#176108=CARTESIAN_POINT('Ctrl Pts',(-21.845742680186,-3.12619666607363,
135.830257907741));
#176109=CARTESIAN_POINT('Ctrl Pts',(-21.8383408585105,-3.25770653532805,
135.743518308122));
#176110=CARTESIAN_POINT('Ctrl Pts',(-21.8309429441991,-3.38914698154654,
135.656824497663));
#176111=CARTESIAN_POINT('Ctrl Pts',(-21.8235450298877,-3.51719526162264,
135.564833503806));
#176112=CARTESIAN_POINT('Ctrl Pts',(-21.8161471155763,-3.64140375070958,
135.467847433975));
#176113=CARTESIAN_POINT('Ctrl Pts',(-21.8087504306641,-3.7655915985983,
135.37087748147));
#176114=CARTESIAN_POINT('Ctrl Pts',(-21.8013537457518,-3.88594062800541,
135.268914329994));
#176115=CARTESIAN_POINT('Ctrl Pts',(-21.7939570608396,-4.0020340600782,
135.162302097723));
#176116=CARTESIAN_POINT('Ctrl Pts',(-21.7865607039042,-4.11812234444605,
135.055694592751));
#176117=CARTESIAN_POINT('Ctrl Pts',(-21.7791643469687,-4.22995513172452,
134.944438669363));
#176118=CARTESIAN_POINT('Ctrl Pts',(-21.7717679900333,-4.33715068128002,
134.828917056526));
#176119=CARTESIAN_POINT('Ctrl Pts',(-21.7643705006967,-4.44436264274842,
134.713377757034));
#176120=CARTESIAN_POINT('Ctrl Pts',(-21.75697301136,-4.54693569891078,134.593571741362));
#176121=CARTESIAN_POINT('Ctrl Pts',(-21.7495755220234,-4.64452686892937,
134.469916608994));
#176122=CARTESIAN_POINT('Ctrl Pts',(-21.7421754395084,-4.74215224938077,
134.346218129512));
#176123=CARTESIAN_POINT('Ctrl Pts',(-21.7347753569935,-4.83479203551193,
134.218668139732));
#176124=CARTESIAN_POINT('Ctrl Pts',(-21.7273752744785,-4.92214531890378,
134.087715003266));
#176125=CARTESIAN_POINT('Ctrl Pts',(-21.719967054812,-5.00959465621136,
133.956617870363));
#176126=CARTESIAN_POINT('Ctrl Pts',(-21.7125588351455,-5.09174567445106,
133.822110428272));
#176127=CARTESIAN_POINT('Ctrl Pts',(-21.705150615479,-5.16834199435097,
133.684668169188));
#176128=CARTESIAN_POINT('Ctrl Pts',(-21.697737836177,-5.24498545800748,
133.547141316687));
#176129=CARTESIAN_POINT('Ctrl Pts',(-21.690325056875,-5.31606724272622,
133.406676380159));
#176130=CARTESIAN_POINT('Ctrl Pts',(-21.6829122775729,-5.38137848385342,
133.263770338621));
#176131=CARTESIAN_POINT('Ctrl Pts',(-21.6754889065441,-5.446783044745,133.120660106229));
#176132=CARTESIAN_POINT('Ctrl Pts',(-21.6680655355153,-5.50640045337233,
132.975102147108));
#176133=CARTESIAN_POINT('Ctrl Pts',(-21.6606421644865,-5.56007092836429,
132.827610931803));
#176134=CARTESIAN_POINT('Ctrl Pts',(-21.6567061150459,-5.58852830200886,
132.749407550449));
#176135=CARTESIAN_POINT('Ctrl Pts',(-21.6527700656052,-5.61531462151302,
132.670660884153));
#176136=CARTESIAN_POINT('Ctrl Pts',(-21.6488340161646,-5.64041188726546,
132.591448837127));
#176137=CARTESIAN_POINT('Ctrl Pts',(-21.6398564824062,-5.69765495647397,
132.410778132406));
#176138=CARTESIAN_POINT('Ctrl Pts',(-21.6308789486478,-5.74624880988774,
132.227243494478));
#176139=CARTESIAN_POINT('Ctrl Pts',(-21.6219014148894,-5.78594647018682,
132.041597056826));
#176140=CARTESIAN_POINT('Ctrl Pts',(-21.6129769272198,-5.82540956655472,
131.857047559343));
#176141=CARTESIAN_POINT('Ctrl Pts',(-21.6040524395501,-5.85608123096748,
131.670411147484));
#176142=CARTESIAN_POINT('Ctrl Pts',(-21.5951279518804,-5.8777655631654,
131.482448035947));
#176143=CARTESIAN_POINT('Ctrl Pts',(-21.5862995925613,-5.8992163268758,
131.296509531821));
#176144=CARTESIAN_POINT('Ctrl Pts',(-21.5774712332422,-5.91187226502017,
131.109272779503));
#176145=CARTESIAN_POINT('Ctrl Pts',(-21.5686428739231,-5.91559043864777,
130.921494407222));
#176146=CARTESIAN_POINT('Ctrl Pts',(-21.5668869983483,-5.91632994754399,
130.884147098912));
#176147=CARTESIAN_POINT('Ctrl Pts',(-21.5651311227735,-5.91671605321219,
130.846778431061));
#176148=CARTESIAN_POINT('Ctrl Pts',(-21.5633752471987,-5.91674785866266,
130.809394454159));
#176149=CARTESIAN_POINT('',(-19.8133751630259,-5.91241589777291,130.801494312422));
#176150=CARTESIAN_POINT('Ctrl Pts',(-21.5633751922043,-5.91249924175333,
130.809389669497));
#176151=CARTESIAN_POINT('Ctrl Pts',(-21.4990455922534,-5.90151877568405,
129.440734853295));
#176152=CARTESIAN_POINT('Ctrl Pts',(-21.3419001176983,-4.74664212764213,
126.080642320765));
#176153=CARTESIAN_POINT('Ctrl Pts',(-21.0919387685389,0.850611657590301,
123.857849238585));
#176154=CARTESIAN_POINT('Ctrl Pts',(-20.813491144726,6.30407313683402,127.765245217356));
#176155=CARTESIAN_POINT('Ctrl Pts',(-20.5350435209133,5.96439937442269,
134.46543977988));
#176156=CARTESIAN_POINT('Ctrl Pts',(-20.2565958971003,0.143733964024427,
137.801281445897));
#176157=CARTESIAN_POINT('Ctrl Pts',(-20.0160397875307,-4.99895800061713,
135.128328424986));
#176158=CARTESIAN_POINT('Ctrl Pts',(-19.8682995525653,-5.90317744802826,
131.97214796945));
#176159=CARTESIAN_POINT('Ctrl Pts',(-19.8133751922042,-5.90827769618411,
130.801496940956));
#176160=CARTESIAN_POINT('',(-18.0633751922043,-5.91997941989959,130.800355646857));
#176161=CARTESIAN_POINT('Ctrl Pts',(-19.8133751324712,-5.91674930439072,
130.801491559896));
#176162=CARTESIAN_POINT('Ctrl Pts',(-19.805254061995,-5.91666525141781,
130.628152287518));
#176163=CARTESIAN_POINT('Ctrl Pts',(-19.7971329915187,-5.90895978560523,
130.455069894106));
#176164=CARTESIAN_POINT('Ctrl Pts',(-19.7890119210425,-5.89372508479234,
130.282886565106));
#176165=CARTESIAN_POINT('Ctrl Pts',(-19.780850939307,-5.8784155125575,130.109857035655));
#176166=CARTESIAN_POINT('Ctrl Pts',(-19.7726899575716,-5.85550259932545,
129.937735664064));
#176167=CARTESIAN_POINT('Ctrl Pts',(-19.764528975836,-5.82513029749076,
129.767158814755));
#176168=CARTESIAN_POINT('Ctrl Pts',(-19.7563478049367,-5.79468285869375,
129.596159981416));
#176169=CARTESIAN_POINT('Ctrl Pts',(-19.7481666340374,-5.75673919147736,
129.426713542274));
#176170=CARTESIAN_POINT('Ctrl Pts',(-19.7399854631381,-5.7114933612633,
129.259441801982));
#176171=CARTESIAN_POINT('Ctrl Pts',(-19.7317751853,-5.6660865556063,129.091574942928));
#176172=CARTESIAN_POINT('Ctrl Pts',(-19.7235649074619,-5.61332565032963,
128.925898501203));
#176173=CARTESIAN_POINT('Ctrl Pts',(-19.7153546296238,-5.5534544170368,
128.763019244744));
#176174=CARTESIAN_POINT('Ctrl Pts',(-19.7101366362407,-5.5154036098262,
128.659502299372));
#176175=CARTESIAN_POINT('Ctrl Pts',(-19.7049186428575,-5.47448177662029,
128.557114725779));
#176176=CARTESIAN_POINT('Ctrl Pts',(-19.6997006494744,-5.43076109945184,
128.456007057477));
#176177=CARTESIAN_POINT('Ctrl Pts',(-19.692277383069,-5.36856281551098,
128.312168401059));
#176178=CARTESIAN_POINT('Ctrl Pts',(-19.6848541166636,-5.30055198667891,
128.170585018124));
#176179=CARTESIAN_POINT('Ctrl Pts',(-19.6774308502582,-5.22691332803574,
128.031761183154));
#176180=CARTESIAN_POINT('Ctrl Pts',(-19.6700163575372,-5.15336170417167,
127.893101426428));
#176181=CARTESIAN_POINT('Ctrl Pts',(-19.6626018648161,-5.07419566381752,
127.757195052076));
#176182=CARTESIAN_POINT('Ctrl Pts',(-19.6551873720952,-4.98964822034993,
127.624527099965));
#176183=CARTESIAN_POINT('Ctrl Pts',(-19.6477800257414,-4.90518226689174,
127.491987018222));
#176184=CARTESIAN_POINT('Ctrl Pts',(-19.6403726793877,-4.81534543548999,
127.362679457492));
#176185=CARTESIAN_POINT('Ctrl Pts',(-19.632965333034,-4.72041689796875,
127.237065441684));
#176186=CARTESIAN_POINT('Ctrl Pts',(-19.6255635113586,-4.62555916173197,
127.111545113548));
#176187=CARTESIAN_POINT('Ctrl Pts',(-19.6181616896832,-4.52561750498102,
126.989713141722));
#176188=CARTESIAN_POINT('Ctrl Pts',(-19.6107598680078,-4.42091463852936,
126.872001996924));
#176189=CARTESIAN_POINT('Ctrl Pts',(-19.6033619536965,-4.31626704390605,
126.754352990923));
#176190=CARTESIAN_POINT('Ctrl Pts',(-19.5959640393852,-4.20686349262083,
126.640820757849));
#176191=CARTESIAN_POINT('Ctrl Pts',(-19.5885661250739,-4.09306716331315,
126.531804970286));
#176192=CARTESIAN_POINT('Ctrl Pts',(-19.5811694401617,-3.97928974489091,
126.422807299169));
#176193=CARTESIAN_POINT('Ctrl Pts',(-19.5737727552495,-3.86112126657913,
126.318324841927));
#176194=CARTESIAN_POINT('Ctrl Pts',(-19.5663760703374,-3.73896205988283,
126.218720719225));
#176195=CARTESIAN_POINT('Ctrl Pts',(-19.5589797134019,-3.61680826985394,
126.119121013074));
#176196=CARTESIAN_POINT('Ctrl Pts',(-19.5515833564665,-3.49066439259866,
126.024399447261));
#176197=CARTESIAN_POINT('Ctrl Pts',(-19.5441869995311,-3.36096394646326,
125.934878929226));
#176198=CARTESIAN_POINT('Ctrl Pts',(-19.5367895101945,-3.23124364285826,
125.845344705372));
#176199=CARTESIAN_POINT('Ctrl Pts',(-19.529392020858,-3.09796599340552,
125.761013326884));
#176200=CARTESIAN_POINT('Ctrl Pts',(-19.5219945315215,-2.96159346797302,
125.682164341264));
#176201=CARTESIAN_POINT('Ctrl Pts',(-19.5145944490065,-2.82517313736313,
125.603287715255));
#176202=CARTESIAN_POINT('Ctrl Pts',(-19.5071943664916,-2.68565609370416,
125.529897495227));
#176203=CARTESIAN_POINT('Ctrl Pts',(-19.4997942839766,-2.54352921937556,
125.462227179259));
#176204=CARTESIAN_POINT('Ctrl Pts',(-19.4923860643102,-2.40124606193763,
125.394482452821));
#176205=CARTESIAN_POINT('Ctrl Pts',(-19.4849778446437,-2.25634767994791,
125.332470351808));
#176206=CARTESIAN_POINT('Ctrl Pts',(-19.4775696249772,-2.10934141801378,
125.276376414916));
#176207=CARTESIAN_POINT('Ctrl Pts',(-19.4701568456752,-1.96224467617836,
125.220247953141));
#176208=CARTESIAN_POINT('Ctrl Pts',(-19.4627440663732,-1.81303782222359,
125.170045032456));
#176209=CARTESIAN_POINT('Ctrl Pts',(-19.4553312870711,-1.66224265139249,
125.125903086652));
#176210=CARTESIAN_POINT('Ctrl Pts',(-19.4479079160424,-1.51123201734951,
125.081698068766));
#176211=CARTESIAN_POINT('Ctrl Pts',(-19.4404845450136,-1.35862889501245,
125.043571412378));
#176212=CARTESIAN_POINT('Ctrl Pts',(-19.4330611739849,-1.20496535129876,
125.01160746689));
#176213=CARTESIAN_POINT('Ctrl Pts',(-19.4291251245438,-1.12348925330885,
124.994659416026));
#176214=CARTESIAN_POINT('Ctrl Pts',(-19.4251890751027,-1.04171513246566,
124.979443058799));
#176215=CARTESIAN_POINT('Ctrl Pts',(-19.4212530256616,-0.959722669037745,
124.965965036498));
#176216=CARTESIAN_POINT('Ctrl Pts',(-19.4138297592562,-0.805087441922301,
124.940545907076));
#176217=CARTESIAN_POINT('Ctrl Pts',(-19.4064064928507,-0.649207817768075,
124.921236066696));
#176218=CARTESIAN_POINT('Ctrl Pts',(-19.3989832264453,-0.492607899991114,
124.908152682006));
#176219=CARTESIAN_POINT('Ctrl Pts',(-19.3915687337243,-0.336193070312152,
124.895084760789));
#176220=CARTESIAN_POINT('Ctrl Pts',(-19.3841542410033,-0.179060009951245,
124.888228677603));
#176221=CARTESIAN_POINT('Ctrl Pts',(-19.3767397482823,-0.0217427461081744,
124.88765056759));
#176222=CARTESIAN_POINT('Ctrl Pts',(-19.3693324019285,0.135422889433114,
124.88707301478));
#176223=CARTESIAN_POINT('Ctrl Pts',(-19.3619250555747,0.292772004215519,
124.892761390263));
#176224=CARTESIAN_POINT('Ctrl Pts',(-19.354517709221,0.449765826577879,
124.904730013558));
#176225=CARTESIAN_POINT('Ctrl Pts',(-19.3471158875456,0.606642557024484,
124.916689710203));
#176226=CARTESIAN_POINT('Ctrl Pts',(-19.3397140658702,0.763164152067051,
124.93492029984));
#176227=CARTESIAN_POINT('Ctrl Pts',(-19.3323122441948,0.918792328765516,
124.959384037707));
#176228=CARTESIAN_POINT('Ctrl Pts',(-19.3249143298834,1.07433835056069,
124.983834861357));
#176229=CARTESIAN_POINT('Ctrl Pts',(-19.3175164155721,1.22899152544658,
125.014512222368));
#176230=CARTESIAN_POINT('Ctrl Pts',(-19.3101185012607,1.38221929063171,
125.051326601057));
#176231=CARTESIAN_POINT('Ctrl Pts',(-19.3027218163485,1.53542159214232,
125.088134861865));
#176232=CARTESIAN_POINT('Ctrl Pts',(-19.2953251314363,1.68719859146999,
125.13107802911));
#176233=CARTESIAN_POINT('Ctrl Pts',(-19.2879284465241,1.83702839595899,
125.180015568146));
#176234=CARTESIAN_POINT('Ctrl Pts',(-19.2805320895887,1.98685155683745,
125.22895093724));
#176235=CARTESIAN_POINT('Ctrl Pts',(-19.2731357326532,2.13472733970239,
125.283880033731));
#176236=CARTESIAN_POINT('Ctrl Pts',(-19.2657393757178,2.28014974612413,
125.344612665714));
#176237=CARTESIAN_POINT('Ctrl Pts',(-19.2583418863812,2.42559441708775,
125.405354596019));
#176238=CARTESIAN_POINT('Ctrl Pts',(-19.2509443970446,2.56858461921539,
125.471901687142));
#176239=CARTESIAN_POINT('Ctrl Pts',(-19.2435469077081,2.70863518501748,
125.544015952339));
#176240=CARTESIAN_POINT('Ctrl Pts',(-19.2361468251931,2.8487348453281,125.616155497079));
#176241=CARTESIAN_POINT('Ctrl Pts',(-19.228746742678,2.98589248594806,125.693865930657));
#176242=CARTESIAN_POINT('Ctrl Pts',(-19.2213466601631,3.11964848651157,
125.776863836552));
#176243=CARTESIAN_POINT('Ctrl Pts',(-19.2139384404966,3.25355156554814,
125.859953007177));
#176244=CARTESIAN_POINT('Ctrl Pts',(-19.2065302208301,3.38404521721012,
125.948341064354));
#176245=CARTESIAN_POINT('Ctrl Pts',(-19.1991220011637,3.51069911038355,
126.041701452892));
#176246=CARTESIAN_POINT('Ctrl Pts',(-19.1917092218616,3.63743095691508,
126.135119303192));
#176247=CARTESIAN_POINT('Ctrl Pts',(-19.1842964425595,3.76031804505089,
126.233515350278));
#176248=CARTESIAN_POINT('Ctrl Pts',(-19.1768836632575,3.87896438743185,
126.336523798306));
#176249=CARTESIAN_POINT('Ctrl Pts',(-19.1694602922287,3.99778025727076,
126.439679429635));
#176250=CARTESIAN_POINT('Ctrl Pts',(-19.1620369212,4.11234300825503,126.54746036933));
#176251=CARTESIAN_POINT('Ctrl Pts',(-19.1546135501712,4.2222940796779,126.659464567335));
#176252=CARTESIAN_POINT('Ctrl Pts',(-19.1506775007304,4.28059277598683,
126.718851880623));
#176253=CARTESIAN_POINT('Ctrl Pts',(-19.1467414512895,4.33759563802791,
126.779425951686));
#176254=CARTESIAN_POINT('Ctrl Pts',(-19.1428054018486,4.39325400916325,
126.841123333038));
#176255=CARTESIAN_POINT('Ctrl Pts',(-19.1353821354432,4.49822396008497,
126.957482668758));
#176256=CARTESIAN_POINT('Ctrl Pts',(-19.1279588690378,4.59872662010651,
127.078191170905));
#176257=CARTESIAN_POINT('Ctrl Pts',(-19.1205356026323,4.69438012291138,
127.202871227867));
#176258=CARTESIAN_POINT('Ctrl Pts',(-19.1131211099113,4.78992057121961,
127.327403923355));
#176259=CARTESIAN_POINT('Ctrl Pts',(-19.1057066171903,4.8806230454924,127.455898536846));
#176260=CARTESIAN_POINT('Ctrl Pts',(-19.0982921244693,4.96614324961477,
127.58794152379));
#176261=CARTESIAN_POINT('Ctrl Pts',(-19.0908847781155,5.0515810261445,127.719857242733));
#176262=CARTESIAN_POINT('Ctrl Pts',(-19.0834774317617,5.13184627475372,
127.855314215252));
#176263=CARTESIAN_POINT('Ctrl Pts',(-19.0760700854079,5.20663572878033,
127.993866897543));
#176264=CARTESIAN_POINT('Ctrl Pts',(-19.0686682637325,5.28136940201058,
128.132316242016));
#176265=CARTESIAN_POINT('Ctrl Pts',(-19.0612664420571,5.35063523600553,
128.273856371853));
#176266=CARTESIAN_POINT('Ctrl Pts',(-19.0538646203816,5.41417403142384,
128.418014012407));
#176267=CARTESIAN_POINT('Ctrl Pts',(-19.0464667060703,5.47767928520665,
128.562095553263));
#176268=CARTESIAN_POINT('Ctrl Pts',(-19.0390687917589,5.53546337120056,
128.708791512263));
#176269=CARTESIAN_POINT('Ctrl Pts',(-19.0316708774475,5.58731374165029,
128.857605441673));
#176270=CARTESIAN_POINT('Ctrl Pts',(-19.0242741925353,5.63915549550904,
129.006394640907));
#176271=CARTESIAN_POINT('Ctrl Pts',(-19.0168775076232,5.68506536818857,
129.157300759831));
#176272=CARTESIAN_POINT('Ctrl Pts',(-19.009480822711,5.72487949973719,129.309808752963));
#176273=CARTESIAN_POINT('Ctrl Pts',(-19.0020844657755,5.76469186588549,
129.462309983731));
#176274=CARTESIAN_POINT('Ctrl Pts',(-18.99468810884,5.79840893404005,129.616412586286));
#176275=CARTESIAN_POINT('Ctrl Pts',(-18.9872917519045,5.82591721352525,
129.77158804645));
#176276=CARTESIAN_POINT('Ctrl Pts',(-18.9798942625679,5.85342970459826,
129.926787264372));
#176277=CARTESIAN_POINT('Ctrl Pts',(-18.9724967732313,5.87473144910435,
130.083059299371));
#176278=CARTESIAN_POINT('Ctrl Pts',(-18.9650992838947,5.88976042715353,
130.239867328645));
#176279=CARTESIAN_POINT('Ctrl Pts',(-18.9576992013797,5.90479467358766,
130.396730326732));
#176280=CARTESIAN_POINT('Ctrl Pts',(-18.9502991188648,5.91355173996144,
130.554129321824));
#176281=CARTESIAN_POINT('Ctrl Pts',(-18.9428990363498,5.91602163658517,
130.711524428738));
#176282=CARTESIAN_POINT('Ctrl Pts',(-18.9354908166833,5.91849424911415,
130.869092607753));
#176283=CARTESIAN_POINT('Ctrl Pts',(-18.9280825970168,5.91466587953959,
131.026656516571));
#176284=CARTESIAN_POINT('Ctrl Pts',(-18.9206743773503,5.90457866351184,
131.183677594382));
#176285=CARTESIAN_POINT('Ctrl Pts',(-18.9132615980483,5.89448523897093,
131.340795316047));
#176286=CARTESIAN_POINT('Ctrl Pts',(-18.9058488187462,5.87812533065798,
131.497369170545));
#176287=CARTESIAN_POINT('Ctrl Pts',(-18.8984360394441,5.85559265213575,
131.65286828091));
#176288=CARTESIAN_POINT('Ctrl Pts',(-18.8910126684153,5.83302777786578,
131.808589575696));
#176289=CARTESIAN_POINT('Ctrl Pts',(-18.8835892973866,5.80427258604344,
131.963232693286));
#176290=CARTESIAN_POINT('Ctrl Pts',(-18.8761659263578,5.76947152194551,
132.116278648527));
#176291=CARTESIAN_POINT('Ctrl Pts',(-18.8722298769172,5.75101916272129,
132.19742728628));
#176292=CARTESIAN_POINT('Ctrl Pts',(-18.8682938274765,5.7308679204954,132.27812717353));
#176293=CARTESIAN_POINT('Ctrl Pts',(-18.8643577780358,5.70904487533382,
132.358303079154));
#176294=CARTESIAN_POINT('Ctrl Pts',(-18.8569345116303,5.66788729323179,
132.509512334959));
#176295=CARTESIAN_POINT('Ctrl Pts',(-18.8495112452249,5.62065595438862,
132.659313963098));
#176296=CARTESIAN_POINT('Ctrl Pts',(-18.8420879788194,5.56746214607701,
132.807182580322));
#176297=CARTESIAN_POINT('Ctrl Pts',(-18.8346734860984,5.51433120842935,
132.954876429122));
#176298=CARTESIAN_POINT('Ctrl Pts',(-18.8272589933775,5.45525195381932,
133.100641466801));
#176299=CARTESIAN_POINT('Ctrl Pts',(-18.8198445006565,5.39038620852657,
133.24396449636));
#176300=CARTESIAN_POINT('Ctrl Pts',(-18.8124371543027,5.32558298328118,
133.387149385787));
#176301=CARTESIAN_POINT('Ctrl Pts',(-18.8050298079489,5.25500452342057,
133.527896615039));
#176302=CARTESIAN_POINT('Ctrl Pts',(-18.7976224615952,5.17886175452877,
133.665710209975));
#176303=CARTESIAN_POINT('Ctrl Pts',(-18.7902206399198,5.10277577578681,
133.803421018332));
#176304=CARTESIAN_POINT('Ctrl Pts',(-18.7828188182444,5.02113393111676,
133.938202223669));
#176305=CARTESIAN_POINT('Ctrl Pts',(-18.775416996569,4.93419429630813,134.069579937731));
#176306=CARTESIAN_POINT('Ctrl Pts',(-18.7680190822576,4.84730055625585,
134.200888298521));
#176307=CARTESIAN_POINT('Ctrl Pts',(-18.7606211679462,4.7551148012385,134.328796435686));
#176308=CARTESIAN_POINT('Ctrl Pts',(-18.7532232536348,4.65793981954055,
134.452857184652));
#176309=CARTESIAN_POINT('Ctrl Pts',(-18.7458265687226,4.56078098656177,
134.576897316972));
#176310=CARTESIAN_POINT('Ctrl Pts',(-18.7384298838105,4.4586348024227,134.697091036458));
#176311=CARTESIAN_POINT('Ctrl Pts',(-18.7310331988983,4.3518460191663,134.813022088427));
#176312=CARTESIAN_POINT('Ctrl Pts',(-18.7236368419628,4.24506197103646,
134.928947999892));
#176313=CARTESIAN_POINT('Ctrl Pts',(-18.7162404850274,4.13363598601705,
135.040611345094));
#176314=CARTESIAN_POINT('Ctrl Pts',(-18.7088441280919,4.0179513735731,135.14763096629));
#176315=CARTESIAN_POINT('Ctrl Pts',(-18.7014466387554,3.90224904951965,
135.254666972462));
#176316=CARTESIAN_POINT('Ctrl Pts',(-18.6940491494187,3.78228707385151,
135.357057585485));
#176317=CARTESIAN_POINT('Ctrl Pts',(-18.6866516600822,3.65848356752733,
135.454460460433));
#176318=CARTESIAN_POINT('Ctrl Pts',(-18.6792515775672,3.53463666207592,
135.551897479808));
#176319=CARTESIAN_POINT('Ctrl Pts',(-18.6718514950523,3.40694583801266,
135.644343049292));
#176320=CARTESIAN_POINT('Ctrl Pts',(-18.6644514125373,3.27585991636076,
135.731496943149));
#176321=CARTESIAN_POINT('Ctrl Pts',(-18.6570431928708,3.14462985226186,
135.818746671672));
#176322=CARTESIAN_POINT('Ctrl Pts',(-18.6496349732043,3.00999754606355,
135.900692897353));
#176323=CARTESIAN_POINT('Ctrl Pts',(-18.6422267535379,2.87243887957627,
135.977079964834));
#176324=CARTESIAN_POINT('Ctrl Pts',(-18.6348139742358,2.73479554802506,
136.05351404728));
#176325=CARTESIAN_POINT('Ctrl Pts',(-18.6274011949337,2.59422259977726,
136.124381985966));
#176326=CARTESIAN_POINT('Ctrl Pts',(-18.6199884156316,2.45121733113151,
136.189475672796));
#176327=CARTESIAN_POINT('Ctrl Pts',(-18.6125650446028,2.30800772985163,
136.254662368538));
#176328=CARTESIAN_POINT('Ctrl Pts',(-18.6051416735741,2.1623592117385,136.314058193694));
#176329=CARTESIAN_POINT('Ctrl Pts',(-18.5977183025454,2.01478648989958,
136.367504150014));
#176330=CARTESIAN_POINT('Ctrl Pts',(-18.5937822531046,1.9365398918211,136.395842478473));
#176331=CARTESIAN_POINT('Ctrl Pts',(-18.5898462036637,1.85775255249047,
136.42250892794));
#176332=CARTESIAN_POINT('Ctrl Pts',(-18.5859101542229,1.77850240341984,
136.44748561738));
#176333=CARTESIAN_POINT('Ctrl Pts',(-18.5784868878175,1.62903909558629,
136.494590874169));
#176334=CARTESIAN_POINT('Ctrl Pts',(-18.571063621412,1.47747705089621,136.535825250256));
#176335=CARTESIAN_POINT('Ctrl Pts',(-18.5636403550066,1.32431844264458,
136.570998392298));
#176336=CARTESIAN_POINT('Ctrl Pts',(-18.5562258622856,1.17134085514886,
136.606129962608));
#176337=CARTESIAN_POINT('Ctrl Pts',(-18.5488113695646,1.01677082046078,
136.635214475868));
#176338=CARTESIAN_POINT('Ctrl Pts',(-18.5413968768436,0.861127576809288,
136.658110685596));
#176339=CARTESIAN_POINT('Ctrl Pts',(-18.5339895304898,0.705634347975893,
136.680984827095));
#176340=CARTESIAN_POINT('Ctrl Pts',(-18.526582184136,0.549070336308056,
136.697682485281));
#176341=CARTESIAN_POINT('Ctrl Pts',(-18.5191748377823,0.391966829328503,
136.708113031684));
#176342=CARTESIAN_POINT('Ctrl Pts',(-18.5117730161069,0.234980496071408,
136.718535798592));
#176343=CARTESIAN_POINT('Ctrl Pts',(-18.5043711944314,0.0774558395621827,
136.722700736153));
#176344=CARTESIAN_POINT('Ctrl Pts',(-18.496969372756,-0.0800689483216963,
136.720568822659));
#176345=CARTESIAN_POINT('Ctrl Pts',(-18.4895714584446,-0.237510580095773,
136.718438034587));
#176346=CARTESIAN_POINT('Ctrl Pts',(-18.4821735441333,-0.394951970787518,
136.710017020522));
#176347=CARTESIAN_POINT('Ctrl Pts',(-18.474775629822,-0.551853243714099,
136.695318821449));
#176348=CARTESIAN_POINT('Ctrl Pts',(-18.4673789449098,-0.708728442495824,
136.680623064951));
#176349=CARTESIAN_POINT('Ctrl Pts',(-18.4599822599976,-0.86506333034826,
136.659652228581));
#176350=CARTESIAN_POINT('Ctrl Pts',(-18.4525855750854,-1.02032135351922,
136.632471366175));
#176351=CARTESIAN_POINT('Ctrl Pts',(-18.4451892181499,-1.17557249238673,
136.605291708997));
#176352=CARTESIAN_POINT('Ctrl Pts',(-18.4377928612145,-1.32974649380934,
136.571902637663));
#176353=CARTESIAN_POINT('Ctrl Pts',(-18.430396504279,-1.48231549085407,
136.532420616211));
#176354=CARTESIAN_POINT('Ctrl Pts',(-18.4229990149425,-1.63490784660174,
136.492932549961));
#176355=CARTESIAN_POINT('Ctrl Pts',(-18.415601525606,-1.78589434727353,
136.4473497697));
#176356=CARTESIAN_POINT('Ctrl Pts',(-18.4082040362694,-1.9347609637968,
136.395839006639));
#176357=CARTESIAN_POINT('Ctrl Pts',(-18.4008039537544,-2.08367976528151,
136.344310186559));
#176358=CARTESIAN_POINT('Ctrl Pts',(-18.3934038712394,-2.23047685051118,
136.286849368298));
#176359=CARTESIAN_POINT('Ctrl Pts',(-18.3860037887244,-2.37465703234387,
136.223671878348));
#176360=CARTESIAN_POINT('Ctrl Pts',(-18.378595569058,-2.51899575510878,
136.160424918253));
#176361=CARTESIAN_POINT('Ctrl Pts',(-18.3711873493915,-2.66071148568839,
136.091448882692));
#176362=CARTESIAN_POINT('Ctrl Pts',(-18.3637791297251,-2.79933190824786,
136.017005956544));
#176363=CARTESIAN_POINT('Ctrl Pts',(-18.356366350423,-2.93803764936441,
135.942517212017));
#176364=CARTESIAN_POINT('Ctrl Pts',(-18.348953571121,-3.07364396547769,
135.862555061328));
#176365=CARTESIAN_POINT('Ctrl Pts',(-18.341540791819,-3.20570696855736,
135.77742540643));
#176366=CARTESIAN_POINT('Ctrl Pts',(-18.3341174207902,-3.33795866944916,
135.692174114289));
#176367=CARTESIAN_POINT('Ctrl Pts',(-18.3266940497614,-3.46665664103307,
135.601740785341));
#176368=CARTESIAN_POINT('Ctrl Pts',(-18.3192706787326,-3.59138889857157,
135.506472519862));
#176369=CARTESIAN_POINT('Ctrl Pts',(-18.3153346292918,-3.65752493442915,
135.455958999574));
#176370=CARTESIAN_POINT('Ctrl Pts',(-18.3113985798509,-3.72254665499518,
135.404086846922));
#176371=CARTESIAN_POINT('Ctrl Pts',(-18.30746253041,-3.78639689256382,135.35091196276));
#176372=CARTESIAN_POINT('Ctrl Pts',(-18.3001424141559,-3.9051431555055,
135.252019319332));
#176373=CARTESIAN_POINT('Ctrl Pts',(-18.2928222979017,-4.02021616790234,
135.148301554346));
#176374=CARTESIAN_POINT('Ctrl Pts',(-18.2855021816476,-4.13119046426338,
135.040065507012));
#176375=CARTESIAN_POINT('Ctrl Pts',(-18.2781907686664,-4.24203281742192,
134.931958147232));
#176376=CARTESIAN_POINT('Ctrl Pts',(-18.2708793556851,-4.34878587753108,
134.819343458631));
#176377=CARTESIAN_POINT('Ctrl Pts',(-18.2635679427039,-4.45105574861657,
134.702569601857));
#176378=CARTESIAN_POINT('Ctrl Pts',(-18.2562635213531,-4.55322782285328,
134.585907411551));
#176379=CARTESIAN_POINT('Ctrl Pts',(-18.2489591000023,-4.65092498734133,
134.465094254707));
#176380=CARTESIAN_POINT('Ctrl Pts',(-18.2416546786515,-4.74378905259512,
134.34051615529));
#176381=CARTESIAN_POINT('Ctrl Pts',(-18.2342263667162,-4.8382281889974,
134.213825081716));
#176382=CARTESIAN_POINT('Ctrl Pts',(-18.226798054781,-4.92766849113517,
134.083240461263));
#176383=CARTESIAN_POINT('Ctrl Pts',(-18.2193697428457,-5.01177438429781,
133.949205301075));
#176384=CARTESIAN_POINT('Ctrl Pts',(-18.212073836435,-5.09438113673903,
133.817559242996));
#176385=CARTESIAN_POINT('Ctrl Pts',(-18.2047779300244,-5.17184184502397,
133.682584966104));
#176386=CARTESIAN_POINT('Ctrl Pts',(-18.1974820236138,-5.24388129092448,
133.544732776451));
#176387=CARTESIAN_POINT('Ctrl Pts',(-18.1901875500544,-5.31590658891714,
133.406907659745));
#176388=CARTESIAN_POINT('Ctrl Pts',(-18.1828930764951,-5.38251256475605,
133.266206095432));
#176389=CARTESIAN_POINT('Ctrl Pts',(-18.1755986029358,-5.4434696449894,
133.123103549971));
#176390=CARTESIAN_POINT('Ctrl Pts',(-18.1683040281309,-5.50442757129209,
132.979999018282));
#176391=CARTESIAN_POINT('Ctrl Pts',(-18.161009453326,-5.55973629600026,
132.834493793265));
#176392=CARTESIAN_POINT('Ctrl Pts',(-18.1537148785212,-5.60921426509306,
132.687083616516));
#176393=CARTESIAN_POINT('Ctrl Pts',(-18.1461865713281,-5.66027760470986,
132.534950130517));
#176394=CARTESIAN_POINT('Ctrl Pts',(-18.138658264135,-5.70513013885221,
132.380787987925));
#176395=CARTESIAN_POINT('Ctrl Pts',(-18.1311299569419,-5.7436280871913,
132.225158618172));
#176396=CARTESIAN_POINT('Ctrl Pts',(-18.1238273542451,-5.78097183714094,
132.07419513779));
#176397=CARTESIAN_POINT('Ctrl Pts',(-18.1165247515484,-5.81233652687398,
131.921851535299));
#176398=CARTESIAN_POINT('Ctrl Pts',(-18.1092221488516,-5.83764314806235,
131.768649494605));
#176399=CARTESIAN_POINT('Ctrl Pts',(-18.1015809894104,-5.86412301222138,
131.608344837722));
#176400=CARTESIAN_POINT('Ctrl Pts',(-18.0939398299692,-5.88396960496991,
131.447100723953));
#176401=CARTESIAN_POINT('Ctrl Pts',(-18.086298670528,-5.89715334372373,
131.285518599011));
#176402=CARTESIAN_POINT('Ctrl Pts',(-18.0786575110868,-5.91033708247756,
131.123936474068));
#176403=CARTESIAN_POINT('Ctrl Pts',(-18.0710163516455,-5.91685801118231,
130.962016816047));
#176404=CARTESIAN_POINT('Ctrl Pts',(-18.0633751922043,-5.91674864602274,
130.800357832532));
#176405=CARTESIAN_POINT('',(-16.3133751922043,-5.92097783986537,130.809153648924));
#176406=CARTESIAN_POINT('Ctrl Pts',(-18.0633751922043,-5.92301518338556,
130.800353593109));
#176407=CARTESIAN_POINT('Ctrl Pts',(-18.0519217636686,-5.92489819397444,
130.557782917589));
#176408=CARTESIAN_POINT('Ctrl Pts',(-17.9476524605274,-5.80104331945593,
128.351415487931));
#176409=CARTESIAN_POINT('Ctrl Pts',(-17.7505672827852,-3.02951815479332,
124.495669764465));
#176410=CARTESIAN_POINT('Ctrl Pts',(-17.4721196589708,3.6701517233714,124.845539689074));
#176411=CARTESIAN_POINT('Ctrl Pts',(-17.1936720351586,6.99713146463687,
130.671274942398));
#176412=CARTESIAN_POINT('Ctrl Pts',(-16.9152244113454,3.89408921877592,
136.619309429597));
#176413=CARTESIAN_POINT('Ctrl Pts',(-16.6367767875328,-2.78743078230602,
137.223690034585));
#176414=CARTESIAN_POINT('Ctrl Pts',(-16.4361603811523,-5.75582047298202,
133.408977741301));
#176415=CARTESIAN_POINT('Ctrl Pts',(-16.3283598493761,-5.92377094759506,
131.126796202098));
#176416=CARTESIAN_POINT('Ctrl Pts',(-16.3133751922043,-5.92097783986537,
130.809153648924));
#176417=CARTESIAN_POINT('',(-14.5633751922042,-5.90740060865866,130.806092547028));
#176418=CARTESIAN_POINT('Ctrl Pts',(-16.3133751922043,-5.92097783986537,
130.809153648924));
#176419=CARTESIAN_POINT('Ctrl Pts',(-16.2355439747718,-5.90647026905285,
129.159298978353));
#176420=CARTESIAN_POINT('Ctrl Pts',(-16.064896882735,-4.32853530421092,
125.517624031903));
#176421=CARTESIAN_POINT('Ctrl Pts',(-15.8014339160941,1.84829460391826,
124.054444500495));
#176422=CARTESIAN_POINT('Ctrl Pts',(-15.522986292281,6.67794397737314,128.710888677124));
#176423=CARTESIAN_POINT('Ctrl Pts',(-15.2445386684683,5.37088907132037,
135.291131295225));
#176424=CARTESIAN_POINT('Ctrl Pts',(-14.9660910446553,-0.871750508755442,
137.748250851493));
#176425=CARTESIAN_POINT('Ctrl Pts',(-14.7390365525673,-5.30894723277776,
134.548523582037));
#176426=CARTESIAN_POINT('Ctrl Pts',(-14.6047979350836,-5.90970731248103,
131.689299166102));
#176427=CARTESIAN_POINT('Ctrl Pts',(-14.5633751922042,-5.90740060865866,
130.806092547028));
#176428=CARTESIAN_POINT('',(-12.8133751922043,-5.9146051397711,130.798967998767));
#176429=CARTESIAN_POINT('Ctrl Pts',(-14.5633751922042,-5.90740060865866,
130.806092547028));
#176430=CARTESIAN_POINT('Ctrl Pts',(-14.5119820604793,-5.90453868486625,
129.710299488454));
#176431=CARTESIAN_POINT('Ctrl Pts',(-14.3677730541501,-5.08582181367531,
126.631532353636));
#176432=CARTESIAN_POINT('Ctrl Pts',(-14.1307481732166,-0.122437078091865,
123.80703472175));
#176433=CARTESIAN_POINT('Ctrl Pts',(-13.8523005494037,5.82086821931613,
126.919125270293));
#176434=CARTESIAN_POINT('Ctrl Pts',(-13.5738529255909,6.41507998839504,
133.601557298682));
#176435=CARTESIAN_POINT('Ctrl Pts',(-13.2954053017781,1.11414664221958,
137.713502227777));
#176436=CARTESIAN_POINT('Ctrl Pts',(-13.0419127239824,-4.643793337457,135.676787665054));
#176437=CARTESIAN_POINT('Ctrl Pts',(-12.8812360207912,-5.90184908491918,
132.241450451055));
#176438=CARTESIAN_POINT('Ctrl Pts',(-12.8133751922043,-5.9146051397711,
130.798967998767));
#176439=CARTESIAN_POINT('',(-11.0633751922043,-5.92207844733352,130.804950250625));
#176440=CARTESIAN_POINT('Ctrl Pts',(-12.8133751922043,-5.9146051397711,
130.798967998767));
#176441=CARTESIAN_POINT('Ctrl Pts',(-12.7884201461869,-5.91929603350845,
130.268511522982));
#176442=CARTESIAN_POINT('Ctrl Pts',(-12.6706492255654,-5.61047757032242,
127.770484247143));
#176443=CARTESIAN_POINT('Ctrl Pts',(-12.4600624303391,-2.08330682229084,
124.123238465223));
#176444=CARTESIAN_POINT('Ctrl Pts',(-12.1816148065263,4.49493906093286,
125.440305866834));
#176445=CARTESIAN_POINT('Ctrl Pts',(-11.9031671827135,6.94255553713972,
131.686677535726));
#176446=CARTESIAN_POINT('Ctrl Pts',(-11.6247195589006,3.01030263740934,
137.122243060405));
#176447=CARTESIAN_POINT('Ctrl Pts',(-11.3462719350876,-3.6882713246427,
136.751983265833));
#176448=CARTESIAN_POINT('Ctrl Pts',(-11.159157146189,-5.91205182492537,
132.830344731594));
#176449=CARTESIAN_POINT('Ctrl Pts',(-11.0648582318944,-5.92650494164408,
130.836311522113));
#176450=CARTESIAN_POINT('Ctrl Pts',(-11.0633751922043,-5.92646057751854,
130.804950686933));
#176451=CARTESIAN_POINT('',(-9.31337521180815,-5.91431177079138,130.809468401107));
#176452=CARTESIAN_POINT('Ctrl Pts',(-11.0633751922043,-5.91674997067294,
130.804949720094));
#176453=CARTESIAN_POINT('Ctrl Pts',(-11.0559725385279,-5.91676553096338,
130.648667335256));
#176454=CARTESIAN_POINT('Ctrl Pts',(-11.0485698848515,-5.91058485695991,
130.492142119407));
#176455=CARTESIAN_POINT('Ctrl Pts',(-11.0411672311751,-5.89817619223044,
130.33590766592));
#176456=CARTESIAN_POINT('Ctrl Pts',(-11.0337733149295,-5.88578217357992,
130.17985761762));
#176457=CARTESIAN_POINT('Ctrl Pts',(-11.026379398684,-5.86717482433238,
130.024098019341));
#176458=CARTESIAN_POINT('Ctrl Pts',(-11.0189854824384,-5.8423743511813,
129.869164112462));
#176459=CARTESIAN_POINT('Ctrl Pts',(-11.0115986568399,-5.81759766128598,
129.714378784714));
#176460=CARTESIAN_POINT('Ctrl Pts',(-11.0042118312414,-5.78663972892824,
129.56041794053));
#176461=CARTESIAN_POINT('Ctrl Pts',(-10.9968250056428,-5.74957266881999,
129.407813200377));
#176462=CARTESIAN_POINT('Ctrl Pts',(-10.9894436296807,-5.71253295496425,
129.25532104449));
#176463=CARTESIAN_POINT('Ctrl Pts',(-10.9820622537184,-5.66939317491942,
129.104183364184));
#176464=CARTESIAN_POINT('Ctrl Pts',(-10.9746808777562,-5.62027675265298,
128.954922922998));
#176465=CARTESIAN_POINT('Ctrl Pts',(-10.9669598698273,-5.56890038492651,
128.798794708451));
#176466=CARTESIAN_POINT('Ctrl Pts',(-10.9592388618985,-5.51098439803554,
128.644721000573));
#176467=CARTESIAN_POINT('Ctrl Pts',(-10.9515178539696,-5.44672909903955,
128.493284529642));
#176468=CARTESIAN_POINT('Ctrl Pts',(-10.9441414338751,-5.38534150780139,
128.34860665371));
#176469=CARTESIAN_POINT('Ctrl Pts',(-10.9367650137806,-5.31816835142111,
128.206336096069));
#176470=CARTESIAN_POINT('Ctrl Pts',(-10.9293885936862,-5.24543405326975,
128.066961823949));
#176471=CARTESIAN_POINT('Ctrl Pts',(-10.9220123116993,-5.17270111691086,
127.92759016131));
#176472=CARTESIAN_POINT('Ctrl Pts',(-10.9146360297123,-5.0944074193427,
127.791115009524));
#176473=CARTESIAN_POINT('Ctrl Pts',(-10.9072597477254,-5.01082368071441,
127.658001355929));
#176474=CARTESIAN_POINT('Ctrl Pts',(-10.8998821260389,-4.92722476138972,
127.524863525884));
#176475=CARTESIAN_POINT('Ctrl Pts',(-10.8925045043525,-4.83833408803295,
127.395088727551));
#176476=CARTESIAN_POINT('Ctrl Pts',(-10.885126882666,-4.74446599590369,
127.269113387709));
#176477=CARTESIAN_POINT('Ctrl Pts',(-10.8777464429199,-4.65056204860439,
127.143089928563));
#176478=CARTESIAN_POINT('Ctrl Pts',(-10.8703660031739,-4.55167712190346,
127.020869117988));
#176479=CARTESIAN_POINT('Ctrl Pts',(-10.8629855634278,-4.4481660206591,
126.90285454745));
#176480=CARTESIAN_POINT('Ctrl Pts',(-10.8555969500128,-4.34454028322792,
126.784709278463));
#176481=CARTESIAN_POINT('Ctrl Pts',(-10.8482083365977,-4.23627838943202,
126.670779832888));
#176482=CARTESIAN_POINT('Ctrl Pts',(-10.8408197231827,-4.12377266546004,
126.561433612997));
#176483=CARTESIAN_POINT('Ctrl Pts',(-10.8334263149394,-4.01119393108678,
126.452016433059));
#176484=CARTESIAN_POINT('Ctrl Pts',(-10.8260329066962,-3.89436615855799,
126.34718865428));
#176485=CARTESIAN_POINT('Ctrl Pts',(-10.8186394984529,-3.77371450048516,
126.24727718281));
#176486=CARTESIAN_POINT('Ctrl Pts',(-10.8112359444123,-3.65289727502847,
126.147228605218));
#176487=CARTESIAN_POINT('Ctrl Pts',(-10.8038323903717,-3.52824598511995,
126.052110030891));
#176488=CARTESIAN_POINT('Ctrl Pts',(-10.7964288363311,-3.40021498322093,
125.96220524724));
#176489=CARTESIAN_POINT('Ctrl Pts',(-10.7940781200414,-3.35956362036101,
125.93365941124));
#176490=CARTESIAN_POINT('Ctrl Pts',(-10.7917274037517,-3.31857172301088,
125.905638850208));
#176491=CARTESIAN_POINT('Ctrl Pts',(-10.7893766874619,-3.27725432932366,
125.878151667123));
#176492=CARTESIAN_POINT('Ctrl Pts',(-10.7819534210565,-3.14677919633695,
125.791350599861));
#176493=CARTESIAN_POINT('Ctrl Pts',(-10.7745301546511,-3.01265587994184,
125.709605488931));
#176494=CARTESIAN_POINT('Ctrl Pts',(-10.7671068882456,-2.87531383550085,
125.633238794414));
#176495=CARTESIAN_POINT('Ctrl Pts',(-10.7596923955246,-2.73813411795046,
125.556962358988));
#176496=CARTESIAN_POINT('Ctrl Pts',(-10.7522779028036,-2.59774356784212,
125.486051866285));
#176497=CARTESIAN_POINT('Ctrl Pts',(-10.7448634100826,-2.45460168509987,
125.420787349744));
#176498=CARTESIAN_POINT('Ctrl Pts',(-10.7374560637288,-2.31159776789361,
125.355585737602));
#176499=CARTESIAN_POINT('Ctrl Pts',(-10.7300487173751,-2.16584813471945,
125.296019421885));
#176500=CARTESIAN_POINT('Ctrl Pts',(-10.7226413710213,-2.017837932274,125.242323163397));
#176501=CARTESIAN_POINT('Ctrl Pts',(-10.7152395493459,-1.86993812142143,
125.188666953605));
#176502=CARTESIAN_POINT('Ctrl Pts',(-10.7078377276705,-1.71978144779477,
125.140872210394));
#176503=CARTESIAN_POINT('Ctrl Pts',(-10.7004359059951,-1.56787403763929,
125.099126041793));
#176504=CARTESIAN_POINT('Ctrl Pts',(-10.6930379916837,-1.41604681822383,
125.05740191067));
#176505=CARTESIAN_POINT('Ctrl Pts',(-10.6856400773724,-1.26247106191039,
125.021720093822));
#176506=CARTESIAN_POINT('Ctrl Pts',(-10.678242163061,-1.10766898746678,
124.992218157448));
#176507=CARTESIAN_POINT('Ctrl Pts',(-10.6708454781488,-0.952892638319105,
124.96272112376));
#176508=CARTESIAN_POINT('Ctrl Pts',(-10.6634487932367,-0.796890741846708,
124.939402002103));
#176509=CARTESIAN_POINT('Ctrl Pts',(-10.6560521083244,-0.640196785166688,
124.922347472497));
#176510=CARTESIAN_POINT('Ctrl Pts',(-10.648655751389,-0.483509776461135,
124.905293699108));
#176511=CARTESIAN_POINT('Ctrl Pts',(-10.6412593944536,-0.326131139669395,
124.894504005844));
#176512=CARTESIAN_POINT('Ctrl Pts',(-10.6338630375182,-0.168600310285228,
124.890013274209));
#176513=CARTESIAN_POINT('Ctrl Pts',(-10.6264655481816,-0.0110453625287005,
124.885521855032));
#176514=CARTESIAN_POINT('Ctrl Pts',(-10.619068058845,0.146661451045509,
124.887331328345));
#176515=CARTESIAN_POINT('Ctrl Pts',(-10.6116705695084,0.303980012317705,
124.895424443041));
#176516=CARTESIAN_POINT('Ctrl Pts',(-10.6042704869934,0.461353721367905,
124.903520394766));
#176517=CARTESIAN_POINT('Ctrl Pts',(-10.5968704044785,0.61833853456716,
124.917904354309));
#176518=CARTESIAN_POINT('Ctrl Pts',(-10.5894703219635,0.774398922773036,
124.938507152732));
#176519=CARTESIAN_POINT('Ctrl Pts',(-10.582062102297,0.930630915418698,
124.959132606049));
#176520=CARTESIAN_POINT('Ctrl Pts',(-10.5746538826305,1.08593608273927,
124.985990505799));
#176521=CARTESIAN_POINT('Ctrl Pts',(-10.567245662964,1.23978783797754,125.018960313412));
#176522=CARTESIAN_POINT('Ctrl Pts',(-10.559832883662,1.39373428640401,125.051950413392));
#176523=CARTESIAN_POINT('Ctrl Pts',(-10.55242010436,1.54622517948682,125.091059824526));
#176524=CARTESIAN_POINT('Ctrl Pts',(-10.5450073250579,1.69674908362636,
125.136118111311));
#176525=CARTESIAN_POINT('Ctrl Pts',(-10.5375839540292,1.84748806337922,
125.181240779489));
#176526=CARTESIAN_POINT('Ctrl Pts',(-10.5301605830004,1.99625408881397,
125.232329178865));
#176527=CARTESIAN_POINT('Ctrl Pts',(-10.5227372119717,2.14255491820914,
125.289164430216));
#176528=CARTESIAN_POINT('Ctrl Pts',(-10.5188011625308,2.22012712839686,
125.319299844227));
#176529=CARTESIAN_POINT('Ctrl Pts',(-10.5148651130899,2.29700667109292,
125.351050124242));
#176530=CARTESIAN_POINT('Ctrl Pts',(-10.510929063649,2.37312309110805,125.384377466582));
#176531=CARTESIAN_POINT('Ctrl Pts',(-10.5035057972436,2.51667628374082,
125.447231794123));
#176532=CARTESIAN_POINT('Ctrl Pts',(-10.4960825308381,2.65794768936465,
125.515888309583));
#176533=CARTESIAN_POINT('Ctrl Pts',(-10.4886592644326,2.79643388206537,
125.590159997554));
#176534=CARTESIAN_POINT('Ctrl Pts',(-10.4812447717116,2.93475639558649,
125.664343902557));
#176535=CARTESIAN_POINT('Ctrl Pts',(-10.4738302789907,3.07029992295007,
125.744129595039));
#176536=CARTESIAN_POINT('Ctrl Pts',(-10.4664157862697,3.20258049315985,
125.829281849613));
#176537=CARTESIAN_POINT('Ctrl Pts',(-10.4590084399159,3.33473356637598,
125.914352031239));
#176538=CARTESIAN_POINT('Ctrl Pts',(-10.4516010935622,3.46362963165732,
126.00477827684));
#176539=CARTESIAN_POINT('Ctrl Pts',(-10.4441937472084,3.58880894445214,
126.100279312707));
#176540=CARTESIAN_POINT('Ctrl Pts',(-10.436791925533,3.71389489379274,126.195709120299));
#176541=CARTESIAN_POINT('Ctrl Pts',(-10.4293901038576,3.8352693147493,126.296205956322));
#176542=CARTESIAN_POINT('Ctrl Pts',(-10.4219882821822,3.95250121443982,
126.401445138891));
#176543=CARTESIAN_POINT('Ctrl Pts',(-10.4145903678708,4.06967122832319,
126.506628766516));
#176544=CARTESIAN_POINT('Ctrl Pts',(-10.4071924535595,4.18270279898259,
126.616549506211));
#176545=CARTESIAN_POINT('Ctrl Pts',(-10.3997945392481,4.29119791608063,
126.730842358429));
#176546=CARTESIAN_POINT('Ctrl Pts',(-10.3923978543359,4.39967500325837,
126.845116217247));
#176547=CARTESIAN_POINT('Ctrl Pts',(-10.3850011694237,4.50361687634247,
126.963760476095));
#176548=CARTESIAN_POINT('Ctrl Pts',(-10.3776044845115,4.60266224615703,
127.086373149822));
#176549=CARTESIAN_POINT('Ctrl Pts',(-10.3702081275761,4.70170322419625,
127.208980386774));
#176550=CARTESIAN_POINT('Ctrl Pts',(-10.3628117706406,4.79584789609205,
127.33555539834));
#176551=CARTESIAN_POINT('Ctrl Pts',(-10.3554154137051,4.88477533698727,
127.465663196466));
#176552=CARTESIAN_POINT('Ctrl Pts',(-10.3480179243686,4.97371639290084,
127.595790914427));
#176553=CARTESIAN_POINT('Ctrl Pts',(-10.340620435032,5.05743841669607,127.729452187701));
#176554=CARTESIAN_POINT('Ctrl Pts',(-10.3332229456954,5.13566397518045,
127.866183274972));
#176555=CARTESIAN_POINT('Ctrl Pts',(-10.3258228631804,5.21391695551287,
128.002962293113));
#176556=CARTESIAN_POINT('Ctrl Pts',(-10.3184227806654,5.28666944907581,
128.142812943979));
#176557=CARTESIAN_POINT('Ctrl Pts',(-10.3110226981504,5.3536901830731,128.285247284235));
#176558=CARTESIAN_POINT('Ctrl Pts',(-10.3036144784839,5.42078461325731,
128.427838245691));
#176559=CARTESIAN_POINT('Ctrl Pts',(-10.2962062588175,5.48213453801958,
128.573018232284));
#176560=CARTESIAN_POINT('Ctrl Pts',(-10.288798039151,5.53755673686508,128.720279057622));
#176561=CARTESIAN_POINT('Ctrl Pts',(-10.2813852598489,5.59301304714952,
128.867630519541));
#176562=CARTESIAN_POINT('Ctrl Pts',(-10.2739724805468,5.64253424443491,
129.017065018678));
#176563=CARTESIAN_POINT('Ctrl Pts',(-10.2665597012447,5.6859872785842,129.168060146907));
#176564=CARTESIAN_POINT('Ctrl Pts',(-10.2591363302159,5.72950240046618,
129.319271024056));
#176565=CARTESIAN_POINT('Ctrl Pts',(-10.2517129591872,5.76693195373218,
129.472046622293));
#176566=CARTESIAN_POINT('Ctrl Pts',(-10.2442895881585,5.79819401899688,
129.625854495151));
#176567=CARTESIAN_POINT('Ctrl Pts',(-10.2403535387177,5.81476991612321,
129.70740711991));
#176568=CARTESIAN_POINT('Ctrl Pts',(-10.2364174892769,5.82961277704559,
129.789249858412));
#176569=CARTESIAN_POINT('Ctrl Pts',(-10.2324814398361,5.84271632432023,
129.871303000898));
#176570=CARTESIAN_POINT('Ctrl Pts',(-10.2250581734307,5.86742920553252,
130.026052666836));
#176571=CARTESIAN_POINT('Ctrl Pts',(-10.2176349070252,5.88602718010824,
130.182018825036));
#176572=CARTESIAN_POINT('Ctrl Pts',(-10.2102116406198,5.89839547540299,
130.338676842623));
#176573=CARTESIAN_POINT('Ctrl Pts',(-10.2027971478988,5.91074915239983,
130.495149703442));
#176574=CARTESIAN_POINT('Ctrl Pts',(-10.1953826551778,5.91688777704139,
130.652312427466));
#176575=CARTESIAN_POINT('Ctrl Pts',(-10.1879681624568,5.91674765296144,
130.809630691122));
#176576=CARTESIAN_POINT('Ctrl Pts',(-10.180560816103,5.91660766393836,130.966797325512));
#176577=CARTESIAN_POINT('Ctrl Pts',(-10.1731534697492,5.91020097425619,
131.12411883029));
#176578=CARTESIAN_POINT('Ctrl Pts',(-10.1657461233955,5.89751572429131,
131.281056374036));
#176579=CARTESIAN_POINT('Ctrl Pts',(-10.1583443017201,5.8848399354645,131.43787686784));
#176580=CARTESIAN_POINT('Ctrl Pts',(-10.1509424800447,5.86589494036225,
131.594313600335));
#176581=CARTESIAN_POINT('Ctrl Pts',(-10.1435406583693,5.84072094086921,
131.749828466513));
#176582=CARTESIAN_POINT('Ctrl Pts',(-10.136142744058,5.81556023053434,131.905261237605));
#176583=CARTESIAN_POINT('Ctrl Pts',(-10.1287448297466,5.78417712400211,
132.05977274399));
#176584=CARTESIAN_POINT('Ctrl Pts',(-10.1213469154352,5.74666357142174,
132.212830837128));
#176585=CARTESIAN_POINT('Ctrl Pts',(-10.113950230523,5.70915625291342,132.365863494788));
#176586=CARTESIAN_POINT('Ctrl Pts',(-10.1065535456107,5.66552059908761,
132.517442856355));
#176587=CARTESIAN_POINT('Ctrl Pts',(-10.0991568606985,5.6158995258123,132.667047676221));
#176588=CARTESIAN_POINT('Ctrl Pts',(-10.0917605037631,5.56628065278753,
132.816645862452));
#176589=CARTESIAN_POINT('Ctrl Pts',(-10.0843641468277,5.5106770055377,132.964269326751));
#176590=CARTESIAN_POINT('Ctrl Pts',(-10.0769677898923,5.44928108410796,
133.109412944279));
#176591=CARTESIAN_POINT('Ctrl Pts',(-10.0695703005556,5.38787576280555,
133.254578783665));
#176592=CARTESIAN_POINT('Ctrl Pts',(-10.0621728112191,5.32067654700163,
133.397263676478));
#176593=CARTESIAN_POINT('Ctrl Pts',(-10.0547753218825,5.24792363598143,
133.536983546806));
#176594=CARTESIAN_POINT('Ctrl Pts',(-10.0473752393675,5.17514522154135,
133.676752395717));
#176595=CARTESIAN_POINT('Ctrl Pts',(-10.0399751568525,5.09680940804071,
133.813553821845));
#176596=CARTESIAN_POINT('Ctrl Pts',(-10.0325750743375,5.01320170743094,
133.946929503543));
#176597=CARTESIAN_POINT('Ctrl Pts',(-10.025166854671,4.92950207155915,134.080451845515));
#176598=CARTESIAN_POINT('Ctrl Pts',(-10.0177586350045,4.8405191700166,134.21054060371));
#176599=CARTESIAN_POINT('Ctrl Pts',(-10.010350415338,4.74658151925483,134.336766942378));
#176600=CARTESIAN_POINT('Ctrl Pts',(-10.002937636036,4.65258605143658,134.46307097125));
#176601=CARTESIAN_POINT('Ctrl Pts',(-9.99552485673399,4.55362999186371,
134.585507553963));
#176602=CARTESIAN_POINT('Ctrl Pts',(-9.98811207743194,4.45008094043782,
134.703682377315));
#176603=CARTESIAN_POINT('Ctrl Pts',(-9.98068870640318,4.34638393327112,
134.822026054397));
#176604=CARTESIAN_POINT('Ctrl Pts',(-9.97326533537441,4.23808108345211,
134.936095540218));
#176605=CARTESIAN_POINT('Ctrl Pts',(-9.96584196434566,4.12557607384473,
135.045534113359));
#176606=CARTESIAN_POINT('Ctrl Pts',(-9.96190591490489,4.06592321823056,
135.103561070781));
#176607=CARTESIAN_POINT('Ctrl Pts',(-9.95796986546407,4.00508953330804,
135.160286789327));
#176608=CARTESIAN_POINT('Ctrl Pts',(-9.9540338160233,3.94313868804302,135.215662902533));
#176609=CARTESIAN_POINT('Ctrl Pts',(-9.94661054961786,3.82630132729226,
135.320100523812));
#176610=CARTESIAN_POINT('Ctrl Pts',(-9.93918728321246,3.7051352407465,135.420051044737));
#176611=CARTESIAN_POINT('Ctrl Pts',(-9.93176401680702,3.58001977948435,
135.515134326948));
#176612=CARTESIAN_POINT('Ctrl Pts',(-9.924349524086,3.45505219430705,135.610105228615));
#176613=CARTESIAN_POINT('Ctrl Pts',(-9.91693503136498,3.32614482006905,
135.700220118628));
#176614=CARTESIAN_POINT('Ctrl Pts',(-9.90952053864396,3.193712768883,135.785136592489));
#176615=CARTESIAN_POINT('Ctrl Pts',(-9.90211319229019,3.06140836069405,
135.869971220656));
#176616=CARTESIAN_POINT('Ctrl Pts',(-9.89470584593635,2.92558635088209,
135.949617207303));
#176617=CARTESIAN_POINT('Ctrl Pts',(-9.88729849958258,2.78669366316633,
136.02377332305));
#176618=CARTESIAN_POINT('Ctrl Pts',(-9.87989667790721,2.64790456685758,
136.097874130368));
#176619=CARTESIAN_POINT('Ctrl Pts',(-9.87249485623189,2.50604968068134,
136.166493044531));
#176620=CARTESIAN_POINT('Ctrl Pts',(-9.86509303455651,2.36160345772091,
136.229373029624));
#176621=CARTESIAN_POINT('Ctrl Pts',(-9.85769512024507,2.21723348679515,
136.292219820863));
#176622=CARTESIAN_POINT('Ctrl Pts',(-9.85029720593362,2.07027524482308,
136.349333567877));
#176623=CARTESIAN_POINT('Ctrl Pts',(-9.84289929162219,1.9212261447454,136.400503991645));
#176624=CARTESIAN_POINT('Ctrl Pts',(-9.83550260670999,1.77220181392583,
136.451665911817));
#176625=CARTESIAN_POINT('Ctrl Pts',(-9.8281059217978,1.6210876673359,136.496886347886));
#176626=CARTESIAN_POINT('Ctrl Pts',(-9.82070923688559,1.46839949318662,
136.536003793036));
#176627=CARTESIAN_POINT('Ctrl Pts',(-9.81331287995015,1.315718089391,136.575119503677));
#176628=CARTESIAN_POINT('Ctrl Pts',(-9.80591652301471,1.16146315842902,
136.608132668826));
#176629=CARTESIAN_POINT('Ctrl Pts',(-9.79852016607927,1.00616372711077,
136.634932211908));
#176630=CARTESIAN_POINT('Ctrl Pts',(-9.7911226767427,0.850840519053114,
136.661735858068));
#176631=CARTESIAN_POINT('Ctrl Pts',(-9.78372518740613,0.694472860110188,
136.682323924469));
#176632=CARTESIAN_POINT('Ctrl Pts',(-9.77632769806957,0.537597850636254,
136.696636842718));
#176633=CARTESIAN_POINT('Ctrl Pts',(-9.76892761555455,0.380667848870265,
136.710954778338));
#176634=CARTESIAN_POINT('Ctrl Pts',(-9.76152753303949,0.223230513995242,
136.718993152237));
#176635=CARTESIAN_POINT('Ctrl Pts',(-9.75412745052446,0.0658257711749089,
136.720744439661));
#176636=CARTESIAN_POINT('Ctrl Pts',(-9.746719230858,-0.091752054341082,
136.722497652806));
#176637=CARTESIAN_POINT('Ctrl Pts',(-9.73931101119156,-0.249296842727074,
136.71794996901));
#176638=CARTESIAN_POINT('Ctrl Pts',(-9.7319027915251,-0.406270231155212,
136.707145982271));
#176639=CARTESIAN_POINT('Ctrl Pts',(-9.72449001222301,-0.563340234085357,
136.696335345859));
#176640=CARTESIAN_POINT('Ctrl Pts',(-9.71707723292087,-0.719837766041626,
136.679260773995));
#176641=CARTESIAN_POINT('Ctrl Pts',(-9.70966445361879,-0.875232383435107,
136.656018402971));
#176642=CARTESIAN_POINT('Ctrl Pts',(-9.70224108259003,-1.03084903594476,
136.632742822157));
#176643=CARTESIAN_POINT('Ctrl Pts',(-9.69481771156129,-1.18535926075348,
136.603281910697));
#176644=CARTESIAN_POINT('Ctrl Pts',(-9.68739434053253,-1.33824473757904,
136.567782481775));
#176645=CARTESIAN_POINT('Ctrl Pts',(-9.68345829109182,-1.41930828582709,
136.548959832764));
#176646=CARTESIAN_POINT('Ctrl Pts',(-9.67952224165109,-1.49991533204027,
136.528440367216));
#176647=CARTESIAN_POINT('Ctrl Pts',(-9.67558619221037,-1.5799907695123,
136.506251508381));
#176648=CARTESIAN_POINT('Ctrl Pts',(-9.66816292580495,-1.73101054551834,
136.464404013107));
#176649=CARTESIAN_POINT('Ctrl Pts',(-9.66073965939949,-1.88059497894224,
136.416489250882));
#176650=CARTESIAN_POINT('Ctrl Pts',(-9.65331639299407,-2.02821920009124,
136.362620906441));
#176651=CARTESIAN_POINT('Ctrl Pts',(-9.64590190027308,-2.17566894167027,
136.308816229909));
#176652=CARTESIAN_POINT('Ctrl Pts',(-9.63848740755215,-2.32116273533804,
136.249072104348));
#176653=CARTESIAN_POINT('Ctrl Pts',(-9.63107291483115,-2.4641881282552,
136.183552697337));
#176654=CARTESIAN_POINT('Ctrl Pts',(-9.62366556847732,-2.60707566791507,
136.118096440396));
#176655=CARTESIAN_POINT('Ctrl Pts',(-9.61625822212349,-2.7474992061147,
136.046876138106));
#176656=CARTESIAN_POINT('Ctrl Pts',(-9.60885087576966,-2.88496373685656,
135.97010497821));
#176657=CARTESIAN_POINT('Ctrl Pts',(-9.60144905409428,-3.02232574136377,
135.893391077142));
#176658=CARTESIAN_POINT('Ctrl Pts',(-9.59404723241887,-3.15673280821445,
135.811134743078));
#176659=CARTESIAN_POINT('Ctrl Pts',(-9.5866454107435,-3.2877122323319,135.723596212643));
#176660=CARTESIAN_POINT('Ctrl Pts',(-9.57924749643216,-3.41862251343128,
135.636103893117));
#176661=CARTESIAN_POINT('Ctrl Pts',(-9.57184958212081,-3.54610844577842,
135.543335137415));
#176662=CARTESIAN_POINT('Ctrl Pts',(-9.56445166780946,-3.66972425183371,
135.445594772185));
#176663=CARTESIAN_POINT('Ctrl Pts',(-9.55705498289727,-3.79331951518448,
135.347870649631));
#176664=CARTESIAN_POINT('Ctrl Pts',(-9.54965829798511,-3.91304563615874,
135.245176788596));
#176665=CARTESIAN_POINT('Ctrl Pts',(-9.54226161307292,-4.02848793837069,
135.137859837931));
#176666=CARTESIAN_POINT('Ctrl Pts',(-9.5348652561375,-4.14392512174999,
135.030547645812));
#176667=CARTESIAN_POINT('Ctrl Pts',(-9.52746889920204,-4.25507859064215,
134.918613025821));
#176668=CARTESIAN_POINT('Ctrl Pts',(-9.5200725422666,-4.36156894126619,
134.802441023596));
#176669=CARTESIAN_POINT('Ctrl Pts',(-9.51267505293002,-4.46807559583507,
134.68625123514));
#176670=CARTESIAN_POINT('Ctrl Pts',(-9.50527756359342,-4.56991745833369,
134.565823047891));
#176671=CARTESIAN_POINT('Ctrl Pts',(-9.49788007425684,-4.66675409632555,
134.441576141415));
#176672=CARTESIAN_POINT('Ctrl Pts',(-9.49047999174186,-4.76362468025047,
134.317285680379));
#176673=CARTESIAN_POINT('Ctrl Pts',(-9.48307990922691,-4.85548631699029,
134.189174129133));
#176674=CARTESIAN_POINT('Ctrl Pts',(-9.47567982671194,-4.94204083301768,
134.057691674696));
#176675=CARTESIAN_POINT('Ctrl Pts',(-9.4682716070455,-5.02869052463333,
133.926064641783));
#176676=CARTESIAN_POINT('Ctrl Pts',(-9.46086338737904,-5.11002123582678,
133.791059615239));
#176677=CARTESIAN_POINT('Ctrl Pts',(-9.4534551677126,-5.1857794865322,133.653153639104));
#176678=CARTESIAN_POINT('Ctrl Pts',(-9.44604238841058,-5.26158436517683,
133.515162784141));
#176679=CARTESIAN_POINT('Ctrl Pts',(-9.43862960910857,-5.33180978297738,
133.374267755105));
#176680=CARTESIAN_POINT('Ctrl Pts',(-9.43121682980654,-5.39624990440219,
133.230966793224));
#176681=CARTESIAN_POINT('Ctrl Pts',(-9.42379345877782,-5.46078210089444,
133.087461076208));
#176682=CARTESIAN_POINT('Ctrl Pts',(-9.41637008774905,-5.51951235233774,
132.941542905853));
#176683=CARTESIAN_POINT('Ctrl Pts',(-9.40894671672032,-5.57228401204957,
132.793727715805));
#176684=CARTESIAN_POINT('Ctrl Pts',(-9.40501066727938,-5.60026481226855,
132.715352555262));
#176685=CARTESIAN_POINT('Ctrl Pts',(-9.4010746178385,-5.62657128217795,
132.636444292024));
#176686=CARTESIAN_POINT('Ctrl Pts',(-9.39713856839757,-5.651185896725,132.557080938426));
#176687=CARTESIAN_POINT('Ctrl Pts',(-9.38809573540457,-5.70773646903769,
132.374748484753));
#176688=CARTESIAN_POINT('Ctrl Pts',(-9.37905290241155,-5.75549286966623,
132.189567681947));
#176689=CARTESIAN_POINT('Ctrl Pts',(-9.37001006941856,-5.7942091403477,
132.00230510727));
#176690=CARTESIAN_POINT('Ctrl Pts',(-9.36057093182716,-5.83462216204914,
131.806835699677));
#176691=CARTESIAN_POINT('Ctrl Pts',(-9.35113179423582,-5.86518480503675,
131.609097826369));
#176692=CARTESIAN_POINT('Ctrl Pts',(-9.34169265664443,-5.8856728759424,
131.409988688164));
#176693=CARTESIAN_POINT('Ctrl Pts',(-9.3328127637492,-5.90494708118736,
131.222676255793));
#176694=CARTESIAN_POINT('Ctrl Pts',(-9.32393287085396,-5.91530547341419,
131.034150421048));
#176695=CARTESIAN_POINT('Ctrl Pts',(-9.31505297795874,-5.91660919492221,
130.845179694748));
#176696=CARTESIAN_POINT('Ctrl Pts',(-9.31449373326259,-5.9166913016939,
130.833278551608));
#176697=CARTESIAN_POINT('Ctrl Pts',(-9.31393448856645,-5.91673751044455,
130.821375650849));
#176698=CARTESIAN_POINT('Ctrl Pts',(-9.3133752438703,-5.91674779288229,
130.809471187257));
#176699=CARTESIAN_POINT('',(-7.56337516349587,-5.91244826925484,130.801667160838));
#176700=CARTESIAN_POINT('Ctrl Pts',(-9.3133751922043,-5.9128223061593,130.809466697563));
#176701=CARTESIAN_POINT('Ctrl Pts',(-9.24848044299772,-5.90153186961771,
129.428978555947));
#176702=CARTESIAN_POINT('Ctrl Pts',(-9.09076981918684,-4.73048501898084,
126.056784170589));
#176703=CARTESIAN_POINT('Ctrl Pts',(-8.84024332077167,0.892881284146524,
123.863155855944));
#176704=CARTESIAN_POINT('Ctrl Pts',(-8.56179569695882,6.32245629500537,
127.80367620762));
#176705=CARTESIAN_POINT('Ctrl Pts',(-8.28334807314588,5.9420028399166,134.501678940454));
#176706=CARTESIAN_POINT('Ctrl Pts',(-8.00490044933302,0.101139057920626,
137.802026758594));
#176707=CARTESIAN_POINT('Ctrl Pts',(-7.76490948901916,-5.01314309408,135.104171354005));
#176708=CARTESIAN_POINT('Ctrl Pts',(-7.61773440330959,-5.90337292098504,
131.960358330193));
#176709=CARTESIAN_POINT('Ctrl Pts',(-7.56337519220432,-5.90810821042033,
130.801669750358));
#176710=CARTESIAN_POINT('',(-5.81337519220429,-5.91970862835117,130.800211422335));
#176711=CARTESIAN_POINT('Ctrl Pts',(-7.56337513504499,-5.9167493857658,
130.801664594553));
#176712=CARTESIAN_POINT('Ctrl Pts',(-7.55528446404787,-5.91667068981716,
130.628956793656));
#176713=CARTESIAN_POINT('Ctrl Pts',(-7.5471937930507,-5.90902596019284,
130.456497795035));
#176714=CARTESIAN_POINT('Ctrl Pts',(-7.53910312205358,-5.89390511114336,
130.284925247825));
#176715=CARTESIAN_POINT('Ctrl Pts',(-7.53097456335621,-5.87871345286232,
130.112549245717));
#176716=CARTESIAN_POINT('Ctrl Pts',(-7.52284600465886,-5.85597557211895,
129.941068258802));
#176717=CARTESIAN_POINT('Ctrl Pts',(-7.51471744596151,-5.82583314817139,
129.771113942194));
#176718=CARTESIAN_POINT('Ctrl Pts',(-7.50656981588184,-5.79562000348323,
129.600760875467));
#176719=CARTESIAN_POINT('Ctrl Pts',(-7.49842218580217,-5.75796764258631,
129.431941879387));
#176720=CARTESIAN_POINT('Ctrl Pts',(-7.49027455572249,-5.71306787093264,
129.265274504115));
#176721=CARTESIAN_POINT('Ctrl Pts',(-7.48209847134111,-5.66801129397036,
129.098025069553));
#176722=CARTESIAN_POINT('Ctrl Pts',(-7.47392238695973,-5.61565671350522,
128.932942534547));
#176723=CARTESIAN_POINT('Ctrl Pts',(-7.46574630257834,-5.55624564874628,
128.770628862076));
#176724=CARTESIAN_POINT('Ctrl Pts',(-7.45983260228799,-5.51327407280285,
128.653228604539));
#176725=CARTESIAN_POINT('Ctrl Pts',(-7.45391890199762,-5.46661188495489,
128.53727643129));
#176726=CARTESIAN_POINT('Ctrl Pts',(-7.44800520170728,-5.41636538536468,
128.422991982784));
#176727=CARTESIAN_POINT('Ctrl Pts',(-7.4405819353018,-5.35329266708549,
128.27953460997));
#176728=CARTESIAN_POINT('Ctrl Pts',(-7.43315866889636,-5.28442124009781,
128.138367851464));
#176729=CARTESIAN_POINT('Ctrl Pts',(-7.42573540249089,-5.20993888572132,
127.999994847994));
#176730=CARTESIAN_POINT('Ctrl Pts',(-7.41832090976983,-5.13554456330222,
127.861785389922));
#176731=CARTESIAN_POINT('Ctrl Pts',(-7.41090641704874,-5.05555268903511,
127.726363439756));
#176732=CARTESIAN_POINT('Ctrl Pts',(-7.40349192432768,-4.97019922455477,
127.59421260996));
#176733=CARTESIAN_POINT('Ctrl Pts',(-7.39608457797386,-4.884928026957,127.462189152109));
#176734=CARTESIAN_POINT('Ctrl Pts',(-7.38867723162001,-4.79430572819841,
127.333430849439));
#176735=CARTESIAN_POINT('Ctrl Pts',(-7.38126988526619,-4.69861430131405,
127.208397017919));
#176736=CARTESIAN_POINT('Ctrl Pts',(-7.37386806359074,-4.60299424470596,
127.083456441347));
#176737=CARTESIAN_POINT('Ctrl Pts',(-7.36646624191535,-4.50231281384863,
126.962235100016));
#176738=CARTESIAN_POINT('Ctrl Pts',(-7.35906442023989,-4.39689534614848,
126.845163492199));
#176739=CARTESIAN_POINT('Ctrl Pts',(-7.35166650592851,-4.29153352750941,
126.728153685572));
#176740=CARTESIAN_POINT('Ctrl Pts',(-7.34426859161715,-4.18144090029054,
126.615289526455));
#176741=CARTESIAN_POINT('Ctrl Pts',(-7.33687067730577,-4.06698306932293,
126.506968469258));
#176742=CARTESIAN_POINT('Ctrl Pts',(-7.32947399239352,-3.95254425917018,
126.398665413055));
#176743=CARTESIAN_POINT('Ctrl Pts',(-7.32207730748121,-3.83374195587244,
126.294904216699));
#176744=CARTESIAN_POINT('Ctrl Pts',(-7.31468062256897,-3.71097869393608,
126.196045557194));
#176745=CARTESIAN_POINT('Ctrl Pts',(-7.30728426563349,-3.58822087545141,
126.097191281186));
#176746=CARTESIAN_POINT('Ctrl Pts',(-7.29988790869808,-3.46150273829219,
126.003239343929));
#176747=CARTESIAN_POINT('Ctrl Pts',(-7.29249155176259,-3.33125975840187,
125.914510007931));
#176748=CARTESIAN_POINT('Ctrl Pts',(-7.28509406242597,-3.20099683797864,
125.825767087244));
#176749=CARTESIAN_POINT('Ctrl Pts',(-7.27769657308931,-3.06720830881352,
125.742248570103));
#176750=CARTESIAN_POINT('Ctrl Pts',(-7.27029908375269,-2.93035833389096,
125.664231183642));
#176751=CARTESIAN_POINT('Ctrl Pts',(-7.26289900123764,-2.79346038642164,
125.586186448306));
#176752=CARTESIAN_POINT('Ctrl Pts',(-7.25549891872264,-2.65349918058857,
125.513646867873));
#176753=CARTESIAN_POINT('Ctrl Pts',(-7.24809883620759,-2.51096301111948,
125.446842972304));
#176754=CARTESIAN_POINT('Ctrl Pts',(-7.24069061654108,-2.36827010847918,
125.379965618985));
#176755=CARTESIAN_POINT('Ctrl Pts',(-7.23328239687457,-2.2229969258592,
125.31883670449));
#176756=CARTESIAN_POINT('Ctrl Pts',(-7.22587417720806,-2.07565192789372,
125.263638675731));
#176757=CARTESIAN_POINT('Ctrl Pts',(-7.21846139790595,-1.92821624154057,
125.208406673506));
#176758=CARTESIAN_POINT('Ctrl Pts',(-7.21104861860382,-1.77870655261404,
125.159112947436));
#176759=CARTESIAN_POINT('Ctrl Pts',(-7.20363583930171,-1.62764547111343,
125.115889752486));
#176760=CARTESIAN_POINT('Ctrl Pts',(-7.19621246827291,-1.47636854645551,
125.072604798209));
#176761=CARTESIAN_POINT('Ctrl Pts',(-7.18878909724414,-1.32353616372034,
125.035407786739));
#176762=CARTESIAN_POINT('Ctrl Pts',(-7.18136572621535,-1.16968089342613,
125.004379827076));
#176763=CARTESIAN_POINT('Ctrl Pts',(-7.17742967677499,-1.08810313741903,
124.987928058359));
#176764=CARTESIAN_POINT('Ctrl Pts',(-7.17349362733462,-1.00623790539112,
124.973209765342));
#176765=CARTESIAN_POINT('Ctrl Pts',(-7.16955757789427,-0.924164916562035,
124.960231104157));
#176766=CARTESIAN_POINT('Ctrl Pts',(-7.16213431148884,-0.769377821023641,
124.935753754211));
#176767=CARTESIAN_POINT('Ctrl Pts',(-7.15471104508342,-0.613383540478684,
124.917393155114));
#176768=CARTESIAN_POINT('Ctrl Pts',(-7.14728777867799,-0.456706881859427,
124.905263280976));
#176769=CARTESIAN_POINT('Ctrl Pts',(-7.13987328595699,-0.30021540203947,
124.893147743342));
#176770=CARTESIAN_POINT('Ctrl Pts',(-7.13245879323596,-0.143043518065936,
124.887248300721));
#176771=CARTESIAN_POINT('Ctrl Pts',(-7.12504430051496,0.0142743501722947,
124.887627836256));
#176772=CARTESIAN_POINT('Ctrl Pts',(-7.11763695416119,0.171440589526204,
124.88800700598));
#176773=CARTESIAN_POINT('Ctrl Pts',(-7.11022960780743,0.328752162237795,
124.894653104793));
#176774=CARTESIAN_POINT('Ctrl Pts',(-7.10282226145367,0.4856702194611,124.907577172294));
#176775=CARTESIAN_POINT('Ctrl Pts',(-7.09542043977828,0.642471241277148,
124.920491600539));
#176776=CARTESIAN_POINT('Ctrl Pts',(-7.08801861810287,0.798878961563464,
124.93967464378));
#176777=CARTESIAN_POINT('Ctrl Pts',(-7.08061679642748,0.954355337116193,
124.965085281275));
#176778=CARTESIAN_POINT('Ctrl Pts',(-7.07321888211614,1.10974963790049,
124.990482504692));
#176779=CARTESIAN_POINT('Ctrl Pts',(-7.06582096780479,1.26421320561768,
125.022100715093));
#176780=CARTESIAN_POINT('Ctrl Pts',(-7.05842305349344,1.41721403227515,
125.059847152596));
#176781=CARTESIAN_POINT('Ctrl Pts',(-7.05102636858124,1.57018943297094,
125.097587317325));
#176782=CARTESIAN_POINT('Ctrl Pts',(-7.04362968366908,1.72170221297456,
125.141453598607));
#176783=CARTESIAN_POINT('Ctrl Pts',(-7.03623299875687,1.87123134477403,
125.19130228749));
#176784=CARTESIAN_POINT('Ctrl Pts',(-7.02883664182143,2.02075384629509,
125.24114876603));
#176785=CARTESIAN_POINT('Ctrl Pts',(-7.02144028488599,2.16829252036316,
125.296977006675));
#176786=CARTESIAN_POINT('Ctrl Pts',(-7.01404392795055,2.31334253567563,
125.358593740887));
#176787=CARTESIAN_POINT('Ctrl Pts',(-7.00664643861397,2.45841475851594,
125.420219908779));
#176788=CARTESIAN_POINT('Ctrl Pts',(-6.9992489492774,2.60099722033429,125.487636188884));
#176789=CARTESIAN_POINT('Ctrl Pts',(-6.99185145994082,2.74060621132301,
125.560601645516));
#176790=CARTESIAN_POINT('Ctrl Pts',(-6.98445137742582,2.8802641420271,125.633592680075));
#176791=CARTESIAN_POINT('Ctrl Pts',(-6.97705129491078,3.01694619596777,
125.712136591347));
#176792=CARTESIAN_POINT('Ctrl Pts',(-6.96965121239577,3.15019448653172,
125.795947170223));
#176793=CARTESIAN_POINT('Ctrl Pts',(-6.96224299272931,3.28358929728922,
125.879849907447));
#176794=CARTESIAN_POINT('Ctrl Pts',(-6.95483477306293,3.41354248801447,
125.969030678893));
#176795=CARTESIAN_POINT('Ctrl Pts',(-6.94742655339647,3.53962572340069,
126.063160315877));
#176796=CARTESIAN_POINT('Ctrl Pts',(-6.94001377409441,3.66578656091466,
126.157347888081));
#176797=CARTESIAN_POINT('Ctrl Pts',(-6.93260099479233,3.78807240757056,
126.256490160701));
#176798=CARTESIAN_POINT('Ctrl Pts',(-6.92518821549027,3.90608951004912,
126.360218934183));
#176799=CARTESIAN_POINT('Ctrl Pts',(-6.91776484446151,4.02427524089816,
126.464095920201));
#176800=CARTESIAN_POINT('Ctrl Pts',(-6.91034147343269,4.13817977612814,
126.572572238946));
#176801=CARTESIAN_POINT('Ctrl Pts',(-6.90291810240393,4.24744700906844,
126.685243665153));
#176802=CARTESIAN_POINT('Ctrl Pts',(-6.89898205296311,4.30538311780511,
126.744984758842));
#176803=CARTESIAN_POINT('Ctrl Pts',(-6.89504600352228,4.36201619215133,
126.805904700208));
#176804=CARTESIAN_POINT('Ctrl Pts',(-6.89110995408146,4.41729796259356,
126.867939746754));
#176805=CARTESIAN_POINT('Ctrl Pts',(-6.88368668767603,4.52155765636165,
126.98493590849));
#176806=CARTESIAN_POINT('Ctrl Pts',(-6.8762634212706,4.62132366738767,127.106253962405));
#176807=CARTESIAN_POINT('Ctrl Pts',(-6.86884015486518,4.7162164350593,127.231513979355));
#176808=CARTESIAN_POINT('Ctrl Pts',(-6.86142566214419,4.81099704735989,
127.356625949367));
#176809=CARTESIAN_POINT('Ctrl Pts',(-6.85401116942323,4.90091565794216,
127.485670313854));
#176810=CARTESIAN_POINT('Ctrl Pts',(-6.84659667670223,4.98563049443313,
127.618231440103));
#176811=CARTESIAN_POINT('Ctrl Pts',(-6.83918933034846,5.07026367957537,
127.750664798949));
#176812=CARTESIAN_POINT('Ctrl Pts',(-6.83178198399465,5.14970287601641,
127.886607859114));
#176813=CARTESIAN_POINT('Ctrl Pts',(-6.82437463764089,5.22364753486462,
128.025613238979));
#176814=CARTESIAN_POINT('Ctrl Pts',(-6.81697281596549,5.29753704299648,
128.164514943387));
#176815=CARTESIAN_POINT('Ctrl Pts',(-6.80957099429009,5.36593999871168,
128.306474091605));
#176816=CARTESIAN_POINT('Ctrl Pts',(-6.8021691726147,5.42860008842839,128.451015839932));
#176817=CARTESIAN_POINT('Ctrl Pts',(-6.79477125830335,5.49122710037147,
128.595481285796));
#176818=CARTESIAN_POINT('Ctrl Pts',(-6.78737334399204,5.5481171358204,128.742526274992));
#176819=CARTESIAN_POINT('Ctrl Pts',(-6.77997542968069,5.59906067297614,
128.891653075146));
#176820=CARTESIAN_POINT('Ctrl Pts',(-6.7725787447685,5.64999574424015,129.04075509313));
#176821=CARTESIAN_POINT('Ctrl Pts',(-6.76518205985623,5.69498615793799,
129.191937882538));
#176822=CARTESIAN_POINT('Ctrl Pts',(-6.75778537494404,5.73387119238194,
129.344685409969));
#176823=CARTESIAN_POINT('Ctrl Pts',(-6.7503890180086,5.77275450262271,129.497426164415));
#176824=CARTESIAN_POINT('Ctrl Pts',(-6.7429926610732,5.80553287979693,129.65173115717));
#176825=CARTESIAN_POINT('Ctrl Pts',(-6.73559630413777,5.83209605254753,
129.807071192996));
#176826=CARTESIAN_POINT('Ctrl Pts',(-6.7281988148012,5.85866329218773,129.962435011778));
#176827=CARTESIAN_POINT('Ctrl Pts',(-6.72080132546463,5.87901336978973,
130.118833821182));
#176828=CARTESIAN_POINT('Ctrl Pts',(-6.71340383612807,5.89308753440536,
130.275730430823));
#176829=CARTESIAN_POINT('Ctrl Pts',(-6.70600375361309,5.90716663269756,
130.432682040326));
#176830=CARTESIAN_POINT('Ctrl Pts',(-6.69860367109814,5.91496540446514,
130.590131425927));
#176831=CARTESIAN_POINT('Ctrl Pts',(-6.69120358858316,5.91647714663784,
130.747538651636));
#176832=CARTESIAN_POINT('Ctrl Pts',(-6.6837953689167,5.91799055112647,130.905118962771));
#176833=CARTESIAN_POINT('Ctrl Pts',(-6.67638714925018,5.9132031162481,131.062656647922));
#176834=CARTESIAN_POINT('Ctrl Pts',(-6.66897892958372,5.9021602552449,131.219613412749));
#176835=CARTESIAN_POINT('Ctrl Pts',(-6.66156615028166,5.89111059754501,
131.376666781846));
#176836=CARTESIAN_POINT('Ctrl Pts',(-6.65415337097965,5.87379788285035,
131.533138147988));
#176837=CARTESIAN_POINT('Ctrl Pts',(-6.6467405916776,5.85031905458617,131.688497214504));
#176838=CARTESIAN_POINT('Ctrl Pts',(-6.63931722064885,5.82680667867113,
131.844078265341));
#176839=CARTESIAN_POINT('Ctrl Pts',(-6.6318938496201,5.7971106630666,131.998543476737));
#176840=CARTESIAN_POINT('Ctrl Pts',(-6.62447047859135,5.76137860958308,
132.151374752436));
#176841=CARTESIAN_POINT('Ctrl Pts',(-6.62053442915043,5.74243261744663,
132.23240956195));
#176842=CARTESIAN_POINT('Ctrl Pts',(-6.61659837970951,5.72179050545635,
132.312985287692));
#176843=CARTESIAN_POINT('Ctrl Pts',(-6.61266233026859,5.6994798111297,132.393026864776));
#176844=CARTESIAN_POINT('Ctrl Pts',(-6.60523906386315,5.65740253792386,
132.54398278114));
#176845=CARTESIAN_POINT('Ctrl Pts',(-6.59781579745767,5.60926018913864,
132.693494123237));
#176846=CARTESIAN_POINT('Ctrl Pts',(-6.59039253105223,5.55516724814181,
132.841036194989));
#176847=CARTESIAN_POINT('Ctrl Pts',(-6.58297803833122,5.5011382405091,132.988403884266));
#176848=CARTESIAN_POINT('Ctrl Pts',(-6.57556354561025,5.44117276734328,
133.133806589066));
#176849=CARTESIAN_POINT('Ctrl Pts',(-6.56814905288923,5.37543577590156,
133.276732106978));
#176850=CARTESIAN_POINT('Ctrl Pts',(-6.56074170653544,5.30976214424714,
133.419519867895));
#176851=CARTESIAN_POINT('Ctrl Pts',(-6.55333436018166,5.23832822370858,
133.55983485831));
#176852=CARTESIAN_POINT('Ctrl Pts',(-6.54592701382788,5.16134795509735,
133.697182397232));
#176853=CARTESIAN_POINT('Ctrl Pts',(-6.53852519215247,5.08442510127475,
133.834427497179));
#176854=CARTESIAN_POINT('Ctrl Pts',(-6.53112337047707,5.00196431778647,
133.968709228251));
#176855=CARTESIAN_POINT('Ctrl Pts',(-6.52372154880166,4.91422656033279,
134.099555281955));
#176856=CARTESIAN_POINT('Ctrl Pts',(-6.51632363449031,4.82653511895844,
134.230332263046));
#176857=CARTESIAN_POINT('Ctrl Pts',(-6.50892572017889,4.73357245879413,
134.357676869513));
#176858=CARTESIAN_POINT('Ctrl Pts',(-6.50152780586754,4.63564408453204,
134.481143788225));
#176859=CARTESIAN_POINT('Ctrl Pts',(-6.49413112095533,4.53773198418901,
134.604590188976));
#176860=CARTESIAN_POINT('Ctrl Pts',(-6.48673443604315,4.43485603929642,
134.724159888735));
#176861=CARTESIAN_POINT('Ctrl Pts',(-6.47933775113094,4.32736352937015,
134.839438739137));
#176862=CARTESIAN_POINT('Ctrl Pts',(-6.47194139419549,4.21987578577442,
134.954712477953));
#176863=CARTESIAN_POINT('Ctrl Pts',(-6.46454503726002,4.10777213874416,
135.065695472695));
#176864=CARTESIAN_POINT('Ctrl Pts',(-6.45714868032456,3.99143821085792,
135.172008905993));
#176865=CARTESIAN_POINT('Ctrl Pts',(-6.44975119098798,3.87508647195033,
135.27833861615));
#176866=CARTESIAN_POINT('Ctrl Pts',(-6.44235370165139,3.75450343817615,
135.379997089517));
#176867=CARTESIAN_POINT('Ctrl Pts',(-6.4349562123148,3.63010930669793,135.476644532733));
#176868=CARTESIAN_POINT('Ctrl Pts',(-6.4275561297998,3.50567156904975,135.57332585556));
#176869=CARTESIAN_POINT('Ctrl Pts',(-6.42015604728487,3.37742036838085,
135.664992421953));
#176870=CARTESIAN_POINT('Ctrl Pts',(-6.41275596476987,3.24580634495809,
135.751346743838));
#176871=CARTESIAN_POINT('Ctrl Pts',(-6.4053477451034,3.11404759838633,135.837796021178));
#176872=CARTESIAN_POINT('Ctrl Pts',(-6.39793952543684,2.97891895667795,
135.918921183524));
#176873=CARTESIAN_POINT('Ctrl Pts',(-6.39053130577037,2.84089784907312,
135.994469477083));
#176874=CARTESIAN_POINT('Ctrl Pts',(-6.38311852646829,2.70279179177936,
136.070064269356));
#176875=CARTESIAN_POINT('Ctrl Pts',(-6.37570574716627,2.56179005476495,
136.140075187587));
#176876=CARTESIAN_POINT('Ctrl Pts',(-6.36829296786419,2.41839119192782,
136.204297154721));
#176877=CARTESIAN_POINT('Ctrl Pts',(-6.36086959683542,2.27478743407074,
136.268610885214));
#176878=CARTESIAN_POINT('Ctrl Pts',(-6.35344622580663,2.12878005524076,
136.327119006033));
#176879=CARTESIAN_POINT('Ctrl Pts',(-6.34602285477786,1.98088472687642,
136.37966565508));
#176880=CARTESIAN_POINT('Ctrl Pts',(-6.34208680533712,1.90246707507912,
136.407527149243));
#176881=CARTESIAN_POINT('Ctrl Pts',(-6.33815075589638,1.82351886925034,
136.433713503745));
#176882=CARTESIAN_POINT('Ctrl Pts',(-6.33421470645564,1.74411814830525,
136.458207312273));
#176883=CARTESIAN_POINT('Ctrl Pts',(-6.32679144005021,1.59437086661246,
136.504401870733));
#176884=CARTESIAN_POINT('Ctrl Pts',(-6.31936817364477,1.44256062466505,
136.544712881658));
#176885=CARTESIAN_POINT('Ctrl Pts',(-6.31194490723934,1.28919074518874,
136.578953052104));
#176886=CARTESIAN_POINT('Ctrl Pts',(-6.30453041451832,1.13600213617317,
136.613152753511));
#176887=CARTESIAN_POINT('Ctrl Pts',(-6.29711592179732,0.981257919622204,
136.641295816229));
#176888=CARTESIAN_POINT('Ctrl Pts',(-6.2897014290763,0.82547818395196,136.663244157142));
#176889=CARTESIAN_POINT('Ctrl Pts',(-6.28229408272252,0.669848594655958,
136.685171343418));
#176890=CARTESIAN_POINT('Ctrl Pts',(-6.27488673636877,0.513185840371659,
136.700915642659));
#176891=CARTESIAN_POINT('Ctrl Pts',(-6.26747939001498,0.356021750459489,
136.710389662169));
#176892=CARTESIAN_POINT('Ctrl Pts',(-6.26007756833959,0.198974879455262,
136.719856615599));
#176893=CARTESIAN_POINT('Ctrl Pts',(-6.25267574666416,0.0414277883562145,
136.723062578698));
#176894=CARTESIAN_POINT('Ctrl Pts',(-6.24527392498877,-0.116081103395428,
136.719971806609));
#176895=CARTESIAN_POINT('Ctrl Pts',(-6.23787601067742,-0.273506847429162,
136.716882666115));
#176896=CARTESIAN_POINT('Ctrl Pts',(-6.23047809636608,-0.430894059994037,
136.70750341764));
#176897=CARTESIAN_POINT('Ctrl Pts',(-6.22308018205473,-0.587702953794054,
136.691850388309));
#176898=CARTESIAN_POINT('Ctrl Pts',(-6.21568349714252,-0.744485788800949,
136.676199960227));
#176899=CARTESIAN_POINT('Ctrl Pts',(-6.20828681223032,-0.900690124697001,
136.654277857563));
#176900=CARTESIAN_POINT('Ctrl Pts',(-6.2008901273181,-1.05577981367228,
136.6261523991));
#176901=CARTESIAN_POINT('Ctrl Pts',(-6.19349377038265,-1.21086262580822,
136.59802818775));
#176902=CARTESIAN_POINT('Ctrl Pts',(-6.18609741344724,-1.36483052198972,
136.563701234132));
#176903=CARTESIAN_POINT('Ctrl Pts',(-6.17870105651178,-1.51715635401359,
136.523291213401));
#176904=CARTESIAN_POINT('Ctrl Pts',(-6.1713035671752,-1.66950550751121,
136.482875005793));
#176905=CARTESIAN_POINT('Ctrl Pts',(-6.16390607783857,-1.82021173543165,
136.436373972391));
#176906=CARTESIAN_POINT('Ctrl Pts',(-6.15650858850199,-1.96876203316624,
136.383957970356));
#176907=CARTESIAN_POINT('Ctrl Pts',(-6.14910850598699,-2.11736440497743,
136.331523593973));
#176908=CARTESIAN_POINT('Ctrl Pts',(-6.14170842347198,-2.26380899008739,
136.273170244804));
#176909=CARTESIAN_POINT('Ctrl Pts',(-6.13430834095698,-2.40760192128238,
136.209116259696));
#176910=CARTESIAN_POINT('Ctrl Pts',(-6.1269001212905,-2.55155296758749,
136.144991840647));
#176911=CARTESIAN_POINT('Ctrl Pts',(-6.11949190162403,-2.69284619579678,
136.075154419176));
#176912=CARTESIAN_POINT('Ctrl Pts',(-6.11208368195756,-2.83101089482012,
135.999869050425));
#176913=CARTESIAN_POINT('Ctrl Pts',(-6.10467090265549,-2.96926063191031,
135.924537344786));
#176914=CARTESIAN_POINT('Ctrl Pts',(-6.09725812335342,-3.10437768324554,
135.843751201475));
#176915=CARTESIAN_POINT('Ctrl Pts',(-6.08984534405135,-3.23592003113169,
135.757819218849));
#176916=CARTESIAN_POINT('Ctrl Pts',(-6.0824219730226,-3.36765033289323,
135.671764452575));
#176917=CARTESIAN_POINT('Ctrl Pts',(-6.07499860199389,-3.49579542666038,
135.580549378065));
#176918=CARTESIAN_POINT('Ctrl Pts',(-6.06757523096513,-3.61994544822661,
135.484523597032));
#176919=CARTESIAN_POINT('Ctrl Pts',(-6.06363918152437,-3.68577276859955,
135.433608423821));
#176920=CARTESIAN_POINT('Ctrl Pts',(-6.05970313208357,-3.75047752394584,
135.381341426573));
#176921=CARTESIAN_POINT('Ctrl Pts',(-6.0557670826428,-3.8140028879032,135.327778853101));
#176922=CARTESIAN_POINT('Ctrl Pts',(-6.04844892319008,-3.93211338161724,
135.228191828275));
#176923=CARTESIAN_POINT('Ctrl Pts',(-6.04113076373738,-4.04652378683626,
135.123804285533));
#176924=CARTESIAN_POINT('Ctrl Pts',(-6.03381260428466,-4.15681063084074,
135.014925418377));
#176925=CARTESIAN_POINT('Ctrl Pts',(-6.02650314913099,-4.26696629846438,
134.906176052939));
#176926=CARTESIAN_POINT('Ctrl Pts',(-6.01919369397733,-4.37300789179196,
134.792946258656));
#176927=CARTESIAN_POINT('Ctrl Pts',(-6.01188423882365,-4.4745437509958,
134.675586364397));
#176928=CARTESIAN_POINT('Ctrl Pts',(-6.0045817750019,-4.57598249339982,
134.558338722276));
#176929=CARTESIAN_POINT('Ctrl Pts',(-5.99727931118016,-4.67292382734191,
134.436969129899));
#176930=CARTESIAN_POINT('Ctrl Pts',(-5.98997684735841,-4.76501202442191,
134.311865566902));
#176931=CARTESIAN_POINT('Ctrl Pts',(-5.98261844506032,-4.85780563731206,
134.185803683142));
#176932=CARTESIAN_POINT('Ctrl Pts',(-5.97526004276216,-4.94567115456138,
134.055950647106));
#176933=CARTESIAN_POINT('Ctrl Pts',(-5.96790164046408,-5.02828466217561,
133.922739029278));
#176934=CARTESIAN_POINT('Ctrl Pts',(-5.96060768547709,-5.11017461347822,
133.790694122677));
#176935=CARTESIAN_POINT('Ctrl Pts',(-5.95331373049013,-5.18690398224569,
133.655349566142));
#176936=CARTESIAN_POINT('Ctrl Pts',(-5.94601977550315,-5.25819998616286,
133.517156862774));
#176937=CARTESIAN_POINT('Ctrl Pts',(-5.93872726715306,-5.32948184968156,
133.378991567674));
#176938=CARTESIAN_POINT('Ctrl Pts',(-5.93143475880301,-5.39533231605664,
133.237979591406));
#176939=CARTESIAN_POINT('Ctrl Pts',(-5.92414225045292,-5.45552437627061,
133.094597361315));
#176940=CARTESIAN_POINT('Ctrl Pts',(-5.91684965354754,-5.51571716741625,
132.951213390087));
#176941=CARTESIAN_POINT('Ctrl Pts',(-5.90955705664208,-5.5702512675601,
132.805459462894));
#176942=CARTESIAN_POINT('Ctrl Pts',(-5.9022644597367,-5.61894779131388,
132.657832031154));
#176943=CARTESIAN_POINT('Ctrl Pts',(-5.89485702077567,-5.6684111761685,
132.507879798256));
#176944=CARTESIAN_POINT('Ctrl Pts',(-5.88744958181468,-5.71185143378304,
132.355994940758));
#176945=CARTESIAN_POINT('Ctrl Pts',(-5.88004214285365,-5.74913392966919,
132.202713084302));
#176946=CARTESIAN_POINT('Ctrl Pts',(-5.87274168883747,-5.78587795797063,
132.051645063295));
#176947=CARTESIAN_POINT('Ctrl Pts',(-5.86544123482127,-5.8166408791501,
131.899220517167));
#176948=CARTESIAN_POINT('Ctrl Pts',(-5.85814078080509,-5.84134564715325,
131.745961166092));
#176949=CARTESIAN_POINT('Ctrl Pts',(-5.85067984937163,-5.86659347143138,
131.589332892374));
#176950=CARTESIAN_POINT('Ctrl Pts',(-5.84321891793812,-5.88551366306476,
131.431833112249));
#176951=CARTESIAN_POINT('Ctrl Pts',(-5.83575798650466,-5.89808008625693,
131.274022047321));
#176952=CARTESIAN_POINT('Ctrl Pts',(-5.82829705507119,-5.91064650944911,
131.116210982393));
#176953=CARTESIAN_POINT('Ctrl Pts',(-5.82083612363776,-5.91685920350292,
130.958089057843));
#176954=CARTESIAN_POINT('Ctrl Pts',(-5.81337519220429,-5.91674854661678,
130.800213497092));
#176955=CARTESIAN_POINT('',(-4.06337519220434,-5.92132048307296,130.809046855528));
#176956=CARTESIAN_POINT('Ctrl Pts',(-5.81337519220429,-5.92270786400364,
130.800209320135));
#176957=CARTESIAN_POINT('Ctrl Pts',(-5.80135661441281,-5.92473620102161,
130.545634893806));
#176958=CARTESIAN_POINT('Ctrl Pts',(-5.69652216201681,-5.79401867711778,
128.327156252607));
#176959=CARTESIAN_POINT('Ctrl Pts',(-5.49887183501715,-2.99105923299359,
124.477345113001));
#176960=CARTESIAN_POINT('Ctrl Pts',(-5.22042421120391,3.70635675827079,
124.86799134748));
#176961=CARTESIAN_POINT('Ctrl Pts',(-4.94197658739132,6.99781195427446,
130.713870933415));
#176962=CARTESIAN_POINT('Ctrl Pts',(-4.66352896357833,3.85861982642432,
136.642906118412));
#176963=CARTESIAN_POINT('Ctrl Pts',(-4.38508133976539,-2.82645541785551,
137.20660321694));
#176964=CARTESIAN_POINT('Ctrl Pts',(-4.18503008264081,-5.7632723015822,
133.384689163164));
#176965=CARTESIAN_POINT('Ctrl Pts',(-4.07779470012041,-5.92396940801648,
131.114663565642));
#176966=CARTESIAN_POINT('Ctrl Pts',(-4.06337519220434,-5.92132048307296,
130.809046855528));
#176967=CARTESIAN_POINT('',(-2.31337593551284,-5.91165713928214,130.806298299166));
#176968=CARTESIAN_POINT('Ctrl Pts',(-4.06337519220434,-5.92132048307296,
130.809046855528));
#176969=CARTESIAN_POINT('Ctrl Pts',(-3.98497882551612,-5.90691873702097,
129.147461743774));
#176970=CARTESIAN_POINT('Ctrl Pts',(-3.81376658422367,-4.30954189761841,
125.494430884269));
#176971=CARTESIAN_POINT('Ctrl Pts',(-3.54973846832673,1.88934901456002,
124.065820654671));
#176972=CARTESIAN_POINT('Ctrl Pts',(-3.27129084451378,6.6905638084388,128.751578004728));
#176973=CARTESIAN_POINT('Ctrl Pts',(-2.99284322070105,5.34347731457243,
135.323742291973));
#176974=CARTESIAN_POINT('Ctrl Pts',(-2.7143955968881,-0.914003788003028,
137.74281560451));
#176975=CARTESIAN_POINT('Ctrl Pts',(-2.48790670352819,-5.32063620302637,
134.524174883853));
#176976=CARTESIAN_POINT('Ctrl Pts',(-2.35423368477254,-5.91003297744418,
131.677416134064));
#176977=CARTESIAN_POINT('Ctrl Pts',(-2.31337654062121,-5.90751142670208,
130.806309852799));
#176978=CARTESIAN_POINT('',(-0.563374439001446,-5.91502852340845,130.79899021336));
#176979=CARTESIAN_POINT('Ctrl Pts',(-2.31337519220432,-5.91674968734432,
130.80628410681));
#176980=CARTESIAN_POINT('Ctrl Pts',(-2.3057930075727,-5.91680232326788,
130.644373357754));
#176981=CARTESIAN_POINT('Ctrl Pts',(-2.29821082294107,-5.91020461859756,
130.482517862187));
#176982=CARTESIAN_POINT('Ctrl Pts',(-2.29062863830944,-5.89699648063777,
130.321283946792));
#176983=CARTESIAN_POINT('Ctrl Pts',(-2.28304210500759,-5.88378076731029,
130.159957557637));
#176984=CARTESIAN_POINT('Ctrl Pts',(-2.27545557170574,-5.86394708961438,
129.999253804566));
#176985=CARTESIAN_POINT('Ctrl Pts',(-2.26786903840389,-5.83758710464856,
129.839732524392));
#176986=CARTESIAN_POINT('Ctrl Pts',(-2.26027699856307,-5.81120798679575,
129.680095458771));
#176987=CARTESIAN_POINT('Ctrl Pts',(-2.25268495872227,-5.77829317310447,
129.521642918593));
#176988=CARTESIAN_POINT('Ctrl Pts',(-2.24509291888145,-5.73898519239538,
129.364923392826));
#176989=CARTESIAN_POINT('Ctrl Pts',(-2.23748852633052,-5.6996132552133,
129.207948874869));
#176990=CARTESIAN_POINT('Ctrl Pts',(-2.22988413377958,-5.65382744716086,
129.052713342816));
#176991=CARTESIAN_POINT('Ctrl Pts',(-2.22227974122865,-5.60182027501037,
128.899750376865));
#176992=CARTESIAN_POINT('Ctrl Pts',(-2.2146688457404,-5.54976862864605,
128.746656603808));
#176993=CARTESIAN_POINT('Ctrl Pts',(-2.20705795025213,-5.49148513093914,
128.595839595603));
#176994=CARTESIAN_POINT('Ctrl Pts',(-2.19944705476388,-5.4272100320278,
128.447811905836));
#176995=CARTESIAN_POINT('Ctrl Pts',(-2.191821899877,-5.36281451045945,128.299506878686));
#176996=CARTESIAN_POINT('Ctrl Pts',(-2.18419674499019,-5.29240509848426,
128.154001928447));
#176997=CARTESIAN_POINT('Ctrl Pts',(-2.17657159010332,-5.21626825515832,
128.011785452467));
#176998=CARTESIAN_POINT('Ctrl Pts',(-2.170214509823,-5.15279308219536,127.89321978811));
#176999=CARTESIAN_POINT('Ctrl Pts',(-2.16385742954263,-5.08533789991428,
127.776939382873));
#177000=CARTESIAN_POINT('Ctrl Pts',(-2.15750034926231,-5.01409095860777,
127.663210761015));
#177001=CARTESIAN_POINT('Ctrl Pts',(-2.15007708285687,-4.93089474233096,
127.530407992961));
#177002=CARTESIAN_POINT('Ctrl Pts',(-2.14265381645139,-4.84229297604232,
127.400711986189));
#177003=CARTESIAN_POINT('Ctrl Pts',(-2.13523055004595,-4.7485443720732,
127.274593357682));
#177004=CARTESIAN_POINT('Ctrl Pts',(-2.12781605732493,-4.65490657116863,
127.148623790919));
#177005=CARTESIAN_POINT('Ctrl Pts',(-2.12040156460396,-4.55613426162116,
127.026223482906));
#177006=CARTESIAN_POINT('Ctrl Pts',(-2.11298707188294,-4.45253099752081,
126.907836746394));
#177007=CARTESIAN_POINT('Ctrl Pts',(-2.10557972552916,-4.349027590147,126.789564115475));
#177008=CARTESIAN_POINT('Ctrl Pts',(-2.09817237917537,-4.24070274209709,
126.675297633804));
#177009=CARTESIAN_POINT('Ctrl Pts',(-2.09076503282159,-4.12790201220618,
126.565450906317));
#177010=CARTESIAN_POINT('Ctrl Pts',(-2.08336321114618,-4.01518541335518,
126.455686106663));
#177011=CARTESIAN_POINT('Ctrl Pts',(-2.07596138947079,-3.89799984592126,
126.350334756892));
#177012=CARTESIAN_POINT('Ctrl Pts',(-2.06855956779538,-3.77672959920243,
126.249775664246));
#177013=CARTESIAN_POINT('Ctrl Pts',(-2.06116165348401,-3.65552337010287,
126.149269655962));
#177014=CARTESIAN_POINT('Ctrl Pts',(-2.0537637391726,-3.53023704266339,
126.053551104272));
#177015=CARTESIAN_POINT('Ctrl Pts',(-2.04636582486123,-3.40128995994975,
125.962960285963));
#177016=CARTESIAN_POINT('Ctrl Pts',(-2.03896913994901,-3.27236430590211,
125.872384522205));
#177017=CARTESIAN_POINT('Ctrl Pts',(-2.03157245503679,-3.13977940913043,
125.786935014975));
#177018=CARTESIAN_POINT('Ctrl Pts',(-2.02417577012457,-3.00398582290172,
125.706910300171));
#177019=CARTESIAN_POINT('Ctrl Pts',(-2.0167794131891,-2.86819825790272,
125.626889133748));
#177020=CARTESIAN_POINT('Ctrl Pts',(-2.00938305625366,-2.72920260794733,
125.552292471002));
#177021=CARTESIAN_POINT('Ctrl Pts',(-2.00198669931819,-2.58747616329207,
125.483374086208));
#177022=CARTESIAN_POINT('Ctrl Pts',(-1.99458920998161,-2.44572801995653,
125.414445149833));
#177023=CARTESIAN_POINT('Ctrl Pts',(-1.98719172064502,-2.30124858517679,
125.351196385678));
#177024=CARTESIAN_POINT('Ctrl Pts',(-1.97979423130843,-2.15453722444724,
125.293834334989));
#177025=CARTESIAN_POINT('Ctrl Pts',(-1.97239414879345,-2.00777443427803,
125.236452176123));
#177026=CARTESIAN_POINT('Ctrl Pts',(-1.96499406627848,-1.85877850786164,
125.184960975141));
#177027=CARTESIAN_POINT('Ctrl Pts',(-1.9575939837635,-1.70806599298024,
125.139518066698));
#177028=CARTESIAN_POINT('Ctrl Pts',(-1.95018576409703,-1.55718775419468,
125.094025189105));
#177029=CARTESIAN_POINT('Ctrl Pts',(-1.94277754443058,-1.40458951497581,
125.054593993804));
#177030=CARTESIAN_POINT('Ctrl Pts',(-1.93536932476411,-1.25080081208395,
125.021331317019));
#177031=CARTESIAN_POINT('Ctrl Pts',(-1.92795654546203,-1.09691745481113,
124.98804816761));
#177032=CARTESIAN_POINT('Ctrl Pts',(-1.92054376615991,-0.941842540717448,
124.960941166087));
#177033=CARTESIAN_POINT('Ctrl Pts',(-1.91313098685782,-0.786112328983106,
124.940065436667));
#177034=CARTESIAN_POINT('Ctrl Pts',(-1.90570761582904,-0.630159602619215,
124.919159879025));
#177035=CARTESIAN_POINT('Ctrl Pts',(-1.89828424480029,-0.473550079262816,
124.904503410531));
#177036=CARTESIAN_POINT('Ctrl Pts',(-1.89086087377152,-0.316822461589335,
124.896099105892));
#177037=CARTESIAN_POINT('Ctrl Pts',(-1.88692482433083,-0.233721718073758,
124.891642941914));
#177038=CARTESIAN_POINT('Ctrl Pts',(-1.88298877489015,-0.150587741872396,
124.888943614882));
#177039=CARTESIAN_POINT('Ctrl Pts',(-1.87905272544947,-0.0675003028066515,
124.887995663338));
#177040=CARTESIAN_POINT('Ctrl Pts',(-1.87162945904403,0.0892000142053658,
124.886207856309));
#177041=CARTESIAN_POINT('Ctrl Pts',(-1.86420619263863,0.246208356781524,
124.890647171959));
#177042=CARTESIAN_POINT('Ctrl Pts',(-1.85678292623319,0.402988941192107,
124.901350328249));
#177043=CARTESIAN_POINT('Ctrl Pts',(-1.84936843351219,0.559584223971734,
124.912040834298));
#177044=CARTESIAN_POINT('Ctrl Pts',(-1.84195394079111,0.715951915618239,
124.928980419423));
#177045=CARTESIAN_POINT('Ctrl Pts',(-1.8345394480701,0.871554124829254,
124.952153856865));
#177046=CARTESIAN_POINT('Ctrl Pts',(-1.82713210171632,1.02700635877293,
124.975304958876));
#177047=CARTESIAN_POINT('Ctrl Pts',(-1.81972475536254,1.18169421235017,
125.004677897003));
#177048=CARTESIAN_POINT('Ctrl Pts',(-1.81231740900876,1.33508292502333,
125.04020550638));
#177049=CARTESIAN_POINT('Ctrl Pts',(-1.80491558733332,1.4883572346082,125.075706617926));
#177050=CARTESIAN_POINT('Ctrl Pts',(-1.79751376565783,1.64033397049057,
125.117353176775));
#177051=CARTESIAN_POINT('Ctrl Pts',(-1.7901119439824,1.79048671365771,125.165026624024));
#177052=CARTESIAN_POINT('Ctrl Pts',(-1.78271402967108,1.94056019235902,
125.212674904831));
#177053=CARTESIAN_POINT('Ctrl Pts',(-1.77531611535977,2.08881124105536,
125.266343625154));
#177054=CARTESIAN_POINT('Ctrl Pts',(-1.76791820104845,2.2347269100769,125.325863907712));
#177055=CARTESIAN_POINT('Ctrl Pts',(-1.76052151613624,2.38061833056206,
125.38537429908));
#177056=CARTESIAN_POINT('Ctrl Pts',(-1.75312483122411,2.52417479632223,
125.450734181854));
#177057=CARTESIAN_POINT('Ctrl Pts',(-1.7457281463119,2.66490160560296,125.521725858759));
#177058=CARTESIAN_POINT('Ctrl Pts',(-1.73833178937645,2.8056221749097,125.592714387819));
#177059=CARTESIAN_POINT('Ctrl Pts',(-1.73093543244098,2.94351300392341,
125.669334046348));
#177060=CARTESIAN_POINT('Ctrl Pts',(-1.72353907550553,3.07810259811792,
125.751320447732));
#177061=CARTESIAN_POINT('Ctrl Pts',(-1.71614158616895,3.2127127983229,125.833319401442));
#177062=CARTESIAN_POINT('Ctrl Pts',(-1.70874409683235,3.34402043850989,
125.92068653983));
#177063=CARTESIAN_POINT('Ctrl Pts',(-1.70134660749576,3.47158183043043,
126.01311337315));
#177064=CARTESIAN_POINT('Ctrl Pts',(-1.69394652498075,3.59918793879934,
126.105572606553));
#177065=CARTESIAN_POINT('Ctrl Pts',(-1.6865464424657,3.7230448821481,126.203094847359));
#177066=CARTESIAN_POINT('Ctrl Pts',(-1.67914635995069,3.84274108368343,
126.305330552511));
#177067=CARTESIAN_POINT('Ctrl Pts',(-1.67173814028423,3.96256890349707,
126.40767867633));
#177068=CARTESIAN_POINT('Ctrl Pts',(-1.6643299206178,4.07822656056999,126.514750372571));
#177069=CARTESIAN_POINT('Ctrl Pts',(-1.65692170095133,4.18933794300868,
126.626157874547));
#177070=CARTESIAN_POINT('Ctrl Pts',(-1.64950892164925,4.30051771264958,
126.737633945983));
#177071=CARTESIAN_POINT('Ctrl Pts',(-1.64209614234712,4.40714537972399,
126.853450866711));
#177072=CARTESIAN_POINT('Ctrl Pts',(-1.63468336304504,4.50888470548128,
126.973187262682));
#177073=CARTESIAN_POINT('Ctrl Pts',(-1.62725999201627,4.61076940115831,
127.09309474363));
#177074=CARTESIAN_POINT('Ctrl Pts',(-1.61983662098756,4.70775157596957,
127.216932591816));
#177075=CARTESIAN_POINT('Ctrl Pts',(-1.61241324995879,4.79953746112196,
127.344249243378));
#177076=CARTESIAN_POINT('Ctrl Pts',(-1.60847720051802,4.8482045398015,127.411755586956));
#177077=CARTESIAN_POINT('Ctrl Pts',(-1.60454115107726,4.89541150488017,
127.480239503417));
#177078=CARTESIAN_POINT('Ctrl Pts',(-1.60060510163649,4.94111983370151,
127.549630928098));
#177079=CARTESIAN_POINT('Ctrl Pts',(-1.59318183523107,5.02732431535081,
127.680500989416));
#177080=CARTESIAN_POINT('Ctrl Pts',(-1.5857585688257,5.10845623767103,127.814996113277));
#177081=CARTESIAN_POINT('Ctrl Pts',(-1.57833530242027,5.18419510460719,
127.952685376613));
#177082=CARTESIAN_POINT('Ctrl Pts',(-1.57092080969925,5.25984445449256,
128.090211902674));
#177083=CARTESIAN_POINT('Ctrl Pts',(-1.56350631697814,5.33011325860168,
128.230924729751));
#177084=CARTESIAN_POINT('Ctrl Pts',(-1.55609182425712,5.39472358424925,
128.374363084225));
#177085=CARTESIAN_POINT('Ctrl Pts',(-1.54868447790336,5.45927163603234,
128.517663187412));
#177086=CARTESIAN_POINT('Ctrl Pts',(-1.54127713154963,5.51817191462117,
128.663683250145));
#177087=CARTESIAN_POINT('Ctrl Pts',(-1.53386978519586,5.57119187658512,
128.811937058989));
#177088=CARTESIAN_POINT('Ctrl Pts',(-1.52646796352046,5.62417229426118,
128.96008029455));
#177089=CARTESIAN_POINT('Ctrl Pts',(-1.51906614184496,5.67128100279193,
129.110453608984));
#177090=CARTESIAN_POINT('Ctrl Pts',(-1.51166432016956,5.71233320680563,
129.262550027083));
#177091=CARTESIAN_POINT('Ctrl Pts',(-1.50426640585821,5.75336373968031,
129.414566154667));
#177092=CARTESIAN_POINT('Ctrl Pts',(-1.49686849154693,5.78834403834904,
129.56830321489));
#177093=CARTESIAN_POINT('Ctrl Pts',(-1.48947057723558,5.81713892222552,
129.723238366371));
#177094=CARTESIAN_POINT('Ctrl Pts',(-1.48207389232338,5.84592902091465,
129.878147770441));
#177095=CARTESIAN_POINT('Ctrl Pts',(-1.47467720741118,5.86853567675316,
130.034254503959));
#177096=CARTESIAN_POINT('Ctrl Pts',(-1.46728052249898,5.88487464624398,
130.191024689632));
#177097=CARTESIAN_POINT('Ctrl Pts',(-1.45988416556353,5.90121289124782,
130.347787923951));
#177098=CARTESIAN_POINT('Ctrl Pts',(-1.45248780862806,5.911283963798,130.505214180646));
#177099=CARTESIAN_POINT('Ctrl Pts',(-1.4450914516926,5.91505544553447,130.662763870594));
#177100=CARTESIAN_POINT('Ctrl Pts',(-1.43769396235606,5.91882750469441,
130.820337681801));
#177101=CARTESIAN_POINT('Ctrl Pts',(-1.43029647301953,5.91629804369174,
130.978034590675));
#177102=CARTESIAN_POINT('Ctrl Pts',(-1.42289898368298,5.90748677934887,
131.135314563483));
#177103=CARTESIAN_POINT('Ctrl Pts',(-1.41549890116797,5.89867242623088,
131.292649670544));
#177104=CARTESIAN_POINT('Ctrl Pts',(-1.40809881865298,5.88357190632204,
131.449567178063));
#177105=CARTESIAN_POINT('Ctrl Pts',(-1.40069873613797,5.86225683278428,
131.605531878268));
#177106=CARTESIAN_POINT('Ctrl Pts',(-1.3932905164715,5.84091832113198,131.761668077693));
#177107=CARTESIAN_POINT('Ctrl Pts',(-1.38588229680507,5.81335165939988,
131.916849007374));
#177108=CARTESIAN_POINT('Ctrl Pts',(-1.37847407713861,5.77967978901732,
132.070548636355));
#177109=CARTESIAN_POINT('Ctrl Pts',(-1.37106129783653,5.74598719416029,
132.224342864894));
#177110=CARTESIAN_POINT('Ctrl Pts',(-1.36364851853442,5.70618199722547,
132.376653615695));
#177111=CARTESIAN_POINT('Ctrl Pts',(-1.35623573923235,5.6604369668774,132.526970238608));
#177112=CARTESIAN_POINT('Ctrl Pts',(-1.34881236820361,5.61462657388495,
132.677501640961));
#177113=CARTESIAN_POINT('Ctrl Pts',(-1.34138899717489,5.56285951934267,
132.826032873159));
#177114=CARTESIAN_POINT('Ctrl Pts',(-1.33396562614615,5.50535692750925,
132.9720726979));
#177115=CARTESIAN_POINT('Ctrl Pts',(-1.3300295767053,5.47486767356284,133.049506517156));
#177116=CARTESIAN_POINT('Ctrl Pts',(-1.32609352726445,5.44276673279752,
133.126240303509));
#177117=CARTESIAN_POINT('Ctrl Pts',(-1.32215747782359,5.40909223016113,
133.202203775095));
#177118=CARTESIAN_POINT('Ctrl Pts',(-1.31473421141816,5.34558316913515,
133.345468511766));
#177119=CARTESIAN_POINT('Ctrl Pts',(-1.30731094501272,5.27628239810198,
133.486424995463));
#177120=CARTESIAN_POINT('Ctrl Pts',(-1.29988767860729,5.2013792288988,133.624570659332));
#177121=CARTESIAN_POINT('Ctrl Pts',(-1.29247318588628,5.1265645890212,133.7625530465));
#177122=CARTESIAN_POINT('Ctrl Pts',(-1.2850586931653,5.04616090743831,133.89773090165));
#177123=CARTESIAN_POINT('Ctrl Pts',(-1.27764420044429,4.96040561664195,
134.029621332747));
#177124=CARTESIAN_POINT('Ctrl Pts',(-1.27023685409053,4.87473298002385,
134.161384642879));
#177125=CARTESIAN_POINT('Ctrl Pts',(-1.26282950773677,4.78371920504016,
134.289866526044));
#177126=CARTESIAN_POINT('Ctrl Pts',(-1.25542216138302,4.68764766141966,
134.414608526628));
#177127=CARTESIAN_POINT('Ctrl Pts',(-1.24802033970763,4.59164777158069,
134.539257489922));
#177128=CARTESIAN_POINT('Ctrl Pts',(-1.24061851803223,4.49059785100919,
134.660171830121));
#177129=CARTESIAN_POINT('Ctrl Pts',(-1.23321669635683,4.38482454589331,
134.776922041161));
#177130=CARTESIAN_POINT('Ctrl Pts',(-1.22581878204542,4.27910707768095,
134.893610620674));
#177131=CARTESIAN_POINT('Ctrl Pts',(-1.21842086773407,4.1686714407265,135.006139172925));
#177132=CARTESIAN_POINT('Ctrl Pts',(-1.21102295342266,4.05388444788204,
135.114111358122));
#177133=CARTESIAN_POINT('Ctrl Pts',(-1.20362626851044,3.93911653055418,
135.222065600299));
#177134=CARTESIAN_POINT('Ctrl Pts',(-1.19622958359819,3.81999896415178,
135.325464722696));
#177135=CARTESIAN_POINT('Ctrl Pts',(-1.18883289868597,3.69693537909345,
135.423949275153));
#177136=CARTESIAN_POINT('Ctrl Pts',(-1.18143654175054,3.57387725080378,
135.522429460702));
#177137=CARTESIAN_POINT('Ctrl Pts',(-1.17404018481509,3.44687374321637,
135.615995276359));
#177138=CARTESIAN_POINT('Ctrl Pts',(-1.16664382787965,3.31636130502646,
135.70432778654));
#177139=CARTESIAN_POINT('Ctrl Pts',(-1.15924633854305,3.18582888504832,
135.792673820654));
#177140=CARTESIAN_POINT('Ctrl Pts',(-1.15184884920649,3.05178677394595,
135.875784744682));
#177141=CARTESIAN_POINT('Ctrl Pts',(-1.14445135986989,2.91469997481603,
135.953385245523));
#177142=CARTESIAN_POINT('Ctrl Pts',(-1.13705127735488,2.77756512012139,
136.031012949099));
#177143=CARTESIAN_POINT('Ctrl Pts',(-1.12965119483986,2.63738377704964,
136.103126199768));
#177144=CARTESIAN_POINT('Ctrl Pts',(-1.12225111232485,2.49464493972069,
136.169495954836));
#177145=CARTESIAN_POINT('Ctrl Pts',(-1.11484289265838,2.35174914636659,
136.235938690273));
#177146=CARTESIAN_POINT('Ctrl Pts',(-1.10743467299194,2.20629058125491,
136.296625160027));
#177147=CARTESIAN_POINT('Ctrl Pts',(-1.10002645332548,2.0587782619703,136.351374465623));
#177148=CARTESIAN_POINT('Ctrl Pts',(-1.09261367402341,1.91117515131413,
136.406157468504));
#177149=CARTESIAN_POINT('Ctrl Pts',(-1.0852008947213,1.76151612176115,136.454995910186));
#177150=CARTESIAN_POINT('Ctrl Pts',(-1.07778811541922,1.6103241834286,136.49775912696));
#177151=CARTESIAN_POINT('Ctrl Pts',(-1.07036474439047,1.45891621496458,
136.540583445823));
#177152=CARTESIAN_POINT('Ctrl Pts',(-1.06294137336175,1.30597132523184,
136.577315115797));
#177153=CARTESIAN_POINT('Ctrl Pts',(-1.055518002333,1.15202232914964,136.607874649223));
#177154=CARTESIAN_POINT('Ctrl Pts',(-1.05158195289228,1.07039487747272,
136.624078047111));
#177155=CARTESIAN_POINT('Ctrl Pts',(-1.04764590345148,0.988485227210227,
136.638547102349));
#177156=CARTESIAN_POINT('Ctrl Pts',(-1.04370985401076,0.906373115949746,
136.651275901473));
#177157=CARTESIAN_POINT('Ctrl Pts',(-1.03628658760532,0.751512236741009,
136.675282019368));
#177158=CARTESIAN_POINT('Ctrl Pts',(-1.02886332119983,0.595462795402828,
136.693167740489));
#177159=CARTESIAN_POINT('Ctrl Pts',(-1.0214400547944,0.438749943334577,
136.704820688588));
#177160=CARTESIAN_POINT('Ctrl Pts',(-1.01402556207338,0.282222312843054,
136.716459863869));
#177161=CARTESIAN_POINT('Ctrl Pts',(-1.00661106935241,0.125033201004514,
136.721880902015));
#177162=CARTESIAN_POINT('Ctrl Pts',(-0.999196576631391,-0.0322827833728939,
136.721022546762));
#177163=CARTESIAN_POINT('Ctrl Pts',(-0.991789230277595,-0.189447140681941,
136.720165018825));
#177164=CARTESIAN_POINT('Ctrl Pts',(-0.984381883923756,-0.346737756299064,
136.713040148482));
#177165=CARTESIAN_POINT('Ctrl Pts',(-0.976974537569959,-0.503615750273477,
136.699638536255));
#177166=CARTESIAN_POINT('Ctrl Pts',(-0.969572715894546,-0.660376738721094,
136.686246919456));
#177167=CARTESIAN_POINT('Ctrl Pts',(-0.962170894219245,-0.816725347952993,
136.66658791377));
#177168=CARTESIAN_POINT('Ctrl Pts',(-0.954769072543826,-0.972123662110491,
136.64070417737));
#177169=CARTESIAN_POINT('Ctrl Pts',(-0.94737115823238,-1.12743994270911,
136.614834104792));
#177170=CARTESIAN_POINT('Ctrl Pts',(-0.939973243920947,-1.28180656000724,
136.582745906877));
#177171=CARTESIAN_POINT('Ctrl Pts',(-0.932575329609506,-1.43469179080562,
136.544533962326));
#177172=CARTESIAN_POINT('Ctrl Pts',(-0.925178644697286,-1.58755161485074,
136.506328367908));
#177173=CARTESIAN_POINT('Ctrl Pts',(-0.917781959785012,-1.73893017918694,
136.462001137028));
#177174=CARTESIAN_POINT('Ctrl Pts',(-0.910385274872795,-1.88830689611621,
136.411697563798));
#177175=CARTESIAN_POINT('Ctrl Pts',(-0.902988917937337,-2.03767698952532,
136.361396221082));
#177176=CARTESIAN_POINT('Ctrl Pts',(-0.895592561001907,-2.18504505824414,
136.305119182057));
#177177=CARTESIAN_POINT('Ctrl Pts',(-0.888196204066446,-2.32990686155138,
136.243061250897));
#177178=CARTESIAN_POINT('Ctrl Pts',(-0.880798714729856,-2.47479084357051,
136.18099381851));
#177179=CARTESIAN_POINT('Ctrl Pts',(-0.873401225393216,-2.6171674529902,
136.113143878704));
#177180=CARTESIAN_POINT('Ctrl Pts',(-0.866003736056626,-2.75655371556865,
136.039753838298));
#177181=CARTESIAN_POINT('Ctrl Pts',(-0.858603653541681,-2.89598883978418,
135.966338071128));
#177182=CARTESIAN_POINT('Ctrl Pts',(-0.851203571026781,-3.03243119997379,
135.887378510511));
#177183=CARTESIAN_POINT('Ctrl Pts',(-0.843803488511838,-3.16542378276714,
135.803162757878));
#177184=CARTESIAN_POINT('Ctrl Pts',(-0.836395268845371,-3.29856260457818,
135.718854401368));
#177185=CARTESIAN_POINT('Ctrl Pts',(-0.828987049178865,-3.42824375777772,
135.62927851019));
#177186=CARTESIAN_POINT('Ctrl Pts',(-0.82157882951239,-3.55403991091922,
135.534765555211));
#177187=CARTESIAN_POINT('Ctrl Pts',(-0.814166050210334,-3.67991348949378,
135.440194429085));
#177188=CARTESIAN_POINT('Ctrl Pts',(-0.806753270908295,-3.80189701475527,
135.340680419632));
#177189=CARTESIAN_POINT('Ctrl Pts',(-0.799340491606245,-3.91959785588101,
135.236592923151));
#177190=CARTESIAN_POINT('Ctrl Pts',(-0.791917120577471,-4.03746687348868,
135.132356701573));
#177191=CARTESIAN_POINT('Ctrl Pts',(-0.78449374954874,-4.15104071652076,
135.023534199059));
#177192=CARTESIAN_POINT('Ctrl Pts',(-0.777070378519966,-4.25996451027873,
134.910530722867));
#177193=CARTESIAN_POINT('Ctrl Pts',(-0.773134329079252,-4.31771851931851,
134.85061356831));
#177194=CARTESIAN_POINT('Ctrl Pts',(-0.769198279638492,-4.37416591199664,
134.789521537525));
#177195=CARTESIAN_POINT('Ctrl Pts',(-0.765262230197777,-4.42925861303343,
134.72731851963));
#177196=CARTESIAN_POINT('Ctrl Pts',(-0.757905128544479,-4.53223562284684,
134.611051198123));
#177197=CARTESIAN_POINT('Ctrl Pts',(-0.750548026891183,-4.63080249576435,
134.490533175901));
#177198=CARTESIAN_POINT('Ctrl Pts',(-0.743190925237883,-4.72458291754208,
134.366136413117));
#177199=CARTESIAN_POINT('Ctrl Pts',(-0.735698603028151,-4.8200869855888,
134.239453288083));
#177200=CARTESIAN_POINT('Ctrl Pts',(-0.728206280818478,-4.91062661734549,
134.108747682586));
#177201=CARTESIAN_POINT('Ctrl Pts',(-0.720713958608741,-4.99584315379781,
133.974452374148));
#177202=CARTESIAN_POINT('Ctrl Pts',(-0.71337486278037,-5.07931691662832,
133.842903555193));
#177203=CARTESIAN_POINT('Ctrl Pts',(-0.706035766951913,-5.15768296477155,
133.707910767536));
#177204=CARTESIAN_POINT('Ctrl Pts',(-0.698696671123543,-5.23064471034456,
133.569914174568));
#177205=CARTESIAN_POINT('Ctrl Pts',(-0.691362564756517,-5.30355685310305,
133.432011398151));
#177206=CARTESIAN_POINT('Ctrl Pts',(-0.68402845838953,-5.37107182671326,
133.291109214693));
#177207=CARTESIAN_POINT('Ctrl Pts',(-0.676694352022508,-5.43293719121724,
133.147675372094));
#177208=CARTESIAN_POINT('Ctrl Pts',(-0.669363719094841,-5.4947732562291,
133.004309459891));
#177209=CARTESIAN_POINT('Ctrl Pts',(-0.66203308616718,-5.55096488716106,
132.858414623623));
#177210=CARTESIAN_POINT('Ctrl Pts',(-0.654702453239508,-5.60130642736868,
132.710481513317));
#177211=CARTESIAN_POINT('Ctrl Pts',(-0.647091848153241,-5.6535706159776,
132.556898529033));
#177212=CARTESIAN_POINT('Ctrl Pts',(-0.639481243066946,-5.69952882857686,
132.401118882871));
#177213=CARTESIAN_POINT('Ctrl Pts',(-0.631870637980683,-5.73900659669919,
132.243712501416));
#177214=CARTESIAN_POINT('Ctrl Pts',(-0.624540907355159,-5.77702741143781,
132.092115307537));
#177215=CARTESIAN_POINT('Ctrl Pts',(-0.617211176729692,-5.80903751536817,
131.939009708147));
#177216=CARTESIAN_POINT('Ctrl Pts',(-0.609881446104168,-5.83493256653342,
131.784917860417));
#177217=CARTESIAN_POINT('Ctrl Pts',(-0.60255090713329,-5.86083047348497,
131.630809018962));
#177218=CARTESIAN_POINT('Ctrl Pts',(-0.595220368162337,-5.88061192932304,
131.475714089102));
#177219=CARTESIAN_POINT('Ctrl Pts',(-0.587889829191454,-5.8942242033676,
131.320162520369));
#177220=CARTESIAN_POINT('Ctrl Pts',(-0.580555320412306,-5.9078438490554,
131.164526713642));
#177221=CARTESIAN_POINT('Ctrl Pts',(-0.57322081163314,-5.91528762124507,
131.008434154064));
#177222=CARTESIAN_POINT('Ctrl Pts',(-0.565886302853983,-5.91655484099832,
130.852416584515));
#177223=CARTESIAN_POINT('Ctrl Pts',(-0.565049265970727,-5.9166994600457,
130.83461137573));
#177224=CARTESIAN_POINT('Ctrl Pts',(-0.564212229087517,-5.91676369097117,
130.816807141521));
#177225=CARTESIAN_POINT('Ctrl Pts',(-0.563375192204262,-5.91674757584986,
130.79900466996));
#177226=CARTESIAN_POINT('',(1.18662480779564,-5.92210060015532,130.804726096251));
#177227=CARTESIAN_POINT('Ctrl Pts',(-0.563374100425627,-5.91425578389467,
130.798983714904));
#177228=CARTESIAN_POINT('Ctrl Pts',(-0.537854269078733,-5.91899404643966,
130.256440525358));
#177229=CARTESIAN_POINT('Ctrl Pts',(-0.419518563127545,-5.60142465403446,
127.746111889883));
#177230=CARTESIAN_POINT('Ctrl Pts',(-0.2083669825721,-2.04259833657134,
124.110680571));
#177231=CARTESIAN_POINT('Ctrl Pts',(0.0700806412408244,4.5275083038907,
125.467767220224));
#177232=CARTESIAN_POINT('Ctrl Pts',(0.348528265053751,6.93705599415352,
131.728922494524));
#177233=CARTESIAN_POINT('Ctrl Pts',(0.626975888866651,2.97178811981426,
137.140450571258));
#177234=CARTESIAN_POINT('Ctrl Pts',(0.905423512679459,-3.72440785671249,
136.72942151575));
#177235=CARTESIAN_POINT('Ctrl Pts',(1.09197315232256,-5.91763069388933,
132.806204183693));
#177236=CARTESIAN_POINT('Ctrl Pts',(1.18570691736122,-5.92652215037093,
130.824135984152));
#177237=CARTESIAN_POINT('Ctrl Pts',(1.18662480779563,-5.92650486509969,
130.804726368057));
#177238=CARTESIAN_POINT('',(2.93662479004875,-5.91447619583082,130.809538251585));
#177239=CARTESIAN_POINT('Ctrl Pts',(1.18662480779565,-5.91674998873255,
130.804725766041));
#177240=CARTESIAN_POINT('Ctrl Pts',(1.1940350854322,-5.91675964326844,130.648286730755));
#177241=CARTESIAN_POINT('Ctrl Pts',(1.20144536306876,-5.91056063453475,
130.491606878693));
#177242=CARTESIAN_POINT('Ctrl Pts',(1.20885564070531,-5.89812159424516,
130.335220742903));
#177243=CARTESIAN_POINT('Ctrl Pts',(1.21625716100478,-5.88569725419679,
130.179019421525));
#177244=CARTESIAN_POINT('Ctrl Pts',(1.2236586813042,-5.86704758979576,130.023111495431));
#177245=CARTESIAN_POINT('Ctrl Pts',(1.23106020160367,-5.84219319642566,
129.868033101075));
#177246=CARTESIAN_POINT('Ctrl Pts',(1.23845460439431,-5.817362703735,129.713103834439));
#177247=CARTESIAN_POINT('Ctrl Pts',(1.24584900718498,-5.78633941867362,
129.559002879114));
#177248=CARTESIAN_POINT('Ctrl Pts',(1.25324340997562,-5.74919584151621,
129.40626271742));
#177249=CARTESIAN_POINT('Ctrl Pts',(1.2606323293674,-5.71207980857768,129.253635821835));
#177250=CARTESIAN_POINT('Ctrl Pts',(1.26802124875918,-5.66885260811299,
129.102368073306));
#177251=CARTESIAN_POINT('Ctrl Pts',(1.27541016815096,-5.61963804525913,
128.952983075632));
#177252=CARTESIAN_POINT('Ctrl Pts',(1.28279523383285,-5.57044915038689,
128.803675990088));
#177253=CARTESIAN_POINT('Ctrl Pts',(1.29018029951475,-5.51527922885192,
128.656250054947));
#177254=CARTESIAN_POINT('Ctrl Pts',(1.29756536519665,-5.45430225584897,
128.51121486024));
#177255=CARTESIAN_POINT('Ctrl Pts',(1.30494927592191,-5.39333481908606,
128.366202347709));
#177256=CARTESIAN_POINT('Ctrl Pts',(1.31233318664717,-5.32656227780676,
128.223580178958));
#177257=CARTESIAN_POINT('Ctrl Pts',(1.31971709737243,-5.2542072203174,128.083839151291));
#177258=CARTESIAN_POINT('Ctrl Pts',(1.3271007517007,-5.18185467526619,127.944102975955));
#177259=CARTESIAN_POINT('Ctrl Pts',(1.33448440602898,-5.10392017165668,
127.807248075647));
#177260=CARTESIAN_POINT('Ctrl Pts',(1.34186806035726,-5.02067271393934,
127.673741499563));
#177261=CARTESIAN_POINT('Ctrl Pts',(1.34925292985532,-4.93741155571667,
127.540212951547));
#177262=CARTESIAN_POINT('Ctrl Pts',(1.35663779935341,-4.84883590086788,
127.410034142876));
#177263=CARTESIAN_POINT('Ctrl Pts',(1.36402266885148,-4.75525851876446,
127.283643789672));
#177264=CARTESIAN_POINT('Ctrl Pts',(1.37141022555093,-4.66164708578567,
127.15720744563));
#177265=CARTESIAN_POINT('Ctrl Pts',(1.37879778225042,-4.56303052504015,
127.034562602469));
#177266=CARTESIAN_POINT('Ctrl Pts',(1.38618533894987,-4.45976225609666,
126.916115360179));
#177267=CARTESIAN_POINT('Ctrl Pts',(1.39358103742541,-4.35638017589496,
126.797537577986));
#177268=CARTESIAN_POINT('Ctrl Pts',(1.40097673590085,-4.24833639680506,
126.683166916957));
#177269=CARTESIAN_POINT('Ctrl Pts',(1.40837243437639,-4.13602208551581,
126.57337351399));
#177270=CARTESIAN_POINT('Ctrl Pts',(1.41577279822131,-4.02363692388693,
126.463510850928));
#177271=CARTESIAN_POINT('Ctrl Pts',(1.42317316206625,-3.90697614011333,
126.358231449219));
#177272=CARTESIAN_POINT('Ctrl Pts',(1.43057352591117,-3.78646397365026,
126.257865138766));
#177273=CARTESIAN_POINT('Ctrl Pts',(1.43798426079176,-3.66578291873755,
126.157358172717));
#177274=CARTESIAN_POINT('Ctrl Pts',(1.44539499567228,-3.54123999963713,
126.061778274154));
#177275=CARTESIAN_POINT('Ctrl Pts',(1.45280573055285,-3.41328899580607,
125.971412366901));
#177276=CARTESIAN_POINT('Ctrl Pts',(1.45597674047032,-3.35853951297656,
125.932745326085));
#177277=CARTESIAN_POINT('Ctrl Pts',(1.45914775038788,-3.30316634952253,
125.895032363853));
#177278=CARTESIAN_POINT('Ctrl Pts',(1.46231876030535,-3.24720637728398,
125.858293361066));
#177279=CARTESIAN_POINT('Ctrl Pts',(1.46974202671077,-3.11620527896578,
125.772288141195));
#177280=CARTESIAN_POINT('Ctrl Pts',(1.4771652931162,-2.9815868418728,125.691360991508));
#177281=CARTESIAN_POINT('Ctrl Pts',(1.48458855952163,-2.84378247631683,
125.615831751896));
#177282=CARTESIAN_POINT('Ctrl Pts',(1.49200305224264,-2.7061409840766,125.540391781573));
#177283=CARTESIAN_POINT('Ctrl Pts',(1.49941754496364,-2.56532138278411,
125.470337199803));
#177284=CARTESIAN_POINT('Ctrl Pts',(1.50683203768466,-2.42178486849296,
125.405945237731));
#177285=CARTESIAN_POINT('Ctrl Pts',(1.51423938403844,-2.27838670009834,
125.341615339057));
#177286=CARTESIAN_POINT('Ctrl Pts',(1.52164673039226,-2.13227717025643,
125.282937346352));
#177287=CARTESIAN_POINT('Ctrl Pts',(1.52905407674604,-1.98394284573079,
125.230143062844));
#177288=CARTESIAN_POINT('Ctrl Pts',(1.53645589842143,-1.83571915454092,
125.177388155304));
#177289=CARTESIAN_POINT('Ctrl Pts',(1.54385772009686,-1.68527432280217,
125.130508343911));
#177290=CARTESIAN_POINT('Ctrl Pts',(1.55125954177225,-1.53311560636215,
125.089687652292));
#177291=CARTESIAN_POINT('Ctrl Pts',(1.5586574560836,-1.38103721332414,125.048888509599));
#177292=CARTESIAN_POINT('Ctrl Pts',(1.56605537039489,-1.22724709706649,
125.014142213072));
#177293=CARTESIAN_POINT('Ctrl Pts',(1.57345328470623,-1.072268304086,124.985583147465));
#177294=CARTESIAN_POINT('Ctrl Pts',(1.58084996961843,-0.917315265769306,
124.957028827857));
#177295=CARTESIAN_POINT('Ctrl Pts',(1.58824665453057,-0.76117430953846,
124.934659766071));
#177296=CARTESIAN_POINT('Ctrl Pts',(1.59564333944277,-0.604379440272201,
124.918559393036));
#177297=CARTESIAN_POINT('Ctrl Pts',(1.60303969637822,-0.447591523454532,
124.902459733909));
#177298=CARTESIAN_POINT('Ctrl Pts',(1.61043605331375,-0.290150122598635,
124.892628248985));
#177299=CARTESIAN_POINT('Ctrl Pts',(1.61783241024921,-0.132594875537374,
124.889096535424));
#177300=CARTESIAN_POINT('Ctrl Pts',(1.62522989958578,0.0249844936342075,
124.885564281149));
#177301=CARTESIAN_POINT('Ctrl Pts',(1.63262738892231,0.182677370488753,
124.888333727073));
#177302=CARTESIAN_POINT('Ctrl Pts',(1.64002487825888,0.339943751926087,
124.897384334557));
#177303=CARTESIAN_POINT('Ctrl Pts',(1.64742496077388,0.497265262849863,
124.906438114718));
#177304=CARTESIAN_POINT('Ctrl Pts',(1.6548250432889,0.654159608239698,124.921777418875));
#177305=CARTESIAN_POINT('Ctrl Pts',(1.6622251258039,0.810091689926226,124.943329819454));
#177306=CARTESIAN_POINT('Ctrl Pts',(1.66963334547036,0.966195234966553,
124.964905919114));
#177307=CARTESIAN_POINT('Ctrl Pts',(1.67704156513685,1.12133403318331,124.992708707882));
#177308=CARTESIAN_POINT('Ctrl Pts',(1.68444978480332,1.27498224132818,125.026614443945));
#177309=CARTESIAN_POINT('Ctrl Pts',(1.6918625641054,1.42872501738185,125.060541048421));
#177310=CARTESIAN_POINT('Ctrl Pts',(1.69927534340744,1.58097501507603,125.100577990297));
#177311=CARTESIAN_POINT('Ctrl Pts',(1.70668812270952,1.73122184777611,125.146551723985));
#177312=CARTESIAN_POINT('Ctrl Pts',(1.71411149373828,1.88168336019642,125.192591147099));
#177313=CARTESIAN_POINT('Ctrl Pts',(1.72153486476699,2.03013563975381,125.244584180947));
#177314=CARTESIAN_POINT('Ctrl Pts',(1.72895823579574,2.17608778622686,125.302308953947));
#177315=CARTESIAN_POINT('Ctrl Pts',(1.73289428523654,2.25347511636075,125.332916013678));
#177316=CARTESIAN_POINT('Ctrl Pts',(1.73683033467736,2.33015996168881,125.365133693031));
#177317=CARTESIAN_POINT('Ctrl Pts',(1.74076638411816,2.40607209844888,125.398923760145));
#177318=CARTESIAN_POINT('Ctrl Pts',(1.74818965052359,2.54924001924134,125.46265077217));
#177319=CARTESIAN_POINT('Ctrl Pts',(1.755612916929,2.69009087573639,125.532165974727));
#177320=CARTESIAN_POINT('Ctrl Pts',(1.76303618333444,2.82812238976302,125.607279291377));
#177321=CARTESIAN_POINT('Ctrl Pts',(1.77045067605546,2.96599076200327,125.682303830325));
#177322=CARTESIAN_POINT('Ctrl Pts',(1.77786516877653,3.10104609990376,125.762913136486));
#177323=CARTESIAN_POINT('Ctrl Pts',(1.78527966149755,3.2328058733188,125.848869042764));
#177324=CARTESIAN_POINT('Ctrl Pts',(1.79268700785134,3.36443865170356,125.934742101503));
#177325=CARTESIAN_POINT('Ctrl Pts',(1.80009435420517,3.49278187861667,126.025951298649));
#177326=CARTESIAN_POINT('Ctrl Pts',(1.80750170055896,3.61737753021731,126.122212567111));
#177327=CARTESIAN_POINT('Ctrl Pts',(1.81490352223436,3.74188025368009,126.218402040287));
#177328=CARTESIAN_POINT('Ctrl Pts',(1.82230534390971,3.86264067308458,126.319635854887));
#177329=CARTESIAN_POINT('Ctrl Pts',(1.82970716558512,3.97922977996487,126.425586711466));
#177330=CARTESIAN_POINT('Ctrl Pts',(1.83710507989642,4.09575734036218,126.531481637412));
#177331=CARTESIAN_POINT('Ctrl Pts',(1.84450299420769,4.20811769806562,126.642088395783));
#177332=CARTESIAN_POINT('Ctrl Pts',(1.85190090851899,4.31591507196789,126.75703957099));
#177333=CARTESIAN_POINT('Ctrl Pts',(1.8592975934312,4.42369453190318,126.871971643398));
#177334=CARTESIAN_POINT('Ctrl Pts',(1.86669427834345,4.52691225790639,126.991246427726));
#177335=CARTESIAN_POINT('Ctrl Pts',(1.87409096325567,4.62520941449318,127.114459747003));
#177336=CARTESIAN_POINT('Ctrl Pts',(1.88148732019112,4.72350221248104,127.237667602871));
#177337=CARTESIAN_POINT('Ctrl Pts',(1.88888367712659,4.81687464207243,127.364813354635));
#177338=CARTESIAN_POINT('Ctrl Pts',(1.89628003406204,4.90500843225194,127.495460068738));
#177339=CARTESIAN_POINT('Ctrl Pts',(1.90367752339863,4.99315571593972,127.626126785186));
#177340=CARTESIAN_POINT('Ctrl Pts',(1.9110750127352,5.07606255445162,127.760295221747));
#177341=CARTESIAN_POINT('Ctrl Pts',(1.91847250207178,5.15345434266035,127.897499956885));
#177342=CARTESIAN_POINT('Ctrl Pts',(1.92587258458679,5.23087326044057,128.03475278893));
#177343=CARTESIAN_POINT('Ctrl Pts',(1.93327266710181,5.30277309546234,128.175043713766));
#177344=CARTESIAN_POINT('Ctrl Pts',(1.94067274961682,5.36892554946398,128.317883389274));
#177345=CARTESIAN_POINT('Ctrl Pts',(1.9480809692833,5.43515074488934,128.46088013169));
#177346=CARTESIAN_POINT('Ctrl Pts',(1.95548918894971,5.49561578119426,128.60643088284));
#177347=CARTESIAN_POINT('Ctrl Pts',(1.96289740861619,5.55014053475337,128.754026350431));
#177348=CARTESIAN_POINT('Ctrl Pts',(1.97031018791826,5.60469884738858,128.90171266057));
#177349=CARTESIAN_POINT('Ctrl Pts',(1.97772296722037,5.6533094769499,129.051445840615));
#177350=CARTESIAN_POINT('Ctrl Pts',(1.98513574652245,5.69584255581191,129.202702682206));
#177351=CARTESIAN_POINT('Ctrl Pts',(1.99255911755121,5.73843640793154,129.354175646665));
#177352=CARTESIAN_POINT('Ctrl Pts',(1.99998248857994,5.77493527928529,129.507176258639));
#177353=CARTESIAN_POINT('Ctrl Pts',(2.0074058596087,5.80526049315837,129.661171582859));
#177354=CARTESIAN_POINT('Ctrl Pts',(2.01134190904947,5.82133964919735,129.742823598827));
#177355=CARTESIAN_POINT('Ctrl Pts',(2.0152779584903,5.83568403513684,129.82475517368));
#177356=CARTESIAN_POINT('Ctrl Pts',(2.01921400793108,5.84828785886529,129.906886560922));
#177357=CARTESIAN_POINT('Ctrl Pts',(2.02663727433653,5.87205827706538,130.061783794029));
#177358=CARTESIAN_POINT('Ctrl Pts',(2.03406054074194,5.88970649679028,130.217860273688));
#177359=CARTESIAN_POINT('Ctrl Pts',(2.04148380714739,5.90112094111124,130.374590678089));
#177360=CARTESIAN_POINT('Ctrl Pts',(2.04889829986839,5.91252189450691,130.531135840167));
#177361=CARTESIAN_POINT('Ctrl Pts',(2.05631279258944,5.9177037113047,130.68833301988));
#177362=CARTESIAN_POINT('Ctrl Pts',(2.06372728531045,5.9166059488978,130.845647515817));
#177363=CARTESIAN_POINT('Ctrl Pts',(2.07113463166422,5.91550924455563,131.00281038612));
#177364=CARTESIAN_POINT('Ctrl Pts',(2.07854197801803,5.90814501292183,131.160089976757));
#177365=CARTESIAN_POINT('Ctrl Pts',(2.0859493243718,5.89450467461231,131.316947394096));
#177366=CARTESIAN_POINT('Ctrl Pts',(2.09335114604718,5.88087450978173,131.473687821256));
#177367=CARTESIAN_POINT('Ctrl Pts',(2.10075296772251,5.86097759089359,131.630006331778));
#177368=CARTESIAN_POINT('Ctrl Pts',(2.1081547893979,5.83485739468559,131.785365075345));
#177369=CARTESIAN_POINT('Ctrl Pts',(2.11555270370928,5.80875098712571,131.940641806242));
#177370=CARTESIAN_POINT('Ctrl Pts',(2.12295061802067,5.77642790665482,132.09495941201));
#177371=CARTESIAN_POINT('Ctrl Pts',(2.13034853233205,5.73798334105775,132.247786313694));
#177372=CARTESIAN_POINT('Ctrl Pts',(2.13774521724426,5.69954516425014,132.400587818319));
#177373=CARTESIAN_POINT('Ctrl Pts',(2.14514190215647,5.65498761229471,132.551898748862));
#177374=CARTESIAN_POINT('Ctrl Pts',(2.15253858706868,5.60445677138152,132.70119873934));
#177375=CARTESIAN_POINT('Ctrl Pts',(2.1599349440041,5.55392817105891,132.8504921097));
#177376=CARTESIAN_POINT('Ctrl Pts',(2.16733130093954,5.49742692808816,132.997774363695));
#177377=CARTESIAN_POINT('Ctrl Pts',(2.17472765787497,5.43514861378607,133.142541557647));
#177378=CARTESIAN_POINT('Ctrl Pts',(2.18212514721153,5.37286076451498,133.287330915827));
#177379=CARTESIAN_POINT('Ctrl Pts',(2.18952263654819,5.30479423031583,133.429604104318));
#177380=CARTESIAN_POINT('Ctrl Pts',(2.19692012588476,5.231192152731,133.568878518341));
#177381=CARTESIAN_POINT('Ctrl Pts',(2.2043202083997,5.15756427405248,133.708201754793));
#177382=CARTESIAN_POINT('Ctrl Pts',(2.21172029091452,5.07839716282394,133.844523793975));
#177383=CARTESIAN_POINT('Ctrl Pts',(2.21912037342946,4.99397911564089,133.977388060725));
#177384=CARTESIAN_POINT('Ctrl Pts',(2.22652859309594,4.90946824213586,134.110398425397));
#177385=CARTESIAN_POINT('Ctrl Pts',(2.23393681276249,4.81969510204575,134.239943109171));
#177386=CARTESIAN_POINT('Ctrl Pts',(2.24134503242897,4.72499081618039,134.365595284014));
#177387=CARTESIAN_POINT('Ctrl Pts',(2.24875781173106,4.63022824140704,134.491324795675));
#177388=CARTESIAN_POINT('Ctrl Pts',(2.25617059103314,4.5305287090298,134.6131567363));
#177389=CARTESIAN_POINT('Ctrl Pts',(2.26358337033523,4.42626221243583,134.73069903768));
#177390=CARTESIAN_POINT('Ctrl Pts',(2.27100674136397,4.32184673498236,134.848409289012));
#177391=CARTESIAN_POINT('Ctrl Pts',(2.27843011239267,4.21285151842754,134.961817391203));
#177392=CARTESIAN_POINT('Ctrl Pts',(2.28585348342142,4.09968240962053,135.070569086775));
#177393=CARTESIAN_POINT('Ctrl Pts',(2.28978953286226,4.03967743267468,135.128231845229));
#177394=CARTESIAN_POINT('Ctrl Pts',(2.29372558230313,3.97849956930882,135.184586200873));
#177395=CARTESIAN_POINT('Ctrl Pts',(2.29766163174398,3.9162127817296,135.23958417571));
#177396=CARTESIAN_POINT('Ctrl Pts',(2.3050848981494,3.79874184426099,135.343308639825));
#177397=CARTESIAN_POINT('Ctrl Pts',(2.31250816455476,3.67696957545211,135.442519736538));
#177398=CARTESIAN_POINT('Ctrl Pts',(2.3199314309602,3.55127763336318,135.53683964375));
#177399=CARTESIAN_POINT('Ctrl Pts',(2.32734592368122,3.42573424871136,135.631048072665));
#177400=CARTESIAN_POINT('Ctrl Pts',(2.3347604164023,3.29628070791526,135.720376597284));
#177401=CARTESIAN_POINT('Ctrl Pts',(2.34217490912332,3.16333419970981,135.804485346355));
#177402=CARTESIAN_POINT('Ctrl Pts',(2.34958225547707,3.03051583035488,135.888513028247));
#177403=CARTESIAN_POINT('Ctrl Pts',(2.3569896018308,2.8942115092836,135.967330752114));
#177404=CARTESIAN_POINT('Ctrl Pts',(2.36439694818455,2.75486998560348,136.040640014707));
#177405=CARTESIAN_POINT('Ctrl Pts',(2.37179876985996,2.61563238808818,136.113894600486));
#177406=CARTESIAN_POINT('Ctrl Pts',(2.37920059153536,2.47336242734692,136.181648732345));
#177407=CARTESIAN_POINT('Ctrl Pts',(2.38660241321077,2.32853611232308,136.243648267259));
#177408=CARTESIAN_POINT('Ctrl Pts',(2.39400032752223,2.18378624998154,136.305615073103));
#177409=CARTESIAN_POINT('Ctrl Pts',(2.40139824183376,2.03648306321578,136.361833185401));
#177410=CARTESIAN_POINT('Ctrl Pts',(2.40879615614523,1.88712523577866,136.412095356923));
#177411=CARTESIAN_POINT('Ctrl Pts',(2.41619284105743,1.73779222890518,136.462349175782));
#177412=CARTESIAN_POINT('Ctrl Pts',(2.42358952596956,1.58640561248091,136.50664889932));
#177413=CARTESIAN_POINT('Ctrl Pts',(2.43098621088177,1.43348214829835,136.54483616346));
#177414=CARTESIAN_POINT('Ctrl Pts',(2.43838256781722,1.28056546490244,136.583021734337));
#177415=CARTESIAN_POINT('Ctrl Pts',(2.44577892475267,1.12611243142052,136.615095294281));
#177416=CARTESIAN_POINT('Ctrl Pts',(2.45317528168812,0.97065274101566,136.640948989111));
#177417=CARTESIAN_POINT('Ctrl Pts',(2.46057277102466,0.815169249335995,
136.666806642208));
#177418=CARTESIAN_POINT('Ctrl Pts',(2.46797026036123,0.658679162120519,
136.686442472838));
#177419=CARTESIAN_POINT('Ctrl Pts',(2.47536774969777,0.501719932381965,
136.699800183192));
#177420=CARTESIAN_POINT('Ctrl Pts',(2.48276783221279,0.3447056808274,136.713162576072));
#177421=CARTESIAN_POINT('Ctrl Pts',(2.49016791472778,0.187222331038063,
136.720242435294));
#177422=CARTESIAN_POINT('Ctrl Pts',(2.49756799724281,0.0298098439794243,
136.721035522925));
#177423=CARTESIAN_POINT('Ctrl Pts',(2.50497621690927,-0.127775734290234,
136.721829482636));
#177424=CARTESIAN_POINT('Ctrl Pts',(2.51238443657572,-0.285289920693903,
136.716322863255));
#177425=CARTESIAN_POINT('Ctrl Pts',(2.51979265624217,-0.442194633834676,
136.70456353512));
#177426=CARTESIAN_POINT('Ctrl Pts',(2.52720543554424,-0.599195919208739,
136.692796969314));
#177427=CARTESIAN_POINT('Ctrl Pts',(2.53461821484636,-0.755586613862468,
136.674770068906));
#177428=CARTESIAN_POINT('Ctrl Pts',(2.54203099414843,-0.910836869243758,
136.650582197367));
#177429=CARTESIAN_POINT('Ctrl Pts',(2.54945436517718,-1.06630895347023,
136.626359765062));
#177430=CARTESIAN_POINT('Ctrl Pts',(2.55687773620583,-1.22063697863208,
136.595958851851));
#177431=CARTESIAN_POINT('Ctrl Pts',(2.56430110723457,-1.37330352774386,
136.55952942336));
#177432=CARTESIAN_POINT('Ctrl Pts',(2.56823715667533,-1.45425099526594,
136.540213666262));
#177433=CARTESIAN_POINT('Ctrl Pts',(2.57217320611614,-1.5347316402072,136.519203902923));
#177434=CARTESIAN_POINT('Ctrl Pts',(2.5761092555569,-1.614670524186,136.49652801328));
#177435=CARTESIAN_POINT('Ctrl Pts',(2.58353252196235,-1.76543276456432,
136.453761993102));
#177436=CARTESIAN_POINT('Ctrl Pts',(2.59095578836782,-1.91472275577802,
136.404937555722));
#177437=CARTESIAN_POINT('Ctrl Pts',(2.59837905477326,-2.06201632989022,
136.350171578802));
#177438=CARTESIAN_POINT('Ctrl Pts',(2.60579354749427,-2.20913581522959,
136.295470330719));
#177439=CARTESIAN_POINT('Ctrl Pts',(2.61320804021524,-2.35426323378479,
136.234841650059));
#177440=CARTESIAN_POINT('Ctrl Pts',(2.62062253293624,-2.49688714154573,
136.168452820808));
#177441=CARTESIAN_POINT('Ctrl Pts',(2.62802987929002,-2.63937358301488,
136.102127979611));
#177442=CARTESIAN_POINT('Ctrl Pts',(2.63543722564383,-2.77936098129598,
136.030054198934));
#177443=CARTESIAN_POINT('Ctrl Pts',(2.64284457199761,-2.91635563729711,
135.952447675814));
#177444=CARTESIAN_POINT('Ctrl Pts',(2.65024639367301,-3.05324811751509,
135.874899034568));
#177445=CARTESIAN_POINT('Ctrl Pts',(2.65764821534844,-3.18715197646189,
135.791826050558));
#177446=CARTESIAN_POINT('Ctrl Pts',(2.66505003702383,-3.31759610195315,
135.703491833078));
#177447=CARTESIAN_POINT('Ctrl Pts',(2.67244795133514,-3.4479713670052,135.615204246545));
#177448=CARTESIAN_POINT('Ctrl Pts',(2.67984586564639,-3.57489022758569,
135.521661166579));
#177449=CARTESIAN_POINT('Ctrl Pts',(2.6872437799577,-3.69790876998053,135.423170127754));
#177450=CARTESIAN_POINT('Ctrl Pts',(2.6946404648699,-3.8209068689261,135.324695456352));
#177451=CARTESIAN_POINT('Ctrl Pts',(2.70203714978218,-3.94000564497269,
135.221274691116));
#177452=CARTESIAN_POINT('Ctrl Pts',(2.70943383469438,-4.05479253956745,
135.113256998725));
#177453=CARTESIAN_POINT('Ctrl Pts',(2.71683019162982,-4.16957434439101,
135.005244095952));
#177454=CARTESIAN_POINT('Ctrl Pts',(2.7242265485652,-4.28004437606428,134.892634927137));
#177455=CARTESIAN_POINT('Ctrl Pts',(2.73162290550064,-4.38582558171782,
134.77581684032));
#177456=CARTESIAN_POINT('Ctrl Pts',(2.73902039483721,-4.49162298274399,
134.658980868355));
#177457=CARTESIAN_POINT('Ctrl Pts',(2.74641788417378,-4.59272987779126,
134.537934972038));
#177458=CARTESIAN_POINT('Ctrl Pts',(2.75381537351035,-4.68880839543919,
134.413100895469));
#177459=CARTESIAN_POINT('Ctrl Pts',(2.76121545602542,-4.78492059326364,
134.288223058507));
#177460=CARTESIAN_POINT('Ctrl Pts',(2.76861553854049,-4.8760006766464,134.159554693013));
#177461=CARTESIAN_POINT('Ctrl Pts',(2.77601562105556,-4.96175321800073,
134.027547792733));
#177462=CARTESIAN_POINT('Ctrl Pts',(2.78342384072205,-5.04760005308911,
133.895395737296));
#177463=CARTESIAN_POINT('Ctrl Pts',(2.79083206038853,-5.1281074434976,133.759898128959));
#177464=CARTESIAN_POINT('Ctrl Pts',(2.79824028005501,-5.20302481775922,
133.621533545926));
#177465=CARTESIAN_POINT('Ctrl Pts',(2.80565305935704,-5.2779883024141,133.483083801801));
#177466=CARTESIAN_POINT('Ctrl Pts',(2.81306583865903,-5.34735475106751,
133.341763901173));
#177467=CARTESIAN_POINT('Ctrl Pts',(2.82047861796104,-5.41092136493723,
133.198073329018));
#177468=CARTESIAN_POINT('Ctrl Pts',(2.82790198898978,-5.4745788057661,133.054177445034));
#177469=CARTESIAN_POINT('Ctrl Pts',(2.83532536001858,-5.53241972375438,
132.907904470494));
#177470=CARTESIAN_POINT('Ctrl Pts',(2.84274873104732,-5.58429061271274,
132.759770783048));
#177471=CARTESIAN_POINT('Ctrl Pts',(2.84668478048813,-5.61179380266354,
132.681226747544));
#177472=CARTESIAN_POINT('Ctrl Pts',(2.8506208299289,-5.63761944817894,132.602159811346));
#177473=CARTESIAN_POINT('Ctrl Pts',(2.85455687936971,-5.66175049941405,
132.522648092026));
#177474=CARTESIAN_POINT('Ctrl Pts',(2.86366808789622,-5.71760930989739,
132.33859353023));
#177475=CARTESIAN_POINT('Ctrl Pts',(2.87277929642273,-5.76452188978835,
132.151705729902));
#177476=CARTESIAN_POINT('Ctrl Pts',(2.88189050494924,-5.80224320684398,
131.962766561583));
#177477=CARTESIAN_POINT('Ctrl Pts',(2.89101288072823,-5.84001075744482,
131.773595817903));
#177478=CARTESIAN_POINT('Ctrl Pts',(2.90013525650721,-5.86856438465176,
131.582368600916));
#177479=CARTESIAN_POINT('Ctrl Pts',(2.9092576322862,-5.88770617541872,131.38989161968));
#177480=CARTESIAN_POINT('Ctrl Pts',(2.91838000806519,-5.90684796618569,
131.197414638443));
#177481=CARTESIAN_POINT('Ctrl Pts',(2.92750238384411,-5.91657775146001,
131.00368782821));
#177482=CARTESIAN_POINT('Ctrl Pts',(2.9366247596231,-5.9167477322684,130.809540887515));
#177483=CARTESIAN_POINT('',(4.68662480779567,-5.90794960642534,130.801846066134));
#177484=CARTESIAN_POINT('Ctrl Pts',(2.93662480779568,-5.91315123421776,
130.809536714076));
#177485=CARTESIAN_POINT('Ctrl Pts',(3.002084706258,-5.90155967865228,129.41722218474));
#177486=CARTESIAN_POINT('Ctrl Pts',(3.16036047932472,-4.71421286616052,
126.032947503737));
#177487=CARTESIAN_POINT('Ctrl Pts',(3.41145212699552,0.935117824657439,
123.868719682199));
#177488=CARTESIAN_POINT('Ctrl Pts',(3.6898997508085,6.34060517223504,127.842218389349));
#177489=CARTESIAN_POINT('Ctrl Pts',(3.96834737462117,5.91938612231001,134.537781095536));
#177490=CARTESIAN_POINT('Ctrl Pts',(4.24679499843421,0.0585404040744741,
137.802512770201));
#177491=CARTESIAN_POINT('Ctrl Pts',(4.48622080949229,-5.02721977015144,
135.080001576444));
#177492=CARTESIAN_POINT('Ctrl Pts',(4.63283074594615,-5.90357735060225,
131.948565170342));
#177493=CARTESIAN_POINT('Ctrl Pts',(4.68662480779567,-5.90794960642534,
130.801846066134));
#177494=CARTESIAN_POINT('',(6.43662480779561,-5.92239257047651,130.800071874156));
#177495=CARTESIAN_POINT('Ctrl Pts',(4.68662480779567,-5.90794960642534,
130.801846066134));
#177496=CARTESIAN_POINT('Ctrl Pts',(4.72564662055044,-5.91112120831184,
129.970024548512));
#177497=CARTESIAN_POINT('Ctrl Pts',(4.85748430790944,-5.357959038813,127.163691475044));
#177498=CARTESIAN_POINT('Ctrl Pts',(5.082137869873,-1.05101382462193,123.885333917891));
#177499=CARTESIAN_POINT('Ctrl Pts',(5.36058549368563,5.25307447480259,126.180209982854));
#177500=CARTESIAN_POINT('Ctrl Pts',(5.63903311749881,6.72984395884472,132.724454578803));
#177501=CARTESIAN_POINT('Ctrl Pts',(5.91748074131143,2.02221561585842,137.504226626174));
#177502=CARTESIAN_POINT('Ctrl Pts',(6.18334463807725,-4.24699899157585,
136.189382608541));
#177503=CARTESIAN_POINT('Ctrl Pts',(6.35639266023856,-5.90852833851104,
132.49976478573));
#177504=CARTESIAN_POINT('Ctrl Pts',(6.43662480779561,-5.92239257047651,
130.800071874156));
#177505=CARTESIAN_POINT('',(8.18662480779565,-5.92165762541258,130.808932636213));
#177506=CARTESIAN_POINT('Ctrl Pts',(6.43662480779561,-5.92239257047651,
130.800071874156));
#177507=CARTESIAN_POINT('Ctrl Pts',(6.44920853484286,-5.92456705683997,
130.53348955878));
#177508=CARTESIAN_POINT('Ctrl Pts',(6.55460813649462,-5.78691335188716,
128.302891236576));
#177509=CARTESIAN_POINT('Ctrl Pts',(6.75282361275006,-2.95248947639563,
124.459254911432));
#177510=CARTESIAN_POINT('Ctrl Pts',(7.03127123656321,3.74242445275167,124.890662980229));
#177511=CARTESIAN_POINT('Ctrl Pts',(7.30971886037598,6.99823313741991,130.756470277563));
#177512=CARTESIAN_POINT('Ctrl Pts',(7.588166484189,3.82300745149239,136.66628645778));
#177513=CARTESIAN_POINT('Ctrl Pts',(7.86661410800171,-2.86537531805696,
137.189279161839));
#177514=CARTESIAN_POINT('Ctrl Pts',(8.06610021587067,-5.77064201872146,
133.360405977193));
#177515=CARTESIAN_POINT('Ctrl Pts',(8.17277044913534,-5.92416113212367,
131.102527757664));
#177516=CARTESIAN_POINT('Ctrl Pts',(8.18662480779565,-5.92165762541258,
130.808932636213));
#177517=CARTESIAN_POINT('',(9.93662400132317,-5.91171822603858,130.806485822397));
#177518=CARTESIAN_POINT('Ctrl Pts',(8.18662480779565,-5.92165762541258,
130.808932636213));
#177519=CARTESIAN_POINT('Ctrl Pts',(8.26558632373962,-5.90738914211935,
129.135616935941));
#177520=CARTESIAN_POINT('Ctrl Pts',(8.4373637142878,-4.29042602827262,125.471272957867));
#177521=CARTESIAN_POINT('Ctrl Pts',(8.70195697944047,1.93033341467937,124.077446507921));
#177522=CARTESIAN_POINT('Ctrl Pts',(8.98040460325343,6.7029357182005,128.792343398947));
#177523=CARTESIAN_POINT('Ctrl Pts',(9.25885222706628,5.3158675533077,135.356185821374));
#177524=CARTESIAN_POINT('Ctrl Pts',(9.53729985087913,-0.956223198505886,
137.737123250526));
#177525=CARTESIAN_POINT('Ctrl Pts',(9.76322355739578,-5.33223384913622,
134.499816419021));
#177526=CARTESIAN_POINT('Ctrl Pts',(9.89633138930801,-5.91036449412479,
131.665510020757));
#177527=CARTESIAN_POINT('Ctrl Pts',(9.93662334661598,-5.90763365731545,
130.806498324047));
#177528=CARTESIAN_POINT('',(11.6866256258633,-5.91485588054631,130.79903509886));
#177529=CARTESIAN_POINT('Ctrl Pts',(9.93662480779568,-5.91674962384094,
130.806470422784));
#177530=CARTESIAN_POINT('Ctrl Pts',(9.94419276580098,-5.91680724575811,
130.644875194101));
#177531=CARTESIAN_POINT('Ctrl Pts',(9.95176072380631,-5.91024040341668,
130.48332735637));
#177532=CARTESIAN_POINT('Ctrl Pts',(9.9593286818116,-5.89708709072551,130.322391316782));
#177533=CARTESIAN_POINT('Ctrl Pts',(9.96690056530931,-5.88392695542389,
130.161371799827));
#177534=CARTESIAN_POINT('Ctrl Pts',(9.97447244880701,-5.86417356697056,
130.000965061026));
#177535=CARTESIAN_POINT('Ctrl Pts',(9.98204433230472,-5.83791669394471,
129.841729204687));
#177536=CARTESIAN_POINT('Ctrl Pts',(9.98962133024956,-5.81164208565014,
129.682385792102));
#177537=CARTESIAN_POINT('Ctrl Pts',(9.99719832819441,-5.77885529158964,
129.524215182232));
#177538=CARTESIAN_POINT('Ctrl Pts',(10.0047753261393,-5.73969699141968,
129.367764289717));
#177539=CARTESIAN_POINT('Ctrl Pts',(10.0123643149607,-5.70047672180609,
129.211065807938));
#177540=CARTESIAN_POINT('Ctrl Pts',(10.0199533037822,-5.65486488004793,
129.056092820959));
#177541=CARTESIAN_POINT('Ctrl Pts',(10.0275422926037,-5.6030521688323,128.9033774625));
#177542=CARTESIAN_POINT('Ctrl Pts',(10.0351374993923,-5.5511970053554,128.750536978138));
#177543=CARTESIAN_POINT('Ctrl Pts',(10.042732706181,-5.49313096425641,128.599958136316));
#177544=CARTESIAN_POINT('Ctrl Pts',(10.0503279129696,-5.42909254872292,
128.452152153186));
#177545=CARTESIAN_POINT('Ctrl Pts',(10.0579373914952,-5.3649338021114,128.304068435931));
#177546=CARTESIAN_POINT('Ctrl Pts',(10.0655468700207,-5.2947803979279,128.158768307418));
#177547=CARTESIAN_POINT('Ctrl Pts',(10.0731563485463,-5.21891713299337,
128.016738957181));
#177548=CARTESIAN_POINT('Ctrl Pts',(10.0801692651992,-5.14900133623913,
127.885844311493));
#177549=CARTESIAN_POINT('Ctrl Pts',(10.0871821818521,-5.07423647615101,
127.75772757786));
#177550=CARTESIAN_POINT('Ctrl Pts',(10.0941950985049,-4.99487698837381,
127.632746764413));
#177551=CARTESIAN_POINT('Ctrl Pts',(10.1016183649104,-4.9108739053874,127.500452895869));
#177552=CARTESIAN_POINT('Ctrl Pts',(10.1090416313157,-4.82148428427923,
127.371298636164));
#177553=CARTESIAN_POINT('Ctrl Pts',(10.1164648977212,-4.72696969736647,
127.245753018704));
#177554=CARTESIAN_POINT('Ctrl Pts',(10.1238793904422,-4.63256681884621,
127.120355785738));
#177555=CARTESIAN_POINT('Ctrl Pts',(10.1312938831632,-4.53305125390469,
126.998559000602));
#177556=CARTESIAN_POINT('Ctrl Pts',(10.1387083758842,-4.4287292556656,126.880805119996));
#177557=CARTESIAN_POINT('Ctrl Pts',(10.146115722238,-4.32450780689622,126.763164735014));
#177558=CARTESIAN_POINT('Ctrl Pts',(10.1535230685917,-4.21548939334842,
126.649559774533));
#177559=CARTESIAN_POINT('Ctrl Pts',(10.1609304149455,-4.10202208518554,
126.54040173231));
#177560=CARTESIAN_POINT('Ctrl Pts',(10.1683322366209,-3.98863940522165,
126.431325104274));
#177561=CARTESIAN_POINT('Ctrl Pts',(10.1757340582964,-3.87081470539658,
126.32668904823));
#177562=CARTESIAN_POINT('Ctrl Pts',(10.1831358799718,-3.74893457379556,
126.226870025123));
#177563=CARTESIAN_POINT('Ctrl Pts',(10.1905337942832,-3.62711878176765,
126.127103695702));
#177564=CARTESIAN_POINT('Ctrl Pts',(10.1979317085945,-3.50125210960173,
126.032149570891));
#177565=CARTESIAN_POINT('Ctrl Pts',(10.2053296229059,-3.3717559639555,125.942345368512));
#177566=CARTESIAN_POINT('Ctrl Pts',(10.2127263078181,-3.24228133821939,
125.852556089963));
#177567=CARTESIAN_POINT('Ctrl Pts',(10.2201229927302,-3.10917874253501,
125.767915247813));
#177568=CARTESIAN_POINT('Ctrl Pts',(10.2275196776424,-2.97290053909443,
125.688718629785));
#177569=CARTESIAN_POINT('Ctrl Pts',(10.2349160345779,-2.8366283783722,125.609525523417));
#177570=CARTESIAN_POINT('Ctrl Pts',(10.2423123915133,-2.69718121262551,
125.535776348748));
#177571=CARTESIAN_POINT('Ctrl Pts',(10.2497087484487,-2.55503786806384,
125.467721969947));
#177572=CARTESIAN_POINT('Ctrl Pts',(10.2571062377853,-2.41287276099325,
125.399657171847));
#177573=CARTESIAN_POINT('Ctrl Pts',(10.2645037271219,-2.26801098990349,
125.337289066872));
#177574=CARTESIAN_POINT('Ctrl Pts',(10.2719012164585,-2.12095316831205,
125.280821152664));
#177575=CARTESIAN_POINT('Ctrl Pts',(10.2793012989735,-1.97384379582901,
125.224333443716));
#177576=CARTESIAN_POINT('Ctrl Pts',(10.2867013814885,-1.82453718840631,
125.173750177241));
#177577=CARTESIAN_POINT('Ctrl Pts',(10.2941014640035,-1.67355084199639,
125.129225540605));
#177578=CARTESIAN_POINT('Ctrl Pts',(10.30150968367,-1.52239847057702,125.084651944553));
#177579=CARTESIAN_POINT('Ctrl Pts',(10.3089179033365,-1.36956302977261,
125.046150388616));
#177580=CARTESIAN_POINT('Ctrl Pts',(10.3163261230029,-1.21557469687477,
125.013824483596));
#177581=CARTESIAN_POINT('Ctrl Pts',(10.323738902305,-1.06149158672746,124.98147868252));
#177582=CARTESIAN_POINT('Ctrl Pts',(10.331151681607,-0.90625453780127,124.955316168244));
#177583=CARTESIAN_POINT('Ctrl Pts',(10.3385644609091,-0.7504001348975,124.935388799603));
#177584=CARTESIAN_POINT('Ctrl Pts',(10.3459878319378,-0.59432303991357,
124.915432957802));
#177585=CARTESIAN_POINT('Ctrl Pts',(10.3534112029666,-0.437627200085401,
124.901730087478));
#177586=CARTESIAN_POINT('Ctrl Pts',(10.3608345739954,-0.280851326824123,
124.894279984045));
#177587=CARTESIAN_POINT('Ctrl Pts',(10.3647706234362,-0.197724997035228,
124.890329760442));
#177588=CARTESIAN_POINT('Ctrl Pts',(10.368706672877,-0.114576129541411,
124.888136543532));
#177589=CARTESIAN_POINT('Ctrl Pts',(10.3726427223178,-0.0314844594406813,
124.887694386375));
#177590=CARTESIAN_POINT('Ctrl Pts',(10.3800659887232,0.125223837166229,
124.886860491777));
#177591=CARTESIAN_POINT('Ctrl Pts',(10.3874892551287,0.28220224736707,124.892255479522));
#177592=CARTESIAN_POINT('Ctrl Pts',(10.3949125215341,0.438914773846293,
124.903912805425));
#177593=CARTESIAN_POINT('Ctrl Pts',(10.4023270142551,0.595442079133384,
124.915556353337));
#177594=CARTESIAN_POINT('Ctrl Pts',(10.4097415069761,0.751703757586047,
124.933447479131));
#177595=CARTESIAN_POINT('Ctrl Pts',(10.4171559996971,0.907162020557403,
124.957567682036));
#177596=CARTESIAN_POINT('Ctrl Pts',(10.4245633460509,1.06247044700223,124.981664636982));
#177597=CARTESIAN_POINT('Ctrl Pts',(10.4319706924046,1.2169766331604,125.011978659766));
#177598=CARTESIAN_POINT('Ctrl Pts',(10.4393780387584,1.37014623725376,125.04843933153));
#177599=CARTESIAN_POINT('Ctrl Pts',(10.4467798604338,1.52320160167784,125.08487280955));
#177600=CARTESIAN_POINT('Ctrl Pts',(10.4541816821093,1.67492200735845,125.127443722312));
#177601=CARTESIAN_POINT('Ctrl Pts',(10.4615835037847,1.82478176673787,125.176030308648));
#177602=CARTESIAN_POINT('Ctrl Pts',(10.4689814180961,1.97456241631661,125.224591246504));
#177603=CARTESIAN_POINT('Ctrl Pts',(10.4763793324075,2.1224840215316,125.279161418682));
#177604=CARTESIAN_POINT('Ctrl Pts',(10.4837772467188,2.26803467022076,125.339568828561));
#177605=CARTESIAN_POINT('Ctrl Pts',(10.491173931631,2.41356113103246,125.399966199824));
#177606=CARTESIAN_POINT('Ctrl Pts',(10.4985706165432,2.55671707286601,125.466198740585));
#177607=CARTESIAN_POINT('Ctrl Pts',(10.5059673014554,2.69700912831771,125.538045746209));
#177608=CARTESIAN_POINT('Ctrl Pts',(10.5133636583908,2.83729496307266,125.609889566063));
#177609=CARTESIAN_POINT('Ctrl Pts',(10.5207600153262,2.97471683167974,125.687347185622));
#177610=CARTESIAN_POINT('Ctrl Pts',(10.5281563722617,3.10880485774485,125.770151353048));
#177611=CARTESIAN_POINT('Ctrl Pts',(10.5355538615983,3.24291341302963,125.852968198003));
#177612=CARTESIAN_POINT('Ctrl Pts',(10.542951350935,3.37368679182139,125.941133024556));
#177613=CARTESIAN_POINT('Ctrl Pts',(10.5503488402716,3.5006831919568,126.03433464782));
#177614=CARTESIAN_POINT('Ctrl Pts',(10.5577489227866,3.62772411048287,126.127568942768));
#177615=CARTESIAN_POINT('Ctrl Pts',(10.5651490053016,3.75098511348906,126.225843329081));
#177616=CARTESIAN_POINT('Ctrl Pts',(10.5725490878166,3.87005675957541,126.328805764795));
#177617=CARTESIAN_POINT('Ctrl Pts',(10.579957307483,3.9892593371775,126.431881418291));
#177618=CARTESIAN_POINT('Ctrl Pts',(10.5873655271494,4.10426307557628,126.539655171727));
#177619=CARTESIAN_POINT('Ctrl Pts',(10.5947737468159,4.21469423029261,126.651736976103));
#177620=CARTESIAN_POINT('Ctrl Pts',(10.602186526118,4.32519335354219,126.763887764959));
#177621=CARTESIAN_POINT('Ctrl Pts',(10.60959930542,4.43111403458347,126.880351612742));
#177622=CARTESIAN_POINT('Ctrl Pts',(10.6170120847221,4.53212260591901,127.000705106427));
#177623=CARTESIAN_POINT('Ctrl Pts',(10.6244354557508,4.6332755030381,127.121230566828));
#177624=CARTESIAN_POINT('Ctrl Pts',(10.6318588267796,4.72950204486285,127.245656478611));
#177625=CARTESIAN_POINT('Ctrl Pts',(10.6392821978083,4.8205112168404,127.373529498024));
#177626=CARTESIAN_POINT('Ctrl Pts',(10.6432182472491,4.86876646355787,127.441330841188));
#177627=CARTESIAN_POINT('Ctrl Pts',(10.64715429669,4.91555567296337,127.510100850996));
#177628=CARTESIAN_POINT('Ctrl Pts',(10.6510903461308,4.96084074961768,127.579769229586));
#177629=CARTESIAN_POINT('Ctrl Pts',(10.6585136125362,5.04624699088922,127.711161617332));
#177630=CARTESIAN_POINT('Ctrl Pts',(10.6659368789416,5.12655870002981,127.84614812235));
#177631=CARTESIAN_POINT('Ctrl Pts',(10.6733601453471,5.20145801007354,127.984295878603));
#177632=CARTESIAN_POINT('Ctrl Pts',(10.6807746380681,5.2762687953528,128.122280355681));
#177633=CARTESIAN_POINT('Ctrl Pts',(10.6881891307891,5.34567973862619,128.263418321831));
#177634=CARTESIAN_POINT('Ctrl Pts',(10.6956036235102,5.40941571721768,128.407247320115));
#177635=CARTESIAN_POINT('Ctrl Pts',(10.7030109698639,5.47309026467339,128.550937690595));
#177636=CARTESIAN_POINT('Ctrl Pts',(10.7104183162176,5.5311005864092,128.697313590628));
#177637=CARTESIAN_POINT('Ctrl Pts',(10.7178256625714,5.58321710302218,128.84588740023));
#177638=CARTESIAN_POINT('Ctrl Pts',(10.7252274842468,5.63529474917068,128.99435039788));
#177639=CARTESIAN_POINT('Ctrl Pts',(10.7326293059222,5.68148721984,129.145007690324));
#177640=CARTESIAN_POINT('Ctrl Pts',(10.7400311275976,5.72161280918421,129.297351186846));
#177641=CARTESIAN_POINT('Ctrl Pts',(10.747429041909,5.76171721654226,129.449614262423));
#177642=CARTESIAN_POINT('Ctrl Pts',(10.7548269562203,5.79576102598574,129.603561409261));
#177643=CARTESIAN_POINT('Ctrl Pts',(10.7622248705317,5.82361224211681,129.758668972784));
#177644=CARTESIAN_POINT('Ctrl Pts',(10.7696215554439,5.85145882988107,129.913750760244));
#177645=CARTESIAN_POINT('Ctrl Pts',(10.7770182403562,5.87311480087535,130.069992214597));
#177646=CARTESIAN_POINT('Ctrl Pts',(10.7844149252684,5.88849916302601,130.226858955627));
#177647=CARTESIAN_POINT('Ctrl Pts',(10.7918112822038,5.90388284301787,130.383718741021));
#177648=CARTESIAN_POINT('Ctrl Pts',(10.7992076391392,5.91299543066692,130.541203386449));
#177649=CARTESIAN_POINT('Ctrl Pts',(10.8066039960746,5.91580779284587,130.698773115445));
#177650=CARTESIAN_POINT('Ctrl Pts',(10.8140014854112,5.91862058560467,130.856366968771));
#177651=CARTESIAN_POINT('Ctrl Pts',(10.8213989747479,5.9151312256229,131.01404555834));
#177652=CARTESIAN_POINT('Ctrl Pts',(10.8287964640845,5.90536271669626,131.171268980449));
#177653=CARTESIAN_POINT('Ctrl Pts',(10.8361965465995,5.89559078343395,131.328547516986));
#177654=CARTESIAN_POINT('Ctrl Pts',(10.8435966291146,5.87953534189579,131.485370196036));
#177655=CARTESIAN_POINT('Ctrl Pts',(10.8509967116296,5.85727126187853,131.641202255674));
#177656=CARTESIAN_POINT('Ctrl Pts',(10.8584049312961,5.83498270021658,131.797205668681));
#177657=CARTESIAN_POINT('Ctrl Pts',(10.8658131509625,5.80647191886609,131.952215917124));
#177658=CARTESIAN_POINT('Ctrl Pts',(10.873221370629,5.77186505907829,132.105707728175));
#177659=CARTESIAN_POINT('Ctrl Pts',(10.8806341499311,5.7372368993457,132.259294010875));
#177660=CARTESIAN_POINT('Ctrl Pts',(10.8880469292331,5.69650528113772,132.411359634179));
#177661=CARTESIAN_POINT('Ctrl Pts',(10.8954597085352,5.64984607839031,132.56139500909));
#177662=CARTESIAN_POINT('Ctrl Pts',(10.902883079564,5.60312020678591,132.71164476158));
#177663=CARTESIAN_POINT('Ctrl Pts',(10.9103064505928,5.55044995959825,132.859858121085));
#177664=CARTESIAN_POINT('Ctrl Pts',(10.9177298216216,5.49205944728994,133.005545205449));
#177665=CARTESIAN_POINT('Ctrl Pts',(10.9216658710623,5.46109939660376,133.08279199329));
#177666=CARTESIAN_POINT('Ctrl Pts',(10.9256019205029,5.42853195025858,133.159328950403));
#177667=CARTESIAN_POINT('Ctrl Pts',(10.9295379699436,5.39439566032155,133.235086028303));
#177668=CARTESIAN_POINT('Ctrl Pts',(10.936961236349,5.33001568285598,133.377961512929));
#177669=CARTESIAN_POINT('Ctrl Pts',(10.9443845027544,5.25985815368121,133.518493531566));
#177670=CARTESIAN_POINT('Ctrl Pts',(10.9518077691599,5.18411544039399,133.656180679065));
#177671=CARTESIAN_POINT('Ctrl Pts',(10.9592222618809,5.10846224870362,133.793705091791));
#177672=CARTESIAN_POINT('Ctrl Pts',(10.966636754602,5.02723719084237,133.928391002378));
#177673=CARTESIAN_POINT('Ctrl Pts',(10.974051247323,4.94068063440387,134.059756973054));
#177674=CARTESIAN_POINT('Ctrl Pts',(10.9814585936767,4.85420750443351,134.190996328262));
#177675=CARTESIAN_POINT('Ctrl Pts',(10.9888659400305,4.76241331003379,134.318921804274));
#177676=CARTESIAN_POINT('Ctrl Pts',(10.9962732863842,4.66558420643275,134.443076678924));
#177677=CARTESIAN_POINT('Ctrl Pts',(11.0036751080596,4.56882732163019,134.567138954184));
#177678=CARTESIAN_POINT('Ctrl Pts',(11.011076929735,4.46704323337127,134.687435934572));
#177679=CARTESIAN_POINT('Ctrl Pts',(11.0184787514104,4.36056119631744,134.803540110371));
#177680=CARTESIAN_POINT('Ctrl Pts',(11.0258766657218,4.25413537030136,134.919582995679));
#177681=CARTESIAN_POINT('Ctrl Pts',(11.0332745800332,4.14301678622663,135.03143720997));
#177682=CARTESIAN_POINT('Ctrl Pts',(11.0406724943446,4.02757466278196,135.138708653686));
#177683=CARTESIAN_POINT('Ctrl Pts',(11.0480691792568,3.9121517237247,135.245962270834));
#177684=CARTESIAN_POINT('Ctrl Pts',(11.0554658641691,3.79240694448886,135.348634375047));
#177685=CARTESIAN_POINT('Ctrl Pts',(11.0628625490813,3.6687461360898,135.446367979842));
#177686=CARTESIAN_POINT('Ctrl Pts',(11.0702589060167,3.54509081094057,135.544097251027));
#177687=CARTESIAN_POINT('Ctrl Pts',(11.0776552629521,3.41752009475671,135.636888226728));
#177688=CARTESIAN_POINT('Ctrl Pts',(11.0850516198875,3.28647236959852,135.724424634057));
#177689=CARTESIAN_POINT('Ctrl Pts',(11.0924491092241,3.15540458069868,135.811974443433));
#177690=CARTESIAN_POINT('Ctrl Pts',(11.0998465985608,3.02085903330203,135.894267875232));
#177691=CARTESIAN_POINT('Ctrl Pts',(11.1072440878974,2.88330239779886,135.971032452059));
#177692=CARTESIAN_POINT('Ctrl Pts',(11.1146441704124,2.74569754202996,136.04782393859));
#177693=CARTESIAN_POINT('Ctrl Pts',(11.1220442529274,2.60507982236836,136.119082529544));
#177694=CARTESIAN_POINT('Ctrl Pts',(11.1294443354424,2.46193961812188,136.184582163118));
#177695=CARTESIAN_POINT('Ctrl Pts',(11.1368525551089,2.31864201650667,136.250153820272));
#177696=CARTESIAN_POINT('Ctrl Pts',(11.1442607747753,2.17281673063916,136.309953718074));
#177697=CARTESIAN_POINT('Ctrl Pts',(11.1516689944418,2.02497386985343,136.363804059936));
#177698=CARTESIAN_POINT('Ctrl Pts',(11.1590817737438,1.87704001425334,136.417687545785));
#177699=CARTESIAN_POINT('Ctrl Pts',(11.166494553046,1.72708646407916,136.465614065613));
#177700=CARTESIAN_POINT('Ctrl Pts',(11.173907332348,1.57563701514503,136.507456141841));
#177701=CARTESIAN_POINT('Ctrl Pts',(11.1813307033768,1.42397116813621,136.54935800399));
#177702=CARTESIAN_POINT('Ctrl Pts',(11.1887540744055,1.27080551601733,136.585157974457));
#177703=CARTESIAN_POINT('Ctrl Pts',(11.1961774454342,1.11667334769981,136.61477981045));
#177704=CARTESIAN_POINT('Ctrl Pts',(11.200113494875,1.03494877370778,136.63048601866));
#177705=CARTESIAN_POINT('Ctrl Pts',(11.2040495443158,0.952952563794645,
136.64445619853));
#177706=CARTESIAN_POINT('Ctrl Pts',(11.2079855937565,0.870764490067564,
136.656684922091));
#177707=CARTESIAN_POINT('Ctrl Pts',(11.215408860162,0.71576034801899,136.679747913082));
#177708=CARTESIAN_POINT('Ctrl Pts',(11.2228321265674,0.559604922454607,
136.696683385581));
#177709=CARTESIAN_POINT('Ctrl Pts',(11.2302553929728,0.402824039110081,
136.707382162166));
#177710=CARTESIAN_POINT('Ctrl Pts',(11.2376698856938,0.246228457749604,
136.718068293686));
#177711=CARTESIAN_POINT('Ctrl Pts',(11.2450843784149,0.0890092588634893,
136.722532376653));
#177712=CARTESIAN_POINT('Ctrl Pts',(11.2524988711359,-0.0682985857609222,
136.720716410255));
#177713=CARTESIAN_POINT('Ctrl Pts',(11.2599062174897,-0.225454811162149,
136.718902194154));
#177714=CARTESIAN_POINT('Ctrl Pts',(11.2673135638434,-0.382699141440079,
136.710819983197));
#177715=CARTESIAN_POINT('Ctrl Pts',(11.2747209101972,-0.53949264941082,
136.696463658394));
#177716=CARTESIAN_POINT('Ctrl Pts',(11.2821227318726,-0.696169214867613,
136.68211804108));
#177717=CARTESIAN_POINT('Ctrl Pts',(11.2895245535481,-0.852395257374062,
136.661507661269));
#177718=CARTESIAN_POINT('Ctrl Pts',(11.2969263752234,-1.00763313071025,
136.634678450789));
#177719=CARTESIAN_POINT('Ctrl Pts',(11.3043242895348,-1.16278905518213,
136.60786340324));
#177720=CARTESIAN_POINT('Ctrl Pts',(11.3117222038461,-1.31695748245476,
136.574836126431));
#177721=CARTESIAN_POINT('Ctrl Pts',(11.3191201181575,-1.46960727369043,
136.535694234065));
#177722=CARTESIAN_POINT('Ctrl Pts',(11.3265168030697,-1.6222316972995,136.496558846373));
#177723=CARTESIAN_POINT('Ctrl Pts',(11.333913487982,-1.77333762450528,136.451310952486));
#177724=CARTESIAN_POINT('Ctrl Pts',(11.3413101728942,-1.92240536170159,
136.400099012792));
#177725=CARTESIAN_POINT('Ctrl Pts',(11.3487065298296,-2.07146648907822,
136.348889343888));
#177726=CARTESIAN_POINT('Ctrl Pts',(11.356102886765,-2.21848925309794,136.291716276284));
#177727=CARTESIAN_POINT('Ctrl Pts',(11.3634992437005,-2.36297060821013,
136.228777680001));
#177728=CARTESIAN_POINT('Ctrl Pts',(11.3708967330371,-2.50747408378725,
136.165829447658));
#177729=CARTESIAN_POINT('Ctrl Pts',(11.3782942223737,-2.64943503345679,
136.097114078121));
#177730=CARTESIAN_POINT('Ctrl Pts',(11.3856917117103,-2.78837196752447,
136.02287691372));
#177731=CARTESIAN_POINT('Ctrl Pts',(11.3930917942253,-2.927357605719,135.948613725596));
#177732=CARTESIAN_POINT('Ctrl Pts',(11.4004918767404,-3.0633167886923,135.868825064542));
#177733=CARTESIAN_POINT('Ctrl Pts',(11.4078919592554,-3.19579426225298,
135.783801308633));
#177734=CARTESIAN_POINT('Ctrl Pts',(11.4153001789218,-3.32841740841409,
135.698684060363));
#177735=CARTESIAN_POINT('Ctrl Pts',(11.4227083985882,-3.45755088504768,
135.608320422832));
#177736=CARTESIAN_POINT('Ctrl Pts',(11.4301166182547,-3.58276938029463,
135.51304346207));
#177737=CARTESIAN_POINT('Ctrl Pts',(11.4375293975567,-3.70806494543602,
135.417707859928));
#177738=CARTESIAN_POINT('Ctrl Pts',(11.4449421768588,-3.82944044060424,
135.317453145898));
#177739=CARTESIAN_POINT('Ctrl Pts',(11.4523549561609,-3.94650549087129,
135.21265109949));
#177740=CARTESIAN_POINT('Ctrl Pts',(11.4597783271896,-4.06373780917214,
135.107699307003));
#177741=CARTESIAN_POINT('Ctrl Pts',(11.4672016982183,-4.17664711448327,
134.998187464499));
#177742=CARTESIAN_POINT('Ctrl Pts',(11.474625069247,-4.28488100590149,134.884523031952));
#177743=CARTESIAN_POINT('Ctrl Pts',(11.4785611186878,-4.34226921216777,
134.824255422475));
#177744=CARTESIAN_POINT('Ctrl Pts',(11.4824971681286,-4.39834367447588,
134.762820912282));
#177745=CARTESIAN_POINT('Ctrl Pts',(11.4864332175694,-4.45305670734803,
134.700283681956));
#177746=CARTESIAN_POINT('Ctrl Pts',(11.4937956702431,-4.55539843887839,
134.583306645577));
#177747=CARTESIAN_POINT('Ctrl Pts',(11.5011581229168,-4.65329686455237,
134.462100747582));
#177748=CARTESIAN_POINT('Ctrl Pts',(11.5085205755906,-4.74637765054397,
134.337040869289));
#177749=CARTESIAN_POINT('Ctrl Pts',(11.5159415852658,-4.8401987512058,134.210986331771));
#177750=CARTESIAN_POINT('Ctrl Pts',(11.523362594941,-4.92912493136729,134.081016476417));
#177751=CARTESIAN_POINT('Ctrl Pts',(11.5307836046162,-5.01281050267483,
133.947553488959));
#177752=CARTESIAN_POINT('Ctrl Pts',(11.5381280065076,-5.09563217992484,
133.815468252527));
#177753=CARTESIAN_POINT('Ctrl Pts',(11.5454724083989,-5.1733207042299,133.679961977886));
#177754=CARTESIAN_POINT('Ctrl Pts',(11.5528168102903,-5.24558146672041,
133.541476917342));
#177755=CARTESIAN_POINT('Ctrl Pts',(11.5601561603024,-5.3177925243272,133.403087114356));
#177756=CARTESIAN_POINT('Ctrl Pts',(11.5674955103146,-5.38458307413891,
133.261722937933));
#177757=CARTESIAN_POINT('Ctrl Pts',(11.5748348603267,-5.44570279726505,
133.117853994768));
#177758=CARTESIAN_POINT('Ctrl Pts',(11.5821706709072,-5.50679304515347,
132.974054432993));
#177759=CARTESIAN_POINT('Ctrl Pts',(11.5895064814877,-5.56221776140611,
132.827752857696));
#177760=CARTESIAN_POINT('Ctrl Pts',(11.5968422920681,-5.61177352462589,
132.679441541368));
#177761=CARTESIAN_POINT('Ctrl Pts',(11.6043241683788,-5.66231600889853,
132.528177149784));
#177762=CARTESIAN_POINT('Ctrl Pts',(11.6118060446894,-5.70675318012188,
132.374822504533));
#177763=CARTESIAN_POINT('Ctrl Pts',(11.619287921,-5.74492160186354,132.21991928853));
#177764=CARTESIAN_POINT('Ctrl Pts',(11.6266225812379,-5.78233900809533,
132.068064003577));
#177765=CARTESIAN_POINT('Ctrl Pts',(11.6339572414757,-5.8137320057929,131.914720911414));
#177766=CARTESIAN_POINT('Ctrl Pts',(11.6412919017136,-5.83899770548043,
131.760413104564));
#177767=CARTESIAN_POINT('Ctrl Pts',(11.6488473860606,-5.86502407784319,
131.601459563231));
#177768=CARTESIAN_POINT('Ctrl Pts',(11.6564028704076,-5.88454831827244,
131.44148272438));
#177769=CARTESIAN_POINT('Ctrl Pts',(11.6639583547546,-5.8975152635197,131.28106207451));
#177770=CARTESIAN_POINT('Ctrl Pts',(11.6715138391016,-5.91048220876697,
131.120641424639));
#177771=CARTESIAN_POINT('Ctrl Pts',(11.6790693234486,-5.9168918570892,130.959777403725));
#177772=CARTESIAN_POINT('Ctrl Pts',(11.6866248077956,-5.91674761742372,
130.799050795463));
#177773=CARTESIAN_POINT('',(13.4366248077956,-5.9221125045945,130.804501180565));
#177774=CARTESIAN_POINT('Ctrl Pts',(11.6866260347045,-5.91391045748492,
130.799027254254));
#177775=CARTESIAN_POINT('Ctrl Pts',(11.7127109702638,-5.91868981499976,
130.244388001879));
#177776=CARTESIAN_POINT('Ctrl Pts',(11.8316117804274,-5.59228796829895,
127.72174242367));
#177777=CARTESIAN_POINT('Ctrl Pts',(12.0433284651951,-2.00181416161862,
124.098370713555));
#177778=CARTESIAN_POINT('Ctrl Pts',(12.3217760890081,4.55990977836376,125.495426323045));
#177779=CARTESIAN_POINT('Ctrl Pts',(12.600223712821,6.93129939600614,131.771133193343));
#177780=CARTESIAN_POINT('Ctrl Pts',(12.8786713366339,2.93316348151725,137.158423295966));
#177781=CARTESIAN_POINT('Ctrl Pts',(13.1571189604468,-3.76040637948188,
136.706640210358));
#177782=CARTESIAN_POINT('Ctrl Pts',(13.343103450834,-5.92313498158111,132.782070348646));
#177783=CARTESIAN_POINT('Ctrl Pts',(13.436272066617,-5.92653126023725,130.811960232984));
#177784=CARTESIAN_POINT('Ctrl Pts',(13.4366248077956,-5.92652866437588,
130.804501285384));
#177785=CARTESIAN_POINT('',(15.186624792037,-5.91464336866557,130.809600954502));
#177786=CARTESIAN_POINT('Ctrl Pts',(13.4366248077956,-5.91674999833336,
130.804501053285));
#177787=CARTESIAN_POINT('Ctrl Pts',(13.4440429936624,-5.9167537153653,130.647897384805));
#177788=CARTESIAN_POINT('Ctrl Pts',(13.4514611795291,-5.91053569384905,
130.491055185319));
#177789=CARTESIAN_POINT('Ctrl Pts',(13.4588793653959,-5.89806501653408,
130.334509978281));
#177790=CARTESIAN_POINT('Ctrl Pts',(13.4662887814253,-5.8856090821513,130.17814984021));
#177791=CARTESIAN_POINT('Ctrl Pts',(13.4736981974548,-5.86691523469698,
130.022086364759));
#177792=CARTESIAN_POINT('Ctrl Pts',(13.4811076134842,-5.84200452152495,
129.866856626651));
#177793=CARTESIAN_POINT('Ctrl Pts',(13.4885098919879,-5.81711780496167,
129.711776422089));
#177794=CARTESIAN_POINT('Ctrl Pts',(13.4959121704916,-5.78602620363372,
129.557528722674));
#177795=CARTESIAN_POINT('Ctrl Pts',(13.5033144489953,-5.7488026662856,129.404646908764));
#177796=CARTESIAN_POINT('Ctrl Pts',(13.5107112166218,-5.71160684126162,
129.251878912903));
#177797=CARTESIAN_POINT('Ctrl Pts',(13.5181079842483,-5.66828825786702,
129.100475139549));
#177798=CARTESIAN_POINT('Ctrl Pts',(13.5255047518748,-5.61897116429073,
128.95096006254));
#177799=CARTESIAN_POINT('Ctrl Pts',(13.5328976308802,-5.56967999764619,
128.801523588445));
#177800=CARTESIAN_POINT('Ctrl Pts',(13.5402905098857,-5.51439671792575,
128.653974187445));
#177801=CARTESIAN_POINT('Ctrl Pts',(13.5476833888911,-5.45329573856649,
128.508822303742));
#177802=CARTESIAN_POINT('Ctrl Pts',(13.5550750649302,-5.39220470153485,
128.363694039098));
#177803=CARTESIAN_POINT('Ctrl Pts',(13.5624667409693,-5.32529798838409,
128.220962861824));
#177804=CARTESIAN_POINT('Ctrl Pts',(13.5698584170083,-5.25279862348526,
128.081120418169));
#177805=CARTESIAN_POINT('Ctrl Pts',(13.5772497912476,-5.18030221871185,
127.941283684235));
#177806=CARTESIAN_POINT('Ctrl Pts',(13.5846411654869,-5.10221378826202,
127.804335781348));
#177807=CARTESIAN_POINT('Ctrl Pts',(13.5920325397262,-5.01880277670205,
127.670744615075));
#177808=CARTESIAN_POINT('Ctrl Pts',(13.5994250770067,-4.9353786403247,127.53713242808));
#177809=CARTESIAN_POINT('Ctrl Pts',(13.6068176142871,-4.84663045333017,
127.406878346496));
#177810=CARTESIAN_POINT('Ctrl Pts',(13.6142101515676,-4.75287143714511,
127.28042195969));
#177811=CARTESIAN_POINT('Ctrl Pts',(13.6216053171532,-4.65907908635613,
127.153920613224));
#177812=CARTESIAN_POINT('Ctrl Pts',(13.6290004827387,-4.56027258201902,
127.031219949844));
#177813=CARTESIAN_POINT('Ctrl Pts',(13.6363956483242,-4.4568058175647,126.912726967411));
#177814=CARTESIAN_POINT('Ctrl Pts',(13.6437989522555,-4.35322518841236,
126.794103583996));
#177815=CARTESIAN_POINT('Ctrl Pts',(13.6512022561868,-4.24497430347026,
126.67969741039));
#177816=CARTESIAN_POINT('Ctrl Pts',(13.658605560118,-4.13244484685284,126.569879521821));
#177817=CARTESIAN_POINT('Ctrl Pts',(13.6660134637275,-4.01984547560077,
126.459993403317));
#177818=CARTESIAN_POINT('Ctrl Pts',(13.673421367337,-3.90296251305144,126.354701499595));
#177819=CARTESIAN_POINT('Ctrl Pts',(13.6808292709464,-3.78222076458437,
126.254334612097));
#177820=CARTESIAN_POINT('Ctrl Pts',(13.6882476815014,-3.66130776294873,
126.153825369964));
#177821=CARTESIAN_POINT('Ctrl Pts',(13.6956660920563,-3.53652534116423,
126.058255321024));
#177822=CARTESIAN_POINT('Ctrl Pts',(13.7030845026112,-3.40832794592024,
125.967912419192));
#177823=CARTESIAN_POINT('Ctrl Pts',(13.706727737765,-3.34536927660466,125.923544365764));
#177824=CARTESIAN_POINT('Ctrl Pts',(13.7103709729188,-3.28158735658004,
125.88043633549));
#177825=CARTESIAN_POINT('Ctrl Pts',(13.7140142080725,-3.21703809881979,
125.838618333351));
#177826=CARTESIAN_POINT('Ctrl Pts',(13.721437474478,-3.08551588946378,125.753412147826));
#177827=CARTESIAN_POINT('Ctrl Pts',(13.7288607408834,-2.95040732000841,
125.673305958167));
#177828=CARTESIAN_POINT('Ctrl Pts',(13.7362840072888,-2.81214573972864,
125.598616972223));
#177829=CARTESIAN_POINT('Ctrl Pts',(13.7436985000098,-2.67404757315466,
125.524016262459));
#177830=CARTESIAN_POINT('Ctrl Pts',(13.7511129927308,-2.53280413880009,
125.45482018752));
#177831=CARTESIAN_POINT('Ctrl Pts',(13.7585274854519,-2.38887831175831,
125.391303165986));
#177832=CARTESIAN_POINT('Ctrl Pts',(13.7659348318056,-2.24509120584755,
125.327847364547));
#177833=CARTESIAN_POINT('Ctrl Pts',(13.7733421781595,-2.09862719348059,
125.270059869189));
#177834=CARTESIAN_POINT('Ctrl Pts',(13.7807495245132,-1.94997424345807,
125.218169516972));
#177835=CARTESIAN_POINT('Ctrl Pts',(13.7881513461886,-1.80143216441404,
125.166317866538));
#177836=CARTESIAN_POINT('Ctrl Pts',(13.795553167864,-1.65070474935151,125.120354724112));
#177837=CARTESIAN_POINT('Ctrl Pts',(13.8029549895394,-1.49830036492387,
125.080461022101));
#177838=CARTESIAN_POINT('Ctrl Pts',(13.8103529038507,-1.34597643358468,
125.040588379664));
#177839=CARTESIAN_POINT('Ctrl Pts',(13.8177508181621,-1.19197765613274,
125.006778890994));
#177840=CARTESIAN_POINT('Ctrl Pts',(13.8251487324734,-1.03682788741214,
124.979163754422));
#177841=CARTESIAN_POINT('Ctrl Pts',(13.8325454173856,-0.881703901768178,
124.951553206984));
#177842=CARTESIAN_POINT('Ctrl Pts',(13.8399421022978,-0.725429671639387,
124.930135033964));
#177843=CARTESIAN_POINT('Ctrl Pts',(13.84733878721,-0.568539699878368,124.914989414104));
#177844=CARTESIAN_POINT('Ctrl Pts',(13.8547351441455,-0.411656684782658,
124.899844465818));
#177845=CARTESIAN_POINT('Ctrl Pts',(13.8621315010809,-0.254158353911757,
124.890971553542));
#177846=CARTESIAN_POINT('Ctrl Pts',(13.8695278580164,-0.0965845274411798,
124.888398988924));
#177847=CARTESIAN_POINT('Ctrl Pts',(13.8769253473529,0.061013423984047,
124.88582603044));
#177848=CARTESIAN_POINT('Ctrl Pts',(13.8843228366896,0.218686520751447,
124.889555346353));
#177849=CARTESIAN_POINT('Ctrl Pts',(13.8917203260261,0.375894894790388,
124.899563111252));
#177850=CARTESIAN_POINT('Ctrl Pts',(13.8991204085411,0.533158377980696,
124.909574384358));
#177851=CARTESIAN_POINT('Ctrl Pts',(13.906520491056,0.689956441782852,124.925868464725));
#177852=CARTESIAN_POINT('Ctrl Pts',(13.913920573571,0.845754438828811,124.948369668828));
#177853=CARTESIAN_POINT('Ctrl Pts',(13.9213287932375,1.00172375178961,124.970895615318));
#177854=CARTESIAN_POINT('Ctrl Pts',(13.928737012904,1.15669043217741,124.999642262864));
#177855=CARTESIAN_POINT('Ctrl Pts',(13.9361452325704,1.3101293997381,125.034482670985));
#177856=CARTESIAN_POINT('Ctrl Pts',(13.9435580118725,1.46366280642284,125.069344522796));
#177857=CARTESIAN_POINT('Ctrl Pts',(13.9509707911745,1.61566626704777,125.110307511829));
#177858=CARTESIAN_POINT('Ctrl Pts',(13.9583835704766,1.76563046085579,125.157194988846));
#177859=CARTESIAN_POINT('Ctrl Pts',(13.9658069415053,1.91580893053656,125.204149460888));
#177860=CARTESIAN_POINT('Ctrl Pts',(13.973230312534,2.06394196326246,125.257045202587));
#177861=CARTESIAN_POINT('Ctrl Pts',(13.9806536835628,2.20954001850263,125.315657358222));
#177862=CARTESIAN_POINT('Ctrl Pts',(13.9845897330036,2.28673960096969,125.346734929519));
#177863=CARTESIAN_POINT('Ctrl Pts',(13.9885257824445,2.36322690734754,125.379418814373));
#177864=CARTESIAN_POINT('Ctrl Pts',(13.9924618318854,2.43893194790328,125.413670354158));
#177865=CARTESIAN_POINT('Ctrl Pts',(13.9998850982908,2.58170929171549,125.478267689239));
#177866=CARTESIAN_POINT('Ctrl Pts',(14.0073083646962,2.72213437980149,125.548639002982));
#177867=CARTESIAN_POINT('Ctrl Pts',(14.0147316311016,2.85970610034554,125.62459116496));
#177868=CARTESIAN_POINT('Ctrl Pts',(14.0221461238226,2.99711522254071,125.700453557791));
#177869=CARTESIAN_POINT('Ctrl Pts',(14.0295606165437,3.131677366452,125.781883490623));
#177870=CARTESIAN_POINT('Ctrl Pts',(14.0369751092647,3.26291146066457,125.868639863475));
#177871=CARTESIAN_POINT('Ctrl Pts',(14.0443824556184,3.39401906651588,125.955312617269));
#177872=CARTESIAN_POINT('Ctrl Pts',(14.0517898019722,3.52180469925431,126.04730138617));
#177873=CARTESIAN_POINT('Ctrl Pts',(14.0591971483259,3.64581207272215,126.144319320228));
#177874=CARTESIAN_POINT('Ctrl Pts',(14.0665989700013,3.76972695681267,126.241264894652));
#177875=CARTESIAN_POINT('Ctrl Pts',(14.0740007916767,3.88986889984315,126.343231936572));
#177876=CARTESIAN_POINT('Ctrl Pts',(14.0814026133521,4.00581089366082,126.449890541113));
#177877=CARTESIAN_POINT('Ctrl Pts',(14.0888005276634,4.12169168260212,126.556492841406));
#177878=CARTESIAN_POINT('Ctrl Pts',(14.0961984419748,4.23337666379677,126.667781519879));
#177879=CARTESIAN_POINT('Ctrl Pts',(14.1035963562861,4.34047230003337,126.783386758519));
#177880=CARTESIAN_POINT('Ctrl Pts',(14.1109930411983,4.44755013891845,126.898972785665));
#177881=CARTESIAN_POINT('Ctrl Pts',(14.1183897261105,4.55003989306975,127.018873675703));
#177882=CARTESIAN_POINT('Ctrl Pts',(14.1257864110227,4.64758519399128,127.142683074814));
#177883=CARTESIAN_POINT('Ctrl Pts',(14.1331827679581,4.74512616965181,127.266486984086));
#177884=CARTESIAN_POINT('Ctrl Pts',(14.1405791248936,4.8377228969889,127.394198764614));
#177885=CARTESIAN_POINT('Ctrl Pts',(14.147975481829,4.92505977062255,127.525379553532));
#177886=CARTESIAN_POINT('Ctrl Pts',(14.1553729711656,5.01241001575426,127.656580426562));
#177887=CARTESIAN_POINT('Ctrl Pts',(14.1627704605021,5.09449859683924,127.791251054751));
#177888=CARTESIAN_POINT('Ctrl Pts',(14.1701679498386,5.17105374699097,127.928924353583));
#177889=CARTESIAN_POINT('Ctrl Pts',(14.1775680323536,5.24763573343257,128.066645913577));
#177890=CARTESIAN_POINT('Ctrl Pts',(14.1849681148686,5.31868024563838,128.20737191385));
#177891=CARTESIAN_POINT('Ctrl Pts',(14.1923681973836,5.38396196834096,128.350611631635));
#177892=CARTESIAN_POINT('Ctrl Pts',(14.1997764170501,5.44931547500848,128.494008856214));
#177893=CARTESIAN_POINT('Ctrl Pts',(14.2071846367166,5.50889338230191,128.639924978483));
#177894=CARTESIAN_POINT('Ctrl Pts',(14.2145928563831,5.5625186701399,128.787849619122));
#177895=CARTESIAN_POINT('Ctrl Pts',(14.2220056356851,5.61617696344769,128.935865304909));
#177896=CARTESIAN_POINT('Ctrl Pts',(14.2294184149872,5.66387522400035,129.085891617444));
#177897=CARTESIAN_POINT('Ctrl Pts',(14.2368311942892,5.70548677149639,129.237404567519));
#177898=CARTESIAN_POINT('Ctrl Pts',(14.244254565318,5.74715777552295,129.389134006402));
#177899=CARTESIAN_POINT('Ctrl Pts',(14.2516779363467,5.7827246124855,129.542353962618));
#177900=CARTESIAN_POINT('Ctrl Pts',(14.2591013073754,5.8121118512552,129.696531031845));
#177901=CARTESIAN_POINT('Ctrl Pts',(14.2630373568164,5.82769367038867,129.77827941338));
#177902=CARTESIAN_POINT('Ctrl Pts',(14.2669734062573,5.84153904980948,129.860296788583));
#177903=CARTESIAN_POINT('Ctrl Pts',(14.2709094556983,5.85364268295297,129.942503377177));
#177904=CARTESIAN_POINT('Ctrl Pts',(14.2783327221038,5.87646975731931,130.09754243768));
#177905=CARTESIAN_POINT('Ctrl Pts',(14.2857559885092,5.89316756823212,130.253723455326));
#177906=CARTESIAN_POINT('Ctrl Pts',(14.2931792549146,5.90362773861287,130.410520438838));
#177907=CARTESIAN_POINT('Ctrl Pts',(14.3005937476357,5.9140755459409,130.567132101337));
#177908=CARTESIAN_POINT('Ctrl Pts',(14.3080082403568,5.9183003628808,130.72435791174));
#177909=CARTESIAN_POINT('Ctrl Pts',(14.3154227330778,5.91624500282486,130.881662810613));
#177910=CARTESIAN_POINT('Ctrl Pts',(14.3228300794316,5.91419162380233,131.038816093102));
#177911=CARTESIAN_POINT('Ctrl Pts',(14.3302374257853,5.9058701231011,131.196047941545));
#177912=CARTESIAN_POINT('Ctrl Pts',(14.3376447721391,5.89127520189453,131.352819420069));
#177913=CARTESIAN_POINT('Ctrl Pts',(14.3450465938145,5.8766911661309,131.509473972509));
#177914=CARTESIAN_POINT('Ctrl Pts',(14.3524484154899,5.85584306074447,131.665668468618));
#177915=CARTESIAN_POINT('Ctrl Pts',(14.3598502371653,5.82877763571499,131.8208653327));
#177916=CARTESIAN_POINT('Ctrl Pts',(14.3672481514766,5.80172649831251,131.975980269566));
#177917=CARTESIAN_POINT('Ctrl Pts',(14.374646065788,5.76846464164647,132.130098256421));
#177918=CARTESIAN_POINT('Ctrl Pts',(14.3820439800994,5.72909048761005,132.282688303594));
#177919=CARTESIAN_POINT('Ctrl Pts',(14.3894406650116,5.68972287684377,132.435252993069));
#177920=CARTESIAN_POINT('Ctrl Pts',(14.3968373499239,5.64424507785501,132.586289885705));
#177921=CARTESIAN_POINT('Ctrl Pts',(14.4042340348361,5.59280634174263,132.735279514429));
#177922=CARTESIAN_POINT('Ctrl Pts',(14.4116303917716,5.54136988647778,132.884262536797));
#177923=CARTESIAN_POINT('Ctrl Pts',(14.419026748707,5.48397314146012,133.031198122891));
#177924=CARTESIAN_POINT('Ctrl Pts',(14.4264231056425,5.42081474203117,133.175583528867));
#177925=CARTESIAN_POINT('Ctrl Pts',(14.4338205949791,5.35764667288985,133.319991040617));
#177926=CARTESIAN_POINT('Ctrl Pts',(14.4412180843157,5.28871534252514,133.461847252803));
#177927=CARTESIAN_POINT('Ctrl Pts',(14.4486155736523,5.21426682572683,133.600671049658));
#177928=CARTESIAN_POINT('Ctrl Pts',(14.4560156561673,5.13979221111637,133.739543510979));
#177929=CARTESIAN_POINT('Ctrl Pts',(14.4634157386823,5.05979673572452,133.875381111754));
#177930=CARTESIAN_POINT('Ctrl Pts',(14.4708158211974,4.97457147010795,134.007729040225));
#177931=CARTESIAN_POINT('Ctrl Pts',(14.4782240408639,4.88925249055057,134.140222498849));
#177932=CARTESIAN_POINT('Ctrl Pts',(14.4856322605304,4.79869243848905,134.269218307875));
#177933=CARTESIAN_POINT('Ctrl Pts',(14.4930404801969,4.70322502682163,134.394291662806));
#177934=CARTESIAN_POINT('Ctrl Pts',(14.5004532594989,4.60769885655543,134.5194419983));
#177935=CARTESIAN_POINT('Ctrl Pts',(14.507866038801,4.5072595457769,134.64066478231));
#177936=CARTESIAN_POINT('Ctrl Pts',(14.5152788181031,4.40227946764858,134.757570206143));
#177937=CARTESIAN_POINT('Ctrl Pts',(14.5227021891319,4.29714938906111,134.87464266993));
#177938=CARTESIAN_POINT('Ctrl Pts',(14.5301255601606,4.18746584462711,134.987385186112));
#177939=CARTESIAN_POINT('Ctrl Pts',(14.5375489311894,4.07363683014216,135.09544597428));
#177940=CARTESIAN_POINT('Ctrl Pts',(14.54148498063,4.01328195537579,135.152742397047));
#177941=CARTESIAN_POINT('Ctrl Pts',(14.5454210300707,3.95176218053971,135.208723301553));
#177942=CARTESIAN_POINT('Ctrl Pts',(14.5493570795113,3.88914175871114,135.263341100047));
#177943=CARTESIAN_POINT('Ctrl Pts',(14.5567803459167,3.77104159745337,135.366348563449));
#177944=CARTESIAN_POINT('Ctrl Pts',(14.564203612322,3.64866765869746,135.464816559647));
#177945=CARTESIAN_POINT('Ctrl Pts',(14.5716268787275,3.52240389334273,135.558369596803));
#177946=CARTESIAN_POINT('Ctrl Pts',(14.5790413714485,3.39628936127274,135.651812062038));
#177947=CARTESIAN_POINT('Ctrl Pts',(14.5864558641695,3.26629445086713,135.740350911159));
#177948=CARTESIAN_POINT('Ctrl Pts',(14.5938703568906,3.13283841202407,135.82364881876));
#177949=CARTESIAN_POINT('Ctrl Pts',(14.6012777032443,2.99951100313579,135.906866440701));
#177950=CARTESIAN_POINT('Ctrl Pts',(14.6086850495981,2.862729421611,135.984852981169));
#177951=CARTESIAN_POINT('Ctrl Pts',(14.6160923959519,2.72294422531694,136.057312674106));
#177952=CARTESIAN_POINT('Ctrl Pts',(14.6234942176273,2.58326328609667,136.129718323871));
#177953=CARTESIAN_POINT('Ctrl Pts',(14.6308960393026,2.44058352265737,136.19660516277));
#177954=CARTESIAN_POINT('Ctrl Pts',(14.638297860978,2.29538248216377,136.257721950091));
#177955=CARTESIAN_POINT('Ctrl Pts',(14.6456957752894,2.15025809216776,136.318806474335));
#177956=CARTESIAN_POINT('Ctrl Pts',(14.6530936896008,2.00261541898403,136.374126868734));
#177957=CARTESIAN_POINT('Ctrl Pts',(14.6604916039122,1.85295439869872,136.423478925525));
#177958=CARTESIAN_POINT('Ctrl Pts',(14.6678882888244,1.70331824936092,136.4728227809));
#177959=CARTESIAN_POINT('Ctrl Pts',(14.6752849737366,1.55166477278916,136.516200150363));
#177960=CARTESIAN_POINT('Ctrl Pts',(14.6826816586488,1.3985116852086,136.553455818451));
#177961=CARTESIAN_POINT('Ctrl Pts',(14.6900780155843,1.24536538859666,136.590709834583));
#177962=CARTESIAN_POINT('Ctrl Pts',(14.6974743725197,1.09071997590906,136.621842600824));
#177963=CARTESIAN_POINT('Ctrl Pts',(14.7048707294551,0.935105787033889,
136.646749489385));
#177964=CARTESIAN_POINT('Ctrl Pts',(14.7122682187917,0.779467773228917,
136.671660191255));
#177965=CARTESIAN_POINT('Ctrl Pts',(14.7196657081283,0.62286105653735,136.690343058499));
#177966=CARTESIAN_POINT('Ctrl Pts',(14.7270631974649,0.465823422714856,
136.702745065985));
#177967=CARTESIAN_POINT('Ctrl Pts',(14.7344632799798,0.30873073959416,136.715151420975));
#177968=CARTESIAN_POINT('Ctrl Pts',(14.7418633624948,0.151207210495546,
136.721272503175));
#177969=CARTESIAN_POINT('Ctrl Pts',(14.7492634450097,-0.00620718782220476,
136.721107361624));
#177970=CARTESIAN_POINT('Ctrl Pts',(14.7566716646762,-0.163794679454623,
136.720942038482));
#177971=CARTESIAN_POINT('Ctrl Pts',(14.7640798843426,-0.321272427130523,
136.714476687566));
#177972=CARTESIAN_POINT('Ctrl Pts',(14.7714881040091,-0.478102650822751,
136.70176245378));
#177973=CARTESIAN_POINT('Ctrl Pts',(14.7789008833112,-0.635029400900809,
136.689040394595));
#177974=CARTESIAN_POINT('Ctrl Pts',(14.7863136626133,-0.791307463137764,
136.670061833636));
#177975=CARTESIAN_POINT('Ctrl Pts',(14.7937264419153,-0.946407603652012,
136.644929357873));
#177976=CARTESIAN_POINT('Ctrl Pts',(14.8011498129441,-1.10172935852028,
136.61976097165));
#177977=CARTESIAN_POINT('Ctrl Pts',(14.8085731839728,-1.25586946535376,
136.588421183204));
#177978=CARTESIAN_POINT('Ctrl Pts',(14.8159965550016,-1.40831142963687,
136.55106310505));
#177979=CARTESIAN_POINT('Ctrl Pts',(14.8199326044424,-1.48913981689591,
136.531254955617));
#177980=CARTESIAN_POINT('Ctrl Pts',(14.8238686538833,-1.56949107832643,
136.509755673011));
#177981=CARTESIAN_POINT('Ctrl Pts',(14.8278047033241,-1.64929044664833,
136.486593592823));
#177982=CARTESIAN_POINT('Ctrl Pts',(14.8352279697296,-1.7997895648476,136.442910632452));
#177983=CARTESIAN_POINT('Ctrl Pts',(14.842651236135,-1.94877958185454,136.393178329126));
#177984=CARTESIAN_POINT('Ctrl Pts',(14.8500745025404,-2.09573705091141,
136.3375167491));
#177985=CARTESIAN_POINT('Ctrl Pts',(14.8574889952614,-2.24252082844392,
136.28192095644));
#177986=CARTESIAN_POINT('Ctrl Pts',(14.8649034879824,-2.38727649413616,
136.2204099673));
#177987=CARTESIAN_POINT('Ctrl Pts',(14.8723179807034,-2.52949363175903,
136.153154175873));
#177988=CARTESIAN_POINT('Ctrl Pts',(14.8797253270571,-2.67157369515048,
136.08596320811));
#177989=CARTESIAN_POINT('Ctrl Pts',(14.8871326734108,-2.81111976622904,
136.013038619768));
#177990=CARTESIAN_POINT('Ctrl Pts',(14.8945400197646,-2.94763947110261,
135.934599609163));
#177991=CARTESIAN_POINT('Ctrl Pts',(14.90194184144,-3.08405735442892,135.856219101331));
#177992=CARTESIAN_POINT('Ctrl Pts',(14.9093436631153,-3.21745304361395,
135.772332545676));
#177993=CARTESIAN_POINT('Ctrl Pts',(14.9167454847906,-3.34735703682289,
135.68320591441));
#177994=CARTESIAN_POINT('Ctrl Pts',(14.9241433991019,-3.4771924547259,135.594126332397));
#177995=CARTESIAN_POINT('Ctrl Pts',(14.9315413134133,-3.60353954051628,
135.499812394439));
#177996=CARTESIAN_POINT('Ctrl Pts',(14.9389392277246,-3.72595626075486,
135.40057433164));
#177997=CARTESIAN_POINT('Ctrl Pts',(14.9463359126368,-3.84835263755524,
135.301352760407));
#177998=CARTESIAN_POINT('Ctrl Pts',(14.9537325975491,-3.96681965542502,
135.197208923264));
#177999=CARTESIAN_POINT('Ctrl Pts',(14.9611292824613,-4.08094688893181,
135.088494491784));
#178000=CARTESIAN_POINT('Ctrl Pts',(14.9685256393967,-4.1950690619173,134.979784880815));
#178001=CARTESIAN_POINT('Ctrl Pts',(14.9759219963321,-4.30485156286373,
134.866505335949));
#178002=CARTESIAN_POINT('Ctrl Pts',(14.9833183532675,-4.40991970378503,
134.749045493278));
#178003=CARTESIAN_POINT('Ctrl Pts',(14.9907158426041,-4.51500393090708,
134.631567667204));
#178004=CARTESIAN_POINT('Ctrl Pts',(14.9981133319406,-4.61537211194998,
134.50990854722));
#178005=CARTESIAN_POINT('Ctrl Pts',(15.0055108212772,-4.71068894902936,
134.38449192633));
#178006=CARTESIAN_POINT('Ctrl Pts',(15.0129109037922,-4.80603919927794,
134.259031340839));
#178007=CARTESIAN_POINT('Ctrl Pts',(15.0203109863071,-4.89633435429538,
134.129810928955));
#178008=CARTESIAN_POINT('Ctrl Pts',(15.027711068822,-4.98128174338273,133.9972844744));
#178009=CARTESIAN_POINT('Ctrl Pts',(15.0351192884885,-5.06632254085743,
133.864612293385));
#178010=CARTESIAN_POINT('Ctrl Pts',(15.042527508155,-5.14600362724973,133.728627124168));
#178011=CARTESIAN_POINT('Ctrl Pts',(15.0499357278214,-5.22007734897655,
133.58980906139));
#178012=CARTESIAN_POINT('Ctrl Pts',(15.0573485071235,-5.29419666184331,
133.45090555841));
#178013=CARTESIAN_POINT('Ctrl Pts',(15.0647612864255,-5.36270157095136,
133.30916602285));
#178014=CARTESIAN_POINT('Ctrl Pts',(15.0721740657276,-5.4253923217827,133.165091164927));
#178015=CARTESIAN_POINT('Ctrl Pts',(15.0795974367563,-5.48817264809856,
133.02081044609));
#178016=CARTESIAN_POINT('Ctrl Pts',(15.0870208077851,-5.54512208931563,
132.874188087565));
#178017=CARTESIAN_POINT('Ctrl Pts',(15.0944441788138,-5.596090285426,132.725741391869));
#178018=CARTESIAN_POINT('Ctrl Pts',(15.0983802282549,-5.62311484597069,
132.647031391876));
#178019=CARTESIAN_POINT('Ctrl Pts',(15.1023162776959,-5.64845871011584,
132.567808712566));
#178020=CARTESIAN_POINT('Ctrl Pts',(15.1062523271369,-5.67210530385628,
132.488151573851));
#178021=CARTESIAN_POINT('Ctrl Pts',(15.1154352247266,-5.72727337324023,
132.302309561938));
#178022=CARTESIAN_POINT('Ctrl Pts',(15.1246181223163,-5.77333541830667,
132.113648895864));
#178023=CARTESIAN_POINT('Ctrl Pts',(15.1338010199059,-5.81004723006746,
131.922967674081));
#178024=CARTESIAN_POINT('Ctrl Pts',(15.1428586604398,-5.84625828339016,
131.734887392601));
#178025=CARTESIAN_POINT('Ctrl Pts',(15.1519163009736,-5.87337244800413,
131.544841256533));
#178026=CARTESIAN_POINT('Ctrl Pts',(15.1609739415075,-5.89120098166726,
131.353616073709));
#178027=CARTESIAN_POINT('Ctrl Pts',(15.1695242154695,-5.90803084443243,
131.173102429403));
#178028=CARTESIAN_POINT('Ctrl Pts',(15.1780744894315,-5.91658646534607,
130.991538235456));
#178029=CARTESIAN_POINT('Ctrl Pts',(15.1866247633935,-5.91674767718177,
130.80960342827));
#178030=CARTESIAN_POINT('',(16.9366248077956,-5.90780204387767,130.802025653359));
#178031=CARTESIAN_POINT('Ctrl Pts',(15.1866248077956,-5.91348565267583,
130.809599593522));
#178032=CARTESIAN_POINT('Ctrl Pts',(15.2526498555137,-5.9016025138533,129.405465492393));
#178033=CARTESIAN_POINT('Ctrl Pts',(15.4114907778362,-4.69782533091822,
126.00913283962));
#178034=CARTESIAN_POINT('Ctrl Pts',(15.6631475747628,0.977319714034647,
123.874540511177));
#178035=CARTESIAN_POINT('Ctrl Pts',(15.9415951985758,6.35851909600637,127.880870334347));
#178036=CARTESIAN_POINT('Ctrl Pts',(16.2200428223884,5.89655005967416,134.57374490735));
#178037=CARTESIAN_POINT('Ctrl Pts',(16.4984904462014,0.0159395809900309,
137.802739462705));
#178038=CARTESIAN_POINT('Ctrl Pts',(16.7373511080038,-5.04118839832629,
135.055819514375));
#178039=CARTESIAN_POINT('Ctrl Pts',(16.8833958952019,-5.90379043459487,
131.936768349731));
#178040=CARTESIAN_POINT('Ctrl Pts',(16.9366248077956,-5.90780204387767,
130.802025653359));
#178041=CARTESIAN_POINT('',(18.6866248077956,-5.92206989474538,130.799941417168));
#178042=CARTESIAN_POINT('Ctrl Pts',(16.9366248077956,-5.90780204387767,
130.802025653359));
#178043=CARTESIAN_POINT('Ctrl Pts',(16.9762117698061,-5.91078552440622,
129.958104298891));
#178044=CARTESIAN_POINT('Ctrl Pts',(17.1086146064211,-5.34658274166464,
127.139324596949));
#178045=CARTESIAN_POINT('Ctrl Pts',(17.33383331764,-1.00887627239691,123.879064291967));
#178046=CARTESIAN_POINT('Ctrl Pts',(17.6122809414531,5.28112566490743,126.212272612985));
#178047=CARTESIAN_POINT('Ctrl Pts',(17.8907285652659,6.7180311134912,132.765385474242));
#178048=CARTESIAN_POINT('Ctrl Pts',(18.1691761890789,1.98139416284149,137.516412293604));
#178049=CARTESIAN_POINT('Ctrl Pts',(18.4344749365886,-4.26639119716458,
136.166306194459));
#178050=CARTESIAN_POINT('Ctrl Pts',(18.6069578094943,-5.90800757224012,
132.487901526767));
#178051=CARTESIAN_POINT('Ctrl Pts',(18.6866248077956,-5.92206989474538,
130.799941417168));
#178052=CARTESIAN_POINT('',(20.4366248077956,-5.92198869469903,130.808811111152));
#178053=CARTESIAN_POINT('Ctrl Pts',(18.6866248077956,-5.92206989474538,
130.799941417168));
#178054=CARTESIAN_POINT('Ctrl Pts',(18.6997736840986,-5.92439085252084,
130.521347028541));
#178055=CARTESIAN_POINT('Ctrl Pts',(18.8057384350059,-5.7797270106078,128.27862052501));
#178056=CARTESIAN_POINT('Ctrl Pts',(19.0045190605175,-2.91381031421446,
124.441399830078));
#178057=CARTESIAN_POINT('Ctrl Pts',(19.2829666843302,3.77835347032134,124.913553747223));
#178058=CARTESIAN_POINT('Ctrl Pts',(19.5614143081434,6.99839499846111,130.799071396303));
#178059=CARTESIAN_POINT('Ctrl Pts',(19.839861931956,3.78725341361693,136.689449581327));
#178060=CARTESIAN_POINT('Ctrl Pts',(20.1183095557691,-2.9041890407256,137.171718511235));
#178061=CARTESIAN_POINT('Ctrl Pts',(20.3172305143822,-5.7779299637371,133.336128281175));
#178062=CARTESIAN_POINT('Ctrl Pts',(20.423335598391,-5.92434601569743,131.090388889328));
#178063=CARTESIAN_POINT('Ctrl Pts',(20.4366248077956,-5.92198869469903,
130.808811111152));
#178064=CARTESIAN_POINT('',(22.1866248077956,-5.90776713110451,130.806650508727));
#178065=CARTESIAN_POINT('Ctrl Pts',(20.4366248077956,-5.92198869469903,
130.808811111152));
#178066=CARTESIAN_POINT('Ctrl Pts',(20.5161514729953,-5.90788176989252,
129.123764167348));
#178067=CARTESIAN_POINT('Ctrl Pts',(20.6884940127994,-4.27118742048918,
125.448150887193));
#178068=CARTESIAN_POINT('Ctrl Pts',(20.9536524272077,1.97124628558328,124.089321629448));
#178069=CARTESIAN_POINT('Ctrl Pts',(21.2321000510206,6.71505924821413,128.8331833492));
#178070=CARTESIAN_POINT('Ctrl Pts',(21.5105476748335,5.28806081061698,135.388460681217));
#178071=CARTESIAN_POINT('Ctrl Pts',(21.7889952986464,-0.99840717580492,
137.731174000475));
#178072=CARTESIAN_POINT('Ctrl Pts',(22.0143543429672,-5.34374262142005,
134.475446717348));
#178073=CARTESIAN_POINT('Ctrl Pts',(22.1468975126835,-5.9107024042326,131.653576004858));
#178074=CARTESIAN_POINT('Ctrl Pts',(22.1866248077956,-5.90776713110451,
130.806650508727));
#178075=CARTESIAN_POINT('',(23.9366248230411,-5.91468528336671,130.799105832252));
#178076=CARTESIAN_POINT('Ctrl Pts',(22.1866248077956,-5.90776713110451,
130.806650508727));
#178077=CARTESIAN_POINT('Ctrl Pts',(22.2397133872878,-5.90384465210482,
129.674882755639));
#178078=CARTESIAN_POINT('Ctrl Pts',(22.3856178413844,-5.04464026757503,
126.558908262004));
#178079=CARTESIAN_POINT('Ctrl Pts',(22.6243381700852,0.00536115071223864,
123.805965673837));
#178080=CARTESIAN_POINT('Ctrl Pts',(22.9027857938979,5.89084570391381,127.026067693108));
#178081=CARTESIAN_POINT('Ctrl Pts',(23.1812334177107,6.36293083903494,133.718236330083));
#178082=CARTESIAN_POINT('Ctrl Pts',(23.4596810415237,0.987793379532795,
137.732695537999));
#178083=CARTESIAN_POINT('Ctrl Pts',(23.7114781715519,-4.69373819460421,
135.605498381351));
#178084=CARTESIAN_POINT('Ctrl Pts',(23.8704594269759,-5.90161551527517,
132.206175144537));
#178085=CARTESIAN_POINT('Ctrl Pts',(23.9366248077956,-5.91356949928869,
130.799107147868));
#178086=CARTESIAN_POINT('',(25.6866248077955,-5.92211383359681,130.804275968097));
#178087=CARTESIAN_POINT('Ctrl Pts',(23.9366248512203,-5.91674766439881,
130.799103400509));
#178088=CARTESIAN_POINT('Ctrl Pts',(23.9456716507033,-5.91657663065078,
130.606613054719));
#178089=CARTESIAN_POINT('Ctrl Pts',(23.9547184501863,-5.90700848198333,
130.414538242424));
#178090=CARTESIAN_POINT('Ctrl Pts',(23.9637652496693,-5.88818678512448,
130.22368261214));
#178091=CARTESIAN_POINT('Ctrl Pts',(23.9729451091623,-5.86908825940729,
130.030019883928));
#178092=CARTESIAN_POINT('Ctrl Pts',(23.9821249686552,-5.84046202858799,
129.837612422055));
#178093=CARTESIAN_POINT('Ctrl Pts',(23.9913048281483,-5.80250701712613,
129.647276835508));
#178094=CARTESIAN_POINT('Ctrl Pts',(23.999728648482,-5.76767792224026,129.472616996169));
#178095=CARTESIAN_POINT('Ctrl Pts',(24.0081524688158,-5.72499397722651,
129.299701495139));
#178096=CARTESIAN_POINT('Ctrl Pts',(24.0165762891496,-5.6746439613045,129.129145265759));
#178097=CARTESIAN_POINT('Ctrl Pts',(24.023999555555,-5.63027435619705,128.97884714951));
#178098=CARTESIAN_POINT('Ctrl Pts',(24.0314228219604,-5.57986236094382,
128.83008573685));
#178099=CARTESIAN_POINT('Ctrl Pts',(24.0388460883658,-5.52353043033182,
128.683383920924));
#178100=CARTESIAN_POINT('Ctrl Pts',(24.0462605810868,-5.46726507938364,
128.536855494361));
#178101=CARTESIAN_POINT('Ctrl Pts',(24.0536750738078,-5.40509385289825,
128.392382164185));
#178102=CARTESIAN_POINT('Ctrl Pts',(24.0610895665288,-5.33718947358348,
128.250473563374));
#178103=CARTESIAN_POINT('Ctrl Pts',(24.0684969128826,-5.26935054306615,
128.108701739416));
#178104=CARTESIAN_POINT('Ctrl Pts',(24.0759042592364,-5.19578962060363,
127.969490058064));
#178105=CARTESIAN_POINT('Ctrl Pts',(24.0833116055901,-5.11672815014872,
127.833329887335));
#178106=CARTESIAN_POINT('Ctrl Pts',(24.0907134272655,-5.03772564672119,
127.697271269999));
#178107=CARTESIAN_POINT('Ctrl Pts',(24.0981152489409,-4.95323095060532,
127.564259953031));
#178108=CARTESIAN_POINT('Ctrl Pts',(24.1055170706163,-4.86351217474033,
127.434764219086));
#178109=CARTESIAN_POINT('Ctrl Pts',(24.1129149849276,-4.77384076071849,
127.305336844929));
#178110=CARTESIAN_POINT('Ctrl Pts',(24.120312899239,-4.67895097119628,127.179421663853));
#178111=CARTESIAN_POINT('Ctrl Pts',(24.1277108135503,-4.57915505213842,
127.057459288337));
#178112=CARTESIAN_POINT('Ctrl Pts',(24.1351074984625,-4.47937571735225,
126.935517180756));
#178113=CARTESIAN_POINT('Ctrl Pts',(24.1425041833746,-4.37469210734596,
126.817526863637));
#178114=CARTESIAN_POINT('Ctrl Pts',(24.1499008682868,-4.26545776381407,
126.703897152588));
#178115=CARTESIAN_POINT('Ctrl Pts',(24.1572972252222,-4.15622826384744,
126.590272479999));
#178116=CARTESIAN_POINT('Ctrl Pts',(24.1646935821577,-4.04244869027558,
126.481008298142));
#178117=CARTESIAN_POINT('Ctrl Pts',(24.1720899390931,-3.92451038575863,
126.376477512224));
#178118=CARTESIAN_POINT('Ctrl Pts',(24.1794874284297,-3.80655402458584,
126.271930722375));
#178119=CARTESIAN_POINT('Ctrl Pts',(24.1868849177662,-3.68443794406968,
126.17211901905));
#178120=CARTESIAN_POINT('Ctrl Pts',(24.1942824071028,-3.55858746359443,
126.07737576182));
#178121=CARTESIAN_POINT('Ctrl Pts',(24.2016824896177,-3.4326928664287,125.982599292489));
#178122=CARTESIAN_POINT('Ctrl Pts',(24.2090825721327,-3.30306156096661,
125.892895031101));
#178123=CARTESIAN_POINT('Ctrl Pts',(24.2164826546477,-3.17014866238169,
125.808553573564));
#178124=CARTESIAN_POINT('Ctrl Pts',(24.2238908743141,-3.03708961240101,
125.724119373924));
#178125=CARTESIAN_POINT('Ctrl Pts',(24.2312990939805,-2.90074207837538,
125.645059954875));
#178126=CARTESIAN_POINT('Ctrl Pts',(24.238707313647,-2.76158728059598,125.571620775557));
#178127=CARTESIAN_POINT('Ctrl Pts',(24.246120092949,-2.62234683536006,125.498136395649));
#178128=CARTESIAN_POINT('Ctrl Pts',(24.2535328722511,-2.48029601952231,
125.430279308824));
#178129=CARTESIAN_POINT('Ctrl Pts',(24.2609456515532,-2.33593645005443,
125.368246981538));
#178130=CARTESIAN_POINT('Ctrl Pts',(24.2683690225819,-2.19137061286431,
125.306126019554));
#178131=CARTESIAN_POINT('Ctrl Pts',(24.2757923936106,-2.04448978115152,
125.249846572598));
#178132=CARTESIAN_POINT('Ctrl Pts',(24.2832157646394,-1.895811938507,125.19955663738));
#178133=CARTESIAN_POINT('Ctrl Pts',(24.2871518140804,-1.81697937885602,
125.172891707034));
#178134=CARTESIAN_POINT('Ctrl Pts',(24.2910878635214,-1.73764181840951,
125.147909796198));
#178135=CARTESIAN_POINT('Ctrl Pts',(24.2950239129624,-1.65787755193035,
125.124627121591));
#178136=CARTESIAN_POINT('Ctrl Pts',(24.3024471793678,-1.50744463471726,
125.080716723912));
#178137=CARTESIAN_POINT('Ctrl Pts',(24.3098704457732,-1.3550385302888,125.042720586018));
#178138=CARTESIAN_POINT('Ctrl Pts',(24.3172937121787,-1.20116535325871,
125.010818319746));
#178139=CARTESIAN_POINT('Ctrl Pts',(24.3247082048997,-1.04747404154529,
124.978953759303));
#178140=CARTESIAN_POINT('Ctrl Pts',(24.3321226976207,-0.892319470638296,
124.953168809008));
#178141=CARTESIAN_POINT('Ctrl Pts',(24.3395371903417,-0.736223770039259,
124.933593621429));
#178142=CARTESIAN_POINT('Ctrl Pts',(24.3469445366954,-0.580278520353359,
124.914037301153));
#178143=CARTESIAN_POINT('Ctrl Pts',(24.3543518830492,-0.423394314735643,
124.900678874369));
#178144=CARTESIAN_POINT('Ctrl Pts',(24.361759229403,-0.266104250879958,
124.893597630424));
#178145=CARTESIAN_POINT('Ctrl Pts',(24.3691610510784,-0.108931499888111,
124.886521667938));
#178146=CARTESIAN_POINT('Ctrl Pts',(24.3765628727537,0.0486461353012634,
124.885713582992));
#178147=CARTESIAN_POINT('Ctrl Pts',(24.3839646944291,0.206089753637759,
124.891200922788));
#178148=CARTESIAN_POINT('Ctrl Pts',(24.3913626087405,0.363450258713448,
124.89668536586));
#178149=CARTESIAN_POINT('Ctrl Pts',(24.3987605230519,0.520676515704192,
124.908458602183));
#178150=CARTESIAN_POINT('Ctrl Pts',(24.4061584373632,0.677229048280863,
124.926496092191));
#178151=CARTESIAN_POINT('Ctrl Pts',(24.4135551222754,0.833755564666995,
124.944530584695));
#178152=CARTESIAN_POINT('Ctrl Pts',(24.4209518071876,0.98960820836661,124.968827222111));
#178153=CARTESIAN_POINT('Ctrl Pts',(24.4283484920998,1.1442519333095,124.99930953462));
#178154=CARTESIAN_POINT('Ctrl Pts',(24.4357448490353,1.29888880118756,125.029790495511));
#178155=CARTESIAN_POINT('Ctrl Pts',(24.4431412059707,1.4523164906429,125.066456513942));
#178156=CARTESIAN_POINT('Ctrl Pts',(24.4505375629061,1.60400973569663,125.109179906624));
#178157=CARTESIAN_POINT('Ctrl Pts',(24.4579350522427,1.75572620537343,125.151909840366));
#178158=CARTESIAN_POINT('Ctrl Pts',(24.4653325415793,1.90570734256569,125.200698893727));
#178159=CARTESIAN_POINT('Ctrl Pts',(24.4727300309159,2.05344278690677,125.255369422457));
#178160=CARTESIAN_POINT('Ctrl Pts',(24.4801301134309,2.20123001967885,125.310059115855));
#178161=CARTESIAN_POINT('Ctrl Pts',(24.4875301959458,2.34676964236528,125.370634260061));
#178162=CARTESIAN_POINT('Ctrl Pts',(24.4949302784608,2.48957116752841,125.436869027977));
#178163=CARTESIAN_POINT('Ctrl Pts',(24.5023384981273,2.63252971764881,125.503176627829));
#178164=CARTESIAN_POINT('Ctrl Pts',(24.5097467177938,2.77274381858923,125.575156122638));
#178165=CARTESIAN_POINT('Ctrl Pts',(24.5171549374602,2.90974684729997,125.652535324805));
#178166=CARTESIAN_POINT('Ctrl Pts',(24.5245677167623,3.04683419908907,125.729962152581));
#178167=CARTESIAN_POINT('Ctrl Pts',(24.5319804960644,3.18070622379183,125.812795114103));
#178168=CARTESIAN_POINT('Ctrl Pts',(24.5393932753664,3.3109256510603,125.900718920251));
#178169=CARTESIAN_POINT('Ctrl Pts',(24.5468166463952,3.44133114195296,125.988768356055));
#178170=CARTESIAN_POINT('Ctrl Pts',(24.5542400174239,3.56807331189845,126.081922943875));
#178171=CARTESIAN_POINT('Ctrl Pts',(24.5616633884526,3.69074766429063,126.179826885282));
#178172=CARTESIAN_POINT('Ctrl Pts',(24.5655994378935,3.75579254946112,126.23173790419));
#178173=CARTESIAN_POINT('Ctrl Pts',(24.5695354873344,3.81969442791911,126.284983507724));
#178174=CARTESIAN_POINT('Ctrl Pts',(24.5734715367753,3.88239733584584,126.339506589816));
#178175=CARTESIAN_POINT('Ctrl Pts',(24.5808948031808,4.00065306330287,126.442335421033));
#178176=CARTESIAN_POINT('Ctrl Pts',(24.5883180695862,4.11499951238944,126.550021152415));
#178177=CARTESIAN_POINT('Ctrl Pts',(24.5957413359917,4.22501200326998,126.66223505999));
#178178=CARTESIAN_POINT('Ctrl Pts',(24.6031558287127,4.33489446852228,126.774316340045));
#178179=CARTESIAN_POINT('Ctrl Pts',(24.6105703214338,4.44045291290973,126.890914879288));
#178180=CARTESIAN_POINT('Ctrl Pts',(24.6179848141548,4.5412956116416,127.011661746025));
#178181=CARTESIAN_POINT('Ctrl Pts',(24.6253921605086,4.64204111438377,127.132292232387));
#178182=CARTESIAN_POINT('Ctrl Pts',(24.6327995068624,4.73807968241352,127.257062801791));
#178183=CARTESIAN_POINT('Ctrl Pts',(24.6402068532162,4.82905645503334,127.385567801878));
#178184=CARTESIAN_POINT('Ctrl Pts',(24.6476086748916,4.91996537374391,127.513976958088));
#178185=CARTESIAN_POINT('Ctrl Pts',(24.655010496567,5.0058197993633,127.646114695752));
#178186=CARTESIAN_POINT('Ctrl Pts',(24.6624123182425,5.08630526646846,127.78154251209));
#178187=CARTESIAN_POINT('Ctrl Pts',(24.6698102325539,5.16674824592203,127.916898837137));
#178188=CARTESIAN_POINT('Ctrl Pts',(24.6772081468652,5.24182772113697,128.055541461833));
#178189=CARTESIAN_POINT('Ctrl Pts',(24.6846060611766,5.31127273781135,128.197003245229));
#178190=CARTESIAN_POINT('Ctrl Pts',(24.6920027460888,5.38070621398372,128.338441520242));
#178191=CARTESIAN_POINT('Ctrl Pts',(24.6993994310011,5.44450692564126,128.482697689365));
#178192=CARTESIAN_POINT('Ctrl Pts',(24.7067961159133,5.50245000353816,128.62928026938));
#178193=CARTESIAN_POINT('Ctrl Pts',(24.7141924728488,5.56039051217835,128.775856349771));
#178194=CARTESIAN_POINT('Ctrl Pts',(24.7215888297843,5.61247376626662,128.924758288788));
#178195=CARTESIAN_POINT('Ctrl Pts',(24.7289851867198,5.65852327027925,129.07547514935));
#178196=CARTESIAN_POINT('Ctrl Pts',(24.7363826760564,5.70457982458843,129.226215085048));
#178197=CARTESIAN_POINT('Ctrl Pts',(24.743780165393,5.74460068036273,129.378770138535));
#178198=CARTESIAN_POINT('Ctrl Pts',(24.7511776547296,5.77845943249758,129.532614908126));
#178199=CARTESIAN_POINT('Ctrl Pts',(24.7585777372446,5.81233005376556,129.686513607762));
#178200=CARTESIAN_POINT('Ctrl Pts',(24.7659778197597,5.84003419043265,129.841702559298));
#178201=CARTESIAN_POINT('Ctrl Pts',(24.7733779022747,5.86149671679066,129.997647036701));
#178202=CARTESIAN_POINT('Ctrl Pts',(24.7807861219412,5.8829828434028,130.153762991088));
#178203=CARTESIAN_POINT('Ctrl Pts',(24.7881943416076,5.89821360233257,130.31063576042));
#178204=CARTESIAN_POINT('Ctrl Pts',(24.7956025612741,5.90716577155861,130.467725637467));
#178205=CARTESIAN_POINT('Ctrl Pts',(24.8030153405762,5.91612345069544,130.624912200711));
#178206=CARTESIAN_POINT('Ctrl Pts',(24.8104281198783,5.9187948335726,130.782315765558));
#178207=CARTESIAN_POINT('Ctrl Pts',(24.8178408991804,5.91520882655381,130.939398022606));
#178208=CARTESIAN_POINT('Ctrl Pts',(24.8252642702092,5.91161769568003,131.096704726149));
#178209=CARTESIAN_POINT('Ctrl Pts',(24.832687641238,5.90175134137646,131.253688833394));
#178210=CARTESIAN_POINT('Ctrl Pts',(24.8401110122668,5.885690466642,131.409817712148));
#178211=CARTESIAN_POINT('Ctrl Pts',(24.8440470617073,5.87717460548304,131.492600989918));
#178212=CARTESIAN_POINT('Ctrl Pts',(24.8479831111478,5.86691809743371,131.575143999358));
#178213=CARTESIAN_POINT('Ctrl Pts',(24.8519191605883,5.85493873763482,131.657368789299));
#178214=CARTESIAN_POINT('Ctrl Pts',(24.8593424269937,5.83234603891552,131.812442176991));
#178215=CARTESIAN_POINT('Ctrl Pts',(24.8667656933991,5.80355403208354,131.966851851249));
#178216=CARTESIAN_POINT('Ctrl Pts',(24.8741889598045,5.76860973210365,132.120062833563));
#178217=CARTESIAN_POINT('Ctrl Pts',(24.8816034525255,5.73370673338439,132.273092733219));
#178218=CARTESIAN_POINT('Ctrl Pts',(24.8890179452466,5.69266599767656,132.424926400591));
#178219=CARTESIAN_POINT('Ctrl Pts',(24.8964324379676,5.64558618084606,132.575034849925));
#178220=CARTESIAN_POINT('Ctrl Pts',(24.9038397843214,5.59855174131547,132.724998619084));
#178221=CARTESIAN_POINT('Ctrl Pts',(24.9112471306751,5.54548991948243,132.873240126774));
#178222=CARTESIAN_POINT('Ctrl Pts',(24.9186544770289,5.48655019129086,133.019241553631));
#178223=CARTESIAN_POINT('Ctrl Pts',(24.9260562987043,5.42765442257233,133.165134087116));
#178224=CARTESIAN_POINT('Ctrl Pts',(24.9334581203797,5.36288961569906,133.308789521764));
#178225=CARTESIAN_POINT('Ctrl Pts',(24.9408599420551,5.29245471923663,133.449706267444));
#178226=CARTESIAN_POINT('Ctrl Pts',(24.9482578563664,5.22205700480778,133.590548624272));
#178227=CARTESIAN_POINT('Ctrl Pts',(24.9556557706778,5.14599532836024,133.728654838313));
#178228=CARTESIAN_POINT('Ctrl Pts',(24.9630536849891,5.06451625138588,133.863544446947));
#178229=CARTESIAN_POINT('Ctrl Pts',(24.9704503699014,4.98305071475594,133.998411639375));
#178230=CARTESIAN_POINT('Ctrl Pts',(24.9778470548135,4.89616975719619,134.130062968087));
#178231=CARTESIAN_POINT('Ctrl Pts',(24.9852437397257,4.80416533013663,134.258043585531));
#178232=CARTESIAN_POINT('Ctrl Pts',(24.9926400966611,4.71216498264979,134.386018528181));
#178233=CARTESIAN_POINT('Ctrl Pts',(25.0000364535966,4.61504183527233,134.510322780091));
#178234=CARTESIAN_POINT('Ctrl Pts',(25.0074328105321,4.5131303536997,134.630531676603));
#178235=CARTESIAN_POINT('Ctrl Pts',(25.0148302998686,4.41120326921907,134.750758977405));
#178236=CARTESIAN_POINT('Ctrl Pts',(25.0222277892052,4.30448663224654,134.866889389592));
#178237=CARTESIAN_POINT('Ctrl Pts',(25.0296252785417,4.1933541530555,134.978532572523));
#178238=CARTESIAN_POINT('Ctrl Pts',(25.0370253610567,4.08218271654616,135.0902148918));
#178239=CARTESIAN_POINT('Ctrl Pts',(25.0444254435717,3.96659261901945,135.197406585606));
#178240=CARTESIAN_POINT('Ctrl Pts',(25.0518255260867,3.84699313335238,135.299755416073));
#178241=CARTESIAN_POINT('Ctrl Pts',(25.0592337457532,3.72726213575569,135.4022167896));
#178242=CARTESIAN_POINT('Ctrl Pts',(25.0666419654197,3.60351322928271,135.4998244221));
#178243=CARTESIAN_POINT('Ctrl Pts',(25.0740501850862,3.47618793284358,135.592267051286));
#178244=CARTESIAN_POINT('Ctrl Pts',(25.0814629643882,3.34878426980885,135.684766577367));
#178245=CARTESIAN_POINT('Ctrl Pts',(25.0888757436903,3.21780014050114,135.772094559034));
#178246=CARTESIAN_POINT('Ctrl Pts',(25.0962885229924,3.08370406445976,135.853984346651));
#178247=CARTESIAN_POINT('Ctrl Pts',(25.1037118940211,2.94941638565646,135.935991142236));
#178248=CARTESIAN_POINT('Ctrl Pts',(25.1111352650498,2.81200820471106,136.012544043446));
#178249=CARTESIAN_POINT('Ctrl Pts',(25.1185586360786,2.6719712621141,136.083423047291));
#178250=CARTESIAN_POINT('Ctrl Pts',(25.1224946855194,2.59772031500809,136.121004795849));
#178251=CARTESIAN_POINT('Ctrl Pts',(25.1264307349603,2.52273065029043,136.156992217978));
#178252=CARTESIAN_POINT('Ctrl Pts',(25.1303667844011,2.44707746919643,136.191358150724));
#178253=CARTESIAN_POINT('Ctrl Pts',(25.1377900508066,2.30439793070983,136.256171227358));
#178254=CARTESIAN_POINT('Ctrl Pts',(25.145213317212,2.15892591567081,136.315409897181));
#178255=CARTESIAN_POINT('Ctrl Pts',(25.1526365836174,2.01113692938864,136.368824546261));
#178256=CARTESIAN_POINT('Ctrl Pts',(25.1600510763384,1.86352261741495,136.422176063662));
#178257=CARTESIAN_POINT('Ctrl Pts',(25.1674655690594,1.71359713277626,136.469717136335));
#178258=CARTESIAN_POINT('Ctrl Pts',(25.1748800617804,1.56185885207399,136.511244836533));
#178259=CARTESIAN_POINT('Ctrl Pts',(25.1822874081341,1.41026682243951,136.552732510771));
#178260=CARTESIAN_POINT('Ctrl Pts',(25.189694754488,1.25686583279447,136.588218253181));
#178261=CARTESIAN_POINT('Ctrl Pts',(25.1971021008418,1.10217233463407,136.617547928093));
#178262=CARTESIAN_POINT('Ctrl Pts',(25.2045039225171,0.947594212721068,
136.646855727826));
#178263=CARTESIAN_POINT('Ctrl Pts',(25.2119057441925,0.791725866935453,
136.670016532975));
#178264=CARTESIAN_POINT('Ctrl Pts',(25.2193075658679,0.63509683581886,136.686926602885));
#178265=CARTESIAN_POINT('Ctrl Pts',(25.2267054801792,0.478550487948597,
136.7038277461));
#178266=CARTESIAN_POINT('Ctrl Pts',(25.2341033944905,0.321244624674761,
136.714484685648));
#178267=CARTESIAN_POINT('Ctrl Pts',(25.2415013088019,0.163716745317209,
136.71884515891));
#178268=CARTESIAN_POINT('Ctrl Pts',(25.2488979937141,0.00621504423535982,
136.723204907542));
#178269=CARTESIAN_POINT('Ctrl Pts',(25.2562946786262,-0.151508226914853,
136.721270256281));
#178270=CARTESIAN_POINT('Ctrl Pts',(25.2636913635384,-0.308912585129157,
136.713040975924));
#178271=CARTESIAN_POINT('Ctrl Pts',(25.2710877204738,-0.466309963869269,
136.704812060463));
#178272=CARTESIAN_POINT('Ctrl Pts',(25.2784840774093,-0.623388085001987,
136.690289090361));
#178273=CARTESIAN_POINT('Ctrl Pts',(25.2858804343447,-0.779608879247233,
136.669523919461));
#178274=CARTESIAN_POINT('Ctrl Pts',(25.2932779236813,-0.935853591294892,
136.648755569361));
#178275=CARTESIAN_POINT('Ctrl Pts',(25.3006754130179,-1.0912403450341,136.621743164734));
#178276=CARTESIAN_POINT('Ctrl Pts',(25.3080729023544,-1.24523873629802,
136.588590129966));
#178277=CARTESIAN_POINT('Ctrl Pts',(25.3154729848694,-1.39929111145949,
136.555425473454));
#178278=CARTESIAN_POINT('Ctrl Pts',(25.3228730673844,-1.5519537904435,136.516115979528));
#178279=CARTESIAN_POINT('Ctrl Pts',(25.3302731498994,-1.70270920356773,
136.470815587879));
#178280=CARTESIAN_POINT('Ctrl Pts',(25.3376813695658,-1.85363038776651,
136.425465383793));
#178281=CARTESIAN_POINT('Ctrl Pts',(25.3450895892323,-2.00263976006402,
136.374111233591));
#178282=CARTESIAN_POINT('Ctrl Pts',(25.3524978088987,-2.14923679492765,
136.316956354769));
#178283=CARTESIAN_POINT('Ctrl Pts',(25.3599105882008,-2.29592405782034,
136.259766298072));
#178284=CARTESIAN_POINT('Ctrl Pts',(25.3673233675028,-2.44019568341001,
136.196768547618));
#178285=CARTESIAN_POINT('Ctrl Pts',(25.3747361468049,-2.58157408554993,
136.128213151523));
#178286=CARTESIAN_POINT('Ctrl Pts',(25.3821595178337,-2.72315449578081,
136.059559800262));
#178287=CARTESIAN_POINT('Ctrl Pts',(25.3895828888624,-2.86183309784256,
135.985333119044));
#178288=CARTESIAN_POINT('Ctrl Pts',(25.3970062598912,-2.99715899924097,
135.905827906079));
#178289=CARTESIAN_POINT('Ctrl Pts',(25.4009423093321,-3.06891203926582,
135.863672334462));
#178290=CARTESIAN_POINT('Ctrl Pts',(25.404878358773,-3.13972302222651,135.820033486419));
#178291=CARTESIAN_POINT('Ctrl Pts',(25.408814408214,-3.20952844705469,135.774959948637));
#178292=CARTESIAN_POINT('Ctrl Pts',(25.4162346050843,-3.34112486183839,
135.68998781376));
#178293=CARTESIAN_POINT('Ctrl Pts',(25.4236548019546,-3.4695443034646,135.599657033977));
#178294=CARTESIAN_POINT('Ctrl Pts',(25.4310749988249,-3.59431996881035,
135.504232373722));
#178295=CARTESIAN_POINT('Ctrl Pts',(25.4384864234167,-3.71894812231803,
135.408920526065));
#178296=CARTESIAN_POINT('Ctrl Pts',(25.4458978480086,-3.83994078008817,
135.308527009478));
#178297=CARTESIAN_POINT('Ctrl Pts',(25.4533092726004,-3.9568580362525,135.203361077153));
#178298=CARTESIAN_POINT('Ctrl Pts',(25.4607135552692,-4.07366262662126,
135.098296486613));
#178299=CARTESIAN_POINT('Ctrl Pts',(25.4681178379381,-4.18639935763738,
134.988468883858));
#178300=CARTESIAN_POINT('Ctrl Pts',(25.4755221206069,-4.29465958995777,
134.874229112847));
#178301=CARTESIAN_POINT('Ctrl Pts',(25.4829208860585,-4.40283915339494,
134.760074466305));
#178302=CARTESIAN_POINT('Ctrl Pts',(25.4903196515101,-4.50654860379132,
134.64151446767));
#178303=CARTESIAN_POINT('Ctrl Pts',(25.4977184169617,-4.60541461751424,
134.518938219836));
#178304=CARTESIAN_POINT('Ctrl Pts',(25.5051132855161,-4.70422855894348,
134.396426532371));
#178305=CARTESIAN_POINT('Ctrl Pts',(25.5125081540706,-4.79820391012449,
134.269903098562));
#178306=CARTESIAN_POINT('Ctrl Pts',(25.519903022625,-4.88700634916399,134.139791550104));
#178307=CARTESIAN_POINT('Ctrl Pts',(25.527296676565,-4.97579420231431,134.009701372598));
#178308=CARTESIAN_POINT('Ctrl Pts',(25.5346903305049,-5.05941061909563,
133.876024558373));
#178309=CARTESIAN_POINT('Ctrl Pts',(25.5420839844448,-5.13756344001877,
133.739215377564));
#178310=CARTESIAN_POINT('Ctrl Pts',(25.5494773254721,-5.21571295337497,
133.602411986764));
#178311=CARTESIAN_POINT('Ctrl Pts',(25.5568706664994,-5.28839914527273,
133.462476817398));
#178312=CARTESIAN_POINT('Ctrl Pts',(25.5642640075267,-5.35537498064481,
133.319890259447));
#178313=CARTESIAN_POINT('Ctrl Pts',(25.5716584987318,-5.42236123540883,
133.177281519388));
#178314=CARTESIAN_POINT('Ctrl Pts',(25.5790529899368,-5.48363520598969,
133.032020907689));
#178315=CARTESIAN_POINT('Ctrl Pts',(25.5864474811419,-5.53899739066159,
132.884610234498));
#178316=CARTESIAN_POINT('Ctrl Pts',(25.5938445860284,-5.5943791438355,132.737147457039));
#178317=CARTESIAN_POINT('Ctrl Pts',(25.601241690915,-5.64384481952122,132.587533454593));
#178318=CARTESIAN_POINT('Ctrl Pts',(25.6086387958015,-5.68724435633118,
132.436286533127));
#178319=CARTESIAN_POINT('Ctrl Pts',(25.6160440377224,-5.73069163391611,
132.28487323557));
#178320=CARTESIAN_POINT('Ctrl Pts',(25.6234492796433,-5.76805934356134,
132.131823791191));
#178321=CARTESIAN_POINT('Ctrl Pts',(25.6308545215641,-5.79924809922357,
131.977668780902));
#178322=CARTESIAN_POINT('Ctrl Pts',(25.6382643467168,-5.83045615814433,
131.82341836142));
#178323=CARTESIAN_POINT('Ctrl Pts',(25.6456741718695,-5.85547758370099,
131.668061380605));
#178324=CARTESIAN_POINT('Ctrl Pts',(25.6530839970223,-5.87426478966554,
131.512134411511));
#178325=CARTESIAN_POINT('Ctrl Pts',(25.6605043622138,-5.89307871932133,
131.355985645511));
#178326=CARTESIAN_POINT('Ctrl Pts',(25.6679247274053,-5.90564068938807,
131.199265643398));
#178327=CARTESIAN_POINT('Ctrl Pts',(25.6753450925968,-5.91195518967298,
131.042512665214));
#178328=CARTESIAN_POINT('Ctrl Pts',(25.6791049976631,-5.91515475209332,
130.963085803919));
#178329=CARTESIAN_POINT('Ctrl Pts',(25.6828649027293,-5.91675113395662,
130.883650431332));
#178330=CARTESIAN_POINT('Ctrl Pts',(25.6866248077955,-5.91674999939557,
130.804276044766));
#178331=CARTESIAN_POINT('',(27.4366239742277,-5.91481336151323,130.809673827526));
#178332=CARTESIAN_POINT('Ctrl Pts',(25.6866248077955,-5.92653132131743,
130.804275904954));
#178333=CARTESIAN_POINT('Ctrl Pts',(25.6868372158726,-5.92653226647307,
130.799784399869));
#178334=CARTESIAN_POINT('Ctrl Pts',(25.6870496239497,-5.92652760397538,
130.795292896806));
#178335=CARTESIAN_POINT('Ctrl Pts',(25.7800779066311,-5.92202701559398,
128.828156677032));
#178336=CARTESIAN_POINT('Ctrl Pts',(25.9657096558399,-3.76932368489478,
124.907771816502));
#178337=CARTESIAN_POINT('Ctrl Pts',(26.2441572796525,2.92355563587315,124.445871569505));
#178338=CARTESIAN_POINT('Ctrl Pts',(26.5226049034657,6.92983015090643,129.827112128218));
#178339=CARTESIAN_POINT('Ctrl Pts',(26.8010525272784,4.56792929827948,136.1063963074));
#178340=CARTESIAN_POINT('Ctrl Pts',(27.0795001510913,-1.99167542371128,
137.513368706464));
#178341=CARTESIAN_POINT('Ctrl Pts',(27.2913571581557,-5.59000537624551,
133.893030412084));
#178342=CARTESIAN_POINT('Ctrl Pts',(27.4103982906157,-5.91861368694706,
131.367325223928));
#178343=CARTESIAN_POINT('Ctrl Pts',(27.4366235484716,-5.91382540835153,
130.809681996055));
#178344=CARTESIAN_POINT('',(29.1866256294184,-5.9117342771041,130.802189275152));
#178345=CARTESIAN_POINT('Ctrl Pts',(27.4366248077956,-5.91674762872223,
130.809657834746));
#178346=CARTESIAN_POINT('Ctrl Pts',(27.443965016876,-5.91688743308838,130.65350279638));
#178347=CARTESIAN_POINT('Ctrl Pts',(27.4513052259564,-5.91084113374822,
130.497219595639));
#178348=CARTESIAN_POINT('Ctrl Pts',(27.4586454350368,-5.89860518297208,
130.341340685042));
#178349=CARTESIAN_POINT('Ctrl Pts',(27.4660516835234,-5.88625914610499,
130.184059341544));
#178350=CARTESIAN_POINT('Ctrl Pts',(27.4734579320102,-5.86761150181308,
130.027189989693));
#178351=CARTESIAN_POINT('Ctrl Pts',(27.4808641804968,-5.84271241096424,
129.871278496172));
#178352=CARTESIAN_POINT('Ctrl Pts',(27.4882001791284,-5.81804949333168,
129.716845856602));
#178353=CARTESIAN_POINT('Ctrl Pts',(27.4955361777599,-5.78725328873107,
129.563353362203));
#178354=CARTESIAN_POINT('Ctrl Pts',(27.5028721763914,-5.75042446463643,
129.411324710272));
#178355=CARTESIAN_POINT('Ctrl Pts',(27.5102083131135,-5.71359494728757,
129.259293196601));
#178356=CARTESIAN_POINT('Ctrl Pts',(27.5175444498355,-5.67073267353985,
129.108725949671));
#178357=CARTESIAN_POINT('Ctrl Pts',(27.5248805865576,-5.62198896756605,
128.960134326932));
#178358=CARTESIAN_POINT('Ctrl Pts',(27.5322183682366,-5.57323433195728,
128.811509386));
#178359=CARTESIAN_POINT('Ctrl Pts',(27.5395561499156,-5.51859575789823,
128.664861311901));
#178360=CARTESIAN_POINT('Ctrl Pts',(27.5468939315946,-5.45827368163428,
128.520683981333));
#178361=CARTESIAN_POINT('Ctrl Pts',(27.5543523871881,-5.39695957516337,
128.374135574105));
#178362=CARTESIAN_POINT('Ctrl Pts',(27.5618108427816,-5.3297735441911,128.230140266825));
#178363=CARTESIAN_POINT('Ctrl Pts',(27.5692692983752,-5.25697551298712,
128.089192295278));
#178364=CARTESIAN_POINT('Ctrl Pts',(27.5766186203589,-5.18524267709565,
127.950306702565));
#178365=CARTESIAN_POINT('Ctrl Pts',(27.5839679423425,-5.10806120040344,
127.814380171892));
#178366=CARTESIAN_POINT('Ctrl Pts',(27.5913172643262,-5.02572412757875,
127.681857205883));
#178367=CARTESIAN_POINT('Ctrl Pts',(27.5988302867247,-4.94155306067873,
127.546382394172));
#178368=CARTESIAN_POINT('Ctrl Pts',(27.6063433091232,-4.85199427692997,
127.414464896858));
#178369=CARTESIAN_POINT('Ctrl Pts',(27.6138563315217,-4.75740460400089,
127.286544249941));
#178370=CARTESIAN_POINT('Ctrl Pts',(27.6213693539202,-4.66281493107167,
127.158623603023));
#178371=CARTESIAN_POINT('Ctrl Pts',(27.6288823763187,-4.56319468257101,
127.034700088833));
#178372=CARTESIAN_POINT('Ctrl Pts',(27.6363953987172,-4.45894050967834,
126.915173029695));
#178373=CARTESIAN_POINT('Ctrl Pts',(27.6438186651226,-4.3559318324494,126.797073927153));
#178374=CARTESIAN_POINT('Ctrl Pts',(27.651241931528,-4.2480722099351,126.68289148983));
#178375=CARTESIAN_POINT('Ctrl Pts',(27.6586651979334,-4.13569101201919,
126.573049896808));
#178376=CARTESIAN_POINT('Ctrl Pts',(27.6660796906545,-4.02344263934621,
126.463338127426));
#178377=CARTESIAN_POINT('Ctrl Pts',(27.6734941833755,-3.90668359313888,
126.357957248402));
#178378=CARTESIAN_POINT('Ctrl Pts',(27.6809086760965,-3.78578340080344,
126.257298422621));
#178379=CARTESIAN_POINT('Ctrl Pts',(27.6883160224503,-3.66499973662536,
126.156736615606));
#178380=CARTESIAN_POINT('Ctrl Pts',(27.6957233688041,-3.54008315735201,
126.060888038354));
#178381=CARTESIAN_POINT('Ctrl Pts',(27.7031307151579,-3.41143985491094,
125.970106933819));
#178382=CARTESIAN_POINT('Ctrl Pts',(27.7105325368333,-3.28289249949808,
125.879393537256));
#178383=CARTESIAN_POINT('Ctrl Pts',(27.7179343585087,-3.15062425902694,
125.793740302197));
#178384=CARTESIAN_POINT('Ctrl Pts',(27.7253361801841,-3.01507411433273,
125.713461026376));
#178385=CARTESIAN_POINT('Ctrl Pts',(27.7327340944955,-2.87959552550517,
125.633224129359));
#178386=CARTESIAN_POINT('Ctrl Pts',(27.7401320088068,-2.74083880317532,
125.558355731559));
#178387=CARTESIAN_POINT('Ctrl Pts',(27.7475299231182,-2.59927150009754,
125.489126076054));
#178388=CARTESIAN_POINT('Ctrl Pts',(27.7549266080304,-2.45772772293704,
125.419907925262));
#178389=CARTESIAN_POINT('Ctrl Pts',(27.7623232929426,-2.31337462703835,
125.356326820817));
#178390=CARTESIAN_POINT('Ctrl Pts',(27.7697199778548,-2.16670403726219,
125.298606883752));
#178391=CARTESIAN_POINT('Ctrl Pts',(27.7771163347903,-2.02003995101388,
125.240889506048));
#178392=CARTESIAN_POINT('Ctrl Pts',(27.7845126917257,-1.87105892257703,
125.189032915675));
#178393=CARTESIAN_POINT('Ctrl Pts',(27.7919090486611,-1.72027215703767,
125.143212830392));
#178394=CARTESIAN_POINT('Ctrl Pts',(27.7993065379977,-1.56946230565956,
125.097385729937));
#178395=CARTESIAN_POINT('Ctrl Pts',(27.8067040273342,-1.41684652389887,
125.057597083329));
#178396=CARTESIAN_POINT('Ctrl Pts',(27.8141015166708,-1.26295040520195,
125.023972495952));
#178397=CARTESIAN_POINT('Ctrl Pts',(27.8215015991858,-1.10900033845896,
124.990336121528));
#178398=CARTESIAN_POINT('Ctrl Pts',(27.8289016817008,-0.953769405649258,
124.962868188108));
#178399=CARTESIAN_POINT('Ctrl Pts',(27.8363017642158,-0.797792446516978,
124.941643007551));
#178400=CARTESIAN_POINT('Ctrl Pts',(27.8437099838823,-0.641643974683311,
124.920394487726));
#178401=CARTESIAN_POINT('Ctrl Pts',(27.8511182035487,-0.484748208384811,
124.905402480083));
#178402=CARTESIAN_POINT('Ctrl Pts',(27.8585264232152,-0.32764488956888,
124.896689385275));
#178403=CARTESIAN_POINT('Ctrl Pts',(27.8659392025172,-0.170444876281628,
124.887970927702));
#178404=CARTESIAN_POINT('Ctrl Pts',(27.8733519818193,-0.0130374283167435,
124.885539089349));
#178405=CARTESIAN_POINT('Ctrl Pts',(27.8807647611214,0.144039189540048,
124.88936414467));
#178406=CARTESIAN_POINT('Ctrl Pts',(27.8881881321502,0.301340245834596,
124.893194665409));
#178407=CARTESIAN_POINT('Ctrl Pts',(27.8956115031789,0.458309156382128,
124.903299911375));
#178408=CARTESIAN_POINT('Ctrl Pts',(27.9030348742077,0.614413412423298,
124.919598369086));
#178409=CARTESIAN_POINT('Ctrl Pts',(27.9069709236484,0.697183634646086,
124.928240202441));
#178410=CARTESIAN_POINT('Ctrl Pts',(27.9109069730892,0.779710939849281,
124.938622315023));
#178411=CARTESIAN_POINT('Ctrl Pts',(27.91484302253,0.861917404034309,124.950726793084));
#178412=CARTESIAN_POINT('Ctrl Pts',(27.9222662889354,1.01695622991221,124.973555460939));
#178413=CARTESIAN_POINT('Ctrl Pts',(27.9296895553408,1.17132190883347,125.002582419669));
#178414=CARTESIAN_POINT('Ctrl Pts',(27.9371128217462,1.32447953445568,125.037759840218));
#178415=CARTESIAN_POINT('Ctrl Pts',(27.9445273144673,1.47745614048356,125.072895683977));
#178416=CARTESIAN_POINT('Ctrl Pts',(27.9519418071883,1.62922717502141,125.114167437156));
#178417=CARTESIAN_POINT('Ctrl Pts',(27.9593562999093,1.7792638030657,125.161475638976));
#178418=CARTESIAN_POINT('Ctrl Pts',(27.9667636462631,1.92915582015953,125.20873824337));
#178419=CARTESIAN_POINT('Ctrl Pts',(27.9741709926169,2.0773164051288,125.262025602098));
#178420=CARTESIAN_POINT('Ctrl Pts',(27.9815783389707,2.22322796668605,125.321187451356));
#178421=CARTESIAN_POINT('Ctrl Pts',(27.9889801606462,2.36903070189555,125.380305175475));
#178422=CARTESIAN_POINT('Ctrl Pts',(27.9963819823215,2.51258740918187,125.445288526469));
#178423=CARTESIAN_POINT('Ctrl Pts',(28.003783803997,2.65339680176143,125.515937792668));
#178424=CARTESIAN_POINT('Ctrl Pts',(28.0111817183084,2.79413186215931,125.58654976367));
#178425=CARTESIAN_POINT('Ctrl Pts',(28.0185796326198,2.93212216335348,125.662821526187));
#178426=CARTESIAN_POINT('Ctrl Pts',(28.0259775469312,3.0668876185034,125.744505787833));
#178427=CARTESIAN_POINT('Ctrl Pts',(28.0333742318434,3.20163067807899,125.826176475036));
#178428=CARTESIAN_POINT('Ctrl Pts',(28.0407709167557,3.33314963631253,125.913257682901));
#178429=CARTESIAN_POINT('Ctrl Pts',(28.0481676016679,3.46099009048201,126.005456768135));
#178430=CARTESIAN_POINT('Ctrl Pts',(28.0555639586034,3.58882487607142,126.097651765164));
#178431=CARTESIAN_POINT('Ctrl Pts',(28.0629603155388,3.71298117914123,126.194963969986));
#178432=CARTESIAN_POINT('Ctrl Pts',(28.0703566724743,3.83303484452738,126.297058271024));
#178433=CARTESIAN_POINT('Ctrl Pts',(28.0777541618109,3.95310689043654,126.399168202961));
#178434=CARTESIAN_POINT('Ctrl Pts',(28.0851516511474,4.0690747635913,126.506061447077));
#178435=CARTESIAN_POINT('Ctrl Pts',(28.092549140484,4.1805486925268,126.617363699498));
#178436=CARTESIAN_POINT('Ctrl Pts',(28.099949222999,4.29206169847481,126.728704968751));
#178437=CARTESIAN_POINT('Ctrl Pts',(28.107349305514,4.3990773597029,126.844458059937));
#178438=CARTESIAN_POINT('Ctrl Pts',(28.114749388029,4.50124406159337,126.964213164607));
#178439=CARTESIAN_POINT('Ctrl Pts',(28.1221576076954,4.60352310627586,127.084099952326));
#178440=CARTESIAN_POINT('Ctrl Pts',(28.1295658273619,4.70094230097773,127.207997257701));
#178441=CARTESIAN_POINT('Ctrl Pts',(28.1369740470284,4.79319105568959,127.335463088645));
#178442=CARTESIAN_POINT('Ctrl Pts',(28.1443868263304,4.88549658797059,127.46300737268));
#178443=CARTESIAN_POINT('Ctrl Pts',(28.1517996056325,4.9726251329659,127.594124248633));
#178444=CARTESIAN_POINT('Ctrl Pts',(28.1592123849345,5.05431075435431,127.72834479171));
#178445=CARTESIAN_POINT('Ctrl Pts',(28.1666357559633,5.13611309198947,127.862757115393));
#178446=CARTESIAN_POINT('Ctrl Pts',(28.1740591269921,5.21245679269273,128.000281637707));
#178447=CARTESIAN_POINT('Ctrl Pts',(28.1814824980209,5.28312260207257,128.140426283921));
#178448=CARTESIAN_POINT('Ctrl Pts',(28.1854185474616,5.32059130980751,128.214734338067));
#178449=CARTESIAN_POINT('Ctrl Pts',(28.1893545969023,5.35646456875852,128.289778682676));
#178450=CARTESIAN_POINT('Ctrl Pts',(28.1932906463429,5.39071533044503,128.365484075261));
#178451=CARTESIAN_POINT('Ctrl Pts',(28.2007139127484,5.45531119805775,128.508262082997));
#178452=CARTESIAN_POINT('Ctrl Pts',(28.2081371791538,5.51432841563994,128.653824080753));
#178453=CARTESIAN_POINT('Ctrl Pts',(28.2155604455592,5.56751809318757,128.801694183901));
#178454=CARTESIAN_POINT('Ctrl Pts',(28.2229749382802,5.62064490495354,128.949389516867));
#178455=CARTESIAN_POINT('Ctrl Pts',(28.2303894310012,5.66795776150901,129.099387177314));
#178456=CARTESIAN_POINT('Ctrl Pts',(28.2378039237222,5.70925449378641,129.251188480396));
#178457=CARTESIAN_POINT('Ctrl Pts',(28.245211270076,5.75051142271838,129.402843471667));
#178458=CARTESIAN_POINT('Ctrl Pts',(28.2526186164298,5.78576367384332,129.556298286936));
#178459=CARTESIAN_POINT('Ctrl Pts',(28.2600259627835,5.81485789762128,129.711036240736));
#178460=CARTESIAN_POINT('Ctrl Pts',(28.2674277844589,5.84393042182966,129.865658785133));
#178461=CARTESIAN_POINT('Ctrl Pts',(28.2748296061344,5.8668539950702,130.021562197229));
#178462=CARTESIAN_POINT('Ctrl Pts',(28.2822314278098,5.88352568267587,130.17821678122));
#178463=CARTESIAN_POINT('Ctrl Pts',(28.2896293421211,5.90018856942726,130.334788668475));
#178464=CARTESIAN_POINT('Ctrl Pts',(28.2970272564324,5.91060610388832,130.492110567638));
#178465=CARTESIAN_POINT('Ctrl Pts',(28.3044251707437,5.91472684148525,130.649644900478));
#178466=CARTESIAN_POINT('Ctrl Pts',(28.3118218556558,5.91884689429037,130.807153053971));
#178467=CARTESIAN_POINT('Ctrl Pts',(28.3192185405681,5.9166722173005,130.964873198271));
#178468=CARTESIAN_POINT('Ctrl Pts',(28.3266152254803,5.90820340383502,131.122264850649));
#178469=CARTESIAN_POINT('Ctrl Pts',(28.3340115824157,5.89973496588562,131.279649524117));
#178470=CARTESIAN_POINT('Ctrl Pts',(28.3414079393512,5.88497296644016,131.436705361867));
#178471=CARTESIAN_POINT('Ctrl Pts',(28.3488042962866,5.8639700781312,131.592894374156));
#178472=CARTESIAN_POINT('Ctrl Pts',(28.3562017856231,5.84296397422646,131.749107299381));
#178473=CARTESIAN_POINT('Ctrl Pts',(28.3635992749596,5.81571512869173,131.904452764903));
#178474=CARTESIAN_POINT('Ctrl Pts',(28.3709967642961,5.78232777297846,132.058400524563));
#178475=CARTESIAN_POINT('Ctrl Pts',(28.3783968468111,5.7489287133792,132.212402250373));
#178476=CARTESIAN_POINT('Ctrl Pts',(28.3857969293261,5.70938693836345,132.365004930219));
#178477=CARTESIAN_POINT('Ctrl Pts',(28.3931970118411,5.66385717509631,132.515691229286));
#178478=CARTESIAN_POINT('Ctrl Pts',(28.4006052315076,5.61827734717395,132.66654322343));
#178479=CARTESIAN_POINT('Ctrl Pts',(28.408013451174,5.56669648954086,132.815474270903));
#178480=CARTESIAN_POINT('Ctrl Pts',(28.4154216708405,5.50931858117112,132.961984156014));
#178481=CARTESIAN_POINT('Ctrl Pts',(28.4228344501426,5.45190535765593,133.108584215514));
#178482=CARTESIAN_POINT('Ctrl Pts',(28.4302472294447,5.38868812329735,133.252759802188));
#178483=CARTESIAN_POINT('Ctrl Pts',(28.4376600087468,5.31991765272615,133.394033710972));
#178484=CARTESIAN_POINT('Ctrl Pts',(28.4450833797755,5.25104891968187,133.535509478542));
#178485=CARTESIAN_POINT('Ctrl Pts',(28.4525067508043,5.17661127919204,133.674074959643));
#178486=CARTESIAN_POINT('Ctrl Pts',(28.459930121833,5.09690021530756,133.809279710936));
#178487=CARTESIAN_POINT('Ctrl Pts',(28.4638661712739,5.05463549659387,133.880968514267));
#178488=CARTESIAN_POINT('Ctrl Pts',(28.4678022207148,5.01088893682213,133.951713004331));
#178489=CARTESIAN_POINT('Ctrl Pts',(28.4717382701558,4.96570921926207,134.021449754074));
#178490=CARTESIAN_POINT('Ctrl Pts',(28.4791615365612,4.88050168195686,134.152971087675));
#178491=CARTESIAN_POINT('Ctrl Pts',(28.4865848029667,4.78993649839303,134.281303759618));
#178492=CARTESIAN_POINT('Ctrl Pts',(28.4940080693721,4.69427951265969,134.405981144429));
#178493=CARTESIAN_POINT('Ctrl Pts',(28.5014225620932,4.59873558553967,134.530511170925));
#178494=CARTESIAN_POINT('Ctrl Pts',(28.5088370548142,4.49811206029958,134.651394216484));
#178495=CARTESIAN_POINT('Ctrl Pts',(28.5162515475352,4.39271921730441,134.768190639202));
#178496=CARTESIAN_POINT('Ctrl Pts',(28.523658893889,4.28742795589973,134.884874489131));
#178497=CARTESIAN_POINT('Ctrl Pts',(28.5310662402428,4.17737677656537,134.997479282392));
#178498=CARTESIAN_POINT('Ctrl Pts',(28.5384735865966,4.06291749224456,135.105596720562));
#178499=CARTESIAN_POINT('Ctrl Pts',(28.5458754082719,3.9485435759763,135.213633520666));
#178500=CARTESIAN_POINT('Ctrl Pts',(28.5532772299473,3.82976837124208,135.317189374453));
#178501=CARTESIAN_POINT('Ctrl Pts',(28.5606790516227,3.70698188742178,135.41589136655));
#178502=CARTESIAN_POINT('Ctrl Pts',(28.5680769659341,3.58426022163018,135.514541254634));
#178503=CARTESIAN_POINT('Ctrl Pts',(28.5754748802455,3.45753178411389,135.608342150716));
#178504=CARTESIAN_POINT('Ctrl Pts',(28.5828727945568,3.32722104761594,135.696960198852));
#178505=CARTESIAN_POINT('Ctrl Pts',(28.5902694794691,3.19693196639815,135.785563520277));
#178506=CARTESIAN_POINT('Ctrl Pts',(28.5976661643813,3.06306207609928,135.868985493458));
#178507=CARTESIAN_POINT('Ctrl Pts',(28.6050628492935,2.92606642084863,135.946934473456));
#178508=CARTESIAN_POINT('Ctrl Pts',(28.612459206229,2.7890768401287,136.024879997115));
#178509=CARTESIAN_POINT('Ctrl Pts',(28.6198555631645,2.64896209449349,136.097352825506));
#178510=CARTESIAN_POINT('Ctrl Pts',(28.6272519201,2.50620328079606,136.16410647701));
#178511=CARTESIAN_POINT('Ctrl Pts',(28.6346494094366,2.36342261035959,136.230870348669));
#178512=CARTESIAN_POINT('Ctrl Pts',(28.6420468987732,2.2179974040005,136.291913141832));
#178513=CARTESIAN_POINT('Ctrl Pts',(28.6494443881098,2.07043011247464,136.347035938371));
#178514=CARTESIAN_POINT('Ctrl Pts',(28.6568444706249,1.92281109146329,136.402178058121));
#178515=CARTESIAN_POINT('Ctrl Pts',(28.6642445531399,1.77304883971829,136.451395918903));
#178516=CARTESIAN_POINT('Ctrl Pts',(28.671644635655,1.62166223948166,136.494540064959));
#178517=CARTESIAN_POINT('Ctrl Pts',(28.6790528553215,1.47010917411581,136.53773165244));
#178518=CARTESIAN_POINT('Ctrl Pts',(28.6864610749879,1.31692855244665,136.574836085069));
#178519=CARTESIAN_POINT('Ctrl Pts',(28.6938692946544,1.16265147571948,136.605754597336));
#178520=CARTESIAN_POINT('Ctrl Pts',(28.7012820739565,1.0082794440254,136.636692139431));
#178521=CARTESIAN_POINT('Ctrl Pts',(28.7086948532586,0.852809980353635,
136.661436116041));
#178522=CARTESIAN_POINT('Ctrl Pts',(28.7161076325607,0.696780120652307,
136.679939569973));
#178523=CARTESIAN_POINT('Ctrl Pts',(28.7235310035895,0.540527318170587,
136.698469462507));
#178524=CARTESIAN_POINT('Ctrl Pts',(28.7309543746183,0.383712891615819,
136.710740994564));
#178525=CARTESIAN_POINT('Ctrl Pts',(28.7383777456471,0.226875528073778,
136.716759289616));
#178526=CARTESIAN_POINT('Ctrl Pts',(28.7423137950877,0.143716594668171,
136.71995033406));
#178527=CARTESIAN_POINT('Ctrl Pts',(28.7462498445283,0.0605511674709851,
136.721384239266));
#178528=CARTESIAN_POINT('Ctrl Pts',(28.7501858939688,-0.0225410760443611,
136.721067679978));
#178529=CARTESIAN_POINT('Ctrl Pts',(28.7576091603742,-0.179250454103204,
136.720470659038));
#178530=CARTESIAN_POINT('Ctrl Pts',(28.7650324267796,-0.336173059472607,
136.713642549052));
#178531=CARTESIAN_POINT('Ctrl Pts',(28.7724556931851,-0.492772611700997,
136.700554789713));
#178532=CARTESIAN_POINT('Ctrl Pts',(28.7798701859061,-0.649187076263437,
136.687482499018));
#178533=CARTESIAN_POINT('Ctrl Pts',(28.7872846786271,-0.805278879335282,
136.668165316284));
#178534=CARTESIAN_POINT('Ctrl Pts',(28.7946991713481,-0.960510423616398,
136.642626651983));
#178535=CARTESIAN_POINT('Ctrl Pts',(28.8021065177018,-1.11559234989033,
136.617112602807));
#178536=CARTESIAN_POINT('Ctrl Pts',(28.8095138640555,-1.26981530217414,
136.585389070105));
#178537=CARTESIAN_POINT('Ctrl Pts',(28.8169212104093,-1.42264560394922,
136.547531348797));
#178538=CARTESIAN_POINT('Ctrl Pts',(28.8243230320847,-1.57536191912015,
136.509701863205));
#178539=CARTESIAN_POINT('Ctrl Pts',(28.8317248537601,-1.72668729116989,
136.465747388037));
#178540=CARTESIAN_POINT('Ctrl Pts',(28.8391266754356,-1.87609716623874,
136.415794479364));
#178541=CARTESIAN_POINT('Ctrl Pts',(28.8465245897469,-2.02542816899692,
136.365867940442));
#178542=CARTESIAN_POINT('Ctrl Pts',(28.8539225040582,-2.17284533544077,
136.309949392371));
#178543=CARTESIAN_POINT('Ctrl Pts',(28.8613204183695,-2.31783834522459,
136.248215498797));
#178544=CARTESIAN_POINT('Ctrl Pts',(28.8687171032817,-2.46280725980105,
136.186491864277));
#178545=CARTESIAN_POINT('Ctrl Pts',(28.8761137881939,-2.60535247413135,
136.118954948376));
#178546=CARTESIAN_POINT('Ctrl Pts',(28.8835104731061,-2.74498265660099,
136.045829951394));
#178547=CARTESIAN_POINT('Ctrl Pts',(28.8909068300416,-2.88460664772181,
135.972708196851));
#178548=CARTESIAN_POINT('Ctrl Pts',(28.898303186977,-3.02131553329272,135.893999027086));
#178549=CARTESIAN_POINT('Ctrl Pts',(28.9056995439125,-3.15464189674526,
135.80997397317));
#178550=CARTESIAN_POINT('Ctrl Pts',(28.9130970332491,-3.28798867280498,
135.725936054803));
#178551=CARTESIAN_POINT('Ctrl Pts',(28.9204945225856,-3.41795157975971,
135.636580830796));
#178552=CARTESIAN_POINT('Ctrl Pts',(28.9278920119222,-3.54409167524775,
135.542223507091));
#178553=CARTESIAN_POINT('Ctrl Pts',(28.9352920944372,-3.67027598895036,
135.447833106573));
#178554=CARTESIAN_POINT('Ctrl Pts',(28.9426921769522,-3.79263452436216,
135.34843733866));
#178555=CARTESIAN_POINT('Ctrl Pts',(28.9500922594672,-3.91076107159585,
135.244391969188));
#178556=CARTESIAN_POINT('Ctrl Pts',(28.9575004791336,-4.02901751111209,
135.140232191137));
#178557=CARTESIAN_POINT('Ctrl Pts',(28.9649086988002,-4.143032388792,135.031412847989));
#178558=CARTESIAN_POINT('Ctrl Pts',(28.9723169184666,-4.25243553721774,
134.918327385092));
#178559=CARTESIAN_POINT('Ctrl Pts',(28.9797296977688,-4.36190602145663,
134.805172319978));
#178560=CARTESIAN_POINT('Ctrl Pts',(28.9871424770708,-4.46675887243248,
134.687746180831));
#178561=CARTESIAN_POINT('Ctrl Pts',(28.994555256373,-4.56666430268049,134.566475409691));
#178562=CARTESIAN_POINT('Ctrl Pts',(29.0019786274017,-4.66671248249163,
134.445031361187));
#178563=CARTESIAN_POINT('Ctrl Pts',(29.0094019984305,-4.761798897917,134.319732005737));
#178564=CARTESIAN_POINT('Ctrl Pts',(29.0168253694593,-4.85163668595149,
134.191033325406));
#178565=CARTESIAN_POINT('Ctrl Pts',(29.0207614189,-4.899270836795,134.122794197013));
#178566=CARTESIAN_POINT('Ctrl Pts',(29.0246974683408,-4.94543016668652,
134.053599828531));
#178567=CARTESIAN_POINT('Ctrl Pts',(29.0286335177815,-4.99007722365454,
133.983520862735));
#178568=CARTESIAN_POINT('Ctrl Pts',(29.0362400418879,-5.07635889267805,
133.848091328453));
#178569=CARTESIAN_POINT('Ctrl Pts',(29.0438465659943,-5.15724064230757,
133.708963349913));
#178570=CARTESIAN_POINT('Ctrl Pts',(29.0514530901007,-5.2323984196574,133.566594738792));
#178571=CARTESIAN_POINT('Ctrl Pts',(29.0590492970541,-5.30745425632099,
133.424419230161));
#178572=CARTESIAN_POINT('Ctrl Pts',(29.0666455040075,-5.37680142326697,
133.279012149228));
#178573=CARTESIAN_POINT('Ctrl Pts',(29.0742417109609,-5.44015902814017,
133.130860200855));
#178574=CARTESIAN_POINT('Ctrl Pts',(29.0818288199004,-5.50344074930285,
132.98288569479));
#178575=CARTESIAN_POINT('Ctrl Pts',(29.0894159288399,-5.56074706272857,
132.83217318864));
#178576=CARTESIAN_POINT('Ctrl Pts',(29.0970030377794,-5.61184284714001,
132.679234059029));
#178577=CARTESIAN_POINT('Ctrl Pts',(29.1045799859559,-5.66287020335803,
132.526499747652));
#178578=CARTESIAN_POINT('Ctrl Pts',(29.1121569341324,-5.7077035037439,132.371545087259));
#178579=CARTESIAN_POINT('Ctrl Pts',(29.1197338823088,-5.74615574642359,
132.214901187824));
#178580=CARTESIAN_POINT('Ctrl Pts',(29.1273048899565,-5.78457784152278,
132.05838010137));
#178581=CARTESIAN_POINT('Ctrl Pts',(29.1348758976042,-5.81662876103272,
131.900172750996));
#178582=CARTESIAN_POINT('Ctrl Pts',(29.1424469052518,-5.84217110628933,
131.740825954532));
#178583=CARTESIAN_POINT('Ctrl Pts',(29.1500122319244,-5.86769428561259,
131.5815987254));
#178584=CARTESIAN_POINT('Ctrl Pts',(29.1575775585969,-5.88671857053288,
131.421234097781));
#178585=CARTESIAN_POINT('Ctrl Pts',(29.1651428852695,-5.89915750936803,
131.260289605641));
#178586=CARTESIAN_POINT('Ctrl Pts',(29.1723035261115,-5.91093106222438,
131.107954385549));
#178587=CARTESIAN_POINT('Ctrl Pts',(29.1794641669536,-5.91680531166713,
130.955100016775));
#178588=CARTESIAN_POINT('Ctrl Pts',(29.1866248077956,-5.91674960731476,
130.802204964392));
#178589=CARTESIAN_POINT('',(30.9366248077955,-5.92174042288377,130.7998180981));
#178590=CARTESIAN_POINT('Ctrl Pts',(29.1866262959298,-5.90766577404403,
130.80217654783));
#178591=CARTESIAN_POINT('Ctrl Pts',(29.2267779111514,-5.91044712185902,
129.946168516127));
#178592=CARTESIAN_POINT('Ctrl Pts',(29.3597454009771,-5.33509832877074,
127.114953888422));
#178593=CARTESIAN_POINT('Ctrl Pts',(29.5855287654075,-0.96670133588667,
123.873051285443));
#178594=CARTESIAN_POINT('Ctrl Pts',(29.8639763892201,5.30898116095411,126.244505404626));
#178595=CARTESIAN_POINT('Ctrl Pts',(30.1424240130331,6.70596932902698,132.806243703186));
#178596=CARTESIAN_POINT('Ctrl Pts',(30.420871636846,1.94049928853783,137.528349243488));
#178597=CARTESIAN_POINT('Ctrl Pts',(30.6856052351002,-4.28566032468232,
136.143193126057));
#178598=CARTESIAN_POINT('Ctrl Pts',(30.85752295875,-5.90750938229346,132.476046720674));
#178599=CARTESIAN_POINT('Ctrl Pts',(30.9366248077955,-5.92174042288377,
130.7998180981));
#178600=CARTESIAN_POINT('',(32.6866248077956,-5.92231311245214,130.808682413197));
#178601=CARTESIAN_POINT('Ctrl Pts',(30.9366248077955,-5.92174042288377,
130.7998180981));
#178602=CARTESIAN_POINT('Ctrl Pts',(30.9503388333543,-5.92420768321634,
130.509207417696));
#178603=CARTESIAN_POINT('Ctrl Pts',(31.0568687335175,-5.77245931818093,
128.254344206899));
#178604=CARTESIAN_POINT('Ctrl Pts',(31.2562145082845,-2.87502317972114,
124.423780530593));
#178605=CARTESIAN_POINT('Ctrl Pts',(31.5346621320976,3.8141424796121,124.936662800225));
#178606=CARTESIAN_POINT('Ctrl Pts',(31.8131097559105,6.99829753140275,130.841672711039));
#178607=CARTESIAN_POINT('Ctrl Pts',(32.0915573797234,3.75135903767198,136.712394630739));
#178608=CARTESIAN_POINT('Ctrl Pts',(32.3700050035363,-2.94289514760019,
137.153921915842));
#178609=CARTESIAN_POINT('Ctrl Pts',(32.5683608128937,-5.78513647409968,
133.311856168978));
#178610=CARTESIAN_POINT('Ctrl Pts',(32.6739007476468,-5.92452395854052,
131.07824707337));
#178611=CARTESIAN_POINT('Ctrl Pts',(32.6866248077956,-5.92231311245214,
130.808682413197));
#178612=CARTESIAN_POINT('',(34.4366248077956,-5.90791192852897,130.806830871508));
#178613=CARTESIAN_POINT('Ctrl Pts',(32.6866248077956,-5.92231311245214,
130.808682413197));
#178614=CARTESIAN_POINT('Ctrl Pts',(32.7667166222511,-5.90839690389693,
129.111903044516));
#178615=CARTESIAN_POINT('Ctrl Pts',(32.939624311311,-4.25182580178573,125.425065311405));
#178616=CARTESIAN_POINT('Ctrl Pts',(33.2053478749749,2.01208611123176,124.101445579217));
#178617=CARTESIAN_POINT('Ctrl Pts',(33.4837954987878,6.7269339492388,128.874096342156));
#178618=CARTESIAN_POINT('Ctrl Pts',(33.7622431226007,5.26005811688714,135.420565675545));
#178619=CARTESIAN_POINT('Ctrl Pts',(34.0406907464136,-1.0405541567591,137.724968074804));
#178620=CARTESIAN_POINT('Ctrl Pts',(34.2654846414787,-5.35514334605665,
134.451080629057));
#178621=CARTESIAN_POINT('Ctrl Pts',(34.3974626619392,-5.91103772112295,
131.641657145399));
#178622=CARTESIAN_POINT('Ctrl Pts',(34.4366248077956,-5.90791192852897,
130.806830871508));
#178623=CARTESIAN_POINT('',(36.1866248250608,-5.91451745769036,130.799166741936));
#178624=CARTESIAN_POINT('Ctrl Pts',(34.4366248077956,-5.90791192852897,
130.806830871508));
#178625=CARTESIAN_POINT('Ctrl Pts',(34.4902785365435,-5.90362946585253,
129.663085004891));
#178626=CARTESIAN_POINT('Ctrl Pts',(34.6367481398959,-5.03069841154749,
126.53472321439));
#178627=CARTESIAN_POINT('Ctrl Pts',(34.8760336178522,0.047962267785614,
123.806127972732));
#178628=CARTESIAN_POINT('Ctrl Pts',(35.1544812416653,5.91373610162903,127.061996945949));
#178629=CARTESIAN_POINT('Ctrl Pts',(35.432928865478,6.34507536014334,133.756915308749));
#178630=CARTESIAN_POINT('Ctrl Pts',(35.711376489291,0.945600336853253,137.73858015067));
#178631=CARTESIAN_POINT('Ctrl Pts',(35.9626084700635,-4.71015443282379,
135.581689261836));
#178632=CARTESIAN_POINT('Ctrl Pts',(36.1210245762317,-5.90156890071962,
132.19441833346));
#178633=CARTESIAN_POINT('Ctrl Pts',(36.1866248077956,-5.91323377650414,
130.799168236558));
#178634=CARTESIAN_POINT('',(37.9366248077955,-5.92210452553072,130.804050934745));
#178635=CARTESIAN_POINT('Ctrl Pts',(36.1866248550572,-5.91674771806056,
130.799164145188));
#178636=CARTESIAN_POINT('Ctrl Pts',(36.1956075840384,-5.91657982411567,
130.607998669251));
#178637=CARTESIAN_POINT('Ctrl Pts',(36.2045903130197,-5.90714364554391,
130.417241009972));
#178638=CARTESIAN_POINT('Ctrl Pts',(36.2135730420009,-5.88857986329382,
130.227682409108));
#178639=CARTESIAN_POINT('Ctrl Pts',(36.2226894911536,-5.86973973382792,
130.035301969952));
#178640=CARTESIAN_POINT('Ctrl Pts',(36.2318059403062,-5.84149826826958,
129.8441565403));
#178641=CARTESIAN_POINT('Ctrl Pts',(36.2409223894589,-5.80405176354405,
129.655050525119));
#178642=CARTESIAN_POINT('Ctrl Pts',(36.2500388386115,-5.76660525881853,
129.465944509937));
#178643=CARTESIAN_POINT('Ctrl Pts',(36.2591552877641,-5.71995381969959,
129.278877833967));
#178644=CARTESIAN_POINT('Ctrl Pts',(36.2682717369168,-5.66434131196571,
129.09463313517));
#178645=CARTESIAN_POINT('Ctrl Pts',(36.2756950033222,-5.61905762163104,
128.944607893977));
#178646=CARTESIAN_POINT('Ctrl Pts',(36.2831182697276,-5.56774100745304,
128.796156109647));
#178647=CARTESIAN_POINT('Ctrl Pts',(36.290541536133,-5.51051710494887,128.649799920216));
#178648=CARTESIAN_POINT('Ctrl Pts',(36.297956028854,-5.45336083634523,128.503616711647));
#178649=CARTESIAN_POINT('Ctrl Pts',(36.305370521575,-5.3903113115816,128.359524512129));
#178650=CARTESIAN_POINT('Ctrl Pts',(36.3127850142959,-5.32154435244625,
128.218031893786));
#178651=CARTESIAN_POINT('Ctrl Pts',(36.3201923606497,-5.25284367349506,
128.076675651357));
#178652=CARTESIAN_POINT('Ctrl Pts',(36.3275997070035,-5.17843669292861,
127.937914335489));
#178653=CARTESIAN_POINT('Ctrl Pts',(36.3350070533572,-5.09854784169346,
127.802237957103));
#178654=CARTESIAN_POINT('Ctrl Pts',(36.3424088750326,-5.01871857457771,
127.66666277128));
#178655=CARTESIAN_POINT('Ctrl Pts',(36.3498106967079,-4.93341576631353,
127.534168261902));
#178656=CARTESIAN_POINT('Ctrl Pts',(36.3572125183833,-4.84291037544202,
127.405221070867));
#178657=CARTESIAN_POINT('Ctrl Pts',(36.3646104326946,-4.752452761662,127.27634195005));
#178658=CARTESIAN_POINT('Ctrl Pts',(36.3720083470059,-4.65679824878223,
127.151006722973));
#178659=CARTESIAN_POINT('Ctrl Pts',(36.3794062613172,-4.55626175911545,
127.029654093222));
#178660=CARTESIAN_POINT('Ctrl Pts',(36.3868029462294,-4.45574197678934,
126.908321630078));
#178661=CARTESIAN_POINT('Ctrl Pts',(36.3941996311416,-4.35034206577818,
126.790970737893));
#178662=CARTESIAN_POINT('Ctrl Pts',(36.4015963160537,-4.2404180498028,126.678008072593));
#178663=CARTESIAN_POINT('Ctrl Pts',(36.4089926729892,-4.13049890797349,
126.565050416175));
#178664=CARTESIAN_POINT('Ctrl Pts',(36.4163890299246,-4.01605632038603,
126.456480867289));
#178665=CARTESIAN_POINT('Ctrl Pts',(36.42378538686,-3.8974838924297,126.352669942019));
#178666=CARTESIAN_POINT('Ctrl Pts',(36.4311828761966,-3.77889331073178,
126.248843123031));
#178667=CARTESIAN_POINT('Ctrl Pts',(36.4385803655331,-3.65617191057611,
126.149776624228));
#178668=CARTESIAN_POINT('Ctrl Pts',(36.4459778548697,-3.52974703272114,
126.055801209967));
#178669=CARTESIAN_POINT('Ctrl Pts',(36.4533779373846,-3.40327783682139,
125.961792852771));
#178670=CARTESIAN_POINT('Ctrl Pts',(36.4607780198996,-3.27310287782725,
125.872879355944));
#178671=CARTESIAN_POINT('Ctrl Pts',(36.4681781024146,-3.13967903141979,
125.789348539598));
#178672=CARTESIAN_POINT('Ctrl Pts',(36.475586322081,-3.00610847177691,125.705725872533));
#178673=CARTESIAN_POINT('Ctrl Pts',(36.4829945417474,-2.86928220683207,
125.62749790441));
#178674=CARTESIAN_POINT('Ctrl Pts',(36.4904027614138,-2.72968294214001,
125.554907160501));
#178675=CARTESIAN_POINT('Ctrl Pts',(36.4978155407158,-2.58999775642967,
125.4822717382));
#178676=CARTESIAN_POINT('Ctrl Pts',(36.5052283200179,-2.44753650711736,
125.415280612245));
#178677=CARTESIAN_POINT('Ctrl Pts',(36.5126410993199,-2.30280200391537,
125.354128191947));
#178678=CARTESIAN_POINT('Ctrl Pts',(36.5200644703487,-2.15786069726782,
125.292888394204));
#178679=CARTESIAN_POINT('Ctrl Pts',(36.5274878413774,-2.01063999794909,
125.237504095288));
#178680=CARTESIAN_POINT('Ctrl Pts',(36.5349112124061,-1.86165878085102,
125.188120136053));
#178681=CARTESIAN_POINT('Ctrl Pts',(36.5388472618473,-1.78266536478243,
125.161935575913));
#178682=CARTESIAN_POINT('Ctrl Pts',(36.5427833112885,-1.7031772022922,125.137437078181));
#178683=CARTESIAN_POINT('Ctrl Pts',(36.5467193607296,-1.6232726854084,125.114640382677));
#178684=CARTESIAN_POINT('Ctrl Pts',(36.5541426271351,-1.47257526031468,
125.071646526421));
#178685=CARTESIAN_POINT('Ctrl Pts',(36.5615658935405,-1.31994068634216,
125.034578831723));
#178686=CARTESIAN_POINT('Ctrl Pts',(36.5689891599459,-1.16587616207567,
125.003613826229));
#178687=CARTESIAN_POINT('Ctrl Pts',(36.5764036526669,-1.01199372928239,
124.9726854188));
#178688=CARTESIAN_POINT('Ctrl Pts',(36.583818145388,-0.85668507271891,124.947845416152));
#178689=CARTESIAN_POINT('Ctrl Pts',(36.591232638109,-0.700473104488531,
124.929220790091));
#178690=CARTESIAN_POINT('Ctrl Pts',(36.5986399844627,-0.544411699234631,
124.910614115145));
#178691=CARTESIAN_POINT('Ctrl Pts',(36.6060473308166,-0.387449083782456,
124.898210934551));
#178692=CARTESIAN_POINT('Ctrl Pts',(36.6134546771703,-0.230118828605541,
124.892087291068));
#178693=CARTESIAN_POINT('Ctrl Pts',(36.6208564988457,-0.0729059162684447,
124.885968214829));
#178694=CARTESIAN_POINT('Ctrl Pts',(36.6282583205211,0.0846737184149918,
124.886119364646));
#178695=CARTESIAN_POINT('Ctrl Pts',(36.6356601421965,0.242081016691307,
124.892565006767));
#178696=CARTESIAN_POINT('Ctrl Pts',(36.6430580565079,0.399405220879894,
124.899007246284));
#178697=CARTESIAN_POINT('Ctrl Pts',(36.6504559708192,0.556556897801354,
124.911737345329));
#178698=CARTESIAN_POINT('Ctrl Pts',(36.6578538851306,0.712996730501101,
124.930727480844));
#178699=CARTESIAN_POINT('Ctrl Pts',(36.6652505700428,0.869410565738761,
124.949714460544));
#178700=CARTESIAN_POINT('Ctrl Pts',(36.672647254955,1.02511242132171,124.974959367078));
#178701=CARTESIAN_POINT('Ctrl Pts',(36.6800439398672,1.1795677265864,125.006382475067));
#178702=CARTESIAN_POINT('Ctrl Pts',(36.6874402968026,1.33401618314101,125.037804189723));
#178703=CARTESIAN_POINT('Ctrl Pts',(36.6948366537381,1.48721783347539,125.075403486711));
#178704=CARTESIAN_POINT('Ctrl Pts',(36.7022330106735,1.63864819858704,125.119049487666));
#178705=CARTESIAN_POINT('Ctrl Pts',(36.7096305000101,1.79010174807438,125.162702170934));
#178706=CARTESIAN_POINT('Ctrl Pts',(36.7170279893467,1.93978311364797,125.2124032981));
#178707=CARTESIAN_POINT('Ctrl Pts',(36.7244254786833,2.08718302576793,125.267972121493));
#178708=CARTESIAN_POINT('Ctrl Pts',(36.7318255611983,2.23463460869859,125.323560424452));
#178709=CARTESIAN_POINT('Ctrl Pts',(36.7392256437132,2.37980279677705,125.385020387333));
#178710=CARTESIAN_POINT('Ctrl Pts',(36.7466257262282,2.52219848632689,125.452123201488));
#178711=CARTESIAN_POINT('Ctrl Pts',(36.7540339458947,2.66475075457582,125.519299802084));
#178712=CARTESIAN_POINT('Ctrl Pts',(36.7614421655612,2.80452409805858,125.59213148631));
#178713=CARTESIAN_POINT('Ctrl Pts',(36.7688503852277,2.94105355925407,125.670343231142));
#178714=CARTESIAN_POINT('Ctrl Pts',(36.7762631645297,3.07766705205501,125.748603113999));
#178715=CARTESIAN_POINT('Ctrl Pts',(36.7836759438318,3.21103236867163,125.83224945783));
#178716=CARTESIAN_POINT('Ctrl Pts',(36.7910887231338,3.34071416611194,125.920964317568));
#178717=CARTESIAN_POINT('Ctrl Pts',(36.7985120941626,3.4705812589859,126.009805937257));
#178718=CARTESIAN_POINT('Ctrl Pts',(36.8059354651913,3.5967540222762,126.1037303147));
#178719=CARTESIAN_POINT('Ctrl Pts',(36.8133588362201,3.7188301327171,126.202379195777));
#178720=CARTESIAN_POINT('Ctrl Pts',(36.8172948856609,3.7835578156491,126.254685199571));
#178721=CARTESIAN_POINT('Ctrl Pts',(36.8212309351017,3.84713438905048,126.308318805457));
#178722=CARTESIAN_POINT('Ctrl Pts',(36.8251669845425,3.90950423776022,126.36322256776));
#178723=CARTESIAN_POINT('Ctrl Pts',(36.8325902509479,4.02713182593014,126.466769349974));
#178724=CARTESIAN_POINT('Ctrl Pts',(36.8400135173534,4.14082064282964,126.575149145481));
#178725=CARTESIAN_POINT('Ctrl Pts',(36.8474367837588,4.25014801752764,126.688030651248));
#178726=CARTESIAN_POINT('Ctrl Pts',(36.8548512764798,4.35934617634797,126.80077874045));
#178727=CARTESIAN_POINT('Ctrl Pts',(36.8622657692008,4.46419289657875,126.918017683605));
#178728=CARTESIAN_POINT('Ctrl Pts',(36.8696802619218,4.56429870647891,127.039376171312));
#178729=CARTESIAN_POINT('Ctrl Pts',(36.8770876082756,4.66430803063057,127.16061768914));
#178730=CARTESIAN_POINT('Ctrl Pts',(36.8844949546294,4.75958530541786,127.285970560856));
#178731=CARTESIAN_POINT('Ctrl Pts',(36.8919023009832,4.84977814603905,127.41502698148));
#178732=CARTESIAN_POINT('Ctrl Pts',(36.8993041226586,4.93990371743693,127.543987146957));
#178733=CARTESIAN_POINT('Ctrl Pts',(36.906705944334,5.02495219245812,127.676645056671));
#178734=CARTESIAN_POINT('Ctrl Pts',(36.9141077660094,5.10461178079674,127.812560301728));
#178735=CARTESIAN_POINT('Ctrl Pts',(36.9215056803208,5.18422931745863,127.948403798184));
#178736=CARTESIAN_POINT('Ctrl Pts',(36.9289035946321,5.25846344461655,128.087500884228));
#178737=CARTESIAN_POINT('Ctrl Pts',(36.9363015089434,5.32704605660825,128.229382778191));
#178738=CARTESIAN_POINT('Ctrl Pts',(36.9436981938556,5.39561727141405,128.371241093956));
#178739=CARTESIAN_POINT('Ctrl Pts',(36.9510948787679,5.45853867274588,128.515882963387));
#178740=CARTESIAN_POINT('Ctrl Pts',(36.9584915636801,5.51558838732208,128.662815543528));
#178741=CARTESIAN_POINT('Ctrl Pts',(36.9658879206155,5.57263557225415,128.809741608524));
#178742=CARTESIAN_POINT('Ctrl Pts',(36.973284277551,5.62381145299412,128.958957834283));
#178743=CARTESIAN_POINT('Ctrl Pts',(36.9806806344864,5.66894264750733,129.109952218811));
#178744=CARTESIAN_POINT('Ctrl Pts',(36.988078123823,5.71408075172164,129.260969720964));
#178745=CARTESIAN_POINT('Ctrl Pts',(36.9954756131596,5.75317222009143,129.413765566268));
#178746=CARTESIAN_POINT('Ctrl Pts',(37.0028731024962,5.78609384812336,129.567813593305));
#178747=CARTESIAN_POINT('Ctrl Pts',(37.0102731850112,5.81902701678101,129.721915621639));
#178748=CARTESIAN_POINT('Ctrl Pts',(37.0176732675261,5.84578596095896,129.877270340826));
#178749=CARTESIAN_POINT('Ctrl Pts',(37.0250733500411,5.86629881137007,130.033342577428));
#178750=CARTESIAN_POINT('Ctrl Pts',(37.0324815697076,5.88683421776897,130.189586431498));
#178751=CARTESIAN_POINT('Ctrl Pts',(37.0398897893741,5.90110976543565,130.346549008294));
#178752=CARTESIAN_POINT('Ctrl Pts',(37.0472980090406,5.9091055181301,130.503690469223));
#178753=CARTESIAN_POINT('Ctrl Pts',(37.0547107883427,5.91710619207691,130.6609286481));
#178754=CARTESIAN_POINT('Ctrl Pts',(37.0621235676446,5.91881936528427,130.818345558087));
#178755=CARTESIAN_POINT('Ctrl Pts',(37.0695363469467,5.91427722042245,130.975403075722));
#178756=CARTESIAN_POINT('Ctrl Pts',(37.0769597179755,5.90972858553104,131.132685004503));
#178757=CARTESIAN_POINT('Ctrl Pts',(37.0843830890043,5.89890680721048,131.289606143896));
#178758=CARTESIAN_POINT('Ctrl Pts',(37.091806460033,5.88189582924777,131.44563436284));
#178759=CARTESIAN_POINT('Ctrl Pts',(37.0957425094738,5.87287620055913,131.528364268369));
#178760=CARTESIAN_POINT('Ctrl Pts',(37.0996785589146,5.86211741981153,131.610843314209));
#178761=CARTESIAN_POINT('Ctrl Pts',(37.1036146083554,5.84963775632701,131.692993658958));
#178762=CARTESIAN_POINT('Ctrl Pts',(37.1110378747608,5.82610150047212,131.84792664533));
#178763=CARTESIAN_POINT('Ctrl Pts',(37.1184611411662,5.79637009157543,132.002158193617));
#178764=CARTESIAN_POINT('Ctrl Pts',(37.1258844075717,5.76049380029665,132.155153621414));
#178765=CARTESIAN_POINT('Ctrl Pts',(37.1332989002927,5.72465991181477,132.307968221321));
#178766=CARTESIAN_POINT('Ctrl Pts',(37.1407133930137,5.68269568186778,132.45954924896));
#178767=CARTESIAN_POINT('Ctrl Pts',(37.1481278857347,5.63470298458015,132.609368328924));
#178768=CARTESIAN_POINT('Ctrl Pts',(37.1555352320885,5.58675654446106,132.759043007619));
#178769=CARTESIAN_POINT('Ctrl Pts',(37.1629425784423,5.53279331760733,132.906958766367));
#178770=CARTESIAN_POINT('Ctrl Pts',(37.1703499247961,5.4729659293069,133.052598705302));
#178771=CARTESIAN_POINT('Ctrl Pts',(37.1777517464715,5.41318316252982,133.198130020475));
#178772=CARTESIAN_POINT('Ctrl Pts',(37.1851535681469,5.34754508419324,133.341388551759));
#178773=CARTESIAN_POINT('Ctrl Pts',(37.1925553898223,5.27625369249818,133.481873929372));
#178774=CARTESIAN_POINT('Ctrl Pts',(37.1999533041337,5.20499993497386,133.622285145848));
#178775=CARTESIAN_POINT('Ctrl Pts',(37.207351218445,5.12809897604868,133.759925792089));
#178776=CARTESIAN_POINT('Ctrl Pts',(37.2147491327564,5.04580029735864,133.894316915263));
#178777=CARTESIAN_POINT('Ctrl Pts',(37.2221458176686,4.96351529521606,134.02868570507));
#178778=CARTESIAN_POINT('Ctrl Pts',(37.2295425025809,4.87583454835409,134.159805725539));
#178779=CARTESIAN_POINT('Ctrl Pts',(37.2369391874931,4.78305277157969,134.287223914737));
#178780=CARTESIAN_POINT('Ctrl Pts',(37.2443355444285,4.69027510884636,134.41463645408));
#178781=CARTESIAN_POINT('Ctrl Pts',(37.251731901364,4.59239708567242,134.538347186755));
#178782=CARTESIAN_POINT('Ctrl Pts',(37.2591282582995,4.48975574661072,134.657933491961));
#178783=CARTESIAN_POINT('Ctrl Pts',(37.266525747636,4.38709869289799,134.777538106136));
#178784=CARTESIAN_POINT('Ctrl Pts',(37.2739232369726,4.27967711435648,134.893016752237));
#178785=CARTESIAN_POINT('Ctrl Pts',(37.2813207263092,4.16786709044987,135.003981371735));
#178786=CARTESIAN_POINT('Ctrl Pts',(37.2887208088242,4.05601787171271,135.114984889708));
#178787=CARTESIAN_POINT('Ctrl Pts',(37.2961208913392,3.93977740953756,135.221470967769));
#178788=CARTESIAN_POINT('Ctrl Pts',(37.3035209738543,3.81955711339041,135.323089865933));
#178789=CARTESIAN_POINT('Ctrl Pts',(37.3109291935207,3.69920462266887,135.424820504523));
#178790=CARTESIAN_POINT('Ctrl Pts',(37.3183374131872,3.57486384361288,135.521673033861));
#178791=CARTESIAN_POINT('Ctrl Pts',(37.3257456328536,3.44697818169413,135.61333888508));
#178792=CARTESIAN_POINT('Ctrl Pts',(37.3331584121557,3.31901380828399,135.705061155101));
#178793=CARTESIAN_POINT('Ctrl Pts',(37.3405711914578,3.18750051559732,135.791590181211));
#178794=CARTESIAN_POINT('Ctrl Pts',(37.3479839707599,3.05290843766486,135.872662170723));
#178795=CARTESIAN_POINT('Ctrl Pts',(37.3554073417886,2.91812404825991,135.953849999696));
#178796=CARTESIAN_POINT('Ctrl Pts',(37.3628307128174,2.78025241393159,136.02956503996));
#178797=CARTESIAN_POINT('Ctrl Pts',(37.3702540838461,2.63978660528028,136.099590285964));
#178798=CARTESIAN_POINT('Ctrl Pts',(37.3741901332869,2.56530826310386,136.136719351627));
#178799=CARTESIAN_POINT('Ctrl Pts',(37.3781261827276,2.49010092212003,136.172249623619));
#178800=CARTESIAN_POINT('Ctrl Pts',(37.3820622321684,2.41423994751945,136.206154397256));
#178801=CARTESIAN_POINT('Ctrl Pts',(37.3894854985738,2.27116851696018,136.270097742207));
#178802=CARTESIAN_POINT('Ctrl Pts',(37.3969087649793,2.12533859458309,136.328449785029));
#178803=CARTESIAN_POINT('Ctrl Pts',(37.4043320313847,1.97722719635829,136.380963810952));
#178804=CARTESIAN_POINT('Ctrl Pts',(37.4117465241057,1.8292908535063,136.433415769657));
#178805=CARTESIAN_POINT('Ctrl Pts',(37.4191610168267,1.67907875063627,136.480043322525));
#178806=CARTESIAN_POINT('Ctrl Pts',(37.4265755095477,1.52709049039462,136.520646579329));
#178807=CARTESIAN_POINT('Ctrl Pts',(37.4339828559015,1.37524872216024,136.561210701185));
#178808=CARTESIAN_POINT('Ctrl Pts',(37.4413902022553,1.22163456289373,136.595761990761));
#178809=CARTESIAN_POINT('Ctrl Pts',(37.4487975486091,1.06676539278921,136.624149459032));
#178810=CARTESIAN_POINT('Ctrl Pts',(37.4561993702845,0.912011729954633,
136.652515754857));
#178811=CARTESIAN_POINT('Ctrl Pts',(37.4636011919599,0.75600528565307,136.674727316029));
#178812=CARTESIAN_POINT('Ctrl Pts',(37.4710030136353,0.599276220113848,
136.690683627265));
#178813=CARTESIAN_POINT('Ctrl Pts',(37.4784009279467,0.44262989062857,136.706631515288));
#178814=CARTESIAN_POINT('Ctrl Pts',(37.485798842258,0.28526207005183,136.716330691948));
#178815=CARTESIAN_POINT('Ctrl Pts',(37.4931967565693,0.127710565882259,
136.719732167508));
#178816=CARTESIAN_POINT('Ctrl Pts',(37.5005934414816,-0.0298147560858202,
136.723133077804));
#178817=CARTESIAN_POINT('Ctrl Pts',(37.5079901263939,-0.187523328218363,
136.720238356069));
#178818=CARTESIAN_POINT('Ctrl Pts',(37.5153868113061,-0.344874676129766,
136.711051063176));
#178819=CARTESIAN_POINT('Ctrl Pts',(37.5227831682415,-0.50221904691751,
136.701864177658));
#178820=CARTESIAN_POINT('Ctrl Pts',(37.530179525177,-0.659205852315889,
136.686385297525));
#178821=CARTESIAN_POINT('Ctrl Pts',(37.5375758821124,-0.815297348663056,
136.664669551041));
#178822=CARTESIAN_POINT('Ctrl Pts',(37.544973371449,-0.971412743016796,
136.64295047982));
#178823=CARTESIAN_POINT('Ctrl Pts',(37.5523708607856,-1.12663218562586,
136.614992692396));
#178824=CARTESIAN_POINT('Ctrl Pts',(37.5597683501222,-1.28042591172418,
136.580902839959));
#178825=CARTESIAN_POINT('Ctrl Pts',(37.5671684326372,-1.43427354997455,
136.546801037377));
#178826=CARTESIAN_POINT('Ctrl Pts',(37.5745685151522,-1.58669411242584,
136.506562970707));
#178827=CARTESIAN_POINT('Ctrl Pts',(37.5819685976672,-1.73717097605971,
136.46034572738));
#178828=CARTESIAN_POINT('Ctrl Pts',(37.5893768173337,-1.88781330447453,
136.414077663443));
#178829=CARTESIAN_POINT('Ctrl Pts',(37.5967850370001,-2.03650730868539,
136.361817402371));
#178830=CARTESIAN_POINT('Ctrl Pts',(37.6041932566666,-2.18275370947581,
136.303771204735));
#178831=CARTESIAN_POINT('Ctrl Pts',(37.6116060359687,-2.32909012248588,
136.245689280633));
#178832=CARTESIAN_POINT('Ctrl Pts',(37.6190188152708,-2.47297558986873,
136.181814475047));
#178833=CARTESIAN_POINT('Ctrl Pts',(37.6264315945728,-2.61393405644007,
136.112399738662));
#178834=CARTESIAN_POINT('Ctrl Pts',(37.6338549656016,-2.75509393107895,
136.042885819246));
#178835=CARTESIAN_POINT('Ctrl Pts',(37.6412783366304,-2.8933181248711,135.967816337263));
#178836=CARTESIAN_POINT('Ctrl Pts',(37.6487017076592,-3.02815754819667,
135.887488830173));
#178837=CARTESIAN_POINT('Ctrl Pts',(37.6526377570999,-3.09965264586894,
135.844897258483));
#178838=CARTESIAN_POINT('Ctrl Pts',(37.6565738065405,-3.17019667480669,
135.800828172418));
#178839=CARTESIAN_POINT('Ctrl Pts',(37.6605098559812,-3.2397264308791,135.755330544314));
#178840=CARTESIAN_POINT('Ctrl Pts',(37.6679221115746,-3.37066287645052,
135.669650713946));
#178841=CARTESIAN_POINT('Ctrl Pts',(37.675334367168,-3.49839897233822,135.578641572179));
#178842=CARTESIAN_POINT('Ctrl Pts',(37.6827466227614,-3.62247011547864,
135.482569764768));
#178843=CARTESIAN_POINT('Ctrl Pts',(37.6901501101258,-3.74639449031427,
135.386611604221));
#178844=CARTESIAN_POINT('Ctrl Pts',(37.6975535974902,-3.86666224837065,
135.285602925195));
#178845=CARTESIAN_POINT('Ctrl Pts',(37.7049570848546,-3.98283590640176,
135.179854727398));
#178846=CARTESIAN_POINT('Ctrl Pts',(37.7123534420334,-4.09889767935609,
135.074208374077));
#178847=CARTESIAN_POINT('Ctrl Pts',(37.7197497992122,-4.21087292643776,
134.963831839071));
#178848=CARTESIAN_POINT('Ctrl Pts',(37.7271461563909,-4.3183556485216,134.849077548994));
#178849=CARTESIAN_POINT('Ctrl Pts',(37.734537015717,-4.42575847665778,134.734408557959));
#178850=CARTESIAN_POINT('Ctrl Pts',(37.7419278750431,-4.52867517368807,
134.615368563017));
#178851=CARTESIAN_POINT('Ctrl Pts',(37.7493187343692,-4.6267352650982,134.492348056427));
#178852=CARTESIAN_POINT('Ctrl Pts',(37.756705723756,-4.72474401111272,134.369391964794));
#178853=CARTESIAN_POINT('Ctrl Pts',(37.7640927131428,-4.81790098287275,
134.242459804359));
#178854=CARTESIAN_POINT('Ctrl Pts',(37.7714797025296,-4.90587490393759,
134.111976373577));
#178855=CARTESIAN_POINT('Ctrl Pts',(37.7788655139203,-4.9938347958847,133.981513750864));
#178856=CARTESIAN_POINT('Ctrl Pts',(37.7862513253109,-5.07661306799916,
133.847501291781));
#178857=CARTESIAN_POINT('Ctrl Pts',(37.7936371367016,-5.15392078710318,
133.710394182886));
#178858=CARTESIAN_POINT('Ctrl Pts',(37.8010226735015,-5.2312256320508,133.573292171376));
#178859=CARTESIAN_POINT('Ctrl Pts',(37.8084082103015,-5.30306014434898,
133.433096065046));
#178860=CARTESIAN_POINT('Ctrl Pts',(37.8157937471015,-5.36918067557369,
133.290286890718));
#178861=CARTESIAN_POINT('Ctrl Pts',(37.8231804792538,-5.43531190843543,
133.147454602662));
#178862=CARTESIAN_POINT('Ctrl Pts',(37.8305672114062,-5.49572716160444,
133.002008744488));
#178863=CARTESIAN_POINT('Ctrl Pts',(37.8379539435586,-5.55023045568705,
132.854451457325));
#178864=CARTESIAN_POINT('Ctrl Pts',(37.8453433414564,-5.60475341907727,
132.706840919258));
#178865=CARTESIAN_POINT('Ctrl Pts',(37.8527327393541,-5.65336004616993,
132.557117786319));
#178866=CARTESIAN_POINT('Ctrl Pts',(37.8601221372519,-5.69590390508168,
132.405800365598));
#178867=CARTESIAN_POINT('Ctrl Pts',(37.8675196661198,-5.7384945773941,132.254316441808));
#178868=CARTESIAN_POINT('Ctrl Pts',(37.8749171949877,-5.77500905850871,
132.101235087859));
#178869=CARTESIAN_POINT('Ctrl Pts',(37.8823147238556,-5.80535167515036,
131.947086520978));
#178870=CARTESIAN_POINT('Ctrl Pts',(37.8897168959795,-5.83571333714352,
131.792841198643));
#178871=CARTESIAN_POINT('Ctrl Pts',(37.8971190681034,-5.85989535865037,
131.637527697812));
#178872=CARTESIAN_POINT('Ctrl Pts',(37.9045212402273,-5.87785390268125,
131.481681856887));
#178873=CARTESIAN_POINT('Ctrl Pts',(37.911933808771,-5.89583766965469,131.325617129025));
#178874=CARTESIAN_POINT('Ctrl Pts',(37.9193463773147,-5.90758047647729,
131.16901894028));
#178875=CARTESIAN_POINT('Ctrl Pts',(37.9267589458584,-5.91309056511575,
131.012424384809));
#178876=CARTESIAN_POINT('Ctrl Pts',(37.9300475665041,-5.91553514166833,
130.94295047909));
#178877=CARTESIAN_POINT('Ctrl Pts',(37.9333361871498,-5.91675362238445,
130.873477241184));
#178878=CARTESIAN_POINT('Ctrl Pts',(37.9366248077955,-5.91674999191025,
130.804051214748));
#178879=CARTESIAN_POINT('',(39.6866240381297,-5.91498544959244,130.809720579457));
#178880=CARTESIAN_POINT('Ctrl Pts',(37.9366248077955,-5.92651271267239,
130.804050704229));
#178881=CARTESIAN_POINT('Ctrl Pts',(37.9374023651284,-5.92652516855156,
130.787608616101));
#178882=CARTESIAN_POINT('Ctrl Pts',(37.9381799224613,-5.92646268754296,
130.771166625385));
#178883=CARTESIAN_POINT('Ctrl Pts',(38.0317733543984,-5.90988757984946,
128.792144232197));
#178884=CARTESIAN_POINT('Ctrl Pts',(38.217405103607,-3.7333596383727,124.884936123503));
#178885=CARTESIAN_POINT('Ctrl Pts',(38.4958527274199,2.96220739674919,124.46378589054));
#178886=CARTESIAN_POINT('Ctrl Pts',(38.7743003512328,6.93565054613509,129.869314077418));
#178887=CARTESIAN_POINT('Ctrl Pts',(39.0527479750457,4.53556966898844,136.134104355128));
#178888=CARTESIAN_POINT('Ctrl Pts',(39.3311955988587,-2.03247815906468,
137.501120510476));
#178889=CARTESIAN_POINT('Ctrl Pts',(39.5424875011082,-5.59916423616403,
133.868660331039));
#178890=CARTESIAN_POINT('Ctrl Pts',(39.6609635287535,-5.91891885957568,
131.355273964503));
#178891=CARTESIAN_POINT('Ctrl Pts',(39.6866236817946,-5.9141696267495,130.80972741823));
#178892=CARTESIAN_POINT('',(41.4366255671013,-5.91167177449429,130.80237612265));
#178893=CARTESIAN_POINT('Ctrl Pts',(39.6866248077955,-5.91674758557763,
130.809705808054));
#178894=CARTESIAN_POINT('Ctrl Pts',(39.6939603857742,-5.91688853801437,
130.653681435918));
#178895=CARTESIAN_POINT('Ctrl Pts',(39.701295963753,-5.91085373526745,130.497522968287));
#178896=CARTESIAN_POINT('Ctrl Pts',(39.7086315417317,-5.89863824892961,
130.34176211912));
#178897=CARTESIAN_POINT('Ctrl Pts',(39.716109012763,-5.88618647682792,130.182988367297));
#178898=CARTESIAN_POINT('Ctrl Pts',(39.7235864837944,-5.86731242361618,
130.024628175413));
#178899=CARTESIAN_POINT('Ctrl Pts',(39.7310639548258,-5.84206663858188,
129.867243787673));
#178900=CARTESIAN_POINT('Ctrl Pts',(39.7383948603265,-5.81731569490013,
129.712944283338));
#178901=CARTESIAN_POINT('Ctrl Pts',(39.7457257658273,-5.78644057510626,
129.55958307169));
#178902=CARTESIAN_POINT('Ctrl Pts',(39.7530566713281,-5.74954111903638,
129.407683316609));
#178903=CARTESIAN_POINT('Ctrl Pts',(39.7603875560361,-5.71264176762486,
129.255783992362));
#178904=CARTESIAN_POINT('Ctrl Pts',(39.7677184407442,-5.66971820337799,
129.105346486387));
#178905=CARTESIAN_POINT('Ctrl Pts',(39.7750493254522,-5.62092094437509,
128.956881713874));
#178906=CARTESIAN_POINT('Ctrl Pts',(39.7823816999613,-5.57211376866862,
128.808386769972));
#178907=CARTESIAN_POINT('Ctrl Pts',(39.7897140744705,-5.51743064147151,
128.661865718906));
#178908=CARTESIAN_POINT('Ctrl Pts',(39.7970464489796,-5.45707122236629,
128.517812075216));
#178909=CARTESIAN_POINT('Ctrl Pts',(39.804633482105,-5.39461547742173,128.368755345348));
#178910=CARTESIAN_POINT('Ctrl Pts',(39.8122205152304,-5.32608221199373,
128.222340914693));
#178911=CARTESIAN_POINT('Ctrl Pts',(39.8198075483558,-5.2517452856169,128.079089618656));
#178912=CARTESIAN_POINT('Ctrl Pts',(39.8271512980281,-5.17979202408456,
127.940431774284));
#178913=CARTESIAN_POINT('Ctrl Pts',(39.8344950477005,-5.10240180354443,
127.804737635045));
#178914=CARTESIAN_POINT('Ctrl Pts',(39.8418387973729,-5.01986775780857,
127.672450935501));
#178915=CARTESIAN_POINT('Ctrl Pts',(39.8495474722248,-4.93323243509578,
127.533590653014));
#178916=CARTESIAN_POINT('Ctrl Pts',(39.8572561470767,-4.84092929066518,
127.398485515014));
#178917=CARTESIAN_POINT('Ctrl Pts',(39.8649648219286,-4.74334534328168,
127.267609917154));
#178918=CARTESIAN_POINT('Ctrl Pts',(39.8726734967805,-4.64576139589804,
127.136734319293));
#178919=CARTESIAN_POINT('Ctrl Pts',(39.8803821716324,-4.54289700502975,
127.010088583274));
#178920=CARTESIAN_POINT('Ctrl Pts',(39.8880908464843,-4.43518330710743,
126.888102250852));
#178921=CARTESIAN_POINT('Ctrl Pts',(39.8955141128897,-4.33145763563316,
126.770632379469));
#178922=CARTESIAN_POINT('Ctrl Pts',(39.9029373792952,-4.22290495060319,
126.657108629819));
#178923=CARTESIAN_POINT('Ctrl Pts',(39.9103606457006,-4.10985719789727,
126.547953168156));
#178924=CARTESIAN_POINT('Ctrl Pts',(39.9177751384216,-3.99694305824686,
126.438926719184));
#178925=CARTESIAN_POINT('Ctrl Pts',(39.9251896311426,-3.87954469199329,
126.334258538078));
#178926=CARTESIAN_POINT('Ctrl Pts',(39.9326041238636,-3.75803400081586,
126.234337531058));
#178927=CARTESIAN_POINT('Ctrl Pts',(39.9400114702173,-3.63664042621773,
126.134512831667));
#178928=CARTESIAN_POINT('Ctrl Pts',(39.9474188165711,-3.51114270386505,
126.039426432942));
#178929=CARTESIAN_POINT('Ctrl Pts',(39.9548261629248,-3.38194917453696,
125.949430098666));
#178930=CARTESIAN_POINT('Ctrl Pts',(39.9622279846002,-3.25285200261651,
125.859500887051));
#178931=CARTESIAN_POINT('Ctrl Pts',(39.9696298062757,-3.12006481721647,
125.77465439327));
#178932=CARTESIAN_POINT('Ctrl Pts',(39.9770316279511,-2.98402850121463,
125.695201737042));
#178933=CARTESIAN_POINT('Ctrl Pts',(39.9844295422624,-2.84806399772568,
125.615791023253));
#178934=CARTESIAN_POINT('Ctrl Pts',(39.9918274565738,-2.70885410104915,
125.541768664143));
#178935=CARTESIAN_POINT('Ctrl Pts',(39.9992253708851,-2.56686800032308,
125.473402051659));
#178936=CARTESIAN_POINT('Ctrl Pts',(40.0066220557973,-2.42490549511085,
125.405046800465));
#178937=CARTESIAN_POINT('Ctrl Pts',(40.0140187407095,-2.28016803751169,
125.342345592298));
#178938=CARTESIAN_POINT('Ctrl Pts',(40.0214154256217,-2.13314880756229,
125.285519550159));
#178939=CARTESIAN_POINT('Ctrl Pts',(40.0288117825571,-1.98613609659962,
125.228696027746));
#178940=CARTESIAN_POINT('Ctrl Pts',(40.0362081394926,-1.83684216265196,
125.177747287962));
#178941=CARTESIAN_POINT('Ctrl Pts',(40.0436044964281,-1.68577927097773,
125.132845933459));
#178942=CARTESIAN_POINT('Ctrl Pts',(40.0510019857646,-1.53469325118937,
125.087937704444));
#178943=CARTESIAN_POINT('Ctrl Pts',(40.0583994751012,-1.3818380922606,125.049078810608));
#178944=CARTESIAN_POINT('Ctrl Pts',(40.0657969644377,-1.22774014249539,
125.016391655572));
#178945=CARTESIAN_POINT('Ctrl Pts',(40.0731970469527,-1.07358817393255,
124.983693042105));
#178946=CARTESIAN_POINT('Ctrl Pts',(40.0805971294677,-0.918192912085663,
124.95717055235));
#178947=CARTESIAN_POINT('Ctrl Pts',(40.0879972119827,-0.762089639146931,
124.936895241068));
#178948=CARTESIAN_POINT('Ctrl Pts',(40.0954054316492,-0.605814714611795,
124.916597634997));
#178949=CARTESIAN_POINT('Ctrl Pts',(40.1028136513156,-0.448830594622927,
124.902560974183));
#178950=CARTESIAN_POINT('Ctrl Pts',(40.1102218709821,-0.291677147486677,
124.894804373301));
#178951=CARTESIAN_POINT('Ctrl Pts',(40.1176346502841,-0.134426975026185,
124.88704299836));
#178952=CARTESIAN_POINT('Ctrl Pts',(40.1250474295862,0.0229923598331128,
124.885569388876));
#178953=CARTESIAN_POINT('Ctrl Pts',(40.1324602088882,0.180042783226127,
124.890350543284));
#178954=CARTESIAN_POINT('Ctrl Pts',(40.1398835799169,0.337317607629243,
124.89513852923));
#178955=CARTESIAN_POINT('Ctrl Pts',(40.1473069509458,0.494222096405806,
124.90619910228));
#178956=CARTESIAN_POINT('Ctrl Pts',(40.1547303219745,0.650224246858324,
124.923447508932));
#178957=CARTESIAN_POINT('Ctrl Pts',(40.1586663714154,0.732940330251242,
124.93259302801));
#178958=CARTESIAN_POINT('Ctrl Pts',(40.1626024208563,0.81540290755164,124.943477315367));
#178959=CARTESIAN_POINT('Ctrl Pts',(40.1665384702972,0.897534165250741,
124.956081983241));
#178960=CARTESIAN_POINT('Ctrl Pts',(40.1739617367026,1.05243115403726,124.979853993472));
#178961=CARTESIAN_POINT('Ctrl Pts',(40.1813850031081,1.20661727758316,125.009820082102));
#178962=CARTESIAN_POINT('Ctrl Pts',(40.1888082695135,1.35955793060564,125.045929164833));
#178963=CARTESIAN_POINT('Ctrl Pts',(40.1962227622345,1.51231782047762,125.081995569627));
#178964=CARTESIAN_POINT('Ctrl Pts',(40.2036372549555,1.66383481017379,125.1241904315));
#178965=CARTESIAN_POINT('Ctrl Pts',(40.2110517476765,1.81358067993473,125.172411072349));
#178966=CARTESIAN_POINT('Ctrl Pts',(40.2184590940303,1.96318221898834,125.220585236329));
#178967=CARTESIAN_POINT('Ctrl Pts',(40.2258664403841,2.11101568360718,125.274773503299));
#178968=CARTESIAN_POINT('Ctrl Pts',(40.2332737867379,2.25656440679198,125.334822461515));
#178969=CARTESIAN_POINT('Ctrl Pts',(40.2406756084133,2.40200457424758,125.394826632952));
#178970=CARTESIAN_POINT('Ctrl Pts',(40.2480774300886,2.54516304965807,125.460682650378));
#178971=CARTESIAN_POINT('Ctrl Pts',(40.255479251764,2.68553977122917,125.532187754349));
#178972=CARTESIAN_POINT('Ctrl Pts',(40.2628771660754,2.82584238902285,125.603655111332));
#178973=CARTESIAN_POINT('Ctrl Pts',(40.2702750803868,2.96336584570946,125.68076544684));
#178974=CARTESIAN_POINT('Ctrl Pts',(40.2776729946982,3.09763156868231,125.763268550642));
#178975=CARTESIAN_POINT('Ctrl Pts',(40.2850696796104,3.23187497912706,125.845757943925));
#178976=CARTESIAN_POINT('Ctrl Pts',(40.2924663645227,3.36286141258997,125.933638131604));
#178977=CARTESIAN_POINT('Ctrl Pts',(40.2998630494349,3.4901382561708,126.026613709732));
#178978=CARTESIAN_POINT('Ctrl Pts',(40.3072594063703,3.61740945616265,126.119585165226));
#178979=CARTESIAN_POINT('Ctrl Pts',(40.3146557633057,3.74097109189239,126.217651341734));
#178980=CARTESIAN_POINT('Ctrl Pts',(40.3220521202412,3.8604010559739,126.320474551938));
#178981=CARTESIAN_POINT('Ctrl Pts',(40.3294496095777,3.97984930508813,126.423313504638));
#178982=CARTESIAN_POINT('Ctrl Pts',(40.3368470989143,4.0951643401099,126.530910697628));
#178983=CARTESIAN_POINT('Ctrl Pts',(40.3442445882509,4.20595867528984,126.642889461322));
#178984=CARTESIAN_POINT('Ctrl Pts',(40.3516446707659,4.3167918492519,126.754907478997));
#178985=CARTESIAN_POINT('Ctrl Pts',(40.3590447532808,4.42310090580708,126.871309860251));
#178986=CARTESIAN_POINT('Ctrl Pts',(40.3664448357958,4.52453673147266,126.991684663849));
#178987=CARTESIAN_POINT('Ctrl Pts',(40.3738530554623,4.62608409625671,127.112191831918));
#178988=CARTESIAN_POINT('Ctrl Pts',(40.3812612751288,4.7227472879426,127.236679860052));
#178989=CARTESIAN_POINT('Ctrl Pts',(40.3886694947953,4.81421841280676,127.364704873703));
#178990=CARTESIAN_POINT('Ctrl Pts',(40.3960822740973,4.905745836622,127.492808684613));
#178991=CARTESIAN_POINT('Ctrl Pts',(40.4034950533994,4.99207462168811,127.624453507457));
#178992=CARTESIAN_POINT('Ctrl Pts',(40.4109078327014,5.07294169108934,127.759168807301));
#178993=CARTESIAN_POINT('Ctrl Pts',(40.4183312037302,5.15392430715175,127.894076594683));
#178994=CARTESIAN_POINT('Ctrl Pts',(40.425754574759,5.22942944258174,128.03206329476));
#178995=CARTESIAN_POINT('Ctrl Pts',(40.4331779457878,5.29924084244862,128.172635507258));
#178996=CARTESIAN_POINT('Ctrl Pts',(40.4371139952286,5.33625652175943,128.247170267308));
#178997=CARTESIAN_POINT('Ctrl Pts',(40.4410500446693,5.37167229983716,128.32243159223));
#178998=CARTESIAN_POINT('Ctrl Pts',(40.4449860941101,5.40546158672476,128.39834407628));
#178999=CARTESIAN_POINT('Ctrl Pts',(40.4524093605156,5.46918712726751,128.541512652051));
#179000=CARTESIAN_POINT('Ctrl Pts',(40.459832626921,5.5273171742017,128.687431207435));
#179001=CARTESIAN_POINT('Ctrl Pts',(40.4672558933265,5.57960573897948,128.835622351557));
#179002=CARTESIAN_POINT('Ctrl Pts',(40.4746703860475,5.63183250301585,128.983638346053));
#179003=CARTESIAN_POINT('Ctrl Pts',(40.4820848787685,5.67823140463998,129.133921234178));
#179004=CARTESIAN_POINT('Ctrl Pts',(40.4894993714894,5.71860331416626,129.285971109664));
#179005=CARTESIAN_POINT('Ctrl Pts',(40.4969067178432,5.75893631172639,129.437874433757));
#179006=CARTESIAN_POINT('Ctrl Pts',(40.504314064197,5.79325378669266,129.591540996322));
#179007=CARTESIAN_POINT('Ctrl Pts',(40.5117214105508,5.82140553757743,129.746453187985));
#179008=CARTESIAN_POINT('Ctrl Pts',(40.5191232322262,5.84953629182421,129.901249840291));
#179009=CARTESIAN_POINT('Ctrl Pts',(40.5265250539017,5.87151041202376,130.057289906154));
#179010=CARTESIAN_POINT('Ctrl Pts',(40.5339268755771,5.88722818982492,130.214043072993));
#179011=CARTESIAN_POINT('Ctrl Pts',(40.5413247898884,5.90293767033347,130.370713491055));
#179012=CARTESIAN_POINT('Ctrl Pts',(40.5487227041997,5.91239734872819,130.528095889897));
#179013=CARTESIAN_POINT('Ctrl Pts',(40.5561206185111,5.9155590537797,130.685652388091));
#179014=CARTESIAN_POINT('Ctrl Pts',(40.5635173034233,5.9187202334132,130.843182703254));
#179015=CARTESIAN_POINT('Ctrl Pts',(40.5709139883355,5.91558550943023,131.000886687489));
#179016=CARTESIAN_POINT('Ctrl Pts',(40.5783106732477,5.90615876521095,131.158223871694));
#179017=CARTESIAN_POINT('Ctrl Pts',(40.5857070301832,5.8967324389834,131.315554079403));
#179018=CARTESIAN_POINT('Ctrl Pts',(40.5931033871186,5.88101466958121,131.472517146792));
#179019=CARTESIAN_POINT('Ctrl Pts',(40.600499744054,5.85906140355735,131.628575414718));
#179020=CARTESIAN_POINT('Ctrl Pts',(40.6078972333906,5.83710477643234,131.784657575564));
#179021=CARTESIAN_POINT('Ctrl Pts',(40.6152947227272,5.80891080381423,131.939834291438));
#179022=CARTESIAN_POINT('Ctrl Pts',(40.6226922120638,5.77458694298216,132.093575960494));
#179023=CARTESIAN_POINT('Ctrl Pts',(40.6300922945788,5.74025104997384,132.247371523453));
#179024=CARTESIAN_POINT('Ctrl Pts',(40.6374923770939,5.69978107174915,132.399730673917));
#179025=CARTESIAN_POINT('Ctrl Pts',(40.6448924596089,5.65333488177034,132.550137028524));
#179026=CARTESIAN_POINT('Ctrl Pts',(40.6523006792754,5.60683761943092,132.700708770381));
#179027=CARTESIAN_POINT('Ctrl Pts',(40.6597088989418,5.55435113191353,132.849323071186));
#179028=CARTESIAN_POINT('Ctrl Pts',(40.6671171186083,5.4960824393679,132.995480966194));
#179029=CARTESIAN_POINT('Ctrl Pts',(40.6745298979104,5.43777788341435,133.141728818948));
#179030=CARTESIAN_POINT('Ctrl Pts',(40.6819426772125,5.37368418260655,133.285516913133));
#179031=CARTESIAN_POINT('Ctrl Pts',(40.6893554565146,5.30405501181169,133.426369579064));
#179032=CARTESIAN_POINT('Ctrl Pts',(40.6967788275433,5.23432635159222,133.56742350189));
#179033=CARTESIAN_POINT('Ctrl Pts',(40.7042021985721,5.15904660284588,133.705533292648));
#179034=CARTESIAN_POINT('Ctrl Pts',(40.7116255696009,5.07851398612542,133.84025031504));
#179035=CARTESIAN_POINT('Ctrl Pts',(40.7155616190416,5.03581366038748,133.911680512801));
#179036=CARTESIAN_POINT('Ctrl Pts',(40.7194976684823,4.99163726934961,133.982157394404));
#179037=CARTESIAN_POINT('Ctrl Pts',(40.723433717923,4.94603388147802,134.051617830318));
#179038=CARTESIAN_POINT('Ctrl Pts',(40.7308569843284,4.86002731518371,134.182618044669));
#179039=CARTESIAN_POINT('Ctrl Pts',(40.7382802507339,4.76868261218417,134.310397042927));
#179040=CARTESIAN_POINT('Ctrl Pts',(40.7457035171393,4.67226845212472,134.434489826531));
#179041=CARTESIAN_POINT('Ctrl Pts',(40.7531180098603,4.57596824559563,134.55843594277));
#179042=CARTESIAN_POINT('Ctrl Pts',(40.7605325025813,4.4746107352678,134.678704224687));
#179043=CARTESIAN_POINT('Ctrl Pts',(40.7679469953023,4.36850887198248,134.794856927289));
#179044=CARTESIAN_POINT('Ctrl Pts',(40.7753543416561,4.26250927366765,134.910897677542));
#179045=CARTESIAN_POINT('Ctrl Pts',(40.7827616880099,4.15177467598909,135.022830471733));
#179046=CARTESIAN_POINT('Ctrl Pts',(40.7901690343636,4.03665937080015,135.130249160586));
#179047=CARTESIAN_POINT('Ctrl Pts',(40.797570856039,3.92162992294871,135.237587732528));
#179048=CARTESIAN_POINT('Ctrl Pts',(40.8049726777144,3.80222654496907,135.340418649281));
#179049=CARTESIAN_POINT('Ctrl Pts',(40.8123744993898,3.67884150905682,135.438371376481));
#179050=CARTESIAN_POINT('Ctrl Pts',(40.8197724137012,3.55552160714426,135.536272395199));
#179051=CARTESIAN_POINT('Ctrl Pts',(40.8271703280126,3.42822452493381,135.629300121399));
#179052=CARTESIAN_POINT('Ctrl Pts',(40.834568242324,3.29737675957992,135.717123289208));
#179053=CARTESIAN_POINT('Ctrl Pts',(40.8419649272362,3.16655073875137,135.8049318624));
#179054=CARTESIAN_POINT('Ctrl Pts',(40.8493616121484,3.03217551552328,135.887537385946));
#179055=CARTESIAN_POINT('Ctrl Pts',(40.8567582970606,2.89470790091954,135.964650990293));
#179056=CARTESIAN_POINT('Ctrl Pts',(40.864154653996,2.75724638177389,136.041761175341));
#179057=CARTESIAN_POINT('Ctrl Pts',(40.8715510109314,2.61669306946448,136.113379742752));
#179058=CARTESIAN_POINT('Ctrl Pts',(40.8789473678669,2.47353055233435,136.179263144047));
#179059=CARTESIAN_POINT('Ctrl Pts',(40.8863448572035,2.33034611665716,136.245156632258));
#179060=CARTESIAN_POINT('Ctrl Pts',(40.8937423465401,2.18455201988314,136.305313049932));
#179061=CARTESIAN_POINT('Ctrl Pts',(40.9011398358766,2.03665191433,136.359536541185));
#179062=CARTESIAN_POINT('Ctrl Pts',(40.9085399183916,1.88869996262476,136.413779040399));
#179063=CARTESIAN_POINT('Ctrl Pts',(40.9159400009066,1.73864088254088,136.462084343953));
#179064=CARTESIAN_POINT('Ctrl Pts',(40.9233400834216,1.58699445648627,136.504306157445));
#179065=CARTESIAN_POINT('Ctrl Pts',(40.930748303088,1.43518127959615,136.54657439816));
#179066=CARTESIAN_POINT('Ctrl Pts',(40.9381565227545,1.2817776307969,136.582745689409));
#179067=CARTESIAN_POINT('Ctrl Pts',(40.9455647424209,1.12731520270745,136.612724500472));
#179068=CARTESIAN_POINT('Ctrl Pts',(40.952977521723,0.972757705570631,136.642721762993));
#179069=CARTESIAN_POINT('Ctrl Pts',(40.9603903010251,0.817140498780058,
136.666518894402));
#179070=CARTESIAN_POINT('Ctrl Pts',(40.9678030803271,0.661000894175588,
136.684072207466));
#179071=CARTESIAN_POINT('Ctrl Pts',(40.9752264513559,0.504638189981837,
136.701650601526));
#179072=CARTESIAN_POINT('Ctrl Pts',(40.9826498223847,0.347751968537191,
136.712967332296));
#179073=CARTESIAN_POINT('Ctrl Pts',(40.9900731934134,0.190880875758771,
136.718030802296));
#179074=CARTESIAN_POINT('Ctrl Pts',(40.9940092428542,0.107704058296784,
136.720715575587));
#179075=CARTESIAN_POINT('Ctrl Pts',(40.9979452922951,0.0245314433688089,
136.721643202666));
#179076=CARTESIAN_POINT('Ctrl Pts',(41.0018813417359,-0.0585573336590143,
136.720820843172));
#179077=CARTESIAN_POINT('Ctrl Pts',(41.0093046081413,-0.215260174020292,
136.71926989883));
#179078=CARTESIAN_POINT('Ctrl Pts',(41.0167278745468,-0.372138307333893,
136.711486682914));
#179079=CARTESIAN_POINT('Ctrl Pts',(41.0241511409522,-0.528655289229605,
136.697445900138));
#179080=CARTESIAN_POINT('Ctrl Pts',(41.0315656336732,-0.684987281050643,
136.683421712401));
#179081=CARTESIAN_POINT('Ctrl Pts',(41.0389801263942,-0.840958602928902,
136.663154712461));
#179082=CARTESIAN_POINT('Ctrl Pts',(41.0463946191152,-0.996031810030865,
136.636671582862));
#179083=CARTESIAN_POINT('Ctrl Pts',(41.053801965469,-1.15095555173808,136.6102139787));
#179084=CARTESIAN_POINT('Ctrl Pts',(41.0612093118228,-1.30498253648128,
136.577552234876));
#179085=CARTESIAN_POINT('Ctrl Pts',(41.0686166581766,-1.45757955597116,
136.538764893558));
#179086=CARTESIAN_POINT('Ctrl Pts',(41.076018479852,-1.61006276284655,136.500006481302));
#179087=CARTESIAN_POINT('Ctrl Pts',(41.0834203015274,-1.76111776782164,
136.455131660018));
#179088=CARTESIAN_POINT('Ctrl Pts',(41.0908221232029,-1.91022079713827,
136.404270176539));
#179089=CARTESIAN_POINT('Ctrl Pts',(41.0982200375142,-2.05924511612529,
136.353435542442));
#179090=CARTESIAN_POINT('Ctrl Pts',(41.1056179518255,-2.20631915919651,
136.296620660277));
#179091=CARTESIAN_POINT('Ctrl Pts',(41.1130158661368,-2.35093369086305,
136.234005296886));
#179092=CARTESIAN_POINT('Ctrl Pts',(41.120412551049,-2.49552419021863,136.171400339031));
#179093=CARTESIAN_POINT('Ctrl Pts',(41.1278092359612,-2.63765564713984,
136.102996961254));
#179094=CARTESIAN_POINT('Ctrl Pts',(41.1352059208734,-2.77683810997354,
136.029023350556));
#179095=CARTESIAN_POINT('Ctrl Pts',(41.1426022778088,-2.91601440131099,
135.955053019926));
#179096=CARTESIAN_POINT('Ctrl Pts',(41.1499986347443,-3.05224162892631,
135.87551312267));
#179097=CARTESIAN_POINT('Ctrl Pts',(41.1573949916798,-3.1850540377979,135.790678030127));
#179098=CARTESIAN_POINT('Ctrl Pts',(41.1647924810163,-3.31788678058872,
135.705829949114));
#179099=CARTESIAN_POINT('Ctrl Pts',(41.1721899703529,-3.44730334902115,
135.615685259549));
#179100=CARTESIAN_POINT('Ctrl Pts',(41.1795874596895,-3.5728667276141,135.520561833503));
#179101=CARTESIAN_POINT('Ctrl Pts',(41.1869875422044,-3.69847412225334,
135.425405062089));
#179102=CARTESIAN_POINT('Ctrl Pts',(41.1943876247194,-3.82022534039261,
135.325266304615));
#179103=CARTESIAN_POINT('Ctrl Pts',(41.2017877072343,-3.9377163453184,135.220503793043));
#179104=CARTESIAN_POINT('Ctrl Pts',(41.2091959269008,-4.0553365436833,135.115626084319));
#179105=CARTESIAN_POINT('Ctrl Pts',(41.2166041465672,-4.16868689470295,
135.00611471642));
#179106=CARTESIAN_POINT('Ctrl Pts',(41.2240123662337,-4.27739963283134,
134.892365380718));
#179107=CARTESIAN_POINT('Ctrl Pts',(41.2314251455357,-4.38617928183638,
134.778546034198));
#179108=CARTESIAN_POINT('Ctrl Pts',(41.2388379248378,-4.49031538389258,
134.660483801621));
#179109=CARTESIAN_POINT('Ctrl Pts',(41.2462507041399,-4.5894807535191,134.538607124638));
#179110=CARTESIAN_POINT('Ctrl Pts',(41.2536740751686,-4.68878781527613,
134.416556304543));
#179111=CARTESIAN_POINT('Ctrl Pts',(41.2610974461973,-4.78310973622976,
134.290680452602));
#179112=CARTESIAN_POINT('Ctrl Pts',(41.2685208172261,-4.87216243438203,
134.161437288644));
#179113=CARTESIAN_POINT('Ctrl Pts',(41.272456866667,-4.91938031173366,134.092909461965));
#179114=CARTESIAN_POINT('Ctrl Pts',(41.2763929161079,-4.96511758064068,
134.023435390549));
#179115=CARTESIAN_POINT('Ctrl Pts',(41.2803289655488,-5.00933721984806,
133.953085943844));
#179116=CARTESIAN_POINT('Ctrl Pts',(41.2879507990617,-5.09496488614177,
133.816860071033));
#179117=CARTESIAN_POINT('Ctrl Pts',(41.2955726325746,-5.17514684997344,
133.676956375135));
#179118=CARTESIAN_POINT('Ctrl Pts',(41.3031944660875,-5.24956106473146,
133.533836609429));
#179119=CARTESIAN_POINT('Ctrl Pts',(41.3108058128407,-5.32387289415342,
133.390913759935));
#179120=CARTESIAN_POINT('Ctrl Pts',(41.3184171595939,-5.39243262360372,
133.244783959347));
#179121=CARTESIAN_POINT('Ctrl Pts',(41.3260285063472,-5.45496157201488,
133.095937544126));
#179122=CARTESIAN_POINT('Ctrl Pts',(41.3336305557737,-5.51741414076793,
132.947272946105));
#179123=CARTESIAN_POINT('Ctrl Pts',(41.3412326052003,-5.57385047090191,
132.795898661498));
#179124=CARTESIAN_POINT('Ctrl Pts',(41.3488346546268,-5.62403781503907,
132.642329392467));
#179125=CARTESIAN_POINT('Ctrl Pts',(41.3564261680854,-5.67415560263751,
132.488972960895));
#179126=CARTESIAN_POINT('Ctrl Pts',(41.3640176815441,-5.7180415659947,132.333427938303));
#179127=CARTESIAN_POINT('Ctrl Pts',(41.3716091950027,-5.75551120804998,
132.176228430626));
#179128=CARTESIAN_POINT('Ctrl Pts',(41.3791945469146,-5.79295043838896,
132.019156511754));
#179129=CARTESIAN_POINT('Ctrl Pts',(41.3867798988264,-5.823983640756,131.860433118151));
#179130=CARTESIAN_POINT('Ctrl Pts',(41.3943652507382,-5.84847600411157,
131.700607788737));
#179131=CARTESIAN_POINT('Ctrl Pts',(41.4019444458498,-5.87294848775788,
131.5409121847));
#179132=CARTESIAN_POINT('Ctrl Pts',(41.4095236409613,-5.89089066382546,
131.380116769395));
#179133=CARTESIAN_POINT('Ctrl Pts',(41.4171028360728,-5.90221872705661,
131.218781491174));
#179134=CARTESIAN_POINT('Ctrl Pts',(41.4236101599804,-5.91194474355384,
131.080262704199));
#179135=CARTESIAN_POINT('Ctrl Pts',(41.430117483888,-5.91679593767829,130.941346268479));
#179136=CARTESIAN_POINT('Ctrl Pts',(41.4366248077955,-5.91674967204228,
130.802390620728));
#179137=CARTESIAN_POINT('',(43.1866248077955,-5.92140473490589,130.799702052978));
#179138=CARTESIAN_POINT('Ctrl Pts',(41.4366261848254,-5.90754071104223,
130.802364327911));
#179139=CARTESIAN_POINT('Ctrl Pts',(41.4773429863376,-5.91011510315806,
129.934261000353));
#179140=CARTESIAN_POINT('Ctrl Pts',(41.6108756624536,-5.32352528808913,
127.090594479252));
#179141=CARTESIAN_POINT('Ctrl Pts',(41.8372242131748,-0.924490577904954,
123.867295121138));
#179142=CARTESIAN_POINT('Ctrl Pts',(42.1156718369874,5.33663993075326,126.276907163378));
#179143=CARTESIAN_POINT('Ctrl Pts',(42.3941194608004,6.69365905240206,132.847027751616));
#179144=CARTESIAN_POINT('Ctrl Pts',(42.6725670846133,1.8995325083189,137.540037033501));
#179145=CARTESIAN_POINT('Ctrl Pts',(42.9367355336118,-4.30480664579817,
136.120044043652));
#179146=CARTESIAN_POINT('Ctrl Pts',(43.1080881080057,-5.90703348562082,
132.464199972487));
#179147=CARTESIAN_POINT('Ctrl Pts',(43.1866248077955,-5.92140473490589,
130.799702052978));
#179148=CARTESIAN_POINT('',(44.9366248077955,-5.92016258122845,130.808544943896));
#179149=CARTESIAN_POINT('Ctrl Pts',(43.1866248077955,-5.92140473490589,
130.799702052978));
#179150=CARTESIAN_POINT('Ctrl Pts',(43.20090398261,-5.92401764812218,130.497070839358));
#179151=CARTESIAN_POINT('Ctrl Pts',(43.3079990320291,-5.76510993760414,
128.23006237518));
#179152=CARTESIAN_POINT('Ctrl Pts',(43.5079099560517,-2.83612951018477,
124.406397665834));
#179153=CARTESIAN_POINT('Ctrl Pts',(43.786357579865,3.84979015445499,124.959989282935));
#179154=CARTESIAN_POINT('Ctrl Pts',(44.0648052036776,6.99794073985275,130.884272643158));
#179155=CARTESIAN_POINT('Ctrl Pts',(44.3432528274906,3.71532565374068,136.735120755777));
#179156=CARTESIAN_POINT('Ctrl Pts',(44.6217004513035,-2.981492204414,137.135890035122));
#179157=CARTESIAN_POINT('Ctrl Pts',(44.8194911114051,-5.79226188538465,
133.287589730583));
#179158=CARTESIAN_POINT('Ctrl Pts',(44.9244658969025,-5.92469486449521,
131.06610242403));
#179159=CARTESIAN_POINT('Ctrl Pts',(44.9366248077955,-5.92263029408517,
130.808546688057));
#179160=CARTESIAN_POINT('',(46.6866247826357,-5.91193532425354,130.807010291797));
#179161=CARTESIAN_POINT('Ctrl Pts',(44.9366248077955,-5.91674852212777,
130.808542530865));
#179162=CARTESIAN_POINT('Ctrl Pts',(44.9439356290697,-5.91685786750848,
130.653836042839));
#179163=CARTESIAN_POINT('Ctrl Pts',(44.9512464503438,-5.91089535321625,
130.498893564097));
#179164=CARTESIAN_POINT('Ctrl Pts',(44.9585572716179,-5.89883200535206,
130.344239399696));
#179165=CARTESIAN_POINT('Ctrl Pts',(44.9658607352432,-5.88678079810431,
130.189740880055));
#179166=CARTESIAN_POINT('Ctrl Pts',(44.9731641988686,-5.86864100352846,
130.035530478046));
#179167=CARTESIAN_POINT('Ctrl Pts',(44.9804676624939,-5.84443566142174,
129.882133768032));
#179168=CARTESIAN_POINT('Ctrl Pts',(44.9877654758338,-5.82024904564804,
129.728855732559));
#179169=CARTESIAN_POINT('Ctrl Pts',(44.9950632891737,-5.79000628061789,
129.576390514602));
#179170=CARTESIAN_POINT('Ctrl Pts',(45.0023611025136,-5.75378230755912,
129.425259562632));
#179171=CARTESIAN_POINT('Ctrl Pts',(45.0097042106975,-5.71733350561856,
129.273190596412));
#179172=CARTESIAN_POINT('Ctrl Pts',(45.0170473188815,-5.67482902238523,
129.122472908791));
#179173=CARTESIAN_POINT('Ctrl Pts',(45.0243904270655,-5.62639776554055,
128.973628865938));
#179174=CARTESIAN_POINT('Ctrl Pts',(45.0316830372035,-5.57829956709244,
128.82580841325));
#179175=CARTESIAN_POINT('Ctrl Pts',(45.0389756473414,-5.52435599133673,
128.679836282438));
#179176=CARTESIAN_POINT('Ctrl Pts',(45.0462682574794,-5.46474358155259,
128.536209795777));
#179177=CARTESIAN_POINT('Ctrl Pts',(45.0535606612411,-5.40513285876214,
128.392587373657));
#179178=CARTESIAN_POINT('Ctrl Pts',(45.0608530650027,-5.33985376844323,
128.251310819223));
#179179=CARTESIAN_POINT('Ctrl Pts',(45.0681454687644,-5.26913108006282,
128.112857650149));
#179180=CARTESIAN_POINT('Ctrl Pts',(45.0754392015105,-5.19839550301742,
127.974379249052));
#179181=CARTESIAN_POINT('Ctrl Pts',(45.0827329342566,-5.12221452936977,
127.838725599691));
#179182=CARTESIAN_POINT('Ctrl Pts',(45.0900266670027,-5.04085882516912,
127.7063495028));
#179183=CARTESIAN_POINT('Ctrl Pts',(45.0974074196632,-4.95853248403015,
127.572394055934));
#179184=CARTESIAN_POINT('Ctrl Pts',(45.1047881723237,-4.87090734677987,
127.441795221017));
#179185=CARTESIAN_POINT('Ctrl Pts',(45.1121689249843,-4.77830835698527,
127.314991074502));
#179186=CARTESIAN_POINT('Ctrl Pts',(45.1194735190076,-4.68666485414325,
127.189495362429));
#179187=CARTESIAN_POINT('Ctrl Pts',(45.126778113031,-4.59014995067122,127.067716658515));
#179188=CARTESIAN_POINT('Ctrl Pts',(45.1340827070544,-4.48911806096891,
126.950044906939));
#179189=CARTESIAN_POINT('Ctrl Pts',(45.1415015390335,-4.38650611404346,
126.830532864129));
#179190=CARTESIAN_POINT('Ctrl Pts',(45.1489203710127,-4.27923500777099,
126.715257603372));
#179191=CARTESIAN_POINT('Ctrl Pts',(45.1563392029919,-4.16771300727604,
126.604586950869));
#179192=CARTESIAN_POINT('Ctrl Pts',(45.163758034971,-4.05619100678108,126.493916298365));
#179193=CARTESIAN_POINT('Ctrl Pts',(45.1711768669501,-3.94041845823231,
126.387850480556));
#179194=CARTESIAN_POINT('Ctrl Pts',(45.1785956989293,-3.82083591173472,
126.286712612453));
#179195=CARTESIAN_POINT('Ctrl Pts',(45.1860189653347,-3.70118188768014,
126.185514291651));
#179196=CARTESIAN_POINT('Ctrl Pts',(45.1934422317401,-3.5773236613378,126.088919949533));
#179197=CARTESIAN_POINT('Ctrl Pts',(45.2008654981455,-3.44965085327522,
125.997299191601));
#179198=CARTESIAN_POINT('Ctrl Pts',(45.2082799908665,-3.32212894386903,
125.905786721796));
#179199=CARTESIAN_POINT('Ctrl Pts',(45.2156944835875,-3.19080172729827,
125.819236350781));
#179200=CARTESIAN_POINT('Ctrl Pts',(45.2231089763085,-3.05609353823588,
125.737978984877));
#179201=CARTESIAN_POINT('Ctrl Pts',(45.2305163226623,-2.92151518599797,
125.65679993788));
#179202=CARTESIAN_POINT('Ctrl Pts',(45.2379236690161,-2.78356266621654,
125.580903931238));
#179203=CARTESIAN_POINT('Ctrl Pts',(45.2453310153699,-2.64269098546984,
125.510579840294));
#179204=CARTESIAN_POINT('Ctrl Pts',(45.2527328370453,-2.50192437213682,
125.44030819971));
#179205=CARTESIAN_POINT('Ctrl Pts',(45.2601346587207,-2.35824326553433,
125.37560036619));
#179206=CARTESIAN_POINT('Ctrl Pts',(45.2675364803961,-2.21212898083884,
125.316700284179));
#179207=CARTESIAN_POINT('Ctrl Pts',(45.2749343947074,-2.06609182873709,
125.257831295062));
#179208=CARTESIAN_POINT('Ctrl Pts',(45.2823323090188,-1.91762440194704,
125.204764090846));
#179209=CARTESIAN_POINT('Ctrl Pts',(45.2897302233302,-1.76722968623992,
125.157695247759));
#179210=CARTESIAN_POINT('Ctrl Pts',(45.2971269082424,-1.61685996340631,
125.110634226661));
#179211=CARTESIAN_POINT('Ctrl Pts',(45.3045235931546,-1.46456394322652,
125.069569699691));
#179212=CARTESIAN_POINT('Ctrl Pts',(45.3119202780668,-1.31086164400109,
125.034648985882));
#179213=CARTESIAN_POINT('Ctrl Pts',(45.3193166350022,-1.15716616009645,
124.999729820494));
#179214=CARTESIAN_POINT('Ctrl Pts',(45.3267129919377,-1.00206488515139,
124.970954009303));
#179215=CARTESIAN_POINT('Ctrl Pts',(45.3341093488732,-0.846089689838693,
124.94841809742));
#179216=CARTESIAN_POINT('Ctrl Pts',(45.3415068382097,-0.690090614325849,
124.925878735232));
#179217=CARTESIAN_POINT('Ctrl Pts',(45.3489043275463,-0.533217721518071,
124.909581227955));
#179218=CARTESIAN_POINT('Ctrl Pts',(45.3563018168828,-0.376009541818982,
124.899570410712));
#179219=CARTESIAN_POINT('Ctrl Pts',(45.3637018993978,-0.218746253035978,
124.889556084192));
#179220=CARTESIAN_POINT('Ctrl Pts',(45.3711019819128,-0.0611478156626729,
124.885832859144));
#179221=CARTESIAN_POINT('Ctrl Pts',(45.3785020644278,0.096245841597927,
124.888393469206));
#179222=CARTESIAN_POINT('Ctrl Pts',(45.3859102840943,0.253812569365371,
124.890956894922));
#179223=CARTESIAN_POINT('Ctrl Pts',(45.3933185037608,0.411173693849745,
124.899817948841));
#179224=CARTESIAN_POINT('Ctrl Pts',(45.4007267234272,0.567792275605391,
124.914917308198));
#179225=CARTESIAN_POINT('Ctrl Pts',(45.4081395027293,0.724507253484786,
124.930025960958));
#179226=CARTESIAN_POINT('Ctrl Pts',(45.4155522820314,0.88047840897048,124.951380519465));
#179227=CARTESIAN_POINT('Ctrl Pts',(45.4229650613335,1.03517813060349,124.9788703549));
#179228=CARTESIAN_POINT('Ctrl Pts',(45.4303884323622,1.19009889445346,125.0063994691));
#179229=CARTESIAN_POINT('Ctrl Pts',(45.437811803391,1.3437442324516,125.040081288913));
#179230=CARTESIAN_POINT('Ctrl Pts',(45.4452351744197,1.49560003991316,125.07975485969));
#179231=CARTESIAN_POINT('Ctrl Pts',(45.4491712238606,1.57611763276001,125.10079073887));
#179232=CARTESIAN_POINT('Ctrl Pts',(45.4531072733014,1.65613241984305,125.123510294631));
#179233=CARTESIAN_POINT('Ctrl Pts',(45.4570433227422,1.73557007374295,125.147884056877));
#179234=CARTESIAN_POINT('Ctrl Pts',(45.4644665891476,1.88538700983267,125.193852211792));
#179235=CARTESIAN_POINT('Ctrl Pts',(45.4718898555531,2.03360296229411,125.245846044098));
#179236=CARTESIAN_POINT('Ctrl Pts',(45.4793131219585,2.17969637211682,125.30373753578));
#179237=CARTESIAN_POINT('Ctrl Pts',(45.4867276146795,2.32561711166163,125.361560604525));
#179238=CARTESIAN_POINT('Ctrl Pts',(45.4941421074005,2.46941995843265,125.425267321563));
#179239=CARTESIAN_POINT('Ctrl Pts',(45.5015566001215,2.61059714831543,125.494679545062));
#179240=CARTESIAN_POINT('Ctrl Pts',(45.5089639464753,2.75163826630716,125.564024866447));
#179241=CARTESIAN_POINT('Ctrl Pts',(45.5163712928292,2.890058432802,125.639064582904));
#179242=CARTESIAN_POINT('Ctrl Pts',(45.5237786391829,3.0253686666206,125.719572028693));
#179243=CARTESIAN_POINT('Ctrl Pts',(45.5311804608583,3.16057798096165,125.800019428992));
#179244=CARTESIAN_POINT('Ctrl Pts',(45.5385822825336,3.29268166164688,125.885926248643));
#179245=CARTESIAN_POINT('Ctrl Pts',(45.545984104209,3.4212143086976,125.977019401486));
#179246=CARTESIAN_POINT('Ctrl Pts',(45.5533820185204,3.54967910436535,126.068064466964));
#179247=CARTESIAN_POINT('Ctrl Pts',(45.5607799328318,3.67457631691279,126.164290197822));
#179248=CARTESIAN_POINT('Ctrl Pts',(45.5681778471432,3.79546868509539,126.265379672138));
#179249=CARTESIAN_POINT('Ctrl Pts',(45.5755745320554,3.91634096315892,126.366452347217));
#179250=CARTESIAN_POINT('Ctrl Pts',(45.5829712169676,4.03320943165098,126.472386922357));
#179251=CARTESIAN_POINT('Ctrl Pts',(45.5903679018798,4.14566906430304,126.582825520971));
#179252=CARTESIAN_POINT('Ctrl Pts',(45.5977642588152,4.25812371037713,126.693259222622));
#179253=CARTESIAN_POINT('Ctrl Pts',(45.6051606157507,4.3661696429725,126.808196289093));
#179254=CARTESIAN_POINT('Ctrl Pts',(45.6125569726861,4.46943814686197,126.927241427513));
#179255=CARTESIAN_POINT('Ctrl Pts',(45.6199544620227,4.57272246142317,127.046304792049));
#179256=CARTESIAN_POINT('Ctrl Pts',(45.6273519513593,4.67122764626124,127.169477198867));
#179257=CARTESIAN_POINT('Ctrl Pts',(45.6347494406959,4.76462489147967,127.296329801568));
#179258=CARTESIAN_POINT('Ctrl Pts',(45.6421495232109,4.85805487695762,127.423226872252));
#179259=CARTESIAN_POINT('Ctrl Pts',(45.6495496057259,4.94637313659405,127.55380640695));
#179260=CARTESIAN_POINT('Ctrl Pts',(45.6569496882409,5.02929393913205,127.687610220709));
#179261=CARTESIAN_POINT('Ctrl Pts',(45.6643579079074,5.11230592161691,127.821561165516));
#179262=CARTESIAN_POINT('Ctrl Pts',(45.6717661275738,5.18990839753916,127.95874315233));
#179263=CARTESIAN_POINT('Ctrl Pts',(45.6791743472403,5.26186104793697,128.098672373384));
#179264=CARTESIAN_POINT('Ctrl Pts',(45.6865871265424,5.3338579839904,128.238687718539));
#179265=CARTESIAN_POINT('Ctrl Pts',(45.6939999058444,5.40019800847263,128.381453329469));
#179266=CARTESIAN_POINT('Ctrl Pts',(45.7014126851465,5.46068900966242,128.526465514131));
#179267=CARTESIAN_POINT('Ctrl Pts',(45.7088360561752,5.52126644323154,128.671684899004));
#179268=CARTESIAN_POINT('Ctrl Pts',(45.716259427204,5.57597803248774,128.819156919657));
#179269=CARTESIAN_POINT('Ctrl Pts',(45.7236827982327,5.6246813069971,128.96836204534));
#179270=CARTESIAN_POINT('Ctrl Pts',(45.7276188476735,5.65050495176093,129.047474183104));
#179271=CARTESIAN_POINT('Ctrl Pts',(45.7315548971143,5.67464029293529,129.127073364458));
#179272=CARTESIAN_POINT('Ctrl Pts',(45.7354909465551,5.69707194876263,129.20708112633));
#179273=CARTESIAN_POINT('Ctrl Pts',(45.7429142129605,5.73937735158505,129.357973268265));
#179274=CARTESIAN_POINT('Ctrl Pts',(45.750337479366,5.77574781060515,129.510775483146));
#179275=CARTESIAN_POINT('Ctrl Pts',(45.7577607457714,5.80600911562059,129.664979771742));
#179276=CARTESIAN_POINT('Ctrl Pts',(45.7651752384924,5.83623465428658,129.819001803675));
#179277=CARTESIAN_POINT('Ctrl Pts',(45.7725897312134,5.86036534023474,129.974422248053));
#179278=CARTESIAN_POINT('Ctrl Pts',(45.7800042239344,5.87827659032461,130.130717618536));
#179279=CARTESIAN_POINT('Ctrl Pts',(45.7874115702882,5.89617057687732,130.286862345657));
#179280=CARTESIAN_POINT('Ctrl Pts',(45.794818916642,5.90785701927774,130.443879951684));
#179281=CARTESIAN_POINT('Ctrl Pts',(45.8022262629957,5.91326231156118,130.601236524534));
#179282=CARTESIAN_POINT('Ctrl Pts',(45.8096280846711,5.9186635723737,130.758475734914));
#179283=CARTESIAN_POINT('Ctrl Pts',(45.8170299063465,5.91779299821617,130.916053037257));
#179284=CARTESIAN_POINT('Ctrl Pts',(45.8244317280219,5.91062878415207,131.073429267641));
#179285=CARTESIAN_POINT('Ctrl Pts',(45.8318296423332,5.90346835202084,131.230722420336));
#179286=CARTESIAN_POINT('Ctrl Pts',(45.8392275566445,5.89002091356227,131.387814340496));
#179287=CARTESIAN_POINT('Ctrl Pts',(45.8466254709558,5.87031675378085,131.544165843811));
#179288=CARTESIAN_POINT('Ctrl Pts',(45.854022155868,5.85061586847319,131.700491364344));
#179289=CARTESIAN_POINT('Ctrl Pts',(45.8614188407802,5.82466037207562,131.856076342233));
#179290=CARTESIAN_POINT('Ctrl Pts',(45.8688155256924,5.79253242970573,132.010386576369));
#179291=CARTESIAN_POINT('Ctrl Pts',(45.8762118826278,5.76040591192252,132.164689968228));
#179292=CARTESIAN_POINT('Ctrl Pts',(45.8836082395633,5.72210756845078,132.317718363261));
#179293=CARTESIAN_POINT('Ctrl Pts',(45.8910045964987,5.67777067078999,132.468947885455));
#179294=CARTESIAN_POINT('Ctrl Pts',(45.8984020858353,5.63342698503679,132.620200561275));
#179295=CARTESIAN_POINT('Ctrl Pts',(45.9057995751719,5.58304300928447,132.76965345763));
#179296=CARTESIAN_POINT('Ctrl Pts',(45.9131970645085,5.52680181437526,132.916798135487));
#179297=CARTESIAN_POINT('Ctrl Pts',(45.9205971470234,5.47054090420276,133.063994394681));
#179298=CARTESIAN_POINT('Ctrl Pts',(45.9279972295384,5.40841882008364,133.208880475903));
#179299=CARTESIAN_POINT('Ctrl Pts',(45.9353973120533,5.34066660127346,133.350968325192));
#179300=CARTESIAN_POINT('Ctrl Pts',(45.9428055317198,5.27283988193331,133.49321241468));
#179301=CARTESIAN_POINT('Ctrl Pts',(45.9502137513862,5.19937082501298,133.632651790219));
#179302=CARTESIAN_POINT('Ctrl Pts',(45.9576219710527,5.12053657342015,133.768822754745));
#179303=CARTESIAN_POINT('Ctrl Pts',(45.9650347503548,5.04165380066066,133.905077530227));
#179304=CARTESIAN_POINT('Ctrl Pts',(45.9724475296569,4.95739945253087,134.038059571623));
#179305=CARTESIAN_POINT('Ctrl Pts',(45.9798603089589,4.86809345833394,134.167334992049));
#179306=CARTESIAN_POINT('Ctrl Pts',(45.9872836799877,4.77865985954472,134.296795127256));
#179307=CARTESIAN_POINT('Ctrl Pts',(45.9947070510164,4.68416042234265,134.422537766178));
#179308=CARTESIAN_POINT('Ctrl Pts',(46.0021304220451,4.58495523391334,134.54416222534));
#179309=CARTESIAN_POINT('Ctrl Pts',(46.0060664714861,4.53235426261025,134.60865043193));
#179310=CARTESIAN_POINT('Ctrl Pts',(46.010002520927,4.47843095841243,134.67198147985));
#179311=CARTESIAN_POINT('Ctrl Pts',(46.0139385703679,4.42324302030786,134.734100016788));
#179312=CARTESIAN_POINT('Ctrl Pts',(46.0213618367734,4.31916029140282,134.851253638795));
#179313=CARTESIAN_POINT('Ctrl Pts',(46.0287851031789,4.2102625819376,134.964446465579));
#179314=CARTESIAN_POINT('Ctrl Pts',(46.0362083695843,4.09688312118325,135.073257343169));
#179315=CARTESIAN_POINT('Ctrl Pts',(46.0436228623053,3.98363766553642,135.181939615337));
#179316=CARTESIAN_POINT('Ctrl Pts',(46.0510373550263,3.86592126912529,135.286249991384));
#179317=CARTESIAN_POINT('Ctrl Pts',(46.0584518477473,3.74410701560329,135.38580069883));
#179318=CARTESIAN_POINT('Ctrl Pts',(46.0658591941011,3.62241017124454,135.485255455557));
#179319=CARTESIAN_POINT('Ctrl Pts',(46.0732665404548,3.49662361989866,135.579959441951));
#179320=CARTESIAN_POINT('Ctrl Pts',(46.0806738868086,3.36715677110134,135.669562138708));
#179321=CARTESIAN_POINT('Ctrl Pts',(46.088075708484,3.23778648356381,135.759098006394));
#179322=CARTESIAN_POINT('Ctrl Pts',(46.0954775301595,3.10474166968327,135.843539948656));
#179323=CARTESIAN_POINT('Ctrl Pts',(46.1028793518349,2.96846415723677,135.922578189114));
#179324=CARTESIAN_POINT('Ctrl Pts',(46.1102772661463,2.83225858462753,136.0015747059));
#179325=CARTESIAN_POINT('Ctrl Pts',(46.1176751804578,2.69282403416121,136.075173015105));
#179326=CARTESIAN_POINT('Ctrl Pts',(46.1250730947692,2.55063050665169,136.14310715407));
#179327=CARTESIAN_POINT('Ctrl Pts',(46.1324697796814,2.40846060912821,136.211030003614));
#179328=CARTESIAN_POINT('Ctrl Pts',(46.1398664645937,2.26353298103326,136.27329039032));
#179329=CARTESIAN_POINT('Ctrl Pts',(46.1472631495059,2.1163414731415,136.329668693281));
#179330=CARTESIAN_POINT('Ctrl Pts',(46.1546595064414,1.96915649187545,136.386044496369));
#179331=CARTESIAN_POINT('Ctrl Pts',(46.1620558633768,1.81970817900835,136.436538600782));
#179332=CARTESIAN_POINT('Ctrl Pts',(46.1694522203123,1.66850932276898,136.480979963826));
#179333=CARTESIAN_POINT('Ctrl Pts',(46.1768497096488,1.51728731759851,136.525428130956));
#179334=CARTESIAN_POINT('Ctrl Pts',(46.1842471989854,1.36431459357758,136.563821606276));
#179335=CARTESIAN_POINT('Ctrl Pts',(46.191644688322,1.21011786912664,136.596039588756));
#179336=CARTESIAN_POINT('Ctrl Pts',(46.199044770837,1.05586709125386,136.628268865198));
#179337=CARTESIAN_POINT('Ctrl Pts',(46.206444853352,0.900391823851985,136.654318262379));
#179338=CARTESIAN_POINT('Ctrl Pts',(46.213844935867,0.744227562900071,136.674118355081));
#179339=CARTESIAN_POINT('Ctrl Pts',(46.2212531555334,0.587891583288495,
136.693940220021));
#179340=CARTESIAN_POINT('Ctrl Pts',(46.2286613751999,0.430865467671833,
136.707499010156));
#179341=CARTESIAN_POINT('Ctrl Pts',(46.2360695948664,0.27368914003429,136.714777254075));
#179342=CARTESIAN_POINT('Ctrl Pts',(46.2434823741684,0.116416072989489,
136.722059977632));
#179343=CARTESIAN_POINT('Ctrl Pts',(46.2508951534706,-0.0410070178754066,
136.723054449985));
#179344=CARTESIAN_POINT('Ctrl Pts',(46.2583079327727,-0.198042161633038,
136.717795310257));
#179345=CARTESIAN_POINT('Ctrl Pts',(46.2657313038014,-0.355301684568288,
136.712528656023));
#179346=CARTESIAN_POINT('Ctrl Pts',(46.2731546748302,-0.512171781994873,
136.700990570913));
#179347=CARTESIAN_POINT('Ctrl Pts',(46.280578045859,-0.668120711639999,
136.683267427269));
#179348=CARTESIAN_POINT('Ctrl Pts',(46.2845140952996,-0.750808576077483,
136.673870191249));
#179349=CARTESIAN_POINT('Ctrl Pts',(46.2884501447402,-0.833237643384159,
136.662734966589));
#179350=CARTESIAN_POINT('Ctrl Pts',(46.2923861941809,-0.915330156377743,
136.649880377803));
#179351=CARTESIAN_POINT('Ctrl Pts',(46.2998094605863,-1.07015407387049,
136.625637024531));
#179352=CARTESIAN_POINT('Ctrl Pts',(46.3072327269918,-1.22424827677132,
136.595201785179));
#179353=CARTESIAN_POINT('Ctrl Pts',(46.3146559933972,-1.37707831775669,
136.558627370964));
#179354=CARTESIAN_POINT('Ctrl Pts',(46.3220704861182,-1.52972772632494,
136.52209618467));
#179355=CARTESIAN_POINT('Ctrl Pts',(46.3294849788391,-1.68111558755918,
136.479440352643));
#179356=CARTESIAN_POINT('Ctrl Pts',(46.3368994715601,-1.83071399666345,
136.430764160232));
#179357=CARTESIAN_POINT('Ctrl Pts',(46.3443068179139,-1.98016821718939,
136.382134883767));
#179358=CARTESIAN_POINT('Ctrl Pts',(46.3517141642678,-2.12783606660938,
136.327496913579));
#179359=CARTESIAN_POINT('Ctrl Pts',(46.3591215106215,-2.27320134724993,
136.267005233259));
#179360=CARTESIAN_POINT('Ctrl Pts',(46.3665233322969,-2.41845820897882,
136.206558669917));
#179361=CARTESIAN_POINT('Ctrl Pts',(46.3739251539723,-2.56141557822503,
136.140267232377));
#179362=CARTESIAN_POINT('Ctrl Pts',(46.3813269756476,-2.7015740126405,136.06833520116));
#179363=CARTESIAN_POINT('Ctrl Pts',(46.3887248899591,-2.84165845851243,
135.996441142302));
#179364=CARTESIAN_POINT('Ctrl Pts',(46.3961228042706,-2.97894658086459,
135.918912589866));
#179365=CARTESIAN_POINT('Ctrl Pts',(46.4035207185821,-3.11296057086087,
135.836001209537));
#179366=CARTESIAN_POINT('Ctrl Pts',(46.4109174034943,-3.24695229016116,
135.753103607576));
#179367=CARTESIAN_POINT('Ctrl Pts',(46.4183140884065,-3.3776706398419,135.664825149305));
#179368=CARTESIAN_POINT('Ctrl Pts',(46.4257107733187,-3.50466390820735,
135.571462614902));
#179369=CARTESIAN_POINT('Ctrl Pts',(46.4331071302542,-3.63165154555802,
135.478104220293));
#179370=CARTESIAN_POINT('Ctrl Pts',(46.4405034871896,-3.75491412925077,
135.379662418904));
#179371=CARTESIAN_POINT('Ctrl Pts',(46.4478998441251,-3.87403058165865,
135.276476181242));
#179372=CARTESIAN_POINT('Ctrl Pts',(46.4552973334616,-3.99316527109948,
135.173274145503));
#179373=CARTESIAN_POINT('Ctrl Pts',(46.4626948227982,-4.10815228314594,
135.065326471596));
#179374=CARTESIAN_POINT('Ctrl Pts',(46.4700923121348,-4.21860528029612,
134.953011006736));
#179375=CARTESIAN_POINT('Ctrl Pts',(46.4774923946498,-4.32909699657292,
134.840656169864));
#179376=CARTESIAN_POINT('Ctrl Pts',(46.4848924771647,-4.43505127190368,
134.723930759578));
#179377=CARTESIAN_POINT('Ctrl Pts',(46.4922925596797,-4.53612024823016,
134.603247777788));
#179378=CARTESIAN_POINT('Ctrl Pts',(46.4997007793462,-4.63730036028668,
134.482432092651));
#179379=CARTESIAN_POINT('Ctrl Pts',(46.5071089990127,-4.73358420549952,
134.357650431633));
#179380=CARTESIAN_POINT('Ctrl Pts',(46.5145172186791,-4.8246652425727,134.229347604346));
#179381=CARTESIAN_POINT('Ctrl Pts',(46.5219299979812,-4.91580233850455,
134.100965808809));
#179382=CARTESIAN_POINT('Ctrl Pts',(46.5293427772834,-5.00173004214471,
133.969058840609));
#179383=CARTESIAN_POINT('Ctrl Pts',(46.5367555565854,-5.08218670994251,
133.834098033215));
#179384=CARTESIAN_POINT('Ctrl Pts',(46.5441789276142,-5.16275833800006,
133.698944387491));
#179385=CARTESIAN_POINT('Ctrl Pts',(46.5516022986429,-5.23784313964544,
133.560728514899));
#179386=CARTESIAN_POINT('Ctrl Pts',(46.5590256696716,-5.30722636269027,
133.419944471635));
#179387=CARTESIAN_POINT('Ctrl Pts',(46.5629617191124,-5.34401501237569,
133.345297393831));
#179388=CARTESIAN_POINT('Ctrl Pts',(46.5668977685531,-5.37920155682514,
133.269928624069));
#179389=CARTESIAN_POINT('Ctrl Pts',(46.5708338179938,-5.41275963571393,
133.193913648676));
#179390=CARTESIAN_POINT('Ctrl Pts',(46.5790075004481,-5.48244704303539,
133.036059363562));
#179391=CARTESIAN_POINT('Ctrl Pts',(46.5871811829024,-5.54529049275333,
132.875006885446));
#179392=CARTESIAN_POINT('Ctrl Pts',(46.5953548653567,-5.60101427766594,
132.711339805675));
#179393=CARTESIAN_POINT('Ctrl Pts',(46.6034977581387,-5.65652815509931,
132.548289247991));
#179394=CARTESIAN_POINT('Ctrl Pts',(46.6116406509207,-5.70497578329349,
132.382643967415));
#179395=CARTESIAN_POINT('Ctrl Pts',(46.6197835437026,-5.74613022296392,
132.215005159341));
#179396=CARTESIAN_POINT('Ctrl Pts',(46.6279070867468,-5.78718686844328,
132.04776470687));
#179397=CARTESIAN_POINT('Ctrl Pts',(46.6360306297911,-5.8209848249271,131.878540410804));
#179398=CARTESIAN_POINT('Ctrl Pts',(46.6441541728353,-5.84734612825664,
131.707950025905));
#179399=CARTESIAN_POINT('Ctrl Pts',(46.6522457214236,-5.87360360797701,
131.538031508751));
#179400=CARTESIAN_POINT('Ctrl Pts',(46.6603372700119,-5.89248280272631,
131.366757875198));
#179401=CARTESIAN_POINT('Ctrl Pts',(46.6684288186002,-5.90385647684864,
131.1947569076));
#179402=CARTESIAN_POINT('Ctrl Pts',(46.6744941295062,-5.91238202284796,
131.065827403781));
#179403=CARTESIAN_POINT('Ctrl Pts',(46.6805594404121,-5.91669136066497,
130.936489603205));
#179404=CARTESIAN_POINT('Ctrl Pts',(46.6866247513181,-5.91674940543741,
130.807013117524));
#179405=CARTESIAN_POINT('',(48.4366248414426,-5.9154484603631,130.799233570558));
#179406=CARTESIAN_POINT('Ctrl Pts',(46.6866248077955,-5.90806780525821,
130.807008021674));
#179407=CARTESIAN_POINT('Ctrl Pts',(46.7408436857992,-5.90342285908467,
129.651290948913));
#179408=CARTESIAN_POINT('Ctrl Pts',(46.8878784384072,-5.01664859954711,
126.510550347247));
#179409=CARTESIAN_POINT('Ctrl Pts',(47.1277290656195,0.0905616076009186,
123.806549593712));
#179410=CARTESIAN_POINT('Ctrl Pts',(47.4061766894324,5.9364073636732,127.098064873448));
#179411=CARTESIAN_POINT('Ctrl Pts',(47.6846243132453,6.32698476215336,133.795484879415));
#179412=CARTESIAN_POINT('Ctrl Pts',(47.9630719370583,0.903372254600805,
137.744207813289));
#179413=CARTESIAN_POINT('Ctrl Pts',(48.2137387685748,-4.72645520494283,
135.557858009853));
#179414=CARTESIAN_POINT('Ctrl Pts',(48.3715897254874,-5.9015373895361,132.182661905809));
#179415=CARTESIAN_POINT('Ctrl Pts',(48.4366248077955,-5.91290344989438,
130.799236492267));
#179416=CARTESIAN_POINT('',(50.1866248077955,-5.92098875812942,130.803826647697));
#179417=CARTESIAN_POINT('Ctrl Pts',(48.4366248586207,-5.91674777733439,
130.799232078923));
#179418=CARTESIAN_POINT('Ctrl Pts',(48.445546196015,-5.91658317823966,130.609335619975));
#179419=CARTESIAN_POINT('Ctrl Pts',(48.4544675334093,-5.90727285882511,
130.419839250733));
#179420=CARTESIAN_POINT('Ctrl Pts',(48.4633888708036,-5.88895466743454,
130.231522518797));
#179421=CARTESIAN_POINT('Ctrl Pts',(48.4728185897837,-5.86959261560288,
130.03247457532));
#179422=CARTESIAN_POINT('Ctrl Pts',(48.4822483087638,-5.84016649034169,
129.834744725379));
#179423=CARTESIAN_POINT('Ctrl Pts',(48.4916780277439,-5.80089613338642,
129.639227744387));
#179424=CARTESIAN_POINT('Ctrl Pts',(48.501107746724,-5.76162577643119,129.443710763395));
#179425=CARTESIAN_POINT('Ctrl Pts',(48.5105374657041,-5.71251132052502,
129.250406591543));
#179426=CARTESIAN_POINT('Ctrl Pts',(48.5199671846841,-5.6538287683761,129.060184359161));
#179427=CARTESIAN_POINT('Ctrl Pts',(48.5273904510895,-5.6076326708179,128.910437552264));
#179428=CARTESIAN_POINT('Ctrl Pts',(48.5348137174949,-5.555413339271,128.762300897197));
#179429=CARTESIAN_POINT('Ctrl Pts',(48.5422369839003,-5.49729958532726,
128.616295757545));
#179430=CARTESIAN_POINT('Ctrl Pts',(48.5496514766213,-5.43925451701456,
128.470463183842));
#179431=CARTESIAN_POINT('Ctrl Pts',(48.5570659693423,-5.37532903029584,
128.326757454371));
#179432=CARTESIAN_POINT('Ctrl Pts',(48.5644804620632,-5.3057020395247,128.185686061558));
#179433=CARTESIAN_POINT('Ctrl Pts',(48.571887808417,-5.23614215786867,128.044750638665));
#179434=CARTESIAN_POINT('Ctrl Pts',(48.5792951547707,-5.16089187637648,
127.906444830133));
#179435=CARTESIAN_POINT('Ctrl Pts',(48.5867025011244,-5.08017860467204,
127.771257271629));
#179436=CARTESIAN_POINT('Ctrl Pts',(48.5941043227998,-4.99952553197077,
127.636170541107));
#179437=CARTESIAN_POINT('Ctrl Pts',(48.6015061444752,-4.91341777248504,
127.504197748952));
#179438=CARTESIAN_POINT('Ctrl Pts',(48.6089079661506,-4.82212912031739,
127.375803879012));
#179439=CARTESIAN_POINT('Ctrl Pts',(48.6163058804619,-4.73088865871902,
127.247477787197));
#179440=CARTESIAN_POINT('Ctrl Pts',(48.6237037947732,-4.63447296699451,
127.122727158461));
#179441=CARTESIAN_POINT('Ctrl Pts',(48.6311017090845,-4.53319963213509,
127.001988771243));
#179442=CARTESIAN_POINT('Ctrl Pts',(48.6384983939967,-4.43194312706619,
126.881270448554));
#179443=CARTESIAN_POINT('Ctrl Pts',(48.6458950789088,-4.32583082068225,
126.764563329783));
#179444=CARTESIAN_POINT('Ctrl Pts',(48.653291763821,-4.21522120553785,126.652271896105));
#179445=CARTESIAN_POINT('Ctrl Pts',(48.6606881207564,-4.1046164949397,126.539985441546));
#179446=CARTESIAN_POINT('Ctrl Pts',(48.6680844776919,-3.98951513404839,
126.432114548716));
#179447=CARTESIAN_POINT('Ctrl Pts',(48.6754808346273,-3.87031297639719,
126.329027330845));
#179448=CARTESIAN_POINT('Ctrl Pts',(48.6828783239638,-3.75109256859135,
126.225924330058));
#179449=CARTESIAN_POINT('Ctrl Pts',(48.6902758133004,-3.62777039628237,
126.127606706723));
#179450=CARTESIAN_POINT('Ctrl Pts',(48.697673302637,-3.50077580576758,126.034402617724));
#179451=CARTESIAN_POINT('Ctrl Pts',(48.7050733851519,-3.37373669749576,
125.941165856177));
#179452=CARTESIAN_POINT('Ctrl Pts',(48.7124734676669,-3.2430229086499,125.853046418634));
#179453=CARTESIAN_POINT('Ctrl Pts',(48.7198735501819,-3.10909305848895,
125.770329338744));
#179454=CARTESIAN_POINT('Ctrl Pts',(48.7272817698484,-2.97501593868961,
125.687521302921));
#179455=CARTESIAN_POINT('Ctrl Pts',(48.7346899895148,-2.83771601297265,
125.610127684493));
#179456=CARTESIAN_POINT('Ctrl Pts',(48.7420982091813,-2.69767745426955,
125.538388065869));
#179457=CARTESIAN_POINT('Ctrl Pts',(48.7495109884833,-2.55755270417024,
125.466604292707));
#179458=CARTESIAN_POINT('Ctrl Pts',(48.7569237677852,-2.41468630033689,
125.400481610002));
#179459=CARTESIAN_POINT('Ctrl Pts',(48.7643365470873,-2.26958222659054,
125.340211362719));
#179460=CARTESIAN_POINT('Ctrl Pts',(48.771759918116,-2.12427082133892,125.27985499848));
#179461=CARTESIAN_POINT('Ctrl Pts',(48.7791832891448,-1.97671570973133,
125.22536789989));
#179462=CARTESIAN_POINT('Ctrl Pts',(48.7866066601735,-1.82743663873346,
125.17689174658));
#179463=CARTESIAN_POINT('Ctrl Pts',(48.7905427096146,-1.7482852933807,125.151188526923));
#179464=CARTESIAN_POINT('Ctrl Pts',(48.7944787590558,-1.66864947431325,
125.127174350099));
#179465=CARTESIAN_POINT('Ctrl Pts',(48.7984148084969,-1.58860766791951,
125.104864478439));
#179466=CARTESIAN_POINT('Ctrl Pts',(48.8058380749024,-1.43765131909392,
125.062788756759));
#179467=CARTESIAN_POINT('Ctrl Pts',(48.8132613413078,-1.28479393150785,
125.026650878815));
#179468=CARTESIAN_POINT('Ctrl Pts',(48.8206846077132,-1.13054376892283,
124.996624281518));
#179469=CARTESIAN_POINT('Ctrl Pts',(48.8280991004342,-0.976475917220308,
124.966633173166));
#179470=CARTESIAN_POINT('Ctrl Pts',(48.8355135931552,-0.821018930020202,
124.94273903862));
#179471=CARTESIAN_POINT('Ctrl Pts',(48.8429280858763,-0.664696482650895,
124.925065664219));
#179472=CARTESIAN_POINT('Ctrl Pts',(48.85033543223,-0.508524704741576,124.907409324081));
#179473=CARTESIAN_POINT('Ctrl Pts',(48.8577427785838,-0.351489495762193,
124.895961849281));
#179474=CARTESIAN_POINT('Ctrl Pts',(48.8651501249376,-0.194124879194325,
124.890796033174));
#179475=CARTESIAN_POINT('Ctrl Pts',(48.872551946613,-0.0368776310945197,
124.885634069927));
#179476=CARTESIAN_POINT('Ctrl Pts',(48.8799537682885,0.120698163911409,
124.886744448906));
#179477=CARTESIAN_POINT('Ctrl Pts',(48.8873555899639,0.278063309341962,
124.894148154507));
#179478=CARTESIAN_POINT('Ctrl Pts',(48.8947535042752,0.435345382937171,
124.901547951749));
#179479=CARTESIAN_POINT('Ctrl Pts',(48.9021514185865,0.592416656476129,
124.915234441797));
#179480=CARTESIAN_POINT('Ctrl Pts',(48.9095493328979,0.74873799236339,124.935176519134));
#179481=CARTESIAN_POINT('Ctrl Pts',(48.9169460178101,0.905033350480361,
124.955115282459));
#179482=CARTESIAN_POINT('Ctrl Pts',(48.9243427027223,1.0605786483571,124.981307522652));
#179483=CARTESIAN_POINT('Ctrl Pts',(48.9317393876345,1.21483981054544,125.013670261726));
#179484=CARTESIAN_POINT('Ctrl Pts',(48.9391357445699,1.36909413263219,125.046031565803));
#179485=CARTESIAN_POINT('Ctrl Pts',(48.9465321015054,1.52206406690208,125.084562748093));
#179486=CARTESIAN_POINT('Ctrl Pts',(48.9539284584408,1.67322594076375,125.129129740002));
#179487=CARTESIAN_POINT('Ctrl Pts',(48.9613259477774,1.82441095789421,125.173703555231));
#179488=CARTESIAN_POINT('Ctrl Pts',(48.968723437114,1.97378700535063,125.224314914506));
#179489=CARTESIAN_POINT('Ctrl Pts',(48.9761209264506,2.12084592329109,125.28077997344));
#179490=CARTESIAN_POINT('Ctrl Pts',(48.9835210089656,2.26795639250747,125.337264826113));
#179491=CARTESIAN_POINT('Ctrl Pts',(48.9909210914806,2.41274776671714,125.399607330248));
#179492=CARTESIAN_POINT('Ctrl Pts',(48.9983211739956,2.55473234412884,125.467575704122));
#179493=CARTESIAN_POINT('Ctrl Pts',(49.0057293936621,2.69687304817977,125.53561881621));
#179494=CARTESIAN_POINT('Ctrl Pts',(49.0131376133285,2.83620045485241,125.609299991048));
#179495=CARTESIAN_POINT('Ctrl Pts',(49.020545832995,2.97225128938345,125.68834138038));
#179496=CARTESIAN_POINT('Ctrl Pts',(49.027958612297,3.10838586093301,125.767431418368));
#179497=CARTESIAN_POINT('Ctrl Pts',(49.0353713915991,3.24123952756261,125.851888044962));
#179498=CARTESIAN_POINT('Ctrl Pts',(49.0427841709011,3.37037888976805,125.941390670928));
#179499=CARTESIAN_POINT('Ctrl Pts',(49.0502075419299,3.49970277235025,126.031021182443));
#179500=CARTESIAN_POINT('Ctrl Pts',(49.0576309129587,3.62530145360704,126.125711869107));
#179501=CARTESIAN_POINT('Ctrl Pts',(49.0650542839875,3.74677479852134,126.225102034382));
#179502=CARTESIAN_POINT('Ctrl Pts',(49.0689903334282,3.81118288070779,126.277801084845));
#179503=CARTESIAN_POINT('Ctrl Pts',(49.072926382869,3.87443179320028,126.331820705672));
#179504=CARTESIAN_POINT('Ctrl Pts',(49.0768624323098,3.93646627155632,126.387103113707));
#179505=CARTESIAN_POINT('Ctrl Pts',(49.0842856987152,4.05346136170605,126.491364009955));
#179506=CARTESIAN_POINT('Ctrl Pts',(49.0917089651207,4.16648833363798,126.600433853532));
#179507=CARTESIAN_POINT('Ctrl Pts',(49.0991322315261,4.27512654098774,126.713978774627));
#179508=CARTESIAN_POINT('Ctrl Pts',(49.1065467242471,4.3836363469984,126.827389495055));
#179509=CARTESIAN_POINT('Ctrl Pts',(49.1139612169682,4.48776745793892,126.945264497789));
#179510=CARTESIAN_POINT('Ctrl Pts',(49.1213757096892,4.58713266954996,127.067230109483));
#179511=CARTESIAN_POINT('Ctrl Pts',(49.128783056043,4.68640210922901,127.189078166128));
#179512=CARTESIAN_POINT('Ctrl Pts',(49.1361904023967,4.78091456023954,127.315008695161));
#179513=CARTESIAN_POINT('Ctrl Pts',(49.1435977487505,4.87032012673337,127.444611754089));
#179514=CARTESIAN_POINT('Ctrl Pts',(49.1509995704259,4.95965901118264,127.574118150166));
#179515=CARTESIAN_POINT('Ctrl Pts',(49.1584013921013,5.04389838410333,127.707291316244));
#179516=CARTESIAN_POINT('Ctrl Pts',(49.1658032137767,5.12272914186027,127.84368895363));
#179517=CARTESIAN_POINT('Ctrl Pts',(49.1732011280881,5.20151828547382,127.980014587765));
#179518=CARTESIAN_POINT('Ctrl Pts',(49.1805990423994,5.27490431380218,128.119560980864));
#179519=CARTESIAN_POINT('Ctrl Pts',(49.1879969567108,5.34262197975757,128.26185772791));
#179520=CARTESIAN_POINT('Ctrl Pts',(49.195393641623,5.4103283922654,128.404130827817));
#179521=CARTESIAN_POINT('Ctrl Pts',(49.2027903265353,5.47236815169598,128.549153037798));
#179522=CARTESIAN_POINT('Ctrl Pts',(49.2101870114475,5.52852238895339,128.696430173424));
#179523=CARTESIAN_POINT('Ctrl Pts',(49.2175833683829,5.58467413627307,128.843700778627));
#179524=CARTESIAN_POINT('Ctrl Pts',(49.2249797253184,5.63494074732371,128.993225761867));
#179525=CARTESIAN_POINT('Ctrl Pts',(49.2323760822538,5.67915195998449,129.14449207521));
#179526=CARTESIAN_POINT('Ctrl Pts',(49.2397735715904,5.72336994149479,129.295781547811));
#179527=CARTESIAN_POINT('Ctrl Pts',(49.247171060927,5.7615305739112,129.448812523025));
#179528=CARTESIAN_POINT('Ctrl Pts',(49.2545685502636,5.79351385791696,129.603058099203));
#179529=CARTESIAN_POINT('Ctrl Pts',(49.2619686327786,5.82550835361335,129.757357745929));
#179530=CARTESIAN_POINT('Ctrl Pts',(49.2693687152936,5.85132111373933,129.912872476042));
#179531=CARTESIAN_POINT('Ctrl Pts',(49.2767687978086,5.87088352809197,130.069066688529));
#179532=CARTESIAN_POINT('Ctrl Pts',(49.2841770174751,5.89046745333025,130.22543265261));
#179533=CARTESIAN_POINT('Ctrl Pts',(49.2915852371415,5.90378726074775,130.382479220564));
#179534=CARTESIAN_POINT('Ctrl Pts',(49.2989934568079,5.91082630062458,130.539666442442));
#179535=CARTESIAN_POINT('Ctrl Pts',(49.30640623611,5.917869672913,130.696950410432));
#179536=CARTESIAN_POINT('Ctrl Pts',(49.3138190154121,5.91862457296778,130.854374832421));
#179537=CARTESIAN_POINT('Ctrl Pts',(49.3212317947142,5.91312645857319,131.011401790818));
#179538=CARTESIAN_POINT('Ctrl Pts',(49.328655165743,5.90762048821491,131.168653116698));
#179539=CARTESIAN_POINT('Ctrl Pts',(49.3360785367717,5.8958436868817,131.32550547347));
#179540=CARTESIAN_POINT('Ctrl Pts',(49.3435019078005,5.87788323603809,131.481427250921));
#179541=CARTESIAN_POINT('Ctrl Pts',(49.3474379572412,5.86836017404581,131.564100718616));
#179542=CARTESIAN_POINT('Ctrl Pts',(49.351374006682,5.8570995192712,131.646512744557));
#179543=CARTESIAN_POINT('Ctrl Pts',(49.3553100561227,5.84412001454051,131.728585599996));
#179544=CARTESIAN_POINT('Ctrl Pts',(49.3627333225281,5.81964107369463,131.883372443948));
#179545=CARTESIAN_POINT('Ctrl Pts',(49.3701565889336,5.7889713644415,132.037420151157));
#179546=CARTESIAN_POINT('Ctrl Pts',(49.377579855339,5.75216441127301,132.190194355135));
#179547=CARTESIAN_POINT('Ctrl Pts',(49.38499434806,5.71540096086654,132.342787992691));
#179548=CARTESIAN_POINT('Ctrl Pts',(49.392408840781,5.67251479168054,132.494110763706));
#179549=CARTESIAN_POINT('Ctrl Pts',(49.399823333502,5.62361099232305,132.643634922699));
#179550=CARTESIAN_POINT('Ctrl Pts',(49.4072306798558,5.57475432828858,132.793014964679));
#179551=CARTESIAN_POINT('Ctrl Pts',(49.4146380262096,5.51989169604158,132.940599493412));
#179552=CARTESIAN_POINT('Ctrl Pts',(49.4220453725634,5.45917886455839,133.085872547681));
#179553=CARTESIAN_POINT('Ctrl Pts',(49.4294471942388,5.39851131499548,133.231037251826));
#179554=CARTESIAN_POINT('Ctrl Pts',(49.4368490159141,5.33200239743908,133.373893571248));
#179555=CARTESIAN_POINT('Ctrl Pts',(49.4442508375895,5.25985715224054,133.513942375056));
#179556=CARTESIAN_POINT('Ctrl Pts',(49.4516487519009,5.18774999195535,133.653917248191));
#179557=CARTESIAN_POINT('Ctrl Pts',(49.4590466662122,5.1100126001463,133.791087226305));
#179558=CARTESIAN_POINT('Ctrl Pts',(49.4664445805236,5.02689736934888,133.924974884106));
#179559=CARTESIAN_POINT('Ctrl Pts',(49.4738412654358,4.94379595079495,134.058840292208));
#179560=CARTESIAN_POINT('Ctrl Pts',(49.481237950348,4.85531866367337,134.189424145733));
#179561=CARTESIAN_POINT('Ctrl Pts',(49.4886346352602,4.76176297524727,134.316275185158));
#179562=CARTESIAN_POINT('Ctrl Pts',(49.4960309921956,4.66821143517857,134.443120599875));
#179563=CARTESIAN_POINT('Ctrl Pts',(49.503427349131,4.56958216311505,134.566233229168));
#179564=CARTESIAN_POINT('Ctrl Pts',(49.5108237060665,4.46621476997766,134.685192511752));
#179565=CARTESIAN_POINT('Ctrl Pts',(49.518221195403,4.36283155102836,134.804170007307));
#179566=CARTESIAN_POINT('Ctrl Pts',(49.5256186847396,4.25470901146467,134.918992608217));
#179567=CARTESIAN_POINT('Ctrl Pts',(49.5330161740762,4.14222558600479,135.029274552446));
#179568=CARTESIAN_POINT('Ctrl Pts',(49.5404162565912,4.02970272965449,135.139595155841));
#179569=CARTESIAN_POINT('Ctrl Pts',(49.5478163391062,3.91281621016474,135.245371672274));
#179570=CARTESIAN_POINT('Ctrl Pts',(49.5552164216212,3.79197955834561,135.346256872611));
#179571=CARTESIAN_POINT('Ctrl Pts',(49.5626246412877,3.67101003420549,135.447253006596));
#179572=CARTESIAN_POINT('Ctrl Pts',(49.5700328609541,3.54608199006025,135.543346843867));
#179573=CARTESIAN_POINT('Ctrl Pts',(49.5774410806205,3.41764070151259,135.634232520408));
#179574=CARTESIAN_POINT('Ctrl Pts',(49.5848538599226,3.28912035949482,135.725174135567));
#179575=CARTESIAN_POINT('Ctrl Pts',(49.5922666392247,3.15708277670348,135.810900999753));
#179576=CARTESIAN_POINT('Ctrl Pts',(49.5996794185268,3.0219996842398,135.891152187009));
#179577=CARTESIAN_POINT('Ctrl Pts',(49.6071027895555,2.88672357871883,135.971518040925));
#179578=CARTESIAN_POINT('Ctrl Pts',(49.6145261605842,2.74839359989224,136.046392414594));
#179579=CARTESIAN_POINT('Ctrl Pts',(49.621949531613,2.60750413019932,136.115561307946));
#179580=CARTESIAN_POINT('Ctrl Pts',(49.6258855810538,2.53280115277032,136.152236314887));
#179581=CARTESIAN_POINT('Ctrl Pts',(49.6298216304947,2.4573789223514,136.187308120155));
#179582=CARTESIAN_POINT('Ctrl Pts',(49.6337576799356,2.38131296529585,136.220750478332));
#179583=CARTESIAN_POINT('Ctrl Pts',(49.641180946341,2.23785494422899,136.283821722154));
#179584=CARTESIAN_POINT('Ctrl Pts',(49.6486042127465,2.09167251829583,136.341284975719));
#179585=CARTESIAN_POINT('Ctrl Pts',(49.6560274791519,1.94324419645132,136.392896432559));
#179586=CARTESIAN_POINT('Ctrl Pts',(49.6634419718729,1.79499130455702,136.444446888943));
#179587=CARTESIAN_POINT('Ctrl Pts',(49.6708564645939,1.64449814962074,136.490159194205));
#179588=CARTESIAN_POINT('Ctrl Pts',(49.6782709573149,1.49226554182097,136.529836503044));
#179589=CARTESIAN_POINT('Ctrl Pts',(49.6856783036687,1.34017966153985,136.5694755694));
#179590=CARTESIAN_POINT('Ctrl Pts',(49.6930856500225,1.18635802488163,136.603091125833));
#179591=CARTESIAN_POINT('Ctrl Pts',(49.7004929963763,1.03131892156764,136.630535335554));
#179592=CARTESIAN_POINT('Ctrl Pts',(49.7078948180517,0.87639545226619,136.657959076347));
#179593=CARTESIAN_POINT('Ctrl Pts',(49.7152966397271,0.720256690325655,
136.679220570484));
#179594=CARTESIAN_POINT('Ctrl Pts',(49.7226984614025,0.563433398017768,
136.694222531779));
#179595=CARTESIAN_POINT('Ctrl Pts',(49.7300963757139,0.406692891505404,
136.709216573656));
#179596=CARTESIAN_POINT('Ctrl Pts',(49.7374942900252,0.249268944948803,
136.717957628023));
#179597=CARTESIAN_POINT('Ctrl Pts',(49.7448922043366,0.0916996540967001,
136.720399979837));
#179598=CARTESIAN_POINT('Ctrl Pts',(49.7522888892488,-0.0658434515980862,
136.722841925776));
#179599=CARTESIAN_POINT('Ctrl Pts',(49.759685574161,-0.223531480763051,
136.718987240832));
#179600=CARTESIAN_POINT('Ctrl Pts',(49.7670822590732,-0.380823987658732,
136.708842275842));
#179601=CARTESIAN_POINT('Ctrl Pts',(49.7744786160086,-0.538109520039827,
136.698697760691));
#179602=CARTESIAN_POINT('Ctrl Pts',(49.7818749729441,-0.694999192499319,
136.682263544104));
#179603=CARTESIAN_POINT('Ctrl Pts',(49.7892713298795,-0.850955606919887,
136.65959802672));
#179604=CARTESIAN_POINT('Ctrl Pts',(49.7966688192161,-1.00693589866586,
136.636929039187));
#179605=CARTESIAN_POINT('Ctrl Pts',(49.8040663085527,-1.16198227843079,
136.608026904952));
#179606=CARTESIAN_POINT('Ctrl Pts',(49.8114637978893,-1.31556564047997,
136.573001498058));
#179607=CARTESIAN_POINT('Ctrl Pts',(49.8188638804043,-1.4692028409384,136.537963813063));
#179608=CARTESIAN_POINT('Ctrl Pts',(49.8262639629193,-1.62137563885699,
136.496798664685));
#179609=CARTESIAN_POINT('Ctrl Pts',(49.8336640454343,-1.77156837702499,
136.449666282278));
#179610=CARTESIAN_POINT('Ctrl Pts',(49.8410722651008,-1.92192626754878,
136.40248207297));
#179611=CARTESIAN_POINT('Ctrl Pts',(49.8484804847673,-2.0702993937618,136.349317637552));
#179612=CARTESIAN_POINT('Ctrl Pts',(49.8558887044338,-2.21618974126468,
136.290382272027));
#179613=CARTESIAN_POINT('Ctrl Pts',(49.8633014837358,-2.36216988184215,
136.231410632767));
#179614=CARTESIAN_POINT('Ctrl Pts',(49.8707142630379,-2.50566385928894,
136.166661138954));
#179615=CARTESIAN_POINT('Ctrl Pts',(49.87812704234,-2.64619716702359,136.096389634468));
#179616=CARTESIAN_POINT('Ctrl Pts',(49.8855504133687,-2.78693127533868,
136.026017722762));
#179617=CARTESIAN_POINT('Ctrl Pts',(49.8929737843975,-2.92469593891223,
135.950108221743));
#179618=CARTESIAN_POINT('Ctrl Pts',(49.9003971554262,-3.05904388763994,
135.868961397094));
#179619=CARTESIAN_POINT('Ctrl Pts',(49.904333204867,-3.13027839368957,135.825935403574));
#179620=CARTESIAN_POINT('Ctrl Pts',(49.9082692543077,-3.20055285457639,
135.781437712479));
#179621=CARTESIAN_POINT('Ctrl Pts',(49.9122053037485,-3.26980436544908,
135.735517679979));
#179622=CARTESIAN_POINT('Ctrl Pts',(49.9196099432231,-3.40008282836062,
135.649131243417));
#179623=CARTESIAN_POINT('Ctrl Pts',(49.9270145826977,-3.52713740843895,
135.557444507087));
#179624=CARTESIAN_POINT('Ctrl Pts',(49.9344192221724,-3.65050568465854,
135.460726025132));
#179625=CARTESIAN_POINT('Ctrl Pts',(49.9418150978359,-3.77372794752092,
135.36412201499));
#179626=CARTESIAN_POINT('Ctrl Pts',(49.9492109734994,-3.89327229771408,
135.262498341619));
#179627=CARTESIAN_POINT('Ctrl Pts',(49.956606849163,-4.00870365838643,135.156167775718));
#179628=CARTESIAN_POINT('Ctrl Pts',(49.963995606204,-4.12402391493515,135.049939554311));
#179629=CARTESIAN_POINT('Ctrl Pts',(49.971384363245,-4.23523878823535,134.939013711422));
#179630=CARTESIAN_POINT('Ctrl Pts',(49.978773120286,-4.34194490417043,134.823744278234));
#179631=CARTESIAN_POINT('Ctrl Pts',(49.9861563981161,-4.44857189105712,
134.708560324314));
#179632=CARTESIAN_POINT('Ctrl Pts',(49.9935396759461,-4.55069652350319,
134.589039467391));
#179633=CARTESIAN_POINT('Ctrl Pts',(50.0009229537762,-4.64795116117806,
134.465573608612));
#179634=CARTESIAN_POINT('Ctrl Pts',(50.008660531027,-4.74987273169511,134.336183025985));
#179635=CARTESIAN_POINT('Ctrl Pts',(50.0163981082779,-4.84644505124757,
134.202459754589));
#179636=CARTESIAN_POINT('Ctrl Pts',(50.0241356855287,-4.93729087406291,
134.06489575576));
#179637=CARTESIAN_POINT('Ctrl Pts',(50.0315139282383,-5.02391779979922,
133.933720254881));
#179638=CARTESIAN_POINT('Ctrl Pts',(50.0388921709478,-5.10533787375355,
133.799053048601));
#179639=CARTESIAN_POINT('Ctrl Pts',(50.0462704136574,-5.18126751669558,
133.661351601615));
#179640=CARTESIAN_POINT('Ctrl Pts',(50.0536484892962,-5.25719544030873,
133.5236532727));
#179641=CARTESIAN_POINT('Ctrl Pts',(50.061026564935,-5.3276329986223,133.38292116834));
#179642=CARTESIAN_POINT('Ctrl Pts',(50.0684046405738,-5.39234218173474,
133.239638087914));
#179643=CARTESIAN_POINT('Ctrl Pts',(50.0757840254405,-5.45706284739009,
133.096329582131));
#179644=CARTESIAN_POINT('Ctrl Pts',(50.0831634103072,-5.51605295970531,
132.950469541257));
#179645=CARTESIAN_POINT('Ctrl Pts',(50.090542795174,-5.56912241309877,132.802561335818));
#179646=CARTESIAN_POINT('Ctrl Pts',(50.0979249660981,-5.62221190265312,
132.654597288224));
#179647=CARTESIAN_POINT('Ctrl Pts',(50.1053071370221,-5.66937615664302,
132.504583889727));
#179648=CARTESIAN_POINT('Ctrl Pts',(50.1126893079463,-5.71047479811216,
132.35304010107));
#179649=CARTESIAN_POINT('Ctrl Pts',(50.1200796238243,-5.75161878485249,
132.201329109947));
#179650=CARTESIAN_POINT('Ctrl Pts',(50.1274699397025,-5.78668369838023,
132.048084719622));
#179651=CARTESIAN_POINT('Ctrl Pts',(50.1348602555805,-5.81558005653692,
131.893837174684));
#179652=CARTESIAN_POINT('Ctrl Pts',(50.1422553353984,-5.84449504184223,
131.73949019881));
#179653=CARTESIAN_POINT('Ctrl Pts',(50.1496504152164,-5.86723349559764,
131.584139150302));
#179654=CARTESIAN_POINT('Ctrl Pts',(50.1570454950343,-5.88375782693143,
131.428319267256));
#179655=CARTESIAN_POINT('Ctrl Pts',(50.1644507263577,-5.90030484183908,
131.272285484371));
#179656=CARTESIAN_POINT('Ctrl Pts',(50.171855957681,-5.91062067882276,131.115781955036));
#179657=CARTESIAN_POINT('Ctrl Pts',(50.1792611890044,-5.91471982211213,
130.959344450316));
#179658=CARTESIAN_POINT('Ctrl Pts',(50.1817157286014,-5.91607852504501,
130.907491640724));
#179659=CARTESIAN_POINT('Ctrl Pts',(50.1841702681985,-5.91675464911097,
130.855646046806));
#179660=CARTESIAN_POINT('Ctrl Pts',(50.1866248077955,-5.91674997593985,
130.803827029961));
#179661=CARTESIAN_POINT('',(51.9366241057987,-5.91515969554757,130.80975978087));
#179662=CARTESIAN_POINT('Ctrl Pts',(50.1866248077955,-5.92647345050323,
130.803826153073));
#179663=CARTESIAN_POINT('Ctrl Pts',(50.1879675143841,-5.92650997018912,
130.775433012952));
#179664=CARTESIAN_POINT('Ctrl Pts',(50.1893102209727,-5.92632365013767,
130.747040365475));
#179665=CARTESIAN_POINT('Ctrl Pts',(50.2834688021656,-5.89752915104776,
128.756206350782));
#179666=CARTESIAN_POINT('Ctrl Pts',(50.4691005513741,-3.69725725083763,
124.862319776956));
#179667=CARTESIAN_POINT('Ctrl Pts',(50.7475481751871,3.00074939194039,124.481935163904));
#179668=CARTESIAN_POINT('Ctrl Pts',(51.025995799,6.94121393828233,129.911550675113));
#179669=CARTESIAN_POINT('Ctrl Pts',(51.3044434228129,4.50304197249439,136.161614907245));
#179670=CARTESIAN_POINT('Ctrl Pts',(51.5828910466258,-2.07320558018495,
137.488624163583));
#179671=CARTESIAN_POINT('Ctrl Pts',(51.7936178464117,-5.60823393350386,
133.844292795978));
#179672=CARTESIAN_POINT('Ctrl Pts',(51.9115287715932,-5.91922017290752,
131.343217642334));
#179673=CARTESIAN_POINT('Ctrl Pts',(51.9366238221706,-5.91451815454292,
130.809765226023));
#179674=CARTESIAN_POINT('',(53.686625479034,-5.9116149950419,130.802566075556));
#179675=CARTESIAN_POINT('Ctrl Pts',(51.9366248077955,-5.9167475488552,130.809746303783));
#179676=CARTESIAN_POINT('Ctrl Pts',(51.9439560591643,-5.91688945578099,
130.653846494255));
#179677=CARTESIAN_POINT('Ctrl Pts',(51.951287310533,-5.91086546482152,130.497806767427));
#179678=CARTESIAN_POINT('Ctrl Pts',(51.9586185619018,-5.89866929285895,
130.342158133818));
#179679=CARTESIAN_POINT('Ctrl Pts',(51.9661672174164,-5.88611145026003,
130.181893827313));
#179680=CARTESIAN_POINT('Ctrl Pts',(51.9737158729309,-5.86700965347304,
130.022044579614));
#179681=CARTESIAN_POINT('Ctrl Pts',(51.9812645284455,-5.84141482151809,
129.863189301891));
#179682=CARTESIAN_POINT('Ctrl Pts',(51.9885906513572,-5.81657451923583,
129.709017040682));
#179683=CARTESIAN_POINT('Ctrl Pts',(51.9959167742689,-5.78561867600374,
129.555781372117));
#179684=CARTESIAN_POINT('Ctrl Pts',(52.0032428971806,-5.74864632721248,
129.404004960197));
#179685=CARTESIAN_POINT('Ctrl Pts',(52.010568844207,-5.71167486605228,129.25223219212));
#179686=CARTESIAN_POINT('Ctrl Pts',(52.0178947912334,-5.66868727655011,
129.101918981409));
#179687=CARTESIAN_POINT('Ctrl Pts',(52.0252207382597,-5.61983329325566,
128.953575833072));
#179688=CARTESIAN_POINT('Ctrl Pts',(52.0325480234181,-5.57097038646265,
128.805205588892));
#179689=CARTESIAN_POINT('Ctrl Pts',(52.0398753085765,-5.51623907267722,
128.658806485197));
#179690=CARTESIAN_POINT('Ctrl Pts',(52.0472025937348,-5.45583825678566,
128.514871705539));
#179691=CARTESIAN_POINT('Ctrl Pts',(52.0549179021112,-5.39223885936663,
128.363314725409));
#179692=CARTESIAN_POINT('Ctrl Pts',(52.0626332104877,-5.32235333157764,
128.214490617775));
#179693=CARTESIAN_POINT('Ctrl Pts',(52.0703485188641,-5.24646991932888,
128.068947678341));
#179694=CARTESIAN_POINT('Ctrl Pts',(52.0776870150263,-5.17429261903222,
127.930512991046));
#179695=CARTESIAN_POINT('Ctrl Pts',(52.0850255111885,-5.09668961357051,
127.79504689232));
#179696=CARTESIAN_POINT('Ctrl Pts',(52.0923640073507,-5.01395414508074,
127.662992381665));
#179697=CARTESIAN_POINT('Ctrl Pts',(52.0997074671847,-4.93116271530131,
127.530848550905));
#179698=CARTESIAN_POINT('Ctrl Pts',(52.1070509270187,-4.84323212316322,
127.402121216907));
#179699=CARTESIAN_POINT('Ctrl Pts',(52.1143943868527,-4.75049683159906,
127.277221491381));
#179700=CARTESIAN_POINT('Ctrl Pts',(52.1217476746734,-4.65763742943423,
127.152154608565));
#179701=CARTESIAN_POINT('Ctrl Pts',(52.1291009624941,-4.55996073382341,
127.030925851244));
#179702=CARTESIAN_POINT('Ctrl Pts',(52.1364542503148,-4.45783936112482,
126.913910927247));
#179703=CARTESIAN_POINT('Ctrl Pts',(52.1375649316271,-4.44241438348144,
126.89623634514));
#179704=CARTESIAN_POINT('Ctrl Pts',(52.1386756129393,-4.42688806529473,
126.878657827617));
#179705=CARTESIAN_POINT('Ctrl Pts',(52.1397862942516,-4.41126175718772,
126.861176590403));
#179706=CARTESIAN_POINT('Ctrl Pts',(52.147209560657,-4.30682293506047,126.744340303067));
#179707=CARTESIAN_POINT('Ctrl Pts',(52.1546328270625,-4.19758120997391,
126.631479447753));
#179708=CARTESIAN_POINT('Ctrl Pts',(52.1620560934679,-4.08387109150341,
126.523014162246));
#179709=CARTESIAN_POINT('Ctrl Pts',(52.1694705861889,-3.97029536895008,
126.414677073698));
#179710=CARTESIAN_POINT('Ctrl Pts',(52.1768850789099,-3.85226203288944,
126.310725469028));
#179711=CARTESIAN_POINT('Ctrl Pts',(52.1842995716309,-3.73014534549287,
126.211545983379));
#179712=CARTESIAN_POINT('Ctrl Pts',(52.1917069179847,-3.60814635875687,
126.112462090653));
#179713=CARTESIAN_POINT('Ctrl Pts',(52.1991142643386,-3.48207214368769,
126.018141393914));
#179714=CARTESIAN_POINT('Ctrl Pts',(52.2065216106924,-3.35233317478483,
125.928933164743));
#179715=CARTESIAN_POINT('Ctrl Pts',(52.2139234323678,-3.22269097010012,
125.839791470436));
#179716=CARTESIAN_POINT('Ctrl Pts',(52.2213252540432,-3.08938976024935,
125.755754861952));
#179717=CARTESIAN_POINT('Ctrl Pts',(52.2287270757186,-2.9528723138158,125.677131769465));
#179718=CARTESIAN_POINT('Ctrl Pts',(52.2361249900299,-2.81642693387919,
125.598550181496));
#179719=CARTESIAN_POINT('Ctrl Pts',(52.2435229043413,-2.67676902132893,
125.525376604003));
#179720=CARTESIAN_POINT('Ctrl Pts',(52.2509208186527,-2.53436938430073,
125.457875567889));
#179721=CARTESIAN_POINT('Ctrl Pts',(52.2583175035649,-2.39199341150901,
125.390385749223));
#179722=CARTESIAN_POINT('Ctrl Pts',(52.2657141884771,-2.24687695550852,
125.32856676075));
#179723=CARTESIAN_POINT('Ctrl Pts',(52.2731108733894,-2.09951453323692,
125.272636719248));
#179724=CARTESIAN_POINT('Ctrl Pts',(52.2805072303248,-1.95215864516933,
125.216709157742));
#179725=CARTESIAN_POINT('Ctrl Pts',(52.2879035872603,-1.80255733785183,
125.16667015647));
#179726=CARTESIAN_POINT('Ctrl Pts',(52.2952999441957,-1.65122391773314,
125.122689196584));
#179727=CARTESIAN_POINT('Ctrl Pts',(52.3026974335323,-1.49986732808149,
125.0787015031));
#179728=CARTESIAN_POINT('Ctrl Pts',(52.3100949228689,-1.34677845608772,
125.040773801967));
#179729=CARTESIAN_POINT('Ctrl Pts',(52.3174924122055,-1.19248438540936,
125.009025290507));
#179730=CARTESIAN_POINT('Ctrl Pts',(52.3248924947206,-1.03813622718349,
124.977265649656));
#179731=CARTESIAN_POINT('Ctrl Pts',(52.3322925772356,-0.88258239452695,
124.951689586367));
#179732=CARTESIAN_POINT('Ctrl Pts',(52.3396926597507,-0.726358592244894,
124.932364895669));
#179733=CARTESIAN_POINT('Ctrl Pts',(52.3471008794171,-0.569963005832477,
124.913018955488));
#179734=CARTESIAN_POINT('Ctrl Pts',(52.3545090990836,-0.412896349256926,
124.899938161637));
#179735=CARTESIAN_POINT('Ctrl Pts',(52.36191731875,-0.255698597178542,124.893138342105));
#179736=CARTESIAN_POINT('Ctrl Pts',(52.3693300980521,-0.098404092506292,
124.886334337398));
#179737=CARTESIAN_POINT('Ctrl Pts',(52.3767428773542,0.0590212960175399,
124.88581901139));
#179738=CARTESIAN_POINT('Ctrl Pts',(52.3841556566563,0.216039705387039,
124.891556087718));
#179739=CARTESIAN_POINT('Ctrl Pts',(52.3915790276851,0.37328247002283,124.897301361449));
#179740=CARTESIAN_POINT('Ctrl Pts',(52.3990023987139,0.53011672287545,124.909316851731));
#179741=CARTESIAN_POINT('Ctrl Pts',(52.4064257697426,0.686010987022784,
124.92751456818));
#179742=CARTESIAN_POINT('Ctrl Pts',(52.4103618191833,0.768669866501998,
124.937163434089));
#179743=CARTESIAN_POINT('Ctrl Pts',(52.4142978686239,0.851064660209557,
124.948549492898));
#179744=CARTESIAN_POINT('Ctrl Pts',(52.4182339180645,0.933117668009956,
124.961653883513));
#179745=CARTESIAN_POINT('Ctrl Pts',(52.42565718447,1.08786707994086,124.98636835524));
#179746=CARTESIAN_POINT('Ctrl Pts',(52.4330804508755,1.24186793468851,125.017272463365));
#179747=CARTESIAN_POINT('Ctrl Pts',(52.4405037172809,1.39458594783973,125.054311870243));
#179748=CARTESIAN_POINT('Ctrl Pts',(52.4479182100019,1.54712346098142,125.091307499619));
#179749=CARTESIAN_POINT('Ctrl Pts',(52.4553327027228,1.69838079131768,125.134423906641));
#179750=CARTESIAN_POINT('Ctrl Pts',(52.4627471954438,1.84783035390649,125.183555199685));
#179751=CARTESIAN_POINT('Ctrl Pts',(52.4701545417976,1.99713587138085,125.232639138139));
#179752=CARTESIAN_POINT('Ctrl Pts',(52.4775618881514,2.14463673762683,125.287726305386));
#179753=CARTESIAN_POINT('Ctrl Pts',(52.4849692345052,2.28981722907865,125.348660147423));
#179754=CARTESIAN_POINT('Ctrl Pts',(52.4923710561806,2.43488943944198,125.409548542702));
#179755=CARTESIAN_POINT('Ctrl Pts',(52.499772877856,2.57764437818717,125.476274786242));
#179756=CARTESIAN_POINT('Ctrl Pts',(52.5071746995314,2.71758322703924,125.548633078337));
#179757=CARTESIAN_POINT('Ctrl Pts',(52.5145726138428,2.85744820326268,125.620953173052));
#179758=CARTESIAN_POINT('Ctrl Pts',(52.5219705281541,2.99449971945855,125.698899224199));
#179759=CARTESIAN_POINT('Ctrl Pts',(52.5293684424655,3.1282607349877,125.782218112974));
#179760=CARTESIAN_POINT('Ctrl Pts',(52.5367651273777,3.26199952186255,125.865523155661));
#179761=CARTESIAN_POINT('Ctrl Pts',(52.5441618122898,3.39244857680424,125.954199066723));
#179762=CARTESIAN_POINT('Ctrl Pts',(52.551558497202,3.51915709350606,126.047947692501));
#179763=CARTESIAN_POINT('Ctrl Pts',(52.5589548541375,3.64585999181964,126.141692161367));
#179764=CARTESIAN_POINT('Ctrl Pts',(52.5663512110729,3.76882238158787,126.240508675684));
#179765=CARTESIAN_POINT('Ctrl Pts',(52.5737475680084,3.88762421884382,126.344056984902));
#179766=CARTESIAN_POINT('Ctrl Pts',(52.581145057345,4.00644424496435,126.44762114763));
#179767=CARTESIAN_POINT('Ctrl Pts',(52.5885425466816,4.12110216881211,126.555918302442));
#179768=CARTESIAN_POINT('Ctrl Pts',(52.5959400360182,4.23121280471162,126.668569427994));
#179769=CARTESIAN_POINT('Ctrl Pts',(52.6033401185331,4.34136203972353,126.781260043223));
#179770=CARTESIAN_POINT('Ctrl Pts',(52.6107402010482,4.44696055228445,126.898307401211));
#179771=CARTESIAN_POINT('Ctrl Pts',(52.6181402835632,4.54766174298314,127.019297443205));
#179772=CARTESIAN_POINT('Ctrl Pts',(52.6255485032296,4.64847366499349,127.140420526187));
#179773=CARTESIAN_POINT('Ctrl Pts',(52.632956722896,4.74437727177301,127.26549466413));
#179774=CARTESIAN_POINT('Ctrl Pts',(52.6403649425625,4.83506737729302,127.394074116473));
#179775=CARTESIAN_POINT('Ctrl Pts',(52.6477777218646,4.92581330106,127.522732707324));
#179776=CARTESIAN_POINT('Ctrl Pts',(52.6551905011666,5.01133912725185,127.654900598912));
#179777=CARTESIAN_POINT('Ctrl Pts',(52.6626032804687,5.09138464810678,127.790105663598));
#179778=CARTESIAN_POINT('Ctrl Pts',(52.6700266514975,5.17154454175555,127.92550391562));
#179779=CARTESIAN_POINT('Ctrl Pts',(52.6774500225262,5.24620831404149,128.063947680314));
#179780=CARTESIAN_POINT('Ctrl Pts',(52.684873393555,5.3151627175081,128.20494225014));
#179781=CARTESIAN_POINT('Ctrl Pts',(52.6888094429958,5.35172399676439,128.27970095418));
#179782=CARTESIAN_POINT('Ctrl Pts',(52.6927454924366,5.38668098162346,128.355176470578));
#179783=CARTESIAN_POINT('Ctrl Pts',(52.6966815418774,5.42000754163706,128.431293233125));
#179784=CARTESIAN_POINT('Ctrl Pts',(52.7041048082828,5.48286039373613,128.574847071766));
#179785=CARTESIAN_POINT('Ctrl Pts',(52.7115280746882,5.54010111599179,128.721116777712));
#179786=CARTESIAN_POINT('Ctrl Pts',(52.7189513410937,5.59148663042751,128.86962347153));
#179787=CARTESIAN_POINT('Ctrl Pts',(52.7263658338147,5.64281141145248,129.017954642769));
#179788=CARTESIAN_POINT('Ctrl Pts',(52.7337803265356,5.68829463881708,129.168517189784));
#179789=CARTESIAN_POINT('Ctrl Pts',(52.7411948192566,5.72774022959643,129.32081000341));
#179790=CARTESIAN_POINT('Ctrl Pts',(52.7486021656104,5.76714780123039,129.472956031489));
#179791=CARTESIAN_POINT('Ctrl Pts',(52.7560095119642,5.80052922839119,129.626828647179));
#179792=CARTESIAN_POINT('Ctrl Pts',(52.763416858318,5.82773746320924,129.781909336376));
#179793=CARTESIAN_POINT('Ctrl Pts',(52.7708186799934,5.85492540509926,129.936874360544));
#179794=CARTESIAN_POINT('Ctrl Pts',(52.7782205016688,5.87594925799897,130.093045298053));
#179795=CARTESIAN_POINT('Ctrl Pts',(52.7856223233442,5.89071254356778,130.249891239193));
#179796=CARTESIAN_POINT('Ctrl Pts',(52.7930202376556,5.90546803571309,130.406654382583));
#179797=CARTESIAN_POINT('Ctrl Pts',(52.8004181519669,5.91396950750976,130.564091449242));
#179798=CARTESIAN_POINT('Ctrl Pts',(52.8078160662783,5.91617206285784,130.721664274476));
#179799=CARTESIAN_POINT('Ctrl Pts',(52.8152127511905,5.91837425218116,130.879210913964));
#179800=CARTESIAN_POINT('Ctrl Pts',(52.8226094361027,5.91427959736362,131.036892894355));
#179801=CARTESIAN_POINT('Ctrl Pts',(52.8300061210149,5.90389527170223,131.194169780198));
#179802=CARTESIAN_POINT('Ctrl Pts',(52.8374024779504,5.89351140649271,131.35143969222));
#179803=CARTESIAN_POINT('Ctrl Pts',(52.8447988348858,5.87683844956178,131.508304172924));
#179804=CARTESIAN_POINT('Ctrl Pts',(52.8521951918212,5.8539356193096,131.66422591369));
#179805=CARTESIAN_POINT('Ctrl Pts',(52.8595926811578,5.83102928257562,131.820171526473));
#179806=CARTESIAN_POINT('Ctrl Pts',(52.8669901704944,5.80189122761264,131.975173742568));
#179807=CARTESIAN_POINT('Ctrl Pts',(52.874387659831,5.76663213354565,132.128703624063));
#179808=CARTESIAN_POINT('Ctrl Pts',(52.881787742346,5.731360679458,132.28228732522));
#179809=CARTESIAN_POINT('Ctrl Pts',(52.8891878248609,5.68996399765501,132.434397300576));
#179810=CARTESIAN_POINT('Ctrl Pts',(52.8965879073759,5.64260310204595,132.584518137361));
#179811=CARTESIAN_POINT('Ctrl Pts',(52.9039961270424,5.59519012826335,132.734804047438));
#179812=CARTESIAN_POINT('Ctrl Pts',(52.9114043467088,5.54179995576858,132.883096094616));
#179813=CARTESIAN_POINT('Ctrl Pts',(52.9188125663753,5.48264263821576,133.028896583586));
#179814=CARTESIAN_POINT('Ctrl Pts',(52.9262253456773,5.42344891032091,133.174786810325));
#179815=CARTESIAN_POINT('Ctrl Pts',(52.9336381249794,5.35848111807983,133.318182083901));
#179816=CARTESIAN_POINT('Ctrl Pts',(52.9410509042814,5.28799582719607,133.458608287633));
#179817=CARTESIAN_POINT('Ctrl Pts',(52.9484742753102,5.21740982362327,133.59923513891));
#179818=CARTESIAN_POINT('Ctrl Pts',(52.955897646339,5.14129075613998,133.736884121616));
#179819=CARTESIAN_POINT('Ctrl Pts',(52.9633210173677,5.05993957075007,133.871108423118));
#179820=CARTESIAN_POINT('Ctrl Pts',(52.9672570668085,5.01680522026109,133.942277368443));
#179821=CARTESIAN_POINT('Ctrl Pts',(52.9711931162494,4.97220063492622,134.012484030043));
#179822=CARTESIAN_POINT('Ctrl Pts',(52.9751291656902,4.92617526658991,134.081665578252));
#179823=CARTESIAN_POINT('Ctrl Pts',(52.9825524320956,4.83937285831089,134.212139819091));
#179824=CARTESIAN_POINT('Ctrl Pts',(52.9899756985011,4.74725202068656,134.339360408767));
#179825=CARTESIAN_POINT('Ctrl Pts',(52.9973989649065,4.6500842589625,134.462863992862));
#179826=CARTESIAN_POINT('Ctrl Pts',(53.0048134576275,4.55303134146338,134.586221605976));
#179827=CARTESIAN_POINT('Ctrl Pts',(53.0122279503485,4.45094360188705,134.705870667667));
#179828=CARTESIAN_POINT('Ctrl Pts',(53.0196424430696,4.34413664995451,134.821375346071));
#179829=CARTESIAN_POINT('Ctrl Pts',(53.0270497894233,4.23743264258361,134.936768696717));
#179830=CARTESIAN_POINT('Ctrl Pts',(53.0344571357771,4.12601872987208,135.048025344126));
#179831=CARTESIAN_POINT('Ctrl Pts',(53.0418644821309,4.01025166945499,135.154741303223));
#179832=CARTESIAN_POINT('Ctrl Pts',(53.0492663038063,3.89457095247904,135.261377669531));
#179833=CARTESIAN_POINT('Ctrl Pts',(53.0566681254817,3.77454382579025,135.363479838813));
#179834=CARTESIAN_POINT('Ctrl Pts',(53.0640699471571,3.65056480986416,135.460679671441));
#179835=CARTESIAN_POINT('Ctrl Pts',(53.0714678614684,3.52665124149642,135.557828193034));
#179836=CARTESIAN_POINT('Ctrl Pts',(53.0788657757797,3.39879023163356,135.650079302173));
#179837=CARTESIAN_POINT('Ctrl Pts',(53.086263690091,3.26741028603743,135.737104335336));
#179838=CARTESIAN_POINT('Ctrl Pts',(53.0936603750032,3.13605217340384,135.824114906517));
#179839=CARTESIAN_POINT('Ctrl Pts',(53.1010570599155,3.00117659656919,135.90590091945));
#179840=CARTESIAN_POINT('Ctrl Pts',(53.1084537448277,2.8632421165247,135.982176290672));
#179841=CARTESIAN_POINT('Ctrl Pts',(53.1158501017631,2.7253137526396,136.058448279764));
#179842=CARTESIAN_POINT('Ctrl Pts',(53.1232464586986,2.58432708190977,136.129209932343));
#179843=CARTESIAN_POINT('Ctrl Pts',(53.130642815634,2.4407661662857,136.194220642095));
#179844=CARTESIAN_POINT('Ctrl Pts',(53.1380403049706,2.29718327111916,136.259241305152));
#179845=CARTESIAN_POINT('Ctrl Pts',(53.1454377943071,2.1510256863835,136.318509118218));
#179846=CARTESIAN_POINT('Ctrl Pts',(53.1528352836437,2.00279824729528,136.371831294914));
#179847=CARTESIAN_POINT('Ctrl Pts',(53.1602353661587,1.85451884730828,136.425172163616));
#179848=CARTESIAN_POINT('Ctrl Pts',(53.1676354486737,1.70416849937797,136.472563119973));
#179849=CARTESIAN_POINT('Ctrl Pts',(53.1750355311887,1.5522678668175,136.513861036354));
#179850=CARTESIAN_POINT('Ctrl Pts',(53.1824437508552,1.40020020389534,136.55520436404));
#179851=CARTESIAN_POINT('Ctrl Pts',(53.1898519705216,1.24657921239373,136.590441173567));
#179852=CARTESIAN_POINT('Ctrl Pts',(53.1972601901881,1.09193715660315,136.619479172551));
#179853=CARTESIAN_POINT('Ctrl Pts',(53.2046729694902,0.937199921207133,
136.648535043939));
#179854=CARTESIAN_POINT('Ctrl Pts',(53.2120857487923,0.781440737749198,
136.671384448335));
#179855=CARTESIAN_POINT('Ctrl Pts',(53.2194985280944,0.62519717405066,136.687986970085));
#179856=CARTESIAN_POINT('Ctrl Pts',(53.2269218991231,0.468730362221436,
136.704613214297));
#179857=CARTESIAN_POINT('Ctrl Pts',(53.2343452701519,0.311778159362604,
136.714974724435));
#179858=CARTESIAN_POINT('Ctrl Pts',(53.2417686411807,0.154879150262876,
136.719083181754));
#179859=CARTESIAN_POINT('Ctrl Pts',(53.2457046906215,0.0716875308978307,
136.721261584405));
#179860=CARTESIAN_POINT('Ctrl Pts',(53.2496407400623,-0.0114891897633528,
136.721682898984));
#179861=CARTESIAN_POINT('Ctrl Pts',(53.2535767895031,-0.0945714214127198,
136.720354769756));
#179862=CARTESIAN_POINT('Ctrl Pts',(53.2610000559085,-0.251261917394923,
136.717849959484));
#179863=CARTESIAN_POINT('Ctrl Pts',(53.268423322314,-0.408089765475678,
136.709111926048));
#179864=CARTESIAN_POINT('Ctrl Pts',(53.2758465887194,-0.564518377244247,
136.694118640121));
#179865=CARTESIAN_POINT('Ctrl Pts',(53.2832610814404,-0.72076210338496,
136.679143075013));
#179866=CARTESIAN_POINT('Ctrl Pts',(53.2906755741615,-0.87660716449545,
136.657927008867));
#179867=CARTESIAN_POINT('Ctrl Pts',(53.2980900668825,-1.03151628812405,
136.630500395312));
#179868=CARTESIAN_POINT('Ctrl Pts',(53.3054974132363,-1.18627610450663,
136.60310021656));
#179869=CARTESIAN_POINT('Ctrl Pts',(53.3129047595901,-1.34010141418094,
136.569501471909));
#179870=CARTESIAN_POINT('Ctrl Pts',(53.3203121059439,-1.49245949684531,
136.52978594786));
#179871=CARTESIAN_POINT('Ctrl Pts',(53.3277139276193,-1.64470394510392,
136.490100045148));
#179872=CARTESIAN_POINT('Ctrl Pts',(53.3351157492948,-1.79548298560572,
136.444306540601));
#179873=CARTESIAN_POINT('Ctrl Pts',(53.3425175709702,-1.94427364410263,
136.392538367007));
#179874=CARTESIAN_POINT('Ctrl Pts',(53.3499154852815,-2.09298575716804,
136.34079752143));
#179875=CARTESIAN_POINT('Ctrl Pts',(53.3573133995928,-2.23971122698436,
136.283088410468));
#179876=CARTESIAN_POINT('Ctrl Pts',(53.3647113139041,-2.38394192178945,
136.219593897494));
#179877=CARTESIAN_POINT('Ctrl Pts',(53.3721079988163,-2.52814864807028,
136.156109936155));
#179878=CARTESIAN_POINT('Ctrl Pts',(53.3795046837286,-2.66986108084924,
136.086842631213));
#179879=CARTESIAN_POINT('Ctrl Pts',(53.3869013686408,-2.8085906665899,136.012023147919));
#179880=CARTESIAN_POINT('Ctrl Pts',(53.3942977255762,-2.94731410091516,
135.937206982199));
#179881=CARTESIAN_POINT('Ctrl Pts',(53.4016940825117,-3.08305462262472,
135.856839304833));
#179882=CARTESIAN_POINT('Ctrl Pts',(53.4090904394471,-3.21534815550256,
135.771197317258));
#179883=CARTESIAN_POINT('Ctrl Pts',(53.4164879287837,-3.34766194285783,
135.685542217676));
#179884=CARTESIAN_POINT('Ctrl Pts',(53.4238854181202,-3.47652737718893,
135.594611402899));
#179885=CARTESIAN_POINT('Ctrl Pts',(53.4312829074568,-3.60150938608916,
135.498725399346));
#179886=CARTESIAN_POINT('Ctrl Pts',(53.4386829899718,-3.72653520723922,
135.402805783102));
#179887=CARTESIAN_POINT('Ctrl Pts',(53.4460830724868,-3.84767459657205,
135.301927746744));
#179888=CARTESIAN_POINT('Ctrl Pts',(53.4534831550018,-3.96452570551961,
135.196451975083));
#179889=CARTESIAN_POINT('Ctrl Pts',(53.4608913746683,-4.08150530427405,
135.090860221967));
#179890=CARTESIAN_POINT('Ctrl Pts',(53.4682995943347,-4.19418692839497,
134.980660887301));
#179891=CARTESIAN_POINT('Ctrl Pts',(53.4757078140012,-4.30220522783594,
134.866251893817));
#179892=CARTESIAN_POINT('Ctrl Pts',(53.4831205933033,-4.41029001073799,
134.751772483506));
#179893=CARTESIAN_POINT('Ctrl Pts',(53.4905333726054,-4.51370550507364,
134.633078532338));
#179894=CARTESIAN_POINT('Ctrl Pts',(53.4979461519075,-4.61212713946999,
134.510600465696));
#179895=CARTESIAN_POINT('Ctrl Pts',(53.5053695229362,-4.7106894033128,134.387947396649));
#179896=CARTESIAN_POINT('Ctrl Pts',(53.5127928939649,-4.8042433346608,134.26149971259));
#179897=CARTESIAN_POINT('Ctrl Pts',(53.5202162649937,-4.89250764304995,
134.13171685416));
#179898=CARTESIAN_POINT('Ctrl Pts',(53.5241523144345,-4.93930749723082,
134.062902868523));
#179899=CARTESIAN_POINT('Ctrl Pts',(53.5280883638753,-4.9846210103391,133.993151668565));
#179900=CARTESIAN_POINT('Ctrl Pts',(53.532024413316,-5.02841159320816,133.922534347779));
#179901=CARTESIAN_POINT('Ctrl Pts',(53.5396620524379,-5.11338427302963,
133.785506187936));
#179902=CARTESIAN_POINT('Ctrl Pts',(53.5472996915599,-5.1928647323864,133.644820790303));
#179903=CARTESIAN_POINT('Ctrl Pts',(53.5549373306818,-5.26653292943453,
133.500943912345));
#179904=CARTESIAN_POINT('Ctrl Pts',(53.5625643034415,-5.34009824499512,
133.357267965967));
#179905=CARTESIAN_POINT('Ctrl Pts',(53.5701912762012,-5.40786731261599,
133.21040972157));
#179906=CARTESIAN_POINT('Ctrl Pts',(53.5778182489609,-5.46956365958501,
133.060863207028));
#179907=CARTESIAN_POINT('Ctrl Pts',(53.5854357124241,-5.53118308365448,
132.911503146823));
#179908=CARTESIAN_POINT('Ctrl Pts',(53.5930531758872,-5.58674474131301,
132.759461810151));
#179909=CARTESIAN_POINT('Ctrl Pts',(53.6006706393504,-5.63601825436551,
132.60525728283));
#179910=CARTESIAN_POINT('Ctrl Pts',(53.608277176095,-5.68522108800988,132.451273951118));
#179911=CARTESIAN_POINT('Ctrl Pts',(53.6158837128396,-5.72815365873106,
132.295133942283));
#179912=CARTESIAN_POINT('Ctrl Pts',(53.6234902495842,-5.76463396731877,
132.137374415445));
#179913=CARTESIAN_POINT('Ctrl Pts',(53.631090387928,-5.80108358971582,131.979747591401));
#179914=CARTESIAN_POINT('Ctrl Pts',(53.6386905262718,-5.83109168432949,
131.82050429686));
#179915=CARTESIAN_POINT('Ctrl Pts',(53.6462906646155,-5.85452601886792,
131.660196850089));
#179916=CARTESIAN_POINT('Ctrl Pts',(53.6538841673983,-5.8779398932582,131.500029365223));
#179917=CARTESIAN_POINT('Ctrl Pts',(53.6614776701811,-5.89479140087716,
131.33879992004));
#179918=CARTESIAN_POINT('Ctrl Pts',(53.6690711729639,-5.90499937150216,
131.177070940819));
#179919=CARTESIAN_POINT('Ctrl Pts',(53.6749223845744,-5.91286517440627,
131.052449865664));
#179920=CARTESIAN_POINT('Ctrl Pts',(53.680773596185,-5.91678736038817,130.927532467533));
#179921=CARTESIAN_POINT('Ctrl Pts',(53.6866248077955,-5.91674973171695,
130.802578841105));
#179922=CARTESIAN_POINT('',(55.4366248077955,-5.92106340457748,130.79959340511));
#179923=CARTESIAN_POINT('Ctrl Pts',(53.686626026497,-5.90742709745722,130.802555663958));
#179924=CARTESIAN_POINT('Ctrl Pts',(53.727908030041,-5.90978532495469,129.922359697697));
#179925=CARTESIAN_POINT('Ctrl Pts',(53.8620059081893,-5.31185327642548,
127.066239178578));
#179926=CARTESIAN_POINT('Ctrl Pts',(54.0889196609419,-0.882245562582123,
123.861796012345));
#179927=CARTESIAN_POINT('Ctrl Pts',(54.3673672847546,5.36410094939406,126.309476688583));
#179928=CARTESIAN_POINT('Ctrl Pts',(54.6458149085676,6.68110073978089,132.887736108264));
#179929=CARTESIAN_POINT('Ctrl Pts',(54.9242625323805,1.858495340223,137.551475230548));
#179930=CARTESIAN_POINT('Ctrl Pts',(55.1878658321232,-4.32383043540707,
136.096859582895));
#179931=CARTESIAN_POINT('Ctrl Pts',(55.3586532572615,-5.90657959716367,
132.452360893221));
#179932=CARTESIAN_POINT('Ctrl Pts',(55.4366248077955,-5.92106340457748,
130.79959340511));
#179933=CARTESIAN_POINT('',(57.1866248077955,-5.92031730829855,130.808402304245));
#179934=CARTESIAN_POINT('Ctrl Pts',(55.4366248077955,-5.92106340457748,
130.79959340511));
#179935=CARTESIAN_POINT('Ctrl Pts',(55.4514691318657,-5.92382085046061,
130.48493740509));
#179936=CARTESIAN_POINT('Ctrl Pts',(55.5591293305407,-5.75767852999927,
128.205775126642));
#179937=CARTESIAN_POINT('Ctrl Pts',(55.7596054038189,-2.79713074682738,
124.389251879948));
#179938=CARTESIAN_POINT('Ctrl Pts',(56.0380530276321,3.88529517390352,124.983532330973));
#179939=CARTESIAN_POINT('Ctrl Pts',(56.3165006514451,6.99732463703978,130.926869614113));
#179940=CARTESIAN_POINT('Ctrl Pts',(56.5949482752577,3.6791545970478,136.757627114317));
#179941=CARTESIAN_POINT('Ctrl Pts',(56.8733958990709,-3.01997878093501,
137.117623537249));
#179942=CARTESIAN_POINT('Ctrl Pts',(57.0706214099165,-5.7993065312336,133.263329052102));
#179943=CARTESIAN_POINT('Ctrl Pts',(57.1750310461582,-5.92485864146025,
131.053955056992));
#179944=CARTESIAN_POINT('Ctrl Pts',(57.1866248077955,-5.9229396490959,130.808404094467));
#179945=CARTESIAN_POINT('',(58.9366247815215,-5.91201869214909,130.807184091162));
#179946=CARTESIAN_POINT('Ctrl Pts',(57.1866248077955,-5.91674862124091,
130.808399867971));
#179947=CARTESIAN_POINT('Ctrl Pts',(57.1939380426069,-5.91685425135328,
130.653671450818));
#179948=CARTESIAN_POINT('Ctrl Pts',(57.2012512774183,-5.91088629876316,
130.498704782712));
#179949=CARTESIAN_POINT('Ctrl Pts',(57.2085645122297,-5.89881522288282,
130.344024296181));
#179950=CARTESIAN_POINT('Ctrl Pts',(57.2158702793011,-5.88675647310165,
130.189501758042));
#179951=CARTESIAN_POINT('Ctrl Pts',(57.2231760463724,-5.86860702960594,
130.035265200377));
#179952=CARTESIAN_POINT('Ctrl Pts',(57.2304818134437,-5.84438936097259,
129.881840395646));
#179953=CARTESIAN_POINT('Ctrl Pts',(57.2377818193403,-5.82019078988507,
129.728536578501));
#179954=CARTESIAN_POINT('Ctrl Pts',(57.2450818252368,-5.78993357634959,
129.576043618411));
#179955=CARTESIAN_POINT('Ctrl Pts',(57.2523818311334,-5.75369209415274,
129.4248832353));
#179956=CARTESIAN_POINT('Ctrl Pts',(57.2597947192818,-5.71689019869302,
129.271385412372));
#179957=CARTESIAN_POINT('Ctrl Pts',(57.2672076074303,-5.67391745113027,
129.119262122311));
#179958=CARTESIAN_POINT('Ctrl Pts',(57.2746204955787,-5.62490602073945,
128.96905061096));
#179959=CARTESIAN_POINT('Ctrl Pts',(57.281915036378,-5.57667706173495,128.82123723834));
#179960=CARTESIAN_POINT('Ctrl Pts',(57.2892095771774,-5.52260093667172,
128.675275429644));
#179961=CARTESIAN_POINT('Ctrl Pts',(57.2965041179767,-5.46285411060139,
128.53166276506));
#179962=CARTESIAN_POINT('Ctrl Pts',(57.3037983637164,-5.40310970125243,
128.388055909517));
#179963=CARTESIAN_POINT('Ctrl Pts',(57.3110926094561,-5.33769519475609,
128.246798364337));
#179964=CARTESIAN_POINT('Ctrl Pts',(57.3183868551958,-5.26683529508206,
128.108367936386));
#179965=CARTESIAN_POINT('Ctrl Pts',(57.3256823401667,-5.19596335690571,
127.969913990266));
#179966=CARTESIAN_POINT('Ctrl Pts',(57.3329778251376,-5.11964436033471,
127.834288459341));
#179967=CARTESIAN_POINT('Ctrl Pts',(57.3402733101084,-5.03814892406815,
127.701944465369));
#179968=CARTESIAN_POINT('Ctrl Pts',(57.3477747964908,-4.95435231454629,
127.565863495766));
#179969=CARTESIAN_POINT('Ctrl Pts',(57.3552762828731,-4.86508283881317,
127.433252493631));
#179970=CARTESIAN_POINT('Ctrl Pts',(57.3627777692554,-4.77068175052153,
127.304571167079));
#179971=CARTESIAN_POINT('Ctrl Pts',(57.370084061884,-4.6787370424514,127.179238215753));
#179972=CARTESIAN_POINT('Ctrl Pts',(57.3773903545127,-4.58192475377393,
127.057633233637));
#179973=CARTESIAN_POINT('Ctrl Pts',(57.3846966471413,-4.48059993087497,
126.940145972655));
#179974=CARTESIAN_POINT('Ctrl Pts',(57.3922957304005,-4.37521464115621,
126.817950555159));
#179975=CARTESIAN_POINT('Ctrl Pts',(57.3998948136597,-4.26494798228707,
126.700210065349));
#179976=CARTESIAN_POINT('Ctrl Pts',(57.4074938969189,-4.15023953349525,
126.587318718662));
#179977=CARTESIAN_POINT('Ctrl Pts',(57.4150929801781,-4.03553108470327,
126.474427371975));
#179978=CARTESIAN_POINT('Ctrl Pts',(57.4226920634373,-3.91638123640206,
126.366385422119));
#179979=CARTESIAN_POINT('Ctrl Pts',(57.4302911466965,-3.79326491482562,
126.26353780133));
#179980=CARTESIAN_POINT('Ctrl Pts',(57.437714413102,-3.67299708478074,126.163069723505));
#179981=CARTESIAN_POINT('Ctrl Pts',(57.4451376795074,-3.54855315606726,
126.067231131235));
#179982=CARTESIAN_POINT('Ctrl Pts',(57.4525609459128,-3.42032499192752,
125.976389251444));
#179983=CARTESIAN_POINT('Ctrl Pts',(57.4599754386338,-3.29224838282892,
125.885654739211));
#179984=CARTESIAN_POINT('Ctrl Pts',(57.4673899313548,-3.16039674277302,
125.799905397816));
#179985=CARTESIAN_POINT('Ctrl Pts',(57.4748044240758,-3.02519641289154,
125.719469544403));
#179986=CARTESIAN_POINT('Ctrl Pts',(57.4822117704296,-2.89012639417781,
125.639111218095));
#179987=CARTESIAN_POINT('Ctrl Pts',(57.4896191167834,-2.75171442980218,
125.564056373772));
#179988=CARTESIAN_POINT('Ctrl Pts',(57.4970264631372,-2.6104172763789,125.494591111676));
#179989=CARTESIAN_POINT('Ctrl Pts',(57.5044282848126,-2.46922550770409,
125.425177659393));
#179990=CARTESIAN_POINT('Ctrl Pts',(57.511830106488,-2.32515316823143,125.361345652437));
#179991=CARTESIAN_POINT('Ctrl Pts',(57.5192319281634,-2.17868304917881,
125.303336100831));
#179992=CARTESIAN_POINT('Ctrl Pts',(57.5266298424747,-2.03229025056129,
125.245357172015));
#179993=CARTESIAN_POINT('Ctrl Pts',(57.5340277567861,-1.88350253939427,
125.193194714378));
#179994=CARTESIAN_POINT('Ctrl Pts',(57.5414256710974,-1.73282408874509,
125.14704223869));
#179995=CARTESIAN_POINT('Ctrl Pts',(57.5488223560096,-1.58217067812126,
125.100897432707));
#179996=CARTESIAN_POINT('Ctrl Pts',(57.5562190409218,-1.42962750820282,
125.060760735669));
#179997=CARTESIAN_POINT('Ctrl Pts',(57.563615725834,-1.27571548442838,125.026776298381));
#179998=CARTESIAN_POINT('Ctrl Pts',(57.5710120827695,-1.12181028527413,
124.992793367999));
#179999=CARTESIAN_POINT('Ctrl Pts',(57.578408439705,-0.966536717466216,
124.964962235441));
#180000=CARTESIAN_POINT('Ctrl Pts',(57.5858047966404,-0.810427229520558,
124.943376206381));
#180001=CARTESIAN_POINT('Ctrl Pts',(57.593202285977,-0.65429384081399,124.921786872445));
#180002=CARTESIAN_POINT('Ctrl Pts',(57.6005997753136,-0.497324646944804,
124.906444596948));
#180003=CARTESIAN_POINT('Ctrl Pts',(57.6079972646502,-0.340058441262998,
124.897390935993));
#180004=CARTESIAN_POINT('Ctrl Pts',(57.6153973471651,-0.182737106157256,
124.888334101291));
#180005=CARTESIAN_POINT('Ctrl Pts',(57.6227974296801,-0.0251189243910171,
124.885570291646));
#180006=CARTESIAN_POINT('Ctrl Pts',(57.630197512195,0.132256229568732,124.889088954131));
#180007=CARTESIAN_POINT('Ctrl Pts',(57.6376057318615,0.289804433689493,
124.892611485747));
#180008=CARTESIAN_POINT('Ctrl Pts',(57.645013951528,0.447108702886177,124.902430277321));
#180009=CARTESIAN_POINT('Ctrl Pts',(57.6524221711944,0.603632468775904,
124.918482738682));
#180010=CARTESIAN_POINT('Ctrl Pts',(57.6598349504965,0.760252572432243,
124.934545080065));
#180011=CARTESIAN_POINT('Ctrl Pts',(57.6672477297986,0.916090846875104,
124.956848683615));
#180012=CARTESIAN_POINT('Ctrl Pts',(57.6746605091007,1.07062036384995,124.985279710841));
#180013=CARTESIAN_POINT('Ctrl Pts',(57.6820838801294,1.22537067984492,125.013751361652));
#180014=CARTESIAN_POINT('Ctrl Pts',(57.6895072511581,1.37880814035333,125.048367840201));
#180015=CARTESIAN_POINT('Ctrl Pts',(57.6969306221869,1.53041962999226,125.08896506532));
#180016=CARTESIAN_POINT('Ctrl Pts',(57.7008666716277,1.61080767966777,125.110490688195));
#180017=CARTESIAN_POINT('Ctrl Pts',(57.7048027210686,1.69068268387806,125.133696895736));
#180018=CARTESIAN_POINT('Ctrl Pts',(57.7087387705094,1.76997049597375,125.158553765939));
#180019=CARTESIAN_POINT('Ctrl Pts',(57.7161620369149,1.91950483509634,125.205433047384));
#180020=CARTESIAN_POINT('Ctrl Pts',(57.7235853033203,2.06740154024459,125.258328148936));
#180021=CARTESIAN_POINT('Ctrl Pts',(57.7310085697257,2.21313984135335,125.317107880074));
#180022=CARTESIAN_POINT('Ctrl Pts',(57.7384230624467,2.35870589189342,125.375818138451));
#180023=CARTESIAN_POINT('Ctrl Pts',(57.7458375551678,2.50211827346222,125.440399043895));
#180024=CARTESIAN_POINT('Ctrl Pts',(57.7532520478888,2.64287031575285,125.510669366972));
#180025=CARTESIAN_POINT('Ctrl Pts',(57.7606593942426,2.7834866959255,125.580871960867));
#180026=CARTESIAN_POINT('Ctrl Pts',(57.7680667405963,2.92144750976236,125.656752889853));
#180027=CARTESIAN_POINT('Ctrl Pts',(57.7754740869501,3.05626516492244,125.738082515825));
#180028=CARTESIAN_POINT('Ctrl Pts',(57.7828759086255,3.19098226798874,125.819351483093));
#180029=CARTESIAN_POINT('Ctrl Pts',(57.7902777303009,3.32256056190424,125.906060863689));
#180030=CARTESIAN_POINT('Ctrl Pts',(57.7976795519763,3.45053631766601,125.997934743492));
#180031=CARTESIAN_POINT('Ctrl Pts',(57.8050774662877,3.57844451602229,126.089760123789));
#180032=CARTESIAN_POINT('Ctrl Pts',(57.812475380599,3.70275366117676,126.186744356588));
#180033=CARTESIAN_POINT('Ctrl Pts',(57.8198732949103,3.82302842918003,126.288567864108));
#180034=CARTESIAN_POINT('Ctrl Pts',(57.8272699798225,3.94328320969938,126.390374450409));
#180035=CARTESIAN_POINT('Ctrl Pts',(57.8346666647347,4.05950465906293,126.497018474366));
#180036=CARTESIAN_POINT('Ctrl Pts',(57.8420633496469,4.17128993700269,126.608139600513));
#180037=CARTESIAN_POINT('Ctrl Pts',(57.8494597065824,4.28307025826609,126.719255799432));
#180038=CARTESIAN_POINT('Ctrl Pts',(57.8568560635178,4.39041453447414,126.834848442644));
#180039=CARTESIAN_POINT('Ctrl Pts',(57.8642524204533,4.492956463491,126.954520000128));
#180040=CARTESIAN_POINT('Ctrl Pts',(57.8716499097899,4.59551409193883,127.074209879633));
#180041=CARTESIAN_POINT('Ctrl Pts',(57.8790473991264,4.69326766630308,127.197979633371));
#180042=CARTESIAN_POINT('Ctrl Pts',(57.886444888463,4.7858909932891,127.325398421328));
#180043=CARTESIAN_POINT('Ctrl Pts',(57.893844970978,4.87854678923855,127.452861875742));
#180044=CARTESIAN_POINT('Ctrl Pts',(57.9012450534929,4.96606853785129,127.583976609418));
#180045=CARTESIAN_POINT('Ctrl Pts',(57.9086451360079,5.04817330226624,127.718282706562));
#180046=CARTESIAN_POINT('Ctrl Pts',(57.9160533556744,5.13036834931048,127.852736487067));
#180047=CARTESIAN_POINT('Ctrl Pts',(57.9234615753408,5.20713432174797,127.990388320514));
#180048=CARTESIAN_POINT('Ctrl Pts',(57.9308697950073,5.27823385014464,128.130752945209));
#180049=CARTESIAN_POINT('Ctrl Pts',(57.9382825743094,5.34937713911489,128.271203961989));
#180050=CARTESIAN_POINT('Ctrl Pts',(57.9456953536114,5.41484687967498,128.414370758362));
#180051=CARTESIAN_POINT('Ctrl Pts',(57.9531081329135,5.4744540297795,128.559748482178));
#180052=CARTESIAN_POINT('Ctrl Pts',(57.9605315039422,5.53414634937529,128.705333928504));
#180053=CARTESIAN_POINT('Ctrl Pts',(57.967954874971,5.5879592209053,128.853136261815));
#180054=CARTESIAN_POINT('Ctrl Pts',(57.9753782459998,5.6357533391064,129.002635093728));
#180055=CARTESIAN_POINT('Ctrl Pts',(57.9793142954406,5.66109492738108,129.081902961584));
#180056=CARTESIAN_POINT('Ctrl Pts',(57.9832503448815,5.68474527857404,129.161647586823));
#180057=CARTESIAN_POINT('Ctrl Pts',(57.9871863943223,5.70668948883968,129.241790414194));
#180058=CARTESIAN_POINT('Ctrl Pts',(57.9946096607278,5.74807558454479,129.392937285441));
#180059=CARTESIAN_POINT('Ctrl Pts',(58.0020329271332,5.78351521925214,129.545958066559));
#180060=CARTESIAN_POINT('Ctrl Pts',(58.0094561935386,5.81283727832263,129.700343707259));
#180061=CARTESIAN_POINT('Ctrl Pts',(58.0168706862596,5.84212468115439,129.854546876954));
#180062=CARTESIAN_POINT('Ctrl Pts',(58.0242851789807,5.86530883165831,130.010111332086));
#180063=CARTESIAN_POINT('Ctrl Pts',(58.0316996717017,5.88226833561215,130.166512837641));
#180064=CARTESIAN_POINT('Ctrl Pts',(58.0391070180555,5.89921149335756,130.322763597537));
#180065=CARTESIAN_POINT('Ctrl Pts',(58.0465143644092,5.90994190850043,130.479849433084));
#180066=CARTESIAN_POINT('Ctrl Pts',(58.053921710763,5.91438922651423,130.637235994029));
#180067=CARTESIAN_POINT('Ctrl Pts',(58.0613235324384,5.91883322755047,130.794505170139));
#180068=CARTESIAN_POINT('Ctrl Pts',(58.0687253541138,5.91700345175747,130.952074253508));
#180069=CARTESIAN_POINT('Ctrl Pts',(58.0761271757892,5.90888137664651,131.10940395747));
#180070=CARTESIAN_POINT('Ctrl Pts',(58.0835250901006,5.90076358911575,131.266650608307));
#180071=CARTESIAN_POINT('Ctrl Pts',(58.090923004412,5.88636013670069,131.423657759545));
#180072=CARTESIAN_POINT('Ctrl Pts',(58.0983209187234,5.86570458601269,131.579886421218));
#180073=CARTESIAN_POINT('Ctrl Pts',(58.1057176036356,5.84505246790256,131.736089120521));
#180074=CARTESIAN_POINT('Ctrl Pts',(58.1131142885478,5.81815036247924,131.891513217307));
#180075=CARTESIAN_POINT('Ctrl Pts',(58.12051097346,5.78508368517174,132.045625020528));
#180076=CARTESIAN_POINT('Ctrl Pts',(58.1279073303955,5.75201847407532,132.19972999027));
#180077=CARTESIAN_POINT('Ctrl Pts',(58.1353036873309,5.71278931290752,132.352522417155));
#180078=CARTESIAN_POINT('Ctrl Pts',(58.1427000442664,5.66753265968059,132.503479246136));
#180079=CARTESIAN_POINT('Ctrl Pts',(58.150097533603,5.62226907754451,132.654459186993));
#180080=CARTESIAN_POINT('Ctrl Pts',(58.1574950229396,5.57097627309034,132.803602612771));
#180081=CARTESIAN_POINT('Ctrl Pts',(58.1648925122762,5.51384040878113,132.950402208261));
#180082=CARTESIAN_POINT('Ctrl Pts',(58.1722925947912,5.45668451558301,133.097253264122));
#180083=CARTESIAN_POINT('Ctrl Pts',(58.1796926773062,5.39368161974116,133.241758506183));
#180084=CARTESIAN_POINT('Ctrl Pts',(58.1870927598213,5.32506572715347,133.38343129593));
#180085=CARTESIAN_POINT('Ctrl Pts',(58.1945009794877,5.25637438433838,133.525259869472));
#180086=CARTESIAN_POINT('Ctrl Pts',(58.2019091991542,5.18205788157243,133.66424943452));
#180087=CARTESIAN_POINT('Ctrl Pts',(58.2093174188207,5.10239617928412,133.799937989648));
#180088=CARTESIAN_POINT('Ctrl Pts',(58.2167301981228,5.02268544654705,133.935710058817));
#180089=CARTESIAN_POINT('Ctrl Pts',(58.2241429774249,4.93762316002383,134.068176756233));
#180090=CARTESIAN_POINT('Ctrl Pts',(58.231555756727,4.84753188428267,134.196906150549));
#180091=CARTESIAN_POINT('Ctrl Pts',(58.2389791277557,4.75731188190199,134.32581947946));
#180092=CARTESIAN_POINT('Ctrl Pts',(58.2464024987845,4.66204876442175,134.450984543766));
#180093=CARTESIAN_POINT('Ctrl Pts',(58.2538258698133,4.56210505142999,134.572002859369));
#180094=CARTESIAN_POINT('Ctrl Pts',(58.2577619192539,4.50911249668749,134.636169674094));
#180095=CARTESIAN_POINT('Ctrl Pts',(58.2616979686946,4.45480467750348,134.699171302174));
#180096=CARTESIAN_POINT('Ctrl Pts',(58.2656340181352,4.39923962874216,134.760952743551));
#180097=CARTESIAN_POINT('Ctrl Pts',(58.2730572845406,4.29444568089989,134.877470613859));
#180098=CARTESIAN_POINT('Ctrl Pts',(58.2804805509461,4.18486095219262,134.989998452176));
#180099=CARTESIAN_POINT('Ctrl Pts',(58.2879038173515,4.07082122940121,135.098117140793));
#180100=CARTESIAN_POINT('Ctrl Pts',(58.2953183100725,3.95691629209141,135.2061080421));
#180101=CARTESIAN_POINT('Ctrl Pts',(58.3027328027936,3.83856710982604,135.3096999124));
#180102=CARTESIAN_POINT('Ctrl Pts',(58.3101472955146,3.71614911982727,135.408507257467));
#180103=CARTESIAN_POINT('Ctrl Pts',(58.3175546418684,3.59384912089656,135.507219368293));
#180104=CARTESIAN_POINT('Ctrl Pts',(58.3249619882221,3.46748841003899,135.601155901602));
#180105=CARTESIAN_POINT('Ctrl Pts',(58.3323693345759,3.33747852291532,135.689968836773));
#180106=CARTESIAN_POINT('Ctrl Pts',(58.3397711562512,3.20756560207102,135.778715531905));
#180107=CARTESIAN_POINT('Ctrl Pts',(58.3471729779266,3.07400923113412,135.862346028108));
#180108=CARTESIAN_POINT('Ctrl Pts',(58.3545747996019,2.9372531153924,135.940553244271));
#180109=CARTESIAN_POINT('Ctrl Pts',(58.3619727139134,2.80056919213752,136.018719175454));
#180110=CARTESIAN_POINT('Ctrl Pts',(58.3693706282249,2.66068921127279,136.091467343368));
#180111=CARTESIAN_POINT('Ctrl Pts',(58.3767685425363,2.51808478389424,136.15853465131));
#180112=CARTESIAN_POINT('Ctrl Pts',(58.3841652274485,2.37550405478604,136.225590813882));
#180113=CARTESIAN_POINT('Ctrl Pts',(58.3915619123607,2.23020011521923,136.286967831439));
#180114=CARTESIAN_POINT('Ctrl Pts',(58.3989585972729,2.08266814371336,136.342449093355));
#180115=CARTESIAN_POINT('Ctrl Pts',(58.4063549542083,1.9351427139295,136.397927895172));
#180116=CARTESIAN_POINT('Ctrl Pts',(58.4137513111438,1.78538979804815,136.447511329748));
#180117=CARTESIAN_POINT('Ctrl Pts',(58.4211476680793,1.63392321598273,136.491031479043));
#180118=CARTESIAN_POINT('Ctrl Pts',(58.4285451574158,1.48243344399757,136.534558291384));
#180119=CARTESIAN_POINT('Ctrl Pts',(58.4359426467523,1.32922984222628,136.572019866972));
#180120=CARTESIAN_POINT('Ctrl Pts',(58.4433401360889,1.17483985468064,136.603298613299));
#180121=CARTESIAN_POINT('Ctrl Pts',(58.4507402186039,1.02039574596376,136.634588324342));
#180122=CARTESIAN_POINT('Ctrl Pts',(58.4581403011189,0.86476478908387,136.659690816806));
#180123=CARTESIAN_POINT('Ctrl Pts',(58.4655403836339,0.708482892709509,
136.678539926477));
#180124=CARTESIAN_POINT('Ctrl Pts',(58.4729486033004,0.552029148323692,
136.697409762682));
#180125=CARTESIAN_POINT('Ctrl Pts',(58.4803568229668,0.394923405833401,
136.71001243907));
#180126=CARTESIAN_POINT('Ctrl Pts',(58.4877650426333,0.23770568557277,136.716333771222));
#180127=CARTESIAN_POINT('Ctrl Pts',(58.4951778219354,0.08039120042774,136.722658994048));
#180128=CARTESIAN_POINT('Ctrl Pts',(58.5025906012376,-0.0770350273878875,
136.72269516894));
#180129=CARTESIAN_POINT('Ctrl Pts',(58.5100033805397,-0.234035247772293,
136.716480209159));
#180130=CARTESIAN_POINT('Ctrl Pts',(58.5174267515684,-0.391259797433267,
136.710256369153));
#180131=CARTESIAN_POINT('Ctrl Pts',(58.5248501225971,-0.548056752820933,
136.697763585009));
#180132=CARTESIAN_POINT('Ctrl Pts',(58.5322734936259,-0.703894907287435,
136.679091464336));
#180133=CARTESIAN_POINT('Ctrl Pts',(58.5362095430666,-0.78652403606943,
136.669191057924));
#180134=CARTESIAN_POINT('Ctrl Pts',(58.5401455925074,-0.868883792885377,
136.657554270445));
#180135=CARTESIAN_POINT('Ctrl Pts',(58.5440816419481,-0.950896535366328,
136.644200199398));
#180136=CARTESIAN_POINT('Ctrl Pts',(58.5515049083535,-1.10557000815762,
136.619014838168));
#180137=CARTESIAN_POINT('Ctrl Pts',(58.5589281747589,-1.25947608810888,
136.587642147561));
#180138=CARTESIAN_POINT('Ctrl Pts',(58.5663514411644,-1.41208065866681,
136.550138091148));
#180139=CARTESIAN_POINT('Ctrl Pts',(58.5737659338854,-1.56450486329579,
136.512678361414));
#180140=CARTESIAN_POINT('Ctrl Pts',(58.5811804266064,-1.71563026150735,
136.469101778821));
#180141=CARTESIAN_POINT('Ctrl Pts',(58.5885949193274,-1.8649295931009,136.419515840289));
#180142=CARTESIAN_POINT('Ctrl Pts',(58.5960022656812,-2.01408502437742,
136.369977694552));
#180143=CARTESIAN_POINT('Ctrl Pts',(58.603409612035,-2.16141754102118,136.314441840567));
#180144=CARTESIAN_POINT('Ctrl Pts',(58.6108169583887,-2.30641189835171,
136.253066401295));
#180145=CARTESIAN_POINT('Ctrl Pts',(58.6182187800641,-2.45129811342042,
136.191736738141));
#180146=CARTESIAN_POINT('Ctrl Pts',(58.6256206017395,-2.59384929920243,
136.124576306744));
#180147=CARTESIAN_POINT('Ctrl Pts',(58.633022423415,-2.73356726611679,136.05179242409));
#180148=CARTESIAN_POINT('Ctrl Pts',(58.6404203377263,-2.87321147700378,
135.97904696348));
#180149=CARTESIAN_POINT('Ctrl Pts',(58.6478182520377,-3.01002511741883,
135.900684135702));
#180150=CARTESIAN_POINT('Ctrl Pts',(58.655216166349,-3.14353191933897,135.816958510335));
#180151=CARTESIAN_POINT('Ctrl Pts',(58.6626128512612,-3.27701653485051,
135.733246798649));
#180152=CARTESIAN_POINT('Ctrl Pts',(58.6700095361734,-3.40719508659085,
135.644174256277));
#180153=CARTESIAN_POINT('Ctrl Pts',(58.6774062210856,-3.5336176778186,135.550040407597));
#180154=CARTESIAN_POINT('Ctrl Pts',(58.684802578021,-3.66003466333635,135.45591073291));
#180155=CARTESIAN_POINT('Ctrl Pts',(58.6921989349565,-3.78269572007288,
135.356720421088));
#180156=CARTESIAN_POINT('Ctrl Pts',(58.6995952918919,-3.90118184161253,
135.252810999572));
#180157=CARTESIAN_POINT('Ctrl Pts',(58.7069927812285,-4.01968610367937,
135.14888566926));
#180158=CARTESIAN_POINT('Ctrl Pts',(58.714390270565,-4.13401387715223,135.040240036794));
#180159=CARTESIAN_POINT('Ctrl Pts',(58.7217877599015,-4.24378113175039,
134.927254294136));
#180160=CARTESIAN_POINT('Ctrl Pts',(58.7291878424165,-4.35358686508995,
134.8142289445));
#180161=CARTESIAN_POINT('Ctrl Pts',(58.7365879249314,-4.45882863663084,
134.696860723119));
#180162=CARTESIAN_POINT('Ctrl Pts',(58.7439880074464,-4.55916110881966,
134.575564741758));
#180163=CARTESIAN_POINT('Ctrl Pts',(58.7513962271129,-4.65960390687621,
134.454135382997));
#180164=CARTESIAN_POINT('Ctrl Pts',(58.7588044467794,-4.7551263867847,134.328769926799));
#180165=CARTESIAN_POINT('Ctrl Pts',(58.7662126664459,-4.84542472061101,
134.199915040542));
#180166=CARTESIAN_POINT('Ctrl Pts',(58.773625445748,-4.93577863155494,134.070980846253));
#180167=CARTESIAN_POINT('Ctrl Pts',(58.78103822505,-5.02090178799864,133.938553255662));
#180168=CARTESIAN_POINT('Ctrl Pts',(58.7884510043521,-5.10053542037966,
133.803105186207));
#180169=CARTESIAN_POINT('Ctrl Pts',(58.7958743753808,-5.18028283702907,
133.667463582198));
#180170=CARTESIAN_POINT('Ctrl Pts',(58.8032977464095,-5.25452488828037,
133.528793207927));
#180171=CARTESIAN_POINT('Ctrl Pts',(58.8107211174382,-5.32304983338438,
133.387589417693));
#180172=CARTESIAN_POINT('Ctrl Pts',(58.8146571668791,-5.35938340351294,
133.312719779971));
#180173=CARTESIAN_POINT('Ctrl Pts',(58.81859321632,-5.39411050494493,133.237138216132));
#180174=CARTESIAN_POINT('Ctrl Pts',(58.8225292657609,-5.42720523735072,
133.160920371566));
#180175=CARTESIAN_POINT('Ctrl Pts',(58.8307364137368,-5.49621183143824,
133.001996776182));
#180176=CARTESIAN_POINT('Ctrl Pts',(58.8389435617126,-5.55829734966145,
132.839894260625));
#180177=CARTESIAN_POINT('Ctrl Pts',(58.8471507096885,-5.61318787800807,
132.67520331771));
#180178=CARTESIAN_POINT('Ctrl Pts',(58.8553258331378,-5.66786422194073,
132.511155003572));
#180179=CARTESIAN_POINT('Ctrl Pts',(58.8635009565872,-5.71540149870125,
132.344538634856));
#180180=CARTESIAN_POINT('Ctrl Pts',(58.8716760800365,-5.75557476425497,
132.1759617606));
#180181=CARTESIAN_POINT('Ctrl Pts',(58.879830802216,-5.79564777619953,132.007805575074));
#180182=CARTESIAN_POINT('Ctrl Pts',(58.8879855243955,-5.8283933671508,131.837698871199));
#180183=CARTESIAN_POINT('Ctrl Pts',(58.896140246575,-5.85363568991775,131.666265352569));
#180184=CARTESIAN_POINT('Ctrl Pts',(58.9042614198469,-5.87877416459087,
131.495537119436));
#180185=CARTESIAN_POINT('Ctrl Pts',(58.9123825931188,-5.89647088813332,
131.323493192654));
#180186=CARTESIAN_POINT('Ctrl Pts',(58.9205037663907,-5.90660082279266,
131.150766856951));
#180187=CARTESIAN_POINT('Ctrl Pts',(58.9258774271522,-5.91330365138323,
131.036476384186));
#180188=CARTESIAN_POINT('Ctrl Pts',(58.9312510879138,-5.91669453246377,
130.921887482986));
#180189=CARTESIAN_POINT('Ctrl Pts',(58.9366247486753,-5.91674932490583,
130.807187051078));
#180190=CARTESIAN_POINT('',(60.6866248421796,-5.91522241010308,130.799308802059));
#180191=CARTESIAN_POINT('Ctrl Pts',(58.9366248077955,-5.90823460448425,
130.807181723492));
#180192=CARTESIAN_POINT('Ctrl Pts',(58.9914088350549,-5.90322513381588,
129.639500448815));
#180193=CARTESIAN_POINT('Ctrl Pts',(59.1390087369187,-5.00249046179937,
126.486390081414));
#180194=CARTESIAN_POINT('Ctrl Pts',(59.3794245133868,0.133157591622454,
123.807230521151));
#180195=CARTESIAN_POINT('Ctrl Pts',(59.6578721371997,5.95885864996216,127.134270139101));
#180196=CARTESIAN_POINT('Ctrl Pts',(59.9363197610124,6.30865971541475,133.83394361287));
#180197=CARTESIAN_POINT('Ctrl Pts',(60.2147673848254,0.861110697562879,
137.749578317314));
#180198=CARTESIAN_POINT('Ctrl Pts',(60.4648690670865,-4.74264084872292,
135.534005146028));
#180199=CARTESIAN_POINT('Ctrl Pts',(60.6221548747431,-5.90152067071388,
132.170905612889));
#180200=CARTESIAN_POINT('Ctrl Pts',(60.6866248077955,-5.91257889518605,
130.79931179142));
#180201=CARTESIAN_POINT('',(62.4366248077954,-5.92102293431065,130.803603394944));
#180202=CARTESIAN_POINT('Ctrl Pts',(60.6866248620209,-5.9167478418662,130.799307077057));
#180203=CARTESIAN_POINT('Ctrl Pts',(60.6954873200923,-5.91658668901759,
130.610627325191));
#180204=CARTESIAN_POINT('Ctrl Pts',(60.7043497781637,-5.90739656084578,
130.422339921947));
#180205=CARTESIAN_POINT('Ctrl Pts',(60.7132122362351,-5.88931252189037,
130.235213376507));
#180206=CARTESIAN_POINT('Ctrl Pts',(60.7221443094069,-5.87108643180472,
130.04661694166));
#180207=CARTESIAN_POINT('Ctrl Pts',(60.7310763825786,-5.84382625345664,
129.859199684484));
#180208=CARTESIAN_POINT('Ctrl Pts',(60.7400084557503,-5.80771882203087,
129.673726880793));
#180209=CARTESIAN_POINT('Ctrl Pts',(60.7490150007341,-5.77131034226002,
129.486707684064));
#180210=CARTESIAN_POINT('Ctrl Pts',(60.7580215457179,-5.72590651421125,
129.30166550607));
#180211=CARTESIAN_POINT('Ctrl Pts',(60.7670280907016,-5.67174697298224,
129.119363039833));
#180212=CARTESIAN_POINT('Ctrl Pts',(60.7685729379515,-5.66245725994887,
129.088093616972));
#180213=CARTESIAN_POINT('Ctrl Pts',(60.7701177852014,-5.65291005942039,
129.056904746874));
#180214=CARTESIAN_POINT('Ctrl Pts',(60.7716626324512,-5.64310672008258,
129.025800214246));
#180215=CARTESIAN_POINT('Ctrl Pts',(60.7790858988566,-5.59599992711428,
128.876337390568));
#180216=CARTESIAN_POINT('Ctrl Pts',(60.786509165262,-5.54287981320506,128.728521354023));
#180217=CARTESIAN_POINT('Ctrl Pts',(60.7939324316674,-5.48387836124831,
128.582872674422));
#180218=CARTESIAN_POINT('Ctrl Pts',(60.8013469243884,-5.42494664410802,
128.437396139466));
#180219=CARTESIAN_POINT('Ctrl Pts',(60.8087614171094,-5.36014756421678,
128.294082205112));
#180220=CARTESIAN_POINT('Ctrl Pts',(60.8161759098303,-5.28966312186374,
128.15343726528));
#180221=CARTESIAN_POINT('Ctrl Pts',(60.8235832561841,-5.21924661506993,
128.012927884337));
#180222=CARTESIAN_POINT('Ctrl Pts',(60.8309906025378,-5.1431558210789,127.875082708114));
#180223=CARTESIAN_POINT('Ctrl Pts',(60.8383979488915,-5.06162111976517,
127.740388978917));
#180224=CARTESIAN_POINT('Ctrl Pts',(60.8457997705669,-4.98014723010781,
127.605795709385));
#180225=CARTESIAN_POINT('Ctrl Pts',(60.8532015922422,-4.8932377101554,127.474349524752));
#180226=CARTESIAN_POINT('Ctrl Pts',(60.8606034139176,-4.80116917942636,
127.346513733589));
#180227=CARTESIAN_POINT('Ctrl Pts',(60.8680013282289,-4.70914925095804,
127.218745425946));
#180228=CARTESIAN_POINT('Ctrl Pts',(60.8753992425403,-4.61197595310718,
127.094584018232));
#180229=CARTESIAN_POINT('Ctrl Pts',(60.8827971568516,-4.50996952577516,
126.97446434755));
#180230=CARTESIAN_POINT('Ctrl Pts',(60.8901938417637,-4.40798005006093,
126.854364638579));
#180231=CARTESIAN_POINT('Ctrl Pts',(60.8975905266759,-4.3011592803352,126.738305617849));
#180232=CARTESIAN_POINT('Ctrl Pts',(60.9049872115881,-4.18986816470222,
126.626689576793));
#180233=CARTESIAN_POINT('Ctrl Pts',(60.9123835685235,-4.07858198383394,
126.515078484909));
#180234=CARTESIAN_POINT('Ctrl Pts',(60.9197799254589,-3.96282611476256,
126.40791024533));
#180235=CARTESIAN_POINT('Ctrl Pts',(60.9271762823943,-3.84299864449683,
126.305550554794));
#180236=CARTESIAN_POINT('Ctrl Pts',(60.9345737717309,-3.72315282833915,
126.203175192728));
#180237=CARTESIAN_POINT('Ctrl Pts',(60.9419712610674,-3.59923445362533,
126.105610088057));
#180238=CARTESIAN_POINT('Ctrl Pts',(60.949368750404,-3.471674856282,126.013180778032));
#180239=CARTESIAN_POINT('Ctrl Pts',(60.9567688329189,-3.34407054311992,
125.920719067056));
#180240=CARTESIAN_POINT('Ctrl Pts',(60.9641689154339,-3.21282276807083,
125.833396954096));
#180241=CARTESIAN_POINT('Ctrl Pts',(60.9715689979489,-3.07839187697724,
125.751496675774));
#180242=CARTESIAN_POINT('Ctrl Pts',(60.9789772176153,-2.94381316529887,
125.669506339676));
#180243=CARTESIAN_POINT('Ctrl Pts',(60.9863854372817,-2.80604466650949,
125.59294993879));
#180244=CARTESIAN_POINT('Ctrl Pts',(60.9937936569482,-2.6655720029761,125.52206410379));
#180245=CARTESIAN_POINT('Ctrl Pts',(61.0012064362502,-2.52501288086183,
125.451134639741));
#180246=CARTESIAN_POINT('Ctrl Pts',(61.0086192155523,-2.38174661647441,
125.385882850486));
#180247=CARTESIAN_POINT('Ctrl Pts',(61.0160319948543,-2.23627834906836,
125.326497009553));
#180248=CARTESIAN_POINT('Ctrl Pts',(61.023455365883,-2.09060222978048,125.267026315346));
#180249=CARTESIAN_POINT('Ctrl Pts',(61.0308787369117,-1.9427181735932,125.213438436121));
#180250=CARTESIAN_POINT('Ctrl Pts',(61.0383021079405,-1.79314678028665,
125.165871885038));
#180251=CARTESIAN_POINT('Ctrl Pts',(61.0422381573817,-1.7138404386294,125.140650958306));
#180252=CARTESIAN_POINT('Ctrl Pts',(61.046174206823,-1.63405991391674,125.117121992242));
#180253=CARTESIAN_POINT('Ctrl Pts',(61.0501102562642,-1.55388378398904,
125.095299771126));
#180254=CARTESIAN_POINT('Ctrl Pts',(61.0575335226697,-1.40267410517459,
125.054143743153));
#180255=CARTESIAN_POINT('Ctrl Pts',(61.0649567890751,-1.24959956816168,
125.018937021065));
#180256=CARTESIAN_POINT('Ctrl Pts',(61.0723800554806,-1.09516948305461,
124.989849944613));
#180257=CARTESIAN_POINT('Ctrl Pts',(61.0797945482016,-0.940921921483288,
124.96079724667));
#180258=CARTESIAN_POINT('Ctrl Pts',(61.0872090409226,-0.785322364161935,
124.937849865632));
#180259=CARTESIAN_POINT('Ctrl Pts',(61.0946235336436,-0.628895230239016,
124.921128397784));
#180260=CARTESIAN_POINT('Ctrl Pts',(61.1020308799974,-0.47261886667715,
124.904423046716));
#180261=CARTESIAN_POINT('Ctrl Pts',(61.1094382263512,-0.315516883168193,
124.8939317019));
#180262=CARTESIAN_POINT('Ctrl Pts',(61.116845572705,-0.158123736413326,
124.88972390459));
#180263=CARTESIAN_POINT('Ctrl Pts',(61.1242473943804,-0.00084797940541162,
124.885519245614));
#180264=CARTESIAN_POINT('Ctrl Pts',(61.1316492160557,0.156718136893979,
124.88758881261));
#180265=CARTESIAN_POINT('Ctrl Pts',(61.1390510377312,0.314035298255438,
124.895950307343));
#180266=CARTESIAN_POINT('Ctrl Pts',(61.1464489520425,0.47126941311197,124.904307388108));
#180267=CARTESIAN_POINT('Ctrl Pts',(61.1538468663538,0.628254462934403,
124.918949762001));
#180268=CARTESIAN_POINT('Ctrl Pts',(61.1612447806652,0.784451509464366,
124.939843042198));
#180269=CARTESIAN_POINT('Ctrl Pts',(61.1686414655774,0.940622598878676,
124.960732850311));
#180270=CARTESIAN_POINT('Ctrl Pts',(61.1760381504896,1.096005575261,124.9878714536));
#180271=CARTESIAN_POINT('Ctrl Pts',(61.1834348354018,1.25006687816888,125.021172624546));
#180272=CARTESIAN_POINT('Ctrl Pts',(61.1908311923373,1.40412134983736,125.054472318884));
#180273=CARTESIAN_POINT('Ctrl Pts',(61.1982275492727,1.55685389968581,125.093933958689));
#180274=CARTESIAN_POINT('Ctrl Pts',(61.2056239062081,1.70774168093889,125.139420290106));
#180275=CARTESIAN_POINT('Ctrl Pts',(61.2130213955447,1.85865256349626,125.184913585596));
#180276=CARTESIAN_POINT('Ctrl Pts',(61.2204188848813,2.00771775765134,125.236433301559));
#180277=CARTESIAN_POINT('Ctrl Pts',(61.2278163742178,2.1544302320902,125.2937925037));
#180278=CARTESIAN_POINT('Ctrl Pts',(61.2352164567328,2.30119413635954,125.351171813021));
#180279=CARTESIAN_POINT('Ctrl Pts',(61.2426165392478,2.44560333140259,125.414394548285));
#180280=CARTESIAN_POINT('Ctrl Pts',(61.2500166217628,2.5871715353852,125.483225963285));
#180281=CARTESIAN_POINT('Ctrl Pts',(61.2574248414292,2.72889540816165,125.552133065502));
#180282=CARTESIAN_POINT('Ctrl Pts',(61.2648330610957,2.86777171519548,125.626661000668));
#180283=CARTESIAN_POINT('Ctrl Pts',(61.2722412807622,3.00333888164796,125.706529105591));
#180284=CARTESIAN_POINT('Ctrl Pts',(61.2796540600642,3.13898948742954,125.786446368001));
#180285=CARTESIAN_POINT('Ctrl Pts',(61.2870668393663,3.27132658113066,125.871710147787));
#180286=CARTESIAN_POINT('Ctrl Pts',(61.2944796186683,3.39991872279468,125.961997223428));
#180287=CARTESIAN_POINT('Ctrl Pts',(61.3019029896971,3.52869460294108,126.052413305476));
#180288=CARTESIAN_POINT('Ctrl Pts',(61.3093263607259,3.65371454805904,126.147866792564));
#180289=CARTESIAN_POINT('Ctrl Pts',(61.3167497317546,3.77458062620727,126.247994559098));
#180290=CARTESIAN_POINT('Ctrl Pts',(61.3206857811954,3.83866672098319,126.301084703447));
#180291=CARTESIAN_POINT('Ctrl Pts',(61.3246218306362,3.90158562885523,126.355488337498));
#180292=CARTESIAN_POINT('Ctrl Pts',(61.328557880077,3.96328243814734,126.411147342755));
#180293=CARTESIAN_POINT('Ctrl Pts',(61.3359811464824,4.07964069498093,126.516118489612));
#180294=CARTESIAN_POINT('Ctrl Pts',(61.3434044128879,4.19200163368944,126.625874339636));
#180295=CARTESIAN_POINT('Ctrl Pts',(61.3508276792933,4.29994664806236,126.740078468611));
#180296=CARTESIAN_POINT('Ctrl Pts',(61.3582421720143,4.40776408039256,126.854147617789));
#180297=CARTESIAN_POINT('Ctrl Pts',(61.3656566647354,4.51117572342619,126.9726543122));
#180298=CARTESIAN_POINT('Ctrl Pts',(61.3730711574564,4.60979665473362,127.095222528399));
#180299=CARTESIAN_POINT('Ctrl Pts',(61.3804785038101,4.70832253147444,127.217672608738));
#180300=CARTESIAN_POINT('Ctrl Pts',(61.3878858501639,4.80206665651455,127.344176128685));
#180301=CARTESIAN_POINT('Ctrl Pts',(61.3952931965177,4.89068163592486,127.474321023428));
#180302=CARTESIAN_POINT('Ctrl Pts',(61.4026950181931,4.97923052294039,127.604368851199));
#180303=CARTESIAN_POINT('Ctrl Pts',(61.4100968398685,5.06265767223972,127.738052338859));
#180304=CARTESIAN_POINT('Ctrl Pts',(61.4174986615439,5.14065667831233,127.87492731431));
#180305=CARTESIAN_POINT('Ctrl Pts',(61.4248965758553,5.21861450931679,128.011730034527));
#180306=CARTESIAN_POINT('Ctrl Pts',(61.4322944901667,5.29114971946928,128.15172056374));
#180307=CARTESIAN_POINT('Ctrl Pts',(61.4396924044781,5.35799993008529,128.294426891009));
#180308=CARTESIAN_POINT('Ctrl Pts',(61.4470890893903,5.42483903140899,128.437109503076));
#180309=CARTESIAN_POINT('Ctrl Pts',(61.4544857743025,5.48599485003209,128.582506679756));
#180310=CARTESIAN_POINT('Ctrl Pts',(61.4618824592147,5.54125152915468,128.730122913459));
#180311=CARTESIAN_POINT('Ctrl Pts',(61.4692788161501,5.59650575813822,128.877732601703));
#180312=CARTESIAN_POINT('Ctrl Pts',(61.4766751730856,5.64586123685168,129.027560801719));
#180313=CARTESIAN_POINT('Ctrl Pts',(61.4840715300211,5.68915082939721,129.179093438648));
#180314=CARTESIAN_POINT('Ctrl Pts',(61.4914690193577,5.73244704968986,129.33064927561));
#180315=CARTESIAN_POINT('Ctrl Pts',(61.4988665086943,5.76967543209657,129.483909710115));
#180316=CARTESIAN_POINT('Ctrl Pts',(61.5062639980309,5.80071918692378,129.638347119808));
#180317=CARTESIAN_POINT('Ctrl Pts',(61.5136640805459,5.83177382409111,129.792838667295));
#180318=CARTESIAN_POINT('Ctrl Pts',(61.5210641630609,5.85663944366383,129.948507645677));
#180319=CARTESIAN_POINT('Ctrl Pts',(61.5284642455759,5.87525069706555,130.104818046216));
#180320=CARTESIAN_POINT('Ctrl Pts',(61.5358724652423,5.8938824154537,130.26130032611));
#180321=CARTESIAN_POINT('Ctrl Pts',(61.5432806849089,5.90624598905169,130.418425065803));
#180322=CARTESIAN_POINT('Ctrl Pts',(61.5506889045753,5.91232805527671,130.575652223999));
#180323=CARTESIAN_POINT('Ctrl Pts',(61.5581016838774,5.918413864912,130.732976152888));
#180324=CARTESIAN_POINT('Ctrl Pts',(61.5655144631794,5.91821046384112,130.890402253458));
#180325=CARTESIAN_POINT('Ctrl Pts',(61.5729272424815,5.91175658364844,131.047392833927));
#180326=CARTESIAN_POINT('Ctrl Pts',(61.5803506135103,5.90529348184907,131.2046077299));
#180327=CARTESIAN_POINT('Ctrl Pts',(61.5877739845391,5.89256209389692,131.361385491828));
#180328=CARTESIAN_POINT('Ctrl Pts',(61.5951973555678,5.87365283570351,131.517195050048));
#180329=CARTESIAN_POINT('Ctrl Pts',(61.5991334050085,5.8636266932882,131.599809016413));
#180330=CARTESIAN_POINT('Ctrl Pts',(61.6030694544492,5.85186458175435,131.682150968647));
#180331=CARTESIAN_POINT('Ctrl Pts',(61.6070055038899,5.83838571673788,131.764143293535));
#180332=CARTESIAN_POINT('Ctrl Pts',(61.6144287702953,5.81296499797722,131.918778259385));
#180333=CARTESIAN_POINT('Ctrl Pts',(61.6218520367008,5.78135812484507,132.072636417221));
#180334=CARTESIAN_POINT('Ctrl Pts',(61.6292753031062,5.74362187368212,132.225183736276));
#180335=CARTESIAN_POINT('Ctrl Pts',(61.6366897958272,5.7059302236342,132.377550757068));
#180336=CARTESIAN_POINT('Ctrl Pts',(61.6441042885482,5.66212370437189,132.528609664138));
#180337=CARTESIAN_POINT('Ctrl Pts',(61.6515187812692,5.61231061509273,132.677833361488));
#180338=CARTESIAN_POINT('Ctrl Pts',(61.658926127623,5.56254553754444,132.82691323142));
#180339=CARTESIAN_POINT('Ctrl Pts',(61.6663334739767,5.50678553285906,132.974161061339));
#180340=CARTESIAN_POINT('Ctrl Pts',(61.6737408203305,5.44518950792927,133.119061847798));
#180341=CARTESIAN_POINT('Ctrl Pts',(61.6811426420059,5.38363942363875,133.263854561783));
#180342=CARTESIAN_POINT('Ctrl Pts',(61.6885444636813,5.31626213137478,133.406303375749));
#180343=CARTESIAN_POINT('Ctrl Pts',(61.6959462853567,5.24326570604115,133.545910416193));
#180344=CARTESIAN_POINT('Ctrl Pts',(61.703344199668,5.17030781495226,133.685443759167));
#180345=CARTESIAN_POINT('Ctrl Pts',(61.7107421139794,5.09173687084677,133.82213798627));
#180346=CARTESIAN_POINT('Ctrl Pts',(61.7181400282907,5.00780816780718,133.955517217442));
#180347=CARTESIAN_POINT('Ctrl Pts',(61.7255367132029,4.92389341219542,134.088874283406));
#180348=CARTESIAN_POINT('Ctrl Pts',(61.7329333981151,4.83462286337252,134.218917131155));
#180349=CARTESIAN_POINT('Ctrl Pts',(61.7403300830273,4.74029673003504,134.345196320295));
#180350=CARTESIAN_POINT('Ctrl Pts',(61.7477264399628,4.64597477921716,134.471469910083));
#180351=CARTESIAN_POINT('Ctrl Pts',(61.7551227968982,4.54659791300742,134.59397987401));
#180352=CARTESIAN_POINT('Ctrl Pts',(61.7625191538336,4.44250829611049,134.712307725894));
#180353=CARTESIAN_POINT('Ctrl Pts',(61.7699166431702,4.33840274282749,134.830653694074));
#180354=CARTESIAN_POINT('Ctrl Pts',(61.7773141325067,4.22958324876174,134.944815995));
#180355=CARTESIAN_POINT('Ctrl Pts',(61.7847116218433,4.11643058986292,135.054411177423));
#180356=CARTESIAN_POINT('Ctrl Pts',(61.7921117043583,4.00323826547494,135.164044778268));
#180357=CARTESIAN_POINT('Ctrl Pts',(61.7995117868733,3.88571001994317,135.269107813487));
#180358=CARTESIAN_POINT('Ctrl Pts',(61.8069118693883,3.76426149009823,135.369255577657));
#180359=CARTESIAN_POINT('Ctrl Pts',(61.8143200890548,3.64267941510951,135.469513464589));
#180360=CARTESIAN_POINT('Ctrl Pts',(61.8217283087212,3.51716873512941,135.564845049001));
#180361=CARTESIAN_POINT('Ctrl Pts',(61.8291365283877,3.38817657939181,135.654947183061));
#180362=CARTESIAN_POINT('Ctrl Pts',(61.8365493076898,3.25910503113451,135.745104773482));
#180363=CARTESIAN_POINT('Ctrl Pts',(61.8439620869918,3.12654805093928,135.830026299104));
#180364=CARTESIAN_POINT('Ctrl Pts',(61.8513748662939,2.99097894949759,135.909453710367));
#180365=CARTESIAN_POINT('Ctrl Pts',(61.8587982373226,2.8552161405664,135.988994611239));
#180366=CARTESIAN_POINT('Ctrl Pts',(61.8662216083514,2.71643294310971,136.063025543815));
#180367=CARTESIAN_POINT('Ctrl Pts',(61.8736449793801,2.57512503308625,136.131335521437));
#180368=CARTESIAN_POINT('Ctrl Pts',(61.877581028821,2.50020018855354,136.167555110648));
#180369=CARTESIAN_POINT('Ctrl Pts',(61.8815170782618,2.42456586350064,136.202167149593));
#180370=CARTESIAN_POINT('Ctrl Pts',(61.8854531277027,2.34829774264479,136.23514585309));
#180371=CARTESIAN_POINT('Ctrl Pts',(61.8928763941081,2.2044584469599,136.297342658656));
#180372=CARTESIAN_POINT('Ctrl Pts',(61.9002996605136,2.05792893431406,136.353914993641));
#180373=CARTESIAN_POINT('Ctrl Pts',(61.907722926919,1.90918918891571,136.404621968916));
#180374=CARTESIAN_POINT('Ctrl Pts',(61.91513741964,1.76062524154414,136.455269012758));
#180375=CARTESIAN_POINT('Ctrl Pts',(61.922551912361,1.60985661112041,136.500064376527));
#180376=CARTESIAN_POINT('Ctrl Pts',(61.929966405082,1.45738529679739,136.538814267146));
#180377=CARTESIAN_POINT('Ctrl Pts',(61.9373737514358,1.30506094006778,136.577526809161));
#180378=CARTESIAN_POINT('Ctrl Pts',(61.9447810977896,1.15103752593519,136.610205386813));
#180379=CARTESIAN_POINT('Ctrl Pts',(61.9521884441434,0.99583423444274,136.636705321029));
#180380=CARTESIAN_POINT('Ctrl Pts',(61.9595902658188,0.840746699420133,
136.663185490594));
#180381=CARTESIAN_POINT('Ctrl Pts',(61.9669920874942,0.684481405619452,
136.683496129843));
#180382=CARTESIAN_POINT('Ctrl Pts',(61.9743939091696,0.527569697687247,
136.697543185295));
#180383=CARTESIAN_POINT('Ctrl Pts',(61.981791823481,0.370740822224485,136.711582825415));
#180384=CARTESIAN_POINT('Ctrl Pts',(61.9891897377924,0.213266583089832,
136.719365433586));
#180385=CARTESIAN_POINT('Ctrl Pts',(61.9965876521038,0.0556853443427907,
136.720848571152));
#180386=CARTESIAN_POINT('Ctrl Pts',(62.003984337016,-0.10186970726096,136.722331462247));
#180387=CARTESIAN_POINT('Ctrl Pts',(62.0113810219281,-0.259531350270411,
136.717516956931));
#180388=CARTESIAN_POINT('Ctrl Pts',(62.0187777068403,-0.416759187618657,
136.706414695769));
#180389=CARTESIAN_POINT('Ctrl Pts',(62.0261740637758,-0.573980053319833,
136.695312926894));
#180390=CARTESIAN_POINT('Ctrl Pts',(62.0335704207112,-0.730766779235901,
136.677923982828));
#180391=CARTESIAN_POINT('Ctrl Pts',(62.0409667776467,-0.886582332707555,
136.654309534423));
#180392=CARTESIAN_POINT('Ctrl Pts',(62.0483642669833,-1.04242174193845,
136.630691470585));
#180393=CARTESIAN_POINT('Ctrl Pts',(62.0557617563198,-1.19728931355836,
136.600846060519));
#180394=CARTESIAN_POINT('Ctrl Pts',(62.0631592456564,-1.3506566204702,136.564886397048));
#180395=CARTESIAN_POINT('Ctrl Pts',(62.0705593281714,-1.50407769005373,
136.528914127973));
#180396=CARTESIAN_POINT('Ctrl Pts',(62.0779594106865,-1.6559970846206,136.486823423278));
#180397=CARTESIAN_POINT('Ctrl Pts',(62.0853594932015,-1.80590013187556,
136.438777648297));
#180398=CARTESIAN_POINT('Ctrl Pts',(62.092767712868,-1.95596801294138,136.390679042047));
#180399=CARTESIAN_POINT('Ctrl Pts',(62.1001759325344,-2.10401476313579,
136.336612402311));
#180400=CARTESIAN_POINT('Ctrl Pts',(62.1075841522009,-2.24954365133065,
136.276790052767));
#180401=CARTESIAN_POINT('Ctrl Pts',(62.1149969315029,-2.39516211012792,
136.216930883566));
#180402=CARTESIAN_POINT('Ctrl Pts',(62.122409710805,-2.53825928041674,136.151309100842));
#180403=CARTESIAN_POINT('Ctrl Pts',(62.1298224901071,-2.67836222180148,
136.080183432192));
#180404=CARTESIAN_POINT('Ctrl Pts',(62.1372458611359,-2.81866534883903,
136.008956135851));
#180405=CARTESIAN_POINT('Ctrl Pts',(62.1446692321646,-2.95596537727408,
135.93220942865));
#180406=CARTESIAN_POINT('Ctrl Pts',(62.1520926031934,-3.08981687309164,
135.850246293367));
#180407=CARTESIAN_POINT('Ctrl Pts',(62.1560286526342,-3.16078814789647,
135.806787472362));
#180408=CARTESIAN_POINT('Ctrl Pts',(62.1599647020749,-3.23079043668502,
135.761862825116));
#180409=CARTESIAN_POINT('Ctrl Pts',(62.1639007515157,-3.2997611362165,135.715522089806));
#180410=CARTESIAN_POINT('Ctrl Pts',(62.1712980963833,-3.4293835044989,135.628430094224));
#180411=CARTESIAN_POINT('Ctrl Pts',(62.1786954412508,-3.55575829884785,
135.536066499443));
#180412=CARTESIAN_POINT('Ctrl Pts',(62.1860927861183,-3.67842526326733,
135.43870179459));
#180413=CARTESIAN_POINT('Ctrl Pts',(62.1934813718664,-3.80094697900442,
135.341452378275));
#180414=CARTESIAN_POINT('Ctrl Pts',(62.2008699576145,-3.91976931110266,
135.239213869239));
#180415=CARTESIAN_POINT('Ctrl Pts',(62.2082585433626,-4.03445957380163,
135.132300833172));
#180416=CARTESIAN_POINT('Ctrl Pts',(62.2156400218208,-4.14903951268851,
135.025490639782));
#180417=CARTESIAN_POINT('Ctrl Pts',(62.223021500279,-4.25949502084972,134.914015124824));
#180418=CARTESIAN_POINT('Ctrl Pts',(62.2304029787372,-4.36542533481602,
134.798229945504));
#180419=CARTESIAN_POINT('Ctrl Pts',(62.2377789958862,-4.47127727448394,
134.682530431769));
#180420=CARTESIAN_POINT('Ctrl Pts',(62.2451550130352,-4.57261043273816,
134.562527878227));
#180421=CARTESIAN_POINT('Ctrl Pts',(62.2525310301842,-4.6690599892814,134.438615613984));
#180422=CARTESIAN_POINT('Ctrl Pts',(62.2602016042513,-4.76936120228845,
134.309754986156));
#180423=CARTESIAN_POINT('Ctrl Pts',(62.2678721783185,-4.86438039852302,
134.176666214058));
#180424=CARTESIAN_POINT('Ctrl Pts',(62.2755427523856,-4.95375217877916,
134.0398312037));
#180425=CARTESIAN_POINT('Ctrl Pts',(62.2829137966036,-5.03963406171821,
133.908339492247));
#180426=CARTESIAN_POINT('Ctrl Pts',(62.2902848408216,-5.1203010331985,133.773388936696));
#180427=CARTESIAN_POINT('Ctrl Pts',(62.2976558850396,-5.19547235895497,
133.635437714686));
#180428=CARTESIAN_POINT('Ctrl Pts',(62.3050267840442,-5.27064220379776,
133.497489210385));
#180429=CARTESIAN_POINT('Ctrl Pts',(62.3123976830489,-5.34031643794952,
133.356540487433));
#180430=CARTESIAN_POINT('Ctrl Pts',(62.3197685820535,-5.40426003168304,
133.213074812412));
#180431=CARTESIAN_POINT('Ctrl Pts',(62.3271408180326,-5.4682152238599,133.069583114792));
#180432=CARTESIAN_POINT('Ctrl Pts',(62.3345130540117,-5.52643755324915,
132.923573899925));
#180433=CARTESIAN_POINT('Ctrl Pts',(62.3418852899909,-5.57874000795137,
132.775550736804));
#180434=CARTESIAN_POINT('Ctrl Pts',(62.3492603456933,-5.63106246722916,
132.627470957975));
#180435=CARTESIAN_POINT('Ctrl Pts',(62.3566354013958,-5.677460419311,132.477376051935));
#180436=CARTESIAN_POINT('Ctrl Pts',(62.3640104570983,-5.71779666927694,
132.32578488821));
#180437=CARTESIAN_POINT('Ctrl Pts',(62.3713936318705,-5.75817732471455,
132.174026840426));
#180438=CARTESIAN_POINT('Ctrl Pts',(62.3787768066428,-5.79248285793303,
132.020769609828));
#180439=CARTESIAN_POINT('Ctrl Pts',(62.386159981415,-5.82062703583033,131.866543027635));
#180440=CARTESIAN_POINT('Ctrl Pts',(62.3935479622602,-5.84878953416268,
131.712216051745));
#180441=CARTESIAN_POINT('Ctrl Pts',(62.4009359431054,-5.87078263465548,
131.556918838468));
#180442=CARTESIAN_POINT('Ctrl Pts',(62.4083239239507,-5.8865720210988,131.401185887571));
#180443=CARTESIAN_POINT('Ctrl Pts',(62.415721914078,-5.90238279910038,131.245241948711));
#180444=CARTESIAN_POINT('Ctrl Pts',(62.4231199042053,-5.91197306176435,
131.088861467507));
#180445=CARTESIAN_POINT('Ctrl Pts',(62.4305178943326,-5.91536056244642,
130.932579098112));
#180446=CARTESIAN_POINT('Ctrl Pts',(62.4325535321535,-5.91629267027411,
130.889576296485));
#180447=CARTESIAN_POINT('Ctrl Pts',(62.4345891699745,-5.91675544781438,
130.846580893109));
#180448=CARTESIAN_POINT('Ctrl Pts',(62.4366248077954,-5.91674995161543,
130.803603941404));
#180449=CARTESIAN_POINT('',(64.1866248077954,-5.91487042073829,130.809777511898));
#180450=CARTESIAN_POINT('Ctrl Pts',(62.4366248077954,-5.92641419966217,
130.803602705471));
#180451=CARTESIAN_POINT('Ctrl Pts',(62.4385326636398,-5.9264866793447,130.763257721606));
#180452=CARTESIAN_POINT('Ctrl Pts',(62.4404405194842,-5.9261104867987,130.722914125487));
#180453=CARTESIAN_POINT('Ctrl Pts',(62.5351642499328,-5.88495218713434,
128.720344364475));
#180454=CARTESIAN_POINT('Ctrl Pts',(62.7207959991417,-3.66101786007206,
124.839923614913));
#180455=CARTESIAN_POINT('Ctrl Pts',(62.9992436229541,3.03918019325866,124.50031871707));
#180456=CARTESIAN_POINT('Ctrl Pts',(63.2776912467674,6.94652012119423,129.953820356205));
#180457=CARTESIAN_POINT('Ctrl Pts',(63.55613887058,4.4703474141243,136.188926944336));
#180458=CARTESIAN_POINT('Ctrl Pts',(63.8345864943932,-2.113856177913,137.475880128848));
#180459=CARTESIAN_POINT('Ctrl Pts',(64.0447484734647,-5.61721949372411,
133.819923126594));
#180460=CARTESIAN_POINT('Ctrl Pts',(64.1620945779322,-5.91951888618433,
131.331144473255));
#180461=CARTESIAN_POINT('Ctrl Pts',(64.1866248077954,-5.91487042073829,
130.809777511898));
#180462=CARTESIAN_POINT('',(65.9366248077954,-5.90732499563075,130.802771912788));
#180463=CARTESIAN_POINT('Ctrl Pts',(64.1866248077954,-5.91487042073829,
130.809777511898));
#180464=CARTESIAN_POINT('Ctrl Pts',(64.2549104525365,-5.90193032756302,
129.358430365884));
#180465=CARTESIAN_POINT('Ctrl Pts',(64.416011971882,-4.63111467414602,125.91410477066));
#180466=CARTESIAN_POINT('Ctrl Pts',(64.6699293658316,1.14574950453723,123.90038939781));
#180467=CARTESIAN_POINT('Ctrl Pts',(64.9483769896447,6.42781211149671,128.036547041898));
#180468=CARTESIAN_POINT('Ctrl Pts',(65.2268246134574,5.80302940406682,134.716190146808));
#180469=CARTESIAN_POINT('Ctrl Pts',(65.5052722372703,-0.154453831949839,
137.801053017846));
#180470=CARTESIAN_POINT('Ctrl Pts',(65.7418723020498,-5.0959898596557,134.958976688939));
#180471=CARTESIAN_POINT('Ctrl Pts',(65.8856564922247,-5.90472330876078,
131.889541835793));
#180472=CARTESIAN_POINT('Ctrl Pts',(65.9366248077954,-5.90732499563075,
130.802771912788));
#180473=CARTESIAN_POINT('',(67.6866248077955,-5.92071699922957,130.79949226525));
#180474=CARTESIAN_POINT('Ctrl Pts',(65.9366248077954,-5.90732499563075,
130.802771912788));
#180475=CARTESIAN_POINT('Ctrl Pts',(65.978472366829,-5.90946111183665,129.910478965698));
#180476=CARTESIAN_POINT('Ctrl Pts',(66.1131358004669,-5.30008853599008,
127.041893018253));
#180477=CARTESIAN_POINT('Ctrl Pts',(66.3406151087089,-0.839967855329431,
123.856554162838));
#180478=CARTESIAN_POINT('Ctrl Pts',(66.619062732522,5.39136319930542,126.342212773363));
#180479=CARTESIAN_POINT('Ctrl Pts',(66.8975103563348,6.66829485651329,132.928367264669));
#180480=CARTESIAN_POINT('Ctrl Pts',(67.1759579801478,1.81738930489791,137.562663410783));
#180481=CARTESIAN_POINT('Ctrl Pts',(67.4389961306345,-4.3427319715742,136.073640374768));
#180482=CARTESIAN_POINT('Ctrl Pts',(67.6092184065172,-5.90614742993307,
132.440529099857));
#180483=CARTESIAN_POINT('Ctrl Pts',(67.6866248077955,-5.92071699922957,
130.79949226525));
#180484=CARTESIAN_POINT('',(69.4366248077955,-5.9204678244194,130.808252981436));
#180485=CARTESIAN_POINT('Ctrl Pts',(67.6866248077955,-5.92071699922957,
130.79949226525));
#180486=CARTESIAN_POINT('Ctrl Pts',(67.7020342811215,-5.92361739746199,
130.472807224837));
#180487=CARTESIAN_POINT('Ctrl Pts',(67.8102596290518,-5.75016475465227,
128.181482562032));
#180488=CARTESIAN_POINT('Ctrl Pts',(68.0113008515862,-2.75802833476207,
124.372343808279));
#180489=CARTESIAN_POINT('Ctrl Pts',(68.2897484753995,3.92065622231303,125.00729107194));
#180490=CARTESIAN_POINT('Ctrl Pts',(68.5681960992121,6.99644924578514,130.969462045448));
#180491=CARTESIAN_POINT('Ctrl Pts',(68.8466437230252,3.64284720793011,136.77991287238));
#180492=CARTESIAN_POINT('Ctrl Pts',(69.1250913468378,-3.05835345103424,
137.099123099097));
#180493=CARTESIAN_POINT('Ctrl Pts',(69.3217517084282,-5.80627074332086,
133.239074215812));
#180494=CARTESIAN_POINT('Ctrl Pts',(69.4255961954139,-5.92501520140697,
131.041805089321));
#180495=CARTESIAN_POINT('Ctrl Pts',(69.4366248077955,-5.92324058126049,
130.808254804363));
#180496=CARTESIAN_POINT('',(71.1866247805454,-5.91210743526078,130.807354196885));
#180497=CARTESIAN_POINT('Ctrl Pts',(69.4366248077955,-5.91674872130226,
130.808250536342));
#180498=CARTESIAN_POINT('Ctrl Pts',(69.4439407278742,-5.91685046494537,
130.653493687942));
#180499=CARTESIAN_POINT('Ctrl Pts',(69.451256647953,-5.91087639187094,130.498496518504));
#180500=CARTESIAN_POINT('Ctrl Pts',(69.4585725680317,-5.89879643630179,
130.343783625551));
#180501=CARTESIAN_POINT('Ctrl Pts',(69.4658809137479,-5.88672898742519,
130.189230910885));
#180502=CARTESIAN_POINT('Ctrl Pts',(69.473189259464,-5.86856826374107,130.034962267138));
#180503=CARTESIAN_POINT('Ctrl Pts',(69.4804976051802,-5.84433620417594,
129.881503697422));
#180504=CARTESIAN_POINT('Ctrl Pts',(69.4878000820948,-5.82012360361777,
129.728168359136));
#180505=CARTESIAN_POINT('Ctrl Pts',(69.4951025590094,-5.78984942927961,
129.575642178058));
#180506=CARTESIAN_POINT('Ctrl Pts',(69.5024050359239,-5.75358752863028,
129.424447173581));
#180507=CARTESIAN_POINT('Ctrl Pts',(69.5098876008631,-5.71643136509835,
129.269523515115));
#180508=CARTESIAN_POINT('Ctrl Pts',(69.5173701658022,-5.67298833895637,
129.115997951889));
#180509=CARTESIAN_POINT('Ctrl Pts',(69.5248527307414,-5.62339394741176,
128.964422826576));
#180510=CARTESIAN_POINT('Ctrl Pts',(69.5321494851218,-5.57503110703688,
128.8166116858));
#180511=CARTESIAN_POINT('Ctrl Pts',(69.5394462395022,-5.52081893454438,
128.670655641708));
#180512=CARTESIAN_POINT('Ctrl Pts',(69.5467429938826,-5.46093385327126,
128.527052554809));
#180513=CARTESIAN_POINT('Ctrl Pts',(69.5540393668669,-5.40105190214901,
128.383456973943));
#180514=CARTESIAN_POINT('Ctrl Pts',(69.5613357398511,-5.3354977798605,128.242214460549));
#180515=CARTESIAN_POINT('Ctrl Pts',(69.5686321128354,-5.26449616021194,
128.103803130377));
#180516=CARTESIAN_POINT('Ctrl Pts',(69.5759296374804,-5.19348333365522,
127.965369953336));
#180517=CARTESIAN_POINT('Ctrl Pts',(69.5832271621254,-5.11702147458102,
127.829769190646));
#180518=CARTESIAN_POINT('Ctrl Pts',(69.5905246867704,-5.03538118839708,
127.69745430259));
#180519=CARTESIAN_POINT('Ctrl Pts',(69.5981465124115,-4.95011281907282,
127.559259359025));
#180520=CARTESIAN_POINT('Ctrl Pts',(69.6057683380526,-4.85919544818148,
127.424649435827));
#180521=CARTESIAN_POINT('Ctrl Pts',(69.6133901636938,-4.76298711651232,
127.294106454341));
#180522=CARTESIAN_POINT('Ctrl Pts',(69.6206984429048,-4.6707366002486,127.168933746034));
#180523=CARTESIAN_POINT('Ctrl Pts',(69.6280067221158,-4.57362205408285,
127.047500299789));
#180524=CARTESIAN_POINT('Ctrl Pts',(69.6353150013268,-4.47199918411649,
126.930195693384));
#180525=CARTESIAN_POINT('Ctrl Pts',(69.6426281226757,-4.37030898339657,
126.812813366211));
#180526=CARTESIAN_POINT('Ctrl Pts',(69.6499412440246,-4.26410477346076,
126.699565604616));
#180527=CARTESIAN_POINT('Ctrl Pts',(69.6572543653735,-4.15377803744627,
126.5908040939));
#180528=CARTESIAN_POINT('Ctrl Pts',(69.6645770915714,-4.04330640138201,
126.481899738858));
#180529=CARTESIAN_POINT('Ctrl Pts',(69.6718998177694,-3.92870171892136,
126.377493647466));
#180530=CARTESIAN_POINT('Ctrl Pts',(69.6792225439673,-3.8103876164212,126.277896569866));
#180531=CARTESIAN_POINT('Ctrl Pts',(69.6801438941328,-3.79550125921326,
126.265365200885));
#180532=CARTESIAN_POINT('Ctrl Pts',(69.6810652442983,-3.78055621475712,
126.252909905282));
#180533=CARTESIAN_POINT('Ctrl Pts',(69.6819865944638,-3.76555335708998,
126.240531252065));
#180534=CARTESIAN_POINT('Ctrl Pts',(69.6894098608692,-3.64467617762322,
126.140797140098));
#180535=CARTESIAN_POINT('Ctrl Pts',(69.6968331272747,-3.51965115785384,
126.045717849011));
#180536=CARTESIAN_POINT('Ctrl Pts',(69.7042563936801,-3.3908723891784,125.95565821354));
#180537=CARTESIAN_POINT('Ctrl Pts',(69.7116708864011,-3.26224582631312,
125.865705021079));
#180538=CARTESIAN_POINT('Ctrl Pts',(69.7190853791222,-3.12987464858298,
125.780759886778));
#180539=CARTESIAN_POINT('Ctrl Pts',(69.7264998718432,-2.99418718778021,
125.701148526438));
#180540=CARTESIAN_POINT('Ctrl Pts',(69.7339072181969,-2.8586305076609,125.621613898525));
#180541=CARTESIAN_POINT('Ctrl Pts',(69.7413145645506,-2.71976422759838,
125.547402997708));
#180542=CARTESIAN_POINT('Ctrl Pts',(69.7487219109044,-2.57804683731763,
125.47879913852));
#180543=CARTESIAN_POINT('Ctrl Pts',(69.7561237325798,-2.43643514521304,
125.410246446678));
#180544=CARTESIAN_POINT('Ctrl Pts',(69.7635255542552,-2.29197691152282,
125.347292631605));
#180545=CARTESIAN_POINT('Ctrl Pts',(69.7709273759306,-2.14515638561624,
125.290175759969));
#180546=CARTESIAN_POINT('Ctrl Pts',(69.778325290242,-1.99841336512276,125.233089039885));
#180547=CARTESIAN_POINT('Ctrl Pts',(69.7857232045533,-1.84931088296295,
125.181833261727));
#180548=CARTESIAN_POINT('Ctrl Pts',(69.7931211188647,-1.69835428081799,
125.136598863635));
#180549=CARTESIAN_POINT('Ctrl Pts',(69.8005178037769,-1.54742276492156,
125.091371982678));
#180550=CARTESIAN_POINT('Ctrl Pts',(69.807914488689,-1.39463809780787,125.052164602853));
#180551=CARTESIAN_POINT('Ctrl Pts',(69.8153111736012,-1.24052205275116,
125.019117701392));
#180552=CARTESIAN_POINT('Ctrl Pts',(69.8227075305367,-1.08641284136107,
124.986072265266));
#180553=CARTESIAN_POINT('Ctrl Pts',(69.8301038874722,-0.930972734409442,
124.959186842633));
#180554=CARTESIAN_POINT('Ctrl Pts',(69.8375002444076,-0.774734738525306,
124.938551496275));
#180555=CARTESIAN_POINT('Ctrl Pts',(69.8448977337442,-0.618472822205254,
124.917912990592));
#180556=CARTESIAN_POINT('Ctrl Pts',(69.8522952230807,-0.461413143825941,
124.903526515388));
#180557=CARTESIAN_POINT('Ctrl Pts',(69.8596927124173,-0.304094739718604,
124.895430346208));
#180558=CARTESIAN_POINT('Ctrl Pts',(69.8670927949323,-0.14672118788802,
124.887331338928));
#180559=CARTESIAN_POINT('Ctrl Pts',(69.8744928774473,0.0109108976734853,
124.885527047099));
#180560=CARTESIAN_POINT('Ctrl Pts',(69.8818929599623,0.168261716740211,
124.890003631622));
#180561=CARTESIAN_POINT('Ctrl Pts',(69.8893011796288,0.325785559207997,
124.89448513861));
#180562=CARTESIAN_POINT('Ctrl Pts',(69.8967093992953,0.483027144149797,
124.905261304));
#180563=CARTESIAN_POINT('Ctrl Pts',(69.9041176189618,0.639450294128235,
124.922266272536));
#180564=CARTESIAN_POINT('Ctrl Pts',(69.9115303982638,0.795969719945647,
124.939281707346));
#180565=CARTESIAN_POINT('Ctrl Pts',(69.9189431775659,0.951669338700781,
124.962533529471));
#180566=CARTESIAN_POINT('Ctrl Pts',(69.926355956868,1.10602292486905,124.991904694966));
#180567=CARTESIAN_POINT('Ctrl Pts',(69.9337793278967,1.26059705867981,125.02131782736));
#180568=CARTESIAN_POINT('Ctrl Pts',(69.9412026989255,1.4138209560176,125.05686768192));
#180569=CARTESIAN_POINT('Ctrl Pts',(69.9486260699543,1.56518250981502,125.098387057036));
#180570=CARTESIAN_POINT('Ctrl Pts',(69.9525621193951,1.64543803750871,125.120401625966));
#180571=CARTESIAN_POINT('Ctrl Pts',(69.9564981688358,1.72517029904688,125.144093625371));
#180572=CARTESIAN_POINT('Ctrl Pts',(69.9604342182766,1.80430533129763,125.16943268245));
#180573=CARTESIAN_POINT('Ctrl Pts',(69.967857484682,1.95355153240296,125.217221353296));
#180574=CARTESIAN_POINT('Ctrl Pts',(69.9752807510875,2.10112350987105,125.271015764047));
#180575=CARTESIAN_POINT('Ctrl Pts',(69.9827040174929,2.24650130187933,125.330681556536));
#180576=CARTESIAN_POINT('Ctrl Pts',(69.9901185102139,2.39170726941065,125.390276829014));
#180577=CARTESIAN_POINT('Ctrl Pts',(69.9975330029349,2.53472387157822,125.455729529795));
#180578=CARTESIAN_POINT('Ctrl Pts',(70.0049474956559,2.67504555065757,125.526855348558));
#180579=CARTESIAN_POINT('Ctrl Pts',(70.0123548420097,2.81523198241931,125.597912613578));
#180580=CARTESIAN_POINT('Ctrl Pts',(70.0197621883634,2.95272833140933,125.674631943299));
#180581=CARTESIAN_POINT('Ctrl Pts',(70.0271695347172,3.08704841219299,125.756780735754));
#180582=CARTESIAN_POINT('Ctrl Pts',(70.0345713563926,3.22126831199298,125.83886825854));
#180583=CARTESIAN_POINT('Ctrl Pts',(70.041973178068,3.35231634345692,125.926376987033));
#180584=CARTESIAN_POINT('Ctrl Pts',(70.0493749997434,3.47973046574129,126.019028189375));
#180585=CARTESIAN_POINT('Ctrl Pts',(70.0567729140548,3.60707732710293,126.11163048187));
#180586=CARTESIAN_POINT('Ctrl Pts',(70.0641708283662,3.73079379854535,126.209369622826));
#180587=CARTESIAN_POINT('Ctrl Pts',(70.0715687426776,3.85044650954543,126.311923390444));
#180588=CARTESIAN_POINT('Ctrl Pts',(70.0789654275898,3.9700793364348,126.414460115486));
#180589=CARTESIAN_POINT('Ctrl Pts',(70.086362112502,4.08564946004065,126.521809636526));
#180590=CARTESIAN_POINT('Ctrl Pts',(70.0937587974142,4.19675624102293,126.63360917257));
#180591=CARTESIAN_POINT('Ctrl Pts',(70.1011551543496,4.30785809541419,126.745403751306));
#180592=CARTESIAN_POINT('Ctrl Pts',(70.108551511285,4.41449673755278,126.861647687931));
#180593=CARTESIAN_POINT('Ctrl Pts',(70.1159478682204,4.51630829196768,126.981941230005));
#180594=CARTESIAN_POINT('Ctrl Pts',(70.123345357557,4.61813543399169,127.102253189327));
#180595=CARTESIAN_POINT('Ctrl Pts',(70.1307428468936,4.71513377558765,127.226615703652));
#180596=CARTESIAN_POINT('Ctrl Pts',(70.1381403362302,4.80697975214996,127.354595955314));
#180597=CARTESIAN_POINT('Ctrl Pts',(70.1455404187452,4.89885792517665,127.482621070255));
#180598=CARTESIAN_POINT('Ctrl Pts',(70.1529405012601,4.98557991961542,127.614266144404));
#180599=CARTESIAN_POINT('Ctrl Pts',(70.1603405837751,5.06686560348531,127.749069548172));
#180600=CARTESIAN_POINT('Ctrl Pts',(70.1677488034416,5.14824066932122,127.884021182141));
#180601=CARTESIAN_POINT('Ctrl Pts',(70.175157023108,5.2241672936826,128.022137761481));
#180602=CARTESIAN_POINT('Ctrl Pts',(70.1825652427745,5.29441106545892,128.162932588555));
#180603=CARTESIAN_POINT('Ctrl Pts',(70.1899780220765,5.36469807110454,128.303814072495));
#180604=CARTESIAN_POINT('Ctrl Pts',(70.1973908013786,5.42929510173657,128.447376749211));
#180605=CARTESIAN_POINT('Ctrl Pts',(70.2048035806806,5.4880161919904,128.593114625156));
#180606=CARTESIAN_POINT('Ctrl Pts',(70.2122269517094,5.54682118569186,128.739060738212));
#180607=CARTESIAN_POINT('Ctrl Pts',(70.2196503227381,5.5997333454398,128.887187907311));
#180608=CARTESIAN_POINT('Ctrl Pts',(70.2270736937669,5.64661653630389,129.036974905719));
#180609=CARTESIAN_POINT('Ctrl Pts',(70.2310097432078,5.67147512904752,129.116395566368));
#180610=CARTESIAN_POINT('Ctrl Pts',(70.2349457926487,5.69463961388656,129.196282680525));
#180611=CARTESIAN_POINT('Ctrl Pts',(70.2388818420896,5.71609556543968,129.276557603673));
#180612=CARTESIAN_POINT('Ctrl Pts',(70.246305108495,5.75656082045037,129.42795360343));
#180613=CARTESIAN_POINT('Ctrl Pts',(70.2537283749005,5.79106831761621,129.581187280543));
#180614=CARTESIAN_POINT('Ctrl Pts',(70.2611516413059,5.81945004420199,129.735748552531));
#180615=CARTESIAN_POINT('Ctrl Pts',(70.2685661340269,5.84779822594401,129.890127145933));
#180616=CARTESIAN_POINT('Ctrl Pts',(70.275980626748,5.87003498190646,130.045829847321));
#180617=CARTESIAN_POINT('Ctrl Pts',(70.283395119469,5.88604211128355,130.202331692433));
#180618=CARTESIAN_POINT('Ctrl Pts',(70.2908024658228,5.90203381238663,130.358682695174));
#180619=CARTESIAN_POINT('Ctrl Pts',(70.2982098121765,5.91180780265241,130.515830939367));
#180620=CARTESIAN_POINT('Ctrl Pts',(70.3056171585303,5.91529698159951,130.67324165639));
#180621=CARTESIAN_POINT('Ctrl Pts',(70.3130189802057,5.91878355818531,130.830534970562));
#180622=CARTESIAN_POINT('Ctrl Pts',(70.3204208018811,5.91599464855981,130.988089996177));
#180623=CARTESIAN_POINT('Ctrl Pts',(70.3278226235566,5.90691501336847,131.145367343808));
#180624=CARTESIAN_POINT('Ctrl Pts',(70.3352205378679,5.8978401712459,131.302561665951));
#180625=CARTESIAN_POINT('Ctrl Pts',(70.3426184521793,5.88248123859997,131.459478230305));
#180626=CARTESIAN_POINT('Ctrl Pts',(70.3500163664906,5.86087506240501,131.615578261222));
#180627=CARTESIAN_POINT('Ctrl Pts',(70.3574130514028,5.83927247676453,131.771652351146));
#180628=CARTESIAN_POINT('Ctrl Pts',(70.3648097363151,5.81142475918317,131.926909807532));
#180629=CARTESIAN_POINT('Ctrl Pts',(70.3722064212272,5.77742057223629,132.080817469168));
#180630=CARTESIAN_POINT('Ctrl Pts',(70.3796027781627,5.74341789307072,132.234718306376));
#180631=CARTESIAN_POINT('Ctrl Pts',(70.3869991350981,5.70325936785843,132.387269103333));
#180632=CARTESIAN_POINT('Ctrl Pts',(70.3943954920335,5.65708463606796,132.537947645339));
#180633=CARTESIAN_POINT('Ctrl Pts',(70.4017929813701,5.61090283480805,132.688649256616));
#180634=CARTESIAN_POINT('Ctrl Pts',(70.4091904707067,5.55870310232612,132.837477685252));
#180635=CARTESIAN_POINT('Ctrl Pts',(70.4165879600433,5.50067468580775,132.983926758662));
#180636=CARTESIAN_POINT('Ctrl Pts',(70.4239880425583,5.44262592751775,133.130427169569));
#180637=CARTESIAN_POINT('Ctrl Pts',(70.4313881250733,5.37874455454987,133.274546217773));
#180638=CARTESIAN_POINT('Ctrl Pts',(70.4387882075884,5.30926753077319,133.415798698237));
#180639=CARTESIAN_POINT('Ctrl Pts',(70.4461964272549,5.23971410986665,133.557206500324));
#180640=CARTESIAN_POINT('Ctrl Pts',(70.4536046469213,5.16455291508093,133.695741104571));
#180641=CARTESIAN_POINT('Ctrl Pts',(70.4610128665878,5.08406671399133,133.830942222312));
#180642=CARTESIAN_POINT('Ctrl Pts',(70.4684256458899,5.00353097498771,133.966226554085));
#180643=CARTESIAN_POINT('Ctrl Pts',(70.475838425192,4.91766390208587,134.098172998918));
#180644=CARTESIAN_POINT('Ctrl Pts',(70.4832512044941,4.82679068316633,134.22635159701));
#180645=CARTESIAN_POINT('Ctrl Pts',(70.4906745755229,4.73578762033045,134.354713342694));
#180646=CARTESIAN_POINT('Ctrl Pts',(70.4980979465516,4.63976435258281,134.479296194346));
#180647=CARTESIAN_POINT('Ctrl Pts',(70.5055213175804,4.53908581848059,134.599703882011));
#180648=CARTESIAN_POINT('Ctrl Pts',(70.509457367021,4.48570364395298,134.663546927152));
#180649=CARTESIAN_POINT('Ctrl Pts',(70.5133934164617,4.43101332217446,134.726216800849));
#180650=CARTESIAN_POINT('Ctrl Pts',(70.5173294659024,4.37507322173496,134.787658857336));
#180651=CARTESIAN_POINT('Ctrl Pts',(70.5247527323078,4.26957193813348,134.903536658334));
#180652=CARTESIAN_POINT('Ctrl Pts',(70.5321759987133,4.15930425088632,135.015395338423));
#180653=CARTESIAN_POINT('Ctrl Pts',(70.5395992651187,4.04460849184142,135.122817831691));
#180654=CARTESIAN_POINT('Ctrl Pts',(70.5470137578397,3.93004829365897,135.230113360492));
#180655=CARTESIAN_POINT('Ctrl Pts',(70.5544282505607,3.81107071101288,135.33298288641));
#180656=CARTESIAN_POINT('Ctrl Pts',(70.5618427432817,3.68805352078212,135.431043207754));
#180657=CARTESIAN_POINT('Ctrl Pts',(70.5692500896354,3.56515489915108,135.529009014867));
#180658=CARTESIAN_POINT('Ctrl Pts',(70.5766574359892,3.4382247111246,135.622174614237));
#180659=CARTESIAN_POINT('Ctrl Pts',(70.5840647823429,3.30767660323895,135.710194496825));
#180660=CARTESIAN_POINT('Ctrl Pts',(70.5914666040183,3.17722586305691,135.798148730865));
#180661=CARTESIAN_POINT('Ctrl Pts',(70.5988684256938,3.04316288404195,135.880964682051));
#180662=CARTESIAN_POINT('Ctrl Pts',(70.6062702473692,2.90593323255091,135.958337975923));
#180663=CARTESIAN_POINT('Ctrl Pts',(70.6136681616805,2.76877602352488,136.035670425036));
#180664=CARTESIAN_POINT('Ctrl Pts',(70.6210660759918,2.62845579556738,136.107565755947));
#180665=CARTESIAN_POINT('Ctrl Pts',(70.6284639903032,2.48544575258087,136.173763747661));
#180666=CARTESIAN_POINT('Ctrl Pts',(70.6358606752154,2.34245947526874,136.239950738471));
#180667=CARTESIAN_POINT('Ctrl Pts',(70.6432573601277,2.1967846085204,136.300442112532));
#180668=CARTESIAN_POINT('Ctrl Pts',(70.6506540450399,2.04891764025126,136.355024277523));
#180669=CARTESIAN_POINT('Ctrl Pts',(70.6580504019754,1.90105722855834,136.409604022284));
#180670=CARTESIAN_POINT('Ctrl Pts',(70.6654467589108,1.75100525881178,136.458274949689));
#180671=CARTESIAN_POINT('Ctrl Pts',(70.6728431158463,1.59927656356989,136.500872272581));
#180672=CARTESIAN_POINT('Ctrl Pts',(70.6802406051828,1.44752463827816,136.54347611723));
#180673=CARTESIAN_POINT('Ctrl Pts',(70.6876380945194,1.29409583577123,136.580004404934));
#180674=CARTESIAN_POINT('Ctrl Pts',(70.6950355838559,1.13951830610753,136.610342756063));
#180675=CARTESIAN_POINT('Ctrl Pts',(70.7024356663709,0.984886589529773,
136.640691742254));
#180676=CARTESIAN_POINT('Ctrl Pts',(70.709835748886,0.829105710134168,136.664846399819));
#180677=CARTESIAN_POINT('Ctrl Pts',(70.717235831401,0.672711969420469,136.682743827999));
#180678=CARTESIAN_POINT('Ctrl Pts',(70.7246440510675,0.516146257711301,
136.700660936241));
#180679=CARTESIAN_POINT('Ctrl Pts',(70.732052270734,0.358966709958309,136.712307031883));
#180680=CARTESIAN_POINT('Ctrl Pts',(70.7394604904004,0.201713422834879,
136.717671218029));
#180681=CARTESIAN_POINT('Ctrl Pts',(70.7468732697025,0.0443633489371363,
136.723038705742));
#180682=CARTESIAN_POINT('Ctrl Pts',(70.7542860490046,-0.113060182341062,
136.722116581831));
#180683=CARTESIAN_POINT('Ctrl Pts',(70.7616988283066,-0.270019661649939,
136.714946032296));
#180684=CARTESIAN_POINT('Ctrl Pts',(70.7691221993354,-0.427203412023969,
136.707765237144));
#180685=CARTESIAN_POINT('Ctrl Pts',(70.7765455703642,-0.583921415204719,
136.694318216891));
#180686=CARTESIAN_POINT('Ctrl Pts',(70.783968941393,-0.739643019853316,
136.674697811091));
#180687=CARTESIAN_POINT('Ctrl Pts',(70.7879049908338,-0.822210351126378,
136.664294601151));
#180688=CARTESIAN_POINT('Ctrl Pts',(70.7918410402745,-0.904497745579814,
136.652156682058));
#180689=CARTESIAN_POINT('Ctrl Pts',(70.7957770897153,-0.98642767853512,
136.638303623589));
#180690=CARTESIAN_POINT('Ctrl Pts',(70.8032003561208,-1.14094497514307,
136.612177187655));
#180691=CARTESIAN_POINT('Ctrl Pts',(70.8106236225262,-1.29465722909891,
136.579868208319));
#180692=CARTESIAN_POINT('Ctrl Pts',(70.8180468889316,-1.4470306744114,136.541435899433));
#180693=CARTESIAN_POINT('Ctrl Pts',(70.8254613816527,-1.59922402696579,
136.503049014345));
#180694=CARTESIAN_POINT('Ctrl Pts',(70.8328758743737,-1.7500813621471,136.458553295931));
#180695=CARTESIAN_POINT('Ctrl Pts',(70.8402903670947,-1.89907608388792,
136.408059448705));
#180696=CARTESIAN_POINT('Ctrl Pts',(70.8476977134485,-2.04792719890596,
136.357614269349));
#180697=CARTESIAN_POINT('Ctrl Pts',(70.8551050598022,-2.19491892331317,
136.301182589468));
#180698=CARTESIAN_POINT('Ctrl Pts',(70.862512406156,-2.3395369845147,136.238925665533));
#180699=CARTESIAN_POINT('Ctrl Pts',(70.8699142278314,-2.48404718411098,
136.176715175161));
#180700=CARTESIAN_POINT('Ctrl Pts',(70.8773160495068,-2.62618690414198,
136.108688238563));
#180701=CARTESIAN_POINT('Ctrl Pts',(70.8847178711823,-2.76545922625434,
136.035055201503));
#180702=CARTESIAN_POINT('Ctrl Pts',(70.8921157854936,-2.90465802759125,
135.96146103475));
#180703=CARTESIAN_POINT('Ctrl Pts',(70.899513699805,-3.04099211639179,135.882266835393));
#180704=CARTESIAN_POINT('Ctrl Pts',(70.9069116141163,-3.17398678309439,
135.797730067471));
#180705=CARTESIAN_POINT('Ctrl Pts',(70.9143082990285,-3.30695934849587,
135.713207348026));
#180706=CARTESIAN_POINT('Ctrl Pts',(70.9217049839407,-3.43659327848189,
135.623344022168));
#180707=CARTESIAN_POINT('Ctrl Pts',(70.9291016688529,-3.5624405079365,135.528442347375));
#180708=CARTESIAN_POINT('Ctrl Pts',(70.9364980257884,-3.68828215719317,
135.433544880621));
#180709=CARTESIAN_POINT('Ctrl Pts',(70.9438943827238,-3.81033714172265,
135.333609733897));
#180710=CARTESIAN_POINT('Ctrl Pts',(70.9512907396592,-3.928188541847,135.228980978931));
#180711=CARTESIAN_POINT('Ctrl Pts',(70.9586882289958,-4.04605798532149,
135.124336205035));
#180712=CARTESIAN_POINT('Ctrl Pts',(70.9660857183324,-4.15972228376363,
135.014996639913));
#180713=CARTESIAN_POINT('Ctrl Pts',(70.9734832076689,-4.26879972834428,
134.901344806184));
#180714=CARTESIAN_POINT('Ctrl Pts',(70.9808832901838,-4.37791540985311,
134.787653131982));
#180715=CARTESIAN_POINT('Ctrl Pts',(70.9882833726988,-4.48244077783003,
134.669646448629));
#180716=CARTESIAN_POINT('Ctrl Pts',(70.9956834552137,-4.58203302802309,
134.547741962367));
#180717=CARTESIAN_POINT('Ctrl Pts',(71.0030916748801,-4.68173479013442,
134.42570342959));
#180718=CARTESIAN_POINT('Ctrl Pts',(71.0104998945465,-4.77649236511753,
134.299758823676));
#180719=CARTESIAN_POINT('Ctrl Pts',(71.017908114213,-4.86600464965862,134.170356653214));
#180720=CARTESIAN_POINT('Ctrl Pts',(71.025320893515,-4.95557202751718,134.040874837876));
#180721=CARTESIAN_POINT('Ctrl Pts',(71.0327336728171,-5.03988748249446,
133.907931532048));
#180722=CARTESIAN_POINT('Ctrl Pts',(71.0401464521191,-5.11869512860509,
133.772001219609));
#180723=CARTESIAN_POINT('Ctrl Pts',(71.0475698231479,-5.19761537877647,
133.635876683564));
#180724=CARTESIAN_POINT('Ctrl Pts',(71.0549931941766,-5.27101192856715,
133.496756946096));
#180725=CARTESIAN_POINT('Ctrl Pts',(71.0624165652054,-5.33867605651321,
133.355138641251));
#180726=CARTESIAN_POINT('Ctrl Pts',(71.0663526146463,-5.37455320072993,
133.280049217935));
#180727=CARTESIAN_POINT('Ctrl Pts',(71.0702886640872,-5.40881957231786,
133.204257660723));
#180728=CARTESIAN_POINT('Ctrl Pts',(71.0742247135281,-5.44144973190216,
133.127839771267));
#180729=CARTESIAN_POINT('Ctrl Pts',(71.0824664643207,-5.50977449449734,
132.967827248446));
#180730=CARTESIAN_POINT('Ctrl Pts',(71.0907082151132,-5.57109886347091,
132.804654973488));
#180731=CARTESIAN_POINT('Ctrl Pts',(71.0989499659057,-5.62515069641183,
132.638920566207));
#180732=CARTESIAN_POINT('Ctrl Pts',(71.1071583725541,-5.67898384861912,
132.473856680531));
#180733=CARTESIAN_POINT('Ctrl Pts',(71.1153667792024,-5.72560307789162,
132.306251557788));
#180734=CARTESIAN_POINT('Ctrl Pts',(71.1235751858508,-5.76478541520492,
132.136719307687));
#180735=CARTESIAN_POINT('Ctrl Pts',(71.1317620467689,-5.80386490526583,
131.967632052125));
#180736=CARTESIAN_POINT('Ctrl Pts',(71.139948907687,-5.83554637754198,131.796627980267));
#180737=CARTESIAN_POINT('Ctrl Pts',(71.1481357686052,-5.85965608173033,
131.624336938164));
#180738=CARTESIAN_POINT('Ctrl Pts',(71.1562874406351,-5.88366215722719,
131.452786439997));
#180739=CARTESIAN_POINT('Ctrl Pts',(71.164439112665,-5.90016132245018,131.279960230598));
#180740=CARTESIAN_POINT('Ctrl Pts',(71.172590784695,-5.90903071560393,131.106497282917));
#180741=CARTESIAN_POINT('Ctrl Pts',(71.1772687719017,-5.91412058030319,
131.006952373956));
#180742=CARTESIAN_POINT('Ctrl Pts',(71.1819467591085,-5.91669867470891,
130.907198071244));
#180743=CARTESIAN_POINT('Ctrl Pts',(71.1866247463153,-5.91674924113994,
130.807357277356));
#180744=CARTESIAN_POINT('',(72.9366248426605,-5.91499535916685,130.799390962839));
#180745=CARTESIAN_POINT('Ctrl Pts',(71.1866248077955,-5.90841215785675,
130.807351744564));
#180746=CARTESIAN_POINT('Ctrl Pts',(71.2419739843107,-5.90303659312473,
129.627713360534));
#180747=CARTESIAN_POINT('Ctrl Pts',(71.3901390354303,-4.98822362966825,
126.46224284269));
#180748=CARTESIAN_POINT('Ctrl Pts',(71.6311199611539,0.175748641439395,
123.808170729825));
#180749=CARTESIAN_POINT('Ctrl Pts',(71.9095675849669,5.98108912855082,127.170611401303));
#180750=CARTESIAN_POINT('Ctrl Pts',(72.1880152087798,6.29010089897139,133.872290084015));
#180751=CARTESIAN_POINT('Ctrl Pts',(72.4664628325927,0.818817231748582,
137.754691463744));
#180752=CARTESIAN_POINT('Ctrl Pts',(72.7159993655978,-4.75871170394957,
135.510131186065));
#180753=CARTESIAN_POINT('Ctrl Pts',(72.8727200239988,-5.90151843304881,
132.159149211696));
#180754=CARTESIAN_POINT('Ctrl Pts',(72.9366248077954,-5.91226047810136,
130.799394002698));
#180755=CARTESIAN_POINT('',(74.6866248077955,-5.92105151543396,130.803381673069));
#180756=CARTESIAN_POINT('Ctrl Pts',(72.9366248650027,-5.91674791128255,
130.799389014852));
#180757=CARTESIAN_POINT('Ctrl Pts',(72.945430803682,-5.91659035247599,130.611876899878));
#180758=CARTESIAN_POINT('Ctrl Pts',(72.9542367423612,-5.90751514879322,
130.424749374994));
#180759=CARTESIAN_POINT('Ctrl Pts',(72.9630426810405,-5.88965462586106,
130.238764515587));
#180760=CARTESIAN_POINT('Ctrl Pts',(72.9719130074933,-5.87166350932068,
130.051419761291));
#180761=CARTESIAN_POINT('Ctrl Pts',(72.9807833339461,-5.84475822811481,
129.865234475));
#180762=CARTESIAN_POINT('Ctrl Pts',(72.989653660399,-5.80912273554289,129.680962377449));
#180763=CARTESIAN_POINT('Ctrl Pts',(72.998594956327,-5.77320213145674,129.495215960533));
#180764=CARTESIAN_POINT('Ctrl Pts',(73.007536252255,-5.72841111589955,129.311413496325));
#180765=CARTESIAN_POINT('Ctrl Pts',(73.0164775481831,-5.67498623746573,
129.130305132501));
#180766=CARTESIAN_POINT('Ctrl Pts',(73.0187710588615,-5.66128234821181,
129.083849454294));
#180767=CARTESIAN_POINT('Ctrl Pts',(73.02106456954,-5.64701062660013,129.037570925487));
#180768=CARTESIAN_POINT('Ctrl Pts',(73.0233580802185,-5.63217556439491,
128.991481974542));
#180769=CARTESIAN_POINT('Ctrl Pts',(73.0307813466239,-5.58415982157597,
128.842308672483));
#180770=CARTESIAN_POINT('Ctrl Pts',(73.0382046130293,-5.53014089368967,
128.694818731837));
#180771=CARTESIAN_POINT('Ctrl Pts',(73.0456278794347,-5.4702539300403,128.549531909354));
#180772=CARTESIAN_POINT('Ctrl Pts',(73.0530423721557,-5.41043774780861,
128.404416803829));
#180773=CARTESIAN_POINT('Ctrl Pts',(73.0604568648767,-5.34476747589827,
128.261499975141));
#180774=CARTESIAN_POINT('Ctrl Pts',(73.0678713575977,-5.27342819378993,
128.121286699941));
#180775=CARTESIAN_POINT('Ctrl Pts',(73.0752787039515,-5.20215767116756,
127.981208567574));
#180776=CARTESIAN_POINT('Ctrl Pts',(73.0826860503052,-5.12522918424966,
127.843829131562));
#180777=CARTESIAN_POINT('Ctrl Pts',(73.090093396659,-5.04287607462456,127.709634222797));
#180778=CARTESIAN_POINT('Ctrl Pts',(73.0974952183343,-4.96058438705569,
127.575539401658));
#180779=CARTESIAN_POINT('Ctrl Pts',(73.1048970400097,-4.87287632710042,
127.444624695334));
#180780=CARTESIAN_POINT('Ctrl Pts',(73.1122988616851,-4.78003132944284,
127.317351719951));
#180781=CARTESIAN_POINT('Ctrl Pts',(73.1196967759964,-4.6872353439367,127.190145930981));
#180782=CARTESIAN_POINT('Ctrl Pts',(73.1270946903077,-4.58930804075162,
127.066578345136));
#180783=CARTESIAN_POINT('Ctrl Pts',(73.1344926046191,-4.48657230083255,
126.947081842069));
#180784=CARTESIAN_POINT('Ctrl Pts',(73.1418892895313,-4.38385363372979,
126.827605197153));
#180785=CARTESIAN_POINT('Ctrl Pts',(73.1492859744434,-4.27632835894441,
126.712198575072));
#180786=CARTESIAN_POINT('Ctrl Pts',(73.1566826593556,-4.16435986675526,
126.601262062612));
#180787=CARTESIAN_POINT('Ctrl Pts',(73.164079016291,-4.05239633936639,126.490330469193));
#180788=CARTESIAN_POINT('Ctrl Pts',(73.1714753732265,-3.9359902514904,126.383868854023));
#180789=CARTESIAN_POINT('Ctrl Pts',(73.1788717301619,-3.81554190886022,
126.282240483798));
#180790=CARTESIAN_POINT('Ctrl Pts',(73.1862692194984,-3.6950751252813,126.18059655401));
#180791=CARTESIAN_POINT('Ctrl Pts',(73.193666708835,-3.57056514000339,126.083787583313));
#180792=CARTESIAN_POINT('Ctrl Pts',(73.2010641981715,-3.44244526259913,
125.992136477264));
#180793=CARTESIAN_POINT('Ctrl Pts',(73.2084642806865,-3.31428047297036,
125.900453243061));
#180794=CARTESIAN_POINT('Ctrl Pts',(73.2158643632015,-3.1825035751514,125.813931690438));
#180795=CARTESIAN_POINT('Ctrl Pts',(73.2232644457165,-3.04757662451002,
125.732851248528));
#180796=CARTESIAN_POINT('Ctrl Pts',(73.2306726653829,-2.91250130781558,
125.651681650337));
#180797=CARTESIAN_POINT('Ctrl Pts',(73.2380808850493,-2.77426934101548,
125.57596530382));
#180798=CARTESIAN_POINT('Ctrl Pts',(73.2454891047157,-2.63336777791731,
125.505935879144));
#180799=CARTESIAN_POINT('Ctrl Pts',(73.2529018840178,-2.49237949225783,
125.435863352525));
#180800=CARTESIAN_POINT('Ctrl Pts',(73.2603146633198,-2.34871867610027,
125.37148487465));
#180801=CARTESIAN_POINT('Ctrl Pts',(73.2677274426219,-2.2028916054145,125.312985640632));
#180802=CARTESIAN_POINT('Ctrl Pts',(73.2751508136506,-2.05685617017173,
125.254402820165));
#180803=CARTESIAN_POINT('Ctrl Pts',(73.2825741846794,-1.90864864930206,
125.201716146024));
#180804=CARTESIAN_POINT('Ctrl Pts',(73.2899975557081,-1.75879047610902,
125.155060959763));
#180805=CARTESIAN_POINT('Ctrl Pts',(73.2939336051492,-1.67933207687891,
125.13032326053));
#180806=CARTESIAN_POINT('Ctrl Pts',(73.2978696545902,-1.59940980282377,
125.107280377103));
#180807=CARTESIAN_POINT('Ctrl Pts',(73.3018057040313,-1.51910232032421,
125.085946615162));
#180808=CARTESIAN_POINT('Ctrl Pts',(73.3092289704367,-1.36764491465122,
125.045711805949));
#180809=CARTESIAN_POINT('Ctrl Pts',(73.3166522368422,-1.2143589004448,125.011437544314));
#180810=CARTESIAN_POINT('Ctrl Pts',(73.3240755032476,-1.05975461527935,
124.983291066539));
#180811=CARTESIAN_POINT('Ctrl Pts',(73.3314899959686,-0.905333059539768,
124.955177855563));
#180812=CARTESIAN_POINT('Ctrl Pts',(73.3389044886896,-0.749596697896401,
124.933178078357));
#180813=CARTESIAN_POINT('Ctrl Pts',(73.3463189814106,-0.593070673885265,
124.917409136682));
#180814=CARTESIAN_POINT('Ctrl Pts',(73.3537263277644,-0.436695515549284,
124.901655393708));
#180815=CARTESIAN_POINT('Ctrl Pts',(73.3611336741181,-0.27953257898284,
124.892120567636));
#180816=CARTESIAN_POINT('Ctrl Pts',(73.3685410204719,-0.122116734302222,
124.888870945045));
#180817=CARTESIAN_POINT('Ctrl Pts',(73.3759428421473,0.0351817037025853,
124.885623746145));
#180818=CARTESIAN_POINT('Ctrl Pts',(73.3833446638227,0.192732302624848,
124.888652424469));
#180819=CARTESIAN_POINT('Ctrl Pts',(73.3907464854981,0.349995650471745,
124.897971398496));
#180820=CARTESIAN_POINT('Ctrl Pts',(73.3981443998094,0.507175980221113,
124.907285453109));
#180821=CARTESIAN_POINT('Ctrl Pts',(73.4055423141208,0.664068989187735,
124.922883168268));
#180822=CARTESIAN_POINT('Ctrl Pts',(73.4129402284321,0.820135958420872,
124.944726877117));
#180823=CARTESIAN_POINT('Ctrl Pts',(73.4203369133443,0.976176992155399,
124.966566955938));
#180824=CARTESIAN_POINT('Ctrl Pts',(73.4277335982566,1.13139188926999,124.994650916692));
#180825=CARTESIAN_POINT('Ctrl Pts',(73.4351302831688,1.28524762409922,125.028889285523));
#180826=CARTESIAN_POINT('Ctrl Pts',(73.4425266401042,1.43909653680393,125.06312613619));
#180827=CARTESIAN_POINT('Ctrl Pts',(73.4499229970396,1.59158604266972,125.103516771243));
#180828=CARTESIAN_POINT('Ctrl Pts',(73.457319353975,1.7421941401116,125.149920756655));
#180829=CARTESIAN_POINT('Ctrl Pts',(73.4647168433116,1.89282529603757,125.196331846635));
#180830=CARTESIAN_POINT('Ctrl Pts',(73.4721143326482,2.04157411322565,125.248758010204));
#180831=CARTESIAN_POINT('Ctrl Pts',(73.4795118219848,2.18793470767816,125.307009230085));
#180832=CARTESIAN_POINT('Ctrl Pts',(73.4869119044998,2.33434660861027,125.365280869842));
#180833=CARTESIAN_POINT('Ctrl Pts',(73.4943119870148,2.47836827335111,125.429381493493));
#180834=CARTESIAN_POINT('Ctrl Pts',(73.5017120695298,2.61951485804302,125.499073399046));
#180835=CARTESIAN_POINT('Ctrl Pts',(73.5091202891963,2.76081664791502,125.568841938013));
#180836=CARTESIAN_POINT('Ctrl Pts',(73.5165285088627,2.89923670919764,125.644213871848));
#180837=CARTESIAN_POINT('Ctrl Pts',(73.5239367285292,3.0343151840806,125.724905732821));
#180838=CARTESIAN_POINT('Ctrl Pts',(73.5313495078312,3.16947679751105,125.805647258289));
#180839=CARTESIAN_POINT('Ctrl Pts',(73.5387622871333,3.30129241448396,125.891715031785));
#180840=CARTESIAN_POINT('Ctrl Pts',(73.5461750664354,3.42933257057741,125.98278321148));
#180841=CARTESIAN_POINT('Ctrl Pts',(73.5535984374641,3.55755567645037,126.073981513662));
#180842=CARTESIAN_POINT('Ctrl Pts',(73.5610218084928,3.68199225276942,126.170194264108));
#180843=CARTESIAN_POINT('Ctrl Pts',(73.5684451795216,3.80224658541458,126.271055921629));
#180844=CARTESIAN_POINT('Ctrl Pts',(73.5723812289625,3.86600831804772,126.324535192591));
#180845=CARTESIAN_POINT('Ctrl Pts',(73.5763172784034,3.92859488981757,126.379320823921));
#180846=CARTESIAN_POINT('Ctrl Pts',(73.5802533278442,3.98995174384923,126.435354363936));
#180847=CARTESIAN_POINT('Ctrl Pts',(73.5876765942497,4.10566885566872,126.541031871657));
#180848=CARTESIAN_POINT('Ctrl Pts',(73.5950998606552,4.21735959757791,126.651469661085));
#180849=CARTESIAN_POINT('Ctrl Pts',(73.6025231270606,4.32460741903181,126.766328766063));
#180850=CARTESIAN_POINT('Ctrl Pts',(73.6099376197817,4.4317284824672,126.881052117117));
#180851=CARTESIAN_POINT('Ctrl Pts',(73.6173521125027,4.53441682563771,127.000186111896));
#180852=CARTESIAN_POINT('Ctrl Pts',(73.6247666052237,4.63228982220687,127.123352390792));
#180853=CARTESIAN_POINT('Ctrl Pts',(73.6321739515775,4.73006848509707,127.246399957391));
#180854=CARTESIAN_POINT('Ctrl Pts',(73.6395812979313,4.82304081044393,127.373471780618));
#180855=CARTESIAN_POINT('Ctrl Pts',(73.6469886442851,4.91086191911022,127.504153688609));
#180856=CARTESIAN_POINT('Ctrl Pts',(73.6543904659605,4.99861752748036,127.634738129104));
#180857=CARTESIAN_POINT('Ctrl Pts',(73.661792287636,5.08122936173455,127.768926984656));
#180858=CARTESIAN_POINT('Ctrl Pts',(73.6691941093114,5.15839372584091,127.90627422622));
#180859=CARTESIAN_POINT('Ctrl Pts',(73.6765920236228,5.23551735548016,128.043548963244));
#180860=CARTESIAN_POINT('Ctrl Pts',(73.6839899379341,5.30719905963787,128.183978441169));
#180861=CARTESIAN_POINT('Ctrl Pts',(73.6913878522455,5.37317933775536,128.327089060627));
#180862=CARTESIAN_POINT('Ctrl Pts',(73.6987845371577,5.43914865114758,128.470175897697));
#180863=CARTESIAN_POINT('Ctrl Pts',(73.70618122207,5.49941826281195,128.61594265333));
#180864=CARTESIAN_POINT('Ctrl Pts',(73.7135779069822,5.55377533624324,128.763892515136));
#180865=CARTESIAN_POINT('Ctrl Pts',(73.7209742639176,5.6081299994249,128.911835816689));
#180866=CARTESIAN_POINT('Ctrl Pts',(73.7283706208531,5.6565725169158,129.061961681544));
#180867=CARTESIAN_POINT('Ctrl Pts',(73.7357669777886,5.6989388852343,129.213755026961));
#180868=CARTESIAN_POINT('Ctrl Pts',(73.7431644671252,5.74131173995197,129.365571612326));
#180869=CARTESIAN_POINT('Ctrl Pts',(73.7505619564618,5.7776064928376,129.519055827002));
#180870=CARTESIAN_POINT('Ctrl Pts',(73.7579594457983,5.80770956814848,129.673679347474));
#180871=CARTESIAN_POINT('Ctrl Pts',(73.7653595283134,5.83782319604574,129.828357070982));
#180872=CARTESIAN_POINT('Ctrl Pts',(73.7727596108284,5.86174075366047,129.984174529263));
#180873=CARTESIAN_POINT('Ctrl Pts',(73.7801596933434,5.87940015646438,130.140595325715));
#180874=CARTESIAN_POINT('Ctrl Pts',(73.7875679130099,5.89707897759708,130.297188122912));
#180875=CARTESIAN_POINT('Ctrl Pts',(73.7949761326763,5.90848585923868,130.454385212029));
#180876=CARTESIAN_POINT('Ctrl Pts',(73.8023843523428,5.91361072643859,130.611646480434));
#180877=CARTESIAN_POINT('Ctrl Pts',(73.8097971316449,5.91873874790875,130.769004540526));
#180878=CARTESIAN_POINT('Ctrl Pts',(73.817209910947,5.9175770532492,130.926426486195));
#180879=CARTESIAN_POINT('Ctrl Pts',(73.8246226902491,5.91016764640917,131.083374871392));
#180880=CARTESIAN_POINT('Ctrl Pts',(73.8320460612779,5.90274765266118,131.240547511802));
#180881=CARTESIAN_POINT('Ctrl Pts',(73.8394694323067,5.88906214985623,131.39724486943));
#180882=CARTESIAN_POINT('Ctrl Pts',(73.8468928033354,5.86920478500243,131.552936434838));
#180883=CARTESIAN_POINT('Ctrl Pts',(73.850828852776,5.85867593368659,131.635487838581));
#180884=CARTESIAN_POINT('Ctrl Pts',(73.8547649022166,5.84641280124301,131.717756665896));
#180885=CARTESIAN_POINT('Ctrl Pts',(73.8587009516572,5.83243507540528,131.799665421976));
#180886=CARTESIAN_POINT('Ctrl Pts',(73.8661242180626,5.80607352070382,131.954142779668));
#180887=CARTESIAN_POINT('Ctrl Pts',(73.873547484468,5.77353065489684,132.107805686861));
#180888=CARTESIAN_POINT('Ctrl Pts',(73.8809707508734,5.73486650406995,132.260120468296));
#180889=CARTESIAN_POINT('Ctrl Pts',(73.8883852435944,5.69624805105844,132.412255226308));
#180890=CARTESIAN_POINT('Ctrl Pts',(73.8957997363155,5.65152280498643,132.56304467189));
#180891=CARTESIAN_POINT('Ctrl Pts',(73.9032142290365,5.60080227162785,132.711962378057));
#180892=CARTESIAN_POINT('Ctrl Pts',(73.9106215753903,5.55013062462896,132.860736551732));
#180893=CARTESIAN_POINT('Ctrl Pts',(73.918028921744,5.49347531371264,133.007642226515));
#180894=CARTESIAN_POINT('Ctrl Pts',(73.9254362680978,5.43099837779956,133.152165375811));
#180895=CARTESIAN_POINT('Ctrl Pts',(73.9328380897732,5.36856803954236,133.29658073429));
#180896=CARTESIAN_POINT('Ctrl Pts',(73.9402399114486,5.30032486926107,133.438616764308));
#180897=CARTESIAN_POINT('Ctrl Pts',(73.947641733124,5.22647996870166,133.577776868196));
#180898=CARTESIAN_POINT('Ctrl Pts',(73.9550396474354,5.1526740502905,133.716863510549));
#180899=CARTESIAN_POINT('Ctrl Pts',(73.9624375617467,5.07327246536376,133.853076921387));
#180900=CARTESIAN_POINT('Ctrl Pts',(73.9698354760581,4.98853340009094,133.985942783514));
#180901=CARTESIAN_POINT('Ctrl Pts',(73.9772321609703,4.90380841691344,134.118786565745));
#180902=CARTESIAN_POINT('Ctrl Pts',(73.9846288458825,4.8137479143422,134.248283588933));
#180903=CARTESIAN_POINT('Ctrl Pts',(73.9920255307947,4.71865483138288,134.373986248464));
#180904=CARTESIAN_POINT('Ctrl Pts',(73.9994218877301,4.6235659649505,134.499683334209));
#180905=CARTESIAN_POINT('Ctrl Pts',(74.0068182446656,4.523445187041,134.621586093119));
#180906=CARTESIAN_POINT('Ctrl Pts',(74.014214601601,4.4186372034637,134.73927812962));
#180907=CARTESIAN_POINT('Ctrl Pts',(74.0216120909376,4.31381317351656,134.856988185071));
#180908=CARTESIAN_POINT('Ctrl Pts',(74.0290095802742,4.20430075729512,134.970485955687));
#180909=CARTESIAN_POINT('Ctrl Pts',(74.0364070696108,4.09048305787075,135.079390315214));
#180910=CARTESIAN_POINT('Ctrl Pts',(74.0438071521258,3.97662545982813,135.188332850996));
#180911=CARTESIAN_POINT('Ctrl Pts',(74.0512072346407,3.85845984330652,135.292678511851));
#180912=CARTESIAN_POINT('Ctrl Pts',(74.0586073171557,3.73640393575553,135.392085128843));
#180913=CARTESIAN_POINT('Ctrl Pts',(74.0660155368222,3.61421381518662,135.491601053629));
#180914=CARTESIAN_POINT('Ctrl Pts',(74.0734237564887,3.48812515021597,135.586166852634));
#180915=CARTESIAN_POINT('Ctrl Pts',(74.0808319761552,3.35858690714007,135.675482105446));
#180916=CARTESIAN_POINT('Ctrl Pts',(74.0882447554572,3.22896893543684,135.764852330306));
#180917=CARTESIAN_POINT('Ctrl Pts',(74.0956575347593,3.09589746978524,135.848965370567));
#180918=CARTESIAN_POINT('Ctrl Pts',(74.1030703140613,2.95984738292835,135.927566062624));
#180919=CARTESIAN_POINT('Ctrl Pts',(74.1104936850901,2.82360290132734,136.006279063036));
#180920=CARTESIAN_POINT('Ctrl Pts',(74.1179170561189,2.68437162790257,136.079463811276));
#180921=CARTESIAN_POINT('Ctrl Pts',(74.1253404271476,2.5426505137647,136.146912341916));
#180922=CARTESIAN_POINT('Ctrl Pts',(74.1292764765885,2.46750657849685,136.182675171266));
#180923=CARTESIAN_POINT('Ctrl Pts',(74.1332125260293,2.3916629614686,136.216826161325));
#180924=CARTESIAN_POINT('Ctrl Pts',(74.1371485754701,2.31519550295665,136.249339988104));
#180925=CARTESIAN_POINT('Ctrl Pts',(74.1445718418755,2.17098026267194,136.310660050688));
#180926=CARTESIAN_POINT('Ctrl Pts',(74.1519951082809,2.0241090930186,136.366339370785));
#180927=CARTESIAN_POINT('Ctrl Pts',(74.1594183746864,1.87506343567259,136.41613998553));
#180928=CARTESIAN_POINT('Ctrl Pts',(74.1668328674074,1.726193937916,136.465881740083));
#180929=CARTESIAN_POINT('Ctrl Pts',(74.1742473601283,1.57515541879241,136.509758502452));
#180930=CARTESIAN_POINT('Ctrl Pts',(74.1816618528493,1.4224510478273,136.547579538958));
#180931=CARTESIAN_POINT('Ctrl Pts',(74.1890691992031,1.26989385908415,136.585364122125));
#180932=CARTESIAN_POINT('Ctrl Pts',(74.1964765455569,1.11567437487134,136.61710451008));
#180933=CARTESIAN_POINT('Ctrl Pts',(74.2038838919107,0.960312646315376,
136.642659186826));
#180934=CARTESIAN_POINT('Ctrl Pts',(74.2112857135861,0.805066792397916,
136.668194803931));
#180935=CARTESIAN_POINT('Ctrl Pts',(74.2186875352614,0.648680757205681,
136.687553835673));
#180936=CARTESIAN_POINT('Ctrl Pts',(74.2260893569368,0.491686448070869,
136.700645464763));
#180937=CARTESIAN_POINT('Ctrl Pts',(74.2334872712482,0.334775015009695,
136.713730182883));
#180938=CARTESIAN_POINT('Ctrl Pts',(74.2408851855595,0.177256318563158,
136.72055405647));
#180939=CARTESIAN_POINT('Ctrl Pts',(74.2482830998709,0.0196689711522565,
136.72107792483));
#180940=CARTESIAN_POINT('Ctrl Pts',(74.2556797847831,-0.137892188100206,
136.721601706132));
#180941=CARTESIAN_POINT('Ctrl Pts',(74.2630764696953,-0.295521602744105,
136.715827558846));
#180942=CARTESIAN_POINT('Ctrl Pts',(74.2704731546075,-0.452678944409718,
136.703768412912));
#180943=CARTESIAN_POINT('Ctrl Pts',(74.2778695115429,-0.609829317554113,
136.691709801693));
#180944=CARTESIAN_POINT('Ctrl Pts',(74.2852658684783,-0.76650728713711,
136.673366774501));
#180945=CARTESIAN_POINT('Ctrl Pts',(74.2926622254137,-0.922176205857355,
136.648804270118));
#180946=CARTESIAN_POINT('Ctrl Pts',(74.3000597147503,-1.07786895788646,
136.624238005152));
#180947=CARTESIAN_POINT('Ctrl Pts',(74.3074572040869,-1.23255198268647,
136.593450425187));
#180948=CARTESIAN_POINT('Ctrl Pts',(74.3148546934235,-1.38569755137894,
136.556557837638));
#180949=CARTESIAN_POINT('Ctrl Pts',(74.3222547759385,-1.53889680501311,
136.519652317449));
#180950=CARTESIAN_POINT('Ctrl Pts',(74.3296548584534,-1.69055716679896,
136.476637616123));
#180951=CARTESIAN_POINT('Ctrl Pts',(74.3370549409684,-1.84016496842807,
136.427680228923));
#180952=CARTESIAN_POINT('Ctrl Pts',(74.3444631606348,-1.98993727921513,
136.378669008043));
#180953=CARTESIAN_POINT('Ctrl Pts',(74.3518713803013,-2.13765216746389,
136.323702167447));
#180954=CARTESIAN_POINT('Ctrl Pts',(74.3592795999678,-2.28281420372402,
136.262995050625));
#180955=CARTESIAN_POINT('Ctrl Pts',(74.3666923792698,-2.42806558479541,
136.202250569585));
#180956=CARTESIAN_POINT('Ctrl Pts',(74.3741051585719,-2.57076064540786,
136.13575892959));
#180957=CARTESIAN_POINT('Ctrl Pts',(74.3815179378739,-2.71042802887655,
136.063781732364));
#180958=CARTESIAN_POINT('Ctrl Pts',(74.3889413089027,-2.85029497565258,
135.991701690743));
#180959=CARTESIAN_POINT('Ctrl Pts',(74.3963646799315,-2.98712528124606,
135.914120621237));
#180960=CARTESIAN_POINT('Ctrl Pts',(74.4037880509602,-3.12047536423706,
135.831344212495));
#180961=CARTESIAN_POINT('Ctrl Pts',(74.4077241004011,-3.19118077793225,
135.787454174387));
#180962=CARTESIAN_POINT('Ctrl Pts',(74.411660149842,-3.26090830066379,135.742104235688));
#180963=CARTESIAN_POINT('Ctrl Pts',(74.4155961992829,-3.32959563312116,
135.695344514738));
#180964=CARTESIAN_POINT('Ctrl Pts',(74.4229865676082,-3.45856369964765,
135.607547964975));
#180965=CARTESIAN_POINT('Ctrl Pts',(74.4303769359336,-3.58426034178358,
135.514508215958));
#180966=CARTESIAN_POINT('Ctrl Pts',(74.4377673042589,-3.70622745252568,
135.41649771794));
#180967=CARTESIAN_POINT('Ctrl Pts',(74.4451489183431,-3.82805008745028,
135.318603317997));
#180968=CARTESIAN_POINT('Ctrl Pts',(74.4525305324272,-3.94615169233114,
135.215750121195));
#180969=CARTESIAN_POINT('Ctrl Pts',(74.4599121465114,-4.06010195808091,
135.108254511761));
#180970=CARTESIAN_POINT('Ctrl Pts',(74.4672866643554,-4.1739426788938,135.000862242145));
#180971=CARTESIAN_POINT('Ctrl Pts',(74.4746611821994,-4.2836397319908,134.888836700284));
#180972=CARTESIAN_POINT('Ctrl Pts',(74.4820357000435,-4.38879495099896,
134.772535190413));
#180973=CARTESIAN_POINT('Ctrl Pts',(74.4894047737232,-4.49387254021456,
134.656319538972));
#180974=CARTESIAN_POINT('Ctrl Pts',(74.4967738474029,-4.59441471883195,
134.53583448246));
#180975=CARTESIAN_POINT('Ctrl Pts',(74.5041429210826,-4.69005947318445,
134.411474796587));
#180976=CARTESIAN_POINT('Ctrl Pts',(74.511746333029,-4.7887457530969,134.283160443615));
#180977=CARTESIAN_POINT('Ctrl Pts',(74.5193497449753,-4.88221766942739,
134.1507212306));
#180978=CARTESIAN_POINT('Ctrl Pts',(74.5269531569216,-4.97012145377866,
134.014629032697));
#180979=CARTESIAN_POINT('Ctrl Pts',(74.5343173147514,-5.05525919803919,
133.882819204185));
#180980=CARTESIAN_POINT('Ctrl Pts',(74.5416814725812,-5.13517372494517,
133.747583154343));
#180981=CARTESIAN_POINT('Ctrl Pts',(74.549045630411,-5.20958712413971,133.609379790138));
#180982=CARTESIAN_POINT('Ctrl Pts',(74.5564096624141,-5.28399925187906,
133.471178787328));
#180983=CARTESIAN_POINT('Ctrl Pts',(74.5637736944171,-5.35291025985287,
133.330010902823));
#180984=CARTESIAN_POINT('Ctrl Pts',(74.5711377264201,-5.41608807588343,
133.18635988641));
#180985=CARTESIAN_POINT('Ctrl Pts',(74.5785031202411,-5.47927757528023,
133.042682304859));
#180986=CARTESIAN_POINT('Ctrl Pts',(74.585868514062,-5.53673162053088,132.896521022438));
#180987=CARTESIAN_POINT('Ctrl Pts',(74.593233907883,-5.58826626889062,132.748379822841));
#180988=CARTESIAN_POINT('Ctrl Pts',(74.6006021517574,-5.63982085868267,
132.60018129972));
#180989=CARTESIAN_POINT('Ctrl Pts',(74.6079703956318,-5.68545136843434,
132.450001690142));
#180990=CARTESIAN_POINT('Ctrl Pts',(74.6153386395062,-5.72502375860916,
132.298359789541));
#180991=CARTESIAN_POINT('Ctrl Pts',(74.6227149696233,-5.76463957730755,
132.146551470286));
#180992=CARTESIAN_POINT('Ctrl Pts',(74.6300912997405,-5.79818390819066,
131.993278020939));
#180993=CARTESIAN_POINT('Ctrl Pts',(74.6374676298576,-5.82557373822989,
131.839068877389));
#180994=CARTESIAN_POINT('Ctrl Pts',(74.6448488045965,-5.85298155734553,
131.684758452449));
#180995=CARTESIAN_POINT('Ctrl Pts',(74.6522299793354,-5.87422677263048,
131.529511481286));
#180996=CARTESIAN_POINT('Ctrl Pts',(74.6596111540743,-5.88927831124794,
131.373861745892));
#180997=CARTESIAN_POINT('Ctrl Pts',(74.6670021893174,-5.9043499572014,131.218004078166));
#180998=CARTESIAN_POINT('Ctrl Pts',(74.6743932245606,-5.91321138974546,
131.061742946688));
#180999=CARTESIAN_POINT('Ctrl Pts',(74.6817842598037,-5.91588359738916,
130.905611912086));
#181000=CARTESIAN_POINT('Ctrl Pts',(74.683397775801,-5.91646695948111,130.871527387562));
#181001=CARTESIAN_POINT('Ctrl Pts',(74.6850112917982,-5.91675555147155,
130.837449041975));
#181002=CARTESIAN_POINT('Ctrl Pts',(74.6866248077955,-5.91674991913294,
130.803382384264));
#181003=CARTESIAN_POINT('',(76.4366248077954,-5.91522634936544,130.8098031079));
#181004=CARTESIAN_POINT('Ctrl Pts',(74.6866248077955,-5.92633562348113,
130.803380799432));
#181005=CARTESIAN_POINT('Ctrl Pts',(74.6890978128956,-5.92645530821839,
130.751082873092));
#181006=CARTESIAN_POINT('Ctrl Pts',(74.6915708179957,-5.92582318992127,
130.698787913914));
#181007=CARTESIAN_POINT('Ctrl Pts',(74.7868596977001,-5.87215715415332,
128.684559602157));
#181008=CARTESIAN_POINT('Ctrl Pts',(74.9724914469087,-3.62464280894678,
124.817748467285));
#181009=CARTESIAN_POINT('Ctrl Pts',(75.2509390707216,3.07749837663965,124.518935868821));
#181010=CARTESIAN_POINT('Ctrl Pts',(75.5293866945345,6.95156889824953,129.996121554386));
#181011=CARTESIAN_POINT('Ctrl Pts',(75.8078343183472,4.43748720538687,136.216039454336));
#181012=CARTESIAN_POINT('Ctrl Pts',(76.0862819421603,-2.1544284459224,137.462888878506));
#181013=CARTESIAN_POINT('Ctrl Pts',(76.2958787719761,-5.62611108597975,
133.795562092127));
#181014=CARTESIAN_POINT('Ctrl Pts',(76.412659727188,-5.91981165034088,131.319080415719));
#181015=CARTESIAN_POINT('Ctrl Pts',(76.4366248077954,-5.91522634936544,
130.8098031079));
#181016=CARTESIAN_POINT('',(78.1866248462858,-5.91289176011554,130.802962071976));
#181017=CARTESIAN_POINT('Ctrl Pts',(76.4366248077954,-5.91522634936544,
130.8098031079));
#181018=CARTESIAN_POINT('Ctrl Pts',(76.5054756017923,-5.9020529485309,129.346668158248));
#181019=CARTESIAN_POINT('Ctrl Pts',(76.6671422703935,-4.61414522720397,
125.890408083284));
#181020=CARTESIAN_POINT('Ctrl Pts',(76.9216248135988,1.18775470884825,123.907491814845));
#181021=CARTESIAN_POINT('Ctrl Pts',(77.200072437412,6.444541485859,128.075726239824));
#181022=CARTESIAN_POINT('Ctrl Pts',(77.4785200612247,5.77910947071827,134.751442356751));
#181023=CARTESIAN_POINT('Ctrl Pts',(77.7569676850376,-0.197041822817637,
137.799983181025));
#181024=CARTESIAN_POINT('Ctrl Pts',(77.9930026005611,-5.10942382781107,
134.934739361913));
#181025=CARTESIAN_POINT('Ctrl Pts',(78.1362216414804,-5.9049751713417,131.877724787875));
#181026=CARTESIAN_POINT('Ctrl Pts',(78.1866248077954,-5.90723462883533,
130.802964231305));
#181027=CARTESIAN_POINT('',(79.9366248077955,-5.91765730409607,130.799401002026));
#181028=CARTESIAN_POINT('Ctrl Pts',(78.1866248725357,-5.91674983436422,
130.802960599348));
#181029=CARTESIAN_POINT('Ctrl Pts',(78.1945270335779,-5.91670989979542,
130.634189328837));
#181030=CARTESIAN_POINT('Ctrl Pts',(78.2024291946202,-5.90944460636754,
130.465609897226));
#181031=CARTESIAN_POINT('Ctrl Pts',(78.2103313556624,-5.89502840903797,
130.297832613271));
#181032=CARTESIAN_POINT('Ctrl Pts',(78.2182492070647,-5.88058358721903,
130.129722194372));
#181033=CARTESIAN_POINT('Ctrl Pts',(78.2261670584669,-5.85895952068674,
129.962417391742));
#181034=CARTESIAN_POINT('Ctrl Pts',(78.2340849098691,-5.83028189352874,
129.79651955644));
#181035=CARTESIAN_POINT('Ctrl Pts',(78.2420266193473,-5.80151785492241,
129.630121837653));
#181036=CARTESIAN_POINT('Ctrl Pts',(78.2499683288254,-5.76565778336446,
129.465139853294));
#181037=CARTESIAN_POINT('Ctrl Pts',(78.2579100383036,-5.72287817090009,
129.302163558743));
#181038=CARTESIAN_POINT('Ctrl Pts',(78.2658646621798,-5.68002899243783,
129.138922240554));
#181039=CARTESIAN_POINT('Ctrl Pts',(78.2738192860561,-5.63023788296061,
128.977693401605));
#181040=CARTESIAN_POINT('Ctrl Pts',(78.2817739099323,-5.57373019043886,
128.819048972839));
#181041=CARTESIAN_POINT('Ctrl Pts',(78.2897479198207,-5.51708478445259,
128.660017915758));
#181042=CARTESIAN_POINT('Ctrl Pts',(78.2977219297091,-5.45369016527998,
128.503584133401));
#181043=CARTESIAN_POINT('Ctrl Pts',(78.3056959395974,-5.38381942457843,
128.350298889322));
#181044=CARTESIAN_POINT('Ctrl Pts',(78.3084182706194,-5.35996551825003,
128.297967229215));
#181045=CARTESIAN_POINT('Ctrl Pts',(78.3111406016414,-5.33535717654536,
128.246002314849));
#181046=CARTESIAN_POINT('Ctrl Pts',(78.3138629326633,-5.31000644233234,
128.19442534157));
#181047=CARTESIAN_POINT('Ctrl Pts',(78.3212861990688,-5.24087992828296,
128.05378498228));
#181048=CARTESIAN_POINT('Ctrl Pts',(78.3287094654741,-5.1660575455445,127.915680173518));
#181049=CARTESIAN_POINT('Ctrl Pts',(78.3361327318796,-5.08574833795125,
127.780605600121));
#181050=CARTESIAN_POINT('Ctrl Pts',(78.3435472246006,-5.0055340491721,127.645690673652));
#181051=CARTESIAN_POINT('Ctrl Pts',(78.3509617173216,-4.91984603282031,
127.513799171315));
#181052=CARTESIAN_POINT('Ctrl Pts',(78.3583762100426,-4.82894063743904,
127.385404215008));
#181053=CARTESIAN_POINT('Ctrl Pts',(78.3657835563964,-4.73812286010017,
127.257133010595));
#181054=CARTESIAN_POINT('Ctrl Pts',(78.3731909027502,-4.64209792915583,
127.132351945622));
#181055=CARTESIAN_POINT('Ctrl Pts',(78.380598249104,-4.54116712779319,127.01150790754));
#181056=CARTESIAN_POINT('Ctrl Pts',(78.3880000707794,-4.44031160443018,
126.890753999501));
#181057=CARTESIAN_POINT('Ctrl Pts',(78.3954018924548,-4.33455773444595,
126.773931556894));
#181058=CARTESIAN_POINT('Ctrl Pts',(78.4028037141302,-4.22424889844974,
126.661456828381));
#181059=CARTESIAN_POINT('Ctrl Pts',(78.4102016284416,-4.11399829362917,
126.549041474401));
#181060=CARTESIAN_POINT('Ctrl Pts',(78.417599542753,-3.99919777225675,126.440969529504));
#181061=CARTESIAN_POINT('Ctrl Pts',(78.4249974570644,-3.88022953820049,
126.337622513157));
#181062=CARTESIAN_POINT('Ctrl Pts',(78.4323941419766,-3.76128107450676,
126.23429267121));
#181063=CARTESIAN_POINT('Ctrl Pts',(78.4397908268889,-3.63816655426999,
126.135686443999));
#181064=CARTESIAN_POINT('Ctrl Pts',(78.4471875118011,-3.51130351085463,
126.042147033826));
#181065=CARTESIAN_POINT('Ctrl Pts',(78.4545838687365,-3.38444609267964,
125.948611771288));
#181066=CARTESIAN_POINT('Ctrl Pts',(78.461980225672,-3.2538407822705,125.860143100606));
#181067=CARTESIAN_POINT('Ctrl Pts',(78.4693765826074,-3.11993630293593,
125.77704244302));
#181068=CARTESIAN_POINT('Ctrl Pts',(78.476774071944,-2.98601132248373,125.69392906251));
#181069=CARTESIAN_POINT('Ctrl Pts',(78.4841715612806,-2.84878648456505,
125.616185528377));
#181070=CARTESIAN_POINT('Ctrl Pts',(78.4915690506172,-2.7087373189545,125.544068543983));
#181071=CARTESIAN_POINT('Ctrl Pts',(78.4989691331322,-2.56863905932585,
125.471926279092));
#181072=CARTESIAN_POINT('Ctrl Pts',(78.5063692156472,-2.42571483246961,
125.405414661724));
#181073=CARTESIAN_POINT('Ctrl Pts',(78.5137692981623,-2.28046231007505,
125.34474321203));
#181074=CARTESIAN_POINT('Ctrl Pts',(78.5211775178287,-2.1350500675999,125.284005047841));
#181075=CARTESIAN_POINT('Ctrl Pts',(78.5285857374952,-1.98730476136634,
125.229120020179));
#181076=CARTESIAN_POINT('Ctrl Pts',(78.5359939571617,-1.83774216640246,
125.180248750584));
#181077=CARTESIAN_POINT('Ctrl Pts',(78.5434067364638,-1.68808751815687,
125.131347401538));
#181078=CARTESIAN_POINT('Ctrl Pts',(78.5508195157658,-1.53661371075818,
125.088467287444));
#181079=CARTESIAN_POINT('Ctrl Pts',(78.5582322950679,-1.38384851366532,
125.051718280889));
#181080=CARTESIAN_POINT('Ctrl Pts',(78.5656556660967,-1.23086503849498,
125.014916765631));
#181081=CARTESIAN_POINT('Ctrl Pts',(78.5730790371254,-1.07658685352688,
124.984263926978));
#181082=CARTESIAN_POINT('Ctrl Pts',(78.5805024081542,-0.921549500963253,
124.959818113676));
#181083=CARTESIAN_POINT('Ctrl Pts',(78.5844384575949,-0.839344976565465,
124.946856356895));
#181084=CARTESIAN_POINT('Ctrl Pts',(78.5883745070356,-0.756927080310396,
124.935638748306));
#181085=CARTESIAN_POINT('Ctrl Pts',(78.5923105564763,-0.674375721295938,
124.926168042545));
#181086=CARTESIAN_POINT('Ctrl Pts',(78.5997338228818,-0.518686434531233,
124.908306587052));
#181087=CARTESIAN_POINT('Ctrl Pts',(78.6071570892872,-0.362051622079567,
124.896607754196));
#181088=CARTESIAN_POINT('Ctrl Pts',(78.6145803556926,-0.205000469604143,
124.891163058718));
#181089=CARTESIAN_POINT('Ctrl Pts',(78.6219948484136,-0.0481349385484352,
124.885724798418));
#181090=CARTESIAN_POINT('Ctrl Pts',(78.6294093411346,0.109145583613756,
124.886525974743));
#181091=CARTESIAN_POINT('Ctrl Pts',(78.6368238338557,0.266304483379695,
124.893606648348));
#181092=CARTESIAN_POINT('Ctrl Pts',(78.6442311802094,0.423311907481,124.900680497332));
#181093=CARTESIAN_POINT('Ctrl Pts',(78.6516385265633,0.580197572140323,
124.914021777738));
#181094=CARTESIAN_POINT('Ctrl Pts',(78.659045872917,0.736422647367805,124.93361856507));
#181095=CARTESIAN_POINT('Ctrl Pts',(78.6664476945924,0.892531204040482,
124.953200736379));
#181096=CARTESIAN_POINT('Ctrl Pts',(78.6738495162679,1.04797978349757,124.979029078526));
#181097=CARTESIAN_POINT('Ctrl Pts',(78.6812513379433,1.20223257834504,125.011039688249));
#181098=CARTESIAN_POINT('Ctrl Pts',(78.6886492522546,1.35640394434237,125.04303339982));
#181099=CARTESIAN_POINT('Ctrl Pts',(78.696047166566,1.50938041830019,125.081202803749));
#181100=CARTESIAN_POINT('Ctrl Pts',(78.7034450808773,1.66063442655972,125.125432561689));
#181101=CARTESIAN_POINT('Ctrl Pts',(78.7108417657895,1.81186329914721,125.169654969446));
#181102=CARTESIAN_POINT('Ctrl Pts',(78.7182384507017,1.96136991620067,125.219935627707));
#181103=CARTESIAN_POINT('Ctrl Pts',(78.7256351356139,2.10863984492123,125.276108763054));
#181104=CARTESIAN_POINT('Ctrl Pts',(78.7330314925494,2.25590324353882,125.332279407626));
#181105=CARTESIAN_POINT('Ctrl Pts',(78.7404278494848,2.40092980223452,125.394341876737));
#181106=CARTESIAN_POINT('Ctrl Pts',(78.7478242064203,2.54322338087415,125.462081572301));
#181107=CARTESIAN_POINT('Ctrl Pts',(78.7552216957569,2.68553874502392,125.529831638986));
#181108=CARTESIAN_POINT('Ctrl Pts',(78.7626191850934,2.82511995890015,125.603260502345));
#181109=CARTESIAN_POINT('Ctrl Pts',(78.77001667443,2.96149401523343,125.682106840152));
#181110=CARTESIAN_POINT('Ctrl Pts',(78.777416756945,3.09791587728085,125.76098081742));
#181111=CARTESIAN_POINT('Ctrl Pts',(78.78481683946,3.23112802041357,125.845275863474));
#181112=CARTESIAN_POINT('Ctrl Pts',(78.792216921975,3.36068516568954,125.934686523788));
#181113=CARTESIAN_POINT('Ctrl Pts',(78.7996251416415,3.49038477236554,126.024195500314));
#181114=CARTESIAN_POINT('Ctrl Pts',(78.807033361308,3.61642104746169,126.11883111272));
#181115=CARTESIAN_POINT('Ctrl Pts',(78.8144415809744,3.73838006652545,126.218246244733));
#181116=CARTESIAN_POINT('Ctrl Pts',(78.8218543602765,3.86041414933046,126.317722565101));
#181117=CARTESIAN_POINT('Ctrl Pts',(78.8292671395786,3.97836569659867,126.421984020153));
#181118=CARTESIAN_POINT('Ctrl Pts',(78.8366799188806,4.09185699712507,126.530645971315));
#181119=CARTESIAN_POINT('Ctrl Pts',(78.8441032899094,4.20551045934395,126.639463183769));
#181120=CARTESIAN_POINT('Ctrl Pts',(78.8515266609381,4.31469068806539,126.752693182139));
#181121=CARTESIAN_POINT('Ctrl Pts',(78.8589500319669,4.41905911919642,126.869916938525));
#181122=CARTESIAN_POINT('Ctrl Pts',(78.8628860814077,4.47439776566789,126.932071786906));
#181123=CARTESIAN_POINT('Ctrl Pts',(78.8668221308484,4.52838434356865,126.995348905774));
#181124=CARTESIAN_POINT('Ctrl Pts',(78.8707581802892,4.5809733425261,127.059682554292));
#181125=CARTESIAN_POINT('Ctrl Pts',(78.8781814466946,4.68015455331391,127.181013807612));
#181126=CARTESIAN_POINT('Ctrl Pts',(78.8856047131,4.77466205487176,127.306471606538));
#181127=CARTESIAN_POINT('Ctrl Pts',(78.8930279795055,4.86413281547984,127.435660198135));
#181128=CARTESIAN_POINT('Ctrl Pts',(78.9004424722265,4.95349782907904,127.564696099546));
#181129=CARTESIAN_POINT('Ctrl Pts',(78.9078569649475,5.03783774076514,127.69745371263));
#181130=CARTESIAN_POINT('Ctrl Pts',(78.9152714576685,5.11682879366983,127.833503223013));
#181131=CARTESIAN_POINT('Ctrl Pts',(78.9226788040223,5.19574371202383,127.969421603755));
#181132=CARTESIAN_POINT('Ctrl Pts',(78.9300861503761,5.2693198488673,128.108625244604));
#181133=CARTESIAN_POINT('Ctrl Pts',(78.9374934967298,5.33727598584508,128.250654367149));
#181134=CARTESIAN_POINT('Ctrl Pts',(78.9448953184052,5.40518143857207,128.392577559015));
#181135=CARTESIAN_POINT('Ctrl Pts',(78.9522971400807,5.46747507706612,128.537321701267));
#181136=CARTESIAN_POINT('Ctrl Pts',(78.9596989617561,5.52392104796787,128.684401462696));
#181137=CARTESIAN_POINT('Ctrl Pts',(78.9670968760674,5.58033722148095,128.831403581864));
#181138=CARTESIAN_POINT('Ctrl Pts',(78.9744947903788,5.63091174177378,128.980738517087));
#181139=CARTESIAN_POINT('Ctrl Pts',(78.9818927046902,5.67545647981579,129.13190006251));
#181140=CARTESIAN_POINT('Ctrl Pts',(78.9892893896024,5.71999381533041,129.283036487627));
#181141=CARTESIAN_POINT('Ctrl Pts',(78.9966860745146,5.75850325193283,129.435998562765));
#181142=CARTESIAN_POINT('Ctrl Pts',(79.0040827594268,5.79084619600052,129.590263876459));
#181143=CARTESIAN_POINT('Ctrl Pts',(79.0114791163622,5.82318770594818,129.744522349868));
#181144=CARTESIAN_POINT('Ctrl Pts',(79.0188754732976,5.84936319043042,129.900083581578));
#181145=CARTESIAN_POINT('Ctrl Pts',(79.0262718302331,5.86928502103311,130.056414159338));
#181146=CARTESIAN_POINT('Ctrl Pts',(79.0336693195697,5.88920990171894,130.212768671708));
#181147=CARTESIAN_POINT('Ctrl Pts',(79.0410668089063,5.90287917492191,130.369892394333));
#181148=CARTESIAN_POINT('Ctrl Pts',(79.0484642982428,5.91025702645075,130.527246121753));
#181149=CARTESIAN_POINT('Ctrl Pts',(79.0558643807578,5.91763746427399,130.684655009279));
#181150=CARTESIAN_POINT('Ctrl Pts',(79.0632644632728,5.91872207191936,130.842293689474));
#181151=CARTESIAN_POINT('Ctrl Pts',(79.0706645457878,5.91352715278672,130.99962243092));
#181152=CARTESIAN_POINT('Ctrl Pts',(79.0780727654543,5.90832652130644,131.157124171491));
#181153=CARTESIAN_POINT('Ctrl Pts',(79.0854809851207,5.89683258566624,131.314314919371));
#181154=CARTESIAN_POINT('Ctrl Pts',(79.0928892047872,5.87911364833969,131.47065880337));
#181155=CARTESIAN_POINT('Ctrl Pts',(79.1003019840893,5.86138380530286,131.627098914422));
#181156=CARTESIAN_POINT('Ctrl Pts',(79.1077147633914,5.83742138275471,131.782690754884));
#181157=CARTESIAN_POINT('Ctrl Pts',(79.1151275426934,5.80734582588931,131.936908639076));
#181158=CARTESIAN_POINT('Ctrl Pts',(79.1225509137222,5.77722729565787,132.091346877013));
#181159=CARTESIAN_POINT('Ctrl Pts',(79.129974284751,5.74097827168832,132.244406875497));
#181160=CARTESIAN_POINT('Ctrl Pts',(79.1373976557797,5.69876829185863,132.395577296151));
#181161=CARTESIAN_POINT('Ctrl Pts',(79.1413337052205,5.67638754773837,132.475731480466));
#181162=CARTESIAN_POINT('Ctrl Pts',(79.1452697546613,5.65233177958366,132.555354745812));
#181163=CARTESIAN_POINT('Ctrl Pts',(79.1492058041021,5.62663169755628,132.634373268494));
#181164=CARTESIAN_POINT('Ctrl Pts',(79.1566290705075,5.57816214492473,132.783399736188));
#181165=CARTESIAN_POINT('Ctrl Pts',(79.1640523369129,5.52369455860523,132.930724578636));
#181166=CARTESIAN_POINT('Ctrl Pts',(79.1714756033183,5.4633656692368,133.075828452844));
#181167=CARTESIAN_POINT('Ctrl Pts',(79.1788900960393,5.40310808360552,133.220760826324));
#181168=CARTESIAN_POINT('Ctrl Pts',(79.1863045887604,5.33700312620981,133.363477115313));
#181169=CARTESIAN_POINT('Ctrl Pts',(79.1937190814814,5.26523741356136,133.50347260882));
#181170=CARTESIAN_POINT('Ctrl Pts',(79.2011264278352,5.19354087140873,133.6433331694));
#181171=CARTESIAN_POINT('Ctrl Pts',(79.208533774189,5.11619460507125,133.780477825228));
#181172=CARTESIAN_POINT('Ctrl Pts',(79.2159411205427,5.03343343375855,133.914421457875));
#181173=CARTESIAN_POINT('Ctrl Pts',(79.2233429422181,4.95073398884981,134.048265190307));
#181174=CARTESIAN_POINT('Ctrl Pts',(79.2307447638935,4.86262787581848,134.178912337079));
#181175=CARTESIAN_POINT('Ctrl Pts',(79.2381465855689,4.76939593305506,134.305902134706));
#181176=CARTESIAN_POINT('Ctrl Pts',(79.2455444998803,4.67621320670851,134.432824895408));
#181177=CARTESIAN_POINT('Ctrl Pts',(79.2529424141917,4.57791025988974,134.556093851872));
#181178=CARTESIAN_POINT('Ctrl Pts',(79.260340328503,4.47481128958491,134.675277109187));
#181179=CARTESIAN_POINT('Ctrl Pts',(79.2677370134152,4.37172945245855,134.794440560407));
#181180=CARTESIAN_POINT('Ctrl Pts',(79.2751336983274,4.26385341766289,134.909519377983));
#181181=CARTESIAN_POINT('Ctrl Pts',(79.2825303832396,4.15154779152017,135.020114583018));
#181182=CARTESIAN_POINT('Ctrl Pts',(79.289926740175,4.03924714512659,135.130704884146));
#181183=CARTESIAN_POINT('Ctrl Pts',(79.2973230971105,3.9225175638997,135.236811706103));
#181184=CARTESIAN_POINT('Ctrl Pts',(79.3047194540459,3.80176045737709,135.338073002271));
#181185=CARTESIAN_POINT('Ctrl Pts',(79.3121169433825,3.68098486263312,135.439349801801));
#181186=CARTESIAN_POINT('Ctrl Pts',(79.3195144327191,3.5561808008703,135.53577935852));
#181187=CARTESIAN_POINT('Ctrl Pts',(79.3269119220557,3.42778256246763,135.627040087212));
#181188=CARTESIAN_POINT('Ctrl Pts',(79.3343120045707,3.29933931426163,135.718332807211));
#181189=CARTESIAN_POINT('Ctrl Pts',(79.3417120870857,3.16729968497964,135.804452875525));
#181190=CARTESIAN_POINT('Ctrl Pts',(79.3491121696007,3.03212657833541,135.88512227065));
#181191=CARTESIAN_POINT('Ctrl Pts',(79.3565203892671,2.89680483496421,135.965880370069));
#181192=CARTESIAN_POINT('Ctrl Pts',(79.3639286089336,2.75834305393096,136.041175635316));
#181193=CARTESIAN_POINT('Ctrl Pts',(79.3713368286001,2.61722899799891,136.110775879731));
#181194=CARTESIAN_POINT('Ctrl Pts',(79.3787496079022,2.47602808871995,136.180418961934));
#181195=CARTESIAN_POINT('Ctrl Pts',(79.3861623872043,2.3321719920476,136.244359887505));
#181196=CARTESIAN_POINT('Ctrl Pts',(79.3935751665063,2.18616754527691,136.302415003117));
#181197=CARTESIAN_POINT('Ctrl Pts',(79.4009985375351,2.03995448050585,136.360553070601));
#181198=CARTESIAN_POINT('Ctrl Pts',(79.4084219085638,1.89158728601007,136.412788407988));
#181199=CARTESIAN_POINT('Ctrl Pts',(79.4158452795926,1.741587804611,136.458987261415));
#181200=CARTESIAN_POINT('Ctrl Pts',(79.4197813290334,1.66205448038528,136.483483002028));
#181201=CARTESIAN_POINT('Ctrl Pts',(79.4237173784741,1.58206244191956,136.506282522811));
#181202=CARTESIAN_POINT('Ctrl Pts',(79.4276534279149,1.50169039877162,136.527371757581));
#181203=CARTESIAN_POINT('Ctrl Pts',(79.4350766943203,1.35011123372,136.567145396185));
#181204=CARTESIAN_POINT('Ctrl Pts',(79.4424999607257,1.19672161046144,136.600952949165));
#181205=CARTESIAN_POINT('Ctrl Pts',(79.4499232271312,1.04203237321619,136.628628734306));
#181206=CARTESIAN_POINT('Ctrl Pts',(79.4573377198522,0.887525965802995,
136.656271808966));
#181207=CARTESIAN_POINT('Ctrl Pts',(79.4647522125732,0.731723365765574,
136.677797476357));
#181208=CARTESIAN_POINT('Ctrl Pts',(79.4721667052942,0.575150071538092,
136.693089933616));
#181209=CARTESIAN_POINT('Ctrl Pts',(79.479574051648,0.418727688546467,136.708367651429));
#181210=CARTESIAN_POINT('Ctrl Pts',(79.4869813980017,0.261536459217152,
136.717424083419));
#181211=CARTESIAN_POINT('Ctrl Pts',(79.4943887443555,0.104111452942493,
136.720194571276));
#181212=CARTESIAN_POINT('Ctrl Pts',(79.5017905660309,-0.0531961398232929,
136.722962992798));
#181213=CARTESIAN_POINT('Ctrl Pts',(79.5091923877063,-0.210736790727082,
136.719454798675));
#181214=CARTESIAN_POINT('Ctrl Pts',(79.5165942093817,-0.367971046389676,
136.709657212278));
#181215=CARTESIAN_POINT('Ctrl Pts',(79.5239921236931,-0.525122299312614,
136.699864797951));
#181216=CARTESIAN_POINT('Ctrl Pts',(79.5313900380044,-0.681967107482434,
136.683789626689));
#181217=CARTESIAN_POINT('Ctrl Pts',(79.5387879523158,-0.837966869088659,
136.661471004848));
#181218=CARTESIAN_POINT('Ctrl Pts',(79.546184637228,-0.993940706364406,
136.639156091958));
#181219=CARTESIAN_POINT('Ctrl Pts',(79.5535813221401,-1.14906940661803,
136.610599840533));
#181220=CARTESIAN_POINT('Ctrl Pts',(79.5609780070523,-1.30282021898066,
136.575893346358));
#181221=CARTESIAN_POINT('Ctrl Pts',(79.5683743639878,-1.45656421387115,
136.541188391105));
#181222=CARTESIAN_POINT('Ctrl Pts',(79.5757707209233,-1.60893007821654,
136.500333817537));
#181223=CARTESIAN_POINT('Ctrl Pts',(79.5831670778587,-1.75939624028258,
136.453471647824));
#181224=CARTESIAN_POINT('Ctrl Pts',(79.5905645671953,-1.90988543910226,
136.406602303393));
#181225=CARTESIAN_POINT('Ctrl Pts',(79.5979620565318,-2.058474000088,136.353723642426));
#181226=CARTESIAN_POINT('Ctrl Pts',(79.6053595458684,-2.20465661993256,
136.295027221057));
#181227=CARTESIAN_POINT('Ctrl Pts',(79.6127596283834,-2.350890483868,136.236310223747));
#181228=CARTESIAN_POINT('Ctrl Pts',(79.6201597108984,-2.49471638126169,
136.171771544599));
#181229=CARTESIAN_POINT('Ctrl Pts',(79.6275597934134,-2.63565019398481,
136.101650360203));
#181230=CARTESIAN_POINT('Ctrl Pts',(79.6349680130798,-2.77673897792317,
136.031452070356));
#181231=CARTESIAN_POINT('Ctrl Pts',(79.6423762327463,-2.91492899181364,
135.955659182587));
#181232=CARTESIAN_POINT('Ctrl Pts',(79.6497844524127,-3.04976124275421,
135.87455656296));
#181233=CARTESIAN_POINT('Ctrl Pts',(79.6571972317148,-3.18467648069582,
135.793404026024));
#181234=CARTESIAN_POINT('Ctrl Pts',(79.6646100110169,-3.31622952641147,
135.706935449793));
#181235=CARTESIAN_POINT('Ctrl Pts',(79.672022790319,-3.4439919092189,135.615477981727));
#181236=CARTESIAN_POINT('Ctrl Pts',(79.6794461613477,-3.57193684491018,
135.523889834943));
#181237=CARTESIAN_POINT('Ctrl Pts',(79.6868695323765,-3.69608000633086,
135.427298788013));
#181238=CARTESIAN_POINT('Ctrl Pts',(79.6942929034052,-3.81602679377552,
135.326071584853));
#181239=CARTESIAN_POINT('Ctrl Pts',(79.6982289528461,-3.87962545856341,
135.272398492824));
#181240=CARTESIAN_POINT('Ctrl Pts',(79.702165002287,-3.94204499181968,135.217422623261));
#181241=CARTESIAN_POINT('Ctrl Pts',(79.7061010517278,-4.00323101482898,
135.161202593632));
#181242=CARTESIAN_POINT('Ctrl Pts',(79.7134134904188,-4.11690312406568,
135.056756364984));
#181243=CARTESIAN_POINT('Ctrl Pts',(79.7207259291098,-4.22668148481328,
134.947677566942));
#181244=CARTESIAN_POINT('Ctrl Pts',(79.7280383678008,-4.3321564831283,134.834292474085));
#181245=CARTESIAN_POINT('Ctrl Pts',(79.7353420711127,-4.43750548187835,
134.721042830127));
#181246=CARTESIAN_POINT('Ctrl Pts',(79.7426457744246,-4.53856108607832,
134.60349740517));
#181247=CARTESIAN_POINT('Ctrl Pts',(79.7499494777365,-4.63494720400953,
134.482022235843));
#181248=CARTESIAN_POINT('Ctrl Pts',(79.7572461627114,-4.73124070176747,
134.360663795474));
#181249=CARTESIAN_POINT('Ctrl Pts',(79.7645428476862,-4.82287340406486,
134.235383424818));
#181250=CARTESIAN_POINT('Ctrl Pts',(79.771839532661,-4.90950671483698,134.106583259889));
#181251=CARTESIAN_POINT('Ctrl Pts',(79.7791305735189,-4.99607301318684,
133.977882724201));
#181252=CARTESIAN_POINT('Ctrl Pts',(79.7864216143768,-5.07764740490519,
133.845668133241));
#181253=CARTESIAN_POINT('Ctrl Pts',(79.7937126552347,-5.15393239403828,
133.71037359761));
#181254=CARTESIAN_POINT('Ctrl Pts',(79.8010006578554,-5.23018559458332,
133.575135440335));
#181255=CARTESIAN_POINT('Ctrl Pts',(79.8082886604761,-5.30115358817978,
133.436820226451));
#181256=CARTESIAN_POINT('Ctrl Pts',(79.8155766630968,-5.36658298783485,
133.295889786005));
#181257=CARTESIAN_POINT('Ctrl Pts',(79.8228631672246,-5.43199893449135,
133.154988322395));
#181258=CARTESIAN_POINT('Ctrl Pts',(79.8301496713525,-5.49187839129512,
133.011473051662));
#181259=CARTESIAN_POINT('Ctrl Pts',(79.8374361754803,-5.54601474745979,
132.865828779692));
#181260=CARTESIAN_POINT('Ctrl Pts',(79.8447227195084,-5.60015140007108,
132.720183710184));
#181261=CARTESIAN_POINT('Ctrl Pts',(79.8520092635366,-5.64854475669413,
132.572409977985));
#181262=CARTESIAN_POINT('Ctrl Pts',(79.8592958075647,-5.69103712586775,
132.423010361796));
#181263=CARTESIAN_POINT('Ctrl Pts',(79.866586863467,-5.733555806585,132.273518236419));
#181264=CARTESIAN_POINT('Ctrl Pts',(79.8738779193693,-5.77016609637652,
132.122398587331));
#181265=CARTESIAN_POINT('Ctrl Pts',(79.8811689752716,-5.80076069769532,
131.970167587254));
#181266=CARTESIAN_POINT('Ctrl Pts',(79.8884625230659,-5.83136575544766,
131.817884558608));
#181267=CARTESIAN_POINT('Ctrl Pts',(79.8957560708601,-5.85595096667871,
131.664489802451));
#181268=CARTESIAN_POINT('Ctrl Pts',(79.9030496186544,-5.87446066816507,
131.510506792718));
#181269=CARTESIAN_POINT('Ctrl Pts',(79.9103508269902,-5.89298981071651,
131.356362051921));
#181270=CARTESIAN_POINT('Ctrl Pts',(79.917652035326,-5.90543066925387,131.201628207417));
#181271=CARTESIAN_POINT('Ctrl Pts',(79.9249532436618,-5.91177963798963,
131.046831387663));
#181272=CARTESIAN_POINT('Ctrl Pts',(79.9288437650397,-5.91516274903892,
130.964346364803));
#181273=CARTESIAN_POINT('Ctrl Pts',(79.9327342864175,-5.91681701672771,
130.88184344256));
#181274=CARTESIAN_POINT('Ctrl Pts',(79.9366248077954,-5.91674792198156,
130.799401764183));
#181275=CARTESIAN_POINT('',(81.6866248077954,-5.92353248883006,130.808099003046));
#181276=CARTESIAN_POINT('Ctrl Pts',(79.9366248077954,-5.92036607957503,
130.799398731789));
#181277=CARTESIAN_POINT('Ctrl Pts',(79.9525994303772,-5.92340740034602,
130.460680406864));
#181278=CARTESIAN_POINT('Ctrl Pts',(80.061389927564,-5.74256826904676,128.157184786054));
#181279=CARTESIAN_POINT('Ctrl Pts',(80.2629962993529,-2.71882372294293,
124.355674077366));
#181280=CARTESIAN_POINT('Ctrl Pts',(80.5414439231668,3.95587198936288,125.031264625449));
#181281=CARTESIAN_POINT('Ctrl Pts',(80.8198915469792,6.99531459853266,131.012048358891));
#181282=CARTESIAN_POINT('Ctrl Pts',(81.0983391707924,3.60640483176838,136.801977204155));
#181283=CARTESIAN_POINT('Ctrl Pts',(81.3767867946052,-3.09661479272062,
137.080389406207));
#181284=CARTESIAN_POINT('Ctrl Pts',(81.5728820069396,-5.81315485131558,
133.214825300187));
#181285=CARTESIAN_POINT('Ctrl Pts',(81.6761613446696,-5.92516446039476,
131.029652639399));
#181286=CARTESIAN_POINT('Ctrl Pts',(81.6866248077954,-5.92353248883006,
130.808099003046));
#181287=CARTESIAN_POINT('',(83.4366248077954,-5.90860028553273,130.807517856062));
#181288=CARTESIAN_POINT('Ctrl Pts',(81.6866248077954,-5.92353248883006,
130.808099003046));
#181289=CARTESIAN_POINT('Ctrl Pts',(81.7689772192739,-5.91068809952968,
129.064366932107));
#181290=CARTESIAN_POINT('Ctrl Pts',(81.944145505357,-4.17314388298674,125.333100902792));
#181291=CARTESIAN_POINT('Ctrl Pts',(82.2121296660436,2.17468473634867,124.152420537573));
#181292=CARTESIAN_POINT('Ctrl Pts',(82.4905772898569,6.77193580165642,129.038448380621));
#181293=CARTESIAN_POINT('Ctrl Pts',(82.7690249136695,5.1461086926968,135.547263299818));
#181294=CARTESIAN_POINT('Ctrl Pts',(83.0474725374827,-1.20874090346615,
137.697582357697));
#181295=CARTESIAN_POINT('Ctrl Pts',(83.2700058355244,-5.39976777314671,
134.353588453385));
#181296=CARTESIAN_POINT('Ctrl Pts',(83.3997232589621,-5.91239030108813,
131.593925525655));
#181297=CARTESIAN_POINT('Ctrl Pts',(83.4366248077954,-5.90860028553273,
130.807517856062));
#181298=CARTESIAN_POINT('',(85.1866248077954,-5.91194855424759,130.79948298725));
#181299=CARTESIAN_POINT('Ctrl Pts',(83.4366248077954,-5.90860028553273,
130.807517856062));
#181300=CARTESIAN_POINT('Ctrl Pts',(83.4925391335664,-5.90285754109132,
129.615929534796));
#181301=CARTESIAN_POINT('Ctrl Pts',(83.6412693339418,-4.97384773570943,
126.438109061856));
#181302=CARTESIAN_POINT('Ctrl Pts',(83.8828154089211,0.218333178828223,
123.80937018488));
#181303=CARTESIAN_POINT('Ctrl Pts',(84.1612630327344,6.00309797568514,127.207087313424));
#181304=CARTESIAN_POINT('Ctrl Pts',(84.4397106565468,6.27130900052438,133.910522871902));
#181305=CARTESIAN_POINT('Ctrl Pts',(84.71815828036,0.776493424362582,137.759547063109));
#181306=CARTESIAN_POINT('Ctrl Pts',(84.9671296641093,-4.7746681124197,135.486236640735));
#181307=CARTESIAN_POINT('Ctrl Pts',(85.1232851732545,-5.90153036521254,
132.147392464895));
#181308=CARTESIAN_POINT('Ctrl Pts',(85.1866248077954,-5.91194855424759,
130.79948298725));
#181309=CARTESIAN_POINT('',(86.9366241207765,-5.92196730184553,130.803176251173));
#181310=CARTESIAN_POINT('Ctrl Pts',(85.1866248077954,-5.91194855424759,
130.79948298725));
#181311=CARTESIAN_POINT('Ctrl Pts',(85.2161010478588,-5.91679684620963,
130.172209027827));
#181312=CARTESIAN_POINT('Ctrl Pts',(85.3383931625264,-5.53558770671179,
127.575492174767));
#181313=CARTESIAN_POINT('Ctrl Pts',(85.5535011517986,-1.75560445854355,
124.029745239887));
#181314=CARTESIAN_POINT('Ctrl Pts',(85.8319487756115,4.7507286914536,125.665475774475));
#181315=CARTESIAN_POINT('Ctrl Pts',(86.1103963994243,6.8913742600039,132.023590431382));
#181316=CARTESIAN_POINT('Ctrl Pts',(86.3888440232373,2.69918354595779,137.261292452082));
#181317=CARTESIAN_POINT('Ctrl Pts',(86.6642530762223,-3.90060987699965,
136.572983623696));
#181318=CARTESIAN_POINT('Ctrl Pts',(86.846846254603,-5.92098433078664,132.701838245013));
#181319=CARTESIAN_POINT('Ctrl Pts',(86.9366235583794,-5.9262383104758,130.803187280332));
#181320=CARTESIAN_POINT('',(88.6866248062304,-5.91569305183782,130.809821120246));
#181321=CARTESIAN_POINT('Ctrl Pts',(86.9366248077953,-5.91674987874936,
130.803162778058));
#181322=CARTESIAN_POINT('Ctrl Pts',(86.9396629621512,-5.91673689178478,
130.739013432001));
#181323=CARTESIAN_POINT('Ctrl Pts',(86.9427011165071,-5.91568067838148,
130.67487583135));
#181324=CARTESIAN_POINT('Ctrl Pts',(86.945739270863,-5.91358218154266,130.610772537765));
#181325=CARTESIAN_POINT('Ctrl Pts',(86.9531625372684,-5.90845482484487,
130.454145925023));
#181326=CARTESIAN_POINT('Ctrl Pts',(86.9605858036738,-5.89709281915318,
130.297486319545));
#181327=CARTESIAN_POINT('Ctrl Pts',(86.9680090700793,-5.87948312036875,
130.141330603314));
#181328=CARTESIAN_POINT('Ctrl Pts',(86.9754235628003,-5.86189423478589,
129.985359450172));
#181329=CARTESIAN_POINT('Ctrl Pts',(86.9828380555213,-5.83807239593259,
129.829891368147));
#181330=CARTESIAN_POINT('Ctrl Pts',(86.9902525482423,-5.80805654683473,
129.675463053006));
#181331=CARTESIAN_POINT('Ctrl Pts',(86.9976598945961,-5.77806962814226,
129.521183581689));
#181332=CARTESIAN_POINT('Ctrl Pts',(87.0050672409499,-5.74190065508616,
129.367942246121));
#181333=CARTESIAN_POINT('Ctrl Pts',(87.0124745873037,-5.69964032010081,
129.21627032291));
#181334=CARTESIAN_POINT('Ctrl Pts',(87.0198764089791,-5.65741150446767,
129.064711522341));
#181335=CARTESIAN_POINT('Ctrl Pts',(87.0272782306545,-5.60910047272904,
128.914720161505));
#181336=CARTESIAN_POINT('Ctrl Pts',(87.0346800523299,-5.55484889329824,
128.766816916164));
#181337=CARTESIAN_POINT('Ctrl Pts',(87.0420779666413,-5.50062595285393,
128.618991747795));
#181338=CARTESIAN_POINT('Ctrl Pts',(87.0494758809526,-5.44046883837646,
128.473252849217));
#181339=CARTESIAN_POINT('Ctrl Pts',(87.056873795264,-5.37456889341132,128.330105219982));
#181340=CARTESIAN_POINT('Ctrl Pts',(87.0642704801762,-5.30867989982158,
128.186981379285));
#181341=CARTESIAN_POINT('Ctrl Pts',(87.0716671650885,-5.23705012580709,
128.046448292034));
#181342=CARTESIAN_POINT('Ctrl Pts',(87.0790638500007,-5.15991888229762,
127.908990573753));
#181343=CARTESIAN_POINT('Ctrl Pts',(87.0864602069362,-5.08279105886826,
127.771538950492));
#181344=CARTESIAN_POINT('Ctrl Pts',(87.0938565638716,-5.00016243365457,
127.637162750611));
#181345=CARTESIAN_POINT('Ctrl Pts',(87.1012529208071,-4.91231793758966,
127.506321345129));
#181346=CARTESIAN_POINT('Ctrl Pts',(87.1086504101436,-4.82445999230827,
127.375459907495));
#181347=CARTESIAN_POINT('Ctrl Pts',(87.1160478994802,-4.73138479422256,
127.248134651781));
#181348=CARTESIAN_POINT('Ctrl Pts',(87.1234453888168,-4.63342010767118,
127.124775224029));
#181349=CARTESIAN_POINT('Ctrl Pts',(87.1308454713318,-4.53542107975067,
127.001372552822));
#181350=CARTESIAN_POINT('Ctrl Pts',(87.1382455538468,-4.4325293828044,126.881938769633));
#181351=CARTESIAN_POINT('Ctrl Pts',(87.1456456363618,-4.32511237779127,
126.766869629096));
#181352=CARTESIAN_POINT('Ctrl Pts',(87.1530538560283,-4.21757725673839,
126.65167395821));
#181353=CARTESIAN_POINT('Ctrl Pts',(87.1604620756948,-4.10550714502573,
126.540852787686));
#181354=CARTESIAN_POINT('Ctrl Pts',(87.1678702953613,-3.9893060253567,126.434764755412));
#181355=CARTESIAN_POINT('Ctrl Pts',(87.1752830746634,-3.87303338583718,
126.328611427724));
#181356=CARTESIAN_POINT('Ctrl Pts',(87.1826958539654,-3.75262495683606,
126.227197283059));
#181357=CARTESIAN_POINT('Ctrl Pts',(87.1901086332675,-3.62851653654409,
126.130839642271));
#181358=CARTESIAN_POINT('Ctrl Pts',(87.1975320042963,-3.50423078432128,
126.034344321167));
#181359=CARTESIAN_POINT('Ctrl Pts',(87.204955375325,-3.37623478500182,125.942920150223));
#181360=CARTESIAN_POINT('Ctrl Pts',(87.2123787463538,-3.2449926234718,125.856840689752));
#181361=CARTESIAN_POINT('Ctrl Pts',(87.2163147957945,-3.17540488031723,
125.811199294363));
#181362=CARTESIAN_POINT('Ctrl Pts',(87.2202508452353,-3.10490493454365,
125.767059720152));
#181363=CARTESIAN_POINT('Ctrl Pts',(87.224186894676,-3.03356448216249,125.724457361099));
#181364=CARTESIAN_POINT('Ctrl Pts',(87.2316101610815,-2.89901861542882,
125.644110641499));
#181365=CARTESIAN_POINT('Ctrl Pts',(87.2390334274869,-2.76107501090047,
125.568991475291));
#181366=CARTESIAN_POINT('Ctrl Pts',(87.2464566938924,-2.62017831194225,
125.499401034673));
#181367=CARTESIAN_POINT('Ctrl Pts',(87.2538711866134,-2.47944814118135,
125.429892844177));
#181368=CARTESIAN_POINT('Ctrl Pts',(87.2612856793344,-2.33577215490723,
125.36590053602));
#181369=CARTESIAN_POINT('Ctrl Pts',(87.2687001720554,-2.18962294012674,
125.307681443504));
#181370=CARTESIAN_POINT('Ctrl Pts',(87.2761075184092,-2.04361458946177,
125.249518464741));
#181371=CARTESIAN_POINT('Ctrl Pts',(87.2835148647629,-1.89513810041531,
125.19711776113));
#181372=CARTESIAN_POINT('Ctrl Pts',(87.2909222111167,-1.74468947252004,
125.150690198539));
#181373=CARTESIAN_POINT('Ctrl Pts',(87.2983240327921,-1.59435305488766,
125.104297263377));
#181374=CARTESIAN_POINT('Ctrl Pts',(87.3057258544675,-1.44204778232258,
125.063868708343));
#181375=CARTESIAN_POINT('Ctrl Pts',(87.3131276761429,-1.28828828932917,
125.029566781759));
#181376=CARTESIAN_POINT('Ctrl Pts',(87.3205255904543,-1.13460996477558,
124.995282962894));
#181377=CARTESIAN_POINT('Ctrl Pts',(87.3279235047656,-0.979479312067915,
124.96711941249));
#181378=CARTESIAN_POINT('Ctrl Pts',(87.335321419077,-0.823424627491789,
124.945188112396));
#181379=CARTESIAN_POINT('Ctrl Pts',(87.3427181039892,-0.667395876372897,
124.923260456886));
#181380=CARTESIAN_POINT('Ctrl Pts',(87.3501147889014,-0.510443767454701,
124.907563048054));
#181381=CARTESIAN_POINT('Ctrl Pts',(87.3575114738136,-0.353105374908404,
124.898156493367));
#181382=CARTESIAN_POINT('Ctrl Pts',(87.364907830749,-0.195773958911312,
124.888750355776));
#181383=CARTESIAN_POINT('Ctrl Pts',(87.3723041876844,-0.0380566659750203,
124.885634539975));
#181384=CARTESIAN_POINT('Ctrl Pts',(87.3797005446199,0.119506009921639,
124.888817626758));
#181385=CARTESIAN_POINT('Ctrl Pts',(87.3870980339564,0.277092809066217,
124.89200120088));
#181386=CARTESIAN_POINT('Ctrl Pts',(87.3944955232931,0.434524570790814,
124.90148559025));
#181387=CARTESIAN_POINT('Ctrl Pts',(87.4018930126296,0.591262657080174,
124.917227271629));
#181388=CARTESIAN_POINT('Ctrl Pts',(87.4092930951446,0.748055687662819,
124.93297447123));
#181389=CARTESIAN_POINT('Ctrl Pts',(87.4166931776596,0.904154187469182,
124.954983292769));
#181390=CARTESIAN_POINT('Ctrl Pts',(87.4240932601746,1.05902662934586,124.983158580114));
#181391=CARTESIAN_POINT('Ctrl Pts',(87.4315014798411,1.21406936939365,125.011364849084));
#181392=CARTESIAN_POINT('Ctrl Pts',(87.4389096995075,1.36788299161932,125.045751058433));
#181393=CARTESIAN_POINT('Ctrl Pts',(87.446317919174,1.51994740129198,125.086171178608));
#181394=CARTESIAN_POINT('Ctrl Pts',(87.4537306984761,1.67210540407156,125.126616176694));
#181395=CARTESIAN_POINT('Ctrl Pts',(87.4611434777781,1.82251169319055,125.173102375787));
#181396=CARTESIAN_POINT('Ctrl Pts',(87.4685562570802,1.97066373806021,125.225434646199));
#181397=CARTESIAN_POINT('Ctrl Pts',(87.4759796281089,2.11902746951911,125.277841691413));
#181398=CARTESIAN_POINT('Ctrl Pts',(87.4834029991377,2.26513017790937,125.336111353121));
#181399=CARTESIAN_POINT('Ctrl Pts',(87.4908263701665,2.40849085997515,125.400001049595));
#181400=CARTESIAN_POINT('Ctrl Pts',(87.4947624196073,2.48450413349837,125.433876899678));
#181401=CARTESIAN_POINT('Ctrl Pts',(87.498698469048,2.55974695012835,125.46933198269));
#181402=CARTESIAN_POINT('Ctrl Pts',(87.5026345184888,2.63415077846103,125.506325110056));
#181403=CARTESIAN_POINT('Ctrl Pts',(87.5100577848942,2.77447407663323,125.576092993754));
#181404=CARTESIAN_POINT('Ctrl Pts',(87.5174810512996,2.91223584635632,125.651545110787));
#181405=CARTESIAN_POINT('Ctrl Pts',(87.5249043177051,3.04694236233204,125.732470161027));
#181406=CARTESIAN_POINT('Ctrl Pts',(87.5323188104261,3.18148966639265,125.813299564579));
#181407=CARTESIAN_POINT('Ctrl Pts',(87.5397333031471,3.31298858766372,125.899588835289));
#181408=CARTESIAN_POINT('Ctrl Pts',(87.5471477958681,3.44096717952954,125.991079467259));
#181409=CARTESIAN_POINT('Ctrl Pts',(87.5545551422219,3.56882242081021,126.082481917114));
#181410=CARTESIAN_POINT('Ctrl Pts',(87.5619624885757,3.69316378589292,126.179075532161));
#181411=CARTESIAN_POINT('Ctrl Pts',(87.5693698349295,3.81354576748629,126.280556992099));
#181412=CARTESIAN_POINT('Ctrl Pts',(87.5767716566049,3.93383796365611,126.381962763336));
#181413=CARTESIAN_POINT('Ctrl Pts',(87.5841734782803,4.05017637208661,126.488248881137));
#181414=CARTESIAN_POINT('Ctrl Pts',(87.5915752999557,4.1621463161506,126.599070068097));
#181415=CARTESIAN_POINT('Ctrl Pts',(87.598973214267,4.27405715215269,126.709832753415));
#181416=CARTESIAN_POINT('Ctrl Pts',(87.6063711285784,4.38160385180637,126.825125478141));
#181417=CARTESIAN_POINT('Ctrl Pts',(87.6137690428898,4.48440664456365,126.94456430057));
#181418=CARTESIAN_POINT('Ctrl Pts',(87.621165727802,4.58719235336167,127.063983274434));
#181419=CARTESIAN_POINT('Ctrl Pts',(87.6285624127141,4.68523547662453,127.187546695878));
#181420=CARTESIAN_POINT('Ctrl Pts',(87.6359590976264,4.7781947218654,127.314835469005));
#181421=CARTESIAN_POINT('Ctrl Pts',(87.6433554545618,4.87114984519592,127.442118598015));
#181422=CARTESIAN_POINT('Ctrl Pts',(87.6507518114973,4.95902131856453,127.5731264488));
#181423=CARTESIAN_POINT('Ctrl Pts',(87.6581481684327,5.04150977250863,127.707408926596));
#181424=CARTESIAN_POINT('Ctrl Pts',(87.6655456577693,5.12401085564567,127.841711963383));
#181425=CARTESIAN_POINT('Ctrl Pts',(87.6729431471059,5.20112708295338,127.979290307344));
#181426=CARTESIAN_POINT('Ctrl Pts',(87.6803406364425,5.272603924762,128.11966726169));
#181427=CARTESIAN_POINT('Ctrl Pts',(87.6877407189575,5.34410582266671,128.260093424959));
#181428=CARTESIAN_POINT('Ctrl Pts',(87.6951408014724,5.40996422984681,128.403319819423));
#181429=CARTESIAN_POINT('Ctrl Pts',(87.7025408839874,5.46997190044179,128.548847822019));
#181430=CARTESIAN_POINT('Ctrl Pts',(87.7099491036539,5.53004555563953,128.694535847614));
#181431=CARTESIAN_POINT('Ctrl Pts',(87.7173573233204,5.58425548376604,128.842530190304));
#181432=CARTESIAN_POINT('Ctrl Pts',(87.7247655429869,5.63244341971258,128.99231434712));
#181433=CARTESIAN_POINT('Ctrl Pts',(87.7321783222889,5.68066101452968,129.142190693586));
#181434=CARTESIAN_POINT('Ctrl Pts',(87.739591101591,5.72284913182212,129.293858690448));
#181435=CARTESIAN_POINT('Ctrl Pts',(87.7470038808931,5.75890030966424,129.446790072125));
#181436=CARTESIAN_POINT('Ctrl Pts',(87.7544272519218,5.79500299911989,129.599939969332));
#181437=CARTESIAN_POINT('Ctrl Pts',(87.7618506229506,5.82495116508458,129.754356491213));
#181438=CARTESIAN_POINT('Ctrl Pts',(87.7692739939793,5.84868890442652,129.909503834758));
#181439=CARTESIAN_POINT('Ctrl Pts',(87.7732100434201,5.86127522340487,129.991766679014));
#181440=CARTESIAN_POINT('Ctrl Pts',(87.7771460928609,5.87211643822368,130.074234930039));
#181441=CARTESIAN_POINT('Ctrl Pts',(87.7810821423017,5.88121015909862,130.156828666991));
#181442=CARTESIAN_POINT('Ctrl Pts',(87.7885054087072,5.89836063286343,130.31259787722));
#181443=CARTESIAN_POINT('Ctrl Pts',(87.7959286751126,5.90934423144243,130.469284467981));
#181444=CARTESIAN_POINT('Ctrl Pts',(87.8033519415181,5.91407185703321,130.626358841317));
#181445=CARTESIAN_POINT('Ctrl Pts',(87.8107664342391,5.91879389496316,130.783247565789));
#181446=CARTESIAN_POINT('Ctrl Pts',(87.8181809269601,5.91727466666259,130.940522791048));
#181447=CARTESIAN_POINT('Ctrl Pts',(87.8255954196811,5.90947656179092,131.09764772629));
#181448=CARTESIAN_POINT('Ctrl Pts',(87.8330027660349,5.90168597302632,131.254621218604));
#181449=CARTESIAN_POINT('Ctrl Pts',(87.8404101123887,5.88762857404784,131.411444338941));
#181450=CARTESIAN_POINT('Ctrl Pts',(87.8478174587424,5.86731874924192,131.56757831737));
#181451=CARTESIAN_POINT('Ctrl Pts',(87.8552192804178,5.84702407226958,131.723595845187));
#181452=CARTESIAN_POINT('Ctrl Pts',(87.8626211020932,5.82048630266507,131.878924885928));
#181453=CARTESIAN_POINT('Ctrl Pts',(87.8700229237686,5.78777178924067,132.033029929533));
#181454=CARTESIAN_POINT('Ctrl Pts',(87.87742083808,5.75507454555326,132.187053622285));
#181455=CARTESIAN_POINT('Ctrl Pts',(87.8848187523914,5.71620712911922,132.33985424048));
#181456=CARTESIAN_POINT('Ctrl Pts',(87.8922166667027,5.67128728570899,132.490904742531));
#181457=CARTESIAN_POINT('Ctrl Pts',(87.8996133516149,5.62637490716184,132.64193014273));
#181458=CARTESIAN_POINT('Ctrl Pts',(87.9070100365271,5.57541220416368,132.791205646551));
#181459=CARTESIAN_POINT('Ctrl Pts',(87.9144067214393,5.51856729703439,132.938217583392));
#181460=CARTESIAN_POINT('Ctrl Pts',(87.9218030783748,5.46172491046786,133.085223001569));
#181461=CARTESIAN_POINT('Ctrl Pts',(87.9291994353102,5.39900097300319,133.229964704157));
#181462=CARTESIAN_POINT('Ctrl Pts',(87.9365957922457,5.33061234560512,133.371947535936));
#181463=CARTESIAN_POINT('Ctrl Pts',(87.9439932815823,5.26221324773357,133.513952105648));
#181464=CARTESIAN_POINT('Ctrl Pts',(87.9513907709188,5.18814789506565,133.653196627176));
#181465=CARTESIAN_POINT('Ctrl Pts',(87.9587882602554,5.10867976660914,133.789209291241));
#181466=CARTESIAN_POINT('Ctrl Pts',(87.9661883427704,5.0291837807234,133.925269634334));
#181467=CARTESIAN_POINT('Ctrl Pts',(87.9735884252854,4.94428143644078,134.058095542208));
#181468=CARTESIAN_POINT('Ctrl Pts',(87.9809885078004,4.85428021801495,134.187243135108));
#181469=CARTESIAN_POINT('Ctrl Pts',(87.9883967274669,4.76418003399711,134.316532739062));
#181470=CARTESIAN_POINT('Ctrl Pts',(87.9958049471333,4.66896999237839,134.442135644086));
#181471=CARTESIAN_POINT('Ctrl Pts',(88.0032131667998,4.56899909557546,134.563639514792));
#181472=CARTESIAN_POINT('Ctrl Pts',(88.0106259461019,4.46896666835359,134.685218169103));
#181473=CARTESIAN_POINT('Ctrl Pts',(88.018038725404,4.3641677950318,134.802692484011));
#181474=CARTESIAN_POINT('Ctrl Pts',(88.0254515047061,4.25498883460737,134.915686508306));
#181475=CARTESIAN_POINT('Ctrl Pts',(88.0328748757348,4.14565387416439,135.028841983761));
#181476=CARTESIAN_POINT('Ctrl Pts',(88.0402982467635,4.03192659623113,135.137504125873));
#181477=CARTESIAN_POINT('Ctrl Pts',(88.0477216177923,3.91422757004694,135.241336287139));
#181478=CARTESIAN_POINT('Ctrl Pts',(88.051657667233,3.85182072221531,135.296390590461));
#181479=CARTESIAN_POINT('Ctrl Pts',(88.0555937166738,3.7882977884274,135.350087715604));
#181480=CARTESIAN_POINT('Ctrl Pts',(88.0595297661146,3.72372471661368,135.40238245281));
#181481=CARTESIAN_POINT('Ctrl Pts',(88.06695303252,3.60194191842861,135.501008695118));
#181482=CARTESIAN_POINT('Ctrl Pts',(88.0743762989254,3.47605395534822,135.594942437263));
#181483=CARTESIAN_POINT('Ctrl Pts',(88.0817995653309,3.34645823359367,135.683822458109));
#181484=CARTESIAN_POINT('Ctrl Pts',(88.0892140580519,3.2170156832198,135.772597430151));
#181485=CARTESIAN_POINT('Ctrl Pts',(88.0966285507728,3.0838744019375,135.856330361269));
#181486=CARTESIAN_POINT('Ctrl Pts',(88.1040430434938,2.94746567774693,135.934699460275));
#181487=CARTESIAN_POINT('Ctrl Pts',(88.1114503898476,2.81118842942062,136.012993024192));
#181488=CARTESIAN_POINT('Ctrl Pts',(88.1188577362013,2.67165032930038,136.085932863465));
#181489=CARTESIAN_POINT('Ctrl Pts',(88.1262650825551,2.52931243490207,136.153239861777));
#181490=CARTESIAN_POINT('Ctrl Pts',(88.1336669042305,2.38708070147531,136.22049665999));
#181491=CARTESIAN_POINT('Ctrl Pts',(88.1410687259059,2.24205366766045,136.282128823476));
#181492=CARTESIAN_POINT('Ctrl Pts',(88.1484705475813,2.09471773639211,136.337902717103));
#181493=CARTESIAN_POINT('Ctrl Pts',(88.1558684618926,1.94745958261503,136.393647168125));
#181494=CARTESIAN_POINT('Ctrl Pts',(88.163266376204,1.79789530701756,136.443539376393));
#181495=CARTESIAN_POINT('Ctrl Pts',(88.1706642905153,1.64653196907772,136.487393525909));
#181496=CARTESIAN_POINT('Ctrl Pts',(88.1780609754275,1.49519378497874,136.53124038766));
#181497=CARTESIAN_POINT('Ctrl Pts',(88.1854576603397,1.34205749010861,136.569051078361));
#181498=CARTESIAN_POINT('Ctrl Pts',(88.1928543452519,1.18764612323309,136.60068939089));
#181499=CARTESIAN_POINT('Ctrl Pts',(88.2002507021873,1.0332416031195,136.632326300544));
#181500=CARTESIAN_POINT('Ctrl Pts',(88.2076470591228,0.877562489117202,
136.657791301282));
#181501=CARTESIAN_POINT('Ctrl Pts',(88.2150434160582,0.721142587985943,
136.676999200886));
#181502=CARTESIAN_POINT('Ctrl Pts',(88.2224409053948,0.564698738568276,
136.696210041267));
#181503=CARTESIAN_POINT('Ctrl Pts',(88.2298383947314,0.407514246733144,
136.709161827551));
#181504=CARTESIAN_POINT('Ctrl Pts',(88.2372358840679,0.250128475829376,
136.715821207647));
#181505=CARTESIAN_POINT('Ctrl Pts',(88.2446359665829,0.0926875335874854,
136.722482922179));
#181506=CARTESIAN_POINT('Ctrl Pts',(88.2520360490979,-0.0649544554721071,
136.722847823034));
#181507=CARTESIAN_POINT('Ctrl Pts',(88.2594361316129,-0.222257839989229,
136.716934677573));
#181508=CARTESIAN_POINT('Ctrl Pts',(88.2668443512794,-0.379734195748697,
136.71101503));
#181509=CARTESIAN_POINT('Ctrl Pts',(88.2742525709459,-0.536870830133897,
136.698803563685));
#181510=CARTESIAN_POINT('Ctrl Pts',(88.2816607906123,-0.693132189373962,
136.680371026896));
#181511=CARTESIAN_POINT('Ctrl Pts',(88.2890735699144,-0.849489724873278,
136.661927145188));
#181512=CARTESIAN_POINT('Ctrl Pts',(88.2964863492164,-1.00497054393579,
136.637254621682));
#181513=CARTESIAN_POINT('Ctrl Pts',(88.3038991285185,-1.15904951168507,
136.606475300331));
#181514=CARTESIAN_POINT('Ctrl Pts',(88.3113224995472,-1.31334863468906,
136.575652000044));
#181515=CARTESIAN_POINT('Ctrl Pts',(88.318745870576,-1.46624154398572,136.538704562227));
#181516=CARTESIAN_POINT('Ctrl Pts',(88.3261692416047,-1.61721768054957,
136.495804857495));
#181517=CARTESIAN_POINT('Ctrl Pts',(88.3301052910456,-1.69726885078065,
136.473058404681));
#181518=CARTESIAN_POINT('Ctrl Pts',(88.3340413404865,-1.77678146029476,
136.448639369187));
#181519=CARTESIAN_POINT('Ctrl Pts',(88.3379773899274,-1.85568182637297,
136.422578797894));
#181520=CARTESIAN_POINT('Ctrl Pts',(88.3454006563329,-2.00448545439682,
136.37342937376));
#181521=CARTESIAN_POINT('Ctrl Pts',(88.3528239227383,-2.15156009103515,
136.318289747177));
#181522=CARTESIAN_POINT('Ctrl Pts',(88.3602471891438,-2.2963870229461,136.257299018405));
#181523=CARTESIAN_POINT('Ctrl Pts',(88.3676616818648,-2.44104278145067,
136.19638037561));
#181524=CARTESIAN_POINT('Ctrl Pts',(88.3750761745858,-2.5834557825298,136.12962453947));
#181525=CARTESIAN_POINT('Ctrl Pts',(88.3824906673068,-2.72312217244512,
136.057220428796));
#181526=CARTESIAN_POINT('Ctrl Pts',(88.3898980136606,-2.86265394663559,
135.984886103931));
#181527=CARTESIAN_POINT('Ctrl Pts',(88.3973053600144,-2.9994440507029,135.906914513157));
#181528=CARTESIAN_POINT('Ctrl Pts',(88.4047127063682,-3.13300844333492,
135.823542688032));
#181529=CARTESIAN_POINT('Ctrl Pts',(88.4121145280437,-3.26647321860391,
135.740233044761));
#181530=CARTESIAN_POINT('Ctrl Pts',(88.4195163497191,-3.39671675751825,
135.651531383647));
#181531=CARTESIAN_POINT('Ctrl Pts',(88.4269181713945,-3.52327958355582,
135.557720643758));
#181532=CARTESIAN_POINT('Ctrl Pts',(88.4343160857059,-3.64977559806242,
135.463959425829));
#181533=CARTESIAN_POINT('Ctrl Pts',(88.4417140000172,-3.77259447017055,
135.365094722142));
#181534=CARTESIAN_POINT('Ctrl Pts',(88.4491119143286,-3.89130578958367,
135.261452698111));
#181535=CARTESIAN_POINT('Ctrl Pts',(88.4565085992408,-4.00999738132931,
135.157827897503));
#181536=CARTESIAN_POINT('Ctrl Pts',(88.463905284153,-4.12458249421014,135.049427597485));
#181537=CARTESIAN_POINT('Ctrl Pts',(88.4713019690653,-4.23466381808838,
134.936618222105));
#181538=CARTESIAN_POINT('Ctrl Pts',(88.4786983260007,-4.34474026084537,
134.823813848812));
#181539=CARTESIAN_POINT('Ctrl Pts',(88.4860946829362,-4.45031305096526,
134.706601056056));
#181540=CARTESIAN_POINT('Ctrl Pts',(88.4934910398717,-4.55102197822761,
134.585382902106));
#181541=CARTESIAN_POINT('Ctrl Pts',(88.5008885292083,-4.65174632428396,
134.464146189347));
#181542=CARTESIAN_POINT('Ctrl Pts',(88.5082860185449,-4.74760508617959,
134.338903181521));
#181543=CARTESIAN_POINT('Ctrl Pts',(88.5156835078815,-4.83827866479283,
134.210089632668));
#181544=CARTESIAN_POINT('Ctrl Pts',(88.5230835903965,-4.92898402888836,
134.081230928426));
#181545=CARTESIAN_POINT('Ctrl Pts',(88.5304836729115,-5.0145003760186,133.948799496202));
#181546=CARTESIAN_POINT('Ctrl Pts',(88.5378837554266,-5.09455180095346,
133.813259504186));
#181547=CARTESIAN_POINT('Ctrl Pts',(88.5452919750931,-5.17469125065952,
133.677570472014));
#181548=CARTESIAN_POINT('Ctrl Pts',(88.5527001947595,-5.24935358736278,
133.53876637534));
#181549=CARTESIAN_POINT('Ctrl Pts',(88.560108414426,-5.31830885369035,133.397336031884));
#181550=CARTESIAN_POINT('Ctrl Pts',(88.5675211937281,-5.38730656083386,
133.255818640412));
#181551=CARTESIAN_POINT('Ctrl Pts',(88.5749339730302,-5.45059004857925,
133.111672122273));
#181552=CARTESIAN_POINT('Ctrl Pts',(88.5823467523323,-5.50797797946812,
132.965404147945));
#181553=CARTESIAN_POINT('Ctrl Pts',(88.5897701233611,-5.56544790892379,
132.818927179077));
#181554=CARTESIAN_POINT('Ctrl Pts',(88.5971934943899,-5.61700533517418,
132.670323051701));
#181555=CARTESIAN_POINT('Ctrl Pts',(88.6046168654186,-5.66251888820989,
132.520114213851));
#181556=CARTESIAN_POINT('Ctrl Pts',(88.6085529148593,-5.68665126611114,
132.440469883815));
#181557=CARTESIAN_POINT('Ctrl Pts',(88.6124889642999,-5.70908534761106,
132.360374588369));
#181558=CARTESIAN_POINT('Ctrl Pts',(88.6164250137405,-5.72980742602137,
132.27990710047));
#181559=CARTESIAN_POINT('Ctrl Pts',(88.6261250355039,-5.78087502936128,
132.081602583305));
#181560=CARTESIAN_POINT('Ctrl Pts',(88.6358250572672,-5.82166799180386,
131.880551790034));
#181561=CARTESIAN_POINT('Ctrl Pts',(88.6455250790304,-5.85194413610283,
131.677676362547));
#181562=CARTESIAN_POINT('Ctrl Pts',(88.6550245796708,-5.88159440485232,
131.478994823436));
#181563=CARTESIAN_POINT('Ctrl Pts',(88.6645240803113,-5.90115822620598,
131.278563068723));
#181564=CARTESIAN_POINT('Ctrl Pts',(88.6740235809517,-5.91045275283364,
131.077268695536));
#181565=CARTESIAN_POINT('Ctrl Pts',(88.678223984272,-5.91456252259787,130.988262169246));
#181566=CARTESIAN_POINT('Ctrl Pts',(88.6824243875923,-5.91666507788678,
130.899087300844));
#181567=CARTESIAN_POINT('Ctrl Pts',(88.6866247909126,-5.9167474790821,130.80982241906));
#181568=CARTESIAN_POINT('',(90.4366248408691,-5.91280601562254,130.803156497514));
#181569=CARTESIAN_POINT('Ctrl Pts',(88.6866248077954,-5.91558532475283,
130.809820987551));
#181570=CARTESIAN_POINT('Ctrl Pts',(88.756040751048,-5.90219245444721,129.3349040253));
#181571=CARTESIAN_POINT('Ctrl Pts',(88.918272568905,-4.59705841354693,125.866736618183));
#181572=CARTESIAN_POINT('Ctrl Pts',(89.1733202613661,1.22971590047256,123.914849797887));
#181573=CARTESIAN_POINT('Ctrl Pts',(89.451767885179,6.46103205536798,128.115006548304));
#181574=CARTESIAN_POINT('Ctrl Pts',(89.7302155089922,5.75497539034297,134.786548306122));
#181575=CARTESIAN_POINT('Ctrl Pts',(90.0086631328047,-0.239622512229257,
137.79865411884));
#181576=CARTESIAN_POINT('Ctrl Pts',(90.2441328990728,-5.12275198661228,
134.910492178741));
#181577=CARTESIAN_POINT('Ctrl Pts',(90.3867867907362,-5.90523390002275,
131.865903345122));
#181578=CARTESIAN_POINT('Ctrl Pts',(90.4366248077954,-5.90715601702778,
130.803158353846));
#181579=CARTESIAN_POINT('',(92.1866248077953,-5.91752627892735,130.799315009708));
#181580=CARTESIAN_POINT('Ctrl Pts',(90.4366248639554,-5.91674987721069,
130.80315520174));
#181581=CARTESIAN_POINT('Ctrl Pts',(90.4445032138975,-5.91671559555037,
130.634884630583));
#181582=CARTESIAN_POINT('Ctrl Pts',(90.4523815638397,-5.90949872441783,
130.466797726228));
#181583=CARTESIAN_POINT('Ctrl Pts',(90.4602599137817,-5.89517156383314,
130.29950143376));
#181584=CARTESIAN_POINT('Ctrl Pts',(90.4681529579633,-5.88081768106298,
130.131893109991));
#181585=CARTESIAN_POINT('Ctrl Pts',(90.4760460021448,-5.85932704389707,
129.965078635201));
#181586=CARTESIAN_POINT('Ctrl Pts',(90.4839390463263,-5.83082321380477,
129.799656077985));
#181587=CARTESIAN_POINT('Ctrl Pts',(90.491854985065,-5.80223670552753,129.633753696242));
#181588=CARTESIAN_POINT('Ctrl Pts',(90.4997709238037,-5.76659635918975,
129.46925159903));
#181589=CARTESIAN_POINT('Ctrl Pts',(90.5076868625424,-5.72407656219687,
129.306736474929));
#181590=CARTESIAN_POINT('Ctrl Pts',(90.5156151112129,-5.6814906434436,129.143968626525));
#181591=CARTESIAN_POINT('Ctrl Pts',(90.5235433598835,-5.6320039940697,128.983194201965));
#181592=CARTESIAN_POINT('Ctrl Pts',(90.531471608554,-5.57583988714239,128.824981898005));
#181593=CARTESIAN_POINT('Ctrl Pts',(90.5394190372223,-5.5195399081597,128.666386847268));
#181594=CARTESIAN_POINT('Ctrl Pts',(90.5473664658905,-5.45653027275169,
128.510366586071));
#181595=CARTESIAN_POINT('Ctrl Pts',(90.5553138945588,-5.38708203898443,
128.357469188068));
#181596=CARTESIAN_POINT('Ctrl Pts',(90.5587287231827,-5.3572417187441,128.291772667468));
#181597=CARTESIAN_POINT('Ctrl Pts',(90.5621435518066,-5.32621325346571,
128.226652364695));
#181598=CARTESIAN_POINT('Ctrl Pts',(90.5655583804305,-5.2940206433992,128.162150181253));
#181599=CARTESIAN_POINT('Ctrl Pts',(90.572981646836,-5.22403929231815,128.021933220414));
#181600=CARTESIAN_POINT('Ctrl Pts',(90.5804049132415,-5.14837761269494,
127.884286435494));
#181601=CARTESIAN_POINT('Ctrl Pts',(90.5878281796469,-5.06724765577779,
127.749703229656));
#181602=CARTESIAN_POINT('Ctrl Pts',(90.595242672368,-4.98621358773235,127.615279089991));
#181603=CARTESIAN_POINT('Ctrl Pts',(90.6026571650891,-4.89972429797056,
127.483911638574));
#181604=CARTESIAN_POINT('Ctrl Pts',(90.6100716578101,-4.80803901031332,
127.356072428072));
#181605=CARTESIAN_POINT('Ctrl Pts',(90.6174790041639,-4.71644209238809,
127.228356433814));
#181606=CARTESIAN_POINT('Ctrl Pts',(90.6248863505178,-4.61965936280325,
127.104162211755));
#181607=CARTESIAN_POINT('Ctrl Pts',(90.6322936968716,-4.51799481949465,
126.983934807068));
#181608=CARTESIAN_POINT('Ctrl Pts',(90.639695518547,-4.41640610143804,126.863797072516));
#181609=CARTESIAN_POINT('Ctrl Pts',(90.6470973402225,-4.30994305946116,
126.747620548181));
#181610=CARTESIAN_POINT('Ctrl Pts',(90.6544991618979,-4.19895160163495,
126.635819384757));
#181611=CARTESIAN_POINT('Ctrl Pts',(90.6618970762093,-4.08801873533561,
126.524077240298));
#181612=CARTESIAN_POINT('Ctrl Pts',(90.6692949905207,-3.97256247634775,
126.416706121082));
#181613=CARTESIAN_POINT('Ctrl Pts',(90.6766929048321,-3.85296734387529,
126.314085212924));
#181614=CARTESIAN_POINT('Ctrl Pts',(90.6840895897443,-3.73339208594409,
126.2114813585));
#181615=CARTESIAN_POINT('Ctrl Pts',(90.6914862746566,-3.60967960264082,
126.113626391262));
#181616=CARTESIAN_POINT('Ctrl Pts',(90.6988829595688,-3.48224950876385,
126.020860965511));
#181617=CARTESIAN_POINT('Ctrl Pts',(90.7062793165043,-3.35482506527059,
125.928099653075));
#181618=CARTESIAN_POINT('Ctrl Pts',(90.7136756734398,-3.22368364076562,
125.840427653108));
#181619=CARTESIAN_POINT('Ctrl Pts',(90.7210720303753,-3.08927578508048,
125.758143649756));
#181620=CARTESIAN_POINT('Ctrl Pts',(90.7284695197119,-2.9548473512095,125.675847048513));
#181621=CARTESIAN_POINT('Ctrl Pts',(90.7358670090485,-2.81715180878977,
125.598940281324));
#181622=CARTESIAN_POINT('Ctrl Pts',(90.7432644983851,-2.67666624141168,
125.527677152113));
#181623=CARTESIAN_POINT('Ctrl Pts',(90.7506645809002,-2.53613142703582,
125.456389041722));
#181624=CARTESIAN_POINT('Ctrl Pts',(90.7580646634152,-2.39280497314063,
125.390748676996));
#181625=CARTESIAN_POINT('Ctrl Pts',(90.7654647459302,-2.24718581760332,
125.330962544736));
#181626=CARTESIAN_POINT('Ctrl Pts',(90.7728729655967,-2.10140653883449,
125.271110671477));
#181627=CARTESIAN_POINT('Ctrl Pts',(90.7802811852632,-1.95332986923686,
125.217126028321));
#181628=CARTESIAN_POINT('Ctrl Pts',(90.7876894049297,-1.80347255203134,
125.169166094165));
#181629=CARTESIAN_POINT('Ctrl Pts',(90.7951021842319,-1.65352300014715,
125.121176641469));
#181630=CARTESIAN_POINT('Ctrl Pts',(90.802514963534,-1.50179097578084,125.079219385903));
#181631=CARTESIAN_POINT('Ctrl Pts',(90.8099277428361,-1.34880490743863,
125.043400985337));
#181632=CARTESIAN_POINT('Ctrl Pts',(90.8173511138649,-1.19560024542797,
125.007531405761));
#181633=CARTESIAN_POINT('Ctrl Pts',(90.8247744848937,-1.04113832634722,
124.977818270137));
#181634=CARTESIAN_POINT('Ctrl Pts',(90.8321978559225,-0.885955037661632,
124.954316666129));
#181635=CARTESIAN_POINT('Ctrl Pts',(90.8361339053628,-0.803673134438044,
124.941855551773));
#181636=CARTESIAN_POINT('Ctrl Pts',(90.8400699548032,-0.721188480435601,
124.931139852149));
#181637=CARTESIAN_POINT('Ctrl Pts',(90.8440060042436,-0.63858100003989,
124.922171835413));
#181638=CARTESIAN_POINT('Ctrl Pts',(90.851429270649,-0.48278587008773,124.905258435729));
#181639=CARTESIAN_POINT('Ctrl Pts',(90.8588525370545,-0.326082745600167,
124.894513300188));
#181640=CARTESIAN_POINT('Ctrl Pts',(90.8662758034599,-0.16900135951202,
124.890024720529));
#181641=CARTESIAN_POINT('Ctrl Pts',(90.8736902961809,-0.0121056305772075,
124.885541445998));
#181642=CARTESIAN_POINT('Ctrl Pts',(90.881104788902,0.14516710055356,124.88730001866));
#181643=CARTESIAN_POINT('Ctrl Pts',(90.888519281623,0.302279986459184,124.895337231905));
#181644=CARTESIAN_POINT('Ctrl Pts',(90.8959266279768,0.459241441050176,
124.903366698582));
#181645=CARTESIAN_POINT('Ctrl Pts',(90.9033339743306,0.616042986821128,
124.917662739376));
#181646=CARTESIAN_POINT('Ctrl Pts',(90.9107413206843,0.772145876353247,
124.93821015));
#181647=CARTESIAN_POINT('Ctrl Pts',(90.9181431423597,0.928132338460816,
124.958742235589));
#181648=CARTESIAN_POINT('Ctrl Pts',(90.9255449640351,1.08342081336588,124.985516358822));
#181649=CARTESIAN_POINT('Ctrl Pts',(90.9329467857105,1.23747589259897,125.018465356007));
#181650=CARTESIAN_POINT('Ctrl Pts',(90.9403447000218,1.39144964735457,125.051396959672));
#181651=CARTESIAN_POINT('Ctrl Pts',(90.9477426143332,1.54419093901699,125.090496867628));
#181652=CARTESIAN_POINT('Ctrl Pts',(90.9551405286445,1.69517290579942,125.135646532172));
#181653=CARTESIAN_POINT('Ctrl Pts',(90.9625372135568,1.84612978211828,125.180788693661));
#181654=CARTESIAN_POINT('Ctrl Pts',(90.969933898469,1.99532755652216,125.231978509551));
#181655=CARTESIAN_POINT('Ctrl Pts',(90.9773305833812,2.14225281485328,125.289047077997));
#181656=CARTESIAN_POINT('Ctrl Pts',(90.9847269403166,2.28917155836448,125.346113115963));
#181657=CARTESIAN_POINT('Ctrl Pts',(90.992123297252,2.43381763818899,125.409057253026));
#181658=CARTESIAN_POINT('Ctrl Pts',(90.9995196541875,2.5756962297044,125.477661874931));
#181659=CARTESIAN_POINT('Ctrl Pts',(91.006917143524,2.71759654319447,125.546277000379));
#181660=CARTESIAN_POINT('Ctrl Pts',(91.0143146328607,2.85672818862127,125.620554173739));
#181661=CARTESIAN_POINT('Ctrl Pts',(91.0217121221972,2.9926197582217,125.700229198294));
#181662=CARTESIAN_POINT('Ctrl Pts',(91.0291122047122,3.12855896440119,125.779932152805));
#181663=CARTESIAN_POINT('Ctrl Pts',(91.0365122872273,3.26125551155026,125.865036537193));
#181664=CARTESIAN_POINT('Ctrl Pts',(91.0439123697423,3.39026598836524,125.95523419205));
#181665=CARTESIAN_POINT('Ctrl Pts',(91.0513205894087,3.51941832546209,126.045531028502));
#181666=CARTESIAN_POINT('Ctrl Pts',(91.0587288090752,3.64487619156441,126.140932106109));
#181667=CARTESIAN_POINT('Ctrl Pts',(91.0661370287417,3.76622778288404,126.241087795355));
#181668=CARTESIAN_POINT('Ctrl Pts',(91.0735498080438,3.88765406408343,126.341305128756));
#181669=CARTESIAN_POINT('Ctrl Pts',(91.0809625873458,4.00496875691294,126.446282656632));
#181670=CARTESIAN_POINT('Ctrl Pts',(91.0883753666479,4.11779649856984,126.555633448299));
#181671=CARTESIAN_POINT('Ctrl Pts',(91.0957987376766,4.23078545379503,126.665140485505));
#181672=CARTESIAN_POINT('Ctrl Pts',(91.1032221087054,4.33927439652106,126.779032997027));
#181673=CARTESIAN_POINT('Ctrl Pts',(91.1106454797341,4.44292731966955,126.896889901792));
#181674=CARTESIAN_POINT('Ctrl Pts',(91.1145815291749,4.49788658664,126.959380460635));
#181675=CARTESIAN_POINT('Ctrl Pts',(91.1185175786157,4.55148697851146,127.022985038748));
#181676=CARTESIAN_POINT('Ctrl Pts',(91.1224536280564,4.60368338593768,127.087637619475));
#181677=CARTESIAN_POINT('Ctrl Pts',(91.1298768944618,4.70212418135033,127.209570368989));
#181678=CARTESIAN_POINT('Ctrl Pts',(91.1373001608672,4.79586623467169,127.335601137458));
#181679=CARTESIAN_POINT('Ctrl Pts',(91.1447234272727,4.88454892996854,127.465331969405));
#181680=CARTESIAN_POINT('Ctrl Pts',(91.1521379199937,4.97312680968425,127.594909470281));
#181681=CARTESIAN_POINT('Ctrl Pts',(91.1595524127147,5.05665702547508,127.728178024655));
#181682=CARTESIAN_POINT('Ctrl Pts',(91.1669669054357,5.13481844287327,127.864705855314));
#181683=CARTESIAN_POINT('Ctrl Pts',(91.1743742517894,5.21290452535465,128.00110209531));
#181684=CARTESIAN_POINT('Ctrl Pts',(91.1817815981432,5.28563192693006,128.140751035867));
#181685=CARTESIAN_POINT('Ctrl Pts',(91.189188944497,5.35272223325634,128.283191195234));
#181686=CARTESIAN_POINT('Ctrl Pts',(91.1965907661724,5.41976250110099,128.425525117356));
#181687=CARTESIAN_POINT('Ctrl Pts',(91.2039925878478,5.48117388676096,128.570645776893));
#181688=CARTESIAN_POINT('Ctrl Pts',(91.2113944095231,5.53672349559555,128.71806641592));
#181689=CARTESIAN_POINT('Ctrl Pts',(91.2187923238345,5.59224378022399,128.86540923274));
#181690=CARTESIAN_POINT('Ctrl Pts',(91.2261902381458,5.64190831935104,129.015049262592));
#181691=CARTESIAN_POINT('Ctrl Pts',(91.2335881524572,5.68553206885048,129.166479163805));
#181692=CARTESIAN_POINT('Ctrl Pts',(91.2409848373694,5.72914856887417,129.317883900117));
#181693=CARTESIAN_POINT('Ctrl Pts',(91.2483815222816,5.76672616841884,129.471077559092));
#181694=CARTESIAN_POINT('Ctrl Pts',(91.2557782071938,5.79812945649661,129.625536895288));
#181695=CARTESIAN_POINT('Ctrl Pts',(91.2631745641292,5.82953135211968,129.779989382594));
#181696=CARTESIAN_POINT('Ctrl Pts',(91.2705709210646,5.85475940625998,129.935707069719));
#181697=CARTESIAN_POINT('Ctrl Pts',(91.277967278,5.8737292391587,130.092156020872));
#181698=CARTESIAN_POINT('Ctrl Pts',(91.2853647673366,5.89270197638728,130.248628924759));
#181699=CARTESIAN_POINT('Ctrl Pts',(91.2927622566732,5.90541453963378,130.405832944991));
#181700=CARTESIAN_POINT('Ctrl Pts',(91.3001597460097,5.91183439766716,130.563228668087));
#181701=CARTESIAN_POINT('Ctrl Pts',(91.3075598285247,5.91825650617181,130.72067956601));
#181702=CARTESIAN_POINT('Ctrl Pts',(91.3149599110397,5.91838150233257,130.87832192784));
#181703=CARTESIAN_POINT('Ctrl Pts',(91.3223599935547,5.91222897474555,131.035616131401));
#181704=CARTESIAN_POINT('Ctrl Pts',(91.3297682132211,5.90606968182196,131.19308329611));
#181705=CARTESIAN_POINT('Ctrl Pts',(91.3371764328876,5.89361909443958,131.35020116476));
#181706=CARTESIAN_POINT('Ctrl Pts',(91.344584652554,5.87494877580655,131.506434291869));
#181707=CARTESIAN_POINT('Ctrl Pts',(91.3519974318561,5.85626696590393,131.66276357786));
#181708=CARTESIAN_POINT('Ctrl Pts',(91.3594102111581,5.83135785562912,131.818206669498));
#181709=CARTESIAN_POINT('Ctrl Pts',(91.3668229904602,5.8003440879611,131.972238617939));
#181710=CARTESIAN_POINT('Ctrl Pts',(91.3742463614889,5.76928600636741,132.126490654451));
#181711=CARTESIAN_POINT('Ctrl Pts',(91.3816697325177,5.73210593435422,132.27932715899));
#181712=CARTESIAN_POINT('Ctrl Pts',(91.3890931035464,5.6889765193202,132.430237834678));
#181713=CARTESIAN_POINT('Ctrl Pts',(91.3930291529874,5.6661082685921,132.510254295983));
#181714=CARTESIAN_POINT('Ctrl Pts',(91.3969652024283,5.64156825671818,132.589729651809));
#181715=CARTESIAN_POINT('Ctrl Pts',(91.4009012518693,5.61538764267704,132.66859026677));
#181716=CARTESIAN_POINT('Ctrl Pts',(91.4083245182747,5.56601182166638,132.817318925424));
#181717=CARTESIAN_POINT('Ctrl Pts',(91.4157477846802,5.51064843637328,132.964309478627));
#181718=CARTESIAN_POINT('Ctrl Pts',(91.4231710510857,5.44943737629167,133.109043425324));
#181719=CARTESIAN_POINT('Ctrl Pts',(91.4305855438067,5.38829866259978,133.253606308515));
#181720=CARTESIAN_POINT('Ctrl Pts',(91.4380000365277,5.32132617541701,133.395917553664));
#181721=CARTESIAN_POINT('Ctrl Pts',(91.4454145292487,5.24870960011652,133.535473595116));
#181722=CARTESIAN_POINT('Ctrl Pts',(91.4528218756025,5.17616301540528,133.674895127202));
#181723=CARTESIAN_POINT('Ctrl Pts',(91.4602292219562,5.09798334366856,133.811566413381));
#181724=CARTESIAN_POINT('Ctrl Pts',(91.46763656831,5.01440835281893,133.945003773622));
#181725=CARTESIAN_POINT('Ctrl Pts',(91.4750383899854,4.93089569535057,134.078341611245));
#181726=CARTESIAN_POINT('Ctrl Pts',(91.4824402116608,4.84199592845688,134.208450010511));
#181727=CARTESIAN_POINT('Ctrl Pts',(91.4898420333362,4.74799269012315,134.334869926014));
#181728=CARTESIAN_POINT('Ctrl Pts',(91.4972399476476,4.65403907536715,134.461223105428));
#181729=CARTESIAN_POINT('Ctrl Pts',(91.504637861959,4.55498757674822,134.583891380064));
#181730=CARTESIAN_POINT('Ctrl Pts',(91.5120357762703,4.45116501431281,134.702444836494));
#181731=CARTESIAN_POINT('Ctrl Pts',(91.5194324611825,4.34735970530389,134.82097859149));
#181732=CARTESIAN_POINT('Ctrl Pts',(91.5268291460947,4.23878515177542,134.93539860488));
#181733=CARTESIAN_POINT('Ctrl Pts',(91.5342258310069,4.12580838199207,135.04530812462));
#181734=CARTESIAN_POINT('Ctrl Pts',(91.5416221879424,4.01283662171701,135.155212770856));
#181735=CARTESIAN_POINT('Ctrl Pts',(91.5490185448779,3.8954633008768,135.260607060807));
#181736=CARTESIAN_POINT('Ctrl Pts',(91.5564149018133,3.77409202545241,135.361131398055));
#181737=CARTESIAN_POINT('Ctrl Pts',(91.5638123911499,3.65270216777599,135.461671125835));
#181738=CARTESIAN_POINT('Ctrl Pts',(91.5712098804865,3.5273134242617,135.55733917819));
#181739=CARTESIAN_POINT('Ctrl Pts',(91.578607369823,3.39836203482263,135.647816619511));
#181740=CARTESIAN_POINT('Ctrl Pts',(91.5860074523381,3.2693654416738,135.738325777559));
#181741=CARTESIAN_POINT('Ctrl Pts',(91.5934075348531,3.13680402148058,135.823640487567));
#181742=CARTESIAN_POINT('Ctrl Pts',(91.6008076173681,3.00114236177598,135.903485551008));
#181743=CARTESIAN_POINT('Ctrl Pts',(91.6082158370345,2.86533152813027,135.983418412306));
#181744=CARTESIAN_POINT('Ctrl Pts',(91.615624056701,2.7264139688223,136.057869426345));
#181745=CARTESIAN_POINT('Ctrl Pts',(91.6230322763675,2.58487885096429,136.126609379916));
#181746=CARTESIAN_POINT('Ctrl Pts',(91.6304450556695,2.44325662060257,136.195391641782));
#181747=CARTESIAN_POINT('Ctrl Pts',(91.6378578349716,2.29901396268784,136.258455689784));
#181748=CARTESIAN_POINT('Ctrl Pts',(91.6452706142737,2.15265882307452,136.315620959261));
#181749=CARTESIAN_POINT('Ctrl Pts',(91.6526939853025,2.00609456437444,136.372867909156));
#181750=CARTESIAN_POINT('Ctrl Pts',(91.6601173563312,1.85741214745418,136.424199125519));
#181751=CARTESIAN_POINT('Ctrl Pts',(91.66754072736,1.70713421966435,136.46948403357));
#181752=CARTESIAN_POINT('Ctrl Pts',(91.6714767768007,1.62745325648183,136.493495178414));
#181753=CARTESIAN_POINT('Ctrl Pts',(91.6754128262415,1.54732391292978,136.515807342531));
#181754=CARTESIAN_POINT('Ctrl Pts',(91.6793488756822,1.46682498273252,136.536406939128));
#181755=CARTESIAN_POINT('Ctrl Pts',(91.6867721420876,1.31500651266434,136.575257135418));
#181756=CARTESIAN_POINT('Ctrl Pts',(91.6941954084931,1.1614139351894,136.608130335848));
#181757=CARTESIAN_POINT('Ctrl Pts',(91.7016186748985,1.00655909361785,136.634863970927));
#181758=CARTESIAN_POINT('Ctrl Pts',(91.7090331676195,0.851887277608911,
136.661566009069));
#181759=CARTESIAN_POINT('Ctrl Pts',(91.7164476603405,0.695956531385569,
136.682142862991));
#181760=CARTESIAN_POINT('Ctrl Pts',(91.7238621530615,0.539293048570612,
136.696481930834));
#181761=CARTESIAN_POINT('Ctrl Pts',(91.7312694994153,0.382780563918668,
136.710807178143));
#181762=CARTESIAN_POINT('Ctrl Pts',(91.7386768457691,0.225537117906594,
136.718906574708));
#181763=CARTESIAN_POINT('Ctrl Pts',(91.7460841921229,0.0680981636066172,
136.720718720539));
#181764=CARTESIAN_POINT('Ctrl Pts',(91.7534860137983,-0.0892233667816346,
136.722529514803));
#181765=CARTESIAN_POINT('Ctrl Pts',(91.7608878354737,-0.246739743448905,
136.71806239102));
#181766=CARTESIAN_POINT('Ctrl Pts',(91.7682896571491,-0.403911445235869,
136.707307856607));
#181767=CARTESIAN_POINT('Ctrl Pts',(91.7756875714605,-0.561000177304546,
136.69655899943));
#181768=CARTESIAN_POINT('Ctrl Pts',(91.7830854857718,-0.717744225373094,
136.679529367138));
#181769=CARTESIAN_POINT('Ctrl Pts',(91.7904834000831,-0.873605236879032,
136.656261543983));
#181770=CARTESIAN_POINT('Ctrl Pts',(91.7978800849954,-1.02944034711246,
136.632997587518));
#181771=CARTESIAN_POINT('Ctrl Pts',(91.8052767699075,-1.18439234318304,
136.603497552744));
#181772=CARTESIAN_POINT('Ctrl Pts',(91.8126734548197,-1.33792903861843,
136.567855776766));
#181773=CARTESIAN_POINT('Ctrl Pts',(91.8200698117552,-1.49145892607585,
136.532215581181));
#181774=CARTESIAN_POINT('Ctrl Pts',(91.8274661686906,-1.64357327404957,
136.49043427029));
#181775=CARTESIAN_POINT('Ctrl Pts',(91.8348625256261,-1.79375138499813,
136.442657038589));
#181776=CARTESIAN_POINT('Ctrl Pts',(91.8422600149627,-1.94395248859886,
136.394872492071));
#181777=CARTESIAN_POINT('Ctrl Pts',(91.8496575042993,-2.09221640916468,
136.341090310078));
#181778=CARTESIAN_POINT('Ctrl Pts',(91.8570549936358,-2.23803901880698,
136.281505121119));
#181779=CARTESIAN_POINT('Ctrl Pts',(91.8644550761508,-2.38391274633883,
136.221899044663));
#181780=CARTESIAN_POINT('Ctrl Pts',(91.8718551586658,-2.52734311371323,
136.156486052207));
#181781=CARTESIAN_POINT('Ctrl Pts',(91.8792552411808,-2.66784746770677,
136.085508262875));
#181782=CARTESIAN_POINT('Ctrl Pts',(91.8866634608472,-2.80850632068193,
136.014452426166));
#181783=CARTESIAN_POINT('Ctrl Pts',(91.8940716805137,-2.94623240141119,
135.937819740826));
#181784=CARTESIAN_POINT('Ctrl Pts',(91.9014799001802,-3.08056845955723,
135.855897861661));
#181785=CARTESIAN_POINT('Ctrl Pts',(91.9088926794822,-3.21498719930563,
135.773925560947));
#181786=CARTESIAN_POINT('Ctrl Pts',(91.9163054587843,-3.34601144888164,
135.686657786049));
#181787=CARTESIAN_POINT('Ctrl Pts',(91.9237182380863,-3.47321473698105,
135.594424286591));
#181788=CARTESIAN_POINT('Ctrl Pts',(91.9311416091151,-3.60059977910374,
135.502058999584));
#181789=CARTESIAN_POINT('Ctrl Pts',(91.9385649801439,-3.72415266332074,
135.404714047604));
#181790=CARTESIAN_POINT('Ctrl Pts',(91.9459883511726,-3.84348102971194,
135.302758569809));
#181791=CARTESIAN_POINT('Ctrl Pts',(91.9499244006134,-3.90675179281829,
135.248699329093));
#181792=CARTESIAN_POINT('Ctrl Pts',(91.9538604500543,-3.968835515863,135.193344512691));
#181793=CARTESIAN_POINT('Ctrl Pts',(91.9577964994951,-4.02967817795937,
135.136753068));
#181794=CARTESIAN_POINT('Ctrl Pts',(91.9651092607808,-4.14271737387972,
135.031612181927));
#181795=CARTESIAN_POINT('Ctrl Pts',(91.9724220220665,-4.25183428317431,
134.921862168348));
#181796=CARTESIAN_POINT('Ctrl Pts',(91.9797347833521,-4.35662126326586,
134.807831827773));
#181797=CARTESIAN_POINT('Ctrl Pts',(91.9870388008535,-4.46128295077362,
134.693937831962));
#181798=CARTESIAN_POINT('Ctrl Pts',(91.9943428183548,-4.5616247513243,134.575773972212));
#181799=CARTESIAN_POINT('Ctrl Pts',(92.0016468358561,-4.6572727888953,134.453708604853));
#181800=CARTESIAN_POINT('Ctrl Pts',(92.008943826474,-4.7528288075724,134.331760671373));
#181801=CARTESIAN_POINT('Ctrl Pts',(92.0162408170919,-4.84369981294541,
134.205919000611));
#181802=CARTESIAN_POINT('Ctrl Pts',(92.0235378077098,-4.92954964602831,
134.076587817783));
#181803=CARTESIAN_POINT('Ctrl Pts',(92.030829124937,-5.01533273109574,133.947357189604));
#181804=CARTESIAN_POINT('Ctrl Pts',(92.0381204421642,-5.09610220423257,
133.814642770773));
#181805=CARTESIAN_POINT('Ctrl Pts',(92.0454117593914,-5.17156320462958,
133.67888050496));
#181806=CARTESIAN_POINT('Ctrl Pts',(92.0527000265024,-5.24699263805258,
133.543175031448));
#181807=CARTESIAN_POINT('Ctrl Pts',(92.0599882936134,-5.31711782937492,
133.404424583361));
#181808=CARTESIAN_POINT('Ctrl Pts',(92.0672765607244,-5.38168819565519,
133.263092552374));
#181809=CARTESIAN_POINT('Ctrl Pts',(92.0745633173205,-5.44624517953679,
133.121789812867));
#181810=CARTESIAN_POINT('Ctrl Pts',(92.0818500739167,-5.50524946949846,
132.97790690556));
#181811=CARTESIAN_POINT('Ctrl Pts',(92.0891368305128,-5.55849739808825,
132.831929910573));
#181812=CARTESIAN_POINT('Ctrl Pts',(92.0964236148311,-5.61174552925784,
132.685952360223));
#181813=CARTESIAN_POINT('Ctrl Pts',(92.1037103991495,-5.65923712502633,
132.537881068885));
#181814=CARTESIAN_POINT('Ctrl Pts',(92.1109971834678,-5.70081754541245,
132.388219789468));
#181815=CARTESIAN_POINT('Ctrl Pts',(92.1182883586633,-5.74242302136636,
132.23846832702));
#181816=CARTESIAN_POINT('Ctrl Pts',(92.1255795338589,-5.7781101049333,132.08712533467));
#181817=CARTESIAN_POINT('Ctrl Pts',(92.1328707090544,-5.80777463398576,
131.934707627706));
#181818=CARTESIAN_POINT('Ctrl Pts',(92.140164370051,-5.8374492766502,131.78223795654));
#181819=CARTESIAN_POINT('Ctrl Pts',(92.1474580310474,-5.86109721452016,
131.628693221285));
#181820=CARTESIAN_POINT('Ctrl Pts',(92.154751692044,-5.87866595867811,131.474597224131));
#181821=CARTESIAN_POINT('Ctrl Pts',(92.1620527420383,-5.89625250122448,
131.320345116762));
#181822=CARTESIAN_POINT('Ctrl Pts',(92.1693537920326,-5.90774752402002,
131.16554101612));
#181823=CARTESIAN_POINT('Ctrl Pts',(92.1766548420269,-5.91315060519789,
131.010711005857));
#181824=CARTESIAN_POINT('Ctrl Pts',(92.1799781639497,-5.91561000187961,
130.940234845878));
#181825=CARTESIAN_POINT('Ctrl Pts',(92.1833014858725,-5.91680790818329,
130.869753291447));
#181826=CARTESIAN_POINT('Ctrl Pts',(92.1866248077953,-5.91674784920219,
130.79931567344));
#181827=CARTESIAN_POINT('',(93.9366248077954,-5.92381476472989,130.807936889348));
#181828=CARTESIAN_POINT('Ctrl Pts',(92.1866248077953,-5.92001119952791,
130.799312890928));
#181829=CARTESIAN_POINT('Ctrl Pts',(92.2031645796329,-5.92319097430219,
130.448557057701));
#181830=CARTESIAN_POINT('Ctrl Pts',(92.3125202260744,-5.73488872890447,
128.132881907437));
#181831=CARTESIAN_POINT('Ctrl Pts',(92.514691747121,-2.67951836410898,124.339243304882));
#181832=CARTESIAN_POINT('Ctrl Pts',(92.7931393709338,3.99094117012314,125.055452103163));
#181833=CARTESIAN_POINT('Ctrl Pts',(93.0715869947465,6.99392073732381,131.054626976383));
#181834=CARTESIAN_POINT('Ctrl Pts',(93.3500346185597,3.56982881895088,136.823819292042));
#181835=CARTESIAN_POINT('Ctrl Pts',(93.6284822423723,-3.13476138820806,
137.061423152762));
#181836=CARTESIAN_POINT('Ctrl Pts',(93.8240123054511,-5.8199591828543,133.190582379912));
#181837=CARTESIAN_POINT('Ctrl Pts',(93.9267264939254,-5.92530633858584,
131.017497826861));
#181838=CARTESIAN_POINT('Ctrl Pts',(93.9366248077954,-5.92381476472989,
130.807936889348));
#181839=CARTESIAN_POINT('',(95.6866248077953,-5.90879879622959,130.807679832969));
#181840=CARTESIAN_POINT('Ctrl Pts',(93.9366248077954,-5.92381476472989,
130.807936889348));
#181841=CARTESIAN_POINT('Ctrl Pts',(94.0195423685297,-5.91131994314571,
129.052457926775));
#181842=CARTESIAN_POINT('Ctrl Pts',(94.1952758038683,-4.15316323793241,
125.310207551055));
#181843=CARTESIAN_POINT('Ctrl Pts',(94.463825113811,2.21513669179455,124.165781705854));
#181844=CARTESIAN_POINT('Ctrl Pts',(94.7422727376241,6.78255994238161,129.079703794217));
#181845=CARTESIAN_POINT('Ctrl Pts',(95.0207203614368,5.11714195239869,135.578501249066));
#181846=CARTESIAN_POINT('Ctrl Pts',(95.2991679852499,-1.25067950555994,
137.690096693304));
#181847=CARTESIAN_POINT('Ctrl Pts',(95.521136134036,-5.41068117704307,134.329209871018));
#181848=CARTESIAN_POINT('Ctrl Pts',(95.6502884082178,-5.91273003071525,
131.581978529553));
#181849=CARTESIAN_POINT('Ctrl Pts',(95.6866248077953,-5.90879879622959,
130.807679832969));
#181850=CARTESIAN_POINT('',(97.4366248077953,-5.91164346900976,130.799578598919));
#181851=CARTESIAN_POINT('Ctrl Pts',(95.6866248077953,-5.90879879622959,
130.807679832969));
#181852=CARTESIAN_POINT('Ctrl Pts',(95.743104282822,-5.90268828273519,129.60414881709));
#181853=CARTESIAN_POINT('Ctrl Pts',(95.8923996324532,-4.95936241370667,
126.413989174633));
#181854=CARTESIAN_POINT('Ctrl Pts',(96.1345108566885,0.26090962579987,123.810828841882));
#181855=CARTESIAN_POINT('Ctrl Pts',(96.4129584805014,6.02488437581224,127.243696523827));
#181856=CARTESIAN_POINT('Ctrl Pts',(96.6914061043143,6.25228471641837,133.94864055981));
#181857=CARTESIAN_POINT('Ctrl Pts',(96.969853728127,0.734140843724936,137.764144935481));
#181858=CARTESIAN_POINT('Ctrl Pts',(97.2182599626209,-4.79051041786796,
135.462322015875));
#181859=CARTESIAN_POINT('Ctrl Pts',(97.3738503225103,-5.90155615582126,
132.135635140803));
#181860=CARTESIAN_POINT('Ctrl Pts',(97.4366248077953,-5.91164346900976,
130.799578598919));
#181861=CARTESIAN_POINT('',(99.1866239901644,-5.92190965301424,130.802961585215));
#181862=CARTESIAN_POINT('Ctrl Pts',(97.4366248077953,-5.91164346900976,
130.799578598919));
#181863=CARTESIAN_POINT('Ctrl Pts',(97.4666661971145,-5.9164708586937,130.160194706803));
#181864=CARTESIAN_POINT('Ctrl Pts',(97.5895234610379,-5.52581770990293,
127.551110354335));
#181865=CARTESIAN_POINT('Ctrl Pts',(97.8051965995659,-1.71433292458932,
124.019183895178));
#181866=CARTESIAN_POINT('Ctrl Pts',(98.0836442233787,4.78192252208498,125.694490020073));
#181867=CARTESIAN_POINT('Ctrl Pts',(98.3620918471916,6.88382478086414,132.065517593005));
#181868=CARTESIAN_POINT('Ctrl Pts',(98.6405394710045,2.6598283595664,137.277603516453));
#181869=CARTESIAN_POINT('Ctrl Pts',(98.9153832961096,-3.92211680638712,
136.550627681392));
#181870=CARTESIAN_POINT('Ctrl Pts',(99.0974112466104,-5.92004009495408,
132.689770205197));
#181871=CARTESIAN_POINT('Ctrl Pts',(99.1866233225069,-5.92612303819684,
130.802974698158));
#181872=CARTESIAN_POINT('',(100.936624807795,-5.91594690676652,130.809831085281));
#181873=CARTESIAN_POINT('Ctrl Pts',(99.1866248077953,-5.91674983077855,
130.802945526759));
#181874=CARTESIAN_POINT('Ctrl Pts',(99.190228111407,-5.91673163312845,130.7268578703));
#181875=CARTESIAN_POINT('Ctrl Pts',(99.1938314150186,-5.91524580007589,
130.650789527188));
#181876=CARTESIAN_POINT('Ctrl Pts',(99.1974347186303,-5.91229419097278,
130.574778471288));
#181877=CARTESIAN_POINT('Ctrl Pts',(99.2048579850357,-5.90621349862531,
130.41818597215));
#181878=CARTESIAN_POINT('Ctrl Pts',(99.2122812514411,-5.89389807196139,
130.261598432965));
#181879=CARTESIAN_POINT('Ctrl Pts',(99.2197045178466,-5.8753381352769,130.105552805173));
#181880=CARTESIAN_POINT('Ctrl Pts',(99.2271190105676,-5.85680013489626,
129.949691610355));
#181881=CARTESIAN_POINT('Ctrl Pts',(99.2345335032886,-5.83203235906404,
129.794371419087));
#181882=CARTESIAN_POINT('Ctrl Pts',(99.2419479960096,-5.80107701710407,
129.640128680138));
#181883=CARTESIAN_POINT('Ctrl Pts',(99.2493553423634,-5.77015151106811,
129.486034606148));
#181884=CARTESIAN_POINT('Ctrl Pts',(99.2567626887172,-5.73305038463465,
129.333016280592));
#181885=CARTESIAN_POINT('Ctrl Pts',(99.264170035071,-5.68986756258922,129.181604418165));
#181886=CARTESIAN_POINT('Ctrl Pts',(99.2715718567464,-5.64671694792167,
129.030305484417));
#181887=CARTESIAN_POINT('Ctrl Pts',(99.2789736784218,-5.59749377128855,
128.880610985535));
#181888=CARTESIAN_POINT('Ctrl Pts',(99.2863755000972,-5.54234286797957,
128.733040725262));
#181889=CARTESIAN_POINT('Ctrl Pts',(99.2937734144086,-5.48722107840303,
128.585548366179));
#181890=CARTESIAN_POINT('Ctrl Pts',(99.3011713287199,-5.42617792445619,
128.440178361236));
#181891=CARTESIAN_POINT('Ctrl Pts',(99.3085692430313,-5.35940782021498,
128.297434535864));
#181892=CARTESIAN_POINT('Ctrl Pts',(99.3159659279435,-5.29264881195401,
128.154714431927));
#181893=CARTESIAN_POINT('Ctrl Pts',(99.3233626128557,-5.22016490028322,
128.014619979193));
#181894=CARTESIAN_POINT('Ctrl Pts',(99.3307592977679,-5.14219834169077,
127.877634327457));
#181895=CARTESIAN_POINT('Ctrl Pts',(99.3381556547034,-5.06423524021717,
127.740654749809));
#181896=CARTESIAN_POINT('Ctrl Pts',(99.3455520116389,-4.98079015985139,
127.606784023502));
#181897=CARTESIAN_POINT('Ctrl Pts',(99.3529483685743,-4.8921508225692,127.47647977659));
#181898=CARTESIAN_POINT('Ctrl Pts',(99.3603458579109,-4.80349791437826,
127.346155579765));
#181899=CARTESIAN_POINT('Ctrl Pts',(99.3677433472474,-4.70964937578964,
127.219399258241));
#181900=CARTESIAN_POINT('Ctrl Pts',(99.375140836584,-4.61093558044671,127.096638454907));
#181901=CARTESIAN_POINT('Ctrl Pts',(99.382540919099,-4.51218718113584,126.973834617964));
#181902=CARTESIAN_POINT('Ctrl Pts',(99.389941001614,-4.40857036319694,126.85502937857));
#181903=CARTESIAN_POINT('Ctrl Pts',(99.397341084129,-4.30045488985332,126.740616247796));
#181904=CARTESIAN_POINT('Ctrl Pts',(99.4047493037955,-4.19222053243215,
126.626077308023));
#181905=CARTESIAN_POINT('Ctrl Pts',(99.4121575234619,-4.0794778971994,126.515940393338));
#181906=CARTESIAN_POINT('Ctrl Pts',(99.4195657431284,-3.96263314250425,
126.410561675827));
#181907=CARTESIAN_POINT('Ctrl Pts',(99.4269785224305,-3.84571647181216,
126.305118099473));
#181908=CARTESIAN_POINT('Ctrl Pts',(99.4343913017325,-3.72469293701729,
126.204438794061));
#181909=CARTESIAN_POINT('Ctrl Pts',(99.4418040810346,-3.60000025985815,
126.108838421737));
#181910=CARTESIAN_POINT('Ctrl Pts',(99.4492274520634,-3.47512941595448,
126.013101451118));
#181911=CARTESIAN_POINT('Ctrl Pts',(99.4566508230921,-3.34657926322684,
125.92245812203));
#181912=CARTESIAN_POINT('Ctrl Pts',(99.4640741941209,-3.21481554320218,
125.837179164701));
#181913=CARTESIAN_POINT('Ctrl Pts',(99.4680102435616,-3.14495125721809,
125.791962215285));
#181914=CARTESIAN_POINT('Ctrl Pts',(99.4719462930024,-3.07418392752774,
125.748252612057));
#181915=CARTESIAN_POINT('Ctrl Pts',(99.4758823424432,-3.00258546426742,
125.706085311909));
#181916=CARTESIAN_POINT('Ctrl Pts',(99.4833056088486,-2.8675529970698,125.626559099827));
#181917=CARTESIAN_POINT('Ctrl Pts',(99.4907288752541,-2.72915467663098,
125.552281027277));
#181918=CARTESIAN_POINT('Ctrl Pts',(99.4981521416595,-2.58783697139819,
125.483549554207));
#181919=CARTESIAN_POINT('Ctrl Pts',(99.5055666343805,-2.44668629195717,
125.41489931603));
#181920=CARTESIAN_POINT('Ctrl Pts',(99.5129811271015,-2.30262342832347,
125.35178279001));
#181921=CARTESIAN_POINT('Ctrl Pts',(99.5203956198226,-2.15612252520884,
125.294454427912));
#181922=CARTESIAN_POINT('Ctrl Pts',(99.5278029661763,-2.00976282518029,
125.237181321047));
#181923=CARTESIAN_POINT('Ctrl Pts',(99.5352103125301,-1.86097010910352,
125.185685406831));
#181924=CARTESIAN_POINT('Ctrl Pts',(99.5426176588839,-1.71024165092188,
125.140174527937));
#181925=CARTESIAN_POINT('Ctrl Pts',(99.5500194805593,-1.5596256117108,125.094697592772));
#181926=CARTESIAN_POINT('Ctrl Pts',(99.5574213022347,-1.40707706092008,
125.05519691221));
#181927=CARTESIAN_POINT('Ctrl Pts',(99.5648231239101,-1.25311161117067,
125.021831598836));
#181928=CARTESIAN_POINT('Ctrl Pts',(99.5722210382215,-1.09922743858373,
124.988483898752));
#181929=CARTESIAN_POINT('Ctrl Pts',(99.5796189525328,-0.943928220562229,
124.961265194468));
#181930=CARTESIAN_POINT('Ctrl Pts',(99.5870168668442,-0.787742925268995,
124.940284249868));
#181931=CARTESIAN_POINT('Ctrl Pts',(99.5944135517564,-0.631583585138571,
124.919306791921));
#181932=CARTESIAN_POINT('Ctrl Pts',(99.6018102366686,-0.474538829596409,
124.904565085961));
#181933=CARTESIAN_POINT('Ctrl Pts',(99.6092069215808,-0.317146091797828,
124.896116469009));
#181934=CARTESIAN_POINT('Ctrl Pts',(99.6166032785163,-0.159760332958178,
124.887668226678));
#181935=CARTESIAN_POINT('Ctrl Pts',(99.6239996354517,-0.00202699530287781,
124.885512538533));
#181936=CARTESIAN_POINT('Ctrl Pts',(99.6313959923871,0.155513384969617,
124.889654695071));
#181937=CARTESIAN_POINT('Ctrl Pts',(99.6387934817237,0.313077885076512,
124.893797485784));
#181938=CARTESIAN_POINT('Ctrl Pts',(99.6461909710603,0.470448995785109,
124.904240031248));
#181939=CARTESIAN_POINT('Ctrl Pts',(99.6535884603969,0.627088353998179,
124.920935530189));
#181940=CARTESIAN_POINT('Ctrl Pts',(99.6609885429119,0.783782621895561,
124.937636881711));
#181941=CARTESIAN_POINT('Ctrl Pts',(99.6683886254269,0.939744255614704,
124.960595511352));
#181942=CARTESIAN_POINT('Ctrl Pts',(99.6757887079419,1.09444231709256,124.989713029186));
#181943=CARTESIAN_POINT('Ctrl Pts',(99.6831969276084,1.24931048499225,125.018862564724));
#181944=CARTESIAN_POINT('Ctrl Pts',(99.6906051472749,1.40291193879136,125.054184444152));
#181945=CARTESIAN_POINT('Ctrl Pts',(99.6980133669413,1.55472748231848,125.095529474659));
#181946=CARTESIAN_POINT('Ctrl Pts',(99.7054261462434,1.70663646577957,125.136899952343));
#181947=CARTESIAN_POINT('Ctrl Pts',(99.7128389255454,1.85675699353004,125.184300855926));
#181948=CARTESIAN_POINT('Ctrl Pts',(99.7202517048475,2.00458773210166,125.23753400029));
#181949=CARTESIAN_POINT('Ctrl Pts',(99.7276750758762,2.15262969816523,125.290843206668));
#181950=CARTESIAN_POINT('Ctrl Pts',(99.735098446905,2.29837499564107,125.350001157429));
#181951=CARTESIAN_POINT('Ctrl Pts',(99.7425218179338,2.44134410684905,125.414762347337));
#181952=CARTESIAN_POINT('Ctrl Pts',(99.7464578673746,2.51714976010779,125.44910028415));
#181953=CARTESIAN_POINT('Ctrl Pts',(99.7503939168153,2.592175357509,125.485012734642));
#181954=CARTESIAN_POINT('Ctrl Pts',(99.7543299662561,2.66635261964488,125.522458093833));
#181955=CARTESIAN_POINT('Ctrl Pts',(99.7617532326615,2.8062486210409,125.593078872639));
#181956=CARTESIAN_POINT('Ctrl Pts',(99.7691764990669,2.9435485399053,125.669368186712));
#181957=CARTESIAN_POINT('Ctrl Pts',(99.7765997654724,3.07775994633127,125.751111734396));
#181958=CARTESIAN_POINT('Ctrl Pts',(99.7840142581934,3.2118127260205,125.832758667995));
#181959=CARTESIAN_POINT('Ctrl Pts',(99.7914287509144,3.34278394363856,125.919846811222));
#181960=CARTESIAN_POINT('Ctrl Pts',(99.7988432436354,3.4702032349126,126.012114790096));
#181961=CARTESIAN_POINT('Ctrl Pts',(99.8062505899892,3.59749971467655,126.104293837619));
#181962=CARTESIAN_POINT('Ctrl Pts',(99.813657936343,3.72125078325056,126.201642564191));
#181963=CARTESIAN_POINT('Ctrl Pts',(99.8210652826968,3.84101278799423,126.303854943204));
#181964=CARTESIAN_POINT('Ctrl Pts',(99.8284671043722,3.96068546971632,126.405991088368));
#181965=CARTESIAN_POINT('Ctrl Pts',(99.8358689260476,4.07637472889887,126.512983421846));
#181966=CARTESIAN_POINT('Ctrl Pts',(99.843270747723,4.18766799839924,126.624484148377));
#181967=CARTESIAN_POINT('Ctrl Pts',(99.8506686620344,4.29890251704895,126.735926014542));
#181968=CARTESIAN_POINT('Ctrl Pts',(99.8580665763457,4.40574540457195,126.851871270446));
#181969=CARTESIAN_POINT('Ctrl Pts',(99.865464490657,4.50781923461863,126.97193366973));
#181970=CARTESIAN_POINT('Ctrl Pts',(99.8728611755693,4.60987610184649,127.09197611682));
#181971=CARTESIAN_POINT('Ctrl Pts',(99.8802578604815,4.70716524297956,127.216134065239));
#181972=CARTESIAN_POINT('Ctrl Pts',(99.8876545453937,4.79934792301003,127.343986349311));
#181973=CARTESIAN_POINT('Ctrl Pts',(99.8950509023291,4.89152651556394,127.47183296428));
#181974=CARTESIAN_POINT('Ctrl Pts',(99.9024472592646,4.97859887890554,127.603373286392));
#181975=CARTESIAN_POINT('Ctrl Pts',(99.9098436162,5.06026838897342,127.738155406877));
#181976=CARTESIAN_POINT('Ctrl Pts',(99.9172411055366,5.14195040285179,127.872958162849));
#181977=CARTESIAN_POINT('Ctrl Pts',(99.9246385948732,5.21822772294531,128.011003386167));
#181978=CARTESIAN_POINT('Ctrl Pts',(99.9320360842097,5.28884872608873,128.151812839476));
#181979=CARTESIAN_POINT('Ctrl Pts',(99.9394361667247,5.35949448531528,128.292671653321));
#181980=CARTESIAN_POINT('Ctrl Pts',(99.9468362492398,5.42447981257595,128.436296292949));
#181981=CARTESIAN_POINT('Ctrl Pts',(99.9542363317547,5.48360050111013,128.582186882971));
#181982=CARTESIAN_POINT('Ctrl Pts',(99.9616445514212,5.54278619891914,128.728237894695));
#181983=CARTESIAN_POINT('Ctrl Pts',(99.9690527710876,5.59609423909144,128.876559486611));
#181984=CARTESIAN_POINT('Ctrl Pts',(99.9764609907541,5.64336950355073,129.026634201918));
#181985=CARTESIAN_POINT('Ctrl Pts',(99.9838737700562,5.69067386514649,129.176801285708));
#181986=CARTESIAN_POINT('Ctrl Pts',(99.9912865493583,5.73193795464536,129.328723283557));
#181987=CARTESIAN_POINT('Ctrl Pts',(99.9986993286603,5.76705752781521,129.481871285522));
#181988=CARTESIAN_POINT('Ctrl Pts',(100.006122699689,5.80222728147815,129.635238112534));
#181989=CARTESIAN_POINT('Ctrl Pts',(100.013546070718,5.83123491537528,129.789834076422));
#181990=CARTESIAN_POINT('Ctrl Pts',(100.020969441747,5.85402778899558,129.945123043802));
#181991=CARTESIAN_POINT('Ctrl Pts',(100.024905491187,5.86611311749639,130.027460980414));
#181992=CARTESIAN_POINT('Ctrl Pts',(100.028841540628,5.87645212380115,130.109993697044));
#181993=CARTESIAN_POINT('Ctrl Pts',(100.032777590069,5.88504290467065,130.192641259784));
#181994=CARTESIAN_POINT('Ctrl Pts',(100.040200856474,5.90124484928165,130.348511983771));
#181995=CARTESIAN_POINT('Ctrl Pts',(100.04762412288,5.91127444860908,130.505262531775));
#181996=CARTESIAN_POINT('Ctrl Pts',(100.055047389285,5.91504583031439,130.662362773285));
#181997=CARTESIAN_POINT('Ctrl Pts',(100.062461882006,5.91881275455972,130.819277335357));
#181998=CARTESIAN_POINT('Ctrl Pts',(100.069876374727,5.91633617547076,130.976540398697));
#181999=CARTESIAN_POINT('Ctrl Pts',(100.077290867448,5.90758175100173,131.1336149535));
#182000=CARTESIAN_POINT('Ctrl Pts',(100.084698213802,5.89883576437661,131.290538113933));
#182001=CARTESIAN_POINT('Ctrl Pts',(100.092105560156,5.88382399900399,131.447272757324));
#182002=CARTESIAN_POINT('Ctrl Pts',(100.099512906509,5.86256411864931,131.603280211283));
#182003=CARTESIAN_POINT('Ctrl Pts',(100.106914728185,5.8413200947155,131.759171308998));
#182004=CARTESIAN_POINT('Ctrl Pts',(100.11431654986,5.81383728483579,131.914335928916));
#182005=CARTESIAN_POINT('Ctrl Pts',(100.121718371535,5.78018529639496,132.068238974782));
#182006=CARTESIAN_POINT('Ctrl Pts',(100.129116285847,5.7465510725769,132.222060776429));
#182007=CARTESIAN_POINT('Ctrl Pts',(100.136514200158,5.70675423553321,132.374621966586));
#182008=CARTESIAN_POINT('Ctrl Pts',(100.14391211447,5.66091573710451,132.525396230185));
#182009=CARTESIAN_POINT('Ctrl Pts',(100.151308799382,5.61508485620265,132.676145437837));
#182010=CARTESIAN_POINT('Ctrl Pts',(100.158705484294,5.56321441506422,132.82510795149));
#182011=CARTESIAN_POINT('Ctrl Pts',(100.166102169206,5.50547565775297,132.971771133456));
#182012=CARTESIAN_POINT('Ctrl Pts',(100.173498526141,5.44773946063873,133.118427812222));
#182013=CARTESIAN_POINT('Ctrl Pts',(100.180894883077,5.38413560147719,133.262785014671));
#182014=CARTESIAN_POINT('Ctrl Pts',(100.188291240012,5.31488395136552,133.404348914851));
#182015=CARTESIAN_POINT('Ctrl Pts',(100.195688729349,5.24562169864942,133.545934488824));
#182016=CARTESIAN_POINT('Ctrl Pts',(100.203086218685,5.17071009731625,133.68472557365));
#182017=CARTESIAN_POINT('Ctrl Pts',(100.210483708022,5.09041549352912,133.820251972661));
#182018=CARTESIAN_POINT('Ctrl Pts',(100.217883790537,5.01009274259305,133.955825880242));
#182019=CARTESIAN_POINT('Ctrl Pts',(100.225283873052,4.92438342235262,134.088132502492));
#182020=CARTESIAN_POINT('Ctrl Pts',(100.232683955567,4.8335977133866,134.216729839623));
#182021=CARTESIAN_POINT('Ctrl Pts',(100.240092175233,4.74271217620058,134.345468582747));
#182022=CARTESIAN_POINT('Ctrl Pts',(100.2475003949,4.6467393180703,134.470489590093));
#182023=CARTESIAN_POINT('Ctrl Pts',(100.254908614566,4.54603064494879,134.59138265839));
#182024=CARTESIAN_POINT('Ctrl Pts',(100.262321393868,4.4452599873193,134.712350134353));
#182025=CARTESIAN_POINT('Ctrl Pts',(100.269734173171,4.33974795618001,134.829184332247));
#182026=CARTESIAN_POINT('Ctrl Pts',(100.277146952473,4.22988319189158,134.941511659703));
#182027=CARTESIAN_POINT('Ctrl Pts',(100.284570323501,4.11986144767587,135.053999485712));
#182028=CARTESIAN_POINT('Ctrl Pts',(100.29199369453,4.00547481954478,135.161967324346));
#182029=CARTESIAN_POINT('Ctrl Pts',(100.299417065559,3.88714591821438,135.265081094463));
#182030=CARTESIAN_POINT('Ctrl Pts',(100.303353115,3.82440509546536,135.319754489561));
#182031=CARTESIAN_POINT('Ctrl Pts',(100.30728916444,3.76055646896729,135.373063937694));
#182032=CARTESIAN_POINT('Ctrl Pts',(100.311225213881,3.69566626063343,135.424964631385));
#182033=CARTESIAN_POINT('Ctrl Pts',(100.318648480287,3.57328535287096,135.522847719918));
#182034=CARTESIAN_POINT('Ctrl Pts',(100.326071746692,3.44682792085274,135.616013405926));
#182035=CARTESIAN_POINT('Ctrl Pts',(100.333495013098,3.3166935622925,135.704102894089));
#182036=CARTESIAN_POINT('Ctrl Pts',(100.340909505819,3.18671301173692,135.792088267793));
#182037=CARTESIAN_POINT('Ctrl Pts',(100.34832399854,3.05306449113602,135.875009178764));
#182038=CARTESIAN_POINT('Ctrl Pts',(100.355738491261,2.9161812393335,135.95254646715));
#182039=CARTESIAN_POINT('Ctrl Pts',(100.363145837614,2.77942992076272,136.030009022179));
#182040=CARTESIAN_POINT('Ctrl Pts',(100.370553183968,2.63945040045551,136.102098102025));
#182041=CARTESIAN_POINT('Ctrl Pts',(100.377960530322,2.49670542644565,136.16853740213));
#182042=CARTESIAN_POINT('Ctrl Pts',(100.385362351997,2.35406691702286,136.234927149299));
#182043=CARTESIAN_POINT('Ctrl Pts',(100.392764173673,2.20866739775046,136.295675350166));
#182044=CARTESIAN_POINT('Ctrl Pts',(100.400165995348,2.06099468475453,136.350551334798));
#182045=CARTESIAN_POINT('Ctrl Pts',(100.40756390966,1.9133999270344,136.405398350826));
#182046=CARTESIAN_POINT('Ctrl Pts',(100.414961823971,1.76353471448369,136.45437919451));
#182047=CARTESIAN_POINT('Ctrl Pts',(100.422359738282,1.6119072283005,136.49731113991));
#182048=CARTESIAN_POINT('Ctrl Pts',(100.429756423194,1.4603049398546,136.540235950799));
#182049=CARTESIAN_POINT('Ctrl Pts',(100.437153108107,1.30694131783884,136.577113756863));
#182050=CARTESIAN_POINT('Ctrl Pts',(100.444549793019,1.15234022045967,136.60781153739));
#182051=CARTESIAN_POINT('Ctrl Pts',(100.451946149954,0.997745978255167,
136.638507956746));
#182052=CARTESIAN_POINT('Ctrl Pts',(100.45934250689,0.841914735938592,136.663024822723));
#182053=CARTESIAN_POINT('Ctrl Pts',(100.466738863825,0.685380808968709,
136.681280194113));
#182054=CARTESIAN_POINT('Ctrl Pts',(100.474136353162,0.528822916254995,
136.699538360446));
#182055=CARTESIAN_POINT('Ctrl Pts',(100.481533842498,0.371562495485032,
136.711533080147));
#182056=CARTESIAN_POINT('Ctrl Pts',(100.488931331835,0.21413910303813,136.717234285001));
#182057=CARTESIAN_POINT('Ctrl Pts',(100.49633141435,0.0566605260651548,
136.722937488404));
#182058=CARTESIAN_POINT('Ctrl Pts',(100.503731496865,-0.10098076350849,
136.722342770967));
#182059=CARTESIAN_POINT('Ctrl Pts',(100.51113157938,-0.258245238563375,
136.715472184713));
#182060=CARTESIAN_POINT('Ctrl Pts',(100.518539799047,-0.415682642075875,
136.708594043543));
#182061=CARTESIAN_POINT('Ctrl Pts',(100.525948018713,-0.572742030421845,
136.695426268184));
#182062=CARTESIAN_POINT('Ctrl Pts',(100.533356238379,-0.728888290417765,
136.676042865661));
#182063=CARTESIAN_POINT('Ctrl Pts',(100.540769017682,-0.885130655831496,
136.656647532977));
#182064=CARTESIAN_POINT('Ctrl Pts',(100.548181796984,-1.04045840554142,
136.631029010719));
#182065=CARTESIAN_POINT('Ctrl Pts',(100.555594576286,-1.19434715609937,
136.599312337228));
#182066=CARTESIAN_POINT('Ctrl Pts',(100.563017947314,-1.34845579012067,
136.567550345468));
#182067=CARTESIAN_POINT('Ctrl Pts',(100.570441318343,-1.50112095712515,
136.529672889666));
#182068=CARTESIAN_POINT('Ctrl Pts',(100.577864689372,-1.651833153772,136.48585494517));
#182069=CARTESIAN_POINT('Ctrl Pts',(100.581800738813,-1.73174437672379,
136.462621619602));
#182070=CARTESIAN_POINT('Ctrl Pts',(100.585736788254,-1.81110686745139,
136.437719020714));
#182071=CARTESIAN_POINT('Ctrl Pts',(100.589672837694,-1.88984713359227,
136.411178643341));
#182072=CARTESIAN_POINT('Ctrl Pts',(100.5970961041,-2.0383488181342,136.361124319913));
#182073=CARTESIAN_POINT('Ctrl Pts',(100.604519370505,-2.18508507926232,
136.305090429881));
#182074=CARTESIAN_POINT('Ctrl Pts',(100.611942636911,-2.32953805998807,
136.243219228485));
#182075=CARTESIAN_POINT('Ctrl Pts',(100.619357129632,-2.47382030928688,
136.181421153711));
#182076=CARTESIAN_POINT('Ctrl Pts',(100.626771622353,-2.61582431006067,
136.113799646043));
#182077=CARTESIAN_POINT('Ctrl Pts',(100.634186115074,-2.75504736790875,
136.040546687892));
#182078=CARTESIAN_POINT('Ctrl Pts',(100.641593461428,-2.89413623733203,
135.967364333701));
#182079=CARTESIAN_POINT('Ctrl Pts',(100.649000807781,-3.0304491717913,135.888561507371));
#182080=CARTESIAN_POINT('Ctrl Pts',(100.656408154135,-3.16350358182101,
135.804378182566));
#182081=CARTESIAN_POINT('Ctrl Pts',(100.663809975811,-3.29645875485178,
135.72025764486));
#182082=CARTESIAN_POINT('Ctrl Pts',(100.671211797486,-3.42615992846691,
135.630764797794));
#182083=CARTESIAN_POINT('Ctrl Pts',(100.678613619161,-3.55214935698775,
135.536185372156));
#182084=CARTESIAN_POINT('Ctrl Pts',(100.686011533473,-3.67807227667005,
135.441655874261));
#182085=CARTESIAN_POINT('Ctrl Pts',(100.693409447784,-3.80028705571648,
135.342045368973));
#182086=CARTESIAN_POINT('Ctrl Pts',(100.700807362095,-3.91836527726643,
135.237682635693));
#182087=CARTESIAN_POINT('Ctrl Pts',(100.708204047008,-4.03642387635795,
135.133337245606));
#182088=CARTESIAN_POINT('Ctrl Pts',(100.71560073192,-4.15034700284785,135.024241441889));
#182089=CARTESIAN_POINT('Ctrl Pts',(100.722997416832,-4.2597395844868,134.910764060344));
#182090=CARTESIAN_POINT('Ctrl Pts',(100.730393773767,-4.36912731554406,
134.797291710504));
#182091=CARTESIAN_POINT('Ctrl Pts',(100.737790130703,-4.47398464210597,
134.679438437891));
#182092=CARTESIAN_POINT('Ctrl Pts',(100.745186487638,-4.57395381415604,
134.557609486009));
#182093=CARTESIAN_POINT('Ctrl Pts',(100.752583976975,-4.6739382917417,134.435761881803));
#182094=CARTESIAN_POINT('Ctrl Pts',(100.759981466312,-4.76903288785948,
134.309937674948));
#182095=CARTESIAN_POINT('Ctrl Pts',(100.767378955648,-4.85892066186766,
134.180574556903));
#182096=CARTESIAN_POINT('Ctrl Pts',(100.774779038163,-4.94883994589581,
134.051166090818));
#182097=CARTESIAN_POINT('Ctrl Pts',(100.782179120678,-5.03354856088985,
133.918216549965));
#182098=CARTESIAN_POINT('Ctrl Pts',(100.789579203193,-5.11277343225509,
133.782191773445));
#182099=CARTESIAN_POINT('Ctrl Pts',(100.79698742286,-5.19208541951074,133.646017423701));
#182100=CARTESIAN_POINT('Ctrl Pts',(100.804395642526,-5.26590143296005,
133.50676140791));
#182101=CARTESIAN_POINT('Ctrl Pts',(100.811803862193,-5.33399449506292,
133.364913934554));
#182102=CARTESIAN_POINT('Ctrl Pts',(100.819216641495,-5.40212946730932,
133.222979156445));
#182103=CARTESIAN_POINT('Ctrl Pts',(100.826629420797,-5.46453432178863,
133.078450084456));
#182104=CARTESIAN_POINT('Ctrl Pts',(100.834042200099,-5.52103081473653,
132.931835483511));
#182105=CARTESIAN_POINT('Ctrl Pts',(100.841465571127,-5.57760803252298,
132.78501139275));
#182106=CARTESIAN_POINT('Ctrl Pts',(100.848888942156,-5.62825990803157,
132.636096173978));
#182107=CARTESIAN_POINT('Ctrl Pts',(100.856312313185,-5.67285825397636,
132.485613065235));
#182108=CARTESIAN_POINT('Ctrl Pts',(100.860248362626,-5.69650536711889,
132.405823310187));
#182109=CARTESIAN_POINT('Ctrl Pts',(100.864184412066,-5.71845147017101,
132.325592936097));
#182110=CARTESIAN_POINT('Ctrl Pts',(100.868120461507,-5.73868333621174,
132.245000797898));
#182111=CARTESIAN_POINT('Ctrl Pts',(100.877925013815,-5.78908015969434,
132.044248788432));
#182112=CARTESIAN_POINT('Ctrl Pts',(100.887729566123,-5.82896187484381,
131.840759098584));
#182113=CARTESIAN_POINT('Ctrl Pts',(100.897534118431,-5.85808598425451,
131.635479841012));
#182114=CARTESIAN_POINT('Ctrl Pts',(100.907119184766,-5.88655811759235,
131.434795991399));
#182115=CARTESIAN_POINT('Ctrl Pts',(100.9167042511,-5.90474895845509,131.232401516521));
#182116=CARTESIAN_POINT('Ctrl Pts',(100.926289317435,-5.91247627987531,
131.029204568812));
#182117=CARTESIAN_POINT('Ctrl Pts',(100.929734473082,-5.91525370718769,
130.956169590497));
#182118=CARTESIAN_POINT('Ctrl Pts',(100.933179628729,-5.91667977690174,
130.883031174209));
#182119=CARTESIAN_POINT('Ctrl Pts',(100.936624784376,-5.91674746993127,
130.809832323138));
#182120=CARTESIAN_POINT('',(102.686624807795,-5.90708923804999,130.803354028443));
#182121=CARTESIAN_POINT('Ctrl Pts',(100.936624807795,-5.91594690676652,
130.809831085281));
#182122=CARTESIAN_POINT('Ctrl Pts',(101.006605900304,-5.90234915318238,
129.323137679429));
#182123=CARTESIAN_POINT('Ctrl Pts',(101.169402867416,-4.57985391044984,
125.843090929061));
#182124=CARTESIAN_POINT('Ctrl Pts',(101.425015709134,1.27163152452042,123.922463074289));
#182125=CARTESIAN_POINT('Ctrl Pts',(101.703463332946,6.47728320895777,128.154386511786));
#182126=CARTESIAN_POINT('Ctrl Pts',(101.981910956759,5.73062805723803,134.821506694067));
#182127=CARTESIAN_POINT('Ctrl Pts',(102.260358580572,-0.282194322339087,
137.797065880537));
#182128=CARTESIAN_POINT('Ctrl Pts',(102.495263197585,-5.13597471230578,
134.886235526842));
#182129=CARTESIAN_POINT('Ctrl Pts',(102.637351939992,-5.90549920155596,
131.854077402682));
#182130=CARTESIAN_POINT('Ctrl Pts',(102.686624807795,-5.90708923804999,
130.803354028443));
#182131=CARTESIAN_POINT('',(104.436623928268,-5.91867361597261,130.799254319557));
#182132=CARTESIAN_POINT('Ctrl Pts',(102.686624807795,-5.90708923804999,
130.803354028443));
#182133=CARTESIAN_POINT('Ctrl Pts',(102.730167814596,-5.90849437180735,
129.874817552491));
#182134=CARTESIAN_POINT('Ctrl Pts',(102.866526696002,-5.26416868365254,
126.968865704744));
#182135=CARTESIAN_POINT('Ctrl Pts',(103.09570145201,-0.712954253829686,
123.842374064699));
#182136=CARTESIAN_POINT('Ctrl Pts',(103.374149075824,5.47194727155702,126.441408224103));
#182137=CARTESIAN_POINT('Ctrl Pts',(103.652596699636,6.62839657387416,133.049782491025));
#182138=CARTESIAN_POINT('Ctrl Pts',(103.931044323449,1.69367323997139,137.594723751195));
#182139=CARTESIAN_POINT('Ctrl Pts',(104.192386583952,-4.39869557774552,
136.00378319751));
#182140=CARTESIAN_POINT('Ctrl Pts',(104.36091296985,-5.90497045334534,132.405092580601));
#182141=CARTESIAN_POINT('Ctrl Pts',(104.436623481144,-5.91965264882207,
130.799262955289));
#182142=CARTESIAN_POINT('',(106.186626238041,-5.92089107076249,130.807736560839));
#182143=CARTESIAN_POINT('Ctrl Pts',(104.436624807795,-5.91674778188568,
130.799237332397));
#182144=CARTESIAN_POINT('Ctrl Pts',(104.447754512545,-5.9165434785673,130.563292783946));
#182145=CARTESIAN_POINT('Ctrl Pts',(104.458884217295,-5.90222283262232,
130.32793572196));
#182146=CARTESIAN_POINT('Ctrl Pts',(104.470013922045,-5.87401388310876,
130.094507489415));
#182147=CARTESIAN_POINT('Ctrl Pts',(104.475989138389,-5.85886931459173,
129.969186627684));
#182148=CARTESIAN_POINT('Ctrl Pts',(104.481964354732,-5.83972243368569,
129.844421012513));
#182149=CARTESIAN_POINT('Ctrl Pts',(104.487939571075,-5.81661343588987,
129.720414724117));
#182150=CARTESIAN_POINT('Ctrl Pts',(104.49536283748,-5.78790414117255,129.566356416966));
#182151=CARTESIAN_POINT('Ctrl Pts',(104.502786103886,-5.7530266451983,129.413206531442));
#182152=CARTESIAN_POINT('Ctrl Pts',(104.510209370291,-5.71204908842056,
129.261497767545));
#182153=CARTESIAN_POINT('Ctrl Pts',(104.517623863012,-5.67111996371195,
129.109968310809));
#182154=CARTESIAN_POINT('Ctrl Pts',(104.525038355733,-5.62410522566874,
128.959876942165));
#182155=CARTESIAN_POINT('Ctrl Pts',(104.532452848454,-5.57112437816934,
128.811748330776));
#182156=CARTESIAN_POINT('Ctrl Pts',(104.539860194807,-5.51819459560541,
128.663762491319));
#182157=CARTESIAN_POINT('Ctrl Pts',(104.547267541161,-5.45931027629513,
128.517735992088));
#182158=CARTESIAN_POINT('Ctrl Pts',(104.554674887515,-5.39464126270649,
128.374180334294));
#182159=CARTESIAN_POINT('Ctrl Pts',(104.56207670919,-5.330020481708,128.230731745725));
#182160=CARTESIAN_POINT('Ctrl Pts',(104.569478530866,-5.2596237497342,128.089750668129));
#182161=CARTESIAN_POINT('Ctrl Pts',(104.576880352541,-5.18366970116864,
127.951730429181));
#182162=CARTESIAN_POINT('Ctrl Pts',(104.584278266852,-5.10775574815394,
127.813783050043));
#182163=CARTESIAN_POINT('Ctrl Pts',(104.591676181164,-5.02629050060196,
127.678793722975));
#182164=CARTESIAN_POINT('Ctrl Pts',(104.599074095475,-4.93953933280967,
127.547232781247));
#182165=CARTESIAN_POINT('Ctrl Pts',(104.606470780387,-4.85280258148795,
127.41569370256));
#182166=CARTESIAN_POINT('Ctrl Pts',(104.613867465299,-4.76078185863432,
127.287582189795));
#182167=CARTESIAN_POINT('Ctrl Pts',(104.621264150212,-4.66378687969518,
127.163341185692));
#182168=CARTESIAN_POINT('Ctrl Pts',(104.628660507147,-4.56679620161498,
127.039105690566));
#182169=CARTESIAN_POINT('Ctrl Pts',(104.636056864082,-4.46483193572243,
126.918740657105));
#182170=CARTESIAN_POINT('Ctrl Pts',(104.643453221018,-4.35824508450094,
126.802657187035));
#182171=CARTESIAN_POINT('Ctrl Pts',(104.650850710355,-4.25164191456034,
126.686555944289));
#182172=CARTESIAN_POINT('Ctrl Pts',(104.658248199691,-4.14041500259756,
126.574737845144));
#182173=CARTESIAN_POINT('Ctrl Pts',(104.665645689028,-4.02495320719324,
126.467578141766));
#182174=CARTESIAN_POINT('Ctrl Pts',(104.673045771543,-3.90945093683552,
126.36038087372));
#182175=CARTESIAN_POINT('Ctrl Pts',(104.680445854058,-3.78971110078864,
126.257845506502));
#182176=CARTESIAN_POINT('Ctrl Pts',(104.687845936573,-3.66615658516074,
126.160307812571));
#182177=CARTESIAN_POINT('Ctrl Pts',(104.695254156239,-3.54246620864119,
126.062662865918));
#182178=CARTESIAN_POINT('Ctrl Pts',(104.702662375906,-3.41495306876543,
125.970026798783));
#182179=CARTESIAN_POINT('Ctrl Pts',(104.710070595572,-3.28407065155395,
125.882693164547));
#182180=CARTESIAN_POINT('Ctrl Pts',(104.717483374874,-3.15310767839848,
125.795305777918));
#182181=CARTESIAN_POINT('Ctrl Pts',(104.724896154176,-3.01877161353898,
125.713227521416));
#182182=CARTESIAN_POINT('Ctrl Pts',(104.732308933478,-2.88154115773741,
125.636706302621));
#182183=CARTESIAN_POINT('Ctrl Pts',(104.739732304507,-2.74411462062511,
125.560075746721));
#182184=CARTESIAN_POINT('Ctrl Pts',(104.747155675536,-2.60378576492046,
125.489018254992));
#182185=CARTESIAN_POINT('Ctrl Pts',(104.754579046565,-2.46105464894796,
125.423734206321));
#182186=CARTESIAN_POINT('Ctrl Pts',(104.758515096006,-2.38537518646285,
125.389119037241));
#182187=CARTESIAN_POINT('Ctrl Pts',(104.762451145447,-2.30902065175045,
125.356126168367));
#182188=CARTESIAN_POINT('Ctrl Pts',(104.766387194889,-2.23206726167876,
125.324779766639));
#182189=CARTESIAN_POINT('Ctrl Pts',(104.773810461294,-2.08693556965547,
125.265661431276));
#182190=CARTESIAN_POINT('Ctrl Pts',(104.7812337277,-1.939234095028,125.212223602401));
#182191=CARTESIAN_POINT('Ctrl Pts',(104.788656994105,-1.78944784497462,
125.164696888884));
#182192=CARTESIAN_POINT('Ctrl Pts',(104.796071486826,-1.63983862982983,
125.117226347995));
#182193=CARTESIAN_POINT('Ctrl Pts',(104.803485979547,-1.48814989626871,
125.0756531277));
#182194=CARTESIAN_POINT('Ctrl Pts',(104.810900472268,-1.33488765808264,
125.040160282498));
#182195=CARTESIAN_POINT('Ctrl Pts',(104.818307818622,-1.18177313981183,
125.004701646637));
#182196=CARTESIAN_POINT('Ctrl Pts',(104.825715164976,-1.02708849740593,
124.975311802433));
#182197=CARTESIAN_POINT('Ctrl Pts',(104.83312251133,-0.871355875321791,
124.952124335507));
#182198=CARTESIAN_POINT('Ctrl Pts',(104.840524333005,-0.715739404502658,
124.928954162669));
#182199=CARTESIAN_POINT('Ctrl Pts',(104.84792615468,-0.559076877960228,
124.911977210923));
#182200=CARTESIAN_POINT('Ctrl Pts',(104.855327976356,-0.401901523465638,
124.901276192629));
#182201=CARTESIAN_POINT('Ctrl Pts',(104.862725890667,-0.244809140617348,
124.890580823319));
#182202=CARTESIAN_POINT('Ctrl Pts',(104.870123804979,-0.0872048404574969,
124.886154814723));
#182203=CARTESIAN_POINT('Ctrl Pts',(104.87752171929,0.0703722310258373,
124.888029126549));
#182204=CARTESIAN_POINT('Ctrl Pts',(104.884918404202,0.22792311605863,124.889903126898));
#182205=CARTESIAN_POINT('Ctrl Pts',(104.892315089114,0.385446408489498,
124.89807536525));
#182206=CARTESIAN_POINT('Ctrl Pts',(104.899711774026,0.542402039280793,
124.9125246906));
#182207=CARTESIAN_POINT('Ctrl Pts',(104.907108130962,0.69935071049494,124.926973375252));
#182208=CARTESIAN_POINT('Ctrl Pts',(104.914504487897,0.855731398391698,
124.947698559261));
#182209=CARTESIAN_POINT('Ctrl Pts',(104.921900844833,1.01100850603132,124.974627144822));
#182210=CARTESIAN_POINT('Ctrl Pts',(104.929298334169,1.16630938699253,125.001559853218));
#182211=CARTESIAN_POINT('Ctrl Pts',(104.936695823506,1.32050598344136,125.034697790466));
#182212=CARTESIAN_POINT('Ctrl Pts',(104.944093312842,1.47307239754155,125.073916631791));
#182213=CARTESIAN_POINT('Ctrl Pts',(104.951493395357,1.62569229356169,125.113149221221));
#182214=CARTESIAN_POINT('Ctrl Pts',(104.958893477872,1.77668050814672,125.15846686595));
#182215=CARTESIAN_POINT('Ctrl Pts',(104.966293560387,1.92552596614671,125.209695273133));
#182216=CARTESIAN_POINT('Ctrl Pts',(104.973701780054,2.07453509502946,125.260980011217));
#182217=CARTESIAN_POINT('Ctrl Pts',(104.98110999972,2.22139640868509,125.318188370107));
#182218=CARTESIAN_POINT('Ctrl Pts',(104.988518219387,2.36561781206822,125.381097491945));
#182219=CARTESIAN_POINT('Ctrl Pts',(104.995930998689,2.50992798131898,125.444045333297));
#182220=CARTESIAN_POINT('Ctrl Pts',(105.003343777991,2.65159466748911,125.512700766747));
#182221=CARTESIAN_POINT('Ctrl Pts',(105.010756557293,2.79015054945589,125.58679504789));
#182222=CARTESIAN_POINT('Ctrl Pts',(105.018179928322,2.92890440656424,125.660995198416));
#182223=CARTESIAN_POINT('Ctrl Pts',(105.02560329935,3.06453826104044,125.740649529086));
#182224=CARTESIAN_POINT('Ctrl Pts',(105.033026670379,3.19661323471266,125.825445636352));
#182225=CARTESIAN_POINT('Ctrl Pts',(105.03696271982,3.2666425548477,125.870406567078));
#182226=CARTESIAN_POINT('Ctrl Pts',(105.04089876926,3.3356718809024,125.916812348075));
#182227=CARTESIAN_POINT('Ctrl Pts',(105.044834818701,3.40363968346692,125.964611918756));
#182228=CARTESIAN_POINT('Ctrl Pts',(105.052258085107,3.53182483790369,126.054760417289));
#182229=CARTESIAN_POINT('Ctrl Pts',(105.059681351512,3.65661985161943,126.150141399217));
#182230=CARTESIAN_POINT('Ctrl Pts',(105.067104617917,3.77756854861396,126.250471463994));
#182231=CARTESIAN_POINT('Ctrl Pts',(105.074519110638,3.89837429429289,126.350682946966));
#182232=CARTESIAN_POINT('Ctrl Pts',(105.081933603359,4.0153424876353,126.455831633507));
#182233=CARTESIAN_POINT('Ctrl Pts',(105.08934809608,4.128045606891,126.565590745312));
#182234=CARTESIAN_POINT('Ctrl Pts',(105.096755442434,4.24064009863725,126.675244067153));
#182235=CARTESIAN_POINT('Ctrl Pts',(105.104162788788,4.34897743453195,126.789498709027));
#182236=CARTESIAN_POINT('Ctrl Pts',(105.111570135142,4.45266299337704,126.907987582305));
#182237=CARTESIAN_POINT('Ctrl Pts',(105.118971956817,4.55627121962051,127.02638808211));
#182238=CARTESIAN_POINT('Ctrl Pts',(105.126373778493,4.65523433222816,127.1490162455));
#182239=CARTESIAN_POINT('Ctrl Pts',(105.133775600168,4.74919452031331,127.275468160898));
#182240=CARTESIAN_POINT('Ctrl Pts',(105.141173514479,4.84310510754649,127.401853323315));
#182241=CARTESIAN_POINT('Ctrl Pts',(105.148571428791,4.93201780786472,127.532057918868));
#182242=CARTESIAN_POINT('Ctrl Pts',(105.155969343102,5.01561515241312,127.665645083246));
#182243=CARTESIAN_POINT('Ctrl Pts',(105.163366028014,5.09919860459946,127.79921004786));
#182244=CARTESIAN_POINT('Ctrl Pts',(105.170762712927,5.17746825630318,127.936156149521));
#182245=CARTESIAN_POINT('Ctrl Pts',(105.178159397839,5.25014998195715,128.076017580216));
#182246=CARTESIAN_POINT('Ctrl Pts',(105.185555754774,5.32282848482725,128.215872809309));
#182247=CARTESIAN_POINT('Ctrl Pts',(105.19295211171,5.38991938217132,128.358642779165));
#182248=CARTESIAN_POINT('Ctrl Pts',(105.200348468645,5.45119467001556,128.503837365761));
#182249=CARTESIAN_POINT('Ctrl Pts',(105.207745957982,5.51247933926285,128.649054182019));
#182250=CARTESIAN_POINT('Ctrl Pts',(105.215143447318,5.56794648098274,128.796696010208));
#182251=CARTESIAN_POINT('Ctrl Pts',(105.222540936655,5.61741643250335,128.946253197006));
#182252=CARTESIAN_POINT('Ctrl Pts',(105.22994101917,5.66690372563873,129.095862810843));
#182253=CARTESIAN_POINT('Ctrl Pts',(105.237341101685,5.71038952574151,129.247388765903));
#182254=CARTESIAN_POINT('Ctrl Pts',(105.2447411842,5.74774422171534,129.400306870647));
#182255=CARTESIAN_POINT('Ctrl Pts',(105.252149403867,5.78513999301754,129.553393124567));
#182256=CARTESIAN_POINT('Ctrl Pts',(105.259557623533,5.81639110777643,129.707874222446));
#182257=CARTESIAN_POINT('Ctrl Pts',(105.2669658432,5.84141907322822,129.863215690668));
#182258=CARTESIAN_POINT('Ctrl Pts',(105.274378622502,5.86646244297514,130.018652768972));
#182259=CARTESIAN_POINT('Ctrl Pts',(105.281791401804,5.88527498666656,130.174950903038));
#182260=CARTESIAN_POINT('Ctrl Pts',(105.289204181106,5.89783020810086,130.331571659454));
#182261=CARTESIAN_POINT('Ctrl Pts',(105.296627552135,5.91040336902432,130.488416202951));
#182262=CARTESIAN_POINT('Ctrl Pts',(105.304050923163,5.91670133608945,130.645583917464));
#182263=CARTESIAN_POINT('Ctrl Pts',(105.311474294192,5.91674971887665,130.802536700609));
#182264=CARTESIAN_POINT('Ctrl Pts',(105.315410343633,5.91677537259135,130.885756832263));
#182265=CARTESIAN_POINT('Ctrl Pts',(105.319346393074,5.91504491162565,130.96891661744));
#182266=CARTESIAN_POINT('Ctrl Pts',(105.323282442514,5.91156803654956,131.051936690209));
#182267=CARTESIAN_POINT('Ctrl Pts',(105.33070570892,5.90501075866559,131.208509956486));
#182268=CARTESIAN_POINT('Ctrl Pts',(105.338128975325,5.89221879044042,131.365059286446));
#182269=CARTESIAN_POINT('Ctrl Pts',(105.345552241731,5.87318399051068,131.521047701382));
#182270=CARTESIAN_POINT('Ctrl Pts',(105.352966734452,5.85417168813369,131.676851750967));
#182271=CARTESIAN_POINT('Ctrl Pts',(105.360381227173,5.82893128578972,131.832095838212));
#182272=CARTESIAN_POINT('Ctrl Pts',(105.367795719894,5.79750662537259,131.986243645306));
#182273=CARTESIAN_POINT('Ctrl Pts',(105.375203066248,5.76611225322631,132.140242878941));
#182274=CARTESIAN_POINT('Ctrl Pts',(105.382610412601,5.72854556349577,132.293147572659));
#182275=CARTESIAN_POINT('Ctrl Pts',(105.390017758955,5.68490209584444,132.444427300102));
#182276=CARTESIAN_POINT('Ctrl Pts',(105.397419580631,5.64129117913782,132.595594197416));
#182277=CARTESIAN_POINT('Ctrl Pts',(105.404821402306,5.59161261194114,132.745138184505));
#182278=CARTESIAN_POINT('Ctrl Pts',(105.412223223981,5.53601281097703,132.892539900865));
#182279=CARTESIAN_POINT('Ctrl Pts',(105.419621138293,5.4804423607151,133.039863805006));
#182280=CARTESIAN_POINT('Ctrl Pts',(105.427019052604,5.41895703322618,133.185047342242));
#182281=CARTESIAN_POINT('Ctrl Pts',(105.434416966915,5.35175277515702,133.327587281205));
#182282=CARTESIAN_POINT('Ctrl Pts',(105.441813651828,5.28455968521634,133.470103532616));
#182283=CARTESIAN_POINT('Ctrl Pts',(105.44921033674,5.21164970996226,133.609976720348));
#182284=CARTESIAN_POINT('Ctrl Pts',(105.456607021652,5.13326657530261,133.74672443419));
#182285=CARTESIAN_POINT('Ctrl Pts',(105.464003378588,5.05488691623329,133.883466084496));
#182286=CARTESIAN_POINT('Ctrl Pts',(105.471399735523,4.97103476593801,134.017082212602));
#182287=CARTESIAN_POINT('Ctrl Pts',(105.478796092458,4.88199923792222,134.147116068302));
#182288=CARTESIAN_POINT('Ctrl Pts',(105.486193581795,4.7929500783398,134.277169832517));
#182289=CARTESIAN_POINT('Ctrl Pts',(105.493591071132,4.69871617181061,134.403639924246));
#182290=CARTESIAN_POINT('Ctrl Pts',(105.500988560468,4.59962919204559,134.526099708123));
#182291=CARTESIAN_POINT('Ctrl Pts',(105.508388642983,4.50050747749342,134.648602420088));
#182292=CARTESIAN_POINT('Ctrl Pts',(105.515788725498,4.39652953721887,134.767091735234));
#182293=CARTESIAN_POINT('Ctrl Pts',(105.523188808013,4.28806633044486,134.881175269743));
#182294=CARTESIAN_POINT('Ctrl Pts',(105.53059702768,4.17948385722472,134.995384250827));
#182295=CARTESIAN_POINT('Ctrl Pts',(105.538005247346,4.06640652532517,135.105177505565));
#182296=CARTESIAN_POINT('Ctrl Pts',(105.545413467012,3.94924157527939,135.210200099729));
#182297=CARTESIAN_POINT('Ctrl Pts',(105.552826246315,3.83200451216169,135.315287333547));
#182298=CARTESIAN_POINT('Ctrl Pts',(105.560239025617,3.71067510476582,135.415597818611));
#182299=CARTESIAN_POINT('Ctrl Pts',(105.567651804919,3.58569203052612,135.510818226503));
#182300=CARTESIAN_POINT('Ctrl Pts',(105.575075175947,3.46053037460892,135.60617468978));
#182301=CARTESIAN_POINT('Ctrl Pts',(105.582498546976,3.33170493020274,135.696426336569));
#182302=CARTESIAN_POINT('Ctrl Pts',(105.589921918005,3.19968226068691,135.781303855453));
#182303=CARTESIAN_POINT('Ctrl Pts',(105.593857967446,3.12968067347,135.826307952573));
#182304=CARTESIAN_POINT('Ctrl Pts',(105.597794016886,3.05878063457298,135.869801961931));
#182305=CARTESIAN_POINT('Ctrl Pts',(105.601730066327,2.98705416019581,135.911751145669));
#182306=CARTESIAN_POINT('Ctrl Pts',(105.609153332733,2.85178026802552,135.99086599701));
#182307=CARTESIAN_POINT('Ctrl Pts',(105.616576599138,2.71315651173587,136.064722488628));
#182308=CARTESIAN_POINT('Ctrl Pts',(105.623999865543,2.57163026611553,136.133023520856));
#182309=CARTESIAN_POINT('Ctrl Pts',(105.631414358264,2.43027129276448,136.201243826935));
#182310=CARTESIAN_POINT('Ctrl Pts',(105.638828850985,2.28601699142607,136.263921582802));
#182311=CARTESIAN_POINT('Ctrl Pts',(105.646243343706,2.1393422790795,136.320803781004));
#182312=CARTESIAN_POINT('Ctrl Pts',(105.65365069006,1.9928089373428,136.377631154002));
#182313=CARTESIAN_POINT('Ctrl Pts',(105.661058036414,1.84386017461458,136.428673955848));
#182314=CARTESIAN_POINT('Ctrl Pts',(105.668465382768,1.69299389513649,136.473725858361));
#182315=CARTESIAN_POINT('Ctrl Pts',(105.675867204443,1.54224013742148,136.518744159465));
#182316=CARTESIAN_POINT('Ctrl Pts',(105.683269026118,1.38957206674136,136.557780351749));
#182317=CARTESIAN_POINT('Ctrl Pts',(105.690670847794,1.23550577761279,136.590676892709));
#182318=CARTESIAN_POINT('Ctrl Pts',(105.698068762105,1.08152081887889,136.623556067841));
#182319=CARTESIAN_POINT('Ctrl Pts',(105.705466676416,0.926139475819769,
136.650301968651));
#182320=CARTESIAN_POINT('Ctrl Pts',(105.712864590728,0.769891045187945,
136.670807441755));
#182321=CARTESIAN_POINT('Ctrl Pts',(105.72026127564,0.61366858021088,136.691309507221));
#182322=CARTESIAN_POINT('Ctrl Pts',(105.727657960552,0.456579683407301,
136.705573154684));
#182323=CARTESIAN_POINT('Ctrl Pts',(105.735054645464,0.299161959957347,
136.71354268315));
#182324=CARTESIAN_POINT('Ctrl Pts',(105.7424510024,0.141751216574213,136.721511858238));
#182325=CARTESIAN_POINT('Ctrl Pts',(105.749847359335,-0.0159879516442059,
136.723187450375));
#182326=CARTESIAN_POINT('Ctrl Pts',(105.757243716271,-0.17351499490074,
136.718565814297));
#182327=CARTESIAN_POINT('Ctrl Pts',(105.764641205607,-0.331066155949856,
136.713943470636));
#182328=CARTESIAN_POINT('Ctrl Pts',(105.772038694944,-0.488404754209991,
136.703021990012));
#182329=CARTESIAN_POINT('Ctrl Pts',(105.77943618428,-0.644992571524573,
136.685849812079));
#182330=CARTESIAN_POINT('Ctrl Pts',(105.786836266795,-0.801635280455549,
136.668671614466));
#182331=CARTESIAN_POINT('Ctrl Pts',(105.79423634931,-0.957526313599619,
136.645238397603));
#182332=CARTESIAN_POINT('Ctrl Pts',(105.801636431825,-1.11213503481809,
136.615650166954));
#182333=CARTESIAN_POINT('Ctrl Pts',(105.809044651492,-1.26691376421993,
136.586029401004));
#182334=CARTESIAN_POINT('Ctrl Pts',(105.816452871158,-1.42040699889691,
136.550240175196));
#182335=CARTESIAN_POINT('Ctrl Pts',(105.823861090825,-1.57209599917411,
136.508433261904));
#182336=CARTESIAN_POINT('Ctrl Pts',(105.831273870127,-1.7238783614999,136.466600617154));
#182337=CARTESIAN_POINT('Ctrl Pts',(105.838686649429,-1.87385392185703,
136.418743017881));
#182338=CARTESIAN_POINT('Ctrl Pts',(105.846099428731,-2.02152195230672,
136.365060174172));
#182339=CARTESIAN_POINT('Ctrl Pts',(105.853522799759,-2.16940097776336,
136.311300625899));
#182340=CARTESIAN_POINT('Ctrl Pts',(105.860946170788,-2.31496554370426,
136.251699350603));
#182341=CARTESIAN_POINT('Ctrl Pts',(105.868369541817,-2.45773688190387,
136.186503311868));
#182342=CARTESIAN_POINT('Ctrl Pts',(105.872305591258,-2.53343767116798,
136.151934807774));
#182343=CARTESIAN_POINT('Ctrl Pts',(105.876241640698,-2.6083536159097,136.115794171515));
#182344=CARTESIAN_POINT('Ctrl Pts',(105.880177690139,-2.68241656366872,
136.078123215698));
#182345=CARTESIAN_POINT('Ctrl Pts',(105.887600956545,-2.82209697171773,
136.007076968697));
#182346=CARTESIAN_POINT('Ctrl Pts',(105.89502422295,-2.95916405618854,135.930370114267));
#182347=CARTESIAN_POINT('Ctrl Pts',(105.902447489356,-3.09312604171576,
135.848218451859));
#182348=CARTESIAN_POINT('Ctrl Pts',(105.909861982077,-3.22692969530103,
135.766163885894));
#182349=CARTESIAN_POINT('Ctrl Pts',(105.917276474798,-3.35763523991832,
135.678677514719));
#182350=CARTESIAN_POINT('Ctrl Pts',(105.924690967519,-3.48477310900594,
135.586022142732));
#182351=CARTESIAN_POINT('Ctrl Pts',(105.932098313872,-3.6117884378286,135.49345607548));
#182352=CARTESIAN_POINT('Ctrl Pts',(105.939505660226,-3.7352426371587,135.395731144136));
#182353=CARTESIAN_POINT('Ctrl Pts',(105.94691300658,-3.85469298785055,135.293154724218));
#182354=CARTESIAN_POINT('Ctrl Pts',(105.954314828255,-3.97405424796441,
135.190654809664));
#182355=CARTESIAN_POINT('Ctrl Pts',(105.961716649931,-4.08941732342291,
135.083310853458));
#182356=CARTESIAN_POINT('Ctrl Pts',(105.969118471606,-4.20037070756353,
134.971471904962));
#182357=CARTESIAN_POINT('Ctrl Pts',(105.976516385917,-4.311265520276,134.859691995376));
#182358=CARTESIAN_POINT('Ctrl Pts',(105.983914300229,-4.41775501543425,
134.743422083526));
#182359=CARTESIAN_POINT('Ctrl Pts',(105.99131221454,-4.51946294403796,134.623049562737));
#182360=CARTESIAN_POINT('Ctrl Pts',(105.998708899452,-4.62115397062931,
134.502697045676));
#182361=CARTESIAN_POINT('Ctrl Pts',(106.006105584365,-4.7180647670393,134.378243557669));
#182362=CARTESIAN_POINT('Ctrl Pts',(106.013502269277,-4.80985788171252,
134.250111293432));
#182363=CARTESIAN_POINT('Ctrl Pts',(106.020898626212,-4.90164692618279,
134.121984710713));
#182364=CARTESIAN_POINT('Ctrl Pts',(106.028294983148,-4.98831852271849,
133.990179979564));
#182365=CARTESIAN_POINT('Ctrl Pts',(106.035691340083,-5.06957742408703,
133.855149909485));
#182366=CARTESIAN_POINT('Ctrl Pts',(106.04308882942,-5.15084876640076,133.720099165958));
#182367=CARTESIAN_POINT('Ctrl Pts',(106.050486318756,-5.22670557100859,
133.581822420132));
#182368=CARTESIAN_POINT('Ctrl Pts',(106.057883808093,-5.29689767150079,
133.440798673002));
#182369=CARTESIAN_POINT('Ctrl Pts',(106.065283890608,-5.3671143777252,133.299725490215));
#182370=CARTESIAN_POINT('Ctrl Pts',(106.072683973123,-5.43166225998016,
133.155903722865));
#182371=CARTESIAN_POINT('Ctrl Pts',(106.080084055638,-5.49033863389968,
133.009833865558));
#182372=CARTESIAN_POINT('Ctrl Pts',(106.087492275304,-5.54907952852431,
132.863603389427));
#182373=CARTESIAN_POINT('Ctrl Pts',(106.094900494971,-5.60193588187207,
132.71512023319));
#182374=CARTESIAN_POINT('Ctrl Pts',(106.102308714637,-5.64875415154569,
132.564902323376));
#182375=CARTESIAN_POINT('Ctrl Pts',(106.10972149394,-5.69560123708312,132.414591956945));
#182376=CARTESIAN_POINT('Ctrl Pts',(106.117134273242,-5.73640273714705,
132.262545069094));
#182377=CARTESIAN_POINT('Ctrl Pts',(106.124547052544,-5.77105601780815,
132.1092908846));
#182378=CARTESIAN_POINT('Ctrl Pts',(106.131970423572,-5.80575881270173,
131.95581772334));
#182379=CARTESIAN_POINT('Ctrl Pts',(106.139393794601,-5.83429577530219,
131.801134186271));
#182380=CARTESIAN_POINT('Ctrl Pts',(106.14681716563,-5.85661589714791,131.645776564512));
#182381=CARTESIAN_POINT('Ctrl Pts',(106.150753215071,-5.86845056131456,
131.563402225699));
#182382=CARTESIAN_POINT('Ctrl Pts',(106.154689264512,-5.87853831853057,
131.480838422975));
#182383=CARTESIAN_POINT('Ctrl Pts',(106.158625313952,-5.88687750885685,
131.398165095669));
#182384=CARTESIAN_POINT('Ctrl Pts',(106.167958478567,-5.90665140581494,
131.202130014161));
#182385=CARTESIAN_POINT('Ctrl Pts',(106.177291643181,-5.91663550124626,
131.005090988402));
#182386=CARTESIAN_POINT('Ctrl Pts',(106.186624807795,-5.91674902090619,
130.807764454462));
#182387=CARTESIAN_POINT('',(107.936623643011,-5.91240499895973,130.80786427171));
#182388=CARTESIAN_POINT('Ctrl Pts',(106.186627341394,-5.92408642895685,
130.80771504248));
#182389=CARTESIAN_POINT('Ctrl Pts',(106.270109206851,-5.91195890497154,
129.040502122754));
#182390=CARTESIAN_POINT('Ctrl Pts',(106.446406946912,-4.13303796844123,
125.287351149234));
#182391=CARTESIAN_POINT('Ctrl Pts',(106.715520561579,2.25550656452963,124.17938886912));
#182392=CARTESIAN_POINT('Ctrl Pts',(106.993968185391,6.79293275285633,129.121023115604));
#182393=CARTESIAN_POINT('Ctrl Pts',(107.272415809204,5.0879855945222,135.609562290782));
#182394=CARTESIAN_POINT('Ctrl Pts',(107.550863433017,-1.29257176326585,
137.682355875427));
#182395=CARTESIAN_POINT('Ctrl Pts',(107.772265740639,-5.42148536177523,
134.304840178653));
#182396=CARTESIAN_POINT('Ctrl Pts',(107.900852173658,-5.9130646159241,131.570055323628));
#182397=CARTESIAN_POINT('Ctrl Pts',(107.936622732073,-5.90900772285622,
130.807881682323));
#182398=CARTESIAN_POINT('',(109.686626001159,-5.91357378928978,130.799653518455));
#182399=CARTESIAN_POINT('Ctrl Pts',(107.936624807795,-5.91674897578147,
130.807842009375));
#182400=CARTESIAN_POINT('Ctrl Pts',(107.94409446103,-5.91684274612946,130.648475973948));
#182401=CARTESIAN_POINT('Ctrl Pts',(107.951564114265,-5.91049345477139,
130.489096138341));
#182402=CARTESIAN_POINT('Ctrl Pts',(107.9590337675,-5.89772439811517,130.330253576512));
#182403=CARTESIAN_POINT('Ctrl Pts',(107.966504510164,-5.88495347912462,
130.1713878479));
#182404=CARTESIAN_POINT('Ctrl Pts',(107.973975252829,-5.86576095780414,
130.013059911091));
#182405=CARTESIAN_POINT('Ctrl Pts',(107.981445995494,-5.84022206841509,
129.855816072435));
#182406=CARTESIAN_POINT('Ctrl Pts',(107.98891919135,-5.81467479273977,129.69852059912));
#182407=CARTESIAN_POINT('Ctrl Pts',(107.996392387206,-5.7827770550703,129.542310291412));
#182408=CARTESIAN_POINT('Ctrl Pts',(108.003865583063,-5.74465529499681,
129.38772160068));
#182409=CARTESIAN_POINT('Ctrl Pts',(108.011342597095,-5.70651405790379,
129.233053928102));
#182410=CARTESIAN_POINT('Ctrl Pts',(108.018819611127,-5.6621425497145,129.080009875145));
#182411=CARTESIAN_POINT('Ctrl Pts',(108.026296625159,-5.61171717273773,
128.929111051321));
#182412=CARTESIAN_POINT('Ctrl Pts',(108.033783535364,-5.5612250554452,128.778012505934));
#182413=CARTESIAN_POINT('Ctrl Pts',(108.04127044557,-5.50466317855855,128.629065205899));
#182414=CARTESIAN_POINT('Ctrl Pts',(108.048757355775,-5.44225660651554,
128.482772025387));
#182415=CARTESIAN_POINT('Ctrl Pts',(108.056249706816,-5.37980468279946,
128.336372531704));
#182416=CARTESIAN_POINT('Ctrl Pts',(108.063742057857,-5.31149975231297,
128.192631329411));
#182417=CARTESIAN_POINT('Ctrl Pts',(108.071234408898,-5.23761287276468,
128.052026706582));
#182418=CARTESIAN_POINT('Ctrl Pts',(108.078738864129,-5.16360662604355,
127.911194931432));
#182419=CARTESIAN_POINT('Ctrl Pts',(108.086243319359,-5.08400059452109,
127.773510173305));
#182420=CARTESIAN_POINT('Ctrl Pts',(108.093747774589,-4.99910978103279,
127.639422709852));
#182421=CARTESIAN_POINT('Ctrl Pts',(108.098418076607,-4.94627906576286,
127.55597508682));
#182422=CARTESIAN_POINT('Ctrl Pts',(108.103088378625,-4.89140236815802,
127.473920090637));
#182423=CARTESIAN_POINT('Ctrl Pts',(108.107758680642,-4.83456333426392,
127.39335960181));
#182424=CARTESIAN_POINT('Ctrl Pts',(108.115181947048,-4.74421986413769,
127.265311786478));
#182425=CARTESIAN_POINT('Ctrl Pts',(108.122605213453,-4.64864907589165,
127.14066207089));
#182426=CARTESIAN_POINT('Ctrl Pts',(108.130028479859,-4.54813506396797,
127.019866199231));
#182427=CARTESIAN_POINT('Ctrl Pts',(108.13744297258,-4.44773985125906,126.899213098261));
#182428=CARTESIAN_POINT('Ctrl Pts',(108.144857465301,-4.34241328079953,
126.782405058767));
#182429=CARTESIAN_POINT('Ctrl Pts',(108.152271958022,-4.23248278113099,
126.669869104704));
#182430=CARTESIAN_POINT('Ctrl Pts',(108.159679304375,-4.122658236617,126.55744161703));
#182431=CARTESIAN_POINT('Ctrl Pts',(108.167086650729,-4.00823885606507,
126.449278282703));
#182432=CARTESIAN_POINT('Ctrl Pts',(108.174493997083,-3.88959232822549,
126.345773163819));
#182433=CARTESIAN_POINT('Ctrl Pts',(108.181895818758,-3.77103429144233,
126.242345242957));
#182434=CARTESIAN_POINT('Ctrl Pts',(108.189297640434,-3.64825566504315,
126.143568864137));
#182435=CARTESIAN_POINT('Ctrl Pts',(108.196699462109,-3.52166090466189,
126.049801223145));
#182436=CARTESIAN_POINT('Ctrl Pts',(108.204097376421,-3.39513297266975,
125.956083081362));
#182437=CARTESIAN_POINT('Ctrl Pts',(108.211495290732,-3.26479321789758,
125.867368633233));
#182438=CARTESIAN_POINT('Ctrl Pts',(108.218893205043,-3.13107898728395,
125.783974682412));
#182439=CARTESIAN_POINT('Ctrl Pts',(108.226289889956,-2.99738697754934,
125.700594590154));
#182440=CARTESIAN_POINT('Ctrl Pts',(108.233686574868,-2.86032192138361,
125.622533437739));
#182441=CARTESIAN_POINT('Ctrl Pts',(108.24108325978,-2.72035004343166,125.550064641538));
#182442=CARTESIAN_POINT('Ctrl Pts',(108.248479616715,-2.58038437197945,
125.47759905868));
#182443=CARTESIAN_POINT('Ctrl Pts',(108.255875973651,-2.43751246652316,
125.410725510616));
#182444=CARTESIAN_POINT('Ctrl Pts',(108.263272330586,-2.29222479750266,
125.349671255172));
#182445=CARTESIAN_POINT('Ctrl Pts',(108.270669819923,-2.14691488456913,
125.288607652166));
#182446=CARTESIAN_POINT('Ctrl Pts',(108.27806730926,-1.99918881579962,125.233365260405));
#182447=CARTESIAN_POINT('Ctrl Pts',(108.285464798596,-1.84955651734156,
125.184122966749));
#182448=CARTESIAN_POINT('Ctrl Pts',(108.292864881111,-1.69987176551313,
125.134863411283));
#182449=CARTESIAN_POINT('Ctrl Pts',(108.300264963626,-1.5482798079326,125.091608258246));
#182450=CARTESIAN_POINT('Ctrl Pts',(108.307665046141,-1.39530503277655,
125.054486320852));
#182451=CARTESIAN_POINT('Ctrl Pts',(108.315073265808,-1.24216204612914,
125.017323564072));
#182452=CARTESIAN_POINT('Ctrl Pts',(108.322481485474,-1.08763356825991,
124.986307579436));
#182453=CARTESIAN_POINT('Ctrl Pts',(108.329889705141,-0.932254191617432,
124.961516046237));
#182454=CARTESIAN_POINT('Ctrl Pts',(108.337302484443,-0.776779181561499,
124.936709254263));
#182455=CARTESIAN_POINT('Ctrl Pts',(108.344715263745,-0.620452598997422,
124.91813459151));
#182456=CARTESIAN_POINT('Ctrl Pts',(108.352128043047,-0.463812917036198,
124.905817734744));
#182457=CARTESIAN_POINT('Ctrl Pts',(108.359551414076,-0.306949420951381,
124.893483279076));
#182458=CARTESIAN_POINT('Ctrl Pts',(108.366974785105,-0.149772304001651,
124.88742450181));
#182459=CARTESIAN_POINT('Ctrl Pts',(108.374398156133,0.00718037102544568,
124.887614974497));
#182460=CARTESIAN_POINT('Ctrl Pts',(108.378334205574,0.0904004453502009,
124.887715967686));
#182461=CARTESIAN_POINT('Ctrl Pts',(108.382270255015,0.173557500760324,
124.889572981685));
#182462=CARTESIAN_POINT('Ctrl Pts',(108.386206304455,0.256572186180075,
124.893176195153));
#182463=CARTESIAN_POINT('Ctrl Pts',(108.393629570861,0.41313529208642,124.899971743302));
#182464=CARTESIAN_POINT('Ctrl Pts',(108.401052837266,0.56966497356679,124.913001938145));
#182465=CARTESIAN_POINT('Ctrl Pts',(108.408476103672,0.725624240145992,
124.932274103846));
#182466=CARTESIAN_POINT('Ctrl Pts',(108.415890596393,0.881399175823931,
124.951523491448));
#182467=CARTESIAN_POINT('Ctrl Pts',(108.423305089114,1.03660467170355,124.977000119638));
#182468=CARTESIAN_POINT('Ctrl Pts',(108.430719581835,1.19070447731366,125.008659330387));
#182469=CARTESIAN_POINT('Ctrl Pts',(108.438126928189,1.34465575572914,125.040288026798));
#182470=CARTESIAN_POINT('Ctrl Pts',(108.445534274542,1.49750310227977,125.078087367941));
#182471=CARTESIAN_POINT('Ctrl Pts',(108.452941620896,1.64871623661404,125.121961007047));
#182472=CARTESIAN_POINT('Ctrl Pts',(108.460343442572,1.79981659048746,125.165801923537));
#182473=CARTESIAN_POINT('Ctrl Pts',(108.467745264247,1.94928480208421,125.215708013698));
#182474=CARTESIAN_POINT('Ctrl Pts',(108.475147085922,2.09660173432233,125.271532070599));
#182475=CARTESIAN_POINT('Ctrl Pts',(108.482545000234,2.24384089909842,125.327326658414));
#182476=CARTESIAN_POINT('Ctrl Pts',(108.489942914545,2.38893069801256,125.389032859332));
#182477=CARTESIAN_POINT('Ctrl Pts',(108.497340828856,2.53136819847509,125.456453961102));
#182478=CARTESIAN_POINT('Ctrl Pts',(108.504737513769,2.67378202840953,125.523863858708));
#182479=CARTESIAN_POINT('Ctrl Pts',(108.512134198681,2.81354409759998,125.596986612715));
#182480=CARTESIAN_POINT('Ctrl Pts',(108.519530883593,2.95017236730276,125.67557776335));
#182481=CARTESIAN_POINT('Ctrl Pts',(108.526927240528,3.08679457876498,125.754165429171));
#182482=CARTESIAN_POINT('Ctrl Pts',(108.534323597464,3.22028294344749,125.838220823368));
#182483=CARTESIAN_POINT('Ctrl Pts',(108.541719954399,3.35018115165315,125.927454137674));
#182484=CARTESIAN_POINT('Ctrl Pts',(108.549117443736,3.480099247606,126.016701113829));
#182485=CARTESIAN_POINT('Ctrl Pts',(108.556514933072,3.60642578491945,126.111127377187));
#182486=CARTESIAN_POINT('Ctrl Pts',(108.563912422409,3.72873463347499,126.210400605156));
#182487=CARTESIAN_POINT('Ctrl Pts',(108.571312504924,3.85108635720804,126.309708633201));
#182488=CARTESIAN_POINT('Ctrl Pts',(108.578712587439,3.96941729841992,126.413866773637));
#182489=CARTESIAN_POINT('Ctrl Pts',(108.586112669954,4.0833356382855,126.522503470532));
#182490=CARTESIAN_POINT('Ctrl Pts',(108.59352088962,4.19737924307678,126.631259624643));
#182491=CARTESIAN_POINT('Ctrl Pts',(108.600929109287,4.30700028622644,126.744503912244));
#182492=CARTESIAN_POINT('Ctrl Pts',(108.608337328953,4.41184445366697,126.861828553125));
#182493=CARTESIAN_POINT('Ctrl Pts',(108.615750108256,4.51675315094359,126.979225405365));
#182494=CARTESIAN_POINT('Ctrl Pts',(108.623162887558,4.61687887714527,127.100707327746));
#182495=CARTESIAN_POINT('Ctrl Pts',(108.63057566686,4.71190897181134,127.225835166509));
#182496=CARTESIAN_POINT('Ctrl Pts',(108.637999037888,4.80707484993294,127.351141793796));
#182497=CARTESIAN_POINT('Ctrl Pts',(108.645422408917,4.8971303418157,127.480104436667));
#182498=CARTESIAN_POINT('Ctrl Pts',(108.652845779946,4.98180684638433,127.612256122438));
#182499=CARTESIAN_POINT('Ctrl Pts',(108.656781829387,5.02670436089111,127.682326117169));
#182500=CARTESIAN_POINT('Ctrl Pts',(108.660717878828,5.07009042209485,127.753292264444));
#182501=CARTESIAN_POINT('Ctrl Pts',(108.664653928268,5.11193040177253,127.82508249528));
#182502=CARTESIAN_POINT('Ctrl Pts',(108.672077194674,5.19083929766396,127.960476630141));
#182503=CARTESIAN_POINT('Ctrl Pts',(108.679500461079,5.26448474199825,128.099212622914));
#182504=CARTESIAN_POINT('Ctrl Pts',(108.686923727485,5.33257031628044,128.240842647193));
#182505=CARTESIAN_POINT('Ctrl Pts',(108.694338220206,5.40057541906814,128.382305276546));
#182506=CARTESIAN_POINT('Ctrl Pts',(108.701752712927,5.46303357186457,128.526654795715));
#182507=CARTESIAN_POINT('Ctrl Pts',(108.709167205648,5.51969249025468,128.673415903237));
#182508=CARTESIAN_POINT('Ctrl Pts',(108.716574552001,5.57629679864595,128.820035556878));
#182509=CARTESIAN_POINT('Ctrl Pts',(108.723981898355,5.62711286672333,128.969061825581));
#182510=CARTESIAN_POINT('Ctrl Pts',(108.731389244709,5.67193512427151,129.119996491685));
#182511=CARTESIAN_POINT('Ctrl Pts',(108.738791066384,5.71672395168899,129.27081858502));
#182512=CARTESIAN_POINT('Ctrl Pts',(108.74619288806,5.75552776395484,129.423545885352));
#182513=CARTESIAN_POINT('Ctrl Pts',(108.753594709735,5.78818980415609,129.57766205901));
#182514=CARTESIAN_POINT('Ctrl Pts',(108.760992624046,5.82083460232035,129.731696875938));
#182515=CARTESIAN_POINT('Ctrl Pts',(108.768390538358,5.8473440082055,129.887118741775));
#182516=CARTESIAN_POINT('Ctrl Pts',(108.775788452669,5.86761167405109,130.043398197312));
#182517=CARTESIAN_POINT('Ctrl Pts',(108.783185137581,5.88787597177845,130.199651682039));
#182518=CARTESIAN_POINT('Ctrl Pts',(108.790581822493,5.90190054016471,130.35676210378));
#182519=CARTESIAN_POINT('Ctrl Pts',(108.797978507406,5.90963049642396,130.514191773208));
#182520=CARTESIAN_POINT('Ctrl Pts',(108.805374864341,5.91736010992885,130.67161446204));
#182521=CARTESIAN_POINT('Ctrl Pts',(108.812771221277,5.91879564796385,130.829355997565));
#182522=CARTESIAN_POINT('Ctrl Pts',(108.820167578212,5.91393428789429,130.986875825065));
#182523=CARTESIAN_POINT('Ctrl Pts',(108.827565067549,5.90907218353808,131.144419769252));
#182524=CARTESIAN_POINT('Ctrl Pts',(108.834962556885,5.89791127299929,131.301741564682));
#182525=CARTESIAN_POINT('Ctrl Pts',(108.842360046222,5.88050081494962,131.458303067539));
#182526=CARTESIAN_POINT('Ctrl Pts',(108.849760128737,5.86308425369089,131.614919452788));
#182527=CARTESIAN_POINT('Ctrl Pts',(108.857160211252,5.83941382434853,131.770774644046));
#182528=CARTESIAN_POINT('Ctrl Pts',(108.864560293767,5.80959033980777,131.92533815798));
#182529=CARTESIAN_POINT('Ctrl Pts',(108.871968513433,5.77973406127979,132.080071630387));
#182530=CARTESIAN_POINT('Ctrl Pts',(108.8793767331,5.74371128634123,132.233510222212));
#182531=CARTESIAN_POINT('Ctrl Pts',(108.886784952766,5.7016735766245,132.385135423831));
#182532=CARTESIAN_POINT('Ctrl Pts',(108.894197732068,5.65960999339889,132.536853948231));
#182533=CARTESIAN_POINT('Ctrl Pts',(108.90161051137,5.61152421227203,132.6867565038));
#182534=CARTESIAN_POINT('Ctrl Pts',(108.909023290672,5.55761670512263,132.834342667103));
#182535=CARTESIAN_POINT('Ctrl Pts',(108.916446661701,5.50363217239908,132.982139708437));
#182536=CARTESIAN_POINT('Ctrl Pts',(108.92387003273,5.44380944163022,133.127613402821));
#182537=CARTESIAN_POINT('Ctrl Pts',(108.931293403759,5.3783962047193,133.270285358421));
#182538=CARTESIAN_POINT('Ctrl Pts',(108.9352294532,5.34371253693922,133.345933452649));
#182539=CARTESIAN_POINT('Ctrl Pts',(108.939165502641,5.30745793321449,133.420794310745));
#182540=CARTESIAN_POINT('Ctrl Pts',(108.943101552081,5.2696743098201,133.49479984396));
#182541=CARTESIAN_POINT('Ctrl Pts',(108.950524818487,5.19841557528643,133.634371969968));
#182542=CARTESIAN_POINT('Ctrl Pts',(108.957948084892,5.12150021691154,133.771322160943));
#182543=CARTESIAN_POINT('Ctrl Pts',(108.965371351298,5.03914478229674,133.905158970499));
#182544=CARTESIAN_POINT('Ctrl Pts',(108.972785844019,4.95688668496634,134.038837596061));
#182545=CARTESIAN_POINT('Ctrl Pts',(108.98020033674,4.86920150351011,134.169409849959));
#182546=CARTESIAN_POINT('Ctrl Pts',(108.987614829461,4.77635275662183,134.29640656612));
#182547=CARTESIAN_POINT('Ctrl Pts',(108.995022175815,4.68359350085161,134.423280878064));
#182548=CARTESIAN_POINT('Ctrl Pts',(109.002429522168,4.58568080639566,134.546586213726));
#182549=CARTESIAN_POINT('Ctrl Pts',(109.009836868522,4.48292272216005,134.665880322247));
#182550=CARTESIAN_POINT('Ctrl Pts',(109.017238690197,4.3802412787808,134.785085456721));
#182551=CARTESIAN_POINT('Ctrl Pts',(109.024640511873,4.27272188391508,134.900285039362));
#182552=CARTESIAN_POINT('Ctrl Pts',(109.032042333548,4.16071421276395,135.011068095179));
#182553=CARTESIAN_POINT('Ctrl Pts',(109.03944024786,4.04876566958952,135.121792669484));
#182554=CARTESIAN_POINT('Ctrl Pts',(109.046838162171,3.93233383349262,135.228105098317));
#182555=CARTESIAN_POINT('Ctrl Pts',(109.054236076482,3.81180666993848,135.329629722659));
#182556=CARTESIAN_POINT('Ctrl Pts',(109.061632761395,3.69129953581284,135.431137475451));
#182557=CARTESIAN_POINT('Ctrl Pts',(109.069029446307,3.56669871018576,135.527858762617));
#182558=CARTESIAN_POINT('Ctrl Pts',(109.076426131219,3.43842690082814,135.619456775501));
#182559=CARTESIAN_POINT('Ctrl Pts',(109.083822488154,3.31016077917751,135.711050726833));
#182560=CARTESIAN_POINT('Ctrl Pts',(109.09121884509,3.17822430124098,135.797521638641));
#182561=CARTESIAN_POINT('Ctrl Pts',(109.098615202025,3.04307072530972,135.878574953132));
#182562=CARTESIAN_POINT('Ctrl Pts',(109.106012691362,2.90789645702027,135.959640677093));
#182563=CARTESIAN_POINT('Ctrl Pts',(109.113410180699,2.76950443017307,136.035286960192));
#182564=CARTESIAN_POINT('Ctrl Pts',(109.120807670035,2.62837402591716,136.105264365266));
#182565=CARTESIAN_POINT('Ctrl Pts',(109.12820775255,2.48719414861702,136.175266300812));
#182566=CARTESIAN_POINT('Ctrl Pts',(109.135607835065,2.34327431692121,136.239595236074));
#182567=CARTESIAN_POINT('Ctrl Pts',(109.14300791758,2.19711533330873,136.29804924859));
#182568=CARTESIAN_POINT('Ctrl Pts',(109.150416137247,2.05079563286817,136.356567537302));
#182569=CARTESIAN_POINT('Ctrl Pts',(109.157824356913,1.9022322101993,136.409197863355));
#182570=CARTESIAN_POINT('Ctrl Pts',(109.16523257658,1.75194322489847,136.455787472727));
#182571=CARTESIAN_POINT('Ctrl Pts',(109.172645355882,1.60156173923575,136.502405757225));
#182572=CARTESIAN_POINT('Ctrl Pts',(109.180058135184,1.44945293451599,136.542975820561));
#182573=CARTESIAN_POINT('Ctrl Pts',(109.187470914486,1.29614619109431,136.577395834314));
#182574=CARTESIAN_POINT('Ctrl Pts',(109.194894285514,1.14262039580749,136.611865028997));
#182575=CARTESIAN_POINT('Ctrl Pts',(109.202317656543,0.987893609460659,
136.64016655654));
#182576=CARTESIAN_POINT('Ctrl Pts',(109.209741027572,0.832502200176965,
136.662250224686));
#182577=CARTESIAN_POINT('Ctrl Pts',(109.213677077013,0.750109946408958,
136.673959515427));
#182578=CARTESIAN_POINT('Ctrl Pts',(109.217613126454,0.667530887443442,
136.683921612908));
#182579=CARTESIAN_POINT('Ctrl Pts',(109.221549175894,0.584844965044413,
136.692134978847));
#182580=CARTESIAN_POINT('Ctrl Pts',(109.2289724423,0.428901895939548,136.707625130678));
#182581=CARTESIAN_POINT('Ctrl Pts',(109.236395708705,0.272107191678051,
136.716938984737));
#182582=CARTESIAN_POINT('Ctrl Pts',(109.243818975111,0.114991369290807,
136.719993089879));
#182583=CARTESIAN_POINT('Ctrl Pts',(109.251233467832,-0.0419387552421442,
136.723043585323));
#182584=CARTESIAN_POINT('Ctrl Pts',(109.258647960553,-0.199188872851643,
136.719849051427));
#182585=CARTESIAN_POINT('Ctrl Pts',(109.266062453274,-0.356221822541083,
136.710377598209));
#182586=CARTESIAN_POINT('Ctrl Pts',(109.273469799627,-0.513103417961313,
136.700915273934));
#182587=CARTESIAN_POINT('Ctrl Pts',(109.280877145981,-0.669767892046414,
136.685188096883));
#182588=CARTESIAN_POINT('Ctrl Pts',(109.288284492335,-0.825676658664553,
136.663216189931));
#182589=CARTESIAN_POINT('Ctrl Pts',(109.29568631401,-0.981469142642558,
136.641260670457));
#182590=CARTESIAN_POINT('Ctrl Pts',(109.303088135686,-1.1365066733729,136.613069746773));
#182591=CARTESIAN_POINT('Ctrl Pts',(109.310489957361,-1.29025447796769,
136.578715468507));
#182592=CARTESIAN_POINT('Ctrl Pts',(109.317887871672,-1.44392112029299,
136.544379325597));
#182593=CARTESIAN_POINT('Ctrl Pts',(109.325285785984,-1.59629902900928,
136.503886388978));
#182594=CARTESIAN_POINT('Ctrl Pts',(109.332683700295,-1.74686244673501,
136.457360012108));
#182595=CARTESIAN_POINT('Ctrl Pts',(109.340080385207,-1.89740084355233,
136.410841367077));
#182596=CARTESIAN_POINT('Ctrl Pts',(109.34747707012,-2.04612499152957,136.358291381861));
#182597=CARTESIAN_POINT('Ctrl Pts',(109.354873755032,-2.19252304013005,
136.299883639172));
#182598=CARTESIAN_POINT('Ctrl Pts',(109.362270111967,-2.33891459728753,
136.241478486343));
#182599=CARTESIAN_POINT('Ctrl Pts',(109.369666468903,-2.48297991342709,
136.177216230822));
#182600=CARTESIAN_POINT('Ctrl Pts',(109.377062825838,-2.6242261715584,136.107318995963));
#182601=CARTESIAN_POINT('Ctrl Pts',(109.384460315175,-2.76549405485232,
136.037411059659));
#182602=CARTESIAN_POINT('Ctrl Pts',(109.391857804511,-2.90394168616086,
135.961866591785));
#182603=CARTESIAN_POINT('Ctrl Pts',(109.399255293848,-3.03910008971452,
135.8809540824));
#182604=CARTESIAN_POINT('Ctrl Pts',(109.406655376363,-3.17430587283665,
135.800013209261));
#182605=CARTESIAN_POINT('Ctrl Pts',(109.414055458878,-3.30621981243113,
135.713700739666));
#182606=CARTESIAN_POINT('Ctrl Pts',(109.421455541392,-3.43440132943781,
135.622328868899));
#182607=CARTESIAN_POINT('Ctrl Pts',(109.428863761059,-3.56272379520065,
135.530856525367));
#182608=CARTESIAN_POINT('Ctrl Pts',(109.436271980725,-3.68730533789365,
135.434313887141));
#182609=CARTESIAN_POINT('Ctrl Pts',(109.443680200392,-3.80773736331207,
135.333054329282));
#182610=CARTESIAN_POINT('Ctrl Pts',(109.451092979694,-3.92824351263296,
135.231732447855));
#182611=CARTESIAN_POINT('Ctrl Pts',(109.458505758996,-4.04459478033752,
135.125688112711));
#182612=CARTESIAN_POINT('Ctrl Pts',(109.465918538298,-4.15641935227887,
135.015311665786));
#182613=CARTESIAN_POINT('Ctrl Pts',(109.473341909327,-4.26840370441258,
134.904777507817));
#182614=CARTESIAN_POINT('Ctrl Pts',(109.480765280356,-4.37584818850849,
134.789899147314));
#182615=CARTESIAN_POINT('Ctrl Pts',(109.488188651384,-4.47842065632573,
134.671100715826));
#182616=CARTESIAN_POINT('Ctrl Pts',(109.492124700825,-4.53280703995719,
134.60811093692));
#182617=CARTESIAN_POINT('Ctrl Pts',(109.496060750266,-4.58582443318841,
134.544019592876));
#182618=CARTESIAN_POINT('Ctrl Pts',(109.499996799707,-4.63742833134212,
134.478893109485));
#182619=CARTESIAN_POINT('Ctrl Pts',(109.507772966711,-4.73937840491298,
134.350227446411));
#182620=CARTESIAN_POINT('Ctrl Pts',(109.515549133715,-4.83613835824615,
134.217102726659));
#182621=CARTESIAN_POINT('Ctrl Pts',(109.523325300718,-4.92729617052023,
134.079980102561));
#182622=CARTESIAN_POINT('Ctrl Pts',(109.530729946761,-5.01409874736348,
133.949408768976));
#182623=CARTESIAN_POINT('Ctrl Pts',(109.538134592803,-5.09582174505376,
133.815213002727));
#182624=CARTESIAN_POINT('Ctrl Pts',(109.545539238845,-5.17214874724491,
133.677826799527));
#182625=CARTESIAN_POINT('Ctrl Pts',(109.552936918627,-5.24840394130658,
133.540569848701));
#182626=CARTESIAN_POINT('Ctrl Pts',(109.560334598409,-5.31927306273739,
133.400128758789));
#182627=CARTESIAN_POINT('Ctrl Pts',(109.567732278191,-5.38448260220117,
133.256966918849));
#182628=CARTESIAN_POINT('Ctrl Pts',(109.575124465065,-5.44964372243038,
133.113911379103));
#182629=CARTESIAN_POINT('Ctrl Pts',(109.582516651939,-5.50915347148947,
132.968139449289));
#182630=CARTESIAN_POINT('Ctrl Pts',(109.589908838812,-5.56278404411905,
132.820139435044));
#182631=CARTESIAN_POINT('Ctrl Pts',(109.597297002377,-5.616385427498,132.672219972047));
#182632=CARTESIAN_POINT('Ctrl Pts',(109.604685165941,-5.6641138786913,132.522075189744));
#182633=CARTESIAN_POINT('Ctrl Pts',(109.612073329506,-5.70578961301687,
132.370213565479));
#182634=CARTESIAN_POINT('Ctrl Pts',(109.619459567761,-5.74745448690789,
132.2183915154));
#182635=CARTESIAN_POINT('Ctrl Pts',(109.626845806016,-5.78306968274208,
132.064853873456));
#182636=CARTESIAN_POINT('Ctrl Pts',(109.634232044272,-5.8125052155614,131.910124462865));
#182637=CARTESIAN_POINT('Ctrl Pts',(109.641617182809,-5.84193636580126,
131.755418089532));
#182638=CARTESIAN_POINT('Ctrl Pts',(109.649002321347,-5.86518961886955,
131.599520668681));
#182639=CARTESIAN_POINT('Ctrl Pts',(109.656387459885,-5.88218612271177,
131.442966114158));
#182640=CARTESIAN_POINT('Ctrl Pts',(109.663774300717,-5.8991865442944,131.286375473383));
#182641=CARTESIAN_POINT('Ctrl Pts',(109.671161141549,-5.90992729760968,
131.129127768272));
#182642=CARTESIAN_POINT('Ctrl Pts',(109.678547982381,-5.91438139765927,
130.971762067745));
#182643=CARTESIAN_POINT('Ctrl Pts',(109.681240257519,-5.9160047794402,130.914407134462));
#182644=CARTESIAN_POINT('Ctrl Pts',(109.683932532657,-5.91679355703985,
130.857036545142));
#182645=CARTESIAN_POINT('Ctrl Pts',(109.686624807795,-5.91674814578703,
130.79967640731));
#182646=CARTESIAN_POINT('',(111.436624807795,-5.92599054836748,130.802728473828));
#182647=CARTESIAN_POINT('Ctrl Pts',(109.686626838718,-5.9113458756003,130.799637453972));
#182648=CARTESIAN_POINT('Ctrl Pts',(109.717232700319,-5.91613812751391,
130.148157013076));
#182649=CARTESIAN_POINT('Ctrl Pts',(109.840654436524,-5.5159435970196,127.526716476239));
#182650=CARTESIAN_POINT('Ctrl Pts',(110.056892047334,-1.67299786539814,
124.008873977688));
#182651=CARTESIAN_POINT('Ctrl Pts',(110.335339671146,4.81293915681766,125.723693613804));
#182652=CARTESIAN_POINT('Ctrl Pts',(110.613787294959,6.87602021906624,132.107398021992));
#182653=CARTESIAN_POINT('Ctrl Pts',(110.892234918771,2.62037461225579,137.293674712428));
#182654=CARTESIAN_POINT('Ctrl Pts',(111.166514089717,-3.94351033188604,
136.528222003439));
#182655=CARTESIAN_POINT('Ctrl Pts',(111.347977386058,-5.9191353605258,132.677693844969));
#182656=CARTESIAN_POINT('Ctrl Pts',(111.436624807795,-5.92599054836748,
130.802728473828));
#182657=CARTESIAN_POINT('',(113.186624807795,-5.9163106462342,130.809833344935));
#182658=CARTESIAN_POINT('Ctrl Pts',(111.436624807795,-5.92599054836748,
130.802728473828));
#182659=CARTESIAN_POINT('Ctrl Pts',(111.440793260663,-5.92631289871739,
130.714562291163));
#182660=CARTESIAN_POINT('Ctrl Pts',(111.44496171353,-5.92451638237235,130.626409536429));
#182661=CARTESIAN_POINT('Ctrl Pts',(111.541946041002,-5.83246842234974,
128.577681904707));
#182662=CARTESIAN_POINT('Ctrl Pts',(111.72757779021,-3.51471719713118,124.752557286777));
#182663=CARTESIAN_POINT('Ctrl Pts',(112.006025414023,3.19176304137608,124.57618197385));
#182664=CARTESIAN_POINT('Ctrl Pts',(112.284473037836,6.96516897115486,130.123198571052));
#182665=CARTESIAN_POINT('Ctrl Pts',(112.562920661649,4.33792488386143,136.296169812387));
#182666=CARTESIAN_POINT('Ctrl Pts',(112.841368285462,-2.27566025228867,
137.422436693472));
#182667=CARTESIAN_POINT('Ctrl Pts',(113.049269667511,-5.65225878233849,
133.722498405386));
#182668=CARTESIAN_POINT('Ctrl Pts',(113.164355174955,-5.92066294021549,
131.282860026435));
#182669=CARTESIAN_POINT('Ctrl Pts',(113.186624807795,-5.9163106462342,130.809833344935));
#182670=CARTESIAN_POINT('',(114.936624807795,-5.90703435793375,130.803551001656));
#182671=CARTESIAN_POINT('Ctrl Pts',(113.186624807795,-5.9163106462342,130.809833344935));
#182672=CARTESIAN_POINT('Ctrl Pts',(113.257171049559,-5.90252335186627,
129.311368827196));
#182673=CARTESIAN_POINT('Ctrl Pts',(113.420533165929,-4.56253139760311,
125.819471574505));
#182674=CARTESIAN_POINT('Ctrl Pts',(113.676711156899,1.31350002779897,123.93033136193));
#182675=CARTESIAN_POINT('Ctrl Pts',(113.955158780714,6.49329434443499,128.193864671035));
#182676=CARTESIAN_POINT('Ctrl Pts',(114.233606404526,5.70606837360377,134.856316225183));
#182677=CARTESIAN_POINT('Ctrl Pts',(114.512054028339,-0.324755675635378,
137.795218524968));
#182678=CARTESIAN_POINT('Ctrl Pts',(114.746393496096,-5.14909238192378,
134.861969788687));
#182679=CARTESIAN_POINT('Ctrl Pts',(114.887917089248,-5.90577078422116,
131.842246860606));
#182680=CARTESIAN_POINT('Ctrl Pts',(114.936624807795,-5.90703435793375,
130.803551001656));
#182681=CARTESIAN_POINT('',(116.686624005233,-5.91849301305788,130.799182298099));
#182682=CARTESIAN_POINT('Ctrl Pts',(114.936624807795,-5.90703435793375,
130.803551001656));
#182683=CARTESIAN_POINT('Ctrl Pts',(114.980732963852,-5.9081786099777,129.86294116798));
#182684=CARTESIAN_POINT('Ctrl Pts',(115.117656994514,-5.25199350988407,
126.944533803055));
#182685=CARTESIAN_POINT('Ctrl Pts',(115.347396899778,-0.670561456245021,
123.838163099281));
#182686=CARTESIAN_POINT('Ctrl Pts',(115.625844523592,5.49840441862291,126.474798355674));
#182687=CARTESIAN_POINT('Ctrl Pts',(115.904292147403,6.61460524476664,133.09008981987));
#182688=CARTESIAN_POINT('Ctrl Pts',(116.182739771217,1.65230699240024,137.604907811225));
#182689=CARTESIAN_POINT('Ctrl Pts',(116.443516934764,-4.41711217639929,
135.980430952529));
#182690=CARTESIAN_POINT('Ctrl Pts',(116.611478223709,-5.90462326373388,
132.393283988731));
#182691=CARTESIAN_POINT('Ctrl Pts',(116.686623638048,-5.91929151057414,
130.799189386355));
#182692=CARTESIAN_POINT('',(118.436626221702,-5.92102170304425,130.807562845889));
#182693=CARTESIAN_POINT('Ctrl Pts',(116.686624807795,-5.91674772039611,
130.79916680515));
#182694=CARTESIAN_POINT('Ctrl Pts',(116.697559326435,-5.91654419251059,
130.567309538048));
#182695=CARTESIAN_POINT('Ctrl Pts',(116.708493845074,-5.9027089717455,130.336026612641));
#182696=CARTESIAN_POINT('Ctrl Pts',(116.719428363714,-5.87546247901726,
130.10659903926));
#182697=CARTESIAN_POINT('Ctrl Pts',(116.726163915423,-5.85867891800975,
129.965273999261));
#182698=CARTESIAN_POINT('Ctrl Pts',(116.732899467133,-5.8368073903389,129.824652131221));
#182699=CARTESIAN_POINT('Ctrl Pts',(116.739635018842,-5.80990738120078,
129.685027430187));
#182700=CARTESIAN_POINT('Ctrl Pts',(116.747058285247,-5.78026082175766,
129.531146739006));
#182701=CARTESIAN_POINT('Ctrl Pts',(116.754481551653,-5.74445170516041,
129.378212000212));
#182702=CARTESIAN_POINT('Ctrl Pts',(116.761904818058,-5.70255141329609,
129.226755489147));
#182703=CARTESIAN_POINT('Ctrl Pts',(116.769319310779,-5.66070064409708,
129.0754779871));
#182704=CARTESIAN_POINT('Ctrl Pts',(116.7767338035,-5.6127731283662,128.925675591356));
#182705=CARTESIAN_POINT('Ctrl Pts',(116.784148296221,-5.55889156157783,
128.777872233904));
#182706=CARTESIAN_POINT('Ctrl Pts',(116.791555642575,-5.50506192787217,
128.630211334891));
#182707=CARTESIAN_POINT('Ctrl Pts',(116.798962988928,-5.44528979480404,
128.484545986759));
#182708=CARTESIAN_POINT('Ctrl Pts',(116.806370335282,-5.37974811534769,
128.34138664736));
#182709=CARTESIAN_POINT('Ctrl Pts',(116.813772156957,-5.31425531934863,
128.198334081597));
#182710=CARTESIAN_POINT('Ctrl Pts',(116.821173978633,-5.24300169982891,
128.057784140942));
#182711=CARTESIAN_POINT('Ctrl Pts',(116.828575800308,-5.16620889014691,
127.920228813042));
#182712=CARTESIAN_POINT('Ctrl Pts',(116.835973714619,-5.08945661879133,
127.782746099529));
#182713=CARTESIAN_POINT('Ctrl Pts',(116.843371628931,-5.00717116225369,
127.648255175586));
#182714=CARTESIAN_POINT('Ctrl Pts',(116.850769543242,-4.91962075296629,
127.517224750358));
#182715=CARTESIAN_POINT('Ctrl Pts',(116.858166228154,-4.83208489296877,
127.386216100011));
#182716=CARTESIAN_POINT('Ctrl Pts',(116.865562913066,-4.73928602390572,
127.258667117113));
#182717=CARTESIAN_POINT('Ctrl Pts',(116.872959597979,-4.64153655180344,
127.135018850876));
#182718=CARTESIAN_POINT('Ctrl Pts',(116.880355954914,-4.54379141401512,
127.011376067333));
#182719=CARTESIAN_POINT('Ctrl Pts',(116.887752311849,-4.44109634116225,
126.891633949385));
#182720=CARTESIAN_POINT('Ctrl Pts',(116.895148668785,-4.33380483171786,
126.776201454489));
#182721=CARTESIAN_POINT('Ctrl Pts',(116.902546158121,-4.22649689566947,
126.660751286584));
#182722=CARTESIAN_POINT('Ctrl Pts',(116.909943647458,-4.11459137597694,
126.549612328952));
#182723=CARTESIAN_POINT('Ctrl Pts',(116.917341136794,-3.99847940828271,
126.443157459716));
#182724=CARTESIAN_POINT('Ctrl Pts',(116.924741219309,-3.88232673771803,
126.336665272891));
#182725=CARTESIAN_POINT('Ctrl Pts',(116.932141301824,-3.76196495829002,
126.234860695784));
#182726=CARTESIAN_POINT('Ctrl Pts',(116.939541384339,-3.63781899221396,
126.138076920405));
#182727=CARTESIAN_POINT('Ctrl Pts',(116.946949604006,-3.51353651488587,
126.041186721316));
#182728=CARTESIAN_POINT('Ctrl Pts',(116.954357823672,-3.38546183549985,
125.949328579188));
#182729=CARTESIAN_POINT('Ctrl Pts',(116.961766043339,-3.25405021861709,
125.862793281465));
#182730=CARTESIAN_POINT('Ctrl Pts',(116.969178822641,-3.12255772007668,
125.776204722711));
#182731=CARTESIAN_POINT('Ctrl Pts',(116.976591601943,-2.98772451050982,
125.694945728685));
#182732=CARTESIAN_POINT('Ctrl Pts',(116.984004381245,-2.85003079089306,
125.619261288386));
#182733=CARTESIAN_POINT('Ctrl Pts',(116.991427752274,-2.71214032803271,
125.54346870661));
#182734=CARTESIAN_POINT('Ctrl Pts',(116.998851123302,-2.57138152517667,
125.473266752986));
#182735=CARTESIAN_POINT('Ctrl Pts',(117.006274494331,-2.42825565114771,
125.408852758692));
#182736=CARTESIAN_POINT('Ctrl Pts',(117.010210543773,-2.35236687846472,
125.374698913318));
#182737=CARTESIAN_POINT('Ctrl Pts',(117.014146593214,-2.2758129214637,125.342171447449));
#182738=CARTESIAN_POINT('Ctrl Pts',(117.018082642656,-2.19867014271157,
125.311294063623));
#182739=CARTESIAN_POINT('Ctrl Pts',(117.025505909061,-2.05318126955525,
125.253060281388));
#182740=CARTESIAN_POINT('Ctrl Pts',(117.032929175466,-1.90515724026218,
125.20052254339));
#182741=CARTESIAN_POINT('Ctrl Pts',(117.040352441872,-1.75508445680622,
125.153908501852));
#182742=CARTESIAN_POINT('Ctrl Pts',(117.047766934593,-1.60518904691754,
125.10734955424));
#182743=CARTESIAN_POINT('Ctrl Pts',(117.055181427314,-1.4532500558055,125.066700476575));
#182744=CARTESIAN_POINT('Ctrl Pts',(117.062595920035,-1.29977460219091,
125.032141239718));
#182745=CARTESIAN_POINT('Ctrl Pts',(117.070003266389,-1.14644707399665,
124.997615312355));
#182746=CARTESIAN_POINT('Ctrl Pts',(117.077410612743,-0.991586393215401,
124.969167622001));
#182747=CARTESIAN_POINT('Ctrl Pts',(117.084817959096,-0.835715507803487,
124.946928573358));
#182748=CARTESIAN_POINT('Ctrl Pts',(117.092219780772,-0.679960876778697,
124.924706111436));
#182749=CARTESIAN_POINT('Ctrl Pts',(117.099621602447,-0.523197909306233,
124.908683123499));
#182750=CARTESIAN_POINT('Ctrl Pts',(117.107023424123,-0.365960326771369,
124.898939074464));
#182751=CARTESIAN_POINT('Ctrl Pts',(117.114421338434,-0.20880574873239,
124.889200169237));
#182752=CARTESIAN_POINT('Ctrl Pts',(117.121819252745,-0.0511774262446159,
124.885733624754));
#182753=CARTESIAN_POINT('Ctrl Pts',(117.129217167057,0.106385316232477,
124.888567118213));
#182754=CARTESIAN_POINT('Ctrl Pts',(117.136613851969,0.263921874640249,
124.891400140796));
#182755=CARTESIAN_POINT('Ctrl Pts',(117.144010536881,0.421392501794947,
124.900531116727));
#182756=CARTESIAN_POINT('Ctrl Pts',(117.151407221793,0.578257267417322,
124.915935607839));
#182757=CARTESIAN_POINT('Ctrl Pts',(117.158803578729,0.735115077491607,
124.931339415899));
#182758=CARTESIAN_POINT('Ctrl Pts',(117.166199935664,0.891366707938846,
124.953016149552));
#182759=CARTESIAN_POINT('Ctrl Pts',(117.1735962926,1.04647701670976,124.980889452015));
#182760=CARTESIAN_POINT('Ctrl Pts',(117.180993781936,1.20161107326492,125.008767021953));
#182761=CARTESIAN_POINT('Ctrl Pts',(117.188391271273,1.35560309277827,125.04284298368));
#182762=CARTESIAN_POINT('Ctrl Pts',(117.195788760609,1.50792794395739,125.082989813438));
#182763=CARTESIAN_POINT('Ctrl Pts',(117.203188843124,1.66030619237707,125.123150716604));
#182764=CARTESIAN_POINT('Ctrl Pts',(117.210588925639,1.81101574813416,125.169386629819));
#182765=CARTESIAN_POINT('Ctrl Pts',(117.217989008154,1.95954660651778,125.22152015241));
#182766=CARTESIAN_POINT('Ctrl Pts',(117.225397227821,2.10824078984943,125.273711001168));
#182767=CARTESIAN_POINT('Ctrl Pts',(117.232805447487,2.25475113898685,125.33181228662));
#182768=CARTESIAN_POINT('Ctrl Pts',(117.240213667154,2.39858692460105,125.395598159514));
#182769=CARTESIAN_POINT('Ctrl Pts',(117.247626446456,2.54251123874147,125.459423291549));
#182770=CARTESIAN_POINT('Ctrl Pts',(117.255039225758,2.68375737504578,125.528939818301));
#182771=CARTESIAN_POINT('Ctrl Pts',(117.26245200506,2.82185965697311,125.603876155629));
#182772=CARTESIAN_POINT('Ctrl Pts',(117.269875376089,2.96015926591721,125.67891956551));
#182773=CARTESIAN_POINT('Ctrl Pts',(117.277298747117,3.09530572889295,125.759398062139));
#182774=CARTESIAN_POINT('Ctrl Pts',(117.284722118146,3.22686207754897,125.844996576182));
#182775=CARTESIAN_POINT('Ctrl Pts',(117.288658167587,3.29661641025614,125.890382962234));
#182776=CARTESIAN_POINT('Ctrl Pts',(117.292594217028,3.36536197219685,125.937208084541));
#182777=CARTESIAN_POINT('Ctrl Pts',(117.296530266468,3.43303754592154,125.985420508912));
#182778=CARTESIAN_POINT('Ctrl Pts',(117.303953532874,3.56067156588671,126.07634763662));
#182779=CARTESIAN_POINT('Ctrl Pts',(117.311376799279,3.68488365633071,126.17248651403));
#182780=CARTESIAN_POINT('Ctrl Pts',(117.318800065685,3.80521937484481,126.273550968971));
#182781=CARTESIAN_POINT('Ctrl Pts',(117.326214558406,3.92541286653305,126.374495974119));
#182782=CARTESIAN_POINT('Ctrl Pts',(117.333629051127,4.04173882282624,126.480354731091));
#182783=CARTESIAN_POINT('Ctrl Pts',(117.341043543848,4.15377171908746,126.59079786519));
#182784=CARTESIAN_POINT('Ctrl Pts',(117.348450890201,4.2656966338253,126.701134550039));
#182785=CARTESIAN_POINT('Ctrl Pts',(117.355858236555,4.37333646204576,126.816046555153));
#182786=CARTESIAN_POINT('Ctrl Pts',(117.363265582909,4.47629882443489,126.935164396532));
#182787=CARTESIAN_POINT('Ctrl Pts',(117.370667404584,4.5791843936096,127.054193395332));
#182788=CARTESIAN_POINT('Ctrl Pts',(117.37806922626,4.67739920022347,127.177421703261));
#182789=CARTESIAN_POINT('Ctrl Pts',(117.385471047935,4.77058789874365,127.304443238133));
#182790=CARTESIAN_POINT('Ctrl Pts',(117.392868962247,4.86372740367526,127.431397719325));
#182791=CARTESIAN_POINT('Ctrl Pts',(117.400266876558,4.95184586431757,127.562141139332));
#182792=CARTESIAN_POINT('Ctrl Pts',(117.407664790869,5.03462847701474,127.696234709413));
#182793=CARTESIAN_POINT('Ctrl Pts',(117.415061475782,5.11739733274345,127.830305995576));
#182794=CARTESIAN_POINT('Ctrl Pts',(117.422458160694,5.19483190450104,127.967726009528));
#182795=CARTESIAN_POINT('Ctrl Pts',(117.429854845606,5.2666609073049,128.108027283209));
#182796=CARTESIAN_POINT('Ctrl Pts',(117.437251202542,5.33848672513551,128.248322335784));
#182797=CARTESIAN_POINT('Ctrl Pts',(117.444647559477,5.40470729811113,128.391498061778));
#182798=CARTESIAN_POINT('Ctrl Pts',(117.452043916412,5.46509761000641,128.537062958324));
#182799=CARTESIAN_POINT('Ctrl Pts',(117.459441405749,5.52549716781264,128.682650141228));
#182800=CARTESIAN_POINT('Ctrl Pts',(117.466838895086,5.58006454414085,128.830626878191));
#182801=CARTESIAN_POINT('Ctrl Pts',(117.474236384422,5.6286231820523,128.980482431677));
#182802=CARTESIAN_POINT('Ctrl Pts',(117.481636466937,5.677198842119,129.130390516794));
#182803=CARTESIAN_POINT('Ctrl Pts',(117.489036549452,5.71976145503388,129.282178374837));
#182804=CARTESIAN_POINT('Ctrl Pts',(117.496436631967,5.75618460300468,129.435321035));
#182805=CARTESIAN_POINT('Ctrl Pts',(117.503844851634,5.79264780197107,129.588632091261));
#182806=CARTESIAN_POINT('Ctrl Pts',(117.5112530713,5.82295796742928,129.743300561369));
#182807=CARTESIAN_POINT('Ctrl Pts',(117.518661290967,5.84703986156242,129.898791503804));
#182808=CARTESIAN_POINT('Ctrl Pts',(117.526074070269,5.87113657769958,130.054378148319));
#182809=CARTESIAN_POINT('Ctrl Pts',(117.533486849571,5.88899734173318,130.210787903836));
#182810=CARTESIAN_POINT('Ctrl Pts',(117.540899628873,5.90059893554949,130.367482185628));
#182811=CARTESIAN_POINT('Ctrl Pts',(117.548322999902,5.91221710626711,130.524400359559));
#182812=CARTESIAN_POINT('Ctrl Pts',(117.555746370931,5.91755823215747,130.681603499632));
#182813=CARTESIAN_POINT('Ctrl Pts',(117.563169741959,5.91665119790844,130.838553669326));
#182814=CARTESIAN_POINT('Ctrl Pts',(117.5671057914,5.91617026658563,130.921772415262));
#182815=CARTESIAN_POINT('Ctrl Pts',(117.571041840841,5.91393362046543,131.00492012587));
#182816=CARTESIAN_POINT('Ctrl Pts',(117.574977890281,5.90995144306108,131.087917495741));
#182817=CARTESIAN_POINT('Ctrl Pts',(117.582401156687,5.90244118075565,131.244447945065));
#182818=CARTESIAN_POINT('Ctrl Pts',(117.589824423092,5.88869648933059,131.400916506187));
#182819=CARTESIAN_POINT('Ctrl Pts',(117.597247689498,5.86871249631517,131.556786160789));
#182820=CARTESIAN_POINT('Ctrl Pts',(117.604662182219,5.84875212271991,131.712471590403));
#182821=CARTESIAN_POINT('Ctrl Pts',(117.61207667494,5.82256717319967,131.867559155842));
#182822=CARTESIAN_POINT('Ctrl Pts',(117.619491167661,5.79020475355474,132.021512816107));
#182823=CARTESIAN_POINT('Ctrl Pts',(117.626898514014,5.75787352602829,132.175318090037));
#182824=CARTESIAN_POINT('Ctrl Pts',(117.634305860368,5.7193767580515,132.327991271683));
#182825=CARTESIAN_POINT('Ctrl Pts',(117.641713206722,5.6748132163735,132.479002526086));
#182826=CARTESIAN_POINT('Ctrl Pts',(117.649115028397,5.63028291186618,132.629901150599));
#182827=CARTESIAN_POINT('Ctrl Pts',(117.656516850073,5.57969494840352,132.779139959445));
#182828=CARTESIAN_POINT('Ctrl Pts',(117.663918671748,5.5231989014902,132.926200493023));
#182829=CARTESIAN_POINT('Ctrl Pts',(117.671316586059,5.46673267840028,133.073183394489));
#182830=CARTESIAN_POINT('Ctrl Pts',(117.678714500371,5.40436471669324,133.217989963171));
#182831=CARTESIAN_POINT('Ctrl Pts',(117.686112414682,5.33629402269755,133.360118169804));
#182832=CARTESIAN_POINT('Ctrl Pts',(117.693509099594,5.26823464081633,133.502222757308));
#182833=CARTESIAN_POINT('Ctrl Pts',(117.700905784506,5.19447456862119,133.6416495298));
#182834=CARTESIAN_POINT('Ctrl Pts',(117.708302469419,5.11526046407216,133.777917569635));
#182835=CARTESIAN_POINT('Ctrl Pts',(117.715698826354,5.03604987195955,133.914179567203));
#182836=CARTESIAN_POINT('Ctrl Pts',(117.72309518329,4.95138591595434,134.047282787873));
#182837=CARTESIAN_POINT('Ctrl Pts',(117.730491540225,4.86156048457356,134.176772249816));
#182838=CARTESIAN_POINT('Ctrl Pts',(117.737889029561,4.77172130068986,134.306281536926));
#182839=CARTESIAN_POINT('Ctrl Pts',(117.745286518898,4.67671928075236,134.43217565692));
#182840=CARTESIAN_POINT('Ctrl Pts',(117.752684008235,4.57688868937742,134.554030001332));
#182841=CARTESIAN_POINT('Ctrl Pts',(117.76008409075,4.4770231025435,134.675927061594));
#182842=CARTESIAN_POINT('Ctrl Pts',(117.767484173265,4.37232581064742,134.793781238172));
#182843=CARTESIAN_POINT('Ctrl Pts',(117.77488425578,4.26317015459075,134.907202412652));
#182844=CARTESIAN_POINT('Ctrl Pts',(117.782292475446,4.1538944706687,135.020748305374));
#182845=CARTESIAN_POINT('Ctrl Pts',(117.789700695112,4.04015089112619,135.129851192083));
#182846=CARTESIAN_POINT('Ctrl Pts',(117.797108914779,3.92234880953655,135.234158624115));
#182847=CARTESIAN_POINT('Ctrl Pts',(117.804521694081,3.80447422273125,135.338530255631));
#182848=CARTESIAN_POINT('Ctrl Pts',(117.811934473383,3.68253644489493,135.438100315633));
#182849=CARTESIAN_POINT('Ctrl Pts',(117.819347252685,3.55697605265327,135.532558151865));
#182850=CARTESIAN_POINT('Ctrl Pts',(117.826770623714,3.43123625383499,135.627150953883));
#182851=CARTESIAN_POINT('Ctrl Pts',(117.834193994743,3.30186380887613,135.716616731473));
#182852=CARTESIAN_POINT('Ctrl Pts',(117.841617365771,3.16932691188674,135.800689018311));
#182853=CARTESIAN_POINT('Ctrl Pts',(117.845553415212,3.09905266891977,135.845266162082));
#182854=CARTESIAN_POINT('Ctrl Pts',(117.849489464653,3.02788918325162,135.88832777694));
#182855=CARTESIAN_POINT('Ctrl Pts',(117.853425514094,2.95590868120716,135.929839564051));
#182856=CARTESIAN_POINT('Ctrl Pts',(117.8608487805,2.82015570079294,136.008129499001));
#182857=CARTESIAN_POINT('Ctrl Pts',(117.868272046905,2.68108492745272,136.081140780079));
#182858=CARTESIAN_POINT('Ctrl Pts',(117.875695313311,2.53914553621633,136.148579036419));
#182859=CARTESIAN_POINT('Ctrl Pts',(117.883109806032,2.39737390555306,136.215937586342));
#182860=CARTESIAN_POINT('Ctrl Pts',(117.890524298753,2.25274073962245,136.277736064058));
#182861=CARTESIAN_POINT('Ctrl Pts',(117.897938791474,2.10572248673276,136.33372435776));
#182862=CARTESIAN_POINT('Ctrl Pts',(117.905346137827,1.95884593557024,136.389658687836));
#182863=CARTESIAN_POINT('Ctrl Pts',(117.912753484181,1.80958922049484,136.439793850581));
#182864=CARTESIAN_POINT('Ctrl Pts',(117.920160830535,1.65845149250135,136.483926552523));
#182865=CARTESIAN_POINT('Ctrl Pts',(117.927562652211,1.50742648872749,136.52802633863));
#182866=CARTESIAN_POINT('Ctrl Pts',(117.934964473886,1.35452362225062,136.566132473785));
#182867=CARTESIAN_POINT('Ctrl Pts',(117.942366295561,1.2002599370313,136.598090560017));
#182868=CARTESIAN_POINT('Ctrl Pts',(117.949764209873,1.04607768641041,136.630031775825));
#182869=CARTESIAN_POINT('Ctrl Pts',(117.957162124184,0.890536412317678,
136.655831330758));
#182870=CARTESIAN_POINT('Ctrl Pts',(117.964560038495,0.734166053972068,
136.675385295397));
#182871=CARTESIAN_POINT('Ctrl Pts',(117.971956723408,0.577821681543391,
136.694936010521));
#182872=CARTESIAN_POINT('Ctrl Pts',(117.97935340832,0.420648868362236,136.70824314901));
#182873=CARTESIAN_POINT('Ctrl Pts',(117.986750093232,0.263185548715929,
136.715254283455));
#182874=CARTESIAN_POINT('Ctrl Pts',(117.994146450168,0.105729211158112,
136.722265107019));
#182875=CARTESIAN_POINT('Ctrl Pts',(118.001542807103,-0.0520172343242812,
136.722980465023));
#182876=CARTESIAN_POINT('Ctrl Pts',(118.008939164039,-0.209513225759455,
136.71740000275));
#182877=CARTESIAN_POINT('Ctrl Pts',(118.016336653375,-0.367033330232874,
136.711818686093));
#182878=CARTESIAN_POINT('Ctrl Pts',(118.023734142712,-0.524302531221012,
136.699939643114));
#182879=CARTESIAN_POINT('Ctrl Pts',(118.031131632048,-0.680782915405135,
136.681814588853));
#182880=CARTESIAN_POINT('Ctrl Pts',(118.038531714563,-0.837318153545358,
136.663683180882));
#182881=CARTESIAN_POINT('Ctrl Pts',(118.045931797078,-0.993063653747919,
136.639301445216));
#182882=CARTESIAN_POINT('Ctrl Pts',(118.053331879593,-1.14748939846722,
136.608772615599));
#182883=CARTESIAN_POINT('Ctrl Pts',(118.06074009926,-1.3020849501683,136.578210216395));
#182884=CARTESIAN_POINT('Ctrl Pts',(118.068148318926,-1.45535748179579,
136.541487296792));
#182885=CARTESIAN_POINT('Ctrl Pts',(118.075556538593,-1.60678918108002,
136.498757784085));
#182886=CARTESIAN_POINT('Ctrl Pts',(118.082969317895,-1.75831408404838,
136.456001972077));
#182887=CARTESIAN_POINT('Ctrl Pts',(118.090382097197,-1.90799554291565,
136.40723231569));
#182888=CARTESIAN_POINT('Ctrl Pts',(118.097794876499,-2.05533405471236,
136.352651569385));
#182889=CARTESIAN_POINT('Ctrl Pts',(118.105218247528,-2.20288309068433,
136.297992835551));
#182890=CARTESIAN_POINT('Ctrl Pts',(118.112641618557,-2.34808214977163,
136.237506571698));
#182891=CARTESIAN_POINT('Ctrl Pts',(118.120064989585,-2.49045397595665,
136.171442651236));
#182892=CARTESIAN_POINT('Ctrl Pts',(118.124001039026,-2.56594293436141,
136.136413975426));
#182893=CARTESIAN_POINT('Ctrl Pts',(118.127937088467,-2.64063749277048,
136.099817974152));
#182894=CARTESIAN_POINT('Ctrl Pts',(118.131873137907,-2.71446975451147,
136.061696874107));
#182895=CARTESIAN_POINT('Ctrl Pts',(118.139296404313,-2.85371509593537,
135.989801669139));
#182896=CARTESIAN_POINT('Ctrl Pts',(118.146719670718,-2.99031270447579,
135.912261869661));
#182897=CARTESIAN_POINT('Ctrl Pts',(118.154142937123,-3.12377212751132,
135.829296264705));
#182898=CARTESIAN_POINT('Ctrl Pts',(118.161557429844,-3.25707381259186,
135.746428718203));
#182899=CARTESIAN_POINT('Ctrl Pts',(118.168971922565,-3.38724438116514,
135.658148326199));
#182900=CARTESIAN_POINT('Ctrl Pts',(118.176386415286,-3.51381587513444,
135.564720746606));
#182901=CARTESIAN_POINT('Ctrl Pts',(118.18379376164,-3.6402653747327,135.471383216031));
#182902=CARTESIAN_POINT('Ctrl Pts',(118.191201107994,-3.76312240734789,
135.372908594552));
#182903=CARTESIAN_POINT('Ctrl Pts',(118.198608454348,-3.88194613311887,
135.269606946948));
#182904=CARTESIAN_POINT('Ctrl Pts',(118.206010276023,-4.00068123567213,
135.166382345611));
#182905=CARTESIAN_POINT('Ctrl Pts',(118.213412097698,-4.11538874059069,
135.058338130456));
#182906=CARTESIAN_POINT('Ctrl Pts',(118.220813919374,-4.22565927359882,
134.945825849335));
#182907=CARTESIAN_POINT('Ctrl Pts',(118.228211833685,-4.33587159565062,
134.833372962571));
#182908=CARTESIAN_POINT('Ctrl Pts',(118.235609747996,-4.44165134985032,
134.71645697315));
#182909=CARTESIAN_POINT('Ctrl Pts',(118.243007662308,-4.54262465234175,
134.595467557556));
#182910=CARTESIAN_POINT('Ctrl Pts',(118.25040434722,-4.64358117490245,134.474498248207));
#182911=CARTESIAN_POINT('Ctrl Pts',(118.257801032132,-4.73973259207421,
134.34945714251));
#182912=CARTESIAN_POINT('Ctrl Pts',(118.265197717044,-4.83074402857291,
134.220768481523));
#182913=CARTESIAN_POINT('Ctrl Pts',(118.27259407398,-4.92175142952915,134.092085526726));
#182914=CARTESIAN_POINT('Ctrl Pts',(118.279990430915,-5.0076190874318,133.959755643005));
#182915=CARTESIAN_POINT('Ctrl Pts',(118.287386787851,-5.08805451689844,
133.824233428724));
#182916=CARTESIAN_POINT('Ctrl Pts',(118.294784277187,-5.16850226123474,
133.688690465645));
#182917=CARTESIAN_POINT('Ctrl Pts',(118.302181766524,-5.24351593059231,
133.549954519867));
#182918=CARTESIAN_POINT('Ctrl Pts',(118.30957925586,-5.31284827901142,133.408506106341));
#182919=CARTESIAN_POINT('Ctrl Pts',(118.316979338375,-5.38220493177775,
133.267008108293));
#182920=CARTESIAN_POINT('Ctrl Pts',(118.32437942089,-5.44587613419044,133.122796084346));
#182921=CARTESIAN_POINT('Ctrl Pts',(118.331779503405,-5.50366225229148,
132.976371753634));
#182922=CARTESIAN_POINT('Ctrl Pts',(118.339187723072,-5.56151191216997,
132.829786414316));
#182923=CARTESIAN_POINT('Ctrl Pts',(118.346595942738,-5.61346342709531,
132.680984257502));
#182924=CARTESIAN_POINT('Ctrl Pts',(118.354004162405,-5.65936641028078,
132.530484134782));
#182925=CARTESIAN_POINT('Ctrl Pts',(118.361416941707,-5.70529764598653,
132.379891381747));
#182926=CARTESIAN_POINT('Ctrl Pts',(118.368829721009,-5.7451728375307,132.227598940661));
#182927=CARTESIAN_POINT('Ctrl Pts',(118.376242500311,-5.77889257442692,
132.074136651256));
#182928=CARTESIAN_POINT('Ctrl Pts',(118.38366587134,-5.81266049166447,131.920455087736));
#182929=CARTESIAN_POINT('Ctrl Pts',(118.391089242369,-5.84025532294638,
131.765600704004));
#182930=CARTESIAN_POINT('Ctrl Pts',(118.398512613398,-5.86162932531237,
131.610110091744));
#182931=CARTESIAN_POINT('Ctrl Pts',(118.402448662838,-5.87296233422877,
131.527665238179));
#182932=CARTESIAN_POINT('Ctrl Pts',(118.406384712279,-5.88254731524014,
131.445041558131));
#182933=CARTESIAN_POINT('Ctrl Pts',(118.41032076172,-5.89038309505153,131.362318999554));
#182934=CARTESIAN_POINT('Ctrl Pts',(118.419088777078,-5.90783822074711,
131.178044722765));
#182935=CARTESIAN_POINT('Ctrl Pts',(118.427856792437,-5.91664794092523,
130.992938687461));
#182936=CARTESIAN_POINT('Ctrl Pts',(118.436624807795,-5.91674911845536,
130.807590440738));
#182937=CARTESIAN_POINT('',(120.186623619739,-5.91251430151314,130.808017835056));
#182938=CARTESIAN_POINT('Ctrl Pts',(118.436627322331,-5.92434761776706,
130.807541365187));
#182939=CARTESIAN_POINT('Ctrl Pts',(118.520674343399,-5.91263932333013,
129.028571282425));
#182940=CARTESIAN_POINT('Ctrl Pts',(118.69753723907,-4.11280805307987,125.264539470063));
#182941=CARTESIAN_POINT('Ctrl Pts',(118.967216009345,2.29579285864173,124.193241523149));
#182942=CARTESIAN_POINT('Ctrl Pts',(119.245663633159,6.80305384870884,129.162404813681));
#182943=CARTESIAN_POINT('Ctrl Pts',(119.524111256971,5.05864069946902,135.640445273981));
#182944=CARTESIAN_POINT('Ctrl Pts',(119.802558880784,-1.33441612424553,
137.674360190906));
#182945=CARTESIAN_POINT('Ctrl Pts',(120.023396027555,-5.4322063654912,134.280458789483));
#182946=CARTESIAN_POINT('Ctrl Pts',(120.151417299721,-5.91340439953517,
131.558097539106));
#182947=CARTESIAN_POINT('Ctrl Pts',(120.186622697283,-5.90922639532864,
130.808035468526));
#182948=CARTESIAN_POINT('',(121.936626022957,-5.91342861064485,130.799761379028));
#182949=CARTESIAN_POINT('Ctrl Pts',(120.186624807795,-5.91674888370799,
130.807995124438));
#182950=CARTESIAN_POINT('Ctrl Pts',(120.194083991,-5.9168466282442,130.648873159404));
#182951=CARTESIAN_POINT('Ctrl Pts',(120.201543174204,-5.91052102208661,
130.489729998654));
#182952=CARTESIAN_POINT('Ctrl Pts',(120.209002357409,-5.89779360542141,
130.331115279131));
#182953=CARTESIAN_POINT('Ctrl Pts',(120.216462331572,-5.88506483916271,
130.172483740374));
#182954=CARTESIAN_POINT('Ctrl Pts',(120.223922305736,-5.86593293838123,
130.014381117835));
#182955=CARTESIAN_POINT('Ctrl Pts',(120.231382279899,-5.84047139694184,
129.857352473987));
#182956=CARTESIAN_POINT('Ctrl Pts',(120.238844423679,-5.81500245041472,
129.700278160835));
#182957=CARTESIAN_POINT('Ctrl Pts',(120.246306567458,-5.78320025401866,
129.544278808323));
#182958=CARTESIAN_POINT('Ctrl Pts',(120.253768711238,-5.74518954052248,
129.389889795678));
#182959=CARTESIAN_POINT('Ctrl Pts',(120.261234404323,-5.70716074755135,
129.235427349203));
#182960=CARTESIAN_POINT('Ctrl Pts',(120.268700097408,-5.66291764158275,
129.082577121966));
#182961=CARTESIAN_POINT('Ctrl Pts',(120.276165790493,-5.61263496516564,
128.931859800397));
#182962=CARTESIAN_POINT('Ctrl Pts',(120.28364116073,-5.56228711153645,128.780947116616));
#182963=CARTESIAN_POINT('Ctrl Pts',(120.291116530966,-5.50588416412254,
128.63217320733));
#182964=CARTESIAN_POINT('Ctrl Pts',(120.298591901202,-5.44364958479852,
128.486040156451));
#182965=CARTESIAN_POINT('Ctrl Pts',(120.306072502209,-5.38137145782292,
128.339804851307));
#182966=CARTESIAN_POINT('Ctrl Pts',(120.313553103216,-5.3132537206381,128.196214416576));
#182967=CARTESIAN_POINT('Ctrl Pts',(120.321033704224,-5.23956589460368,
128.05574645792));
#182968=CARTESIAN_POINT('Ctrl Pts',(120.32852648743,-5.16575806754871,127.915049746439));
#182969=CARTESIAN_POINT('Ctrl Pts',(120.336019270636,-5.08636220911963,
127.777485986279));
#182970=CARTESIAN_POINT('Ctrl Pts',(120.343512053842,-5.00169188693494,
127.64350490579));
#182971=CARTESIAN_POINT('Ctrl Pts',(120.348826078698,-4.94164207843157,
127.548482966356));
#182972=CARTESIAN_POINT('Ctrl Pts',(120.354140103554,-4.87894016049074,
127.455262458878));
#182973=CARTESIAN_POINT('Ctrl Pts',(120.359454128411,-4.81371002966179,
127.363993440529));
#182974=CARTESIAN_POINT('Ctrl Pts',(120.366877394816,-4.72258876999511,
127.236497943973));
#182975=CARTESIAN_POINT('Ctrl Pts',(120.374300661221,-4.6262609742564,127.11243230437));
#182976=CARTESIAN_POINT('Ctrl Pts',(120.381723927627,-4.52501350586842,
126.9922505281));
#182977=CARTESIAN_POINT('Ctrl Pts',(120.389138420348,-4.42388570358,126.872210796709));
#182978=CARTESIAN_POINT('Ctrl Pts',(120.396552913069,-4.3178500408882,126.756046074127));
#182979=CARTESIAN_POINT('Ctrl Pts',(120.40396740579,-4.20723653968417,126.644181383249));
#182980=CARTESIAN_POINT('Ctrl Pts',(120.411374752144,-4.09672965193697,
126.53242451177));
#182981=CARTESIAN_POINT('Ctrl Pts',(120.418782098497,-3.98165397039524,
126.424959684706));
#182982=CARTESIAN_POINT('Ctrl Pts',(120.426189444851,-3.8623795757647,126.322178718623));
#182983=CARTESIAN_POINT('Ctrl Pts',(120.433591266527,-3.7431941404779,126.219474410462));
#182984=CARTESIAN_POINT('Ctrl Pts',(120.440993088202,-3.61981650902956,
126.121447250087));
#182985=CARTESIAN_POINT('Ctrl Pts',(120.448394909877,-3.49265330391212,
126.028451964632));
#182986=CARTESIAN_POINT('Ctrl Pts',(120.455792824189,-3.36555722726127,
125.935505770664));
#182987=CARTESIAN_POINT('Ctrl Pts',(120.4631907385,-3.23467985735817,125.847586381291));
#182988=CARTESIAN_POINT('Ctrl Pts',(120.470588652811,-3.10046046151212,
125.765007932042));
#182989=CARTESIAN_POINT('Ctrl Pts',(120.477985337723,-2.96626337049419,
125.682443205833));
#182990=CARTESIAN_POINT('Ctrl Pts',(120.485382022635,-2.82872567343642,
125.605217853611));
#182991=CARTESIAN_POINT('Ctrl Pts',(120.492778707548,-2.68831525070869,
125.533602448639));
#182992=CARTESIAN_POINT('Ctrl Pts',(120.500175064483,-2.54791105392604,
125.461990219169));
#182993=CARTESIAN_POINT('Ctrl Pts',(120.507571421418,-2.40463471728811,
125.395987611958));
#182994=CARTESIAN_POINT('Ctrl Pts',(120.514967778354,-2.25897808553035,
125.335818894986));
#182995=CARTESIAN_POINT('Ctrl Pts',(120.52236526769,-2.11329915337054,125.275640966031));
#182996=CARTESIAN_POINT('Ctrl Pts',(120.529762757027,-1.96523954550562,
125.221298848294));
#182997=CARTESIAN_POINT('Ctrl Pts',(120.537160246363,-1.81531026757037,
125.172968321255));
#182998=CARTESIAN_POINT('Ctrl Pts',(120.544560328878,-1.66532843215927,
125.124620852024));
#182999=CARTESIAN_POINT('Ctrl Pts',(120.551960411393,-1.513475976834,125.082289283677));
#183000=CARTESIAN_POINT('Ctrl Pts',(120.559360493908,-1.36027806417806,
125.046099234942));
#183001=CARTESIAN_POINT('Ctrl Pts',(120.566768713574,-1.20691169466769,
125.009869391529));
#183002=CARTESIAN_POINT('Ctrl Pts',(120.574176933241,-1.05219727675213,
124.979794640251));
#183003=CARTESIAN_POINT('Ctrl Pts',(120.581585152907,-0.896669865831108,
124.955949404748));
#183004=CARTESIAN_POINT('Ctrl Pts',(120.588997932209,-0.74104673038411,
124.932089492902));
#183005=CARTESIAN_POINT('Ctrl Pts',(120.596410711511,-0.584609974946085,
124.914466778572));
#183006=CARTESIAN_POINT('Ctrl Pts',(120.603823490813,-0.427898218953112,
124.903103660212));
#183007=CARTESIAN_POINT('Ctrl Pts',(120.611246861842,-0.270962545854011,
124.891724305696));
#183008=CARTESIAN_POINT('Ctrl Pts',(120.618670232871,-0.113751459536328,
124.886622422408));
#183009=CARTESIAN_POINT('Ctrl Pts',(120.626093603899,0.0431971480589227,
124.887768307046));
#183010=CARTESIAN_POINT('Ctrl Pts',(120.630029653341,0.126415065745407,
124.888375882577));
#183011=CARTESIAN_POINT('Ctrl Pts',(120.633965702782,0.209559276287754,
124.890739062768));
#183012=CARTESIAN_POINT('Ctrl Pts',(120.637901752223,0.292550489865668,
124.89484754343));
#183013=CARTESIAN_POINT('Ctrl Pts',(120.645325018628,0.449069328589629,
124.902596009737));
#183014=CARTESIAN_POINT('Ctrl Pts',(120.652748285034,0.605516791442864,
124.91657880376));
#183015=CARTESIAN_POINT('Ctrl Pts',(120.660171551439,0.761355853315115,
124.936799980715));
#183016=CARTESIAN_POINT('Ctrl Pts',(120.66758604416,0.917010726358304,124.956997257918));
#183017=CARTESIAN_POINT('Ctrl Pts',(120.675000536881,1.07205826317264,124.983418193991));
#183018=CARTESIAN_POINT('Ctrl Pts',(120.682415029602,1.22596249506846,125.016014867424));
#183019=CARTESIAN_POINT('Ctrl Pts',(120.689822375956,1.37971838827108,125.048580122956));
#183020=CARTESIAN_POINT('Ctrl Pts',(120.69722972231,1.53233280759622,125.087309188948));
#183021=CARTESIAN_POINT('Ctrl Pts',(120.704637068663,1.68327606900739,125.132102492444));
#183022=CARTESIAN_POINT('Ctrl Pts',(120.712038890339,1.83410675123923,125.176862387406));
#183023=CARTESIAN_POINT('Ctrl Pts',(120.719440712014,1.98326840100057,125.227677408351));
#183024=CARTESIAN_POINT('Ctrl Pts',(120.72684253369,2.13024278691824,125.284397190941));
#183025=CARTESIAN_POINT('Ctrl Pts',(120.734240448001,2.27713958620143,125.341087031599));
#183026=CARTESIAN_POINT('Ctrl Pts',(120.741638362312,2.42185107377855,125.403675292032));
#183027=CARTESIAN_POINT('Ctrl Pts',(120.749036276624,2.56387552382144,125.471962202139));
#183028=CARTESIAN_POINT('Ctrl Pts',(120.756432961536,2.70587637197733,125.5402377642));
#183029=CARTESIAN_POINT('Ctrl Pts',(120.763829646448,2.84519073274181,125.614209934796));
#183030=CARTESIAN_POINT('Ctrl Pts',(120.77122633136,2.98133806439828,125.693631324376));
#183031=CARTESIAN_POINT('Ctrl Pts',(120.778622688295,3.11747935913958,125.773049192329));
#183032=CARTESIAN_POINT('Ctrl Pts',(120.786019045231,3.25045358154954,125.857915610738));
#183033=CARTESIAN_POINT('Ctrl Pts',(120.793415402166,3.37980619453057,125.947937999021));
#183034=CARTESIAN_POINT('Ctrl Pts',(120.800812891503,3.5091786117264,126.037974169961));
#183035=CARTESIAN_POINT('Ctrl Pts',(120.808210380839,3.63492800903486,126.133167669307));
#183036=CARTESIAN_POINT('Ctrl Pts',(120.815607870176,3.75663028717459,126.233183586649));
#183037=CARTESIAN_POINT('Ctrl Pts',(120.823007952691,3.87837522785968,126.333234564416));
#183038=CARTESIAN_POINT('Ctrl Pts',(120.830408035206,3.99606993650866,126.438111089069));
#183039=CARTESIAN_POINT('Ctrl Pts',(120.837808117721,4.10932486332231,126.547439226445));
#183040=CARTESIAN_POINT('Ctrl Pts',(120.845216337387,4.22270432557088,126.656887581348));
#183041=CARTESIAN_POINT('Ctrl Pts',(120.852624557054,4.33163398757523,126.770797065199));
#183042=CARTESIAN_POINT('Ctrl Pts',(120.86003277672,4.43576202410635,126.888757748531));
#183043=CARTESIAN_POINT('Ctrl Pts',(120.867445556022,4.53995414970641,127.006791034695));
#183044=CARTESIAN_POINT('Ctrl Pts',(120.874858335325,4.63933852586753,127.128880200011));
#183045=CARTESIAN_POINT('Ctrl Pts',(120.882271114627,4.73360517117553,127.254584195604));
#183046=CARTESIAN_POINT('Ctrl Pts',(120.889694485655,4.82800650908714,127.38046780296));
#183047=CARTESIAN_POINT('Ctrl Pts',(120.897117856684,4.917275300239,127.509976249791));
#183048=CARTESIAN_POINT('Ctrl Pts',(120.904541227713,5.00114579112764,127.642640937015));
#183049=CARTESIAN_POINT('Ctrl Pts',(120.908477277154,5.04561593784276,127.712982937428));
#183050=CARTESIAN_POINT('Ctrl Pts',(120.912413326595,5.08856920412359,127.784211873135));
#183051=CARTESIAN_POINT('Ctrl Pts',(120.916349376036,5.12997140109303,127.856255465699));
#183052=CARTESIAN_POINT('Ctrl Pts',(120.923772642441,5.20805465245714,127.992127432866));
#183053=CARTESIAN_POINT('Ctrl Pts',(120.931195908846,5.28085420694602,128.131309155906));
#183054=CARTESIAN_POINT('Ctrl Pts',(120.938619175252,5.34807637760309,128.273351012325));
#183055=CARTESIAN_POINT('Ctrl Pts',(120.946033667973,5.41521909723699,128.415224987065));
#183056=CARTESIAN_POINT('Ctrl Pts',(120.953448160694,5.47679739633404,128.559952032276));
#183057=CARTESIAN_POINT('Ctrl Pts',(120.960862653415,5.53256188844834,128.707055319573));
#183058=CARTESIAN_POINT('Ctrl Pts',(120.968269999769,5.58827263264549,128.854016823183));
#183059=CARTESIAN_POINT('Ctrl Pts',(120.975677346123,5.63818059402247,129.003349662604));
#183060=CARTESIAN_POINT('Ctrl Pts',(120.983084692476,5.68208323896502,129.154554378042));
#183061=CARTESIAN_POINT('Ctrl Pts',(120.990486514152,5.72595313965853,129.305646319298));
#183062=CARTESIAN_POINT('Ctrl Pts',(120.997888335827,5.76382653855316,129.458606999766));
#183063=CARTESIAN_POINT('Ctrl Pts',(121.005290157503,5.79554982470989,129.612919141116));
#183064=CARTESIAN_POINT('Ctrl Pts',(121.012688071814,5.82725636439077,129.767149822288));
#183065=CARTESIAN_POINT('Ctrl Pts',(121.020085986125,5.85281918210673,129.922730178796));
#183066=CARTESIAN_POINT('Ctrl Pts',(121.027483900437,5.87213515503615,130.079130113872));
#183067=CARTESIAN_POINT('Ctrl Pts',(121.034880585349,5.89144791800142,130.235504058116));
#183068=CARTESIAN_POINT('Ctrl Pts',(121.042277270261,5.90451585081448,130.392696940494));
#183069=CARTESIAN_POINT('Ctrl Pts',(121.049673955173,5.91128734477379,130.550170747553));
#183070=CARTESIAN_POINT('Ctrl Pts',(121.057070312109,5.91805853847797,130.707637572059));
#183071=CARTESIAN_POINT('Ctrl Pts',(121.064466669044,5.91853383241655,130.865384923527));
#183072=CARTESIAN_POINT('Ctrl Pts',(121.07186302598,5.91271369451713,131.022872240071));
#183073=CARTESIAN_POINT('Ctrl Pts',(121.079260515317,5.90689266553974,131.180383668325));
#183074=CARTESIAN_POINT('Ctrl Pts',(121.086658004653,5.89477429936458,131.337634609316));
#183075=CARTESIAN_POINT('Ctrl Pts',(121.09405549399,5.87641112958486,131.494087229051));
#183076=CARTESIAN_POINT('Ctrl Pts',(121.101455576505,5.8580415226243,131.650594693011));
#183077=CARTESIAN_POINT('Ctrl Pts',(121.10885565902,5.83342279705357,131.806302908013));
#183078=CARTESIAN_POINT('Ctrl Pts',(121.116255741535,5.80265899309267,131.960682014229));
#183079=CARTESIAN_POINT('Ctrl Pts',(121.123663961202,5.77186136116694,132.115230876142));
#183080=CARTESIAN_POINT('Ctrl Pts',(121.131072180868,5.73490522938715,132.26844734425));
#183081=CARTESIAN_POINT('Ctrl Pts',(121.138480400535,5.69194531289289,132.419813841134));
#183082=CARTESIAN_POINT('Ctrl Pts',(121.145893179837,5.64895895528682,132.571273501572));
#183083=CARTESIAN_POINT('Ctrl Pts',(121.153305959139,5.59996156567458,132.720880567995));
#183084=CARTESIAN_POINT('Ctrl Pts',(121.160718738441,5.54515665844007,132.868135846572));
#183085=CARTESIAN_POINT('Ctrl Pts',(121.16814210947,5.49027344338409,133.015601530396));
#183086=CARTESIAN_POINT('Ctrl Pts',(121.175565480498,5.42956628132339,133.160708371548));
#183087=CARTESIAN_POINT('Ctrl Pts',(121.182988851527,5.36328577167897,133.302979494827));
#183088=CARTESIAN_POINT('Ctrl Pts',(121.186924900968,5.32814225508741,133.378415058137));
#183089=CARTESIAN_POINT('Ctrl Pts',(121.190860950409,5.29143262378694,133.453053837168));
#183090=CARTESIAN_POINT('Ctrl Pts',(121.194796999849,5.25319920775148,133.526827999589));
#183091=CARTESIAN_POINT('Ctrl Pts',(121.202220266255,5.18109217833081,133.665963767506));
#183092=CARTESIAN_POINT('Ctrl Pts',(121.20964353266,5.10334459033582,133.802443215493));
#183093=CARTESIAN_POINT('Ctrl Pts',(121.217066799066,5.0201759789293,133.935776224457));
#183094=CARTESIAN_POINT('Ctrl Pts',(121.224481291787,4.93710566591456,134.068951644878));
#183095=CARTESIAN_POINT('Ctrl Pts',(121.231895784508,4.84862727869129,134.198987714987));
#183096=CARTESIAN_POINT('Ctrl Pts',(121.239310277229,4.75500718701793,134.325416881517));
#183097=CARTESIAN_POINT('Ctrl Pts',(121.246717623582,4.66147732991412,134.451724190855));
#183098=CARTESIAN_POINT('Ctrl Pts',(121.254124969936,4.56281585497749,134.574431219593));
#183099=CARTESIAN_POINT('Ctrl Pts',(121.26153231629,4.45933349751323,134.693097600245));
#183100=CARTESIAN_POINT('Ctrl Pts',(121.268934137965,4.35592832109475,134.811675475034));
#183101=CARTESIAN_POINT('Ctrl Pts',(121.276335959641,4.2477096657567,134.92621842222));
#183102=CARTESIAN_POINT('Ctrl Pts',(121.283737781316,4.13502970194288,135.036317602998));
#183103=CARTESIAN_POINT('Ctrl Pts',(121.291135695627,4.02240922100567,135.146358663275));
#183104=CARTESIAN_POINT('Ctrl Pts',(121.298533609938,3.9053323881929,135.25196036875));
#183105=CARTESIAN_POINT('Ctrl Pts',(121.30593152425,3.78418944852479,135.352749429022));
#183106=CARTESIAN_POINT('Ctrl Pts',(121.313328209162,3.66306664061498,135.45352173998));
#183107=CARTESIAN_POINT('Ctrl Pts',(121.320724894074,3.53787935362518,135.549482754533));
#183108=CARTESIAN_POINT('Ctrl Pts',(121.328121578986,3.40905233774438,135.640298243406));
#183109=CARTESIAN_POINT('Ctrl Pts',(121.335517935922,3.28023103418856,135.731109705426));
#183110=CARTESIAN_POINT('Ctrl Pts',(121.342914292857,3.1477706277457,135.816775880339));
#183111=CARTESIAN_POINT('Ctrl Pts',(121.350310649792,3.01212616136603,135.897004974922));
#183112=CARTESIAN_POINT('Ctrl Pts',(121.357708139129,2.87646092747217,135.977246352785));
#183113=CARTESIAN_POINT('Ctrl Pts',(121.365105628466,2.73761098431293,136.052048802786));
#183114=CARTESIAN_POINT('Ctrl Pts',(121.372503117802,2.59605722255035,136.121165810513));
#183115=CARTESIAN_POINT('Ctrl Pts',(121.379903200317,2.4544538393353,136.1903070471));
#183116=CARTESIAN_POINT('Ctrl Pts',(121.387303282832,2.31014508565248,136.253758709631));
#183117=CARTESIAN_POINT('Ctrl Pts',(121.394703365347,2.16363298386153,136.311321927912));
#183118=CARTESIAN_POINT('Ctrl Pts',(121.402111585013,2.0169597769537,136.368948442868));
#183119=CARTESIAN_POINT('Ctrl Pts',(121.40951980468,1.86807873108844,136.420673446083));
#183120=CARTESIAN_POINT('Ctrl Pts',(121.416928024346,1.71750892611891,136.466347340546));
#183121=CARTESIAN_POINT('Ctrl Pts',(121.424340803648,1.5668464479467,136.512049346529));
#183122=CARTESIAN_POINT('Ctrl Pts',(121.43175358295,1.41449349995957,136.551692728728));
#183123=CARTESIAN_POINT('Ctrl Pts',(121.439166362252,1.26098007256295,136.585178883097));
#183124=CARTESIAN_POINT('Ctrl Pts',(121.446589733281,1.10724729798208,136.618712884054));
#183125=CARTESIAN_POINT('Ctrl Pts',(121.45401310431,0.952351098933248,136.64607202137));
#183126=CARTESIAN_POINT('Ctrl Pts',(121.461436475339,0.796828139136472,
136.667209368743));
#183127=CARTESIAN_POINT('Ctrl Pts',(121.465372524779,0.714366134128753,
136.678416897504));
#183128=CARTESIAN_POINT('Ctrl Pts',(121.46930857422,0.631727963045877,136.687876128241));
#183129=CARTESIAN_POINT('Ctrl Pts',(121.473244623661,0.54899357553466,136.695586009326));
#183130=CARTESIAN_POINT('Ctrl Pts',(121.480667890067,0.392959102742847,
136.710126604437));
#183131=CARTESIAN_POINT('Ctrl Pts',(121.488091156472,0.236110607450815,
136.718485832063));
#183132=CARTESIAN_POINT('Ctrl Pts',(121.495514422877,0.078979104850994,
136.720583472014));
#183133=CARTESIAN_POINT('Ctrl Pts',(121.502928915598,-0.0779666813618246,
136.722678632729));
#183134=CARTESIAN_POINT('Ctrl Pts',(121.510343408319,-0.23519443945632,
136.718526931922));
#183135=CARTESIAN_POINT('Ctrl Pts',(121.51775790104,-0.392166824264851,
136.708099750052));
#183136=CARTESIAN_POINT('Ctrl Pts',(121.525165247394,-0.548987913178997,
136.697682618292));
#183137=CARTESIAN_POINT('Ctrl Pts',(121.532572593748,-0.705553748843742,
136.681002071509));
#183138=CARTESIAN_POINT('Ctrl Pts',(121.539979940102,-0.861325877599658,
136.658081510731));
#183139=CARTESIAN_POINT('Ctrl Pts',(121.547381761777,-1.01698182562545,
136.635178044972));
#183140=CARTESIAN_POINT('Ctrl Pts',(121.554783583453,-1.17184487771584,
136.606043886146));
#183141=CARTESIAN_POINT('Ctrl Pts',(121.562185405128,-1.32538070947762,
136.57075433786));
#183142=CARTESIAN_POINT('Ctrl Pts',(121.569583319439,-1.47883549086751,
136.535483418652));
#183143=CARTESIAN_POINT('Ctrl Pts',(121.576981233751,-1.63096408437483,
136.494063664693));
#183144=CARTESIAN_POINT('Ctrl Pts',(121.584379148062,-1.78124149324664,
136.44662162759));
#183145=CARTESIAN_POINT('Ctrl Pts',(121.591775832974,-1.93149392874036,
136.399187474493));
#183146=CARTESIAN_POINT('Ctrl Pts',(121.599172517886,-2.07989543452824,
136.345733136804));
#183147=CARTESIAN_POINT('Ctrl Pts',(121.606569202799,-2.2259352262042,136.286435309801));
#183148=CARTESIAN_POINT('Ctrl Pts',(121.613965559734,-2.37196854232265,
136.227140112126));
#183149=CARTESIAN_POINT('Ctrl Pts',(121.621361916669,-2.5156400066765,136.162002080765));
#183150=CARTESIAN_POINT('Ctrl Pts',(121.628758273605,-2.6564581635341,136.091246334876));
#183151=CARTESIAN_POINT('Ctrl Pts',(121.636155762941,-2.7972978800106,136.020479756102));
#183152=CARTESIAN_POINT('Ctrl Pts',(121.643553252278,-2.93528308558697,
135.944093917864));
#183153=CARTESIAN_POINT('Ctrl Pts',(121.650950741615,-3.06994644755794,
135.862360160036));
#183154=CARTESIAN_POINT('Ctrl Pts',(121.65835082413,-3.20465701556178,135.780597750566));
#183155=CARTESIAN_POINT('Ctrl Pts',(121.665750906645,-3.33604310259594,
135.693483882548));
#183156=CARTESIAN_POINT('Ctrl Pts',(121.67315098916,-3.46366603818448,135.601333427415));
#183157=CARTESIAN_POINT('Ctrl Pts',(121.680559208826,-3.59142930831138,
135.509081643382));
#183158=CARTESIAN_POINT('Ctrl Pts',(121.687967428493,-3.71542086035615,
135.411782430656));
#183159=CARTESIAN_POINT('Ctrl Pts',(121.695375648159,-3.83523425877866,
135.309791644981));
#183160=CARTESIAN_POINT('Ctrl Pts',(121.702788427461,-3.95512140034852,
135.207738085679));
#183161=CARTESIAN_POINT('Ctrl Pts',(121.710201206763,-4.07082499036623,
135.1009874521));
#183162=CARTESIAN_POINT('Ctrl Pts',(121.717613986065,-4.18197559769595,
134.989932342286));
#183163=CARTESIAN_POINT('Ctrl Pts',(121.725037357094,-4.29328502222603,
134.878718551723));
#183164=CARTESIAN_POINT('Ctrl Pts',(121.732460728123,-4.4000282184377,134.763188274579));
#183165=CARTESIAN_POINT('Ctrl Pts',(121.739884099152,-4.50187562605314,
134.643767656426));
#183166=CARTESIAN_POINT('Ctrl Pts',(121.743820148593,-4.5558775653682,134.58044797922));
#183167=CARTESIAN_POINT('Ctrl Pts',(121.747756198034,-4.60850383410758,
134.51603509072));
#183168=CARTESIAN_POINT('Ctrl Pts',(121.751692247475,-4.65971033277122,
134.450595686396));
#183169=CARTESIAN_POINT('Ctrl Pts',(121.759397770821,-4.75995624605906,
134.322486305309));
#183170=CARTESIAN_POINT('Ctrl Pts',(121.767103294168,-4.855078114618,134.190031390031));
#183171=CARTESIAN_POINT('Ctrl Pts',(121.774808817515,-4.94467841284417,
134.05368146292));
#183172=CARTESIAN_POINT('Ctrl Pts',(121.782221809932,-5.03087714347355,
133.92250789686));
#183173=CARTESIAN_POINT('Ctrl Pts',(121.789634802349,-5.11196556567067,
133.787729956513));
#183174=CARTESIAN_POINT('Ctrl Pts',(121.797047794766,-5.18762905297334,
133.649784201366));
#183175=CARTESIAN_POINT('Ctrl Pts',(121.804453731265,-5.26322052139986,
133.511969747308));
#183176=CARTESIAN_POINT('Ctrl Pts',(121.811859667764,-5.33339715386406,
133.370993803931));
#183177=CARTESIAN_POINT('Ctrl Pts',(121.819265604263,-5.39788738894737,
133.22732209038));
#183178=CARTESIAN_POINT('Ctrl Pts',(121.826665950708,-5.46232894634043,
133.083758821266));
#183179=CARTESIAN_POINT('Ctrl Pts',(121.834066297153,-5.52109249856701,
132.937504171086));
#183180=CARTESIAN_POINT('Ctrl Pts',(121.841466643598,-5.5739523158509,132.789048538404));
#183181=CARTESIAN_POINT('Ctrl Pts',(121.848862862064,-5.62678264746364,
132.64067571558));
#183182=CARTESIAN_POINT('Ctrl Pts',(121.856259080531,-5.67371567677217,
132.490104705223));
#183183=CARTESIAN_POINT('Ctrl Pts',(121.863655298998,-5.71457379272419,
132.337845840843));
#183184=CARTESIAN_POINT('Ctrl Pts',(121.871049372158,-5.75542005759352,
132.185631139841));
#183185=CARTESIAN_POINT('Ctrl Pts',(121.878443445317,-5.79019481915347,
132.031729918762));
#183186=CARTESIAN_POINT('Ctrl Pts',(121.885837518477,-5.81877034216444,
131.876667601432));
#183187=CARTESIAN_POINT('Ctrl Pts',(121.893230393674,-5.84734123546433,
131.721630406781));
#183188=CARTESIAN_POINT('Ctrl Pts',(121.90062326887,-5.86971482614708,131.565432857629));
#183189=CARTESIAN_POINT('Ctrl Pts',(121.908016144067,-5.8858145526158,131.408610247037));
#183190=CARTESIAN_POINT('Ctrl Pts',(121.915410427234,-5.9019173452718,131.251757769634));
#183191=CARTESIAN_POINT('Ctrl Pts',(121.922804710401,-5.91174385098551,
131.094280364091));
#183192=CARTESIAN_POINT('Ctrl Pts',(121.930198993569,-5.91526939587632,
130.93671822675));
#183193=CARTESIAN_POINT('Ctrl Pts',(121.932340931644,-5.916290657663,130.891076433814));
#183194=CARTESIAN_POINT('Ctrl Pts',(121.93448286972,-5.91678353011378,130.845427540589));
#183195=CARTESIAN_POINT('Ctrl Pts',(121.936624807795,-5.91674823051506,
130.799784680839));
#183196=CARTESIAN_POINT('',(123.686624807795,-5.92584126535119,130.802516799045));
#183197=CARTESIAN_POINT('Ctrl Pts',(121.936626891659,-5.91105546203302,
130.799744720898));
#183198=CARTESIAN_POINT('Ctrl Pts',(121.967797884869,-5.91580744003664,
130.136152748363));
#183199=CARTESIAN_POINT('Ctrl Pts',(122.091784752684,-5.50598867124265,
127.502332575195));
#183200=CARTESIAN_POINT('Ctrl Pts',(122.308587495099,-1.63160081265663,
123.998815869465));
#183201=CARTESIAN_POINT('Ctrl Pts',(122.587035118914,4.84377744631919,125.753085473515));
#183202=CARTESIAN_POINT('Ctrl Pts',(122.865482742726,6.86796086381084,132.14923016645));
#183203=CARTESIAN_POINT('Ctrl Pts',(123.143930366539,2.58082376599965,137.309505444483));
#183204=CARTESIAN_POINT('Ctrl Pts',(123.417644388228,-3.96476507443635,
136.505770194011));
#183205=CARTESIAN_POINT('Ctrl Pts',(123.598542535314,-5.91824650158347,
132.665654016414));
#183206=CARTESIAN_POINT('Ctrl Pts',(123.686624807795,-5.92584126535119,
130.802516799045));
#183207=CARTESIAN_POINT('',(125.436624807795,-5.91667608508364,130.809827719978));
#183208=CARTESIAN_POINT('Ctrl Pts',(123.686624807795,-5.92584126535119,
130.802516799045));
#183209=CARTESIAN_POINT('Ctrl Pts',(123.691358409918,-5.92624941319846,
130.702390518927));
#183210=CARTESIAN_POINT('Ctrl Pts',(123.696092012042,-5.92393242245176,
130.602283526104));
#183211=CARTESIAN_POINT('Ctrl Pts',(123.793641488769,-5.81880593488637,
128.542219269167));
#183212=CARTESIAN_POINT('Ctrl Pts',(123.979273237977,-3.47781303298138,
124.731274331503));
#183213=CARTESIAN_POINT('Ctrl Pts',(124.257720861791,3.22961659657427,124.595726535137));
#183214=CARTESIAN_POINT('Ctrl Pts',(124.536168485603,6.96918634942095,130.16561015189));
#183215=CARTESIAN_POINT('Ctrl Pts',(124.814616109416,4.30441431082963,136.322474241898));
#183216=CARTESIAN_POINT('Ctrl Pts',(125.093063733229,-2.31590419708269,
137.408461485986));
#183217=CARTESIAN_POINT('Ctrl Pts',(125.300399966022,-5.66080020113054,
133.698150859813));
#183218=CARTESIAN_POINT('Ctrl Pts',(125.414920324211,-5.92093715202594,
131.270777417702));
#183219=CARTESIAN_POINT('Ctrl Pts',(125.436624807795,-5.91667608508364,
130.809827719978));
#183220=CARTESIAN_POINT('',(127.186624807795,-5.90699143088146,130.803749018818));
#183221=CARTESIAN_POINT('Ctrl Pts',(125.436624807795,-5.91667608508364,
130.809827719978));
#183222=CARTESIAN_POINT('Ctrl Pts',(125.507736198815,-5.90271535681672,
129.299597169321));
#183223=CARTESIAN_POINT('Ctrl Pts',(125.671663464439,-4.54509055714801,
125.795879117947));
#183224=CARTESIAN_POINT('Ctrl Pts',(125.928406604669,1.35531985884536,123.938454369257));
#183225=CARTESIAN_POINT('Ctrl Pts',(126.206854228481,6.50906486850591,128.23343956317));
#183226=CARTESIAN_POINT('Ctrl Pts',(126.485301852293,5.68129724950531,134.890975609601));
#183227=CARTESIAN_POINT('Ctrl Pts',(126.763749476106,-0.367304994988542,
137.793112120586));
#183228=CARTESIAN_POINT('Ctrl Pts',(126.997523794607,-5.16210537323063,
134.837695341821));
#183229=CARTESIAN_POINT('Ctrl Pts',(127.138482238503,-5.90604835788347,
131.830411623805));
#183230=CARTESIAN_POINT('Ctrl Pts',(127.186624807795,-5.90699143088146,
130.803749018818));
#183231=CARTESIAN_POINT('',(128.936624084929,-5.91831124264779,130.799118091926));
#183232=CARTESIAN_POINT('Ctrl Pts',(127.186624807795,-5.90699143088146,
130.803749018818));
#183233=CARTESIAN_POINT('Ctrl Pts',(127.231298113108,-5.90786654387585,
129.851070076254));
#183234=CARTESIAN_POINT('Ctrl Pts',(127.368787293024,-5.23971675382112,
126.920207720007));
#183235=CARTESIAN_POINT('Ctrl Pts',(127.599092347546,-0.628143810757646,
123.834210268875));
#183236=CARTESIAN_POINT('Ctrl Pts',(127.877539971358,5.52465782028921,126.508348920764));
#183237=CARTESIAN_POINT('Ctrl Pts',(128.155987595171,6.60056880902916,133.130312450174));
#183238=CARTESIAN_POINT('Ctrl Pts',(128.434435218984,1.61087951798409,137.614839874481));
#183239=CARTESIAN_POINT('Ctrl Pts',(128.694647287185,-4.43540799159065,
135.957047019246));
#183240=CARTESIAN_POINT('Ctrl Pts',(128.862043480784,-5.90429634502181,
132.381480787606));
#183241=CARTESIAN_POINT('Ctrl Pts',(128.936623799777,-5.9189280327544,130.799123593926));
#183242=CARTESIAN_POINT('',(130.686626174971,-5.92114659639425,130.807384154776));
#183243=CARTESIAN_POINT('Ctrl Pts',(128.936624807795,-5.91674766505958,
130.799104144226));
#183244=CARTESIAN_POINT('Ctrl Pts',(128.947379588894,-5.91654502312587,
130.571008021481));
#183245=CARTESIAN_POINT('Ctrl Pts',(128.958134369993,-5.90314918816152,
130.343473921271));
#183246=CARTESIAN_POINT('Ctrl Pts',(128.968889151092,-5.87677360007643,
130.117729263822));
#183247=CARTESIAN_POINT('Ctrl Pts',(128.976369589598,-5.85842818114997,
129.960713606087));
#183248=CARTESIAN_POINT('Ctrl Pts',(128.983850028104,-5.8338043041974,129.804562724547));
#183249=CARTESIAN_POINT('Ctrl Pts',(128.99133046661,-5.80298603825706,129.649681613559));
#183250=CARTESIAN_POINT('Ctrl Pts',(128.998753733015,-5.77240331265216,
129.495984240453));
#183251=CARTESIAN_POINT('Ctrl Pts',(129.006176999421,-5.73566390235169,
129.343270315442));
#183252=CARTESIAN_POINT('Ctrl Pts',(129.013600265826,-5.69284242803125,
129.192071669484));
#183253=CARTESIAN_POINT('Ctrl Pts',(129.021014758547,-5.65007156513736,
129.04105172777));
#183254=CARTESIAN_POINT('Ctrl Pts',(129.028429251268,-5.60123304769037,
128.891543855909));
#183255=CARTESIAN_POINT('Ctrl Pts',(129.035843743989,-5.54645275821413,
128.744071229301));
#183256=CARTESIAN_POINT('Ctrl Pts',(129.043251090343,-5.49172526804333,
128.596740742362));
#183257=CARTESIAN_POINT('Ctrl Pts',(129.050658436697,-5.43106753609541,
128.45144194301));
#183258=CARTESIAN_POINT('Ctrl Pts',(129.05806578305,-5.36465561944204,128.308684226828));
#183259=CARTESIAN_POINT('Ctrl Pts',(129.065467604726,-5.29829323530168,
128.166032984736));
#183260=CARTESIAN_POINT('Ctrl Pts',(129.072869426401,-5.22618536856474,
128.025919389152));
#183261=CARTESIAN_POINT('Ctrl Pts',(129.080271248076,-5.14855664335168,
127.888834069462));
#183262=CARTESIAN_POINT('Ctrl Pts',(129.087669162388,-5.07096889773812,
127.751821116045));
#183263=CARTESIAN_POINT('Ctrl Pts',(129.095067076699,-4.98786628133185,
127.617833578836));
#183264=CARTESIAN_POINT('Ctrl Pts',(129.10246499101,-4.89951987476105,127.48733852549));
#183265=CARTESIAN_POINT('Ctrl Pts',(129.109861675922,-4.81118814976063,
127.356865158054));
#183266=CARTESIAN_POINT('Ctrl Pts',(129.117258360835,-4.71761457318377,
127.2298834314));
#183267=CARTESIAN_POINT('Ctrl Pts',(129.124655045747,-4.61911423006035,
127.10683248486));
#183268=CARTESIAN_POINT('Ctrl Pts',(129.132051402682,-4.52061825454543,
126.983786994528));
#183269=CARTESIAN_POINT('Ctrl Pts',(129.139447759617,-4.41719618013541,
126.864672229181));
#183270=CARTESIAN_POINT('Ctrl Pts',(129.146844116553,-4.30920398819393,
126.749894986853));
#183271=CARTESIAN_POINT('Ctrl Pts',(129.154241605889,-4.20119526237202,
126.635100171836));
#183272=CARTESIAN_POINT('Ctrl Pts',(129.161639095226,-4.08861528164914,
126.524644474013));
#183273=CARTESIAN_POINT('Ctrl Pts',(129.169036584562,-3.97185744423585,
126.418898383643));
#183274=CARTESIAN_POINT('Ctrl Pts',(129.176436667077,-3.8550586775434,126.313115224144));
#183275=CARTESIAN_POINT('Ctrl Pts',(129.183836749592,-3.7340794147835,126.212045209555));
#183276=CARTESIAN_POINT('Ctrl Pts',(129.191236832107,-3.60934659853295,
126.116018939087));
#183277=CARTESIAN_POINT('Ctrl Pts',(129.198645051773,-3.48447662572835,
126.019887077865));
#183278=CARTESIAN_POINT('Ctrl Pts',(129.20605327144,-3.35584515268553,125.92881026458));
#183279=CARTESIAN_POINT('Ctrl Pts',(129.213461491106,-3.22390920563638,
125.843076509967));
#183280=CARTESIAN_POINT('Ctrl Pts',(129.220874270408,-3.0918920542133,125.757289987659));
#183281=CARTESIAN_POINT('Ctrl Pts',(129.22828704971,-2.95656669623262,125.676853267191));
#183282=CARTESIAN_POINT('Ctrl Pts',(129.235699829012,-2.81841481509146,
125.602008409903));
#183283=CARTESIAN_POINT('Ctrl Pts',(129.243123200041,-2.68006553606374,
125.527056610774));
#183284=CARTESIAN_POINT('Ctrl Pts',(129.250546571069,-2.5388820019244,125.457712796615));
#183285=CARTESIAN_POINT('Ctrl Pts',(129.257969942098,-2.39536667341973,
125.394171243582));
#183286=CARTESIAN_POINT('Ctrl Pts',(129.261905991539,-2.31927140263232,
125.3604799875));
#183287=CARTESIAN_POINT('Ctrl Pts',(129.265842040981,-2.24252086008494,
125.328419129956));
#183288=CARTESIAN_POINT('Ctrl Pts',(129.269778090422,-2.16519155121374,
125.298011908208));
#183289=CARTESIAN_POINT('Ctrl Pts',(129.277201356828,-2.01935088806817,
125.240664836975));
#183290=CARTESIAN_POINT('Ctrl Pts',(129.284624623233,-1.87100978919444,
125.189029136661));
#183291=CARTESIAN_POINT('Ctrl Pts',(129.292047889638,-1.72065603333818,
125.143329494402));
#183292=CARTESIAN_POINT('Ctrl Pts',(129.299462382359,-1.57047998313492,
125.097683865324));
#183293=CARTESIAN_POINT('Ctrl Pts',(129.30687687508,-1.41829636462693,125.057960436557));
#183294=CARTESIAN_POINT('Ctrl Pts',(129.314291367801,-1.26461338267296,
125.024336088651));
#183295=CARTESIAN_POINT('Ctrl Pts',(129.321698714155,-1.11107852616328,
124.990744149157));
#183296=CARTESIAN_POINT('Ctrl Pts',(129.329106060509,-0.956047545426268,
124.963239666791));
#183297=CARTESIAN_POINT('Ctrl Pts',(129.336513406863,-0.800044172539664,
124.941949860507));
#183298=CARTESIAN_POINT('Ctrl Pts',(129.343915228538,-0.644157152854006,
124.920675932963));
#183299=CARTESIAN_POINT('Ctrl Pts',(129.351317050214,-0.487299553360572,
124.905607502572));
#183300=CARTESIAN_POINT('Ctrl Pts',(129.358718871889,-0.330005569281536,
124.896820783867));
#183301=CARTESIAN_POINT('Ctrl Pts',(129.3661167862,-0.172794619472546,124.888038703602));
#183302=CARTESIAN_POINT('Ctrl Pts',(129.373514700512,-0.0151481156323031,
124.885531751684));
#183303=CARTESIAN_POINT('Ctrl Pts',(129.380912614823,0.142394459293183,
124.88932432178));
#183304=CARTESIAN_POINT('Ctrl Pts',(129.388309299735,0.29991085350083,124.89311626162));
#183305=CARTESIAN_POINT('Ctrl Pts',(129.395705984648,0.457322980247357,
124.903205636778));
#183306=CARTESIAN_POINT('Ctrl Pts',(129.40310266956,0.614091068019229,124.919564722832));
#183307=CARTESIAN_POINT('Ctrl Pts',(129.410499026495,0.770852204529808,
124.935923083507));
#183308=CARTESIAN_POINT('Ctrl Pts',(129.417895383431,0.926968987565892,
124.958550563564));
#183309=CARTESIAN_POINT('Ctrl Pts',(129.425291740366,1.08190674979855,124.987367550075));
#183310=CARTESIAN_POINT('Ctrl Pts',(129.432689229703,1.23686823339825,125.01618894854));
#183311=CARTESIAN_POINT('Ctrl Pts',(129.44008671904,1.39064996974529,125.05120167205));
#183312=CARTESIAN_POINT('Ctrl Pts',(129.447484208376,1.54272761355005,125.092275002583));
#183313=CARTESIAN_POINT('Ctrl Pts',(129.454884290891,1.6948585679371,125.13336273131));
#183314=CARTESIAN_POINT('Ctrl Pts',(129.462284373406,1.84528388026811,125.180515199723));
#183315=CARTESIAN_POINT('Ctrl Pts',(129.469684455921,1.99349463516965,125.233551905893));
#183316=CARTESIAN_POINT('Ctrl Pts',(129.477092675588,2.14186836303254,125.286646931374));
#183317=CARTESIAN_POINT('Ctrl Pts',(129.484500895254,2.28802231865685,125.345638990424));
#183318=CARTESIAN_POINT('Ctrl Pts',(129.491909114921,2.43146715661416,125.410299250766));
#183319=CARTESIAN_POINT('Ctrl Pts',(129.499321894223,2.57500028247584,125.474999308419));
#183320=CARTESIAN_POINT('Ctrl Pts',(129.506734673525,2.71582063498677,125.545374352514));
#183321=CARTESIAN_POINT('Ctrl Pts',(129.514147452827,2.85346419944377,125.621149969233));
#183322=CARTESIAN_POINT('Ctrl Pts',(129.521570823856,2.9913044354806,125.697033857707));
#183323=CARTESIAN_POINT('Ctrl Pts',(129.528994194885,3.12595849905387,125.778333538135));
#183324=CARTESIAN_POINT('Ctrl Pts',(129.536417565913,3.25699134782469,125.86473128707));
#183325=CARTESIAN_POINT('Ctrl Pts',(129.540353615354,3.32646810833134,125.91054144664));
#183326=CARTESIAN_POINT('Ctrl Pts',(129.544289664795,3.39492735876577,125.957784175133));
#183327=CARTESIAN_POINT('Ctrl Pts',(129.548225714235,3.46230819590717,126.006407666666));
#183328=CARTESIAN_POINT('Ctrl Pts',(129.555648980641,3.5893863518749,126.098110054211));
#183329=CARTESIAN_POINT('Ctrl Pts',(129.563072247046,3.7130109163222,126.19500326464));
#183330=CARTESIAN_POINT('Ctrl Pts',(129.570495513452,3.83272919727131,126.296798364764));
#183331=CARTESIAN_POINT('Ctrl Pts',(129.577910006173,3.95230598115442,126.398473151534));
#183332=CARTESIAN_POINT('Ctrl Pts',(129.585324498894,4.06798538989691,126.505038056301));
#183333=CARTESIAN_POINT('Ctrl Pts',(129.592738991615,4.17934391174314,126.616161120183));
#183334=CARTESIAN_POINT('Ctrl Pts',(129.600146337969,4.29059510205344,126.727177079473));
#183335=CARTESIAN_POINT('Ctrl Pts',(129.607553684322,4.39753343396602,126.842742189719));
#183336=CARTESIAN_POINT('Ctrl Pts',(129.614961030676,4.49976878459078,126.962484585245));
#183337=CARTESIAN_POINT('Ctrl Pts',(129.622362852352,4.601927884234,127.082137672375));
#183338=CARTESIAN_POINT('Ctrl Pts',(129.629764674027,4.69939074546822,127.205961558573));
#183339=CARTESIAN_POINT('Ctrl Pts',(129.637166495702,4.79180450128185,127.333548006088));
#183340=CARTESIAN_POINT('Ctrl Pts',(129.644564410014,4.88416947259307,127.46106710171));
#183341=CARTESIAN_POINT('Ctrl Pts',(129.651962324325,4.97149042829734,127.592344501425));
#183342=CARTESIAN_POINT('Ctrl Pts',(129.659360238637,5.053455241603,127.726939508323));
#183343=CARTESIAN_POINT('Ctrl Pts',(129.666756923549,5.13540643384361,127.861512147972));
#183344=CARTESIAN_POINT('Ctrl Pts',(129.674153608461,5.21200305628852,127.999400982067));
#183345=CARTESIAN_POINT('Ctrl Pts',(129.681550293373,5.28297667459216,128.140136899817));
#183346=CARTESIAN_POINT('Ctrl Pts',(129.688946650309,5.35394714585119,128.280866577189));
#183347=CARTESIAN_POINT('Ctrl Pts',(129.696343007244,5.41929494063072,128.424442753893));
#183348=CARTESIAN_POINT('Ctrl Pts',(129.703739364179,5.47879803879187,128.570372566427));
#183349=CARTESIAN_POINT('Ctrl Pts',(129.711136853516,5.53831024702926,128.716324721189));
#183350=CARTESIAN_POINT('Ctrl Pts',(129.718534342853,5.59197583595167,128.864630883593));
#183351=CARTESIAN_POINT('Ctrl Pts',(129.725931832189,5.6396213608959,129.014779250814));
#183352=CARTESIAN_POINT('Ctrl Pts',(129.733331914704,5.68728358790507,129.164980252312));
#183353=CARTESIAN_POINT('Ctrl Pts',(129.740731997219,5.72892143645894,129.317024388783));
#183354=CARTESIAN_POINT('Ctrl Pts',(129.748132079734,5.76441168675377,129.470385929607));
#183355=CARTESIAN_POINT('Ctrl Pts',(129.755540299401,5.79994096222729,129.62391610721));
#183356=CARTESIAN_POINT('Ctrl Pts',(129.762948519067,5.82930905523075,129.77876621825));
#183357=CARTESIAN_POINT('Ctrl Pts',(129.770356738734,5.85244398568209,129.934400873122));
#183358=CARTESIAN_POINT('Ctrl Pts',(129.777769518036,5.87559315529713,130.090131318527));
#183359=CARTESIAN_POINT('Ctrl Pts',(129.785182297338,5.89250147783606,130.246646899673));
#183360=CARTESIAN_POINT('Ctrl Pts',(129.79259507664,5.90314901413344,130.403408900479));
#183361=CARTESIAN_POINT('Ctrl Pts',(129.800018447669,5.91381176413,130.560394890182));
#183362=CARTESIAN_POINT('Ctrl Pts',(129.807441818697,5.91819585092863,130.717627630594));
#183363=CARTESIAN_POINT('Ctrl Pts',(129.814865189726,5.91633343325431,130.874569370989));
#183364=CARTESIAN_POINT('Ctrl Pts',(129.818801239167,5.9153459347153,130.957783647511));
#183365=CARTESIAN_POINT('Ctrl Pts',(129.822737288608,5.91260318632033,131.040916202488));
#183366=CARTESIAN_POINT('Ctrl Pts',(129.826673338048,5.90811585414848,131.123887793968));
#183367=CARTESIAN_POINT('Ctrl Pts',(129.834096604454,5.8996528857171,131.280369626048));
#183368=CARTESIAN_POINT('Ctrl Pts',(129.841519870859,5.88495598040664,131.436751620332));
#183369=CARTESIAN_POINT('Ctrl Pts',(129.848943137265,5.86402353481957,131.592496738793));
#183370=CARTESIAN_POINT('Ctrl Pts',(129.856357629986,5.84311582964484,131.748057779458));
#183371=CARTESIAN_POINT('Ctrl Pts',(129.863772122707,5.81598730324102,131.902983076263));
#183372=CARTESIAN_POINT('Ctrl Pts',(129.871186615428,5.78268832356932,132.056736884889));
#183373=CARTESIAN_POINT('Ctrl Pts',(129.878593961781,5.74942143870794,132.210342499806));
#183374=CARTESIAN_POINT('Ctrl Pts',(129.886001308135,5.70999601899646,132.362778512018));
#183375=CARTESIAN_POINT('Ctrl Pts',(129.893408654489,5.66451405460985,132.513515697606));
#183376=CARTESIAN_POINT('Ctrl Pts',(129.900810476164,5.61906601238819,132.664140457715));
#183377=CARTESIAN_POINT('Ctrl Pts',(129.90821229784,5.56757052721464,132.813068558219));
#183378=CARTESIAN_POINT('Ctrl Pts',(129.915614119515,5.51018032783333,132.959782459633));
#183379=CARTESIAN_POINT('Ctrl Pts',(129.923012033827,5.45282042429159,133.10641891192));
#183380=CARTESIAN_POINT('Ctrl Pts',(129.930409948138,5.38957213943364,133.250843146186));
#183381=CARTESIAN_POINT('Ctrl Pts',(129.937807862449,5.32063753189545,133.392554353878));
#183382=CARTESIAN_POINT('Ctrl Pts',(129.945204547361,5.25171438003843,133.534242011739));
#183383=CARTESIAN_POINT('Ctrl Pts',(129.952601232274,5.1771069441081,133.673217202481));
#183384=CARTESIAN_POINT('Ctrl Pts',(129.959997917186,5.09706480497668,133.809000518847));
#183385=CARTESIAN_POINT('Ctrl Pts',(129.967394274121,5.01702621499759,133.944777814438));
#183386=CARTESIAN_POINT('Ctrl Pts',(129.974790631057,4.93155359053565,134.077363195483));
#183387=CARTESIAN_POINT('Ctrl Pts',(129.982186987992,4.84094158430336,134.20630346539));
#183388=CARTESIAN_POINT('Ctrl Pts',(129.989584477329,4.75031570514154,134.335263476382));
#183389=CARTESIAN_POINT('Ctrl Pts',(129.996981966665,4.65454909212963,134.46057695959));
#183390=CARTESIAN_POINT('Ctrl Pts',(130.004379456002,4.55397858840311,134.581821349177));
#183391=CARTESIAN_POINT('Ctrl Pts',(130.011779538517,4.45337282984241,134.703108240798));
#183392=CARTESIAN_POINT('Ctrl Pts',(130.019179621032,4.34796006592033,134.820322911678));
#183393=CARTESIAN_POINT('Ctrl Pts',(130.026579703547,4.23811600538281,134.933077523267));
#183394=CARTESIAN_POINT('Ctrl Pts',(130.033987923213,4.12815116000849,135.045956120142));
#183395=CARTESIAN_POINT('Ctrl Pts',(130.04139614288,4.01374554763212,135.154364595974));
#183396=CARTESIAN_POINT('Ctrl Pts',(130.048804362546,3.89531069969698,135.257953000724));
#183397=CARTESIAN_POINT('Ctrl Pts',(130.056217141848,3.77680295708913,135.361605162409));
#183398=CARTESIAN_POINT('Ctrl Pts',(130.063629921151,3.65426132726043,135.460431107745));
#183399=CARTESIAN_POINT('Ctrl Pts',(130.071042700453,3.52812826970216,135.554122872146));
#183400=CARTESIAN_POINT('Ctrl Pts',(130.078466071481,3.4018149873162,135.647948507733));
#183401=CARTESIAN_POINT('Ctrl Pts',(130.08588944251,3.2719003357471,135.736625100936));
#183402=CARTESIAN_POINT('Ctrl Pts',(130.093312813539,3.13885412248647,135.819889040399));
#183403=CARTESIAN_POINT('Ctrl Pts',(130.09724886298,3.06830982781482,135.864037578994));
#183404=CARTESIAN_POINT('Ctrl Pts',(130.101184912421,2.99688553237233,135.906665203682));
#183405=CARTESIAN_POINT('Ctrl Pts',(130.105120961861,2.92465366993242,135.947738055928));
#183406=CARTESIAN_POINT('Ctrl Pts',(130.112544228267,2.78842663165143,136.025200173423));
#183407=CARTESIAN_POINT('Ctrl Pts',(130.119967494672,2.64891399457985,136.097363538501));
#183408=CARTESIAN_POINT('Ctrl Pts',(130.127390761078,2.50656671734434,136.163936520005));
#183409=CARTESIAN_POINT('Ctrl Pts',(130.134805253799,2.36438768276912,136.230430817773));
#183410=CARTESIAN_POINT('Ctrl Pts',(130.14221974652,2.21938101168184,136.291347727374));
#183411=CARTESIAN_POINT('Ctrl Pts',(130.149634239241,2.07202466606484,136.346440041908));
#183412=CARTESIAN_POINT('Ctrl Pts',(130.157041585595,1.92481034804172,136.401479256396));
#183413=CARTESIAN_POINT('Ctrl Pts',(130.164448931948,1.77525121138219,136.450704922263));
#183414=CARTESIAN_POINT('Ctrl Pts',(130.171856278302,1.62384763533801,136.49391678828));
#183415=CARTESIAN_POINT('Ctrl Pts',(130.179258099978,1.47255698179307,136.537096425256));
#183416=CARTESIAN_POINT('Ctrl Pts',(130.186659921653,1.31942498539211,136.574271091245));
#183417=CARTESIAN_POINT('Ctrl Pts',(130.194061743328,1.16496962038035,136.605289538531));
#183418=CARTESIAN_POINT('Ctrl Pts',(130.20145965764,1.01059579115362,136.63629161142));
#183419=CARTESIAN_POINT('Ctrl Pts',(130.208857571951,0.854900349667567,
136.661143864464));
#183420=CARTESIAN_POINT('Ctrl Pts',(130.216255486262,0.698413857970478,
136.679745596058));
#183421=CARTESIAN_POINT('Ctrl Pts',(130.223652171175,0.541953371489244,
136.698344236383));
#183422=CARTESIAN_POINT('Ctrl Pts',(130.231048856087,0.384702466027742,
136.710694372796));
#183423=CARTESIAN_POINT('Ctrl Pts',(130.238445540999,0.227199385047126,
136.716746853422));
#183424=CARTESIAN_POINT('Ctrl Pts',(130.245841897934,0.0697032879180588,
136.722799065674));
#183425=CARTESIAN_POINT('Ctrl Pts',(130.25323825487,-0.0880445894748271,
136.722554163036));
#183426=CARTESIAN_POINT('Ctrl Pts',(130.260634611805,-0.245503693015841,
136.716015081353));
#183427=CARTESIAN_POINT('Ctrl Pts',(130.268032101142,-0.40298690394747,
136.709474998521));
#183428=CARTESIAN_POINT('Ctrl Pts',(130.275429590478,-0.56018087999485,
136.696638833368));
#183429=CARTESIAN_POINT('Ctrl Pts',(130.282827079815,-0.716548032609668,
136.677561574409));
#183430=CARTESIAN_POINT('Ctrl Pts',(130.29022716233,-0.872969999487436,
136.658477627947));
#183431=CARTESIAN_POINT('Ctrl Pts',(130.297627244845,-1.02856419554083,
136.633148276953));
#183432=CARTESIAN_POINT('Ctrl Pts',(130.30502732736,-1.18280124145736,136.601679979625));
#183433=CARTESIAN_POINT('Ctrl Pts',(130.312435547026,-1.33720788686194,
136.57017707967));
#183434=CARTESIAN_POINT('Ctrl Pts',(130.319843766693,-1.4902540358692,136.532521827054));
#183435=CARTESIAN_POINT('Ctrl Pts',(130.327251986359,-1.64142282280249,
136.488871298292));
#183436=CARTESIAN_POINT('Ctrl Pts',(130.334664765661,-1.79268465160185,
136.445193903357));
#183437=CARTESIAN_POINT('Ctrl Pts',(130.342077544964,-1.9420664624772,136.395513997035));
#183438=CARTESIAN_POINT('Ctrl Pts',(130.349490324266,-2.0890699959377,136.340037370644));
#183439=CARTESIAN_POINT('Ctrl Pts',(130.356913695294,-2.23628357494058,
136.284481476649));
#183440=CARTESIAN_POINT('Ctrl Pts',(130.364337066323,-2.38111174676919,
136.223112465582));
#183441=CARTESIAN_POINT('Ctrl Pts',(130.371760437352,-2.52307878529869,
136.156183111416));
#183442=CARTESIAN_POINT('Ctrl Pts',(130.375696486793,-2.59835311557997,
136.120695561889));
#183443=CARTESIAN_POINT('Ctrl Pts',(130.379632536234,-2.67282351982889,
136.083645551673));
#183444=CARTESIAN_POINT('Ctrl Pts',(130.383568585674,-2.74642235967692,
136.045075719989));
#183445=CARTESIAN_POINT('Ctrl Pts',(130.39099185208,-2.88522747468796,135.972334221157));
#183446=CARTESIAN_POINT('Ctrl Pts',(130.398415118485,-3.02135054562298,
135.893964349898));
#183447=CARTESIAN_POINT('Ctrl Pts',(130.405838384891,-3.15430246077847,
135.810187876714));
#183448=CARTESIAN_POINT('Ctrl Pts',(130.413252877612,-3.28709723781139,
135.726510420364));
#183449=CARTESIAN_POINT('Ctrl Pts',(130.420667370333,-3.41672800682248,
135.637439278793));
#183450=CARTESIAN_POINT('Ctrl Pts',(130.428081863054,-3.5427284355203,135.543242953587));
#183451=CARTESIAN_POINT('Ctrl Pts',(130.435489209407,-3.66860742026092,
135.449137418347));
#183452=CARTESIAN_POINT('Ctrl Pts',(130.442896555761,-3.79086273364817,
135.349916755745));
#183453=CARTESIAN_POINT('Ctrl Pts',(130.450303902115,-3.90905543144098,
135.245893708338));
#183454=CARTESIAN_POINT('Ctrl Pts',(130.45770572379,-4.0271599766607,135.141948245244));
#183455=CARTESIAN_POINT('Ctrl Pts',(130.465107545466,-4.1412076605105,135.033207774757));
#183456=CARTESIAN_POINT('Ctrl Pts',(130.472509367141,-4.25079125627099,
134.920026330195));
#183457=CARTESIAN_POINT('Ctrl Pts',(130.479907281453,-4.36031700370395,
134.806904633237));
#183458=CARTESIAN_POINT('Ctrl Pts',(130.487305195764,-4.4653830972374,134.689346898611));
#183459=CARTESIAN_POINT('Ctrl Pts',(130.494703110075,-4.56561803201373,
134.567745071518));
#183460=CARTESIAN_POINT('Ctrl Pts',(130.502099794987,-4.66583630956262,
134.446163452443));
#183461=CARTESIAN_POINT('Ctrl Pts',(130.5094964799,-4.76122478456999,134.320539362502));
#183462=CARTESIAN_POINT('Ctrl Pts',(130.516893164812,-4.8514511704319,134.191299073372));
#183463=CARTESIAN_POINT('Ctrl Pts',(130.524289521747,-4.94167355556137,
134.062064514891));
#183464=CARTESIAN_POINT('Ctrl Pts',(130.531685878683,-5.02673409297332,
133.929214382131));
#183465=CARTESIAN_POINT('Ctrl Pts',(130.539082235618,-5.10634306997367,
133.793205045473));
#183466=CARTESIAN_POINT('Ctrl Pts',(130.546479724955,-5.18596423531163,
133.657174885439));
#183467=CARTESIAN_POINT('Ctrl Pts',(130.553877214291,-5.26013198975974,
133.517984880619));
#183468=CARTESIAN_POINT('Ctrl Pts',(130.561274703628,-5.32860201697006,
133.376117042122));
#183469=CARTESIAN_POINT('Ctrl Pts',(130.568674786143,-5.39709604624213,
133.234199472073));
#183470=CARTESIAN_POINT('Ctrl Pts',(130.576074868658,-5.45988820945286,
133.089602535361));
#183471=CARTESIAN_POINT('Ctrl Pts',(130.583474951173,-5.51678193044974,
132.94282915705));
#183472=CARTESIAN_POINT('Ctrl Pts',(130.590883170839,-5.5737382119418,132.795894386321));
#183473=CARTESIAN_POINT('Ctrl Pts',(130.598291390506,-5.62478296336238,
132.646778742849));
#183474=CARTESIAN_POINT('Ctrl Pts',(130.605699610172,-5.66976895910799,
132.496001984061));
#183475=CARTESIAN_POINT('Ctrl Pts',(130.613112389474,-5.71478264298338,
132.345132424692));
#183476=CARTESIAN_POINT('Ctrl Pts',(130.620525168776,-5.75373004841809,
132.192600073624));
#183477=CARTESIAN_POINT('Ctrl Pts',(130.627937948079,-5.78651499205246,
132.038935365911));
#183478=CARTESIAN_POINT('Ctrl Pts',(130.635361319107,-5.81934678035175,
131.885051094858));
#183479=CARTESIAN_POINT('Ctrl Pts',(130.642784690136,-5.8459984577789,131.730031602649));
#183480=CARTESIAN_POINT('Ctrl Pts',(130.650208061165,-5.86642554864406,
131.574413761652));
#183481=CARTESIAN_POINT('Ctrl Pts',(130.654144110606,-5.87725648236231,
131.491901448354));
#183482=CARTESIAN_POINT('Ctrl Pts',(130.658080160047,-5.88633833199474,
131.409220952629));
#183483=CARTESIAN_POINT('Ctrl Pts',(130.662016209487,-5.89367041093406,
131.326452228091));
#183484=CARTESIAN_POINT('Ctrl Pts',(130.67021907559,-5.9089507224997,131.153959281779));
#183485=CARTESIAN_POINT('Ctrl Pts',(130.678421941693,-5.91665983543796,
130.980785795447));
#183486=CARTESIAN_POINT('Ctrl Pts',(130.686624807795,-5.91674921377853,
130.807410822667));
#183487=CARTESIAN_POINT('',(132.436623601775,-5.91262847433545,130.80816648937));
#183488=CARTESIAN_POINT('Ctrl Pts',(130.686627247827,-5.92459733177465,
130.807363227819));
#183489=CARTESIAN_POINT('Ctrl Pts',(130.771239442985,-5.91334481668904,
129.016629511582));
#183490=CARTESIAN_POINT('Ctrl Pts',(130.948667512746,-4.09245350856522,
125.241769634098));
#183491=CARTESIAN_POINT('Ctrl Pts',(131.218911457113,2.33599408130523,124.207339154629));
#183492=CARTESIAN_POINT('Ctrl Pts',(131.497359080925,6.81292285489911,129.203847355033));
#183493=CARTESIAN_POINT('Ctrl Pts',(131.775806704738,5.02910835462435,135.671149054285));
#183494=CARTESIAN_POINT('Ctrl Pts',(132.054254328551,-1.37621103794747,
137.666109936025));
#183495=CARTESIAN_POINT('Ctrl Pts',(132.274526317919,-5.44283188373582,
134.256076213049));
#183496=CARTESIAN_POINT('Ctrl Pts',(132.401982432682,-5.91374388142558,
131.546133979802));
#183497=CARTESIAN_POINT('Ctrl Pts',(132.43662267284,-5.90945480774847,130.808184249578));
#183498=CARTESIAN_POINT('',(134.186626039157,-5.9132873379319,130.799875516716));
#183499=CARTESIAN_POINT('Ctrl Pts',(132.436624807795,-5.91674879074801,
130.8081434316));
#183500=CARTESIAN_POINT('Ctrl Pts',(132.44407390138,-5.91685037237187,130.649258288229));
#183501=CARTESIAN_POINT('Ctrl Pts',(132.451522994964,-5.91054770060562,
130.490344618787));
#183502=CARTESIAN_POINT('Ctrl Pts',(132.458972088549,-5.89786057853249,
130.331950669859));
#183503=CARTESIAN_POINT('Ctrl Pts',(132.466421684772,-5.88517260037755,
130.173546033072));
#183504=CARTESIAN_POINT('Ctrl Pts',(132.473871280995,-5.86609934203964,
130.015661551399));
#183505=CARTESIAN_POINT('Ctrl Pts',(132.481320877217,-5.84071257509522,
129.858841089674));
#183506=CARTESIAN_POINT('Ctrl Pts',(132.488772368481,-5.81531935022228,
129.701980735697));
#183507=CARTESIAN_POINT('Ctrl Pts',(132.496223859745,-5.78360947568675,
129.546185301953));
#183508=CARTESIAN_POINT('Ctrl Pts',(132.503675351009,-5.74570599473036,
129.391989142132));
#183509=CARTESIAN_POINT('Ctrl Pts',(132.511130130572,-5.70778578719094,
129.237724936454));
#183510=CARTESIAN_POINT('Ctrl Pts',(132.518584910135,-5.66366661589122,
129.085061765474));
#183511=CARTESIAN_POINT('Ctrl Pts',(132.526039689697,-5.61352158044227,
128.934519440244));
#183512=CARTESIAN_POINT('Ctrl Pts',(132.53350393347,-5.56331288340478,128.783785994129));
#183513=CARTESIAN_POINT('Ctrl Pts',(132.540968177242,-5.50706315523841,
128.635179119972));
#183514=CARTESIAN_POINT('Ctrl Pts',(132.548432421014,-5.44499427198543,
128.489200160806));
#183515=CARTESIAN_POINT('Ctrl Pts',(132.555901690165,-5.38288360022045,
128.343122919809));
#183516=CARTESIAN_POINT('Ctrl Pts',(132.563370959316,-5.31494612024657,
128.199677450412));
#183517=CARTESIAN_POINT('Ctrl Pts',(132.570840228467,-5.24144983426337,
128.059340727401));
#183518=CARTESIAN_POINT('Ctrl Pts',(132.578321762038,-5.16783286855118,
127.91877357373));
#183519=CARTESIAN_POINT('Ctrl Pts',(132.58580329561,-5.08863904046948,127.781325683021));
#183520=CARTESIAN_POINT('Ctrl Pts',(132.593284829182,-5.00418050062325,
127.647446288719));
#183521=CARTESIAN_POINT('Ctrl Pts',(132.599239744847,-4.93695584979939,
127.54088518133));
#183522=CARTESIAN_POINT('Ctrl Pts',(132.605194660512,-4.86639670527273,
127.436584300791));
#183523=CARTESIAN_POINT('Ctrl Pts',(132.611149576177,-4.79267835126431,
127.334754763319));
#183524=CARTESIAN_POINT('Ctrl Pts',(132.618572842582,-4.7007826785881,127.20781630993));
#183525=CARTESIAN_POINT('Ctrl Pts',(132.625996108988,-4.60370144481768,
127.08433934361));
#183526=CARTESIAN_POINT('Ctrl Pts',(132.633419375393,-4.50172427172658,
126.964776116107));
#183527=CARTESIAN_POINT('Ctrl Pts',(132.640833868114,-4.39986762718525,
126.845354202409));
#183528=CARTESIAN_POINT('Ctrl Pts',(132.648248360835,-4.29312680145029,
126.729837101266));
#183529=CARTESIAN_POINT('Ctrl Pts',(132.655662853556,-4.18183439753327,
126.618647818758));
#183530=CARTESIAN_POINT('Ctrl Pts',(132.66307019991,-4.07064926142554,126.507565704667));
#183531=CARTESIAN_POINT('Ctrl Pts',(132.670477546264,-3.95492154306506,
126.400803367012));
#183532=CARTESIAN_POINT('Ctrl Pts',(132.677884892618,-3.83502370139943,
126.298750362317));
#183533=CARTESIAN_POINT('Ctrl Pts',(132.685286714293,-3.71521528406725,
126.196773472603));
#183534=CARTESIAN_POINT('Ctrl Pts',(132.692688535969,-3.59124321937131,
126.099499163105));
#183535=CARTESIAN_POINT('Ctrl Pts',(132.700090357644,-3.463516281595,126.007279679159));
#183536=CARTESIAN_POINT('Ctrl Pts',(132.707488271955,-3.335856769874,125.91510887716));
#183537=CARTESIAN_POINT('Ctrl Pts',(132.714886186267,-3.20444663454561,
125.827987804427));
#183538=CARTESIAN_POINT('Ctrl Pts',(132.722284100578,-3.06972704701265,
125.746227916723));
#183539=CARTESIAN_POINT('Ctrl Pts',(132.72968078549,-2.93502984743204,125.66448161603));
#183540=CARTESIAN_POINT('Ctrl Pts',(132.737077470403,-2.79702460599024,
125.588094925615));
#183541=CARTESIAN_POINT('Ctrl Pts',(132.744474155315,-2.65618084144462,
125.517335565607));
#183542=CARTESIAN_POINT('Ctrl Pts',(132.75187051225,-2.51534332205942,125.446579343143));
#183543=CARTESIAN_POINT('Ctrl Pts',(132.759266869186,-2.37166786339592,
125.381450122535));
#183544=CARTESIAN_POINT('Ctrl Pts',(132.766663226121,-2.22564766625974,
125.322169173611));
#183545=CARTESIAN_POINT('Ctrl Pts',(132.774060715458,-2.07960511305829,
125.262879148622));
#183546=CARTESIAN_POINT('Ctrl Pts',(132.781458204794,-1.93121745249945,
125.209439318576));
#183547=CARTESIAN_POINT('Ctrl Pts',(132.788855694131,-1.7809967507698,125.16202234906));
#183548=CARTESIAN_POINT('Ctrl Pts',(132.796255776646,-1.63072338940593,
125.114588757598));
#183549=CARTESIAN_POINT('Ctrl Pts',(132.803655859161,-1.47861606328235,
125.073182342554));
#183550=CARTESIAN_POINT('Ctrl Pts',(132.811055941676,-1.32520068992937,
125.037925523514));
#183551=CARTESIAN_POINT('Ctrl Pts',(132.818464161342,-1.17161662060201,
125.002629935978));
#183552=CARTESIAN_POINT('Ctrl Pts',(132.825872381009,-1.01672199563854,
124.973497532491));
#183553=CARTESIAN_POINT('Ctrl Pts',(132.833280600675,-0.861052313563191,
124.950599478281));
#183554=CARTESIAN_POINT('Ctrl Pts',(132.840693379978,-0.705286819396123,
124.9276873307));
#183555=CARTESIAN_POINT('Ctrl Pts',(132.84810615928,-0.548745687904146,
124.911017217811));
#183556=CARTESIAN_POINT('Ctrl Pts',(132.855518938582,-0.391967664889735,
124.900608258923));
#183557=CARTESIAN_POINT('Ctrl Pts',(132.86294230961,-0.234965630083658,
124.890184427226));
#183558=CARTESIAN_POINT('Ctrl Pts',(132.870365680639,-0.0777263999109395,
124.88603962697));
#183559=CARTESIAN_POINT('Ctrl Pts',(132.877789051668,0.0792123244657625,
124.8881408811));
#183560=CARTESIAN_POINT('Ctrl Pts',(132.881725101109,0.162425001823287,
124.889255016459));
#183561=CARTESIAN_POINT('Ctrl Pts',(132.88566115055,0.245553286538442,124.892124275274));
#183562=CARTESIAN_POINT('Ctrl Pts',(132.88959719999,0.328517952984534,124.896737870888));
#183563=CARTESIAN_POINT('Ctrl Pts',(132.897020466396,0.484986724663619,
124.90543896823));
#183564=CARTESIAN_POINT('Ctrl Pts',(132.904443732801,0.641346171672067,
124.920373843296));
#183565=CARTESIAN_POINT('Ctrl Pts',(132.911866999207,0.79705925416422,124.941543282201));
#183566=CARTESIAN_POINT('Ctrl Pts',(132.919281491928,0.952588296724034,
124.962687700588));
#183567=CARTESIAN_POINT('Ctrl Pts',(132.926695984649,1.10747212912949,124.990051965506));
#183568=CARTESIAN_POINT('Ctrl Pts',(132.93411047737,1.26117508433303,125.023584893742));
#183569=CARTESIAN_POINT('Ctrl Pts',(132.941517823724,1.41472989484175,125.057085501678));
#183570=CARTESIAN_POINT('Ctrl Pts',(132.948925170077,1.5671057317581,125.096742857397));
#183571=CARTESIAN_POINT('Ctrl Pts',(132.956332516431,1.71777352698821,125.142454165453));
#183572=CARTESIAN_POINT('Ctrl Pts',(132.963734338107,1.86832894849248,125.188131380291));
#183573=CARTESIAN_POINT('Ctrl Pts',(132.971136159782,2.01717850917903,125.239853449051));
#183574=CARTESIAN_POINT('Ctrl Pts',(132.978537981457,2.16380490258672,125.297466855558));
#183575=CARTESIAN_POINT('Ctrl Pts',(132.985935895769,2.31035389306298,125.355049848397));
#183576=CARTESIAN_POINT('Ctrl Pts',(132.99333381008,2.45468170696657,125.418517849114));
#183577=CARTESIAN_POINT('Ctrl Pts',(133.000731724392,2.59628784382242,125.487668037162));
#183578=CARTESIAN_POINT('Ctrl Pts',(133.008128409304,2.73787044830651,125.556806733703));
#183579=CARTESIAN_POINT('Ctrl Pts',(133.015525094216,2.87673193830053,125.631625579822));
#183580=CARTESIAN_POINT('Ctrl Pts',(133.022921779128,3.0123932869216,125.711874265359));
#183581=CARTESIAN_POINT('Ctrl Pts',(133.030318136064,3.1480486201766,125.792119392586));
#183582=CARTESIAN_POINT('Ctrl Pts',(133.037714492999,3.28050377290562,125.877793690452));
#183583=CARTESIAN_POINT('Ctrl Pts',(133.045110849935,3.40930599745367,125.968601816899));
#183584=CARTESIAN_POINT('Ctrl Pts',(133.052508339271,3.53812794195056,126.059423846302));
#183585=CARTESIAN_POINT('Ctrl Pts',(133.059905828608,3.66329553956439,126.155381054207));
#183586=CARTESIAN_POINT('Ctrl Pts',(133.067303317944,3.7843867375661,126.256135954796));
#183587=CARTESIAN_POINT('Ctrl Pts',(133.074703400459,3.90552038390059,126.35692617486));
#183588=CARTESIAN_POINT('Ctrl Pts',(133.082103482974,4.02257449876675,126.462517197492));
#183589=CARTESIAN_POINT('Ctrl Pts',(133.089503565489,4.13516181582623,126.572532724157));
#183590=CARTESIAN_POINT('Ctrl Pts',(133.096911785156,4.24787293421459,126.682669224204));
#183591=CARTESIAN_POINT('Ctrl Pts',(133.104320004822,4.35610717864507,126.797239683346));
#183592=CARTESIAN_POINT('Ctrl Pts',(133.111728224489,4.45951522576416,126.915832038055));
#183593=CARTESIAN_POINT('Ctrl Pts',(133.119141003791,4.56298691881095,127.034497384378));
#183594=CARTESIAN_POINT('Ctrl Pts',(133.126553783093,4.66162626220762,127.157189268572));
#183595=CARTESIAN_POINT('Ctrl Pts',(133.133966562395,4.75512596507289,127.283464762987));
#183596=CARTESIAN_POINT('Ctrl Pts',(133.141389933424,4.84875926469812,127.40992068575));
#183597=CARTESIAN_POINT('Ctrl Pts',(133.148813304453,4.93723804723103,127.53997013756));
#183598=CARTESIAN_POINT('Ctrl Pts',(133.156236675481,5.0202994165876,127.673142910298));
#183599=CARTESIAN_POINT('Ctrl Pts',(133.160172724922,5.06434054764887,127.743754309837));
#183600=CARTESIAN_POINT('Ctrl Pts',(133.164108774363,5.10685942735345,127.815243394556));
#183601=CARTESIAN_POINT('Ctrl Pts',(133.168044823803,5.14782230743705,127.887537679238));
#183602=CARTESIAN_POINT('Ctrl Pts',(133.175468090209,5.22507702087024,128.023882443928));
#183603=CARTESIAN_POINT('Ctrl Pts',(133.182891356614,5.29702798789942,128.163504739803));
#183604=CARTESIAN_POINT('Ctrl Pts',(133.19031462302,5.3633842639891,128.305953164949));
#183605=CARTESIAN_POINT('Ctrl Pts',(133.197729115741,5.42966211247099,128.448233227885));
#183606=CARTESIAN_POINT('Ctrl Pts',(133.205143608462,5.4903582760621,128.593332436224));
#183607=CARTESIAN_POINT('Ctrl Pts',(133.212558101183,5.5452262755268,128.740772452329));
#183608=CARTESIAN_POINT('Ctrl Pts',(133.219965447537,5.60004139114794,128.888070360196));
#183609=CARTESIAN_POINT('Ctrl Pts',(133.22737279389,5.64903939646685,129.037704236752));
#183610=CARTESIAN_POINT('Ctrl Pts',(133.234780140244,5.69202080197526,129.189173398578));
#183611=CARTESIAN_POINT('Ctrl Pts',(133.24218196192,5.73497015032987,129.340529588989));
#183612=CARTESIAN_POINT('Ctrl Pts',(133.249583783595,5.77191173244081,129.49371798158));
#183613=CARTESIAN_POINT('Ctrl Pts',(133.256985605271,5.80269508903512,129.648220372532));
#183614=CARTESIAN_POINT('Ctrl Pts',(133.264383519582,5.83346219533502,129.802641202874));
#183615=CARTESIAN_POINT('Ctrl Pts',(133.271781433893,5.858077477642,129.958374284966));
#183616=CARTESIAN_POINT('Ctrl Pts',(133.279179348205,5.87644104189458,130.114888904124));
#183617=CARTESIAN_POINT('Ctrl Pts',(133.286576033117,5.89480155445593,130.271377513391));
#183618=CARTESIAN_POINT('Ctrl Pts',(133.293972718029,5.90691236745847,130.428647031564));
#183619=CARTESIAN_POINT('Ctrl Pts',(133.301369402941,5.91272514819743,130.586159141004));
#183620=CARTESIAN_POINT('Ctrl Pts',(133.308765759877,5.91853767119159,130.743664266192));
#183621=CARTESIAN_POINT('Ctrl Pts',(133.316162116812,5.91805270342139,130.901411588216));
#183622=CARTESIAN_POINT('Ctrl Pts',(133.323558473748,5.91127400335937,131.058860558053));
#183623=CARTESIAN_POINT('Ctrl Pts',(133.330955963084,5.90449426546107,131.216333633729));
#183624=CARTESIAN_POINT('Ctrl Pts',(133.338353452421,5.89141889269998,131.37350789329));
#183625=CARTESIAN_POINT('Ctrl Pts',(133.345750941757,5.87210369164419,131.529845832494));
#183626=CARTESIAN_POINT('Ctrl Pts',(133.353151024272,5.85278171967458,131.68623857572));
#183627=CARTESIAN_POINT('Ctrl Pts',(133.360551106787,5.82721561013181,131.841794044638));
#183628=CARTESIAN_POINT('Ctrl Pts',(133.367951189302,5.79551262671546,131.995983022559));
#183629=CARTESIAN_POINT('Ctrl Pts',(133.375359408969,5.7637747826097,132.150341547113));
#183630=CARTESIAN_POINT('Ctrl Pts',(133.382767628635,5.72588666341188,132.303330214011));
#183631=CARTESIAN_POINT('Ctrl Pts',(133.390175848302,5.68200613203574,132.454432397219));
#183632=CARTESIAN_POINT('Ctrl Pts',(133.397588627604,5.63809859292471,132.6056275813));
#183633=CARTESIAN_POINT('Ctrl Pts',(133.405001406906,5.58819141044362,132.754933614834));
#183634=CARTESIAN_POINT('Ctrl Pts',(133.412414186208,5.53249113394025,132.901852552085));
#183635=CARTESIAN_POINT('Ctrl Pts',(133.419837557237,5.47671127026969,133.048981414004));
#183636=CARTESIAN_POINT('Ctrl Pts',(133.427260928266,5.41512192644351,133.193716024936));
#183637=CARTESIAN_POINT('Ctrl Pts',(133.434684299295,5.34797660011437,133.335581043987));
#183638=CARTESIAN_POINT('Ctrl Pts',(133.438620348735,5.31237453696658,133.410801281088));
#183639=CARTESIAN_POINT('Ctrl Pts',(133.442556398176,5.27521123837849,133.485215215288));
#183640=CARTESIAN_POINT('Ctrl Pts',(133.446492447616,5.2365294464544,133.558755273187));
#183641=CARTESIAN_POINT('Ctrl Pts',(133.453915714022,5.1635767940994,133.697449527286));
#183642=CARTESIAN_POINT('Ctrl Pts',(133.461338980427,5.08499985744994,133.833453174989));
#183643=CARTESIAN_POINT('Ctrl Pts',(133.468762246833,5.00102115109538,133.966277442657));
#183644=CARTESIAN_POINT('Ctrl Pts',(133.476176739554,4.91714170059768,134.098944723072));
#183645=CARTESIAN_POINT('Ctrl Pts',(133.483591232275,4.82787338620697,134.228439790858));
#183646=CARTESIAN_POINT('Ctrl Pts',(133.491005724996,4.73348541887591,134.354296722877));
#183647=CARTESIAN_POINT('Ctrl Pts',(133.498413071349,4.63918842622115,134.480032349247));
#183648=CARTESIAN_POINT('Ctrl Pts',(133.505820417703,4.53978182674042,134.602136524107));
#183649=CARTESIAN_POINT('Ctrl Pts',(133.513227764057,4.43557903062356,134.720170779664));
#183650=CARTESIAN_POINT('Ctrl Pts',(133.520629585732,4.33145395288362,134.838117000821));
#183651=CARTESIAN_POINT('Ctrl Pts',(133.528031407408,4.22254004715631,134.95199906812));
#183652=CARTESIAN_POINT('Ctrl Pts',(133.535433229083,4.1091919660784,135.061410294093));
#183653=CARTESIAN_POINT('Ctrl Pts',(133.542831143395,3.99590372056947,135.170763762732));
#183654=CARTESIAN_POINT('Ctrl Pts',(133.550229057706,3.8781862293635,135.275650831741));
#183655=CARTESIAN_POINT('Ctrl Pts',(133.557626972017,3.75643200257498,135.375700593167));
#183656=CARTESIAN_POINT('Ctrl Pts',(133.56502365693,3.63469800913089,135.475733728138));
#183657=CARTESIAN_POINT('Ctrl Pts',(133.572420341842,3.50892889963901,135.570930914207));
#183658=CARTESIAN_POINT('Ctrl Pts',(133.579817026754,3.37955145096719,135.660960513869));
#183659=CARTESIAN_POINT('Ctrl Pts',(133.587213383689,3.25017973902701,135.750986121523));
#183660=CARTESIAN_POINT('Ctrl Pts',(133.594609740625,3.11720031244699,135.83584438515));
#183661=CARTESIAN_POINT('Ctrl Pts',(133.60200609756,2.98106998197459,135.915246286906));
#183662=CARTESIAN_POINT('Ctrl Pts',(133.609403586897,2.84491880960145,135.994660345297));
#183663=CARTESIAN_POINT('Ctrl Pts',(133.616801076233,2.70561609526588,136.068616190367));
#183664=CARTESIAN_POINT('Ctrl Pts',(133.62419856557,2.56364422132333,136.13687023959));
#183665=CARTESIAN_POINT('Ctrl Pts',(133.631598648085,2.42162257935944,136.205148215164));
#183666=CARTESIAN_POINT('Ctrl Pts',(133.6389987306,2.2769302511042,136.26772025374));
#183667=CARTESIAN_POINT('Ctrl Pts',(133.646398813115,2.13007046019527,136.324390544759));
#183668=CARTESIAN_POINT('Ctrl Pts',(133.653807032781,1.98304918184942,136.381123150588));
#183669=CARTESIAN_POINT('Ctrl Pts',(133.661215252448,1.83385602962931,136.431940914274));
#183670=CARTESIAN_POINT('Ctrl Pts',(133.668623472114,1.68301098441021,136.476697401366));
#183671=CARTESIAN_POINT('Ctrl Pts',(133.676036251416,1.53207309658211,136.52148143533));
#183672=CARTESIAN_POINT('Ctrl Pts',(133.683449030718,1.3794816508222,136.560196667391));
#183673=CARTESIAN_POINT('Ctrl Pts',(133.69086181002,1.22576722794721,136.592747721535));
#183674=CARTESIAN_POINT('Ctrl Pts',(133.698285181049,1.07183317069698,136.62534528615));
#183675=CARTESIAN_POINT('Ctrl Pts',(133.705708552078,0.916773298681986,
136.651761019437));
#183676=CARTESIAN_POINT('Ctrl Pts',(133.713131923107,0.761124551332805,
136.671951262785));
#183677=CARTESIAN_POINT('Ctrl Pts',(133.717067972547,0.678595850746283,
136.682656614266));
#183678=CARTESIAN_POINT('Ctrl Pts',(133.721004021988,0.595901629734843,
136.691612627742));
#183679=CARTESIAN_POINT('Ctrl Pts',(133.724940071429,0.513121842865592,
136.698818738282));
#183680=CARTESIAN_POINT('Ctrl Pts',(133.732363337835,0.357001748301379,
136.712409237865));
#183681=CARTESIAN_POINT('Ctrl Pts',(133.73978660424,0.200105274057244,136.719813529305));
#183682=CARTESIAN_POINT('Ctrl Pts',(133.747209870645,0.0429639138102346,
136.720954626336));
#183683=CARTESIAN_POINT('Ctrl Pts',(133.754624363366,-0.113991718398853,
136.722094374685));
#183684=CARTESIAN_POINT('Ctrl Pts',(133.762038856087,-0.271191290846173,
136.716985660809));
#183685=CARTESIAN_POINT('Ctrl Pts',(133.769453348808,-0.428097294104577,
136.70560313667));
#183686=CARTESIAN_POINT('Ctrl Pts',(133.776860695162,-0.584852065449522,
136.694231583436));
#183687=CARTESIAN_POINT('Ctrl Pts',(133.784268041516,-0.741313461089294,
136.676598285024));
#183688=CARTESIAN_POINT('Ctrl Pts',(133.79167538787,-0.896943179789474,
136.65272991975));
#183689=CARTESIAN_POINT('Ctrl Pts',(133.799077209545,-1.05245682397432,
136.628879356404));
#183690=CARTESIAN_POINT('Ctrl Pts',(133.80647903122,-1.20713965891711,136.598803042012));
#183691=CARTESIAN_POINT('Ctrl Pts',(133.813880852896,-1.36045782851884,
136.562579531373));
#183692=CARTESIAN_POINT('Ctrl Pts',(133.821278767207,-1.5136950626515,136.526375142843));
#183693=CARTESIAN_POINT('Ctrl Pts',(133.828676681518,-1.66556870377039,
136.484030106367));
#183694=CARTESIAN_POINT('Ctrl Pts',(133.83607459583,-1.81555453520508,136.435674167014));
#183695=CARTESIAN_POINT('Ctrl Pts',(133.843471280742,-1.96551544171603,
136.38732626354));
#183696=CARTESIAN_POINT('Ctrl Pts',(133.850867965654,-2.11358880624222,
136.332969554149));
#183697=CARTESIAN_POINT('Ctrl Pts',(133.858264650566,-2.25926492943554,
136.272783840134));
#183698=CARTESIAN_POINT('Ctrl Pts',(133.865661007502,-2.40493459319669,
136.212600794817));
#183699=CARTESIAN_POINT('Ctrl Pts',(133.873057364437,-2.54820688196584,
136.14658940133));
#183700=CARTESIAN_POINT('Ctrl Pts',(133.880453721372,-2.68859171948106,
136.074977766291));
#183701=CARTESIAN_POINT('Ctrl Pts',(133.887851210709,-2.8289980502734,136.003355167328));
#183702=CARTESIAN_POINT('Ctrl Pts',(133.895248700046,-2.96651571702576,
135.926130789232));
#183703=CARTESIAN_POINT('Ctrl Pts',(133.902646189382,-3.10067904741429,
135.843578811634));
#183704=CARTESIAN_POINT('Ctrl Pts',(133.910046271897,-3.23488940854992,
135.760997895569));
#183705=CARTESIAN_POINT('Ctrl Pts',(133.917446354412,-3.36574277446368,
135.673085857166));
#183706=CARTESIAN_POINT('Ctrl Pts',(133.924846436927,-3.49280239951895,
135.580160232334));
#183707=CARTESIAN_POINT('Ctrl Pts',(133.932254656593,-3.62000173969448,
135.487132426224));
#183708=CARTESIAN_POINT('Ctrl Pts',(133.93966287626,-3.74339870653799,135.389080244456));
#183709=CARTESIAN_POINT('Ctrl Pts',(133.947071095926,-3.86258903823458,
135.286362010271));
#183710=CARTESIAN_POINT('Ctrl Pts',(133.954483875228,-3.98185272959161,
135.183580554726));
#183711=CARTESIAN_POINT('Ctrl Pts',(133.96189665453,-4.09690435448368,135.076127578396));
#183712=CARTESIAN_POINT('Ctrl Pts',(133.969309433832,-4.20737687847538,
134.964397920881));
#183713=CARTESIAN_POINT('Ctrl Pts',(133.976732804861,-4.31800725079001,
134.852508618791));
#183714=CARTESIAN_POINT('Ctrl Pts',(133.98415617589,-4.42404520370888,134.736330706023));
#183715=CARTESIAN_POINT('Ctrl Pts',(133.991579546919,-4.52516377712922,
134.616292326379));
#183716=CARTESIAN_POINT('Ctrl Pts',(133.99551559636,-4.57877927106441,134.55264509721));
#183717=CARTESIAN_POINT('Ctrl Pts',(133.9994516458,-4.63101246522455,134.487913051098));
#183718=CARTESIAN_POINT('Ctrl Pts',(134.003387695241,-4.68181966692091,
134.422163150725));
#183719=CARTESIAN_POINT('Ctrl Pts',(134.011022574931,-4.7803720042715,134.294625987765));
#183720=CARTESIAN_POINT('Ctrl Pts',(134.018657454621,-4.87386670141188,
134.162855095918));
#183721=CARTESIAN_POINT('Ctrl Pts',(134.02629233431,-4.96192037701707,134.027290454631));
#183722=CARTESIAN_POINT('Ctrl Pts',(134.033714027795,-5.04751535913498,
133.895511139718));
#183723=CARTESIAN_POINT('Ctrl Pts',(134.041135721279,-5.12796884959424,
133.760147423981));
#183724=CARTESIAN_POINT('Ctrl Pts',(134.048557414764,-5.20296800714661,
133.62163846668));
#183725=CARTESIAN_POINT('Ctrl Pts',(134.05597195836,-5.27789491224383,133.483262945708));
#183726=CARTESIAN_POINT('Ctrl Pts',(134.063386501956,-5.34737776716814,
133.341748538514));
#183727=CARTESIAN_POINT('Ctrl Pts',(134.070801045553,-5.41114695277371,
133.197563328994));
#183728=CARTESIAN_POINT('Ctrl Pts',(134.078209897014,-5.47486718285919,
133.053488810271));
#183729=CARTESIAN_POINT('Ctrl Pts',(134.085618748475,-5.53288232615693,
132.906747909422));
#183730=CARTESIAN_POINT('Ctrl Pts',(134.093027599936,-5.58496872146775,
132.757833151984));
#183731=CARTESIAN_POINT('Ctrl Pts',(134.100432213184,-5.63702532090011,
132.609003580822));
#183732=CARTESIAN_POINT('Ctrl Pts',(134.107836826432,-5.68315980345566,
132.458002979346));
#183733=CARTESIAN_POINT('Ctrl Pts',(134.11524143968,-5.72319672339956,132.305343571423));
#183734=CARTESIAN_POINT('Ctrl Pts',(134.12264368252,-5.7632208264932,132.152733033712));
#183735=CARTESIAN_POINT('Ctrl Pts',(134.130045925361,-5.79715115857646,
131.998465105857));
#183736=CARTESIAN_POINT('Ctrl Pts',(134.137448168201,-5.82486222414745,
131.843066847546));
#183737=CARTESIAN_POINT('Ctrl Pts',(134.144849108908,-5.85256841504679,
131.687695925445));
#183738=CARTESIAN_POINT('Ctrl Pts',(134.152250049615,-5.87405745611901,
131.531195435284));
#183739=CARTESIAN_POINT('Ctrl Pts',(134.159650990322,-5.88925506503365,
131.374102086546));
#183740=CARTESIAN_POINT('Ctrl Pts',(134.167053047952,-5.90445496751447,
131.216985029869));
#183741=CARTESIAN_POINT('Ctrl Pts',(134.174455105581,-5.91336150741497,
131.0592753061));
#183742=CARTESIAN_POINT('Ctrl Pts',(134.18185716321,-5.91595230949239,130.901514280964));
#183743=CARTESIAN_POINT('Ctrl Pts',(134.183446378072,-5.91650855227934,
130.867643136172));
#183744=CARTESIAN_POINT('Ctrl Pts',(134.185035592933,-5.91677385779731,
130.833769631019));
#183745=CARTESIAN_POINT('Ctrl Pts',(134.186624807795,-5.91674831791726,
130.799899124178));
#183746=CARTESIAN_POINT('',(135.936624807795,-5.92567594249246,130.802308620648));
#183747=CARTESIAN_POINT('Ctrl Pts',(134.186626933769,-5.91077285849561,
130.799858365367));
#183748=CARTESIAN_POINT('Ctrl Pts',(134.218363062198,-5.91547483959939,
130.124154099521));
#183749=CARTESIAN_POINT('Ctrl Pts',(134.342915065229,-5.49594096797783,
127.477948136323));
#183750=CARTESIAN_POINT('Ctrl Pts',(134.560282942868,-1.5901433003448,123.989009943189));
#183751=CARTESIAN_POINT('Ctrl Pts',(134.83873056668,4.87443624786771,125.782664510092));
#183752=CARTESIAN_POINT('Ctrl Pts',(135.117178190494,6.8596470137397,132.19101247627));
#183753=CARTESIAN_POINT('Ctrl Pts',(135.395625814306,2.54117728637125,137.325095126005));
#183754=CARTESIAN_POINT('Ctrl Pts',(135.66877468674,-3.98589310494111,136.483271655578));
#183755=CARTESIAN_POINT('Ctrl Pts',(135.84910768457,-5.91738414547342,132.653629227728));
#183756=CARTESIAN_POINT('Ctrl Pts',(135.936624807795,-5.92567594249246,
130.802308620648));
#183757=CARTESIAN_POINT('',(137.686624807795,-5.91704275648427,130.809814173709));
#183758=CARTESIAN_POINT('Ctrl Pts',(135.936624807795,-5.92567594249246,
130.802308620648));
#183759=CARTESIAN_POINT('Ctrl Pts',(135.941923559174,-5.92617797191561,
130.690219840098));
#183760=CARTESIAN_POINT('Ctrl Pts',(135.947222310553,-5.92327425135077,
130.578157588943));
#183761=CARTESIAN_POINT('Ctrl Pts',(136.045336936536,-5.80492782942922,
128.506840458106));
#183762=CARTESIAN_POINT('Ctrl Pts',(136.230968685746,-3.44077999718933,
124.710216416672));
#183763=CARTESIAN_POINT('Ctrl Pts',(136.509416309557,3.26735047713948,124.615501159646));
#183764=CARTESIAN_POINT('Ctrl Pts',(136.787863933371,6.97294548192195,130.208045401854));
#183765=CARTESIAN_POINT('Ctrl Pts',(137.066311557183,4.27074423614178,136.348574195687));
#183766=CARTESIAN_POINT('Ctrl Pts',(137.344759180996,-2.35606232519568,
137.394241561112));
#183767=CARTESIAN_POINT('Ctrl Pts',(137.551530264534,-5.66925498345734,
133.67380708407));
#183768=CARTESIAN_POINT('Ctrl Pts',(137.665485473467,-5.92120632191818,
131.258690372421));
#183769=CARTESIAN_POINT('Ctrl Pts',(137.686624807795,-5.91704275648427,
130.809814173709));
#183770=CARTESIAN_POINT('',(139.436624807833,-5.91674998555252,130.803947139341));
#183771=CARTESIAN_POINT('Ctrl Pts',(137.686624807795,-5.91674748693855,
130.809813901568));
#183772=CARTESIAN_POINT('Ctrl Pts',(137.69393408468,-5.91689052743576,130.654616684241));
#183773=CARTESIAN_POINT('Ctrl Pts',(137.701243361564,-5.91092312658041,
130.499242156393));
#183774=CARTESIAN_POINT('Ctrl Pts',(137.708552638449,-5.89883028694207,
130.344217369919));
#183775=CARTESIAN_POINT('Ctrl Pts',(137.715856751963,-5.8867459898465,130.189302095017));
#183776=CARTESIAN_POINT('Ctrl Pts',(137.723160865477,-5.86854489581824,
130.034736451036));
#183777=CARTESIAN_POINT('Ctrl Pts',(137.730464978992,-5.84426407875375,
129.881047052038));
#183778=CARTESIAN_POINT('Ctrl Pts',(137.737766293394,-5.81999256668224,
129.727416550513));
#183779=CARTESIAN_POINT('Ctrl Pts',(137.745067607796,-5.78964602436644,
129.574662004816));
#183780=CARTESIAN_POINT('Ctrl Pts',(137.752368922199,-5.7533133206347,129.423304356182));
#183781=CARTESIAN_POINT('Ctrl Pts',(137.759668915328,-5.71698719180307,
129.271974097787));
#183782=CARTESIAN_POINT('Ctrl Pts',(137.766968908458,-5.67467714561526,
129.122040606972));
#183783=CARTESIAN_POINT('Ctrl Pts',(137.774268901587,-5.62652299648003,
128.974013783608));
#183784=CARTESIAN_POINT('Ctrl Pts',(137.781569104416,-5.57836746407182,
128.825982708035));
#183785=CARTESIAN_POINT('Ctrl Pts',(137.788869307244,-5.52436761338954,
128.679858774188));
#183786=CARTESIAN_POINT('Ctrl Pts',(137.796169510073,-5.46471278755805,
128.536135604037));
#183787=CARTESIAN_POINT('Ctrl Pts',(137.80347145356,-5.40504373764388,128.392378164567));
#183788=CARTESIAN_POINT('Ctrl Pts',(137.810773397047,-5.33971717708414,
128.251022982321));
#183789=CARTESIAN_POINT('Ctrl Pts',(137.818075340535,-5.26897000914988,
128.112542346364));
#183790=CARTESIAN_POINT('Ctrl Pts',(137.825384779612,-5.19815021783941,
127.973919557277));
#183791=CARTESIAN_POINT('Ctrl Pts',(137.83269421869,-5.12189888135447,127.838177549932));
#183792=CARTESIAN_POINT('Ctrl Pts',(137.840003657768,-5.04049846765269,
127.705763231636));
#183793=CARTESIAN_POINT('Ctrl Pts',(137.847317023562,-4.95905432468774,
127.573277778806));
#183794=CARTESIAN_POINT('Ctrl Pts',(137.854630389357,-4.87245580897648,
127.444123893767));
#183795=CARTESIAN_POINT('Ctrl Pts',(137.861943755151,-4.78102743035337,
127.318717596155));
#183796=CARTESIAN_POINT('Ctrl Pts',(137.869268052795,-4.68946238671831,
127.19312384413));
#183797=CARTESIAN_POINT('Ctrl Pts',(137.876592350438,-4.59305329741779,
127.07128916947));
#183798=CARTESIAN_POINT('Ctrl Pts',(137.883916648082,-4.49216403964663,
126.95359539447));
#183799=CARTESIAN_POINT('Ctrl Pts',(137.889829241595,-4.4107204391639,126.858586223006));
#183800=CARTESIAN_POINT('Ctrl Pts',(137.895741835109,-4.3263580580978,126.766274891852));
#183801=CARTESIAN_POINT('Ctrl Pts',(137.901654428623,-4.23928440043606,
126.676843405643));
#183802=CARTESIAN_POINT('Ctrl Pts',(137.909077695028,-4.12996334593991,
126.564562095313));
#183803=CARTESIAN_POINT('Ctrl Pts',(137.916500961434,-4.01601309505411,
126.456457204189));
#183804=CARTESIAN_POINT('Ctrl Pts',(137.923924227839,-3.89778575089131,
126.352934239129));
#183805=CARTESIAN_POINT('Ctrl Pts',(137.93133872056,-3.77969814163099,126.249533629616));
#183806=CARTESIAN_POINT('Ctrl Pts',(137.938753213281,-3.65734377954116,
126.150704410188));
#183807=CARTESIAN_POINT('Ctrl Pts',(137.946167706002,-3.53111305708877,
126.056816922079));
#183808=CARTESIAN_POINT('Ctrl Pts',(137.953575052356,-3.40500400055936,
125.963019926266));
#183809=CARTESIAN_POINT('Ctrl Pts',(137.96098239871,-3.27502631919018,125.874155400811));
#183810=CARTESIAN_POINT('Ctrl Pts',(137.968389745063,-3.14160499327923,
125.790554814715));
#183811=CARTESIAN_POINT('Ctrl Pts',(137.975791566739,-3.00828317802684,
125.70701658109));
#183812=CARTESIAN_POINT('Ctrl Pts',(137.983193388414,-2.87152314723186,
125.628734666894));
#183813=CARTESIAN_POINT('Ctrl Pts',(137.990595210089,-2.73178040618521,
125.55599836112));
#183814=CARTESIAN_POINT('Ctrl Pts',(137.997993124401,-2.5921114342442,125.483300452276));
#183815=CARTESIAN_POINT('Ctrl Pts',(138.005391038712,-2.44946321813233,
125.416142493546));
#183816=CARTESIAN_POINT('Ctrl Pts',(138.012788953023,-2.30431740720409,
125.354768720061));
#183817=CARTESIAN_POINT('Ctrl Pts',(138.020185637936,-2.15919571687599,
125.293405145783));
#183818=CARTESIAN_POINT('Ctrl Pts',(138.027582322848,-2.01157759898021,
125.237823994241));
#183819=CARTESIAN_POINT('Ctrl Pts',(138.03497900776,-1.86196641298671,125.188222118614));
#183820=CARTESIAN_POINT('Ctrl Pts',(138.042375364695,-1.71236186091009,
125.138622442387));
#183821=CARTESIAN_POINT('Ctrl Pts',(138.049771721631,-1.56076477078605,
125.095001632386));
#183822=CARTESIAN_POINT('Ctrl Pts',(138.057168078566,-1.40769520274225,
125.057507149913));
#183823=CARTESIAN_POINT('Ctrl Pts',(138.064565567903,-1.25460219935681,
125.020006926938));
#183824=CARTESIAN_POINT('Ctrl Pts',(138.071963057239,-1.10003663177245,
124.988634987906));
#183825=CARTESIAN_POINT('Ctrl Pts',(138.079360546576,-0.944530182811315,
124.963487969043));
#183826=CARTESIAN_POINT('Ctrl Pts',(138.086760629091,-0.788969221304679,
124.938332134932));
#183827=CARTESIAN_POINT('Ctrl Pts',(138.094160711606,-0.632467090023876,
124.919405625163));
#183828=CARTESIAN_POINT('Ctrl Pts',(138.101560794121,-0.475561895459883,
124.906753353083));
#183829=CARTESIAN_POINT('Ctrl Pts',(138.108969013787,-0.31848416750478,
124.894087168528));
#183830=CARTESIAN_POINT('Ctrl Pts',(138.116377233454,-0.161002863466468,
124.887709029779));
#183831=CARTESIAN_POINT('Ctrl Pts',(138.12378545312,-0.00365814210466802,
124.887611748424));
#183832=CARTESIAN_POINT('Ctrl Pts',(138.131198232422,0.153783422307805,
124.887514407193));
#183833=CARTESIAN_POINT('Ctrl Pts',(138.138611011724,0.311087864390723,
124.893705611727));
#183834=CARTESIAN_POINT('Ctrl Pts',(138.146023791026,0.4677193546816,124.906126206511));
#183835=CARTESIAN_POINT('Ctrl Pts',(138.153447162055,0.624574647391092,
124.918564548423));
#183836=CARTESIAN_POINT('Ctrl Pts',(138.160870533084,0.780754698214678,
124.937250013342));
#183837=CARTESIAN_POINT('Ctrl Pts',(138.168293904113,0.935732260909257,
124.962072050712));
#183838=CARTESIAN_POINT('Ctrl Pts',(138.172229953553,1.01790508328725,124.975233290522));
#183839=CARTESIAN_POINT('Ctrl Pts',(138.176166002994,1.09974005804813,124.990118896725));
#183840=CARTESIAN_POINT('Ctrl Pts',(138.180102052435,1.18116035903808,125.006706715449));
#183841=CARTESIAN_POINT('Ctrl Pts',(138.187525318841,1.33471650566103,125.037990823872));
#183842=CARTESIAN_POINT('Ctrl Pts',(138.194948585246,1.48726110624673,125.07542706292));
#183843=CARTESIAN_POINT('Ctrl Pts',(138.202371851651,1.63826267605801,125.118938384632));
#183844=CARTESIAN_POINT('Ctrl Pts',(138.209786344373,1.7890857745541,125.162398279576));
#183845=CARTESIAN_POINT('Ctrl Pts',(138.217200837094,1.93836911722859,125.211918862519));
#183846=CARTESIAN_POINT('Ctrl Pts',(138.224615329815,2.08559010884906,125.267371863706));
#183847=CARTESIAN_POINT('Ctrl Pts',(138.232022676168,2.23266920333493,125.322771417202));
#183848=CARTESIAN_POINT('Ctrl Pts',(138.239430022522,2.37768955703574,125.384091875053));
#183849=CARTESIAN_POINT('Ctrl Pts',(138.246837368876,2.52014258346241,125.451154856387));
#183850=CARTESIAN_POINT('Ctrl Pts',(138.254239190551,2.66248936304763,125.51816781962));
#183851=CARTESIAN_POINT('Ctrl Pts',(138.261641012227,2.80227229171358,125.590914620009));
#183852=CARTESIAN_POINT('Ctrl Pts',(138.269042833902,2.93900177070275,125.669168395818));
#183853=CARTESIAN_POINT('Ctrl Pts',(138.276440748213,3.07565907126367,125.747380862067));
#183854=CARTESIAN_POINT('Ctrl Pts',(138.283838662525,3.20926580914066,125.831094329171));
#183855=CARTESIAN_POINT('Ctrl Pts',(138.291236576836,3.33935615915975,125.920035586942));
#183856=CARTESIAN_POINT('Ctrl Pts',(138.298633261748,3.46942489052312,126.008962064289));
#183857=CARTESIAN_POINT('Ctrl Pts',(138.306029946661,3.59597808595126,126.103114397584));
#183858=CARTESIAN_POINT('Ctrl Pts',(138.313426631573,3.71857804920002,126.2021755002));
#183859=CARTESIAN_POINT('Ctrl Pts',(138.320822988508,3.84117257623801,126.301232210343));
#183860=CARTESIAN_POINT('Ctrl Pts',(138.328219345444,3.95981392927376,126.405197022414));
#183861=CARTESIAN_POINT('Ctrl Pts',(138.335615702379,4.07409693973764,126.513712101535));
#183862=CARTESIAN_POINT('Ctrl Pts',(138.343013191716,4.18839744722169,126.62224379459));
#183863=CARTESIAN_POINT('Ctrl Pts',(138.350410681052,4.29833801278211,126.735326884774));
#183864=CARTESIAN_POINT('Ctrl Pts',(138.357808170389,4.4035499460711,126.852566286511));
#183865=CARTESIAN_POINT('Ctrl Pts',(138.365208252904,4.50879876124089,126.96984678634));
#183866=CARTESIAN_POINT('Ctrl Pts',(138.372608335419,4.60931539467053,127.091286220921));
#183867=CARTESIAN_POINT('Ctrl Pts',(138.380008417934,4.70477119978698,127.216456142785));
#183868=CARTESIAN_POINT('Ctrl Pts',(138.3874166376,4.80033196837398,127.341763701845));
#183869=CARTESIAN_POINT('Ctrl Pts',(138.394824857267,4.89082056866922,127.470809643247));
#183870=CARTESIAN_POINT('Ctrl Pts',(138.402233076933,4.97595107948322,127.603135630613));
#183871=CARTESIAN_POINT('Ctrl Pts',(138.409645856235,5.06113398670645,127.735543062418));
#183872=CARTESIAN_POINT('Ctrl Pts',(138.417058635538,5.14095204430903,127.871234241915));
#183873=CARTESIAN_POINT('Ctrl Pts',(138.42447141484,5.21516539258678,128.009726385602));
#183874=CARTESIAN_POINT('Ctrl Pts',(138.431894785868,5.28948478037655,128.148416413358));
#183875=CARTESIAN_POINT('Ctrl Pts',(138.439318156897,5.35818330192005,128.289915063571));
#183876=CARTESIAN_POINT('Ctrl Pts',(138.446741527926,5.4210689770581,128.433718993769));
#183877=CARTESIAN_POINT('Ctrl Pts',(138.450677577367,5.45441247093785,128.509967288089));
#183878=CARTESIAN_POINT('Ctrl Pts',(138.454613626808,5.48612259164549,128.586863403795));
#183879=CARTESIAN_POINT('Ctrl Pts',(138.458549676248,5.51617645144817,128.664330730161));
#183880=CARTESIAN_POINT('Ctrl Pts',(138.465972942654,5.57285709308646,128.810431690011));
#183881=CARTESIAN_POINT('Ctrl Pts',(138.473396209059,5.62381500765201,128.959006984408));
#183882=CARTESIAN_POINT('Ctrl Pts',(138.480819475465,5.66882773729218,129.109567813886));
#183883=CARTESIAN_POINT('Ctrl Pts',(138.488233968186,5.71378726562398,129.259950692966));
#183884=CARTESIAN_POINT('Ctrl Pts',(138.495648460907,5.75281548986186,129.412314081771));
#183885=CARTESIAN_POINT('Ctrl Pts',(138.503062953628,5.78573785149633,129.566148973192));
#183886=CARTESIAN_POINT('Ctrl Pts',(138.510470299982,5.81862848131925,129.719835592754));
#183887=CARTESIAN_POINT('Ctrl Pts',(138.517877646335,5.84542488693863,129.874990528817));
#183888=CARTESIAN_POINT('Ctrl Pts',(138.525284992689,5.86600224181193,130.031089473945));
#183889=CARTESIAN_POINT('Ctrl Pts',(138.532686814365,5.88656424931753,130.18707199459));
#183890=CARTESIAN_POINT('Ctrl Pts',(138.54008863604,5.90091639318574,130.343996753884));
#183891=CARTESIAN_POINT('Ctrl Pts',(138.547490457715,5.90898489853239,130.501329214216));
#183892=CARTESIAN_POINT('Ctrl Pts',(138.554888372027,5.91704914457791,130.658578619969));
#183893=CARTESIAN_POINT('Ctrl Pts',(138.562286286338,5.91883633916288,130.81623492627));
#183894=CARTESIAN_POINT('Ctrl Pts',(138.569684200649,5.91432455187191,130.973758544428));
#183895=CARTESIAN_POINT('Ctrl Pts',(138.577080885562,5.90981351435814,131.131255985018));
#183896=CARTESIAN_POINT('Ctrl Pts',(138.584477570474,5.89900558318721,131.288620408449));
#183897=CARTESIAN_POINT('Ctrl Pts',(138.591874255386,5.8819309468065,131.445312175408));
#183898=CARTESIAN_POINT('Ctrl Pts',(138.599270612322,5.86485706753306,131.601996994489));
#183899=CARTESIAN_POINT('Ctrl Pts',(138.606666969257,5.84151707599249,131.758008845303));
#183900=CARTESIAN_POINT('Ctrl Pts',(138.614063326192,5.81199302529507,131.912813429562));
#183901=CARTESIAN_POINT('Ctrl Pts',(138.621460815529,5.7824644543901,132.067641714798));
#183902=CARTESIAN_POINT('Ctrl Pts',(138.628858304866,5.74675000907169,132.221261998736));
#183903=CARTESIAN_POINT('Ctrl Pts',(138.636255794202,5.70498279988453,132.37315053834));
#183904=CARTESIAN_POINT('Ctrl Pts',(138.643655876717,5.66320094926714,132.525092322235));
#183905=CARTESIAN_POINT('Ctrl Pts',(138.651055959232,5.61536220923463,132.675300793432));
#183906=CARTESIAN_POINT('Ctrl Pts',(138.658456041747,5.56164940327724,132.823267865937));
#183907=CARTESIAN_POINT('Ctrl Pts',(138.665864261414,5.50787753456762,132.971397643451));
#183908=CARTESIAN_POINT('Ctrl Pts',(138.67327248108,5.44821882806217,133.1172807491));
#183909=CARTESIAN_POINT('Ctrl Pts',(138.680680700747,5.38290434774678,133.260428887283));
#183910=CARTESIAN_POINT('Ctrl Pts',(138.688093480049,5.31754966745868,133.403665130756));
#183911=CARTESIAN_POINT('Ctrl Pts',(138.695506259351,5.24653244497277,133.544162720141));
#183912=CARTESIAN_POINT('Ctrl Pts',(138.702919038653,5.17012920969352,133.681458898399));
#183913=CARTESIAN_POINT('Ctrl Pts',(138.710342409682,5.09361680588854,133.818951251876));
#183914=CARTESIAN_POINT('Ctrl Pts',(138.71776578071,5.01170321296263,133.953232740431));
#183915=CARTESIAN_POINT('Ctrl Pts',(138.725189151739,4.92470813722807,134.083869776818));
#183916=CARTESIAN_POINT('Ctrl Pts',(138.72912520118,4.87858126065594,134.153136668103));
#183917=CARTESIAN_POINT('Ctrl Pts',(138.733061250621,4.83102647550725,134.221379519561));
#183918=CARTESIAN_POINT('Ctrl Pts',(138.736997300061,4.78209586517842,134.288537665126));
#183919=CARTESIAN_POINT('Ctrl Pts',(138.744420566467,4.6898142611695,134.415195831729));
#183920=CARTESIAN_POINT('Ctrl Pts',(138.751843832872,4.59235765566148,134.53837674423));
#183921=CARTESIAN_POINT('Ctrl Pts',(138.759267099278,4.49001704558511,134.657629034489));
#183922=CARTESIAN_POINT('Ctrl Pts',(138.766681591999,4.38779739361071,134.776740378444));
#183923=CARTESIAN_POINT('Ctrl Pts',(138.77409608472,4.28070546797207,134.891932062163));
#183924=CARTESIAN_POINT('Ctrl Pts',(138.781510577441,4.16907515762518,135.002782093856));
#183925=CARTESIAN_POINT('Ctrl Pts',(138.788917923794,4.05755244077452,135.113525284114));
#183926=CARTESIAN_POINT('Ctrl Pts',(138.796325270148,3.94150031062554,135.219934891887));
#183927=CARTESIAN_POINT('Ctrl Pts',(138.803732616502,3.82129241007672,135.321622496093));
#183928=CARTESIAN_POINT('Ctrl Pts',(138.811134438177,3.70117416511497,135.423234257847));
#183929=CARTESIAN_POINT('Ctrl Pts',(138.818536259853,3.57690660511175,135.520130788457));
#183930=CARTESIAN_POINT('Ctrl Pts',(138.825938081528,3.44889957457064,135.611961088386));
#183931=CARTESIAN_POINT('Ctrl Pts',(138.83333599584,3.32096011794519,135.703742911814));
#183932=CARTESIAN_POINT('Ctrl Pts',(138.840733910151,3.18928542472388,135.790463613759));
#183933=CARTESIAN_POINT('Ctrl Pts',(138.848131824462,3.05431761223031,135.871813082673));
#183934=CARTESIAN_POINT('Ctrl Pts',(138.855528509374,2.91937222893831,135.953149032781));
#183935=CARTESIAN_POINT('Ctrl Pts',(138.862925194287,2.78113513191781,136.029115328895));
#183936=CARTESIAN_POINT('Ctrl Pts',(138.870321879199,2.64007665259938,136.099445681179));
#183937=CARTESIAN_POINT('Ctrl Pts',(138.877718236134,2.49902442796164,136.169772914942));
#183938=CARTESIAN_POINT('Ctrl Pts',(138.88511459307,2.35515140384878,136.234464535202));
#183939=CARTESIAN_POINT('Ctrl Pts',(138.892510950005,2.20895145225117,136.29330077429));
#183940=CARTESIAN_POINT('Ctrl Pts',(138.899908439342,2.06272911706785,136.352146021356));
#183941=CARTESIAN_POINT('Ctrl Pts',(138.907305928678,1.91417949137052,136.405133962877));
#183942=CARTESIAN_POINT('Ctrl Pts',(138.914703418015,1.7638151645086,136.452093492619));
#183943=CARTESIAN_POINT('Ctrl Pts',(138.92210350053,1.61339812766402,136.499069483951));
#183944=CARTESIAN_POINT('Ctrl Pts',(138.929503583045,1.46116547920626,136.540012744826));
#183945=CARTESIAN_POINT('Ctrl Pts',(138.93690366556,1.30764350683274,136.574802456935));
#183946=CARTESIAN_POINT('Ctrl Pts',(138.944311885226,1.15395272126881,136.609630423908));
#183947=CARTESIAN_POINT('Ctrl Pts',(138.951720104893,0.998970144751367,
136.638291246499));
#183948=CARTESIAN_POINT('Ctrl Pts',(138.959128324559,0.843231489926721,
136.660715389683));
#183949=CARTESIAN_POINT('Ctrl Pts',(138.966541103861,0.687396980558781,
136.683153334553));
#183950=CARTESIAN_POINT('Ctrl Pts',(138.973953883163,0.530805836065061,
136.69934691287));
#183951=CARTESIAN_POINT('Ctrl Pts',(138.981366662465,0.373996857945198,
136.709278645172));
#183952=CARTESIAN_POINT('Ctrl Pts',(138.988790033494,0.216963823803561,
136.719224568399));
#183953=CARTESIAN_POINT('Ctrl Pts',(138.996213404523,0.0597127066057581,
136.722890767328));
#183954=CARTESIAN_POINT('Ctrl Pts',(139.003636775552,-0.0972188953469484,
136.720311855439));
#183955=CARTESIAN_POINT('Ctrl Pts',(139.007572824993,-0.180427796224534,
136.718944454475));
#183956=CARTESIAN_POINT('Ctrl Pts',(139.011508874433,-0.263546962858581,
136.715822195045));
#183957=CARTESIAN_POINT('Ctrl Pts',(139.015444923874,-0.346497202820251,
136.710956104895));
#183958=CARTESIAN_POINT('Ctrl Pts',(139.022868190279,-0.502938766598866,
136.701778810738));
#183959=CARTESIAN_POINT('Ctrl Pts',(139.030291456685,-0.659252032738175,
136.686368100478));
#183960=CARTESIAN_POINT('Ctrl Pts',(139.03771472309,-0.814899961487367,
136.664724822568));
#183961=CARTESIAN_POINT('Ctrl Pts',(139.045129215811,-0.970363927311087,
136.643107125215));
#183962=CARTESIAN_POINT('Ctrl Pts',(139.052543708532,-1.12516375489571,
136.615271573938));
#183963=CARTESIAN_POINT('Ctrl Pts',(139.059958201253,-1.27876393545895,
136.581270982101));
#183964=CARTESIAN_POINT('Ctrl Pts',(139.067365547607,-1.43221607038478,
136.547303161314));
#183965=CARTESIAN_POINT('Ctrl Pts',(139.074772893961,-1.58447049815674,
136.507182209653));
#183966=CARTESIAN_POINT('Ctrl Pts',(139.082180240315,-1.73499846600558,
136.461012532388));
#183967=CARTESIAN_POINT('Ctrl Pts',(139.08958206199,-1.8854141644169,136.41487729021));
#183968=CARTESIAN_POINT('Ctrl Pts',(139.096983883665,-2.03410561145598,
136.362702414163));
#183969=CARTESIAN_POINT('Ctrl Pts',(139.104385705341,-2.18055597030818,
136.304642994213));
#183970=CARTESIAN_POINT('Ctrl Pts',(139.111783619652,-2.32692901915716,
136.246614223378));
#183971=CARTESIAN_POINT('Ctrl Pts',(139.119181533963,-2.47106298978218,
136.182707232422));
#183972=CARTESIAN_POINT('Ctrl Pts',(139.126579448275,-2.61245800134243,
136.113126364302));
#183973=CARTESIAN_POINT('Ctrl Pts',(139.133976133187,-2.75382951561592,
136.043557059261));
#183974=CARTESIAN_POINT('Ctrl Pts',(139.141372818099,-2.89246263958192,
135.968315913089));
#183975=CARTESIAN_POINT('Ctrl Pts',(139.148769503011,-3.02787911043441,
135.887654692779));
#183976=CARTESIAN_POINT('Ctrl Pts',(139.156165859947,-3.16328957677839,
135.806997049072));
#183977=CARTESIAN_POINT('Ctrl Pts',(139.163562216882,-3.29548335289159,
135.720920000121));
#183978=CARTESIAN_POINT('Ctrl Pts',(139.170958573817,-3.42400859213571,
135.629720264627));
#183979=CARTESIAN_POINT('Ctrl Pts',(139.178356063154,-3.55255350892234,
135.538506566219));
#183980=CARTESIAN_POINT('Ctrl Pts',(139.185753552491,-3.67742846603564,
135.44216883567));
#183981=CARTESIAN_POINT('Ctrl Pts',(139.193151041827,-3.79821243989223,
135.341045841818));
#183982=CARTESIAN_POINT('Ctrl Pts',(139.200551124342,-3.91903875438439,
135.239887399457));
#183983=CARTESIAN_POINT('Ctrl Pts',(139.207951206857,-4.03577094431272,
135.133940593454));
#183984=CARTESIAN_POINT('Ctrl Pts',(139.215351289372,-4.14802289045598,
135.023582899309));
#183985=CARTESIAN_POINT('Ctrl Pts',(139.222759509039,-4.26039826915299,
134.913103855534));
#183986=CARTESIAN_POINT('Ctrl Pts',(139.230167728705,-4.36828329918245,
134.798204499265));
#183987=CARTESIAN_POINT('Ctrl Pts',(139.237575948372,-4.47132991298856,
134.679297955345));
#183988=CARTESIAN_POINT('Ctrl Pts',(139.244988727674,-4.57443995026648,
134.56031822643));
#183989=CARTESIAN_POINT('Ctrl Pts',(139.252401506976,-4.6727054048812,134.437326686306));
#183990=CARTESIAN_POINT('Ctrl Pts',(139.259814286278,-4.7658203354942,134.310767195858));
#183991=CARTESIAN_POINT('Ctrl Pts',(139.267237657306,-4.85906831308645,
134.184026871275));
#183992=CARTESIAN_POINT('Ctrl Pts',(139.274661028335,-4.94715085999547,
134.053708722867));
#183993=CARTESIAN_POINT('Ctrl Pts',(139.282084399364,-5.02980651250673,
133.920283756741));
#183994=CARTESIAN_POINT('Ctrl Pts',(139.286020448805,-5.0736325227633,133.849538638213));
#183995=CARTESIAN_POINT('Ctrl Pts',(139.289956498246,-5.11593361734224,
133.77792047178));
#183996=CARTESIAN_POINT('Ctrl Pts',(139.293892547686,-5.15667626875567,
133.70550184504));
#183997=CARTESIAN_POINT('Ctrl Pts',(139.301655844179,-5.23703534137144,
133.562666426064));
#183998=CARTESIAN_POINT('Ctrl Pts',(139.309419140672,-5.31155351039293,
133.416316834427));
#183999=CARTESIAN_POINT('Ctrl Pts',(139.317182437165,-5.37992469322463,
133.26694886121));
#184000=CARTESIAN_POINT('Ctrl Pts',(139.324933467789,-5.44818785081589,
133.117816886707));
#184001=CARTESIAN_POINT('Ctrl Pts',(139.332684498413,-5.5103232440121,132.965676328053));
#184002=CARTESIAN_POINT('Ctrl Pts',(139.340435529037,-5.56606974513515,
132.81104897274));
#184003=CARTESIAN_POINT('Ctrl Pts',(139.348451302267,-5.62372031227101,
132.65114019732));
#184004=CARTESIAN_POINT('Ctrl Pts',(139.356467075497,-5.67453761797106,
132.488572011555));
#184005=CARTESIAN_POINT('Ctrl Pts',(139.364482848727,-5.71828491622516,
132.323948778671));
#184006=CARTESIAN_POINT('Ctrl Pts',(139.37220791147,-5.76044561790614,132.165295986652));
#184007=CARTESIAN_POINT('Ctrl Pts',(139.379932974214,-5.79603998975774,
132.004734941028));
#184008=CARTESIAN_POINT('Ctrl Pts',(139.387658036958,-5.82490506791931,
131.842826559342));
#184009=CARTESIAN_POINT('Ctrl Pts',(139.395374508062,-5.85373804299438,
131.681098248492));
#184010=CARTESIAN_POINT('Ctrl Pts',(139.403090979166,-5.87585658124932,
131.518025905713));
#184011=CARTESIAN_POINT('Ctrl Pts',(139.41080745027,-5.89114804590412,131.354183556102));
#184012=CARTESIAN_POINT('Ctrl Pts',(139.418513889541,-5.90641963082197,
131.190554210469));
#184013=CARTESIAN_POINT('Ctrl Pts',(139.426220328812,-5.91488181128325,
131.026157176566));
#184014=CARTESIAN_POINT('Ctrl Pts',(139.433926768083,-5.91647336974226,
130.861574493773));
#184015=CARTESIAN_POINT('Ctrl Pts',(139.434826114654,-5.91665910566928,
130.84236758561));
#184016=CARTESIAN_POINT('Ctrl Pts',(139.435725461224,-5.9167513280669,130.82315815739));
#184017=CARTESIAN_POINT('Ctrl Pts',(139.436624807795,-5.91674998555258,
130.80394714016));
#184018=CARTESIAN_POINT('',(141.186624807795,-5.91699976706494,130.799049164418));
#184019=CARTESIAN_POINT('Ctrl Pts',(139.436624807833,-5.91674998555252,
130.803947139341));
#184020=CARTESIAN_POINT('Ctrl Pts',(139.444414740142,-5.9167383569805,130.637545744475));
#184021=CARTESIAN_POINT('Ctrl Pts',(139.452204672452,-5.90970268366904,
130.471295336118));
#184022=CARTESIAN_POINT('Ctrl Pts',(139.459994604761,-5.8957067789312,130.30579052283));
#184023=CARTESIAN_POINT('Ctrl Pts',(139.467795773126,-5.8816906867568,130.140046988432));
#184024=CARTESIAN_POINT('Ctrl Pts',(139.475596941491,-5.86069434653312,
129.975051505079));
#184025=CARTESIAN_POINT('Ctrl Pts',(139.483398109855,-5.83283296513644,
129.811390243729));
#184026=CARTESIAN_POINT('Ctrl Pts',(139.491218767466,-5.80490197912712,
129.647320116124));
#184027=CARTESIAN_POINT('Ctrl Pts',(139.499039425076,-5.77007170382882,
129.484591184027));
#184028=CARTESIAN_POINT('Ctrl Pts',(139.506860082686,-5.72850826458461,
129.323778426303));
#184029=CARTESIAN_POINT('Ctrl Pts',(139.514690882978,-5.68689092134039,
129.162757109059));
#184030=CARTESIAN_POINT('Ctrl Pts',(139.52252168327,-5.63852307109696,129.003657224133));
#184031=CARTESIAN_POINT('Ctrl Pts',(139.530352483562,-5.58361987152639,
128.847035991247));
#184032=CARTESIAN_POINT('Ctrl Pts',(139.538201730399,-5.5285873397904,128.690045815141));
#184033=CARTESIAN_POINT('Ctrl Pts',(139.546050977236,-5.46698878344372,
128.535546258075));
#184034=CARTESIAN_POINT('Ctrl Pts',(139.553900224074,-5.39908734484855,
128.384074187162));
#184035=CARTESIAN_POINT('Ctrl Pts',(139.560046873215,-5.34591455923882,
128.265458262093));
#184036=CARTESIAN_POINT('Ctrl Pts',(139.566193522357,-5.28887763188302,
128.148698427508));
#184037=CARTESIAN_POINT('Ctrl Pts',(139.572340171499,-5.22812176134569,
128.034040525764));
#184038=CARTESIAN_POINT('Ctrl Pts',(139.579763437905,-5.15474730930144,
127.895568956866));
#184039=CARTESIAN_POINT('Ctrl Pts',(139.58718670431,-5.07575678829435,127.759805100288));
#184040=CARTESIAN_POINT('Ctrl Pts',(139.594609970715,-4.99137419954193,
127.627237050147));
#184041=CARTESIAN_POINT('Ctrl Pts',(139.602024463436,-4.90709134400182,
127.494825684433));
#184042=CARTESIAN_POINT('Ctrl Pts',(139.609438956157,-4.81742930465359,
127.365602918501));
#184043=CARTESIAN_POINT('Ctrl Pts',(139.616853448878,-4.72265870931268,
127.240033853947));
#184044=CARTESIAN_POINT('Ctrl Pts',(139.624260795232,-4.62797945743952,
127.114585817584));
#184045=CARTESIAN_POINT('Ctrl Pts',(139.631668141586,-4.52820167529697,
126.992784767797));
#184046=CARTESIAN_POINT('Ctrl Pts',(139.63907548794,-4.42364010616832,126.875068216433));
#184047=CARTESIAN_POINT('Ctrl Pts',(139.646477309615,-4.3191565230031,126.757439462515));
#184048=CARTESIAN_POINT('Ctrl Pts',(139.653879131291,-4.20989650391839,
126.643889419174));
#184049=CARTESIAN_POINT('Ctrl Pts',(139.661280952966,-4.09621593772498,
126.534823692556));
#184050=CARTESIAN_POINT('Ctrl Pts',(139.668678867277,-3.98259538261721,
126.425815540885));
#184051=CARTESIAN_POINT('Ctrl Pts',(139.676076781589,-3.8645591965125,126.321287249256));
#184052=CARTESIAN_POINT('Ctrl Pts',(139.6834746959,-3.74250101662348,126.221608529238));
#184053=CARTESIAN_POINT('Ctrl Pts',(139.690871380812,-3.62046312058982,
126.121946374016));
#184054=CARTESIAN_POINT('Ctrl Pts',(139.698268065725,-3.49440484616371,
126.0271324268));
#184055=CARTESIAN_POINT('Ctrl Pts',(139.705664750637,-3.36475397762668,
125.937497024599));
#184056=CARTESIAN_POINT('Ctrl Pts',(139.713061107572,-3.23510885794502,
125.847865596926));
#184057=CARTESIAN_POINT('Ctrl Pts',(139.720457464508,-3.10187176795193,
125.763412469989));
#184058=CARTESIAN_POINT('Ctrl Pts',(139.727853821443,-2.96550039594985,
125.684425269915));
#184059=CARTESIAN_POINT('Ctrl Pts',(139.73525131078,-2.82910814514249,125.6054259767));
#184060=CARTESIAN_POINT('Ctrl Pts',(139.742648800116,-2.68958097989421,
125.531894463733));
#184061=CARTESIAN_POINT('Ctrl Pts',(139.750046289453,-2.5474020217075,125.464072844206));
#184062=CARTESIAN_POINT('Ctrl Pts',(139.757446371968,-2.40517322290756,
125.396227449915));
#184063=CARTESIAN_POINT('Ctrl Pts',(139.764846454483,-2.26029111709618,
125.334096094844));
#184064=CARTESIAN_POINT('Ctrl Pts',(139.772246536998,-2.11325952156014,
125.277873057005));
#184065=CARTESIAN_POINT('Ctrl Pts',(139.779654756665,-1.96606624966948,
125.221588196156));
#184066=CARTESIAN_POINT('Ctrl Pts',(139.787062976331,-1.81671911670941,
125.171224760489));
#184067=CARTESIAN_POINT('Ctrl Pts',(139.794471195998,-1.66573854684275,
125.126927601135));
#184068=CARTESIAN_POINT('Ctrl Pts',(139.8018839753,-1.51466505095442,125.082603177618));
#184069=CARTESIAN_POINT('Ctrl Pts',(139.809296754602,-1.36195647613885,
125.044352560755));
#184070=CARTESIAN_POINT('Ctrl Pts',(139.816709533904,-1.20814369104697,
125.012269511214));
#184071=CARTESIAN_POINT('Ctrl Pts',(139.824132904933,-1.05411113103469,
124.980140619907));
#184072=CARTESIAN_POINT('Ctrl Pts',(139.831556275961,-0.898971576840442,
124.954196957889));
#184073=CARTESIAN_POINT('Ctrl Pts',(139.83897964699,-0.743262098289538,
124.934480549307));
#184074=CARTESIAN_POINT('Ctrl Pts',(139.842915696431,-0.660701196564727,
124.924026436388));
#184075=CARTESIAN_POINT('Ctrl Pts',(139.846851745872,-0.577980099564831,
124.915322157159));
#184076=CARTESIAN_POINT('Ctrl Pts',(139.850787795312,-0.495178763206054,
124.908368033194));
#184077=CARTESIAN_POINT('Ctrl Pts',(139.858211061718,-0.339018026973734,
124.895252772426));
#184078=CARTESIAN_POINT('Ctrl Pts',(139.865634328123,-0.182099743347254,
124.88832605418));
#184079=CARTESIAN_POINT('Ctrl Pts',(139.873057594529,-0.0249556378615223,
124.887663246681));
#184080=CARTESIAN_POINT('Ctrl Pts',(139.88047208725,0.132002736341643,124.887001222565));
#184081=CARTESIAN_POINT('Ctrl Pts',(139.887886579971,0.289186031483495,
124.892588374202));
#184082=CARTESIAN_POINT('Ctrl Pts',(139.895301072692,0.446056663475881,
124.904448413518));
#184083=CARTESIAN_POINT('Ctrl Pts',(139.902708419046,0.60277609764719,124.916297021683));
#184084=CARTESIAN_POINT('Ctrl Pts',(139.910115765399,0.759183098873836,
124.934406453087));
#184085=CARTESIAN_POINT('Ctrl Pts',(139.917523111753,0.914739449614415,
124.958748391133));
#184086=CARTESIAN_POINT('Ctrl Pts',(139.924924933429,1.07017978055975,124.983072174044));
#184087=CARTESIAN_POINT('Ctrl Pts',(139.932326755104,1.22477035706669,125.013619150465));
#184088=CARTESIAN_POINT('Ctrl Pts',(139.939728576779,1.37797756460276,125.050309141089));
#184089=CARTESIAN_POINT('Ctrl Pts',(139.947126491091,1.53110389524665,125.086979763352));
#184090=CARTESIAN_POINT('Ctrl Pts',(139.954524405402,1.68284794917277,125.129786854809));
#184091=CARTESIAN_POINT('Ctrl Pts',(139.961922319713,1.83268590703819,125.17859907546));
#184092=CARTESIAN_POINT('Ctrl Pts',(139.969319004626,1.98249896455313,125.227403184404));
#184093=CARTESIAN_POINT('Ctrl Pts',(139.976715689538,2.13040620008801,125.282210326405));
#184094=CARTESIAN_POINT('Ctrl Pts',(139.98411237445,2.27589846390889,125.342839149653));
#184095=CARTESIAN_POINT('Ctrl Pts',(139.991508731385,2.42138427645033,125.403465284555));
#184096=CARTESIAN_POINT('Ctrl Pts',(139.998905088321,2.56445498561727,125.469912443845));
#184097=CARTESIAN_POINT('Ctrl Pts',(140.006301445256,2.70462121169588,125.541951030338));
#184098=CARTESIAN_POINT('Ctrl Pts',(140.013698934593,2.84480889758158,125.614000646124));
#184099=CARTESIAN_POINT('Ctrl Pts',(140.021096423929,2.98209088291864,125.691643222996));
#184100=CARTESIAN_POINT('Ctrl Pts',(140.028493913266,3.11600233204865,125.774603165246));
#184101=CARTESIAN_POINT('Ctrl Pts',(140.035893995781,3.24996072362956,125.857592188976));
#184102=CARTESIAN_POINT('Ctrl Pts',(140.043294078296,3.38054590943538,125.94590209281));
#184103=CARTESIAN_POINT('Ctrl Pts',(140.050694160811,3.50732211232254,126.03921401301));
#184104=CARTESIAN_POINT('Ctrl Pts',(140.058102380477,3.63423771867769,126.132628539258));
#184105=CARTESIAN_POINT('Ctrl Pts',(140.065510600144,3.75733567684197,126.231055844775));
#184106=CARTESIAN_POINT('Ctrl Pts',(140.07291881981,3.87621281748567,126.334136377546));
#184107=CARTESIAN_POINT('Ctrl Pts',(140.080331599112,3.99516312502599,126.437280354666));
#184108=CARTESIAN_POINT('Ctrl Pts',(140.087744378415,4.10988716710901,126.545083010852));
#184109=CARTESIAN_POINT('Ctrl Pts',(140.095157157717,4.22001911275532,126.657148391205));
#184110=CARTESIAN_POINT('Ctrl Pts',(140.102580528745,4.33030842009029,126.769373895829));
#184111=CARTESIAN_POINT('Ctrl Pts',(140.110003899774,4.43599227624557,126.885874013523));
#184112=CARTESIAN_POINT('Ctrl Pts',(140.117427270803,4.53674502575533,127.006219607311));
#184113=CARTESIAN_POINT('Ctrl Pts',(140.121363320244,4.59016655107471,127.07002972879));
#184114=CARTESIAN_POINT('Ctrl Pts',(140.125299369685,4.64220248121217,127.134920454943));
#184115=CARTESIAN_POINT('Ctrl Pts',(140.129235419125,4.69280932749273,127.200824690411));
#184116=CARTESIAN_POINT('Ctrl Pts',(140.136658685531,4.78825226019181,127.325118021702));
#184117=CARTESIAN_POINT('Ctrl Pts',(140.144081951936,4.87889806966939,127.453393757467));
#184118=CARTESIAN_POINT('Ctrl Pts',(140.151505218342,4.96439593586349,127.585245280322));
#184119=CARTESIAN_POINT('Ctrl Pts',(140.158919711063,5.04979275068001,127.716940965626));
#184120=CARTESIAN_POINT('Ctrl Pts',(140.166334203784,5.1300535322111,127.852203715424));
#184121=CARTESIAN_POINT('Ctrl Pts',(140.173748696505,5.20486775361052,127.990594061875));
#184122=CARTESIAN_POINT('Ctrl Pts',(140.181156042858,5.27960986624664,128.128851022499));
#184123=CARTESIAN_POINT('Ctrl Pts',(140.188563389212,5.348915693337,128.270229252329));
#184124=CARTESIAN_POINT('Ctrl Pts',(140.195970735566,5.41251813870924,128.414260627891));
#184125=CARTESIAN_POINT('Ctrl Pts',(140.203372557241,5.47607314697814,128.558184579419));
#184126=CARTESIAN_POINT('Ctrl Pts',(140.210774378917,5.5339330932668,128.704757396574));
#184127=CARTESIAN_POINT('Ctrl Pts',(140.218176200592,5.58587700300791,128.853486795463));
#184128=CARTESIAN_POINT('Ctrl Pts',(140.225574114904,5.63779349196338,129.00213768126));
#184129=CARTESIAN_POINT('Ctrl Pts',(140.232972029215,5.68380004126205,129.152942529997));
#184130=CARTESIAN_POINT('Ctrl Pts',(140.240369943526,5.72372401381683,129.305389645146));
#184131=CARTESIAN_POINT('Ctrl Pts',(140.247766628439,5.76364135173166,129.457811426351));
#184132=CARTESIAN_POINT('Ctrl Pts',(140.255163313351,5.79747802458901,129.611874571548));
#184133=CARTESIAN_POINT('Ctrl Pts',(140.262559998263,5.82511140093468,129.767052693562));
#184134=CARTESIAN_POINT('Ctrl Pts',(140.269956355198,5.85274355198747,129.922223934816));
#184135=CARTESIAN_POINT('Ctrl Pts',(140.277352712134,5.87417288799663,130.07850968707));
#184136=CARTESIAN_POINT('Ctrl Pts',(140.284749069069,5.88932805388643,130.235374118424));
#184137=CARTESIAN_POINT('Ctrl Pts',(140.292146558406,5.90448554007083,130.392262566123));
#184138=CARTESIAN_POINT('Ctrl Pts',(140.299544047743,5.91336690756985,130.54972949774));
#184139=CARTESIAN_POINT('Ctrl Pts',(140.306941537079,5.91595276783079,130.707234867658));
#184140=CARTESIAN_POINT('Ctrl Pts',(140.314341619594,5.91853953456102,130.864795450839));
#184141=CARTESIAN_POINT('Ctrl Pts',(140.321741702109,5.91482639404668,131.022394126134));
#184142=CARTESIAN_POINT('Ctrl Pts',(140.329141784624,5.90484606719343,131.17949190825));
#184143=CARTESIAN_POINT('Ctrl Pts',(140.336550004291,5.89485476594481,131.336762435527));
#184144=CARTESIAN_POINT('Ctrl Pts',(140.343958223957,5.87858253942994,131.493530596899));
#184145=CARTESIAN_POINT('Ctrl Pts',(140.351366443624,5.85611396607032,131.649262847943));
#184146=CARTESIAN_POINT('Ctrl Pts',(140.358779222926,5.83363156367869,131.805090949589));
#184147=CARTESIAN_POINT('Ctrl Pts',(140.366192002228,5.80494528293594,131.959881504242));
#184148=CARTESIAN_POINT('Ctrl Pts',(140.37360478153,5.77019051133239,132.113112704643));
#184149=CARTESIAN_POINT('Ctrl Pts',(140.381028152559,5.73538608048134,132.26656284897));
#184150=CARTESIAN_POINT('Ctrl Pts',(140.388451523587,5.69449593773427,132.418448829562));
#184151=CARTESIAN_POINT('Ctrl Pts',(140.395874894616,5.64770510344878,132.568264704238));
#184152=CARTESIAN_POINT('Ctrl Pts',(140.399810944057,5.62289548038023,132.647700675773));
#184153=CARTESIAN_POINT('Ctrl Pts',(140.403746993498,5.59642776595489,132.72655500006));
#184154=CARTESIAN_POINT('Ctrl Pts',(140.407683042938,5.56833490270679,132.804754822166));
#184155=CARTESIAN_POINT('Ctrl Pts',(140.415106309344,5.5153526393686,132.952237246126));
#184156=CARTESIAN_POINT('Ctrl Pts',(140.422529575749,5.45642690408131,133.097836301353));
#184157=CARTESIAN_POINT('Ctrl Pts',(140.429952842155,5.39171016875434,133.241037046362));
#184158=CARTESIAN_POINT('Ctrl Pts',(140.437367334876,5.32706992323409,133.384068539983));
#184159=CARTESIAN_POINT('Ctrl Pts',(140.444781827597,5.25665245388446,133.524707028831));
#184160=CARTESIAN_POINT('Ctrl Pts',(140.452196320318,5.18065965010269,133.662453714772));
#184161=CARTESIAN_POINT('Ctrl Pts',(140.459603666671,5.10474009104626,133.800067635271));
#184162=CARTESIAN_POINT('Ctrl Pts',(140.467011013025,5.02325607468222,133.934794977023));
#184163=CARTESIAN_POINT('Ctrl Pts',(140.474418359379,4.93645707454128,134.066157992283));
#184164=CARTESIAN_POINT('Ctrl Pts',(140.481820181054,4.84972281236938,134.19742303205));
#184165=CARTESIAN_POINT('Ctrl Pts',(140.48922200273,4.757681664416,134.325328431454));
#184166=CARTESIAN_POINT('Ctrl Pts',(140.496623824405,4.66062836091113,134.449422186864));
#184167=CARTESIAN_POINT('Ctrl Pts',(140.504021738717,4.56362629108983,134.573450434146));
#184168=CARTESIAN_POINT('Ctrl Pts',(140.511419653028,4.4616175645007,134.6936707514));
#184169=CARTESIAN_POINT('Ctrl Pts',(140.518817567339,4.35493937136174,134.809661309682));
#184170=CARTESIAN_POINT('Ctrl Pts',(140.526214252251,4.2482789062031,134.925632592438));
#184171=CARTESIAN_POINT('Ctrl Pts',(140.533610937164,4.13695076704041,135.037375236797));
#184172=CARTESIAN_POINT('Ctrl Pts',(140.541007622076,4.02133153301469,135.14450154432));
#184173=CARTESIAN_POINT('Ctrl Pts',(140.548403979011,3.90571742566694,135.251623101749));
#184174=CARTESIAN_POINT('Ctrl Pts',(140.555800335947,3.78581287560716,135.354128475629));
#184175=CARTESIAN_POINT('Ctrl Pts',(140.563196692882,3.66203012422643,135.451668002682));
#184176=CARTESIAN_POINT('Ctrl Pts',(140.570594182219,3.53822842139034,135.549222463287));
#184177=CARTESIAN_POINT('Ctrl Pts',(140.577991671555,3.41054762819856,135.641809332179));
#184178=CARTESIAN_POINT('Ctrl Pts',(140.585389160892,3.27943162033682,135.729120389376));
#184179=CARTESIAN_POINT('Ctrl Pts',(140.592789243407,3.14826964996188,135.816462053328));
#184180=CARTESIAN_POINT('Ctrl Pts',(140.600189325922,3.01367037786306,135.89852401661));
#184181=CARTESIAN_POINT('Ctrl Pts',(140.607589408437,2.87610495408147,135.975042473531));
#184182=CARTESIAN_POINT('Ctrl Pts',(140.614997628103,2.73838826297432,136.051645070362));
#184183=CARTESIAN_POINT('Ctrl Pts',(140.62240584777,2.59769923300498,136.122691805838));
#184184=CARTESIAN_POINT('Ctrl Pts',(140.629814067436,2.45453246690868,136.187965444389));
#184185=CARTESIAN_POINT('Ctrl Pts',(140.637226846738,2.31127758405667,136.253279257775));
#184186=CARTESIAN_POINT('Ctrl Pts',(140.644639626041,2.16554227108809,136.312812753108));
#184187=CARTESIAN_POINT('Ctrl Pts',(140.652052405343,2.01783871947345,136.366397786149));
#184188=CARTESIAN_POINT('Ctrl Pts',(140.659475776371,1.8699241220977,136.420059383997));
#184189=CARTESIAN_POINT('Ctrl Pts',(140.6668991474,1.72003602403849,136.467755431367));
#184190=CARTESIAN_POINT('Ctrl Pts',(140.674322518429,1.56870009680697,136.509368117016));
#184191=CARTESIAN_POINT('Ctrl Pts',(140.67825856787,1.48845815693258,136.53143216143));
#184192=CARTESIAN_POINT('Ctrl Pts',(140.682194617311,1.40780933448111,136.55178681208));
#184193=CARTESIAN_POINT('Ctrl Pts',(140.686130666751,1.32683273061614,136.570420404584));
#184194=CARTESIAN_POINT('Ctrl Pts',(140.693553933157,1.17411338292093,136.605562778511));
#184195=CARTESIAN_POINT('Ctrl Pts',(140.700977199562,1.01976597491551,136.634686734355));
#184196=CARTESIAN_POINT('Ctrl Pts',(140.708400465968,0.864306156244563,
136.657642212601));
#184197=CARTESIAN_POINT('Ctrl Pts',(140.715814958689,0.7090300781691,136.680570559379));
#184198=CARTESIAN_POINT('Ctrl Pts',(140.72322945141,0.552644572186405,136.697344886597));
#184199=CARTESIAN_POINT('Ctrl Pts',(140.730643944131,0.395678417444024,
136.707865436948));
#184200=CARTESIAN_POINT('Ctrl Pts',(140.738051290484,0.238863552591311,
136.718375847197));
#184201=CARTESIAN_POINT('Ctrl Pts',(140.745458636838,0.081469523095977,
136.722644455598));
#184202=CARTESIAN_POINT('Ctrl Pts',(140.752865983192,-0.0759668817954667,
136.720622916972));
#184203=CARTESIAN_POINT('Ctrl Pts',(140.760267804867,-0.233285864676519,
136.718602886085));
#184204=CARTESIAN_POINT('Ctrl Pts',(140.767669626543,-0.390646788362894,
136.710302054212));
#184205=CARTESIAN_POINT('Ctrl Pts',(140.775071448218,-0.547510060510293,
136.695724067239));
#184206=CARTESIAN_POINT('Ctrl Pts',(140.78246936253,-0.704290525757123,
136.681153775871));
#184207=CARTESIAN_POINT('Ctrl Pts',(140.789867276841,-0.860573491901972,
136.660312963175));
#184208=CARTESIAN_POINT('Ctrl Pts',(140.797265191152,-1.01582180275943,
136.633257307982));
#184209=CARTESIAN_POINT('Ctrl Pts',(140.804661876065,-1.17104431416416,
136.606206148948));
#184210=CARTESIAN_POINT('Ctrl Pts',(140.812058560977,-1.32523214413837,
136.572942261236));
#184211=CARTESIAN_POINT('Ctrl Pts',(140.819455245889,-1.47785556077945,
136.533572911064));
#184212=CARTESIAN_POINT('Ctrl Pts',(140.826851602824,-1.63047220993841,
136.494205306571));
#184213=CARTESIAN_POINT('Ctrl Pts',(140.83424795976,-1.78152422222521,136.448732871148));
#184214=CARTESIAN_POINT('Ctrl Pts',(140.841644316695,-1.93049458948127,
136.397313433609));
#184215=CARTESIAN_POINT('Ctrl Pts',(140.849041806032,-2.07948776448096,
136.345886123623));
#184216=CARTESIAN_POINT('Ctrl Pts',(140.856439295368,-2.22639830697387,
136.2885101204));
#184217=CARTESIAN_POINT('Ctrl Pts',(140.863836784705,-2.37072697710647,
136.225392268693));
#184218=CARTESIAN_POINT('Ctrl Pts',(140.87123686722,-2.51510624143075,136.162252291121));
#184219=CARTESIAN_POINT('Ctrl Pts',(140.878636949735,-2.65690148959547,
136.093366607084));
#184220=CARTESIAN_POINT('Ctrl Pts',(140.88603703225,-2.79563610629492,136.018989015034));
#184221=CARTESIAN_POINT('Ctrl Pts',(140.893445251916,-2.9345232759676,135.944529637176));
#184222=CARTESIAN_POINT('Ctrl Pts',(140.900853471583,-3.07034276389088,
135.86456646768));
#184223=CARTESIAN_POINT('Ctrl Pts',(140.908261691249,-3.2026444587668,135.779398208703));
#184224=CARTESIAN_POINT('Ctrl Pts',(140.915674470551,-3.33502758312833,
135.694177530085));
#184225=CARTESIAN_POINT('Ctrl Pts',(140.923087249853,-3.46388829527051,
135.603745592259));
#184226=CARTESIAN_POINT('Ctrl Pts',(140.930500029155,-3.58880827868209,
135.50844243035));
#184227=CARTESIAN_POINT('Ctrl Pts',(140.937923400184,-3.71390675362418,
135.413003094813));
#184228=CARTESIAN_POINT('Ctrl Pts',(140.945346771213,-3.83505296731995,
135.312678871508));
#184229=CARTESIAN_POINT('Ctrl Pts',(140.952770142242,-3.95186366354295,
135.207848342912));
#184230=CARTESIAN_POINT('Ctrl Pts',(140.956706191682,-4.01379949751447,
135.152264681276));
#184231=CARTESIAN_POINT('Ctrl Pts',(140.960642241123,-4.0745171000723,135.095414728721));
#184232=CARTESIAN_POINT('Ctrl Pts',(140.964578290564,-4.13396390152835,
135.037358730412));
#184233=CARTESIAN_POINT('Ctrl Pts',(140.971895211055,-4.24447255398932,
134.929435511951));
#184234=CARTESIAN_POINT('Ctrl Pts',(140.979212131547,-4.35094241740044,
134.816995737345));
#184235=CARTESIAN_POINT('Ctrl Pts',(140.986529052038,-4.45297372612522,
134.70037852781));
#184236=CARTESIAN_POINT('Ctrl Pts',(140.993837183181,-4.55488247116387,
134.58390140307));
#184237=CARTESIAN_POINT('Ctrl Pts',(141.001145314324,-4.65236301871726,
134.463257114099));
#184238=CARTESIAN_POINT('Ctrl Pts',(141.008453445466,-4.74505034526125,
134.338823488136));
#184239=CARTESIAN_POINT('Ctrl Pts',(141.01587725223,-4.83920475878625,134.212420283812));
#184240=CARTESIAN_POINT('Ctrl Pts',(141.023301058994,-4.92841261661277,
134.082107020091));
#184241=CARTESIAN_POINT('Ctrl Pts',(141.030724865757,-5.01233110107955,
133.948317916203));
#184242=CARTESIAN_POINT('Ctrl Pts',(141.038020045489,-5.09479558950856,
133.81684688119));
#184243=CARTESIAN_POINT('Ctrl Pts',(141.04531522522,-5.17215228161119,133.682019809762));
#184244=CARTESIAN_POINT('Ctrl Pts',(141.052610404951,-5.24411756057458,
133.544280611539));
#184245=CARTESIAN_POINT('Ctrl Pts',(141.05990249636,-5.31605237394326,133.406599723472));
#184246=CARTESIAN_POINT('Ctrl Pts',(141.067194587769,-5.38260013705376,
133.266009501727));
#184247=CARTESIAN_POINT('Ctrl Pts',(141.074486679178,-5.4435222173952,133.122980127366));
#184248=CARTESIAN_POINT('Ctrl Pts',(141.081777219704,-5.50443134082765,
132.979981172494));
#184249=CARTESIAN_POINT('Ctrl Pts',(141.089067760231,-5.55971701232054,
132.834544451499));
#184250=CARTESIAN_POINT('Ctrl Pts',(141.096358300758,-5.60918809127039,
132.687161594635));
#184251=CARTESIAN_POINT('Ctrl Pts',(141.103880509677,-5.6602311915705,132.535095415664));
#184252=CARTESIAN_POINT('Ctrl Pts',(141.111402718597,-5.70508387488403,
132.380957767139));
#184253=CARTESIAN_POINT('Ctrl Pts',(141.118924927517,-5.74359140978907,
132.225306879709));
#184254=CARTESIAN_POINT('Ctrl Pts',(141.126219416928,-5.78093320773838,
132.074368004931));
#184255=CARTESIAN_POINT('Ctrl Pts',(141.133513906339,-5.81230840630384,
131.922006577658));
#184256=CARTESIAN_POINT('Ctrl Pts',(141.14080839575,-5.83762777962395,131.768742527943));
#184257=CARTESIAN_POINT('Ctrl Pts',(141.148444464425,-5.86413278395792,
131.608301578218));
#184258=CARTESIAN_POINT('Ctrl Pts',(141.156080533099,-5.88400104460627,
131.44687190088));
#184259=CARTESIAN_POINT('Ctrl Pts',(141.163716601773,-5.89719109893007,
131.285055640632));
#184260=CARTESIAN_POINT('Ctrl Pts',(141.171352670447,-5.91038115325386,
131.123239380383));
#184261=CARTESIAN_POINT('Ctrl Pts',(141.178988739121,-5.91689302595348,
130.961037018775));
#184262=CARTESIAN_POINT('Ctrl Pts',(141.186624807795,-5.91674761616294,
130.799049390764));
#184263=CARTESIAN_POINT('',(142.936624807795,-5.92483523511467,130.807229770117));
#184264=CARTESIAN_POINT('Ctrl Pts',(141.186624807795,-5.91856290585919,
130.799047761251));
#184265=CARTESIAN_POINT('Ctrl Pts',(141.205425176656,-5.92226342242035,
130.400100415301));
#184266=CARTESIAN_POINT('Ctrl Pts',(141.317041420117,-5.70333307753058,
128.03562168117));
#184267=CARTESIAN_POINT('Ctrl Pts',(141.521473538194,-2.52131864300096,
124.275921843184));
#184268=CARTESIAN_POINT('Ctrl Pts',(141.799921162,4.12972612270149,125.154323212222));
#184269=CARTESIAN_POINT('Ctrl Pts',(142.078368785816,6.98575432998188,131.22483293709));
#184270=CARTESIAN_POINT('Ctrl Pts',(142.356816409628,3.42221558107838,136.908949141534));
#184271=CARTESIAN_POINT('Ctrl Pts',(142.635264033442,-3.28617210231038,
136.983246718178));
#184272=CARTESIAN_POINT('Ctrl Pts',(142.828533499497,-5.84638522401492,
133.093672015244));
#184273=CARTESIAN_POINT('Ctrl Pts',(142.928987090948,-5.92579859098698,
130.968857383612));
#184274=CARTESIAN_POINT('Ctrl Pts',(142.936624807795,-5.92483523511467,
130.807229770117));
#184275=CARTESIAN_POINT('',(144.686624807795,-5.90969244644754,130.808282040953));
#184276=CARTESIAN_POINT('Ctrl Pts',(142.936624807795,-5.92483523511467,
130.807229770117));
#184277=CARTESIAN_POINT('Ctrl Pts',(143.021802965552,-5.91409159534479,
129.004709116883));
#184278=CARTESIAN_POINT('Ctrl Pts',(143.199796997915,-4.07199242933219,
125.219045149632));
#184279=CARTESIAN_POINT('Ctrl Pts',(143.47060690488,2.37610874285143,124.221681241164));
#184280=CARTESIAN_POINT('Ctrl Pts',(143.749054528693,6.82253940572497,129.245349203993));
#184281=CARTESIAN_POINT('Ctrl Pts',(144.027502152506,4.99938965432202,135.701672493953));
#184282=CARTESIAN_POINT('Ctrl Pts',(144.305949776318,-1.41795495564429,
137.6576054165));
#184283=CARTESIAN_POINT('Ctrl Pts',(144.525657328082,-5.45337545441397,
134.231681535502));
#184284=CARTESIAN_POINT('Ctrl Pts',(144.652549005241,-5.91408802850884,
131.534134200586));
#184285=CARTESIAN_POINT('Ctrl Pts',(144.686624807795,-5.90969244644754,
130.808282040953));
#184286=CARTESIAN_POINT('',(146.436624824885,-5.9136271076536,130.800021490431));
#184287=CARTESIAN_POINT('Ctrl Pts',(144.686624807795,-5.90969244644754,
130.808282040953));
#184288=CARTESIAN_POINT('Ctrl Pts',(144.745364879845,-5.90211531582624,
129.557053751139));
#184289=CARTESIAN_POINT('Ctrl Pts',(144.8969208265,-4.90031956675752,126.317657450322));
#184290=CARTESIAN_POINT('Ctrl Pts',(145.141292647757,0.431102961529391,
123.819254264266));
#184291=CARTESIAN_POINT('Ctrl Pts',(145.419740271571,6.10978948450507,127.391439143905));
#184292=CARTESIAN_POINT('Ctrl Pts',(145.698187895383,6.17387795102984,134.099932127357));
#184293=CARTESIAN_POINT('Ctrl Pts',(145.976635519196,0.564474191264713,
137.779955890925));
#184294=CARTESIAN_POINT('Ctrl Pts',(146.222781156667,-4.85274554974043,
135.366472664822));
#184295=CARTESIAN_POINT('Ctrl Pts',(146.376110919533,-5.90179167691209,
132.088595634264));
#184296=CARTESIAN_POINT('Ctrl Pts',(146.436624807795,-5.91049805840725,
130.800024150482));
#184297=CARTESIAN_POINT('',(148.186624807795,-5.92111847692839,130.802105950051));
#184298=CARTESIAN_POINT('Ctrl Pts',(146.436624841933,-5.916748406975,130.800018836969));
#184299=CARTESIAN_POINT('Ctrl Pts',(146.445134157759,-5.91661530346575,
130.618632431374));
#184300=CARTESIAN_POINT('Ctrl Pts',(146.453643473586,-5.90813728831268,
130.437583582325));
#184301=CARTESIAN_POINT('Ctrl Pts',(146.462152789412,-5.89143102435819,
130.257578167473));
#184302=CARTESIAN_POINT('Ctrl Pts',(146.47070354915,-5.87464339393995,130.076696051277));
#184303=CARTESIAN_POINT('Ctrl Pts',(146.479254308889,-5.84954727551356,
129.896867686644));
#184304=CARTESIAN_POINT('Ctrl Pts',(146.487805068627,-5.81631051165087,
129.718790447305));
#184305=CARTESIAN_POINT('Ctrl Pts',(146.496410202756,-5.78286239478047,
129.539580812518));
#184306=CARTESIAN_POINT('Ctrl Pts',(146.505015336886,-5.74116985229078,
129.362144772545));
#184307=CARTESIAN_POINT('Ctrl Pts',(146.513620471015,-5.6914525224521,129.187172085831));
#184308=CARTESIAN_POINT('Ctrl Pts',(146.520257236284,-5.65310771073977,
129.052223271231));
#184309=CARTESIAN_POINT('Ctrl Pts',(146.526894001554,-5.60999045453091,
128.918739338434));
#184310=CARTESIAN_POINT('Ctrl Pts',(146.533530766823,-5.56222059870605,
128.787027582633));
#184311=CARTESIAN_POINT('Ctrl Pts',(146.540954033228,-5.50878969501127,
128.639707101586));
#184312=CARTESIAN_POINT('Ctrl Pts',(146.548377299634,-5.44942107922372,
128.494288070434));
#184313=CARTESIAN_POINT('Ctrl Pts',(146.555800566039,-5.38426878985133,
128.351284964201));
#184314=CARTESIAN_POINT('Ctrl Pts',(146.56321505876,-5.31919350507435,128.208450875764));
#184315=CARTESIAN_POINT('Ctrl Pts',(146.570629551481,-5.24834830671106,
128.068027364898));
#184316=CARTESIAN_POINT('Ctrl Pts',(146.578044044202,-5.17193660139352,
127.930512612945));
#184317=CARTESIAN_POINT('Ctrl Pts',(146.585451390556,-5.09559854455438,
127.793130402887));
#184318=CARTESIAN_POINT('Ctrl Pts',(146.59285873691,-5.01370484193458,127.658651694499));
#184319=CARTESIAN_POINT('Ctrl Pts',(146.600266083264,-4.92650642000909,
127.527553474002));
#184320=CARTESIAN_POINT('Ctrl Pts',(146.607667904939,-4.83937303395645,
127.396553031505));
#184321=CARTESIAN_POINT('Ctrl Pts',(146.615069726615,-4.74694301229305,
127.268928366144));
#184322=CARTESIAN_POINT('Ctrl Pts',(146.62247154829,-4.64951245962729,127.145130582399));
#184323=CARTESIAN_POINT('Ctrl Pts',(146.629869462601,-4.55213333979178,
127.02139815054));
#184324=CARTESIAN_POINT('Ctrl Pts',(146.637267376913,-4.44975917640805,
126.901488869612));
#184325=CARTESIAN_POINT('Ctrl Pts',(146.644665291224,-4.34272844203446,
126.785823540315));
#184326=CARTESIAN_POINT('Ctrl Pts',(146.652061976136,-4.23571549422752,
126.670177432496));
#184327=CARTESIAN_POINT('Ctrl Pts',(146.659458661048,-4.12404776455757,
126.558774150282));
#184328=CARTESIAN_POINT('Ctrl Pts',(146.666855345961,-4.00810301044205,
126.452000244138));
#184329=CARTESIAN_POINT('Ctrl Pts',(146.674251702896,-3.8921633974384,126.345231072461));
#184330=CARTESIAN_POINT('Ctrl Pts',(146.681648059831,-3.77194741167059,
126.243091121585));
#184331=CARTESIAN_POINT('Ctrl Pts',(146.689044416767,-3.64786835687497,
126.145928798444));
#184332=CARTESIAN_POINT('Ctrl Pts',(146.696441906103,-3.52377030525935,
126.048751599503));
#184333=CARTESIAN_POINT('Ctrl Pts',(146.70383939544,-3.39580830089613,125.956553775881));
#184334=CARTESIAN_POINT('Ctrl Pts',(146.711236884776,-3.26442715553067,
125.86964219513));
#184335=CARTESIAN_POINT('Ctrl Pts',(146.718636967291,-3.13299995470803,
125.782700147658));
#184336=CARTESIAN_POINT('Ctrl Pts',(146.726037049806,-2.99815153767556,
125.701048238365));
#184337=CARTESIAN_POINT('Ctrl Pts',(146.733437132321,-2.86035385522582,
125.624948837702));
#184338=CARTESIAN_POINT('Ctrl Pts',(146.740845351987,-2.72240465005856,
125.548765757924));
#184339=CARTESIAN_POINT('Ctrl Pts',(146.748253571654,-2.58150002992763,
125.478147560544));
#184340=CARTESIAN_POINT('Ctrl Pts',(146.75566179132,-2.43813525646765,125.413309974726));
#184341=CARTESIAN_POINT('Ctrl Pts',(146.763074570622,-2.29468224438167,
125.348432482455));
#184342=CARTESIAN_POINT('Ctrl Pts',(146.770487349924,-2.14876640696812,
125.289342831039));
#184343=CARTESIAN_POINT('Ctrl Pts',(146.777900129226,-2.0009004450983,125.236207605004));
#184344=CARTESIAN_POINT('Ctrl Pts',(146.785323500255,-1.85282320540788,
125.182996456866));
#184345=CARTESIAN_POINT('Ctrl Pts',(146.792746871284,-1.70279063125872,
125.135756838232));
#184346=CARTESIAN_POINT('Ctrl Pts',(146.800170242312,-1.551328750304,125.094604959836));
#184347=CARTESIAN_POINT('Ctrl Pts',(146.804106291753,-1.47102002674315,
125.072785246484));
#184348=CARTESIAN_POINT('Ctrl Pts',(146.808042341194,-1.39030962529649,
125.052676157388));
#184349=CARTESIAN_POINT('Ctrl Pts',(146.811978390635,-1.30927668226356,
125.034289116122));
#184350=CARTESIAN_POINT('Ctrl Pts',(146.81940165704,-1.1564510806562,124.999611730133));
#184351=CARTESIAN_POINT('Ctrl Pts',(146.826824923445,-1.00201574427408,
124.970957689606));
#184352=CARTESIAN_POINT('Ctrl Pts',(146.834248189851,-0.846486777102989,
124.9484754839));
#184353=CARTESIAN_POINT('Ctrl Pts',(146.841662682572,-0.691141632255162,
124.926019850294));
#184354=CARTESIAN_POINT('Ctrl Pts',(146.849077175293,-0.534705795357542,
124.909721584459));
#184355=CARTESIAN_POINT('Ctrl Pts',(146.856491668014,-0.37770834673534,
124.89967883382));
#184356=CARTESIAN_POINT('Ctrl Pts',(146.863899014368,-0.22086221816497,
124.889645762761));
#184357=CARTESIAN_POINT('Ctrl Pts',(146.871306360721,-0.0634559255323632,
124.885856227417));
#184358=CARTESIAN_POINT('Ctrl Pts',(146.878713707075,0.0939735972562396,
124.88835693894));
#184359=CARTESIAN_POINT('Ctrl Pts',(146.88611552875,0.251285703167327,124.890855785338));
#184360=CARTESIAN_POINT('Ctrl Pts',(146.893517350426,0.40862063309177,124.899635531284));
#184361=CARTESIAN_POINT('Ctrl Pts',(146.900919172101,0.565438808281448,
124.914690888575));
#184362=CARTESIAN_POINT('Ctrl Pts',(146.908317086413,0.722174200377338,
124.92973829826));
#184363=CARTESIAN_POINT('Ctrl Pts',(146.915715000724,0.878393010365668,
124.951054686014));
#184364=CARTESIAN_POINT('Ctrl Pts',(146.923112915035,1.0335582540163,124.978582738342));
#184365=CARTESIAN_POINT('Ctrl Pts',(146.930509599948,1.18869771201809,125.006106216007));
#184366=CARTESIAN_POINT('Ctrl Pts',(146.93790628486,1.34278358397292,125.03983924436));
#184367=CARTESIAN_POINT('Ctrl Pts',(146.945302969772,1.49528646691333,125.079672945355));
#184368=CARTESIAN_POINT('Ctrl Pts',(146.952699326707,1.64778258771611,125.119504880082));
#184369=CARTESIAN_POINT('Ctrl Pts',(146.960095683643,1.79869549788864,125.165436855246));
#184370=CARTESIAN_POINT('Ctrl Pts',(146.967492040578,1.9475086720437,125.217309469168));
#184371=CARTESIAN_POINT('Ctrl Pts',(146.974889529915,2.09634462987568,125.269190024919));
#184372=CARTESIAN_POINT('Ctrl Pts',(146.982287019251,2.24307985907154,125.327012907538));
#184373=CARTESIAN_POINT('Ctrl Pts',(146.989684508588,2.38721575165447,125.390569753712));
#184374=CARTESIAN_POINT('Ctrl Pts',(146.997084591103,2.53140217085101,125.45414887964));
#184375=CARTESIAN_POINT('Ctrl Pts',(147.004484673618,2.67298709790295,125.523465820563));
#184376=CARTESIAN_POINT('Ctrl Pts',(147.011884756133,2.8114946921874,125.598265328551));
#184377=CARTESIAN_POINT('Ctrl Pts',(147.0192929758,2.9501545898108,125.673147086288));
#184378=CARTESIAN_POINT('Ctrl Pts',(147.026701195466,3.08573006824559,125.753523273201));
#184379=CARTESIAN_POINT('Ctrl Pts',(147.034109415132,3.21777192742527,125.839093818534));
#184380=CARTESIAN_POINT('Ctrl Pts',(147.041522194435,3.34989505616613,125.924717031109));
#184381=CARTESIAN_POINT('Ctrl Pts',(147.048934973737,3.47847992772278,126.015540757741));
#184382=CARTESIAN_POINT('Ctrl Pts',(147.056347753039,3.60310926247154,126.111223691672));
#184383=CARTESIAN_POINT('Ctrl Pts',(147.063771124068,3.72791667345833,126.207043341866));
#184384=CARTESIAN_POINT('Ctrl Pts',(147.071194495096,3.84875697358736,126.307735827878));
#184385=CARTESIAN_POINT('Ctrl Pts',(147.078617866125,3.96524806068224,126.412921402484));
#184386=CARTESIAN_POINT('Ctrl Pts',(147.082553915566,4.02701443022521,126.468693318034));
#184387=CARTESIAN_POINT('Ctrl Pts',(147.086489965007,4.0875587198433,126.52572781076));
#184388=CARTESIAN_POINT('Ctrl Pts',(147.090426014447,4.14682854345745,126.583964475772));
#184389=CARTESIAN_POINT('Ctrl Pts',(147.097849280853,4.25860958104587,126.693797008481));
#184390=CARTESIAN_POINT('Ctrl Pts',(147.105272547258,4.36619310847296,126.808239621997));
#184391=CARTESIAN_POINT('Ctrl Pts',(147.112695813664,4.4691752306249,126.926938365545));
#184392=CARTESIAN_POINT('Ctrl Pts',(147.120110306385,4.5720356364607,127.045496817035));
#184393=CARTESIAN_POINT('Ctrl Pts',(147.127524799106,4.67030522009927,127.168301106319));
#184394=CARTESIAN_POINT('Ctrl Pts',(147.134939291827,4.76361542649413,127.294959154215));
#184395=CARTESIAN_POINT('Ctrl Pts',(147.142346638181,4.85683569699896,127.421495124316));
#184396=CARTESIAN_POINT('Ctrl Pts',(147.149753984534,4.94510588643994,127.551877159868));
#184397=CARTESIAN_POINT('Ctrl Pts',(147.157161330888,5.02809646950872,127.685678771687));
#184398=CARTESIAN_POINT('Ctrl Pts',(147.164563152564,5.11102515506961,127.819380589217));
#184399=CARTESIAN_POINT('Ctrl Pts',(147.171964974239,5.18868187889322,127.95649658886));
#184400=CARTESIAN_POINT('Ctrl Pts',(147.179366795914,5.2607794346013,128.096569949332));
#184401=CARTESIAN_POINT('Ctrl Pts',(147.186764710226,5.33283893057094,128.236569366167));
#184402=CARTESIAN_POINT('Ctrl Pts',(147.194162624537,5.39934493249765,128.379522703619));
#184403=CARTESIAN_POINT('Ctrl Pts',(147.201560538848,5.46005540675389,128.524947202304));
#184404=CARTESIAN_POINT('Ctrl Pts',(147.208957223761,5.52075579203069,128.670347534075));
#184405=CARTESIAN_POINT('Ctrl Pts',(147.216353908673,5.57566241745714,128.818217867889));
#184406=CARTESIAN_POINT('Ctrl Pts',(147.223750593585,5.62458072998013,128.968053950793));
#184407=CARTESIAN_POINT('Ctrl Pts',(147.23114695052,5.67349687341389,129.117883389808));
#184408=CARTESIAN_POINT('Ctrl Pts',(147.238543307456,5.71642511604805,129.269678049739));
#184409=CARTESIAN_POINT('Ctrl Pts',(147.245939664391,5.75322037244169,129.422917202647));
#184410=CARTESIAN_POINT('Ctrl Pts',(147.253337153728,5.79002126228304,129.576179816861));
#184411=CARTESIAN_POINT('Ctrl Pts',(147.260734643065,5.82068720909482,129.730887001399));
#184412=CARTESIAN_POINT('Ctrl Pts',(147.268132132401,5.84512400504113,129.886506637789));
#184413=CARTESIAN_POINT('Ctrl Pts',(147.275532214916,5.86956936726836,130.042180826402));
#184414=CARTESIAN_POINT('Ctrl Pts',(147.282932297431,5.88778117318749,130.198767735153));
#184415=CARTESIAN_POINT('Ctrl Pts',(147.290332379946,5.89971696663163,130.355729058111));
#184416=CARTESIAN_POINT('Ctrl Pts',(147.297740599613,5.9116658847077,130.51286297618));
#184417=CARTESIAN_POINT('Ctrl Pts',(147.305148819279,5.91732497999493,130.670371758208));
#184418=CARTESIAN_POINT('Ctrl Pts',(147.312557038945,5.91670390691144,130.827715283885));
#184419=CARTESIAN_POINT('Ctrl Pts',(147.319969818248,5.91608245156783,130.985155651876));
#184420=CARTESIAN_POINT('Ctrl Pts',(147.32738259755,5.90917314202703,131.142430188767));
#184421=CARTESIAN_POINT('Ctrl Pts',(147.334795376852,5.89603757950191,131.299003340752));
#184422=CARTESIAN_POINT('Ctrl Pts',(147.34221874788,5.88288324826905,131.4558002118));
#184423=CARTESIAN_POINT('Ctrl Pts',(147.349642118909,5.86348494193607,131.611893326914));
#184424=CARTESIAN_POINT('Ctrl Pts',(147.357065489938,5.83795561703674,131.766755950062));
#184425=CARTESIAN_POINT('Ctrl Pts',(147.361001539379,5.82441935640741,131.848867828732));
#184426=CARTESIAN_POINT('Ctrl Pts',(147.36493758882,5.80916028979156,131.930633990754));
#184427=CARTESIAN_POINT('Ctrl Pts',(147.36887363826,5.79220092157807,132.011977711918));
#184428=CARTESIAN_POINT('Ctrl Pts',(147.376296904666,5.7602160824111,132.165389431382));
#184429=CARTESIAN_POINT('Ctrl Pts',(147.383720171071,5.72208379492518,132.317761527952));
#184430=CARTESIAN_POINT('Ctrl Pts',(147.391143437477,5.67788353275672,132.468562874189));
#184431=CARTESIAN_POINT('Ctrl Pts',(147.398557930198,5.63373551162751,132.619185985759));
#184432=CARTESIAN_POINT('Ctrl Pts',(147.405972422919,5.58353389537917,132.768241687633));
#184433=CARTESIAN_POINT('Ctrl Pts',(147.41338691564,5.52740933832674,132.915207975638));
#184434=CARTESIAN_POINT('Ctrl Pts',(147.420794261993,5.47133887623547,133.062032612001));
#184435=CARTESIAN_POINT('Ctrl Pts',(147.428201608347,5.40935697062705,133.206771497293));
#184436=CARTESIAN_POINT('Ctrl Pts',(147.435608954701,5.34164432245116,133.348916864719));
#184437=CARTESIAN_POINT('Ctrl Pts',(147.443010776376,5.27398217692291,133.490956214767));
#184438=CARTESIAN_POINT('Ctrl Pts',(147.450412598052,5.20059795919364,133.630405562924));
#184439=CARTESIAN_POINT('Ctrl Pts',(147.457814419727,5.12172076388581,133.766776351267));
#184440=CARTESIAN_POINT('Ctrl Pts',(147.465212334039,5.04288520723543,133.903075150533));
#184441=CARTESIAN_POINT('Ctrl Pts',(147.47261024835,4.95856263432894,134.036298304224));
#184442=CARTESIAN_POINT('Ctrl Pts',(147.480008162661,4.86902837922111,134.165981239355));
#184443=CARTESIAN_POINT('Ctrl Pts',(147.487404847574,4.77950900308215,134.295642623536));
#184444=CARTESIAN_POINT('Ctrl Pts',(147.494801532486,4.68477987555104,134.421764649904));
#184445=CARTESIAN_POINT('Ctrl Pts',(147.502198217398,4.58516007824034,134.543911074427));
#184446=CARTESIAN_POINT('Ctrl Pts',(147.509594574333,4.48554469817586,134.66605208285));
#184447=CARTESIAN_POINT('Ctrl Pts',(147.516990931269,4.38103931545204,134.784217550653));
#184448=CARTESIAN_POINT('Ctrl Pts',(147.524387288204,4.27200361100666,134.898003947174));
#184449=CARTESIAN_POINT('Ctrl Pts',(147.531784777541,4.16295121291654,135.011807764683));
#184450=CARTESIAN_POINT('Ctrl Pts',(147.539182266877,4.04936737033896,135.121230906417));
#184451=CARTESIAN_POINT('Ctrl Pts',(147.546579756214,3.93164884797777,135.225906489622));
#184452=CARTESIAN_POINT('Ctrl Pts',(147.553979838729,3.81388905957093,135.330618766691));
#184453=CARTESIAN_POINT('Ctrl Pts',(147.561379921244,3.69199198441348,135.430579923824));
#184454=CARTESIAN_POINT('Ctrl Pts',(147.568780003759,3.56638756593778,135.52546327394));
#184455=CARTESIAN_POINT('Ctrl Pts',(147.576188223426,3.44064503249161,135.620450958054));
#184456=CARTESIAN_POINT('Ctrl Pts',(147.583596443092,3.31118731252439,135.710349459245));
#184457=CARTESIAN_POINT('Ctrl Pts',(147.591004662759,3.17847404300024,135.794874951828));
#184458=CARTESIAN_POINT('Ctrl Pts',(147.598417442061,3.04567909067309,135.879452468441));
#184459=CARTESIAN_POINT('Ctrl Pts',(147.605830221363,2.90962491796424,135.958650199476));
#184460=CARTESIAN_POINT('Ctrl Pts',(147.613243000665,2.77079539841787,136.032230491865));
#184461=CARTESIAN_POINT('Ctrl Pts',(147.620666371694,2.6317675127435,136.105915919227));
#184462=CARTESIAN_POINT('Ctrl Pts',(147.628089742722,2.48995669580852,136.173967716226));
#184463=CARTESIAN_POINT('Ctrl Pts',(147.635513113751,2.34586716132055,136.236196202701));
#184464=CARTESIAN_POINT('Ctrl Pts',(147.639449163192,2.2694674327546,136.269191239382));
#184465=CARTESIAN_POINT('Ctrl Pts',(147.643385212633,2.19242734667834,136.300549962301));
#184466=CARTESIAN_POINT('Ctrl Pts',(147.647321262073,2.11482361751463,136.330249833729));
#184467=CARTESIAN_POINT('Ctrl Pts',(147.654744528479,1.96846540624065,136.38626286434));
#184468=CARTESIAN_POINT('Ctrl Pts',(147.662167794884,1.81965901317569,136.436541931007));
#184469=CARTESIAN_POINT('Ctrl Pts',(147.66959106129,1.66889424831701,136.480866809797));
#184470=CARTESIAN_POINT('Ctrl Pts',(147.677005554011,1.51830767489006,136.525139300261));
#184471=CARTESIAN_POINT('Ctrl Pts',(147.684420046732,1.365767691602,136.563471506478));
#184472=CARTESIAN_POINT('Ctrl Pts',(147.691834539453,1.21178409719669,136.595691195618));
#184473=CARTESIAN_POINT('Ctrl Pts',(147.699241885806,1.05794891797699,136.627879830208));
#184474=CARTESIAN_POINT('Ctrl Pts',(147.70664923216,0.90267326058903,136.653967600545));
#184475=CARTESIAN_POINT('Ctrl Pts',(147.714056578514,0.746481996895511,
136.6738320751));
#184476=CARTESIAN_POINT('Ctrl Pts',(147.721458400189,0.590407226539157,
136.693681733981));
#184477=CARTESIAN_POINT('Ctrl Pts',(147.728860221865,0.433418578332028,
136.707317292175));
#184478=CARTESIAN_POINT('Ctrl Pts',(147.73626204354,0.276050921131112,136.714667415985));
#184479=CARTESIAN_POINT('Ctrl Pts',(147.743659957852,0.118766337091485,
136.722013659723));
#184480=CARTESIAN_POINT('Ctrl Pts',(147.751057872163,-0.0388964855337151,
136.723081059724));
#184481=CARTESIAN_POINT('Ctrl Pts',(147.758455786474,-0.196397863552939,
136.71785014928));
#184482=CARTESIAN_POINT('Ctrl Pts',(147.765852471386,-0.353873067700333,
136.712620108119));
#184483=CARTESIAN_POINT('Ctrl Pts',(147.773249156299,-0.51118650776281,
136.701093846212));
#184484=CARTESIAN_POINT('Ctrl Pts',(147.780645841211,-0.667798687876059,
136.683304015403));
#184485=CARTESIAN_POINT('Ctrl Pts',(147.788042198146,-0.824403923641123,
136.665514973413));
#184486=CARTESIAN_POINT('Ctrl Pts',(147.795438555082,-0.980307590371243,
136.641462956881));
#184487=CARTESIAN_POINT('Ctrl Pts',(147.802834912017,-1.13497576996038,
136.611232457387));
#184488=CARTESIAN_POINT('Ctrl Pts',(147.810232401354,-1.2896676296426,136.580997329526));
#184489=CARTESIAN_POINT('Ctrl Pts',(147.81762989069,-1.44312325915959,136.544581906819));
#184490=CARTESIAN_POINT('Ctrl Pts',(147.825027380027,-1.59481952864751,
136.502121689561));
#184491=CARTESIAN_POINT('Ctrl Pts',(147.832427462542,-1.74656897502743,
136.45964658794));
#184492=CARTESIAN_POINT('Ctrl Pts',(147.839827545057,-1.89655747419436,
136.411122573423));
#184493=CARTESIAN_POINT('Ctrl Pts',(147.847227627572,-2.04427778012711,
136.35673478725));
#184494=CARTESIAN_POINT('Ctrl Pts',(147.854635847238,-2.19216051972247,
136.302287196115));
#184495=CARTESIAN_POINT('Ctrl Pts',(147.862044066905,-2.33776973465519,
136.241963085661));
#184496=CARTESIAN_POINT('Ctrl Pts',(147.869452286571,-2.48061818933069,
136.175995746767));
#184497=CARTESIAN_POINT('Ctrl Pts',(147.876865065873,-2.62355456484653,
136.109987806076));
#184498=CARTESIAN_POINT('Ctrl Pts',(147.884277845175,-2.76372646261958,
136.038329885458));
#184499=CARTESIAN_POINT('Ctrl Pts',(147.891690624477,-2.90067239292292,
135.961300624143));
#184500=CARTESIAN_POINT('Ctrl Pts',(147.899113995506,-3.03781399799365,
135.884161299807));
#184501=CARTESIAN_POINT('Ctrl Pts',(147.906537366535,-3.17172011261075,
135.801635501764));
#184502=CARTESIAN_POINT('Ctrl Pts',(147.913960737564,-3.30195861365784,
135.714044912527));
#184503=CARTESIAN_POINT('Ctrl Pts',(147.917896787004,-3.37101419194558,
135.667602280405));
#184504=CARTESIAN_POINT('Ctrl Pts',(147.921832836445,-3.43903922199857,
135.619736429816));
#184505=CARTESIAN_POINT('Ctrl Pts',(147.925768885886,-3.50597327616687,
135.570499720583));
#184506=CARTESIAN_POINT('Ctrl Pts',(147.933123905128,-3.63104824377164,
135.478494538933));
#184507=CARTESIAN_POINT('Ctrl Pts',(147.940478924369,-3.75270524870596,
135.381410785428));
#184508=CARTESIAN_POINT('Ctrl Pts',(147.947833943611,-3.8704987908315,135.279533203363));
#184509=CARTESIAN_POINT('Ctrl Pts',(147.955180237663,-3.98815259559593,
135.177776477707));
#184510=CARTESIAN_POINT('Ctrl Pts',(147.962526531715,-4.10195177232589,
135.071237486037));
#184511=CARTESIAN_POINT('Ctrl Pts',(147.969872825766,-4.21148001421642,
134.960243995665));
#184512=CARTESIAN_POINT('Ctrl Pts',(147.97721208139,-4.3209033179346,134.849356847308));
#184513=CARTESIAN_POINT('Ctrl Pts',(147.984551337014,-4.42606356485535,
134.734023963175));
#184514=CARTESIAN_POINT('Ctrl Pts',(147.991890592638,-4.52657792759927,
134.614612948826));
#184515=CARTESIAN_POINT('Ctrl Pts',(147.999224490157,-4.62701890873292,
134.495289111794));
#184516=CARTESIAN_POINT('Ctrl Pts',(148.006558387677,-4.72282051299202,
134.37189336114));
#184517=CARTESIAN_POINT('Ctrl Pts',(148.013892285197,-4.81363732265844,
134.244829522877));
#184518=CARTESIAN_POINT('Ctrl Pts',(148.021223039868,-4.90441521392979,
134.117820136214));
#184519=CARTESIAN_POINT('Ctrl Pts',(148.028553794539,-4.99021233941579,
133.987146098375));
#184520=CARTESIAN_POINT('Ctrl Pts',(148.035884549209,-5.07072415600133,
133.853243543532));
#184521=CARTESIAN_POINT('Ctrl Pts',(148.043213762271,-5.15121904148193,
133.719369147514));
#184522=CARTESIAN_POINT('Ctrl Pts',(148.050542975332,-5.22643063297417,
133.582267911324));
#184523=CARTESIAN_POINT('Ctrl Pts',(148.057872188393,-5.29609838416044,
133.442403920431));
#184524=CARTESIAN_POINT('Ctrl Pts',(148.065201372892,-5.36576586384708,
133.302540474598));
#184525=CARTESIAN_POINT('Ctrl Pts',(148.072530557391,-5.42988937632489,
133.159914636398));
#184526=CARTESIAN_POINT('Ctrl Pts',(148.07985974189,-5.48825502631292,133.015013762827));
#184527=CARTESIAN_POINT('Ctrl Pts',(148.087190410633,-5.54663249601668,
132.870083545161));
#184528=CARTESIAN_POINT('Ctrl Pts',(148.094521079376,-5.59924964074774,
132.72287772861));
#184529=CARTESIAN_POINT('Ctrl Pts',(148.101851748119,-5.64594135944282,
132.573902006806));
#184530=CARTESIAN_POINT('Ctrl Pts',(148.109189520302,-5.69267832254938,
132.424781927093));
#184531=CARTESIAN_POINT('Ctrl Pts',(148.116527292484,-5.73347827712869,
132.273888880453));
#184532=CARTESIAN_POINT('Ctrl Pts',(148.123865064667,-5.76822634556614,
132.1217426384));
#184533=CARTESIAN_POINT('Ctrl Pts',(148.13120651168,-5.80299181618652,131.969520199975));
#184534=CARTESIAN_POINT('Ctrl Pts',(148.138547958692,-5.83169929265059,
131.816043689774));
#184535=CARTESIAN_POINT('Ctrl Pts',(148.145889405705,-5.85428548751921,
131.661840642477));
#184536=CARTESIAN_POINT('Ctrl Pts',(148.153241485596,-5.87690439477602,
131.50741425743));
#184537=CARTESIAN_POINT('Ctrl Pts',(148.160593565487,-5.89338426854782,
131.352259611532));
#184538=CARTESIAN_POINT('Ctrl Pts',(148.167945645379,-5.90371385336624,
131.196907812272));
#184539=CARTESIAN_POINT('Ctrl Pts',(148.174172032851,-5.91246185372226,
131.065342253818));
#184540=CARTESIAN_POINT('Ctrl Pts',(148.180398420323,-5.91679965474399,
130.93363543647));
#184541=CARTESIAN_POINT('Ctrl Pts',(148.186624807795,-5.91674957104603,
130.802107613661));
#184542=CARTESIAN_POINT('',(149.936624807795,-5.91741018499184,130.809792679456));
#184543=CARTESIAN_POINT('Ctrl Pts',(148.186624807795,-5.92549522901829,
130.802104283454));
#184544=CARTESIAN_POINT('Ctrl Pts',(148.19248870843,-5.9260986124455,130.678050383426));
#184545=CARTESIAN_POINT('Ctrl Pts',(148.198352609065,-5.92254184562957,
130.554031734584));
#184546=CARTESIAN_POINT('Ctrl Pts',(148.297032384304,-5.79083462023666,
128.4715467825));
#184547=CARTESIAN_POINT('Ctrl Pts',(148.482664133512,-3.40361946202966,
124.689384322596));
#184548=CARTESIAN_POINT('Ctrl Pts',(148.761111757326,3.30496328483161,124.635505114617));
#184549=CARTESIAN_POINT('Ctrl Pts',(149.039559381138,6.97644622936501,130.250502748502));
#184550=CARTESIAN_POINT('Ctrl Pts',(149.31800700495,4.23691590745723,136.374468706597));
#184551=CARTESIAN_POINT('Ctrl Pts',(149.596454628764,-2.39613314855434,
137.379777445777));
#184552=CARTESIAN_POINT('Ctrl Pts',(149.802660563045,-5.67762348943452,
133.649467228661));
#184553=CARTESIAN_POINT('Ctrl Pts',(149.916050622722,-5.92147029572398,
131.246598976015));
#184554=CARTESIAN_POINT('Ctrl Pts',(149.936624807795,-5.91741018499184,
130.809792679456));
#184555=CARTESIAN_POINT('',(151.686624807835,-5.91674999613679,130.804146806335));
#184556=CARTESIAN_POINT('Ctrl Pts',(149.936624807795,-5.91674750701871,
130.809792071131));
#184557=CARTESIAN_POINT('Ctrl Pts',(149.943932106311,-5.91688990486533,
130.654671145612));
#184558=CARTESIAN_POINT('Ctrl Pts',(149.951239404828,-5.91092786845665,
130.499368082824));
#184559=CARTESIAN_POINT('Ctrl Pts',(149.958546703344,-5.89884527149,130.344409505468));
#184560=CARTESIAN_POINT('Ctrl Pts',(149.965848675255,-5.88677148205011,
130.189563884111));
#184561=CARTESIAN_POINT('Ctrl Pts',(149.973150647166,-5.86858604119047,
130.035062629882));
#184562=CARTESIAN_POINT('Ctrl Pts',(149.980452619077,-5.84432489231685,
129.881432063698));
#184563=CARTESIAN_POINT('Ctrl Pts',(149.987751576981,-5.82007375762373,
129.727864911008));
#184564=CARTESIAN_POINT('Ctrl Pts',(149.995050534885,-5.78975196218206,
129.575168110421));
#184565=CARTESIAN_POINT('Ctrl Pts',(150.002349492789,-5.75344725503109,
129.423862429927));
#184566=CARTESIAN_POINT('Ctrl Pts',(150.009646984945,-5.7171498384515,129.272587134056));
#184567=CARTESIAN_POINT('Ctrl Pts',(150.016944477101,-5.67487198927059,
129.122702776197));
#184568=CARTESIAN_POINT('Ctrl Pts',(150.024241969256,-5.62675242818888,
128.974719211615));
#184569=CARTESIAN_POINT('Ctrl Pts',(150.031539528218,-5.57863242658976,
128.826734292296));
#184570=CARTESIAN_POINT('Ctrl Pts',(150.038837087179,-5.52467072538557,
128.680650566464));
#184571=CARTESIAN_POINT('Ctrl Pts',(150.046134646141,-5.46505561347183,
128.536961732464));
#184572=CARTESIAN_POINT('Ctrl Pts',(150.053433804352,-5.40542743699231,
128.393241409264));
#184573=CARTESIAN_POINT('Ctrl Pts',(150.060732962563,-5.34014353216303,
128.251917377002));
#184574=CARTESIAN_POINT('Ctrl Pts',(150.068032120774,-5.26943979956252,
128.113462113109));
#184575=CARTESIAN_POINT('Ctrl Pts',(150.075338692602,-5.1986642545184,127.974866222825));
#184576=CARTESIAN_POINT('Ctrl Pts',(150.082645264429,-5.12245806211543,
127.839145263181));
#184577=CARTESIAN_POINT('Ctrl Pts',(150.089951836257,-5.0411027552245,127.706746443114));
#184578=CARTESIAN_POINT('Ctrl Pts',(150.097262210755,-4.95970510735594,
127.574278716719));
#184579=CARTESIAN_POINT('Ctrl Pts',(150.104572585253,-4.87315322139015,
127.445136892233));
#184580=CARTESIAN_POINT('Ctrl Pts',(150.111882959752,-4.78177074702681,
127.319737383215));
#184581=CARTESIAN_POINT('Ctrl Pts',(150.119204413597,-4.69024977658409,
127.19414782309));
#184582=CARTESIAN_POINT('Ctrl Pts',(150.126525867443,-4.59388383081696,
127.072312209756));
#184583=CARTESIAN_POINT('Ctrl Pts',(150.133847321289,-4.49303604899263,
126.95461288233));
#184584=CARTESIAN_POINT('Ctrl Pts',(150.140348172989,-4.40349147386482,
126.850105514131));
#184585=CARTESIAN_POINT('Ctrl Pts',(150.146849024689,-4.31041409756609,
126.748858792964));
#184586=CARTESIAN_POINT('Ctrl Pts',(150.153349876389,-4.21408048751599,
126.651114151579));
#184587=CARTESIAN_POINT('Ctrl Pts',(150.160773142795,-4.10407797028059,
126.539500389849));
#184588=CARTESIAN_POINT('Ctrl Pts',(150.1681964092,-3.98947176547295,126.432091149178));
#184589=CARTESIAN_POINT('Ctrl Pts',(150.175619675606,-3.87061643811742,
126.32928978556));
#184590=CARTESIAN_POINT('Ctrl Pts',(150.183034168327,-3.75190158788854,
126.226609924616));
#184591=CARTESIAN_POINT('Ctrl Pts',(150.190448661048,-3.62894789123219,
126.128527341995));
#184592=CARTESIAN_POINT('Ctrl Pts',(150.197863153769,-3.50214798775444,
126.03540999564));
#184593=CARTESIAN_POINT('Ctrl Pts',(150.205270500122,-3.37547029879769,
125.942382399289));
#184594=CARTESIAN_POINT('Ctrl Pts',(150.212677846476,-3.2449540820249,125.854310731327));
#184595=CARTESIAN_POINT('Ctrl Pts',(150.22008519283,-3.11102632760607,125.771523867636));
#184596=CARTESIAN_POINT('Ctrl Pts',(150.227487014505,-2.97719846155896,
125.688798749512));
#184597=CARTESIAN_POINT('Ctrl Pts',(150.234888836181,-2.83996444037969,
125.611350782824));
#184598=CARTESIAN_POINT('Ctrl Pts',(150.242290657856,-2.69978152190396,
125.539466478413));
#184599=CARTESIAN_POINT('Ctrl Pts',(150.249688572167,-2.55967260489901,
125.467620121167));
#184600=CARTESIAN_POINT('Ctrl Pts',(150.257086486479,-2.41661822217042,
125.401331746898));
#184601=CARTESIAN_POINT('Ctrl Pts',(150.26448440079,-2.27110150087739,125.340842654274));
#184602=CARTESIAN_POINT('Ctrl Pts',(150.271881085702,-2.12560896182449,
125.280363613841));
#184603=CARTESIAN_POINT('Ctrl Pts',(150.279277770615,-1.97765524070537,
125.225682085472));
#184604=CARTESIAN_POINT('Ctrl Pts',(150.286674455527,-1.82774488596508,
125.176991854607));
#184605=CARTESIAN_POINT('Ctrl Pts',(150.294070812462,-1.67784117840697,
125.128303782718));
#184606=CARTESIAN_POINT('Ctrl Pts',(150.301467169398,-1.52598136477429,
125.085606595426));
#184607=CARTESIAN_POINT('Ctrl Pts',(150.308863526333,-1.37268639319796,
125.049044585546));
#184608=CARTESIAN_POINT('Ctrl Pts',(150.31626101567,-1.21936795177014,125.012476977928));
#184609=CARTESIAN_POINT('Ctrl Pts',(150.323658505006,-1.06461427803038,
124.982046504626));
#184610=CARTESIAN_POINT('Ctrl Pts',(150.331055994343,-0.908957633202125,
124.957846563573));
#184611=CARTESIAN_POINT('Ctrl Pts',(150.338456076858,-0.753246423178655,
124.933638139267));
#184612=CARTESIAN_POINT('Ctrl Pts',(150.345856159373,-0.596631980484085,
124.915664653056));
#184613=CARTESIAN_POINT('Ctrl Pts',(150.353256241888,-0.439652675039819,
124.903967741847));
#184614=CARTESIAN_POINT('Ctrl Pts',(150.360664461554,-0.282500754710905,
124.892257968682));
#184615=CARTESIAN_POINT('Ctrl Pts',(150.368072681221,-0.124983542895683,
124.886838581501));
#184616=CARTESIAN_POINT('Ctrl Pts',(150.375480900887,0.0323588554119081,
124.887699103927));
#184617=CARTESIAN_POINT('Ctrl Pts',(150.382893680189,0.189798095340595,
124.88856015599));
#184618=CARTESIAN_POINT('Ctrl Pts',(150.390306459491,0.347061935317314,
124.895708802602));
#184619=CARTESIAN_POINT('Ctrl Pts',(150.397719238793,0.503614915903667,
124.9090826276));
#184620=CARTESIAN_POINT('Ctrl Pts',(150.405142609822,0.660391586730009,
124.922475561746));
#184621=CARTESIAN_POINT('Ctrl Pts',(150.412565980851,0.816455000170236,
124.942111392765));
#184622=CARTESIAN_POINT('Ctrl Pts',(150.41998935188,0.9712785927025,124.967876362652));
#184623=CARTESIAN_POINT('Ctrl Pts',(150.423925401321,1.05336977640659,124.981537567908));
#184624=CARTESIAN_POINT('Ctrl Pts',(150.427861450762,1.1351126220454,124.996921051034));
#184625=CARTESIAN_POINT('Ctrl Pts',(150.431797500202,1.21643043974548,125.014004190906));
#184626=CARTESIAN_POINT('Ctrl Pts',(150.439220766608,1.36979330608149,125.046222459557));
#184627=CARTESIAN_POINT('Ctrl Pts',(150.446644033013,1.52210719535654,125.084586587279));
#184628=CARTESIAN_POINT('Ctrl Pts',(150.454067299419,1.67284110169347,125.129016292242));
#184629=CARTESIAN_POINT('Ctrl Pts',(150.46148179214,1.82339685307062,125.173393484984));
#184630=CARTESIAN_POINT('Ctrl Pts',(150.468896284861,1.9723759840262,125.223821880504));
#184631=CARTESIAN_POINT('Ctrl Pts',(150.476310777582,2.11925668982468,125.280170030237));
#184632=CARTESIAN_POINT('Ctrl Pts',(150.483718123936,2.26599582646911,125.336463869502));
#184633=CARTESIAN_POINT('Ctrl Pts',(150.491125470289,2.41064021824683,125.398665971281));
#184634=CARTESIAN_POINT('Ctrl Pts',(150.498532816643,2.55268237394668,125.466594862098));
#184635=CARTESIAN_POINT('Ctrl Pts',(150.505934638318,2.6946185892478,125.534473088986));
#184636=CARTESIAN_POINT('Ctrl Pts',(150.513336459994,2.83395609763766,125.608069439907));
#184637=CARTESIAN_POINT('Ctrl Pts',(150.520738281669,2.97020669040165,125.687154077002));
#184638=CARTESIAN_POINT('Ctrl Pts',(150.528136195981,3.10638535753878,125.766196965932));
#184639=CARTESIAN_POINT('Ctrl Pts',(150.535534110292,3.23948003235821,125.850722184156));
#184640=CARTESIAN_POINT('Ctrl Pts',(150.542932024603,3.36902656142461,125.940453690936));
#184641=CARTESIAN_POINT('Ctrl Pts',(150.550328709516,3.49855156220764,126.030170285968));
#184642=CARTESIAN_POINT('Ctrl Pts',(150.557725394428,3.62452928092174,126.125091240058));
#184643=CARTESIAN_POINT('Ctrl Pts',(150.56512207934,3.74652395962857,126.224896808076));
#184644=CARTESIAN_POINT('Ctrl Pts',(150.572518436275,3.86851322896337,126.32469795061));
#184645=CARTESIAN_POINT('Ctrl Pts',(150.579914793211,3.98651952052958,126.429383040045));
#184646=CARTESIAN_POINT('Ctrl Pts',(150.587311150146,4.10013985150687,126.538591781754));
#184647=CARTESIAN_POINT('Ctrl Pts',(150.594708639483,4.21377757804723,126.647817243601));
#184648=CARTESIAN_POINT('Ctrl Pts',(150.602106128819,4.32302773779736,126.761567478045));
#184649=CARTESIAN_POINT('Ctrl Pts',(150.609503618156,4.42752405223851,126.879445162508));
#184650=CARTESIAN_POINT('Ctrl Pts',(150.616903700671,4.5320569977008,126.997364168812));
#184651=CARTESIAN_POINT('Ctrl Pts',(150.624303783186,4.63183253248303,127.119413226679));
#184652=CARTESIAN_POINT('Ctrl Pts',(150.631703865701,4.72652462418257,127.245161896014));
#184653=CARTESIAN_POINT('Ctrl Pts',(150.639112085368,4.82132083957137,127.371048838938));
#184654=CARTESIAN_POINT('Ctrl Pts',(150.646520305034,4.91102222404954,127.500643219211));
#184655=CARTESIAN_POINT('Ctrl Pts',(150.653928524701,4.99534565174867,127.633484968466));
#184656=CARTESIAN_POINT('Ctrl Pts',(150.661341304003,5.07972097911038,127.766408479601));
#184657=CARTESIAN_POINT('Ctrl Pts',(150.668754083305,5.15871156714548,127.902583020226));
#184658=CARTESIAN_POINT('Ctrl Pts',(150.676166862607,5.23208049943405,128.041524355689));
#184659=CARTESIAN_POINT('Ctrl Pts',(150.683590233635,5.30555426469391,128.180664217048));
#184660=CARTESIAN_POINT('Ctrl Pts',(150.691013604664,5.37339017096703,128.322578433019));
#184661=CARTESIAN_POINT('Ctrl Pts',(150.698436975693,5.43539930563968,128.466762501817));
#184662=CARTESIAN_POINT('Ctrl Pts',(150.702373025134,5.46827803673185,128.543212354743));
#184663=CARTESIAN_POINT('Ctrl Pts',(150.706309074575,5.49951948144194,128.620300074247));
#184664=CARTESIAN_POINT('Ctrl Pts',(150.710245124015,5.52910121881237,128.697948911696));
#184665=CARTESIAN_POINT('Ctrl Pts',(150.717668390421,5.58489145227859,128.844392195787));
#184666=CARTESIAN_POINT('Ctrl Pts',(150.725091656826,5.63494400272429,128.993274932717));
#184667=CARTESIAN_POINT('Ctrl Pts',(150.732514923232,5.6790393918795,129.144106977913));
#184668=CARTESIAN_POINT('Ctrl Pts',(150.739929415953,5.72308266394661,129.294760752157));
#184669=CARTESIAN_POINT('Ctrl Pts',(150.747343908674,5.76118268588832,129.447358893899));
#184670=CARTESIAN_POINT('Ctrl Pts',(150.754758401395,5.79316800090004,129.601391342876));
#184671=CARTESIAN_POINT('Ctrl Pts',(150.762165747748,5.82512248726093,129.75527532958));
#184672=CARTESIAN_POINT('Ctrl Pts',(150.769573094102,5.85097392427088,129.910590508307));
#184673=CARTESIAN_POINT('Ctrl Pts',(150.776980440456,5.87060067930828,130.066811821482));
#184674=CARTESIAN_POINT('Ctrl Pts',(150.784382262131,5.89021279597131,130.222916618908));
#184675=CARTESIAN_POINT('Ctrl Pts',(150.791784083807,5.90360942837723,130.379925836323));
#184676=CARTESIAN_POINT('Ctrl Pts',(150.799185905482,5.91072005689088,130.537304496932));
#184677=CARTESIAN_POINT('Ctrl Pts',(150.806583819794,5.91782693175914,130.694600078573));
#184678=CARTESIAN_POINT('Ctrl Pts',(150.813981734105,5.91865439454688,130.852264343029));
#184679=CARTESIAN_POINT('Ctrl Pts',(150.821379648416,5.91318379987458,131.00975757811));
#184680=CARTESIAN_POINT('Ctrl Pts',(150.828776333329,5.9077141143159,131.167224640672));
#184681=CARTESIAN_POINT('Ctrl Pts',(150.836173018241,5.89594846148009,131.32452035756));
#184682=CARTESIAN_POINT('Ctrl Pts',(150.843569703153,5.87792031419289,131.481105283225));
#184683=CARTESIAN_POINT('Ctrl Pts',(150.850966060088,5.85989296629269,131.637683265751));
#184684=CARTESIAN_POINT('Ctrl Pts',(150.858362417024,5.8356037187708,131.793550148872));
#184685=CARTESIAN_POINT('Ctrl Pts',(150.865758773959,5.80513787564255,131.948172143684));
#184686=CARTESIAN_POINT('Ctrl Pts',(150.873156263296,5.77466736811589,132.102817811518));
#184687=CARTESIAN_POINT('Ctrl Pts',(150.880553752633,5.7380184542325,132.256217845262));
#184688=CARTESIAN_POINT('Ctrl Pts',(150.887951241969,5.69532743024335,132.407849321866));
#184689=CARTESIAN_POINT('Ctrl Pts',(150.895351324484,5.65262144098211,132.559533952648));
#184690=CARTESIAN_POINT('Ctrl Pts',(150.902751406999,5.60386922569224,132.709448432841));
#184691=CARTESIAN_POINT('Ctrl Pts',(150.910151489514,5.54925669734036,132.857085798764));
#184692=CARTESIAN_POINT('Ctrl Pts',(150.917559709181,5.49458411689897,133.004885507149));
#184693=CARTESIAN_POINT('Ctrl Pts',(150.924967928847,5.43403848386057,133.150402750441));
#184694=CARTESIAN_POINT('Ctrl Pts',(150.932376148513,5.36785383032385,133.293150648641));
#184695=CARTESIAN_POINT('Ctrl Pts',(150.939788927816,5.30162844123736,133.43598640579));
#184696=CARTESIAN_POINT('Ctrl Pts',(150.947201707118,5.22975728583163,133.576049090089));
#184697=CARTESIAN_POINT('Ctrl Pts',(150.95461448642,5.15251970532112,133.712877636388));
#184698=CARTESIAN_POINT('Ctrl Pts',(150.962037857448,5.0751717641333,133.849901689731));
#184699=CARTESIAN_POINT('Ctrl Pts',(150.969461228477,4.99244227934222,133.983682059071));
#184700=CARTESIAN_POINT('Ctrl Pts',(150.976884599506,4.90465359070537,134.113787111338));
#184701=CARTESIAN_POINT('Ctrl Pts',(150.980820648947,4.85810592152945,134.182771931878));
#184702=CARTESIAN_POINT('Ctrl Pts',(150.984756698388,4.81013660385384,134.25072403948));
#184703=CARTESIAN_POINT('Ctrl Pts',(150.988692747828,4.76079808940158,134.317583086248));
#184704=CARTESIAN_POINT('Ctrl Pts',(150.996116014234,4.66774719094704,134.443677161852));
#184705=CARTESIAN_POINT('Ctrl Pts',(151.003539280639,4.56954255390688,134.566262546077));
#184706=CARTESIAN_POINT('Ctrl Pts',(151.010962547045,4.46647791742634,134.684889650526));
#184707=CARTESIAN_POINT('Ctrl Pts',(151.018377039766,4.36353509478691,134.803376547588));
#184708=CARTESIAN_POINT('Ctrl Pts',(151.025791532487,4.25574394883958,134.917914198125));
#184709=CARTESIAN_POINT('Ctrl Pts',(151.033206025208,4.14344093113797,135.02808265064));
#184710=CARTESIAN_POINT('Ctrl Pts',(151.040613371561,4.03124615531315,135.138144918652));
#184711=CARTESIAN_POINT('Ctrl Pts',(151.048020717915,3.91454842985615,135.243846112645));
#184712=CARTESIAN_POINT('Ctrl Pts',(151.055428064269,3.79372375517209,135.344800093205));
#184713=CARTESIAN_POINT('Ctrl Pts',(151.062829885944,3.67298919608848,135.445678778479));
#184714=CARTESIAN_POINT('Ctrl Pts',(151.07023170762,3.54813410179089,135.541817061911));
#184715=CARTESIAN_POINT('Ctrl Pts',(151.077633529295,3.41957044582327,135.632866445309));
#184716=CARTESIAN_POINT('Ctrl Pts',(151.085031443607,3.29107465760982,135.723867764447));
#184717=CARTESIAN_POINT('Ctrl Pts',(151.092429357918,3.15887451048879,135.809785318427));
#184718=CARTESIAN_POINT('Ctrl Pts',(151.099827272229,3.02341400132938,135.89031169274));
#184719=CARTESIAN_POINT('Ctrl Pts',(151.107223957141,2.88797600324841,135.970824685032));
#184720=CARTESIAN_POINT('Ctrl Pts',(151.114620642054,2.74927903903473,136.04594808522));
#184721=CARTESIAN_POINT('Ctrl Pts',(151.122017326966,2.60779505238653,136.115418471445));
#184722=CARTESIAN_POINT('Ctrl Pts',(151.129413683901,2.46631733928662,136.18488577728));
#184723=CARTESIAN_POINT('Ctrl Pts',(151.136810040837,2.32205318455341,136.24870040302));
#184724=CARTESIAN_POINT('Ctrl Pts',(151.144206397772,2.1754977888152,136.306645591407));
#184725=CARTESIAN_POINT('Ctrl Pts',(151.151603887109,2.02891995507124,136.364599651351));
#184726=CARTESIAN_POINT('Ctrl Pts',(151.159001376445,1.88005052901395,136.416682347392));
#184727=CARTESIAN_POINT('Ctrl Pts',(151.166398865782,1.7294031320678,136.462725696747));
#184728=CARTESIAN_POINT('Ctrl Pts',(151.173798948297,1.57870292591083,136.508785186526));
#184729=CARTESIAN_POINT('Ctrl Pts',(151.181199030812,1.42622386472237,136.548801005477));
#184730=CARTESIAN_POINT('Ctrl Pts',(151.188599113327,1.27249296190427,136.582655541192));
#184731=CARTESIAN_POINT('Ctrl Pts',(151.196007332993,1.11859301615438,136.61654730345));
#184732=CARTESIAN_POINT('Ctrl Pts',(151.20341555266,0.963438844543162,136.644264172089));
#184733=CARTESIAN_POINT('Ctrl Pts',(151.210823772326,0.807566573070859,
136.66573987441));
#184734=CARTESIAN_POINT('Ctrl Pts',(151.218236551628,0.6515983648165,136.687228794667));
#184735=CARTESIAN_POINT('Ctrl Pts',(151.225649330931,0.494911546686642,
136.702468858212));
#184736=CARTESIAN_POINT('Ctrl Pts',(151.233062110233,0.338045016600596,
136.711445865745));
#184737=CARTESIAN_POINT('Ctrl Pts',(151.240485481261,0.180954348259829,
136.720435700046));
#184738=CARTESIAN_POINT('Ctrl Pts',(151.24790885229,0.0236838273676483,
136.723144598866));
#184739=CARTESIAN_POINT('Ctrl Pts',(151.255332223319,-0.133229168437175,
136.719610447554));
#184740=CARTESIAN_POINT('Ctrl Pts',(151.25926827276,-0.21642820388921,136.717736555728));
#184741=CARTESIAN_POINT('Ctrl Pts',(151.2632043222,-0.299526824438706,136.714108384187));
#184742=CARTESIAN_POINT('Ctrl Pts',(151.267140371641,-0.382445906253092,
136.70873744254));
#184743=CARTESIAN_POINT('Ctrl Pts',(151.274563638047,-0.538828706737724,
136.698608014215));
#184744=CARTESIAN_POINT('Ctrl Pts',(151.281986904452,-0.695045267387024,
136.682246066261));
#184745=CARTESIAN_POINT('Ctrl Pts',(151.289410170858,-0.850558563565077,
136.659655716231));
#184746=CARTESIAN_POINT('Ctrl Pts',(151.296824663579,-1.00588805594146,
136.637092066118));
#184747=CARTESIAN_POINT('Ctrl Pts',(151.3042391563,-1.16051557254203,136.608314720081));
#184748=CARTESIAN_POINT('Ctrl Pts',(151.311653649021,-1.31390593599615,
136.5733797503));
#184749=CARTESIAN_POINT('Ctrl Pts',(151.319060995374,-1.46714845604283,
136.538478452159));
#184750=CARTESIAN_POINT('Ctrl Pts',(151.326468341728,-1.61915583527227,
136.497431427929));
#184751=CARTESIAN_POINT('Ctrl Pts',(151.333875688082,-1.76939996625633,
136.450346299616));
#184752=CARTESIAN_POINT('Ctrl Pts',(151.341277509757,-1.91953203949932,
136.403296289168));
#184753=CARTESIAN_POINT('Ctrl Pts',(151.348679331433,-2.06790312835083,
136.350217252759));
#184754=CARTESIAN_POINT('Ctrl Pts',(151.356081153108,-2.21399734964868,
136.291267423613));
#184755=CARTESIAN_POINT('Ctrl Pts',(151.363479067419,-2.36001444894535,
136.232348713624));
#184756=CARTESIAN_POINT('Ctrl Pts',(151.370876981731,-2.50375672910866,
136.167565522326));
#184757=CARTESIAN_POINT('Ctrl Pts',(151.378274896042,-2.64472556245306,
136.097125231811));
#184758=CARTESIAN_POINT('Ctrl Pts',(151.385671580954,-2.78567096933374,
136.026696647195));
#184759=CARTESIAN_POINT('Ctrl Pts',(151.393068265867,-2.92384351053614,
135.950612995893));
#184760=CARTESIAN_POINT('Ctrl Pts',(151.400464950779,-3.0587664646925,135.869128951555));
#184761=CARTESIAN_POINT('Ctrl Pts',(151.407861307714,-3.19368343622383,
135.787648520304));
#184762=CARTESIAN_POINT('Ctrl Pts',(151.41525766465,-3.32535078766426,135.700768365125));
#184763=CARTESIAN_POINT('Ctrl Pts',(151.422654021585,-3.4533184869581,135.608787949739));
#184764=CARTESIAN_POINT('Ctrl Pts',(151.430051510922,-3.58130577843335,
135.516793451917));
#184765=CARTESIAN_POINT('Ctrl Pts',(151.437449000258,-3.7055919867931,135.419697356975));
#184766=CARTESIAN_POINT('Ctrl Pts',(151.444846489595,-3.82575815843665,
135.317840990367));
#184767=CARTESIAN_POINT('Ctrl Pts',(151.45224657211,-3.94596645414534,135.215948918166));
#184768=CARTESIAN_POINT('Ctrl Pts',(151.459646654625,-4.06205155301634,
135.109293493141));
#184769=CARTESIAN_POINT('Ctrl Pts',(151.46704673714,-4.17362964078278,134.998254534212));
#184770=CARTESIAN_POINT('Ctrl Pts',(151.474454956806,-4.28533042012754,
134.887093476532));
#184771=CARTESIAN_POINT('Ctrl Pts',(151.481863176473,-4.3925140263037,134.771539522283));
#184772=CARTESIAN_POINT('Ctrl Pts',(151.489271396139,-4.49483491301252,
134.652007907439));
#184773=CARTESIAN_POINT('Ctrl Pts',(151.496684175441,-4.59721877651929,
134.532402722881));
#184774=CARTESIAN_POINT('Ctrl Pts',(151.504096954743,-4.69473372608831,
134.408815291793));
#184775=CARTESIAN_POINT('Ctrl Pts',(151.511509734045,-4.78707652795662,
134.281691329188));
#184776=CARTESIAN_POINT('Ctrl Pts',(151.518933105074,-4.87955127355102,
134.154385725903));
#184777=CARTESIAN_POINT('Ctrl Pts',(151.526356476103,-4.96683890493653,
134.023533808525));
#184778=CARTESIAN_POINT('Ctrl Pts',(151.533779847131,-5.04868083039081,
133.889608166037));
#184779=CARTESIAN_POINT('Ctrl Pts',(151.537715896572,-5.09207538303798,
133.818597576886));
#184780=CARTESIAN_POINT('Ctrl Pts',(151.541651946013,-5.13393973377019,
133.7467232386));
#184781=CARTESIAN_POINT('Ctrl Pts',(151.545587995454,-5.17424079758205,
133.674057941525));
#184782=CARTESIAN_POINT('Ctrl Pts',(151.553371571041,-5.25393653848299,
133.53036161839));
#184783=CARTESIAN_POINT('Ctrl Pts',(151.561155146628,-5.32773786595042,
133.38317140476));
#184784=CARTESIAN_POINT('Ctrl Pts',(151.568938722215,-5.39534067565741,
133.23298771041));
#184785=CARTESIAN_POINT('Ctrl Pts',(151.576709743611,-5.46283444825421,
133.083046248537));
#184786=CARTESIAN_POINT('Ctrl Pts',(151.584480765007,-5.52414949831497,
132.930121219899));
#184787=CARTESIAN_POINT('Ctrl Pts',(151.592251786403,-5.57902686897509,
132.774738692392));
#184788=CARTESIAN_POINT('Ctrl Pts',(151.600116204852,-5.63456379060807,
132.617488679326));
#184789=CARTESIAN_POINT('Ctrl Pts',(151.607980623302,-5.6835070853738,132.457721980328));
#184790=CARTESIAN_POINT('Ctrl Pts',(151.615845041751,-5.72563672666113,
132.296008912845));
#184791=CARTESIAN_POINT('Ctrl Pts',(151.623589367304,-5.76712303104186,
132.136765270247));
#184792=CARTESIAN_POINT('Ctrl Pts',(151.631333692857,-5.80200216877751,
131.97563459611));
#184793=CARTESIAN_POINT('Ctrl Pts',(151.63907801841,-5.83011250681481,131.8131810775));
#184794=CARTESIAN_POINT('Ctrl Pts',(151.647002483308,-5.85887671429841,
131.646948757222));
#184795=CARTESIAN_POINT('Ctrl Pts',(151.654926948205,-5.8805532369963,131.479331604281));
#184796=CARTESIAN_POINT('Ctrl Pts',(151.662851413103,-5.89502310973353,
131.310950291965));
#184797=CARTESIAN_POINT('Ctrl Pts',(151.670775878,-5.90949298247077,131.142568979649));
#184798=CARTESIAN_POINT('Ctrl Pts',(151.678700342898,-5.91675611320991,
130.973423862282));
#184799=CARTESIAN_POINT('Ctrl Pts',(151.686624807795,-5.91674999613682,
130.804146807182));
#184800=CARTESIAN_POINT('',(153.436624807795,-5.91686882972502,130.799002464883));
#184801=CARTESIAN_POINT('Ctrl Pts',(151.686624807835,-5.91674999613679,
130.804146806335));
#184802=CARTESIAN_POINT('Ctrl Pts',(151.694394241467,-5.91674399871208,
130.638181424187));
#184803=CARTESIAN_POINT('Ctrl Pts',(151.702163675099,-5.90975068576896,
130.472358873233));
#184804=CARTESIAN_POINT('Ctrl Pts',(151.709933108731,-5.89583178258735,
130.307270933572));
#184805=CARTESIAN_POINT('Ctrl Pts',(151.717713027261,-5.88189409576128,
130.141960206734));
#184806=CARTESIAN_POINT('Ctrl Pts',(151.725492945791,-5.86101218853056,
129.977386382935));
#184807=CARTESIAN_POINT('Ctrl Pts',(151.733272864321,-5.83329921270253,
129.814132937896));
#184808=CARTESIAN_POINT('Ctrl Pts',(151.741071519732,-5.8055194939216,129.650486319022));
#184809=CARTESIAN_POINT('Ctrl Pts',(151.748870175143,-5.77087585845673,
129.488166749331));
#184810=CARTESIAN_POINT('Ctrl Pts',(151.756668830555,-5.72953240368024,
129.327746586183));
#184811=CARTESIAN_POINT('Ctrl Pts',(151.764477142575,-5.68813775577232,
129.167127784325));
#184812=CARTESIAN_POINT('Ctrl Pts',(151.772285454596,-5.64002681891617,
129.008413384443));
#184813=CARTESIAN_POINT('Ctrl Pts',(151.780093766616,-5.58541276505045,
128.852158064932));
#184814=CARTESIAN_POINT('Ctrl Pts',(151.787920366743,-5.53067079780044,
128.695536774662));
#184815=CARTESIAN_POINT('Ctrl Pts',(151.79574696687,-5.46939536664615,128.541386377018));
#184816=CARTESIAN_POINT('Ctrl Pts',(151.803573566996,-5.40184768559138,
128.390241286594));
#184817=CARTESIAN_POINT('Ctrl Pts',(151.810394251087,-5.34298158970802,
128.25852216247));
#184818=CARTESIAN_POINT('Ctrl Pts',(151.817214935177,-5.27935270885023,
128.129085204907));
#184819=CARTESIAN_POINT('Ctrl Pts',(151.824035619267,-5.21116117164875,
128.002266792299));
#184820=CARTESIAN_POINT('Ctrl Pts',(151.831458885672,-5.13694516332012,
127.864244440074));
#184821=CARTESIAN_POINT('Ctrl Pts',(151.838882152078,-5.05712967269481,
127.728963936607));
#184822=CARTESIAN_POINT('Ctrl Pts',(151.846305418483,-4.97194166800753,
127.596912003413));
#184823=CARTESIAN_POINT('Ctrl Pts',(151.853719911204,-4.88685434846738,
127.465016144638));
#184824=CARTESIAN_POINT('Ctrl Pts',(151.861134403925,-4.79640735469481,
127.336341571188));
#184825=CARTESIAN_POINT('Ctrl Pts',(151.868548896646,-4.70087414069661,
127.21135172865));
#184826=CARTESIAN_POINT('Ctrl Pts',(151.875956243,-4.60543300520682,127.086482356028));
#184827=CARTESIAN_POINT('Ctrl Pts',(151.883363589354,-4.50491563415403,
126.965290938613));
#184828=CARTESIAN_POINT('Ctrl Pts',(151.890770935708,-4.39963942824886,
126.848213064213));
#184829=CARTESIAN_POINT('Ctrl Pts',(151.898172757383,-4.29444174130989,
126.73122251091));
#184830=CARTESIAN_POINT('Ctrl Pts',(151.905574579058,-4.18449253521667,
126.618339668136));
#184831=CARTESIAN_POINT('Ctrl Pts',(151.912976400734,-4.07015016122592,
126.509967968125));
#184832=CARTESIAN_POINT('Ctrl Pts',(151.920374315045,-3.95586814768432,
126.401653476691));
#184833=CARTESIAN_POINT('Ctrl Pts',(151.927772229356,-3.83719785513682,
126.297845641497));
#184834=CARTESIAN_POINT('Ctrl Pts',(151.935170143668,-3.71453516404212,
126.198911771081));
#184835=CARTESIAN_POINT('Ctrl Pts',(151.94256682858,-3.59189285726126,126.099994341679));
#184836=CARTESIAN_POINT('Ctrl Pts',(151.949963513492,-3.46525975899447,
126.005949503642));
#184837=CARTESIAN_POINT('Ctrl Pts',(151.957360198404,-3.33506565645255,
125.917104983813));
#184838=CARTESIAN_POINT('Ctrl Pts',(151.96475655534,-3.20487732685367,125.828264403444));
#184839=CARTESIAN_POINT('Ctrl Pts',(151.972152912275,-3.0711286152806,125.744623893211));
#184840=CARTESIAN_POINT('Ctrl Pts',(151.979549269211,-2.93427895241776,
125.666468287836));
#184841=CARTESIAN_POINT('Ctrl Pts',(151.986946758547,-2.79740833752209,
125.588300716638));
#184842=CARTESIAN_POINT('Ctrl Pts',(151.994344247884,-2.65743615019851,
125.515619907497));
#184843=CARTESIAN_POINT('Ctrl Pts',(152.001741737221,-2.51484697681013,
125.448665028221));
#184844=CARTESIAN_POINT('Ctrl Pts',(152.009141819736,-2.37220781900786,
125.381686678016));
#184845=CARTESIAN_POINT('Ctrl Pts',(152.016541902251,-2.22695018633235,
125.320438412596));
#184846=CARTESIAN_POINT('Ctrl Pts',(152.023941984766,-2.07957906936119,
125.265111439494));
#184847=CARTESIAN_POINT('Ctrl Pts',(152.031350204432,-1.93204590269703,
125.209723628697));
#184848=CARTESIAN_POINT('Ctrl Pts',(152.038758424098,-1.78239496026529,
125.160270244536));
#184849=CARTESIAN_POINT('Ctrl Pts',(152.046166643765,-1.6311475383365,125.116892967488));
#184850=CARTESIAN_POINT('Ctrl Pts',(152.053579423067,-1.47980702614295,
125.07348899245));
#184851=CARTESIAN_POINT('Ctrl Pts',(152.060992202369,-1.32686843830145,
125.036168664721));
#184852=CARTESIAN_POINT('Ctrl Pts',(152.068404981671,-1.17286320437495,
125.005022511685));
#184853=CARTESIAN_POINT('Ctrl Pts',(152.0758283527,-1.01863792054824,124.973831855565));
#184854=CARTESIAN_POINT('Ctrl Pts',(152.083251723729,-0.86334331429587,
124.948833052723));
#184855=CARTESIAN_POINT('Ctrl Pts',(152.090675094757,-0.707516701305408,
124.930064857232));
#184856=CARTESIAN_POINT('Ctrl Pts',(152.094611144198,-0.624893692094613,
124.920113509647));
#184857=CARTESIAN_POINT('Ctrl Pts',(152.098547193639,-0.542121142311129,
124.911912938485));
#184858=CARTESIAN_POINT('Ctrl Pts',(152.102483243079,-0.459279008347264,
124.905462978601));
#184859=CARTESIAN_POINT('Ctrl Pts',(152.109906509485,-0.303041329096324,
124.893298555553));
#184860=CARTESIAN_POINT('Ctrl Pts',(152.11732977589,-0.146083787901677,
124.887327171775));
#184861=CARTESIAN_POINT('Ctrl Pts',(152.124753042296,0.0110614407656326,
124.887620957328));
#184862=CARTESIAN_POINT('Ctrl Pts',(152.132167535017,0.168020936822925,
124.887914395652));
#184863=CARTESIAN_POINT('Ctrl Pts',(152.139582027738,0.325167309145095,
124.894458263104));
#184864=CARTESIAN_POINT('Ctrl Pts',(152.146996520459,0.481962839262947,
124.907272998744));
#184865=CARTESIAN_POINT('Ctrl Pts',(152.154403866812,0.638607243945569,
124.920075383059));
#184866=CARTESIAN_POINT('Ctrl Pts',(152.161811213166,0.794901110064077,
124.939136572747));
#184867=CARTESIAN_POINT('Ctrl Pts',(152.16921855952,0.950306402420161,124.964424975453));
#184868=CARTESIAN_POINT('Ctrl Pts',(152.176620381195,1.1055957876461,124.989694517115));
#184869=CARTESIAN_POINT('Ctrl Pts',(152.184022202871,1.25999755183236,125.021181964288));
#184870=CARTESIAN_POINT('Ctrl Pts',(152.191424024546,1.41297857840731,125.058803890889));
#184871=CARTESIAN_POINT('Ctrl Pts',(152.198821938858,1.56587884748914,125.096405957168));
#184872=CARTESIAN_POINT('Ctrl Pts',(152.206219853169,1.71735951103385,125.140135964636));
#184873=CARTESIAN_POINT('Ctrl Pts',(152.21361776748,1.86689755890752,125.189859387087));
#184874=CARTESIAN_POINT('Ctrl Pts',(152.221014452393,2.01641075627049,125.239574546408));
#184875=CARTESIAN_POINT('Ctrl Pts',(152.228411137305,2.16398162479775,125.295281026284));
#184876=CARTESIAN_POINT('Ctrl Pts',(152.235807822217,2.30910212812869,125.356794378926));
#184877=CARTESIAN_POINT('Ctrl Pts',(152.243204179153,2.45421619666444,125.418305004001));
#184878=CARTESIAN_POINT('Ctrl Pts',(152.250600536088,2.59687977234429,125.485621844194));
#184879=CARTESIAN_POINT('Ctrl Pts',(152.257996893024,2.7366048821447,125.558512327583));
#184880=CARTESIAN_POINT('Ctrl Pts',(152.26539438236,2.87635138421607,125.63141397069));
#184881=CARTESIAN_POINT('Ctrl Pts',(152.272791871697,3.01315819363307,125.709890783435));
#184882=CARTESIAN_POINT('Ctrl Pts',(152.280189361033,3.14656216097893,125.79366434563));
#184883=CARTESIAN_POINT('Ctrl Pts',(152.287589443548,3.28001289287883,125.877467274517));
#184884=CARTESIAN_POINT('Ctrl Pts',(152.294989526063,3.41005809179386,125.966570451265));
#184885=CARTESIAN_POINT('Ctrl Pts',(152.302389608579,3.53626392966847,126.060652365341));
#184886=CARTESIAN_POINT('Ctrl Pts',(152.309797828245,3.66260854383611,126.154837732154));
#184887=CARTESIAN_POINT('Ctrl Pts',(152.317206047912,3.78510506633482,126.254012546252));
#184888=CARTESIAN_POINT('Ctrl Pts',(152.324614267578,3.90335252399985,126.357814808077));
#184889=CARTESIAN_POINT('Ctrl Pts',(152.33202704688,4.02167276100213,126.461680958462));
#184890=CARTESIAN_POINT('Ctrl Pts',(152.339439826182,4.13573845214823,126.570179975122));
#184891=CARTESIAN_POINT('Ctrl Pts',(152.346852605484,4.24518618352658,126.682913683576));
#184892=CARTESIAN_POINT('Ctrl Pts',(152.354275976513,4.35479029895607,126.795808471239));
#184893=CARTESIAN_POINT('Ctrl Pts',(152.361699347542,4.45976302775116,126.912949758086));
#184894=CARTESIAN_POINT('Ctrl Pts',(152.369122718571,4.55978133275822,127.033906432732));
#184895=CARTESIAN_POINT('Ctrl Pts',(152.373058768011,4.61281343797622,127.098040563942));
#184896=CARTESIAN_POINT('Ctrl Pts',(152.376994817452,4.66445339573696,127.163246845292));
#184897=CARTESIAN_POINT('Ctrl Pts',(152.380930866892,4.71465812659974,127.229457917941));
#184898=CARTESIAN_POINT('Ctrl Pts',(152.388354133298,4.80934268217594,127.354329934586));
#184899=CARTESIAN_POINT('Ctrl Pts',(152.395777399703,4.89920596138387,127.483155080469));
#184900=CARTESIAN_POINT('Ctrl Pts',(152.403200666109,4.98389962585687,127.615524610198));
#184901=CARTESIAN_POINT('Ctrl Pts',(152.41061515883,5.06849318945193,127.747737690136));
#184902=CARTESIAN_POINT('Ctrl Pts',(152.418029651551,5.14792910118636,127.883486503988));
#184903=CARTESIAN_POINT('Ctrl Pts',(152.425444144272,5.22189951513272,128.022329701786));
#184904=CARTESIAN_POINT('Ctrl Pts',(152.432851490626,5.29579863360919,128.161039077283));
#184905=CARTESIAN_POINT('Ctrl Pts',(152.440258836979,5.36424256721013,128.302836571942));
#184906=CARTESIAN_POINT('Ctrl Pts',(152.447666183333,5.42696707431228,128.447252445074));
#184907=CARTESIAN_POINT('Ctrl Pts',(152.455068005008,5.48964479911058,128.591560607398));
#184908=CARTESIAN_POINT('Ctrl Pts',(152.462469826684,5.54661144304806,128.738482918814));
#184909=CARTESIAN_POINT('Ctrl Pts',(152.469871648359,5.59764903232333,128.887525759413));
#184910=CARTESIAN_POINT('Ctrl Pts',(152.477269562671,5.6486596792525,129.036489921457));
#184911=CARTESIAN_POINT('Ctrl Pts',(152.484667476982,5.69374738423859,129.187572031053));
#184912=CARTESIAN_POINT('Ctrl Pts',(152.492065391293,5.73274262823508,129.340259350264));
#184913=CARTESIAN_POINT('Ctrl Pts',(152.499462076206,5.77173139192943,129.492921295612));
#184914=CARTESIAN_POINT('Ctrl Pts',(152.506858761118,5.80462961177846,129.647187559806));
#184915=CARTESIAN_POINT('Ctrl Pts',(152.51425544603,5.83131786286819,129.802531018934));
#184916=CARTESIAN_POINT('Ctrl Pts',(152.521651802965,5.8580049305729,129.957867589971));
#184917=CARTESIAN_POINT('Ctrl Pts',(152.529048159901,5.87848251381301,130.114280893062));
#184918=CARTESIAN_POINT('Ctrl Pts',(152.536444516836,5.89268252059566,130.271234671877));
#184919=CARTESIAN_POINT('Ctrl Pts',(152.543842006173,5.90688470143562,130.428212480717));
#184920=CARTESIAN_POINT('Ctrl Pts',(152.551239495509,5.91480735847635,130.585730558241));
#184921=CARTESIAN_POINT('Ctrl Pts',(152.558636984846,5.91643439093532,130.743248750815));
#184922=CARTESIAN_POINT('Ctrl Pts',(152.566037067361,5.918061993748,130.900822161147));
#184923=CARTESIAN_POINT('Ctrl Pts',(152.573437149876,5.91338957416129,131.058395313563));
#184924=CARTESIAN_POINT('Ctrl Pts',(152.580837232391,5.90245313343109,131.215429431938));
#184925=CARTESIAN_POINT('Ctrl Pts',(152.588245452057,5.89150466696001,131.37263622547));
#184926=CARTESIAN_POINT('Ctrl Pts',(152.595653671724,5.87427844963756,131.529302428629));
#184927=CARTESIAN_POINT('Ctrl Pts',(152.60306189139,5.85086230615452,131.684895021732));
#184928=CARTESIAN_POINT('Ctrl Pts',(152.610474670692,5.82743175042586,131.84058337948));
#184929=CARTESIAN_POINT('Ctrl Pts',(152.617887449994,5.79780374713262,131.995196444689));
#184930=CARTESIAN_POINT('Ctrl Pts',(152.625300229297,5.76211685764562,132.148213243912));
#184931=CARTESIAN_POINT('Ctrl Pts',(152.632723600325,5.72637897705737,132.301448680713));
#184932=CARTESIAN_POINT('Ctrl Pts',(152.640146971354,5.68456501883588,132.453082937305));
#184933=CARTESIAN_POINT('Ctrl Pts',(152.647570342383,5.63686307972441,132.60261120715));
#184934=CARTESIAN_POINT('Ctrl Pts',(152.651506391824,5.61157036701482,132.681894683705));
#184935=CARTESIAN_POINT('Ctrl Pts',(152.655442441264,5.58462313432085,132.760586430516));
#184936=CARTESIAN_POINT('Ctrl Pts',(152.659378490705,5.55605476705483,132.83861379453));
#184937=CARTESIAN_POINT('Ctrl Pts',(152.666801757111,5.50217571798014,132.985770967907));
#184938=CARTESIAN_POINT('Ctrl Pts',(152.674225023516,5.44236477167517,133.131008627844));
#184939=CARTESIAN_POINT('Ctrl Pts',(152.681648289922,5.37677753181936,133.273812770539));
#184940=CARTESIAN_POINT('Ctrl Pts',(152.689062782643,5.31126781063433,133.416448130596));
#184941=CARTESIAN_POINT('Ctrl Pts',(152.696477275364,5.23999553955777,133.556655362616));
#184942=CARTESIAN_POINT('Ctrl Pts',(152.703891768085,5.16316564057221,133.693936906664));
#184943=CARTESIAN_POINT('Ctrl Pts',(152.711299114438,5.08640979313591,133.83108613359));
#184944=CARTESIAN_POINT('Ctrl Pts',(152.718706460792,5.00410716291266,133.965314962822));
#184945=CARTESIAN_POINT('Ctrl Pts',(152.726113807146,4.91651012699712,134.096147174078));
#184946=CARTESIAN_POINT('Ctrl Pts',(152.733515628821,4.82897842425573,134.226881805736));
#184947=CARTESIAN_POINT('Ctrl Pts',(152.740917450497,4.73616038514163,134.354224554757));
#184948=CARTESIAN_POINT('Ctrl Pts',(152.748319272172,4.63835348589855,134.477725219992));
#184949=CARTESIAN_POINT('Ctrl Pts',(152.755717186483,4.54059821815634,134.601160690186));
#184950=CARTESIAN_POINT('Ctrl Pts',(152.763115100795,4.43785956635898,134.720757823964));
#184951=CARTESIAN_POINT('Ctrl Pts',(152.770513015106,4.33047728226959,134.836096852769));
#184952=CARTESIAN_POINT('Ctrl Pts',(152.777909700018,4.22311284316767,134.95141671432));
#184953=CARTESIAN_POINT('Ctrl Pts',(152.785306384931,4.11110655746502,135.062479602365));
#184954=CARTESIAN_POINT('Ctrl Pts',(152.792703069843,3.99483735735602,135.168900117991));
#184955=CARTESIAN_POINT('Ctrl Pts',(152.800099426778,3.87857331274518,135.27531591482));
#184956=CARTESIAN_POINT('Ctrl Pts',(152.807495783714,3.7580470049338,135.377089496483));
#184957=CARTESIAN_POINT('Ctrl Pts',(152.814892140649,3.63367279617466,135.473873715614));
#184958=CARTESIAN_POINT('Ctrl Pts',(152.822289629986,3.50927954540669,135.570672752655));
#184959=CARTESIAN_POINT('Ctrl Pts',(152.829687119322,3.38103751529433,135.662480676899));
#184960=CARTESIAN_POINT('Ctrl Pts',(152.837084608659,3.24939244952186,135.748991976069));
#184961=CARTESIAN_POINT('Ctrl Pts',(152.844484691174,3.11770123577574,135.83553360164));
#184962=CARTESIAN_POINT('Ctrl Pts',(152.851884773689,2.98260492302754,135.916774700531));
#184963=CARTESIAN_POINT('Ctrl Pts',(152.859284856204,2.84457625844915,135.992454339962));
#184964=CARTESIAN_POINT('Ctrl Pts',(152.86669307587,2.70639581716417,136.068217196937));
#184965=CARTESIAN_POINT('Ctrl Pts',(152.874101295537,2.56527691219257,136.138406202024));
#184966=CARTESIAN_POINT('Ctrl Pts',(152.881509515203,2.42171545948031,136.202807134465));
#184967=CARTESIAN_POINT('Ctrl Pts',(152.888922294505,2.27806564708916,136.267247704605));
#184968=CARTESIAN_POINT('Ctrl Pts',(152.896335073807,2.13197063697471,136.325892964705));
#184969=CARTESIAN_POINT('Ctrl Pts',(152.903747853109,1.98394363465944,136.378577891497));
#184970=CARTESIAN_POINT('Ctrl Pts',(152.911171224138,1.83570512442169,136.431338096984));
#184971=CARTESIAN_POINT('Ctrl Pts',(152.918594595167,1.68552946406388,136.47812084926));
#184972=CARTESIAN_POINT('Ctrl Pts',(152.926017966196,1.53394303250813,136.518811539179));
#184973=CARTESIAN_POINT('Ctrl Pts',(152.929954015637,1.45356826922851,136.540386719334));
#184974=CARTESIAN_POINT('Ctrl Pts',(152.933890065077,1.3727970364754,136.560250060588));
#184975=CARTESIAN_POINT('Ctrl Pts',(152.937826114518,1.29170850495124,136.578390380283));
#184976=CARTESIAN_POINT('Ctrl Pts',(152.945249380924,1.1387780651872,136.612602457086));
#184977=CARTESIAN_POINT('Ctrl Pts',(152.952672647329,0.984256231096225,
136.640786316849));
#184978=CARTESIAN_POINT('Ctrl Pts',(152.960095913735,0.828659556224084,
136.662795041743));
#184979=CARTESIAN_POINT('Ctrl Pts',(152.967510406456,0.673246783700032,
136.684777754151));
#184980=CARTESIAN_POINT('Ctrl Pts',(152.974924899177,0.516762065087655,
136.700599807618));
#184981=CARTESIAN_POINT('Ctrl Pts',(152.982339391898,0.35973477698849,136.710164665511));
#184982=CARTESIAN_POINT('Ctrl Pts',(152.989746738251,0.202858837701513,
136.719720304435));
#184983=CARTESIAN_POINT('Ctrl Pts',(152.997154084605,0.0454417401219702,
136.723030731617));
#184984=CARTESIAN_POINT('Ctrl Pts',(153.004561430959,-0.11197944215825,
136.720050870363));
#184985=CARTESIAN_POINT('Ctrl Pts',(153.011963252634,-0.269283213781397,
136.717073231602));
#184986=CARTESIAN_POINT('Ctrl Pts',(153.01936507431,-0.426590692414489,
136.707814652917));
#184987=CARTESIAN_POINT('Ctrl Pts',(153.026766895985,-0.583362317904174,
136.692282064779));
#184988=CARTESIAN_POINT('Ctrl Pts',(153.034164810297,-0.740051184873071,
136.676757676173));
#184989=CARTESIAN_POINT('Ctrl Pts',(153.041562724608,-0.896204391514378,
136.654965910835));
#184990=CARTESIAN_POINT('Ctrl Pts',(153.048960638919,-1.0512851305278,136.626965716388));
#184991=CARTESIAN_POINT('Ctrl Pts',(153.056357323832,-1.2063400979359,136.598970175065));
#184992=CARTESIAN_POINT('Ctrl Pts',(153.063754008744,-1.36032258444087,
136.564768318571));
#184993=CARTESIAN_POINT('Ctrl Pts',(153.071150693656,-1.51270352091475,
136.524470635766));
#184994=CARTESIAN_POINT('Ctrl Pts',(153.078547050591,-1.66507770065822,
136.484174739802));
#184995=CARTESIAN_POINT('Ctrl Pts',(153.085943407527,-1.81585011068001,
136.437783650405));
#184996=CARTESIAN_POINT('Ctrl Pts',(153.093339764462,-1.96450471314927,
136.385458340641));
#184997=CARTESIAN_POINT('Ctrl Pts',(153.100737253799,-2.11318207501793,
136.333125019739));
#184998=CARTESIAN_POINT('Ctrl Pts',(153.108134743135,-2.25974063158198,
136.274855793389));
#184999=CARTESIAN_POINT('Ctrl Pts',(153.115532232472,-2.40368241136039,
136.210860541529));
#185000=CARTESIAN_POINT('Ctrl Pts',(153.122932314987,-2.5476746497063,136.146842856234));
#185001=CARTESIAN_POINT('Ctrl Pts',(153.130332397502,-2.68904794402243,
136.077095300567));
#185002=CARTESIAN_POINT('Ctrl Pts',(153.137732480017,-2.82732723277683,
136.001874569572));
#185003=CARTESIAN_POINT('Ctrl Pts',(153.145140699683,-2.96575857382483,
135.926571125651));
#185004=CARTESIAN_POINT('Ctrl Pts',(153.15254891935,-3.10108878681862,135.845782665914));
#185005=CARTESIAN_POINT('Ctrl Pts',(153.159957139016,-3.23286958708453,
135.75981062694));
#185006=CARTESIAN_POINT('Ctrl Pts',(153.167369918318,-3.36473149623409,
135.67378567361));
#185007=CARTESIAN_POINT('Ctrl Pts',(153.174782697621,-3.4930393360125,135.582570999549));
#185008=CARTESIAN_POINT('Ctrl Pts',(153.182195476923,-3.61737686754928,
135.486509179991));
#185009=CARTESIAN_POINT('Ctrl Pts',(153.189618847951,-3.74189205838202,
135.3903101028));
#185010=CARTESIAN_POINT('Ctrl Pts',(153.19704221898,-3.86242532549634,135.289250286883));
#185011=CARTESIAN_POINT('Ctrl Pts',(153.204465590009,-3.97859572430564,
135.18371064069));
#185012=CARTESIAN_POINT('Ctrl Pts',(153.20840163945,-4.04019205722495,135.12775098789));
#185013=CARTESIAN_POINT('Ctrl Pts',(153.21233768889,-4.10056247302935,135.070532483352));
#185014=CARTESIAN_POINT('Ctrl Pts',(153.216273738331,-4.15965476973412,
135.012115691133));
#185015=CARTESIAN_POINT('Ctrl Pts',(153.223592420534,-4.26953086420184,
134.90349562831));
#185016=CARTESIAN_POINT('Ctrl Pts',(153.230911102736,-4.37533843268223,
134.790381873428));
#185017=CARTESIAN_POINT('Ctrl Pts',(153.238229784938,-4.47667967794884,
134.673116182801));
#185018=CARTESIAN_POINT('Ctrl Pts',(153.245539663129,-4.57789901472265,
134.555991556986));
#185019=CARTESIAN_POINT('Ctrl Pts',(153.252849541319,-4.67466246908713,
134.434725220875));
#185020=CARTESIAN_POINT('Ctrl Pts',(153.26015941951,-4.76660722913028,134.309697418175));
#185021=CARTESIAN_POINT('Ctrl Pts',(153.267512144022,-4.85909091672224,
134.183936774069));
#185022=CARTESIAN_POINT('Ctrl Pts',(153.274864868534,-4.94669893677471,
134.054370679206));
#185023=CARTESIAN_POINT('Ctrl Pts',(153.282217593045,-5.02910073848491,
133.921422747949));
#185024=CARTESIAN_POINT('Ctrl Pts',(153.289514502521,-5.11087702246753,
133.789484033556));
#185025=CARTESIAN_POINT('Ctrl Pts',(153.296811411997,-5.18752564005307,
133.654214974863));
#185026=CARTESIAN_POINT('Ctrl Pts',(153.304108321473,-5.25876516238274,
133.516061104237));
#185027=CARTESIAN_POINT('Ctrl Pts',(153.311402106787,-5.32997418361129,
133.377966383996));
#185028=CARTESIAN_POINT('Ctrl Pts',(153.318695892102,-5.39577854117277,
133.236989650387));
#185029=CARTESIAN_POINT('Ctrl Pts',(153.325989677416,-5.45594192358712,
133.093602476554));
#185030=CARTESIAN_POINT('Ctrl Pts',(153.333281875092,-5.51609221023646,
132.950246513812));
#185031=CARTESIAN_POINT('Ctrl Pts',(153.340574072768,-5.57060381713691,
132.804481509788));
#185032=CARTESIAN_POINT('Ctrl Pts',(153.347866270444,-5.61928803196595,
132.656800245814));
#185033=CARTESIAN_POINT('Ctrl Pts',(153.355262815223,-5.66866888956578,
132.507005748932));
#185034=CARTESIAN_POINT('Ctrl Pts',(153.362659360003,-5.71205414157252,
132.355240103339));
#185035=CARTESIAN_POINT('Ctrl Pts',(153.370055904782,-5.74929893923802,
132.202034495757));
#185036=CARTESIAN_POINT('Ctrl Pts',(153.377351841901,-5.78603713388111,
132.050912787906));
#185037=CARTESIAN_POINT('Ctrl Pts',(153.38464777902,-5.81680082570675,131.898390434799));
#185038=CARTESIAN_POINT('Ctrl Pts',(153.391943716139,-5.84150245883854,
131.744987847601));
#185039=CARTESIAN_POINT('Ctrl Pts',(153.399390564749,-5.86671502842724,
131.58841223237));
#185040=CARTESIAN_POINT('Ctrl Pts',(153.406837413358,-5.8856119489608,131.430919987324));
#185041=CARTESIAN_POINT('Ctrl Pts',(153.414284261967,-5.89815585201501,
131.273069597468));
#185042=CARTESIAN_POINT('Ctrl Pts',(153.421731110576,-5.91069975506921,
131.115219207613));
#185043=CARTESIAN_POINT('Ctrl Pts',(153.429177959186,-5.91689066209841,
130.957011097166));
#185044=CARTESIAN_POINT('Ctrl Pts',(153.436624807795,-5.91674757395282,
130.799002574689));
#185045=CARTESIAN_POINT('',(155.186624807795,-5.92506007442198,130.807039561929));
#185046=CARTESIAN_POINT('Ctrl Pts',(153.436624807795,-5.91819628231606,
130.799001262779));
#185047=CARTESIAN_POINT('Ctrl Pts',(153.455990325912,-5.92201671705791,
130.387995942853));
#185048=CARTESIAN_POINT('Ctrl Pts',(153.568171718631,-5.69523304119842,
128.011295060988));
#185049=CARTESIAN_POINT('Ctrl Pts',(153.773168985959,-2.48153146899543,
124.260694817819));
#185050=CARTESIAN_POINT('Ctrl Pts',(154.05161660977,4.16404298980398,125.179566709394));
#185051=CARTESIAN_POINT('Ctrl Pts',(154.330064233584,6.98306536577905,131.267349416113));
#185052=CARTESIAN_POINT('Ctrl Pts',(154.608511857395,3.38499181231609,136.92966803523));
#185053=CARTESIAN_POINT('Ctrl Pts',(154.886959481209,-3.32372385062522,
136.963128375415));
#185054=CARTESIAN_POINT('Ctrl Pts',(155.079663798008,-5.85279551419678,
133.069460061617));
#185055=CARTESIAN_POINT('Ctrl Pts',(155.179552240204,-5.92590251216317,
130.956692591981));
#185056=CARTESIAN_POINT('Ctrl Pts',(155.186624807795,-5.92506007442198,
130.807039561929));
#185057=CARTESIAN_POINT('',(156.936624807795,-5.90993960677025,130.808420119559));
#185058=CARTESIAN_POINT('Ctrl Pts',(155.186624807795,-5.92506007442198,
130.807039561929));
#185059=CARTESIAN_POINT('Ctrl Pts',(155.272368114808,-5.91484689555162,
128.992741496091));
#185060=CARTESIAN_POINT('Ctrl Pts',(155.450927296425,-4.05138645339299,
125.196360691353));
#185061=CARTESIAN_POINT('Ctrl Pts',(155.722302352647,2.41613535680962,124.236267251306));
#185062=CARTESIAN_POINT('Ctrl Pts',(156.00074997646,6.83190314484835,129.286908822695));
#185063=CARTESIAN_POINT('Ctrl Pts',(156.279197600274,4.96948569979414,135.732014461931));
#185064=CARTESIAN_POINT('Ctrl Pts',(156.557645224086,-1.45964633049555,
137.648846947465));
#185065=CARTESIAN_POINT('Ctrl Pts',(156.776787626594,-5.46381109745409,
134.20729724922));
#185066=CARTESIAN_POINT('Ctrl Pts',(156.903114154496,-5.9144261227287,131.522159083227));
#185067=CARTESIAN_POINT('Ctrl Pts',(156.936624807795,-5.90993960677025,
130.808420119559));
#185068=CARTESIAN_POINT('',(158.686624841308,-5.91340240352139,130.800147492464));
#185069=CARTESIAN_POINT('Ctrl Pts',(156.936624807795,-5.90993960677025,
130.808420119559));
#185070=CARTESIAN_POINT('Ctrl Pts',(156.995930029101,-5.90199962961032,
129.545286070295));
#185071=CARTESIAN_POINT('Ctrl Pts',(157.148051125009,-4.88528165776799,
126.293613740952));
#185072=CARTESIAN_POINT('Ctrl Pts',(157.392988095525,0.473615299172821,
123.822007928195));
#185073=CARTESIAN_POINT('Ctrl Pts',(157.671435719337,6.13045170597051,127.428694400194));
#185074=CARTESIAN_POINT('Ctrl Pts',(157.94988334315,6.15370248419541,134.13745321549));
#185075=CARTESIAN_POINT('Ctrl Pts',(158.228330966963,0.522001304524755,
137.783262763922));
#185076=CARTESIAN_POINT('Ctrl Pts',(158.473911455178,-4.86802256101213,
135.342465056774));
#185077=CARTESIAN_POINT('Ctrl Pts',(158.626676068789,-5.90188209181897,
132.076832144556));
#185078=CARTESIAN_POINT('Ctrl Pts',(158.686624807795,-5.91023198214956,
130.800150465391));
#185079=CARTESIAN_POINT('',(160.436624807795,-5.92111242539784,130.80190585319));
#185080=CARTESIAN_POINT('Ctrl Pts',(158.686624876677,-5.91674849775012,
130.800144354807));
#185081=CARTESIAN_POINT('Ctrl Pts',(158.695090859125,-5.91661988002312,
130.619653055616));
#185082=CARTESIAN_POINT('Ctrl Pts',(158.703556841572,-5.90822844586705,
130.43949138511));
#185083=CARTESIAN_POINT('Ctrl Pts',(158.712022824019,-5.89168835379828,
130.260357948255));
#185084=CARTESIAN_POINT('Ctrl Pts',(158.720527460507,-5.87507274286249,
130.080406622712));
#185085=CARTESIAN_POINT('Ctrl Pts',(158.729032096996,-5.85023399995928,
129.901493083318));
#185086=CARTESIAN_POINT('Ctrl Pts',(158.737536733484,-5.81733743584099,
129.724307044791));
#185087=CARTESIAN_POINT('Ctrl Pts',(158.746093572354,-5.78423894904418,
129.546033419143));
#185088=CARTESIAN_POINT('Ctrl Pts',(158.754650411224,-5.74298350254313,
129.369508707574));
#185089=CARTESIAN_POINT('Ctrl Pts',(158.763207250093,-5.69378812398778,
129.195414576943));
#185090=CARTESIAN_POINT('Ctrl Pts',(158.770546904925,-5.65159063687621,
129.04608480148));
#185091=CARTESIAN_POINT('Ctrl Pts',(158.777886559757,-5.60355225430021,
128.898543003698));
#185092=CARTESIAN_POINT('Ctrl Pts',(158.785226214589,-5.54983746486989,
128.753206143611));
#185093=CARTESIAN_POINT('Ctrl Pts',(158.792649480994,-5.49551076954329,
128.606213641147));
#185094=CARTESIAN_POINT('Ctrl Pts',(158.8000727474,-5.43525804680119,128.461158697887));
#185095=CARTESIAN_POINT('Ctrl Pts',(158.807496013805,-5.36923646405302,
128.318554841649));
#185096=CARTESIAN_POINT('Ctrl Pts',(158.814910506526,-5.30329291333286,
128.176119531326));
#185097=CARTESIAN_POINT('Ctrl Pts',(158.822324999247,-5.23159422979941,
128.036129877013));
#185098=CARTESIAN_POINT('Ctrl Pts',(158.829739491968,-5.15434684888729,
127.899082812628));
#185099=CARTESIAN_POINT('Ctrl Pts',(158.837146838322,-5.07717392190918,
127.762167839363));
#185100=CARTESIAN_POINT('Ctrl Pts',(158.844554184676,-4.99446312652244,
127.628190132767));
#185101=CARTESIAN_POINT('Ctrl Pts',(158.85196153103,-4.90646828810346,127.497625142761));
#185102=CARTESIAN_POINT('Ctrl Pts',(158.859363352705,-4.81853907955477,
127.36715753305));
#185103=CARTESIAN_POINT('Ctrl Pts',(158.866765174381,-4.7253338828433,127.240097880055));
#185104=CARTESIAN_POINT('Ctrl Pts',(158.874166996056,-4.62715154309232,
127.116895477425));
#185105=CARTESIAN_POINT('Ctrl Pts',(158.881564910367,-4.5290210330342,126.993758112383));
#185106=CARTESIAN_POINT('Ctrl Pts',(158.888962824679,-4.42591884457932,
126.874474233687));
#185107=CARTESIAN_POINT('Ctrl Pts',(158.89636073899,-4.31818600554819,126.759462573859));
#185108=CARTESIAN_POINT('Ctrl Pts',(158.903757423902,-4.21047106976063,
126.644470026882));
#185109=CARTESIAN_POINT('Ctrl Pts',(158.911154108815,-4.09812726563609,
126.533748561878));
#185110=CARTESIAN_POINT('Ctrl Pts',(158.918550793727,-3.98153469663544,
126.427682422635));
#185111=CARTESIAN_POINT('Ctrl Pts',(158.925947150662,-3.86494729747148,
126.321620986475));
#185112=CARTESIAN_POINT('Ctrl Pts',(158.933343507598,-3.74411178415559,
126.220214716842));
#185113=CARTESIAN_POINT('Ctrl Pts',(158.940739864533,-3.61944357361845,
126.123809498318));
#185114=CARTESIAN_POINT('Ctrl Pts',(158.94813735387,-3.49475627605998,126.027389519909));
#185115=CARTESIAN_POINT('Ctrl Pts',(158.955534843206,-3.36623540821487,
125.935972345539));
#185116=CARTESIAN_POINT('Ctrl Pts',(158.962932332543,-3.23432764157704,
125.849862129381));
#185117=CARTESIAN_POINT('Ctrl Pts',(158.970332415058,-3.10237363487604,
125.763721727419));
#185118=CARTESIAN_POINT('Ctrl Pts',(158.977732497573,-2.96703067792505,
125.682892191536));
#185119=CARTESIAN_POINT('Ctrl Pts',(158.985132580088,-2.82877230989586,
125.607633014423));
#185120=CARTESIAN_POINT('Ctrl Pts',(158.992540799755,-2.69036191257786,
125.532291082108));
#185121=CARTESIAN_POINT('Ctrl Pts',(158.999949019421,-2.54903003007183,
125.462531919536));
#185122=CARTESIAN_POINT('Ctrl Pts',(159.007357239088,-2.40527322804099,
125.398568237075));
#185123=CARTESIAN_POINT('Ctrl Pts',(159.01477001839,-2.26142794609707,125.334565186036));
#185124=CARTESIAN_POINT('Ctrl Pts',(159.022182797692,-2.11515511668609,
125.276364860532));
#185125=CARTESIAN_POINT('Ctrl Pts',(159.029595576994,-1.96696844522749,
125.224130721049));
#185126=CARTESIAN_POINT('Ctrl Pts',(159.037018948023,-1.81857003770349,
125.171821946978));
#185127=CARTESIAN_POINT('Ctrl Pts',(159.044442319051,-1.6682526823436,125.125496494448));
#185128=CARTESIAN_POINT('Ctrl Pts',(159.05186569008,-1.5165431044626,125.08526736996));
#185129=CARTESIAN_POINT('Ctrl Pts',(159.055801739521,-1.43610304604864,
125.063936922872));
#185130=CARTESIAN_POINT('Ctrl Pts',(159.059737788962,-1.35527173024639,
125.044319513473));
#185131=CARTESIAN_POINT('Ctrl Pts',(159.063673838402,-1.27412836142776,
125.0264260834));
#185132=CARTESIAN_POINT('Ctrl Pts',(159.071097104808,-1.12109450023375,
124.992679632717));
#185133=CARTESIAN_POINT('Ctrl Pts',(159.078520371213,-0.966487599903085,
124.96496621481));
#185134=CARTESIAN_POINT('Ctrl Pts',(159.085943637619,-0.810824658756232,
124.943431174615));
#185135=CARTESIAN_POINT('Ctrl Pts',(159.09335813034,-0.655345698278701,
124.921921587048));
#185136=CARTESIAN_POINT('Ctrl Pts',(159.100772623061,-0.498813547604672,
124.906575892524));
#185137=CARTESIAN_POINT('Ctrl Pts',(159.108187115782,-0.341757874707942,
124.897489015984));
#185138=CARTESIAN_POINT('Ctrl Pts',(159.115594462136,-0.184853577981791,
124.888410897718));
#185139=CARTESIAN_POINT('Ctrl Pts',(159.123001808489,-0.0274271337459625,
124.885579609365));
#185140=CARTESIAN_POINT('Ctrl Pts',(159.130409154843,0.129984249697388,
124.889038592745));
#185141=CARTESIAN_POINT('Ctrl Pts',(159.137810976519,0.287278229792342,
124.892494996285));
#185142=CARTESIAN_POINT('Ctrl Pts',(159.145212798194,0.444556799859494,
124.902232321938));
#185143=CARTESIAN_POINT('Ctrl Pts',(159.152614619869,0.601280423338662,
124.918241997031));
#185144=CARTESIAN_POINT('Ctrl Pts',(159.160012534181,0.757921313636707,
124.934243220741));
#185145=CARTESIAN_POINT('Ctrl Pts',(159.167410448492,0.914007470349413,
124.956510161788));
#185146=CARTESIAN_POINT('Ctrl Pts',(159.174808362803,1.06900226807922,124.984982238964));
#185147=CARTESIAN_POINT('Ctrl Pts',(159.182205047716,1.22397130848554,125.013449584598));
#185148=CARTESIAN_POINT('Ctrl Pts',(159.189601732628,1.37784898306789,125.048119952392));
#185149=CARTESIAN_POINT('Ctrl Pts',(159.19699841754,1.53010656143899,125.088881243695));
#185150=CARTESIAN_POINT('Ctrl Pts',(159.204394774475,1.68235738854946,125.1296407276));
#185151=CARTESIAN_POINT('Ctrl Pts',(159.211791131411,1.83298790168538,125.17649050147));
#185152=CARTESIAN_POINT('Ctrl Pts',(159.219187488346,1.9814825553528,125.229268022341));
#185153=CARTESIAN_POINT('Ctrl Pts',(159.226584977683,2.12999994393089,125.282053623586));
#185154=CARTESIAN_POINT('Ctrl Pts',(159.233982467019,2.27638047016422,125.340768653868));
#185155=CARTESIAN_POINT('Ctrl Pts',(159.241379956356,2.42012680368066,125.40520171857));
#185156=CARTESIAN_POINT('Ctrl Pts',(159.248780038871,2.56392352725143,125.469657370183));
#185157=CARTESIAN_POINT('Ctrl Pts',(159.256180121386,2.70508387916875,125.539834894461));
#185158=CARTESIAN_POINT('Ctrl Pts',(159.263580203901,2.84313358139258,125.615476151628));
#185159=CARTESIAN_POINT('Ctrl Pts',(159.270988423567,2.98133508345591,125.691200584132));
#185160=CARTESIAN_POINT('Ctrl Pts',(159.278396643234,3.11641877732786,125.772400568279));
#185161=CARTESIAN_POINT('Ctrl Pts',(159.2858048629,3.24793729788046,125.858773304462));
#185162=CARTESIAN_POINT('Ctrl Pts',(159.293217642202,3.379536765888,125.945199201623));
#185163=CARTESIAN_POINT('Ctrl Pts',(159.300630421504,3.5075663852619,126.036803978112));
#185164=CARTESIAN_POINT('Ctrl Pts',(159.308043200806,3.6316109617408,126.133243793394));
#185165=CARTESIAN_POINT('Ctrl Pts',(159.315466571835,3.75583277892774,126.229821406407));
#185166=CARTESIAN_POINT('Ctrl Pts',(159.322889942864,3.8760578964236,126.331247616026));
#185167=CARTESIAN_POINT('Ctrl Pts',(159.330313313893,3.99190653076059,126.437140356099));
#185168=CARTESIAN_POINT('Ctrl Pts',(159.334249363333,4.05333225643613,126.493287227747));
#185169=CARTESIAN_POINT('Ctrl Pts',(159.338185412774,4.11352823916345,126.550689214031));
#185170=CARTESIAN_POINT('Ctrl Pts',(159.342121462215,4.1724424615358,126.609285592293));
#185171=CARTESIAN_POINT('Ctrl Pts',(159.34954472862,4.28355284627977,126.719796532962));
#185172=CARTESIAN_POINT('Ctrl Pts',(159.356967995026,4.39043773576217,126.834891917589));
#185173=CARTESIAN_POINT('Ctrl Pts',(159.364391261431,4.49269539695125,126.954215343331));
#185174=CARTESIAN_POINT('Ctrl Pts',(159.371805754152,4.59483219807689,127.073397738694));
#185175=CARTESIAN_POINT('Ctrl Pts',(159.379220246873,4.69235241644284,127.196797947547));
#185176=CARTESIAN_POINT('Ctrl Pts',(159.386634739594,4.78488989052833,127.324021654474));
#185177=CARTESIAN_POINT('Ctrl Pts',(159.394042085948,4.87733817351233,127.451122738402));
#185178=CARTESIAN_POINT('Ctrl Pts',(159.401449432302,4.96481305505397,127.582039683973));
#185179=CARTESIAN_POINT('Ctrl Pts',(159.408856778656,5.04698761211093,127.716344003994));
#185180=CARTESIAN_POINT('Ctrl Pts',(159.416258600331,5.12910088028297,127.850548154785));
#185181=CARTESIAN_POINT('Ctrl Pts',(159.423660422006,5.20592150129936,127.988134332506));
#185182=CARTESIAN_POINT('Ctrl Pts',(159.431062243682,5.27716505490398,128.128643976029));
#185183=CARTESIAN_POINT('Ctrl Pts',(159.438460157993,5.3483709995912,128.269079445604));
#185184=CARTESIAN_POINT('Ctrl Pts',(159.445858072304,5.41400557177566,128.412434975372));
#185185=CARTESIAN_POINT('Ctrl Pts',(159.453255986616,5.47382968100753,128.558226341566));
#185186=CARTESIAN_POINT('Ctrl Pts',(159.460652671528,5.53364384855771,128.70399347988));
#185187=CARTESIAN_POINT('Ctrl Pts',(159.46804935644,5.587649327999,128.852195306212));
#185188=CARTESIAN_POINT('Ctrl Pts',(159.475446041352,5.63565463941373,129.002326392654));
#185189=CARTESIAN_POINT('Ctrl Pts',(159.482842398288,5.68365782222265,129.152450822126));
#185190=CARTESIAN_POINT('Ctrl Pts',(159.490238755223,5.72566125231639,129.304503986051));
#185191=CARTESIAN_POINT('Ctrl Pts',(159.497635112159,5.7615230167609,129.457964282962));
#185192=CARTESIAN_POINT('Ctrl Pts',(159.505032601495,5.79739027173312,129.611448075037));
#185193=CARTESIAN_POINT('Ctrl Pts',(159.512430090832,5.82711390383247,129.766339065531));
#185194=CARTESIAN_POINT('Ctrl Pts',(159.519827580168,5.85060294612467,129.922104572363));
#185195=CARTESIAN_POINT('Ctrl Pts',(159.527227662683,5.87410022246421,130.077924682551));
#185196=CARTESIAN_POINT('Ctrl Pts',(159.534627745198,5.89135850200246,130.234619550542));
#185197=CARTESIAN_POINT('Ctrl Pts',(159.542027827713,5.90233860618015,130.391650621933));
#185198=CARTESIAN_POINT('Ctrl Pts',(159.54943604738,5.91333078411117,130.54885436513));
#185199=CARTESIAN_POINT('Ctrl Pts',(159.556844267046,5.91803097388586,130.706394677405));
#185200=CARTESIAN_POINT('Ctrl Pts',(159.564252486713,5.91645211760912,130.863731507222));
#185201=CARTESIAN_POINT('Ctrl Pts',(159.571665266015,5.91487228957268,131.021165175233));
#185202=CARTESIAN_POINT('Ctrl Pts',(159.579078045317,5.90700573329939,131.178394739263));
#185203=CARTESIAN_POINT('Ctrl Pts',(159.586490824619,5.89291730892882,131.334885030413));
#185204=CARTESIAN_POINT('Ctrl Pts',(159.593914195648,5.87880875435682,131.491598922231));
#185205=CARTESIAN_POINT('Ctrl Pts',(159.601337566676,5.85846062433322,131.647571062304));
#185206=CARTESIAN_POINT('Ctrl Pts',(159.608760937705,5.83198907969069,131.802275411959));
#185207=CARTESIAN_POINT('Ctrl Pts',(159.612696987146,5.81795323154548,131.884303370225));
#185208=CARTESIAN_POINT('Ctrl Pts',(159.616633036587,5.80219671380875,131.965975131038));
#185209=CARTESIAN_POINT('Ctrl Pts',(159.620569086027,5.78474249749451,132.047214108602));
#185210=CARTESIAN_POINT('Ctrl Pts',(159.627992352433,5.75182439025273,132.200428284909));
#185211=CARTESIAN_POINT('Ctrl Pts',(159.635415618838,5.71276527706964,132.352565436319));
#185212=CARTESIAN_POINT('Ctrl Pts',(159.642838885244,5.66764786323264,132.503094929015));
#185213=CARTESIAN_POINT('Ctrl Pts',(159.650253377965,5.62258377443199,132.653446508352));
#185214=CARTESIAN_POINT('Ctrl Pts',(159.657667870686,5.57147574393903,132.802193857082));
#185215=CARTESIAN_POINT('Ctrl Pts',(159.665082363407,5.51445760123563,132.948815776033));
#185216=CARTESIAN_POINT('Ctrl Pts',(159.67248970976,5.45749441476486,133.095296375258));
#185217=CARTESIAN_POINT('Ctrl Pts',(159.679897056114,5.39463259086107,133.239655277422));
#185218=CARTESIAN_POINT('Ctrl Pts',(159.687304402468,5.3260559180466,133.381385825115));
#185219=CARTESIAN_POINT('Ctrl Pts',(159.694706224143,5.25753039230196,133.523010664818));
#185220=CARTESIAN_POINT('Ctrl Pts',(159.702108045819,5.18329866644969,133.662010718739));
#185221=CARTESIAN_POINT('Ctrl Pts',(159.709509867494,5.1035928048584,133.797898832571));
#185222=CARTESIAN_POINT('Ctrl Pts',(159.716907781805,5.02392901937096,133.933715212126));
#185223=CARTESIAN_POINT('Ctrl Pts',(159.724305696117,4.93879704161671,134.066422602066));
#185224=CARTESIAN_POINT('Ctrl Pts',(159.731703610428,4.8484750285367,134.19555811405));
#185225=CARTESIAN_POINT('Ctrl Pts',(159.73910029534,4.75816802533676,134.324672166054));
#185226=CARTESIAN_POINT('Ctrl Pts',(159.746496980253,4.66267291234489,134.450215212586));
#185227=CARTESIAN_POINT('Ctrl Pts',(159.753893665165,4.56231142080306,134.571752960037));
#185228=CARTESIAN_POINT('Ctrl Pts',(159.7612900221,4.46195437939494,134.693285318378));
#185229=CARTESIAN_POINT('Ctrl Pts',(159.768686379036,4.35673162617207,134.810812442921));
#185230=CARTESIAN_POINT('Ctrl Pts',(159.776082735971,4.24700529181384,134.923932999963));
#185231=CARTESIAN_POINT('Ctrl Pts',(159.783480225308,4.13726215807369,135.037070876051));
#185232=CARTESIAN_POINT('Ctrl Pts',(159.790877714644,4.02301433022011,135.145800573338));
#185233=CARTESIAN_POINT('Ctrl Pts',(159.798275203981,3.90466079892524,135.249757631089));
#185234=CARTESIAN_POINT('Ctrl Pts',(159.805675286496,3.78626577898337,135.353751130825));
#185235=CARTESIAN_POINT('Ctrl Pts',(159.813075369011,3.6637624703608,135.452968413815));
#185236=CARTESIAN_POINT('Ctrl Pts',(159.820475451526,3.53758279716106,135.547085416216));
#185237=CARTESIAN_POINT('Ctrl Pts',(159.827883671192,3.41126437643905,135.641305909937));
#185238=CARTESIAN_POINT('Ctrl Pts',(159.835291890859,3.28126181733074,135.730414699631));
#185239=CARTESIAN_POINT('Ctrl Pts',(159.842700110525,3.14803647601173,135.814130762812));
#185240=CARTESIAN_POINT('Ctrl Pts',(159.850112889827,3.01472913671803,135.897898351833));
#185241=CARTESIAN_POINT('Ctrl Pts',(159.857525669129,2.87819538571021,135.976266415152));
#185242=CARTESIAN_POINT('Ctrl Pts',(159.864938448432,2.73892053422907,136.049000249579));
#185243=CARTESIAN_POINT('Ctrl Pts',(159.87236181946,2.59944668030884,136.121838009519));
#185244=CARTESIAN_POINT('Ctrl Pts',(159.879785190489,2.45722424019631,136.189025302982));
#185245=CARTESIAN_POINT('Ctrl Pts',(159.887208561518,2.31275857289416,136.250375522614));
#185246=CARTESIAN_POINT('Ctrl Pts',(159.891144610959,2.23615940968312,136.282904881142));
#185247=CARTESIAN_POINT('Ctrl Pts',(159.8950806604,2.1589298615324,136.313794058186));
#185248=CARTESIAN_POINT('Ctrl Pts',(159.89901670984,2.08114677863706,136.343020983419));
#185249=CARTESIAN_POINT('Ctrl Pts',(159.906439976246,1.93445031182582,136.398142052265));
#185250=CARTESIAN_POINT('Ctrl Pts',(159.913863242651,1.78534061284876,136.447514360626));
#185251=CARTESIAN_POINT('Ctrl Pts',(159.921286509057,1.63430882319367,136.490920670263));
#185252=CARTESIAN_POINT('Ctrl Pts',(159.928701001778,1.48345554057138,136.534275677247));
#185253=CARTESIAN_POINT('Ctrl Pts',(159.936115494499,1.33068504447641,136.571678619083));
#185254=CARTESIAN_POINT('Ctrl Pts',(159.94352998722,1.17650817263736,136.602960369421));
#185255=CARTESIAN_POINT('Ctrl Pts',(159.950937333574,1.02247990227215,136.634211969231));
#185256=CARTESIAN_POINT('Ctrl Pts',(159.958344679927,0.86704831811973,136.659354049223));
#185257=CARTESIAN_POINT('Ctrl Pts',(159.965752026281,0.710739027593632,
136.678267375181));
#185258=CARTESIAN_POINT('Ctrl Pts',(159.973153847957,0.554546318433565,
136.697166594867));
#185259=CARTESIAN_POINT('Ctrl Pts',(159.980555669632,0.397477575349415,
136.709846265965));
#185260=CARTESIAN_POINT('Ctrl Pts',(159.987957491307,0.240068091516747,
136.716238311999));
#185261=CARTESIAN_POINT('Ctrl Pts',(159.995355405619,0.0827417029254899,
136.722626983722));
#185262=CARTESIAN_POINT('Ctrl Pts',(160.00275331993,-0.0749246961394813,
136.722734625595));
#185263=CARTESIAN_POINT('Ctrl Pts',(160.010151234241,-0.232391313986322,
136.716545056476));
#185264=CARTESIAN_POINT('Ctrl Pts',(160.017547919154,-0.389831763738124,
136.71035651595));
#185265=CARTESIAN_POINT('Ctrl Pts',(160.024944604066,-0.547072125519367,
136.697872856038));
#185266=CARTESIAN_POINT('Ctrl Pts',(160.032341288978,-0.703573112222377,
136.679130012041));
#185267=CARTESIAN_POINT('Ctrl Pts',(160.039737645913,-0.860067159507634,
136.660387999121));
#185268=CARTESIAN_POINT('Ctrl Pts',(160.047134002849,-1.01582152625271,
136.635387398346));
#185269=CARTESIAN_POINT('Ctrl Pts',(160.054530359784,-1.17030281856806,
136.604215949844));
#185270=CARTESIAN_POINT('Ctrl Pts',(160.061927849121,-1.3248077623638,136.573039728913));
#185271=CARTESIAN_POINT('Ctrl Pts',(160.069325338457,-1.47803887768987,
136.535690852927));
#185272=CARTESIAN_POINT('Ctrl Pts',(160.076722827794,-1.62947386920359,
136.492308004109));
#185273=CARTESIAN_POINT('Ctrl Pts',(160.084122910309,-1.7809619460186,136.448909947501));
#185274=CARTESIAN_POINT('Ctrl Pts',(160.091522992824,-1.93065228679722,
136.399473809455));
#185275=CARTESIAN_POINT('Ctrl Pts',(160.098923075339,-2.0780387819236,136.344187815532));
#185276=CARTESIAN_POINT('Ctrl Pts',(160.106331295005,-2.22558734365329,
136.288841028974));
#185277=CARTESIAN_POINT('Ctrl Pts',(160.113739514672,-2.37082665080243,
136.227631671566));
#185278=CARTESIAN_POINT('Ctrl Pts',(160.121147734338,-2.51327089691157,
136.160795995804));
#185279=CARTESIAN_POINT('Ctrl Pts',(160.12856051364,-2.65580281507737,136.093919183799));
#185280=CARTESIAN_POINT('Ctrl Pts',(160.135973292943,-2.79553591368827,
136.021409324709));
#185281=CARTESIAN_POINT('Ctrl Pts',(160.143386072245,-2.93201040772376,
135.94354786182));
#185282=CARTESIAN_POINT('Ctrl Pts',(160.150809443273,-3.06867990291634,
135.865575146821));
#185283=CARTESIAN_POINT('Ctrl Pts',(160.158232814302,-3.20208117860711,
135.782235753263));
#185284=CARTESIAN_POINT('Ctrl Pts',(160.165656185331,-3.33178407785868,
135.693853988154));
#185285=CARTESIAN_POINT('Ctrl Pts',(160.169592234772,-3.40055566722048,
135.646991855602));
#185286=CARTESIAN_POINT('Ctrl Pts',(160.173528284212,-3.4682880639065,135.598712804192));
#185287=CARTESIAN_POINT('Ctrl Pts',(160.177464333653,-3.5349211601155,135.549069560617));
#185288=CARTESIAN_POINT('Ctrl Pts',(160.184814521984,-3.65935196658665,
135.456365646416));
#185289=CARTESIAN_POINT('Ctrl Pts',(160.192164710316,-3.78033979812036,
135.358609719615));
#185290=CARTESIAN_POINT('Ctrl Pts',(160.199514898647,-3.89744121542264,
135.256088656746));
#185291=CARTESIAN_POINT('Ctrl Pts',(160.206856366003,-4.01440369225802,
135.1536892348));
#185292=CARTESIAN_POINT('Ctrl Pts',(160.214197833358,-4.12748864631828,
135.046536175349));
#185293=CARTESIAN_POINT('Ctrl Pts',(160.221539300714,-4.23628206835796,
134.93495921823));
#185294=CARTESIAN_POINT('Ctrl Pts',(160.228873737485,-4.3449713039615,134.82348911321));
#185295=CARTESIAN_POINT('Ctrl Pts',(160.236208174257,-4.44937692219924,
134.70760381301));
#185296=CARTESIAN_POINT('Ctrl Pts',(160.243542611028,-4.54911861775299,
134.587672706743));
#185297=CARTESIAN_POINT('Ctrl Pts',(160.250871701082,-4.64878760279232,
134.467829028831));
#185298=CARTESIAN_POINT('Ctrl Pts',(160.258200791136,-4.74379918996974,
134.343945707568));
#185299=CARTESIAN_POINT('Ctrl Pts',(160.26552988119,-4.83381069254079,134.216428136121));
#185300=CARTESIAN_POINT('Ctrl Pts',(160.272855833505,-4.9237836592839,134.088965157643));
#185301=CARTESIAN_POINT('Ctrl Pts',(160.280181785821,-5.00876058062966,
133.957871335271));
#185302=CARTESIAN_POINT('Ctrl Pts',(160.287507738136,-5.08843983619722,
133.823584126335));
#185303=CARTESIAN_POINT('Ctrl Pts',(160.294832163464,-5.16810248378662,
133.689324907607));
#185304=CARTESIAN_POINT('Ctrl Pts',(160.302156588792,-5.24246946773354,
133.551873954233));
#185305=CARTESIAN_POINT('Ctrl Pts',(160.309481014119,-5.31128333298679,
133.411696407072));
#185306=CARTESIAN_POINT('Ctrl Pts',(160.316805428625,-5.38009709656539,
133.271519067027));
#185307=CARTESIAN_POINT('Ctrl Pts',(160.32412984313,-5.4433575896976,133.1286154836));
#185308=CARTESIAN_POINT('Ctrl Pts',(160.331454257636,-5.5008541512746,132.983473778672));
#185309=CARTESIAN_POINT('Ctrl Pts',(160.338780177261,-5.55836252802465,
132.838302248058));
#185310=CARTESIAN_POINT('Ctrl Pts',(160.346106096887,-5.6101044760651,132.690892035358));
#185311=CARTESIAN_POINT('Ctrl Pts',(160.353432016512,-5.65591824276781,
132.541749288424));
#185312=CARTESIAN_POINT('Ctrl Pts',(160.360764971615,-5.70177600690807,
132.392463311645));
#185313=CARTESIAN_POINT('Ctrl Pts',(160.368097926717,-5.74169410699057,
132.24144184254));
#185314=CARTESIAN_POINT('Ctrl Pts',(160.375430881819,-5.77556110624976,
132.08920476005));
#185315=CARTESIAN_POINT('Ctrl Pts',(160.382767538779,-5.8094452024113,131.936890824499));
#185316=CARTESIAN_POINT('Ctrl Pts',(160.39010419574,-5.83727204445423,131.783360427865));
#185317=CARTESIAN_POINT('Ctrl Pts',(160.3974408527,-5.85898183122031,131.62914086947));
#185318=CARTESIAN_POINT('Ctrl Pts',(160.404787910665,-5.88072239543675,
131.47470267766));
#185319=CARTESIAN_POINT('Ctrl Pts',(160.412134968629,-5.89632854334946,
131.319573751473));
#185320=CARTESIAN_POINT('Ctrl Pts',(160.419482026594,-5.90579252285111,
131.16428455333));
#185321=CARTESIAN_POINT('Ctrl Pts',(160.425196286995,-5.91315324377544,
131.04350656032));
#185322=CARTESIAN_POINT('Ctrl Pts',(160.430910547395,-5.91679954108405,
130.922631689549));
#185323=CARTESIAN_POINT('Ctrl Pts',(160.436624807795,-5.91674949152901,
130.801907661968));
#185324=CARTESIAN_POINT('',(162.186624807795,-5.91777788669619,130.809763220789));
#185325=CARTESIAN_POINT('Ctrl Pts',(160.436624807795,-5.92529977099551,
130.801904117208));
#185326=CARTESIAN_POINT('Ctrl Pts',(160.443053857686,-5.92601137657551,
130.665882277054));
#185327=CARTESIAN_POINT('Ctrl Pts',(160.449482907576,-5.9217351792167,130.529905972966));
#185328=CARTESIAN_POINT('Ctrl Pts',(160.548727832071,-5.77652682953759,
128.436339550169));
#185329=CARTESIAN_POINT('Ctrl Pts',(160.734359581279,-3.3663328045,124.668778821217));
#185330=CARTESIAN_POINT('Ctrl Pts',(161.012807205092,3.34245362589332,124.655737658797));
#185331=CARTESIAN_POINT('Ctrl Pts',(161.291254828905,6.97968846202762,130.292980618556));
#185332=CARTESIAN_POINT('Ctrl Pts',(161.569702452718,4.20293057829504,136.400156815103));
#185333=CARTESIAN_POINT('Ctrl Pts',(161.848150076531,-2.43611518231675,
137.365069675955));
#185334=CARTESIAN_POINT('Ctrl Pts',(162.053790861556,-5.68590607778289,
133.625131439863));
#185335=CARTESIAN_POINT('Ctrl Pts',(162.166615771978,-5.92172892300598,
131.234503316265));
#185336=CARTESIAN_POINT('Ctrl Pts',(162.186624807795,-5.91777788669619,
130.809763220789));
#185337=CARTESIAN_POINT('',(163.936624807795,-5.90693473238044,130.804346773966));
#185338=CARTESIAN_POINT('Ctrl Pts',(162.186624807795,-5.91777788669619,
130.809763220789));
#185339=CARTESIAN_POINT('Ctrl Pts',(162.259431646582,-5.90340125874275,
129.264262281094));
#185340=CARTESIAN_POINT('Ctrl Pts',(162.425054359975,-4.4920549294218,125.725268843379));
#185341=CARTESIAN_POINT('Ctrl Pts',(162.683492947968,1.48047183150485,123.96434865219));
#185342=CARTESIAN_POINT('Ctrl Pts',(162.961940571783,6.5549269731353,128.352729954683));
#185343=CARTESIAN_POINT('Ctrl Pts',(163.240388195595,5.60572445244513,134.994040067549));
#185344=CARTESIAN_POINT('Ctrl Pts',(163.518835819408,-0.49486498518204,
137.785239443099));
#185345=CARTESIAN_POINT('Ctrl Pts',(163.750914690142,-5.20052006496424,
134.764823450537));
#185346=CARTESIAN_POINT('Ctrl Pts',(163.89017768627,-5.90691414848796,131.794876866286));
#185347=CARTESIAN_POINT('Ctrl Pts',(163.936624807795,-5.90693473238044,
130.804346773966));
#185348=CARTESIAN_POINT('',(165.686624807795,-5.9178288693344,130.79896272858));
#185349=CARTESIAN_POINT('Ctrl Pts',(163.936624807795,-5.90693473238044,
130.804346773966));
#185350=CARTESIAN_POINT('Ctrl Pts',(163.982993560875,-5.90695528154252,
129.815487965044));
#185351=CARTESIAN_POINT('Ctrl Pts',(164.122178188557,-5.20227317339492,
126.847267783513));
#185352=CARTESIAN_POINT('Ctrl Pts',(164.354178690849,-0.500757509154189,
123.823902004597));
#185353=CARTESIAN_POINT('Ctrl Pts',(164.632626314658,5.60218586257347,126.609950755435));
#185354=CARTESIAN_POINT('Ctrl Pts',(164.911073938473,6.55699410858763,133.250457261255));
#185355=CARTESIAN_POINT('Ctrl Pts',(165.189521562285,1.48624509578439,137.643120449992));
#185356=CARTESIAN_POINT('Ctrl Pts',(165.448038518726,-4.48957751367164,
135.886709966933));
#185357=CARTESIAN_POINT('Ctrl Pts',(165.613739600563,-5.90343703981052,
132.346093050683));
#185358=CARTESIAN_POINT('Ctrl Pts',(165.686624807795,-5.9178288693344,130.79896272858));
#185359=CARTESIAN_POINT('',(167.436624807795,-5.92148368288513,130.806842939611));
#185360=CARTESIAN_POINT('Ctrl Pts',(165.686624807795,-5.9178288693344,130.79896272858));
#185361=CARTESIAN_POINT('Ctrl Pts',(165.706555475167,-5.92176435608143,
130.375895538377));
#185362=CARTESIAN_POINT('Ctrl Pts',(165.819302017143,-5.6870478495866,127.986964075457));
#185363=CARTESIAN_POINT('Ctrl Pts',(166.024864433725,-2.44165234092735,
124.245710270396));
#185364=CARTESIAN_POINT('Ctrl Pts',(166.303312057537,4.19820555675649,125.205018635372));
#185365=CARTESIAN_POINT('Ctrl Pts',(166.581759681351,6.98011764152404,131.309848738916));
#185366=CARTESIAN_POINT('Ctrl Pts',(166.860207305163,3.34764261143406,136.950159953411));
#185367=CARTESIAN_POINT('Ctrl Pts',(167.138654928975,-3.36115243712761,
136.942781817248));
#185368=CARTESIAN_POINT('Ctrl Pts',(167.33079409652,-5.85912794910789,133.045254473615));
#185369=CARTESIAN_POINT('Ctrl Pts',(167.43011738946,-5.92599866040667,130.944526178327));
#185370=CARTESIAN_POINT('Ctrl Pts',(167.436624807795,-5.92527153925886,
130.806844527503));
#185371=CARTESIAN_POINT('',(169.186624778302,-5.9129989234673,130.808555423824));
#185372=CARTESIAN_POINT('Ctrl Pts',(167.436624807795,-5.91674948011374,
130.806840955004));
#185373=CARTESIAN_POINT('Ctrl Pts',(167.443972012379,-5.91681455163261,
130.651615351601));
#185374=CARTESIAN_POINT('Ctrl Pts',(167.451319216962,-5.91076692399308,
130.496140163611));
#185375=CARTESIAN_POINT('Ctrl Pts',(167.458666421546,-5.89857393061799,
130.34094272027));
#185376=CARTESIAN_POINT('Ctrl Pts',(167.466005334366,-5.88639469777177,
130.185920426611));
#185377=CARTESIAN_POINT('Ctrl Pts',(167.473344247186,-5.86808392919402,
130.031175630505));
#185378=CARTESIAN_POINT('Ctrl Pts',(167.480683160006,-5.84366093305929,
129.877237399252));
#185379=CARTESIAN_POINT('Ctrl Pts',(167.488015470109,-5.81925990995148,
129.723437664066));
#185380=CARTESIAN_POINT('Ctrl Pts',(167.495347780212,-5.78875766286815,
129.570443423924));
#185381=CARTESIAN_POINT('Ctrl Pts',(167.502680090315,-5.75222542074246,
129.418780135795));
#185382=CARTESIAN_POINT('Ctrl Pts',(167.510007480636,-5.71571769076565,
129.267218609641));
#185383=CARTESIAN_POINT('Ctrl Pts',(167.517334870957,-5.67318810855586,
129.116986627315));
#185384=CARTESIAN_POINT('Ctrl Pts',(167.524662261277,-5.62475920940763,
128.96860072077));
#185385=CARTESIAN_POINT('Ctrl Pts',(167.531987158873,-5.57634678541911,
128.820265294032));
#185386=CARTESIAN_POINT('Ctrl Pts',(167.539312056469,-5.5220391529434,128.673775056407));
#185387=CARTESIAN_POINT('Ctrl Pts',(167.546636954065,-5.46200904102642,
128.529632546291));
#185388=CARTESIAN_POINT('Ctrl Pts',(167.553960722033,-5.40198818680619,
128.38551226548));
#185389=CARTESIAN_POINT('Ctrl Pts',(167.561284490001,-5.33624675509488,
128.243739344073));
#185390=CARTESIAN_POINT('Ctrl Pts',(167.568608257969,-5.26500596497368,
128.104797180399));
#185391=CARTESIAN_POINT('Ctrl Pts',(167.575932412763,-5.19376141206259,
127.965847678088));
#185392=CARTESIAN_POINT('Ctrl Pts',(167.583256567557,-5.117017096654,127.829729570625));
#185393=CARTESIAN_POINT('Ctrl Pts',(167.590580722352,-5.03504049750885,
127.696902210613));
#185394=CARTESIAN_POINT('Ctrl Pts',(167.597906780482,-4.95304259501328,
127.564040332606));
#185395=CARTESIAN_POINT('Ctrl Pts',(167.605232838613,-4.86580990330667,
127.434471228328));
#185396=CARTESIAN_POINT('Ctrl Pts',(167.612558896743,-4.77365342222497,
127.308625563678));
#185397=CARTESIAN_POINT('Ctrl Pts',(167.619892590845,-4.68140088617454,
127.182648729726));
#185398=CARTESIAN_POINT('Ctrl Pts',(167.627226284948,-4.5842145368701,127.060403394326));
#185399=CARTESIAN_POINT('Ctrl Pts',(167.63455997905,-4.48244629727542,126.942287889802));
#185400=CARTESIAN_POINT('Ctrl Pts',(167.641897718933,-4.38062191517208,
126.824107224469));
#185401=CARTESIAN_POINT('Ctrl Pts',(167.649235458816,-4.27421086771408,
126.710061206532));
#185402=CARTESIAN_POINT('Ctrl Pts',(167.656573198699,-4.16360166614498,
126.600510985601));
#185403=CARTESIAN_POINT('Ctrl Pts',(167.663921850295,-4.0528279812466,126.490797856116));
#185404=CARTESIAN_POINT('Ctrl Pts',(167.671270501891,-3.93784395315123,
126.385594134857));
#185405=CARTESIAN_POINT('Ctrl Pts',(167.678619153487,-3.81907152118827,
126.285220956242));
#185406=CARTESIAN_POINT('Ctrl Pts',(167.684262827859,-3.72785574894204,
126.208135585093));
#185407=CARTESIAN_POINT('Ctrl Pts',(167.68990650223,-3.63440624112913,126.133898470931));
#185408=CARTESIAN_POINT('Ctrl Pts',(167.695550176602,-3.53892500501756,
126.062637262987));
#185409=CARTESIAN_POINT('Ctrl Pts',(167.702973443007,-3.41333614114691,
125.968905609436));
#185410=CARTESIAN_POINT('Ctrl Pts',(167.710396709413,-3.28383094794813,
125.880025172351));
#185411=CARTESIAN_POINT('Ctrl Pts',(167.717819975818,-3.15082080951499,
125.796341169837));
#185412=CARTESIAN_POINT('Ctrl Pts',(167.725234468539,-3.01796787801939,
125.712756074865));
#185413=CARTESIAN_POINT('Ctrl Pts',(167.73264896126,-2.88161855994549,125.634355386119));
#185414=CARTESIAN_POINT('Ctrl Pts',(167.740063453981,-2.74221653490598,
125.561443582347));
#185415=CARTESIAN_POINT('Ctrl Pts',(167.747470800335,-2.60294887078684,
125.488602053717));
#185416=CARTESIAN_POINT('Ctrl Pts',(167.754878146689,-2.46063468583382,
125.421239049779));
#185417=CARTESIAN_POINT('Ctrl Pts',(167.762285493042,-2.3157457177737,125.359615230212));
#185418=CARTESIAN_POINT('Ctrl Pts',(167.769687314718,-2.17096481337226,
125.298037372015));
#185419=CARTESIAN_POINT('Ctrl Pts',(167.777089136393,-2.02361329162015,
125.242190320611));
#185420=CARTESIAN_POINT('Ctrl Pts',(167.784490958069,-1.8741864167139,125.192288287499));
#185421=CARTESIAN_POINT('Ctrl Pts',(167.79188887238,-1.72483842309231,125.142412597282));
#185422=CARTESIAN_POINT('Ctrl Pts',(167.799286786691,-1.57341761136135,
125.098475793171));
#185423=CARTESIAN_POINT('Ctrl Pts',(167.806684701002,-1.42043799449899,
125.060643487842));
#185424=CARTESIAN_POINT('Ctrl Pts',(167.814081385915,-1.26748380007303,
125.022817469556));
#185425=CARTESIAN_POINT('Ctrl Pts',(167.821478070827,-1.11297167666974,
124.991094026185));
#185426=CARTESIAN_POINT('Ctrl Pts',(167.828874755739,-0.957429641656374,
124.965588568258));
#185427=CARTESIAN_POINT('Ctrl Pts',(167.836271112675,-0.801894503539834,
124.940084241271));
#185428=CARTESIAN_POINT('Ctrl Pts',(167.84366746961,-0.645329912993157,
124.920797411925));
#185429=CARTESIAN_POINT('Ctrl Pts',(167.851063826545,-0.488272628939536,
124.907792089826));
#185430=CARTESIAN_POINT('Ctrl Pts',(167.858461315882,-0.331191299014834,
124.89478477658));
#185431=CARTESIAN_POINT('Ctrl Pts',(167.865858805218,-0.1736174974353,124.888060916291));
#185432=CARTESIAN_POINT('Ctrl Pts',(167.873256294555,-0.0160914847102347,
124.887632499204));
#185433=CARTESIAN_POINT('Ctrl Pts',(167.88065637707,0.14148974851462,124.887203931936));
#185434=CARTESIAN_POINT('Ctrl Pts',(167.888056459585,0.29902278646763,124.893075202722));
#185435=CARTESIAN_POINT('Ctrl Pts',(167.8954565421,0.45596914255646,124.90520621176));
#185436=CARTESIAN_POINT('Ctrl Pts',(167.902864761766,0.613088077298231,
124.91735056009));
#185437=CARTESIAN_POINT('Ctrl Pts',(167.910272981433,0.769618669418635,
124.935768364139));
#185438=CARTESIAN_POINT('Ctrl Pts',(167.917681201099,0.925028582930064,
124.96036774597));
#185439=CARTESIAN_POINT('Ctrl Pts',(167.925093980401,1.08053414865005,124.984982268311));
#185440=CARTESIAN_POINT('Ctrl Pts',(167.932506759704,1.23491729609663,125.015785876818));
#185441=CARTESIAN_POINT('Ctrl Pts',(167.939919539006,1.38765812122744,125.052636050004));
#185442=CARTESIAN_POINT('Ctrl Pts',(167.947342910034,1.5406171896123,125.089538876447));
#185443=CARTESIAN_POINT('Ctrl Pts',(167.954766281063,1.69192889079118,125.132505421117));
#185444=CARTESIAN_POINT('Ctrl Pts',(167.962189652092,1.84108986408209,125.181343751606));
#185445=CARTESIAN_POINT('Ctrl Pts',(167.966125701533,1.92017859118967,125.20723900629));
#185446=CARTESIAN_POINT('Ctrl Pts',(167.970061750973,1.99866301631166,125.234784230544));
#185447=CARTESIAN_POINT('Ctrl Pts',(167.973997800414,2.07647074253002,125.263945487098));
#185448=CARTESIAN_POINT('Ctrl Pts',(167.98142106682,2.22321368588102,125.318942706867));
#185449=CARTESIAN_POINT('Ctrl Pts',(167.988844333225,2.36799203508985,125.379857046413));
#185450=CARTESIAN_POINT('Ctrl Pts',(167.996267599631,2.51029298523497,125.446528995465));
#185451=CARTESIAN_POINT('Ctrl Pts',(168.003682092352,2.65242574747452,125.513122143811));
#185452=CARTESIAN_POINT('Ctrl Pts',(168.011096585073,2.79208660427583,125.585459199409));
#185453=CARTESIAN_POINT('Ctrl Pts',(168.018511077794,2.92877956937595,125.663331460237));
#185454=CARTESIAN_POINT('Ctrl Pts',(168.025918424147,3.06534078464996,125.741128664848));
#185455=CARTESIAN_POINT('Ctrl Pts',(168.033325770501,3.19893948086716,125.824450270135));
#185456=CARTESIAN_POINT('Ctrl Pts',(168.040733116855,3.32910137189247,125.913040282711));
#185457=CARTESIAN_POINT('Ctrl Pts',(168.04813493853,3.45916618326872,126.001564221514));
#185458=CARTESIAN_POINT('Ctrl Pts',(168.055536760206,3.58579898605364,126.095348534552));
#185459=CARTESIAN_POINT('Ctrl Pts',(168.062938581881,3.70855185565093,126.194092328578));
#185460=CARTESIAN_POINT('Ctrl Pts',(168.070336496192,3.83123992496291,126.292783996523));
#185461=CARTESIAN_POINT('Ctrl Pts',(168.077734410504,3.95005185001548,126.396429698054));
#185462=CARTESIAN_POINT('Ctrl Pts',(168.085132324815,4.06457045960395,126.504686497192));
#185463=CARTESIAN_POINT('Ctrl Pts',(168.092529009727,4.17907003827798,126.612925306015));
#185464=CARTESIAN_POINT('Ctrl Pts',(168.09992569464,4.28927744650871,126.725773435414));
#185465=CARTESIAN_POINT('Ctrl Pts',(168.107322379552,4.3948101798645,126.842849031636));
#185466=CARTESIAN_POINT('Ctrl Pts',(168.114718736487,4.50033823378823,126.959919436603));
#185467=CARTESIAN_POINT('Ctrl Pts',(168.122115093423,4.60119177504133,127.081216658401));
#185468=CARTESIAN_POINT('Ctrl Pts',(168.129511450358,4.69702681922106,127.206323705301));
#185469=CARTESIAN_POINT('Ctrl Pts',(168.136908939695,4.79287653599075,127.331449906411));
#185470=CARTESIAN_POINT('Ctrl Pts',(168.144306429031,4.88370599878966,127.460386797676));
#185471=CARTESIAN_POINT('Ctrl Pts',(168.151703918368,4.96921309588313,127.59268632365));
#185472=CARTESIAN_POINT('Ctrl Pts',(168.159104000883,5.05475016735696,127.725032227017));
#185473=CARTESIAN_POINT('Ctrl Pts',(168.166504083398,5.13496095593303,127.860742798688));
#185474=CARTESIAN_POINT('Ctrl Pts',(168.173904165913,5.20958813355524,127.999343319719));
#185475=CARTESIAN_POINT('Ctrl Pts',(168.181312385579,5.28429737143119,128.138096246271));
#185476=CARTESIAN_POINT('Ctrl Pts',(168.188720605246,5.35341055977898,128.279745139567));
#185477=CARTESIAN_POINT('Ctrl Pts',(168.196128824912,5.41671725750466,128.423792467995));
#185478=CARTESIAN_POINT('Ctrl Pts',(168.203541604214,5.48006291944636,128.56792845515));
#185479=CARTESIAN_POINT('Ctrl Pts',(168.210954383516,5.53759483341865,128.714465472273));
#185480=CARTESIAN_POINT('Ctrl Pts',(168.218367162819,5.58915188595099,128.862889073023));
#185481=CARTESIAN_POINT('Ctrl Pts',(168.225790533847,5.64078260561777,129.011524748374));
#185482=CARTESIAN_POINT('Ctrl Pts',(168.233213904876,5.68642130519154,129.162052034856));
#185483=CARTESIAN_POINT('Ctrl Pts',(168.240637275905,5.72595738410117,129.313943696716));
#185484=CARTESIAN_POINT('Ctrl Pts',(168.244573325346,5.74692036179461,129.394480300425));
#185485=CARTESIAN_POINT('Ctrl Pts',(168.248509374786,5.76616853337601,129.475400336614));
#185486=CARTESIAN_POINT('Ctrl Pts',(168.252445424227,5.78369131892802,129.556624551783));
#185487=CARTESIAN_POINT('Ctrl Pts',(168.259868690633,5.81673874561114,129.709810886667));
#185488=CARTESIAN_POINT('Ctrl Pts',(168.267291957038,5.8437460207227,129.864542700632));
#185489=CARTESIAN_POINT('Ctrl Pts',(168.274715223444,5.86457016118434,130.020302337177));
#185490=CARTESIAN_POINT('Ctrl Pts',(168.282129716165,5.88536968924135,130.175877878767));
#185491=CARTESIAN_POINT('Ctrl Pts',(168.289544208886,5.90000058018201,130.332478458477));
#185492=CARTESIAN_POINT('Ctrl Pts',(168.296958701607,5.90837032823849,130.489573980475));
#185493=CARTESIAN_POINT('Ctrl Pts',(168.30436604796,5.91673200921669,130.646518087894));
#185494=CARTESIAN_POINT('Ctrl Pts',(168.311773394314,5.91884454153348,130.803955817635));
#185495=CARTESIAN_POINT('Ctrl Pts',(168.319180740668,5.91466693643344,130.961349768659));
#185496=CARTESIAN_POINT('Ctrl Pts',(168.326582562343,5.91049244714892,131.118626329337));
#185497=CARTESIAN_POINT('Ctrl Pts',(168.333984384019,5.90003717156359,131.275858804753));
#185498=CARTESIAN_POINT('Ctrl Pts',(168.341386205694,5.88331214550307,131.432507703109));
#185499=CARTESIAN_POINT('Ctrl Pts',(168.348784120006,5.86659594845354,131.589073907731));
#185500=CARTESIAN_POINT('Ctrl Pts',(168.356182034317,5.84361663198994,131.745056778573));
#185501=CARTESIAN_POINT('Ctrl Pts',(168.363579948628,5.81443722663803,131.89991997241));
#185502=CARTESIAN_POINT('Ctrl Pts',(168.370976633541,5.78526267037401,132.054757430793));
#185503=CARTESIAN_POINT('Ctrl Pts',(168.378373318453,5.74989013919929,132.208475214983));
#185504=CARTESIAN_POINT('Ctrl Pts',(168.385770003365,5.70843414450413,132.360545111885));
#185505=CARTESIAN_POINT('Ctrl Pts',(168.3931663603,5.66697998801119,132.512608265849));
#185506=CARTESIAN_POINT('Ctrl Pts',(168.400562717236,5.61944300252852,132.663023317657));
#185507=CARTESIAN_POINT('Ctrl Pts',(168.407959074171,5.56598808303539,132.811275469274));
#185508=CARTESIAN_POINT('Ctrl Pts',(168.415356563508,5.51252497945723,132.959550318676));
#185509=CARTESIAN_POINT('Ctrl Pts',(168.422754052845,5.4531422644287,133.105661257341));
#185510=CARTESIAN_POINT('Ctrl Pts',(168.430151542181,5.38805360091495,133.249111925198));
#185511=CARTESIAN_POINT('Ctrl Pts',(168.437551624696,5.32294212067166,133.392612879463));
#185512=CARTESIAN_POINT('Ctrl Pts',(168.444951707211,5.25212086368438,133.533451366482));
#185513=CARTESIAN_POINT('Ctrl Pts',(168.452351789726,5.17585013234562,133.67115429169));
#185514=CARTESIAN_POINT('Ctrl Pts',(168.459760009393,5.09949553349667,133.809008635421));
#185515=CARTESIAN_POINT('Ctrl Pts',(168.467168229059,5.01767967434691,133.943720204958));
#185516=CARTESIAN_POINT('Ctrl Pts',(168.474576448726,4.9307073937808,134.07484302226));
#185517=CARTESIAN_POINT('Ctrl Pts',(168.481989228028,4.84368158322695,134.206046543469));
#185518=CARTESIAN_POINT('Ctrl Pts',(168.48940200733,4.75149324537416,134.333656609204));
#185519=CARTESIAN_POINT('Ctrl Pts',(168.496814786632,4.6544881127323,134.457259599325));
#185520=CARTESIAN_POINT('Ctrl Pts',(168.504238157661,4.5573443746082,134.581039199194));
#185521=CARTESIAN_POINT('Ctrl Pts',(168.511661528689,4.45537033724308,134.700800004877));
#185522=CARTESIAN_POINT('Ctrl Pts',(168.519084899718,4.34894979669837,134.816163981179));
#185523=CARTESIAN_POINT('Ctrl Pts',(168.523020949159,4.2925230725765,134.877332729534));
#185524=CARTESIAN_POINT('Ctrl Pts',(168.5269569986,4.23484686126025,134.937266017562));
#185525=CARTESIAN_POINT('Ctrl Pts',(168.53089304804,4.17598212226016,134.995912105627));
#185526=CARTESIAN_POINT('Ctrl Pts',(168.538316314446,4.06496506161014,135.106516797436));
#185527=CARTESIAN_POINT('Ctrl Pts',(168.545739580851,3.94938289617561,135.212875107856));
#185528=CARTESIAN_POINT('Ctrl Pts',(168.553162847257,3.82959385918532,135.31458693519));
#185529=CARTESIAN_POINT('Ctrl Pts',(168.560577339978,3.70994640288897,135.416178547591));
#185530=CARTESIAN_POINT('Ctrl Pts',(168.567991832699,3.58610225395346,135.513134369022));
#185531=CARTESIAN_POINT('Ctrl Pts',(168.57540632542,3.45845739538752,135.605090042017));
#185532=CARTESIAN_POINT('Ctrl Pts',(168.582813671773,3.33093556574234,135.696957084672));
#185533=CARTESIAN_POINT('Ctrl Pts',(168.590221018127,3.19962062016315,135.783833356494));
#185534=CARTESIAN_POINT('Ctrl Pts',(168.597628364481,3.064942533938,135.865393894097));
#185535=CARTESIAN_POINT('Ctrl Pts',(168.605030186156,2.93036489571015,135.946893600775));
#185536=CARTESIAN_POINT('Ctrl Pts',(168.612432007832,2.79242942924893,136.023085274895));
#185537=CARTESIAN_POINT('Ctrl Pts',(168.619833829507,2.65159598941728,136.093686592717));
#185538=CARTESIAN_POINT('Ctrl Pts',(168.627231743819,2.51083689446027,136.164250640653));
#185539=CARTESIAN_POINT('Ctrl Pts',(168.63462965813,2.36718320570566,136.229230042688));
#185540=CARTESIAN_POINT('Ctrl Pts',(168.642027572441,2.22112023343574,136.288387921576));
#185541=CARTESIAN_POINT('Ctrl Pts',(168.649424257354,2.07508153418408,136.347535969496));
#185542=CARTESIAN_POINT('Ctrl Pts',(168.656820942266,1.92663469170935,136.400864274336));
#185543=CARTESIAN_POINT('Ctrl Pts',(168.664217627178,1.77628600285024,136.448183665694));
#185544=CARTESIAN_POINT('Ctrl Pts',(168.671613984114,1.62594398060959,136.49550095886));
#185545=CARTESIAN_POINT('Ctrl Pts',(168.679010341049,1.47370063573898,136.53680975625));
#185546=CARTESIAN_POINT('Ctrl Pts',(168.686406697984,1.32007821216927,136.571970527768));
#185547=CARTESIAN_POINT('Ctrl Pts',(168.693804187321,1.16643226861439,136.607136682489));
#185548=CARTESIAN_POINT('Ctrl Pts',(168.701201676658,1.01140718986344,136.636152853836));
#185549=CARTESIAN_POINT('Ctrl Pts',(168.708599165994,0.855536067754428,
136.658930507769));
#185550=CARTESIAN_POINT('Ctrl Pts',(168.715999248509,0.699610305265305,
136.681716146373));
#185551=CARTESIAN_POINT('Ctrl Pts',(168.723399331024,0.542838278075566,
136.698258859513));
#185552=CARTESIAN_POINT('Ctrl Pts',(168.730799413539,0.385758713844092,
136.708521927794));
#185553=CARTESIAN_POINT('Ctrl Pts',(168.738207633206,0.228506424483239,
136.718796281374));
#185554=CARTESIAN_POINT('Ctrl Pts',(168.745615852872,0.0709462954679959,
136.722777175773));
#185555=CARTESIAN_POINT('Ctrl Pts',(168.753024072538,-0.0863816863814132,
136.720480018555));
#185556=CARTESIAN_POINT('Ctrl Pts',(168.760436851841,-0.243806500978941,
136.718181447475));
#185557=CARTESIAN_POINT('Ctrl Pts',(168.767849631143,-0.400998511820644,
136.709597145508));
#185558=CARTESIAN_POINT('Ctrl Pts',(168.775262410445,-0.55742285170284,
136.69479441542));
#185559=CARTESIAN_POINT('Ctrl Pts',(168.782685781474,-0.714070698017043,
136.679970534497));
#185560=CARTESIAN_POINT('Ctrl Pts',(168.790109152502,-0.869948313691009,
136.658910529599));
#185561=CARTESIAN_POINT('Ctrl Pts',(168.797532523531,-1.02453019586171,
136.631732961965));
#185562=CARTESIAN_POINT('Ctrl Pts',(168.801468572972,-1.1064932189296,136.617322763489));
#185563=CARTESIAN_POINT('Ctrl Pts',(168.805404622413,-1.18809219258352,
136.601193539564));
#185564=CARTESIAN_POINT('Ctrl Pts',(168.809340671853,-1.26925063669719,
136.583368610617));
#185565=CARTESIAN_POINT('Ctrl Pts',(168.816763938259,-1.42231292942813,
136.549751350918));
#185566=CARTESIAN_POINT('Ctrl Pts',(168.824187204664,-1.57427017187731,
136.509998066409));
#185567=CARTESIAN_POINT('Ctrl Pts',(168.83161047107,-1.72459211334545,136.464193884111));
#185568=CARTESIAN_POINT('Ctrl Pts',(168.839024963791,-1.87473638676212,
136.418443838552));
#185569=CARTESIAN_POINT('Ctrl Pts',(168.846439456512,-2.02324885282527,
136.366657238365));
#185570=CARTESIAN_POINT('Ctrl Pts',(168.853853949233,-2.16960892878973,
136.308970291159));
#185571=CARTESIAN_POINT('Ctrl Pts',(168.861261295586,-2.31582793740229,
136.251338944805));
#185572=CARTESIAN_POINT('Ctrl Pts',(168.86866864194,-2.45989834098218,136.187818709047));
#185573=CARTESIAN_POINT('Ctrl Pts',(168.876075988294,-2.60131432648213,
136.118595683626));
#185574=CARTESIAN_POINT('Ctrl Pts',(168.883477809969,-2.74262483860503,
136.049424287348));
#185575=CARTESIAN_POINT('Ctrl Pts',(168.890879631645,-2.88128454078637,
135.974558733826));
#185576=CARTESIAN_POINT('Ctrl Pts',(168.89828145332,-3.01680734327979,135.894233309101));
#185577=CARTESIAN_POINT('Ctrl Pts',(168.905679367632,-3.15225860434103,
135.813950287542));
#185578=CARTESIAN_POINT('Ctrl Pts',(168.913077281943,-3.28457594329207,
135.72821332472));
#185579=CARTESIAN_POINT('Ctrl Pts',(168.920475196254,-3.41329774653486,
135.637302687982));
#185580=CARTESIAN_POINT('Ctrl Pts',(168.927871881166,-3.54199815854864,
135.546407158943));
#185581=CARTESIAN_POINT('Ctrl Pts',(168.935268566079,-3.66710391612022,
135.450339877519));
#185582=CARTESIAN_POINT('Ctrl Pts',(168.942665250991,-3.78818219902325,
135.349424554355));
#185583=CARTESIAN_POINT('Ctrl Pts',(168.950061607926,-3.90925511318838,
135.248513705883));
#185584=CARTESIAN_POINT('Ctrl Pts',(168.957457964862,-4.02630062101159,
135.1427554821));
#185585=CARTESIAN_POINT('Ctrl Pts',(168.964854321797,-4.1389190462698,135.032513842193));
#185586=CARTESIAN_POINT('Ctrl Pts',(168.972251811134,-4.25155471369718,
134.922255324009));
#185587=CARTESIAN_POINT('Ctrl Pts',(168.97964930047,-4.35976168219568,134.807512284089));
#185588=CARTESIAN_POINT('Ctrl Pts',(168.987046789807,-4.4631773164106,134.688685372884));
#185589=CARTESIAN_POINT('Ctrl Pts',(168.994446872322,-4.56662920281481,
134.569816807091));
#185590=CARTESIAN_POINT('Ctrl Pts',(169.001846954837,-4.66528616595876,
134.446861801133));
#185591=CARTESIAN_POINT('Ctrl Pts',(169.009247037352,-4.7588261173174,134.320253754116));
#185592=CARTESIAN_POINT('Ctrl Pts',(169.016655257018,-4.85246892546906,
134.193506488535));
#185593=CARTESIAN_POINT('Ctrl Pts',(169.024063476685,-4.94098326302515,
134.063098460322));
#185594=CARTESIAN_POINT('Ctrl Pts',(169.031471696351,-5.02409021673763,
133.929492303844));
#185595=CARTESIAN_POINT('Ctrl Pts',(169.038884475653,-5.10724832139393,
133.795803915006));
#185596=CARTESIAN_POINT('Ctrl Pts',(169.046297254955,-5.18499222651813,
133.658913799479));
#185597=CARTESIAN_POINT('Ctrl Pts',(169.053710034257,-5.25708944704321,
133.519308334979));
#185598=CARTESIAN_POINT('Ctrl Pts',(169.061133405286,-5.32928968345753,
133.379503395645));
#185599=CARTESIAN_POINT('Ctrl Pts',(169.068556776315,-5.39582696368089,
133.236975695829));
#185600=CARTESIAN_POINT('Ctrl Pts',(169.075980147344,-5.45651698950754,
133.092231441217));
#185601=CARTESIAN_POINT('Ctrl Pts',(169.079916196784,-5.48869629743827,
133.015484564331));
#185602=CARTESIAN_POINT('Ctrl Pts',(169.083852246225,-5.51923256297325,
132.938114797283));
#185603=CARTESIAN_POINT('Ctrl Pts',(169.087788295666,-5.54810406687026,
132.860199090228));
#185604=CARTESIAN_POINT('Ctrl Pts',(169.096337488275,-5.61081365713913,
132.690964329118));
#185605=CARTESIAN_POINT('Ctrl Pts',(169.104886680883,-5.66582349201742,
132.518730504111));
#185606=CARTESIAN_POINT('Ctrl Pts',(169.113435873491,-5.71287611630099,
132.344158345288));
#185607=CARTESIAN_POINT('Ctrl Pts',(169.1219544283,-5.75976011777493,132.170211801898));
#185608=CARTESIAN_POINT('Ctrl Pts',(169.130472983109,-5.79874374486091,
131.993943781956));
#185609=CARTESIAN_POINT('Ctrl Pts',(169.138991537918,-5.82961881215657,
131.816030063309));
#185610=CARTESIAN_POINT('Ctrl Pts',(169.147449767728,-5.86027523457195,
131.639376258474));
#185611=CARTESIAN_POINT('Ctrl Pts',(169.155907997538,-5.88293745840983,
131.461100123086));
#185612=CARTESIAN_POINT('Ctrl Pts',(169.164366227348,-5.89744884930004,
131.281883006978));
#185613=CARTESIAN_POINT('Ctrl Pts',(169.171785731182,-5.91017814641917,
131.124674925614));
#185614=CARTESIAN_POINT('Ctrl Pts',(169.179205235017,-5.91663626882271,
130.966743136856));
#185615=CARTESIAN_POINT('Ctrl Pts',(169.186624738851,-5.91674851051812,
130.808558924556));
#185616=CARTESIAN_POINT('',(170.936624807795,-5.90997459655701,130.800282389652));
#185617=CARTESIAN_POINT('Ctrl Pts',(169.186624807795,-5.91019576558979,
130.808552806709));
#185618=CARTESIAN_POINT('Ctrl Pts',(169.246495178356,-5.90189558337006,
129.533520458627));
#185619=CARTESIAN_POINT('Ctrl Pts',(169.399181423523,-4.87013215197593,
126.269586643864));
#185620=CARTESIAN_POINT('Ctrl Pts',(169.64468354329,0.516110086827318,123.825020325773));
#185621=CARTESIAN_POINT('Ctrl Pts',(169.923131167105,6.15088676129293,127.466074743035));
#185622=CARTESIAN_POINT('Ctrl Pts',(170.201578790917,6.13329898965285,134.174850794656));
#185623=CARTESIAN_POINT('Ctrl Pts',(170.48002641473,0.479509074835291,137.786311031131));
#185624=CARTESIAN_POINT('Ctrl Pts',(170.72504175369,-4.88318756993693,135.318440300322));
#185625=CARTESIAN_POINT('Ctrl Pts',(170.877241218044,-5.9019844995111,132.065066804779));
#185626=CARTESIAN_POINT('Ctrl Pts',(170.936624807795,-5.90997459655701,
130.800282389652));
#185627=CARTESIAN_POINT('',(172.686624807795,-5.92509021110593,130.801708436727));
#185628=CARTESIAN_POINT('Ctrl Pts',(170.936624807795,-5.90997459655701,
130.800282389652));
#185629=CARTESIAN_POINT('Ctrl Pts',(170.970057092649,-5.91447293021401,
130.088223165501));
#185630=CARTESIAN_POINT('Ctrl Pts',(171.096305252108,-5.46525073119121,
127.404805355658));
#185631=CARTESIAN_POINT('Ctrl Pts',(171.315369286168,-1.46542337909948,
123.961108842987));
#185632=CARTESIAN_POINT('Ctrl Pts',(171.593816909983,4.96532439755938,125.872513685901));
#185633=CARTESIAN_POINT('Ctrl Pts',(171.872264533795,6.83318162244277,132.316044924908));
#185634=CARTESIAN_POINT('Ctrl Pts',(172.150712157608,2.4216787557808,137.370412135345));
#185635=CARTESIAN_POINT('Ctrl Pts',(172.422165582275,-4.04851912677806,
136.415502720852));
#185636=CARTESIAN_POINT('Ctrl Pts',(172.600803132337,-5.91495363718931,
132.617640293932));
#185637=CARTESIAN_POINT('Ctrl Pts',(172.686624807795,-5.92509021110593,
130.801708436727));
#185638=CARTESIAN_POINT('',(174.436624807795,-5.9179196420516,130.809725587076));
#185639=CARTESIAN_POINT('Ctrl Pts',(172.686624807795,-5.92509021110593,
130.801708436727));
#185640=CARTESIAN_POINT('Ctrl Pts',(172.693619006941,-5.92591631029654,
130.653715648455));
#185641=CARTESIAN_POINT('Ctrl Pts',(172.793429080688,-5.85367826635182,
128.542618109344));
#185642=CARTESIAN_POINT('Ctrl Pts',(172.986055029049,-3.32892140626788,
124.648400676076));
#185643=CARTESIAN_POINT('Ctrl Pts',(173.264502652858,3.37982011111009,124.676198042461));
#185644=CARTESIAN_POINT('Ctrl Pts',(173.542950276673,6.9826720597651,130.335477437983));
#185645=CARTESIAN_POINT('Ctrl Pts',(173.821397900485,4.16878950799601,136.425637569324));
#185646=CARTESIAN_POINT('Ctrl Pts',(174.099845524299,-2.47600694493612,
137.350118796645));
#185647=CARTESIAN_POINT('Ctrl Pts',(174.304921160068,-5.69410310579832,
133.600799859742));
#185648=CARTESIAN_POINT('Ctrl Pts',(174.417180921234,-5.92198205708473,
131.22240348325));
#185649=CARTESIAN_POINT('Ctrl Pts',(174.436624807795,-5.91814536937201,
130.809725791712));
#185650=CARTESIAN_POINT('',(176.18662480776,-5.91674999707342,130.804546713429));
#185651=CARTESIAN_POINT('Ctrl Pts',(174.436624807795,-5.91674756863957,
130.809724524517));
#185652=CARTESIAN_POINT('Ctrl Pts',(174.443929001547,-5.9168880736424,130.654738123466));
#185653=CARTESIAN_POINT('Ctrl Pts',(174.451233195298,-5.91093472951897,
130.49956034794));
#185654=CARTESIAN_POINT('Ctrl Pts',(174.45853738905,-5.8988692447101,130.344717064023));
#185655=CARTESIAN_POINT('Ctrl Pts',(174.46583594041,-5.88681308032585,130.18999339446));
#185656=CARTESIAN_POINT('Ctrl Pts',(174.47313449177,-5.86865420127859,130.035604084019));
#185657=CARTESIAN_POINT('Ctrl Pts',(174.48043304313,-5.84442638127245,129.882074958789));
#185658=CARTESIAN_POINT('Ctrl Pts',(174.487779198497,-5.82004053794948,
129.727544456563));
#185659=CARTESIAN_POINT('Ctrl Pts',(174.495125353863,-5.78950629686442,
129.57388579532));
#185660=CARTESIAN_POINT('Ctrl Pts',(174.502471509229,-5.75291125004384,
129.421630451692));
#185661=CARTESIAN_POINT('Ctrl Pts',(174.509764874657,-5.71657917755128,
129.270469224622));
#185662=CARTESIAN_POINT('Ctrl Pts',(174.517058240085,-5.67427322768761,
129.120691588368));
#185663=CARTESIAN_POINT('Ctrl Pts',(174.524351605513,-5.62613037306831,
128.972807291086));
#185664=CARTESIAN_POINT('Ctrl Pts',(174.531644770911,-5.57798883883177,
128.824927049732));
#185665=CARTESIAN_POINT('Ctrl Pts',(174.538937936308,-5.52401083722427,
128.678940410037));
#185666=CARTESIAN_POINT('Ctrl Pts',(174.546231101706,-5.46438297325061,
128.535341163231));
#185667=CARTESIAN_POINT('Ctrl Pts',(174.553525601954,-5.40474419573206,
128.391715633801));
#185668=CARTESIAN_POINT('Ctrl Pts',(174.560820102202,-5.33945364616344,
128.25047872192));
#185669=CARTESIAN_POINT('Ctrl Pts',(174.56811460245,-5.26874562569991,128.112103182964));
#185670=CARTESIAN_POINT('Ctrl Pts',(174.575500116573,-5.1971553774347,127.972001124914));
#185671=CARTESIAN_POINT('Ctrl Pts',(174.582885630696,-5.12001174020782,
127.83483268724));
#185672=CARTESIAN_POINT('Ctrl Pts',(174.590271144818,-5.0376047641483,127.701060953864));
#185673=CARTESIAN_POINT('Ctrl Pts',(174.59757652405,-4.95609192679949,127.568740681165));
#185674=CARTESIAN_POINT('Ctrl Pts',(174.604881903281,-4.86942966911613,
127.439744052297));
#185675=CARTESIAN_POINT('Ctrl Pts',(174.612187282513,-4.77794074362902,
127.314487724054));
#185676=CARTESIAN_POINT('Ctrl Pts',(174.619612864081,-4.68494646403069,
127.187170434578));
#185677=CARTESIAN_POINT('Ctrl Pts',(174.62703844565,-4.58696555586886,127.063717931935));
#185678=CARTESIAN_POINT('Ctrl Pts',(174.634464027218,-4.48437712179394,
126.944530000553));
#185679=CARTESIAN_POINT('Ctrl Pts',(174.641889608787,-4.38178868771901,
126.825342069171));
#185680=CARTESIAN_POINT('Ctrl Pts',(174.649315190355,-4.27459305631298,
126.710418962902));
#185681=CARTESIAN_POINT('Ctrl Pts',(174.656740771924,-4.16320513849686,
126.60011829138));
#185682=CARTESIAN_POINT('Ctrl Pts',(174.664164038329,-4.05185194943482,
126.489852009629));
#185683=CARTESIAN_POINT('Ctrl Pts',(174.671587304735,-3.93594660125779,
126.383845984206));
#185684=CARTESIAN_POINT('Ctrl Pts',(174.67901057114,-3.81584854330713,126.282499224617));
#185685=CARTESIAN_POINT('Ctrl Pts',(174.686425063861,-3.69589243128723,
126.181272248482));
#185686=CARTESIAN_POINT('Ctrl Pts',(174.693839556582,-3.57175375582001,
126.084693815132));
#185687=CARTESIAN_POINT('Ctrl Pts',(174.701254049303,-3.44382960705885,
125.993127075111));
#185688=CARTESIAN_POINT('Ctrl Pts',(174.708661395657,-3.3160287564088,125.901648590562));
#185689=CARTESIAN_POINT('Ctrl Pts',(174.716068742011,-3.18444999758383,
125.815172398668));
#185690=CARTESIAN_POINT('Ctrl Pts',(174.723476088364,-3.04952429295717,
125.734022152615));
#185691=CARTESIAN_POINT('Ctrl Pts',(174.73087791004,-2.91469922101105,125.652932431477));
#185692=CARTESIAN_POINT('Ctrl Pts',(174.738279731715,-2.77653249221001,
125.577160938383));
#185693=CARTESIAN_POINT('Ctrl Pts',(174.745681553391,-2.63548481858331,
125.506988596128));
#185694=CARTESIAN_POINT('Ctrl Pts',(174.753079467702,-2.49451160292591,
125.436853297306));
#185695=CARTESIAN_POINT('Ctrl Pts',(174.760477382013,-2.35066080461964,
125.372311428666));
#185696=CARTESIAN_POINT('Ctrl Pts',(174.767875296325,-2.20441845267172,
125.313598389239));
#185697=CARTESIAN_POINT('Ctrl Pts',(174.775271981237,-2.05820040354942,
125.254895106854));
#185698=CARTESIAN_POINT('Ctrl Pts',(174.782668666149,-1.90959193565443,
125.202018870151));
#185699=CARTESIAN_POINT('Ctrl Pts',(174.790065351061,-1.75909991924992,
125.155157307665));
#185700=CARTESIAN_POINT('Ctrl Pts',(174.797461707997,-1.6086145758194,125.10829782307));
#185701=CARTESIAN_POINT('Ctrl Pts',(174.804858064932,-1.45624620636001,
125.067452593391));
#185702=CARTESIAN_POINT('Ctrl Pts',(174.812254421867,-1.30251747706525,
125.03275955855));
#185703=CARTESIAN_POINT('Ctrl Pts',(174.819651911204,-1.14876521150936,
124.998061212116));
#185704=CARTESIAN_POINT('Ctrl Pts',(174.827049400541,-0.993652535579348,
124.969517018183));
#185705=CARTESIAN_POINT('Ctrl Pts',(174.834446889877,-0.837712808111135,
124.947213887833));
#185706=CARTESIAN_POINT('Ctrl Pts',(174.841846972392,-0.681718416213029,
124.924902939155));
#185707=CARTESIAN_POINT('Ctrl Pts',(174.849247054907,-0.524896764851784,
124.908837462763));
#185708=CARTESIAN_POINT('Ctrl Pts',(174.856647137422,-0.367786690952134,
124.89905253818));
#185709=CARTESIAN_POINT('Ctrl Pts',(174.864055357088,-0.210503858375036,
124.889256854067));
#185710=CARTESIAN_POINT('Ctrl Pts',(174.871463576755,-0.0529323426943236,
124.885755536941));
#185711=CARTESIAN_POINT('Ctrl Pts',(174.878871796421,0.104387918666272,
124.888531535777));
#185712=CARTESIAN_POINT('Ctrl Pts',(174.886284575723,0.261805008023041,
124.891309243195));
#185713=CARTESIAN_POINT('Ctrl Pts',(174.893697355026,0.418970163099699,
124.900371943808));
#185714=CARTESIAN_POINT('Ctrl Pts',(174.901110134328,0.575348724016495,
124.915650707214));
#185715=CARTESIAN_POINT('Ctrl Pts',(174.908533505356,0.73195072595411,124.930951301634));
#185716=CARTESIAN_POINT('Ctrl Pts',(174.915956876385,0.887763520202904,
124.952485646826));
#185717=CARTESIAN_POINT('Ctrl Pts',(174.923380247414,1.04226196719356,124.98013358265));
#185718=CARTESIAN_POINT('Ctrl Pts',(174.927316296855,1.12418075092763,124.994793181628));
#185719=CARTESIAN_POINT('Ctrl Pts',(174.931252346295,1.20573025481183,125.01117069005));
#185720=CARTESIAN_POINT('Ctrl Pts',(174.935188395736,1.28683407005348,125.02924255482));
#185721=CARTESIAN_POINT('Ctrl Pts',(174.942611662142,1.43979333443543,125.063325527774));
#185722=CARTESIAN_POINT('Ctrl Pts',(174.950034928547,1.59162887770532,125.103541133724));
#185723=CARTESIAN_POINT('Ctrl Pts',(174.957458194952,1.74181071071733,125.149802632141));
#185724=CARTESIAN_POINT('Ctrl Pts',(174.964872687674,1.89181504127466,125.19600945331));
#185725=CARTESIAN_POINT('Ctrl Pts',(174.972287180395,2.04016919884106,125.248247834485));
#185726=CARTESIAN_POINT('Ctrl Pts',(174.979701673116,2.18635301765181,125.306379984215));
#185727=CARTESIAN_POINT('Ctrl Pts',(174.987109019469,2.33239593899437,125.36445610399));
#185728=CARTESIAN_POINT('Ctrl Pts',(174.994516365823,2.47627234150279,125.428414546277));
#185729=CARTESIAN_POINT('Ctrl Pts',(175.001923712177,2.61747698089627,125.498067672677));
#185730=CARTESIAN_POINT('Ctrl Pts',(175.009325533852,2.75857630454238,125.567668849148));
#185731=CARTESIAN_POINT('Ctrl Pts',(175.016727355528,2.89700749946936,125.642956088335));
#185732=CARTESIAN_POINT('Ctrl Pts',(175.024129177203,3.03228519126849,125.723693625791));
#185733=CARTESIAN_POINT('Ctrl Pts',(175.031527091514,3.16749147102659,125.804388542529));
#185734=CARTESIAN_POINT('Ctrl Pts',(175.038925005826,3.29954724326952,125.890527836688));
#185735=CARTESIAN_POINT('Ctrl Pts',(175.046322920137,3.42799174957475,125.981829837224));
#185736=CARTESIAN_POINT('Ctrl Pts',(175.053719605049,3.55641491073356,126.073116665024));
#185737=CARTESIAN_POINT('Ctrl Pts',(175.061116289962,3.6812276930651,126.169564280363));
#185738=CARTESIAN_POINT('Ctrl Pts',(175.068512974874,3.80199826361165,126.270847656738));
#185739=CARTESIAN_POINT('Ctrl Pts',(175.075909331809,3.92276347906459,126.372126542102));
#185740=CARTESIAN_POINT('Ctrl Pts',(175.083305688745,4.03948655308724,126.478240522284));
#185741=CARTESIAN_POINT('Ctrl Pts',(175.09070204568,4.15176891907437,126.588824423307));
#185742=CARTESIAN_POINT('Ctrl Pts',(175.098099535017,4.26406847577848,126.699425255008));
#185743=CARTESIAN_POINT('Ctrl Pts',(175.105497024353,4.37192570472563,126.814497108236));
#185744=CARTESIAN_POINT('Ctrl Pts',(175.11289451369,4.47497919168296,126.933638230659));
#185745=CARTESIAN_POINT('Ctrl Pts',(175.120294596205,4.57806880388083,127.052821117818));
#185746=CARTESIAN_POINT('Ctrl Pts',(175.12769467872,4.6763510773099,127.176075832118));
#185747=CARTESIAN_POINT('Ctrl Pts',(175.135094761235,4.76950524405483,127.302967996132));
#185748=CARTESIAN_POINT('Ctrl Pts',(175.142502980902,4.86276184338219,127.429999691124));
#185749=CARTESIAN_POINT('Ctrl Pts',(175.149911200568,4.95087885376649,127.560676522493));
#185750=CARTESIAN_POINT('Ctrl Pts',(175.157319420235,5.03357877135145,127.694535009095));
#185751=CARTESIAN_POINT('Ctrl Pts',(175.164732199537,5.11632958935577,127.828475883363));
#185752=CARTESIAN_POINT('Ctrl Pts',(175.172144978839,5.19365648795154,127.965601990528));
#185753=CARTESIAN_POINT('Ctrl Pts',(175.179557758141,5.26532846351507,128.105426247523));
#185754=CARTESIAN_POINT('Ctrl Pts',(175.18698112917,5.33710284735834,128.245450291974));
#185755=CARTESIAN_POINT('Ctrl Pts',(175.194404500198,5.40320601409473,128.388179848205));
#185756=CARTESIAN_POINT('Ctrl Pts',(175.201827871227,5.46345520708816,128.533108151934));
#185757=CARTESIAN_POINT('Ctrl Pts',(175.205763920668,5.49540077487273,128.609952616077));
#185758=CARTESIAN_POINT('Ctrl Pts',(175.209699970109,5.52570141200866,128.687414966641));
#185759=CARTESIAN_POINT('Ctrl Pts',(175.213636019549,5.55433563356411,128.765418187722));
#185760=CARTESIAN_POINT('Ctrl Pts',(175.221059285955,5.60833888177444,128.912529828282));
#185761=CARTESIAN_POINT('Ctrl Pts',(175.22848255236,5.6565751734508,129.062010888378));
#185762=CARTESIAN_POINT('Ctrl Pts',(175.235905818766,5.6988310137765,129.213368587756));
#185763=CARTESIAN_POINT('Ctrl Pts',(175.243320311487,5.74103691120799,129.364547394903));
#185764=CARTESIAN_POINT('Ctrl Pts',(175.250734804208,5.77727632757357,129.51759807029));
#185765=CARTESIAN_POINT('Ctrl Pts',(175.258149296929,5.80738402842343,129.672008504082));
#185766=CARTESIAN_POINT('Ctrl Pts',(175.265556643283,5.8374627103377,129.826270111284));
#185767=CARTESIAN_POINT('Ctrl Pts',(175.272963989636,5.86142137137703,129.981888503833));
#185768=CARTESIAN_POINT('Ctrl Pts',(175.28037133599,5.87914478016453,130.138337182269));
#185769=CARTESIAN_POINT('Ctrl Pts',(175.287773157665,5.89685497016506,130.294669175379));
#185770=CARTESIAN_POINT('Ctrl Pts',(175.295174979341,5.90833912582,130.451829852019));
#185771=CARTESIAN_POINT('Ctrl Pts',(175.302576801016,5.91353324571094,130.609283416511));
#185772=CARTESIAN_POINT('Ctrl Pts',(175.309974715328,5.91872462366646,130.766653862494));
#185773=CARTESIAN_POINT('Ctrl Pts',(175.317372629639,5.9176325664383,130.924316516258));
#185774=CARTESIAN_POINT('Ctrl Pts',(175.32477054395,5.91024500066961,131.081731478616));
#185775=CARTESIAN_POINT('Ctrl Pts',(175.332167228863,5.90285866258037,131.239120281463));
#185776=CARTESIAN_POINT('Ctrl Pts',(175.339563913775,5.88917890982933,131.396261102075));
#185777=CARTESIAN_POINT('Ctrl Pts',(175.346960598687,5.86924578015624,131.55261494239));
#185778=CARTESIAN_POINT('Ctrl Pts',(175.354356955622,5.84931353433896,131.708961849813));
#185779=CARTESIAN_POINT('Ctrl Pts',(175.361753312558,5.82312851013706,131.864521476024));
#185780=CARTESIAN_POINT('Ctrl Pts',(175.369149669493,5.79078250377275,132.018761110196));
#185781=CARTESIAN_POINT('Ctrl Pts',(175.37654715883,5.75843154515223,132.17302435885));
#185782=CARTESIAN_POINT('Ctrl Pts',(175.383944648166,5.71991780283251,132.325966847695));
#185783=CARTESIAN_POINT('Ctrl Pts',(175.391342137503,5.67538392920773,132.477067351752));
#185784=CARTESIAN_POINT('Ctrl Pts',(175.398742220018,5.63083444430259,132.628220823857));
#185785=CARTESIAN_POINT('Ctrl Pts',(175.406142302533,5.58026073187371,132.777530667734));
#185786=CARTESIAN_POINT('Ctrl Pts',(175.413542385048,5.52385486305895,132.924492220642));
#185787=CARTESIAN_POINT('Ctrl Pts',(175.420950604715,5.46738697019292,133.071615372885));
#185788=CARTESIAN_POINT('Ctrl Pts',(175.428358824381,5.40507424749297,133.216384728638));
#185789=CARTESIAN_POINT('Ctrl Pts',(175.435767044047,5.33715663715738,133.358316293169));
#185790=CARTESIAN_POINT('Ctrl Pts',(175.44317982335,5.26919722466591,133.500335214211));
#185791=CARTESIAN_POINT('Ctrl Pts',(175.450592602652,5.19562622460076,133.639512534424));
#185792=CARTESIAN_POINT('Ctrl Pts',(175.458005381954,5.11672857063927,133.775390623625));
#185793=CARTESIAN_POINT('Ctrl Pts',(175.465428752982,5.03771818400969,133.911462861812));
#185794=CARTESIAN_POINT('Ctrl Pts',(175.472852124011,4.95336614232203,134.044226139633));
#185795=CARTESIAN_POINT('Ctrl Pts',(175.48027549504,4.86400001629385,134.17325278028));
#185796=CARTESIAN_POINT('Ctrl Pts',(175.484211544481,4.81661595196297,134.241665801102));
#185797=CARTESIAN_POINT('Ctrl Pts',(175.488147593921,4.76782291709144,134.309028877887));
#185798=CARTESIAN_POINT('Ctrl Pts',(175.492083643362,4.71767409421103,134.375282305773));
#185799=CARTESIAN_POINT('Ctrl Pts',(175.499506909768,4.62309497934961,134.500234203069));
#185800=CARTESIAN_POINT('Ctrl Pts',(175.506930176173,4.52340522385552,134.621614925639));
#185801=CARTESIAN_POINT('Ctrl Pts',(175.514353442579,4.41890401854798,134.738978494484));
#185802=CARTESIAN_POINT('Ctrl Pts',(175.5217679353,4.31452632498669,134.856203349337));
#185803=CARTESIAN_POINT('Ctrl Pts',(175.529182428021,4.20534874690522,134.969420225197));
#185804=CARTESIAN_POINT('Ctrl Pts',(175.536596920742,4.09171282355591,135.078213297765));
#185805=CARTESIAN_POINT('Ctrl Pts',(175.544004267095,3.97818642678798,135.186901511475));
#185806=CARTESIAN_POINT('Ctrl Pts',(175.551411613449,3.8602105073087,135.291174153915));
#185807=CARTESIAN_POINT('Ctrl Pts',(175.558818959803,3.73816573865111,135.390649691848));
#185808=CARTESIAN_POINT('Ctrl Pts',(175.566220781478,3.6162119955864,135.490051037171));
#185809=CARTESIAN_POINT('Ctrl Pts',(175.573622603154,3.49019573395453,135.584662167159));
#185810=CARTESIAN_POINT('Ctrl Pts',(175.581024424829,3.36053313950423,135.674139624954));
#185811=CARTESIAN_POINT('Ctrl Pts',(175.588422339141,3.2309389929287,135.763569848295));
#185812=CARTESIAN_POINT('Ctrl Pts',(175.595820253452,3.097702653472,135.847871585104));
#185813=CARTESIAN_POINT('Ctrl Pts',(175.603218167763,2.96127182766808,135.926742849024));
#185814=CARTESIAN_POINT('Ctrl Pts',(175.610614852676,2.82486367419191,136.005601005972));
#185815=CARTESIAN_POINT('Ctrl Pts',(175.618011537588,2.68526241084319,136.07903029447));
#185816=CARTESIAN_POINT('Ctrl Pts',(175.6254082225,2.54294315333224,136.146773057786));
#185817=CARTESIAN_POINT('Ctrl Pts',(175.632804579435,2.4006302064062,136.214512817317));
#185818=CARTESIAN_POINT('Ctrl Pts',(175.640200936371,2.25559984201149,136.27656639258));
#185819=CARTESIAN_POINT('Ctrl Pts',(175.647597293306,2.108349862954,136.332723071121));
#185820=CARTESIAN_POINT('Ctrl Pts',(175.654994782643,1.96107733954886,136.388888347394));
#185821=CARTESIAN_POINT('Ctrl Pts',(175.66239227198,1.81158487365314,136.439154796263));
#185822=CARTESIAN_POINT('Ctrl Pts',(175.669789761316,1.66038809370673,136.483360700395));
#185823=CARTESIAN_POINT('Ctrl Pts',(175.677189843831,1.50913831196425,136.527582100839));
#185824=CARTESIAN_POINT('Ctrl Pts',(175.684589926346,1.35618338473752,136.565738621961));
#185825=CARTESIAN_POINT('Ctrl Pts',(175.691990008861,1.20205171822511,136.597719076112));
#185826=CARTESIAN_POINT('Ctrl Pts',(175.699398228528,1.04775056809937,136.629734696061));
#185827=CARTESIAN_POINT('Ctrl Pts',(175.706806448194,0.89227046033038,136.655560610638));
#185828=CARTESIAN_POINT('Ctrl Pts',(175.71421466786,0.736148288012586,136.675137079037));
#185829=CARTESIAN_POINT('Ctrl Pts',(175.721627447163,0.579930025102714,
136.694725596425));
#185830=CARTESIAN_POINT('Ctrl Pts',(175.729040226465,0.423069281292891,
136.708056971602));
#185831=CARTESIAN_POINT('Ctrl Pts',(175.736453005767,0.266105087431851,
136.715123567046));
#185832=CARTESIAN_POINT('Ctrl Pts',(175.743876376796,0.108916615769398,
136.722200259573));
#185833=CARTESIAN_POINT('Ctrl Pts',(175.751299747824,-0.0483752288583152,
136.722994292513));
#185834=CARTESIAN_POINT('Ctrl Pts',(175.758723118853,-0.205233569866812,
136.717550090625));
#185835=CARTESIAN_POINT('Ctrl Pts',(175.762659168294,-0.288403626033039,
136.714663444153));
#185836=CARTESIAN_POINT('Ctrl Pts',(175.766595217735,-0.371451917537092,
136.710023870462));
#185837=CARTESIAN_POINT('Ctrl Pts',(175.770531267175,-0.454299466532195,
136.703643841586));
#185838=CARTESIAN_POINT('Ctrl Pts',(175.777954533581,-0.610547358354118,
136.691611306242));
#185839=CARTESIAN_POINT('Ctrl Pts',(175.785377799986,-0.766553145834642,
136.673348737022));
#185840=CARTESIAN_POINT('Ctrl Pts',(175.792801066392,-0.921779894265251,
136.648866789094));
#185841=CARTESIAN_POINT('Ctrl Pts',(175.800215559113,-1.07682317756969,
136.624413776796));
#185842=CARTESIAN_POINT('Ctrl Pts',(175.807630051834,-1.2310888894619,136.593756075164));
#185843=CARTESIAN_POINT('Ctrl Pts',(175.815044544555,-1.38404257487515,
136.556956267656));
#185844=CARTESIAN_POINT('Ctrl Pts',(175.822451890908,-1.53684883776815,
136.520191929188));
#185845=CARTESIAN_POINT('Ctrl Pts',(175.829859237262,-1.68834523120841,
136.477297357118));
#185846=CARTESIAN_POINT('Ctrl Pts',(175.837266583616,-1.83800499713292,
136.428386594837));
#185847=CARTESIAN_POINT('Ctrl Pts',(175.844668405291,-1.98755314115846,
136.379512312047));
#185848=CARTESIAN_POINT('Ctrl Pts',(175.852070226967,-2.13526703187452,
136.324630888933));
#185849=CARTESIAN_POINT('Ctrl Pts',(175.859472048642,-2.2806327507365,136.263906827533));
#185850=CARTESIAN_POINT('Ctrl Pts',(175.866869962954,-2.42592173216508,
136.203214821893));
#185851=CARTESIAN_POINT('Ctrl Pts',(175.874267877265,-2.56886466684566,
136.136686463989));
#185852=CARTESIAN_POINT('Ctrl Pts',(175.881665791576,-2.70896548878649,
136.064535191006));
#185853=CARTESIAN_POINT('Ctrl Pts',(175.889062476488,-2.84904302851353,
135.992395908255));
#185854=CARTESIAN_POINT('Ctrl Pts',(175.896459161401,-2.98627906134308,
135.91463573573));
#185855=CARTESIAN_POINT('Ctrl Pts',(175.903855846313,-3.12020000172131,
135.831515131977));
#185856=CARTESIAN_POINT('Ctrl Pts',(175.911252203248,-3.25411500390483,
135.748398213878));
#185857=CARTESIAN_POINT('Ctrl Pts',(175.918648560184,-3.38471488874059,
135.659921534012));
#185858=CARTESIAN_POINT('Ctrl Pts',(175.926044917119,-3.51155330329859,
135.56639001275));
#185859=CARTESIAN_POINT('Ctrl Pts',(175.933442406456,-3.63841113714163,
135.472844171573));
#185860=CARTESIAN_POINT('Ctrl Pts',(175.940839895792,-3.76150605356803,
135.374242169608));
#185861=CARTESIAN_POINT('Ctrl Pts',(175.948237385129,-3.88042328543855,
135.270930407497));
#185862=CARTESIAN_POINT('Ctrl Pts',(175.955637467644,-3.99938220356058,
135.167582429608));
#185863=CARTESIAN_POINT('Ctrl Pts',(175.963037550159,-4.11416023972835,
135.059521649114));
#185864=CARTESIAN_POINT('Ctrl Pts',(175.970437632674,-4.224378232165,134.947132529476));
#185865=CARTESIAN_POINT('Ctrl Pts',(175.97784585234,-4.33471742061488,134.834619826447));
#185866=CARTESIAN_POINT('Ctrl Pts',(175.985254072007,-4.44048629003844,
134.717769546018));
#185867=CARTESIAN_POINT('Ctrl Pts',(175.992662291673,-4.5413443749702,134.597001100188));
#185868=CARTESIAN_POINT('Ctrl Pts',(176.000075070975,-4.64226453636987,
134.476158323397));
#185869=CARTESIAN_POINT('Ctrl Pts',(176.007487850277,-4.73826766343565,
134.351392871023));
#185870=CARTESIAN_POINT('Ctrl Pts',(176.014900629579,-4.82905597116431,
134.223154116721));
#185871=CARTESIAN_POINT('Ctrl Pts',(176.022324000608,-4.9199740014849,134.094732128872));
#185872=CARTESIAN_POINT('Ctrl Pts',(176.029747371637,-5.00566212797293,
133.96282723945));
#185873=CARTESIAN_POINT('Ctrl Pts',(176.037170742666,-5.08586753153024,
133.827915150599));
#185874=CARTESIAN_POINT('Ctrl Pts',(176.041106792106,-5.12839436099982,
133.756381523917));
#185875=CARTESIAN_POINT('Ctrl Pts',(176.045042841547,-5.16938058638033,
133.684002841315));
#185876=CARTESIAN_POINT('Ctrl Pts',(176.048978890988,-5.20879401129288,
133.610852290531));
#185877=CARTESIAN_POINT('Ctrl Pts',(176.056804946312,-5.28715980636309,
133.465406897628));
#185878=CARTESIAN_POINT('Ctrl Pts',(176.064631001636,-5.35952100433335,
133.316508050305));
#185879=CARTESIAN_POINT('Ctrl Pts',(176.07245705696,-5.42557744025171,133.164665683089));
#185880=CARTESIAN_POINT('Ctrl Pts',(176.080269925152,-5.49152256914748,
133.013079174693));
#185881=CARTESIAN_POINT('Ctrl Pts',(176.088082793345,-5.55118398804998,
132.858559319343));
#185882=CARTESIAN_POINT('Ctrl Pts',(176.095895661537,-5.60430706077633,
132.701641021469));
#185883=CARTESIAN_POINT('Ctrl Pts',(176.103690540573,-5.65730781744522,
132.545084028514));
#185884=CARTESIAN_POINT('Ctrl Pts',(176.11148541961,-5.70380015565364,132.386139904117));
#185885=CARTESIAN_POINT('Ctrl Pts',(176.119280298646,-5.74357746203557,
132.225363256584));
#185886=CARTESIAN_POINT('Ctrl Pts',(176.127064591086,-5.78330074496215,
132.064804967479));
#185887=CARTESIAN_POINT('Ctrl Pts',(176.134848883526,-5.81632709643767,
131.902419418109));
#185888=CARTESIAN_POINT('Ctrl Pts',(176.142633175966,-5.84249900201333,
131.738778069229));
#185889=CARTESIAN_POINT('Ctrl Pts',(176.150402849986,-5.86862175837175,
131.575444028665));
#185890=CARTESIAN_POINT('Ctrl Pts',(176.158172524007,-5.88791569417547,
131.410859201104));
#185891=CARTESIAN_POINT('Ctrl Pts',(176.165942198028,-5.9002739477779,131.245606471567));
#185892=CARTESIAN_POINT('Ctrl Pts',(176.172836401272,-5.91123969895993,
131.098974077335));
#185893=CARTESIAN_POINT('Ctrl Pts',(176.179730604516,-5.91674536509889,
130.951816162445));
#185894=CARTESIAN_POINT('Ctrl Pts',(176.18662480776,-5.91674999707342,130.804546713429));
#185895=CARTESIAN_POINT('',(177.936624807795,-5.91674751037323,130.798932819469));
#185896=CARTESIAN_POINT('Ctrl Pts',(176.186624807795,-5.91674999707345,
130.804546712692));
#185897=CARTESIAN_POINT('Ctrl Pts',(176.194355043842,-5.91675519072865,
130.639418479146));
#185898=CARTESIAN_POINT('Ctrl Pts',(176.202085279889,-5.90984332064331,
130.474416800835));
#185899=CARTESIAN_POINT('Ctrl Pts',(176.209815515936,-5.89607197714202,
130.310128078309));
#185900=CARTESIAN_POINT('Ctrl Pts',(176.217554849163,-5.88228442709847,
130.145646015741));
#185901=CARTESIAN_POINT('Ctrl Pts',(176.225294182391,-5.86162132030127,
129.981878903413));
#185902=CARTESIAN_POINT('Ctrl Pts',(176.233033515618,-5.8341917385858,129.819405126228));
#185903=CARTESIAN_POINT('Ctrl Pts',(176.240899598884,-5.80631293205789,
129.654270453487));
#185904=CARTESIAN_POINT('Ctrl Pts',(176.248765682149,-5.77144417701273,
129.490472187952));
#185905=CARTESIAN_POINT('Ctrl Pts',(176.256631765414,-5.72975279112999,
129.328601993997));
#185906=CARTESIAN_POINT('Ctrl Pts',(176.264397304788,-5.68859430250429,
129.168800816951));
#185907=CARTESIAN_POINT('Ctrl Pts',(176.272162844161,-5.64078673126599,
129.010878994164));
#185908=CARTESIAN_POINT('Ctrl Pts',(176.279928383534,-5.5865400071046,128.855386191998));
#185909=CARTESIAN_POINT('Ctrl Pts',(176.287844738745,-5.53123974824816,
128.696873538136));
#185910=CARTESIAN_POINT('Ctrl Pts',(176.295761093957,-5.46924781901711,
128.540885545812));
#185911=CARTESIAN_POINT('Ctrl Pts',(176.303677449168,-5.40083612746166,
128.387979089991));
#185912=CARTESIAN_POINT('Ctrl Pts',(176.311593804379,-5.3324244359062,128.23507263417));
#185913=CARTESIAN_POINT('Ctrl Pts',(176.31951015959,-5.25759319491068,128.085247996554));
#185914=CARTESIAN_POINT('Ctrl Pts',(176.327426514802,-5.17666132341062,
127.939031996761));
#185915=CARTESIAN_POINT('Ctrl Pts',(176.334849781207,-5.10077048390061,
127.801923404455));
#185916=CARTESIAN_POINT('Ctrl Pts',(176.342273047613,-5.01931395727661,
127.667624627721));
#185917=CARTESIAN_POINT('Ctrl Pts',(176.349696314018,-4.93252462046695,
127.536619588814));
#185918=CARTESIAN_POINT('Ctrl Pts',(176.357110806739,-4.84583786144609,
127.405769386985));
#185919=CARTESIAN_POINT('Ctrl Pts',(176.36452529946,-4.75383104242812,127.278205482258));
#185920=CARTESIAN_POINT('Ctrl Pts',(176.371939792181,-4.65678323929925,
127.154387956753));
#185921=CARTESIAN_POINT('Ctrl Pts',(176.379347138535,-4.55982897449686,
127.030689771241));
#185922=CARTESIAN_POINT('Ctrl Pts',(176.386754484889,-4.45784362701647,
126.91073106819));
#185923=CARTESIAN_POINT('Ctrl Pts',(176.394161831242,-4.35114987704113,
126.794943538984));
#185924=CARTESIAN_POINT('Ctrl Pts',(176.401563652918,-4.24453570328974,
126.679242368485));
#185925=CARTESIAN_POINT('Ctrl Pts',(176.408965474593,-4.13322037119265,
126.567706450713));
#185926=CARTESIAN_POINT('Ctrl Pts',(176.416367296269,-4.01756711697121,
126.460734825312));
#185927=CARTESIAN_POINT('Ctrl Pts',(176.42376521058,-3.90197491520212,126.353819669399));
#185928=CARTESIAN_POINT('Ctrl Pts',(176.431163124891,-3.78204962521748,
126.251464260148));
#185929=CARTESIAN_POINT('Ctrl Pts',(176.438561039203,-3.65819156987707,
126.154031059289));
#185930=CARTESIAN_POINT('Ctrl Pts',(176.445957724115,-3.53435409749872,
126.056614050062));
#185931=CARTESIAN_POINT('Ctrl Pts',(176.453354409027,-3.40658544998641,
125.964117856352));
#185932=CARTESIAN_POINT('Ctrl Pts',(176.460751093939,-3.27531937255807,
125.87686494834));
#185933=CARTESIAN_POINT('Ctrl Pts',(176.468147450875,-3.1440591156053,125.789615909212));
#185934=CARTESIAN_POINT('Ctrl Pts',(176.47554380781,-3.00930204797122,125.707609900153));
#185935=CARTESIAN_POINT('Ctrl Pts',(176.482940164745,-2.87151103396717,
125.631126141505));
#185936=CARTESIAN_POINT('Ctrl Pts',(176.490337654082,-2.73369892380657,
125.554630672999));
#185937=CARTESIAN_POINT('Ctrl Pts',(176.497735143419,-2.59285226879406,
125.483659319529));
#185938=CARTESIAN_POINT('Ctrl Pts',(176.505132632755,-2.44945853109072,
125.418445331659));
#185939=CARTESIAN_POINT('Ctrl Pts',(176.51253271527,-2.30601452693502,125.353208483127));
#185940=CARTESIAN_POINT('Ctrl Pts',(176.519932797785,-2.16002200197382,
125.293733172932));
#185941=CARTESIAN_POINT('Ctrl Pts',(176.5273328803,-2.01198823718576,125.240204446508));
#185942=CARTESIAN_POINT('Ctrl Pts',(176.534741099967,-1.86379169405521,
125.186616859746));
#185943=CARTESIAN_POINT('Ctrl Pts',(176.542149319633,-1.71354977984559,
125.138989042347));
#185944=CARTESIAN_POINT('Ctrl Pts',(176.549557539299,-1.56178547706073,
125.097456317848));
#185945=CARTESIAN_POINT('Ctrl Pts',(176.556970318601,-1.4099277658798,125.055898030649));
#185946=CARTESIAN_POINT('Ctrl Pts',(176.564383097904,-1.25654616188793,
125.02044239542));
#185947=CARTESIAN_POINT('Ctrl Pts',(176.571795877206,-1.10217315737517,
124.99117346303));
#185948=CARTESIAN_POINT('Ctrl Pts',(176.579219248234,-0.947579577474068,
124.961862709817));
#185949=CARTESIAN_POINT('Ctrl Pts',(176.586642619263,-0.791992136134873,
124.9387563693));
#185950=CARTESIAN_POINT('Ctrl Pts',(176.594065990292,-0.635948581030021,
124.921886651216));
#185951=CARTESIAN_POINT('Ctrl Pts',(176.598002039733,-0.553210543900006,
124.912941921905));
#185952=CARTESIAN_POINT('Ctrl Pts',(176.601938089173,-0.470344291830868,
124.905749659825));
#185953=CARTESIAN_POINT('Ctrl Pts',(176.605874138614,-0.387429773278801,
124.900308726426));
#185954=CARTESIAN_POINT('Ctrl Pts',(176.61329740502,-0.231055578962694,
124.890047295841));
#185955=CARTESIAN_POINT('Ctrl Pts',(176.620720671425,-0.0740369722305812,
124.885987209403));
#185956=CARTESIAN_POINT('Ctrl Pts',(176.62814393783,0.0830930337498934,
124.888194112958));
#185957=CARTESIAN_POINT('Ctrl Pts',(176.635558430551,0.240037325112162,
124.890398408136));
#185958=CARTESIAN_POINT('Ctrl Pts',(176.642972923272,0.397092384027427,
124.898854944318));
#185959=CARTESIAN_POINT('Ctrl Pts',(176.650387415993,0.553720283044722,
124.913577612681));
#185960=CARTESIAN_POINT('Ctrl Pts',(176.657794762347,0.710197218196119,
124.928286090781));
#185961=CARTESIAN_POINT('Ctrl Pts',(176.665202108701,0.866247443924086,
124.949248642838));
#185962=CARTESIAN_POINT('Ctrl Pts',(176.672609455055,1.02133334952026,124.976427128613));
#185963=CARTESIAN_POINT('Ctrl Pts',(176.68001127673,1.17630358619691,125.003585343648));
#185964=CARTESIAN_POINT('Ctrl Pts',(176.687413098406,1.33031056870666,125.036950197183));
#185965=CARTESIAN_POINT('Ctrl Pts',(176.694814920081,1.4828222356449,125.076431778974));
#185966=CARTESIAN_POINT('Ctrl Pts',(176.702212834392,1.63525339286118,125.115892518745));
#185967=CARTESIAN_POINT('Ctrl Pts',(176.709610748704,1.78619044609497,125.161463462799));
#185968=CARTESIAN_POINT('Ctrl Pts',(176.717008663015,1.93511206174074,125.213003727597));
#185969=CARTESIAN_POINT('Ctrl Pts',(176.724405347927,2.08400892931559,125.264535427338));
#185970=CARTESIAN_POINT('Ctrl Pts',(176.73180203284,2.23089067161478,125.322034357041));
#185971=CARTESIAN_POINT('Ctrl Pts',(176.739198717752,2.37525153545877,125.385309897578));
#185972=CARTESIAN_POINT('Ctrl Pts',(176.746595074687,2.51960599819104,125.448582632412));
#185973=CARTESIAN_POINT('Ctrl Pts',(176.753991431623,2.66143946282441,125.517631318926));
#185974=CARTESIAN_POINT('Ctrl Pts',(176.761387788558,2.8002668239092,125.592217461683));
#185975=CARTESIAN_POINT('Ctrl Pts',(176.768785277895,2.93911543981793,125.66681502377));
#185976=CARTESIAN_POINT('Ctrl Pts',(176.776182767231,3.0749567069106,125.746951553495));
#185977=CARTESIAN_POINT('Ctrl Pts',(176.783580256568,3.20733089967709,125.832343012762));
#185978=CARTESIAN_POINT('Ctrl Pts',(176.790980339083,3.33975149601111,125.917764405874));
#185979=CARTESIAN_POINT('Ctrl Pts',(176.798380421598,3.4687022847138,126.008444193921));
#185980=CARTESIAN_POINT('Ctrl Pts',(176.805780504113,3.59375338405989,126.104055608627));
#185981=CARTESIAN_POINT('Ctrl Pts',(176.81318872378,3.71894198994533,126.199772157913));
#185982=CARTESIAN_POINT('Ctrl Pts',(176.820596943446,3.84022204610599,126.300430936731));
#185983=CARTESIAN_POINT('Ctrl Pts',(176.828005163113,3.95719701619971,126.405665090767));
#185984=CARTESIAN_POINT('Ctrl Pts',(176.835417942415,4.07424398243563,126.510964014669));
#185985=CARTESIAN_POINT('Ctrl Pts',(176.842830721717,4.18698031602106,126.620843665207));
#185986=CARTESIAN_POINT('Ctrl Pts',(176.850243501019,4.29504747748942,126.734901473084));
#185987=CARTESIAN_POINT('Ctrl Pts',(176.857666872048,4.4032690503861,126.849122252105));
#185988=CARTESIAN_POINT('Ctrl Pts',(176.865090243076,4.50680788154691,126.967532831516));
#185989=CARTESIAN_POINT('Ctrl Pts',(176.872513614105,4.60534620625596,127.089698199119));
#185990=CARTESIAN_POINT('Ctrl Pts',(176.876449663546,4.65759359041109,127.154473208339));
#185991=CARTESIAN_POINT('Ctrl Pts',(176.880385712987,4.70843587755835,127.220303339764));
#185992=CARTESIAN_POINT('Ctrl Pts',(176.884321762427,4.75783081149922,127.287120715079));
#185993=CARTESIAN_POINT('Ctrl Pts',(176.891745028833,4.850988115349,127.413136199624));
#185994=CARTESIAN_POINT('Ctrl Pts',(176.899168295238,4.93927637338779,127.543045824573));
#185995=CARTESIAN_POINT('Ctrl Pts',(176.906591561644,5.02235224927055,127.676436634035));
#185996=CARTESIAN_POINT('Ctrl Pts',(176.914006054365,5.10532993636708,127.809669786638));
#185997=CARTESIAN_POINT('Ctrl Pts',(176.921420547086,5.18310730860256,127.946375620103));
#185998=CARTESIAN_POINT('Ctrl Pts',(176.928835039807,5.25538191600952,128.08610906935));
#185999=CARTESIAN_POINT('Ctrl Pts',(176.936242386161,5.32758686242861,128.225707838237));
#186000=CARTESIAN_POINT('Ctrl Pts',(176.943649732514,5.39429943243706,128.368328084139));
#186001=CARTESIAN_POINT('Ctrl Pts',(176.951057078868,5.45526112277846,128.513496884211));
#186002=CARTESIAN_POINT('Ctrl Pts',(176.958458900543,5.51617734559132,128.658557411914));
#186003=CARTESIAN_POINT('Ctrl Pts',(176.965860722219,5.57135108524651,128.806162366322));
#186004=CARTESIAN_POINT('Ctrl Pts',(176.973262543894,5.62057039359431,128.955815510421));
#186005=CARTESIAN_POINT('Ctrl Pts',(176.980660458206,5.66976371945242,129.10538965379));
#186006=CARTESIAN_POINT('Ctrl Pts',(176.988058372517,5.7130087576989,129.257009479828));
#186007=CARTESIAN_POINT('Ctrl Pts',(176.995456286828,5.75014224409737,129.410160224815));
#186008=CARTESIAN_POINT('Ctrl Pts',(177.002852971741,5.78726955958403,129.563285518926));
#186009=CARTESIAN_POINT('Ctrl Pts',(177.010249656653,5.81828725106939,129.717940864624));
#186010=CARTESIAN_POINT('Ctrl Pts',(177.017646341565,5.84308231987691,129.873597723139));
#186011=CARTESIAN_POINT('Ctrl Pts',(177.0250426985,5.86787628924509,130.029247679666));
#186012=CARTESIAN_POINT('Ctrl Pts',(177.032439055436,5.88644812582946,130.185898692064));
#186013=CARTESIAN_POINT('Ctrl Pts',(177.039835412371,5.89873627125152,130.343013714768));
#186014=CARTESIAN_POINT('Ctrl Pts',(177.047232901708,5.91102629802002,130.500152792183));
#186015=CARTESIAN_POINT('Ctrl Pts',(177.054630391044,5.91703068894933,130.657755649171));
#186016=CARTESIAN_POINT('Ctrl Pts',(177.062027880381,5.91673992046528,130.815281976114));
#186017=CARTESIAN_POINT('Ctrl Pts',(177.069427962896,5.91644905005278,130.972863523666));
#186018=CARTESIAN_POINT('Ctrl Pts',(177.076828045411,5.90985862727574,131.130368114695));
#186019=CARTESIAN_POINT('Ctrl Pts',(177.084228127926,5.89701120996687,131.287257451295));
#186020=CARTESIAN_POINT('Ctrl Pts',(177.091636347592,5.88414966560198,131.444319303847));
#186021=CARTESIAN_POINT('Ctrl Pts',(177.099044567259,5.86501741696226,131.600764178604));
#186022=CARTESIAN_POINT('Ctrl Pts',(177.106452786925,5.83970877139378,131.75606016459));
#186023=CARTESIAN_POINT('Ctrl Pts',(177.113865566227,5.81438454877628,131.911451732665));
#186024=CARTESIAN_POINT('Ctrl Pts',(177.121278345529,5.78287642886657,132.065692638045));
#186025=CARTESIAN_POINT('Ctrl Pts',(177.128691124831,5.74532930527565,132.218263632783));
#186026=CARTESIAN_POINT('Ctrl Pts',(177.13611449586,5.70772853259378,132.371052628114));
#186027=CARTESIAN_POINT('Ctrl Pts',(177.143537866889,5.66407162589269,132.522166589652));
#186028=CARTESIAN_POINT('Ctrl Pts',(177.150961237918,5.61455281366331,132.671103038224));
#186029=CARTESIAN_POINT('Ctrl Pts',(177.154897287358,5.58829675123149,132.750072716939));
#186030=CARTESIAN_POINT('Ctrl Pts',(177.158833336799,5.5603934953522,132.828430567071));
#186031=CARTESIAN_POINT('Ctrl Pts',(177.16276938624,5.53087731346671,132.906104347396));
#186032=CARTESIAN_POINT('Ctrl Pts',(177.170192652645,5.47521071559956,133.052594672972));
#186033=CARTESIAN_POINT('Ctrl Pts',(177.177615919051,5.4136360289286,133.197093410418));
#186034=CARTESIAN_POINT('Ctrl Pts',(177.185039185456,5.34631510325961,133.339088488395));
#186035=CARTESIAN_POINT('Ctrl Pts',(177.192453678177,5.27907374533417,133.480915739982));
#186036=CARTESIAN_POINT('Ctrl Pts',(177.199868170898,5.20609982544146,133.620244888226));
#186037=CARTESIAN_POINT('Ctrl Pts',(177.207282663619,5.12760430784209,133.756580904858));
#186038=CARTESIAN_POINT('Ctrl Pts',(177.214690009973,5.04918444717779,133.892785515704));
#186039=CARTESIAN_POINT('Ctrl Pts',(177.222097356327,4.96525376871951,134.026002416854));
#186040=CARTESIAN_POINT('Ctrl Pts',(177.22950470268,4.8760704285268,134.155758495847));
#186041=CARTESIAN_POINT('Ctrl Pts',(177.236906524356,4.78695360463412,134.28541779786));
#186042=CARTESIAN_POINT('Ctrl Pts',(177.244308346031,4.69259213007899,134.411621110942));
#186043=CARTESIAN_POINT('Ctrl Pts',(177.251710167707,4.59328893996197,134.533921888885));
#186044=CARTESIAN_POINT('Ctrl Pts',(177.259108082018,4.49403817122483,134.656158105201));
#186045=CARTESIAN_POINT('Ctrl Pts',(177.266505996329,4.38985111697191,134.774495600136));
#186046=CARTESIAN_POINT('Ctrl Pts',(177.273903910641,4.28107261419333,134.888518772499));
#186047=CARTESIAN_POINT('Ctrl Pts',(177.281300595553,4.17231218842958,135.002522996278));
#186048=CARTESIAN_POINT('Ctrl Pts',(177.288697280465,4.05896208592436,135.112214050608));
#186049=CARTESIAN_POINT('Ctrl Pts',(177.296093965377,3.94140590276758,135.217211178386));
#186050=CARTESIAN_POINT('Ctrl Pts',(177.303490322313,3.82385493217522,135.322203650482));
#186051=CARTESIAN_POINT('Ctrl Pts',(177.310886679248,3.70209853017439,135.422502361196));
#186052=CARTESIAN_POINT('Ctrl Pts',(177.318283036184,3.57655525460029,135.517765233477));
#186053=CARTESIAN_POINT('Ctrl Pts',(177.32568052552,3.4509927580304,135.613042690747));
#186054=CARTESIAN_POINT('Ctrl Pts',(177.333078014857,3.32164253086402,135.703282548755));
#186055=CARTESIAN_POINT('Ctrl Pts',(177.340475504193,3.18895400316233,135.788184744501));
#186056=CARTESIAN_POINT('Ctrl Pts',(177.347875586708,3.05621896170209,135.87311670258));
#186057=CARTESIAN_POINT('Ctrl Pts',(177.355275669223,2.92014360401691,135.952707071962));
#186058=CARTESIAN_POINT('Ctrl Pts',(177.362675751738,2.78120381892832,136.026700694589));
#186059=CARTESIAN_POINT('Ctrl Pts',(177.370083971405,2.64211125526319,136.10077568081));
#186060=CARTESIAN_POINT('Ctrl Pts',(177.377492191071,2.50014830366085,136.169241454361));
#186061=CARTESIAN_POINT('Ctrl Pts',(177.384900410737,2.35581345131169,136.231889847807));
#186062=CARTESIAN_POINT('Ctrl Pts',(177.39231319004,2.21138976326912,136.294576800294));
#186063=CARTESIAN_POINT('Ctrl Pts',(177.399725969342,2.06459161280398,136.351439103559));
#186064=CARTESIAN_POINT('Ctrl Pts',(177.407138748644,1.91593417645481,136.402317994502));
#186065=CARTESIAN_POINT('Ctrl Pts',(177.414562119672,1.76706433138938,136.45326958359));
#186066=CARTESIAN_POINT('Ctrl Pts',(177.421985490701,1.61633025132645,136.49822057893));
#186067=CARTESIAN_POINT('Ctrl Pts',(177.42940886173,1.46425967146917,136.537062788184));
#186068=CARTESIAN_POINT('Ctrl Pts',(177.433344911171,1.38362820114492,136.557657859537));
#186069=CARTESIAN_POINT('Ctrl Pts',(177.437280960611,1.30262113124199,136.576536392097));
#186070=CARTESIAN_POINT('Ctrl Pts',(177.441217010052,1.22131776273696,136.593688167889));
#186071=CARTESIAN_POINT('Ctrl Pts',(177.448640276458,1.06798214712807,136.626035881742));
#186072=CARTESIAN_POINT('Ctrl Pts',(177.456063542863,0.913128644707063,
136.652336451127));
#186073=CARTESIAN_POINT('Ctrl Pts',(177.463486809269,0.757275559365821,
136.672449257804));
#186074=CARTESIAN_POINT('Ctrl Pts',(177.47090130199,0.601606679428604,136.692538292813));
#186075=CARTESIAN_POINT('Ctrl Pts',(177.478315794711,0.444940934814573,
136.706454075208));
#186076=CARTESIAN_POINT('Ctrl Pts',(177.485730287432,0.287808838163108,
136.714106520325));
#186077=CARTESIAN_POINT('Ctrl Pts',(177.493137633785,0.130828191341923,
136.721751589727));
#186078=CARTESIAN_POINT('Ctrl Pts',(177.500544980139,-0.0266175423223238,
136.723145321975));
#186079=CARTESIAN_POINT('Ctrl Pts',(177.507952326493,-0.18399078026119,
136.718249182231));
#186080=CARTESIAN_POINT('Ctrl Pts',(177.515354148168,-0.341246643301121,
136.713356694213));
#186081=CARTESIAN_POINT('Ctrl Pts',(177.522755969844,-0.498429746764934,
136.702183686622));
#186082=CARTESIAN_POINT('Ctrl Pts',(177.530157791519,-0.655000654859997,
136.684743658205));
#186083=CARTESIAN_POINT('Ctrl Pts',(177.537555705831,-0.811488910392845,
136.667312836243));
#186084=CARTESIAN_POINT('Ctrl Pts',(177.544953620142,-0.96736524410747,
136.643621623335));
#186085=CARTESIAN_POINT('Ctrl Pts',(177.552351534454,-1.12209360613494,
136.613735498013));
#186086=CARTESIAN_POINT('Ctrl Pts',(177.559748219366,-1.27679625511462,
136.583854339223));
#186087=CARTESIAN_POINT('Ctrl Pts',(177.567144904278,-1.4303509448687,136.547780381962));
#186088=CARTESIAN_POINT('Ctrl Pts',(177.57454158919,-1.58222999060772,136.505630547969));
#186089=CARTESIAN_POINT('Ctrl Pts',(177.581937946126,-1.73410230187086,
136.463482582945));
#186090=CARTESIAN_POINT('Ctrl Pts',(177.589334303061,-1.88429875714948,
136.415259376694));
#186091=CARTESIAN_POINT('Ctrl Pts',(177.596730659997,-2.03230531659756,
136.361128172776));
#186092=CARTESIAN_POINT('Ctrl Pts',(177.604128149333,-2.18033453622717,
136.306988681232));
#186093=CARTESIAN_POINT('Ctrl Pts',(177.61152563867,-2.32617284183337,136.246939519212));
#186094=CARTESIAN_POINT('Ctrl Pts',(177.618923128006,-2.46932485398994,
136.181196613574));
#186095=CARTESIAN_POINT('Ctrl Pts',(177.626323210521,-2.61252704786361,
136.115430661862));
#186096=CARTESIAN_POINT('Ctrl Pts',(177.633723293036,-2.75304073439541,
136.04396714834));
#186097=CARTESIAN_POINT('Ctrl Pts',(177.641123375552,-2.89039401235355,
135.96706853259));
#186098=CARTESIAN_POINT('Ctrl Pts',(177.648531595218,-3.02789832436052,
135.890085358907));
#186099=CARTESIAN_POINT('Ctrl Pts',(177.655939814885,-3.16223496167907,
135.807655330097));
#186100=CARTESIAN_POINT('Ctrl Pts',(177.663348034551,-3.29295934264992,
135.720085317969));
#186101=CARTESIAN_POINT('Ctrl Pts',(177.670760813853,-3.42376418229605,
135.63246140796));
#186102=CARTESIAN_POINT('Ctrl Pts',(177.678173593155,-3.55095203452769,
135.539691430287));
#186103=CARTESIAN_POINT('Ctrl Pts',(177.685586372457,-3.67411086194991,
135.44212300223));
#186104=CARTESIAN_POINT('Ctrl Pts',(177.693009743486,-3.79744566448051,
135.344415163826));
#186105=CARTESIAN_POINT('Ctrl Pts',(177.700433114515,-3.91673966209711,
135.241895424228));
#186106=CARTESIAN_POINT('Ctrl Pts',(177.707856485544,-4.03161657575471,
135.134949301406));
#186107=CARTESIAN_POINT('Ctrl Pts',(177.711792534984,-4.09252707180661,
135.078243900951));
#186108=CARTESIAN_POINT('Ctrl Pts',(177.715728584425,-4.15219641590479,
135.020294666788));
#186109=CARTESIAN_POINT('Ctrl Pts',(177.719664633866,-4.21057314726077,
134.961162794007));
#186110=CARTESIAN_POINT('Ctrl Pts',(177.726987714394,-4.31918395389978,
134.851147035132));
#186111=CARTESIAN_POINT('Ctrl Pts',(177.734310794923,-4.42366599101378,
134.736683004449));
#186112=CARTESIAN_POINT('Ctrl Pts',(177.741633875452,-4.52362539881567,
134.61811779569));
#186113=CARTESIAN_POINT('Ctrl Pts',(177.748948118279,-4.62346417276795,
134.499695674788));
#186114=CARTESIAN_POINT('Ctrl Pts',(177.756262361106,-4.71879093201483,
134.377182514416));
#186115=CARTESIAN_POINT('Ctrl Pts',(177.763576603933,-4.80924728733108,
134.250963451053));
#186116=CARTESIAN_POINT('Ctrl Pts',(177.770882500434,-4.89960042235674,
134.124888417022));
#186117=CARTESIAN_POINT('Ctrl Pts',(177.778188396935,-4.985093998768,133.995116211621));
#186118=CARTESIAN_POINT('Ctrl Pts',(177.785494293436,-5.06540902935797,
133.862065954546));
#186119=CARTESIAN_POINT('Ctrl Pts',(177.792795471415,-5.14567218839746,
133.729101628126));
#186120=CARTESIAN_POINT('Ctrl Pts',(177.800096649395,-5.22076325672502,
133.592863788803));
#186121=CARTESIAN_POINT('Ctrl Pts',(177.807397827374,-5.29040573463265,
133.453801638888));
#186122=CARTESIAN_POINT('Ctrl Pts',(177.814695823601,-5.36001786330739,
133.314800090344));
#186123=CARTESIAN_POINT('Ctrl Pts',(177.821993819828,-5.42418595412213,
133.172977022927));
#186124=CARTESIAN_POINT('Ctrl Pts',(177.829291816054,-5.48267892226044,
133.028807155));
#186125=CARTESIAN_POINT('Ctrl Pts',(177.836588164671,-5.54115868490669,
132.884669835157));
#186126=CARTESIAN_POINT('Ctrl Pts',(177.843884513287,-5.59396573107036,
132.738187125347));
#186127=CARTESIAN_POINT('Ctrl Pts',(177.851180861903,-5.64091681357705,
132.589854404955));
#186128=CARTESIAN_POINT('Ctrl Pts',(177.85847957844,-5.68788313335843,132.441473545386));
#186129=CARTESIAN_POINT('Ctrl Pts',(177.865778294978,-5.72898957039591,
132.291241840484));
#186130=CARTESIAN_POINT('Ctrl Pts',(177.873077011515,-5.76410247697536,
132.139670767841));
#186131=CARTESIAN_POINT('Ctrl Pts',(177.88037674119,-5.79922025759192,131.988078655554));
#186132=CARTESIAN_POINT('Ctrl Pts',(177.887676470866,-5.82834277242975,
131.835147181732));
#186133=CARTESIAN_POINT('Ctrl Pts',(177.894976200541,-5.85138751742267,
131.681398064572));
#186134=CARTESIAN_POINT('Ctrl Pts',(177.902282487808,-5.87445296428058,
131.527510829438));
#186135=CARTESIAN_POINT('Ctrl Pts',(177.909588775074,-5.89142968455054,
131.372804865184));
#186136=CARTESIAN_POINT('Ctrl Pts',(177.916895062341,-5.90228702617907,
131.217807619125));
#186137=CARTESIAN_POINT('Ctrl Pts',(177.923471644159,-5.91206000566133,
131.078290511037));
#186138=CARTESIAN_POINT('Ctrl Pts',(177.930048225977,-5.91687557850981,
130.938537649031));
#186139=CARTESIAN_POINT('Ctrl Pts',(177.936624807795,-5.91674751037323,
130.798932819469));
#186140=CARTESIAN_POINT('',(179.686624807795,-5.92158244890185,130.806643466513));
#186141=CARTESIAN_POINT('Ctrl Pts',(177.936624807795,-5.91746116842021,
130.798932164786));
#186142=CARTESIAN_POINT('Ctrl Pts',(177.957120624423,-5.9215064818599,130.363799294495));
#186143=CARTESIAN_POINT('Ctrl Pts',(178.070432315656,-5.6787771470729,127.962628861881));
#186144=CARTESIAN_POINT('Ctrl Pts',(178.276559881491,-2.40168273653391,
124.230968756176));
#186145=CARTESIAN_POINT('Ctrl Pts',(178.555007505305,4.23221255766007,125.230678047027));
#186146=CARTESIAN_POINT('Ctrl Pts',(178.833455129117,6.97691126644166,131.352329330672));
#186147=CARTESIAN_POINT('Ctrl Pts',(179.11190275293,3.31016936242742,136.970424136732));
#186148=CARTESIAN_POINT('Ctrl Pts',(179.390350376743,-3.39845647489431,
136.922207797627));
#186149=CARTESIAN_POINT('Ctrl Pts',(179.581924395032,-5.86538284120287,
133.021055300245));
#186150=CARTESIAN_POINT('Ctrl Pts',(179.680682538715,-5.92608698495012,
130.932358269279));
#186151=CARTESIAN_POINT('Ctrl Pts',(179.686624807795,-5.92546899106887,
130.806644964827));
#186152=CARTESIAN_POINT('',(181.436624793272,-5.91313131605275,130.808682171932));
#186153=CARTESIAN_POINT('Ctrl Pts',(179.686624807795,-5.9167495603248,130.80664160337));
#186154=CARTESIAN_POINT('Ctrl Pts',(179.693977154138,-5.91680943647244,
130.651326226339));
#186155=CARTESIAN_POINT('Ctrl Pts',(179.701329500482,-5.91074953815374,
130.495761078002));
#186156=CARTESIAN_POINT('Ctrl Pts',(179.708681846825,-5.89853708827506,
130.340474014242));
#186157=CARTESIAN_POINT('Ctrl Pts',(179.716025830516,-5.88633852899205,
130.185363575961));
#186158=CARTESIAN_POINT('Ctrl Pts',(179.723369814208,-5.86800137290794,
130.030530968938));
#186159=CARTESIAN_POINT('Ctrl Pts',(179.730713797899,-5.84354481501677,
129.876505802743));
#186160=CARTESIAN_POINT('Ctrl Pts',(179.738051104691,-5.81911049219403,
129.722620670976));
#186161=CARTESIAN_POINT('Ctrl Pts',(179.745388411482,-5.78856789958858,
129.569541892852));
#186162=CARTESIAN_POINT('Ctrl Pts',(179.752725718274,-5.75198815284064,
129.417795490325));
#186163=CARTESIAN_POINT('Ctrl Pts',(179.760058027822,-5.71543331957921,
129.266152438212));
#186164=CARTESIAN_POINT('Ctrl Pts',(179.767390337371,-5.6728496059675,129.11584032425));
#186165=CARTESIAN_POINT('Ctrl Pts',(179.774722646919,-5.62435943793095,
128.96737627483));
#186166=CARTESIAN_POINT('Ctrl Pts',(179.782052360326,-5.57588643874756,
128.818964791891));
#186167=CARTESIAN_POINT('Ctrl Pts',(179.789382073733,-5.52151126173289,
128.672400433808));
#186168=CARTESIAN_POINT('Ctrl Pts',(179.796711787139,-5.46140653421223,
128.528186364447));
#186169=CARTESIAN_POINT('Ctrl Pts',(179.804040294966,-5.40131169262705,
128.383996015199));
#186170=CARTESIAN_POINT('Ctrl Pts',(179.811368802792,-5.33548932152652,
128.24215553726));
#186171=CARTESIAN_POINT('Ctrl Pts',(179.818697310619,-5.26416055459471,
128.103148997209));
#186172=CARTESIAN_POINT('Ctrl Pts',(179.826026126248,-5.19282879179809,
127.964136618774));
#186173=CARTESIAN_POINT('Ctrl Pts',(179.833354941878,-5.11599034668846,
127.827958754184));
#186174=CARTESIAN_POINT('Ctrl Pts',(179.840683757508,-5.03391263741617,
127.695075471208));
#186175=CARTESIAN_POINT('Ctrl Pts',(179.848014394317,-4.95181453217909,
127.562159167297));
#186176=CARTESIAN_POINT('Ctrl Pts',(179.855345031126,-4.86447477205808,
127.432539398244));
#186177=CARTESIAN_POINT('Ctrl Pts',(179.862675667936,-4.77220433056239,
127.306647594766));
#186178=CARTESIAN_POINT('Ctrl Pts',(179.870013917591,-4.67983806647012,
127.180625053001));
#186179=CARTESIAN_POINT('Ctrl Pts',(179.877352167246,-4.58253111937658,
127.058338516905));
#186180=CARTESIAN_POINT('Ctrl Pts',(179.884690416902,-4.48063543929967,
126.940187145452));
#186181=CARTESIAN_POINT('Ctrl Pts',(179.892032632595,-4.37868468856922,
126.821971917776));
#186182=CARTESIAN_POINT('Ctrl Pts',(179.899374848289,-4.27214052426441,
126.707896584654));
#186183=CARTESIAN_POINT('Ctrl Pts',(179.906717063983,-4.16139154293925,
126.598323172553));
#186184=CARTESIAN_POINT('Ctrl Pts',(179.914070345708,-4.05047564310977,
126.48858461374));
#186185=CARTESIAN_POINT('Ctrl Pts',(179.921423627433,-3.93534254692211,
126.383361787399));
#186186=CARTESIAN_POINT('Ctrl Pts',(179.928776909158,-3.81641438967868,
126.282976784186));
#186187=CARTESIAN_POINT('Ctrl Pts',(179.934933147562,-3.71684658903447,
126.198933490997));
#186188=CARTESIAN_POINT('Ctrl Pts',(179.941089385965,-3.61461941093371,
126.118280447087));
#186189=CARTESIAN_POINT('Ctrl Pts',(179.947245624368,-3.50999522101216,
126.041182675165));
#186190=CARTESIAN_POINT('Ctrl Pts',(179.954668890774,-3.38383811283284,
125.948217253306));
#186191=CARTESIAN_POINT('Ctrl Pts',(179.962092157179,-3.25379427861745,
125.860126797838));
#186192=CARTESIAN_POINT('Ctrl Pts',(179.969515423585,-3.12027719627839,
125.777254016261));
#186193=CARTESIAN_POINT('Ctrl Pts',(179.976929916306,-2.98691792004263,
125.694479183429));
#186194=CARTESIAN_POINT('Ctrl Pts',(179.984344409027,-2.85009388096072,
125.616909944266));
#186195=CARTESIAN_POINT('Ctrl Pts',(179.991758901748,-2.71025060387357,
125.544848071074));
#186196=CARTESIAN_POINT('Ctrl Pts',(179.999166248101,-2.5705421130023,125.47285565383));
#186197=CARTESIAN_POINT('Ctrl Pts',(180.006573594455,-2.42782050707694,
125.406360204809));
#186198=CARTESIAN_POINT('Ctrl Pts',(180.013980940809,-2.28255910179349,
125.345619507262));
#186199=CARTESIAN_POINT('Ctrl Pts',(180.021382762484,-2.13740603794629,
125.284924112419));
#186200=CARTESIAN_POINT('Ctrl Pts',(180.02878458416,-1.98971728942356,125.229975066268));
#186201=CARTESIAN_POINT('Ctrl Pts',(180.036186405835,-1.83998941521192,
125.180983561525));
#186202=CARTESIAN_POINT('Ctrl Pts',(180.043584320146,-1.69034058117979,
125.132017919016));
#186203=CARTESIAN_POINT('Ctrl Pts',(180.050982234458,-1.53865511912818,
125.089003670412));
#186204=CARTESIAN_POINT('Ctrl Pts',(180.058380148769,-1.38544804064297,
125.052103296376));
#186205=CARTESIAN_POINT('Ctrl Pts',(180.065776833681,-1.23226642239424,
125.015209054514));
#186206=CARTESIAN_POINT('Ctrl Pts',(180.073173518594,-1.07756405213862,
124.984426758055));
#186207=CARTESIAN_POINT('Ctrl Pts',(180.080570203506,-0.921869639997064,
124.959868601201));
#186208=CARTESIAN_POINT('Ctrl Pts',(180.087966560441,-0.76618213150912,
124.935311533282));
#186209=CARTESIAN_POINT('Ctrl Pts',(180.095362917377,-0.609503037337292,
124.916978114377));
#186210=CARTESIAN_POINT('Ctrl Pts',(180.102759274312,-0.452369496104509,
124.904929085503));
#186211=CARTESIAN_POINT('Ctrl Pts',(180.110156763649,-0.295211897325392,
124.892878211893));
#186212=CARTESIAN_POINT('Ctrl Pts',(180.117554252985,-0.137600085177405,
124.887113672636));
#186213=CARTESIAN_POINT('Ctrl Pts',(180.124951742322,0.0199256168518951,
124.887644169037));
#186214=CARTESIAN_POINT('Ctrl Pts',(180.132351824837,0.177506539271902,
124.888174851403));
#186215=CARTESIAN_POINT('Ctrl Pts',(180.139751907352,0.335000918410661,
124.895004961724));
#186216=CARTESIAN_POINT('Ctrl Pts',(180.147151989867,0.491870521751642,
124.908091123018));
#186217=CARTESIAN_POINT('Ctrl Pts',(180.154560209533,0.648912619348167,
124.921191673893));
#186218=CARTESIAN_POINT('Ctrl Pts',(180.1619684292,0.805328196918372,124.940561982845));
#186219=CARTESIAN_POINT('Ctrl Pts',(180.169376648866,0.960585487624677,
124.966106933161));
#186220=CARTESIAN_POINT('Ctrl Pts',(180.176789428168,1.115938336603,124.991667605968));
#186221=CARTESIAN_POINT('Ctrl Pts',(180.184202207471,1.27013111337955,125.023410417793));
#186222=CARTESIAN_POINT('Ctrl Pts',(180.191614986773,1.42264479111333,125.061189684987));
#186223=CARTESIAN_POINT('Ctrl Pts',(180.199038357801,1.57537638754186,125.09902293297));
#186224=CARTESIAN_POINT('Ctrl Pts',(180.20646172883,1.72642373571236,125.142909758842));
#186225=CARTESIAN_POINT('Ctrl Pts',(180.213885099859,1.87528465261602,125.192655169651));
#186226=CARTESIAN_POINT('Ctrl Pts',(180.2178211493,1.95421428262784,125.219031380086));
#186227=CARTESIAN_POINT('Ctrl Pts',(180.221757198741,2.03252957801731,125.247053850963));
#186228=CARTESIAN_POINT('Ctrl Pts',(180.225693248181,2.11015834979351,125.276688204941));
#186229=CARTESIAN_POINT('Ctrl Pts',(180.233116514587,2.25656379065098,125.332577671686));
#186230=CARTESIAN_POINT('Ctrl Pts',(180.240539780992,2.40096865457811,125.394372189534));
#186231=CARTESIAN_POINT('Ctrl Pts',(180.247963047398,2.5428611171387,125.461909129584));
#186232=CARTESIAN_POINT('Ctrl Pts',(180.255377540119,2.68458587459203,125.529366246579));
#186233=CARTESIAN_POINT('Ctrl Pts',(180.26279203284,2.82380380761203,125.602552117214));
#186234=CARTESIAN_POINT('Ctrl Pts',(180.270206525561,2.9600202095537,125.681255024126));
#186235=CARTESIAN_POINT('Ctrl Pts',(180.277613871915,3.09610532099887,125.759882074213));
#186236=CARTESIAN_POINT('Ctrl Pts',(180.285021218268,3.22919433968091,125.844015388928));
#186237=CARTESIAN_POINT('Ctrl Pts',(180.292428564622,3.35881454655656,125.933396092511));
#186238=CARTESIAN_POINT('Ctrl Pts',(180.299830386298,3.48833807779142,126.022710132594));
#186239=CARTESIAN_POINT('Ctrl Pts',(180.307232207973,3.61439764263109,126.11726355784));
#186240=CARTESIAN_POINT('Ctrl Pts',(180.314634029648,3.73654715640086,126.21675275393));
#186241=CARTESIAN_POINT('Ctrl Pts',(180.32203194396,3.8586321883935,126.316189430449));
#186242=CARTESIAN_POINT('Ctrl Pts',(180.329429858271,3.97681099133407,126.420556453577));
#186243=CARTESIAN_POINT('Ctrl Pts',(180.336827772583,4.09066848929571,126.529508354249));
#186244=CARTESIAN_POINT('Ctrl Pts',(180.344224457495,4.20450706620659,126.638442149092));
#186245=CARTESIAN_POINT('Ctrl Pts',(180.351621142407,4.31402549395549,126.751959051452));
#186246=CARTESIAN_POINT('Ctrl Pts',(180.359017827319,4.4188435996499,126.869674886236));
#186247=CARTESIAN_POINT('Ctrl Pts',(180.366414184255,4.52365705759943,126.987385501376));
#186248=CARTESIAN_POINT('Ctrl Pts',(180.37381054119,4.62377035965245,127.109294399949));
#186249=CARTESIAN_POINT('Ctrl Pts',(180.381206898125,4.71884206612648,127.234982504021));
#186250=CARTESIAN_POINT('Ctrl Pts',(180.388604387462,4.81392832832141,127.360689851263));
#186251=CARTESIAN_POINT('Ctrl Pts',(180.396001876799,4.90397123280667,127.490177258346));
#186252=CARTESIAN_POINT('Ctrl Pts',(180.403399366135,4.98867140088571,127.622994839086));
#186253=CARTESIAN_POINT('Ctrl Pts',(180.41079944865,5.07340126047743,127.755858978823));
#186254=CARTESIAN_POINT('Ctrl Pts',(180.418199531165,5.15278445416412,127.892055301928));
#186255=CARTESIAN_POINT('Ctrl Pts',(180.42559961368,5.22656654840633,128.031107531824));
#186256=CARTESIAN_POINT('Ctrl Pts',(180.433007833347,5.30042977364622,128.170312663941));
#186257=CARTESIAN_POINT('Ctrl Pts',(180.440416053013,5.36867942446826,128.312379644405));
#186258=CARTESIAN_POINT('Ctrl Pts',(180.44782427268,5.43110809229362,128.456809669807));
#186259=CARTESIAN_POINT('Ctrl Pts',(180.455237051982,5.49357518392232,128.60132858948));
#186260=CARTESIAN_POINT('Ctrl Pts',(180.462649831284,5.55021401954599,128.748213104701));
#186261=CARTESIAN_POINT('Ctrl Pts',(180.470062610586,5.60086662026004,128.896947797918));
#186262=CARTESIAN_POINT('Ctrl Pts',(180.477485981615,5.65159159578549,129.04589501024));
#186263=CARTESIAN_POINT('Ctrl Pts',(180.484909352643,5.69631314746229,129.196697323519));
#186264=CARTESIAN_POINT('Ctrl Pts',(180.492332723672,5.73492388620217,129.348826838512));
#186265=CARTESIAN_POINT('Ctrl Pts',(180.496268773113,5.75539622633393,129.429489557658));
#186266=CARTESIAN_POINT('Ctrl Pts',(180.500204822554,5.77415145806278,129.510525263669));
#186267=CARTESIAN_POINT('Ctrl Pts',(180.504140871994,5.79117948410592,129.591854640108));
#186268=CARTESIAN_POINT('Ctrl Pts',(180.5115641384,5.82329380979685,129.745239305871));
#186269=CARTESIAN_POINT('Ctrl Pts',(180.518987404805,5.84935868805641,129.900132653963));
#186270=CARTESIAN_POINT('Ctrl Pts',(180.526410671211,5.86923428957744,130.056016167097));
#186271=CARTESIAN_POINT('Ctrl Pts',(180.533825163932,5.88908639978802,130.211715438863));
#186272=CARTESIAN_POINT('Ctrl Pts',(180.541239656653,5.90276374747488,130.368402179512));
#186273=CARTESIAN_POINT('Ctrl Pts',(180.548654149374,5.91017705542789,130.525545739925));
#186274=CARTESIAN_POINT('Ctrl Pts',(180.556061495727,5.91758321815559,130.682537839459));
#186275=CARTESIAN_POINT('Ctrl Pts',(180.563468842081,5.91873734318499,130.839985511826));
#186276=CARTESIAN_POINT('Ctrl Pts',(180.570876188435,5.91360171383272,130.997351116438));
#186277=CARTESIAN_POINT('Ctrl Pts',(180.57827801011,5.90846991482658,131.154599351844));
#186278=CARTESIAN_POINT('Ctrl Pts',(180.585679831786,5.89705771424754,131.311765269877));
#186279=CARTESIAN_POINT('Ctrl Pts',(180.593081653461,5.87937943175644,131.468309455911));
#186280=CARTESIAN_POINT('Ctrl Pts',(180.600479567773,5.86171048149293,131.624771003489));
#186281=CARTESIAN_POINT('Ctrl Pts',(180.607877482084,5.83778207877467,131.780611102708));
#186282=CARTESIAN_POINT('Ctrl Pts',(180.615275396395,5.80766051783306,131.935293803967));
#186283=CARTESIAN_POINT('Ctrl Pts',(180.622672081308,5.77754396254863,132.089950799766));
#186284=CARTESIAN_POINT('Ctrl Pts',(180.63006876622,5.74123636296223,132.243450413284));
#186285=CARTESIAN_POINT('Ctrl Pts',(180.637465451132,5.69885544372551,132.395265138277));
#186286=CARTESIAN_POINT('Ctrl Pts',(180.644861808067,5.65647640370319,132.547073131647));
#186287=CARTESIAN_POINT('Ctrl Pts',(180.652258165003,5.60802467985748,132.697196025489));
#186288=CARTESIAN_POINT('Ctrl Pts',(180.659654521938,5.55366829783429,132.84512003507));
#186289=CARTESIAN_POINT('Ctrl Pts',(180.667052011275,5.49930359371009,132.993066692195));
#186290=CARTESIAN_POINT('Ctrl Pts',(180.674449500611,5.4390325601511,133.138813444321));
#186291=CARTESIAN_POINT('Ctrl Pts',(180.681846989948,5.37307187764845,133.281865241199));
#186292=CARTESIAN_POINT('Ctrl Pts',(180.689247072463,5.30708807273077,133.424967184663));
#186293=CARTESIAN_POINT('Ctrl Pts',(180.696647154978,5.23541080405183,133.56537195318));
#186294=CARTESIAN_POINT('Ctrl Pts',(180.704047237493,5.15830324904222,133.702608045482));
#186295=CARTESIAN_POINT('Ctrl Pts',(180.71145545716,5.08111090634927,133.839995042975));
#186296=CARTESIAN_POINT('Ctrl Pts',(180.718863676826,4.99847653549861,133.974206080262));
#186297=CARTESIAN_POINT('Ctrl Pts',(180.726271896493,4.91070768452162,134.104797043204));
#186298=CARTESIAN_POINT('Ctrl Pts',(180.733684675795,4.82288481328128,134.235468382706));
#186299=CARTESIAN_POINT('Ctrl Pts',(180.741097455097,4.72992138477512,134.362514907542));
#186300=CARTESIAN_POINT('Ctrl Pts',(180.748510234399,4.6321656429306,134.485525109809));
#186301=CARTESIAN_POINT('Ctrl Pts',(180.755933605427,4.53427022309773,134.608711074823));
#186302=CARTESIAN_POINT('Ctrl Pts',(180.763356976456,4.43156905705897,134.727848916707));
#186303=CARTESIAN_POINT('Ctrl Pts',(180.770780347485,4.32444823497244,134.842562943545));
#186304=CARTESIAN_POINT('Ctrl Pts',(180.774716396926,4.26765020477355,134.9033870731));
#186305=CARTESIAN_POINT('Ctrl Pts',(180.778652446367,4.20961023112803,134.962968159235));
#186306=CARTESIAN_POINT('Ctrl Pts',(180.782588495807,4.15038958737084,135.02125483435));
#186307=CARTESIAN_POINT('Ctrl Pts',(180.790011762213,4.03870130145738,135.131181684552));
#186308=CARTESIAN_POINT('Ctrl Pts',(180.797435028618,3.92247384426901,135.236834442952));
#186309=CARTESIAN_POINT('Ctrl Pts',(180.804858295024,3.80206787792984,135.337815195933));
#186310=CARTESIAN_POINT('Ctrl Pts',(180.812272787745,3.68180422144385,135.43867659805));
#186311=CARTESIAN_POINT('Ctrl Pts',(180.819687280466,3.5573721694491,135.534876748629));
#186312=CARTESIAN_POINT('Ctrl Pts',(180.827101773187,3.42916991556503,135.626053707414));
#186313=CARTESIAN_POINT('Ctrl Pts',(180.83450911954,3.30109122784012,135.717142786413));
#186314=CARTESIAN_POINT('Ctrl Pts',(180.841916465894,3.16924987469744,135.803218097274));
#186315=CARTESIAN_POINT('Ctrl Pts',(180.849323812248,3.03407780160299,135.883957300012));
#186316=CARTESIAN_POINT('Ctrl Pts',(180.856725633923,2.89900654493989,135.964636284407));
#186317=CARTESIAN_POINT('Ctrl Pts',(180.864127455599,2.76060983375698,136.039986894538));
#186318=CARTESIAN_POINT('Ctrl Pts',(180.871529277274,2.61934923298189,136.109729611159));
#186319=CARTESIAN_POINT('Ctrl Pts',(180.878927191586,2.47816320257805,136.179435511143));
#186320=CARTESIAN_POINT('Ctrl Pts',(180.886325105897,2.33411662733151,136.243539248482));
#186321=CARTESIAN_POINT('Ctrl Pts',(180.893723020208,2.18769625047188,136.301806904541));
#186322=CARTESIAN_POINT('Ctrl Pts',(180.901119705121,2.04130020602305,136.360064877571));
#186323=CARTESIAN_POINT('Ctrl Pts',(180.908516390033,1.8925314893964,136.412488556298));
#186324=CARTESIAN_POINT('Ctrl Pts',(180.915913074945,1.74189753958409,136.458891855794));
#186325=CARTESIAN_POINT('Ctrl Pts',(180.92330943188,1.59127026903901,136.505293097718));
#186326=CARTESIAN_POINT('Ctrl Pts',(180.930705788816,1.43877828651029,136.5456743813));
#186327=CARTESIAN_POINT('Ctrl Pts',(180.938102145751,1.28494467561209,136.579899358075));
#186328=CARTESIAN_POINT('Ctrl Pts',(180.945499635088,1.13108751239619,136.61412957478));
#186329=CARTESIAN_POINT('Ctrl Pts',(180.952897124424,0.97588867623078,136.642201526869));
#186330=CARTESIAN_POINT('Ctrl Pts',(180.960294613761,0.819881788008743,
136.664029927023));
#186331=CARTESIAN_POINT('Ctrl Pts',(180.967694696276,0.663820211813073,
136.685865979089));
#186332=CARTESIAN_POINT('Ctrl Pts',(180.975094778791,0.50695038905536,136.701454069904));
#186333=CARTESIAN_POINT('Ctrl Pts',(180.982494861306,0.34981126093449,136.710760760142));
#186334=CARTESIAN_POINT('Ctrl Pts',(180.989903080972,0.192499342187787,
136.720077684043));
#186335=CARTESIAN_POINT('Ctrl Pts',(180.997311300639,0.0349178995625732,
136.72309939146));
#186336=CARTESIAN_POINT('Ctrl Pts',(181.004719520305,-0.122393183915837,
136.719844576722));
#186337=CARTESIAN_POINT('Ctrl Pts',(181.012132299607,-0.279801089741335,
136.7165877587));
#186338=CARTESIAN_POINT('Ctrl Pts',(181.01954507891,-0.436937933096332,
136.707046743394));
#186339=CARTESIAN_POINT('Ctrl Pts',(181.026957858212,-0.593269266378005,
136.691292088211));
#186340=CARTESIAN_POINT('Ctrl Pts',(181.03438122924,-0.749823973199911,
136.675514922038));
#186341=CARTESIAN_POINT('Ctrl Pts',(181.041804600269,-0.905570502595506,
136.653506436043));
#186342=CARTESIAN_POINT('Ctrl Pts',(181.049227971298,-1.05998408315404,
136.625388388154));
#186343=CARTESIAN_POINT('Ctrl Pts',(181.053164020739,-1.14185786866959,
136.61047952448));
#186344=CARTESIAN_POINT('Ctrl Pts',(181.05710007018,-1.22335714732034,136.59385388328));
#186345=CARTESIAN_POINT('Ctrl Pts',(181.06103611962,-1.30440558235503,136.575535250101));
#186346=CARTESIAN_POINT('Ctrl Pts',(181.068459386026,-1.45726040139478,
136.540986879633));
#186347=CARTESIAN_POINT('Ctrl Pts',(181.075882652431,-1.60897283890215,
136.500309324795));
#186348=CARTESIAN_POINT('Ctrl Pts',(181.083305918837,-1.75901317219453,
136.453590938817));
#186349=CARTESIAN_POINT('Ctrl Pts',(181.090720411558,-1.90887617027225,
136.406927770093));
#186350=CARTESIAN_POINT('Ctrl Pts',(181.098134904279,-2.05707064500866,
136.354238091858));
#186351=CARTESIAN_POINT('Ctrl Pts',(181.105549397,-2.20307685243817,136.295661278134));
#186352=CARTESIAN_POINT('Ctrl Pts',(181.112956743353,-2.34894233358859,
136.237140922947));
#186353=CARTESIAN_POINT('Ctrl Pts',(181.120364089707,-2.49262340217373,
136.172744866634));
#186354=CARTESIAN_POINT('Ctrl Pts',(181.127771436061,-2.6336153873598,136.102662284512));
#186355=CARTESIAN_POINT('Ctrl Pts',(181.135173257736,-2.77450221540357,
136.032631972624));
#186356=CARTESIAN_POINT('Ctrl Pts',(181.142575079412,-2.91270362066783,
135.956923745224));
#186357=CARTESIAN_POINT('Ctrl Pts',(181.149976901087,-3.04773494857795,
135.875774842979));
#186358=CARTESIAN_POINT('Ctrl Pts',(181.157374815399,-3.1826949945026,135.794668778606));
#186359=CARTESIAN_POINT('Ctrl Pts',(181.16477272971,-3.31448797669285,135.708127951092));
#186360=CARTESIAN_POINT('Ctrl Pts',(181.172170644021,-3.44265399617015,
135.616435432566));
#186361=CARTESIAN_POINT('Ctrl Pts',(181.179567328934,-3.57079871677919,
135.524758151673));
#186362=CARTESIAN_POINT('Ctrl Pts',(181.186964013846,-3.69531736762194,
135.427931095897));
#186363=CARTESIAN_POINT('Ctrl Pts',(181.194360698758,-3.81577910700978,
135.326280604586));
#186364=CARTESIAN_POINT('Ctrl Pts',(181.201757055694,-3.93623550499821,
135.224634620564));
#186365=CARTESIAN_POINT('Ctrl Pts',(181.209153412629,-4.0526350639138,135.118165867008));
#186366=CARTESIAN_POINT('Ctrl Pts',(181.216549769564,-4.16458033046145,
135.007240729303));
#186367=CARTESIAN_POINT('Ctrl Pts',(181.223947258901,-4.27654273611478,
134.896298608676));
#186368=CARTESIAN_POINT('Ctrl Pts',(181.231344748238,-4.38404922633616,
134.78089900815));
#186369=CARTESIAN_POINT('Ctrl Pts',(181.238742237574,-4.48673961136266,
134.661444778215));
#186370=CARTESIAN_POINT('Ctrl Pts',(181.246142320089,-4.58946599434432,
134.541948673785));
#186371=CARTESIAN_POINT('Ctrl Pts',(181.253542402604,-4.68737266758336,
134.418395392961));
#186372=CARTESIAN_POINT('Ctrl Pts',(181.260942485119,-4.78014018674565,
134.291220287464));
#186373=CARTESIAN_POINT('Ctrl Pts',(181.268350704786,-4.87300971333234,
134.163905339864));
#186374=CARTESIAN_POINT('Ctrl Pts',(181.275758924452,-4.96072858024092,
134.032960915913));
#186375=CARTESIAN_POINT('Ctrl Pts',(181.283167144119,-5.04302069557768,
133.898851339232));
#186376=CARTESIAN_POINT('Ctrl Pts',(181.290579923421,-5.12536346033855,
133.764659220344));
#186377=CARTESIAN_POINT('Ctrl Pts',(181.297992702723,-5.20227263606082,
133.627298391857));
#186378=CARTESIAN_POINT('Ctrl Pts',(181.305405482025,-5.27351870270403,
133.487256637678));
#186379=CARTESIAN_POINT('Ctrl Pts',(181.312828853054,-5.34486656906833,
133.347014785273));
#186380=CARTESIAN_POINT('Ctrl Pts',(181.320252224083,-5.4105350099472,133.204084694854));
#186381=CARTESIAN_POINT('Ctrl Pts',(181.327675595111,-5.47034281196722,
133.058973684604));
#186382=CARTESIAN_POINT('Ctrl Pts',(181.331611644552,-5.50205434366603,
132.982032345081));
#186383=CARTESIAN_POINT('Ctrl Pts',(181.335547693993,-5.53211907170173,
132.904478128601));
#186384=CARTESIAN_POINT('Ctrl Pts',(181.339483743433,-5.56051574565194,
132.826388116107));
#186385=CARTESIAN_POINT('Ctrl Pts',(181.348080014218,-5.622533640077,132.655840742883));
#186386=CARTESIAN_POINT('Ctrl Pts',(181.356676285003,-5.67674712583689,
132.482312359138));
#186387=CARTESIAN_POINT('Ctrl Pts',(181.365272555788,-5.7229002646624,132.306473503879));
#186388=CARTESIAN_POINT('Ctrl Pts',(181.373836240798,-5.76887845136683,
132.13130119875));
#186389=CARTESIAN_POINT('Ctrl Pts',(181.382399925807,-5.8068571937891,131.953836020863));
#186390=CARTESIAN_POINT('Ctrl Pts',(181.390963610817,-5.83663002103799,
131.774762884679));
#186391=CARTESIAN_POINT('Ctrl Pts',(181.399463586485,-5.86618135400975,
131.597021959055));
#186392=CARTESIAN_POINT('Ctrl Pts',(181.407963562153,-5.88764834009424,
131.417697041437));
#186393=CARTESIAN_POINT('Ctrl Pts',(181.416463537821,-5.90087621830845,
131.237477713398));
#186394=CARTESIAN_POINT('Ctrl Pts',(181.423183949748,-5.91133469418984,
131.094989291209));
#186395=CARTESIAN_POINT('Ctrl Pts',(181.429904361675,-5.91664371146173,
130.95194217167));
#186396=CARTESIAN_POINT('Ctrl Pts',(181.436624773602,-5.91674841954496,
130.808685234569));
#186397=CARTESIAN_POINT('',(183.186624807795,-5.9097261727316,130.800419732287));
#186398=CARTESIAN_POINT('Ctrl Pts',(181.436624807795,-5.91046065331948,
130.808679910655));
#186399=CARTESIAN_POINT('Ctrl Pts',(181.497060327612,-5.90180348691877,
129.521756724088));
#186400=CARTESIAN_POINT('Ctrl Pts',(181.650311722033,-4.85487069311502,
126.24557662955));
#186401=CARTESIAN_POINT('Ctrl Pts',(181.89637899106,0.558585749835051,123.828291345372));
#186402=CARTESIAN_POINT('Ctrl Pts',(182.174826614872,6.17109389324245,127.503578787286));
#186403=CARTESIAN_POINT('Ctrl Pts',(182.453274238685,6.11266822346165,134.212123479067));
#186404=CARTESIAN_POINT('Ctrl Pts',(182.731721862497,0.436999076760051,
137.789100579601));
#186405=CARTESIAN_POINT('Ctrl Pts',(182.976172052201,-4.89824093256168,
135.294398866638));
#186406=CARTESIAN_POINT('Ctrl Pts',(183.1278063673,-5.90209859011289,132.053299422131));
#186407=CARTESIAN_POINT('Ctrl Pts',(183.186624807795,-5.9097261727316,130.800419732287));
#186408=CARTESIAN_POINT('',(184.936624807795,-5.92486718842363,130.801517542038));
#186409=CARTESIAN_POINT('Ctrl Pts',(183.186624807795,-5.9097261727316,130.800419732287));
#186410=CARTESIAN_POINT('Ctrl Pts',(183.220622241905,-5.91413496418055,
130.076247273033));
#186411=CARTESIAN_POINT('Ctrl Pts',(183.347435550617,-5.4548282023846,127.380421002293));
#186412=CARTESIAN_POINT('Ctrl Pts',(183.567064733937,-1.42373941229825,
123.952315184543));
#186413=CARTESIAN_POINT('Ctrl Pts',(183.845512357749,4.99525395369783,125.90283040054));
#186414=CARTESIAN_POINT('Ctrl Pts',(184.123959981563,6.82385296796736,132.357612432922));
#186415=CARTESIAN_POINT('Ctrl Pts',(184.402407605375,2.38166446842562,137.385031927559));
#186416=CARTESIAN_POINT('Ctrl Pts',(184.673295880787,-4.06914253102304,
136.392824298985));
#186417=CARTESIAN_POINT('Ctrl Pts',(184.851368281593,-5.91419482002716,
132.605670887374));
#186418=CARTESIAN_POINT('Ctrl Pts',(184.936624807795,-5.92486718842363,
130.801517542038));
#186419=CARTESIAN_POINT('',(186.686624807795,-5.91810304431807,130.809680029163));
#186420=CARTESIAN_POINT('Ctrl Pts',(184.936624807795,-5.92486718842363,
130.801517542038));
#186421=CARTESIAN_POINT('Ctrl Pts',(184.944184156197,-5.92581346379487,
130.641550624367));
#186422=CARTESIAN_POINT('Ctrl Pts',(185.044559379204,-5.84727879099301,
128.518407035367));
#186423=CARTESIAN_POINT('Ctrl Pts',(185.237750476814,-3.29138665363019,
124.628250642296));
#186424=CARTESIAN_POINT('Ctrl Pts',(185.516198100626,3.4170613558443,124.696885507443));
#186425=CARTESIAN_POINT('Ctrl Pts',(185.794645724439,6.98539691202545,130.377991632052));
#186426=CARTESIAN_POINT('Ctrl Pts',(186.073093348252,4.13449396166582,136.450910025061));
#186427=CARTESIAN_POINT('Ctrl Pts',(186.351540972065,-2.5158069582057,137.334925361857));
#186428=CARTESIAN_POINT('Ctrl Pts',(186.55605145858,-5.7022149293107,133.576472626177));
#186429=CARTESIAN_POINT('Ctrl Pts',(186.667746070489,-5.92222955506447,
131.210299569289));
#186430=CARTESIAN_POINT('Ctrl Pts',(186.686624807795,-5.91851213263273,
130.809680396867));
#186431=CARTESIAN_POINT('',(188.436624807759,-5.91674998742092,130.804746434304));
#186432=CARTESIAN_POINT('Ctrl Pts',(186.686624807795,-5.91674760990531,
130.809678810848));
#186433=CARTESIAN_POINT('Ctrl Pts',(186.693927872074,-5.91688686513407,
130.654750624113));
#186434=CARTESIAN_POINT('Ctrl Pts',(186.701230936354,-5.91093684901184,
130.499626658566));
#186435=CARTESIAN_POINT('Ctrl Pts',(186.708534000633,-5.89887823475046,
130.344832452937));
#186436=CARTESIAN_POINT('Ctrl Pts',(186.71583126983,-5.88682918916652,130.190161078655));
#186437=CARTESIAN_POINT('Ctrl Pts',(186.723128539027,-5.86868122137412,
130.035819325382));
#186438=CARTESIAN_POINT('Ctrl Pts',(186.730425808224,-5.84446706708341,
129.882332817401));
#186439=CARTESIAN_POINT('Ctrl Pts',(186.737842908702,-5.81985528279573,
129.726325848082));
#186440=CARTESIAN_POINT('Ctrl Pts',(186.745260009179,-5.78897632400346,
129.57120286325));
#186441=CARTESIAN_POINT('Ctrl Pts',(186.752677109657,-5.75191958714079,
129.417511085149));
#186442=CARTESIAN_POINT('Ctrl Pts',(186.759968840886,-5.71548921030546,
129.266417117715));
#186443=CARTESIAN_POINT('Ctrl Pts',(186.767260572116,-5.67308835349849,
129.116706741788));
#186444=CARTESIAN_POINT('Ctrl Pts',(186.774552303345,-5.62485348468246,
128.968889604895));
#186445=CARTESIAN_POINT('Ctrl Pts',(186.781843715033,-5.57662072963386,
128.821078945703));
#186446=CARTESIAN_POINT('Ctrl Pts',(186.789135126721,-5.52255459037707,
128.675161726577));
#186447=CARTESIAN_POINT('Ctrl Pts',(186.796426538409,-5.46284118724312,
128.531631701602));
#186448=CARTESIAN_POINT('Ctrl Pts',(186.803719166403,-5.40311782310642,
128.388077733878));
#186449=CARTESIAN_POINT('Ctrl Pts',(186.811011794397,-5.33774546886925,
128.246912107963));
#186450=CARTESIAN_POINT('Ctrl Pts',(186.818304422391,-5.26695796755661,
128.108607600227));
#186451=CARTESIAN_POINT('Ctrl Pts',(186.8258154055,-5.19405095418979,127.966161993203));
#186452=CARTESIAN_POINT('Ctrl Pts',(186.833326388608,-5.11539964036747,
127.826751909787));
#186453=CARTESIAN_POINT('Ctrl Pts',(186.840837371716,-5.03130930734334,
127.690864637748));
#186454=CARTESIAN_POINT('Ctrl Pts',(186.84814077682,-4.949542944875,127.558732827339));
#186455=CARTESIAN_POINT('Ctrl Pts',(186.855444181923,-4.86263449198645,
127.429931967507));
#186456=CARTESIAN_POINT('Ctrl Pts',(186.862747587026,-4.77090702822886,
127.30487827149));
#186457=CARTESIAN_POINT('Ctrl Pts',(186.870362359137,-4.6752689357269,127.174493145188));
#186458=CARTESIAN_POINT('Ctrl Pts',(186.877977131248,-4.57439219292684,
127.048182094909));
#186459=CARTESIAN_POINT('Ctrl Pts',(186.885591903359,-4.46868683856503,
126.926375509119));
#186460=CARTESIAN_POINT('Ctrl Pts',(186.89320667547,-4.3629814842032,126.80456892333));
#186461=CARTESIAN_POINT('Ctrl Pts',(186.900821447581,-4.25244789244555,
126.687267089292));
#186462=CARTESIAN_POINT('Ctrl Pts',(186.908436219692,-4.13753558760197,
126.574853574916));
#186463=CARTESIAN_POINT('Ctrl Pts',(186.915859486097,-4.02551323950221,
126.465267174611));
#186464=CARTESIAN_POINT('Ctrl Pts',(186.923282752503,-3.9089647500179,126.359968661986));
#186465=CARTESIAN_POINT('Ctrl Pts',(186.930706018908,-3.78825199071475,
126.259354851085));
#186466=CARTESIAN_POINT('Ctrl Pts',(186.938120511629,-3.66768190386831,
126.158859957352));
#186467=CARTESIAN_POINT('Ctrl Pts',(186.94553500435,-3.54295762806711,126.063038980729));
#186468=CARTESIAN_POINT('Ctrl Pts',(186.952949497071,-3.4144784567078,125.972252647831));
#186469=CARTESIAN_POINT('Ctrl Pts',(186.960356843425,-3.28612311841112,
125.881553818218));
#186470=CARTESIAN_POINT('Ctrl Pts',(186.967764189779,-3.15402039231062,
125.795880185779));
#186471=CARTESIAN_POINT('Ctrl Pts',(186.975171536132,-3.01860320296358,
125.715552774313));
#186472=CARTESIAN_POINT('Ctrl Pts',(186.982573357808,-2.88328701286552,
125.63528527406));
#186473=CARTESIAN_POINT('Ctrl Pts',(186.989975179483,-2.74466160138934,
125.560356244931));
#186474=CARTESIAN_POINT('Ctrl Pts',(186.997377001159,-2.60318938208514,
125.491043800031));
#186475=CARTESIAN_POINT('Ctrl Pts',(187.00477491547,-2.46179184486368,125.421767944631));
#186476=CARTESIAN_POINT('Ctrl Pts',(187.012172829781,-2.3175508271054,125.358102932441));
#186477=CARTESIAN_POINT('Ctrl Pts',(187.019570744093,-2.17095378175324,
125.300281199535));
#186478=CARTESIAN_POINT('Ctrl Pts',(187.026967429005,-2.02438109817091,
125.242469075553));
#186479=CARTESIAN_POINT('Ctrl Pts',(187.034364113917,-1.87545351098578,
125.190498440448));
#186480=CARTESIAN_POINT('Ctrl Pts',(187.041760798829,-1.72467902321808,
125.144553833817));
#186481=CARTESIAN_POINT('Ctrl Pts',(187.049157155765,-1.573911220949,125.098611264417));
#186482=CARTESIAN_POINT('Ctrl Pts',(187.0565535127,-1.42129703801589,125.058694301019));
#186483=CARTESIAN_POINT('Ctrl Pts',(187.063949869636,-1.2673599706079,125.024937699367));
#186484=CARTESIAN_POINT('Ctrl Pts',(187.071347358972,-1.11339933504184,
124.991175929494));
#186485=CARTESIAN_POINT('Ctrl Pts',(187.078744848309,-0.958115776379954,
124.963576479304));
#186486=CARTESIAN_POINT('Ctrl Pts',(187.086142337645,-0.802043172628662,
124.942223011561));
#186487=CARTESIAN_POINT('Ctrl Pts',(187.09354242016,-0.645915857868791,
124.920862058393));
#186488=CARTESIAN_POINT('Ctrl Pts',(187.100942502675,-0.488999316935465,
124.905751497561));
#186489=CARTESIAN_POINT('Ctrl Pts',(187.10834258519,-0.331832590309043,
124.896923127883));
#186490=CARTESIAN_POINT('Ctrl Pts',(187.115750804857,-0.174493042708975,
124.888085050506));
#186491=CARTESIAN_POINT('Ctrl Pts',(187.123159024523,-0.016903132952331,
124.885542980791));
#186492=CARTESIAN_POINT('Ctrl Pts',(187.13056724419,0.140397315335382,124.889276581278));
#186493=CARTESIAN_POINT('Ctrl Pts',(187.137980023492,0.297794579424681,
124.893012479734));
#186494=CARTESIAN_POINT('Ctrl Pts',(187.145392802794,0.454901655364147,
124.903031721345));
#186495=CARTESIAN_POINT('Ctrl Pts',(187.152805582096,0.611184312778971,
124.919262122357));
#186496=CARTESIAN_POINT('Ctrl Pts',(187.160228953124,0.767690274183362,
124.935515714127));
#186497=CARTESIAN_POINT('Ctrl Pts',(187.167652324153,0.923369095910833,
124.957998137041));
#186498=CARTESIAN_POINT('Ctrl Pts',(187.175075695182,1.07769637957054,124.986586036512));
#186499=CARTESIAN_POINT('Ctrl Pts',(187.179011744623,1.15952440839869,125.001744026769));
#186500=CARTESIAN_POINT('Ctrl Pts',(187.182947794064,1.24097270681647,125.01861764673));
#186501=CARTESIAN_POINT('Ctrl Pts',(187.186883843504,1.32196501082129,125.037182878614));
#186502=CARTESIAN_POINT('Ctrl Pts',(187.19430710991,1.47471396849223,125.072196326546));
#186503=CARTESIAN_POINT('Ctrl Pts',(187.201730376315,1.62630189479336,125.113335453442));
#186504=CARTESIAN_POINT('Ctrl Pts',(187.209153642721,1.77619933841254,125.160510294185));
#186505=CARTESIAN_POINT('Ctrl Pts',(187.216568135442,1.92591961570148,125.207629378185));
#186506=CARTESIAN_POINT('Ctrl Pts',(187.223982628163,2.07395303475566,125.260769865369));
#186507=CARTESIAN_POINT('Ctrl Pts',(187.231397120884,2.21978027822349,125.319790800442));
#186508=CARTESIAN_POINT('Ctrl Pts',(187.238804467237,2.36546696790406,125.378754848915));
#186509=CARTESIAN_POINT('Ctrl Pts',(187.246211813591,2.50895137152433,125.443587922699));
#186510=CARTESIAN_POINT('Ctrl Pts',(187.253619159945,2.64972939637269,125.514099311307));
#186511=CARTESIAN_POINT('Ctrl Pts',(187.26102098162,2.79040242365833,125.584558109861));
#186512=CARTESIAN_POINT('Ctrl Pts',(187.268422803296,2.92837275898145,125.660686624124));
#186513=CARTESIAN_POINT('Ctrl Pts',(187.275824624971,3.0631564720913,125.742246139407));
#186514=CARTESIAN_POINT('Ctrl Pts',(187.283222539282,3.19786903392806,125.823762600057));
#186515=CARTESIAN_POINT('Ctrl Pts',(187.290620453594,3.3293980051506,125.910704159221));
#186516=CARTESIAN_POINT('Ctrl Pts',(187.298018367905,3.45728435048477,126.002786346309));
#186517=CARTESIAN_POINT('Ctrl Pts',(187.305415052817,3.58514944342875,126.094853231009));
#186518=CARTESIAN_POINT('Ctrl Pts',(187.31281173773,3.70937280925888,126.192058830229));
#186519=CARTESIAN_POINT('Ctrl Pts',(187.320208422642,3.82952460154685,126.2940754948));
#186520=CARTESIAN_POINT('Ctrl Pts',(187.327604779577,3.94967106617857,126.396087635844));
#186521=CARTESIAN_POINT('Ctrl Pts',(187.335001136513,4.06574603167699,126.502910176461));
#186522=CARTESIAN_POINT('Ctrl Pts',(187.342397493448,4.17735316173905,126.614175523252));
#186523=CARTESIAN_POINT('Ctrl Pts',(187.349794982785,4.28897737913757,126.725457905052));
#186524=CARTESIAN_POINT('Ctrl Pts',(187.357192472121,4.39613213470813,126.841184183831));
#186525=CARTESIAN_POINT('Ctrl Pts',(187.364589961458,4.4984584664945,126.96095041467));
#186526=CARTESIAN_POINT('Ctrl Pts',(187.371990043973,4.6008206686173,127.080758629375));
#186527=CARTESIAN_POINT('Ctrl Pts',(187.379390126488,4.69835083467273,127.204609332144));
#186528=CARTESIAN_POINT('Ctrl Pts',(187.386790209003,4.79073084686722,127.332066200991));
#186529=CARTESIAN_POINT('Ctrl Pts',(187.394198428669,4.88321244038255,127.45966322177));
#186530=CARTESIAN_POINT('Ctrl Pts',(187.401606648336,4.97053235119977,127.590874025252));
#186531=CARTESIAN_POINT('Ctrl Pts',(187.409014868002,5.05241590194538,127.725233449638));
#186532=CARTESIAN_POINT('Ctrl Pts',(187.416427647304,5.13434985065019,127.859675570009));
#186533=CARTESIAN_POINT('Ctrl Pts',(187.423840426606,5.21084059102242,127.997269847324));
#186534=CARTESIAN_POINT('Ctrl Pts',(187.431253205909,5.28166008873117,128.137527801358));
#186535=CARTESIAN_POINT('Ctrl Pts',(187.438676576937,5.35258077665936,128.277986162534));
#186536=CARTESIAN_POINT('Ctrl Pts',(187.446099947966,5.41781388333707,128.421115463055));
#186537=CARTESIAN_POINT('Ctrl Pts',(187.453523318995,5.47717974033229,128.566407835537));
#186538=CARTESIAN_POINT('Ctrl Pts',(187.457459368436,5.50865694217581,128.64344533767));
#186539=CARTESIAN_POINT('Ctrl Pts',(187.461395417877,5.53848548259736,128.721090701616));
#186540=CARTESIAN_POINT('Ctrl Pts',(187.465331467317,5.56664434588085,128.799266782113));
#186541=CARTESIAN_POINT('Ctrl Pts',(187.472754733723,5.61975108322465,128.946704430135));
#186542=CARTESIAN_POINT('Ctrl Pts',(187.480178000128,5.66707654755361,129.096476348691));
#186543=CARTESIAN_POINT('Ctrl Pts',(187.487601266534,5.70841024769987,129.248088467055));
#186544=CARTESIAN_POINT('Ctrl Pts',(187.495015759255,5.74969509484514,129.399521392486));
#186545=CARTESIAN_POINT('Ctrl Pts',(187.502430251976,5.78500217687627,129.552789831813));
#186546=CARTESIAN_POINT('Ctrl Pts',(187.509844744697,5.81416937976279,129.707380678858));
#186547=CARTESIAN_POINT('Ctrl Pts',(187.517252091051,5.84330847020106,129.861822525424));
#186548=CARTESIAN_POINT('Ctrl Pts',(187.524659437404,5.86631939401667,130.017583877895));
#186549=CARTESIAN_POINT('Ctrl Pts',(187.532066783758,5.88309012691937,130.17413754512));
#186550=CARTESIAN_POINT('Ctrl Pts',(187.539468605433,5.89984835157674,130.330574448713));
#186551=CARTESIAN_POINT('Ctrl Pts',(187.546870427109,5.91037561281063,130.487802120845));
#186552=CARTESIAN_POINT('Ctrl Pts',(187.554272248784,5.91461117192879,130.64528438617));
#186553=CARTESIAN_POINT('Ctrl Pts',(187.561670163096,5.91884449512825,130.802683517833));
#186554=CARTESIAN_POINT('Ctrl Pts',(187.569068077407,5.91679272080989,130.960336602811));
#186555=CARTESIAN_POINT('Ctrl Pts',(187.576465991718,5.90844706236015,131.117703678424));
#186556=CARTESIAN_POINT('Ctrl Pts',(187.583862676631,5.90010279080743,131.275044602484));
#186557=CARTESIAN_POINT('Ctrl Pts',(187.591259361543,5.88546673073356,131.432099239102));
#186558=CARTESIAN_POINT('Ctrl Pts',(187.598656046455,5.86458220017064,131.588328843926));
#186559=CARTESIAN_POINT('Ctrl Pts',(187.60605240339,5.84369859564966,131.744551521365));
#186560=CARTESIAN_POINT('Ctrl Pts',(187.613448760326,5.81656712099775,131.899948869742));
#186561=CARTESIAN_POINT('Ctrl Pts',(187.620845117261,5.78328281349836,132.053988746889));
#186562=CARTESIAN_POINT('Ctrl Pts',(187.628242606598,5.74999341008647,132.208052207934));
#186563=CARTESIAN_POINT('Ctrl Pts',(187.635640095934,5.71054937699733,132.360757419028));
#186564=CARTESIAN_POINT('Ctrl Pts',(187.643037585271,5.66509653682644,132.511584033214));
#186565=CARTESIAN_POINT('Ctrl Pts',(187.650437667786,5.61962776323287,132.662463519436));
#186566=CARTESIAN_POINT('Ctrl Pts',(187.657837750301,5.56814609641887,132.811462740405));
#186567=CARTESIAN_POINT('Ctrl Pts',(187.665237832816,5.51084667598898,132.958078211923));
#186568=CARTESIAN_POINT('Ctrl Pts',(187.672646052482,5.45348424895594,133.104854902223));
#186569=CARTESIAN_POINT('Ctrl Pts',(187.680054272149,5.39029142860743,133.249242260506));
#186570=CARTESIAN_POINT('Ctrl Pts',(187.687462491815,5.3215110989095,133.390757761603));
#186571=CARTESIAN_POINT('Ctrl Pts',(187.694875271117,5.2526884360661,133.53236036313));
#186572=CARTESIAN_POINT('Ctrl Pts',(187.702288050419,5.17827158724947,133.671087257152));
#186573=CARTESIAN_POINT('Ctrl Pts',(187.709700829722,5.09854826658263,133.806482556433));
#186574=CARTESIAN_POINT('Ctrl Pts',(187.71712420075,5.01871103349667,133.942071314867));
#186575=CARTESIAN_POINT('Ctrl Pts',(187.724547571779,4.93355238690208,134.074318658072));
#186576=CARTESIAN_POINT('Ctrl Pts',(187.731970942808,4.84340249483737,134.20279891118));
#186577=CARTESIAN_POINT('Ctrl Pts',(187.735906992249,4.79560285894802,134.270922224219));
#186578=CARTESIAN_POINT('Ctrl Pts',(187.739843041689,4.74640066993037,134.337987035869));
#186579=CARTESIAN_POINT('Ctrl Pts',(187.74377909113,4.69584947277127,134.403933966114));
#186580=CARTESIAN_POINT('Ctrl Pts',(187.751202357536,4.6005114925774,134.528307818423));
#186581=CARTESIAN_POINT('Ctrl Pts',(187.758625623941,4.50008470519337,134.649079452252));
#186582=CARTESIAN_POINT('Ctrl Pts',(187.766048890346,4.39487101069584,134.765804718124));
#186583=CARTESIAN_POINT('Ctrl Pts',(187.773463383067,4.28978167004782,134.882392024425));
#186584=CARTESIAN_POINT('Ctrl Pts',(187.780877875788,4.17991693151612,134.994942207732));
#186585=CARTESIAN_POINT('Ctrl Pts',(187.788292368509,4.06562085926568,135.103041530498));
#186586=CARTESIAN_POINT('Ctrl Pts',(187.795699714863,3.95143494987295,135.211036663066));
#186587=CARTESIAN_POINT('Ctrl Pts',(187.803107061217,3.83282647904385,135.314589220668));
#186588=CARTESIAN_POINT('Ctrl Pts',(187.810514407571,3.71017843575953,135.413319994402));
#186589=CARTESIAN_POINT('Ctrl Pts',(187.817916229246,3.58762186801298,135.511977131));
#186590=CARTESIAN_POINT('Ctrl Pts',(187.825318050921,3.4610320163687,135.60581941131));
#186591=CARTESIAN_POINT('Ctrl Pts',(187.832719872597,3.33082714958386,135.69450591828));
#186592=CARTESIAN_POINT('Ctrl Pts',(187.840117786908,3.20069101693379,135.783145608334));
#186593=CARTESIAN_POINT('Ctrl Pts',(187.847515701219,3.06694397743706,135.866634735812));
#186594=CARTESIAN_POINT('Ctrl Pts',(187.854913615531,2.93003556760929,135.944674045271));
#186595=CARTESIAN_POINT('Ctrl Pts',(187.862310300443,2.79314990947657,136.022700386012));
#186596=CARTESIAN_POINT('Ctrl Pts',(187.869706985355,2.65310424769539,136.095278521522));
#186597=CARTESIAN_POINT('Ctrl Pts',(187.877103670267,2.51037525760295,136.162153692006));
#186598=CARTESIAN_POINT('Ctrl Pts',(187.884500027203,2.36765259626331,136.229025897175));
#186599=CARTESIAN_POINT('Ctrl Pts',(187.891896384138,2.22224718122004,136.290195481735));
#186600=CARTESIAN_POINT('Ctrl Pts',(187.899292741074,2.0746580887224,136.345454767407));
#186601=CARTESIAN_POINT('Ctrl Pts',(187.90669023041,1.92704639995784,136.400722513416));
#186602=CARTESIAN_POINT('Ctrl Pts',(187.914087719747,1.77725071766979,136.450078027893));
#186603=CARTESIAN_POINT('Ctrl Pts',(187.921485209083,1.62578764516406,136.493362735278));
#186604=CARTESIAN_POINT('Ctrl Pts',(187.928885291598,1.47427147751353,136.53666261605));
#186605=CARTESIAN_POINT('Ctrl Pts',(187.936285374113,1.32108711461301,136.573887350165));
#186606=CARTESIAN_POINT('Ctrl Pts',(187.943685456628,1.16676362970169,136.60492896859));
#186607=CARTESIAN_POINT('Ctrl Pts',(187.951093676295,1.01227045025355,136.636004720467));
#186608=CARTESIAN_POINT('Ctrl Pts',(187.958501895961,0.856636013498965,
136.660883705003));
#186609=CARTESIAN_POINT('Ctrl Pts',(187.965910115627,0.700397566244245,
136.679509450719));
#186610=CARTESIAN_POINT('Ctrl Pts',(187.973322894929,0.544062956832329,
136.698146660271));
#186611=CARTESIAN_POINT('Ctrl Pts',(187.980735674231,0.387123967424787,
136.710522932578));
#186612=CARTESIAN_POINT('Ctrl Pts',(187.988148453534,0.23011966537511,136.716633911495));
#186613=CARTESIAN_POINT('Ctrl Pts',(187.995571824562,0.072891028215697,
136.722753622065));
#186614=CARTESIAN_POINT('Ctrl Pts',(188.002995195591,-0.0844027356615752,
136.72259016019));
#186615=CARTESIAN_POINT('Ctrl Pts',(188.01041856662,-0.241225030045429,
136.716191217928));
#186616=CARTESIAN_POINT('Ctrl Pts',(188.014354616061,-0.324375973428068,
136.7127983452));
#186617=CARTESIAN_POINT('Ctrl Pts',(188.018290665501,-0.407394483839031,
136.707653318947));
#186618=CARTESIAN_POINT('Ctrl Pts',(188.022226714942,-0.490201660815617,
136.700769091733));
#186619=CARTESIAN_POINT('Ctrl Pts',(188.029649981348,-0.646373412268205,
136.687785654058));
#186620=CARTESIAN_POINT('Ctrl Pts',(188.037073247753,-0.80226513988054,
136.668573771693));
#186621=CARTESIAN_POINT('Ctrl Pts',(188.044496514159,-0.957339983753277,
136.643147368083));
#186622=CARTESIAN_POINT('Ctrl Pts',(188.051911006879,-1.11223154203839,
136.61775101637));
#186623=CARTESIAN_POINT('Ctrl Pts',(188.0593254996,-1.26630777361279,136.58615482358));
#186624=CARTESIAN_POINT('Ctrl Pts',(188.066739992321,-1.41903461427524,
136.548424625391));
#186625=CARTESIAN_POINT('Ctrl Pts',(188.074147338675,-1.57161425105952,
136.510730792987));
#186626=CARTESIAN_POINT('Ctrl Pts',(188.081554685029,-1.72284672618799,
136.466914814107));
#186627=CARTESIAN_POINT('Ctrl Pts',(188.088962031383,-1.87220598557174,
136.417093936555));
#186628=CARTESIAN_POINT('Ctrl Pts',(188.096363853058,-2.02145384718316,
136.367310217293));
#186629=CARTESIAN_POINT('Ctrl Pts',(188.103765674734,-2.16883092230147,
136.311530634628));
#186630=CARTESIAN_POINT('Ctrl Pts',(188.111167496409,-2.31382430327432,
136.249922815914));
#186631=CARTESIAN_POINT('Ctrl Pts',(188.11856541072,-2.45874114337115,136.188347519488));
#186632=CARTESIAN_POINT('Ctrl Pts',(188.125963325032,-2.60127645265397,
136.120950259984));
#186633=CARTESIAN_POINT('Ctrl Pts',(188.133361239343,-2.7409354735747,136.047947490328));
#186634=CARTESIAN_POINT('Ctrl Pts',(188.140757924255,-2.88057128569987,
135.974956852407));
#186635=CARTESIAN_POINT('Ctrl Pts',(188.148154609167,-3.01733142762264,
135.896362725914));
#186636=CARTESIAN_POINT('Ctrl Pts',(188.15555129408,-3.1507439080487,135.812428447418));
#186637=CARTESIAN_POINT('Ctrl Pts',(188.162947651015,-3.28415047282601,
135.728497890655));
#186638=CARTESIAN_POINT('Ctrl Pts',(188.170344007951,-3.41420935528581,
135.639227851488));
#186639=CARTESIAN_POINT('Ctrl Pts',(188.177740364886,-3.54047606690486,
135.544925961718));
#186640=CARTESIAN_POINT('Ctrl Pts',(188.185137854223,-3.66676211027926,
135.450609634088));
#186641=CARTESIAN_POINT('Ctrl Pts',(188.192535343559,-3.78925452766934,
135.351260145295));
#186642=CARTESIAN_POINT('Ctrl Pts',(188.199932832896,-3.90754066825958,
135.247226414368));
#186643=CARTESIAN_POINT('Ctrl Pts',(188.207332915411,-4.02586827387267,
135.143156214579));
#186644=CARTESIAN_POINT('Ctrl Pts',(188.214732997926,-4.13998638682651,
135.034398749718));
#186645=CARTESIAN_POINT('Ctrl Pts',(188.222133080441,-4.24951819270741,
134.921340784187));
#186646=CARTESIAN_POINT('Ctrl Pts',(188.229541300107,-4.35917044006939,
134.808158499799));
#186647=CARTESIAN_POINT('Ctrl Pts',(188.236949519774,-4.4642260490177,134.690666539206));
#186648=CARTESIAN_POINT('Ctrl Pts',(188.24435773944,-4.56434711347478,134.569286379147));
#186649=CARTESIAN_POINT('Ctrl Pts',(188.251770518742,-4.66452980077634,
134.447831511624));
#186650=CARTESIAN_POINT('Ctrl Pts',(188.259183298044,-4.75977166640558,
134.322483972582));
#186651=CARTESIAN_POINT('Ctrl Pts',(188.266596077347,-4.84977766634151,
134.193694940048));
#186652=CARTESIAN_POINT('Ctrl Pts',(188.274019448375,-4.93991227107106,
134.064721887705));
#186653=CARTESIAN_POINT('Ctrl Pts',(188.281442819404,-5.02479586745561,
133.932297834228));
#186654=CARTESIAN_POINT('Ctrl Pts',(188.288866190433,-5.10417853681512,
133.796900011929));
#186655=CARTESIAN_POINT('Ctrl Pts',(188.292802239874,-5.14626913287155,
133.725108837719));
#186656=CARTESIAN_POINT('Ctrl Pts',(188.296738289315,-5.18681400928749,
133.652482001339));
#186657=CARTESIAN_POINT('Ctrl Pts',(188.300674338755,-5.22578141579513,
133.579092885161));
#186658=CARTESIAN_POINT('Ctrl Pts',(188.308522635262,-5.30348058216972,
133.432758457005));
#186659=CARTESIAN_POINT('Ctrl Pts',(188.316370931769,-5.37511838685106,
133.282990724991));
#186660=CARTESIAN_POINT('Ctrl Pts',(188.324219228275,-5.44039662476336,
133.130304539453));
#186661=CARTESIAN_POINT('Ctrl Pts',(188.332053990155,-5.50556228836188,
132.977881665902));
#186662=CARTESIAN_POINT('Ctrl Pts',(188.339888752035,-5.56439012663925,
132.822550655319));
#186663=CARTESIAN_POINT('Ctrl Pts',(188.347723513915,-5.61662765213832,
132.664850977588));
#186664=CARTESIAN_POINT('Ctrl Pts',(188.355539641514,-5.6687409353559,132.507526374433));
#186665=CARTESIAN_POINT('Ctrl Pts',(188.363355769114,-5.71429507358988,
132.347844634376));
#186666=CARTESIAN_POINT('Ctrl Pts',(188.371171896713,-5.75308575484795,
132.1863645466));
#186667=CARTESIAN_POINT('Ctrl Pts',(188.378976980979,-5.7918216291147,132.025112612533));
#186668=CARTESIAN_POINT('Ctrl Pts',(188.386782065244,-5.82381301965768,
131.862067694374));
#186669=CARTESIAN_POINT('Ctrl Pts',(188.39458714951,-5.8489048080885,131.697805136503));
#186670=CARTESIAN_POINT('Ctrl Pts',(188.402376866656,-5.87394719429565,
131.533865988645));
#186671=CARTESIAN_POINT('Ctrl Pts',(188.410166583802,-5.89211702687552,
131.368714288067));
#186672=CARTESIAN_POINT('Ctrl Pts',(188.417956300948,-5.90330990566078,
131.20293648265));
#186673=CARTESIAN_POINT('Ctrl Pts',(188.424179136552,-5.91225136570458,
131.070504455847));
#186674=CARTESIAN_POINT('Ctrl Pts',(188.430401972156,-5.91674131959235,
130.937673208914));
#186675=CARTESIAN_POINT('Ctrl Pts',(188.436624807759,-5.91674998742092,
130.804746434304));
#186676=CARTESIAN_POINT('',(190.186624807795,-5.9167474892903,130.798909885783));
#186677=CARTESIAN_POINT('Ctrl Pts',(188.436624807795,-5.91674998742097,
130.80474643354));
#186678=CARTESIAN_POINT('Ctrl Pts',(188.444336312247,-5.91676072880488,
130.640020016287));
#186679=CARTESIAN_POINT('Ctrl Pts',(188.452047816698,-5.9098880006331,130.475412038668));
#186680=CARTESIAN_POINT('Ctrl Pts',(188.45975932115,-5.89618734660479,130.311506342716));
#186681=CARTESIAN_POINT('Ctrl Pts',(188.467479281045,-5.88247167020258,
130.147420928874));
#186682=CARTESIAN_POINT('Ctrl Pts',(188.47519924094,-5.86191315565751,129.984039656638));
#186683=CARTESIAN_POINT('Ctrl Pts',(188.482919200835,-5.83461887000143,
129.821938506494));
#186684=CARTESIAN_POINT('Ctrl Pts',(188.490936097646,-5.80627474974523,
129.65360237375));
#186685=CARTESIAN_POINT('Ctrl Pts',(188.498952994457,-5.77066650315088,
129.486647185334));
#186686=CARTESIAN_POINT('Ctrl Pts',(188.506969891268,-5.72797103557548,
129.321701392353));
#186687=CARTESIAN_POINT('Ctrl Pts',(188.514715160958,-5.6867221685032,129.162344264416));
#186688=CARTESIAN_POINT('Ctrl Pts',(188.522460430647,-5.63885863849107,
129.004862872487));
#186689=CARTESIAN_POINT('Ctrl Pts',(188.530205700337,-5.5845895056426,128.849804244379));
#186690=CARTESIAN_POINT('Ctrl Pts',(188.538358410709,-5.52746553966337,
128.686588741718));
#186691=CARTESIAN_POINT('Ctrl Pts',(188.546511121081,-5.46324405110737,
128.526058178221));
#186692=CARTESIAN_POINT('Ctrl Pts',(188.554663831453,-5.39222426567471,
128.368822067026));
#186693=CARTESIAN_POINT('Ctrl Pts',(188.562816541824,-5.32120448024206,
128.21158595583));
#186694=CARTESIAN_POINT('Ctrl Pts',(188.570969252196,-5.24338665044448,
128.057644630733));
#186695=CARTESIAN_POINT('Ctrl Pts',(188.579121962568,-5.15912334327355,
127.907573277876));
#186696=CARTESIAN_POINT('Ctrl Pts',(188.586545228974,-5.08239929092767,
127.770929194955));
#186697=CARTESIAN_POINT('Ctrl Pts',(188.593968495379,-5.00012675873199,
127.637128755464));
#186698=CARTESIAN_POINT('Ctrl Pts',(188.601391761784,-4.91254156507233,
127.506654455104));
#186699=CARTESIAN_POINT('Ctrl Pts',(188.608806254505,-4.82505988983811,
127.376334364533));
#186700=CARTESIAN_POINT('Ctrl Pts',(188.616220747226,-4.73227825779838,
127.249332894892));
#186701=CARTESIAN_POINT('Ctrl Pts',(188.623635239947,-4.6344785403192,127.126108420962));
#186702=CARTESIAN_POINT('Ctrl Pts',(188.631042586301,-4.53677308588965,
127.00300271542));
#186703=CARTESIAN_POINT('Ctrl Pts',(188.638449932655,-4.43405940528752,
126.883667048682));
#186704=CARTESIAN_POINT('Ctrl Pts',(188.645857279009,-4.32666280054533,
126.76853113989));
#186705=CARTESIAN_POINT('Ctrl Pts',(188.653259100684,-4.21934629624284,
126.653481103803));
#186706=CARTESIAN_POINT('Ctrl Pts',(188.66066092236,-4.10735407577181,126.542624860554));
#186707=CARTESIAN_POINT('Ctrl Pts',(188.668062744035,-3.99105179769123,
126.436359231274));
#186708=CARTESIAN_POINT('Ctrl Pts',(188.675460658346,-3.87481091467824,
126.330149698793));
#186709=CARTESIAN_POINT('Ctrl Pts',(188.682858572658,-3.75426478020397,
126.22852620523));
#186710=CARTESIAN_POINT('Ctrl Pts',(188.690256486969,-3.62981591611858,
126.131848768722));
#186711=CARTESIAN_POINT('Ctrl Pts',(188.697653171881,-3.50538773317637,
126.035187398249));
#186712=CARTESIAN_POINT('Ctrl Pts',(188.705049856793,-3.3770584023365,125.943470682302));
#186713=CARTESIAN_POINT('Ctrl Pts',(188.712446541706,-3.24526362374814,
125.857018444755));
#186714=CARTESIAN_POINT('Ctrl Pts',(188.719842898641,-3.11347468907845,
125.77057004059));
#186715=CARTESIAN_POINT('Ctrl Pts',(188.727239255577,-2.97822092432744,
125.689385855431));
#186716=CARTESIAN_POINT('Ctrl Pts',(188.734635612512,-2.83996688492409,
125.613742286863));
#186717=CARTESIAN_POINT('Ctrl Pts',(188.742033101849,-2.70169167847449,
125.53808713707));
#186718=CARTESIAN_POINT('Ctrl Pts',(188.749430591185,-2.56041561025224,
125.467974472102));
#186719=CARTESIAN_POINT('Ctrl Pts',(188.756828080522,-2.41662755324927,
125.403634570878));
#186720=CARTESIAN_POINT('Ctrl Pts',(188.764228163037,-2.27278909156605,
125.339272115401));
#186721=CARTESIAN_POINT('Ctrl Pts',(188.771628245552,-2.1264372284147,125.280686605083));
#186722=CARTESIAN_POINT('Ctrl Pts',(188.779028328067,-1.97808036179923,
125.228059993966));
#186723=CARTESIAN_POINT('Ctrl Pts',(188.786436547733,-1.82956036155703,
125.175375514479));
#186724=CARTESIAN_POINT('Ctrl Pts',(188.7938447674,-1.67903130693944,125.128663144689));
#186725=CARTESIAN_POINT('Ctrl Pts',(188.801252987066,-1.52701699451342,
125.088055022082));
#186726=CARTESIAN_POINT('Ctrl Pts',(188.808665766368,-1.37490911981405,
125.047421905852));
#186727=CARTESIAN_POINT('Ctrl Pts',(188.81607854567,-1.22131452911263,125.012900604892));
#186728=CARTESIAN_POINT('Ctrl Pts',(188.823491324972,-1.06676621647483,
124.984571927082));
#186729=CARTESIAN_POINT('Ctrl Pts',(188.830914696001,-0.911997077960795,
124.956202771929));
#186730=CARTESIAN_POINT('Ctrl Pts',(188.83833806703,-0.75627186444372,124.934043964435));
#186731=CARTESIAN_POINT('Ctrl Pts',(188.845761438059,-0.600128509702636,
124.918124440318));
#186732=CARTESIAN_POINT('Ctrl Pts',(188.8496974875,-0.517337556408728,124.909683526647));
#186733=CARTESIAN_POINT('Ctrl Pts',(188.853633536941,-0.434429058316661,
124.90299582822));
#186734=CARTESIAN_POINT('Ctrl Pts',(188.857569586381,-0.3514829554707,124.898059719837));
#186735=CARTESIAN_POINT('Ctrl Pts',(188.864992852787,-0.195049194165717,
124.888750373478));
#186736=CARTESIAN_POINT('Ctrl Pts',(188.872416119192,-0.0380087817261698,
124.885646179091));
#186737=CARTESIAN_POINT('Ctrl Pts',(188.879839385598,0.1191048789509,124.888809536702));
#186738=CARTESIAN_POINT('Ctrl Pts',(188.887253878319,0.276032844328527,
124.891969155487));
#186739=CARTESIAN_POINT('Ctrl Pts',(188.89466837104,0.433033516041292,124.90138157371));
#186740=CARTESIAN_POINT('Ctrl Pts',(188.902082863761,0.589568892045253,
124.917057407774));
#186741=CARTESIAN_POINT('Ctrl Pts',(188.909490210115,0.745953393360701,
124.932718132878));
#186742=CARTESIAN_POINT('Ctrl Pts',(188.916897556468,0.901873122835364,
124.954630218564));
#186743=CARTESIAN_POINT('Ctrl Pts',(188.924304902822,1.05679071189202,124.98275225271));
#186744=CARTESIAN_POINT('Ctrl Pts',(188.931706724498,1.21159275756575,125.010853312383));
#186745=CARTESIAN_POINT('Ctrl Pts',(188.939108546173,1.36539378534926,125.045155031959));
#186746=CARTESIAN_POINT('Ctrl Pts',(188.946510367848,1.51766229100495,125.085564264052));
#186747=CARTESIAN_POINT('Ctrl Pts',(188.95390828216,1.66985041530155,125.125952164426));
#186748=CARTESIAN_POINT('Ctrl Pts',(188.961306196471,1.8205072687502,125.17244106084));
#186749=CARTESIAN_POINT('Ctrl Pts',(188.968704110782,1.96911238500255,125.22488689886));
#186750=CARTESIAN_POINT('Ctrl Pts',(188.976100795695,2.11769280578066,125.277324021333));
#186751=CARTESIAN_POINT('Ctrl Pts',(188.983497480607,2.26422181439622,125.33571599657));
#186752=CARTESIAN_POINT('Ctrl Pts',(188.990894165519,2.40819482739287,125.39986913031));
#186753=CARTESIAN_POINT('Ctrl Pts',(188.998290522454,2.55216145647515,125.464019419434));
#186754=CARTESIAN_POINT('Ctrl Pts',(189.00568687939,2.69357197430951,125.533930207192));
#186755=CARTESIAN_POINT('Ctrl Pts',(189.013083236325,2.83194273622357,125.609360049592));
#186756=CARTESIAN_POINT('Ctrl Pts',(189.020480725662,2.97033468305507,125.684801440493));
#186757=CARTESIAN_POINT('Ctrl Pts',(189.027878214998,3.10568561952156,125.765763389823));
#186758=CARTESIAN_POINT('Ctrl Pts',(189.035275704335,3.23753755765109,125.851959066268));
#186759=CARTESIAN_POINT('Ctrl Pts',(189.04267578685,3.36943571627262,125.938184958474));
#186760=CARTESIAN_POINT('Ctrl Pts',(189.050075869365,3.49783212220785,126.029648026486));
#186761=CARTESIAN_POINT('Ctrl Pts',(189.05747595188,3.62229889082746,126.126018891269));
#186762=CARTESIAN_POINT('Ctrl Pts',(189.064884171547,3.74690252345494,126.222495725726));
#186763=CARTESIAN_POINT('Ctrl Pts',(189.072292391213,3.86756759402008,126.323890905695));
#186764=CARTESIAN_POINT('Ctrl Pts',(189.079700610879,3.98389980667395,126.429835169831));
#186765=CARTESIAN_POINT('Ctrl Pts',(189.087113390182,4.10030361986379,126.535844640893));
#186766=CARTESIAN_POINT('Ctrl Pts',(189.094526169484,4.21236899608596,126.646408513676));
#186767=CARTESIAN_POINT('Ctrl Pts',(189.101938948786,4.31973985307035,126.761122043812));
#186768=CARTESIAN_POINT('Ctrl Pts',(189.109362319814,4.42726412657015,126.875999482018));
#186769=CARTESIAN_POINT('Ctrl Pts',(189.116785690843,4.53008024059027,126.995038137808));
#186770=CARTESIAN_POINT('Ctrl Pts',(189.124209061872,4.627873084345,127.11780107272));
#186771=CARTESIAN_POINT('Ctrl Pts',(189.128145111313,4.6797251966109,127.182892926467));
#186772=CARTESIAN_POINT('Ctrl Pts',(189.132081160754,4.73016581507376,127.249031329645));
#186773=CARTESIAN_POINT('Ctrl Pts',(189.136017210194,4.77915309751256,127.316148147971));
#186774=CARTESIAN_POINT('Ctrl Pts',(189.1434404766,4.87154158335144,127.442728372691));
#186775=CARTESIAN_POINT('Ctrl Pts',(189.150863743005,4.95903740885353,127.573173026402));
#186776=CARTESIAN_POINT('Ctrl Pts',(189.158287009411,5.04129975781475,127.707067070878));
#186777=CARTESIAN_POINT('Ctrl Pts',(189.165701502132,5.12346487951111,127.840802863713));
#186778=CARTESIAN_POINT('Ctrl Pts',(189.173115994853,5.20040864350211,127.977979617276));
#186779=CARTESIAN_POINT('Ctrl Pts',(189.180530487574,5.27183131466145,128.118150433635));
#186780=CARTESIAN_POINT('Ctrl Pts',(189.187937833927,5.34318514596105,128.258186148084));
#186781=CARTESIAN_POINT('Ctrl Pts',(189.195345180281,5.40902831002284,128.401209849912));
#186782=CARTESIAN_POINT('Ctrl Pts',(189.202752526635,5.46910518719545,128.546747051454));
#186783=CARTESIAN_POINT('Ctrl Pts',(189.21015434831,5.52913725676648,128.692175705861));
#186784=CARTESIAN_POINT('Ctrl Pts',(189.217556169986,5.58341146092722,128.840113783703));
#186785=CARTESIAN_POINT('Ctrl Pts',(189.224957991661,5.6317188761904,128.990063766976));
#186786=CARTESIAN_POINT('Ctrl Pts',(189.232355905972,5.68000079034474,129.139934592819));
#186787=CARTESIAN_POINT('Ctrl Pts',(189.239753820284,5.72232207444452,129.291814854514));
#186788=CARTESIAN_POINT('Ctrl Pts',(189.247151734595,5.75852260079111,129.445188804042));
#186789=CARTESIAN_POINT('Ctrl Pts',(189.254548419507,5.79471711126733,129.598537265604));
#186790=CARTESIAN_POINT('Ctrl Pts',(189.26194510442,5.82479279708112,129.753378559388));
#186791=CARTESIAN_POINT('Ctrl Pts',(189.269341789332,5.84863987901503,129.909183468564));
#186792=CARTESIAN_POINT('Ctrl Pts',(189.276738146267,5.8724859035443,130.064981469187));
#186793=CARTESIAN_POINT('Ctrl Pts',(189.284134503203,5.89010381686027,130.221742631245));
#186794=CARTESIAN_POINT('Ctrl Pts',(189.291530860138,5.90143533087373,130.3789295444));
#186795=CARTESIAN_POINT('Ctrl Pts',(189.298928349475,5.91276857977092,130.536140523273));
#186796=CARTESIAN_POINT('Ctrl Pts',(189.306325838811,5.9178134861293,130.693777010678));
#186797=CARTESIAN_POINT('Ctrl Pts',(189.313723328148,5.91656381556915,130.851298649032));
#186798=CARTESIAN_POINT('Ctrl Pts',(189.321123410663,5.91531370693891,131.008875506353));
#186799=CARTESIAN_POINT('Ctrl Pts',(189.328523493178,5.90776463111646,131.166337061412));
#186800=CARTESIAN_POINT('Ctrl Pts',(189.335923575693,5.89396242191814,131.323145285339));
#186801=CARTESIAN_POINT('Ctrl Pts',(189.343331795359,5.88014503577195,131.480125936029));
#186802=CARTESIAN_POINT('Ctrl Pts',(189.350740015026,5.86006081725151,131.636451448796));
#186803=CARTESIAN_POINT('Ctrl Pts',(189.358148234692,5.83380730984865,131.791590496599));
#186804=CARTESIAN_POINT('Ctrl Pts',(189.365561013994,5.80753764385015,131.946825029897));
#186805=CARTESIAN_POINT('Ctrl Pts',(189.372973793296,5.77509119954317,132.100871278681));
#186806=CARTESIAN_POINT('Ctrl Pts',(189.380386572599,5.7366160286638,132.253210886634));
#186807=CARTESIAN_POINT('Ctrl Pts',(189.387809943627,5.69808588265588,132.405768164563));
#186808=CARTESIAN_POINT('Ctrl Pts',(189.395233314656,5.65350991124101,132.556613574327));
#186809=CARTESIAN_POINT('Ctrl Pts',(189.402656685685,5.60308539804483,132.705245828387));
#186810=CARTESIAN_POINT('Ctrl Pts',(189.406592735126,5.57634911122828,132.784054215872));
#186811=CARTESIAN_POINT('Ctrl Pts',(189.410528784567,5.54796938585717,132.862240759177));
#186812=CARTESIAN_POINT('Ctrl Pts',(189.414464834007,5.51798092849068,132.93973342701));
#186813=CARTESIAN_POINT('Ctrl Pts',(189.421888100413,5.46142363380593,133.085882180079));
#186814=CARTESIAN_POINT('Ctrl Pts',(189.429311366818,5.39897048314281,133.230003417703));
#186815=CARTESIAN_POINT('Ctrl Pts',(189.436734633224,5.33078644043194,133.371586063258));
#186816=CARTESIAN_POINT('Ctrl Pts',(189.444149125945,5.26268298559709,133.513001369884));
#186817=CARTESIAN_POINT('Ctrl Pts',(189.451563618666,5.18886228167012,133.651883723719));
#186818=CARTESIAN_POINT('Ctrl Pts',(189.458978111387,5.10953830238054,133.787739389865));
#186819=CARTESIAN_POINT('Ctrl Pts',(189.466385457741,5.03029077852894,133.923464113205));
#186820=CARTESIAN_POINT('Ctrl Pts',(189.473792804094,4.94555072602297,134.056167636292));
#186821=CARTESIAN_POINT('Ctrl Pts',(189.481200150448,4.85557917610903,134.1853784269));
#186822=CARTESIAN_POINT('Ctrl Pts',(189.488601972123,4.76567473037149,134.314492847226));
#186823=CARTESIAN_POINT('Ctrl Pts',(189.496003793799,4.67054676872829,134.440119416974));
#186824=CARTESIAN_POINT('Ctrl Pts',(189.503405615474,4.57050093892078,134.561813442263));
#186825=CARTESIAN_POINT('Ctrl Pts',(189.510803529786,4.470507922528,134.683443226223));
#186826=CARTESIAN_POINT('Ctrl Pts',(189.518201444097,4.36560244470111,134.801144312466));
#186827=CARTESIAN_POINT('Ctrl Pts',(189.525599358408,4.25613186592361,134.914503206622));
#186828=CARTESIAN_POINT('Ctrl Pts',(189.53299604332,4.1466794791702,135.027843262585));
#186829=CARTESIAN_POINT('Ctrl Pts',(189.540392728233,4.03266375619807,135.136842290347));
#186830=CARTESIAN_POINT('Ctrl Pts',(189.547789413145,3.9144706037665,135.241121874919));
#186831=CARTESIAN_POINT('Ctrl Pts',(189.55518577008,3.79628269214324,135.345396835624));
#186832=CARTESIAN_POINT('Ctrl Pts',(189.562582127016,3.67391799928616,135.444952522259));
#186833=CARTESIAN_POINT('Ctrl Pts',(189.569978483951,3.5477971575957,135.539449411987));
#186834=CARTESIAN_POINT('Ctrl Pts',(189.577375973288,3.42165700648274,135.633960769431));
#186835=CARTESIAN_POINT('Ctrl Pts',(189.584773462624,3.2917598602477,135.723411563957));
#186836=CARTESIAN_POINT('Ctrl Pts',(189.592170951961,3.15855696719353,135.807504473932));
#186837=CARTESIAN_POINT('Ctrl Pts',(189.599571034476,3.02530738007121,135.891626862547));
#186838=CARTESIAN_POINT('Ctrl Pts',(189.606971116991,2.88875005437881,135.970387427978));
#186839=CARTESIAN_POINT('Ctrl Pts',(189.614371199506,2.74936242334025,136.043533913767));
#186840=CARTESIAN_POINT('Ctrl Pts',(189.621779419172,2.6098215212719,136.116760831637));
#186841=CARTESIAN_POINT('Ctrl Pts',(189.629187638839,2.46744442931756,136.184361167894));
#186842=CARTESIAN_POINT('Ctrl Pts',(189.636595858505,2.3227308926061,136.246129793398));
#186843=CARTESIAN_POINT('Ctrl Pts',(189.644008637807,2.17792828712777,136.307936436459));
#186844=CARTESIAN_POINT('Ctrl Pts',(189.651421417109,2.03078671951321,136.363904084189));
#186845=CARTESIAN_POINT('Ctrl Pts',(189.658834196411,1.88182232319197,136.413877112455));
#186846=CARTESIAN_POINT('Ctrl Pts',(189.66625756744,1.73264507955527,136.463921544528));
#186847=CARTESIAN_POINT('Ctrl Pts',(189.673680938469,1.58164016277834,136.507954145901));
#186848=CARTESIAN_POINT('Ctrl Pts',(189.681104309498,1.42933595688406,136.545869938717));
#186849=CARTESIAN_POINT('Ctrl Pts',(189.685040358939,1.3485806124279,136.565973801845));
#186850=CARTESIAN_POINT('Ctrl Pts',(189.688976408379,1.26746012441086,136.584358871603));
#186851=CARTESIAN_POINT('Ctrl Pts',(189.69291245782,1.18605385454001,136.601015412931));
#186852=CARTESIAN_POINT('Ctrl Pts',(189.700335724226,1.03252417016951,136.632429130043));
#186853=CARTESIAN_POINT('Ctrl Pts',(189.707758990631,0.877513437794605,
136.657786574917));
#186854=CARTESIAN_POINT('Ctrl Pts',(189.715182257037,0.721540807687306,
136.676950286983));
#186855=CARTESIAN_POINT('Ctrl Pts',(189.722596749758,0.56575252427599,136.696091349132));
#186856=CARTESIAN_POINT('Ctrl Pts',(189.730011242479,0.409004972998288,
136.709053204846));
#186857=CARTESIAN_POINT('Ctrl Pts',(189.7374257352,0.251829205035335,136.715749000509));
#186858=CARTESIAN_POINT('Ctrl Pts',(189.744833081553,0.0948049289951359,
136.722438342512));
#186859=CARTESIAN_POINT('Ctrl Pts',(189.752240427907,-0.0626463716075346,
136.722873632068));
#186860=CARTESIAN_POINT('Ctrl Pts',(189.759647774261,-0.219986889591926,
136.717019607471));
#186861=CARTESIAN_POINT('Ctrl Pts',(189.767049595936,-0.377210057081186,
136.711169949027));
#186862=CARTESIAN_POINT('Ctrl Pts',(189.774451417612,-0.534322235037135,
136.699040330281));
#186863=CARTESIAN_POINT('Ctrl Pts',(189.781853239287,-0.690784079832339,
136.68064753343));
#186864=CARTESIAN_POINT('Ctrl Pts',(189.789251153599,-0.847163329639719,
136.662264445992));
#186865=CARTESIAN_POINT('Ctrl Pts',(189.79664906791,-1.00289256018978,136.637624808542));
#186866=CARTESIAN_POINT('Ctrl Pts',(189.804046982221,-1.15743613013174,
136.606797361484));
#186867=CARTESIAN_POINT('Ctrl Pts',(189.811443667134,-1.31195401773457,
136.575975037388));
#186868=CARTESIAN_POINT('Ctrl Pts',(189.818840352046,-1.4652862700588,136.538967017513));
#186869=CARTESIAN_POINT('Ctrl Pts',(189.826237036958,-1.61690592382758,
136.4958934336));
#186870=CARTESIAN_POINT('Ctrl Pts',(189.833633393893,-1.76851885462208,
136.452821759614));
#186871=CARTESIAN_POINT('Ctrl Pts',(189.841029750829,-1.91841897876412,
136.403685158374));
#186872=CARTESIAN_POINT('Ctrl Pts',(189.848426107764,-2.0660932839906,136.348653999445));
#186873=CARTESIAN_POINT('Ctrl Pts',(189.855823597101,-2.21379019853027,
136.293614415105));
#186874=CARTESIAN_POINT('Ctrl Pts',(189.863221086437,-2.35926026579751,
136.232678606497));
#186875=CARTESIAN_POINT('Ctrl Pts',(189.870618575774,-2.50200942995244,
136.166065511994));
#186876=CARTESIAN_POINT('Ctrl Pts',(189.878018658289,-2.64480863460694,
136.099429066372));
#186877=CARTESIAN_POINT('Ctrl Pts',(189.885418740804,-2.78488469905547,
136.027111530211));
#186878=CARTESIAN_POINT('Ctrl Pts',(189.892818823319,-2.92176732847544,
135.949378230826));
#186879=CARTESIAN_POINT('Ctrl Pts',(189.900227042986,-3.05880047441704,
135.871559455687));
#186880=CARTESIAN_POINT('Ctrl Pts',(189.907635262652,-3.19263284780672,
135.788313208874));
#186881=CARTESIAN_POINT('Ctrl Pts',(189.915043482319,-3.32282174323811,
135.699949062806));
#186882=CARTESIAN_POINT('Ctrl Pts',(189.922456261621,-3.45309076776235,
135.611530530079));
#186883=CARTESIAN_POINT('Ctrl Pts',(189.929869040923,-3.579711546312,135.517988042663));
#186884=CARTESIAN_POINT('Ctrl Pts',(189.937281820225,-3.70227416517129,
135.419671719583));
#186885=CARTESIAN_POINT('Ctrl Pts',(189.944705191254,-3.82501190724813,
135.321214917531));
#186886=CARTESIAN_POINT('Ctrl Pts',(189.952128562282,-3.94367962786938,
135.217970900963));
#186887=CARTESIAN_POINT('Ctrl Pts',(189.959551933311,-4.05790340171897,
135.110327471226));
#186888=CARTESIAN_POINT('Ctrl Pts',(189.963487982752,-4.1184675873743,135.053252341912));
#186889=CARTESIAN_POINT('Ctrl Pts',(189.967424032192,-4.17778307250271,
134.994940957179));
#186890=CARTESIAN_POINT('Ctrl Pts',(189.971360081633,-4.23579876978104,
134.935454824241));
#186891=CARTESIAN_POINT('Ctrl Pts',(189.97868580183,-4.34377677455446,134.824740065172));
#186892=CARTESIAN_POINT('Ctrl Pts',(189.986011522027,-4.44759549208393,
134.709599597571));
#186893=CARTESIAN_POINT('Ctrl Pts',(189.993337242224,-4.54686303201109,
134.590383217952));
#186894=CARTESIAN_POINT('Ctrl Pts',(190.000654105557,-4.6460105565541,134.471310972051));
#186895=CARTESIAN_POINT('Ctrl Pts',(190.00797096889,-4.74061760854022,134.348172911224));
#186896=CARTESIAN_POINT('Ctrl Pts',(190.015287832222,-4.83032801012746,
134.221356648743));
#186897=CARTESIAN_POINT('Ctrl Pts',(190.022596306275,-4.91993555265535,
134.094685789707));
#186898=CARTESIAN_POINT('Ctrl Pts',(190.029904780328,-5.00465740532908,
133.964345439033));
#186899=CARTESIAN_POINT('Ctrl Pts',(190.037213254381,-5.08417700870137,
133.830756941033));
#186900=CARTESIAN_POINT('Ctrl Pts',(190.044516984866,-5.16364499985177,
133.697255148686));
#186901=CARTESIAN_POINT('Ctrl Pts',(190.051820715352,-5.23791726272298,
133.560509731128));
#186902=CARTESIAN_POINT('Ctrl Pts',(190.059124445837,-5.30671991172705,
133.420971849862));
#186903=CARTESIAN_POINT('Ctrl Pts',(190.06642496806,-5.3754923382356,133.281495262502));
#186904=CARTESIAN_POINT('Ctrl Pts',(190.073725490283,-5.43879976191837,
133.139228995741));
#186905=CARTESIAN_POINT('Ctrl Pts',(190.081026012506,-5.49641386784294,
132.994649446895));
#186906=CARTESIAN_POINT('Ctrl Pts',(190.088324859137,-5.55401475037018,
132.850103081465));
#186907=CARTESIAN_POINT('Ctrl Pts',(190.095623705769,-5.60592477449524,
132.703244847386));
#186908=CARTESIAN_POINT('Ctrl Pts',(190.1029225524,-5.65196358703582,132.554571511522));
#186909=CARTESIAN_POINT('Ctrl Pts',(190.110223624323,-5.69801643600718,
132.405852847751));
#186910=CARTESIAN_POINT('Ctrl Pts',(190.117524696245,-5.73819437761977,
132.255318341899));
#186911=CARTESIAN_POINT('Ctrl Pts',(190.124825768168,-5.77236675875697,
132.103480536934));
#186912=CARTESIAN_POINT('Ctrl Pts',(190.132127831751,-5.80654378132449,
131.951622108746));
#186913=CARTESIAN_POINT('Ctrl Pts',(190.139429895335,-5.83471354286302,
131.79846040554));
#186914=CARTESIAN_POINT('Ctrl Pts',(190.146731958918,-5.85679658929349,
131.644517908875));
#186915=CARTESIAN_POINT('Ctrl Pts',(190.154040273153,-5.87889853906686,
131.490443635655));
#186916=CARTESIAN_POINT('Ctrl Pts',(190.161348587387,-5.89490331910291,
131.33558761541));
#186917=CARTESIAN_POINT('Ctrl Pts',(190.168656901621,-5.90478335808391,
131.180477695875));
#186918=CARTESIAN_POINT('Ctrl Pts',(190.174646203679,-5.91288023732375,
131.053362176412));
#186919=CARTESIAN_POINT('Ctrl Pts',(190.180635505737,-5.91686463980822,
130.926076303123));
#186920=CARTESIAN_POINT('Ctrl Pts',(190.186624807795,-5.9167474892903,130.798909885783));
#186921=CARTESIAN_POINT('',(191.936624807795,-5.92167388468568,130.806439789968));
#186922=CARTESIAN_POINT('Ctrl Pts',(190.186624807795,-5.91709367293974,
130.798909566865));
#186923=CARTESIAN_POINT('Ctrl Pts',(190.207685773679,-5.92124324054971,
130.351707301601));
#186924=CARTESIAN_POINT('Ctrl Pts',(190.321562614164,-5.67042057656234,
127.938289561738));
#186925=CARTESIAN_POINT('Ctrl Pts',(190.52825532926,-2.36162413690314,124.216470821409));
#186926=CARTESIAN_POINT('Ctrl Pts',(190.80670295307,4.26606273237082,125.256543993538));
#186927=CARTESIAN_POINT('Ctrl Pts',(191.085150576885,6.97344635934664,131.394789617243));
#186928=CARTESIAN_POINT('Ctrl Pts',(191.363598200697,3.27257345387652,136.990459834304));
#186929=CARTESIAN_POINT('Ctrl Pts',(191.64204582451,-3.43563458160472,136.901407078928));
#186930=CARTESIAN_POINT('Ctrl Pts',(191.833054693543,-5.87156050063434,
132.996862586964));
#186931=CARTESIAN_POINT('Ctrl Pts',(191.931247687971,-5.92616743922034,
130.920188992212));
#186932=CARTESIAN_POINT('Ctrl Pts',(191.936624807795,-5.92565178765728,
130.806441186659));
#186933=CARTESIAN_POINT('',(193.686624807763,-5.91674833022066,130.808805764476));
#186934=CARTESIAN_POINT('Ctrl Pts',(191.936624807795,-5.91674963529206,
130.806438061004));
#186935=CARTESIAN_POINT('Ctrl Pts',(191.943982571507,-5.91680420246894,
130.651025731606));
#186936=CARTESIAN_POINT('Ctrl Pts',(191.95134033522,-5.91073134974623,130.495363673782));
#186937=CARTESIAN_POINT('Ctrl Pts',(191.958698098932,-5.89849824070525,
130.3399803134));
#186938=CARTESIAN_POINT('Ctrl Pts',(191.966047433817,-5.88627914553708,
130.184774955408));
#186939=CARTESIAN_POINT('Ctrl Pts',(191.973396768702,-5.86791386650228,
130.029848035039));
#186940=CARTESIAN_POINT('Ctrl Pts',(191.980746103587,-5.84342153691622,
129.875729741274));
#186941=CARTESIAN_POINT('Ctrl Pts',(191.988088691781,-5.81895169129261,
129.721752928126));
#186942=CARTESIAN_POINT('Ctrl Pts',(191.995431279975,-5.7883660488743,129.568583637425));
#186943=CARTESIAN_POINT('Ctrl Pts',(192.00277386817,-5.7517356631725,129.416748487506));
#186944=CARTESIAN_POINT('Ctrl Pts',(192.010111385737,-5.71513057359504,
129.265018191543));
#186945=CARTESIAN_POINT('Ctrl Pts',(192.017448903304,-5.67248913923677,
129.114620570674));
#186946=CARTESIAN_POINT('Ctrl Pts',(192.024786420871,-5.62393372693014,
128.966073371895));
#186947=CARTESIAN_POINT('Ctrl Pts',(192.032121243465,-5.57539614838435,
128.817580732537));
#186948=CARTESIAN_POINT('Ctrl Pts',(192.03945606606,-5.52094902955856,128.670937524576));
#186949=CARTESIAN_POINT('Ctrl Pts',(192.046790888654,-5.46076494507694,
128.52664755901));
#186950=CARTESIAN_POINT('Ctrl Pts',(192.054124432835,-5.40059135029389,
128.382382742256));
#186951=CARTESIAN_POINT('Ctrl Pts',(192.061457977017,-5.33468292520694,
128.240470702987));
#186952=CARTESIAN_POINT('Ctrl Pts',(192.068791521199,-5.2632607654466,128.101396193566));
#186953=CARTESIAN_POINT('Ctrl Pts',(192.076125297015,-5.19183634977695,
127.962317291398));
#186954=CARTESIAN_POINT('Ctrl Pts',(192.083459072831,-5.11489802642811,
127.826076435999));
#186955=CARTESIAN_POINT('Ctrl Pts',(192.090792848647,-5.03271319836429,
127.693134424325));
#186956=CARTESIAN_POINT('Ctrl Pts',(192.098128366077,-4.95050885317121,
127.560160841782));
#186957=CARTESIAN_POINT('Ctrl Pts',(192.105463883507,-4.86305572373874,
127.43048798552));
#186958=CARTESIAN_POINT('Ctrl Pts',(192.112799400937,-4.77066480062535,
127.304548062218));
#186959=CARTESIAN_POINT('Ctrl Pts',(192.120142509709,-4.67817826447584,
127.178477806865));
#186960=CARTESIAN_POINT('Ctrl Pts',(192.12748561848,-4.58074395310877,127.056148507902));
#186961=CARTESIAN_POINT('Ctrl Pts',(192.134828727252,-4.47871388483845,
126.937960159743));
#186962=CARTESIAN_POINT('Ctrl Pts',(192.142175724157,-4.37662979224858,
126.81970923155));
#186963=CARTESIAN_POINT('Ctrl Pts',(192.149522721062,-4.26994535451669,
126.705603899663));
#186964=CARTESIAN_POINT('Ctrl Pts',(192.156869717967,-4.15904929270293,
126.596007074508));
#186965=CARTESIAN_POINT('Ctrl Pts',(192.164227936362,-4.04798385296286,
126.486242855825));
#186966=CARTESIAN_POINT('Ctrl Pts',(192.171586154757,-3.93269421798494,
126.381001158029));
#186967=CARTESIAN_POINT('Ctrl Pts',(192.178944373152,-3.81360275633488,
126.280605034052));
#186968=CARTESIAN_POINT('Ctrl Pts',(192.18560993948,-3.70572174572714,126.189659510622));
#186969=CARTESIAN_POINT('Ctrl Pts',(192.192275505808,-3.59472154676677,
126.102689823874));
#186970=CARTESIAN_POINT('Ctrl Pts',(192.198941072137,-3.48093537284348,
126.019904588655));
#186971=CARTESIAN_POINT('Ctrl Pts',(192.206364338542,-3.35421469515357,
125.927708843354));
#186972=CARTESIAN_POINT('Ctrl Pts',(192.213787604947,-3.22363703874374,
125.840411633728));
#186973=CARTESIAN_POINT('Ctrl Pts',(192.221210871353,-3.08961796002339,
125.758353143969));
#186974=CARTESIAN_POINT('Ctrl Pts',(192.228625364074,-2.95575728072412,
125.676391640529));
#186975=CARTESIAN_POINT('Ctrl Pts',(192.236039856795,-2.8184635906989,125.599656725305));
#186976=CARTESIAN_POINT('Ctrl Pts',(192.243454349516,-2.67818424350777,
125.528447452973));
#186977=CARTESIAN_POINT('Ctrl Pts',(192.25086169587,-2.53804010283326,125.457306814819));
#186978=CARTESIAN_POINT('Ctrl Pts',(192.258269042224,-2.39491636453648,
125.39168138473));
#186979=CARTESIAN_POINT('Ctrl Pts',(192.265676388577,-2.24928790474382,
125.331826059971));
#186980=CARTESIAN_POINT('Ctrl Pts',(192.273078210253,-2.10376806015,125.272015377571));
#186981=CARTESIAN_POINT('Ctrl Pts',(192.280480031928,-1.95574755751648,
125.21796637283));
#186982=CARTESIAN_POINT('Ctrl Pts',(192.287881853604,-1.80572423221982,
125.169887211854));
#186983=CARTESIAN_POINT('Ctrl Pts',(192.295279767915,-1.65578010306985,
125.121833431494));
#186984=CARTESIAN_POINT('Ctrl Pts',(192.302677682226,-1.5038356114583,125.079743332305));
#186985=CARTESIAN_POINT('Ctrl Pts',(192.310075596538,-1.35040674849502,
125.04377625692));
#186986=CARTESIAN_POINT('Ctrl Pts',(192.31747228145,-1.19700338262484,125.007815158611));
#186987=CARTESIAN_POINT('Ctrl Pts',(192.324868966362,-1.04211649807024,
124.977975149715));
#186988=CARTESIAN_POINT('Ctrl Pts',(192.332265651274,-0.886275478114352,
124.954365203944));
#186989=CARTESIAN_POINT('Ctrl Pts',(192.33966200821,-0.73044136831249,124.930756305064));
#186990=CARTESIAN_POINT('Ctrl Pts',(192.347058365145,-0.573653576316578,
124.913376975953));
#186991=CARTESIAN_POINT('Ctrl Pts',(192.354454722081,-0.416449600545396,
124.902284686785));
#186992=CARTESIAN_POINT('Ctrl Pts',(192.361852211417,-0.259221556444396,
124.891190699359));
#186993=CARTESIAN_POINT('Ctrl Pts',(192.369249700754,-0.10157757409154,
124.886385694742));
#186994=CARTESIAN_POINT('Ctrl Pts',(192.37664719009,0.0559419800692496,
124.887875084974));
#186995=CARTESIAN_POINT('Ctrl Pts',(192.384047272605,0.213516752465648,
124.88936499731));
#186996=CARTESIAN_POINT('Ctrl Pts',(192.39144735512,0.370966636778287,124.897153694073));
#186997=CARTESIAN_POINT('Ctrl Pts',(192.398847437635,0.527753674510833,
124.911194522712));
#186998=CARTESIAN_POINT('Ctrl Pts',(192.406255657302,0.684713115709465,
124.925250790685));
#186999=CARTESIAN_POINT('Ctrl Pts',(192.413663876968,0.841007882692738,
124.945572886768));
#187000=CARTESIAN_POINT('Ctrl Pts',(192.421072096635,0.996106797477932,
124.972062458991));
#187001=CARTESIAN_POINT('Ctrl Pts',(192.428484875937,1.15130117305738,124.998568335104));
#187002=CARTESIAN_POINT('Ctrl Pts',(192.435897655239,1.30529786549359,125.031249174006));
#187003=CARTESIAN_POINT('Ctrl Pts',(192.443310434541,1.45757874437968,125.069956135283));
#187004=CARTESIAN_POINT('Ctrl Pts',(192.45073380557,1.61007720932673,125.108718402881));
#187005=CARTESIAN_POINT('Ctrl Pts',(192.458157176598,1.76085460737413,125.153523883713));
#187006=CARTESIAN_POINT('Ctrl Pts',(192.465580547627,1.90940995179483,125.204174531507));
#187007=CARTESIAN_POINT('Ctrl Pts',(192.469516597068,1.9881775599421,125.231030720313));
#187008=CARTESIAN_POINT('Ctrl Pts',(192.473452646509,2.06632082359468,125.259529399429));
#187009=CARTESIAN_POINT('Ctrl Pts',(192.477388695949,2.14376776436376,125.289635752718));
#187010=CARTESIAN_POINT('Ctrl Pts',(192.484811962355,2.28983027762013,125.346415395433));
#187011=CARTESIAN_POINT('Ctrl Pts',(192.49223522876,2.43385630529008,125.409087801767));
#187012=CARTESIAN_POINT('Ctrl Pts',(192.499658495166,2.57533502238865,125.477487230207));
#187013=CARTESIAN_POINT('Ctrl Pts',(192.507072987887,2.71664652339273,125.545805816202));
#187014=CARTESIAN_POINT('Ctrl Pts',(192.514487480608,2.85541637385971,125.619837789946));
#187015=CARTESIAN_POINT('Ctrl Pts',(192.521901973329,2.99115116509402,125.699368426577));
#187016=CARTESIAN_POINT('Ctrl Pts',(192.529309319682,3.1267551300262,125.778822408586));
#187017=CARTESIAN_POINT('Ctrl Pts',(192.536716666036,3.25932953951027,125.863764315137));
#187018=CARTESIAN_POINT('Ctrl Pts',(192.54412401239,3.38840325911156,125.953932397693));
#187019=CARTESIAN_POINT('Ctrl Pts',(192.551525834065,3.51738071066331,126.044033229491));
#187020=CARTESIAN_POINT('Ctrl Pts',(192.558927655741,3.64286236637453,126.139352263232));
#187021=CARTESIAN_POINT('Ctrl Pts',(192.566329477416,3.76440399802195,126.239583174779));
#187022=CARTESIAN_POINT('Ctrl Pts',(192.573727391728,3.88588146878789,126.339761175208));
#187023=CARTESIAN_POINT('Ctrl Pts',(192.581125306039,4.00342277045593,126.444845652573));
#187024=CARTESIAN_POINT('Ctrl Pts',(192.58852322035,4.11661493775789,126.554488617525));
#187025=CARTESIAN_POINT('Ctrl Pts',(192.595919905262,4.22978829457512,126.664113361806));
#187026=CARTESIAN_POINT('Ctrl Pts',(192.603316590175,4.33861368359645,126.778294830715));
#187027=CARTESIAN_POINT('Ctrl Pts',(192.610713275087,4.44271327755592,126.896646542057));
#187028=CARTESIAN_POINT('Ctrl Pts',(192.618109632022,4.54680825563025,127.01499300556));
#187029=CARTESIAN_POINT('Ctrl Pts',(192.625505988958,4.64617760874819,127.137509063529));
#187030=CARTESIAN_POINT('Ctrl Pts',(192.632902345893,4.74048245459971,127.263773567354));
#187031=CARTESIAN_POINT('Ctrl Pts',(192.64029983523,4.83480173876412,127.390057402596));
#187032=CARTESIAN_POINT('Ctrl Pts',(192.647697324566,4.92405474836339,127.520090527295));
#187033=CARTESIAN_POINT('Ctrl Pts',(192.655094813903,5.00794484883268,127.653421241197));
#187034=CARTESIAN_POINT('Ctrl Pts',(192.662494896418,5.09186435684631,127.786798693974));
#187035=CARTESIAN_POINT('Ctrl Pts',(192.669894978933,5.1704170140703,127.923475721708));
#187036=CARTESIAN_POINT('Ctrl Pts',(192.677295061448,5.24335129090999,128.062974507837));
#187037=CARTESIAN_POINT('Ctrl Pts',(192.684703281114,5.31636576648502,128.202626687223));
#187038=CARTESIAN_POINT('Ctrl Pts',(192.692111500781,5.38374935076555,128.345106490511));
#187039=CARTESIAN_POINT('Ctrl Pts',(192.699519720447,5.4452976753735,128.48991386098));
#187040=CARTESIAN_POINT('Ctrl Pts',(192.706932499749,5.50688388194844,128.634810357969));
#187041=CARTESIAN_POINT('Ctrl Pts',(192.714345279052,5.56262754045087,128.782036928429));
#187042=CARTESIAN_POINT('Ctrl Pts',(192.721758058354,5.61237381239609,128.931077202695));
#187043=CARTESIAN_POINT('Ctrl Pts',(192.729181429382,5.66219116414747,129.080330432694));
#187044=CARTESIAN_POINT('Ctrl Pts',(192.736604800411,5.70599391075369,129.231402184733));
#187045=CARTESIAN_POINT('Ctrl Pts',(192.74402817144,5.74367787858866,129.383763915644));
#187046=CARTESIAN_POINT('Ctrl Pts',(192.747964220881,5.76365882254902,129.464549761242));
#187047=CARTESIAN_POINT('Ctrl Pts',(192.751900270321,5.7819204194436,129.545698134267));
#187048=CARTESIAN_POINT('Ctrl Pts',(192.755836319762,5.79845305499836,129.627129658289));
#187049=CARTESIAN_POINT('Ctrl Pts',(192.763259586168,5.82963308968896,129.780706971204));
#187050=CARTESIAN_POINT('Ctrl Pts',(192.770682852573,5.85475460525286,129.935756113794));
#187051=CARTESIAN_POINT('Ctrl Pts',(192.778106118978,5.87368093133555,130.091757727195));
#187052=CARTESIAN_POINT('Ctrl Pts',(192.785520611699,5.89258488807253,130.247574959644));
#187053=CARTESIAN_POINT('Ctrl Pts',(192.79293510442,5.90530818568646,130.404342055148));
#187054=CARTESIAN_POINT('Ctrl Pts',(192.800349597141,5.91176477883311,130.561527830965));
#187055=CARTESIAN_POINT('Ctrl Pts',(192.807756943495,5.91821514887222,130.718562105214));
#187056=CARTESIAN_POINT('Ctrl Pts',(192.815164289849,5.91841082384763,130.876013885927));
#187057=CARTESIAN_POINT('Ctrl Pts',(192.822571636203,5.91231736054565,131.033345312885));
#187058=CARTESIAN_POINT('Ctrl Pts',(192.829973457878,5.90622844197851,131.190559396129));
#187059=CARTESIAN_POINT('Ctrl Pts',(192.837375279553,5.89385973928897,131.347652932937));
#187060=CARTESIAN_POINT('Ctrl Pts',(192.844777101229,5.8752288554425,131.504086605847));
#187061=CARTESIAN_POINT('Ctrl Pts',(192.85217501554,5.8566078066946,131.660437698638));
#187062=CARTESIAN_POINT('Ctrl Pts',(192.859572929851,5.83173120439777,131.816129251521));
#187063=CARTESIAN_POINT('Ctrl Pts',(192.866970844163,5.80066860403245,131.970625728376));
#187064=CARTESIAN_POINT('Ctrl Pts',(192.874367529075,5.76961116570776,132.125096530719));
#187065=CARTESIAN_POINT('Ctrl Pts',(192.881764213987,5.73236984310127,132.278372285581));
#187066=CARTESIAN_POINT('Ctrl Pts',(192.889160898899,5.6890655697637,132.429926213114));
#187067=CARTESIAN_POINT('Ctrl Pts',(192.896557255835,5.64576321658296,132.581473420587));
#187068=CARTESIAN_POINT('Ctrl Pts',(192.90395361277,5.5963985497707,132.731298593605));
#187069=CARTESIAN_POINT('Ctrl Pts',(192.911349969705,5.54114271941322,132.878888979771));
#187070=CARTESIAN_POINT('Ctrl Pts',(192.918747459042,5.48587842924699,133.026501962402));
#187071=CARTESIAN_POINT('Ctrl Pts',(192.926144948379,5.42472131052274,133.17187912729));
#187072=CARTESIAN_POINT('Ctrl Pts',(192.933542437715,5.35789105322837,133.314526752354));
#187073=CARTESIAN_POINT('Ctrl Pts',(192.94094252023,5.29103736869093,133.457224382321));
#187074=CARTESIAN_POINT('Ctrl Pts',(192.948342602745,5.21850674434839,133.597190229583));
#187075=CARTESIAN_POINT('Ctrl Pts',(192.95574268526,5.14056522291733,133.733954403645));
#187076=CARTESIAN_POINT('Ctrl Pts',(192.963150904926,5.06253799677085,133.870868963976));
#187077=CARTESIAN_POINT('Ctrl Pts',(192.970559124593,4.97908817626604,134.004574495774));
#187078=CARTESIAN_POINT('Ctrl Pts',(192.977967344259,4.89052600718495,134.13462876526));
#187079=CARTESIAN_POINT('Ctrl Pts',(192.985380123561,4.80190932956638,134.26476308098));
#187080=CARTESIAN_POINT('Ctrl Pts',(192.992792902864,4.70817425520031,134.391241357163));
#187081=CARTESIAN_POINT('Ctrl Pts',(193.000205682166,4.60967152652743,134.51365421339));
#187082=CARTESIAN_POINT('Ctrl Pts',(193.007629053194,4.51102805253667,134.636241978846));
#187083=CARTESIAN_POINT('Ctrl Pts',(193.015052424223,4.40760356345385,134.754752442234));
#187084=CARTESIAN_POINT('Ctrl Pts',(193.022475795252,4.29978642922707,134.868812268839));
#187085=CARTESIAN_POINT('Ctrl Pts',(193.026411844693,4.24261919762311,134.929289525733));
#187086=CARTESIAN_POINT('Ctrl Pts',(193.030347894133,4.18421761234096,134.988516202176));
#187087=CARTESIAN_POINT('Ctrl Pts',(193.034283943574,4.12464325826948,135.046441304506));
#187088=CARTESIAN_POINT('Ctrl Pts',(193.04170720998,4.01228788574312,135.155686239721));
#187089=CARTESIAN_POINT('Ctrl Pts',(193.049130476385,3.89541944365211,135.260629531099));
#187090=CARTESIAN_POINT('Ctrl Pts',(193.05655374279,3.77440100965145,135.360875467848));
#187091=CARTESIAN_POINT('Ctrl Pts',(193.063968235512,3.65352560938941,135.461002922225));
#187092=CARTESIAN_POINT('Ctrl Pts',(193.071382728233,3.52851026521044,135.55644383722));
#187093=CARTESIAN_POINT('Ctrl Pts',(193.078797220954,3.39975536658942,135.6468387032));
#187094=CARTESIAN_POINT('Ctrl Pts',(193.086204567307,3.27112456678774,135.737146443204));
#187095=CARTESIAN_POINT('Ctrl Pts',(193.093611913661,3.13876169151149,135.822417603552));
#187096=CARTESIAN_POINT('Ctrl Pts',(193.101019260015,3.0031006403987,135.902332479605));
#187097=CARTESIAN_POINT('Ctrl Pts',(193.10842108169,2.86754077041626,135.982187752127));
#187098=CARTESIAN_POINT('Ctrl Pts',(193.115822903366,2.72868794285352,136.056694506122));
#187099=CARTESIAN_POINT('Ctrl Pts',(193.123224725041,2.58700541559937,136.125576037201));
#187100=CARTESIAN_POINT('Ctrl Pts',(193.130622639352,2.44539768144717,136.194421206256));
#187101=CARTESIAN_POINT('Ctrl Pts',(193.138020553664,2.30096355740562,136.257646903513));
#187102=CARTESIAN_POINT('Ctrl Pts',(193.145418467975,2.15419120161526,136.315022177613));
#187103=CARTESIAN_POINT('Ctrl Pts',(193.152815152887,2.00744323672871,136.372387916984));
#187104=CARTESIAN_POINT('Ctrl Pts',(193.1602118378,1.85835815862988,136.423905027017));
#187105=CARTESIAN_POINT('Ctrl Pts',(193.167608522712,1.70744452966099,136.46939051516));
#187106=CARTESIAN_POINT('Ctrl Pts',(193.175004879647,1.55653759236051,136.514873986428));
#187107=CARTESIAN_POINT('Ctrl Pts',(193.182401236583,1.40380262282025,136.554326259858));
#187108=CARTESIAN_POINT('Ctrl Pts',(193.189797593518,1.24976352495471,136.58761417367));
#187109=CARTESIAN_POINT('Ctrl Pts',(193.197195082855,1.09570084331009,136.620907183947));
#187110=CARTESIAN_POINT('Ctrl Pts',(193.204592572191,0.94033400067869,136.648033876561));
#187111=CARTESIAN_POINT('Ctrl Pts',(193.211990061528,0.78419712723474,136.668912214077));
#187112=CARTESIAN_POINT('Ctrl Pts',(193.219390144043,0.628005520252473,
136.689797870461));
#187113=CARTESIAN_POINT('Ctrl Pts',(193.226790226558,0.471043714796622,
136.704430761329));
#187114=CARTESIAN_POINT('Ctrl Pts',(193.234190309073,0.313850845635412,
136.712780728661));
#187115=CARTESIAN_POINT('Ctrl Pts',(193.241598528739,0.156485126754066,
136.721139877641));
#187116=CARTESIAN_POINT('Ctrl Pts',(193.249006748406,-0.00111179024260466,
136.723202286104));
#187117=CARTESIAN_POINT('Ctrl Pts',(193.256414968072,-0.15840014612975,
136.718989934455));
#187118=CARTESIAN_POINT('Ctrl Pts',(193.263827747375,-0.315785310375573,
136.714774990174));
#187119=CARTESIAN_POINT('Ctrl Pts',(193.271240526677,-0.472861163480505,
136.704277615075));
#187120=CARTESIAN_POINT('Ctrl Pts',(193.278653305979,-0.629093697246785,
136.687571618591));
#187121=CARTESIAN_POINT('Ctrl Pts',(193.286076677007,-0.785549463383723,
136.670841751796));
#187122=CARTESIAN_POINT('Ctrl Pts',(193.293500048036,-0.941159135255626,
136.647885600237));
#187123=CARTESIAN_POINT('Ctrl Pts',(193.300923419065,-1.09539869234955,
136.618828114018));
#187124=CARTESIAN_POINT('Ctrl Pts',(193.304859468506,-1.17718020644852,
136.6034211376));
#187125=CARTESIAN_POINT('Ctrl Pts',(193.308795517947,-1.25857677010934,
136.586299695192));
#187126=CARTESIAN_POINT('Ctrl Pts',(193.312731567387,-1.33951219278451,
136.567488036588));
#187127=CARTESIAN_POINT('Ctrl Pts',(193.320154833793,-1.49215387404138,
136.532009835551));
#187128=CARTESIAN_POINT('Ctrl Pts',(193.327578100198,-1.64361588484665,
136.490409517706));
#187129=CARTESIAN_POINT('Ctrl Pts',(193.335001366604,-1.79336905016339,
136.442778659217));
#187130=CARTESIAN_POINT('Ctrl Pts',(193.342415859325,-1.94294521967514,
136.395204096447));
#187131=CARTESIAN_POINT('Ctrl Pts',(193.349830352046,-2.0908162116855,136.3416132926));
#187132=CARTESIAN_POINT('Ctrl Pts',(193.357244844767,-2.23646314026778,
136.282148782941));
#187133=CARTESIAN_POINT('Ctrl Pts',(193.364652191121,-2.38196968885627,
136.222741587416));
#187134=CARTESIAN_POINT('Ctrl Pts',(193.372059537474,-2.52525609829113,
136.157472096766));
#187135=CARTESIAN_POINT('Ctrl Pts',(193.379466883828,-2.66581885865279,
136.08653255488));
#187136=CARTESIAN_POINT('Ctrl Pts',(193.386868705504,-2.80627678200372,
136.015645922381));
#187137=CARTESIAN_POINT('Ctrl Pts',(193.394270527179,-2.94401476924652,
135.9390978265));
#187138=CARTESIAN_POINT('Ctrl Pts',(193.401672348854,-3.07854961893739,
135.857128453737));
#187139=CARTESIAN_POINT('Ctrl Pts',(193.409070263166,-3.21301344872921,
135.775202351967));
#187140=CARTESIAN_POINT('Ctrl Pts',(193.416468177477,-3.34427719051927,
135.687860866565));
#187141=CARTESIAN_POINT('Ctrl Pts',(193.423866091788,-3.47188267699022,
135.595389863951));
#187142=CARTESIAN_POINT('Ctrl Pts',(193.4312627767,-3.59946695774474,135.502934228339));
#187143=CARTESIAN_POINT('Ctrl Pts',(193.438659461613,-3.72339388777422,
135.405350986174));
#187144=CARTESIAN_POINT('Ctrl Pts',(193.446056146525,-3.84323461989282,
135.302969093412));
#187145=CARTESIAN_POINT('Ctrl Pts',(193.45345250346,-3.96307003814781,135.200591740371));
#187146=CARTESIAN_POINT('Ctrl Pts',(193.460848860396,-4.07881933492679,
135.093416402282));
#187147=CARTESIAN_POINT('Ctrl Pts',(193.468245217331,-4.19008729459038,
134.981811877151));
#187148=CARTESIAN_POINT('Ctrl Pts',(193.475642706668,-4.30137228966243,
134.870190265084));
#187149=CARTESIAN_POINT('Ctrl Pts',(193.483040196004,-4.40817431791499,
134.754138380124));
#187150=CARTESIAN_POINT('Ctrl Pts',(193.490437685341,-4.51013564852389,
134.634061257879));
#187151=CARTESIAN_POINT('Ctrl Pts',(193.497837767856,-4.61213272151835,
134.513942042786));
#187152=CARTESIAN_POINT('Ctrl Pts',(193.505237850371,-4.70928547688403,
134.389795065409));
#187153=CARTESIAN_POINT('Ctrl Pts',(193.512637932886,-4.80127712631488,
134.262057613953));
#187154=CARTESIAN_POINT('Ctrl Pts',(193.520046152552,-4.89336993002218,
134.134179702037));
#187155=CARTESIAN_POINT('Ctrl Pts',(193.527454372219,-4.98029007582845,
134.002703734542));
#187156=CARTESIAN_POINT('Ctrl Pts',(193.534862591885,-5.06176430342499,
133.868095707138));
#187157=CARTESIAN_POINT('Ctrl Pts',(193.542275371188,-5.14328867704949,
133.733404830738));
#187158=CARTESIAN_POINT('Ctrl Pts',(193.54968815049,-5.21936027347246,133.595578379247));
#187159=CARTESIAN_POINT('Ctrl Pts',(193.557100929792,-5.28975254618504,
133.455105524687));
#187160=CARTESIAN_POINT('Ctrl Pts',(193.564524300821,-5.36024539867765,
133.314431955926));
#187161=CARTESIAN_POINT('Ctrl Pts',(193.571947671849,-5.42504256684365,
133.171104771232));
#187162=CARTESIAN_POINT('Ctrl Pts',(193.579371042878,-5.48396592885686,
133.025632382487));
#187163=CARTESIAN_POINT('Ctrl Pts',(193.583307092319,-5.51520850924322,
132.948499431412));
#187164=CARTESIAN_POINT('Ctrl Pts',(193.58724314176,-5.54480058572185,132.870763639298));
#187165=CARTESIAN_POINT('Ctrl Pts',(193.591179191201,-5.57272137747765,
132.792502215014));
#187166=CARTESIAN_POINT('Ctrl Pts',(193.59982438893,-5.63404702115283,132.62060765482));
#187167=CARTESIAN_POINT('Ctrl Pts',(193.60846958666,-5.6874596691831,132.445749915596));
#187168=CARTESIAN_POINT('Ctrl Pts',(193.61711478439,-5.7327048543804,132.268609781835));
#187169=CARTESIAN_POINT('Ctrl Pts',(193.625725250551,-5.77776826973561,
132.092181298032));
#187170=CARTESIAN_POINT('Ctrl Pts',(193.634335716713,-5.81472962923724,
131.913488824043));
#187171=CARTESIAN_POINT('Ctrl Pts',(193.642946182875,-5.84338413695381,
131.733226803029));
#187172=CARTESIAN_POINT('Ctrl Pts',(193.651489290023,-5.87181448266578,
131.554374957907));
#187173=CARTESIAN_POINT('Ctrl Pts',(193.660032397172,-5.89206736515099,
131.373978144609));
#187174=CARTESIAN_POINT('Ctrl Pts',(193.668575504321,-5.90398986112245,
131.192734512496));
#187175=CARTESIAN_POINT('Ctrl Pts',(193.674591938801,-5.91238621090631,
131.065094718366));
#187176=CARTESIAN_POINT('Ctrl Pts',(193.680608373282,-5.91665199363111,
130.937035352127));
#187177=CARTESIAN_POINT('Ctrl Pts',(193.686624807763,-5.91674833022066,
130.808805764476));
#187178=CARTESIAN_POINT('',(195.436626015881,-5.91264468443637,130.800534531502));
#187179=CARTESIAN_POINT('Ctrl Pts',(193.686624807795,-5.91674833022117,
130.808805763797));
#187180=CARTESIAN_POINT('Ctrl Pts',(193.694249891429,-5.91687042486749,
130.646290683926));
#187181=CARTESIAN_POINT('Ctrl Pts',(193.701874975063,-5.91029198571113,
130.483707620702));
#187182=CARTESIAN_POINT('Ctrl Pts',(193.709500058697,-5.89702633263468,
130.321648493507));
#187183=CARTESIAN_POINT('Ctrl Pts',(193.716903394445,-5.8841464629385,130.164302267934));
#187184=CARTESIAN_POINT('Ctrl Pts',(193.724306730192,-5.86496295699468,
130.007450318832));
#187185=CARTESIAN_POINT('Ctrl Pts',(193.731710065939,-5.839540805705,129.851630991173));
#187186=CARTESIAN_POINT('Ctrl Pts',(193.739114086533,-5.81411630273351,
129.695797249413));
#187187=CARTESIAN_POINT('Ctrl Pts',(193.746518107128,-5.78245206455313,
129.540996686389));
#187188=CARTESIAN_POINT('Ctrl Pts',(193.753922127722,-5.74466447835844,
129.387758840923));
#187189=CARTESIAN_POINT('Ctrl Pts',(193.761328280158,-5.70686601197486,
129.234476873648));
#187190=CARTESIAN_POINT('Ctrl Pts',(193.768734432594,-5.66294077563007,
129.082758880831));
#187191=CARTESIAN_POINT('Ctrl Pts',(193.776140585029,-5.61305539489754,
128.933120468277));
#187192=CARTESIAN_POINT('Ctrl Pts',(193.783931104195,-5.56058104765214,
128.775716076322));
#187193=CARTESIAN_POINT('Ctrl Pts',(193.79172162336,-5.50151156375219,128.620613319595));
#187194=CARTESIAN_POINT('Ctrl Pts',(193.799512142525,-5.43609843388967,
128.468388789919));
#187195=CARTESIAN_POINT('Ctrl Pts',(193.806931140232,-5.37380478565584,
128.32342368392));
#187196=CARTESIAN_POINT('Ctrl Pts',(193.814350137939,-5.3057587036248,128.181068965662));
#187197=CARTESIAN_POINT('Ctrl Pts',(193.821769135646,-5.23222448513309,
128.041797043696));
#187198=CARTESIAN_POINT('Ctrl Pts',(193.829193605055,-5.15863603325452,
127.902422405087));
#187199=CARTESIAN_POINT('Ctrl Pts',(193.836618074465,-5.07955156595895,
127.766135413061));
#187200=CARTESIAN_POINT('Ctrl Pts',(193.844042543874,-4.99527888296432,
127.633379784462));
#187201=CARTESIAN_POINT('Ctrl Pts',(193.851477405336,-4.91088824323663,
127.500438337403));
#187202=CARTESIAN_POINT('Ctrl Pts',(193.858912266798,-4.82129510231583,
127.371038424274));
#187203=CARTESIAN_POINT('Ctrl Pts',(193.86634712826,-4.72684806539047,127.245591458262));
#187204=CARTESIAN_POINT('Ctrl Pts',(193.867440357178,-4.71296048557474,
127.227145620151));
#187205=CARTESIAN_POINT('Ctrl Pts',(193.868533586096,-4.69896802508309,
127.20878518446));
#187206=CARTESIAN_POINT('Ctrl Pts',(193.869626815014,-4.68487185884326,
127.190511391503));
#187207=CARTESIAN_POINT('Ctrl Pts',(193.877050081419,-4.58915576902482,
127.066428291302));
#187208=CARTESIAN_POINT('Ctrl Pts',(193.884473347825,-4.48836185950119,
126.945962881474));
#187209=CARTESIAN_POINT('Ctrl Pts',(193.89189661423,-4.38279338078887,126.82955839056));
#187210=CARTESIAN_POINT('Ctrl Pts',(193.899311106951,-4.27734967525132,
126.713291480087));
#187211=CARTESIAN_POINT('Ctrl Pts',(193.906725599672,-4.16714288156309,
126.601076208577));
#187212=CARTESIAN_POINT('Ctrl Pts',(193.914140092393,-4.0525183215702,126.493325264447));
#187213=CARTESIAN_POINT('Ctrl Pts',(193.921547438747,-3.93800424104399,
126.385678174735));
#187214=CARTESIAN_POINT('Ctrl Pts',(193.928954785101,-3.81908114123644,
126.282487100167));
#187215=CARTESIAN_POINT('Ctrl Pts',(193.936362131454,-3.69613316353616,
126.184130082202));
#187216=CARTESIAN_POINT('Ctrl Pts',(193.94376395313,-3.57327688507596,126.085846422612));
#187217=CARTESIAN_POINT('Ctrl Pts',(193.951165774805,-3.44640199616621,
125.992389872936));
#187218=CARTESIAN_POINT('Ctrl Pts',(193.958567596481,-3.31592780126095,
125.904100075582));
#187219=CARTESIAN_POINT('Ctrl Pts',(193.965965510792,-3.18552248266734,
125.815856885725));
#187220=CARTESIAN_POINT('Ctrl Pts',(193.973363425103,-3.05152195049331,
125.732775224944));
#187221=CARTESIAN_POINT('Ctrl Pts',(193.980761339415,-2.91437665000294,
125.655152979063));
#187222=CARTESIAN_POINT('Ctrl Pts',(193.988158024327,-2.77725414057385,
125.577543632592));
#187223=CARTESIAN_POINT('Ctrl Pts',(193.995554709239,-2.63698822459584,
125.505392084079));
#187224=CARTESIAN_POINT('Ctrl Pts',(194.002951394151,-2.49405635059935,
125.438951641306));
#187225=CARTESIAN_POINT('Ctrl Pts',(194.010347751087,-2.35113081435208,
125.372514144571));
#187226=CARTESIAN_POINT('Ctrl Pts',(194.017744108022,-2.20553989364301,
125.31178740741));
#187227=CARTESIAN_POINT('Ctrl Pts',(194.025140464957,-2.057783294511,125.256977588125));
#187228=CARTESIAN_POINT('Ctrl Pts',(194.032537954294,-1.9100040734663,125.202159377317));
#187229=CARTESIAN_POINT('Ctrl Pts',(194.039935443631,-1.76005886381328,
125.15326001798));
#187230=CARTESIAN_POINT('Ctrl Pts',(194.047332932967,-1.60846474911433,
125.110436512579));
#187231=CARTESIAN_POINT('Ctrl Pts',(194.054733015482,-1.45681749333343,
125.067597995464));
#187232=CARTESIAN_POINT('Ctrl Pts',(194.062133097997,-1.30352054068615,
125.030839674279));
#187233=CARTESIAN_POINT('Ctrl Pts',(194.069533180512,-1.14910329058166,
125.000267907239));
#187234=CARTESIAN_POINT('Ctrl Pts',(194.076941400178,-0.994516242836139,
124.969662523398));
#187235=CARTESIAN_POINT('Ctrl Pts',(194.084349619845,-0.838806803898584,
124.945257351789));
#187236=CARTESIAN_POINT('Ctrl Pts',(194.091757839511,-0.68251238996658,
124.927107228436));
#187237=CARTESIAN_POINT('Ctrl Pts',(194.099170618813,-0.526121779430448,
124.908945933984));
#187238=CARTESIAN_POINT('Ctrl Pts',(194.106583398116,-0.369145847837443,
124.897047387302));
#187239=CARTESIAN_POINT('Ctrl Pts',(194.113996177418,-0.212123673302736,
124.891414303779));
#187240=CARTESIAN_POINT('Ctrl Pts',(194.121419548446,-0.0548771381217091,
124.885773171442));
#187241=CARTESIAN_POINT('Ctrl Pts',(194.128842919475,0.102415399659899,
124.886415380671));
#187242=CARTESIAN_POINT('Ctrl Pts',(194.136266290504,0.259217491474521,
124.893291606413));
#187243=CARTESIAN_POINT('Ctrl Pts',(194.140202339945,0.342357722969995,
124.896937546294));
#187244=CARTESIAN_POINT('Ctrl Pts',(194.144138389385,0.425360189154594,
124.902335228505));
#187245=CARTESIAN_POINT('Ctrl Pts',(194.148074438826,0.508146029354237,
124.909471460393));
#187246=CARTESIAN_POINT('Ctrl Pts',(194.155497705232,0.664277540311929,
124.922930171021));
#187247=CARTESIAN_POINT('Ctrl Pts',(194.162920971637,0.820110071483281,
124.942616445193));
#187248=CARTESIAN_POINT('Ctrl Pts',(194.170344238043,0.975106807833801,
124.968514725511));
#187249=CARTESIAN_POINT('Ctrl Pts',(194.177758730764,1.12992035091363,124.994382396213));
#187250=CARTESIAN_POINT('Ctrl Pts',(194.185173223485,1.28389970087569,125.0264473977));
#187251=CARTESIAN_POINT('Ctrl Pts',(194.192587716206,1.43651099637365,125.064642269093));
#187252=CARTESIAN_POINT('Ctrl Pts',(194.199995062559,1.58897519935966,125.102800326831));
#187253=CARTESIAN_POINT('Ctrl Pts',(194.207402408913,1.74007361322188,125.147076402391));
#187254=CARTESIAN_POINT('Ctrl Pts',(194.214809755267,1.88928054317001,125.197351647384));
#187255=CARTESIAN_POINT('Ctrl Pts',(194.222211576942,2.03837618896044,125.247589395203));
#187256=CARTESIAN_POINT('Ctrl Pts',(194.229613398618,2.18558280757734,125.303817284624));
#187257=CARTESIAN_POINT('Ctrl Pts',(194.237015220293,2.33038800394414,125.365866127951));
#187258=CARTESIAN_POINT('Ctrl Pts',(194.244413134605,2.47511675877508,125.427882216177));
#187259=CARTESIAN_POINT('Ctrl Pts',(194.251811048916,2.61744627377012,125.495712991953));
#187260=CARTESIAN_POINT('Ctrl Pts',(194.259208963227,2.75688245248113,125.569140497485));
#187261=CARTESIAN_POINT('Ctrl Pts',(194.26660564814,2.89629545942845,125.642555800698));
#187262=CARTESIAN_POINT('Ctrl Pts',(194.274002333052,3.03281575440156,125.721565813977));
#187263=CARTESIAN_POINT('Ctrl Pts',(194.281399017964,3.16597214979834,125.805905765394));
#187264=CARTESIAN_POINT('Ctrl Pts',(194.2887953749,3.29912264090107,125.89024197709));
#187265=CARTESIAN_POINT('Ctrl Pts',(194.296191731835,3.42890921364481,125.979907457263));
#187266=CARTESIAN_POINT('Ctrl Pts',(194.30358808877,3.55488831789053,126.07459322267));
#187267=CARTESIAN_POINT('Ctrl Pts',(194.310985578107,3.68088670985897,126.169293484709));
#187268=CARTESIAN_POINT('Ctrl Pts',(194.318383067444,3.80307617420363,126.269015338105));
#187269=CARTESIAN_POINT('Ctrl Pts',(194.32578055678,3.92104512400985,126.373408609478));
#187270=CARTESIAN_POINT('Ctrl Pts',(194.333180639295,4.03905542764841,126.477838475751));
#187271=CARTESIAN_POINT('Ctrl Pts',(194.34058072181,4.15284199170322,126.586942773136));
#187272=CARTESIAN_POINT('Ctrl Pts',(194.347980804325,4.26202918068377,126.700333592131));
#187273=CARTESIAN_POINT('Ctrl Pts',(194.355389023992,4.37133643220337,126.813849095989));
#187274=CARTESIAN_POINT('Ctrl Pts',(194.362797243658,4.47603394942869,126.931660265503));
#187275=CARTESIAN_POINT('Ctrl Pts',(194.370205463325,4.57578511067753,127.053344597419));
#187276=CARTESIAN_POINT('Ctrl Pts',(194.377618242627,4.67559766710175,127.17510382401));
#187277=CARTESIAN_POINT('Ctrl Pts',(194.385031021929,4.77045757678608,127.300740665929));
#187278=CARTESIAN_POINT('Ctrl Pts',(194.392443801231,4.86007117030686,127.429803049224));
#187279=CARTESIAN_POINT('Ctrl Pts',(194.39986717226,4.94981280793254,127.559049842905));
#187280=CARTESIAN_POINT('Ctrl Pts',(194.407290543289,5.03429295787514,127.691731639473));
#187281=CARTESIAN_POINT('Ctrl Pts',(194.414713914317,5.11326315514323,127.827370448158));
#187282=CARTESIAN_POINT('Ctrl Pts',(194.418649963758,5.15513504859709,127.899289399128));
#187283=CARTESIAN_POINT('Ctrl Pts',(194.422586013199,5.19545868610213,127.972039303758));
#187284=CARTESIAN_POINT('Ctrl Pts',(194.426522062639,5.23420254088829,128.04554668338));
#187285=CARTESIAN_POINT('Ctrl Pts',(194.433945329045,5.30727224186316,128.184179307264));
#187286=CARTESIAN_POINT('Ctrl Pts',(194.44136859545,5.37494091137785,128.325926541199));
#187287=CARTESIAN_POINT('Ctrl Pts',(194.448791861856,5.4369314766717,128.470328338338));
#187288=CARTESIAN_POINT('Ctrl Pts',(194.456206354577,5.49884877426541,128.614559464546));
#187289=CARTESIAN_POINT('Ctrl Pts',(194.463620847298,5.55510118019554,128.761438569126));
#187290=CARTESIAN_POINT('Ctrl Pts',(194.471035340019,5.60545688611216,128.910480035154));
#187291=CARTESIAN_POINT('Ctrl Pts',(194.478442686372,5.6557640573036,129.059377849406));
#187292=CARTESIAN_POINT('Ctrl Pts',(194.485850032726,5.70018572444837,129.21043352466));
#187293=CARTESIAN_POINT('Ctrl Pts',(194.49325737908,5.73853772718516,129.363140538545));
#187294=CARTESIAN_POINT('Ctrl Pts',(194.500659200755,5.77686112555123,129.515733657777));
#187295=CARTESIAN_POINT('Ctrl Pts',(194.508061022431,5.80912378280913,129.669975302801));
#187296=CARTESIAN_POINT('Ctrl Pts',(194.515462844106,5.83519107930323,129.825342931045));
#187297=CARTESIAN_POINT('Ctrl Pts',(194.522860758417,5.86124461507446,129.980628541928));
#187298=CARTESIAN_POINT('Ctrl Pts',(194.530258672729,5.88110924179336,130.13703858504));
#187299=CARTESIAN_POINT('Ctrl Pts',(194.53765658704,5.8947012623256,130.294039551533));
#187300=CARTESIAN_POINT('Ctrl Pts',(194.545053271952,5.90829102411064,130.451014427314));
#187301=CARTESIAN_POINT('Ctrl Pts',(194.552449956865,5.91561021638582,130.608579660035));
#187302=CARTESIAN_POINT('Ctrl Pts',(194.559846641777,5.91662691086489,130.766195710526));
#187303=CARTESIAN_POINT('Ctrl Pts',(194.567242998712,5.91764356026267,130.923804772156));
#187304=CARTESIAN_POINT('Ctrl Pts',(194.574639355648,5.91235826511605,131.081464273787));
#187305=CARTESIAN_POINT('Ctrl Pts',(194.582035712583,5.90079123209493,131.238634031134));
#187306=CARTESIAN_POINT('Ctrl Pts',(194.58943320192,5.88922242813151,131.395827851571));
#187307=CARTESIAN_POINT('Ctrl Pts',(194.596830691256,5.87136999872203,131.552531406112));
#187308=CARTESIAN_POINT('Ctrl Pts',(194.604228180593,5.84730608186697,131.708209137763));
#187309=CARTESIAN_POINT('Ctrl Pts',(194.611628263108,5.82323372944323,131.863941442));
#187310=CARTESIAN_POINT('Ctrl Pts',(194.619028345623,5.79294561132196,132.0186468387));
#187311=CARTESIAN_POINT('Ctrl Pts',(194.626428428138,5.75656504659628,132.171799620522));
#187312=CARTESIAN_POINT('Ctrl Pts',(194.633836647804,5.72014447769965,132.325120809573));
#187313=CARTESIAN_POINT('Ctrl Pts',(194.641244867471,5.67761816964086,132.476885610823));
#187314=CARTESIAN_POINT('Ctrl Pts',(194.648653087137,5.62915963413416,132.626582441586));
#187315=CARTESIAN_POINT('Ctrl Pts',(194.656065866439,5.58067127320736,132.776371408251));
#187316=CARTESIAN_POINT('Ctrl Pts',(194.663478645741,5.52624353814764,132.924089518748));
#187317=CARTESIAN_POINT('Ctrl Pts',(194.670891425043,5.46609803607665,133.069245343661));
#187318=CARTESIAN_POINT('Ctrl Pts',(194.678314796072,5.4058665952918,133.214608574024));
#187319=CARTESIAN_POINT('Ctrl Pts',(194.685738167101,5.33990122668302,133.35740186875));
#187320=CARTESIAN_POINT('Ctrl Pts',(194.69316153813,5.26846977602395,133.49715782152));
#187321=CARTESIAN_POINT('Ctrl Pts',(194.697097587571,5.23059510690934,133.571259781079));
#187322=CARTESIAN_POINT('Ctrl Pts',(194.701033637011,5.19118446278821,133.644508299809));
#187323=CARTESIAN_POINT('Ctrl Pts',(194.704969686452,5.15028262235604,133.716837136331));
#187324=CARTESIAN_POINT('Ctrl Pts',(194.712392952858,5.07314302780579,133.853247064702));
#187325=CARTESIAN_POINT('Ctrl Pts',(194.719816219263,4.99046363417835,133.986796475152));
#187326=CARTESIAN_POINT('Ctrl Pts',(194.727239485669,4.90248172731818,134.117003591961));
#187327=CARTESIAN_POINT('Ctrl Pts',(194.73465397839,4.81460380776549,134.247056814772));
#187328=CARTESIAN_POINT('Ctrl Pts',(194.742068471111,4.7214360566969,134.373775300779));
#187329=CARTESIAN_POINT('Ctrl Pts',(194.749482963832,4.62326173930799,134.496701535243));
#187330=CARTESIAN_POINT('Ctrl Pts',(194.756890310185,4.52518204602216,134.619509288774));
#187331=CARTESIAN_POINT('Ctrl Pts',(194.764297656539,4.4221056244628,134.738531777645));
#187332=CARTESIAN_POINT('Ctrl Pts',(194.771705002893,4.31435908307288,134.853340274814));
#187333=CARTESIAN_POINT('Ctrl Pts',(194.779106824568,4.2066929031187,134.968063143474));
#187334=CARTESIAN_POINT('Ctrl Pts',(194.786508646244,4.0943637931164,135.078578007448));
#187335=CARTESIAN_POINT('Ctrl Pts',(194.793910467919,3.97773861771825,135.184489160384));
#187336=CARTESIAN_POINT('Ctrl Pts',(194.801308382231,3.86117500784292,135.290344403647));
#187337=CARTESIAN_POINT('Ctrl Pts',(194.808706296542,3.74032012477287,135.39160052553));
#187338=CARTESIAN_POINT('Ctrl Pts',(194.816104210853,3.61557758426522,135.487898734701));
#187339=CARTESIAN_POINT('Ctrl Pts',(194.823500895765,3.49085577370419,135.584180940857));
#187340=CARTESIAN_POINT('Ctrl Pts',(194.830897580678,3.36224788314285,135.675506641639));
#187341=CARTESIAN_POINT('Ctrl Pts',(194.83829426559,3.23019058414608,135.761557340775));
#187342=CARTESIAN_POINT('Ctrl Pts',(194.845690622525,3.09813914070806,135.847604224333));
#187343=CARTESIAN_POINT('Ctrl Pts',(194.853086979461,2.96263890570939,135.928376367518));
#187344=CARTESIAN_POINT('Ctrl Pts',(194.860483336396,2.82415527368646,136.003598787972));
#187345=CARTESIAN_POINT('Ctrl Pts',(194.867880825733,2.68565043946621,136.078832725171));
#187346=CARTESIAN_POINT('Ctrl Pts',(194.875278315069,2.54416162679036,136.148515069628));
#187347=CARTESIAN_POINT('Ctrl Pts',(194.882675804406,2.40017840727624,136.212417031449));
#187348=CARTESIAN_POINT('Ctrl Pts',(194.890075886921,2.25614471466828,136.276341394004));
#187349=CARTESIAN_POINT('Ctrl Pts',(194.897475969436,2.10961521526799,136.33448118823));
#187350=CARTESIAN_POINT('Ctrl Pts',(194.904876051951,1.96109885853,136.386656008315));
#187351=CARTESIAN_POINT('Ctrl Pts',(194.912284271617,1.81241919278925,136.438888199978));
#187352=CARTESIAN_POINT('Ctrl Pts',(194.919692491284,1.66174865902651,136.485142194737));
#187353=CARTESIAN_POINT('Ctrl Pts',(194.92710071095,1.50961145356359,136.525287449974));
#187354=CARTESIAN_POINT('Ctrl Pts',(194.934513490252,1.35738061018877,136.565457413946));
#187355=CARTESIAN_POINT('Ctrl Pts',(194.941926269555,1.20368165996157,136.599511065906));
#187356=CARTESIAN_POINT('Ctrl Pts',(194.949339048857,1.04904784043026,136.627369220598));
#187357=CARTESIAN_POINT('Ctrl Pts',(194.956762419885,0.894193072846361,
136.655267180328));
#187358=CARTESIAN_POINT('Ctrl Pts',(194.964185790914,0.738401136849904,
136.676951911201));
#187359=CARTESIAN_POINT('Ctrl Pts',(194.971609161943,0.582210051798615,
136.692396114919));
#187360=CARTESIAN_POINT('Ctrl Pts',(194.975545211384,0.499393790750225,
136.700585002308));
#187361=CARTESIAN_POINT('Ctrl Pts',(194.979481260825,0.416465321632257,
136.70702032481));
#187362=CARTESIAN_POINT('Ctrl Pts',(194.983417310265,0.333504579172153,
136.711703950924));
#187363=CARTESIAN_POINT('Ctrl Pts',(194.990840576671,0.177043208009956,
136.720537123605));
#187364=CARTESIAN_POINT('Ctrl Pts',(194.998263843076,0.0199940748712888,
136.723163326617));
#187365=CARTESIAN_POINT('Ctrl Pts',(195.005687109482,-0.137109229893286,
136.71952178372));
#187366=CARTESIAN_POINT('Ctrl Pts',(195.013101602203,-0.294026851598554,
136.715884544824));
#187367=CARTESIAN_POINT('Ctrl Pts',(195.020516094924,-0.450998147931574,
136.70599431416));
#187368=CARTESIAN_POINT('Ctrl Pts',(195.027930587645,-0.607485087027711,
136.689842112868));
#187369=CARTESIAN_POINT('Ctrl Pts',(195.035337933998,-0.763821198120527,
136.673705479675));
#187370=CARTESIAN_POINT('Ctrl Pts',(195.042745280352,-0.919673512534122,
136.651318929462));
#187371=CARTESIAN_POINT('Ctrl Pts',(195.050152626706,-1.07450479022457,
136.622725509723));
#187372=CARTESIAN_POINT('Ctrl Pts',(195.057554448381,-1.22922058890767,
136.594153416035));
#187373=CARTESIAN_POINT('Ctrl Pts',(195.064956270057,-1.38291650166136,
136.559383737918));
#187374=CARTESIAN_POINT('Ctrl Pts',(195.072358091732,-1.53506131021855,
136.518511240044));
#187375=CARTESIAN_POINT('Ctrl Pts',(195.079756006044,-1.68712580271452,
136.477660318445));
#187376=CARTESIAN_POINT('Ctrl Pts',(195.087153920355,-1.83764046212198,
136.430713089725));
#187377=CARTESIAN_POINT('Ctrl Pts',(195.094551834666,-1.98608526295548,
136.377815191775));
#187378=CARTESIAN_POINT('Ctrl Pts',(195.101948519579,-2.13450539495601,
136.324926084496));
#187379=CARTESIAN_POINT('Ctrl Pts',(195.109345204491,-2.28085599977257,
136.266088395828));
#187380=CARTESIAN_POINT('Ctrl Pts',(195.116741889403,-2.42463308582467,
136.201497354913));
#187381=CARTESIAN_POINT('Ctrl Pts',(195.124138246339,-2.56840379665031,
136.136909178033));
#187382=CARTESIAN_POINT('Ctrl Pts',(195.131534603274,-2.70960087509142,
136.066568309123));
#187383=CARTESIAN_POINT('Ctrl Pts',(195.138930960209,-2.84774141358831,
135.990717663107));
#187384=CARTESIAN_POINT('Ctrl Pts',(195.146328449546,-2.98590310175456,
135.914855404164));
#187385=CARTESIAN_POINT('Ctrl Pts',(195.153725938883,-3.1210069909607,135.833481868153));
#187386=CARTESIAN_POINT('Ctrl Pts',(195.161123428219,-3.25259596837197,
135.746885279015));
#187387=CARTESIAN_POINT('Ctrl Pts',(195.168523510734,-3.38423107409569,
135.660258333577));
#187388=CARTESIAN_POINT('Ctrl Pts',(195.175923593249,-3.51234850319129,
135.568404894722));
#187389=CARTESIAN_POINT('Ctrl Pts',(195.183323675764,-3.63652137552785,
135.471655642292));
#187390=CARTESIAN_POINT('Ctrl Pts',(195.190731895431,-3.76083078870214,
135.374800004113));
#187391=CARTESIAN_POINT('Ctrl Pts',(195.198140115097,-3.88118668830531,
135.273038030831));
#187392=CARTESIAN_POINT('Ctrl Pts',(195.205548334764,-3.99719590421933,
135.166740182184));
#187393=CARTESIAN_POINT('Ctrl Pts',(195.212961114066,-4.11327652186949,
135.060376908984));
#187394=CARTESIAN_POINT('Ctrl Pts',(195.220373893368,-4.2250048606152,134.949472459869));
#187395=CARTESIAN_POINT('Ctrl Pts',(195.22778667267,-4.33202607173832,134.834432661125));
#187396=CARTESIAN_POINT('Ctrl Pts',(195.235210043698,-4.43920019978721,
134.719228488122));
#187397=CARTESIAN_POINT('Ctrl Pts',(195.242633414727,-4.54165352484936,
134.599877446827));
#187398=CARTESIAN_POINT('Ctrl Pts',(195.250056785756,-4.63907226748901,
134.476817432767));
#187399=CARTESIAN_POINT('Ctrl Pts',(195.253992835197,-4.6907260223665,134.411568060529));
#187400=CARTESIAN_POINT('Ctrl Pts',(195.257928884637,-4.7409651046425,134.345276439808));
#187401=CARTESIAN_POINT('Ctrl Pts',(195.261864934078,-4.78974787966705,
134.278010831926));
#187402=CARTESIAN_POINT('Ctrl Pts',(195.269344497194,-4.88244840344199,
134.150187905093));
#187403=CARTESIAN_POINT('Ctrl Pts',(195.27682406031,-4.97016722581075,134.018460598548));
#187404=CARTESIAN_POINT('Ctrl Pts',(195.284303623426,-5.05256043017122,
133.883250622416));
#187405=CARTESIAN_POINT('Ctrl Pts',(195.291774119838,-5.13485375774175,
133.748204547404));
#187406=CARTESIAN_POINT('Ctrl Pts',(195.29924461625,-5.21183412944589,133.609684515291));
#187407=CARTESIAN_POINT('Ctrl Pts',(195.306715112662,-5.28319868593022,
133.468144056114));
#187408=CARTESIAN_POINT('Ctrl Pts',(195.314177953125,-5.35449010624771,
133.326748651109));
#187409=CARTESIAN_POINT('Ctrl Pts',(195.321640793587,-5.42017700590164,
133.182339305798));
#187410=CARTESIAN_POINT('Ctrl Pts',(195.329103634049,-5.48000059220959,
133.03539716408));
#187411=CARTESIAN_POINT('Ctrl Pts',(195.336560224284,-5.53977407546993,
132.888578088357));
#187412=CARTESIAN_POINT('Ctrl Pts',(195.344016814518,-5.59369388645601,
132.739230777314));
#187413=CARTESIAN_POINT('Ctrl Pts',(195.351473404753,-5.64154786489769,
132.587859496334));
#187414=CARTESIAN_POINT('Ctrl Pts',(195.358924751708,-5.68936819367592,
132.436594655673));
#187415=CARTESIAN_POINT('Ctrl Pts',(195.366376098664,-5.73113107811833,
132.28330902832));
#187416=CARTESIAN_POINT('Ctrl Pts',(195.373827445619,-5.76667310995969,
132.128525186405));
#187417=CARTESIAN_POINT('Ctrl Pts',(195.381275645374,-5.80220013002815,
131.97380672004));
#187418=CARTESIAN_POINT('Ctrl Pts',(195.388723845128,-5.83151144890194,
131.817591655312));
#187419=CARTESIAN_POINT('Ctrl Pts',(195.396172044882,-5.85449396429676,
131.660416097376));
#187420=CARTESIAN_POINT('Ctrl Pts',(195.403619442704,-5.87747400521164,
131.503257462208));
#187421=CARTESIAN_POINT('Ctrl Pts',(195.411066840526,-5.89412654082032,
131.345138900639));
#187422=CARTESIAN_POINT('Ctrl Pts',(195.418514238348,-5.90438986155658,
131.186605205818));
#187423=CARTESIAN_POINT('Ctrl Pts',(195.424551094831,-5.91270930356792,
131.058097882038));
#187424=CARTESIAN_POINT('Ctrl Pts',(195.430587951313,-5.91683153852153,
130.929318034017));
#187425=CARTESIAN_POINT('Ctrl Pts',(195.436624807795,-5.91674877781543,
130.800557629312));
#187426=CARTESIAN_POINT('',(197.186623444831,-5.92116344383671,130.801362336707));
#187427=CARTESIAN_POINT('Ctrl Pts',(195.436626945312,-5.90948723714756,
130.800516761409));
#187428=CARTESIAN_POINT('Ctrl Pts',(195.471188816171,-5.9137909198465,130.064246680543));
#187429=CARTESIAN_POINT('Ctrl Pts',(195.598566561638,-5.44429779229546,
127.356026198653));
#187430=CARTESIAN_POINT('Ctrl Pts',(195.818760181701,-1.38200268831043,
123.943775431166));
#187431=CARTESIAN_POINT('Ctrl Pts',(196.097207805517,5.0249984088633,125.933328743181));
#187432=CARTESIAN_POINT('Ctrl Pts',(196.375655429329,6.81427145311116,132.39912238462));
#187433=CARTESIAN_POINT('Ctrl Pts',(196.654103053143,2.34156192761705,137.399407870579));
#187434=CARTESIAN_POINT('Ctrl Pts',(196.924425368086,-4.08962105397609,
136.370105731155));
#187435=CARTESIAN_POINT('Ctrl Pts',(197.101931808425,-5.91344458449586,
132.593748677927));
#187436=CARTESIAN_POINT('Ctrl Pts',(197.18662237416,-5.92463101698242,130.801383223244));
#187437=CARTESIAN_POINT('',(198.936625519421,-5.91828595945227,130.809611426597));
#187438=CARTESIAN_POINT('Ctrl Pts',(197.186624807795,-5.91674922678536,
130.801335748166));
#187439=CARTESIAN_POINT('Ctrl Pts',(197.194749305453,-5.91666143946249,
130.629620706627));
#187440=CARTESIAN_POINT('Ctrl Pts',(197.20287380311,-5.90909912685711,130.458101858393));
#187441=CARTESIAN_POINT('Ctrl Pts',(197.210998300767,-5.89410901923282,
130.287244158827));
#187442=CARTESIAN_POINT('Ctrl Pts',(197.218421567172,-5.88041271860844,
130.131133310534));
#187443=CARTESIAN_POINT('Ctrl Pts',(197.225844833577,-5.86048931664855,
129.975330918972));
#187444=CARTESIAN_POINT('Ctrl Pts',(197.233268099982,-5.83435518767231,
129.820373774879));
#187445=CARTESIAN_POINT('Ctrl Pts',(197.240682592703,-5.80825194706619,
129.665599777262));
#187446=CARTESIAN_POINT('Ctrl Pts',(197.248097085424,-5.77595265235115,
129.511669403079));
#187447=CARTESIAN_POINT('Ctrl Pts',(197.255511578145,-5.73752557677412,
129.359116410395));
#187448=CARTESIAN_POINT('Ctrl Pts',(197.262918924498,-5.69913553865926,
129.206710454028));
#187449=CARTESIAN_POINT('Ctrl Pts',(197.270326270852,-5.65462956830657,
129.055679595785));
#187450=CARTESIAN_POINT('Ctrl Pts',(197.277733617205,-5.60412731398305,
128.906549348981));
#187451=CARTESIAN_POINT('Ctrl Pts',(197.285135438881,-5.55366272614622,
128.757530329141));
#187452=CARTESIAN_POINT('Ctrl Pts',(197.292537260556,-5.49721087842226,
128.610409450263));
#187453=CARTESIAN_POINT('Ctrl Pts',(197.299939082232,-5.43494173808804,
128.465698849356));
#187454=CARTESIAN_POINT('Ctrl Pts',(197.307336996543,-5.37270546914825,
128.321064640048));
#187455=CARTESIAN_POINT('Ctrl Pts',(197.314734910855,-5.3046581706263,128.178838516762));
#187456=CARTESIAN_POINT('Ctrl Pts',(197.322132825166,-5.23101855199436,
128.03951424368));
#187457=CARTESIAN_POINT('Ctrl Pts',(197.329529510078,-5.15739117093109,
127.900213123764));
#187458=CARTESIAN_POINT('Ctrl Pts',(197.336926194991,-5.07817348849507,
127.76381322667));
#187459=CARTESIAN_POINT('Ctrl Pts',(197.344322879903,-4.9936309933754,127.630785336515));
#187460=CARTESIAN_POINT('Ctrl Pts',(197.351719236839,-4.90909224695859,
127.497763344956));
#187461=CARTESIAN_POINT('Ctrl Pts',(197.359115593775,-4.81922935754628,
127.368113378099));
#187462=CARTESIAN_POINT('Ctrl Pts',(197.36651195071,-4.72435198303289,127.242278515352));
#187463=CARTESIAN_POINT('Ctrl Pts',(197.373909440047,-4.62946008255125,
127.116424386966));
#187464=CARTESIAN_POINT('Ctrl Pts',(197.381306929384,-4.52955239306734,
126.9943868238));
#187465=CARTESIAN_POINT('Ctrl Pts',(197.388704418721,-4.42497971392021,
126.876576879388));
#187466=CARTESIAN_POINT('Ctrl Pts',(197.396104501236,-4.32037037698219,
126.758725636883));
#187467=CARTESIAN_POINT('Ctrl Pts',(197.403504583751,-4.21109304215689,
126.645105242758));
#187468=CARTESIAN_POINT('Ctrl Pts',(197.410904666267,-4.09753619015153,
126.536090741738));
#187469=CARTESIAN_POINT('Ctrl Pts',(197.418312885934,-3.9838544707137,126.426956368068));
#187470=CARTESIAN_POINT('Ctrl Pts',(197.4257211056,-3.86588410582371,126.322438260625));
#187471=CARTESIAN_POINT('Ctrl Pts',(197.433129325267,-3.74404811053006,
126.222872397726));
#187472=CARTESIAN_POINT('Ctrl Pts',(197.440542104569,-3.62213712721409,
126.123245253698));
#187473=CARTESIAN_POINT('Ctrl Pts',(197.447954883872,-3.49635607014594,
126.028576651746));
#187474=CARTESIAN_POINT('Ctrl Pts',(197.455367663174,-3.36715745966806,
125.939159572974));
#187475=CARTESIAN_POINT('Ctrl Pts',(197.462791034203,-3.23777424415678,
125.849614730886));
#187476=CARTESIAN_POINT('Ctrl Pts',(197.470214405232,-3.10496403682583,
125.765336597878));
#187477=CARTESIAN_POINT('Ctrl Pts',(197.477637776261,-2.96920520601125,
125.686572911233));
#187478=CARTESIAN_POINT('Ctrl Pts',(197.481573825702,-2.89722261642787,
125.644810514667));
#187479=CARTESIAN_POINT('Ctrl Pts',(197.485509875143,-2.82441143032903,
125.604597636826));
#187480=CARTESIAN_POINT('Ctrl Pts',(197.489445924583,-2.75084517427645,
125.565965692624));
#187481=CARTESIAN_POINT('Ctrl Pts',(197.496869190989,-2.61210151128014,
125.493107051516));
#187482=CARTESIAN_POINT('Ctrl Pts',(197.504292457394,-2.47025146129094,
125.425654175521));
#187483=CARTESIAN_POINT('Ctrl Pts',(197.5117157238,-2.32575549227818,125.363883436965));
#187484=CARTESIAN_POINT('Ctrl Pts',(197.519130216521,-2.18143030550119,
125.302185706292));
#187485=CARTESIAN_POINT('Ctrl Pts',(197.526544709242,-2.03446576441921,
125.246156890495));
#187486=CARTESIAN_POINT('Ctrl Pts',(197.533959201963,-1.88534783816607,
125.19602805863));
#187487=CARTESIAN_POINT('Ctrl Pts',(197.541366548317,-1.73637363738422,
125.14594754282));
#187488=CARTESIAN_POINT('Ctrl Pts',(197.548773894671,-1.58525053483429,
125.101755808138));
#187489=CARTESIAN_POINT('Ctrl Pts',(197.556181241024,-1.432485332562,125.063636243892));
#187490=CARTESIAN_POINT('Ctrl Pts',(197.5635830627,-1.27983406834118,125.025545110655));
#187491=CARTESIAN_POINT('Ctrl Pts',(197.570984884375,-1.12554350365379,
124.993517220284));
#187492=CARTESIAN_POINT('Ctrl Pts',(197.57838670605,-0.970136385334234,
124.967686397057));
#187493=CARTESIAN_POINT('Ctrl Pts',(197.585784620362,-0.814811305222937,
124.941869209721));
#187494=CARTESIAN_POINT('Ctrl Pts',(197.593182534673,-0.658371212651233,
124.922242635465));
#187495=CARTESIAN_POINT('Ctrl Pts',(197.600580448984,-0.501349743220964,
124.908889559417));
#187496=CARTESIAN_POINT('Ctrl Pts',(197.607977133896,-0.3443543679101,124.895538702408));
#187497=CARTESIAN_POINT('Ctrl Pts',(197.615373818808,-0.186778179082625,
124.88845930607));
#187498=CARTESIAN_POINT('Ctrl Pts',(197.622770503721,-0.0291607638722707,
124.887682477566));
#187499=CARTESIAN_POINT('Ctrl Pts',(197.630166860656,0.128449662416806,
124.886905683508));
#187500=CARTESIAN_POINT('Ctrl Pts',(197.637563217591,0.286100938161007,
124.892430903457));
#187501=CARTESIAN_POINT('Ctrl Pts',(197.644959574526,0.443252910452061,
124.9042371087));
#187502=CARTESIAN_POINT('Ctrl Pts',(197.652357063863,0.600428943111264,
124.916045121502));
#187503=CARTESIAN_POINT('Ctrl Pts',(197.659754553199,0.757105147833064,
124.934136006373));
#187504=CARTESIAN_POINT('Ctrl Pts',(197.667152042536,0.912746078026357,
124.958436810369));
#187505=CARTESIAN_POINT('Ctrl Pts',(197.674552125051,1.06844156790636,124.982746132975));
#187506=CARTESIAN_POINT('Ctrl Pts',(197.681952207565,1.2231006920997,125.013269651301));
#187507=CARTESIAN_POINT('Ctrl Pts',(197.68935229008,1.37619793154745,125.049883246362));
#187508=CARTESIAN_POINT('Ctrl Pts',(197.696760509747,1.52946351714884,125.086537101834));
#187509=CARTESIAN_POINT('Ctrl Pts',(197.704168729413,1.68116342485591,125.12929432084));
#187510=CARTESIAN_POINT('Ctrl Pts',(197.711576949079,1.83078633663098,125.177980613327));
#187511=CARTESIAN_POINT('Ctrl Pts',(197.718989728381,1.98050133881175,125.226696871413));
#187512=CARTESIAN_POINT('Ctrl Pts',(197.726402507683,2.12813644850627,125.281349345265));
#187513=CARTESIAN_POINT('Ctrl Pts',(197.733815286985,2.27320057411559,125.341715680144));
#187514=CARTESIAN_POINT('Ctrl Pts',(197.741238658014,2.41847197415036,125.402168269274));
#187515=CARTESIAN_POINT('Ctrl Pts',(197.748662029042,2.56116471546263,125.468350868582));
#187516=CARTESIAN_POINT('Ctrl Pts',(197.756085400071,2.7008117998894,125.539994921295));
#187517=CARTESIAN_POINT('Ctrl Pts',(197.760021449512,2.77485603483877,125.577982317118));
#187518=CARTESIAN_POINT('Ctrl Pts',(197.763957498952,2.84804449245546,125.617504387378));
#187519=CARTESIAN_POINT('Ctrl Pts',(197.767893548393,2.92031099958208,125.658516252623));
#187520=CARTESIAN_POINT('Ctrl Pts',(197.775316814799,3.05660337666153,125.735863350536));
#187521=CARTESIAN_POINT('Ctrl Pts',(197.782740081204,3.19002680850025,125.818745887891));
#187522=CARTESIAN_POINT('Ctrl Pts',(197.790163347609,3.32009988104743,125.906925845936));
#187523=CARTESIAN_POINT('Ctrl Pts',(197.79757784033,3.4500192180248,125.995001582594));
#187524=CARTESIAN_POINT('Ctrl Pts',(197.804992333051,3.57659577183659,126.08836206974));
#187525=CARTESIAN_POINT('Ctrl Pts',(197.812406825772,3.69937245935516,126.186723346248));
#187526=CARTESIAN_POINT('Ctrl Pts',(197.819814172126,3.82203081007992,126.284989818454));
#187527=CARTESIAN_POINT('Ctrl Pts',(197.82722151848,3.94089629635784,126.38824725262));
#187528=CARTESIAN_POINT('Ctrl Pts',(197.834628864833,4.05554068868584,126.49616838823));
#187529=CARTESIAN_POINT('Ctrl Pts',(197.842030686509,4.17009957490073,126.604009032185));
#187530=CARTESIAN_POINT('Ctrl Pts',(197.849432508184,4.28044336511714,126.716506196922));
#187531=CARTESIAN_POINT('Ctrl Pts',(197.85683432986,4.38617691174633,126.833292416016));
#187532=CARTESIAN_POINT('Ctrl Pts',(197.864232244171,4.49185464245934,126.950016984573));
#187533=CARTESIAN_POINT('Ctrl Pts',(197.871630158482,4.59292672653128,127.071025822277));
#187534=CARTESIAN_POINT('Ctrl Pts',(197.879028072794,4.68903498727919,127.195914767817));
#187535=CARTESIAN_POINT('Ctrl Pts',(197.886424757706,4.78512727657764,127.32078295908));
#187536=CARTESIAN_POINT('Ctrl Pts',(197.893821442618,4.87625715228911,127.449529682885));
#187537=CARTESIAN_POINT('Ctrl Pts',(197.90121812753,4.96210678305087,127.581717783478));
#187538=CARTESIAN_POINT('Ctrl Pts',(197.908614484466,5.04795260715005,127.713900022711));
#187539=CARTESIAN_POINT('Ctrl Pts',(197.916010841401,5.12851844851035,127.849523022255));
#187540=CARTESIAN_POINT('Ctrl Pts',(197.923407198337,5.20353003334438,127.988120969634));
#187541=CARTESIAN_POINT('Ctrl Pts',(197.930804687674,5.27855310264355,128.126740136713));
#187542=CARTESIAN_POINT('Ctrl Pts',(197.93820217701,5.34802004452218,128.268334830214));
#187543=CARTESIAN_POINT('Ctrl Pts',(197.945599666347,5.41170281439631,128.412415130906));
#187544=CARTESIAN_POINT('Ctrl Pts',(197.952999748862,5.47540790816671,128.556545938723));
#187545=CARTESIAN_POINT('Ctrl Pts',(197.960399831377,5.5333246421133,128.703163747315));
#187546=CARTESIAN_POINT('Ctrl Pts',(197.967799913892,5.58527338516755,128.851759333269));
#187547=CARTESIAN_POINT('Ctrl Pts',(197.975208133559,5.63727925120526,129.000518315345));
#187548=CARTESIAN_POINT('Ctrl Pts',(197.982616353225,5.68330389749944,129.15125906534));
#187549=CARTESIAN_POINT('Ctrl Pts',(197.990024572892,5.72321757932056,129.303457188875));
#187550=CARTESIAN_POINT('Ctrl Pts',(197.997437352194,5.76315582734688,129.455748987816));
#187551=CARTESIAN_POINT('Ctrl Pts',(198.004850131496,5.79697553623499,129.609499583923));
#187552=CARTESIAN_POINT('Ctrl Pts',(198.012262910798,5.82459833231772,129.76417561976));
#187553=CARTESIAN_POINT('Ctrl Pts',(198.019686281827,5.85226059714686,129.91907266397));
#187554=CARTESIAN_POINT('Ctrl Pts',(198.027109652855,5.87370821410285,130.074897420031));
#187555=CARTESIAN_POINT('Ctrl Pts',(198.034533023884,5.88891470369336,130.231111827664));
#187556=CARTESIAN_POINT('Ctrl Pts',(198.038469073325,5.89697754934896,130.313940454904));
#187557=CARTESIAN_POINT('Ctrl Pts',(198.042405122766,5.90328666138535,130.396878621457));
#187558=CARTESIAN_POINT('Ctrl Pts',(198.046341172207,5.90784402994841,130.479846395531));
#187559=CARTESIAN_POINT('Ctrl Pts',(198.053764438612,5.91643908482775,130.636321028099));
#187560=CARTESIAN_POINT('Ctrl Pts',(198.061187705018,5.9188262827532,130.793373976012));
#187561=CARTESIAN_POINT('Ctrl Pts',(198.068610971423,5.91494565958679,130.950471557045));
#187562=CARTESIAN_POINT('Ctrl Pts',(198.076025464144,5.91106962299469,131.107383461784));
#187563=CARTESIAN_POINT('Ctrl Pts',(198.083439956865,5.90094052019157,131.264339525099));
#187564=CARTESIAN_POINT('Ctrl Pts',(198.090854449586,5.88455019112052,131.420801702085));
#187565=CARTESIAN_POINT('Ctrl Pts',(198.09826179594,5.86817565966571,131.577113074935));
#187566=CARTESIAN_POINT('Ctrl Pts',(198.105669142294,5.84555195468406,131.732931140355));
#187567=CARTESIAN_POINT('Ctrl Pts',(198.113076488647,5.81672294120831,131.887718724436));
#187568=CARTESIAN_POINT('Ctrl Pts',(198.120478310323,5.78791542949845,132.042390862097));
#187569=CARTESIAN_POINT('Ctrl Pts',(198.127880131998,5.75291189262878,132.196033683341));
#187570=CARTESIAN_POINT('Ctrl Pts',(198.135281953674,5.71180790358625,132.348116114732));
#187571=CARTESIAN_POINT('Ctrl Pts',(198.142679867985,5.67072561301959,132.500118262991));
#187572=CARTESIAN_POINT('Ctrl Pts',(198.150077782296,5.6235493809752,132.650561302415));
#187573=CARTESIAN_POINT('Ctrl Pts',(198.157475696608,5.57042563656271,132.798925429756));
#187574=CARTESIAN_POINT('Ctrl Pts',(198.16487238152,5.5173107203528,132.94726490167));
#187575=CARTESIAN_POINT('Ctrl Pts',(198.172269066432,5.45825037911139,133.093525796069));
#187576=CARTESIAN_POINT('Ctrl Pts',(198.179665751344,5.39344060874215,133.237204419061));
#187577=CARTESIAN_POINT('Ctrl Pts',(198.18706210828,5.32863371210605,133.380876671192));
#187578=CARTESIAN_POINT('Ctrl Pts',(198.194458465215,5.25807804673258,133.5219665393));
#187579=CARTESIAN_POINT('Ctrl Pts',(198.20185482215,5.18201726216687,133.659991486062));
#187580=CARTESIAN_POINT('Ctrl Pts',(198.209252311487,5.1059448325008,133.798037564794));
#187581=CARTESIAN_POINT('Ctrl Pts',(198.216649800824,5.02436578559861,133.933017460883));
#187582=CARTESIAN_POINT('Ctrl Pts',(198.22404729016,4.93756904071554,134.064474500649));
#187583=CARTESIAN_POINT('Ctrl Pts',(198.231447372675,4.85074186936809,134.195977622476));
#187584=CARTESIAN_POINT('Ctrl Pts',(198.23884745519,4.75869356396067,134.323955117915));
#187585=CARTESIAN_POINT('Ctrl Pts',(198.246247537705,4.66175545359166,134.447980610569));
#187586=CARTESIAN_POINT('Ctrl Pts',(198.253655757372,4.56471074980486,134.572142482001));
#187587=CARTESIAN_POINT('Ctrl Pts',(198.261063977038,4.4627657331708,134.692343377834));
#187588=CARTESIAN_POINT('Ctrl Pts',(198.268472196704,4.35629146133617,134.808190692181));
#187589=CARTESIAN_POINT('Ctrl Pts',(198.275884976006,4.24975165636372,134.924109308617));
#187590=CARTESIAN_POINT('Ctrl Pts',(198.283297755308,4.13867730416189,135.035668740291));
#187591=CARTESIAN_POINT('Ctrl Pts',(198.290710534611,4.0234747705666,135.142514756496));
#187592=CARTESIAN_POINT('Ctrl Pts',(198.298133905639,3.9081076301889,135.249513439299));
#187593=CARTESIAN_POINT('Ctrl Pts',(198.305557276668,3.7886008105804,135.351785013754));
#187594=CARTESIAN_POINT('Ctrl Pts',(198.312980647697,3.6653926842793,135.449016367192));
#187595=CARTESIAN_POINT('Ctrl Pts',(198.316916697138,3.60006477937584,135.500570763819));
#187596=CARTESIAN_POINT('Ctrl Pts',(198.320852746578,3.53369678008804,135.550708903358));
#187597=CARTESIAN_POINT('Ctrl Pts',(198.324788796019,3.4663570110182,135.599389255089));
#187598=CARTESIAN_POINT('Ctrl Pts',(198.332212062425,3.33935630815509,135.691198879192));
#187599=CARTESIAN_POINT('Ctrl Pts',(198.33963532883,3.2085135538949,135.778098250994));
#187600=CARTESIAN_POINT('Ctrl Pts',(198.347058595235,3.07424533812585,135.859748452689));
#187601=CARTESIAN_POINT('Ctrl Pts',(198.354473087956,2.94013581623739,135.941302150627));
#187602=CARTESIAN_POINT('Ctrl Pts',(198.361887580677,2.80260920746114,136.017618835655));
#187603=CARTESIAN_POINT('Ctrl Pts',(198.369302073398,2.66211377350456,136.088400816071));
#187604=CARTESIAN_POINT('Ctrl Pts',(198.376709419752,2.52175375433678,136.15911457415));
#187605=CARTESIAN_POINT('Ctrl Pts',(198.384116766106,2.37843093774423,136.22430408084));
#187606=CARTESIAN_POINT('Ctrl Pts',(198.39152411246,2.23262097347329,136.283715885415));
#187607=CARTESIAN_POINT('Ctrl Pts',(198.398925934135,2.08691975977482,136.343083378425));
#187608=CARTESIAN_POINT('Ctrl Pts',(198.406327755811,1.93873543618441,136.396681609322));
#187609=CARTESIAN_POINT('Ctrl Pts',(198.413729577486,1.7885664693587,136.444303928202));
#187610=CARTESIAN_POINT('Ctrl Pts',(198.421127491797,1.63847677556185,136.49190110763));
#187611=CARTESIAN_POINT('Ctrl Pts',(198.428525406109,1.48640487996303,136.533528545095));
#187612=CARTESIAN_POINT('Ctrl Pts',(198.43592332042,1.33286725626621,136.569028469201));
#187613=CARTESIAN_POINT('Ctrl Pts',(198.443320005332,1.17935514773689,136.604522493864));
#187614=CARTESIAN_POINT('Ctrl Pts',(198.450716690245,1.02437815788533,136.633890942145));
#187615=CARTESIAN_POINT('Ctrl Pts',(198.458113375157,0.868465999221073,
136.657026452098));
#187616=CARTESIAN_POINT('Ctrl Pts',(198.465509732092,0.712560753865369,
136.680160936198));
#187617=CARTESIAN_POINT('Ctrl Pts',(198.472906089028,0.555720791400502,
136.697062976703));
#187618=CARTESIAN_POINT('Ctrl Pts',(198.480302445963,0.398483782675044,
136.707676739666));
#187619=CARTESIAN_POINT('Ctrl Pts',(198.4876999353,0.241222700562017,136.718292127623));
#187620=CARTESIAN_POINT('Ctrl Pts',(198.495097424636,0.0835648236240816,
136.722617295928));
#187621=CARTESIAN_POINT('Ctrl Pts',(198.502494913973,-0.0739494677253907,
136.720648477257));
#187622=CARTESIAN_POINT('Ctrl Pts',(198.509894996488,-0.231518975465559,
136.718678968419));
#187623=CARTESIAN_POINT('Ctrl Pts',(198.517295079003,-0.388944424367331,
136.710411084445));
#187624=CARTESIAN_POINT('Ctrl Pts',(198.524695161518,-0.545688000420484,
136.695893115032));
#187625=CARTESIAN_POINT('Ctrl Pts',(198.532103381184,-0.702603932149111,
136.681359181619));
#187626=CARTESIAN_POINT('Ctrl Pts',(198.539511600851,-0.858836121715699,
136.660561472159));
#187627=CARTESIAN_POINT('Ctrl Pts',(198.546919820517,-1.01385369294746,
136.633599954889));
#187628=CARTESIAN_POINT('Ctrl Pts',(198.55433259982,-1.16896667490789,136.606621843255));
#187629=CARTESIAN_POINT('Ctrl Pts',(198.561745379122,-1.32286318481004,
136.573472442769));
#187630=CARTESIAN_POINT('Ctrl Pts',(198.569158158424,-1.47502554766598,
136.534302170168));
#187631=CARTESIAN_POINT('Ctrl Pts',(198.576581529452,-1.62740532724162,
136.495075929244));
#187632=CARTESIAN_POINT('Ctrl Pts',(198.584004900481,-1.77804565442718,
136.449811741413));
#187633=CARTESIAN_POINT('Ctrl Pts',(198.59142827151,-1.92644614760085,136.398709176862));
#187634=CARTESIAN_POINT('Ctrl Pts',(198.595364320951,-2.00513164990258,
136.371613370947));
#187635=CARTESIAN_POINT('Ctrl Pts',(198.599300370392,-2.083187811426,136.34287698262));
#187636=CARTESIAN_POINT('Ctrl Pts',(198.603236419832,-2.16054276008407,
136.312535046934));
#187637=CARTESIAN_POINT('Ctrl Pts',(198.610659686238,-2.30643177908773,
136.255311103171));
#187638=CARTESIAN_POINT('Ctrl Pts',(198.618082952643,-2.4502663863924,136.192200621447));
#187639=CARTESIAN_POINT('Ctrl Pts',(198.625506219049,-2.59153626383937,
136.12337089728));
#187640=CARTESIAN_POINT('Ctrl Pts',(198.63292071177,-2.73263917202303,136.054622524132));
#187641=CARTESIAN_POINT('Ctrl Pts',(198.640335204491,-2.87118305185535,
135.980168525608));
#187642=CARTESIAN_POINT('Ctrl Pts',(198.647749697212,-3.00667515047484,
135.900225127344));
#187643=CARTESIAN_POINT('Ctrl Pts',(198.655157043566,-3.14203665670858,
135.820358781537));
#187644=CARTESIAN_POINT('Ctrl Pts',(198.662564389919,-3.27435191817235,
135.735013757533));
#187645=CARTESIAN_POINT('Ctrl Pts',(198.669971736273,-3.40315059928627,
135.644453236626));
#187646=CARTESIAN_POINT('Ctrl Pts',(198.677373557949,-3.53185321748438,
135.553960259172));
#187647=CARTESIAN_POINT('Ctrl Pts',(198.684775379624,-3.65704417362253,
135.458259743947));
#187648=CARTESIAN_POINT('Ctrl Pts',(198.692177201299,-3.77828017388039,
135.357659365744));
#187649=CARTESIAN_POINT('Ctrl Pts',(198.699575115611,-3.89945217459736,
135.257112093699));
#187650=CARTESIAN_POINT('Ctrl Pts',(198.706973029922,-4.01667309082048,
135.151670347788));
#187651=CARTESIAN_POINT('Ctrl Pts',(198.714370944233,-4.12953101835425,
135.041683372673));
#187652=CARTESIAN_POINT('Ctrl Pts',(198.721767629146,-4.24237019094798,
134.931714675399));
#187653=CARTESIAN_POINT('Ctrl Pts',(198.729164314058,-4.35084754678297,
134.81720250832));
#187654=CARTESIAN_POINT('Ctrl Pts',(198.73656099897,-4.45458643666219,134.69853450182));
#187655=CARTESIAN_POINT('Ctrl Pts',(198.743957355906,-4.55832072665023,
134.579871757183));
#187656=CARTESIAN_POINT('Ctrl Pts',(198.751353712841,-4.65731672275938,
134.457053820572));
#187657=CARTESIAN_POINT('Ctrl Pts',(198.758750069776,-4.75123682608077,
134.330502870084));
#187658=CARTESIAN_POINT('Ctrl Pts',(198.766147559113,-4.84517130880985,
134.203932544323));
#187659=CARTESIAN_POINT('Ctrl Pts',(198.77354504845,-4.93402812889303,134.073628366469));
#187660=CARTESIAN_POINT('Ctrl Pts',(198.780942537786,-5.01751202795966,
133.940042937537));
#187661=CARTESIAN_POINT('Ctrl Pts',(198.788342620301,-5.10102519217775,
133.80641068044));
#187662=CARTESIAN_POINT('Ctrl Pts',(198.795742702816,-5.17916148769389,
133.669495198516));
#187663=CARTESIAN_POINT('Ctrl Pts',(198.803142785331,-5.25167084038773,
133.529775071685));
#187664=CARTESIAN_POINT('Ctrl Pts',(198.810551004998,-5.32425992456896,
133.389901308211));
#187665=CARTESIAN_POINT('Ctrl Pts',(198.817959224664,-5.39120953722308,
133.247217072428));
#187666=CARTESIAN_POINT('Ctrl Pts',(198.825367444331,-5.45231683291927,
133.102223040768));
#187667=CARTESIAN_POINT('Ctrl Pts',(198.832780223633,-5.51346173913636,
132.957139767702));
#187668=CARTESIAN_POINT('Ctrl Pts',(198.840193002935,-5.56875703240109,
132.809744214664));
#187669=CARTESIAN_POINT('Ctrl Pts',(198.847605782237,-5.61804944659764,
132.660553220203));
#187670=CARTESIAN_POINT('Ctrl Pts',(198.855029153265,-5.66741229210717,
132.511149054653));
#187671=CARTESIAN_POINT('Ctrl Pts',(198.862452524294,-5.71075502537524,
132.359944681874));
#187672=CARTESIAN_POINT('Ctrl Pts',(198.869875895323,-5.74797508196189,
132.207468959657));
#187673=CARTESIAN_POINT('Ctrl Pts',(198.873811944764,-5.76771004904698,
132.126622673133));
#187674=CARTESIAN_POINT('Ctrl Pts',(198.877747994205,-5.78572457362142,
132.045419093963));
#187675=CARTESIAN_POINT('Ctrl Pts',(198.881684043645,-5.80200928305024,
131.96393762747));
#187676=CARTESIAN_POINT('Ctrl Pts',(198.892415019576,-5.84640680080297,
131.741792131358));
#187677=CARTESIAN_POINT('Ctrl Pts',(198.903145995507,-5.87805736973165,
131.517021225439));
#187678=CARTESIAN_POINT('Ctrl Pts',(198.913876971438,-5.89671799543621,
131.290824845232));
#187679=CARTESIAN_POINT('Ctrl Pts',(198.921459583557,-5.90990377532492,
131.130992279687));
#187680=CARTESIAN_POINT('Ctrl Pts',(198.929042195676,-5.91660456247561,
130.970448251875));
#187681=CARTESIAN_POINT('Ctrl Pts',(198.936624807795,-5.91674765788855,
130.809625156515));
#187682=CARTESIAN_POINT('',(200.686624807795,-5.90698642445631,130.80494468951));
#187683=CARTESIAN_POINT('Ctrl Pts',(198.936625793059,-5.9188774747153,130.809606147102));
#187684=CARTESIAN_POINT('Ctrl Pts',(199.011127751193,-5.90425259497605,
129.228876773919));
#187685=CARTESIAN_POINT('Ctrl Pts',(199.178445583929,-4.43793552679426,
125.654919300417));
#187686=CARTESIAN_POINT('Ctrl Pts',(199.438579291272,1.60513008150291,123.992524011201));
#187687=CARTESIAN_POINT('Ctrl Pts',(199.717026915084,6.59860307470548,128.472837940681));
#187688=CARTESIAN_POINT('Ctrl Pts',(199.995474538897,5.52828220193623,135.095707309003));
#187689=CARTESIAN_POINT('Ctrl Pts',(200.27392216271,-0.622259942815148,
137.775038711833));
#187690=CARTESIAN_POINT('Ctrl Pts',(200.504305585676,-5.2380063121806,134.691886300211));
#187691=CARTESIAN_POINT('Ctrl Pts',(200.641873134038,-5.90782357734734,
131.759296891607));
#187692=CARTESIAN_POINT('Ctrl Pts',(200.686624807795,-5.90698642445631,
130.80494468951));
#187693=CARTESIAN_POINT('',(202.436624807795,-5.91672686803579,130.798894919773));
#187694=CARTESIAN_POINT('Ctrl Pts',(200.686624807795,-5.90698642445631,
130.80494468951));
#187695=CARTESIAN_POINT('Ctrl Pts',(200.734689008642,-5.90608730535493,
129.77995116259));
#187696=CARTESIAN_POINT('Ctrl Pts',(200.875569084094,-5.16390162333142,
126.774392662908));
#187697=CARTESIAN_POINT('Ctrl Pts',(201.109265034148,-0.373204209884669,
123.815921653964));
#187698=CARTESIAN_POINT('Ctrl Pts',(201.387712657962,5.67784563147399,126.712951384136));
#187699=CARTESIAN_POINT('Ctrl Pts',(201.666160281774,6.5112327157493,133.369786323417));
#187700=CARTESIAN_POINT('Ctrl Pts',(201.944607905587,1.36111502553663,137.669120366955));
#187701=CARTESIAN_POINT('Ctrl Pts',(202.201429414261,-4.54266270085758,
135.816111494225));
#187702=CARTESIAN_POINT('Ctrl Pts',(202.36543504833,-5.90274340491685,132.310756663458));
#187703=CARTESIAN_POINT('Ctrl Pts',(202.436624807795,-5.91672686803579,
130.798894919773));
#187704=CARTESIAN_POINT('',(204.186624807795,-5.92581928566479,130.806233519117));
#187705=CARTESIAN_POINT('Ctrl Pts',(202.436624807795,-5.91672686803579,
130.798894919773));
#187706=CARTESIAN_POINT('Ctrl Pts',(202.458250922934,-5.9209747821421,130.339619647749));
#187707=CARTESIAN_POINT('Ctrl Pts',(202.572692912681,-5.66197777958727,
127.913946320691));
#187708=CARTESIAN_POINT('Ctrl Pts',(202.779950777024,-2.32147802600033,
124.202217003606));
#187709=CARTESIAN_POINT('Ctrl Pts',(203.058398400839,4.2997548257633,125.28261551589));
#187710=CARTESIAN_POINT('Ctrl Pts',(203.336846024651,6.96972305013295,131.437228026285));
#187711=CARTESIAN_POINT('Ctrl Pts',(203.615293648464,3.23485627607878,137.010266301744));
#187712=CARTESIAN_POINT('Ctrl Pts',(203.893741272277,-3.4726853742618,136.880380435614));
#187713=CARTESIAN_POINT('Ctrl Pts',(204.084184992054,-5.87766124044895,
132.972676372107));
#187714=CARTESIAN_POINT('Ctrl Pts',(204.181812837227,-5.92623998325372,
130.908018473525));
#187715=CARTESIAN_POINT('Ctrl Pts',(204.186624807795,-5.92581928566479,
130.806233519117));
#187716=CARTESIAN_POINT('',(205.936623590202,-5.91340924895264,130.808944439334));
#187717=CARTESIAN_POINT('Ctrl Pts',(204.186624807795,-5.92581928566479,
130.806233519117));
#187718=CARTESIAN_POINT('Ctrl Pts',(204.274628711831,-5.91812534204668,
128.944735566654));
#187719=CARTESIAN_POINT('Ctrl Pts',(204.455448490471,-3.96770241261772,
125.106068119418));
#187720=CARTESIAN_POINT('Ctrl Pts',(204.729084143717,2.57533168687046,124.297039558175));
#187721=CARTESIAN_POINT('Ctrl Pts',(205.007531767529,6.86682325353852,129.453694210665));
#187722=CARTESIAN_POINT('Ctrl Pts',(205.285979391342,4.84803947518153,135.851545143624));
#187723=CARTESIAN_POINT('Ctrl Pts',(205.564427015155,-1.62585529160082,
137.611280375001));
#187724=CARTESIAN_POINT('Ctrl Pts',(205.781308123836,-5.50460122239126,
134.109769780245));
#187725=CARTESIAN_POINT('Ctrl Pts',(205.905373357914,-5.91576144076024,
131.474232650613));
#187726=CARTESIAN_POINT('Ctrl Pts',(205.936622717388,-5.911015738934,130.80896117583));
#187727=CARTESIAN_POINT('',(207.686626030528,-5.91241378256136,130.800689035563));
#187728=CARTESIAN_POINT('Ctrl Pts',(205.936624807795,-5.91674824245351,
130.808921091594));
#187729=CARTESIAN_POINT('Ctrl Pts',(205.944320535086,-5.91687464410253,
130.644927890423));
#187730=CARTESIAN_POINT('Ctrl Pts',(205.952016262377,-5.91017796225583,
130.480857837863));
#187731=CARTESIAN_POINT('Ctrl Pts',(205.959711989668,-5.89667042808694,
130.31732014181));
#187732=CARTESIAN_POINT('Ctrl Pts',(205.967107144318,-5.8836904587688,130.160169750732));
#187733=CARTESIAN_POINT('Ctrl Pts',(205.974502298968,-5.86442165241146,
130.003511317041));
#187734=CARTESIAN_POINT('Ctrl Pts',(205.981897453618,-5.83892794642443,
129.847882181341));
#187735=CARTESIAN_POINT('Ctrl Pts',(205.989293079306,-5.81343261660182,
129.692243132757));
#187736=CARTESIAN_POINT('Ctrl Pts',(205.996688704995,-5.78171165733105,
129.53763388078));
#187737=CARTESIAN_POINT('Ctrl Pts',(206.004084330683,-5.74388042102671,
129.384583074623));
#187738=CARTESIAN_POINT('Ctrl Pts',(206.011481882822,-5.70603933025007,
129.231492401015));
#187739=CARTESIAN_POINT('Ctrl Pts',(206.01887943496,-5.66208488256809,129.079961343446));
#187740=CARTESIAN_POINT('Ctrl Pts',(206.026276987099,-5.61218269697228,
128.930504716408));
#187741=CARTESIAN_POINT('Ctrl Pts',(206.033677921977,-5.56225769219368,
128.780979746109));
#187742=CARTESIAN_POINT('Ctrl Pts',(206.041078856855,-5.50637965184727,
128.633531448377));
#187743=CARTESIAN_POINT('Ctrl Pts',(206.048479791733,-5.44476278582211,
128.488655807227));
#187744=CARTESIAN_POINT('Ctrl Pts',(206.055889603669,-5.38307201339005,
128.343606394855));
#187745=CARTESIAN_POINT('Ctrl Pts',(206.063299415605,-5.31562881696656,
128.201136143459));
#187746=CARTESIAN_POINT('Ctrl Pts',(206.070709227541,-5.24269425134762,
128.06171817835));
#187747=CARTESIAN_POINT('Ctrl Pts',(206.078124284764,-5.16970805651977,
127.922201521501));
#187748=CARTESIAN_POINT('Ctrl Pts',(206.085539341988,-5.09122293266157,
127.785741777807));
#187749=CARTESIAN_POINT('Ctrl Pts',(206.092954399211,-5.00754363174057,
127.652783656945));
#187750=CARTESIAN_POINT('Ctrl Pts',(206.100380033849,-4.92374496414771,
127.519635874265));
#187751=CARTESIAN_POINT('Ctrl Pts',(206.107805668488,-4.83473753693092,
127.389999992524));
#187752=CARTESIAN_POINT('Ctrl Pts',(206.115231303126,-4.74086717656672,
127.264288728938));
#187753=CARTESIAN_POINT('Ctrl Pts',(206.117261623011,-4.71520110645441,
127.229916706794));
#187754=CARTESIAN_POINT('Ctrl Pts',(206.119291942896,-4.68917170648531,
127.195837875561));
#187755=CARTESIAN_POINT('Ctrl Pts',(206.121322262781,-4.66278652276695,
127.162060189869));
#187756=CARTESIAN_POINT('Ctrl Pts',(206.128745542087,-4.56631670550191,
127.038561820438));
#187757=CARTESIAN_POINT('Ctrl Pts',(206.136168821393,-4.46479117026267,
126.918712002184));
#187758=CARTESIAN_POINT('Ctrl Pts',(206.1435921007,-4.35851586193957,126.802952110088));
#187759=CARTESIAN_POINT('Ctrl Pts',(206.151006606373,-4.25236616125308,
126.687329035533));
#187760=CARTESIAN_POINT('Ctrl Pts',(206.158421112046,-4.14147811176257,
126.575786537499));
#187761=CARTESIAN_POINT('Ctrl Pts',(206.165835617719,-4.02619954292322,
126.4687351952));
#187762=CARTESIAN_POINT('Ctrl Pts',(206.173242977064,-3.9110320831151,126.361787032278));
#187763=CARTESIAN_POINT('Ctrl Pts',(206.180650336408,-3.79148280018012,
126.259321659787));
#187764=CARTESIAN_POINT('Ctrl Pts',(206.188057695753,-3.66793813141363,
126.161714774232));
#187765=CARTESIAN_POINT('Ctrl Pts',(206.195459530445,-3.54448560632645,
126.064180687105));
#187766=CARTESIAN_POINT('Ctrl Pts',(206.202861365137,-3.41704392042245,
125.971498102217));
#187767=CARTESIAN_POINT('Ctrl Pts',(206.210263199829,-3.28603443959317,
125.884004103622));
#187768=CARTESIAN_POINT('Ctrl Pts',(206.217661127171,-3.15509411728722,
125.796556292186));
#187769=CARTESIAN_POINT('Ctrl Pts',(206.225059054513,-3.02059006058692,
125.714291818989));
#187770=CARTESIAN_POINT('Ctrl Pts',(206.232456981854,-2.88297452136991,
125.637505822661));
#187771=CARTESIAN_POINT('Ctrl Pts',(206.239853679775,-2.74538185171612,
125.560732586972));
#187772=CARTESIAN_POINT('Ctrl Pts',(206.247250377697,-2.60467905146201,
125.489436202917));
#187773=CARTESIAN_POINT('Ctrl Pts',(206.254647075618,-2.4613451038374,125.423867067499));
#187774=CARTESIAN_POINT('Ctrl Pts',(206.262043445548,-2.3180175120597,125.358300839608));
#187775=CARTESIAN_POINT('Ctrl Pts',(206.269439815478,-2.1720593443594,125.298461510681));
#187776=CARTESIAN_POINT('Ctrl Pts',(206.276836185407,-2.02397155401354,
125.244552193614));
#187777=CARTESIAN_POINT('Ctrl Pts',(206.284233687713,-1.87586109160203,
125.190634623095));
#187778=CARTESIAN_POINT('Ctrl Pts',(206.291631190018,-1.72562070814953,
125.142648999845));
#187779=CARTESIAN_POINT('Ctrl Pts',(206.299028692324,-1.57376843488975,
125.100749176045));
#187780=CARTESIAN_POINT('Ctrl Pts',(206.306428787771,-1.42186293089913,
125.058834664561));
#187781=CARTESIAN_POINT('Ctrl Pts',(206.313828883218,-1.26834477174244,
125.023010299208));
#187782=CARTESIAN_POINT('Ctrl Pts',(206.321228978665,-1.1137439959854,124.993379213887));
#187783=CARTESIAN_POINT('Ctrl Pts',(206.328637211142,-0.958973223613178,
124.963715546683));
#187784=CARTESIAN_POINT('Ctrl Pts',(206.336045443619,-0.803117824125187,
124.940258829909));
#187785=CARTESIAN_POINT('Ctrl Pts',(206.343453676096,-0.646715539100822,
124.923060627429));
#187786=CARTESIAN_POINT('Ctrl Pts',(206.35086646816,-0.490216992290331,
124.905851839875));
#187787=CARTESIAN_POINT('Ctrl Pts',(206.358279260223,-0.333171260766503,
124.894909268023));
#187788=CARTESIAN_POINT('Ctrl Pts',(206.365692052287,-0.176117430763197,
124.890232345954));
#187789=CARTESIAN_POINT('Ctrl Pts',(206.373115435889,-0.0188391992448544,
124.885548741409));
#187790=CARTESIAN_POINT('Ctrl Pts',(206.380538819491,0.13844678157505,124.887148662973));
#187791=CARTESIAN_POINT('Ctrl Pts',(206.387962203094,0.295204371712296,
124.894979521256));
#187792=CARTESIAN_POINT('Ctrl Pts',(206.391898097594,0.378317594721756,
124.899131459738));
#187793=CARTESIAN_POINT('Ctrl Pts',(206.395833992093,0.461282402246363,
124.905034131635));
#187794=CARTESIAN_POINT('Ctrl Pts',(206.399769886593,0.544020024813092,
124.912673866295));
#187795=CARTESIAN_POINT('Ctrl Pts',(206.407193124759,0.700066147897168,
124.927082679821));
#187796=CARTESIAN_POINT('Ctrl Pts',(206.414616362924,0.855775400938864,
124.947717077111));
#187797=CARTESIAN_POINT('Ctrl Pts',(206.42203960109,1.0106110768226,124.974558235503));
#187798=CARTESIAN_POINT('Ctrl Pts',(206.429454065568,1.1652637490334,125.001367669744));
#187799=CARTESIAN_POINT('Ctrl Pts',(206.436868530046,1.31904453505951,125.034369199787));
#187800=CARTESIAN_POINT('Ctrl Pts',(206.444282994524,1.47141999714576,125.07349211842));
#187801=CARTESIAN_POINT('Ctrl Pts',(206.451690312658,1.62364859393998,125.11257732889));
#187802=CARTESIAN_POINT('Ctrl Pts',(206.459097630792,1.77447420420068,125.157772089943));
#187803=CARTESIAN_POINT('Ctrl Pts',(206.466504948926,1.92337186920565,125.208954357494));
#187804=CARTESIAN_POINT('Ctrl Pts',(206.47390674243,2.07215848127999,125.260098451574));
#187805=CARTESIAN_POINT('Ctrl Pts',(206.481308535935,2.21901965969763,125.317221039542));
#187806=CARTESIAN_POINT('Ctrl Pts',(206.48871032944,2.36344405149433,125.380149819859));
#187807=CARTESIAN_POINT('Ctrl Pts',(206.496108215656,2.50779220395472,125.443045381076));
#187808=CARTESIAN_POINT('Ctrl Pts',(206.503506101871,2.64970579024399,125.511740881817));
#187809=CARTESIAN_POINT('Ctrl Pts',(206.510903988087,2.78869205246822,125.586015362698));
#187810=CARTESIAN_POINT('Ctrl Pts',(206.518300645105,2.92765522138042,125.660277502477));
#187811=CARTESIAN_POINT('Ctrl Pts',(206.525697302122,3.06369170265306,125.740116606851));
#187812=CARTESIAN_POINT('Ctrl Pts',(206.533093959139,3.19633193171053,125.825265042582));
#187813=CARTESIAN_POINT('Ctrl Pts',(206.540490288307,3.32896628161558,125.910409704189));
#187814=CARTESIAN_POINT('Ctrl Pts',(206.547886617474,3.45820436447894,126.000863027573));
#187815=CARTESIAN_POINT('Ctrl Pts',(206.555282946642,3.58360452178626,126.096313337224));
#187816=CARTESIAN_POINT('Ctrl Pts',(206.562680408361,3.70902388080001,126.191778262557));
#187817=CARTESIAN_POINT('Ctrl Pts',(206.57007787008,3.83060384705553,126.292241471571));
#187818=CARTESIAN_POINT('Ctrl Pts',(206.577475331799,3.94793497542389,126.397350293965));
#187819=CARTESIAN_POINT('Ctrl Pts',(206.584875386871,4.06530723695059,126.502495964703));
#187820=CARTESIAN_POINT('Ctrl Pts',(206.592275441942,4.17842741707443,126.612290242479));
#187821=CARTESIAN_POINT('Ctrl Pts',(206.599675497014,4.28692225118017,126.726342940454));
#187822=CARTESIAN_POINT('Ctrl Pts',(206.607083689639,4.39553639284793,126.840521057759));
#187823=CARTESIAN_POINT('Ctrl Pts',(206.614491882264,4.49951477334651,126.958966676524));
#187824=CARTESIAN_POINT('Ctrl Pts',(206.621900074889,4.59852335176967,127.081255254334));
#187825=CARTESIAN_POINT('Ctrl Pts',(206.629312827337,4.69759287104336,127.203619102085));
#187826=CARTESIAN_POINT('Ctrl Pts',(206.636725579785,4.79168627026316,127.329830323613));
#187827=CARTESIAN_POINT('Ctrl Pts',(206.644138332232,4.88051264007905,127.459435067942));
#187828=CARTESIAN_POINT('Ctrl Pts',(206.651561676931,4.96946593591552,127.589225007439));
#187829=CARTESIAN_POINT('Ctrl Pts',(206.658985021629,5.05313697283413,127.722417839174));
#187830=CARTESIAN_POINT('Ctrl Pts',(206.666408366327,5.13128020290801,127.85853407112));
#187831=CARTESIAN_POINT('Ctrl Pts',(206.670344747687,5.17271725948344,127.930712505499));
#187832=CARTESIAN_POINT('Ctrl Pts',(206.674281129047,5.21260076983565,128.003712593246));
#187833=CARTESIAN_POINT('Ctrl Pts',(206.678217510406,5.25089964747057,128.077460646043));
#187834=CARTESIAN_POINT('Ctrl Pts',(206.685640788461,5.32312415823054,128.216535662379));
#187835=CARTESIAN_POINT('Ctrl Pts',(206.693064066516,5.38992876580882,128.358692359875));
#187836=CARTESIAN_POINT('Ctrl Pts',(206.70048734457,5.45103920233565,128.503469012753));
#187837=CARTESIAN_POINT('Ctrl Pts',(206.707901848764,5.51207741006388,128.648074548481));
#187838=CARTESIAN_POINT('Ctrl Pts',(206.715316352958,5.56743469941649,128.795293535183));
#187839=CARTESIAN_POINT('Ctrl Pts',(206.722730857152,5.61688222173231,128.944638952992));
#187840=CARTESIAN_POINT('Ctrl Pts',(206.730138214794,5.66628208350656,129.093840422567));
#187841=CARTESIAN_POINT('Ctrl Pts',(206.737545572436,5.70978340170099,129.245163890933));
#187842=CARTESIAN_POINT('Ctrl Pts',(206.744952930079,5.74720510199896,129.398101723174));
#187843=CARTESIAN_POINT('Ctrl Pts',(206.752354762849,5.78459889084789,129.550925484796));
#187844=CARTESIAN_POINT('Ctrl Pts',(206.75975659562,5.81592200238041,129.705360851741));
#187845=CARTESIAN_POINT('Ctrl Pts',(206.76715842839,5.84104299956862,129.860884470708));
#187846=CARTESIAN_POINT('Ctrl Pts',(206.774556353595,5.86615073491324,130.016325985852));
#187847=CARTESIAN_POINT('Ctrl Pts',(206.7819542788,5.88506281728915,130.172854241269));
#187848=CARTESIAN_POINT('Ctrl Pts',(206.789352204005,5.89769879798555,130.3299352275));
#187849=CARTESIAN_POINT('Ctrl Pts',(206.796748899477,5.91033267824449,130.486990102675));
#187850=CARTESIAN_POINT('Ctrl Pts',(206.804145594949,5.916692497478,130.644597154582));
#187851=CARTESIAN_POINT('Ctrl Pts',(206.811542290421,5.91674961156377,130.802216658626));
#187852=CARTESIAN_POINT('Ctrl Pts',(206.818938657709,5.91680672311545,130.959829169243));
#187853=CARTESIAN_POINT('Ctrl Pts',(206.826335024996,5.91056168541346,131.117453757603));
#187854=CARTESIAN_POINT('Ctrl Pts',(206.833731392284,5.89803799224905,131.274550371269));
#187855=CARTESIAN_POINT('Ctrl Pts',(206.841128891757,5.88551238204311,131.431671032212));
#187856=CARTESIAN_POINT('Ctrl Pts',(206.84852639123,5.86670623237614,131.588263185401));
#187857=CARTESIAN_POINT('Ctrl Pts',(206.855923890704,5.84169493924943,131.743791721611));
#187858=CARTESIAN_POINT('Ctrl Pts',(206.863323983131,5.81667487922173,131.899374773326));
#187859=CARTESIAN_POINT('Ctrl Pts',(206.870724075559,5.78544540453325,132.053893097456));
#187860=CARTESIAN_POINT('Ctrl Pts',(206.878124167987,5.74813303139715,132.206821745677));
#187861=CARTESIAN_POINT('Ctrl Pts',(206.885532397177,5.71077963148513,132.359918546412));
#187862=CARTESIAN_POINT('Ctrl Pts',(206.892940626368,5.66733006440155,132.511421817633));
#187863=CARTESIAN_POINT('Ctrl Pts',(206.900348855559,5.61796095210065,132.660821040837));
#187864=CARTESIAN_POINT('Ctrl Pts',(206.907761644179,5.56856145534386,132.810312212507));
#187865=CARTESIAN_POINT('Ctrl Pts',(206.9151744328,5.51323528469942,132.957696407142));
#187866=CARTESIAN_POINT('Ctrl Pts',(206.922587221421,5.4522070340239,133.102483551754));
#187867=CARTESIAN_POINT('Ctrl Pts',(206.930010601367,5.39109158672778,133.247477566947));
#187868=CARTESIAN_POINT('Ctrl Pts',(206.937433981314,5.32425794604404,133.389866784103));
#187869=CARTESIAN_POINT('Ctrl Pts',(206.944857361261,5.25197679745634,133.529185434225));
#187870=CARTESIAN_POINT('Ctrl Pts',(206.948793285581,5.21365286245805,133.603053088456));
#187871=CARTESIAN_POINT('Ctrl Pts',(206.9527292099,5.17379827248528,133.67605802251));
#187872=CARTESIAN_POINT('Ctrl Pts',(206.956665134219,5.13245820404137,133.748134275011));
#187873=CARTESIAN_POINT('Ctrl Pts',(206.964088477532,5.05448883884311,133.884073567444));
#187874=CARTESIAN_POINT('Ctrl Pts',(206.971511820845,4.97099709000868,134.017118578131));
#187875=CARTESIAN_POINT('Ctrl Pts',(206.978935164159,4.8822231829641,134.146788979435));
#187876=CARTESIAN_POINT('Ctrl Pts',(206.986349734158,4.79355419377888,134.276306129166));
#187877=CARTESIAN_POINT('Ctrl Pts',(206.993764304158,4.69961568142008,134.402456303235));
#187878=CARTESIAN_POINT('Ctrl Pts',(207.001178874158,4.60069370173865,134.524783715183));
#187879=CARTESIAN_POINT('Ctrl Pts',(207.008586298086,4.50186706186089,134.646993229456));
#187880=CARTESIAN_POINT('Ctrl Pts',(207.015993722013,4.39806674964955,134.76538702808));
#187881=CARTESIAN_POINT('Ctrl Pts',(207.02340114594,4.2896219877561,134.879538376224));
#187882=CARTESIAN_POINT('Ctrl Pts',(207.030803045408,4.18125810400504,134.993604590251));
#187883=CARTESIAN_POINT('Ctrl Pts',(207.038204944876,4.06825692352974,135.103434384324));
#187884=CARTESIAN_POINT('Ctrl Pts',(207.045606844344,3.9509877230448,135.208634289223));
#187885=CARTESIAN_POINT('Ctrl Pts',(207.053004836591,3.8337804251313,135.313778662536));
#187886=CARTESIAN_POINT('Ctrl Pts',(207.060402828839,3.71230987122733,135.414297765317));
#187887=CARTESIAN_POINT('Ctrl Pts',(207.067800821086,3.58698186339951,135.509835266753));
#187888=CARTESIAN_POINT('Ctrl Pts',(207.0751975839,3.46167468317873,135.605356891311));
#187889=CARTESIAN_POINT('Ctrl Pts',(207.082594346714,3.33251161790928,135.695898331514));
#187890=CARTESIAN_POINT('Ctrl Pts',(207.089991109528,3.19993127924519,135.781143752344));
#187891=CARTESIAN_POINT('Ctrl Pts',(207.097387544336,3.06735681979036,135.866385393008));
#187892=CARTESIAN_POINT('Ctrl Pts',(207.104783979144,2.93136570223466,135.946331279376));
#187893=CARTESIAN_POINT('Ctrl Pts',(207.112180413952,2.79242499555474,136.020709264532));
#187894=CARTESIAN_POINT('Ctrl Pts',(207.119577981065,2.65346301872775,136.095098636061));
#187895=CARTESIAN_POINT('Ctrl Pts',(207.126975548178,2.51155088280885,136.163918232992));
#187896=CARTESIAN_POINT('Ctrl Pts',(207.134373115291,2.36717955207727,136.226942247263));
#187897=CARTESIAN_POINT('Ctrl Pts',(207.141773275419,2.22275761591827,136.289988352881));
#187898=CARTESIAN_POINT('Ctrl Pts',(207.149173435547,2.07587511060173,136.347234681915));
#187899=CARTESIAN_POINT('Ctrl Pts',(207.156573595675,1.92704208331791,136.398503927459));
#187900=CARTESIAN_POINT('Ctrl Pts',(207.163981892314,1.7780454134245,136.449829543778));
#187901=CARTESIAN_POINT('Ctrl Pts',(207.171390188953,1.62709429179282,136.495164830576));
#187902=CARTESIAN_POINT('Ctrl Pts',(207.178798485592,1.47471370865867,136.534382436023));
#187903=CARTESIAN_POINT('Ctrl Pts',(207.186211341619,1.32223934388331,136.573624177691));
#187904=CARTESIAN_POINT('Ctrl Pts',(207.193624197646,1.16833412867738,136.606740657254));
#187905=CARTESIAN_POINT('Ctrl Pts',(207.201037053673,1.01353178190939,136.633655934288));
#187906=CARTESIAN_POINT('Ctrl Pts',(207.208460500376,0.858508270520578,
136.660609664919));
#187907=CARTESIAN_POINT('Ctrl Pts',(207.215883947078,0.702585436732427,
136.681344449338));
#187908=CARTESIAN_POINT('Ctrl Pts',(207.223307393781,0.546301465452972,
136.695836262202));
#187909=CARTESIAN_POINT('Ctrl Pts',(207.227242515198,0.463456336076836,
136.703518279122));
#187910=CARTESIAN_POINT('Ctrl Pts',(207.231177636615,0.38050972967095,136.709446907009));
#187911=CARTESIAN_POINT('Ctrl Pts',(207.235112758032,0.297541510646655,
136.713624498283));
#187912=CARTESIAN_POINT('Ctrl Pts',(207.242535825934,0.141033322402311,
136.72150495238));
#187913=CARTESIAN_POINT('Ctrl Pts',(207.249958893836,-0.0160248826544751,
136.723175299195));
#187914=CARTESIAN_POINT('Ctrl Pts',(207.257381961737,-0.17309917929533,
136.71857799915));
#187915=CARTESIAN_POINT('Ctrl Pts',(207.264796255826,-0.329987819465992,
136.713986132956));
#187916=CARTESIAN_POINT('Ctrl Pts',(207.272210549914,-0.486892143847507,
136.703141376656));
#187917=CARTESIAN_POINT('Ctrl Pts',(207.279624844002,-0.643274099441511,
136.68603801398));
#187918=CARTESIAN_POINT('Ctrl Pts',(207.28703199178,-0.799505325385146,
136.668951136479));
#187919=CARTESIAN_POINT('Ctrl Pts',(207.294439139558,-0.955214816271548,
136.645617702214));
#187920=CARTESIAN_POINT('Ctrl Pts',(207.301846287336,-1.10986562624154,
136.616084015508));
#187921=CARTESIAN_POINT('Ctrl Pts',(207.309247910677,-1.26440109375863,
136.586572355766));
#187922=CARTESIAN_POINT('Ctrl Pts',(207.316649534019,-1.41787908742527,
136.550869720914));
#187923=CARTESIAN_POINT('Ctrl Pts',(207.32405115736,-1.56976899679204,136.509074094964));
#187924=CARTESIAN_POINT('Ctrl Pts',(207.331448873763,-1.72157873124577,
136.467300530788));
#187925=CARTESIAN_POINT('Ctrl Pts',(207.338846590166,-1.87180169182007,
136.419440479476));
#187926=CARTESIAN_POINT('Ctrl Pts',(207.34624430657,-2.01991876954609,136.365642729358));
#187927=CARTESIAN_POINT('Ctrl Pts',(207.353640794833,-2.16801125746096,
136.311853910529));
#187928=CARTESIAN_POINT('Ctrl Pts',(207.361037283097,-2.31399820584744,
136.252129476629));
#187929=CARTESIAN_POINT('Ctrl Pts',(207.36843377136,-2.4573768406137,136.186667708927));
#187930=CARTESIAN_POINT('Ctrl Pts',(207.375829932446,-2.60074913313828,
136.121208836875));
#187931=CARTESIAN_POINT('Ctrl Pts',(207.383226093531,-2.7415130018506,136.050013290682));
#187932=CARTESIAN_POINT('Ctrl Pts',(207.390622254617,-2.87918704637743,
135.973326908274));
#187933=CARTESIAN_POINT('Ctrl Pts',(207.398019549068,-3.01688218766657,
135.896628774672));
#187934=CARTESIAN_POINT('Ctrl Pts',(207.40541684352,-3.15148623585924,135.814438311193));
#187935=CARTESIAN_POINT('Ctrl Pts',(207.412814137971,-3.28254386071344,
135.727046506894));
#187936=CARTESIAN_POINT('Ctrl Pts',(207.420214026732,-3.41364744886641,
135.639624053363));
#187937=CARTESIAN_POINT('Ctrl Pts',(207.427613915493,-3.5412018269446,135.546996834099));
#187938=CARTESIAN_POINT('Ctrl Pts',(207.435013804254,-3.66478215559698,
135.449498109021));
#187939=CARTESIAN_POINT('Ctrl Pts',(207.442421832859,-3.78849842204456,
135.351892135792));
#187940=CARTESIAN_POINT('Ctrl Pts',(207.449829861464,-3.90823161575698,
135.249404186581));
#187941=CARTESIAN_POINT('Ctrl Pts',(207.457237890069,-4.02359084921884,
135.142407095024));
#187942=CARTESIAN_POINT('Ctrl Pts',(207.464650479546,-4.13902110546382,
135.035344128971));
#187943=CARTESIAN_POINT('Ctrl Pts',(207.472063069024,-4.25007177278625,
134.923766752786));
#187944=CARTESIAN_POINT('Ctrl Pts',(207.479475658502,-4.35639050034371,
134.80808293199));
#187945=CARTESIAN_POINT('Ctrl Pts',(207.486898843278,-4.4628611961998,134.692233756756));
#187946=CARTESIAN_POINT('Ctrl Pts',(207.494322028054,-4.56458620292865,
134.572266697968));
#187947=CARTESIAN_POINT('Ctrl Pts',(207.501745212829,-4.66125443395861,
134.448621539125));
#187948=CARTESIAN_POINT('Ctrl Pts',(207.505683602501,-4.71254201121785,
134.383021283805));
#187949=CARTESIAN_POINT('Ctrl Pts',(207.509621992173,-4.76240691754465,
134.316386173422));
#187950=CARTESIAN_POINT('Ctrl Pts',(207.513560381845,-4.81080786236673,
134.248784847229));
#187951=CARTESIAN_POINT('Ctrl Pts',(207.521051269147,-4.90286732147384,
134.120205920782));
#187952=CARTESIAN_POINT('Ctrl Pts',(207.528542156449,-4.98990483109686,
133.987743324545));
#187953=CARTESIAN_POINT('Ctrl Pts',(207.53603304375,-5.07157846591888,133.851822254163));
#187954=CARTESIAN_POINT('Ctrl Pts',(207.54351476451,-5.15315215733145,133.716067509366));
#187955=CARTESIAN_POINT('Ctrl Pts',(207.55099648527,-5.22937485457269,133.576863024161));
#187956=CARTESIAN_POINT('Ctrl Pts',(207.558478206029,-5.29994590927854,
133.43466552788));
#187957=CARTESIAN_POINT('Ctrl Pts',(207.565952157474,-5.37044368021443,
133.292615695094));
#187958=CARTESIAN_POINT('Ctrl Pts',(207.57342610892,-5.43530133283299,133.14757936331));
#187959=CARTESIAN_POINT('Ctrl Pts',(207.580900060365,-5.49426246614916,
133.000040584129));
#187960=CARTESIAN_POINT('Ctrl Pts',(207.588367634612,-5.55317329048832,
132.852627693386));
#187961=CARTESIAN_POINT('Ctrl Pts',(207.595835208858,-5.60619748008959,
132.702716943955));
#187962=CARTESIAN_POINT('Ctrl Pts',(207.603302783105,-5.65312540941891,
132.550815216999));
#187963=CARTESIAN_POINT('Ctrl Pts',(207.610764849886,-5.70001872858317,
132.399025520213));
#187964=CARTESIAN_POINT('Ctrl Pts',(207.618226916666,-5.74082463923422,
132.245248118835));
#187965=CARTESIAN_POINT('Ctrl Pts',(207.625688983447,-5.7753823822878,132.090007886789));
#187966=CARTESIAN_POINT('Ctrl Pts',(207.633147775048,-5.80992495758146,
131.934835791327));
#187967=CARTESIAN_POINT('Ctrl Pts',(207.640606566648,-5.83822474834227,
131.77820249896));
#187968=CARTESIAN_POINT('Ctrl Pts',(207.648065358248,-5.86017137152786,
131.620646142873));
#187969=CARTESIAN_POINT('Ctrl Pts',(207.655522975005,-5.88211453787134,
131.463114603699));
#187970=CARTESIAN_POINT('Ctrl Pts',(207.662980591761,-5.89770647524173,
131.304660650403));
#187971=CARTESIAN_POINT('Ctrl Pts',(207.670438208517,-5.9068882401741,131.145830792827));
#187972=CARTESIAN_POINT('Ctrl Pts',(207.67583374161,-5.9135311823046,131.030918511774));
#187973=CARTESIAN_POINT('Ctrl Pts',(207.681229274702,-5.91681984302548,
130.91580966449));
#187974=CARTESIAN_POINT('Ctrl Pts',(207.686624807795,-5.91674887527788,
130.800712412811));
#187975=CARTESIAN_POINT('Ctrl Pts',(207.686626923708,-5.90924709096476,
130.800671958988));
#187976=CARTESIAN_POINT('Ctrl Pts',(207.721753951025,-5.91343857842015,
130.052291188706));
#187977=CARTESIAN_POINT('Ctrl Pts',(207.849696852946,-5.433669738664,127.331654299026));
#187978=CARTESIAN_POINT('Ctrl Pts',(208.070455629472,-1.34028874287017,
123.935438990336));
#187979=CARTESIAN_POINT('Ctrl Pts',(208.348903253284,5.054696368039,125.964103710928));
#187980=CARTESIAN_POINT('Ctrl Pts',(208.627350877096,6.80417363260146,132.440391727885));
#187981=CARTESIAN_POINT('Ctrl Pts',(208.90579850091,2.30187076695336,137.413882217603));
#187982=CARTESIAN_POINT('Ctrl Pts',(209.175555710051,-4.11089059224102,
136.346724719354));
#187983=CARTESIAN_POINT('Ctrl Pts',(209.352497044589,-5.91202822503604,
132.582291201825));
#187984=CARTESIAN_POINT('Ctrl Pts',(209.436622504522,-5.92383576977198,
130.80157570118));
#187985=CARTESIAN_POINT('Origin',(213.235140564004,0.,130.804360617566));
#187986=CARTESIAN_POINT('',(-258.389859436029,-4.91824857376509,130.800615065845));
#187987=CARTESIAN_POINT('Ctrl Pts',(-258.319801180436,-4.76405452823419,
129.582490119309));
#187988=CARTESIAN_POINT('Ctrl Pts',(-258.327575080909,-4.79806489326847,
129.715096016398));
#187989=CARTESIAN_POINT('Ctrl Pts',(-258.335348981381,-4.82649184728085,
129.8489564752));
#187990=CARTESIAN_POINT('Ctrl Pts',(-258.343122881853,-4.84927537315292,
129.983561362064));
#187991=CARTESIAN_POINT('Ctrl Pts',(-258.34504967233,-4.85492235574935,
130.016923689642));
#187992=CARTESIAN_POINT('Ctrl Pts',(-258.346976462806,-4.86022290448851,
130.050331736036));
#187993=CARTESIAN_POINT('Ctrl Pts',(-258.348903253283,-4.86517660022172,
130.08377772077));
#187994=CARTESIAN_POINT('Ctrl Pts',(-258.362555314187,-4.90027546368103,
130.320755547965));
#187995=CARTESIAN_POINT('Ctrl Pts',(-258.376207375092,-4.91806560196264,
130.560356557379));
#187996=CARTESIAN_POINT('Ctrl Pts',(-258.389859435997,-4.91824857376465,
130.800615065277));
#187997=CARTESIAN_POINT('',(-259.999992532581,-4.31287516290238,128.44040399958));
#187998=CARTESIAN_POINT('Ctrl Pts',(-258.389859436029,-4.91824857376509,
130.800615065845));
#187999=CARTESIAN_POINT('Ctrl Pts',(-258.397511447859,-4.91835112986932,
130.935280517276));
#188000=CARTESIAN_POINT('Ctrl Pts',(-258.40516345969,-4.91291866327918,
131.070155068034));
#188001=CARTESIAN_POINT('Ctrl Pts',(-258.41281547152,-4.90192624921011,
131.204738076728));
#188002=CARTESIAN_POINT('Ctrl Pts',(-258.420459778954,-4.89094490280721,
131.339185581082));
#188003=CARTESIAN_POINT('Ctrl Pts',(-258.428104086388,-4.87441477518558,
131.473341728033));
#188004=CARTESIAN_POINT('Ctrl Pts',(-258.435748393821,-4.85236297429289,
131.606705074898));
#188005=CARTESIAN_POINT('Ctrl Pts',(-258.443731830625,-4.82933287505326,
131.745984906426));
#188006=CARTESIAN_POINT('Ctrl Pts',(-258.451715267428,-4.80027990481861,
131.884399532785));
#188007=CARTESIAN_POINT('Ctrl Pts',(-258.459698704231,-4.76529553161854,
132.02138221098));
#188008=CARTESIAN_POINT('Ctrl Pts',(-258.467334088494,-4.73183636620147,
132.152392878594));
#188009=CARTESIAN_POINT('Ctrl Pts',(-258.474969472757,-4.69295217675676,
132.282093385481));
#188010=CARTESIAN_POINT('Ctrl Pts',(-258.48260485702,-4.64877526646828,
132.409998056209));
#188011=CARTESIAN_POINT('Ctrl Pts',(-258.490238971884,-4.60460570069148,
132.537881462495));
#188012=CARTESIAN_POINT('Ctrl Pts',(-258.497873086747,-4.55514529512487,
132.663969245013));
#188013=CARTESIAN_POINT('Ctrl Pts',(-258.50550720161,-4.50057593422793,
132.787791816965));
#188014=CARTESIAN_POINT('Ctrl Pts',(-258.513141812779,-4.44600302568972,
132.91162243882));
#188015=CARTESIAN_POINT('Ctrl Pts',(-258.520776423949,-4.3863206644437,
133.033187188249));
#188016=CARTESIAN_POINT('Ctrl Pts',(-258.528411035118,-4.32175826677667,
133.152037883727));
#188017=CARTESIAN_POINT('Ctrl Pts',(-258.536047908509,-4.25717673853753,
133.270923796016));
#188018=CARTESIAN_POINT('Ctrl Pts',(-258.543684781901,-4.18771249147707,
133.387093701195));
#188019=CARTESIAN_POINT('Ctrl Pts',(-258.551321655292,-4.11363984045046,
133.50012587544));
#188020=CARTESIAN_POINT('Ctrl Pts',(-258.558966652433,-4.03948839439416,
133.613278288037));
#188021=CARTESIAN_POINT('Ctrl Pts',(-258.566611649574,-3.96071898158943,
133.723285970572));
#188022=CARTESIAN_POINT('Ctrl Pts',(-258.574256646714,-3.87764815134681,
133.829757761224));
#188023=CARTESIAN_POINT('Ctrl Pts',(-258.581906426395,-3.79452535384532,
133.936296158255));
#188024=CARTESIAN_POINT('Ctrl Pts',(-258.589556206076,-3.70709604330389,
134.039293954262));
#188025=CARTESIAN_POINT('Ctrl Pts',(-258.597205985756,-3.61571472858466,
134.13839571996));
#188026=CARTESIAN_POINT('Ctrl Pts',(-258.604866500394,-3.52420517820673,
134.237636555448));
#188027=CARTESIAN_POINT('Ctrl Pts',(-258.612527015032,-3.42873284137469,
134.332970167501));
#188028=CARTESIAN_POINT('Ctrl Pts',(-258.62018752967,-3.32968663806097,
134.424080213725));
#188029=CARTESIAN_POINT('Ctrl Pts',(-258.622575312145,-3.2988139356827,
134.452479215874));
#188030=CARTESIAN_POINT('Ctrl Pts',(-258.624963094621,-3.26759422865444,
134.48046818036));
#188031=CARTESIAN_POINT('Ctrl Pts',(-258.627350877096,-3.23603986999501,
134.508038387338));
#188032=CARTESIAN_POINT('Ctrl Pts',(-258.635127709651,-3.13326963599956,
134.597832531249));
#188033=CARTESIAN_POINT('Ctrl Pts',(-258.642904542206,-3.02659721906916,
134.683487383169));
#188034=CARTESIAN_POINT('Ctrl Pts',(-258.650681374762,-2.91639018574448,
134.764644868348));
#188035=CARTESIAN_POINT('Ctrl Pts',(-258.658448646073,-2.80631864669946,
134.845702574279));
#188036=CARTESIAN_POINT('Ctrl Pts',(-258.666215917384,-2.69272144950787,
134.922273685838));
#188037=CARTESIAN_POINT('Ctrl Pts',(-258.673983188696,-2.57600128484593,
134.994038462338));
#188038=CARTESIAN_POINT('Ctrl Pts',(-258.681742765027,-2.45939675401745,
135.065732141986));
#188039=CARTESIAN_POINT('Ctrl Pts',(-258.689502341359,-2.33967574347888,
135.132628759213));
#188040=CARTESIAN_POINT('Ctrl Pts',(-258.69726191769,-2.21727186503747,
135.194450427469));
#188041=CARTESIAN_POINT('Ctrl Pts',(-258.705015658649,-2.09496003701437,
135.256225604465));
#188042=CARTESIAN_POINT('Ctrl Pts',(-258.712769399607,-1.96996970432977,
135.312933253643));
#188043=CARTESIAN_POINT('Ctrl Pts',(-258.720523140566,-1.84276084284099,
135.36434039149));
#188044=CARTESIAN_POINT('Ctrl Pts',(-258.728273599587,-1.71560582524482,
135.415725770157));
#188045=CARTESIAN_POINT('Ctrl Pts',(-258.736024058607,-1.58623450800852,
135.461814953734));
#188046=CARTESIAN_POINT('Ctrl Pts',(-258.743774517628,-1.45512850411597,
135.502422356093));
#188047=CARTESIAN_POINT('Ctrl Pts',(-258.751523363193,-1.32404979326963,
135.543021304989));
#188048=CARTESIAN_POINT('Ctrl Pts',(-258.759272208759,-1.19123748701413,
135.578140627048));
#188049=CARTESIAN_POINT('Ctrl Pts',(-258.767021054325,-1.05718970734705,
135.60764418042));
#188050=CARTESIAN_POINT('Ctrl Pts',(-258.774769961837,-0.923140856050142,
135.637147969654));
#188051=CARTESIAN_POINT('Ctrl Pts',(-258.78251886935,-0.7878568931795,135.661035816665));
#188052=CARTESIAN_POINT('Ctrl Pts',(-258.790267776863,-0.651847129970203,
135.679222500907));
#188053=CARTESIAN_POINT('Ctrl Pts',(-258.79801842141,-0.515806878143327,
135.697413261966));
#188054=CARTESIAN_POINT('Ctrl Pts',(-258.805769065956,-0.379040889373938,
135.709900265377));
#188055=CARTESIAN_POINT('Ctrl Pts',(-258.813519710502,-0.24206421517884,
135.716650101934));
#188056=CARTESIAN_POINT('Ctrl Pts',(-258.821278578715,-0.104942204614877,
135.72340710027));
#188057=CARTESIAN_POINT('Ctrl Pts',(-258.829037446928,0.032390547106922,
135.724414752418));
#188058=CARTESIAN_POINT('Ctrl Pts',(-258.836796315141,0.169417802337889,
135.719691803839));
#188059=CARTESIAN_POINT('Ctrl Pts',(-258.844559321162,0.306518134269045,
135.71496633651));
#188060=CARTESIAN_POINT('Ctrl Pts',(-258.852322327183,0.443312255718664,
135.704504208516));
#188061=CARTESIAN_POINT('Ctrl Pts',(-258.860085333204,0.579289416653436,
135.688376059214));
#188062=CARTESIAN_POINT('Ctrl Pts',(-258.867860767497,0.715484271752939,
135.67222208937));
#188063=CARTESIAN_POINT('Ctrl Pts',(-258.87563620179,0.85085916677422,135.650384033521));
#188064=CARTESIAN_POINT('Ctrl Pts',(-258.883411636083,0.984913016375688,
135.622983803983));
#188065=CARTESIAN_POINT('Ctrl Pts',(-258.890873924358,1.11356801266962,
135.596687084864));
#188066=CARTESIAN_POINT('Ctrl Pts',(-258.898336212633,1.24100602086473,
135.565267616871));
#188067=CARTESIAN_POINT('Ctrl Pts',(-258.905798500908,1.36679936031642,
135.528875679574));
#188068=CARTESIAN_POINT('Ctrl Pts',(-258.913563209033,1.49769065382591,
135.49100890724));
#188069=CARTESIAN_POINT('Ctrl Pts',(-258.921327917158,1.6272174403873,135.447637701225));
#188070=CARTESIAN_POINT('Ctrl Pts',(-258.929092625283,1.75488088859039,
135.398876492972));
#188071=CARTESIAN_POINT('Ctrl Pts',(-258.936847736376,1.88238654720433,
135.350175552643));
#188072=CARTESIAN_POINT('Ctrl Pts',(-258.94460284747,2.00803308696774,135.296098003159));
#188073=CARTESIAN_POINT('Ctrl Pts',(-258.952357958563,2.13133483328165,
135.236808574501));
#188074=CARTESIAN_POINT('Ctrl Pts',(-258.960105351597,2.25451386693592,
135.177578152011));
#188075=CARTESIAN_POINT('Ctrl Pts',(-258.96785274463,2.37535239987729,135.1131463409));
#188076=CARTESIAN_POINT('Ctrl Pts',(-258.975600137663,2.49338316794614,
135.043726541888));
#188077=CARTESIAN_POINT('Ctrl Pts',(-258.983341684822,2.61132487469468,
134.974359124294));
#188078=CARTESIAN_POINT('Ctrl Pts',(-258.991083231981,2.72646269683481,
134.900011407841));
#188079=CARTESIAN_POINT('Ctrl Pts',(-258.99882477914,2.83835282906841,134.820943279509));
#188080=CARTESIAN_POINT('Ctrl Pts',(-259.006563070912,2.95019591054144,
134.741908400003));
#188081=CARTESIAN_POINT('Ctrl Pts',(-259.014301362683,3.05879369856792,
134.658157281911));
#188082=CARTESIAN_POINT('Ctrl Pts',(-259.022039654455,3.16373051564571,
134.569993670171));
#188083=CARTESIAN_POINT('Ctrl Pts',(-259.029776350361,3.26864569163368,
134.481848240388));
#188084=CARTESIAN_POINT('Ctrl Pts',(-259.037513046267,3.36990109832788,
134.389292378848));
#188085=CARTESIAN_POINT('Ctrl Pts',(-259.045249742173,3.46711370159911,
134.292670472307));
#188086=CARTESIAN_POINT('Ctrl Pts',(-259.052986528804,3.56432744483308,
134.19604743273));
#188087=CARTESIAN_POINT('Ctrl Pts',(-259.060723315434,3.65749801206921,
134.095358529446));
#188088=CARTESIAN_POINT('Ctrl Pts',(-259.068460102065,3.74627914665232,
133.99098510405));
#188089=CARTESIAN_POINT('Ctrl Pts',(-259.076198665721,3.83508067295352,
133.886587705616));
#188090=CARTESIAN_POINT('Ctrl Pts',(-259.083937229377,3.91949050655106,
133.778504399685));
#188091=CARTESIAN_POINT('Ctrl Pts',(-259.091675793033,3.99920287563806,
133.667149366669));
#188092=CARTESIAN_POINT('Ctrl Pts',(-259.099422711592,4.07900130579743,
133.555674109731));
#188093=CARTESIAN_POINT('Ctrl Pts',(-259.107169630151,4.1540919119548,133.440920388912));
#188094=CARTESIAN_POINT('Ctrl Pts',(-259.11491654871,4.22421216047996,133.323331575269));
#188095=CARTESIAN_POINT('Ctrl Pts',(-259.122667657237,4.29437033396256,
133.205679163011));
#188096=CARTESIAN_POINT('Ctrl Pts',(-259.130418765763,4.35955260727491,
133.085188947405));
#188097=CARTESIAN_POINT('Ctrl Pts',(-259.138169874289,4.41954308950522,
132.96232770316));
#188098=CARTESIAN_POINT('Ctrl Pts',(-259.145933621294,4.47963138850846,
132.839266128962));
#188099=CARTESIAN_POINT('Ctrl Pts',(-259.153697368299,4.53451082282979,
132.713826159953));
#188100=CARTESIAN_POINT('Ctrl Pts',(-259.161461115304,4.58401387421637,
132.586494132063));
#188101=CARTESIAN_POINT('Ctrl Pts',(-259.169056118443,4.63244098427488,
132.461929646523));
#188102=CARTESIAN_POINT('Ctrl Pts',(-259.176651121582,4.67572299195017,
132.33555485375));
#188103=CARTESIAN_POINT('Ctrl Pts',(-259.184246124721,4.71375015242697,
132.207835791196));
#188104=CARTESIAN_POINT('Ctrl Pts',(-259.192031309133,4.75272952499007,
132.076918603052));
#188105=CARTESIAN_POINT('Ctrl Pts',(-259.199816493545,4.78631181980715,
131.944171146245));
#188106=CARTESIAN_POINT('Ctrl Pts',(-259.207601677957,4.81432412344634,
131.810077425073));
#188107=CARTESIAN_POINT('Ctrl Pts',(-259.215377243051,4.84230181528276,
131.676149389148));
#188108=CARTESIAN_POINT('Ctrl Pts',(-259.223152808144,4.86472313132261,
131.540878776735));
#188109=CARTESIAN_POINT('Ctrl Pts',(-259.230928373238,4.88146463124323,
131.404765577923));
#188110=CARTESIAN_POINT('Ctrl Pts',(-259.238696177382,4.89818942113344,
131.268788236454));
#188111=CARTESIAN_POINT('Ctrl Pts',(-259.246463981527,4.90924563005071,
131.131970366726));
#188112=CARTESIAN_POINT('Ctrl Pts',(-259.254231785671,4.91456074023952,
130.994822668895));
#188113=CARTESIAN_POINT('Ctrl Pts',(-259.26199368058,4.91987180704147,130.857779304028));
#188114=CARTESIAN_POINT('Ctrl Pts',(-259.269755575489,4.91945045365875,
130.720406998459));
#188115=CARTESIAN_POINT('Ctrl Pts',(-259.277517470398,4.9132759609789,130.583221761263));
#188116=CARTESIAN_POINT('Ctrl Pts',(-259.285275943259,4.90710419049708,
130.446097006021));
#188117=CARTESIAN_POINT('Ctrl Pts',(-259.293034416119,4.89518434386338,
130.309159543684));
#188118=CARTESIAN_POINT('Ctrl Pts',(-259.300792888979,4.87754780323644,
130.172925355925));
#188119=CARTESIAN_POINT('Ctrl Pts',(-259.308549661931,4.8599151268374,130.036721017555));
#188120=CARTESIAN_POINT('Ctrl Pts',(-259.316306434883,4.83656829808708,
129.901220033568));
#188121=CARTESIAN_POINT('Ctrl Pts',(-259.324063207834,4.80759053215213,
129.766932866992));
#188122=CARTESIAN_POINT('Ctrl Pts',(-259.331819949055,4.77861288475751,
129.632646249749));
#188123=CARTESIAN_POINT('Ctrl Pts',(-259.339576690276,4.74400442807287,
129.499573821107));
#188124=CARTESIAN_POINT('Ctrl Pts',(-259.347333431497,4.7038993472714,129.368215084119));
#188125=CARTESIAN_POINT('Ctrl Pts',(-259.355091808782,4.66378580744186,
129.236828640735));
#188126=CARTESIAN_POINT('Ctrl Pts',(-259.362850186067,4.61817345026256,
129.107156981035));
#188127=CARTESIAN_POINT('Ctrl Pts',(-259.370608563352,4.56724598277686,
128.979683332316));
#188128=CARTESIAN_POINT('Ctrl Pts',(-259.378374961998,4.51626586154739,
128.852077889003));
#188129=CARTESIAN_POINT('Ctrl Pts',(-259.386141360644,4.45995979725993,
128.726675358917));
#188130=CARTESIAN_POINT('Ctrl Pts',(-259.393907759291,4.39855943860582,
128.603938401819));
#188131=CARTESIAN_POINT('Ctrl Pts',(-259.401678197314,4.33712714504929,
128.481137608079));
#188132=CARTESIAN_POINT('Ctrl Pts',(-259.409448635337,4.27059546581696,
128.361005491011));
#188133=CARTESIAN_POINT('Ctrl Pts',(-259.41721907336,4.19924100054342,128.243978208266));
#188134=CARTESIAN_POINT('Ctrl Pts',(-259.425001697521,4.12777463226247,
128.126767395242));
#188135=CARTESIAN_POINT('Ctrl Pts',(-259.432784321682,4.05147058038222,
128.012671471211));
#188136=CARTESIAN_POINT('Ctrl Pts',(-259.440566945844,3.97064809108426,
127.902096535979));
#188137=CARTESIAN_POINT('Ctrl Pts',(-259.447942546741,3.8940525351133,127.797304556493));
#188138=CARTESIAN_POINT('Ctrl Pts',(-259.455318147638,3.81339932404087,
127.695674852864));
#188139=CARTESIAN_POINT('Ctrl Pts',(-259.462693748534,3.72899119397172,
127.597522963773));
#188140=CARTESIAN_POINT('Ctrl Pts',(-259.470480941117,3.639872710803,127.493893758047));
#188141=CARTESIAN_POINT('Ctrl Pts',(-259.4782681337,3.54629431034451,127.393823152026));
#188142=CARTESIAN_POINT('Ctrl Pts',(-259.486055326282,3.44857082400634,
127.297718016115));
#188143=CARTESIAN_POINT('Ctrl Pts',(-259.493833075873,3.35096584020889,
127.201729420282));
#188144=CARTESIAN_POINT('Ctrl Pts',(-259.501610825463,3.24922604762373,
127.109696996534));
#188145=CARTESIAN_POINT('Ctrl Pts',(-259.509388575054,3.14370639443858,
127.021994536914));
#188146=CARTESIAN_POINT('Ctrl Pts',(-259.517158735265,3.03828970530945,
126.934377655674));
#188147=CARTESIAN_POINT('Ctrl Pts',(-259.524928895477,2.92910079372457,
126.851082577125));
#188148=CARTESIAN_POINT('Ctrl Pts',(-259.532699055688,2.81653106311716,
126.772445956639));
#188149=CARTESIAN_POINT('Ctrl Pts',(-259.540463473649,2.70404452301452,
126.693867449646));
#188150=CARTESIAN_POINT('Ctrl Pts',(-259.548227891611,2.58818245534753,
126.619940769906));
#188151=CARTESIAN_POINT('Ctrl Pts',(-259.555992309572,2.46936864366422,
126.550961792604));
#188152=CARTESIAN_POINT('Ctrl Pts',(-259.563753547399,2.35060349549515,
126.482011067568));
#188153=CARTESIAN_POINT('Ctrl Pts',(-259.571514785227,2.2288893440266,126.418004209507));
#188154=CARTESIAN_POINT('Ctrl Pts',(-259.579276023054,2.10467803831177,
126.359193194673));
#188155=CARTESIAN_POINT('Ctrl Pts',(-259.587035707387,1.98049159479754,
126.300393951483));
#188156=CARTESIAN_POINT('Ctrl Pts',(-259.594795391721,1.85380934306757,
126.246788649275));
#188157=CARTESIAN_POINT('Ctrl Pts',(-259.602555076055,1.72510641635312,
126.198582625222));
#188158=CARTESIAN_POINT('Ctrl Pts',(-259.610314871376,1.59640164878467,
126.150375911673));
#188159=CARTESIAN_POINT('Ctrl Pts',(-259.618074666698,1.46567651331978,
126.107568766764));
#188160=CARTESIAN_POINT('Ctrl Pts',(-259.625834462019,1.33342438310065,
126.070317686091));
#188161=CARTESIAN_POINT('Ctrl Pts',(-259.63359603252,1.20114199805461,126.033058083626));
#188162=CARTESIAN_POINT('Ctrl Pts',(-259.641357603021,1.06733229784172,
126.001357180389));
#188163=CARTESIAN_POINT('Ctrl Pts',(-259.649119173522,0.932501642178328,
125.975320987387));
#188164=CARTESIAN_POINT('Ctrl Pts',(-259.656888964626,0.797528181744626,
125.949257218368));
#188165=CARTESIAN_POINT('Ctrl Pts',(-259.66465875573,0.661531988718544,
125.92887021873));
#188166=CARTESIAN_POINT('Ctrl Pts',(-259.672428546834,0.525027960616441,
125.914214535589));
#188167=CARTESIAN_POINT('Ctrl Pts',(-259.680202491048,0.388450968345654,
125.899551018689));
#188168=CARTESIAN_POINT('Ctrl Pts',(-259.687976435263,0.251365988490296,
125.890624948406));
#188169=CARTESIAN_POINT('Ctrl Pts',(-259.695750379478,0.114289834376831,
125.887438725136));
#188170=CARTESIAN_POINT('Ctrl Pts',(-259.703536666297,-0.0230039540221484,
125.884247443135));
#188171=CARTESIAN_POINT('Ctrl Pts',(-259.711322953117,-0.160288499093245,
125.8868142119));
#188172=CARTESIAN_POINT('Ctrl Pts',(-259.719109239936,-0.297049294226065,
125.895089309184));
#188173=CARTESIAN_POINT('Ctrl Pts',(-259.726453284073,-0.426042399538032,
125.902894400508));
#188174=CARTESIAN_POINT('Ctrl Pts',(-259.73379732821,-0.554569337392523,
125.915777299511));
#188175=CARTESIAN_POINT('Ctrl Pts',(-259.741141372348,-0.682206894920373,
125.933654630235));
#188176=CARTESIAN_POINT('Ctrl Pts',(-259.748774629122,-0.814870892104533,
125.952235980417));
#188177=CARTESIAN_POINT('Ctrl Pts',(-259.756407885897,-0.947026750298924,
125.976276897283));
#188178=CARTESIAN_POINT('Ctrl Pts',(-259.764041142672,-1.07817805427494,
126.005744656085));
#188179=CARTESIAN_POINT('Ctrl Pts',(-259.771664808356,-1.209164568287,126.035175389019));
#188180=CARTESIAN_POINT('Ctrl Pts',(-259.77928847404,-1.33914864612342,
126.070019318878));
#188181=CARTESIAN_POINT('Ctrl Pts',(-259.786912139724,-1.46763882087358,
126.110191963378));
#188182=CARTESIAN_POINT('Ctrl Pts',(-259.794528200188,-1.5960008163482,
126.150324532435));
#188183=CARTESIAN_POINT('Ctrl Pts',(-259.802144260653,-1.72287148776318,
126.195775124874));
#188184=CARTESIAN_POINT('Ctrl Pts',(-259.809760321117,-1.8477699479343,
126.246408305177));
#188185=CARTESIAN_POINT('Ctrl Pts',(-259.817686663262,-1.97775682674349,
126.299104303693));
#188186=CARTESIAN_POINT('Ctrl Pts',(-259.825613005406,-2.10560695858319,
126.357414024714));
#188187=CARTESIAN_POINT('Ctrl Pts',(-259.83353934755,-2.23079566345197,
126.42112736226));
#188188=CARTESIAN_POINT('Ctrl Pts',(-259.841146810408,-2.35094798656864,
126.482277491799));
#188189=CARTESIAN_POINT('Ctrl Pts',(-259.848754273265,-2.46864846641231,
126.548404698225));
#188190=CARTESIAN_POINT('Ctrl Pts',(-259.856361736122,-2.58345457280964,
126.619274533299));
#188191=CARTESIAN_POINT('Ctrl Pts',(-259.863968055281,-2.69824341935702,
126.690133713862));
#188192=CARTESIAN_POINT('Ctrl Pts',(-259.871574374439,-2.81013841209187,
126.765733892621));
#188193=CARTESIAN_POINT('Ctrl Pts',(-259.879180693597,-2.91872362369027,
126.845795792909));
#188194=CARTESIAN_POINT('Ctrl Pts',(-259.886787647209,-3.0273178925455,
126.925864371281));
#188195=CARTESIAN_POINT('Ctrl Pts',(-259.894394600822,-3.13260150486788,
127.010395169864));
#188196=CARTESIAN_POINT('Ctrl Pts',(-259.902001554435,-3.2341898996486,
127.099067274859));
#188197=CARTESIAN_POINT('Ctrl Pts',(-259.9096109211,-3.33581051996215,127.187767508124));
#188198=CARTESIAN_POINT('Ctrl Pts',(-259.917220287765,-3.43373328697769,
127.280611392494));
#188199=CARTESIAN_POINT('Ctrl Pts',(-259.92482965443,-3.52760937784773,
127.377240085717));
#188200=CARTESIAN_POINT('Ctrl Pts',(-259.932447357799,-3.62158831789155,
127.473974643821));
#188201=CARTESIAN_POINT('Ctrl Pts',(-259.940065061167,-3.71151145141156,
127.574501994588));
#188202=CARTESIAN_POINT('Ctrl Pts',(-259.947682764535,-3.79706912348943,
127.678428895032));
#188203=CARTESIAN_POINT('Ctrl Pts',(-259.955305402399,-3.88268221700061,
127.782423115889));
#188204=CARTESIAN_POINT('Ctrl Pts',(-259.962928040264,-3.96392397811463,
127.889820945947));
#188205=CARTESIAN_POINT('Ctrl Pts',(-259.970550678129,-4.04052803945671,
128.000200097042));
#188206=CARTESIAN_POINT('Ctrl Pts',(-259.978184189506,-4.1172413746782,
128.110736701382));
#188207=CARTESIAN_POINT('Ctrl Pts',(-259.985817700883,-4.18930359531733,
128.224262770745));
#188208=CARTESIAN_POINT('Ctrl Pts',(-259.99345121226,-4.25649411764769,
128.340331216579));
#188209=CARTESIAN_POINT('Ctrl Pts',(-259.995631652367,-4.27568645292739,
128.373485067011));
#188210=CARTESIAN_POINT('Ctrl Pts',(-259.997812092474,-4.29448160516882,
128.406846227114));
#188211=CARTESIAN_POINT('Ctrl Pts',(-259.999992532581,-4.31287516290238,
128.44040399958));
#188212=CARTESIAN_POINT('',(-260.,0.837162017623962,125.957883255734));
#188213=CARTESIAN_POINT('Origin',(-260.,0.,130.804360617566));
#188214=CARTESIAN_POINT('',(-258.735140563986,-4.91824979995562,130.802957857252));
#188215=CARTESIAN_POINT('Ctrl Pts',(-258.735140564015,-4.91824979995577,
130.802957857762));
#188216=CARTESIAN_POINT('Ctrl Pts',(-258.743125920418,-4.91829022612684,
130.944697025984));
#188217=CARTESIAN_POINT('Ctrl Pts',(-258.751111276821,-4.91219912563647,
131.086370582116));
#188218=CARTESIAN_POINT('Ctrl Pts',(-258.759096633224,-4.9000197173338,
131.227432517176));
#188219=CARTESIAN_POINT('Ctrl Pts',(-258.767087865585,-4.88783134691572,
131.368598251478));
#188220=CARTESIAN_POINT('Ctrl Pts',(-258.775079097945,-4.86954576746095,
131.509151113065));
#188221=CARTESIAN_POINT('Ctrl Pts',(-258.783070330306,-4.84525785291376,
131.64855218426));
#188222=CARTESIAN_POINT('Ctrl Pts',(-258.791068654905,-4.82094838278348,
131.788076974244));
#188223=CARTESIAN_POINT('Ctrl Pts',(-258.799066979503,-4.79062601762179,
131.926447585823));
#188224=CARTESIAN_POINT('Ctrl Pts',(-258.807065304102,-4.75443630802797,
132.06313718845));
#188225=CARTESIAN_POINT('Ctrl Pts',(-258.815077527633,-4.71818371047263,
132.200064320765));
#188226=CARTESIAN_POINT('Ctrl Pts',(-258.823089751164,-4.67604348840026,
132.335304263536));
#188227=CARTESIAN_POINT('Ctrl Pts',(-258.831101974695,-4.62821082354395,
132.468346084849));
#188228=CARTESIAN_POINT('Ctrl Pts',(-258.83912215898,-4.58033063329716,
132.601520093331));
#188229=CARTESIAN_POINT('Ctrl Pts',(-258.847142343264,-4.52674685385319,
132.732491295973));
#188230=CARTESIAN_POINT('Ctrl Pts',(-258.855162527549,-4.46770190836591,
132.860770771325));
#188231=CARTESIAN_POINT('Ctrl Pts',(-258.863196907718,-4.40855245215567,
132.989277303889));
#188232=CARTESIAN_POINT('Ctrl Pts',(-258.871231287888,-4.34392267902974,
133.115082274356));
#188233=CARTESIAN_POINT('Ctrl Pts',(-258.879265668057,-4.27410033019235,
133.237722372413));
#188234=CARTESIAN_POINT('Ctrl Pts',(-258.881580280287,-4.25398531706869,
133.273053569701));
#188235=CARTESIAN_POINT('Ctrl Pts',(-258.883894892518,-4.23343961435544,
133.30812229263));
#188236=CARTESIAN_POINT('Ctrl Pts',(-258.886209504748,-4.2124707400616,
133.342917949325));
#188237=CARTESIAN_POINT('Ctrl Pts',(-258.89399669733,-4.14192386389677,
133.459983121708));
#188238=CARTESIAN_POINT('Ctrl Pts',(-258.901783889913,-4.06638508417377,
133.574285072608));
#188239=CARTESIAN_POINT('Ctrl Pts',(-258.909571082495,-3.98609680935438,
133.685370039445));
#188240=CARTESIAN_POINT('Ctrl Pts',(-258.917348832086,-3.90590589459564,
133.796320301194));
#188241=CARTESIAN_POINT('Ctrl Pts',(-258.925126581676,-3.82097717117305,
133.904061028655));
#188242=CARTESIAN_POINT('Ctrl Pts',(-258.932904331267,-3.73159812815367,
134.008164368182));
#188243=CARTESIAN_POINT('Ctrl Pts',(-258.940674491478,-3.64230629949165,
134.112166125665));
#188244=CARTESIAN_POINT('Ctrl Pts',(-258.94844465169,-3.54857304588502,
134.212537265401));
#188245=CARTESIAN_POINT('Ctrl Pts',(-258.956214811901,-3.45072800518379,
134.308880455823));
#188246=CARTESIAN_POINT('Ctrl Pts',(-258.963979229863,-3.35295527324923,
134.405152447366));
#188247=CARTESIAN_POINT('Ctrl Pts',(-258.971743647824,-3.25107707939238,
134.497402142855));
#188248=CARTESIAN_POINT('Ctrl Pts',(-258.979508065785,-3.14546180132275,
134.585267006108));
#188249=CARTESIAN_POINT('Ctrl Pts',(-258.987269303613,-3.03988978093909,
134.673095881854));
#188250=CARTESIAN_POINT('Ctrl Pts',(-258.99503054144,-2.93058401949167,
134.756543248864));
#188251=CARTESIAN_POINT('Ctrl Pts',(-259.002791779267,-2.8179479018152,
134.835285162277));
#188252=CARTESIAN_POINT('Ctrl Pts',(-259.010551463601,-2.70533432944358,
134.914011314667));
#188253=CARTESIAN_POINT('Ctrl Pts',(-259.018311147935,-2.58939204584363,
134.988033664008));
#188254=CARTESIAN_POINT('Ctrl Pts',(-259.026070832268,-2.47055518681673,
135.057070357413));
#188255=CARTESIAN_POINT('Ctrl Pts',(-259.03383062759,-2.35171662805145,
135.12610803826));
#188256=CARTESIAN_POINT('Ctrl Pts',(-259.041590422911,-2.22998374808351,
135.190159725453));
#188257=CARTESIAN_POINT('Ctrl Pts',(-259.049350218233,-2.1058168284298,
135.248988672601));
#188258=CARTESIAN_POINT('Ctrl Pts',(-259.057111788734,-1.98162150357265,
135.307831077827));
#188259=CARTESIAN_POINT('Ctrl Pts',(-259.064873359235,-1.85499138276835,
135.361448198621));
#188260=CARTESIAN_POINT('Ctrl Pts',(-259.072634929736,-1.72640798836747,
135.409650892913));
#188261=CARTESIAN_POINT('Ctrl Pts',(-259.08040472084,-1.59768840593121,
135.457904640688));
#188262=CARTESIAN_POINT('Ctrl Pts',(-259.088174511943,-1.46701178244654,
135.500732369397));
#188263=CARTESIAN_POINT('Ctrl Pts',(-259.095944303047,-1.33487665854731,
135.537994250302));
#188264=CARTESIAN_POINT('Ctrl Pts',(-259.103718247262,-1.20267090574684,
135.575276048436));
#188265=CARTESIAN_POINT('Ctrl Pts',(-259.111492191477,-1.06900547771351,
135.60698598034));
#188266=CARTESIAN_POINT('Ctrl Pts',(-259.119266135692,-0.934389518613181,
135.633035310482));
#188267=CARTESIAN_POINT('Ctrl Pts',(-259.127052422511,-0.79955983125197,
135.659125998855));
#188268=CARTESIAN_POINT('Ctrl Pts',(-259.134838709331,-0.6637769823593,
135.679538067927));
#188269=CARTESIAN_POINT('Ctrl Pts',(-259.14262499615,-0.527556552464962,
135.694234557296));
#188270=CARTESIAN_POINT('Ctrl Pts',(-259.149969040287,-0.399073120923145,
135.708096320816));
#188271=CARTESIAN_POINT('Ctrl Pts',(-259.157313084425,-0.270200707173242,
135.716873781456));
#188272=CARTESIAN_POINT('Ctrl Pts',(-259.164657128562,-0.141370506025531,
135.72057841609));
#188273=CARTESIAN_POINT('Ctrl Pts',(-259.172363388608,-0.00618626512051576,
135.724465767165));
#188274=CARTESIAN_POINT('Ctrl Pts',(-259.180069648654,0.129394565249223,
135.722779750212));
#188275=CARTESIAN_POINT('Ctrl Pts',(-259.187775908701,0.264868809592343,
135.715473279296));
#188276=CARTESIAN_POINT('Ctrl Pts',(-259.195472507276,0.400173207544053,
135.708175968628));
#188277=CARTESIAN_POINT('Ctrl Pts',(-259.203169105852,0.535370891849149,
135.695272240219));
#188278=CARTESIAN_POINT('Ctrl Pts',(-259.210865704427,0.669955370441971,
135.676766887995));
#188279=CARTESIAN_POINT('Ctrl Pts',(-259.218554573727,0.804404693166619,
135.65828011969));
#188280=CARTESIAN_POINT('Ctrl Pts',(-259.226243443028,0.938241643463367,
135.634202972054));
#188281=CARTESIAN_POINT('Ctrl Pts',(-259.233932312328,1.07096199527409,
135.604592223143));
#188282=CARTESIAN_POINT('Ctrl Pts',(-259.241615376899,1.20358214954474,
135.575003828936));
#188283=CARTESIAN_POINT('Ctrl Pts',(-259.249298441469,1.33508699557577,
135.539890232041));
#188284=CARTESIAN_POINT('Ctrl Pts',(-259.256981506039,1.4649801353849,135.499359687367));
#188285=CARTESIAN_POINT('Ctrl Pts',(-259.264736641303,1.59609173282675,
135.458448947467));
#188286=CARTESIAN_POINT('Ctrl Pts',(-259.272491776567,1.72556082352701,
135.412019167305));
#188287=CARTESIAN_POINT('Ctrl Pts',(-259.280246911831,1.85288991576312,
135.360233972101));
#188288=CARTESIAN_POINT('Ctrl Pts',(-259.287925523627,1.97896259357931,
135.308959765116));
#188289=CARTESIAN_POINT('Ctrl Pts',(-259.295604135422,2.10293694822109,
135.252435530452));
#188290=CARTESIAN_POINT('Ctrl Pts',(-259.303282747218,2.22434846112939,
135.190869136419));
#188291=CARTESIAN_POINT('Ctrl Pts',(-259.310961664611,2.34576480604577,
135.12930029213));
#188292=CARTESIAN_POINT('Ctrl Pts',(-259.318640582005,2.46461775081044,
135.06268906903));
#188293=CARTESIAN_POINT('Ctrl Pts',(-259.326319499398,2.58046650838747,
134.991289762129));
#188294=CARTESIAN_POINT('Ctrl Pts',(-259.334000455379,2.69634602131912,
134.919871500247));
#188295=CARTESIAN_POINT('Ctrl Pts',(-259.34168141136,2.80921942148387,134.843662834839));
#188296=CARTESIAN_POINT('Ctrl Pts',(-259.349362367341,2.91867451310751,
134.762961651901));
#188297=CARTESIAN_POINT('Ctrl Pts',(-259.35717423276,3.02999508926459,134.680885048172));
#188298=CARTESIAN_POINT('Ctrl Pts',(-259.36498609818,3.13777942900704,134.594161648671));
#188299=CARTESIAN_POINT('Ctrl Pts',(-259.372797963599,3.24162963026778,
134.503146959418));
#188300=CARTESIAN_POINT('Ctrl Pts',(-259.380492559669,3.34392086386956,
134.413498555019));
#188301=CARTESIAN_POINT('Ctrl Pts',(-259.388187155739,3.44239501607596,
134.319687131659));
#188302=CARTESIAN_POINT('Ctrl Pts',(-259.395881751809,3.53671030809215,
134.222088409409));
#188303=CARTESIAN_POINT('Ctrl Pts',(-259.403752251903,3.63318171581071,
134.122258509869));
#188304=CARTESIAN_POINT('Ctrl Pts',(-259.411622751998,3.72530153017333,
134.01846640365));
#188305=CARTESIAN_POINT('Ctrl Pts',(-259.419493252092,3.8127493250714,133.911147647066));
#188306=CARTESIAN_POINT('Ctrl Pts',(-259.427363752186,3.90019711996948,
133.803828890482));
#188307=CARTESIAN_POINT('Ctrl Pts',(-259.43523425228,3.98297269501011,133.69298387897));
#188308=CARTESIAN_POINT('Ctrl Pts',(-259.443104752374,4.06080482670846,
133.579076318657));
#188309=CARTESIAN_POINT('Ctrl Pts',(-259.450996306946,4.13884516815917,
133.464864042741));
#188310=CARTESIAN_POINT('Ctrl Pts',(-259.458887861518,4.21217532934342,
133.347193335508));
#188311=CARTESIAN_POINT('Ctrl Pts',(-259.46677941609,4.28047914998072,133.226483923486));
#188312=CARTESIAN_POINT('Ctrl Pts',(-259.474660674075,4.3486938505123,133.105932008299));
#188313=CARTESIAN_POINT('Ctrl Pts',(-259.482541932061,4.41189508226405,
132.98234960711));
#188314=CARTESIAN_POINT('Ctrl Pts',(-259.490423190047,4.46980916533012,
132.856186411348));
#188315=CARTESIAN_POINT('Ctrl Pts',(-259.498295871439,4.52766022475709,
132.730160509718));
#188316=CARTESIAN_POINT('Ctrl Pts',(-259.506168552831,4.58023543508844,
132.601559746475));
#188317=CARTESIAN_POINT('Ctrl Pts',(-259.514041234222,4.62730647137447,
132.470859307177));
#188318=CARTESIAN_POINT('Ctrl Pts',(-259.52190705186,4.67433646903304,132.340272818348));
#188319=CARTESIAN_POINT('Ctrl Pts',(-259.529772869497,4.71587172181415,
132.207590652673));
#188320=CARTESIAN_POINT('Ctrl Pts',(-259.537638687135,4.75173165413759,
132.073308744783));
#188321=CARTESIAN_POINT('Ctrl Pts',(-259.545499205399,4.78756742684223,
131.939117305544));
#188322=CARTESIAN_POINT('Ctrl Pts',(-259.553359723664,4.8177353988466,131.803328634847));
#188323=CARTESIAN_POINT('Ctrl Pts',(-259.561220241928,4.84210463919843,
131.666454420788));
#188324=CARTESIAN_POINT('Ctrl Pts',(-259.569077860488,4.8664648898651,131.529630698909));
#188325=CARTESIAN_POINT('Ctrl Pts',(-259.576935479049,4.88503060150653,
131.391722602004));
#188326=CARTESIAN_POINT('Ctrl Pts',(-259.584793097609,4.89772182492112,
131.253252573599));
#188327=CARTESIAN_POINT('Ctrl Pts',(-259.592649357877,4.91041085449106,
131.114806481558));
#188328=CARTESIAN_POINT('Ctrl Pts',(-259.600505618145,4.91722738378753,
130.97579902716));
#188329=CARTESIAN_POINT('Ctrl Pts',(-259.608361878413,4.9181432943351,130.836758131155));
#188330=CARTESIAN_POINT('Ctrl Pts',(-259.616218320535,4.91905922608383,
130.69771401668));
#188331=CARTESIAN_POINT('Ctrl Pts',(-259.624074762657,4.91407426562755,
130.558636836429));
#188332=CARTESIAN_POINT('Ctrl Pts',(-259.631931204778,4.90321241491024,
130.420054649918));
#188333=CARTESIAN_POINT('Ctrl Pts',(-259.639792798094,4.89234344245782,
130.28138159992));
#188334=CARTESIAN_POINT('Ctrl Pts',(-259.64765439141,4.87558990925817,130.143204568982));
#188335=CARTESIAN_POINT('Ctrl Pts',(-259.655515984725,4.85302777544528,
130.006047099419));
#188336=CARTESIAN_POINT('Ctrl Pts',(-259.66338015352,4.83045825021641,129.868844696698));
#188337=CARTESIAN_POINT('Ctrl Pts',(-259.671244322315,4.80207640315996,
129.732662891872));
#188338=CARTESIAN_POINT('Ctrl Pts',(-259.67910849111,4.76800926284416,129.598014592608));
#188339=CARTESIAN_POINT('Ctrl Pts',(-259.68698147486,4.73390393663589,129.463215365927));
#188340=CARTESIAN_POINT('Ctrl Pts',(-259.69485445861,4.69410068626818,129.32995344318));
#188341=CARTESIAN_POINT('Ctrl Pts',(-259.70272744236,4.64877652418144,129.198726820363));
#188342=CARTESIAN_POINT('Ctrl Pts',(-259.709002420302,4.61265195865421,
129.094135703471));
#188343=CARTESIAN_POINT('Ctrl Pts',(-259.715277398245,4.57302122015438,
128.990837253891));
#188344=CARTESIAN_POINT('Ctrl Pts',(-259.721552376188,4.52999553129857,
128.88907381165));
#188345=CARTESIAN_POINT('Ctrl Pts',(-259.729340865402,4.47659213822368,
128.762765244579));
#188346=CARTESIAN_POINT('Ctrl Pts',(-259.737129354617,4.41784166832893,
128.63854916123));
#188347=CARTESIAN_POINT('Ctrl Pts',(-259.744917843832,4.35393345271473,
128.51690645369));
#188348=CARTESIAN_POINT('Ctrl Pts',(-259.752699932249,4.29007775865146,
128.395363715515));
#188349=CARTESIAN_POINT('Ctrl Pts',(-259.760482020667,4.2210729339634,128.276390486525));
#188350=CARTESIAN_POINT('Ctrl Pts',(-259.768264109084,4.14715602421871,
128.160446857005));
#188351=CARTESIAN_POINT('Ctrl Pts',(-259.776041625002,4.07328254561895,
128.044571352147));
#188352=CARTESIAN_POINT('Ctrl Pts',(-259.78381914092,3.99450293455686,127.931722230335));
#188353=CARTESIAN_POINT('Ctrl Pts',(-259.791596656838,3.91109954323073,
127.822333886391));
#188354=CARTESIAN_POINT('Ctrl Pts',(-259.799371306898,3.82772688437878,
127.712985849855));
#188355=CARTESIAN_POINT('Ctrl Pts',(-259.807145956958,3.73973407267837,
127.607096360549));
#188356=CARTESIAN_POINT('Ctrl Pts',(-259.814920607018,3.64744583509542,
127.505069490287));
#188357=CARTESIAN_POINT('Ctrl Pts',(-259.822696039392,3.55514831113214,
127.403032353707));
#188358=CARTESIAN_POINT('Ctrl Pts',(-259.830471471765,3.45855475148024,
127.304858906876));
#188359=CARTESIAN_POINT('Ctrl Pts',(-259.838246904139,3.35802912226606,
127.210918886229));
#188360=CARTESIAN_POINT('Ctrl Pts',(-259.845756665457,3.26093825380846,
127.120188609196));
#188361=CARTESIAN_POINT('Ctrl Pts',(-259.853266426776,3.16017986615663,
127.03340743426));
#188362=CARTESIAN_POINT('Ctrl Pts',(-259.860776188094,3.05611296324695,
126.950874323523));
#188363=CARTESIAN_POINT('Ctrl Pts',(-259.86984693344,2.93041464406388,126.851185825005));
#188364=CARTESIAN_POINT('Ctrl Pts',(-259.878917678785,2.79997527753095,
126.757761425072));
#188365=CARTESIAN_POINT('Ctrl Pts',(-259.887988424131,2.66539424307775,
126.670977428039));
#188366=CARTESIAN_POINT('Ctrl Pts',(-259.89732272212,2.52690292495375,126.58167190152));
#188367=CARTESIAN_POINT('Ctrl Pts',(-259.906657020109,2.38402579214265,
126.499398505981));
#188368=CARTESIAN_POINT('Ctrl Pts',(-259.915991318098,2.2374405325973,126.424515537476));
#188369=CARTESIAN_POINT('Ctrl Pts',(-259.925109869169,2.09424334979852,
126.351363365404));
#188370=CARTESIAN_POINT('Ctrl Pts',(-259.93422842024,1.9475076731623,126.285263762748));
#188371=CARTESIAN_POINT('Ctrl Pts',(-259.943346971312,1.79788636277355,
126.226502200243));
#188372=CARTESIAN_POINT('Ctrl Pts',(-259.95278914276,1.64295494286366,126.165655170556));
#188373=CARTESIAN_POINT('Ctrl Pts',(-259.962231314208,1.48492941989842,
126.112676642776));
#188374=CARTESIAN_POINT('Ctrl Pts',(-259.971673485656,1.32455638043327,
126.067828821246));
#188375=CARTESIAN_POINT('Ctrl Pts',(-259.981115657104,1.16418334096776,
126.022980999715));
#188376=CARTESIAN_POINT('Ctrl Pts',(-259.990557828552,1.00146289783601,
125.986263963227));
#188377=CARTESIAN_POINT('Ctrl Pts',(-260.,0.837162017624996,125.957883255734));
#188378=CARTESIAN_POINT('Ctrl Pts',(-258.665423831404,-4.76405452823398,
129.582490119308));
#188379=CARTESIAN_POINT('Ctrl Pts',(-258.673755749879,-4.80055740878989,
129.724814296587));
#188380=CARTESIAN_POINT('Ctrl Pts',(-258.682087668354,-4.83071962826672,
129.868936410275));
#188381=CARTESIAN_POINT('Ctrl Pts',(-258.690419586829,-4.8543766360945,
130.014290660258));
#188382=CARTESIAN_POINT('Ctrl Pts',(-258.698727113262,-4.87796438703723,
130.159219379564));
#188383=CARTESIAN_POINT('Ctrl Pts',(-258.707034639695,-4.89508485697752,
130.305372751092));
#188384=CARTESIAN_POINT('Ctrl Pts',(-258.715342166129,-4.90562406003518,
130.452173672743));
#188385=CARTESIAN_POINT('Ctrl Pts',(-258.721941632081,-4.9139963610206,
130.568791740947));
#188386=CARTESIAN_POINT('Ctrl Pts',(-258.728541098034,-4.91821638989561,
130.685818086956));
#188387=CARTESIAN_POINT('Ctrl Pts',(-258.735140563986,-4.91824979995562,
130.802957857252));
#188388=CARTESIAN_POINT('Origin',(212.,0.,130.804360617566));
#188389=CARTESIAN_POINT('',(212.,-9.,130.804360617566));
#188390=CARTESIAN_POINT('Origin',(212.,0.,130.804360617566));
#188391=CARTESIAN_POINT('',(212.,-7.,130.804360617566));
#188392=CARTESIAN_POINT('Origin',(212.,0.,130.804360617566));
#188393=CARTESIAN_POINT('Origin',(210.,0.,130.804360617566));
#188394=CARTESIAN_POINT('',(210.,-9.,130.804360617566));
#188395=CARTESIAN_POINT('',(210.,-9.,130.804360617566));
#188396=CARTESIAN_POINT('Origin',(210.,0.,130.804360617566));
#188397=CARTESIAN_POINT('Origin',(210.,0.,130.804360617566));
#188398=CARTESIAN_POINT('Ctrl Pts',(210.,-2.8641783061622,134.81100053397));
#188399=CARTESIAN_POINT('Ctrl Pts',(210.,-2.96502472716555,134.75378484428));
#188400=CARTESIAN_POINT('Ctrl Pts',(210.,-3.06346128541938,134.692924280852));
#188401=CARTESIAN_POINT('Ctrl Pts',(210.,-3.15926168328819,134.628476370697));
#188402=CARTESIAN_POINT('Ctrl Pts',(210.,-3.27563203468335,134.550190412411));
#188403=CARTESIAN_POINT('Ctrl Pts',(210.,-3.38811397812997,134.466613066522));
#188404=CARTESIAN_POINT('Ctrl Pts',(210.,-3.49662687492886,134.378182862155));
#188405=CARTESIAN_POINT('Ctrl Pts',(210.,-3.60844752995494,134.287057072797));
#188406=CARTESIAN_POINT('Ctrl Pts',(210.,-3.7160539550275,134.190777777457));
#188407=CARTESIAN_POINT('Ctrl Pts',(210.,-3.81933617822931,134.089772607624));
#188408=CARTESIAN_POINT('Ctrl Pts',(210.,-3.92261840143113,133.988767437792));
#188409=CARTESIAN_POINT('Ctrl Pts',(210.,-4.02157682130595,133.883035820798));
#188410=CARTESIAN_POINT('Ctrl Pts',(210.,-4.11607356234994,133.772960819414));
#188411=CARTESIAN_POINT('Ctrl Pts',(210.,-4.169132731693,133.711154580655));
#188412=CARTESIAN_POINT('Ctrl Pts',(210.,-4.22078471769379,133.647978234656));
#188413=CARTESIAN_POINT('Ctrl Pts',(210.,-4.27100052841727,133.583494472577));
#188414=CARTESIAN_POINT('Ctrl Pts',(210.,-4.28346862121088,133.567483787542));
#188415=CARTESIAN_POINT('Ctrl Pts',(210.,-4.29584950541028,133.551390713183));
#188416=CARTESIAN_POINT('Ctrl Pts',(210.,-4.30813839293311,133.535221857428));
#188417=CARTESIAN_POINT('Ctrl Pts',(210.,-4.40009216432484,133.414235538449));
#188418=CARTESIAN_POINT('Ctrl Pts',(210.,-4.48665891050019,133.289326577391));
#188419=CARTESIAN_POINT('Ctrl Pts',(210.,-4.56773849979461,133.160993194298));
#188420=CARTESIAN_POINT('Ctrl Pts',(210.,-4.64849084265369,133.03317777932));
#188421=CARTESIAN_POINT('Ctrl Pts',(210.,-4.72380062867781,132.901964837969));
#188422=CARTESIAN_POINT('Ctrl Pts',(210.,-4.79353962578297,132.767799500622));
#188423=CARTESIAN_POINT('Ctrl Pts',(210.,-4.86402484104165,132.632198573225));
#188424=CARTESIAN_POINT('Ctrl Pts',(210.,-4.928819916136,132.493581111616));
#188425=CARTESIAN_POINT('Ctrl Pts',(210.,-4.98775557446357,132.352368204748));
#188426=CARTESIAN_POINT('Ctrl Pts',(210.,-5.04615226330057,132.21244669685));
#188427=CARTESIAN_POINT('Ctrl Pts',(210.,-5.09879659579809,132.069976268777));
#188428=CARTESIAN_POINT('Ctrl Pts',(210.,-5.14548145371836,131.925339242337));
#188429=CARTESIAN_POINT('Ctrl Pts',(210.,-5.15890833504517,131.88374065393));
#188430=CARTESIAN_POINT('Ctrl Pts',(210.,-5.17184197206715,131.84196271352));
#188431=CARTESIAN_POINT('Ctrl Pts',(210.,-5.18427670924701,131.800014223967));
#188432=CARTESIAN_POINT('Ctrl Pts',(210.,-5.19020423391478,131.780017765416));
#188433=CARTESIAN_POINT('Ctrl Pts',(210.,-5.19601887800011,131.75998081631));
#188434=CARTESIAN_POINT('Ctrl Pts',(210.,-5.20171845467757,131.739909779336));
#188435=CARTESIAN_POINT('Ctrl Pts',(210.,-5.244666117862,131.588669751436));
#188436=CARTESIAN_POINT('Ctrl Pts',(210.,-5.28095619241888,131.4359495813));
#188437=CARTESIAN_POINT('Ctrl Pts',(210.,-5.31045568168286,131.282214375908));
#188438=CARTESIAN_POINT('Ctrl Pts',(210.,-5.34002140650602,131.128133987004));
#188439=CARTESIAN_POINT('Ctrl Pts',(210.,-5.36276647177015,130.973033269566));
#188440=CARTESIAN_POINT('Ctrl Pts',(210.,-5.37851503032129,130.817349238262));
#188441=CARTESIAN_POINT('Ctrl Pts',(210.,-5.39406434679863,130.663634835425));
#188442=CARTESIAN_POINT('Ctrl Pts',(210.,-5.40279340123895,130.509351025403));
#188443=CARTESIAN_POINT('Ctrl Pts',(210.,-5.40448640685994,130.354899211369));
#188444=CARTESIAN_POINT('Ctrl Pts',(210.,-5.40520651984511,130.289203766836));
#188445=CARTESIAN_POINT('Ctrl Pts',(210.,-5.40465306852236,130.223477753562));
#188446=CARTESIAN_POINT('Ctrl Pts',(210.,-5.40280661787305,130.157751497854));
#188447=CARTESIAN_POINT('Ctrl Pts',(210.,-5.39955346179212,130.041952156823));
#188448=CARTESIAN_POINT('Ctrl Pts',(210.,-5.39228769078652,129.926152028858));
#188449=CARTESIAN_POINT('Ctrl Pts',(210.,-5.38110695373693,129.810516944227));
#188450=CARTESIAN_POINT('Ctrl Pts',(210.,-5.37798956653967,129.778275837868));
#188451=CARTESIAN_POINT('Ctrl Pts',(210.,-5.37456773065206,129.746047563338));
#188452=CARTESIAN_POINT('Ctrl Pts',(210.,-5.37084332865221,129.713835726721));
#188453=CARTESIAN_POINT('Ctrl Pts',(210.,-5.36786151250135,129.688046412175));
#188454=CARTESIAN_POINT('Ctrl Pts',(210.,-5.36468519189614,129.662263949371));
#188455=CARTESIAN_POINT('Ctrl Pts',(210.,-5.36131905158111,129.636517152514));
#188456=CARTESIAN_POINT('Ctrl Pts',(210.,-5.34132632447221,129.483597596195));
#188457=CARTESIAN_POINT('Ctrl Pts',(210.,-5.31462277703016,129.331755121105));
#188458=CARTESIAN_POINT('Ctrl Pts',(210.,-5.28154289170897,129.181379978409));
#188459=CARTESIAN_POINT('Ctrl Pts',(210.,-5.24788597458129,129.028381754061));
#188460=CARTESIAN_POINT('Ctrl Pts',(210.,-5.20762823228242,128.876901854454));
#188461=CARTESIAN_POINT('Ctrl Pts',(210.,-5.16106759031274,128.727341113289));
#188462=CARTESIAN_POINT('Ctrl Pts',(210.,-5.1136565897567,128.575048874982));
#188463=CARTESIAN_POINT('Ctrl Pts',(210.,-5.05971025362034,128.424745789725));
#188464=CARTESIAN_POINT('Ctrl Pts',(210.,-4.99948878343386,128.276855218127));
#188465=CARTESIAN_POINT('Ctrl Pts',(210.,-4.94601440467812,128.145534006347));
#188466=CARTESIAN_POINT('Ctrl Pts',(210.,-4.88759133985197,128.01611464299));
#188467=CARTESIAN_POINT('Ctrl Pts',(210.,-4.82436816053947,127.88890102204));
#188468=CARTESIAN_POINT('Ctrl Pts',(210.,-4.79249149405723,127.824760841));
#188469=CARTESIAN_POINT('Ctrl Pts',(210.,-4.75939410526878,127.761181537784));
#188470=CARTESIAN_POINT('Ctrl Pts',(210.,-4.7250921856227,127.698203303454));
#188471=CARTESIAN_POINT('Ctrl Pts',(210.,-4.71478448273727,127.679278388044));
#188472=CARTESIAN_POINT('Ctrl Pts',(210.,-4.70436799826693,127.660407756002));
#188473=CARTESIAN_POINT('Ctrl Pts',(210.,-4.69384313927245,127.641592516773));
#188474=CARTESIAN_POINT('Ctrl Pts',(210.,-4.68242422337511,127.621178976367));
#188475=CARTESIAN_POINT('Ctrl Pts',(210.,-4.67088203968081,127.60083836979));
#188476=CARTESIAN_POINT('Ctrl Pts',(210.,-4.65921993791005,127.580576301963));
#188477=CARTESIAN_POINT('Ctrl Pts',(210.,-4.64586056367047,127.5573653446));
#188478=CARTESIAN_POINT('Ctrl Pts',(210.,-4.63234280926635,127.534255628605));
#188479=CARTESIAN_POINT('Ctrl Pts',(210.,-4.61866803274399,127.511249065334));
#188480=CARTESIAN_POINT('Ctrl Pts',(210.,-4.53526957206909,127.370938767826));
#188481=CARTESIAN_POINT('Ctrl Pts',(210.,-4.44603502941789,127.234464045224));
#188482=CARTESIAN_POINT('Ctrl Pts',(210.,-4.35129440682451,127.102081779137));
#188483=CARTESIAN_POINT('Ctrl Pts',(210.,-4.25655378423112,126.969699513049));
#188484=CARTESIAN_POINT('Ctrl Pts',(210.,-4.15630670922515,126.841409133477));
#188485=CARTESIAN_POINT('Ctrl Pts',(210.,-4.05083428316753,126.71748608273));
#188486=CARTESIAN_POINT('Ctrl Pts',(210.,-3.99881145153813,126.656362732817));
#188487=CARTESIAN_POINT('Ctrl Pts',(210.,-3.94551667042523,126.596302213789));
#188488=CARTESIAN_POINT('Ctrl Pts',(210.,-3.8909797140714,126.537339895932));
#188489=CARTESIAN_POINT('Ctrl Pts',(210.,-3.86497510378344,126.509225160529));
#188490=CARTESIAN_POINT('Ctrl Pts',(210.,-3.8386880328713,126.481360140095));
#188491=CARTESIAN_POINT('Ctrl Pts',(210.,-3.81212153503869,126.453748815486));
#188492=CARTESIAN_POINT('Ctrl Pts',(210.,-3.79363314055594,126.43453329582));
#188493=CARTESIAN_POINT('Ctrl Pts',(210.,-3.77500857133956,126.41543988829));
#188494=CARTESIAN_POINT('Ctrl Pts',(210.,-3.75626121342458,126.396482227117));
#188495=CARTESIAN_POINT('Ctrl Pts',(210.,-3.6393612358576,126.278270894304));
#188496=CARTESIAN_POINT('Ctrl Pts',(210.,-3.51758395568067,126.165223350996));
#188497=CARTESIAN_POINT('Ctrl Pts',(210.,-3.39124299655272,126.057613808602));
#188498=CARTESIAN_POINT('Ctrl Pts',(210.,-3.26529717903502,125.950340823791));
#188499=CARTESIAN_POINT('Ctrl Pts',(210.,-3.13481576057488,125.848471304097));
#188500=CARTESIAN_POINT('Ctrl Pts',(210.,-3.00006601075642,125.752304395756));
#188501=CARTESIAN_POINT('Ctrl Pts',(210.,-2.86552956545396,125.656289716534));
#188502=CARTESIAN_POINT('Ctrl Pts',(210.,-2.72673788371416,125.565959020801));
#188503=CARTESIAN_POINT('Ctrl Pts',(210.,-2.58391981636417,125.481646183644));
#188504=CARTESIAN_POINT('Ctrl Pts',(210.,2.59168471337878,125.476247689738));
#188505=CARTESIAN_POINT('Ctrl Pts',(210.,2.71111266644001,125.545959660002));
#188506=CARTESIAN_POINT('Ctrl Pts',(210.,2.82764132334605,125.619975219606));
#188507=CARTESIAN_POINT('Ctrl Pts',(210.,2.94101107271424,125.698291576074));
#188508=CARTESIAN_POINT('Ctrl Pts',(210.,3.07489319746795,125.790777978005));
#188509=CARTESIAN_POINT('Ctrl Pts',(210.,3.20437111666488,125.889261565323));
#188510=CARTESIAN_POINT('Ctrl Pts',(210.,3.32928169753943,125.993299430327));
#188511=CARTESIAN_POINT('Ctrl Pts',(210.,3.45638475582413,126.099163406996));
#188512=CARTESIAN_POINT('Ctrl Pts',(210.,3.57875916616007,126.210779035122));
#188513=CARTESIAN_POINT('Ctrl Pts',(210.,3.69619194875321,126.327715160383));
#188514=CARTESIAN_POINT('Ctrl Pts',(210.,3.81326715672415,126.444295223309));
#188515=CARTESIAN_POINT('Ctrl Pts',(210.,3.9254310827064,126.566164219876));
#188516=CARTESIAN_POINT('Ctrl Pts',(210.,4.03242689161515,126.692918634597));
#188517=CARTESIAN_POINT('Ctrl Pts',(210.,4.08855183263102,126.759408005744));
#188518=CARTESIAN_POINT('Ctrl Pts',(210.,4.14325394828036,126.827241949012));
#188519=CARTESIAN_POINT('Ctrl Pts',(210.,4.19649068322839,126.896363740591));
#188520=CARTESIAN_POINT('Ctrl Pts',(210.,4.213627944191,126.918614507503));
#188521=CARTESIAN_POINT('Ctrl Pts',(210.,4.23061332624127,126.940998731528));
#188522=CARTESIAN_POINT('Ctrl Pts',(210.,4.24744532208237,126.963514532833));
#188523=CARTESIAN_POINT('Ctrl Pts',(210.,4.25948801745557,126.979623789201));
#188524=CARTESIAN_POINT('Ctrl Pts',(210.,4.2714501552323,126.995797726654));
#188525=CARTESIAN_POINT('Ctrl Pts',(210.,4.28332546167438,127.012027509189));
#188526=CARTESIAN_POINT('Ctrl Pts',(210.,4.37956101060926,127.143551023039));
#188527=CARTESIAN_POINT('Ctrl Pts',(210.,4.47021273499132,127.278892841946));
#188528=CARTESIAN_POINT('Ctrl Pts',(210.,4.55510872905159,127.417626057086));
#188529=CARTESIAN_POINT('Ctrl Pts',(210.,4.64006233451871,127.556453418196));
#188530=CARTESIAN_POINT('Ctrl Pts',(210.,4.71925268848836,127.69867755979));
#188531=CARTESIAN_POINT('Ctrl Pts',(210.,4.79246067878325,127.843893787959));
#188532=CARTESIAN_POINT('Ctrl Pts',(210.,4.86453983676611,127.986870851115));
#188533=CARTESIAN_POINT('Ctrl Pts',(210.,4.93081984635459,128.1327491888));
#188534=CARTESIAN_POINT('Ctrl Pts',(210.,4.99104310450031,128.281153501978));
#188535=CARTESIAN_POINT('Ctrl Pts',(210.,5.05072900641638,128.428233642658));
#188536=CARTESIAN_POINT('Ctrl Pts',(210.,5.10446594616894,128.577795554527));
#188537=CARTESIAN_POINT('Ctrl Pts',(210.,5.15195263203104,128.729474268576));
#188538=CARTESIAN_POINT('Ctrl Pts',(210.,5.16621208753242,128.775020843036));
#188539=CARTESIAN_POINT('Ctrl Pts',(210.,5.17990759903754,128.820758254765));
#188540=CARTESIAN_POINT('Ctrl Pts',(210.,5.1930300689057,128.866676489988));
#188541=CARTESIAN_POINT('Ctrl Pts',(210.,5.19914764870326,128.888083166548));
#188542=CARTESIAN_POINT('Ctrl Pts',(210.,5.2051406806358,128.90952914099));
#188543=CARTESIAN_POINT('Ctrl Pts',(210.,5.21100820960353,128.931013391454));
#188544=CARTESIAN_POINT('Ctrl Pts',(210.,5.21620337908719,128.950035764076));
#188545=CARTESIAN_POINT('Ctrl Pts',(210.,5.22129750196036,128.96907841561));
#188546=CARTESIAN_POINT('Ctrl Pts',(210.,5.22629012191461,128.988140212046));
#188547=CARTESIAN_POINT('Ctrl Pts',(210.,5.26614820913265,129.140318177088));
#188548=CARTESIAN_POINT('Ctrl Pts',(210.,5.29954350738592,129.293724156363));
#188549=CARTESIAN_POINT('Ctrl Pts',(210.,5.32627173644381,129.447991892391));
#188550=CARTESIAN_POINT('Ctrl Pts',(210.,5.35267492411837,129.600383582004));
#188551=CARTESIAN_POINT('Ctrl Pts',(210.,5.37257233544242,129.753616870713));
#188552=CARTESIAN_POINT('Ctrl Pts',(210.,5.38571671980561,129.907341042028));
#188553=CARTESIAN_POINT('Ctrl Pts',(210.,5.39854800023754,130.057403448666));
#188554=CARTESIAN_POINT('Ctrl Pts',(210.,5.40494414667608,130.207934192936));
#188555=CARTESIAN_POINT('Ctrl Pts',(210.,5.40462612405376,130.358600246709));
#188556=CARTESIAN_POINT('Ctrl Pts',(210.,5.4044980822189,130.41926120798));
#188557=CARTESIAN_POINT('Ctrl Pts',(210.,5.40328109662435,130.479943979233));
#188558=CARTESIAN_POINT('Ctrl Pts',(210.,5.40095462579041,130.540626197016));
#188559=CARTESIAN_POINT('Ctrl Pts',(210.,5.39555663845411,130.681423940254));
#188560=CARTESIAN_POINT('Ctrl Pts',(210.,5.38418746158711,130.82222005765));
#188561=CARTESIAN_POINT('Ctrl Pts',(210.,5.36695826250822,130.962655854025));
#188562=CARTESIAN_POINT('Ctrl Pts',(210.,5.36453283903126,130.982425564501));
#188563=CARTESIAN_POINT('Ctrl Pts',(210.,5.36199124033403,131.002188101967));
#188564=CARTESIAN_POINT('Ctrl Pts',(210.,5.35933373296221,131.021942432198));
#188565=CARTESIAN_POINT('Ctrl Pts',(210.,5.35674292549998,131.041200954947));
#188566=CARTESIAN_POINT('Ctrl Pts',(210.,5.35404312369154,131.060442922715));
#188567=CARTESIAN_POINT('Ctrl Pts',(210.,5.35123522163466,131.079665129237));
#188568=CARTESIAN_POINT('Ctrl Pts',(210.,5.32917189754803,131.23070521666));
#188569=CARTESIAN_POINT('Ctrl Pts',(210.,5.30043229141883,131.380573392734));
#188570=CARTESIAN_POINT('Ctrl Pts',(210.,5.26526672076462,131.52884789957));
#188571=CARTESIAN_POINT('Ctrl Pts',(210.,5.22989628612353,131.677986208872));
#188572=CARTESIAN_POINT('Ctrl Pts',(210.,5.18802438233364,131.825513008037));
#188573=CARTESIAN_POINT('Ctrl Pts',(210.,5.13985568266502,131.970981511079));
#188574=CARTESIAN_POINT('Ctrl Pts',(210.,5.09214210403352,132.115075557753));
#188575=CARTESIAN_POINT('Ctrl Pts',(210.,5.03824965696429,132.257150705429));
#188576=CARTESIAN_POINT('Ctrl Pts',(210.,4.97833532758118,132.396744612767));
#188577=CARTESIAN_POINT('Ctrl Pts',(210.,4.92981628697671,132.509788729726));
#188578=CARTESIAN_POINT('Ctrl Pts',(210.,4.87734729734596,132.621205309558));
#188579=CARTESIAN_POINT('Ctrl Pts',(210.,4.82099454674417,132.730730504221));
#188580=CARTESIAN_POINT('Ctrl Pts',(210.,4.79165588826149,132.787752073659));
#188581=CARTESIAN_POINT('Ctrl Pts',(210.,4.76126429707162,132.844260685062));
#188582=CARTESIAN_POINT('Ctrl Pts',(210.,4.72982767878697,132.900216977775));
#188583=CARTESIAN_POINT('Ctrl Pts',(210.,4.71933699539195,132.91889009794));
#188584=CARTESIAN_POINT('Ctrl Pts',(210.,4.70872882129724,132.937503608749));
#188585=CARTESIAN_POINT('Ctrl Pts',(210.,4.69800701316631,132.956049819302));
#188586=CARTESIAN_POINT('Ctrl Pts',(210.,4.67896109085937,132.988994792853));
#188587=CARTESIAN_POINT('Ctrl Pts',(210.,4.65956569768156,133.021711868397));
#188588=CARTESIAN_POINT('Ctrl Pts',(210.,4.63982391216924,133.054194020027));
#188589=CARTESIAN_POINT('Ctrl Pts',(210.,4.56178429176233,133.182596528585));
#188590=CARTESIAN_POINT('Ctrl Pts',(210.,4.47833472600848,133.30733089509));
#188591=CARTESIAN_POINT('Ctrl Pts',(210.,4.3897187404882,133.4281029892));
#188592=CARTESIAN_POINT('Ctrl Pts',(210.,4.30158605741235,133.548216404765));
#188593=CARTESIAN_POINT('Ctrl Pts',(210.,4.20834258956795,133.66441109461));
#188594=CARTESIAN_POINT('Ctrl Pts',(210.,4.11019598182694,133.776357668134));
#188595=CARTESIAN_POINT('Ctrl Pts',(210.,4.06527327633945,133.827596759005));
#188596=CARTESIAN_POINT('Ctrl Pts',(210.,4.01932297958479,133.877945279926));
#188597=CARTESIAN_POINT('Ctrl Pts',(210.,3.9723632412024,133.927368436226));
#188598=CARTESIAN_POINT('Ctrl Pts',(210.,3.95145209377834,133.949376542386));
#188599=CARTESIAN_POINT('Ctrl Pts',(210.,3.93034076955951,133.971201128248));
#188600=CARTESIAN_POINT('Ctrl Pts',(210.,3.90903081243557,133.992838982041));
#188601=CARTESIAN_POINT('Ctrl Pts',(210.,3.89187183158307,134.010261988421));
#188602=CARTESIAN_POINT('Ctrl Pts',(210.,3.87458340886331,134.027564474838));
#188603=CARTESIAN_POINT('Ctrl Pts',(210.,3.85717820998098,134.044733292105));
#188604=CARTESIAN_POINT('Ctrl Pts',(210.,3.75307497292274,134.147422693473));
#188605=CARTESIAN_POINT('Ctrl Pts',(210.,3.64469941185318,134.245433426635));
#188606=CARTESIAN_POINT('Ctrl Pts',(210.,3.5322642813685,134.338467234451));
#188607=CARTESIAN_POINT('Ctrl Pts',(210.000000000001,3.42170402111848,134.429949691579));
#188608=CARTESIAN_POINT('Ctrl Pts',(210.000000000001,3.30721789468442,134.516620114227));
#188609=CARTESIAN_POINT('Ctrl Pts',(210.000000000001,3.18898565748847,134.598150619545));
#188610=CARTESIAN_POINT('Ctrl Pts',(210.000000000001,3.0814058769606,134.672335411075));
#188611=CARTESIAN_POINT('Ctrl Pts',(210.000000000001,2.97072408738642,134.742264450146));
#188612=CARTESIAN_POINT('Ctrl Pts',(210.000000000001,2.85706463458494,134.807654853105));
#188613=CARTESIAN_POINT('Origin',(236.,4.44872159004524,125.399836936956));
#188614=CARTESIAN_POINT('',(236.,4.44872159004524,125.399836936956));
#188615=CARTESIAN_POINT('',(236.,4.44872159004524,136.208884298175));
#188616=CARTESIAN_POINT('',(236.,4.44872159004524,128.102098777261));
#188617=CARTESIAN_POINT('',(224.,4.44872159004524,125.399836936956));
#188618=CARTESIAN_POINT('',(210.,4.44872159004524,125.399836936956));
#188619=CARTESIAN_POINT('',(224.,4.44872159004524,136.208884298175));
#188620=CARTESIAN_POINT('',(224.,4.44872159004524,143.664891345585));
#188621=CARTESIAN_POINT('',(210.,4.44872159004524,136.208884298175));
#188622=CARTESIAN_POINT('Origin',(224.,5.72436079502262,130.804360617566));
#188623=CARTESIAN_POINT('Origin',(224.,0.,130.804360617566));
#188624=CARTESIAN_POINT('Origin',(236.,-4.44872159004524,136.208884298175));
#188625=CARTESIAN_POINT('',(236.,-4.44872159004524,136.208884298175));
#188626=CARTESIAN_POINT('',(236.,-4.44872159004524,125.399836936956));
#188627=CARTESIAN_POINT('',(236.,-4.44872159004524,133.50662245787));
#188628=CARTESIAN_POINT('',(224.,-4.44872159004524,136.208884298175));
#188629=CARTESIAN_POINT('',(210.,-4.44872159004524,136.208884298175));
#188630=CARTESIAN_POINT('',(224.,-4.44872159004524,125.399836936956));
#188631=CARTESIAN_POINT('',(224.,-4.44872159004524,117.943829889547));
#188632=CARTESIAN_POINT('',(210.,-4.44872159004524,125.399836936956));
#188633=CARTESIAN_POINT('Origin',(224.,-5.72436079502262,130.804360617566));
#188634=CARTESIAN_POINT('',(224.,-7.,130.804360617566));
#188635=CARTESIAN_POINT('Origin',(224.,0.,130.804360617566));
#188636=CARTESIAN_POINT('Origin',(224.,0.,130.804360617566));
#188637=CARTESIAN_POINT('Origin',(210.,0.,130.804360617566));
#188638=CARTESIAN_POINT('',(210.,-7.,130.804360617566));
#188639=CARTESIAN_POINT('Origin',(236.,0.,130.804360617566));
#188640=CARTESIAN_POINT('Origin',(236.,0.,130.804360617566));
#188641=CARTESIAN_POINT('Origin',(236.,0.,130.804360617566));
#188642=CARTESIAN_POINT('Ctrl Pts',(210.579426101437,-2.14555810197798,
126.384433368448));
#188643=CARTESIAN_POINT('Ctrl Pts',(210.533016425084,-2.88204635455982,
126.741945114569));
#188644=CARTESIAN_POINT('Ctrl Pts',(210.440198811428,-4.16073755837059,
127.832228156677));
#188645=CARTESIAN_POINT('Ctrl Pts',(210.254565323169,-5.41774734084591,
130.983824311839));
#188646=CARTESIAN_POINT('Ctrl Pts',(210.022525636658,-3.70466367662459,
135.280954889074));
#188647=CARTESIAN_POINT('Ctrl Pts',(209.744078012845,1.77278938863763,136.341871604603));
#188648=CARTESIAN_POINT('Ctrl Pts',(209.465630389032,5.61248518735455,132.305536381355));
#188649=CARTESIAN_POINT('Ctrl Pts',(209.187182765219,4.2990952821384,126.894094626803));
#188650=CARTESIAN_POINT('Ctrl Pts',(208.908735141406,-0.967335548355457,
125.073681250508));
#188651=CARTESIAN_POINT('Ctrl Pts',(208.630287517594,-5.34357155608916,
128.520706403956));
#188652=CARTESIAN_POINT('Ctrl Pts',(208.351839893781,-4.80999390579215,
134.065650134797));
#188653=CARTESIAN_POINT('Ctrl Pts',(208.073392269968,0.144086686833323,
136.613971320579));
#188654=CARTESIAN_POINT('Ctrl Pts',(207.794944646155,4.96557142732685,133.823362329787));
#188655=CARTESIAN_POINT('Ctrl Pts',(207.516497022342,5.22403776314189,128.258534510045));
#188656=CARTESIAN_POINT('Ctrl Pts',(207.238049398529,0.681816090004523,
125.033145533949));
#188657=CARTESIAN_POINT('Ctrl Pts',(206.959601774716,-4.48693345015888,
127.111248278652));
#188658=CARTESIAN_POINT('Ctrl Pts',(206.681154150904,-5.53242507739068,
132.583126545744));
#188659=CARTESIAN_POINT('Ctrl Pts',(206.40270652709,-1.49388053201802,136.420413394932));
#188660=CARTESIAN_POINT('Ctrl Pts',(206.124258903278,3.91746311099657,135.0968180907));
#188661=CARTESIAN_POINT('Ctrl Pts',(205.845811279465,5.72885172159717,129.828666190814));
#188662=CARTESIAN_POINT('Ctrl Pts',(205.567363655652,2.27570431130586,125.457128678938));
#188663=CARTESIAN_POINT('Ctrl Pts',(205.288916031839,-3.26870357308214,
125.999436687584));
#188664=CARTESIAN_POINT('Ctrl Pts',(205.010468408026,-5.80933288384994,
130.9572347388));
#188665=CARTESIAN_POINT('Ctrl Pts',(204.732020784213,-3.01146890392974,
135.774549108008));
#188666=CARTESIAN_POINT('Ctrl Pts',(204.4535731604,2.5537877891123,136.024502973214));
#188667=CARTESIAN_POINT('Ctrl Pts',(204.175125536587,5.77223831170541,131.477401078575));
#188668=CARTESIAN_POINT('Ctrl Pts',(203.896677912775,3.6862837897924,126.311807855303));
#188669=CARTESIAN_POINT('Ctrl Pts',(203.618230288961,-1.78718543642468,
125.274651160291));
#188670=CARTESIAN_POINT('Ctrl Pts',(203.339782665149,-5.61831856260093,
129.319027308227));
#188671=CARTESIAN_POINT('Ctrl Pts',(203.061335041336,-4.28649139606962,
134.728352208566));
#188672=CARTESIAN_POINT('Ctrl Pts',(202.782887417523,0.984411954691954,
136.531720532469));
#188673=CARTESIAN_POINT('Ctrl Pts',(202.50443979371,5.3506888113544,133.071924892697));
#188674=CARTESIAN_POINT('Ctrl Pts',(202.225992169897,4.79994404549834,127.528348460205));
#188675=CARTESIAN_POINT('Ctrl Pts',(201.947544546084,-0.161714807569177,
124.995267158526));
#188676=CARTESIAN_POINT('Ctrl Pts',(201.669096922271,-4.97476565284641,
127.800458955558));
#188677=CARTESIAN_POINT('Ctrl Pts',(201.390649298458,-5.21624989388704,
133.366089631302));
#188678=CARTESIAN_POINT('Ctrl Pts',(201.112201674645,-0.664255310463968,
136.577616490799));
#188679=CARTESIAN_POINT('Ctrl Pts',(200.833754050833,4.49815745262305,134.483803242045));
#188680=CARTESIAN_POINT('Ctrl Pts',(200.55530642702,5.52698326394509,129.008761972148));
#188681=CARTESIAN_POINT('Ctrl Pts',(200.276858803207,1.47678146385132,125.183788137525));
#188682=CARTESIAN_POINT('Ctrl Pts',(199.998411179394,-3.93051035674001,
126.523845831826));
#188683=CARTESIAN_POINT('Ctrl Pts',(199.719963555581,-5.7258551755912,131.79748749945));
#188684=CARTESIAN_POINT('Ctrl Pts',(199.441515931768,-2.25941881165118,
136.158494079568));
#188685=CARTESIAN_POINT('Ctrl Pts',(199.163068307955,3.28331306145151,135.599313572066));
#188686=CARTESIAN_POINT('Ctrl Pts',(198.884620684142,5.80884062984016,130.633805545853));
#188687=CARTESIAN_POINT('Ctrl Pts',(198.606173060329,2.99632743704681,125.825029298466));
#188688=CARTESIAN_POINT('Ctrl Pts',(198.327725436517,-2.56966429165962,
125.592015279473));
#188689=CARTESIAN_POINT('Ctrl Pts',(198.049277812704,-5.77426007141042,
130.148891988961));
#188690=CARTESIAN_POINT('Ctrl Pts',(197.770830188891,-3.6725929338218,135.308112346714));
#188691=CARTESIAN_POINT('Ctrl Pts',(197.492382565078,1.80400769380988,136.328604885883));
#188692=CARTESIAN_POINT('Ctrl Pts',(197.213934941265,5.62281338150559,132.272586816804));
#188693=CARTESIAN_POINT('Ctrl Pts',(196.935487317452,4.27452826130232,126.867340597462));
#188694=CARTESIAN_POINT('Ctrl Pts',(196.657039693639,-1.00183950872307,
125.080023442474));
#188695=CARTESIAN_POINT('Ctrl Pts',(196.378592069827,-5.35756571281285,
128.553092501978));
#188696=CARTESIAN_POINT('Ctrl Pts',(196.100144446013,-4.78995075846325,
134.094966979145));
#188697=CARTESIAN_POINT('Ctrl Pts',(195.821696822201,0.179394940810534,
136.612934965078));
#188698=CARTESIAN_POINT('Ctrl Pts',(195.543249198387,4.98388545340951,133.79310689028));
#188699=CARTESIAN_POINT('Ctrl Pts',(195.264801574575,5.20842871066526,128.22676699923));
#188700=CARTESIAN_POINT('Ctrl Pts',(194.986353950762,0.64668042870769,125.029109720981));
#188701=CARTESIAN_POINT('Ctrl Pts',(194.70790632695,-4.50933557513701,127.138625880003));
#188702=CARTESIAN_POINT('Ctrl Pts',(194.429458703136,-5.52149247872048,
132.616773181746));
#188703=CARTESIAN_POINT('Ctrl Pts',(194.151011079324,-1.4596675342632,136.429401878284));
#188704=CARTESIAN_POINT('Ctrl Pts',(193.87256345551,3.9435205654586,135.072892454764));
#188705=CARTESIAN_POINT('Ctrl Pts',(193.594115831698,5.72280591721378,129.793810802232));
#188706=CARTESIAN_POINT('Ctrl Pts',(193.315668207884,2.24311220566103,125.443375061888));
#188707=CARTESIAN_POINT('Ctrl Pts',(193.037220584072,-3.29789204077089,
126.019423148508));
#188708=CARTESIAN_POINT('Ctrl Pts',(192.758772960259,-5.80829461271728,
130.992595012001));
#188709=CARTESIAN_POINT('Ctrl Pts',(192.480325336446,-2.98115818654302,
135.792788662769));
#188710=CARTESIAN_POINT('Ctrl Pts',(192.201877712633,2.58551697539033,136.008860638253));
#188711=CARTESIAN_POINT('Ctrl Pts',(191.92343008882,5.77622834646622,131.442251348686));
#188712=CARTESIAN_POINT('Ctrl Pts',(191.644982465007,3.658868051582,126.289451639914));
#188713=CARTESIAN_POINT('Ctrl Pts',(191.366534841194,-1.82081323706467,
125.285632716038));
#188714=CARTESIAN_POINT('Ctrl Pts',(191.088087217381,-5.6272561125207,129.35325512882));
#188715=CARTESIAN_POINT('Ctrl Pts',(190.809639593569,-4.26252552731426,
134.754372595315));
#188716=CARTESIAN_POINT('Ctrl Pts',(190.531191969755,1.01925778154541,136.525622023071));
#188717=CARTESIAN_POINT('Ctrl Pts',(190.252744345943,5.36439298267566,133.039311718326));
#188718=CARTESIAN_POINT('Ctrl Pts',(189.974296722129,4.77991309789331,127.499190535413));
#188719=CARTESIAN_POINT('Ctrl Pts',(189.695849098317,-0.197073412116412,
124.996359191464));
#188720=CARTESIAN_POINT('Ctrl Pts',(189.417401474504,-4.99295908396257,
127.830797421458));
#188721=CARTESIAN_POINT('Ctrl Pts',(189.138953850692,-5.20055927725872,
133.397794962038));
#188722=CARTESIAN_POINT('Ctrl Pts',(188.860506226878,-0.629099556198964,
136.581553036358));
#188723=CARTESIAN_POINT('Ctrl Pts',(188.582058603065,4.52047192378579,134.456353509349));
#188724=CARTESIAN_POINT('Ctrl Pts',(188.303610979253,5.51595054314194,128.975150924561));
#188725=CARTESIAN_POINT('Ctrl Pts',(188.02516335544,1.44254008251539,125.174902685784));
#188726=CARTESIAN_POINT('Ctrl Pts',(187.746715731627,-3.95649424194195,
126.547851272005));
#188727=CARTESIAN_POINT('Ctrl Pts',(187.468268107814,-5.71970364354381,
131.832324004755));
#188728=CARTESIAN_POINT('Ctrl Pts',(187.189820484001,-2.22678481978599,
136.172148603481));
#188729=CARTESIAN_POINT('Ctrl Pts',(186.911372860188,3.312440468869,135.579238274173));
#188730=CARTESIAN_POINT('Ctrl Pts',(186.632925236375,5.80769478834652,130.598448644184));
#188731=CARTESIAN_POINT('Ctrl Pts',(186.354477612562,2.96596131899707,125.806882058373));
#188732=CARTESIAN_POINT('Ctrl Pts',(186.076029988749,-2.60134570724499,
125.607754128061));
#188733=CARTESIAN_POINT('Ctrl Pts',(185.797582364937,-5.7781431113317,130.184053693262));
#188734=CARTESIAN_POINT('Ctrl Pts',(185.519134741124,-3.64510927408837,
135.33038501822));
#188735=CARTESIAN_POINT('Ctrl Pts',(185.240687117311,1.83760191255446,136.317521027561));
#188736=CARTESIAN_POINT('Ctrl Pts',(184.962239493498,5.63164671340385,132.238331952975));
#188737=CARTESIAN_POINT('Ctrl Pts',(184.683791869685,4.25048330587202,126.841393274542));
#188738=CARTESIAN_POINT('Ctrl Pts',(184.405344245872,-1.03666661210287,
125.086227982629));
#188739=CARTESIAN_POINT('Ctrl Pts',(184.126896622059,-5.37117055753467,
128.585747235914));
#188740=CARTESIAN_POINT('Ctrl Pts',(183.848448998247,-4.7698311568614,134.124063801647));
#188741=CARTESIAN_POINT('Ctrl Pts',(183.570001374433,0.214750057761129,
136.611735317726));
#188742=CARTESIAN_POINT('Ctrl Pts',(183.291553750621,5.00198646042476,133.762713190383));
#188743=CARTESIAN_POINT('Ctrl Pts',(183.013106126807,5.19264166658148,128.195109572179));
#188744=CARTESIAN_POINT('Ctrl Pts',(182.734658502995,0.611512855797894,
125.025280195685));
#188745=CARTESIAN_POINT('Ctrl Pts',(182.456210879182,-4.53156639540017,
127.166143403126));
#188746=CARTESIAN_POINT('Ctrl Pts',(182.177763255369,-5.5103575085511,132.650350493844));
#188747=CARTESIAN_POINT('Ctrl Pts',(181.899315631556,-1.42539926727337,
136.438183069882));
#188748=CARTESIAN_POINT('Ctrl Pts',(181.620868007743,3.96943126600311,135.048808039769));
#188749=CARTESIAN_POINT('Ctrl Pts',(181.34242038393,5.71654838332065,129.758993181434));
#188750=CARTESIAN_POINT('Ctrl Pts',(181.063972760118,2.21043680528058,125.429819927867));
#188751=CARTESIAN_POINT('Ctrl Pts',(180.785525136304,-3.32695821097111,
126.039587007222));
#188752=CARTESIAN_POINT('Ctrl Pts',(180.507077512492,-5.80704116228462,
131.027948262352));
#188753=CARTESIAN_POINT('Ctrl Pts',(180.228629888679,-2.95073697519064,
135.810843394787));
#188754=CARTESIAN_POINT('Ctrl Pts',(179.950182264866,2.61715034058839,135.993025435236));
#188755=CARTESIAN_POINT('Ctrl Pts',(179.671734641053,5.78000434826875,131.407077988614));
#188756=CARTESIAN_POINT('Ctrl Pts',(179.39328701724,3.63131672880039,126.26726272238));
#188757=CARTESIAN_POINT('Ctrl Pts',(179.114839393428,-1.8543735647511,125.296818772266));
#188758=CARTESIAN_POINT('Ctrl Pts',(178.836391769614,-5.63598514348121,
129.387536719606));
#188759=CARTESIAN_POINT('Ctrl Pts',(178.557944145802,-4.23840170853308,
134.780246613475));
#188760=CARTESIAN_POINT('Ctrl Pts',(178.279496521988,1.05406583912245,136.519311509933));
#188761=CARTESIAN_POINT('Ctrl Pts',(178.001048898175,5.3778983746034,133.006615727177));
#188762=CARTESIAN_POINT('Ctrl Pts',(177.722601274363,4.75970502876524,127.470155084831));
#188763=CARTESIAN_POINT('Ctrl Pts',(177.44415365055,-0.232424713990654,
124.997666442073));
#188764=CARTESIAN_POINT('Ctrl Pts',(177.165706026737,-5.01096749916768,
127.861246073811));
#188765=CARTESIAN_POINT('Ctrl Pts',(176.887258402924,-5.18467595198119,
133.429404192122));
#188766=CARTESIAN_POINT('Ctrl Pts',(176.608810779111,-0.593920490425269,
136.585275505922));
#188767=CARTESIAN_POINT('Ctrl Pts',(176.330363155298,4.54261888720253,134.428768450716));
#188768=CARTESIAN_POINT('Ctrl Pts',(176.051915531486,5.50471342676105,128.941607659011));
#188769=CARTESIAN_POINT('Ctrl Pts',(175.773467907672,1.40824524732727,125.166225835676));
#188770=CARTESIAN_POINT('Ctrl Pts',(175.49502028386,-3.98233151779528,126.572014438702));
#188771=CARTESIAN_POINT('Ctrl Pts',(175.216572660047,-5.7133401657742,131.867122418498));
#188772=CARTESIAN_POINT('Ctrl Pts',(174.938125036234,-2.19406831359054,
136.185604222037));
#188773=CARTESIAN_POINT('Ctrl Pts',(174.659677412421,3.34144513258691,135.558986041432));
#188774=CARTESIAN_POINT('Ctrl Pts',(174.381229788608,5.80633374058666,130.563099372659));
#188775=CARTESIAN_POINT('Ctrl Pts',(174.102782164795,2.93548529615992,125.788920001687));
#188776=CARTESIAN_POINT('Ctrl Pts',(173.824334540982,-2.63293072900865,
125.623685538813));
#188777=CARTESIAN_POINT('Ctrl Pts',(173.54588691717,-5.7818120400351,130.219238383264));
#188778=CARTESIAN_POINT('Ctrl Pts',(173.267439293356,-3.61749054349026,
135.352489976228));
#188779=CARTESIAN_POINT('Ctrl Pts',(172.988991669544,1.87112803828436,136.306232877052));
#188780=CARTESIAN_POINT('Ctrl Pts',(172.71054404573,5.64027136256211,132.204023952811));
#188781=CARTESIAN_POINT('Ctrl Pts',(172.432096421918,4.22628084721974,126.815592800833));
#188782=CARTESIAN_POINT('Ctrl Pts',(172.153648798105,-1.07145530142008,
125.092644410292));
#188783=CARTESIAN_POINT('Ctrl Pts',(171.875201174292,-5.38457637155629,
128.618484181386));
#188784=CARTESIAN_POINT('Ctrl Pts',(171.596753550479,-4.74953480741189,
134.153037611328));
#188785=CARTESIAN_POINT('Ctrl Pts',(171.318305926666,0.25009721706947,136.610320475968));
#188786=CARTESIAN_POINT('Ctrl Pts',(171.039858302853,5.01990211699227,133.732209867644));
#188787=CARTESIAN_POINT('Ctrl Pts',(170.76141067904,5.1766622072511,128.163548831885));
#188788=CARTESIAN_POINT('Ctrl Pts',(170.482963055228,0.576322623054293,
125.021664816339));
#188789=CARTESIAN_POINT('Ctrl Pts',(170.204515431414,-4.55362929680409,
127.193795741725));
#188790=CARTESIAN_POINT('Ctrl Pts',(169.926067807602,-5.4990183500578,132.683859402108));
#188791=CARTESIAN_POINT('Ctrl Pts',(169.647620183788,-1.39107818158956,
136.446755498118));
#188792=CARTESIAN_POINT('Ctrl Pts',(169.369172559976,3.99519487781229,135.024566345214));
#188793=CARTESIAN_POINT('Ctrl Pts',(169.090724936163,5.71007902062496,129.724214297113));
#188794=CARTESIAN_POINT('Ctrl Pts',(168.81227731235,2.17767949635139,125.416463949427));
#188795=CARTESIAN_POINT('Ctrl Pts',(168.533829688537,-3.35590109951139,
126.059927426375));
#188796=CARTESIAN_POINT('Ctrl Pts',(168.255382064725,-5.80557252980615,
131.063293227581));
#188797=CARTESIAN_POINT('Ctrl Pts',(167.976934440911,-2.92020642319446,
135.828712609743));
#188798=CARTESIAN_POINT('Ctrl Pts',(167.698486817099,2.64868672631821,135.976997964335));
#188799=CARTESIAN_POINT('Ctrl Pts',(167.420039193286,5.78356616988455,131.371882294628));
#188800=CARTESIAN_POINT('Ctrl Pts',(167.141591569473,3.60363084624196,126.245241928676));
#188801=CARTESIAN_POINT('Ctrl Pts',(166.86314394566,-1.88786517794308,125.308208912483));
#188802=CARTESIAN_POINT('Ctrl Pts',(166.584696321847,-5.64450533093961,
129.421870811324));
#188803=CARTESIAN_POINT('Ctrl Pts',(166.306248698034,-4.21412083421794,
134.805973303719));
#188804=CARTESIAN_POINT('Ctrl Pts',(166.027801074221,1.08883483790225,136.512789227187));
#188805=CARTESIAN_POINT('Ctrl Pts',(165.749353450409,5.3912044865292,132.973838130654));
#188806=CARTESIAN_POINT('Ctrl Pts',(165.470905826595,4.73932058701693,127.441243184462));
#188807=CARTESIAN_POINT('Ctrl Pts',(165.192458202783,-0.267767403281747,
124.999188861871));
#188808=CARTESIAN_POINT('Ctrl Pts',(164.914010578969,-5.02879023112935,
127.891803784357));
#188809=CARTESIAN_POINT('Ctrl Pts',(164.635562955157,-5.16860050662956,
133.46091615025));
#188810=CARTESIAN_POINT('Ctrl Pts',(164.357115331344,-0.55871941670932,
136.588783761558));
#188811=CARTESIAN_POINT('Ctrl Pts',(164.078667707531,4.56459752220588,134.401049088318));
#188812=CARTESIAN_POINT('Ctrl Pts',(163.800220083718,5.49327233119978,128.908133418456));
#188813=CARTESIAN_POINT('Ctrl Pts',(163.521772459905,1.37389822909362,125.157757908727));
#188814=CARTESIAN_POINT('Ctrl Pts',(163.243324836092,-4.00802122688977,
126.596334436543));
#188815=CARTESIAN_POINT('Ctrl Pts',(162.964877212279,-5.70676497808368,
131.901881451211));
#188816=CARTESIAN_POINT('Ctrl Pts',(162.686429588467,-2.16127050538683,
136.198860436632));
#188817=CARTESIAN_POINT('Ctrl Pts',(162.407981964654,3.37032597782655,135.538557624299));
#188818=CARTESIAN_POINT('Ctrl Pts',(162.129534340841,5.80475753699479,130.527759041158));
#188819=CARTESIAN_POINT('Ctrl Pts',(161.851086717028,2.90490049783562,125.771143793998));
#188820=CARTESIAN_POINT('Ctrl Pts',(161.572639093215,-2.66441818655578,
125.639808921385));
#188821=CARTESIAN_POINT('Ctrl Pts',(161.294191469402,-5.7852667215671,130.254444755185));
#188822=CARTESIAN_POINT('Ctrl Pts',(161.015743845589,-3.58973776544978,
135.37442640163));
#188823=CARTESIAN_POINT('Ctrl Pts',(160.737296221776,1.90458482867669,136.294740852644));
#188824=CARTESIAN_POINT('Ctrl Pts',(160.458848597964,5.64868700939082,132.169664087608));
#188825=CARTESIAN_POINT('Ctrl Pts',(160.18040097415,4.20192178217643,126.789940132385));
#188826=CARTESIAN_POINT('Ctrl Pts',(159.901953350338,-1.10620428756715,
125.099272487699));
#188827=CARTESIAN_POINT('Ctrl Pts',(159.623505726525,-5.39778265812024,
128.651302125312));
#188828=CARTESIAN_POINT('Ctrl Pts',(159.345058102712,-4.72906246220349,
134.18188733455));
#188829=CARTESIAN_POINT('Ctrl Pts',(159.066610478899,0.285435108933367,
136.608690492233));
#188830=CARTESIAN_POINT('Ctrl Pts',(158.788162855086,5.03763175924073,133.701598052375));
#188831=CARTESIAN_POINT('Ctrl Pts',(158.509715231273,5.16049092479898,128.132085947844));
#188832=CARTESIAN_POINT('Ctrl Pts',(158.23126760746,0.541111034464008,125.018263716911));
#188833=CARTESIAN_POINT('Ctrl Pts',(157.952819983648,-4.57552346179978,
127.221581871133));
#188834=CARTESIAN_POINT('Ctrl Pts',(157.674372359834,-5.48747542341729,
132.717298664853));
#188835=CARTESIAN_POINT('Ctrl Pts',(157.395924736022,-1.35670554899215,
136.455118845335));
#188836=CARTESIAN_POINT('Ctrl Pts',(157.117477112209,4.02081044620608,135.000168269382));
#188837=CARTESIAN_POINT('Ctrl Pts',(156.839029488396,5.70339806885126,129.68947543801));
#188838=CARTESIAN_POINT('Ctrl Pts',(156.560581864583,2.1448414927076,125.403307621479));
#188839=CARTESIAN_POINT('Ctrl Pts',(156.28213424077,-3.38471963390224,126.080443652244));
#188840=CARTESIAN_POINT('Ctrl Pts',(156.003686616957,-5.8038887697026,131.098628597966));
#188841=CARTESIAN_POINT('Ctrl Pts',(155.725238993144,-2.88956766187541,
135.846395645489));
#188842=CARTESIAN_POINT('Ctrl Pts',(155.446791369331,2.68012496398725,135.960778819456));
#188843=CARTESIAN_POINT('Ctrl Pts',(155.168343745519,5.78691367932904,131.336665570917));
#188844=CARTESIAN_POINT('Ctrl Pts',(154.889896121706,3.57581142981733,126.223390074792));
#188845=CARTESIAN_POINT('Ctrl Pts',(154.611448497893,-1.92128683559663,
125.319802714623));
#188846=CARTESIAN_POINT('Ctrl Pts',(154.33300087408,-5.65281635917722,129.456256131708));
#188847=CARTESIAN_POINT('Ctrl Pts',(154.054553250267,-4.18968380410554,
134.831551712731));
#188848=CARTESIAN_POINT('Ctrl Pts',(153.776105626454,1.12356348950664,136.50605541652));
#188849=CARTESIAN_POINT('Ctrl Pts',(153.497658002641,5.40431082539012,132.940980143345));
#188850=CARTESIAN_POINT('Ctrl Pts',(153.219210378828,4.71876052800142,127.412455905645));
#188851=CARTESIAN_POINT('Ctrl Pts',(152.940762755016,-0.303100170353132,
125.000926394444));
#188852=CARTESIAN_POINT('Ctrl Pts',(152.662315131202,-5.04642661941966,
127.922469420767));
#188853=CARTESIAN_POINT('Ctrl Pts',(152.38386750739,-5.15233353688545,133.492329668737));
#188854=CARTESIAN_POINT('Ctrl Pts',(152.105419883576,-0.523497639439988,
136.592077673268));
#188855=CARTESIAN_POINT('Ctrl Pts',(151.826972259764,4.58640701436939,134.373196449306));
#188856=CARTESIAN_POINT('Ctrl Pts',(151.548524635951,5.48162768041213,128.874729443297));
#188857=CARTESIAN_POINT('Ctrl Pts',(151.270077012138,1.33950030055583,125.149499218718));
#188858=CARTESIAN_POINT('Ctrl Pts',(150.991629388325,-4.03356241728369,
126.620810364342));
#188859=CARTESIAN_POINT('Ctrl Pts',(150.713181764512,-5.69997832411825,
131.936599814887));
#188860=CARTESIAN_POINT('Ctrl Pts',(150.434734140699,-2.1283926105098,136.211916756054));
#188861=CARTESIAN_POINT('Ctrl Pts',(150.156286516886,3.39908193439765,135.517953779753));
#188862=CARTESIAN_POINT('Ctrl Pts',(149.877838893074,5.8029662359777,130.49242895923));
#188863=CARTESIAN_POINT('Ctrl Pts',(149.599391269261,2.87420805735513,125.753554094008));
#188864=CARTESIAN_POINT('Ctrl Pts',(149.320943645448,-2.69580691310719,
125.65612367832));
#188865=CARTESIAN_POINT('Ctrl Pts',(149.042496021635,-5.7885070279132,130.289671504441));
#188866=CARTESIAN_POINT('Ctrl Pts',(148.764048397822,-3.56185196835627,
135.396193481562));
#188867=CARTESIAN_POINT('Ctrl Pts',(148.485600774009,1.93797104397778,136.283045380177));
#188868=CARTESIAN_POINT('Ctrl Pts',(148.207153150196,5.6568933420451,132.135253630582));
#188869=CARTESIAN_POINT('Ctrl Pts',(147.928705526383,4.17740701337624,126.764436219762));
#188870=CARTESIAN_POINT('Ctrl Pts',(147.65025790257,-1.14091228290746,125.106111969245));
#188871=CARTESIAN_POINT('Ctrl Pts',(147.371810278758,-5.41078892786276,
128.684199851613));
#188872=CARTESIAN_POINT('Ctrl Pts',(147.093362654945,-4.70841487984645,
134.210611902278));
#188873=CARTESIAN_POINT('Ctrl Pts',(146.814915031132,0.320762423894332,
136.60684542692));
#188874=CARTESIAN_POINT('Ctrl Pts',(146.536467407319,5.05517473019176,133.670878878906));
#188875=CARTESIAN_POINT('Ctrl Pts',(146.258019783506,5.14412841845787,128.100722085923));
#188876=CARTESIAN_POINT('Ctrl Pts',(145.979572159693,0.505879394805349,
125.015077023433));
#188877=CARTESIAN_POINT('Ctrl Pts',(145.70112453588,-4.59724807909095,127.249500761725));
#188878=CARTESIAN_POINT('Ctrl Pts',(145.422676912067,-5.47572915635697,
132.750667042976));
#188879=CARTESIAN_POINT('Ctrl Pts',(145.144229288255,-1.32228264317164,
136.463272801628));
#188880=CARTESIAN_POINT('Ctrl Pts',(144.865781664442,4.0462770219901,134.975614716357));
#188881=CARTESIAN_POINT('Ctrl Pts',(144.587334040629,5.69650577556471,129.654777891387));
#188882=CARTESIAN_POINT('Ctrl Pts',(144.308886416816,2.11192401117359,125.390351431538));
#188883=CARTESIAN_POINT('Ctrl Pts',(144.030438793003,-3.41341274626234,
126.101134924595));
#188884=CARTESIAN_POINT('Ctrl Pts',(143.75199116919,-5.80198994436631,131.133953064144));
#188885=CARTESIAN_POINT('Ctrl Pts',(143.473543545377,-2.85882182656403,
135.863891846773));
#188886=CARTESIAN_POINT('Ctrl Pts',(143.195095921564,2.71146388864014,135.944368601604));
#188887=CARTESIAN_POINT('Ctrl Pts',(142.916648297751,5.790046752559,131.301429122451));
#188888=CARTESIAN_POINT('Ctrl Pts',(142.638200673938,3.54785951038517,126.201707970457));
#188889=CARTESIAN_POINT('Ctrl Pts',(142.359753050125,-1.95463729925998,
125.331599749072));
#188890=CARTESIAN_POINT('Ctrl Pts',(142.081305426313,-5.66091792022584,
129.490691406602));
#188891=CARTESIAN_POINT('Ctrl Pts',(141.8028578025,-4.16509152371897,134.856980892698));
#188892=CARTESIAN_POINT('Ctrl Pts',(141.524410178687,1.15825050705268,136.499110327454));
#188893=CARTESIAN_POINT('Ctrl Pts',(141.245962554874,5.41721690552589,132.908042982814));
#188894=CARTESIAN_POINT('Ctrl Pts',(140.967514931061,4.69802561357932,127.383794315106));
#188895=CARTESIAN_POINT('Ctrl Pts',(140.689067307248,-0.338421705936203,
125.002878975406));
#188896=CARTESIAN_POINT('Ctrl Pts',(140.410619683435,-5.06387601051571,
127.953241846716));
#188897=CARTESIAN_POINT('Ctrl Pts',(140.132172059623,-5.13587564552739,
133.523643583541));
#188898=CARTESIAN_POINT('Ctrl Pts',(139.85372443581,-0.48825646377323,136.595157118993));
#188899=CARTESIAN_POINT('Ctrl Pts',(139.575276811997,4.60804655553434,134.34521156577));
#188900=CARTESIAN_POINT('Ctrl Pts',(139.296829188184,5.46977990589493,128.841396971331));
#188901=CARTESIAN_POINT('Ctrl Pts',(139.018381564371,1.30505273634171,125.141450071677));
#188902=CARTESIAN_POINT('Ctrl Pts',(138.739933940558,-4.05895414253892,
126.645441315135));
#188903=CARTESIAN_POINT('Ctrl Pts',(138.461486316745,-5.69298045535984,
131.971276223022));
#188904=CARTESIAN_POINT('Ctrl Pts',(138.183038692932,-2.09543584726193,
136.224772696493));
#188905=CARTESIAN_POINT('Ctrl Pts',(137.904591069119,3.42771193673771,135.49717527128));
#188906=CARTESIAN_POINT('Ctrl Pts',(137.626143445306,5.80095990391266,130.457110436044));
#188907=CARTESIAN_POINT('Ctrl Pts',(137.347695821494,2.84340911203807,125.736151553513));
#188908=CARTESIAN_POINT('Ctrl Pts',(137.069248197681,-2.727095745542,125.672629205068));
#188909=CARTESIAN_POINT('Ctrl Pts',(136.790800573868,-5.7915328390027,130.324917325691));
#188910=CARTESIAN_POINT('Ctrl Pts',(136.512352950055,-3.53383418552815,
135.417790409441));
#188911=CARTESIAN_POINT('Ctrl Pts',(136.233905326242,1.97128544704926,136.271146893031));
#188912=CARTESIAN_POINT('Ctrl Pts',(135.955457702429,5.66489005643625,132.100793856825));
#188913=CARTESIAN_POINT('Ctrl Pts',(135.677010078616,4.15273744922295,126.739082008025));
#188914=CARTESIAN_POINT('Ctrl Pts',(135.398562454803,-1.17557800132362,
125.113162601491));
#188915=CARTESIAN_POINT('Ctrl Pts',(135.12011483099,-5.42359469883174,128.717176141249));
#188916=CARTESIAN_POINT('Ctrl Pts',(134.841667207177,-4.68759282544451,
134.239210250113));
#188917=CARTESIAN_POINT('Ctrl Pts',(134.563219583365,0.356077852885664,
136.604785348398));
#188918=CARTESIAN_POINT('Ctrl Pts',(134.284771959552,5.0725303797842,133.640053485549));
#188919=CARTESIAN_POINT('Ctrl Pts',(134.006324335739,5.12757529454644,128.069458408322));
#188920=CARTESIAN_POINT('Ctrl Pts',(133.727876711926,0.470629009599695,
125.012104853988));
#188921=CARTESIAN_POINT('Ctrl Pts',(133.449429088113,-4.61880234366392,
127.277551378957));
#188922=CARTESIAN_POINT('Ctrl Pts',(133.1709814643,-5.46377998413907,132.783963299997));
#188923=CARTESIAN_POINT('Ctrl Pts',(132.892533840487,-1.28781073968153,
136.47121706485));
#188924=CARTESIAN_POINT('Ctrl Pts',(132.614086216674,4.07159366149105,134.950906595976));
#188925=CARTESIAN_POINT('Ctrl Pts',(132.335638592862,5.68940239616175,129.620122942976));
#188926=CARTESIAN_POINT('Ctrl Pts',(132.057190969048,2.07892827151876,125.377595859696));
#188927=CARTESIAN_POINT('Ctrl Pts',(131.778743345236,-3.44197937335791,
126.122000476702));
#188928=CARTESIAN_POINT('Ctrl Pts',(131.500295721423,-5.79987612415893,
131.169265317152));
#188929=CARTESIAN_POINT('Ctrl Pts',(131.22184809761,-2.82797005655853,135.881200565267));
#188930=CARTESIAN_POINT('Ctrl Pts',(130.943400473797,2.74270233900145,135.927767918864));
#188931=CARTESIAN_POINT('Ctrl Pts',(130.664952849984,5.79296527347731,131.26617425493));
#188932=CARTESIAN_POINT('Ctrl Pts',(130.386505226171,3.51977612371406,126.180196419108));
#188933=CARTESIAN_POINT('Ctrl Pts',(130.108057602358,-1.98791533311939,
125.343599578688));
#188934=CARTESIAN_POINT('Ctrl Pts',(129.829609978546,-5.66880971387908,
129.52517535999));
#188935=CARTESIAN_POINT('Ctrl Pts',(129.551162354732,-4.14034490433441,
134.882259901329));
#188936=CARTESIAN_POINT('Ctrl Pts',(129.27271473092,1.19289460520041,136.491954217345));
#188937=CARTESIAN_POINT('Ctrl Pts',(128.994267107107,5.42992224869717,132.875027869557));
#188938=CARTESIAN_POINT('Ctrl Pts',(128.715819483294,4.67711661209022,127.355259474909));
#188939=CARTESIAN_POINT('Ctrl Pts',(128.437371859481,-0.373730701178542,
125.005046532403));
#188940=CARTESIAN_POINT('Ctrl Pts',(128.158924235668,-5.0811377578241,127.984119921918));
#188941=CARTESIAN_POINT('Ctrl Pts',(127.880476611855,-5.11922744240848,
133.554856734316));
#188942=CARTESIAN_POINT('Ctrl Pts',(127.602028988042,-0.452997195583419,
136.598021984625));
#188943=CARTESIAN_POINT('Ctrl Pts',(127.323581364229,4.62951534383955,134.3170954747));
#188944=CARTESIAN_POINT('Ctrl Pts',(127.045133740417,5.45772944667181,128.808137237705));
#188945=CARTESIAN_POINT('Ctrl Pts',(126.766686116604,1.2705568129186,125.133610765869));
#188946=CARTESIAN_POINT('Ctrl Pts',(126.488238492791,-4.08419546175569,
126.67022637621));
#188947=CARTESIAN_POINT('Ctrl Pts',(126.209790868978,-5.68577163111709,
132.005909390672));
#188948=CARTESIAN_POINT('Ctrl Pts',(125.931343245165,-2.06240143686808,
136.237427781569));
#188949=CARTESIAN_POINT('Ctrl Pts',(125.652895621352,3.45621492395137,135.476222868834));
#188950=CARTESIAN_POINT('Ctrl Pts',(125.374447997539,5.79873861514512,130.421804780342));
#188951=CARTESIAN_POINT('Ctrl Pts',(125.096000373726,2.8125048031507,125.718936817367));
#188952=CARTESIAN_POINT('Ctrl Pts',(124.817552749914,-2.75828352444112,
125.68932489001));
#188953=CARTESIAN_POINT('Ctrl Pts',(124.5391051261,-5.79434404271298,130.36018091289));
#188954=CARTESIAN_POINT('Ctrl Pts',(124.260657502288,-3.50568545517477,
135.439216384981));
#188955=CARTESIAN_POINT('Ctrl Pts',(123.982209878475,2.00452680341345,136.25904583211));
#188956=CARTESIAN_POINT('Ctrl Pts',(123.703762254662,5.67267685624313,132.066286043259));
#188957=CARTESIAN_POINT('Ctrl Pts',(123.425314630849,4.12791400385628,126.71387843668));
#188958=CARTESIAN_POINT('Ctrl Pts',(123.146867007036,-1.21020015826455,
125.120424123171));
#188959=CARTESIAN_POINT('Ctrl Pts',(122.868419383223,-5.43619949650465,
128.750229772276));
#188960=CARTESIAN_POINT('Ctrl Pts',(122.58997175941,-4.66659707056658,134.267681318331));
#188961=CARTESIAN_POINT('Ctrl Pts',(122.311524135597,0.391380087281262,
136.602510333005));
#188962=CARTESIAN_POINT('Ctrl Pts',(122.033076511785,5.08969806489794,133.609123014551));
#188963=CARTESIAN_POINT('Ctrl Pts',(121.754628887972,5.11083216644683,128.038296073528));
#188964=CARTESIAN_POINT('Ctrl Pts',(121.476181264159,0.435361185062875,
125.00934731871));
#188965=CARTESIAN_POINT('Ctrl Pts',(121.197733640346,-4.64018545681751,
127.305732683402));
#188966=CARTESIAN_POINT('Ctrl Pts',(120.919286016533,-5.45162834954452,
132.817186202114));
#188967=CARTESIAN_POINT('Ctrl Pts',(120.64083839272,-1.25329111589093,136.478951340622));
#188968=CARTESIAN_POINT('Ctrl Pts',(120.362390768907,4.09675942659154,134.92604482381));
#188969=CARTESIAN_POINT('Ctrl Pts',(120.083943145094,5.68208819386074,129.585511876926));
#188970=CARTESIAN_POINT('Ctrl Pts',(119.805495521281,2.04585549641223,125.36504137862));
#188971=CARTESIAN_POINT('Ctrl Pts',(119.527047897469,-3.47041845664194,
126.143039535386));
#188972=CARTESIAN_POINT('Ctrl Pts',(119.248600273655,-5.79754738740892,
131.204564048482));
#188973=CARTESIAN_POINT('Ctrl Pts',(118.970152649843,-2.7970134950826,135.898321159589));
#188974=CARTESIAN_POINT('Ctrl Pts',(118.69170502603,2.77383915751901,135.910977386384));
#188975=CARTESIAN_POINT('Ctrl Pts',(118.413257402217,5.795669133937,131.230902274733));
#188976=CARTESIAN_POINT('Ctrl Pts',(118.134809778404,3.49156231044436,126.158856217863));
#188977=CARTESIAN_POINT('Ctrl Pts',(117.856362154591,-2.02111970404504,
125.355801758813));
#188978=CARTESIAN_POINT('Ctrl Pts',(117.577914530778,-5.67649144770371,
129.559706714059));
#188979=CARTESIAN_POINT('Ctrl Pts',(117.299466906965,-4.11544486294674,
134.907387801903));
#188980=CARTESIAN_POINT('Ctrl Pts',(117.021019283153,1.22749450019975,136.484587351363));
#188981=CARTESIAN_POINT('Ctrl Pts',(116.74257165934,5.44242638410263,132.841936026965));
#188982=CARTESIAN_POINT('Ctrl Pts',(116.464124035527,4.65603429832517,127.326852442422));
#188983=CARTESIAN_POINT('Ctrl Pts',(116.185676411714,-0.409025847692317,
125.007428985116));
#188984=CARTESIAN_POINT('Ctrl Pts',(115.907228787901,-5.09821122170419,
128.015102502178));
#188985=CARTESIAN_POINT('Ctrl Pts',(115.628781164088,-5.10238954443416,
133.585967964446));
#188986=CARTESIAN_POINT('Ctrl Pts',(115.350333540275,-0.417721141415912,
136.600672164005));
#188987=CARTESIAN_POINT('Ctrl Pts',(115.071885916462,4.65081258375125,134.288849217947));
#188988=CARTESIAN_POINT('Ctrl Pts',(114.793438292649,5.44547674927697,128.77495147487));
#188989=CARTESIAN_POINT('Ctrl Pts',(114.514990668836,1.23601380854556,125.125981591782));
#188990=CARTESIAN_POINT('Ctrl Pts',(114.236543045024,-4.10928543960769,
126.695164629152));
#188991=CARTESIAN_POINT('Ctrl Pts',(113.958095421211,-5.67835211851559,
132.040498034489));
#188992=CARTESIAN_POINT('Ctrl Pts',(113.679647797398,-2.02929060343055,
136.249881542344));
#188993=CARTESIAN_POINT('Ctrl Pts',(113.401200173585,3.48458983985001,135.455097348814));
#188994=CARTESIAN_POINT('Ctrl Pts',(113.122752549772,5.79630245198571,130.386513300387));
#188995=CARTESIAN_POINT('Ctrl Pts',(112.844304925959,2.78149627586357,125.701910523471));
#188996=CARTESIAN_POINT('Ctrl Pts',(112.565857302146,-2.78936909412988,
125.706210114483));
#188997=CARTESIAN_POINT('Ctrl Pts',(112.287409678333,-5.7969405348739,130.395460959329));
#188998=CARTESIAN_POINT('Ctrl Pts',(112.008962054521,-3.47740682035766,
135.460470614237));
#188999=CARTESIAN_POINT('Ctrl Pts',(111.730514430707,2.03769388129978,136.246742645822));
#189000=CARTESIAN_POINT('Ctrl Pts',(111.452066806895,5.68025345292297,132.031731468582));
#189001=CARTESIAN_POINT('Ctrl Pts',(111.173619183082,4.10293759711819,126.688826439658));
#189002=CARTESIAN_POINT('Ctrl Pts',(110.895171559269,-1.24477747079359,
125.127896265209));
#189003=CARTESIAN_POINT('Ctrl Pts',(110.616723935456,-5.44860285380605,
128.783359519875));
#189004=CARTESIAN_POINT('Ctrl Pts',(110.338276311643,-4.64542839321807,
134.296024051927));
#189005=CARTESIAN_POINT('Ctrl Pts',(110.05982868783,0.426667818943798,136.600020465042));
#189006=CARTESIAN_POINT('Ctrl Pts',(109.781381064017,5.10667714937814,133.57808861205));
#189007=CARTESIAN_POINT('Ctrl Pts',(109.502933440204,5.0938996545818,128.007236236273));
#189008=CARTESIAN_POINT('Ctrl Pts',(109.224485816392,0.400077228057368,
125.006804519781));
#189009=CARTESIAN_POINT('Ctrl Pts',(108.946038192578,-4.66139662619255,
127.334043630792));
#189010=CARTESIAN_POINT('Ctrl Pts',(108.667590568766,-5.43927470285667,
132.850334518237));
#189011=CARTESIAN_POINT('Ctrl Pts',(108.389142944953,-1.21872505093712,
136.486475342347));
#189012=CARTESIAN_POINT('Ctrl Pts',(108.11069532114,4.1217733847649,134.901030321119));
#189013=CARTESIAN_POINT('Ctrl Pts',(107.832247697327,5.67456343969215,129.550945975765));
#189014=CARTESIAN_POINT('Ctrl Pts',(107.553800073514,2.01270691137792,125.352688453517));
#189015=CARTESIAN_POINT('Ctrl Pts',(107.275352449701,-3.49872894229381,
126.164251321038));
#189016=CARTESIAN_POINT('Ctrl Pts',(106.996904825888,-5.7950038204084,131.239847950126));
#189017=CARTESIAN_POINT('Ctrl Pts',(106.718457202076,-2.76595328924301,
135.91525299533));
#189018=CARTESIAN_POINT('Ctrl Pts',(106.440009578262,2.80487319040651,135.893997626342));
#189019=CARTESIAN_POINT('Ctrl Pts',(106.16156195445,5.7981582337456,131.195614488879));
#189020=CARTESIAN_POINT('Ctrl Pts',(105.883114330637,3.46321911604922,126.137688157493));
#189021=CARTESIAN_POINT('Ctrl Pts',(105.604666706824,-2.05424918163679,
125.36820583729));
#189022=CARTESIAN_POINT('Ctrl Pts',(105.326219083011,-5.68396283705021,
129.594284189235));
#189023=CARTESIAN_POINT('Ctrl Pts',(105.047771459198,-4.09039232223623,
134.932363663296));
#189024=CARTESIAN_POINT('Ctrl Pts',(104.769323835385,1.26204890993897,136.47701000249));
#189025=CARTESIAN_POINT('Ctrl Pts',(104.490876211572,5.45472884839698,132.808768681268));
#189026=CARTESIAN_POINT('Ctrl Pts',(104.21242858776,4.63477945349693,127.29857427028));
#189027=CARTESIAN_POINT('Ctrl Pts',(103.933980963947,-0.444305837602887,
125.010026245263));
#189028=CARTESIAN_POINT('Ctrl Pts',(103.655533340134,-5.1150957694926,128.046188439421));
#189029=CARTESIAN_POINT('Ctrl Pts',(103.377085716321,-5.08536257553889,
133.616976121092));
#189030=CARTESIAN_POINT('Ctrl Pts',(103.098638092508,-0.38242960843803,
136.603107558928));
#189031=CARTESIAN_POINT('Ctrl Pts',(102.820190468695,4.6719374860923,134.260473842188));
#189032=CARTESIAN_POINT('Ctrl Pts',(102.541742844882,5.4330222677386,128.741840912539));
#189033=CARTESIAN_POINT('Ctrl Pts',(102.263295221069,1.2014250032263,125.118562832119));
#189034=CARTESIAN_POINT('Ctrl Pts',(101.984847597256,-4.13422314637653,
126.720255149861));
#189035=CARTESIAN_POINT('Ctrl Pts',(101.706399973443,-5.67072219248816,
132.07504087278));
#189036=CARTESIAN_POINT('Ctrl Pts',(101.427952349631,-1.99610457388343,
136.262133517338));
#189037=CARTESIAN_POINT('Ctrl Pts',(101.149504725818,3.51283563299066,135.433799494034));
#189038=CARTESIAN_POINT('Ctrl Pts',(100.871057102005,5.7936515047074,130.351237303918));
#189039=CARTESIAN_POINT('Ctrl Pts',(100.592609478192,2.75038467920892,125.685073302739));
#189040=CARTESIAN_POINT('Ctrl Pts',(100.314161854379,-2.82035130272114,
125.723284252797));
#189041=CARTESIAN_POINT('Ctrl Pts',(100.035714230566,-5.79932221927147,
130.430756157697));
#189042=CARTESIAN_POINT('Ctrl Pts',(99.7572666067534,-3.44899932895201,
135.481552309624));
#189043=CARTESIAN_POINT('Ctrl Pts',(99.4788189829407,2.07078545168999,136.234237790066));
#189044=CARTESIAN_POINT('Ctrl Pts',(99.2003713591278,5.6876195657222,131.997131413226));
#189045=CARTESIAN_POINT('Ctrl Pts',(98.9219237353147,4.07780915451857,126.663926945268));
#189046=CARTESIAN_POINT('Ctrl Pts',(98.6434761115021,-1.27930865763567,
125.13557875072));
#189047=CARTESIAN_POINT('Ctrl Pts',(98.3650284876889,-5.460804311125,128.816564156414));
#189048=CARTESIAN_POINT('Ctrl Pts',(98.0865808638763,-4.62408757781209,
134.324237400649));
#189049=CARTESIAN_POINT('Ctrl Pts',(97.8081332400632,0.461939740273397,
136.597315836771));
#189050=CARTESIAN_POINT('Ctrl Pts',(97.5296856162504,5.12346700405862,133.546951428038));
#189051=CARTESIAN_POINT('Ctrl Pts',(97.2512379924375,5.07677838639178,127.97628004749));
#189052=CARTESIAN_POINT('Ctrl Pts',(96.9727903686245,0.364778446043045,
125.004476551425));
#189053=CARTESIAN_POINT('Ctrl Pts',(96.6943427448119,-4.68243506580139,
127.362483172053));
#189054=CARTESIAN_POINT('Ctrl Pts',(96.4158951209985,-5.42671950184442,
132.883407020047));
#189055=CARTESIAN_POINT('Ctrl Pts',(96.1374474971861,-1.18411382567837,
136.493788791223));
#189056=CARTESIAN_POINT('Ctrl Pts',(95.8589998733729,4.14663460910971,134.875864014826));
#189057=CARTESIAN_POINT('Ctrl Pts',(95.5805522495601,5.66682841248846,129.516426520346));
#189058=CARTESIAN_POINT('Ctrl Pts',(95.3021046257473,1.97948374474885,125.340537542131));
#189059=CARTESIAN_POINT('Ctrl Pts',(95.0236570019342,-3.52690978125809,
126.185635047646));
#189060=CARTESIAN_POINT('Ctrl Pts',(94.7452093781216,-5.79224551741027,
131.275115714627));
#189061=CARTESIAN_POINT('Ctrl Pts',(94.4667617543085,-2.73479058998699,
135.931995445075));
#189062=CARTESIAN_POINT('Ctrl Pts',(94.1883141304955,2.8358032876865,135.876829267928));
#189063=CARTESIAN_POINT('Ctrl Pts',(93.909866506683,5.80043248066857,131.160312204968));
#189064=CARTESIAN_POINT('Ctrl Pts',(93.6314188828698,3.43474759079615,126.116693022386));
#189065=CARTESIAN_POINT('Ctrl Pts',(93.352971259057,-2.08730253826965,125.380811354481));
#189066=CARTESIAN_POINT('Ctrl Pts',(93.0745236352441,-5.69122360506351,
129.628906504239));
#189067=CARTESIAN_POINT('Ctrl Pts',(92.7960760114314,-4.06518821053398,
134.957186560018));
#189068=CARTESIAN_POINT('Ctrl Pts',(92.5176283876181,1.29655655399172,136.469222451509));
#189069=CARTESIAN_POINT('Ctrl Pts',(92.2391807638055,5.46682918570788,132.775527061492));
#189070=CARTESIAN_POINT('Ctrl Pts',(91.9607331399925,4.61335286521161,127.270426006341));
#189071=CARTESIAN_POINT('Ctrl Pts',(91.6822855161797,-0.479569363597252,
125.012838216602));
#189072=CARTESIAN_POINT('Ctrl Pts',(91.4038378923669,-5.13179077552621,
128.077376581749));
#189073=CARTESIAN_POINT('Ctrl Pts',(91.1253902685539,-5.06814716666323,
133.647880055237));
#189074=CARTESIAN_POINT('Ctrl Pts',(90.846942644741,-0.347123904390365,
136.605328079151));
#189075=CARTESIAN_POINT('Ctrl Pts',(90.5684950209282,4.69288926807169,134.231970398883));
#189076=CARTESIAN_POINT('Ctrl Pts',(90.2900473971151,5.42036646356212,128.708806777632));
#189077=CARTESIAN_POINT('Ctrl Pts',(90.0115997733025,1.16679167866171,125.111354761782));
#189078=CARTESIAN_POINT('Ctrl Pts',(89.7331521494893,-4.15900765798632,
126.7454970086));
#189079=CARTESIAN_POINT('Ctrl Pts',(89.4547045256766,-5.66288213576447,
132.109536625546));
#189080=CARTESIAN_POINT('Ctrl Pts',(89.1762569018636,-1.96284457794726,
136.274183252551));
#189081=CARTESIAN_POINT('Ctrl Pts',(88.8978092780507,3.5409512567151,135.412330093694));
#189082=CARTESIAN_POINT('Ctrl Pts',(88.619361654238,5.79078587154194,130.3159780981));
#189083=CARTESIAN_POINT('Ctrl Pts',(88.3409140304249,2.71917116603865,125.668425779081));
#189084=CARTESIAN_POINT('Ctrl Pts',(88.0624664066122,-2.85122900215762,
125.740546672265));
#189085=CARTESIAN_POINT('Ctrl Pts',(87.7840187827991,-5.80148900765152,
130.466065200115));
#189086=CARTESIAN_POINT('Ctrl Pts',(87.5055711589863,-3.42046403360785,
135.502460689953));
#189087=CARTESIAN_POINT('Ctrl Pts',(87.2271235351733,2.10380028836375,136.221531728214));
#189088=CARTESIAN_POINT('Ctrl Pts',(86.9486759113605,5.69477492168681,131.962487159311));
#189089=CARTESIAN_POINT('Ctrl Pts',(86.6702282875477,4.05252960720113,126.63918087617));
#189090=CARTESIAN_POINT('Ctrl Pts',(86.3917806637346,-1.31379243922498,
125.14347129503));
#189091=CARTESIAN_POINT('Ctrl Pts',(86.113333039922,-5.47280341633199,128.849842451481));
#189092=CARTESIAN_POINT('Ctrl Pts',(85.8348854161089,-4.6025754151404,134.352320319043));
#189093=CARTESIAN_POINT('Ctrl Pts',(85.5564377922961,0.497194544256039,
136.594396548415));
#189094=CARTESIAN_POINT('Ctrl Pts',(85.2779901684829,5.1400670067851,133.515712616316));
#189095=CARTESIAN_POINT('Ctrl Pts',(84.9995425446705,5.05946899631168,127.945428654274));
#189096=CARTESIAN_POINT('Ctrl Pts',(84.7210949208572,0.329466147029263,
125.002363499906));
#189097=CARTESIAN_POINT('Ctrl Pts',(84.4426472970446,-4.70329999605691,
127.391050253351));
#189098=CARTESIAN_POINT('Ctrl Pts',(84.1641996732315,-5.41396321174535,
132.916402482027));
#189099=CARTESIAN_POINT('Ctrl Pts',(83.8857520494189,-1.14945872264635,
136.500891416245));
#189100=CARTESIAN_POINT('Ctrl Pts',(83.6073044256056,4.17134217838416,134.850546837477));
#189101=CARTESIAN_POINT('Ctrl Pts',(83.328856801793,5.65888339887398,129.481954789796));
#189102=CARTESIAN_POINT('Ctrl Pts',(83.05040917798,1.94618722762166,125.328589094719));
#189103=CARTESIAN_POINT('Ctrl Pts',(82.7719615541671,-3.5549599292834,126.207189922827));
#189104=CARTESIAN_POINT('Ctrl Pts',(82.4935139303543,-5.78927258062435,
131.310366035126));
#189105=CARTESIAN_POINT('Ctrl Pts',(82.2150663065413,-2.70352655206008,
135.948547888425));
#189106=CARTESIAN_POINT('Ctrl Pts',(81.9366186827285,2.86662830323276,135.859472947324));
#189107=CARTESIAN_POINT('Ctrl Pts',(81.6581710589156,5.80249179043285,131.124996731141));
#189108=CARTESIAN_POINT('Ctrl Pts',(81.3797234351026,3.40614878970799,126.095871590527));
#189109=CARTESIAN_POINT('Ctrl Pts',(81.1012758112897,-2.12027854913937,
125.393617843285));
#189110=CARTESIAN_POINT('Ctrl Pts',(80.822828187477,-5.6982734826932,129.663572376127));
#189111=CARTESIAN_POINT('Ctrl Pts',(80.5443805636639,-4.03983346178761,
134.981855572247));
#189112=CARTESIAN_POINT('Ctrl Pts',(80.2659329398512,1.33101615366455,136.461224986989));
#189113=CARTESIAN_POINT('Ctrl Pts',(79.9874853160382,5.47872694765296,132.742212399419));
#189114=CARTESIAN_POINT('Ctrl Pts',(79.7090376922254,4.59175532743923,127.242408693648));
#189115=CARTESIAN_POINT('Ctrl Pts',(79.4305900684125,-0.514815118972584,
125.015864794932));
#189116=CARTESIAN_POINT('Ctrl Pts',(79.1521424445996,-5.1482956211654,128.108665773475));
#189117=CARTESIAN_POINT('Ctrl Pts',(78.8736948207867,-5.05074395573051,
133.678678621723));
#189118=CARTESIAN_POINT('Ctrl Pts',(78.5952471969738,-0.31180533753877,
136.607333642391));
#189119=CARTESIAN_POINT('Ctrl Pts',(78.3167995731609,4.71366715331346,134.203339944237));
#189120=CARTESIAN_POINT('Ctrl Pts',(78.0383519493481,5.407509805713,128.675850294243));
#189121=CARTESIAN_POINT('Ctrl Pts',(77.7599043255351,1.1321151182024,125.104357647873));
#189122=CARTESIAN_POINT('Ctrl Pts',(77.4814567017223,-4.18363805603787,
126.770889270024));
#189123=CARTESIAN_POINT('Ctrl Pts',(77.2030090779094,-5.65483223886072,
132.143984014535));
#189124=CARTESIAN_POINT('Ctrl Pts',(76.9245614540965,-1.92951184808342,
136.286030301474));
#189125=CARTESIAN_POINT('Ctrl Pts',(76.6461138302835,3.56893566918854,135.390689943351));
#189126=CARTESIAN_POINT('Ctrl Pts',(76.3676662064707,5.78770565867644,130.280736989476));
#189127=CARTESIAN_POINT('Ctrl Pts',(76.0892185826578,2.68785689298084,125.651968569378));
#189128=CARTESIAN_POINT('Ctrl Pts',(75.8107709588449,-2.8820010482549,125.75799673322));
#189129=CARTESIAN_POINT('Ctrl Pts',(75.532323335032,-5.8034408197229,130.501386778194));
#189130=CARTESIAN_POINT('Ctrl Pts',(75.2538757112192,-3.39180199171105,
135.523194980456));
#189131=CARTESIAN_POINT('Ctrl Pts',(74.9754280874062,2.13673716794415,136.208624931095));
#189132=CARTESIAN_POINT('Ctrl Pts',(74.6969804635933,5.70171925567246,131.92779999059));
#189133=CARTESIAN_POINT('Ctrl Pts',(74.4185328397805,4.02709989190878,126.61458914934));
#189134=CARTESIAN_POINT('Ctrl Pts',(74.1400852159675,-1.34822753775231,
125.151573605674));
#189135=CARTESIAN_POINT('Ctrl Pts',(73.8616375921548,-5.48459972479585,
128.883193171938));
#189136=CARTESIAN_POINT('Ctrl Pts',(73.5831899683417,-4.58089270234404,
134.380271766487));
#189137=CARTESIAN_POINT('Ctrl Pts',(73.3047423445289,0.532430924512096,
136.591262708148));
#189138=CARTESIAN_POINT('Ctrl Pts',(73.026294720716,5.15647654243839,133.484373334449));
#189139=CARTESIAN_POINT('Ctrl Pts',(72.7478470969032,5.04197212574731,127.914683199832));
#189140=CARTESIAN_POINT('Ctrl Pts',(72.46939947309,0.294141639526237,125.000465443524));
#189141=CARTESIAN_POINT('Ctrl Pts',(72.1909518492774,-4.72399064380143,
127.419743816117));
#189142=CARTESIAN_POINT('Ctrl Pts',(71.9125042254643,-5.40100630524849,
132.949319681519));
#189143=CARTESIAN_POINT('Ctrl Pts',(71.6340566016516,-1.11476102599866,
136.507782954223));
#189144=CARTESIAN_POINT('Ctrl Pts',(71.3556089778387,4.19589517704018,134.82507972721));
#189145=CARTESIAN_POINT('Ctrl Pts',(71.0771613540258,5.65072869325411,129.447532061481));
#189146=CARTESIAN_POINT('Ctrl Pts',(70.7987137302128,1.91281859381102,125.316843554035));
#189147=CARTESIAN_POINT('Ctrl Pts',(70.5202661064001,-3.58287834696108,
126.22891514786));
#189148=CARTESIAN_POINT('Ctrl Pts',(70.241818482587,-5.78608512021397,131.345597605407));
#189149=CARTESIAN_POINT('Ctrl Pts',(69.9633708587742,-2.67216233396265,
135.964909712024));
#189150=CARTESIAN_POINT('Ctrl Pts',(69.6849232349613,2.89734709481291,135.841929307673));
#189151=CARTESIAN_POINT('Ctrl Pts',(69.4064756111484,5.80433608672999,131.089669376025));
#189152=CARTESIAN_POINT('Ctrl Pts',(69.1280279873355,3.37742377252397,126.07522463346));
#189153=CARTESIAN_POINT('Ctrl Pts',(68.8495803635227,-2.15317599230747,
125.406624829152));
#189154=CARTESIAN_POINT('Ctrl Pts',(68.5711327397097,-5.70511220870344,
129.698280520343));
#189155=CARTESIAN_POINT('Ctrl Pts',(68.2926851158969,-4.01432901552682,
135.006369785865));
#189156=CARTESIAN_POINT('Ctrl Pts',(68.014237492084,1.36542643204398,136.45301790528));
#189157=CARTESIAN_POINT('Ctrl Pts',(67.735789868271,5.49042169335597,132.708825929535));
#189158=CARTESIAN_POINT('Ctrl Pts',(67.4573422444582,4.56998764048497,127.214523370394));
#189159=CARTESIAN_POINT('Ctrl Pts',(67.1788946206453,-0.550041797684044,
125.019105868103));
#189160=CARTESIAN_POINT('Ctrl Pts',(66.9004469968323,-5.164609694817,128.140054855163));
#189161=CARTESIAN_POINT('Ctrl Pts',(66.6219993730196,-5.03315358762317,
133.709370679297));
#189162=CARTESIAN_POINT('Ctrl Pts',(66.3435517492066,-0.2764752166261,136.609124174332));
#189163=CARTESIAN_POINT('Ctrl Pts',(66.0651041253938,4.73427037188528,134.174583539162));
#189164=CARTESIAN_POINT('Ctrl Pts',(65.7866565015808,5.39445277059944,128.642972683589));
#189165=CARTESIAN_POINT('Ctrl Pts',(65.508208877768,1.0973966068015,125.097571749668));
#189166=CARTESIAN_POINT('Ctrl Pts',(65.2297612539551,-4.20811342784249,
126.796430993211));
#189167=CARTESIAN_POINT('Ctrl Pts',(64.9513136301422,-5.64657280006891,
132.178381763287));
#189168=CARTESIAN_POINT('Ctrl Pts',(64.6728660063292,-1.89610761944867,
136.297674225111));
#189169=CARTESIAN_POINT('Ctrl Pts',(64.3944183825164,3.59678783343796,135.368879844889));
#189170=CARTESIAN_POINT('Ctrl Pts',(64.1159707587035,5.78441098024938,130.245515283918));
#189171=CARTESIAN_POINT('Ctrl Pts',(63.8375231348906,2.65644302039782,125.635702283457));
#189172=CARTESIAN_POINT('Ctrl Pts',(63.5590755110777,-2.91266630074331,
125.775633789045));
#189173=CARTESIAN_POINT('Ctrl Pts',(63.2806278872649,-5.80517758316048,
130.53671958308));
#189174=CARTESIAN_POINT('Ctrl Pts',(63.0021802634519,-3.36301426534433,
135.543754412816));
#189175=CARTESIAN_POINT('Ctrl Pts',(62.723732639639,2.16959486994269,136.195517876976));
#189176=CARTESIAN_POINT('Ctrl Pts',(62.4452850158262,5.70845231035428,131.893071192411));
#189177=CARTESIAN_POINT('Ctrl Pts',(62.1668373920132,4.00152095094907,126.590152676031));
#189178=CARTESIAN_POINT('Ctrl Pts',(61.8883897682004,-1.38261267721222,
125.159885382419));
#189179=CARTESIAN_POINT('Ctrl Pts',(61.6099421443874,-5.49619279939966,
128.916615081961));
#189180=CARTESIAN_POINT('Ctrl Pts',(61.3314945205747,-4.55904024288434,
134.408090707227));
#189181=CARTESIAN_POINT('Ctrl Pts',(61.0530468967616,0.567647575344072,
136.587914432096));
#189182=CARTESIAN_POINT('Ctrl Pts',(60.7745992729488,5.17269500295686,133.452934743723));
#189183=CARTESIAN_POINT('Ctrl Pts',(60.496151649136,5.02428842305186,127.884044823451));
#189184=CARTESIAN_POINT('Ctrl Pts',(60.2177040253229,0.258806232497024,
124.998782452612));
#189185=CARTESIAN_POINT('Ctrl Pts',(59.9392564015102,-4.74450624233532,
127.448562797104));
#189186=CARTESIAN_POINT('Ctrl Pts',(59.6608087776971,-5.38784926247686,
132.982157398764));
#189187=CARTESIAN_POINT('Ctrl Pts',(59.3823611538844,-1.08002202147149,
136.514463149789));
#189188=CARTESIAN_POINT('Ctrl Pts',(59.1039135300714,4.22029269525717,134.799463627718));
#189189=CARTESIAN_POINT('Ctrl Pts',(58.8254659062585,5.64236459780459,129.413159610949));
#189190=CARTESIAN_POINT('Ctrl Pts',(58.5470182824457,1.8793790798041,125.305301355313));
#189191=CARTESIAN_POINT('Ctrl Pts',(58.2685706586328,-3.61066399976409,
126.250809917708));
#189192=CARTESIAN_POINT('Ctrl Pts',(57.9901230348199,-5.78268325429153,
131.380809119953));
#189193=CARTESIAN_POINT('Ctrl Pts',(57.711675411007,-2.64069909790739,135.981080309579));
#189194=CARTESIAN_POINT('Ctrl Pts',(57.4332277871941,2.92795852413098,135.824198999061));
#189195=CARTESIAN_POINT('Ctrl Pts',(57.1547801633813,5.80596530121877,131.054331448687));
#189196=CARTESIAN_POINT('Ctrl Pts',(56.8763325395683,3.34857360366007,126.054752916266));
#189197=CARTESIAN_POINT('Ctrl Pts',(56.5978849157555,-2.18599364874745,
125.419831830104));
#189198=CARTESIAN_POINT('Ctrl Pts',(56.3194372919424,-5.71173952968275,
129.733029650764));
#189199=CARTESIAN_POINT('Ctrl Pts',(56.0409896681298,-3.98867581682796,
135.030728292487));
#189200=CARTESIAN_POINT('Ctrl Pts',(55.7625420443167,1.39978611404518,136.444601510497));
#189201=CARTESIAN_POINT('Ctrl Pts',(55.4840944205039,5.50191298946419,132.675368888989));
#189202=CARTESIAN_POINT('Ctrl Pts',(55.2056467966909,4.54805061095778,127.186771069878));
#189203=CARTESIAN_POINT('Ctrl Pts',(54.9271991728781,-0.585248094394635,
125.022561316018));
#189204=CARTESIAN_POINT('Ctrl Pts',(54.6487515490652,-5.18073239195715,
128.171542663682));
#189205=CARTESIAN_POINT('Ctrl Pts',(54.3703039252523,-5.01537671415865,
133.739955090657));
#189206=CARTESIAN_POINT('Ctrl Pts',(54.0918563014394,-0.241134850822232,
136.610699608625));
#189207=CARTESIAN_POINT('Ctrl Pts',(53.8134086776265,4.75469816032759,134.145702249237));
#189208=CARTESIAN_POINT('Ctrl Pts',(53.5349610538137,5.38119584205463,128.610175163959));
#189209=CARTESIAN_POINT('Ctrl Pts',(53.2565134300007,1.06263743096531,125.090997318624));
#189210=CARTESIAN_POINT('Ctrl Pts',(52.9780658061879,-4.23243286645675,
126.822121231705));
#189211=CARTESIAN_POINT('Ctrl Pts',(52.6996181823749,-5.63810412544538,
132.21272859718));
#189212=CARTESIAN_POINT('Ctrl Pts',(52.4211705585621,-1.86263312984859,
136.309114591992));
#189213=CARTESIAN_POINT('Ctrl Pts',(52.1427229347491,3.62450671739182,135.346900606486));
#189214=CARTESIAN_POINT('Ctrl Pts',(51.8642753109363,5.7809019583462,130.210314286579));
#189215=CARTESIAN_POINT('Ctrl Pts',(51.5858276871234,2.62493071234137,125.619627524071));
#189216=CARTESIAN_POINT('Ctrl Pts',(51.3073800633105,-2.94322362331098,
125.793457186192));
#189217=CARTESIAN_POINT('Ctrl Pts',(51.0289324394976,-5.80669923360788,
130.572062305503));
#189218=CARTESIAN_POINT('Ctrl Pts',(50.7504848156848,-3.33410192124705,
135.564138225197));
#189219=CARTESIAN_POINT('Ctrl Pts',(50.4720371918718,2.20237217680579,136.182211051539));
#189220=CARTESIAN_POINT('Ctrl Pts',(50.193589568059,5.71497383623647,131.858302051661));
#189221=CARTESIAN_POINT('Ctrl Pts',(49.915141944246,3.97579373215887,126.565872361749));
#189222=CARTESIAN_POINT('Ctrl Pts',(49.6366943204332,-1.41694658345112,
125.168406317271));
#189223=CARTESIAN_POINT('Ctrl Pts',(49.3582466966203,-5.50758221055828,
128.950106943089));
#189224=CARTESIAN_POINT('Ctrl Pts',(49.0797990728074,-4.53701884651156,
134.435776110423));
#189225=CARTESIAN_POINT('Ctrl Pts',(48.8013514489945,0.602843191786665,
136.584351844331));
#189226=CARTESIAN_POINT('Ctrl Pts',(48.5229038251815,5.18872178735999,133.421398009111));
#189227=CARTESIAN_POINT('Ctrl Pts',(48.2444562013688,5.006418543501,127.853514660444));
#189228=CARTESIAN_POINT('Ctrl Pts',(47.9660085775558,0.223461235307256,
124.997314589534));
#189229=CARTESIAN_POINT('Ctrl Pts',(47.6875609537429,-4.7648460314457,127.477506128414));
#189230=CARTESIAN_POINT('Ctrl Pts',(47.40911332993,-5.37449257096935,133.014914416948));
#189231=CARTESIAN_POINT('Ctrl Pts',(47.1306657061172,-1.04524299633083,
136.520931755405));
#189232=CARTESIAN_POINT('Ctrl Pts',(46.8522180823042,4.24453382897653,134.773699488214));
#189233=CARTESIAN_POINT('Ctrl Pts',(46.5737704584914,5.6337914224598,129.378838711881));
#189234=CARTESIAN_POINT('Ctrl Pts',(46.2953228346785,1.84586992471411,125.293962926255));
#189235=CARTESIAN_POINT('Ctrl Pts',(46.0168752108656,-3.63831585808481,
126.272873421051));
#189236=CARTESIAN_POINT('Ctrl Pts',(45.7384275870526,-5.77906710891461,
131.415999273987));
#189237=CARTESIAN_POINT('Ctrl Pts',(45.4599799632399,-2.60913800977569,
135.997059081882));
#189238=CARTESIAN_POINT('Ctrl Pts',(45.1815323394269,2.95846145686929,135.806282678493));
#189239=CARTESIAN_POINT('Ctrl Pts',(44.903084715614,5.80737937352832,131.018984258588));
#189240=CARTESIAN_POINT('Ctrl Pts',(44.6246370918012,3.31959935216964,126.034457197533));
#189241=CARTESIAN_POINT('Ctrl Pts',(44.3461894679882,-2.21873030238901,
125.43323835675));
#189242=CARTESIAN_POINT('Ctrl Pts',(44.0677418441753,-5.7181552000533,129.767818479747));
#189243=CARTESIAN_POINT('Ctrl Pts',(43.7892942203624,-3.96287481627985,
135.054930189501));
#189244=CARTESIAN_POINT('Ctrl Pts',(43.5108465965496,1.43409392645716,136.435976114513));
#189245=CARTESIAN_POINT('Ctrl Pts',(43.2323989727367,5.51320041016325,132.641842517543));
#189246=CARTESIAN_POINT('Ctrl Pts',(42.9539513489238,4.52594505174265,127.159152820475));
#189247=CARTESIAN_POINT('Ctrl Pts',(42.6755037251109,-0.620432704521861,
125.026231010632));
#189248=CARTESIAN_POINT('Ctrl Pts',(42.397056101298,-5.19666311515333,128.203128032237));
#189249=CARTESIAN_POINT('Ctrl Pts',(42.1186084774851,-4.99741399406557,
133.770430722483));
#189250=CARTESIAN_POINT('Ctrl Pts',(41.8401608536722,-0.205785549677785,
136.612059886891));
#189251=CARTESIAN_POINT('Ctrl Pts',(41.5617132298594,4.77494976168102,134.11669714467));
#189252=CARTESIAN_POINT('Ctrl Pts',(41.2832656060464,5.36773951131901,128.577458950676));
#189253=CARTESIAN_POINT('Ctrl Pts',(41.0048179822336,1.02783887870806,125.084634598359));
#189254=CARTESIAN_POINT('Ctrl Pts',(40.7263703584206,-4.25659547071474,
126.847959033542));
#189255=CARTESIAN_POINT('Ctrl Pts',(40.4479227346078,-5.62942652880005,
132.24702324348));
#189256=CARTESIAN_POINT('Ctrl Pts',(40.1694751107948,-1.82908961969292,
136.320350978189));
#189257=CARTESIAN_POINT('Ctrl Pts',(39.891027486982,3.65209129391637,135.324753042595));
#189258=CARTESIAN_POINT('Ctrl Pts',(39.6125798631691,5.77717872299504,130.175135301845));
#189259=CARTESIAN_POINT('Ctrl Pts',(39.3341322393562,2.59332113651206,125.603744886877));
#189260=CARTESIAN_POINT('Ctrl Pts',(39.0556846155433,-2.97367188364494,
125.811466264208));
#189261=CARTESIAN_POINT('Ctrl Pts',(38.7772369917304,-5.80800571467979,
130.607413635826));
#189262=CARTESIAN_POINT('Ctrl Pts',(38.4987893679175,-3.30506603077697,
135.584345662267));
#189263=CARTESIAN_POINT('Ctrl Pts',(38.2203417441046,2.23506787395795,136.16870494788));
#189264=CARTESIAN_POINT('Ctrl Pts',(37.9418941202917,5.72128359166147,131.823493856722));
#189265=CARTESIAN_POINT('Ctrl Pts',(37.6634464964789,3.94991918886983,126.541749106207));
#189266=CARTESIAN_POINT('Ctrl Pts',(37.3849988726659,-1.45122798421329,
125.177136094481));
#189267=CARTESIAN_POINT('Ctrl Pts',(37.1065512488531,-5.51876753623267,
128.983667514269));
#189268=CARTESIAN_POINT('Ctrl Pts',(36.8281036250402,-4.51482932923697,
134.463326950183));
#189269=CARTESIAN_POINT('Ctrl Pts',(36.5496560012273,0.6380164696531,136.580575076865));
#189270=CARTESIAN_POINT('Ctrl Pts',(36.2712083774144,5.20455630176915,133.389764299214));
#189271=CARTESIAN_POINT('Ctrl Pts',(35.9927607536015,4.9883631492699,127.82309384212));
#189272=CARTESIAN_POINT('Ctrl Pts',(35.7143131297886,0.188107957679239,
124.996061908681));
#189273=CARTESIAN_POINT('Ctrl Pts',(35.4358655059757,-4.78500925743413,
127.50657273754));
#189274=CARTESIAN_POINT('Ctrl Pts',(35.1574178821628,-5.36093672566315,
133.047589522248));
#189275=CARTESIAN_POINT('Ctrl Pts',(34.87897025835,-1.01042523932657,136.527188531377));
#189276=CARTESIAN_POINT('Ctrl Pts',(34.6005226345371,4.26861767993396,134.747788263399));
#189277=CARTESIAN_POINT('Ctrl Pts',(34.3220750107242,5.62500948490202,129.34457063605));
#189278=CARTESIAN_POINT('Ctrl Pts',(34.0436273869112,1.81229237023524,125.282828687009));
#189279=CARTESIAN_POINT('Ctrl Pts',(33.7651797630984,-3.66583289727342,
126.295104840318));
#189280=CARTESIAN_POINT('Ctrl Pts',(33.4867321392855,-5.77523681808073,
131.451166763527));
#189281=CARTESIAN_POINT('Ctrl Pts',(33.2082845154725,-2.57748023907555,
136.012845436834));
#189282=CARTESIAN_POINT('Ctrl Pts',(32.9298368916598,2.98885476273036,135.788181009863));
#189283=CARTESIAN_POINT('Ctrl Pts',(32.6513892678468,5.80857825125962,130.983629115531));
#189284=CARTESIAN_POINT('Ctrl Pts',(32.3729416440339,3.29050209170421,126.014338229324));
#189285=CARTESIAN_POINT('Ctrl Pts',(32.094494020221,-2.25138474016344,125.446843912307));
#189286=CARTESIAN_POINT('Ctrl Pts',(31.8160463964081,-5.72435898208005,
129.802645718181));
#189287=CARTESIAN_POINT('Ctrl Pts',(31.5375987725953,-3.93692696994811,
135.078974580096));
#189288=CARTESIAN_POINT('Ctrl Pts',(31.2591511487823,1.46834859799131,136.427142036947));
#189289=CARTESIAN_POINT('Ctrl Pts',(30.9807035249695,5.52428353719365,132.608248057529));
#189290=CARTESIAN_POINT('Ctrl Pts',(30.7022559011566,4.50367178196922,127.131669645585));
#189291=CARTESIAN_POINT('Ctrl Pts',(30.4238082773436,-0.655594324287056,
125.030114815962));
#189292=CARTESIAN_POINT('Ctrl Pts',(30.1453606535308,-5.21240127408669,
128.234809790423));
#189293=CARTESIAN_POINT('Ctrl Pts',(29.8669130297179,-4.97926609295916,
133.80079644549));
#189294=CARTESIAN_POINT('Ctrl Pts',(29.588465405905,-0.170428623074124,
136.613204958723));
#189295=CARTESIAN_POINT('Ctrl Pts',(29.3100177820921,4.79502442551506,134.087569300254));
#189296=CARTESIAN_POINT('Ctrl Pts',(29.0315701582792,5.35408427702179,128.544825256054));
#189297=CARTESIAN_POINT('Ctrl Pts',(28.7531225344664,0.99300223950345,125.078483824645));
#189298=CARTESIAN_POINT('Ctrl Pts',(28.4746749106534,-4.28060034526213,
126.873943441297));
#189299=CARTESIAN_POINT('Ctrl Pts',(28.1962272868406,-5.6205403316845,132.281264431386));
#189300=CARTESIAN_POINT('Ctrl Pts',(27.9177796630277,-1.79547833194873,
136.331382967337));
#189301=CARTESIAN_POINT('Ctrl Pts',(27.6393320392148,3.67954054085496,135.3024379739));
#189302=CARTESIAN_POINT('Ctrl Pts',(27.3608844154018,5.77324141216173,130.139979633288));
#189303=CARTESIAN_POINT('Ctrl Pts',(27.082436791589,2.56161546421434,125.58805496041));
#189304=CARTESIAN_POINT('Ctrl Pts',(26.8039891677761,-3.00400995347367,
125.82966035576));
#189305=CARTESIAN_POINT('Ctrl Pts',(26.5255415439632,-5.80909697796402,
130.642772264091));
#189306=CARTESIAN_POINT('Ctrl Pts',(26.2470939201503,-3.27590766986969,
135.604375975235));
#189307=CARTESIAN_POINT('Ctrl Pts',(25.9686462963375,2.2676807498481,136.155000066467));
#189308=CARTESIAN_POINT('Ctrl Pts',(25.6901986725246,5.727381342819,131.788647897428));
#189309=CARTESIAN_POINT('Ctrl Pts',(25.4117510487116,3.92389827987267,126.517783803302));
#189310=CARTESIAN_POINT('Ctrl Pts',(25.1333034248988,-1.48545560918882,
125.186074390566));
#189311=CARTESIAN_POINT('Ctrl Pts',(24.8548558010858,-5.5297483619465,129.017295551901));
#189312=CARTESIAN_POINT('Ctrl Pts',(24.576408177273,-4.49247251330123,134.490742205601));
#189313=CARTESIAN_POINT('Ctrl Pts',(24.2979605534601,0.673166105584617,
136.576584269648));
#189314=CARTESIAN_POINT('Ctrl Pts',(24.0195129296472,5.22019795943058,133.358034786234));
#189315=CARTESIAN_POINT('Ctrl Pts',(23.7410653058343,4.97012290940784,127.792783495733));
#189316=CARTESIAN_POINT('Ctrl Pts',(23.4626176820214,0.152747709641667,
124.995024456474));
#189317=CARTESIAN_POINT('Ctrl Pts',(23.1841700582085,-4.80499517314482,
127.53576154741));
#189318=CARTESIAN_POINT('Ctrl Pts',(22.9057224343956,-5.34718222887511,
133.080181503877));
#189319=CARTESIAN_POINT('Ctrl Pts',(22.6272748105827,-0.975570040643468,
136.533233245855));
#189320=CARTESIAN_POINT('Ctrl Pts',(22.3488271867698,4.29254335569345,134.721730913422));
#189321=CARTESIAN_POINT('Ctrl Pts',(22.070379562957,5.61601911054919,129.310356653276));
#189322=CARTESIAN_POINT('Ctrl Pts',(21.791931939144,1.77864766059611,125.27189905016));
#189323=CARTESIAN_POINT('Ctrl Pts',(21.5134843153312,-3.69321409767591,
126.317503351717));
#189324=CARTESIAN_POINT('Ctrl Pts',(21.2350366915183,-5.77119252372273,
131.486310285425));
#189325=CARTESIAN_POINT('Ctrl Pts',(20.9565890677054,-2.54572695889727,
136.028438789465));
#189326=CARTESIAN_POINT('Ctrl Pts',(20.6781414438925,3.01913731547902,135.769894663934));
#189327=CARTESIAN_POINT('Ctrl Pts',(20.3996938200796,5.80956188998761,130.948267329615));
#189328=CARTESIAN_POINT('Ctrl Pts',(20.1212461962667,3.26128290047392,125.994396757156));
#189329=CARTESIAN_POINT('Ctrl Pts',(19.8427985724538,-2.28395575204823,
125.460647992615));
#189330=CARTESIAN_POINT('Ctrl Pts',(19.5643509486409,-5.7303506458796,129.837510075529));
#189331=CARTESIAN_POINT('Ctrl Pts',(19.285903324828,-3.91083323933969,135.102860573299));
#189332=CARTESIAN_POINT('Ctrl Pts',(19.0074557010152,1.50254885932817,136.418099605148));
#189333=CARTESIAN_POINT('Ctrl Pts',(18.7290080772022,5.53516195986603,132.574586753804));
#189334=CARTESIAN_POINT('Ctrl Pts',(18.4505604533894,4.48123162698169,127.104322563612));
#189335=CARTESIAN_POINT('Ctrl Pts',(18.1721128295765,-0.690731650763477,
125.034212588094));
#189336=CARTESIAN_POINT('Ctrl Pts',(17.8936652057636,-5.22794628557398,
128.26658676426));
#189337=CARTESIAN_POINT('Ctrl Pts',(17.6152175819507,-4.96093368331654,
133.831051134467));
#189338=CARTESIAN_POINT('Ctrl Pts',(17.3367699581378,-0.135065381175154,
136.614134781694));
#189339=CARTESIAN_POINT('Ctrl Pts',(17.0583223343249,4.81492140795562,134.058319795333));
#189340=CARTESIAN_POINT('Ctrl Pts',(16.779874710512,5.34023064516271,128.512275289347));
#189341=CARTESIAN_POINT('Ctrl Pts',(16.5014270866992,0.958128804235671,
125.0725452254));
#189342=CARTESIAN_POINT('Ctrl Pts',(16.2229794628862,-4.30444660058956,
126.900073492105));
#189343=CARTESIAN_POINT('Ctrl Pts',(15.9445318390734,-5.61144586338,132.315450892077));
#189344=CARTESIAN_POINT('Ctrl Pts',(15.6660842152604,-1.76180051209467,
136.342210150638));
#189345=CARTESIAN_POINT('Ctrl Pts',(15.3876365914476,3.70685344106567,135.279956227294));
#189346=CARTESIAN_POINT('Ctrl Pts',(15.1091889676347,5.76909017174479,130.104848583611));
#189347=CARTESIAN_POINT('Ctrl Pts',(14.8307413438218,2.52981487031356,125.572558326068));
#189348=CARTESIAN_POINT('Ctrl Pts',(14.5522937200089,-3.03423670860886,
125.848038786661));
#189349=CARTESIAN_POINT('Ctrl Pts',(14.273846096196,-5.80997298302346,130.678136880072));
#189350=CARTESIAN_POINT('Ctrl Pts',(13.9953984723831,-3.24662791899898,
135.624228421867));
#189351=CARTESIAN_POINT('Ctrl Pts',(13.7169508485702,2.30020959599411,136.141096915141));
#189352=CARTESIAN_POINT('Ctrl Pts',(13.4385032247574,5.73326686375462,131.753765465006));
#189353=CARTESIAN_POINT('Ctrl Pts',(13.1600556009444,3.89773196938174,126.493977341077));
#189354=CARTESIAN_POINT('Ctrl Pts',(12.8816079771316,-1.51962819006047,
125.195220874312));
#189355=CARTESIAN_POINT('Ctrl Pts',(12.6031603533186,-5.54052428080121,
129.050989809886));
#189356=CARTESIAN_POINT('Ctrl Pts',(12.3247127295058,-4.46994922714442,
134.518020860792));
#189357=CARTESIAN_POINT('Ctrl Pts',(12.0462651056929,0.708290797098533,
136.572379570561));
#189358=CARTESIAN_POINT('Ctrl Pts',(11.76781748188,5.23564618073708,133.326210645918));
#189359=CARTESIAN_POINT('Ctrl Pts',(11.4893698580671,4.95169849981347,127.762584744442));
#189360=CARTESIAN_POINT('Ctrl Pts',(11.2109222342542,0.117381801481337,
124.994202271355));
#189361=CARTESIAN_POINT('Ctrl Pts',(10.9324746104413,-4.82480303799234,
127.565071476419));
#189362=CARTESIAN_POINT('Ctrl Pts',(10.6540269866284,-5.33322959028317,
133.112689154126));
#189363=CARTESIAN_POINT('Ctrl Pts',(10.3755793628155,-0.940678691853753,
136.539065674851));
#189364=CARTESIAN_POINT('Ctrl Pts',(10.0971317390026,4.31630996968034,134.695528403849));
#189365=CARTESIAN_POINT('Ctrl Pts',(9.81868411518972,5.60682063254294,129.276198031366));
#189366=CARTESIAN_POINT('Ctrl Pts',(9.54023649137686,1.74493704251384,125.261174420708));
#189367=CARTESIAN_POINT('Ctrl Pts',(9.26178886756394,-3.72045844467185,
126.340068125262));
#189368=CARTESIAN_POINT('Ctrl Pts',(8.98334124375105,-5.76693437570339,
131.52142853743));
#189369=CARTESIAN_POINT('Ctrl Pts',(8.70489361993813,-2.51387934587036,
136.043838561958));
#189370=CARTESIAN_POINT('Ctrl Pts',(8.42644599612531,3.0493079929842,135.751424318317));
#189371=CARTESIAN_POINT('Ctrl Pts',(8.14799837231237,5.81033025326331,130.912900211183));
#189372=CARTESIAN_POINT('Ctrl Pts',(7.86955074849947,3.23194286120641,125.974633519968));
#189373=CARTESIAN_POINT('Ctrl Pts',(7.59110312468663,-2.3164421311127,125.47465008616));
#189374=CARTESIAN_POINT('Ctrl Pts',(7.31265550087371,-5.73612996942864,
129.872410259879));
#189375=CARTESIAN_POINT('Ctrl Pts',(7.0342078770608,-3.88459459136738,135.126587284006));
#189376=CARTESIAN_POINT('Ctrl Pts',(6.75576025324794,1.53669344316449,136.408849154185));
#189377=CARTESIAN_POINT('Ctrl Pts',(6.47731262943506,5.54583527507644,132.540859853697));
#189378=CARTESIAN_POINT('Ctrl Pts',(6.19886500562214,4.45862541830825,127.077112587908));
#189379=CARTESIAN_POINT('Ctrl Pts',(5.92041738180924,-0.725843381924555,
125.038524175185));
#189380=CARTESIAN_POINT('Ctrl Pts',(5.64196975799638,-5.24329757358911,
128.29845777624));
#189381=CARTESIAN_POINT('Ctrl Pts',(5.36352213418349,-4.94241744445191,
133.861193668313));
#189382=CARTESIAN_POINT('Ctrl Pts',(5.08507451037056,-0.0996971343788212,
136.614849321347));
#189383=CARTESIAN_POINT('Ctrl Pts',(4.80662688655771,4.83463997171276,134.028949713759));
#189384=CARTESIAN_POINT('Ctrl Pts',(4.5281792627448,5.32617912909322,128.479810256704));
#189385=CARTESIAN_POINT('Ctrl Pts',(4.24973163893191,0.923219865152705,
125.066819020683));
#189386=CARTESIAN_POINT('Ctrl Pts',(3.97128401511898,-4.32813335306523,
126.926348217707));
#189387=CARTESIAN_POINT('Ctrl Pts',(3.69283639130614,-5.60214346088543,
132.349581358763));
#189388=CARTESIAN_POINT('Ctrl Pts',(3.41438876749324,-1.72805740807474,
136.352832126888));
#189389=CARTESIAN_POINT('Ctrl Pts',(3.13594114368033,3.73402898245891,135.257308635848));
#189390=CARTESIAN_POINT('Ctrl Pts',(2.85749351986744,5.76472515556999,130.06974345461));
#189391=CARTESIAN_POINT('Ctrl Pts',(2.5790458960546,2.49792053319242,125.557255558086));
#189392=CARTESIAN_POINT('Ctrl Pts',(2.30059827224166,-3.06435102898697,
125.866600875889));
#189393=CARTESIAN_POINT('Ctrl Pts',(2.02215064842876,-5.81063369739741,
130.713506173321));
#189394=CARTESIAN_POINT('Ctrl Pts',(1.74370302461591,-3.21722786313679,
135.643902266527));
#189395=CARTESIAN_POINT('Ctrl Pts',(1.46525540080302,2.33265320702766,136.12699600909));
#189396=CARTESIAN_POINT('Ctrl Pts',(1.18680777699008,5.73893993637821,131.718847852038));
#189397=CARTESIAN_POINT('Ctrl Pts',(0.908360153177235,3.87142122699929,
126.47033060169));
#189398=CARTESIAN_POINT('Ctrl Pts',(0.629912529364331,-1.55374446055069,
125.204575206795));
#189399=CARTESIAN_POINT('Ctrl Pts',(0.351464905551429,-5.55109489349118,
129.084749039672));
#189400=CARTESIAN_POINT('Ctrl Pts',(0.0730172817385382,-4.44726030537518,
134.545161904937));
#189401=CARTESIAN_POINT('Ctrl Pts',(-0.205430342074321,0.743389242636492,
136.56796113541));
#189402=CARTESIAN_POINT('Ctrl Pts',(-0.48387796588724,5.25090039324876,
133.294293057522));
#189403=CARTESIAN_POINT('Ctrl Pts',(-0.762325589700153,4.93309060321035,
127.732498707276));
#189404=CARTESIAN_POINT('Ctrl Pts',(-1.040773213513,0.0820115436953976,
124.993595383789));
#189405=CARTESIAN_POINT('Ctrl Pts',(-1.3192208373259,-4.84443211798899,
127.594501438479));
#189406=CARTESIAN_POINT('Ctrl Pts',(-1.5976684611388,-5.31907932690746,
133.145111268411));
#189407=CARTESIAN_POINT('Ctrl Pts',(-1.8761160849517,-0.905752485869179,
136.544685602242));
#189408=CARTESIAN_POINT('Ctrl Pts',(-2.15456370876455,4.33991664121397,
134.669181705622));
#189409=CARTESIAN_POINT('Ctrl Pts',(-2.43301133257747,5.59741439173625,
129.242096036083));
#189410=CARTESIAN_POINT('Ctrl Pts',(-2.71145895639038,1.71116176514775,
125.250655196059));
#189411=CARTESIAN_POINT('Ctrl Pts',(-2.98990658020324,-3.74756492871192,
126.362798324807));
#189412=CARTESIAN_POINT('Ctrl Pts',(-3.26835420401613,-5.76246253181,131.556520218218));
#189413=CARTESIAN_POINT('Ctrl Pts',(-3.54680182782904,-2.48193858011979,
136.059044183669));
#189414=CARTESIAN_POINT('Ctrl Pts',(-3.82524945164193,3.0793656772603,135.732770657435));
#189415=CARTESIAN_POINT('Ctrl Pts',(-4.1036970754548,5.81088331261472,130.877529070775));
#189416=CARTESIAN_POINT('Ctrl Pts',(-4.38214469926771,3.20248306110764,
125.955049250094));
#189417=CARTESIAN_POINT('Ctrl Pts',(-4.66059232308062,-2.34884267356213,
125.488849674089));
#189418=CARTESIAN_POINT('Ctrl Pts',(-4.93903994689347,-5.7416967385722,
129.907344977992));
#189419=CARTESIAN_POINT('Ctrl Pts',(-5.21748757070636,-3.85821199831392,
135.150153833014));
#189420=CARTESIAN_POINT('Ctrl Pts',(-5.49593519451928,1.57078108426016,
136.399391026839));
#189421=CARTESIAN_POINT('Ctrl Pts',(-5.77438281833216,5.55630308732125,
132.507068606974));
#189422=CARTESIAN_POINT('Ctrl Pts',(-6.05283044214503,4.43585399363028,
127.050040726751));
#189423=CARTESIAN_POINT('Ctrl Pts',(-6.33127806595794,-0.76092821669219,
125.043049417465));
#189424=CARTESIAN_POINT('Ctrl Pts',(-6.60972568977086,-5.25845456928442,
128.330421645371));
#189425=CARTESIAN_POINT('Ctrl Pts',(-6.88817331358369,-4.92371806249131,
133.891222930087));
#189426=CARTESIAN_POINT('Ctrl Pts',(-7.16662093739661,-0.0643251932685087,
136.615348551203));
#189427=CARTESIAN_POINT('Ctrl Pts',(-7.44506856120951,4.8541793861078,133.999460143849));
#189428=CARTESIAN_POINT('Ctrl Pts',(-7.72351618502242,5.3119302494974,128.44743136113));
#189429=CARTESIAN_POINT('Ctrl Pts',(-8.00196380883526,0.888276715818123,
125.06130542268));
#189430=CARTESIAN_POINT('Ctrl Pts',(-8.28041143264819,-4.35165972496785,
126.952766644486));
#189431=CARTESIAN_POINT('Ctrl Pts',(-8.55885905646108,-5.59263346890473,
132.383654566726));
#189432=CARTESIAN_POINT('Ctrl Pts',(-8.83730668027396,-1.69425027025207,
136.363248502487));
#189433=CARTESIAN_POINT('Ctrl Pts',(-9.11575430408684,3.76106615803527,
135.234496038775));
#189434=CARTESIAN_POINT('Ctrl Pts',(-9.39420192789976,5.7601465253845,130.034665547118));
#189435=CARTESIAN_POINT('Ctrl Pts',(-9.67264955171265,2.4659336347071,125.542147223509));
#189436=CARTESIAN_POINT('Ctrl Pts',(-9.95109717552551,-3.09435179871079,
125.885345935621));
#189437=CARTESIAN_POINT('Ctrl Pts',(-10.2295447993384,-5.81107909660284,
130.748878833214));
#189438=CARTESIAN_POINT('Ctrl Pts',(-10.5079924231513,-3.18770859171301,
135.663396780189));
#189439=CARTESIAN_POINT('Ctrl Pts',(-10.7864400469642,2.36501038073878,
136.112697870828));
#189440=CARTESIAN_POINT('Ctrl Pts',(-11.0648876707771,5.74440035047196,
131.683896352409));
#189441=CARTESIAN_POINT('Ctrl Pts',(-11.34333529459,3.84496702767957,126.446844461378));
#189442=CARTESIAN_POINT('Ctrl Pts',(-11.6217829184029,-1.58780315646856,
125.214137041385));
#189443=CARTESIAN_POINT('Ctrl Pts',(-11.9002305422157,-5.56145980831845,
129.118571990297));
#189444=CARTESIAN_POINT('Ctrl Pts',(-12.1786781660286,-4.42440658873985,
134.572164332316));
#189445=CARTESIAN_POINT('Ctrl Pts',(-12.4571257898416,0.778460141612691,
136.563329127923));
#189446=CARTESIAN_POINT('Ctrl Pts',(-12.7355734136544,5.26596003171537,
133.262283203764));
#189447=CARTESIAN_POINT('Ctrl Pts',(-13.0140210374673,4.91429990912079,
127.702526499083));
#189448=CARTESIAN_POINT('Ctrl Pts',(-13.2924686612802,0.0466382469415425,
124.993203816266));
#189449=CARTESIAN_POINT('Ctrl Pts',(-13.5709162850931,-4.86388168577195,
127.624050343051));
#189450=CARTESIAN_POINT('Ctrl Pts',(-13.849363908906,-5.30473196309121,
133.177446645321));
#189451=CARTESIAN_POINT('Ctrl Pts',(-14.1278115327188,-0.87079271689315,
136.550092819781));
#189452=CARTESIAN_POINT('Ctrl Pts',(-14.4062591565318,4.36336249554048,
134.642691795028));
#189453=CARTESIAN_POINT('Ctrl Pts',(-14.6847067803446,5.58780073668082,
129.20805193109));
#189454=CARTESIAN_POINT('Ctrl Pts',(-14.9631544041576,1.67732308005318,
125.240341766008));
#189455=CARTESIAN_POINT('Ctrl Pts',(-15.2416020279704,-3.77453254535539,
126.385693108075));
#189456=CARTESIAN_POINT('Ctrl Pts',(-15.5200496517834,-5.75777715774833,
131.591584027456));
#189457=CARTESIAN_POINT('Ctrl Pts',(-15.7984972755962,-2.44990584522241,
136.074055091149));
#189458=CARTESIAN_POINT('Ctrl Pts',(-16.0769448994091,3.1093092545088,135.713934372506));
#189459=CARTESIAN_POINT('Ctrl Pts',(-16.355392523222,5.81122104754806,130.842155219084));
#189460=CARTESIAN_POINT('Ctrl Pts',(-16.6338401470349,3.17290459182133,
125.935644673236));
#189461=CARTESIAN_POINT('Ctrl Pts',(-16.9122877708478,-2.38115617878252,
125.50324623023));
#189462=CARTESIAN_POINT('Ctrl Pts',(-17.1907353946607,-5.74705074703162,
129.94231293535));
#189463=CARTESIAN_POINT('Ctrl Pts',(-17.4691830184736,-3.83168643779603,
135.173559347056));
#189464=CARTESIAN_POINT('Ctrl Pts',(-17.7476306422864,1.6048105194851,136.389725573584));
#189465=CARTESIAN_POINT('Ctrl Pts',(-18.0260782660994,5.56656500871184,
132.473214265779));
#189466=CARTESIAN_POINT('Ctrl Pts',(-18.3045258899123,4.4129181967513,127.023107983299));
#189467=CARTESIAN_POINT('Ctrl Pts',(-18.5829735137251,-0.795984854984928,
125.047788147249));
#189468=CARTESIAN_POINT('Ctrl Pts',(-18.861421137538,-5.27341671101187,
128.362477187221));
#189469=CARTESIAN_POINT('Ctrl Pts',(-19.1398687613509,-4.90483623034722,
133.921137807042));
#189470=CARTESIAN_POINT('Ctrl Pts',(-19.4183163851638,-0.0289508685644962,
136.615632452765));
#189471=CARTESIAN_POINT('Ctrl Pts',(-19.6967640089767,4.87353892710056,
133.969852178351));
#189472=CARTESIAN_POINT('Ctrl Pts',(-19.9752116327896,5.29748453437273,
128.415139802436));
#189473=CARTESIAN_POINT('Ctrl Pts',(-20.2536592566025,0.853300651063172,
125.056004635698));
#189474=CARTESIAN_POINT('Ctrl Pts',(-20.5321068804154,-4.37502484451904,
126.979327793496));
#189475=CARTESIAN_POINT('Ctrl Pts',(-20.8105545042282,-5.58291623983416,
132.417669253371));
#189476=CARTESIAN_POINT('Ctrl Pts',(-21.0890021280412,-1.66038035136256,
136.37345889145));
#189477=CARTESIAN_POINT('Ctrl Pts',(-21.367449751854,3.78796396592178,135.211519281404));
#189478=CARTESIAN_POINT('Ctrl Pts',(-21.6458973756669,5.75535445085128,
129.999616160961));
#189479=CARTESIAN_POINT('Ctrl Pts',(-21.9243449994798,2.43385536014432,
125.527233882186));
#189480=CARTESIAN_POINT('Ctrl Pts',(-22.2027926232928,-3.12423790609075,
125.904273271251));
#189481=CARTESIAN_POINT('Ctrl Pts',(-22.4812402471056,-5.81130916413533,
130.784253549004));
#189482=CARTESIAN_POINT('Ctrl Pts',(-22.7596878709185,-3.15807119857507,
135.682711240481));
#189483=CARTESIAN_POINT('Ctrl Pts',(-23.0381354947314,2.39727991812053,
136.098203030175));
#189484=CARTESIAN_POINT('Ctrl Pts',(-23.3165831185443,5.74964790369824,
131.648912261261));
#189485=CARTESIAN_POINT('Ctrl Pts',(-23.5950307423572,3.81837035169266,
126.423519790431));
#189486=CARTESIAN_POINT('Ctrl Pts',(-23.8734783661701,-1.62180301575654,
125.223906023766));
#189487=CARTESIAN_POINT('Ctrl Pts',(-24.151925989983,-5.57161864120731,
129.15245740844));
#189488=CARTESIAN_POINT('Ctrl Pts',(-24.4303736137958,-4.4013889240913,
134.599027142342));
#189489=CARTESIAN_POINT('Ctrl Pts',(-24.7088212376087,0.813502194462058,
136.558483719739));
#189490=CARTESIAN_POINT('Ctrl Pts',(-24.9872688614217,5.28082453809644,
133.230182270781));
#189491=CARTESIAN_POINT('Ctrl Pts',(-25.2657164852345,4.89532711384086,
127.672669230493));
#189492=CARTESIAN_POINT('Ctrl Pts',(-25.5441641090475,0.0112632219902977,
124.993027583295));
#189493=CARTESIAN_POINT('Ctrl Pts',(-25.8226117328602,-4.88315102063038,
127.65371709519));
#189494=CARTESIAN_POINT('Ctrl Pts',(-26.1010593566733,-5.29018803048126,
133.209694086655));
#189495=CARTESIAN_POINT('Ctrl Pts',(-26.3795069804861,-0.835800680372761,
136.555287127099));
#189496=CARTESIAN_POINT('Ctrl Pts',(-26.6579546042989,4.38664666386508,
134.616059653661));
#189497=CARTESIAN_POINT('Ctrl Pts',(-26.9364022281119,5.57798002361419,
129.174066977901));
#189498=CARTESIAN_POINT('Ctrl Pts',(-27.2148498519247,1.64342224113504,
125.23023451272));
#189499=CARTESIAN_POINT('Ctrl Pts',(-27.4932974757377,-3.80136029530733,
126.408751626694));
#189500=CARTESIAN_POINT('Ctrl Pts',(-27.7717450995505,-5.75287842713667,
131.626618665841));
#189501=CARTESIAN_POINT('Ctrl Pts',(-28.0501927233634,-2.41778232816299,
136.088870728161));
#189502=CARTESIAN_POINT('Ctrl Pts',(-28.3286403471763,3.13913761515943,
135.694916161515));
#189503=CARTESIAN_POINT('Ctrl Pts',(-28.6070879709892,5.8113434455484,130.8067799669));
#189504=CARTESIAN_POINT('Ctrl Pts',(-28.8855355948021,3.14320854938853,
125.916420508438));
#189505=CARTESIAN_POINT('Ctrl Pts',(-29.163983218615,-2.41338144938502,
125.517839221114));
#189506=CARTESIAN_POINT('Ctrl Pts',(-29.4424308424279,-5.75219179641212,
129.977312836202));
#189507=CARTESIAN_POINT('Ctrl Pts',(-29.7208784662408,-3.80501889272807,
135.196802958832));
#189508=CARTESIAN_POINT('Ctrl Pts',(-29.9993260900537,1.6387804878663,136.379853152576));
#189509=CARTESIAN_POINT('Ctrl Pts',(-30.2777737138665,5.576620658989,132.439298084597));
#189510=CARTESIAN_POINT('Ctrl Pts',(-30.5562213376795,4.38981887756547,
126.996315355552));
#189511=CARTESIAN_POINT('Ctrl Pts',(-30.8346689614924,-0.831011997766135,
125.052740188944));
#189512=CARTESIAN_POINT('Ctrl Pts',(-31.1131165853052,-5.2881834443438,
128.394623213959));
#189513=CARTESIAN_POINT('Ctrl Pts',(-31.3915642091181,-4.88577264769286,
133.950937190672));
#189514=CARTESIAN_POINT('Ctrl Pts',(-31.670011832931,0.00642452892459172,
136.615701015511));
#189515=CARTESIAN_POINT('Ctrl Pts',(-31.9484594567439,4.89271787731614,
133.940126914399));
#189516=CARTESIAN_POINT('Ctrl Pts',(-32.2269070805568,5.28284251901049,
128.382936777197));
#189517=CARTESIAN_POINT('Ctrl Pts',(-32.5053547043697,0.818292966938792,
125.050916856162));
#189518=CARTESIAN_POINT('Ctrl Pts',(-32.7838023281826,-4.3982278459157,
127.006030680504));
#189519=CARTESIAN_POINT('Ctrl Pts',(-33.0622499519955,-5.57299213374921,
132.451624158271));
#189520=CARTESIAN_POINT('Ctrl Pts',(-33.3406975758084,-1.62644890646854,
136.383462915428));
#189521=CARTESIAN_POINT('Ctrl Pts',(-33.6191451996212,3.81472140941051,
135.188379215148));
#189522=CARTESIAN_POINT('Ctrl Pts',(-33.8975928234342,5.75034910954236,
129.964596594906));
#189523=CARTESIAN_POINT('Ctrl Pts',(-34.176040447247,2.40168689817613,125.512516086734));
#189524=CARTESIAN_POINT('Ctrl Pts',(-34.4544880710599,-3.15400824368619,
125.923382181419));
#189525=CARTESIAN_POINT('Ctrl Pts',(-34.7329356948729,-5.81132389146964,
130.81962900987));
#189526=CARTESIAN_POINT('Ctrl Pts',(-35.0113833186857,-3.1283167819475,
135.701844931696));
#189527=CARTESIAN_POINT('Ctrl Pts',(-35.2898309424986,2.42946062341331,
136.083512024245));
#189528=CARTESIAN_POINT('Ctrl Pts',(-35.5682785663115,5.75468240160701,
131.613896874941));
#189529=CARTESIAN_POINT('Ctrl Pts',(-35.8467261901244,3.79163218458816,
126.400357453152));
#189530=CARTESIAN_POINT('Ctrl Pts',(-36.1251738139373,-1.65574277853735,
125.233881791944));
#189531=CARTESIAN_POINT('Ctrl Pts',(-36.4036214377501,-5.58157101571846,
129.186404038463));
#189532=CARTESIAN_POINT('Ctrl Pts',(-36.6820690615631,-4.37820816435757,
134.625749339604));
#189533=CARTESIAN_POINT('Ctrl Pts',(-36.960516685376,0.848514102688449,
136.553425090409));
#189534=CARTESIAN_POINT('Ctrl Pts',(-37.2389643091888,5.29549336158222,
133.197991448084));
#189535=CARTESIAN_POINT('Ctrl Pts',(-37.5174119330018,4.87617292041449,
127.64292800788));
#189536=CARTESIAN_POINT('Ctrl Pts',(-37.7958595568146,-0.0241122203237842,
124.993066691407));
#189537=CARTESIAN_POINT('Ctrl Pts',(-38.0743071806275,-4.90223940853195,
127.683500595584));
#189538=CARTESIAN_POINT('Ctrl Pts',(-38.3527548044404,-5.27544806800837,
133.241852397473));
#189539=CARTESIAN_POINT('Ctrl Pts',(-38.6312024282533,-0.800777672950798,
136.560268331721));
#189540=CARTESIAN_POINT('Ctrl Pts',(-38.9096500520661,4.40976828338437,
134.589286268384));
#189541=CARTESIAN_POINT('Ctrl Pts',(-39.1880976758791,5.56795261644649,
129.140142435842));
#189542=CARTESIAN_POINT('Ctrl Pts',(-39.4665452996919,1.6094605046014,125.220333810727));
#189543=CARTESIAN_POINT('Ctrl Pts',(-39.7449929235049,-3.82804718445556,
126.43197302622));
#189544=CARTESIAN_POINT('Ctrl Pts',(-40.0234405473177,-5.74776652149929,
131.661622835152));
#189545=CARTESIAN_POINT('Ctrl Pts',(-40.3018881711306,-2.38556921929025,
136.103490545709));
#189546=CARTESIAN_POINT('Ctrl Pts',(-40.5803357949436,3.16884965391132,
135.675716729192));
#189547=CARTESIAN_POINT('Ctrl Pts',(-40.8587834187564,5.81125050208024,
130.771404625066));
#189548=CARTESIAN_POINT('Ctrl Pts',(-41.1372310425694,3.11339603420704,
125.897377468058));
#189549=CARTESIAN_POINT('Ctrl Pts',(-41.4156786663821,-2.4455172912504,
125.532628105994));
#189550=CARTESIAN_POINT('Ctrl Pts',(-41.6941262901951,-5.75711969621025,
130.012343383614));
#189551=CARTESIAN_POINT('Ctrl Pts',(-41.9725739140079,-3.77821035128576,
135.219883807042));
#189552=CARTESIAN_POINT('Ctrl Pts',(-42.2510215378209,1.67268973063362,
136.369774129642));
#189553=CARTESIAN_POINT('Ctrl Pts',(-42.5294691616338,5.58646966553678,
132.405321320208));
#189554=CARTESIAN_POINT('Ctrl Pts',(-42.8079167854466,4.366556892027,126.969663836325));
#189555=CARTESIAN_POINT('Ctrl Pts',(-43.0863644092596,-0.866008347092154,
125.057905359049));
#189556=CARTESIAN_POINT('Ctrl Pts',(-43.3648120330724,-5.3027542220935,
128.426858534403));
#189557=CARTESIAN_POINT('Ctrl Pts',(-43.6432596568854,-4.86652802093628,
133.98061997675));
#189558=CARTESIAN_POINT('Ctrl Pts',(-43.9217072806982,0.0417996883503892,
136.615554236903));
#189559=CARTESIAN_POINT('Ctrl Pts',(-44.2001549045111,4.9117155260715,133.910285453475));
#189560=CARTESIAN_POINT('Ctrl Pts',(-44.478602528324,5.26800474597596,128.350823478709));
#189561=CARTESIAN_POINT('Ctrl Pts',(-44.7570501521369,0.783254960667603,
125.046042272601));
#189562=CARTESIAN_POINT('Ctrl Pts',(-45.0354977759497,-4.42126786936209,
127.032874316024));
#189563=CARTESIAN_POINT('Ctrl Pts',(-45.3139453997627,-5.56286151839129,
132.485518023215));
#189564=CARTESIAN_POINT('Ctrl Pts',(-45.5923930235756,-1.59245719291215,
136.393260203719));
#189565=CARTESIAN_POINT('Ctrl Pts',(-45.8708406473885,3.84133749699455,
135.165076697471));
#189566=CARTESIAN_POINT('Ctrl Pts',(-46.1492882712014,5.74513068693249,
129.929608146614));
#189567=CARTESIAN_POINT('Ctrl Pts',(-46.4277358950142,2.3694294408167,125.497994382526));
#189568=CARTESIAN_POINT('Ctrl Pts',(-46.7061835188271,-3.18366170834627,
125.942671958037));
#189569=CARTESIAN_POINT('Ctrl Pts',(-46.98463114264,-5.81112327806003,130.85500390496));
#189570=CARTESIAN_POINT('Ctrl Pts',(-47.263078766453,-3.09844644439114,
135.720797144829));
#189571=CARTESIAN_POINT('Ctrl Pts',(-47.5415263902657,2.46155130414924,
136.068625397419));
#189572=CARTESIAN_POINT('Ctrl Pts',(-47.8199740140787,5.75950365764311,
131.578851490957));
#189573=CARTESIAN_POINT('Ctrl Pts',(-48.0984216378915,3.76475351715869,
126.377358307829));
#189574=CARTESIAN_POINT('Ctrl Pts',(-48.3768692617045,-1.6896211871606,
125.244063976264));
#189575=CARTESIAN_POINT('Ctrl Pts',(-48.6553168855173,-5.59131656306301,
129.220410622463));
#189576=CARTESIAN_POINT('Ctrl Pts',(-48.9337645093303,-4.35486516851022,
134.652329933902));
#189577=CARTESIAN_POINT('Ctrl Pts',(-49.2122121331431,0.883494568912716,
136.548153427379));
#189578=CARTESIAN_POINT('Ctrl Pts',(-49.4906597569561,5.3099659586141,133.165711928516));
#189579=CARTESIAN_POINT('Ctrl Pts',(-49.7691073807689,4.85683803860733,
127.613303933314));
#189580=CARTESIAN_POINT('Ctrl Pts',(-50.0475550045819,-0.0594867691506708,
124.993321139153));
#189581=CARTESIAN_POINT('Ctrl Pts',(-50.3260026283946,-4.92114614214944,
127.713399740592));
#189582=CARTESIAN_POINT('Ctrl Pts',(-50.6044502522077,-5.26051262186729,
133.273920386136));
#189583=CARTESIAN_POINT('Ctrl Pts',(-50.8828978760204,-0.765724992417492,
136.565036249065));
#189584=CARTESIAN_POINT('Ctrl Pts',(-51.1613454998334,4.4327264973184,134.562372631296));
#189585=CARTESIAN_POINT('Ctrl Pts',(-51.4397931236463,5.55771888674681,
129.106279562002));
#189586=CARTESIAN_POINT('Ctrl Pts',(-51.7182407474591,1.57543912891688,
125.210640026899));
#189587=CARTESIAN_POINT('Ctrl Pts',(-51.9966883712721,-3.85459222390762,
126.455356446176));
#189588=CARTESIAN_POINT('Ctrl Pts',(-52.2751359950849,-5.7424416302597,
131.696595238295));
#189589=CARTESIAN_POINT('Ctrl Pts',(-52.5535836188979,-2.35326771227282,
136.117914002047));
#189590=CARTESIAN_POINT('Ctrl Pts',(-52.8320312427106,3.19844426977395,
135.656336786975));
#189591=CARTESIAN_POINT('Ctrl Pts',(-53.1104788665238,5.81094222058764,
130.736030504428));
#189592=CARTESIAN_POINT('Ctrl Pts',(-53.3889264903363,3.08346815099054,
125.878516257743));
#189593=CARTESIAN_POINT('Ctrl Pts',(-53.6673741141495,-2.47756251357323,
125.547612336859));
#189594=CARTESIAN_POINT('Ctrl Pts',(-53.9458217379622,-5.76183426382087,
130.047403279515));
#189595=CARTESIAN_POINT('Ctrl Pts',(-54.2242693617753,-3.75126180686946,
135.242801036416));
#189596=CARTESIAN_POINT('Ctrl Pts',(-54.502716985588,1.70653699126786,136.359488878264));
#189597=CARTESIAN_POINT('Ctrl Pts',(-54.7811646094011,5.59611166339667,
132.371285231631));
#189598=CARTESIAN_POINT('Ctrl Pts',(-55.0596122332138,4.3431331021171,126.943154413196));
#189599=CARTESIAN_POINT('Ctrl Pts',(-55.3380598570268,-0.900972606160421,
125.063283466166));
#189600=CARTESIAN_POINT('Ctrl Pts',(-55.6165074808396,-5.31712850433539,
128.459181954061));
#189601=CARTESIAN_POINT('Ctrl Pts',(-55.8949551046525,-4.84710306319425,
134.01018506537));
#189602=CARTESIAN_POINT('Ctrl Pts',(-56.1734027284654,0.0771732988733811,
136.615192122377));
#189603=CARTESIAN_POINT('Ctrl Pts',(-56.4518503522783,4.93053116940174,
133.880328901363));
#189604=CARTESIAN_POINT('Ctrl Pts',(-56.7302979760911,5.25297176508825,
128.318801096944));
#189605=CARTESIAN_POINT('Ctrl Pts',(-57.0087455999042,0.748187930595796,
125.041381065643));
#189606=CARTESIAN_POINT('Ctrl Pts',(-57.2871932237169,-4.44414406110167,
127.059857705357));
#189607=CARTESIAN_POINT('Ctrl Pts',(-57.5656408475299,-5.55252476915405,
132.519349592253));
#189608=CARTESIAN_POINT('Ctrl Pts',(-57.8440884713427,-1.55840647026886,
136.402850393281));
#189609=CARTESIAN_POINT('Ctrl Pts',(-58.1225360951557,3.867811242405,135.141612591857));
#189610=CARTESIAN_POINT('Ctrl Pts',(-58.4009837189685,5.73969937639226,
129.894652112598));
#189611=CARTESIAN_POINT('Ctrl Pts',(-58.6794313427815,2.33708418337799,
125.483669307672));
#189612=CARTESIAN_POINT('Ctrl Pts',(-58.9578789665944,-3.21319720125095,
125.962141886319));
#189613=CARTESIAN_POINT('Ctrl Pts',(-59.2363265904072,-5.81070733134035,
130.890376923444));
#189614=CARTESIAN_POINT('Ctrl Pts',(-59.5147742142201,-3.06846129276222,
135.739567177598));
#189615=CARTESIAN_POINT('Ctrl Pts',(-59.793221838033,2.49355077119662,136.053543701326));
#189616=CARTESIAN_POINT('Ctrl Pts',(-60.071669461846,5.76411149315304,131.543777407928));
#189617=CARTESIAN_POINT('Ctrl Pts',(-60.3501170856587,3.73773534540316,
126.354523206705));
#189618=CARTESIAN_POINT('Ctrl Pts',(-60.6285647094717,-1.72343698624942,
125.254452199421));
#189619=CARTESIAN_POINT('Ctrl Pts',(-60.9070123332846,-5.6008549221161,
129.254475900312));
#189620=CARTESIAN_POINT('Ctrl Pts',(-61.1854599570975,-4.33136080153256,
134.678767940282));
#189621=CARTESIAN_POINT('Ctrl Pts',(-61.4639075809103,0.918442296920838,
136.542668925995));
#189622=CARTESIAN_POINT('Ctrl Pts',(-61.7423552047232,5.32424179290464,
133.133344908207));
#189623=CARTESIAN_POINT('Ctrl Pts',(-62.0208028285362,4.83732318488056,
127.583798104527));
#189624=CARTESIAN_POINT('Ctrl Pts',(-62.299250452349,-0.0948591136734494,
124.993790917104));
#189625=CARTESIAN_POINT('Ctrl Pts',(-62.5776980761619,-4.93987052088691,
127.743413422294));
#189626=CARTESIAN_POINT('Ctrl Pts',(-62.8561456999749,-5.24538224549645,
133.305896864355));
#189627=CARTESIAN_POINT('Ctrl Pts',(-63.1345933237877,-0.730643937663188,
136.569590702456));
#189628=CARTESIAN_POINT('Ctrl Pts',(-63.4130409476006,4.45552045494177,
134.53531973969));
#189629=CARTESIAN_POINT('Ctrl Pts',(-63.6914885714135,5.5472792137301,129.072479611178));
#189630=CARTESIAN_POINT('Ctrl Pts',(-63.9699361952264,1.54135937475606,
125.201153520444));
#189631=CARTESIAN_POINT('Ctrl Pts',(-64.2483838190392,-3.88099443002729,
126.478901020081));
#189632=CARTESIAN_POINT('Ctrl Pts',(-64.5268314428522,-5.73690395073373,
131.731534579357));
#189633=CARTESIAN_POINT('Ctrl Pts',(-64.805279066665,-2.32087900405488,
136.132140562712));
#189634=CARTESIAN_POINT('Ctrl Pts',(-65.083726690478,3.22792036610792,135.636777052998));
#189635=CARTESIAN_POINT('Ctrl Pts',(-65.3621743142908,5.81041861249411,
130.700658915789));
#189636=CARTESIAN_POINT('Ctrl Pts',(-65.6406219381037,3.05342600872776,
125.859837576403));
#189637=CARTESIAN_POINT('Ctrl Pts',(-65.9190695619166,-2.50951592890599,
125.562791358466));
#189638=CARTESIAN_POINT('Ctrl Pts',(-66.1975171857295,-5.76633532454392,
130.082491224748));
#189639=CARTESIAN_POINT('Ctrl Pts',(-66.4759648095424,-3.72417425806736,
135.26555379775));
#189640=CARTESIAN_POINT('Ctrl Pts',(-66.7544124333553,1.74032101554631,
136.348997779564));
#189641=CARTESIAN_POINT('Ctrl Pts',(-67.0328600571681,5.60554629528092,
132.337191080086));
#189642=CARTESIAN_POINT('Ctrl Pts',(-67.3113076809811,4.31954837581292,
126.916788068483));
#189643=CARTESIAN_POINT('Ctrl Pts',(-67.5897553047939,-0.935903479357421,
125.068874311009));
#189644=CARTESIAN_POINT('Ctrl Pts',(-67.8682029286069,-5.33130575842519,
128.491592275178));
#189645=CARTESIAN_POINT('Ctrl Pts',(-68.1466505524197,-4.82749849426569,
134.039631360986));
#189646=CARTESIAN_POINT('Ctrl Pts',(-68.4250981762326,0.112544049711387,
136.614614685353));
#189647=CARTESIAN_POINT('Ctrl Pts',(-68.7035458000455,4.94916411008632,
133.850258368115));
#189648=CARTESIAN_POINT('Ctrl Pts',(-68.9819934238584,5.23774413340002,
128.286870818499));
#189649=CARTESIAN_POINT('Ctrl Pts',(-69.2604410476712,0.713093176145084,
125.036933408012));
#189650=CARTESIAN_POINT('Ctrl Pts',(-69.5388886714842,-4.46685557344872,
127.086979848621));
#189651=CARTESIAN_POINT('Ctrl Pts',(-69.8173362952971,-5.54198226906957,
132.553117611744));
#189652=CARTESIAN_POINT('Ctrl Pts',(-70.09578391911,-1.52429800030071,136.412233128746));
#189653=CARTESIAN_POINT('Ctrl Pts',(-70.3742315429229,3.89414166464747,
135.117987767775));
#189654=CARTESIAN_POINT('Ctrl Pts',(-70.6526791667357,5.73405537918087,
129.859729788164));
#189655=CARTESIAN_POINT('Ctrl Pts',(-70.9311267905487,2.3046523244254,125.469541392991));
#189656=CARTESIAN_POINT('Ctrl Pts',(-71.2095744143614,-3.24261362795168,
125.981791244794));
#189657=CARTESIAN_POINT('Ctrl Pts',(-71.4880220381746,-5.81007606672361,
130.925746754563));
#189658=CARTESIAN_POINT('Ctrl Pts',(-71.7664696619872,-3.03836243817177,
135.758154334473));
#189659=CARTESIAN_POINT('Ctrl Pts',(-72.0449172858002,2.52545783880292,
136.038267494822));
#189660=CARTESIAN_POINT('Ctrl Pts',(-72.3233649096131,5.76850573739207,
131.508675925537));
#189661=CARTESIAN_POINT('Ctrl Pts',(-72.601812533426,3.71057867048956,126.331852995942));
#189662=CARTESIAN_POINT('Ctrl Pts',(-72.8802601572389,-1.75718892274731,
125.265046076474));
#189663=CARTESIAN_POINT('Ctrl Pts',(-73.1587077810518,-5.61018573943046,
129.28859860971));
#189664=CARTESIAN_POINT('Ctrl Pts',(-73.4371554048648,-4.30769593438731,
134.705062379074));
#189665=CARTESIAN_POINT('Ctrl Pts',(-73.7156030286775,0.953355991712339,
136.536971789486));
#189666=CARTESIAN_POINT('Ctrl Pts',(-73.9940506524905,5.33832033545752,
133.100891586529));
#189667=CARTESIAN_POINT('Ctrl Pts',(-74.2724982763033,4.81762908236426,
127.554411614868));
#189668=CARTESIAN_POINT('Ctrl Pts',(-74.5509459001162,-0.130227943157576,
124.994476007852));
#189669=CARTESIAN_POINT('Ctrl Pts',(-74.8293935239292,-4.95841185090586,
127.77354052852));
#189670=CARTESIAN_POINT('Ctrl Pts',(-75.107841147742,-5.23005749955717,
133.337780647228));
#189671=CARTESIAN_POINT('Ctrl Pts',(-75.3862887715549,-0.695535808628632,
136.573931523126));
#189672=CARTESIAN_POINT('Ctrl Pts',(-75.6647363953679,4.4781493116164,134.508128596022));
#189673=CARTESIAN_POINT('Ctrl Pts',(-75.9431840191806,5.53663398424198,
129.038743835842));
#189674=CARTESIAN_POINT('Ctrl Pts',(-76.2216316429937,1.50722250495638,
125.191874642891));
#189675=CARTESIAN_POINT('Ctrl Pts',(-76.5000792668064,-3.90725282447187,
126.502605875483));
#189676=CARTESIAN_POINT('Ctrl Pts',(-76.7785268906195,-5.73115368812196,
131.766439563647));
#189677=CARTESIAN_POINT('Ctrl Pts',(-77.0569745144322,-2.28840429481114,
136.146169700531));
#189678=CARTESIAN_POINT('Ctrl Pts',(-77.3354221382452,3.25727685066645,
135.617038252052));
#189679=CARTESIAN_POINT('Ctrl Pts',(-77.613869762058,5.80967969720196,130.665291169852));
#189680=CARTESIAN_POINT('Ctrl Pts',(-77.8923173858709,3.0232707206408,125.841342116181));
#189681=CARTESIAN_POINT('Ctrl Pts',(-78.1707650096839,-2.54137635320382,
125.57816460835));
#189682=CARTESIAN_POINT('Ctrl Pts',(-78.4492126334967,-5.77062271159095,
130.117605919119));
#189683=CARTESIAN_POINT('Ctrl Pts',(-78.7276602573096,-3.69694870861804,
135.288141247929));
#189684=CARTESIAN_POINT('Ctrl Pts',(-79.0061078811224,1.77404055158998,
136.338301222296));
#189685=CARTESIAN_POINT('Ctrl Pts',(-79.2845555049354,5.61477321158579,
132.303040128944));
#189686=CARTESIAN_POINT('Ctrl Pts',(-79.5630031287483,4.29580358705489,
126.8905657792));
#189687=CARTESIAN_POINT('Ctrl Pts',(-79.8414507525611,-0.970799672307275,
125.074677686406));
#189688=CARTESIAN_POINT('Ctrl Pts',(-80.1198983763742,-5.34528545901998,
128.524088296775));
#189689=CARTESIAN_POINT('Ctrl Pts',(-80.3983460001869,-4.80771504060458,
134.068957772455));
#189690=CARTESIAN_POINT('Ctrl Pts',(-80.6767936239998,0.147910630189091,
136.613821947228));
#189691=CARTESIAN_POINT('Ctrl Pts',(-80.9552412478128,4.96761365767528,
133.820074968005));
#189692=CARTESIAN_POINT('Ctrl Pts',(-81.2336888716256,5.22232241517632,
128.255033826564));
#189693=CARTESIAN_POINT('Ctrl Pts',(-81.5121364954386,0.6779719977639,125.032699464516));
#189694=CARTESIAN_POINT('Ctrl Pts',(-81.7905841192513,-4.48940156482041,
127.114239740797));
#189695=CARTESIAN_POINT('Ctrl Pts',(-82.0690317430644,-5.53123440879372,
132.586820830401));
#189696=CARTESIAN_POINT('Ctrl Pts',(-82.3474793668772,-1.490133046909,136.421408062431));
#189697=CARTESIAN_POINT('Ctrl Pts',(-82.62592699069,3.92032778803891,135.094203100652));
#189698=CARTESIAN_POINT('Ctrl Pts',(-82.9043746145031,5.72819890443852,
129.824842467372));
#189699=CARTESIAN_POINT('Ctrl Pts',(-83.1828222383158,2.27213506573304,
125.455611161998));
#189700=CARTESIAN_POINT('Ctrl Pts',(-83.4612698621288,-3.27190989841242,
126.001619305352));
#189701=CARTESIAN_POINT('Ctrl Pts',(-83.7397174859417,-5.80922950760163,
130.961112087674));
#189702=CARTESIAN_POINT('Ctrl Pts',(-84.0181651097544,-3.00815099594316,
135.776557926701));
#189703=CARTESIAN_POINT('Ctrl Pts',(-84.2966127335676,2.55727132464077,
136.022797343974));
#189704=CARTESIAN_POINT('Ctrl Pts',(-84.5750603573801,5.77268622752965,
131.473548344486));
#189705=CARTESIAN_POINT('Ctrl Pts',(-84.8535079811934,3.68328449871872,
126.309348515594));
#189706=CARTESIAN_POINT('Ctrl Pts',(-85.131955605006,-1.79087574596318,
125.275845214866));
#189707=CARTESIAN_POINT('Ctrl Pts',(-85.4104032288191,-5.61930866924928,
129.322777486226));
#189708=CARTESIAN_POINT('Ctrl Pts',(-85.6888508526319,-4.28387144398495,
134.731212275928));
#189709=CARTESIAN_POINT('Ctrl Pts',(-85.9672984764448,0.98823435954663,
136.531062228962));
#189710=CARTESIAN_POINT('Ctrl Pts',(-86.2457461002577,5.35220106458756,
133.068353166051));
#189711=CARTESIAN_POINT('Ctrl Pts',(-86.5241937240705,4.79775646083024,
127.525145553266));
#189712=CARTESIAN_POINT('Ctrl Pts',(-86.8026413478836,-0.165591946996939,
124.995376386011));
#189713=CARTESIAN_POINT('Ctrl Pts',(-87.0810889716963,-4.97676944515001,
127.803779942897));
#189714=CARTESIAN_POINT('Ctrl Pts',(-87.3595365955093,-5.21453895191432,
133.36957055329));
#189715=CARTESIAN_POINT('Ctrl Pts',(-87.6379842193221,-0.660401906259044,
136.578058550223));
#189716=CARTESIAN_POINT('Ctrl Pts',(-87.916431843135,4.50061222882128,134.480800207869));
#189717=CARTESIAN_POINT('Ctrl Pts',(-88.1948794669479,5.52578359274576,
129.005073486085));
#189718=CARTESIAN_POINT('Ctrl Pts',(-88.4733270907608,1.47302978447255,
125.182803738068));
#189719=CARTESIAN_POINT('Ctrl Pts',(-88.7517747145737,-3.93336643422502,
126.526470133988));
#189720=CARTESIAN_POINT('Ctrl Pts',(-89.0302223383866,-5.7251910555031,
131.801308897747));
#189721=CARTESIAN_POINT('Ctrl Pts',(-89.3086699621995,-2.25584478790559,
136.16000089565));
#189722=CARTESIAN_POINT('Ctrl Pts',(-89.5871175860123,3.28651263563227,
135.597121115567));
#189723=CARTESIAN_POINT('Ctrl Pts',(-89.8655652098253,5.80872550209253,
130.629928577187));
#189724=CARTESIAN_POINT('Ctrl Pts',(-90.1440128336381,2.99300340414587,
125.823030562435));
#189725=CARTESIAN_POINT('Ctrl Pts',(-90.4224604574511,-2.57314260586573,
125.593731516848));
#189726=CARTESIAN_POINT('Ctrl Pts',(-90.7009080812639,-5.77469626609129,
130.152746061436));
#189727=CARTESIAN_POINT('Ctrl Pts',(-90.9793557050769,-3.66958616737523,
135.310562549967));
#189728=CARTESIAN_POINT('Ctrl Pts',(-91.2578033288896,1.80769434990835,
136.327399602824));
#189729=CARTESIAN_POINT('Ctrl Pts',(-91.5362509527026,5.62379207040447,
132.268833643682));
#189730=CARTESIAN_POINT('Ctrl Pts',(-91.8146985765155,4.27189961571542,
126.864488517025));
#189731=CARTESIAN_POINT('Ctrl Pts',(-92.0931462003284,-1.00565989191805,
125.080693377311));
#189732=CARTESIAN_POINT('Ctrl Pts',(-92.3715938241412,-5.3590670880956,
128.556668814702));
#189733=CARTESIAN_POINT('Ctrl Pts',(-92.6500414479542,-4.78775343529548,
134.098163213075));
#189734=CARTESIAN_POINT('Ctrl Pts',(-92.928489071767,0.183271729783054,
136.612813937377));
#189735=CARTESIAN_POINT('Ctrl Pts',(-93.2069366955801,4.98587912851244,
133.789779819492));
#189736=CARTESIAN_POINT('Ctrl Pts',(-93.4853843193926,5.2067071818758,128.223291300872));
#189737=CARTESIAN_POINT('Ctrl Pts',(-93.7638319432059,0.642825696881324,
125.028679392048));
#189738=CARTESIAN_POINT('Ctrl Pts',(-94.0422795670186,-4.51178119976554,
127.14163637176));
#189739=CARTESIAN_POINT('Ctrl Pts',(-94.3207271908314,-5.52028158659305,
132.62045799934));
#189740=CARTESIAN_POINT('Ctrl Pts',(-94.5991748146444,-1.45591287608963,
136.430374854359));
#189741=CARTESIAN_POINT('Ctrl Pts',(-94.8776224384574,3.94636864224209,
135.07025947184));
#189742=CARTESIAN_POINT('Ctrl Pts',(-95.1560700622702,5.7221301691794,129.789991442987));
#189743=CARTESIAN_POINT('Ctrl Pts',(-95.4345176860831,2.23953361224044,
125.441879130882));
#189744=CARTESIAN_POINT('Ctrl Pts',(-95.7129653098959,-3.30108492704829,
126.021625333256));
#189745=CARTESIAN_POINT('Ctrl Pts',(-95.9914129337089,-5.80816768534362,
130.996471612301));
#189746=CARTESIAN_POINT('Ctrl Pts',(-96.2698605575217,-2.97782808557417,
135.794777272329));
#189747=CARTESIAN_POINT('Ctrl Pts',(-96.5483081813347,2.58899004984866,
136.007133822036));
#189748=CARTESIAN_POINT('Ctrl Pts',(-96.8267558051475,5.77665280865574,
131.438395966436));
#189749=CARTESIAN_POINT('Ctrl Pts',(-97.1052034289604,3.65585384148698,
126.287010599573));
#189750=CARTESIAN_POINT('Ctrl Pts',(-97.3836510527732,-1.82449620761995,
125.286849214428));
#189751=CARTESIAN_POINT('Ctrl Pts',(-97.6620986765863,-5.62822337351841,
129.35701126335));
#189752=CARTESIAN_POINT('Ctrl Pts',(-97.9405463003989,-4.25988821315111,
134.757216661848));
#189753=CARTESIAN_POINT('Ctrl Pts',(-98.2189939242121,1.02307610799351,
136.524940463405));
#189754=CARTESIAN_POINT('Ctrl Pts',(-98.4974415480248,5.36588346593846,
133.035730852497));
#189755=CARTESIAN_POINT('Ctrl Pts',(-98.7758891718378,4.77770605666655,
127.496001004183));
#189756=CARTESIAN_POINT('Ctrl Pts',(-99.0543367956506,-0.200949814765295,
124.996492018215));
#189757=CARTESIAN_POINT('Ctrl Pts',(-99.3327844194636,-4.99494262337204,
127.834130544897));
#189758=CARTESIAN_POINT('Ctrl Pts',(-99.6112320432764,-5.19882717761281,
133.401265404553));
#189759=CARTESIAN_POINT('Ctrl Pts',(-99.8896796670892,-0.625243532454567,
136.581971630822));
#189760=CARTESIAN_POINT('Ctrl Pts',(-100.168127290903,4.5229083741848,134.453335587896));
#189761=CARTESIAN_POINT('Ctrl Pts',(-100.446574914715,5.51472844130613,
128.971469809575));
#189762=CARTESIAN_POINT('Ctrl Pts',(-100.725022538528,1.43878248032906,
125.173941142103));
#189763=CARTESIAN_POINT('Ctrl Pts',(-101.003470162341,-3.95933429163924,
126.550492911299));
#189764=CARTESIAN_POINT('Ctrl Pts',(-101.281917786154,-5.71901627382367,
131.836141289563));
#189765=CARTESIAN_POINT('Ctrl Pts',(-101.560365409967,-2.22320168984167,
136.17363363555));
#189766=CARTESIAN_POINT('Ctrl Pts',(-101.83881303378,3.31562663766449,135.577026381578));
#189767=CARTESIAN_POINT('Ctrl Pts',(-102.117260657593,5.80755606252295,
130.594572448163));
#189768=CARTESIAN_POINT('Ctrl Pts',(-102.395708281405,2.96262518080941,
125.804903593708));
#189769=CARTESIAN_POINT('Ctrl Pts',(-102.674155905219,-2.60481350978186,
125.609491507123));
#189770=CARTESIAN_POINT('Ctrl Pts',(-102.952603529031,-5.77855583709781,
130.187910349571));
#189771=CARTESIAN_POINT('Ctrl Pts',(-103.231051152844,-3.64208764826766,
135.332816873036));
#189772=CARTESIAN_POINT('Ctrl Pts',(-103.509498776657,1.84128116344741,
136.316293325111));
#189773=CARTESIAN_POINT('Ctrl Pts',(-103.78794640047,5.63260253753978,132.234572891835));
#189774=CARTESIAN_POINT('Ctrl Pts',(-104.066394024283,4.24783734756473,
126.838557248259));
#189775=CARTESIAN_POINT('Ctrl Pts',(-104.344841648096,-1.04048284643121,
125.086921160811));
#189776=CARTESIAN_POINT('Ctrl Pts',(-104.623289271909,-5.3726501349701,
128.589332621676));
#189777=CARTESIAN_POINT('Ctrl Pts',(-104.901736895722,-4.76761441802147,
134.12724660063));
#189778=CARTESIAN_POINT('Ctrl Pts',(-105.180184519534,0.218626038175886,
136.611590693152));
#189779=CARTESIAN_POINT('Ctrl Pts',(-105.458632143348,5.00395984576562,
133.759374045173));
#189780=CARTESIAN_POINT('Ctrl Pts',(-105.73707976716,5.1908990121252,128.191644417652));
#189781=CARTESIAN_POINT('Ctrl Pts',(-106.015527390973,0.607655575856702,
125.024873339572));
#189782=CARTESIAN_POINT('Ctrl Pts',(-106.293975014786,-4.53399364899913,
127.169168726316));
#189783=CARTESIAN_POINT('Ctrl Pts',(-106.572422638599,-5.50912420832816,
132.654027872123));
#189784=CARTESIAN_POINT('Ctrl Pts',(-106.850870262412,-1.42163875588365,
136.43913317226));
#189785=CARTESIAN_POINT('Ctrl Pts',(-107.129317886225,3.97226326230387,
135.046157768576));
#189786=CARTESIAN_POINT('Ctrl Pts',(-107.407765510038,5.71584939828273,
129.755178006424));
#189787=CARTESIAN_POINT('Ctrl Pts',(-107.686213133851,2.20684917200607,
125.428345808491));
#189788=CARTESIAN_POINT('Ctrl Pts',(-107.964660757664,-3.3301376327682,
126.041808587174));
#189789=CARTESIAN_POINT('Ctrl Pts',(-108.243108381476,-5.80689063929651,
131.031824018185));
#189790=CARTESIAN_POINT('Ctrl Pts',(-108.521556005289,-2.94739483068967,
135.812811696231));
#189791=CARTESIAN_POINT('Ctrl Pts',(-108.800003629102,2.62061283907833,
135.991277509423));
#189792=CARTESIAN_POINT('Ctrl Pts',(-109.078451252915,5.7804053337882,131.403220093974));
#189793=CARTESIAN_POINT('Ctrl Pts',(-109.356898876728,3.62828771524594,
126.264840075618));
#189794=CARTESIAN_POINT('Ctrl Pts',(-109.635346500541,-1.85804906189805,
125.298057667405));
#189795=CARTESIAN_POINT('Ctrl Pts',(-109.913794124354,-5.636929521901,129.391298672536));
#189796=CARTESIAN_POINT('Ctrl Pts',(-110.192241748167,-4.2357471305931,
134.783074573235));
#189797=CARTESIAN_POINT('Ctrl Pts',(-110.470689371979,1.05787994597834,
136.518606719657));
#189798=CARTESIAN_POINT('Ctrl Pts',(-110.749136995792,5.37936703250445,
133.003025854698));
#189799=CARTESIAN_POINT('Ctrl Pts',(-111.027584619605,4.75747861284798,
127.466979047582));
#189800=CARTESIAN_POINT('Ctrl Pts',(-111.306032243418,-0.23630023626489,
124.997822863128));
#189801=CARTESIAN_POINT('Ctrl Pts',(-111.584479867231,-5.01293071215839,
127.864591209862));
#189802=CARTESIAN_POINT('Ctrl Pts',(-111.862927491044,-5.18292275885852,
133.432864026556));
#189803=CARTESIAN_POINT('Ctrl Pts',(-112.141375114857,-0.590061990020461,
136.585670619917));
#189804=CARTESIAN_POINT('Ctrl Pts',(-112.41982273867,4.54503692151536,134.425735753813));
#189805=CARTESIAN_POINT('Ctrl Pts',(-112.698270362483,5.50346893957634,
128.937934051507));
#189806=CARTESIAN_POINT('Ctrl Pts',(-112.976717986295,1.40448186157095,
125.165287183403));
#189807=CARTESIAN_POINT('Ctrl Pts',(-113.255165610108,-3.98515543446448,
126.574673317241));
#189808=CARTESIAN_POINT('Ctrl Pts',(-113.533613233921,-5.71262957189362,
131.870935448366));
#189809=CARTESIAN_POINT('Ctrl Pts',(-113.812060857734,-2.19047621022174,
136.187067415062));
#189810=CARTESIAN_POINT('Ctrl Pts',(-114.090508481547,3.34461777793161,
135.556754794705));
#189811=CARTESIAN_POINT('Ctrl Pts',(-114.36895610536,5.80617142182825,130.559224092919));
#189812=CARTESIAN_POINT('Ctrl Pts',(-114.647403729173,2.9321371763071,125.786961881698));
#189813=CARTESIAN_POINT('Ctrl Pts',(-114.925851352986,-2.63638789137572,
125.625443995184));
#189814=CARTESIAN_POINT('Ctrl Pts',(-115.204298976799,-5.78220128159277,
130.223097480497));
#189815=CARTESIAN_POINT('Ctrl Pts',(-115.482746600612,-3.61445417026275,
135.354903392492));
#189816=CARTESIAN_POINT('Ctrl Pts',(-115.761194224424,1.87479974763623,
136.304982800703));
#189817=CARTESIAN_POINT('Ctrl Pts',(-116.039641848237,5.64120428651674,
132.200259142944));
#189818=CARTESIAN_POINT('Ctrl Pts',(-116.31808947205,4.22361767423897,126.812772933795));
#189819=CARTESIAN_POINT('Ctrl Pts',(-116.596537095863,-1.07526724547036,
125.093360806132));
#189820=CARTESIAN_POINT('Ctrl Pts',(-116.874984719676,-5.38603409631742,
128.622078507325));
#189821=CARTESIAN_POINT('Ctrl Pts',(-117.153432343489,-4.7472987350426,
134.156206857421));
#189822=CARTESIAN_POINT('Ctrl Pts',(-117.431879967302,0.253972245300257,
136.610152259881));
#189823=CARTESIAN_POINT('Ctrl Pts',(-117.710327591115,5.02185513944583,
133.728858771743));
#189824=CARTESIAN_POINT('Ctrl Pts',(-117.988775214928,5.17489849170343,
128.160094349593));
#189825=CARTESIAN_POINT('Ctrl Pts',(-118.26722283874,0.572462937930709,
125.021281448121));
#189826=CARTESIAN_POINT('Ctrl Pts',(-118.545670462553,-4.55603808943068,
127.196835784245));
#189827=CARTESIAN_POINT('Ctrl Pts',(-118.824118086366,-5.49776268743969,
132.687529204804));
#189828=CARTESIAN_POINT('Ctrl Pts',(-119.102565710179,-1.38731195633035,
136.447682691592));
#189829=CARTESIAN_POINT('Ctrl Pts',(-119.381013333992,3.99801068868978,
135.021898883958));
#189830=CARTESIAN_POINT('Ctrl Pts',(-119.659460957805,5.70935682448427,
129.720403447709));
#189831=CARTESIAN_POINT('Ctrl Pts',(-119.937908581618,2.17408295616475,
125.415011696306));
#189832=CARTESIAN_POINT('Ctrl Pts',(-120.216356205431,-3.3590669390133,
126.062168319208));
#189833=CARTESIAN_POINT('Ctrl Pts',(-120.494803829244,-5.80539841678086,
131.067167995328));
#189834=CARTESIAN_POINT('Ctrl Pts',(-120.773251453056,-2.91685235900652,
135.830660530138));
#189835=CARTESIAN_POINT('Ctrl Pts',(-121.051699076869,2.65213852053535,
135.975228993696));
#189836=CARTESIAN_POINT('Ctrl Pts',(-121.330146700682,5.78394366387473,
131.368022030553));
#189837=CARTESIAN_POINT('Ctrl Pts',(-121.608594324495,3.60058714147007,
126.242837765265));
#189838=CARTESIAN_POINT('Ctrl Pts',(-121.887041948308,-1.89153306548558,
125.309470158462));
#189839=CARTESIAN_POINT('Ctrl Pts',(-122.165489572121,-5.64542679178685,
129.425638443252));
#189840=CARTESIAN_POINT('Ctrl Pts',(-122.443937195934,-4.21144909086733,
134.808785051914));
#189841=CARTESIAN_POINT('Ctrl Pts',(-122.722384819747,1.09264458383337,
136.512061232418));
#189842=CARTESIAN_POINT('Ctrl Pts',(-123.00083244356,5.39265126464657,132.97023938455));
#189843=CARTESIAN_POINT('Ctrl Pts',(-123.279280067372,4.73707487890982,
127.438080758883));
#189844=CARTESIAN_POINT('Ctrl Pts',(-123.557727691185,-0.27164190157181,
124.999368871432));
#189845=CARTESIAN_POINT('Ctrl Pts',(-123.836175314998,-5.03073304495359,
127.895160809065));
#189846=CARTESIAN_POINT('Ctrl Pts',(-124.114622938811,-5.16682628499523,
133.464365248398));
#189847=CARTESIAN_POINT('Ctrl Pts',(-124.393070562624,-0.554858582622917,
136.589155380447));
#189848=CARTESIAN_POINT('Ctrl Pts',(-124.671518186437,4.56699705083122,
134.398001728342));
#189849=CARTESIAN_POINT('Ctrl Pts',(-124.94996581025,5.49200550478084,128.904467454562));
#189850=CARTESIAN_POINT('Ctrl Pts',(-125.228413434063,1.37012919922165,
125.156842182641));
#189851=CARTESIAN_POINT('Ctrl Pts',(-125.506861057876,-4.0108289058903,
126.599010455801));
#189852=CARTESIAN_POINT('Ctrl Pts',(-125.785308681688,-5.70603118637341,
131.905690084846));
#189853=CARTESIAN_POINT('Ctrl Pts',(-126.063756305501,-2.1576695617001,
136.200301736396));
#189854=CARTESIAN_POINT('Ctrl Pts',(-126.342203929314,3.37348498215772,
135.536307106118));
#189855=CARTESIAN_POINT('Ctrl Pts',(-126.620651553127,5.8045716313158,130.523884821299));
#189856=CARTESIAN_POINT('Ctrl Pts',(-126.89909917694,2.90154052038371,125.769206091244));
#189857=CARTESIAN_POINT('Ctrl Pts',(-127.177546800753,-2.66786458064647,
125.641588389905));
#189858=CARTESIAN_POINT('Ctrl Pts',(-127.455994424566,-5.7856324644928,
130.258306150342));
#189859=CARTESIAN_POINT('Ctrl Pts',(-127.734442048379,-3.5866867573295,
135.376821289913));
#189860=CARTESIAN_POINT('Ctrl Pts',(-128.012889672192,1.90824886043053,
136.293468448719));
#189861=CARTESIAN_POINT('Ctrl Pts',(-128.291337296005,5.64959699859458,
132.16589366852));
#189862=CARTESIAN_POINT('Ctrl Pts',(-128.569784919818,4.19924149320669,
126.787136529081));
#189863=CARTESIAN_POINT('Ctrl Pts',(-128.84823254363,-1.11001180008614,
125.100012074652));
#189864=CARTESIAN_POINT('Ctrl Pts',(-129.126680167443,-5.39921847619124,
128.654905258242));
#189865=CARTESIAN_POINT('Ctrl Pts',(-129.405127791256,-4.72680713916258,
134.185042910317));
#189866=CARTESIAN_POINT('Ctrl Pts',(-129.683575415069,0.289309041389885,
136.608498690867));
#189867=CARTESIAN_POINT('Ctrl Pts',(-129.962023038882,5.03956434643776,
133.69823512996));
#189868=CARTESIAN_POINT('Ctrl Pts',(-130.240470662695,5.15870621351431,
128.128642265792));
#189869=CARTESIAN_POINT('Ctrl Pts',(-130.518918286508,0.537249087180579,
125.017903850796));
#189870=CARTESIAN_POINT('Ctrl Pts',(-130.79736591032,-4.57791370419536,
127.224636520332));
#189871=CARTESIAN_POINT('Ctrl Pts',(-131.075813534134,-5.4861974449331,
132.720960755981));
#189872=CARTESIAN_POINT('Ctrl Pts',(-131.354261157946,-1.35293374942274,
136.456023095549));
#189873=CARTESIAN_POINT('Ctrl Pts',(-131.632708781759,4.02360996731925,
134.99748371691));
#189874=CARTESIAN_POINT('Ctrl Pts',(-131.911156405572,5.7026526883694,129.685669055425));
#189875=CARTESIAN_POINT('Ctrl Pts',(-132.189604029385,2.1412361788793,125.401877288427));
#189876=CARTESIAN_POINT('Ctrl Pts',(-132.468051653198,-3.38787177379785,
126.082703774923));
#189877=CARTESIAN_POINT('Ctrl Pts',(-132.746499277011,-5.80369107309236,
131.102502234048));
#189878=CARTESIAN_POINT('Ctrl Pts',(-133.024946900823,-2.88620180228584,
135.848323112653));
#189879=CARTESIAN_POINT('Ctrl Pts',(-133.303394524637,2.68356592602436,
135.95898886954));
#189880=CARTESIAN_POINT('Ctrl Pts',(-133.581842148449,5.78726766780228,
131.332803080451));
#189881=CARTESIAN_POINT('Ctrl Pts',(-133.860289772262,3.57275314661281,
126.221004483821));
#189882=CARTESIAN_POINT('Ctrl Pts',(-134.138737396075,-1.92494697761906,
125.321086264707));
#189883=CARTESIAN_POINT('Ctrl Pts',(-134.417185019888,-5.65371486830715,
129.460029303025));
#189884=CARTESIAN_POINT('Ctrl Pts',(-134.695632643701,-4.1869949943469,
134.834347145171));
#189885=CARTESIAN_POINT('Ctrl Pts',(-134.974080267514,1.1273687333409,136.505304244234));
#189886=CARTESIAN_POINT('Ctrl Pts',(-135.252527891327,5.40573567011315,
132.937372656969));
#189887=CARTESIAN_POINT('Ctrl Pts',(-135.53097551514,4.71649561092,127.409307208922));
#189888=CARTESIAN_POINT('Ctrl Pts',(-135.809423138953,-0.306973501088704,
125.001129985841));
#189889=CARTESIAN_POINT('Ctrl Pts',(-136.087870762765,-5.04834896208586,
127.925838209736));
#189890=CARTESIAN_POINT('Ctrl Pts',(-136.366318386578,-5.15053835248403,
133.49576790279));
#189891=CARTESIAN_POINT('Ctrl Pts',(-136.644766010391,-0.519634614735935,
136.592425783278));
#189892=CARTESIAN_POINT('Ctrl Pts',(-136.923213634204,4.58878794839197,
134.37013453918));
#189893=CARTESIAN_POINT('Ctrl Pts',(-137.201661258017,5.48033856170195,
128.871071258858));
#189894=CARTESIAN_POINT('Ctrl Pts',(-137.48010888183,1.33572576623031,125.148606452753));
#189895=CARTESIAN_POINT('Ctrl Pts',(-137.758556505643,-4.03635375457527,
126.623503425159));
#189896=CARTESIAN_POINT('Ctrl Pts',(-138.037004129456,-5.69922136176977,
131.940403911158));
#189897=CARTESIAN_POINT('Ctrl Pts',(-138.315451753269,-2.12478295993955,
136.213336109146));
#189898=CARTESIAN_POINT('Ctrl Pts',(-138.593899377082,3.40222718065648,
135.515684073514));
#189899=CARTESIAN_POINT('Ctrl Pts',(-138.872347000894,5.80275675026745,
130.488555942812));
#189900=CARTESIAN_POINT('Ctrl Pts',(-139.150794624707,2.870836346809,125.751636880291));
#189901=CARTESIAN_POINT('Ctrl Pts',(-139.42924224852,-2.69924241121433,
125.65792409305));
#189902=CARTESIAN_POINT('Ctrl Pts',(-139.707689872333,-5.78884925865424,
130.293535054436));
#189903=CARTESIAN_POINT('Ctrl Pts',(-139.986137496146,-3.55878643839929,
135.398569753122));
#189904=CARTESIAN_POINT('Ctrl Pts',(-140.264585119959,1.94162726236197,
136.281750695826));
#189905=CARTESIAN_POINT('Ctrl Pts',(-140.543032743772,5.65778036277742,
132.131477741989));
#189906=CARTESIAN_POINT('Ctrl Pts',(-140.821480367585,4.17470970773734,
126.761648984083));
#189907=CARTESIAN_POINT('Ctrl Pts',(-141.099927991397,-1.14471522280625,
125.106874719905));
#189908=CARTESIAN_POINT('Ctrl Pts',(-141.37837561521,-5.41220278603824,
128.687811658017));
#189909=CARTESIAN_POINT('Ctrl Pts',(-141.656823239023,-4.70614038970644,
134.213753690789));
#189910=CARTESIAN_POINT('Ctrl Pts',(-141.935270862836,0.324635117026387,
136.60663004738));
#189911=CARTESIAN_POINT('Ctrl Pts',(-142.213718486649,5.05708681051884,
133.667504254592));
#189912=CARTESIAN_POINT('Ctrl Pts',(-142.492166110462,5.14232277757003,
128.097289331719));
#189913=CARTESIAN_POINT('Ctrl Pts',(-142.770613734275,0.502015328467386,
125.014740672754));
#189914=CARTESIAN_POINT('Ctrl Pts',(-143.049061358088,-4.59961968268416,
127.252569904414));
#189915=CARTESIAN_POINT('Ctrl Pts',(-143.327508981901,-5.4744289093626,
132.754321286837));
#189916=CARTESIAN_POINT('Ctrl Pts',(-143.605956605714,-1.31850540905707,
136.464154075075));
#189917=CARTESIAN_POINT('Ctrl Pts',(-143.884404229526,4.04906014960179,
134.972913172143));
#189918=CARTESIAN_POINT('Ctrl Pts',(-144.162851853339,5.69573723836169,
129.650976116669));
#189919=CARTESIAN_POINT('Ctrl Pts',(-144.441299477152,2.10831005730047,
125.388943071553));
#189920=CARTESIAN_POINT('Ctrl Pts',(-144.719747100965,-3.41655106974776,
126.103414193369));
#189921=CARTESIAN_POINT('Ctrl Pts',(-144.998194724778,-5.80176867149642,
131.13782542502));
#189922=CARTESIAN_POINT('Ctrl Pts',(-145.276642348591,-2.85544429629671,
135.865798789283));
#189923=CARTESIAN_POINT('Ctrl Pts',(-145.555089972404,2.71489389099137,
135.942557738738));
#189924=CARTESIAN_POINT('Ctrl Pts',(-145.833537596217,5.79037722239768,
131.29756454872));
#189925=CARTESIAN_POINT('Ctrl Pts',(-146.111985220029,3.54478676207412,
126.199341040322));
#189926=CARTESIAN_POINT('Ctrl Pts',(-146.390432843843,-1.95828956013508,
125.332905555698));
#189927=CARTESIAN_POINT('Ctrl Pts',(-146.668880467655,-5.66179344434354,
129.49446997749));
#189928=CARTESIAN_POINT('Ctrl Pts',(-146.947328091469,-4.16238574718705,
134.859759905796));
#189929=CARTESIAN_POINT('Ctrl Pts',(-147.225775715281,1.16205110778606,
136.498336005488));
#189930=CARTESIAN_POINT('Ctrl Pts',(-147.504223339094,5.41861976405632,
132.904426889841));
#189931=CARTESIAN_POINT('Ctrl Pts',(-147.782670962907,4.6957415714508,127.380659463914));
#189932=CARTESIAN_POINT('Ctrl Pts',(-148.06111858672,-0.342293725589094,
125.003106141093));
#189933=CARTESIAN_POINT('Ctrl Pts',(-148.339566210533,-5.06577781079073,
127.956622275114));
#189934=CARTESIAN_POINT('Ctrl Pts',(-148.618013834346,-5.1340595648799,
133.527070826096));
#189935=CARTESIAN_POINT('Ctrl Pts',(-148.896461458158,-0.48439139159784,
136.595481707227));
#189936=CARTESIAN_POINT('Ctrl Pts',(-149.174909081971,4.61040880672808,
134.342135218952));
#189937=CARTESIAN_POINT('Ctrl Pts',(-149.453356705784,5.4684685426618,128.837746701901));
#189938=CARTESIAN_POINT('Ctrl Pts',(-149.731804329597,1.30127283742975,
125.140580298914));
#189939=CARTESIAN_POINT('Ctrl Pts',(-150.01025195341,-4.06172903468827,
126.648151317718));
#189940=CARTESIAN_POINT('Ctrl Pts',(-150.288699577223,-5.69220035042211,
131.975075640969));
#189941=CARTESIAN_POINT('Ctrl Pts',(-150.567147201036,-2.09181762356486,
136.226170050321));
#189942=CARTESIAN_POINT('Ctrl Pts',(-150.845594824849,3.43084330837664,
135.494886461086));
#189943=CARTESIAN_POINT('Ctrl Pts',(-151.124042448661,5.80072684593324,
130.453238766583));
#189944=CARTESIAN_POINT('Ctrl Pts',(-151.402490072475,2.84002579333802,
125.734254899877));
#189945=CARTESIAN_POINT('Ctrl Pts',(-151.680937696287,-2.73052022036177,
125.674450499292));
#189946=CARTESIAN_POINT('Ctrl Pts',(-151.9593853201,-5.79185154487752,130.32878288736));
#189947=CARTESIAN_POINT('Ctrl Pts',(-152.237832943913,-3.53075424732904,
135.420147976222));
#189948=CARTESIAN_POINT('Ctrl Pts',(-152.516280567726,1.97493371658077,
136.269829976228));
#189949=CARTESIAN_POINT('Ctrl Pts',(-152.794728191539,5.66575407582884,
132.097012638644));
#189950=CARTESIAN_POINT('Ctrl Pts',(-153.073175815352,4.15002322686382,
126.736311243251));
#189951=CARTESIAN_POINT('Ctrl Pts',(-153.351623439165,-1.17937622768304,
125.113948487592));
#189952=CARTESIAN_POINT('Ctrl Pts',(-153.630071062978,-5.42498654472129,
128.720796487292));
#189953=CARTESIAN_POINT('Ctrl Pts',(-153.90851868679,-4.6852992524868,134.242338134946));
#189954=CARTESIAN_POINT('Ctrl Pts',(-154.186966310604,0.359949163189457,
136.604546398667));
#189955=CARTESIAN_POINT('Ctrl Pts',(-154.465413934416,5.0744218823891,133.636667284384));
#189956=CARTESIAN_POINT('Ctrl Pts',(-154.743861558229,5.12574879096345,
128.066036709167));
#189957=CARTESIAN_POINT('Ctrl Pts',(-155.022309182042,0.466762967392146,
125.011792031209));
#189958=CARTESIAN_POINT('Ctrl Pts',(-155.300756805855,-4.62115522057418,
127.280634901405));
#189959=CARTESIAN_POINT('Ctrl Pts',(-155.579204429668,-5.46245751681569,
132.787609561181));
#189960=CARTESIAN_POINT('Ctrl Pts',(-155.857652053481,-1.28402821098903,
136.472075328871));
#189961=CARTESIAN_POINT('Ctrl Pts',(-156.136099677293,4.07436029247137,
134.948188160129));
#189962=CARTESIAN_POINT('Ctrl Pts',(-156.414547301107,5.68861073071636,
129.616325916999));
#189963=CARTESIAN_POINT('Ctrl Pts',(-156.692994924919,2.07530581151645,
125.376209524969));
#189964=CARTESIAN_POINT('Ctrl Pts',(-156.971442548732,-3.44510376414151,
126.124298807112));
#189965=CARTESIAN_POINT('Ctrl Pts',(-157.249890172545,-5.79963128322921,
131.173136259331));
#189966=CARTESIAN_POINT('Ctrl Pts',(-157.528337796358,-2.82458098076833,
135.883086912459));
#189967=CARTESIAN_POINT('Ctrl Pts',(-157.806785420171,2.74612125456611,
135.925936210153));
#189968=CARTESIAN_POINT('Ctrl Pts',(-158.085233043984,5.79327221243612,
131.262307741136));
#189969=CARTESIAN_POINT('Ctrl Pts',(-158.363680667797,3.51668902415852,
126.177848237519));
#189970=CARTESIAN_POINT('Ctrl Pts',(-158.64212829161,-1.9915595775106,125.344927593469));
#189971=CARTESIAN_POINT('Ctrl Pts',(-158.920575915422,-5.66966222054205,
129.528959190434));
#189972=CARTESIAN_POINT('Ctrl Pts',(-159.199023539236,-4.13762226129274,
134.885022392109));
#189973=CARTESIAN_POINT('Ctrl Pts',(-159.477471163048,1.19669042199943,
136.491156774389));
#189974=CARTESIAN_POINT('Ctrl Pts',(-159.755918786861,5.43130306905165,
132.871403303985));
#189975=CARTESIAN_POINT('Ctrl Pts',(-160.034366410674,4.67481352955083,
127.352138585409));
#189976=CARTESIAN_POINT('Ctrl Pts',(-160.312814034487,-0.377601266270116,
125.005297263965));
#189977=CARTESIAN_POINT('Ctrl Pts',(-160.5912616583,-5.08301894523598,127.987511864483));
#189978=CARTESIAN_POINT('Ctrl Pts',(-160.869709282113,-5.1173905328107,
133.558272858373));
#189979=CARTESIAN_POINT('Ctrl Pts',(-161.148156905926,-0.449130219157962,
136.598323039052));
#189980=CARTESIAN_POINT('Ctrl Pts',(-161.426604529739,4.63185882466967,
134.314004805186));
#189981=CARTESIAN_POINT('Ctrl Pts',(-161.705052153551,5.45639588750942,
128.804495018547));
#189982=CARTESIAN_POINT('Ctrl Pts',(-161.983499777364,1.26677168948586,
125.13276401854));
#189983=CARTESIAN_POINT('Ctrl Pts',(-162.261947401177,-4.08695380593746,
126.67295322014));
#189984=CARTESIAN_POINT('Ctrl Pts',(-162.54039502499,-5.68496841249774,
132.009703989503));
#189985=CARTESIAN_POINT('Ctrl Pts',(-162.818842648803,-2.05877477411906,
136.238803084352));
#189986=CARTESIAN_POINT('Ctrl Pts',(-163.097290272616,3.45933230493559,
135.473915039499));
#189987=CARTESIAN_POINT('Ctrl Pts',(-163.375737896429,5.79848199353304,
130.417934601304));
#189988=CARTESIAN_POINT('Ctrl Pts',(-163.654185520242,2.80911000166655,
125.717060794092));
#189989=CARTESIAN_POINT('Ctrl Pts',(-163.932633144055,-2.76169684907854,
125.691166996241));
#189990=CARTESIAN_POINT('Ctrl Pts',(-164.211080767867,-5.79463921191188,
130.36404834299));
#189991=CARTESIAN_POINT('Ctrl Pts',(-164.489528391681,-3.50259122286156,
135.441555159625));
#189992=CARTESIAN_POINT('Ctrl Pts',(-164.767976015493,2.00816698890481,
136.257706731653));
#189993=CARTESIAN_POINT('Ctrl Pts',(-165.046423639306,5.67351784227885,
132.062499635604));
#189994=CARTESIAN_POINT('Ctrl Pts',(-165.324871263119,4.12518296535417,
126.711124245485));
#189995=CARTESIAN_POINT('Ctrl Pts',(-165.603318886932,-1.21399353033979,
125.121233115594));
#189996=CARTESIAN_POINT('Ctrl Pts',(-165.881766510745,-5.43756927853226,
128.753858523801));
#189997=CARTESIAN_POINT('Ctrl Pts',(-166.160214134558,-4.66428449978105,
134.270795183582));
#189998=CARTESIAN_POINT('Ctrl Pts',(-166.438661758371,0.395249871304121,
136.602247821935));
#189999=CARTESIAN_POINT('Ctrl Pts',(-166.717109382183,5.09156891968999,
133.60572536201));
#190000=CARTESIAN_POINT('Ctrl Pts',(-166.995557005996,5.10898486785074,
128.034885556215));
#190001=CARTESIAN_POINT('Ctrl Pts',(-167.274004629809,0.431493310242956,
125.009058035423));
#190002=CARTESIAN_POINT('Ctrl Pts',(-167.552452253622,-4.64251951985801,
127.30883047135));
#190003=CARTESIAN_POINT('Ctrl Pts',(-167.830899877435,-5.45028371089662,
132.820824345507));
#190004=CARTESIAN_POINT('Ctrl Pts',(-168.109347501248,-1.24950343278299,
136.479786563416));
#190005=CARTESIAN_POINT('Ctrl Pts',(-168.387795125061,4.09950945842204,
134.923309597059));
#190006=CARTESIAN_POINT('Ctrl Pts',(-168.666242748874,5.68127342950807,
129.581719740392));
#190007=CARTESIAN_POINT('Ctrl Pts',(-168.944690372687,2.04222466451309,
125.36367712052));
#190008=CARTESIAN_POINT('Ctrl Pts',(-169.223137996499,-3.47352879894819,
126.145356842267));
#190009=CARTESIAN_POINT('Ctrl Pts',(-169.501585620313,-5.79727898749155,
131.208433428525));
#190010=CARTESIAN_POINT('Ctrl Pts',(-169.780033244125,-2.79361299935373,
135.900186841566));
#190011=CARTESIAN_POINT('Ctrl Pts',(-170.058480867939,2.77724685960862,
135.909124899701));
#190012=CARTESIAN_POINT('Ctrl Pts',(-170.336928491751,5.79595253064181,
131.227033964152));
#190013=CARTESIAN_POINT('Ctrl Pts',(-170.615376115564,3.48846097403773,
126.156526871832));
#190014=CARTESIAN_POINT('Ctrl Pts',(-170.893823739377,-2.02475579691427,
125.357151932539));
#190015=CARTESIAN_POINT('Ctrl Pts',(-171.17227136319,-5.67732090532164,
129.563495663847));
#190016=CARTESIAN_POINT('Ctrl Pts',(-171.450718987003,-4.11270545428381,
134.910133667999));
#190017=CARTESIAN_POINT('Ctrl Pts',(-171.729166610815,1.23128539240979,
136.483766816968));
#190018=CARTESIAN_POINT('Ctrl Pts',(-172.007614234629,5.44378511511418,
132.838303123102));
#190019=CARTESIAN_POINT('Ctrl Pts',(-172.286061858441,4.65371226071637,
127.323745630264));
#190020=CARTESIAN_POINT('Ctrl Pts',(-172.564509482254,-0.412894814796852,
125.00770327326));
#190021=CARTESIAN_POINT('Ctrl Pts',(-172.842957106067,-5.10007172654484,
128.018505833219));
#190022=CARTESIAN_POINT('Ctrl Pts',(-173.12140472988,-5.10053187395325,
133.589372843419));
#190023=CARTESIAN_POINT('Ctrl Pts',(-173.399852353693,-0.413852404033268,
136.600949673471));
#190024=CARTESIAN_POINT('Ctrl Pts',(-173.678299977506,4.65313720737985,
134.285744340263));
#190025=CARTESIAN_POINT('Ctrl Pts',(-173.956747601319,5.44412104360021,
128.771317440947));
#190026=CARTESIAN_POINT('Ctrl Pts',(-174.235195225131,1.23222360085094,
125.125157901261));
#190027=CARTESIAN_POINT('Ctrl Pts',(-174.513642848945,-4.11202713361109,
126.697908213384));
#190028=CARTESIAN_POINT('Ctrl Pts',(-174.792090472757,-5.67752581597763,
132.044287673595));
#190029=CARTESIAN_POINT('Ctrl Pts',(-175.070538096571,-2.02565563601667,
136.251234743121));
#190030=CARTESIAN_POINT('Ctrl Pts',(-175.348985720383,3.48769311466452,
135.452770585855));
#190031=CARTESIAN_POINT('Ctrl Pts',(-175.627433344196,5.79602227624969,
130.382644755183));
#190032=CARTESIAN_POINT('Ctrl Pts',(-175.905880968009,2.77809011739122,
125.700055200075));
#190033=CARTESIAN_POINT('Ctrl Pts',(-176.184328591822,-2.79277114210269,
125.708072964459));
#190034=CARTESIAN_POINT('Ctrl Pts',(-176.462776215635,-5.79721215645926,
130.399330114555));
#190035=CARTESIAN_POINT('Ctrl Pts',(-176.741223839448,-3.47429840858841,
135.462790510077));
#190036=CARTESIAN_POINT('Ctrl Pts',(-177.019671463261,2.04132584786218,
136.245381411334));
#190037=CARTESIAN_POINT('Ctrl Pts',(-177.298119087073,5.68107137443935,
132.02794001176));
#190038=CARTESIAN_POINT('Ctrl Pts',(-177.576566710886,4.10018984367198,
126.686088924097));
#190039=CARTESIAN_POINT('Ctrl Pts',(-177.855014334699,-1.24856584802001,
125.128728333976));
#190040=CARTESIAN_POINT('Ctrl Pts',(-178.133461958512,-5.4499505212146,
128.786996542421));
#190041=CARTESIAN_POINT('Ctrl Pts',(-178.411909582325,-4.64309691029714,
134.29912378221));
#190042=CARTESIAN_POINT('Ctrl Pts',(-178.690357206138,0.430535933288815,
136.599734402363));
#190043=CARTESIAN_POINT('Ctrl Pts',(-178.968804829951,5.10852728703229,
133.574679634036));
#190044=CARTESIAN_POINT('Ctrl Pts',(-179.247252453763,5.09203162942501,
128.00383702718));
#190045=CARTESIAN_POINT('Ctrl Pts',(-179.525700077576,0.396207663951002,
125.006538786706));
#190046=CARTESIAN_POINT('Ctrl Pts',(-179.80414770139,-4.66371178887382,
127.337155569449));
#190047=CARTESIAN_POINT('Ctrl Pts',(-180.082595325202,-5.43790794271038,
132.853964409027));
#190048=CARTESIAN_POINT('Ctrl Pts',(-180.361042949015,-1.2149323537682,
136.487287492965));
#190049=CARTESIAN_POINT('Ctrl Pts',(-180.639490572828,4.12450671554208,
134.898278404822));
#190050=CARTESIAN_POINT('Ctrl Pts',(-180.917938196641,5.67372560662389,
129.547158869193));
#190051=CARTESIAN_POINT('Ctrl Pts',(-181.196385820454,2.00906784212309,
125.351346322599));
#190052=CARTESIAN_POINT('Ctrl Pts',(-181.474833444267,-3.50182512086801,
126.166587518521));
#190053=CARTESIAN_POINT('Ctrl Pts',(-181.75328106808,-5.79471187144949,
131.243715624654));
#190054=CARTESIAN_POINT('Ctrl Pts',(-182.031728691892,-2.76254149958135,
135.917097942958));
#190055=CARTESIAN_POINT('Ctrl Pts',(-182.310176315705,2.80826955274668,
135.892124430331));
#190056=CARTESIAN_POINT('Ctrl Pts',(-182.588623939518,5.79841807769547,
131.191744524852));
#190057=CARTESIAN_POINT('Ctrl Pts',(-182.867071563331,3.46010365771282,
126.135377733334));
#190058=CARTESIAN_POINT('Ctrl Pts',(-183.145519187144,-2.05787698824661,
125.369578119929));
#190059=CARTESIAN_POINT('Ctrl Pts',(-183.423966810957,-5.68476921488759,
129.598078117967));
#190060=CARTESIAN_POINT('Ctrl Pts',(-183.70241443477,-4.08763624946197,
134.93509280296));
#190061=CARTESIAN_POINT('Ctrl Pts',(-183.980862058583,1.26583473708647,
136.476166407061));
#190062=CARTESIAN_POINT('Ctrl Pts',(-184.259309682396,5.45606543971754,
132.805127573733));
#190063=CARTESIAN_POINT('Ctrl Pts',(-184.537757306209,4.63243854686269,
127.295481650585));
#190064=CARTESIAN_POINT('Ctrl Pts',(-184.816204930021,-0.448173063354899,
125.010324079826));
#190065=CARTESIAN_POINT('Ctrl Pts',(-185.094652553834,-5.11693552282041,
128.049603032828));
#190066=CARTESIAN_POINT('Ctrl Pts',(-185.373100177647,-5.08348421301165,
133.620369628814));
#190067=CARTESIAN_POINT('Ctrl Pts',(-185.65154780146,-0.378559253454916,
136.60336151315));
#190068=CARTESIAN_POINT('Ctrl Pts',(-185.929995425273,4.67424316637891,
134.257354871388));
#190069=CARTESIAN_POINT('Ctrl Pts',(-186.208443049086,5.4316444657843,128.73821519851));
#190070=CARTESIAN_POINT('Ctrl Pts',(-186.486890672899,1.19762985171755,
125.117762228929));
#190071=CARTESIAN_POINT('Ctrl Pts',(-186.765338296712,-4.13694808860639,
126.72301537273));
#190072=CARTESIAN_POINT('Ctrl Pts',(-187.043785920525,-5.66987283665109,
132.078825411735));
#190073=CARTESIAN_POINT('Ctrl Pts',(-187.322233544337,-1.99246143649967,
136.263464565965));
#190074=CARTESIAN_POINT('Ctrl Pts',(-187.600681168151,3.51592468664221,
135.43145388367));
#190075=CARTESIAN_POINT('Ctrl Pts',(-187.879128791963,5.79334778522967,
130.347370535898));
#190076=CARTESIAN_POINT('Ctrl Pts',(-188.157576415776,2.74696728996466,
125.683238747971));
#190077=CARTESIAN_POINT('Ctrl Pts',(-188.436024039589,-2.82374194796541,
125.72516777749));
#190078=CARTESIAN_POINT('Ctrl Pts',(-188.714471663402,-5.79957028317828,
130.434626894674));
#190079=CARTESIAN_POINT('Ctrl Pts',(-188.992919287215,-3.44587685290989,
135.483853240698));
#190080=CARTESIAN_POINT('Ctrl Pts',(-189.271366911028,2.07440906473995,
136.232854471987));
#190081=CARTESIAN_POINT('Ctrl Pts',(-189.54981453484,5.68841439241029,131.993335047731));
#190082=CARTESIAN_POINT('Ctrl Pts',(-189.828262158654,4.07504478794802,
126.661206206783));
#190083=CARTESIAN_POINT('Ctrl Pts',(-190.106709782466,-1.28309189963338,
125.136433864998));
#190084=CARTESIAN_POINT('Ctrl Pts',(-190.385157406279,-5.46212981397553,
128.820209315208));
#190085=CARTESIAN_POINT('Ctrl Pts',(-190.663605030092,-4.62173726915045,
134.327322881104));
#190086=CARTESIAN_POINT('Ctrl Pts',(-190.942052653905,0.465806041606811,
136.597006233083));
#190087=CARTESIAN_POINT('Ctrl Pts',(-191.220500277718,5.12529635601715,
133.543531250871));
#190088=CARTESIAN_POINT('Ctrl Pts',(-191.49894790153,5.07488970389458,127.972892272577));
#190089=CARTESIAN_POINT('Ctrl Pts',(-191.777395525344,0.360907336037817,
125.004234378408));
#190090=CARTESIAN_POINT('Ctrl Pts',(-192.055843149156,-4.68473124233415,
127.365609146106));
#190091=CARTESIAN_POINT('Ctrl Pts',(-192.33429077297,-5.42533067084548,
132.887028523726));
#190092=CARTESIAN_POINT('Ctrl Pts',(-192.612738396782,-1.1803162549878,
136.494577839569));
#190093=CARTESIAN_POINT('Ctrl Pts',(-192.891186020595,4.14935113754904,
134.873095510955));
#190094=CARTESIAN_POINT('Ctrl Pts',(-193.169633644408,5.66596754175055,
129.512644584067));
#190095=CARTESIAN_POINT('Ctrl Pts',(-193.448081268221,1.97583657298603,
125.339217588127));
#190096=CARTESIAN_POINT('Ctrl Pts',(-193.726528892034,-3.52999168137001,
126.187990049162));
#190097=CARTESIAN_POINT('Ctrl Pts',(-194.004976515847,-5.79193003022761,
131.27898154032));
#190098=CARTESIAN_POINT('Ctrl Pts',(-194.28342413966,-2.73136763281852,
135.933819589987));
#190099=CARTESIAN_POINT('Ctrl Pts',(-194.561871763472,2.83918818442447,
135.874935432001));
#190100=CARTESIAN_POINT('Ctrl Pts',(-194.840319387286,5.80066876223446,
131.156440730899));
#190101=CARTESIAN_POINT('Ctrl Pts',(-195.118767011098,3.43161812597426,
126.114401605713));
#190102=CARTESIAN_POINT('Ctrl Pts',(-195.397214634911,-2.09092192419104,
125.382205695184));
#190103=CARTESIAN_POINT('Ctrl Pts',(-195.675662258724,-5.69200687323938,
129.63270527133));
#190104=CARTESIAN_POINT('Ctrl Pts',(-195.954109882537,-4.06241557577554,
134.95989887212));
#190105=CARTESIAN_POINT('Ctrl Pts',(-196.23255750635,1.30033717579212,136.468355826305));
#190106=CARTESIAN_POINT('Ctrl Pts',(-196.511005130163,5.46814358780935,
132.771877885207));
#190107=CARTESIAN_POINT('Ctrl Pts',(-196.789452753976,4.61099317629508,
127.267347693709));
#190108=CARTESIAN_POINT('Ctrl Pts',(-197.067900377789,-0.483434704694746,
125.013159586548));
#190109=CARTESIAN_POINT('Ctrl Pts',(-197.346348001602,-5.13360970916836,
128.080802310993));
#190110=CARTESIAN_POINT('Ctrl Pts',(-197.624795625414,-5.06624818169292,
133.651262065958));
#190111=CARTESIAN_POINT('Ctrl Pts',(-197.903243249227,-0.343252075224855,
136.605558468718));
#190112=CARTESIAN_POINT('Ctrl Pts',(-198.18169087304,4.69517591957924,134.228837450539));
#190113=CARTESIAN_POINT('Ctrl Pts',(-198.460138496853,5.41896661638458,
128.705189517851));
#190114=CARTESIAN_POINT('Ctrl Pts',(-198.738586120666,1.1629917239694,125.110577275591));
#190115=CARTESIAN_POINT('Ctrl Pts',(-199.017033744479,-4.16171574746965,
126.748273767825));
#190116=CARTESIAN_POINT('Ctrl Pts',(-199.295481368292,-5.6620097581009,
132.113315924113));
#190117=CARTESIAN_POINT('Ctrl Pts',(-199.573928992105,-1.95919340559182,
136.275492099704));
#190118=CARTESIAN_POINT('Ctrl Pts',(-199.852376615917,3.54402597473752,
135.409965722843));
#190119=CARTESIAN_POINT('Ctrl Pts',(-200.13082423973,5.79045861957696,130.312113250549));
#190120=CARTESIAN_POINT('Ctrl Pts',(-200.409271863544,2.71574267265526,
125.666612060922));
#190121=CARTESIAN_POINT('Ctrl Pts',(-200.687719487356,-2.85460811903155,
125.742450801881));
#190122=CARTESIAN_POINT('Ctrl Pts',(-200.966167111169,-5.80171350468764,
130.469937375411));
#190123=CARTESIAN_POINT('Ctrl Pts',(-201.244614734982,-3.41732760899753,
135.504742570997));
#190124=CARTESIAN_POINT('Ctrl Pts',(-201.523062358795,2.10741541362659,
136.220126377805));
#190125=CARTESIAN_POINT('Ctrl Pts',(-201.801509982608,5.69554662409457,
131.958686025817));
#190126=CARTESIAN_POINT('Ctrl Pts',(-202.079957606421,4.04974872994014,
126.636477015578));
#190127=CARTESIAN_POINT('Ctrl Pts',(-202.358405230234,-1.31757040580477,
125.144349423131));
#190128=CARTESIAN_POINT('Ctrl Pts',(-202.636852854047,-5.47410670550813,
128.853495611451));
#190129=CARTESIAN_POINT('Ctrl Pts',(-202.915300477859,-4.6002063678289,
134.355391435336));
#190130=CARTESIAN_POINT('Ctrl Pts',(-203.193748101672,0.501058889310003,
136.594063415189));
#190131=CARTESIAN_POINT('Ctrl Pts',(-203.472195725485,5.14187550526088,
133.512281366733));
#190132=CARTESIAN_POINT('Ctrl Pts',(-203.750643349298,5.05755972645996,
127.942052439074));
#190133=CARTESIAN_POINT('Ctrl Pts',(-204.029090973111,0.325593634571106,
125.002144895921));
#190134=CARTESIAN_POINT('Ctrl Pts',(-204.307538596924,-4.70557710135553,
127.394190146963));
#190135=CARTESIAN_POINT('Ctrl Pts',(-204.585986220737,-5.41255236135747,
132.920015464399));
#190136=CARTESIAN_POINT('Ctrl Pts',(-204.864433844549,-1.14565641915494,
136.50165733308));
#190137=CARTESIAN_POINT('Ctrl Pts',(-205.142881468362,4.17404180382362,
134.847761848621));
#190138=CARTESIAN_POINT('Ctrl Pts',(-205.421329092175,5.6579995223666,129.478178163952));
#190139=CARTESIAN_POINT('Ctrl Pts',(-205.699776715988,1.94253208849746,
125.327291366541));
#190140=CARTESIAN_POINT('Ctrl Pts',(-205.978224339801,-3.55802743673226,
126.209563641112));
#190141=CARTESIAN_POINT('Ctrl Pts',(-206.256671963614,-5.78893356690891,
131.314229868733));
#190142=CARTESIAN_POINT('Ctrl Pts',(-206.535119587427,-2.70009255422283,
135.950351163029));
#190143=CARTESIAN_POINT('Ctrl Pts',(-206.81356721124,2.87000160893922,135.857558541658));
#190144=CARTESIAN_POINT('Ctrl Pts',(-207.092014835053,5.80270450085972,
131.121123890489));
#190145=CARTESIAN_POINT('Ctrl Pts',(-207.370462458865,3.40300543436423,
126.09359926625));
#190146=CARTESIAN_POINT('Ctrl Pts',(-207.648910082679,-2.12388938025395,
125.395034190384));
#190147=CARTESIAN_POINT('Ctrl Pts',(-207.927357706491,-5.69903361218359,
129.667375840811));
#190148=CARTESIAN_POINT('Ctrl Pts',(-208.205805330304,-4.03704436778601,
134.984550956282));
#190149=CARTESIAN_POINT('Ctrl Pts',(-208.484252954117,1.33479143002538,
136.460335364123));
#190150=CARTESIAN_POINT('Ctrl Pts',(-208.76270057793,5.48001911182977,132.738555289606));
#190151=CARTESIAN_POINT('Ctrl Pts',(-209.041148201743,4.58937694367963,
127.239344802146));
#190152=CARTESIAN_POINT('Ctrl Pts',(-209.319595825556,-0.518678432184342,
125.016209688352));
#190153=CARTESIAN_POINT('Ctrl Pts',(-209.598043449369,-5.15009366772074,
128.112102511612));
#190154=CARTESIAN_POINT('Ctrl Pts',(-209.876491073182,-5.04882441868487,
133.682049010123));
#190155=CARTESIAN_POINT('Ctrl Pts',(-210.154938696994,-0.307932177662294,
136.607540458767));
#190156=CARTESIAN_POINT('Ctrl Pts',(-210.433386320807,4.71593469130848,
134.200193134443));
#190157=CARTESIAN_POINT('Ctrl Pts',(-210.71183394462,5.40608796518471,128.672241622749));
#190158=CARTESIAN_POINT('Ctrl Pts',(-210.990281568433,1.12831050113542,
125.103603307488));
#190159=CARTESIAN_POINT('Ctrl Pts',(-211.268729192246,-4.18632919242468,
126.773682462711));
#190160=CARTESIAN_POINT('Ctrl Pts',(-211.547176816059,-5.65393687169752,
132.14775793267));
#190161=CARTESIAN_POINT('Ctrl Pts',(-211.825624439872,-1.92585277605142,
136.287316898656));
#190162=CARTESIAN_POINT('Ctrl Pts',(-212.104072063685,3.57199593764717,
135.388306899624));
#190163=CARTESIAN_POINT('Ctrl Pts',(-212.382519687498,5.78735488635066,
130.276874205606));
#190164=CARTESIAN_POINT('Ctrl Pts',(-212.660967311311,2.68441742250212,
125.650175755035));
#190165=CARTESIAN_POINT('Ctrl Pts',(-212.939414935123,-2.88536851154432,
125.759921397201));
#190166=CARTESIAN_POINT('Ctrl Pts',(-213.217862558936,-5.80364174156953,
130.505260248325));
#190167=CARTESIAN_POINT('Ctrl Pts',(-213.496310182749,-3.38865173475374,
135.525457726916));
#190168=CARTESIAN_POINT('Ctrl Pts',(-213.774757806562,2.14034367146046,
136.20719760043));
#190169=CARTESIAN_POINT('Ctrl Pts',(-214.053205430375,5.7024678052036,131.923994229952));
#190170=CARTESIAN_POINT('Ctrl Pts',(-214.331653054188,4.02430260700449,
126.611902266833));
#190171=CARTESIAN_POINT('Ctrl Pts',(-214.610100678001,-1.35200008892003,
125.152474715061));
#190172=CARTESIAN_POINT('Ctrl Pts',(-214.888548301814,-5.48588075200302,
128.886854197714));
#190173=CARTESIAN_POINT('Ctrl Pts',(-215.166995925626,-4.5785050041694,
134.383328404815));
#190174=CARTESIAN_POINT('Ctrl Pts',(-215.445443549439,0.536293170092427,
136.59090605773));
#190175=CARTESIAN_POINT('Ctrl Pts',(-215.723891173253,5.15826412041666,
133.480931139593));
#190176=CARTESIAN_POINT('Ctrl Pts',(-216.002338797065,5.04004233928969,
127.911318669453));
#190177=CARTESIAN_POINT('Ctrl Pts',(-216.280786420879,0.290267868112,125.000270416672));
#190178=CARTESIAN_POINT('Ctrl Pts',(-216.559234044691,-4.72624859348692,
127.422897512942));
#190179=CARTESIAN_POINT('Ctrl Pts',(-216.837681668504,-5.39957348775117,
132.952924008705));
#190180=CARTESIAN_POINT('Ctrl Pts',(-217.116129292317,-1.11095413060172,
136.508525711168));
#190181=CARTESIAN_POINT('Ctrl Pts',(-217.39457691613,4.19857779944424,134.822278356567));
#190182=CARTESIAN_POINT('Ctrl Pts',(-217.673024539943,5.64982184372931,
129.443760886018));
#190183=CARTESIAN_POINT('Ctrl Pts',(-217.951472163756,1.90915562276867,
125.315568099769));
#190184=CARTESIAN_POINT('Ctrl Pts',(-218.229919787568,-3.58593134807924,
126.231307494954));
#190185=CARTESIAN_POINT('Ctrl Pts',(-218.508367411381,-5.78572259252759,
131.349459303753));
#190186=CARTESIAN_POINT('Ctrl Pts',(-218.786815035194,-2.66871742270537,
135.966692049498));
#190187=CARTESIAN_POINT('Ctrl Pts',(-219.065262659007,2.90070868448967,
135.839994403207));
#190188=CARTESIAN_POINT('Ctrl Pts',(-219.34371028282,5.80452521813531,131.085795312298));
#190189=CARTESIAN_POINT('Ctrl Pts',(-219.622157906633,3.37426664313623,
126.07297148578));
#190190=CARTESIAN_POINT('Ctrl Pts',(-219.900605530446,-2.15677813481551,
125.408063130162));
#190191=CARTESIAN_POINT('Ctrl Pts',(-220.179053154259,-5.70584917134113,
129.702088541682));
#190192=CARTESIAN_POINT('Ctrl Pts',(-220.457500778071,-4.01152356563293,
135.009048141953));
#190193=CARTESIAN_POINT('Ctrl Pts',(-220.735948401884,1.36919622307095,
136.452105317718));
#190194=CARTESIAN_POINT('Ctrl Pts',(-221.014396025697,5.49169157172664,
132.705161021709));
#190195=CARTESIAN_POINT('Ctrl Pts',(-221.29284364951,4.56759065001379,127.211474013555));
#190196=CARTESIAN_POINT('Ctrl Pts',(-221.571291273323,-0.553902939853376,
125.019474272218));
#190197=CARTESIAN_POINT('Ctrl Pts',(-221.849738897136,-5.16638678765824,
128.143502474846));
#190198=CARTESIAN_POINT('Ctrl Pts',(-222.128186520948,-5.03121356963114,
133.712729320486));
#190199=CARTESIAN_POINT('Ctrl Pts',(-222.406634144762,-0.272600869560251,
136.609307409853));
#190200=CARTESIAN_POINT('Ctrl Pts',(-222.685081768574,4.73651871234416,
134.171422984523));
#190201=CARTESIAN_POINT('Ctrl Pts',(-222.963529392388,5.39300898940659,
128.639372734101));
#190202=CARTESIAN_POINT('Ctrl Pts',(-223.2419770162,1.09358746834067,125.096840583045));
#190203=CARTESIAN_POINT('Ctrl Pts',(-223.520424640014,-4.21078751141269,
126.799240515859));
#190204=CARTESIAN_POINT('Ctrl Pts',(-223.798872263826,-5.64565447658353,
132.182150161146));
#190205=CARTESIAN_POINT('Ctrl Pts',(-224.077319887639,-1.89244078332859,
136.298938524645));
#190206=CARTESIAN_POINT('Ctrl Pts',(-224.355767511452,3.59983353893359,
135.366478216591));
#190207=CARTESIAN_POINT('Ctrl Pts',(-224.634215135265,5.78403670056078,
130.241654706868));
#190208=CARTESIAN_POINT('Ctrl Pts',(-224.912662759078,2.65299270027449,
125.633930439363));
#190209=CARTESIAN_POINT('Ctrl Pts',(-225.191110382891,-2.91602198566553,
125.77757891607));
#190210=CARTESIAN_POINT('Ctrl Pts',(-225.469558006704,-5.8053549223724,
130.540594204513));
#190211=CARTESIAN_POINT('Ctrl Pts',(-225.748005630516,-3.35985029277391,
135.545997940844));
#190212=CARTESIAN_POINT('Ctrl Pts',(-226.026453254329,2.17319261807209,
136.194068618944));
#190213=CARTESIAN_POINT('Ctrl Pts',(-226.304900878142,5.7091776792716,131.88926094565));
#190214=CARTESIAN_POINT('Ctrl Pts',(-226.583348501955,3.99870736205508,
126.587482871174));
#190215=CARTESIAN_POINT('Ctrl Pts',(-226.861796125768,-1.38637967317499,
125.160809439701));
#190216=CARTESIAN_POINT('Ctrl Pts',(-227.140243749581,-5.49745151716988,
128.920283837883));
#190217=CARTESIAN_POINT('Ctrl Pts',(-227.418691373394,-4.55663398232247,
134.411132754326));
#190218=CARTESIAN_POINT('Ctrl Pts',(-227.697138997207,0.571507578333558,
136.5875342777));
#190219=CARTESIAN_POINT('Ctrl Pts',(-227.97558662102,5.17446159419872,133.44948173115));
#190220=CARTESIAN_POINT('Ctrl Pts',(-228.254034244832,5.02233819149715,
127.880692102567));
#190221=CARTESIAN_POINT('Ctrl Pts',(-228.532481868645,0.254931345670833,
124.998611010119));
#190222=CARTESIAN_POINT('Ctrl Pts',(-228.810929492458,-4.74674495273865,
127.451730180279));
#190223=CARTESIAN_POINT('Ctrl Pts',(-229.089377116271,-5.38639453096373,
132.985752937203));
#190224=CARTESIAN_POINT('Ctrl Pts',(-229.367824740084,-1.07621067523457,
136.515182719319));
#190225=CARTESIAN_POINT('Ctrl Pts',(-229.646272363897,4.22295821522052,
134.796645979094));
#190226=CARTESIAN_POINT('Ctrl Pts',(-229.92471998771,5.64143480886619,129.409394025606));
#190227=CARTESIAN_POINT('Ctrl Pts',(-230.203167611523,1.87570841257552,
125.304048222223));
#190228=CARTESIAN_POINT('Ctrl Pts',(-230.481615235336,-3.61370238142155,
126.25322080496));
#190229=CARTESIAN_POINT('Ctrl Pts',(-230.760062859148,-5.78229722606833,
131.384668539942));
#190230=CARTESIAN_POINT('Ctrl Pts',(-231.038510482961,-2.63724340088164,
135.982841643878));
#190231=CARTESIAN_POINT('Ctrl Pts',(-231.316958106774,2.93130827321233,
135.822243667495));
#190232=CARTESIAN_POINT('Ctrl Pts',(-231.595405730587,5.80613084659478,
131.050456305442));
#190233=CARTESIAN_POINT('Ctrl Pts',(-231.8738533544,3.34540281721704,126.052519028673));
#190234=CARTESIAN_POINT('Ctrl Pts',(-232.152300978213,-2.18958696916944,
125.42129203173));
#190235=CARTESIAN_POINT('Ctrl Pts',(-232.430748602025,-5.71245329815966,
129.736842087648));
#190236=CARTESIAN_POINT('Ctrl Pts',(-232.709196225839,-3.98585411499877,
135.033389521383));
#190237=CARTESIAN_POINT('Ctrl Pts',(-232.987643849651,1.40355028004735,
136.443665992055));
#190238=CARTESIAN_POINT('Ctrl Pts',(-233.266091473464,5.50316053497282,
132.671696318956));
#190239=CARTESIAN_POINT('Ctrl Pts',(-233.544539097277,4.5456351025967,127.183736360699));
#190240=CARTESIAN_POINT('Ctrl Pts',(-233.82298672109,-0.589106922445798,
125.022953217175));
#190241=CARTESIAN_POINT('Ctrl Pts',(-234.101434344904,-5.18248846523346,
128.175001037157));
#190242=CARTESIAN_POINT('Ctrl Pts',(-234.379881968716,-5.01341628710851,
133.743301860178));
#190243=CARTESIAN_POINT('Ctrl Pts',(-234.658329592529,-0.237259460132118,
136.610859256499));
#190244=CARTESIAN_POINT('Ctrl Pts',(-234.936777216342,4.75692721993639,
134.14252806687));
#190245=CARTESIAN_POINT('Ctrl Pts',(-235.215224840155,5.37973017369771,
128.606584069875));
#190246=CARTESIAN_POINT('Ctrl Pts',(-235.493672463967,1.05882391226032,
125.090289352854));
#190247=CARTESIAN_POINT('Ctrl Pts',(-235.772120087781,-4.23508979812022,
126.824946980203));
#190248=CARTESIAN_POINT('Ctrl Pts',(-236.050567711593,-5.63716287966734,
132.216491335124));
#190249=CARTESIAN_POINT('Ctrl Pts',(-236.329015335406,-1.85895866551617,
136.310356547029));
#190250=CARTESIAN_POINT('Ctrl Pts',(-236.607462959219,3.62753774706455,
135.344480482612));
#190251=CARTESIAN_POINT('Ctrl Pts',(-236.885910583032,5.78050418516386,
130.206456059403));
#190252=CARTESIAN_POINT('Ctrl Pts',(-237.164358206845,2.62146967042642,
125.617876715884));
#190253=CARTESIAN_POINT('Ctrl Pts',(-237.442805830658,-2.94656740551997,
125.795422704185));
#190254=CARTESIAN_POINT('Ctrl Pts',(-237.72125345447,-5.80685298361372,
130.575937934662));
#190255=CARTESIAN_POINT('Ctrl Pts',(-237.999701078284,-3.33092435030571,
135.566362451659));
#190256=CARTESIAN_POINT('Ctrl Pts',(-238.278148702096,2.20596103623244,
136.180739919846));
#190257=CARTESIAN_POINT('Ctrl Pts',(-238.55659632591,5.7156759976606,131.854487459968));
#190258=CARTESIAN_POINT('Ctrl Pts',(-238.835043949722,3.97296394353457,
126.56321973347));
#190259=CARTESIAN_POINT('Ctrl Pts',(-239.113491573535,-1.42070788462113,
125.169353288205));
#190260=CARTESIAN_POINT('Ctrl Pts',(-239.391939197348,-5.50881857224844,
128.95378329321));
#190261=CARTESIAN_POINT('Ctrl Pts',(-239.670386821161,-4.53459411272838,
134.438803453569));
#190262=CARTESIAN_POINT('Ctrl Pts',(-239.948834444974,0.606700809151854,
136.583948200045));
#190263=CARTESIAN_POINT('Ctrl Pts',(-240.227282068787,5.1904673264033,133.417934306771));
#190264=CARTESIAN_POINT('Ctrl Pts',(-240.5057296926,5.00444793911587,127.850173873291));
#190265=CARTESIAN_POINT('Ctrl Pts',(-240.784177316413,0.21958537665436,
124.997166737753));
#190266=CARTESIAN_POINT('Ctrl Pts',(-241.062624940225,-4.76706541961049,
127.48068708057));
#190267=CARTESIAN_POINT('Ctrl Pts',(-241.341072564039,-5.37301597934592,
133.018501033406));
#190268=CARTESIAN_POINT('Ctrl Pts',(-241.619520187851,-1.04142734048567,
136.521628110858));
#190269=CARTESIAN_POINT('Ctrl Pts',(-241.897967811664,4.24718214772698,
134.770865666018));
#190270=CARTESIAN_POINT('Ctrl Pts',(-242.176415435477,5.63283872856131,
129.375078856195));
#190271=CARTESIAN_POINT('Ctrl Pts',(-242.45486305929,1.84219169731802,125.292732160775));
#190272=CARTESIAN_POINT('Ctrl Pts',(-242.733310683103,-3.64133950769301,
126.275302759127));
#190273=CARTESIAN_POINT('Ctrl Pts',(-243.011758306915,-5.77865759445851,
131.419856272607));
#190274=CARTESIAN_POINT('Ctrl Pts',(-243.290205930729,-2.60567165503458,
135.998799347738));
#190275=CARTESIAN_POINT('Ctrl Pts',(-243.568653554541,2.96179924122969,
135.80430699228));
#190276=CARTESIAN_POINT('Ctrl Pts',(-243.847101178355,5.80752132674009,
131.015108179419));
#190277=CARTESIAN_POINT('Ctrl Pts',(-244.125548802166,3.31641502616601,
126.032242652805));
#190278=CARTESIAN_POINT('Ctrl Pts',(-244.403996425981,-2.22231466757369,
125.434720404883));
#190279=CARTESIAN_POINT('Ctrl Pts',(-244.682444049792,-5.71884574792013,
129.771635190908));
#190280=CARTESIAN_POINT('Ctrl Pts',(-244.960891673606,-3.96003696707471,
135.05757419259));
#190281=CARTESIAN_POINT('Ctrl Pts',(-245.239339297418,1.43785232795156,
136.435017699859));
#190282=CARTESIAN_POINT('Ctrl Pts',(-245.517786921232,5.51442557658153,
132.638162421391));
#190283=CARTESIAN_POINT('Ctrl Pts',(-245.796234545044,4.52351111499922,
127.156132871406));
#190284=CARTESIAN_POINT('Ctrl Pts',(-246.074682168857,-0.624289075464052,
125.026646394309));
#190285=CARTESIAN_POINT('Ctrl Pts',(-246.353129792671,-5.19839810379266,
128.206597031353));
#190286=CARTESIAN_POINT('Ctrl Pts',(-246.631577416483,-4.99543323060155,
133.773765496319));
#190287=CARTESIAN_POINT('Ctrl Pts',(-246.910025040296,-0.201909258968066,
136.612195941205));
#190288=CARTESIAN_POINT('Ctrl Pts',(-247.188472664109,4.77715945784187,
134.113509452194));
#190289=CARTESIAN_POINT('Ctrl Pts',(-247.466920287922,5.36625201010822,
128.573876845067));
#190290=CARTESIAN_POINT('Ctrl Pts',(-247.745367911734,1.02402112107033,
125.083949859676));
#190291=CARTESIAN_POINT('Ctrl Pts',(-248.023815535548,-4.25923515201858,
126.850800903184));
#190292=CARTESIAN_POINT('Ctrl Pts',(-248.30226315936,-5.62846239560694,
132.250780182078));
#190293=CARTESIAN_POINT('Ctrl Pts',(-248.580710783174,-1.82540766330725,
136.32157054271));
#190294=CARTESIAN_POINT('Ctrl Pts',(-248.859158406986,3.65510753545023,
135.322314512822));
#190295=CARTESIAN_POINT('Ctrl Pts',(-249.137606030799,5.7767574710584,130.171279567513));
#190296=CARTESIAN_POINT('Ctrl Pts',(-249.416053654612,2.58984950105633,
125.602015179472));
#190297=CARTESIAN_POINT('Ctrl Pts',(-249.694501278425,-2.97700363923603,
125.813452100338));
#190298=CARTESIAN_POINT('Ctrl Pts',(-249.972948902238,-5.80813586978118,
130.611290129096));
#190299=CARTESIAN_POINT('Ctrl Pts',(-250.251396526051,-3.30187497921299,
135.586550504748));
#190300=CARTESIAN_POINT('Ctrl Pts',(-250.529844149864,2.23864771169993,
136.167211997028));
#190301=CARTESIAN_POINT('Ctrl Pts',(-250.808291773676,5.72196251956533,
131.819675061465));
#190302=CARTESIAN_POINT('Ctrl Pts',(-251.08673939749,3.94707330538994,126.539113752772));
#190303=CARTESIAN_POINT('Ctrl Pts',(-251.365187021302,-1.45498345124562,
125.178105944033));
#190304=CARTESIAN_POINT('Ctrl Pts',(-251.643634645115,-5.5199814959705,
128.987351322257));
#190305=CARTESIAN_POINT('Ctrl Pts',(-251.922082268928,-4.51238621219265,
134.466339477392));
#190306=CARTESIAN_POINT('Ctrl Pts',(-252.200529892741,0.641871558658502,
136.580147957277));
#190307=CARTESIAN_POINT('Ctrl Pts',(-252.478977516554,5.20628072353487,
133.386290036154));
#190308=CARTESIAN_POINT('Ctrl Pts',(-252.757425140367,4.98637224582674,
127.819765111179));
#190309=CARTESIAN_POINT('Ctrl Pts',(-253.035872764179,0.184231269403876,
124.995937655572));
#190310=CARTESIAN_POINT('Ctrl Pts',(-253.314320387993,-4.78720923844335,
127.509767136124));
#190311=CARTESIAN_POINT('Ctrl Pts',(-253.592768011806,-5.35943833369967,
133.051167092665));
#190312=CARTESIAN_POINT('Ctrl Pts',(-253.871215635618,-1.00660540571931,
136.527861630253));
#190313=CARTESIAN_POINT('Ctrl Pts',(-254.149663259431,4.27124868131666,
134.744938404161));
#190314=CARTESIAN_POINT('Ctrl Pts',(-254.428110883244,5.62403395537261,
129.340816589823));
#190315=CARTESIAN_POINT('Ctrl Pts',(-254.706558507057,1.80860665472018,
125.281620447135));
#190316=CARTESIAN_POINT('Ctrl Pts',(-254.98500613087,-3.66884158147516,
126.297552326988));
#190317=CARTESIAN_POINT('Ctrl Pts',(-255.263453754682,-5.77480406163408,
131.45502159855));
#190318=CARTESIAN_POINT('Ctrl Pts',(-255.541901378496,-2.57400292253984,
136.014563813166));
#190319=CARTESIAN_POINT('Ctrl Pts',(-255.820349002309,2.99217964199006,
135.78618647082));
#190320=CARTESIAN_POINT('Ctrl Pts',(-256.098796626121,5.80869814913581,
130.979749546569));
#190321=CARTESIAN_POINT('Ctrl Pts',(-256.377244249934,3.28730143236016,
126.01214820295));
#190322=CARTESIAN_POINT('Ctrl Pts',(-256.655691873747,-2.25495451926359,
125.448338134603));
#190323=CARTESIAN_POINT('Ctrl Pts',(-256.93413949756,-5.72503666514098,
129.806484721847));
#190324=CARTESIAN_POINT('Ctrl Pts',(-257.212587121373,-3.93405347634203,
135.081566970265));
#190325=CARTESIAN_POINT('Ctrl Pts',(-257.491034745186,1.47206408278265,
136.426225506557));
#190326=CARTESIAN_POINT('Ctrl Pts',(-257.769482368999,5.52555616721843,
132.604438319186));
#190327=CARTESIAN_POINT('Ctrl Pts',(-258.047929992812,4.50108754276566,
127.128895412351));
#190328=CARTESIAN_POINT('Ctrl Pts',(-258.326377616624,-0.659198908970111,
125.030117734768));
#190329=CARTESIAN_POINT('Ctrl Pts',(-258.604825240438,-5.21458571703409,
128.239112839452));
#190330=CARTESIAN_POINT('Ctrl Pts',(-258.883272864251,-4.97637574492231,
133.802560593787));
#190331=CARTESIAN_POINT('Ctrl Pts',(-259.161720488063,-0.168236736403017,
136.616288572087));
#190332=CARTESIAN_POINT('Ctrl Pts',(-259.440168111876,4.80044487344316,
134.078525892203));
#190333=CARTESIAN_POINT('Ctrl Pts',(-259.672207798387,5.25516631655033,
129.4749169549));
#190334=CARTESIAN_POINT('Ctrl Pts',(-259.857849473896,3.17366342871357,
126.795179433485));
#190335=CARTESIAN_POINT('Ctrl Pts',(-259.9506752748,1.64266665146648,126.102093112095));
#190336=CARTESIAN_POINT('Ctrl Pts',(-259.997093138402,0.835778587061721,
125.962806053044));
#190337=CARTESIAN_POINT('Ctrl Pts',(210.385579563201,-2.29217962691353,
126.082387726892));
#190338=CARTESIAN_POINT('Ctrl Pts',(210.339169886847,-3.0789974560272,126.464330840008));
#190339=CARTESIAN_POINT('Ctrl Pts',(210.246352273192,-4.44507089109247,
127.629120819077));
#190340=CARTESIAN_POINT('Ctrl Pts',(210.060718784933,-5.78798125627161,
130.996088365878));
#190341=CARTESIAN_POINT('Ctrl Pts',(209.828679098422,-3.95783017776954,
135.586872998689));
#190342=CARTESIAN_POINT('Ctrl Pts',(209.550231474609,1.89393692750204,136.720289837399));
#190343=CARTESIAN_POINT('Ctrl Pts',(209.271783850796,5.99602695027556,132.40812259401));
#190344=CARTESIAN_POINT('Ctrl Pts',(208.993336226983,4.59288360023261,126.626877830413));
#190345=CARTESIAN_POINT('Ctrl Pts',(208.71488860317,-1.03344059257722,124.682062423228));
#190346=CARTESIAN_POINT('Ctrl Pts',(208.436440979357,-5.70873650289865,
128.364647771496));
#190347=CARTESIAN_POINT('Ctrl Pts',(208.157993355544,-5.13869562717284,
134.288517668348));
#190348=CARTESIAN_POINT('Ctrl Pts',(207.879545731732,0.153933173725622,
137.010984097728));
#190349=CARTESIAN_POINT('Ctrl Pts',(207.601098107919,5.30490488755997,134.029672582798));
#190350=CARTESIAN_POINT('Ctrl Pts',(207.322650484106,5.58103410012833,128.084559773234));
#190351=CARTESIAN_POINT('Ctrl Pts',(207.044202860293,0.728409521696789,
124.638756607567));
#190352=CARTESIAN_POINT('Ctrl Pts',(206.76575523648,-4.79355811073501,126.858871164077));
#190353=CARTESIAN_POINT('Ctrl Pts',(206.487307612667,-5.91049575314416,
132.704682504842));
#190354=CARTESIAN_POINT('Ctrl Pts',(206.208859988854,-1.59596820864792,
136.804198957117));
#190355=CARTESIAN_POINT('Ctrl Pts',(205.930412365042,4.1851717387407,135.390152799229));
#190356=CARTESIAN_POINT('Ctrl Pts',(205.651964741228,6.12034565262566,129.76198992389));
#190357=CARTESIAN_POINT('Ctrl Pts',(205.373517117416,2.43121966936229,125.091713591677));
#190358=CARTESIAN_POINT('Ctrl Pts',(205.095069493603,-3.49207776276838,
125.671081434371));
#190359=CARTESIAN_POINT('Ctrl Pts',(204.81662186979,-6.20632667560231,130.96768173473));
#190360=CARTESIAN_POINT('Ctrl Pts',(204.538174245977,-3.21726438559061,
136.114198085604));
#190361=CARTESIAN_POINT('Ctrl Pts',(204.259726622164,2.72830660529182,136.381233108793));
#190362=CARTESIAN_POINT('Ctrl Pts',(203.981278998351,6.16669716267351,131.523394807979));
#190363=CARTESIAN_POINT('Ctrl Pts',(203.702831374538,3.9381942601484,126.004799186432));
#190364=CARTESIAN_POINT('Ctrl Pts',(203.424383750725,-1.909316761502,124.896766062528));
#190365=CARTESIAN_POINT('Ctrl Pts',(203.145936126912,-6.00225896230248,
129.217523725228));
#190366=CARTESIAN_POINT('Ctrl Pts',(202.867488503099,-4.57941839934143,
134.996506974633));
#190367=CARTESIAN_POINT('Ctrl Pts',(202.589040879287,1.05168395343957,136.923112517541));
#190368=CARTESIAN_POINT('Ctrl Pts',(202.310593255474,5.71634013176502,133.226883983125));
#190369=CARTESIAN_POINT('Ctrl Pts',(202.032145631661,5.12795898713612,127.30447482202));
#190370=CARTESIAN_POINT('Ctrl Pts',(201.753698007848,-0.172765951628197,
124.598289728405));
#190371=CARTESIAN_POINT('Ctrl Pts',(201.475250384035,-5.31472742110118,
127.595180598346));
#190372=CARTESIAN_POINT('Ctrl Pts',(201.196802760222,-5.57271402936141,
133.541151128878));
#190373=CARTESIAN_POINT('Ctrl Pts',(200.918355136409,-0.709648686901125,
136.972144879116));
#190374=CARTESIAN_POINT('Ctrl Pts',(200.639907512596,4.80554913058071,134.735246206027));
#190375=CARTESIAN_POINT('Ctrl Pts',(200.361459888783,5.90468206117194,128.886055711564));
#190376=CARTESIAN_POINT('Ctrl Pts',(200.083012264971,1.57770063730838,124.799693711321));
#190377=CARTESIAN_POINT('Ctrl Pts',(199.804564641158,-4.19911059728431,
126.231327253625));
#190378=CARTESIAN_POINT('Ctrl Pts',(199.526117017345,-6.11714433092778,
131.865355052293));
#190379=CARTESIAN_POINT('Ctrl Pts',(199.247669393532,-2.4138212635637,136.524380797905));
#190380=CARTESIAN_POINT('Ctrl Pts',(198.969221769719,3.50768562329156,135.926987436306));
#190381=CARTESIAN_POINT('Ctrl Pts',(198.690774145906,6.20580078231077,130.622150282517));
#190382=CARTESIAN_POINT('Ctrl Pts',(198.412326522093,3.20108819260905,125.484755525167));
#190383=CARTESIAN_POINT('Ctrl Pts',(198.13387889828,-2.74526806424844,125.235817970576));
#190384=CARTESIAN_POINT('Ctrl Pts',(197.855431274468,-6.16885708386238,
130.104099070135));
#190385=CARTESIAN_POINT('Ctrl Pts',(197.576983650655,-3.92356780882929,
135.615886322105));
#190386=CARTESIAN_POINT('Ctrl Pts',(197.298536026841,1.92728860557448,136.706116507701));
#190387=CARTESIAN_POINT('Ctrl Pts',(197.020088403029,6.00706094473797,132.372921347066));
#190388=CARTESIAN_POINT('Ctrl Pts',(196.741640779216,4.56663773692898,126.598295504472));
#190389=CARTESIAN_POINT('Ctrl Pts',(196.463193155403,-1.07030245846182,
124.688838023107));
#190390=CARTESIAN_POINT('Ctrl Pts',(196.184745531591,-5.72368698170812,
128.399247046161));
#190391=CARTESIAN_POINT('Ctrl Pts',(195.906297907777,-5.11728278641862,
134.319837945007));
#190392=CARTESIAN_POINT('Ctrl Pts',(195.627850283965,0.191654296427489,
137.009876920548));
#190393=CARTESIAN_POINT('Ctrl Pts',(195.349402660151,5.32447044368961,133.997349569974));
#190394=CARTESIAN_POINT('Ctrl Pts',(195.070955036339,5.56435836804288,128.050621358318));
#190395=CARTESIAN_POINT('Ctrl Pts',(194.792507412526,0.690872786183208,
124.634444998269));
#190396=CARTESIAN_POINT('Ctrl Pts',(194.514059788713,-4.81749113516689,
126.888119675218));
#190397=CARTESIAN_POINT('Ctrl Pts',(194.2356121649,-5.89881605082435,132.740628459178));
#190398=CARTESIAN_POINT('Ctrl Pts',(193.957164541087,-1.55941718895885,
136.81380168864));
#190399=CARTESIAN_POINT('Ctrl Pts',(193.678716917274,4.21300988779493,135.364592151301));
#190400=CARTESIAN_POINT('Ctrl Pts',(193.400269293461,6.11388669464029,129.724752614155));
#190401=CARTESIAN_POINT('Ctrl Pts',(193.121821669648,2.39640030908087,125.077020090361));
#190402=CARTESIAN_POINT('Ctrl Pts',(192.843374045836,-3.52326088986039,
125.692433714928));
#190403=CARTESIAN_POINT('Ctrl Pts',(192.564926422022,-6.20521745188322,
131.005458431507));
#190404=CARTESIAN_POINT('Ctrl Pts',(192.28647879821,-3.1848823173506,136.133684081248));
#190405=CARTESIAN_POINT('Ctrl Pts',(192.008031174397,2.76220407667619,136.36452181979));
#190406=CARTESIAN_POINT('Ctrl Pts',(191.729583550584,6.17095986540858,131.485843042463));
#190407=CARTESIAN_POINT('Ctrl Pts',(191.451135926771,3.90890500597959,125.980915208923));
#190408=CARTESIAN_POINT('Ctrl Pts',(191.172688302958,-1.94524259331895,
124.908498067517));
#190409=CARTESIAN_POINT('Ctrl Pts',(190.894240679145,-6.01180727974115,
129.254090580708));
#190410=CARTESIAN_POINT('Ctrl Pts',(190.615793055332,-4.5538147691942,135.024305522869));
#190411=CARTESIAN_POINT('Ctrl Pts',(190.337345431519,1.08891104802307,136.916597252826));
#190412=CARTESIAN_POINT('Ctrl Pts',(190.058897807707,5.73098080836918,133.192042114338));
#190413=CARTESIAN_POINT('Ctrl Pts',(189.780450183893,5.10655917980125,127.273324325042));
#190414=CARTESIAN_POINT('Ctrl Pts',(189.502002560081,-0.210540865719208,
124.599456387862));
#190415=CARTESIAN_POINT('Ctrl Pts',(189.223554936268,-5.33416414113684,
127.627592311355));
#190416=CARTESIAN_POINT('Ctrl Pts',(188.945107312455,-5.55595115925501,
133.575023114497));
#190417=CARTESIAN_POINT('Ctrl Pts',(188.666659688642,-0.672090485321342,
136.976350437346));
#190418=CARTESIAN_POINT('Ctrl Pts',(188.388212064829,4.82938851117716,134.705920634282));
#190419=CARTESIAN_POINT('Ctrl Pts',(188.109764441016,5.89289539464864,128.850147777659));
#190420=CARTESIAN_POINT('Ctrl Pts',(187.831316817203,1.54111929438253,124.790201052305));
#190421=CARTESIAN_POINT('Ctrl Pts',(187.552869193391,-4.22687014955807,
126.256973159398));
#190422=CARTESIAN_POINT('Ctrl Pts',(187.274421569578,-6.11057242014135,
131.902572188318));
#190423=CARTESIAN_POINT('Ctrl Pts',(186.995973945765,-2.37895715467313,
136.538968434335));
#190424=CARTESIAN_POINT('Ctrl Pts',(186.717526321952,3.53880351742172,135.905540247907));
#190425=CARTESIAN_POINT('Ctrl Pts',(186.439078698139,6.20457663716883,130.584377187674));
#190426=CARTESIAN_POINT('Ctrl Pts',(186.160631074326,3.16864693777749,125.465368152723));
#190427=CARTESIAN_POINT('Ctrl Pts',(185.882183450513,-2.77911450042273,
125.25263236868));
#190428=CARTESIAN_POINT('Ctrl Pts',(185.6037358267,-6.17300548002561,130.14166362836));
#190429=CARTESIAN_POINT('Ctrl Pts',(185.325288202887,-3.89420599156785,
135.639681046572));
#190430=CARTESIAN_POINT('Ctrl Pts',(185.046840579075,1.96317856060187,136.694275209062));
#190431=CARTESIAN_POINT('Ctrl Pts',(184.768392955261,6.0164979221829,132.336325600291));
#190432=CARTESIAN_POINT('Ctrl Pts',(184.489945331449,4.54094961554151,126.570575013045));
#190433=CARTESIAN_POINT('Ctrl Pts',(184.211497707636,-1.10750955006109,
124.695466564429));
#190434=CARTESIAN_POINT('Ctrl Pts',(183.933050083823,-5.73822154400692,
128.434133314579));
#190435=CARTESIAN_POINT('Ctrl Pts',(183.65460246001,-5.09578826671723,134.350923164133));
#190436=CARTESIAN_POINT('Ctrl Pts',(183.376154836197,0.229425484589131,
137.008595292604));
#190437=CARTESIAN_POINT('Ctrl Pts',(183.097707212384,5.34380842361613,133.964878848429));
#190438=CARTESIAN_POINT('Ctrl Pts',(182.819259588571,5.54749248089459,128.016800549989));
#190439=CARTESIAN_POINT('Ctrl Pts',(182.540811964758,0.653301958305029,
124.630353773773));
#190440=CARTESIAN_POINT('Ctrl Pts',(182.262364340946,-4.84124114839195,
126.917517669999));
#190441=CARTESIAN_POINT('Ctrl Pts',(181.983916717133,-5.88692014749505,
132.776500352206));
#190442=CARTESIAN_POINT('Ctrl Pts',(181.70546909332,-1.52280712308763,136.82318296266));
#190443=CARTESIAN_POINT('Ctrl Pts',(181.427021469507,4.24069125417353,135.33886187379));
#190444=CARTESIAN_POINT('Ctrl Pts',(181.148573845694,6.10720153813428,129.687555653153));
#190445=CARTESIAN_POINT('Ctrl Pts',(180.870126221881,2.36149196193127,125.062538635854));
#190446=CARTESIAN_POINT('Ctrl Pts',(180.591678598068,-3.55431336199069,
125.713975516152));
#190447=CARTESIAN_POINT('Ctrl Pts',(180.313230974255,-6.20387834410407,
131.04322762551));
#190448=CARTESIAN_POINT('Ctrl Pts',(180.034783350442,-3.15238220429199,
136.15297262387));
#190449=CARTESIAN_POINT('Ctrl Pts',(179.75633572663,2.79599917883219,136.347604482659));
#190450=CARTESIAN_POINT('Ctrl Pts',(179.477888102817,6.17499390876314,131.448266031944));
#190451=CARTESIAN_POINT('Ctrl Pts',(179.199440479004,3.8794709017638,125.957209961944));
#190452=CARTESIAN_POINT('Ctrl Pts',(178.920992855191,-1.98109634126673,
124.920448547985));
#190453=CARTESIAN_POINT('Ctrl Pts',(178.642545231378,-6.02113282860982,
129.290714880887));
#190454=CARTESIAN_POINT('Ctrl Pts',(178.364097607565,-4.52804239515191,
135.051947700091));
#190455=CARTESIAN_POINT('Ctrl Pts',(178.085649983752,1.12609779228193,136.909855496619));
#190456=CARTESIAN_POINT('Ctrl Pts',(177.807202359939,5.74540912154417,133.157111769304));
#190457=CARTESIAN_POINT('Ctrl Pts',(177.528754736127,5.08497014694685,127.242304671825));
#190458=CARTESIAN_POINT('Ctrl Pts',(177.250307112313,-0.248307978092709,
124.600852972375));
#190459=CARTESIAN_POINT('Ctrl Pts',(176.971859488501,-5.35340320178418,
127.660121740658));
#190460=CARTESIAN_POINT('Ctrl Pts',(176.693411864688,-5.53898241132168,
133.608792432211));
#190461=CARTESIAN_POINT('Ctrl Pts',(176.414964240875,-0.634507379188621,
136.980327290216));
#190462=CARTESIAN_POINT('Ctrl Pts',(176.136516617062,4.85304893701009,134.676450488799));
#190463=CARTESIAN_POINT('Ctrl Pts',(175.858068993249,5.88089036471739,128.814312257825));
#190464=CARTESIAN_POINT('Ctrl Pts',(175.579621369436,1.50448084471559,124.780931250186));
#190465=CARTESIAN_POINT('Ctrl Pts',(175.301173745623,-4.25447307360455,
126.282787570284));
#190466=CARTESIAN_POINT('Ctrl Pts',(175.02272612181,-6.10377407984646,131.939748629711));
#190467=CARTESIAN_POINT('Ctrl Pts',(174.744278497998,-2.34400489265046,
136.553343572764));
#190468=CARTESIAN_POINT('Ctrl Pts',(174.465830874185,3.56979027988629,135.883904033421));
#190469=CARTESIAN_POINT('Ctrl Pts',(174.187383250372,6.20312257915782,130.546612244398));
#190470=CARTESIAN_POINT('Ctrl Pts',(173.908935626559,3.13608826756835,125.446178618609));
#190471=CARTESIAN_POINT('Ctrl Pts',(173.630488002746,-2.81285795548731,
125.269652488117));
#190472=CARTESIAN_POINT('Ctrl Pts',(173.352040378933,-6.17692513320066,
130.179252743065));
#190473=CARTESIAN_POINT('Ctrl Pts',(173.07359275512,-3.86469987307124,135.663296596462));
#190474=CARTESIAN_POINT('Ctrl Pts',(172.795145131307,1.99899576932572,136.682215657471));
#190475=CARTESIAN_POINT('Ctrl Pts',(172.516697507494,6.02571195608475,132.29967308599));
#190476=CARTESIAN_POINT('Ctrl Pts',(172.238249883681,4.51509322759614,126.543011406101));
#190477=CARTESIAN_POINT('Ctrl Pts',(171.959802259869,-1.14467560248665,
124.702321473066));
#190478=CARTESIAN_POINT('Ctrl Pts',(171.681354636056,-5.75254347439624,
128.469107412642));
#190479=CARTESIAN_POINT('Ctrl Pts',(171.402907012243,-5.07410492070761,
134.38187696408));
#190480=CARTESIAN_POINT('Ctrl Pts',(171.12445938843,0.267188171305193,137.007083764462));
#190481=CARTESIAN_POINT('Ctrl Pts',(170.846011764617,5.36294838675633,133.932291012718));
#190482=CARTESIAN_POINT('Ctrl Pts',(170.567564140804,5.53042102937231,127.983083035723));
#190483=CARTESIAN_POINT('Ctrl Pts',(170.289116516991,0.615706922082464,
124.62649132937));
#190484=CARTESIAN_POINT('Ctrl Pts',(170.010668893178,-4.86481176764585,
126.947059693175));
#190485=CARTESIAN_POINT('Ctrl Pts',(169.732221269365,-5.87480610217478,
132.812299166869));
#190486=CARTESIAN_POINT('Ctrl Pts',(169.453773645553,-1.48614062903852,
136.832341207004));
#190487=CARTESIAN_POINT('Ctrl Pts',(169.17532602174,4.26821548017818,135.312963568669));
#190488=CARTESIAN_POINT('Ctrl Pts',(168.896878397927,6.10029007702938,129.650400075769));
#190489=CARTESIAN_POINT('Ctrl Pts',(168.618430774114,2.32649610882855,125.048269946673));
#190490=CARTESIAN_POINT('Ctrl Pts',(168.339983150301,-3.58523412773234,
125.735705943466));
#190491=CARTESIAN_POINT('Ctrl Pts',(168.061535526488,-6.2023093493314,131.08098796821));
#190492=CARTESIAN_POINT('Ctrl Pts',(167.783087902675,-3.11976527855146,
136.172062971709));
#190493=CARTESIAN_POINT('Ctrl Pts',(167.504640278862,2.82969067421049,136.330481738588));
#190494=CARTESIAN_POINT('Ctrl Pts',(167.22619265505,6.17879913544756,131.410665161273));
#190495=CARTESIAN_POINT('Ctrl Pts',(166.947745031236,3.84989304232704,125.933684327914));
#190496=CARTESIAN_POINT('Ctrl Pts',(166.669297407424,-2.01687667896098,
124.93261705898));
#190497=CARTESIAN_POINT('Ctrl Pts',(166.39084978361,-6.03023526218728,129.327395269766));
#190498=CARTESIAN_POINT('Ctrl Pts',(166.112402159798,-4.50210223283349,
135.079432481411));
#190499=CARTESIAN_POINT('Ctrl Pts',(165.833954535985,1.16324280857304,136.902887499053));
#190500=CARTESIAN_POINT('Ctrl Pts',(165.555506912173,5.75962453647134,133.122094242209));
#190501=CARTESIAN_POINT('Ctrl Pts',(165.277059288359,5.06319268865361,127.2114170119));
#190502=CARTESIAN_POINT('Ctrl Pts',(164.998611664547,-0.286065889322858,
124.602479430144));
#190503=CARTESIAN_POINT('Ctrl Pts',(164.720164040733,-5.37244389010723,
127.692767680889));
#190504=CARTESIAN_POINT('Ctrl Pts',(164.441716416921,-5.52180841435808,
133.642457830674));
#190505=CARTESIAN_POINT('Ctrl Pts',(164.163268793108,-0.596900761151562,
136.984075290369));
#190506=CARTESIAN_POINT('Ctrl Pts',(163.884821169295,4.87652953132996,134.646836861603));
#190507=CARTESIAN_POINT('Ctrl Pts',(163.606373545482,5.86866741623098,128.778550479967));
#190508=CARTESIAN_POINT('Ctrl Pts',(163.327925921669,1.46778664595768,124.771884648456));
#190509=CARTESIAN_POINT('Ctrl Pts',(163.049478297856,-4.28191834658676,
126.308769529723));
#190510=CARTESIAN_POINT('Ctrl Pts',(162.771030674043,-6.09674956195837,
131.976882998882));
#190511=CARTESIAN_POINT('Ctrl Pts',(162.49258305023,-2.30896577266445,136.567505680515));
#190512=CARTESIAN_POINT('Ctrl Pts',(162.214135426418,3.60064476245918,135.862079594585));
#190513=CARTESIAN_POINT('Ctrl Pts',(161.935687802605,6.20143866215845,130.508856852083));
#190514=CARTESIAN_POINT('Ctrl Pts',(161.657240178792,3.10341338845521,125.427187633898));
#190515=CARTESIAN_POINT('Ctrl Pts',(161.378792554979,-2.84649717906582,
125.2868776982));
#190516=CARTESIAN_POINT('Ctrl Pts',(161.100344931166,-6.18061589814333,
130.216865021372));
#190517=CARTESIAN_POINT('Ctrl Pts',(160.821897307353,-3.83505054669964,
135.686732096692));
#190518=CARTESIAN_POINT('Ctrl Pts',(160.54344968354,2.0347389045262,136.6699382998));
#190519=CARTESIAN_POINT('Ctrl Pts',(160.265002059727,6.03470270501411,132.262965162335));
#190520=CARTESIAN_POINT('Ctrl Pts',(159.986554435914,4.48906953121078,126.51560570502));
#190521=CARTESIAN_POINT('Ctrl Pts',(159.708106812101,-1.18179923853688,
124.709402495009));
#190522=CARTESIAN_POINT('Ctrl Pts',(159.429659188289,-5.76665224217155,
128.50416804437));
#190523=CARTESIAN_POINT('Ctrl Pts',(159.151211564475,-5.05223355187421,
134.412698197843));
#190524=CARTESIAN_POINT('Ctrl Pts',(158.872763940663,0.304940957265202,
137.005342392132));
#190525=CARTESIAN_POINT('Ctrl Pts',(158.59431631685,5.38188962387183,133.899587270395));
#190526=CARTESIAN_POINT('Ctrl Pts',(158.315868693037,5.51314464606502,127.949470064936));
#190527=CARTESIAN_POINT('Ctrl Pts',(158.037421069224,0.57808907061355,124.622857808186));
#190528=CARTESIAN_POINT('Ctrl Pts',(157.758973445411,-4.88820211951067,
126.976744650055));
#190529=CARTESIAN_POINT('Ctrl Pts',(157.480525821598,-5.86247436375394,
132.848023576631));
#190530=CARTESIAN_POINT('Ctrl Pts',(157.202078197785,-1.44941906550188,
136.841276082311));
#190531=CARTESIAN_POINT('Ctrl Pts',(156.923630573973,4.29558154588865,135.286898195607));
#190532=CARTESIAN_POINT('Ctrl Pts',(156.645182950159,6.09315256743229,129.613287258817));
#190533=CARTESIAN_POINT('Ctrl Pts',(156.366735326347,2.29141404655692,125.034214551549));
#190534=CARTESIAN_POINT('Ctrl Pts',(156.088287702534,-3.61602204130483,
125.757624191644));
#190535=CARTESIAN_POINT('Ctrl Pts',(155.809840078721,-6.2005105257049,131.11873806038));
#190536=CARTESIAN_POINT('Ctrl Pts',(155.531392454908,-3.08703274876129,
136.190954417361));
#190537=CARTESIAN_POINT('Ctrl Pts',(155.252944831095,2.86327731436015,136.313154222067));
#190538=CARTESIAN_POINT('Ctrl Pts',(154.974497207282,6.18237540445775,131.373041823765));
#190539=CARTESIAN_POINT('Ctrl Pts',(154.696049583469,3.82017252368788,125.910339178587));
#190540=CARTESIAN_POINT('Ctrl Pts',(154.417601959656,-2.05258228054818,
124.945003149591));
#190541=CARTESIAN_POINT('Ctrl Pts',(154.139154335844,-6.03911424317947,
129.364130388138));
#190542=CARTESIAN_POINT('Ctrl Pts',(153.860706712031,-4.47599524346119,
135.106758848372));
#190543=CARTESIAN_POINT('Ctrl Pts',(153.582259088218,1.20034472047403,136.895693518332));
#190544=CARTESIAN_POINT('Ctrl Pts',(153.303811464405,5.77362652639317,133.086990830643));
#190545=CARTESIAN_POINT('Ctrl Pts',(153.025363840592,5.04122761189337,127.180662489822));
#190546=CARTESIAN_POINT('Ctrl Pts',(152.746916216779,-0.323813200276178,
124.604335700902));
#190547=CARTESIAN_POINT('Ctrl Pts',(152.468468592966,-5.39128550054617,
127.725528922339));
#190548=CARTESIAN_POINT('Ctrl Pts',(152.190020969154,-5.5044298047531,133.6760180624));
#190549=CARTESIAN_POINT('Ctrl Pts',(151.91157334534,-0.55927202473736,136.987594298923));
#190550=CARTESIAN_POINT('Ctrl Pts',(151.633125721528,4.89982942405471,134.617080850036));
#190551=CARTESIAN_POINT('Ctrl Pts',(151.354678097715,5.85622700211526,128.742863769248));
#190552=CARTESIAN_POINT('Ctrl Pts',(151.076230473902,1.43103805782584,124.763061582343));
#190553=CARTESIAN_POINT('Ctrl Pts',(150.797782850089,-4.3092049515099,126.334918074943));
#190554=CARTESIAN_POINT('Ctrl Pts',(150.519335226276,-6.0894991267732,132.013973919806));
#190555=CARTESIAN_POINT('Ctrl Pts',(150.240887602463,-2.27384109310269,
136.581454232806));
#190556=CARTESIAN_POINT('Ctrl Pts',(149.96243997865,3.63136582181627,135.840067740113));
#190557=CARTESIAN_POINT('Ctrl Pts',(149.683992354837,6.19952494856889,130.471112409769));
#190558=CARTESIAN_POINT('Ctrl Pts',(149.405544731024,3.0706235112177,125.40839590231));
#190559=CARTESIAN_POINT('Ctrl Pts',(149.127097107212,-2.88003092464457,
125.30430736064));
#190560=CARTESIAN_POINT('Ctrl Pts',(148.848649483398,-6.18407763809098,
130.254499069545));
#190561=CARTESIAN_POINT('Ctrl Pts',(148.570201859586,-3.80525911111971,
135.709986678852));
#190562=CARTESIAN_POINT('Ctrl Pts',(148.291754235773,2.07040664172831,136.657443590992));
#190563=CARTESIAN_POINT('Ctrl Pts',(148.01330661196,6.04346983581547,132.226203189553));
#190564=CARTESIAN_POINT('Ctrl Pts',(147.734858988147,4.46287949070312,126.488358925329));
#190565=CARTESIAN_POINT('Ctrl Pts',(147.456411364334,-1.21887908258166,
124.716709367866));
#190566=CARTESIAN_POINT('Ctrl Pts',(147.177963740522,-5.78054732452736,
128.53931391058));
#190567=CARTESIAN_POINT('Ctrl Pts',(146.899516116708,-5.03017497066859,
134.44338572333));
#190568=CARTESIAN_POINT('Ctrl Pts',(146.621068492896,0.342682443525903,
137.003371240143));
#190569=CARTESIAN_POINT('Ctrl Pts',(146.342620869082,5.40063143308812,133.866768833311));
#190570=CARTESIAN_POINT('Ctrl Pts',(146.06417324527,5.49566397115542,127.915962883168));
#190571=CARTESIAN_POINT('Ctrl Pts',(145.785725621457,0.540449797841529,
124.619453344862));
#190572=CARTESIAN_POINT('Ctrl Pts',(145.507277997644,-4.91141133724831,
127.006571440652));
#190573=CARTESIAN_POINT('Ctrl Pts',(145.228830373831,-5.84992538918966,
132.883672257711));
#190574=CARTESIAN_POINT('Ctrl Pts',(144.950382750018,-1.41264379320865,
136.849987257496));
#190575=CARTESIAN_POINT('Ctrl Pts',(144.671935126205,4.32278843724517,135.260666720466));
#190576=CARTESIAN_POINT('Ctrl Pts',(144.393487502392,6.08578927382608,129.576218577526));
#190577=CARTESIAN_POINT('Ctrl Pts',(144.11503987858,2.25624707509518,125.020372971309));
#190578=CARTESIAN_POINT('Ctrl Pts',(143.836592254767,-3.64667596185081,
125.779729448496));
#190579=CARTESIAN_POINT('Ctrl Pts',(143.558144630954,-6.19848193988065,
131.156476503179));
#190580=CARTESIAN_POINT('Ctrl Pts',(143.279697007141,-3.05418582783736,
136.209646260801));
#190581=CARTESIAN_POINT('Ctrl Pts',(143.001249383328,2.89675785471595,136.295622575173));
#190582=CARTESIAN_POINT('Ctrl Pts',(142.722801759515,6.18572258327378,131.335397413564));
#190583=CARTESIAN_POINT('Ctrl Pts',(142.444354135702,3.79031044715096,125.887175379022));
#190584=CARTESIAN_POINT('Ctrl Pts',(142.165906511889,-2.0882118229442,124.957606360848));
#190585=CARTESIAN_POINT('Ctrl Pts',(141.887458888076,-6.04776944257254,
129.400918874772));
#190586=CARTESIAN_POINT('Ctrl Pts',(141.609011264264,-4.44972239443904,
135.133925788383));
#190587=CARTESIAN_POINT('Ctrl Pts',(141.33056364045,1.2374021531599,136.888273821029));
#190588=CARTESIAN_POINT('Ctrl Pts',(141.052116016638,5.78741457246075,133.051802835376));
#190589=CARTESIAN_POINT('Ctrl Pts',(140.773668392825,5.01907573059014,127.15004224521));
#190590=CARTESIAN_POINT('Ctrl Pts',(140.495220769012,-0.361548512212229,
124.606421715863));
#190591=CARTESIAN_POINT('Ctrl Pts',(140.216773145199,-5.4099273349182,127.758404251031));
#190592=CARTESIAN_POINT('Ctrl Pts',(139.938325521386,-5.48684722647749,
133.709471883804));
#190593=CARTESIAN_POINT('Ctrl Pts',(139.659877897573,-0.521622564292735,
136.990884185479));
#190594=CARTESIAN_POINT('Ctrl Pts',(139.38143027376,4.92294775179823,134.58718355672));
#190595=CARTESIAN_POINT('Ctrl Pts',(139.102982649947,5.84356958335437,128.707253448052));
#190596=CARTESIAN_POINT('Ctrl Pts',(138.824535026135,1.39423644205237,124.754462378786));
#190597=CARTESIAN_POINT('Ctrl Pts',(138.546087402322,-4.33633187725888,
126.361232236999));
#190598=CARTESIAN_POINT('Ctrl Pts',(138.267639778509,-6.08202304295846,
132.051020018064));
#190599=CARTESIAN_POINT('Ctrl Pts',(137.989192154696,-2.23863215552307,
136.595188712768));
#190600=CARTESIAN_POINT('Ctrl Pts',(137.710744530883,3.66195231957746,135.817869285661));
#190601=CARTESIAN_POINT('Ctrl Pts',(137.43229690707,6.19738150930245,130.433380316089));
#190602=CARTESIAN_POINT('Ctrl Pts',(137.153849283257,3.03771985089675,125.389804120178));
#190603=CARTESIAN_POINT('Ctrl Pts',(136.875401659444,-2.91345794961824,
125.321940829576));
#190604=CARTESIAN_POINT('Ctrl Pts',(136.596954035631,-6.1873102247676,130.29215349304));
#190605=CARTESIAN_POINT('Ctrl Pts',(136.318506411819,-3.77532667026395,
135.733059481234));
#190606=CARTESIAN_POINT('Ctrl Pts',(136.040058788006,2.10599765925102,136.644731994041));
#190607=CARTESIAN_POINT('Ctrl Pts',(135.761611164193,6.05201302361958,132.189388529871));
#190608=CARTESIAN_POINT('Ctrl Pts',(135.48316354038,4.4365240765547,126.461272076668));
#190609=CARTESIAN_POINT('Ctrl Pts',(135.204715916567,-1.25591376061384,
124.724241820878));
#190610=CARTESIAN_POINT('Ctrl Pts',(134.926268292754,-5.79422820657625,
128.574543708929));
#190611=CARTESIAN_POINT('Ctrl Pts',(134.647820668941,-5.00792999447956,
134.473938403405));
#190612=CARTESIAN_POINT('Ctrl Pts',(134.369373045128,0.380411231562576,
137.001170381535));
#190613=CARTESIAN_POINT('Ctrl Pts',(134.090925421316,5.41917311992063,133.833836917565));
#190614=CARTESIAN_POINT('Ctrl Pts',(133.812477797503,5.4779796523963,127.88256273204));
#190615=CARTESIAN_POINT('Ctrl Pts',(133.53403017369,0.502790498503515,124.616278065551));
#190616=CARTESIAN_POINT('Ctrl Pts',(133.255582549877,-4.93443856083268,
127.036538959725));
#190617=CARTESIAN_POINT('Ctrl Pts',(132.977134926064,-5.83715964348875,
132.919243889133));
#190618=CARTESIAN_POINT('Ctrl Pts',(132.698687302251,-1.37581617488021,
136.858474409763));
#190619=CARTESIAN_POINT('Ctrl Pts',(132.420239678438,4.34983514608645,135.234270115264));
#190620=CARTESIAN_POINT('Ctrl Pts',(132.141792054625,6.07820046906025,129.539195405491));
#190621=CARTESIAN_POINT('Ctrl Pts',(131.863344430812,2.22099649756843,125.006745718858));
#190622=CARTESIAN_POINT('Ctrl Pts',(131.584896806999,-3.67719475347803,
125.802020894903));
#190623=CARTESIAN_POINT('Ctrl Pts',(131.306449183186,-6.1962236670286,131.194201898194));
#190624=CARTESIAN_POINT('Ctrl Pts',(131.028001559374,-3.02122573293442,
136.228137809392));
#190625=CARTESIAN_POINT('Ctrl Pts',(130.749553935561,2.93013105464412,136.277887447547));
#190626=CARTESIAN_POINT('Ctrl Pts',(130.471106311748,6.18884054786473,131.2977333256));
#190627=CARTESIAN_POINT('Ctrl Pts',(130.192658687935,3.76030791926647,125.864193787566));
#190628=CARTESIAN_POINT('Ctrl Pts',(129.914211064122,-2.12376398588317,
124.970426225734));
#190629=CARTESIAN_POINT('Ctrl Pts',(129.635763440309,-6.05620053964477,
129.437759366456));
#190630=CARTESIAN_POINT('Ctrl Pts',(129.357315816496,-4.42328465931731,
135.160932294765));
#190631=CARTESIAN_POINT('Ctrl Pts',(129.078868192683,1.27441373345414,136.880628682086));
#190632=CARTESIAN_POINT('Ctrl Pts',(128.800420568871,5.80098816375315,133.01653156031));
#190633=CARTESIAN_POINT('Ctrl Pts',(128.521972945058,4.99673786558976,127.11955741271));
#190634=CARTESIAN_POINT('Ctrl Pts',(128.243525321245,-0.399270426835251,
124.608737397728));
#190635=CARTESIAN_POINT('Ctrl Pts',(127.965077697432,-5.42836870244348,
127.791392448756));
#190636=CARTESIAN_POINT('Ctrl Pts',(127.686630073619,-5.46906133106002,
133.742818055242));
#190637=CARTESIAN_POINT('Ctrl Pts',(127.408182449806,-0.483953774931917,
136.993944828129));
#190638=CARTESIAN_POINT('Ctrl Pts',(127.129734825993,4.9458836579024,134.557146089508));
#190639=CARTESIAN_POINT('Ctrl Pts',(126.85128720218,5.8306956289736,128.671720835934));
#190640=CARTESIAN_POINT('Ctrl Pts',(126.572839578367,1.35738316233494,124.746087356435));
#190641=CARTESIAN_POINT('Ctrl Pts',(126.294391954555,-4.36329811863544,
126.387711040812));
#190642=CARTESIAN_POINT('Ctrl Pts',(126.015944330741,-6.07432158754323,
132.088019920899));
#190643=CARTESIAN_POINT('Ctrl Pts',(125.737496706929,-2.20334026460562,
136.608708611466));
#190644=CARTESIAN_POINT('Ctrl Pts',(125.459049083116,3.69240312234872,135.795485053802));
#190645=CARTESIAN_POINT('Ctrl Pts',(125.180601459303,6.19500842378515,130.39566196922));
#190646=CARTESIAN_POINT('Ctrl Pts',(124.90215383549,3.00470362674961,125.371412976429));
#190647=CARTESIAN_POINT('Ctrl Pts',(124.623706211677,-2.9467770153362,125.339777451594));
#190648=CARTESIAN_POINT('Ctrl Pts',(124.345258587864,-6.19031353838844,
130.329826896558));
#190649=CARTESIAN_POINT('Ctrl Pts',(124.066810964051,-3.74525433329013,
135.755949648866));
#190650=CARTESIAN_POINT('Ctrl Pts',(123.788363340238,2.14151063825588,136.631803979981));
#190651=CARTESIAN_POINT('Ctrl Pts',(123.509915716426,6.0603319518555,132.152522547471));
#190652=CARTESIAN_POINT('Ctrl Pts',(123.231468092613,4.4100042653751,126.43434616275));
#190653=CARTESIAN_POINT('Ctrl Pts',(122.9530204688,-1.29290190029971,124.731999574929));
#190654=CARTESIAN_POINT('Ctrl Pts',(122.674572844987,-5.80769438136815,
128.609856133963));
#190655=CARTESIAN_POINT('Ctrl Pts',(122.396125221174,-4.98549944760296,
134.504355105923));
#190656=CARTESIAN_POINT('Ctrl Pts',(122.117677597361,0.418125923321227,
136.998739897863));
#190657=CARTESIAN_POINT('Ctrl Pts',(121.839229973548,5.43751399730024,133.80079274346));
#190658=CARTESIAN_POINT('Ctrl Pts',(121.560782349735,5.46009234508668,127.849270849208));
#190659=CARTESIAN_POINT('Ctrl Pts',(121.282334725922,0.465112568078527,
124.613332087916));
#190660=CARTESIAN_POINT('Ctrl Pts',(121.00388710211,-4.95728293698158,127.066646096814));
#190661=CARTESIAN_POINT('Ctrl Pts',(120.725439478297,-5.82417759969065,
132.954737152777));
#190662=CARTESIAN_POINT('Ctrl Pts',(120.446991854484,-1.33893757517749,
136.866737224615));
#190663=CARTESIAN_POINT('Ctrl Pts',(120.168544230671,4.37672067018674,135.207709358136));
#190664=CARTESIAN_POINT('Ctrl Pts',(119.890096606858,6.07038643434081,129.502219114618));
#190665=CARTESIAN_POINT('Ctrl Pts',(119.611648983045,2.18566362019961,124.993333299159));
#190666=CARTESIAN_POINT('Ctrl Pts',(119.333201359232,-3.7075772853013,125.82449770485));
#190667=CARTESIAN_POINT('Ctrl Pts',(119.054753735419,-6.19373579082994,
131.231912847497));
#190668=CARTESIAN_POINT('Ctrl Pts',(118.776306111606,-2.98815368540088,
136.246428377926));
#190669=CARTESIAN_POINT('Ctrl Pts',(118.497858487794,2.96339567748857,136.259949496373));
#190670=CARTESIAN_POINT('Ctrl Pts',(118.219410863981,6.1917291826932,131.26005095553));
#190671=CARTESIAN_POINT('Ctrl Pts',(117.940963240168,3.73016605178927,125.841395255808));
#190672=CARTESIAN_POINT('Ctrl Pts',(117.662515616355,-2.15923745196658,
124.983462269205));
#190673=CARTESIAN_POINT('Ctrl Pts',(117.384067992542,-6.06440722197891,
129.474650498052));
#190674=CARTESIAN_POINT('Ctrl Pts',(117.105620368729,-4.39668301775581,
135.187777366781));
#190675=CARTESIAN_POINT('Ctrl Pts',(116.827172744916,1.31137808987868,136.872758384795));
#190676=CARTESIAN_POINT('Ctrl Pts',(116.548725121103,5.81434679729579,132.981178312436));
#190677=CARTESIAN_POINT('Ctrl Pts',(116.27027749729,4.97421484463032,127.089209121948));
#190678=CARTESIAN_POINT('Ctrl Pts',(115.991829873478,-0.436977546345769,
124.611282660692));
#190679=CARTESIAN_POINT('Ctrl Pts',(115.713382249665,-5.44660891977013,
127.824492293124));
#190680=CARTESIAN_POINT('Ctrl Pts',(115.434934625852,-5.45107277756375,
133.776055341058));
#190681=CARTESIAN_POINT('Ctrl Pts',(115.156487002039,-0.446267052485976,
136.99677611346));
#190682=CARTESIAN_POINT('Ctrl Pts',(114.878039378226,4.9686362924688,134.526969561451));
#190683=CARTESIAN_POINT('Ctrl Pts',(114.599591754413,5.81760561602206,128.636267249567));
#190684=CARTESIAN_POINT('Ctrl Pts',(114.3211441306,1.32047958428524,124.737936825626));
#190685=CARTESIAN_POINT('Ctrl Pts',(114.042696506787,-4.39010267639563,
126.414353505198));
#190686=CARTESIAN_POINT('Ctrl Pts',(113.764248882975,-6.06639504590774,
132.124972257267));
#190687=CARTESIAN_POINT('Ctrl Pts',(113.485801259161,-2.16796672810439,
136.622013427915));
#190688=CARTESIAN_POINT('Ctrl Pts',(113.207353635349,3.72271710176439,135.772915873991));
#190689=CARTESIAN_POINT('Ctrl Pts',(112.928906011536,6.19240577995249,130.357958766832));
#190690=CARTESIAN_POINT('Ctrl Pts',(112.650458387723,2.97157606220462,125.353223152553));
#190691=CARTESIAN_POINT('Ctrl Pts',(112.37201076391,-2.9799868871482,125.357816565752));
#190692=CARTESIAN_POINT('Ctrl Pts',(112.093563140097,-6.19308746766462,
130.367517884098));
#190693=CARTESIAN_POINT('Ctrl Pts',(111.815115516284,-3.71504321453968,
135.778656333547));
#190694=CARTESIAN_POINT('Ctrl Pts',(111.536667892471,2.1769442627965,136.618660027865));
#190695=CARTESIAN_POINT('Ctrl Pts',(111.258220268658,6.06842631226225,132.115606608435));
#190696=CARTESIAN_POINT('Ctrl Pts',(110.979772644846,4.38332103986566,126.407582181323));
#190697=CARTESIAN_POINT('Ctrl Pts',(110.701325021032,-1.32984213103019,
124.739982342551));
#190698=CARTESIAN_POINT('Ctrl Pts',(110.42287739722,-5.82094534990898,128.645249877167));
#190699=CARTESIAN_POINT('Ctrl Pts',(110.144429773407,-4.96288416121089,
134.534634703787));
#190700=CARTESIAN_POINT('Ctrl Pts',(109.865982149594,0.455825121270016,
136.996079879188));
#190701=CARTESIAN_POINT('Ctrl Pts',(109.587534525781,5.45565338559904,133.767637535461));
#190702=CARTESIAN_POINT('Ctrl Pts',(109.309086901968,5.44200271204727,127.816088468313));
#190703=CARTESIAN_POINT('Ctrl Pts',(109.030639278155,0.427417402736423,
124.610615521118));
#190704=CARTESIAN_POINT('Ctrl Pts',(108.752191654342,-4.97994361918818,
127.096891736289));
#190705=CARTESIAN_POINT('Ctrl Pts',(108.473744030529,-5.81097973884976,
132.990150733429));
#190706=CARTESIAN_POINT('Ctrl Pts',(108.195296406717,-1.30200936065053,
136.874775395874));
#190707=CARTESIAN_POINT('Ctrl Pts',(107.916848782904,4.40344401329306,135.180985433302));
#190708=CARTESIAN_POINT('Ctrl Pts',(107.638401159091,6.06234745921968,129.465291075077));
#190709=CARTESIAN_POINT('Ctrl Pts',(107.359953535278,2.15024975226158,124.980136209215));
#190710=CARTESIAN_POINT('Ctrl Pts',(107.081505911465,-3.73782243148481,
125.847159045447));
#190711=CARTESIAN_POINT('Ctrl Pts',(106.803058287652,-6.19101840347381,
131.269607953695));
#190712=CARTESIAN_POINT('Ctrl Pts',(106.524610663839,-2.95497091073364,
136.264517288637));
#190713=CARTESIAN_POINT('Ctrl Pts',(106.246163040026,2.99655049061638,136.241809386346));
#190714=CARTESIAN_POINT('Ctrl Pts',(105.967715416213,6.1943883807198,131.222351699685));
#190715=CARTESIAN_POINT('Ctrl Pts',(105.689267792401,3.69988596163724,125.818780628557));
#190716=CARTESIAN_POINT('Ctrl Pts',(105.410820168588,-2.19463090671215,
124.996714008204));
#190717=CARTESIAN_POINT('Ctrl Pts',(105.132372544775,-6.07238918547325,
129.511590902545));
#190718=CARTESIAN_POINT('Ctrl Pts',(104.853924920962,-4.36991845548819,
135.214460009678));
#190719=CARTESIAN_POINT('Ctrl Pts',(104.575477297149,1.34829385270585,136.864663220793));
#190720=CARTESIAN_POINT('Ctrl Pts',(104.297029673336,5.82748997807964,132.945744401783));
#190721=CARTESIAN_POINT('Ctrl Pts',(104.018582049523,4.95150750231056,127.058998497491));
#190722=CARTESIAN_POINT('Ctrl Pts',(103.74013442571,-0.474668473492613,
124.614057410436));
#190723=CARTESIAN_POINT('Ctrl Pts',(103.461686801897,-5.46464731100027,
127.857702557609));
#190724=CARTESIAN_POINT('Ctrl Pts',(103.183239178085,-5.43288223256107,
133.809182509633));
#190725=CARTESIAN_POINT('Ctrl Pts',(102.904791554272,-0.408563793450433,
136.999377936557));
#190726=CARTESIAN_POINT('Ctrl Pts',(102.626343930459,4.99120481239017,134.496655090749));
#190727=CARTESIAN_POINT('Ctrl Pts',(102.347896306646,5.80430002955499,128.600894002697));
#190728=CARTESIAN_POINT('Ctrl Pts',(102.069448682833,1.28352707537895,124.730011088381));
#190729=CARTESIAN_POINT('Ctrl Pts',(101.79100105902,-4.41674455728669,126.441158642913));
#190730=CARTESIAN_POINT('Ctrl Pts',(101.512553435207,-6.05824371177293,
132.161875657885));
#190731=CARTESIAN_POINT('Ctrl Pts',(101.234105811394,-2.13251285679878,
136.635102669099));
#190732=CARTESIAN_POINT('Ctrl Pts',(100.955658187581,3.75289313452884,135.750162582539));
#190733=CARTESIAN_POINT('Ctrl Pts',(100.677210563769,6.18957367424645,130.320272106026));
#190734=CARTESIAN_POINT('Ctrl Pts',(100.398762939956,2.93833838481571,125.33523532258));
#190735=CARTESIAN_POINT('Ctrl Pts',(100.120315316143,-3.01308633445025,
125.376057503601));
#190736=CARTESIAN_POINT('Ctrl Pts',(99.8418676923298,-6.19563190980719,
130.405225059005));
#190737=CARTESIAN_POINT('Ctrl Pts',(99.5634200685172,-3.68469443349671,
135.801178693871));
#190738=CARTESIAN_POINT('Ctrl Pts',(99.2849724447041,2.2122972198669,136.605300624745));
#190739=CARTESIAN_POINT('Ctrl Pts',(99.0065248208913,6.07629580490035,132.078642080696));
#190740=CARTESIAN_POINT('Ctrl Pts',(98.7280771970783,4.35647538878314,126.380981124141));
#190741=CARTESIAN_POINT('Ctrl Pts',(98.4496295732656,-1.36673308397146,
124.748189827941));
#190742=CARTESIAN_POINT('Ctrl Pts',(98.1711819494526,-5.8339806211792,128.680723627015));
#190743=CARTESIAN_POINT('Ctrl Pts',(97.8927343256397,-4.94008497332115,
134.564776074971));
#190744=CARTESIAN_POINT('Ctrl Pts',(97.6142867018267,0.493507428451318,
136.993190424079));
#190745=CARTESIAN_POINT('Ctrl Pts',(97.3358390780141,5.47359061265531,133.734372522146));
#190746=CARTESIAN_POINT('Ctrl Pts',(97.0573914542009,5.42371142359607,127.783016818942));
#190747=CARTESIAN_POINT('Ctrl Pts',(96.7789438303882,0.389706399285272,
124.608128465823));
#190748=CARTESIAN_POINT('Ctrl Pts',(96.5004962065753,-5.0024197677526,127.127274757387));
#190749=CARTESIAN_POINT('Ctrl Pts',(96.2220485827623,-5.79756655001767,
133.025483318824));
#190750=CARTESIAN_POINT('Ctrl Pts',(95.9436009589496,-1.26503289968789,
136.882588625681));
#190751=CARTESIAN_POINT('Ctrl Pts',(95.6651533351365,4.4300041851621,135.154099331026));
#190752=CARTESIAN_POINT('Ctrl Pts',(95.3867057113237,6.05408384158403,129.428412655251));
#190753=CARTESIAN_POINT('Ctrl Pts',(95.1082580875108,2.11475620602821,124.967154938047));
#190754=CARTESIAN_POINT('Ctrl Pts',(94.8298104636979,-3.76792907128354,
125.870004076972));
#190755=CARTESIAN_POINT('Ctrl Pts',(94.5513628398851,-6.18807160565406,
131.307285819983));
#190756=CARTESIAN_POINT('Ctrl Pts',(94.2729152160721,-2.92167863853249,
136.282403871234));
#190757=CARTESIAN_POINT('Ctrl Pts',(93.9944675922592,3.02959426546386,136.223467789656));
#190758=CARTESIAN_POINT('Ctrl Pts',(93.7160199684464,6.19681804340696,131.184636955029));
#190759=CARTESIAN_POINT('Ctrl Pts',(93.4375723446334,3.66946877085029,125.796350743805));
#190760=CARTESIAN_POINT('Ctrl Pts',(93.1591247208205,-2.22994303860241,
125.010180951684));
#190761=CARTESIAN_POINT('Ctrl Pts',(92.8806770970077,-6.08014613435319,
129.548579211095));
#190762=CARTESIAN_POINT('Ctrl Pts',(92.6022294731947,-4.3429919642852,135.24097923472));
#190763=CARTESIAN_POINT('Ctrl Pts',(92.323781849382,1.38515965400848,136.856343490049));
#190764=CARTESIAN_POINT('Ctrl Pts',(92.045334225569,5.84041721907928,132.910231141365));
#190765=CARTESIAN_POINT('Ctrl Pts',(91.7668866017561,4.9286166800594,127.028926658805));
#190766=CARTESIAN_POINT('Ctrl Pts',(91.4884389779432,-0.512341811624615,
124.617061544141));
#190767=CARTESIAN_POINT('Ctrl Pts',(91.2099913541303,-5.48248320771468,
127.891022011592));
#190768=CARTESIAN_POINT('Ctrl Pts',(90.9315437303175,-5.41449037010934,
133.842198333429));
#190769=CARTESIAN_POINT('Ctrl Pts',(90.6530961065044,-0.370845394933272,
137.00175020101));
#190770=CARTESIAN_POINT('Ctrl Pts',(90.3746484826917,5.01358838138169,134.466203800718));
#190771=CARTESIAN_POINT('Ctrl Pts',(90.0962008588786,5.79077936261581,128.565602406094));
#190772=CARTESIAN_POINT('Ctrl Pts',(89.817753235066,1.24652700490487,124.722310438393));
#190773=CARTESIAN_POINT('Ctrl Pts',(89.5393056112528,-4.44322277408392,
126.468125460682));
#190774=CARTESIAN_POINT('Ctrl Pts',(89.2608579874402,-6.04986788718945,
132.198728755283));
#190775=CARTESIAN_POINT('Ctrl Pts',(88.9824103636271,-2.09697996444503,
136.647975849991));
#190776=CARTESIAN_POINT('Ctrl Pts',(88.7039627398144,3.78293010245805,135.727226022576));
#190777=CARTESIAN_POINT('Ctrl Pts',(88.4255151160013,6.18651221161165,130.282603383299));
#190778=CARTESIAN_POINT('Ctrl Pts',(88.1470674921886,2.9049918262175,125.317450153056));
#190779=CARTESIAN_POINT('Ctrl Pts',(87.8686198683756,-3.04607413073006,
125.394499589218));
#190780=CARTESIAN_POINT('Ctrl Pts',(87.5901722445627,-6.19794677053091,
130.442947024027));
#190781=CARTESIAN_POINT('Ctrl Pts',(87.3117246207499,-3.65420911474647,
135.823515895262));
#190782=CARTESIAN_POINT('Ctrl Pts',(87.033276996937,2.24756819945024,136.59172626566));
#190783=CARTESIAN_POINT('Ctrl Pts',(86.754829373124,6.08394013816284,132.041630333989));
#190784=CARTESIAN_POINT('Ctrl Pts',(86.4763817493112,4.32946830690299,126.35454397691));
#190785=CARTESIAN_POINT('Ctrl Pts',(86.1979341254982,-1.40357339211569,
124.756621726966));
#190786=CARTESIAN_POINT('Ctrl Pts',(85.9194865016854,-5.84679971215209,
128.716276069012));
#190787=CARTESIAN_POINT('Ctrl Pts',(85.6410388778725,-4.91710272876601,
134.594778102578));
#190788=CARTESIAN_POINT('Ctrl Pts',(85.3625912540596,0.531171448533366,
136.990071639606));
#190789=CARTESIAN_POINT('Ctrl Pts',(85.0841436302467,5.49132501379855,133.700998936161));
#190790=CARTESIAN_POINT('Ctrl Pts',(84.8056960064338,5.4052191575235,127.750057126576));
#190791=CARTESIAN_POINT('Ctrl Pts',(84.527248382621,0.351980955120191,124.60587101419));
#190792=CARTESIAN_POINT('Ctrl Pts',(84.2488007588079,-5.02471054981291,
127.157794034254));
#190793=CARTESIAN_POINT('Ctrl Pts',(83.9703531349953,-5.78393853022499,
133.0607335997));
#190794=CARTESIAN_POINT('Ctrl Pts',(83.6919055111822,-1.22800956246596,
136.890176624513));
#190795=CARTESIAN_POINT('Ctrl Pts',(83.4134578873695,4.45640020159694,135.127052047582));
#190796=CARTESIAN_POINT('Ctrl Pts',(83.1350102635564,6.04559588764522,129.391585221682));
#190797=CARTESIAN_POINT('Ctrl Pts',(82.8565626397436,2.07918429672594,124.954389966684));
#190798=CARTESIAN_POINT('Ctrl Pts',(82.5781150159307,-3.79789608908488,
125.893031952893));
#190799=CARTESIAN_POINT('Ctrl Pts',(82.2996673921181,-6.18489550656524,
131.344945050191));
#190800=CARTESIAN_POINT('Ctrl Pts',(82.0212197683047,-2.88827810245507,
136.300087462925));
#190801=CARTESIAN_POINT('Ctrl Pts',(81.7427721444922,3.06252577758164,136.204925385956));
#190802=CARTESIAN_POINT('Ctrl Pts',(81.464324520679,6.19901808072266,131.146908119091));
#190803=CARTESIAN_POINT('Ctrl Pts',(81.1858768968663,3.6389156065486,125.774106432701));
#190804=CARTESIAN_POINT('Ctrl Pts',(80.9074292730533,-2.26517253913331,
125.023862600622));
#190805=CARTESIAN_POINT('Ctrl Pts',(80.6289816492404,-6.08767778118217,
129.585614053086));
#190806=CARTESIAN_POINT('Ctrl Pts',(80.3505340254275,-4.31590454191782,
135.267334059228));
#190807=CARTESIAN_POINT('Ctrl Pts',(80.0720864016147,1.42197412771073,136.847799500855));
#190808=CARTESIAN_POINT('Ctrl Pts',(79.7936387778018,5.85312804127117,132.874639847142));
#190809=CARTESIAN_POINT('Ctrl Pts',(79.5151911539889,4.90554322610457,126.998994720211));
#190810=CARTESIAN_POINT('Ctrl Pts',(79.236743530176,-0.54999616474248,124.62029495049));
#190811=CARTESIAN_POINT('Ctrl Pts',(78.9582959063631,-5.50011594899764,
127.924449420408));
#190812=CARTESIAN_POINT('Ctrl Pts',(78.6798482825503,-5.39589787172579,
133.87510158903));
#190813=CARTESIAN_POINT('Ctrl Pts',(78.4014006587372,-0.333113254603616,
137.003892818912));
#190814=CARTESIAN_POINT('Ctrl Pts',(78.1229530349246,5.035786170012,134.435616819741));
#190815=CARTESIAN_POINT('Ctrl Pts',(77.8445054111114,5.77704411621779,128.530393767498));
#190816=CARTESIAN_POINT('Ctrl Pts',(77.5660577872988,1.20948074391421,124.71483516101));
#190817=CARTESIAN_POINT('Ctrl Pts',(77.2876101634857,-4.46953634562727,
126.49525295924));
#190818=CARTESIAN_POINT('Ctrl Pts',(77.009162539673,-6.04126788252658,132.235530183857));
#190819=CARTESIAN_POINT('Ctrl Pts',(76.73071491586,-2.06136936772754,136.660632493573));
#190820=CARTESIAN_POINT('Ctrl Pts',(76.4522672920471,3.81282689252116,135.704107044024));
#190821=CARTESIAN_POINT('Ctrl Pts',(76.1738196682342,6.18322150549176,130.244953994479));
#190822=CARTESIAN_POINT('Ctrl Pts',(75.8953720444213,2.87153762207887,125.299868303017));
#190823=CARTESIAN_POINT('Ctrl Pts',(75.6169244206085,-3.07894905361277,
125.413142139227));
#190824=CARTESIAN_POINT('Ctrl Pts',(75.3384767967955,-6.20003196405775,
130.480682381363));
#190825=CARTESIAN_POINT('Ctrl Pts',(75.0600291729826,-3.62358838793365,
135.84566711001));
#190826=CARTESIAN_POINT('Ctrl Pts',(74.7815815491698,2.28275589456742,136.577937453613));
#190827=CARTESIAN_POINT('Ctrl Pts',(74.5031339253568,6.09135902878616,132.004572739798));
#190828=CARTESIAN_POINT('Ctrl Pts',(74.224686301544,4.30230079498258,126.328271719272));
#190829=CARTESIAN_POINT('Ctrl Pts',(73.946238677731,-1.44036169033171,124.76527772718));
#190830=CARTESIAN_POINT('Ctrl Pts',(73.6677910539182,-5.85940214781156,
128.75190588575));
#190831=CARTESIAN_POINT('Ctrl Pts',(73.3893434301052,-4.89393827916089,
134.624639674871));
#190832=CARTESIAN_POINT('Ctrl Pts',(73.1108958062924,0.56881578586215,136.986723641335));
#190833=CARTESIAN_POINT('Ctrl Pts',(72.8324481824796,5.50885593187395,133.66751801418));
#190834=CARTESIAN_POINT('Ctrl Pts',(72.5540005586665,5.38652659906729,127.717210612549));
#190835=CARTESIAN_POINT('Ctrl Pts',(72.2755529348538,0.314242468171368,
124.603843249867));
#190836=CARTESIAN_POINT('Ctrl Pts',(71.9971053110409,-5.04681513937595,
127.188448435987));
#190837=CARTESIAN_POINT('Ctrl Pts',(71.7186576872279,-5.77009618446306,
133.095900269846));
#190838=CARTESIAN_POINT('Ctrl Pts',(71.4402100634152,-1.19094072089807,
136.897539111196));
#190839=CARTESIAN_POINT('Ctrl Pts',(71.1617624396021,4.48263108448347,135.099844585217));
#190840=CARTESIAN_POINT('Ctrl Pts',(70.8833148157894,6.03688391192757,129.354810139024));
#190841=CARTESIAN_POINT('Ctrl Pts',(70.6048671919763,2.04353534248492,124.941841768133));
#190842=CARTESIAN_POINT('Ctrl Pts',(70.3264195681636,-3.82772237444985,
125.916241819903));
#190843=CARTESIAN_POINT('Ctrl Pts',(70.0479719443506,-6.18149022389895,
131.382584248845));
#190844=CARTESIAN_POINT('Ctrl Pts',(69.7695243205378,-2.85477054017052,
136.317567408437));
#190845=CARTESIAN_POINT('Ctrl Pts',(69.4910766967249,3.09534380668036,136.186182862342));
#190846=CARTESIAN_POINT('Ctrl Pts',(69.2126290729119,6.20098841114368,131.109166589932));
#190847=CARTESIAN_POINT('Ctrl Pts',(68.934181449099,3.60822760089105,125.752048519516));
#190848=CARTESIAN_POINT('Ctrl Pts',(68.6557338252862,-2.30031810286251,
125.037758448041));
#190849=CARTESIAN_POINT('Ctrl Pts',(68.3772862014732,-6.09498384687224,
129.622694056181));
#190850=CARTESIAN_POINT('Ctrl Pts',(68.0988385776604,-4.28865719212064,
135.293523506613));
#190851=CARTESIAN_POINT('Ctrl Pts',(67.8203909538475,1.45873590963839,136.83903156981));
#190852=CARTESIAN_POINT('Ctrl Pts',(67.5419433300346,5.86562197365073,132.83897183796));
#190853=CARTESIAN_POINT('Ctrl Pts',(67.2634957062218,4.88228799544191,126.969203790852));
#190854=CARTESIAN_POINT('Ctrl Pts',(66.9850480824087,-0.587630137549865,
124.623757509667));
#190855=CARTESIAN_POINT('Ctrl Pts',(66.706600458596,-5.51754488146136,127.957983545393));
#190856=CARTESIAN_POINT('Ctrl Pts',(66.428152834783,-5.37710542636232,133.907891057196));
#190857=CARTESIAN_POINT('Ctrl Pts',(66.1497052109702,-0.295368770640213,
137.00580571087));
#190858=CARTESIAN_POINT('Ctrl Pts',(65.8712575871573,5.05779735573374,134.404895281231));
#190859=CARTESIAN_POINT('Ctrl Pts',(65.5928099633443,5.76309479932555,128.495269391582));
#190860=CARTESIAN_POINT('Ctrl Pts',(65.3143623395316,1.17238966517029,124.707585533234));
#190861=CARTESIAN_POINT('Ctrl Pts',(65.0359147157185,-4.49568429685739,
126.522540133366));
#190862=CARTESIAN_POINT('Ctrl Pts',(64.7574670919057,-6.03244401646077,
132.272278579917));
#190863=CARTESIAN_POINT('Ctrl Pts',(64.4790194680927,-2.02568238621027,
136.673072130848));
#190864=CARTESIAN_POINT('Ctrl Pts',(64.20057184428,3.84258239688126,135.680806503568));
#190865=CARTESIAN_POINT('Ctrl Pts',(63.922124220467,6.17970167782515,130.207325334677));
#190866=CARTESIAN_POINT('Ctrl Pts',(63.6436765966542,2.8379770120581,125.282490423967));
#190867=CARTESIAN_POINT('Ctrl Pts',(63.3652289728412,-3.11170988490585,
125.431984462817));
#190868=CARTESIAN_POINT('Ctrl Pts',(63.0867813490283,-6.20188741312008,
130.518429732716));
#190869=CARTESIAN_POINT('Ctrl Pts',(62.8083337252156,-3.59283338772076,
135.86763151729));
#190870=CARTESIAN_POINT('Ctrl Pts',(62.5298861014024,2.31785900132509,136.563934699553));
#190871=CARTESIAN_POINT('Ctrl Pts',(62.2514384775899,6.09855220186056,131.967470671305));
#190872=CARTESIAN_POINT('Ctrl Pts',(61.9729908537767,4.27497385972414,126.302165324755));
#190873=CARTESIAN_POINT('Ctrl Pts',(61.6945432299639,-1.47709661541541,
124.774157507831));
#190874=CARTESIAN_POINT('Ctrl Pts',(61.416095606151,-5.87178746116934,128.787611756953));
#190875=CARTESIAN_POINT('Ctrl Pts',(61.1376479823382,-4.8705924828735,134.65435968532));
#190876=CARTESIAN_POINT('Ctrl Pts',(60.8592003585251,0.606439045512412,
136.983146553331));
#190877=CARTESIAN_POINT('Ctrl Pts',(60.5807527347125,5.52618271726667,133.633930996847));
#190878=CARTESIAN_POINT('Ctrl Pts',(60.3023051108993,5.36763444088732,127.684478494003));
#190879=CARTESIAN_POINT('Ctrl Pts',(60.0238574870866,0.276492336852797,
124.602045247997));
#190880=CARTESIAN_POINT('Ctrl Pts',(59.7454098632736,-5.06873271734795,
127.219236826675));
#190881=CARTESIAN_POINT('Ctrl Pts',(59.4669622394608,-5.75604002566515,
133.130982026147));
#190882=CARTESIAN_POINT('Ctrl Pts',(59.1885146156479,-1.15382774858414,
136.904675812908));
#190883=CARTESIAN_POINT('Ctrl Pts',(58.9100669918351,4.50869586182645,135.072477952114));
#190884=CARTESIAN_POINT('Ctrl Pts',(58.6316193680221,6.02794823725661,129.318088769994));
#190885=CARTESIAN_POINT('Ctrl Pts',(58.3531717442092,2.00781066429043,124.929510807376));
#190886=CARTESIAN_POINT('Ctrl Pts',(58.0747241203963,-3.85740682215468,
125.939632817953));
#190887=CARTESIAN_POINT('Ctrl Pts',(57.7962764965834,-6.17785588383907,
131.42020202121));
#190888=CARTESIAN_POINT('Ctrl Pts',(57.5178288727705,-2.82115719331391,
136.334843060042));
#190889=CARTESIAN_POINT('Ctrl Pts',(57.2393812489577,3.12804713667602,136.167240913326));
#190890=CARTESIAN_POINT('Ctrl Pts',(56.9609336251447,6.20272896165862,131.071413766074));
#190891=CARTESIAN_POINT('Ctrl Pts',(56.6824860013319,3.57740589103289,125.730177821614));
#190892=CARTESIAN_POINT('Ctrl Pts',(56.404038377519,-2.33537842745856,125.051867979023));
#190893=CARTESIAN_POINT('Ctrl Pts',(56.125590753706,-6.10206406069443,129.659817846364));
#190894=CARTESIAN_POINT('Ctrl Pts',(55.8471431298932,-4.26125092455389,
135.319546606417));
#190895=CARTESIAN_POINT('Ctrl Pts',(55.5686955060803,1.49544363757083,136.830040021814));
#190896=CARTESIAN_POINT('Ctrl Pts',(55.2902478822675,5.87789855325116,132.80322843551));
#190897=CARTESIAN_POINT('Ctrl Pts',(55.0118002584545,4.85885184980179,126.939554974638));
#190898=CARTESIAN_POINT('Ctrl Pts',(54.7333526346416,-0.625242335506623,
124.627449093364));
#190899=CARTESIAN_POINT('Ctrl Pts',(54.4549050108287,-5.53476935927053,
127.991623143927));
#190900=CARTESIAN_POINT('Ctrl Pts',(54.1764573870159,-5.35811373037978,
133.9405655229));
#190901=CARTESIAN_POINT('Ctrl Pts',(53.8980097632029,-0.257613341678002,
137.007488805997));
#190902=CARTESIAN_POINT('Ctrl Pts',(53.61956213939,5.07962112291461,134.374040323585));
#190903=CARTESIAN_POINT('Ctrl Pts',(53.3411145155772,5.74893192883615,128.460230579889));
#190904=CARTESIAN_POINT('Ctrl Pts',(53.0626668917642,1.13525514309568,124.7005618237));
#190905=CARTESIAN_POINT('Ctrl Pts',(52.7842192679514,-4.52166565885288,
126.549985971924));
#190906=CARTESIAN_POINT('Ctrl Pts',(52.5057716441385,-6.0233966159634,132.308972581737));
#190907=CARTESIAN_POINT('Ctrl Pts',(52.2273240203255,-1.98992034228702,
136.685294300858));
#190908=CARTESIAN_POINT('Ctrl Pts',(51.9488763965128,3.87219551293788,135.657325264614));
#190909=CARTESIAN_POINT('Ctrl Pts',(51.6704287726998,6.17595285904027,130.169718798237));
#190910=CARTESIAN_POINT('Ctrl Pts',(51.391981148887,2.80431123975502,125.265317159845));
#190911=CARTESIAN_POINT('Ctrl Pts',(51.113533525074,-3.14435541064497,125.451025861782));
#190912=CARTESIAN_POINT('Ctrl Pts',(50.8350859012611,-6.20351304896362,
130.556187679343));
#190913=CARTESIAN_POINT('Ctrl Pts',(50.5566382774483,-3.5619452537452,135.889408303207));
#190914=CARTESIAN_POINT('Ctrl Pts',(50.2781906536353,2.35287621896542,136.549718522358));
#190915=CARTESIAN_POINT('Ctrl Pts',(49.9997430298226,6.10551939084041,131.930325503341));
#190916=CARTESIAN_POINT('Ctrl Pts',(49.7212954060095,4.2474885137371,126.27622576074));
#190917=CARTESIAN_POINT('Ctrl Pts',(49.4428477821967,-1.51377680614101,
124.783260739875));
#190918=CARTESIAN_POINT('Ctrl Pts',(49.1644001583838,-5.88395519328364,
128.823392359526));
#190919=CARTESIAN_POINT('Ctrl Pts',(48.8859525345709,-4.84706620499019,
134.683937032636));
#190920=CARTESIAN_POINT('Ctrl Pts',(48.607504910758,0.644039833341117,136.97934050814));
#190921=CARTESIAN_POINT('Ctrl Pts',(48.3290572869451,5.54330472792681,133.600239128744));
#190922=CARTESIAN_POINT('Ctrl Pts',(48.0506096631323,5.34854338303893,127.651861983834));
#190923=CARTESIAN_POINT('Ctrl Pts',(47.7721620393193,0.23873196000854,124.600477075203));
#190924=CARTESIAN_POINT('Ctrl Pts',(47.4937144155065,-5.09046247156518,
127.250158065443));
#190925=CARTESIAN_POINT('Ctrl Pts',(47.2152667916935,-5.74177057468722,
133.165977568637));
#190926=CARTESIAN_POINT('Ctrl Pts',(46.9368191678807,-1.11667202075834,
136.911586465198));
#190927=CARTESIAN_POINT('Ctrl Pts',(46.6583715440677,4.53459356778643,135.044953162355));
#190928=CARTESIAN_POINT('Ctrl Pts',(46.379923920255,6.01878919474683,129.281422475313));
#190929=CARTESIAN_POINT('Ctrl Pts',(46.101476296442,1.97201158593325,124.917397541337));
#190930=CARTESIAN_POINT('Ctrl Pts',(45.8230286726291,-3.88694833223118,
125.963204080281));
#190931=CARTESIAN_POINT('Ctrl Pts',(45.5445810488162,-6.17399262105761,
131.457796973343));
#190932=CARTESIAN_POINT('Ctrl Pts',(45.2661334250033,-2.78743930743976,
136.351913777587));
#190933=CARTESIAN_POINT('Ctrl Pts',(44.9876858011905,3.16063455573481,136.148100240809));
#190934=CARTESIAN_POINT('Ctrl Pts',(44.7092381773775,6.20423966777097,131.033651046464));
#190935=CARTESIAN_POINT('Ctrl Pts',(44.4307905535647,3.54645161908363,125.708495149421));
#190936=CARTESIAN_POINT('Ctrl Pts',(44.1523429297517,-2.37035221374829,
125.066190670735));
#190937=CARTESIAN_POINT('Ctrl Pts',(43.8738953059389,-6.10891816028884,
129.696984048001));
#190938=CARTESIAN_POINT('Ctrl Pts',(43.5954476821259,-4.23368675476706,
135.345402394343));
#190939=CARTESIAN_POINT('Ctrl Pts',(43.3170000583131,1.53209595128933,136.820825190051));
#190940=CARTESIAN_POINT('Ctrl Pts',(43.0385524345002,5.88995732515911,132.767410964279));
#190941=CARTESIAN_POINT('Ctrl Pts',(42.7601048106873,4.83523565761953,126.910049370218));
#190942=CARTESIAN_POINT('Ctrl Pts',(42.4816571868744,-0.662831364878718,
124.631369564788));
#190943=CARTESIAN_POINT('Ctrl Pts',(42.2032095630615,-5.55178874416567,
128.025366969483));
#190944=CARTESIAN_POINT('Ctrl Pts',(41.9247619392486,-5.33892348752252,
133.973123775378));
#190945=CARTESIAN_POINT('Ctrl Pts',(41.6463143154357,-0.219848366758665,
137.008942041929));
#190946=CARTESIAN_POINT('Ctrl Pts',(41.3678666916229,5.10125666286673,134.343053090145));
#190947=CARTESIAN_POINT('Ctrl Pts',(41.0894190678099,5.73455602955998,128.425278630796));
#190948=CARTESIAN_POINT('Ctrl Pts',(40.8109714439971,1.09807855372398,124.693764292674));
#190949=CARTESIAN_POINT('Ctrl Pts',(40.5325238201841,-4.5474794688646,126.5775894579));
#190950=CARTESIAN_POINT('Ctrl Pts',(40.2540761963713,-6.01412601628932,
132.345610829607));
#190951=CARTESIAN_POINT('Ctrl Pts',(39.9756285725584,-1.95408456113369,
136.697298550707));
#190952=CARTESIAN_POINT('Ctrl Pts',(39.6971809487455,3.90166514336576,135.633664197272));
#190953=CARTESIAN_POINT('Ctrl Pts',(39.4187333249326,6.171975188051,130.132135778682));
#190954=CARTESIAN_POINT('Ctrl Pts',(39.1402857011198,2.77054155266769,125.248349147017));
#190955=CARTESIAN_POINT('Ctrl Pts',(38.8618380773068,-3.17688442113803,
125.470265630536));
#190956=CARTESIAN_POINT('Ctrl Pts',(38.583390453494,-6.20490881134979,130.593954822108));
#190957=CARTESIAN_POINT('Ctrl Pts',(38.304942829681,-3.53092513057837,135.910996660811));
#190958=CARTESIAN_POINT('Ctrl Pts',(38.0264952058682,2.38780624991219,136.535289448812));
#190959=CARTESIAN_POINT('Ctrl Pts',(37.7480475820552,6.11226033755391,131.893138612335));
#190960=CARTESIAN_POINT('Ctrl Pts',(37.4695999582424,4.21984577550119,126.250453988427));
#190961=CARTESIAN_POINT('Ctrl Pts',(37.1911523344295,-1.55040090331038,
124.792587085991));
#190962=CARTESIAN_POINT('Ctrl Pts',(36.9127047106166,-5.89590489327443,
128.859246367608));
#190963=CARTESIAN_POINT('Ctrl Pts',(36.6342570868037,-4.82336031728617,
134.713370620821));
#190964=CARTESIAN_POINT('Ctrl Pts',(36.3558094629908,0.681616756036961,
136.975305646799));
#190965=CARTESIAN_POINT('Ctrl Pts',(36.0773618391779,5.56022132939171,133.566443658335));
#190966=CARTESIAN_POINT('Ctrl Pts',(35.798914215365,5.32925413294858,127.619362290662));
#190967=CARTESIAN_POINT('Ctrl Pts',(35.5204665915522,0.200962736863706,
124.599138789596));
#190968=CARTESIAN_POINT('Ctrl Pts',(35.2420189677392,-5.11200359682353,
127.281211006494));
#190969=CARTESIAN_POINT('Ctrl Pts',(34.9635713439263,-5.72728836028912,
133.200885600541));
#190970=CARTESIAN_POINT('Ctrl Pts',(34.6851237201134,-1.07947491424015,
136.918270811987));
#190971=CARTESIAN_POINT('Ctrl Pts',(34.4066760963006,4.56032324271418,135.017271235878));
#190972=CARTESIAN_POINT('Ctrl Pts',(34.1282284724876,6.00940712379002,129.244812613665));
#190973=CARTESIAN_POINT('Ctrl Pts',(33.8497808486748,1.93613943396156,124.905502418881));
#190974=CARTESIAN_POINT('Ctrl Pts',(33.5713332248619,-3.91634581000783,
125.986954733445));
#190975=CARTESIAN_POINT('Ctrl Pts',(33.292885601049,-6.16990057870911,131.495367712155));
#190976=CARTESIAN_POINT('Ctrl Pts',(33.0144379772361,-2.753618131977,136.368778928511));
#190977=CARTESIAN_POINT('Ctrl Pts',(32.7359903534233,3.19310485631782,136.128761554055));
#190978=CARTESIAN_POINT('Ctrl Pts',(32.4575427296103,6.20552047350092,130.995879830412));
#190979=CARTESIAN_POINT('Ctrl Pts',(32.1790951057975,3.51536593206519,125.687001306397));
#190980=CARTESIAN_POINT('Ctrl Pts',(31.9006474819845,-2.40523816576522,
125.080725992446));
#190981=CARTESIAN_POINT('Ctrl Pts',(31.6221998581717,-6.11554589167424,
129.734191283883));
#190982=CARTESIAN_POINT('Ctrl Pts',(31.3437522343588,-4.20596570416061,
135.371089912296));
#190983=CARTESIAN_POINT('Ctrl Pts',(31.0653046105458,1.56869149262894,136.811387415981));
#190984=CARTESIAN_POINT('Ctrl Pts',(30.786856986733,5.90179784253235,132.731520751495));
#190985=CARTESIAN_POINT('Ctrl Pts',(30.5084093629201,4.81144029400183,126.880688070935));
#190986=CARTESIAN_POINT('Ctrl Pts',(30.2299617391072,-0.700395832790832,
124.635518778667));
#190987=CARTESIAN_POINT('Ctrl Pts',(29.9515141152943,-5.56860240548724,
128.05921377167));
#190988=CARTESIAN_POINT('Ctrl Pts',(29.6730664914815,-5.31953540889204,
134.005564608172));
#190989=CARTESIAN_POINT('Ctrl Pts',(29.3946188676685,-0.182075245277261,
137.010165364815));
#190990=CARTESIAN_POINT('Ctrl Pts',(29.1161712438556,5.12270317387725,134.311934729152));
#190991=CARTESIAN_POINT('Ctrl Pts',(28.8377236200427,5.71996763420123,128.390414839463));
#190992=CARTESIAN_POINT('Ctrl Pts',(28.5592759962298,1.06086127464794,124.687193192043));
#190993=CARTESIAN_POINT('Ctrl Pts',(28.280828372417,-4.57312477035222,126.605349568435));
#190994=CARTESIAN_POINT('Ctrl Pts',(28.0023807486041,-6.00463256096402,
132.382191965885));
#190995=CARTESIAN_POINT('Ctrl Pts',(27.7239331247912,-1.91817637065835,
136.709084435575));
#190996=CARTESIAN_POINT('Ctrl Pts',(27.4454855009783,3.93099019615694,135.60982417831));
#190997=CARTESIAN_POINT('Ctrl Pts',(27.1670378771654,6.16776881225138,130.094577668667));
#190998=CARTESIAN_POINT('Ctrl Pts',(26.8885902533525,2.73666920214424,125.231587014236));
#190999=CARTESIAN_POINT('Ctrl Pts',(26.6101426295396,-3.20929571101057,
125.48970305614));
#191000=CARTESIAN_POINT('Ctrl Pts',(26.3316950057267,-6.2060746485581,130.631729761538));
#191001=CARTESIAN_POINT('Ctrl Pts',(26.0532473819138,-3.49977416768234,
135.932395790139));
#191002=CARTESIAN_POINT('Ctrl Pts',(25.774799758101,2.42264779982026,136.52064801359));
#191003=CARTESIAN_POINT('Ctrl Pts',(25.4963521342881,6.11877479221284,131.85591137626));
#191004=CARTESIAN_POINT('Ctrl Pts',(25.2179045104751,4.19204666932822,126.224850962798));
#191005=CARTESIAN_POINT('Ctrl Pts',(24.9394568866623,-1.58696754980412,
124.802136200585));
#191006=CARTESIAN_POINT('Ctrl Pts',(24.6610092628494,-5.90763611834117,
128.895172452612));
#191007=CARTESIAN_POINT('Ctrl Pts',(24.3825616390365,-4.79947569819179,
134.742659359205));
#191008=CARTESIAN_POINT('Ctrl Pts',(24.1041140152236,0.719168421173241,
136.97104211882));
#191009=CARTESIAN_POINT('Ctrl Pts',(23.8256663914108,5.57693189481048,133.532545837923));
#191010=CARTESIAN_POINT('Ctrl Pts',(23.5472187675978,5.3097674053865,127.586980618775));
#191011=CARTESIAN_POINT('Ctrl Pts',(23.2687711437849,0.163186066970757,
124.598030440764));
#191012=CARTESIAN_POINT('Ctrl Pts',(22.990323519972,-5.13335529490864,127.312394499151));
#191013=CARTESIAN_POINT('Ctrl Pts',(22.7118758961592,-5.71259391911463,
133.235704828331));
#191014=CARTESIAN_POINT('Ctrl Pts',(22.4334282723462,-1.04223780738205,
136.924728605587));
#191015=CARTESIAN_POINT('Ctrl Pts',(22.1549806485334,4.58588393318709,134.98943319845));
#191016=CARTESIAN_POINT('Ctrl Pts',(21.8765330247205,5.9998023720423,129.208260541641));
#191017=CARTESIAN_POINT('Ctrl Pts',(21.5980854009075,1.90019553763114,124.893825880784));
#191018=CARTESIAN_POINT('Ctrl Pts',(21.3196377770947,-3.94559816615024,
126.010883897355));
#191019=CARTESIAN_POINT('Ctrl Pts',(21.0411901532818,-6.16557990842568,
131.532912845442));
#191020=CARTESIAN_POINT('Ctrl Pts',(20.7627425294689,-2.71969492018171,
136.385437887866));
#191021=CARTESIAN_POINT('Ctrl Pts',(20.484294905656,3.22545683522612,136.109225569666));
#191022=CARTESIAN_POINT('Ctrl Pts',(20.2058472818431,6.20657133138755,130.958101517545));
#191023=CARTESIAN_POINT('Ctrl Pts',(19.9273996580302,3.48414998186958,125.665697089004));
#191024=CARTESIAN_POINT('Ctrl Pts',(19.6489520342174,-2.44003499079723,
125.095473405541));
#191025=CARTESIAN_POINT('Ctrl Pts',(19.3705044104044,-6.12194700925765,
129.771438175283));
#191026=CARTESIAN_POINT('Ctrl Pts',(19.0920567865916,-4.17808879994825,
135.396608208416));
#191027=CARTESIAN_POINT('Ctrl Pts',(18.8136091627787,1.60522890552839,136.801727049323));
#191028=CARTESIAN_POINT('Ctrl Pts',(18.5351615389658,5.91341966661616,132.695559127084));
#191029=CARTESIAN_POINT('Ctrl Pts',(18.2567139151529,4.78746664069464,126.85147216478));
#191030=CARTESIAN_POINT('Ctrl Pts',(17.97826629134,-0.737934347277788,124.63989658125));
#191031=CARTESIAN_POINT('Ctrl Pts',(17.6998186675271,-5.58520972019883,
128.093162296283));
#191032=CARTESIAN_POINT('Ctrl Pts',(17.4213710437142,-5.29995021292075,
134.037886819174));
#191033=CARTESIAN_POINT('Ctrl Pts',(17.1429234199013,-0.144295376930669,
137.011158729324));
#191034=CARTESIAN_POINT('Ctrl Pts',(16.8644757960885,5.14395986123776,134.280686393713));
#191035=CARTESIAN_POINT('Ctrl Pts',(16.5860281722755,5.70516728333829,128.355640497777));
#191036=CARTESIAN_POINT('Ctrl Pts',(16.3075805484627,1.02360468496723,124.6808487653));
#191037=CARTESIAN_POINT('Ctrl Pts',(16.0291329246498,-4.5986006130197,126.633265274869));
#191038=CARTESIAN_POINT('Ctrl Pts',(15.7506853008369,-5.99491660177097,
132.418714635041));
#191039=CARTESIAN_POINT('Ctrl Pts',(15.472237677024,-1.88219710145218,136.720651518731));
#191040=CARTESIAN_POINT('Ctrl Pts',(15.1937900532111,3.96016958466077,135.585806091128));
#191041=CARTESIAN_POINT('Ctrl Pts',(14.9153424293982,6.16333388751023,130.057045859918));
#191042=CARTESIAN_POINT('Ctrl Pts',(14.6368948055853,2.70269544333712,125.215031382631));
#191043=CARTESIAN_POINT('Ctrl Pts',(14.3584471817724,-3.24158807925031,
125.509337418335));
#191044=CARTESIAN_POINT('Ctrl Pts',(14.0799995579596,-6.20701051738803,
130.669511097867));
#191045=CARTESIAN_POINT('Ctrl Pts',(13.8015519341466,-3.46849351936748,
135.953604898237));
#191046=CARTESIAN_POINT('Ctrl Pts',(13.5231043103337,2.45739957762318,136.505794759238));
#191047=CARTESIAN_POINT('Ctrl Pts',(13.2446566865208,6.12506251342167,131.818645174584));
#191048=CARTESIAN_POINT('Ctrl Pts',(12.966209062708,4.16409222532429,126.199417632585));
#191049=CARTESIAN_POINT('Ctrl Pts',(12.687761438895,-1.62347539063169,124.811907729812));
#191050=CARTESIAN_POINT('Ctrl Pts',(12.4093138150822,-5.91914843377905,
128.931169283287));
#191051=CARTESIAN_POINT('Ctrl Pts',(12.1308661912693,-4.77541323276041,
134.771802162479));
#191052=CARTESIAN_POINT('Ctrl Pts',(11.8524185674564,0.756693437259193,
136.96655008219));
#191053=CARTESIAN_POINT('Ctrl Pts',(11.5739709436435,5.59343580496719,133.498546923603));
#191054=CARTESIAN_POINT('Ctrl Pts',(11.2955233198306,5.2900839224404,127.554718168085));
#191055=CARTESIAN_POINT('Ctrl Pts',(11.0170756960177,0.125403350157864,
124.597152069781));
#191056=CARTESIAN_POINT('Ctrl Pts',(10.7386280722048,-5.15451677462551,
127.343707387895));
#191057=CARTESIAN_POINT('Ctrl Pts',(10.460180448392,-5.69768779567166,133.270433961767));
#191058=CARTESIAN_POINT('Ctrl Pts',(10.1817328245791,-1.0049620800187,136.930959606699));
#191059=CARTESIAN_POINT('Ctrl Pts',(9.90328520076621,4.61127469204443,134.961440081617));
#191060=CARTESIAN_POINT('Ctrl Pts',(9.62483757695328,5.98997529541125,129.171767613693));
#191061=CARTESIAN_POINT('Ctrl Pts',(9.34638995314043,1.86418122885626,124.882368359726));
#191062=CARTESIAN_POINT('Ctrl Pts',(9.0679423293275,-3.97470431670162,126.034990685308));
#191063=CARTESIAN_POINT('Ctrl Pts',(8.78949470551463,-6.16103077031137,
131.57043098196));
#191064=CARTESIAN_POINT('Ctrl Pts',(8.5110470817017,-2.68567092909101,136.401890038352));
#191065=CARTESIAN_POINT('Ctrl Pts',(8.2325994578889,3.25768929364524,136.089493011555));
#191066=CARTESIAN_POINT('Ctrl Pts',(7.95415183407592,6.20739220249103,130.920317507753));
#191067=CARTESIAN_POINT('Ctrl Pts',(7.67570421026306,3.45280492521512,125.644583286679));
#191068=CARTESIAN_POINT('Ctrl Pts',(7.39725658645018,-2.47474139943534,
125.110432363552));
#191069=CARTESIAN_POINT('Ctrl Pts',(7.11880896263729,-6.1281212758433,129.808723342005));
#191070=CARTESIAN_POINT('Ctrl Pts',(6.84036133882437,-4.15005707511893,
135.421956337113));
#191071=CARTESIAN_POINT('Ctrl Pts',(6.56191371501151,1.64170683608044,136.791844448048));
#191072=CARTESIAN_POINT('Ctrl Pts',(6.28346609119863,5.92482236675955,132.659527423617));
#191073=CARTESIAN_POINT('Ctrl Pts',(6.00501846738572,4.76331558605049,126.822402734361));
#191074=CARTESIAN_POINT('Ctrl Pts',(5.72657084357281,-0.775445517336138,
124.644502810313));
#191075=CARTESIAN_POINT('Ctrl Pts',(5.44812321975995,-5.60161007291028,
128.127211285347));
#191076=CARTESIAN_POINT('Ctrl Pts',(5.16967559594705,-5.28016862534525,
134.070089210674));
#191077=CARTESIAN_POINT('Ctrl Pts',(4.89122797213414,-0.106510161665837,
137.011922098645));
#191078=CARTESIAN_POINT('Ctrl Pts',(4.6127803483213,5.16502593727395,134.249309241742));
#191079=CARTESIAN_POINT('Ctrl Pts',(4.33433272450837,5.69015552540359,128.320956894316));
#191080=CARTESIAN_POINT('Ctrl Pts',(4.05588510069549,0.986310165238503,
124.674731247541));
#191081=CARTESIAN_POINT('Ctrl Pts',(3.77743747688256,-4.62390605285035,
126.661335542776));
#191082=CARTESIAN_POINT('Ctrl Pts',(3.49898985306972,-5.98497849873861,
132.455177483715));
#191083=CARTESIAN_POINT('Ctrl Pts',(3.22054222925682,-1.84614808674025,
136.731999371551));
#191084=CARTESIAN_POINT('Ctrl Pts',(2.94209460544391,3.9892022276243,135.561610825727));
#191085=CARTESIAN_POINT('Ctrl Pts',(2.66364698163102,6.15867057816533,130.019541743194));
#191086=CARTESIAN_POINT('Ctrl Pts',(2.38519935781816,2.66862153515642,125.198682865676));
#191087=CARTESIAN_POINT('Ctrl Pts',(2.10675173400524,-3.27376032925169,
125.529167989562));
#191088=CARTESIAN_POINT('Ctrl Pts',(1.82830411019233,-6.20771638316062,
130.707297431096));
#191089=CARTESIAN_POINT('Ctrl Pts',(1.54985648637947,-3.43708434474973,
135.974623199195));
#191090=CARTESIAN_POINT('Ctrl Pts',(1.27140886256659,2.49206029558105,136.490730236146));
#191091=CARTESIAN_POINT('Ctrl Pts',(0.992961238753657,6.13112326818657,
131.78134138822));
#191092=CARTESIAN_POINT('Ctrl Pts',(0.714513614940807,4.13598347935162,
126.174154940227));
#191093=CARTESIAN_POINT('Ctrl Pts',(0.436065991127901,-1.65992307298164,
124.821901311585));
#191094=CARTESIAN_POINT('Ctrl Pts',(0.157618367314999,-5.93044141299494,
128.967235525755));
#191095=CARTESIAN_POINT('Ctrl Pts',(-0.120829256497892,-4.75117381263555,
134.800797950748));
#191096=CARTESIAN_POINT('Ctrl Pts',(-0.399276880310752,0.794190413791566,
136.961829703365));
#191097=CARTESIAN_POINT('Ctrl Pts',(-0.67772450412367,5.60973244830296,
133.464448175219));
#191098=CARTESIAN_POINT('Ctrl Pts',(-0.956172127936585,5.27020441348929,
127.522576134092));
#191099=CARTESIAN_POINT('Ctrl Pts',(-1.23461975174943,0.0876159864779326,
124.596503709192));
#191100=CARTESIAN_POINT('Ctrl Pts',(-1.51306737556233,-5.17548725182775,
127.375148512417));
#191101=CARTESIAN_POINT('Ctrl Pts',(-1.79151499937523,-5.6825705423121,
133.305071713949));
#191102=CARTESIAN_POINT('Ctrl Pts',(-2.06996262318813,-0.967649113415911,
136.936963584433));
#191103=CARTESIAN_POINT('Ctrl Pts',(-2.34841024700098,4.63649457842225,
134.933292922676));
#191104=CARTESIAN_POINT('Ctrl Pts',(-2.62685787081389,5.97992625804282,
129.13533518208));
#191105=CARTESIAN_POINT('Ctrl Pts',(-2.90530549462681,1.82809784216042,
124.871130280269));
#191106=CARTESIAN_POINT('Ctrl Pts',(-3.18375311843967,-4.00366318312286,
126.059274204017));
#191107=CARTESIAN_POINT('Ctrl Pts',(-3.46220074225256,-6.15625333293613,
131.607920731459));
#191108=CARTESIAN_POINT('Ctrl Pts',(-3.74064836606547,-2.65154741947636,
136.418134770325));
#191109=CARTESIAN_POINT('Ctrl Pts',(-4.01909598987837,3.28980103718956,
136.06956461092));
#191110=CARTESIAN_POINT('Ctrl Pts',(-4.29754361369122,6.20798305639367,
130.882529201136));
#191111=CARTESIAN_POINT('Ctrl Pts',(-4.57599123750414,3.42133192360438,
125.623660681799));
#191112=CARTESIAN_POINT('Ctrl Pts',(-4.85443886131705,-2.5093561056208,
125.125602312169));
#191113=CARTESIAN_POINT('Ctrl Pts',(-5.13288648512991,-6.13406846264146,
129.846045402432));
#191114=CARTESIAN_POINT('Ctrl Pts',(-5.41133410894279,-4.12187156839848,
135.447133359102));
#191115=CARTESIAN_POINT('Ctrl Pts',(-5.68978173275571,1.67812393258193,
136.781739978358));
#191116=CARTESIAN_POINT('Ctrl Pts',(-5.9682293565686,5.93600552043131,132.623426976261));
#191117=CARTESIAN_POINT('Ctrl Pts',(-6.24667698038146,4.73898802499559,
126.793480856855));
#191118=CARTESIAN_POINT('Ctrl Pts',(-6.52512460419438,-0.812927952975666,
124.649337295173));
#191119=CARTESIAN_POINT('Ctrl Pts',(-6.80357222800728,-5.61780285590049,
128.161359477164));
#191120=CARTESIAN_POINT('Ctrl Pts',(-7.08201985182013,-5.26019137917956,
134.1021705894));
#191121=CARTESIAN_POINT('Ctrl Pts',(-7.36046747563304,-0.0687209996277829,
137.012455444495));
#191122=CARTESIAN_POINT('Ctrl Pts',(-7.63891509944595,5.18590062137458,
134.217804435933));
#191123=CARTESIAN_POINT('Ctrl Pts',(-7.91736272325884,5.67493291666336,
128.286365314294));
#191124=CARTESIAN_POINT('Ctrl Pts',(-8.1958103470717,0.948979097423875,
124.668840865451));
#191125=CARTESIAN_POINT('Ctrl Pts',(-8.47425797088461,-4.64904015214177,
126.689559331999));
#191126=CARTESIAN_POINT('Ctrl Pts',(-8.75270559469752,-5.97481862012702,
132.491579160764));
#191127=CARTESIAN_POINT('Ctrl Pts',(-9.03115321851038,-1.81003066233205,
136.743127573537));
#191128=CARTESIAN_POINT('Ctrl Pts',(-9.30960084232328,4.0180870492325,135.537239278668));
#191129=CARTESIAN_POINT('Ctrl Pts',(-9.58804846613619,6.15377905701727,
129.982066708221));
#191130=CARTESIAN_POINT('Ctrl Pts',(-9.86649608994908,2.63444874022312,
125.182542069172));
#191131=CARTESIAN_POINT('Ctrl Pts',(-10.144943713762,-3.30581126886015,
125.549194034992));
#191132=CARTESIAN_POINT('Ctrl Pts',(-10.4233913375749,-6.20819221971975,
130.745087361036));
#191133=CARTESIAN_POINT('Ctrl Pts',(-10.7018389613878,-3.40554780770759,
135.995449914173));
#191134=CARTESIAN_POINT('Ctrl Pts',(-10.9802865852006,2.52662866932821,
136.475455002538));
#191135=CARTESIAN_POINT('Ctrl Pts',(-11.2587342090136,6.13695683192405,
131.744001399476));
#191136=CARTESIAN_POINT('Ctrl Pts',(-11.5371818328265,4.10772147299012,
126.149063821843));
#191137=CARTESIAN_POINT('Ctrl Pts',(-11.8156294566394,-1.69630924627168,
124.832116575588));
#191138=CARTESIAN_POINT('Ctrl Pts',(-12.0940770804522,-5.94151463752335,
129.003369843568));
#191139=CARTESIAN_POINT('Ctrl Pts',(-12.3725247042651,-4.72675833601782,
134.829645649562));
#191140=CARTESIAN_POINT('Ctrl Pts',(-12.6509723280781,0.83165796130609,
136.956881157257));
#191141=CARTESIAN_POINT('Ctrl Pts',(-12.9294199518909,5.62582122093989,
133.430250856313));
#191142=CARTESIAN_POINT('Ctrl Pts',(-13.2078675757038,5.25012961517551,
127.490555707831));
#191143=CARTESIAN_POINT('Ctrl Pts',(-13.4863151995167,0.0498253761554086,
124.596085383024));
#191144=CARTESIAN_POINT('Ctrl Pts',(-13.7647628233296,-5.19626594944658,
127.406716707655));
#191145=CARTESIAN_POINT('Ctrl Pts',(-14.0432104471424,-5.66724271921134,
133.339616801361));
#191146=CARTESIAN_POINT('Ctrl Pts',(-14.3216580709554,-0.930300290219375,
136.942740316309));
#191147=CARTESIAN_POINT('Ctrl Pts',(-14.6001056947683,4.6615426577884,134.904992764631));
#191148=CARTESIAN_POINT('Ctrl Pts',(-14.8785533185811,5.96965563230779,
129.098964596818));
#191149=CARTESIAN_POINT('Ctrl Pts',(-15.157000942394,1.79194671462675,124.860112058844));
#191150=CARTESIAN_POINT('Ctrl Pts',(-15.4354485662069,-4.03247369233249,
126.08373355365));
#191151=CARTESIAN_POINT('Ctrl Pts',(-15.7138961900198,-6.15124777332969,
131.645380704742));
#191152=CARTESIAN_POINT('Ctrl Pts',(-15.9923438138327,-2.61732565579698,
136.434171481834));
#191153=CARTESIAN_POINT('Ctrl Pts',(-16.2707914376456,3.32179087594663,
136.049441106215));
#191154=CARTESIAN_POINT('Ctrl Pts',(-16.5492390614585,6.2083438712012,130.844737997954));
#191155=CARTESIAN_POINT('Ctrl Pts',(-16.8276866852714,3.38973214328102,
125.602930049661));
#191156=CARTESIAN_POINT('Ctrl Pts',(-17.1061343090842,-2.54387782669295,
125.140982689263));
#191157=CARTESIAN_POINT('Ctrl Pts',(-17.3845819328972,-6.13978834927694,
129.883402973582));
#191158=CARTESIAN_POINT('Ctrl Pts',(-17.66302955671,-4.09353332421128,135.47213834144));
#191159=CARTESIAN_POINT('Ctrl Pts',(-17.9414771805229,1.71447884558397,
136.771414014676));
#191160=CARTESIAN_POINT('Ctrl Pts',(-18.2199248043358,5.94696871323555,
132.587259122732));
#191161=CARTESIAN_POINT('Ctrl Pts',(-18.4983724281487,4.71448485899666,
126.764707603974));
#191162=CARTESIAN_POINT('Ctrl Pts',(-18.7768200519616,-0.850380265270943,
124.654399856686));
#191163=CARTESIAN_POINT('Ctrl Pts',(-19.0552676757745,-5.63378746913994,
128.19560560636));
#191164=CARTESIAN_POINT('Ctrl Pts',(-19.3337152995874,-5.24001921468789,
134.134129766565));
#191165=CARTESIAN_POINT('Ctrl Pts',(-19.6121629234003,-0.0309292911078312,
137.012758747106));
#191166=CARTESIAN_POINT('Ctrl Pts',(-19.8906105472132,5.2065831400206,134.18617314371));
#191167=CARTESIAN_POINT('Ctrl Pts',(-20.1690581710261,5.65950002119693,
128.251867039513));
#191168=CARTESIAN_POINT('Ctrl Pts',(-20.447505794839,0.911612864839816,
124.663177837304));
#191169=CARTESIAN_POINT('Ctrl Pts',(-20.7259534186518,-4.67400197954067,
126.717935596697));
#191170=CARTESIAN_POINT('Ctrl Pts',(-21.0044010424647,-5.96443734241423,
132.527918317308));
#191171=CARTESIAN_POINT('Ctrl Pts',(-21.2828486662776,-1.77384616657202,
136.754035712331));
#191172=CARTESIAN_POINT('Ctrl Pts',(-21.5612962900905,4.0468229791472,135.512692353051));
#191173=CARTESIAN_POINT('Ctrl Pts',(-21.8397439139034,6.14865950532324,
129.944622143653));
#191174=CARTESIAN_POINT('Ctrl Pts',(-22.1181915377163,2.60017832482316,
125.166609591221));
#191175=CARTESIAN_POINT('Ctrl Pts',(-22.3966391615293,-3.33773971041633,
125.569414812551));
#191176=CARTESIAN_POINT('Ctrl Pts',(-22.6750867853421,-6.20843800943312,
130.782879487369));
#191177=CARTESIAN_POINT('Ctrl Pts',(-22.953534409155,-3.37388507683905,
136.016084271426));
#191178=CARTESIAN_POINT('Ctrl Pts',(-23.2319820329679,2.56110341792085,
136.45996962444));
#191179=CARTESIAN_POINT('Ctrl Pts',(-23.5104296567807,6.14256298846929,
131.706626591997));
#191180=CARTESIAN_POINT('Ctrl Pts',(-23.7888772805937,4.07930725349882,
126.124145207193));
#191181=CARTESIAN_POINT('Ctrl Pts',(-24.0673249044065,-1.73263256219878,
124.842553143289));
#191182=CARTESIAN_POINT('Ctrl Pts',(-24.3457725282195,-5.95236769704188,
129.039570897758));
#191183=CARTESIAN_POINT('Ctrl Pts',(-24.6242201520323,-4.70216770763169,
134.858344189959));
#191184=CARTESIAN_POINT('Ctrl Pts',(-24.9026677758452,0.86909469142902,
136.951704627238));
#191185=CARTESIAN_POINT('Ctrl Pts',(-25.1811153996581,5.64170152670257,
133.395956234079));
#191186=CARTESIAN_POINT('Ctrl Pts',(-25.459563023471,5.22986027137813,127.458658075828));
#191187=CARTESIAN_POINT('Ctrl Pts',(-25.7380106472839,0.0120329195352371,
124.595897106778));
#191188=CARTESIAN_POINT('Ctrl Pts',(-26.0164582710968,-5.21685209751974,
127.438410803838));
#191189=CARTESIAN_POINT('Ctrl Pts',(-26.2949058949097,-5.6517048943475,
133.374067943923));
#191190=CARTESIAN_POINT('Ctrl Pts',(-26.5733535187226,-0.892916994403456,
136.948289588268));
#191191=CARTESIAN_POINT('Ctrl Pts',(-26.8518011425354,4.68641800197708,
134.876540656153));
#191192=CARTESIAN_POINT('Ctrl Pts',(-27.1302487663484,5.95916379878798,
129.062657205632));
#191193=CARTESIAN_POINT('Ctrl Pts',(-27.4086963901612,1.75572918584856,
124.849314103734));
#191194=CARTESIAN_POINT('Ctrl Pts',(-27.6871440139742,-4.06113477674652,
126.108367827853));
#191195=CARTESIAN_POINT('Ctrl Pts',(-27.965591637787,-6.1460142769749,131.682809513716));
#191196=CARTESIAN_POINT('Ctrl Pts',(-28.2440392616,-2.5830069061529,136.449999578631));
#191197=CARTESIAN_POINT('Ctrl Pts',(-28.5224868854127,3.3536576245212,136.029123243122));
#191198=CARTESIAN_POINT('Ctrl Pts',(-28.8009345092257,6.20847463354345,
130.806945298572));
#191199=CARTESIAN_POINT('Ctrl Pts',(-29.0793821330386,3.35800675518651,
125.582392158445));
#191200=CARTESIAN_POINT('Ctrl Pts',(-29.3578297568515,-2.57830528343674,
125.156572924908));
#191201=CARTESIAN_POINT('Ctrl Pts',(-29.6362773806644,-6.14528072379723,
129.920794671155));
#191202=CARTESIAN_POINT('Ctrl Pts',(-29.9147250044772,-4.06504339264135,
135.496970357558));
#191203=CARTESIAN_POINT('Ctrl Pts',(-30.1931726282902,1.75077022794215,
136.760866939637));
#191204=CARTESIAN_POINT('Ctrl Pts',(-30.471620252103,5.95771153892721,132.551025203244));
#191205=CARTESIAN_POINT('Ctrl Pts',(-30.750067875916,4.68980699602731,126.736084041921));
#191206=CARTESIAN_POINT('Ctrl Pts',(-31.0285154997288,-0.887801066412759,
124.659690307256));
#191207=CARTESIAN_POINT('Ctrl Pts',(-31.3069631235417,-5.6495633203129,
128.229948403933));
#191208=CARTESIAN_POINT('Ctrl Pts',(-31.5854107473546,-5.21965287935721,
134.16596555791));
#191209=CARTESIAN_POINT('Ctrl Pts',(-31.8638583711675,0.00686356350839004,
137.012831995241));
#191210=CARTESIAN_POINT('Ctrl Pts',(-32.1423059949804,5.22707272681363,
134.154416537178));
#191211=CARTESIAN_POINT('Ctrl Pts',(-32.4207536187933,5.64385741087595,
128.217463348321));
#191212=CARTESIAN_POINT('Ctrl Pts',(-32.6992012426062,0.874212852105795,
124.657742372942));
#191213=CARTESIAN_POINT('Ctrl Pts',(-32.9776488664191,-4.69879061007736,
126.746463285377));
#191214=CARTESIAN_POINT('Ctrl Pts',(-33.2560964902319,-5.9538350502823,
132.564193606789));
#191215=CARTESIAN_POINT('Ctrl Pts',(-33.5345441140448,-1.73759594028995,
136.764723383724));
#191216=CARTESIAN_POINT('Ctrl Pts',(-33.8129917378578,4.07540895254819,
135.487970958469));
#191217=CARTESIAN_POINT('Ctrl Pts',(-34.0914393616706,6.14331211279008,
129.907209437008));
#191218=CARTESIAN_POINT('Ctrl Pts',(-34.3698869854835,2.56581155885918,
125.150886022208));
#191219=CARTESIAN_POINT('Ctrl Pts',(-34.6483346092964,-3.3695444708001,
125.589829572953));
#191220=CARTESIAN_POINT('Ctrl Pts',(-34.9267822331094,-6.2084537431929,
130.820672409693));
#191221=CARTESIAN_POINT('Ctrl Pts',(-35.2052298569221,-3.34209732541825,
136.036525506343));
#191222=CARTESIAN_POINT('Ctrl Pts',(-35.4836774807351,2.59548326388451,
136.444274675672));
#191223=CARTESIAN_POINT('Ctrl Pts',(-35.7621251045479,6.14794153008404,
131.66921835072));
#191224=CARTESIAN_POINT('Ctrl Pts',(-36.0405727283609,4.05074187377708,
126.099400019648));
#191225=CARTESIAN_POINT('Ctrl Pts',(-36.3190203521737,-1.76889167478912,
124.85321062796));
#191226=CARTESIAN_POINT('Ctrl Pts',(-36.5974679759867,-5.96300018938643,
129.075837346879));
#191227=CARTESIAN_POINT('Ctrl Pts',(-36.8759155997995,-4.67740283869194,
134.886892508504));
#191228=CARTESIAN_POINT('Ctrl Pts',(-37.1543632236125,0.906499216928551,
136.946300305126));
#191229=CARTESIAN_POINT('Ctrl Pts',(-37.4328108474252,5.65737277714046,
133.361565579315));
#191230=CARTESIAN_POINT('Ctrl Pts',(-37.7112584712383,5.2093971331851,127.426884420063));
#191231=CARTESIAN_POINT('Ctrl Pts',(-37.9897060950511,-0.0257599829691867,
124.595938887431));
#191232=CARTESIAN_POINT('Ctrl Pts',(-38.268153718864,-5.23724493321992,
127.470229626529));
#191233=CARTESIAN_POINT('Ctrl Pts',(-38.5466013426768,-5.63595764348039,
133.408423865036));
#191234=CARTESIAN_POINT('Ctrl Pts',(-38.8250489664898,-0.855500611219946,
136.953611194679));
#191235=CARTESIAN_POINT('Ctrl Pts',(-39.1034965903026,4.71111968922328,
134.847937651547));
#191236=CARTESIAN_POINT('Ctrl Pts',(-39.3819442141156,5.94845114626212,
129.026414353905));
#191237=CARTESIAN_POINT('Ctrl Pts',(-39.6603918379284,1.71944659787975,
124.838736815064));
#191238=CARTESIAN_POINT('Ctrl Pts',(-39.9388394617414,-4.08964537431793,
126.133176113797));
#191239=CARTESIAN_POINT('Ctrl Pts',(-40.2172870855541,-6.14055303780089,
131.720205771443));
#191240=CARTESIAN_POINT('Ctrl Pts',(-40.495734709367,-2.54859244223803,
136.465618474199));
#191241=CARTESIAN_POINT('Ctrl Pts',(-40.7741823331801,3.3854001020792,136.008611774531));
#191242=CARTESIAN_POINT('Ctrl Pts',(-41.0526299569928,6.20837533857501,
130.769152503414));
#191243=CARTESIAN_POINT('Ctrl Pts',(-41.3310775808058,3.3261569349168,125.562047769191));
#191244=CARTESIAN_POINT('Ctrl Pts',(-41.6095252046187,-2.61263720013008,
125.172372441404));
#191245=CARTESIAN_POINT('Ctrl Pts',(-41.8879728284316,-6.15054538268038,
129.958219109591));
#191246=CARTESIAN_POINT('Ctrl Pts',(-42.1664204522444,-4.03640282939359,
135.521628487296));
#191247=CARTESIAN_POINT('Ctrl Pts',(-42.4448680760573,1.78699673486542,
136.750099144066));
#191248=CARTESIAN_POINT('Ctrl Pts',(-42.7233156998703,5.96823359942677,
132.514726560457));
#191249=CARTESIAN_POINT('Ctrl Pts',(-43.0017633236831,4.66495535053527,
126.707611231352));
#191250=CARTESIAN_POINT('Ctrl Pts',(-43.2802109474961,-0.925188969759574,
124.665208450844));
#191251=CARTESIAN_POINT('Ctrl Pts',(-43.5586585713089,-5.6651298248394,
128.264386597296));
#191252=CARTESIAN_POINT('Ctrl Pts',(-43.8371061951219,-5.19909312786956,
134.197676783747));
#191253=CARTESIAN_POINT('Ctrl Pts',(-44.1155538189346,0.0446561637927345,
137.012675186187));
#191254=CARTESIAN_POINT('Ctrl Pts',(-44.3940014427476,5.24736862250453,
134.122535793092));
#191255=CARTESIAN_POINT('Ctrl Pts',(-44.6724490665605,5.62800566534308,
128.183155515557));
#191256=CARTESIAN_POINT('Ctrl Pts',(-44.9508966903734,0.836780445093053,
124.65253467378));
#191257=CARTESIAN_POINT('Ctrl Pts',(-45.2293443141862,-4.72340512520001,
126.775141340936));
#191258=CARTESIAN_POINT('Ctrl Pts',(-45.5077919379991,-5.94301213660306,
132.600403685011));
#191259=CARTESIAN_POINT('Ctrl Pts',(-45.7862395618121,-1.7012813267513,
136.775190191685));
#191260=CARTESIAN_POINT('Ctrl Pts',(-46.0646871856249,4.10384391017172,
135.463076010984));
#191261=CARTESIAN_POINT('Ctrl Pts',(-46.3431348094379,6.13773707756737,
129.869829974632));
#191262=CARTESIAN_POINT('Ctrl Pts',(-46.6215824332507,2.5313497158043,125.135371944775));
#191263=CARTESIAN_POINT('Ctrl Pts',(-46.9000300570636,-3.40122437147435,
125.610437559721));
#191264=CARTESIAN_POINT('Ctrl Pts',(-47.1784776808764,-6.20823942041608,
130.858464727578));
#191265=CARTESIAN_POINT('Ctrl Pts',(-47.4569253046894,-3.31018573135201,
136.056772861467));
#191266=CARTESIAN_POINT('Ctrl Pts',(-47.7353729285023,2.62976693326135,
136.428370737814));
#191267=CARTESIAN_POINT('Ctrl Pts',(-48.0138205523151,6.15309225746451,
131.631778061822));
#191268=CARTESIAN_POINT('Ctrl Pts',(-48.2922681761281,4.02202639232555,
126.074829176147));
#191269=CARTESIAN_POINT('Ctrl Pts',(-48.570715799941,-1.80508524044794,
124.864088634681));
#191270=CARTESIAN_POINT('Ctrl Pts',(-48.8491634237538,-5.97341172056607,
129.112167847066));
#191271=CARTESIAN_POINT('Ctrl Pts',(-49.1276110475668,-4.65246464686987,
134.915289547327));
#191272=CARTESIAN_POINT('Ctrl Pts',(-49.4060586713796,0.943870151766231,
136.940668391181));
#191273=CARTESIAN_POINT('Ctrl Pts',(-49.6845062951925,5.6728343915496,133.327080166382));
#191274=CARTESIAN_POINT('Ctrl Pts',(-49.9629539190054,5.18874095886556,
127.395235917922));
#191275=CARTESIAN_POINT('Ctrl Pts',(-50.2414015428183,-0.0635519309279763,
124.596210723434));
#191276=CARTESIAN_POINT('Ctrl Pts',(-50.5198491666312,-5.25744370088312,
127.50217199667));
#191277=CARTESIAN_POINT('Ctrl Pts',(-50.798296790444,-5.6200015501302,133.442683291627));
#191278=CARTESIAN_POINT('Ctrl Pts',(-51.076744414257,-0.818052527146474,
136.958704938348));
#191279=CARTESIAN_POINT('Ctrl Pts',(-51.3551920380699,4.73564680419706,
134.819184810706));
#191280=CARTESIAN_POINT('Ctrl Pts',(-51.6336396618827,5.93751807169133,
128.990237384633));
#191281=CARTESIAN_POINT('Ctrl Pts',(-51.9120872856956,1.68310029518491,
124.828380584778));
#191282=CARTESIAN_POINT('Ctrl Pts',(-52.1905349095086,-4.11800442857602,
126.1581574922));
#191283=CARTESIAN_POINT('Ctrl Pts',(-52.4689825333214,-6.13486425817587,
131.757568092191));
#191284=CARTESIAN_POINT('Ctrl Pts',(-52.7474301571343,-2.51408353929296,
136.481027589776));
#191285=CARTESIAN_POINT('Ctrl Pts',(-53.0258777809472,3.41701713239144,
135.987907460498));
#191286=CARTESIAN_POINT('Ctrl Pts',(-53.3043254047601,6.20804598997526,
130.731361012906));
#191287=CARTESIAN_POINT('Ctrl Pts',(-53.5827730285729,3.29418386267868,
125.541897635768));
#191288=CARTESIAN_POINT('Ctrl Pts',(-53.8612206523859,-2.64687230459117,
125.188380653292));
#191289=CARTESIAN_POINT('Ctrl Pts',(-54.1396682761987,-6.15558213084251,
129.995674902111));
#191290=CARTESIAN_POINT('Ctrl Pts',(-54.4181159000117,-4.0076126957546,
135.546111816938));
#191291=CARTESIAN_POINT('Ctrl Pts',(-54.6965635238244,1.82315702396754,
136.739111026966));
#191292=CARTESIAN_POINT('Ctrl Pts',(-54.9750111476374,5.97853450483549,
132.478364539431));
#191293=CARTESIAN_POINT('Ctrl Pts',(-55.2534587714502,4.63993084340721,
126.679290227339));
#191294=CARTESIAN_POINT('Ctrl Pts',(-55.5319063952633,-0.962542589888887,
124.670954082973));
#191295=CARTESIAN_POINT('Ctrl Pts',(-55.810354019076,-5.68048640589689,
128.298918910331));
#191296=CARTESIAN_POINT('Ctrl Pts',(-56.088801642889,-5.1783407220741,134.229262269005));
#191297=CARTESIAN_POINT('Ctrl Pts',(-56.3672492667019,0.0824471093265141,
137.012288325754));
#191298=CARTESIAN_POINT('Ctrl Pts',(-56.6456968905149,5.26747007502141,
134.090532092806));
#191299=CARTESIAN_POINT('Ctrl Pts',(-56.9241445143275,5.6119453719906,128.148944812513));
#191300=CARTESIAN_POINT('Ctrl Pts',(-57.2025921381407,0.799317030873196,
124.64755493279));
#191301=CARTESIAN_POINT('Ctrl Pts',(-57.4810397619534,-4.74784461280872,
126.803968700697));
#191302=CARTESIAN_POINT('Ctrl Pts',(-57.7594873857663,-5.93196900242356,
132.636547210196));
#191303=CARTESIAN_POINT('Ctrl Pts',(-58.0379350095792,-1.66490367160747,
136.785435748359));
#191304=CARTESIAN_POINT('Ctrl Pts',(-58.3163826333922,4.13212679834998,
135.438008433087));
#191305=CARTESIAN_POINT('Ctrl Pts',(-58.5948302572049,6.13193460624012,
129.832485141631));
#191306=CARTESIAN_POINT('Ctrl Pts',(-58.873277881018,2.49679407265481,125.120067933803));
#191307=CARTESIAN_POINT('Ctrl Pts',(-59.1517255048308,-3.43277823852872,
125.631238009216));
#191308=CARTESIAN_POINT('Ctrl Pts',(-59.4301731286437,-6.20779504904446,
130.896255040614));
#191309=CARTESIAN_POINT('Ctrl Pts',(-59.7086207524566,-3.27815147713605,
136.076825586523));
#191310=CARTESIAN_POINT('Ctrl Pts',(-59.9870683762695,2.66395315565763,
136.412258400192));
#191311=CARTESIAN_POINT('Ctrl Pts',(-60.2655160000824,6.15801497974849,
131.594307112665));
#191312=CARTESIAN_POINT('Ctrl Pts',(-60.5439636238952,3.99316187320697,
126.050433587173));
#191313=CARTESIAN_POINT('Ctrl Pts',(-60.8224112477081,-1.84121191800936,
124.875186760365));
#191314=CARTESIAN_POINT('Ctrl Pts',(-61.1008588715211,-5.98360190477769,
129.148561052078));
#191315=CARTESIAN_POINT('Ctrl Pts',(-61.3793064953339,-4.62735405625939,
134.943534254169));
#191316=CARTESIAN_POINT('Ctrl Pts',(-61.6577541191468,0.981206111148332,
136.934809094094));
#191317=CARTESIAN_POINT('Ctrl Pts',(-61.9362017429597,5.68808579699418,
133.292501273148));
#191318=CARTESIAN_POINT('Ctrl Pts',(-62.2146493667725,5.16789251384163,
127.36371374215));
#191319=CARTESIAN_POINT('Ctrl Pts',(-62.4930969905855,-0.10134152394658,
124.596712604715));
#191320=CARTESIAN_POINT('Ctrl Pts',(-62.7715446143984,-5.27744765203657,
127.534236730624));
#191321=CARTESIAN_POINT('Ctrl Pts',(-63.0499922382113,-5.60383720555579,
133.476844954201));
#191322=CARTESIAN_POINT('Ctrl Pts',(-63.3284398620242,-0.780574129835986,
136.963570630527));
#191323=CARTESIAN_POINT('Ctrl Pts',(-63.606887485837,4.75999843803683,134.790283199078));
#191324=CARTESIAN_POINT('Ctrl Pts',(-63.88533510965,5.92636498020503,128.954127638363));
#191325=CARTESIAN_POINT('Ctrl Pts',(-64.1637827334628,1.64669162458969,
124.818245796629));
#191326=CARTESIAN_POINT('Ctrl Pts',(-64.4422303572757,-4.14621088866563,
126.183311037368));
#191327=CARTESIAN_POINT('Ctrl Pts',(-64.7206779810887,-6.12894814889968,
131.794895091487));
#191328=CARTESIAN_POINT('Ctrl Pts',(-64.9991256049015,-2.47948147605779,
136.49622635437));
#191329=CARTESIAN_POINT('Ctrl Pts',(-65.2775732287142,3.44850754387722,
135.967011068231));
#191330=CARTESIAN_POINT('Ctrl Pts',(-65.5560208525274,6.20748659994837,
130.693572227424));
#191331=CARTESIAN_POINT('Ctrl Pts',(-65.83446847634,3.26208872324607,125.521942504845));
#191332=CARTESIAN_POINT('Ctrl Pts',(-66.1129161001531,-2.68100932822562,
125.204596967384));
#191333=CARTESIAN_POINT('Ctrl Pts',(-66.3913637239659,-6.1603907816451,
130.033160660777));
#191334=CARTESIAN_POINT('Ctrl Pts',(-66.6698113477789,-3.97867405855336,
135.570419439246));
#191335=CARTESIAN_POINT('Ctrl Pts',(-66.9482589715917,1.85924975531565,
136.727902995508));
#191336=CARTESIAN_POINT('Ctrl Pts',(-67.2267065954047,5.98861387344954,
132.441940487574));
#191337=CARTESIAN_POINT('Ctrl Pts',(-67.5051542192175,4.61473440193538,
126.651122079325));
#191338=CARTESIAN_POINT('Ctrl Pts',(-67.7836018430304,-0.999860542648545,
124.676926990737));
#191339=CARTESIAN_POINT('Ctrl Pts',(-68.0620494668433,-5.69563249444164,
128.33354406343));
#191340=CARTESIAN_POINT('Ctrl Pts',(-68.3404970906562,-5.15739643095884,
134.260720843274));
#191341=CARTESIAN_POINT('Ctrl Pts',(-68.618944714469,0.120234999752325,
137.011671428276));
#191342=CARTESIAN_POINT('Ctrl Pts',(-68.8973923382821,5.28737633949755,
134.058406622227));
#191343=CARTESIAN_POINT('Ctrl Pts',(-69.1758399620947,5.59567712593856,
128.114832506878));
#191344=CARTESIAN_POINT('Ctrl Pts',(-69.4542875859078,0.761823997666808,
124.642803334499));
#191345=CARTESIAN_POINT('Ctrl Pts',(-69.7327352097205,-4.77210816728929,
126.832944296451));
#191346=CARTESIAN_POINT('Ctrl Pts',(-70.0111828335336,-5.92070605695121,
132.672622843033));
#191347=CARTESIAN_POINT('Ctrl Pts',(-70.2896304573463,-1.62846432284579,
136.795459674095));
#191348=CARTESIAN_POINT('Ctrl Pts',(-70.5680780811594,4.16025656905012,
135.412769153666));
#191349=CARTESIAN_POINT('Ctrl Pts',(-70.8465257049722,6.12590491382102,
129.795176321834));
#191350=CARTESIAN_POINT('Ctrl Pts',(-71.1249733287852,2.46214590988275,
125.104974556385));
#191351=CARTESIAN_POINT('Ctrl Pts',(-71.4034209525978,-3.46420490272305,
125.652230150673));
#191352=CARTESIAN_POINT('Ctrl Pts',(-71.681868576411,-6.20712064554441,
130.93404194847));
#191353=CARTESIAN_POINT('Ctrl Pts',(-71.9603162002238,-3.24599574981168,
136.09668293845));
#191354=CARTESIAN_POINT('Ctrl Pts',(-72.2387638240367,2.69804066428979,
136.395938259856));
#191355=CARTESIAN_POINT('Ctrl Pts',(-72.5172114478495,6.16270951452303,
131.556806891751));
#191356=CARTESIAN_POINT('Ctrl Pts',(-72.7956590716624,3.96414938600637,
126.026214156713));
#191357=CARTESIAN_POINT('Ctrl Pts',(-73.0741066954753,-1.87727036878649,
124.886504593767));
#191358=CARTESIAN_POINT('Ctrl Pts',(-73.3525543192881,-5.99357036442037,
129.185015613353));
#191359=CARTESIAN_POINT('Ctrl Pts',(-73.6310019431012,-4.60207199734241,
134.971625582408));
#191360=CARTESIAN_POINT('Ctrl Pts',(-73.909449566914,1.01850571157763,136.928722630985));
#191361=CARTESIAN_POINT('Ctrl Pts',(-74.187897190727,5.70312642832773,133.257830180947));
#191362=CARTESIAN_POINT('Ctrl Pts',(-74.4663448145398,5.14685257066011,
127.332319060812));
#191363=CARTESIAN_POINT('Ctrl Pts',(-74.7447924383527,-0.139127361718492,
124.597444512675));
#191364=CARTESIAN_POINT('Ctrl Pts',(-75.0232400621657,-5.29725604542678,
127.566422640223));
#191365=CARTESIAN_POINT('Ctrl Pts',(-75.3016876859784,-5.58746520873256,
133.510907586884));
#191366=CARTESIAN_POINT('Ctrl Pts',(-75.5801353097915,-0.743066808063574,
136.968208090913));
#191367=CARTESIAN_POINT('Ctrl Pts',(-75.8585829336042,4.7841736883842,134.761233887624));
#191368=CARTESIAN_POINT('Ctrl Pts',(-76.1370305574171,5.91499228508486,
128.918086453158));
#191369=CARTESIAN_POINT('Ctrl Pts',(-76.41547818123,1.61022193523031,124.808332826166));
#191370=CARTESIAN_POINT('Ctrl Pts',(-76.693925805043,-4.17426370938676,
126.208635817229));
#191371=CARTESIAN_POINT('Ctrl Pts',(-76.9723734288558,-6.12280492919574,
131.832185386163));
#191372=CARTESIAN_POINT('Ctrl Pts',(-77.2508210526686,-2.44478753472383,
136.511214204787));
#191373=CARTESIAN_POINT('Ctrl Pts',(-77.5292686764817,3.47987016964863,
135.945923372052));
#191374=CARTESIAN_POINT('Ctrl Pts',(-77.8077163002943,6.20669718922256,
130.655787547247));
#191375=CARTESIAN_POINT('Ctrl Pts',(-78.0861639241075,3.22987270591563,
125.502183115868));
#191376=CARTESIAN_POINT('Ctrl Pts',(-78.3646115479203,-2.71504700607423,
125.221020782777));
#191377=CARTESIAN_POINT('Ctrl Pts',(-78.6430591717333,-6.16497115690175,
130.070674996542));
#191378=CARTESIAN_POINT('Ctrl Pts',(-78.921506795546,-3.94958799012119,
135.594550453492));
#191379=CARTESIAN_POINT('Ctrl Pts',(-79.199954419359,1.89527359148086,136.71647546501));
#191380=CARTESIAN_POINT('Ctrl Pts',(-79.4784020431719,5.9984713317742,132.405455754592));
#191381=CARTESIAN_POINT('Ctrl Pts',(-79.7568496669848,4.58936695978296,
126.623107831093));
#191382=CARTESIAN_POINT('Ctrl Pts',(-80.0352972907976,-1.0371414452086,
124.683126952807));
#191383=CARTESIAN_POINT('Ctrl Pts',(-80.3137449146107,-5.71056752923021,
128.368260773546));
#191384=CARTESIAN_POINT('Ctrl Pts',(-80.5921925384234,-5.13626103062165,
134.292051340844));
#191385=CARTESIAN_POINT('Ctrl Pts',(-80.8706401622364,0.158018434826916,
137.010824516613));
#191386=CARTESIAN_POINT('Ctrl Pts',(-81.1490877860493,5.30708667829958,
134.026160571776));
#191387=CARTESIAN_POINT('Ctrl Pts',(-81.4275354098621,5.57920153001237,
128.080819862696));
#191388=CARTESIAN_POINT('Ctrl Pts',(-81.705983033675,0.724302734791404,
124.63828005498));
#191389=CARTESIAN_POINT('Ctrl Pts',(-81.984430657488,-4.79619488954742,
126.862067054498));
#191390=CARTESIAN_POINT('Ctrl Pts',(-82.2628782813007,-5.90922371753823,
132.708629246728));
#191391=CARTESIAN_POINT('Ctrl Pts',(-82.5413259051138,-1.59196463073914,
136.805261597452));
#191392=CARTESIAN_POINT('Ctrl Pts',(-82.8197735289264,4.18823217991362,
135.387359107972));
#191393=CARTESIAN_POINT('Ctrl Pts',(-83.0982211527395,6.11964822374235,
129.757904897731));
#191394=CARTESIAN_POINT('Ctrl Pts',(-83.3766687765523,2.42740651138818,
125.090092371815));
#191395=CARTESIAN_POINT('Ctrl Pts',(-83.6551164003652,-3.49550319953123,
125.67341320622));
#191396=CARTESIAN_POINT('Ctrl Pts',(-83.9335640241781,-6.20621623490623,
130.971824050937));
#191397=CARTESIAN_POINT('Ctrl Pts',(-84.2120116479911,-3.21371974092037,
136.116344181428));
#191398=CARTESIAN_POINT('Ctrl Pts',(-84.4904592718038,2.73202819603347,
136.379410921554));
#191399=CARTESIAN_POINT('Ctrl Pts',(-84.7689068956169,6.16717568783019,
131.519278788663));
#191400=CARTESIAN_POINT('Ctrl Pts',(-85.0473545194296,3.9349900057924,126.002171782228));
#191401=CARTESIAN_POINT('Ctrl Pts',(-85.3258021432425,-1.91325925661942,
124.898041715501));
#191402=CARTESIAN_POINT('Ctrl Pts',(-85.6042497670555,-6.00331673010926,
129.221530180052));
#191403=CARTESIAN_POINT('Ctrl Pts',(-85.8826973908683,-4.57661940695503,
134.999562491112));
#191404=CARTESIAN_POINT('Ctrl Pts',(-86.1611450146813,1.05576757090286,
136.922409227389));
#191405=CARTESIAN_POINT('Ctrl Pts',(-86.4395926384942,5.71795572821454,
133.223068174528));
#191406=CARTESIAN_POINT('Ctrl Pts',(-86.718040262307,5.12562190896342,127.301053037252));
#191407=CARTESIAN_POINT('Ctrl Pts',(-86.9964878861199,-0.176908044074368,
124.598406420195));
#191408=CARTESIAN_POINT('Ctrl Pts',(-87.2749355099329,-5.31686814704595,
127.598728532803));
#191409=CARTESIAN_POINT('Ctrl Pts',(-87.5533831337457,-5.57088616633168,
133.544869927476));
#191410=CARTESIAN_POINT('Ctrl Pts',(-87.8318307575586,-0.70553195167748,
136.972617147663));
#191411=CARTESIAN_POINT('Ctrl Pts',(-88.1102783813713,4.80817165941601,
134.732037952774));
#191412=CARTESIAN_POINT('Ctrl Pts',(-88.3887260051845,5.90340040775061,
128.882115164534));
#191413=CARTESIAN_POINT('Ctrl Pts',(-88.6671736289971,1.57369257850503,
124.798642040718));
#191414=CARTESIAN_POINT('Ctrl Pts',(-88.9456212528103,-4.20216185122988,
126.234130893362));
#191415=CARTESIAN_POINT('Ctrl Pts',(-89.2240688766231,-6.11643482670397,
131.869437594414));
#191416=CARTESIAN_POINT('Ctrl Pts',(-89.5025165004358,-2.41000300088966,
136.525990585645));
#191417=CARTESIAN_POINT('Ctrl Pts',(-89.7809641242489,3.51110384754994,
135.924645153375));
#191418=CARTESIAN_POINT('Ctrl Pts',(-90.0594117480617,6.20567778705031,
130.618008372501));
#191419=CARTESIAN_POINT('Ctrl Pts',(-90.3378593718745,3.19753700446471,
125.482620201028));
#191420=CARTESIAN_POINT('Ctrl Pts',(-90.6163069956876,-2.74898407685696,
125.237651490881));
#191421=CARTESIAN_POINT('Ctrl Pts',(-90.8947546195002,-6.16932308688508,
130.108216519297));
#191422=CARTESIAN_POINT('Ctrl Pts',(-91.1732022433134,-3.92035556825405,
135.618503965492));
#191423=CARTESIAN_POINT('Ctrl Pts',(-91.4516498671261,1.93122719758584,
136.70482885892));
#191424=CARTESIAN_POINT('Ctrl Pts',(-91.7300974909391,6.00810651453776,
132.368911692441));
#191425=CARTESIAN_POINT('Ctrl Pts',(-92.0085451147519,4.56382945695037,
126.595248520721));
#191426=CARTESIAN_POINT('Ctrl Pts',(-92.2869927385648,-1.07438391611076,
124.689553739443));
#191427=CARTESIAN_POINT('Ctrl Pts',(-92.5654403623776,-5.72529095683809,
128.403067754236));
#191428=CARTESIAN_POINT('Ctrl Pts',(-92.8438879861907,-5.11493530424405,
134.323252600751));
#191429=CARTESIAN_POINT('Ctrl Pts',(-93.1223356100035,0.195796014469281,
137.009747622148));
#191430=CARTESIAN_POINT('Ctrl Pts',(-93.4007832338166,5.32660036105212,
133.993795136343));
#191431=CARTESIAN_POINT('Ctrl Pts',(-93.6792308576291,5.56251919472255,
128.046908140318));
#191432=CARTESIAN_POINT('Ctrl Pts',(-93.9576784814422,0.686754632612129,
124.633985261843));
#191433=CARTESIAN_POINT('Ctrl Pts',(-94.2361261052551,-4.82010388703947,
126.891335895681));
#191434=CARTESIAN_POINT('Ctrl Pts',(-94.5145737290679,-5.8975224096676,
132.744565087048));
#191435=CARTESIAN_POINT('Ctrl Pts',(-94.7930213528811,-1.55540594779807,
136.814841155217));
#191436=CARTESIAN_POINT('Ctrl Pts',(-95.0714689766937,4.21605259429308,
135.361779237583));
#191437=CARTESIAN_POINT('Ctrl Pts',(-95.3499166005066,6.11316476784841,
129.720672250431));
#191438=CARTESIAN_POINT('Ctrl Pts',(-95.6283642243196,2.39257716445285,
125.075421931555));
#191439=CARTESIAN_POINT('Ctrl Pts',(-95.9068118481323,-3.52667196918255,
125.694786390909));
#191440=CARTESIAN_POINT('Ctrl Pts',(-96.1852594719453,-6.20508185064282,
131.009599947983));
#191441=CARTESIAN_POINT('Ctrl Pts',(-96.4637070957582,-3.18132464646333,
136.135808586901));
#191442=CARTESIAN_POINT('Ctrl Pts',(-96.742154719571,2.76591449146702,136.362676997713));
#191443=CARTESIAN_POINT('Ctrl Pts',(-97.020602343384,6.17141333417382,131.481724194021));
#191444=CARTESIAN_POINT('Ctrl Pts',(-97.299049967197,3.90568481307747,125.978307354616));
#191445=CARTESIAN_POINT('Ctrl Pts',(-97.5774975910097,-1.94917724792726,
124.909797698053));
#191446=CARTESIAN_POINT('Ctrl Pts',(-97.8559452148228,-6.01284064068852,
129.258103399115));
#191447=CARTESIAN_POINT('Ctrl Pts',(-98.1343928386354,-4.55099722825276,
135.027343945068));
#191448=CARTESIAN_POINT('Ctrl Pts',(-98.4128404624484,1.09299030837272,
136.915869117251));
#191449=CARTESIAN_POINT('Ctrl Pts',(-98.6912880862614,5.73257314714861,
133.188216542011));
#191450=CARTESIAN_POINT('Ctrl Pts',(-98.9697357100741,5.10420131546234,
127.269916830042));
#191451=CARTESIAN_POINT('Ctrl Pts',(-99.2481833338871,-0.214682171037078,
124.599598291628));
#191452=CARTESIAN_POINT('Ctrl Pts',(-99.5266309576999,-5.33628323016052,
127.631153211259));
#191453=CARTESIAN_POINT('Ctrl Pts',(-99.8050785815131,-5.55410069269506,
133.578730717485));
#191454=CARTESIAN_POINT('Ctrl Pts',(-100.083526205326,-0.667970951546107,
136.976797637399));
#191455=CARTESIAN_POINT('Ctrl Pts',(-100.361973829139,4.83199146187865,
134.702696476397));
#191456=CARTESIAN_POINT('Ctrl Pts',(-100.640421452952,5.89158977774298,
128.846215105423));
#191457=CARTESIAN_POINT('Ctrl Pts',(-100.918869076765,1.53710490802326,
124.789173799381));
#191458=CARTESIAN_POINT('Ctrl Pts',(-101.197316700577,-4.22990428042106,
126.259795321038));
#191459=CARTESIAN_POINT('Ctrl Pts',(-101.47576432439,-6.10983807746976,
131.906650335846));
#191460=CARTESIAN_POINT('Ctrl Pts',(-101.754211948203,-2.37512916350784,
136.540554949401));
#191461=CARTESIAN_POINT('Ctrl Pts',(-102.032659572016,3.54220742020778,
135.903177200671));
#191462=CARTESIAN_POINT('Ctrl Pts',(-102.311107195829,6.20442843120499,
130.580236103105));
#191463=CARTESIAN_POINT('Ctrl Pts',(-102.589554819642,3.16508281710451,
125.463254485237));
#191464=CARTESIAN_POINT('Ctrl Pts',(-102.868002443455,-2.78281928302352,
125.254488475437));
#191465=CARTESIAN_POINT('Ctrl Pts',(-103.146450067268,-6.1734464103326,
130.145783837928));
#191466=CARTESIAN_POINT('Ctrl Pts',(-103.424897691081,-3.8909778761698,
135.642279087639));
#191467=CARTESIAN_POINT('Ctrl Pts',(-103.703345314893,1.96710924135641,
136.69296360881));
#191468=CARTESIAN_POINT('Ctrl Pts',(-103.981792938706,6.01751906470488,
132.332309655276));
#191469=CARTESIAN_POINT('Ctrl Pts',(-104.260240562519,4.53812283973896,
126.567545180546));
#191470=CARTESIAN_POINT('Ctrl Pts',(-104.538688186332,-1.11158657532129,
124.696207112496));
#191471=CARTESIAN_POINT('Ctrl Pts',(-104.817135810145,-5.73980223168479,
128.437963715717));
#191472=CARTESIAN_POINT('Ctrl Pts',(-105.095583433958,-5.093420042057,134.354323466822));
#191473=CARTESIAN_POINT('Ctrl Pts',(-105.374031057771,0.233566338818549,
137.008440784786));
#191474=CARTESIAN_POINT('Ctrl Pts',(-105.652478681584,5.34591666467016,
133.961311515241));
#191475=CARTESIAN_POINT('Ctrl Pts',(-105.930926305397,5.54563073823764,
128.013098596357));
#191476=CARTESIAN_POINT('Ctrl Pts',(-106.20937392921,0.649181082487974,
124.629919114234));
#191477=CARTESIAN_POINT('Ctrl Pts',(-106.487821553022,-4.84383427380942,
126.920749735436));
#191478=CARTESIAN_POINT('Ctrl Pts',(-106.766269176835,-5.88560256693534,
132.780429032376));
#191479=CARTESIAN_POINT('Ctrl Pts',(-107.044716800648,-1.51878962871805,
136.824197992414));
#191480=CARTESIAN_POINT('Ctrl Pts',(-107.323164424461,4.2437167812931,135.336030490371));
#191481=CARTESIAN_POINT('Ctrl Pts',(-107.601612048274,6.10645478638612,
129.683479759601));
#191482=CARTESIAN_POINT('Ctrl Pts',(-107.880059672087,2.35765915969063,
125.060963779225));
#191483=CARTESIAN_POINT('Ctrl Pts',(-108.1585072959,-3.55771005670707,125.716348912751));
#191484=CARTESIAN_POINT('Ctrl Pts',(-108.436954919713,-6.20371753478999,
131.04736823981));
#191485=CARTESIAN_POINT('Ctrl Pts',(-108.715402543526,-3.14881166685081,
136.155075433609));
#191486=CARTESIAN_POINT('Ctrl Pts',(-108.993850167338,2.79969829492213,
136.345737108415));
#191487=CARTESIAN_POINT('Ctrl Pts',(-109.272297791151,6.17542229652738,
131.444144499421));
#191488=CARTESIAN_POINT('Ctrl Pts',(-109.550745414964,3.87623489377466,
125.954621758183));
#191489=CARTESIAN_POINT('Ctrl Pts',(-109.829193038777,-1.98502301175461,
124.921772105802));
#191490=CARTESIAN_POINT('Ctrl Pts',(-110.10764066259,-6.02214174324697,
129.294733915307));
#191491=CARTESIAN_POINT('Ctrl Pts',(-110.386088286403,-4.52520641067474,
135.054968914823));
#191492=CARTESIAN_POINT('Ctrl Pts',(-110.664535910216,1.13017254468408,
136.909102542919));
#191493=CARTESIAN_POINT('Ctrl Pts',(-110.942983534029,5.74697814347679,
133.153276574838));
#191494=CARTESIAN_POINT('Ctrl Pts',(-111.221431157841,5.08259158390449,
127.238911592946));
#191495=CARTESIAN_POINT('Ctrl Pts',(-111.499878781655,-0.252448342873548,
124.601020082813));
#191496=CARTESIAN_POINT('Ctrl Pts',(-111.778326405467,-5.3555005753377,
127.663695474083));
#191497=CARTESIAN_POINT('Ctrl Pts',(-112.05677402928,-5.53710940981492,
133.612488702192));
#191498=CARTESIAN_POINT('Ctrl Pts',(-112.335221653093,-0.630385199504834,
136.980749405212));
#191499=CARTESIAN_POINT('Ctrl Pts',(-112.613669276906,4.85563221312083,
134.673210545752));
#191500=CARTESIAN_POINT('Ctrl Pts',(-112.892116900719,5.8795608327098,128.810387606114));
#191501=CARTESIAN_POINT('Ctrl Pts',(-113.170564524532,1.50046027955312,
124.779928453004));
#191502=CARTESIAN_POINT('Ctrl Pts',(-113.449012148345,-4.25748996895278,
126.285628149252));
#191503=CARTESIAN_POINT('Ctrl Pts',(-113.727459772158,-6.10301492593933,
131.943822231527));
#191504=CARTESIAN_POINT('Ctrl Pts',(-114.00590739597,-2.3401673148416,136.554906756366));
#191505=CARTESIAN_POINT('Ctrl Pts',(-114.284355019783,3.57317973506622,
135.881520309444));
#191506=CARTESIAN_POINT('Ctrl Pts',(-114.562802643596,6.202949167983,130.542472138726));
#191507=CARTESIAN_POINT('Ctrl Pts',(-114.841250267409,3.13251134643626,
125.444086686097));
#191508=CARTESIAN_POINT('Ctrl Pts',(-115.119697891222,-2.81655137079845,
125.271531112549));
#191509=CARTESIAN_POINT('Ctrl Pts',(-115.398145515035,-6.17734097445314,
130.183375560363));
#191510=CARTESIAN_POINT('Ctrl Pts',(-115.676593138848,-3.86145600246928,
135.665874938939));
#191511=CARTESIAN_POINT('Ctrl Pts',(-115.955040762661,2.00291839317105,
136.680880154352));
#191512=CARTESIAN_POINT('Ctrl Pts',(-116.233488386474,6.02670863349017,
132.295650999397));
#191513=CARTESIAN_POINT('Ctrl Pts',(-116.511936010287,4.51224806071678,
126.539998837124));
#191514=CARTESIAN_POINT('Ctrl Pts',(-116.790383634099,-1.14874804428301,
124.703086825424));
#191515=CARTESIAN_POINT('Ctrl Pts',(-117.068831257912,-5.75410081604829,
128.472947364906));
#191516=CARTESIAN_POINT('Ctrl Pts',(-117.347278881725,-5.07171604131793,
134.385262787713));
#191517=CARTESIAN_POINT('Ctrl Pts',(-117.625726505538,0.271328008281021,
137.006904052952));
#191518=CARTESIAN_POINT('Ctrl Pts',(-117.904174129351,5.3650348733795,133.928710912162));
#191519=CARTESIAN_POINT('Ctrl Pts',(-118.182621753164,5.52853678636705,
127.979392483636));
#191520=CARTESIAN_POINT('Ctrl Pts',(-118.461069376977,0.611583476719488,
124.626081762825));
#191521=CARTESIAN_POINT('Ctrl Pts',(-118.73951700079,-4.86738517051901,
126.95030748382));
#191522=CARTESIAN_POINT('Ctrl Pts',(-119.017964624603,-5.87346463103546,
132.816219753764));
#191523=CARTESIAN_POINT('Ctrl Pts',(-119.296412248415,-1.48211703032935,
136.833331762325));
#191524=CARTESIAN_POINT('Ctrl Pts',(-119.574859872228,4.27122371580729,
135.310113820466));
#191525=CARTESIAN_POINT('Ctrl Pts',(-119.853307496041,6.09951852799569,
129.646328803424));
#191526=CARTESIAN_POINT('Ctrl Pts',(-120.131755119854,2.32265379100196,
125.046718450578));
#191527=CARTESIAN_POINT('Ctrl Pts',(-120.410202743667,-3.58861631197691,
125.738099972737));
#191528=CARTESIAN_POINT('Ctrl Pts',(-120.68865036748,-6.20212333790203,
131.085127526901));
#191529=CARTESIAN_POINT('Ctrl Pts',(-120.967097991293,-3.11618200686478,
136.174144007612));
#191530=CARTESIAN_POINT('Ctrl Pts',(-121.245545615105,2.83337835452712,
136.328591881372));
#191531=CARTESIAN_POINT('Ctrl Pts',(-121.523993238919,6.17920242633619,
131.406541097396));
#191532=CARTESIAN_POINT('Ctrl Pts',(-121.802440862731,3.84664133916317,
125.931115870606));
#191533=CARTESIAN_POINT('Ctrl Pts',(-122.080888486544,-2.02079521982502,
124.933964495032));
#191534=CARTESIAN_POINT('Ctrl Pts',(-122.359336110357,-6.03121969312815,
129.331420371272));
#191535=CARTESIAN_POINT('Ctrl Pts',(-122.63778373417,-4.49924790990888,
135.082436376724));
#191536=CARTESIAN_POINT('Ctrl Pts',(-122.916231357983,1.16731290203685,
136.90210975513));
#191537=CARTESIAN_POINT('Ctrl Pts',(-123.194678981796,5.76117018341619,
133.118249567719));
#191538=CARTESIAN_POINT('Ctrl Pts',(-123.473126605609,5.06079351504635,
127.208038474877));
#191539=CARTESIAN_POINT('Ctrl Pts',(-123.751574229422,-0.290205160143283,
124.602671741062));
#191540=CARTESIAN_POINT('Ctrl Pts',(-124.030021853235,-5.37451947047147,
127.696354115408));
#191541=CARTESIAN_POINT('Ctrl Pts',(-124.308469477047,-5.51991294730918,
133.646142630679));
#191542=CARTESIAN_POINT('Ctrl Pts',(-124.58691710086,-0.592776088308802,
136.984472304668));
#191543=CARTESIAN_POINT('Ctrl Pts',(-124.865364724673,4.87909303712557,
134.64358125345));
#191544=CARTESIAN_POINT('Ctrl Pts',(-125.143812348486,5.86731401838748,
128.774633994209));
#191545=CARTESIAN_POINT('Ctrl Pts',(-125.422259972299,1.46376005097626,
124.770906344175));
#191546=CARTESIAN_POINT('Ctrl Pts',(-125.700707596112,-4.28491789462882,
126.311628420759));
#191547=CARTESIAN_POINT('Ctrl Pts',(-125.979155219925,-6.09596562494584,
131.980951904039));
#191548=CARTESIAN_POINT('Ctrl Pts',(-126.257602843738,-2.30511875041471,
136.569045474729));
#191549=CARTESIAN_POINT('Ctrl Pts',(-126.536050467551,3.60401964443632,
135.859675282198));
#191550=CARTESIAN_POINT('Ctrl Pts',(-126.814498091363,6.20124005219796,
130.50471787872));
#191551=CARTESIAN_POINT('Ctrl Pts',(-127.092945715177,3.09982379940838,
125.42511751388));
#191552=CARTESIAN_POINT('Ctrl Pts',(-127.371393338989,-2.85017909022625,
125.288778770691));
#191553=CARTESIAN_POINT('Ctrl Pts',(-127.649840962802,-6.18100663493216,
130.220990293627));
#191554=CARTESIAN_POINT('Ctrl Pts',(-127.928288586615,-3.83179104109667,
135.689290645038));
#191555=CARTESIAN_POINT('Ctrl Pts',(-128.206736210428,2.03865332610762,
136.6685789433));
#191556=CARTESIAN_POINT('Ctrl Pts',(-128.485183834241,6.03567488037103,
132.258937083203));
#191557=CARTESIAN_POINT('Ctrl Pts',(-128.763631458054,4.48620607868298,
126.512610511197));
#191558=CARTESIAN_POINT('Ctrl Pts',(-129.042079081867,-1.18586694596332,
124.710192623294));
#191559=CARTESIAN_POINT('Ctrl Pts',(-129.32052670568,-5.76818618009069,
128.508017405469));
#191560=CARTESIAN_POINT('Ctrl Pts',(-129.598974329492,-5.04982410627509,
134.416069416958));
#191561=CARTESIAN_POINT('Ctrl Pts',(-129.877421953305,0.30907962358457,
137.005137483589));
#191562=CARTESIAN_POINT('Ctrl Pts',(-130.155869577118,5.38395427874936,
133.895994535135));
#191563=CARTESIAN_POINT('Ctrl Pts',(-130.434317200931,5.51123797253198,
127.945791051148));
#191564=CARTESIAN_POINT('Ctrl Pts',(-130.712764824744,0.573963208500954,
124.622473349811));
#191565=CARTESIAN_POINT('Ctrl Pts',(-130.991212448557,-4.89075570448117,
126.980008045559));
#191566=CARTESIAN_POINT('Ctrl Pts',(-131.26966007237,-5.8611090517438,132.851935924971));
#191567=CARTESIAN_POINT('Ctrl Pts',(-131.548107696183,-1.44538951154951,
136.842242126491));
#191568=CARTESIAN_POINT('Ctrl Pts',(-131.826555319995,4.29857237855583,
135.28403018822));
#191569=CARTESIAN_POINT('Ctrl Pts',(-132.105002943808,6.09235624970348,
129.609220758541));
#191570=CARTESIAN_POINT('Ctrl Pts',(-132.383450567622,2.28756235552218,
125.032686473479));
#191571=CARTESIAN_POINT('Ctrl Pts',(-132.661898191434,-3.6193895897498,
125.760038764874));
#191572=CARTESIAN_POINT('Ctrl Pts',(-132.940345815247,-6.20029931905343,
131.122876410071));
#191573=CARTESIAN_POINT('Ctrl Pts',(-133.21879343906,-3.08343687560774,
136.193013602317));
#191574=CARTESIAN_POINT('Ctrl Pts',(-133.497241062873,2.86695342225543,
136.311241951909));
#191575=CARTESIAN_POINT('Ctrl Pts',(-133.775688686686,6.18275358352724,
131.368915381349));
#191576=CARTESIAN_POINT('Ctrl Pts',(-134.054136310499,3.81690524584148,
125.907790562906));
#191577=CARTESIAN_POINT('Ctrl Pts',(-134.332583934311,-2.05649254658467,
124.946374413949));
#191578=CARTESIAN_POINT('Ctrl Pts',(-134.611031558124,-6.04007415394596,
129.36816140758));
#191579=CARTESIAN_POINT('Ctrl Pts',(-134.889479181937,-4.47312268785726,
135.109745312956));
#191580=CARTESIAN_POINT('Ctrl Pts',(-135.16792680575,1.20441000418008,136.894891013003));
#191581=CARTESIAN_POINT('Ctrl Pts',(-135.446374429563,5.775148741076,133.083136818595));
#191582=CARTESIAN_POINT('Ctrl Pts',(-135.724822053376,5.03880791662344,
127.177298619846));
#191583=CARTESIAN_POINT('Ctrl Pts',(-136.003269677189,-0.327951223754644,
124.604553205172));
#191584=CARTESIAN_POINT('Ctrl Pts',(-136.281717301002,-5.39333921080989,
127.729127925058));
#191585=CARTESIAN_POINT('Ctrl Pts',(-136.560164924815,-5.50251194239939,
133.679691255889));
#191586=CARTESIAN_POINT('Ctrl Pts',(-136.838612548628,-0.555145011576188,
136.987966197812));
#191587=CARTESIAN_POINT('Ctrl Pts',(-137.117060172441,4.90237306454367,
134.613809697415));
#191588=CARTESIAN_POINT('Ctrl Pts',(-137.395507796253,5.8548497885868,128.73895559457));
#191589=CARTESIAN_POINT('Ctrl Pts',(-137.673955420066,1.42700558223168,
124.762107807213));
#191590=CARTESIAN_POINT('Ctrl Pts',(-137.952403043879,-4.3121870410957,
126.33779517211));
#191591=CARTESIAN_POINT('Ctrl Pts',(-138.230850667692,-6.08869043570493,
132.018037977528));
#191592=CARTESIAN_POINT('Ctrl Pts',(-138.509298291505,-2.26998476896503,
136.582970580575));
#191593=CARTESIAN_POINT('Ctrl Pts',(-138.787745915318,3.63472600553235,
135.837642928407));
#191594=CARTESIAN_POINT('Ctrl Pts',(-139.066193539131,6.1993011471828,130.466974722087));
#191595=CARTESIAN_POINT('Ctrl Pts',(-139.344641162943,3.06702138726935,
125.406347671494));
#191596=CARTESIAN_POINT('Ctrl Pts',(-139.623088786757,-2.88370119522,125.306230810748));
#191597=CARTESIAN_POINT('Ctrl Pts',(-139.901536410569,-6.18444325593727,
130.258626643894));
#191598=CARTESIAN_POINT('Ctrl Pts',(-140.179984034382,-3.80198409129777,
135.712525338258));
#191599=CARTESIAN_POINT('Ctrl Pts',(-140.458431658195,2.07431271599591,
136.656060431482));
#191600=CARTESIAN_POINT('Ctrl Pts',(-140.736879282008,6.04441747309895,
132.222169267145));
#191601=CARTESIAN_POINT('Ctrl Pts',(-141.015326905821,4.45999785863389,
126.485381217648));
#191602=CARTESIAN_POINT('Ctrl Pts',(-141.293774529634,-1.22294190490765,
124.717524242802));
#191603=CARTESIAN_POINT('Ctrl Pts',(-141.572222153447,-5.78205780187226,
128.543172537875));
#191604=CARTESIAN_POINT('Ctrl Pts',(-141.85066977726,-5.02774504814366,
134.446742213005));
#191605=CARTESIAN_POINT('Ctrl Pts',(-142.129117401072,0.346819785828787,
137.003141142159));
#191606=CARTESIAN_POINT('Ctrl Pts',(-142.407565024885,5.40267417971275,
133.863163596476));
#191607=CARTESIAN_POINT('Ctrl Pts',(-142.686012648698,5.49373493774783,
127.912295544006));
#191608=CARTESIAN_POINT('Ctrl Pts',(-142.964460272511,0.536321671864061,
124.619094008905));
#191609=CARTESIAN_POINT('Ctrl Pts',(-143.242907896324,-4.91394500969209,
127.00985032009));
#191610=CARTESIAN_POINT('Ctrl Pts',(-143.521355520137,-5.84853628690073,
132.887576222521));
#191611=CARTESIAN_POINT('Ctrl Pts',(-143.79980314395,-1.40860843332932,
136.850928754739));
#191612=CARTESIAN_POINT('Ctrl Pts',(-144.078250767763,4.32576175612421,
135.257780560169));
#191613=CARTESIAN_POINT('Ctrl Pts',(-144.356698391576,6.08496821690962,
129.572157000006));
#191614=CARTESIAN_POINT('Ctrl Pts',(-144.635146015388,2.2523861535788,125.018868367886));
#191615=CARTESIAN_POINT('Ctrl Pts',(-144.913593639201,-3.65002874971022,
125.782164476213));
#191616=CARTESIAN_POINT('Ctrl Pts',(-145.192041263014,-6.19824554583293,
131.160613490521));
#191617=CARTESIAN_POINT('Ctrl Pts',(-145.470488886827,-3.05057748646412,
136.211683518503));
#191618=CARTESIAN_POINT('Ctrl Pts',(-145.74893651064,2.90042225397064,136.293687962933));
#191619=CARTESIAN_POINT('Ctrl Pts',(-146.027384134453,6.18607563651005,
131.33126874552));
#191620=CARTESIAN_POINT('Ctrl Pts',(-146.305831758266,3.78702771569254,
125.884646699409));
#191621=CARTESIAN_POINT('Ctrl Pts',(-146.584279382079,-2.09211366925746,
124.959001402698));
#191622=CARTESIAN_POINT('Ctrl Pts',(-146.862727005891,-6.04870479759444,
129.404955662777));
#191623=CARTESIAN_POINT('Ctrl Pts',(-147.141174629705,-4.4468317125993,
135.136894711575));
#191624=CARTESIAN_POINT('Ctrl Pts',(-147.419622253517,1.24146247646836,
136.887446584034));
#191625=CARTESIAN_POINT('Ctrl Pts',(-147.69806987733,5.78891329847519,133.04793962858));
#191626=CARTESIAN_POINT('Ctrl Pts',(-147.976517501143,5.01663560332014,
127.146693166932));
#191627=CARTESIAN_POINT('Ctrl Pts',(-148.254965124956,-0.365685135012239,
124.606664405427));
#191628=CARTESIAN_POINT('Ctrl Pts',(-148.533412748769,-5.41195909898036,
127.762015688586));
#191629=CARTESIAN_POINT('Ctrl Pts',(-148.811860372582,-5.48490703988586,
133.713133334664));
#191630=CARTESIAN_POINT('Ctrl Pts',(-149.090307996395,-0.517493363741682,
136.991230955176));
#191631=CARTESIAN_POINT('Ctrl Pts',(-149.368755620208,4.92547143272535,
134.583896980843));
#191632=CARTESIAN_POINT('Ctrl Pts',(-149.647203244021,5.84216860517359,
128.703353729273));
#191633=CARTESIAN_POINT('Ctrl Pts',(-149.925650867833,1.39019823527075,
124.753533168151));
#191634=CARTESIAN_POINT('Ctrl Pts',(-150.204098491647,-4.33929639788676,
126.364127433687));
#191635=CARTESIAN_POINT('Ctrl Pts',(-150.482546115459,-6.08118962780021,
132.055079077756));
#191636=CARTESIAN_POINT('Ctrl Pts',(-150.760993739272,-2.23476667239474,
136.596681557904));
#191637=CARTESIAN_POINT('Ctrl Pts',(-151.039441363085,3.66529768052036,
135.81542406449));
#191638=CARTESIAN_POINT('Ctrl Pts',(-151.317888986898,6.19713252478332,
130.429244067412));
#191639=CARTESIAN_POINT('Ctrl Pts',(-151.596336610711,3.03410532552526,
125.387777854462));
#191640=CARTESIAN_POINT('Ctrl Pts',(-151.874784234524,-2.91711644360522,
125.323886586026));
#191641=CARTESIAN_POINT('Ctrl Pts',(-152.153231858337,-6.18765071012318,
130.296283216534));
#191642=CARTESIAN_POINT('Ctrl Pts',(-152.431679482149,-3.77203625758034,
135.735578157629));
#191643=CARTESIAN_POINT('Ctrl Pts',(-152.710127105962,2.10989524146327,
136.643325082775));
#191644=CARTESIAN_POINT('Ctrl Pts',(-152.988574729775,6.0529360877152,132.185348913665));
#191645=CARTESIAN_POINT('Ctrl Pts',(-153.267022353588,4.43362437172323,
126.458311965469));
#191646=CARTESIAN_POINT('Ctrl Pts',(-153.545469977401,-1.25997154729018,
124.725081412269));
#191647=CARTESIAN_POINT('Ctrl Pts',(-153.823917601214,-5.79571516737629,
128.578411459437));
#191648=CARTESIAN_POINT('Ctrl Pts',(-154.102365225027,-5.00547968506979,
134.477280039263));
#191649=CARTESIAN_POINT('Ctrl Pts',(-154.38081284884,0.38454709653853,137.000915102638));
#191650=CARTESIAN_POINT('Ctrl Pts',(-154.659260472653,5.4211938825983,133.830219312748));
#191651=CARTESIAN_POINT('Ctrl Pts',(-154.937708096465,5.47602833059452,
127.8789072034));
#191652=CARTESIAN_POINT('Ctrl Pts',(-155.216155720278,0.498660261630971,
124.615943865326));
#191653=CARTESIAN_POINT('Ctrl Pts',(-155.494603344091,-4.93695222686361,
127.039833201595));
#191654=CARTESIAN_POINT('Ctrl Pts',(-155.773050967904,-5.83574680239484,
132.923139325752));
#191655=CARTESIAN_POINT('Ctrl Pts',(-156.051498591717,-1.37177515860606,
136.85939132518));
#191656=CARTESIAN_POINT('Ctrl Pts',(-156.32994621553,4.3527908409998,135.231365909006));
#191657=CARTESIAN_POINT('Ctrl Pts',(-156.608393839343,6.0773547033811,129.535138901228));
#191658=CARTESIAN_POINT('Ctrl Pts',(-156.886841463156,2.21712648863745,
125.005264645838));
#191659=CARTESIAN_POINT('Ctrl Pts',(-157.165289086968,-3.68053265651321,
125.804476286877));
#191660=CARTESIAN_POINT('Ctrl Pts',(-157.443736710782,-6.19596209434481,
131.19833736989));
#191661=CARTESIAN_POINT('Ctrl Pts',(-157.722184334594,-3.0176050570491,
136.230153064351));
#191662=CARTESIAN_POINT('Ctrl Pts',(-158.000631958407,2.93378360947182,
136.275930564914));
#191663=CARTESIAN_POINT('Ctrl Pts',(-158.27907958222,6.18916846218569,131.293602584915));
#191664=CARTESIAN_POINT('Ctrl Pts',(-158.557527206033,3.7570098558391,125.861685137721));
#191665=CARTESIAN_POINT('Ctrl Pts',(-158.835974829846,-2.12765726788813,
124.971844993383));
#191666=CARTESIAN_POINT('Ctrl Pts',(-159.114422453659,-6.05711130426257,
129.44180177344));
#191667=CARTESIAN_POINT('Ctrl Pts',(-159.392870077472,-4.42037595835707,
135.163883566548));
#191668=CARTESIAN_POINT('Ctrl Pts',(-159.671317701285,1.27846894590735,
136.879776744077));
#191669=CARTESIAN_POINT('Ctrl Pts',(-159.949765325097,5.80246334556346,
133.01265930192));
#191670=CARTESIAN_POINT('Ctrl Pts',(-160.22821294891,4.9942773967397,127.116223250229));
#191671=CARTESIAN_POINT('Ctrl Pts',(-160.506660572723,-0.403405495673234,
124.609005263594));
#191672=CARTESIAN_POINT('Ctrl Pts',(-160.785108196536,-5.43037844501628,
127.795016187323));
#191673=CARTESIAN_POINT('Ctrl Pts',(-161.063555820349,-5.46709889212507,
133.746467627798));
#191674=CARTESIAN_POINT('Ctrl Pts',(-161.342003444162,-0.479822539999598,
136.994266455786));
#191675=CARTESIAN_POINT('Ctrl Pts',(-161.620451067975,4.94838728575097,
134.553844212161));
#191676=CARTESIAN_POINT('Ctrl Pts',(-161.898898691787,5.82927093805496,
128.66782971756));
#191677=CARTESIAN_POINT('Ctrl Pts',(-162.177346315601,1.35333937400316,
124.745182744726));
#191678=CARTESIAN_POINT('Ctrl Pts',(-162.455793939413,-4.36624496045326,
126.390624229737));
#191679=CARTESIAN_POINT('Ctrl Pts',(-162.734241563226,-6.07346347917808,
132.092073832152));
#191680=CARTESIAN_POINT('Ctrl Pts',(-163.012689187039,-2.19946576572379,
136.61017789865));
#191681=CARTESIAN_POINT('Ctrl Pts',(-163.291136810852,3.69573353655413,
135.793019513774));
#191682=CARTESIAN_POINT('Ctrl Pts',(-163.569584434665,6.19473426535967,
130.391527312818));
#191683=CARTESIAN_POINT('Ctrl Pts',(-163.848032058478,3.0010768338922,125.369408750896));
#191684=CARTESIAN_POINT('Ctrl Pts',(-164.126479682291,-2.95042359716811,
125.341745442286));
#191685=CARTESIAN_POINT('Ctrl Pts',(-164.404927306104,-6.19062887863655,
130.333958616169));
#191686=CARTESIAN_POINT('Ctrl Pts',(-164.683374929917,-3.74194864967208,
135.758448248921));
#191687=CARTESIAN_POINT('Ctrl Pts',(-164.961822553729,2.14539958398697,
136.630373369092));
#191688=CARTESIAN_POINT('Ctrl Pts',(-165.240270177542,6.06123040855813,
132.148477387157));
#191689=CARTESIAN_POINT('Ctrl Pts',(-165.518717801355,4.40708659523179,
126.431403757722));
#191690=CARTESIAN_POINT('Ctrl Pts',(-165.797165425168,-1.29695450096345,
124.732863851664));
#191691=CARTESIAN_POINT('Ctrl Pts',(-166.075613048981,-5.80915777052276,
128.613732864363));
#191692=CARTESIAN_POINT('Ctrl Pts',(-166.354060672794,-4.98302884210618,
134.50768176414));
#191693=CARTESIAN_POINT('Ctrl Pts',(-166.632508296607,0.422260157714416,
136.998459447511));
#191694=CARTESIAN_POINT('Ctrl Pts',(-166.91095592042,5.43951270115045,133.797162904712));
#191695=CARTESIAN_POINT('Ctrl Pts',(-167.189403544233,5.45811880719792,
127.845627266545));
#191696=CARTESIAN_POINT('Ctrl Pts',(-167.467851168046,0.460980373357943,
124.613023035806));
#191697=CARTESIAN_POINT('Ctrl Pts',(-167.746298791858,-4.95977650345479,
127.069955579048));
#191698=CARTESIAN_POINT('Ctrl Pts',(-168.024746415672,-5.822741072145,132.958623916859));
#191699=CARTESIAN_POINT('Ctrl Pts',(-168.303194039484,-1.33489105224939,
136.867629524233));
#191700=CARTESIAN_POINT('Ctrl Pts',(-168.581641663297,4.37965863161014,
135.204787213532));
#191701=CARTESIAN_POINT('Ctrl Pts',(-168.86008928711,6.06951599123876,129.498167833929));
#191702=CARTESIAN_POINT('Ctrl Pts',(-169.138536910923,2.18178466725943,
124.991875811423));
#191703=CARTESIAN_POINT('Ctrl Pts',(-169.416984534736,-3.71090017982492,
125.826973370093));
#191704=CARTESIAN_POINT('Ctrl Pts',(-169.695432158549,-6.19344904920226,
131.236046650305));
#191705=CARTESIAN_POINT('Ctrl Pts',(-169.973879782361,-2.98452080916978,
136.248421555465));
#191706=CARTESIAN_POINT('Ctrl Pts',(-170.252327406175,2.96703625254325,
136.257970415857));
#191707=CARTESIAN_POINT('Ctrl Pts',(-170.530775029987,6.19203194594742,
131.25591829527));
#191708=CARTESIAN_POINT('Ctrl Pts',(-170.8092226538,3.72685277860365,125.838906728691));
#191709=CARTESIAN_POINT('Ctrl Pts',(-171.087670277614,-2.16312202539704,
124.984904710079));
#191710=CARTESIAN_POINT('Ctrl Pts',(-171.366117901426,-6.06529336244348,
129.478698374222));
#191711=CARTESIAN_POINT('Ctrl Pts',(-171.644565525239,-4.39375640545797,
135.190710877796));
#191712=CARTESIAN_POINT('Ctrl Pts',(-171.923013149052,1.31542804121008,
136.871881777341));
#191713=CARTESIAN_POINT('Ctrl Pts',(-172.201460772865,5.81579838023838,
132.977297145939));
#191714=CARTESIAN_POINT('Ctrl Pts',(-172.479908396678,4.97173412537368,
127.085889998814));
#191715=CARTESIAN_POINT('Ctrl Pts',(-172.75835602049,-0.441110907994683,
124.611575692932));
#191716=CARTESIAN_POINT('Ctrl Pts',(-173.036803644304,-5.4485965663818,
127.828128198426));
#191717=CARTESIAN_POINT('Ctrl Pts',(-173.315251268116,-5.44908815900415,
133.779692900072));
#191718=CARTESIAN_POINT('Ctrl Pts',(-173.593698891929,-0.442133936257506,
136.997072587158));
#191719=CARTESIAN_POINT('Ctrl Pts',(-173.872146515742,4.97111977446672,
134.523652504987));
#191720=CARTESIAN_POINT('Ctrl Pts',(-174.150594139555,5.81615726515733,
128.632384875785));
#191721=CARTESIAN_POINT('Ctrl Pts',(-174.429041763368,1.31643036424716,
124.737056846366));
#191722=CARTESIAN_POINT('Ctrl Pts',(-174.707489387181,-4.39303173020782,
126.417284578411));
#191723=CARTESIAN_POINT('Ctrl Pts',(-174.985937010994,-6.06551227613263,
132.129020869861));
#191724=CARTESIAN_POINT('Ctrl Pts',(-175.264384634806,-2.16408335703982,
136.623459102702));
#191725=CARTESIAN_POINT('Ctrl Pts',(-175.542832258619,3.72603244582337,
135.770430106468));
#191726=CARTESIAN_POINT('Ctrl Pts',(-175.821279882432,6.19210645777918,
130.353825855915));
#191727=CARTESIAN_POINT('Ctrl Pts',(-176.099727506245,2.96793713625374,
125.351241041473));
#191728=CARTESIAN_POINT('Ctrl Pts',(-176.378175130058,-2.98362142169932,
125.359806717758));
#191729=CARTESIAN_POINT('Ctrl Pts',(-176.656622753871,-6.19337765112022,
130.371651446723));
#191730=CARTESIAN_POINT('Ctrl Pts',(-176.935070377684,-3.71172238248064,
135.781134764673));
#191731=CARTESIAN_POINT('Ctrl Pts',(-177.213518001496,2.18082442793968,
136.617205770365));
#191732=CARTESIAN_POINT('Ctrl Pts',(-177.49196562531,6.06930012827989,132.111556053907));
#191733=CARTESIAN_POINT('Ctrl Pts',(-177.770413249122,4.38038551252508,
126.404657591498));
#191734=CARTESIAN_POINT('Ctrl Pts',(-178.048860872936,-1.33388939551094,
124.740871272604));
#191735=CARTESIAN_POINT('Ctrl Pts',(-178.327308496748,-5.82238511319243,
128.649135443807));
#191736=CARTESIAN_POINT('Ctrl Pts',(-178.605756120561,-4.96039335117553,
134.537946261091));
#191737=CARTESIAN_POINT('Ctrl Pts',(-178.884203744374,0.459957571884186,
136.995774267775));
#191738=CARTESIAN_POINT('Ctrl Pts',(-179.162651368187,5.45762995655925,
133.763995597288));
#191739=CARTESIAN_POINT('Ctrl Pts',(-179.441098991999,5.44000703120181,
127.812456966643));
#191740=CARTESIAN_POINT('Ctrl Pts',(-179.719546615813,0.423283403288203,
124.610331628578));
#191741=CARTESIAN_POINT('Ctrl Pts',(-179.997994239625,-4.98241699370369,
127.100216336253));
#191742=CARTESIAN_POINT('Ctrl Pts',(-180.276441863438,-5.80951957808352,
132.994028680947));
#191743=CARTESIAN_POINT('Ctrl Pts',(-180.554889487251,-1.29795748101432,
136.875643046625));
#191744=CARTESIAN_POINT('Ctrl Pts',(-180.833337111064,4.40636413235919,
135.178045458633));
#191745=CARTESIAN_POINT('Ctrl Pts',(-181.111784734877,6.06145237094964,
129.461245168083));
#191746=CARTESIAN_POINT('Ctrl Pts',(-181.39023235869,2.14636199904753,124.97870236077));
#191747=CARTESIAN_POINT('Ctrl Pts',(-181.668679982503,-3.74113019436597,
125.849654892224));
#191748=CARTESIAN_POINT('Ctrl Pts',(-181.947127606316,-6.19070650352801,
131.273739934436));
#191749=CARTESIAN_POINT('Ctrl Pts',(-182.225575230128,-2.95132596877351,
136.266488314898));
#191750=CARTESIAN_POINT('Ctrl Pts',(-182.504022853942,3.00017895099442,
136.239808181284));
#191751=CARTESIAN_POINT('Ctrl Pts',(-182.782470477755,6.19466598168877,
131.218217272988));
#191752=CARTESIAN_POINT('Ctrl Pts',(-183.060918101567,3.6965576014681,125.81631231638));
#191753=CARTESIAN_POINT('Ctrl Pts',(-183.33936572538,-2.19850662762309,
124.998180068855));
#191754=CARTESIAN_POINT('Ctrl Pts',(-183.617813349193,-6.07325066894868,
129.515644097905));
#191755=CARTESIAN_POINT('Ctrl Pts',(-183.896260973006,-4.36697404029963,
135.217375651221));
#191756=CARTESIAN_POINT('Ctrl Pts',(-184.174708596819,1.35233839284232,
136.863761976378));
#191757=CARTESIAN_POINT('Ctrl Pts',(-184.453156220632,5.8289179083658,132.941854470998));
#191758=CARTESIAN_POINT('Ctrl Pts',(-184.731603844444,4.94900662457131,
127.055694536694));
#191759=CARTESIAN_POINT('Ctrl Pts',(-185.010051468258,-0.478799974789776,
124.614375598192));
#191760=CARTESIAN_POINT('Ctrl Pts',(-185.28849909207,-5.46661278799793,
127.861350494915));
#191761=CARTESIAN_POINT('Ctrl Pts',(-185.566946715884,-5.43087550791776,
133.812807920317));
#191762=CARTESIAN_POINT('Ctrl Pts',(-185.845394339696,-0.404428949079144,
136.999649245311));
#191763=CARTESIAN_POINT('Ctrl Pts',(-186.123841963509,4.99366805651034,
134.493322978084));
#191764=CARTESIAN_POINT('Ctrl Pts',(-186.402289587322,5.80282807241402,
128.59702051737));
#191765=CARTESIAN_POINT('Ctrl Pts',(-186.680737211135,1.27947257368013,
124.729155774178));
#191766=CARTESIAN_POINT('Ctrl Pts',(-186.959184834948,-4.41965571455532,
126.444107491802));
#191767=CARTESIAN_POINT('Ctrl Pts',(-187.237632458761,-6.0573363132998,
132.165918821797));
#191768=CARTESIAN_POINT('Ctrl Pts',(-187.516080082574,-2.12862075745111,
136.636524677919));
#191769=CARTESIAN_POINT('Ctrl Pts',(-187.794527706387,3.75619328558978,
135.74765667963));
#191770=CARTESIAN_POINT('Ctrl Pts',(-188.072975330199,6.18924919941703,
130.316141093742));
#191771=CARTESIAN_POINT('Ctrl Pts',(-188.351422954013,2.93468746061294,
125.333275399398));
#191772=CARTESIAN_POINT('Ctrl Pts',(-188.629870577825,-3.01670868704181,
125.378069743179));
#191773=CARTESIAN_POINT('Ctrl Pts',(-188.908318201638,-6.19589692571743,
130.409360311474));
#191774=CARTESIAN_POINT('Ctrl Pts',(-189.186765825451,-3.68135857605119,
135.80363686423));
#191775=CARTESIAN_POINT('Ctrl Pts',(-189.465213449264,2.21616846064164,
136.603822774524));
#191776=CARTESIAN_POINT('Ctrl Pts',(-189.743661073077,6.07714494785282,
132.07458628205));
#191777=CARTESIAN_POINT('Ctrl Pts',(-190.02210869689,4.35352211302309,126.378074457888));
#191778=CARTESIAN_POINT('Ctrl Pts',(-190.300556320702,-1.37077486229612,
124.749103378371));
#191779=CARTESIAN_POINT('Ctrl Pts',(-190.579003944516,-5.83539670523986,
128.684617885911));
#191780=CARTESIAN_POINT('Ctrl Pts',(-190.857451568328,-4.93757405104588,
134.568072408653));
#191781=CARTESIAN_POINT('Ctrl Pts',(-191.135899192141,0.497637942157669,
136.992859662928));
#191782=CARTESIAN_POINT('Ctrl Pts',(-191.414346815954,5.47554497748281,
133.730718619501));
#191783=CARTESIAN_POINT('Ctrl Pts',(-191.692794439767,5.42169367374449,
127.779397532831));
#191784=CARTESIAN_POINT('Ctrl Pts',(-191.97124206358,0.385570748295746,
124.60786974337));
#191785=CARTESIAN_POINT('Ctrl Pts',(-192.249689687393,-5.00487285865859,
127.130614351886));
#191786=CARTESIAN_POINT('Ctrl Pts',(-192.528137311206,-5.79608281013753,
133.029352306079));
#191787=CARTESIAN_POINT('Ctrl Pts',(-192.806584935019,-1.26097581348702,
136.883431595415));
#191788=CARTESIAN_POINT('Ctrl Pts',(-193.085032558831,4.43290635366497,
135.151141635234));
#191789=CARTESIAN_POINT('Ctrl Pts',(-193.363480182644,6.05316414131348,
129.424372271875));
#191790=CARTESIAN_POINT('Ctrl Pts',(-193.641927806457,2.11085979660312,
124.965744782026));
#191791=CARTESIAN_POINT('Ctrl Pts',(-193.92037543027,-3.77122157995168,
125.872520012798));
#191792=CARTESIAN_POINT('Ctrl Pts',(-194.198823054083,-6.1877345589472,
131.311415825543));
#191793=CARTESIAN_POINT('Ctrl Pts',(-194.477270677896,-2.91802176590892,
136.284352673182));
#191794=CARTESIAN_POINT('Ctrl Pts',(-194.755718301709,3.03321047671203,
136.221444534203));
#191795=CARTESIAN_POINT('Ctrl Pts',(-195.034165925522,6.19707047180361,
131.180500915096));
#191796=CARTESIAN_POINT('Ctrl Pts',(-195.312613549334,3.66612544703105,
125.793902738034));
#191797=CARTESIAN_POINT('Ctrl Pts',(-195.591061173148,-2.23380976337827,
125.011670577786));
#191798=CARTESIAN_POINT('Ctrl Pts',(-195.86950879696,-6.08098292891658,
129.552637575454));
#191799=CARTESIAN_POINT('Ctrl Pts',(-196.147956420774,-4.3400298553121,
135.243876898752));
#191800=CARTESIAN_POINT('Ctrl Pts',(-196.426404044586,1.38919863307876,
136.855417642068));
#191801=CARTESIAN_POINT('Ctrl Pts',(-196.704851668399,5.84182144379631,
132.906332590435));
#191802=CARTESIAN_POINT('Ctrl Pts',(-196.983299292212,4.92609573650846,
127.025637982775));
#191803=CARTESIAN_POINT('Ctrl Pts',(-197.261746916025,-0.516471299475173,
124.617404875624));
#191804=CARTESIAN_POINT('Ctrl Pts',(-197.540194539838,-5.48442644226676,
127.894681845726));
#191805=CARTESIAN_POINT('Ctrl Pts',(-197.81864216365,-5.41246161374207,
133.845811461438));
#191806=CARTESIAN_POINT('Ctrl Pts',(-198.097089787464,-0.36670897563802,
137.001996334766));
#191807=CARTESIAN_POINT('Ctrl Pts',(-198.375537411276,5.01603129634849,
134.462856755322));
#191808=CARTESIAN_POINT('Ctrl Pts',(-198.65398503509,5.78928385374183,128.561737952753));
#191809=CARTESIAN_POINT('Ctrl Pts',(-198.932432658902,1.24246737178614,
124.721479820939));
#191810=CARTESIAN_POINT('Ctrl Pts',(-199.210880282716,-4.44611592693577,
126.471091975977));
#191811=CARTESIAN_POINT('Ctrl Pts',(-199.489327906528,-6.04893589364168,
132.202766320694));
#191812=CARTESIAN_POINT('Ctrl Pts',(-199.767775530341,-2.09307928103787,
136.649374140152));
#191813=CARTESIAN_POINT('Ctrl Pts',(-200.046223154153,3.7862149382325,135.724700077139));
#191814=CARTESIAN_POINT('Ctrl Pts',(-200.324670777967,6.18616259614969,
130.278474422724));
#191815=CARTESIAN_POINT('Ctrl Pts',(-200.603118401779,2.90132903904936,
125.315512490399));
#191816=CARTESIAN_POINT('Ctrl Pts',(-200.881566025592,-3.04968416713424,
125.396533841802));
#191817=CARTESIAN_POINT('Ctrl Pts',(-201.160013649405,-6.1981866090755,
130.447083813107));
#191818=CARTESIAN_POINT('Ctrl Pts',(-201.438461273218,-3.65085835552605,
135.825953713766));
#191819=CARTESIAN_POINT('Ctrl Pts',(-201.716908897031,2.2514303724059,136.590224877478));
#191820=CARTESIAN_POINT('Ctrl Pts',(-201.995356520844,6.08476457658541,
132.037569441512));
#191821=CARTESIAN_POINT('Ctrl Pts',(-202.273804144657,4.32649739215744,
126.35165534194));
#191822=CARTESIAN_POINT('Ctrl Pts',(-202.55225176847,-1.40760953451491,
124.757559863922));
#191823=CARTESIAN_POINT('Ctrl Pts',(-202.830699392283,-5.84819206451709,
128.720178875862));
#191824=CARTESIAN_POINT('Ctrl Pts',(-203.109147016096,-4.91457178729319,
134.59805909049));
#191825=CARTESIAN_POINT('Ctrl Pts',(-203.387594639908,0.535299872273523,
136.989715740974));
#191826=CARTESIAN_POINT('Ctrl Pts',(-203.666042263721,5.49325710007376,
133.697333204442));
#191827=CARTESIAN_POINT('Ctrl Pts',(-203.944489887534,5.40317941343439,
127.746450190138));
#191828=CARTESIAN_POINT('Ctrl Pts',(-204.222937511347,0.347843805837959,
124.605637471411));
#191829=CARTESIAN_POINT('Ctrl Pts',(-204.50138513516,-5.0271432662092,127.161148499539));
#191830=CARTESIAN_POINT('Ctrl Pts',(-204.779832758973,-5.78243126621161,
133.064593483327));
#191831=CARTESIAN_POINT('Ctrl Pts',(-205.058280382786,-1.22394742003769,
136.890994881994));
#191832=CARTESIAN_POINT('Ctrl Pts',(-205.336728006599,4.45928431199552,
135.124076740266));
#191833=CARTESIAN_POINT('Ctrl Pts',(-205.615175630412,6.04465160945437,
129.387550511641));
#191834=CARTESIAN_POINT('Ctrl Pts',(-205.893623254225,2.07527937547198,
124.953003555339));
#191835=CARTESIAN_POINT('Ctrl Pts',(-206.172070878037,-3.80117322153507,
125.89556788454));
#191836=CARTESIAN_POINT('Ctrl Pts',(-206.45051850185,-6.18453332558722,
131.349072927534));
#191837=CARTESIAN_POINT('Ctrl Pts',(-206.728966125663,-2.8846094346739,
136.302013968343));
#191838=CARTESIAN_POINT('Ctrl Pts',(-207.007413749476,3.06612960569919,
136.202880155086));
#191839=CARTESIAN_POINT('Ctrl Pts',(-207.285861373289,6.19924532719362,
131.142770619188));
#191840=CARTESIAN_POINT('Ctrl Pts',(-207.564308997102,3.63555744296752,
125.771678824048));
#191841=CARTESIAN_POINT('Ctrl Pts',(-207.842756620915,-2.26903012449045,
125.025375736976));
#191842=CARTESIAN_POINT('Ctrl Pts',(-208.121204244728,-6.08848985582611,
129.58967743606));
#191843=CARTESIAN_POINT('Ctrl Pts',(-208.399651868541,-4.31292484892225,
135.270213638376));
#191844=CARTESIAN_POINT('Ctrl Pts',(-208.678099492353,1.42600739604885,
136.846849083615));
#191845=CARTESIAN_POINT('Ctrl Pts',(-208.956547116166,5.85450850838505,
132.870732820528));
#191846=CARTESIAN_POINT('Ctrl Pts',(-209.234994739979,4.90300231015654,
126.995721450812));
#191847=CARTESIAN_POINT('Ctrl Pts',(-209.513442363792,-0.554123486127181,
124.620663412976));
#191848=CARTESIAN_POINT('Ctrl Pts',(-209.791889987605,-5.50203686909699,
127.928121015754));
#191849=CARTESIAN_POINT('Ctrl Pts',(-210.070337611418,-5.393847158811,133.878702300482));
#191850=CARTESIAN_POINT('Ctrl Pts',(-210.348785235231,-0.328975413660277,
137.004113768549));
#191851=CARTESIAN_POINT('Ctrl Pts',(-210.627232859043,5.03820866530154,
134.432254965643));
#191852=CARTESIAN_POINT('Ctrl Pts',(-210.905680482857,5.77552511102812,
128.526538489345));
#191853=CARTESIAN_POINT('Ctrl Pts',(-211.184128106669,1.20541612980698,
124.714029271085));
#191854=CARTESIAN_POINT('Ctrl Pts',(-211.462575730482,-4.47241138685473,
126.498237031013));
#191855=CARTESIAN_POINT('Ctrl Pts',(-211.741023354295,-6.04031132844015,
132.239562001151));
#191856=CARTESIAN_POINT('Ctrl Pts',(-212.019470978108,-2.05746024480169,
136.66200701326));
#191857=CARTESIAN_POINT('Ctrl Pts',(-212.297918601921,3.81609629128846,
135.701561149659));
#191858=CARTESIAN_POINT('Ctrl Pts',(-212.576366225734,6.1828467623524,130.240827238612));
#191859=CARTESIAN_POINT('Ctrl Pts',(-212.854813849547,2.86786310767097,
125.297952972686));
#191860=CARTESIAN_POINT('Ctrl Pts',(-213.133261473359,-3.0825466400586,
125.415198329437));
#191861=CARTESIAN_POINT('Ctrl Pts',(-213.411709097173,-6.20024661634941,
130.484820553763));
#191862=CARTESIAN_POINT('Ctrl Pts',(-213.690156720985,-3.62022285110177,
135.848084486325));
#191863=CARTESIAN_POINT('Ctrl Pts',(-213.968604344798,2.28660885659016,
136.576412583105));
#191864=CARTESIAN_POINT('Ctrl Pts',(-214.247051968611,6.09215873212836,
132.00050690397));
#191865=CARTESIAN_POINT('Ctrl Pts',(-214.525499592424,4.29931235134063,
126.325401222624));
#191866=CARTESIAN_POINT('Ctrl Pts',(-214.803947216237,-1.44439204724454,
124.766240415898));
#191867=CARTESIAN_POINT('Ctrl Pts',(-215.08239484005,-5.86077071688603,
128.755817095934));
#191868=CARTESIAN_POINT('Ctrl Pts',(-215.360842463863,-4.89138741227638,
134.627905195436));
#191869=CARTESIAN_POINT('Ctrl Pts',(-215.639290087675,0.572941966656434,
136.986342618411));
#191870=CARTESIAN_POINT('Ctrl Pts',(-215.917737711489,5.51076566800256,
133.66384058922));
#191871=CARTESIAN_POINT('Ctrl Pts',(-216.196185335301,5.38446493632399,
127.713616159441));
#191872=CARTESIAN_POINT('Ctrl Pts',(-216.474632959115,0.310103973899474,
124.603634895418));
#191873=CARTESIAN_POINT('Ctrl Pts',(-216.753080582927,-5.04922739111732,
127.191817647757));
#191874=CARTESIAN_POINT('Ctrl Pts',(-217.031528206741,-5.76856545216855,
133.099750906814));
#191875=CARTESIAN_POINT('Ctrl Pts',(-217.309975830553,-1.18687367276612,
136.898332626102));
#191876=CARTESIAN_POINT('Ctrl Pts',(-217.588423454366,4.48549702990607,
135.096851776628));
#191877=CARTESIAN_POINT('Ctrl Pts',(-217.866871078179,6.03591509080661,
129.350781251827));
#191878=CARTESIAN_POINT('Ctrl Pts',(-218.145318701992,2.03962205410111,
124.94047915284));
#191879=CARTESIAN_POINT('Ctrl Pts',(-218.423766325804,-3.83098400924668,
125.9187976534));
#191880=CARTESIAN_POINT('Ctrl Pts',(-218.702213949618,-6.18110292207006,
131.386709845009));
#191881=CARTESIAN_POINT('Ctrl Pts',(-218.98066157343,-2.85109021317626,
136.319471545938));
#191882=CARTESIAN_POINT('Ctrl Pts',(-219.259109197243,3.09893511812703,
136.18411573184));
#191883=CARTESIAN_POINT('Ctrl Pts',(-219.537556821056,6.20119046726778,
131.105027783371));
#191884=CARTESIAN_POINT('Ctrl Pts',(-219.816004444869,3.6048547219858,125.749641397935));
#191885=CARTESIAN_POINT('Ctrl Pts',(-220.094452068682,-2.30416640585769,
125.039295038577));
#191886=CARTESIAN_POINT('Ctrl Pts',(-220.372899692494,-6.09577117150464,
129.626762307198));
#191887=CARTESIAN_POINT('Ctrl Pts',(-220.651347316308,-4.28566002551621,
135.296384894171));
#191888=CARTESIAN_POINT('Ctrl Pts',(-220.929794940121,1.46276331779004,
136.83805661853));
#191889=CARTESIAN_POINT('Ctrl Pts',(-221.208242563933,5.86697863200795,
132.835056480438));
#191890=CARTESIAN_POINT('Ctrl Pts',(-221.486690187747,4.87972720125093,
126.965946049375));
#191891=CARTESIAN_POINT('Ctrl Pts',(-221.765137811559,-0.591755139529082,
124.624151089502));
#191892=CARTESIAN_POINT('Ctrl Pts',(-222.043585435373,-5.51944341592756,
127.961666765899));
#191893=CARTESIAN_POINT('Ctrl Pts',(-222.322033059185,-5.37503283288975,
133.911479218663));
#191894=CARTESIAN_POINT('Ctrl Pts',(-222.600480682998,-0.29122966137826,
137.006001468201));
#191895=CARTESIAN_POINT('Ctrl Pts',(-222.878928306811,5.06019934158045,
134.401518743003));
#191896=CARTESIAN_POINT('Ctrl Pts',(-223.157375930624,5.7615523541068,128.491423431472));
#191897=CARTESIAN_POINT('Ctrl Pts',(-223.435823554437,1.16832022068962,
124.706804400699));
#191898=CARTESIAN_POINT('Ctrl Pts',(-223.71427117825,-4.49854111992577,
126.525541651043));
#191899=CARTESIAN_POINT('Ctrl Pts',(-223.992718802062,-6.03146293728042,
132.276304499695));
#191900=CARTESIAN_POINT('Ctrl Pts',(-224.271166425875,-2.02176496861996,
136.674422829126));
#191901=CARTESIAN_POINT('Ctrl Pts',(-224.549614049688,3.84583623749284,
135.678240754614));
#191902=CARTESIAN_POINT('Ctrl Pts',(-224.828061673501,6.1793018208946,130.203200936436));
#191903=CARTESIAN_POINT('Ctrl Pts',(-225.106509297314,2.83429090657077,
125.280597496933));
#191904=CARTESIAN_POINT('Ctrl Pts',(-225.384956921127,-3.11529488808334,
125.434062514461));
#191905=CARTESIAN_POINT('Ctrl Pts',(-225.66340454494,-6.20207687120481,
130.522569135094));
#191906=CARTESIAN_POINT('Ctrl Pts',(-225.941852168753,-3.5894531979886,
135.87002836184));
#191907=CARTESIAN_POINT('Ctrl Pts',(-226.220299792565,2.32170260964191,
136.562386403224));
#191908=CARTESIAN_POINT('Ctrl Pts',(-226.498747416378,6.09932714048972,
131.963400042786));
#191909=CARTESIAN_POINT('Ctrl Pts',(-226.777195040191,4.27196799792278,
126.299313072794));
#191910=CARTESIAN_POINT('Ctrl Pts',(-227.055642664004,-1.48112103749588,
124.775144712639));
#191911=CARTESIAN_POINT('Ctrl Pts',(-227.334090287817,-5.87313219624144,
128.79153122554));
#191912=CARTESIAN_POINT('Ctrl Pts',(-227.61253791163,-4.8680217850994,134.65760961753));
#191913=CARTESIAN_POINT('Ctrl Pts',(-227.890985535443,0.610562830463375,
136.982740420231));
#191914=CARTESIAN_POINT('Ctrl Pts',(-228.169433159256,5.52807003248314,
133.630242014917));
#191915=CARTESIAN_POINT('Ctrl Pts',(-228.447880783069,5.36555093588535,
127.680896657417));
#191916=CARTESIAN_POINT('Ctrl Pts',(-228.726328406882,0.272352650944771,
124.601862089598));
#191917=CARTESIAN_POINT('Ctrl Pts',(-229.004776030695,-5.07112441504767,
127.222620660081));
#191918=CARTESIAN_POINT('Ctrl Pts',(-229.283223654507,-5.75448588181141,
133.134823273769));
#191919=CARTESIAN_POINT('Ctrl Pts',(-229.561671278321,-1.14975594545406,
136.905444555836));
#191920=CARTESIAN_POINT('Ctrl Pts',(-229.840118902133,4.51154353607471,
135.069467753152));
#191921=CARTESIAN_POINT('Ctrl Pts',(-230.118566525947,6.0269549091058,129.314065854931));
#191922=CARTESIAN_POINT('Ctrl Pts',(-230.397014149759,2.00388915378425,
124.928172038625));
#191923=CARTESIAN_POINT('Ctrl Pts',(-230.675461773572,-3.86065283843716,
125.942208458593));
#191924=CARTESIAN_POINT('Ctrl Pts',(-230.953909397385,-6.17744347551146,
131.424325183319));
#191925=CARTESIAN_POINT('Ctrl Pts',(-231.232357021197,-2.81746534348149,
136.33672475907));
#191926=CARTESIAN_POINT('Ctrl Pts',(-231.510804645011,3.13162579837364,
136.165151959792));
#191927=CARTESIAN_POINT('Ctrl Pts',(-231.789252268823,6.20290581994918,
131.067273806224));
#191928=CARTESIAN_POINT('Ctrl Pts',(-232.067699892636,3.57401842178686,
125.727791276302));
#191929=CARTESIAN_POINT('Ctrl Pts',(-232.346147516449,-2.33921730549066,
125.053427966802));
#191930=CARTESIAN_POINT('Ctrl Pts',(-232.624595140262,-6.10282660614105,
129.663890814674));
#191931=CARTESIAN_POINT('Ctrl Pts',(-232.903042764075,-4.25823639540172,
135.322389696357));
#191932=CARTESIAN_POINT('Ctrl Pts',(-233.181490387888,1.499465036299,136.829040572621));
#191933=CARTESIAN_POINT('Ctrl Pts',(-233.459938011701,5.87923135258013,
132.799304892167));
#191934=CARTESIAN_POINT('Ctrl Pts',(-233.738385635514,4.85627127225937,
126.9363128818));
#191935=CARTESIAN_POINT('Ctrl Pts',(-234.016833259326,-0.629364865227224,
124.627867775965));
#191936=CARTESIAN_POINT('Ctrl Pts',(-234.29528088314,-5.53664543775268,
127.99531785311));
#191937=CARTESIAN_POINT('Ctrl Pts',(-234.573728506952,-5.35601933315035,
133.944141001422));
#191938=CARTESIAN_POINT('Ctrl Pts',(-234.852176130765,-0.253473117473377,
137.007659363768));
#191939=CARTESIAN_POINT('Ctrl Pts',(-235.130623754578,5.08200251031112,
134.370649226346));
#191940=CARTESIAN_POINT('Ctrl Pts',(-235.409071378391,5.74736610074488,
128.456394080338));
#191941=CARTESIAN_POINT('Ctrl Pts',(-235.687519002204,1.13118101903705,
124.699805477501));
#191942=CARTESIAN_POINT('Ctrl Pts',(-235.965966626017,-4.52450415790052,
126.553004824284));
#191943=CARTESIAN_POINT('Ctrl Pts',(-236.24441424983,-6.0223910480441,132.312992454817));
#191944=CARTESIAN_POINT('Ctrl Pts',(-236.522861873642,-1.98599477519336,
136.686621127679));
#191945=CARTESIAN_POINT('Ctrl Pts',(-236.801309497456,3.87543367482126,
135.654739756147));
#191946=CARTESIAN_POINT('Ctrl Pts',(-237.079757121268,6.1755279031354,130.165596910454));
#191947=CARTESIAN_POINT('Ctrl Pts',(-237.358204745081,2.80061367977841,
125.263446706254));
#191948=CARTESIAN_POINT('Ctrl Pts',(-237.636652368894,-3.14792769771062,
125.453125697856));
#191949=CARTESIAN_POINT('Ctrl Pts',(-237.915099992707,-6.20367730582095,
130.560328158313));
#191950=CARTESIAN_POINT('Ctrl Pts',(-238.19354761652,-3.55855053636696,
135.891784527174));
#191951=CARTESIAN_POINT('Ctrl Pts',(-238.471995240333,2.35671033115007,
136.54814685758));
#191952=CARTESIAN_POINT('Ctrl Pts',(-238.750442864146,6.10626953604027,
131.92625023297));
#191953=CARTESIAN_POINT('Ctrl Pts',(-239.028890487959,4.24446534516054,
126.273391859158));
#191954=CARTESIAN_POINT('Ctrl Pts',(-239.307338111771,-1.51779514426229,
124.784272424193));
#191955=CARTESIAN_POINT('Ctrl Pts',(-239.585785735585,-5.88527604452282,
128.827319941278));
#191956=CARTESIAN_POINT('Ctrl Pts',(-239.864233359397,-4.84447577158576,
134.687171256065));
#191957=CARTESIAN_POINT('Ctrl Pts',(-240.14268098321,0.648161069640796,
136.978909279916));
#191958=CARTESIAN_POINT('Ctrl Pts',(-240.421128607023,5.54516955229552,
133.596538726537));
#191959=CARTESIAN_POINT('Ctrl Pts',(-240.699576230836,5.34643811298351,
127.648292896498));
#191960=CARTESIAN_POINT('Ctrl Pts',(-240.978023854649,0.234591235861842,
124.600319119639));
#191961=CARTESIAN_POINT('Ctrl Pts',(-241.256471478461,-5.09283352659785,
127.253556395099));
#191962=CARTESIAN_POINT('Ctrl Pts',(-241.534919102275,-5.74019307686353,
133.169809284574));
#191963=CARTESIAN_POINT('Ctrl Pts',(-241.813366726087,-1.11259561351327,
136.912330407661));
#191964=CARTESIAN_POINT('Ctrl Pts',(-242.0918143499,4.53742286533832,135.041925684563));
#191965=CARTESIAN_POINT('Ctrl Pts',(-242.370261973713,6.01777139637409,
129.277405681456));
#191966=CARTESIAN_POINT('Ctrl Pts',(-242.648709597526,1.96808199861856,
124.916082668738));
#191967=CARTESIAN_POINT('Ctrl Pts',(-242.927157221339,-3.89017860971679,
125.965799432623));
#191968=CARTESIAN_POINT('Ctrl Pts',(-243.205604845152,-6.1735551215127,
131.461917548614));
#191969=CARTESIAN_POINT('Ctrl Pts',(-243.484052468965,-2.78373607157309,
136.353772968415));
#191970=CARTESIAN_POINT('Ctrl Pts',(-243.762500092778,3.16420043507544,
136.145989541648));
#191971=CARTESIAN_POINT('Ctrl Pts',(-244.040947716591,6.20439132167383,
131.029510086731));
#191972=CARTESIAN_POINT('Ctrl Pts',(-244.319395340403,3.54304968502077,
125.706129268813));
#191973=CARTESIAN_POINT('Ctrl Pts',(-244.597842964216,-2.37418152456686,
125.067773997952));
#191974=CARTESIAN_POINT('Ctrl Pts',(-244.876290588029,-6.10965589829292,
129.701061582678));
#191975=CARTESIAN_POINT('Ctrl Pts',(-245.154738211842,-4.23065497477177,
135.348227081313));
#191976=CARTESIAN_POINT('Ctrl Pts',(-245.433185835655,1.53611119157916,
136.819801279981));
#191977=CARTESIAN_POINT('Ctrl Pts',(-245.711633459468,5.89126621607239,
132.763479380503));
#191978=CARTESIAN_POINT('Ctrl Pts',(-245.990081083281,4.83263539234992,
126.906823046158));
#191979=CARTESIAN_POINT('Ctrl Pts',(-246.268528707094,-0.666951269578287,
124.631813334641));
#191980=CARTESIAN_POINT('Ctrl Pts',(-246.546976330906,-5.55364229714491,
128.029073030433));
#191981=CARTESIAN_POINT('Ctrl Pts',(-246.825423954719,-5.33680736414475,
133.976686438464));
#191982=CARTESIAN_POINT('Ctrl Pts',(-247.103871578532,-0.215707181029578,
137.009087393821));
#191983=CARTESIAN_POINT('Ctrl Pts',(-247.382319202345,5.10361736357064,
134.339647559554));
#191984=CARTESIAN_POINT('Ctrl Pts',(-247.660766826158,5.73296687661779,
128.421451733968));
#191985=CARTESIAN_POINT('Ctrl Pts',(-247.939214449971,1.09399990105564,
124.693032760838));
#191986=CARTESIAN_POINT('Ctrl Pts',(-248.217662073784,-4.55029953871062,
126.580625533077));
#191987=CARTESIAN_POINT('Ctrl Pts',(-248.496109697597,-6.01309599689209,
132.349624507031));
#191988=CARTESIAN_POINT('Ctrl Pts',(-248.77455732141,-1.95015099000055,
136.698601456905));
#191989=CARTESIAN_POINT('Ctrl Pts',(-249.053004945222,3.90488750652966,
135.631059025098));
#191990=CARTESIAN_POINT('Ctrl Pts',(-249.331452569036,6.17152514891849,
130.128016554096));
#191991=CARTESIAN_POINT('Ctrl Pts',(-249.609900192848,2.76683267521693,
125.246501236177));
#191992=CARTESIAN_POINT('Ctrl Pts',(-249.888347816661,-3.18044385971988,
125.472387173231));
#191993=CARTESIAN_POINT('Ctrl Pts',(-250.166795440474,-6.20504786089197,
130.598096224241));
#191994=CARTESIAN_POINT('Ctrl Pts',(-250.445243064287,-3.5275160113489,
135.913352176149));
#191995=CARTESIAN_POINT('Ctrl Pts',(-250.7236906881,2.39163072389511,136.533694473816));
#191996=CARTESIAN_POINT('Ctrl Pts',(-251.002138311913,6.11298566151878,
131.889058851139));
#191997=CARTESIAN_POINT('Ctrl Pts',(-251.280585935725,4.21680541219097,
126.247638542206));
#191998=CARTESIAN_POINT('Ctrl Pts',(-251.559033559539,-1.5544130086051,
124.793623212388));
#191999=CARTESIAN_POINT('Ctrl Pts',(-251.837481183351,-5.89720181167361,
128.863181916876));
#192000=CARTESIAN_POINT('Ctrl Pts',(-252.115928807165,-4.82075024435922,
134.716589015834));
#192001=CARTESIAN_POINT('Ctrl Pts',(-252.394376430977,0.685735291195708,
136.974849339035));
#192002=CARTESIAN_POINT('Ctrl Pts',(-252.67282405479,5.56206359338632,133.562731973716));
#192003=CARTESIAN_POINT('Ctrl Pts',(-252.951271678603,5.32712717665345,
127.615806083426));
#192004=CARTESIAN_POINT('Ctrl Pts',(-253.229719302416,0.196821126400439,
124.599006045371));
#192005=CARTESIAN_POINT('Ctrl Pts',(-253.508166926229,-5.11435391846912,
127.284623701469));
#192006=CARTESIAN_POINT('Ctrl Pts',(-253.786614550041,-5.72568757235024,
133.204707652256));
#192007=CARTESIAN_POINT('Ctrl Pts',(-254.065062173855,-1.07539404373626,
136.918989908584));
#192008=CARTESIAN_POINT('Ctrl Pts',(-254.343509797667,4.56313403947717,
135.014226625117));
#192009=CARTESIAN_POINT('Ctrl Pts',(-254.621957421481,6.00836492926231,
129.240802026269));
#192010=CARTESIAN_POINT('Ctrl Pts',(-254.900405045293,1.9322018468105,124.904211611225));
#192011=CARTESIAN_POINT('Ctrl Pts',(-255.178852669106,-3.91956009939235,
125.989569474605));
#192012=CARTESIAN_POINT('Ctrl Pts',(-255.457300292919,-6.16943824888009,
131.499485975975));
#192013=CARTESIAN_POINT('Ctrl Pts',(-255.735747916732,-2.74990318521692,
136.370614733943));
#192014=CARTESIAN_POINT('Ctrl Pts',(-256.014195540545,3.19665694865877,
136.126630713714));
#192015=CARTESIAN_POINT('Ctrl Pts',(-256.292643164358,6.20564856486739,
130.991735142402));
#192016=CARTESIAN_POINT('Ctrl Pts',(-256.571090788171,3.51194654848645,
125.68466161966));
#192017=CARTESIAN_POINT('Ctrl Pts',(-256.849538411983,-2.40905189372645,
125.082322325773));
#192018=CARTESIAN_POINT('Ctrl Pts',(-257.127986035797,-6.11626988572704,
129.738292634474));
#192019=CARTESIAN_POINT('Ctrl Pts',(-257.406433659609,-4.20289584392431,
135.373859459261));
#192020=CARTESIAN_POINT('Ctrl Pts',(-257.684881283423,1.57266088340656,
136.810408252432));
#192021=CARTESIAN_POINT('Ctrl Pts',(-257.963328907235,5.90315744058412,
132.727450666138));
#192022=CARTESIAN_POINT('Ctrl Pts',(-258.241776531048,4.80867945501638,
126.87772425425));
#192023=CARTESIAN_POINT('Ctrl Pts',(-258.520224154861,-0.704246744852541,
124.635521896935));
#192024=CARTESIAN_POINT('Ctrl Pts',(-258.798671778674,-5.5709361272427,
128.063810879205));
#192025=CARTESIAN_POINT('Ctrl Pts',(-259.077119402487,-5.31644754243966,
134.007449313497));
#192026=CARTESIAN_POINT('Ctrl Pts',(-259.355567026299,-0.179733571114533,
137.013459703814));
#192027=CARTESIAN_POINT('Ctrl Pts',(-259.634014650113,5.12849404027147,
134.30227331953));
#192028=CARTESIAN_POINT('Ctrl Pts',(-259.866054336623,5.61428989304695,
129.384066440553));
#192029=CARTESIAN_POINT('Ctrl Pts',(-260.051696012132,3.39054283699284,
126.521203045511));
#192030=CARTESIAN_POINT('Ctrl Pts',(-260.144521813036,1.754921961264,125.780753115897));
#192031=CARTESIAN_POINT('Ctrl Pts',(-260.190939676638,0.892893391295023,
125.631947563271));
#192032=CARTESIAN_POINT('Ctrl Pts',(210.191733024964,-2.43880115184907,
125.780342085335));
#192033=CARTESIAN_POINT('Ctrl Pts',(210.145323348611,-3.27594855749458,
126.186716565447));
#192034=CARTESIAN_POINT('Ctrl Pts',(210.052505734956,-4.72940422381435,
127.426013481475));
#192035=CARTESIAN_POINT('Ctrl Pts',(209.866872246696,-6.15821517169733,
131.008352419918));
#192036=CARTESIAN_POINT('Ctrl Pts',(209.634832560185,-4.21099667891447,
135.892791108304));
#192037=CARTESIAN_POINT('Ctrl Pts',(209.356384936373,2.01508446636645,137.098708070195));
#192038=CARTESIAN_POINT('Ctrl Pts',(209.07793731256,6.37956871319657,132.510708806665));
#192039=CARTESIAN_POINT('Ctrl Pts',(208.799489688747,4.8866719183268,126.359661034021));
#192040=CARTESIAN_POINT('Ctrl Pts',(208.521042064934,-1.09954563679898,
124.290443595948));
#192041=CARTESIAN_POINT('Ctrl Pts',(208.242594441121,-6.07390144970816,
128.208589139036));
#192042=CARTESIAN_POINT('Ctrl Pts',(207.964146817309,-5.46739734855352,
134.511385201899));
#192043=CARTESIAN_POINT('Ctrl Pts',(207.685699193495,0.163779660617915,
137.407996874876));
#192044=CARTESIAN_POINT('Ctrl Pts',(207.407251569682,5.6442383477931,134.235982835808));
#192045=CARTESIAN_POINT('Ctrl Pts',(207.128803945869,5.93803043711477,127.910585036422));
#192046=CARTESIAN_POINT('Ctrl Pts',(206.850356322057,0.775002953389061,
124.244367681185));
#192047=CARTESIAN_POINT('Ctrl Pts',(206.571908698243,-5.10018277131114,
126.606494049502));
#192048=CARTESIAN_POINT('Ctrl Pts',(206.293461074431,-6.28856642889766,
132.82623846394));
#192049=CARTESIAN_POINT('Ctrl Pts',(206.015013450618,-1.69805588527783,
137.187984519302));
#192050=CARTESIAN_POINT('Ctrl Pts',(205.736565826805,4.45288036648484,135.683487507757));
#192051=CARTESIAN_POINT('Ctrl Pts',(205.458118202992,6.51183958365415,129.695313656966));
#192052=CARTESIAN_POINT('Ctrl Pts',(205.179670579179,2.58673502741873,124.726298504418));
#192053=CARTESIAN_POINT('Ctrl Pts',(204.901222955366,-3.71545195245463,
125.342726181157));
#192054=CARTESIAN_POINT('Ctrl Pts',(204.622775331554,-6.60332046735468,
130.978128730661));
#192055=CARTESIAN_POINT('Ctrl Pts',(204.344327707741,-3.42305986725146,
136.4538470632));
#192056=CARTESIAN_POINT('Ctrl Pts',(204.065880083927,2.90282542147133,136.737963244372));
#192057=CARTESIAN_POINT('Ctrl Pts',(203.787432460115,6.56115601364161,131.569388537382));
#192058=CARTESIAN_POINT('Ctrl Pts',(203.508984836302,4.1901047305044,125.69779051756));
#192059=CARTESIAN_POINT('Ctrl Pts',(203.230537212489,-2.03144808657932,
124.518880964767));
#192060=CARTESIAN_POINT('Ctrl Pts',(202.952089588676,-6.38619936200403,
129.116020142231));
#192061=CARTESIAN_POINT('Ctrl Pts',(202.673641964863,-4.87234540261322,
135.2646617407));
#192062=CARTESIAN_POINT('Ctrl Pts',(202.39519434105,1.1189559521872,137.314504502614));
#192063=CARTESIAN_POINT('Ctrl Pts',(202.116746717238,6.08199145217563,133.381843073553));
#192064=CARTESIAN_POINT('Ctrl Pts',(201.838299093424,5.45597392877388,127.080601183836));
#192065=CARTESIAN_POINT('Ctrl Pts',(201.559851469612,-0.183817095687214,
124.201312298284));
#192066=CARTESIAN_POINT('Ctrl Pts',(201.281403845799,-5.65468918935595,
127.389902241135));
#192067=CARTESIAN_POINT('Ctrl Pts',(201.002956221986,-5.92917816483575,
133.716212626452));
#192068=CARTESIAN_POINT('Ctrl Pts',(200.724508598173,-0.755042063338292,
137.366673267433));
#192069=CARTESIAN_POINT('Ctrl Pts',(200.44606097436,5.11294080853837,134.986689170007));
#192070=CARTESIAN_POINT('Ctrl Pts',(200.167613350547,6.2823808583988,128.763349450982));
#192071=CARTESIAN_POINT('Ctrl Pts',(199.889165726734,1.67861981076543,124.415599285115));
#192072=CARTESIAN_POINT('Ctrl Pts',(199.610718102921,-4.46771083782862,
125.938808675424));
#192073=CARTESIAN_POINT('Ctrl Pts',(199.332270479108,-6.50843348626435,
131.933222605136));
#192074=CARTESIAN_POINT('Ctrl Pts',(199.053822855296,-2.56822371547623,
136.890267516244));
#192075=CARTESIAN_POINT('Ctrl Pts',(198.775375231483,3.73205818513161,136.254661300547));
#192076=CARTESIAN_POINT('Ctrl Pts',(198.49692760767,6.60276093478139,130.610495019181));
#192077=CARTESIAN_POINT('Ctrl Pts',(198.218479983857,3.4058489481713,125.14448175187));
#192078=CARTESIAN_POINT('Ctrl Pts',(197.940032360044,-2.92087183683725,
124.879620661678));
#192079=CARTESIAN_POINT('Ctrl Pts',(197.661584736231,-6.56345409631434,
130.05930615131));
#192080=CARTESIAN_POINT('Ctrl Pts',(197.383137112418,-4.1745426838368,135.923660297497));
#192081=CARTESIAN_POINT('Ctrl Pts',(197.104689488605,2.05056951733907,137.083628129519));
#192082=CARTESIAN_POINT('Ctrl Pts',(196.826241864792,6.39130850797037,132.473255877329));
#192083=CARTESIAN_POINT('Ctrl Pts',(196.54779424098,4.85874721255563,126.329250411482));
#192084=CARTESIAN_POINT('Ctrl Pts',(196.269346617166,-1.13876540820057,
124.297652603739));
#192085=CARTESIAN_POINT('Ctrl Pts',(195.990898993354,-6.0898082506034,128.245401590344));
#192086=CARTESIAN_POINT('Ctrl Pts',(195.712451369541,-5.44461481437399,
134.544708910868));
#192087=CARTESIAN_POINT('Ctrl Pts',(195.434003745728,0.203913652044436,
137.406818876019));
#192088=CARTESIAN_POINT('Ctrl Pts',(195.155556121915,5.66505543396973,134.201592249669));
#192089=CARTESIAN_POINT('Ctrl Pts',(194.877108498102,5.92028802542049,127.874475717408));
#192090=CARTESIAN_POINT('Ctrl Pts',(194.59866087429,0.735065143658737,124.239780275557));
#192091=CARTESIAN_POINT('Ctrl Pts',(194.320213250476,-5.1256466951968,126.637613470433));
#192092=CARTESIAN_POINT('Ctrl Pts',(194.041765626664,-6.2761396229282,132.86448373661));
#192093=CARTESIAN_POINT('Ctrl Pts',(193.763318002851,-1.6591668436545,137.198201498994));
#192094=CARTESIAN_POINT('Ctrl Pts',(193.484870379038,4.48249921013125,135.656291847837));
#192095=CARTESIAN_POINT('Ctrl Pts',(193.206422755225,6.50496747206681,129.655694426079));
#192096=CARTESIAN_POINT('Ctrl Pts',(192.927975131412,2.54968841250072,124.710665118833));
#192097=CARTESIAN_POINT('Ctrl Pts',(192.649527507599,-3.74862973894988,
125.365444281348));
#192098=CARTESIAN_POINT('Ctrl Pts',(192.371079883787,-6.60214029104917,
131.018321851013));
#192099=CARTESIAN_POINT('Ctrl Pts',(192.092632259973,-3.38860644815819,
136.474579499726));
#192100=CARTESIAN_POINT('Ctrl Pts',(191.814184636161,2.93889117796205,136.720183001327));
#192101=CARTESIAN_POINT('Ctrl Pts',(191.535737012347,6.56569138435095,131.529434736241));
#192102=CARTESIAN_POINT('Ctrl Pts',(191.257289388535,4.15894196037717,125.672378777932));
#192103=CARTESIAN_POINT('Ctrl Pts',(190.978841764722,-2.06967194957323,
124.531363418996));
#192104=CARTESIAN_POINT('Ctrl Pts',(190.700394140909,-6.3963584469616,129.154926032595));
#192105=CARTESIAN_POINT('Ctrl Pts',(190.421946517096,-4.84510401107414,
135.294238450423));
#192106=CARTESIAN_POINT('Ctrl Pts',(190.143498893283,1.15856431450073,137.307572482581));
#192107=CARTESIAN_POINT('Ctrl Pts',(189.86505126947,6.09756863406271,133.344772510351));
#192108=CARTESIAN_POINT('Ctrl Pts',(189.586603645657,5.4332052617092,127.047458114672));
#192109=CARTESIAN_POINT('Ctrl Pts',(189.308156021844,-0.224008319322015,
124.202553584261));
#192110=CARTESIAN_POINT('Ctrl Pts',(189.029708398032,-5.67536919831109,
127.424387201254));
#192111=CARTESIAN_POINT('Ctrl Pts',(188.751260774218,-5.91134304125131,
133.752251266956));
#192112=CARTESIAN_POINT('Ctrl Pts',(188.472813150406,-0.71508141444371,
137.371147838333));
#192113=CARTESIAN_POINT('Ctrl Pts',(188.194365526593,5.13830509856852,134.955487759214));
#192114=CARTESIAN_POINT('Ctrl Pts',(187.91591790278,6.26984024615536,128.725144630756));
#192115=CARTESIAN_POINT('Ctrl Pts',(187.637470278967,1.63969850624965,124.405499418827));
#192116=CARTESIAN_POINT('Ctrl Pts',(187.359022655154,-4.49724605717418,
125.966095046791));
#192117=CARTESIAN_POINT('Ctrl Pts',(187.080575031341,-6.5014411967389,131.972820371883));
#192118=CARTESIAN_POINT('Ctrl Pts',(186.802127407528,-2.53112948956026,
136.905788265189));
#192119=CARTESIAN_POINT('Ctrl Pts',(186.523679783716,3.76516656597443,136.231842221641));
#192120=CARTESIAN_POINT('Ctrl Pts',(186.245232159903,6.60145848599114,130.570305731164));
#192121=CARTESIAN_POINT('Ctrl Pts',(185.96678453609,3.3713325565579,125.123854247073));
#192122=CARTESIAN_POINT('Ctrl Pts',(185.688336912277,-2.95688329360047,
124.897510609301));
#192123=CARTESIAN_POINT('Ctrl Pts',(185.409889288464,-6.5678678487195,130.099273563458));
#192124=CARTESIAN_POINT('Ctrl Pts',(185.131441664651,-4.14330270904733,
135.948977074923));
#192125=CARTESIAN_POINT('Ctrl Pts',(184.852994040838,2.08875520864929,137.071029390563));
#192126=CARTESIAN_POINT('Ctrl Pts',(184.574546417025,6.40134913096194,132.434319247607));
#192127=CARTESIAN_POINT('Ctrl Pts',(184.296098793212,4.831415925211,126.299756751549));
#192128=CARTESIAN_POINT('Ctrl Pts',(184.017651169399,-1.17835248801931,
124.304705146227));
#192129=CARTESIAN_POINT('Ctrl Pts',(183.739203545587,-6.10527253047917,
128.282519393244));
#192130=CARTESIAN_POINT('Ctrl Pts',(183.460755921774,-5.42174537657308,
134.577782526619));
#192131=CARTESIAN_POINT('Ctrl Pts',(183.182308297961,0.244100911417136,
137.405455267482));
#192132=CARTESIAN_POINT('Ctrl Pts',(182.903860674148,5.68563038680749,134.167044506474));
#192133=CARTESIAN_POINT('Ctrl Pts',(182.625413050335,5.90234329520773,127.838491527799));
#192134=CARTESIAN_POINT('Ctrl Pts',(182.346965426522,0.695091060812155,
124.23542735186));
#192135=CARTESIAN_POINT('Ctrl Pts',(182.068517802709,-5.15091590138369,
126.668891936874));
#192136=CARTESIAN_POINT('Ctrl Pts',(181.790070178896,-6.263482786439,132.902650210566));
#192137=CARTESIAN_POINT('Ctrl Pts',(181.511622555083,-1.62021497890189,
137.208182855437));
#192138=CARTESIAN_POINT('Ctrl Pts',(181.233174931271,4.51195124234396,135.628915707812));
#192139=CARTESIAN_POINT('Ctrl Pts',(180.954727307458,6.49785469294791,129.61611812487));
#192140=CARTESIAN_POINT('Ctrl Pts',(180.676279683645,2.51254711858197,124.695257343842));
#192141=CARTESIAN_POINT('Ctrl Pts',(180.397832059832,-3.78166851301026,
125.388364025079));
#192142=CARTESIAN_POINT('Ctrl Pts',(180.119384436019,-6.60071552592353,
131.058506988669));
#192143=CARTESIAN_POINT('Ctrl Pts',(179.840936812206,-3.35402743339335,
136.495101852955));
#192144=CARTESIAN_POINT('Ctrl Pts',(179.562489188393,2.97484801707599,136.702183530083));
#192145=CARTESIAN_POINT('Ctrl Pts',(179.28404156458,6.56998346925752,131.489454075275));
#192146=CARTESIAN_POINT('Ctrl Pts',(179.005593940767,4.12762507472721,125.647157201507));
#192147=CARTESIAN_POINT('Ctrl Pts',(178.727146316955,-2.10781911778238,
124.544078323705));
#192148=CARTESIAN_POINT('Ctrl Pts',(178.448698693142,-6.40628051373842,
129.193893042167));
#192149=CARTESIAN_POINT('Ctrl Pts',(178.170251069329,-4.81768308177075,
135.323648786705));
#192150=CARTESIAN_POINT('Ctrl Pts',(177.891803445516,1.19812974544141,137.300399483306));
#192151=CARTESIAN_POINT('Ctrl Pts',(177.613355821703,6.11291986848493,133.307607811431));
#192152=CARTESIAN_POINT('Ctrl Pts',(177.33490819789,5.41023526512845,127.014454258818));
#192153=CARTESIAN_POINT('Ctrl Pts',(177.056460574078,-0.264191242194762,
124.204039502676));
#192154=CARTESIAN_POINT('Ctrl Pts',(176.778012950264,-5.69583890440069,
127.458997407505));
#192155=CARTESIAN_POINT('Ctrl Pts',(176.499565326452,-5.89328887066216,
133.788180672302));
#192156=CARTESIAN_POINT('Ctrl Pts',(176.221117702638,-0.675094267951971,
137.375379074508));
#192157=CARTESIAN_POINT('Ctrl Pts',(175.942670078826,5.16347898681764,134.924132526884));
#192158=CARTESIAN_POINT('Ctrl Pts',(175.664222455013,6.25706730267374,128.687016856641));
#192159=CARTESIAN_POINT('Ctrl Pts',(175.3857748312,1.60071644210391,124.395636664696));
#192160=CARTESIAN_POINT('Ctrl Pts',(175.107327207387,-4.5266146294138,125.993560701866));
#192161=CARTESIAN_POINT('Ctrl Pts',(174.828879583574,-6.49420799391872,
132.012374840923));
#192162=CARTESIAN_POINT('Ctrl Pts',(174.550431959762,-2.49394147171037,
136.92108292349));
#192163=CARTESIAN_POINT('Ctrl Pts',(174.271984335948,3.79813542718566,136.208822025409));
#192164=CARTESIAN_POINT('Ctrl Pts',(173.993536712136,6.59991141772898,130.530125116137));
#192165=CARTESIAN_POINT('Ctrl Pts',(173.715089088322,3.33669123897678,125.103437235529));
#192166=CARTESIAN_POINT('Ctrl Pts',(173.43664146451,-2.99278518196597,124.915619437422));
#192167=CARTESIAN_POINT('Ctrl Pts',(173.158193840697,-6.5720382263662,130.139267102866));
#192168=CARTESIAN_POINT('Ctrl Pts',(172.879746216884,-4.11190920265221,
135.974103216695));
#192169=CARTESIAN_POINT('Ctrl Pts',(172.601298593071,2.12686350036709,137.058198437889));
#192170=CARTESIAN_POINT('Ctrl Pts',(172.322850969258,6.41115254960738,132.395322219168));
#192171=CARTESIAN_POINT('Ctrl Pts',(172.044403345445,4.80390560797255,126.270430011369));
#192172=CARTESIAN_POINT('Ctrl Pts',(171.765955721632,-1.21789590355323,
124.31199853584));
#192173=CARTESIAN_POINT('Ctrl Pts',(171.487508097819,-6.12051057723618,
128.319730643897));
#192174=CARTESIAN_POINT('Ctrl Pts',(171.209060474007,-5.39867503400336,
134.610716316833));
#192175=CARTESIAN_POINT('Ctrl Pts',(170.930612850193,0.284279125540913,
137.403847052956));
#192176=CARTESIAN_POINT('Ctrl Pts',(170.652165226381,5.70599465652041,134.13237215779));
#192177=CARTESIAN_POINT('Ctrl Pts',(170.373717602568,5.88417985149351,127.802617239562));
#192178=CARTESIAN_POINT('Ctrl Pts',(170.095269978755,0.655091221110643,
124.231317842401));
#192179=CARTESIAN_POINT('Ctrl Pts',(169.816822354942,-5.17599423848763,
126.700323644626));
#192180=CARTESIAN_POINT('Ctrl Pts',(169.538374731129,-6.25059385429175,
132.940738931629));
#192181=CARTESIAN_POINT('Ctrl Pts',(169.259927107316,-1.58120307648749,
137.217926915891));
#192182=CARTESIAN_POINT('Ctrl Pts',(168.981479483503,4.54123608254409,135.601360792124));
#192183=CARTESIAN_POINT('Ctrl Pts',(168.703031859691,6.49050113343381,129.576585854424));
#192184=CARTESIAN_POINT('Ctrl Pts',(168.424584235878,2.47531272130571,124.680075943919));
#192185=CARTESIAN_POINT('Ctrl Pts',(168.146136612065,-3.81456715595326,
125.411484460556));
#192186=CARTESIAN_POINT('Ctrl Pts',(167.867688988252,-6.59904616885666,
131.098682708838));
#192187=CARTESIAN_POINT('Ctrl Pts',(167.589241364439,-3.31932413390846,
136.515413333674));
#192188=CARTESIAN_POINT('Ctrl Pts',(167.310793740626,3.01069462210276,136.683965512842));
#192189=CARTESIAN_POINT('Ctrl Pts',(167.032346116813,6.57403210101054,131.449448027918));
#192190=CARTESIAN_POINT('Ctrl Pts',(166.753898493,4.09615523841214,125.622126727152));
#192191=CARTESIAN_POINT('Ctrl Pts',(166.475450869187,-2.14588817997888,
124.557025205477));
#192192=CARTESIAN_POINT('Ctrl Pts',(166.197003245374,-6.41596519343492,
129.232919728208));
#192193=CARTESIAN_POINT('Ctrl Pts',(165.918555621562,-4.79008363144905,
135.352891659104));
#192194=CARTESIAN_POINT('Ctrl Pts',(165.640107997748,1.23765077924384,137.292985770921));
#192195=CARTESIAN_POINT('Ctrl Pts',(165.361660373936,6.12804458641347,133.270350353765));
#192196=CARTESIAN_POINT('Ctrl Pts',(165.083212750123,5.38706479029029,126.981590839339));
#192197=CARTESIAN_POINT('Ctrl Pts',(164.80476512631,-0.304364375363971,
124.205769998417));
#192198=CARTESIAN_POINT('Ctrl Pts',(164.526317502497,-5.71609754908509,
127.493731577419));
#192199=CARTESIAN_POINT('Ctrl Pts',(164.247869878684,-5.8750163220866,133.823999511097));
#192200=CARTESIAN_POINT('Ctrl Pts',(163.969422254871,-0.635082105593798,
137.37936681918));
#192201=CARTESIAN_POINT('Ctrl Pts',(163.690974631059,5.18846154045405,134.892624634889));
#192202=CARTESIAN_POINT('Ctrl Pts',(163.412527007245,6.24406250126218,128.648967541478));
#192203=CARTESIAN_POINT('Ctrl Pts',(163.134079383433,1.56167506282176,124.386011388187));
#192204=CARTESIAN_POINT('Ctrl Pts',(162.85563175962,-4.55581546628373,126.021204622902));
#192205=CARTESIAN_POINT('Ctrl Pts',(162.577184135807,-6.48673414583306,
132.051884546553));
#192206=CARTESIAN_POINT('Ctrl Pts',(162.298736511994,-2.45666103994207,
136.936150924396));
#192207=CARTESIAN_POINT('Ctrl Pts',(162.020288888181,3.83096354709181,136.185601564872));
#192208=CARTESIAN_POINT('Ctrl Pts',(161.741841264368,6.59811978732212,130.489954663008));
#192209=CARTESIAN_POINT('Ctrl Pts',(161.463393640556,3.30192627907479,125.083231473798));
#192210=CARTESIAN_POINT('Ctrl Pts',(161.184946016742,-3.02857617157586,
124.933946475014));
#192211=CARTESIAN_POINT('Ctrl Pts',(160.90649839293,-6.57596507471956,130.179285287561));
#192212=CARTESIAN_POINT('Ctrl Pts',(160.628050769116,-4.08036332794952,
135.999037791754));
#192213=CARTESIAN_POINT('Ctrl Pts',(160.349603145304,2.16489298037573,137.045135746957));
#192214=CARTESIAN_POINT('Ctrl Pts',(160.07115552149,6.42071840063739,132.356266237063));
#192215=CARTESIAN_POINT('Ctrl Pts',(159.792707897678,4.77621728024515,126.241271277656));
#192216=CARTESIAN_POINT('Ctrl Pts',(159.514260273865,-1.25739418950663,
124.319532502318));
#192217=CARTESIAN_POINT('Ctrl Pts',(159.235812650052,-6.13552182622286,
128.357033963427));
#192218=CARTESIAN_POINT('Ctrl Pts',(158.957365026239,-5.37540464154493,
134.643509061136));
#192219=CARTESIAN_POINT('Ctrl Pts',(158.678917402427,0.324446805597038,
137.401994292032));
#192220=CARTESIAN_POINT('Ctrl Pts',(158.400469778613,5.72614748850293,134.097576488416));
#192221=CARTESIAN_POINT('Ctrl Pts',(158.122022154801,5.86579836733105,127.766854182028));
#192222=CARTESIAN_POINT('Ctrl Pts',(157.843574530988,0.615067106763091,
124.22745189946));
#192223=CARTESIAN_POINT('Ctrl Pts',(157.565126907175,-5.20088077722156,
126.731907428977));
#192224=CARTESIAN_POINT('Ctrl Pts',(157.286679283362,-6.23747330409059,
132.978748488409));
#192225=CARTESIAN_POINT('Ctrl Pts',(157.008231659549,-1.54213258201158,
137.227433319288));
#192226=CARTESIAN_POINT('Ctrl Pts',(156.729784035736,4.5703526455712,135.57362812183));
#192227=CARTESIAN_POINT('Ctrl Pts',(156.451336411923,6.48290706601333,129.537099079623));
#192228=CARTESIAN_POINT('Ctrl Pts',(156.172888788111,2.43798660040623,124.665121481617));
#192229=CARTESIAN_POINT('Ctrl Pts',(155.894441164297,-3.84732444870741,
125.434804731043));
#192230=CARTESIAN_POINT('Ctrl Pts',(155.615993540485,-6.59713228170722,
131.138847522794));
#192231=CARTESIAN_POINT('Ctrl Pts',(155.337545916672,-3.28449783564716,
136.535513189234));
#192232=CARTESIAN_POINT('Ctrl Pts',(155.059098292859,3.04642966473303,136.665529624679));
#192233=CARTESIAN_POINT('Ctrl Pts',(154.780650669046,6.57783712958646,131.409418076611));
#192234=CARTESIAN_POINT('Ctrl Pts',(154.502203045233,4.06453361755842,125.597288282381));
#192235=CARTESIAN_POINT('Ctrl Pts',(154.22375542142,-2.18387772549973,124.57020358456));
#192236=CARTESIAN_POINT('Ctrl Pts',(153.945307797607,-6.42541212718171,
129.272004644569));
#192237=CARTESIAN_POINT('Ctrl Pts',(153.666860173794,-4.76230668281685,
135.381965984011));
#192238=CARTESIAN_POINT('Ctrl Pts',(153.388412549982,1.27712595144142,137.285331620145));
#192239=CARTESIAN_POINT('Ctrl Pts',(153.109964926169,6.14294222739622,133.233001517943));
#192240=CARTESIAN_POINT('Ctrl Pts',(152.831517302356,5.36369469578529,126.948869073999));
#192241=CARTESIAN_POINT('Ctrl Pts',(152.553069678543,-0.344526230199219,
124.207745007359));
#192242=CARTESIAN_POINT('Ctrl Pts',(152.27462205473,-5.73614438167267,127.528588423912));
#192243=CARTESIAN_POINT('Ctrl Pts',(151.996174430917,-5.85652607262075,
133.859706456064));
#192244=CARTESIAN_POINT('Ctrl Pts',(151.717726807104,-0.595046410034728,
137.383110924578));
#192245=CARTESIAN_POINT('Ctrl Pts',(151.439279183291,5.21325183374003,134.860965250768));
#192246=CARTESIAN_POINT('Ctrl Pts',(151.160831559478,6.23082632381839,128.610998095198));
#192247=CARTESIAN_POINT('Ctrl Pts',(150.882383935665,1.52257581509584,124.376623945969));
#192248=CARTESIAN_POINT('Ctrl Pts',(150.603936311853,-4.58484748573611,
126.049025785542));
#192249=CARTESIAN_POINT('Ctrl Pts',(150.32548868804,-6.47901992942814,132.091348024725));
#192250=CARTESIAN_POINT('Ctrl Pts',(150.047041064227,-2.41928957569559,
136.950991709558));
#192251=CARTESIAN_POINT('Ctrl Pts',(149.768593440414,3.8636497092349,136.162181700472));
#192252=CARTESIAN_POINT('Ctrl Pts',(149.490145816601,6.59608366116008,130.449795860306));
#192253=CARTESIAN_POINT('Ctrl Pts',(149.211698192788,3.26703896508027,125.06323771061));
#192254=CARTESIAN_POINT('Ctrl Pts',(148.933250568975,-3.06425493618196,
124.95249104296));
#192255=CARTESIAN_POINT('Ctrl Pts',(148.654802945162,-6.57964824826877,
130.219326634649));
#192256=CARTESIAN_POINT('Ctrl Pts',(148.376355321349,-4.04866625388314,
136.02377987614));
#192257=CARTESIAN_POINT('Ctrl Pts',(148.097907697537,2.20284223947883,137.031841801807));
#192258=CARTESIAN_POINT('Ctrl Pts',(147.819460073724,6.43004632958585,132.317152748525));
#192259=CARTESIAN_POINT('Ctrl Pts',(147.541012449911,4.74835196802999,126.212281630895));
#192260=CARTESIAN_POINT('Ctrl Pts',(147.262564826098,-1.29684588225586,
124.327306766486));
#192261=CARTESIAN_POINT('Ctrl Pts',(146.984117202285,-6.15030572119196,
128.394427969547));
#192262=CARTESIAN_POINT('Ctrl Pts',(146.705669578472,-5.35193506149072,
134.676159544383));
#192263=CARTESIAN_POINT('Ctrl Pts',(146.427221954659,0.364602463157475,
137.399897053366));
#192264=CARTESIAN_POINT('Ctrl Pts',(146.148774330846,5.74608813598446,134.062658787717));
#192265=CARTESIAN_POINT('Ctrl Pts',(145.870326707034,5.84719952385297,127.731203680413));
#192266=CARTESIAN_POINT('Ctrl Pts',(145.59187908322,0.575020200877703,124.22382966629));
#192267=CARTESIAN_POINT('Ctrl Pts',(145.313431459408,-5.22557459540567,
126.76364211958));
#192268=CARTESIAN_POINT('Ctrl Pts',(145.034983835595,-6.22412162202233,
133.016677472446));
#192269=CARTESIAN_POINT('Ctrl Pts',(144.756536211782,-1.50300494324566,
137.236701713364));
#192270=CARTESIAN_POINT('Ctrl Pts',(144.478088587969,4.59929985250025,135.545718724575));
#192271=CARTESIAN_POINT('Ctrl Pts',(144.199640964156,6.47507277208744,129.497659263665));
#192272=CARTESIAN_POINT('Ctrl Pts',(143.921193340343,2.40057013901678,124.65039451108));
#192273=CARTESIAN_POINT('Ctrl Pts',(143.64274571653,-3.87993917743928,125.458323972397));
#192274=CARTESIAN_POINT('Ctrl Pts',(143.364298092718,-6.594973935395,131.178999942215));
#192275=CARTESIAN_POINT('Ctrl Pts',(143.085850468904,-3.2495498291107,136.555400674828));
#192276=CARTESIAN_POINT('Ctrl Pts',(142.807402845092,3.08205182079176,136.646876548744));
#192277=CARTESIAN_POINT('Ctrl Pts',(142.528955221279,6.58139841398854,131.369365704677));
#192278=CARTESIAN_POINT('Ctrl Pts',(142.250507597466,4.03276138391676,125.572642787588));
#192279=CARTESIAN_POINT('Ctrl Pts',(141.972059973653,-2.2217863466284,124.583612972623));
#192280=CARTESIAN_POINT('Ctrl Pts',(141.69361234984,-6.43462096491922,129.311146342943));
#192281=CARTESIAN_POINT('Ctrl Pts',(141.415164726027,-4.7343532651591,135.410870684068));
#192282=CARTESIAN_POINT('Ctrl Pts',(141.136717102214,1.31655379926713,137.277437314604));
#192283=CARTESIAN_POINT('Ctrl Pts',(140.858269478402,6.15761223939561,133.195562687939));
#192284=CARTESIAN_POINT('Ctrl Pts',(140.579821854588,5.34012584760095,126.916290175316));
#192285=CARTESIAN_POINT('Ctrl Pts',(140.301374230776,-0.384675318488256,
124.20996445632));
#192286=CARTESIAN_POINT('Ctrl Pts',(140.022926606963,-5.75597865932068,
127.563566655346));
#192287=CARTESIAN_POINT('Ctrl Pts',(139.74447898315,-5.83781880742758,133.895300184066));
#192288=CARTESIAN_POINT('Ctrl Pts',(139.466031359337,-0.554988664812238,
137.386611251964));
#192289=CARTESIAN_POINT('Ctrl Pts',(139.187583735524,5.23784894806212,134.829155547671));
#192290=CARTESIAN_POINT('Ctrl Pts',(138.909136111711,6.21735926081381,128.573109924773));
#192291=CARTESIAN_POINT('Ctrl Pts',(138.630688487898,1.48342014776303,124.367474685896));
#192292=CARTESIAN_POINT('Ctrl Pts',(138.352240864086,-4.61370961197883,
126.077023158863));
#192293=CARTESIAN_POINT('Ctrl Pts',(138.073793240272,-6.47106563055709,
132.130763813104));
#192294=CARTESIAN_POINT('Ctrl Pts',(137.79534561646,-2.38182846378423,136.965604729043));
#192295=CARTESIAN_POINT('Ctrl Pts',(137.516897992647,3.89619270241722,136.138563300043));
#192296=CARTESIAN_POINT('Ctrl Pts',(137.238450368834,6.59380311469226,130.409650196134));
#192297=CARTESIAN_POINT('Ctrl Pts',(136.960002745021,3.23203058975544,125.043456686844));
#192298=CARTESIAN_POINT('Ctrl Pts',(136.681555121208,-3.09982015369448,
124.971252454085));
#192299=CARTESIAN_POINT('Ctrl Pts',(136.403107497395,-6.58308761053252,
130.259389660389));
#192300=CARTESIAN_POINT('Ctrl Pts',(136.124659873582,-4.01681915499975,
136.048328553027));
#192301=CARTESIAN_POINT('Ctrl Pts',(135.846212249769,2.24070987145278,137.018317095051));
#192302=CARTESIAN_POINT('Ctrl Pts',(135.567764625956,6.43913599080291,132.277983202917));
#192303=CARTESIAN_POINT('Ctrl Pts',(135.289317002144,4.72031070388647,126.183462145311));
#192304=CARTESIAN_POINT('Ctrl Pts',(135.010869378331,-1.33624951990408,
124.335321040266));
#192305=CARTESIAN_POINT('Ctrl Pts',(134.732421754518,-6.16486171432077,
128.431911276607));
#192306=CARTESIAN_POINT('Ctrl Pts',(134.453974130705,-5.32826716351462,
134.708666556695));
#192307=CARTESIAN_POINT('Ctrl Pts',(134.175526506892,0.404744610239488,
137.397555414672));
#192308=CARTESIAN_POINT('Ctrl Pts',(133.897078883079,5.76581586005707,134.027620349581));
#192309=CARTESIAN_POINT('Ctrl Pts',(133.618631259266,5.82838401024617,127.695667055759));
#192310=CARTESIAN_POINT('Ctrl Pts',(133.340183635453,0.534951987407334,
124.220451277114));
#192311=CARTESIAN_POINT('Ctrl Pts',(133.06173601164,-5.25007477800144,126.795526540492));
#192312=CARTESIAN_POINT('Ctrl Pts',(132.783288387828,-6.21053930283845,
133.054524478268));
#192313=CARTESIAN_POINT('Ctrl Pts',(132.504840764015,-1.46382161007886,
137.245731754674));
#192314=CARTESIAN_POINT('Ctrl Pts',(132.226393140202,4.62807663068185,135.517633634551));
#192315=CARTESIAN_POINT('Ctrl Pts',(131.947945516389,6.46699854195874,129.458267868007));
#192316=CARTESIAN_POINT('Ctrl Pts',(131.669497892576,2.3630647236181,124.635895578019));
#192317=CARTESIAN_POINT('Ctrl Pts',(131.391050268763,-3.91241013359816,
125.482041313105));
#192318=CARTESIAN_POINT('Ctrl Pts',(131.11260264495,-6.59257120989826,131.219138479237));
#192319=CARTESIAN_POINT('Ctrl Pts',(130.834155021138,-3.2144814093103,136.575075053519));
#192320=CARTESIAN_POINT('Ctrl Pts',(130.555707397324,3.1175597702868,136.628006976231));
#192321=CARTESIAN_POINT('Ctrl Pts',(130.277259773512,6.58471582225214,131.329292396271));
#192322=CARTESIAN_POINT('Ctrl Pts',(129.998812149698,4.0008397148189,125.548191156024));
#192323=CARTESIAN_POINT('Ctrl Pts',(129.720364525886,-2.25961263864694,
124.59725287278));
#192324=CARTESIAN_POINT('Ctrl Pts',(129.441916902073,-6.44359136541048,
129.350343372922));
#192325=CARTESIAN_POINT('Ctrl Pts',(129.16346927826,-4.70622441430021,135.439604688201));
#192326=CARTESIAN_POINT('Ctrl Pts',(128.885021654447,1.35593286170785,137.269303146827));
#192327=CARTESIAN_POINT('Ctrl Pts',(128.606574030634,6.17205407880915,133.158035251063));
#192328=CARTESIAN_POINT('Ctrl Pts',(128.328126406821,5.31635911908928,126.883855350513));
#192329=CARTESIAN_POINT('Ctrl Pts',(128.049678783009,-0.424810152491945,
124.212428263054));
#192330=CARTESIAN_POINT('Ctrl Pts',(127.771231159195,-5.77559964706288,
127.598664975593));
#192331=CARTESIAN_POINT('Ctrl Pts',(127.492783535383,-5.81889521971155,
133.930779376167));
#192332=CARTESIAN_POINT('Ctrl Pts',(127.21433591157,-0.514910354280421,
137.389867671632));
#192333=CARTESIAN_POINT('Ctrl Pts',(126.935888287757,5.26225197196523,134.797196704317));
#192334=CARTESIAN_POINT('Ctrl Pts',(126.657440663944,6.20366181127538,128.535304434163));
#192335=CARTESIAN_POINT('Ctrl Pts',(126.378993040131,1.44420951175126,124.358563947));
#192336=CARTESIAN_POINT('Ctrl Pts',(126.100545416318,-4.64240077551519,
126.105195705413));
#192337=CARTESIAN_POINT('Ctrl Pts',(125.822097792505,-6.46287154396936,
132.170130451126));
#192338=CARTESIAN_POINT('Ctrl Pts',(125.543650168692,-2.34427909234318,
136.979989441362));
#192339=CARTESIAN_POINT('Ctrl Pts',(125.26520254488,3.92859132074607,136.114747238771));
#192340=CARTESIAN_POINT('Ctrl Pts',(124.986754921067,6.59127823242518,130.369519158099));
#192341=CARTESIAN_POINT('Ctrl Pts',(124.708307297254,3.19690245034852,125.023889135492));
#192342=CARTESIAN_POINT('Ctrl Pts',(124.429859673441,-3.13527050623128,
124.990230013179));
#192343=CARTESIAN_POINT('Ctrl Pts',(124.151412049628,-6.58628303406391,
130.299472880227));
#192344=CARTESIAN_POINT('Ctrl Pts',(123.872964425815,-3.98482321140548,
136.072682912751));
#192345=CARTESIAN_POINT('Ctrl Pts',(123.594516802002,2.2784944730983,137.004562127853));
#192346=CARTESIAN_POINT('Ctrl Pts',(123.316069178189,6.44798704746787,132.238759051683));
#192347=CARTESIAN_POINT('Ctrl Pts',(123.037621554376,4.6920945268939,126.154813888819));
#192348=CARTESIAN_POINT('Ctrl Pts',(122.759173930564,-1.37560364233486,
124.343575026687));
#192349=CARTESIAN_POINT('Ctrl Pts',(122.480726306751,-6.17918926623166,
128.46948249565));
#192350=CARTESIAN_POINT('Ctrl Pts',(122.202278682938,-5.30440182463932,
134.741028893516));
#192351=CARTESIAN_POINT('Ctrl Pts',(121.923831059125,0.444871759361186,
137.394969462721));
#192352=CARTESIAN_POINT('Ctrl Pts',(121.645383435312,5.78532992970255,133.992462472369));
#192353=CARTESIAN_POINT('Ctrl Pts',(121.366935811499,5.80935252372653,127.660245624887));
#192354=CARTESIAN_POINT('Ctrl Pts',(121.088488187686,0.494863951094175,
124.21731685712));
#192355=CARTESIAN_POINT('Ctrl Pts',(120.810040563873,-5.27438041714564,
126.827559510225));
#192356=CARTESIAN_POINT('Ctrl Pts',(120.53159294006,-6.19672684983677,133.092288103441));
#192357=CARTESIAN_POINT('Ctrl Pts',(120.253145316248,-1.42458403446405,
137.254523108609));
#192358=CARTESIAN_POINT('Ctrl Pts',(119.974697692435,4.65668191378195,135.489373892464));
#192359=CARTESIAN_POINT('Ctrl Pts',(119.696250068622,6.45868467482089,129.418926352309));
#192360=CARTESIAN_POINT('Ctrl Pts',(119.417802444809,2.32547174398699,124.621625219699));
#192361=CARTESIAN_POINT('Ctrl Pts',(119.139354820996,-3.94473611396066,
125.505955874312));
#192362=CARTESIAN_POINT('Ctrl Pts',(118.860907197183,-6.58992419425096,
131.259261646514));
#192363=CARTESIAN_POINT('Ctrl Pts',(118.58245957337,-3.17929387571916,136.594535596262));
#192364=CARTESIAN_POINT('Ctrl Pts',(118.304011949557,3.15295219745811,136.608921606362));
#192365=CARTESIAN_POINT('Ctrl Pts',(118.025564325744,6.58778923144938,131.289199636326));
#192366=CARTESIAN_POINT('Ctrl Pts',(117.747116701932,3.96876979313418,125.523934293753));
#192367=CARTESIAN_POINT('Ctrl Pts',(117.468669078118,-2.29735519988813,
124.611122779595));
#192368=CARTESIAN_POINT('Ctrl Pts',(117.190221454306,-6.45232299625411,
129.389594282045));
#192369=CARTESIAN_POINT('Ctrl Pts',(116.911773830493,-4.67792117256487,
135.468166931659));
#192370=CARTESIAN_POINT('Ctrl Pts',(116.63332620668,1.39526167955762,137.260929418227));
#192371=CARTESIAN_POINT('Ctrl Pts',(116.354878582867,6.18626721048894,133.120420597908));
#192372=CARTESIAN_POINT('Ctrl Pts',(116.076430959054,5.29239539093549,126.851565801475));
#192373=CARTESIAN_POINT('Ctrl Pts',(115.797983335241,-0.464929244999223,
124.215136336267));
#192374=CARTESIAN_POINT('Ctrl Pts',(115.519535711428,-5.79500661783607,
127.633882084071));
#192375=CARTESIAN_POINT('Ctrl Pts',(115.241088087616,-5.79975601069334,
133.96614271767));
#192376=CARTESIAN_POINT('Ctrl Pts',(114.962640463802,-0.474812963556037,
137.392880062915));
#192377=CARTESIAN_POINT('Ctrl Pts',(114.68419283999,5.28646000118636,134.765089904953));
#192378=CARTESIAN_POINT('Ctrl Pts',(114.405745216177,6.18973448276714,128.497583024264));
#192379=CARTESIAN_POINT('Ctrl Pts',(114.127297592364,1.40494536002493,124.349892059469));
#192380=CARTESIAN_POINT('Ctrl Pts',(113.848849968551,-4.67091991318358,
126.133542381245));
#192381=CARTESIAN_POINT('Ctrl Pts',(113.570402344738,-6.45443797329988,
132.209446480045));
#192382=CARTESIAN_POINT('Ctrl Pts',(113.291954720925,-2.30664285277824,
136.994145313484));
#192383=CARTESIAN_POINT('Ctrl Pts',(113.013507097112,3.96084436367879,136.09073439917));
#192384=CARTESIAN_POINT('Ctrl Pts',(112.735059473299,6.58850910791926,130.329404233275));
#192385=CARTESIAN_POINT('Ctrl Pts',(112.456611849487,3.16165584854565,125.004535781636));
#192386=CARTESIAN_POINT('Ctrl Pts',(112.178164225674,-3.1706046801665,125.00942301702));
#192387=CARTESIAN_POINT('Ctrl Pts',(111.899716601861,-6.58923440045535,
130.339574808866));
#192388=CARTESIAN_POINT('Ctrl Pts',(111.621268978048,-3.9526796087217,136.096842052857));
#192389=CARTESIAN_POINT('Ctrl Pts',(111.342821354235,2.31619464429322,136.990577409908));
#192390=CARTESIAN_POINT('Ctrl Pts',(111.064373730422,6.45659917160154,132.199481748287));
#192391=CARTESIAN_POINT('Ctrl Pts',(110.785926106609,4.66370448261314,126.12633792299));
#192392=CARTESIAN_POINT('Ctrl Pts',(110.507478482796,-1.41490679126679,
124.352068419894));
#192393=CARTESIAN_POINT('Ctrl Pts',(110.229030858983,-6.19328784601188,
128.50714023446));
#192394=CARTESIAN_POINT('Ctrl Pts',(109.950583235171,-5.28033992920373,
134.773245355646));
#192395=CARTESIAN_POINT('Ctrl Pts',(109.672135611358,0.484982423596243,
137.392139293334));
#192396=CARTESIAN_POINT('Ctrl Pts',(109.393687987545,5.80462962181993,133.957186458871));
#192397=CARTESIAN_POINT('Ctrl Pts',(109.115240363732,5.79010576951274,127.624940700352));
#192398=CARTESIAN_POINT('Ctrl Pts',(108.836792739919,0.454757577415474,
124.214426522456));
#192399=CARTESIAN_POINT('Ctrl Pts',(108.558345116106,-5.29849061218381,
126.859739841786));
#192400=CARTESIAN_POINT('Ctrl Pts',(108.279897492293,-6.18268477484283,
133.12996694862));
#192401=CARTESIAN_POINT('Ctrl Pts',(108.00144986848,-1.38529367036394,137.2630754494));
#192402=CARTESIAN_POINT('Ctrl Pts',(107.723002244667,4.68511464182123,135.460940545486));
#192403=CARTESIAN_POINT('Ctrl Pts',(107.444554620855,6.45013147874722,129.379636174388));
#192404=CARTESIAN_POINT('Ctrl Pts',(107.166106997042,2.28779259314522,124.607583964913));
#192405=CARTESIAN_POINT('Ctrl Pts',(106.887659373229,-3.97691592067581,
125.530066769856));
#192406=CARTESIAN_POINT('Ctrl Pts',(106.609211749416,-6.58703298653922,
131.299367957265));
#192407=CARTESIAN_POINT('Ctrl Pts',(106.330764125603,-3.14398853222427,
136.613781581943));
#192408=CARTESIAN_POINT('Ctrl Pts',(106.05231650179,3.18822779082625,136.589621146351));
#192409=CARTESIAN_POINT('Ctrl Pts',(105.773868877977,6.59061852769399,131.249088910493));
#192410=CARTESIAN_POINT('Ctrl Pts',(105.495421254164,3.93655280722527,125.49987309962));
#192411=CARTESIAN_POINT('Ctrl Pts',(105.216973630351,-2.33501263178752,
124.625222179118));
#192412=CARTESIAN_POINT('Ctrl Pts',(104.938526006539,-6.46081553389627,
129.428897615854));
#192413=CARTESIAN_POINT('Ctrl Pts',(104.660078382726,-4.64944458874018,
135.49655635606));
#192414=CARTESIAN_POINT('Ctrl Pts',(104.381630758913,1.43453879547275,137.252316439095));
#192415=CARTESIAN_POINT('Ctrl Pts',(104.1031831351,6.20025110776228,133.082720122298));
#192416=CARTESIAN_POINT('Ctrl Pts',(103.824735511287,5.26823555112421,126.819422724701));
#192417=CARTESIAN_POINT('Ctrl Pts',(103.546287887474,-0.505031109382345,
124.218088575609));
#192418=CARTESIAN_POINT('Ctrl Pts',(103.267840263661,-5.81419885250792,
127.669216675797));
#192419=CARTESIAN_POINT('Ctrl Pts',(102.989392639848,-5.78040188958328,
134.001388898174));
#192420=CARTESIAN_POINT('Ctrl Pts',(102.710945016035,-0.434697978462825,
137.395648314187));
#192421=CARTESIAN_POINT('Ctrl Pts',(102.432497392222,5.31047213868803,134.732836339309));
#192422=CARTESIAN_POINT('Ctrl Pts',(102.15404976841,6.17557779137139,128.459947092858));
#192423=CARTESIAN_POINT('Ctrl Pts',(101.875602144597,1.3656291475316,124.341459344644));
#192424=CARTESIAN_POINT('Ctrl Pts',(101.597154520784,-4.69926596819684,
126.162062135967));
#192425=CARTESIAN_POINT('Ctrl Pts',(101.318706896971,-6.44576523105769,
132.248710442988));
#192426=CARTESIAN_POINT('Ctrl Pts',(101.040259273158,-2.26892113971413,
137.008071820859));
#192427=CARTESIAN_POINT('Ctrl Pts',(100.761811649345,3.99295063606701,136.066525671043));
#192428=CARTESIAN_POINT('Ctrl Pts',(100.483364025532,6.58549584378548,130.289306908136));
#192429=CARTESIAN_POINT('Ctrl Pts',(100.204916401719,3.12629209042249,124.985397342422));
#192430=CARTESIAN_POINT('Ctrl Pts',(99.9264687779064,-3.20582136617937,
125.028830754405));
#192431=CARTESIAN_POINT('Ctrl Pts',(99.6480211540935,-6.5919416003429,130.379693960313));
#192432=CARTESIAN_POINT('Ctrl Pts',(99.3695735302808,-3.92038953804142,
136.120805078117));
#192433=CARTESIAN_POINT('Ctrl Pts',(99.0911259064677,2.35380898804382,136.976363459425));
#192434=CARTESIAN_POINT('Ctrl Pts',(98.812678282655,6.46497204407849,132.160152748165));
#192435=CARTESIAN_POINT('Ctrl Pts',(98.5342306588419,4.63514162304771,126.098035303012));
#192436=CARTESIAN_POINT('Ctrl Pts',(98.2557830350292,-1.45415751030726,
124.36080090516));
#192437=CARTESIAN_POINT('Ctrl Pts',(97.9773354112161,-6.20715693123341,
128.544883097616));
#192438=CARTESIAN_POINT('Ctrl Pts',(97.6988877874034,-5.25608236883021,
134.805314749293));
#192439=CARTESIAN_POINT('Ctrl Pts',(97.4204401635904,0.525075116629235,
137.389065011387));
#192440=CARTESIAN_POINT('Ctrl Pts',(97.1419925397775,5.82371422125203,133.921793616252));
#192441=CARTESIAN_POINT('Ctrl Pts',(96.8635449159648,5.77064446080036,127.589753590393));
#192442=CARTESIAN_POINT('Ctrl Pts',(96.5850972921516,0.414634352527504,
124.211780380221));
#192443=CARTESIAN_POINT('Ctrl Pts',(96.306649668339,-5.32240446970382,126.89206634272));
#192444=CARTESIAN_POINT('Ctrl Pts',(96.0282020445258,-6.16841359819089,
133.1675596176));
#192445=CARTESIAN_POINT('Ctrl Pts',(95.7497544207132,-1.34595197369742,
137.271388460138));
#192446=CARTESIAN_POINT('Ctrl Pts',(95.4713067969001,4.7133737612145,135.432334647225));
#192447=CARTESIAN_POINT('Ctrl Pts',(95.1928591730874,6.44133927067958,129.340398790155));
#192448=CARTESIAN_POINT('Ctrl Pts',(94.9144115492744,2.25002866730758,124.593772333964));
#192449=CARTESIAN_POINT('Ctrl Pts',(94.6359639254615,-4.008948361309,125.554373106298));
#192450=CARTESIAN_POINT('Ctrl Pts',(94.3575163016487,-6.58389769389783,
131.339455925338));
#192451=CARTESIAN_POINT('Ctrl Pts',(94.0790686778357,-3.10856668707799,
136.632812297395));
#192452=CARTESIAN_POINT('Ctrl Pts',(93.8006210540229,3.22338524324122,136.570106311383));
#192453=CARTESIAN_POINT('Ctrl Pts',(93.52217343021,6.59320360614536,131.208961705089));
#192454=CARTESIAN_POINT('Ctrl Pts',(93.2437258063971,3.90418995090443,125.476008465224));
#192455=CARTESIAN_POINT('Ctrl Pts',(92.9652781825842,-2.37258353893516,
124.639550548886));
#192456=CARTESIAN_POINT('Ctrl Pts',(92.6868305587713,-6.46906866364288,
129.468251917951));
#192457=CARTESIAN_POINT('Ctrl Pts',(92.4083829349583,-4.62079571803641,
135.524771909422));
#192458=CARTESIAN_POINT('Ctrl Pts',(92.1299353111456,1.47376275402524,137.24346452859));
#192459=CARTESIAN_POINT('Ctrl Pts',(91.8514876873325,6.21400525245068,133.04493522124));
#192460=CARTESIAN_POINT('Ctrl Pts',(91.5730400635199,5.24388049490719,126.787427311268));
#192461=CARTESIAN_POINT('Ctrl Pts',(91.2945924397067,-0.545114259651984,
124.221284871682));
#192462=CARTESIAN_POINT('Ctrl Pts',(91.016144815894,-5.83317563990314,127.704667441434));
#192463=CARTESIAN_POINT('Ctrl Pts',(90.7376971920811,-5.76083357355547,
134.036516611621));
#192464=CARTESIAN_POINT('Ctrl Pts',(90.4592495682681,-0.394566885476172,
137.398172322869));
#192465=CARTESIAN_POINT('Ctrl Pts',(90.1808019444553,5.33428749469169,134.700437202553));
#192466=CARTESIAN_POINT('Ctrl Pts',(89.9023543206424,6.16119226166949,128.422398034556));
#192467=CARTESIAN_POINT('Ctrl Pts',(89.6239066968295,1.32626233114802,124.333266115003));
#192468=CARTESIAN_POINT('Ctrl Pts',(89.3454590730166,-4.72743789018152,
126.190753912764));
#192469=CARTESIAN_POINT('Ctrl Pts',(89.0670114492037,-6.43685363861442,
132.28792088502));
#192470=CARTESIAN_POINT('Ctrl Pts',(88.7885638253908,-2.23111535094281,
137.021768447433));
#192471=CARTESIAN_POINT('Ctrl Pts',(88.5101162015778,4.02490894820102,136.042121951457));
#192472=CARTESIAN_POINT('Ctrl Pts',(88.2316685777651,6.58223855168135,130.2492286685));
#192473=CARTESIAN_POINT('Ctrl Pts',(87.9532209539521,3.09081248639635,124.966474527032));
#192474=CARTESIAN_POINT('Ctrl Pts',(87.6747733301392,-3.2409192593025,125.048452506173));
#192475=CARTESIAN_POINT('Ctrl Pts',(87.3963257063264,-6.59440453341028,
130.41982884794));
#192476=CARTESIAN_POINT('Ctrl Pts',(87.1178780825135,-3.88795419588509,
136.144571100572));
#192477=CARTESIAN_POINT('Ctrl Pts',(86.8394304587006,2.39133611053674,136.961920803106));
#192478=CARTESIAN_POINT('Ctrl Pts',(86.5609828348878,6.47310535463887,132.120773508667));
#192479=CARTESIAN_POINT('Ctrl Pts',(86.2825352110747,4.60640700660486,126.06990707765));
#192480=CARTESIAN_POINT('Ctrl Pts',(86.004087587262,-1.49335434500641,124.369772158902));
#192481=CARTESIAN_POINT('Ctrl Pts',(85.725639963449,-6.22079600797217,128.582709686544));
#192482=CARTESIAN_POINT('Ctrl Pts',(85.4471923396362,-5.23163004239161,
134.837235886113));
#192483=CARTESIAN_POINT('Ctrl Pts',(85.1687447158232,0.565148352810691,
137.385746730796));
#192484=CARTESIAN_POINT('Ctrl Pts',(84.8902970920103,5.842583020812,133.886285256006));
#192485=CARTESIAN_POINT('Ctrl Pts',(84.6118494681974,5.75096931873532,127.554685598878));
#192486=CARTESIAN_POINT('Ctrl Pts',(84.3334018443846,0.374495763211118,
124.209378528473));
#192487=CARTESIAN_POINT('Ctrl Pts',(84.0549542205716,-5.34612110356891,
126.924537815158));
#192488=CARTESIAN_POINT('Ctrl Pts',(83.7765065967588,-6.15391384870464,
133.205064717373));
#192489=CARTESIAN_POINT('Ctrl Pts',(83.498058972946,-1.30656040228555,137.279461832782));
#192490=CARTESIAN_POINT('Ctrl Pts',(83.2196113491328,4.74145822480973,135.403557257686));
#192491=CARTESIAN_POINT('Ctrl Pts',(82.9411637253203,6.43230837641647,129.301215653567));
#192492=CARTESIAN_POINT('Ctrl Pts',(82.6627161015071,2.21218136583022,124.580190838648));
#192493=CARTESIAN_POINT('Ctrl Pts',(82.3842684776944,-4.04083224888638,
125.578873982957));
#192494=CARTESIAN_POINT('Ctrl Pts',(82.1058208538814,-6.58051843250612,
131.379524065257));
#192495=CARTESIAN_POINT('Ctrl Pts',(81.8273732300686,-3.07302965285007,
136.651627037425));
#192496=CARTESIAN_POINT('Ctrl Pts',(81.5489256062556,3.25842325193051,136.550377824588));
#192497=CARTESIAN_POINT('Ctrl Pts',(81.270477982443,6.59554437101248,131.168819507043));
#192498=CARTESIAN_POINT('Ctrl Pts',(80.9920303586297,3.87168242338918,125.452341274876));
#192499=CARTESIAN_POINT('Ctrl Pts',(80.713582734817,-2.41006652912724,124.654107357959));
#192500=CARTESIAN_POINT('Ctrl Pts',(80.435135111004,-6.47708207967116,129.507655730047));
#192501=CARTESIAN_POINT('Ctrl Pts',(80.1566874871913,-4.59197562204804,
135.552812546207));
#192502=CARTESIAN_POINT('Ctrl Pts',(79.8782398633782,1.51293210175691,137.234374014721));
#192503=CARTESIAN_POINT('Ctrl Pts',(79.5997922395654,6.22752913488936,133.007067294864));
#192504=CARTESIAN_POINT('Ctrl Pts',(79.3213446157525,5.2193311247699,126.755580746775));
#192505=CARTESIAN_POINT('Ctrl Pts',(79.0428969919396,-0.585177210512381,
124.224725106049));
#192506=CARTESIAN_POINT('Ctrl Pts',(78.7644493681267,-5.85193627682986,
127.740233067343));
#192507=CARTESIAN_POINT('Ctrl Pts',(78.4860017443139,-5.74105178772106,
134.071524556339));
#192508=CARTESIAN_POINT('Ctrl Pts',(78.2075541205009,-0.354421171668466,
137.400451995434));
#192509=CARTESIAN_POINT('Ctrl Pts',(77.9291064966881,5.35790518671055,134.667893695246));
#192510=CARTESIAN_POINT('Ctrl Pts',(77.6506588728751,6.14657842672258,128.384937240753));
#192511=CARTESIAN_POINT('Ctrl Pts',(77.3722112490624,1.28684636962602,124.325312674148));
#192512=CARTESIAN_POINT('Ctrl Pts',(77.0937636252493,-4.75543463521666,
126.219616648455));
#192513=CARTESIAN_POINT('Ctrl Pts',(76.8153160014366,-6.42770352619243,
132.327076353179));
#192514=CARTESIAN_POINT('Ctrl Pts',(76.5368683776235,-2.19322688737167,
137.035234685673));
#192515=CARTESIAN_POINT('Ctrl Pts',(76.2584207538107,4.05671811585379,136.017524144697));
#192516=CARTESIAN_POINT('Ctrl Pts',(75.9799731299978,6.57873735230709,130.209170999483));
#192517=CARTESIAN_POINT('Ctrl Pts',(75.7015255061849,3.05521835117689,124.947768036657));
#192518=CARTESIAN_POINT('Ctrl Pts',(75.423077882372,-3.27589705897064,125.068287545233));
#192519=CARTESIAN_POINT('Ctrl Pts',(75.1446302585591,-6.5966231083926,130.459977984534));
#192520=CARTESIAN_POINT('Ctrl Pts',(74.8661826347462,-3.85537478415624,
136.168139239563));
#192521=CARTESIAN_POINT('Ctrl Pts',(74.5877350109334,2.42877462119068,136.94724997613));
#192522=CARTESIAN_POINT('Ctrl Pts',(74.3092873871204,6.48099880189986,132.081345489005));
#192523=CARTESIAN_POINT('Ctrl Pts',(74.0308397633076,4.57750169805637,126.041954289206));
#192524=CARTESIAN_POINT('Ctrl Pts',(73.7523921394947,-1.53249584291112,
124.378981848686));
#192525=CARTESIAN_POINT('Ctrl Pts',(73.4739445156818,-6.23420457082727,
128.620618599563));
#192526=CARTESIAN_POINT('Ctrl Pts',(73.1954968918689,-5.20698385597775,
134.869007583256));
#192527=CARTESIAN_POINT('Ctrl Pts',(72.917049268056,0.605200647212208,137.382184574524));
#192528=CARTESIAN_POINT('Ctrl Pts',(72.6386016442432,5.86123532130951,133.850662693911));
#192529=CARTESIAN_POINT('Ctrl Pts',(72.3601540204302,5.73108107238729,127.519738025268));
#192530=CARTESIAN_POINT('Ctrl Pts',(72.0817063966174,0.334343296816498,
124.207221056211));
#192531=CARTESIAN_POINT('Ctrl Pts',(71.8032587728044,-5.36963963495047,
126.957153055855));
#192532=CARTESIAN_POINT('Ctrl Pts',(71.5248111489915,-6.13918606367764,
133.242480858172));
#192533=CARTESIAN_POINT('Ctrl Pts',(71.2463635251787,-1.26712041579749,
137.287295268168));
#192534=CARTESIAN_POINT('Ctrl Pts',(70.9679159013657,4.76936699192676,135.374609443224));
#192535=CARTESIAN_POINT('Ctrl Pts',(70.689468277553,6.423039130601,129.262088216567));
#192536=CARTESIAN_POINT('Ctrl Pts',(70.4110206537399,2.17425209115883,124.566839982233));
#192537=CARTESIAN_POINT('Ctrl Pts',(70.1325730299272,-4.07256640193864,
125.603568491945));
#192538=CARTESIAN_POINT('Ctrl Pts',(69.8541254061142,-6.57689532758393,
131.419570892283));
#192539=CARTESIAN_POINT('Ctrl Pts',(69.5756777823013,-3.03737874637841,
136.670225104848));
#192540=CARTESIAN_POINT('Ctrl Pts',(69.2972301584884,3.2933405185478,136.530436417012));
#192541=CARTESIAN_POINT('Ctrl Pts',(69.0187825346755,6.5976407355574,131.128663803839));
#192542=CARTESIAN_POINT('Ctrl Pts',(68.7403349108627,3.83903142925813,125.428872405572));
#192543=CARTESIAN_POINT('Ctrl Pts',(68.4618872870498,-2.44746021341752,
124.668892066929));
#192544=CARTESIAN_POINT('Ctrl Pts',(68.1834396632368,-6.48485548504104,
129.547107592018));
#192545=CARTESIAN_POINT('Ctrl Pts',(67.904992039424,-4.56298536871445,135.580677227361));
#192546=CARTESIAN_POINT('Ctrl Pts',(67.6265444156111,1.55204538723279,137.225045234339));
#192547=CARTESIAN_POINT('Ctrl Pts',(67.3480967917982,6.2408222539455,132.969117746385));
#192548=CARTESIAN_POINT('Ctrl Pts',(67.0696491679854,5.19458835039884,126.723884211309));
#192549=CARTESIAN_POINT('Ctrl Pts',(66.7912015441724,-0.625218477415679,
124.228409151229));
#192550=CARTESIAN_POINT('Ctrl Pts',(66.5127539203596,-5.87048006810572,
127.775912235624));
#192551=CARTESIAN_POINT('Ctrl Pts',(66.2343062965465,-5.72105726510147,
134.106411435094));
#192552=CARTESIAN_POINT('Ctrl Pts',(65.9558586727338,-0.314262324654327,
137.402487247406));
#192553=CARTESIAN_POINT('Ctrl Pts',(65.6774110489208,5.3813243395822,134.6352070233));
#192554=CARTESIAN_POINT('Ctrl Pts',(65.398963425108,6.13173682805169,128.347566099575));
#192555=CARTESIAN_POINT('Ctrl Pts',(65.120515801295,1.24738272353907,124.317599316798));
#192556=CARTESIAN_POINT('Ctrl Pts',(64.8420681774823,-4.78325516587229,
126.248649273519));
#192557=CARTESIAN_POINT('Ctrl Pts',(64.5636205536692,-6.41831523285262,
132.366175396547));
#192558=CARTESIAN_POINT('Ctrl Pts',(64.2851729298565,-2.15525715297185,
137.048470036584));
#192559=CARTESIAN_POINT('Ctrl Pts',(64.0067253060435,4.08837696032456,135.992733162246));
#192560=CARTESIAN_POINT('Ctrl Pts',(63.7282776822307,6.57499237540094,130.169135385437));
#192561=CARTESIAN_POINT('Ctrl Pts',(63.4498300584178,3.01951100371835,124.929278564476));
#192562=CARTESIAN_POINT('Ctrl Pts',(63.1713824346048,-3.31075346906837,
125.088335136589));
#192563=CARTESIAN_POINT('Ctrl Pts',(62.892934810792,-6.59859724307971,130.500139882352));
#192564=CARTESIAN_POINT('Ctrl Pts',(62.614487186979,-3.82265251009718,136.191508621766));
#192565=CARTESIAN_POINT('Ctrl Pts',(62.3360395631662,2.46612313270748,136.932351522132));
#192566=CARTESIAN_POINT('Ctrl Pts',(62.0575919393533,6.48865209336687,132.041870150199));
#192567=CARTESIAN_POINT('Ctrl Pts',(61.7791443155403,4.5484267684992,126.014177973478));
#192568=CARTESIAN_POINT('Ctrl Pts',(61.5006966917276,-1.57158055361859,
124.388429633243));
#192569=CARTESIAN_POINT('Ctrl Pts',(61.2222490679146,-6.24738212293903,
128.658608431946));
#192570=CARTESIAN_POINT('Ctrl Pts',(60.9438014441017,-5.18214472286266,
134.900628663412));
#192571=CARTESIAN_POINT('Ctrl Pts',(60.6653538202889,0.645230515680748,
137.378378674564));
#192572=CARTESIAN_POINT('Ctrl Pts',(60.3869061964759,5.87967043157647,133.814927249971));
#192573=CARTESIAN_POINT('Ctrl Pts',(60.108458572663,5.71098045872276,127.484912164554));
#192574=CARTESIAN_POINT('Ctrl Pts',(59.8300109488502,0.294178441208572,
124.205308043382));
#192575=CARTESIAN_POINT('Ctrl Pts',(59.5515633250373,-5.39295919236059,
126.989910856244));
#192576=CARTESIAN_POINT('Ctrl Pts',(59.2731157012244,-6.12423078885343,
133.27980665353));
#192577=CARTESIAN_POINT('Ctrl Pts',(58.9946680774115,-1.2276334756968,137.294888476026));
#192578=CARTESIAN_POINT('Ctrl Pts',(58.7162204535986,4.79709902839574,135.345492276511));
#192579=CARTESIAN_POINT('Ctrl Pts',(58.4377728297857,6.41353187670863,129.223017929039));
#192580=CARTESIAN_POINT('Ctrl Pts',(58.1593252059728,2.13624224877676,124.553720259438));
#192581=CARTESIAN_POINT('Ctrl Pts',(57.8808775821599,-4.10414964454526,
125.628455718198));
#192582=CARTESIAN_POINT('Ctrl Pts',(57.602429958347,-6.57302851338661,131.459594922466));
#192583=CARTESIAN_POINT('Ctrl Pts',(57.3239823345341,-3.00161528872044,
136.688605810505));
#192584=CARTESIAN_POINT('Ctrl Pts',(57.0455347107212,3.32813574922106,136.510282827592));
#192585=CARTESIAN_POINT('Ctrl Pts',(56.7670870869083,6.59949262209846,131.088496083461));
#192586=CARTESIAN_POINT('Ctrl Pts',(56.4886394630955,3.80623817840574,125.405602726962));
#192587=CARTESIAN_POINT('Ctrl Pts',(56.2101918392826,-2.48476320616966,
124.683904127941));
#192588=CARTESIAN_POINT('Ctrl Pts',(55.9317442154696,-6.49238859170611,
129.586606041964));
#192589=CARTESIAN_POINT('Ctrl Pts',(55.6532965916568,-4.53382603227983,
135.608364920346));
#192590=CARTESIAN_POINT('Ctrl Pts',(55.3748489678439,1.59110116109648,137.215478533129));
#192591=CARTESIAN_POINT('Ctrl Pts',(55.096401344031,6.25388411703813,132.931087982032));
#192592=CARTESIAN_POINT('Ctrl Pts',(54.8179537202181,5.1696530886458,126.692338879397));
#192593=CARTESIAN_POINT('Ctrl Pts',(54.5395060964052,-0.665236576618623,
124.23233687071));
#192594=CARTESIAN_POINT('Ctrl Pts',(54.2610584725923,-5.88880632658389,
127.811703624173));
#192595=CARTESIAN_POINT('Ctrl Pts',(53.9826108487795,-5.70085074660091,
134.141175955143));
#192596=CARTESIAN_POINT('Ctrl Pts',(53.7041632249665,-0.274091832533765,
137.40427800337));
#192597=CARTESIAN_POINT('Ctrl Pts',(53.4257156011537,5.40454408550164,134.602378397932));
#192598=CARTESIAN_POINT('Ctrl Pts',(53.1472679773408,6.11666801561766,128.310285995821));
#192599=CARTESIAN_POINT('Ctrl Pts',(52.8688203535278,1.20787285522606,124.310126328773));
#192600=CARTESIAN_POINT('Ctrl Pts',(52.590372729715,-4.81089845124901,126.277850712144));
#192601=CARTESIAN_POINT('Ctrl Pts',(52.3119251059021,-6.40868910648141,
132.405216566294));
#192602=CARTESIAN_POINT('Ctrl Pts',(52.0334774820892,-2.11720755472543,
137.061474009724));
#192603=CARTESIAN_POINT('Ctrl Pts',(51.7550298582764,4.11988430848393,135.967749922743));
#192604=CARTESIAN_POINT('Ctrl Pts',(51.4765822344634,6.57100375973434,130.129123309894));
#192605=CARTESIAN_POINT('Ctrl Pts',(51.1981346106506,2.98369176716867,124.91100679562));
#192606=CARTESIAN_POINT('Ctrl Pts',(50.9196869868376,-3.34548719797895,
125.108594537373));
#192607=CARTESIAN_POINT('Ctrl Pts',(50.6412393630248,-6.60032686431936,
130.540313053181));
#192608=CARTESIAN_POINT('Ctrl Pts',(50.3627917392119,-3.78978858624336,
136.214678381218));
#192609=CARTESIAN_POINT('Ctrl Pts',(50.0843441153989,2.50338026112505,136.917225993175));
#192610=CARTESIAN_POINT('Ctrl Pts',(49.8058964915862,6.49606494544435,132.002348955022));
#192611=CARTESIAN_POINT('Ctrl Pts',(49.5274488677731,4.51918329531533,125.986579159731));
#192612=CARTESIAN_POINT('Ctrl Pts',(49.2490012439603,-1.6106070288309,124.39811516248));
#192613=CARTESIAN_POINT('Ctrl Pts',(48.9705536201474,-6.26032817600901,
128.696677775965));
#192614=CARTESIAN_POINT('Ctrl Pts',(48.6921059963345,-5.15711356346882,
134.932097954848));
#192615=CARTESIAN_POINT('Ctrl Pts',(48.4136583725217,0.685236474895564,
137.374329171949));
#192616=CARTESIAN_POINT('Ctrl Pts',(48.1352107487087,5.89788766849362,133.779080248378));
#192617=CARTESIAN_POINT('Ctrl Pts',(47.8567631248959,5.69066822257687,127.450209307224));
#192618=CARTESIAN_POINT('Ctrl Pts',(47.578315501083,0.254002684709825,124.203639560873));
#192619=CARTESIAN_POINT('Ctrl Pts',(47.29986787727,-5.41607891168467,127.022810002472));
#192620=CARTESIAN_POINT('Ctrl Pts',(47.0214202534572,-6.10904857840509,
133.317040720324));
#192621=CARTESIAN_POINT('Ctrl Pts',(46.7429726296443,-1.18810104518584,
137.302241174989));
#192622=CARTESIAN_POINT('Ctrl Pts',(46.4645250058313,4.82465330659632,135.316206836494));
#192623=CARTESIAN_POINT('Ctrl Pts',(46.1860773820186,6.40378696703385,129.184006238746));
#192624=CARTESIAN_POINT('Ctrl Pts',(45.9076297582056,2.09815324715241,124.54083215642));
#192625=CARTESIAN_POINT('Ctrl Pts',(45.6291821343927,-4.13558080637756,
125.653534739511));
#192626=CARTESIAN_POINT('Ctrl Pts',(45.3507345105798,-6.56891813320061,
131.499594672701));
#192627=CARTESIAN_POINT('Ctrl Pts',(45.072286886767,-2.96574060510383,136.706768473292));
#192628=CARTESIAN_POINT('Ctrl Pts',(44.793839262954,3.36280765460034,136.489917803126));
#192629=CARTESIAN_POINT('Ctrl Pts',(44.5153916391412,6.60109996201359,131.048317834339));
#192630=CARTESIAN_POINT('Ctrl Pts',(44.2369440153282,3.77330388599763,125.38253310131));
#192631=CARTESIAN_POINT('Ctrl Pts',(43.9584963915154,-2.52197412510756,
124.699142984721));
#192632=CARTESIAN_POINT('Ctrl Pts',(43.6800487677024,-6.49968112052436,
129.626149616253));
#192633=CARTESIAN_POINT('Ctrl Pts',(43.4016011438896,-4.50449869325427,
135.635874599185));
#192634=CARTESIAN_POINT('Ctrl Pts',(43.1231535200766,1.6300979761215,137.205674265588));
#192635=CARTESIAN_POINT('Ctrl Pts',(42.8447058962639,6.26671424015497,132.892979411015));
#192636=CARTESIAN_POINT('Ctrl Pts',(42.5662582724509,5.14452626349642,126.660945919963));
#192637=CARTESIAN_POINT('Ctrl Pts',(42.287810648638,-0.705230025235587,
124.236508118946));
#192638=CARTESIAN_POINT('Ctrl Pts',(42.0093630248251,-5.90691437317801,
127.847605906729));
#192639=CARTESIAN_POINT('Ctrl Pts',(41.7309154010123,-5.68043298097947,
134.175816828272));
#192640=CARTESIAN_POINT('Ctrl Pts',(41.4524677771993,-0.233911183839542,
137.405824196969));
#192641=CARTESIAN_POINT('Ctrl Pts',(41.1740201533865,5.42756356405245,134.569409035618));
#192642=CARTESIAN_POINT('Ctrl Pts',(40.8955725295735,6.10137254780096,128.273098310918));
#192643=CARTESIAN_POINT('Ctrl Pts',(40.6171249057607,1.1683182287399,124.302893986988));
#192644=CARTESIAN_POINT('Ctrl Pts',(40.3386772819477,-4.83836346701448,
126.307219882257));
#192645=CARTESIAN_POINT('Ctrl Pts',(40.060229658135,-6.39882550377857,132.444198415735));
#192646=CARTESIAN_POINT('Ctrl Pts',(39.781782034322,-2.07907950257448,137.074246123225));
#192647=CARTESIAN_POINT('Ctrl Pts',(39.5033344105091,4.15123899281517,135.94257535195));
#192648=CARTESIAN_POINT('Ctrl Pts',(39.2248867866962,6.56677165310695,130.089136255519));
#192649=CARTESIAN_POINT('Ctrl Pts',(38.9464391628834,2.94776196882331,124.892953407157));
#192650=CARTESIAN_POINT('Ctrl Pts',(38.6679915390704,-3.38009695863112,
125.129064996863));
#192651=CARTESIAN_POINT('Ctrl Pts',(38.3895439152575,-6.6018119080198,130.58049600839));
#192652=CARTESIAN_POINT('Ctrl Pts',(38.1110962914447,-3.75678423037978,
136.237647659355));
#192653=CARTESIAN_POINT('Ctrl Pts',(37.8326486676317,2.54054462586645,136.901873949744));
#192654=CARTESIAN_POINT('Ctrl Pts',(37.5542010438189,6.50323708344635,131.962783367948));
#192655=CARTESIAN_POINT('Ctrl Pts',(37.275753420006,4.48977236213255,125.959158870647));
#192656=CARTESIAN_POINT('Ctrl Pts',(36.9973057961931,-1.64957382240749,
124.4080380775));
#192657=CARTESIAN_POINT('Ctrl Pts',(36.7188581723802,-6.27304225031618,
128.734825220947));
#192658=CARTESIAN_POINT('Ctrl Pts',(36.4404105485673,-5.13189130533538,
134.96341429146));
#192659=CARTESIAN_POINT('Ctrl Pts',(36.1619629247544,0.725217042420823,
137.370036216732));
#192660=CARTESIAN_POINT('Ctrl Pts',(35.8835153009416,5.91588635701427,133.743123017455));
#192661=CARTESIAN_POINT('Ctrl Pts',(35.6050676771286,5.67014511662727,127.415630739204));
#192662=CARTESIAN_POINT('Ctrl Pts',(35.3266200533158,0.213817516048174,
124.202215670509));
#192663=CARTESIAN_POINT('Ctrl Pts',(35.0481724295028,-5.43899793621292,
127.055849275448));
#192664=CARTESIAN_POINT('Ctrl Pts',(34.76972480569,-6.09363999491508,133.354181678833));
#192665=CARTESIAN_POINT('Ctrl Pts',(34.4912771818771,-1.14852458915375,
137.309353092597));
#192666=CARTESIAN_POINT('Ctrl Pts',(34.2128295580642,4.85202880549439,135.286754208357));
#192667=CARTESIAN_POINT('Ctrl Pts',(33.9343819342512,6.393804762678,129.145054591279));
#192668=CARTESIAN_POINT('Ctrl Pts',(33.6559343104384,2.05998649768791,124.528176150753));
#192669=CARTESIAN_POINT('Ctrl Pts',(33.3774866866255,-4.16685872274224,
125.678804626571));
#192670=CARTESIAN_POINT('Ctrl Pts',(33.0990390628127,-6.56456433933747,
131.539568660782));
#192671=CARTESIAN_POINT('Ctrl Pts',(32.8205914389997,-2.92975602487846,
136.724712420187));
#192672=CARTESIAN_POINT('Ctrl Pts',(32.5421438151868,3.39735494990529,136.469342098247));
#192673=CARTESIAN_POINT('Ctrl Pts',(32.263696191374,6.60246269574222,131.008130545292));
#192674=CARTESIAN_POINT('Ctrl Pts',(31.985248567561,3.74022977242616,125.359664383471));
#192675=CARTESIAN_POINT('Ctrl Pts',(31.7068009437482,-2.55909159136699,
124.714608072585));
#192676=CARTESIAN_POINT('Ctrl Pts',(31.4283533199352,-6.50673280126843,
129.665736849585));
#192677=CARTESIAN_POINT('Ctrl Pts',(31.1499056961224,-4.47500443837311,
135.663205244496));
#192678=CARTESIAN_POINT('Ctrl Pts',(30.8714580723094,1.66903438726656,137.195632795014));
#192679=CARTESIAN_POINT('Ctrl Pts',(30.5930104484966,6.27931214787105,132.854793445461));
#192680=CARTESIAN_POINT('Ctrl Pts',(30.3145628246837,5.11920880603445,126.629706496284));
#192681=CARTESIAN_POINT('Ctrl Pts',(30.0361152008708,-0.745197341294603,
124.240922741373));
#192682=CARTESIAN_POINT('Ctrl Pts',(29.7576675770579,-5.9248035368878,127.883617752917));
#192683=CARTESIAN_POINT('Ctrl Pts',(29.4792199532451,-5.65980472482494,
134.210332770852));
#192684=CARTESIAN_POINT('Ctrl Pts',(29.2007723294321,-0.193721867480399,
137.407125770907));
#192685=CARTESIAN_POINT('Ctrl Pts',(28.9223247056193,5.45038192223944,134.536300158051));
#192686=CARTESIAN_POINT('Ctrl Pts',(28.6438770818064,6.08585099138068,128.236004422871));
#192687=CARTESIAN_POINT('Ctrl Pts',(28.3654294579935,1.12872030979243,124.29590255944));
#192688=CARTESIAN_POINT('Ctrl Pts',(28.0869818341806,-4.86564919544231,
126.336755695574));
#192689=CARTESIAN_POINT('Ctrl Pts',(27.8085342103677,-6.38872479024353,
132.483119500384));
#192690=CARTESIAN_POINT('Ctrl Pts',(27.5300865865548,-2.04087440936798,
137.086785903815));
#192691=CARTESIAN_POINT('Ctrl Pts',(27.2516389627419,4.18243985145892,135.91721038272));
#192692=CARTESIAN_POINT('Ctrl Pts',(26.973191338929,6.56229621234102,130.049175704046));
#192693=CARTESIAN_POINT('Ctrl Pts',(26.6947437151162,2.91172294007416,124.875119068062));
#192694=CARTESIAN_POINT('Ctrl Pts',(26.4162960913032,-3.41458146854746,
125.149745756519));
#192695=CARTESIAN_POINT('Ctrl Pts',(26.1378484674903,-6.60305231915217,
130.620687258984));
#192696=CARTESIAN_POINT('Ctrl Pts',(25.8594008436774,-3.72364066549499,
136.260415605043));
#192697=CARTESIAN_POINT('Ctrl Pts',(25.5809532198646,2.57761484979243,136.886295960714));
#192698=CARTESIAN_POINT('Ctrl Pts',(25.3025055960517,6.51016824160669,131.92317485509));
#192699=CARTESIAN_POINT('Ctrl Pts',(25.0240579722387,4.46019505878377,125.931918122295));
#192700=CARTESIAN_POINT('Ctrl Pts',(24.7456103484259,-1.68847949041943,
124.418198010604));
#192701=CARTESIAN_POINT('Ctrl Pts',(24.467162724613,-6.28552387473587,128.773049353324));
#192702=CARTESIAN_POINT('Ctrl Pts',(24.1887151008001,-5.10647888308236,
134.994576512808));
#192703=CARTESIAN_POINT('Ctrl Pts',(23.9102674769872,0.765170736761864,
137.365499967992));
#192704=CARTESIAN_POINT('Ctrl Pts',(23.6318198531744,5.93366583019039,133.707056889611));
#192705=CARTESIAN_POINT('Ctrl Pts',(23.3533722293614,5.64941190136517,127.381177741815));
#192706=CARTESIAN_POINT('Ctrl Pts',(23.0749246055485,0.173624424299845,
124.201036425055));
#192707=CARTESIAN_POINT('Ctrl Pts',(22.7964769817356,-5.46171541667246,
127.08902745089));
#192708=CARTESIAN_POINT('Ctrl Pts',(22.5180293579228,-6.07800560935413,
133.391228152785));
#192709=CARTESIAN_POINT('Ctrl Pts',(22.2395817341099,-1.10890557412062,
137.316223965318));
#192710=CARTESIAN_POINT('Ctrl Pts',(21.9611341102969,4.87922451068073,135.257135483476));
#192711=CARTESIAN_POINT('Ctrl Pts',(21.6826864864842,6.38358563353538,129.106164430008));
#192712=CARTESIAN_POINT('Ctrl Pts',(21.4042388626712,2.02174341466617,124.515752711409));
#192713=CARTESIAN_POINT('Ctrl Pts',(21.1257912388583,-4.19798223462457,
125.704264442993));
#192714=CARTESIAN_POINT('Ctrl Pts',(20.8473436150454,-6.55996729312864,
131.579515405459));
#192715=CARTESIAN_POINT('Ctrl Pts',(20.5688959912325,-2.89366288146616,
136.742436986267));
#192716=CARTESIAN_POINT('Ctrl Pts',(20.2904483674196,3.43177635497322,136.448556475397));
#192717=CARTESIAN_POINT('Ctrl Pts',(20.0120007436067,6.60358077278748,130.967935705476));
#192718=CARTESIAN_POINT('Ctrl Pts',(19.7335531197938,3.70701706326526,125.336997420853));
#192719=CARTESIAN_POINT('Ctrl Pts',(19.455105495981,-2.59611422954622,124.730298818468));
#192720=CARTESIAN_POINT('Ctrl Pts',(19.176657872168,-6.51354337263571,129.705366275038));
#192721=CARTESIAN_POINT('Ctrl Pts',(18.8982102483552,-4.4453443605568,135.690355843533));
#192722=CARTESIAN_POINT('Ctrl Pts',(18.6197626245423,1.70790895172861,137.1853544935));
#192723=CARTESIAN_POINT('Ctrl Pts',(18.3413150007294,6.29167737336628,132.816531500364));
#192724=CARTESIAN_POINT('Ctrl Pts',(18.0628673769165,5.09370165440758,126.598621765949));
#192725=CARTESIAN_POINT('Ctrl Pts',(17.7844197531036,-0.785137043792105,
124.245580574404));
#192726=CARTESIAN_POINT('Ctrl Pts',(17.5059721292907,-5.94247315482366,
127.919737828307));
#192727=CARTESIAN_POINT('Ctrl Pts',(17.2275245054778,-5.63896674252494,
134.244722503881));
#192728=CARTESIAN_POINT('Ctrl Pts',(16.949076881665,-0.15352537268619,137.408182676953));
#192729=CARTESIAN_POINT('Ctrl Pts',(16.6706292578521,5.47299831451989,134.503052992091));
#192730=CARTESIAN_POINT('Ctrl Pts',(16.3921816340391,6.07010392151387,128.199005706208));
#192731=CARTESIAN_POINT('Ctrl Pts',(16.1137340102263,1.08908056569879,124.289152305198));
#192732=CARTESIAN_POINT('Ctrl Pts',(15.8352863864134,-4.89275462544986,
126.366457057635));
#192733=CARTESIAN_POINT('Ctrl Pts',(15.5568387626005,-6.37838734016194,
132.521978378005));
#192734=CARTESIAN_POINT('Ctrl Pts',(15.2783911387876,-2.00259369080969,
137.099092886824));
#192735=CARTESIAN_POINT('Ctrl Pts',(14.9999435149747,4.21348572825588,135.891655954962));
#192736=CARTESIAN_POINT('Ctrl Pts',(14.7214958911618,6.55757760327567,130.009243136227));
#192737=CARTESIAN_POINT('Ctrl Pts',(14.4430482673489,2.87557601636067,124.857504439193));
#192738=CARTESIAN_POINT('Ctrl Pts',(14.164600643536,-3.44893944989177,125.170636050008));
#192739=CARTESIAN_POINT('Ctrl Pts',(13.8861530197231,-6.60404805175259,
130.660885315664));
#192740=CARTESIAN_POINT('Ctrl Pts',(13.6077053959103,-3.69035911973598,
136.282981374608));
#192741=CARTESIAN_POINT('Ctrl Pts',(13.3292577720973,2.61458955925225,136.870492603333));
#192742=CARTESIAN_POINT('Ctrl Pts',(13.0508101482845,6.5168581630887,131.883524884162));
#192743=CARTESIAN_POINT('Ctrl Pts',(12.7723625244716,4.43045248126686,125.904857924092));
#192744=CARTESIAN_POINT('Ctrl Pts',(12.4939149006587,-1.72732259120293,
124.428594585312));
#192745=CARTESIAN_POINT('Ctrl Pts',(12.2154672768458,-6.29777258675688,
128.811348756686));
#192746=CARTESIAN_POINT('Ctrl Pts',(11.9370196530329,-5.08087723837641,
135.025583464166));
#192747=CARTESIAN_POINT('Ctrl Pts',(11.65857202922,0.805096077419857,137.36072059382));
#192748=CARTESIAN_POINT('Ctrl Pts',(11.3801244054071,5.95122542919731,133.670883201288));
#192749=CARTESIAN_POINT('Ctrl Pts',(11.1016767815943,5.62846934506734,127.346851591727));
#192750=CARTESIAN_POINT('Ctrl Pts',(10.8232291577813,0.13342489883439,124.200101868207));
#192751=CARTESIAN_POINT('Ctrl Pts',(10.5447815339684,-5.4842305112587,127.12234329937));
#192752=CARTESIAN_POINT('Ctrl Pts',(10.2663339101556,-6.06214600106014,
133.428178769409));
#192753=CARTESIAN_POINT('Ctrl Pts',(9.98788628634267,-1.06924546818365,
137.322853538546));
#192754=CARTESIAN_POINT('Ctrl Pts',(9.70943866252976,4.90623941440849,135.227351759386));
#192755=CARTESIAN_POINT('Ctrl Pts',(9.43099103871685,6.37312995827954,129.067337196021));
#192756=CARTESIAN_POINT('Ctrl Pts',(9.15254341490403,1.98342541519871,124.503562298745));
#192757=CARTESIAN_POINT('Ctrl Pts',(8.87409579109107,-4.22895018873139,
125.729913245354));
#192758=CARTESIAN_POINT('Ctrl Pts',(8.59564816727821,-6.55512716491932,
131.61943342649));
#192759=CARTESIAN_POINT('Ctrl Pts',(8.31720054346528,-2.85746251231165,
136.759941514744));
#192760=CARTESIAN_POINT('Ctrl Pts',(8.03875291965246,3.46607059430627,136.427561704794));
#192761=CARTESIAN_POINT('Ctrl Pts',(7.76030529583951,6.60445415171875,130.927734804324));
#192762=CARTESIAN_POINT('Ctrl Pts',(7.48185767202662,3.67366698922382,125.314533053388));
#192763=CARTESIAN_POINT('Ctrl Pts',(7.20341004821377,-2.63304066775796,
124.746214640945));
#192764=CARTESIAN_POINT('Ctrl Pts',(6.92496242440086,-6.52011258225796,
129.745036424131));
#192765=CARTESIAN_POINT('Ctrl Pts',(6.64651480058794,-4.41551955887045,
135.71732539022));
#192766=CARTESIAN_POINT('Ctrl Pts',(6.36806717677509,1.74672022899638,137.174839741911));
#192767=CARTESIAN_POINT('Ctrl Pts',(6.08961955296221,6.30380945844269,132.778194993536));
#192768=CARTESIAN_POINT('Ctrl Pts',(5.81117192914928,5.06800575379271,126.567692880813));
#192769=CARTESIAN_POINT('Ctrl Pts',(5.53272430533639,-0.825047652747706,
124.250481445441));
#192770=CARTESIAN_POINT('Ctrl Pts',(5.25427668152353,-5.95992257223146,
127.955964794454));
#192771=CARTESIAN_POINT('Ctrl Pts',(4.97582905771062,-5.61791980623858,
134.278984753035));
#192772=CARTESIAN_POINT('Ctrl Pts',(4.69738143389771,-0.113323188952861,
137.408994875945));
#192773=CARTESIAN_POINT('Ctrl Pts',(4.41893381008486,5.49541190283514,134.469668769726));
#192774=CARTESIAN_POINT('Ctrl Pts',(4.14048618627195,6.05413192171396,128.162103531929));
#192775=CARTESIAN_POINT('Ctrl Pts',(3.86203856245905,1.0494004653243,124.282643474398));
#192776=CARTESIAN_POINT('Ctrl Pts',(3.58359093864613,-4.91967875263547,
126.396322867843));
#192777=CARTESIAN_POINT('Ctrl Pts',(3.30514331483329,-6.36781353659179,
132.560773608667));
#192778=CARTESIAN_POINT('Ctrl Pts',(3.02669569102039,-1.96423876540577,
137.111166616214));
#192779=CARTESIAN_POINT('Ctrl Pts',(2.74824806720748,4.24437547278969,135.865913015604));
#192780=CARTESIAN_POINT('Ctrl Pts',(2.46980044339459,6.55261600076067,129.969340031779));
#192781=CARTESIAN_POINT('Ctrl Pts',(2.19135281958173,2.83932253712042,124.840110173268));
#192782=CARTESIAN_POINT('Ctrl Pts',(1.91290519576881,-3.48316962951642,
125.191735103234));
#192783=CARTESIAN_POINT('Ctrl Pts',(1.6344575719559,-6.60479906892382,130.701088688872));
#192784=CARTESIAN_POINT('Ctrl Pts',(1.35600994814304,-3.65694082636265,
136.305344131865));
#192785=CARTESIAN_POINT('Ctrl Pts',(1.07756232433016,2.65146738413444,136.854464463202));
#192786=CARTESIAN_POINT('Ctrl Pts',(0.799114700517227,6.52330659999492,
131.843834924404));
#192787=CARTESIAN_POINT('Ctrl Pts',(0.520667076704378,4.40054573170394,
125.877979278764));
#192788=CARTESIAN_POINT('Ctrl Pts',(0.242219452891471,-1.76610168541259,
124.439227416375));
#192789=CARTESIAN_POINT('Ctrl Pts',(-0.03622817092143,-6.30978793249869,
128.849722011837));
#192790=CARTESIAN_POINT('Ctrl Pts',(-0.314675794734322,-5.05508731989592,
135.056433996558));
#192791=CARTESIAN_POINT('Ctrl Pts',(-0.593123418547181,0.844991584946641,
137.355698271319));
#192792=CARTESIAN_POINT('Ctrl Pts',(-0.871571042360099,5.96856450335716,
133.634603292916));
#192793=CARTESIAN_POINT('Ctrl Pts',(-1.15001866617301,5.60731822376822,
127.312653560908));
#192794=CARTESIAN_POINT('Ctrl Pts',(-1.42846628998586,0.0932204292604712,
124.199412034595));
#192795=CARTESIAN_POINT('Ctrl Pts',(-1.70691391379876,-5.50654238566651,
127.155795586355));
#192796=CARTESIAN_POINT('Ctrl Pts',(-1.98536153761166,-6.04606175771675,
133.465032159487));
#192797=CARTESIAN_POINT('Ctrl Pts',(-2.26380916142456,-1.02954574096264,
137.329241566624));
#192798=CARTESIAN_POINT('Ctrl Pts',(-2.5422567852374,4.9330725156305,135.197404139731));
#192799=CARTESIAN_POINT('Ctrl Pts',(-2.82070440905033,6.36243812434939,
129.028574328076));
#192800=CARTESIAN_POINT('Ctrl Pts',(-3.09915203286324,1.94503391917308,
124.491605364478));
#192801=CARTESIAN_POINT('Ctrl Pts',(-3.3775996566761,-4.25976143753379,
125.755750083229));
#192802=CARTESIAN_POINT('Ctrl Pts',(-3.65604728048899,-6.55004413406227,
131.659321244699));
#192803=CARTESIAN_POINT('Ctrl Pts',(-3.9344949043019,-2.82115625883292,
136.777225356981));
#192804=CARTESIAN_POINT('Ctrl Pts',(-4.2129425281148,3.50023639711881,136.406358564405));
#192805=CARTESIAN_POINT('Ctrl Pts',(-4.49139015192765,6.60508280017262,
130.887529331496));
#192806=CARTESIAN_POINT('Ctrl Pts',(-4.76983777574057,3.64018078610111,
125.292272113504));
#192807=CARTESIAN_POINT('Ctrl Pts',(-5.04828539955349,-2.66986953767946,
124.762354950249));
#192808=CARTESIAN_POINT('Ctrl Pts',(-5.32673302336633,-6.52644018671072,
129.784745826872));
#192809=CARTESIAN_POINT('Ctrl Pts',(-5.60518064717923,-4.38553113848304,
135.74411288519));
#192810=CARTESIAN_POINT('Ctrl Pts',(-5.88362827099213,1.7854667809037,137.164088929876));
#192811=CARTESIAN_POINT('Ctrl Pts',(-6.16207589480503,6.31570795354138,
132.739785345549));
#192812=CARTESIAN_POINT('Ctrl Pts',(-6.44052351861788,5.04212205636089,
126.536920986959));
#192813=CARTESIAN_POINT('Ctrl Pts',(-6.71897114243081,-0.864927689259141,
124.255625172881));
#192814=CARTESIAN_POINT('Ctrl Pts',(-6.99741876624371,-5.97715114251656,
127.992297308957));
#192815=CARTESIAN_POINT('Ctrl Pts',(-7.27586639005655,-5.59666469586782,
134.313118248714));
#192816=CARTESIAN_POINT('Ctrl Pts',(-7.55431401386947,-0.0731168059870705,
137.409562337785));
#192817=CARTESIAN_POINT('Ctrl Pts',(-7.83276163768236,5.51762185664139,
134.436148728019));
#192818=CARTESIAN_POINT('Ctrl Pts',(-8.11120926149529,6.03793558382929,
128.125299267457));
#192819=CARTESIAN_POINT('Ctrl Pts',(-8.38965688530811,1.00968147902963,
124.276376308223));
#192820=CARTESIAN_POINT('Ctrl Pts',(-8.66810450912106,-4.94642057931569,
126.426352019512));
#192821=CARTESIAN_POINT('Ctrl Pts',(-8.94655213293394,-6.3570037713493,
132.599503754801));
#192822=CARTESIAN_POINT('Ctrl Pts',(-9.22499975674682,-1.92581105441205,
137.123006644589));
#192823=CARTESIAN_POINT('Ctrl Pts',(-9.50344738055969,4.27510794042973,
135.839982518561));
#192824=CARTESIAN_POINT('Ctrl Pts',(-9.78189500437264,6.54741158865002,
129.929467869325));
#192825=CARTESIAN_POINT('Ctrl Pts',(-10.0603426281855,2.80296384573913,
124.822936914835));
#192826=CARTESIAN_POINT('Ctrl Pts',(-10.3387902519984,-3.51727073900952,
125.213042134361));
#192827=CARTESIAN_POINT('Ctrl Pts',(-10.6172378758113,-6.60530534283666,
130.74129588886));
#192828=CARTESIAN_POINT('Ctrl Pts',(-10.8956854996242,-3.62338702370218,
136.327503048155));
#192829=CARTESIAN_POINT('Ctrl Pts',(-11.174133123437,2.68824695791763,136.838212134247));
#192830=CARTESIAN_POINT('Ctrl Pts',(-11.4525807472499,6.52951331337615,
131.804106446543));
#192831=CARTESIAN_POINT('Ctrl Pts',(-11.7310283710628,4.37047591830066,
125.851283182307));
#192832=CARTESIAN_POINT('Ctrl Pts',(-12.0094759948757,-1.80481533607482,
124.450096109789));
#192833=CARTESIAN_POINT('Ctrl Pts',(-12.2879236186886,-6.32156946672825,
128.88816769684));
#192834=CARTESIAN_POINT('Ctrl Pts',(-12.5663712425015,-5.02911008329581,
135.087126966809));
#192835=CARTESIAN_POINT('Ctrl Pts',(-12.8448188663144,0.884855780999501,
137.350433186591));
#192836=CARTESIAN_POINT('Ctrl Pts',(-13.1232664901273,5.98568241016441,
133.598218508862));
#192837=CARTESIAN_POINT('Ctrl Pts',(-13.4017141139402,5.58595932123025,
127.278584916578));
#192838=CARTESIAN_POINT('Ctrl Pts',(-13.6801617377531,0.0530125053692662,
124.198966949783));
#192839=CARTESIAN_POINT('Ctrl Pts',(-13.958609361566,-5.5286502131212,127.189383072259));
#192840=CARTESIAN_POINT('Ctrl Pts',(-14.2370569853788,-6.02975347533148,
133.501786957402));
#192841=CARTESIAN_POINT('Ctrl Pts',(-14.5155046091917,-0.989807863545592,
137.335387812837));
#192842=CARTESIAN_POINT('Ctrl Pts',(-14.7939522330047,4.95972282003631,
135.167293734234));
#192843=CARTESIAN_POINT('Ctrl Pts',(-15.0723998568175,6.35151052793477,
128.989877262545));
#192844=CARTESIAN_POINT('Ctrl Pts',(-15.3508474806304,1.9065703492003,124.479882351679));
#192845=CARTESIAN_POINT('Ctrl Pts',(-15.6292951044433,-4.29041483930959,
125.781773999224));
#192846=CARTESIAN_POINT('Ctrl Pts',(-15.9077427282562,-6.54471838891106,
131.699177382027));
#192847=CARTESIAN_POINT('Ctrl Pts',(-16.186190352069,-2.78474546637155,
136.794287872519));
#192848=CARTESIAN_POINT('Ctrl Pts',(-16.464637975882,3.53427249738445,136.384947839923));
#192849=CARTESIAN_POINT('Ctrl Pts',(-16.7430855996949,6.60546669485434,
130.847320776822));
#192850=CARTESIAN_POINT('Ctrl Pts',(-17.0215332235078,3.6065596947407,125.270215426085));
#192851=CARTESIAN_POINT('Ctrl Pts',(-17.2999808473206,-2.7065994746034,
124.778719148295));
#192852=CARTESIAN_POINT('Ctrl Pts',(-17.5784284711336,-6.53252595152224,
129.824493011814));
#192853=CARTESIAN_POINT('Ctrl Pts',(-17.8568760949464,-4.35538021062653,
135.770717335825));
#192854=CARTESIAN_POINT('Ctrl Pts',(-18.1353237187593,1.82414717168286,
137.153102455769));
#192855=CARTESIAN_POINT('Ctrl Pts',(-18.4137713425722,6.32737241775927,
132.701303979686));
#192856=CARTESIAN_POINT('Ctrl Pts',(-18.6922189663851,5.01605152124203,
126.506307224649));
#192857=CARTESIAN_POINT('Ctrl Pts',(-18.9706665901979,-0.904775675556959,
124.261011566121));
#192858=CARTESIAN_POINT('Ctrl Pts',(-19.2491142140109,-5.99415822726801,
128.028734025499));
#192859=CARTESIAN_POINT('Ctrl Pts',(-19.5275618378238,-5.57520219902858,
134.347121726088));
#192860=CARTESIAN_POINT('Ctrl Pts',(-19.8060094616367,-0.0329077136511566,
137.409885041447));
#192861=CARTESIAN_POINT('Ctrl Pts',(-20.0844570854496,5.53962735294063,
134.402494109067));
#192862=CARTESIAN_POINT('Ctrl Pts',(-20.3629047092624,6.02151550802112,
128.08859427659));
#192863=CARTESIAN_POINT('Ctrl Pts',(-20.6413523330754,0.969925078616457,
124.270351038909));
#192864=CARTESIAN_POINT('Ctrl Pts',(-20.9197999568882,-4.9729791145623,
126.456543399899));
#192865=CARTESIAN_POINT('Ctrl Pts',(-21.1982475807011,-6.34595844499429,
132.638167381246));
#192866=CARTESIAN_POINT('Ctrl Pts',(-21.476695204514,-1.88731198178147,
137.134612533211));
#192867=CARTESIAN_POINT('Ctrl Pts',(-21.7551428283269,4.30568199237261,
135.813865424697));
#192868=CARTESIAN_POINT('Ctrl Pts',(-22.0335904521398,6.54196455979519,
129.889628126344));
#192869=CARTESIAN_POINT('Ctrl Pts',(-22.3120380759527,2.766501289502,124.805985300257));
#192870=CARTESIAN_POINT('Ctrl Pts',(-22.5904856997656,-3.5512415147419,
125.234556353852));
#192871=CARTESIAN_POINT('Ctrl Pts',(-22.8689333235784,-6.60556685473091,
130.781505425734));
#192872=CARTESIAN_POINT('Ctrl Pts',(-23.1473809473914,-3.58969895510304,
136.349457302372));
#192873=CARTESIAN_POINT('Ctrl Pts',(-23.4258285712042,2.7249269177212,136.821736218705));
#192874=CARTESIAN_POINT('Ctrl Pts',(-23.7042761950172,6.53547807324032,
131.764340922733));
#192875=CARTESIAN_POINT('Ctrl Pts',(-23.98272381883,4.34024415530499,125.824770623956));
#192876=CARTESIAN_POINT('Ctrl Pts',(-24.2611714426429,-1.84346210864104,
124.461200262812));
#192877=CARTESIAN_POINT('Ctrl Pts',(-24.5396190664558,-6.33311675287646,
128.926684387076));
#192878=CARTESIAN_POINT('Ctrl Pts',(-24.8180666902687,-5.00294649117208,
135.117661237576));
#192879=CARTESIAN_POINT('Ctrl Pts',(-25.0965143140816,0.924687188395989,
137.344925534737));
#192880=CARTESIAN_POINT('Ctrl Pts',(-25.3749619378945,6.00257851530871,
133.561730197376));
#192881=CARTESIAN_POINT('Ctrl Pts',(-25.6534095617074,5.56439342891538,
127.244646921163));
#192882=CARTESIAN_POINT('Ctrl Pts',(-25.9318571855203,0.0128026170801758,
124.198766630261));
#192883=CARTESIAN_POINT('Ctrl Pts',(-26.2103048093331,-5.5505531744091,
127.223104512485));
#192884=CARTESIAN_POINT('Ctrl Pts',(-26.4887524331461,-6.01322175821376,
133.538441801192));
#192885=CARTESIAN_POINT('Ctrl Pts',(-26.7672000569589,-0.950033308434149,
137.341292049436));
#192886=CARTESIAN_POINT('Ctrl Pts',(-27.0456476807718,4.98618934008908,
135.137021658645));
#192887=CARTESIAN_POINT('Ctrl Pts',(-27.3240953045847,6.34034757396176,
128.951247433362));
#192888=CARTESIAN_POINT('Ctrl Pts',(-27.6025429283976,1.86803613056208,
124.468393694749));
#192889=CARTESIAN_POINT('Ctrl Pts',(-27.8809905522105,-4.32090925818572,
125.807984029013));
#192890=CARTESIAN_POINT('Ctrl Pts',(-28.1594381760234,-6.53915012681315,
131.739000361591));
#192891=CARTESIAN_POINT('Ctrl Pts',(-28.4378857998363,-2.74823148414282,
136.811128429099));
#192892=CARTESIAN_POINT('Ctrl Pts',(-28.7163334236492,3.56817763388296,
136.36333032473));
#192893=CARTESIAN_POINT('Ctrl Pts',(-28.994781047462,6.60560582153853,130.807110630244));
#192894=CARTESIAN_POINT('Ctrl Pts',(-29.273228671275,3.5728049609845,125.248363808452));
#192895=CARTESIAN_POINT('Ctrl Pts',(-29.5516762950878,-2.74322911748845,
124.795306628702));
#192896=CARTESIAN_POINT('Ctrl Pts',(-29.8301239189007,-6.53836965118233,
129.86427650611));
#192897=CARTESIAN_POINT('Ctrl Pts',(-30.1085715427137,-4.32506789255462,
135.797137756284));
#192898=CARTESIAN_POINT('Ctrl Pts',(-30.3870191665265,1.862759968018,137.141880726698));
#192899=CARTESIAN_POINT('Ctrl Pts',(-30.6654667903394,6.33880241886542,
132.662752321889));
#192900=CARTESIAN_POINT('Ctrl Pts',(-30.9439144141524,4.98979511448915,
126.475852728289));
#192901=CARTESIAN_POINT('Ctrl Pts',(-31.2223620379652,-0.944590135059391,
124.266640425567));
#192902=CARTESIAN_POINT('Ctrl Pts',(-31.5008096617781,-6.01094319628198,
128.065273593905));
#192903=CARTESIAN_POINT('Ctrl Pts',(-31.7792572855909,-5.55353311102158,
134.380993925146));
#192904=CARTESIAN_POINT('Ctrl Pts',(-32.0577049094039,0.00730259809219468,
137.409962974972));
#192905=CARTESIAN_POINT('Ctrl Pts',(-32.3361525332168,5.56142757631112,
134.368706159956));
#192906=CARTESIAN_POINT('Ctrl Pts',(-32.6146001570296,6.0048723027414,128.051989919443));
#192907=CARTESIAN_POINT('Ctrl Pts',(-32.8930477808425,0.930132737272799,
124.264567889721));
#192908=CARTESIAN_POINT('Ctrl Pts',(-33.1714954046555,-4.99935337423901,
126.486895890252));
#192909=CARTESIAN_POINT('Ctrl Pts',(-33.4499430284683,-6.33467796681538,
132.676763055306));
#192910=CARTESIAN_POINT('Ctrl Pts',(-33.7283906522812,-1.84874297411136,
137.145983852021));
#192911=CARTESIAN_POINT('Ctrl Pts',(-34.0068382760941,4.33609649568588,
135.787562701789));
#192912=CARTESIAN_POINT('Ctrl Pts',(-34.285285899907,6.53627511603778,129.849822279112));
#192913=CARTESIAN_POINT('Ctrl Pts',(-34.5637335237199,2.72993621954223,
124.789255957683));
#192914=CARTESIAN_POINT('Ctrl Pts',(-34.8421811475328,-3.58508069791401,
125.256276964487));
#192915=CARTESIAN_POINT('Ctrl Pts',(-35.1206287713457,-6.60558359491616,
130.821715809516));
#192916=CARTESIAN_POINT('Ctrl Pts',(-35.3990763951586,-3.55587786888901,
136.37120608099));
#192917=CARTESIAN_POINT('Ctrl Pts',(-35.6775240189714,2.76150590435573,
136.805037327097));
#192918=CARTESIAN_POINT('Ctrl Pts',(-35.9559716427844,6.54120065856107,
131.724539826499));
#192919=CARTESIAN_POINT('Ctrl Pts',(-36.2344192665972,4.30985156296601,
125.798442586144));
#192920=CARTESIAN_POINT('Ctrl Pts',(-36.5128668904101,-1.8820405710409,
124.472539463974));
#192921=CARTESIAN_POINT('Ctrl Pts',(-36.791314514223,-6.3444293630544,128.965270655295));
#192922=CARTESIAN_POINT('Ctrl Pts',(-37.0697621380359,-4.9765975130263,
135.148035677403));
#192923=CARTESIAN_POINT('Ctrl Pts',(-37.3482097618488,0.964484331168655,
137.339175519844));
#192924=CARTESIAN_POINT('Ctrl Pts',(-37.6266573856617,6.0192521926987,133.525139710547));
#192925=CARTESIAN_POINT('Ctrl Pts',(-37.9051050094746,5.54262134595571,
127.210840832248));
#192926=CARTESIAN_POINT('Ctrl Pts',(-38.1835526332875,-0.0274077456145885,
124.198811083455));
#192927=CARTESIAN_POINT('Ctrl Pts',(-38.4620002571004,-5.5722504579079,
127.256958657474));
#192928=CARTESIAN_POINT('Ctrl Pts',(-38.7404478809132,-5.99646721895241,
133.574995332598));
#192929=CARTESIAN_POINT('Ctrl Pts',(-39.0188955047262,-0.910223549489097,
137.346954057637));
#192930=CARTESIAN_POINT('Ctrl Pts',(-39.297343128539,5.0124710950622,135.106589034709));
#192931=CARTESIAN_POINT('Ctrl Pts',(-39.5757907523519,6.32894967607775,
128.912686271968));
#192932=CARTESIAN_POINT('Ctrl Pts',(-39.8542383761648,1.82943269115809,
124.457139819403));
#192933=CARTESIAN_POINT('Ctrl Pts',(-40.1326859999777,-4.35124356418029,
125.834379201373));
#192934=CARTESIAN_POINT('Ctrl Pts',(-40.4111336237906,-6.53333955410249,
131.778788707735));
#192935=CARTESIAN_POINT('Ctrl Pts',(-40.6895812476035,-2.7116156651858,
136.827746402689));
#192936=CARTESIAN_POINT('Ctrl Pts',(-40.9680288714165,3.60195055024708,
136.34150681987));
#192937=CARTESIAN_POINT('Ctrl Pts',(-41.2464764952292,6.60550017506977,
130.766900381762));
#192938=CARTESIAN_POINT('Ctrl Pts',(-41.5249241190422,3.53891783562657,
125.226718070324));
#192939=CARTESIAN_POINT('Ctrl Pts',(-41.803371742855,-2.77975710900975,
124.812116776814));
#192940=CARTESIAN_POINT('Ctrl Pts',(-42.081819366668,-6.5439710691505,129.904094835568));
#192941=CARTESIAN_POINT('Ctrl Pts',(-42.3602669904808,-4.2945953075014,
135.82337316755));
#192942=CARTESIAN_POINT('Ctrl Pts',(-42.6387146142937,1.90130373909722,
137.130424158489));
#192943=CARTESIAN_POINT('Ctrl Pts',(-42.9171622381066,6.34999753331677,
132.624131800705));
#192944=CARTESIAN_POINT('Ctrl Pts',(-43.1956098619195,4.96335380904355,
126.44555862638));
#192945=CARTESIAN_POINT('Ctrl Pts',(-43.4740574857324,-0.984369592426984,
124.272511542639));
#192946=CARTESIAN_POINT('Ctrl Pts',(-43.7525051095453,-6.02750542758532,
128.101914660188));
#192947=CARTESIAN_POINT('Ctrl Pts',(-44.0309527333582,-5.53165823480283,
134.414733590743));
#192948=CARTESIAN_POINT('Ctrl Pts',(-44.3094003571711,0.0475126392350714,
137.409796135472));
#192949=CARTESIAN_POINT('Ctrl Pts',(-44.5878479809839,5.58302171893757,
134.334786132711));
#192950=CARTESIAN_POINT('Ctrl Pts',(-44.8662956047969,5.98800658471021,
128.015487552405));
#192951=CARTESIAN_POINT('Ctrl Pts',(-45.1447432286098,0.890305929518511,
124.259027074959));
#192952=CARTESIAN_POINT('Ctrl Pts',(-45.4231908524226,-5.02554238103793,
126.517408365848));
#192953=CARTESIAN_POINT('Ctrl Pts',(-45.7016384762356,-6.32316275481482,
132.715289346806));
#192954=CARTESIAN_POINT('Ctrl Pts',(-45.9800861000484,-1.81010546059046,
137.15712017965));
#192955=CARTESIAN_POINT('Ctrl Pts',(-46.2585337238614,4.36635032334889,
135.761075324496));
#192956=CARTESIAN_POINT('Ctrl Pts',(-46.5369813476741,6.53034346820225,
129.810051802649));
#192957=CARTESIAN_POINT('Ctrl Pts',(-46.8154289714873,2.6932699907919,124.772749507024));
#192958=CARTESIAN_POINT('Ctrl Pts',(-47.0938765952999,-3.61878703460243,
125.278203161403));
#192959=CARTESIAN_POINT('Ctrl Pts',(-47.3723242191129,-6.60535556277213,
130.861925550195));
#192960=CARTESIAN_POINT('Ctrl Pts',(-47.6507718429257,-3.52192501831287,
136.392748578105));
#192961=CARTESIAN_POINT('Ctrl Pts',(-47.9292194667387,2.79798256237344,
136.788116078208));
#192962=CARTESIAN_POINT('Ctrl Pts',(-48.2076670905515,6.54668085728591,
131.684704632686));
#192963=CARTESIAN_POINT('Ctrl Pts',(-48.4861147143645,4.27929926749242,
125.772300044465));
#192964=CARTESIAN_POINT('Ctrl Pts',(-48.7645623381774,-1.92054929373528,
124.484113293097));
#192965=CARTESIAN_POINT('Ctrl Pts',(-49.0430099619902,-6.35550687806913,
129.003925071669));
#192966=CARTESIAN_POINT('Ctrl Pts',(-49.3214575858032,-4.95006412522954,
135.178249160753));
#192967=CARTESIAN_POINT('Ctrl Pts',(-49.5999052096159,1.00424573461974,
137.333183354982));
#192968=CARTESIAN_POINT('Ctrl Pts',(-49.878352833429,6.03570282448511,133.488448404247));
#192969=CARTESIAN_POINT('Ctrl Pts',(-50.1568004572417,5.52064387912377,
127.17716790253));
#192970=CARTESIAN_POINT('Ctrl Pts',(-50.4352480810547,-0.0676170927052693,
124.199100307716));
#192971=CARTESIAN_POINT('Ctrl Pts',(-50.7136957048675,-5.5937412596168,
127.290944252747));
#192972=CARTESIAN_POINT('Ctrl Pts',(-50.9921433286805,-5.97949047839309,
133.611446197116));
#192973=CARTESIAN_POINT('Ctrl Pts',(-51.2705909524933,-0.870380061875472,
137.352373627632));
#192974=CARTESIAN_POINT('Ctrl Pts',(-51.5490385763063,5.03856711107574,
135.075996990117));
#192975=CARTESIAN_POINT('Ctrl Pts',(-51.8274862001192,6.31731725663583,
128.874195207264));
#192976=CARTESIAN_POINT('Ctrl Pts',(-52.105933823932,1.79076146145295,124.446121142656));
#192977=CARTESIAN_POINT('Ctrl Pts',(-52.3843814477449,-4.38141663324442,
125.860958538224));
#192978=CARTESIAN_POINT('Ctrl Pts',(-52.6628290715579,-6.52728688609205,
131.818540946088));
#192979=CARTESIAN_POINT('Ctrl Pts',(-52.9412766953706,-2.67489936631311,
136.844141177504));
#192980=CARTESIAN_POINT('Ctrl Pts',(-53.2197243191836,3.63558999500893,
136.319478134021));
#192981=CARTESIAN_POINT('Ctrl Pts',(-53.4981719429964,6.60514975936288,
130.726691521383));
#192982=CARTESIAN_POINT('Ctrl Pts',(-53.7766195668094,3.50489957436681,
125.205279013792));
#192983=CARTESIAN_POINT('Ctrl Pts',(-54.0550671906223,-2.8161820956091,
124.829148969725));
#192984=CARTESIAN_POINT('Ctrl Pts',(-54.3335148144351,-6.54932999786417,
129.943946524707));
#192985=CARTESIAN_POINT('Ctrl Pts',(-54.6119624382481,-4.26396358463975,
135.849422597461));
#192986=CARTESIAN_POINT('Ctrl Pts',(-54.890410062061,1.93977705666721,137.11873317567));
#192987=CARTESIAN_POINT('Ctrl Pts',(-55.1688576858738,6.3609573462743,132.58544384723));
#192988=CARTESIAN_POINT('Ctrl Pts',(-55.4473053096868,4.93672858469731,
126.415426041482));
#192989=CARTESIAN_POINT('Ctrl Pts',(-55.7257529334997,-1.02411257361735,
124.278624699781));
#192990=CARTESIAN_POINT('Ctrl Pts',(-56.0042005573125,-6.0438443074584,
128.138655866601));
#192991=CARTESIAN_POINT('Ctrl Pts',(-56.2826481811254,-5.50957838095395,
134.448339472641));
#192992=CARTESIAN_POINT('Ctrl Pts',(-56.5610958049383,0.0877209197796484,
137.40938452913));
#192993=CARTESIAN_POINT('Ctrl Pts',(-56.8395434287512,5.60440898064107,
134.300735284249));
#192994=CARTESIAN_POINT('Ctrl Pts',(-57.117991052564,5.97091897889293,127.979088528083));
#192995=CARTESIAN_POINT('Ctrl Pts',(-57.396438676377,0.850446131150592,
124.253728799937));
#192996=CARTESIAN_POINT('Ctrl Pts',(-57.6748863001899,-5.05154516451579,
126.548079696037));
#192997=CARTESIAN_POINT('Ctrl Pts',(-57.9533339240027,-6.31141323569307,
132.753744828139));
#192998=CARTESIAN_POINT('Ctrl Pts',(-58.2317815478157,-1.77140087294607,
137.168021103437));
#192999=CARTESIAN_POINT('Ctrl Pts',(-58.5102291716285,4.39644235429495,
135.734404274317));
#193000=CARTESIAN_POINT('Ctrl Pts',(-58.7886767954414,6.52416983608798,
129.770318170665));
#193001=CARTESIAN_POINT('Ctrl Pts',(-59.0671244192543,2.65650396193163,
124.756466559932));
#193002=CARTESIAN_POINT('Ctrl Pts',(-59.3455720430672,-3.6523592758065,
125.300334132115));
#193003=CARTESIAN_POINT('Ctrl Pts',(-59.62401966688,-6.60488276674858,130.902133157784));
#193004=CARTESIAN_POINT('Ctrl Pts',(-59.902467290693,-3.48784166150989,
136.414083995446));
#193005=CARTESIAN_POINT('Ctrl Pts',(-60.1809149145059,2.83435554011865,
136.770973099059));
#193006=CARTESIAN_POINT('Ctrl Pts',(-60.4593625383188,6.55191846634393,
131.644836817403));
#193007=CARTESIAN_POINT('Ctrl Pts',(-60.7378101621316,4.24858840101079,
125.746343967642));
#193008=CARTESIAN_POINT('Ctrl Pts',(-61.0162577859445,-1.95898684976931,
124.49592132131));
#193009=CARTESIAN_POINT('Ctrl Pts',(-61.2947054097575,-6.36634888743926,
129.042646203845));
#193010=CARTESIAN_POINT('Ctrl Pts',(-61.5731530335703,-4.92334731098624,
135.208300568055));
#193011=CARTESIAN_POINT('Ctrl Pts',(-61.8516006573832,1.04396992537583,
137.326949262193));
#193012=CARTESIAN_POINT('Ctrl Pts',(-62.1300482811962,6.05192980108374,
133.451657638088));
#193013=CARTESIAN_POINT('Ctrl Pts',(-62.408495905009,5.49846184280268,127.143629379772));
#193014=CARTESIAN_POINT('Ctrl Pts',(-62.6869435288219,-0.107823934219708,
124.199634292325));
#193015=CARTESIAN_POINT('Ctrl Pts',(-62.9653911526347,-5.61502478318622,
127.325060038955));
#193016=CARTESIAN_POINT('Ctrl Pts',(-63.2438387764477,-5.96229216561512,
133.647793044045));
#193017=CARTESIAN_POINT('Ctrl Pts',(-63.5222864002605,-0.830504322008783,
137.357550558596));
#193018=CARTESIAN_POINT('Ctrl Pts',(-63.8007340240734,5.06447642113188,
135.045246658467));
#193019=CARTESIAN_POINT('Ctrl Pts',(-64.0791816478864,6.30545074667997,
128.835775665549));
#193020=CARTESIAN_POINT('Ctrl Pts',(-64.3576292716992,1.75202387442331,
124.435338072814));
#193021=CARTESIAN_POINT('Ctrl Pts',(-64.6360768955121,-4.41142734730395,
125.887721054655));
#193022=CARTESIAN_POINT('Ctrl Pts',(-64.914524519325,-6.52099234706562,
131.858255603616));
#193023=CARTESIAN_POINT('Ctrl Pts',(-65.1929721431379,-2.63808394806071,
136.860312146029));
#193024=CARTESIAN_POINT('Ctrl Pts',(-65.4714197669508,3.66909472164654,
136.297245083462));
#193025=CARTESIAN_POINT('Ctrl Pts',(-65.7498673907637,6.60455458740261,
130.686485539062));
#193026=CARTESIAN_POINT('Ctrl Pts',(-66.0283150145766,3.4707514377644,125.184047433287));
#193027=CARTESIAN_POINT('Ctrl Pts',(-66.3067626383895,-2.85250272754526,
124.846402576302));
#193028=CARTESIAN_POINT('Ctrl Pts',(-66.5852102622024,-6.55444623874626,
129.983830096806));
#193029=CARTESIAN_POINT('Ctrl Pts',(-66.8636578860152,-4.23317385903938,
135.875285080744));
#193030=CARTESIAN_POINT('Ctrl Pts',(-67.1421055098281,1.978178495085,137.106808211453));
#193031=CARTESIAN_POINT('Ctrl Pts',(-67.4205531336411,6.37168145161813,
132.546689895061));
#193032=CARTESIAN_POINT('Ctrl Pts',(-67.6990007574539,4.90992042805787,
126.385456090168));
#193033=CARTESIAN_POINT('Ctrl Pts',(-67.9774483812669,-1.06381760593968,
124.284979670466));
#193034=CARTESIAN_POINT('Ctrl Pts',(-68.2558960050797,-6.05995923045808,
128.175495851683));
#193035=CARTESIAN_POINT('Ctrl Pts',(-68.5343436288926,-5.48729436765201,
134.481810325563));
#193036=CARTESIAN_POINT('Ctrl Pts',(-68.8127912527054,0.12792594979327,
137.408728171199));
#193037=CARTESIAN_POINT('Ctrl Pts',(-69.0912388765185,5.62558856890878,
134.266554876337));
#193038=CARTESIAN_POINT('Ctrl Pts',(-69.3696865003312,5.9536101184771,127.942794195258));
#193039=CARTESIAN_POINT('Ctrl Pts',(-69.6481341241442,0.810554819188534,
124.248673260987));
#193040=CARTESIAN_POINT('Ctrl Pts',(-69.9265817479571,-5.07736076112986,
126.578908744281));
#193041=CARTESIAN_POINT('Ctrl Pts',(-70.2050293717699,-6.29942984483285,
132.792128074323));
#193042=CARTESIAN_POINT('Ctrl Pts',(-70.4834769955829,-1.73263064539088,
137.178686219444));
#193043=CARTESIAN_POINT('Ctrl Pts',(-70.7619246193956,4.42637147345276,
135.707550539556));
#193044=CARTESIAN_POINT('Ctrl Pts',(-71.0403722432087,6.51775444846118,
129.730622855503));
#193045=CARTESIAN_POINT('Ctrl Pts',(-71.3188198670216,2.6196394953401,124.740407719779));
#193046=CARTESIAN_POINT('Ctrl Pts',(-71.5972674908343,-3.68579617749442,
125.322669056552));
#193047=CARTESIAN_POINT('Ctrl Pts',(-71.8757151146474,-6.6041652243652,
130.942337142376));
#193048=CARTESIAN_POINT('Ctrl Pts',(-72.1541627384602,-3.45362906145158,
136.435211542427));
#193049=CARTESIAN_POINT('Ctrl Pts',(-72.4326103622731,2.87062348977667,
136.753609024891));
#193050=CARTESIAN_POINT('Ctrl Pts',(-72.711057986086,6.55691329165398,131.604937857965));
#193051=CARTESIAN_POINT('Ctrl Pts',(-72.9895056098989,4.21772010152317,
125.720575317484));
#193052=CARTESIAN_POINT('Ctrl Pts',(-73.2679532337117,-1.99735181482566,
124.50796311106));
#193053=CARTESIAN_POINT('Ctrl Pts',(-73.5464008575247,-6.37695498941029,
129.081432616995));
#193054=CARTESIAN_POINT('Ctrl Pts',(-73.8248484813376,-4.89644806029751,
135.238188785743));
#193055=CARTESIAN_POINT('Ctrl Pts',(-74.1032961051504,1.08365543144292,
137.320473472483));
#193056=CARTESIAN_POINT('Ctrl Pts',(-74.3817437289633,6.06793252119795,
133.414768775364));
#193057=CARTESIAN_POINT('Ctrl Pts',(-74.6601913527762,5.47607605895596,
127.110226506756));
#193058=CARTESIAN_POINT('Ctrl Pts',(-74.9386389765891,-0.148026780279403,
124.200413017498));
#193059=CARTESIAN_POINT('Ctrl Pts',(-75.217086600402,-5.63610023994771,
127.359304751927));
#193060=CARTESIAN_POINT('Ctrl Pts',(-75.4955342242149,-5.94487291790794,
133.684034526541));
#193061=CARTESIAN_POINT('Ctrl Pts',(-75.7739818480278,-0.790597807498519,
137.362484658699));
#193062=CARTESIAN_POINT('Ctrl Pts',(-76.0524294718406,5.09019806515201,
135.014339179226));
#193063=CARTESIAN_POINT('Ctrl Pts',(-76.3308770956536,6.29335058592772,
128.797429070474));
#193064=CARTESIAN_POINT('Ctrl Pts',(-76.6093247194664,1.71322136550425,
124.424791009442));
#193065=CARTESIAN_POINT('Ctrl Pts',(-76.8877723432794,-4.44127459430165,
125.914665758975));
#193066=CARTESIAN_POINT('Ctrl Pts',(-77.1662199670922,-6.51445617026952,
131.89793120868));
#193067=CARTESIAN_POINT('Ctrl Pts',(-77.4446675909052,-2.60117077463652,
136.876258709042));
#193068=CARTESIAN_POINT('Ctrl Pts',(-77.7231152147181,3.7024634886308,136.274808492052));
#193069=CARTESIAN_POINT('Ctrl Pts',(-78.0015628385308,6.60371468124315,
130.646283924643));
#193070=CARTESIAN_POINT('Ctrl Pts',(-78.2800104623438,3.43647469119047,
125.163024115555));
#193071=CARTESIAN_POINT('Ctrl Pts',(-78.5584580861567,-2.88871765894464,
124.863876957204));
#193072=CARTESIAN_POINT('Ctrl Pts',(-78.8369057099696,-6.55931960221255,
130.023744073965));
#193073=CARTESIAN_POINT('Ctrl Pts',(-79.1153533337825,-4.20222727162433,
135.900959659057));
#193074=CARTESIAN_POINT('Ctrl Pts',(-79.3938009575953,2.01650663137172,
137.094649707722));
#193075=CARTESIAN_POINT('Ctrl Pts',(-79.6722485814083,6.38216945196263,
132.507871380239));
#193076=CARTESIAN_POINT('Ctrl Pts',(-79.9506962052212,4.88293033251105,
126.355649882987));
#193077=CARTESIAN_POINT('Ctrl Pts',(-80.229143829034,-1.10348321810992,
124.29157621921));
#193078=CARTESIAN_POINT('Ctrl Pts',(-80.507591452847,-6.07584959944043,
128.212433250316));
#193079=CARTESIAN_POINT('Ctrl Pts',(-80.7860390766598,-5.46480702063872,
134.515144909234));
#193080=CARTESIAN_POINT('Ctrl Pts',(-81.0644867004727,0.168126239464741,
137.407827085998));
#193081=CARTESIAN_POINT('Ctrl Pts',(-81.3429343242857,5.64655969892388,
134.232246175545));
#193082=CARTESIAN_POINT('Ctrl Pts',(-81.6213819480984,5.93608064484842,
127.906605898828));
#193083=CARTESIAN_POINT('Ctrl Pts',(-81.8998295719115,0.770633471818905,
124.243860645443));
#193084=CARTESIAN_POINT('Ctrl Pts',(-82.1782771957242,-5.10298821427442,
126.609894368197));
#193085=CARTESIAN_POINT('Ctrl Pts',(-82.4567248195372,-6.28721302628274,
132.830437663053));
#193086=CARTESIAN_POINT('Ctrl Pts',(-82.7351724433501,-1.69379621456928,
137.189115132473));
#193087=CARTESIAN_POINT('Ctrl Pts',(-83.0136200671628,4.45613657178832,
135.680515115291));
#193088=CARTESIAN_POINT('Ctrl Pts',(-83.2920676909759,6.51109754304618,
129.690967328089));
#193089=CARTESIAN_POINT('Ctrl Pts',(-83.5705153147887,2.58267795704331,
124.724573581631));
#193090=CARTESIAN_POINT('Ctrl Pts',(-83.8489629386017,-3.71909650065006,
125.345207107088));
#193091=CARTESIAN_POINT('Ctrl Pts',(-84.1274105624144,-6.60320296221082,
130.982536014198));
#193092=CARTESIAN_POINT('Ctrl Pts',(-84.4058581862275,-3.41928848589759,
136.456130436155));
#193093=CARTESIAN_POINT('Ctrl Pts',(-84.6843058100402,2.90678506742617,
136.736024499134));
#193094=CARTESIAN_POINT('Ctrl Pts',(-84.9627534338533,6.56166514813073,
131.565009232842));
#193095=CARTESIAN_POINT('Ctrl Pts',(-85.241201057666,4.1866955128661,125.694995048862));
#193096=CARTESIAN_POINT('Ctrl Pts',(-85.519648681479,-2.03564276727566,
124.520238216135));
#193097=CARTESIAN_POINT('Ctrl Pts',(-85.7980963052919,-6.38732479096924,
129.120282873878));
#193098=CARTESIAN_POINT('Ctrl Pts',(-86.0765439291047,-4.8693673699251,
135.267912706297));
#193099=CARTESIAN_POINT('Ctrl Pts',(-86.3549915529177,1.12330078225909,
137.313756225814));
#193100=CARTESIAN_POINT('Ctrl Pts',(-86.6334391767305,6.08371039184151,
133.377783183006));
#193101=CARTESIAN_POINT('Ctrl Pts',(-86.9118868005434,5.45348735709659,
127.076960521238));
#193102=CARTESIAN_POINT('Ctrl Pts',(-87.1903344243564,-0.188224141151809,
124.201436454379));
#193103=CARTESIAN_POINT('Ctrl Pts',(-87.4687820481692,-5.65696684894189,
127.39367712271));
#193104=CARTESIAN_POINT('Ctrl Pts',(-87.7472296719821,-5.92723338074904,
133.720169301662));
#193105=CARTESIAN_POINT('Ctrl Pts',(-88.0256772957949,-0.750661997095914,
137.367175745102));
#193106=CARTESIAN_POINT('Ctrl Pts',(-88.3041249196079,5.11573109001074,
134.983275697681));
#193107=CARTESIAN_POINT('Ctrl Pts',(-88.5825725434208,6.28101722275544,
128.759156842984));
#193108=CARTESIAN_POINT('Ctrl Pts',(-88.8610201672337,1.67435537253749,
124.414480343369));
#193109=CARTESIAN_POINT('Ctrl Pts',(-89.1394677910466,-4.47095726823472,
125.941791652735));
#193110=CARTESIAN_POINT('Ctrl Pts',(-89.4179154148595,-6.50767859790483,
131.93756629108));
#193111=CARTESIAN_POINT('Ctrl Pts',(-89.6963630386723,-2.56416121387375,
136.891980275641));
#193112=CARTESIAN_POINT('Ctrl Pts',(-89.9748106624853,3.73569505946763,
136.252169191183));
#193113=CARTESIAN_POINT('Ctrl Pts',(-90.253258286298,6.60263007200808,130.606088167816));
#193114=CARTESIAN_POINT('Ctrl Pts',(-90.5317059101111,3.40207060478355,
125.142209839621));
#193115=CARTESIAN_POINT('Ctrl Pts',(-90.8101535339238,-2.9248255478482,
124.881571464914));
#193116=CARTESIAN_POINT('Ctrl Pts',(-91.0886011577368,-6.56394990767886,
130.063686977158));
#193117=CARTESIAN_POINT('Ctrl Pts',(-91.3670487815497,-4.17112496913288,
135.926445381018));
#193118=CARTESIAN_POINT('Ctrl Pts',(-91.6454964053626,2.05476004526333,
137.082258115016));
#193119=CARTESIAN_POINT('Ctrl Pts',(-91.9239440291755,6.39242095867105,
132.468989741201));
#193120=CARTESIAN_POINT('Ctrl Pts',(-92.2023916529884,4.85575929818535,
126.326008524418));
#193121=CARTESIAN_POINT('Ctrl Pts',(-92.4808392768012,-1.14310794030347,
124.298414101576));
#193122=CARTESIAN_POINT('Ctrl Pts',(-92.7592869006141,-6.09151482558059,
128.249466693771));
#193123=CARTESIAN_POINT('Ctrl Pts',(-93.0377345244271,-5.44211717319261,
134.548341988427));
#193124=CARTESIAN_POINT('Ctrl Pts',(-93.3161821482399,0.208320299155509,
137.406681306919));
#193125=CARTESIAN_POINT('Ctrl Pts',(-93.5946297720528,5.6673215935918,134.197810453193));
#193126=CARTESIAN_POINT('Ctrl Pts',(-93.8730773958657,5.91833120756931,
127.870524979765));
#193127=CARTESIAN_POINT('Ctrl Pts',(-94.1515250196785,0.730683568342929,
124.239291131637));
#193128=CARTESIAN_POINT('Ctrl Pts',(-94.4299726434915,-5.12842657431339,
126.641035419604));
#193129=CARTESIAN_POINT('Ctrl Pts',(-94.7084202673044,-6.27476323274215,
132.868672174754));
#193130=CARTESIAN_POINT('Ctrl Pts',(-94.9868678911172,-1.6548990195065,
137.199307456074));
#193131=CARTESIAN_POINT('Ctrl Pts',(-95.2653155149302,4.48573654634406,
135.653299003326));
#193132=CARTESIAN_POINT('Ctrl Pts',(-95.543763138743,6.50419936651746,129.651353057874));
#193133=CARTESIAN_POINT('Ctrl Pts',(-95.822210762556,2.54562071666526,124.708964732227));
#193134=CARTESIAN_POINT('Ctrl Pts',(-96.1006583863688,-3.75225901131679,
125.367947448562));
#193135=CARTESIAN_POINT('Ctrl Pts',(-96.3791060101818,-6.60199601594203,
131.022728283664));
#193136=CARTESIAN_POINT('Ctrl Pts',(-96.6575536339946,-3.38482120735248,
136.476839901474));
#193137=CARTESIAN_POINT('Ctrl Pts',(-96.9360012578075,2.94283893308538,
136.718220173391));
#193138=CARTESIAN_POINT('Ctrl Pts',(-97.2144488816204,6.5661738596919,131.525052421605));
#193139=CARTESIAN_POINT('Ctrl Pts',(-97.4928965054334,4.15551578466796,
125.669604109659));
#193140=CARTESIAN_POINT('Ctrl Pts',(-97.771344129246,-2.07385828823457,
124.532746181678));
#193141=CARTESIAN_POINT('Ctrl Pts',(-98.0497917530593,-6.39745790785863,
129.15919553488));
#193142=CARTESIAN_POINT('Ctrl Pts',(-98.3282393768718,-4.84210624335443,
135.297471228287));
#193143=CARTESIAN_POINT('Ctrl Pts',(-98.606687000685,1.16290450875192,137.306797771098));
#193144=CARTESIAN_POINT('Ctrl Pts',(-98.8851346244975,6.09926282835875,
133.340702231527));
#193145=CARTESIAN_POINT('Ctrl Pts',(-99.1635822483109,5.43069657425812,
127.043832655902));
#193146=CARTESIAN_POINT('Ctrl Pts',(-99.4420298721233,-0.228414527308866,
124.202704565042));
#193147=CARTESIAN_POINT('Ctrl Pts',(-99.7204774959365,-5.67762383694899,
127.428175877623));
#193148=CARTESIAN_POINT('Ctrl Pts',(-99.9989251197493,-5.90937420777732,
133.756196030418));
#193149=CARTESIAN_POINT('Ctrl Pts',(-100.277372743562,-0.710698370637635,
137.371623643978));
#193150=CARTESIAN_POINT('Ctrl Pts',(-100.555820367375,5.14107454957247,
134.9520573649));
#193151=CARTESIAN_POINT('Ctrl Pts',(-100.834267991188,6.26845111417983,
128.720960401273));
#193152=CARTESIAN_POINT('Ctrl Pts',(-101.112715615001,1.63542733571746,
124.404406456659));
#193153=CARTESIAN_POINT('Ctrl Pts',(-101.391163238814,-4.50047426920288,
125.969097730777));
#193154=CARTESIAN_POINT('Ctrl Pts',(-101.669610862627,-6.50065988111587,
131.977159382129));
#193155=CARTESIAN_POINT('Ctrl Pts',(-101.94805848644,-2.52705663717401,
136.907476263252));
#193156=CARTESIAN_POINT('Ctrl Pts',(-102.226506110253,3.76878820275105,
136.229328019765));
#193157=CARTESIAN_POINT('Ctrl Pts',(-102.504953734065,6.60130079988703,
130.565899758046));
#193158=CARTESIAN_POINT('Ctrl Pts',(-102.783401357878,3.36754045339959,
125.121605376767));
#193159=CARTESIAN_POINT('Ctrl Pts',(-103.061848981691,-2.96082505626518,
124.899485443752));
#193160=CARTESIAN_POINT('Ctrl Pts',(-103.340296605504,-6.56833698356739,
130.103657326284));
#193161=CARTESIAN_POINT('Ctrl Pts',(-103.618744229317,-4.13986810407194,
135.951741302244));
#193162=CARTESIAN_POINT('Ctrl Pts',(-103.89719185313,2.0929373192654,137.06963389251));
#193163=CARTESIAN_POINT('Ctrl Pts',(-104.175639476943,6.40243559186997,
132.430046418718));
#193164=CARTESIAN_POINT('Ctrl Pts',(-104.454087100755,4.82840833191319,
126.296533112833));
#193165=CARTESIAN_POINT('Ctrl Pts',(-104.732534724569,-1.18269030421136,
124.305493064181));
#193166=CARTESIAN_POINT('Ctrl Pts',(-105.010982348381,-6.10695432839948,
128.286594809759));
#193167=CARTESIAN_POINT('Ctrl Pts',(-105.289429972194,-5.41922566609253,
134.581400333014));
#193168=CARTESIAN_POINT('Ctrl Pts',(-105.567877596007,0.248506639461218,
137.40529087642));
#193169=CARTESIAN_POINT('Ctrl Pts',(-105.84632521982,5.68787348357469,134.163248985309));
#193170=CARTESIAN_POINT('Ctrl Pts',(-106.124772843633,5.90036246435008,
127.834552775061));
#193171=CARTESIAN_POINT('Ctrl Pts',(-106.403220467446,0.690706589119241,
124.234964888896));
#193172=CARTESIAN_POINT('Ctrl Pts',(-106.681668091259,-5.1536748986197,
126.672330744555));
#193173=CARTESIAN_POINT('Ctrl Pts',(-106.960115715072,-6.26208092554253,
132.906830192629));
#193174=CARTESIAN_POINT('Ctrl Pts',(-107.238563338885,-1.61594050155245,
137.209262812568));
#193175=CARTESIAN_POINT('Ctrl Pts',(-107.517010962697,4.51517030028232,
135.625903212168));
#193176=CARTESIAN_POINT('Ctrl Pts',(-107.79545858651,6.49706017448951,129.611781512777));
#193177=CARTESIAN_POINT('Ctrl Pts',(-108.073906210323,2.50846914737518,
124.69358174996));
#193178=CARTESIAN_POINT('Ctrl Pts',(-108.352353834136,-3.78528248064593,
125.390889238328));
#193179=CARTESIAN_POINT('Ctrl Pts',(-108.630801457949,-6.60054443028347,
131.062912461436));
#193180=CARTESIAN_POINT('Ctrl Pts',(-108.909249081762,-3.35022850301195,
136.497339170987));
#193181=CARTESIAN_POINT('Ctrl Pts',(-109.187696705575,2.97878375076591,
136.700196707408));
#193182=CARTESIAN_POINT('Ctrl Pts',(-109.466144329388,6.57043925926657,
131.485068904869));
#193183=CARTESIAN_POINT('Ctrl Pts',(-109.7445919532,4.12418207230337,125.644403440746));
#193184=CARTESIAN_POINT('Ctrl Pts',(-110.023039577014,-2.11199696161116,
124.5454865442));
#193185=CARTESIAN_POINT('Ctrl Pts',(-110.301487200826,-6.40735396459295,
129.198169158078));
#193186=CARTESIAN_POINT('Ctrl Pts',(-110.579934824639,-4.81466569075636,
135.326863256411));
#193187=CARTESIAN_POINT('Ctrl Pts',(-110.858382448452,1.20246514338981,
137.299598366182));
#193188=CARTESIAN_POINT('Ctrl Pts',(-111.136830072265,6.11458925444912,
133.303527294979));
#193189=CARTESIAN_POINT('Ctrl Pts',(-111.415277696078,5.407704554961,127.010844138312));
#193190=CARTESIAN_POINT('Ctrl Pts',(-111.693725319891,-0.268596449482207,
124.204217302498));
#193191=CARTESIAN_POINT('Ctrl Pts',(-111.972172943703,-5.69807043851701,
127.462799738304));
#193192=CARTESIAN_POINT('Ctrl Pts',(-112.250620567517,-5.89129606077132,
133.792113377828));
#193193=CARTESIAN_POINT('Ctrl Pts',(-112.529068191329,-0.670708408989202,
137.375828190507));
#193194=CARTESIAN_POINT('Ctrl Pts',(-112.807515815142,5.16622750472631,
134.920685337692));
#193195=CARTESIAN_POINT('Ctrl Pts',(-113.085963438955,6.25565272584325,
128.682841160722));
#193196=CARTESIAN_POINT('Ctrl Pts',(-113.364411062768,1.5964386975353,124.394569722605));
#193197=CARTESIAN_POINT('Ctrl Pts',(-113.642858686581,-4.52982450344111,
125.996582981263));
#193198=CARTESIAN_POINT('Ctrl Pts',(-113.921306310394,-6.49340027998504,
132.016709014688));
#193199=CARTESIAN_POINT('Ctrl Pts',(-114.199753934207,-2.48985841946147,
136.922746097669));
#193200=CARTESIAN_POINT('Ctrl Pts',(-114.47820155802,3.80174169220082,136.206285824184));
#193201=CARTESIAN_POINT('Ctrl Pts',(-114.756649181833,6.59972691413776,
130.525720184532));
#193202=CARTESIAN_POINT('Ctrl Pts',(-115.035096805645,3.3328855165654,125.101211490497));
#193203=CARTESIAN_POINT('Ctrl Pts',(-115.313544429458,-2.99671485022117,
124.917618229914));
#193204=CARTESIAN_POINT('Ctrl Pts',(-115.591992053271,-6.57248066731354,
130.143653640229));
#193205=CARTESIAN_POINT('Ctrl Pts',(-115.870439677084,-4.10845783467579,
135.976846485386));
#193206=CARTESIAN_POINT('Ctrl Pts',(-116.148887300897,2.13103703870585,
137.056777507999));
#193207=CARTESIAN_POINT('Ctrl Pts',(-116.42733492471,6.41221298046361,132.391042855849));
#193208=CARTESIAN_POINT('Ctrl Pts',(-116.705782548523,4.8008784471946,126.267224740454));
#193209=CARTESIAN_POINT('Ctrl Pts',(-116.984230172336,-1.22222884309565,
124.312812844714));
#193210=CARTESIAN_POINT('Ctrl Pts',(-117.262677796149,-6.12216753577917,
128.323816222486));
#193211=CARTESIAN_POINT('Ctrl Pts',(-117.541125419961,-5.39613334759327,
134.614318718005));
#193212=CARTESIAN_POINT('Ctrl Pts',(-117.819573043774,0.288683771261777,
137.403655846021));
#193213=CARTESIAN_POINT('Ctrl Pts',(-118.098020667587,5.70821460731317,
134.128563052582));
#193214=CARTESIAN_POINT('Ctrl Pts',(-118.3764682914,5.88217508103065,127.79869061768));
#193215=CARTESIAN_POINT('Ctrl Pts',(-118.654915915213,0.650704015508265,
124.230882077529));
#193216=CARTESIAN_POINT('Ctrl Pts',(-118.933363539026,-5.17873225160735,
126.703779183394));
#193217=CARTESIAN_POINT('Ctrl Pts',(-119.211811162839,-6.24916657463125,
132.944910302722));
#193218=CARTESIAN_POINT('Ctrl Pts',(-119.490258786652,-1.57692210432836,
137.218980833058));
#193219=CARTESIAN_POINT('Ctrl Pts',(-119.768706410464,4.54443674292479,
135.598328756974));
#193220=CARTESIAN_POINT('Ctrl Pts',(-120.047154034278,6.48968023150711,
129.572254159139));
#193221=CARTESIAN_POINT('Ctrl Pts',(-120.32560165809,2.47122462583917,124.67842520485));
#193222=CARTESIAN_POINT('Ctrl Pts',(-120.604049281903,-3.81816568494053,
125.414031626265));
#193223=CARTESIAN_POINT('Ctrl Pts',(-120.882496905716,-6.59884825902321,
131.103087058474));
#193224=CARTESIAN_POINT('Ctrl Pts',(-121.160944529529,-3.31551165472302,
136.517627485086));
#193225=CARTESIAN_POINT('Ctrl Pts',(-121.439392153342,3.0146181885189,136.68195476905));
#193226=CARTESIAN_POINT('Ctrl Pts',(-121.717839777155,6.57446118879764,
131.445060164237));
#193227=CARTESIAN_POINT('Ctrl Pts',(-121.996287400968,4.0926955368563,125.619393975946));
#193228=CARTESIAN_POINT('Ctrl Pts',(-122.274735024781,-2.15005737416446,
124.5584588316));
#193229=CARTESIAN_POINT('Ctrl Pts',(-122.553182648593,-6.41701259446945,
129.237202299292));
#193230=CARTESIAN_POINT('Ctrl Pts',(-122.831630272406,-4.7870467289504,
135.356087701536));
#193231=CARTESIAN_POINT('Ctrl Pts',(-123.110077896219,1.24198122024032,
137.292158277842));
#193232=CARTESIAN_POINT('Ctrl Pts',(-123.388525520032,6.1296891021858,133.266259750888));
#193233=CARTESIAN_POINT('Ctrl Pts',(-123.666973143845,5.38451215118288,
126.97799619087));
#193234=CARTESIAN_POINT('Ctrl Pts',(-123.945420767658,-0.30876841871475,
124.20597461069));
#193235=CARTESIAN_POINT('Ctrl Pts',(-124.223868391471,-5.71830589598935,
127.497547421752));
#193236=CARTESIAN_POINT('Ctrl Pts',(-124.502316015284,-5.87299960962311,
133.827920012961));
#193237=CARTESIAN_POINT('Ctrl Pts',(-124.780763639097,-0.630693593994696,
137.379789228888));
#193238=CARTESIAN_POINT('Ctrl Pts',(-125.059211262909,5.19118902341993,
134.889160778557));
#193239=CARTESIAN_POINT('Ctrl Pts',(-125.337658886723,6.24262253199412,
128.644800533857));
#193240=CARTESIAN_POINT('Ctrl Pts',(-125.616106510535,1.55739090273089,
124.384970505708));
#193241=CARTESIAN_POINT('Ctrl Pts',(-125.894554134348,-4.55900688336737,
126.024246385717));
#193242=CARTESIAN_POINT('Ctrl Pts',(-126.173001758161,-6.48590006351826,
132.056213723232));
#193243=CARTESIAN_POINT('Ctrl Pts',(-126.451449381974,-2.45256793912933,
136.937789213063));
#193244=CARTESIAN_POINT('Ctrl Pts',(-126.729897005787,3.83455430671493,
136.183043458277));
#193245=CARTESIAN_POINT('Ctrl Pts',(-127.0083446296,6.5979084730801,130.485550936142));
#193246=CARTESIAN_POINT('Ctrl Pts',(-127.286792253413,3.29810707843306,
125.081028936517));
#193247=CARTESIAN_POINT('Ctrl Pts',(-127.565239877225,-3.03249359980603,
124.935969151478));
#193248=CARTESIAN_POINT('Ctrl Pts',(-127.843687501038,-6.57638080537151,
130.183674436914));
#193249=CARTESIAN_POINT('Ctrl Pts',(-128.122135124851,-4.07689532486387,
136.001760000162));
#193250=CARTESIAN_POINT('Ctrl Pts',(-128.400582748664,2.1690577917847,137.043689437881));
#193251=CARTESIAN_POINT('Ctrl Pts',(-128.679030372477,6.42175276214748,
132.351980497887));
#193252=CARTESIAN_POINT('Ctrl Pts',(-128.95747799629,4.77317066415926,126.238084493312));
#193253=CARTESIAN_POINT('Ctrl Pts',(-129.235925620103,-1.26172209184052,
124.320373171937));
#193254=CARTESIAN_POINT('Ctrl Pts',(-129.514373243916,-6.13715388399014,
128.361129552696));
#193255=CARTESIAN_POINT('Ctrl Pts',(-129.792820867728,-5.37284107338758,
134.647095923599));
#193256=CARTESIAN_POINT('Ctrl Pts',(-130.071268491542,0.328850205779251,
137.401776276312));
#193257=CARTESIAN_POINT('Ctrl Pts',(-130.349716115354,5.72834421106097,
134.093753940311));
#193258=CARTESIAN_POINT('Ctrl Pts',(-130.628163739167,5.86376973154965,
127.762939836503));
#193259=CARTESIAN_POINT('Ctrl Pts',(-130.90661136298,0.610677329821333,
124.227042848828));
#193260=CARTESIAN_POINT('Ctrl Pts',(-131.185058986793,-5.20359770476699,
126.735379570785));
#193261=CARTESIAN_POINT('Ctrl Pts',(-131.463506610606,-6.23602065855449,
132.982911093959));
#193262=CARTESIAN_POINT('Ctrl Pts',(-131.741954234419,-1.53784527367628,
137.228461157434));
#193263=CARTESIAN_POINT('Ctrl Pts',(-132.020401858232,4.57353478979242,
135.57057665953));
#193264=CARTESIAN_POINT('Ctrl Pts',(-132.298849482045,6.48205981103755,
129.532772461657));
#193265=CARTESIAN_POINT('Ctrl Pts',(-132.577297105858,2.43388853216508,
124.66349565853));
#193266=CARTESIAN_POINT('Ctrl Pts',(-132.85574472967,-3.85090740570176,
125.437373754826));
#193267=CARTESIAN_POINT('Ctrl Pts',(-133.134192353483,-6.59690756501448,
131.143250586095));
#193268=CARTESIAN_POINT('Ctrl Pts',(-133.412639977296,-3.28067194892964,
136.53770409198));
#193269=CARTESIAN_POINT('Ctrl Pts',(-133.691087601109,3.0503409184865,136.663495034279));
#193270=CARTESIAN_POINT('Ctrl Pts',(-133.969535224922,6.5782394992522,131.405027682246));
#193271=CARTESIAN_POINT('Ctrl Pts',(-134.247982848735,4.06105734507014,
125.59457664199));
#193272=CARTESIAN_POINT('Ctrl Pts',(-134.526430472548,-2.18803811555026,
124.57166256319));
#193273=CARTESIAN_POINT('Ctrl Pts',(-134.804878096361,-6.42643343958478,
129.276293512134));
#193274=CARTESIAN_POINT('Ctrl Pts',(-135.083325720174,-4.75925038136761,
135.385143480741));
#193275=CARTESIAN_POINT('Ctrl Pts',(-135.361773343986,1.28145127501926,
137.284477781773));
#193276=CARTESIAN_POINT('Ctrl Pts',(-135.640220967799,6.14456181203885,
133.228900980221));
#193277=CARTESIAN_POINT('Ctrl Pts',(-135.918668591612,5.36112022232688,
126.945290030769));
#193278=CARTESIAN_POINT('Ctrl Pts',(-136.197116215425,-0.348928946420584,
124.207976424505));
#193279=CARTESIAN_POINT('Ctrl Pts',(-136.475563839238,-5.73832945953392,
127.53241764038));
#193280=CARTESIAN_POINT('Ctrl Pts',(-136.754011463051,-5.85448553231475,
133.863614608987));
#193281=CARTESIAN_POINT('Ctrl Pts',(-137.032459086864,-0.590655408416443,
137.383506612345));
#193282=CARTESIAN_POINT('Ctrl Pts',(-137.310906710677,5.21595818069537,
134.857484855651));
#193283=CARTESIAN_POINT('Ctrl Pts',(-137.58935433449,6.22936101547165,128.606839930282));
#193284=CARTESIAN_POINT('Ctrl Pts',(-137.867801958302,1.51828539823306,
124.375609161675));
#193285=CARTESIAN_POINT('Ctrl Pts',(-138.146249582115,-4.58802032761614,
126.052086919061));
#193286=CARTESIAN_POINT('Ctrl Pts',(-138.424697205928,-6.47815950964009,
132.095672043897));
#193287=CARTESIAN_POINT('Ctrl Pts',(-138.703144829741,-2.41518657799051,
136.952605052004));
#193288=CARTESIAN_POINT('Ctrl Pts',(-138.981592453554,3.86722483040823,
136.159601783301));
#193289=CARTESIAN_POINT('Ctrl Pts',(-139.260040077367,6.59584554409815,
130.445393501362));
#193290=CARTESIAN_POINT('Ctrl Pts',(-139.53848770118,3.26320642772972,125.061058462695));
#193291=CARTESIAN_POINT('Ctrl Pts',(-139.816935324993,-3.06815997922566,
124.954537528447));
#193292=CARTESIAN_POINT('Ctrl Pts',(-140.095382948806,-6.58003725322031,
130.223718233352));
#193293=CARTESIAN_POINT('Ctrl Pts',(-140.373830572619,-4.04518174419624,
136.026480923393));
#193294=CARTESIAN_POINT('Ctrl Pts',(-140.652278196431,2.20699816962987,
137.030370167137));
#193295=CARTESIAN_POINT('Ctrl Pts',(-140.930725820244,6.43105458342049,
132.312860792301));
#193296=CARTESIAN_POINT('Ctrl Pts',(-141.209173444057,4.74528600953044,
126.209113451214));
#193297=CARTESIAN_POINT('Ctrl Pts',(-141.48762106787,-1.30116858700904,
124.328173765698));
#193298=CARTESIAN_POINT('Ctrl Pts',(-141.766068691683,-6.15191281770628,
128.398533417733));
#193299=CARTESIAN_POINT('Ctrl Pts',(-142.044516315496,-5.34934970658085,
134.679730735221));
#193300=CARTESIAN_POINT('Ctrl Pts',(-142.322963939309,0.369004454631186,
137.399652236939));
#193301=CARTESIAN_POINT('Ctrl Pts',(-142.601411563122,5.74826154890666,
134.058822938361));
#193302=CARTESIAN_POINT('Ctrl Pts',(-142.879859186934,5.84514709792562,
127.727301756295));
#193303=CARTESIAN_POINT('Ctrl Pts',(-143.158306810748,0.570628015260733,
124.223447345055));
#193304=CARTESIAN_POINT('Ctrl Pts',(-143.43675443456,-5.22827033670001,
126.767130735766));
#193305=CARTESIAN_POINT('Ctrl Pts',(-143.715202058373,-6.22264366443886,
133.020831158207));
#193306=CARTESIAN_POINT('Ctrl Pts',(-143.993649682186,-1.49871145760156,
137.237703434405));
#193307=CARTESIAN_POINT('Ctrl Pts',(-144.272097305999,4.60246336264661,
135.542647948195));
#193308=CARTESIAN_POINT('Ctrl Pts',(-144.550544929812,6.47419919545755,
129.493337883343));
#193309=CARTESIAN_POINT('Ctrl Pts',(-144.828992553625,2.39646224985712,
124.648793664219));
#193310=CARTESIAN_POINT('Ctrl Pts',(-145.107440177438,-3.8835064296727,
125.460914759058));
#193311=CARTESIAN_POINT('Ctrl Pts',(-145.38588780125,-6.59472242016944,
131.183401556022));
#193312=CARTESIAN_POINT('Ctrl Pts',(-145.664335425064,-3.24571067663155,
136.557568247724));
#193313=CARTESIAN_POINT('Ctrl Pts',(-145.942783048876,3.08595061694992,
136.644818187128));
#193314=CARTESIAN_POINT('Ctrl Pts',(-146.221230672689,6.58177405062243,
131.364972942318));
#193315=CARTESIAN_POINT('Ctrl Pts',(-146.499678296502,4.02926866931097,
125.569952358496));
#193316=CARTESIAN_POINT('Ctrl Pts',(-146.778125920315,-2.22593777837984,
124.585097249699));
#193317=CARTESIAN_POINT('Ctrl Pts',(-147.056573544128,-6.43561615084533,
129.315441348065));
#193318=CARTESIAN_POINT('Ctrl Pts',(-147.335021167941,-4.73127767801157,
135.414029517352));
#193319=CARTESIAN_POINT('Ctrl Pts',(-147.613468791753,1.32087384515067,
137.276557162581));
#193320=CARTESIAN_POINT('Ctrl Pts',(-147.891916415567,6.15920683289404,
133.191452367319));
#193321=CARTESIAN_POINT('Ctrl Pts',(-148.170364039379,5.33752963518947,
126.91272686995));
#193322=CARTESIAN_POINT('Ctrl Pts',(-148.448811663193,-0.389076544435395,
124.210222669761));
#193323=CARTESIAN_POINT('Ctrl Pts',(-148.727259287005,-5.75814038716998,
127.567409102056));
#193324=CARTESIAN_POINT('Ctrl Pts',(-149.005706910818,-5.83575451489182,
133.899195843233));
#193325=CARTESIAN_POINT('Ctrl Pts',(-149.284154534631,-0.550595335885521,
137.386980203127));
#193326=CARTESIAN_POINT('Ctrl Pts',(-149.562602158444,5.24053405872261,
134.825658742734));
#193327=CARTESIAN_POINT('Ctrl Pts',(-149.841049782257,6.21586866768539,
128.568960756646));
#193328=CARTESIAN_POINT('Ctrl Pts',(-150.119497406069,1.47912363311174,
124.366486037389));
#193329=CARTESIAN_POINT('Ctrl Pts',(-150.397945029883,-4.61686376108527,
126.080103549656));
#193330=CARTESIAN_POINT('Ctrl Pts',(-150.676392653695,-6.4701789051783,
132.135082514543));
#193331=CARTESIAN_POINT('Ctrl Pts',(-150.954840277509,-2.37771572122463,
136.967193065487));
#193332=CARTESIAN_POINT('Ctrl Pts',(-151.233287901321,3.89975205266408,
136.135961667893));
#193333=CARTESIAN_POINT('Ctrl Pts',(-151.511735525134,6.59353820363339,
130.405249368239));
#193334=CARTESIAN_POINT('Ctrl Pts',(-151.790183148947,3.22818485771248,
125.041300809049));
#193335=CARTESIAN_POINT('Ctrl Pts',(-152.06863077276,-3.10371266684865,
124.97332267276));
#193336=CARTESIAN_POINT('Ctrl Pts',(-152.347078396573,-6.58344987536885,
130.263783545709));
#193337=CARTESIAN_POINT('Ctrl Pts',(-152.625526020386,-4.01331826783166,
136.051008339035));
#193338=CARTESIAN_POINT('Ctrl Pts',(-152.903973644199,2.24485676634579,
137.016820189321));
#193339=CARTESIAN_POINT('Ctrl Pts',(-153.182421268012,6.44011809960154,
132.273685188686));
#193340=CARTESIAN_POINT('Ctrl Pts',(-153.460868891824,4.71722551658265,
126.180312687687));
#193341=CARTESIAN_POINT('Ctrl Pts',(-153.739316515637,-1.34056686689732,
124.336214336947));
#193342=CARTESIAN_POINT('Ctrl Pts',(-154.01776413945,-6.16644379003131,
128.436026431582));
#193343=CARTESIAN_POINT('Ctrl Pts',(-154.296211763263,-5.32566011765276,
134.712221943579));
#193344=CARTESIAN_POINT('Ctrl Pts',(-154.574659387076,0.409145029887599,
137.397283806609));
#193345=CARTESIAN_POINT('Ctrl Pts',(-154.853107010889,5.7679658828075,134.023771341112));
#193346=CARTESIAN_POINT('Ctrl Pts',(-155.131554634702,5.82630787022557,
127.691777697632));
#193347=CARTESIAN_POINT('Ctrl Pts',(-155.410002258515,0.530557555869813,
124.220095699443));
#193348=CARTESIAN_POINT('Ctrl Pts',(-155.688449882327,-5.25274923315307,
126.799031501784));
#193349=CARTESIAN_POINT('Ctrl Pts',(-155.96689750614,-6.20903608797397,
133.058669090323));
#193350=CARTESIAN_POINT('Ctrl Pts',(-156.245345129953,-1.4595221062231,
137.246707321489));
#193351=CARTESIAN_POINT('Ctrl Pts',(-156.523792753766,4.63122138952822,
135.514543657883));
#193352=CARTESIAN_POINT('Ctrl Pts',(-156.802240377579,6.46609867604585,
129.453951885458));
#193353=CARTESIAN_POINT('Ctrl Pts',(-157.080688001392,2.35894716575843,
124.634319766706));
#193354=CARTESIAN_POINT('Ctrl Pts',(-157.359135625205,-3.9159615488849,
125.484653766641));
#193355=CARTESIAN_POINT('Ctrl Pts',(-157.637583249018,-6.59229290546042,
131.223538480449));
#193356=CARTESIAN_POINT('Ctrl Pts',(-157.916030872831,-3.21062913332988,
136.577219216243));
#193357=CARTESIAN_POINT('Ctrl Pts',(-158.194478496644,3.12144596437753,
136.625924919674));
#193358=CARTESIAN_POINT('Ctrl Pts',(-158.472926120456,6.58506471193526,
131.324897428694));
#193359=CARTESIAN_POINT('Ctrl Pts',(-158.751373744269,3.99733068751967,
125.545522037924));
#193360=CARTESIAN_POINT('Ctrl Pts',(-159.029821368082,-2.26375495826568,
124.598762393297));
#193361=CARTESIAN_POINT('Ctrl Pts',(-159.308268991895,-6.44456038798308,
129.354644356446));
#193362=CARTESIAN_POINT('Ctrl Pts',(-159.586716615708,-4.7031296554214,
135.442744740987));
#193363=CARTESIAN_POINT('Ctrl Pts',(-159.865164239521,1.36024746981527,
137.268396713766));
#193364=CARTESIAN_POINT('Ctrl Pts',(-160.143611863334,6.17362362207528,
133.153915299856));
#193365=CARTESIAN_POINT('Ctrl Pts',(-160.422059487147,5.31374126392856,
126.880307915048));
#193366=CARTESIAN_POINT('Ctrl Pts',(-160.70050711096,-0.429209725076344,
124.212713263223));
#193367=CARTESIAN_POINT('Ctrl Pts',(-160.978954734773,-5.77773794479658,
127.602520510164));
#193368=CARTESIAN_POINT('Ctrl Pts',(-161.257402358585,-5.81680725143943,
133.934662397221));
#193369=CARTESIAN_POINT('Ctrl Pts',(-161.535849982398,-0.51051486084124,
137.390209872519));
#193370=CARTESIAN_POINT('Ctrl Pts',(-161.814297606211,5.26491574683228,
134.793683619137));
#193371=CARTESIAN_POINT('Ctrl Pts',(-162.092745230024,6.20214598860049,
128.531164416574));
#193372=CARTESIAN_POINT('Ctrl Pts',(-162.371192853837,1.43990705852047,
124.357601470914));
#193373=CARTESIAN_POINT('Ctrl Pts',(-162.64964047765,-4.64553611496906,
126.108295239334));
#193374=CARTESIAN_POINT('Ctrl Pts',(-162.928088101462,-6.46195854585841,
132.1744436748));
#193375=CARTESIAN_POINT('Ctrl Pts',(-163.206535725276,-2.34015675732853,
136.981552712947));
#193376=CARTESIAN_POINT('Ctrl Pts',(-163.484983349088,3.93213476817268,
136.112123988049));
#193377=CARTESIAN_POINT('Ctrl Pts',(-163.763430972902,6.5909865371863,130.365120024332));
#193378=CARTESIAN_POINT('Ctrl Pts',(-164.041878596714,3.19304366611785,
125.021756707701));
#193379=CARTESIAN_POINT('Ctrl Pts',(-164.320326220527,-3.13915034525769,
124.99232388833));
#193380=CARTESIAN_POINT('Ctrl Pts',(-164.59877384434,-6.58661854536123,
130.303868889347));
#193381=CARTESIAN_POINT('Ctrl Pts',(-164.877221468153,-3.98130607648258,
136.075341338217));
#193382=CARTESIAN_POINT('Ctrl Pts',(-165.155669091966,2.28263217906914,
137.003040006531));
#193383=CARTESIAN_POINT('Ctrl Pts',(-165.434116715779,6.44894297483741,
132.23445513871));
#193384=CARTESIAN_POINT('Ctrl Pts',(-165.712564339591,4.6889902251094,126.151683269957));
#193385=CARTESIAN_POINT('Ctrl Pts',(-165.991011963405,-1.37991547158711,
124.344494587733));
#193386=CARTESIAN_POINT('Ctrl Pts',(-166.269459587217,-6.18074626251326,
128.473607204924));
#193387=CARTESIAN_POINT('Ctrl Pts',(-166.54790721103,-5.3017731844313,134.744568344699));
#193388=CARTESIAN_POINT('Ctrl Pts',(-166.826354834843,0.449270444124704,
137.394671073086));
#193389=CARTESIAN_POINT('Ctrl Pts',(-167.104802458656,5.78745648261092,
133.988600447415));
#193390=CARTESIAN_POINT('Ctrl Pts',(-167.383250082469,5.8072527465451,127.656368976875));
#193391=CARTESIAN_POINT('Ctrl Pts',(-167.661697706282,0.490467436472931,
124.216988036188));
#193392=CARTESIAN_POINT('Ctrl Pts',(-167.940145330095,-5.27703348705155,
126.831080686747));
#193393=CARTESIAN_POINT('Ctrl Pts',(-168.218592953908,-6.19519843339338,
133.096423488211));
#193394=CARTESIAN_POINT('Ctrl Pts',(-168.49704057772,-1.42027867171577,
137.255472485049));
#193395=CARTESIAN_POINT('Ctrl Pts',(-168.775488201534,4.65980780479824,
135.486264830004));
#193396=CARTESIAN_POINT('Ctrl Pts',(-169.053935825346,6.45775855296945,
129.414615927465));
#193397=CARTESIAN_POINT('Ctrl Pts',(-169.332383449159,2.32134467000579,
124.620074502325));
#193398=CARTESIAN_POINT('Ctrl Pts',(-169.610831072972,-3.94827156070164,
125.508589897919));
#193399=CARTESIAN_POINT('Ctrl Pts',(-169.889278696785,-6.58961911091297,
131.263659872085));
#193400=CARTESIAN_POINT('Ctrl Pts',(-170.167726320598,-3.17542861898582,
136.596656269364));
#193401=CARTESIAN_POINT('Ctrl Pts',(-170.446173944411,3.15682564547787,
136.606815932013));
#193402=CARTESIAN_POINT('Ctrl Pts',(-170.724621568223,6.58811136125304,
131.284802626386));
#193403=CARTESIAN_POINT('Ctrl Pts',(-171.003069192037,3.96524458316956,
125.521286585549));
#193404=CARTESIAN_POINT('Ctrl Pts',(-171.28151681585,-2.30148825387982,
124.612657487621));
#193405=CARTESIAN_POINT('Ctrl Pts',(-171.559964439662,-6.45326581956532,
129.393901084596));
#193406=CARTESIAN_POINT('Ctrl Pts',(-171.838412063475,-4.67480735663214,
135.471288087592));
#193407=CARTESIAN_POINT('Ctrl Pts',(-172.116859687288,1.39957069001038,
137.259996737715));
#193408=CARTESIAN_POINT('Ctrl Pts',(-172.395307311101,6.18781164536257,
133.116291168777));
#193409=CARTESIAN_POINT('Ctrl Pts',(-172.673754934914,5.289755990031,126.848034367363));
#193410=CARTESIAN_POINT('Ctrl Pts',(-172.952202558727,-0.469327001192524,
124.215448112602));
#193411=CARTESIAN_POINT('Ctrl Pts',(-173.23065018254,-5.79712140621875,
127.637750563632));
#193412=CARTESIAN_POINT('Ctrl Pts',(-173.509097806352,-5.79764444405506,
133.970012956726));
#193413=CARTESIAN_POINT('Ctrl Pts',(-173.787545430165,-0.470415468481743,
137.393195500846));
#193414=CARTESIAN_POINT('Ctrl Pts',(-174.065993053978,5.28910234155359,
134.76156066971));
#193415=CARTESIAN_POINT('Ctrl Pts',(-174.344440677791,6.18819348671444,
128.493452310623));
#193416=CARTESIAN_POINT('Ctrl Pts',(-174.622888301604,1.40063712764339,
124.34895579147));
#193417=CARTESIAN_POINT('Ctrl Pts',(-174.901335925417,-4.67403632680454,
126.13666094344));
#193418=CARTESIAN_POINT('Ctrl Pts',(-175.17978354923,-6.45349873628761,
132.213754066126));
#193419=CARTESIAN_POINT('Ctrl Pts',(-175.458231173043,-2.30251107806296,
136.995683462282));
#193420=CARTESIAN_POINT('Ctrl Pts',(-175.736678796856,3.96437177698222,
136.088089627079));
#193421=CARTESIAN_POINT('Ctrl Pts',(-176.015126420669,6.58819063930867,
130.325006956645));
#193422=CARTESIAN_POINT('Ctrl Pts',(-176.293574044481,3.15778415511627,
125.002426882869));
#193423=CARTESIAN_POINT('Ctrl Pts',(-176.572021668294,-3.17447170129595,
125.011540471058));
#193424=CARTESIAN_POINT('Ctrl Pts',(-176.850469292107,-6.58954314578118,
130.343972778891));
#193425=CARTESIAN_POINT('Ctrl Pts',(-177.12891691592,-3.94914635637289,
136.099479019269));
#193426=CARTESIAN_POINT('Ctrl Pts',(-177.407364539733,2.32032300801719,
136.989030129397));
#193427=CARTESIAN_POINT('Ctrl Pts',(-177.685812163546,6.45752888212044,
132.195172096054));
#193428=CARTESIAN_POINT('Ctrl Pts',(-177.964259787359,4.66058118137817,
126.123226258898));
#193429=CARTESIAN_POINT('Ctrl Pts',(-178.242707411172,-1.41921294300185,
124.353014211231));
#193430=CARTESIAN_POINT('Ctrl Pts',(-178.521155034985,-6.19481970517025,
128.511274345191));
#193431=CARTESIAN_POINT('Ctrl Pts',(-178.799602658797,-5.27768979205393,
134.776768739972));
#193432=CARTESIAN_POINT('Ctrl Pts',(-179.078050282611,0.489379210479558,
137.391814133187));
#193433=CARTESIAN_POINT('Ctrl Pts',(-179.356497906423,5.80673262608622,
133.95331156054));
#193434=CARTESIAN_POINT('Ctrl Pts',(-179.634945530236,5.7879824329786,127.621076906106));
#193435=CARTESIAN_POINT('Ctrl Pts',(-179.913393154049,0.450359142625426,
124.214124470449));
#193436=CARTESIAN_POINT('Ctrl Pts',(-180.191840777862,-5.30112219853358,
126.863277103057));
#193437=CARTESIAN_POINT('Ctrl Pts',(-180.470288401675,-6.18113121345664,
133.134092952866));
#193438=CARTESIAN_POINT('Ctrl Pts',(-180.748736025488,-1.38098260826046,
137.263998600285));
#193439=CARTESIAN_POINT('Ctrl Pts',(-181.0271836493,4.68822154917632,135.457812512445));
#193440=CARTESIAN_POINT('Ctrl Pts',(-181.305631273113,6.44917913527537,
129.375331466973));
#193441=CARTESIAN_POINT('Ctrl Pts',(-181.584078896926,2.28365615597197,
124.606058398942));
#193442=CARTESIAN_POINT('Ctrl Pts',(-181.862526520739,-3.98043526786393,
125.532722265928));
#193443=CARTESIAN_POINT('Ctrl Pts',(-182.140974144552,-6.58670113560653,
131.303764244219));
#193444=CARTESIAN_POINT('Ctrl Pts',(-182.419421768365,-3.14011043796568,
136.615878686839));
#193445=CARTESIAN_POINT('Ctrl Pts',(-182.697869392178,3.19208834924215,
136.587491932238));
#193446=CARTESIAN_POINT('Ctrl Pts',(-182.976317015991,6.59091388568205,
131.244690021124));
#193447=CARTESIAN_POINT('Ctrl Pts',(-183.254764639804,3.93301154522339,
125.497246899427));
#193448=CARTESIAN_POINT('Ctrl Pts',(-183.533212263617,-2.33913626699958,
124.626782017781));
#193449=CARTESIAN_POINT('Ctrl Pts',(-183.811659887429,-6.46173212300977,
129.433210077844));
#193450=CARTESIAN_POINT('Ctrl Pts',(-184.090107511242,-4.64631183113728,
135.499658499484));
#193451=CARTESIAN_POINT('Ctrl Pts',(-184.368555135055,1.43884204859816,
137.251357545694));
#193452=CARTESIAN_POINT('Ctrl Pts',(-184.647002758868,6.20177037701405,
133.078581368264));
#193453=CARTESIAN_POINT('Ctrl Pts',(-184.925450382681,5.26557470227994,
126.815907422802));
#193454=CARTESIAN_POINT('Ctrl Pts',(-185.203898006494,-0.50942688622466,
124.218427116558));
#193455=CARTESIAN_POINT('Ctrl Pts',(-185.482345630307,-5.81629005317544,
127.673097957001));
#193456=CARTESIAN_POINT('Ctrl Pts',(-185.76079325412,-5.77826680282389,
134.005246211819));
#193457=CARTESIAN_POINT('Ctrl Pts',(-186.039240877932,-0.430298644703365,
137.395936977472));
#193458=CARTESIAN_POINT('Ctrl Pts',(-186.317688501746,5.31309294664177,
134.729291084778));
#193459=CARTESIAN_POINT('Ctrl Pts',(-186.596136125558,6.17401167904375,
128.455825836229));
#193460=CARTESIAN_POINT('Ctrl Pts',(-186.874583749371,1.36131529564269,
124.340549319425));
#193461=CARTESIAN_POINT('Ctrl Pts',(-187.153031373184,-4.70236334050424,
126.165199610876));
#193462=CARTESIAN_POINT('Ctrl Pts',(-187.431478996997,-6.44479978994851,
132.253012231859));
#193463=CARTESIAN_POINT('Ctrl Pts',(-187.70992662081,-2.26478007840253,
137.009584789872));
#193464=CARTESIAN_POINT('Ctrl Pts',(-187.988374244623,3.99646188453734,
136.063859475589));
#193465=CARTESIAN_POINT('Ctrl Pts',(-188.266821868436,6.58515061360439,
130.284911651585));
#193466=CARTESIAN_POINT('Ctrl Pts',(-188.545269492249,3.12240763126122,
124.983312050825));
#193467=CARTESIAN_POINT('Ctrl Pts',(-188.823717116061,-3.20967542611822,
125.030971708867));
#193468=CARTESIAN_POINT('Ctrl Pts',(-189.102164739874,-6.59222356825658,
130.384093728275));
#193469=CARTESIAN_POINT('Ctrl Pts',(-189.380612363687,-3.91684029919248,
136.123420487763));
#193470=CARTESIAN_POINT('Ctrl Pts',(-189.6590599875,2.35792785654334,136.974791077059));
#193471=CARTESIAN_POINT('Ctrl Pts',(-189.937507611313,6.46587550329532,
132.155837516369));
#193472=CARTESIAN_POINT('Ctrl Pts',(-190.215955235126,4.63199943809816,
126.094942708994));
#193473=CARTESIAN_POINT('Ctrl Pts',(-190.494402858939,-1.45845782495887,
124.361772891742));
#193474=CARTESIAN_POINT('Ctrl Pts',(-190.772850482752,-6.2086635965042,
128.549026456613));
#193475=CARTESIAN_POINT('Ctrl Pts',(-191.051298106565,-5.25341083294129,
134.808821936201));
#193476=CARTESIAN_POINT('Ctrl Pts',(-191.329745730377,0.529469842708527,
137.388713092773));
#193477=CARTESIAN_POINT('Ctrl Pts',(-191.60819335419,5.82579359894846,133.91790598813));
#193478=CARTESIAN_POINT('Ctrl Pts',(-191.886640978003,5.76849764359442,
127.585902793086));
#193479=CARTESIAN_POINT('Ctrl Pts',(-192.165088601816,0.410234160553658,
124.211505108333));
#193480=CARTESIAN_POINT('Ctrl Pts',(-192.443536225629,-5.32501447498302,
126.895619557667));
#193481=CARTESIAN_POINT('Ctrl Pts',(-192.721983849442,-6.16683494942961,
133.171676088433));
#193482=CARTESIAN_POINT('Ctrl Pts',(-193.000431473255,-1.34163537198624,
137.272285351261));
#193483=CARTESIAN_POINT('Ctrl Pts',(-193.278879097068,4.71646156978089,
135.429187759513));
#193484=CARTESIAN_POINT('Ctrl Pts',(-193.557326720881,6.44036074087642,
129.336099959682));
#193485=CARTESIAN_POINT('Ctrl Pts',(-193.835774344694,2.24588302022023,
124.592271975924));
#193486=CARTESIAN_POINT('Ctrl Pts',(-194.114221968506,-4.01245147853337,
125.557049976435));
#193487=CARTESIAN_POINT('Ctrl Pts',(-194.392669592319,-6.58353908766677,
131.343850110767));
#193488=CARTESIAN_POINT('Ctrl Pts',(-194.671117216133,-3.10467589899933,
136.634885756375));
#193489=CARTESIAN_POINT('Ctrl Pts',(-194.949564839945,3.22723276899961,
136.567953636405));
#193490=CARTESIAN_POINT('Ctrl Pts',(-195.228012463758,6.59347218137276,
131.204561099293));
#193491=CARTESIAN_POINT('Ctrl Pts',(-195.506460087571,3.90063276808784,
125.473403870355));
#193492=CARTESIAN_POINT('Ctrl Pts',(-195.784907711384,-2.3766976025655,
124.641135460387));
#193493=CARTESIAN_POINT('Ctrl Pts',(-196.063355335197,-6.46995898459376,
129.472569879579));
#193494=CARTESIAN_POINT('Ctrl Pts',(-196.34180295901,-4.61764413484867,
135.527854925386));
#193495=CARTESIAN_POINT('Ctrl Pts',(-196.620250582823,1.47806009036541,
137.242479457832));
#193496=CARTESIAN_POINT('Ctrl Pts',(-196.898698206635,6.21549929978325,
133.040787295662));
#193497=CARTESIAN_POINT('Ctrl Pts',(-197.177145830448,5.24119829672186,
126.783928271841));
#193498=CARTESIAN_POINT('Ctrl Pts',(-197.455593454261,-0.5495078942556,
124.2216501647));
#193499=CARTESIAN_POINT('Ctrl Pts',(-197.734041078074,-5.83524317536515,
127.708561380459));
#193500=CARTESIAN_POINT('Ctrl Pts',(-198.012488701887,-5.75867504579123,
134.040360856918));
#193501=CARTESIAN_POINT('Ctrl Pts',(-198.2909363257,-0.390165876051177,
137.398434200813));
#193502=CARTESIAN_POINT('Ctrl Pts',(-198.569383949513,5.33688667311775,
134.696876060105));
#193503=CARTESIAN_POINT('Ctrl Pts',(-198.847831573325,6.15960109109908,
128.418286387655));
#193504=CARTESIAN_POINT('Ctrl Pts',(-199.126279197139,1.32194301960288,
124.332382366286));
#193505=CARTESIAN_POINT('Ctrl Pts',(-199.404726820951,-4.73051610640191,
126.193910184127));
#193506=CARTESIAN_POINT('Ctrl Pts',(-199.683174444764,-6.43586202918244,
132.292216717274));
#193507=CARTESIAN_POINT('Ctrl Pts',(-199.961622068577,-2.22696515648391,
137.023256180599));
#193508=CARTESIAN_POINT('Ctrl Pts',(-200.24006969239,4.02840390172748,136.039434431435));
#193509=CARTESIAN_POINT('Ctrl Pts',(-200.518517316203,6.58186657272242,
130.244835594899));
#193510=CARTESIAN_POINT('Ctrl Pts',(-200.796964940016,3.08691540544346,
124.964412919876));
#193511=CARTESIAN_POINT('Ctrl Pts',(-201.075412563829,-3.24476021523692,
125.050616881724));
#193512=CARTESIAN_POINT('Ctrl Pts',(-201.353860187642,-6.59465971346335,
130.424230250803));
#193513=CARTESIAN_POINT('Ctrl Pts',(-201.632307811455,-3.88438910205457,
136.147164856536));
#193514=CARTESIAN_POINT('Ctrl Pts',(-201.910755435267,2.39544533118521,
136.960323377152));
#193515=CARTESIAN_POINT('Ctrl Pts',(-202.18920305908,6.47398252907625,132.116452857208));
#193516=CARTESIAN_POINT('Ctrl Pts',(-202.467650682893,4.60324605437475,
126.066833668302));
#193517=CARTESIAN_POINT('Ctrl Pts',(-202.746098306706,-1.49764866322506,
124.370770304711));
#193518=CARTESIAN_POINT('Ctrl Pts',(-203.024545930519,-6.22227742352606,
128.586862140274));
#193519=CARTESIAN_POINT('Ctrl Pts',(-203.302993554332,-5.22893720675747,
134.840726745644));
#193520=CARTESIAN_POINT('Ctrl Pts',(-203.581441178145,0.569540855237039,
137.385368066758));
#193521=CARTESIAN_POINT('Ctrl Pts',(-203.859888801958,5.84463869488665,
133.882385042152));
#193522=CARTESIAN_POINT('Ctrl Pts',(-204.138336425771,5.7487991004088,127.550847941203));
#193523=CARTESIAN_POINT('Ctrl Pts',(-204.416784049583,0.370093977104817,
124.209130046901));
#193524=CARTESIAN_POINT('Ctrl Pts',(-204.695231673396,-5.34870943106288,
126.928106852114));
#193525=CARTESIAN_POINT('Ctrl Pts',(-204.973679297209,-6.15231017106575,
133.209171502253));
#193526=CARTESIAN_POINT('Ctrl Pts',(-205.252126921022,-1.30223842092043,
137.280332430907));
#193527=CARTESIAN_POINT('Ctrl Pts',(-205.530574544835,4.74452682016742,
135.400391631911));
#193528=CARTESIAN_POINT('Ctrl Pts',(-205.809022168648,6.43130369654214,
129.296922859329));
#193529=CARTESIAN_POINT('Ctrl Pts',(-206.087469792461,2.20802666244648,
124.578715744137));
#193530=CARTESIAN_POINT('Ctrl Pts',(-206.365917416273,-4.04431900633787,
125.581572127967));
#193531=CARTESIAN_POINT('Ctrl Pts',(-206.644365040087,-6.58013308426553,
131.383915986335));
#193532=CARTESIAN_POINT('Ctrl Pts',(-206.922812663899,-3.06912631512495,
136.653676773657));
#193533=CARTESIAN_POINT('Ctrl Pts',(-207.201260287713,3.26225760245914,
136.548201768512));
#193534=CARTESIAN_POINT('Ctrl Pts',(-207.479707911525,6.59578615352751,
131.164417347887));
#193535=CARTESIAN_POINT('Ctrl Pts',(-207.758155535338,3.86810945157081,
125.449758381845));
#193536=CARTESIAN_POINT('Ctrl Pts',(-208.036603159151,-2.41417086872696,
124.655717283569));
#193537=CARTESIAN_POINT('Ctrl Pts',(-208.315050782964,-6.47794609946865,
129.511979031309));
#193538=CARTESIAN_POINT('Ctrl Pts',(-208.593498406777,-4.58880533005852,
135.555876320469));
#193539=CARTESIAN_POINT('Ctrl Pts',(-208.87194603059,1.51722336207232,137.233362803106));
#193540=CARTESIAN_POINT('Ctrl Pts',(-209.150393654402,6.22899790494034,
133.00291035145));
#193541=CARTESIAN_POINT('Ctrl Pts',(-209.428841278216,5.21662767663345,
126.752098099478));
#193542=CARTESIAN_POINT('Ctrl Pts',(-209.707288902028,-0.589568540070009,
124.225117137599));
#193543=CARTESIAN_POINT('Ctrl Pts',(-209.985736525842,-5.85398007047323,
127.744139519898));
#193544=CARTESIAN_POINT('Ctrl Pts',(-210.264184149654,-5.73886989893714,
134.07535559084));
#193545=CARTESIAN_POINT('Ctrl Pts',(-210.542631773467,-0.350018649658268,
137.400687078332));
#193546=CARTESIAN_POINT('Ctrl Pts',(-210.82107939728,5.36048263929459,134.664316796842));
#193547=CARTESIAN_POINT('Ctrl Pts',(-211.099527021093,6.14496225687153,
128.38083535594));
#193548=CARTESIAN_POINT('Ctrl Pts',(-211.377974644906,1.28252175847855,
124.324455234681));
#193549=CARTESIAN_POINT('Ctrl Pts',(-211.656422268719,-4.75849358128477,
126.222791599316));
#193550=CARTESIAN_POINT('Ctrl Pts',(-211.934869892531,-6.4266857851828,
132.331366069634));
#193551=CARTESIAN_POINT('Ctrl Pts',(-212.213317516344,-2.18906771355195,
137.036697127864));
#193552=CARTESIAN_POINT('Ctrl Pts',(-212.491765140157,4.06019664492976,
136.014815399695));
#193553=CARTESIAN_POINT('Ctrl Pts',(-212.770212763971,6.57833863835413,
130.204780271616));
#193554=CARTESIAN_POINT('Ctrl Pts',(-213.048660387783,3.05130879283982,
124.945730190337));
#193555=CARTESIAN_POINT('Ctrl Pts',(-213.327108011596,-3.27972476857289,
125.070475261673));
#193556=CARTESIAN_POINT('Ctrl Pts',(-213.605555635409,-6.59685149112928,
130.464380859201));
#193557=CARTESIAN_POINT('Ctrl Pts',(-213.884003259222,-3.85179396744981,
136.170711245733));
#193558=CARTESIAN_POINT('Ctrl Pts',(-214.162450883035,2.43287404171984,
136.94562756578));
#193559=CARTESIAN_POINT('Ctrl Pts',(-214.440898506847,6.48184965905313,
132.077019577989));
#193560=CARTESIAN_POINT('Ctrl Pts',(-214.71934613066,4.57432209567675,126.038900178414));
#193561=CARTESIAN_POINT('Ctrl Pts',(-214.997793754473,-1.53678400556905,
124.380006116735));
#193562=CARTESIAN_POINT('Ctrl Pts',(-215.276241378286,-6.23566068176903,
128.624779994154));
#193563=CARTESIAN_POINT('Ctrl Pts',(-215.554689002099,-5.20426982038336,
134.872481986055));
#193564=CARTESIAN_POINT('Ctrl Pts',(-215.833136625912,0.609590763220439,
137.381779179092));
#193565=CARTESIAN_POINT('Ctrl Pts',(-216.111584249725,5.86326721558844,
133.846750038845));
#193566=CARTESIAN_POINT('Ctrl Pts',(-216.390031873537,5.72888753335829,
127.51591364943));
#193567=CARTESIAN_POINT('Ctrl Pts',(-216.668479497351,0.329940079686948,
124.206999374164));
#193568=CARTESIAN_POINT('Ctrl Pts',(-216.946927121163,-5.37220618874772,
126.960737782571));
#193569=CARTESIAN_POINT('Ctrl Pts',(-217.225374744977,-6.13755741658593,
133.246577804923));
#193570=CARTESIAN_POINT('Ctrl Pts',(-217.503822368789,-1.26279321493052,
137.288139541036));
#193571=CARTESIAN_POINT('Ctrl Pts',(-217.782269992602,4.77241626036792,
135.37142519669));
#193572=CARTESIAN_POINT('Ctrl Pts',(-218.060717616415,6.4220083378839,129.257801617636));
#193573=CARTESIAN_POINT('Ctrl Pts',(-218.339165240228,2.17008848543354,
124.565390205911));
#193574=CARTESIAN_POINT('Ctrl Pts',(-218.617612864041,-4.07603667041411,
125.606287811847));
#193575=CARTESIAN_POINT('Ctrl Pts',(-218.896060487854,-6.57648325161253,
131.423960386264));
#193576=CARTESIAN_POINT('Ctrl Pts',(-219.174508111666,-3.03346300364714,
136.672251042379));
#193577=CARTESIAN_POINT('Ctrl Pts',(-219.45295573548,3.29716155176439,136.528237060474));
#193578=CARTESIAN_POINT('Ctrl Pts',(-219.731403359293,6.59785571640026,
131.124260254445));
#193579=CARTESIAN_POINT('Ctrl Pts',(-220.009850983105,3.83544280083539,
125.426311310091));
#193580=CARTESIAN_POINT('Ctrl Pts',(-220.288298606918,-2.45155467689987,
124.67052694699));
#193581=CARTESIAN_POINT('Ctrl Pts',(-220.566746230731,-6.48569317166813,
129.551436072715));
#193582=CARTESIAN_POINT('Ctrl Pts',(-220.845193854544,-4.55979648539947,
135.58372164639));
#193583=CARTESIAN_POINT('Ctrl Pts',(-221.123641478357,1.55633041250914,
137.224007919343));
#193584=CARTESIAN_POINT('Ctrl Pts',(-221.40208910217,6.24226569228925,132.964951939167));
#193585=CARTESIAN_POINT('Ctrl Pts',(-221.680536725983,5.19186375248807,
126.720418085194));
#193586=CARTESIAN_POINT('Ctrl Pts',(-221.958984349796,-0.629607339204784,
124.228827906785));
#193587=CARTESIAN_POINT('Ctrl Pts',(-222.237431973609,-5.87250004419688,
127.779831056953));
#193588=CARTESIAN_POINT('Ctrl Pts',(-222.515879597421,-5.71885209614835,
134.110229116839));
#193589=CARTESIAN_POINT('Ctrl Pts',(-222.794327221234,-0.309858453196267,
137.402695526548));
#193590=CARTESIAN_POINT('Ctrl Pts',(-223.072774845047,5.38387997081673,
134.631614501482));
#193591=CARTESIAN_POINT('Ctrl Pts',(-223.35122246886,6.13009571880702,128.343474128844));
#193592=CARTESIAN_POINT('Ctrl Pts',(-223.629670092673,1.24305297303857,
124.316768218352));
#193593=CARTESIAN_POINT('Ctrl Pts',(-223.908117716486,-4.78629472843886,
126.25184278623));
#193594=CARTESIAN_POINT('Ctrl Pts',(-224.186565340298,-6.41727139797729,
132.370458838244));
#193595=CARTESIAN_POINT('Ctrl Pts',(-224.465012964112,-2.15108915391133,
137.049907133607));
#193596=CARTESIAN_POINT('Ctrl Pts',(-224.743460587925,4.09183893605206,
135.990003292637));
#193597=CARTESIAN_POINT('Ctrl Pts',(-225.021908211737,6.57456694122844,
130.164747166004));
#193598=CARTESIAN_POINT('Ctrl Pts',(-225.300355835551,3.01558911286705,
124.927264554503));
#193599=CARTESIAN_POINT('Ctrl Pts',(-225.578803459363,-3.31456779050113,
125.090546112851));
#193600=CARTESIAN_POINT('Ctrl Pts',(-225.857251083176,-6.5987988200372,
130.504544065675));
#193601=CARTESIAN_POINT('Ctrl Pts',(-226.135698706989,-3.8190561032033,
136.194058782834));
#193602=CARTESIAN_POINT('Ctrl Pts',(-226.414146330802,2.47021260121173,
136.930704187504));
#193603=CARTESIAN_POINT('Ctrl Pts',(-226.692593954615,6.48947660170784,
132.037539139922));
#193604=CARTESIAN_POINT('Ctrl Pts',(-226.971041578427,4.54522863379049,
126.011143274415));
#193605=CARTESIAN_POINT('Ctrl Pts',(-227.24948920224,-1.57586240181677,
124.389479985577));
#193606=CARTESIAN_POINT('Ctrl Pts',(-227.527936826054,-6.24881287531301,
128.662778613197));
#193607=CARTESIAN_POINT('Ctrl Pts',(-227.806384449866,-5.17940958787633,
134.904086480733));
#193608=CARTESIAN_POINT('Ctrl Pts',(-228.084832073679,0.649618082593193,
137.377946562762));
#193609=CARTESIAN_POINT('Ctrl Pts',(-228.363279697492,5.88167847076755,
133.811002298682));
#193610=CARTESIAN_POINT('Ctrl Pts',(-228.641727321305,5.70876368027354,
127.481101212267));
#193611=CARTESIAN_POINT('Ctrl Pts',(-228.920174945118,0.289773956218704,
124.205113169075));
#193612=CARTESIAN_POINT('Ctrl Pts',(-229.198622568931,-5.39550387735667,
126.993511139885));
#193613=CARTESIAN_POINT('Ctrl Pts',(-229.477070192744,-6.12257723265909,
133.283893610337));
#193614=CARTESIAN_POINT('Ctrl Pts',(-229.755517816557,-1.22330121567356,
137.295706392352));
#193615=CARTESIAN_POINT('Ctrl Pts',(-230.033965440369,4.80012885692891,
135.34228952721));
#193616=CARTESIAN_POINT('Ctrl Pts',(-230.312413064183,6.41247500934538,
129.218737684256));
#193617=CARTESIAN_POINT('Ctrl Pts',(-230.590860687995,2.13206989499296,
124.552295855027));
#193618=CARTESIAN_POINT('Ctrl Pts',(-230.869308311808,-4.10760329545278,
125.631196112227));
#193619=CARTESIAN_POINT('Ctrl Pts',(-231.147755935621,-6.5725897249546,
131.463981826697));
#193620=CARTESIAN_POINT('Ctrl Pts',(-231.426203559434,-2.99768728608136,
136.690607874263));
#193621=CARTESIAN_POINT('Ctrl Pts',(-231.704651183247,3.33194332353496,
136.508060252089));
#193622=CARTESIAN_POINT('Ctrl Pts',(-231.98309880706,6.59968079330357,131.084091307006));
#193623=CARTESIAN_POINT('Ctrl Pts',(-232.261546430872,3.80263402635669,
125.403063523931));
#193624=CARTESIAN_POINT('Ctrl Pts',(-232.539994054686,-2.48884764181187,
124.685563901874));
#193625=CARTESIAN_POINT('Ctrl Pts',(-232.818441678498,-6.49319991412244,
129.5909395417));
#193626=CARTESIAN_POINT('Ctrl Pts',(-233.096889302311,-4.53061867580467,
135.611389871331));
#193627=CARTESIAN_POINT('Ctrl Pts',(-233.375336926124,1.59537979255065,
137.214415153187));
#193628=CARTESIAN_POINT('Ctrl Pts',(-233.653784549937,6.25530217018742,
132.926913465378));
#193629=CARTESIAN_POINT('Ctrl Pts',(-233.93223217375,5.16690744192206,126.688889402902));
#193630=CARTESIAN_POINT('Ctrl Pts',(-234.210679797563,-0.669622808008655,
124.232782334755));
#193631=CARTESIAN_POINT('Ctrl Pts',(-234.489127421376,-5.89080241027189,
127.815634669064));
#193632=CARTESIAN_POINT('Ctrl Pts',(-234.767575045188,-5.69862237919218,
134.144980142666));
#193633=CARTESIAN_POINT('Ctrl Pts',(-235.046022669002,-0.269686774814632,
137.404459471037));
#193634=CARTESIAN_POINT('Ctrl Pts',(-235.324470292814,5.40707780068583,
134.598770385822));
#193635=CARTESIAN_POINT('Ctrl Pts',(-235.602917916627,6.11500202779203,
128.306204090801));
#193636=CARTESIAN_POINT('Ctrl Pts',(-235.88136554044,1.20353812581378,124.309321602146));
#193637=CARTESIAN_POINT('Ctrl Pts',(-236.159813164253,-4.81391851768082,
126.281062668365));
#193638=CARTESIAN_POINT('Ctrl Pts',(-236.438260788066,-6.40761921642086,
132.40949357451));
#193639=CARTESIAN_POINT('Ctrl Pts',(-236.716708411879,-2.11303088487057,
137.062885708328));
#193640=CARTESIAN_POINT('Ctrl Pts',(-236.995156035692,4.12332960257798,
135.964999029683));
#193641=CARTESIAN_POINT('Ctrl Pts',(-237.273603659505,6.57055162110693,
130.124737761504));
#193642=CARTESIAN_POINT('Ctrl Pts',(-237.552051283318,2.97975768913041,
124.909016696624));
#193643=CARTESIAN_POINT('Ctrl Pts',(-237.83049890713,-3.34928798990126,
125.110828691528));
#193644=CARTESIAN_POINT('Ctrl Pts',(-238.108946530943,-6.60050162802816,
130.544718381962));
#193645=CARTESIAN_POINT('Ctrl Pts',(-238.387394154756,-3.7861767224282,
136.217206602688));
#193646=CARTESIAN_POINT('Ctrl Pts',(-238.665841778569,2.5074596260677,136.915553795314));
#193647=CARTESIAN_POINT('Ctrl Pts',(-238.944289402382,6.49686307441993,
131.998013005973));
#193648=CARTESIAN_POINT('Ctrl Pts',(-239.222737026195,4.51596674678651,
125.983563984846));
#193649=CARTESIAN_POINT('Ctrl Pts',(-239.501184650008,-1.61488240390346,
124.399191560181));
#193650=CARTESIAN_POINT('Ctrl Pts',(-239.77963227382,-6.26173351679718,
128.700856589348));
#193651=CARTESIAN_POINT('Ctrl Pts',(-240.058079897633,-5.15435743044315,
134.935539058562));
#193652=CARTESIAN_POINT('Ctrl Pts',(-240.336527521446,0.689621330129741,
137.373870359787));
#193653=CARTESIAN_POINT('Ctrl Pts',(-240.614975145259,5.89987177818775,
133.775143146303));
#193654=CARTESIAN_POINT('Ctrl Pts',(-240.893422769072,5.68842828685113,
127.446411919705));
#193655=CARTESIAN_POINT('Ctrl Pts',(-241.171870392886,0.249597095069331,
124.203471501526));
#193656=CARTESIAN_POINT('Ctrl Pts',(-241.450318016698,-5.41860163358522,
127.026425709627));
#193657=CARTESIAN_POINT('Ctrl Pts',(-241.728765640511,-6.10737017438111,
133.321117535742));
#193658=CARTESIAN_POINT('Ctrl Pts',(-242.007213264324,-1.18376388654087,
137.303032704464));
#193659=CARTESIAN_POINT('Ctrl Pts',(-242.285660888137,4.82766358294966,
135.312985703106));
#193660=CARTESIAN_POINT('Ctrl Pts',(-242.56410851195,6.40270406418687,129.179732506718));
#193661=CARTESIAN_POINT('Ctrl Pts',(-242.842556135762,2.09397229991911,
124.539433176702));
#193662=CARTESIAN_POINT('Ctrl Pts',(-243.121003759575,-4.13901771174057,
125.65629610612));
#193663=CARTESIAN_POINT('Ctrl Pts',(-243.399451383388,-6.56845264856689,
131.503978824623));
#193664=CARTESIAN_POINT('Ctrl Pts',(-243.677899007202,-2.9618004881116,
136.70874658909));
#193665=CARTESIAN_POINT('Ctrl Pts',(-243.956346631013,3.36660162892119,
136.487672091016));
#193666=CARTESIAN_POINT('Ctrl Pts',(-244.234794254827,6.60126131660758,
131.043911994042));
#193667=CARTESIAN_POINT('Ctrl Pts',(-244.513241878639,3.76968434387551,
125.380015884821));
#193668=CARTESIAN_POINT('Ctrl Pts',(-244.791689502453,-2.52604838156001,
124.70082759102));
#193669=CARTESIAN_POINT('Ctrl Pts',(-245.070137126265,-6.50046604866569,
129.630487974449));
#193670=CARTESIAN_POINT('Ctrl Pts',(-245.348584750079,-4.50127298246883,
135.638879970036));
#193671=CARTESIAN_POINT('Ctrl Pts',(-245.627032373891,1.63437005520677,
137.204584860103));
#193672=CARTESIAN_POINT('Ctrl Pts',(-245.905479997704,6.26810685556324,
132.888796339615));
#193673=CARTESIAN_POINT('Ctrl Pts',(-246.183927621517,5.14175966970064,
126.65751322091));
#193674=CARTESIAN_POINT('Ctrl Pts',(-246.46237524533,-0.709613463692526,
124.236980274974));
#193675=CARTESIAN_POINT('Ctrl Pts',(-246.740822869143,-5.90888649049716,
127.851549029514));
#193676=CARTESIAN_POINT('Ctrl Pts',(-247.019270492956,-5.67818149768794,
134.179607380607));
#193677=CARTESIAN_POINT('Ctrl Pts',(-247.297718116769,-0.229505103091092,
137.405978846438));
#193678=CARTESIAN_POINT('Ctrl Pts',(-247.576165740581,5.43007526929941,
134.565785666913));
#193679=CARTESIAN_POINT('Ctrl Pts',(-247.854613364394,6.09968174312738,
128.269026622868));
#193680=CARTESIAN_POINT('Ctrl Pts',(-248.133060988207,1.16397868104094,
124.302115661998));
#193681=CARTESIAN_POINT('Ctrl Pts',(-248.41150861202,-4.84136392540264,
126.31045016297));
#193682=CARTESIAN_POINT('Ctrl Pts',(-248.689956235833,-6.39772959817725,
132.448468831983));
#193683=CARTESIAN_POINT('Ctrl Pts',(-248.968403859646,-2.07489431669385,
137.075632371099));
#193684=CARTESIAN_POINT('Ctrl Pts',(-249.246851483459,4.15466747760909,
135.939803537374));
#193685=CARTESIAN_POINT('Ctrl Pts',(-249.525299107272,6.56629282677857,
130.08475354068));
#193686=CARTESIAN_POINT('Ctrl Pts',(-249.803746731085,2.94381584937754,
124.890987292882));
#193687=CARTESIAN_POINT('Ctrl Pts',(-250.082194354898,-3.38388408020374,
125.131322246124));
#193688=CARTESIAN_POINT('Ctrl Pts',(-250.36064197871,-6.60195985200274,
130.584902319384));
#193689=CARTESIAN_POINT('Ctrl Pts',(-250.639089602524,-3.75315704348482,
136.240153847548));
#193690=CARTESIAN_POINT('Ctrl Pts',(-250.917537226336,2.54461373609029,
136.900176950603));
#193691=CARTESIAN_POINT('Ctrl Pts',(-251.19598485015,6.50400880347224,131.958442640812));
#193692=CARTESIAN_POINT('Ctrl Pts',(-251.474432473962,4.48653751899202,
125.956163331638));
#193693=CARTESIAN_POINT('Ctrl Pts',(-251.752880097775,-1.65384256596459,
124.409140480742));
#193694=CARTESIAN_POINT('Ctrl Pts',(-252.031327721588,-6.27442212737671,
128.739012511497));
#193695=CARTESIAN_POINT('Ctrl Pts',(-252.309775345401,-5.12911427652582,
134.966838554275));
#193696=CARTESIAN_POINT('Ctrl Pts',(-252.588222969213,0.729599023732927,
137.369550720794));
#193697=CARTESIAN_POINT('Ctrl Pts',(-252.866670593027,5.91784646323776,
133.739173911277));
#193698=CARTESIAN_POINT('Ctrl Pts',(-253.145118216839,5.66788210748017,
127.411847055674));
#193699=CARTESIAN_POINT('Ctrl Pts',(-253.423565840652,0.209410983396998,
124.20207443517));
#193700=CARTESIAN_POINT('Ctrl Pts',(-253.702013464465,-5.44149859849489,
127.059480266814));
#193701=CARTESIAN_POINT('Ctrl Pts',(-253.980461088278,-6.0919368110008,
133.358248211846));
#193702=CARTESIAN_POINT('Ctrl Pts',(-254.258908712091,-1.1441826817532,
137.310118186916));
#193703=CARTESIAN_POINT('Ctrl Pts',(-254.537356335904,4.85501939763767,
135.283514846073));
#193704=CARTESIAN_POINT('Ctrl Pts',(-254.815803959717,6.39269590315201,
129.140787462715));
#193705=CARTESIAN_POINT('Ctrl Pts',(-255.09425158353,2.05579703890082,124.526802775315));
#193706=CARTESIAN_POINT('Ctrl Pts',(-255.372699207342,-4.17027861730954,
125.681586622223));
#193707=CARTESIAN_POINT('Ctrl Pts',(-255.651146831155,-6.5640724361261,
131.5439503534));
#193708=CARTESIAN_POINT('Ctrl Pts',(-255.929594454968,-2.925803447894,136.726665654721));
#193709=CARTESIAN_POINT('Ctrl Pts',(-256.208042078781,3.40113425532747,
136.467074956607));
#193710=CARTESIAN_POINT('Ctrl Pts',(-256.486489702594,6.60259898059897,
131.003720738236));
#193711=CARTESIAN_POINT('Ctrl Pts',(-256.764937326407,3.73659166461274,
125.357175036369));
#193712=CARTESIAN_POINT('Ctrl Pts',(-257.04338495022,-2.56314926818932,
124.716306516944));
#193713=CARTESIAN_POINT('Ctrl Pts',(-257.321832574033,-6.5075031063131,
129.670100547101));
#193714=CARTESIAN_POINT('Ctrl Pts',(-257.600280197845,-4.47173821150659,
135.666151948257));
#193715=CARTESIAN_POINT('Ctrl Pts',(-257.878727821659,1.67325768403046,
137.194590998305));
#193716=CARTESIAN_POINT('Ctrl Pts',(-258.157175445471,6.28075871394982,
132.850463013089));
#193717=CARTESIAN_POINT('Ctrl Pts',(-258.435623069284,5.1162713672671,126.626553096149));
#193718=CARTESIAN_POINT('Ctrl Pts',(-258.714070693097,-0.749294580734974,
124.240926059104));
#193719=CARTESIAN_POINT('Ctrl Pts',(-258.99251831691,-5.92728653745133,
127.888508918958));
#193720=CARTESIAN_POINT('Ctrl Pts',(-259.270965940723,-5.656519339957,134.212338033208));
#193721=CARTESIAN_POINT('Ctrl Pts',(-259.549413564536,-0.191230405826049,
137.41063083554));
#193722=CARTESIAN_POINT('Ctrl Pts',(-259.827861188349,5.45654320709978,
134.526020746857));
#193723=CARTESIAN_POINT('Ctrl Pts',(-260.059900874859,5.97341346954355,
129.293215926205));
#193724=CARTESIAN_POINT('Ctrl Pts',(-260.245542550368,3.60742224527213,
126.247226657536));
#193725=CARTESIAN_POINT('Ctrl Pts',(-260.338368351272,1.86717727106152,
125.459413119698));
#193726=CARTESIAN_POINT('Ctrl Pts',(-260.384786214875,0.950008195528324,
125.301089073499));
#193727=CARTESIAN_POINT('Ctrl Pts',(209.997886486728,-2.58542267678463,
125.478296443779));
#193728=CARTESIAN_POINT('Ctrl Pts',(209.951476810375,-3.47289965896197,
125.909102290886));
#193729=CARTESIAN_POINT('Ctrl Pts',(209.85865919672,-5.01373755653622,127.222906143875));
#193730=CARTESIAN_POINT('Ctrl Pts',(209.67302570846,-6.52844908712303,131.020616473957));
#193731=CARTESIAN_POINT('Ctrl Pts',(209.440986021949,-4.4641631800594,136.198709217918));
#193732=CARTESIAN_POINT('Ctrl Pts',(209.162538398136,2.13623200523086,137.47712630299));
#193733=CARTESIAN_POINT('Ctrl Pts',(208.884090774324,6.76311047611758,132.61329501932));
#193734=CARTESIAN_POINT('Ctrl Pts',(208.60564315051,5.180460236421,126.09244423763));
#193735=CARTESIAN_POINT('Ctrl Pts',(208.327195526698,-1.16565068102074,
123.898824768668));
#193736=CARTESIAN_POINT('Ctrl Pts',(208.048747902884,-6.43906639651766,
128.052530506575));
#193737=CARTESIAN_POINT('Ctrl Pts',(207.770300279072,-5.79609906993421,
134.734252735451));
#193738=CARTESIAN_POINT('Ctrl Pts',(207.491852655259,0.173626147510206,
137.805009652024));
#193739=CARTESIAN_POINT('Ctrl Pts',(207.213405031446,5.98357180802623,134.442293088818));
#193740=CARTESIAN_POINT('Ctrl Pts',(206.934957407633,6.29502677410122,127.736610299611));
#193741=CARTESIAN_POINT('Ctrl Pts',(206.65650978382,0.821596385081328,123.849978754804));
#193742=CARTESIAN_POINT('Ctrl Pts',(206.378062160007,-5.40680743188727,
126.354116934927));
#193743=CARTESIAN_POINT('Ctrl Pts',(206.099614536195,-6.66663710465116,
132.947794423038));
#193744=CARTESIAN_POINT('Ctrl Pts',(205.821166912381,-1.80014356190772,
137.571770081489));
#193745=CARTESIAN_POINT('Ctrl Pts',(205.542719288569,4.72058899422897,135.976822216287));
#193746=CARTESIAN_POINT('Ctrl Pts',(205.264271664756,6.90333351468265,129.628637390042));
#193747=CARTESIAN_POINT('Ctrl Pts',(204.985824040943,2.74225038547515,124.360883417158));
#193748=CARTESIAN_POINT('Ctrl Pts',(204.70737641713,-3.93882614214087,125.014370927945));
#193749=CARTESIAN_POINT('Ctrl Pts',(204.428928793317,-7.00031425910704,
130.988575726592));
#193750=CARTESIAN_POINT('Ctrl Pts',(204.150481169504,-3.62885534891233,
136.793496040797));
#193751=CARTESIAN_POINT('Ctrl Pts',(203.872033545692,3.07734423765085,137.09469337995));
#193752=CARTESIAN_POINT('Ctrl Pts',(203.593585921878,6.95561486460971,131.615382266785));
#193753=CARTESIAN_POINT('Ctrl Pts',(203.315138298066,4.44201520086038,125.390781848689));
#193754=CARTESIAN_POINT('Ctrl Pts',(203.036690674253,-2.15357941165663,
124.140995867004));
#193755=CARTESIAN_POINT('Ctrl Pts',(202.75824305044,-6.77013976170558,129.014516559232));
#193756=CARTESIAN_POINT('Ctrl Pts',(202.479795426627,-5.16527240588502,
135.532816506767));
#193757=CARTESIAN_POINT('Ctrl Pts',(202.201347802814,1.18622795093483,137.705896487686));
#193758=CARTESIAN_POINT('Ctrl Pts',(201.922900179001,6.44764277258624,133.536802163981));
#193759=CARTESIAN_POINT('Ctrl Pts',(201.644452555188,5.78398887041165,126.856727545651));
#193760=CARTESIAN_POINT('Ctrl Pts',(201.366004931376,-0.194868239746226,
123.804334868162));
#193761=CARTESIAN_POINT('Ctrl Pts',(201.087557307562,-5.99465095761073,
127.184623883922));
#193762=CARTESIAN_POINT('Ctrl Pts',(200.80910968375,-6.2856423003101,133.891274124028));
#193763=CARTESIAN_POINT('Ctrl Pts',(200.530662059936,-0.80043543977546,
137.76120165575));
#193764=CARTESIAN_POINT('Ctrl Pts',(200.252214436124,5.42033248649604,135.238132133988));
#193765=CARTESIAN_POINT('Ctrl Pts',(199.973766812311,6.66007965562565,128.640643190398));
#193766=CARTESIAN_POINT('Ctrl Pts',(199.695319188498,1.77953898422249,124.031504858911));
#193767=CARTESIAN_POINT('Ctrl Pts',(199.416871564685,-4.73631107837294,
125.646290097223));
#193768=CARTESIAN_POINT('Ctrl Pts',(199.138423940872,-6.89972264160091,
132.00109015798));
#193769=CARTESIAN_POINT('Ctrl Pts',(198.859976317059,-2.72262616738874,
137.256154234582));
#193770=CARTESIAN_POINT('Ctrl Pts',(198.581528693247,3.95643074697165,136.582335164788));
#193771=CARTESIAN_POINT('Ctrl Pts',(198.303081069434,6.999721087252,130.598839755845));
#193772=CARTESIAN_POINT('Ctrl Pts',(198.024633445621,3.61060970373355,124.804207978572));
#193773=CARTESIAN_POINT('Ctrl Pts',(197.746185821808,-3.09647560942607,
124.523423352781));
#193774=CARTESIAN_POINT('Ctrl Pts',(197.467738197995,-6.9580511087663,130.014513232485));
#193775=CARTESIAN_POINT('Ctrl Pts',(197.189290574182,-4.4255175588443,136.231434272887));
#193776=CARTESIAN_POINT('Ctrl Pts',(196.910842950369,2.17385042910367,137.461139751337));
#193777=CARTESIAN_POINT('Ctrl Pts',(196.632395326556,6.77555607120273,132.573590407591));
#193778=CARTESIAN_POINT('Ctrl Pts',(196.353947702743,5.15085668818228,126.060205318492));
#193779=CARTESIAN_POINT('Ctrl Pts',(196.07550007893,-1.20722835793932,123.90646718437));
#193780=CARTESIAN_POINT('Ctrl Pts',(195.797052455118,-6.45592951949867,
128.091556134528));
#193781=CARTESIAN_POINT('Ctrl Pts',(195.518604831305,-5.77194684232935,
134.769579876729));
#193782=CARTESIAN_POINT('Ctrl Pts',(195.240157207492,0.216173007661386,
137.80376083149));
#193783=CARTESIAN_POINT('Ctrl Pts',(194.961709583679,6.00564042424985,134.405834929363));
#193784=CARTESIAN_POINT('Ctrl Pts',(194.683261959866,6.2762176827981,127.698330076496));
#193785=CARTESIAN_POINT('Ctrl Pts',(194.404814336053,0.779257501134259,
123.845115552844));
#193786=CARTESIAN_POINT('Ctrl Pts',(194.12636671224,-5.43380225522669,126.387107265649));
#193787=CARTESIAN_POINT('Ctrl Pts',(193.847919088427,-6.65346319503207,
132.988339014042));
#193788=CARTESIAN_POINT('Ctrl Pts',(193.569471464615,-1.75891649835014,
137.58260130935));
#193789=CARTESIAN_POINT('Ctrl Pts',(193.291023840801,4.75198853246758,135.947991544374));
#193790=CARTESIAN_POINT('Ctrl Pts',(193.012576216989,6.89604824949333,129.586636238002));
#193791=CARTESIAN_POINT('Ctrl Pts',(192.734128593176,2.70297651592057,124.344310147306));
#193792=CARTESIAN_POINT('Ctrl Pts',(192.455680969363,-3.97399858803937,
125.038454847768));
#193793=CARTESIAN_POINT('Ctrl Pts',(192.17723334555,-6.99906313021511,131.031185270517));
#193794=CARTESIAN_POINT('Ctrl Pts',(191.898785721737,-3.59233057896577,
136.815474918205));
#193795=CARTESIAN_POINT('Ctrl Pts',(191.620338097924,3.11557827924791,137.075844182864));
#193796=CARTESIAN_POINT('Ctrl Pts',(191.341890474111,6.96042290329331,131.573026430018));
#193797=CARTESIAN_POINT('Ctrl Pts',(191.063442850298,4.40897891477476,125.363842346942));
#193798=CARTESIAN_POINT('Ctrl Pts',(190.784995226486,-2.19410130582752,
124.154228770475));
#193799=CARTESIAN_POINT('Ctrl Pts',(190.506547602672,-6.78090961418206,
129.055761484483));
#193800=CARTESIAN_POINT('Ctrl Pts',(190.22809997886,-5.13639325295408,135.564171377977));
#193801=CARTESIAN_POINT('Ctrl Pts',(189.949652355047,1.22821758097839,137.698547712335));
#193802=CARTESIAN_POINT('Ctrl Pts',(189.671204731234,6.46415645975623,133.497502906364));
#193803=CARTESIAN_POINT('Ctrl Pts',(189.392757107421,5.75985134361714,126.821591904301));
#193804=CARTESIAN_POINT('Ctrl Pts',(189.114309483608,-0.237475772924818,
123.80565078066));
#193805=CARTESIAN_POINT('Ctrl Pts',(188.835861859795,-6.01657425548534,
127.221182091151));
#193806=CARTESIAN_POINT('Ctrl Pts',(188.557414235982,-6.2667349232476,133.929479419415));
#193807=CARTESIAN_POINT('Ctrl Pts',(188.278966612169,-0.758072343566082,
137.76594523932));
#193808=CARTESIAN_POINT('Ctrl Pts',(188.000518988357,5.44722168595988,135.205054884148));
#193809=CARTESIAN_POINT('Ctrl Pts',(187.722071364544,6.64678509766207,128.600141483854));
#193810=CARTESIAN_POINT('Ctrl Pts',(187.443623740731,1.73827771811677,124.02079778535));
#193811=CARTESIAN_POINT('Ctrl Pts',(187.165176116918,-4.76762196479028,
125.675216934184));
#193812=CARTESIAN_POINT('Ctrl Pts',(186.886728493105,-6.89230997333645,
132.043068555446));
#193813=CARTESIAN_POINT('Ctrl Pts',(186.608280869292,-2.68330182444739,
137.272608096043));
#193814=CARTESIAN_POINT('Ctrl Pts',(186.329833245479,3.99152961452714,136.558144195375));
#193815=CARTESIAN_POINT('Ctrl Pts',(186.051385621667,6.99834033481346,130.556234274655));
#193816=CARTESIAN_POINT('Ctrl Pts',(185.772937997853,3.5740181753383,124.782340341422));
#193817=CARTESIAN_POINT('Ctrl Pts',(185.494490374041,-3.13465208677821,
124.542388849921));
#193818=CARTESIAN_POINT('Ctrl Pts',(185.216042750227,-6.96273021741339,
130.056883498557));
#193819=CARTESIAN_POINT('Ctrl Pts',(184.937595126415,-4.39239942652681,
136.258273103275));
#193820=CARTESIAN_POINT('Ctrl Pts',(184.659147502602,2.21433185669671,137.447783572063));
#193821=CARTESIAN_POINT('Ctrl Pts',(184.380699878789,6.78620033974098,132.532312894923));
#193822=CARTESIAN_POINT('Ctrl Pts',(184.102252254976,5.12188223488049,126.028938490053));
#193823=CARTESIAN_POINT('Ctrl Pts',(183.823804631163,-1.24919542597752,
123.913943728027));
#193824=CARTESIAN_POINT('Ctrl Pts',(183.54535700735,-6.47232351695142,128.130905471908));
#193825=CARTESIAN_POINT('Ctrl Pts',(183.266909383538,-5.74770248642891,
134.804641889104));
#193826=CARTESIAN_POINT('Ctrl Pts',(182.988461759724,0.258776338245136,
137.80231524236));
#193827=CARTESIAN_POINT('Ctrl Pts',(182.710014135912,6.02745234999885,134.369210164519));
#193828=CARTESIAN_POINT('Ctrl Pts',(182.431566512099,6.25719410952084,127.66018250561));
#193829=CARTESIAN_POINT('Ctrl Pts',(182.153118888286,0.73688016331929,123.840500929948));
#193830=CARTESIAN_POINT('Ctrl Pts',(181.874671264473,-5.46059065437546,
126.420266203747));
#193831=CARTESIAN_POINT('Ctrl Pts',(181.59622364066,-6.64004542538295,133.028800068927));
#193832=CARTESIAN_POINT('Ctrl Pts',(181.317776016847,-1.71762283471616,
137.593182748215));
#193833=CARTESIAN_POINT('Ctrl Pts',(181.039328393035,4.78321123051439,135.918969541833));
#193834=CARTESIAN_POINT('Ctrl Pts',(180.760880769221,6.88850784776155,129.544680596588));
#193835=CARTESIAN_POINT('Ctrl Pts',(180.482433145409,2.66360227523266,124.32797605183));
#193836=CARTESIAN_POINT('Ctrl Pts',(180.203985521595,-4.00902366402984,
125.062752534008));
#193837=CARTESIAN_POINT('Ctrl Pts',(179.925537897783,-6.99755270774298,
131.073786351827));
#193838=CARTESIAN_POINT('Ctrl Pts',(179.64709027397,-3.5556726624947,136.837231082039));
#193839=CARTESIAN_POINT('Ctrl Pts',(179.368642650157,3.15369685531979,137.056762577506));
#193840=CARTESIAN_POINT('Ctrl Pts',(179.090195026344,6.96497302975191,131.530642118605));
#193841=CARTESIAN_POINT('Ctrl Pts',(178.811747402531,4.37577924769062,125.337104441072));
#193842=CARTESIAN_POINT('Ctrl Pts',(178.533299778718,-2.23454189429802,
124.167708099424));
#193843=CARTESIAN_POINT('Ctrl Pts',(178.254852154906,-6.79142819886702,
129.097071203448));
#193844=CARTESIAN_POINT('Ctrl Pts',(177.976404531092,-5.10732376838957,
135.595349873321));
#193845=CARTESIAN_POINT('Ctrl Pts',(177.69795690728,1.27016169860089,137.690943469992));
#193846=CARTESIAN_POINT('Ctrl Pts',(177.419509283467,6.48043061542571,133.458103853558));
#193847=CARTESIAN_POINT('Ctrl Pts',(177.141061659654,5.73550038331004,126.786603845811));
#193848=CARTESIAN_POINT('Ctrl Pts',(176.862614035841,-0.280074506296806,
123.807226032976));
#193849=CARTESIAN_POINT('Ctrl Pts',(176.584166412028,-6.0382746070172,127.257873074351));
#193850=CARTESIAN_POINT('Ctrl Pts',(176.305718788215,-6.24759533000263,
133.967568912391));
#193851=CARTESIAN_POINT('Ctrl Pts',(176.027271164402,-0.71568115671533,
137.770430858802));
#193852=CARTESIAN_POINT('Ctrl Pts',(175.748823540589,5.4739090366252,135.171814564968));
#193853=CARTESIAN_POINT('Ctrl Pts',(175.470375916777,6.63324424063007,128.559721455457));
#193854=CARTESIAN_POINT('Ctrl Pts',(175.191928292964,1.69695203949225,124.010342079205));
#193855=CARTESIAN_POINT('Ctrl Pts',(174.913480669151,-4.79875618522306,
125.704333833448));
#193856=CARTESIAN_POINT('Ctrl Pts',(174.635033045338,-6.88464190799096,
132.085001052137));
#193857=CARTESIAN_POINT('Ctrl Pts',(174.356585421525,-2.64387805077028,
137.288822274217));
#193858=CARTESIAN_POINT('Ctrl Pts',(174.078137797712,4.02648057448505,136.533740017397));
#193859=CARTESIAN_POINT('Ctrl Pts',(173.799690173899,6.99670025630013,130.513637987877));
#193860=CARTESIAN_POINT('Ctrl Pts',(173.521242550086,3.53729421038521,124.76069585245));
#193861=CARTESIAN_POINT('Ctrl Pts',(173.242794926273,-3.17271240844464,
124.561586386726));
#193862=CARTESIAN_POINT('Ctrl Pts',(172.96434730246,-6.96715131953175,130.099281462668));
#193863=CARTESIAN_POINT('Ctrl Pts',(172.685899678648,-4.35911853223319,
136.284909836929));
#193864=CARTESIAN_POINT('Ctrl Pts',(172.407452054835,2.25473123140845,137.434181218309));
#193865=CARTESIAN_POINT('Ctrl Pts',(172.129004431022,6.79659314313001,132.490971352347));
#193866=CARTESIAN_POINT('Ctrl Pts',(171.850556807209,5.09271798834896,125.997848616637));
#193867=CARTESIAN_POINT('Ctrl Pts',(171.572109183396,-1.29111620461978,
123.921675598615));
#193868=CARTESIAN_POINT('Ctrl Pts',(171.293661559583,-6.48847768007612,
128.170353875152));
#193869=CARTESIAN_POINT('Ctrl Pts',(171.01521393577,-5.72324514729908,134.839555669585));
#193870=CARTESIAN_POINT('Ctrl Pts',(170.736766311957,0.301370079776633,
137.800610341449));
#193871=CARTESIAN_POINT('Ctrl Pts',(170.458318688145,6.04904092628448,134.332453302864));
#193872=CARTESIAN_POINT('Ctrl Pts',(170.179871064331,6.23793867361471,127.6221514434));
#193873=CARTESIAN_POINT('Ctrl Pts',(169.901423440519,0.694475520138818,
123.836144355433));
#193874=CARTESIAN_POINT('Ctrl Pts',(169.622975816706,-5.4871767093294,126.453587596077));
#193875=CARTESIAN_POINT('Ctrl Pts',(169.344528192893,-6.62638160640872,
133.06917869639));
#193876=CARTESIAN_POINT('Ctrl Pts',(169.06608056908,-1.67626552393645,137.603512624779));
#193877=CARTESIAN_POINT('Ctrl Pts',(168.787632945267,4.81425668490999,135.88975801558));
#193878=CARTESIAN_POINT('Ctrl Pts',(168.509185321454,6.88071218983824,129.50277163308));
#193879=CARTESIAN_POINT('Ctrl Pts',(168.230737697641,2.62412933378287,124.311881941165));
#193880=CARTESIAN_POINT('Ctrl Pts',(167.952290073828,-4.0439001841742,125.087262977647));
#193881=CARTESIAN_POINT('Ctrl Pts',(167.673842450016,-6.99578298838191,
131.116377449467));
#193882=CARTESIAN_POINT('Ctrl Pts',(167.395394826203,-3.51888298926545,
136.858763695638));
#193883=CARTESIAN_POINT('Ctrl Pts',(167.11694720239,3.19169856999505,137.037449287095));
#193884=CARTESIAN_POINT('Ctrl Pts',(166.838499578577,6.96926506657354,131.488230894564));
#193885=CARTESIAN_POINT('Ctrl Pts',(166.560051954764,4.34241743449723,125.310569126392));
#193886=CARTESIAN_POINT('Ctrl Pts',(166.281604330951,-2.27489968099678,
124.181433351974));
#193887=CARTESIAN_POINT('Ctrl Pts',(166.003156707138,-6.80169512468258,
129.13844418665));
#193888=CARTESIAN_POINT('Ctrl Pts',(165.724709083325,-5.0780650300646,135.626350836796));
#193889=CARTESIAN_POINT('Ctrl Pts',(165.446261459512,1.31205874991464,137.683084042787));
#193890=CARTESIAN_POINT('Ctrl Pts',(165.1678138357,6.49646463635559,133.418606465321));
#193891=CARTESIAN_POINT('Ctrl Pts',(164.889366211887,5.71093689192698,126.751764666776));
#193892=CARTESIAN_POINT('Ctrl Pts',(164.610918588074,-0.322662861405092,
123.809060566689));
#193893=CARTESIAN_POINT('Ctrl Pts',(164.332470964261,-6.05975120806294,
127.29469547395));
#193894=CARTESIAN_POINT('Ctrl Pts',(164.054023340448,-6.22822422981513,
134.00554119152));
#193895=CARTESIAN_POINT('Ctrl Pts',(163.775575716635,-0.673263450036036,
137.774658347991));
#193896=CARTESIAN_POINT('Ctrl Pts',(163.497128092822,5.50039354957815,135.138412408175));
#193897=CARTESIAN_POINT('Ctrl Pts',(163.218680469009,6.61945758629338,128.51938460299));
#193898=CARTESIAN_POINT('Ctrl Pts',(162.940232845196,1.65556347968583,124.000138127916));
#193899=CARTESIAN_POINT('Ctrl Pts',(162.661785221384,-4.82971258598073,
125.733639716082));
#193900=CARTESIAN_POINT('Ctrl Pts',(162.383337597571,-6.87671872970774,
132.126886094224));
#193901=CARTESIAN_POINT('Ctrl Pts',(162.104889973758,-2.60435630721971,
137.304796168278));
#193902=CARTESIAN_POINT('Ctrl Pts',(161.826442349945,4.06128233172446,136.509123535159));
#193903=CARTESIAN_POINT('Ctrl Pts',(161.547994726132,6.99480091248578,130.471052473933));
#193904=CARTESIAN_POINT('Ctrl Pts',(161.269547102319,3.50043916969439,124.739275313697));
#193905=CARTESIAN_POINT('Ctrl Pts',(160.991099478506,-3.21065516408591,
124.581015251828));
#193906=CARTESIAN_POINT('Ctrl Pts',(160.712651854693,-6.97131425129578,
130.141705553748));
#193907=CARTESIAN_POINT('Ctrl Pts',(160.434204230881,-4.32567610919938,
136.311343486817));
#193908=CARTESIAN_POINT('Ctrl Pts',(160.155756607067,2.29504705622523,137.420333194114));
#193909=CARTESIAN_POINT('Ctrl Pts',(159.877308983254,6.80673409626067,132.449567311792));
#193910=CARTESIAN_POINT('Ctrl Pts',(159.598861359442,5.06336502927952,125.966936850291));
#193911=CARTESIAN_POINT('Ctrl Pts',(159.320413735629,-1.33298914047637,
123.929662509627));
#193912=CARTESIAN_POINT('Ctrl Pts',(159.041966111816,-6.50439141027418,
128.209899882485));
#193913=CARTESIAN_POINT('Ctrl Pts',(158.763518488003,-5.69857573121565,
134.874319924428));
#193914=CARTESIAN_POINT('Ctrl Pts',(158.48507086419,0.343952653928878,137.798646191931));
#193915=CARTESIAN_POINT('Ctrl Pts',(158.206623240377,6.07040535313402,134.295565706438));
#193916=CARTESIAN_POINT('Ctrl Pts',(157.928175616564,6.2184520885971,127.584238299121));
#193917=CARTESIAN_POINT('Ctrl Pts',(157.649727992752,0.652045142912632,
123.832045990734));
#193918=CARTESIAN_POINT('Ctrl Pts',(157.371280368939,-5.51355943493244,
126.487070207899));
#193919=CARTESIAN_POINT('Ctrl Pts',(157.092832745126,-6.61247224442723,
133.109473400187));
#193920=CARTESIAN_POINT('Ctrl Pts',(156.814385121313,-1.63484609852131,
137.613590556265));
#193921=CARTESIAN_POINT('Ctrl Pts',(156.5359374975,4.84512374525377,135.860358048054));
#193922=CARTESIAN_POINT('Ctrl Pts',(156.257489873687,6.87266156459436,129.46091090043));
#193923=CARTESIAN_POINT('Ctrl Pts',(155.979042249874,2.58455915425555,124.296028411687));
#193924=CARTESIAN_POINT('Ctrl Pts',(155.700594626061,-4.07862685611001,
125.111985270442));
#193925=CARTESIAN_POINT('Ctrl Pts',(155.422147002248,-6.99375403770952,
131.158956985208));
#193926=CARTESIAN_POINT('Ctrl Pts',(155.143699378435,-3.48196292253304,
136.880071961106));
#193927=CARTESIAN_POINT('Ctrl Pts',(154.865251754623,3.22958201510593,137.017905027291));
#193928=CARTESIAN_POINT('Ctrl Pts',(154.58680413081,6.97329885471516,131.445794329457));
#193929=CARTESIAN_POINT('Ctrl Pts',(154.308356506997,4.30889471142897,125.284237386175));
#193930=CARTESIAN_POINT('Ctrl Pts',(154.029908883184,-2.31517317045128,
124.195404019528));
#193931=CARTESIAN_POINT('Ctrl Pts',(153.751461259371,-6.81171001118396,
129.179878900999));
#193932=CARTESIAN_POINT('Ctrl Pts',(153.473013635558,-5.04861812217248,
135.65717311965));
#193933=CARTESIAN_POINT('Ctrl Pts',(153.194566011745,1.3539071824088,137.674969721956));
#193934=CARTESIAN_POINT('Ctrl Pts',(152.916118387933,6.51225792839928,133.379012205241));
#193935=CARTESIAN_POINT('Ctrl Pts',(152.637670764119,5.68616177967723,126.717075658174));
#193936=CARTESIAN_POINT('Ctrl Pts',(152.359223140307,-0.365239260122265,
123.811154313817));
#193937=CARTESIAN_POINT('Ctrl Pts',(152.080775516494,-6.08100326279917,
127.331647925483));
#193938=CARTESIAN_POINT('Ctrl Pts',(151.802327892681,-6.20862234048841,
134.043394849727));
#193939=CARTESIAN_POINT('Ctrl Pts',(151.523880268868,-0.630820795332096,
137.778627550233));
#193940=CARTESIAN_POINT('Ctrl Pts',(151.245432645055,5.52667424342534,135.104849651499));
#193941=CARTESIAN_POINT('Ctrl Pts',(150.966985021242,6.60542564552152,128.479132421149));
#193942=CARTESIAN_POINT('Ctrl Pts',(150.688537397429,1.61411357236584,123.990186309594));
#193943=CARTESIAN_POINT('Ctrl Pts',(150.410089773616,-4.86049001996232,
125.763133496143));
#193944=CARTESIAN_POINT('Ctrl Pts',(150.131642149803,-6.8685407320831,132.168722129643));
#193945=CARTESIAN_POINT('Ctrl Pts',(149.853194525991,-2.56473805828847,
137.32052918631));
#193946=CARTESIAN_POINT('Ctrl Pts',(149.574746902178,4.09593359665354,136.484295660832));
#193947=CARTESIAN_POINT('Ctrl Pts',(149.296299278365,6.99264237375128,130.428479310845));
#193948=CARTESIAN_POINT('Ctrl Pts',(149.017851654552,3.46345441894284,124.718079518912));
#193949=CARTESIAN_POINT('Ctrl Pts',(148.739404030739,-3.24847894771935,
124.600674725279));
#193950=CARTESIAN_POINT('Ctrl Pts',(148.460956406926,-6.97521885844655,
130.184154199754));
#193951=CARTESIAN_POINT('Ctrl Pts',(148.182508783113,-4.29207339664657,
136.337573073429));
#193952=CARTESIAN_POINT('Ctrl Pts',(147.9040611593,2.33527783722936,137.406240012622));
#193953=CARTESIAN_POINT('Ctrl Pts',(147.625613535487,6.81662282335624,132.408102307496));
#193954=CARTESIAN_POINT('Ctrl Pts',(147.347165911675,5.03382444535687,125.936204336462));
#193955=CARTESIAN_POINT('Ctrl Pts',(147.068718287862,-1.37481268193005,
123.937904165105));
#193956=CARTESIAN_POINT('Ctrl Pts',(146.790270664049,-6.52006411785656,
128.249542028514));
#193957=CARTESIAN_POINT('Ctrl Pts',(146.511823040236,-5.67369515231286,
134.908933365434));
#193958=CARTESIAN_POINT('Ctrl Pts',(146.233375416423,0.386522482789046,
137.796422866589));
#193959=CARTESIAN_POINT('Ctrl Pts',(145.95492779261,6.09154483888081,134.258548742122));
#193960=CARTESIAN_POINT('Ctrl Pts',(145.676480168797,6.19873507655051,127.546444477659));
#193961=CARTESIAN_POINT('Ctrl Pts',(145.398032544984,0.609590603913882,
123.828205987717));
#193962=CARTESIAN_POINT('Ctrl Pts',(145.119584921171,-5.53973785356302,
126.520712798507));
#193963=CARTESIAN_POINT('Ctrl Pts',(144.841137297358,-6.59831785485502,
133.149682687181));
#193964=CARTESIAN_POINT('Ctrl Pts',(144.562689673546,-1.59336609328267,
137.623416169231));
#193965=CARTESIAN_POINT('Ctrl Pts',(144.284242049733,4.87581126775532,135.830770728684));
#193966=CARTESIAN_POINT('Ctrl Pts',(144.00579442592,6.86435627034879,129.419099949804));
#193967=CARTESIAN_POINT('Ctrl Pts',(143.727346802107,2.54489320293839,124.280416050852));
#193968=CARTESIAN_POINT('Ctrl Pts',(143.448899178294,-4.11320239302776,
125.136918496298));
#193969=CARTESIAN_POINT('Ctrl Pts',(143.170451554481,-6.99146593090932,
131.201523381251));
#193970=CARTESIAN_POINT('Ctrl Pts',(142.892003930668,-3.44491383038404,
136.901155088855));
#193971=CARTESIAN_POINT('Ctrl Pts',(142.613556306855,3.26734578686757,136.998130522314));
#193972=CARTESIAN_POINT('Ctrl Pts',(142.335108683042,6.97707424470332,131.403333995789));
#193973=CARTESIAN_POINT('Ctrl Pts',(142.05666105923,4.27521232068256,125.258110196154));
#193974=CARTESIAN_POINT('Ctrl Pts',(141.778213435417,-2.35536087031262,
124.209619584399));
#193975=CARTESIAN_POINT('Ctrl Pts',(141.499765811604,-6.8214724872659,129.221373811115));
#193976=CARTESIAN_POINT('Ctrl Pts',(141.221318187791,-5.01898413587917,
135.687815579753));
#193977=CARTESIAN_POINT('Ctrl Pts',(140.942870563978,1.39570544537436,137.666600808179));
#193978=CARTESIAN_POINT('Ctrl Pts',(140.664422940165,6.52780990633047,133.339322540502));
#193979=CARTESIAN_POINT('Ctrl Pts',(140.385975316352,5.66117596461176,126.68253810542));
#193980=CARTESIAN_POINT('Ctrl Pts',(140.10752769254,-0.407802124764288,
123.813507196776));
#193981=CARTESIAN_POINT('Ctrl Pts',(139.829080068726,-6.10202998372316,
127.368729059661));
#193982=CARTESIAN_POINT('Ctrl Pts',(139.550632444914,-6.18879038837768,
134.081128484328));
#193983=CARTESIAN_POINT('Ctrl Pts',(139.272184821101,-0.588354765331746,
137.78233831845));
#193984=CARTESIAN_POINT('Ctrl Pts',(138.993737197288,5.55275014432601,135.071127538621));
#193985=CARTESIAN_POINT('Ctrl Pts',(138.715289573475,6.59114893827324,128.438966401494));
#193986=CARTESIAN_POINT('Ctrl Pts',(138.436841949662,1.57260385347371,123.980486993006));
#193987=CARTESIAN_POINT('Ctrl Pts',(138.158394325849,-4.8910873466988,125.792814080728));
#193988=CARTESIAN_POINT('Ctrl Pts',(137.879946702036,-6.86010821815569,
132.210507608145));
#193989=CARTESIAN_POINT('Ctrl Pts',(137.601499078223,-2.52502477204539,
137.336020745319));
#193990=CARTESIAN_POINT('Ctrl Pts',(137.32305145441,4.13043308525698,136.459257314423));
#193991=CARTESIAN_POINT('Ctrl Pts',(137.044603830598,6.99022472008204,130.385920076178));
#193992=CARTESIAN_POINT('Ctrl Pts',(136.766156206785,3.42634132861412,124.69710925351));
#193993=CARTESIAN_POINT('Ctrl Pts',(136.487708582972,-3.28618235777073,
124.620564078594));
#193994=CARTESIAN_POINT('Ctrl Pts',(136.209260959159,-6.97886499629743,
130.226625827737));
#193995=CARTESIAN_POINT('Ctrl Pts',(135.930813335346,-4.25831163973555,
136.363597624819));
#193996=CARTESIAN_POINT('Ctrl Pts',(135.652365711533,2.37542208365453,137.391902196061));
#193997=CARTESIAN_POINT('Ctrl Pts',(135.37391808772,6.82625895798624,132.366577875963));
#193998=CARTESIAN_POINT('Ctrl Pts',(135.095470463907,5.00409733121823,125.905652213954));
#193999=CARTESIAN_POINT('Ctrl Pts',(134.817022840094,-1.4165852791943,123.946400259653));
#194000=CARTESIAN_POINT('Ctrl Pts',(134.538575216282,-6.53549522206528,
128.289278844285));
#194001=CARTESIAN_POINT('Ctrl Pts',(134.260127592469,-5.64860433254967,
134.943394709987));
#194002=CARTESIAN_POINT('Ctrl Pts',(133.981679968656,0.429077988916399,
137.793940447809));
#194003=CARTESIAN_POINT('Ctrl Pts',(133.703232344843,6.1124586001935,134.221403781595));
#194004=CARTESIAN_POINT('Ctrl Pts',(133.42478472103,6.17878836809604,127.508771379477));
#194005=CARTESIAN_POINT('Ctrl Pts',(133.146337097217,0.567113476311158,
123.824624488677));
#194006=CARTESIAN_POINT('Ctrl Pts',(132.867889473404,-5.5657109951702,126.554514121259));
#194007=CARTESIAN_POINT('Ctrl Pts',(132.589441849591,-6.58391896218814,
133.189805067404));
#194008=CARTESIAN_POINT('Ctrl Pts',(132.310994225778,-1.55182704527753,
137.632989099587));
#194009=CARTESIAN_POINT('Ctrl Pts',(132.032546601965,4.90631811527725,135.800997153839));
#194010=CARTESIAN_POINT('Ctrl Pts',(131.754098978153,6.85579661485726,129.377340330521));
#194011=CARTESIAN_POINT('Ctrl Pts',(131.47565135434,2.50513294966777,124.265045437181));
#194012=CARTESIAN_POINT('Ctrl Pts',(131.197203730527,-4.14762551371829,
125.162061731307));
#194013=CARTESIAN_POINT('Ctrl Pts',(130.918756106714,-6.98891875276791,
131.244075060281));
#194014=CARTESIAN_POINT('Ctrl Pts',(130.640308482901,-3.4077370856862,136.922012297644));
#194015=CARTESIAN_POINT('Ctrl Pts',(130.361860859088,3.30498848592948,136.978126504915));
#194016=CARTESIAN_POINT('Ctrl Pts',(130.083413235275,6.98059109663955,131.360851466943));
#194017=CARTESIAN_POINT('Ctrl Pts',(129.804965611462,4.24137151037132,125.232188524482));
#194018=CARTESIAN_POINT('Ctrl Pts',(129.526517987649,-2.39546129141071,
124.224079519825));
#194019=CARTESIAN_POINT('Ctrl Pts',(129.248070363836,-6.83098219117618,
129.262927379388));
#194020=CARTESIAN_POINT('Ctrl Pts',(128.969622740024,-4.98916416928312,
135.718277081636));
#194021=CARTESIAN_POINT('Ctrl Pts',(128.691175116211,1.43745198996158,137.657977611568));
#194022=CARTESIAN_POINT('Ctrl Pts',(128.412727492398,6.54311999386511,133.299538941816));
#194023=CARTESIAN_POINT('Ctrl Pts',(128.134279868585,5.63598037258881,126.648153288314));
#194024=CARTESIAN_POINT('Ctrl Pts',(127.855832244772,-0.450349878148651,
123.81611912838));
#194025=CARTESIAN_POINT('Ctrl Pts',(127.577384620959,-6.12283059168226,
127.40593750243));
#194026=CARTESIAN_POINT('Ctrl Pts',(127.298936997146,-6.16872910836309,
134.118740697091));
#194027=CARTESIAN_POINT('Ctrl Pts',(127.020489373333,-0.545866933628919,
137.785790515136));
#194028=CARTESIAN_POINT('Ctrl Pts',(126.742041749521,5.57862028602806,135.037247319125));
#194029=CARTESIAN_POINT('Ctrl Pts',(126.463594125708,6.57662799357718,128.398888032392));
#194030=CARTESIAN_POINT('Ctrl Pts',(126.185146501895,1.53103586116759,123.971040537565));
#194031=CARTESIAN_POINT('Ctrl Pts',(125.906698878082,-4.92150343239493,
125.822680370014));
#194032=CARTESIAN_POINT('Ctrl Pts',(125.628251254269,-6.85142150039552,
132.252240981353));
#194033=CARTESIAN_POINT('Ctrl Pts',(125.349803630456,-2.48521792008072,
137.351270271259));
#194034=CARTESIAN_POINT('Ctrl Pts',(125.071356006643,4.16477951914341,136.434009423738));
#194035=CARTESIAN_POINT('Ctrl Pts',(124.79290838283,6.98754804106521,130.343376346978));
#194036=CARTESIAN_POINT('Ctrl Pts',(124.514460759018,3.38910127394743,124.676365294554));
#194037=CARTESIAN_POINT('Ctrl Pts',(124.236013135205,-3.32376399712637,
124.640682574762));
#194038=CARTESIAN_POINT('Ctrl Pts',(123.957565511392,-6.98225252973936,
130.269118863895));
#194039=CARTESIAN_POINT('Ctrl Pts',(123.679117887579,-4.22439208952083,
136.389416176637));
#194040=CARTESIAN_POINT('Ctrl Pts',(123.400670263766,2.41547830794073,137.377320275725));
#194041=CARTESIAN_POINT('Ctrl Pts',(123.122222639953,6.83564214308024,132.324995555895));
#194042=CARTESIAN_POINT('Ctrl Pts',(122.84377501614,4.97418478841272,125.875281614887));
#194043=CARTESIAN_POINT('Ctrl Pts',(122.565327392328,-1.45830538437,123.955150478444));
#194044=CARTESIAN_POINT('Ctrl Pts',(122.286879768514,-6.55068415109515,
128.329108857337));
#194045=CARTESIAN_POINT('Ctrl Pts',(122.008432144702,-5.62330420167569,
134.977702681109));
#194046=CARTESIAN_POINT('Ctrl Pts',(121.729984520888,0.471617595401148,
137.791199027578));
#194047=CARTESIAN_POINT('Ctrl Pts',(121.451536897076,6.13314586210485,134.184132201278));
#194048=CARTESIAN_POINT('Ctrl Pts',(121.173089273263,6.15861270236637,127.471220400567));
#194049=CARTESIAN_POINT('Ctrl Pts',(120.89464164945,0.52461533410983,123.821301626325));
#194050=CARTESIAN_POINT('Ctrl Pts',(120.616194025637,-5.5914778973097,126.588472923636));
#194051=CARTESIAN_POINT('Ctrl Pts',(120.337746401824,-6.56927609998288,
133.229839054105));
#194052=CARTESIAN_POINT('Ctrl Pts',(120.059298778011,-1.51023049375061,
137.642308992603));
#194053=CARTESIAN_POINT('Ctrl Pts',(119.780851154198,4.93664315737715,135.77103842679));
#194054=CARTESIAN_POINT('Ctrl Pts',(119.502403530385,6.84698291530094,129.33563359));
#194055=CARTESIAN_POINT('Ctrl Pts',(119.223955906573,2.46527986777437,124.249917140239));
#194056=CARTESIAN_POINT('Ctrl Pts',(118.94550828276,-4.18189494262004,125.187414043775));
#194057=CARTESIAN_POINT('Ctrl Pts',(118.667060658947,-6.98611259767199,
131.28661044553));
#194058=CARTESIAN_POINT('Ctrl Pts',(118.388613035134,-3.37043406603744,
136.942642814599));
#194059=CARTESIAN_POINT('Ctrl Pts',(118.110165411321,3.34250871742766,136.95789371635));
#194060=CARTESIAN_POINT('Ctrl Pts',(117.831717787508,6.98384928020556,131.318348317123));
#194061=CARTESIAN_POINT('Ctrl Pts',(117.553270163695,4.20737353447909,125.206473331696));
#194062=CARTESIAN_POINT('Ctrl Pts',(117.274822539882,-2.43547294780967,
124.238783289987));
#194063=CARTESIAN_POINT('Ctrl Pts',(116.99637491607,-6.84023877052931,129.304538066038));
#194064=CARTESIAN_POINT('Ctrl Pts',(116.717927292256,-4.95915932737393,
135.748556496538));
#194065=CARTESIAN_POINT('Ctrl Pts',(116.439479668444,1.47914526923655,137.649100451659));
#194066=CARTESIAN_POINT('Ctrl Pts',(116.161032044631,6.55818762368211,133.259662883379));
#194067=CARTESIAN_POINT('Ctrl Pts',(115.882584420818,5.61057593724064,126.613922481));
#194068=CARTESIAN_POINT('Ctrl Pts',(115.604136797005,-0.49288094365267,
123.818990011842));
#194069=CARTESIAN_POINT('Ctrl Pts',(115.325689173192,-6.14340431590201,
127.443271875017));
#194070=CARTESIAN_POINT('Ctrl Pts',(115.047241549379,-6.14843924382291,
134.156230094282));
#194071=CARTESIAN_POINT('Ctrl Pts',(114.768793925566,-0.5033588746261,137.78898401237));
#194072=CARTESIAN_POINT('Ctrl Pts',(114.490346301753,5.60428370990391,135.003210248456));
#194073=CARTESIAN_POINT('Ctrl Pts',(114.211898677941,6.56186334951224,128.358898798961));
#194074=CARTESIAN_POINT('Ctrl Pts',(113.933451054127,1.48941113576461,123.961847293312));
#194075=CARTESIAN_POINT('Ctrl Pts',(113.655003430315,-4.95173714997151,
125.852731257293));
#194076=CARTESIAN_POINT('Ctrl Pts',(113.376555806502,-6.84248090069202,
132.293920702821));
#194077=CARTESIAN_POINT('Ctrl Pts',(113.098108182689,-2.4453189774521,137.366277199056));
#194078=CARTESIAN_POINT('Ctrl Pts',(112.819660558876,4.19897162559319,136.408552924347));
#194079=CARTESIAN_POINT('Ctrl Pts',(112.541212935063,6.98461243588604,130.300849699721));
#194080=CARTESIAN_POINT('Ctrl Pts',(112.26276531125,3.35173563488669,124.655848410718));
#194081=CARTESIAN_POINT('Ctrl Pts',(111.984317687437,-3.3612224731848,124.661029468288));
#194082=CARTESIAN_POINT('Ctrl Pts',(111.705870063624,-6.98538133324609,
130.311631733633));
#194083=CARTESIAN_POINT('Ctrl Pts',(111.427422439812,-4.1903160029037,136.415027772168));
#194084=CARTESIAN_POINT('Ctrl Pts',(111.148974815999,2.45544502578993,137.362494791951));
#194085=CARTESIAN_POINT('Ctrl Pts',(110.870527192186,6.84477203094083,132.28335688814));
#194086=CARTESIAN_POINT('Ctrl Pts',(110.592079568373,4.94408792536061,125.845093664656));
#194087=CARTESIAN_POINT('Ctrl Pts',(110.31363194456,-1.49997145150339,123.964154497236));
#194088=CARTESIAN_POINT('Ctrl Pts',(110.035184320747,-6.56563034211481,
128.369030591753));
#194089=CARTESIAN_POINT('Ctrl Pts',(109.756736696934,-5.59779569719655,
135.011856007506));
#194090=CARTESIAN_POINT('Ctrl Pts',(109.478289073121,0.514139725922464,
137.788198707481));
#194091=CARTESIAN_POINT('Ctrl Pts',(109.199841449309,6.15360585804082,134.146735382281));
#194092=CARTESIAN_POINT('Ctrl Pts',(108.921393825496,6.13820882697821,127.433792932393));
#194093=CARTESIAN_POINT('Ctrl Pts',(108.642946201683,0.482097752094529,
123.818237523792));
#194094=CARTESIAN_POINT('Ctrl Pts',(108.36449857787,-5.61703760517944,126.622587947283));
#194095=CARTESIAN_POINT('Ctrl Pts',(108.086050954057,-6.5543898108359,133.26978316381));
#194096=CARTESIAN_POINT('Ctrl Pts',(107.807603330244,-1.46857798007734,
137.651375502926));
#194097=CARTESIAN_POINT('Ctrl Pts',(107.529155706431,4.96678527034939,135.740895657668));
#194098=CARTESIAN_POINT('Ctrl Pts',(107.250708082618,6.83791549827476,129.2939812737));
#194099=CARTESIAN_POINT('Ctrl Pts',(106.972260458805,2.42533543402888,124.23503172061));
#194100=CARTESIAN_POINT('Ctrl Pts',(106.693812834992,-4.21600940986681,
125.212974494265));
#194101=CARTESIAN_POINT('Ctrl Pts',(106.415365211179,-6.98304756960462,
131.329127960835));
#194102=CARTESIAN_POINT('Ctrl Pts',(106.136917587367,-3.33300615371489,
136.96304587525));
#194103=CARTESIAN_POINT('Ctrl Pts',(105.858469963554,3.37990509103613,136.937432906355));
#194104=CARTESIAN_POINT('Ctrl Pts',(105.580022339741,6.98684867466819,131.275826121299));
#194105=CARTESIAN_POINT('Ctrl Pts',(105.301574715928,4.1732196528133,125.180965570684));
#194106=CARTESIAN_POINT('Ctrl Pts',(105.023127092115,-2.4753943568629,124.253730350031));
#194107=CARTESIAN_POINT('Ctrl Pts',(104.744679468302,-6.84924188231931,
129.346204329164));
#194108=CARTESIAN_POINT('Ctrl Pts',(104.466231844489,-4.92897072199215,
135.778652702442));
#194109=CARTESIAN_POINT('Ctrl Pts',(104.187784220676,1.52078373823962,137.639969657397));
#194110=CARTESIAN_POINT('Ctrl Pts',(103.909336596864,6.57301223744494,133.219695842813));
#194111=CARTESIAN_POINT('Ctrl Pts',(103.63088897305,5.58496359993783,126.579846951912));
#194112=CARTESIAN_POINT('Ctrl Pts',(103.352441349238,-0.535393745272065,
123.82211974078));
#194113=CARTESIAN_POINT('Ctrl Pts',(103.073993725425,-6.1637503940156,127.480730793984));
#194114=CARTESIAN_POINT('Ctrl Pts',(102.795546101612,-6.12792154660547,
134.193595286717));
#194115=CARTESIAN_POINT('Ctrl Pts',(102.517098477799,-0.460832163475232,
137.791918691816));
#194116=CARTESIAN_POINT('Ctrl Pts',(102.238650853986,5.6297394649859,134.96901758787));
#194117=CARTESIAN_POINT('Ctrl Pts',(101.960203230173,6.54685555318778,128.319000183017));
#194118=CARTESIAN_POINT('Ctrl Pts',(101.68175560636,1.44773121968427,123.952907600908));
#194119=CARTESIAN_POINT('Ctrl Pts',(101.403307982548,-4.981787379107,125.882965629019));
#194120=CARTESIAN_POINT('Ctrl Pts',(101.124860358735,-6.83328675034245,
132.335545228093));
#194121=CARTESIAN_POINT('Ctrl Pts',(100.846412734922,-2.4053294226295,137.38104097262));
#194122=CARTESIAN_POINT('Ctrl Pts',(100.567965111109,4.23300813760519,136.382888759548));
#194123=CARTESIAN_POINT('Ctrl Pts',(100.289517487296,6.98141801332452,130.258341710245));
#194124=CARTESIAN_POINT('Ctrl Pts',(100.011069863483,3.31424579602927,124.635559362262));
#194125=CARTESIAN_POINT('Ctrl Pts',(99.7326222396699,-3.39855639790849,
124.681604005209));
#194126=CARTESIAN_POINT('Ctrl Pts',(99.4541746158571,-6.98825129087862,
130.354162861621));
#194127=CARTESIAN_POINT('Ctrl Pts',(99.1757269920442,-4.15608464258612,
136.440431462363));
#194128=CARTESIAN_POINT('Ctrl Pts',(98.8972793682313,2.49532075622072,137.347426294104));
#194129=CARTESIAN_POINT('Ctrl Pts',(98.6188317444184,6.85364828325664,132.241663415635));
#194130=CARTESIAN_POINT('Ctrl Pts',(98.3403841206056,4.91380785731226,125.815089481885));
#194131=CARTESIAN_POINT('Ctrl Pts',(98.0619364967926,-1.54158193664305,
123.97341198238));
#194132=CARTESIAN_POINT('Ctrl Pts',(97.7834888729798,-6.58033324128762,
128.409042568218));
#194133=CARTESIAN_POINT('Ctrl Pts',(97.5050412491668,-5.57207976433927,
135.045853423614));
#194134=CARTESIAN_POINT('Ctrl Pts',(97.226593625354,0.55664280480716,137.784939598694));
#194135=CARTESIAN_POINT('Ctrl Pts',(96.948146001541,6.17383782984873,134.109214710358));
#194136=CARTESIAN_POINT('Ctrl Pts',(96.6696983777281,6.11757749800464,127.396490361844));
#194137=CARTESIAN_POINT('Ctrl Pts',(96.3912507539153,0.43956230576973,123.815432294619));
#194138=CARTESIAN_POINT('Ctrl Pts',(96.1128031301024,-5.64238917165504,
126.656857928054));
#194139=CARTESIAN_POINT('Ctrl Pts',(95.8343555062895,-6.53926064636413,
133.309635916377));
#194140=CARTESIAN_POINT('Ctrl Pts',(95.5559078824767,-1.42687104770695,
137.660188294596));
#194141=CARTESIAN_POINT('Ctrl Pts',(95.2774602586637,4.99674333726689,135.710569963425));
#194142=CARTESIAN_POINT('Ctrl Pts',(94.9990126348508,6.82859469977515,129.252384925061));
#194143=CARTESIAN_POINT('Ctrl Pts',(94.720565011038,2.38530112858694,124.22038972988));
#194144=CARTESIAN_POINT('Ctrl Pts',(94.442117387225,-4.24996765133445,125.238742135624));
#194145=CARTESIAN_POINT('Ctrl Pts',(94.1636697634123,-6.97972378214161,
131.371626030693));
#194146=CARTESIAN_POINT('Ctrl Pts',(93.885222139599,-3.29545473562348,136.983220723554));
#194147=CARTESIAN_POINT('Ctrl Pts',(93.6067745157866,3.41717622101856,136.91674483311));
#194148=CARTESIAN_POINT('Ctrl Pts',(93.3283268919733,6.98958916888377,131.233286455149));
#194149=CARTESIAN_POINT('Ctrl Pts',(93.0498792681607,4.13891113095855,125.155666186642));
#194150=CARTESIAN_POINT('Ctrl Pts',(92.7714316443476,-2.51522403926791,
124.268920146089));
#194151=CARTESIAN_POINT('Ctrl Pts',(92.4929840205349,-6.85799119293255,
129.387924624807));
#194152=CARTESIAN_POINT('Ctrl Pts',(92.2145363967218,-4.89859947178764,
135.808564584124));
#194153=CARTESIAN_POINT('Ctrl Pts',(91.9360887729091,1.562365854042,137.63058556713));
#194154=CARTESIAN_POINT('Ctrl Pts',(91.6576411490961,6.58759328582208,133.179639301113));
#194155=CARTESIAN_POINT('Ctrl Pts',(91.3791935252832,5.55914430975498,126.545927963732));
#194156=CARTESIAN_POINT('Ctrl Pts',(91.1007459014705,-0.57788670767935,
123.825508199223));
#194157=CARTESIAN_POINT('Ctrl Pts',(90.8222982776573,-6.18386807209161,
127.518312871276));
#194158=CARTESIAN_POINT('Ctrl Pts',(90.5438506538447,-6.10717677700159,
134.230834889814));
#194159=CARTESIAN_POINT('Ctrl Pts',(90.2654030300316,-0.41828837601907,
137.794594444728));
#194160=CARTESIAN_POINT('Ctrl Pts',(89.9869554062187,5.65498660800168,134.934670604388));
#194161=CARTESIAN_POINT('Ctrl Pts',(89.708507782406,6.53160516072318,128.279193663018));
#194162=CARTESIAN_POINT('Ctrl Pts',(89.430060158593,1.40599765739116,123.944221791613));
#194163=CARTESIAN_POINT('Ctrl Pts',(89.1516125347801,-5.01165300627911,
125.913382364846));
#194164=CARTESIAN_POINT('Ctrl Pts',(88.8731649109673,-6.82383939003939,
132.377113014756));
#194165=CARTESIAN_POINT('Ctrl Pts',(88.5947172871542,-2.36525073744058,
137.395561044874));
#194166=CARTESIAN_POINT('Ctrl Pts',(88.3162696633415,4.26688779394398,136.357017880338));
#194167=CARTESIAN_POINT('Ctrl Pts',(88.0378220395285,6.97796489175107,130.2158539537));
#194168=CARTESIAN_POINT('Ctrl Pts',(87.7593744157156,3.2766331465752,124.615498901007));
#194169=CARTESIAN_POINT('Ctrl Pts',(87.4809267919028,-3.43576438787495,
124.702405423128));
#194170=CARTESIAN_POINT('Ctrl Pts',(87.2024791680898,-6.99086229628967,
130.396710671853));
#194171=CARTESIAN_POINT('Ctrl Pts',(86.924031544277,-4.1216992770237,136.465626305881));
#194172=CARTESIAN_POINT('Ctrl Pts',(86.6455839204641,2.53510402162323,137.332115340552));
#194173=CARTESIAN_POINT('Ctrl Pts',(86.3671362966513,6.8622705711149,132.199916683345));
#194174=CARTESIAN_POINT('Ctrl Pts',(86.0886886728382,4.88334570630671,125.785270178391));
#194175=CARTESIAN_POINT('Ctrl Pts',(85.8102410490255,-1.58313529789712,
123.982922590838));
#194176=CARTESIAN_POINT('Ctrl Pts',(85.5317934252125,-6.59479230379227,
128.449143304076));
#194177=CARTESIAN_POINT('Ctrl Pts',(85.2533458013996,-5.5461573560172,135.079693669646));
#194178=CARTESIAN_POINT('Ctrl Pts',(84.9748981775869,0.599125257088023,
137.781421821987));
#194179=CARTESIAN_POINT('Ctrl Pts',(84.6964505537737,6.19384102782544,134.071571575853));
#194180=CARTESIAN_POINT('Ctrl Pts',(84.418002929961,6.09671947994716,127.359314071181));
#194181=CARTESIAN_POINT('Ctrl Pts',(84.1395553061481,0.397010571302045,
123.812886042756));
#194182=CARTESIAN_POINT('Ctrl Pts',(83.8611076823352,-5.66753165732491,
126.691281596061));
#194183=CARTESIAN_POINT('Ctrl Pts',(83.5826600585222,-6.52388916718428,
133.349395835046));
#194184=CARTESIAN_POINT('Ctrl Pts',(83.3042124347095,-1.38511124210516,
137.66874704105));
#194185=CARTESIAN_POINT('Ctrl Pts',(83.0257648108964,5.02651624802251,135.68006246779));
#194186=CARTESIAN_POINT('Ctrl Pts',(82.7473171870836,6.81902086518772,129.210846085452));
#194187=CARTESIAN_POINT('Ctrl Pts',(82.4688695632707,2.34517843493451,124.205991710613));
#194188=CARTESIAN_POINT('Ctrl Pts',(82.1904219394578,-4.28376840868787,
125.264716013022));
#194189=CARTESIAN_POINT('Ctrl Pts',(81.9119743156449,-6.97614135844701,
131.414103080323));
#194190=CARTESIAN_POINT('Ctrl Pts',(81.6335266918322,-3.25778120324508,
137.003166611925));
#194191=CARTESIAN_POINT('Ctrl Pts',(81.355079068019,3.45432072627939,136.895830263219));
#194192=CARTESIAN_POINT('Ctrl Pts',(81.0766314442065,6.99207066130227,131.190730894994));
#194193=CARTESIAN_POINT('Ctrl Pts',(80.7981838203932,4.10444924022979,125.130576117049));
#194194=CARTESIAN_POINT('Ctrl Pts',(80.5197361965806,-2.55496051912119,
124.284352115297));
#194195=CARTESIAN_POINT('Ctrl Pts',(80.2412885727675,-6.86648637816013,
129.429697407007));
#194196=CARTESIAN_POINT('Ctrl Pts',(79.9628409489547,-4.86804670217826,
135.838291033188));
#194197=CARTESIAN_POINT('Ctrl Pts',(79.6843933251418,1.6038900758031,137.620948528586));
#194198=CARTESIAN_POINT('Ctrl Pts',(79.405945701329,6.60193022850756,133.139494742587));
#194199=CARTESIAN_POINT('Ctrl Pts',(79.1274980775159,5.53311902343524,126.512166773338));
#194200=CARTESIAN_POINT('Ctrl Pts',(78.8490504537032,-0.620358256282274,
123.829155261608));
#194201=CARTESIAN_POINT('Ctrl Pts',(78.5706028298902,-6.2037566046621,127.556016714277));
#194202=CARTESIAN_POINT('Ctrl Pts',(78.2921552060774,-6.08620570371632,
134.267947523646));
#194203=CARTESIAN_POINT('Ctrl Pts',(78.0137075822645,-0.375729088733312,
137.797011171955));
#194204=CARTESIAN_POINT('Ctrl Pts',(77.7352599584516,5.68002420340909,134.90017057075));
#194205=CARTESIAN_POINT('Ctrl Pts',(77.4568123346387,6.51611273722737,128.23948071401));
#194206=CARTESIAN_POINT('Ctrl Pts',(77.1783647108257,1.36421199533782,123.935790187287));
#194207=CARTESIAN_POINT('Ctrl Pts',(76.8999170870129,-5.04133292480603,
125.94398033767));
#194208=CARTESIAN_POINT('Ctrl Pts',(76.6214694632,-6.81413916985829,132.418622522501));
#194209=CARTESIAN_POINT('Ctrl Pts',(76.3430218393871,-2.32508440701577,
137.409836877774));
#194210=CARTESIAN_POINT('Ctrl Pts',(76.0645742155741,4.30060933918641,136.33094124537));
#194211=CARTESIAN_POINT('Ctrl Pts',(75.7861265917614,6.97425319912241,130.173388004487));
#194212=CARTESIAN_POINT('Ctrl Pts',(75.5076789679483,3.23889908027492,124.595667770297));
#194213=CARTESIAN_POINT('Ctrl Pts',(75.2292313441357,-3.47284506432852,
124.72343295124));
#194214=CARTESIAN_POINT('Ctrl Pts',(74.9507837203226,-6.99321425272744,
130.439273587703));
#194215=CARTESIAN_POINT('Ctrl Pts',(74.6723360965098,-4.08716118037883,
136.490611369118));
#194216=CARTESIAN_POINT('Ctrl Pts',(74.3938884726969,2.57479334781394,137.316562498648));
#194217=CARTESIAN_POINT('Ctrl Pts',(74.1154408488841,6.87063857501356,132.158118238212));
#194218=CARTESIAN_POINT('Ctrl Pts',(73.836993225071,4.85270260113016,125.755636859138));
#194219=CARTESIAN_POINT('Ctrl Pts',(73.5585456012583,-1.62462999549052,
123.992685970191));
#194220=CARTESIAN_POINT('Ctrl Pts',(73.2800979774453,-6.60900699384299,
128.489331313375));
#194221=CARTESIAN_POINT('Ctrl Pts',(73.0016503536324,-5.52002943279461,
135.113375491641));
#194222=CARTESIAN_POINT('Ctrl Pts',(72.7232027298196,0.641585508562261,
137.777645507711));
#194223=CARTESIAN_POINT('Ctrl Pts',(72.4447551060067,6.21361471074508,134.033807373642));
#194224=CARTESIAN_POINT('Ctrl Pts',(72.1663074821937,6.07563554570727,127.322265437984));
#194225=CARTESIAN_POINT('Ctrl Pts',(71.8878598583809,0.354444125461637,
123.810598862555));
#194226=CARTESIAN_POINT('Ctrl Pts',(71.609412234568,-5.69246413052499,126.725857675724));
#194227=CARTESIAN_POINT('Ctrl Pts',(71.330964610755,-6.5082759428922,133.3890614465));
#194228=CARTESIAN_POINT('Ctrl Pts',(71.0525169869423,-1.34330011069692,
137.677051425141));
#194229=CARTESIAN_POINT('Ctrl Pts',(70.7740693631292,5.05610289937005,135.649374301231));
#194230=CARTESIAN_POINT('Ctrl Pts',(70.4956217393166,6.80919434927445,129.16936629411));
#194231=CARTESIAN_POINT('Ctrl Pts',(70.2171741155033,2.30496883983272,124.191838196331));
#194232=CARTESIAN_POINT('Ctrl Pts',(69.9387264916908,-4.31741042942741,
125.290895163988));
#194233=CARTESIAN_POINT('Ctrl Pts',(69.6602788678776,-6.97230043126892,
131.456557535721));
#194234=CARTESIAN_POINT('Ctrl Pts',(69.3818312440649,-3.21998695258627,
137.02288280126));
#194235=CARTESIAN_POINT('Ctrl Pts',(69.1033836202519,3.49133723041524,136.874689971681));
#194236=CARTESIAN_POINT('Ctrl Pts',(68.8249359964391,6.9942930599711,131.148161017746));
#194237=CARTESIAN_POINT('Ctrl Pts',(68.5464883726262,4.0698352576252,125.105696291628));
#194238=CARTESIAN_POINT('Ctrl Pts',(68.2680407488133,-2.59460232397255,
124.300025685817));
#194239=CARTESIAN_POINT('Ctrl Pts',(67.9895931250004,-6.87472712320984,
129.471521127857));
#194240=CARTESIAN_POINT('Ctrl Pts',(67.7111455011875,-4.83731354530826,
135.867830948109));
#194241=CARTESIAN_POINT('Ctrl Pts',(67.4326978773747,1.64535486482719,137.61105889887));
#194242=CARTESIAN_POINT('Ctrl Pts',(67.1542502535617,6.61602253424027,133.099263654809));
#194243=CARTESIAN_POINT('Ctrl Pts',(66.8758026297489,5.50688870535577,126.478564631767));
#194244=CARTESIAN_POINT('Ctrl Pts',(66.5973550059358,-0.662806817281494,
123.833060792792));
#194245=CARTESIAN_POINT('Ctrl Pts',(66.3189073821232,-6.22341525475008,
127.593840925854));
#194246=CARTESIAN_POINT('Ctrl Pts',(66.0404597583101,-6.0650091038406,134.304931812993));
#194247=CARTESIAN_POINT('Ctrl Pts',(65.7620121344974,-0.333155878668442,
137.799168783944));
#194248=CARTESIAN_POINT('Ctrl Pts',(65.4835645106842,5.70485132343066,134.865518765369));
#194249=CARTESIAN_POINT('Ctrl Pts',(65.2051168868716,6.50037885677781,128.199862807569));
#194250=CARTESIAN_POINT('Ctrl Pts',(64.9266692630585,1.32237578190785,123.927613100363));
#194251=CARTESIAN_POINT('Ctrl Pts',(64.6482216392459,-5.07082603488719,
125.974758413674));
#194252=CARTESIAN_POINT('Ctrl Pts',(64.3697740154327,-6.80418644924447,
132.460072213177));
#194253=CARTESIAN_POINT('Ctrl Pts',(64.09132639162,-2.28483191973344,137.423867942321));
#194254=CARTESIAN_POINT('Ctrl Pts',(63.812878767807,4.33417152376786,136.304659820925));
#194255=CARTESIAN_POINT('Ctrl Pts',(63.5344311439942,6.97028307297671,130.130945436197));
#194256=CARTESIAN_POINT('Ctrl Pts',(63.2559835201813,3.20104499537862,124.576066704985));
#194257=CARTESIAN_POINT('Ctrl Pts',(62.9775358963684,-3.5097970532309,124.744685810362));
#194258=CARTESIAN_POINT('Ctrl Pts',(62.6990882725555,-6.9953070730393,130.481850031987));
#194259=CARTESIAN_POINT('Ctrl Pts',(62.4206406487427,-4.05247163247362,
136.51538572624));
#194260=CARTESIAN_POINT('Ctrl Pts',(62.1421930249296,2.61438726408988,137.300768344709));
#194261=CARTESIAN_POINT('Ctrl Pts',(61.8637454011169,6.87875198487314,132.116269629093));
#194262=CARTESIAN_POINT('Ctrl Pts',(61.5852977773038,4.82187967727427,125.726190622201));
#194263=CARTESIAN_POINT('Ctrl Pts',(61.3068501534911,-1.66606449182178,
124.002701758653));
#194264=CARTESIAN_POINT('Ctrl Pts',(61.0284025296781,-6.62297678470872,
128.529605106938));
#194265=CARTESIAN_POINT('Ctrl Pts',(60.7499549058653,-5.49369696285183,
135.146897641504));
#194266=CARTESIAN_POINT('Ctrl Pts',(60.4715072820523,0.684021985849089,
137.773610795799));
#194267=CARTESIAN_POINT('Ctrl Pts',(60.1930596582395,6.23315814588628,133.995923503096));
#194268=CARTESIAN_POINT('Ctrl Pts',(59.9146120344266,6.05432647655821,127.285345835106));
#194269=CARTESIAN_POINT('Ctrl Pts',(59.6361644106137,0.311864545564345,
123.808570838767));
#194270=CARTESIAN_POINT('Ctrl Pts',(59.3577167868007,-5.71718566737322,
126.760584885814));
#194271=CARTESIAN_POINT('Ctrl Pts',(59.0792691629879,-6.49242155204172,
133.428631280914));
#194272=CARTESIAN_POINT('Ctrl Pts',(58.800821539175,-1.30143920280946,137.685101139145));
#194273=CARTESIAN_POINT('Ctrl Pts',(58.5223739153621,5.08550219496502,135.618506600908));
#194274=CARTESIAN_POINT('Ctrl Pts',(58.2439262915492,6.79911551616065,129.127947088084));
#194275=CARTESIAN_POINT('Ctrl Pts',(57.9654786677363,2.26467383326308,124.1779297115));
#194276=CARTESIAN_POINT('Ctrl Pts',(57.6870310439234,-4.35089246693584,
125.317278618444));
#194277=CARTESIAN_POINT('Ctrl Pts',(57.4085834201106,-6.96820114293417,
131.498987823723));
#194278=CARTESIAN_POINT('Ctrl Pts',(57.1301357962976,-3.18207338412696,
137.042368560968));
#194279=CARTESIAN_POINT('Ctrl Pts',(56.8516881724848,3.52822436176609,136.853324741857));
#194280=CARTESIAN_POINT('Ctrl Pts',(56.5732405486719,6.9962562825383,131.105578400848));
#194281=CARTESIAN_POINT('Ctrl Pts',(56.294792924859,4.03507046577855,125.081027632309));
#194282=CARTESIAN_POINT('Ctrl Pts',(56.0163453010462,-2.63414798488075,
124.315940276861));
#194283=CARTESIAN_POINT('Ctrl Pts',(55.7378976772331,-6.8827131227178,129.513394237565));
#194284=CARTESIAN_POINT('Ctrl Pts',(55.4594500534204,-4.80640114000575,
135.897183234276));
#194285=CARTESIAN_POINT('Ctrl Pts',(55.1810024296073,1.68675868462211,137.600917044446));
#194286=CARTESIAN_POINT('Ctrl Pts',(54.9025548057946,6.62986968082513,133.058947528554));
#194287=CARTESIAN_POINT('Ctrl Pts',(54.6241071819816,5.4804543274898,126.445122784157));
#194288=CARTESIAN_POINT('Ctrl Pts',(54.3456595581689,-0.705230817730614,
123.837224648055));
#194289=CARTESIAN_POINT('Ctrl Pts',(54.0672119343557,-6.24284329389726,
127.63178410442));
#194290=CARTESIAN_POINT('Ctrl Pts',(53.7887643105431,-6.04358776282204,
134.341786387386));
#194291=CARTESIAN_POINT('Ctrl Pts',(53.51031668673,-0.290570323389535,137.801067200743));
#194292=CARTESIAN_POINT('Ctrl Pts',(53.2318690629172,5.72946704808866,134.830716472279));
#194293=CARTESIAN_POINT('Ctrl Pts',(52.9534214391043,6.48440410239917,128.160341411752));
#194294=CARTESIAN_POINT('Ctrl Pts',(52.6749738152913,1.28049056735643,123.919690833848));
#194295=CARTESIAN_POINT('Ctrl Pts',(52.3965261914786,-5.10013124364513,
126.005715452363));
#194296=CARTESIAN_POINT('Ctrl Pts',(52.1180785676656,-6.79398159699943,
132.501460550851));
#194297=CARTESIAN_POINT('Ctrl Pts',(51.8396309438527,-2.24449476716385,
137.43765371859));
#194298=CARTESIAN_POINT('Ctrl Pts',(51.5611833200399,4.36757310402998,136.278174580871));
#194299=CARTESIAN_POINT('Ctrl Pts',(51.2827356962269,6.96605466042841,130.088527821552));
#194300=CARTESIAN_POINT('Ctrl Pts',(51.0042880724141,3.16307229458231,124.556696431394));
#194301=CARTESIAN_POINT('Ctrl Pts',(50.7258404486012,-3.54661898531293,
124.766163212963));
#194302=CARTESIAN_POINT('Ctrl Pts',(50.4473928247883,-6.99714067967511,
130.52443842702));
#194303=CARTESIAN_POINT('Ctrl Pts',(50.1689452009753,-4.0176319187415,136.539948459229));
#194304=CARTESIAN_POINT('Ctrl Pts',(49.8904975771625,2.65388430328469,137.284733463992));
#194305=CARTESIAN_POINT('Ctrl Pts',(49.6120499533496,6.88661050004828,132.074372406703));
#194306=CARTESIAN_POINT('Ctrl Pts',(49.3336023295367,4.79087807689359,125.696932558722));
#194307=CARTESIAN_POINT('Ctrl Pts',(49.0551547057238,-1.7074372515208,124.012969585086));
#194308=CARTESIAN_POINT('Ctrl Pts',(48.776707081911,-6.63670115873435,128.569963192402));
#194309=CARTESIAN_POINT('Ctrl Pts',(48.498259458098,-5.46716092194746,135.180258877061));
#194310=CARTESIAN_POINT('Ctrl Pts',(48.2198118342852,0.72643311645002,137.769317835757));
#194311=CARTESIAN_POINT('Ctrl Pts',(47.9413642104722,6.25247060906043,133.957921368012));
#194312=CARTESIAN_POINT('Ctrl Pts',(47.6629165866595,6.03279306211481,127.248556630613));
#194313=CARTESIAN_POINT('Ctrl Pts',(47.3844689628464,0.269273409411107,
123.806802046542));
#194314=CARTESIAN_POINT('Ctrl Pts',(47.1060213390337,-5.74169535180415,
126.7954619395));
#194315=CARTESIAN_POINT('Ctrl Pts',(46.8275737152206,-6.47632658212296,
133.468103872012));
#194316=CARTESIAN_POINT('Ctrl Pts',(46.5491260914079,-1.25953006961336,
137.69289588478));
#194317=CARTESIAN_POINT('Ctrl Pts',(46.2706784675948,5.11471304540623,135.587460510634));
#194318=CARTESIAN_POINT('Ctrl Pts',(45.9922308437821,6.78878473932087,129.086590002178));
#194319=CARTESIAN_POINT('Ctrl Pts',(45.7137832199691,2.22429490837156,124.164266771503));
#194320=CARTESIAN_POINT('Ctrl Pts',(45.4353355961562,-4.38421328052394,
125.343865398741));
#194321=CARTESIAN_POINT('Ctrl Pts',(45.1568879723434,-6.96384364534361,
131.541392372057));
#194322=CARTESIAN_POINT('Ctrl Pts',(44.8784403485304,-3.1440419027679,137.061623168999));
#194323=CARTESIAN_POINT('Ctrl Pts',(44.5999927247176,3.56498075346585,136.831735365442));
#194324=CARTESIAN_POINT('Ctrl Pts',(44.3215451009046,6.99796025625624,131.062984622213));
#194325=CARTESIAN_POINT('Ctrl Pts',(44.0430974770918,4.00015615291162,125.056571053198));
#194326=CARTESIAN_POINT('Ctrl Pts',(43.7646498532789,-2.67359603646683,
124.332095298706));
#194327=CARTESIAN_POINT('Ctrl Pts',(43.486202229466,-6.8904440807599,129.555315184507));
#194328=CARTESIAN_POINT('Ctrl Pts',(43.2077546056531,-4.77531063174146,
135.926346804027));
#194329=CARTESIAN_POINT('Ctrl Pts',(42.9293069818402,1.72810000095366,137.590523341125));
#194330=CARTESIAN_POINT('Ctrl Pts',(42.6508593580274,6.64347115515083,133.018547857752));
#194331=CARTESIAN_POINT('Ctrl Pts',(42.3724117342144,5.4538168693733,126.411842469708));
#194332=CARTESIAN_POINT('Ctrl Pts',(42.0939641104015,-0.74762868559244,
123.841646673103));
#194333=CARTESIAN_POINT('Ctrl Pts',(41.8155164865887,-6.26204000219037,
127.669844843974));
#194334=CARTESIAN_POINT('Ctrl Pts',(41.5370688627757,-6.02194247443641,
134.378509881167));
#194335=CARTESIAN_POINT('Ctrl Pts',(41.2586212389629,-0.247974000920424,
137.802706352008));
#194336=CARTESIAN_POINT('Ctrl Pts',(40.9801736151499,5.75387046523817,134.795764981093));
#194337=CARTESIAN_POINT('Ctrl Pts',(40.7017259913371,6.46818906604193,128.120917991039));
#194338=CARTESIAN_POINT('Ctrl Pts',(40.4232783675241,1.23855790375582,123.912023681303));
#194339=CARTESIAN_POINT('Ctrl Pts',(40.1448307437113,-5.12924746516435,
126.036850306614));
#194340=CARTESIAN_POINT('Ctrl Pts',(39.8663831198984,-6.78352499126783,
132.542786001862));
#194341=CARTESIAN_POINT('Ctrl Pts',(39.5879354960856,-2.20407444401526,
137.451193695743));
#194342=CARTESIAN_POINT('Ctrl Pts',(39.3094878722726,4.40081284226458,136.251486506627));
#194343=CARTESIAN_POINT('Ctrl Pts',(39.0310402484598,6.96156811816289,130.046136732356));
#194344=CARTESIAN_POINT('Ctrl Pts',(38.7525926246468,3.12498238497894,124.537557667297));
#194345=CARTESIAN_POINT('Ctrl Pts',(38.474145000834,-3.58330949612422,124.78786436319));
#194346=CARTESIAN_POINT('Ctrl Pts',(38.195697377021,-6.9987150046898,130.567037194673));
#194347=CARTESIAN_POINT('Ctrl Pts',(37.9172497532082,-3.98264333018119,
136.564298657899));
#194348=CARTESIAN_POINT('Ctrl Pts',(37.6388021293952,2.69328300182069,137.268458450676));
#194349=CARTESIAN_POINT('Ctrl Pts',(37.3603545055824,6.89421382933879,132.032428123559));
#194350=CARTESIAN_POINT('Ctrl Pts',(37.0819068817695,4.7596989487639,125.667863752866));
#194351=CARTESIAN_POINT('Ctrl Pts',(36.8034592579566,-1.74874674150458,
124.02348906901));
#194352=CARTESIAN_POINT('Ctrl Pts',(36.5250116341437,-6.65017960735793,
128.610404074285));
#194353=CARTESIAN_POINT('Ctrl Pts',(36.2465640103308,-5.44042229338459,
135.213457962098));
#194354=CARTESIAN_POINT('Ctrl Pts',(35.968116386518,0.768817328804687,137.764766786667));
#194355=CARTESIAN_POINT('Ctrl Pts',(35.689668762705,6.27155138463682,133.919802376575));
#194356=CARTESIAN_POINT('Ctrl Pts',(35.4112211388921,6.01103610030595,127.211899187745));
#194357=CARTESIAN_POINT('Ctrl Pts',(35.1327735150793,0.226672295232647,
123.805292551423));
#194358=CARTESIAN_POINT('Ctrl Pts',(34.8543258912663,-5.76599227560232,
126.830487544402));
#194359=CARTESIAN_POINT('Ctrl Pts',(34.5758782674535,-6.45999162954105,
133.507477757125));
#194360=CARTESIAN_POINT('Ctrl Pts',(34.2974306436406,-1.21757426406734,
137.700435373207));
#194361=CARTESIAN_POINT('Ctrl Pts',(34.0189830198277,5.1437343682746,135.556237180835));
#194362=CARTESIAN_POINT('Ctrl Pts',(33.7405353960148,6.778202401566,129.045296568894));
#194363=CARTESIAN_POINT('Ctrl Pts',(33.4620877722019,2.18383356141425,124.150849882625));
#194364=CARTESIAN_POINT('Ctrl Pts',(33.1836401483891,-4.41737163547663,
125.370654519698));
#194365=CARTESIAN_POINT('Ctrl Pts',(32.9051925245761,-6.95922809996586,
131.58376960941));
#194366=CARTESIAN_POINT('Ctrl Pts',(32.6267449007632,-3.10589391777991,
137.080645911863));
#194367=CARTESIAN_POINT('Ctrl Pts',(32.3482972769504,3.60160504349277,136.80992264244));
#194368=CARTESIAN_POINT('Ctrl Pts',(32.0698496531375,6.99940491798352,131.020381260171));
#194369=CARTESIAN_POINT('Ctrl Pts',(31.7914020293246,3.96509361278713,125.032327460544));
#194370=CARTESIAN_POINT('Ctrl Pts',(31.5129544055117,-2.71294501696876,
124.348490152723));
#194371=CARTESIAN_POINT('Ctrl Pts',(31.2345067816988,-6.89791971086261,
129.597282415287));
#194372=CARTESIAN_POINT('Ctrl Pts',(30.9560591578859,-4.74404317258561,
135.955320576696));
#194373=CARTESIAN_POINT('Ctrl Pts',(30.677611534073,1.76937728190418,137.579878174048));
#194374=CARTESIAN_POINT('Ctrl Pts',(30.3991639102601,6.65682645320975,132.978066139427));
#194375=CARTESIAN_POINT('Ctrl Pts',(30.1207162864473,5.42697731806706,126.378724921634));
#194376=CARTESIAN_POINT('Ctrl Pts',(29.8422686626343,-0.789998849798377,
123.846326704078));
#194377=CARTESIAN_POINT('Ctrl Pts',(29.5638210388214,-6.28100466828836,
127.708021734164));
#194378=CARTESIAN_POINT('Ctrl Pts',(29.2853734150086,-6.00007404075783,
134.415100933532));
#194379=CARTESIAN_POINT('Ctrl Pts',(29.0069257911957,-0.205368489683527,
137.804086176998));
#194380=CARTESIAN_POINT('Ctrl Pts',(28.7284781673828,5.77806067060162,134.760665586949));
#194381=CARTESIAN_POINT('Ctrl Pts',(28.4500305435699,6.45173434856014,128.08159400628));
#194382=CARTESIAN_POINT('Ctrl Pts',(28.171582919757,1.19657934493693,123.904611926838));
#194383=CARTESIAN_POINT('Ctrl Pts',(27.8931352959441,-5.15817362053239,
126.068161822712));
#194384=CARTESIAN_POINT('Ctrl Pts',(27.6146876721312,-6.77281701952304,
132.584047034882));
#194385=CARTESIAN_POINT('Ctrl Pts',(27.3362400483183,-2.16357244807759,
137.464487372053));
#194386=CARTESIAN_POINT('Ctrl Pts',(27.0577924245054,4.4338895067609,136.22459658713));
#194387=CARTESIAN_POINT('Ctrl Pts',(26.7793448006925,6.95682361243065,130.003773739425));
#194388=CARTESIAN_POINT('Ctrl Pts',(26.5008971768797,3.08677667800406,124.518651121888));
#194389=CARTESIAN_POINT('Ctrl Pts',(26.2224495530668,-3.61986722608435,
124.809788456898));
#194390=CARTESIAN_POINT('Ctrl Pts',(25.9440019292538,-7.00002998974624,
130.609644756432));
#194391=CARTESIAN_POINT('Ctrl Pts',(25.665554305441,-3.94750716330764,136.588435419948));
#194392=CARTESIAN_POINT('Ctrl Pts',(25.3871066816281,2.7325818997646,137.251943907838));
#194393=CARTESIAN_POINT('Ctrl Pts',(25.1086590578152,6.90156169100052,131.990438333922));
#194394=CARTESIAN_POINT('Ctrl Pts',(24.8302114340022,4.72834344823931,125.638985281792));
#194395=CARTESIAN_POINT('Ctrl Pts',(24.5517638101894,-1.78999143103474,
124.034259820624));
#194396=CARTESIAN_POINT('Ctrl Pts',(24.2733161863765,-6.66341163113055,
128.650926254035));
#194397=CARTESIAN_POINT('Ctrl Pts',(23.9948685625636,-5.41348206797292,
135.246493666413));
#194398=CARTESIAN_POINT('Ctrl Pts',(23.7164209387507,0.811173052350488,
137.759957817164));
#194399=CARTESIAN_POINT('Ctrl Pts',(23.4379733149379,6.29039976557031,133.881567941299));
#194400=CARTESIAN_POINT('Ctrl Pts',(23.159525691125,5.98905639734383,127.175374864857));
#194401=CARTESIAN_POINT('Ctrl Pts',(22.8810780673121,0.184062781628937,
123.804042409345));
#194402=CARTESIAN_POINT('Ctrl Pts',(22.6026304434992,-5.79007553843628,
126.865660402631));
#194403=CARTESIAN_POINT('Ctrl Pts',(22.3241828196863,-6.44341729959363,
133.546751477239));
#194404=CARTESIAN_POINT('Ctrl Pts',(22.0457351958734,-1.17557334085921,
137.707719325048));
#194405=CARTESIAN_POINT('Ctrl Pts',(21.7672875720605,5.17256508817436,135.524837768503));
#194406=CARTESIAN_POINT('Ctrl Pts',(21.4888399482477,6.76736889502847,129.004068318375));
#194407=CARTESIAN_POINT('Ctrl Pts',(21.2103923244347,2.14329129170119,124.137679542035));
#194408=CARTESIAN_POINT('Ctrl Pts',(20.9319447006219,-4.45036630309889,
125.397644988631));
#194409=CARTESIAN_POINT('Ctrl Pts',(20.6534970768089,-6.95435467783159,
131.626117965476));
#194410=CARTESIAN_POINT('Ctrl Pts',(20.3750494529961,-3.06763084275059,
137.099436084669));
#194411=CARTESIAN_POINT('Ctrl Pts',(20.0966018291831,3.6380958747203,136.787887381128));
#194412=CARTESIAN_POINT('Ctrl Pts',(19.8181542053702,7.00059021418742,130.977769893405));
#194413=CARTESIAN_POINT('Ctrl Pts',(19.5397065815574,3.92988414466092,125.0082977527));
#194414=CARTESIAN_POINT('Ctrl Pts',(19.2612589577445,-2.75219346829522,
124.365124231394));
#194415=CARTESIAN_POINT('Ctrl Pts',(18.9828113339316,-6.90513973601376,
129.639294374793));
#194416=CARTESIAN_POINT('Ctrl Pts',(18.7043637101187,-4.71259992116536,
135.98410347865));
#194417=CARTESIAN_POINT('Ctrl Pts',(18.4259160863058,1.81058899792882,137.568981937677));
#194418=CARTESIAN_POINT('Ctrl Pts',(18.1474684624929,6.6699350801164,132.937503873645));
#194419=CARTESIAN_POINT('Ctrl Pts',(17.86902083868,5.39993666812053,126.345771367118));
#194420=CARTESIAN_POINT('Ctrl Pts',(17.5905732148672,-0.832339740306418,
123.851264567558));
#194421=CARTESIAN_POINT('Ctrl Pts',(17.3121255910542,-6.29973658944851,
127.746313360329));
#194422=CARTESIAN_POINT('Ctrl Pts',(17.0336779672413,-5.97798327212915,
134.451558188587));
#194423=CARTESIAN_POINT('Ctrl Pts',(16.7552303434285,-0.162755368441711,
137.805206624583));
#194424=CARTESIAN_POINT('Ctrl Pts',(16.4767827196156,5.80203676780203,134.72541959047));
#194425=CARTESIAN_POINT('Ctrl Pts',(16.1983350958026,6.43504055968944,128.042370914639));
#194426=CARTESIAN_POINT('Ctrl Pts',(15.9198874719898,1.15455644643036,123.897455845098));
#194427=CARTESIAN_POINT('Ctrl Pts',(15.6414398481769,-5.18690863788001,
126.0996488404));
#194428=CARTESIAN_POINT('Ctrl Pts',(15.362992224364,-6.7618580785529,132.625242120967));
#194429=CARTESIAN_POINT('Ctrl Pts',(15.0845446005511,-2.12299028016722,
137.477534254917));
#194430=CARTESIAN_POINT('Ctrl Pts',(14.8060969767383,4.466801871851,136.197505818795));
#194431=CARTESIAN_POINT('Ctrl Pts',(14.5276493529253,6.95182131904109,129.961440412534));
#194432=CARTESIAN_POINT('Ctrl Pts',(14.2492017291125,3.04845658938423,124.499977495755));
#194433=CARTESIAN_POINT('Ctrl Pts',(13.9707541052995,-3.65629082053323,
124.831934681683));
#194434=CARTESIAN_POINT('Ctrl Pts',(13.6923064814867,-7.00108558611715,
130.652259533458));
#194435=CARTESIAN_POINT('Ctrl Pts',(13.4138588576738,-3.91222472010448,
136.612357850978));
#194436=CARTESIAN_POINT('Ctrl Pts',(13.1354112338608,2.77177954088132,137.23519044743));
#194437=CARTESIAN_POINT('Ctrl Pts',(12.856963610048,6.90865381275575,131.94840459374));
#194438=CARTESIAN_POINT('Ctrl Pts',(12.5785159862351,4.6968127372094,125.6102982156));
#194439=CARTESIAN_POINT('Ctrl Pts',(12.3000683624222,-1.83116979177416,
124.045281440813));
#194440=CARTESIAN_POINT('Ctrl Pts',(12.0216207386093,-6.67639673973472,
128.691528230086));
#194441=CARTESIAN_POINT('Ctrl Pts',(11.7431731147965,-5.38634124399241,
135.279364765853));
#194442=CARTESIAN_POINT('Ctrl Pts',(11.4647254909835,0.853498717580522,
137.75489110545));
#194443=CARTESIAN_POINT('Ctrl Pts',(11.1862778671706,6.30901505342741,133.843219478972));
#194444=CARTESIAN_POINT('Ctrl Pts',(10.9078302433578,5.96685476769427,127.13898501537));
#194445=CARTESIAN_POINT('Ctrl Pts',(10.6293826195448,0.141446447510913,
123.803051666633));
#194446=CARTESIAN_POINT('Ctrl Pts',(10.350934995732,-5.81394424789186,126.900979210845));
#194447=CARTESIAN_POINT('Ctrl Pts',(10.0724873719191,-6.42660420644864,
133.585923577051));
#194448=CARTESIAN_POINT('Ctrl Pts',(9.79403974810624,-1.1335288563486,137.714747470394));
#194449=CARTESIAN_POINT('Ctrl Pts',(9.51559212429333,5.20120413677258,135.493263437154));
#194450=CARTESIAN_POINT('Ctrl Pts',(9.23714450048043,6.75628462114785,128.962906778349));
#194451=CARTESIAN_POINT('Ctrl Pts',(8.95869687666756,2.10266960154115,124.124756237763));
#194452=CARTESIAN_POINT('Ctrl Pts',(8.68024925285465,-4.48319606076117,
125.4248358054));
#194453=CARTESIAN_POINT('Ctrl Pts',(8.40180162904178,-6.94922355952728,
131.66843587102));
#194454=CARTESIAN_POINT('Ctrl Pts',(8.12335400522884,-3.0292540955323,137.117992991138));
#194455=CARTESIAN_POINT('Ctrl Pts',(7.84490638141603,3.67445189496732,136.765630398031));
#194456=CARTESIAN_POINT('Ctrl Pts',(7.56645875760307,7.00151610094645,130.935152100895));
#194457=CARTESIAN_POINT('Ctrl Pts',(7.2880111337902,3.89452905323253,124.984482820099));
#194458=CARTESIAN_POINT('Ctrl Pts',(7.00956350997733,-2.79133993608059,
124.381996918337));
#194459=CARTESIAN_POINT('Ctrl Pts',(6.73111588616443,-6.91210388867261,
129.681349506257));
#194460=CARTESIAN_POINT('Ctrl Pts',(6.45266826235151,-4.68098204262199,
136.012694443327));
#194461=CARTESIAN_POINT('Ctrl Pts',(6.17422063853866,1.85173362191231,137.557835035774));
#194462=CARTESIAN_POINT('Ctrl Pts',(5.89577301472578,6.68279655012581,132.896862563455));
#194463=CARTESIAN_POINT('Ctrl Pts',(5.61732539091285,5.37269592153495,126.312983027266));
#194464=CARTESIAN_POINT('Ctrl Pts',(5.33887776709996,-0.874649788159289,
123.856460080569));
#194465=CARTESIAN_POINT('Ctrl Pts',(5.06043014328709,-6.31823507155263,
127.784718303561));
#194466=CARTESIAN_POINT('Ctrl Pts',(4.7819825194742,-5.95567098713191,134.487880295395));
#194467=CARTESIAN_POINT('Ctrl Pts',(4.50353489566127,-0.120136216239877,
137.806067653244));
#194468=CARTESIAN_POINT('Ctrl Pts',(4.22508727184843,5.82579786839633,134.690028297709));
#194469=CARTESIAN_POINT('Ctrl Pts',(3.94663964803551,6.41810831802433,128.003250169541));
#194470=CARTESIAN_POINT('Ctrl Pts',(3.66819202422262,1.11249076541009,123.890555701254));
#194471=CARTESIAN_POINT('Ctrl Pts',(3.3897444004097,-5.21545145242058,126.131310192911));
#194472=CARTESIAN_POINT('Ctrl Pts',(3.11129677659686,-6.75064857444498,
132.666369733619));
#194473=CARTESIAN_POINT('Ctrl Pts',(2.83284915278395,-2.08232944407128,
137.490333860877));
#194474=CARTESIAN_POINT('Ctrl Pts',(2.55440152897106,4.49954871795507,136.170215205482));
#194475=CARTESIAN_POINT('Ctrl Pts',(2.27595390515816,6.94656142335602,129.919138320362));
#194476=CARTESIAN_POINT('Ctrl Pts',(1.9975062813453,3.01002353908442,124.481537480858));
#194477=CARTESIAN_POINT('Ctrl Pts',(1.71905865753238,-3.69257892978116,
124.854302216906));
#194478=CARTESIAN_POINT('Ctrl Pts',(1.44061103371947,-7.00188175468703,
130.694879946647));
#194479=CARTESIAN_POINT('Ctrl Pts',(1.16216340990662,-3.87679730797559,
136.636065064534));
#194480=CARTESIAN_POINT('Ctrl Pts',(0.883715786093727,2.81087447268782,
137.218198690258));
#194481=CARTESIAN_POINT('Ctrl Pts',(0.605268162280799,6.91548993180329,
131.906328460586));
#194482=CARTESIAN_POINT('Ctrl Pts',(0.326820538467947,4.66510798405627,
125.5818036173));
#194483=CARTESIAN_POINT('Ctrl Pts',(0.0483729146550416,-1.87228029784353,
124.056553521165));
#194484=CARTESIAN_POINT('Ctrl Pts',(-0.23007470915786,-6.68913445200245,
128.732208497919));
#194485=CARTESIAN_POINT('Ctrl Pts',(-0.508522332970751,-5.35900082715629,
135.312070042369));
#194486=CARTESIAN_POINT('Ctrl Pts',(-0.786969956783612,0.895792756101716,
137.749566839272));
#194487=CARTESIAN_POINT('Ctrl Pts',(-1.06541758059653,6.32739655841135,
133.804758410613));
#194488=CARTESIAN_POINT('Ctrl Pts',(-1.34386520440944,5.94443203404716,
127.102730987725));
#194489=CARTESIAN_POINT('Ctrl Pts',(-1.62231282822229,0.0988248720430084,
123.802320359999));
#194490=CARTESIAN_POINT('Ctrl Pts',(-1.90076045203519,-5.83759751950527,
126.936442660293));
#194491=CARTESIAN_POINT('Ctrl Pts',(-2.17920807584809,-6.40955297312139,
133.624992605024));
#194492=CARTESIAN_POINT('Ctrl Pts',(-2.45765569966099,-1.09144236850938,
137.721519548813));
#194493=CARTESIAN_POINT('Ctrl Pts',(-2.73610332347384,5.22965045283876,
135.461515356786));
#194494=CARTESIAN_POINT('Ctrl Pts',(-3.01455094728676,6.74494999065597,
128.921813474073));
#194495=CARTESIAN_POINT('Ctrl Pts',(-3.29299857109967,2.06196999618574,
124.112080448687));
#194496=CARTESIAN_POINT('Ctrl Pts',(-3.57144619491253,-4.51585969194472,
125.452225962441));
#194497=CARTESIAN_POINT('Ctrl Pts',(-3.84989381872542,-6.94383493518842,
131.710721757939));
#194498=CARTESIAN_POINT('Ctrl Pts',(-4.12834144253832,-2.99076509818949,
137.136315943637));
#194499=CARTESIAN_POINT('Ctrl Pts',(-4.40678906635123,3.71067175704807,
136.743152517891));
#194500=CARTESIAN_POINT('Ctrl Pts',(-4.68523669016409,7.00218254395157,
130.892529461858));
#194501=CARTESIAN_POINT('Ctrl Pts',(-4.963684313977,3.85902964859785,124.960883545208));
#194502=CARTESIAN_POINT('Ctrl Pts',(-5.24213193778992,-2.83038296973812,
124.399107588329));
#194503=CARTESIAN_POINT('Ctrl Pts',(-5.52057956160276,-6.91881191077996,
129.723446251312));
#194504=CARTESIAN_POINT('Ctrl Pts',(-5.79902718541567,-4.6491907085676,
136.041092411279));
#194505=CARTESIAN_POINT('Ctrl Pts',(-6.07747480922856,1.89280962922548,
137.546437881394));
#194506=CARTESIAN_POINT('Ctrl Pts',(-6.35592243304147,6.69541038665145,
132.856143714835));
#194507=CARTESIAN_POINT('Ctrl Pts',(-6.63437005685431,5.34525608772619,
126.280361117063));
#194508=CARTESIAN_POINT('Ctrl Pts',(-6.91281768066725,-0.916927425542613,
123.86191305059));
#194509=CARTESIAN_POINT('Ctrl Pts',(-7.19126530448013,-6.33649942913263,
127.823235140749));
#194510=CARTESIAN_POINT('Ctrl Pts',(-7.469712928293,-5.93313801255607,134.524065908027));
#194511=CARTESIAN_POINT('Ctrl Pts',(-7.74816055210589,-0.0775126123463511,
137.806669231077));
#194512=CARTESIAN_POINT('Ctrl Pts',(-8.02660817591882,5.84934309190818,
134.654493020103));
#194513=CARTESIAN_POINT('Ctrl Pts',(-8.3050557997317,6.40093825099524,127.964233220621));
#194514=CARTESIAN_POINT('Ctrl Pts',(-8.58350342354456,1.07038386063539,
123.883911750995));
#194515=CARTESIAN_POINT('Ctrl Pts',(-8.86195104735747,-5.2438010064896,
126.163144707024));
#194516=CARTESIAN_POINT('Ctrl Pts',(-9.14039867117038,-6.73918892257159,
132.707428348838));
#194517=CARTESIAN_POINT('Ctrl Pts',(-9.41884629498326,-2.04159144649203,
137.50288571564));
#194518=CARTESIAN_POINT('Ctrl Pts',(-9.69729391879612,4.53212883162697,
136.142725758454));
#194519=CARTESIAN_POINT('Ctrl Pts',(-9.97574154260907,6.94104412028278,
129.876869030427));
#194520=CARTESIAN_POINT('Ctrl Pts',(-10.254189166422,2.97147895125515,124.463331760497));
#194521=CARTESIAN_POINT('Ctrl Pts',(-10.5326367902348,-3.72873020915888,
124.876890233732));
#194522=CARTESIAN_POINT('Ctrl Pts',(-10.8110844140478,-7.00241846595355,
130.737504416682));
#194523=CARTESIAN_POINT('Ctrl Pts',(-11.0895320378606,-3.84122623969676,
136.659556182137));
#194524=CARTESIAN_POINT('Ctrl Pts',(-11.3679796616735,2.84986524650705,
137.200969265957));
#194525=CARTESIAN_POINT('Ctrl Pts',(-11.6464272854864,6.92206979482823,
131.864211493609));
#194526=CARTESIAN_POINT('Ctrl Pts',(-11.9248749092993,4.6332303636112,125.553502542771));
#194527=CARTESIAN_POINT('Ctrl Pts',(-12.2033225331122,-1.91332142587795,
124.068075643991));
#194528=CARTESIAN_POINT('Ctrl Pts',(-12.4817701569251,-6.70162429593314,
128.77296555011));
#194529=CARTESIAN_POINT('Ctrl Pts',(-12.760217780738,-5.33146183057377,
135.344608284054));
#194530=CARTESIAN_POINT('Ctrl Pts',(-13.0386654045509,0.938053600692905,
137.743985215925));
#194531=CARTESIAN_POINT('Ctrl Pts',(-13.3171130283637,6.34554359938892,
133.766186161411));
#194532=CARTESIAN_POINT('Ctrl Pts',(-13.5955606521767,5.92178902728497,
127.066614125326));
#194533=CARTESIAN_POINT('Ctrl Pts',(-13.8740082759896,0.0561996345831295,
123.801848516541));
#194534=CARTESIAN_POINT('Ctrl Pts',(-14.1524558998025,-5.86103447679583,
126.972049436864));
#194535=CARTESIAN_POINT('Ctrl Pts',(-14.4309035236153,-6.39226423145161,
133.663957113442));
#194536=CARTESIAN_POINT('Ctrl Pts',(-14.7093511474282,-1.04931543687181,
137.728035309365));
#194537=CARTESIAN_POINT('Ctrl Pts',(-14.9877987712411,5.25790298228423,
135.429594703837));
#194538=CARTESIAN_POINT('Ctrl Pts',(-15.266246395054,6.73336542356173,128.880789928272));
#194539=CARTESIAN_POINT('Ctrl Pts',(-15.5446940188669,2.02119398377386,
124.099652644515));
#194540=CARTESIAN_POINT('Ctrl Pts',(-15.8231416426798,-4.54835598628669,
125.479814444798));
#194541=CARTESIAN_POINT('Ctrl Pts',(-16.1015892664927,-6.93818900449243,
131.752974059312));
#194542=CARTESIAN_POINT('Ctrl Pts',(-16.3800368903055,-2.95216527694612,
137.154404263204));
#194543=CARTESIAN_POINT('Ctrl Pts',(-16.6584845141185,3.74675411882228,
136.720454573632));
#194544=CARTESIAN_POINT('Ctrl Pts',(-16.9369321379314,7.00258951850748,
130.849903555692));
#194545=CARTESIAN_POINT('Ctrl Pts',(-17.2153797617442,3.82338724620039,
124.93750080251));
#194546=CARTESIAN_POINT('Ctrl Pts',(-17.4938273855571,-2.86932112251383,
124.416455607327));
#194547=CARTESIAN_POINT('Ctrl Pts',(-17.77227500937,-6.92526355376757,129.765583050046));
#194548=CARTESIAN_POINT('Ctrl Pts',(-18.0507226331829,-4.61722709704176,
136.069296330209));
#194549=CARTESIAN_POINT('Ctrl Pts',(-18.3291702569958,1.93381549778173,
137.534790896862));
#194550=CARTESIAN_POINT('Ctrl Pts',(-18.6076178808087,6.70777612228299,
132.81534883664));
#194551=CARTESIAN_POINT('Ctrl Pts',(-18.8860655046216,5.31761818348739,
126.247906845325));
#194552=CARTESIAN_POINT('Ctrl Pts',(-19.1645131284344,-0.959171085842972,
123.867623275557));
#194553=CARTESIAN_POINT('Ctrl Pts',(-19.4429607522474,-6.35452898539608,
127.861862444637));
#194554=CARTESIAN_POINT('Ctrl Pts',(-19.7214083760603,-5.91038518336925,
134.560113685611));
#194555=CARTESIAN_POINT('Ctrl Pts',(-19.9998559998732,-0.0348861361944895,
137.807011335788));
#194556=CARTESIAN_POINT('Ctrl Pts',(-20.278303623686,5.87267156586067,134.618815074426));
#194557=CARTESIAN_POINT('Ctrl Pts',(-20.5567512474989,6.38353099484532,
127.925321513668));
#194558=CARTESIAN_POINT('Ctrl Pts',(-20.8351988713118,1.02823729239309,
123.877524240513));
#194559=CARTESIAN_POINT('Ctrl Pts',(-21.1136464951247,-5.27195624958391,
126.1951512031));
#194560=CARTESIAN_POINT('Ctrl Pts',(-21.3920941189376,-6.72747954757436,
132.748416445183));
#194561=CARTESIAN_POINT('Ctrl Pts',(-21.6705417427505,-2.00077779699093,
137.515189354092));
#194562=CARTESIAN_POINT('Ctrl Pts',(-21.9489893665634,4.56454100559805,
136.115038496344));
#194563=CARTESIAN_POINT('Ctrl Pts',(-22.2274369903762,6.93526961426714,
129.834634109035));
#194564=CARTESIAN_POINT('Ctrl Pts',(-22.5058846141892,2.93282425418085,
124.445361009293));
#194565=CARTESIAN_POINT('Ctrl Pts',(-22.784332238002,-3.76474331906749,
124.899697895151));
#194566=CARTESIAN_POINT('Ctrl Pts',(-23.062779861815,-7.0026957000287,130.780131364099));
#194567=CARTESIAN_POINT('Ctrl Pts',(-23.3412274856278,-3.80551283336702,
136.682830333316));
#194568=CARTESIAN_POINT('Ctrl Pts',(-23.6196751094408,2.88875041752152,
137.183502812971));
#194569=CARTESIAN_POINT('Ctrl Pts',(-23.8981227332536,6.92839315801137,
131.822055253468));
#194570=CARTESIAN_POINT('Ctrl Pts',(-24.1765703570665,4.60118105711114,
125.525396040718));
#194571=CARTESIAN_POINT('Ctrl Pts',(-24.4550179808794,-1.95429165508329,
124.079847382335));
#194572=CARTESIAN_POINT('Ctrl Pts',(-24.7334656046923,-6.71386580871103,
128.813797876394));
#194573=CARTESIAN_POINT('Ctrl Pts',(-25.0119132285052,-5.30372527471246,
135.376978285193));
#194574=CARTESIAN_POINT('Ctrl Pts',(-25.290360852318,0.980279685362951,
137.738146442235));
#194575=CARTESIAN_POINT('Ctrl Pts',(-25.568808476131,6.36345550391485,133.727504160674));
#194576=CARTESIAN_POINT('Ctrl Pts',(-25.8472560999438,5.89892658645264,
127.030635766497));
#194577=CARTESIAN_POINT('Ctrl Pts',(-26.1257037237567,0.0135723146251221,
123.801636153745));
#194578=CARTESIAN_POINT('Ctrl Pts',(-26.4041513475696,-5.88425425129846,
127.007798221134));
#194579=CARTESIAN_POINT('Ctrl Pts',(-26.6825989713826,-6.37473862207999,
133.70281565846));
#194580=CARTESIAN_POINT('Ctrl Pts',(-26.9610465951954,-1.00714962246484,
137.734294510605));
#194581=CARTESIAN_POINT('Ctrl Pts',(-27.2394942190083,5.28596067820108,
135.397502661138));
#194582=CARTESIAN_POINT('Ctrl Pts',(-27.5179418428212,6.72153134913555,
128.839837661092));
#194583=CARTESIAN_POINT('Ctrl Pts',(-27.7963894666341,1.98034307527561,
124.087473285763));
#194584=CARTESIAN_POINT('Ctrl Pts',(-28.0748370904469,-4.58068373962494,
125.507600230172));
#194585=CARTESIAN_POINT('Ctrl Pts',(-28.3532847142599,-6.93228597665136,
131.795191209466));
#194586=CARTESIAN_POINT('Ctrl Pts',(-28.6317323380727,-2.91345606213275,
137.172257279568));
#194587=CARTESIAN_POINT('Ctrl Pts',(-28.9101799618857,3.78269764324474,
136.697537406337));
#194588=CARTESIAN_POINT('Ctrl Pts',(-29.1886275856985,7.00273700953358,
130.807275961916));
#194589=CARTESIAN_POINT('Ctrl Pts',(-29.4670752095115,3.78760316678249,
124.914335458459));
#194590=CARTESIAN_POINT('Ctrl Pts',(-29.7455228333243,-2.90815295154017,
124.434040332496));
#194591=CARTESIAN_POINT('Ctrl Pts',(-30.0239704571372,-6.93145857856742,
129.807758341064));
#194592=CARTESIAN_POINT('Ctrl Pts',(-30.3024180809501,-4.5850923924679,
136.097305155009));
#194593=CARTESIAN_POINT('Ctrl Pts',(-30.580865704763,1.97474970809384,137.52289451376));
#194594=CARTESIAN_POINT('Ctrl Pts',(-30.8593133285759,6.71989329880362,
132.774479440534));
#194595=CARTESIAN_POINT('Ctrl Pts',(-31.1377609523888,5.28978323295099,
126.215621414657));
#194596=CARTESIAN_POINT('Ctrl Pts',(-31.4162085762017,-1.00137920370602,
123.873590543879));
#194597=CARTESIAN_POINT('Ctrl Pts',(-31.6946562000146,-6.37232307225107,
127.900598783877));
#194598=CARTESIAN_POINT('Ctrl Pts',(-31.9731038238274,-5.88741334268594,
134.596022292384));
#194599=CARTESIAN_POINT('Ctrl Pts',(-32.2515514476404,0.00774163267598956,
137.807093954702));
#194600=CARTESIAN_POINT('Ctrl Pts',(-32.5299990714533,5.89578242580862,
134.582995782735));
#194601=CARTESIAN_POINT('Ctrl Pts',(-32.8084466952661,6.36588719460685,
127.886516490566));
#194602=CARTESIAN_POINT('Ctrl Pts',(-33.086894319079,0.9860526224398,123.8713934065));
#194603=CARTESIAN_POINT('Ctrl Pts',(-33.365341942892,-5.29991613840065,
126.227328495126));
#194604=CARTESIAN_POINT('Ctrl Pts',(-33.6437895667048,-6.71552088334846,
132.789332503824));
#194605=CARTESIAN_POINT('Ctrl Pts',(-33.9222371905177,-1.95989000793276,
137.527244320318));
#194606=CARTESIAN_POINT('Ctrl Pts',(-34.2006848143306,4.59678403882356,
136.08715444511));
#194607=CARTESIAN_POINT('Ctrl Pts',(-34.4791324381435,6.9292381192855,129.792435121214));
#194608=CARTESIAN_POINT('Ctrl Pts',(-34.7575800619564,2.89406088022529,
124.427625893158));
#194609=CARTESIAN_POINT('Ctrl Pts',(-35.0360276857693,-3.80061692502793,
124.922724356021));
#194610=CARTESIAN_POINT('Ctrl Pts',(-35.3144753095821,-7.00271344663942,
130.822759209339));
#194611=CARTESIAN_POINT('Ctrl Pts',(-35.592922933395,-3.76965841235978,
136.705886655638));
#194612=CARTESIAN_POINT('Ctrl Pts',(-35.8713705572079,2.92752854482695,
137.165799978524));
#194613=CARTESIAN_POINT('Ctrl Pts',(-36.1498181810209,6.9344597870381,131.779861302279));
#194614=CARTESIAN_POINT('Ctrl Pts',(-36.4282658048337,4.56896125215494,
125.49748515264));
#194615=CARTESIAN_POINT('Ctrl Pts',(-36.7067134286466,-1.99518946729269,
124.091868299989));
#194616=CARTESIAN_POINT('Ctrl Pts',(-36.9851610524595,-6.72585853672236,
128.854703963711));
#194617=CARTESIAN_POINT('Ctrl Pts',(-37.2636086762724,-5.27579218736066,
135.409178846303));
#194618=CARTESIAN_POINT('Ctrl Pts',(-37.5420563000852,1.02246944540875,
137.732050734562));
#194619=CARTESIAN_POINT('Ctrl Pts',(-37.8205039238982,6.38113160825695,
133.688713841779));
#194620=CARTESIAN_POINT('Ctrl Pts',(-38.0989515477111,5.87584555872632,
126.994797244432));
#194621=CARTESIAN_POINT('Ctrl Pts',(-38.377399171524,-0.0290555082599903,
123.801683279478));
#194622=CARTESIAN_POINT('Ctrl Pts',(-38.6558467953367,-5.90725598259587,
127.04368768842));
#194623=CARTESIAN_POINT('Ctrl Pts',(-38.9342944191497,-6.35697679442443,
133.741566800161));
#194624=CARTESIAN_POINT('Ctrl Pts',(-39.2127420429625,-0.964946487758246,
137.740296920595));
#194625=CARTESIAN_POINT('Ctrl Pts',(-39.4911896667755,5.31382250090111,
135.365240417872));
#194626=CARTESIAN_POINT('Ctrl Pts',(-39.7696372905882,6.70944820589337,
128.798958190032));
#194627=CARTESIAN_POINT('Ctrl Pts',(-40.0480849144012,1.93941878443644,
124.07554282374));
#194628=CARTESIAN_POINT('Ctrl Pts',(-40.3265325382142,-4.61284175404266,
125.535582288951));
#194629=CARTESIAN_POINT('Ctrl Pts',(-40.604980162027,-6.9261260704041,131.837371644027));
#194630=CARTESIAN_POINT('Ctrl Pts',(-40.8834277858398,-2.87463888813357,
137.18987433118));
#194631=CARTESIAN_POINT('Ctrl Pts',(-41.1618754096529,3.81850099841496,
136.674401865208));
#194632=CARTESIAN_POINT('Ctrl Pts',(-41.4403230334656,7.00262501156454,
130.76464826011));
#194633=CARTESIAN_POINT('Ctrl Pts',(-41.7187706572786,3.75167873633635,
124.891388371457));
#194634=CARTESIAN_POINT('Ctrl Pts',(-41.9972182810916,-2.94687701788942,
124.451861112224));
#194635=CARTESIAN_POINT('Ctrl Pts',(-42.2756659049044,-6.93739675562063,
129.849970561546));
#194636=CARTESIAN_POINT('Ctrl Pts',(-42.5541135287174,-4.55278778560923,
136.125117847804));
#194637=CARTESIAN_POINT('Ctrl Pts',(-42.8325611525302,2.01561074332903,
137.510749172913));
#194638=CARTESIAN_POINT('Ctrl Pts',(-43.1110087763431,6.73176146720674,
132.733537040953));
#194639=CARTESIAN_POINT('Ctrl Pts',(-43.389456400156,5.26175226755184,126.183506021407));
#194640=CARTESIAN_POINT('Ctrl Pts',(-43.6679040239687,-1.0435502150944,
123.879814634434));
#194641=CARTESIAN_POINT('Ctrl Pts',(-43.9463516477818,-6.38988103033122,
127.93944272308));
#194642=CARTESIAN_POINT('Ctrl Pts',(-44.2247992715946,-5.86422334173611,
134.631790397739));
#194643=CARTESIAN_POINT('Ctrl Pts',(-44.5032468954075,0.050369114677416,
137.806917084757));
#194644=CARTESIAN_POINT('Ctrl Pts',(-44.7816945192204,5.91867481537061,
134.547036472328));
#194645=CARTESIAN_POINT('Ctrl Pts',(-45.0601421430334,6.34800750407734,
127.847819589252));
#194646=CARTESIAN_POINT('Ctrl Pts',(-45.3385897668461,0.943831413943965,
123.865519476137));
#194647=CARTESIAN_POINT('Ctrl Pts',(-45.6170373906592,-5.32767963687585,
126.25967539076));
#194648=CARTESIAN_POINT('Ctrl Pts',(-45.895485014472,-6.7033133730266,132.830175008601));
#194649=CARTESIAN_POINT('Ctrl Pts',(-46.1739326382849,-1.91892959442962,
137.539050167615));
#194650=CARTESIAN_POINT('Ctrl Pts',(-46.4523802620978,4.62885673652604,
136.059074638009));
#194651=CARTESIAN_POINT('Ctrl Pts',(-46.7308278859106,6.92294985883713,
129.750273630666));
#194652=CARTESIAN_POINT('Ctrl Pts',(-47.0092755097235,2.8551902657795,124.410127069272));
#194653=CARTESIAN_POINT('Ctrl Pts',(-47.2877231335364,-3.83634969773052,
124.945968763085));
#194654=CARTESIAN_POINT('Ctrl Pts',(-47.5661707573492,-7.00247170512816,
130.865386372813));
#194655=CARTESIAN_POINT('Ctrl Pts',(-47.8446183811622,-3.73366430527375,
136.728724294741));
#194656=CARTESIAN_POINT('Ctrl Pts',(-48.123066004975,2.96619819148554,137.147861418602));
#194657=CARTESIAN_POINT('Ctrl Pts',(-48.4015136287881,6.9402694571073,131.737631203552));
#194658=CARTESIAN_POINT('Ctrl Pts',(-48.6799612526008,4.53657214265928,
125.469770912784));
#194659=CARTESIAN_POINT('Ctrl Pts',(-48.9584088764139,-2.03601334702262,
124.104137951514));
#194660=CARTESIAN_POINT('Ctrl Pts',(-49.2368565002267,-6.7376020355722,
128.895682296272));
#194661=CARTESIAN_POINT('Ctrl Pts',(-49.5153041240395,-5.24766360358919,
135.441208774179));
#194662=CARTESIAN_POINT('Ctrl Pts',(-49.7937517478526,1.06462131747325,
137.725698318783));
#194663=CARTESIAN_POINT('Ctrl Pts',(-50.0721993716652,6.39857125742062,
133.649816642113));
#194664=CARTESIAN_POINT('Ctrl Pts',(-50.3506469954783,5.85254679938199,
126.959099887138));
#194665=CARTESIAN_POINT('Ctrl Pts',(-50.6290946192911,-0.0716822544825644,
123.801989891996));
#194666=CARTESIAN_POINT('Ctrl Pts',(-50.907542243104,-5.93003881835047,
127.079716508824));
#194667=CARTESIAN_POINT('Ctrl Pts',(-51.1859898669169,-6.33897940665598,
133.780209102606));
#194668=CARTESIAN_POINT('Ctrl Pts',(-51.4644374907297,-0.922707596604453,
137.746042316915));
#194669=CARTESIAN_POINT('Ctrl Pts',(-51.7428851145428,5.34148741795441,
135.332809169526));
#194670=CARTESIAN_POINT('Ctrl Pts',(-52.0213327383556,6.69711644158035,
128.758153029896));
#194671=CARTESIAN_POINT('Ctrl Pts',(-52.2997803621686,1.89842262772099,
124.063861700536));
#194672=CARTESIAN_POINT('Ctrl Pts',(-52.5782279859813,-4.64482883791282,
125.563759584248));
#194673=CARTESIAN_POINT('Ctrl Pts',(-52.8566756097944,-6.91970951400822,
131.879513799985));
#194674=CARTESIAN_POINT('Ctrl Pts',(-53.135123233607,-2.83571519333325,
137.207254765232));
#194675=CARTESIAN_POINT('Ctrl Pts',(-53.4135708574202,3.85416285762642,
136.651048807542));
#194676=CARTESIAN_POINT('Ctrl Pts',(-53.6920184812329,7.0022535287505,130.72202202986));
#194677=CARTESIAN_POINT('Ctrl Pts',(-53.9704661050458,3.71561528605495,
124.868660391816));
#194678=CARTESIAN_POINT('Ctrl Pts',(-54.2489137288587,-2.98549188662705,
124.469917286158));
#194679=CARTESIAN_POINT('Ctrl Pts',(-54.5273613526715,-6.94307786488582,
129.892218147303));
#194680=CARTESIAN_POINT('Ctrl Pts',(-54.8058089764845,-4.5203144735249,
136.152733377983));
#194681=CARTESIAN_POINT('Ctrl Pts',(-55.0842566002972,2.05639708936689,
137.498355324372));
#194682=CARTESIAN_POINT('Ctrl Pts',(-55.3627042241104,6.74338018771311,
132.69252315503));
#194683=CARTESIAN_POINT('Ctrl Pts',(-55.6411518479232,5.23352632598741,
126.151561855625));
#194684=CARTESIAN_POINT('Ctrl Pts',(-55.919599471736,-1.08568255734582,
123.886295316588));
#194685=CARTESIAN_POINT('Ctrl Pts',(-56.1980470955489,-6.40720220901991,
127.978392822871));
#194686=CARTESIAN_POINT('Ctrl Pts',(-56.4764947193619,-5.8408160398338,
134.667416676276));
#194687=CARTESIAN_POINT('Ctrl Pts',(-56.7549423431748,0.0929947302327828,
137.806480732508));
#194688=CARTESIAN_POINT('Ctrl Pts',(-57.0333899669875,5.94134788626073,
134.510938475691));
#194689=CARTESIAN_POINT('Ctrl Pts',(-57.3118375908005,6.32989258579528,
127.809232243652));
#194690=CARTESIAN_POINT('Ctrl Pts',(-57.5902852146133,0.901575231427987,
123.859902667085));
#194691=CARTESIAN_POINT('Ctrl Pts',(-57.8687328384263,-5.35524571622284,
126.292190691378));
#194692=CARTESIAN_POINT('Ctrl Pts',(-58.1471804622391,-6.69085746896258,
132.870942446081));
#194693=CARTESIAN_POINT('Ctrl Pts',(-58.4256280860521,-1.87789807428466,
137.550606458515));
#194694=CARTESIAN_POINT('Ctrl Pts',(-58.7040757098649,4.6607579102399,136.030800115547));
#194695=CARTESIAN_POINT('Ctrl Pts',(-58.9825233336777,6.91640506593584,
129.708151199698));
#194696=CARTESIAN_POINT('Ctrl Pts',(-59.2609709574908,2.81621385120844,
124.392865186062));
#194697=CARTESIAN_POINT('Ctrl Pts',(-59.5394185813036,-3.87194031308425,
124.969430255013));
#194698=CARTESIAN_POINT('Ctrl Pts',(-59.8178662051166,-7.00197048445272,
130.908011274954));
#194699=CARTESIAN_POINT('Ctrl Pts',(-60.0963138289294,-3.69753184588372,
136.751342404371));
#194700=CARTESIAN_POINT('Ctrl Pts',(-60.3747614527424,3.00475792457964,
137.129687797925));
#194701=CARTESIAN_POINT('Ctrl Pts',(-60.6532090765552,6.94582195293937,
131.695366522141));
#194702=CARTESIAN_POINT('Ctrl Pts',(-60.9316567003681,4.50401492881459,
125.442254348109));
#194703=CARTESIAN_POINT('Ctrl Pts',(-61.210104324181,-2.07676178152925,
124.116655882255));
#194704=CARTESIAN_POINT('Ctrl Pts',(-61.4885519479939,-6.74909587010084,
128.93673135561));
#194705=CARTESIAN_POINT('Ctrl Pts',(-61.7669995718066,-5.21934056571308,
135.473066881942));
#194706=CARTESIAN_POINT('Ctrl Pts',(-62.0454471956197,1.10673373960332,
137.719089430292));
#194707=CARTESIAN_POINT('Ctrl Pts',(-62.3238948194324,6.41577380517329,
133.610814003028));
#194708=CARTESIAN_POINT('Ctrl Pts',(-62.6023424432454,5.82903117176375,
126.923545017394));
#194709=CARTESIAN_POINT('Ctrl Pts',(-62.8807900670583,-0.114306344492842,
123.802555979936));
#194710=CARTESIAN_POINT('Ctrl Pts',(-63.1592376908712,-5.95260191433588,
127.115883347286));
#194711=CARTESIAN_POINT('Ctrl Pts',(-63.4376853146842,-6.32074712567447,
133.818741133891));
#194712=CARTESIAN_POINT('Ctrl Pts',(-63.716132938497,-0.880434514181572,
137.751530486667));
#194713=CARTESIAN_POINT('Ctrl Pts',(-63.99458056231,5.36895440422691,135.300210117855));
#194714=CARTESIAN_POINT('Ctrl Pts',(-64.2730281861228,6.6845365131549,128.717423692735));
#194715=CARTESIAN_POINT('Ctrl Pts',(-64.5514758099358,1.85735612425694,
124.052430348997));
#194716=CARTESIAN_POINT('Ctrl Pts',(-64.8299234337484,-4.67664380594228,
125.592131071942));
#194717=CARTESIAN_POINT('Ctrl Pts',(-65.1083710575615,-6.91303654523158,
131.921616115747));
#194718=CARTESIAN_POINT('Ctrl Pts',(-65.3868186813742,-2.79668642006362,
137.224397937687));
#194719=CARTESIAN_POINT('Ctrl Pts',(-65.6652663051872,3.88968189941585,
136.627479098696));
#194720=CARTESIAN_POINT('Ctrl Pts',(-65.9437139290001,7.00162257485687,
130.679398850698));
#194721=CARTESIAN_POINT('Ctrl Pts',(-66.2221615528129,3.67941415228271,
124.846152361731));
#194722=CARTESIAN_POINT('Ctrl Pts',(-66.500609176626,-3.02399612686491,
124.48820818522));
#194723=CARTESIAN_POINT('Ctrl Pts',(-66.7790568004388,-6.94850169584742,
129.934499532835));
#194724=CARTESIAN_POINT('Ctrl Pts',(-67.0575044242516,-4.48767365952541,
136.180150722241));
#194725=CARTESIAN_POINT('Ctrl Pts',(-67.3359520480646,2.09710723485436,
137.485713427398));
#194726=CARTESIAN_POINT('Ctrl Pts',(-67.6143996718775,6.75474902978674,
132.651439302549));
#194727=CARTESIAN_POINT('Ctrl Pts',(-67.8928472956903,5.20510645418034,
126.119790101011));
#194728=CARTESIAN_POINT('Ctrl Pts',(-68.1712949195033,-1.12777466923081,
123.893032350195));
#194729=CARTESIAN_POINT('Ctrl Pts',(-68.449742543316,-6.42428596647451,
128.017447639935));
#194730=CARTESIAN_POINT('Ctrl Pts',(-68.728190167129,-5.81719230434518,
134.702899807851));
#194731=CARTESIAN_POINT('Ctrl Pts',(-69.0066377909419,0.135616899834216,
137.805784914121));
#194732=CARTESIAN_POINT('Ctrl Pts',(-69.2850854147548,5.96380079832,134.474703130449));
#194733=CARTESIAN_POINT('Ctrl Pts',(-69.5635330385676,6.31154311101565,
127.770755883637));
#194734=CARTESIAN_POINT('Ctrl Pts',(-69.8419806623805,0.859285640710264,
123.854543187474));
#194735=CARTESIAN_POINT('Ctrl Pts',(-70.1204282861936,-5.38261335497044,
126.324873192109));
#194736=CARTESIAN_POINT('Ctrl Pts',(-70.3988759100064,-6.67815363271447,
132.911633305611));
#194737=CARTESIAN_POINT('Ctrl Pts',(-70.6773235338194,-1.83679696793597,
137.561912764793));
#194738=CARTESIAN_POINT('Ctrl Pts',(-70.9557711576322,4.69248637785542,
136.002331925448));
#194739=CARTESIAN_POINT('Ctrl Pts',(-71.2342187814451,6.90960398310133,
129.666069389173));
#194740=CARTESIAN_POINT('Ctrl Pts',(-71.5126664052579,2.77713308079745,
124.375840883174));
#194741=CARTESIAN_POINT('Ctrl Pts',(-71.7911140290708,-3.90738745226578,
124.993107962432));
#194742=CARTESIAN_POINT('Ctrl Pts',(-72.0695616528837,-7.00120980318599,
130.950632336283));
#194743=CARTESIAN_POINT('Ctrl Pts',(-72.3480092766965,-3.66126237309149,
136.773740146404));
#194744=CARTESIAN_POINT('Ctrl Pts',(-72.6264569005095,3.04320631526353,
137.111279789924));
#194745=CARTESIAN_POINT('Ctrl Pts',(-72.9049045243223,6.95111706878496,
131.653068824177));
#194746=CARTESIAN_POINT('Ctrl Pts',(-73.1833521481353,4.47129081703998,
125.414936478256));
#194747=CARTESIAN_POINT('Ctrl Pts',(-73.4617997719481,-2.11743326086482,
124.129421628353));
#194748=CARTESIAN_POINT('Ctrl Pts',(-73.7402473957612,-6.76033961440018,
128.977849620639));
#194749=CARTESIAN_POINT('Ctrl Pts',(-74.018695019574,-5.19082412325261,
135.504751989078));
#194750=CARTESIAN_POINT('Ctrl Pts',(-74.2971426433868,1.14880515130821,
137.712224313981));
#194751=CARTESIAN_POINT('Ctrl Pts',(-74.5755902671998,6.43273861406817,
133.571707369781));
#194752=CARTESIAN_POINT('Ctrl Pts',(-74.8540378910127,5.80529954725181,
126.8881339527));
#194753=CARTESIAN_POINT('Ctrl Pts',(-75.1324855148255,-0.156926198840311,
123.803381522322));
#194754=CARTESIAN_POINT('Ctrl Pts',(-75.4109331386384,-5.97494443446864,
127.15218686363));
#194755=CARTESIAN_POINT('Ctrl Pts',(-75.6893807624512,-6.30228062708332,
133.857161466198));
#194756=CARTESIAN_POINT('Ctrl Pts',(-75.9678283862644,-0.838128806933456,
137.756761226486));
#194757=CARTESIAN_POINT('Ctrl Pts',(-76.2462760100769,5.3962224419198,135.267444470826));
#194758=CARTESIAN_POINT('Ctrl Pts',(-76.52472363389,6.67170888677059,128.676771687789));
#194759=CARTESIAN_POINT('Ctrl Pts',(-76.8031712577027,1.81622079577817,
124.041249192718));
#194760=CARTESIAN_POINT('Ctrl Pts',(-77.0816188815158,-4.70828547921653,
125.620695700721));
#194761=CARTESIAN_POINT('Ctrl Pts',(-77.3600665053286,-6.90610741134329,
131.963677031195));
#194762=CARTESIAN_POINT('Ctrl Pts',(-77.6385141291417,-2.75755401454922,
137.241303213299));
#194763=CARTESIAN_POINT('Ctrl Pts',(-77.9169617529544,3.92505680761298,
136.603693612052));
#194764=CARTESIAN_POINT('Ctrl Pts',(-78.1954093767674,7.00073217326374,
130.636780302039));
#194765=CARTESIAN_POINT('Ctrl Pts',(-78.4738570005803,3.6430766764653,124.823865115242));
#194766=CARTESIAN_POINT('Ctrl Pts',(-78.7523046243931,-3.06238831181505,
124.506733131632));
#194767=CARTESIAN_POINT('Ctrl Pts',(-79.0307522482061,-6.95366804752337,
129.976813151389));
#194768=CARTESIAN_POINT('Ctrl Pts',(-79.3091998720188,-4.45486655312747,
136.207368864621));
#194769=CARTESIAN_POINT('Ctrl Pts',(-79.5876474958318,2.13773967126259,
137.472823950436));
#194770=CARTESIAN_POINT('Ctrl Pts',(-79.8660951196445,6.76586757215105,
132.610287005887));
#194771=CARTESIAN_POINT('Ctrl Pts',(-80.1445427434577,5.17649370523912,
126.08819193488));
#194772=CARTESIAN_POINT('Ctrl Pts',(-80.4229903672703,-1.16982499101125,
123.900025485612));
#194773=CARTESIAN_POINT('Ctrl Pts',(-80.7014379910835,-6.44113166965063,
128.056605727087));
#194774=CARTESIAN_POINT('Ctrl Pts',(-80.9798856148961,-5.7933530106558,
134.738238477622));
#194775=CARTESIAN_POINT('Ctrl Pts',(-81.2583332387092,0.17823404410257,
137.804829655383));
#194776=CARTESIAN_POINT('Ctrl Pts',(-81.5367808625219,5.98603271954817,
134.438331779315));
#194777=CARTESIAN_POINT('Ctrl Pts',(-81.815228486335,6.29295975968447,127.732391934959));
#194778=CARTESIAN_POINT('Ctrl Pts',(-82.0936761101477,0.816964208846405,
123.849441235906));
#194779=CARTESIAN_POINT('Ctrl Pts',(-82.3721237339607,-5.40978153900143,
126.357721681897));
#194780=CARTESIAN_POINT('Ctrl Pts',(-82.6505713577735,-6.66520233502723,
132.952246079378));
#194781=CARTESIAN_POINT('Ctrl Pts',(-82.9290189815866,-1.79562779839943,
137.572968667493));
#194782=CARTESIAN_POINT('Ctrl Pts',(-83.2074666053992,4.72404096366304,
135.97367112261));
#194783=CARTESIAN_POINT('Ctrl Pts',(-83.4859142292123,6.90254686235,129.624029758449));
#194784=CARTESIAN_POINT('Ctrl Pts',(-83.7643618530252,2.73794940269844,
124.359054791448));
#194785=CARTESIAN_POINT('Ctrl Pts',(-84.0428094768383,-3.94268980176888,
125.017001007954));
#194786=CARTESIAN_POINT('Ctrl Pts',(-84.3212571006508,-7.00018968951541,
130.99324797746));
#194787=CARTESIAN_POINT('Ctrl Pts',(-84.5997047244641,-3.62485723087481,
136.795916690882));
#194788=CARTESIAN_POINT('Ctrl Pts',(-84.8781523482765,3.08154193881888,
137.092638076712));
#194789=CARTESIAN_POINT('Ctrl Pts',(-85.1565999720898,6.95615460843127,
131.61073967702));
#194790=CARTESIAN_POINT('Ctrl Pts',(-85.4350475959023,4.4384010199398,125.387818315495));
#194791=CARTESIAN_POINT('Ctrl Pts',(-85.7134952197154,-2.1580262779319,
124.142434716771));
#194792=CARTESIAN_POINT('Ctrl Pts',(-85.9919428435283,-6.7713328518292,
129.019035567703));
#194793=CARTESIAN_POINT('Ctrl Pts',(-86.2703904673411,-5.16211533289519,
135.536262921482));
#194794=CARTESIAN_POINT('Ctrl Pts',(-86.5488380911541,1.19083399361533,
137.70510322424));
#194795=CARTESIAN_POINT('Ctrl Pts',(-86.827285714967,6.4494650554685,133.532498191482));
#194796=CARTESIAN_POINT('Ctrl Pts',(-87.1057333387799,5.78135280522977,
126.852868005224));
#194797=CARTESIAN_POINT('Ctrl Pts',(-87.3841809625928,-0.199540238229241,
123.804466488563));
#194798=CARTESIAN_POINT('Ctrl Pts',(-87.6626285864056,-5.99706555083783,
127.188625712615));
#194799=CARTESIAN_POINT('Ctrl Pts',(-87.9410762102187,-6.28358059516641,
133.895468675847));
#194800=CARTESIAN_POINT('Ctrl Pts',(-88.2195238340314,-0.795792042514341,
137.761734342542));
#194801=CARTESIAN_POINT('Ctrl Pts',(-88.4979714578443,5.42329052060546,
135.234513442586));
#194802=CARTESIAN_POINT('Ctrl Pts',(-88.7764190816572,6.65863403776028,
128.636198521433));
#194803=CARTESIAN_POINT('Ctrl Pts',(-89.0548667054699,1.77501816656995,
124.03031864602));
#194804=CARTESIAN_POINT('Ctrl Pts',(-89.3333143292831,-4.73975268523957,
125.649452412109));
#194805=CARTESIAN_POINT('Ctrl Pts',(-89.6117619530957,-6.8989223691057,
132.005694987746));
#194806=CARTESIAN_POINT('Ctrl Pts',(-89.8902095769088,-2.71831942685781,
137.257969965635));
#194807=CARTESIAN_POINT('Ctrl Pts',(-90.1686572007216,3.9602862713853,136.579693228991));
#194808=CARTESIAN_POINT('Ctrl Pts',(-90.4471048245344,6.99958235696585,
130.59416796313));
#194809=CARTESIAN_POINT('Ctrl Pts',(-90.7255524483476,3.60660420510239,
124.801799478213));
#194810=CARTESIAN_POINT('Ctrl Pts',(-91.0040000721602,-3.10066701883943,
124.525491438947));
#194811=CARTESIAN_POINT('Ctrl Pts',(-91.2824476959735,-6.95857672847263,
130.019157435019));
#194812=CARTESIAN_POINT('Ctrl Pts',(-91.560895319786,-4.4218943700117,136.234386796543));
#194813=CARTESIAN_POINT('Ctrl Pts',(-91.8393429435991,2.17829289294083,
137.459687371113));
#194814=CARTESIAN_POINT('Ctrl Pts',(-92.1177905674117,6.77673540280433,
132.56906778996));
#194815=CARTESIAN_POINT('Ctrl Pts',(-92.3962381912249,5.14768913942031,
126.056768528114));
#194816=CARTESIAN_POINT('Ctrl Pts',(-92.6746858150375,-1.21183196449619,
123.907274463707));
#194817=CARTESIAN_POINT('Ctrl Pts',(-92.9531334388505,-6.45773869432309,
128.095865633305));
#194818=CARTESIAN_POINT('Ctrl Pts',(-93.2315810626634,-5.76929904214118,
134.773431376103));
#194819=CARTESIAN_POINT('Ctrl Pts',(-93.5100286864763,0.220844583841736,
137.803614991691));
#194820=CARTESIAN_POINT('Ctrl Pts',(-93.7884763102892,6.00804282613147,
134.401825770043));
#194821=CARTESIAN_POINT('Ctrl Pts',(-94.0669239341021,6.27414322041607,
127.694141819211));
#194822=CARTESIAN_POINT('Ctrl Pts',(-94.3453715579151,0.774612504073732,
123.844597001431));
#194823=CARTESIAN_POINT('Ctrl Pts',(-94.6238191817278,-5.43674926158731,
126.390734943524));
#194824=CARTESIAN_POINT('Ctrl Pts',(-94.9022668055408,-6.65200405581671,
132.99277926246));
#194825=CARTESIAN_POINT('Ctrl Pts',(-95.1807144293538,-1.75439209121494,
137.583773756932));
#194826=CARTESIAN_POINT('Ctrl Pts',(-95.4591620531666,4.75542049839504,
135.94481876907));
#194827=CARTESIAN_POINT('Ctrl Pts',(-95.7376096769794,6.89523396518648,
129.582033865318));
#194828=CARTESIAN_POINT('Ctrl Pts',(-96.0160573007924,2.69866426887766,
124.342507532899));
#194829=CARTESIAN_POINT('Ctrl Pts',(-96.2945049246052,-3.97784605345104,
125.041108506217));
#194830=CARTESIAN_POINT('Ctrl Pts',(-96.5729525484182,-6.99891018124123,
131.035856619345));
#194831=CARTESIAN_POINT('Ctrl Pts',(-96.8514001722308,-3.58831776824163,
136.817871216047));
#194832=CARTESIAN_POINT('Ctrl Pts',(-97.129847796044,3.11976337470375,137.073763349068));
#194833=CARTESIAN_POINT('Ctrl Pts',(-97.4082954198568,6.96093438520996,
131.56838064919));
#194834=CARTESIAN_POINT('Ctrl Pts',(-97.6867430436697,4.40534675625846,
125.360900864701));
#194835=CARTESIAN_POINT('Ctrl Pts',(-97.9651906674826,-2.1985393285419,
124.155694665303));
#194836=CARTESIAN_POINT('Ctrl Pts',(-98.2436382912955,-6.78207517502872,
129.060287670645));
#194837=CARTESIAN_POINT('Ctrl Pts',(-98.5220859151084,-5.13321525845608,
135.567598511506));
#194838=CARTESIAN_POINT('Ctrl Pts',(-98.8005335389213,1.23281870913114,
137.697726424945));
#194839=CARTESIAN_POINT('Ctrl Pts',(-99.0789811627341,6.4659525095689,133.493187921042));
#194840=CARTESIAN_POINT('Ctrl Pts',(-99.3574287865471,5.7571918330539,126.817748481762));
#194841=CARTESIAN_POINT('Ctrl Pts',(-99.6358764103599,-0.242146883580649,
123.805810838454));
#194842=CARTESIAN_POINT('Ctrl Pts',(-99.9143240341728,-6.01896444373747,
127.225198543987));
#194843=CARTESIAN_POINT('Ctrl Pts',(-100.192771657986,-6.26464772285957,
133.93366134335));
#194844=CARTESIAN_POINT('Ctrl Pts',(-100.471219281798,-0.753425789729175,
137.766449650557));
#194845=CARTESIAN_POINT('Ctrl Pts',(-100.749666905611,5.45015763726631,
135.201418253402));
#194846=CARTESIAN_POINT('Ctrl Pts',(-101.028114529424,6.64531245061667,
128.595705697122));
#194847=CARTESIAN_POINT('Ctrl Pts',(-101.306562153237,1.73374976341167,
124.019639113937));
#194848=CARTESIAN_POINT('Ctrl Pts',(-101.58500977705,-4.77104425798471,
125.678400140516));
#194849=CARTESIAN_POINT('Ctrl Pts',(-101.863457400863,-6.89148168476197,
132.047668428412));
#194850=CARTESIAN_POINT('Ctrl Pts',(-102.141905024676,-2.67898411084018,
137.274397577103));
#194851=CARTESIAN_POINT('Ctrl Pts',(-102.420352648489,3.99536898529432,
136.555478838857));
#194852=CARTESIAN_POINT('Ctrl Pts',(-102.698800272302,6.99817316856906,
130.551563412989));
#194853=CARTESIAN_POINT('Ctrl Pts',(-102.977247896115,3.56999808969468,
124.779956268296));
#194854=CARTESIAN_POINT('Ctrl Pts',(-103.255695519928,-3.13883082950684,
124.544482412068));
#194855=CARTESIAN_POINT('Ctrl Pts',(-103.53414314374,-6.96322755680218,
130.061530814641));
#194856=CARTESIAN_POINT('Ctrl Pts',(-103.812590767553,-4.38875833197407,
136.261203516848));
#194857=CARTESIAN_POINT('Ctrl Pts',(-104.091038391366,2.21876539717438,
137.44630417621));
#194858=CARTESIAN_POINT('Ctrl Pts',(-104.369486015179,6.78735211903507,
132.52778318216));
#194859=CARTESIAN_POINT('Ctrl Pts',(-104.647933638992,5.11869382408742,
126.02552104512));
#194860=CARTESIAN_POINT('Ctrl Pts',(-104.926381262805,-1.25379403310144,
123.914779015865));
#194861=CARTESIAN_POINT('Ctrl Pts',(-105.204828886617,-6.47410642511416,
128.135225903801));
#194862=CARTESIAN_POINT('Ctrl Pts',(-105.483276510431,-5.74503129012806,
134.808477199207));
#194863=CARTESIAN_POINT('Ctrl Pts',(-105.761724134243,0.263446940103889,
137.802140968053));
#194864=CARTESIAN_POINT('Ctrl Pts',(-106.040171758056,6.02983030247923,
134.365186455377));
#194865=CARTESIAN_POINT('Ctrl Pts',(-106.318619381869,6.25509419046252,
127.656006953765));
#194866=CARTESIAN_POINT('Ctrl Pts',(-106.597067005682,0.732232095750508,
123.840010663559));
#194867=CARTESIAN_POINT('Ctrl Pts',(-106.875514629495,-5.46351552342998,
126.423911753675));
#194868=CARTESIAN_POINT('Ctrl Pts',(-107.153962253308,-6.63855928414971,
133.033231352883));
#194869=CARTESIAN_POINT('Ctrl Pts',(-107.432409877121,-1.71309137438684,
137.594327632723));
#194870=CARTESIAN_POINT('Ctrl Pts',(-107.710857500934,4.78662381927155,
135.915775933963));
#194871=CARTESIAN_POINT('Ctrl Pts',(-107.989305124746,6.8876655625929,129.540083265954));
#194872=CARTESIAN_POINT('Ctrl Pts',(-108.26775274856,2.65927913505975,124.326199720693));
#194873=CARTESIAN_POINT('Ctrl Pts',(-108.546200372372,-4.0128549045848,
125.065429563905));
#194874=CARTESIAN_POINT('Ctrl Pts',(-108.824647996185,-6.99737132577695,
131.078456683062));
#194875=CARTESIAN_POINT('Ctrl Pts',(-109.103095619998,-3.5516453391731,
136.839602908365));
#194876=CARTESIAN_POINT('Ctrl Pts',(-109.381543243811,3.1578692066097,137.054656306401));
#194877=CARTESIAN_POINT('Ctrl Pts',(-109.659990867624,6.96545622200577,
131.525993310316));
#194878=CARTESIAN_POINT('Ctrl Pts',(-109.938438491437,4.37212925083209,
125.334185123311));
#194879=CARTESIAN_POINT('Ctrl Pts',(-110.21688611525,-2.23897091146772,
124.169200982596));
#194880=CARTESIAN_POINT('Ctrl Pts',(-110.495333739063,-6.79256618593892,
129.10160440085));
#194881=CARTESIAN_POINT('Ctrl Pts',(-110.773781362875,-5.10412497083799,
135.598757597999));
#194882=CARTESIAN_POINT('Ctrl Pts',(-111.052228986688,1.27475774209554,
137.690094189444));
#194883=CARTESIAN_POINT('Ctrl Pts',(-111.330676610501,6.48220036542147,
133.453778015119));
#194884=CARTESIAN_POINT('Ctrl Pts',(-111.609124234314,5.73281752601749,
126.782776683677));
#194885=CARTESIAN_POINT('Ctrl Pts',(-111.887571858127,-0.284744556090853,
123.807414522182));
#194886=CARTESIAN_POINT('Ctrl Pts',(-112.16601948194,-6.04064030169634,
127.261904002525));
#194887=CARTESIAN_POINT('Ctrl Pts',(-112.444467105753,-6.24548271172772,
133.971738053464));
#194888=CARTESIAN_POINT('Ctrl Pts',(-112.722914729566,-0.71103161847358,
137.770906975801));
#194889=CARTESIAN_POINT('Ctrl Pts',(-113.001362353379,5.47682279633179,
135.16816012963));
#194890=CARTESIAN_POINT('Ctrl Pts',(-113.279809977192,6.63174461897671,
128.55529471533));
#194891=CARTESIAN_POINT('Ctrl Pts',(-113.558257601004,1.69241711551747,
124.009210992206));
#194892=CARTESIAN_POINT('Ctrl Pts',(-113.836705224817,-4.80215903792943,
125.707537813274));
#194893=CARTESIAN_POINT('Ctrl Pts',(-114.11515284863,-6.88378563403075,
132.089595797848));
#194894=CARTESIAN_POINT('Ctrl Pts',(-114.393600472443,-2.63954952408134,
137.290585438973));
#194895=CARTESIAN_POINT('Ctrl Pts',(-114.672048096256,4.03030364933543,
136.531051338922));
#194896=CARTESIAN_POINT('Ctrl Pts',(-114.950495720069,6.99650466029252,
130.508968230339));
#194897=CARTESIAN_POINT('Ctrl Pts',(-115.228943343882,3.53325968669456,
124.758336294896));
#194898=CARTESIAN_POINT('Ctrl Pts',(-115.507390967695,-3.17687832964389,
124.563705347279));
#194899=CARTESIAN_POINT('Ctrl Pts',(-115.785838591507,-6.96762036017394,
130.103931720095));
#194900=CARTESIAN_POINT('Ctrl Pts',(-116.06428621532,-4.35545966688232,
136.287818031834));
#194901=CARTESIAN_POINT('Ctrl Pts',(-116.342733839133,2.25915568424066,
137.432674861647));
#194902=CARTESIAN_POINT('Ctrl Pts',(-116.621181462946,6.79771732743703,
132.486434712303));
#194903=CARTESIAN_POINT('Ctrl Pts',(-116.899629086759,5.08950883367243,
125.994450643782));
#194904=CARTESIAN_POINT('Ctrl Pts',(-117.178076710572,-1.2957096419083,
123.922538864004));
#194905=CARTESIAN_POINT('Ctrl Pts',(-117.456524334385,-6.49023425551004,
128.174685080065));
#194906=CARTESIAN_POINT('Ctrl Pts',(-117.734971958198,-5.7205506538686,
134.843374648297));
#194907=CARTESIAN_POINT('Ctrl Pts',(-118.013419582011,0.306039534242538,
137.800407639092));
#194908=CARTESIAN_POINT('Ctrl Pts',(-118.291867205823,6.05139434124684,
134.328415193001));
#194909=CARTESIAN_POINT('Ctrl Pts',(-118.570314829636,6.23581337569426,
127.617988751722));
#194910=CARTESIAN_POINT('Ctrl Pts',(-118.848762453449,0.689824554297045,
123.835682392233));
#194911=CARTESIAN_POINT('Ctrl Pts',(-119.127210077262,-5.49007933269568,
126.457250882969));
#194912=CARTESIAN_POINT('Ctrl Pts',(-119.405657701075,-6.62486851822702,
133.073600851681));
#194913=CARTESIAN_POINT('Ctrl Pts',(-119.684105324888,-1.67172717832737,
137.60462990379));
#194914=CARTESIAN_POINT('Ctrl Pts',(-119.962552948701,4.81764977004229,
135.886543693482));
#194915=CARTESIAN_POINT('Ctrl Pts',(-120.241000572514,6.87984193501854,
129.498179514853));
#194916=CARTESIAN_POINT('Ctrl Pts',(-120.519448196327,2.61979546067638,
124.310131959122));
#194917=CARTESIAN_POINT('Ctrl Pts',(-120.79789582014,-4.04771505790416,
125.089963279793));
#194918=CARTESIAN_POINT('Ctrl Pts',(-121.076343443952,-6.9955731801444,
131.121046590047));
#194919=CARTESIAN_POINT('Ctrl Pts',(-121.354791067765,-3.51484130258126,
136.86111096256));
#194920=CARTESIAN_POINT('Ctrl Pts',(-121.633238691578,3.19585802251066,
137.035317656727));
#194921=CARTESIAN_POINT('Ctrl Pts',(-121.911686315391,6.96971995125911,
131.483579231079));
#194922=CARTESIAN_POINT('Ctrl Pts',(-122.190133939204,4.3387497345494,125.307672081285));
#194923=CARTESIAN_POINT('Ctrl Pts',(-122.468581563017,-2.2793195285039,
124.182953168171));
#194924=CARTESIAN_POINT('Ctrl Pts',(-122.74702918683,-6.80280549581075,
129.142984227312));
#194925=CARTESIAN_POINT('Ctrl Pts',(-123.025476810643,-5.07484554799192,
135.629739026348));
#194926=CARTESIAN_POINT('Ctrl Pts',(-123.303924434456,1.31664953844379,
137.682206800553));
#194927=CARTESIAN_POINT('Ctrl Pts',(-123.582372058268,6.49820802095541,
133.414269934058));
#194928=CARTESIAN_POINT('Ctrl Pts',(-123.860819682081,5.7082307873194,126.747953906865));
#194929=CARTESIAN_POINT('Ctrl Pts',(-124.139267305894,-0.327331677286216,
123.809277480321));
#194930=CARTESIAN_POINT('Ctrl Pts',(-124.417714929707,-6.06209232150722,
127.298740728095));
#194931=CARTESIAN_POINT('Ctrl Pts',(-124.69616255352,-6.22608627193705,
134.009697395242));
#194932=CARTESIAN_POINT('Ctrl Pts',(-124.974610177333,-0.668611099680587,
137.77510615311));
#194933=CARTESIAN_POINT('Ctrl Pts',(-125.253057801146,5.50328500971429,
135.134740303665));
#194934=CARTESIAN_POINT('Ctrl Pts',(-125.531505424959,6.61793104560076,
128.514967073503));
#194935=CARTESIAN_POINT('Ctrl Pts',(-125.809953048772,1.6510217544855,123.999034667242));
#194936=CARTESIAN_POINT('Ctrl Pts',(-126.088400672584,-4.8330958721059,
125.736864350674));
#194937=CARTESIAN_POINT('Ctrl Pts',(-126.366848296398,-6.87583450209069,
132.131475542423));
#194938=CARTESIAN_POINT('Ctrl Pts',(-126.64529592021,-2.60001712784396,
137.306532951397));
#194939=CARTESIAN_POINT('Ctrl Pts',(-126.923743544023,4.06508896899354,
136.506411634357));
#194940=CARTESIAN_POINT('Ctrl Pts',(-127.202191167836,6.99457689396224,
130.466383993564));
#194941=CARTESIAN_POINT('Ctrl Pts',(-127.480638791649,3.49639035745773,
124.736940359153));
#194942=CARTESIAN_POINT('Ctrl Pts',(-127.759086415462,-3.21480810938582,
124.583159532264));
#194943=CARTESIAN_POINT('Ctrl Pts',(-128.037534039275,-6.97175497581086,
130.146358580199));
#194944=CARTESIAN_POINT('Ctrl Pts',(-128.315981663087,-4.32199960863106,
136.314229355287));
#194945=CARTESIAN_POINT('Ctrl Pts',(-128.594429286901,2.29946225746178,
137.418799932461));
#194946=CARTESIAN_POINT('Ctrl Pts',(-128.872876910713,6.80783064392392,
132.44502391257));
#194947=CARTESIAN_POINT('Ctrl Pts',(-129.151324534526,5.06013524963555,
125.963558475429));
#194948=CARTESIAN_POINT('Ctrl Pts',(-129.429772158339,-1.33757723771771,
123.930553720578));
#194949=CARTESIAN_POINT('Ctrl Pts',(-129.708219782152,-6.50612158788957,
128.214241699924));
#194950=CARTESIAN_POINT('Ctrl Pts',(-129.986667405965,-5.69585804050008,
134.878122430239));
#194951=CARTESIAN_POINT('Ctrl Pts',(-130.265115029778,0.348620787973942,
137.798415069035));
#194952=CARTESIAN_POINT('Ctrl Pts',(-130.543562653591,6.07273414337257,
134.291513345486));
#194953=CARTESIAN_POINT('Ctrl Pts',(-130.822010277403,6.21630149056731,
127.58008862186));
#194954=CARTESIAN_POINT('Ctrl Pts',(-131.100457901217,0.647391451141708,
123.831612347843));
#194955=CARTESIAN_POINT('Ctrl Pts',(-131.378905525029,-5.5164397050528,
126.490751096011));
#194956=CARTESIAN_POINT('Ctrl Pts',(-131.657353148842,-6.61093226536518,
133.113886262947));
#194957=CARTESIAN_POINT('Ctrl Pts',(-131.935800772655,-1.63030103580305,
137.614680188378));
#194958=CARTESIAN_POINT('Ctrl Pts',(-132.214248396468,4.848497201029,135.857123130838));
#194959=CARTESIAN_POINT('Ctrl Pts',(-132.492696020281,6.87176337237162,
129.456324164773));
#194960=CARTESIAN_POINT('Ctrl Pts',(-132.771143644094,2.58021470880796,
124.294304843582));
#194961=CARTESIAN_POINT('Ctrl Pts',(-133.049591267907,-4.08242522165371,
125.114708744776));
#194962=CARTESIAN_POINT('Ctrl Pts',(-133.32803889172,-6.99351581097555,
131.163624762118));
#194963=CARTESIAN_POINT('Ctrl Pts',(-133.606486515532,-3.47790702225152,
136.882394581644));
#194964=CARTESIAN_POINT('Ctrl Pts',(-133.884934139345,3.23372841471757,
137.015748116649));
#194965=CARTESIAN_POINT('Ctrl Pts',(-134.163381763158,6.97372541497715,
131.441139983145));
#194966=CARTESIAN_POINT('Ctrl Pts',(-134.441829386971,4.30520944429882,
125.281362721075));
#194967=CARTESIAN_POINT('Ctrl Pts',(-134.720277010784,-2.31958368451587,
124.196950712432));
#194968=CARTESIAN_POINT('Ctrl Pts',(-134.998724634597,-6.81279272522359,
129.184425616688));
#194969=CARTESIAN_POINT('Ctrl Pts',(-135.27717225841,-5.04537807487797,
135.660541648527));
#194970=CARTESIAN_POINT('Ctrl Pts',(-135.555619882223,1.35849254585843,
137.674064550544));
#194971=CARTESIAN_POINT('Ctrl Pts',(-135.834067506036,6.51397488300169,
133.374665141848));
#194972=CARTESIAN_POINT('Ctrl Pts',(-136.112515129848,5.68343252803032,
126.713281441693));
#194973=CARTESIAN_POINT('Ctrl Pts',(-136.390962753662,-0.369906669086523,
123.811399643837));
#194974=CARTESIAN_POINT('Ctrl Pts',(-136.669410377474,-6.08331970825794,
127.335707355701));
#194975=CARTESIAN_POINT('Ctrl Pts',(-136.947858001288,-6.20645912223011,
134.047537962086));
#194976=CARTESIAN_POINT('Ctrl Pts',(-137.2263056251,-0.626165805256695,
137.779047026878));
#194977=CARTESIAN_POINT('Ctrl Pts',(-137.504753248913,5.52954329684707,
135.101160013885));
#194978=CARTESIAN_POINT('Ctrl Pts',(-137.783200872726,6.60387224235649,
128.474724265995));
#194979=CARTESIAN_POINT('Ctrl Pts',(-138.061648496539,1.60956521423443,
123.989110516135));
#194980=CARTESIAN_POINT('Ctrl Pts',(-138.340096120352,-4.86385361413656,
125.766378666012));
#194981=CARTESIAN_POINT('Ctrl Pts',(-138.618543744165,-6.86762858357524,
132.173306110266));
#194982=CARTESIAN_POINT('Ctrl Pts',(-138.896991367977,-2.56038838701599,
137.322239523433));
#194983=CARTESIAN_POINT('Ctrl Pts',(-139.17543899179,4.09972365528409,136.481560638194));
#194984=CARTESIAN_POINT('Ctrl Pts',(-139.453886615603,6.99238994101352,
130.423812280637));
#194985=CARTESIAN_POINT('Ctrl Pts',(-139.732334239416,3.45939146819007,
124.715769253897));
#194986=CARTESIAN_POINT('Ctrl Pts',(-140.010781863229,-3.25261876323132,
124.602844246145));
#194987=CARTESIAN_POINT('Ctrl Pts',(-140.289229487042,-6.97563125050334,
130.188809822811));
#194988=CARTESIAN_POINT('Ctrl Pts',(-140.567677110855,-4.28837939709471,
136.340436508528));
#194989=CARTESIAN_POINT('Ctrl Pts',(-140.846124734668,2.33968362326381,
137.404679902793));
#194990=CARTESIAN_POINT('Ctrl Pts',(-141.124572358481,6.81769169374202,
132.403552317457));
#194991=CARTESIAN_POINT('Ctrl Pts',(-141.403019982293,5.03057416042698,
125.932845684778));
#194992=CARTESIAN_POINT('Ctrl Pts',(-141.681467606106,-1.37939526911043,
123.938823288595));
#194993=CARTESIAN_POINT('Ctrl Pts',(-141.959915229919,-6.52176783354029,
128.253894297592));
#194994=CARTESIAN_POINT('Ctrl Pts',(-142.238362853732,-5.67095436501806,
134.912719257437));
#194995=CARTESIAN_POINT('Ctrl Pts',(-142.516810477545,0.39118912343359,
137.796163331718));
#194996=CARTESIAN_POINT('Ctrl Pts',(-142.795258101358,6.09384891810056,
134.254482280245));
#194997=CARTESIAN_POINT('Ctrl Pts',(-143.073705725171,6.19655925810344,
127.542307968582));
#194998=CARTESIAN_POINT('Ctrl Pts',(-143.352153348984,0.604934358657401,
123.827800681205));
#194999=CARTESIAN_POINT('Ctrl Pts',(-143.630600972796,-5.54259566370794,
126.524411151443));
#195000=CARTESIAN_POINT('Ctrl Pts',(-143.90904859661,-6.59675104197701,
133.154086093891));
#195001=CARTESIAN_POINT('Ctrl Pts',(-144.187496220422,-1.58881448187379,
137.624478114069));
#195002=CARTESIAN_POINT('Ctrl Pts',(-144.465943844235,4.87916496916901,
135.827515336221));
#195003=CARTESIAN_POINT('Ctrl Pts',(-144.744391468048,6.86343017400547,
129.41451876668));
#195004=CARTESIAN_POINT('Ctrl Pts',(-145.022839091861,2.54053834613545,
124.278718960552));
#195005=CARTESIAN_POINT('Ctrl Pts',(-145.301286715674,-4.11698410963516,
125.139665041902));
#195006=CARTESIAN_POINT('Ctrl Pts',(-145.579734339487,-6.99119929450595,
131.206189621523));
#195007=CARTESIAN_POINT('Ctrl Pts',(-145.8581819633,-3.44084386679896,136.903452976945));
#195008=CARTESIAN_POINT('Ctrl Pts',(-146.136629587113,3.27147897992919,
136.995948411323));
#195009=CARTESIAN_POINT('Ctrl Pts',(-146.415077210925,6.97747246473481,
131.398677139117));
#195010=CARTESIAN_POINT('Ctrl Pts',(-146.693524834738,4.27150962292939,
125.255258017582));
#195011=CARTESIAN_POINT('Ctrl Pts',(-146.971972458551,-2.35976188750221,
124.211193096699));
#195012=CARTESIAN_POINT('Ctrl Pts',(-147.250420082364,-6.82252750409623,
129.225927033352));
#195013=CARTESIAN_POINT('Ctrl Pts',(-147.528867706177,-5.01572364342383,
135.69116432313));
#195014=CARTESIAN_POINT('Ctrl Pts',(-147.80731532999,1.40028521383297,137.665667741127));
#195015=CARTESIAN_POINT('Ctrl Pts',(-148.085762953803,6.52950036731291,
133.334965106058));
#195016=CARTESIAN_POINT('Ctrl Pts',(-148.364210577616,5.65842366705879,
126.678760572968));
#195017=CARTESIAN_POINT('Ctrl Pts',(-148.642658201429,-0.412467953858535,
123.813780934094));
#195018=CARTESIAN_POINT('Ctrl Pts',(-148.921105825242,-6.10432167535963,
127.372802515528));
#195019=CARTESIAN_POINT('Ctrl Pts',(-149.199553449054,-6.18660198989778,
134.085258351801));
#195020=CARTESIAN_POINT('Ctrl Pts',(-149.478001072867,-0.583697308029368,
137.782729451077));
#195021=CARTESIAN_POINT('Ctrl Pts',(-149.75644869668,5.55559668471987,135.067420504625));
#195022=CARTESIAN_POINT('Ctrl Pts',(-150.034896320493,6.58956873019717,
128.434567784019));
#195023=CARTESIAN_POINT('Ctrl Pts',(-150.313343944306,1.56804903095274,
123.979438906626));
#195024=CARTESIAN_POINT('Ctrl Pts',(-150.591791568119,-4.89443112428377,
125.796079665625));
#195025=CARTESIAN_POINT('Ctrl Pts',(-150.870239191931,-6.85916818255639,
132.21508595133));
#195026=CARTESIAN_POINT('Ctrl Pts',(-151.148686815745,-2.52066477005453,
137.33770457307));
#195027=CARTESIAN_POINT('Ctrl Pts',(-151.427134439557,4.13420642480782,
136.456499271296));
#195028=CARTESIAN_POINT('Ctrl Pts',(-151.705582063371,6.98994388248347,
130.381254669068));
#195029=CARTESIAN_POINT('Ctrl Pts',(-151.984029687183,3.42226438989971,
124.694823763634));
#195030=CARTESIAN_POINT('Ctrl Pts',(-152.262477310996,-3.29030889009209,
124.622758759495));
#195031=CARTESIAN_POINT('Ctrl Pts',(-152.540924934809,-6.97924904061452,
130.231283874884));
#195032=CARTESIAN_POINT('Ctrl Pts',(-152.819372558622,-4.25460027808296,
136.366438520441));
#195033=CARTESIAN_POINT('Ctrl Pts',(-153.097820182435,2.37981829122829,
137.390315295868));
#195034=CARTESIAN_POINT('Ctrl Pts',(-153.376267806248,6.82730011148789,
132.362021463707));
#195035=CARTESIAN_POINT('Ctrl Pts',(-153.654715430061,5.00082666144207,
125.902313409905));
#195036=CARTESIAN_POINT('Ctrl Pts',(-153.933163053873,-1.42116218650446,
123.947347261623));
#195037=CARTESIAN_POINT('Ctrl Pts',(-154.211610677687,-6.53717241268631,
128.293641403726));
#195038=CARTESIAN_POINT('Ctrl Pts',(-154.490058301499,-5.64584055023574,
134.947163847896));
#195039=CARTESIAN_POINT('Ctrl Pts',(-154.768505925312,0.433742963236675,
137.79365251058));
#195040=CARTESIAN_POINT('Ctrl Pts',(-155.046953549125,6.11473788301669,
134.217323369476));
#195041=CARTESIAN_POINT('Ctrl Pts',(-155.325401172938,6.17658740985663,
127.504648191865));
#195042=CARTESIAN_POINT('Ctrl Pts',(-155.603848796751,0.562454850108638,
123.824247533559));
#195043=CARTESIAN_POINT('Ctrl Pts',(-155.882296420564,-5.5685462394425,
126.558229801974));
#195044=CARTESIAN_POINT('Ctrl Pts',(-156.160744044376,-6.5823253735531,
133.194198854895));
#195045=CARTESIAN_POINT('Ctrl Pts',(-156.43919166819,-1.54726905384013,
137.634023317798));
#195046=CARTESIAN_POINT('Ctrl Pts',(-156.717639292002,4.90965193805665,
135.79772140676));
#195047=CARTESIAN_POINT('Ctrl Pts',(-156.996086915816,6.8548426487106,129.372764869687));
#195048=CARTESIAN_POINT('Ctrl Pts',(-157.274534539628,2.50076784287941,
124.263374887574));
#195049=CARTESIAN_POINT('Ctrl Pts',(-157.552982163441,-4.15139044125659,
125.164831246407));
#195050=CARTESIAN_POINT('Ctrl Pts',(-157.831429787254,-6.98862371657603,
131.248739591007));
#195051=CARTESIAN_POINT('Ctrl Pts',(-158.109877411067,-3.40365320961064,
136.924285368134));
#195052=CARTESIAN_POINT('Ctrl Pts',(-158.38832503488,3.30910831928323,136.975919274434));
#195053=CARTESIAN_POINT('Ctrl Pts',(-158.666772658693,6.98096096168483,
131.356192272474));
#195054=CARTESIAN_POINT('Ctrl Pts',(-158.945220282506,4.23765151920024,
125.229358938127));
#195055=CARTESIAN_POINT('Ctrl Pts',(-159.223667906319,-2.39985264864321,
124.225679793212));
#195056=CARTESIAN_POINT('Ctrl Pts',(-159.502115530131,-6.8320094717036,
129.267486939452));
#195057=CARTESIAN_POINT('Ctrl Pts',(-159.780563153944,-4.98588335248574,
135.721605915426));
#195058=CARTESIAN_POINT('Ctrl Pts',(-160.059010777757,1.44202599372318,
137.657016683454));
#195059=CARTESIAN_POINT('Ctrl Pts',(-160.33745840157,6.54478389858708,133.295171297791));
#195060=CARTESIAN_POINT('Ctrl Pts',(-160.615906025383,5.63320513111742,
126.644392579866));
#195061=CARTESIAN_POINT('Ctrl Pts',(-160.894353649196,-0.455013954479453,
123.816421262852));
#195062=CARTESIAN_POINT('Ctrl Pts',(-161.172801273009,-6.12509744457689,
127.410024833003));
#195063=CARTESIAN_POINT('Ctrl Pts',(-161.451248896821,-6.16651561075379,
134.122857166646));
#195064=CARTESIAN_POINT('Ctrl Pts',(-161.729696520635,-0.541207181682879,
137.786153289251));
#195065=CARTESIAN_POINT('Ctrl Pts',(-162.008144144447,5.58144420791359,
135.033523026113));
#195066=CARTESIAN_POINT('Ctrl Pts',(-162.286591768261,6.57502103914602,
128.394499115588));
#195067=CARTESIAN_POINT('Ctrl Pts',(-162.565039392073,1.52647474303778,
123.970020197102));
#195068=CARTESIAN_POINT('Ctrl Pts',(-162.843487015886,-4.92482726948487,
125.825966248931));
#195069=CARTESIAN_POINT('Ctrl Pts',(-163.121934639699,-6.85045361253876,
132.256813517449));
#195070=CARTESIAN_POINT('Ctrl Pts',(-163.400382263512,-2.48084774893327,
137.352927527244));
#195071=CARTESIAN_POINT('Ctrl Pts',(-163.678829887325,4.16853599979124,
136.431228462323));
#195072=CARTESIAN_POINT('Ctrl Pts',(-163.957277511138,6.98723880901292,
130.338712735846));
#195073=CARTESIAN_POINT('Ctrl Pts',(-164.23572513495,3.3850104983435,124.674104664506));
#195074=CARTESIAN_POINT('Ctrl Pts',(-164.514172758764,-3.32787709334726,
124.642902334375));
#195075=CARTESIAN_POINT('Ctrl Pts',(-164.792620382576,-6.98260821208591,
130.273779162525));
#195076=CARTESIAN_POINT('Ctrl Pts',(-165.07106800639,-4.22066350329308,
136.392234427513));
#195077=CARTESIAN_POINT('Ctrl Pts',(-165.349515630202,2.4198647741513,137.37570664397));
#195078=CARTESIAN_POINT('Ctrl Pts',(-165.627963254015,6.83665554111671,
132.320432890263));
#195079=CARTESIAN_POINT('Ctrl Pts',(-165.906410877828,4.97089385498702,
125.871962782194));
#195080=CARTESIAN_POINT('Ctrl Pts',(-166.184858501641,-1.46287644221077,
123.956125323802));
#195081=CARTESIAN_POINT('Ctrl Pts',(-166.463306125454,-6.55233475450377,
128.333481545486));
#195082=CARTESIAN_POINT('Ctrl Pts',(-166.741753749267,-5.62051752675643,
134.981454925258));
#195083=CARTESIAN_POINT('Ctrl Pts',(-167.020201373079,0.476280730534997,
137.790882698662));
#195084=CARTESIAN_POINT('Ctrl Pts',(-167.298648996893,6.13540026407138,
134.180037990117));
#195085=CARTESIAN_POINT('Ctrl Pts',(-167.577096620705,6.15638668589229,
127.467110687205));
#195086=CARTESIAN_POINT('Ctrl Pts',(-167.855544244518,0.519954499587912,
123.820953036571));
#195087=CARTESIAN_POINT('Ctrl Pts',(-168.133991868331,-5.5942904706483,
126.592205794446));
#195088=CARTESIAN_POINT('Ctrl Pts',(-168.412439492144,-6.56765579464175,
133.234223059563));
#195089=CARTESIAN_POINT('Ctrl Pts',(-168.690887115956,-1.50566629118217,
137.643315445865));
#195090=CARTESIAN_POINT('Ctrl Pts',(-168.96933473977,4.93995697798634,135.767742446477));
#195091=CARTESIAN_POINT('Ctrl Pts',(-169.247782363582,6.84600111470013,
129.331064021001));
#195092=CARTESIAN_POINT('Ctrl Pts',(-169.526229987396,2.46090467275213,
124.248273193229));
#195093=CARTESIAN_POINT('Ctrl Pts',(-169.804677611208,-4.18564294157836,
125.190206425745));
#195094=CARTESIAN_POINT('Ctrl Pts',(-170.083125235021,-6.98578917262369,
131.291273093865));
#195095=CARTESIAN_POINT('Ctrl Pts',(-170.361572858834,-3.36633642880185,
136.944890983262));
#195096=CARTESIAN_POINT('Ctrl Pts',(-170.640020482647,3.34661503841248,
136.955661448171));
#195097=CARTESIAN_POINT('Ctrl Pts',(-170.91846810646,6.98419077655865,131.313686957504));
#195098=CARTESIAN_POINT('Ctrl Pts',(-171.196915730273,4.20363638773547,
125.203666442409));
#195099=CARTESIAN_POINT('Ctrl Pts',(-171.475363354086,-2.43985448236259,
124.240410265162));
#195100=CARTESIAN_POINT('Ctrl Pts',(-171.753810977898,-6.84123827668714,
129.309103794972));
#195101=CARTESIAN_POINT('Ctrl Pts',(-172.032258601712,-4.9558583078063,
135.751865297389));
#195102=CARTESIAN_POINT('Ctrl Pts',(-172.310706225524,1.48371333881067,
137.648111698089));
#195103=CARTESIAN_POINT('Ctrl Pts',(-172.589153849337,6.55982491048677,
133.255285191615));
#195104=CARTESIAN_POINT('Ctrl Pts',(-172.86760147315,5.60777785468832,126.610178735912));
#195105=CARTESIAN_POINT('Ctrl Pts',(-173.146049096963,-0.497543094390354,
123.819320532272));
#195106=CARTESIAN_POINT('Ctrl Pts',(-173.424496720776,-6.14564624605571,
127.447372928838));
#195107=CARTESIAN_POINT('Ctrl Pts',(-173.702944344589,-6.14620072910595,
134.160333013378));
#195108=CARTESIAN_POINT('Ctrl Pts',(-173.981391968402,-0.498697000705985,
137.789318414533));
#195109=CARTESIAN_POINT('Ctrl Pts',(-174.259839592215,5.60708490864046,
134.999468834432));
#195110=CARTESIAN_POINT('Ctrl Pts',(-174.538287216028,6.56022970827155,
128.354519745462));
#195111=CARTESIAN_POINT('Ctrl Pts',(-174.81673483984,1.48484389103961,123.960854736574));
#195112=CARTESIAN_POINT('Ctrl Pts',(-175.095182463654,-4.95504092340126,
125.85603730847));
#195113=CARTESIAN_POINT('Ctrl Pts',(-175.373630087466,-6.8414851964426,
132.298487262391));
#195114=CARTESIAN_POINT('Ctrl Pts',(-175.652077711279,-2.44093879908611,
137.367907821863));
#195115=CARTESIAN_POINT('Ctrl Pts',(-175.930525335092,4.20271110814107,
136.405749147692));
#195116=CARTESIAN_POINT('Ctrl Pts',(-176.208972958905,6.98427482083815,
130.296188057377));
#195117=CARTESIAN_POINT('Ctrl Pts',(-176.487420582718,3.3476311739788,124.653612724266));
#195118=CARTESIAN_POINT('Ctrl Pts',(-176.765868206531,-3.36532198089259,
124.663274224357));
#195119=CARTESIAN_POINT('Ctrl Pts',(-177.044315830343,-6.98570864044213,
130.316294111058));
#195120=CARTESIAN_POINT('Ctrl Pts',(-177.322763454156,-4.18657033026512,
136.417823273865));
#195121=CARTESIAN_POINT('Ctrl Pts',(-177.601211077969,2.4598215880947,137.360854488428));
#195122=CARTESIAN_POINT('Ctrl Pts',(-177.879658701782,6.84575763596098,
132.278788138201));
#195123=CARTESIAN_POINT('Ctrl Pts',(-178.158106325595,4.94077685023126,
125.841794926299));
#195124=CARTESIAN_POINT('Ctrl Pts',(-178.436553949408,-1.50453649049278,
123.965157149858));
#195125=CARTESIAN_POINT('Ctrl Pts',(-178.715001573221,-6.56725429714808,
128.373413246577));
#195126=CARTESIAN_POINT('Ctrl Pts',(-178.993449197033,-5.59498623293233,
135.015591218853));
#195127=CARTESIAN_POINT('Ctrl Pts',(-179.271896820847,0.518800849074927,
137.787853998597));
#195128=CARTESIAN_POINT('Ctrl Pts',(-179.550344444659,6.15583529561319,
134.142627523792));
#195129=CARTESIAN_POINT('Ctrl Pts',(-179.828792068472,6.13595783475539,
127.429696845569));
#195130=CARTESIAN_POINT('Ctrl Pts',(-180.107239692285,0.477434881962636,
123.81791731232));
#195131=CARTESIAN_POINT('Ctrl Pts',(-180.385687316098,-5.61982740336347,
126.626337869861));
#195132=CARTESIAN_POINT('Ctrl Pts',(-180.664134939911,-6.55274284882976,
133.274157224785));
#195133=CARTESIAN_POINT('Ctrl Pts',(-180.942582563724,-1.4640077355066,
137.652354153945));
#195134=CARTESIAN_POINT('Ctrl Pts',(-181.221030187537,4.97007896599344,
135.737579566256));
#195135=CARTESIAN_POINT('Ctrl Pts',(-181.499477811349,6.83690589960112,
129.289417765863));
#195136=CARTESIAN_POINT('Ctrl Pts',(-181.777925435163,2.42095031289641,
124.233414437113));
#195137=CARTESIAN_POINT('Ctrl Pts',(-182.056373058975,-4.21974034136189,
125.215789639631));
#195138=CARTESIAN_POINT('Ctrl Pts',(-182.334820682789,-6.98269576768506,
131.333788554001));
#195139=CARTESIAN_POINT('Ctrl Pts',(-182.613268306601,-3.32889490715784,
136.965269058779));
#195140=CARTESIAN_POINT('Ctrl Pts',(-182.891715930414,3.38399774748988,
136.935175683191));
#195141=CARTESIAN_POINT('Ctrl Pts',(-183.170163554227,6.98716178967534,
131.27116276926));
#195142=CARTESIAN_POINT('Ctrl Pts',(-183.44861117804,4.16946548897866,125.178181482475));
#195143=CARTESIAN_POINT('Ctrl Pts',(-183.727058801853,-2.47976590637605,
124.255383966707));
#195144=CARTESIAN_POINT('Ctrl Pts',(-184.005506425666,-6.85021357707087,
129.350776057783));
#195145=CARTESIAN_POINT('Ctrl Pts',(-184.283954049479,-4.92564962197493,
135.781941347746));
#195146=CARTESIAN_POINT('Ctrl Pts',(-184.562401673291,1.52534570435398,
137.63895311501));
#195147=CARTESIAN_POINT('Ctrl Pts',(-184.840849297105,6.5746228456623,133.215308265529));
#195148=CARTESIAN_POINT('Ctrl Pts',(-185.119296920917,5.58214277998856,
126.576120308909));
#195149=CARTESIAN_POINT('Ctrl Pts',(-185.39774454473,-0.540053797659538,
123.822478634922));
#195150=CARTESIAN_POINT('Ctrl Pts',(-185.676192168543,-6.16596731835295,
127.484845419088));
#195151=CARTESIAN_POINT('Ctrl Pts',(-185.954639792356,-6.12565809773001,
134.197684503321));
#195152=CARTESIAN_POINT('Ctrl Pts',(-186.233087416169,-0.456168340327589,
137.792224709632));
#195153=CARTESIAN_POINT('Ctrl Pts',(-186.511535039982,5.63251783677319,
134.965259191474));
#195154=CARTESIAN_POINT('Ctrl Pts',(-186.789982663795,6.54519528567348,
128.314631155089));
#195155=CARTESIAN_POINT('Ctrl Pts',(-187.068430287608,1.44315801760525,
123.951942864674));
#195156=CARTESIAN_POINT('Ctrl Pts',(-187.346877911421,-4.98507096645316,
125.886291729948));
#195157=CARTESIAN_POINT('Ctrl Pts',(-187.625325535233,-6.83226326659722,
132.340105641921));
#195158=CARTESIAN_POINT('Ctrl Pts',(-187.903773159046,-2.40093939935397,
137.382644901827));
#195159=CARTESIAN_POINT('Ctrl Pts',(-188.182220782859,4.23673048348491,
136.380062271549));
#195160=CARTESIAN_POINT('Ctrl Pts',(-188.460668406672,6.98105202779173,
130.25368220943));
#195161=CARTESIAN_POINT('Ctrl Pts',(-188.739116030485,3.31012780190951,
124.633348702251));
#195162=CARTESIAN_POINT('Ctrl Pts',(-189.017563654298,-3.40264216519462,
124.683873674555));
#195163=CARTESIAN_POINT('Ctrl Pts',(-189.296011278111,-6.98855021079573,
130.358827145076));
#195164=CARTESIAN_POINT('Ctrl Pts',(-189.574458901924,-4.15232202233378,
136.443204111294));
#195165=CARTESIAN_POINT('Ctrl Pts',(-189.852906525736,2.49968725244504,
137.345759379595));
#195166=CARTESIAN_POINT('Ctrl Pts',(-190.13135414955,6.85460605873784,132.237088750687));
#195167=CARTESIAN_POINT('Ctrl Pts',(-190.409801773362,4.91047676317321,
125.8118109601));
#195168=CARTESIAN_POINT('Ctrl Pts',(-190.688249397175,-1.5461407876216,
123.974442405114));
#195169=CARTESIAN_POINT('Ctrl Pts',(-190.966697020988,-6.58193048776853,
128.413435027317));
#195170=CARTESIAN_POINT('Ctrl Pts',(-191.245144644801,-5.56924761483672,
135.049571463749));
#195171=CARTESIAN_POINT('Ctrl Pts',(-191.523592268614,0.561301743259386,
137.784566522618));
#195172=CARTESIAN_POINT('Ctrl Pts',(-191.802039892427,6.17604222041412,
134.105093356759));
#195173=CARTESIAN_POINT('Ctrl Pts',(-192.08048751624,6.11530161344434,127.39240805334));
#195174=CARTESIAN_POINT('Ctrl Pts',(-192.358935140053,0.43489757281158,
123.815140473294));
#195175=CARTESIAN_POINT('Ctrl Pts',(-192.637382763865,-5.64515609130746,
126.660624763449));
#195176=CARTESIAN_POINT('Ctrl Pts',(-192.915830387678,-6.53758708872167,
133.313999870785));
#195177=CARTESIAN_POINT('Ctrl Pts',(-193.194278011491,-1.42229493048546,
137.661139107108));
#195178=CARTESIAN_POINT('Ctrl Pts',(-193.472725635304,5.00001678589681,
135.707233883791));
#195179=CARTESIAN_POINT('Ctrl Pts',(-193.751173259117,6.82755734043935,
129.247827647489));
#195180=CARTESIAN_POINT('Ctrl Pts',(-194.02962088293,2.38090624383734,124.218799169824));
#195181=CARTESIAN_POINT('Ctrl Pts',(-194.308068506743,-4.25368137711504,
125.241579940071));
#195182=CARTESIAN_POINT('Ctrl Pts',(-194.586516130556,-6.97934361638637,
131.376284395991));
#195183=CARTESIAN_POINT('Ctrl Pts',(-194.864963754369,-3.29133003208973,
136.985418839569));
#195184=CARTESIAN_POINT('Ctrl Pts',(-195.143411378181,3.42125506128717,
136.914462738605));
#195185=CARTESIAN_POINT('Ctrl Pts',(-195.421859001994,6.98987389094189,
131.22862128349));
#195186=CARTESIAN_POINT('Ctrl Pts',(-195.700306625807,4.13514008914463,
125.152905002676));
#195187=CARTESIAN_POINT('Ctrl Pts',(-195.97875424962,-2.51958544175274,
124.270600342989));
#195188=CARTESIAN_POINT('Ctrl Pts',(-196.257201873433,-6.85893504027095,
129.392502183704));
#195189=CARTESIAN_POINT('Ctrl Pts',(-196.535649497246,-4.89525841438522,
135.811832952018));
#195190=CARTESIAN_POINT('Ctrl Pts',(-196.814097121059,1.56692154765205,
137.629541273595));
#195191=CARTESIAN_POINT('Ctrl Pts',(-197.092544744872,6.58917715577019,
133.175242000891));
#195192=CARTESIAN_POINT('Ctrl Pts',(-197.370992368684,5.55630085693524,
126.542218560906));
#195193=CARTESIAN_POINT('Ctrl Pts',(-197.649439992498,-0.582544489036021,
123.825895453776));
#195194=CARTESIAN_POINT('Ctrl Pts',(-197.92788761631,-6.18605990846357,
127.522440915193));
#195195=CARTESIAN_POINT('Ctrl Pts',(-198.206335240123,-6.10488847784037,
134.234910252398));
#195196=CARTESIAN_POINT('Ctrl Pts',(-198.484782863936,-0.413622776464342,
137.79487206686));
#195197=CARTESIAN_POINT('Ctrl Pts',(-198.763230487749,5.657742049887,134.930895364888));
#195198=CARTESIAN_POINT('Ctrl Pts',(-199.041678111562,6.52991832845634,
128.274834822558));
#195199=CARTESIAN_POINT('Ctrl Pts',(-199.320125735375,1.40141866741961,
123.943284911633));
#195200=CARTESIAN_POINT('Ctrl Pts',(-199.598573359188,-5.01491628586802,
125.916728392279));
#195201=CARTESIAN_POINT('Ctrl Pts',(-199.877020983,-6.82278816472322,132.381667113854));
#195202=CARTESIAN_POINT('Ctrl Pts',(-200.155468606814,-2.36085103192995,
137.397138221046));
#195203=CARTESIAN_POINT('Ctrl Pts',(-200.433916230626,4.27059286522247,
136.354168785731));
#195204=CARTESIAN_POINT('Ctrl Pts',(-200.712363854439,6.97757054929515,
130.211196767073));
#195205=CARTESIAN_POINT('Ctrl Pts',(-200.990811478252,3.27250177183757,
124.613313349352));
#195206=CARTESIAN_POINT('Ctrl Pts',(-201.269259102065,-3.43983626333961,
124.704699921646));
#195207=CARTESIAN_POINT('Ctrl Pts',(-201.547706725878,-6.9911328178512,
130.401376688499));
#195208=CARTESIAN_POINT('Ctrl Pts',(-201.826154349691,-4.1179198485831,
136.468375999304));
#195209=CARTESIAN_POINT('Ctrl Pts',(-202.104601973504,2.53946028996452,
137.330421876826));
#195210=CARTESIAN_POINT('Ctrl Pts',(-202.383049597317,6.86320048156709,
132.195336272904));
#195211=CARTESIAN_POINT('Ctrl Pts',(-202.66149722113,4.87999471659204,125.782011994664));
#195212=CARTESIAN_POINT('Ctrl Pts',(-202.939944844942,-1.5876877919352,
123.983980745501));
#195213=CARTESIAN_POINT('Ctrl Pts',(-203.218392468755,-6.59636278253501,
128.453545404684));
#195214=CARTESIAN_POINT('Ctrl Pts',(-203.496840092568,-5.54330262622176,
135.083394400798));
#195215=CARTESIAN_POINT('Ctrl Pts',(-203.775287716381,0.603781838200554,
137.781020392543));
#195216=CARTESIAN_POINT('Ctrl Pts',(-204.053735340194,6.19602028969954,
134.067436879861));
#195217=CARTESIAN_POINT('Ctrl Pts',(-204.332182964007,6.09441878738321,
127.355245692268));
#195218=CARTESIAN_POINT('Ctrl Pts',(-204.61063058782,0.392344148371673,
123.812622622391));
#195219=CARTESIAN_POINT('Ctrl Pts',(-204.889078211633,-5.67027559591653,
126.69506520469));
#195220=CARTESIAN_POINT('Ctrl Pts',(-205.167525835445,-6.5221890759199,
133.353749521179));
#195221=CARTESIAN_POINT('Ctrl Pts',(-205.445973459259,-1.38052942180316,
137.66966997982));
#195222=CARTESIAN_POINT('Ctrl Pts',(-205.724421083071,5.02976932833932,
135.676706523556));
#195223=CARTESIAN_POINT('Ctrl Pts',(-206.002868706884,6.8179557836299,129.206295207017));
#195224=CARTESIAN_POINT('Ctrl Pts',(-206.281316330697,2.340773949421,124.204427932937));
#195225=CARTESIAN_POINT('Ctrl Pts',(-206.55976395451,-4.28746479114066,
125.267576371395));
#195226=CARTESIAN_POINT('Ctrl Pts',(-206.838211578323,-6.97573284294384,
131.418759045136));
#195227=CARTESIAN_POINT('Ctrl Pts',(-207.116659202136,-3.253643195576,137.005339578972));
#195228=CARTESIAN_POINT('Ctrl Pts',(-207.395106825949,3.4583855992191,136.893523381939));
#195229=CARTESIAN_POINT('Ctrl Pts',(-207.673554449762,6.99232697986142,
131.186064076586));
#195230=CARTESIAN_POINT('Ctrl Pts',(-207.952002073574,4.10066146017411,
125.127837939644));
#195231=CARTESIAN_POINT('Ctrl Pts',(-208.230449697387,-2.55931161296347,
124.286058830161));
#195232=CARTESIAN_POINT('Ctrl Pts',(-208.5088973212,-6.86740234311116,129.434280626559));
#195233=CARTESIAN_POINT('Ctrl Pts',(-208.787344945013,-4.86468581119477,
135.841539002563));
#195234=CARTESIAN_POINT('Ctrl Pts',(-209.065792568826,1.60843932809579,
137.619876522599));
#195235=CARTESIAN_POINT('Ctrl Pts',(-209.344240192639,6.60348730149562,
133.135087882371));
#195236=CARTESIAN_POINT('Ctrl Pts',(-209.622687816452,5.53025304311036,
126.508474748144));
#195237=CARTESIAN_POINT('Ctrl Pts',(-209.901135440264,-0.625013594012848,
123.829570862223));
#195238=CARTESIAN_POINT('Ctrl Pts',(-210.179583064078,-6.20592327184948,
127.56015802404));
#195239=CARTESIAN_POINT('Ctrl Pts',(-210.45803068789,-6.08389263906328,
134.272008881199));
#195240=CARTESIAN_POINT('Ctrl Pts',(-210.736478311703,-0.371061885656257,
137.797260388114));
#195241=CARTESIAN_POINT('Ctrl Pts',(-211.014925935516,5.68275661328764,
134.896378628042));
#195242=CARTESIAN_POINT('Ctrl Pts',(-211.293373559329,6.51439940271492,
128.235132222534));
#195243=CARTESIAN_POINT('Ctrl Pts',(-211.571821183142,1.35962738715011,
123.934881198276));
#195244=CARTESIAN_POINT('Ctrl Pts',(-211.850268806955,-5.04457577571481,
125.947346167619));
#195245=CARTESIAN_POINT('Ctrl Pts',(-212.128716430768,-6.81306024192543,
132.423170138115));
#195246=CARTESIAN_POINT('Ctrl Pts',(-212.40716405458,-2.32067518230222,
137.411387242468));
#195247=CARTESIAN_POINT('Ctrl Pts',(-212.685611678394,4.30429699857105,
136.32806964973));
#195248=CARTESIAN_POINT('Ctrl Pts',(-212.964059302206,6.97383051435588,
130.168733304621));
#195249=CARTESIAN_POINT('Ctrl Pts',(-213.24250692602,3.23475447800865,124.593507407987));
#195250=CARTESIAN_POINT('Ctrl Pts',(-213.520954549832,-3.47690289708716,
124.725752193909));
#195251=CARTESIAN_POINT('Ctrl Pts',(-213.799402173646,-6.99345636590915,
130.443941164641));
#195252=CARTESIAN_POINT('Ctrl Pts',(-214.077849797458,-4.08336508379785,
136.49333800514));
#195253=CARTESIAN_POINT('Ctrl Pts',(-214.356297421271,2.57913922684953,
137.314842548456));
#195254=CARTESIAN_POINT('Ctrl Pts',(-214.634745045084,6.87154058597789,
132.153532252007));
#195255=CARTESIAN_POINT('Ctrl Pts',(-214.913192668897,4.84933184001288,
125.752399134204));
#195256=CARTESIAN_POINT('Ctrl Pts',(-215.19164029271,-1.62917596389355,
123.993771817573));
#195257=CARTESIAN_POINT('Ctrl Pts',(-215.470087916522,-6.61055064665203,
128.493742892374));
#195258=CARTESIAN_POINT('Ctrl Pts',(-215.748535540335,-5.51715222849034,
135.117058776675));
#195259=CARTESIAN_POINT('Ctrl Pts',(-216.026983164148,0.646239559784443,
137.777215739773));
#195260=CARTESIAN_POINT('Ctrl Pts',(-216.305430787961,6.21576876317433,
134.029659488472));
#195261=CARTESIAN_POINT('Ctrl Pts',(-216.583878411774,6.0733101303926,127.318211139417));
#195262=CARTESIAN_POINT('Ctrl Pts',(-216.862326035587,0.349776185474419,
123.810363852911));
#195263=CARTESIAN_POINT('Ctrl Pts',(-217.1407736594,-5.69518498637811,126.729657917385));
#195264=CARTESIAN_POINT('Ctrl Pts',(-217.419221283213,-6.50654938100331,
133.393404703032));
#195265=CARTESIAN_POINT('Ctrl Pts',(-217.697668907026,-1.33871275709491,
137.67794645597));
#195266=CARTESIAN_POINT('Ctrl Pts',(-217.976116530838,5.05933549082977,
135.64599861675));
#195267=CARTESIAN_POINT('Ctrl Pts',(-218.254564154652,6.80810158496121,
129.164821983446));
#195268=CARTESIAN_POINT('Ctrl Pts',(-218.533011778464,2.30055491676597,
124.190301258982));
#195269=CARTESIAN_POINT('Ctrl Pts',(-218.811459402277,-4.32108933158155,
125.293777970294));
#195270=CARTESIAN_POINT('Ctrl Pts',(-219.08990702609,-6.97186358115499,
131.461210927519));
#195271=CARTESIAN_POINT('Ctrl Pts',(-219.368354649903,-3.21583579411804,
137.02503053882));
#195272=CARTESIAN_POINT('Ctrl Pts',(-219.646802273716,3.49538798540175,
136.872358389107));
#195273=CARTESIAN_POINT('Ctrl Pts',(-219.925249897529,6.99452096553273,
131.143492725519));
#195274=CARTESIAN_POINT('Ctrl Pts',(-220.203697521342,4.06603087968498,
125.102981222246));
#195275=CARTESIAN_POINT('Ctrl Pts',(-220.482145145155,-2.59894294794204,
124.301758855404));
#195276=CARTESIAN_POINT('Ctrl Pts',(-220.760592768967,-6.87561517183164,
129.476109838232));
#195277=CARTESIAN_POINT('Ctrl Pts',(-221.03904039278,-4.83393294528274,
135.87105839861));
#195278=CARTESIAN_POINT('Ctrl Pts',(-221.317488016593,1.64989750722823,
137.609959220154));
#195279=CARTESIAN_POINT('Ctrl Pts',(-221.595935640406,6.61755275257056,
133.094847397895));
#195280=CARTESIAN_POINT('Ctrl Pts',(-221.874383264219,5.5040003037252,126.474890121013));
#195281=CARTESIAN_POINT('Ctrl Pts',(-222.152830888031,-0.667459538880483,
123.83350472407));
#195282=CARTESIAN_POINT('Ctrl Pts',(-222.431278511845,-6.22555667246622,
127.597995348007));
#195283=CARTESIAN_POINT('Ctrl Pts',(-222.709726135657,-6.06267135940695,
134.308979015016));
#195284=CARTESIAN_POINT('Ctrl Pts',(-222.988173759471,-0.328487245014279,
137.799389584896));
#195285=CARTESIAN_POINT('Ctrl Pts',(-223.266621383283,5.70756060005303,
134.861710259961));
#195286=CARTESIAN_POINT('Ctrl Pts',(-223.545069007096,6.49863908350723,
128.195524826214));
#195287=CARTESIAN_POINT('Ctrl Pts',(-223.823516630909,1.31778572538753,
123.926732036005));
#195288=CARTESIAN_POINT('Ctrl Pts',(-224.101964254722,-5.07404833695195,
125.978143921416));
#195289=CARTESIAN_POINT('Ctrl Pts',(-224.380411878535,-6.80307985867417,
132.464613176793));
#195290=CARTESIAN_POINT('Ctrl Pts',(-224.658859502348,-2.28041333920269,
137.425391438088));
#195291=CARTESIAN_POINT('Ctrl Pts',(-224.937307126161,4.33784163461131,
136.30176583066));
#195292=CARTESIAN_POINT('Ctrl Pts',(-225.215754749974,6.96983206156226,
130.126293395573));
#195293=CARTESIAN_POINT('Ctrl Pts',(-225.494202373786,3.19688731916334,
124.573931612073));
#195294=CARTESIAN_POINT('Ctrl Pts',(-225.7726499976,-3.51384069291894,124.747029711241));
#195295=CARTESIAN_POINT('Ctrl Pts',(-226.051097621412,-6.9955207688696,
130.486518996257));
#195296=CARTESIAN_POINT('Ctrl Pts',(-226.329545245225,-4.04865900841799,
136.518089203828));
#195297=CARTESIAN_POINT('Ctrl Pts',(-226.607992869038,2.61872259278156,
137.299021971784));
#195298=CARTESIAN_POINT('Ctrl Pts',(-226.886440492851,6.87962606292594,
132.111678237058));
#195299=CARTESIAN_POINT('Ctrl Pts',(-227.164888116664,4.81848926965818,
125.722973476035));
#195300=CARTESIAN_POINT('Ctrl Pts',(-227.443335740477,-1.67060376613766,
124.003815258517));
#195301=CARTESIAN_POINT('Ctrl Pts',(-227.72178336429,-6.62449355438458,
128.534026000853));
#195302=CARTESIAN_POINT('Ctrl Pts',(-228.000230988102,-5.49079739065326,
135.150563343936));
#195303=CARTESIAN_POINT('Ctrl Pts',(-228.278678611916,0.688673334723007,
137.773152705292));
#195304=CARTESIAN_POINT('Ctrl Pts',(-228.557126235728,6.23528690905198,
133.991762582447));
#195305=CARTESIAN_POINT('Ctrl Pts',(-228.835573859542,6.05197642466173,
127.281305767118));
#195306=CARTESIAN_POINT('Ctrl Pts',(-229.114021483354,0.307195261492642,
123.808364248553));
#195307=CARTESIAN_POINT('Ctrl Pts',(-229.392469107167,-5.7198833396657,
126.764401619687));
#195308=CARTESIAN_POINT('Ctrl Pts',(-229.670916730979,-6.49066858350677,
133.432963946903));
#195309=CARTESIAN_POINT('Ctrl Pts',(-229.949364354793,-1.29684648589306,
137.685968228869));
#195310=CARTESIAN_POINT('Ctrl Pts',(-230.227811978605,5.0887141777831,135.615111301269));
#195311=CARTESIAN_POINT('Ctrl Pts',(-230.506259602419,6.79799510958498,
129.123409513582));
#195312=CARTESIAN_POINT('Ctrl Pts',(-230.784707226231,2.26025063620168,
124.176419671429));
#195313=CARTESIAN_POINT('Ctrl Pts',(-231.063154850045,-4.35455375246839,
125.32018376586));
#195314=CARTESIAN_POINT('Ctrl Pts',(-231.341602473857,-6.96773597439774,
131.503638470075));
#195315=CARTESIAN_POINT('Ctrl Pts',(-231.62005009767,-3.17790922868121,
137.044490989456));
#195316=CARTESIAN_POINT('Ctrl Pts',(-231.898497721483,3.53226084869627,
136.850968544386));
#195317=CARTESIAN_POINT('Ctrl Pts',(-232.176945345296,6.99645576665798,
131.100908807788));
#195318=CARTESIAN_POINT('Ctrl Pts',(-232.455392969109,4.03124963092651,
125.078335771559));
#195319=CARTESIAN_POINT('Ctrl Pts',(-232.733840592922,-2.63847797813309,
124.317699836946));
#195320=CARTESIAN_POINT('Ctrl Pts',(-233.012288216734,-6.88357322210384,
129.517988268725));
#195321=CARTESIAN_POINT('Ctrl Pts',(-233.290735840548,-4.80300095620762,
135.900390046307));
#195322=CARTESIAN_POINT('Ctrl Pts',(-233.56918346436,1.6912945488023,137.599789733751));
#195323=CARTESIAN_POINT('Ctrl Pts',(-233.847631088173,6.63137298779474,
133.05452203859));
#195324=CARTESIAN_POINT('Ctrl Pts',(-234.126078711986,5.47754361158473,
126.441465924004));
#195325=CARTESIAN_POINT('Ctrl Pts',(-234.404526335799,-0.709880750790079,
123.837696893545));
#195326=CARTESIAN_POINT('Ctrl Pts',(-234.682973959612,-6.24495938279112,
127.635951485018));
#195327=CARTESIAN_POINT('Ctrl Pts',(-234.961421583425,-6.04122542523402,
134.345819283911));
#195328=CARTESIAN_POINT('Ctrl Pts',(-235.239869207238,-0.285900432155891,
137.801259578306));
#195329=CARTESIAN_POINT('Ctrl Pts',(-235.518316831051,5.73215309106056,
134.826891545298));
#195330=CARTESIAN_POINT('Ctrl Pts',(-235.796764454864,6.48263795483918,
128.156014101264));
#195331=CARTESIAN_POINT('Ctrl Pts',(-236.075212078676,1.27589523259052,
123.918837726791));
#195332=CARTESIAN_POINT('Ctrl Pts',(-236.353659702489,-5.10333287746112,
126.009120512446));
#195333=CARTESIAN_POINT('Ctrl Pts',(-236.632107326302,-6.79284738479763,
132.505994694203));
#195334=CARTESIAN_POINT('Ctrl Pts',(-236.910554950115,-2.24006699454776,
137.439150288976));
#195335=CARTESIAN_POINT('Ctrl Pts',(-237.189002573928,4.3712255303347,136.275258303218));
#195336=CARTESIAN_POINT('Ctrl Pts',(-237.467450197741,6.96557533907847,
130.083878612554));
#195337=CARTESIAN_POINT('Ctrl Pts',(-237.745897821554,3.15890169848239,
124.554586686994));
#195338=CARTESIAN_POINT('Ctrl Pts',(-238.024345445366,-3.55064828209192,
124.768531685198));
#195339=CARTESIAN_POINT('Ctrl Pts',(-238.30279306918,-6.99732595023538,
130.529108605612));
#195340=CARTESIAN_POINT('Ctrl Pts',(-238.581240692992,-4.01380290848946,
136.542628678202));
#195341=CARTESIAN_POINT('Ctrl Pts',(-238.859688316805,2.65820892098533,
137.282960733047));
#195342=CARTESIAN_POINT('Ctrl Pts',(-239.138135940618,6.88745661279959,
132.069775778975));
#195343=CARTESIAN_POINT('Ctrl Pts',(-239.416583564431,4.78746814841248,
125.693736110535));
#195344=CARTESIAN_POINT('Ctrl Pts',(-239.695031188244,-1.71196966354462,
124.014110696169));
#195345=CARTESIAN_POINT('Ctrl Pts',(-239.973478812057,-6.63819098907155,
128.574393237416));
#195346=CARTESIAN_POINT('Ctrl Pts',(-240.25192643587,-5.46423908930053,
135.183906861057));
#195347=CARTESIAN_POINT('Ctrl Pts',(-240.530374059683,0.731081590618679,
137.768831439659));
#195348=CARTESIAN_POINT('Ctrl Pts',(-240.808821683496,6.25457400407998,
133.95374756607));
#195349=CARTESIAN_POINT('Ctrl Pts',(-241.087269307308,6.03041846071876,
127.244530942912));
#195350=CARTESIAN_POINT('Ctrl Pts',(-241.365716931122,0.264602954276818,
123.806623883412));
#195351=CARTESIAN_POINT('Ctrl Pts',(-241.644164554934,-5.74436974057257,
126.799295024156));
#195352=CARTESIAN_POINT('Ctrl Pts',(-241.922612178747,-6.47454727189872,
133.472425786911));
#195353=CARTESIAN_POINT('Ctrl Pts',(-242.20105980256,-1.25493215956847,
137.693735001267));
#195354=CARTESIAN_POINT('Ctrl Pts',(-242.479507426373,5.11790430056101,
135.584045721651));
#195355=CARTESIAN_POINT('Ctrl Pts',(-242.757955050186,6.78763673199965,
129.082059331979));
#195356=CARTESIAN_POINT('Ctrl Pts',(-243.036402673998,2.21986260121965,
124.162783684665));
#195357=CARTESIAN_POINT('Ctrl Pts',(-243.314850297812,-4.38785681376436,
125.346792779616));
#195358=CARTESIAN_POINT('Ctrl Pts',(-243.593297921624,-6.96335017562108,
131.54604010063));
#195359=CARTESIAN_POINT('Ctrl Pts',(-243.871745545438,-3.13986490465013,
137.063720209766));
#195360=CARTESIAN_POINT('Ctrl Pts',(-244.15019316925,3.56900282276695,136.829354640385));
#195361=CARTESIAN_POINT('Ctrl Pts',(-244.428640793064,6.99813131154132,
131.058313901354));
#195362=CARTESIAN_POINT('Ctrl Pts',(-244.707088416876,3.99631900273028,
125.053902500829));
#195363=CARTESIAN_POINT('Ctrl Pts',(-244.985536040689,-2.67791523855318,
124.333881184089));
#195364=CARTESIAN_POINT('Ctrl Pts',(-245.263983664501,-6.89127619903846,
129.559914366219));
#195365=CARTESIAN_POINT('Ctrl Pts',(-245.542431288315,-4.7718909901659,
135.929532858758));
#195366=CARTESIAN_POINT('Ctrl Pts',(-245.820878912128,1.73262891883438,
137.589368440225));
#195367=CARTESIAN_POINT('Ctrl Pts',(-246.09932653594,6.6449474950541,133.014113298726));
#195368=CARTESIAN_POINT('Ctrl Pts',(-246.377774159753,5.45088394705135,
126.408203395661));
#195369=CARTESIAN_POINT('Ctrl Pts',(-246.656221783566,-0.752275657806765,
123.842147215306));
#195370=CARTESIAN_POINT('Ctrl Pts',(-246.934669407379,-6.26413068384941,
127.674025028594));
#195371=CARTESIAN_POINT('Ctrl Pts',(-247.213117031192,-6.01955563123113,
134.382528322752));
#195372=CARTESIAN_POINT('Ctrl Pts',(-247.491564655005,-0.243303025152602,
137.802870299053));
#195373=CARTESIAN_POINT('Ctrl Pts',(-247.770012278818,5.75653317502817,
134.791923774272));
#195374=CARTESIAN_POINT('Ctrl Pts',(-248.048459902631,6.46639660963695,
128.116601511768));
#195375=CARTESIAN_POINT('Ctrl Pts',(-248.326907526444,1.23395746102625,
123.91119856316));
#195376=CARTESIAN_POINT('Ctrl Pts',(-248.605355150257,-5.13242831209467,
126.040274792862));
#195377=CARTESIAN_POINT('Ctrl Pts',(-248.883802774069,-6.78236319946242,
132.547313156937));
#195378=CARTESIAN_POINT('Ctrl Pts',(-249.162250397883,-2.19963764338714,
137.452663285294));
#195379=CARTESIAN_POINT('Ctrl Pts',(-249.440698021695,4.40444744868852,
136.24854804965));
#195380=CARTESIAN_POINT('Ctrl Pts',(-249.719145645508,6.96106050463867,
130.041490527264));
#195381=CARTESIAN_POINT('Ctrl Pts',(-249.997593269321,3.12079902353814,
124.535473349588));
#195382=CARTESIAN_POINT('Ctrl Pts',(-250.276040893134,-3.58732430068758,
124.790257319018));
#195383=CARTESIAN_POINT('Ctrl Pts',(-250.554488516946,-6.99887184311352,
130.571708414529));
#195384=CARTESIAN_POINT('Ctrl Pts',(-250.83293614076,-3.97879807562073,
136.566955518948));
#195385=CARTESIAN_POINT('Ctrl Pts',(-251.111383764572,2.69759674828547,
137.26665942739));
#195386=CARTESIAN_POINT('Ctrl Pts',(-251.389831388386,6.89503194542569,
132.027826430486));
#195387=CARTESIAN_POINT('Ctrl Pts',(-251.668279012198,4.75626962579305,
125.66468812107));
#195388=CARTESIAN_POINT('Ctrl Pts',(-251.946726636011,-1.75327212332407,
124.024657749096));
#195389=CARTESIAN_POINT('Ctrl Pts',(-252.225174259824,-6.65164244307981,
128.614843106116));
#195390=CARTESIAN_POINT('Ctrl Pts',(-252.503621883637,-5.43747830869239,
135.217088092717));
#195391=CARTESIAN_POINT('Ctrl Pts',(-252.78206950745,0.773462756270139,
137.764252102553));
#195392=CARTESIAN_POINT('Ctrl Pts',(-253.060517131263,6.2736293330892,133.91561584884));
#195393=CARTESIAN_POINT('Ctrl Pts',(-253.338964755075,6.00863703830687,
127.207888027921));
#195394=CARTESIAN_POINT('Ctrl Pts',(-253.617412378889,0.222000840393564,
123.805142824969));
#195395=CARTESIAN_POINT('Ctrl Pts',(-253.895860002702,-5.76864327852066,
126.83433683216));
#195396=CARTESIAN_POINT('Ctrl Pts',(-254.174307626514,-6.45818604965135,
133.511788771436));
#195397=CARTESIAN_POINT('Ctrl Pts',(-254.452755250327,-1.21297131977014,
137.701246465247));
#195398=CARTESIAN_POINT('Ctrl Pts',(-254.73120287414,5.14690475579816,135.55280306703));
#195399=CARTESIAN_POINT('Ctrl Pts',(-255.009650497953,6.7770268770417,129.040772899161));
#195400=CARTESIAN_POINT('Ctrl Pts',(-255.288098121766,2.17939223099114,
124.149393939406));
#195401=CARTESIAN_POINT('Ctrl Pts',(-255.566545745579,-4.42099713522674,
125.37360376984));
#195402=CARTESIAN_POINT('Ctrl Pts',(-255.844993369392,-6.95870662337211,
131.588414730824));
#195403=CARTESIAN_POINT('Ctrl Pts',(-256.123440993205,-3.10170371057109,
137.082716575498));
#195404=CARTESIAN_POINT('Ctrl Pts',(-256.401888617018,3.60561156199617,
136.807519199501));
#195405=CARTESIAN_POINT('Ctrl Pts',(-256.68033624083,6.99954939633056,131.01570633407));
#195406=CARTESIAN_POINT('Ctrl Pts',(-256.958783864643,3.96123678073902,
125.029688453078));
#195407=CARTESIAN_POINT('Ctrl Pts',(-257.237231488456,-2.71724664265218,
124.350290708114));
#195408=CARTESIAN_POINT('Ctrl Pts',(-257.515679112269,-6.89873632689917,
129.601908459729));
#195409=CARTESIAN_POINT('Ctrl Pts',(-257.794126736082,-4.74058057908887,
135.958444437253));
#195410=CARTESIAN_POINT('Ctrl Pts',(-258.072574359895,1.77385448465437,
137.578773744179));
#195411=CARTESIAN_POINT('Ctrl Pts',(-258.351021983707,6.6583599873155,132.973475360041));
#195412=CARTESIAN_POINT('Ctrl Pts',(-258.629469607521,5.42386327951784,
126.375381938049));
#195413=CARTESIAN_POINT('Ctrl Pts',(-258.907917231333,-0.794342416617398,
123.846330221273));
#195414=CARTESIAN_POINT('Ctrl Pts',(-259.186364855146,-6.28363694765996,
127.713206958712));
#195415=CARTESIAN_POINT('Ctrl Pts',(-259.464812478959,-5.99659113747434,
134.41722675292));
#195416=CARTESIAN_POINT('Ctrl Pts',(-259.743260102772,-0.202727240537578,
137.807801967267));
#195417=CARTESIAN_POINT('Ctrl Pts',(-260.021707726585,5.7845923739281,134.749768174183));
#195418=CARTESIAN_POINT('Ctrl Pts',(-260.253747413096,6.33253704604016,
129.202365411857));
#195419=CARTESIAN_POINT('Ctrl Pts',(-260.439389088604,3.82430165355141,
125.973250269562));
#195420=CARTESIAN_POINT('Ctrl Pts',(-260.532214889509,1.97943258085903,
125.138073123498));
#195421=CARTESIAN_POINT('Ctrl Pts',(-260.578632753112,1.00712299976162,
124.970230583726));
#195422=CARTESIAN_POINT('Ctrl Pts',(-260.,4.64727355878983,134.479645829435));
#195423=CARTESIAN_POINT('Ctrl Pts',(-260.,4.72445468230523,134.365238782885));
#195424=CARTESIAN_POINT('Ctrl Pts',(-260.,4.79717385008238,134.248223015737));
#195425=CARTESIAN_POINT('Ctrl Pts',(-260.,4.86519974457552,134.128712980314));
#195426=CARTESIAN_POINT('Ctrl Pts',(-260.,4.94591766572252,133.986905192449));
#195427=CARTESIAN_POINT('Ctrl Pts',(-260.,5.02002908188102,133.841585703171));
#195428=CARTESIAN_POINT('Ctrl Pts',(-260.,5.08757949274479,133.693228223168));
#195429=CARTESIAN_POINT('Ctrl Pts',(-260.,5.15592794008602,133.543118056849));
#195430=CARTESIAN_POINT('Ctrl Pts',(-260.,5.21755948895336,133.389896884846));
#195431=CARTESIAN_POINT('Ctrl Pts',(-260.,5.2724692973062,133.234041404611));
#195432=CARTESIAN_POINT('Ctrl Pts',(-260.,5.32751299525585,133.077805893413));
#195433=CARTESIAN_POINT('Ctrl Pts',(-260.,5.37580210608346,132.918922369593));
#195434=CARTESIAN_POINT('Ctrl Pts',(-260.,5.41727981065124,132.757869539038));
#195435=CARTESIAN_POINT('Ctrl Pts',(-260.,5.4388804792077,132.673996797064));
#195436=CARTESIAN_POINT('Ctrl Pts',(-260.,5.4586329773621,132.589535771846));
#195437=CARTESIAN_POINT('Ctrl Pts',(-260.,5.47652375629486,132.504555076365));
#195438=CARTESIAN_POINT('Ctrl Pts',(-260.,5.48230964795087,132.477072254138));
#195439=CARTESIAN_POINT('Ctrl Pts',(-260.,5.48790079663348,132.449535089018));
#195440=CARTESIAN_POINT('Ctrl Pts',(-260.,5.49329665994448,132.421945928666));
#195441=CARTESIAN_POINT('Ctrl Pts',(-260.,5.49715720698584,132.402206872054));
#195442=CARTESIAN_POINT('Ctrl Pts',(-260.,5.50091711018986,132.382444492444));
#195443=CARTESIAN_POINT('Ctrl Pts',(-260.,5.50457455091086,132.362669472875));
#195444=CARTESIAN_POINT('Ctrl Pts',(-260.,5.53421387188956,132.202415842791));
#195445=CARTESIAN_POINT('Ctrl Pts',(-260.,5.55716564037324,132.041144769358));
#195446=CARTESIAN_POINT('Ctrl Pts',(-260.,5.57346020341767,131.879315471242));
#195447=CARTESIAN_POINT('Ctrl Pts',(-260.,5.58976582436389,131.717376351679));
#195448=CARTESIAN_POINT('Ctrl Pts',(-260.,5.59940512720595,131.554877419695));
#195449=CARTESIAN_POINT('Ctrl Pts',(-260.,5.60235628880471,131.392278361123));
#195450=CARTESIAN_POINT('Ctrl Pts',(-260.,5.60526194489148,131.232186502907));
#195451=CARTESIAN_POINT('Ctrl Pts',(-260.,5.6016839329031,131.071996842801));
#195452=CARTESIAN_POINT('Ctrl Pts',(-260.,5.59155299666625,130.912159283332));
#195453=CARTESIAN_POINT('Ctrl Pts',(-260.,5.58151245621597,130.753747914057));
#195454=CARTESIAN_POINT('Ctrl Pts',(-260.,5.56503528598279,130.595681704101));
#195455=CARTESIAN_POINT('Ctrl Pts',(-260.,5.542008385626,130.438420204743));
#195456=CARTESIAN_POINT('Ctrl Pts',(-260.,5.53509379108037,130.391197196485));
#195457=CARTESIAN_POINT('Ctrl Pts',(-260.,5.52758829894611,130.344046935964));
#195458=CARTESIAN_POINT('Ctrl Pts',(-260.,5.51948805734336,130.296982392616));
#195459=CARTESIAN_POINT('Ctrl Pts',(-260.,5.51571179868533,130.275041332334));
#195460=CARTESIAN_POINT('Ctrl Pts',(-260.,5.51180627565152,130.253118905161));
#195461=CARTESIAN_POINT('Ctrl Pts',(-260.,5.50777107109651,130.23121644617));
#195462=CARTESIAN_POINT('Ctrl Pts',(-260.,5.50419825781951,130.211823774692));
#195463=CARTESIAN_POINT('Ctrl Pts',(-260.,5.50052560593342,130.192456675027));
#195464=CARTESIAN_POINT('Ctrl Pts',(-260.,5.49675319635138,130.173116366892));
#195465=CARTESIAN_POINT('Ctrl Pts',(-260.,5.4666002147623,130.018528710794));
#195466=CARTESIAN_POINT('Ctrl Pts',(-260.,5.43007631185038,129.865642846568));
#195467=CARTESIAN_POINT('Ctrl Pts',(-260.,5.38715622994236,129.714878921409));
#195468=CARTESIAN_POINT('Ctrl Pts',(-260.,5.34514940182371,129.567322952057));
#195469=CARTESIAN_POINT('Ctrl Pts',(-260.,5.29701544650841,129.421798967472));
#195470=CARTESIAN_POINT('Ctrl Pts',(-260.,5.24268558046692,129.278720038982));
#195471=CARTESIAN_POINT('Ctrl Pts',(-260.,5.18884719914122,129.136935446585));
#195472=CARTESIAN_POINT('Ctrl Pts',(-260.,5.12892436413587,128.997551287232));
#195473=CARTESIAN_POINT('Ctrl Pts',(-260.,5.06280805876399,128.860997446897));
#195474=CARTESIAN_POINT('Ctrl Pts',(-260.,5.03637289178243,128.806399363249));
#195475=CARTESIAN_POINT('Ctrl Pts',(-260.,5.00894715733214,128.752254104499));
#195476=CARTESIAN_POINT('Ctrl Pts',(-260.,4.98052205131543,128.698590732034));
#195477=CARTESIAN_POINT('Ctrl Pts',(-260.,4.92892839867658,128.601187774354));
#195478=CARTESIAN_POINT('Ctrl Pts',(-260.,4.87404261145725,128.505371761023));
#195479=CARTESIAN_POINT('Ctrl Pts',(-260.,4.81598802038452,128.411272751585));
#195480=CARTESIAN_POINT('Ctrl Pts',(-260.,4.79983018598994,128.385082984625));
#195481=CARTESIAN_POINT('Ctrl Pts',(-260.,4.78342684813515,128.359026287272));
#195482=CARTESIAN_POINT('Ctrl Pts',(-260.,4.76678058132004,128.333105619803));
#195483=CARTESIAN_POINT('Ctrl Pts',(-260.,4.75601759437824,128.316346077944));
#195484=CARTESIAN_POINT('Ctrl Pts',(-260.,4.74515304943485,128.299643405288));
#195485=CARTESIAN_POINT('Ctrl Pts',(-260.,4.73418763536694,128.282998417979));
#195486=CARTESIAN_POINT('Ctrl Pts',(-260.,4.72349743847076,128.266771197505));
#195487=CARTESIAN_POINT('Ctrl Pts',(-260.,4.71271622399387,128.250606183426));
#195488=CARTESIAN_POINT('Ctrl Pts',(-260.,4.70184618864053,128.23450587656));
#195489=CARTESIAN_POINT('Ctrl Pts',(-260.,4.61643398223665,128.107996376954));
#195490=CARTESIAN_POINT('Ctrl Pts',(-260.,4.52551512678615,127.985439463241));
#195491=CARTESIAN_POINT('Ctrl Pts',(-260.,4.42949814447551,127.867106517455));
#195492=CARTESIAN_POINT('Ctrl Pts',(-260.,4.3329217980936,127.748084201967));
#195493=CARTESIAN_POINT('Ctrl Pts',(-260.,4.23118703860946,127.633334688566));
#195494=CARTESIAN_POINT('Ctrl Pts',(-260.,4.12467212342404,127.523171713096));
#195495=CARTESIAN_POINT('Ctrl Pts',(-260.,4.01916361053234,127.414049608484));
#195496=CARTESIAN_POINT('Ctrl Pts',(-260.,3.90896409695521,127.309427379582));
#195497=CARTESIAN_POINT('Ctrl Pts',(-260.,3.79441562469337,127.209653467817));
#195498=CARTESIAN_POINT('Ctrl Pts',(-260.,3.70165347482906,127.128855859844));
#195499=CARTESIAN_POINT('Ctrl Pts',(-260.,3.60603870571396,127.051238430853));
#195500=CARTESIAN_POINT('Ctrl Pts',(-260.,3.50774543010271,126.977010181796));
#195501=CARTESIAN_POINT('Ctrl Pts',(-260.,3.45657148047279,126.938365089802));
#195502=CARTESIAN_POINT('Ctrl Pts',(-260.,3.40467143540377,126.900639007406));
#195503=CARTESIAN_POINT('Ctrl Pts',(-260.,3.35206949555686,126.863863967217));
#195504=CARTESIAN_POINT('Ctrl Pts',(-260.,3.33451576292437,126.851591811002));
#195505=CARTESIAN_POINT('Ctrl Pts',(-260.,3.31688203845638,126.839424338156));
#195506=CARTESIAN_POINT('Ctrl Pts',(-260.,3.2991751338089,126.82736680457));
#195507=CARTESIAN_POINT('Ctrl Pts',(-260.,3.26772105256822,126.805948117989));
#195508=CARTESIAN_POINT('Ctrl Pts',(-260.,3.2360509900514,126.78488639037));
#195509=CARTESIAN_POINT('Ctrl Pts',(-260.,3.20417076835762,126.764186616116));
#195510=CARTESIAN_POINT('Ctrl Pts',(-260.,3.07819216095848,126.682388918501));
#195511=CARTESIAN_POINT('Ctrl Pts',(-260.,2.94893322126365,126.606239408971));
#195512=CARTESIAN_POINT('Ctrl Pts',(-260.,2.81674061255645,126.535897250836));
#195513=CARTESIAN_POINT('Ctrl Pts',(-260.,2.6849707683341,126.465780053586));
#195514=CARTESIAN_POINT('Ctrl Pts',(-260.,2.55028528681488,126.401432946769));
#195515=CARTESIAN_POINT('Ctrl Pts',(-260.,2.41301606338223,126.343063828293));
#195516=CARTESIAN_POINT('Ctrl Pts',(-260.,2.35052041203885,126.316489655392));
#195517=CARTESIAN_POINT('Ctrl Pts',(-260.,2.28748911504771,126.291155293666));
#195518=CARTESIAN_POINT('Ctrl Pts',(-260.,2.22395330100519,126.267083981877));
#195519=CARTESIAN_POINT('Ctrl Pts',(-260.,2.19556404838833,126.256328370077));
#195520=CARTESIAN_POINT('Ctrl Pts',(-260.,2.16707406918085,126.245824957815));
#195521=CARTESIAN_POINT('Ctrl Pts',(-260.,2.13848614791516,126.235575968929));
#195522=CARTESIAN_POINT('Ctrl Pts',(-260.,2.1154668765457,126.227323383712));
#195523=CARTESIAN_POINT('Ctrl Pts',(-260.,2.09238327371483,126.219235546019));
#195524=CARTESIAN_POINT('Ctrl Pts',(-260.,2.06925245604652,126.211318807416));
#195525=CARTESIAN_POINT('Ctrl Pts',(-260.,1.93090341986312,126.163967556319));
#195526=CARTESIAN_POINT('Ctrl Pts',(-260.,1.79073515085027,126.122685331451));
#195527=CARTESIAN_POINT('Ctrl Pts',(-260.,1.64906874319027,126.087648542449));
#195528=CARTESIAN_POINT('Ctrl Pts',(-260.,1.50976463913972,126.053195995926));
#195529=CARTESIAN_POINT('Ctrl Pts',(-260.,1.36901131538522,126.024782312242));
#195530=CARTESIAN_POINT('Ctrl Pts',(-260.,1.22711298900573,126.002624910688));
#195531=CARTESIAN_POINT('Ctrl Pts',(-260.,1.09799938680752,125.982463841823));
#195532=CARTESIAN_POINT('Ctrl Pts',(-260.,0.967937472914146,125.967482984268));
#195533=CARTESIAN_POINT('Ctrl Pts',(-260.,0.837162017623963,125.957883255734));
#195534=CARTESIAN_POINT('Ctrl Pts',(210.578629502474,3.43871735229388,135.623751273273));
#195535=CARTESIAN_POINT('Ctrl Pts',(210.532211638871,4.24191310225744,135.050661598608));
#195536=CARTESIAN_POINT('Ctrl Pts',(210.439385837966,5.5417116830592,133.497735776206));
#195537=CARTESIAN_POINT('Ctrl Pts',(210.253744162458,6.40049231640402,129.500124813146));
#195538=CARTESIAN_POINT('Ctrl Pts',(210.021704475947,3.49988613106459,124.739836436729));
#195539=CARTESIAN_POINT('Ctrl Pts',(209.743256852134,-3.22132718841443,
124.582443963435));
#195540=CARTESIAN_POINT('Ctrl Pts',(209.464809228321,-6.97029916743427,
130.151104711613));
#195541=CARTESIAN_POINT('Ctrl Pts',(209.186361604508,-4.320155850937,136.315756482887));
#195542=CARTESIAN_POINT('Ctrl Pts',(208.907913980696,2.30329626696544,137.417975354914));
#195543=CARTESIAN_POINT('Ctrl Pts',(208.629466356883,6.80838731381026,132.441404887444));
#195544=CARTESIAN_POINT('Ctrl Pts',(208.35101873307,5.05782663488002,125.961106241921));
#195545=CARTESIAN_POINT('Ctrl Pts',(208.072571109257,-1.34111875541754,
123.931185212061));
#195546=CARTESIAN_POINT('Ctrl Pts',(207.794123485444,-6.50738248846785,
128.217554840719));
#195547=CARTESIAN_POINT('Ctrl Pts',(207.515675861631,-5.69381680528821,
134.880978212762));
#195548=CARTESIAN_POINT('Ctrl Pts',(207.237228237818,0.352161018465804,
137.798239159538));
#195549=CARTESIAN_POINT('Ctrl Pts',(206.958780614005,6.07448159193836,134.288440920842));
#195550=CARTESIAN_POINT('Ctrl Pts',(206.680332990192,6.21467071562046,127.576957111676));
#195551=CARTESIAN_POINT('Ctrl Pts',(206.40188536638,0.643870262773591,123.831292031177));
#195552=CARTESIAN_POINT('Ctrl Pts',(206.123437742567,-5.51860979104455,
126.493540260974));
#195553=CARTESIAN_POINT('Ctrl Pts',(205.844990118754,-6.60976007302988,
133.117219720399));
#195554=CARTESIAN_POINT('Ctrl Pts',(205.566542494941,-1.62686214948821,
137.615495756827));
#195555=CARTESIAN_POINT('Ctrl Pts',(205.288094871128,4.8510417637676,135.85467075854));
#195556=CARTESIAN_POINT('Ctrl Pts',(205.009647247315,6.87107573233629,129.452857771449));
#195557=CARTESIAN_POINT('Ctrl Pts',(204.731199623502,2.57692653546199,124.293009711503));
#195558=CARTESIAN_POINT('Ctrl Pts',(204.452751999689,-4.08529213152394,
125.116775123829));
#195559=CARTESIAN_POINT('Ctrl Pts',(204.174304375876,-6.9933269740478,131.167153704944));
#195560=CARTESIAN_POINT('Ctrl Pts',(203.895856752063,-3.47483593506387,
136.884143186524));
#195561=CARTESIAN_POINT('Ctrl Pts',(203.617409128251,3.23685955433703,137.014109488232));
#195562=CARTESIAN_POINT('Ctrl Pts',(203.338961504438,6.97403925260401,131.437619947721));
#195563=CARTESIAN_POINT('Ctrl Pts',(203.060513880625,4.30241757323156,125.27919601562));
#195564=CARTESIAN_POINT('Ctrl Pts',(202.782066256812,-2.32291566837452,
124.198128435325));
#195565=CARTESIAN_POINT('Ctrl Pts',(202.503618632999,-6.81360289295739,
129.18786549711));
#195566=CARTESIAN_POINT('Ctrl Pts',(202.225171009186,-5.0429219211382,135.663082604955));
#195567=CARTESIAN_POINT('Ctrl Pts',(201.946723385373,1.36195793536179,137.673371567868));
#195568=CARTESIAN_POINT('Ctrl Pts',(201.66827576156,6.51526498482727,133.371375037445));
#195569=CARTESIAN_POINT('Ctrl Pts',(201.389828137747,5.6813618015098,126.710417660699));
#195570=CARTESIAN_POINT('Ctrl Pts',(201.111380513935,-0.373435327379839,
123.811593861123));
#195571=CARTESIAN_POINT('Ctrl Pts',(200.832932890122,-6.08506363376988,
127.338781095048));
#195572=CARTESIAN_POINT('Ctrl Pts',(200.554485266309,-6.20481573259303,
134.050666607207));
#195573=CARTESIAN_POINT('Ctrl Pts',(200.276037642496,-0.622645295272457,
137.779355505743));
#195574=CARTESIAN_POINT('Ctrl Pts',(199.997590018683,5.53170575049466,135.098364849491));
#195575=CARTESIAN_POINT('Ctrl Pts',(199.71914239487,6.60268945040398,128.471394077867));
#195576=CARTESIAN_POINT('Ctrl Pts',(199.440694771057,1.60612410470526,123.988305584475));
#195577=CARTESIAN_POINT('Ctrl Pts',(199.162247147244,-4.86639082969376,
125.768838683693));
#195578=CARTESIAN_POINT('Ctrl Pts',(198.883799523432,-6.86693032801245,
132.176770441218));
#195579=CARTESIAN_POINT('Ctrl Pts',(198.605351899619,-2.5570963230842,137.323524616753));
#195580=CARTESIAN_POINT('Ctrl Pts',(198.326904275806,4.10258428165832,136.479485555902));
#195581=CARTESIAN_POINT('Ctrl Pts',(198.048456651993,6.99219035394115,130.420283921986));
#195582=CARTESIAN_POINT('Ctrl Pts',(197.77000902818,3.45631507844086,124.714030008118));
#195583=CARTESIAN_POINT('Ctrl Pts',(197.491561404367,-3.25574490376804,
124.604492395141));
#195584=CARTESIAN_POINT('Ctrl Pts',(197.213113780554,-6.97593437139489,
130.192330798173));
#195585=CARTESIAN_POINT('Ctrl Pts',(196.934666156741,-4.28558094504976,
136.342594705906));
#195586=CARTESIAN_POINT('Ctrl Pts',(196.656218532928,2.3430120075278,137.403492044232));
#195587=CARTESIAN_POINT('Ctrl Pts',(196.377770909115,6.81849138768721,132.400109986944));
#195588=CARTESIAN_POINT('Ctrl Pts',(196.099323285303,5.02811028438465,125.930312215887));
#195589=CARTESIAN_POINT('Ctrl Pts',(195.82087566149,-1.38285853342424,123.939526815472));
#195590=CARTESIAN_POINT('Ctrl Pts',(195.542428037677,-6.5230479154113,128.257188313404));
#195591=CARTESIAN_POINT('Ctrl Pts',(195.263980413864,-5.66887493174189,
134.915576722577));
#195592=CARTESIAN_POINT('Ctrl Pts',(194.985532790051,0.394717174261835,
137.795958375315));
#195593=CARTESIAN_POINT('Ctrl Pts',(194.707085166238,6.09558348012494,134.251403247221));
#195594=CARTESIAN_POINT('Ctrl Pts',(194.428637542425,6.19490635356113,127.539184339867));
#195595=CARTESIAN_POINT('Ctrl Pts',(194.150189918612,0.601412926074683,
123.827502918989));
#195596=CARTESIAN_POINT('Ctrl Pts',(193.871742294799,-5.54474959981957,
126.527212884656));
#195597=CARTESIAN_POINT('Ctrl Pts',(193.593294670987,-6.59555811955654,
133.157412666584));
#195598=CARTESIAN_POINT('Ctrl Pts',(193.314847047174,-1.58537093834796,
137.625272568447));
#195599=CARTESIAN_POINT('Ctrl Pts',(193.036399423361,4.88169468552635,135.825047607524));
#195600=CARTESIAN_POINT('Ctrl Pts',(192.757951799548,6.86272137744547,129.411056577024));
#195601=CARTESIAN_POINT('Ctrl Pts',(192.479504175735,2.53724238606986,124.277443893095));
#195602=CARTESIAN_POINT('Ctrl Pts',(192.201056551922,-4.11983840692253,
125.141748821346));
#195603=CARTESIAN_POINT('Ctrl Pts',(191.922608928109,-6.99098896924831,
131.209717356357));
#195604=CARTESIAN_POINT('Ctrl Pts',(191.644161304296,-3.43776219763276,
136.905182851196));
#195605=CARTESIAN_POINT('Ctrl Pts',(191.365713680483,3.27460008958736,136.994290755064));
#195606=CARTESIAN_POINT('Ctrl Pts',(191.08726605667,6.9777648675845,131.395155257469));
#195607=CARTESIAN_POINT('Ctrl Pts',(190.808818432858,4.26870461503614,125.253108347726));
#195608=CARTESIAN_POINT('Ctrl Pts',(190.530370809044,-2.36308664091672,
124.212391080215));
#195609=CARTESIAN_POINT('Ctrl Pts',(190.251923185232,-6.82331671706736,
129.229371781915));
#195610=CARTESIAN_POINT('Ctrl Pts',(189.973475561419,-5.01325206778612,
135.693690281095));
#195611=CARTESIAN_POINT('Ctrl Pts',(189.695027937606,1.40374632081163,137.664953676525));
#195612=CARTESIAN_POINT('Ctrl Pts',(189.416580313793,6.53077041740369,133.331667209374));
#195613=CARTESIAN_POINT('Ctrl Pts',(189.13813268998,5.65633554627347,126.675909450142));
#195614=CARTESIAN_POINT('Ctrl Pts',(188.859685066167,-0.41599536452862,
123.81399662772));
#195615=CARTESIAN_POINT('Ctrl Pts',(188.581237442354,-6.10604685783229,
127.375886813701));
#195616=CARTESIAN_POINT('Ctrl Pts',(188.302789818542,-6.18493958576042,
134.088376935175));
#195617=CARTESIAN_POINT('Ctrl Pts',(188.024342194729,-0.580174985471077,
137.783016493883));
#195618=CARTESIAN_POINT('Ctrl Pts',(187.745894570916,5.55774208334242,135.064612228548));
#195619=CARTESIAN_POINT('Ctrl Pts',(187.467446947103,6.58836568835925,128.431244857581));
#195620=CARTESIAN_POINT('Ctrl Pts',(187.18899932329,1.56460308533104,123.97865493689));
#195621=CARTESIAN_POINT('Ctrl Pts',(186.910551699478,-4.89695331800637,
125.798555082479));
#195622=CARTESIAN_POINT('Ctrl Pts',(186.632104075664,-6.85844885156509,
132.218545967617));
#195623=CARTESIAN_POINT('Ctrl Pts',(186.353656451852,-2.51736494438869,
137.338969602853));
#195624=CARTESIAN_POINT('Ctrl Pts',(186.075208828038,4.13705436656654,136.454406814005));
#195625=CARTESIAN_POINT('Ctrl Pts',(185.796761204226,6.98972282098866,130.377727590732));
#195626=CARTESIAN_POINT('Ctrl Pts',(185.518313580413,3.41917746986535,124.693103276936));
#195627=CARTESIAN_POINT('Ctrl Pts',(185.2398659566,-3.29342493995873,124.62442590766));
#195628=CARTESIAN_POINT('Ctrl Pts',(184.961418332787,-6.97953072271363,
130.234806630193));
#195629=CARTESIAN_POINT('Ctrl Pts',(184.682970708974,-4.25178874032612,
136.368579642862));
#195630=CARTESIAN_POINT('Ctrl Pts',(184.404523085161,2.38313938299372,137.389107198495));
#195631=CARTESIAN_POINT('Ctrl Pts',(184.126075461348,6.82807883617355,132.358574329007));
#195632=CARTESIAN_POINT('Ctrl Pts',(183.847627837535,4.99834740910532,125.899794986266));
#195633=CARTESIAN_POINT('Ctrl Pts',(183.569180213722,-1.42462110408482,
123.948071857337));
#195634=CARTESIAN_POINT('Ctrl Pts',(183.290732589909,-6.53843241923107,
128.296943150732));
#195635=CARTESIAN_POINT('Ctrl Pts',(183.012284966097,-5.64374376128527,
134.950008601993));
#195636=CARTESIAN_POINT('Ctrl Pts',(182.733837342284,0.437269701071178,
137.793426081729));
#195637=CARTESIAN_POINT('Ctrl Pts',(182.455389718471,6.11645366995566,134.214233834728));
#195638=CARTESIAN_POINT('Ctrl Pts',(182.176942094658,6.17491552152431,127.501534682722));
#195639=CARTESIAN_POINT('Ctrl Pts',(181.898494470845,0.558931670205695,
123.82397121282));
#195640=CARTESIAN_POINT('Ctrl Pts',(181.620046847032,-5.57068308070185,
126.561044594899));
#195641=CARTESIAN_POINT('Ctrl Pts',(181.341599223219,-6.58111222344223,
133.197518104296));
#195642=CARTESIAN_POINT('Ctrl Pts',(181.063151599407,-1.54382073804491,
137.634796795631));
#195643=CARTESIAN_POINT('Ctrl Pts',(180.784703975594,4.91216658577983,135.795238324681));
#195644=CARTESIAN_POINT('Ctrl Pts',(180.506256351781,6.85411278995147,129.369307058824));
#195645=CARTESIAN_POINT('Ctrl Pts',(180.227808727968,2.49746418218255,124.262119907186));
#195646=CARTESIAN_POINT('Ctrl Pts',(179.949361104155,-4.15423200110403,
125.16693236216));
#195647=CARTESIAN_POINT('Ctrl Pts',(179.670913480342,-6.98839192089168,
131.252265980172));
#195648=CARTESIAN_POINT('Ctrl Pts',(179.392465856529,-3.40056106730489,
136.925996451342));
#195649=CARTESIAN_POINT('Ctrl Pts',(179.114018232716,3.31221928049139,136.974242649806));
#195650=CARTESIAN_POINT('Ctrl Pts',(178.835570608904,6.98123192042358,131.352668676138));
#195651=CARTESIAN_POINT('Ctrl Pts',(178.55712298509,4.23483347762603,125.227226382977));
#195652=CARTESIAN_POINT('Ctrl Pts',(178.278675361277,-2.40317004799311,
124.22689799325));
#195653=CARTESIAN_POINT('Ctrl Pts',(178.000227737465,-6.83277770089014,
129.270936428355));
#195654=CARTESIAN_POINT('Ctrl Pts',(177.721780113652,-4.98339644641697,
135.724116781409));
#195655=CARTESIAN_POINT('Ctrl Pts',(177.443332489839,1.44548268986267,137.65628156334));
#195656=CARTESIAN_POINT('Ctrl Pts',(177.164884866026,6.54603384991367,133.291865731052));
#195657=CARTESIAN_POINT('Ctrl Pts',(176.886437242213,5.63109969342586,126.64155422085));
#195658=CARTESIAN_POINT('Ctrl Pts',(176.6079896184,-0.458539986806858,123.816658424832));
#195659=CARTESIAN_POINT('Ctrl Pts',(176.329541994587,-6.12680382008778,
127.413119575705));
#195660=CARTESIAN_POINT('Ctrl Pts',(176.051094370774,-6.16483425371434,
134.125965572714));
#195661=CARTESIAN_POINT('Ctrl Pts',(175.772646746962,-0.537683177073775,
137.786418885364));
#195662=CARTESIAN_POINT('Ctrl Pts',(175.494199123148,5.58357247201413,135.030701742416));
#195663=CARTESIAN_POINT('Ctrl Pts',(175.215751499336,6.57379779200069,128.391183573973));
#195664=CARTESIAN_POINT('Ctrl Pts',(174.937303875523,1.5230240890144,123.969257218339));
#195665=CARTESIAN_POINT('Ctrl Pts',(174.65885625171,-4.92733434791298,125.82845697323));
#195666=CARTESIAN_POINT('Ctrl Pts',(174.380408627897,-6.84971323277332,
132.260269090858));
#195667=CARTESIAN_POINT('Ctrl Pts',(174.101961004084,-2.4775402838095,137.354172446613));
#195668=CARTESIAN_POINT('Ctrl Pts',(173.823513380271,4.1713711514037,136.429118707571));
#195669=CARTESIAN_POINT('Ctrl Pts',(173.545065756458,6.98699628128659,130.335187068521));
#195670=CARTESIAN_POINT('Ctrl Pts',(173.266618132645,3.38191316241135,124.672403000642));
#195671=CARTESIAN_POINT('Ctrl Pts',(172.988170508833,-3.33098293707706,
124.644588419932));
#195672=CARTESIAN_POINT('Ctrl Pts',(172.709722885019,-6.98286844495469,
130.277303567246));
#195673=CARTESIAN_POINT('Ctrl Pts',(172.431275261207,-4.21783898400718,
136.394358395635));
#195674=CARTESIAN_POINT('Ctrl Pts',(172.152827637394,2.42317845035331,137.374478352552));
#195675=CARTESIAN_POINT('Ctrl Pts',(171.874380013581,6.83741326768756,132.316981079111));
#195676=CARTESIAN_POINT('Ctrl Pts',(171.595932389768,4.96839931822471,125.869459497128));
#195677=CARTESIAN_POINT('Ctrl Pts',(171.317484765955,-1.46633088488636,
123.956870961504));
#195678=CARTESIAN_POINT('Ctrl Pts',(171.039037142142,-6.55357463903296,
128.336790901335));
#195679=CARTESIAN_POINT('Ctrl Pts',(170.760589518329,-5.61840345982816,
134.984286862899));
#195680=CARTESIAN_POINT('Ctrl Pts',(170.482141894517,0.479806024690783,
137.79063480575));
#195681=CARTESIAN_POINT('Ctrl Pts',(170.203694270703,6.13709721234627,134.176938068128));
#195682=CARTESIAN_POINT('Ctrl Pts',(169.925246646891,6.15469587572206,127.464007413007));
#195683=CARTESIAN_POINT('Ctrl Pts',(169.646799023078,0.51642970291829,123.820698167548));
#195684=CARTESIAN_POINT('Ctrl Pts',(169.368351399265,-5.59641013787386,
126.595033542778));
#195685=CARTESIAN_POINT('Ctrl Pts',(169.089903775452,-6.56642246179436,
133.237534862678));
#195686=CARTESIAN_POINT('Ctrl Pts',(168.811456151639,-1.50221333089678,
137.644067918489));
#195687=CARTESIAN_POINT('Ctrl Pts',(168.533008527826,4.94245646389391,135.76524410303));
#195688=CARTESIAN_POINT('Ctrl Pts',(168.254560904013,6.84525022078748,129.32761071706));
#195689=CARTESIAN_POINT('Ctrl Pts',(167.976113280201,2.45759343384159,124.247038346411));
#195690=CARTESIAN_POINT('Ctrl Pts',(167.697665656387,-4.1884716586909,125.192324799951));
#195691=CARTESIAN_POINT('Ctrl Pts',(167.419218032575,-6.98553591510243,
131.294798006688));
#195692=CARTESIAN_POINT('Ctrl Pts',(167.140770408762,-3.36323392793624,
136.946583212019));
#195693=CARTESIAN_POINT('Ctrl Pts',(166.862322784949,3.34971573589186,136.953965917302));
#195694=CARTESIAN_POINT('Ctrl Pts',(166.583875161136,6.98444028114645,131.310161777048));
#195695=CARTESIAN_POINT('Ctrl Pts',(166.305427537323,4.20080541690416,125.20155108099));
#195696=CARTESIAN_POINT('Ctrl Pts',(166.02697991351,-2.44316440471955,124.241648636582));
#195697=CARTESIAN_POINT('Ctrl Pts',(165.748532289697,-6.84198549362249,
129.312557896394));
#195698=CARTESIAN_POINT('Ctrl Pts',(165.470084665885,-4.95335616345982,
135.754360978348));
#195699=CARTESIAN_POINT('Ctrl Pts',(165.191637042072,1.48716549602113,137.647355549705));
#195700=CARTESIAN_POINT('Ctrl Pts',(164.913189418259,6.56105471673207,133.251972077313));
#195701=CARTESIAN_POINT('Ctrl Pts',(164.634741794446,5.60565517810829,126.60735324588));
#195702=CARTESIAN_POINT('Ctrl Pts',(164.356294170633,-0.501067617717217,
123.819579153818));
#195703=CARTESIAN_POINT('Ctrl Pts',(164.07784654682,-6.1473337513746,127.450478001396));
#195704=CARTESIAN_POINT('Ctrl Pts',(163.799398923007,-6.14450048146789,
134.163431126959));
#195705=CARTESIAN_POINT('Ctrl Pts',(163.520951299194,-0.495171444628521,
137.789562554107));
#195706=CARTESIAN_POINT('Ctrl Pts',(163.242503675381,5.60919595935461,134.996634647659));
#195707=CARTESIAN_POINT('Ctrl Pts',(162.964056051569,6.55898630114736,128.351211711527));
#195708=CARTESIAN_POINT('Ctrl Pts',(162.685608427755,1.48138865648,123.960112777059));
#195709=CARTESIAN_POINT('Ctrl Pts',(162.407160803943,-4.95753279363329,
125.85854324792));
#195710=CARTESIAN_POINT('Ctrl Pts',(162.12871318013,-6.84072379533872,132.301938264875));
#195711=CARTESIAN_POINT('Ctrl Pts',(161.850265556317,-2.4376238170639,137.369132584688));
#195712=CARTESIAN_POINT('Ctrl Pts',(161.571817932504,4.20553336454888,136.403622173655));
#195713=CARTESIAN_POINT('Ctrl Pts',(161.293370308691,6.98401083586784,130.292663931709));
#195714=CARTESIAN_POINT('Ctrl Pts',(161.014922684878,3.34452353692138,124.651929946293));
#195715=CARTESIAN_POINT('Ctrl Pts',(160.736475061065,-3.36841750339773,
124.664979184829));
#195716=CARTESIAN_POINT('Ctrl Pts',(160.458027437253,-6.98594741443756,
130.319820034592));
#195717=CARTESIAN_POINT('Ctrl Pts',(160.179579813439,-4.18373293411359,
136.419930008985));
#195718=CARTESIAN_POINT('Ctrl Pts',(159.901132189627,2.46312772594441,137.35960604848));
#195719=CARTESIAN_POINT('Ctrl Pts',(159.622684565814,6.84649433633851,132.275331778507));
#195720=CARTESIAN_POINT('Ctrl Pts',(159.344236942001,4.93826712148011,125.839306872565));
#195721=CARTESIAN_POINT('Ctrl Pts',(159.065789318188,-1.50798633025781,
123.965923801919));
#195722=CARTESIAN_POINT('Ctrl Pts',(158.787341694375,-6.56847401371661,
128.376730088641));
#195723=CARTESIAN_POINT('Ctrl Pts',(158.508894070562,-5.59285496636459,
135.018410235101));
#195724=CARTESIAN_POINT('Ctrl Pts',(158.230446446749,0.522324568921774,
137.787584650814));
#195725=CARTESIAN_POINT('Ctrl Pts',(157.951998822937,6.15751334234277,134.139517329431));
#195726=CARTESIAN_POINT('Ctrl Pts',(157.673551199123,6.13424816540071,127.426603921307));
#195727=CARTESIAN_POINT('Ctrl Pts',(157.395103575311,0.473908599138188,
123.817683904457));
#195728=CARTESIAN_POINT('Ctrl Pts',(157.116655951498,-5.62192981801017,
126.62917846882));
#195729=CARTESIAN_POINT('Ctrl Pts',(156.838208327685,-6.55148937894732,
133.277461458893));
#195730=CARTESIAN_POINT('Ctrl Pts',(156.559760703872,-1.46055025868114,
137.653085593479));
#195731=CARTESIAN_POINT('Ctrl Pts',(156.281313080059,4.97256319746619,135.735066054016));
#195732=CARTESIAN_POINT('Ctrl Pts',(156.002865456246,6.83613399835919,129.285969096806));
#195733=CARTESIAN_POINT('Ctrl Pts',(155.724417832433,2.4176316184721,124.232199769625));
#195734=CARTESIAN_POINT('Ctrl Pts',(155.44597020862,-4.2225561109203,125.217925193794));
#195735=CARTESIAN_POINT('Ctrl Pts',(155.167522584808,-6.98242105771092,
131.337311859867));
#195736=CARTESIAN_POINT('Ctrl Pts',(154.889074960995,-3.3257821626974,136.96694237038));
#195737=CARTESIAN_POINT('Ctrl Pts',(154.610627337182,3.38708806634394,136.933461308912));
#195738=CARTESIAN_POINT('Ctrl Pts',(154.332179713369,6.98738983086623,131.267636135312));
#195739=CARTESIAN_POINT('Ctrl Pts',(154.053732089556,4.1666216937926,125.17608339317));
#195740=CARTESIAN_POINT('Ctrl Pts',(153.775284465743,-2.48306822909056,
124.256642463619));
#195741=CARTESIAN_POINT('Ctrl Pts',(153.49683684193,-6.85093975406627,129.354234643731));
#195742=CARTESIAN_POINT('Ctrl Pts',(153.218389218117,-4.92313233206838,
135.784421751204));
#195743=CARTESIAN_POINT('Ctrl Pts',(152.939941594304,1.52879319471521,137.638175966376));
#195744=CARTESIAN_POINT('Ctrl Pts',(152.661493970491,6.57583246125511,133.21198772643));
#195745=CARTESIAN_POINT('Ctrl Pts',(152.383046346679,5.58000294317656,126.573307792561));
#195746=CARTESIAN_POINT('Ctrl Pts',(152.104598722866,-0.543576681382813,
123.822758706449));
#195747=CARTESIAN_POINT('Ctrl Pts',(151.826151099053,-6.16763589094857,
127.487960706439));
#195748=CARTESIAN_POINT('Ctrl Pts',(151.54770347524,-6.12393902249645,134.200772209611));
#195749=CARTESIAN_POINT('Ctrl Pts',(151.269255851427,-0.452641363423277,
137.792447383624));
#195750=CARTESIAN_POINT('Ctrl Pts',(150.990808227614,5.63461159587598,134.962412206646));
#195751=CARTESIAN_POINT('Ctrl Pts',(150.712360603801,6.54393176464461,128.311330751416));
#195752=CARTESIAN_POINT('Ctrl Pts',(150.433912979988,1.4396983305442,123.951221951899));
#195753=CARTESIAN_POINT('Ctrl Pts',(150.155465356176,-4.98754753615285,
125.888812791691));
#195754=CARTESIAN_POINT('Ctrl Pts',(149.877017732362,-6.83148087236823,
132.343551945603));
#195755=CARTESIAN_POINT('Ctrl Pts',(149.59857010855,-2.39761702327129,137.383849462723));
#195756=CARTESIAN_POINT('Ctrl Pts',(149.320122484737,4.23953974010866,136.377918157044));
#195757=CARTESIAN_POINT('Ctrl Pts',(149.041674860924,6.98076659535922,130.250159756006));
#195758=CARTESIAN_POINT('Ctrl Pts',(148.763227237111,3.30700997888175,124.631684872525));
#195759=CARTESIAN_POINT('Ctrl Pts',(148.484779613298,-3.40572725176907,
124.685597446761));
#195760=CARTESIAN_POINT('Ctrl Pts',(148.206331989485,-6.98876751706998,
130.362354456768));
#195761=CARTESIAN_POINT('Ctrl Pts',(147.927884365672,-4.14947185445744,
136.445293535346));
#195762=CARTESIAN_POINT('Ctrl Pts',(147.649436741859,2.50298572943186,137.344490837378));
#195763=CARTESIAN_POINT('Ctrl Pts',(147.370989118047,6.85532170562399,132.233627970525));
#195764=CARTESIAN_POINT('Ctrl Pts',(147.092541494233,4.90795193543132,125.809338229895));
#195765=CARTESIAN_POINT('Ctrl Pts',(146.814093870421,-1.54958589664124,
123.975230043125));
#195766=CARTESIAN_POINT('Ctrl Pts',(146.535646246608,-6.58312999118006,
128.41675923269));
#195767=CARTESIAN_POINT('Ctrl Pts',(146.257198622795,-5.56709922760349,
135.052377454143));
#195768=CARTESIAN_POINT('Ctrl Pts',(145.978750998982,0.564823758223794,
137.784275729942));
#195769=CARTESIAN_POINT('Ctrl Pts',(145.700303375169,6.17770130341801,134.101973005276));
#195770=CARTESIAN_POINT('Ctrl Pts',(145.421855751356,6.11357314825767,127.389325593625));
#195771=CARTESIAN_POINT('Ctrl Pts',(145.143408127543,0.431369934500661,
123.81492853524));
#195772=CARTESIAN_POINT('Ctrl Pts',(144.864960503731,-5.64724117546963,
126.663478107772));
#195773=CARTESIAN_POINT('Ctrl Pts',(144.586512879918,-6.53631352825206,
133.317296413447));
#195774=CARTESIAN_POINT('Ctrl Pts',(144.308065256105,-1.41883306523854,
137.661849486446));
#195775=CARTESIAN_POINT('Ctrl Pts',(144.029617632292,5.00248567088053,135.704705295899));
#195776=CARTESIAN_POINT('Ctrl Pts',(143.751170008479,6.82676446047164,129.244383741109));
#195777=CARTESIAN_POINT('Ctrl Pts',(143.472722384666,2.37758021687388,124.217604726676));
#195778=CARTESIAN_POINT('Ctrl Pts',(143.194274760853,-4.25648409478009,
125.243732595056));
#195779=CARTESIAN_POINT('Ctrl Pts',(142.91582713704,-6.97904746413934,131.379805964341));
#195780=CARTESIAN_POINT('Ctrl Pts',(142.637379513228,-3.28820715937746,
136.987073172008));
#195781=CARTESIAN_POINT('Ctrl Pts',(142.358931889414,3.42433488700229,136.912729584442));
#195782=CARTESIAN_POINT('Ctrl Pts',(142.080484265602,6.99008046028611,131.225093326731));
#195783=CARTESIAN_POINT('Ctrl Pts',(141.802036641788,4.13228357498186,125.150824263232));
#195784=CARTESIAN_POINT('Ctrl Pts',(141.523589017976,-2.52288004245522,
124.271878918761));
#195785=CARTESIAN_POINT('Ctrl Pts',(141.245141394163,-6.859640150418,129.395965126019));
#195786=CARTESIAN_POINT('Ctrl Pts',(140.96669377035,-4.89272607219785,135.814297986063));
#195787=CARTESIAN_POINT('Ctrl Pts',(140.688246146537,1.57036424341533,137.628743153505));
#195788=CARTESIAN_POINT('Ctrl Pts',(140.409798522724,6.59036653588803,133.17191416004));
#195789=CARTESIAN_POINT('Ctrl Pts',(140.131350898911,5.55414393918375,126.539419122461));
#195790=CARTESIAN_POINT('Ctrl Pts',(139.852903275098,-0.586065602614643,
123.826196964908));
#195791=CARTESIAN_POINT('Ctrl Pts',(139.574455651286,-6.18770948650656,
127.525566301902));
#195792=CARTESIAN_POINT('Ctrl Pts',(139.296008027473,-6.10315063871238,
134.237987436982));
#195793=CARTESIAN_POINT('Ctrl Pts',(139.01756040366,-0.410094509425858,
137.795073267016));
#195794=CARTESIAN_POINT('Ctrl Pts',(138.739112779847,5.65981843979252,134.928035687503));
#195795=CARTESIAN_POINT('Ctrl Pts',(138.460665156034,6.52863474034383,128.271542171445));
#195796=CARTESIAN_POINT('Ctrl Pts',(138.182217532221,1.39795465605713,123.942585072312));
#195797=CARTESIAN_POINT('Ctrl Pts',(137.903769908408,-5.01737746326431,
125.919264482896));
#195798=CARTESIAN_POINT('Ctrl Pts',(137.625322284595,-6.82198480636163,
132.385108591028));
#195799=CARTESIAN_POINT('Ctrl Pts',(137.346874660782,-2.35752138489827,
137.39832253538));
#195800=CARTESIAN_POINT('Ctrl Pts',(137.06842703697,4.27338901796432,136.352007610208));
#195801=CARTESIAN_POINT('Ctrl Pts',(136.789979413157,6.9772636799772,130.20767611642));
#195802=CARTESIAN_POINT('Ctrl Pts',(136.511531789344,3.26937387837121,124.611668529527));
#195803=CARTESIAN_POINT('Ctrl Pts',(136.233084165531,-3.44291079966457,
124.706442441713));
#195804=CARTESIAN_POINT('Ctrl Pts',(135.954636541718,-6.99132864835187,
130.404905257644));
#195805=CARTESIAN_POINT('Ctrl Pts',(135.676188917905,-4.1150570145959,136.470448034864));
#195806=CARTESIAN_POINT('Ctrl Pts',(135.397741294092,2.54275098386259,137.329133279345));
#195807=CARTESIAN_POINT('Ctrl Pts',(135.11929367028,6.8638950484427,132.191871200516));
#195808=CARTESIAN_POINT('Ctrl Pts',(134.840846046466,4.87745488341857,125.779554679616));
#195809=CARTESIAN_POINT('Ctrl Pts',(134.562398422654,-1.59112804254939,
123.984789340275));
#195810=CARTESIAN_POINT('Ctrl Pts',(134.283950798841,-6.59754202834077,
128.456876850186));
#195811=CARTESIAN_POINT('Ctrl Pts',(134.005503175028,-5.54113719793324,
135.086187261361));
#195812=CARTESIAN_POINT('Ctrl Pts',(133.727055551215,0.607302017773813,
137.780708165749));
#195813=CARTESIAN_POINT('Ctrl Pts',(133.448607927402,6.19766034749954,134.064306486881));
#195814=CARTESIAN_POINT('Ctrl Pts',(133.170160303589,6.09267159041341,127.352173811322));
#195815=CARTESIAN_POINT('Ctrl Pts',(132.891712679776,0.388815285291658,
123.812432161999));
#195816=CARTESIAN_POINT('Ctrl Pts',(132.613265055963,-5.67234327233058,
126.697931188648));
#195817=CARTESIAN_POINT('Ctrl Pts',(132.334817432151,-6.52089547205522,
133.357038250242));
#195818=CARTESIAN_POINT('Ctrl Pts',(132.056369808337,-1.37706329641493,
137.670359272641));
#195819=CARTESIAN_POINT('Ctrl Pts',(131.777922184525,5.0322227753486,135.674162953708));
#195820=CARTESIAN_POINT('Ctrl Pts',(131.499474560712,6.81714195431646,129.20285619093));
#195821=CARTESIAN_POINT('Ctrl Pts',(131.221026936899,2.33744071316646,124.203253758389));
#195822=CARTESIAN_POINT('Ctrl Pts',(130.942579313086,-4.29025435305649,
125.269746047434));
#195823=CARTESIAN_POINT('Ctrl Pts',(130.664131689273,-6.97541525939744,
131.422278745477));
#195824=CARTESIAN_POINT('Ctrl Pts',(130.38568406546,-3.25051031033198,137.006974870947));
#195825=CARTESIAN_POINT('Ctrl Pts',(130.107236441647,3.46145481767177,136.891771512113));
#195826=CARTESIAN_POINT('Ctrl Pts',(129.828788817834,6.99251206970404,131.182534927744));
#195827=CARTESIAN_POINT('Ctrl Pts',(129.550341194022,4.09779233288376,125.125774627163));
#195828=CARTESIAN_POINT('Ctrl Pts',(129.271893570209,-2.5625983695722,124.287357437414));
#195829=CARTESIAN_POINT('Ctrl Pts',(128.993445946396,-6.86808636028122,
129.43774779692));
#195830=CARTESIAN_POINT('Ctrl Pts',(128.714998322583,-4.86213851056362,
135.84398857585));
#195831=CARTESIAN_POINT('Ctrl Pts',(128.43655069877,1.61187710169066,137.61905746063));
#195832=CARTESIAN_POINT('Ctrl Pts',(128.158103074957,6.60465640206541,133.131752863082));
#195833=CARTESIAN_POINT('Ctrl Pts',(127.879655451144,5.52807912434469,126.505688491336));
#195834=CARTESIAN_POINT('Ctrl Pts',(127.601207827331,-0.628532806970051,
123.829893801787));
#195835=CARTESIAN_POINT('Ctrl Pts',(127.322760203518,-6.20755379421381,
127.563293394292));
#195836=CARTESIAN_POINT('Ctrl Pts',(127.044312579706,-6.08213610043705,
134.275075430049));
#195837=CARTESIAN_POINT('Ctrl Pts',(126.765864955893,-0.367532459225645,
137.797440106979));
#195838=CARTESIAN_POINT('Ctrl Pts',(126.48741733208,5.68481555705546,134.893506364063));
#195839=CARTESIAN_POINT('Ctrl Pts',(126.208969708267,6.51309579508176,128.231847445991));
#195840=CARTESIAN_POINT('Ctrl Pts',(125.930522084454,1.35615917984635,123.934202458341));
#195841=CARTESIAN_POINT('Ctrl Pts',(125.652074460641,-5.04702146960864,
125.949897193134));
#195842=CARTESIAN_POINT('Ctrl Pts',(125.373626836828,-6.81223594919939,
132.426606661257));
#195843=CARTESIAN_POINT('Ctrl Pts',(125.095179213015,-2.3173383877032,137.412551266352));
#195844=CARTESIAN_POINT('Ctrl Pts',(124.816731589202,4.3070799438184,136.325891493273));
#195845=CARTESIAN_POINT('Ctrl Pts',(124.538283965389,6.97350221952356,130.165214587198));
#195846=CARTESIAN_POINT('Ctrl Pts',(124.259836341577,3.2316166300094,124.591881659011));
#195847=CARTESIAN_POINT('Ctrl Pts',(123.981388717764,-3.47996676923432,
124.727513397266));
#195848=CARTESIAN_POINT('Ctrl Pts',(123.702941093951,-6.99363071337966,
130.447470860486));
#195849=CARTESIAN_POINT('Ctrl Pts',(123.424493470138,-4.08048968978323,
136.495392575427));
#195850=CARTESIAN_POINT('Ctrl Pts',(123.146045846325,2.58242201572056,137.313533943462));
#195851=CARTESIAN_POINT('Ctrl Pts',(122.867598222512,6.87221404710605,132.150063015792));
#195852=CARTESIAN_POINT('Ctrl Pts',(122.589150598699,4.84677709552158,125.749957325369));
#195853=CARTESIAN_POINT('Ctrl Pts',(122.310702974886,-1.63261122862275,
123.994601339147));
#195854=CARTESIAN_POINT('Ctrl Pts',(122.032255351073,-6.6117095911554,128.497081454556));
#195855=CARTESIAN_POINT('Ctrl Pts',(121.753807727261,-5.51496983938628,
135.119838403918));
#195856=CARTESIAN_POINT('Ctrl Pts',(121.475360103447,0.649757773524084,
137.776882090432));
#195857=CARTESIAN_POINT('Ctrl Pts',(121.196912479635,6.21738973499768,134.026519169992));
#195858=CARTESIAN_POINT('Ctrl Pts',(120.918464855822,6.07154426638285,127.315149951069));
#195859=CARTESIAN_POINT('Ctrl Pts',(120.640017232009,0.346246228389124,
123.810194877238));
#195860=CARTESIAN_POINT('Ctrl Pts',(120.361569608196,-5.69723517842559,
126.732536434776));
#195861=CARTESIAN_POINT('Ctrl Pts',(120.083121984383,-6.50523578167861,
133.396685496627));
#195862=CARTESIAN_POINT('Ctrl Pts',(119.80467436057,-1.3352425000044,137.678614636731));
#195863=CARTESIAN_POINT('Ctrl Pts',(119.526226736757,5.06177340895125,135.6434401592));
#195864=CARTESIAN_POINT('Ctrl Pts',(119.247779112945,6.8072668364591,129.161387985085));
#195865=CARTESIAN_POINT('Ctrl Pts',(118.969331489131,2.29721459473369,124.189147396544));
#195866=CARTESIAN_POINT('Ctrl Pts',(118.690883865319,-4.32386563438011,
125.29596458699));
#195867=CARTESIAN_POINT('Ctrl Pts',(118.412436241506,-6.97152457807781,
131.464728629428));
#195868=CARTESIAN_POINT('Ctrl Pts',(118.133988617693,-3.21269301243169,
137.026646729736));
#195869=CARTESIAN_POINT('Ctrl Pts',(117.85554099388,3.49844648286018,136.870587868534));
#195870=CARTESIAN_POINT('Ctrl Pts',(117.577093370067,6.99468456901571,131.139962515369));
#195871=CARTESIAN_POINT('Ctrl Pts',(117.298645746254,4.06314924558364,125.100935413187));
#195872=CARTESIAN_POINT('Ctrl Pts',(117.020198122441,-2.60222173866402,
124.303077446017));
#195873=CARTESIAN_POINT('Ctrl Pts',(116.741750498628,-6.8762780706787,129.479581108162));
#195874=CARTESIAN_POINT('Ctrl Pts',(116.463302874816,-4.83137078059878,
135.873492420371));
#195875=CARTESIAN_POINT('Ctrl Pts',(116.184855251003,1.65333023126747,137.609119246659));
#195876=CARTESIAN_POINT('Ctrl Pts',(115.90640762719,6.61870153027093,133.09150532375));
#195877=CARTESIAN_POINT('Ctrl Pts',(115.627960003377,5.5018094645007,126.472117149089));
#195878=CARTESIAN_POINT('Ctrl Pts',(115.349512379564,-0.670976720811003,
123.833849080098));
#195879=CARTESIAN_POINT('Ctrl Pts',(115.071064755751,-6.22716807873245,
127.601140585621));
#195880=CARTESIAN_POINT('Ctrl Pts',(114.792617131938,-6.06089618637186,
134.312034814502));
#195881=CARTESIAN_POINT('Ctrl Pts',(114.514169508125,-0.324956789974863,
137.79954781581));
#195882=CARTESIAN_POINT('Ctrl Pts',(114.235721884312,5.70960202138734,134.858825515823));
#195883=CARTESIAN_POINT('Ctrl Pts',(113.957274260499,6.4973155046598,128.192248045959));
#195884=CARTESIAN_POINT('Ctrl Pts',(113.678826636687,1.31431345065849,123.926074420608));
#195885=CARTESIAN_POINT('Ctrl Pts',(113.400379012874,-5.07647845671644,
125.980709787299));
#195886=CARTESIAN_POINT('Ctrl Pts',(113.121931389061,-6.80223466212876,
132.468044618562));
#195887=CARTESIAN_POINT('Ctrl Pts',(112.843483765248,-2.27706952068197,
137.42653512839));
#195888=CARTESIAN_POINT('Ctrl Pts',(112.565036141435,4.34061126924124,136.299570773982));
#195889=CARTESIAN_POINT('Ctrl Pts',(112.286588517622,6.96948235338073,130.122776741767));
#195890=CARTESIAN_POINT('Ctrl Pts',(112.008140893809,3.1937396329048,124.572324994188));
#195891=CARTESIAN_POINT('Ctrl Pts',(111.729693269996,-3.51689378735575,
124.748809532627));
#195892=CARTESIAN_POINT('Ctrl Pts',(111.451245646184,-6.99567362684944,
130.490049688009));
#195893=CARTESIAN_POINT('Ctrl Pts',(111.172798022371,-4.0457711609245,136.52012623271));
#195894=CARTESIAN_POINT('Ctrl Pts',(110.894350398558,2.62199735498092,137.297693407768));
#195895=CARTESIAN_POINT('Ctrl Pts',(110.615902774745,6.88027839335069,132.108204965571));
#195896=CARTESIAN_POINT('Ctrl Pts',(110.337455150932,4.81591970851693,125.720547263895));
#195897=CARTESIAN_POINT('Ctrl Pts',(110.059007527119,-1.67403391768677,
124.004665676154));
#195898=CARTESIAN_POINT('Ctrl Pts',(109.780559903306,-6.62563215463966,
128.537371556004));
#195899=CARTESIAN_POINT('Ctrl Pts',(109.502112279493,-5.48859812160383,
135.153329634858));
#195900=CARTESIAN_POINT('Ctrl Pts',(109.22366465568,0.692189452261082,137.772797645767));
#195901=CARTESIAN_POINT('Ctrl Pts',(108.945217031867,6.23688873483282,133.988612454835));
#195902=CARTESIAN_POINT('Ctrl Pts',(108.666769408055,6.05019195904657,127.278255384801));
#195903=CARTESIAN_POINT('Ctrl Pts',(108.388321784241,0.303664341205276,
123.808216763862));
#195904=CARTESIAN_POINT('Ctrl Pts',(108.109874160429,-5.72191597137591,
126.767292563848));
#195905=CARTESIAN_POINT('Ctrl Pts',(107.831426536616,-6.48933503739778,
133.436236683461));
#195906=CARTESIAN_POINT('Ctrl Pts',(107.552978912803,-1.29337222569216,
137.68661527281));
#195907=CARTESIAN_POINT('Ctrl Pts',(107.27453128899,5.09113647667873,135.612538050821));
#195908=CARTESIAN_POINT('Ctrl Pts',(106.996083665177,6.79713947282576,129.119980660195));
#195909=CARTESIAN_POINT('Ctrl Pts',(106.717636041364,2.25690335216928,124.175286163858));
#195910=CARTESIAN_POINT('Ctrl Pts',(106.439188417551,-4.35731669327239,
125.322387242187));
#195911=CARTESIAN_POINT('Ctrl Pts',(106.160740793739,-6.96737556435125,
131.5071540432));
#195912=CARTESIAN_POINT('Ctrl Pts',(105.882293169926,-3.17475666701035,
137.046088019424));
#195913=CARTESIAN_POINT('Ctrl Pts',(105.603845546113,3.53530851182771,136.849179438675));
#195914=CARTESIAN_POINT('Ctrl Pts',(105.3253979223,6.99659787771835,131.097377667143));
#195915=CARTESIAN_POINT('Ctrl Pts',(105.046950298487,4.02835559679407,125.076307541727));
#195916=CARTESIAN_POINT('Ctrl Pts',(104.768502674674,-2.64174868147234,
124.319038362058));
#195917=CARTESIAN_POINT('Ctrl Pts',(104.490055050861,-6.88421497806359,
129.521463509594));
#195918=CARTESIAN_POINT('Ctrl Pts',(104.211607427049,-4.80042402241278,
135.902808426348));
#195919=CARTESIAN_POINT('Ctrl Pts',(103.933159803235,1.69472209608453,137.598928879852));
#195920=CARTESIAN_POINT('Ctrl Pts',(103.654712179423,6.63250140005722,133.051173033428));
#195921=CARTESIAN_POINT('Ctrl Pts',(103.37626455561,5.47533593308374,126.438706339714));
#195922=CARTESIAN_POINT('Ctrl Pts',(103.097816931797,-0.713395771362793,
123.838062653278));
#195923=CARTESIAN_POINT('Ctrl Pts',(102.819369307984,-6.24655161324796,
127.639106473447));
#195924=CARTESIAN_POINT('Ctrl Pts',(102.540921684171,-6.03943168356949,
134.348864220799));
#195925=CARTESIAN_POINT('Ctrl Pts',(102.262474060358,-0.282369079330704,
137.801396315408));
#195926=CARTESIAN_POINT('Ctrl Pts',(101.984026436545,5.73417691431645,134.823994427897));
#195927=CARTESIAN_POINT('Ctrl Pts',(101.705578812732,6.48129445382252,128.15274543872));
#195928=CARTESIAN_POINT('Ctrl Pts',(101.427131188919,1.27241901910234,123.9182012603));
#195929=CARTESIAN_POINT('Ctrl Pts',(101.148683565106,-5.1057473330482,126.01170112362));
#195930=CARTESIAN_POINT('Ctrl Pts',(100.870235941294,-6.7919813157512,132.509420927444));
#195931=CARTESIAN_POINT('Ctrl Pts',(100.591788317481,-2.23671627601227,
137.440273603317));
#195932=CARTESIAN_POINT('Ctrl Pts',(100.313340693668,4.37398175171709,136.273046427655));
#195933=CARTESIAN_POINT('Ctrl Pts',(100.034893069855,6.96520423050629,130.080364152676));
#195934=CARTESIAN_POINT('Ctrl Pts',(99.7564454460421,3.15574429060373,124.552999259737));
#195935=CARTESIAN_POINT('Ctrl Pts',(99.4779978222292,-3.55369048568456,
124.770330058661));
#195936=CARTESIAN_POINT('Ctrl Pts',(99.1995501984162,-6.99745731306031,
130.532640162439));
#195937=CARTESIAN_POINT('Ctrl Pts',(98.9211025746034,-4.01090271452764,
136.544648090195));
#195938=CARTESIAN_POINT('Ctrl Pts',(98.6426549507905,2.66147553516503,137.281612259238));
#195939=CARTESIAN_POINT('Ctrl Pts',(98.3642073269776,6.88808778834931,132.066298600918));
#195940=CARTESIAN_POINT('Ctrl Pts',(98.0857597031646,4.78488386583629,125.691325584995));
#195941=CARTESIAN_POINT('Ctrl Pts',(97.8073120793519,-1.71539457480834,
124.014981978356));
#195942=CARTESIAN_POINT('Ctrl Pts',(97.5288644555388,-6.63930920288774,
128.577745661565));
#195943=CARTESIAN_POINT('Ctrl Pts',(97.2504168317261,-5.46202302179963,
135.186659713151));
#195944=CARTESIAN_POINT('Ctrl Pts',(96.9719692079131,0.734595481663425,
137.768454983106));
#195945=CARTESIAN_POINT('Ctrl Pts',(96.6935215841003,6.25615662446226,133.950587746053));
#195946=CARTESIAN_POINT('Ctrl Pts',(96.4150739602873,6.0286154596223,127.24149147966));
#195947=CARTESIAN_POINT('Ctrl Pts',(96.1366263364746,0.26107120162757,123.806497895168));
#195948=CARTESIAN_POINT('Ctrl Pts',(95.8581787126614,-5.74638473662552,
126.80219828796));
#195949=CARTESIAN_POINT('Ctrl Pts',(95.5797310888487,-6.47319382842077,
133.47569034516));
#195950=CARTESIAN_POINT('Ctrl Pts',(95.3012834650358,-1.25145402499642,
137.694360884412));
#195951=CARTESIAN_POINT('Ctrl Pts',(95.0228358412229,5.12031089047184,135.581457773658));
#195952=CARTESIAN_POINT('Ctrl Pts',(94.7443882174101,6.78676023868958,129.078635750625));
#195953=CARTESIAN_POINT('Ctrl Pts',(94.465940593597,2.21650847922131,124.161670573963));
#195954=CARTESIAN_POINT('Ctrl Pts',(94.1874929697842,-4.39060629019222,
125.349013033923));
#195955=CARTESIAN_POINT('Ctrl Pts',(93.9090453459715,-6.96296837196094,
131.549553414704));
#195956=CARTESIAN_POINT('Ctrl Pts',(93.6305977221583,-3.13670267981308,
137.065298019608));
#195957=CARTESIAN_POINT('Ctrl Pts',(93.3521500983456,3.5720395386382,136.82754701583));
#195958=CARTESIAN_POINT('Ctrl Pts',(93.0737024745325,6.99825192491364,131.054781961061));
#195959=CARTESIAN_POINT('Ctrl Pts',(92.7952548507199,3.99341267580637,125.051891925383));
#195960=CARTESIAN_POINT('Ctrl Pts',(92.5168072269068,-2.68117773331193,
124.335239594101));
#195961=CARTESIAN_POINT('Ctrl Pts',(92.238359603094,-6.89189678833074,129.563393449252));
#195962=CARTESIAN_POINT('Ctrl Pts',(91.959911979281,-4.7692993827493,135.931935507467));
#195963=CARTESIAN_POINT('Ctrl Pts',(91.6814643554683,1.73605116235111,137.588486737821));
#195964=CARTESIAN_POINT('Ctrl Pts',(91.4030167316553,6.6460555000649,133.010757486647));
#195965=CARTESIAN_POINT('Ctrl Pts',(91.1245691078424,5.44865951108031,126.405457301267));
#195966=CARTESIAN_POINT('Ctrl Pts',(90.8461214840295,-0.755788386771977,
123.84253436519));
#195967=CARTESIAN_POINT('Ctrl Pts',(90.5676738602166,-6.26570367949625,
127.677189650927));
#195968=CARTESIAN_POINT('Ctrl Pts',(90.2892262364038,-6.01774338740505,
134.38556228421));
#195969=CARTESIAN_POINT('Ctrl Pts',(90.0107786125907,-0.239770905396614,
137.802985537273));
#195970=CARTESIAN_POINT('Ctrl Pts',(89.7323309887781,5.75853932521132,134.78901439096));
#195971=CARTESIAN_POINT('Ctrl Pts',(89.453883364965,6.46503323623579,128.113341088056));
#195972=CARTESIAN_POINT('Ctrl Pts',(89.1754357411521,1.23047743759138,123.910583269158));
#195973=CARTESIAN_POINT('Ctrl Pts',(88.8969881173393,-5.13482701403487,
126.042870053701));
#195974=CARTESIAN_POINT('Ctrl Pts',(88.6185404935264,-6.78147629000823,
132.550734054689));
#195975=CARTESIAN_POINT('Ctrl Pts',(88.3400928697134,-2.19628014899849,
137.453766182047));
#195976=CARTESIAN_POINT('Ctrl Pts',(88.0616452459006,4.4071901546906,136.246319437167));
#195977=CARTESIAN_POINT('Ctrl Pts',(87.7831976220877,6.96066800942769,130.037978391542));
#195978=CARTESIAN_POINT('Ctrl Pts',(87.5047499982748,3.1176320110373,124.533905171779));
#195979=CARTESIAN_POINT('Ctrl Pts',(87.2263023744621,-3.59035550070555,
124.792074177916));
#195980=CARTESIAN_POINT('Ctrl Pts',(86.9478547506488,-6.99898170591706,
130.57524070557));
#195981=CARTESIAN_POINT('Ctrl Pts',(86.6694071268362,-3.97588564265574,
136.568957239218));
#195982=CARTESIAN_POINT('Ctrl Pts',(86.3909595030232,2.70085509339449,137.265291093768));
#195983=CARTESIAN_POINT('Ctrl Pts',(86.1125118792103,6.89564194272181,132.024345474689));
#195984=CARTESIAN_POINT('Ctrl Pts',(85.8340642553976,4.75367071752436,125.662293371487));
#195985=CARTESIAN_POINT('Ctrl Pts',(85.5556166315845,-1.75669166735309,
124.025549863481));
#195986=CARTESIAN_POINT('Ctrl Pts',(85.2771690077717,-6.65274022909182,
128.618202275162));
#195987=CARTESIAN_POINT('Ctrl Pts',(84.9987213839588,-5.4352455247236,135.21982740374));
#195988=CARTESIAN_POINT('Ctrl Pts',(84.7202737601459,0.776974290360158,
137.763854263368));
#195989=CARTESIAN_POINT('Ctrl Pts',(84.4418261363329,6.27519268990729,133.912446452669));
#195990=CARTESIAN_POINT('Ctrl Pts',(84.1633785125202,6.00681556763514,127.204859597945));
#195991=CARTESIAN_POINT('Ctrl Pts',(83.8849308887072,0.218468387960617,
123.805038334852));
#195992=CARTESIAN_POINT('Ctrl Pts',(83.6064832648944,-5.77064056747553,
126.837252313669));
#195993=CARTESIAN_POINT('Ctrl Pts',(83.3280356410814,-6.45681275286598,
133.515045019753));
#195994=CARTESIAN_POINT('Ctrl Pts',(83.0495880172686,-1.20948945121144,
137.701851184522));
#195995=CARTESIAN_POINT('Ctrl Pts',(82.7711403934555,5.14929556926191,135.550200479404));
#195996=CARTESIAN_POINT('Ctrl Pts',(82.4926927696429,6.77612951865689,129.037354788424));
#195997=CARTESIAN_POINT('Ctrl Pts',(82.2142451458298,2.17603147273656,124.148301131391));
#195998=CARTESIAN_POINT('Ctrl Pts',(81.9357975220171,-4.42373319158141,
125.375840975569));
#195999=CARTESIAN_POINT('Ctrl Pts',(81.6573498982041,-6.95830316421689,
131.591925172815));
#196000=CARTESIAN_POINT('Ctrl Pts',(81.3789022743912,-3.09853246094448,
137.084276018453));
#196001=CARTESIAN_POINT('Ctrl Pts',(81.1004546505783,3.60863820220999,136.805691401599));
#196002=CARTESIAN_POINT('Ctrl Pts',(80.8220070267654,6.99964664931016,131.012176975526));
#196003=CARTESIAN_POINT('Ctrl Pts',(80.5435594029525,3.95832177744353,125.02768946888));
#196004=CARTESIAN_POINT('Ctrl Pts',(80.2651117791397,-2.72050743312451,
124.351680541802));
#196005=CARTESIAN_POINT('Ctrl Pts',(79.9866641553267,-6.89932321682792,
129.605369373404));
#196006=CARTESIAN_POINT('Ctrl Pts',(79.7082165315139,-4.73799801494326,
135.960872584412));
#196007=CARTESIAN_POINT('Ctrl Pts',(79.4297689077009,1.77731589860328,137.577793207502));
#196008=CARTESIAN_POINT('Ctrl Pts',(79.1513212838881,6.65936332804202,132.970260181018));
#196009=CARTESIAN_POINT('Ctrl Pts',(78.8728736600752,5.42178118699497,126.372371265798));
#196010=CARTESIAN_POINT('Ctrl Pts',(78.5944260362623,-0.798152996164653,
123.847264050135));
#196011=CARTESIAN_POINT('Ctrl Pts',(78.3159784124494,-6.28462356779051,
127.715388706879));
#196012=CARTESIAN_POINT('Ctrl Pts',(78.0375307886365,-5.99583210154638,
134.422127644877));
#196013=CARTESIAN_POINT('Ctrl Pts',(77.7590831648237,-0.197163846663491,
137.804315422519));
#196014=CARTESIAN_POINT('Ctrl Pts',(77.4806355410107,5.78268835131386,134.753886701214));
#196015=CARTESIAN_POINT('Ctrl Pts',(77.2021879171979,6.44853245446487,128.07403645411));
#196016=CARTESIAN_POINT('Ctrl Pts',(76.9237402933849,1.18849026028645,123.903220729472));
#196017=CARTESIAN_POINT('Ctrl Pts',(76.6452926695721,-5.16371642211823,
126.074215422566));
#196018=CARTESIAN_POINT('Ctrl Pts',(76.3668450457591,-6.77071997416741,
132.591982469425));
#196019=CARTESIAN_POINT('Ctrl Pts',(76.0883974219463,-2.15576263801617,
137.467012364608));
#196020=CARTESIAN_POINT('Ctrl Pts',(75.8099497981334,4.44023524761227,136.219390792892));
#196021=CARTESIAN_POINT('Ctrl Pts',(75.5315021743204,6.95587385823614,129.995621028982));
#196022=CARTESIAN_POINT('Ctrl Pts',(75.2530545505077,3.0794042064702,124.515043437855));
#196023=CARTESIAN_POINT('Ctrl Pts',(74.9746069266946,-3.62688747378295,
124.814041084656));
#196024=CARTESIAN_POINT('Ctrl Pts',(74.6961593028819,-7.0002467489329,130.617849738824));
#196025=CARTESIAN_POINT('Ctrl Pts',(74.4177116790688,-3.94072124287924,
136.593052778991));
#196026=CARTESIAN_POINT('Ctrl Pts',(74.1392640552561,2.74013457044532,137.248730516143));
#196027=CARTESIAN_POINT('Ctrl Pts',(73.860816431443,6.90294057654623,131.982347141473));
#196028=CARTESIAN_POINT('Ctrl Pts',(73.5823688076304,4.72228142019582,125.633451699173));
#196029=CARTESIAN_POINT('Ctrl Pts',(73.3039211838172,-1.79792366504193,
124.036368939932));
#196030=CARTESIAN_POINT('Ctrl Pts',(73.0254735600045,-6.66592473556012,
128.658739897661));
#196031=CARTESIAN_POINT('Ctrl Pts',(72.7470259361915,-5.40826662262595,
135.252831477583));
#196032=CARTESIAN_POINT('Ctrl Pts',(72.4685783123786,0.819324307988826,
137.758995657032));
#196033=CARTESIAN_POINT('Ctrl Pts',(72.1901306885658,6.2939962257795,133.87418998802));
#196034=CARTESIAN_POINT('Ctrl Pts',(71.9116830647529,5.98479309088811,127.168361097063));
#196035=CARTESIAN_POINT('Ctrl Pts',(71.63323544094,0.17585747886725,123.803838136996));
#196036=CARTESIAN_POINT('Ctrl Pts',(71.3547878171271,-5.79468256511725,
126.872453342036));
#196037=CARTESIAN_POINT('Ctrl Pts',(71.0763401933142,-6.44019241774003,
133.554299248939));
#196038=CARTESIAN_POINT('Ctrl Pts',(70.7978925695013,-1.16748005934989,
137.709085895581));
#196039=CARTESIAN_POINT('Ctrl Pts',(70.5194449456884,5.17808943901089,135.518767326308));
#196040=CARTESIAN_POINT('Ctrl Pts',(70.2409973218756,6.76524770665308,128.996139303274));
#196041=CARTESIAN_POINT('Ctrl Pts',(69.9625496980626,2.1354738326052,124.135178331551));
#196042=CARTESIAN_POINT('Ctrl Pts',(69.6841020742497,-4.45669616991057,
125.402870073008));
#196043=CARTESIAN_POINT('Ctrl Pts',(69.4056544504369,-6.95338011399016,
131.634267747431));
#196044=CARTESIAN_POINT('Ctrl Pts',(69.1272068266238,-3.06024742481583,
137.103021312725));
#196045=CARTESIAN_POINT('Ctrl Pts',(68.8487592028112,3.64510314636624,136.783613405848));
#196046=CARTESIAN_POINT('Ctrl Pts',(68.5703115789981,7.00078199922599,130.969564289278));
#196047=CARTESIAN_POINT('Ctrl Pts',(68.2918639551854,3.92308420201135,125.003701069051));
#196048=CARTESIAN_POINT('Ctrl Pts',(68.0134163313723,-2.75973632353393,
124.368360595937));
#196049=CARTESIAN_POINT('Ctrl Pts',(67.7349687075595,-6.90649398836592,
129.647389726619));
#196050=CARTESIAN_POINT('Ctrl Pts',(67.4565210837467,-4.70652107887851,
135.98961858491));
#196051=CARTESIAN_POINT('Ctrl Pts',(67.1780734599337,1.81851477576126,137.566848685147));
#196052=CARTESIAN_POINT('Ctrl Pts',(66.8996258361208,6.67242439086218,132.929682617185));
#196053=CARTESIAN_POINT('Ctrl Pts',(66.6211782123079,5.39470195681365,126.339449459324));
#196054=CARTESIAN_POINT('Ctrl Pts',(66.3427305884951,-0.840488029704522,
123.852251532852));
#196055=CARTESIAN_POINT('Ctrl Pts',(66.0642829646821,-6.30331057704718,
127.753702225821));
#196056=CARTESIAN_POINT('Ctrl Pts',(65.7858353408693,-5.97369863792435,
134.458558947856));
#196057=CARTESIAN_POINT('Ctrl Pts',(65.5073877170563,-0.154549481951222,
137.805385921867));
#196058=CARTESIAN_POINT('Ctrl Pts',(65.2289400932435,5.80662309777304,134.718612660325));
#196059=CARTESIAN_POINT('Ctrl Pts',(64.9504924694306,6.43179271995227,128.03483299333));
#196060=CARTESIAN_POINT('Ctrl Pts',(64.6720448456177,1.14645904303803,123.896113914062));
#196061=CARTESIAN_POINT('Ctrl Pts',(64.3935972218049,-5.19241448679041,
126.1057360687));
#196062=CARTESIAN_POINT('Ctrl Pts',(64.1151495979918,-6.75971276680813,
132.633164643176));
#196063=CARTESIAN_POINT('Ctrl Pts',(63.8367019741791,-2.11516524445634,
137.480011660159));
#196064=CARTESIAN_POINT('Ctrl Pts',(63.5582543503661,4.47311580598391,136.192261492683));
#196065=CARTESIAN_POINT('Ctrl Pts',(63.2798067265533,6.95082195458075,129.953293634565));
#196066=CARTESIAN_POINT('Ctrl Pts',(63.0013591027403,3.041062293448,124.496414756892));
#196067=CARTESIAN_POINT('Ctrl Pts',(62.7229114789275,-3.66328505121137,
124.836229964889));
#196068=CARTESIAN_POINT('Ctrl Pts',(62.4444638551145,-7.00125239523119,
130.660465683307));
#196069=CARTESIAN_POINT('Ctrl Pts',(62.1660162313017,-3.90541081822766,
136.616933816649));
#196070=CARTESIAN_POINT('Ctrl Pts',(61.8875686074887,2.77931251080179,137.231931140021));
#196071=CARTESIAN_POINT('Ctrl Pts',(61.609120983676,6.909983419369,131.940305157533));
#196072=CARTESIAN_POINT('Ctrl Pts',(61.3306733598629,4.69071713699276,125.604801636791));
#196073=CARTESIAN_POINT('Ctrl Pts',(61.0522257360502,-1.83908904000824,
124.047438806804));
#196074=CARTESIAN_POINT('Ctrl Pts',(60.7737781122372,-6.67886223373588,
128.699357026925));
#196075=CARTESIAN_POINT('Ctrl Pts',(60.4953304884244,-5.38108731521968,
135.285670711703));
#196076=CARTESIAN_POINT('Ctrl Pts',(60.2168828646114,0.861643965253713,
137.753879344138));
#196077=CARTESIAN_POINT('Ctrl Pts',(59.9384352407986,6.31256653530686,133.835819769716));
#196078=CARTESIAN_POINT('Ctrl Pts',(59.6599876169856,5.96254884543232,127.131997329482));
#196079=CARTESIAN_POINT('Ctrl Pts',(59.3815399931728,0.133240053310041,
123.802897346075));
#196080=CARTESIAN_POINT('Ctrl Pts',(59.1030923693598,-5.81850983866561,
126.907800068673));
#196081=CARTESIAN_POINT('Ctrl Pts',(58.824644745547,-6.42333343891552,133.593451578138));
#196082=CARTESIAN_POINT('Ctrl Pts',(58.5461971217341,-1.12542740608588,
137.716064749505));
#196083=CARTESIAN_POINT('Ctrl Pts',(58.2677494979212,5.20669143275151,135.487159479138));
#196084=CARTESIAN_POINT('Ctrl Pts',(57.9893018741083,6.75411520590753,128.954990822428));
#196085=CARTESIAN_POINT('Ctrl Pts',(57.7108542502954,2.09483706170563,124.122302660713));
#196086=CARTESIAN_POINT('Ctrl Pts',(57.4324066264825,-4.48949400372376,
125.430099324666));
#196087=CARTESIAN_POINT('Ctrl Pts',(57.1539590026696,-6.94819940370625,
131.676579569534));
#196088=CARTESIAN_POINT('Ctrl Pts',(56.8755113788568,-3.02184899009409,
137.121533207807));
#196089=CARTESIAN_POINT('Ctrl Pts',(56.5970637550437,3.68143301988451,136.761313846687));
#196090=CARTESIAN_POINT('Ctrl Pts',(56.318616131231,7.00165793259049,130.926945481348));
#196091=CARTESIAN_POINT('Ctrl Pts',(56.040168507418,3.88770125525153,124.979927614796));
#196092=CARTESIAN_POINT('Ctrl Pts',(55.7617208836052,-2.79886295089852,
124.385279138419));
#196093=CARTESIAN_POINT('Ctrl Pts',(55.4832732597923,-6.91340883722955,
129.689452951814));
#196094=CARTESIAN_POINT('Ctrl Pts',(55.2048256359794,-4.67486974094423,
136.018172443767));
#196095=CARTESIAN_POINT('Ctrl Pts',(54.9263780121665,1.85964626718557,137.555653576309));
#196096=CARTESIAN_POINT('Ctrl Pts',(54.6479303883536,6.68523820454244,132.889026298762));
#196097=CARTESIAN_POINT('Ctrl Pts',(54.3694827645407,5.36742282396772,126.306693101776));
#196098=CARTESIAN_POINT('Ctrl Pts',(54.0910351407278,-0.882791918651148,
123.857496628527));
#196099=CARTESIAN_POINT('Ctrl Pts',(53.8125875169149,-6.32176401481248,
127.792128788032));
#196100=CARTESIAN_POINT('Ctrl Pts',(53.534139893102,-5.95134381670231,134.494854843172));
#196101=CARTESIAN_POINT('Ctrl Pts',(53.2556922692892,-0.111929390351441,
137.806196995646));
#196102=CARTESIAN_POINT('Ctrl Pts',(52.9772446454762,5.83034267767769,134.683193575387));
#196103=CARTESIAN_POINT('Ctrl Pts',(52.6987970216634,6.41481465299549,127.995732158415));
#196104=CARTESIAN_POINT('Ctrl Pts',(52.4203493978505,1.10438534332797,123.889263086274));
#196105=CARTESIAN_POINT('Ctrl Pts',(52.1419017740376,-5.22092014463445,
126.137430824095));
#196106=CARTESIAN_POINT('Ctrl Pts',(51.8634541502246,-6.74845507580631,
132.674279049921));
#196107=CARTESIAN_POINT('Ctrl Pts',(51.5850065264118,-2.07448947267055,
137.492763587005));
#196108=CARTESIAN_POINT('Ctrl Pts',(51.3065589025989,4.50583061140446,136.164932541826));
#196109=CARTESIAN_POINT('Ctrl Pts',(51.028111278786,6.94551248566166,129.910997776748));
#196110=CARTESIAN_POINT('Ctrl Pts',(50.7496636549731,3.00260769274395,124.478019819181));
#196111=CARTESIAN_POINT('Ctrl Pts',(50.4712160311602,-3.69954688426507,
124.858639996399));
#196112=CARTESIAN_POINT('Ctrl Pts',(50.1927684073473,-7.00199860754717,
130.70308695987));
#196113=CARTESIAN_POINT('Ctrl Pts',(49.9143207835345,-3.86995567714208,
136.640599467269));
#196114=CARTESIAN_POINT('Ctrl Pts',(49.6358731597215,2.81838746271124,137.214893587909));
#196115=CARTESIAN_POINT('Ctrl Pts',(49.3574255359087,6.91677021021505,131.89822108075));
#196116=CARTESIAN_POINT('Ctrl Pts',(49.0789779120958,4.65897903754105,125.576344245977));
#196117=CARTESIAN_POINT('Ctrl Pts',(48.8005302882828,-1.88018626685394,
124.058759053897));
#196118=CARTESIAN_POINT('Ctrl Pts',(48.5220826644701,-6.69155224421552,
128.740052157871));
#196119=CARTESIAN_POINT('Ctrl Pts',(48.243635040657,-5.35370860964396,135.318343889229));
#196120=CARTESIAN_POINT('Ctrl Pts',(47.9651874168443,0.903931693984841,
137.748505514272));
#196121=CARTESIAN_POINT('Ctrl Pts',(47.6867397930313,6.33090293035988,133.797337219578));
#196122=CARTESIAN_POINT('Ctrl Pts',(47.4082921692184,5.94008365553619,127.095769642671));
#196123=CARTESIAN_POINT('Ctrl Pts',(47.1298445454056,0.0906176904940206,
123.80221599695));
#196124=CARTESIAN_POINT('Ctrl Pts',(46.8513969215926,-5.84212150519187,
126.943291183793));
#196125=CARTESIAN_POINT('Ctrl Pts',(46.5729492977799,-6.40623644110861,
133.632500556544));
#196126=CARTESIAN_POINT('Ctrl Pts',(46.2945016739667,-1.08333304969514,
137.722787487691));
#196127=CARTESIAN_POINT('Ctrl Pts',(46.016054050154,5.23510049062639,135.455378109134));
#196128=CARTESIAN_POINT('Ctrl Pts',(45.737606426341,6.7427324289391,128.913910870662));
#196129=CARTESIAN_POINT('Ctrl Pts',(45.4591588025282,2.0541226658487,124.10967459599));
#196130=CARTESIAN_POINT('Ctrl Pts',(45.1807111787153,-4.5221254776858,125.457527721552));
#196131=CARTESIAN_POINT('Ctrl Pts',(44.9022635549024,-6.94276122533821,
131.718859071242));
#196132=CARTESIAN_POINT('Ctrl Pts',(44.6238159310895,-2.98333857964632,
137.139811017737));
#196133=CARTESIAN_POINT('Ctrl Pts',(44.3453683072766,3.71762647654865,136.738793550433));
#196134=CARTESIAN_POINT('Ctrl Pts',(44.0669206834637,7.00227441694529,130.88432213099));
#196135=CARTESIAN_POINT('Ctrl Pts',(43.7884730596509,3.85217424829189,124.956369987047));
#196136=CARTESIAN_POINT('Ctrl Pts',(43.5100254358379,-2.8378858653675,124.402435542326));
#196137=CARTESIAN_POINT('Ctrl Pts',(43.2315778120251,-6.92006750718621,
129.731557490323));
#196138=CARTESIAN_POINT('Ctrl Pts',(42.9531301882121,-4.64304517399252,
136.04653310291));
#196139=CARTESIAN_POINT('Ctrl Pts',(42.6746825643993,1.90070884873357,137.544208295828));
#196140=CARTESIAN_POINT('Ctrl Pts',(42.3962349405864,6.69780429426274,132.848292732287));
#196141=CARTESIAN_POINT('Ctrl Pts',(42.1177873167735,5.33994479929498,126.274103406951));
#196142=CARTESIAN_POINT('Ctrl Pts',(41.8393396929606,-0.925063095418803,
123.862999142802));
#196143=CARTESIAN_POINT('Ctrl Pts',(41.5608920691476,-6.33998319728738,
127.8306669696));
#196144=CARTESIAN_POINT('Ctrl Pts',(41.2824444453348,-5.92876846624656,
134.531013985867));
#196145=CARTESIAN_POINT('Ctrl Pts',(41.0039968215219,-0.069305151166692,
137.806748613804));
#196146=CARTESIAN_POINT('Ctrl Pts',(40.725549197709,5.85384621209049,134.647630758868));
#196147=CARTESIAN_POINT('Ctrl Pts',(40.4471015738961,6.39759888272248,127.956735398261));
#196148=CARTESIAN_POINT('Ctrl Pts',(40.1686539500832,1.06227072021291,123.882668499967));
#196149=CARTESIAN_POINT('Ctrl Pts',(39.8902063262704,-5.24923233936253,
126.169298514289));
#196150=CARTESIAN_POINT('Ctrl Pts',(39.6117587024575,-6.73694731831984,
132.715324166149));
#196151=CARTESIAN_POINT('Ctrl Pts',(39.3333110786445,-2.03373682991476,
137.505267672621));
#196152=CARTESIAN_POINT('Ctrl Pts',(39.0548634548317,4.53837845161457,136.137404953004));
#196153=CARTESIAN_POINT('Ctrl Pts',(38.7764158310188,6.9399456482232,129.86873502282));
#196154=CARTESIAN_POINT('Ctrl Pts',(38.4979682072059,2.96404182930761,124.459859306355));
#196155=CARTESIAN_POINT('Ctrl Pts',(38.219520583393,-3.73567162924815,124.881270348773));
#196156=CARTESIAN_POINT('Ctrl Pts',(37.9410729595801,-7.00248535822977,
130.745711989165));
#196157=CARTESIAN_POINT('Ctrl Pts',(37.6626253357672,-3.83435713342598,
136.664048853912));
#196158=CARTESIAN_POINT('Ctrl Pts',(37.3841777119543,2.8573579782368,137.197618491141));
#196159=CARTESIAN_POINT('Ctrl Pts',(37.1057300881414,6.92330069759731,131.856096470565));
#196160=CARTESIAN_POINT('Ctrl Pts',(36.8272824643285,4.62706829790778,125.548080581235));
#196161=CARTESIAN_POINT('Ctrl Pts',(36.5488348405156,-1.92121382270608,
124.070329261737));
#196162=CARTESIAN_POINT('Ctrl Pts',(36.2703872167028,-6.70399429676593,
128.780823782526));
#196163=CARTESIAN_POINT('Ctrl Pts',(35.9919395928899,-5.32613152042688,
135.350849799446));
#196164=CARTESIAN_POINT('Ctrl Pts',(35.7134919690769,0.946185927194629,
137.742874366562));
#196165=CARTESIAN_POINT('Ctrl Pts',(35.4350443452641,6.34900473147662,133.758743763591));
#196166=CARTESIAN_POINT('Ctrl Pts',(35.1565967214512,5.91739835365575,127.059679379064));
#196167=CARTESIAN_POINT('Ctrl Pts',(34.8781490976383,0.0479919698059151,
123.80179411487));
#196168=CARTESIAN_POINT('Ctrl Pts',(34.5997014738253,-5.8655166897575,126.978925372262));
#196169=CARTESIAN_POINT('Ctrl Pts',(34.3212538500126,-6.38890205785425,
133.671444737187));
#196170=CARTESIAN_POINT('Ctrl Pts',(34.0428062261996,-1.04119854999986,
137.729253861025));
#196171=CARTESIAN_POINT('Ctrl Pts',(33.7643586023867,5.26331555992738,135.423424393967));
#196172=CARTESIAN_POINT('Ctrl Pts',(33.4859109785738,6.73109979754094,128.872900970206));
#196173=CARTESIAN_POINT('Ctrl Pts',(33.207463354761,2.01333215372067,124.097294605319));
#196174=CARTESIAN_POINT('Ctrl Pts',(32.9290157309481,-4.55458938262534,
125.485154247296));
#196175=CARTESIAN_POINT('Ctrl Pts',(32.6505681071352,-6.93706578039975,
131.761104685873));
#196176=CARTESIAN_POINT('Ctrl Pts',(32.3721204833222,-2.94471762049033,
137.157854065221));
#196177=CARTESIAN_POINT('Ctrl Pts',(32.0936728595094,3.75368217519627,136.716053351584));
#196178=CARTESIAN_POINT('Ctrl Pts',(31.8152252356965,7.00263142944649,130.84169581763));
#196179=CARTESIAN_POINT('Ctrl Pts',(31.5367776118836,3.8165044975991,124.933029058741));
#196180=CARTESIAN_POINT('Ctrl Pts',(31.2583299880707,-2.87680362093211,
124.41982917192));
#196181=CARTESIAN_POINT('Ctrl Pts',(30.9798823642578,-6.92646975149653,
129.773701781947));
#196182=CARTESIAN_POINT('Ctrl Pts',(30.7014347404449,-4.6110485572945,136.074699511423));
#196183=CARTESIAN_POINT('Ctrl Pts',(30.422987116632,1.94170099881587,137.532513267813));
#196184=CARTESIAN_POINT('Ctrl Pts',(30.1445394928192,6.71012219438185,132.807483427156));
#196185=CARTESIAN_POINT('Ctrl Pts',(29.8660918690062,5.31226890100394,126.241681582474));
#196186=CARTESIAN_POINT('Ctrl Pts',(29.5876442451933,-0.967299993633269,
123.868758871779));
#196187=CARTESIAN_POINT('Ctrl Pts',(29.3091966213805,-6.35796744935336,
127.869315342481));
#196188=CARTESIAN_POINT('Ctrl Pts',(29.0307489975676,-5.90597342309497,
134.567035036052));
#196189=CARTESIAN_POINT('Ctrl Pts',(28.7523013737546,-0.026678343854083,
137.807040755898));
#196190=CARTESIAN_POINT('Ctrl Pts',(28.4738537499418,5.87713283007914,134.611925528561));
#196191=CARTESIAN_POINT('Ctrl Pts',(28.1954061261289,6.38014604707014,127.917844157905));
#196192=CARTESIAN_POINT('Ctrl Pts',(27.916958502316,1.02011673426565,123.876330399509));
#196193=CARTESIAN_POINT('Ctrl Pts',(27.6385108785031,-5.27735002185588,
126.201337958415));
#196194=CARTESIAN_POINT('Ctrl Pts',(27.3600632546902,-6.72518992077305,
132.756298470923));
#196195=CARTESIAN_POINT('Ctrl Pts',(27.0816156308773,-1.99290882629253,
137.51752345366));
#196196=CARTESIAN_POINT('Ctrl Pts',(26.8031680070644,4.57075812054227,136.109679746264));
#196197=CARTESIAN_POINT('Ctrl Pts',(26.5247203832516,6.93412164854658,129.826506938842));
#196198=CARTESIAN_POINT('Ctrl Pts',(26.2462727594386,2.92536613221128,124.441933891359));
#196199=CARTESIAN_POINT('Ctrl Pts',(25.9678251356258,-3.7716579475455,124.904120183435));
#196200=CARTESIAN_POINT('Ctrl Pts',(25.6893775118128,-7.00271262924226,
130.788339191706));
#196201=CARTESIAN_POINT('Ctrl Pts',(25.410929888,-3.79861650619593,136.687281107654));
#196202=CARTESIAN_POINT('Ctrl Pts',(25.1324822641871,2.89622261331168,137.180106489852));
#196203=CARTESIAN_POINT('Ctrl Pts',(24.8540346403742,6.92957463952618,131.813932887921));
#196204=CARTESIAN_POINT('Ctrl Pts',(24.5755870165613,4.59498610055721,125.520011689881));
#196205=CARTESIAN_POINT('Ctrl Pts',(24.2971393927484,-1.96217018727317,
124.082149001586));
#196206=CARTESIAN_POINT('Ctrl Pts',(24.0186917689355,-6.71618793034234,
128.821670390082));
#196207=CARTESIAN_POINT('Ctrl Pts',(23.7402441451226,-5.29835706944761,
135.383187237832));
#196208=CARTESIAN_POINT('Ctrl Pts',(23.4617965213097,0.988405099136929,
137.736986109674));
#196209=CARTESIAN_POINT('Ctrl Pts',(23.1833488974968,6.36687126788796,133.720040831851));
#196210=CARTESIAN_POINT('Ctrl Pts',(22.9049012736839,5.89449378040337,127.023727875996));
#196211=CARTESIAN_POINT('Ctrl Pts',(22.6264536498711,0.00536447075796404,
123.801631715467));
#196212=CARTESIAN_POINT('Ctrl Pts',(22.3480060260581,-5.88869452544514,
127.01470131364));
#196213=CARTESIAN_POINT('Ctrl Pts',(22.0695584022453,-6.3713309314846,133.710282676972));
#196214=CARTESIAN_POINT('Ctrl Pts',(21.7911107784324,-0.999025468309402,
137.735463629893));
#196215=CARTESIAN_POINT('Ctrl Pts',(21.5126631546195,5.29133559513472,135.391299517692));
#196216=CARTESIAN_POINT('Ctrl Pts',(21.2342155308066,6.71921774276442,128.831962640697));
#196217=CARTESIAN_POINT('Ctrl Pts',(20.9557679069937,1.97246703682929,124.085163147446));
#196218=CARTESIAN_POINT('Ctrl Pts',(20.6773202831809,-4.58688451558038,
125.51297787819));
#196219=CARTESIAN_POINT('Ctrl Pts',(20.3988726593679,-6.93111327993769,
131.803314848003));
#196220=CARTESIAN_POINT('Ctrl Pts',(20.120425035555,-2.90598754374001,137.175661681671));
#196221=CARTESIAN_POINT('Ctrl Pts',(19.8419774117421,3.78959877977074,136.693094092787));
#196222=CARTESIAN_POINT('Ctrl Pts',(19.5635297879293,7.00272895686486,130.799068120799));
#196223=CARTESIAN_POINT('Ctrl Pts',(19.2850821641163,3.78069332492835,124.909905694786));
#196224=CARTESIAN_POINT('Ctrl Pts',(19.0066345403035,-2.91561477548059,
124.437459382677));
#196225=CARTESIAN_POINT('Ctrl Pts',(18.7281869164906,-6.932615332923,129.815884265012));
#196226=CARTESIAN_POINT('Ctrl Pts',(18.4497392926777,-4.57888107649638,
136.102670625591));
#196227=CARTESIAN_POINT('Ctrl Pts',(18.1712916688647,1.98262119845391,137.520568925627));
#196228=CARTESIAN_POINT('Ctrl Pts',(17.892844045052,6.72219144845534,132.766599895572));
#196229=CARTESIAN_POINT('Ctrl Pts',(17.614396421239,5.28439615463518,126.209428829746));
#196230=CARTESIAN_POINT('Ctrl Pts',(17.3359487974261,-1.00950104819076,
123.87477560203));
#196231=CARTESIAN_POINT('Ctrl Pts',(17.0575011736132,-6.37571610459714,
127.908072474542));
#196232=CARTESIAN_POINT('Ctrl Pts',(16.7790535498004,-5.88295953192644,
134.602916658952));
#196233=CARTESIAN_POINT('Ctrl Pts',(16.5006059259874,0.0159494520341194,
137.807073411106));
#196234=CARTESIAN_POINT('Ctrl Pts',(16.2221583021745,5.90020166874948,134.576079207535));
#196235=CARTESIAN_POINT('Ctrl Pts',(15.9437106783617,6.3624567927597,127.879059878479));
#196236=CARTESIAN_POINT('Ctrl Pts',(15.6652630545488,0.977924947517885,
123.870249019757));
#196237=CARTESIAN_POINT('Ctrl Pts',(15.3868154307359,-5.3052721502032,126.233547969238));
#196238=CARTESIAN_POINT('Ctrl Pts',(15.108367806923,-6.71318331884074,132.797200445919));
#196239=CARTESIAN_POINT('Ctrl Pts',(14.8299201831101,-1.95200697470083,
137.529530475982));
#196240=CARTESIAN_POINT('Ctrl Pts',(14.5514725592972,4.6029684183469,136.081757948972));
#196241=CARTESIAN_POINT('Ctrl Pts',(14.2730249354843,6.92804070244224,129.784315089592));
#196242=CARTESIAN_POINT('Ctrl Pts',(13.9945773116714,2.88658203459712,124.424244238425));
#196243=CARTESIAN_POINT('Ctrl Pts',(13.7161296878585,-3.80750450567058,
124.927188653676));
#196244=CARTESIAN_POINT('Ctrl Pts',(13.4376820640456,-7.00268041216303,
130.830966987928));
#196245=CARTESIAN_POINT('Ctrl Pts',(13.1592344402328,-3.7627351198343,136.710295367612));
#196246=CARTESIAN_POINT('Ctrl Pts',(12.8807868164199,2.93497992779253,137.162358232954));
#196247=CARTESIAN_POINT('Ctrl Pts',(12.602339192607,6.93559180351842,131.771731895206));
#196248=CARTESIAN_POINT('Ctrl Pts',(12.323891568794,4.56273363430679,125.49213861202));
#196249=CARTESIAN_POINT('Ctrl Pts',(12.0454439449812,-2.00305384290271,
124.094217835458));
#196250=CARTESIAN_POINT('Ctrl Pts',(11.7669963211683,-6.72813269310505,
128.862590466954));
#196251=CARTESIAN_POINT('Ctrl Pts',(11.4885486973554,-5.27038628589867,
135.415355006116));
#196252=CARTESIAN_POINT('Ctrl Pts',(11.2101010735425,1.03058764536478,137.730840961799));
#196253=CARTESIAN_POINT('Ctrl Pts',(10.9316534497296,6.38450187754329,133.681229858508));
#196254=CARTESIAN_POINT('Ctrl Pts',(10.6532058259167,5.87137078451608,126.987916465666));
#196255=CARTESIAN_POINT('Ctrl Pts',(10.3747582021038,-0.0372632270726686,
123.801728804758));
#196256=CARTESIAN_POINT('Ctrl Pts',(10.0963105782909,-5.91165415339157,
127.050617682238));
#196257=CARTESIAN_POINT('Ctrl Pts',(9.81786295447806,-6.35352371310424,
133.749012936746));
#196258=CARTESIAN_POINT('Ctrl Pts',(9.53941533066515,-0.956815367363035,
137.741416564191));
#196259=CARTESIAN_POINT('Ctrl Pts',(9.26096770685226,5.31915955795546,135.35900467071));
#196260=CARTESIAN_POINT('Ctrl Pts',(8.98252008303941,6.70708670490366,128.791097399121));
#196261=CARTESIAN_POINT('Ctrl Pts',(8.70407245922646,1.93152882944647,124.073280671906));
#196262=CARTESIAN_POINT('Ctrl Pts',(8.42562483541358,-4.61900967984285,
125.540997583217));
#196263=CARTESIAN_POINT('Ctrl Pts',(8.14717721160073,-6.92490394452403,
131.845487993513));
#196264=CARTESIAN_POINT('Ctrl Pts',(7.86872958778781,-2.86714978455288,
137.193233207215));
#196265=CARTESIAN_POINT('Ctrl Pts',(7.59028196397491,3.82537495936868,136.669916624805));
#196266=CARTESIAN_POINT('Ctrl Pts',(7.31183434016203,7.00256699558648,130.756440620084));
#196267=CARTESIAN_POINT('Ctrl Pts',(7.03338671634916,3.7447420572761,124.887000752025));
#196268=CARTESIAN_POINT('Ctrl Pts',(6.75493909253623,-2.95431789085107,
124.455325521299));
#196269=CARTESIAN_POINT('Ctrl Pts',(6.47649146872337,-6.9385040237388,129.858103376433));
#196270=CARTESIAN_POINT('Ctrl Pts',(6.19804384491048,-4.54654392357636,
136.130445408932));
#196271=CARTESIAN_POINT('Ctrl Pts',(5.91959622109758,2.02346793133434,137.508375711873));
#196272=CARTESIAN_POINT('Ctrl Pts',(5.64114859728465,6.73401160925262,132.725643652489));
#196273=CARTESIAN_POINT('Ctrl Pts',(5.36270097347181,5.25632759302358,126.177346343905));
#196274=CARTESIAN_POINT('Ctrl Pts',(5.08425334965889,-1.05166469531565,
123.881049110601));
#196275=CARTESIAN_POINT('Ctrl Pts',(4.80580572584599,-6.39322850533622,
127.946936929627));
#196276=CARTESIAN_POINT('Ctrl Pts',(4.5273581020331,-5.85972764552883,134.638657524961));
#196277=CARTESIAN_POINT('Ctrl Pts',(4.24891047822024,0.0585766569097649,
137.806846578216));
#196278=CARTESIAN_POINT('Ctrl Pts',(3.97046285440732,5.92305187327717,134.54009312409));
#196279=CARTESIAN_POINT('Ctrl Pts',(3.69201523059441,6.34453177527304,127.840383997147));
#196280=CARTESIAN_POINT('Ctrl Pts',(3.41356760678156,0.935696923401329,
123.864424586062));
#196281=CARTESIAN_POINT('Ctrl Pts',(3.13511998296867,-5.33299768974021,
126.265927353204));
#196282=CARTESIAN_POINT('Ctrl Pts',(2.85667235915575,-6.70092795743158,
132.838028575505));
#196283=CARTESIAN_POINT('Ctrl Pts',(2.57822473534285,-1.91103279077285,
137.541288294661));
#196284=CARTESIAN_POINT('Ctrl Pts',(2.29977711153,4.63500815146407,136.053640595781));
#196285=CARTESIAN_POINT('Ctrl Pts',(2.02132948771708,6.92170303524179,129.742161038504));
#196286=CARTESIAN_POINT('Ctrl Pts',(1.74288186390418,2.84769097362441,124.40679100305));
#196287=CARTESIAN_POINT('Ctrl Pts',(1.46443424009131,-3.84320997531586,
124.950474904685));
#196288=CARTESIAN_POINT('Ctrl Pts',(1.18598661627842,-7.00238870818588,
130.873593798241));
#196289=CARTESIAN_POINT('Ctrl Pts',(0.907538992465495,-3.72671430393905,
136.733090780986));
#196290=CARTESIAN_POINT('Ctrl Pts',(0.629091368652655,2.97362848551254,
137.144374378117));
#196291=CARTESIAN_POINT('Ctrl Pts',(0.350643744839755,6.94135196660579,
131.729495056193));
#196292=CARTESIAN_POINT('Ctrl Pts',(0.0721961210268491,4.53031209428387,
125.4644623805));
#196293=CARTESIAN_POINT('Ctrl Pts',(-0.206251502786054,-2.04386327463549,
124.106535316138));
#196294=CARTESIAN_POINT('Ctrl Pts',(-0.484699126598912,-6.73982814243653,
128.903582496833));
#196295=CARTESIAN_POINT('Ctrl Pts',(-0.763146750411823,-5.24222020624778,
135.447351912307));
#196296=CARTESIAN_POINT('Ctrl Pts',(-1.04159437422473,1.07273200278813,
137.724439150648));
#196297=CARTESIAN_POINT('Ctrl Pts',(-1.32004199803759,6.40189590713365,
133.642312281717));
#196298=CARTESIAN_POINT('Ctrl Pts',(-1.59848962185049,5.84803022282516,
126.952246475077));
#196299=CARTESIAN_POINT('Ctrl Pts',(-1.87693724566341,-0.0798895441007186,
123.802085379146));
#196300=CARTESIAN_POINT('Ctrl Pts',(-2.1553848694763,-5.93439472281934,
127.08667314716));
#196301=CARTESIAN_POINT('Ctrl Pts',(-2.43383249328916,-6.33548106256618,
133.787634081347));
#196302=CARTESIAN_POINT('Ctrl Pts',(-2.71228011710207,-0.914569811271147,
137.747112443329));
#196303=CARTESIAN_POINT('Ctrl Pts',(-2.99072774091498,5.34678641736288,
135.326541049718));
#196304=CARTESIAN_POINT('Ctrl Pts',(-3.26917536472784,6.6947071334783,128.750306759754));
#196305=CARTESIAN_POINT('Ctrl Pts',(-3.54762298854074,1.89051904855254,
124.061647619009));
#196306=CARTESIAN_POINT('Ctrl Pts',(-3.82607061235365,-4.65096368500298,
125.569212324096));
#196307=CARTESIAN_POINT('Ctrl Pts',(-4.10451823616654,-6.91843800424817,
131.887622559669));
#196308=CARTESIAN_POINT('Ctrl Pts',(-4.38296585997939,-2.82820578207579,
137.210567990736));
#196309=CARTESIAN_POINT('Ctrl Pts',(-4.66141348379231,3.86100938829084,
136.646521806489));
#196310=CARTESIAN_POINT('Ctrl Pts',(-4.93986110760522,7.00214555161287,
130.713814895061));
#196311=CARTESIAN_POINT('Ctrl Pts',(-5.21830873141809,3.70865202682979,
124.864315079211));
#196312=CARTESIAN_POINT('Ctrl Pts',(-5.49675635523098,-2.99291153288594,
124.473426925751));
#196313=CARTESIAN_POINT('Ctrl Pts',(-5.77520397904388,-6.9441356057364,
129.900357551763));
#196314=CARTESIAN_POINT('Ctrl Pts',(-6.05365160285679,-4.51403829679898,
136.158022832244));
#196315=CARTESIAN_POINT('Ctrl Pts',(-6.33209922666964,2.06423968386644,
137.495934078373));
#196316=CARTESIAN_POINT('Ctrl Pts',(-6.61054685048256,6.74558223877327,
132.684616215558));
#196317=CARTESIAN_POINT('Ctrl Pts',(-6.88899447429547,5.22806425626005,
126.145435313781));
#196318=CARTESIAN_POINT('Ctrl Pts',(-7.16744209810832,-1.09378937261818,
123.887579165027));
#196319=CARTESIAN_POINT('Ctrl Pts',(-7.44588972192122,-6.41050400264194,
127.985907267597));
#196320=CARTESIAN_POINT('Ctrl Pts',(-7.72433734573414,-5.8362786247684,
134.674256309687));
#196321=CARTESIAN_POINT('Ctrl Pts',(-8.002784969547,0.101201691205851,137.806360265633));
#196322=CARTESIAN_POINT('Ctrl Pts',(-8.28123259335988,5.94568259693924,
134.503968611703));
#196323=CARTESIAN_POINT('Ctrl Pts',(-8.55968021717279,6.32637165882838,
127.80181794706));
#196324=CARTESIAN_POINT('Ctrl Pts',(-8.8381278409857,0.893434226691435,
123.858857314246));
#196325=CARTESIAN_POINT('Ctrl Pts',(-9.11657546479855,-5.3605256130866,
126.298474910485));
#196326=CARTESIAN_POINT('Ctrl Pts',(-9.39502308861147,-6.68842429067269,
132.878781346775));
#196327=CARTESIAN_POINT('Ctrl Pts',(-9.67347071242438,-1.86998779282204,
137.552796474009));
#196328=CARTESIAN_POINT('Ctrl Pts',(-9.95191833623725,4.66687613264966,
136.025328728591));
#196329=CARTESIAN_POINT('Ctrl Pts',(-10.2303659600501,6.91510888178999,
129.700046347612));
#196330=CARTESIAN_POINT('Ctrl Pts',(-10.508813583863,2.80869439041515,124.389574831969));
#196331=CARTESIAN_POINT('Ctrl Pts',(-10.787261207676,-3.87877303340228,
124.973978073582));
#196332=CARTESIAN_POINT('Ctrl Pts',(-11.0657088314888,-7.00183752812002,
130.916218043094));
#196333=CARTESIAN_POINT('Ctrl Pts',(-11.3441564553017,-3.69055539327479,
136.755666503084));
#196334=CARTESIAN_POINT('Ctrl Pts',(-11.6226040791146,3.01216685433575,
137.126155591738));
#196335=CARTESIAN_POINT('Ctrl Pts',(-11.9010517029275,6.94685491534338,
131.687223935982));
#196336=CARTESIAN_POINT('Ctrl Pts',(-12.1794993267404,4.49772268187999,
125.436984020872));
#196337=CARTESIAN_POINT('Ctrl Pts',(-12.4579469505533,-2.08459697026297,
124.119100987199));
#196338=CARTESIAN_POINT('Ctrl Pts',(-12.7363945743662,-6.75127384495765,
128.944644960744));
#196339=CARTESIAN_POINT('Ctrl Pts',(-13.0148421981791,-5.21385987419926,
135.479176770748));
#196340=CARTESIAN_POINT('Ctrl Pts',(-13.2932898219919,1.11483660973293,
137.717780913442));
#196341=CARTESIAN_POINT('Ctrl Pts',(-13.5717374458049,6.41905271211686,
133.603289543584));
#196342=CARTESIAN_POINT('Ctrl Pts',(-13.8501850696177,5.82447296022373,
126.916719225995));
#196343=CARTESIAN_POINT('Ctrl Pts',(-14.1286326934306,-0.122512900792341,
123.802701425419));
#196344=CARTESIAN_POINT('Ctrl Pts',(-14.4070803172435,-5.95691539106803,
127.122866372359));
#196345=CARTESIAN_POINT('Ctrl Pts',(-14.6855279410564,-6.31720364844761,
133.826144679651));
#196346=CARTESIAN_POINT('Ctrl Pts',(-14.9639755648693,-0.872290365458834,
137.752551056246));
#196347=CARTESIAN_POINT('Ctrl Pts',(-15.2424231886822,5.37421514963333,
135.293909857666));
#196348=CARTESIAN_POINT('Ctrl Pts',(-15.5208708124951,6.68207948721813,
128.709592234107));
#196349=CARTESIAN_POINT('Ctrl Pts',(-15.799318436308,1.84943921378025,124.050264419823));
#196350=CARTESIAN_POINT('Ctrl Pts',(-16.0777660601209,-4.68274534699314,
125.59762105532));
#196351=CARTESIAN_POINT('Ctrl Pts',(-16.3562136839338,-6.91171569870797,
131.929716985153));
#196352=CARTESIAN_POINT('Ctrl Pts',(-16.6346613077467,-2.78915697939336,
137.227665389888));
#196353=CARTESIAN_POINT('Ctrl Pts',(-16.9131089315595,3.89650074609022,
136.622910504741));
#196354=CARTESIAN_POINT('Ctrl Pts',(-17.1915565553724,7.00146464056082,
130.671192525245));
#196355=CARTESIAN_POINT('Ctrl Pts',(-17.4700041791854,3.67242457091876,
124.841849516969));
#196356=CARTESIAN_POINT('Ctrl Pts',(-17.7484518029982,-3.0313942714833,
124.491762925279));
#196357=CARTESIAN_POINT('Ctrl Pts',(-18.0268994268111,-6.94950987023543,
129.942645225261));
#196358=CARTESIAN_POINT('Ctrl Pts',(-18.305347050624,-4.48136540067248,
136.185401873632));
#196359=CARTESIAN_POINT('Ctrl Pts',(-18.5837946744369,2.10493494523792,
137.483244486159));
#196360=CARTESIAN_POINT('Ctrl Pts',(-18.8622422982498,6.75690290826339,
132.643519105064));
#196361=CARTESIAN_POINT('Ctrl Pts',(-19.1406899220627,5.19960719165284,
126.113696921846));
#196362=CARTESIAN_POINT('Ctrl Pts',(-19.4191375458756,-1.1358735191536,
123.894365523333));
#196363=CARTESIAN_POINT('Ctrl Pts',(-19.6975851696885,-6.42754195636435,
128.024982044393));
#196364=CARTESIAN_POINT('Ctrl Pts',(-19.9760327935014,-5.81261333855723,
134.709711694007));
#196365=CARTESIAN_POINT('Ctrl Pts',(-20.2544804173143,0.143822975436045,
137.805614491377));
#196366=CARTESIAN_POINT('Ctrl Pts',(-20.5329280411272,5.96809300114641,
134.467707008981));
#196367=CARTESIAN_POINT('Ctrl Pts',(-20.81137566494,6.30797711635522,127.763363157294));
#196368=CARTESIAN_POINT('Ctrl Pts',(-21.089823288753,0.851138423447451,
123.853547410611));
#196369=CARTESIAN_POINT('Ctrl Pts',(-21.3682709125658,-5.38785490018508,
126.331189435016));
#196370=CARTESIAN_POINT('Ctrl Pts',(-21.6467185363787,-6.67567278189203,
132.919457249623));
#196371=CARTESIAN_POINT('Ctrl Pts',(-21.9251661601916,-1.82887350178604,
137.564054587584));
#196372=CARTESIAN_POINT('Ctrl Pts',(-22.2036137840045,4.69857118102365,
135.996823396506));
#196373=CARTESIAN_POINT('Ctrl Pts',(-22.4820614078173,6.90825848643574,
129.657972577492));
#196374=CARTESIAN_POINT('Ctrl Pts',(-22.7605090316303,2.76959373000234,
124.372596363135));
#196375=CARTESIAN_POINT('Ctrl Pts',(-23.0389566554432,-3.91419236212754,
124.997697289448));
#196376=CARTESIAN_POINT('Ctrl Pts',(-23.3174042792561,-7.0010268923895,
130.958838143028));
#196377=CARTESIAN_POINT('Ctrl Pts',(-23.5958519030689,-3.65425972772349,
136.778021697354));
#196378=CARTESIAN_POINT('Ctrl Pts',(-23.8742995268818,3.05059360620828,
137.107702548922));
#196379=CARTESIAN_POINT('Ctrl Pts',(-24.1527471506948,6.95210044581739,
131.644920100946));
#196380=CARTESIAN_POINT('Ctrl Pts',(-24.4311947745076,4.4649666047081,125.409704551357));
#196381=CARTESIAN_POINT('Ctrl Pts',(-24.7096423983205,-2.12525342038311,
124.131914383013));
#196382=CARTESIAN_POINT('Ctrl Pts',(-24.9880900221334,-6.76246937654364,
128.985776337104));
#196383=CARTESIAN_POINT('Ctrl Pts',(-25.2665376459463,-5.18530634065569,
135.510828402156));
#196384=CARTESIAN_POINT('Ctrl Pts',(-25.5449852697592,1.15689990599717,
137.710866496904));
#196385=CARTESIAN_POINT('Ctrl Pts',(-25.8234328935721,6.43597165674122,
133.564163090109));
#196386=CARTESIAN_POINT('Ctrl Pts',(-26.101880517385,5.8006998696348,126.881336034893));
#196387=CARTESIAN_POINT('Ctrl Pts',(-26.3803281411979,-0.165131717723356,
123.803576920747));
#196388=CARTESIAN_POINT('Ctrl Pts',(-26.6587757650107,-5.9792153236265,
127.15919601668));
#196389=CARTESIAN_POINT('Ctrl Pts',(-26.9372233888237,-6.29869214802456,
133.864543304637));
#196390=CARTESIAN_POINT('Ctrl Pts',(-27.2156710126366,-0.829978596605981,
137.75773220141));
#196391=CARTESIAN_POINT('Ctrl Pts',(-27.4941186364494,5.40144473838504,
135.261112303716));
#196392=CARTESIAN_POINT('Ctrl Pts',(-27.7725662602623,6.66920423404522,
128.668955330874));
#196393=CARTESIAN_POINT('Ctrl Pts',(-28.0510138840753,1.80829084735756,
124.039131496154));
#196394=CARTESIAN_POINT('Ctrl Pts',(-28.3294615078881,-4.71435348813263,
125.626222724194));
#196395=CARTESIAN_POINT('Ctrl Pts',(-28.607909131701,-6.9047372770006,131.971769710144));
#196396=CARTESIAN_POINT('Ctrl Pts',(-28.8863567555139,-2.75000482347336,
137.244524771118));
#196397=CARTESIAN_POINT('Ctrl Pts',(-29.1648043793268,3.93184771762154,
136.599083594488));
#196398=CARTESIAN_POINT('Ctrl Pts',(-29.4432520031397,7.00052428766157,
130.628575090021));
#196399=CARTESIAN_POINT('Ctrl Pts',(-29.7216996269525,3.63606103196502,
124.819604897767));
#196400=CARTESIAN_POINT('Ctrl Pts',(-30.0001472507655,-3.06976468065099,
124.510332840438));
#196401=CARTESIAN_POINT('Ctrl Pts',(-30.2785948745783,-6.95462661809053,
129.984964829937));
#196402=CARTESIAN_POINT('Ctrl Pts',(-30.5570424983912,-4.44852644590303,
136.212581518559));
#196403=CARTESIAN_POINT('Ctrl Pts',(-30.8354901222041,2.14555220747066,
137.470307405446));
#196404=CARTESIAN_POINT('Ctrl Pts',(-31.113937746017,6.7679731982313,132.602353843876));
#196405=CARTESIAN_POINT('Ctrl Pts',(-31.3923853698299,5.17095745368924,
126.082132344179));
#196406=CARTESIAN_POINT('Ctrl Pts',(-31.6708329936428,-1.17791557547805,
123.901407934047));
#196407=CARTESIAN_POINT('Ctrl Pts',(-31.9492806174558,-6.44434173515584,
128.064159812084));
#196408=CARTESIAN_POINT('Ctrl Pts',(-32.2277282412685,-5.78873266382121,
134.745022364106));
#196409=CARTESIAN_POINT('Ctrl Pts',(-32.5061758650815,0.186438930252996,
137.804609283086));
#196410=CARTESIAN_POINT('Ctrl Pts',(-32.7846234888944,5.99028225547263,
134.431309659613));
#196411=CARTESIAN_POINT('Ctrl Pts',(-33.0630711127073,6.28934882947028,
127.725021052809));
#196412=CARTESIAN_POINT('Ctrl Pts',(-33.3415187365202,0.808811080956172,
123.848495071916));
#196413=CARTESIAN_POINT('Ctrl Pts',(-33.619966360333,-5.41498453833882,
126.364069714552));
#196414=CARTESIAN_POINT('Ctrl Pts',(-33.898413984146,-6.66267390360147,
132.960054776787));
#196415=CARTESIAN_POINT('Ctrl Pts',(-34.1768616079588,-1.78769144116968,
137.575062218212));
#196416=CARTESIAN_POINT('Ctrl Pts',(-34.4553092317717,4.73009212211488,
135.968125655805));
#196417=CARTESIAN_POINT('Ctrl Pts',(-34.7337568555846,6.90115210302259,
129.615941287202));
#196418=CARTESIAN_POINT('Ctrl Pts',(-35.0122044793975,2.73039044127535,
124.355856225691));
#196419=CARTESIAN_POINT('Ctrl Pts',(-35.2906521032104,-3.94946664901538,
125.02163167336));
#196420=CARTESIAN_POINT('Ctrl Pts',(-35.5690997270233,-6.99995683103299,
131.00145251874));
#196421=CARTESIAN_POINT('Ctrl Pts',(-35.8475473508362,-3.61782865223385,
136.800155535415));
#196422=CARTESIAN_POINT('Ctrl Pts',(-36.125994974649,3.08890731721304,137.089015933453));
#196423=CARTESIAN_POINT('Ctrl Pts',(-36.404442598462,6.95708836365274,131.60258511867));
#196424=CARTESIAN_POINT('Ctrl Pts',(-36.6828902222748,4.43204507655667,
125.382624982808));
#196425=CARTESIAN_POINT('Ctrl Pts',(-36.9613378460878,-2.16583111845593,
124.144975028777));
#196426=CARTESIAN_POINT('Ctrl Pts',(-37.2397854699006,-6.7734143223399,
129.026975101771));
#196427=CARTESIAN_POINT('Ctrl Pts',(-37.5182330937135,-5.15656066367905,
135.54230563367));
#196428=CARTESIAN_POINT('Ctrl Pts',(-37.7966807175264,1.19892033290996,
137.703696157251));
#196429=CARTESIAN_POINT('Ctrl Pts',(-38.0751283413393,6.45265211406898,
133.524934371139));
#196430=CARTESIAN_POINT('Ctrl Pts',(-38.3535759651522,5.77671183197903,
126.846098212911));
#196431=CARTESIAN_POINT('Ctrl Pts',(-38.6320235889651,-0.207744415637528,
123.80471183269));
#196432=CARTESIAN_POINT('Ctrl Pts',(-38.910471212778,-6.00129369416227,
127.195660733917));
#196433=CARTESIAN_POINT('Ctrl Pts',(-39.1889188365908,-6.27994724724761,
133.902828533427));
#196434=CARTESIAN_POINT('Ctrl Pts',(-39.4673664604039,-0.787636072591,137.762655686833));
#196435=CARTESIAN_POINT('Ctrl Pts',(-39.7458140842166,5.42847417461558,
135.228149603194));
#196436=CARTESIAN_POINT('Ctrl Pts',(-40.0242617080296,6.65608185105682,
128.628397555869));
#196437=CARTESIAN_POINT('Ctrl Pts',(-40.3027093318424,1.76707547405252,
124.028249260538));
#196438=CARTESIAN_POINT('Ctrl Pts',(-40.5811569556554,-4.7457869371699,
125.655016270872));
#196439=CARTESIAN_POINT('Ctrl Pts',(-40.8596045794682,-6.89750299771422,
132.013779176361));
#196440=CARTESIAN_POINT('Ctrl Pts',(-41.1380522032811,-2.7107507651133,
137.261145509698));
#196441=CARTESIAN_POINT('Ctrl Pts',(-41.416499827094,3.96704899308973,136.575041958643));
#196442=CARTESIAN_POINT('Ctrl Pts',(-41.694947450907,6.99932452776054,130.585964168594));
#196443=CARTESIAN_POINT('Ctrl Pts',(-41.9733950747197,3.59956275743227,
124.79758204589));
#196444=CARTESIAN_POINT('Ctrl Pts',(-42.2518426985328,-3.10802133855968,
124.529135983109));
#196445=CARTESIAN_POINT('Ctrl Pts',(-42.5302903223456,-6.95948565969872,
130.027314797628));
#196446=CARTESIAN_POINT('Ctrl Pts',(-42.8087379461585,-4.41552264935019,
136.23956075987));
#196447=CARTESIAN_POINT('Ctrl Pts',(-43.0871855699714,2.18608996547759,
137.457123315624));
#196448=CARTESIAN_POINT('Ctrl Pts',(-43.3656331937842,6.77879269846351,
132.561121957388));
#196449=CARTESIAN_POINT('Ctrl Pts',(-43.6440808175972,5.14211610399531,
126.050742750417));
#196450=CARTESIAN_POINT('Ctrl Pts',(-43.92252844141,-1.21991398370768,123.908706136214));
#196451=CARTESIAN_POINT('Ctrl Pts',(-44.200976065223,-6.46090271649442,
128.103439118922));
#196452=CARTESIAN_POINT('Ctrl Pts',(-44.4794236890358,-5.76463748546755,
134.780187011534));
#196453=CARTESIAN_POINT('Ctrl Pts',(-44.7578713128487,0.229047976506494,
137.803344678006));
#196454=CARTESIAN_POINT('Ctrl Pts',(-45.0363189366615,6.01224953768695,
134.394777912313));
#196455=CARTESIAN_POINT('Ctrl Pts',(-45.3147665604746,6.27048748845154,
127.686793054383));
#196456=CARTESIAN_POINT('Ctrl Pts',(-45.5932141842873,0.766453767672844,
123.843700485376));
#196457=CARTESIAN_POINT('Ctrl Pts',(-45.8716618081003,-5.44191352224889,
126.397114530699));
#196458=CARTESIAN_POINT('Ctrl Pts',(-46.1501094319132,-6.6494281374793,
133.000572423912));
#196459=CARTESIAN_POINT('Ctrl Pts',(-46.4285570557261,-1.74644313698983,
137.585818958004));
#196460=CARTESIAN_POINT('Ctrl Pts',(-46.7070046795389,4.76143778790304,
135.93923656989));
#196461=CARTESIAN_POINT('Ctrl Pts',(-46.9854523033519,6.89378999488032,
129.573954034227));
#196462=CARTESIAN_POINT('Ctrl Pts',(-47.2638999271647,2.69108597692664,
124.339355039948));
#196463=CARTESIAN_POINT('Ctrl Pts',(-47.5423475509777,-3.98459458696386,
125.045780338419));
#196464=CARTESIAN_POINT('Ctrl Pts',(-47.8207951747905,-6.998627383702,131.044059591139));
#196465=CARTESIAN_POINT('Ctrl Pts',(-48.0992427986034,-3.58126351677304,
136.822067197091));
#196466=CARTESIAN_POINT('Ctrl Pts',(-48.3776904224163,3.1271065676212,137.070096437769));
#196467=CARTESIAN_POINT('Ctrl Pts',(-48.6561380462292,6.9618184840203,131.560220557891));
#196468=CARTESIAN_POINT('Ctrl Pts',(-48.9345856700421,4.39895931734504,
125.355746318666));
#196469=CARTESIAN_POINT('Ctrl Pts',(-49.213033293855,-2.20632856086043,
124.158282440523));
#196470=CARTESIAN_POINT('Ctrl Pts',(-49.4914809176678,-6.78410827677761,
129.068239728113));
#196471=CARTESIAN_POINT('Ctrl Pts',(-49.7699285414808,-5.12762390845042,
135.573607298891));
#196472=CARTESIAN_POINT('Ctrl Pts',(-50.0483761652936,1.2408963333889,137.696270160183));
#196473=CARTESIAN_POINT('Ctrl Pts',(-50.3268237891066,6.46909346599971,
133.485604840309));
#196474=CARTESIAN_POINT('Ctrl Pts',(-50.6052714129194,5.7525097361419,126.811007065796));
#196475=CARTESIAN_POINT('Ctrl Pts',(-50.8837190367324,-0.250349415506305,
123.806106119193));
#196476=CARTESIAN_POINT('Ctrl Pts',(-51.1621666605453,-6.02314968455324,
127.232259172855));
#196477=CARTESIAN_POINT('Ctrl Pts',(-51.4406142843581,-6.26096964071598,
133.94099894735));
#196478=CARTESIAN_POINT('Ctrl Pts',(-51.719061908171,-0.745264362431691,
137.767321330073));
#196479=CARTESIAN_POINT('Ctrl Pts',(-51.997509531984,5.45530245673899,135.195022977544));
#196480=CARTESIAN_POINT('Ctrl Pts',(-52.2759571557968,6.64271282450778,
128.587920411975));
#196481=CARTESIAN_POINT('Ctrl Pts',(-52.5544047796097,1.72579462111621,
124.01761811622));
#196482=CARTESIAN_POINT('Ctrl Pts',(-52.8328524034226,-4.77704452932697,
125.684000628399));
#196483=CARTESIAN_POINT('Ctrl Pts',(-53.1113000272355,-6.89001312891767,
132.05574382713));
#196484=CARTESIAN_POINT('Ctrl Pts',(-53.3897476510484,-2.67139625888694,
137.277526989739));
#196485=CARTESIAN_POINT('Ctrl Pts',(-53.6681952748612,4.00210326809833,
136.550786488079));
#196486=CARTESIAN_POINT('Ctrl Pts',(-53.9466428986742,6.99786540531528,
130.543361339928));
#196487=CARTESIAN_POINT('Ctrl Pts',(-54.225090522487,3.56293109977782,124.775781777402));
#196488=CARTESIAN_POINT('Ctrl Pts',(-54.5035381462999,-3.14616282759469,
124.548171656537));
#196489=CARTESIAN_POINT('Ctrl Pts',(-54.7819857701128,-6.9640868150063,
130.069693559035));
#196490=CARTESIAN_POINT('Ctrl Pts',(-55.0604333939257,-4.382355233982,136.266338597842));
#196491=CARTESIAN_POINT('Ctrl Pts',(-55.3388810177386,2.22654671711671,
137.443692705233));
#196492=CARTESIAN_POINT('Ctrl Pts',(-55.6173286415515,6.78936100803939,
132.519824973462));
#196493=CARTESIAN_POINT('Ctrl Pts',(-55.8957762653644,5.11308421129812,
126.019529303714));
#196494=CARTESIAN_POINT('Ctrl Pts',(-56.1742238891773,-1.26186718757599,
123.916259859391));
#196495=CARTESIAN_POINT('Ctrl Pts',(-56.4526715129901,-6.47722428670686,
128.142818509401));
#196496=CARTESIAN_POINT('Ctrl Pts',(-56.7311191368031,-5.74032869635189,
134.815204333253));
#196497=CARTESIAN_POINT('Ctrl Pts',(-57.0095667606159,0.271648535303317,
137.801820722997));
#196498=CARTESIAN_POINT('Ctrl Pts',(-57.2880143844289,6.03399403378365,
134.358113120779));
#196499=CARTESIAN_POINT('Ctrl Pts',(-57.5664620082417,6.25139379221294,
127.64868057857));
#196500=CARTESIAN_POINT('Ctrl Pts',(-57.8449096320546,0.724068053163303,
123.839163828657));
#196501=CARTESIAN_POINT('Ctrl Pts',(-58.1233572558676,-5.46864085405239,
126.430322658971));
#196502=CARTESIAN_POINT('Ctrl Pts',(-58.4018048796803,-6.63593597435208,
133.0410086896));
#196503=CARTESIAN_POINT('Ctrl Pts',(-58.6802525034934,-1.705130117717,137.596324408362));
#196504=CARTESIAN_POINT('Ctrl Pts',(-58.9587001273061,4.79260701686295,
135.910157209259));
#196505=CARTESIAN_POINT('Ctrl Pts',(-59.2371477511191,6.88617243481463,
129.532012374421));
#196506=CARTESIAN_POINT('Ctrl Pts',(-59.515595374932,2.65168179339722,124.323093417365));
#196507=CARTESIAN_POINT('Ctrl Pts',(-59.7940429987449,-4.01957487429483,
125.070142389788));
#196508=CARTESIAN_POINT('Ctrl Pts',(-60.0724906225578,-6.99703859965941,
131.086657781405));
#196509=CARTESIAN_POINT('Ctrl Pts',(-60.3509382463707,-3.5445656762756,
136.843755870437));
#196510=CARTESIAN_POINT('Ctrl Pts',(-60.6293858701835,3.16518994194552,
137.050944762941));
#196511=CARTESIAN_POINT('Ctrl Pts',(-60.9078334939965,6.96629063164357,
131.517827988445));
#196512=CARTESIAN_POINT('Ctrl Pts',(-61.1862811178092,4.36571055307847,
125.32906955493));
#196513=CARTESIAN_POINT('Ctrl Pts',(-61.4647287416223,-2.24674424694855,
124.171836125139));
#196514=CARTESIAN_POINT('Ctrl Pts',(-61.743176365435,-6.79455084358828,
129.109568687053));
#196515=CARTESIAN_POINT('Ctrl Pts',(-62.0216239892481,-5.09849714723216,
135.60473223792));
#196516=CARTESIAN_POINT('Ctrl Pts',(-62.3000716130609,1.2828263519976,137.688588780872));
#196517=CARTESIAN_POINT('Ctrl Pts',(-62.5785192368738,6.48529510329292,
133.446175954988));
#196518=CARTESIAN_POINT('Ctrl Pts',(-62.8569668606868,5.72809447894126,
126.776063893867));
#196519=CARTESIAN_POINT('Ctrl Pts',(-63.1354144844995,-0.292945138585431,
123.80775972859));
#196520=CARTESIAN_POINT('Ctrl Pts',(-63.4138621083125,-6.04478248491762,
127.268989977326));
#196521=CARTESIAN_POINT('Ctrl Pts',(-63.6923097321254,-6.24176003165182,
133.979053131985));
#196522=CARTESIAN_POINT('Ctrl Pts',(-63.9707573559382,-0.702865036227365,
137.771728958244));
#196523=CARTESIAN_POINT('Ctrl Pts',(-64.2492049797512,5.48192859062395,
135.161733654286));
#196524=CARTESIAN_POINT('Ctrl Pts',(-64.527652603564,6.62909764979204,128.547525399088));
#196525=CARTESIAN_POINT('Ctrl Pts',(-64.806100227377,1.68444981822529,124.007238457143));
#196526=CARTESIAN_POINT('Ctrl Pts',(-65.0845478511898,-4.80812510634223,
125.713174722747));
#196527=CARTESIAN_POINT('Ctrl Pts',(-65.3629954750027,-6.88226794815085,
132.097662107432));
#196528=CARTESIAN_POINT('Ctrl Pts',(-65.6414430988157,-2.63194276308962,
137.29366860422));
#196529=CARTESIAN_POINT('Ctrl Pts',(-65.9198907226284,4.03700924369883,
136.526318081592));
#196530=CARTESIAN_POINT('Ctrl Pts',(-66.1983383464414,6.99614697439381,
130.500768182686));
#196531=CARTESIAN_POINT('Ctrl Pts',(-66.4767859702543,3.5261674164012,124.75420490012));
#196532=CARTESIAN_POINT('Ctrl Pts',(-66.7552335940671,-3.18418773440913,
124.567439155348));
#196533=CARTESIAN_POINT('Ctrl Pts',(-67.0336812178801,-6.96842991351606,
130.112099543802));
#196534=CARTESIAN_POINT('Ctrl Pts',(-67.3121288416929,-4.34902542882876,
136.292914040211));
#196535=CARTESIAN_POINT('Ctrl Pts',(-67.5905764655059,2.26692096324861,
137.43001607195));
#196536=CARTESIAN_POINT('Ctrl Pts',(-67.8690240893187,6.79967773534632,
132.478464422373));
#196537=CARTESIAN_POINT('Ctrl Pts',(-68.1474717131316,5.08386285138514,
125.988493160695));
#196538=CARTESIAN_POINT('Ctrl Pts',(-68.4259193369445,-1.30377363249137,
123.924068823677));
#196539=CARTESIAN_POINT('Ctrl Pts',(-68.7043669607574,-6.49330584099122,
128.182296524302));
#196540=CARTESIAN_POINT('Ctrl Pts',(-68.9828145845703,-5.71580719724563,
134.850073031684));
#196541=CARTESIAN_POINT('Ctrl Pts',(-69.2612622083832,0.314239028063776,
137.800037474531));
#196542=CARTESIAN_POINT('Ctrl Pts',(-69.5397098321961,6.05551493801243,
134.32131664364));
#196543=CARTESIAN_POINT('Ctrl Pts',(-69.818157456009,6.23206844827842,127.610685037641));
#196544=CARTESIAN_POINT('Ctrl Pts',(-70.0966050798218,0.681655508046095,
123.834885269867));
#196545=CARTESIAN_POINT('Ctrl Pts',(-70.3750527036349,-5.49516554335789,
126.463692868828));
#196546=CARTESIAN_POINT('Ctrl Pts',(-70.6535003274475,-6.62219791417695,
133.081362075471));
#196547=CARTESIAN_POINT('Ctrl Pts',(-70.9319479512606,-1.66375391422059,
137.606578180005));
#196548=CARTESIAN_POINT('Ctrl Pts',(-71.2103955750734,4.82359865400735,
135.880888651457));
#196549=CARTESIAN_POINT('Ctrl Pts',(-71.4888431988863,6.87829970509706,
129.490117861946));
#196550=CARTESIAN_POINT('Ctrl Pts',(-71.7672908226993,2.6121793508235,124.307071960521));
#196551=CARTESIAN_POINT('Ctrl Pts',(-72.045738446512,-4.05440621480077,
125.094716924722));
#196552=CARTESIAN_POINT('Ctrl Pts',(-72.3241860703251,-6.99519053777849,
131.129245511046));
#196553=CARTESIAN_POINT('Ctrl Pts',(-72.6026336941378,-3.5077364905931,
136.865220751771));
#196554=CARTESIAN_POINT('Ctrl Pts',(-72.8810813179508,3.20315602899298,
137.031561618638));
#196555=CARTESIAN_POINT('Ctrl Pts',(-73.1595289417638,6.97050464080582,
131.475408981201));
#196556=CARTESIAN_POINT('Ctrl Pts',(-73.4379765655765,4.33230001580124,
125.302595680118));
#196557=CARTESIAN_POINT('Ctrl Pts',(-73.7164241893894,-2.28707667910305,
124.18563558039));
#196558=CARTESIAN_POINT('Ctrl Pts',(-73.9948718132024,-6.80474163581863,
129.150960447132));
#196559=CARTESIAN_POINT('Ctrl Pts',(-74.2733194370152,-5.0691814593271,
135.635679297414));
#196560=CARTESIAN_POINT('Ctrl Pts',(-74.5517670608282,1.32470883500465,
137.680652303954));
#196561=CARTESIAN_POINT('Ctrl Pts',(-74.830214684641,6.5012564255912,133.406649176227));
#196562=CARTESIAN_POINT('Ctrl Pts',(-75.108662308454,5.70346696509291,126.741269991954));
#196563=CARTESIAN_POINT('Ctrl Pts',(-75.3871099322667,-0.335530006474783,
123.809672599606));
#196564=CARTESIAN_POINT('Ctrl Pts',(-75.6655575560798,-6.06619129364391,
127.305851786256));
#196565=CARTESIAN_POINT('Ctrl Pts',(-75.9440051798925,-6.22231913187452,
134.016989677222));
#196566=CARTESIAN_POINT('Ctrl Pts',(-76.2224528037055,-0.66043966510086,
137.775878408018));
#196567=CARTESIAN_POINT('Ctrl Pts',(-76.5009004275184,5.50835158962877,
135.128282866967));
#196568=CARTESIAN_POINT('Ctrl Pts',(-76.7793480513312,6.61523683142527,
128.507214014061));
#196569=CARTESIAN_POINT('Ctrl Pts',(-77.0577956751442,1.64304259742666,
123.997110667925));
#196570=CARTESIAN_POINT('Ctrl Pts',(-77.336243298957,-4.83902751651344,
125.742537472861));
#196571=CARTESIAN_POINT('Ctrl Pts',(-77.6146909227699,-6.87426774241415,
132.139532463972));
#196572=CARTESIAN_POINT('Ctrl Pts',(-77.8931385465828,-2.59239173968542,
137.309569755007));
#196573=CARTESIAN_POINT('Ctrl Pts',(-78.1715861703958,4.07176562643718,
136.501637645866));
#196574=CARTESIAN_POINT('Ctrl Pts',(-78.4500337942086,6.99416929867323,
130.458186275174));
#196575=CARTESIAN_POINT('Ctrl Pts',(-78.7284814180215,3.48927306959449,
124.732852213582));
#196576=CARTESIAN_POINT('Ctrl Pts',(-79.0069290418344,-3.22209464997582,
124.586937765577));
#196577=CARTESIAN_POINT('Ctrl Pts',(-79.2853766656473,-6.97251479429268,
130.154531180556));
#196578=CARTESIAN_POINT('Ctrl Pts',(-79.5638242894601,-4.3155344689392,
136.319286102215));
#196579=CARTESIAN_POINT('Ctrl Pts',(-79.8422719132732,2.30721120779087,
137.416093922569));
#196580=CARTESIAN_POINT('Ctrl Pts',(-80.1207195370859,6.80974249809405,
132.437041836753));
#196581=CARTESIAN_POINT('Ctrl Pts',(-80.3991671608989,5.0544531070646,125.957635471416));
#196582=CARTESIAN_POINT('Ctrl Pts',(-80.6776147847117,-1.34563176559565,
123.932132739704));
#196583=CARTESIAN_POINT('Ctrl Pts',(-80.9560624085247,-6.50914678343976,
128.221871700751));
#196584=CARTESIAN_POINT('Ctrl Pts',(-81.2345100323374,-5.69107389680138,
134.884791814753));
#196585=CARTESIAN_POINT('Ctrl Pts',(-81.5129576561506,0.356817876581242,
137.797994998686));
#196586=CARTESIAN_POINT('Ctrl Pts',(-81.7914052799631,6.07681145290804,
134.284389844403));
#196587=CARTESIAN_POINT('Ctrl Pts',(-82.0698529037763,6.21251217275584,
127.572807839535));
#196588=CARTESIAN_POINT('Ctrl Pts',(-82.348300527589,0.639217703933302,
123.830864967548));
#196589=CARTESIAN_POINT('Ctrl Pts',(-82.626748151402,-5.52148660728364,
126.497223923725));
#196590=CARTESIAN_POINT('Ctrl Pts',(-82.9051957752149,-6.60821446602265,
133.121631086217));
#196591=CARTESIAN_POINT('Ctrl Pts',(-83.1836433990278,-1.62231605971109,
137.616579892973));
#196592=CARTESIAN_POINT('Ctrl Pts',(-83.4620910228406,4.85441155092967,
135.851431981043));
#196593=CARTESIAN_POINT('Ctrl Pts',(-83.7405386466535,6.87017209745416,
129.448272049221));
#196594=CARTESIAN_POINT('Ctrl Pts',(-84.0189862704665,2.57258011298421,
124.291291263097));
#196595=CARTESIAN_POINT('Ctrl Pts',(-84.2974338942792,-4.08908731779306,
125.119503032603));
#196596=CARTESIAN_POINT('Ctrl Pts',(-84.5758815180923,-6.99308326653956,
131.171821201958));
#196597=CARTESIAN_POINT('Ctrl Pts',(-84.8543291419051,-3.47077732444568,
136.886461045702));
#196598=CARTESIAN_POINT('Ctrl Pts',(-85.132776765718,3.2410034219148,137.011947723114));
#196599=CARTESIAN_POINT('Ctrl Pts',(-85.4112243895309,6.97446035535538,
131.432965108015));
#196600=CARTESIAN_POINT('Ctrl Pts',(-85.6896720133437,4.29872894355427,
125.27632567523));
#196601=CARTESIAN_POINT('Ctrl Pts',(-85.9681196371569,-2.327324362789,124.19968029493));
#196602=CARTESIAN_POINT('Ctrl Pts',(-86.2465672609694,-6.81468027584547,
129.192413474561));
#196603=CARTESIAN_POINT('Ctrl Pts',(-86.5250148847825,-5.03967793103904,
135.666447330617));
#196604=CARTESIAN_POINT('Ctrl Pts',(-86.8034625085954,1.36654223043768,
137.672461023519));
#196605=CARTESIAN_POINT('Ctrl Pts',(-87.0819101324082,6.51697684144191,
133.367025968708));
#196606=CARTESIAN_POINT('Ctrl Pts',(-87.3603577562212,5.67862810717874,
126.706626649358));
#196607=CARTESIAN_POINT('Ctrl Pts',(-87.638805380034,-0.378102441176264,
123.811844661359));
#196608=CARTESIAN_POINT('Ctrl Pts',(-87.917253003847,-6.08737531742114,
127.342843233717));
#196609=CARTESIAN_POINT('Ctrl Pts',(-88.1957006276599,-6.20264766177327,
134.054807177307));
#196610=CARTESIAN_POINT('Ctrl Pts',(-88.4741482514726,-0.617989821139493,
137.779769525637));
#196611=CARTESIAN_POINT('Ctrl Pts',(-88.7525958752857,5.53457047463998,
135.094671855119));
#196612=CARTESIAN_POINT('Ctrl Pts',(-89.0310434990984,6.6011308830247,128.466987750645));
#196613=CARTESIAN_POINT('Ctrl Pts',(-89.3094911229114,1.60157449308101,
123.987235123859));
#196614=CARTESIAN_POINT('Ctrl Pts',(-89.5879387467241,-4.86975061474005,
125.772087790693));
#196615=CARTESIAN_POINT('Ctrl Pts',(-89.8663863705374,-6.8660128081587,
132.181353345229));
#196616=CARTESIAN_POINT('Ctrl Pts',(-90.1448339943499,-2.55274465425183,
137.325229852876));
#196617=CARTESIAN_POINT('Ctrl Pts',(-90.4232816181632,4.10637112840284,
136.476746095445));
#196618=CARTESIAN_POINT('Ctrl Pts',(-90.7017292419757,6.99193245143733,
130.415617195278));
#196619=CARTESIAN_POINT('Ctrl Pts',(-90.9801768657889,3.45224942649073,
124.711724509022));
#196620=CARTESIAN_POINT('Ctrl Pts',(-91.2586244896016,-3.2598821696406,
124.606666764696));
#196621=CARTESIAN_POINT('Ctrl Pts',(-91.5370721134145,-6.97634130596949,
130.196986896981));
#196622=CARTESIAN_POINT('Ctrl Pts',(-91.8155197372274,-4.28188359533257,
136.345453806627));
#196623=CARTESIAN_POINT('Ctrl Pts',(-92.0939673610402,2.34741595777304,
137.401926772977));
#196624=CARTESIAN_POINT('Ctrl Pts',(-92.3724149848533,6.81955492332935,
132.395558751529));
#196625=CARTESIAN_POINT('Ctrl Pts',(-92.650862608666,5.02485606812542,125.926957379319));
#196626=CARTESIAN_POINT('Ctrl Pts',(-92.929310232479,-1.38744003581995,
123.940451308663));
#196627=CARTESIAN_POINT('Ctrl Pts',(-93.2077578562919,-6.52474652706058,
128.261542572277));
#196628=CARTESIAN_POINT('Ctrl Pts',(-93.4862054801047,-5.66612971152105,
134.919359395943));
#196629=CARTESIAN_POINT('Ctrl Pts',(-93.7646531039176,0.39938350308132,
137.795693371147));
#196630=CARTESIAN_POINT('Ctrl Pts',(-94.0431007277306,6.09788278932073,
134.247334091402));
#196631=CARTESIAN_POINT('Ctrl Pts',(-94.3215483515434,6.19272569030992,
127.535050387806));
#196632=CARTESIAN_POINT('Ctrl Pts',(-94.5999959753563,0.596756213373149,
123.827103070676));
#196633=CARTESIAN_POINT('Ctrl Pts',(-94.8784435991693,-5.54760307049237,
126.530914581157));
#196634=CARTESIAN_POINT('Ctrl Pts',(-95.1568912229821,-6.59398614805128,
133.161814229653));
#196635=CARTESIAN_POINT('Ctrl Pts',(-95.4353388467949,-1.58081808968337,
137.626329176652));
#196636=CARTESIAN_POINT('Ctrl Pts',(-95.7137864706081,4.88504456584684,
135.821788289543));
#196637=CARTESIAN_POINT('Ctrl Pts',(-95.9922340944205,6.86178991305786,
129.406476486855));
#196638=CARTESIAN_POINT('Ctrl Pts',(-96.2706817182339,2.53288554724217,
124.275751909854));
#196639=CARTESIAN_POINT('Ctrl Pts',(-96.5491293420464,-4.12361689815126,
125.144499794972));
#196640=CARTESIAN_POINT('Ctrl Pts',(-96.8275769658595,-6.99071686402826,
131.214383276482));
#196641=CARTESIAN_POINT('Ctrl Pts',(-97.1060245896722,-3.4336895473684,
136.907475965166));
#196642=CARTESIAN_POINT('Ctrl Pts',(-97.3844722134854,3.27873071826322,
136.992103803166));
#196643=CARTESIAN_POINT('Ctrl Pts',(-97.6629198372979,6.9781576287114,131.390497941658));
#196644=CARTESIAN_POINT('Ctrl Pts',(-97.9413674611112,4.26499858032525,
125.250260513709));
#196645=CARTESIAN_POINT('Ctrl Pts',(-98.2198150849237,-2.36748580661544,
124.21396974833));
#196646=CARTESIAN_POINT('Ctrl Pts',(-98.498262708737,-6.82436639538843,
129.233926233285));
#196647=CARTESIAN_POINT('Ctrl Pts',(-98.7767103325495,-5.00998765563179,
135.69703519741));
#196648=CARTESIAN_POINT('Ctrl Pts',(-99.0551579563628,1.40832498814648,
137.664015243098));
#196649=CARTESIAN_POINT('Ctrl Pts',(-99.3336055801754,6.53245576831905,
133.327307800681));
#196650=CARTESIAN_POINT('Ctrl Pts',(-99.6120532039884,5.65357882561176,
126.672135149802));
#196651=CARTESIAN_POINT('Ctrl Pts',(-99.8905008278013,-0.420660865152761,
123.814275833361));
#196652=CARTESIAN_POINT('Ctrl Pts',(-100.168948451614,-6.10833377126732,
127.379962948978));
#196653=CARTESIAN_POINT('Ctrl Pts',(-100.447396075427,-6.18274635028192,
134.092504230901));
#196654=CARTESIAN_POINT('Ctrl Pts',(-100.72584369924,-0.575517077338011,
137.783402166914));
#196655=CARTESIAN_POINT('Ctrl Pts',(-101.004291323053,5.56058427410689,
135.060901864211));
#196656=CARTESIAN_POINT('Ctrl Pts',(-101.282738946866,6.58678032729173,
128.426848099441));
#196657=CARTESIAN_POINT('Ctrl Pts',(-101.561186570679,1.56004704180311,
123.977612190885));
#196658=CARTESIAN_POINT('Ctrl Pts',(-101.839634194492,-4.90029326256724,
125.801824581246));
#196659=CARTESIAN_POINT('Ctrl Pts',(-102.118081818304,-6.85750345127332,
132.223123201514));
#196660=CARTESIAN_POINT('Ctrl Pts',(-102.396529442117,-2.51300297592632,
137.340648317539));
#196661=CARTESIAN_POINT('Ctrl Pts',(-102.67497706593,4.14082446727623,136.451644352694));
#196662=CARTESIAN_POINT('Ctrl Pts',(-102.953424689743,6.98943651557314,
130.373062520413));
#196663=CARTESIAN_POINT('Ctrl Pts',(-103.231872313556,3.41509785901489,
124.690822569333));
#196664=CARTESIAN_POINT('Ctrl Pts',(-103.510319937369,-3.29754889317273,
124.626625421641));
#196665=CARTESIAN_POINT('Ctrl Pts',(-103.788767561182,-6.97990930675369,
130.239465119861));
#196666=CARTESIAN_POINT('Ctrl Pts',(-104.067215184995,-4.24807405495459,
136.371416183792));
#196667=CARTESIAN_POINT('Ctrl Pts',(-104.345662808808,2.38753372339306,
137.387515148146));
#196668=CARTESIAN_POINT('Ctrl Pts',(-104.62411043262,6.82911464744894,132.354016703874));
#196669=CARTESIAN_POINT('Ctrl Pts',(-104.902558056433,4.99507283129728,
125.896460021193));
#196670=CARTESIAN_POINT('Ctrl Pts',(-105.181005680246,-1.42919689394351,
123.949024222305));
#196671=CARTESIAN_POINT('Ctrl Pts',(-105.459453304059,-6.54010449379936,
128.301307668861));
#196672=CARTESIAN_POINT('Ctrl Pts',(-105.737900927872,-5.64097556572054,
134.953774494342));
#196673=CARTESIAN_POINT('Ctrl Pts',(-106.016348551685,0.441934330278796,
137.793132677202));
#196674=CARTESIAN_POINT('Ctrl Pts',(-106.294796175498,6.11872816644418,
134.210150757753));
#196675=CARTESIAN_POINT('Ctrl Pts',(-106.573243799311,6.17270973413615,
127.49741408157));
#196676=CARTESIAN_POINT('Ctrl Pts',(-106.851691423124,0.554272609792058,
123.823599718647));
#196677=CARTESIAN_POINT('Ctrl Pts',(-107.130139046936,-5.57351396522919,
126.564763592701));
#196678=CARTESIAN_POINT('Ctrl Pts',(-107.40858667075,-6.57951348749827,
133.201910016778));
#196679=CARTESIAN_POINT('Ctrl Pts',(-107.687034294562,-1.53926154185996,
137.635825669776));
#196680=CARTESIAN_POINT('Ctrl Pts',(-107.965481918375,4.91549656364115,
135.791958675416));
#196681=CARTESIAN_POINT('Ctrl Pts',(-108.243929542188,6.85315346251289,
129.364732723601));
#196682=CARTESIAN_POINT('Ctrl Pts',(-108.522377166001,2.49309712449469,
124.260454476607));
#196683=CARTESIAN_POINT('Ctrl Pts',(-108.800824789814,-4.15799367636883,
125.169706285567));
#196684=CARTESIAN_POINT('Ctrl Pts',(-109.079272413627,-6.98809141793296,
131.256930157466));
#196685=CARTESIAN_POINT('Ctrl Pts',(-109.35772003744,-3.39647453366164,
136.928264731447));
#196686=CARTESIAN_POINT('Ctrl Pts',(-109.636167661252,3.31633652003941,
136.97203059412));
#196687=CARTESIAN_POINT('Ctrl Pts',(-109.914615285065,6.98159632387027,
131.348009055767));
#196688=CARTESIAN_POINT('Ctrl Pts',(-110.193062908878,4.23111017600536,
125.22440116141));
#196689=CARTESIAN_POINT('Ctrl Pts',(-110.471510532691,-2.40755952238467,
124.228503411086));
#196690=CARTESIAN_POINT('Ctrl Pts',(-110.749958156504,-6.83379963552497,
129.275497185033));
#196691=CARTESIAN_POINT('Ctrl Pts',(-111.028405780317,-4.98011173328953,
135.727441764346));
#196692=CARTESIAN_POINT('Ctrl Pts',(-111.30685340413,1.45005555985492,137.655315275653));
#196693=CARTESIAN_POINT('Ctrl Pts',(-111.585301027943,6.54769263264538,
133.287496143919));
#196694=CARTESIAN_POINT('Ctrl Pts',(-111.863748651756,5.62832004860235,
126.63779677138));
#196695=CARTESIAN_POINT('Ctrl Pts',(-112.142196275568,-0.463203701385527,
123.816966025527));
#196696=CARTESIAN_POINT('Ctrl Pts',(-112.420643899382,-6.12906587855929,
127.417209556553));
#196697=CARTESIAN_POINT('Ctrl Pts',(-112.699091523194,-6.16261593485082,
134.130079441122));
#196698=CARTESIAN_POINT('Ctrl Pts',(-112.977539147007,-0.533023007539609,
137.786776197239));
#196699=CARTESIAN_POINT('Ctrl Pts',(-113.25598677082,5.58639202407863,135.026974145601));
#196700=CARTESIAN_POINT('Ctrl Pts',(-113.534434394633,6.57218569599142,
128.386796547837));
#196701=CARTESIAN_POINT('Ctrl Pts',(-113.812882018446,1.5184617824084,123.968242225583));
#196702=CARTESIAN_POINT('Ctrl Pts',(-114.091329642259,-4.93065432822552,
125.831746742611));
#196703=CARTESIAN_POINT('Ctrl Pts',(-114.369777266072,-6.84873998707567,
132.26484048503));
#196704=CARTESIAN_POINT('Ctrl Pts',(-114.648224889884,-2.4731681773514,
137.355824577657));
#196705=CARTESIAN_POINT('Ctrl Pts',(-114.926672513697,4.17512436637621,
136.426333347767));
#196706=CARTESIAN_POINT('Ctrl Pts',(-115.20512013751,6.98668158356849,130.330523827459));
#196707=CARTESIAN_POINT('Ctrl Pts',(-115.483567761323,3.377819743832,124.670147169045));
#196708=CARTESIAN_POINT('Ctrl Pts',(-115.762015385136,-3.33509342481799,
124.646812996834));
#196709=CARTESIAN_POINT('Ctrl Pts',(-116.040463008949,-6.98321866443162,
130.281964275151));
#196710=CARTESIAN_POINT('Ctrl Pts',(-116.318910632762,-4.21410710063033,
136.397172271667));
#196711=CARTESIAN_POINT('Ctrl Pts',(-116.597358256575,2.42756301807353,
137.372859582102));
#196712=CARTESIAN_POINT('Ctrl Pts',(-116.875805880388,6.83842131621399,
132.312417233142));
#196713=CARTESIAN_POINT('Ctrl Pts',(-117.154253504201,4.96510450020791,
125.866144527128));
#196714=CARTESIAN_POINT('Ctrl Pts',(-117.432701128013,-1.47090079265054,
123.957851162959));
#196715=CARTESIAN_POINT('Ctrl Pts',(-117.711148751826,-6.55522011456102,
128.341165516992));
#196716=CARTESIAN_POINT('Ctrl Pts',(-117.989596375639,-5.61561239149597,
134.988035834682));
#196717=CARTESIAN_POINT('Ctrl Pts',(-118.268043999452,0.484468781437156,
137.790313011739));
#196718=CARTESIAN_POINT('Ctrl Pts',(-118.546491623265,6.13934681184524,
134.172841221298));
#196719=CARTESIAN_POINT('Ctrl Pts',(-118.824939247078,6.15246504593319,
127.459900315453));
#196720=CARTESIAN_POINT('Ctrl Pts',(-119.103386870891,0.511768467435545,
123.820355041281));
#196721=CARTESIAN_POINT('Ctrl Pts',(-119.381834494704,-5.59921833135585,
126.598769704074));
#196722=CARTESIAN_POINT('Ctrl Pts',(-119.660282118516,-6.56479702065358,
133.241916961827));
#196723=CARTESIAN_POINT('Ctrl Pts',(-119.93872974233,-1.49764795613459,
137.645069020452));
#196724=CARTESIAN_POINT('Ctrl Pts',(-120.217177366142,4.94576641590264,
135.761944244007));
#196725=CARTESIAN_POINT('Ctrl Pts',(-120.495624989955,6.84426306584611,
129.323042306287));
#196726=CARTESIAN_POINT('Ctrl Pts',(-120.774072613768,2.45321631911644,
124.245399530209));
#196727=CARTESIAN_POINT('Ctrl Pts',(-121.052520237581,-4.19221637860163,
125.195121570349));
#196728=CARTESIAN_POINT('Ctrl Pts',(-121.330967861394,-6.98520702554029,
131.299460268319));
#196729=CARTESIAN_POINT('Ctrl Pts',(-121.609415485207,-3.35913366234199,
136.948826574209));
#196730=CARTESIAN_POINT('Ctrl Pts',(-121.88786310902,3.3538194337463,136.951728839794));
#196731=CARTESIAN_POINT('Ctrl Pts',(-122.166310732833,6.98477631340985,
131.305500024783));
#196732=CARTESIAN_POINT('Ctrl Pts',(-122.444758356646,4.19706498634193,
125.198748576561));
#196733=CARTESIAN_POINT('Ctrl Pts',(-122.723205980458,-2.44754402515043,
124.24328074465));
#196734=CARTESIAN_POINT('Ctrl Pts',(-123.001653604271,-6.84297964670285,
129.317124789377));
#196735=CARTESIAN_POINT('Ctrl Pts',(-123.280101228084,-4.95005127107555,
135.7576659047));
#196736=CARTESIAN_POINT('Ctrl Pts',(-123.558548851897,1.49173239922134,
137.646361443563));
#196737=CARTESIAN_POINT('Ctrl Pts',(-123.83699647571,6.5626868698133,133.247592473656));
#196738=CARTESIAN_POINT('Ctrl Pts',(-124.115444099523,5.60285271212367,
126.603612786514));
#196739=CARTESIAN_POINT('Ctrl Pts',(-124.393891723336,-0.505729373435472,
123.819915138168));
#196740=CARTESIAN_POINT('Ctrl Pts',(-124.672339347149,-6.14957087106115,
127.454581676257));
#196741=CARTESIAN_POINT('Ctrl Pts',(-124.950786970961,-6.14225716141998,
134.167531415611));
#196742=CARTESIAN_POINT('Ctrl Pts',(-125.229234594775,-0.490509186377616,
137.789891491587));
#196743=CARTESIAN_POINT('Ctrl Pts',(-125.507682218587,5.6119927682395,134.992889956494));
#196744=CARTESIAN_POINT('Ctrl Pts',(-125.786129842401,6.55734752993325,
128.346834579959));
#196745=CARTESIAN_POINT('Ctrl Pts',(-126.064577466213,1.47682025585389,
123.959125575163));
#196746=CARTESIAN_POINT('Ctrl Pts',(-126.343025090026,-4.9608326866744,
125.861853166013));
#196747=CARTESIAN_POINT('Ctrl Pts',(-126.621472713839,-6.8397227402992,
132.306503649927));
#196748=CARTESIAN_POINT('Ctrl Pts',(-126.899920337652,-2.43324173462049,
137.370758070868));
#196749=CARTESIAN_POINT('Ctrl Pts',(-127.178367961465,4.20926955470684,
136.400814018573));
#196750=CARTESIAN_POINT('Ctrl Pts',(-127.456815585278,6.98366775750873,
130.288002692701));
#196751=CARTESIAN_POINT('Ctrl Pts',(-127.73526320909,3.34041646229627,124.649699074291));
#196752=CARTESIAN_POINT('Ctrl Pts',(-128.013710832904,-3.37251437334987,
124.66722874222));
#196753=CARTESIAN_POINT('Ctrl Pts',(-128.292158456716,-6.9862692563739,
130.324482788031));
#196754=CARTESIAN_POINT('Ctrl Pts',(-128.570606080529,-4.17998399101771,
136.422721115849));
#196755=CARTESIAN_POINT('Ctrl Pts',(-128.849053704342,2.46750235851359,
137.357960617914));
#196756=CARTESIAN_POINT('Ctrl Pts',(-129.127501328155,6.84747458476236,
132.270761880817));
#196757=CARTESIAN_POINT('Ctrl Pts',(-129.405948951968,4.93495218534535,
125.836012020477));
#196758=CARTESIAN_POINT('Ctrl Pts',(-129.684396575781,-1.51255018658779,
123.966931803538));
#196759=CARTESIAN_POINT('Ctrl Pts',(-129.962844199593,-6.57009282923063,
128.381114639724));
#196760=CARTESIAN_POINT('Ctrl Pts',(-130.241291823406,-5.59004112868908,
135.022142147398));
#196761=CARTESIAN_POINT('Ctrl Pts',(-130.519739447219,0.52698528042665,
137.78723447924));
#196762=CARTESIAN_POINT('Ctrl Pts',(-130.798187071032,6.15973796149245,
134.135406864555));
#196763=CARTESIAN_POINT('Ctrl Pts',(-131.076634694845,6.13199237587537,
127.422510479544));
#196764=CARTESIAN_POINT('Ctrl Pts',(-131.355082318658,0.4692453613103,123.81736915881));
#196765=CARTESIAN_POINT('Ctrl Pts',(-131.633529942471,-5.62471521638866,
126.632931655165));
#196766=CARTESIAN_POINT('Ctrl Pts',(-131.911977566284,-6.54983729284086,
133.281833582332));
#196767=CARTESIAN_POINT('Ctrl Pts',(-132.190425190097,-1.45597887451291,
137.654058886162));
#196768=CARTESIAN_POINT('Ctrl Pts',(-132.46887281391,4.97585300097076,135.731746107516));
#196769=CARTESIAN_POINT('Ctrl Pts',(-132.747320437723,6.83511905249447,
129.281406779768));
#196770=CARTESIAN_POINT('Ctrl Pts',(-133.025768061535,2.4132446089053,124.230587628526));
#196771=CARTESIAN_POINT('Ctrl Pts',(-133.304215685348,-4.22628373671482,
125.220744707546));
#196772=CARTESIAN_POINT('Ctrl Pts',(-133.582663309161,-6.98206379373247,
131.341972033073));
#196773=CARTESIAN_POINT('Ctrl Pts',(-133.861110932974,-3.32166831708915,
136.969160731525));
#196774=CARTESIAN_POINT('Ctrl Pts',(-134.139558556787,3.39117807044069,
136.931199292478));
#196775=CARTESIAN_POINT('Ctrl Pts',(-134.4180061806,6.98769747949419,131.262972423894));
#196776=CARTESIAN_POINT('Ctrl Pts',(-134.696453804413,4.16286427289247,
125.173303709728));
#196777=CARTESIAN_POINT('Ctrl Pts',(-134.974901428226,-2.48743783327188,
124.25830120144));
#196778=CARTESIAN_POINT('Ctrl Pts',(-135.253349052039,-6.85190608875344,
129.358807503792));
#196779=CARTESIAN_POINT('Ctrl Pts',(-135.531796675851,-4.91980738289134,
135.787706498505));
#196780=CARTESIAN_POINT('Ctrl Pts',(-135.810244299665,1.53335396189511,
137.637154078616));
#196781=CARTESIAN_POINT('Ctrl Pts',(-136.088691923477,6.57743792420584,
133.207598268539));
#196782=CARTESIAN_POINT('Ctrl Pts',(-136.36713954729,5.57717775987727,126.569584461903));
#196783=CARTESIAN_POINT('Ctrl Pts',(-136.645587171103,-0.548236305497475,
123.823123062006));
#196784=CARTESIAN_POINT('Ctrl Pts',(-136.924034794916,-6.1698479889529,
127.492077923251));
#196785=CARTESIAN_POINT('Ctrl Pts',(-137.202482418729,-6.12167078439119,
134.204858766568));
#196786=CARTESIAN_POINT('Ctrl Pts',(-137.480930042542,-0.447977189217358,
137.792747934521));
#196787=CARTESIAN_POINT('Ctrl Pts',(-137.759377666354,5.63738555794455,
134.958650559891));
#196788=CARTESIAN_POINT('Ctrl Pts',(-138.037825290167,6.54226637895086,
128.306963676612));
#196789=CARTESIAN_POINT('Ctrl Pts',(-138.31627291398,1.43512400518173,123.950262577445));
#196790=CARTESIAN_POINT('Ctrl Pts',(-138.594720537793,-4.99082721964375,
125.892142735845));
#196791=CARTESIAN_POINT('Ctrl Pts',(-138.873168161606,-6.83045204508126,
132.348111152362));
#196792=CARTESIAN_POINT('Ctrl Pts',(-139.151615785419,-2.39322512722196,
137.385448243807));
#196793=CARTESIAN_POINT('Ctrl Pts',(-139.430063409232,4.24325876700673,
136.375087310741));
#196794=CARTESIAN_POINT('Ctrl Pts',(-139.708511033045,6.98039514907165,
130.245500691775));
#196795=CARTESIAN_POINT('Ctrl Pts',(-139.986958656858,3.30288940040013,
124.629479042785));
#196796=CARTESIAN_POINT('Ctrl Pts',(-140.26540628067,-3.40981035212143,
124.687871901284));
#196797=CARTESIAN_POINT('Ctrl Pts',(-140.543853904484,-6.98906096953965,
130.36701908296));
#196798=CARTESIAN_POINT('Ctrl Pts',(-140.822301528296,-4.1457059905611,
136.448061769617));
#196799=CARTESIAN_POINT('Ctrl Pts',(-141.100749152109,2.50735026474636,
137.342818807668));
#196800=CARTESIAN_POINT('Ctrl Pts',(-141.379196775922,6.85627411762182,
132.229052190456));
#196801=CARTESIAN_POINT('Ctrl Pts',(-141.657644399735,4.90461700401472,
125.80606361781));
#196802=CARTESIAN_POINT('Ctrl Pts',(-141.936092023548,-1.5541435324211,
123.976265807557));
#196803=CARTESIAN_POINT('Ctrl Pts',(-142.214539647361,-6.58472208669408,
128.421153556726));
#196804=CARTESIAN_POINT('Ctrl Pts',(-142.492987271174,-5.56426272485295,
135.056092168669));
#196805=CARTESIAN_POINT('Ctrl Pts',(-142.771434894987,0.569482251782813,
137.783897193782));
#196806=CARTESIAN_POINT('Ctrl Pts',(-143.0498825188,6.17990085978423,134.097849074668));
#196807=CARTESIAN_POINT('Ctrl Pts',(-143.328330142612,6.11129248258502,
127.385245959334));
#196808=CARTESIAN_POINT('Ctrl Pts',(-143.606777766425,0.426704867125613,
123.814642181877));
#196809=CARTESIAN_POINT('Ctrl Pts',(-143.885225390238,-5.65000367553061,
126.667248180088));
#196810=CARTESIAN_POINT('Ctrl Pts',(-144.163673014051,-6.53463485839856,
133.321658399163));
#196811=CARTESIAN_POINT('Ctrl Pts',(-144.442120637864,-1.4142558410586,
137.662794933783));
#196812=CARTESIAN_POINT('Ctrl Pts',(-144.720568261677,5.00575520397605,
135.701365384942));
#196813=CARTESIAN_POINT('Ctrl Pts',(-144.99901588549,6.82572176129271,129.239827686864));
#196814=CARTESIAN_POINT('Ctrl Pts',(-145.277463509303,2.37318347502772,
124.216019320419));
#196815=CARTESIAN_POINT('Ctrl Pts',(-145.555911133116,-4.26019448832994,
125.246574747685));
#196816=CARTESIAN_POINT('Ctrl Pts',(-145.834358756928,-6.97866183898313,
131.384463876438));
#196817=CARTESIAN_POINT('Ctrl Pts',(-146.112806380741,-3.28407988619528,
136.989266449907));
#196818=CARTESIAN_POINT('Ctrl Pts',(-146.391254004554,3.42841104578457,
136.910442712901));
#196819=CARTESIAN_POINT('Ctrl Pts',(-146.669701628367,6.99035971387901,
131.220427828976));
#196820=CARTESIAN_POINT('Ctrl Pts',(-146.94814925218,4.12850930297597,125.148067503779));
#196821=CARTESIAN_POINT('Ctrl Pts',(-147.226596875993,-2.52723946847004,
124.27356422487));
#196822=CARTESIAN_POINT('Ctrl Pts',(-147.505044499806,-6.86057863090408,
129.400543783708));
#196823=CARTESIAN_POINT('Ctrl Pts',(-147.783492123619,-4.88938118943532,
135.817562432597));
#196824=CARTESIAN_POINT('Ctrl Pts',(-148.061939747432,1.57491870557395,
137.627693521995));
#196825=CARTESIAN_POINT('Ctrl Pts',(-148.340387371245,6.5919452492172,133.167515010566));
#196826=CARTESIAN_POINT('Ctrl Pts',(-148.618834995057,5.55129614325799,
126.535713058481));
#196827=CARTESIAN_POINT('Ctrl Pts',(-148.89728261887,-0.590722922461593,
123.826589678167));
#196828=CARTESIAN_POINT('Ctrl Pts',(-149.175730242683,-6.18989648085842,
127.529696908099));
#196829=CARTESIAN_POINT('Ctrl Pts',(-149.454177866496,-6.10085756660025,
134.242060110815));
#196830=CARTESIAN_POINT('Ctrl Pts',(-149.732625490309,-0.405428592098244,
137.795345420191));
#196831=CARTESIAN_POINT('Ctrl Pts',(-150.011073114122,5.66256945225453,
134.924257224548));
#196832=CARTESIAN_POINT('Ctrl Pts',(-150.289520737935,6.52694280188189,
128.267185315226));
#196833=CARTESIAN_POINT('Ctrl Pts',(-150.567968361748,1.39337457546175,
123.94165356085));
#196834=CARTESIAN_POINT('Ctrl Pts',(-150.84641598556,-5.02063681567507,
125.922614329717));
#196835=CARTESIAN_POINT('Ctrl Pts',(-151.124863609373,-6.8209282449509,
132.389661450552));
#196836=CARTESIAN_POINT('Ctrl Pts',(-151.403311233186,-2.35311983798619,
137.399894552124));
#196837=CARTESIAN_POINT('Ctrl Pts',(-151.681758856999,4.2770907437925,136.349154177582));
#196838=CARTESIAN_POINT('Ctrl Pts',(-151.960206480812,6.97686387952531,
130.20301939961));
#196839=CARTESIAN_POINT('Ctrl Pts',(-152.238654104625,3.26523994872261,
124.609487823786));
#196840=CARTESIAN_POINT('Ctrl Pts',(-152.517101728438,-3.44697997911642,
124.708741709087));
#196841=CARTESIAN_POINT('Ctrl Pts',(-152.795549352251,-6.99159370048095,
130.40957158374));
#196842=CARTESIAN_POINT('Ctrl Pts',(-153.073996976064,-4.11127436944443,
136.473193293963));
#196843=CARTESIAN_POINT('Ctrl Pts',(-153.352444599876,2.54710526019297,
137.327434712448));
#196844=CARTESIAN_POINT('Ctrl Pts',(-153.63089222369,6.86481958872245,132.187289707623));
#196845=CARTESIAN_POINT('Ctrl Pts',(-153.909339847502,4.87410008029735,
125.776300428876));
#196846=CARTESIAN_POINT('Ctrl Pts',(-154.187787471315,-1.5956792888948,
123.98585282914));
#196847=CARTESIAN_POINT('Ctrl Pts',(-154.466235095128,-6.5991073448593,
128.461280784342));
#196848=CARTESIAN_POINT('Ctrl Pts',(-154.744682718941,-5.53827813521478,
135.089884640464));
#196849=CARTESIAN_POINT('Ctrl Pts',(-155.023130342754,0.611958120764675,
137.78030127903));
#196850=CARTESIAN_POINT('Ctrl Pts',(-155.301577966567,6.19983475957701,
134.060169243357));
#196851=CARTESIAN_POINT('Ctrl Pts',(-155.58002559038,6.0903661331043,127.348108135675));
#196852=CARTESIAN_POINT('Ctrl Pts',(-155.858473214192,0.38414856123516,
123.812174211531));
#196853=CARTESIAN_POINT('Ctrl Pts',(-156.136920838005,-5.67508277170857,
126.701718007236));
#196854=CARTESIAN_POINT('Ctrl Pts',(-156.415368461818,-6.51919028065846,
133.3613899366));
#196855=CARTESIAN_POINT('Ctrl Pts',(-156.693816085631,-1.37248040183399,
137.671276839599));
#196856=CARTESIAN_POINT('Ctrl Pts',(-156.972263709444,5.03547191688086,
135.670803202055));
#196857=CARTESIAN_POINT('Ctrl Pts',(-157.250711333257,6.81607154046107,
129.198306568304));
#196858=CARTESIAN_POINT('Ctrl Pts',(-157.52915895707,2.33303440196427,124.201695145721));
#196859=CARTESIAN_POINT('Ctrl Pts',(-157.807606580883,-4.29394737687161,
125.272610733624));
#196860=CARTESIAN_POINT('Ctrl Pts',(-158.086054204696,-6.97500128735293,
131.426934223863));
#196861=CARTESIAN_POINT('Ctrl Pts',(-158.364501828508,-3.2463697625135,
137.009142984327));
#196862=CARTESIAN_POINT('Ctrl Pts',(-158.642949452322,3.46551698009634,
136.889459870208));
#196863=CARTESIAN_POINT('Ctrl Pts',(-158.921397076134,6.99276291791392,
131.177867816534));
#196864=CARTESIAN_POINT('Ctrl Pts',(-159.199844699947,4.09400134962899,
125.123040893851));
#196865=CARTESIAN_POINT('Ctrl Pts',(-159.47829232376,-2.56694745588028,
124.289069249361));
#196866=CARTESIAN_POINT('Ctrl Pts',(-159.756739947573,-6.86899695179061,
129.442332082575));
#196867=CARTESIAN_POINT('Ctrl Pts',(-160.035187571386,-4.85877381816122,
135.84723260065));
#196868=CARTESIAN_POINT('Ctrl Pts',(-160.313635195198,1.61642509006095,
137.617980124263));
#196869=CARTESIAN_POINT('Ctrl Pts',(-160.592082819012,6.60620830727321,
133.12734418504));
#196870=CARTESIAN_POINT('Ctrl Pts',(-160.870530442824,5.52520882131862,
126.501999831362));
#196871=CARTESIAN_POINT('Ctrl Pts',(-161.148978066638,-0.633187649970563,
123.830314858198));
#196872=CARTESIAN_POINT('Ctrl Pts',(-161.42742569045,-6.20971560387352,
127.567437236815));
#196873=CARTESIAN_POINT('Ctrl Pts',(-161.705873314263,-6.07981827928859,
134.279134069845));
#196874=CARTESIAN_POINT('Ctrl Pts',(-161.984320938076,-0.362864971672915,
137.79768385235));
#196875=CARTESIAN_POINT('Ctrl Pts',(-162.262768561889,5.68754351797111,
134.889711224922));
#196876=CARTESIAN_POINT('Ctrl Pts',(-162.541216185702,6.5113773665471,128.227500969805));
#196877=CARTESIAN_POINT('Ctrl Pts',(-162.819663809515,1.35157351373451,
123.93329884439));
#196878=CARTESIAN_POINT('Ctrl Pts',(-163.098111433328,-5.05026037016286,
125.953266818493));
#196879=CARTESIAN_POINT('Ctrl Pts',(-163.376559057141,-6.81115169281603,
132.431153004838));
#196880=CARTESIAN_POINT('Ctrl Pts',(-163.655006680953,-2.31292735302948,
137.414096460505));
#196881=CARTESIAN_POINT('Ctrl Pts',(-163.933454304766,4.31076423140788,
136.323015580059));
#196882=CARTESIAN_POINT('Ctrl Pts',(-164.211901928579,6.97307407972212,
130.160560390364));
#196883=CARTESIAN_POINT('Ctrl Pts',(-164.490349552392,3.2274695023783,124.589726158078));
#196884=CARTESIAN_POINT('Ctrl Pts',(-164.768797176205,-3.4840218770001,
124.729837392289));
#196885=CARTESIAN_POINT('Ctrl Pts',(-165.047244800018,-6.99386735534677,
130.452138713572));
#196886=CARTESIAN_POINT('Ctrl Pts',(-165.325692423831,-4.07669040354407,
136.498114757629));
#196887=CARTESIAN_POINT('Ctrl Pts',(-165.604140047644,2.58676587171747,
137.31180890232));
#196888=CARTESIAN_POINT('Ctrl Pts',(-165.882587671457,6.87311068140868,
132.145475979844));
#196889=CARTESIAN_POINT('Ctrl Pts',(-166.161035295269,4.84340254500906,
125.746723556562));
#196890=CARTESIAN_POINT('Ctrl Pts',(-166.439482919082,-1.63715591688565,
123.995692513036));
#196891=CARTESIAN_POINT('Ctrl Pts',(-166.717930542895,-6.61324807067504,
128.501494835643));
#196892=CARTESIAN_POINT('Ctrl Pts',(-166.996378166708,-5.5120883226436,
135.12351831059));
#196893=CARTESIAN_POINT('Ctrl Pts',(-167.274825790521,0.654411313413328,
137.776446868231));
#196894=CARTESIAN_POINT('Ctrl Pts',(-167.553273414334,6.21953892221278,
134.022368766858));
#196895=CARTESIAN_POINT('Ctrl Pts',(-167.831721038147,6.06921410286677,
127.311098384725));
#196896=CARTESIAN_POINT('Ctrl Pts',(-168.11016866196,0.3415780205785,123.809965339223));
#196897=CARTESIAN_POINT('Ctrl Pts',(-168.388616285773,-5.69995157560742,
126.736339859314));
#196898=CARTESIAN_POINT('Ctrl Pts',(-168.667063909585,-6.50350413192509,
133.401026722375));
#196899=CARTESIAN_POINT('Ctrl Pts',(-168.945511533399,-1.33065410484337,
137.679504289309));
#196900=CARTESIAN_POINT('Ctrl Pts',(-169.223959157211,5.06500203852252,
135.640060691349));
#196901=CARTESIAN_POINT('Ctrl Pts',(-169.502406781024,6.80616874759175,
129.156844962666));
#196902=CARTESIAN_POINT('Ctrl Pts',(-169.780854404837,2.29279887745254,
124.18761563522));
#196903=CARTESIAN_POINT('Ctrl Pts',(-170.05930202865,-4.32754115161411,
125.298851700587));
#196904=CARTESIAN_POINT('Ctrl Pts',(-170.337749652463,-6.97108227448498,
131.469381501595));
#196905=CARTESIAN_POINT('Ctrl Pts',(-170.616197276276,-3.20853934340632,
137.028789598255));
#196906=CARTESIAN_POINT('Ctrl Pts',(-170.894644900089,3.50249449840198,
136.868251541923));
#196907=CARTESIAN_POINT('Ctrl Pts',(-171.173092523901,6.99490700254731,
131.135293963646));
#196908=CARTESIAN_POINT('Ctrl Pts',(-171.451540147715,4.05934169155642,
125.098224807315));
#196909=CARTESIAN_POINT('Ctrl Pts',(-171.729987771527,-2.60656032410858,
124.304815700371));
#196910=CARTESIAN_POINT('Ctrl Pts',(-172.00843539534,-6.87716073946864,
129.484170851909));
#196911=CARTESIAN_POINT('Ctrl Pts',(-172.286883019153,-4.82798640323697,
135.876715903229));
#196912=CARTESIAN_POINT('Ctrl Pts',(-172.565330642966,1.65787157732142,
137.608014245356));
#196913=CARTESIAN_POINT('Ctrl Pts',(-172.843778266779,6.62022656985093,
133.087087280501));
#196914=CARTESIAN_POINT('Ctrl Pts',(-173.122225890592,5.49891676073447,
126.468446029806));
#196915=CARTESIAN_POINT('Ctrl Pts',(-173.400673514405,-0.675628914478315,
123.834298464058));
#196916=CARTESIAN_POINT('Ctrl Pts',(-173.679121138218,-6.22930462359329,
127.605297510917));
#196917=CARTESIAN_POINT('Ctrl Pts',(-173.95756876203,-6.05855370207473,
134.316079269865));
#196918=CARTESIAN_POINT('Ctrl Pts',(-174.236016385844,-0.320287905152608,
137.799763144343));
#196919=CARTESIAN_POINT('Ctrl Pts',(-174.514464009656,5.71230682967103,
134.855013841124));
#196920=CARTESIAN_POINT('Ctrl Pts',(-174.792911633469,6.49557064972945,
128.187912110866));
#196921=CARTESIAN_POINT('Ctrl Pts',(-175.071359257282,1.30972236895365,
123.925198737649));
#196922=CARTESIAN_POINT('Ctrl Pts',(-175.349806881095,-5.07969678539539,
125.984099066334));
#196923=CARTESIAN_POINT('Ctrl Pts',(-175.628254504908,-6.80112275095037,
132.472584277733));
#196924=CARTESIAN_POINT('Ctrl Pts',(-175.906702128721,-2.27264916169912,
137.428053442694));
#196925=CARTESIAN_POINT('Ctrl Pts',(-176.185149752534,4.34427798206938,
136.296672486746));
#196926=CARTESIAN_POINT('Ctrl Pts',(-176.463597376347,6.96902589009458,
130.118125237372));
#196927=CARTESIAN_POINT('Ctrl Pts',(-176.742045000159,3.18957946096438,
124.570194777934));
#196928=CARTESIAN_POINT('Ctrl Pts',(-177.020492623972,-3.52093467317244,
124.751158169184));
#196929=CARTESIAN_POINT('Ctrl Pts',(-177.298940247785,-6.99588184988549,
130.494718895118));
#196930=CARTESIAN_POINT('Ctrl Pts',(-177.577387871598,-4.04195537438161,
136.522825237142));
#196931=CARTESIAN_POINT('Ctrl Pts',(-177.855835495411,2.62633062968132,
137.295941956302));
#196932=CARTESIAN_POINT('Ctrl Pts',(-178.134283119224,6.88114708845103,
132.103612556543));
#196933=CARTESIAN_POINT('Ctrl Pts',(-178.412730743037,4.81252553565828,
125.717334096849));
#196934=CARTESIAN_POINT('Ctrl Pts',(-178.69117836685,-1.67857187946192,
124.005784494632));
#196935=CARTESIAN_POINT('Ctrl Pts',(-178.969625990663,-6.62714374015151,
128.541794220484));
#196936=CARTESIAN_POINT('Ctrl Pts',(-179.248073614475,-5.48569425761253,
135.15699193274));
#196937=CARTESIAN_POINT('Ctrl Pts',(-179.526521238288,0.696840256609583,
137.772334104211));
#196938=CARTESIAN_POINT('Ctrl Pts',(-179.804968862101,6.23901261754625,
133.984449045885));
#196939=CARTESIAN_POINT('Ctrl Pts',(-180.083416485914,6.0478371756692,127.27421807789));
#196940=CARTESIAN_POINT('Ctrl Pts',(-180.361864109727,0.298994822622653,
123.808015646805));
#196941=CARTESIAN_POINT('Ctrl Pts',(-180.64031173354,-5.72460916570447,
126.771112453397));
#196942=CARTESIAN_POINT('Ctrl Pts',(-180.918759357353,-6.48757699345442,
133.440567287733));
#196943=CARTESIAN_POINT('Ctrl Pts',(-181.197206981166,-1.28877849997557,
137.687476978041));
#196944=CARTESIAN_POINT('Ctrl Pts',(-181.475654604978,5.094344474651,135.609138992));
#196945=CARTESIAN_POINT('Ctrl Pts',(-181.754102228792,6.79601374963652,
129.115444406326));
#196946=CARTESIAN_POINT('Ctrl Pts',(-182.032549852604,2.25247839243521,
124.173781310638));
#196947=CARTESIAN_POINT('Ctrl Pts',(-182.310997476417,-4.36097456772779,
125.32529667621));
#196948=CARTESIAN_POINT('Ctrl Pts',(-182.58944510023,-6.96690494559973,
131.511804136733));
#196949=CARTESIAN_POINT('Ctrl Pts',(-182.867892724043,-3.17059003069381,
137.048205563678));
#196950=CARTESIAN_POINT('Ctrl Pts',(-183.146340347856,3.53934223048593,
136.84681851393));
#196951=CARTESIAN_POINT('Ctrl Pts',(-183.424787971669,6.99679188832936,
131.092707847901));
#196952=CARTESIAN_POINT('Ctrl Pts',(-183.703235595482,4.02453161308464,
125.07362016374));
#196953=CARTESIAN_POINT('Ctrl Pts',(-183.981683219295,-2.64607660528548,
124.320802994409));
#196954=CARTESIAN_POINT('Ctrl Pts',(-184.260130843107,-6.88506969142675,
129.52605854136));
#196955=CARTESIAN_POINT('Ctrl Pts',(-184.53857846692,-4.79702008550057,
135.906011247817));
#196956=CARTESIAN_POINT('Ctrl Pts',(-184.817026090733,1.6992566315413,137.597796254561));
#196957=CARTESIAN_POINT('Ctrl Pts',(-185.095473714546,6.63399951749853,
133.046745788687));
#196958=CARTESIAN_POINT('Ctrl Pts',(-185.373921338359,5.47242093576752,
126.435052897159));
#196959=CARTESIAN_POINT('Ctrl Pts',(-185.652368962172,-0.718045143308166,
123.838540348135));
#196960=CARTESIAN_POINT('Ctrl Pts',(-185.930816585985,-6.24866281413942,
127.64327632748));
#196961=CARTESIAN_POINT('Ctrl Pts',(-186.209264209798,-6.03706462292539,
134.35289434186));
#196962=CARTESIAN_POINT('Ctrl Pts',(-186.487711833611,-0.277698970246197,
137.801583219124));
#196963=CARTESIAN_POINT('Ctrl Pts',(-186.766159457423,5.73685846974069,
134.820166358884));
#196964=CARTESIAN_POINT('Ctrl Pts',(-187.044607081237,6.47952323715255,
128.148420205389));
#196965=CARTESIAN_POINT('Ctrl Pts',(-187.323054705049,1.2678226919294,123.917353540782));
#196966=CARTESIAN_POINT('Ctrl Pts',(-187.601502328862,-5.10894497059535,
126.01510993074));
#196967=CARTESIAN_POINT('Ctrl Pts',(-187.879949952675,-6.79084179098006,
132.513953733987));
#196968=CARTESIAN_POINT('Ctrl Pts',(-188.158397576488,-2.23228675651833,
137.44176498151));
#196969=CARTESIAN_POINT('Ctrl Pts',(-188.436845200301,4.37763075391265,
136.270125873797));
#196970=CARTESIAN_POINT('Ctrl Pts',(-188.715292824114,6.96471946064982,
130.075715513085));
#196971=CARTESIAN_POINT('Ctrl Pts',(-188.993740447926,3.15157122851057,
124.550894407098));
#196972=CARTESIAN_POINT('Ctrl Pts',(-189.27218807174,-3.55771699981564,
124.772703249722));
#196973=CARTESIAN_POINT('Ctrl Pts',(-189.550635695553,-6.99763710944952,
130.53731055055));
#196974=CARTESIAN_POINT('Ctrl Pts',(-189.829083319365,-4.00707056907658,
136.547323816845));
#196975=CARTESIAN_POINT('Ctrl Pts',(-190.107530943179,2.66579806799723,
137.279834462351));
#196976=CARTESIAN_POINT('Ctrl Pts',(-190.385978566991,6.88892851205765,
132.061700988983));
#196977=CARTESIAN_POINT('Ctrl Pts',(-190.664426190804,4.78147019640398,
125.688133138775));
#196978=CARTESIAN_POINT('Ctrl Pts',(-190.942873814617,-1.71992564193992,
124.016128399968));
#196979=CARTESIAN_POINT('Ctrl Pts',(-191.22132143843,-6.64079383837953,
128.582177445553));
#196980=CARTESIAN_POINT('Ctrl Pts',(-191.499769062243,-5.45909691816341,
135.190304266535));
#196981=CARTESIAN_POINT('Ctrl Pts',(-191.778216686055,0.739243378134395,
137.767963139373));
#196982=CARTESIAN_POINT('Ctrl Pts',(-192.056664309869,6.25825512397307,
133.946411485565));
#196983=CARTESIAN_POINT('Ctrl Pts',(-192.335111933681,6.0262361436405,127.237468581785));
#196984=CARTESIAN_POINT('Ctrl Pts',(-192.613559557494,0.256400545303713,
123.806325206523));
#196985=CARTESIAN_POINT('Ctrl Pts',(-192.892007181307,-5.74905462830365,
126.806034500975));
#196986=CARTESIAN_POINT('Ctrl Pts',(-193.17045480512,-6.47140945543246,
133.480010167483));
#196987=CARTESIAN_POINT('Ctrl Pts',(-193.448902428933,-1.24685513894648,
137.695194610365));
#196988=CARTESIAN_POINT('Ctrl Pts',(-193.727350052746,5.12349813797151,
135.578039249819));
#196989=CARTESIAN_POINT('Ctrl Pts',(-194.005797676559,6.78560692289256,
129.074106433399));
#196990=CARTESIAN_POINT('Ctrl Pts',(-194.284245300372,2.2120744410027,124.160192684611));
#196991=CARTESIAN_POINT('Ctrl Pts',(-194.562692924184,-4.39424638632456,
125.35194468056));
#196992=CARTESIAN_POINT('Ctrl Pts',(-194.841140547997,-6.9624694554897,
131.554200557291));
#196993=CARTESIAN_POINT('Ctrl Pts',(-195.11958817181,-3.13252323060231,
137.067390161131));
#196994=CARTESIAN_POINT('Ctrl Pts',(-195.398035795623,3.57605881094196,
136.825161580438));
#196995=CARTESIAN_POINT('Ctrl Pts',(-195.676483419436,6.99841750541489,
131.050111047343));
#196996=CARTESIAN_POINT('Ctrl Pts',(-195.954931043249,3.98957240411393,
125.04922787486));
#196997=CARTESIAN_POINT('Ctrl Pts',(-196.233378667062,-2.68549483512068,
124.337030539057));
#196998=CARTESIAN_POINT('Ctrl Pts',(-196.511826290875,-6.89272351459547,
129.567993598765));
#196999=CARTESIAN_POINT('Ctrl Pts',(-196.790273914688,-4.76587601242081,
135.935117548864));
#197000=CARTESIAN_POINT('Ctrl Pts',(-197.0687215385,1.74057871918182,137.58732653051));
#197001=CARTESIAN_POINT('Ctrl Pts',(-197.347169162313,6.64752663985393,
133.006321204467));
#197002=CARTESIAN_POINT('Ctrl Pts',(-197.625616786126,5.44572232823074,
126.401821670817));
#197003=CARTESIAN_POINT('Ctrl Pts',(-197.904064409939,-0.760434764710735,
123.843040353244));
#197004=CARTESIAN_POINT('Ctrl Pts',(-198.182512033752,-6.26778945818702,
127.681372279183));
#197005=CARTESIAN_POINT('Ctrl Pts',(-198.460959657565,-6.01535183812634,
134.389577921633));
#197006=CARTESIAN_POINT('Ctrl Pts',(-198.739407281378,-0.235099745102313,
137.803144009248));
#197007=CARTESIAN_POINT('Ctrl Pts',(-199.017854905191,5.76119752841001,
134.785170069484));
#197008=CARTESIAN_POINT('Ctrl Pts',(-199.296302529004,6.46323572345932,
128.10902671676));
#197009=CARTESIAN_POINT('Ctrl Pts',(-199.574750152817,1.22587603526843,
123.909763544495));
#197010=CARTESIAN_POINT('Ctrl Pts',(-199.853197776629,-5.13800384196074,
126.04629826259));
#197011=CARTESIAN_POINT('Ctrl Pts',(-200.131645400443,-6.78030919386985,
132.555259840639));
#197012=CARTESIAN_POINT('Ctrl Pts',(-200.410093024255,-2.19184163313082,
137.455230568865));
#197013=CARTESIAN_POINT('Ctrl Pts',(-200.688540648069,4.41082131103843,
136.243376724908));
#197014=CARTESIAN_POINT('Ctrl Pts',(-200.96698827188,6.96015495096418,130.03333278901));
#197015=CARTESIAN_POINT('Ctrl Pts',(-201.245435895694,3.11344621342587,
124.531825760752));
#197016=CARTESIAN_POINT('Ctrl Pts',(-201.523883519507,-3.59436749394705,
124.794471835542));
#197017=CARTESIAN_POINT('Ctrl Pts',(-201.80233114332,-6.99913306899709,
130.579912101622));
#197018=CARTESIAN_POINT('Ctrl Pts',(-202.080778767133,-3.97203728029775,
136.571609588935));
#197019=CARTESIAN_POINT('Ctrl Pts',(-202.359226390945,2.705166724186,137.263487017335));
#197020=CARTESIAN_POINT('Ctrl Pts',(-202.637674014758,6.89645466388467,
132.019742830214));
#197021=CARTESIAN_POINT('Ctrl Pts',(-202.916121638571,4.75023767801316,
125.659121764391));
#197022=CARTESIAN_POINT('Ctrl Pts',(-203.194569262384,-1.76121567194074,
124.026723845744));
#197023=CARTESIAN_POINT('Ctrl Pts',(-203.473016886197,-6.65419785954973,
128.622643014438));
#197024=CARTESIAN_POINT('Ctrl Pts',(-203.75146451001,-5.43229728987039,
135.223454077576));
#197025=CARTESIAN_POINT('Ctrl Pts',(-204.029912133822,0.781619106723946,
137.763334135682));
#197026=CARTESIAN_POINT('Ctrl Pts',(-204.308359757636,6.27726572845484,
133.908257495395));
#197027=CARTESIAN_POINT('Ctrl Pts',(-204.586807381448,6.00441180721532,
127.200851258176));
#197028=CARTESIAN_POINT('Ctrl Pts',(-204.865255005262,0.213796766968775,
123.804894081017));
#197029=CARTESIAN_POINT('Ctrl Pts',(-205.143702629074,-5.77328705756903,
126.841104707996));
#197030=CARTESIAN_POINT('Ctrl Pts',(-205.422150252887,-6.4550021169537,
133.519353900054));
#197031=CARTESIAN_POINT('Ctrl Pts',(-205.7005978767,-1.20488557524167,137.702656900301));
#197032=CARTESIAN_POINT('Ctrl Pts',(-205.979045500513,5.15246194818434,
135.546762617222));
#197033=CARTESIAN_POINT('Ctrl Pts',(-206.257493124326,6.77494865298866,
129.032832575676));
#197034=CARTESIAN_POINT('Ctrl Pts',(-206.535940748139,2.17158852033829,
124.14685026067));
#197035=CARTESIAN_POINT('Ctrl Pts',(-206.814388371952,-4.42735537450605,
125.378794726189));
#197036=CARTESIAN_POINT('Ctrl Pts',(-207.092835995765,-6.9577759685135,
131.596569192254));
#197037=CARTESIAN_POINT('Ctrl Pts',(-207.371283619578,-3.09434035370993,
137.086342679721));
#197038=CARTESIAN_POINT('Ctrl Pts',(-207.64973124339,3.61264287922363,136.803281543952));
#197039=CARTESIAN_POINT('Ctrl Pts',(-207.928178867203,6.99978379356611,
131.007505140413));
#197040=CARTESIAN_POINT('Ctrl Pts',(-208.206626491016,3.95446536007061,
125.025048844539));
#197041=CARTESIAN_POINT('Ctrl Pts',(-208.485074114829,-2.72481355295718,
124.353497733001));
#197042=CARTESIAN_POINT('Ctrl Pts',(-208.763521738642,-6.90012192535954,
129.609974470206));
#197043=CARTESIAN_POINT('Ctrl Pts',(-209.041969362455,-4.73455533805275,
135.964033727826));
#197044=CARTESIAN_POINT('Ctrl Pts',(-209.320416986268,1.78183630903778,
137.576605461163));
#197045=CARTESIAN_POINT('Ctrl Pts',(-209.598864610081,6.66080743566547,
132.965815025787));
#197046=CARTESIAN_POINT('Ctrl Pts',(-209.877312233893,5.41882192745001,
126.368753582173));
#197047=CARTESIAN_POINT('Ctrl Pts',(-210.155759857706,-0.802796207923886,
123.847798312635));
#197048=CARTESIAN_POINT('Ctrl Pts',(-210.434207481519,-6.28668384699127,
127.719583954367));
#197049=CARTESIAN_POINT('Ctrl Pts',(-210.712655105332,-5.99341615225276,
134.42612864986));
#197050=CARTESIAN_POINT('Ctrl Pts',(-210.991102729145,-0.19249180825093,
137.804445456879));
#197051=CARTESIAN_POINT('Ctrl Pts',(-211.269550352958,5.78532310378624,
134.750026269725));
#197052=CARTESIAN_POINT('Ctrl Pts',(-211.547997976771,6.44670871218949,
128.069733104719));
#197053=CARTESIAN_POINT('Ctrl Pts',(-211.826445600584,1.18388395332015,
123.902429030038));
#197054=CARTESIAN_POINT('Ctrl Pts',(-212.104893224396,-5.16687232270428,
126.077662906191));
#197055=CARTESIAN_POINT('Ctrl Pts',(-212.38334084821,-6.76952534990887,
132.596501067076));
#197056=CARTESIAN_POINT('Ctrl Pts',(-212.661788472022,-2.15131529024619,
137.468449705789));
#197057=CARTESIAN_POINT('Ctrl Pts',(-212.940236095835,4.44384842355829,
136.216426031276));
#197058=CARTESIAN_POINT('Ctrl Pts',(-213.218683719648,6.95533253017721,
129.990978635656));
#197059=CARTESIAN_POINT('Ctrl Pts',(-213.497131343461,3.0752058284468,124.512989545492));
#197060=CARTESIAN_POINT('Ctrl Pts',(-213.775578967274,-3.63088479746918,
124.81646312));
#197061=CARTESIAN_POINT('Ctrl Pts',(-214.054026591087,-7.00036967309483,
130.622521969716));
#197062=CARTESIAN_POINT('Ctrl Pts',(-214.3324742149,-3.93685680621679,136.595681653493));
#197063=CARTESIAN_POINT('Ctrl Pts',(-214.610921838713,2.74443513942699,
137.246900227015));
#197064=CARTESIAN_POINT('Ctrl Pts',(-214.889369462525,6.90372526504794,
131.977739635008));
#197065=CARTESIAN_POINT('Ctrl Pts',(-215.167817086339,4.71882913781829,
125.630301048724));
#197066=CARTESIAN_POINT('Ctrl Pts',(-215.446264710151,-1.80244043944716,
124.037570439344));
#197067=CARTESIAN_POINT('Ctrl Pts',(-215.724712333964,-6.66735530697114,
128.66318942767));
#197068=CARTESIAN_POINT('Ctrl Pts',(-216.003159957777,-5.40529636580357,
135.256440137483));
#197069=CARTESIAN_POINT('Ctrl Pts',(-216.28160758159,0.823965872130078,
137.758447264668));
#197070=CARTESIAN_POINT('Ctrl Pts',(-216.560055205403,6.29604372654653,
133.869988489185));
#197071=CARTESIAN_POINT('Ctrl Pts',(-216.838502829216,5.98236497510254,
127.164367463932));
#197072=CARTESIAN_POINT('Ctrl Pts',(-217.116950453029,0.171185066315507,
123.803722323317));
#197073=CARTESIAN_POINT('Ctrl Pts',(-217.395398076842,-5.79730555555969,
126.876321774922));
#197074=CARTESIAN_POINT('Ctrl Pts',(-217.673845700654,-6.43835558599724,
133.558597027552));
#197075=CARTESIAN_POINT('Ctrl Pts',(-217.952293324468,-1.16287136405879,
137.709863571333));
#197076=CARTESIAN_POINT('Ctrl Pts',(-218.23074094828,5.18123483202488,135.515310253174));
#197077=CARTESIAN_POINT('Ctrl Pts',(-218.509188572093,6.76403933487094,
128.991624362576));
#197078=CARTESIAN_POINT('Ctrl Pts',(-218.787636195906,2.13102213066266,
124.133754533223));
#197079=CARTESIAN_POINT('Ctrl Pts',(-219.066083819719,-4.46030030540597,
125.405845818157));
#197080=CARTESIAN_POINT('Ctrl Pts',(-219.344531443532,-6.95282465859006,
131.638908471637));
#197081=CARTESIAN_POINT('Ctrl Pts',(-219.622979067345,-3.0560428148978,
137.105062417155));
#197082=CARTESIAN_POINT('Ctrl Pts',(-219.901426691158,3.6490930796943,136.781179215245));
#197083=CARTESIAN_POINT('Ctrl Pts',(-220.179874314971,7.00089070215466,
130.964891705888));
#197084=CARTESIAN_POINT('Ctrl Pts',(-220.458321938783,3.91921178185968,
125.001083968743));
#197085=CARTESIAN_POINT('Ctrl Pts',(-220.736769562596,-2.76403130182543,
124.370203966041));
#197086=CARTESIAN_POINT('Ctrl Pts',(-221.015217186409,-6.90726464956813,
129.651999600063));
#197087=CARTESIAN_POINT('Ctrl Pts',(-221.293664810222,-4.7030592229955,
135.992758713204));
#197088=CARTESIAN_POINT('Ctrl Pts',(-221.572112434035,1.82302787229404,
137.565633443793));
#197089=CARTESIAN_POINT('Ctrl Pts',(-221.850560057848,6.67384141280798,
132.925228753618));
#197090=CARTESIAN_POINT('Ctrl Pts',(-222.129007681661,5.39172073022998,
126.33584985658));
#197091=CARTESIAN_POINT('Ctrl Pts',(-222.407455305474,-0.845127903228338,
123.85281405));
#197092=CARTESIAN_POINT('Ctrl Pts',(-222.685902929286,-6.30534528041361,
127.757909937084));
#197093=CARTESIAN_POINT('Ctrl Pts',(-222.964350553099,-5.9712583781396,
134.462545172141));
#197094=CARTESIAN_POINT('Ctrl Pts',(-223.242798176912,-0.14987673854478,
137.805487513793));
#197095=CARTESIAN_POINT('Ctrl Pts',(-223.521245800725,5.80923430188729,
134.714736261875));
#197096=CARTESIAN_POINT('Ctrl Pts',(-223.799693424538,6.42994281575757,
128.030540825308));
#197097=CARTESIAN_POINT('Ctrl Pts',(-224.078141048351,1.1418480021166,123.895350269195));
#197098=CARTESIAN_POINT('Ctrl Pts',(-224.356588672164,-5.19554934309376,
126.109202699315));
#197099=CARTESIAN_POINT('Ctrl Pts',(-224.635036295977,-6.75849065869668,
132.637675885092));
#197100=CARTESIAN_POINT('Ctrl Pts',(-224.913483919789,-2.11070922958169,
137.481421902441));
#197101=CARTESIAN_POINT('Ctrl Pts',(-225.191931543603,4.47671086764076,
136.189274791569));
#197102=CARTESIAN_POINT('Ctrl Pts',(-225.470379167415,6.95025237698553,
129.948654622468));
#197103=CARTESIAN_POINT('Ctrl Pts',(-225.748826791228,3.03685149058481,
124.494386459301));
#197104=CARTESIAN_POINT('Ctrl Pts',(-226.027274415041,-3.66726755721984,
124.838676288203));
#197105=CARTESIAN_POINT('Ctrl Pts',(-226.305722038854,-7.00134687591997,
130.665138575908));
#197106=CARTESIAN_POINT('Ctrl Pts',(-226.584169662667,-3.9015304504591,
136.619539118521));
#197107=CARTESIAN_POINT('Ctrl Pts',(-226.86261728648,2.78360185861461,137.230074706019));
#197108=CARTESIAN_POINT('Ctrl Pts',(-227.141064910293,6.91074004613266,
131.935692959814));
#197109=CARTESIAN_POINT('Ctrl Pts',(-227.419512534106,4.68724573967455,
125.601672059739));
#197110=CARTESIAN_POINT('Ctrl Pts',(-227.697960157918,-1.8435984168596,
124.048667778841));
#197111=CARTESIAN_POINT('Ctrl Pts',(-227.976407781732,-6.68026569308986,
128.703815182788));
#197112=CARTESIAN_POINT('Ctrl Pts',(-228.254855405544,-5.37809514649209,
135.289261223946));
#197113=CARTESIAN_POINT('Ctrl Pts',(-228.533303029357,0.86628210517778,
137.753302707416));
#197114=CARTESIAN_POINT('Ctrl Pts',(-228.81175065317,6.31458842242258,133.831605885006));
#197115=CARTESIAN_POINT('Ctrl Pts',(-229.090198276983,5.96009646425557,
127.128018550972));
#197116=CARTESIAN_POINT('Ctrl Pts',(-229.368645900796,0.128567022336676,
123.802809976843));
#197117=CARTESIAN_POINT('Ctrl Pts',(-229.647093524609,-5.82110923226107,
126.911684396774));
#197118=CARTESIAN_POINT('Ctrl Pts',(-229.925541148421,-6.42147047940683,
133.597738095807));
#197119=CARTESIAN_POINT('Ctrl Pts',(-230.203988772235,-1.12081406224988,
137.716814356412));
#197120=CARTESIAN_POINT('Ctrl Pts',(-230.482436396047,5.20981572330331,
135.483683323156));
#197121=CARTESIAN_POINT('Ctrl Pts',(-230.76088401986,6.75287937278817,128.950483321085));
#197122=CARTESIAN_POINT('Ctrl Pts',(-231.039331643673,2.0903767751783,124.120905987538));
#197123=CARTESIAN_POINT('Ctrl Pts',(-231.317779267486,-4.49307995823781,
125.433096954076));
#197124=CARTESIAN_POINT('Ctrl Pts',(-231.596226891299,-6.94761570919197,
131.681216826544));
#197125=CARTESIAN_POINT('Ctrl Pts',(-231.874674515112,-3.01763203329532,
137.123548679767));
#197126=CARTESIAN_POINT('Ctrl Pts',(-232.153122138925,3.68540806167951,
136.758855413326));
#197127=CARTESIAN_POINT('Ctrl Pts',(-232.431569762738,7.00173819016367,
130.922272322824));
#197128=CARTESIAN_POINT('Ctrl Pts',(-232.71001738655,3.88381297581431,124.977334135496));
#197129=CARTESIAN_POINT('Ctrl Pts',(-232.988465010364,-2.80314662849731,
124.38714861912));
#197130=CARTESIAN_POINT('Ctrl Pts',(-233.266912634176,-6.914151422545,129.694067431082));
#197131=CARTESIAN_POINT('Ctrl Pts',(-233.545360257989,-4.67138883434919,
136.021291440583));
#197132=CARTESIAN_POINT('Ctrl Pts',(-233.823807881803,1.86415188258208,
137.554410884971));
#197133=CARTESIAN_POINT('Ctrl Pts',(-234.102255505615,6.68662808830262,
132.884563891901));
#197134=CARTESIAN_POINT('Ctrl Pts',(-234.380703129428,5.36441974081549,
126.303111713297));
#197135=CARTESIAN_POINT('Ctrl Pts',(-234.659150753241,-0.887428282007554,
123.858087379481));
#197136=CARTESIAN_POINT('Ctrl Pts',(-234.937598377053,-6.32377306694735,
127.796348807152));
#197137=CARTESIAN_POINT('Ctrl Pts',(-235.216046000867,-5.94887933685163,
134.498826139047));
#197138=CARTESIAN_POINT('Ctrl Pts',(-235.494493624679,-0.107256115101469,
137.806270141374));
#197139=CARTESIAN_POINT('Ctrl Pts',(-235.772941248493,5.83293023667497,
134.679301353618));
#197140=CARTESIAN_POINT('Ctrl Pts',(-236.051388872305,6.41293865542997,
127.991451330808));
#197141=CARTESIAN_POINT('Ctrl Pts',(-236.329836496118,1.09976973931543,
123.88852752427));
#197142=CARTESIAN_POINT('Ctrl Pts',(-236.608284119931,-5.22403384049169,
126.140916473241));
#197143=CARTESIAN_POINT('Ctrl Pts',(-236.886731743744,-6.7472055291277,
132.678782768935));
#197144=CARTESIAN_POINT('Ctrl Pts',(-237.165179367557,-2.07002495581049,
137.494146678133));
#197145=CARTESIAN_POINT('Ctrl Pts',(-237.44362699137,4.50940742555574,136.161924011888));
#197146=CARTESIAN_POINT('Ctrl Pts',(-237.722074615182,6.94491467963605,
129.906362317783));
#197147=CARTESIAN_POINT('Ctrl Pts',(-238.000522238996,2.99838462107406,
124.476017191522));
#197148=CARTESIAN_POINT('Ctrl Pts',(-238.278969862808,-3.70351442502255,
124.861110517033));
#197149=CARTESIAN_POINT('Ctrl Pts',(-238.557417486622,-7.00206464126185,
130.707760341024));
#197150=CARTESIAN_POINT('Ctrl Pts',(-238.835865110434,-3.86605952205578,
136.64318109997));
#197151=CARTESIAN_POINT('Ctrl Pts',(-239.114312734247,2.82266543041169,
137.213011077826));
#197152=CARTESIAN_POINT('Ctrl Pts',(-239.39276035806,6.91749874720356,131.893604362681));
#197153=CARTESIAN_POINT('Ctrl Pts',(-239.671207981873,4.655488653916,125.573235858291));
#197154=CARTESIAN_POINT('Ctrl Pts',(-239.949655605686,-1.88468807905538,
124.060015453022));
#197155=CARTESIAN_POINT('Ctrl Pts',(-240.228103229498,-6.69292853950653,
128.74451877439));
#197156=CARTESIAN_POINT('Ctrl Pts',(-240.506550853312,-5.35069463988719,
135.321916120768));
#197157=CARTESIAN_POINT('Ctrl Pts',(-240.784998477124,0.908566237823527,
137.747900654559));
#197158=CARTESIAN_POINT('Ctrl Pts',(-241.063446100938,6.33289912890243,
133.79311110514));
#197159=CARTESIAN_POINT('Ctrl Pts',(-241.34189372475,5.9376070998423,127.091805866219));
#197160=CARTESIAN_POINT('Ctrl Pts',(-241.620341348563,0.0859442142595387,
123.802157075403));
#197161=CARTESIAN_POINT('Ctrl Pts',(-241.898788972376,-5.84469720561911,
126.947191263173));
#197162=CARTESIAN_POINT('Ctrl Pts',(-242.177236596189,-6.40434742286629,
133.636775654432));
#197163=CARTESIAN_POINT('Ctrl Pts',(-242.455684220002,-1.07871522826414,
137.723508997977));
#197164=CARTESIAN_POINT('Ctrl Pts',(-242.734131843815,5.23820356294377,
135.451882999115));
#197165=CARTESIAN_POINT('Ctrl Pts',(-243.012579467628,6.74146918027728,
128.909410975699));
#197166=CARTESIAN_POINT('Ctrl Pts',(-243.29102709144,2.04965396001378,124.108305099723));
#197167=CARTESIAN_POINT('Ctrl Pts',(-243.569474715254,-4.52569311833944,
125.460547124147));
#197168=CARTESIAN_POINT('Ctrl Pts',(-243.847922339066,-6.94214931333881,
131.72349268922));
#197169=CARTESIAN_POINT('Ctrl Pts',(-244.12636996288,-2.9791094322281,137.141800782542));
#197170=CARTESIAN_POINT('Ctrl Pts',(-244.404817586691,3.72158647951367,
136.736310965414));
#197171=CARTESIAN_POINT('Ctrl Pts',(-244.683265210505,7.00232622618917,
130.879648570499));
#197172=CARTESIAN_POINT('Ctrl Pts',(-244.961712834317,3.84827025365086,
124.953800224859));
#197173=CARTESIAN_POINT('Ctrl Pts',(-245.240160458131,-2.84215808354001,
124.404331064352));
#197174=CARTESIAN_POINT('Ctrl Pts',(-245.518608081943,-6.92078198909823,
129.736176404423));
#197175=CARTESIAN_POINT('Ctrl Pts',(-245.797055705757,-4.63954534567172,
136.049630852671));
#197176=CARTESIAN_POINT('Ctrl Pts',(-246.075503329569,1.90520681603656,
137.542938200555));
#197177=CARTESIAN_POINT('Ctrl Pts',(-246.353950953382,6.69916698833444,
132.843821947487));
#197178=CARTESIAN_POINT('Ctrl Pts',(-246.632398577195,5.33691997085474,
126.270540365447));
#197179=CARTESIAN_POINT('Ctrl Pts',(-246.910846201008,-0.929695776805409,
123.86361810567));
#197180=CARTESIAN_POINT('Ctrl Pts',(-247.189293824821,-6.34196652374499,
127.834899140205));
#197181=CARTESIAN_POINT('Ctrl Pts',(-247.467741448634,-5.9262798576518,
134.534970206175));
#197182=CARTESIAN_POINT('Ctrl Pts',(-247.746189072447,-0.0646315172428821,
137.806793310625));
#197183=CARTESIAN_POINT('Ctrl Pts',(-248.024636696259,5.85641003008765,
134.643722858007));
#197184=CARTESIAN_POINT('Ctrl Pts',(-248.303084320073,6.39569686130214,
127.952466069697));
#197185=CARTESIAN_POINT('Ctrl Pts',(-248.581531943885,1.05765072414216,
123.881961048084));
#197186=CARTESIAN_POINT('Ctrl Pts',(-248.859979567699,-5.25232475939459,
126.172803052805));
#197187=CARTESIAN_POINT('Ctrl Pts',(-249.138427191511,-6.73567037937639,
132.719820195375));
#197188=CARTESIAN_POINT('Ctrl Pts',(-249.416874815324,-2.02926397650361,
137.506623561341));
#197189=CARTESIAN_POINT('Ctrl Pts',(-249.695322439137,4.54193688572079,
136.134374705723));
#197190=CARTESIAN_POINT('Ctrl Pts',(-249.97377006295,6.93931963591783,129.864103288757));
#197191=CARTESIAN_POINT('Ctrl Pts',(-250.252217686763,2.95980664532115,
124.457882422832));
#197192=CARTESIAN_POINT('Ctrl Pts',(-250.530665310576,-3.73962405773988,
124.883764975191));
#197193=CARTESIAN_POINT('Ctrl Pts',(-250.809112934388,-7.00252294251614,
130.750385685678));
#197194=CARTESIAN_POINT('Ctrl Pts',(-251.087560558202,-3.83044533540895,
136.666606721818));
#197195=CARTESIAN_POINT('Ctrl Pts',(-251.366008182014,2.86162440732935,
137.195709974661));
#197196=CARTESIAN_POINT('Ctrl Pts',(-251.644455805827,6.9240011177651,131.851475403357));
#197197=CARTESIAN_POINT('Ctrl Pts',(-251.92290342964,4.62355905740654,125.54499349784));
#197198=CARTESIAN_POINT('Ctrl Pts',(-252.201351053453,-1.92570790361727,
124.071613041873));
#197199=CARTESIAN_POINT('Ctrl Pts',(-252.479798677266,-6.70534337666252,
128.785298693283));
#197200=CARTESIAN_POINT('Ctrl Pts',(-252.758246301079,-5.3230958619522,
135.354403619622));
#197201=CARTESIAN_POINT('Ctrl Pts',(-253.036693924892,0.950816704398073,
137.74224130304));
#197202=CARTESIAN_POINT('Ctrl Pts',(-253.315141548704,6.35097516523885,
133.754505582129));
#197203=CARTESIAN_POINT('Ctrl Pts',(-253.593589172518,5.91489771943887,
127.055730740027));
#197204=CARTESIAN_POINT('Ctrl Pts',(-253.87203679633,0.0433182135112656,
123.801763664947));
#197205=CARTESIAN_POINT('Ctrl Pts',(-254.150484420143,-5.86806858651122,
126.982841017323));
#197206=CARTESIAN_POINT('Ctrl Pts',(-254.428932043956,-6.38698707931617,
133.675708334441));
#197207=CARTESIAN_POINT('Ctrl Pts',(-254.707379667769,-1.03657636838919,
137.729947101491));
#197208=CARTESIAN_POINT('Ctrl Pts',(-254.985827291582,5.26639719763008,
135.41991073597));
#197209=CARTESIAN_POINT('Ctrl Pts',(-255.264274915395,6.72980937160111,
128.868408326187));
#197210=CARTESIAN_POINT('Ctrl Pts',(-255.542722539208,2.00885483266244,
124.095953322692));
#197211=CARTESIAN_POINT('Ctrl Pts',(-255.821170163021,-4.5581378946222,
125.488193449449));
#197212=CARTESIAN_POINT('Ctrl Pts',(-256.099617786833,-6.93642696247006,
131.765738008466));
#197213=CARTESIAN_POINT('Ctrl Pts',(-256.378065410647,-2.94047400549736,
137.159811411449));
#197214=CARTESIAN_POINT('Ctrl Pts',(-256.656513034459,3.7576223973322,136.713559240208));
#197215=CARTESIAN_POINT('Ctrl Pts',(-256.934960658272,7.0026634652268,130.836998362911));
#197216=CARTESIAN_POINT('Ctrl Pts',(-257.213408282085,3.81256854888166,
124.930527794066));
#197217=CARTESIAN_POINT('Ctrl Pts',(-257.491855905898,-2.88103328591622,
124.421666290213));
#197218=CARTESIAN_POINT('Ctrl Pts',(-257.770303529711,-6.92721451599304,
129.778484277494));
#197219=CARTESIAN_POINT('Ctrl Pts',(-258.048751153524,-4.60741964202412,
136.077475067175));
#197220=CARTESIAN_POINT('Ctrl Pts',(-258.327198777336,1.94598288966397,
137.53178391186));
#197221=CARTESIAN_POINT('Ctrl Pts',(-258.60564640115,6.71185090883407,132.801931226644));
#197222=CARTESIAN_POINT('Ctrl Pts',(-258.884094024962,5.30847971878909,
126.240167716581));
#197223=CARTESIAN_POINT('Ctrl Pts',(-259.162541648776,-0.970525071554103,
123.86553674091));
#197224=CARTESIAN_POINT('Ctrl Pts',(-259.440989272588,-6.36258613651914,
127.881151058581));
#197225=CARTESIAN_POINT('Ctrl Pts',(-259.673028959099,-5.97575359986218,
133.442106215535));
#197226=CARTESIAN_POINT('Ctrl Pts',(-259.858689921174,-2.9628379271774,
136.206922793942));
#197227=CARTESIAN_POINT('Ctrl Pts',(-259.951535008647,-1.00384119663989,
136.721969923993));
#197228=CARTESIAN_POINT('Ctrl Pts',(-259.997972158816,-0.016740685831905,
136.724751058381));
#197229=CARTESIAN_POINT('Ctrl Pts',(210.384788400103,3.2437100417032,135.350446923363));
#197230=CARTESIAN_POINT('Ctrl Pts',(210.338370536501,4.00135710969089,134.809856772425));
#197231=CARTESIAN_POINT('Ctrl Pts',(210.245544735596,5.2274450014198,133.344996311945));
#197232=CARTESIAN_POINT('Ctrl Pts',(210.059903060087,6.03752477204218,129.574087134129));
#197233=CARTESIAN_POINT('Ctrl Pts',(209.827863373576,3.30140998082846,125.08375145776));
#197234=CARTESIAN_POINT('Ctrl Pts',(209.549415749763,-3.03864792542705,
124.935284604053));
#197235=CARTESIAN_POINT('Ctrl Pts',(209.27096812595,-6.57501826603042,130.18815040753));
#197236=CARTESIAN_POINT('Ctrl Pts',(208.992520502138,-4.0751627655632,136.003208990552));
#197237=CARTESIAN_POINT('Ctrl Pts',(208.714072878324,2.17267791003586,137.042921783734));
#197238=CARTESIAN_POINT('Ctrl Pts',(208.435625254512,6.42228832295553,132.348569225854));
#197239=CARTESIAN_POINT('Ctrl Pts',(208.157177630698,4.77100074356668,126.235763887068));
#197240=CARTESIAN_POINT('Ctrl Pts',(207.878730006886,-1.26506482749479,
124.320958291314));
#197241=CARTESIAN_POINT('Ctrl Pts',(207.600282383073,-6.13835327551471,
128.364250828182));
#197242=CARTESIAN_POINT('Ctrl Pts',(207.32183475926,-5.37092434612766,134.649796015418));
#197243=CARTESIAN_POINT('Ctrl Pts',(207.043387135447,0.332190207827403,
137.40162108792));
#197244=CARTESIAN_POINT('Ctrl Pts',(206.764939511634,5.73000189292936,134.090861108297));
#197245=CARTESIAN_POINT('Ctrl Pts',(206.486491887821,5.86224098722307,127.759980958474));
#197246=CARTESIAN_POINT('Ctrl Pts',(206.208044264008,0.607356820266201,
124.226729984437));
#197247=CARTESIAN_POINT('Ctrl Pts',(205.929596640195,-5.20565320191231,
126.738003936844));
#197248=CARTESIAN_POINT('Ctrl Pts',(205.651149016382,-6.23492509722864,
132.986059061584));
#197249=CARTESIAN_POINT('Ctrl Pts',(205.37270139257,-1.53460390898592,137.229240938669));
#197250=CARTESIAN_POINT('Ctrl Pts',(205.094253768756,4.57594250116295,135.568271122458));
#197251=CARTESIAN_POINT('Ctrl Pts',(204.815806144944,6.48142172411287,129.529500574057));
#197252=CARTESIAN_POINT('Ctrl Pts',(204.537358521131,2.43079079302514,124.662263970705));
#197253=CARTESIAN_POINT('Ctrl Pts',(204.258910897318,-3.85361800715474,
125.439314209572));
#197254=CARTESIAN_POINT('Ctrl Pts',(203.980463273505,-6.5967401814699,131.146579956944));
#197255=CARTESIAN_POINT('Ctrl Pts',(203.702015649692,-3.27778036432047,
136.539362872731));
#197256=CARTESIAN_POINT('Ctrl Pts',(203.42356802588,3.05329946149495,136.661958874297));
#197257=CARTESIAN_POINT('Ctrl Pts',(203.145120402066,6.5785462535266,131.40170824395));
#197258=CARTESIAN_POINT('Ctrl Pts',(202.866672778254,4.05843041346184,125.592524323598));
#197259=CARTESIAN_POINT('Ctrl Pts',(202.58822515444,-2.19118470860141,124.572763346851));
#197260=CARTESIAN_POINT('Ctrl Pts',(202.309777530628,-6.42720813017419,
129.279535830482));
#197261=CARTESIAN_POINT('Ctrl Pts',(202.031329906815,-4.75694126595338,
135.387547802118));
#197262=CARTESIAN_POINT('Ctrl Pts',(201.752882283002,1.28472223178851,137.283834652022));
#197263=CARTESIAN_POINT('Ctrl Pts',(201.474434659189,6.14578876089344,133.225801404307));
#197264=CARTESIAN_POINT('Ctrl Pts',(201.195987035376,5.35917565710019,126.94258236746));
#197265=CARTESIAN_POINT('Ctrl Pts',(200.917539411563,-0.352258065224466,
124.208148884143));
#197266=CARTESIAN_POINT('Ctrl Pts',(200.63909178775,-5.73998383440169,127.535311740963));
#197267=CARTESIAN_POINT('Ctrl Pts',(200.360644163938,-5.85294487354697,
133.866570813476));
#197268=CARTESIAN_POINT('Ctrl Pts',(200.082196540124,-0.587335506164227,
137.383808313225));
#197269=CARTESIAN_POINT('Ctrl Pts',(199.803748916312,5.2180064984534,134.854854804556));
#197270=CARTESIAN_POINT('Ctrl Pts',(199.525301292498,6.22825544477889,128.603695015683));
#197271=CARTESIAN_POINT('Ctrl Pts',(199.246853668687,1.51504190454761,124.374839406449));
#197272=CARTESIAN_POINT('Ctrl Pts',(198.968406044873,-4.5904211320519,126.054399690658));
#197273=CARTESIAN_POINT('Ctrl Pts',(198.689958421061,-6.47751140283473,
132.098942018204));
#197274=CARTESIAN_POINT('Ctrl Pts',(198.411510797247,-2.41208513843682,
136.95382728238));
#197275=CARTESIAN_POINT('Ctrl Pts',(198.133063173434,3.86992953127461,136.15765309974));
#197276=CARTESIAN_POINT('Ctrl Pts',(197.854615549622,6.59566801831256,130.442064648858));
#197277=CARTESIAN_POINT('Ctrl Pts',(197.576167925809,3.26030981281707,125.059408494076));
#197278=CARTESIAN_POINT('Ctrl Pts',(197.297720301996,-3.07111383566833,
124.956082684267));
#197279=CARTESIAN_POINT('Ctrl Pts',(197.019272678183,-6.58033390142619,
130.227038590899));
#197280=CARTESIAN_POINT('Ctrl Pts',(196.74082505437,-4.04254857895594,136.028525236289));
#197281=CARTESIAN_POINT('Ctrl Pts',(196.462377430557,2.21014139809766,137.029259811701));
#197282=CARTESIAN_POINT('Ctrl Pts',(196.183929806745,6.43181940170927,132.309616130935));
#197283=CARTESIAN_POINT('Ctrl Pts',(195.905482182931,4.74296958699597,126.206716169203));
#197284=CARTESIAN_POINT('Ctrl Pts',(195.627034559119,-1.30443757122094,
124.328826848098));
#197285=CARTESIAN_POINT('Ctrl Pts',(195.348586935305,-6.15313032680387,
128.401636713722));
#197286=CARTESIAN_POINT('Ctrl Pts',(195.070139311493,-5.34739690918169,
134.682432467391));
#197287=CARTESIAN_POINT('Ctrl Pts',(194.791691687679,0.372333033116476,
137.399469645412));
#197288=CARTESIAN_POINT('Ctrl Pts',(194.513244063867,5.74990710746052,134.055923815831));
#197289=CARTESIAN_POINT('Ctrl Pts',(194.234796440054,5.84359744862664,127.724350254736));
#197290=CARTESIAN_POINT('Ctrl Pts',(193.956348816241,0.567307210110782,
124.223155750211));
#197291=CARTESIAN_POINT('Ctrl Pts',(193.677901192428,-5.23031063999889,
126.769767009054));
#197292=CARTESIAN_POINT('Ctrl Pts',(193.399453568615,-6.22152852682933,
133.023972693263));
#197293=CARTESIAN_POINT('Ctrl Pts',(193.121005944802,-1.49546563606909,
137.238463313985));
#197294=CARTESIAN_POINT('Ctrl Pts',(192.84255832099,4.60485711668079,135.540327880088));
#197295=CARTESIAN_POINT('Ctrl Pts',(192.564110697177,6.47354113897745,129.490069896797));
#197296=CARTESIAN_POINT('Ctrl Pts',(192.285663073364,2.39335710461987,124.64758087922));
#197297=CARTESIAN_POINT('Ctrl Pts',(192.007215449551,-3.88620518688872,
125.462871665772));
#197298=CARTESIAN_POINT('Ctrl Pts',(191.728767825738,-6.59453476332446,
131.18672985278));
#197299=CARTESIAN_POINT('Ctrl Pts',(191.450320201925,-3.24280905319821,
136.559209392401));
#197300=CARTESIAN_POINT('Ctrl Pts',(191.171872578112,3.08889975678785,136.643264047941));
#197301=CARTESIAN_POINT('Ctrl Pts',(190.893424954299,6.58206059142805,131.361651697256));
#197302=CARTESIAN_POINT('Ctrl Pts',(190.614977330486,4.02662929408197,125.567916069518));
#197303=CARTESIAN_POINT('Ctrl Pts',(190.336529706674,-2.22907761274862,
124.586217166899));
#197304=CARTESIAN_POINT('Ctrl Pts',(190.05808208286,-6.43637108995848,129.318688322246));
#197305=CARTESIAN_POINT('Ctrl Pts',(189.779634459048,-4.72895396970476,
135.416419737866));
#197306=CARTESIAN_POINT('Ctrl Pts',(189.501186835235,1.32414082646293,137.275894133543));
#197307=CARTESIAN_POINT('Ctrl Pts',(189.222739211422,6.16041489098677,133.188345380025));
#197308=CARTESIAN_POINT('Ctrl Pts',(188.944291587609,5.33556862369218,126.910031093937));
#197309=CARTESIAN_POINT('Ctrl Pts',(188.665843963796,-0.392404551757433,
124.210415391489));
#197310=CARTESIAN_POINT('Ctrl Pts',(188.387396339983,-5.75977711417006,
127.570313219673));
#197311=CARTESIAN_POINT('Ctrl Pts',(188.10894871617,-5.83419588941534,133.902142614521));
#197312=CARTESIAN_POINT('Ctrl Pts',(187.830501092358,-0.547273658602122,
137.387261689231));
#197313=CARTESIAN_POINT('Ctrl Pts',(187.552053468544,5.24256632866185,134.823016271676));
#197314=CARTESIAN_POINT('Ctrl Pts',(187.273605844732,6.214743973489,128.565822630237));
#197315=CARTESIAN_POINT('Ctrl Pts',(186.995158220918,1.47587551380139,124.365736040492));
#197316=CARTESIAN_POINT('Ctrl Pts',(186.716710597106,-4.61925044254253,
126.082430892781));
#197317=CARTESIAN_POINT('Ctrl Pts',(186.438262973293,-6.46951090511933,
132.138348483055));
#197318=CARTESIAN_POINT('Ctrl Pts',(186.15981534948,-2.37460689906969,136.968396393875));
#197319=CARTESIAN_POINT('Ctrl Pts',(185.881367725667,3.90244484122886,136.133996556155));
#197320=CARTESIAN_POINT('Ctrl Pts',(185.602920101854,6.59334041746713,130.401921658061));
#197321=CARTESIAN_POINT('Ctrl Pts',(185.324472478041,3.22527825263932,125.039668503516));
#197322=CARTESIAN_POINT('Ctrl Pts',(185.046024854228,-3.10665706276191,
124.974885780916));
#197323=CARTESIAN_POINT('Ctrl Pts',(184.767577230416,-6.5837263061198,130.26710564752));
#197324=CARTESIAN_POINT('Ctrl Pts',(184.489129606603,-4.01067270706429,
136.05303658523));
#197325=CARTESIAN_POINT('Ctrl Pts',(184.21068198279,2.247993177529,137.015690720733));
#197326=CARTESIAN_POINT('Ctrl Pts',(183.932234358977,6.44086315254518,132.270435931769));
#197327=CARTESIAN_POINT('Ctrl Pts',(183.653786735164,4.71489454403,126.177929550814));
#197328=CARTESIAN_POINT('Ctrl Pts',(183.375339111351,-1.34383181504516,
124.33688730648));
#197329=CARTESIAN_POINT('Ctrl Pts',(183.096891487538,-6.16764238592767,
128.439137081397));
#197330=CARTESIAN_POINT('Ctrl Pts',(182.818443863726,-5.32369091022383,
134.71491173846));
#197331=CARTESIAN_POINT('Ctrl Pts',(182.539996239912,0.412472435216218,
137.397080956463));
#197332=CARTESIAN_POINT('Ctrl Pts',(182.2615486161,5.76959376309122,134.020862255314));
#197333=CARTESIAN_POINT('Ctrl Pts',(181.983100992287,5.82474028301032,127.688835683913));
#197334=CARTESIAN_POINT('Ctrl Pts',(181.704653368474,0.527235037225083,
124.219824324685));
#197335=CARTESIAN_POINT('Ctrl Pts',(181.426205744661,-5.25477345090652,
126.801680146133));
#197336=CARTESIAN_POINT('Ctrl Pts',(181.147758120848,-6.20790184760947,
133.061803779016));
#197337=CARTESIAN_POINT('Ctrl Pts',(180.869310497035,-1.45627171922457,
137.247447428754));
#197338=CARTESIAN_POINT('Ctrl Pts',(180.590862873222,4.63360097629919,135.5122090613));
#197339=CARTESIAN_POINT('Ctrl Pts',(180.31241524941,6.46542073859599,129.450687965235));
#197340=CARTESIAN_POINT('Ctrl Pts',(180.033967625596,2.35583469548556,124.633125906077));
#197341=CARTESIAN_POINT('Ctrl Pts',(179.755520001784,-3.91864834385308,
125.4866270652));
#197342=CARTESIAN_POINT('Ctrl Pts',(179.477072377971,-6.59208499180493,
131.226865573221));
#197343=CARTESIAN_POINT('Ctrl Pts',(179.198624754158,-3.20771757354326,
136.578842667508));
#197344=CARTESIAN_POINT('Ctrl Pts',(178.920177130345,3.12438558908937,136.62435285703));
#197345=CARTESIAN_POINT('Ctrl Pts',(178.641729506532,6.58533103007041,131.32157450091));
#197346=CARTESIAN_POINT('Ctrl Pts',(178.363281882719,3.99467896572256,125.5435018533));
#197347=CARTESIAN_POINT('Ctrl Pts',(178.084834258906,-2.26688791720775,
124.599901402811));
#197348=CARTESIAN_POINT('Ctrl Pts',(177.806386635093,-6.44529554785546,
129.357895865998));
#197349=CARTESIAN_POINT('Ctrl Pts',(177.527939011281,-4.70079144021631,
135.445120772143));
#197350=CARTESIAN_POINT('Ctrl Pts',(177.249491387467,1.36351035455298,137.26771380997));
#197351=CARTESIAN_POINT('Ctrl Pts',(176.971043763655,6.17481274467203,133.150801016333));
#197352=CARTESIAN_POINT('Ctrl Pts',(176.692596139842,5.31176387881016,126.877624126216));
#197353=CARTESIAN_POINT('Ctrl Pts',(176.414148516029,-0.432536497586617,
124.212926239906));
#197354=CARTESIAN_POINT('Ctrl Pts',(176.135700892216,-5.77935696328393,
127.605434537195));
#197355=CARTESIAN_POINT('Ctrl Pts',(175.857253268403,-5.81523071700703,
133.937599626117));
#197356=CARTESIAN_POINT('Ctrl Pts',(175.57880564459,-0.50719153161477,137.390471133416));
#197357=CARTESIAN_POINT('Ctrl Pts',(175.300358020777,5.2669318936477,134.791028826034));
#197358=CARTESIAN_POINT('Ctrl Pts',(175.021910396965,6.20100221257536,128.528033194638));
#197359=CARTESIAN_POINT('Ctrl Pts',(174.743462773151,1.43665443394553,124.356871260137));
#197360=CARTESIAN_POINT('Ctrl Pts',(174.465015149339,-4.64790858500931,
126.110637067746));
#197361=CARTESIAN_POINT('Ctrl Pts',(174.186567525525,-6.46127067729819,
132.177705516496));
#197362=CARTESIAN_POINT('Ctrl Pts',(173.908119901713,-2.33704066777073,
136.982737094758));
#197363=CARTESIAN_POINT('Ctrl Pts',(173.6296722779,3.93481554465429,136.11014252095));
#197364=CARTESIAN_POINT('Ctrl Pts',(173.351224654087,6.59076849796787,130.361793579788));
#197365=CARTESIAN_POINT('Ctrl Pts',(173.072777030274,3.1901271785899,125.020142125741));
#197366=CARTESIAN_POINT('Ctrl Pts',(172.794329406461,-3.14208517153551,
124.993904890899));
#197367=CARTESIAN_POINT('Ctrl Pts',(172.515881782648,-6.58687474841394,
130.30719261232));
#197368=CARTESIAN_POINT('Ctrl Pts',(172.237434158836,-3.97864821822065,
136.077353442554));
#197369=CARTESIAN_POINT('Ctrl Pts',(171.958986535022,2.28576165674636,137.001891466644));
#197370=CARTESIAN_POINT('Ctrl Pts',(171.68053891121,6.44966823482829,132.231201406644));
#197371=CARTESIAN_POINT('Ctrl Pts',(171.402091287397,4.68664478891289,126.149314366529));
#197372=CARTESIAN_POINT('Ctrl Pts',(171.123643663584,-1.38317626268716,
124.345187419464));
#197373=CARTESIAN_POINT('Ctrl Pts',(170.845196039771,-6.18192590079466,
128.476725093301));
#197374=CARTESIAN_POINT('Ctrl Pts',(170.566748415958,-5.29978763994156,
134.747246102621));
#197375=CARTESIAN_POINT('Ctrl Pts',(170.288300792145,0.452596552998033,
137.394447971839));
#197376=CARTESIAN_POINT('Ctrl Pts',(170.009853168332,5.78906662430322,133.985681506144));
#197377=CARTESIAN_POINT('Ctrl Pts',(169.73140554452,5.80566727950083,127.653436560012));
#197378=CARTESIAN_POINT('Ctrl Pts',(169.452957920706,0.487143327451347,
124.216736891574));
#197379=CARTESIAN_POINT('Ctrl Pts',(169.174510296894,-5.27904154425138,
126.833741604011));
#197380=CARTESIAN_POINT('Ctrl Pts',(168.896062673081,-6.19404513230377,
133.099551214382));
#197381=CARTESIAN_POINT('Ctrl Pts',(168.617615049268,-1.41702383969606,
137.256192792574));
#197382=CARTESIAN_POINT('Ctrl Pts',(168.339167425455,4.66217313612931,135.483915791456));
#197383=CARTESIAN_POINT('Ctrl Pts',(168.060719801642,6.45706075967145,129.411356194513));
#197384=CARTESIAN_POINT('Ctrl Pts',(167.782272177829,2.3182249900303,124.618899610305));
#197385=CARTESIAN_POINT('Ctrl Pts',(167.503824554016,-3.95094629386185,
125.510579515201));
#197386=CARTESIAN_POINT('Ctrl Pts',(167.225376930203,-6.58939094815179,
131.266985637585));
#197387=CARTESIAN_POINT('Ctrl Pts',(166.946929306391,-3.1725072307341,136.59826196706));
#197388=CARTESIAN_POINT('Ctrl Pts',(166.668481682578,3.15975564613386,136.605226004165));
#197389=CARTESIAN_POINT('Ctrl Pts',(166.390034058765,6.58835744684964,131.281478139015));
#197390=CARTESIAN_POINT('Ctrl Pts',(166.111586434952,3.96258061306513,125.519282580138));
#197391=CARTESIAN_POINT('Ctrl Pts',(165.833138811139,-2.30461422130139,
124.613815547242));
#197392=CARTESIAN_POINT('Ctrl Pts',(165.554691187326,-6.45398117295568,
129.397157009033));
#197393=CARTESIAN_POINT('Ctrl Pts',(165.276243563513,-4.67245472117232,
135.473649841348));
#197394=CARTESIAN_POINT('Ctrl Pts',(164.9977959397,1.40282935726546,137.259293984466));
#197395=CARTESIAN_POINT('Ctrl Pts',(164.719348315888,6.18898178840028,133.11316970443));
#197396=CARTESIAN_POINT('Ctrl Pts',(164.440900692075,5.2877623045642,126.845362665158));
#197397=CARTESIAN_POINT('Ctrl Pts',(164.162453068262,-0.472652415616787,
124.215681336348));
#197398=CARTESIAN_POINT('Ctrl Pts',(163.884005444449,-5.79872265620017,
127.640674392099));
#197399=CARTESIAN_POINT('Ctrl Pts',(163.605557820636,-5.79605005908598,
133.97294053439));
#197400=CARTESIAN_POINT('Ctrl Pts',(163.327110196823,-0.467090610458611,
137.393436526853));
#197401=CARTESIAN_POINT('Ctrl Pts',(163.04866257301,5.29110229053537,134.758893652935));
#197402=CARTESIAN_POINT('Ctrl Pts',(162.770214949197,6.18703067124424,128.49032810919));
#197403=CARTESIAN_POINT('Ctrl Pts',(162.491767325384,1.39738011833125,124.34824539387));
#197404=CARTESIAN_POINT('Ctrl Pts',(162.213319701571,-4.67639449751423,
126.139017170363));
#197405=CARTESIAN_POINT('Ctrl Pts',(161.934872077759,-6.45279102471594,
132.217011660137));
#197406=CARTESIAN_POINT('Ctrl Pts',(161.656424453946,-2.29938783657033,
136.996848853628));
#197407=CARTESIAN_POINT('Ctrl Pts',(161.377976830133,3.96704044204275,136.086091878046));
#197408=CARTESIAN_POINT('Ctrl Pts',(161.09952920632,6.58795235511813,130.321681900999));
#197409=CARTESIAN_POINT('Ctrl Pts',(160.821081582507,3.15485789320466,125.000830084311));
#197410=CARTESIAN_POINT('Ctrl Pts',(160.542633958694,-3.17739684918762,
125.013139309456));
#197411=CARTESIAN_POINT('Ctrl Pts',(160.264186334881,-6.58977911164196,
130.347297999864));
#197412=CARTESIAN_POINT('Ctrl Pts',(159.985738711068,-3.94647629910411,
136.10147490719));
#197413=CARTESIAN_POINT('Ctrl Pts',(159.707291087255,2.32344543622502,136.98786256077));
#197414=CARTESIAN_POINT('Ctrl Pts',(159.428843463442,6.45823432228318,132.191914009409));
#197415=CARTESIAN_POINT('Ctrl Pts',(159.15039583963,4.65822136844951,126.120871676696));
#197416=CARTESIAN_POINT('Ctrl Pts',(158.871948215817,-1.42246945622416,
124.353726879487));
#197417=CARTESIAN_POINT('Ctrl Pts',(158.593500592004,-6.19598034212407,
128.514399356595));
#197418=CARTESIAN_POINT('Ctrl Pts',(158.315052968191,-5.2756879840792,134.779434361708));
#197419=CARTESIAN_POINT('Ctrl Pts',(158.036605344378,0.49270389964821,137.391570789103));
#197420=CARTESIAN_POINT('Ctrl Pts',(157.758157720565,5.80832496952254,133.950382871961));
#197421=CARTESIAN_POINT('Ctrl Pts',(157.479710096752,5.78637914485521,127.618154194761));
#197422=CARTESIAN_POINT('Ctrl Pts',(157.201262472939,0.447033566402335,
124.213893565282));
#197423=CARTESIAN_POINT('Ctrl Pts',(156.922814849126,-5.3031140207705,126.865950194636));
#197424=CARTESIAN_POINT('Ctrl Pts',(156.644367225313,-6.17995889437779,
133.137213600617));
#197425=CARTESIAN_POINT('Ctrl Pts',(156.365919601501,-1.37772345182797,
137.264699081378));
#197426=CARTESIAN_POINT('Ctrl Pts',(156.087471977688,4.69057253741941,135.455449118975));
#197427=CARTESIAN_POINT('Ctrl Pts',(155.809024353875,6.44846151198586,129.372076042081));
#197428=CARTESIAN_POINT('Ctrl Pts',(155.530576730062,2.28052938189546,124.604902519066));
#197429=CARTESIAN_POINT('Ctrl Pts',(155.252129106249,-3.98309784010292,
125.534728128207));
#197430=CARTESIAN_POINT('Ctrl Pts',(154.973681482436,-6.58645273219382,
131.307088559209));
#197431=CARTESIAN_POINT('Ctrl Pts',(154.695233858623,-3.13717932950269,
136.617466571466));
#197432=CARTESIAN_POINT('Ctrl Pts',(154.41678623481,3.19500861727094,136.585884198101));
#197433=CARTESIAN_POINT('Ctrl Pts',(154.138338610998,6.59113972962085,131.241364097354));
#197434=CARTESIAN_POINT('Ctrl Pts',(153.859890987185,3.93033542552574,125.495259147487));
#197435=CARTESIAN_POINT('Ctrl Pts',(153.581443363372,-2.3422551270676,124.627959084596));
#197436=CARTESIAN_POINT('Ctrl Pts',(153.302995739559,-6.46242764341012,
129.436470296516));
#197437=CARTESIAN_POINT('Ctrl Pts',(153.024548115746,-4.64394486260028,
135.502005888322));
#197438=CARTESIAN_POINT('Ctrl Pts',(152.746100491933,1.44209637762021,137.250634969033));
#197439=CARTESIAN_POINT('Ctrl Pts',(152.46765286812,6.20292149713234,133.075452838754));
#197440=CARTESIAN_POINT('Ctrl Pts',(152.189205244307,5.26356479034146,126.813247906226));
#197441=CARTESIAN_POINT('Ctrl Pts',(151.910757620494,-0.512750819337957,
124.218680578724));
#197442=CARTESIAN_POINT('Ctrl Pts',(151.632309996682,-5.8178734753159,127.676031478561));
#197443=CARTESIAN_POINT('Ctrl Pts',(151.353862372869,-5.77665462639848,
134.008164029768));
#197444=CARTESIAN_POINT('Ctrl Pts',(151.075414749056,-0.4269723810881,137.39615775966));
#197445=CARTESIAN_POINT('Ctrl Pts',(150.796967125243,5.31507662368183,134.72661194316));
#197446=CARTESIAN_POINT('Ctrl Pts',(150.51851950143,6.17282986721635,128.452708771068));
#197447=CARTESIAN_POINT('Ctrl Pts',(150.240071877617,1.35805402228283,124.339858761329));
#197448=CARTESIAN_POINT('Ctrl Pts',(149.961624253804,-4.70470712450132,
126.167570148998));
#197449=CARTESIAN_POINT('Ctrl Pts',(149.683176629991,-6.44407226158927,
132.256265457474));
#197450=CARTESIAN_POINT('Ctrl Pts',(149.404729006178,-2.26164980070799,
137.010731147569));
#197451=CARTESIAN_POINT('Ctrl Pts',(149.126281382365,3.99911833928874,136.061845518646));
#197452=CARTESIAN_POINT('Ctrl Pts',(148.847833758553,6.58489209327119,130.281588108047));
#197453=CARTESIAN_POINT('Ctrl Pts',(148.56938613474,3.11947170339994,124.981733094838));
#197454=CARTESIAN_POINT('Ctrl Pts',(148.290938510927,-3.21259078723097,
125.032588323847));
#197455=CARTESIAN_POINT('Ctrl Pts',(148.012490887114,-6.59243928818165,
130.387420324031));
#197456=CARTESIAN_POINT('Ctrl Pts',(147.734043263301,-3.91415814185689,
136.125400085308));
#197457=CARTESIAN_POINT('Ctrl Pts',(147.455595639488,2.36104311957866,136.973604522958));
#197458=CARTESIAN_POINT('Ctrl Pts',(147.177148015675,6.46656109749016,132.152575195872));
#197459=CARTESIAN_POINT('Ctrl Pts',(146.898700391862,4.6296253358803,126.092602535266));
#197460=CARTESIAN_POINT('Ctrl Pts',(146.62025276805,-1.46170993963237,124.362505370115));
#197461=CARTESIAN_POINT('Ctrl Pts',(146.341805144237,-6.20980518912327,
128.552158475246));
#197462=CARTESIAN_POINT('Ctrl Pts',(146.063357520424,-5.2513928356585,134.811475322978));
#197463=CARTESIAN_POINT('Ctrl Pts',(145.784909896611,0.532792988974217,
137.388449514872));
#197464=CARTESIAN_POINT('Ctrl Pts',(145.506462272798,5.82736808512415,133.914967660766));
#197465=CARTESIAN_POINT('Ctrl Pts',(145.228014648985,5.76687659380242,127.582989895561));
#197466=CARTESIAN_POINT('Ctrl Pts',(144.949567025172,0.406907240360106,
124.211294451169));
#197467=CARTESIAN_POINT('Ctrl Pts',(144.671119401359,-5.32698998844935,
126.898304724507));
#197468=CARTESIAN_POINT('Ctrl Pts',(144.392671777546,-6.16564365580234,
133.174789542127));
#197469=CARTESIAN_POINT('Ctrl Pts',(144.114224153734,-1.33837201191069,
137.272965979966));
#197470=CARTESIAN_POINT('Ctrl Pts',(143.83577652992,4.71879812781917,135.426810098699));
#197471=CARTESIAN_POINT('Ctrl Pts',(143.557328906108,6.43962331418753,129.332848963481));
#197472=CARTESIAN_POINT('Ctrl Pts',(143.278881282295,2.24274926790569,124.591135151027));
#197473=CARTESIAN_POINT('Ctrl Pts',(143.000433658482,-4.01510179118866,
125.559072009383));
#197474=CARTESIAN_POINT('Ctrl Pts',(142.721986034669,-6.58327045280769,
131.347172852065));
#197475=CARTESIAN_POINT('Ctrl Pts',(142.443538410856,-3.10173517893752,
136.636455769093));
#197476=CARTESIAN_POINT('Ctrl Pts',(142.165090787043,3.23014319618891,136.566328155556));
#197477=CARTESIAN_POINT('Ctrl Pts',(141.886643163231,6.5936777752854,131.201233862367));
#197478=CARTESIAN_POINT('Ctrl Pts',(141.608195539417,3.89794459796173,125.471432445543));
#197479=CARTESIAN_POINT('Ctrl Pts',(141.329747915605,-2.37980923970876,
124.642331490782));
#197480=CARTESIAN_POINT('Ctrl Pts',(141.051300291792,-6.47063464623165,
129.475834271677));
#197481=CARTESIAN_POINT('Ctrl Pts',(140.772852667979,-4.61526292094352,
135.530187862324));
#197482=CARTESIAN_POINT('Ctrl Pts',(140.494405044166,1.48130996056343,137.241737084533));
#197483=CARTESIAN_POINT('Ctrl Pts',(140.215957420353,6.21663135432719,133.037651816923));
#197484=CARTESIAN_POINT('Ctrl Pts',(139.93750979654,5.23917223278974,126.781281039444));
#197485=CARTESIAN_POINT('Ctrl Pts',(139.659062172727,-0.552830222889001,
124.221923855894));
#197486=CARTESIAN_POINT('Ctrl Pts',(139.380614548914,-5.83680871099059,
127.711504486408));
#197487=CARTESIAN_POINT('Ctrl Pts',(139.102166925101,-5.75704513764935,
134.043268807033));
#197488=CARTESIAN_POINT('Ctrl Pts',(138.823719301288,-0.386838330098996,
137.398634730999));
#197489=CARTESIAN_POINT('Ctrl Pts',(138.545271677476,5.33885400470937,134.694184892919));
#197490=CARTESIAN_POINT('Ctrl Pts',(138.266824053663,6.15840032670771,128.41517657427));
#197491=CARTESIAN_POINT('Ctrl Pts',(137.98837642985,1.31867760304303,124.331711673279));
#197492=CARTESIAN_POINT('Ctrl Pts',(137.709928806037,-4.7328454168358,126.196294945608));
#197493=CARTESIAN_POINT('Ctrl Pts',(137.431481182224,-6.43511471099507,
132.295465453942));
#197494=CARTESIAN_POINT('Ctrl Pts',(137.153033558411,-2.22382795858067,
137.024383462168));
#197495=CARTESIAN_POINT('Ctrl Pts',(136.874585934598,4.03104804773404,136.037404341212));
#197496=CARTESIAN_POINT('Ctrl Pts',(136.596138310785,6.5815878258261,130.241513686623));
#197497=CARTESIAN_POINT('Ctrl Pts',(136.317690686972,3.08396992042408,124.96285186497));
#197498=CARTESIAN_POINT('Ctrl Pts',(136.03924306316,-3.24766568154122,125.052251213384));
#197499=CARTESIAN_POINT('Ctrl Pts',(135.760795439346,-6.5948551794591,130.427558098075));
#197500=CARTESIAN_POINT('Ctrl Pts',(135.482347815534,-3.88169494404043,
136.149128090351));
#197501=CARTESIAN_POINT('Ctrl Pts',(135.203900191721,2.3985533136112,136.959117881544));
#197502=CARTESIAN_POINT('Ctrl Pts',(134.925452567908,6.47464825189767,132.113186423748));
#197503=CARTESIAN_POINT('Ctrl Pts',(134.647004944095,4.60085775084163,126.064507989766));
#197504=CARTESIAN_POINT('Ctrl Pts',(134.368557320282,-1.50089625884118,
124.371522566057));
#197505=CARTESIAN_POINT('Ctrl Pts',(134.090109696469,-6.22339992950755,
128.590001050074));
#197506=CARTESIAN_POINT('Ctrl Pts',(133.811662072656,-5.22690309494509,
134.843367799137));
#197507=CARTESIAN_POINT('Ctrl Pts',(133.533214448844,0.572862335460145,
137.385084264805));
#197508=CARTESIAN_POINT('Ctrl Pts',(133.25476682503,5.84619526545829,133.879437184883));
#197509=CARTESIAN_POINT('Ctrl Pts',(132.976319201218,5.7471603490167,127.547944965438));
#197510=CARTESIAN_POINT('Ctrl Pts',(132.697871577405,0.366765836220533,
124.208939645549));
#197511=CARTESIAN_POINT('Ctrl Pts',(132.419423953592,-5.35066856255522,
126.930803994717));
#197512=CARTESIAN_POINT('Ctrl Pts',(132.140976329779,-6.15109994703373,
133.212277646521));
#197513=CARTESIAN_POINT('Ctrl Pts',(131.862528705966,-1.29897097812634,
137.280993182001));
#197514=CARTESIAN_POINT('Ctrl Pts',(131.584081082153,4.74684886141891,135.397999791857));
#197515=CARTESIAN_POINT('Ctrl Pts',(131.30563345834,6.43054649377913,129.293676412286));
#197516=CARTESIAN_POINT('Ctrl Pts',(131.027185834528,2.20488604801711,124.577598016342));
#197517=CARTESIAN_POINT('Ctrl Pts',(130.748738210715,-4.04695696120101,
125.583610256657));
#197518=CARTESIAN_POINT('Ctrl Pts',(130.470290586902,-6.57984422791396,
131.387237030814));
#197519=CARTESIAN_POINT('Ctrl Pts',(130.191842963089,-3.06617609243459,
136.65522885629));
#197520=CARTESIAN_POINT('Ctrl Pts',(129.913395339276,3.26515808096253,136.546558601182));
#197521=CARTESIAN_POINT('Ctrl Pts',(129.634947715463,6.59597148979528,131.161088921098));
#197522=CARTESIAN_POINT('Ctrl Pts',(129.35650009165,3.86540933062731,125.447803357213));
#197523=CARTESIAN_POINT('Ctrl Pts',(129.078052467837,-2.41727516764341,
124.656932233223));
#197524=CARTESIAN_POINT('Ctrl Pts',(128.799604844024,-6.47860187730669,
129.515247475871));
#197525=CARTESIAN_POINT('Ctrl Pts',(128.521157220212,-4.58640995902212,
135.558194719059));
#197526=CARTESIAN_POINT('Ctrl Pts',(128.242709596398,1.52046865302106,137.232600660681));
#197527=CARTESIAN_POINT('Ctrl Pts',(127.964261972586,6.23011085196111,132.999768039666));
#197528=CARTESIAN_POINT('Ctrl Pts',(127.685814348773,5.2145855357842,126.749463249355));
#197529=CARTESIAN_POINT('Ctrl Pts',(127.40736672496,-0.592889141112855,
124.225411047681));
#197530=CARTESIAN_POINT('Ctrl Pts',(127.128919101147,-5.85552766157182,
127.747092101177));
#197531=CARTESIAN_POINT('Ctrl Pts',(126.850471477334,-5.7372223194756,134.078253565364));
#197532=CARTESIAN_POINT('Ctrl Pts',(126.572023853521,-0.346689944673359,
137.400867349086));
#197533=CARTESIAN_POINT('Ctrl Pts',(126.293576229708,5.36243355253846,134.66161370381));
#197534=CARTESIAN_POINT('Ctrl Pts',(126.015128605896,6.14374258441013,128.377732909565));
#197535=CARTESIAN_POINT('Ctrl Pts',(125.736680982083,1.27925231971985,124.323804431618));
#197536=CARTESIAN_POINT('Ctrl Pts',(125.45823335827,-4.76080833184274,126.225190495787));
#197537=CARTESIAN_POINT('Ctrl Pts',(125.179785734457,-6.42591870485886,
132.334610196974));
#197538=CARTESIAN_POINT('Ctrl Pts',(124.901338110644,-2.1859237116904,137.037805291532));
#197539=CARTESIAN_POINT('Ctrl Pts',(124.622890486831,4.06282838421153,136.012769251418));
#197540=CARTESIAN_POINT('Ctrl Pts',(124.344442863018,6.5780396752237,130.201460121699));
#197541=CARTESIAN_POINT('Ctrl Pts',(124.065995239205,3.04835385980878,124.944187094356));
#197542=CARTESIAN_POINT('Ctrl Pts',(123.787547615392,-3.28262023240536,
125.07212724945));
#197543=CARTESIAN_POINT('Ctrl Pts',(123.509099991579,-6.59702669595264,
130.467709834674));
#197544=CARTESIAN_POINT('Ctrl Pts',(123.230652367767,-3.84908790859021,
136.17265804307));
#197545=CARTESIAN_POINT('Ctrl Pts',(122.952204743954,2.43597462836867,136.944403173336));
#197546=CARTESIAN_POINT('Ctrl Pts',(122.673757120141,6.48249548583303,132.073749152604));
#197547=CARTESIAN_POINT('Ctrl Pts',(122.395309496328,4.57191967932717,126.036589081248));
#197548=CARTESIAN_POINT('Ctrl Pts',(122.116861872515,-1.54002696178715,
124.380778133181));
#197549=CARTESIAN_POINT('Ctrl Pts',(121.838414248702,-6.23676405951882,
128.627925678811));
#197550=CARTESIAN_POINT('Ctrl Pts',(121.559966624889,-5.20221966941523,
134.8751106084));
#197551=CARTESIAN_POINT('Ctrl Pts',(121.281519001076,0.612910454321425,
137.381475163605));
#197552=CARTESIAN_POINT('Ctrl Pts',(121.003071377263,5.86480581287692,133.843792760907));
#197553=CARTESIAN_POINT('Ctrl Pts',(120.724623753451,5.72723114109079,127.513020702994));
#197554=CARTESIAN_POINT('Ctrl Pts',(120.446176129638,0.326610841437887,
124.206829235678));
#197555=CARTESIAN_POINT('Ctrl Pts',(120.167728505825,-5.3741488656698,126.963446800991));
#197556=CARTESIAN_POINT('Ctrl Pts',(119.889280882012,-6.13632830699453,
133.249676524665));
#197557=CARTESIAN_POINT('Ctrl Pts',(119.610833258199,-1.25952181049465,
137.288780390037));
#197558=CARTESIAN_POINT('Ctrl Pts',(119.332385634386,4.77472369878856,135.369019266025));
#197559=CARTESIAN_POINT('Ctrl Pts',(119.053938010573,6.42123138710552,129.254559840052));
#197560=CARTESIAN_POINT('Ctrl Pts',(118.77549038676,2.16694112526505,124.564291616636));
#197561=CARTESIAN_POINT('Ctrl Pts',(118.497042762948,-4.07866216973492,
125.608341960757));
#197562=CARTESIAN_POINT('Ctrl Pts',(118.218595139134,-6.57617418447253,
131.427279610862));
#197563=CARTESIAN_POINT('Ctrl Pts',(117.940147515322,-3.03050338764912,
136.673785137412));
#197564=CARTESIAN_POINT('Ctrl Pts',(117.661699891509,3.30005197410286,136.526576267552));
#197565=CARTESIAN_POINT('Ctrl Pts',(117.383252267696,6.59802078815589,131.120930761129));
#197566=CARTESIAN_POINT('Ctrl Pts',(117.104804643883,3.83273082912851,125.424372758082));
#197567=CARTESIAN_POINT('Ctrl Pts',(116.82635702007,-2.45465152255762,124.671760770883));
#197568=CARTESIAN_POINT('Ctrl Pts',(116.547909396257,-6.48632904140672,
129.554708448625));
#197569=CARTESIAN_POINT('Ctrl Pts',(116.269461772444,-4.55738704599302,
135.586025420722));
#197570=CARTESIAN_POINT('Ctrl Pts',(115.991014148631,1.55957100395386,137.223226036031));
#197571=CARTESIAN_POINT('Ctrl Pts',(115.712566524818,6.24335949054626,132.961802910777));
#197572=CARTESIAN_POINT('Ctrl Pts',(115.434118901006,5.18980561039392,126.717795714978));
#197573=CARTESIAN_POINT('Ctrl Pts',(115.155671277193,-0.632926089611396,
124.229142024863));
#197574=CARTESIAN_POINT('Ctrl Pts',(114.87722365338,-5.87402963342224,127.782793004156));
#197575=CARTESIAN_POINT('Ctrl Pts',(114.598776029567,-5.71718690641897,
134.113117008387));
#197576=CARTESIAN_POINT('Ctrl Pts',(114.320328405754,-0.306528712524212,
137.40285553119));
#197577=CARTESIAN_POINT('Ctrl Pts',(114.041880781941,5.38581439342023,134.628899582769));
#197578=CARTESIAN_POINT('Ctrl Pts',(113.763433158128,6.12885718347172,128.340379164441));
#197579=CARTESIAN_POINT('Ctrl Pts',(113.484985534315,1.23977963323159,124.316137329349));
#197580=CARTESIAN_POINT('Ctrl Pts',(113.206537910502,-4.78859483334625,
126.254255728798));
#197581=CARTESIAN_POINT('Ctrl Pts',(112.92809028669,-6.41648458394181,132.373698236044));
#197582=CARTESIAN_POINT('Ctrl Pts',(112.649642662877,-2.14793846459313,
137.050996138312));
#197583=CARTESIAN_POINT('Ctrl Pts',(112.371195039064,4.09445817108915,135.987941162125));
#197584=CARTESIAN_POINT('Ctrl Pts',(112.092747415251,6.57424777294209,130.161428897475));
#197585=CARTESIAN_POINT('Ctrl Pts',(111.814299791438,3.01262484132005,124.925739474628));
#197586=CARTESIAN_POINT('Ctrl Pts',(111.535852167625,-3.31745314456969,
125.092215695531));
#197587=CARTESIAN_POINT('Ctrl Pts',(111.257404543812,-6.59895375719588,
130.507874045991));
#197588=CARTESIAN_POINT('Ctrl Pts',(110.978956919999,-3.816338243772,136.195989071554));
#197589=CARTESIAN_POINT('Ctrl Pts',(110.700509296186,2.47330567719032,136.929460943594));
#197590=CARTESIAN_POINT('Ctrl Pts',(110.422061672374,6.49010250851429,132.0342648438));
#197591=CARTESIAN_POINT('Ctrl Pts',(110.143614048561,4.54281219364771,126.008846844259));
#197592=CARTESIAN_POINT('Ctrl Pts',(109.865166424748,-1.57910059846782,
124.390271728514));
#197593=CARTESIAN_POINT('Ctrl Pts',(109.586718800935,-6.24989708394428,
128.665930956147));
#197594=CARTESIAN_POINT('Ctrl Pts',(109.308271177122,-5.17734347372243,
134.906702574525));
#197595=CARTESIAN_POINT('Ctrl Pts',(109.029823553309,0.652935861560398,
137.377622345005));
#197596=CARTESIAN_POINT('Ctrl Pts',(108.751375929496,5.88319903775945,133.808035709655));
#197597=CARTESIAN_POINT('Ctrl Pts',(108.472928305683,5.70708970850866,127.478218402361));
#197598=CARTESIAN_POINT('Ctrl Pts',(108.19448068187,0.286443743970404,124.204963299759));
#197599=CARTESIAN_POINT('Ctrl Pts',(107.916033058058,-5.39743002772183,
126.996231933739));
#197600=CARTESIAN_POINT('Ctrl Pts',(107.637585434244,-6.12132928305326,
133.286984790727));
#197601=CARTESIAN_POINT('Ctrl Pts',(107.359137810432,-1.22002597081922,
137.296327315513));
#197602=CARTESIAN_POINT('Ctrl Pts',(107.080690186619,4.80242160701559,135.339869595089));
#197603=CARTESIAN_POINT('Ctrl Pts',(106.802242562806,6.41167833934146,129.215500696253));
#197604=CARTESIAN_POINT('Ctrl Pts',(106.523794938993,2.12891590571267,124.551216444981));
#197605=CARTESIAN_POINT('Ctrl Pts',(106.24534731518,-4.11021624194206,125.633266205238));
#197606=CARTESIAN_POINT('Ctrl Pts',(105.966899691367,-6.57226045847839,
131.467299108419));
#197607=CARTESIAN_POINT('Ctrl Pts',(105.688452067554,-2.99471838644612,
136.692123924851));
#197608=CARTESIAN_POINT('Ctrl Pts',(105.410004443742,3.33482358260376,136.506381895117));
#197609=CARTESIAN_POINT('Ctrl Pts',(105.131556819929,6.59982559442975,131.080760870538));
#197610=CARTESIAN_POINT('Ctrl Pts',(104.853109196116,3.79991030437941,125.401141516381));
#197611=CARTESIAN_POINT('Ctrl Pts',(104.574661572303,-2.49193691945696,
124.686816554284));
#197612=CARTESIAN_POINT('Ctrl Pts',(104.29621394849,-6.49381585219884,129.594215727701));
#197613=CARTESIAN_POINT('Ctrl Pts',(104.017766324677,-4.52819525731082,
135.613678936038));
#197614=CARTESIAN_POINT('Ctrl Pts',(103.739318700864,1.59861556440955,137.213613557961));
#197615=CARTESIAN_POINT('Ctrl Pts',(103.460871077051,6.25637677914949,132.923757837073));
#197616=CARTESIAN_POINT('Ctrl Pts',(103.182423453238,5.16483337484823,126.686279609768));
#197617=CARTESIAN_POINT('Ctrl Pts',(102.903975829425,-0.672939584800916,
124.233116649188));
#197618=CARTESIAN_POINT('Ctrl Pts',(102.625528205613,-5.89231394094447,
127.818605872432));
#197619=CARTESIAN_POINT('Ctrl Pts',(102.347080581799,-5.69693964089892,
134.147857844226));
#197620=CARTESIAN_POINT('Ctrl Pts',(102.068632957987,-0.266356121840884,
137.40459920364));
#197621=CARTESIAN_POINT('Ctrl Pts',(101.790185334174,5.40899566096888,134.59604374203));
#197622=CARTESIAN_POINT('Ctrl Pts',(101.511737710361,6.11374467547657,128.303116723058));
#197623=CARTESIAN_POINT('Ctrl Pts',(101.233290086548,1.20026100625305,124.308710650579));
#197624=CARTESIAN_POINT('Ctrl Pts',(100.954842462735,-4.81620389170723,
126.28348956762));
#197625=CARTESIAN_POINT('Ctrl Pts',(100.676394838922,-6.40681269782886,
132.412728122731));
#197626=CARTESIAN_POINT('Ctrl Pts',(100.397947215109,-2.10987362484612,
137.063955513716));
#197627=CARTESIAN_POINT('Ctrl Pts',(100.119499591297,4.12593623631335,135.962920993349));
#197628=CARTESIAN_POINT('Ctrl Pts',(99.8410519674839,6.5702122594916,130.121421497322));
#197629=CARTESIAN_POINT('Ctrl Pts',(99.5626043436712,2.97678418891005,124.907509689368));
#197630=CARTESIAN_POINT('Ctrl Pts',(99.2841567198582,-3.35216312728773,
125.112515807244));
#197631=CARTESIAN_POINT('Ctrl Pts',(99.0057090960455,-6.6006362917809,130.548049243728));
#197632=CARTESIAN_POINT('Ctrl Pts',(98.7272614722323,-3.78344716313679,
136.219120311263));
#197633=CARTESIAN_POINT('Ctrl Pts',(98.4488138484198,2.51054507676055,136.914291746006));
#197634=CARTESIAN_POINT('Ctrl Pts',(98.1703662246066,6.49746903806041,131.994734960442));
#197635=CARTESIAN_POINT('Ctrl Pts',(97.8919186007939,4.51353637239165,125.981282306795));
#197636=CARTESIAN_POINT('Ctrl Pts',(97.6134709769809,-1.61811572099509,
124.400003000271));
#197637=CARTESIAN_POINT('Ctrl Pts',(97.335023353168,-6.26279851613479,128.704015473778));
#197638=CARTESIAN_POINT('Ctrl Pts',(97.0565757293552,-5.15227542966332,
134.938142526861));
#197639=CARTESIAN_POINT('Ctrl Pts',(96.7781281055422,0.692937074020952,
137.373525951775));
#197640=CARTESIAN_POINT('Ctrl Pts',(96.4996804817294,5.90137425853808,133.772167356118));
#197641=CARTESIAN_POINT('Ctrl Pts',(96.2212328579164,5.6867367976186,127.443539353151));
#197642=CARTESIAN_POINT('Ctrl Pts',(95.9427852341037,0.246266032224636,
124.203341906934));
#197643=CARTESIAN_POINT('Ctrl Pts',(95.6643376102905,-5.42051118601915,
127.029158178097));
#197644=CARTESIAN_POINT('Ctrl Pts',(95.3858899864779,-6.10610343100435,
133.324201062238));
#197645=CARTESIAN_POINT('Ctrl Pts',(95.1074423626648,-1.18048492263276,
137.303633678775));
#197646=CARTESIAN_POINT('Ctrl Pts',(94.828994738852,4.82994155974394,135.3105518592));
#197647=CARTESIAN_POINT('Ctrl Pts',(94.5505471150391,6.40188770447863,129.176500428244));
#197648=CARTESIAN_POINT('Ctrl Pts',(94.2720994912261,2.09081179839861,124.538372985881));
#197649=CARTESIAN_POINT('Ctrl Pts',(93.9936518674133,-4.14161800857485,
125.658382066524));
#197650=CARTESIAN_POINT('Ctrl Pts',(93.7152042436005,-6.56810319495607,
131.507294040545));
#197651=CARTESIAN_POINT('Ctrl Pts',(93.4367566197874,-2.95882241485189,
136.710244539055));
#197652=CARTESIAN_POINT('Ctrl Pts',(93.1583089959747,3.36947161799043,136.485976232185));
#197653=CARTESIAN_POINT('Ctrl Pts',(92.8798613721617,6.60138584173913,131.040580737834));
#197654=CARTESIAN_POINT('Ctrl Pts',(92.6014137483489,3.76694897255651,125.37811049295));
#197655=CARTESIAN_POINT('Ctrl Pts',(92.3229661245359,-2.5291299767175,124.702099025532));
#197656=CARTESIAN_POINT('Ctrl Pts',(92.044518500723,-6.50106203225643,129.633767849141));
#197657=CARTESIAN_POINT('Ctrl Pts',(91.7660708769102,-4.49883567468812,
135.641154240296));
#197658=CARTESIAN_POINT('Ctrl Pts',(91.4876232530973,1.63760088757763,137.203763582666));
#197659=CARTESIAN_POINT('Ctrl Pts',(91.2091756292845,6.26916223541028,132.885634228324));
#197660=CARTESIAN_POINT('Ctrl Pts',(90.9307280054714,5.13966975450256,126.654916101563));
#197661=CARTESIAN_POINT('Ctrl Pts',(90.6522803816587,-0.71292814396669,
124.237334773374));
#197662=CARTESIAN_POINT('Ctrl Pts',(90.3738327578456,-5.91037990660673,
127.85452937895));
#197663=CARTESIAN_POINT('Ctrl Pts',(90.0953851340328,-5.67648127318543,
134.182474785545));
#197664=CARTESIAN_POINT('Ctrl Pts',(89.8169375102199,-0.226173661233629,
137.406098301819));
#197665=CARTESIAN_POINT('Ctrl Pts',(89.5384898864071,5.43197649619419,134.563047399079));
#197666=CARTESIAN_POINT('Ctrl Pts',(89.260042262594,6.09840562042418,128.265946966186));
#197667=CARTESIAN_POINT('Ctrl Pts',(88.9815946387814,1.1606979031614,124.301524670509));
#197668=CARTESIAN_POINT('Ctrl Pts',(88.7031470149683,-4.84363448386183,
126.312890928981));
#197669=CARTESIAN_POINT('Ctrl Pts',(88.4246993911556,-6.39690340491527,
132.45169841077));
#197670=CARTESIAN_POINT('Ctrl Pts',(88.1462517673426,-2.07173060295614,
137.076682937528));
#197671=CARTESIAN_POINT('Ctrl Pts',(87.8678041435297,4.15726141345302,135.937709672222));
#197672=CARTESIAN_POINT('Ctrl Pts',(87.5893565197169,6.5659332844097,130.081439403729));
#197673=CARTESIAN_POINT('Ctrl Pts',(87.3109088959039,2.94083323066708,124.889498414087));
#197674=CARTESIAN_POINT('Ctrl Pts',(87.032461272091,-3.38674889436835,125.133026832359));
#197675=CARTESIAN_POINT('Ctrl Pts',(86.7540136482781,-6.60207423736065,
130.588233939178));
#197676=CARTESIAN_POINT('Ctrl Pts',(86.4755660244652,-3.75041588547566,
136.242050905059));
#197677=CARTESIAN_POINT('Ctrl Pts',(86.1971184006524,2.54769144715974,136.898896142674));
#197678=CARTESIAN_POINT('Ctrl Pts',(85.9186707768394,6.50459480150186,131.955160967326));
#197679=CARTESIAN_POINT('Ctrl Pts',(85.6402231530266,4.48409330038545,125.953896490271));
#197680=CARTESIAN_POINT('Ctrl Pts',(85.3617755292137,-1.65707088364924,
124.409971587854));
#197681=CARTESIAN_POINT('Ctrl Pts',(85.0833279054008,-6.27546787802325,
128.742177820471));
#197682=CARTESIAN_POINT('Ctrl Pts',(84.8048802815879,-5.12701646614329,
134.969429300388));
#197683=CARTESIAN_POINT('Ctrl Pts',(84.526432657775,0.732912609443495,137.369186135708));
#197684=CARTESIAN_POINT('Ctrl Pts',(84.2479850339622,5.91933080172332,133.73618902941));
#197685=CARTESIAN_POINT('Ctrl Pts',(83.9695374101491,5.6661731626052,127.408984840408));
#197686=CARTESIAN_POINT('Ctrl Pts',(83.6910897863363,0.206079195000604,
124.201965117285));
#197687=CARTESIAN_POINT('Ctrl Pts',(83.4126421625234,-5.44339148528112,
127.062224313968));
#197688=CARTESIAN_POINT('Ctrl Pts',(83.1341945387106,-6.09065131504733,
133.361323960135));
#197689=CARTESIAN_POINT('Ctrl Pts',(82.8557469148977,-1.14090013114324,
137.310699209084));
#197690=CARTESIAN_POINT('Ctrl Pts',(82.5772992910847,4.85728253721157,135.281067144739));
#197691=CARTESIAN_POINT('Ctrl Pts',(82.2988516672719,6.39185984531258,129.137560481192));
#197692=CARTESIAN_POINT('Ctrl Pts',(82.0204040434589,2.05263021528453,124.52576171526));
#197693=CARTESIAN_POINT('Ctrl Pts',(81.7419564196462,-4.17286630602932,
125.683688613938));
#197694=CARTESIAN_POINT('Ctrl Pts',(81.4635087958331,-6.56370254795435,
131.547262925216));
#197695=CARTESIAN_POINT('Ctrl Pts',(81.1850611720204,-2.92281680300497,
136.728146308557));
#197696=CARTESIAN_POINT('Ctrl Pts',(80.9066135482074,3.40399479636718,136.465360034899));
#197697=CARTESIAN_POINT('Ctrl Pts',(80.6281659243945,6.60270147226842,131.000391851905));
#197698=CARTESIAN_POINT('Ctrl Pts',(80.3497183005816,3.73384805505426,125.355280541214));
#197699=CARTESIAN_POINT('Ctrl Pts',(80.0712706767688,-2.56622931613655,
124.717607618327));
#197700=CARTESIAN_POINT('Ctrl Pts',(79.7928230529558,-6.50806731306963,
129.673363347327));
#197701=CARTESIAN_POINT('Ctrl Pts',(79.514375429143,-4.46930938605503,135.668450315387));
#197702=CARTESIAN_POINT('Ctrl Pts',(79.23592780533,1.67652552884245,137.193676475141));
#197703=CARTESIAN_POINT('Ctrl Pts',(78.9574801815173,6.28171538555901,132.847433497217));
#197704=CARTESIAN_POINT('Ctrl Pts',(78.6790325577042,5.11431568180404,126.62370635255));
#197705=CARTESIAN_POINT('Ctrl Pts',(78.4005849338915,-0.752890285318027,
124.241796241119));
#197706=CARTESIAN_POINT('Ctrl Pts',(78.1221373100785,-5.92822686096799,
127.890562192549));
#197707=CARTESIAN_POINT('Ctrl Pts',(77.8436896862655,-5.65581256137084,
134.216966549603));
#197708=CARTESIAN_POINT('Ctrl Pts',(77.5652420624528,-0.185982819678218,
137.407352770183));
#197709=CARTESIAN_POINT('Ctrl Pts',(77.2867944386398,5.45475604753291,134.529911776607));
#197710=CARTESIAN_POINT('Ctrl Pts',(77.008346814827,6.08284058670873,128.228871271165));
#197711=CARTESIAN_POINT('Ctrl Pts',(76.729899191014,1.12109178998211,124.294579655415));
#197712=CARTESIAN_POINT('Ctrl Pts',(76.4514515672013,-4.8708855933594,126.342458723402));
#197713=CARTESIAN_POINT('Ctrl Pts',(76.1730039433881,-6.38675707239351,
132.4906076561));
#197714=CARTESIAN_POINT('Ctrl Pts',(75.8945563195755,-2.03351081232684,
137.089177938131));
#197715=CARTESIAN_POINT('Ctrl Pts',(75.6161086957625,4.18843254174224,135.912308132958));
#197716=CARTESIAN_POINT('Ctrl Pts',(75.3376610719495,6.56141100625526,130.041484098248));
#197717=CARTESIAN_POINT('Ctrl Pts',(75.0592134481368,2.90477329876725,124.871706316201));
#197718=CARTESIAN_POINT('Ctrl Pts',(74.7807658243238,-3.42120916422307,
125.153748010832));
#197719=CARTESIAN_POINT('Ctrl Pts',(74.5023182005109,-6.60326754065171,
130.628426643279));
#197720=CARTESIAN_POINT('Ctrl Pts',(74.223870576698,-3.71724563477466,136.264780003243));
#197721=CARTESIAN_POINT('Ctrl Pts',(73.9454229528852,2.58474341191554,136.883274704086));
#197722=CARTESIAN_POINT('Ctrl Pts',(73.6669753290721,6.51147953479087,131.915544330879));
#197723=CARTESIAN_POINT('Ctrl Pts',(73.3885277052595,4.45448406865298,125.926690409479));
#197724=CARTESIAN_POINT('Ctrl Pts',(73.1100800814464,-1.6959646429323,124.420177121874));
#197725=CARTESIAN_POINT('Ctrl Pts',(72.8316324576336,-6.28790470014163,
128.780416582107));
#197726=CARTESIAN_POINT('Ctrl Pts',(72.5531848338207,-5.1015675191428,135.000561735763));
#197727=CARTESIAN_POINT('Ctrl Pts',(72.2747372100078,0.772860986519783,
137.364603057617));
#197728=CARTESIAN_POINT('Ctrl Pts',(71.996289586195,5.93706800192887,133.700102062723));
#197729=CARTESIAN_POINT('Ctrl Pts',(71.7178419623819,5.64539956546153,127.374556144564));
#197730=CARTESIAN_POINT('Ctrl Pts',(71.4393943385692,0.165884721436248,
124.20083298183));
#197731=CARTESIAN_POINT('Ctrl Pts',(71.1609467147562,-5.46607007766984,
127.095429116077));
#197732=CARTESIAN_POINT('Ctrl Pts',(70.8824990909434,-6.07497350776591,
133.398352108815));
#197733=CARTESIAN_POINT('Ctrl Pts',(70.6040514671303,-1.10127306317963,
137.317523644624));
#197734=CARTESIAN_POINT('Ctrl Pts',(70.3256038433176,4.88444352628841,135.251416544269));
#197735=CARTESIAN_POINT('Ctrl Pts',(70.0471562195047,6.38159513342946,129.098682298033));
#197736=CARTESIAN_POINT('Ctrl Pts',(69.7687085956917,2.01437257120279,124.513383100429));
#197737=CARTESIAN_POINT('Ctrl Pts',(69.4902609718789,-4.20395997638847,
125.709184909736));
#197738=CARTESIAN_POINT('Ctrl Pts',(69.211813348066,-6.5590586805409,131.587204281367));
#197739=CARTESIAN_POINT('Ctrl Pts',(68.9333657242531,-2.88670288510633,
136.745828570004));
#197740=CARTESIAN_POINT('Ctrl Pts',(68.6549181004402,3.43839183846502,136.444534067195));
#197741=CARTESIAN_POINT('Ctrl Pts',(68.3764704766273,6.60377243726651,130.960195701968));
#197742=CARTESIAN_POINT('Ctrl Pts',(68.0980228528144,3.70060877843901,125.332652507142));
#197743=CARTESIAN_POINT('Ctrl Pts',(67.8195752290015,-2.6032335629848,124.733341757993));
#197744=CARTESIAN_POINT('Ctrl Pts',(67.5411276051886,-6.51483143505509,
129.713000755032));
#197745=CARTESIAN_POINT('Ctrl Pts',(67.2626799813758,-4.43961748551916,
135.695566149845));
#197746=CARTESIAN_POINT('Ctrl Pts',(66.9842323575627,1.71538804583728,137.183352609169));
#197747=CARTESIAN_POINT('Ctrl Pts',(66.7057847337499,6.29403576443417,132.809157059292));
#197748=CARTESIAN_POINT('Ctrl Pts',(66.4273371099371,5.08877209625689,126.592651519219));
#197749=CARTESIAN_POINT('Ctrl Pts',(66.1488894861241,-0.792824528042931,
124.246500887099));
#197750=CARTESIAN_POINT('Ctrl Pts',(65.8704418623113,-5.94585414270274,
127.92670297802));
#197751=CARTESIAN_POINT('Ctrl Pts',(65.5919942384984,-5.63493427134196,
134.251331858291));
#197752=CARTESIAN_POINT('Ctrl Pts',(65.3135466146855,-0.145785086460763,
137.408362562243));
#197753=CARTESIAN_POINT('Ctrl Pts',(65.0350989908726,5.47733347088038,134.496638102466));
#197754=CARTESIAN_POINT('Ctrl Pts',(64.7566513670597,6.06705015109826,128.191891011849));
#197755=CARTESIAN_POINT('Ctrl Pts',(64.4782037432468,1.0814441343344,124.28787586265));
#197756=CARTESIAN_POINT('Ctrl Pts',(64.199756119434,-4.89795621039988,126.37219185524));
#197757=CARTESIAN_POINT('Ctrl Pts',(63.921308495621,-6.37637407623982,132.529454416925));
#197758=CARTESIAN_POINT('Ctrl Pts',(63.6428608718081,-1.99521566920641,
137.101440052517));
#197759=CARTESIAN_POINT('Ctrl Pts',(63.3644132479953,4.21944846612332,135.886717316821));
#197760=CARTESIAN_POINT('Ctrl Pts',(63.0859656241823,6.556645592603,130.001557061437));
#197761=CARTESIAN_POINT('Ctrl Pts',(62.8075180003696,2.86860572942485,124.854134055001));
#197762=CARTESIAN_POINT('Ctrl Pts',(62.5290703765565,-3.4555426599142,125.174678574835));
#197763=CARTESIAN_POINT('Ctrl Pts',(62.2506227527437,-6.60421615743575,
130.66862586668));
#197764=CARTESIAN_POINT('Ctrl Pts',(61.9721751289308,-3.68393764016947,
136.287306763578));
#197765=CARTESIAN_POINT('Ctrl Pts',(61.6937275051179,2.62169959805353,136.867428009101));
#197766=CARTESIAN_POINT('Ctrl Pts',(61.415279881305,6.51812298281107,131.875886519111));
#197767=CARTESIAN_POINT('Ctrl Pts',(61.1368322574921,4.42470977437533,125.899665072552));
#197768=CARTESIAN_POINT('Ctrl Pts',(60.8583846336791,-1.73479555762186,
124.430619224162));
#197769=CARTESIAN_POINT('Ctrl Pts',(60.5799370098664,-6.30010852163892,
128.818730341733));
#197770=CARTESIAN_POINT('Ctrl Pts',(60.3014893860534,-5.07592953168175,
135.031538679362));
#197771=CARTESIAN_POINT('Ctrl Pts',(60.0230417622406,0.81278072494776,137.35977688733));
#197772=CARTESIAN_POINT('Ctrl Pts',(59.7445941384276,5.95458520189618,133.663907793273));
#197773=CARTESIAN_POINT('Ctrl Pts',(59.4661465146148,5.62441677596096,127.340254541386));
#197774=CARTESIAN_POINT('Ctrl Pts',(59.1876988908018,0.125684100952275,
124.199945542519));
#197775=CARTESIAN_POINT('Ctrl Pts',(58.909251266989,-5.48854612282181,127.128771354006));
#197776=CARTESIAN_POINT('Ctrl Pts',(58.6308036431761,-6.05907059010694,
133.435284136186));
#197777=CARTESIAN_POINT('Ctrl Pts',(58.3523560193632,-1.06160518713815,
137.324106732513));
#197778=CARTESIAN_POINT('Ctrl Pts',(58.0739083955504,4.91142352051418,135.221601156507));
#197779=CARTESIAN_POINT('Ctrl Pts',(57.7954607717374,6.37109394919177,129.059867319411));
#197780=CARTESIAN_POINT('Ctrl Pts',(57.5170131479246,1.97604028380464,124.501237600083));
#197781=CARTESIAN_POINT('Ctrl Pts',(57.2385655241116,-4.23489786746425,
125.734870009144));
#197782=CARTESIAN_POINT('Ctrl Pts',(56.9601179002987,-6.554171764796,131.627116628959));
#197783=CARTESIAN_POINT('Ctrl Pts',(56.6816702764859,-2.85048199937133,
136.76329066817));
#197784=CARTESIAN_POINT('Ctrl Pts',(56.4032226526729,3.47266146968847,136.423499100792));
#197785=CARTESIAN_POINT('Ctrl Pts',(56.1247750288601,6.60459869704857,130.919993777505));
#197786=CARTESIAN_POINT('Ctrl Pts',(55.8463274050471,3.66723237440476,125.310227229228));
#197787=CARTESIAN_POINT('Ctrl Pts',(55.5678797812343,-2.6401413460556,124.749300861495));
#197788=CARTESIAN_POINT('Ctrl Pts',(55.2894321574214,-6.5213541475661,129.752678603477));
#197789=CARTESIAN_POINT('Ctrl Pts',(55.0109845336085,-4.40976107332459,
135.722500738884));
#197790=CARTESIAN_POINT('Ctrl Pts',(54.7325369097956,1.75418699849736,137.172792367301));
#197791=CARTESIAN_POINT('Ctrl Pts',(54.4540892859827,6.30612291549916,132.770806332897));
#197792=CARTESIAN_POINT('Ctrl Pts',(54.1756416621698,5.06303994438864,126.561752752318));
#197793=CARTESIAN_POINT('Ctrl Pts',(53.897194038357,-0.832729392363195,
124.251448536985));
#197794=CARTESIAN_POINT('Ctrl Pts',(53.618746414544,-5.96326109862574,127.962950396153));
#197795=CARTESIAN_POINT('Ctrl Pts',(53.3402987907312,-5.61384717675129,
134.285569438194));
#197796=CARTESIAN_POINT('Ctrl Pts',(53.0618511669183,-0.105581951123662,
137.409127640582));
#197797=CARTESIAN_POINT('Ctrl Pts',(52.7834035431054,5.49970792962155,134.463227609627));
#197798=CARTESIAN_POINT('Ctrl Pts',(52.5049559192925,6.05103489871361,128.155007558556));
#197799=CARTESIAN_POINT('Ctrl Pts',(52.2265082954796,1.04175640537643,124.281413540623));
#197800=CARTESIAN_POINT('Ctrl Pts',(51.9480606716666,-4.9248453318719,126.402089222721));
#197801=CARTESIAN_POINT('Ctrl Pts',(51.6696130478539,-6.36575480119974,
132.568237253767));
#197802=CARTESIAN_POINT('Ctrl Pts',(51.3911654240409,-1.95684659263562,
137.113468826308));
#197803=CARTESIAN_POINT('Ctrl Pts',(51.112717800228,4.25030803728985,135.860938172086));
#197804=CARTESIAN_POINT('Ctrl Pts',(50.8342701764151,6.55163722003711,129.961659772806));
#197805=CARTESIAN_POINT('Ctrl Pts',(50.5558225526023,2.83233186284197,124.836782281636));
#197806=CARTESIAN_POINT('Ctrl Pts',(50.2773749287893,-3.48974810920128,
125.195817748775));
#197807=CARTESIAN_POINT('Ctrl Pts',(49.9989273049765,-6.60492005256131,
130.708830119782));
#197808=CARTESIAN_POINT('Ctrl Pts',(49.7204796811635,-3.65049313590031,
136.309630351328));
#197809=CARTESIAN_POINT('Ctrl Pts',(49.4420320573507,2.65855863614892,136.851356644924));
#197810=CARTESIAN_POINT('Ctrl Pts',(49.1635844335378,6.52452489938715,131.836189001557));
#197811=CARTESIAN_POINT('Ctrl Pts',(48.8851368097249,4.39477152084969,125.87282148092));
#197812=CARTESIAN_POINT('Ctrl Pts',(48.606689185912,-1.77356218882415,124.441297507781));
#197813=CARTESIAN_POINT('Ctrl Pts',(48.3282415620992,-6.31207889029818,
128.857117679619));
#197814=CARTESIAN_POINT('Ctrl Pts',(48.0497939382862,-5.05010345378512,
135.062358983324));
#197815=CARTESIAN_POINT('Ctrl Pts',(47.7713463144734,0.852670345487299,
137.354707803682));
#197816=CARTESIAN_POINT('Ctrl Pts',(47.4928986906604,5.97188175251911,133.627607562248));
#197817=CARTESIAN_POINT('Ctrl Pts',(47.2144510668476,5.60322557162828,127.306081301933));
#197818=CARTESIAN_POINT('Ctrl Pts',(46.9360034430346,0.0854788231980546,
124.199302832238));
#197819=CARTESIAN_POINT('Ctrl Pts',(46.6575558192218,-5.5108187878785,127.162249792247));
#197820=CARTESIAN_POINT('Ctrl Pts',(46.3791081954089,-6.04294315135938,
133.47211867372));
#197821=CARTESIAN_POINT('Ctrl Pts',(46.100660571596,-1.02189797292572,137.330448228811));
#197822=CARTESIAN_POINT('Ctrl Pts',(45.822212947783,4.93822152013526,135.191622086273));
#197823=CARTESIAN_POINT('Ctrl Pts',(45.5437653239702,6.36035668172477,129.02111698363));
#197824=CARTESIAN_POINT('Ctrl Pts',(45.2653177001572,1.9376347735074,124.489325664279));
#197825=CARTESIAN_POINT('Ctrl Pts',(44.9868700763445,-4.26567883284234,
125.76074296039));
#197826=CARTESIAN_POINT('Ctrl Pts',(44.7084224525315,-6.54904198180601,
131.666998489025));
#197827=CARTESIAN_POINT('Ctrl Pts',(44.4299748287186,-2.81415548797717,
136.780531955991));
#197828=CARTESIAN_POINT('Ctrl Pts',(44.1515272049057,3.50680242016433,136.402255915145));
#197829=CARTESIAN_POINT('Ctrl Pts',(43.8730795810928,6.60518022099696,130.879787568212));
#197830=CARTESIAN_POINT('Ctrl Pts',(43.59463195728,3.63372007972613,125.288005538446));
#197831=CARTESIAN_POINT('Ctrl Pts',(43.316184333467,-2.6769512977182,124.765484337463));
#197832=CARTESIAN_POINT('Ctrl Pts',(43.0377367096542,-6.52763520890084,
129.792395422388));
#197833=CARTESIAN_POINT('Ctrl Pts',(42.7592890858413,-4.37974125581177,
135.749253084432));
#197834=CARTESIAN_POINT('Ctrl Pts',(42.4808414620283,1.79292094911309,137.161996140853));
#197835=CARTESIAN_POINT('Ctrl Pts',(42.2023938382155,6.31797639086063,132.732382739134));
#197836=CARTESIAN_POINT('Ctrl Pts',(41.9239462144025,5.0371201797131,126.531011196811));
#197837=CARTESIAN_POINT('Ctrl Pts',(41.6454985905898,-0.872603399589798,
124.256639007436));
#197838=CARTESIAN_POINT('Ctrl Pts',(41.3670509667768,-5.98044708371573,
127.999303103786));
#197839=CARTESIAN_POINT('Ctrl Pts',(41.0886033429639,-5.592552058989,134.319678020622));
#197840=CARTESIAN_POINT('Ctrl Pts',(40.810155719151,-0.0653749034083074,
137.409647976851));
#197841=CARTESIAN_POINT('Ctrl Pts',(40.5317080953382,5.52187859466303,134.429681536124));
#197842=CARTESIAN_POINT('Ctrl Pts',(40.2532604715252,6.03479542300531,128.118222278014));
#197843=CARTESIAN_POINT('Ctrl Pts',(39.9748128477124,1.00203007375177,124.275192928799));
#197844=CARTESIAN_POINT('Ctrl Pts',(39.6963652238994,-4.95155196138904,
126.432149717987));
#197845=CARTESIAN_POINT('Ctrl Pts',(39.4179176000866,-6.35489964077443,
132.60695472951));
#197846=CARTESIAN_POINT('Ctrl Pts',(39.1394699762736,-1.91840500439501,
137.125263813774));
#197847=CARTESIAN_POINT('Ctrl Pts',(38.8610223524608,4.28101011172891,135.834971654011));
#197848=CARTESIAN_POINT('Ctrl Pts',(38.5825747286478,6.54638607414467,129.921793710766));
#197849=CARTESIAN_POINT('Ctrl Pts',(38.304127104835,2.79595304316033,124.819651639079));
#197850=CARTESIAN_POINT('Ctrl Pts',(38.0256794810221,-3.52382424458856,
125.217164749334));
#197851=CARTESIAN_POINT('Ctrl Pts',(37.7472318572093,-6.60537919994535,
130.749037912801));
#197852=CARTESIAN_POINT('Ctrl Pts',(37.4687842333963,-3.61691336126579,
136.331749939282));
#197853=CARTESIAN_POINT('Ctrl Pts',(37.1903366095834,2.69531916037638,136.835061207086));
#197854=CARTESIAN_POINT('Ctrl Pts',(36.9118889857706,6.53068504729366,131.796453249222));
#197855=CARTESIAN_POINT('Ctrl Pts',(36.6334413619576,4.36467041744916,125.846160629286));
#197856=CARTESIAN_POINT('Ctrl Pts',(36.3549937381448,-1.8122631000273,124.452211577043));
#197857=CARTESIAN_POINT('Ctrl Pts',(36.0765461143319,-6.32381536255287,
128.895577173308));
#197858=CARTESIAN_POINT('Ctrl Pts',(35.798098490519,-5.02409024244786,135.093021505591));
#197859=CARTESIAN_POINT('Ctrl Pts',(35.5196508667061,0.892528370013623,
137.34939599451));
#197860=CARTESIAN_POINT('Ctrl Pts',(35.2412032428932,5.98895701286753,133.591202714771));
#197861=CARTESIAN_POINT('Ctrl Pts',(34.9627556190803,5.58182673771145,127.272037692505));
#197862=CARTESIAN_POINT('Ctrl Pts',(34.6843079952674,0.0452703779943793,
124.198904874802));
#197863=CARTESIAN_POINT('Ctrl Pts',(34.4058603714545,-5.53288724751859,
127.195863190245));
#197864=CARTESIAN_POINT('Ctrl Pts',(34.1274127476417,-6.02659178913083,
133.508854356496));
#197865=CARTESIAN_POINT('Ctrl Pts',(33.8489651238287,-0.982152891908117,
137.336547898535));
#197866=CARTESIAN_POINT('Ctrl Pts',(33.5705175000158,4.96483653214189,135.161480444452));
#197867=CARTESIAN_POINT('Ctrl Pts',(33.292069876203,6.34938372890195,128.982432726597));
#197868=CARTESIAN_POINT('Ctrl Pts',(33.0136222523901,1.89915746344075,124.477647734417));
#197869=CARTESIAN_POINT('Ctrl Pts',(32.7351746285772,-4.29630173192265,
125.786802804744));
#197870=CARTESIAN_POINT('Ctrl Pts',(32.4567270047643,-6.543669521657,131.706848383727));
#197871=CARTESIAN_POINT('Ctrl Pts',(32.1782793809514,-2.77772469701646,
136.797551794587));
#197872=CARTESIAN_POINT('Ctrl Pts',(31.8998317571386,3.54081342478663,136.380805297429));
#197873=CARTESIAN_POINT('Ctrl Pts',(31.6213841333256,6.60551698756319,130.839578563946));
#197874=CARTESIAN_POINT('Ctrl Pts',(31.3429365095127,3.6000731362139,125.26598825823));
#197875=CARTESIAN_POINT('Ctrl Pts',(31.0644888856998,-2.71366205396602,
124.781891586214));
#197876=CARTESIAN_POINT('Ctrl Pts',(30.7860412618869,-6.53367438631237,
129.83214974004));
#197877=CARTESIAN_POINT('Ctrl Pts',(30.507593638074,-4.34955914537615,135.775822195171));
#197878=CARTESIAN_POINT('Ctrl Pts',(30.2291460142612,1.83158846238341,137.150964329883));
#197879=CARTESIAN_POINT('Ctrl Pts',(29.9506983904483,6.32959575128355,132.693887701803));
#197880=CARTESIAN_POINT('Ctrl Pts',(29.6722507666353,5.01101376269691,126.500427991838));
#197881=CARTESIAN_POINT('Ctrl Pts',(29.3938031428225,-0.912445072176531,
124.26207210612));
#197882=CARTESIAN_POINT('Ctrl Pts',(29.1153555190096,-5.99741146113971,
128.035759753857));
#197883=CARTESIAN_POINT('Ctrl Pts',(28.8369078951967,-5.57104970715349,
134.353656341672));
#197884=CARTESIAN_POINT('Ctrl Pts',(28.5584602713837,-0.0251654332018655,
137.409923551768));
#197885=CARTESIAN_POINT('Ctrl Pts',(28.280012647571,5.54384464446253,134.396001125022));
#197886=CARTESIAN_POINT('Ctrl Pts',(28.001565023758,6.0183323257333,128.081536533317));
#197887=CARTESIAN_POINT('Ctrl Pts',(27.7231173999451,0.962266611534229,
124.269214257685));
#197888=CARTESIAN_POINT('Ctrl Pts',(27.4446697761322,-4.97807510932732,
126.462372227135));
#197889=CARTESIAN_POINT('Ctrl Pts',(27.1662221523194,-6.34380899720599,
132.645605409466));
#197890=CARTESIAN_POINT('Ctrl Pts',(26.8877745285064,-1.87989232895117,
137.136824577849));
#197891=CARTESIAN_POINT('Ctrl Pts',(26.6093269046936,4.31155355176403,135.808818724794));
#197892=CARTESIAN_POINT('Ctrl Pts',(26.3308792808807,6.5408923495088,129.881960352566));
#197893=CARTESIAN_POINT('Ctrl Pts',(26.0524316570678,2.75947061841045,124.802742762115));
#197894=CARTESIAN_POINT('Ctrl Pts',(25.7739840332549,-3.55776980337282,
125.238718785491));
#197895=CARTESIAN_POINT('Ctrl Pts',(25.4955364094419,-6.60559358257403,
130.789247755823));
#197896=CARTESIAN_POINT('Ctrl Pts',(25.2170887856292,-3.58319956057628,
136.353664707793));
#197897=CARTESIAN_POINT('Ctrl Pts',(24.9386411618162,2.73197980856112,136.81854229942));
#197898=CARTESIAN_POINT('Ctrl Pts',(24.6601935380033,6.5366031982641,131.756680734531));
#197899=CARTESIAN_POINT('Ctrl Pts',(24.3817459141905,4.3344075795813,125.819683505575));
#197900=CARTESIAN_POINT('Ctrl Pts',(24.1032982903775,-1.85089685715453,
124.463361027524));
#197901=CARTESIAN_POINT('Ctrl Pts',(23.8248506665647,-6.33531750350378,
128.934107397669));
#197902=CARTESIAN_POINT('Ctrl Pts',(23.5464030427517,-4.99789086159903,
135.123525109951));
#197903=CARTESIAN_POINT('Ctrl Pts',(23.2679554189389,0.932353321572971,
137.343841656646));
#197904=CARTESIAN_POINT('Ctrl Pts',(22.9895077951259,6.00581035021119,133.554694599836));
#197905=CARTESIAN_POINT('Ctrl Pts',(22.7110601713131,5.56022106715229,127.238124974604));
#197906=CARTESIAN_POINT('Ctrl Pts',(22.4326125475002,0.00506025528043594,
124.198751684957));
#197907=CARTESIAN_POINT('Ctrl Pts',(22.1541649236873,-5.554750683987,127.229610302442));
#197908=CARTESIAN_POINT('Ctrl Pts',(21.8757172998744,-6.01001710932725,
133.545489823263));
#197909=CARTESIAN_POINT('Ctrl Pts',(21.5972696760615,-0.942371416853923,
137.342405515655));
#197910=CARTESIAN_POINT('Ctrl Pts',(21.3188220522486,4.99126757030501,135.131177347952));
#197911=CARTESIAN_POINT('Ctrl Pts',(21.0403744284357,6.33817549733007,128.943815981773));
#197912=CARTESIAN_POINT('Ctrl Pts',(20.7619268046228,1.86060977939589,124.466204243228));
#197913=CARTESIAN_POINT('Ctrl Pts',(20.48347918081,-4.32676542996233,125.813048576547));
#197914=CARTESIAN_POINT('Ctrl Pts',(20.205031556997,-6.5380545834274,131.746664836412));
#197915=CARTESIAN_POINT('Ctrl Pts',(19.9265839331841,-2.74119097644563,
136.814349553278));
#197916=CARTESIAN_POINT('Ctrl Pts',(19.6481363093713,3.57469322326559,136.359148042506));
#197917=CARTESIAN_POINT('Ctrl Pts',(19.3696886855584,6.60560898426828,130.799368254665));
#197918=CARTESIAN_POINT('Ctrl Pts',(19.0912410617455,3.56629279066743,125.244176204439));
#197919=CARTESIAN_POINT('Ctrl Pts',(18.8127934379326,-2.75027225446848,
124.798521999768));
#197920=CARTESIAN_POINT('Ctrl Pts',(18.5343458141197,-6.53947145601676,
129.871940083324));
#197921=CARTESIAN_POINT('Ctrl Pts',(18.2558981903068,-4.31921586042675,
135.802207086573));
#197922=CARTESIAN_POINT('Ctrl Pts',(17.9774505664939,1.87018810546999,137.139697343177));
#197923=CARTESIAN_POINT('Ctrl Pts',(17.6990029426811,6.34098056620813,132.65532264735));
#197924=CARTESIAN_POINT('Ctrl Pts',(17.4205553188681,4.98472166072295,126.470004270672));
#197925=CARTESIAN_POINT('Ctrl Pts',(17.1421076950552,-0.95225293377558,
124.26774763171));
#197926=CARTESIAN_POINT('Ctrl Pts',(16.8636600712423,-6.01415360227624,
128.072318995452));
#197927=CARTESIAN_POINT('Ctrl Pts',(16.5852124474295,-5.54934091802252,
134.387503142263));
#197928=CARTESIAN_POINT('Ctrl Pts',(16.3067648236166,0.0150449695187284,
137.409954355121));
#197929=CARTESIAN_POINT('Ctrl Pts',(16.0283171998036,5.56560526505998,134.362187624359));
#197930=CARTESIAN_POINT('Ctrl Pts',(15.7498695759908,6.00164621694371,128.044951683866));
#197931=CARTESIAN_POINT('Ctrl Pts',(15.4714219521779,0.922467492173741,
124.263477748823));
#197932=CARTESIAN_POINT('Ctrl Pts',(15.192974328365,-5.00441379286154,126.492755630261));
#197933=CARTESIAN_POINT('Ctrl Pts',(14.9145267045521,-6.33248328146239,
132.684187861418));
#197934=CARTESIAN_POINT('Ctrl Pts',(14.6360790807393,-1.84130999340576,
137.148150690142));
#197935=CARTESIAN_POINT('Ctrl Pts',(14.3576314569263,4.34193722559672,135.782480353541));
#197936=CARTESIAN_POINT('Ctrl Pts',(14.0791838331134,6.53515624970152,129.842161174248));
#197937=CARTESIAN_POINT('Ctrl Pts',(13.8007362093005,2.72288594046203,124.786056277307));
#197938=CARTESIAN_POINT('Ctrl Pts',(13.5222885854877,-3.59158352768866,
125.260479058552));
#197939=CARTESIAN_POINT('Ctrl Pts',(13.2438409616747,-6.60556319250329,
130.829458158858));
#197940=CARTESIAN_POINT('Ctrl Pts',(12.9653933378619,-3.54935298310934,
136.375373844801));
#197941=CARTESIAN_POINT('Ctrl Pts',(12.686945714049,2.76853922222938,136.801800534039));
#197942=CARTESIAN_POINT('Ctrl Pts',(12.4084980902361,6.5422791329992,131.716872931266));
#197943=CARTESIAN_POINT('Ctrl Pts',(12.1300504664232,4.30398412864651,125.793391090908));
#197944=CARTESIAN_POINT('Ctrl Pts',(11.8516028426103,-1.88946202861834,
124.474745446076));
#197945=CARTESIAN_POINT('Ctrl Pts',(11.5731552187974,-6.34658488693473,
128.972706924952));
#197946=CARTESIAN_POINT('Ctrl Pts',(11.2947075949845,-4.97150628206636,
135.153868666082));
#197947=CARTESIAN_POINT('Ctrl Pts',(11.0162599711716,0.972143724437105,
137.338044995907));
#197948=CARTESIAN_POINT('Ctrl Pts',(10.7378123473587,6.0224411400439,133.518084570262));
#197949=CARTESIAN_POINT('Ctrl Pts',(10.4593647235458,5.53840936055655,127.204344404875));
#197950=CARTESIAN_POINT('Ctrl Pts',(10.1809170997329,-0.0351500549433496,
124.198843268382));
#197951=CARTESIAN_POINT('Ctrl Pts',(9.90246947592002,-5.57640828712608,
127.263489878326));
#197952=CARTESIAN_POINT('Ctrl Pts',(9.62402185210712,-5.99321972612948,
133.582023716479));
#197953=CARTESIAN_POINT('Ctrl Pts',(9.34557422829421,-0.902555021880531,
137.348020863117));
#197954=CARTESIAN_POINT('Ctrl Pts',(9.06712660448133,5.01751365521256,135.100713919668));
#197955=CARTESIAN_POINT('Ctrl Pts',(8.78867898066847,6.32673240233446,128.905268180115));
#197956=CARTESIAN_POINT('Ctrl Pts',(8.51023135685555,1.82199314977141,124.454995614755));
#197957=CARTESIAN_POINT('Ctrl Pts',(8.23178373304265,-4.35706879811783,
125.839479303254));
#197958=CARTESIAN_POINT('Ctrl Pts',(7.9533361092298,-6.53219737518076,131.786446371669));
#197959=CARTESIAN_POINT('Ctrl Pts',(7.67488848541689,-2.70455568003535,
136.83092460962));
#197960=CARTESIAN_POINT('Ctrl Pts',(7.39644086160398,3.60844056017245,136.337284952891));
#197961=CARTESIAN_POINT('Ctrl Pts',(7.1179932377911,6.60545620770325,130.759158130379));
#197962=CARTESIAN_POINT('Ctrl Pts',(6.83954561397822,3.53238029483008,125.222570185327));
#197963=CARTESIAN_POINT('Ctrl Pts',(6.5610979901653,-2.78678054262086,124.815374961881));
#197964=CARTESIAN_POINT('Ctrl Pts',(6.28265036635242,-6.54502620320144,
129.911764977794));
#197965=CARTESIAN_POINT('Ctrl Pts',(6.00420274253956,-4.28871252534551,
135.828406780936));
#197966=CARTESIAN_POINT('Ctrl Pts',(5.72575511872663,1.90871844804856,137.128195598241));
#197967=CARTESIAN_POINT('Ctrl Pts',(5.44730749491374,6.35213041376593,132.616689004818));
#197968=CARTESIAN_POINT('Ctrl Pts',(5.16885987110085,4.95824484805471,126.439741160674));
#197969=CARTESIAN_POINT('Ctrl Pts',(4.89041224728798,-0.992025509291961,
124.273665373899));
#197970=CARTESIAN_POINT('Ctrl Pts',(4.61196462347505,-6.03067288673954,
128.108979473854));
#197971=CARTESIAN_POINT('Ctrl Pts',(4.33351699966218,-5.52742649602286,
134.421217168191));
#197972=CARTESIAN_POINT('Ctrl Pts',(4.05506937584931,0.0552548147426717,
137.409740385768));
#197973=CARTESIAN_POINT('Ctrl Pts',(3.77662175203639,5.58715965010757,134.328242287108));
#197974=CARTESIAN_POINT('Ctrl Pts',(3.49817412822347,5.98473771494644,128.008469085329));
#197975=CARTESIAN_POINT('Ctrl Pts',(3.21972650441063,0.882634190440881,
124.25798361478));
#197976=CARTESIAN_POINT('Ctrl Pts',(2.94127888059773,-5.03056703600248,
126.523298801495));
#197977=CARTESIAN_POINT('Ctrl Pts',(2.66283125678483,-6.32092291322184,
132.722700655682));
#197978=CARTESIAN_POINT('Ctrl Pts',(2.38438363297192,-1.80265942744139,
137.159241730961));
#197979=CARTESIAN_POINT('Ctrl Pts',(2.10593600915906,4.37216000734877,135.755957516231));
#197980=CARTESIAN_POINT('Ctrl Pts',(1.82748838534615,6.529177987276,129.802397650584));
#197981=CARTESIAN_POINT('Ctrl Pts',(1.54904076153325,2.68620036497402,124.769592802981));
#197982=CARTESIAN_POINT('Ctrl Pts',(1.27059313772038,-3.62526416455594,
125.282444762183));
#197983=CARTESIAN_POINT('Ctrl Pts',(0.992145513907496,-6.60528803085927,
130.869667631896));
#197984=CARTESIAN_POINT('Ctrl Pts',(0.713697890094564,-3.51537488306232,
136.396876545864));
#197985=CARTESIAN_POINT('Ctrl Pts',(0.435250266281723,2.80499604665836,
136.784836531317));
#197986=CARTESIAN_POINT('Ctrl Pts',(0.156802642468823,6.54771264117505,
131.677031314524));
#197987=CARTESIAN_POINT('Ctrl Pts',(-0.121644981344083,4.27340119199728,
125.767284359559));
#197988=CARTESIAN_POINT('Ctrl Pts',(-0.400092605156985,-1.92795718537184,
124.486364410847));
#197989=CARTESIAN_POINT('Ctrl Pts',(-0.678540228969845,-6.35761709532873,
129.011374324836));
#197990=CARTESIAN_POINT('Ctrl Pts',(-0.956987852782752,-4.94493748154019,
135.184051049593));
#197991=CARTESIAN_POINT('Ctrl Pts',(-1.23543547659566,1.01189810415772,
137.332006227089));
#197992=CARTESIAN_POINT('Ctrl Pts',(-1.51388310040852,6.03884876610542,
133.48137398265));
#197993=CARTESIAN_POINT('Ctrl Pts',(-1.79233072422142,5.51639242616521,
127.170697235071));
#197994=CARTESIAN_POINT('Ctrl Pts',(-2.07077834803434,-0.0753590626689394,
124.19917962168));
#197995=CARTESIAN_POINT('Ctrl Pts',(-2.34922597184723,-5.59785925440532,
127.297500662476));
#197996=CARTESIAN_POINT('Ctrl Pts',(-2.6276735956601,-5.97620026197078,
133.618454682368));
#197997=CARTESIAN_POINT('Ctrl Pts',(-2.906121219473,-0.862705182398668,
137.353393732843));
#197998=CARTESIAN_POINT('Ctrl Pts',(-3.18456884328591,5.04357381430661,
135.070091288433));
#197999=CARTESIAN_POINT('Ctrl Pts',(-3.46301646709877,6.31505486794284,
128.866790750024));
#198000=CARTESIAN_POINT('Ctrl Pts',(-3.74146409091167,1.78330900552073,
124.444022264336));
#198001=CARTESIAN_POINT('Ctrl Pts',(-4.01991171472458,-4.38721071348669,
125.866094005463));
#198002=CARTESIAN_POINT('Ctrl Pts',(-4.29835933853748,-6.52609811395827,
131.826191515377));
#198003=CARTESIAN_POINT('Ctrl Pts',(-4.57680696235032,-2.66782016531947,
136.847276349416));
#198004=CARTESIAN_POINT('Ctrl Pts',(-4.85525458616324,3.64205418498746,
136.31521683873));
#198005=CARTESIAN_POINT('Ctrl Pts',(-5.13370220997616,6.60505866352928,
130.718949681087));
#198006=CARTESIAN_POINT('Ctrl Pts',(-5.41214983378902,3.49833690534187,
125.201171001511));
#198007=CARTESIAN_POINT('Ctrl Pts',(-5.69059745760191,-2.82318556559566,
124.832449848059));
#198008=CARTESIAN_POINT('Ctrl Pts',(-5.96904508141481,-6.55033842203324,
129.951622947723));
#198009=CARTESIAN_POINT('Ctrl Pts',(-6.24749270522772,-4.2580502704442,
135.854420307421));
#198010=CARTESIAN_POINT('Ctrl Pts',(-6.52594032904057,1.9471780623631,137.116459521273));
#198011=CARTESIAN_POINT('Ctrl Pts',(-6.80438795285348,6.36304488079526,
132.577988205793));
#198012=CARTESIAN_POINT('Ctrl Pts',(-7.0828355766664,4.93158430580029,126.409639783256));
#198013=CARTESIAN_POINT('Ctrl Pts',(-7.36128320047925,-1.03176132493798,
124.279825113401));
#198014=CARTESIAN_POINT('Ctrl Pts',(-7.63973082429214,-6.04696870240127,
128.145739830595));
#198015=CARTESIAN_POINT('Ctrl Pts',(-7.91817844810507,-5.50530725320171,
134.454797170168));
#198016=CARTESIAN_POINT('Ctrl Pts',(-8.19662607191793,0.09546261247915,
137.40928165164));
#198017=CARTESIAN_POINT('Ctrl Pts',(-8.47507369573082,5.60850700089942,
134.294166371127));
#198018=CARTESIAN_POINT('Ctrl Pts',(-8.75352131954372,5.96760744629241,
127.972090089581));
#198019=CARTESIAN_POINT('Ctrl Pts',(-9.03196894335663,0.842768182373745,
124.252732059145));
#198020=CARTESIAN_POINT('Ctrl Pts',(-9.31041656716948,-5.05653386963193,
126.554000609049));
#198021=CARTESIAN_POINT('Ctrl Pts',(-9.5888641909824,-6.30912832085822,
132.76114236515));
#198022=CARTESIAN_POINT('Ctrl Pts',(-9.86731181479532,-1.76394206326903,
137.170097289323));
#198023=CARTESIAN_POINT('Ctrl Pts',(-10.1457594386081,4.40222077710389,
135.729251195677));
#198024=CARTESIAN_POINT('Ctrl Pts',(-10.424207062421,6.52295778375913,129.762671255026));
#198025=CARTESIAN_POINT('Ctrl Pts',(-10.7026546862339,2.64941525134336,
124.753352949195));
#198026=CARTESIAN_POINT('Ctrl Pts',(-10.9811023100469,-3.65881046592654,
125.304615082438));
#198027=CARTESIAN_POINT('Ctrl Pts',(-11.2595499338597,-6.60476810783814,
130.909874684957));
#198028=CARTESIAN_POINT('Ctrl Pts',(-11.5379975576726,-3.48126651950624,
136.418172014193));
#198029=CARTESIAN_POINT('Ctrl Pts',(-11.8164451814855,2.84134893092756,
136.767650919861));
#198030=CARTESIAN_POINT('Ctrl Pts',(-12.0948928052984,6.5529035214511,131.637157360647));
#198031=CARTESIAN_POINT('Ctrl Pts',(-12.3733404291112,4.2426599028951,125.741364278924));
#198032=CARTESIAN_POINT('Ctrl Pts',(-12.6517880529242,-1.96638090096281,
124.498217491291));
#198033=CARTESIAN_POINT('Ctrl Pts',(-12.9302356767371,-6.36841371988325,
129.050108164486));
#198034=CARTESIAN_POINT('Ctrl Pts',(-13.2086833005499,-4.91818544453708,
135.214071142064));
#198035=CARTESIAN_POINT('Ctrl Pts',(-13.4871309243628,1.05161498762227,
137.325725573964));
#198036=CARTESIAN_POINT('Ctrl Pts',(-13.7655785481758,6.05503262040511,
133.444564197323));
#198037=CARTESIAN_POINT('Ctrl Pts',(-14.0440261719886,5.49417107982388,
127.137184712));
#198038=CARTESIAN_POINT('Ctrl Pts',(-14.3224737958015,-0.115565277936756,
124.199760732389));
#198039=CARTESIAN_POINT('Ctrl Pts',(-14.6009214196144,-5.61910279095105,
127.331641394614));
#198040=CARTESIAN_POINT('Ctrl Pts',(-14.8793690434273,-5.95895934751375,
133.654781370965));
#198041=CARTESIAN_POINT('Ctrl Pts',(-15.1578166672402,-0.822823375059262,
137.358523925738));
#198042=CARTESIAN_POINT('Ctrl Pts',(-15.4362642910531,5.06944708191823,
135.039310588977));
#198043=CARTESIAN_POINT('Ctrl Pts',(-15.714711914866,6.3031433268707,128.828385117298));
#198044=CARTESIAN_POINT('Ctrl Pts',(-15.9931595386788,1.74455878009922,
124.433284598595));
#198045=CARTESIAN_POINT('Ctrl Pts',(-16.2716071624918,-4.41719005914895,
125.892891696959));
#198046=CARTESIAN_POINT('Ctrl Pts',(-16.5500547863046,-6.51975702577033,
131.865898794765));
#198047=CARTESIAN_POINT('Ctrl Pts',(-16.8285024101176,-2.63098579354628,
136.863404166748));
#198048=CARTESIAN_POINT('Ctrl Pts',(-17.1069500339304,3.67553285214529,
136.292944517765));
#198049=CARTESIAN_POINT('Ctrl Pts',(-17.3853976577434,6.60441636647752,
130.678744396729));
#198050=CARTESIAN_POINT('Ctrl Pts',(-17.6638452815562,3.46416388369313,
125.179979445948));
#198051=CARTESIAN_POINT('Ctrl Pts',(-17.9422929053691,-2.8594859743911,
124.849746025587));
#198052=CARTESIAN_POINT('Ctrl Pts',(-18.220740529182,-6.55540791566593,
129.991512516161));
#198053=CARTESIAN_POINT('Ctrl Pts',(-18.4991881529949,-4.22723023192423,
135.880246702087));
#198054=CARTESIAN_POINT('Ctrl Pts',(-18.7776357768078,1.98556552327847,
137.104489547159));
#198055=CARTESIAN_POINT('Ctrl Pts',(-19.0560834006207,6.37372356285652,
132.539221684343));
#198056=CARTESIAN_POINT('Ctrl Pts',(-19.3345310244336,4.90474102187576,
126.379701253833));
#198057=CARTESIAN_POINT('Ctrl Pts',(-19.6129786482465,-1.07145890828896,
124.286226621967));
#198058=CARTESIAN_POINT('Ctrl Pts',(-19.8914262720594,-6.06304044541393,
128.182598703507));
#198059=CARTESIAN_POINT('Ctrl Pts',(-20.1698738958722,-5.48298400919569,
134.488241903877));
#198060=CARTESIAN_POINT('Ctrl Pts',(-20.4483215196851,0.135666872813404,
137.408578169733));
#198061=CARTESIAN_POINT('Ctrl Pts',(-20.7267691434981,5.62964652640204,
134.25996113911));
#198062=CARTESIAN_POINT('Ctrl Pts',(-21.0052167673109,5.95025604574973,
127.935816044659));
#198063=CARTESIAN_POINT('Ctrl Pts',(-21.2836643911238,0.802870945221437,
124.247723276515));
#198064=CARTESIAN_POINT('Ctrl Pts',(-21.5621120149367,-5.08231333153929,
126.584859915257));
#198065=CARTESIAN_POINT('Ctrl Pts',(-21.8405596387496,-6.29709994142449,
132.79951156535));
#198066=CARTESIAN_POINT('Ctrl Pts',(-22.1190072625625,-1.725159335575,137.180716962973));
#198067=CARTESIAN_POINT('Ctrl Pts',(-22.3974548863754,4.43211842094896,
135.702362381491));
#198068=CARTESIAN_POINT('Ctrl Pts',(-22.6759025101882,6.51649586964294,
129.722983459651));
#198069=CARTESIAN_POINT('Ctrl Pts',(-22.9543501340012,2.61253196265622,
124.737337317723));
#198070=CARTESIAN_POINT('Ctrl Pts',(-23.232797757814,-3.6922211887298,125.326989197785));
#198071=CARTESIAN_POINT('Ctrl Pts',(-23.511245381627,-6.60400344270576,
130.950077828156));
#198072=CARTESIAN_POINT('Ctrl Pts',(-23.7896930054398,-3.4470291563393,
136.439259460675));
#198073=CARTESIAN_POINT('Ctrl Pts',(-24.0681406292527,2.87759652796706,
136.75024433649));
#198074=CARTESIAN_POINT('Ctrl Pts',(-24.3465882530656,6.55785158147733,
131.597252547181));
#198075=CARTESIAN_POINT('Ctrl Pts',(-24.6250358768785,4.21176140046998,
125.715631809479));
#198076=CARTESIAN_POINT('Ctrl Pts',(-24.9034835006914,-2.00473175158637,
124.510304248187));
#198077=CARTESIAN_POINT('Ctrl Pts',(-25.1819311245043,-6.3789743605254,
129.088907008606));
#198078=CARTESIAN_POINT('Ctrl Pts',(-25.4603787483172,-4.89125116236366,
135.24392783109));
#198079=CARTESIAN_POINT('Ctrl Pts',(-25.73882637213,1.09129290310671,137.319203269261));
#198080=CARTESIAN_POINT('Ctrl Pts',(-26.017273995943,6.07099210324431,133.407656578282));
#198081=CARTESIAN_POINT('Ctrl Pts',(-26.2957216197559,5.47174614495268,
127.103808077481));
#198082=CARTESIAN_POINT('Ctrl Pts',(-26.5741692435687,-0.155767210890682,
124.200586578976));
#198083=CARTESIAN_POINT('Ctrl Pts',(-26.8526168673816,-5.64013810957666,
127.365910809639));
#198084=CARTESIAN_POINT('Ctrl Pts',(-27.1310644911945,-5.94149762162655,
133.691002436174));
#198085=CARTESIAN_POINT('Ctrl Pts',(-27.4095121150075,-0.782911077696857,
137.363411251701));
#198086=CARTESIAN_POINT('Ctrl Pts',(-27.6879597388203,5.09513249930392,
135.008372961895));
#198087=CARTESIAN_POINT('Ctrl Pts',(-27.9664073626332,6.29099822050462,
128.79005270507));
#198088=CARTESIAN_POINT('Ctrl Pts',(-28.2448549864461,1.70574390941038,
124.422783015417));
#198089=CARTESIAN_POINT('Ctrl Pts',(-28.523302610259,-4.44700572420938,
125.919871384741));
#198090=CARTESIAN_POINT('Ctrl Pts',(-28.8017502340719,-6.51317434558802,
131.905566738465));
#198091=CARTESIAN_POINT('Ctrl Pts',(-29.0801978578848,-2.59405392962697,
136.879307463993));
#198092=CARTESIAN_POINT('Ctrl Pts',(-29.3586454816977,3.7088753210816,136.270468815306));
#198093=CARTESIAN_POINT('Ctrl Pts',(-29.6370931055106,6.6035293403484,130.638543767126));
#198094=CARTESIAN_POINT('Ctrl Pts',(-29.9155407293234,3.42986249617799,
125.158996303897));
#198095=CARTESIAN_POINT('Ctrl Pts',(-30.1939883531365,-2.89568042388203,
124.86726285355));
#198096=CARTESIAN_POINT('Ctrl Pts',(-30.4724359769491,-6.56023449624756,
130.031432204983));
#198097=CARTESIAN_POINT('Ctrl Pts',(-30.7508836007622,-4.19625355183344,
135.905885007927));
#198098=CARTESIAN_POINT('Ctrl Pts',(-31.029331224575,2.02387940833292,137.092286119451));
#198099=CARTESIAN_POINT('Ctrl Pts',(-31.3077788483879,6.38416606424714,
132.50039087698));
#198100=CARTESIAN_POINT('Ctrl Pts',(-31.5862264722008,4.8777159909692,126.349926681791));
#198101=CARTESIAN_POINT('Ctrl Pts',(-31.8646740960137,-1.11111678833609,
124.292869662384));
#198102=CARTESIAN_POINT('Ctrl Pts',(-32.1431217198266,-6.07888752023319,
128.219554726771));
#198103=CARTESIAN_POINT('Ctrl Pts',(-32.4215693436394,-5.46045759120085,
134.52155013001));
#198104=CARTESIAN_POINT('Ctrl Pts',(-32.7000169674524,0.175866105961793,
137.407629966116));
#198105=CARTESIAN_POINT('Ctrl Pts',(-32.9784645912652,5.65057744328232,
134.225627858545));
#198106=CARTESIAN_POINT('Ctrl Pts',(-33.2569122150782,5.93268415628106,
127.89964829471));
#198107=CARTESIAN_POINT('Ctrl Pts',(-33.535359838891,0.762943957391,124.242957452493));
#198108=CARTESIAN_POINT('Ctrl Pts',(-33.813807462704,-5.10790446645711,
126.615875576613));
#198109=CARTESIAN_POINT('Ctrl Pts',(-34.0922550865168,-6.28483822063666,
132.837806834499));
#198110=CARTESIAN_POINT('Ctrl Pts',(-34.3707027103298,-1.68631268146717,
137.191100358392));
#198111=CARTESIAN_POINT('Ctrl Pts',(-34.6491503341426,4.46185183101625,
135.675292070049));
#198112=CARTESIAN_POINT('Ctrl Pts',(-34.9275979579556,6.5097924843757,129.683335735103));
#198113=CARTESIAN_POINT('Ctrl Pts',(-35.2060455817684,2.57555186563646,
124.721546502031));
#198114=CARTESIAN_POINT('Ctrl Pts',(-35.4844932055813,-3.72549509491909,
125.349566279145));
#198115=CARTESIAN_POINT('Ctrl Pts',(-35.7629408293942,-6.60299406379731,
130.990275571749));
#198116=CARTESIAN_POINT('Ctrl Pts',(-36.0413884532071,-3.41266406223907,
136.460138103909));
#198117=CARTESIAN_POINT('Ctrl Pts',(-36.3198360770199,2.91373749460914,
136.73261742621));
#198118=CARTESIAN_POINT('Ctrl Pts',(-36.5982837008328,6.56255663790157,
131.557318352812));
#198119=CARTESIAN_POINT('Ctrl Pts',(-36.8767313246458,4.18070682967726,
125.690087904753));
#198120=CARTESIAN_POINT('Ctrl Pts',(-37.1551789484586,-2.04300831613737,
124.522624233657));
#198121=CARTESIAN_POINT('Ctrl Pts',(-37.4336265722715,-6.38929862592666,
129.12776941949));
#198122=CARTESIAN_POINT('Ctrl Pts',(-37.7120741960844,-4.86413563307991,
135.273620010322));
#198123=CARTESIAN_POINT('Ctrl Pts',(-37.9905218198973,1.13093038033133,
137.312439554669));
#198124=CARTESIAN_POINT('Ctrl Pts',(-38.2689694437102,6.0867266232385,133.370652493151));
#198125=CARTESIAN_POINT('Ctrl Pts',(-38.5474170675231,5.44911845251588,
127.070568568297));
#198126=CARTESIAN_POINT('Ctrl Pts',(-38.825864691336,-0.195963371833029,
124.201657130839));
#198127=CARTESIAN_POINT('Ctrl Pts',(-39.1043123151489,-5.66096443081045,
127.400307637685));
#198128=CARTESIAN_POINT('Ctrl Pts',(-39.3827599389617,-5.92381573136,133.727116535809));
#198129=CARTESIAN_POINT('Ctrl Pts',(-39.6612075627747,-0.742969769276543,
137.368055529631));
#198130=CARTESIAN_POINT('Ctrl Pts',(-39.9396551865875,5.12062911468111,
134.977279553588));
#198131=CARTESIAN_POINT('Ctrl Pts',(-40.2181028104005,6.27861999888597,
128.751794933764));
#198132=CARTESIAN_POINT('Ctrl Pts',(-40.4965504342133,1.66686583175366,
124.412517903944));
#198133=CARTESIAN_POINT('Ctrl Pts',(-40.7749980580263,-4.47665660383728,
125.947032069068));
#198134=CARTESIAN_POINT('Ctrl Pts',(-41.0534456818391,-6.5063503173351,
131.945193876568));
#198135=CARTESIAN_POINT('Ctrl Pts',(-41.3318933056519,-2.55702594208532,
136.894985651848));
#198136=CARTESIAN_POINT('Ctrl Pts',(-41.6103409294649,3.74208035627896,
136.247790564197));
#198137=CARTESIAN_POINT('Ctrl Pts',(-41.8887885532778,6.60239761801125,
130.598349281928));
#198138=CARTESIAN_POINT('Ctrl Pts',(-42.1672361770906,3.39543401384647,
125.138222352896));
#198139=CARTESIAN_POINT('Ctrl Pts',(-42.4456838009036,-2.93176757287012,
124.884999682853));
#198140=CARTESIAN_POINT('Ctrl Pts',(-42.7241314247165,-6.56481798492739,
130.071380534953));
#198141=CARTESIAN_POINT('Ctrl Pts',(-43.0025790485293,-4.16512137802412,
135.931334274905));
#198142=CARTESIAN_POINT('Ctrl Pts',(-43.2810266723423,2.06211829779186,
137.079849690351));
#198143=CARTESIAN_POINT('Ctrl Pts',(-43.5594742961552,6.39437199801655,
132.461497222591));
#198144=CARTESIAN_POINT('Ctrl Pts',(-43.837921919968,4.85051021450257,126.320317170437));
#198145=CARTESIAN_POINT('Ctrl Pts',(-44.116369543781,-1.150733495542,124.299753988494));
#198146=CARTESIAN_POINT('Ctrl Pts',(-44.3948171675938,-6.09450933963988,
128.256606530968));
#198147=CARTESIAN_POINT('Ctrl Pts',(-44.6732647914067,-5.43772883394191,
134.554720614319));
#198148=CARTESIAN_POINT('Ctrl Pts',(-44.9517124152196,0.216058822326645,
137.406437075925));
#198149=CARTESIAN_POINT('Ctrl Pts',(-45.2301600390324,5.67129897593744,
134.191167801664));
#198150=CARTESIAN_POINT('Ctrl Pts',(-45.5086076628454,5.91489242901924,
127.863588179946));
#198151=CARTESIAN_POINT('Ctrl Pts',(-45.7870552866582,0.722988698391639,
124.238434763679));
#198152=CARTESIAN_POINT('Ctrl Pts',(-46.0655029104712,-5.13330632609627,
126.647046443824));
#198153=CARTESIAN_POINT('Ctrl Pts',(-46.343950534284,-6.27234361285742,
132.876026753548));
#198154=CARTESIAN_POINT('Ctrl Pts',(-46.622398158097,-1.64740354042306,
137.201247090823));
#198155=CARTESIAN_POINT('Ctrl Pts',(-46.9008457819097,4.49141990552312,
135.64804126445));
#198156=CARTESIAN_POINT('Ctrl Pts',(-47.1792934057228,6.50284787635396,
129.643729550545));
#198157=CARTESIAN_POINT('Ctrl Pts',(-47.4577410295356,2.53847633059532,
124.705981087252));
#198158=CARTESIAN_POINT('Ctrl Pts',(-47.7361886533485,-3.75863095151733,
125.372345489915));
#198159=CARTESIAN_POINT('Ctrl Pts',(-48.0146362771614,-6.60174000851572,
131.030466426196));
#198160=CARTESIAN_POINT('Ctrl Pts',(-48.2930839009743,-3.37817251061699,
136.480807170229));
#198161=CARTESIAN_POINT('Ctrl Pts',(-48.5715315247872,2.94977049163681,
136.714770842195));
#198162=CARTESIAN_POINT('Ctrl Pts',(-48.8499791486,6.56701851637621,131.517356257317));
#198163=CARTESIAN_POINT('Ctrl Pts',(-49.128426772413,4.14949734125552,125.664733511282));
#198164=CARTESIAN_POINT('Ctrl Pts',(-49.4068743962258,-2.08120917626415,
124.535176991179));
#198165=CARTESIAN_POINT('Ctrl Pts',(-49.6853220200388,-6.39938613351776,
129.166693957078));
#198166=CARTESIAN_POINT('Ctrl Pts',(-49.9637696438516,-4.83683986146123,
135.303146579501));
#198167=CARTESIAN_POINT('Ctrl Pts',(-50.2422172676646,1.17052595051479,
137.305434680818));
#198168=CARTESIAN_POINT('Ctrl Pts',(-50.5206648914774,6.10223559733929,
133.333553313131));
#198169=CARTESIAN_POINT('Ctrl Pts',(-50.7991125152903,5.42628884099088,
127.03746741615));
#198170=CARTESIAN_POINT('Ctrl Pts',(-51.0775601391032,-0.236152271280866,
124.202972348307));
#198171=CARTESIAN_POINT('Ctrl Pts',(-51.3560077629162,-5.68158098292544,
127.434830604167));
#198172=CARTESIAN_POINT('Ctrl Pts',(-51.634455386729,-5.90591433192304,
133.763122331648));
#198173=CARTESIAN_POINT('Ctrl Pts',(-51.9129030105419,-0.703000929838195,
137.372456587432));
#198174=CARTESIAN_POINT('Ctrl Pts',(-52.1913506343548,5.14593598326309,
134.946031516236));
#198175=CARTESIAN_POINT('Ctrl Pts',(-52.4697982581677,6.26600912069438,
128.713613221033));
#198176=CARTESIAN_POINT('Ctrl Pts',(-52.7482458819806,1.62792598777083,
124.402489644555));
#198177=CARTESIAN_POINT('Ctrl Pts',(-53.0266935057934,-4.50614159930848,
125.97437274349));
#198178=CARTESIAN_POINT('Ctrl Pts',(-53.3051411296064,-6.49928519387843,
131.984778740675));
#198179=CARTESIAN_POINT('Ctrl Pts',(-53.5835887534191,-2.51990320300721,
136.910438149353));
#198180=CARTESIAN_POINT('Ctrl Pts',(-53.8620363772322,3.7751467273123,136.22491060479));
#198181=CARTESIAN_POINT('Ctrl Pts',(-54.140484001045,6.60102124140245,130.558162430556));
#198182=CARTESIAN_POINT('Ctrl Pts',(-54.418931624858,3.36087971245889,125.117658362733));
#198183=CARTESIAN_POINT('Ctrl Pts',(-54.6973792486707,-2.96774608413265,
124.902955856252));
#198184=CARTESIAN_POINT('Ctrl Pts',(-54.9758268724838,-6.56915821186243,
130.111356025769));
#198185=CARTESIAN_POINT('Ctrl Pts',(-55.2542744962966,-4.13383486411065,
135.956593559989));
#198186=CARTESIAN_POINT('Ctrl Pts',(-55.5327221201095,2.10028077469877,
137.067180720695));
#198187=CARTESIAN_POINT('Ctrl Pts',(-55.8111697439224,6.40434098598004,
132.422542162396));
#198188=CARTESIAN_POINT('Ctrl Pts',(-56.0896173677353,4.82312470059616,
126.29087381696));
#198189=CARTESIAN_POINT('Ctrl Pts',(-56.3680649915482,-1.19030756189505,
124.306879345194));
#198190=CARTESIAN_POINT('Ctrl Pts',(-56.646512615361,-6.10990532476174,
128.293752743129));
#198191=CARTESIAN_POINT('Ctrl Pts',(-56.924960239174,-5.41479857964128,
134.587752127659));
#198192=CARTESIAN_POINT('Ctrl Pts',(-57.2034078629868,0.256243532552689,
137.404999543363));
#198193=CARTESIAN_POINT('Ctrl Pts',(-57.4818554867998,5.69181035652338,
134.156582245398));
#198194=CARTESIAN_POINT('Ctrl Pts',(-57.7603031106126,5.89688152324325,
127.827637036585));
#198195=CARTESIAN_POINT('Ctrl Pts',(-58.0387507344255,0.683006648780185,
124.234155377662));
#198196=CARTESIAN_POINT('Ctrl Pts',(-58.3171983582384,-5.15851796918197,
126.67837136184));
#198197=CARTESIAN_POINT('Ctrl Pts',(-58.5956459820513,-6.25961658107885,
132.91416990625));
#198198=CARTESIAN_POINT('Ctrl Pts',(-58.8740936058642,-1.60843335423465,
137.211156784272));
#198199=CARTESIAN_POINT('Ctrl Pts',(-59.1525412296771,4.52082154881365,
135.620610974484));
#198200=CARTESIAN_POINT('Ctrl Pts',(-59.4309888534899,6.49566230291273,
129.604166373598));
#198201=CARTESIAN_POINT('Ctrl Pts',(-59.7094364773029,2.50130673138007,
124.69064165017));
#198202=CARTESIAN_POINT('Ctrl Pts',(-59.9878841011157,-3.79162753066369,
125.395325986002));
#198203=CARTESIAN_POINT('Ctrl Pts',(-60.2663317249287,-6.60024132333016,
131.070648902209));
#198204=CARTESIAN_POINT('Ctrl Pts',(-60.5447793487415,-3.34355577957023,
136.501265893734));
#198205=CARTESIAN_POINT('Ctrl Pts',(-60.8232269725544,2.98569418383416,
136.696705245755));
#198206=CARTESIAN_POINT('Ctrl Pts',(-61.1016745963673,6.57123705156454,
131.477367741508));
#198207=CARTESIAN_POINT('Ctrl Pts',(-61.3801222201802,4.11813409168408,
125.639569568584));
#198208=CARTESIAN_POINT('Ctrl Pts',(-61.6585698439931,-2.11933291641938,
124.547962055604));
#198209=CARTESIAN_POINT('Ctrl Pts',(-61.937017467806,-6.40923650950231,
129.205679179005));
#198210=CARTESIAN_POINT('Ctrl Pts',(-62.2154650916189,-4.80936485896274,
135.332506444514));
#198211=CARTESIAN_POINT('Ctrl Pts',(-62.4939127154318,1.21007814642843,
137.298188907278));
#198212=CARTESIAN_POINT('Ctrl Pts',(-62.7723603392447,6.1175184508558,133.296360412945));
#198213=CARTESIAN_POINT('Ctrl Pts',(-63.0508079630576,5.40325815633759,
127.004505847616));
#198214=CARTESIAN_POINT('Ctrl Pts',(-63.3292555868704,-0.276332420019459,
124.204532182646));
#198215=CARTESIAN_POINT('Ctrl Pts',(-63.6077032106833,-5.70198700196771,
127.469478429822));
#198216=CARTESIAN_POINT('Ctrl Pts',(-63.8861508344962,-5.8877940866586,
133.799018489484));
#198217=CARTESIAN_POINT('Ctrl Pts',(-64.1645984583092,-0.663006040441876,
137.376614262022));
#198218=CARTESIAN_POINT('Ctrl Pts',(-64.4430460821219,5.17105216729505,
134.914630007745));
#198219=CARTESIAN_POINT('Ctrl Pts',(-64.721493705935,6.25316605323042,128.675508981716));
#198220=CARTESIAN_POINT('Ctrl Pts',(-64.9999413297477,1.58892582039159,
124.392698608848));
#198221=CARTESIAN_POINT('Ctrl Pts',(-65.2783889535607,-4.53545961804555,
126.00189239489));
#198222=CARTESIAN_POINT('Ctrl Pts',(-65.5568365773735,-6.49197923701883,
132.024319863954));
#198223=CARTESIAN_POINT('Ctrl Pts',(-65.8352842011867,-2.48268708798906,
136.92566438391));
#198224=CARTESIAN_POINT('Ctrl Pts',(-66.1137318249993,3.80807320889562,
136.201829784909));
#198225=CARTESIAN_POINT('Ctrl Pts',(-66.3921794488124,6.59940026152389,
130.517984702147));
#198226=CARTESIAN_POINT('Ctrl Pts',(-66.6706270726251,3.3262008724376,125.097305095413));
#198227=CARTESIAN_POINT('Ctrl Pts',(-66.9490746964381,-3.00361462447264,
124.921130708376));
#198228=CARTESIAN_POINT('Ctrl Pts',(-67.227522320251,-6.57325501622426,
130.151357196124));
#198229=CARTESIAN_POINT('Ctrl Pts',(-67.5059699440638,-4.10239516942585,
135.981661927186));
#198230=CARTESIAN_POINT('Ctrl Pts',(-67.7844175678767,2.13836542492937,
137.054279679937));
#198231=CARTESIAN_POINT('Ctrl Pts',(-68.0628651916897,6.41407265873309,
132.383527139888));
#198232=CARTESIAN_POINT('Ctrl Pts',(-68.3413128155024,4.79556046403026,
126.261597712398));
#198233=CARTESIAN_POINT('Ctrl Pts',(-68.6197604393155,-1.22983752096341,
124.314245468451));
#198234=CARTESIAN_POINT('Ctrl Pts',(-68.8982080631282,-6.12507490509475,
128.330991986789));
#198235=CARTESIAN_POINT('Ctrl Pts',(-69.1766556869413,-5.39166767798822,
134.620643446035));
#198236=CARTESIAN_POINT('Ctrl Pts',(-69.455103310754,0.296418747580413,
137.403317421698));
#198237=CARTESIAN_POINT('Ctrl Pts',(-69.733550934567,5.7121108249834,134.121872471326));
#198238=CARTESIAN_POINT('Ctrl Pts',(-70.0119985583799,5.87865210635384,
127.791796196812));
#198239=CARTESIAN_POINT('Ctrl Pts',(-70.2904461821926,0.642999290106501,
124.230119453016));
#198240=CARTESIAN_POINT('Ctrl Pts',(-70.5688938060058,-5.18353846148724,
126.709849169906));
#198241=CARTESIAN_POINT('Ctrl Pts',(-70.8473414298183,-6.24665759690589,
132.95223487919));
#198242=CARTESIAN_POINT('Ctrl Pts',(-71.1257890536316,-1.56940356695681,
137.220829071533));
#198243=CARTESIAN_POINT('Ctrl Pts',(-71.4042366774442,4.55005567139915,
135.593002216589));
#198244=CARTESIAN_POINT('Ctrl Pts',(-71.6826843012574,6.48823603031619,
129.56464767029));
#198245=CARTESIAN_POINT('Ctrl Pts',(-71.9611319250699,2.46404444532374,
124.675528759193));
#198246=CARTESIAN_POINT('Ctrl Pts',(-72.2395795488831,-3.82448360965763,
125.418506915858));
#198247=CARTESIAN_POINT('Ctrl Pts',(-72.518027172696,-6.59849806377525,
131.110821510811));
#198248=CARTESIAN_POINT('Ctrl Pts',(-72.7964747965087,-3.30881515183405,
136.52151351632));
#198249=CARTESIAN_POINT('Ctrl Pts',(-73.0749224203217,3.02150724003593,
136.678421306317));
#198250=CARTESIAN_POINT('Ctrl Pts',(-73.3533700441346,6.57521208714753,
131.437354287172));
#198251=CARTESIAN_POINT('Ctrl Pts',(-73.6318176679474,4.08661824313884,
125.614597009117));
#198252=CARTESIAN_POINT('Ctrl Pts',(-73.9102652917603,-2.15737812391465,
124.56097895318));
#198253=CARTESIAN_POINT('Ctrl Pts',(-74.1887129155733,-6.41884938887091,
129.244723640663));
#198254=CARTESIAN_POINT('Ctrl Pts',(-74.4671605393861,-4.78171164368069,
135.361698517417));
#198255=CARTESIAN_POINT('Ctrl Pts',(-74.745608163199,1.24958550245192,137.290702502541));
#198256=CARTESIAN_POINT('Ctrl Pts',(-75.0240557870119,6.13257461747648,
133.25907517079));
#198257=CARTESIAN_POINT('Ctrl Pts',(-75.3025034108249,5.380027251966,126.971685084098));
#198258=CARTESIAN_POINT('Ctrl Pts',(-75.5809510346376,-0.31650232915867,
124.206336576053));
#198259=CARTESIAN_POINT('Ctrl Pts',(-75.8593986584506,-5.72218173178456,
127.504249830764));
#198260=CARTESIAN_POINT('Ctrl Pts',(-76.1378462822634,-5.86945566701928,
133.83480367917));
#198261=CARTESIAN_POINT('Ctrl Pts',(-76.4162939060764,-0.622986583113102,
137.380528399336));
#198262=CARTESIAN_POINT('Ctrl Pts',(-76.6947415298893,5.19597673608708,
134.88307619171));
#198263=CARTESIAN_POINT('Ctrl Pts',(-76.9731891537022,6.24009127239896,
128.637483627779));
#198264=CARTESIAN_POINT('Ctrl Pts',(-77.2516367775151,1.54986677478153,
124.383145159635));
#198265=CARTESIAN_POINT('Ctrl Pts',(-77.5300844013279,-4.56460957365852,
126.029590003516));
#198266=CARTESIAN_POINT('Ctrl Pts',(-77.8085320251407,-6.48443271748106,
132.063815781194));
#198267=CARTESIAN_POINT('Ctrl Pts',(-78.0869796489538,-2.44537897608793,
136.940663791305));
#198268=CARTESIAN_POINT('Ctrl Pts',(-78.3654272727665,3.84085858092573,
136.178548959823));
#198269=CARTESIAN_POINT('Ctrl Pts',(-78.6438748965796,6.5975347384416,130.477817585504));
#198270=CARTESIAN_POINT('Ctrl Pts',(-78.9223225203923,3.29139877882003,
125.077163305135));
#198271=CARTESIAN_POINT('Ctrl Pts',(-79.2007701442053,-3.03937186476788,
124.939523565746));
#198272=CARTESIAN_POINT('Ctrl Pts',(-79.4792177680182,-6.57710824620412,
130.191382563762));
#198273=CARTESIAN_POINT('Ctrl Pts',(-79.7576653918309,-4.07080345897965,
136.00653844758));
#198274=CARTESIAN_POINT('Ctrl Pts',(-80.036113015644,2.17637083724304,137.041147046131));
#198275=CARTESIAN_POINT('Ctrl Pts',(-80.314560639457,6.42356665566488,132.344453600785));
#198276=CARTESIAN_POINT('Ctrl Pts',(-80.5930082632696,4.76781852620778,
126.232489941585));
#198277=CARTESIAN_POINT('Ctrl Pts',(-80.8714558870828,-1.26932190795047,
124.321852085313));
#198278=CARTESIAN_POINT('Ctrl Pts',(-81.1499035108954,-6.14001751852468,
128.368322882032));
#198279=CARTESIAN_POINT('Ctrl Pts',(-81.4283511347085,-5.36833698610627,
134.653393350648));
#198280=CARTESIAN_POINT('Ctrl Pts',(-81.7067987585213,0.336582978702201,
137.401390773263));
#198281=CARTESIAN_POINT('Ctrl Pts',(-81.9852463823341,5.73219962907597,
134.087039765632));
#198282=CARTESIAN_POINT('Ctrl Pts',(-82.2636940061471,5.86020485384888,
127.756066988721));
#198283=CARTESIAN_POINT('Ctrl Pts',(-82.54214162996,0.602968104857597,124.226327139294));
#198284=CARTESIAN_POINT('Ctrl Pts',(-82.8205892537728,-5.20836687586887,
126.741478701599));
#198285=CARTESIAN_POINT('Ctrl Pts',(-83.0990368775859,-6.23346714053832,
132.990220261861));
#198286=CARTESIAN_POINT('Ctrl Pts',(-83.3774845013985,-1.53031562485268,
137.230263594196));
#198287=CARTESIAN_POINT('Ctrl Pts',(-83.6559321252116,4.57912118999838,
135.56521601382));
#198288=CARTESIAN_POINT('Ctrl Pts',(-83.9343797490243,6.48056933374724,
129.525174905002));
#198289=CARTESIAN_POINT('Ctrl Pts',(-84.2128273728376,2.42669085319518,
124.660642974335));
#198290=CARTESIAN_POINT('Ctrl Pts',(-84.4912749966499,-3.85719797100462,
125.441887420503));
#198291=CARTESIAN_POINT('Ctrl Pts',(-84.7697226204634,-6.59651029444787,
131.150982763393));
#198292=CARTESIAN_POINT('Ctrl Pts',(-85.0481702442759,-3.27395191473627,
136.541549287701));
#198293=CARTESIAN_POINT('Ctrl Pts',(-85.326617868089,3.05720833317481,136.659919701402));
#198294=CARTESIAN_POINT('Ctrl Pts',(-85.6050654919017,6.57894347582879,
131.397317377022));
#198295=CARTESIAN_POINT('Ctrl Pts',(-85.8835131157147,4.05495096345227,
125.58981675825));
#198296=CARTESIAN_POINT('Ctrl Pts',(-86.1619607395276,-2.19534338896908,
124.574227201559));
#198297=CARTESIAN_POINT('Ctrl Pts',(-86.4404083633404,-6.42822441541511,
129.283825895241));
#198298=CARTESIAN_POINT('Ctrl Pts',(-86.7188559871533,-4.75388124031539,
135.390721716488));
#198299=CARTESIAN_POINT('Ctrl Pts',(-86.9973036109663,1.28904655462414,
137.282975744021));
#198300=CARTESIAN_POINT('Ctrl Pts',(-87.2757512347791,6.14740353928957,
133.221698968287));
#198301=CARTESIAN_POINT('Ctrl Pts',(-87.554198858592,5.35659698870609,126.939006341782));
#198302=CARTESIAN_POINT('Ctrl Pts',(-87.8326464824051,-0.356660510187587,
124.208385461669));
#198303=CARTESIAN_POINT('Ctrl Pts',(-88.1110941062178,-5.74216442405318,
127.539143518524));
#198304=CARTESIAN_POINT('Ctrl Pts',(-88.3895417300309,-5.85089975254147,
133.870476574676));
#198305=CARTESIAN_POINT('Ctrl Pts',(-88.6679893538435,-0.582944040787213,
137.384198854334));
#198306=CARTESIAN_POINT('Ctrl Pts',(-88.9464369776566,5.22070876605056,
134.851371237371));
#198307=CARTESIAN_POINT('Ctrl Pts',(-89.2248846014694,6.22678526269035,
128.599538568266));
#198308=CARTESIAN_POINT('Ctrl Pts',(-89.5033322252823,1.51075029828878,
124.373829650922));
#198309=CARTESIAN_POINT('Ctrl Pts',(-89.7817798490951,-4.59359038598471,
126.057464543021));
#198310=CARTESIAN_POINT('Ctrl Pts',(-90.0602274729082,-6.47664591490472,
132.103265028861));
#198311=CARTESIAN_POINT('Ctrl Pts',(-90.338675096721,-2.40798024976945,
136.955435815729));
#198312=CARTESIAN_POINT('Ctrl Pts',(-90.6171227205338,3.87350162852866,
136.155068992212));
#198313=CARTESIAN_POINT('Ctrl Pts',(-90.8955703443469,6.59542474128344,
130.437662569033));
#198314=CARTESIAN_POINT('Ctrl Pts',(-91.1740179681596,3.25647472121003,
125.057233738258));
#198315=CARTESIAN_POINT('Ctrl Pts',(-91.4524655919725,-3.07501648002118,
124.958133746811));
#198316=CARTESIAN_POINT('Ctrl Pts',(-91.7309132157855,-6.58071775901922,
130.231430645527));
#198317=CARTESIAN_POINT('Ctrl Pts',(-92.0093608395982,-4.03906090341396,
136.031222199361));
#198318=CARTESIAN_POINT('Ctrl Pts',(-92.2878084634112,2.21429560333469,
137.027783305909));
#198319=CARTESIAN_POINT('Ctrl Pts',(-92.5662560872241,6.4328226249721,132.305322992969));
#198320=CARTESIAN_POINT('Ctrl Pts',(-92.844703711037,4.73989991511645,126.203551583122));
#198321=CARTESIAN_POINT('Ctrl Pts',(-93.1231513348499,-1.30875925974737,
124.329698913911));
#198322=CARTESIAN_POINT('Ctrl Pts',(-93.4015989586628,-6.15473261134757,
128.40574404555));
#198323=CARTESIAN_POINT('Ctrl Pts',(-93.6800465824757,-5.34480736852315,
134.686000627937));
#198324=CARTESIAN_POINT('Ctrl Pts',(-93.9584942062885,0.37673473761816,
137.399219669449));
#198325=CARTESIAN_POINT('Ctrl Pts',(-94.2369418301014,5.75207602440345,
134.052085419056));
#198326=CARTESIAN_POINT('Ctrl Pts',(-94.5153894539144,5.84154044929785,
127.720450736271));
#198327=CARTESIAN_POINT('Ctrl Pts',(-94.7938370777271,0.56291457640357,
124.222778577022));
#198328=CARTESIAN_POINT('Ctrl Pts',(-95.0722847015402,-5.23300229230026,
126.773258784876));
#198329=CARTESIAN_POINT('Ctrl Pts',(-95.350732325353,-6.22004570075364,
133.028124646699));
#198330=CARTESIAN_POINT('Ctrl Pts',(-95.6291799491659,-1.49117097634027,
137.239460002661));
#198331=CARTESIAN_POINT('Ctrl Pts',(-95.9076275729788,4.60801702757804,
135.537253395802));
#198332=CARTESIAN_POINT('Ctrl Pts',(-96.1860751967916,6.47266249729856,
129.48574954041));
#198333=CARTESIAN_POINT('Ctrl Pts',(-96.4645228206046,2.38924733914408,
124.645984847192));
#198334=CARTESIAN_POINT('Ctrl Pts',(-96.7429704444176,-3.88976940246256,
125.465466633565));
#198335=CARTESIAN_POINT('Ctrl Pts',(-97.0214180682302,-6.59427808900543,
131.191131171763));
#198336=CARTESIAN_POINT('Ctrl Pts',(-97.2998656920433,-3.23896736014657,
136.561372465446));
#198337=CARTESIAN_POINT('Ctrl Pts',(-97.5783133158561,3.09279614033489,
136.641201116591));
#198338=CARTESIAN_POINT('Ctrl Pts',(-97.856760939669,6.58243107933991,131.357258494642));
#198339=CARTESIAN_POINT('Ctrl Pts',(-98.135208563482,4.02313342606635,125.565229734223));
#198340=CARTESIAN_POINT('Ctrl Pts',(-98.4136561872948,-2.2332273047675,
124.587706309824));
#198341=CARTESIAN_POINT('Ctrl Pts',(-98.6921038111079,-6.43736124173946,
129.322984493793));
#198342=CARTESIAN_POINT('Ctrl Pts',(-98.9705514349205,-4.72587468013238,
135.419574966262));
#198343=CARTESIAN_POINT('Ctrl Pts',(-99.2489990587337,1.32845984070286,
137.275008918035));
#198344=CARTESIAN_POINT('Ctrl Pts',(-99.5274466825463,6.16200466680371,
133.184233190419));
#198345=CARTESIAN_POINT('Ctrl Pts',(-99.8058943063594,5.3329682347749,126.906470831589));
#198346=CARTESIAN_POINT('Ctrl Pts',(-100.084341930172,-0.396805475030165,
124.210678763569));
#198347=CARTESIAN_POINT('Ctrl Pts',(-100.362789553985,-5.76193433830736,
127.574158200105));
#198348=CARTESIAN_POINT('Ctrl Pts',(-100.641237177798,-5.83212703082168,
133.906035854126));
#198349=CARTESIAN_POINT('Ctrl Pts',(-100.919684801611,-0.542879897255484,
137.387625491007));
#198350=CARTESIAN_POINT('Ctrl Pts',(-101.198132425424,5.24524734073077,
134.819516319564));
#198351=CARTESIAN_POINT('Ctrl Pts',(-101.476580049237,6.21324851716398,
128.561675209245));
#198352=CARTESIAN_POINT('Ctrl Pts',(-101.75502767305,1.47157784038775,124.3647524279));
#198353=CARTESIAN_POINT('Ctrl Pts',(-102.033475296863,-4.62240098113028,
126.085514980508));
#198354=CARTESIAN_POINT('Ctrl Pts',(-102.311922920676,-6.4686191178319,
132.142666145147));
#198355=CARTESIAN_POINT('Ctrl Pts',(-102.590370544489,-2.3704922948573,
136.969979909799));
#198356=CARTESIAN_POINT('Ctrl Pts',(-102.868818168302,3.90600114210426,
136.131390752135));
#198357=CARTESIAN_POINT('Ctrl Pts',(-103.147265792114,6.59307034823604,
130.397521140692));
#198358=CARTESIAN_POINT('Ctrl Pts',(-103.425713415927,3.22142999373166,
125.037517133282));
#198359=CARTESIAN_POINT('Ctrl Pts',(-103.70416103974,-3.11054714940797,
124.976960561963));
#198360=CARTESIAN_POINT('Ctrl Pts',(-103.982608663553,-6.58408342091771,
130.271499957422));
#198361=CARTESIAN_POINT('Ctrl Pts',(-104.261056287366,-4.00716867896111,
136.055712267864));
#198362=CARTESIAN_POINT('Ctrl Pts',(-104.539503911179,2.25213831788793,
137.014188954471));
#198363=CARTESIAN_POINT('Ctrl Pts',(-104.817951534992,6.44184022367115,
132.266136766442));
#198364=CARTESIAN_POINT('Ctrl Pts',(-105.096399158805,4.71180566529118,
126.17478370933));
#198365=CARTESIAN_POINT('Ctrl Pts',(-105.374846782618,-1.34814811498862,
124.337785663482));
#198366=CARTESIAN_POINT('Ctrl Pts',(-105.65329440643,-6.16921963829011,
128.443254090687));
#198367=CARTESIAN_POINT('Ctrl Pts',(-105.931742030243,-5.32107969713743,
134.718464069627));
#198368=CARTESIAN_POINT('Ctrl Pts',(-106.210189654056,0.416872536489867,
137.396804190707));
#198369=CARTESIAN_POINT('Ctrl Pts',(-106.488637277869,5.77173927443855,
134.017010726842));
#198370=CARTESIAN_POINT('Ctrl Pts',(-106.767084901682,5.82265958431723,
127.684948759235));
#198371=CARTESIAN_POINT('Ctrl Pts',(-107.045532525495,0.52284018894291,
124.219473897692));
#198372=CARTESIAN_POINT('Ctrl Pts',(-107.323980149308,-5.25744379790729,
126.805188242113));
#198373=CARTESIAN_POINT('Ctrl Pts',(-107.602427773121,-6.20639377488812,
133.065946629143));
#198374=CARTESIAN_POINT('Ctrl Pts',(-107.880875396933,-1.45197107193893,
137.248417956151));
#198375=CARTESIAN_POINT('Ctrl Pts',(-108.159323020746,4.63674211339212,
135.509115398702));
#198376=CARTESIAN_POINT('Ctrl Pts',(-108.437770644559,6.46451581396073,
129.446373037437));
#198377=CARTESIAN_POINT('Ctrl Pts',(-108.716218268372,2.35171529065418,
124.631554920928));
#198378=CARTESIAN_POINT('Ctrl Pts',(-108.994665892185,-3.92219669708481,
125.489243681306));
#198379=CARTESIAN_POINT('Ctrl Pts',(-109.273113515998,-6.59180153016358,
131.231265248209));
#198380=CARTESIAN_POINT('Ctrl Pts',(-109.551561139811,-3.20386278442967,
136.580982315001));
#198381=CARTESIAN_POINT('Ctrl Pts',(-109.830008763624,3.12826934279688,
136.622266245509));
#198382=CARTESIAN_POINT('Ctrl Pts',(-110.108456387437,6.5856747684467,131.317179124427));
#198383=CARTESIAN_POINT('Ctrl Pts',(-110.38690401125,3.99116680999183,125.540836848117));
#198384=CARTESIAN_POINT('Ctrl Pts',(-110.665351635062,-2.27102846750687,
124.601415778499));
#198385=CARTESIAN_POINT('Ctrl Pts',(-110.943799258875,-6.44625952927566,
129.362197985281));
#198386=CARTESIAN_POINT('Ctrl Pts',(-111.222246882688,-4.69769300092514,
135.448257197571));
#198387=CARTESIAN_POINT('Ctrl Pts',(-111.500694506501,1.36782390021364,
137.266802319797));
#198388=CARTESIAN_POINT('Ctrl Pts',(-111.779142130314,6.17637745896884,
133.1466792255));
#198389=CARTESIAN_POINT('Ctrl Pts',(-112.057589754127,5.30914186574463,
126.874079759138));
#198390=CARTESIAN_POINT('Ctrl Pts',(-112.33603737794,-0.436935736099303,
124.213216396775));
#198391=CARTESIAN_POINT('Ctrl Pts',(-112.614485001753,-5.78149074196569,
127.609292578024));
#198392=CARTESIAN_POINT('Ctrl Pts',(-112.892932625565,-5.81313819748998,
133.94148019986));
#198393=CARTESIAN_POINT('Ctrl Pts',(-113.171380249379,-0.502795637109545,
137.390808182378));
#198394=CARTESIAN_POINT('Ctrl Pts',(-113.449827873191,5.26959155084185,
134.787512618686));
#198395=CARTESIAN_POINT('Ctrl Pts',(-113.728275497004,6.19948153742887,
128.523894953756));
#198396=CARTESIAN_POINT('Ctrl Pts',(-114.006723120817,1.43235085262869,
124.355913826926));
#198397=CARTESIAN_POINT('Ctrl Pts',(-114.28517074463,-4.65104029150761,
126.113740276555));
#198398=CARTESIAN_POINT('Ctrl Pts',(-114.563618368443,-6.46035262369882,
132.182017670029));
#198399=CARTESIAN_POINT('Ctrl Pts',(-114.842065992256,-2.33291650048142,
136.984295534578));
#198400=CARTESIAN_POINT('Ctrl Pts',(-115.120513616069,3.93835591737112,
136.107515116997));
#198401=CARTESIAN_POINT('Ctrl Pts',(-115.398961239881,6.59047164654225,
130.357394787938));
#198402=CARTESIAN_POINT('Ctrl Pts',(-115.677408863695,3.18626589498021,
125.018014220813));
#198403=CARTESIAN_POINT('Ctrl Pts',(-115.955856487507,-3.14596255632626,
124.996003313566));
#198404=CARTESIAN_POINT('Ctrl Pts',(-116.23430411132,-6.58720510718372,
130.311589014666));
#198405=CARTESIAN_POINT('Ctrl Pts',(-116.512751735133,-3.97512796739924,
136.0800077456));
#198406=CARTESIAN_POINT('Ctrl Pts',(-116.791199358946,2.28989757862811,
137.00036449556));
#198407=CARTESIAN_POINT('Ctrl Pts',(-117.069646982759,6.45061911761184,
132.226896373261));
#198408=CARTESIAN_POINT('Ctrl Pts',(-117.348094606572,4.68353681777373,
126.146187386213));
#198409=CARTESIAN_POINT('Ctrl Pts',(-117.626542230384,-1.38748701410568,
124.346112034364));
#198410=CARTESIAN_POINT('Ctrl Pts',(-117.904989854198,-6.18347806253024,
128.480851627495));
#198411=CARTESIAN_POINT('Ctrl Pts',(-118.18343747801,-5.29715485118671,
134.750782472776));
#198412=CARTESIAN_POINT('Ctrl Pts',(-118.461885101824,0.45699488799644,
137.394144426544));
#198413=CARTESIAN_POINT('Ctrl Pts',(-118.740332725636,5.79118865055225,
133.981816988697));
#198414=CARTESIAN_POINT('Ctrl Pts',(-119.018780349449,5.80356295854445,
127.649562373154));
#198415=CARTESIAN_POINT('Ctrl Pts',(-119.297227973262,0.482746427446748,
124.216413223762));
#198416=CARTESIAN_POINT('Ctrl Pts',(-119.575675597075,-5.28169048700048,
126.837265890154));
#198417=CARTESIAN_POINT('Ctrl Pts',(-119.854123220888,-6.19251186881905,
133.103684807684));
#198418=CARTESIAN_POINT('Ctrl Pts',(-120.132570844701,-1.41271736421608,
137.257137122728));
#198419=CARTESIAN_POINT('Ctrl Pts',(-120.411018468513,4.66529538302207,
135.480803065184));
#198420=CARTESIAN_POINT('Ctrl Pts',(-120.689466092327,6.45612958561205,
129.407046855192));
#198421=CARTESIAN_POINT('Ctrl Pts',(-120.967913716139,2.31409609848935,
124.61735373025));
#198422=CARTESIAN_POINT('Ctrl Pts',(-121.246361339953,-3.95447865326606,
125.51321768266));
#198423=CARTESIAN_POINT('Ctrl Pts',(-121.524808963765,-6.5890807096919,
131.271383505546));
#198424=CARTESIAN_POINT('Ctrl Pts',(-121.803256587578,-3.16863948839908,
136.600378109714));
#198425=CARTESIAN_POINT('Ctrl Pts',(-122.081704211391,3.16362662608795,
136.603115789794));
#198426=CARTESIAN_POINT('Ctrl Pts',(-122.360151835204,6.58867442295306,
131.277080751534));
#198427=CARTESIAN_POINT('Ctrl Pts',(-122.638599459017,3.9590522997634,125.51663900382));
#198428=CARTESIAN_POINT('Ctrl Pts',(-122.91704708283,-2.30874547645122,
124.615355099576));
#198429=CARTESIAN_POINT('Ctrl Pts',(-123.195494706643,-6.45491894829438,
129.401464916637));
#198430=CARTESIAN_POINT('Ctrl Pts',(-123.473942330455,-4.66933724697619,
135.476767347585));
#198431=CARTESIAN_POINT('Ctrl Pts',(-123.752389954268,1.40713727450679,
137.258356253404));
#198432=CARTESIAN_POINT('Ctrl Pts',(-124.030837578081,6.19052138319586,
133.109038465103));
#198433=CARTESIAN_POINT('Ctrl Pts',(-124.309285201894,5.28511876451003,
126.841834324687));
#198434=CARTESIAN_POINT('Ctrl Pts',(-124.587732825707,-0.477049806354697,
124.215998267256));
#198435=CARTESIAN_POINT('Ctrl Pts',(-124.86618044952,-5.80083291035842,
127.644545350364));
#198436=CARTESIAN_POINT('Ctrl Pts',(-125.144628073333,-5.79393395618462,
133.976808298475));
#198437=CARTESIAN_POINT('Ctrl Pts',(-125.423075697146,-0.462692745686338,
137.393746810514));
#198438=CARTESIAN_POINT('Ctrl Pts',(-125.701523320958,5.2937404943001,134.755361320645));
#198439=CARTESIAN_POINT('Ctrl Pts',(-125.979970944772,6.18548483362552,
128.486199201761));
#198440=CARTESIAN_POINT('Ctrl Pts',(-126.258418568584,1.39307078858202,
124.34731417552));
#198441=CARTESIAN_POINT('Ctrl Pts',(-126.536866192397,-4.67950725587653,
126.142139385264));
#198442=CARTESIAN_POINT('Ctrl Pts',(-126.81531381621,-6.45184673882346,
132.221318145323));
#198443=CARTESIAN_POINT('Ctrl Pts',(-127.093761440023,-2.29525425902701,
136.998382159598));
#198444=CARTESIAN_POINT('Ctrl Pts',(-127.372209063836,3.97056475541062,
136.083442971518));
#198445=CARTESIAN_POINT('Ctrl Pts',(-127.650656687649,6.58762873249828,
130.317284997668));
#198446=CARTESIAN_POINT('Ctrl Pts',(-127.929104311462,3.15098372797424,
124.998725723536));
#198447=CARTESIAN_POINT('Ctrl Pts',(-128.207551935275,-3.18126138844507,
125.015261295985));
#198448=CARTESIAN_POINT('Ctrl Pts',(-128.485999559087,-6.59008270214206,
130.351696331743));
#198449=CARTESIAN_POINT('Ctrl Pts',(-128.764447182901,-3.94293995600869,
136.104107732291));
#198450=CARTESIAN_POINT('Ctrl Pts',(-129.042894806713,2.32757198637139,
136.986310441447));
#198451=CARTESIAN_POINT('Ctrl Pts',(-129.321342430526,6.45915898148892,
132.187603267495));
#198452=CARTESIAN_POINT('Ctrl Pts',(-129.599790054339,4.6550944200771,126.117763673416));
#198453=CARTESIAN_POINT('Ctrl Pts',(-129.878237678152,-1.42677449938118,
124.354677718024));
#198454=CARTESIAN_POINT('Ctrl Pts',(-130.156685301965,-6.19750735571679,
128.518535262782));
#198455=CARTESIAN_POINT('Ctrl Pts',(-130.435132925778,-5.27303371721495,
134.782954639811));
#198456=CARTESIAN_POINT('Ctrl Pts',(-130.713580549591,0.497100305389368,
137.391240475519));
#198457=CARTESIAN_POINT('Ctrl Pts',(-130.992028173403,5.81042343204081,
133.946505508738));
#198458=CARTESIAN_POINT('Ctrl Pts',(-131.270475797217,5.78425127961196,
127.614292889281));
#198459=CARTESIAN_POINT('Ctrl Pts',(-131.548923421029,0.442634777604211,
124.213596668645));
#198460=CARTESIAN_POINT('Ctrl Pts',(-131.827371044842,-5.30574146111081,
126.869490540348));
#198461=CARTESIAN_POINT('Ctrl Pts',(-132.105818668655,-6.17840049694519,
133.141337783923));
#198462=CARTESIAN_POINT('Ctrl Pts',(-132.384266292468,-1.37341130773126,
137.265617179298));
#198463=CARTESIAN_POINT('Ctrl Pts',(-132.662713916281,4.69367577841589,
135.45231744437));
#198464=CARTESIAN_POINT('Ctrl Pts',(-132.941161540094,6.44750412300737,
129.367772450924));
#198465=CARTESIAN_POINT('Ctrl Pts',(-133.219609163907,2.27639115664257,
124.603381801387));
#198466=CARTESIAN_POINT('Ctrl Pts',(-133.49805678772,-3.98661407478655,
125.537387749261));
#198467=CARTESIAN_POINT('Ctrl Pts',(-133.776504411532,-6.58611572841139,
131.311484457178));
#198468=CARTESIAN_POINT('Ctrl Pts',(-134.054952035345,-3.13329877726696,
136.619559130867));
#198469=CARTESIAN_POINT('Ctrl Pts',(-134.333399659158,3.19886668003099,
136.583750459073));
#198470=CARTESIAN_POINT('Ctrl Pts',(-134.611847282971,6.59142993170542,
131.236964861823));
#198471=CARTESIAN_POINT('Ctrl Pts',(-134.890294906784,3.92679108539655,
125.492637097993));
#198472=CARTESIAN_POINT('Ctrl Pts',(-135.168742530597,-2.34637693398254,
124.629523756529));
#198473=CARTESIAN_POINT('Ctrl Pts',(-135.44719015441,-6.46333917791768,
129.440783832808));
#198474=CARTESIAN_POINT('Ctrl Pts',(-135.725637778223,-4.64080846901838,
135.505104359849));
#198475=CARTESIAN_POINT('Ctrl Pts',(-136.004085402036,1.44639850681073,
137.24967103183));
#198476=CARTESIAN_POINT('Ctrl Pts',(-136.282533025848,6.20443591537649,
133.07131230402));
#198477=CARTESIAN_POINT('Ctrl Pts',(-136.560980649661,5.26089982125598,
126.809735723105));
#198478=CARTESIAN_POINT('Ctrl Pts',(-136.839428273474,-0.517146199354053,
124.219024271924));
#198479=CARTESIAN_POINT('Ctrl Pts',(-137.117875897287,-5.81996012675442,
127.679915210822));
#198480=CARTESIAN_POINT('Ctrl Pts',(-137.3963235211,-5.77451501852576,134.012018840873));
#198481=CARTESIAN_POINT('Ctrl Pts',(-137.674771144913,-0.422572709013315,
137.396441266521));
#198482=CARTESIAN_POINT('Ctrl Pts',(-137.953218768726,5.31769327625758,
134.723063616821));
#198483=CARTESIAN_POINT('Ctrl Pts',(-138.231666392539,6.17125892440694,
128.448589350091));
#198484=CARTESIAN_POINT('Ctrl Pts',(-138.510114016352,1.35373910378499,
124.338953792345));
#198485=CARTESIAN_POINT('Ctrl Pts',(-138.788561640165,-4.70780081938319,
126.170711254294));
#198486=CARTESIAN_POINT('Ctrl Pts',(-139.067009263977,-6.44310177839452,
132.260566114734));
#198487=CARTESIAN_POINT('Ctrl Pts',(-139.34545688779,-2.25750696608163,
137.012239262869));
#198488=CARTESIAN_POINT('Ctrl Pts',(-139.623904511603,4.00262646271346,
136.059175207703));
#198489=CARTESIAN_POINT('Ctrl Pts',(-139.902352135416,6.5845417114487,130.277193256163));
#198490=CARTESIAN_POINT('Ctrl Pts',(-140.180799759229,3.11558480010749,
124.979652356196));
#198491=CARTESIAN_POINT('Ctrl Pts',(-140.459247383042,-3.21644233775325,
125.034733795609));
#198492=CARTESIAN_POINT('Ctrl Pts',(-140.737695006855,-6.59271609916233,
130.391820422461));
#198493=CARTESIAN_POINT('Ctrl Pts',(-141.016142630668,-3.91060583752806,
136.128011334905));
#198494=CARTESIAN_POINT('Ctrl Pts',(-141.294590254481,2.36516014507876,
136.97202731291));
#198495=CARTESIAN_POINT('Ctrl Pts',(-141.573037878293,6.46745949885459,
132.148258905163));
#198496=CARTESIAN_POINT('Ctrl Pts',(-141.851485502106,4.62647952614482,
126.089513624195));
#198497=CARTESIAN_POINT('Ctrl Pts',(-142.129933125919,-1.4660091150024,
124.363482397054));
#198498=CARTESIAN_POINT('Ctrl Pts',(-142.408380749732,-6.21130699798892,
128.556303600169));
#198499=CARTESIAN_POINT('Ctrl Pts',(-142.686828373545,-5.24871718904012,
134.814979378581));
#198500=CARTESIAN_POINT('Ctrl Pts',(-142.965275997358,0.537187302547703,
137.388092445238));
#198501=CARTESIAN_POINT('Ctrl Pts',(-143.243723621171,5.82944290615228,
133.911077595444));
#198502=CARTESIAN_POINT('Ctrl Pts',(-143.522171244983,5.76472526312116,
127.579141614542));
#198503=CARTESIAN_POINT('Ctrl Pts',(-143.800618868797,0.402506725767204,
124.21102433671));
#198504=CARTESIAN_POINT('Ctrl Pts',(-144.079066492609,-5.32959582902011,
126.901860998601));
#198505=CARTESIAN_POINT('Ctrl Pts',(-144.357514116423,-6.1640601821688,
133.178904162615));
#198506=CARTESIAN_POINT('Ctrl Pts',(-144.635961740235,-1.33405435898536,
137.27385781163));
#198507=CARTESIAN_POINT('Ctrl Pts',(-144.914409364048,4.72188224792766,
135.423659591808));
#198508=CARTESIAN_POINT('Ctrl Pts',(-145.192856987861,6.43863974576633,
129.328551279958));
#198509=CARTESIAN_POINT('Ctrl Pts',(-145.471304611674,2.23860186228433,
124.589639652074));
#198510=CARTESIAN_POINT('Ctrl Pts',(-145.749752235487,-4.01860177085642,
125.56175298548));
#198511=CARTESIAN_POINT('Ctrl Pts',(-146.0281998593,-6.58290669619051,131.35156661715));
#198512=CARTESIAN_POINT('Ctrl Pts',(-146.306647483113,-3.09784196059638,
136.638524667701));
#198513=CARTESIAN_POINT('Ctrl Pts',(-146.585095106925,3.2339881987928,136.564170970937));
#198514=CARTESIAN_POINT('Ctrl Pts',(-146.863542730738,6.59394119259793,
131.196832941802));
#198515=CARTESIAN_POINT('Ctrl Pts',(-147.141990354551,3.89438436234147,
125.468832020033));
#198516=CARTESIAN_POINT('Ctrl Pts',(-147.420437978364,-2.38392144565404,
124.643921224334));
#198517=CARTESIAN_POINT('Ctrl Pts',(-147.698885602177,-6.47151990613084,
129.480153276819));
#198518=CARTESIAN_POINT('Ctrl Pts',(-147.97733322599,-4.61210772419611,
135.533267184325));
#198519=CARTESIAN_POINT('Ctrl Pts',(-148.255780849803,1.48560614228611,
137.240746976909));
#198520=CARTESIAN_POINT('Ctrl Pts',(-148.534228473616,6.21812053990256,
133.033502140209));
#198521=CARTESIAN_POINT('Ctrl Pts',(-148.812676097428,5.23648593342438,
126.777785143819));
#198522=CARTESIAN_POINT('Ctrl Pts',(-149.091123721242,-0.557223429310831,
124.222294298654));
#198523=CARTESIAN_POINT('Ctrl Pts',(-149.369571345054,-5.83887168238761,
127.715400848752));
#198524=CARTESIAN_POINT('Ctrl Pts',(-149.648018968867,-5.75488210408933,
134.047110522317));
#198525=CARTESIAN_POINT('Ctrl Pts',(-149.92646659268,-0.382437013753756,
137.398891450554));
#198526=CARTESIAN_POINT('Ctrl Pts',(-150.204914216493,5.34144900913504,
134.690620704017));
#198527=CARTESIAN_POINT('Ctrl Pts',(-150.483361840306,6.15680433691945,
128.411066792389));
#198528=CARTESIAN_POINT('Ctrl Pts',(-150.761809464119,1.31435725568762,
124.330832987197));
#198529=CARTESIAN_POINT('Ctrl Pts',(-151.040257087932,-4.73591993359918,
126.199454824906));
#198530=CARTESIAN_POINT('Ctrl Pts',(-151.318704711745,-6.43411806645975,
132.299760123916));
#198531=CARTESIAN_POINT('Ctrl Pts',(-151.597152335558,-2.21967602038541,
137.025866330917));
#198532=CARTESIAN_POINT('Ctrl Pts',(-151.87559995937,4.03453985122072,136.034712724799));
#198533=CARTESIAN_POINT('Ctrl Pts',(-152.154047583183,6.58121069778455,
130.237121049039));
#198534=CARTESIAN_POINT('Ctrl Pts',(-152.432495206996,3.08007042310019,
124.960794825562));
#198535=CARTESIAN_POINT('Ctrl Pts',(-152.710942830809,-3.25150410060774,
125.054420090877));
#198536=CARTESIAN_POINT('Ctrl Pts',(-152.989390454622,-6.59510520066311,
130.431959800007));
#198537=CARTESIAN_POINT('Ctrl Pts',(-153.267838078435,-3.87812681010997,
136.151717667683));
#198538=CARTESIAN_POINT('Ctrl Pts',(-153.546285702248,2.40266066190714,
136.957515639215));
#198539=CARTESIAN_POINT('Ctrl Pts',(-153.824733326061,6.47552036213011,
132.108864744186));
#198540=CARTESIAN_POINT('Ctrl Pts',(-154.103180949873,4.59769319631231,
126.061438285362));
#198541=CARTESIAN_POINT('Ctrl Pts',(-154.381628573686,-1.50518940711724,
124.372525745196));
#198542=CARTESIAN_POINT('Ctrl Pts',(-154.660076197499,-6.22487647799626,
128.594155240135));
#198543=CARTESIAN_POINT('Ctrl Pts',(-154.938523821312,-5.22420616771914,
134.846855502398));
#198544=CARTESIAN_POINT('Ctrl Pts',(-155.216971445125,0.577254394032953,
137.384700452354));
#198545=CARTESIAN_POINT('Ctrl Pts',(-155.495419068938,5.84824636811312,
133.87553456161));
#198546=CARTESIAN_POINT('Ctrl Pts',(-155.773866692751,5.74498563261573,
127.544109851479));
#198547=CARTESIAN_POINT('Ctrl Pts',(-156.052314316564,0.362363758895462,
124.208696323275));
#198548=CARTESIAN_POINT('Ctrl Pts',(-156.330761940377,-5.353252706796,126.934376065411));
#198549=CARTESIAN_POINT('Ctrl Pts',(-156.60920956419,-6.14949145587554,
133.216382551721));
#198550=CARTESIAN_POINT('Ctrl Pts',(-156.887657188002,-1.29464797636456,
137.281858714364));
#198551=CARTESIAN_POINT('Ctrl Pts',(-157.166104811815,4.74991374635575,
135.394830569423));
#198552=CARTESIAN_POINT('Ctrl Pts',(-157.444552435628,6.42953678236183,
129.28938479565));
#198553=CARTESIAN_POINT('Ctrl Pts',(-157.723000059441,2.20072961571137,
124.576127791533));
#198554=CARTESIAN_POINT('Ctrl Pts',(-158.001447683254,-4.05044055615985,
125.586312488451));
#198555=CARTESIAN_POINT('Ctrl Pts',(-158.279895307067,-6.57945373194114,
131.391628500203));
#198556=CARTESIAN_POINT('Ctrl Pts',(-158.55834293088,-3.06227035225273,
136.657274017441));
#198557=CARTESIAN_POINT('Ctrl Pts',(-158.836790554693,3.2689898809326,136.54437805091));
#198558=CARTESIAN_POINT('Ctrl Pts',(-159.115238178505,6.59620811257463,
131.156686478575));
#198559=CARTESIAN_POINT('Ctrl Pts',(-159.393685802319,3.86183333144169,
125.445224652049));
#198560=CARTESIAN_POINT('Ctrl Pts',(-159.672133426131,-2.42137762023968,
124.658546969484));
#198561=CARTESIAN_POINT('Ctrl Pts',(-159.950581049944,-6.47946082979399,
129.519571789819));
#198562=CARTESIAN_POINT('Ctrl Pts',(-160.229028673757,-4.58323607602601,
135.56125477743));
#198563=CARTESIAN_POINT('Ctrl Pts',(-160.50747629757,1.52475872807955,137.231584419323));
#198564=CARTESIAN_POINT('Ctrl Pts',(-160.785923921383,6.23157474968534,
132.99560937474));
#198565=CARTESIAN_POINT('Ctrl Pts',(-161.064371545196,5.2118780056808,126.745983770767));
#198566=CARTESIAN_POINT('Ctrl Pts',(-161.342819169009,-0.597280011148509,
124.225808226271));
#198567=CARTESIAN_POINT('Ctrl Pts',(-161.621266792821,-5.85756687648338,
127.751000949223));
#198568=CARTESIAN_POINT('Ctrl Pts',(-161.899714416635,-5.73503594038016,
134.08208204247));
#198569=CARTESIAN_POINT('Ctrl Pts',(-162.178162040447,-0.342287147149402,
137.401097271823));
#198570=CARTESIAN_POINT('Ctrl Pts',(-162.45660966426,5.36500681265522,134.658033784415));
#198571=CARTESIAN_POINT('Ctrl Pts',(-162.735057288073,6.14212160678308,
128.373632919072));
#198572=CARTESIAN_POINT('Ctrl Pts',(-163.013504911886,1.27492670359879,
124.322952060995));
#198573=CARTESIAN_POINT('Ctrl Pts',(-163.291952535699,-4.76386355656041,
126.228369031995));
#198574=CARTESIAN_POINT('Ctrl Pts',(-163.570400159512,-6.42489593591386,
132.338898720518));
#198575=CARTESIAN_POINT('Ctrl Pts',(-163.848847783325,-2.18176282377798,
137.039262858781));
#198576=CARTESIAN_POINT('Ctrl Pts',(-164.127295407138,4.06630373837012,
136.010056429275));
#198577=CARTESIAN_POINT('Ctrl Pts',(-164.405743030951,6.57763581493773,
130.197069861187));
#198578=CARTESIAN_POINT('Ctrl Pts',(-164.684190654763,3.04444191295097,
124.942153830408));
#198579=CARTESIAN_POINT('Ctrl Pts',(-164.962638278576,-3.28644537778151,
125.074319452304));
#198580=CARTESIAN_POINT('Ctrl Pts',(-165.241085902389,-6.59724991811553,
130.472112977002));
#198581=CARTESIAN_POINT('Ctrl Pts',(-165.519533526202,-3.84550407727676,
136.175225852179));
#198582=CARTESIAN_POINT('Ctrl Pts',(-165.797981150015,2.44007214726114,
136.942775958099));
#198583=CARTESIAN_POINT('Ctrl Pts',(-166.076428773828,6.48334127261722,
132.069422244329));
#198584=CARTESIAN_POINT('Ctrl Pts',(-166.354876397641,4.56873649726763,
126.03353869726));
#198585=CARTESIAN_POINT('Ctrl Pts',(-166.633324021454,-1.54431392388507,
124.381807427344));
#198586=CARTESIAN_POINT('Ctrl Pts',(-166.911771645267,-6.23821529291649,
128.632088780075));
#198587=CARTESIAN_POINT('Ctrl Pts',(-167.19021926908,-5.19950156151742,
134.878581830081));
#198588=CARTESIAN_POINT('Ctrl Pts',(-167.468666892892,0.617300095144361,
137.381064622557));
#198589=CARTESIAN_POINT('Ctrl Pts',(-167.747114516705,5.86683312115408,
133.839877724298));
#198590=CARTESIAN_POINT('Ctrl Pts',(-168.025562140518,5.72503311955499,
127.509198898206));
#198591=CARTESIAN_POINT('Ctrl Pts',(-168.304009764331,0.32220736450136,
124.206612714607));
#198592=CARTESIAN_POINT('Ctrl Pts',(-168.582457388144,-5.37671121782417,
126.967034535923));
#198593=CARTESIAN_POINT('Ctrl Pts',(-168.860905011957,-6.1346948579149,
133.253771562468));
#198594=CARTESIAN_POINT('Ctrl Pts',(-169.13935263577,-1.25519362008691,
137.289619591024));
#198595=CARTESIAN_POINT('Ctrl Pts',(-169.417800259582,4.77776923498369,
135.365831445486));
#198596=CARTESIAN_POINT('Ctrl Pts',(-169.696247883396,6.42019557010726,
129.250274449328));
#198597=CARTESIAN_POINT('Ctrl Pts',(-169.974695507208,2.16277582029264,
124.562846720449));
#198598=CARTESIAN_POINT('Ctrl Pts',(-170.253143131021,-4.08212925089891,
125.611065348116));
#198599=CARTESIAN_POINT('Ctrl Pts',(-170.531590754834,-6.57575696361412,
131.431668621828));
#198600=CARTESIAN_POINT('Ctrl Pts',(-170.810038378647,-3.02658527035502,
136.675806485322));
#198601=CARTESIAN_POINT('Ctrl Pts',(-171.08848600246,3.30387042945021,136.524372432426));
#198602=CARTESIAN_POINT('Ctrl Pts',(-171.366933626273,6.59823060763395,
131.116526959784));
#198603=CARTESIAN_POINT('Ctrl Pts',(-171.645381250086,3.82913919888762,
125.421815868818));
#198604=CARTESIAN_POINT('Ctrl Pts',(-171.923828873899,-2.45874406978715,
124.673400450021));
#198605=CARTESIAN_POINT('Ctrl Pts',(-172.202276497711,-6.48716165465291,
129.559037911142));
#198606=CARTESIAN_POINT('Ctrl Pts',(-172.480724121525,-4.55419459435809,
135.589066102071));
#198607=CARTESIAN_POINT('Ctrl Pts',(-172.759171745337,1.5638548133772,137.222183698596));
#198608=CARTESIAN_POINT('Ctrl Pts',(-173.03761936915,6.24479804617409,132.957635411742));
#198609=CARTESIAN_POINT('Ctrl Pts',(-173.316066992963,5.18707694988104,
126.714332782362));
#198610=CARTESIAN_POINT('Ctrl Pts',(-173.594514616776,-0.637314460555731,
124.229565924566));
#198611=CARTESIAN_POINT('Ctrl Pts',(-173.872962240589,-5.8760450162844,
127.786714193059));
#198612=CARTESIAN_POINT('Ctrl Pts',(-174.151409864401,-5.71497726280517,
134.11693210545));
#198613=CARTESIAN_POINT('Ctrl Pts',(-174.429857488215,-0.302124596968923,
137.403058648589));
#198614=CARTESIAN_POINT('Ctrl Pts',(-174.708305112027,5.38836581387496,
134.625304065538));
#198615=CARTESIAN_POINT('Ctrl Pts',(-174.98675273584,6.1272112780718,128.336289117263));
#198616=CARTESIAN_POINT('Ctrl Pts',(-175.265200359654,1.2354489086321,124.315311305772));
#198617=CARTESIAN_POINT('Ctrl Pts',(-175.543647983466,-4.79163065280562,
126.257452804136));
#198618=CARTESIAN_POINT('Ctrl Pts',(-175.822095607279,-6.41543572848632,
132.377980454247));
#198619=CARTESIAN_POINT('Ctrl Pts',(-176.100543231092,-2.14376878114676,
137.05242835005));
#198620=CARTESIAN_POINT('Ctrl Pts',(-176.378990854905,4.09791694713909,
135.985207234778));
#198621=CARTESIAN_POINT('Ctrl Pts',(-176.657438478718,6.57381719537689,
130.157041176716));
#198622=CARTESIAN_POINT('Ctrl Pts',(-176.93588610253,3.00870058988678,124.923730061481));
#198623=CARTESIAN_POINT('Ctrl Pts',(-177.214333726344,-3.32126487451375,
125.094431142515));
#198624=CARTESIAN_POINT('Ctrl Pts',(-177.492781350156,-6.59915017204588,
130.512278465557));
#198625=CARTESIAN_POINT('Ctrl Pts',(-177.771228973969,-3.81273884787578,
136.198535017289));
#198626=CARTESIAN_POINT('Ctrl Pts',(-178.049676597782,2.47739321484437,
136.927808815745));
#198627=CARTESIAN_POINT('Ctrl Pts',(-178.328124221595,6.49092194050925,
132.029932867148));
#198628=CARTESIAN_POINT('Ctrl Pts',(-178.606571845408,4.53961050201187,
126.005815893719));
#198629=CARTESIAN_POINT('Ctrl Pts',(-178.885019469221,-1.58338121553252,
124.391327099562));
#198630=CARTESIAN_POINT('Ctrl Pts',(-179.163467093034,-6.25132294847495,
128.670102814346));
#198631=CARTESIAN_POINT('Ctrl Pts',(-179.441914716847,-5.1746042858732,
134.910157185999));
#198632=CARTESIAN_POINT('Ctrl Pts',(-179.72036234066,0.657322921973241,
137.377185090575));
#198633=CARTESIAN_POINT('Ctrl Pts',(-179.998809964472,5.88520247653593,
133.804108404782));
#198634=CARTESIAN_POINT('Ctrl Pts',(-180.277257588285,5.70486846328706,
127.474410048364));
#198635=CARTESIAN_POINT('Ctrl Pts',(-180.555705212098,0.282039030594865,
124.204773587913));
#198636=CARTESIAN_POINT('Ctrl Pts',(-180.834152835911,-5.39997049284089,
126.999835199963));
#198637=CARTESIAN_POINT('Ctrl Pts',(-181.112600459724,-6.11967093658025,
133.291069809391));
#198638=CARTESIAN_POINT('Ctrl Pts',(-181.391048083537,-1.21569275214809,
137.297140154028));
#198639=CARTESIAN_POINT('Ctrl Pts',(-181.669495707349,4.8054476816156,135.336663294571));
#198640=CARTESIAN_POINT('Ctrl Pts',(-181.947943331163,6.41061645514481,
129.21122169024));
#198641=CARTESIAN_POINT('Ctrl Pts',(-182.226390954976,2.12474188242055,
124.549796930959));
#198642=CARTESIAN_POINT('Ctrl Pts',(-182.504838578788,-4.11366668083735,
125.636010647245));
#198643=CARTESIAN_POINT('Ctrl Pts',(-182.783286202602,-6.5718165281946,
131.471685498325));
#198644=CARTESIAN_POINT('Ctrl Pts',(-183.061733826414,-2.99078803722709,
136.694121384618));
#198645=CARTESIAN_POINT('Ctrl Pts',(-183.340181450227,3.33862855183402,
136.5041548568));
#198646=CARTESIAN_POINT('Ctrl Pts',(-183.61862907404,6.60000860283161,131.076355873553));
#198647=CARTESIAN_POINT('Ctrl Pts',(-183.897076697853,3.79630317617236,
125.398606537762));
#198648=CARTESIAN_POINT('Ctrl Pts',(-184.175524321666,-2.49601940966891,
124.68848111554));
#198649=CARTESIAN_POINT('Ctrl Pts',(-184.453971945479,-6.49462209535141,
129.598550178357));
#198650=CARTESIAN_POINT('Ctrl Pts',(-184.732419569291,-4.52498435533419,
135.616700127691));
#198651=CARTESIAN_POINT('Ctrl Pts',(-185.010867193105,1.60289294946002,
137.212545163075));
#198652=CARTESIAN_POINT('Ctrl Pts',(-185.289314816917,6.25778993937471,
132.919581658354));
#198653=CARTESIAN_POINT('Ctrl Pts',(-185.56776244073,5.16208368503734,126.682833351442));
#198654=CARTESIAN_POINT('Ctrl Pts',(-185.846210064543,-0.677325294041226,
124.233567254297));
#198655=CARTESIAN_POINT('Ctrl Pts',(-186.124657688356,-5.89430541707644,
127.822539256894));
#198656=CARTESIAN_POINT('Ctrl Pts',(-186.403105312169,-5.69470681464601,
134.151659419877));
#198657=CARTESIAN_POINT('Ctrl Pts',(-186.681552935982,-0.261950851450417,
137.404775508174));
#198658=CARTESIAN_POINT('Ctrl Pts',(-186.960000559794,5.41152514721792,
134.592432760195));
#198659=CARTESIAN_POINT('Ctrl Pts',(-187.238448183608,6.11207390329327,
128.299036770752));
#198660=CARTESIAN_POINT('Ctrl Pts',(-187.51689580742,1.19592533365239,124.307911004657));
#198661=CARTESIAN_POINT('Ctrl Pts',(-187.795343431234,-4.81922019341476,
126.286705063617));
#198662=CARTESIAN_POINT('Ctrl Pts',(-188.073791055046,-6.40573779472858,
132.417003876913));
#198663=CARTESIAN_POINT('Ctrl Pts',(-188.352238678859,-2.10569530037498,
137.065362316871));
#198664=CARTESIAN_POINT('Ctrl Pts',(-188.630686302672,4.12937830608858,
135.960166062105));
#198665=CARTESIAN_POINT('Ctrl Pts',(-188.909133926485,6.56975498060235,
130.117036478904));
#198666=CARTESIAN_POINT('Ctrl Pts',(-189.187581550298,2.97284777831579,
124.905524201484));
#198667=CARTESIAN_POINT('Ctrl Pts',(-189.466029174111,-3.35596130055467,
125.114754416262));
#198668=CARTESIAN_POINT('Ctrl Pts',(-189.744476797923,-6.60080589203976,
130.552454777323));
#198669=CARTESIAN_POINT('Ctrl Pts',(-190.022924421737,-3.77983233603489,
136.221644299282));
#198670=CARTESIAN_POINT('Ctrl Pts',(-190.301372045549,2.5146224817104,136.912614766765));
#198671=CARTESIAN_POINT('Ctrl Pts',(-190.579819669362,6.49826208490189,
131.990398075938));
#198672=CARTESIAN_POINT('Ctrl Pts',(-190.858267293175,4.51031628981952,
125.978270902017));
#198673=CARTESIAN_POINT('Ctrl Pts',(-191.136714916988,-1.62238983440674,
124.401084409096));
#198674=CARTESIAN_POINT('Ctrl Pts',(-191.415162540801,-6.26419895896261,
128.708195934325));
#198675=CARTESIAN_POINT('Ctrl Pts',(-191.693610164614,-5.14951526336424,
134.941580400114));
#198676=CARTESIAN_POINT('Ctrl Pts',(-191.972057788427,0.697321391460013,
137.373062000163));
#198677=CARTESIAN_POINT('Ctrl Pts',(-192.25050541224,5.90335375357599,133.768227928508));
#198678=CARTESIAN_POINT('Ctrl Pts',(-192.528953036052,5.68449241101982,
127.439744591064));
#198679=CARTESIAN_POINT('Ctrl Pts',(-192.807400659866,0.241860245628379,
124.203179011344));
#198680=CARTESIAN_POINT('Ctrl Pts',(-193.085848283678,-5.42302966996514,
127.032776842093));
#198681=CARTESIAN_POINT('Ctrl Pts',(-193.364295907491,-6.10442024858855,
133.32827591039));
#198682=CARTESIAN_POINT('Ctrl Pts',(-193.642743531304,-1.17614683626724,
137.304420124699));
#198683=CARTESIAN_POINT('Ctrl Pts',(-193.921191155117,4.83294806061645,
135.307327197512));
#198684=CARTESIAN_POINT('Ctrl Pts',(-194.19963877893,6.40079979243214,129.172227965502));
#198685=CARTESIAN_POINT('Ctrl Pts',(-194.478086402743,2.08662921145659,
124.536978906625));
#198686=CARTESIAN_POINT('Ctrl Pts',(-194.756534026555,-4.14505167734362,
125.661147461485));
#198687=CARTESIAN_POINT('Ctrl Pts',(-195.034981650369,-6.5676325716969,
131.511677646851));
#198688=CARTESIAN_POINT('Ctrl Pts',(-195.313429274181,-2.95487997934909,
136.712218036662));
#198689=CARTESIAN_POINT('Ctrl Pts',(-195.591876897994,3.3732629601091,136.483726073203));
#198690=CARTESIAN_POINT('Ctrl Pts',(-195.870324521807,6.60154203228333,
131.03617470844));
#198691=CARTESIAN_POINT('Ctrl Pts',(-196.14877214562,3.76332648004682,125.375597518911));
#198692=CARTESIAN_POINT('Ctrl Pts',(-196.427219769433,-2.53320225863353,
124.703788407225));
#198693=CARTESIAN_POINT('Ctrl Pts',(-196.705667393246,-6.50184187543975,
129.63810712732));
#198694=CARTESIAN_POINT('Ctrl Pts',(-196.984115017059,-4.49560644135098,
135.644155830301));
#198695=CARTESIAN_POINT('Ctrl Pts',(-197.262562640871,1.64187168975517,
137.202669169918));
#198696=CARTESIAN_POINT('Ctrl Pts',(-197.541010264685,6.27054994786743,
132.881449524674));
#198697=CARTESIAN_POINT('Ctrl Pts',(-197.819457888497,5.13689913728475,
126.651486645231));
#198698=CARTESIAN_POINT('Ctrl Pts',(-198.097905512311,-0.717311028988463,
124.237812067191));
#198699=CARTESIAN_POINT('Ctrl Pts',(-198.376353136123,-5.91234740221361,
127.858474813215));
#198700=CARTESIAN_POINT('Ctrl Pts',(-198.654800759936,-5.67422534703162,
134.186262698915));
#198701=CARTESIAN_POINT('Ctrl Pts',(-198.933248383749,-0.221767399246752,
137.406247786956));
#198702=CARTESIAN_POINT('Ctrl Pts',(-199.211696007562,5.43448395450644,
134.559421086446));
#198703=CARTESIAN_POINT('Ctrl Pts',(-199.490143631375,6.09671004336861,
128.261877259937));
#198704=CARTESIAN_POINT('Ctrl Pts',(-199.768591255188,1.15635744321901,
124.300751431872));
#198705=CARTESIAN_POINT('Ctrl Pts',(-200.047038879001,-4.84663115604747,
126.316124726487));
#198706=CARTESIAN_POINT('Ctrl Pts',(-200.325486502814,-6.39580249400115,
132.455967542492));
#198707=CARTESIAN_POINT('Ctrl Pts',(-200.603934126626,-2.06754379228947,
137.078064279972));
#198708=CARTESIAN_POINT('Ctrl Pts',(-200.882381750439,4.16068664940635,
135.934933839164));
#198709=CARTESIAN_POINT('Ctrl Pts',(-201.160829374253,6.56544932114097,
130.077057250143));
#198710=CARTESIAN_POINT('Ctrl Pts',(-201.439276998065,2.9368848067771,124.887536925038));
#198711=CARTESIAN_POINT('Ctrl Pts',(-201.717724621878,-3.39053337021544,
125.13528852046));
#198712=CARTESIAN_POINT('Ctrl Pts',(-201.996172245691,-6.60221701674386,
130.592640423553));
#198713=CARTESIAN_POINT('Ctrl Pts',(-202.274619869504,-3.74678576111652,
136.244552841837));
#198714=CARTESIAN_POINT('Ctrl Pts',(-202.553067493317,2.55175856831618,
136.897194374181));
#198715=CARTESIAN_POINT('Ctrl Pts',(-202.83151511713,6.50536143380309,131.950819335672));
#198716=CARTESIAN_POINT('Ctrl Pts',(-203.109962740942,4.48085494619837,
125.950904742844));
#198717=CARTESIAN_POINT('Ctrl Pts',(-203.388410364755,-1.66133833502902,
124.411078994385));
#198718=CARTESIAN_POINT('Ctrl Pts',(-203.666857988568,-6.27684284725421,
128.746366728457));
#198719=CARTESIAN_POINT('Ctrl Pts',(-203.945305612381,-5.12423542367342,
134.97285030803));
#198720=CARTESIAN_POINT('Ctrl Pts',(-204.223753236194,0.737294021446153,
137.368695504108));
#198721=CARTESIAN_POINT('Ctrl Pts',(-204.502200860007,5.9212862796718,133.732237625041));
#198722=CARTESIAN_POINT('Ctrl Pts',(-204.78064848382,5.66390571779574,127.405203810847));
#198723=CARTESIAN_POINT('Ctrl Pts',(-205.059096107633,0.20167249844203,
124.201829043986));
#198724=CARTESIAN_POINT('Ctrl Pts',(-205.337543731446,-5.44588789473034,
127.065858241646));
#198725=CARTESIAN_POINT('Ctrl Pts',(-205.615991355258,-6.08894335906002,
133.36538848678));
#198726=CARTESIAN_POINT('Ctrl Pts',(-205.894438979071,-1.13655733783284,
137.311459233274));
#198727=CARTESIAN_POINT('Ctrl Pts',(-206.172886602884,4.86026935294961,
135.277824241371));
#198728=CARTESIAN_POINT('Ctrl Pts',(-206.451334226697,6.39074594572923,
129.133294720038));
#198729=CARTESIAN_POINT('Ctrl Pts',(-206.72978185051,2.04843921967989,124.524393122426));
#198730=CARTESIAN_POINT('Ctrl Pts',(-207.008229474323,-4.17628307743617,
125.686474859378));
#198731=CARTESIAN_POINT('Ctrl Pts',(-207.286677098136,-6.56320524915893,
131.551643585487));
#198732=CARTESIAN_POINT('Ctrl Pts',(-207.565124721949,-2.9188624273063,
136.730095770877));
#198733=CARTESIAN_POINT('Ctrl Pts',(-207.843572345762,3.40777237088467,
136.463086838631));
#198734=CARTESIAN_POINT('Ctrl Pts',(-208.122019969575,6.60283083916734,
130.995984953369));
#198735=CARTESIAN_POINT('Ctrl Pts',(-208.400467593387,3.73021033247459,
125.352789664874));
#198736=CARTESIAN_POINT('Ctrl Pts',(-208.678915217201,-2.57029123885685,
124.719321757855));
#198737=CARTESIAN_POINT('Ctrl Pts',(-208.957362841013,-6.50882072738636,
129.677707292235));
#198738=CARTESIAN_POINT('Ctrl Pts',(-209.235810464827,-4.4660619410178,
135.671432192519));
#198739=CARTESIAN_POINT('Ctrl Pts',(-209.514258088639,1.68078958989102,
137.192556085085));
#198740=CARTESIAN_POINT('Ctrl Pts',(-209.792705712452,6.28307759882623,
132.8432404237));
#198741=CARTESIAN_POINT('Ctrl Pts',(-210.071153336265,5.11152423984512,
126.620293825292));
#198742=CARTESIAN_POINT('Ctrl Pts',(-210.349600960078,-0.757270183712145,
124.242300205957));
#198743=CARTESIAN_POINT('Ctrl Pts',(-210.62804858389,-5.93017030314353,
127.894519530418));
#198744=CARTESIAN_POINT('Ctrl Pts',(-210.906496207704,-5.65353361891029,
134.220740660327));
#198745=CARTESIAN_POINT('Ctrl Pts',(-211.184943831516,-0.181575729370575,
137.407475430382));
#198746=CARTESIAN_POINT('Ctrl Pts',(-211.463391455329,5.4572413849935,134.52627026755));
#198747=CARTESIAN_POINT('Ctrl Pts',(-211.741839079142,6.08112026761121,
128.224811961777));
#198748=CARTESIAN_POINT('Ctrl Pts',(-212.020286702955,1.11674670353533,
124.293832852717));
#198749=CARTESIAN_POINT('Ctrl Pts',(-212.298734326768,-4.87386252498038,
126.345710702588));
#198750=CARTESIAN_POINT('Ctrl Pts',(-212.577181950581,-6.38563019446009,
132.494870007167));
#198751=CARTESIAN_POINT('Ctrl Pts',(-212.855629574394,-2.02931567060901,
137.090533768676));
#198752=CARTESIAN_POINT('Ctrl Pts',(-213.134077198207,4.19184081695006,
135.909511500946));
#198753=CARTESIAN_POINT('Ctrl Pts',(-213.412524822019,6.56090037654053,
130.037104971874));
#198754=CARTESIAN_POINT('Ctrl Pts',(-213.690972445832,2.90081300789186,
124.869768898671));
#198755=CARTESIAN_POINT('Ctrl Pts',(-213.969420069645,-3.42497980241531,
125.156032694208));
#198756=CARTESIAN_POINT('Ctrl Pts',(-214.247867693459,-6.60338349386843,
130.632833915152));
#198757=CARTESIAN_POINT('Ctrl Pts',(-214.52631531727,-3.71360034767391,
136.267259796069));
#198758=CARTESIAN_POINT('Ctrl Pts',(-214.804762941084,2.58880009856982,
136.881548209402));
#198759=CARTESIAN_POINT('Ctrl Pts',(-215.083210564897,6.51221972414398,
131.911198112957));
#198760=CARTESIAN_POINT('Ctrl Pts',(-215.36165818871,4.45122756284936,125.923718430264));
#198761=CARTESIAN_POINT('Ctrl Pts',(-215.640105812523,-1.70022527414834,
124.421310485075));
#198762=CARTESIAN_POINT('Ctrl Pts',(-215.918553436335,-6.28925414482577,
128.784613782311));
#198763=CARTESIAN_POINT('Ctrl Pts',(-216.197001060149,-5.09876570355457,
135.003965751026));
#198764=CARTESIAN_POINT('Ctrl Pts',(-216.475448683961,0.77723933073121,
137.364085764208));
#198765=CARTESIAN_POINT('Ctrl Pts',(-216.753896307774,5.93899939032692,
133.696138828015));
#198766=CARTESIAN_POINT('Ctrl Pts',(-217.032343931587,5.64310914646246,
127.370788987637));
#198767=CARTESIAN_POINT('Ctrl Pts',(-217.3107915554,0.161477278206604,124.200723735865));
#198768=CARTESIAN_POINT('Ctrl Pts',(-217.589239179213,-5.46854432011718,
127.099078172778));
#198769=CARTESIAN_POINT('Ctrl Pts',(-217.867686803026,-6.07324084149572,
133.402406163341));
#198770=CARTESIAN_POINT('Ctrl Pts',(-218.146134426838,-1.09692572384833,
137.318257218917));
#198771=CARTESIAN_POINT('Ctrl Pts',(-218.424582050652,4.88741054621452,
135.24815551939));
#198772=CARTESIAN_POINT('Ctrl Pts',(-218.703029674464,6.38045528758512,
129.094423396537));
#198773=CARTESIAN_POINT('Ctrl Pts',(-218.981477298277,2.01017332223456,
124.512040044732));
#198774=CARTESIAN_POINT('Ctrl Pts',(-219.25992492209,-4.20735972382344,
125.711991902411));
#198775=CARTESIAN_POINT('Ctrl Pts',(-219.538372545903,-6.55853472463687,
131.591581833275));
#198776=CARTESIAN_POINT('Ctrl Pts',(-219.816820169716,-2.8827367157428,
136.747753924796));
#198777=CARTESIAN_POINT('Ctrl Pts',(-220.095267793529,3.44215550540127,
136.442237917877));
#198778=CARTESIAN_POINT('Ctrl Pts',(-220.373715417342,6.60387497572639,
130.955788097589));
#198779=CARTESIAN_POINT('Ctrl Pts',(-220.652163041155,3.69695596058723,
125.330183820803));
#198780=CARTESIAN_POINT('Ctrl Pts',(-220.930610664968,-2.60728497599312,
124.735080591838));
#198781=CARTESIAN_POINT('Ctrl Pts',(-221.20905828878,-6.51555839258729,
129.717349205704));
#198782=CARTESIAN_POINT('Ctrl Pts',(-221.487505912593,-4.43635194911701,
135.698528203611));
#198783=CARTESIAN_POINT('Ctrl Pts',(-221.765953536406,1.71964520775051,
137.182206283321));
#198784=CARTESIAN_POINT('Ctrl Pts',(-222.044401160219,6.295372428034,132.804955771283));
#198785=CARTESIAN_POINT('Ctrl Pts',(-222.322848784032,5.08595993299503,
126.589256047487));
#198786=CARTESIAN_POINT('Ctrl Pts',(-222.601296407845,-0.797201277510683,
124.247031504286));
#198787=CARTESIAN_POINT('Ctrl Pts',(-222.879744031658,-5.94777345943203,
127.930672072853));
#198788=CARTESIAN_POINT('Ctrl Pts',(-223.158191655471,-5.63263239702162,
134.255092026522));
#198789=CARTESIAN_POINT('Ctrl Pts',(-223.436639279283,-0.141377331138957,
137.40845839296));
#198790=CARTESIAN_POINT('Ctrl Pts',(-223.715086903097,5.47979659539413,
134.492981531924));
#198791=CARTESIAN_POINT('Ctrl Pts',(-223.993534526909,6.06530515370598,
128.187842249741));
#198792=CARTESIAN_POINT('Ctrl Pts',(-224.271982150722,1.07709458239186,
124.287155523561));
#198793=CARTESIAN_POINT('Ctrl Pts',(-224.550429774535,-4.90091329114502,
126.375461895601));
#198794=CARTESIAN_POINT('Ctrl Pts',(-224.828877398348,-6.37522127304402,
132.533709829396));
#198795=CARTESIAN_POINT('Ctrl Pts',(-225.107325022161,-1.99101235188949,
137.102770320923));
#198796=CARTESIAN_POINT('Ctrl Pts',(-225.385772645974,4.22283965429091,
135.883899989486));
#198797=CARTESIAN_POINT('Ctrl Pts',(-225.664220269787,6.55610831536389,
129.997181124546));
#198798=CARTESIAN_POINT('Ctrl Pts',(-225.9426678936,2.86463371831382,124.852220780782));
#198799=CARTESIAN_POINT('Ctrl Pts',(-226.221115517412,-3.45929932072906,
125.176986168825));
#198800=CARTESIAN_POINT('Ctrl Pts',(-226.499563141226,-6.60430528018926,
130.673033762736));
#198801=CARTESIAN_POINT('Ctrl Pts',(-226.778010765038,-3.68027732540471,
136.289764320562));
#198802=CARTESIAN_POINT('Ctrl Pts',(-227.056458388851,2.62574569988376,
136.865676852203));
#198803=CARTESIAN_POINT('Ctrl Pts',(-227.334906012664,6.51883670178814,
131.871535875972));
#198804=CARTESIAN_POINT('Ctrl Pts',(-227.613353636477,4.42143523762624,
125.896712971676));
#198805=CARTESIAN_POINT('Ctrl Pts',(-227.89180126029,-1.73904921079426,
124.431778502036));
#198806=CARTESIAN_POINT('Ctrl Pts',(-228.170248884103,-6.30143239177224,
128.822935678624));
#198807=CARTESIAN_POINT('Ctrl Pts',(-228.448696507916,-5.07310704679746,
135.034925576111));
#198808=CARTESIAN_POINT('Ctrl Pts',(-228.727144131728,0.81715583912702,
137.359232951281));
#198809=CARTESIAN_POINT('Ctrl Pts',(-229.005591755541,5.95649242917557,
133.659932875084));
#198810=CARTESIAN_POINT('Ctrl Pts',(-229.284039379354,5.62210346764449,
127.336501396687));
#198811=CARTESIAN_POINT('Ctrl Pts',(-229.562487003167,0.121276074371264,
124.199863127936));
#198812=CARTESIAN_POINT('Ctrl Pts',(-229.84093462698,-5.4909981065832,127.132435404515));
#198813=CARTESIAN_POINT('Ctrl Pts',(-230.119382250793,-6.0573132777586,
133.439327568368));
#198814=CARTESIAN_POINT('Ctrl Pts',(-230.397829874606,-1.05725346287773,
137.324813829725));
#198815=CARTESIAN_POINT('Ctrl Pts',(-230.676277498418,4.91437063468431,
135.218322130955));
#198816=CARTESIAN_POINT('Ctrl Pts',(-230.954725122232,6.3699281993239,129.055615435388));
#198817=CARTESIAN_POINT('Ctrl Pts',(-231.233172746044,1.97183293707754,
124.49992013129));
#198818=CARTESIAN_POINT('Ctrl Pts',(-231.511620369858,-4.23828046494889,
125.73769764504));
#198819=CARTESIAN_POINT('Ctrl Pts',(-231.79006799367,-6.55362117119865,
131.631490910294));
#198820=CARTESIAN_POINT('Ctrl Pts',(-232.068515617483,-2.84650418331021,
136.765191844092));
#198821=CARTESIAN_POINT('Ctrl Pts',(-232.346963241296,3.47641108958031,
136.421180083507));
#198822=CARTESIAN_POINT('Ctrl Pts',(-232.625410865109,6.60467440326965,
130.915585630608));
#198823=CARTESIAN_POINT('Ctrl Pts',(-232.903858488922,3.66356459663667,
125.307780824367));
#198824=CARTESIAN_POINT('Ctrl Pts',(-233.182306112735,-2.64418209922576,
124.751064325225));
#198825=CARTESIAN_POINT('Ctrl Pts',(-233.460753736548,-6.52205462137589,
129.75703139878));
#198826=CARTESIAN_POINT('Ctrl Pts',(-233.73920136036,-4.40647756656326,
135.725442859523));
#198827=CARTESIAN_POINT('Ctrl Pts',(-234.017648984174,1.75843710352442,
137.17162014814));
#198828=CARTESIAN_POINT('Ctrl Pts',(-234.296096607986,6.30743397990132,
132.766596986079));
#198829=CARTESIAN_POINT('Ctrl Pts',(-234.574544231799,5.06020716402928,
126.558374461932));
#198830=CARTESIAN_POINT('Ctrl Pts',(-234.852991855612,-0.837102830722735,
124.252005786856));
#198831=CARTESIAN_POINT('Ctrl Pts',(-235.131439479425,-5.96515621878728,
127.966931100874));
#198832=CARTESIAN_POINT('Ctrl Pts',(-235.409887103238,-5.6115224558684,
134.289315524594));
#198833=CARTESIAN_POINT('Ctrl Pts',(-235.688334727051,-0.101173694118813,
137.409196638266));
#198834=CARTESIAN_POINT('Ctrl Pts',(-235.966782350864,5.50214874991674,
134.459556113093));
#198835=CARTESIAN_POINT('Ctrl Pts',(-236.245229974676,6.04926528768773,
128.150969493757));
#198836=CARTESIAN_POINT('Ctrl Pts',(-236.52367759849,1.03740254911254,124.280719691838));
#198837=CARTESIAN_POINT('Ctrl Pts',(-236.802125222302,-4.92778245216537,
126.405377203086));
#198838=CARTESIAN_POINT('Ctrl Pts',(-237.080572846115,-6.36457611545918,
132.572485569954));
#198839=CARTESIAN_POINT('Ctrl Pts',(-237.359020469928,-1.95263525547508,
137.114773483282));
#198840=CARTESIAN_POINT('Ctrl Pts',(-237.637468093741,4.25368201275546,
135.858100253825));
#198841=CARTESIAN_POINT('Ctrl Pts',(-237.915915717553,6.55107331518259,
129.957287187551));
#198842=CARTESIAN_POINT('Ctrl Pts',(-238.194363341367,2.8283482786799,124.834893221623));
#198843=CARTESIAN_POINT('Ctrl Pts',(-238.47281096518,-3.49349065343433,
125.198148167872));
#198844=CARTESIAN_POINT('Ctrl Pts',(-238.751258588993,-6.60498234154917,
130.713238476685));
#198845=CARTESIAN_POINT('Ctrl Pts',(-239.029706212805,-3.64681792910581,
136.312065581403));
#198846=CARTESIAN_POINT('Ctrl Pts',(-239.308153836619,2.66259400322518,
136.8495808907));
#198847=CARTESIAN_POINT('Ctrl Pts',(-239.586601460431,6.52521212154101,
131.831834094415));
#198848=CARTESIAN_POINT('Ctrl Pts',(-239.865049084244,4.39147907449425,
125.869889367774));
#198849=CARTESIAN_POINT('Ctrl Pts',(-240.143496708057,-1.77780870633274,
124.44248265737));
#198850=CARTESIAN_POINT('Ctrl Pts',(-240.42194433187,-6.31337713682396,
128.861330997368));
#198851=CARTESIAN_POINT('Ctrl Pts',(-240.700391955683,-5.04726040419313,
135.065728636055));
#198852=CARTESIAN_POINT('Ctrl Pts',(-240.978839579496,0.857042067512721,
137.354137245149));
#198853=CARTESIAN_POINT('Ctrl Pts',(-241.257287203309,5.97376474800676,
133.623621107872));
#198854=CARTESIAN_POINT('Ctrl Pts',(-241.535734827122,5.60088945971499,
127.302342308534));
#198855=CARTESIAN_POINT('Ctrl Pts',(-241.814182450934,0.0810703766063902,
124.199247252091));
#198856=CARTESIAN_POINT('Ctrl Pts',(-242.092630074747,-5.51324842209508,
127.165928700792));
#198857=CARTESIAN_POINT('Ctrl Pts',(-242.37107769856,-6.04116125805038,
133.476151333726));
#198858=CARTESIAN_POINT('Ctrl Pts',(-242.649525322373,-1.01754202499167,
137.331128822742));
#198859=CARTESIAN_POINT('Ctrl Pts',(-242.927972946186,4.94114861934255,
135.188325181553));
#198860=CARTESIAN_POINT('Ctrl Pts',(-243.206420569999,6.35916507103108,
129.016872274634));
#198861=CARTESIAN_POINT('Ctrl Pts',(-243.484868193812,1.93341948492588,
124.488033831209));
#198862=CARTESIAN_POINT('Ctrl Pts',(-243.763315817625,-4.26904415503308,
125.763591134728));
#198863=CARTESIAN_POINT('Ctrl Pts',(-244.041763441437,-6.54846477091785,
131.671369337695));
#198864=CARTESIAN_POINT('Ctrl Pts',(-244.320211065251,-2.8101661726183,
136.782408882594));
#198865=CARTESIAN_POINT('Ctrl Pts',(-244.598658689063,3.51053785406796,
136.399914115825));
#198866=CARTESIAN_POINT('Ctrl Pts',(-244.877106312876,6.60522909217403,
130.875379042142));
#198867=CARTESIAN_POINT('Ctrl Pts',(-245.155553936689,3.6300374779527,125.285581505715));
#198868=CARTESIAN_POINT('Ctrl Pts',(-245.434001560502,-2.68098124131831,
124.767272365732));
#198869=CARTESIAN_POINT('Ctrl Pts',(-245.712449184315,-6.528309173032,129.796752401026));
#198870=CARTESIAN_POINT('Ctrl Pts',(-245.990896808128,-4.37643990036281,
135.752175162922));
#198871=CARTESIAN_POINT('Ctrl Pts',(-246.269344431941,1.79716383976481,
137.160798071814));
#198872=CARTESIAN_POINT('Ctrl Pts',(-246.547792055753,6.31926180748295,
132.728165489484));
#198873=CARTESIAN_POINT('Ctrl Pts',(-246.826239679567,5.03426688722615,
126.527650212955));
#198874=CARTESIAN_POINT('Ctrl Pts',(-247.104687303379,-0.876973364781528,
124.257222869343));
#198875=CARTESIAN_POINT('Ctrl Pts',(-247.383134927193,-5.98231793708558,
128.003295270889));
#198876=CARTESIAN_POINT('Ctrl Pts',(-247.661582551005,-5.59020457768662,
134.32340988638));
#198877=CARTESIAN_POINT('Ctrl Pts',(-247.940030174818,-0.0609663080697638,
137.409690138946));
#198878=CARTESIAN_POINT('Ctrl Pts',(-248.218477798631,5.524297020294,134.425995249648));
#198879=CARTESIAN_POINT('Ctrl Pts',(-248.496925422444,6.03300126391963,
128.114195060156));
#198880=CARTESIAN_POINT('Ctrl Pts',(-248.775373046256,0.997672074500306,
124.274525596028));
#198881=CARTESIAN_POINT('Ctrl Pts',(-249.05382067007,-4.95446901239483,
126.435455516518));
#198882=CARTESIAN_POINT('Ctrl Pts',(-249.332268293882,-6.35369511616563,
132.611195791991));
#198883=CARTESIAN_POINT('Ctrl Pts',(-249.610715917695,-1.91418580344349,
137.126542810973));
#198884=CARTESIAN_POINT('Ctrl Pts',(-249.889163541508,4.28436674946925,
135.832113249982));
#198885=CARTESIAN_POINT('Ctrl Pts',(-250.167611165321,6.54579556256923,
129.917424639176));
#198886=CARTESIAN_POINT('Ctrl Pts',(-250.446058789134,2.79195803356287,
124.817786863269));
#198887=CARTESIAN_POINT('Ctrl Pts',(-250.724506412947,-3.52755253356211,
125.219517907192));
#198888=CARTESIAN_POINT('Ctrl Pts',(-251.00295403676,-6.60541465285253,
130.75344656718));
#198889=CARTESIAN_POINT('Ctrl Pts',(-251.281401660573,-3.61322339864049,
136.334162752248));
#198890=CARTESIAN_POINT('Ctrl Pts',(-251.559849284386,2.6993436431913,136.83326092127));
#198891=CARTESIAN_POINT('Ctrl Pts',(-251.838296908198,6.53134574711249,
131.792094239578));
#198892=CARTESIAN_POINT('Ctrl Pts',(-252.116744532012,4.3613601835781,125.843248612281));
#198893=CARTESIAN_POINT('Ctrl Pts',(-252.395192155824,-1.81650232468185,
124.453422554885));
#198894=CARTESIAN_POINT('Ctrl Pts',(-252.673639779637,-6.32508793705065,
128.899798314935));
#198895=CARTESIAN_POINT('Ctrl Pts',(-252.95208740345,-5.02122673409033,
135.096373791053));
#198896=CARTESIAN_POINT('Ctrl Pts',(-253.230535027263,0.896896539007115,
137.348798831588));
#198897=CARTESIAN_POINT('Ctrl Pts',(-253.508982651076,5.99081570467794,
133.587204877683));
#198898=CARTESIAN_POINT('Ctrl Pts',(-253.787430274889,5.57946791275175,
127.26831297809));
#198899=CARTESIAN_POINT('Ctrl Pts',(-254.065877898701,0.0408616672245685,
124.198876151673));
#198900=CARTESIAN_POINT('Ctrl Pts',(-254.344325522515,-5.53529442795169,
127.199556781751));
#198901=CARTESIAN_POINT('Ctrl Pts',(-254.622773146327,-6.0247854077167,
133.512876168065));
#198902=CARTESIAN_POINT('Ctrl Pts',(-254.90122077014,-0.977792831057213,
137.337201825807));
#198903=CARTESIAN_POINT('Ctrl Pts',(-255.179668393953,4.96774341227684,
135.158166043599));
#198904=CARTESIAN_POINT('Ctrl Pts',(-255.458116017766,6.34816648213513,
128.97819485735));
#198905=CARTESIAN_POINT('Ctrl Pts',(-255.736563641579,1.89493404819936,
124.476382515012));
#198906=CARTESIAN_POINT('Ctrl Pts',(-256.015011265392,-4.29964901022966,
125.789669655819));
#198907=CARTESIAN_POINT('Ctrl Pts',(-256.293458889205,-6.54306693065544,
131.711218953762));
#198908=CARTESIAN_POINT('Ctrl Pts',(-256.571906513018,-2.77372173452912,
136.799398141047));
#198909=CARTESIAN_POINT('Ctrl Pts',(-256.85035413683,3.54453019961847,136.378452625405));
#198910=CARTESIAN_POINT('Ctrl Pts',(-257.128801760644,6.60554720661629,
130.835147498674));
#198911=CARTESIAN_POINT('Ctrl Pts',(-257.407249384456,3.5963603924579,125.263628838565));
#198912=CARTESIAN_POINT('Ctrl Pts',(-257.685697008269,-2.71765185753996,
124.783624522784));
#198913=CARTESIAN_POINT('Ctrl Pts',(-257.964144632082,-6.53437691572335,
129.836661023534));
#198914=CARTESIAN_POINT('Ctrl Pts',(-258.242592255895,-4.34613602341029,
135.778440351053));
#198915=CARTESIAN_POINT('Ctrl Pts',(-258.521039879708,1.83562753012831,
137.150276335207));
#198916=CARTESIAN_POINT('Ctrl Pts',(-258.799487503521,6.33122643152078,
132.688650362788));
#198917=CARTESIAN_POINT('Ctrl Pts',(-259.077935127334,5.00743946241547,
126.498999976245));
#198918=CARTESIAN_POINT('Ctrl Pts',(-259.356382751147,-0.915487258132909,
124.259032700089));
#198919=CARTESIAN_POINT('Ctrl Pts',(-259.634830374959,-6.00176822571329,
128.046924274587));
#198920=CARTESIAN_POINT('Ctrl Pts',(-259.86687006147,-5.63687269779404,
133.292521465648));
#198921=CARTESIAN_POINT('Ctrl Pts',(-260.052531023546,-2.79481741349804,
135.900547185714));
#198922=CARTESIAN_POINT('Ctrl Pts',(-260.145376111017,-0.946914048523564,
136.386386345067));
#198923=CARTESIAN_POINT('Ctrl Pts',(-260.191813261187,-0.0157913329746497,
136.389009763222));
#198924=CARTESIAN_POINT('Ctrl Pts',(210.190947297731,3.04870273111253,135.077142573452));
#198925=CARTESIAN_POINT('Ctrl Pts',(210.144529434129,3.76080111712433,134.569051946243));
#198926=CARTESIAN_POINT('Ctrl Pts',(210.051703633225,4.91317831978039,133.192256847685));
#198927=CARTESIAN_POINT('Ctrl Pts',(209.866061957716,5.67455722768035,129.648049455111));
#198928=CARTESIAN_POINT('Ctrl Pts',(209.634022271206,3.10293383059235,125.427666478792));
#198929=CARTESIAN_POINT('Ctrl Pts',(209.355574647392,-2.85596866243967,
125.28812524467));
#198930=CARTESIAN_POINT('Ctrl Pts',(209.07712702358,-6.17973736462657,130.225196103446));
#198931=CARTESIAN_POINT('Ctrl Pts',(208.798679399767,-3.83016968018938,
135.690661498217));
#198932=CARTESIAN_POINT('Ctrl Pts',(208.520231775954,2.04205955310628,136.667868212554));
#198933=CARTESIAN_POINT('Ctrl Pts',(208.241784152142,6.03618933210081,132.255733564264));
#198934=CARTESIAN_POINT('Ctrl Pts',(207.963336528328,4.48417485225333,126.510421532214));
#198935=CARTESIAN_POINT('Ctrl Pts',(207.684888904515,-1.18901089957204,
124.710731370568));
#198936=CARTESIAN_POINT('Ctrl Pts',(207.406441280703,-5.76932406256156,
128.510946815645));
#198937=CARTESIAN_POINT('Ctrl Pts',(207.12799365689,-5.04803188696711,134.418613818075));
#198938=CARTESIAN_POINT('Ctrl Pts',(206.849546033077,0.312219397189005,
137.005003016302));
#198939=CARTESIAN_POINT('Ctrl Pts',(206.571098409264,5.38552219392035,133.893281295751));
#198940=CARTESIAN_POINT('Ctrl Pts',(206.292650785451,5.50981125882569,127.943004805273));
#198941=CARTESIAN_POINT('Ctrl Pts',(206.014203161638,0.570843377758803,
124.622167937696));
#198942=CARTESIAN_POINT('Ctrl Pts',(205.735755537825,-4.89269661278007,
126.982467612715));
#198943=CARTESIAN_POINT('Ctrl Pts',(205.457307914013,-5.86009012142741,
132.854898402769));
#198944=CARTESIAN_POINT('Ctrl Pts',(205.178860290199,-1.44234566848361,
136.842986120511));
#198945=CARTESIAN_POINT('Ctrl Pts',(204.900412666387,4.30084323855829,135.281871486376));
#198946=CARTESIAN_POINT('Ctrl Pts',(204.621965042573,6.09176771588946,129.606143376667));
#198947=CARTESIAN_POINT('Ctrl Pts',(204.343517418761,2.28465505058828,125.031518229909));
#198948=CARTESIAN_POINT('Ctrl Pts',(204.065069794948,-3.62194388278553,
125.761853295313));
#198949=CARTESIAN_POINT('Ctrl Pts',(203.786622171135,-6.20015338889199,
131.126006208945));
#198950=CARTESIAN_POINT('Ctrl Pts',(203.508174547322,-3.08072479357708,
136.194582558939));
#198951=CARTESIAN_POINT('Ctrl Pts',(203.229726923509,2.86973936865286,136.309808260363));
#198952=CARTESIAN_POINT('Ctrl Pts',(202.951279299696,6.1830532544492,131.365796540178));
#198953=CARTESIAN_POINT('Ctrl Pts',(202.672831675884,3.81444325369211,125.905852631576));
#198954=CARTESIAN_POINT('Ctrl Pts',(202.39438405207,-2.05945374882828,124.947398258377));
#198955=CARTESIAN_POINT('Ctrl Pts',(202.115936428258,-6.04081336739099,
129.371206163854));
#198956=CARTESIAN_POINT('Ctrl Pts',(201.837488804444,-4.47096061076856,
135.112012999282));
#198957=CARTESIAN_POINT('Ctrl Pts',(201.559041180632,1.20748652821524,136.894297736177));
#198958=CARTESIAN_POINT('Ctrl Pts',(201.280593556819,5.77631253695961,133.08022777117));
#198959=CARTESIAN_POINT('Ctrl Pts',(201.002145933006,5.03698951269057,127.174747074221));
#198960=CARTESIAN_POINT('Ctrl Pts',(200.723698309193,-0.331080803069094,
124.604703907164));
#198961=CARTESIAN_POINT('Ctrl Pts',(200.44525068538,-5.39490403503349,127.731842386878));
#198962=CARTESIAN_POINT('Ctrl Pts',(200.166803061567,-5.50107401450091,
133.682475019745));
#198963=CARTESIAN_POINT('Ctrl Pts',(199.888355437754,-0.552025717056,136.988261120707));
#198964=CARTESIAN_POINT('Ctrl Pts',(199.609907813942,4.90430724641216,134.611344759621));
#198965=CARTESIAN_POINT('Ctrl Pts',(199.331460190128,5.85382143915379,128.735995953499));
#198966=CARTESIAN_POINT('Ctrl Pts',(199.053012566316,1.42395970438994,124.761373228423));
#198967=CARTESIAN_POINT('Ctrl Pts',(198.774564942502,-4.31445143441004,
126.339960697623));
#198968=CARTESIAN_POINT('Ctrl Pts',(198.49611731869,-6.088092477657,132.02111359519));
#198969=CARTESIAN_POINT('Ctrl Pts',(198.217669694877,-2.26707395378944,
136.584129948007));
#198970=CARTESIAN_POINT('Ctrl Pts',(197.939222071064,3.6372747808909,135.835820643578));
#198971=CARTESIAN_POINT('Ctrl Pts',(197.660774447251,6.19914568268399,130.46384537573));
#198972=CARTESIAN_POINT('Ctrl Pts',(197.382326823438,3.06430454719326,125.404786980035));
#198973=CARTESIAN_POINT('Ctrl Pts',(197.103879199626,-2.88648276756863,
125.307672973393));
#198974=CARTESIAN_POINT('Ctrl Pts',(196.825431575812,-6.1847334314575,130.261746383626));
#198975=CARTESIAN_POINT('Ctrl Pts',(196.546983952,-3.79951621286212,135.71445576667));
#198976=CARTESIAN_POINT('Ctrl Pts',(196.268536328187,2.07727078866752,136.65502757917));
#198977=CARTESIAN_POINT('Ctrl Pts',(195.990088704374,6.04514741573133,132.219122274927));
#198978=CARTESIAN_POINT('Ctrl Pts',(195.711641080561,4.45782888960729,126.483120122517));
#198979=CARTESIAN_POINT('Ctrl Pts',(195.433193456748,-1.22601660901765,
124.718126880723));
#198980=CARTESIAN_POINT('Ctrl Pts',(195.154745832935,-5.78321273819644,
128.54608511404));
#198981=CARTESIAN_POINT('Ctrl Pts',(194.876298209123,-5.02591888662151,
134.449288212205));
#198982=CARTESIAN_POINT('Ctrl Pts',(194.597850585309,0.349948891971121,
137.002980915508));
#198983=CARTESIAN_POINT('Ctrl Pts',(194.319402961497,5.40423073479611,133.860444384439));
#198984=CARTESIAN_POINT('Ctrl Pts',(194.040955337684,5.49228854369214,127.909516169605));
#198985=CARTESIAN_POINT('Ctrl Pts',(193.762507713871,0.533201494146887,
124.618808581434));
#198986=CARTESIAN_POINT('Ctrl Pts',(193.484060090058,-4.91587168017823,
127.012321133451));
#198987=CARTESIAN_POINT('Ctrl Pts',(193.205612466245,-5.84749893410212,
132.890532719942));
#198988=CARTESIAN_POINT('Ctrl Pts',(192.927164842432,-1.40556033379022,
136.851654059523));
#198989=CARTESIAN_POINT('Ctrl Pts',(192.648717218619,4.32801954783523,135.255608152653));
#198990=CARTESIAN_POINT('Ctrl Pts',(192.370269594806,6.08436090050943,129.569083216569));
#198991=CARTESIAN_POINT('Ctrl Pts',(192.091821970994,2.24947182316989,125.017717865345));
#198992=CARTESIAN_POINT('Ctrl Pts',(191.81337434718,-3.65257196685492,125.783994510198));
#198993=CARTESIAN_POINT('Ctrl Pts',(191.534926723368,-6.19808055740059,
131.163742349203));
#198994=CARTESIAN_POINT('Ctrl Pts',(191.256479099555,-3.04785590876364,
136.213235933607));
#198995=CARTESIAN_POINT('Ctrl Pts',(190.978031475742,2.90319942398833,136.292237340818));
#198996=CARTESIAN_POINT('Ctrl Pts',(190.699583851929,6.18635631527163,131.328148137043));
#198997=CARTESIAN_POINT('Ctrl Pts',(190.421136228116,3.7845539731278,125.882723791311));
#198998=CARTESIAN_POINT('Ctrl Pts',(190.142688604304,-2.09506858458051,
124.960043253581));
#198999=CARTESIAN_POINT('Ctrl Pts',(189.86424098049,-6.04942546284962,129.408004862578));
#199000=CARTESIAN_POINT('Ctrl Pts',(189.585793356678,-4.44465587162338,
135.139149194637));
#199001=CARTESIAN_POINT('Ctrl Pts',(189.307345732864,1.24453533211424,136.886834590562));
#199002=CARTESIAN_POINT('Ctrl Pts',(189.028898109051,5.79005936456987,133.045023550676));
#199003=CARTESIAN_POINT('Ctrl Pts',(188.750450485239,5.01480170111087,127.144152737732));
#199004=CARTESIAN_POINT('Ctrl Pts',(188.472002861426,-0.368813738986236,
124.606834155258));
#199005=CARTESIAN_POINT('Ctrl Pts',(188.193555237613,-5.41350737050784,
127.764739625646));
#199006=CARTESIAN_POINT('Ctrl Pts',(187.9151076138,-5.48345219307025,133.715908293866));
#199007=CARTESIAN_POINT('Ctrl Pts',(187.636659989987,-0.51437233173317,
136.991506884579));
#199008=CARTESIAN_POINT('Ctrl Pts',(187.358212366174,4.92739057398128,134.581420314804));
#199009=CARTESIAN_POINT('Ctrl Pts',(187.079764742362,5.84112225861874,128.700400402891));
#199010=CARTESIAN_POINT('Ctrl Pts',(186.801317118548,1.38714794227173,124.752817144095));
#199011=CARTESIAN_POINT('Ctrl Pts',(186.522869494736,-4.34154756707868,
126.366306703083));
#199012=CARTESIAN_POINT('Ctrl Pts',(186.244421870923,-6.08057295867359,
132.058150998494));
#199013=CARTESIAN_POINT('Ctrl Pts',(185.96597424711,-2.23184885375068,136.597823184897));
#199014=CARTESIAN_POINT('Ctrl Pts',(185.687526623297,3.66783531589119,135.813586298303));
#199015=CARTESIAN_POINT('Ctrl Pts',(185.409078999484,6.19695801394562,130.42611572539));
#199016=CARTESIAN_POINT('Ctrl Pts',(185.130631375671,3.03137903541329,125.386233730096));
#199017=CARTESIAN_POINT('Ctrl Pts',(184.852183751858,-2.9198891855651,125.325345654173));
#199018=CARTESIAN_POINT('Ctrl Pts',(184.573736128045,-6.18792188952598,
130.299404664846));
#199019=CARTESIAN_POINT('Ctrl Pts',(184.295288504232,-3.76955667380246,
135.737493527599));
#199020=CARTESIAN_POINT('Ctrl Pts',(184.01684088042,2.11284697206427,136.642274242971));
#199021=CARTESIAN_POINT('Ctrl Pts',(183.738393256607,6.05364746891681,132.182297534532));
#199022=CARTESIAN_POINT('Ctrl Pts',(183.459945632794,4.43144167895468,126.456064115361));
#199023=CARTESIAN_POINT('Ctrl Pts',(183.181498008981,-1.2630425260055,124.725702755623));
#199024=CARTESIAN_POINT('Ctrl Pts',(182.903050385168,-5.79685235262429,
128.581331012064));
#199025=CARTESIAN_POINT('Ctrl Pts',(182.624602761355,-5.00363805916239,
134.479814874928));
#199026=CARTESIAN_POINT('Ctrl Pts',(182.346155137542,0.387675169361259,
137.000735831198));
#199027=CARTESIAN_POINT('Ctrl Pts',(182.06770751373,5.42273385622678,133.827490675898));
#199028=CARTESIAN_POINT('Ctrl Pts',(181.789259889916,5.47456504449634,127.876136685104));
#199029=CARTESIAN_POINT('Ctrl Pts',(181.510812266103,0.495538404244469,
124.615677436551));
#199030=CARTESIAN_POINT('Ctrl Pts',(181.232364642291,-4.93886382111119,
127.042315697369));
#199031=CARTESIAN_POINT('Ctrl Pts',(180.953917018477,-5.83469147177671,
132.926089453735));
#199032=CARTESIAN_POINT('Ctrl Pts',(180.675469394665,-1.36872270040423,
136.860098061879));
#199033=CARTESIAN_POINT('Ctrl Pts',(180.397021770852,4.35503536681857,135.229179797918));
#199034=CARTESIAN_POINT('Ctrl Pts',(180.118574147039,6.07672868724052,129.532068871648));
#199035=CARTESIAN_POINT('Ctrl Pts',(179.840126523226,2.21420520878857,125.004131904969));
#199036=CARTESIAN_POINT('Ctrl Pts',(179.561678899413,-3.68306468660213,
125.80632176824));
#199037=CARTESIAN_POINT('Ctrl Pts',(179.2832312756,-6.19577806271818,131.20146516627));
#199038=CARTESIAN_POINT('Ctrl Pts',(179.004783651788,-3.01487407978163,
136.231688883676));
#199039=CARTESIAN_POINT('Ctrl Pts',(178.726336027974,2.93655189768736,136.274463064253));
#199040=CARTESIAN_POINT('Ctrl Pts',(178.447888404162,6.18943013971724,131.290480325685));
#199041=CARTESIAN_POINT('Ctrl Pts',(178.169440780348,3.75452445381909,125.859777323623));
#199042=CARTESIAN_POINT('Ctrl Pts',(177.890993156536,-2.13060578642238,
124.972904812372));
#199043=CARTESIAN_POINT('Ctrl Pts',(177.612545532723,-6.05781339482078,
129.44485530364));
#199044=CARTESIAN_POINT('Ctrl Pts',(177.33409790891,-4.41818643401566,135.166124762878));
#199045=CARTESIAN_POINT('Ctrl Pts',(177.055650285097,1.28153801924328,136.879146056599));
#199046=CARTESIAN_POINT('Ctrl Pts',(176.777202661284,5.80359163943039,133.009736301615));
#199047=CARTESIAN_POINT('Ctrl Pts',(176.498755037472,4.99242806419446,127.113694031581));
#199048=CARTESIAN_POINT('Ctrl Pts',(176.220307413658,-0.406533008366379,
124.60919405498));
#199049=CARTESIAN_POINT('Ctrl Pts',(175.941859789846,-5.43191010648008,
127.797749498684));
#199050=CARTESIAN_POINT('Ctrl Pts',(175.663412166033,-5.46562718029972,
133.749233679521));
#199051=CARTESIAN_POINT('Ctrl Pts',(175.38496454222,-0.476699886155768,
136.994523381468));
#199052=CARTESIAN_POINT('Ctrl Pts',(175.106516918407,4.95029131528126,134.551355909651));
#199053=CARTESIAN_POINT('Ctrl Pts',(174.828069294595,5.82820663315002,128.664882815304));
#199054=CARTESIAN_POINT('Ctrl Pts',(174.549621670781,1.35028477887665,124.744485301934));
#199055=CARTESIAN_POINT('Ctrl Pts',(174.271174046969,-4.36848282210566,
126.392817162263));
#199056=CARTESIAN_POINT('Ctrl Pts',(173.992726423155,-6.07282812182305,
132.095141942134));
#199057=CARTESIAN_POINT('Ctrl Pts',(173.714278799343,-2.19654105173196,
136.611301742902));
#199058=CARTESIAN_POINT('Ctrl Pts',(173.435831175529,3.69825993790488,135.791166334329));
#199059=CARTESIAN_POINT('Ctrl Pts',(173.157383551717,6.19454071464915,130.388400091055));
#199060=CARTESIAN_POINT('Ctrl Pts',(172.878935927904,2.99834119476844,125.367881250842));
#199061=CARTESIAN_POINT('Ctrl Pts',(172.600488304091,-2.95318740599396,
125.343221361866));
#199062=CARTESIAN_POINT('Ctrl Pts',(172.322040680278,-6.1908810518732,130.337081657394));
#199063=CARTESIAN_POINT('Ctrl Pts',(172.043593056465,-3.7394574524341,135.760348489473));
#199064=CARTESIAN_POINT('Ctrl Pts',(171.765145432652,2.14834486313941,136.629304580736));
#199065=CARTESIAN_POINT('Ctrl Pts',(171.486697808839,6.06192320196904,132.145421734178));
#199066=CARTESIAN_POINT('Ctrl Pts',(171.208250185027,4.40489025960108,126.42916923593));
#199067=CARTESIAN_POINT('Ctrl Pts',(170.929802561213,-1.30002164048796,
124.733503877423));
#199068=CARTESIAN_POINT('Ctrl Pts',(170.651354937401,-5.81027716255637,
128.616659285268));
#199069=CARTESIAN_POINT('Ctrl Pts',(170.372907313588,-4.98117182005496,
134.510205342342));
#199070=CARTESIAN_POINT('Ctrl Pts',(170.094459689775,0.42538708130529,136.998261137926));
#199071=CARTESIAN_POINT('Ctrl Pts',(169.816012065962,5.44103603626017,133.794424944161));
#199072=CARTESIAN_POINT('Ctrl Pts',(169.537564442149,5.45663868327959,127.842865707018));
#199073=CARTESIAN_POINT('Ctrl Pts',(169.259116818336,0.457856951984399,
124.612775615598));
#199074=CARTESIAN_POINT('Ctrl Pts',(168.980669194523,-4.9616729506289,127.072449665244));
#199075=CARTESIAN_POINT('Ctrl Pts',(168.702221570711,-5.82166780281318,
132.961567566087));
#199076=CARTESIAN_POINT('Ctrl Pts',(168.423773946897,-1.33183434849535,
136.868317666657));
#199077=CARTESIAN_POINT('Ctrl Pts',(168.145326323085,4.38188980836473,135.202587479883));
#199078=CARTESIAN_POINT('Ctrl Pts',(167.866878699272,6.06887129855542,129.495101671966));
#199079=CARTESIAN_POINT('Ctrl Pts',(167.588431075459,2.17885654621902,124.9907608742));
#199080=CARTESIAN_POINT('Ctrl Pts',(167.309983451646,-3.71342092903282,
125.82883423045));
#199081=CARTESIAN_POINT('Ctrl Pts',(167.031535827833,-6.19324598120115,
131.239173268482));
#199082=CARTESIAN_POINT('Ctrl Pts',(166.75308820402,-2.98178053353198,136.249940722101));
#199083=CARTESIAN_POINT('Ctrl Pts',(166.474640580207,2.96979555637586,136.25648609103));
#199084=CARTESIAN_POINT('Ctrl Pts',(166.196192956395,6.19227461255283,131.252794500981));
#199085=CARTESIAN_POINT('Ctrl Pts',(165.917745332582,3.7243558092261,125.837014079288));
#199086=CARTESIAN_POINT('Ctrl Pts',(165.639297708769,-2.16606403788322,
124.985982457902));
#199087=CARTESIAN_POINT('Ctrl Pts',(165.360850084956,-6.06597685228888,
129.481756121673));
#199088=CARTESIAN_POINT('Ctrl Pts',(165.082402461143,-4.39155327888481,
135.192938704347));
#199089=CARTESIAN_POINT('Ctrl Pts',(164.80395483733,1.31849321850979,136.871232419228));
#199090=CARTESIAN_POINT('Ctrl Pts',(164.525507213517,5.81690886006848,132.974367331546));
#199091=CARTESIAN_POINT('Ctrl Pts',(164.247059589704,4.96986943102014,127.083372084437));
#199092=CARTESIAN_POINT('Ctrl Pts',(163.968611965891,-0.444237213516358,
124.611783518878));
#199093=CARTESIAN_POINT('Ctrl Pts',(163.690164342078,-5.45011156102575,
127.830870782803));
#199094=CARTESIAN_POINT('Ctrl Pts',(163.411716718265,-5.44759963670407,
133.782449941821));
#199095=CARTESIAN_POINT('Ctrl Pts',(163.133269094453,-0.439009776288703,
136.9973104996));
#199096=CARTESIAN_POINT('Ctrl Pts',(162.85482147064,4.97300862171615,134.52115265821));
#199097=CARTESIAN_POINT('Ctrl Pts',(162.576373846827,5.81507504134112,128.629444506854));
#199098=CARTESIAN_POINT('Ctrl Pts',(162.297926223014,1.31337158018249,124.736378010682));
#199099=CARTESIAN_POINT('Ctrl Pts',(162.019478599201,-4.39525620139515,
126.419491092807));
#199100=CARTESIAN_POINT('Ctrl Pts',(161.741030975388,-6.06485825409316,
132.132085055398));
#199101=CARTESIAN_POINT('Ctrl Pts',(161.462583351575,-2.16115185607673,
136.624565122567));
#199102=CARTESIAN_POINT('Ctrl Pts',(161.184135727762,3.72854751953661,135.768561582436));
#199103=CARTESIAN_POINT('Ctrl Pts',(160.905688103949,6.19189387436843,130.350699870288));
#199104=CARTESIAN_POINT('Ctrl Pts',(160.627240480137,2.96519224948793,125.349730222329));
#199105=CARTESIAN_POINT('Ctrl Pts',(160.348792856324,-2.9863761949775,125.361299434083));
#199106=CARTESIAN_POINT('Ctrl Pts',(160.070345232511,-6.19361080884636,
130.374775965136));
#199107=CARTESIAN_POINT('Ctrl Pts',(159.791897608698,-3.70921966409463,
135.783019805394));
#199108=CARTESIAN_POINT('Ctrl Pts',(159.513449984885,2.18376314650564,136.616119073061));
#199109=CARTESIAN_POINT('Ctrl Pts',(159.235002361072,6.06997430822783,132.108496240312));
#199110=CARTESIAN_POINT('Ctrl Pts',(158.956554737259,4.37817561541891,126.402436480826));
#199111=CARTESIAN_POINT('Ctrl Pts',(158.678107113446,-1.3369525821905,124.741529957054));
#199112=CARTESIAN_POINT('Ctrl Pts',(158.399659489633,-5.82348667053154,
128.652068624549));
#199113=CARTESIAN_POINT('Ctrl Pts',(158.121211865821,-4.95852100179383,
134.540458488317));
#199114=CARTESIAN_POINT('Ctrl Pts',(157.842764242008,0.463083230374652,
136.995556927392));
#199115=CARTESIAN_POINT('Ctrl Pts',(157.564316618195,5.45913659670229,133.761248414491));
#199116=CARTESIAN_POINT('Ctrl Pts',(157.285868994382,5.43851012430973,127.809704468215));
#199117=CARTESIAN_POINT('Ctrl Pts',(157.007421370569,0.420158533666468,
124.610103226106));
#199118=CARTESIAN_POINT('Ctrl Pts',(156.728973746756,-4.98429822353081,
127.102721920452));
#199119=CARTESIAN_POINT('Ctrl Pts',(156.450526122943,-5.80842840980828,
132.996965742341));
#199120=CARTESIAN_POINT('Ctrl Pts',(156.172078499131,-1.2948966449748,136.876312569277));
#199121=CARTESIAN_POINT('Ctrl Pts',(155.893630875317,4.40858187737264,135.175832183934));
#199122=CARTESIAN_POINT('Ctrl Pts',(155.615183251505,6.06078902561252,129.458182987356));
#199123=CARTESIAN_POINT('Ctrl Pts',(155.336735627692,2.14342714531882,124.977605268507));
#199124=CARTESIAN_POINT('Ctrl Pts',(155.058288003879,-3.74363956928552,
125.85153106262));
#199125=CARTESIAN_POINT('Ctrl Pts',(154.779840380066,-6.19048440667673,
131.276865258552));
#199126=CARTESIAN_POINT('Ctrl Pts',(154.501392756253,-2.94857649630798,
136.267990772552));
#199127=CARTESIAN_POINT('Ctrl Pts',(154.22294513244,3.00292916819795,136.238307087292));
#199128=CARTESIAN_POINT('Ctrl Pts',(153.944497508627,6.19488962837548,131.215092059396));
#199129=CARTESIAN_POINT('Ctrl Pts',(153.666049884815,3.69404915725887,125.814434901805));
#199130=CARTESIAN_POINT('Ctrl Pts',(153.387602261001,-2.20144202504465,
124.999275705575));
#199131=CARTESIAN_POINT('Ctrl Pts',(153.109154637189,-6.07391553275397,
129.518705949301));
#199132=CARTESIAN_POINT('Ctrl Pts',(152.830707013376,-4.36475739313218,
135.219590025439));
#199133=CARTESIAN_POINT('Ctrl Pts',(152.552259389563,1.3553995605252,136.863093971691));
#199134=CARTESIAN_POINT('Ctrl Pts',(152.27381176575,5.83001053300956,132.93891795108));
#199135=CARTESIAN_POINT('Ctrl Pts',(151.995364141937,4.94712663750637,127.053188019893));
#199136=CARTESIAN_POINT('Ctrl Pts',(151.716916518124,-0.481924957293099,
124.614602450997));
#199137=CARTESIAN_POINT('Ctrl Pts',(151.438468894311,-5.46811105968323,
127.864102250682));
#199138=CARTESIAN_POINT('Ctrl Pts',(151.160021270498,-5.4293702303005,133.815555849925));
#199139=CARTESIAN_POINT('Ctrl Pts',(150.881573646685,-0.40130339875292,
136.999868135696));
#199140=CARTESIAN_POINT('Ctrl Pts',(150.603126022873,4.99554165148768,134.490811679673));
#199141=CARTESIAN_POINT('Ctrl Pts',(150.324678399059,5.80172796978809,128.59408679072));
#199142=CARTESIAN_POINT('Ctrl Pts',(150.046230775247,1.27640971402146,124.728495570759));
#199143=CARTESIAN_POINT('Ctrl Pts',(149.767783151434,-4.42186671284978,
126.446327506304));
#199144=CARTESIAN_POINT('Ctrl Pts',(149.489335527621,-6.05666365081033,
132.168978969345));
#199145=CARTESIAN_POINT('Ctrl Pts',(149.210887903808,-2.12568257814469,
136.637612832414));
#199146=CARTESIAN_POINT('Ctrl Pts',(148.932440279995,3.75869693846883,135.74577288025));
#199147=CARTESIAN_POINT('Ctrl Pts',(148.653992656183,6.18901759118317,130.313016460088));
#199148=CARTESIAN_POINT('Ctrl Pts',(148.375545032369,2.93193342791814,125.331781317152));
#199149=CARTESIAN_POINT('Ctrl Pts',(148.097097408557,-3.01945432269288,
125.379579200934));
#199150=CARTESIAN_POINT('Ctrl Pts',(147.818649784743,-6.19611105929333,
130.412486191295));
#199151=CARTESIAN_POINT('Ctrl Pts',(147.540202160931,-3.67884442925635,
135.805506635269));
#199152=CARTESIAN_POINT('Ctrl Pts',(147.261754537118,2.21910050972548,136.602718208539));
#199153=CARTESIAN_POINT('Ctrl Pts',(146.983306913305,6.07780048935632,132.071522421221));
#199154=CARTESIAN_POINT('Ctrl Pts',(146.704859289492,4.35129873632927,126.375866840638));
#199155=CARTESIAN_POINT('Ctrl Pts',(146.426411665679,-1.37383398262348,
124.749780697104));
#199156=CARTESIAN_POINT('Ctrl Pts',(146.147964041867,-5.83648038706648,
128.687557717801));
#199157=CARTESIAN_POINT('Ctrl Pts',(145.869516418053,-4.93568644371351,
134.570573191811));
#199158=CARTESIAN_POINT('Ctrl Pts',(145.591068794241,0.500762219724632,
136.992623299802));
#199159=CARTESIAN_POINT('Ctrl Pts',(145.312621170428,5.47703486683029,133.727962316256));
#199160=CARTESIAN_POINT('Ctrl Pts',(145.034173546615,5.42018003934715,127.776654197497));
#199161=CARTESIAN_POINT('Ctrl Pts',(144.755725922802,0.382444546219556,
124.607660367099));
#199162=CARTESIAN_POINT('Ctrl Pts',(144.477278298989,-5.00673880142907,
127.133131341243));
#199163=CARTESIAN_POINT('Ctrl Pts',(144.198830675176,-5.79497378335261,
133.032282670807));
#199164=CARTESIAN_POINT('Ctrl Pts',(143.920383051363,-1.25791095858285,
136.884082473484));
#199165=CARTESIAN_POINT('Ctrl Pts',(143.64193542755,4.43511058475782,135.148914901497));
#199166=CARTESIAN_POINT('Ctrl Pts',(143.363487803737,6.05248216790344,129.421314185853));
#199167=CARTESIAN_POINT('Ctrl Pts',(143.085040179924,2.10791831893749,124.964665575378));
#199168=CARTESIAN_POINT('Ctrl Pts',(142.806592556112,-3.77371948759721,
125.87441142371));
#199169=CARTESIAN_POINT('Ctrl Pts',(142.528144932299,-6.18749344147606,
131.314539739788));
#199170=CARTESIAN_POINT('Ctrl Pts',(142.249697308486,-2.91526319849757,
136.285838366179));
#199171=CARTESIAN_POINT('Ctrl Pts',(141.971249684673,3.03595150537554,136.219926726669));
#199172=CARTESIAN_POINT('Ctrl Pts',(141.69280206086,6.19727509028471,131.177374398005));
#199173=CARTESIAN_POINT('Ctrl Pts',(141.414354437047,3.6636056209416,125.792040627854));
#199174=CARTESIAN_POINT('Ctrl Pts',(141.135906813234,-2.23673843696229,
125.012784062803));
#199175=CARTESIAN_POINT('Ctrl Pts',(140.857459189421,-6.0816291420453,129.555703417335));
#199176=CARTESIAN_POINT('Ctrl Pts',(140.579011565609,-4.33779976968917,
135.246077738584));
#199177=CARTESIAN_POINT('Ctrl Pts',(140.300563941795,1.39225567771152,136.854731015561));
#199178=CARTESIAN_POINT('Ctrl Pts',(140.022116317983,5.84289617276637,132.903389473806));
#199179=CARTESIAN_POINT('Ctrl Pts',(139.74366869417,4.92420052639575,127.023142956427));
#199180=CARTESIAN_POINT('Ctrl Pts',(139.465221070357,-0.519594843163371,
124.617650746882));
#199181=CARTESIAN_POINT('Ctrl Pts',(139.186773446544,-5.48590793547459,
127.897442670915));
#199182=CARTESIAN_POINT('Ctrl Pts',(138.908325822731,-5.41093963658633,
133.848550177083));
#199183=CARTESIAN_POINT('Ctrl Pts',(138.629878198918,-0.363582150772119,
137.002196194983));
#199184=CARTESIAN_POINT('Ctrl Pts',(138.351430575105,5.0178895696262,134.460334098336));
#199185=CARTESIAN_POINT('Ctrl Pts',(138.072982951292,5.78816591307159,128.558810977095));
#199186=CARTESIAN_POINT('Ctrl Pts',(137.79453532748,1.23940055002892,124.720838274248));
#199187=CARTESIAN_POINT('Ctrl Pts',(137.516087703667,-4.44831337040726,
126.473325408321));
#199188=CARTESIAN_POINT('Ctrl Pts',(137.237640079854,-6.0482446156285,132.205822316857));
#199189=CARTESIAN_POINT('Ctrl Pts',(136.959192456041,-2.09013453226308,
136.650444388955));
#199190=CARTESIAN_POINT('Ctrl Pts',(136.680744832228,3.78870707750376,135.722801072215));
#199191=CARTESIAN_POINT('Ctrl Pts',(136.402297208415,6.18591197167502,130.275351256826));
#199192=CARTESIAN_POINT('Ctrl Pts',(136.123849584602,2.89856596247695,125.314035200413));
#199193=CARTESIAN_POINT('Ctrl Pts',(135.845401960789,-3.05242056341787,
125.398059985055));
#199194=CARTESIAN_POINT('Ctrl Pts',(135.566954336976,-6.19838171056633,
130.450210938505));
#199195=CARTESIAN_POINT('Ctrl Pts',(135.288506713164,-3.64833287348497,
135.827808145838));
#199196=CARTESIAN_POINT('Ctrl Pts',(135.01005908935,2.25435564335981,136.589102483743));
#199197=CARTESIAN_POINT('Ctrl Pts',(134.731611465538,6.08540145535266,132.034501646982));
#199198=CARTESIAN_POINT('Ctrl Pts',(134.453163841725,4.32426061826468,126.349461299917));
#199199=CARTESIAN_POINT('Ctrl Pts',(134.174716217912,-1.41066447513297,
124.75825579184));
#199200=CARTESIAN_POINT('Ctrl Pts',(133.896268594099,-5.84925783067434,
128.723125249964));
#199201=CARTESIAN_POINT('Ctrl Pts',(133.617820970286,-4.91266899195694,
134.600548336913));
#199202=CARTESIAN_POINT('Ctrl Pts',(133.339373346473,0.538422653146471,
136.989460363863));
#199203=CARTESIAN_POINT('Ctrl Pts',(133.06092572266,5.49473018341705,133.694567882885));
#199204=CARTESIAN_POINT('Ctrl Pts',(132.782478098847,5.40164910761999,127.743716119554));
#199205=CARTESIAN_POINT('Ctrl Pts',(132.504030475035,0.344716387149417,
124.605447129098));
#199206=CARTESIAN_POINT('Ctrl Pts',(132.225582851222,-5.02899385277987,
127.163676800786));
#199207=CARTESIAN_POINT('Ctrl Pts',(131.947135227409,-5.78130442201224,
133.067517042801));
#199208=CARTESIAN_POINT('Ctrl Pts',(131.668687603596,-1.22087865983776,
136.891627091362));
#199209=CARTESIAN_POINT('Ctrl Pts',(131.390239979783,4.46147494748924,135.121836630005));
#199210=CARTESIAN_POINT('Ctrl Pts',(131.11179235597,6.04395103324181,129.384496633644));
#199211=CARTESIAN_POINT('Ctrl Pts',(130.833344732157,2.07233138286776,124.951942274296));
#199212=CARTESIAN_POINT('Ctrl Pts',(130.554897108344,-3.80365956934553,
125.897474465882));
#199213=CARTESIAN_POINT('Ctrl Pts',(130.276449484532,-6.18427319643048,
131.35219531615));
#199214=CARTESIAN_POINT('Ctrl Pts',(129.998001860718,-2.88184187453723,
136.303482841632));
#199215=CARTESIAN_POINT('Ctrl Pts',(129.719554236906,3.0688613442533,136.201345690253));
#199216=CARTESIAN_POINT('Ctrl Pts',(129.441106613093,6.1994309098865,131.139642914452));
#199217=CARTESIAN_POINT('Ctrl Pts',(129.16265898928,3.63302632837089,125.769832087263));
#199218=CARTESIAN_POINT('Ctrl Pts',(128.884211365467,-2.27195196571463,
125.026507029031));
#199219=CARTESIAN_POINT('Ctrl Pts',(128.605763741654,-6.08911739433215,
129.592747154821));
#199220=CARTESIAN_POINT('Ctrl Pts',(128.327316117841,-4.31068140748063,
135.272400862266));
#199221=CARTESIAN_POINT('Ctrl Pts',(128.048868494028,1.42906020435147,136.846143860731));
#199222=CARTESIAN_POINT('Ctrl Pts',(127.770420870216,5.85556530185681,132.867783216248));
#199223=CARTESIAN_POINT('Ctrl Pts',(127.491973246402,4.9010919472237,126.993238007373));
#199224=CARTESIAN_POINT('Ctrl Pts',(127.21352562259,-0.557245475255655,
124.620928293575));
#199225=CARTESIAN_POINT('Ctrl Pts',(126.935077998777,-5.50350152892981,
127.930890808061));
#199226=CARTESIAN_POINT('Ctrl Pts',(126.656630374964,-5.39230853851415,
133.881431700678));
#199227=CARTESIAN_POINT('Ctrl Pts',(126.378182751151,-0.325847430121078,
137.004294591193));
#199228=CARTESIAN_POINT('Ctrl Pts',(126.099735127338,5.04005154802147,134.429721043558));
#199229=CARTESIAN_POINT('Ctrl Pts',(125.821287503525,5.77438937373851,128.523618373138));
#199230=CARTESIAN_POINT('Ctrl Pts',(125.542839879712,1.20234545959337,124.713406404895));
#199231=CARTESIAN_POINT('Ctrl Pts',(125.264392255899,-4.47459519407686,
126.50048379844));
#199232=CARTESIAN_POINT('Ctrl Pts',(124.985944632086,-6.03960146051831,
132.24261373269));
#199233=CARTESIAN_POINT('Ctrl Pts',(124.707497008274,-2.05450903567761,
136.663059316712));
#199234=CARTESIAN_POINT('Ctrl Pts',(124.429049384461,3.81857682460466,135.69964700956));
#199235=CARTESIAN_POINT('Ctrl Pts',(124.150601760648,6.18257713092382,130.237705656202));
#199236=CARTESIAN_POINT('Ctrl Pts',(123.872154136835,2.86509108960817,125.296492529702));
#199237=CARTESIAN_POINT('Ctrl Pts',(123.593706513022,-3.08527369557641,
125.416741101634));
#199238=CARTESIAN_POINT('Ctrl Pts',(123.315258889209,-6.20042267852561,
130.487948808862));
#199239=CARTESIAN_POINT('Ctrl Pts',(123.036811265396,-3.61768612739718,
135.849923510712));
#199240=CARTESIAN_POINT('Ctrl Pts',(122.758363641583,2.28952724101679,136.575272403211));
#199241=CARTESIAN_POINT('Ctrl Pts',(122.47991601777,6.09277692456002,131.997435289415));
#199242=CARTESIAN_POINT('Ctrl Pts',(122.201468393958,4.29706226313277,126.323220837128));
#199243=CARTESIAN_POINT('Ctrl Pts',(121.923020770144,-1.44744269495155,
124.766954927214));
#199244=CARTESIAN_POINT('Ctrl Pts',(121.644573146332,-5.86181852788225,
128.758769903068));
#199245=CARTESIAN_POINT('Ctrl Pts',(121.366125522519,-4.88946949944416,
134.630382812884));
#199246=CARTESIAN_POINT('Ctrl Pts',(121.087677898706,0.576063135118759,
136.986068236777));
#199247=CARTESIAN_POINT('Ctrl Pts',(120.809230274893,5.51222189075617,133.661066351821));
#199248=CARTESIAN_POINT('Ctrl Pts',(120.53078265108,5.38291801579874,127.710891454918));
#199249=CARTESIAN_POINT('Ctrl Pts',(120.252335027267,0.306975454486648,
124.603463594118));
#199250=CARTESIAN_POINT('Ctrl Pts',(119.973887403454,-5.05106255291402,
127.194357167205));
#199251=CARTESIAN_POINT('Ctrl Pts',(119.695439779642,-5.76742083231046,
133.102667552701));
#199252=CARTESIAN_POINT('Ctrl Pts',(119.416992155829,-1.18380112098488,
136.898946143343));
#199253=CARTESIAN_POINT('Ctrl Pts',(119.138544532016,4.48767398862585,135.09459837285));
#199254=CARTESIAN_POINT('Ctrl Pts',(118.860096908203,6.03519593775195,129.347731695017));
#199255=CARTESIAN_POINT('Ctrl Pts',(118.58164928439,2.0366676557964,124.939435836727));
#199256=CARTESIAN_POINT('Ctrl Pts',(118.303201660577,-3.83345870508974,
125.920719334523));
#199257=CARTESIAN_POINT('Ctrl Pts',(118.024754036764,-6.18082379086727,
131.389830592295));
#199258=CARTESIAN_POINT('Ctrl Pts',(117.746306412951,-2.84831376286653,
136.320923545089));
#199259=CARTESIAN_POINT('Ctrl Pts',(117.467858789138,3.10165746534553,136.18256466657));
#199260=CARTESIAN_POINT('Ctrl Pts',(117.189411165326,6.20135700729606,131.101899006891));
#199261=CARTESIAN_POINT('Ctrl Pts',(116.910963541513,3.60231241267338,125.747810102979));
#199262=CARTESIAN_POINT('Ctrl Pts',(116.6325159177,-2.30708130645123,125.040444095748));
#199263=CARTESIAN_POINT('Ctrl Pts',(116.354068293887,-6.09638001213474,
129.62983578909));
#199264=CARTESIAN_POINT('Ctrl Pts',(116.075620670074,-4.28340331138726,
135.298558421074));
#199265=CARTESIAN_POINT('Ctrl Pts',(115.797173046261,1.46581177664024,136.837332825402));
#199266=CARTESIAN_POINT('Ctrl Pts',(115.518725422448,5.86801745082159,132.832100497806));
#199267=CARTESIAN_POINT('Ctrl Pts',(115.240277798635,4.87780175628715,126.963474280869));
#199268=CARTESIAN_POINT('Ctrl Pts',(114.961830174822,-0.594875458411799,
124.624434969628));
#199269=CARTESIAN_POINT('Ctrl Pts',(114.68338255101,-5.52089118811201,127.964445422689));
#199270=CARTESIAN_POINT('Ctrl Pts',(114.404934927196,-5.37347762646609,
133.914199202272));
#199271=CARTESIAN_POINT('Ctrl Pts',(114.126487303384,-0.288100635073559,
137.006163246571));
#199272=CARTESIAN_POINT('Ctrl Pts',(113.848039679571,5.06202676545313,134.398973649715));
#199273=CARTESIAN_POINT('Ctrl Pts',(113.569592055758,5.76039886228364,128.488510282924));
#199274=CARTESIAN_POINT('Ctrl Pts',(113.291144431945,1.16524581580469,124.706200238089));
#199275=CARTESIAN_POINT('Ctrl Pts',(113.012696808132,-4.50071120997606,
126.527801670297));
#199276=CARTESIAN_POINT('Ctrl Pts',(112.734249184319,-6.03073450575487,
132.279351853526));
#199277=CARTESIAN_POINT('Ctrl Pts',(112.455801560506,-2.01880740850426,
136.675457148234));
#199278=CARTESIAN_POINT('Ctrl Pts',(112.177353936694,3.84830507293705,135.676311550269));
#199279=CARTESIAN_POINT('Ctrl Pts',(111.898906312881,6.17901319250346,130.200081053184));
#199280=CARTESIAN_POINT('Ctrl Pts',(111.620458689068,2.8315100497353,125.279153955068));
#199281=CARTESIAN_POINT('Ctrl Pts',(111.342011065255,-3.11801250178361,
125.435621858436));
#199282=CARTESIAN_POINT('Ctrl Pts',(111.063563441442,-6.20223388754234,
130.525698403974));
#199283=CARTESIAN_POINT('Ctrl Pts',(110.785115817629,-3.58690532661952,
135.871851910398));
#199284=CARTESIAN_POINT('Ctrl Pts',(110.506668193816,2.32461399939974,136.56122847942));
#199285=CARTESIAN_POINT('Ctrl Pts',(110.228220570003,6.09992662367788,131.960324722029));
#199286=CARTESIAN_POINT('Ctrl Pts',(109.94977294619,4.26970467877848,126.297146424621));
#199287=CARTESIAN_POINT('Ctrl Pts',(109.671325322378,-1.48416727924886,
124.775877780875));
#199288=CARTESIAN_POINT('Ctrl Pts',(109.392877698565,-5.8741620132489,128.794490356288));
#199289=CARTESIAN_POINT('Ctrl Pts',(109.114430074752,-4.86608882584101,
134.660075514194));
#199290=CARTESIAN_POINT('Ctrl Pts',(108.835982450939,0.61368227085971,136.982447044243));
#199291=CARTESIAN_POINT('Ctrl Pts',(108.557534827126,5.52950934068608,133.627458964475));
#199292=CARTESIAN_POINT('Ctrl Pts',(108.279087203313,5.36398745797076,127.67818141992));
#199293=CARTESIAN_POINT('Ctrl Pts',(108.0006395795,0.269223146735527,124.601709835656));
#199294=CARTESIAN_POINT('Ctrl Pts',(107.722191955687,-5.07294408406776,
127.225171303631));
#199295=CARTESIAN_POINT('Ctrl Pts',(107.443744331874,-5.75332352870873,
133.137732897993));
#199296=CARTESIAN_POINT('Ctrl Pts',(107.165296708062,-1.14667971594628,
136.906039358215));
#199297=CARTESIAN_POINT('Ctrl Pts',(106.886849084249,4.51370673735246,135.067201139359));
#199298=CARTESIAN_POINT('Ctrl Pts',(106.608401460436,6.02621720585718,129.31102073231));
#199299=CARTESIAN_POINT('Ctrl Pts',(106.329953836623,2.00092845925606,124.927146726103));
#199300=CARTESIAN_POINT('Ctrl Pts',(106.05150621281,-3.86311579061174,125.944145168289));
#199301=CARTESIAN_POINT('Ctrl Pts',(105.773058588997,-6.17714535260555,
131.427444173636));
#199302=CARTESIAN_POINT('Ctrl Pts',(105.494610965184,-2.81468010588189,
136.338159830278));
#199303=CARTESIAN_POINT('Ctrl Pts',(105.216163341371,3.13433865337982,136.163584351558));
#199304=CARTESIAN_POINT('Ctrl Pts',(104.937715717558,6.20305331114115,131.064144073934));
#199305=CARTESIAN_POINT('Ctrl Pts',(104.659268093745,3.57146501196475,125.725975491034));
#199306=CARTESIAN_POINT('Ctrl Pts',(104.380820469933,-2.34212515744159,
125.054594746511));
#199307=CARTESIAN_POINT('Ctrl Pts',(104.10237284612,-6.10341672633411,129.666967945808));
#199308=CARTESIAN_POINT('Ctrl Pts',(103.823925222307,-4.25596649220884,
135.324549445729));
#199309=CARTESIAN_POINT('Ctrl Pts',(103.545477598494,1.50250903273456,136.828298236068));
#199310=CARTESIAN_POINT('Ctrl Pts',(103.267029974681,5.88025215824177,132.796342640716));
#199311=CARTESIAN_POINT('Ctrl Pts',(102.988582350868,4.85433081661274,126.933852879821));
#199312=CARTESIAN_POINT('Ctrl Pts',(102.710134727055,-0.63248339823904,
124.628170645098));
#199313=CARTESIAN_POINT('Ctrl Pts',(102.431687103242,-5.53807626864099,
127.998105271418));
#199314=CARTESIAN_POINT('Ctrl Pts',(102.153239479429,-5.35444759822839,
133.946851467654));
#199315=CARTESIAN_POINT('Ctrl Pts',(101.874791855617,-0.250343164351048,
137.00780209187));
#199316=CARTESIAN_POINT('Ctrl Pts',(101.596344231803,5.0838144076213,134.368093056165));
#199317=CARTESIAN_POINT('Ctrl Pts',(101.317896607991,5.74619489713063,128.453488007394));
#199318=CARTESIAN_POINT('Ctrl Pts',(101.039448984178,1.12810299340375,124.69922004086));
#199319=CARTESIAN_POINT('Ctrl Pts',(100.761001360365,-4.52666045036627,
126.55527801162));
#199320=CARTESIAN_POINT('Ctrl Pts',(100.482553736552,-6.0216440799065,132.316035318018));
#199321=CARTESIAN_POINT('Ctrl Pts',(100.204106112739,-1.98303097367997,
136.687637424115));
#199322=CARTESIAN_POINT('Ctrl Pts',(99.9256584889259,3.87789072090961,135.652795559044));
#199323=CARTESIAN_POINT('Ctrl Pts',(99.6472108651132,6.17522028847693,130.162478841968));
#199324=CARTESIAN_POINT('Ctrl Pts',(99.3687632413001,2.79782408721636,125.262020118999));
#199325=CARTESIAN_POINT('Ctrl Pts',(99.0903156174874,-3.15063576889091,
125.454701555827));
#199326=CARTESIAN_POINT('Ctrl Pts',(98.8118679936743,-6.20381527050148,
130.563458325018));
#199327=CARTESIAN_POINT('Ctrl Pts',(98.5334203698616,-3.55599161174595,
135.89359253233));
#199328=CARTESIAN_POINT('Ctrl Pts',(98.2549727460486,2.35961461835606,136.546971232774));
#199329=CARTESIAN_POINT('Ctrl Pts',(97.9765251222358,6.10685028777152,131.923171319966));
#199330=CARTESIAN_POINT('Ctrl Pts',(97.6980774984228,4.24218887894701,126.271239028595));
#199331=CARTESIAN_POINT('Ctrl Pts',(97.4196298746099,-1.52083686718185,
124.785024022185));
#199332=CARTESIAN_POINT('Ctrl Pts',(97.141182250797,-5.88628782938184,128.830285285991));
#199333=CARTESIAN_POINT('Ctrl Pts',(96.8627346269842,-4.842527837527,134.689625340572));
#199334=CARTESIAN_POINT('Ctrl Pts',(96.5842870031713,0.651278666378471,
136.978596920444));
#199335=CARTESIAN_POINT('Ctrl Pts',(96.3058393793584,5.54659189261388,133.593746966183));
#199336=CARTESIAN_POINT('Ctrl Pts',(96.0273917555454,5.34485813561491,127.645587226641));
#199337=CARTESIAN_POINT('Ctrl Pts',(95.7489441317327,0.231460862821695,
124.6001859187));
#199338=CARTESIAN_POINT('Ctrl Pts',(95.4704965079195,-5.09463763541278,
127.256118068232));
#199339=CARTESIAN_POINT('Ctrl Pts',(95.192048884107,-5.73901303358793,133.172711779316));
#199340=CARTESIAN_POINT('Ctrl Pts',(94.9136012602939,-1.10951582026908,
136.912906473138));
#199341=CARTESIAN_POINT('Ctrl Pts',(94.635153636481,4.53957222901603,135.039645944743));
#199342=CARTESIAN_POINT('Ctrl Pts',(94.3567060126683,6.01701517026768,129.274365105863));
#199343=CARTESIAN_POINT('Ctrl Pts',(94.0782583888551,1.96511511757592,124.915075397801));
#199344=CARTESIAN_POINT('Ctrl Pts',(93.7998107650425,-3.89262972695748,
125.967751099126));
#199345=CARTESIAN_POINT('Ctrl Pts',(93.5213631412293,-6.17323801795121,
131.465034666385));
#199346=CARTESIAN_POINT('Ctrl Pts',(93.2429155174167,-2.7809421498907,136.355191058501));
#199347=CARTESIAN_POINT('Ctrl Pts',(92.9644678936037,3.16690369734264,136.14440544854));
#199348=CARTESIAN_POINT('Ctrl Pts',(92.6860202697908,6.20451975856463,131.026379514606));
#199349=CARTESIAN_POINT('Ctrl Pts',(92.4075726459779,3.54048526930663,125.704329060518));
#199350=CARTESIAN_POINT('Ctrl Pts',(92.129125022165,-2.37708222012305,125.068958456964));
#199351=CARTESIAN_POINT('Ctrl Pts',(91.850677398352,-6.1102272761821,129.70414224903));
#199352=CARTESIAN_POINT('Ctrl Pts',(91.5722297745392,-4.22837196662692,
135.350372973126));
#199353=CARTESIAN_POINT('Ctrl Pts',(91.2937821507264,1.53915061280415,136.819040427511));
#199354=CARTESIAN_POINT('Ctrl Pts',(91.0153345269133,5.89226897075567,132.76051097));
#199355=CARTESIAN_POINT('Ctrl Pts',(90.7368869031008,4.8306799979248,126.90437490186));
#199356=CARTESIAN_POINT('Ctrl Pts',(90.4584392792875,-0.670067901161403,
124.632135181558));
#199357=CARTESIAN_POINT('Ctrl Pts',(90.1799916554748,-5.5550561337172,128.031869106972));
#199358=CARTESIAN_POINT('Ctrl Pts',(89.9015440316619,-5.3352191589658,133.979387286881));
#199359=CARTESIAN_POINT('Ctrl Pts',(89.6230964078489,-0.212576417070642,
137.009211066365));
#199360=CARTESIAN_POINT('Ctrl Pts',(89.3446487840362,5.10541366717708,134.337080407198));
#199361=CARTESIAN_POINT('Ctrl Pts',(89.0662011602232,5.73177800461257,128.418552844315));
#199362=CARTESIAN_POINT('Ctrl Pts',(88.7877535364103,1.09091836873142,124.69246607186));
#199363=CARTESIAN_POINT('Ctrl Pts',(88.5093059125973,-4.5524419536888,126.58291180426));
#199364=CARTESIAN_POINT('Ctrl Pts',(88.2308582887847,-6.0123305198223,132.352662766849));
#199365=CARTESIAN_POINT('Ctrl Pts',(87.9524106649715,-1.94718105691378,
136.69959969301));
#199366=CARTESIAN_POINT('Ctrl Pts',(87.6739630411587,3.90733267221543,135.629099907278));
#199367=CARTESIAN_POINT('Ctrl Pts',(87.395515417346,6.17119855939173,130.124900415918));
#199368=CARTESIAN_POINT('Ctrl Pts',(87.1170677935327,2.76403445029686,125.245091656395));
#199369=CARTESIAN_POINT('Ctrl Pts',(86.8386201697203,-3.18314228803115,
125.473979486801));
#199370=CARTESIAN_POINT('Ctrl Pts',(86.5601725459069,-6.20516676880425,
130.601227172784));
#199371=CARTESIAN_POINT('Ctrl Pts',(86.2817249220945,-3.52494612829556,
135.915144570902));
#199372=CARTESIAN_POINT('Ctrl Pts',(86.0032772982812,2.394527800925,136.532501191579));
#199373=CARTESIAN_POINT('Ctrl Pts',(85.7248296744686,6.11354766028192,131.885976459962));
#199374=CARTESIAN_POINT('Ctrl Pts',(85.4463820506556,4.21451588324655,126.245499609054));
#199375=CARTESIAN_POINT('Ctrl Pts',(85.1679344268427,-1.55745009994542,
124.794393312227));
#199376=CARTESIAN_POINT('Ctrl Pts',(84.8894868030298,-5.89819552695468,
128.86615336578));
#199377=CARTESIAN_POINT('Ctrl Pts',(84.611039179217,-4.81878740756302,134.719031197036));
#199378=CARTESIAN_POINT('Ctrl Pts',(84.332591555404,0.68885092852684,136.974518008049));
#199379=CARTESIAN_POINT('Ctrl Pts',(84.0541439315912,5.56346891353935,133.559931606153));
#199380=CARTESIAN_POINT('Ctrl Pts',(83.7756963077782,5.32553075757526,127.613110082872));
#199381=CARTESIAN_POINT('Ctrl Pts',(83.4972486839655,0.193690002040587,
124.598891899719));
#199382=CARTESIAN_POINT('Ctrl Pts',(83.2188010601524,-5.11614240308669,
127.287196314267));
#199383=CARTESIAN_POINT('Ctrl Pts',(82.9403534363397,-5.72448987722869,
133.207602900518));
#199384=CARTESIAN_POINT('Ctrl Pts',(82.6619058125266,-1.07231081107503,
136.919547233648));
#199385=CARTESIAN_POINT('Ctrl Pts',(82.3834581887138,4.56526950516122,135.011933810073));
#199386=CARTESIAN_POINT('Ctrl Pts',(82.1050105649009,6.00759017196827,129.237766173961));
#199387=CARTESIAN_POINT('Ctrl Pts',(81.826562941088,1.92922895783247,124.903222299129));
#199388=CARTESIAN_POINT('Ctrl Pts',(81.5481153172751,-3.92199942047723,
125.991536252305));
#199389=CARTESIAN_POINT('Ctrl Pts',(81.2696676934623,-6.16910193169181,
131.502600677615));
#199390=CARTESIAN_POINT('Ctrl Pts',(80.9912200696492,-2.74710114506546,
136.372016598662));
#199391=CARTESIAN_POINT('Ctrl Pts',(80.7127724458365,3.19935139052435,136.125028668197));
#199392=CARTESIAN_POINT('Ctrl Pts',(80.4343248220235,6.20575629522666,130.988606728286));
#199393=CARTESIAN_POINT('Ctrl Pts',(80.1558771982107,3.50937433266497,125.682871613546));
#199394=CARTESIAN_POINT('Ctrl Pts',(79.8774295743978,-2.41195119914859,
125.083534694853));
#199395=CARTESIAN_POINT('Ctrl Pts',(79.5989819505849,-6.11681140931136,
129.741357321249));
#199396=CARTESIAN_POINT('Ctrl Pts',(79.320534326772,-4.20062075716678,135.376028046362));
#199397=CARTESIAN_POINT('Ctrl Pts',(79.0420867029591,1.57573515908161,136.809559742781));
#199398=CARTESIAN_POINT('Ctrl Pts',(78.7636390791462,5.90406744307602,132.724606813414));
#199399=CARTESIAN_POINT('Ctrl Pts',(78.4851914553333,4.80685017661309,126.875041439303));
#199400=CARTESIAN_POINT('Ctrl Pts',(78.2067438315204,-0.707627574471386,
124.636328432103));
#199401=CARTESIAN_POINT('Ctrl Pts',(77.9282962077074,-5.57183015414549,
128.065735678218));
#199402=CARTESIAN_POINT('Ctrl Pts',(77.6498485838947,-5.31579302119528,
134.011805454327));
#199403=CARTESIAN_POINT('Ctrl Pts',(77.3714009600817,-0.174801792692954,
137.010390117845));
#199404=CARTESIAN_POINT('Ctrl Pts',(77.0929533362689,5.12682374375196,134.305936852001));
#199405=CARTESIAN_POINT('Ctrl Pts',(76.814505712456,5.7171487189526,128.38370608822));
#199406=CARTESIAN_POINT('Ctrl Pts',(76.536058088643,1.05369331967776,124.68593858136));
#199407=CARTESIAN_POINT('Ctrl Pts',(76.2576104648302,-4.57805476460059,
126.610702024239));
#199408=CARTESIAN_POINT('Ctrl Pts',(75.9791628410172,-6.00279417061961,
132.389232842773));
#199409=CARTESIAN_POINT('Ctrl Pts',(75.7007152172044,-1.91125898663751,
136.711343511654));
#199410=CARTESIAN_POINT('Ctrl Pts',(75.4222675933915,3.93662983587222,135.605225473025));
#199411=CARTESIAN_POINT('Ctrl Pts',(75.1438199695785,6.16694815427437,130.087347167514));
#199412=CARTESIAN_POINT('Ctrl Pts',(74.8653723457658,2.73014239106432,125.228369194547));
#199413=CARTESIAN_POINT('Ctrl Pts',(74.5869247219528,-3.21553085466319,
125.493454937009));
#199414=CARTESIAN_POINT('Ctrl Pts',(74.3084770981399,-6.20628833237051,
130.639003547736));
#199415=CARTESIAN_POINT('Ctrl Pts',(74.0300294743271,-3.49377002667009,
135.936507227495));
#199416=CARTESIAN_POINT('Ctrl Pts',(73.7515818505141,2.42935225338577,136.517818892029));
#199417=CARTESIAN_POINT('Ctrl Pts',(73.4731342267013,6.1200184930355,131.848741520285));
#199418=CARTESIAN_POINT('Ctrl Pts',(73.1946866028884,4.18668671711015,126.219929119786));
#199419=CARTESIAN_POINT('Ctrl Pts',(72.9162389790755,-1.59400562082267,
124.803985303816));
#199420=CARTESIAN_POINT('Ctrl Pts',(72.6377913552626,-5.90988466472314,
128.902093266552));
#199421=CARTESIAN_POINT('Ctrl Pts',(72.3593437314497,-4.79486841565966,
134.748291993943));
#199422=CARTESIAN_POINT('Ctrl Pts',(72.0808961076369,0.726397665050741,
136.970210458201));
#199423=CARTESIAN_POINT('Ctrl Pts',(71.8024484838239,5.58013977807825,133.526014137426));
#199424=CARTESIAN_POINT('Ctrl Pts',(71.524000860011,5.30600604003494,127.580751192065));
#199425=CARTESIAN_POINT('Ctrl Pts',(71.2455532361981,0.155911964005252,
124.597827826664));
#199426=CARTESIAN_POINT('Ctrl Pts',(70.9671056123853,-5.13745759022245,
127.318404890117));
#199427=CARTESIAN_POINT('Ctrl Pts',(70.6886579885723,-5.70975459779179,
133.242404968692));
#199428=CARTESIAN_POINT('Ctrl Pts',(70.4102103647595,-1.03506606700937,
136.925961393668));
#199429=CARTESIAN_POINT('Ctrl Pts',(70.1317627409465,4.59079761356593,134.98406576223));
#199430=CARTESIAN_POINT('Ctrl Pts',(69.8533151171337,5.99794256020584,129.201225292793));
#199431=CARTESIAN_POINT('Ctrl Pts',(69.5748674933208,1.89327130980037,124.891587869307));
#199432=CARTESIAN_POINT('Ctrl Pts',(69.2964198695077,-3.95122378286636,
126.015499746463));
#199433=CARTESIAN_POINT('Ctrl Pts',(69.0179722456952,-6.16473724709165,
131.540140815303));
#199434=CARTESIAN_POINT('Ctrl Pts',(68.7395246218819,-2.71315834539685,
136.388635827283));
#199435=CARTESIAN_POINT('Ctrl Pts',(68.4610769980694,3.23168053056381,136.105454728543));
#199436=CARTESIAN_POINT('Ctrl Pts',(68.1826293742561,6.20676287530703,130.950827114659));
#199437=CARTESIAN_POINT('Ctrl Pts',(67.9041817504435,3.47813335486666,125.661603945233));
#199438=CARTESIAN_POINT('Ctrl Pts',(67.6257341266304,-2.44673080243567,
125.09832292005));
#199439=CARTESIAN_POINT('Ctrl Pts',(67.3472865028177,-6.12316888174425,
129.778611783445));
#199440=CARTESIAN_POINT('Ctrl Pts',(67.0688388790048,-4.17271389215982,
135.401513714782));
#199441=CARTESIAN_POINT('Ctrl Pts',(66.7903912551918,1.61226131591331,136.799856533191));
#199442=CARTESIAN_POINT('Ctrl Pts',(66.511943631379,5.91564713800617,132.688631501398));
#199443=CARTESIAN_POINT('Ctrl Pts',(66.233496007566,4.78284223570014,126.845853579115));
#199444=CARTESIAN_POINT('Ctrl Pts',(65.9550483837533,-0.745161026381345,
124.640750241348));
#199445=CARTESIAN_POINT('Ctrl Pts',(65.6766007599402,-5.58839770835831,
128.099703730218));
#199446=CARTESIAN_POINT('Ctrl Pts',(65.3981531361275,-5.2961699047596,134.044104768727));
#199447=CARTESIAN_POINT('Ctrl Pts',(65.1197055123145,-0.137020690970298,
137.011339202618));
#199448=CARTESIAN_POINT('Ctrl Pts',(64.8412578885016,5.14804384398771,134.274663544608));
#199449=CARTESIAN_POINT('Ctrl Pts',(64.5628102646887,5.70230758224426,128.348949030369));
#199450=CARTESIAN_POINT('Ctrl Pts',(64.2843626408759,1.01642922563077,124.679637811238));
#199451=CARTESIAN_POINT('Ctrl Pts',(64.0059150170629,-4.60349793400934,
126.638647641779));
#199452=CARTESIAN_POINT('Ctrl Pts',(63.72746739325,-5.9930353856715,132.425744190676));
#199453=CARTESIAN_POINT('Ctrl Pts',(63.4490197694371,-1.87526609395646,
136.722868444874));
#199454=CARTESIAN_POINT('Ctrl Pts',(63.1705721456243,3.96578112626272,135.581173140958));
#199455=CARTESIAN_POINT('Ctrl Pts',(62.8921245218114,6.16246923062527,130.049820488308));
#199456=CARTESIAN_POINT('Ctrl Pts',(62.6136768979985,2.69614916540168,125.211853353112));
#199457=CARTESIAN_POINT('Ctrl Pts',(62.3352292741856,-3.24780026861702,
125.513127184779));
#199458=CARTESIAN_POINT('Ctrl Pts',(62.0567816503727,-6.20717991964031,
130.676786050054));
#199459=CARTESIAN_POINT('Ctrl Pts',(61.7783340265599,-3.46246446211126,
135.957679710507));
#199460=CARTESIAN_POINT('Ctrl Pts',(61.4998864027468,2.46408668530527,136.502924878181));
#199461=CARTESIAN_POINT('Ctrl Pts',(61.2214387789342,6.12626254625314,131.81146788069));
#199462=CARTESIAN_POINT('Ctrl Pts',(60.942991155121,4.15870241175792,126.194528508313));
#199463=CARTESIAN_POINT('Ctrl Pts',(60.6645435313083,-1.63050207523548,
124.813799641521));
#199464=CARTESIAN_POINT('Ctrl Pts',(60.3860959074953,-5.92135480954196,
128.938103656541));
#199465=CARTESIAN_POINT('Ctrl Pts',(60.1076482836825,-4.77077174814381,
134.777406647022));
#199466=CARTESIAN_POINT('Ctrl Pts',(59.8292006598696,0.763917484641806,
136.965674430521));
#199467=CARTESIAN_POINT('Ctrl Pts',(59.5507530360567,5.59660386848551,133.491995816827));
#199468=CARTESIAN_POINT('Ctrl Pts',(59.2723054122438,5.28628470648961,127.548511753291));
#199469=CARTESIAN_POINT('Ctrl Pts',(58.9938577884309,0.11812814859451,124.596993738963));
#199470=CARTESIAN_POINT('Ctrl Pts',(58.715410164618,-5.15858240697801,127.34974263934));
#199471=CARTESIAN_POINT('Ctrl Pts',(58.4369625408051,-5.69480774129836,
133.277116694236));
#199472=CARTESIAN_POINT('Ctrl Pts',(58.1585149169922,-0.997782968190397,
136.932148715521));
#199473=CARTESIAN_POINT('Ctrl Pts',(57.8800672931793,4.61615560827684,134.956042833877));
#199474=CARTESIAN_POINT('Ctrl Pts',(57.6016196693665,5.98807269247603,129.164743816393));
#199475=CARTESIAN_POINT('Ctrl Pts',(57.3231720455535,1.85724350590365,124.880172539454));
#199476=CARTESIAN_POINT('Ctrl Pts',(57.0447244217407,-3.98030173120474,
126.039640693622));
#199477=CARTESIAN_POINT('Ctrl Pts',(56.7662767979277,-6.16014412588574,
131.577653688385));
#199478=CARTESIAN_POINT('Ctrl Pts',(56.4878291741149,-2.67911500864857,
136.405048128532));
#199479=CARTESIAN_POINT('Ctrl Pts',(56.209381550302,3.26388991949243,136.085684354897));
#199480=CARTESIAN_POINT('Ctrl Pts',(55.9309339264891,6.20753946150667,130.913042073662));
#199481=CARTESIAN_POINT('Ctrl Pts',(55.6524863026762,3.44676349355797,125.640526843659));
#199482=CARTESIAN_POINT('Ctrl Pts',(55.3740386788633,-2.48141974121268,
125.113322584571));
#199483=CARTESIAN_POINT('Ctrl Pts',(55.0955910550504,-6.12929945790263,
129.815904255142));
#199484=CARTESIAN_POINT('Ctrl Pts',(54.8171434312375,-4.14465240570495,
135.426829034002));
#199485=CARTESIAN_POINT('Ctrl Pts',(54.5386958074246,1.64872772980914,136.789931158292));
#199486=CARTESIAN_POINT('Ctrl Pts',(54.2602481836117,5.92700762645589,132.652586367033));
#199487=CARTESIAN_POINT('Ctrl Pts',(53.9818005597989,4.75865706480954,126.81681240286));
#199488=CARTESIAN_POINT('Ctrl Pts',(53.703352935986,-0.78266686607524,124.645400445441));
#199489=CARTESIAN_POINT('Ctrl Pts',(53.4249053121731,-5.604758182439,128.133772004274));
#199490=CARTESIAN_POINT('Ctrl Pts',(53.1464576883601,-5.27635053680027,
134.076284033214));
#199491=CARTESIAN_POINT('Ctrl Pts',(52.8680100645473,-0.0992345118958833,
137.012058285519));
#199492=CARTESIAN_POINT('Ctrl Pts',(52.5895624407343,5.1690731815654,134.243261643865));
#199493=CARTESIAN_POINT('Ctrl Pts',(52.3111148169216,5.68725514443172,128.314282958697));
#199494=CARTESIAN_POINT('Ctrl Pts',(52.0326671931086,0.979127467424884,
124.673563994973));
#199495=CARTESIAN_POINT('Ctrl Pts',(51.7542195692957,-4.62877051910935,
126.666747621346));
#199496=CARTESIAN_POINT('Ctrl Pts',(51.4757719454828,-5.98305452659317,
132.462195457613));
#199497=CARTESIAN_POINT('Ctrl Pts',(51.1973243216699,-1.83920371260068,
136.734174065611));
#199498=CARTESIAN_POINT('Ctrl Pts',(50.9188766978571,3.99478546317524,135.556943802347));
#199499=CARTESIAN_POINT('Ctrl Pts',(50.6404290740441,6.15776195441257,130.012321768865));
#199500=CARTESIAN_POINT('Ctrl Pts',(50.3619814502312,2.66205603294,125.195544744091));
#199501=CARTESIAN_POINT('Ctrl Pts',(50.0835338264184,-3.27994933413751,
125.532995501151));
#199502=CARTESIAN_POINT('Ctrl Pts',(49.8050862026055,-6.20784149757545,
130.714573279694));
#199503=CARTESIAN_POINT('Ctrl Pts',(49.5266385787925,-3.43103059465853,
135.978661235386));
#199504=CARTESIAN_POINT('Ctrl Pts',(49.2481909549797,2.4987298095866,136.487819701939));
#199505=CARTESIAN_POINT('Ctrl Pts',(48.9697433311668,6.13227958855924,131.774156922365));
#199506=CARTESIAN_POINT('Ctrl Pts',(48.6912957073539,4.13056400415832,126.169298715863));
#199507=CARTESIAN_POINT('Ctrl Pts',(48.412848083541,-1.66693811079436,124.823835961664));
#199508=CARTESIAN_POINT('Ctrl Pts',(48.1344004597282,-5.93260553638082,
128.974183201367));
#199509=CARTESIAN_POINT('Ctrl Pts',(47.8559528359152,-4.7464982979263,134.806374077418));
#199510=CARTESIAN_POINT('Ctrl Pts',(47.5775052121024,0.801408996989757,
136.960910093092));
#199511=CARTESIAN_POINT('Ctrl Pts',(47.2990575882894,5.61286057467834,133.457877904919));
#199512=CARTESIAN_POINT('Ctrl Pts',(47.0206099644766,5.26636748772036,127.516392961194));
#199513=CARTESIAN_POINT('Ctrl Pts',(46.7421623406636,0.0803399559020909,
124.596389667526));
#199514=CARTESIAN_POINT('Ctrl Pts',(46.4637147168508,-5.17951607056515,
127.381208400702));
#199515=CARTESIAN_POINT('Ctrl Pts',(46.1852670930379,-5.67964986161014,
133.311736790894));
#199516=CARTESIAN_POINT('Ctrl Pts',(45.9068194692249,-0.960462896156299,
136.938108969933));
#199517=CARTESIAN_POINT('Ctrl Pts',(45.6283718454121,4.64134254964412,134.927866063412));
#199518=CARTESIAN_POINT('Ctrl Pts',(45.3499242215992,5.97798093451044,129.128323096598));
#199519=CARTESIAN_POINT('Ctrl Pts',(45.0714765977863,1.82114688116607,124.868976732569));
#199520=CARTESIAN_POINT('Ctrl Pts',(44.7930289739735,-4.00923218799886,
126.063958199228));
#199521=CARTESIAN_POINT('Ctrl Pts',(44.5145813501605,-6.15532273827383,
131.615137906808));
#199522=CARTESIAN_POINT('Ctrl Pts',(44.2361337263477,-2.644972396308,136.421252894246));
#199523=CARTESIAN_POINT('Ctrl Pts',(43.9576861025347,3.29597836378001,136.065718279858));
#199524=CARTESIAN_POINT('Ctrl Pts',(43.6792384787219,6.20808602504863,130.875253005433));
#199525=CARTESIAN_POINT('Ctrl Pts',(43.4007908549089,3.41526591116036,125.619641089845));
#199526=CARTESIAN_POINT('Ctrl Pts',(43.1223432310961,-2.5160167300689,125.128533132602));
#199527=CARTESIAN_POINT('Ctrl Pts',(42.8438956072832,-6.13520291061547,
129.853233354452));
#199528=CARTESIAN_POINT('Ctrl Pts',(42.5654479834703,-4.11643733763101,
135.451973065955));
#199529=CARTESIAN_POINT('Ctrl Pts',(42.2870003596574,1.68513304949262,136.779783985877));
#199530=CARTESIAN_POINT('Ctrl Pts',(42.0085527358444,5.93814848745852,132.616472745983));
#199531=CARTESIAN_POINT('Ctrl Pts',(41.7301051120316,4.73429556013123,126.787918986671));
#199532=CARTESIAN_POINT('Ctrl Pts',(41.4516574882187,-0.820143703760798,
124.65027887207));
#199533=CARTESIAN_POINT('Ctrl Pts',(41.1732098644058,-5.62091097014408,
128.167939237972));
#199534=CARTESIAN_POINT('Ctrl Pts',(40.8947622405929,-5.25633565173145,
134.108342055376));
#199535=CARTESIAN_POINT('Ctrl Pts',(40.61631461678,-0.0614446556499193,
137.012547339898));
#199536=CARTESIAN_POINT('Ctrl Pts',(40.3378669929672,5.18991097723558,134.211732313379));
#199537=CARTESIAN_POINT('Ctrl Pts',(40.0594193691542,5.67199196328813,128.279709157768));
#199538=CARTESIAN_POINT('Ctrl Pts',(39.7809717453414,0.941789427290636,
124.66771735763));
#199539=CARTESIAN_POINT('Ctrl Pts',(39.5025241215285,-4.65387158341555,
126.695000921683));
#199540=CARTESIAN_POINT('Ctrl Pts',(39.2240764977156,-5.97285196322902,
132.49858529287));
#199541=CARTESIAN_POINT('Ctrl Pts',(38.9456288739027,-1.80307317887526,
136.745259954929));
#199542=CARTESIAN_POINT('Ctrl Pts',(38.6671812500898,4.02364177184326,135.532538355018));
#199543=CARTESIAN_POINT('Ctrl Pts',(38.3887336262769,6.15282650006613,129.974852398711));
#199544=CARTESIAN_POINT('Ctrl Pts',(38.110286002464,2.62786425701304,125.179443971804));
#199545=CARTESIAN_POINT('Ctrl Pts',(37.8318383786511,-3.31197685992897,
125.553059149895));
#199546=CARTESIAN_POINT('Ctrl Pts',(37.5533907548383,-6.20827304166094,
130.752363836438));
#199547=CARTESIAN_POINT('Ctrl Pts',(37.2749431310254,-3.3994695891056,135.999451024653));
#199548=CARTESIAN_POINT('Ctrl Pts',(36.9964955072125,2.53328034251594,136.47250392303));
#199549=CARTESIAN_POINT('Ctrl Pts',(36.7180478833995,6.13806939699002,131.73681002788));
#199550=CARTESIAN_POINT('Ctrl Pts',(36.4396002595867,4.10227253699055,126.144240677337));
#199551=CARTESIAN_POINT('Ctrl Pts',(36.1611526357737,-1.70331237734853,
124.834093892349));
#199552=CARTESIAN_POINT('Ctrl Pts',(35.8827050119609,-5.94363642833981,
129.01033056409));
#199553=CARTESIAN_POINT('Ctrl Pts',(35.604257388148,-4.72204896446884,134.835193211735));
#199554=CARTESIAN_POINT('Ctrl Pts',(35.3258097643351,0.838870812832614,
136.955917622458));
#199555=CARTESIAN_POINT('Ctrl Pts',(35.0473621405222,5.62890929425843,133.423661665951));
#199556=CARTESIAN_POINT('Ctrl Pts',(34.7689145167094,5.24625512176713,127.484396005948));
#199557=CARTESIAN_POINT('Ctrl Pts',(34.4904668928964,0.0425487861828518,
124.596015634733));
#199558=CARTESIAN_POINT('Ctrl Pts',(34.2120192690835,-5.20025780527969,
127.412801008228));
#199559=CARTESIAN_POINT('Ctrl Pts',(33.9335716452707,-5.66428152040741,
133.346263975806));
#199560=CARTESIAN_POINT('Ctrl Pts',(33.6551240214578,-0.923107233816384,
136.943841936043));
#199561=CARTESIAN_POINT('Ctrl Pts',(33.3766763976448,4.66635750435639,134.899536494936));
#199562=CARTESIAN_POINT('Ctrl Pts',(33.098228773832,5.96766766026296,129.091964482989));
#199563=CARTESIAN_POINT('Ctrl Pts',(32.8197811500191,1.78498277316083,124.858000863516));
#199564=CARTESIAN_POINT('Ctrl Pts',(32.5413335262063,-4.03801408121996,
126.08845136219));
#199565=CARTESIAN_POINT('Ctrl Pts',(32.2628859023933,-6.15027326291425,
131.65259208158));
#199566=CARTESIAN_POINT('Ctrl Pts',(31.9844382785804,-2.6107317735426,136.437249523951));
#199567=CARTESIAN_POINT('Ctrl Pts',(31.7059906547675,3.32794467437699,136.045557243275));
#199568=CARTESIAN_POINT('Ctrl Pts',(31.4275430309546,6.20840254567991,130.837461310262));
#199569=CARTESIAN_POINT('Ctrl Pts',(31.1490954071417,3.3836417748287,125.598947457719));
#199570=CARTESIAN_POINT('Ctrl Pts',(30.8706477833288,-2.55052048699994,
125.143954000505));
#199571=CARTESIAN_POINT('Ctrl Pts',(30.5922001595159,-6.14087902112821,
129.890597698133));
#199572=CARTESIAN_POINT('Ctrl Pts',(30.3137525357031,-4.08806973345779,
135.476944878919));
#199573=CARTESIAN_POINT('Ctrl Pts',(30.0353049118902,1.72147592595096,136.769415391952));
#199574=CARTESIAN_POINT('Ctrl Pts',(29.7568572880773,5.94906930818524,132.58029197645));
#199575=CARTESIAN_POINT('Ctrl Pts',(29.4784096642643,4.70975862438989,126.759174401203));
#199576=CARTESIAN_POINT('Ctrl Pts',(29.1999620404515,-0.857590150719802,
124.65538534046));
#199577=CARTESIAN_POINT('Ctrl Pts',(28.9215144166386,-5.63685547292606,
128.202204165235));
#199578=CARTESIAN_POINT('Ctrl Pts',(28.6430667928257,-5.23612599121204,
134.140277647291));
#199579=CARTESIAN_POINT('Ctrl Pts',(28.3646191690128,-0.0236525225496446,
137.012806347637));
#199580=CARTESIAN_POINT('Ctrl Pts',(28.0861715451999,5.2105564588459,134.180076721482));
#199581=CARTESIAN_POINT('Ctrl Pts',(27.807723921387,5.65651860439647,128.245228908728));
#199582=CARTESIAN_POINT('Ctrl Pts',(27.5292762975741,0.904416488802812,
124.662098115861));
#199583=CARTESIAN_POINT('Ctrl Pts',(27.2508286737613,-4.67880019679877,
126.723406495856));
#199584=CARTESIAN_POINT('Ctrl Pts',(26.9723810499484,-5.96242807363892,
132.53491234801));
#199585=CARTESIAN_POINT('Ctrl Pts',(26.6939334261354,-1.76687583160983,
136.756125702037));
#199586=CARTESIAN_POINT('Ctrl Pts',(26.4154858023226,4.05234898298581,135.507957703324));
#199587=CARTESIAN_POINT('Ctrl Pts',(26.1370381785097,6.14766305047102,129.937413766291));
#199588=CARTESIAN_POINT('Ctrl Pts',(25.8585905546968,2.59357510460964,125.163551632871));
#199589=CARTESIAN_POINT('Ctrl Pts',(25.5801429308839,-3.34388165920016,
125.573317387547));
#199590=CARTESIAN_POINT('Ctrl Pts',(25.301695307071,-6.2084745359058,130.790156319941));
#199591=CARTESIAN_POINT('Ctrl Pts',(25.0232476832582,-3.36778261495664,
136.020048307934));
#199592=CARTESIAN_POINT('Ctrl Pts',(24.7448000594452,2.56773700381057,136.456978108987));
#199593=CARTESIAN_POINT('Ctrl Pts',(24.4663524356323,6.14363175700203,131.69942858114));
#199594=CARTESIAN_POINT('Ctrl Pts',(24.1879048118195,4.07382905860539,126.11935532127));
#199595=CARTESIAN_POINT('Ctrl Pts',(23.9094571880065,-1.73962352703587,
124.844573053462));
#199596=CARTESIAN_POINT('Ctrl Pts',(23.6310095641937,-5.95444707666522,
129.046544405257));
#199597=CARTESIAN_POINT('Ctrl Pts',(23.3525619403807,-4.69742465375045,
134.863862982068));
#199598=CARTESIAN_POINT('Ctrl Pts',(23.0741143165679,0.876301544009003,
136.950697203617));
#199599=CARTESIAN_POINT('Ctrl Pts',(22.795666692755,5.64474943253441,133.389348367819));
#199600=CARTESIAN_POINT('Ctrl Pts',(22.5172190689421,5.22594835390121,127.452522073212));
#199601=CARTESIAN_POINT('Ctrl Pts',(22.2387714451292,0.0047560398029127,
124.595871654449));
#199602=CARTESIAN_POINT('Ctrl Pts',(21.9603238213163,-5.22080684252888,
127.444519291243));
#199603=CARTESIAN_POINT('Ctrl Pts',(21.6818761975034,-5.64870328716988,
133.380696969555));
#199604=CARTESIAN_POINT('Ctrl Pts',(21.4034285736905,-0.885717365398449,
136.949347401415));
#199605=CARTESIAN_POINT('Ctrl Pts',(21.1249809498776,4.69119954547528,134.871055178212));
#199606=CARTESIAN_POINT('Ctrl Pts',(20.8465333260648,5.95713325189572,129.055669322849));
#199607=CARTESIAN_POINT('Ctrl Pts',(20.5680857022518,1.74875252196249,124.847245339011));
#199608=CARTESIAN_POINT('Ctrl Pts',(20.289638078439,-4.06664634434428,126.113119274905));
#199609=CARTESIAN_POINT('Ctrl Pts',(20.011190454626,-6.14499588691713,131.690014824823));
#199610=CARTESIAN_POINT('Ctrl Pts',(19.7327428308132,-2.57639440915122,
136.453037424885));
#199611=CARTESIAN_POINT('Ctrl Pts',(19.4542952070003,3.35978766676044,136.025201992224));
#199612=CARTESIAN_POINT('Ctrl Pts',(19.1758475831874,6.20848901167171,130.799668388532));
#199613=CARTESIAN_POINT('Ctrl Pts',(18.8973999593745,3.3518922564065,125.578446714094));
#199614=CARTESIAN_POINT('Ctrl Pts',(18.6189523355616,-2.58492973345636,
125.159584616859));
#199615=CARTESIAN_POINT('Ctrl Pts',(18.3405047117487,-6.14632757911053,
129.927995901635));
#199616=CARTESIAN_POINT('Ctrl Pts',(18.0620570879358,-4.05955064435711,
135.501743547556));
#199617=CARTESIAN_POINT('Ctrl Pts',(17.7836094641229,1.75775501248606,136.758825760728));
#199618=CARTESIAN_POINT('Ctrl Pts',(17.5051618403101,5.95976968396092,132.544045399129));
#199619=CARTESIAN_POINT('Ctrl Pts',(17.2267142164972,4.68504716681072,126.730579711598));
#199620=CARTESIAN_POINT('Ctrl Pts',(16.9482665926842,-0.8950048193604,124.660719661391));
#199621=CARTESIAN_POINT('Ctrl Pts',(16.6698189688713,-5.65259109995534,
128.236565516362));
#199622=CARTESIAN_POINT('Ctrl Pts',(16.3913713450585,-5.21572230411858,
134.172089625574));
#199623=CARTESIAN_POINT('Ctrl Pts',(16.1129237212456,0.0141404870033325,
137.012835299135));
#199624=CARTESIAN_POINT('Ctrl Pts',(15.8344760974327,5.23100886137047,134.148296041183));
#199625=CARTESIAN_POINT('Ctrl Pts',(15.5560284736198,5.64083564112771,128.210843489254));
#199626=CARTESIAN_POINT('Ctrl Pts',(15.2775808498069,0.8670100368296,124.656706477888));
#199627=CARTESIAN_POINT('Ctrl Pts',(14.999133225994,-4.70355543551987,126.751963291284));
#199628=CARTESIAN_POINT('Ctrl Pts',(14.7206856021811,-5.95178324408404,
132.571175276918));
#199629=CARTESIAN_POINT('Ctrl Pts',(14.4422379783683,-1.73061301211068,
136.766770904302));
#199630=CARTESIAN_POINT('Ctrl Pts',(14.1637903545553,4.08090603284655,135.48320275811));
#199631=CARTESIAN_POINT('Ctrl Pts',(13.8853427307424,6.14227179696077,129.900007258904));
#199632=CARTESIAN_POINT('Ctrl Pts',(13.6068951069296,2.55918984632695,125.147868316191));
#199633=CARTESIAN_POINT('Ctrl Pts',(13.3284474831167,-3.37566254970675,
125.593769463429));
#199634=CARTESIAN_POINT('Ctrl Pts',(13.0499998593037,-6.20844597284355,
130.827949329789));
#199635=CARTESIAN_POINT('Ctrl Pts',(12.7715522354909,-3.33597084638438,
136.04045232199));
#199636=CARTESIAN_POINT('Ctrl Pts',(12.493104611678,2.60209851666622,136.441242835124));
#199637=CARTESIAN_POINT('Ctrl Pts',(12.2146569878651,6.14896646247997,131.662013967328));
#199638=CARTESIAN_POINT('Ctrl Pts',(11.9362093640522,4.04523462298623,126.094643569795));
#199639=CARTESIAN_POINT('Ctrl Pts',(11.6577617402393,-1.77587021433397,
124.855273056695));
#199640=CARTESIAN_POINT('Ctrl Pts',(11.3793141164265,-5.96503708076441,
129.08282338295));
#199641=CARTESIAN_POINT('Ctrl Pts',(11.1008664926135,-4.67262627823404,
134.892382326048));
#199642=CARTESIAN_POINT('Ctrl Pts',(10.8224188688007,0.913699803509421,
136.945249030013));
#199643=CARTESIAN_POINT('Ctrl Pts',(10.5439712449878,5.6603804025445,133.354939282016));
#199644=CARTESIAN_POINT('Ctrl Pts',(10.2655236211749,5.20544793659703,127.420772344084));
#199645=CARTESIAN_POINT('Ctrl Pts',(9.98707599736195,-0.0330368828140487,
124.595957732005));
#199646=CARTESIAN_POINT('Ctrl Pts',(9.70862837354909,-5.24116242086055,
127.476362074414));
#199647=CARTESIAN_POINT('Ctrl Pts',(9.43018074973619,-5.63291573915475,
133.415034496211));
#199648=CARTESIAN_POINT('Ctrl Pts',(9.15173312592329,-0.848294676398009,
136.954625162043));
#199649=CARTESIAN_POINT('Ctrl Pts',(8.87328550211039,4.71586775246963,134.842423168626));
#199650=CARTESIAN_POINT('Ctrl Pts',(8.59483787829755,5.94637809976527,129.019438961107));
#199651=CARTESIAN_POINT('Ctrl Pts',(8.3163902544846,1.71245747009635,124.836710557603));
#199652=CARTESIAN_POINT('Ctrl Pts',(8.03794263067172,-4.09512791639282,
126.137961023291));
#199653=CARTESIAN_POINT('Ctrl Pts',(7.75949500685887,-6.1394908058375,131.727404749824));
#199654=CARTESIAN_POINT('Ctrl Pts',(7.48104738304595,-2.54196157551782,
136.468616012024));
#199655=CARTESIAN_POINT('Ctrl Pts',(7.20259975923305,3.39150616097622,136.004653280976));
#199656=CARTESIAN_POINT('Ctrl Pts',(6.92415213542018,6.20834541982004,130.761875640674));
#199657=CARTESIAN_POINT('Ctrl Pts',(6.64570451160728,3.32001853238404,125.558139618628));
#199658=CARTESIAN_POINT('Ctrl Pts',(6.36725688779438,-2.61924319439064,
125.175424402463));
#199659=CARTESIAN_POINT('Ctrl Pts',(6.08880926398148,-6.15154838266407,
129.965426579154));
#199660=CARTESIAN_POINT('Ctrl Pts',(5.81036164016863,-4.03088112711464,
135.52636815294));
#199661=CARTESIAN_POINT('Ctrl Pts',(5.53191401635571,1.79396896476278,136.748015484609));
#199662=CARTESIAN_POINT('Ctrl Pts',(5.2534663925428,5.97024921827925,132.507734357147));
#199663=CARTESIAN_POINT('Ctrl Pts',(4.97501876872993,4.66016210308585,126.702135977443));
#199664=CARTESIAN_POINT('Ctrl Pts',(4.69657114491704,-0.932386323268277,
124.666281637197));
#199665=CARTESIAN_POINT('Ctrl Pts',(4.41812352110413,-5.66811726814286,
128.27102201808));
#199666=CARTESIAN_POINT('Ctrl Pts',(4.13967589729124,-5.19512534651691,
134.203776811419));
#199667=CARTESIAN_POINT('Ctrl Pts',(3.86122827347838,0.051932972575587,
137.012634193321));
#199668=CARTESIAN_POINT('Ctrl Pts',(3.58278064966546,5.25126742693796,134.116391450127));
#199669=CARTESIAN_POINT('Ctrl Pts',(3.30433302585255,5.62494365461986,128.176554173511));
#199670=CARTESIAN_POINT('Ctrl Pts',(3.02588540203969,0.829571457480427,
124.651542643499));
#199671=CARTESIAN_POINT('Ctrl Pts',(2.74743777822681,-4.72813638226476,
126.780670249786));
#199672=CARTESIAN_POINT('Ctrl Pts',(2.46899015441389,-5.9409178690121,132.607372735859));
#199673=CARTESIAN_POINT('Ctrl Pts',(2.19054253060099,-1.69428606410994,
136.77719516726));
#199674=CARTESIAN_POINT('Ctrl Pts',(1.91209490678813,4.10931186323347,135.458274436681));
#199675=CARTESIAN_POINT('Ctrl Pts',(1.63364728297522,6.13665293931019,129.862634262664));
#199676=CARTESIAN_POINT('Ctrl Pts',(1.35519965916232,2.52470975632363,125.132394602912));
#199677=CARTESIAN_POINT('Ctrl Pts',(1.07675203534945,-3.40731835379603,
125.614414619682));
#199678=CARTESIAN_POINT('Ctrl Pts',(0.798304411536565,-6.20818735353264,
130.86574146555));
#199679=CARTESIAN_POINT('Ctrl Pts',(0.519856787723634,-3.30403546218559,
136.060662310741));
#199680=CARTESIAN_POINT('Ctrl Pts',(0.241409163910791,2.63636360780418,
136.425298684517));
#199681=CARTESIAN_POINT('Ctrl Pts',(-0.0370384599021062,6.15407331574431,
131.624567572855));
#199682=CARTESIAN_POINT('Ctrl Pts',(-0.315486083715014,4.01649028971072,
126.070106338619));
#199683=CARTESIAN_POINT('Ctrl Pts',(-0.593933707527915,-1.81205109610819,
124.866193505555));
#199684=CARTESIAN_POINT('Ctrl Pts',(-0.872381331340776,-5.97540604822092,
129.119166152838));
#199685=CARTESIAN_POINT('Ctrl Pts',(-1.15082895515369,-4.6476547568326,
134.920750186879));
#199686=CARTESIAN_POINT('Ctrl Pts',(-1.42927657896659,0.951064205527318,
136.939573303531));
#199687=CARTESIAN_POINT('Ctrl Pts',(-1.70772420277945,5.67580162507719,
133.320435683583));
#199688=CARTESIAN_POINT('Ctrl Pts',(-1.98617182659235,5.18475462950527,
127.389147995065));
#199689=CARTESIAN_POINT('Ctrl Pts',(-2.26461945040527,-0.0708285812371651,
124.596273864213));
#199690=CARTESIAN_POINT('Ctrl Pts',(-2.54306707421816,-5.26132378599129,
127.508328177794));
#199691=CARTESIAN_POINT('Ctrl Pts',(-2.82151469803103,-5.61691946137538,
133.449275283389));
#199692=CARTESIAN_POINT('Ctrl Pts',(-3.09996232184393,-0.810840553526189,
136.959675022356));
#199693=CARTESIAN_POINT('Ctrl Pts',(-3.37840994565684,4.74036121125036,
134.813641527147));
#199694=CARTESIAN_POINT('Ctrl Pts',(-3.6568575694697,5.93540260240737,128.983274740293));
#199695=CARTESIAN_POINT('Ctrl Pts',(-3.9353051932826,1.6760989624889,124.826396909662));
#199696=CARTESIAN_POINT('Ctrl Pts',(-4.21375281709551,-4.12345774197041,
126.162975686831));
#199697=CARTESIAN_POINT('Ctrl Pts',(-4.49220044090841,-6.13375822366836,
131.764760471086));
#199698=CARTESIAN_POINT('Ctrl Pts',(-4.77064806472125,-2.50743454856317,
136.483984708096));
#199699=CARTESIAN_POINT('Ctrl Pts',(-5.04909568853418,3.4230989816841,135.983911870971));
#199700=CARTESIAN_POINT('Ctrl Pts',(-5.32754331234708,6.20797177544568,
130.724084467112));
#199701=CARTESIAN_POINT('Ctrl Pts',(-5.60599093615995,3.28802178385396,
125.538026923812));
#199702=CARTESIAN_POINT('Ctrl Pts',(-5.88443855997284,-2.65345959830539,
125.191472770368));
#199703=CARTESIAN_POINT('Ctrl Pts',(-6.16288618378574,-6.15654123833006,
130.002888343683));
#199704=CARTESIAN_POINT('Ctrl Pts',(-6.44133380759864,-4.00206224408943,
135.550817782599));
#199705=CARTESIAN_POINT('Ctrl Pts',(-6.71978143141151,1.83011644085978,
136.736984964173));
#199706=CARTESIAN_POINT('Ctrl Pts',(-6.9982290552244,5.98050752281724,132.471360196026));
#199707=CARTESIAN_POINT('Ctrl Pts',(-7.27667667903734,4.63510435534053,
126.673844252731));
#199708=CARTESIAN_POINT('Ctrl Pts',(-7.55512430285017,-0.969733277257762,
124.672071061776));
#199709=CARTESIAN_POINT('Ctrl Pts',(-7.83357192666308,-5.68343340216059,
128.305572393592));
#199710=CARTESIAN_POINT('Ctrl Pts',(-8.112019550476,-5.17433588163501,134.235338030648));
#199711=CARTESIAN_POINT('Ctrl Pts',(-8.39046717428886,0.0897235337524442,
137.012203037646));
#199712=CARTESIAN_POINT('Ctrl Pts',(-8.66891479810176,5.27133140485959,
134.084364130551));
#199713=CARTESIAN_POINT('Ctrl Pts',(-8.94736242191464,5.60884323375645,
128.142362232103));
#199714=CARTESIAN_POINT('Ctrl Pts',(-9.22581004572757,0.792102138056052,
124.646606804043));
#199715=CARTESIAN_POINT('Ctrl Pts',(-9.50425766954039,-4.75254212617725,
126.809526307613));
#199716=CARTESIAN_POINT('Ctrl Pts',(-9.78270529335335,-5.92983235104376,
132.643503383524));
#199717=CARTESIAN_POINT('Ctrl Pts',(-10.0611529171662,-1.65789633371603,
136.787398104638));
#199718=CARTESIAN_POINT('Ctrl Pts',(-10.3396005409791,4.13756542155812,
135.433173662763));
#199719=CARTESIAN_POINT('Ctrl Pts',(-10.618048164792,6.13080668572826,129.82529616244));
#199720=CARTESIAN_POINT('Ctrl Pts',(-10.8964957886049,2.49013611227157,
125.11713106642));
#199721=CARTESIAN_POINT('Ctrl Pts',(-11.1749434124178,-3.4388478984508,
125.635252091294));
#199722=CARTESIAN_POINT('Ctrl Pts',(-11.4533910362307,-6.20769868755626,
130.90353132682));
#199723=CARTESIAN_POINT('Ctrl Pts',(-11.7318386600436,-3.2719776457377,
136.080677525301));
#199724=CARTESIAN_POINT('Ctrl Pts',(-12.0102862838565,2.67053100751937,
136.409146247984));
#199725=CARTESIAN_POINT('Ctrl Pts',(-12.2887339076694,6.15895212755882,
131.587090785312));
#199726=CARTESIAN_POINT('Ctrl Pts',(-12.5671815314823,3.98759712391021,
126.045744536976));
#199727=CARTESIAN_POINT('Ctrl Pts',(-12.8456291552951,-1.84816483166266,
124.877333995382));
#199728=CARTESIAN_POINT('Ctrl Pts',(-13.1240767791081,-5.98555359480885,
129.155571368227));
#199729=CARTESIAN_POINT('Ctrl Pts',(-13.4025244029209,-4.62251101487491,
134.948965513381));
#199730=CARTESIAN_POINT('Ctrl Pts',(-13.6809720267338,0.988393365511613,
136.933670234486));
#199731=CARTESIAN_POINT('Ctrl Pts',(-13.9594196505467,5.69101252869335,
133.285838851062));
#199732=CARTESIAN_POINT('Ctrl Pts',(-14.2378672743596,5.16386919942402,
127.357650198006));
#199733=CARTESIAN_POINT('Ctrl Pts',(-14.5163148981725,-0.108617655081171,
124.59682003936));
#199734=CARTESIAN_POINT('Ctrl Pts',(-14.7947625219854,-5.28129019083405,
127.540416416869));
#199735=CARTESIAN_POINT('Ctrl Pts',(-15.0732101457983,-5.60071504657988,
133.483418062279));
#199736=CARTESIAN_POINT('Ctrl Pts',(-15.3516577696111,-0.77335638465969,
136.96449679523));
#199737=CARTESIAN_POINT('Ctrl Pts',(-15.6301053934241,4.76467901420313,
134.784711320289));
#199738=CARTESIAN_POINT('Ctrl Pts',(-15.908553017237,5.92420716652329,128.947178000488));
#199739=CARTESIAN_POINT('Ctrl Pts',(-16.1870006410499,1.63967834641818,
124.816304777366));
#199740=CARTESIAN_POINT('Ctrl Pts',(-16.4654482648627,-4.15163477130477,
126.188162338596));
#199741=CARTESIAN_POINT('Ctrl Pts',(-16.7438958886757,-6.12779835283271,
131.802080604377));
#199742=CARTESIAN_POINT('Ctrl Pts',(-17.0223435124885,-2.4728146076992,
136.499142943608));
#199743=CARTESIAN_POINT('Ctrl Pts',(-17.3007911363014,3.45456495820035,
135.96297853079));
#199744=CARTESIAN_POINT('Ctrl Pts',(-17.5792387601143,6.20736809239421,
130.686296268213));
#199745=CARTESIAN_POINT('Ctrl Pts',(-17.8576863839272,3.25590319646751,
125.518109374927));
#199746=CARTESIAN_POINT('Ctrl Pts',(-18.13613400774,-2.6875776772989,125.207729125896));
#199747=CARTESIAN_POINT('Ctrl Pts',(-18.414581631553,-6.16130596109642,
130.040379807061));
#199748=CARTESIAN_POINT('Ctrl Pts',(-18.6930292553659,-3.97309506317598,
135.575091530542));
#199749=CARTESIAN_POINT('Ctrl Pts',(-18.9714768791788,1.86619610131902,
136.72573460816));
#199750=CARTESIAN_POINT('Ctrl Pts',(-19.2499245029916,5.99054421744964,
132.434924263623));
#199751=CARTESIAN_POINT('Ctrl Pts',(-19.5283721268046,4.6098748520987,126.645705585822));
#199752=CARTESIAN_POINT('Ctrl Pts',(-19.8068197506174,-1.00704429742433,
124.678087720601));
#199753=CARTESIAN_POINT('Ctrl Pts',(-20.0852673744304,-5.6985389344635,
128.340215362621));
#199754=CARTESIAN_POINT('Ctrl Pts',(-20.3637149982432,-5.15335467983417,
134.266772113748));
#199755=CARTESIAN_POINT('Ctrl Pts',(-20.6421626220562,0.127510770190762,
137.011541848088));
#199756=CARTESIAN_POINT('Ctrl Pts',(-20.920610245869,5.29120005165768,134.05221526924));
#199757=CARTESIAN_POINT('Ctrl Pts',(-21.1990578696819,5.59253497514422,
128.108268932023));
#199758=CARTESIAN_POINT('Ctrl Pts',(-21.4775054934948,0.754603466995427,
124.64189914242));
#199759=CARTESIAN_POINT('Ctrl Pts',(-21.7559531173077,-4.77677176289349,
126.838530395495));
#199760=CARTESIAN_POINT('Ctrl Pts',(-22.0344007411205,-5.91852710095694,
132.679565881077));
#199761=CARTESIAN_POINT('Ctrl Pts',(-22.3128483649335,-1.62144516936395,
136.797379338361));
#199762=CARTESIAN_POINT('Ctrl Pts',(-22.5912959887463,4.16566566087426,
135.407901366475));
#199763=CARTESIAN_POINT('Ctrl Pts',(-22.8697436125593,6.12473325285015,
129.787994341809));
#199764=CARTESIAN_POINT('Ctrl Pts',(-23.1481912363721,2.45547019531011,
125.102078272311));
#199765=CARTESIAN_POINT('Ctrl Pts',(-23.426638860185,-3.47025001533206,
125.656281106122));
#199766=CARTESIAN_POINT('Ctrl Pts',(-23.7050864839979,-6.20697999302203,
130.941317513284));
#199767=CARTESIAN_POINT('Ctrl Pts',(-23.9835341078108,-3.23979858495512,
136.100497223997));
#199768=CARTESIAN_POINT('Ctrl Pts',(-24.2619817316237,2.70459944972584,
136.392786124057));
#199769=CARTESIAN_POINT('Ctrl Pts',(-24.5404293554366,6.16360271713728,
131.549584993415));
#199770=CARTESIAN_POINT('Ctrl Pts',(-24.8188769792495,3.95855619623184,
126.021559067602));
#199771=CARTESIAN_POINT('Ctrl Pts',(-25.0973246030624,-1.88421008278963,
124.88869411336));
#199772=CARTESIAN_POINT('Ctrl Pts',(-25.3757722268753,-5.99547934450715,
129.192037680109));
#199773=CARTESIAN_POINT('Ctrl Pts',(-25.6542198506882,-4.59719598407162,
134.977027260026));
#199774=CARTESIAN_POINT('Ctrl Pts',(-25.932667474501,1.02568590021626,136.92754004162));
#199775=CARTESIAN_POINT('Ctrl Pts',(-26.211115098314,5.7060125497474,133.251150066453));
#199776=CARTESIAN_POINT('Ctrl Pts',(-26.4895627221268,5.14279242027056,
127.326280120068));
#199777=CARTESIAN_POINT('Ctrl Pts',(-26.7680103459397,-0.146402704058008,
124.597596237205));
#199778=CARTESIAN_POINT('Ctrl Pts',(-27.0464579697526,-5.30106089552683,
127.572625602596));
#199779=CARTESIAN_POINT('Ctrl Pts',(-27.3249055935655,-5.58430309522854,
133.517461567711));
#199780=CARTESIAN_POINT('Ctrl Pts',(-27.6033532173784,-0.735843558787732,
136.969090301993));
#199781=CARTESIAN_POINT('Ctrl Pts',(-27.8818008411913,4.78882026022281,
134.755633620073));
#199782=CARTESIAN_POINT('Ctrl Pts',(-28.1602484650042,5.91279220696403,
128.911150079267));
#199783=CARTESIAN_POINT('Ctrl Pts',(-28.4386960888171,1.60319697146318,
124.806434534681));
#199784=CARTESIAN_POINT('Ctrl Pts',(-28.7171437126299,-4.17965796028613,
126.213520045287));
#199785=CARTESIAN_POINT('Ctrl Pts',(-28.9955913364429,-6.12161141417542,
131.839363766787));
#199786=CARTESIAN_POINT('Ctrl Pts',(-29.2740389602557,-2.43810303578058,
136.514090156867));
#199787=CARTESIAN_POINT('Ctrl Pts',(-29.5524865840687,3.48590292454168,
135.941854036124));
#199788=CARTESIAN_POINT('Ctrl Pts',(-29.8309342078815,6.20653439303521,
130.648512444231));
#199789=CARTESIAN_POINT('Ctrl Pts',(-30.1093818316944,3.22366396039099,
125.498387710026));
#199790=CARTESIAN_POINT('Ctrl Pts',(-30.3878294555073,-2.72159616711309,
125.224192866663));
#199791=CARTESIAN_POINT('Ctrl Pts',(-30.6662770793202,-6.16584237440457,
130.077899580028));
#199792=CARTESIAN_POINT('Ctrl Pts',(-30.9447247031331,-3.94398065776386,
135.599188497297));
#199793=CARTESIAN_POINT('Ctrl Pts',(-31.2231723269461,1.90220660919519,
136.714264833456));
#199794=CARTESIAN_POINT('Ctrl Pts',(-31.5016199507588,6.00035893026297,
132.398427910084));
#199795=CARTESIAN_POINT('Ctrl Pts',(-31.7800675745718,4.58447452824918,
126.617721019404));
#199796=CARTESIAN_POINT('Ctrl Pts',(-32.0585151983846,-1.04431800119413,
124.68433139072));
#199797=CARTESIAN_POINT('Ctrl Pts',(-32.3369628221976,-5.71343330531054,
128.374949641459));
#199798=CARTESIAN_POINT('Ctrl Pts',(-32.6154104460104,-5.1321825185805,
134.298077895915));
#199799=CARTESIAN_POINT('Ctrl Pts',(-32.8938580698234,0.165293281670594,
137.010650649146));
#199800=CARTESIAN_POINT('Ctrl Pts',(-33.1723056936362,5.31087263109202,
134.019946057479));
#199801=CARTESIAN_POINT('Ctrl Pts',(-33.4507533174492,5.57601948309184,
128.074275536613));
#199802=CARTESIAN_POINT('Ctrl Pts',(-33.729200941262,0.717076833825826,
124.637419833072));
#199803=CARTESIAN_POINT('Ctrl Pts',(-34.0076485650749,-4.80082439457541,
126.867681438675));
#199804=CARTESIAN_POINT('Ctrl Pts',(-34.2860961888878,-5.90700253767186,
132.715558892209));
#199805=CARTESIAN_POINT('Ctrl Pts',(-34.5645438127007,-1.58493392176466,
136.807138498572));
#199806=CARTESIAN_POINT('Ctrl Pts',(-34.8429914365135,4.19361153991761,
135.382458484293));
#199807=CARTESIAN_POINT('Ctrl Pts',(-35.1214390603265,6.11843286572883,
129.750730183006));
#199808=CARTESIAN_POINT('Ctrl Pts',(-35.3998866841394,2.42071328999757,
125.087236778371));
#199809=CARTESIAN_POINT('Ctrl Pts',(-35.6783343079523,-3.50152354082281,
125.677500884929));
#199810=CARTESIAN_POINT('Ctrl Pts',(-35.9567819317651,-6.20603129656164,
130.979098624759));
#199811=CARTESIAN_POINT('Ctrl Pts',(-36.2352295555781,-3.2074994722443,
136.120120672404));
#199812=CARTESIAN_POINT('Ctrl Pts',(-36.5136771793909,2.73856767200523,
136.376218918968));
#199813=CARTESIAN_POINT('Ctrl Pts',(-36.7921248032039,6.1680249121504,131.512051586954));
#199814=CARTESIAN_POINT('Ctrl Pts',(-37.0705724270167,3.92936858279784,
125.997550826698));
#199815=CARTESIAN_POINT('Ctrl Pts',(-37.3490200508296,-1.92018551381882,
124.900273438536));
#199816=CARTESIAN_POINT('Ctrl Pts',(-37.6274676746425,-6.00518292951342,
129.228563737208));
#199817=CARTESIAN_POINT('Ctrl Pts',(-37.9059152984554,-4.57171060248077,
135.004934386972));
#199818=CARTESIAN_POINT('Ctrl Pts',(-38.1843629222683,1.0629404277527,136.921182952087));
#199819=CARTESIAN_POINT('Ctrl Pts',(-38.4628105460811,5.72080113240803,
133.216370615161));
#199820=CARTESIAN_POINT('Ctrl Pts',(-38.7412581698941,5.12152507305273,
127.295038923683));
#199821=CARTESIAN_POINT('Ctrl Pts',(-39.0197057937069,-0.184182328028525,
124.598602428988));
#199822=CARTESIAN_POINT('Ctrl Pts',(-39.2981534175199,-5.32063516745863,
127.604954541453));
#199823=CARTESIAN_POINT('Ctrl Pts',(-39.5766010413327,-5.56768421547239,
133.55140453819));
#199824=CARTESIAN_POINT('Ctrl Pts',(-39.8550486651457,-0.698303465962086,
136.973455372429));
#199825=CARTESIAN_POINT('Ctrl Pts',(-40.1334962889585,4.81278405474664,
134.726409503982));
#199826=CARTESIAN_POINT('Ctrl Pts',(-40.4119439127715,5.90115814671511,
128.875192311658));
#199827=CARTESIAN_POINT('Ctrl Pts',(-40.6903915365843,1.56665618945481,
124.796786547352));
#199828=CARTESIAN_POINT('Ctrl Pts',(-40.9688391603973,-4.20752627050468,
126.239047867263));
#199829=CARTESIAN_POINT('Ctrl Pts',(-41.2472867842101,-6.11519763695597,
131.876608576776));
#199830=CARTESIAN_POINT('Ctrl Pts',(-41.5257344080229,-2.40330111905734,
136.528825793999));
#199831=CARTESIAN_POINT('Ctrl Pts',(-41.8041820318359,3.51711171946819,
135.920539169751));
#199832=CARTESIAN_POINT('Ctrl Pts',(-42.0826296556488,6.20547070826194,
130.610734395262));
#199833=CARTESIAN_POINT('Ctrl Pts',(-42.3610772794617,3.19130527026066,
125.478862659902));
#199834=CARTESIAN_POINT('Ctrl Pts',(-42.6395249032745,-2.75551380718057,
125.240863382598));
#199835=CARTESIAN_POINT('Ctrl Pts',(-42.9179725270875,-6.17015031015604,
130.115446272278));
#199836=CARTESIAN_POINT('Ctrl Pts',(-43.1964201509003,-3.91472010669807,
135.623107789941));
#199837=CARTESIAN_POINT('Ctrl Pts',(-43.4748677747133,1.93814663010615,
136.702576065077));
#199838=CARTESIAN_POINT('Ctrl Pts',(-43.7533153985261,6.00995129756958,
132.361872487794));
#199839=CARTESIAN_POINT('Ctrl Pts',(-44.031763022339,4.55890432500984,126.589891590455));
#199840=CARTESIAN_POINT('Ctrl Pts',(-44.3102106461518,-1.08155300737633,
124.690801840773));
#199841=CARTESIAN_POINT('Ctrl Pts',(-44.5886582699649,-5.72811596278534,
128.409773943013));
#199842=CARTESIAN_POINT('Ctrl Pts',(-44.8671058937777,-5.11082018241628,
134.329254217104));
#199843=CARTESIAN_POINT('Ctrl Pts',(-45.1455535175906,0.2030696681468,137.009529473845));
#199844=CARTESIAN_POINT('Ctrl Pts',(-45.4240011414034,5.33034841418793,
133.987557691017));
#199845=CARTESIAN_POINT('Ctrl Pts',(-45.7024487652165,5.55929736958694,
128.040383305508));
#199846=CARTESIAN_POINT('Ctrl Pts',(-45.9808963890292,0.679523629110432,
124.633169041983));
#199847=CARTESIAN_POINT('Ctrl Pts',(-46.2593440128422,-4.82469912994364,
126.896978356949));
#199848=CARTESIAN_POINT('Ctrl Pts',(-46.537791636655,-5.89525908823553,
132.751481083186));
#199849=CARTESIAN_POINT('Ctrl Pts',(-46.816239260468,-1.54836394385628,
136.816675223641));
#199850=CARTESIAN_POINT('Ctrl Pts',(-47.0946868842807,4.22140202314317,
135.35684595901));
#199851=CARTESIAN_POINT('Ctrl Pts',(-47.3731345080937,6.11190575782758,
129.713505066864));
#199852=CARTESIAN_POINT('Ctrl Pts',(-47.6515821319066,2.38586668426401,
125.072607134557));
#199853=CARTESIAN_POINT('Ctrl Pts',(-47.9300297557195,-3.53266731607082,
125.69891064141));
#199854=CARTESIAN_POINT('Ctrl Pts',(-48.2084773795324,-6.20485263332943,
131.016873261253));
#199855=CARTESIAN_POINT('Ctrl Pts',(-48.4869250033452,-3.17508150446096,
136.139547143367));
#199856=CARTESIAN_POINT('Ctrl Pts',(-48.7653726271582,2.77243441565242,
136.359445246621));
#199857=CARTESIAN_POINT('Ctrl Pts',(-49.043820250971,6.1722185487321,131.474491956744));
#199858=CARTESIAN_POINT('Ctrl Pts',(-49.322267874784,3.900035365166,125.973720703898));
#199859=CARTESIAN_POINT('Ctrl Pts',(-49.6007154985968,-1.95608979166789,
124.912071541833));
#199860=CARTESIAN_POINT('Ctrl Pts',(-49.8791631224098,-6.0146639902579,
129.265148186042));
#199861=CARTESIAN_POINT('Ctrl Pts',(-50.1576107462225,-4.54605581447205,
135.032685860113));
#199862=CARTESIAN_POINT('Ctrl Pts',(-50.4360583700356,1.10015556764067,
136.914599201455));
#199863=CARTESIAN_POINT('Ctrl Pts',(-50.7145059938484,5.73537772867887,
133.181501785951));
#199864=CARTESIAN_POINT('Ctrl Pts',(-50.9929536176612,5.10006794583985,
127.263927766504));
#199865=CARTESIAN_POINT('Ctrl Pts',(-51.2714012414742,-0.221955127055423,
124.599838577421));
#199866=CARTESIAN_POINT('Ctrl Pts',(-51.5498488652871,-5.34001228129766,
127.637402035479));
#199867=CARTESIAN_POINT('Ctrl Pts',(-51.8282964891,-5.5508590231301,133.585245715947));
#199868=CARTESIAN_POINT('Ctrl Pts',(-52.1067441129128,-0.660737497244709,
136.977591844792));
#199869=CARTESIAN_POINT('Ctrl Pts',(-52.3851917367258,4.8365695097872,134.697040054928));
#199870=CARTESIAN_POINT('Ctrl Pts',(-52.6636393605386,5.889305416881,128.83930603009));
#199871=CARTESIAN_POINT('Ctrl Pts',(-52.9420869843516,1.53005735442545,
124.78736117289));
#199872=CARTESIAN_POINT('Ctrl Pts',(-53.2205346081644,-4.23523866929,126.264744858582));
#199873=CARTESIAN_POINT('Ctrl Pts',(-53.4989822319774,-6.1085572588392,
131.913813654221));
#199874=CARTESIAN_POINT('Ctrl Pts',(-53.7774298557902,-2.36841014712749,
136.543349308967));
#199875=CARTESIAN_POINT('Ctrl Pts',(-54.0558774796031,3.54819018652628,
135.8990347215));
#199876=CARTESIAN_POINT('Ctrl Pts',(-54.334325103416,6.20417707748961,130.572963521183));
#199877=CARTESIAN_POINT('Ctrl Pts',(-54.6127727272289,3.15882832513996,
125.459534948064));
#199878=CARTESIAN_POINT('Ctrl Pts',(-54.8912203510417,-2.7893293406706,
125.257740055968));
#199879=CARTESIAN_POINT('Ctrl Pts',(-55.1696679748547,-6.17422960871856,
130.153018492501));
#199880=CARTESIAN_POINT('Ctrl Pts',(-55.4481155986676,-3.88531449423931,
135.646848522136));
#199881=CARTESIAN_POINT('Ctrl Pts',(-55.7265632224805,1.97401483228084,
136.690668736158));
#199882=CARTESIAN_POINT('Ctrl Pts',(-56.0050108462934,6.01932096392068,
132.32525935133));
#199883=CARTESIAN_POINT('Ctrl Pts',(-56.2834584701062,4.53316518989421,
126.562218330207));
#199884=CARTESIAN_POINT('Ctrl Pts',(-56.5619060939192,-1.11874793621411,
124.697498830995));
#199885=CARTESIAN_POINT('Ctrl Pts',(-56.840353717732,-5.74258636281662,
128.444686976857));
#199886=CARTESIAN_POINT('Ctrl Pts',(-57.118801341545,-5.08926846293066,
134.360299922064));
#199887=CARTESIAN_POINT('Ctrl Pts',(-57.3972489653578,0.240838529802063,
137.00817836373));
#199888=CARTESIAN_POINT('Ctrl Pts',(-57.6756965891708,5.34962667926312,
133.955051370017));
#199889=CARTESIAN_POINT('Ctrl Pts',(-57.9541442129836,5.54236925427356,
128.0065934946));
#199890=CARTESIAN_POINT('Ctrl Pts',(-58.2325918367966,0.641945244397073,
124.629146926667));
#199891=CARTESIAN_POINT('Ctrl Pts',(-58.5110394606094,-4.84839508431156,
126.92642006471));
#199892=CARTESIAN_POINT('Ctrl Pts',(-58.7894870844223,-5.88329718780563,
132.787331122898));
#199893=CARTESIAN_POINT('Ctrl Pts',(-59.0679347082352,-1.5117365907523,
136.825989160181));
#199894=CARTESIAN_POINT('Ctrl Pts',(-59.3463823320481,4.24903608076433,
135.331064739709));
#199895=CARTESIAN_POINT('Ctrl Pts',(-59.624829955861,6.10515217101086,129.676320372777));
#199896=CARTESIAN_POINT('Ctrl Pts',(-59.9032775796738,2.3509316693629,125.058189882977));
#199897=CARTESIAN_POINT('Ctrl Pts',(-60.1817252034868,-3.56368018703254,
125.720509582217));
#199898=CARTESIAN_POINT('Ctrl Pts',(-60.4601728272995,-6.20344404700091,
131.054640023013));
#199899=CARTESIAN_POINT('Ctrl Pts',(-60.7386204511126,-3.14254588286485,
136.158775917031));
#199900=CARTESIAN_POINT('Ctrl Pts',(-61.0170680749254,2.80619842572279,
136.342465728569));
#199901=CARTESIAN_POINT('Ctrl Pts',(-61.2955156987383,6.17618347148551,
131.436907494571));
#199902=CARTESIAN_POINT('Ctrl Pts',(-61.5739633225512,3.87055763028967,
125.950069582238));
#199903=CARTESIAN_POINT('Ctrl Pts',(-61.8524109463641,-1.9919215858902,
124.924087986069));
#199904=CARTESIAN_POINT('Ctrl Pts',(-62.130858570177,-6.02392217541635,
129.301789670958));
#199905=CARTESIAN_POINT('Ctrl Pts',(-62.4093061939898,-4.5202325706933,
135.060280651108));
#199906=CARTESIAN_POINT('Ctrl Pts',(-62.6877538178028,1.13732994085927,
136.907789033684));
#199907=CARTESIAN_POINT('Ctrl Pts',(-62.9662014416156,5.74974179841868,
133.146544870902));
#199908=CARTESIAN_POINT('Ctrl Pts',(-63.2446490654287,5.0784218337339,127.232947801366));
#199909=CARTESIAN_POINT('Ctrl Pts',(-63.5230966892413,-0.25971970145348,
124.601304636701));
#199910=CARTESIAN_POINT('Ctrl Pts',(-63.8015443130544,-5.3591915190178,
127.669966882319));
#199911=CARTESIAN_POINT('Ctrl Pts',(-64.0799919368672,-5.53382814166538,
133.618983846983));
#199912=CARTESIAN_POINT('Ctrl Pts',(-64.3584395606801,-0.623147044656387,
136.9814995658));
#199913=CARTESIAN_POINT('Ctrl Pts',(-64.636887184493,4.86017574396616,134.667526361205));
#199914=CARTESIAN_POINT('Ctrl Pts',(-64.9153348083059,5.8772344566688,128.803492564343));
#199915=CARTESIAN_POINT('Ctrl Pts',(-65.1937824321189,1.4934018225579,124.778158760555));
#199916=CARTESIAN_POINT('Ctrl Pts',(-65.4722300559316,-4.26279412974889,
126.290610067033));
#199917=CARTESIAN_POINT('Ctrl Pts',(-65.7506776797446,-6.10169052588679,
131.950977620477));
#199918=CARTESIAN_POINT('Ctrl Pts',(-66.0291253035574,-2.33343141288849,
136.5576601636));
#199919=CARTESIAN_POINT('Ctrl Pts',(-66.3075729273703,3.57913717409239,
135.877341488227));
#199920=CARTESIAN_POINT('Ctrl Pts',(-66.5860205511832,6.20265354865397,
130.535201221608));
#199921=CARTESIAN_POINT('Ctrl Pts',(-66.8644681749961,3.126234328474,125.440405290707));
#199922=CARTESIAN_POINT('Ctrl Pts',(-67.142915798809,-2.82304151453613,
125.274822261403));
#199923=CARTESIAN_POINT('Ctrl Pts',(-67.421363422622,-6.17808011893247,
130.190614848446));
#199924=CARTESIAN_POINT('Ctrl Pts',(-67.6998110464348,-3.85576491002292,
135.670409814162));
#199925=CARTESIAN_POINT('Ctrl Pts',(-67.9782586702478,2.00980988661012,
136.678543287925));
#199926=CARTESIAN_POINT('Ctrl Pts',(-68.2567062940606,6.02846758211988,
132.288589857404));
#199927=CARTESIAN_POINT('Ctrl Pts',(-68.5351539178734,4.50725807667536,
126.534702264101));
#199928=CARTESIAN_POINT('Ctrl Pts',(-68.8136015416864,-1.15590140943545,
124.704422113226));
#199929=CARTESIAN_POINT('Ctrl Pts',(-69.0920491654993,-5.75684396919829,
128.479687449276));
#199930=CARTESIAN_POINT('Ctrl Pts',(-69.3704967893121,-5.0675281587308,
134.391213860386));
#199931=CARTESIAN_POINT('Ctrl Pts',(-69.648944413125,0.278598467097045,
137.006597368867));
#199932=CARTESIAN_POINT('Ctrl Pts',(-69.9273920369379,5.36870671195437,
133.922428299012));
#199933=CARTESIAN_POINT('Ctrl Pts',(-70.2058396607509,5.52523576442926,
127.972907355982));
#199934=CARTESIAN_POINT('Ctrl Pts',(-70.4842872845636,0.604343072166899,
124.625353636165));
#199935=CARTESIAN_POINT('Ctrl Pts',(-70.7627349083767,-4.87191137961658,
126.956005470983));
#199936=CARTESIAN_POINT('Ctrl Pts',(-71.0411825321895,-5.87111727963483,
132.823107682909));
#199937=CARTESIAN_POINT('Ctrl Pts',(-71.3196301560023,-1.47505321969301,
136.835079963061));
#199938=CARTESIAN_POINT('Ctrl Pts',(-71.5980777798154,4.27651268879093,
135.305115781721));
#199939=CARTESIAN_POINT('Ctrl Pts',(-71.8765254036282,6.09817235553532,
129.639177478635));
#199940=CARTESIAN_POINT('Ctrl Pts',(-72.1549730274411,2.31590953982396,
125.043985557866));
#199941=CARTESIAN_POINT('Ctrl Pts',(-72.433420651254,-3.5945610045145,125.742296906994));
#199942=CARTESIAN_POINT('Ctrl Pts',(-72.7118682750669,-6.20180558977201,
131.092397510578));
#199943=CARTESIAN_POINT('Ctrl Pts',(-72.9903158988798,-3.109893813075,136.177806280867));
#199944=CARTESIAN_POINT('Ctrl Pts',(-73.2687635226926,2.8398584510789,136.325280993997));
#199945=CARTESIAN_POINT('Ctrl Pts',(-73.5472111465057,6.17991953348924,
131.399299593141));
#199946=CARTESIAN_POINT('Ctrl Pts',(-73.8256587703184,3.84093647047644,
125.926598338115));
#199947=CARTESIAN_POINT('Ctrl Pts',(-74.1041063941314,-2.02767956872624,
124.93632232597));
#199948=CARTESIAN_POINT('Ctrl Pts',(-74.3825540179442,-6.0329571419232,
129.338486834193));
#199949=CARTESIAN_POINT('Ctrl Pts',(-74.6610016417573,-4.49424182803428,
135.08771773742));
#199950=CARTESIAN_POINT('Ctrl Pts',(-74.9394492655699,1.17446216989917,
136.900752701129));
#199951=CARTESIAN_POINT('Ctrl Pts',(-75.217896889383,5.76389280936176,133.111501165354));
#199952=CARTESIAN_POINT('Ctrl Pts',(-75.4963445131958,5.05658753883907,
127.202100176243));
#199953=CARTESIAN_POINT('Ctrl Pts',(-75.7747921370087,-0.297474651842549,
124.603000552501));
#199954=CARTESIAN_POINT('Ctrl Pts',(-76.0532397608216,-5.37817216992523,
127.702647875272));
#199955=CARTESIAN_POINT('Ctrl Pts',(-76.3316873846344,-5.51659220216403,
133.65261768112));
#199956=CARTESIAN_POINT('Ctrl Pts',(-76.6101350084474,-0.585533501125347,
136.985178390654));
#199957=CARTESIAN_POINT('Ctrl Pts',(-76.8885826322602,4.8836018825454,134.637869516455));
#199958=CARTESIAN_POINT('Ctrl Pts',(-77.1670302560731,5.86494571337264,
128.767753241497));
#199959=CARTESIAN_POINT('Ctrl Pts',(-77.4454778798861,1.4566909521364,124.769179651345));
#199960=CARTESIAN_POINT('Ctrl Pts',(-77.7239255036988,-4.29019163080361,
126.316642534169));
#199961=CARTESIAN_POINT('Ctrl Pts',(-78.0023731275119,-6.09459769254796,
131.988099098418));
#199962=CARTESIAN_POINT('Ctrl Pts',(-78.2808207513247,-2.29836621249045,
136.571757827603));
#199963=CARTESIAN_POINT('Ctrl Pts',(-78.5592683751376,3.60995153541429,
135.855460273781));
#199964=CARTESIAN_POINT('Ctrl Pts',(-78.8377159989505,6.20090017820995,
130.497448895834));
#199965=CARTESIAN_POINT('Ctrl Pts',(-79.1161636227633,3.09352448804556,
125.421474396687));
#199966=CARTESIAN_POINT('Ctrl Pts',(-79.3946112465763,-2.85664907955992,
125.292109365916));
#199967=CARTESIAN_POINT('Ctrl Pts',(-79.6730588703891,-6.18170169811556,
130.228233946967));
#199968=CARTESIAN_POINT('Ctrl Pts',(-79.9515064942021,-3.8260724490201,
135.693790792945));
#199969=CARTESIAN_POINT('Ctrl Pts',(-80.2299541180149,2.04553046669522,
136.666200169693));
#199970=CARTESIAN_POINT('Ctrl Pts',(-80.5084017418279,6.03739081323573,
132.251865364817));
#199971=CARTESIAN_POINT('Ctrl Pts',(-80.7868493656406,4.48118394535095,
126.507344411756));
#199972=CARTESIAN_POINT('Ctrl Pts',(-81.0652969894537,-1.19301205030527,
124.711571430921));
#199973=CARTESIAN_POINT('Ctrl Pts',(-81.3437446132665,-5.77088825360962,
128.514774063314));
#199974=CARTESIAN_POINT('Ctrl Pts',(-81.6221922370794,-5.04560007541116,
134.421994886542));
#199975=CARTESIAN_POINT('Ctrl Pts',(-81.9006398608923,0.316348080823153,
137.00478654784));
#199976=CARTESIAN_POINT('Ctrl Pts',(-82.179087484705,5.38758780524389,133.889689686862));
#199977=CARTESIAN_POINT('Ctrl Pts',(-82.4575351085182,5.50789753494193,
127.939326137905));
#199978=CARTESIAN_POINT('Ctrl Pts',(-82.7359827323308,0.566718505781886,
124.621789311041));
#199979=CARTESIAN_POINT('Ctrl Pts',(-83.0144303561439,-4.89524714445407,
126.985733479472));
#199980=CARTESIAN_POINT('Ctrl Pts',(-83.2928779799568,-5.858719815054,132.858809437506));
#199981=CARTESIAN_POINT('Ctrl Pts',(-83.5713256037696,-1.43831518999427,
136.843947295418));
#199982=CARTESIAN_POINT('Ctrl Pts',(-83.8497732275826,4.30383082906709,
135.279000046597));
#199983=CARTESIAN_POINT('Ctrl Pts',(-84.1282208513953,6.09096657004034,
129.602077760783));
#199984=CARTESIAN_POINT('Ctrl Pts',(-84.4066684752085,2.28080159340614,
125.029994685571));
#199985=CARTESIAN_POINT('Ctrl Pts',(-84.685116099021,-3.6253086242162,125.764271808403));
#199986=CARTESIAN_POINT('Ctrl Pts',(-84.9635637228342,-6.19993732235617,
131.130144324829));
#199987=CARTESIAN_POINT('Ctrl Pts',(-85.242011346647,-3.07712650502686,
136.196637529698));
#199988=CARTESIAN_POINT('Ctrl Pts',(-85.5204589704598,2.87341324443482,
136.307891679689));
#199989=CARTESIAN_POINT('Ctrl Pts',(-85.7989065942728,6.18342659630218,
131.361669646028));
#199990=CARTESIAN_POINT('Ctrl Pts',(-86.0773542180856,3.81117298335027,
125.903307841269));
#199991=CARTESIAN_POINT('Ctrl Pts',(-86.3558018418987,-2.06336241514917,
124.948774108188));
#199992=CARTESIAN_POINT('Ctrl Pts',(-86.6342494657113,-6.04176855498474,
129.375238315919));
#199993=CARTESIAN_POINT('Ctrl Pts',(-86.9126970895244,-4.46808454959173,
135.114996102359));
#199994=CARTESIAN_POINT('Ctrl Pts',(-87.1911447133372,1.2115508788106,136.893490464523));
#199995=CARTESIAN_POINT('Ctrl Pts',(-87.4695923371502,5.77783023713722,
133.076371967865));
#199996=CARTESIAN_POINT('Ctrl Pts',(-87.7480399609628,5.03456587023344,
127.171386034204));
#199997=CARTESIAN_POINT('Ctrl Pts',(-88.026487584776,-0.33521857919891,
124.60492626198));
#199998=CARTESIAN_POINT('Ctrl Pts',(-88.3049352085887,-5.39695353068522,
127.735443803332));
#199999=CARTESIAN_POINT('Ctrl Pts',(-88.5833828324018,-5.49915184330967,
133.686145972045));
#200000=CARTESIAN_POINT('Ctrl Pts',(-88.8618304562145,-0.547898260434929,
136.988628183031));
#200001=CARTESIAN_POINT('Ctrl Pts',(-89.1402780800275,4.90684705746115,
134.608070619623));
#200002=CARTESIAN_POINT('Ctrl Pts',(-89.4187257038403,5.85243964235601,
128.732089385887));
#200003=CARTESIAN_POINT('Ctrl Pts',(-89.6971733276532,1.41992610349655,
124.760424177987));
#200004=CARTESIAN_POINT('Ctrl Pts',(-89.9756209514662,-4.31743015722937,
126.342841295349));
#200005=CARTESIAN_POINT('Ctrl Pts',(-90.254068575279,-6.08727902165076,
132.025176712493));
#200006=CARTESIAN_POINT('Ctrl Pts',(-90.5325161990919,-2.26321584528708,
136.585641778581));
#200007=CARTESIAN_POINT('Ctrl Pts',(-90.8109638229048,3.64063212865448,
135.833391888981));
#200008=CARTESIAN_POINT('Ctrl Pts',(-91.0894114467178,6.19891703112955,
130.459707942787));
#200009=CARTESIAN_POINT('Ctrl Pts',(-91.3678590705306,3.06070001592934,
125.402742967496));
#200010=CARTESIAN_POINT('Ctrl Pts',(-91.6463066943433,-2.89015079040179,
125.309600728926));
#200011=CARTESIAN_POINT('Ctrl Pts',(-91.9247543181566,-6.18509421206894,
130.265874394073));
#200012=CARTESIAN_POINT('Ctrl Pts',(-92.2032019419691,-3.79623821149537,
135.716990592095));
#200013=CARTESIAN_POINT('Ctrl Pts',(-92.4816495657822,2.08117524889636,
136.653639838841));
#200014=CARTESIAN_POINT('Ctrl Pts',(-92.7600971895951,6.04609032661485,
132.21508723441));
#200015=CARTESIAN_POINT('Ctrl Pts',(-93.0385448134079,4.45494376210749,
126.480145786926));
#200016=CARTESIAN_POINT('Ctrl Pts',(-93.3169924372209,-1.23007848367479,
124.718946519161));
#200017=CARTESIAN_POINT('Ctrl Pts',(-93.5954400610337,-5.78471869563455,
128.549945518824));
#200018=CARTESIAN_POINT('Ctrl Pts',(-93.8738876848466,-5.02348502552524,
134.45264185993));
#200019=CARTESIAN_POINT('Ctrl Pts',(-94.1523353086595,0.354085972155003,
137.002745967751));
#200020=CARTESIAN_POINT('Ctrl Pts',(-94.4307829324724,5.40626925948619,
133.85683674671));
#200021=CARTESIAN_POINT('Ctrl Pts',(-94.7092305562852,5.49035520828578,
127.905851084735));
#200022=CARTESIAN_POINT('Ctrl Pts',(-94.9876781800983,0.529072939433998,
124.618454083368));
#200023=CARTESIAN_POINT('Ctrl Pts',(-95.2661258039109,-4.91840151410816,
127.015602988595));
#200024=CARTESIAN_POINT('Ctrl Pts',(-95.5445734277241,-5.84610525345601,
132.894435063746));
#200025=CARTESIAN_POINT('Ctrl Pts',(-95.8230210515366,-1.40152386299717,
136.85259082867));
#200026=CARTESIAN_POINT('Ctrl Pts',(-96.10146867535,4.33098948930923,135.252718502061));
#200027=CARTESIAN_POINT('Ctrl Pts',(-96.3799162991623,6.08353508153927,
129.565022593965));
#200028=CARTESIAN_POINT('Ctrl Pts',(-96.6583639229758,2.245609131046,125.01621778453));
#200029=CARTESIAN_POINT('Ctrl Pts',(-96.9368115467883,-3.65592190677386,
125.786433472156));
#200030=CARTESIAN_POINT('Ctrl Pts',(-97.2152591706015,-6.19783931398261,
131.167879067045));
#200031=CARTESIAN_POINT('Ctrl Pts',(-97.493706794414,-3.04424517292474,
136.215268965725));
#200032=CARTESIAN_POINT('Ctrl Pts',(-97.7721544182274,2.90686156240656,
136.290298430015));
#200033=CARTESIAN_POINT('Ctrl Pts',(-98.0506020420397,6.18670452996842,
131.324019047625));
#200034=CARTESIAN_POINT('Ctrl Pts',(-98.3290496658531,3.78126827180747,
125.880198954735));
#200035=CARTESIAN_POINT('Ctrl Pts',(-98.6074972896656,-2.09896880291958,
124.961442871316));
#200036=CARTESIAN_POINT('Ctrl Pts',(-98.8859449134787,-6.05035608809047,
129.412042754299));
#200037=CARTESIAN_POINT('Ctrl Pts',(-99.1643925372916,-4.44176170463296,
135.142114735114));
#200038=CARTESIAN_POINT('Ctrl Pts',(-99.4428401611044,1.24859469325925,
136.886002592972));
#200039=CARTESIAN_POINT('Ctrl Pts',(-99.7212877849174,5.79155356528836,
133.041158580159));
#200040=CARTESIAN_POINT('Ctrl Pts',(-99.9997354087301,5.01235764393804,
127.140806513377));
#200041=CARTESIAN_POINT('Ctrl Pts',(-100.278183032543,-0.37295008490757,
124.607081693777));
#200042=CARTESIAN_POINT('Ctrl Pts',(-100.556630656356,-5.41553490534739,
127.768353451233));
#200043=CARTESIAN_POINT('Ctrl Pts',(-100.835078280169,-5.48150771136145,
133.719567477352));
#200044=CARTESIAN_POINT('Ctrl Pts',(-101.113525903981,-0.510242717172956,
136.9918488151));
#200045=CARTESIAN_POINT('Ctrl Pts',(-101.391973527794,4.92991040735466,
134.578130774917));
#200046=CARTESIAN_POINT('Ctrl Pts',(-101.670421151607,5.83971670703623,
128.696502319049));
#200047=CARTESIAN_POINT('Ctrl Pts',(-101.94886877542,1.38310863897239,124.751892664915));
#200048=CARTESIAN_POINT('Ctrl Pts',(-102.227316399233,-4.34450869969331,
126.36920537977));
#200049=CARTESIAN_POINT('Ctrl Pts',(-102.505764023046,-6.07973478439049,
132.062209088779));
#200050=CARTESIAN_POINT('Ctrl Pts',(-102.784211646859,-2.22798161378826,
136.599311502058));
#200051=CARTESIAN_POINT('Ctrl Pts',(-103.062659270672,3.6711778169323,135.811137151577));
#200052=CARTESIAN_POINT('Ctrl Pts',(-103.341106894485,6.19670418089893,
130.42197976097));
#200053=CARTESIAN_POINT('Ctrl Pts',(-103.619554518298,3.02776212844844,
125.384211697232));
#200054=CARTESIAN_POINT('Ctrl Pts',(-103.89800214211,-2.92354540564323,
125.327295702285));
#200055=CARTESIAN_POINT('Ctrl Pts',(-104.176449765923,-6.18825753508174,
130.303534794984));
#200056=CARTESIAN_POINT('Ctrl Pts',(-104.454897389736,-3.76626330296762,
135.740008351935));
#200057=CARTESIAN_POINT('Ctrl Pts',(-104.733345013549,2.1167429123828,136.640862760796));
#200058=CARTESIAN_POINT('Ctrl Pts',(-105.011792637362,6.05456579989334,
132.17825682901));
#200059=CARTESIAN_POINT('Ctrl Pts',(-105.290240261175,4.42853849928509,
126.453107397468));
#200060=CARTESIAN_POINT('Ctrl Pts',(-105.568687884988,-1.26709933603374,
124.726547104658));
#200061=CARTESIAN_POINT('Ctrl Pts',(-105.847135508801,-5.79833478278087,
128.585200512514));
#200062=CARTESIAN_POINT('Ctrl Pts',(-106.125583132613,-5.00118382855433,
134.483153644914));
#200063=CARTESIAN_POINT('Ctrl Pts',(-106.404030756427,0.391810742700936,
137.000475704212));
#200064=CARTESIAN_POINT('Ctrl Pts',(-106.682478380239,5.42475038243292,
133.823870695931));
#200065=CARTESIAN_POINT('Ctrl Pts',(-106.960926004052,5.47260943449832,
127.872483436902));
#200066=CARTESIAN_POINT('Ctrl Pts',(-107.239373627865,0.491407768093767,
124.615348076738));
#200067=CARTESIAN_POINT('Ctrl Pts',(-107.517821251678,-4.94137363058539,
127.045612891524));
#200068=CARTESIAN_POINT('Ctrl Pts',(-107.796268875491,-5.83327406227795,
132.929983241508));
#200069=CARTESIAN_POINT('Ctrl Pts',(-108.074716499304,-1.36468060201792,
136.861010242526));
#200070=CARTESIAN_POINT('Ctrl Pts',(-108.353164123117,4.3579876631431,135.22627212199));
#200071=CARTESIAN_POINT('Ctrl Pts',(-108.631611746929,6.07587816540856,
129.528013351273));
#200072=CARTESIAN_POINT('Ctrl Pts',(-108.910059370743,2.21033345681367,
125.00265536525));
#200073=CARTESIAN_POINT('Ctrl Pts',(-109.188506994555,-3.68639971780079,
125.808781077045));
#200074=CARTESIAN_POINT('Ctrl Pts',(-109.466954618368,-6.19551164239422,
131.205600338952));
#200075=CARTESIAN_POINT('Ctrl Pts',(-109.745402242181,-3.01125103519769,
136.233699898554));
#200076=CARTESIAN_POINT('Ctrl Pts',(-110.023849865994,2.94020216555433,
136.272501896897));
#200077=CARTESIAN_POINT('Ctrl Pts',(-110.302297489807,6.18975321302316,
131.286349193086));
#200078=CARTESIAN_POINT('Ctrl Pts',(-110.58074511362,3.75122344397827,125.857272534824));
#200079=CARTESIAN_POINT('Ctrl Pts',(-110.859192737433,-2.13449741262907,
124.974328145912));
#200080=CARTESIAN_POINT('Ctrl Pts',(-111.137640361246,-6.05871942302636,
129.44889878553));
#200081=CARTESIAN_POINT('Ctrl Pts',(-111.416087985058,-4.41527426856075,
135.169072630797));
#200082=CARTESIAN_POINT('Ctrl Pts',(-111.694535608871,1.28559224057236,
136.878289363941));
#200083=CARTESIAN_POINT('Ctrl Pts',(-111.972983232684,5.8050622852923,133.005862307081));
#200084=CARTESIAN_POINT('Ctrl Pts',(-112.251430856497,4.9899636828869,127.110362746893));
#200085=CARTESIAN_POINT('Ctrl Pts',(-112.52987848031,-0.410667770813077,
124.609466768025));
#200086=CARTESIAN_POINT('Ctrl Pts',(-112.808326104123,-5.43391560537209,
127.801375599495));
#200087=CARTESIAN_POINT('Ctrl Pts',(-113.086773727936,-5.46366046012913,
133.752880958598));
#200088=CARTESIAN_POINT('Ctrl Pts',(-113.365221351749,-0.472568266679477,
136.994840167519));
#200089=CARTESIAN_POINT('Ctrl Pts',(-113.643668975562,4.95279107760506,
134.548051091771));
#200090=CARTESIAN_POINT('Ctrl Pts',(-113.922116599375,5.8267773788663,128.660993359675));
#200091=CARTESIAN_POINT('Ctrl Pts',(-114.200564223187,1.34623992284899,
124.74358542827));
#200092=CARTESIAN_POINT('Ctrl Pts',(-114.479011847001,-4.37142625478972,
126.395733810498));
#200093=CARTESIAN_POINT('Ctrl Pts',(-114.757459470813,-6.07196526032194,
132.099194855029));
#200094=CARTESIAN_POINT('Ctrl Pts',(-115.035907094626,-2.19266482361144,
136.612766491501));
#200095=CARTESIAN_POINT('Ctrl Pts',(-115.314354718439,3.70158746836604,
135.788696886227));
#200096=CARTESIAN_POINT('Ctrl Pts',(-115.592802342252,6.19426170951602,
130.384265748418));
#200097=CARTESIAN_POINT('Ctrl Pts',(-115.871249966065,2.99471204612843,
125.36588127258));
#200098=CARTESIAN_POINT('Ctrl Pts',(-116.149697589878,-2.95683168783455,
125.345193630298));
#200099=CARTESIAN_POINT('Ctrl Pts',(-116.428145213691,-6.19119154993583,
130.34121375418));
#200100=CARTESIAN_POINT('Ctrl Pts',(-116.706592837503,-3.73614883416816,
135.762843219532));
#200101=CARTESIAN_POINT('Ctrl Pts',(-116.985040461316,2.1522321391827,136.627869409019));
#200102=CARTESIAN_POINT('Ctrl Pts',(-117.263488085129,6.06281691900968,
132.14137551338));
#200103=CARTESIAN_POINT('Ctrl Pts',(-117.541935708942,4.40196913533955,
126.426230245297));
#200104=CARTESIAN_POINT('Ctrl Pts',(-117.820383332755,-1.30407323556081,
124.73437290577));
#200105=CARTESIAN_POINT('Ctrl Pts',(-118.098830956568,-5.81173601049948,
128.620537737998));
#200106=CARTESIAN_POINT('Ctrl Pts',(-118.377278580381,-4.97869731087745,
134.51352911087));
#200107=CARTESIAN_POINT('Ctrl Pts',(-118.655726204194,0.429520994555717,
136.997975841351));
#200108=CARTESIAN_POINT('Ctrl Pts',(-118.934173828006,5.44303048925927,
133.790792756097));
#200109=CARTESIAN_POINT('Ctrl Pts',(-119.21262145182,5.45466087115571,127.839224430854));
#200110=CARTESIAN_POINT('Ctrl Pts',(-119.491069075632,0.453724387457947,
124.612471406243));
#200111=CARTESIAN_POINT('Ctrl Pts',(-119.769516699445,-4.96416264264509,
127.075762076232));
#200112=CARTESIAN_POINT('Ctrl Pts',(-120.047964323258,-5.82022671698453,
132.965452653541));
#200113=CARTESIAN_POINT('Ctrl Pts',(-120.326411947071,-1.32778677229758,
136.869205225004));
#200114=CARTESIAN_POINT('Ctrl Pts',(-120.604859570884,4.38482435014149,
135.199661886361));
#200115=CARTESIAN_POINT('Ctrl Pts',(-120.883307194697,6.06799610537801,
129.491051404098));
#200116=CARTESIAN_POINT('Ctrl Pts',(-121.16175481851,2.17497587786225,124.989307930291));
#200117=CARTESIAN_POINT('Ctrl Pts',(-121.440202442323,-3.71674092793051,
125.831313794972));
#200118=CARTESIAN_POINT('Ctrl Pts',(-121.718650066136,-6.19295439384353,
131.243306742772));
#200119=CARTESIAN_POINT('Ctrl Pts',(-121.997097689948,-2.97814531445616,
136.251929645219));
#200120=CARTESIAN_POINT('Ctrl Pts',(-122.275545313761,2.97343381842962,
136.254502739794));
#200121=CARTESIAN_POINT('Ctrl Pts',(-122.553992937574,6.19257253249627,
131.248661478285));
#200122=CARTESIAN_POINT('Ctrl Pts',(-122.832440561387,3.72103961318487,
125.83452943108));
#200123=CARTESIAN_POINT('Ctrl Pts',(-123.1108881852,-2.16994692775201,124.987429454503));
#200124=CARTESIAN_POINT('Ctrl Pts',(-123.389335809013,-6.06685824988591,
129.485805043896));
#200125=CARTESIAN_POINT('Ctrl Pts',(-123.667783432826,-4.38862322287681,
135.19586879047));
#200126=CARTESIAN_POINT('Ctrl Pts',(-123.946231056639,1.32254214979223,
136.870351063246));
#200127=CARTESIAN_POINT('Ctrl Pts',(-124.224678680451,5.81835589657845,
132.97048445655));
#200128=CARTESIAN_POINT('Ctrl Pts',(-124.503126304264,4.96738481689638,
127.080055862859));
#200129=CARTESIAN_POINT('Ctrl Pts',(-124.781573928077,-0.448370239273912,
124.612081396343));
#200130=CARTESIAN_POINT('Ctrl Pts',(-125.06002155189,-5.4520949496557,127.834509024472));
#200131=CARTESIAN_POINT('Ctrl Pts',(-125.338469175703,-5.44561075094924,
133.786085181339));
#200132=CARTESIAN_POINT('Ctrl Pts',(-125.616916799516,-0.434876304995071,
136.997602129441));
#200133=CARTESIAN_POINT('Ctrl Pts',(-125.895364423329,4.97548822036069,
134.517832684797));
#200134=CARTESIAN_POINT('Ctrl Pts',(-126.173812047142,5.8136221373178,128.625563823564));
#200135=CARTESIAN_POINT('Ctrl Pts',(-126.452259670955,1.30932132131015,
124.735502775877));
#200136=CARTESIAN_POINT('Ctrl Pts',(-126.730707294768,-4.39818182507867,
126.422425604514));
#200137=CARTESIAN_POINT('Ctrl Pts',(-127.00915491858,-6.0639707373477,132.136132640718));
#200138=CARTESIAN_POINT('Ctrl Pts',(-127.287602542393,-2.15726678343353,
136.626006248326));
#200139=CARTESIAN_POINT('Ctrl Pts',(-127.566050166206,3.73185995611441,
135.766071924465));
#200140=CARTESIAN_POINT('Ctrl Pts',(-127.844497790019,6.19158970748781,
130.346567302635));
#200141=CARTESIAN_POINT('Ctrl Pts',(-128.122945413832,2.96155099365221,
125.34775237278));
#200142=CARTESIAN_POINT('Ctrl Pts',(-128.401393037645,-2.99000840354028,
125.363293849751));
#200143=CARTESIAN_POINT('Ctrl Pts',(-128.679840661458,-6.19389614791022,
130.378909875453));
#200144=CARTESIAN_POINT('Ctrl Pts',(-128.958288285271,-3.70589592099968,
135.785494348734));
#200145=CARTESIAN_POINT('Ctrl Pts',(-129.236735909083,2.18764161422919,
136.614660264981));
#200146=CARTESIAN_POINT('Ctrl Pts',(-129.515183532897,6.07084337821547,
132.104444654172));
#200147=CARTESIAN_POINT('Ctrl Pts',(-129.793631156709,4.37523665480886,
126.399515326358));
#200148=CARTESIAN_POINT('Ctrl Pts',(-130.072078780522,-1.34099881217456,
124.742423632508));
#200149=CARTESIAN_POINT('Ctrl Pts',(-130.350526404335,-5.82492188220296,
128.655955885842));
#200150=CARTESIAN_POINT('Ctrl Pts',(-130.628974028148,-4.95602630574081,
134.543767132223));
#200151=CARTESIAN_POINT('Ctrl Pts',(-130.907421651961,0.467215330352083,
136.995246471799));
#200152=CARTESIAN_POINT('Ctrl Pts',(-131.185869275774,5.46110890258918,
133.757604152921));
#200153=CARTESIAN_POINT('Ctrl Pts',(-131.464316899587,5.43651018334856,
127.80607529902));
#200154=CARTESIAN_POINT('Ctrl Pts',(-131.742764523399,0.416024193898128,
124.60982417848));
#200155=CARTESIAN_POINT('Ctrl Pts',(-132.021212147213,-4.98676770583297,
127.106049425532));
#200156=CARTESIAN_POINT('Ctrl Pts',(-132.299659771025,-5.80696370104951,
133.000841985516));
#200157=CARTESIAN_POINT('Ctrl Pts',(-132.578107394838,-1.2908437409496,
136.877175472434));
#200158=CARTESIAN_POINT('Ctrl Pts',(-132.856555018651,4.41149855586104,
135.172888781227));
#200159=CARTESIAN_POINT('Ctrl Pts',(-133.135002642464,6.05988919352027,
129.454138122079));
#200160=CARTESIAN_POINT('Ctrl Pts',(-133.413450266277,2.13953770437982,
124.976175974248));
#200161=CARTESIAN_POINT('Ctrl Pts',(-133.69189789009,-3.74694441285829,
125.854030790976));
#200162=CARTESIAN_POINT('Ctrl Pts',(-133.970345513903,-6.19016766309031,
131.280996881284));
#200163=CARTESIAN_POINT('Ctrl Pts',(-134.248793137716,-2.94492923744478,
136.269957530209));
#200164=CARTESIAN_POINT('Ctrl Pts',(-134.527240761528,3.00655528962129,
136.236301625668));
#200165=CARTESIAN_POINT('Ctrl Pts',(-134.805688385342,6.19516238391663,
131.210957299752));
#200166=CARTESIAN_POINT('Ctrl Pts',(-135.084136009154,3.69071789790064,
125.811970486258));
#200167=CARTESIAN_POINT('Ctrl Pts',(-135.362583632967,-2.2053160346932,
125.000746311619));
#200168=CARTESIAN_POINT('Ctrl Pts',(-135.64103125678,-6.07477226708194,
129.522760161825));
#200169=CARTESIAN_POINT('Ctrl Pts',(-135.919478880593,-4.36180955514542,
135.222502221193));
#200170=CARTESIAN_POINT('Ctrl Pts',(-136.197926504406,1.35944305172635,
136.862187985044));
#200171=CARTESIAN_POINT('Ctrl Pts',(-136.476374128219,5.83143390654715,
132.935026339502));
#200172=CARTESIAN_POINT('Ctrl Pts',(-136.754821752032,4.9446218826347,127.049886984307));
#200173=CARTESIAN_POINT('Ctrl Pts',(-137.033269375845,-0.486056093210629,
124.614925481843));
#200174=CARTESIAN_POINT('Ctrl Pts',(-137.311716999657,-5.47007226455594,
127.867752498391));
#200175=CARTESIAN_POINT('Ctrl Pts',(-137.59016462347,-5.42735925266033,
133.819178915179));
#200176=CARTESIAN_POINT('Ctrl Pts',(-137.868612247283,-0.397168228809268,
137.000134598521));
#200177=CARTESIAN_POINT('Ctrl Pts',(-138.147059871096,4.99800099457058,
134.487476673751));
#200178=CARTESIAN_POINT('Ctrl Pts',(-138.425507494909,5.80025146986304,
128.590215023569));
#200179=CARTESIAN_POINT('Ctrl Pts',(-138.703955118722,1.27235420238826,
124.727645007244));
#200180=CARTESIAN_POINT('Ctrl Pts',(-138.982402742535,-4.42477441912264,
126.449279772744));
#200181=CARTESIAN_POINT('Ctrl Pts',(-139.260850366348,-6.05575151170779,
132.173021077107));
#200182=CARTESIAN_POINT('Ctrl Pts',(-139.539297990161,-2.12178880494131,
136.639030281933));
#200183=CARTESIAN_POINT('Ctrl Pts',(-139.817745613973,3.76199415842019,
135.743263104665));
#200184=CARTESIAN_POINT('Ctrl Pts',(-140.096193237787,6.18868827382574,
130.308885820552));
#200185=CARTESIAN_POINT('Ctrl Pts',(-140.374640861599,2.92828019981485,
125.329825669606));
#200186=CARTESIAN_POINT('Ctrl Pts',(-140.653088485412,-3.02307432338508,
125.381595689934));
#200187=CARTESIAN_POINT('Ctrl Pts',(-140.931536109225,-6.19637122878504,
130.416621761961));
#200188=CARTESIAN_POINT('Ctrl Pts',(-141.209983733038,-3.675505684495,135.807960900193));
#200189=CARTESIAN_POINT('Ctrl Pts',(-141.488431356851,2.22297002541115,
136.601235818153));
#200190=CARTESIAN_POINT('Ctrl Pts',(-141.766878980664,6.07864488008735,
132.06746561987));
#200191=CARTESIAN_POINT('Ctrl Pts',(-142.045326604476,4.34834204827492,
126.372963630579));
#200192=CARTESIAN_POINT('Ctrl Pts',(-142.32377422829,-1.3778746975837,124.750698986551));
#200193=CARTESIAN_POINT('Ctrl Pts',(-142.602221852102,-5.83789190928377,
128.691453643612));
#200194=CARTESIAN_POINT('Ctrl Pts',(-142.880669475915,-4.93317165322728,
134.573866588494));
#200195=CARTESIAN_POINT('Ctrl Pts',(-143.159117099728,0.504892353312588,
136.992287696695));
#200196=CARTESIAN_POINT('Ctrl Pts',(-143.437564723541,5.47898495252035,
133.72430611622));
#200197=CARTESIAN_POINT('Ctrl Pts',(-143.716012347354,5.4181580436573,127.77303726975));
#200198=CARTESIAN_POINT('Ctrl Pts',(-143.994459971167,0.378308584408798,
124.607406491544));
#200199=CARTESIAN_POINT('Ctrl Pts',(-144.27290759498,-5.00918798250961,
127.136473817112));
#200200=CARTESIAN_POINT('Ctrl Pts',(-144.551355218793,-5.79348550593904,
133.036149926065));
#200201=CARTESIAN_POINT('Ctrl Pts',(-144.829802842605,-1.2538528769121,
136.884920689477));
#200202=CARTESIAN_POINT('Ctrl Pts',(-145.108250466418,4.43800929187927,
135.145953798675));
#200203=CARTESIAN_POINT('Ctrl Pts',(-145.386698090231,6.05155773023994,
129.417274873051));
#200204=CARTESIAN_POINT('Ctrl Pts',(-145.665145714044,2.10402024954095,
124.963259983731));
#200205=CARTESIAN_POINT('Ctrl Pts',(-145.943593337857,-3.77700905338292,
125.876931223274));
#200206=CARTESIAN_POINT('Ctrl Pts',(-146.22204096167,-6.18715155339789,
131.318669357863));
#200207=CARTESIAN_POINT('Ctrl Pts',(-146.500488585483,-2.9116040349975,
136.287782885497));
#200208=CARTESIAN_POINT('Ctrl Pts',(-146.778936209295,3.03956535180104,
136.217899228972));
#200209=CARTESIAN_POINT('Ctrl Pts',(-147.057383833109,6.19752267131684,
131.173238054629));
#200210=CARTESIAN_POINT('Ctrl Pts',(-147.335831456921,3.66025942170698,
125.789596536289));
#200211=CARTESIAN_POINT('Ctrl Pts',(-147.614279080735,-2.24060342283806,
125.014278223797));
#200212=CARTESIAN_POINT('Ctrl Pts',(-147.892726704547,-6.08246118135759,
129.559762769929));
#200213=CARTESIAN_POINT('Ctrl Pts',(-148.17117432836,-4.33483425895693,
135.248971936054));
#200214=CARTESIAN_POINT('Ctrl Pts',(-148.449621952173,1.39629357899829,
136.853800431821));
#200215=CARTESIAN_POINT('Ctrl Pts',(-148.728069575986,5.84429583058792,
132.899489269852));
#200216=CARTESIAN_POINT('Ctrl Pts',(-149.006517199799,4.9216757235908,127.019857229157));
#200217=CARTESIAN_POINT('Ctrl Pts',(-149.284964823612,-0.52372393616008,
124.617998919139));
#200218=CARTESIAN_POINT('Ctrl Pts',(-149.563412447425,-5.48784688391679,
127.901104789406));
#200219=CARTESIAN_POINT('Ctrl Pts',(-149.841860071237,-5.40890664157841,
133.852160933818));
#200220=CARTESIAN_POINT('Ctrl Pts',(-150.12030769505,-0.359445435409253,
137.002437480918));
#200221=CARTESIAN_POINT('Ctrl Pts',(-150.398755318863,5.02032856601553,
134.456984183485));
#200222=CARTESIAN_POINT('Ctrl Pts',(-150.677202942676,5.78666587195703,
128.554948269553));
#200223=CARTESIAN_POINT('Ctrl Pts',(-150.955650566489,1.23533993591347,
124.720012413542));
#200224=CARTESIAN_POINT('Ctrl Pts',(-151.234098190302,-4.45120305152329,
126.476295320094));
#200225=CARTESIAN_POINT('Ctrl Pts',(-151.512545814115,-6.0473078879686,
132.209858797279));
#200226=CARTESIAN_POINT('Ctrl Pts',(-151.790993437928,-2.08623220278462,
136.651838109709));
#200227=CARTESIAN_POINT('Ctrl Pts',(-152.069441061741,3.79198895864895,
135.720271272016));
#200228=CARTESIAN_POINT('Ctrl Pts',(-152.347888685554,6.18555751604382,
130.27122269847));
#200229=CARTESIAN_POINT('Ctrl Pts',(-152.626336309366,2.89490089747778,
125.312101827337));
#200230=CARTESIAN_POINT('Ctrl Pts',(-152.904783933179,-3.05602822209906,
125.400098472666));
#200231=CARTESIAN_POINT('Ctrl Pts',(-153.183231556992,-6.19861670084527,
130.454348016274));
#200232=CARTESIAN_POINT('Ctrl Pts',(-153.461679180805,-3.64497925077551,
135.830242041403));
#200233=CARTESIAN_POINT('Ctrl Pts',(-153.740126804618,2.25821606362131,
136.587596565983));
#200234=CARTESIAN_POINT('Ctrl Pts',(-154.018574428431,6.08622113553776,
132.030439780749));
#200235=CARTESIAN_POINT('Ctrl Pts',(-154.297022052244,4.32128631232727,
126.346576141847));
#200236=CARTESIAN_POINT('Ctrl Pts',(-154.575469676057,-1.41469952533967,
124.759198661251));
#200237=CARTESIAN_POINT('Ctrl Pts',(-154.85391729987,-5.85064561113321,
128.727029695929));
#200238=CARTESIAN_POINT('Ctrl Pts',(-155.132364923682,-4.9101342002235,
134.603826364333));
#200239=CARTESIAN_POINT('Ctrl Pts',(-155.410812547495,0.542550667301237,
136.989099625678));
#200240=CARTESIAN_POINT('Ctrl Pts',(-155.689260171308,5.49665797664923,
133.690899879866));
#200241=CARTESIAN_POINT('Ctrl Pts',(-155.967707795121,5.39960513212718,
127.740111567281));
#200242=CARTESIAN_POINT('Ctrl Pts',(-156.246155418934,0.340578956555753,
124.605218435021));
#200243=CARTESIAN_POINT('Ctrl Pts',(-156.524603042747,-5.03142264188343,
127.167034123586));
#200244=CARTESIAN_POINT('Ctrl Pts',(-156.80305066656,-5.77979263109261,
133.071375166841));
#200245=CARTESIAN_POINT('Ctrl Pts',(-157.081498290373,-1.21681555089514,
136.89244058913));
#200246=CARTESIAN_POINT('Ctrl Pts',(-157.359945914186,4.46435557583064,
135.118857936792));
#200247=CARTESIAN_POINT('Ctrl Pts',(-157.638393537999,6.04300202426259,
129.380463022997));
#200248=CARTESIAN_POINT('Ctrl Pts',(-157.916841161811,2.06842482945845,
124.950560437346));
#200249=CARTESIAN_POINT('Ctrl Pts',(-158.195288785624,-3.80693373544809,
125.900014243279));
#200250=CARTESIAN_POINT('Ctrl Pts',(-158.473736409437,-6.18390617652933,
131.356322776543));
#200251=CARTESIAN_POINT('Ctrl Pts',(-158.75218403325,-2.87817094199197,
136.305405050556));
#200252=CARTESIAN_POINT('Ctrl Pts',(-159.030631657063,3.07246278176887,
136.199296231612));
#200253=CARTESIAN_POINT('Ctrl Pts',(-159.309079280876,6.19965330723533,
131.135505140616));
#200254=CARTESIAN_POINT('Ctrl Pts',(-159.587526904689,3.62966531325439,
125.767408410247));
#200255=CARTESIAN_POINT('Ctrl Pts',(-159.865974528502,-2.27580778459908,
125.028024689608));
#200256=CARTESIAN_POINT('Ctrl Pts',(-160.144422152314,-6.08992470779737,
129.596811497064));
#200257=CARTESIAN_POINT('Ctrl Pts',(-160.422869776128,-4.3076983338908,
135.275276954208));
#200258=CARTESIAN_POINT('Ctrl Pts',(-160.70131739994,1.43309236609815,136.845188714382));
#200259=CARTESIAN_POINT('Ctrl Pts',(-160.979765023753,5.85694119209746,
132.863874564441));
#200260=CARTESIAN_POINT('Ctrl Pts',(-161.258212647566,4.89854719004298,
126.989967710171));
#200261=CARTESIAN_POINT('Ctrl Pts',(-161.536660271379,-0.561372372326459,
124.621301594343));
#200262=CARTESIAN_POINT('Ctrl Pts',(-161.815107895192,-5.50541814909322,
127.934564661631));
#200263=CARTESIAN_POINT('Ctrl Pts',(-162.093555519005,-5.39025360147175,
133.885030015096));
#200264=CARTESIAN_POINT('Ctrl Pts',(-162.372003142818,-0.32170932262588,
137.004510691297));
#200265=CARTESIAN_POINT('Ctrl Pts',(-162.650450766631,5.04247010733932,
134.426356343909));
#200266=CARTESIAN_POINT('Ctrl Pts',(-162.928898390443,5.77286584701905,
128.519764868338));
#200267=CARTESIAN_POINT('Ctrl Pts',(-163.207346014257,1.19827989346308,
124.712605277602));
#200268=CARTESIAN_POINT('Ctrl Pts',(-163.485793638069,-4.47746674295796,
126.503471245498));
#200269=CARTESIAN_POINT('Ctrl Pts',(-163.764241261882,-6.03864017901171,
132.246644436198));
#200270=CARTESIAN_POINT('Ctrl Pts',(-164.042688885695,-2.05059829452646,
136.664429257056));
#200271=CARTESIAN_POINT('Ctrl Pts',(-164.321136509508,3.82184324533235,
135.697097278492));
#200272=CARTESIAN_POINT('Ctrl Pts',(-164.599584133321,6.18219755015336,
130.23357933201));
#200273=CARTESIAN_POINT('Ctrl Pts',(-164.878031757134,2.86141432352365,
125.294581502737));
#200274=CARTESIAN_POINT('Ctrl Pts',(-165.156479380946,-3.08886887856293,
125.418801512319));
#200275=CARTESIAN_POINT('Ctrl Pts',(-165.43492700476,-6.20063248088431,
130.492087240433));
#200276=CARTESIAN_POINT('Ctrl Pts',(-165.713374628572,-3.61431775100944,
135.85233694673));
#200277=CARTESIAN_POINT('Ctrl Pts',(-165.991822252385,2.2933784228048,136.573743013877));
#200278=CARTESIAN_POINT('Ctrl Pts',(-166.270269876198,6.09357186382579,
131.993368508814));
#200279=CARTESIAN_POINT('Ctrl Pts',(-166.548717500011,4.2940704495262,126.320353837957));
#200280=CARTESIAN_POINT('Ctrl Pts',(-166.827165123824,-1.45147193088449,
124.767922341652));
#200281=CARTESIAN_POINT('Ctrl Pts',(-167.105612747637,-5.86318251515793,
128.762682724506));
#200282=CARTESIAN_POINT('Ctrl Pts',(-167.38406037145,-4.88691480039125,
134.633645349573));
#200283=CARTESIAN_POINT('Ctrl Pts',(-167.662507995262,0.580188876875391,
136.985682376883));
#200284=CARTESIAN_POINT('Ctrl Pts',(-167.940955619076,5.51412732009539,
133.657386681736));
#200285=CARTESIAN_POINT('Ctrl Pts',(-168.219403242888,5.38085213624319,
127.707299411689));
#200286=CARTESIAN_POINT('Ctrl Pts',(-168.497850866701,0.302836708424229,
124.60326008999));
#200287=CARTESIAN_POINT('Ctrl Pts',(-168.776298490514,-5.05347086004094,
127.197729212531));
#200288=CARTESIAN_POINT('Ctrl Pts',(-169.054746114327,-5.7658855839047,
133.106516402559));
#200289=CARTESIAN_POINT('Ctrl Pts',(-169.33319373814,-1.17973313533045,
136.899734892741));
#200290=CARTESIAN_POINT('Ctrl Pts',(-169.611641361953,4.49053643144484,
135.091602199623));
#200291=CARTESIAN_POINT('Ctrl Pts',(-169.890088985766,6.03422239262278,
129.34370393599));
#200292=CARTESIAN_POINT('Ctrl Pts',(-170.168536609579,2.03275276313275,
124.938077805679));
#200293=CARTESIAN_POINT('Ctrl Pts',(-170.446984233392,-3.83671735018369,
125.923278995643));
#200294=CARTESIAN_POINT('Ctrl Pts',(-170.725431857205,-6.18043165274327,
131.393955742061));
#200295=CARTESIAN_POINT('Ctrl Pts',(-171.003879481017,-2.84463119730373,
136.32282337239));
#200296=CARTESIAN_POINT('Ctrl Pts',(-171.282327104831,3.10524636049842,
136.180493322929));
#200297=CARTESIAN_POINT('Ctrl Pts',(-171.560774728643,6.20155421272058,
131.097759955922));
#200298=CARTESIAN_POINT('Ctrl Pts',(-171.839222352457,3.59893670621881,
125.745406930321));
#200299=CARTESIAN_POINT('Ctrl Pts',(-172.117669976268,-2.31092781546573,
125.04198519967));
#200300=CARTESIAN_POINT('Ctrl Pts',(-172.396117600082,-6.09716256983718,
129.633904970377));
#200301=CARTESIAN_POINT('Ctrl Pts',(-172.674565223895,-4.2804027854792,
135.301416300912));
#200302=CARTESIAN_POINT('Ctrl Pts',(-172.953012847708,1.469838049433,136.836353151837));
#200303=CARTESIAN_POINT('Ctrl Pts',(-173.23146047152,5.86936952249723,132.828183542982));
#200304=CARTESIAN_POINT('Ctrl Pts',(-173.509908095334,4.8752371390276,126.960219534917));
#200305=CARTESIAN_POINT('Ctrl Pts',(-173.788355719146,-0.599000006633149,
124.624833385073));
#200306=CARTESIAN_POINT('Ctrl Pts',(-174.06680334296,-5.5227854089755,127.968130875202));
#200307=CARTESIAN_POINT('Ctrl Pts',(-174.345250966772,-5.37140082353563,
133.917784941036));
#200308=CARTESIAN_POINT('Ctrl Pts',(-174.623698590585,-0.283961288785237,
137.006354152836));
#200309=CARTESIAN_POINT('Ctrl Pts',(-174.902146214398,5.06442479807889,
134.39559428995));
#200310=CARTESIAN_POINT('Ctrl Pts',(-175.18059383821,5.75885190641417,128.484666123661));
#200311=CARTESIAN_POINT('Ctrl Pts',(-175.459041462024,1.16117544831056,
124.705423873895));
#200312=CARTESIAN_POINT('Ctrl Pts',(-175.737489085836,-4.50356452021585,
126.530806541938));
#200313=CARTESIAN_POINT('Ctrl Pts',(-176.01593670965,-6.02974870602229,
132.28337663076));
#200314=CARTESIAN_POINT('Ctrl Pts',(-176.294384333462,-2.01488840059438,
136.676803257405));
#200315=CARTESIAN_POINT('Ctrl Pts',(-176.572831957276,3.85155591220881,
135.67374198281));
#200316=CARTESIAN_POINT('Ctrl Pts',(-176.851279581088,6.17860850065921,
130.195957116059));
#200317=CARTESIAN_POINT('Ctrl Pts',(-177.129727204901,2.82782171880919,
125.277265345029));
#200318=CARTESIAN_POINT('Ctrl Pts',(-177.408174828714,-3.12159507585506,
125.437704115845));
#200319=CARTESIAN_POINT('Ctrl Pts',(-177.686622452527,-6.20241849420629,
130.529838035997));
#200320=CARTESIAN_POINT('Ctrl Pts',(-177.965070076339,-3.58352232136993,
135.874244797437));
#200321=CARTESIAN_POINT('Ctrl Pts',(-178.243517700153,2.32845580000743,
136.559675675186));
#200322=CARTESIAN_POINT('Ctrl Pts',(-178.521965323965,6.10069679256748,
131.956253177754));
#200323=CARTESIAN_POINT('Ctrl Pts',(-178.800412947778,4.26669546836545,
126.294297690589));
#200324=CARTESIAN_POINT('Ctrl Pts',(-179.078860571591,-1.48819055160311,
124.776869704492));
#200325=CARTESIAN_POINT('Ctrl Pts',(-179.357308195404,-5.8755021567984,
128.798411408209));
#200326=CARTESIAN_POINT('Ctrl Pts',(-179.635755819217,-4.86351431413387,
134.663322439258));
#200327=CARTESIAN_POINT('Ctrl Pts',(-179.91420344303,0.617805587336893,
136.982036076937));
#200328=CARTESIAN_POINT('Ctrl Pts',(-180.192651066843,5.53139233552561,
133.623767763677));
#200329=CARTESIAN_POINT('Ctrl Pts',(-180.471098690656,5.36189975090491,
127.674602018838));
#200330=CARTESIAN_POINT('Ctrl Pts',(-180.749546314469,0.265083238567079,
124.601531529021));
#200331=CARTESIAN_POINT('Ctrl Pts',(-181.027993938281,-5.07533181997731,
127.22855794653));
#200332=CARTESIAN_POINT('Ctrl Pts',(-181.306441562095,-5.75176487970607,
133.141572331048));
#200333=CARTESIAN_POINT('Ctrl Pts',(-181.584889185907,-1.14260700432061,
136.906803330016));
#200334=CARTESIAN_POINT('Ctrl Pts',(-181.86333680972,4.5165508885802,135.064187597142));
#200335=CARTESIAN_POINT('Ctrl Pts',(-182.141784433533,6.02521916065313,
129.306998974155));
#200336=CARTESIAN_POINT('Ctrl Pts',(-182.420232057346,1.99700537240587,
124.925812551278));
#200337=CARTESIAN_POINT('Ctrl Pts',(-182.698679681159,-3.86635879394691,
125.946724618282));
#200338=CARTESIAN_POINT('Ctrl Pts',(-182.977127304972,-6.17672811078948,
131.431566859916));
#200339=CARTESIAN_POINT('Ctrl Pts',(-183.255574928785,-2.81098604376035,
136.340037205557));
#200340=CARTESIAN_POINT('Ctrl Pts',(-183.534022552597,3.13791487318212,
136.161491199671));
#200341=CARTESIAN_POINT('Ctrl Pts',(-183.81247017641,6.20322531733387,131.060003899207));
#200342=CARTESIAN_POINT('Ctrl Pts',(-184.090917800223,3.56807473926006,
125.723592911784));
#200343=CARTESIAN_POINT('Ctrl Pts',(-184.369365424036,-2.34596221405232,
125.056159236672));
#200344=CARTESIAN_POINT('Ctrl Pts',(-184.647813047849,-6.10417449927606,
129.671041815353));
#200345=CARTESIAN_POINT('Ctrl Pts',(-184.926260671662,-4.25294862516783,
135.327389007565));
#200346=CARTESIAN_POINT('Ctrl Pts',(-185.204708295475,1.50652926737877,
136.827294071589));
#200347=CARTESIAN_POINT('Ctrl Pts',(-185.483155919288,5.88158036125089,
132.792417528021));
#200348=CARTESIAN_POINT('Ctrl Pts',(-185.761603543101,4.85174643430717,
126.930613805724));
#200349=CARTESIAN_POINT('Ctrl Pts',(-186.040051166913,-0.6366054447743,
124.628594160457));
#200350=CARTESIAN_POINT('Ctrl Pts',(-186.318498790727,-5.53994802001346,
128.001802186308));
#200351=CARTESIAN_POINT('Ctrl Pts',(-186.596946414539,-5.35234900636664,
133.950424497894));
#200352=CARTESIAN_POINT('Ctrl Pts',(-186.875394038353,-0.246202732654624,
137.007967797222));
#200353=CARTESIAN_POINT('Ctrl Pts',(-187.153841662165,5.08619182469514,
134.364699161505));
#200354=CARTESIAN_POINT('Ctrl Pts',(-187.432289285978,5.744624569434,128.449653336115));
#200355=CARTESIAN_POINT('Ctrl Pts',(-187.71073690979,1.12402797537536,124.698468468532));
#200356=CARTESIAN_POINT('Ctrl Pts',(-187.989184533604,-4.52949541623416,
126.558300196495));
#200357=CARTESIAN_POINT('Ctrl Pts',(-188.267632157416,-6.0206337984771,
132.32005401984));
#200358=CARTESIAN_POINT('Ctrl Pts',(-188.54607978123,-1.97910384423165,
136.688959652232));
#200359=CARTESIAN_POINT('Ctrl Pts',(-188.824527405043,3.88112585826452,
135.650206250412));
#200360=CARTESIAN_POINT('Ctrl Pts',(-189.102975028855,6.17479050055486,
130.158357444724));
#200361=CARTESIAN_POINT('Ctrl Pts',(-189.381422652668,2.79412432812102,
125.260153995869));
#200362=CARTESIAN_POINT('Ctrl Pts',(-189.659870276481,-3.15420560129371,
125.456805582802));
#200363=CARTESIAN_POINT('Ctrl Pts',(-189.938317900294,-6.20397467462999,
130.567599004095));
#200364=CARTESIAN_POINT('Ctrl Pts',(-190.216765524107,-3.55259410299321,
135.89596478172));
#200365=CARTESIAN_POINT('Ctrl Pts',(-190.49521314792,2.36344689542356,136.545395071179));
#200366=CARTESIAN_POINT('Ctrl Pts',(-190.773660771733,6.10759565774615,
131.919095162891));
#200367=CARTESIAN_POINT('Ctrl Pts',(-191.052108395545,4.23916238323504,
126.26840866526));
#200368=CARTESIAN_POINT('Ctrl Pts',(-191.330556019359,-1.52485402687357,
124.786040418225));
#200369=CARTESIAN_POINT('Ctrl Pts',(-191.609003643171,-5.88760407954571,
128.834214423098));
#200370=CARTESIAN_POINT('Ctrl Pts',(-191.887451266984,-4.83993360856504,
134.692856533694));
#200371=CARTESIAN_POINT('Ctrl Pts',(-192.165898890797,0.655399404785621,
136.978160860955));
#200372=CARTESIAN_POINT('Ctrl Pts',(-192.44434651461,5.54845238317892,133.59004437145));
#200373=CARTESIAN_POINT('Ctrl Pts',(-192.722794138423,5.34274867839911,
127.642020600343));
#200374=CARTESIAN_POINT('Ctrl Pts',(-193.001241762236,0.227319945953055,
124.600032816164));
#200375=CARTESIAN_POINT('Ctrl Pts',(-193.279689386049,-5.09700471162664,
127.259519183211));
#200376=CARTESIAN_POINT('Ctrl Pts',(-193.558137009861,-5.73743104174462,
133.176541653297));
#200377=CARTESIAN_POINT('Ctrl Pts',(-193.836584633675,-1.105438533588,136.913645639033));
#200378=CARTESIAN_POINT('Ctrl Pts',(-194.115032257487,4.5423979832614,135.036615145204));
#200379=CARTESIAN_POINT('Ctrl Pts',(-194.3934798813,6.01599266197172,129.270349497605));
#200380=CARTESIAN_POINT('Ctrl Pts',(-194.671927505113,1.96118398191049,
124.913765128639));
#200381=CARTESIAN_POINT('Ctrl Pts',(-194.950375128926,-3.89585696836267,
125.970350242409));
#200382=CARTESIAN_POINT('Ctrl Pts',(-195.228822752739,-6.17279568790409,
131.469154736412));
#200383=CARTESIAN_POINT('Ctrl Pts',(-195.507270376552,-2.77723672809589,
136.357045912194));
#200384=CARTESIAN_POINT('Ctrl Pts',(-195.785718000365,3.17046710927626,
136.142290565968));
#200385=CARTESIAN_POINT('Ctrl Pts',(-196.064165624178,6.20466655915177,
131.022238369536));
#200386=CARTESIAN_POINT('Ctrl Pts',(-196.342613247991,3.5370805559797,125.701967162963));
#200387=CARTESIAN_POINT('Ctrl Pts',(-196.621060871803,-2.38090968214636,
125.070546275391));
#200388=CARTESIAN_POINT('Ctrl Pts',(-196.899508495616,-6.11096023628406,
129.708220655875));
#200389=CARTESIAN_POINT('Ctrl Pts',(-197.177956119429,-4.22533687028115,
135.353194111738));
#200390=CARTESIAN_POINT('Ctrl Pts',(-197.456403743242,1.54316466032852,
136.818011809327));
#200391=CARTESIAN_POINT('Ctrl Pts',(-197.734851367055,5.89357325588093,
132.75657784488));
#200392=CARTESIAN_POINT('Ctrl Pts',(-198.013298990868,4.82807594633875,
126.901151619645));
#200393=CARTESIAN_POINT('Ctrl Pts',(-198.291746614681,-0.674187293266194,
124.632583781138));
#200394=CARTESIAN_POINT('Ctrl Pts',(-198.570194238494,-5.55690534624021,
128.035577347248));
#200395=CARTESIAN_POINT('Ctrl Pts',(-198.848641862306,-5.33309885593691,
133.982947476197));
#200396=CARTESIAN_POINT('Ctrl Pts',(-199.12708948612,-0.2084350533912,137.009351564664));
#200397=CARTESIAN_POINT('Ctrl Pts',(-199.405537109932,5.10777038060287,
134.333672103408));
#200398=CARTESIAN_POINT('Ctrl Pts',(-199.683984733745,5.7301843632779,128.414727803113));
#200399=CARTESIAN_POINT('Ctrl Pts',(-199.962432357558,1.08683885116959,
124.691739319248));
#200400=CARTESIAN_POINT('Ctrl Pts',(-200.240879981371,-4.5552584701342,
126.585951190383));
#200401=CARTESIAN_POINT('Ctrl Pts',(-200.519327605184,-6.01129579413245,
132.356675244344));
#200402=CARTESIAN_POINT('Ctrl Pts',(-200.797775228997,-1.94324595144814,
136.700897991079));
#200403=CARTESIAN_POINT('Ctrl Pts',(-201.076222852809,3.91055198777426,
135.626490953421));
#200404=CARTESIAN_POINT('Ctrl Pts',(-201.354670476623,6.17074369131775,
130.120781711275));
#200405=CARTESIAN_POINT('Ctrl Pts',(-201.633118100435,2.76032340012831,
125.243248089324));
#200406=CARTESIAN_POINT('Ctrl Pts',(-201.911565724248,-3.18669924648382,
125.476105205376));
#200407=CARTESIAN_POINT('Ctrl Pts',(-202.190013348061,-6.20530096449064,
130.605368745483));
#200408=CARTESIAN_POINT('Ctrl Pts',(-202.468460971874,-3.52153424193529,
135.91749609474));
#200409=CARTESIAN_POINT('Ctrl Pts',(-202.746908595687,2.39835041244635,
136.530901731028));
#200410=CARTESIAN_POINT('Ctrl Pts',(-203.0253562195,6.11426820372151,131.881895841131));
#200411=CARTESIAN_POINT('Ctrl Pts',(-203.303803843313,4.21147221438356,
126.242687721299));
#200412=CARTESIAN_POINT('Ctrl Pts',(-203.582251467125,-1.56146099811728,
124.795434143027));
#200413=CARTESIAN_POINT('Ctrl Pts',(-203.860699090939,-5.89948783495869,
128.870090442477));
#200414=CARTESIAN_POINT('Ctrl Pts',(-204.139146714752,-4.81617355747646,
134.722246538484));
#200415=CARTESIAN_POINT('Ctrl Pts',(-204.417594338564,0.69296893616836,
136.974056872534));
#200416=CARTESIAN_POINT('Ctrl Pts',(-204.696041962377,5.56530683088876,
133.556217754686));
#200417=CARTESIAN_POINT('Ctrl Pts',(-204.97448958619,5.32339962837619,127.60955636352));
#200418=CARTESIAN_POINT('Ctrl Pts',(-205.252937210003,0.18954822991528,
124.598764006957));
#200419=CARTESIAN_POINT('Ctrl Pts',(-205.531384833816,-5.11848873189165,
127.290611775294));
#200420=CARTESIAN_POINT('Ctrl Pts',(-205.809832457629,-5.72288460116635,
133.211423073505));
#200421=CARTESIAN_POINT('Ctrl Pts',(-206.088280081441,-1.06822910042401,
136.920261566246));
#200422=CARTESIAN_POINT('Ctrl Pts',(-206.366727705255,4.56807675771487,
135.00888586552));
#200423=CARTESIAN_POINT('Ctrl Pts',(-206.645175329067,6.00654323846982,
129.233756864401));
#200424=CARTESIAN_POINT('Ctrl Pts',(-206.92362295288,1.92528991902147,124.901935984182));
#200425=CARTESIAN_POINT('Ctrl Pts',(-207.202070576693,-3.92521078036628,
125.994154992568));
#200426=CARTESIAN_POINT('Ctrl Pts',(-207.480518200506,-6.16863452980439,
131.506717978718));
#200427=CARTESIAN_POINT('Ctrl Pts',(-207.758965824319,-2.74338450090264,
136.373848862034));
#200428=CARTESIAN_POINT('Ctrl Pts',(-208.037413448132,3.20290186254569,
136.12289213331));
#200429=CARTESIAN_POINT('Ctrl Pts',(-208.315861071945,6.20587788476857,
130.984464766326));
#200430=CARTESIAN_POINT('Ctrl Pts',(-208.594308695758,3.50595530487857,
125.680530485208));
#200431=CARTESIAN_POINT('Ctrl Pts',(-208.872756319571,-2.41576892475653,
125.085145782709));
#200432=CARTESIAN_POINT('Ctrl Pts',(-209.151203943383,-6.11751952941318,
129.745440114266));
#200433=CARTESIAN_POINT('Ctrl Pts',(-209.429651567197,-4.19756854398286,
135.378830657213));
#200434=CARTESIAN_POINT('Ctrl Pts',(-209.708099191009,1.57974287074426,
136.808506709009));
#200435=CARTESIAN_POINT('Ctrl Pts',(-209.986546814822,5.90534776198698,
132.720665821612));
#200436=CARTESIAN_POINT('Ctrl Pts',(-210.264994438635,4.80422655224024,
126.87183406841));
#200437=CARTESIAN_POINT('Ctrl Pts',(-210.543442062448,-0.711744159500396,
124.63680209928));
#200438=CARTESIAN_POINT('Ctrl Pts',(-210.821889686261,-5.57365675929581,
128.06945510647));
#200439=CARTESIAN_POINT('Ctrl Pts',(-211.100337310074,-5.31365108556781,
134.015352670796));
#200440=CARTESIAN_POINT('Ctrl Pts',(-211.378784933887,-0.170659650490228,
137.010505403884));
#200441=CARTESIAN_POINT('Ctrl Pts',(-211.657232557699,5.12915966620077,
134.302514265376));
#200442=CARTESIAN_POINT('Ctrl Pts',(-211.935680181513,5.71553182303293,
128.379890818834));
#200443=CARTESIAN_POINT('Ctrl Pts',(-212.214127805325,1.04960945375051,
124.685236675394));
#200444=CARTESIAN_POINT('Ctrl Pts',(-212.492575429138,-4.58085272725645,
126.613758498985));
#200445=CARTESIAN_POINT('Ctrl Pts',(-212.771023052951,-6.00173503901134,
132.393238947258));
#200446=CARTESIAN_POINT('Ctrl Pts',(-213.049470676764,-1.90731605097184,
136.712617831564));
#200447=CARTESIAN_POINT('Ctrl Pts',(-213.327918300577,3.93983321034183,
135.602596970618));
#200448=CARTESIAN_POINT('Ctrl Pts',(-213.60636592439,6.16646822290386,130.083231308093));
#200449=CARTESIAN_POINT('Ctrl Pts',(-213.884813548203,2.72642018733693,
125.226548251849));
#200450=CARTESIAN_POINT('Ctrl Pts',(-214.163261172015,-3.21907480736146,
125.495602268416));
#200451=CARTESIAN_POINT('Ctrl Pts',(-214.441708795829,-6.20639731464204,
130.643145860587));
#200452=CARTESIAN_POINT('Ctrl Pts',(-214.720156419641,-3.49034388913101,
135.938837938644));
#200453=CARTESIAN_POINT('Ctrl Pts',(-214.998604043455,2.43316505771265,
136.516196191791));
#200454=CARTESIAN_POINT('Ctrl Pts',(-215.277051667267,6.12071418324004,
131.844656590906));
#200455=CARTESIAN_POINT('Ctrl Pts',(-215.55549929108,4.18362598788043,126.217135811804));
#200456=CARTESIAN_POINT('Ctrl Pts',(-215.833946914893,-1.59801010884951,
124.805050530808));
#200457=CARTESIAN_POINT('Ctrl Pts',(-216.112394538706,-5.91115298268039,
128.90603813695));
#200458=CARTESIAN_POINT('Ctrl Pts',(-216.390842162519,-4.79223504130557,
134.75149136457));
#200459=CARTESIAN_POINT('Ctrl Pts',(-216.669289786332,0.730512789332353,
136.969724263749));
#200460=CARTESIAN_POINT('Ctrl Pts',(-216.947737410145,5.5819550541073,133.522289166845));
#200461=CARTESIAN_POINT('Ctrl Pts',(-217.226185033957,5.3038533178224,127.577210511344));
#200462=CARTESIAN_POINT('Ctrl Pts',(-217.50463265777,0.151769490097695,
124.597725148413));
#200463=CARTESIAN_POINT('Ctrl Pts',(-217.783080281583,-5.13978308467467,
127.321834570635));
#200464=CARTESIAN_POINT('Ctrl Pts',(-218.061527905396,-5.70812609699421,
133.24621529913));
#200465=CARTESIAN_POINT('Ctrl Pts',(-218.339975529209,-1.03098008363786,
136.9266508665));
#200466=CARTESIAN_POINT('Ctrl Pts',(-218.618423153022,4.59358626040416,
134.981000785606));
#200467=CARTESIAN_POINT('Ctrl Pts',(-218.896870776835,5.99687124029931,
129.197222430498));
#200468=CARTESIAN_POINT('Ctrl Pts',(-219.175318400648,1.88932451380644,
124.890325556239));
#200469=CARTESIAN_POINT('Ctrl Pts',(-219.45376602446,-3.95441914224089,
126.018137986666));
#200470=CARTESIAN_POINT('Ctrl Pts',(-219.732213648274,-6.16424479068368,
131.544255194914));
#200471=CARTESIAN_POINT('Ctrl Pts',(-220.010661272086,-2.70943061658779,
136.390445432439));
#200472=CARTESIAN_POINT('Ctrl Pts',(-220.289108895899,3.23521793110825,
136.103296620509));
#200473=CARTESIAN_POINT('Ctrl Pts',(-220.567556519712,6.20685924929812,
130.94668448929));
#200474=CARTESIAN_POINT('Ctrl Pts',(-220.846004143525,3.47470013931478,
125.659283672863));
#200475=CARTESIAN_POINT('Ctrl Pts',(-221.124451767337,-2.45053865016082,
125.099957217636));
#200476=CARTESIAN_POINT('Ctrl Pts',(-221.402899391151,-6.12385213560643,
129.782698811345));
#200477=CARTESIAN_POINT('Ctrl Pts',(-221.681347014963,-4.16964467523852,
135.404297694017));
#200478=CARTESIAN_POINT('Ctrl Pts',(-221.959794638777,1.61626254320698,
136.79877912285));
#200479=CARTESIAN_POINT('Ctrl Pts',(-222.238242262589,5.91690344326002,
132.684682788949));
#200480=CARTESIAN_POINT('Ctrl Pts',(-222.516689886402,4.7801991357601,126.842662238393));
#200481=CARTESIAN_POINT('Ctrl Pts',(-222.795137510215,-0.749274651793031,
124.64124895857));
#200482=CARTESIAN_POINT('Ctrl Pts',(-223.073585134028,-5.59020163845046,
128.103434208622));
#200483=CARTESIAN_POINT('Ctrl Pts',(-223.352032757841,-5.29400641590365,
134.047638880903));
#200484=CARTESIAN_POINT('Ctrl Pts',(-223.630480381654,-0.132877923733138,
137.011429272127));
#200485=CARTESIAN_POINT('Ctrl Pts',(-223.908928005467,5.15035888890098,
134.271226801972));
#200486=CARTESIAN_POINT('Ctrl Pts',(-224.187375629279,5.70066749165438,
128.345143674176));
#200487=CARTESIAN_POINT('Ctrl Pts',(-224.465823253093,1.01234116266713,
124.678960777928));
#200488=CARTESIAN_POINT('Ctrl Pts',(-224.744270876905,-4.60627723919628,
126.641721091889));
#200489=CARTESIAN_POINT('Ctrl Pts',(-225.022718500718,-5.99195188739136,
132.4297437737));
#200490=CARTESIAN_POINT('Ctrl Pts',(-225.301166124531,-1.87131547419729,
136.724118739406));
#200491=CARTESIAN_POINT('Ctrl Pts',(-225.579613748344,3.96896844094108,
135.578525187401));
#200492=CARTESIAN_POINT('Ctrl Pts',(-225.858061372157,6.16196425374224,
130.045707626623));
#200493=CARTESIAN_POINT('Ctrl Pts',(-226.13650899597,2.69241594604283,125.210055102262));
#200494=CARTESIAN_POINT('Ctrl Pts',(-226.414956619783,-3.25133108423828,
125.515296049447));
#200495=CARTESIAN_POINT('Ctrl Pts',(-226.693404243596,-6.20726368445854,
130.680928949564));
#200496=CARTESIAN_POINT('Ctrl Pts',(-226.971851867408,-3.45902420035033,
135.959989522602));
#200497=CARTESIAN_POINT('Ctrl Pts',(-227.250299491222,2.46788954115291,
136.501278998386));
#200498=CARTESIAN_POINT('Ctrl Pts',(-227.528747115034,6.12693335744362,
131.80737879213));
#200499=CARTESIAN_POINT('Ctrl Pts',(-227.807194738847,4.15562473557794,
126.191753883612));
#200500=CARTESIAN_POINT('Ctrl Pts',(-228.08564236266,-1.63450000472891,
124.81488922523));
#200501=CARTESIAN_POINT('Ctrl Pts',(-228.364089986473,-5.9225990904546,
128.942056174461));
#200502=CARTESIAN_POINT('Ctrl Pts',(-228.642537610286,-4.76811894710285,
134.780589928275));
#200503=CARTESIAN_POINT('Ctrl Pts',(-228.920985234099,0.768029573076269,
136.965163195147));
#200504=CARTESIAN_POINT('Ctrl Pts',(-229.199432857912,5.59839643592858,
133.48825986516));
#200505=CARTESIAN_POINT('Ctrl Pts',(-229.477880481725,5.28411047103341,
127.544984242401));
#200506=CARTESIAN_POINT('Ctrl Pts',(-229.756328105537,0.11398512640586,
124.59691627903));
#200507=CARTESIAN_POINT('Ctrl Pts',(-230.03477572935,-5.16088698090536,
127.353186412258));
#200508=CARTESIAN_POINT('Ctrl Pts',(-230.313223353163,-5.69315607611037,
133.280917040931));
#200509=CARTESIAN_POINT('Ctrl Pts',(-230.591670976976,-0.993692863505588,
136.932813303039));
#200510=CARTESIAN_POINT('Ctrl Pts',(-230.870118600789,4.6189255460653,134.952960938754));
#200511=CARTESIAN_POINT('Ctrl Pts',(-231.148566224602,5.98697702585963,
129.160747549691));
#200512=CARTESIAN_POINT('Ctrl Pts',(-231.427013848415,1.85328909897679,
124.878934275042));
#200513=CARTESIAN_POINT('Ctrl Pts',(-231.705461472227,-3.98348097165998,
126.042298336002));
#200514=CARTESIAN_POINT('Ctrl Pts',(-231.983909096041,-6.15962663320533,
131.581764994044));
#200515=CARTESIAN_POINT('Ctrl Pts',(-232.262356719853,-2.6753763333251,
136.406835008417));
#200516=CARTESIAN_POINT('Ctrl Pts',(-232.540804343666,3.26741411748112,
136.083504753687));
#200517=CARTESIAN_POINT('Ctrl Pts',(-232.819251967479,6.20761061637562,
130.90889893839));
#200518=CARTESIAN_POINT('Ctrl Pts',(-233.097699591292,3.44331621745904,
125.638227513236));
#200519=CARTESIAN_POINT('Ctrl Pts',(-233.376147215105,-2.48521756995422,
125.114980031328));
#200520=CARTESIAN_POINT('Ctrl Pts',(-233.654594838918,-6.12995782020675,
129.819995366479));
#200521=CARTESIAN_POINT('Ctrl Pts',(-233.933042462731,-4.14156629877734,
135.429594278462));
#200522=CARTESIAN_POINT('Ctrl Pts',(-234.211490086544,1.65272232446679,
136.788829411307));
#200523=CARTESIAN_POINT('Ctrl Pts',(-234.489937710357,5.92823987150001,
132.648630080257));
#200524=CARTESIAN_POINT('Ctrl Pts',(-234.768385334169,4.75599458724306,
126.813637210565));
#200525=CARTESIAN_POINT('Ctrl Pts',(-235.046832957982,-0.786777379437916,
124.64592419423));
#200526=CARTESIAN_POINT('Ctrl Pts',(-235.325280581795,-5.6065393706272,
128.137513394595));
#200527=CARTESIAN_POINT('Ctrl Pts',(-235.603728205608,-5.27416557488518,
134.079804910139));
#200528=CARTESIAN_POINT('Ctrl Pts',(-235.882175829421,-0.0950912731361558,
137.012123135159));
#200529=CARTESIAN_POINT('Ctrl Pts',(-236.160623453234,5.17136726315852,
134.239810872567));
#200530=CARTESIAN_POINT('Ctrl Pts',(-236.439071077047,5.68559191994549,
128.310487656705));
#200531=CARTESIAN_POINT('Ctrl Pts',(-236.71751870086,0.975035358909668,
124.672911859406));
#200532=CARTESIAN_POINT('Ctrl Pts',(-236.995966324673,-4.63153106383903,
126.669837932931));
#200533=CARTESIAN_POINT('Ctrl Pts',(-237.274413948486,-5.98194670179065,
132.466188370973));
#200534=CARTESIAN_POINT('Ctrl Pts',(-237.552861572298,-1.83524555513966,
136.735400288432));
#200535=CARTESIAN_POINT('Ctrl Pts',(-237.831309196112,3.99795659995517,
135.554276495761));
#200536=CARTESIAN_POINT('Ctrl Pts',(-238.109756819924,6.15723195072914,
130.008212057319));
#200537=CARTESIAN_POINT('Ctrl Pts',(-238.388204443737,2.65831193628575,
125.193769251723));
#200538=CARTESIAN_POINT('Ctrl Pts',(-238.66665206755,-3.28346688184612,
125.535185818711));
#200539=CARTESIAN_POINT('Ctrl Pts',(-238.945099691363,-6.20790004183648,
130.718716612347));
#200540=CARTESIAN_POINT('Ctrl Pts',(-239.223547315176,-3.42757633615586,
135.980950062836));
#200541=CARTESIAN_POINT('Ctrl Pts',(-239.501994938989,2.50252257603867,
136.486150703575));
#200542=CARTESIAN_POINT('Ctrl Pts',(-239.780442562802,6.13292549587844,
131.770063826148));
#200543=CARTESIAN_POINT('Ctrl Pts',(-240.058890186614,4.12746949507249,
126.166542877259));
#200544=CARTESIAN_POINT('Ctrl Pts',(-240.337337810428,-1.67092933361012,
124.824949861719));
#200545=CARTESIAN_POINT('Ctrl Pts',(-240.61578543424,-5.93382573414137,
128.978143220346));
#200546=CARTESIAN_POINT('Ctrl Pts',(-240.894233058053,-4.74382616849909,
134.80954115134));
#200547=CARTESIAN_POINT('Ctrl Pts',(-241.172680681866,0.805517897201924,
136.960373835741));
#200548=CARTESIAN_POINT('Ctrl Pts',(-241.451128305679,5.6146303671111,133.454131110603));
#200549=CARTESIAN_POINT('Ctrl Pts',(-241.729575929492,5.26417181958768,
127.512878750849));
#200550=CARTESIAN_POINT('Ctrl Pts',(-242.008023553305,0.0761965389532375,
124.596337428779));
#200551=CARTESIAN_POINT('Ctrl Pts',(-242.286471177117,-5.18179963857104,
127.384666138411));
#200552=CARTESIAN_POINT('Ctrl Pts',(-242.564918800931,-5.67797509323448,
133.315527013022));
#200553=CARTESIAN_POINT('Ctrl Pts',(-242.843366424743,-0.956368821719198,
136.938748647509));
#200554=CARTESIAN_POINT('Ctrl Pts',(-243.121814048556,4.64409367574132,
134.924767363992));
#200555=CARTESIAN_POINT('Ctrl Pts',(-243.400261672369,5.9768609617849,129.124333573571));
#200556=CARTESIAN_POINT('Ctrl Pts',(-243.678709296182,1.81718500983798,
124.867762562695));
#200557=CARTESIAN_POINT('Ctrl Pts',(-243.957156919995,-4.01239519172672,
126.066635145309));
#200558=CARTESIAN_POINT('Ctrl Pts',(-244.235604543808,-6.15478022849689,
131.619245986169));
#200559=CARTESIAN_POINT('Ctrl Pts',(-244.514052167621,-2.64122291300849,
136.423016982646));
#200560=CARTESIAN_POINT('Ctrl Pts',(-244.792499791433,3.29948922862226,
136.063517266237));
#200561=CARTESIAN_POINT('Ctrl Pts',(-245.070947415247,6.20813195815889,
130.871109513785));
#200562=CARTESIAN_POINT('Ctrl Pts',(-245.349395039059,3.41180470225455,
125.617362786572));
#200563=CARTESIAN_POINT('Ctrl Pts',(-245.627842662872,-2.51980439909662,
125.13021366711));
#200564=CARTESIAN_POINT('Ctrl Pts',(-245.906290286685,-6.13583635696575,
129.857328397629));
#200565=CARTESIAN_POINT('Ctrl Pts',(-246.184737910498,-4.1133344550539,
135.454719473173));
#200566=CARTESIAN_POINT('Ctrl Pts',(-246.463185534311,1.68912086349306,
136.778657943074));
#200567=CARTESIAN_POINT('Ctrl Pts',(-246.741633158124,5.93935662663147,
132.612509031482));
#200568=CARTESIAN_POINT('Ctrl Pts',(-247.020080781937,4.73161380359756,
126.784760060463));
#200569=CARTESIAN_POINT('Ctrl Pts',(-247.29852840575,-0.824250952757648,
124.650827633015));
#200570=CARTESIAN_POINT('Ctrl Pts',(-247.576976029562,-5.62266935042617,
128.171691401572));
#200571=CARTESIAN_POINT('Ctrl Pts',(-247.855423653376,-5.25412929772145,
134.111849566585));
#200572=CARTESIAN_POINT('Ctrl Pts',(-248.133871277188,-0.0573010988966442,
137.012586967267));
#200573=CARTESIAN_POINT('Ctrl Pts',(-248.412318901001,5.19218401050035,
134.208267641291));
#200574=CARTESIAN_POINT('Ctrl Pts',(-248.690766524814,5.67030566653712,
128.275924050614));
#200575=CARTESIAN_POINT('Ctrl Pts',(-248.969214148627,0.937693424858449,
124.667090143972));
#200576=CARTESIAN_POINT('Ctrl Pts',(-249.24766177244,-4.65661326539506,
126.698107980232));
#200577=CARTESIAN_POINT('Ctrl Pts',(-249.526109396252,-5.97171985295489,
132.502571388608));
#200578=CARTESIAN_POINT('Ctrl Pts',(-249.804557020066,-1.79910763038337,
136.746462060605));
#200579=CARTESIAN_POINT('Ctrl Pts',(-250.083004643878,4.02679661321771,
135.52985179424));
#200580=CARTESIAN_POINT('Ctrl Pts',(-250.361452267692,6.15227148922063,
129.970745989595));
#200581=CARTESIAN_POINT('Ctrl Pts',(-250.639899891504,2.62410942180459,
125.177691303707));
#200582=CARTESIAN_POINT('Ctrl Pts',(-250.918347515317,-3.31548100938434,
125.555270839195));
#200583=CARTESIAN_POINT('Ctrl Pts',(-251.19679513913,-6.20830636318893,
130.756507448682));
#200584=CARTESIAN_POINT('Ctrl Pts',(-251.475242762943,-3.39600146187203,
136.001718782677));
#200585=CARTESIAN_POINT('Ctrl Pts',(-251.753690386756,2.53706287905323,
136.47081186788));
#200586=CARTESIAN_POINT('Ctrl Pts',(-252.032138010569,6.13869037645988,
131.732713075798));
#200587=CARTESIAN_POINT('Ctrl Pts',(-252.310585634382,4.09916130974965,
126.141503726722));
#200588=CARTESIAN_POINT('Ctrl Pts',(-252.589033258195,-1.70729674574642,
124.835232067896));
#200589=CARTESIAN_POINT('Ctrl Pts',(-252.867480882007,-5.94483249743877,
129.014297936587));
#200590=CARTESIAN_POINT('Ctrl Pts',(-253.14592850582,-4.71935760622846,
134.838343962485));
#200591=CARTESIAN_POINT('Ctrl Pts',(-253.424376129633,0.842976373616159,
136.955356360136));
#200592=CARTESIAN_POINT('Ctrl Pts',(-253.702823753446,5.63065624411703,
133.419904173236));
#200593=CARTESIAN_POINT('Ctrl Pts',(-253.981271377259,5.24403810606461,
127.480895216153));
#200594=CARTESIAN_POINT('Ctrl Pts',(-254.259719001072,0.0384051209378723,
124.595988638398));
#200595=CARTESIAN_POINT('Ctrl Pts',(-254.538166624885,-5.20252026939218,
127.416272546179));
#200596=CARTESIAN_POINT('Ctrl Pts',(-254.816614248698,-5.66258373611722,
133.350044001689));
#200597=CARTESIAN_POINT('Ctrl Pts',(-255.095061872511,-0.919009293725241,
136.944456550123));
#200598=CARTESIAN_POINT('Ctrl Pts',(-255.373509496324,4.6690896269236,134.896421351226));
#200599=CARTESIAN_POINT('Ctrl Pts',(-255.651957120136,5.96652359266914,
129.087981388513));
#200600=CARTESIAN_POINT('Ctrl Pts',(-255.93040474395,1.78101326373629,124.856811707331));
#200601=CARTESIAN_POINT('Ctrl Pts',(-256.208852367762,-4.04116012583712,
126.091145862189));
#200602=CARTESIAN_POINT('Ctrl Pts',(-256.487299991575,-6.14970689884083,
131.656699899059));
#200603=CARTESIAN_POINT('Ctrl Pts',(-256.765747615388,-2.60696946356087,
136.438984870644));
#200604=CARTESIAN_POINT('Ctrl Pts',(-257.044195239201,3.33143800190474,
136.043346010603));
#200605=CARTESIAN_POINT('Ctrl Pts',(-257.322642863014,6.2084309480058,130.833296634437));
#200606=CARTESIAN_POINT('Ctrl Pts',(-257.601090486826,3.38015223603414,
125.596729883064));
#200607=CARTESIAN_POINT('Ctrl Pts',(-257.87953811064,-2.5542704291637,125.145582755354));
#200608=CARTESIAN_POINT('Ctrl Pts',(-258.157985734452,-6.14153931545366,
129.894837769574));
#200609=CARTESIAN_POINT('Ctrl Pts',(-258.436433358265,-4.08485240479644,
135.479405634932));
#200610=CARTESIAN_POINT('Ctrl Pts',(-258.714880982078,1.72527217059264,
136.768768758555));
#200611=CARTESIAN_POINT('Ctrl Pts',(-258.993328605892,5.95060195420752,
132.575369498931));
#200612=CARTESIAN_POINT('Ctrl Pts',(-259.271776229703,4.70639920604184,
126.75783223591));
#200613=CARTESIAN_POINT('Ctrl Pts',(-259.550223853517,-0.860449444711704,
124.652528659269));
#200614=CARTESIAN_POINT('Ctrl Pts',(-259.82867147733,-5.64095031490746,
128.212697490595));
#200615=CARTESIAN_POINT('Ctrl Pts',(-260.060711163841,-5.29799179572588,
133.142936715762));
#200616=CARTESIAN_POINT('Ctrl Pts',(-260.246372125917,-2.62679689981868,
135.594171577488));
#200617=CARTESIAN_POINT('Ctrl Pts',(-260.339217213388,-0.889986900407246,
136.05080276614));
#200618=CARTESIAN_POINT('Ctrl Pts',(-260.385654363559,-0.0148419801173944,
136.053268468065));
#200619=CARTESIAN_POINT('Ctrl Pts',(209.997106195361,2.85369542052185,134.803838223542));
#200620=CARTESIAN_POINT('Ctrl Pts',(209.950688331758,3.52024512455777,134.328247120061));
#200621=CARTESIAN_POINT('Ctrl Pts',(209.857862530854,4.598911638141,133.039517383424));
#200622=CARTESIAN_POINT('Ctrl Pts',(209.672220855345,5.31158968331849,129.722011776094));
#200623=CARTESIAN_POINT('Ctrl Pts',(209.440181168834,2.90445768035623,125.771581499823));
#200624=CARTESIAN_POINT('Ctrl Pts',(209.161733545021,-2.67328939945229,
125.640965885288));
#200625=CARTESIAN_POINT('Ctrl Pts',(208.883285921209,-5.78445646322271,
130.262241799363));
#200626=CARTESIAN_POINT('Ctrl Pts',(208.604838297395,-3.58517659481558,
135.378114005881));
#200627=CARTESIAN_POINT('Ctrl Pts',(208.326390673583,1.91144119617671,136.292814641374));
#200628=CARTESIAN_POINT('Ctrl Pts',(208.04794304977,5.65009034124608,132.162897902674));
#200629=CARTESIAN_POINT('Ctrl Pts',(207.769495425957,4.19734896093999,126.785079177362));
#200630=CARTESIAN_POINT('Ctrl Pts',(207.491047802144,-1.1129569716493,125.100504449821));
#200631=CARTESIAN_POINT('Ctrl Pts',(207.212600178331,-5.4002948496084,128.657642803108));
#200632=CARTESIAN_POINT('Ctrl Pts',(206.934152554519,-4.72513942780656,
134.187431620732));
#200633=CARTESIAN_POINT('Ctrl Pts',(206.655704930705,0.292248586550605,
136.608384944684));
#200634=CARTESIAN_POINT('Ctrl Pts',(206.377257306892,5.04104249491135,133.695701483205));
#200635=CARTESIAN_POINT('Ctrl Pts',(206.09880968308,5.15738153042831,128.12602865207));
#200636=CARTESIAN_POINT('Ctrl Pts',(205.820362059267,0.534329935251406,
125.017605890956));
#200637=CARTESIAN_POINT('Ctrl Pts',(205.541914435454,-4.57974002364783,
127.226931288585));
#200638=CARTESIAN_POINT('Ctrl Pts',(205.263466811641,-5.48525514562618,
132.723737743954));
#200639=CARTESIAN_POINT('Ctrl Pts',(204.985019187828,-1.35008742798131,
136.456731302353));
#200640=CARTESIAN_POINT('Ctrl Pts',(204.706571564015,4.02574397595362,134.995471850294));
#200641=CARTESIAN_POINT('Ctrl Pts',(204.428123940202,5.70211370766606,129.682786179275));
#200642=CARTESIAN_POINT('Ctrl Pts',(204.149676316389,2.13851930815143,125.40077248911));
#200643=CARTESIAN_POINT('Ctrl Pts',(203.871228692576,-3.39026975841633,
126.084392381055));
#200644=CARTESIAN_POINT('Ctrl Pts',(203.592781068764,-5.8035665963141,131.105432460946));
#200645=CARTESIAN_POINT('Ctrl Pts',(203.314333444951,-2.88366922283368,
135.849802245147));
#200646=CARTESIAN_POINT('Ctrl Pts',(203.035885821138,2.68617927581077,135.957657646429));
#200647=CARTESIAN_POINT('Ctrl Pts',(202.757438197325,5.78756025537181,131.329884836407));
#200648=CARTESIAN_POINT('Ctrl Pts',(202.478990573512,3.57045609392238,126.219180939555));
#200649=CARTESIAN_POINT('Ctrl Pts',(202.200542949699,-1.92772278905516,
125.322033169903));
#200650=CARTESIAN_POINT('Ctrl Pts',(201.922095325886,-5.6544186046078,129.462876497226));
#200651=CARTESIAN_POINT('Ctrl Pts',(201.643647702073,-4.18497995558374,
134.836478196445));
#200652=CARTESIAN_POINT('Ctrl Pts',(201.36520007826,1.13025082464198,136.504760820331));
#200653=CARTESIAN_POINT('Ctrl Pts',(201.086752454448,5.4068363130258,132.934654138033));
#200654=CARTESIAN_POINT('Ctrl Pts',(200.808304830635,4.71480336828096,127.406911780982));
#200655=CARTESIAN_POINT('Ctrl Pts',(200.529857206822,-0.309903540913717,
125.001258930184));
#200656=CARTESIAN_POINT('Ctrl Pts',(200.251409583008,-5.04982423566531,
127.928373032793));
#200657=CARTESIAN_POINT('Ctrl Pts',(199.972961959197,-5.14920315545485,
133.498379226012));
#200658=CARTESIAN_POINT('Ctrl Pts',(199.694514335383,-0.516715927947778,
136.59271392819));
#200659=CARTESIAN_POINT('Ctrl Pts',(199.416066711571,4.59060799437092,134.367834714685));
#200660=CARTESIAN_POINT('Ctrl Pts',(199.137619087757,5.47938743352869,128.868296891315));
#200661=CARTESIAN_POINT('Ctrl Pts',(198.859171463945,1.33287750423228,125.147907050397));
#200662=CARTESIAN_POINT('Ctrl Pts',(198.580723840131,-4.03848173676817,
126.625521704588));
#200663=CARTESIAN_POINT('Ctrl Pts',(198.302276216319,-5.69867355247927,
131.943285172176));
#200664=CARTESIAN_POINT('Ctrl Pts',(198.023828592506,-2.12206276914206,
136.214432613634));
#200665=CARTESIAN_POINT('Ctrl Pts',(197.745380968693,3.4046200305072,135.513988187415));
#200666=CARTESIAN_POINT('Ctrl Pts',(197.46693334488,5.80262334705539,130.485626102603));
#200667=CARTESIAN_POINT('Ctrl Pts',(197.188485721067,2.86829928156946,125.750165465994));
#200668=CARTESIAN_POINT('Ctrl Pts',(196.910038097254,-2.70185169946893,
125.65926326252));
#200669=CARTESIAN_POINT('Ctrl Pts',(196.631590473441,-5.78913296148881,
130.296454176353));
#200670=CARTESIAN_POINT('Ctrl Pts',(196.353142849628,-3.5564838467683,135.400386297052));
#200671=CARTESIAN_POINT('Ctrl Pts',(196.074695225815,1.94440017923737,136.280795346639));
#200672=CARTESIAN_POINT('Ctrl Pts',(195.796247602003,5.6584754297534,132.128628418917));
#200673=CARTESIAN_POINT('Ctrl Pts',(195.51779997819,4.17268819221861,126.759524075833));
#200674=CARTESIAN_POINT('Ctrl Pts',(195.239352354377,-1.14759564681435,
125.107426913349));
#200675=CARTESIAN_POINT('Ctrl Pts',(194.960904730564,-5.41329514958902,
128.690533514357));
#200676=CARTESIAN_POINT('Ctrl Pts',(194.682457106751,-4.70444086406131,
134.216143957018));
#200677=CARTESIAN_POINT('Ctrl Pts',(194.404009482938,0.327564750825761,
136.606492185605));
#200678=CARTESIAN_POINT('Ctrl Pts',(194.125561859125,5.0585543621317,133.664964953048));
#200679=CARTESIAN_POINT('Ctrl Pts',(193.847114235312,5.14097963875765,128.094682084473));
#200680=CARTESIAN_POINT('Ctrl Pts',(193.568666611499,0.499095778182989,
125.014461412655));
#200681=CARTESIAN_POINT('Ctrl Pts',(193.290218987687,-4.60143272035756,
127.254875257849));
#200682=CARTESIAN_POINT('Ctrl Pts',(193.011771363874,-5.4734693413749,132.757092746623));
#200683=CARTESIAN_POINT('Ctrl Pts',(192.733323740061,-1.31565503151135,
136.464844805061));
#200684=CARTESIAN_POINT('Ctrl Pts',(192.454876116248,4.05118197898966,134.970888425217));
#200685=CARTESIAN_POINT('Ctrl Pts',(192.176428492435,5.69518066204141,129.648096536341));
#200686=CARTESIAN_POINT('Ctrl Pts',(191.897980868622,2.1055865417199,125.38785485147));
#200687=CARTESIAN_POINT('Ctrl Pts',(191.619533244809,-3.4189387468211,126.105117354624));
#200688=CARTESIAN_POINT('Ctrl Pts',(191.341085620997,-5.80162635147675,
131.140754845624));
#200689=CARTESIAN_POINT('Ctrl Pts',(191.062637997183,-2.85290276432908,
135.867262474811));
#200690=CARTESIAN_POINT('Ctrl Pts',(190.784190373371,2.71749909118881,135.941210633695));
#200691=CARTESIAN_POINT('Ctrl Pts',(190.505742749557,5.79065203911519,131.29464457683));
#200692=CARTESIAN_POINT('Ctrl Pts',(190.227295125745,3.54247865217362,126.197531513104));
#200693=CARTESIAN_POINT('Ctrl Pts',(189.948847501932,-1.96105955641241,
125.333869340265));
#200694=CARTESIAN_POINT('Ctrl Pts',(189.670399878119,-5.66247983574075,
129.497321402909));
#200695=CARTESIAN_POINT('Ctrl Pts',(189.391952254306,-4.160357773542,134.861878651407));
#200696=CARTESIAN_POINT('Ctrl Pts',(189.113504630493,1.16492983776554,136.497775047581));
#200697=CARTESIAN_POINT('Ctrl Pts',(188.83505700668,5.41970383815296,132.901701721328));
#200698=CARTESIAN_POINT('Ctrl Pts',(188.556609382867,4.69403477852959,127.378274381527));
#200699=CARTESIAN_POINT('Ctrl Pts',(188.278161759054,-0.345222926215044,
125.003252919028));
#200700=CARTESIAN_POINT('Ctrl Pts',(187.999714135242,-5.0672376268456,127.959166031618));
#200701=CARTESIAN_POINT('Ctrl Pts',(187.721266511429,-5.13270849672517,
133.529673973213));
#200702=CARTESIAN_POINT('Ctrl Pts',(187.442818887616,-0.48147100486422,
136.595752079925));
#200703=CARTESIAN_POINT('Ctrl Pts',(187.164371263803,4.61221481930072,134.339824357932));
#200704=CARTESIAN_POINT('Ctrl Pts',(186.88592363999,5.4675005437485,128.834978175547));
#200705=CARTESIAN_POINT('Ctrl Pts',(186.607476016177,1.29842037074208,125.139898247696));
#200706=CARTESIAN_POINT('Ctrl Pts',(186.329028392364,-4.06384469161484,
126.650182513385));
#200707=CARTESIAN_POINT('Ctrl Pts',(186.050580768551,-5.69163501222784,
131.977953513933));
#200708=CARTESIAN_POINT('Ctrl Pts',(185.772133144738,-2.08909080843167,
136.227249975919));
#200709=CARTESIAN_POINT('Ctrl Pts',(185.493685520926,3.4332257905535,135.493176040453));
#200710=CARTESIAN_POINT('Ctrl Pts',(185.215237897112,5.80057561042411,130.450309792719));
#200711=CARTESIAN_POINT('Ctrl Pts',(184.9367902733,2.83747981818726,125.732798956676));
#200712=CARTESIAN_POINT('Ctrl Pts',(184.658342649487,-2.73312130836828,
125.675805527429));
#200713=CARTESIAN_POINT('Ctrl Pts',(184.379895025674,-5.79211747293216,
130.331703682172));
#200714=CARTESIAN_POINT('Ctrl Pts',(184.101447401861,-3.52844064054064,
135.421950469967));
#200715=CARTESIAN_POINT('Ctrl Pts',(183.822999778048,1.97770076659953,136.26885776521));
#200716=CARTESIAN_POINT('Ctrl Pts',(183.544552154236,5.66643178528845,132.094159137294));
#200717=CARTESIAN_POINT('Ctrl Pts',(183.266104530422,4.14798881387936,126.734198679909));
#200718=CARTESIAN_POINT('Ctrl Pts',(182.98765690661,-1.18225323696583,125.114518204765));
#200719=CARTESIAN_POINT('Ctrl Pts',(182.709209282797,-5.42606231932092,
128.72352494273));
#200720=CARTESIAN_POINT('Ctrl Pts',(182.430761658984,-4.68358520810093,
134.244718011395));
#200721=CARTESIAN_POINT('Ctrl Pts',(182.152314035171,0.362877903506298,
136.604390705933));
#200722=CARTESIAN_POINT('Ctrl Pts',(181.873866411358,5.07587394936235,133.634119096483));
#200723=CARTESIAN_POINT('Ctrl Pts',(181.595418787545,5.12438980598236,128.063437686296));
#200724=CARTESIAN_POINT('Ctrl Pts',(181.316971163732,0.463841771263853,
125.011530548415));
#200725=CARTESIAN_POINT('Ctrl Pts',(181.038523539919,-4.62295419131585,
127.282951248603));
#200726=CARTESIAN_POINT('Ctrl Pts',(180.760075916106,-5.46148109594396,
132.790375128456));
#200727=CARTESIAN_POINT('Ctrl Pts',(180.481628292294,-1.2811736815839,136.472748695004));
#200728=CARTESIAN_POINT('Ctrl Pts',(180.203180668481,4.07646975733793,134.946150534538));
#200729=CARTESIAN_POINT('Ctrl Pts',(179.924733044668,5.68803663588505,129.61344977806));
#200730=CARTESIAN_POINT('Ctrl Pts',(179.646285420855,2.07257572209157,125.37513790386));
#200731=CARTESIAN_POINT('Ctrl Pts',(179.367837797042,-3.44748102935117,
126.12601647128));
#200732=CARTESIAN_POINT('Ctrl Pts',(179.089390173229,-5.79947113363144,
131.176064759319));
#200733=CARTESIAN_POINT('Ctrl Pts',(178.810942549416,-2.82203058602,135.884535099843));
#200734=CARTESIAN_POINT('Ctrl Pts',(178.532494925603,2.74871820628535,135.924573271475));
#200735=CARTESIAN_POINT('Ctrl Pts',(178.254047301791,5.79352924936408,131.259386150458));
#200736=CARTESIAN_POINT('Ctrl Pts',(177.975599677977,3.51436994191561,126.176052793945));
#200737=CARTESIAN_POINT('Ctrl Pts',(177.697152054165,-1.99432365563702,
125.345908221933));
#200738=CARTESIAN_POINT('Ctrl Pts',(177.418704430351,-5.6703312417861,129.531814741282));
#200739=CARTESIAN_POINT('Ctrl Pts',(177.140256806539,-4.135581427815,134.887128753614));
#200740=CARTESIAN_POINT('Ctrl Pts',(176.861809182726,1.19956568393359,136.490578303229));
#200741=CARTESIAN_POINT('Ctrl Pts',(176.583361558913,5.43237053418876,132.868671586896));
#200742=CARTESIAN_POINT('Ctrl Pts',(176.3049139351,4.67309224957875,127.349763936946));
#200743=CARTESIAN_POINT('Ctrl Pts',(176.026466311287,-0.380529519146142,
125.005461870054));
#200744=CARTESIAN_POINT('Ctrl Pts',(175.748018687475,-5.08446324967622,
127.990064460173));
#200745=CARTESIAN_POINT('Ctrl Pts',(175.469571063661,-5.11602364359241,
133.560867732924));
#200746=CARTESIAN_POINT('Ctrl Pts',(175.191123439849,-0.446208240696769,
136.59857562952));
#200747=CARTESIAN_POINT('Ctrl Pts',(174.912675816035,4.63365073691483,134.311682993269));
#200748=CARTESIAN_POINT('Ctrl Pts',(174.634228192223,5.45541105372469,128.801732435971));
#200749=CARTESIAN_POINT('Ctrl Pts',(174.35578056841,1.26391512380778,125.132099343732));
#200750=CARTESIAN_POINT('Ctrl Pts',(174.077332944597,-4.089057059202,126.674997256779));
#200751=CARTESIAN_POINT('Ctrl Pts',(173.798885320784,-5.68438556634791,
132.012578367773));
#200752=CARTESIAN_POINT('Ctrl Pts',(173.520437696972,-2.0560414356932,136.239866391045));
#200753=CARTESIAN_POINT('Ctrl Pts',(173.241990073158,3.46170433115548,135.472190147709));
#200754=CARTESIAN_POINT('Ctrl Pts',(172.963542449346,5.79831293133042,130.41500660232));
#200755=CARTESIAN_POINT('Ctrl Pts',(172.685094825533,2.80655521094699,125.715620375941));
#200756=CARTESIAN_POINT('Ctrl Pts',(172.40664720172,-2.76428964045241,125.692537832834));
#200757=CARTESIAN_POINT('Ctrl Pts',(172.128199577907,-5.79488735533246,
130.366970702468));
#200758=CARTESIAN_POINT('Ctrl Pts',(171.849751954094,-3.50026668664755,
135.443343536393));
#200759=CARTESIAN_POINT('Ctrl Pts',(171.571304330281,2.01092806953244,136.256717694829));
#200760=CARTESIAN_POINT('Ctrl Pts',(171.292856706468,5.6741781691098,132.059642061713));
#200761=CARTESIAN_POINT('Ctrl Pts',(171.014409082656,4.12313573028927,126.709024105332));
#200762=CARTESIAN_POINT('Ctrl Pts',(170.735961458842,-1.21686701828875,
125.121820335384));
#200763=CARTESIAN_POINT('Ctrl Pts',(170.45751383503,-5.43862842431808,128.756593477234));
#200764=CARTESIAN_POINT('Ctrl Pts',(170.179066211217,-4.66255600016836,
134.273164582064));
#200765=CARTESIAN_POINT('Ctrl Pts',(169.900618587404,0.398177609612544,
136.602074304013));
#200766=CARTESIAN_POINT('Ctrl Pts',(169.62217096359,5.09300544821711,133.603168382178));
#200767=CARTESIAN_POINT('Ctrl Pts',(169.343723339778,5.10761008705837,128.032294854024));
#200768=CARTESIAN_POINT('Ctrl Pts',(169.065275715965,0.428570576517446,
125.008814339624));
#200769=CARTESIAN_POINT('Ctrl Pts',(168.786828092152,-4.64430435700642,
127.311157726477));
#200770=CARTESIAN_POINT('Ctrl Pts',(168.508380468339,-5.4492904733226,132.823583917792));
#200771=CARTESIAN_POINT('Ctrl Pts',(168.229932844526,-1.24664485729461,
136.480442540741));
#200772=CARTESIAN_POINT('Ctrl Pts',(167.951485220714,4.10160648060013,134.92125916831));
#200773=CARTESIAN_POINT('Ctrl Pts',(167.673037596901,5.6806818374394,129.578847149419));
#200774=CARTESIAN_POINT('Ctrl Pts',(167.394589973088,2.03948810240773,125.362622138095));
#200775=CARTESIAN_POINT('Ctrl Pts',(167.116142349275,-3.47589556420378,
126.147088945699));
#200776=CARTESIAN_POINT('Ctrl Pts',(166.837694725462,-5.79710101425052,
131.21136089938));
#200777=CARTESIAN_POINT('Ctrl Pts',(166.559247101649,-2.79105383632985,
135.901619477142));
#200778=CARTESIAN_POINT('Ctrl Pts',(166.280799477836,2.77983546661788,135.907746177893));
#200779=CARTESIAN_POINT('Ctrl Pts',(166.002351854023,5.79619177825601,131.224110862948));
#200780=CARTESIAN_POINT('Ctrl Pts',(165.72390423021,3.48613100538707,126.154745578436));
#200781=CARTESIAN_POINT('Ctrl Pts',(165.445456606397,-2.02751385446508,
125.358149368562));
#200782=CARTESIAN_POINT('Ctrl Pts',(165.167008982585,-5.67797253162207,
129.566355234311));
#200783=CARTESIAN_POINT('Ctrl Pts',(164.888561358772,-4.11065183659732,
134.912227567346));
#200784=CARTESIAN_POINT('Ctrl Pts',(164.610113734959,1.23415707975413,136.483170853989));
#200785=CARTESIAN_POINT('Ctrl Pts',(164.331666111146,5.44483593173667,132.835564958663));
#200786=CARTESIAN_POINT('Ctrl Pts',(164.053218487333,4.65197655747607,127.321381503715));
#200787=CARTESIAN_POINT('Ctrl Pts',(163.77477086352,-0.415822011415935,
125.007885701408));
#200788=CARTESIAN_POINT('Ctrl Pts',(163.496323239708,-5.10150046585131,
128.021067173507));
#200789=CARTESIAN_POINT('Ctrl Pts',(163.217875615894,-5.09914921432216,
133.591959349252));
#200790=CARTESIAN_POINT('Ctrl Pts',(162.939427992082,-0.41092894211879,
136.601184472346));
#200791=CARTESIAN_POINT('Ctrl Pts',(162.660980368268,4.65491495289691,134.283411663486));
#200792=CARTESIAN_POINT('Ctrl Pts',(162.382532744456,5.443119411438,128.768560904517));
#200793=CARTESIAN_POINT('Ctrl Pts',(162.104085120643,1.22936304203373,125.124510627495));
#200794=CARTESIAN_POINT('Ctrl Pts',(161.82563749683,-4.11411790527609,126.69996501525));
#200795=CARTESIAN_POINT('Ctrl Pts',(161.547189873017,-5.67692548347038,
132.04715845066));
#200796=CARTESIAN_POINT('Ctrl Pts',(161.268742249204,-2.02291587558315,
136.252281391507));
#200797=CARTESIAN_POINT('Ctrl Pts',(160.990294625391,3.49005459703047,135.451031286826));
#200798=CARTESIAN_POINT('Ctrl Pts',(160.711847001578,5.79583539361873,130.379717839577));
#200799=CARTESIAN_POINT('Ctrl Pts',(160.433399377766,2.77552660577121,125.698630360346));
#200800=CARTESIAN_POINT('Ctrl Pts',(160.154951753952,-2.79535554076737,
125.70945955871));
#200801=CARTESIAN_POINT('Ctrl Pts',(159.87650413014,-5.79744250605075,130.402253930408));
#200802=CARTESIAN_POINT('Ctrl Pts',(159.598056506327,-3.47196302908515,
135.4645647036));
#200803=CARTESIAN_POINT('Ctrl Pts',(159.319608882514,2.04408085678626,136.244375585352));
#200804=CARTESIAN_POINT('Ctrl Pts',(159.041161258701,5.68171429417248,132.025078471215));
#200805=CARTESIAN_POINT('Ctrl Pts',(158.762713634888,4.09812986238831,126.684001284956));
#200806=CARTESIAN_POINT('Ctrl Pts',(158.484266011075,-1.25143570815684,
125.129333034622));
#200807=CARTESIAN_POINT('Ctrl Pts',(158.205818387262,-5.450992998939,128.789737892503));
#200808=CARTESIAN_POINT('Ctrl Pts',(157.927370763449,-4.64135401950845,
134.301482614925));
#200809=CARTESIAN_POINT('Ctrl Pts',(157.648923139637,0.43346256110109,136.59954306568));
#200810=CARTESIAN_POINT('Ctrl Pts',(157.370475515823,5.10994822388206,133.572113957021));
#200811=CARTESIAN_POINT('Ctrl Pts',(157.092027892011,5.09064110376424,128.001254741669));
#200812=CARTESIAN_POINT('Ctrl Pts',(156.813580268198,0.39328350093061,125.006312886931));
#200813=CARTESIAN_POINT('Ctrl Pts',(156.535132644385,-4.66548242629113,
127.339493646268));
#200814=CARTESIAN_POINT('Ctrl Pts',(156.256685020572,-5.43689792523874,
132.856717884066));
#200815=CARTESIAN_POINT('Ctrl Pts',(155.978237396759,-1.21206983812162,
136.487926057176));
#200816=CARTESIAN_POINT('Ctrl Pts',(155.699789772946,4.12659121732586,134.896215248893));
#200817=CARTESIAN_POINT('Ctrl Pts',(155.421342149133,5.67311653923917,129.544289932631));
#200818=CARTESIAN_POINT('Ctrl Pts',(155.142894525321,2.0063249087422,125.350308017949));
#200819=CARTESIAN_POINT('Ctrl Pts',(154.864446901507,-3.50418129846815,
126.168333997033));
#200820=CARTESIAN_POINT('Ctrl Pts',(154.585999277695,-5.79451608115961,
131.246641957895));
#200821=CARTESIAN_POINT('Ctrl Pts',(154.307551653882,-2.75997366311328,
135.918514973638));
#200822=CARTESIAN_POINT('Ctrl Pts',(154.029104030069,2.81084971912495,135.890729976482));
#200823=CARTESIAN_POINT('Ctrl Pts',(153.750656406256,5.79863952713012,131.188820021437));
#200824=CARTESIAN_POINT('Ctrl Pts',(153.472208782443,3.457762888992,126.133610656121));
#200825=CARTESIAN_POINT('Ctrl Pts',(153.19376115863,-2.0606289230217,125.370592326552));
#200826=CARTESIAN_POINT('Ctrl Pts',(152.915313534817,-5.68540342209783,
129.600941602086));
#200827=CARTESIAN_POINT('Ctrl Pts',(152.636865911004,-4.08556992366409,
134.937174162558));
#200828=CARTESIAN_POINT('Ctrl Pts',(152.358418287191,1.26870274343019,136.475552974349));
#200829=CARTESIAN_POINT('Ctrl Pts',(152.079970663379,5.45709956888678,132.802383063404));
#200830=CARTESIAN_POINT('Ctrl Pts',(151.801523039566,4.63068848467127,127.293128133558));
#200831=CARTESIAN_POINT('Ctrl Pts',(151.523075415753,-0.451099095248245,
125.010524323271));
#200832=CARTESIAN_POINT('Ctrl Pts',(151.24462779194,-5.11834864405056,128.052173022803));
#200833=CARTESIAN_POINT('Ctrl Pts',(150.966180168127,-5.08208583420252,
133.622947670083));
#200834=CARTESIAN_POINT('Ctrl Pts',(150.687732544314,-0.375634416417742,
136.603578511732));
#200835=CARTESIAN_POINT('Ctrl Pts',(150.409284920501,4.67600667929353,134.255011416186));
#200836=CARTESIAN_POINT('Ctrl Pts',(150.130837296688,5.43062607235983,128.735464810371));
#200837=CARTESIAN_POINT('Ctrl Pts',(149.852389672876,1.19476540576009,125.117132380189));
#200838=CARTESIAN_POINT('Ctrl Pts',(149.573942049063,-4.13902630119825,
126.725084863609));
#200839=CARTESIAN_POINT('Ctrl Pts',(149.29549442525,-5.66925504003138,132.081692481218));
#200840=CARTESIAN_POINT('Ctrl Pts',(149.017046801437,-1.98971535558138,
136.264494517259));
#200841=CARTESIAN_POINT('Ctrl Pts',(148.738599177624,3.5182755376489,135.429700241853));
#200842=CARTESIAN_POINT('Ctrl Pts',(148.460151553811,5.79314308909515,130.344444812129));
#200843=CARTESIAN_POINT('Ctrl Pts',(148.181703929998,2.74439515243632,125.681829539465));
#200844=CARTESIAN_POINT('Ctrl Pts',(147.903256306185,-2.82631785815477,
125.726570078021));
#200845=CARTESIAN_POINT('Ctrl Pts',(147.624808682372,-5.79978283040501,
130.437552058559));
#200846=CARTESIAN_POINT('Ctrl Pts',(147.346361058559,-3.4435307166558,135.48561318523));
#200847=CARTESIAN_POINT('Ctrl Pts',(147.067913434747,2.07715789987228,136.23183189412));
#200848=CARTESIAN_POINT('Ctrl Pts',(146.789465810933,5.68903988122249,131.990469646568));
#200849=CARTESIAN_POINT('Ctrl Pts',(146.511018187121,4.07297213677825,126.65913114601));
#200850=CARTESIAN_POINT('Ctrl Pts',(146.232570563308,-1.2859580256146,125.137056024094));
#200851=CARTESIAN_POINT('Ctrl Pts',(145.954122939495,-5.46315558500969,
128.822956960357));
#200852=CARTESIAN_POINT('Ctrl Pts',(145.675675315682,-4.61998005176852,
134.329671060644));
#200853=CARTESIAN_POINT('Ctrl Pts',(145.397227691869,0.468731450475054,
136.596797084732));
#200854=CARTESIAN_POINT('Ctrl Pts',(145.118780068056,5.12670164853643,133.540956971746));
#200855=CARTESIAN_POINT('Ctrl Pts',(144.840332444244,5.07348348489189,127.970318499433));
#200856=CARTESIAN_POINT('Ctrl Pts',(144.56188482043,0.357981852079004,125.004026283029));
#200857=CARTESIAN_POINT('Ctrl Pts',(144.283437196618,-4.6864876144088,127.367957957979));
#200858=CARTESIAN_POINT('Ctrl Pts',(144.004989572805,-5.42430391090288,
132.889775799486));
#200859=CARTESIAN_POINT('Ctrl Pts',(143.726541948992,-1.17744990525502,
136.495198967004));
#200860=CARTESIAN_POINT('Ctrl Pts',(143.448094325179,4.15142304169647,134.871019704297));
#200861=CARTESIAN_POINT('Ctrl Pts',(143.169646701366,5.66534102161933,129.509779408224));
#200862=CARTESIAN_POINT('Ctrl Pts',(142.891199077553,1.9730873699693,125.338195999729));
#200863=CARTESIAN_POINT('Ctrl Pts',(142.61275145374,-3.53233718400576,126.189750838038));
#200864=CARTESIAN_POINT('Ctrl Pts',(142.334303829928,-5.79171643014443,
131.281906627513));
#200865=CARTESIAN_POINT('Ctrl Pts',(142.055856206114,-2.72879121805762,
135.935220963265));
#200866=CARTESIAN_POINT('Ctrl Pts',(141.777408582302,2.84175981456215,135.873525297782));
#200867=CARTESIAN_POINT('Ctrl Pts',(141.498960958489,5.80087240528401,131.153514933643));
#200868=CARTESIAN_POINT('Ctrl Pts',(141.220513334676,3.42926664392146,126.112648810165));
#200869=CARTESIAN_POINT('Ctrl Pts',(140.942065710863,-2.09366763421581,
125.383236634823));
#200870=CARTESIAN_POINT('Ctrl Pts',(140.66361808705,-5.69262363785895,129.635572562993));
#200871=CARTESIAN_POINT('Ctrl Pts',(140.385170463237,-4.06033661843482,
134.961967614844));
#200872=CARTESIAN_POINT('Ctrl Pts',(140.106722839424,1.30320139485961,136.467724946589));
#200873=CARTESIAN_POINT('Ctrl Pts',(139.828275215611,5.46916099120554,132.769127130691));
#200874=CARTESIAN_POINT('Ctrl Pts',(139.549827591798,4.60922882000175,127.26500487341));
#200875=CARTESIAN_POINT('Ctrl Pts',(139.271379967986,-0.486359463437733,
125.013377637868));
#200876=CARTESIAN_POINT('Ctrl Pts',(138.992932344173,-5.13500715995863,
128.083380855422));
#200877=CARTESIAN_POINT('Ctrl Pts',(138.71448472036,-5.06483413552331,133.653831547135));
#200878=CARTESIAN_POINT('Ctrl Pts',(138.436037096547,-0.340325971445257,
136.605757658967));
#200879=CARTESIAN_POINT('Ctrl Pts',(138.157589472734,4.69692513454305,134.226483303753));
#200880=CARTESIAN_POINT('Ctrl Pts',(137.879141848921,5.41793149943546,128.70244537992));
#200881=CARTESIAN_POINT('Ctrl Pts',(137.600694225109,1.16012349701482,125.109964875215));
#200882=CARTESIAN_POINT('Ctrl Pts',(137.322246601295,-4.16378132397874,
126.750355871033));
#200883=CARTESIAN_POINT('Ctrl Pts',(137.043798977483,-5.66137452026194,
132.116179179772));
#200884=CARTESIAN_POINT('Ctrl Pts',(136.765351353669,-1.95644110594549,
136.276505315742));
#200885=CARTESIAN_POINT('Ctrl Pts',(136.486903729857,3.54636610727348,135.408197803219));
#200886=CARTESIAN_POINT('Ctrl Pts',(136.208456106044,5.79023611752392,130.309188827029));
#200887=CARTESIAN_POINT('Ctrl Pts',(135.930008482231,2.71316200452982,125.665218535856));
#200888=CARTESIAN_POINT('Ctrl Pts',(135.651560858418,-2.85717544529452,
125.743868756725));
#200889=CARTESIAN_POINT('Ctrl Pts',(135.373113234605,-5.80190824167357,
130.472863778936));
#200890=CARTESIAN_POINT('Ctrl Pts',(135.094665610792,-3.41497080292952,
135.506488201326));
#200891=CARTESIAN_POINT('Ctrl Pts',(134.816217986979,2.11015797310843,136.219087085943));
#200892=CARTESIAN_POINT('Ctrl Pts',(134.537770363167,5.69615465880763,131.955816870215));
#200893=CARTESIAN_POINT('Ctrl Pts',(134.259322739353,4.04766348568775,126.634414610068));
#200894=CARTESIAN_POINT('Ctrl Pts',(133.980875115541,-1.32043269142476,
125.144989017623));
#200895=CARTESIAN_POINT('Ctrl Pts',(133.702427491728,-5.47511573184112,
128.856249449853));
#200896=CARTESIAN_POINT('Ctrl Pts',(133.423979867915,-4.59843488896879,
134.357728874689));
#200897=CARTESIAN_POINT('Ctrl Pts',(133.145532244102,0.503982970832797,
136.59383646292));
#200898=CARTESIAN_POINT('Ctrl Pts',(132.867084620289,5.14326510137581,133.509698580887));
#200899=CARTESIAN_POINT('Ctrl Pts',(132.588636996476,5.05613786622328,127.93948727367));
#200900=CARTESIAN_POINT('Ctrl Pts',(132.310189372663,0.322666938078297,
125.001954612649));
#200901=CARTESIAN_POINT('Ctrl Pts',(132.03174174885,-4.70731914300451,127.396549606854));
#200902=CARTESIAN_POINT('Ctrl Pts',(131.753294125038,-5.41150889699075,
132.92275643908));
#200903=CARTESIAN_POINT('Ctrl Pts',(131.474846501225,-1.14278634154918,
136.502261000723));
#200904=CARTESIAN_POINT('Ctrl Pts',(131.196398877412,4.17610103355955,134.845673468154));
#200905=CARTESIAN_POINT('Ctrl Pts',(130.917951253599,5.65735557270449,129.475316855001));
#200906=CARTESIAN_POINT('Ctrl Pts',(130.639503629786,1.93977671771839,125.326286532249));
#200907=CARTESIAN_POINT('Ctrl Pts',(130.361056005973,-3.56036217749005,
126.211338675105));
#200908=CARTESIAN_POINT('Ctrl Pts',(130.08260838216,-5.788702164947,131.317153601487));
#200909=CARTESIAN_POINT('Ctrl Pts',(129.804160758347,-2.69750765663984,
135.951736826975));
#200910=CARTESIAN_POINT('Ctrl Pts',(129.525713134534,2.87256460754407,135.856132779323));
#200911=CARTESIAN_POINT('Ctrl Pts',(129.247265510721,5.80289032997773,131.118196907806));
#200912=CARTESIAN_POINT('Ctrl Pts',(128.968817886909,3.40064332611445,126.091860817314));
#200913=CARTESIAN_POINT('Ctrl Pts',(128.690370263096,-2.12662876378584,
125.396081824838));
#200914=CARTESIAN_POINT('Ctrl Pts',(128.411922639283,-5.69963291135762,
129.670246833772));
#200915=CARTESIAN_POINT('Ctrl Pts',(128.13347501547,-4.03495285593914,134.986607005474));
#200916=CARTESIAN_POINT('Ctrl Pts',(127.855027391657,1.33765175568188,136.459687060782));
#200917=CARTESIAN_POINT('Ctrl Pts',(127.576579767844,5.48101975175251,132.73579839283));
#200918=CARTESIAN_POINT('Ctrl Pts',(127.298132144031,4.5875983586632,127.237012765392));
#200919=CARTESIAN_POINT('Ctrl Pts',(127.019684520218,-0.521601809398458,
125.016445539469));
#200920=CARTESIAN_POINT('Ctrl Pts',(126.741236896406,-5.15147539628782,
128.114689514947));
#200921=CARTESIAN_POINT('Ctrl Pts',(126.462789272592,-5.0473947575527,133.684609835992));
#200922=CARTESIAN_POINT('Ctrl Pts',(126.18434164878,-0.305004915568794,
136.607721833301));
#200923=CARTESIAN_POINT('Ctrl Pts',(125.905894024967,4.71766954350447,134.197828383304));
#200924=CARTESIAN_POINT('Ctrl Pts',(125.627446401154,5.40503616306688,128.669503836711));
#200925=CARTESIAN_POINT('Ctrl Pts',(125.348998777341,1.12543859946687,125.10300837817));
#200926=CARTESIAN_POINT('Ctrl Pts',(125.070551153528,-4.18838205631096,
126.775777101093));
#200927=CARTESIAN_POINT('Ctrl Pts',(124.792103529715,-5.65328421617778,
132.150617268407));
#200928=CARTESIAN_POINT('Ctrl Pts',(124.513655905902,-1.9230943596648,136.288313341892));
#200929=CARTESIAN_POINT('Ctrl Pts',(124.23520828209,3.57432526499779,135.386524767704));
#200930=CARTESIAN_POINT('Ctrl Pts',(123.956760658277,5.78711458662396,130.273951190703));
#200931=CARTESIAN_POINT('Ctrl Pts',(123.678313034464,2.68182831940755,125.648797965047));
#200932=CARTESIAN_POINT('Ctrl Pts',(123.399865410651,-2.88792715874745,
125.761354953818));
#200933=CARTESIAN_POINT('Ctrl Pts',(123.121417786838,-5.8038186610986,130.50818778305));
#200934=CARTESIAN_POINT('Ctrl Pts',(122.842970163025,-3.38628434620416,
135.527188978355));
#200935=CARTESIAN_POINT('Ctrl Pts',(122.564522539212,2.1430798536649,136.206141633086));
#200936=CARTESIAN_POINT('Ctrl Pts',(122.286074915399,5.703058363287,131.921121426228));
#200937=CARTESIAN_POINT('Ctrl Pts',(122.007627291586,4.02220484693838,126.609852593007));
#200938=CARTESIAN_POINT('Ctrl Pts',(121.729179667773,-1.35485842811595,
125.153131721247));
#200939=CARTESIAN_POINT('Ctrl Pts',(121.450732043961,-5.48687299624567,
128.889614127324));
#200940=CARTESIAN_POINT('Ctrl Pts',(121.172284420148,-4.57671932947311,
134.385655017367));
#200941=CARTESIAN_POINT('Ctrl Pts',(120.893836796335,0.539215815916097,
136.59066130995));
#200942=CARTESIAN_POINT('Ctrl Pts',(120.615389172522,5.15963796863542,133.478339942736));
#200943=CARTESIAN_POINT('Ctrl Pts',(120.336941548709,5.0386048905067,127.908762206842));
#200944=CARTESIAN_POINT('Ctrl Pts',(120.058493924896,0.287340067535411,
125.000097952557));
#200945=CARTESIAN_POINT('Ctrl Pts',(119.780046301083,-4.72797624015824,
127.42526753342));
#200946=CARTESIAN_POINT('Ctrl Pts',(119.50159867727,-5.39851335762638,132.955658580739));
#200947=CARTESIAN_POINT('Ctrl Pts',(119.223151053457,-1.10808043147514,
136.509111896649));
#200948=CARTESIAN_POINT('Ctrl Pts',(118.944703429644,4.20062427846316,134.820177479675));
#200949=CARTESIAN_POINT('Ctrl Pts',(118.666255805832,5.64916048839838,129.440903549983));
#200950=CARTESIAN_POINT('Ctrl Pts',(118.387808182019,1.90639418632776,125.314580056818));
#200951=CARTESIAN_POINT('Ctrl Pts',(118.109360558206,-3.58825524044456,
126.23309670829));
#200952=CARTESIAN_POINT('Ctrl Pts',(117.830912934393,-5.785473397262,131.352381573729));
#200953=CARTESIAN_POINT('Ctrl Pts',(117.55246531058,-2.66612413808396,135.968061952766));
#200954=CARTESIAN_POINT('Ctrl Pts',(117.274017686767,2.9032629565882,135.838553065588));
#200955=CARTESIAN_POINT('Ctrl Pts',(116.995570062954,5.80469322643624,131.082867252651));
#200956=CARTESIAN_POINT('Ctrl Pts',(116.717122439142,3.37189399621826,126.071247447876));
#200957=CARTESIAN_POINT('Ctrl Pts',(116.438674815328,-2.15951109034483,
125.409127420613));
#200958=CARTESIAN_POINT('Ctrl Pts',(116.160227191516,-5.70643098286277,
129.704963129555));
#200959=CARTESIAN_POINT('Ctrl Pts',(115.881779567703,-4.00941957678149,
135.011091421425));
#200960=CARTESIAN_POINT('Ctrl Pts',(115.60333194389,1.37205254932662,136.451439614773));
#200961=CARTESIAN_POINT('Ctrl Pts',(115.324884320077,5.49267541109693,132.702398084833));
#200962=CARTESIAN_POINT('Ctrl Pts',(115.046436696264,4.56579790218037,127.20915284676));
#200963=CARTESIAN_POINT('Ctrl Pts',(114.767989072451,-0.556824827212187,
125.019727914392));
#200964=CARTESIAN_POINT('Ctrl Pts',(114.489541448638,-5.1677527428018,128.146097841224));
#200965=CARTESIAN_POINT('Ctrl Pts',(114.211093824825,-5.02976834651319,
133.715281396157));
#200966=CARTESIAN_POINT('Ctrl Pts',(113.932646201012,-0.269672557622912,
136.60947096195));
#200967=CARTESIAN_POINT('Ctrl Pts',(113.6541985772,4.73823913748602,134.169047716661));
#200968=CARTESIAN_POINT('Ctrl Pts',(113.375750953387,5.39194054109557,128.636641401405));
#200969=CARTESIAN_POINT('Ctrl Pts',(113.097303329574,1.09071199837779,125.09626314683));
#200970=CARTESIAN_POINT('Ctrl Pts',(112.818855705761,-4.21282758660586,
126.801347611796));
#200971=CARTESIAN_POINT('Ctrl Pts',(112.540408081948,-5.64498442756793,
132.185005471008));
#200972=CARTESIAN_POINT('Ctrl Pts',(112.261960458135,-1.8896763524154,136.299918158156));
#200973=CARTESIAN_POINT('Ctrl Pts',(111.983512834322,3.60215197478495,135.364681938413));
#200974=CARTESIAN_POINT('Ctrl Pts',(111.705065210509,5.78377861206482,130.238733208892));
#200975=CARTESIAN_POINT('Ctrl Pts',(111.426617586696,2.65039525815055,125.632568435507));
#200976=CARTESIAN_POINT('Ctrl Pts',(111.148169962883,-2.91857185899754,
125.77902802134));
#200977=CARTESIAN_POINT('Ctrl Pts',(110.869722339071,-5.80551401788879,
130.543522761958));
#200978=CARTESIAN_POINT('Ctrl Pts',(110.591274715258,-3.35747240946702,
135.547714749242));
#200979=CARTESIAN_POINT('Ctrl Pts',(110.312827091445,2.17592232160915,136.192996015246));
#200980=CARTESIAN_POINT('Ctrl Pts',(110.034379467632,5.70975073884148,131.886384600257));
#200981=CARTESIAN_POINT('Ctrl Pts',(109.755931843819,3.99659716390926,126.585446004984));
#200982=CARTESIAN_POINT('Ctrl Pts',(109.477484220006,-1.38923396002991,
125.161483833236));
#200983=CARTESIAN_POINT('Ctrl Pts',(109.199036596193,-5.49842694255352,
128.923049756431));
#200984=CARTESIAN_POINT('Ctrl Pts',(108.92058897238,-4.55483417795961,134.413448453863));
#200985=CARTESIAN_POINT('Ctrl Pts',(108.642141348568,0.57442868015902,136.58727174348));
#200986=CARTESIAN_POINT('Ctrl Pts',(108.363693724754,5.17581964361271,133.446882219296));
#200987=CARTESIAN_POINT('Ctrl Pts',(108.085246100942,5.02088520743284,127.878144437479));
#200988=CARTESIAN_POINT('Ctrl Pts',(107.806798477129,0.252002549500665,
124.998456371553));
#200989=CARTESIAN_POINT('Ctrl Pts',(107.528350853316,-4.74845814041369,
127.454110673523));
#200990=CARTESIAN_POINT('Ctrl Pts',(107.249903229503,-5.38531777436419,
132.988481005259));
#200991=CARTESIAN_POINT('Ctrl Pts',(106.97145560569,-1.07333346107335,136.515751400918));
#200992=CARTESIAN_POINT('Ctrl Pts',(106.693007981877,4.22499186768932,134.794532683627));
#200993=CARTESIAN_POINT('Ctrl Pts',(106.414560358064,5.64075607237289,129.406540768369));
#200994=CARTESIAN_POINT('Ctrl Pts',(106.136112734251,1.87294101279944,125.303077007226));
#200995=CARTESIAN_POINT('Ctrl Pts',(105.857665110439,-3.61601533928142,
126.25502413134));
#200996=CARTESIAN_POINT('Ctrl Pts',(105.579217486626,-5.78203024673271,
131.387589238853));
#200997=CARTESIAN_POINT('Ctrl Pts',(105.300769862813,-2.63464182531766,
135.984195735705));
#200998=CARTESIAN_POINT('Ctrl Pts',(105.022322239,2.93385372415587,135.820786808));
#200999=CARTESIAN_POINT('Ctrl Pts',(104.743874615187,5.80628102785255,131.047527277329));
#201000=CARTESIAN_POINT('Ctrl Pts',(104.465426991374,3.34301971955009,126.050809465687));
#201001=CARTESIAN_POINT('Ctrl Pts',(104.186979367561,-2.19231339542621,
125.422372938737));
#201002=CARTESIAN_POINT('Ctrl Pts',(103.908531743748,-5.71301760046937,
129.739720163916));
#201003=CARTESIAN_POINT('Ctrl Pts',(103.630084119935,-3.98373772710686,
135.03541995542));
#201004=CARTESIAN_POINT('Ctrl Pts',(103.351636496123,1.40640250105958,136.442982914176));
#201005=CARTESIAN_POINT('Ctrl Pts',(103.07318887231,5.50412753733405,132.66892744436));
#201006=CARTESIAN_POINT('Ctrl Pts',(102.794741248497,4.54382825837723,127.181426149873));
#201007=CARTESIAN_POINT('Ctrl Pts',(102.516293624684,-0.592027211677165,
125.023224641008));
#201008=CARTESIAN_POINT('Ctrl Pts',(102.237846000871,-5.18383859633749,
128.177604670405));
#201009=CARTESIAN_POINT('Ctrl Pts',(101.959398377058,-5.01195555555783,
133.745845091081));
#201010=CARTESIAN_POINT('Ctrl Pts',(101.680950753245,-0.234330206861215,
136.611004980102));
#201011=CARTESIAN_POINT('Ctrl Pts',(101.402503129432,4.75863315427373,134.140142370299));
#201012=CARTESIAN_POINT('Ctrl Pts',(101.124055505619,5.37864511878468,128.603859291732));
#201013=CARTESIAN_POINT('Ctrl Pts',(100.845607881807,1.05594498055446,125.089729431141));
#201014=CARTESIAN_POINT('Ctrl Pts',(100.567160257994,-4.23711700902531,
126.827066455619));
#201015=CARTESIAN_POINT('Ctrl Pts',(100.288712634181,-5.63647546198416,
132.219342513305));
#201016=CARTESIAN_POINT('Ctrl Pts',(100.010265010368,-1.85618832251382,
136.311319334515));
#201017=CARTESIAN_POINT('Ctrl Pts',(99.731817386555,3.62984520550588,135.342670124737));
#201018=CARTESIAN_POINT('Ctrl Pts',(99.4533697627421,5.78022831746224,130.203536186614));
#201019=CARTESIAN_POINT('Ctrl Pts',(99.1749221389292,2.61886398552269,125.616530548629));
#201020=CARTESIAN_POINT('Ctrl Pts',(98.8964745151164,-2.9491084104941,125.796887304409));
#201021=CARTESIAN_POINT('Ctrl Pts',(98.6180268913035,-5.80699424922206,
130.578867406308));
#201022=CARTESIAN_POINT('Ctrl Pts',(98.3395792674906,-3.32853606035512,
135.568064753397));
#201023=CARTESIAN_POINT('Ctrl Pts',(98.0611316436778,2.20868415995158,136.179650719541));
#201024=CARTESIAN_POINT('Ctrl Pts',(97.7826840198649,5.71623153748262,131.851607679491));
#201025=CARTESIAN_POINT('Ctrl Pts',(97.5042363960519,3.97084138550236,126.561195750394));
#201026=CARTESIAN_POINT('Ctrl Pts',(97.2257887722391,-1.42355801336861,
125.170045044101));
#201027=CARTESIAN_POINT('Ctrl Pts',(96.9473411484261,-5.50977714262889,
128.956555098203));
#201028=CARTESIAN_POINT('Ctrl Pts',(96.6688935246133,-4.53278024539068,
134.441108154283));
#201029=CARTESIAN_POINT('Ctrl Pts',(96.3904459008004,0.609620258735999,
136.583667889112));
#201030=CARTESIAN_POINT('Ctrl Pts',(96.1119982769875,5.19180952668969,133.415326576248));
#201031=CARTESIAN_POINT('Ctrl Pts',(95.8335506531746,5.00297947361121,127.847635100131));
#201032=CARTESIAN_POINT('Ctrl Pts',(95.5551030293618,0.216655693418756,
124.997029930466));
#201033=CARTESIAN_POINT('Ctrl Pts',(95.2766554055487,-4.7687640848064,127.483077958369));
#201034=CARTESIAN_POINT('Ctrl Pts',(94.9982077817361,-5.37192263617151,
133.021222496396));
#201035=CARTESIAN_POINT('Ctrl Pts',(94.7197601579228,-1.03854671790542,
136.522179267501));
#201036=CARTESIAN_POINT('Ctrl Pts',(94.4413125341102,4.24920289828813,134.768740030285));
#201037=CARTESIAN_POINT('Ctrl Pts',(94.1628649102971,5.63214263605674,129.372229783482));
#201038=CARTESIAN_POINT('Ctrl Pts',(93.8844172864844,1.83941843675322,125.29177780972));
#201039=CARTESIAN_POINT('Ctrl Pts',(93.6059696626714,-3.6436414453401,126.277120131727));
#201040=CARTESIAN_POINT('Ctrl Pts',(93.3275220388585,-5.77837284094635,
131.422775292226));
#201041=CARTESIAN_POINT('Ctrl Pts',(93.0490744150458,-2.60306188492951,
136.000137577949));
#201042=CARTESIAN_POINT('Ctrl Pts',(92.7706267912327,2.96433577669487,135.802834664895));
#201043=CARTESIAN_POINT('Ctrl Pts',(92.49217916742,5.80765367539012,131.012178291378));
#201044=CARTESIAN_POINT('Ctrl Pts',(92.213731543607,3.31402156605677,126.030547628085));
#201045=CARTESIAN_POINT('Ctrl Pts',(91.9352839197941,-2.22503446352861,
125.435817888395));
#201046=CARTESIAN_POINT('Ctrl Pts',(91.6568362959812,-5.71939252010779,
129.77451664892));
#201047=CARTESIAN_POINT('Ctrl Pts',(91.3783886721684,-3.95790825856573,
135.059591705955));
#201048=CARTESIAN_POINT('Ctrl Pts',(91.0999410483554,1.44070033803066,136.434317272356));
#201049=CARTESIAN_POINT('Ctrl Pts',(90.8214934245425,5.51537570610103,132.635387711677));
#201050=CARTESIAN_POINT('Ctrl Pts',(90.5430458007297,4.52169024134706,127.153833702157));
#201051=CARTESIAN_POINT('Ctrl Pts',(90.2645981769166,-0.627207658356129,
125.026935589742));
#201052=CARTESIAN_POINT('Ctrl Pts',(89.9861505531037,-5.19973236082766,
128.209208834995));
#201053=CARTESIAN_POINT('Ctrl Pts',(89.707702929291,-4.99395704474619,133.776299788217));
#201054=CARTESIAN_POINT('Ctrl Pts',(89.4292553054779,-0.198979172907652,
136.61232383091));
#201055=CARTESIAN_POINT('Ctrl Pts',(89.1508076816652,4.77885083815996,134.111113415317));
#201056=CARTESIAN_POINT('Ctrl Pts',(88.8723600578521,5.36515038880097,128.571158722445));
#201057=CARTESIAN_POINT('Ctrl Pts',(88.5939124340396,1.02113883430145,125.08340747321));
#201058=CARTESIAN_POINT('Ctrl Pts',(88.3154648102263,-4.26124942351577,
126.85293267954));
#201059=CARTESIAN_POINT('Ctrl Pts',(88.0370171864138,-5.62775763472933,
132.253627122929));
#201060=CARTESIAN_POINT('Ctrl Pts',(87.7585695626006,-1.82263151087143,
136.322516448493));
#201061=CARTESIAN_POINT('Ctrl Pts',(87.480121938788,3.65740393097785,135.320490142334));
#201062=CARTESIAN_POINT('Ctrl Pts',(87.2016743149749,5.77646383437373,130.168361428106));
#201063=CARTESIAN_POINT('Ctrl Pts',(86.9232266911622,2.58723566992664,125.600684898703));
#201064=CARTESIAN_POINT('Ctrl Pts',(86.6447790673492,-2.97953568169397,
125.814932141244));
#201065=CARTESIAN_POINT('Ctrl Pts',(86.3663314435363,-5.80825930024783,
130.614220406392));
#201066=CARTESIAN_POINT('Ctrl Pts',(86.0878838197235,-3.29947637111547,
135.588238236744));
#201067=CARTESIAN_POINT('Ctrl Pts',(85.8094361959104,2.24136415469026,136.166106240484));
#201068=CARTESIAN_POINT('Ctrl Pts',(85.5309885720977,5.72250051906197,131.816791952599));
#201069=CARTESIAN_POINT('Ctrl Pts',(85.2525409482847,3.94493846610766,126.537102727838));
#201070=CARTESIAN_POINT('Ctrl Pts',(84.9740933244718,-1.45782931624159,
125.178815036599));
#201071=CARTESIAN_POINT('Ctrl Pts',(84.6956457006588,-5.52092317588609,
128.990128911089));
#201072=CARTESIAN_POINT('Ctrl Pts',(84.417198076846,-4.51055834898274,134.468633093685));
#201073=CARTESIAN_POINT('Ctrl Pts',(84.138750453033,0.644789247610192,136.579849880389));
#201074=CARTESIAN_POINT('Ctrl Pts',(83.8603028292202,5.20760702535536,133.383674182895));
#201075=CARTESIAN_POINT('Ctrl Pts',(83.5818552054073,4.98488835254533,127.817235325336));
#201076=CARTESIAN_POINT('Ctrl Pts',(83.3034075815944,0.181300809080568,
124.995818682153));
#201077=CARTESIAN_POINT('Ctrl Pts',(83.0249599577814,-4.78889332089225,
127.512168314565));
#201078=CARTESIAN_POINT('Ctrl Pts',(82.7465123339688,-5.35832843941005,
133.053881840899));
#201079=CARTESIAN_POINT('Ctrl Pts',(82.4680647101557,-1.00372149100682,
136.528395258211));
#201080=CARTESIAN_POINT('Ctrl Pts',(82.1896170863428,4.27325647311088,134.742800475408));
#201081=CARTESIAN_POINT('Ctrl Pts',(81.91116946253,5.62332049862395,129.337971866731));
#201082=CARTESIAN_POINT('Ctrl Pts',(81.632721838717,1.80582770038043,125.280682882997));
#201083=CARTESIAN_POINT('Ctrl Pts',(81.3542742149043,-3.67113253492515,
126.299383890674));
#201084=CARTESIAN_POINT('Ctrl Pts',(81.0758265910913,-5.77450131542928,
131.457938430015));
#201085=CARTESIAN_POINT('Ctrl Pts',(80.7973789672785,-2.57138548712596,
136.015886888767));
#201086=CARTESIAN_POINT('Ctrl Pts',(80.5189313434656,2.99470798468153,135.784697301496));
#201087=CARTESIAN_POINT('Ctrl Pts',(80.2404837196526,5.80881111818491,130.976821604667));
#201088=CARTESIAN_POINT('Ctrl Pts',(79.9620360958398,3.2849006102757,126.010462685879));
#201089=CARTESIAN_POINT('Ctrl Pts',(79.6835884720269,-2.25767308216064,
125.449461771377));
#201090=CARTESIAN_POINT('Ctrl Pts',(79.4051408482139,-5.72555550555307,
129.809351295171));
#201091=CARTESIAN_POINT('Ctrl Pts',(79.1266932244012,-3.93193212827854,
135.083605777338));
#201092=CARTESIAN_POINT('Ctrl Pts',(78.8482456005881,1.47494478932078,136.425443010422));
#201093=CARTESIAN_POINT('Ctrl Pts',(78.5697979767754,5.526419500593,132.601780129612));
#201094=CARTESIAN_POINT('Ctrl Pts',(78.2913503529625,4.49938467142216,127.126376526057));
#201095=CARTESIAN_POINT('Ctrl Pts',(78.0129027291494,-0.662364863624755,
125.030860623086));
#201096=CARTESIAN_POINT('Ctrl Pts',(77.7344551053368,-5.21543344732299,
128.240909163888));
#201097=CARTESIAN_POINT('Ctrl Pts',(77.4560074815235,-4.97577348101974,
133.806644359053));
#201098=CARTESIAN_POINT('Ctrl Pts',(77.1775598577108,-0.163620765707691,
136.613427465507));
#201099=CARTESIAN_POINT('Ctrl Pts',(76.8991122338979,4.79889143997102,134.081961927395));
#201100=CARTESIAN_POINT('Ctrl Pts',(76.620664610085,5.35145685119646,128.538540905275));
#201101=CARTESIAN_POINT('Ctrl Pts',(76.3422169862721,0.986294849373407,
125.077297507303));
#201102=CARTESIAN_POINT('Ctrl Pts',(76.0637693624593,-4.28522393584178,
126.878945325076));
#201103=CARTESIAN_POINT('Ctrl Pts',(75.7853217386464,-5.61883126884571,
132.287858029448));
#201104=CARTESIAN_POINT('Ctrl Pts',(75.5068741148335,-1.78900716094817,
136.333509085178));
#201105=CARTESIAN_POINT('Ctrl Pts',(75.2284264910206,3.68482713000219,135.298142813091));
#201106=CARTESIAN_POINT('Ctrl Pts',(74.9499788672077,5.77248530229349,130.133210236781));
#201107=CARTESIAN_POINT('Ctrl Pts',(74.6715312433948,2.55551148336137,125.585032072894));
#201108=CARTESIAN_POINT('Ctrl Pts',(74.3930836195819,-3.0098525451033,125.833161863185));
#201109=CARTESIAN_POINT('Ctrl Pts',(74.1146359957691,-5.80930912408932,
130.649580452192));
#201110=CARTESIAN_POINT('Ctrl Pts',(73.8361883719562,-3.27029441856551,
135.608234451746));
#201111=CARTESIAN_POINT('Ctrl Pts',(73.5577407481433,2.273961094856,136.152363079971));
#201112=CARTESIAN_POINT('Ctrl Pts',(73.2792931243304,5.72855745128013,131.781938709691));
#201113=CARTESIAN_POINT('Ctrl Pts',(73.0008455005175,3.91888936556733,126.513167830092));
#201114=CARTESIAN_POINT('Ctrl Pts',(72.7223978767045,-1.49204659871303,
125.187793485758));
#201115=CARTESIAN_POINT('Ctrl Pts',(72.4439502528918,-5.53186462930466,
129.023769950998));
#201116=CARTESIAN_POINT('Ctrl Pts',(72.1655026290786,-4.48816931217651,
134.496022252122));
#201117=CARTESIAN_POINT('Ctrl Pts',(71.8870550052659,0.679934343581693,
136.575817858786));
#201118=CARTESIAN_POINT('Ctrl Pts',(71.6086073814528,5.22321155422762,133.351926212129));
#201119=CARTESIAN_POINT('Ctrl Pts',(71.3301597576401,4.96661251460835,127.786946239566));
#201120=CARTESIAN_POINT('Ctrl Pts',(71.0517121338272,0.145939206574258,
124.994822671498));
#201121=CARTESIAN_POINT('Ctrl Pts',(70.7732645100143,-4.80884510277506,
127.541380664158));
#201122=CARTESIAN_POINT('Ctrl Pts',(70.4948168862015,-5.34453568781766,
133.086457828568));
#201123=CARTESIAN_POINT('Ctrl Pts',(70.2163692623885,-0.968859070839113,
136.534399142713));
#201124=CARTESIAN_POINT('Ctrl Pts',(69.9379216385757,4.29715170084345,134.716714980192));
#201125=CARTESIAN_POINT('Ctrl Pts',(69.6594740147628,5.61428998698222,129.303768287553));
#201126=CARTESIAN_POINT('Ctrl Pts',(69.3810263909498,1.77217004839796,125.269792638185));
#201127=CARTESIAN_POINT('Ctrl Pts',(69.102578767137,-3.69848758934425,126.321814583191));
#201128=CARTESIAN_POINT('Ctrl Pts',(68.8241311433241,-5.77041581364239,
131.493077349239));
#201129=CARTESIAN_POINT('Ctrl Pts',(68.5456835195112,-2.53961380568736,
136.031443084562));
#201130=CARTESIAN_POINT('Ctrl Pts',(68.2672358956983,3.02496922266262,135.76637538989));
#201131=CARTESIAN_POINT('Ctrl Pts',(67.9887882718854,5.80975331334755,130.94145852735));
#201132=CARTESIAN_POINT('Ctrl Pts',(67.7103406480725,3.25565793129432,125.990555383323));
#201133=CARTESIAN_POINT('Ctrl Pts',(67.4318930242597,-2.29022804188655,
125.463304082106));
#201134=CARTESIAN_POINT('Ctrl Pts',(67.1534454004468,-5.73150632843341,
129.844222811859));
#201135=CARTESIAN_POINT('Ctrl Pts',(66.8749977766338,-3.90581029880048,
135.107461279717));
#201136=CARTESIAN_POINT('Ctrl Pts',(66.5965501528209,1.50913458598933,136.416360457212));
#201137=CARTESIAN_POINT('Ctrl Pts',(66.3181025290079,5.53725851157817,132.568105943505));
#201138=CARTESIAN_POINT('Ctrl Pts',(66.0396549051952,4.47691237514338,127.09905563901));
#201139=CARTESIAN_POINT('Ctrl Pts',(65.7612072813823,-0.69749752471975,
125.034999595595));
#201140=CARTESIAN_POINT('Ctrl Pts',(65.4827596575694,-5.23094127401388,
128.272704482416));
#201141=CARTESIAN_POINT('Ctrl Pts',(65.2043120337565,-4.95740553817722,
133.836877679162));
#201142=CARTESIAN_POINT('Ctrl Pts',(64.9258644099437,-0.128256295479839,
136.614315842995));
#201143=CARTESIAN_POINT('Ctrl Pts',(64.6474167861306,4.81875421709505,134.05268898675));
#201144=CARTESIAN_POINT('Ctrl Pts',(64.3689691623179,5.33756501339024,128.506007048888));
#201145=CARTESIAN_POINT('Ctrl Pts',(64.0905215385049,0.951414316927145,
125.071399759827));
#201146=CARTESIAN_POINT('Ctrl Pts',(63.8120739146922,-4.30903965761881,
126.905103428319));
#201147=CARTESIAN_POINT('Ctrl Pts',(63.5336262908791,-5.60969669510319,
132.322033964426));
#201148=CARTESIAN_POINT('Ctrl Pts',(63.2551786670663,-1.75531651870651,
136.344296837232));
#201149=CARTESIAN_POINT('Ctrl Pts',(62.9767310432534,3.71211378640213,135.275628965096));
#201150=CARTESIAN_POINT('Ctrl Pts',(62.6982834194405,5.76829286864752,130.098083915181));
#201151=CARTESIAN_POINT('Ctrl Pts',(62.4198357956276,2.52369260137852,125.569572651222));
#201152=CARTESIAN_POINT('Ctrl Pts',(62.1413881718147,-3.04005787731984,
125.851575794724));
#201153=CARTESIAN_POINT('Ctrl Pts',(61.8629405480017,-5.81014368184488,
130.684946233427));
#201154=CARTESIAN_POINT('Ctrl Pts',(61.5844929241889,-3.24099128405306,
135.628052657436));
#201155=CARTESIAN_POINT('Ctrl Pts',(61.3060453003759,2.306473772557,136.138421747261));
#201156=CARTESIAN_POINT('Ctrl Pts',(61.0275976765631,5.73440210969521,131.747049242268));
#201157=CARTESIAN_POINT('Ctrl Pts',(60.7491500527502,3.89269504914048,126.489391944074));
#201158=CARTESIAN_POINT('Ctrl Pts',(60.4707024289374,-1.5262085928491,125.196980058879));
#201159=CARTESIAN_POINT('Ctrl Pts',(60.1922548051244,-5.54260109744501,
129.057476971348));
#201160=CARTESIAN_POINT('Ctrl Pts',(59.9138071813117,-4.46561396460588,
134.52327461468));
#201161=CARTESIAN_POINT('Ctrl Pts',(59.6353595574987,0.715054244335847,
136.571571973714));
#201162=CARTESIAN_POINT('Ctrl Pts',(59.3569119336859,5.23862253507484,133.320083840384));
#201163=CARTESIAN_POINT('Ctrl Pts',(59.0784643098728,4.94815263701827,127.756768965196));
#201164=CARTESIAN_POINT('Ctrl Pts',(58.80001668606,0.110572196236736,124.994041935407));
#201165=CARTESIAN_POINT('Ctrl Pts',(58.5215690622471,-4.82861869113419,
127.570713924673));
#201166=CARTESIAN_POINT('Ctrl Pts',(58.2431214384343,-5.3305448924898,133.118949252284));
#201167=CARTESIAN_POINT('Ctrl Pts',(57.9646738146213,-0.933960749242644,
136.54019069853));
#201168=CARTESIAN_POINT('Ctrl Pts',(57.6862261908085,4.32088769603949,134.690484511247));
#201169=CARTESIAN_POINT('Ctrl Pts',(57.4077785669955,5.6050514357603,129.269620313377));
#201170=CARTESIAN_POINT('Ctrl Pts',(57.1293309431827,1.73844672800264,125.259107478825));
#201171=CARTESIAN_POINT('Ctrl Pts',(56.8508833193697,-3.72570559494523,
126.3444113781));
#201172=CARTESIAN_POINT('Ctrl Pts',(56.5724356955568,-5.76611648697549,
131.528190747811));
#201173=CARTESIAN_POINT('Ctrl Pts',(56.293988071744,-2.50774801792579,136.046805588895));
#201174=CARTESIAN_POINT('Ctrl Pts',(56.0155404479311,3.05511836929639,135.747869609001));
#201175=CARTESIAN_POINT('Ctrl Pts',(55.7370928241181,5.81048022596477,130.906090369819));
#201176=CARTESIAN_POINT('Ctrl Pts',(55.4586452003054,3.22629461271119,125.97082645809));
#201177=CARTESIAN_POINT('Ctrl Pts',(55.1801975764924,-2.32269813636975,
125.477344307648));
#201178=CARTESIAN_POINT('Ctrl Pts',(54.9017499526795,-5.73724476823917,
129.879129906805));
#201179=CARTESIAN_POINT('Ctrl Pts',(54.6233023288666,-3.87954373808533,
135.131157329118));
#201180=CARTESIAN_POINT('Ctrl Pts',(54.3448547050537,1.54326846112093,136.407069949284));
#201181=CARTESIAN_POINT('Ctrl Pts',(54.0664070812409,5.54789233741261,132.534366401168));
#201182=CARTESIAN_POINT('Ctrl Pts',(53.7879594574279,4.45427418523046,127.071872053402));
#201183=CARTESIAN_POINT('Ctrl Pts',(53.5095118336151,-0.732604339787292,
125.039352353899));
#201184=CARTESIAN_POINT('Ctrl Pts',(53.2310642098022,-5.24625526625226,
128.304593612394));
#201185=CARTESIAN_POINT('Ctrl Pts',(52.9526165859893,-4.93885389684926,
133.866998628235));
#201186=CARTESIAN_POINT('Ctrl Pts',(52.6741689621764,-0.0928870726681018,
136.614988930455));
#201187=CARTESIAN_POINT('Ctrl Pts',(52.3957213383635,4.83843843350925,134.023295678104));
#201188=CARTESIAN_POINT('Ctrl Pts',(52.1172737145507,5.32347539014984,128.473558358838));
#201189=CARTESIAN_POINT('Ctrl Pts',(51.8388260907377,0.91649852947334,125.065714449322));
#201190=CARTESIAN_POINT('Ctrl Pts',(51.5603784669247,-4.33269570634681,
126.931406019971));
#201191=CARTESIAN_POINT('Ctrl Pts',(51.2819308431118,-5.6003542519866,132.356153661459));
#201192=CARTESIAN_POINT('Ctrl Pts',(51.0034832192991,-1.72156083256576,
136.354879304913));
#201193=CARTESIAN_POINT('Ctrl Pts',(50.7250355954861,3.73926288906064,135.252949432607));
#201194=CARTESIAN_POINT('Ctrl Pts',(50.4465879716733,5.76388668878802,130.062983764924));
#201195=CARTESIAN_POINT('Ctrl Pts',(50.1681403478604,2.49178020303801,125.554307206545));
#201196=CARTESIAN_POINT('Ctrl Pts',(49.8896927240475,-3.07015055907373,
125.870173253527));
#201197=CARTESIAN_POINT('Ctrl Pts',(49.6112451002346,-5.81076294258959,
130.720316439607));
#201198=CARTESIAN_POINT('Ctrl Pts',(49.3327974764216,-3.21156805341676,
135.647692119444));
#201199=CARTESIAN_POINT('Ctrl Pts',(49.0543498526089,2.33890098302428,136.124282758954));
#201200=CARTESIAN_POINT('Ctrl Pts',(48.7759022287959,5.74003427773134,131.712124843171));
#201201=CARTESIAN_POINT('Ctrl Pts',(48.497454604983,3.86635648746696,126.465775950806));
#201202=CARTESIAN_POINT('Ctrl Pts',(48.2190069811701,-1.56031403276457,
125.206374415548));
#201203=CARTESIAN_POINT('Ctrl Pts',(47.9405593573573,-5.55313218246346,
129.091248723115));
#201204=CARTESIAN_POINT('Ctrl Pts',(47.6621117335443,-4.44289314206747,
134.550389171513));
#201205=CARTESIAN_POINT('Ctrl Pts',(47.3836641097315,0.750147648492217,
136.567112382502));
#201206=CARTESIAN_POINT('Ctrl Pts',(47.1052164859186,5.25383939683757,133.288148247589));
#201207=CARTESIAN_POINT('Ctrl Pts',(46.8267688621057,4.92950940381243,127.726704620456));
#201208=CARTESIAN_POINT('Ctrl Pts',(46.5483212382927,0.0752010886061242,
124.993476502813));
#201209=CARTESIAN_POINT('Ctrl Pts',(46.2698736144798,-4.84821335325179,
127.600167009156));
#201210=CARTESIAN_POINT('Ctrl Pts',(45.991425990667,-5.31635657186091,133.151354908068));
#201211=CARTESIAN_POINT('Ctrl Pts',(45.7129783668541,-0.899027819386881,
136.545769711054));
#201212=CARTESIAN_POINT('Ctrl Pts',(45.4345307430412,4.344463579153,134.664110040551));
#201213=CARTESIAN_POINT('Ctrl Pts',(45.1560831192283,5.5956051872961,129.235529209567));
#201214=CARTESIAN_POINT('Ctrl Pts',(44.8776354954154,1.70465898882477,125.248627800858));
#201215=CARTESIAN_POINT('Ctrl Pts',(44.5991878716026,-3.7527855431554,126.367173438067));
#201216=CARTESIAN_POINT('Ctrl Pts',(44.3207402477896,-5.76160349474165,
131.563277324591));
#201217=CARTESIAN_POINT('Ctrl Pts',(44.0422926239769,-2.47578930463884,
136.0619738325));
#201218=CARTESIAN_POINT('Ctrl Pts',(43.7638450001637,3.08515430739569,135.72918064457));
#201219=CARTESIAN_POINT('Ctrl Pts',(43.485397376351,5.8109918291003,130.870718442656));
#201220=CARTESIAN_POINT('Ctrl Pts',(43.206949752538,3.19681174259461,125.951276641244));
#201221=CARTESIAN_POINT('Ctrl Pts',(42.9285021287252,-2.3550821624196,125.491581927739));
#201222=CARTESIAN_POINT('Ctrl Pts',(42.6500545049123,-5.74277061233009,
129.914071286517));
#201223=CARTESIAN_POINT('Ctrl Pts',(42.3716068810994,-3.85313341945026,
135.154693047476));
#201224=CARTESIAN_POINT('Ctrl Pts',(42.0931592572865,1.57734514987214,136.397571830902));
#201225=CARTESIAN_POINT('Ctrl Pts',(41.8147116334736,5.5583205840564,132.50056275283));
#201226=CARTESIAN_POINT('Ctrl Pts',(41.5362640096606,4.43147094054935,127.04482677653));
#201227=CARTESIAN_POINT('Ctrl Pts',(41.2578163858478,-0.767684007931795,
125.043918736703));
#201228=CARTESIAN_POINT('Ctrl Pts',(40.9793687620349,-5.26137485657243,
128.336575372158));
#201229=CARTESIAN_POINT('Ctrl Pts',(40.700921138222,-4.9201192444739,133.897006090131));
#201230=CARTESIAN_POINT('Ctrl Pts',(40.4224735144091,-0.0575144078915333,
136.615446702946));
#201231=CARTESIAN_POINT('Ctrl Pts',(40.1440258905964,4.85794335980812,133.993783090635));
#201232=CARTESIAN_POINT('Ctrl Pts',(39.8655782667833,5.30918850357096,128.441196037522));
#201233=CARTESIAN_POINT('Ctrl Pts',(39.5871306429705,0.8815487808295,125.060241786462));
#201234=CARTESIAN_POINT('Ctrl Pts',(39.3086830191576,-4.35619120544207,
126.957852125381));
#201235=CARTESIAN_POINT('Ctrl Pts',(39.0302353953447,-5.59080428568363,
132.39021585623));
#201236=CARTESIAN_POINT('Ctrl Pts',(38.7517877715318,-1.6877413533555,136.365256096082));
#201237=CARTESIAN_POINT('Ctrl Pts',(38.4733401477189,3.76627343195761,135.230105056025));
#201238=CARTESIAN_POINT('Ctrl Pts',(38.194892523906,5.7592669259876,130.027911086658));
#201239=CARTESIAN_POINT('Ctrl Pts',(37.9164449000932,2.45977547086574,125.539236304527));
#201240=CARTESIAN_POINT('Ctrl Pts',(37.6379972762802,-3.10012947526937,
125.888953550457));
#201241=CARTESIAN_POINT('Ctrl Pts',(37.3595496524674,-5.81116688337655,
130.755689760074));
#201242=CARTESIAN_POINT('Ctrl Pts',(37.0811020286545,-3.18202581694541,
135.667152110023));
#201243=CARTESIAN_POINT('Ctrl Pts',(36.8026544048415,2.3712415246555,136.109946638975));
#201244=CARTESIAN_POINT('Ctrl Pts',(36.5242067810287,5.74545374668639,131.677166806538));
#201245=CARTESIAN_POINT('Ctrl Pts',(36.2457591572158,3.83987465653194,126.442320725389));
#201246=CARTESIAN_POINT('Ctrl Pts',(35.9673115334029,-1.59436165466975,
125.215976207654));
#201247=CARTESIAN_POINT('Ctrl Pts',(35.6888639095901,-5.56345749412674,
129.125083954872));
#201248=CARTESIAN_POINT('Ctrl Pts',(35.4104162857771,-4.42000768648982,
134.57736491788));
#201249=CARTESIAN_POINT('Ctrl Pts',(35.1319686619643,0.785213255651605,
136.562439250406));
#201250=CARTESIAN_POINT('Ctrl Pts',(34.8535210381513,5.26886157564935,133.25612061713));
#201251=CARTESIAN_POINT('Ctrl Pts',(34.5750734143385,4.91068350582282,127.69675431939));
#201252=CARTESIAN_POINT('Ctrl Pts',(34.2966257905255,0.0398271943713243,
124.993126394665));
#201253=CARTESIAN_POINT('Ctrl Pts',(34.0181781667127,-4.86762836304081,
127.629738826211));
#201254=CARTESIAN_POINT('Ctrl Pts',(33.7397305428998,-5.30197125168398,
133.183673595116));
#201255=CARTESIAN_POINT('Ctrl Pts',(33.4612829190869,-0.864061575724654,
136.551135973552));
#201256=CARTESIAN_POINT('Ctrl Pts',(33.182835295274,4.36787847657091,134.637592545421));
#201257=CARTESIAN_POINT('Ctrl Pts',(32.9043876714611,5.58595159162396,129.201496239381));
#201258=CARTESIAN_POINT('Ctrl Pts',(32.6259400476482,1.67080808288091,125.238353992614));
#201259=CARTESIAN_POINT('Ctrl Pts',(32.3474924238352,-3.77972643051725,
126.390099919638));
#201260=CARTESIAN_POINT('Ctrl Pts',(32.0690448000224,-5.75687700417149,
131.598335779433));
#201261=CARTESIAN_POINT('Ctrl Pts',(31.7905971762095,-2.44373885006871,
136.076947253315));
#201262=CARTESIAN_POINT('Ctrl Pts',(31.5121495523967,3.11507592396733,135.71030918912));
#201263=CARTESIAN_POINT('Ctrl Pts',(31.2337019285837,5.81128810379662,130.835344056578));
#201264=CARTESIAN_POINT('Ctrl Pts',(30.9552543047708,3.16721041344351,125.931906657209));
#201265=CARTESIAN_POINT('Ctrl Pts',(30.676806680958,-2.38737892003384,125.506016414799));
#201266=CARTESIAN_POINT('Ctrl Pts',(30.398359057145,-5.74808365594406,129.949045656226));
#201267=CARTESIAN_POINT('Ctrl Pts',(30.1199114333322,-3.82658032153943,
135.178067562667));
#201268=CARTESIAN_POINT('Ctrl Pts',(29.8414638095193,1.61136338951851,136.387866454021));
#201269=CARTESIAN_POINT('Ctrl Pts',(29.5630161857064,5.56854286508694,132.466696251098));
#201270=CARTESIAN_POINT('Ctrl Pts',(29.2845685618935,4.40850348608286,127.017920810568));
#201271=CARTESIAN_POINT('Ctrl Pts',(29.0061209380806,-0.802735229263066,
125.048698574801));
#201272=CARTESIAN_POINT('Ctrl Pts',(28.7276733142678,-5.27629948471241,
128.368648576612));
#201273=CARTESIAN_POINT('Ctrl Pts',(28.4492256904548,-4.90120227527057,
133.926898952911));
#201274=CARTESIAN_POINT('Ctrl Pts',(28.170778066642,-0.0221396118974229,
136.615689143506));
#201275=CARTESIAN_POINT('Ctrl Pts',(27.892330442829,4.87726827322928,133.964152317942));
#201276=CARTESIAN_POINT('Ctrl Pts',(27.6138828190162,5.29470488305963,128.408921284139));
#201277=CARTESIAN_POINT('Ctrl Pts',(27.3354351952032,0.846566366071392,
125.054981974037));
#201278=CARTESIAN_POINT('Ctrl Pts',(27.0569875713904,-4.37952528427021,
126.984440764576));
#201279=CARTESIAN_POINT('Ctrl Pts',(26.7785399475775,-5.58104715007188,
132.424219286554));
#201280=CARTESIAN_POINT('Ctrl Pts',(26.5000923237646,-1.65385933426847,
136.375426826225));
#201281=CARTESIAN_POINT('Ctrl Pts',(26.2216446999517,3.79314441420758,135.207096681855));
#201282=CARTESIAN_POINT('Ctrl Pts',(25.9431970761388,5.75443375143326,129.992867180015));
#201283=CARTESIAN_POINT('Ctrl Pts',(25.6647494523259,2.42767959080881,125.524360503627));
#201284=CARTESIAN_POINT('Ctrl Pts',(25.3863018285131,-3.12999351502748,
125.907915989602));
#201285=CARTESIAN_POINT('Ctrl Pts',(25.1078542047001,-5.81135548923757,
130.791064884058));
#201286=CARTESIAN_POINT('Ctrl Pts',(24.8294065808873,-3.152365669337,135.686431908074));
#201287=CARTESIAN_POINT('Ctrl Pts',(24.5509589570743,2.40349419906,136.095413918554));
#201288=CARTESIAN_POINT('Ctrl Pts',(24.2725113332615,5.75066031573997,131.64217642775));
#201289=CARTESIAN_POINT('Ctrl Pts',(23.9940637094486,3.81325053762949,126.419027136963));
#201290=CARTESIAN_POINT('Ctrl Pts',(23.7156160856357,-1.62835019691723,
125.2257850794));
#201291=CARTESIAN_POINT('Ctrl Pts',(23.4371684618228,-5.57357664982666,
129.158981412844));
#201292=CARTESIAN_POINT('Ctrl Pts',(23.1587208380098,-4.39695844590187,
134.604200854185));
#201293=CARTESIAN_POINT('Ctrl Pts',(22.880273214197,0.820249766445046,136.557552750588));
#201294=CARTESIAN_POINT('Ctrl Pts',(22.6018255903841,5.28368851485763,133.224002135804));
#201295=CARTESIAN_POINT('Ctrl Pts',(22.3233779665712,4.89167564065013,127.666919171818));
#201296=CARTESIAN_POINT('Ctrl Pts',(22.0449303427584,0.00445182432539013,
124.992991623939));
#201297=CARTESIAN_POINT('Ctrl Pts',(21.7664827189454,-4.88686300107076,
127.659428280044));
#201298=CARTESIAN_POINT('Ctrl Pts',(21.4880350951325,-5.28738946501251,
133.215904115845));
#201299=CARTESIAN_POINT('Ctrl Pts',(21.2095874713197,-0.829063313942982,
136.556289287176));
#201300=CARTESIAN_POINT('Ctrl Pts',(20.9311398475068,4.39113152064558,134.610933008472));
#201301=CARTESIAN_POINT('Ctrl Pts',(20.6526922236938,5.57609100646137,129.167522663925));
#201302=CARTESIAN_POINT('Ctrl Pts',(20.374244599881,1.6368952645291,125.228286434793));
#201303=CARTESIAN_POINT('Ctrl Pts',(20.0957969760681,-3.80652725872624,
126.413189973261));
#201304=CARTESIAN_POINT('Ctrl Pts',(19.8173493522552,-5.75193719040684,
131.633364813234));
#201305=CARTESIAN_POINT('Ctrl Pts',(19.5389017284423,-2.41159784185683,
136.091725296493));
#201306=CARTESIAN_POINT('Ctrl Pts',(19.2604541046294,3.14488211025528,135.691255941942));
#201307=CARTESIAN_POINT('Ctrl Pts',(18.9820064808165,5.81136903907515,130.799968522399));
#201308=CARTESIAN_POINT('Ctrl Pts',(18.7035588570036,3.13749172214556,125.912717223747));
#201309=CARTESIAN_POINT('Ctrl Pts',(18.4251112331907,-2.41958721244422,
125.52064723395));
#201310=CARTESIAN_POINT('Ctrl Pts',(18.1466636093778,-5.75318370220431,
129.984051719947));
#201311=CARTESIAN_POINT('Ctrl Pts',(17.868215985565,-3.79988542828747,135.201280008538));
#201312=CARTESIAN_POINT('Ctrl Pts',(17.589768361752,1.64532191950215,136.377954178279));
#201313=CARTESIAN_POINT('Ctrl Pts',(17.3113207379392,5.57855880171371,132.432768150908));
#201314=CARTESIAN_POINT('Ctrl Pts',(17.0328731141263,4.38537267289848,126.991155152525));
#201315=CARTESIAN_POINT('Ctrl Pts',(16.7544254903134,-0.83775670494522,
125.053691691071));
#201316=CARTESIAN_POINT('Ctrl Pts',(16.4759778665005,-5.29102859763445,
128.400812037271));
#201317=CARTESIAN_POINT('Ctrl Pts',(16.1975302426876,-4.88210369021464,
133.956676108886));
#201318=CARTESIAN_POINT('Ctrl Pts',(15.9190826188747,0.013236004487936,
136.61571624315));
#201319=CARTESIAN_POINT('Ctrl Pts',(15.6406349950618,4.89641245768097,133.934404458007));
#201320=CARTESIAN_POINT('Ctrl Pts',(15.3621873712489,5.2800250653117,128.376735294641));
#201321=CARTESIAN_POINT('Ctrl Pts',(15.0837397474361,0.811552581485459,
125.049935206953));
#201322=CARTESIAN_POINT('Ctrl Pts',(14.8052921236231,-4.40269707817821,
127.011170952307));
#201323=CARTESIAN_POINT('Ctrl Pts',(14.5268444998103,-5.57108320670569,
132.458162692417));
#201324=CARTESIAN_POINT('Ctrl Pts',(14.2483968759974,-1.6199160308156,136.385391118461));
#201325=CARTESIAN_POINT('Ctrl Pts',(13.9699492521845,3.81987484009636,135.18392516268));
#201326=CARTESIAN_POINT('Ctrl Pts',(13.6915016283715,5.74938734422005,129.95785334356));
#201327=CARTESIAN_POINT('Ctrl Pts',(13.4130540045587,2.39549375219187,125.509680355073));
#201328=CARTESIAN_POINT('Ctrl Pts',(13.1346063807458,-3.15974157172482,
125.927059868305));
#201329=CARTESIAN_POINT('Ctrl Pts',(12.8561587569329,-5.81132875318382,
130.82644050072));
#201330=CARTESIAN_POINT('Ctrl Pts',(12.57771113312,-3.12258870965941,135.705530799178));
#201331=CARTESIAN_POINT('Ctrl Pts',(12.2992635093071,2.43565781110307,136.080685136208));
#201332=CARTESIAN_POINT('Ctrl Pts',(12.0208158854942,5.75565379196074,131.607155003388));
#201333=CARTESIAN_POINT('Ctrl Pts',(11.7423682616813,3.78648511732596,126.395896048684));
#201334=CARTESIAN_POINT('Ctrl Pts',(11.4639206378685,-1.66227840004959,
125.235800667314));
#201335=CARTESIAN_POINT('Ctrl Pts',(11.1854730140555,-5.58348927459409,
129.192939840948));
#201336=CARTESIAN_POINT('Ctrl Pts',(10.9070253902426,-4.37374627440173,
134.630895986013));
#201337=CARTESIAN_POINT('Ctrl Pts',(10.6285777664298,0.855255882581734,
136.552453064119));
#201338=CARTESIAN_POINT('Ctrl Pts',(10.3501301426169,5.29831966504511,133.19179399377));
#201339=CARTESIAN_POINT('Ctrl Pts',(10.071682518804,4.87248651263752,127.637200283293));
#201340=CARTESIAN_POINT('Ctrl Pts',(9.79323489499104,-0.0309237106847325,
124.993072195629));
#201341=CARTESIAN_POINT('Ctrl Pts',(9.51478727117816,-4.90591655459505,
127.689234270502));
#201342=CARTESIAN_POINT('Ctrl Pts',(9.23633964736526,-5.27261175218,133.248045275945));
#201343=CARTESIAN_POINT('Ctrl Pts',(8.95789202355236,-0.794034330915497,
136.561229460968));
#201344=CARTESIAN_POINT('Ctrl Pts',(8.67944439973947,4.41422184972672,134.584132417584));
#201345=CARTESIAN_POINT('Ctrl Pts',(8.40099677592661,5.56602379719609,129.1336097421));
#201346=CARTESIAN_POINT('Ctrl Pts',(8.12254915211368,1.60292179042129,125.218425500451));
#201347=CARTESIAN_POINT('Ctrl Pts',(7.84410152830078,-3.83318703466779,
126.436442743329));
#201348=CARTESIAN_POINT('Ctrl Pts',(7.56565390448795,-5.74678423649425,
131.668363127979));
#201349=CARTESIAN_POINT('Ctrl Pts',(7.28720628067502,-2.37936747100029,
136.106307414428));
#201350=CARTESIAN_POINT('Ctrl Pts',(7.00875865686212,3.17457176177998,135.672021609062));
#201351=CARTESIAN_POINT('Ctrl Pts',(6.73031103304925,5.81123463193681,130.764593150968));
#201352=CARTESIAN_POINT('Ctrl Pts',(6.45186340923634,3.10765676993803,125.89370905193));
#201353=CARTESIAN_POINT('Ctrl Pts',(6.17341578542346,-2.45170584616043,
125.535473843045));
#201354=CARTESIAN_POINT('Ctrl Pts',(5.89496816161054,-5.75807056212669,
130.019088180515));
#201355=CARTESIAN_POINT('Ctrl Pts',(5.61652053779771,-3.77304972888379,
135.224329524944));
#201356=CARTESIAN_POINT('Ctrl Pts',(5.33807291398477,1.67921948147701,136.367835370977));
#201357=CARTESIAN_POINT('Ctrl Pts',(5.05962529017187,5.58836802279258,132.398779709476));
#201358=CARTESIAN_POINT('Ctrl Pts',(4.781177666359,4.36207935811697,126.964530794212));
#201359=CARTESIAN_POINT('Ctrl Pts',(4.50273004254611,-0.872747137244579,
125.058897900495));
#201360=CARTESIAN_POINT('Ctrl Pts',(4.2242824187332,-5.30556164954619,128.433064562307));
#201361=CARTESIAN_POINT('Ctrl Pts',(3.94583479492031,-4.86282419701095,
133.986336454649));
#201362=CARTESIAN_POINT('Ctrl Pts',(3.66738717110745,0.0486111304084952,
136.615528000873));
#201363=CARTESIAN_POINT('Ctrl Pts',(3.38893954729453,4.91537520376836,133.904540613147));
#201364=CARTESIAN_POINT('Ctrl Pts',(3.11049192348162,5.26514959429328,128.344639261694));
#201365=CARTESIAN_POINT('Ctrl Pts',(2.83204429966877,0.776508724519974,
125.045101672218));
#201366=CARTESIAN_POINT('Ctrl Pts',(2.55359667585587,-4.42570572852705,
127.038041698076));
#201367=CARTESIAN_POINT('Ctrl Pts',(2.27514905204296,-5.56091282480238,
132.492044816037));
#201368=CARTESIAN_POINT('Ctrl Pts',(1.99670142823006,-1.58591270077849,
136.395148603559));
#201369=CARTESIAN_POINT('Ctrl Pts',(1.7182538044172,3.84646371911817,135.160591357131));
#201370=CARTESIAN_POINT('Ctrl Pts',(1.43980618060429,5.7441278913444,129.922870874744));
#201371=CARTESIAN_POINT('Ctrl Pts',(1.16135855679139,2.36321914767325,125.495196402842));
#201372=CARTESIAN_POINT('Ctrl Pts',(0.882910932978526,-3.18937254303613,
125.946384477181));
#201373=CARTESIAN_POINT('Ctrl Pts',(0.604463309165634,-5.81108667620601,
130.861815299204));
#201374=CARTESIAN_POINT('Ctrl Pts',(0.326015685352703,-3.09269604130886,
135.724448075619));
#201375=CARTESIAN_POINT('Ctrl Pts',(0.0475680615398608,2.46773116894999,
136.065760837718));
#201376=CARTESIAN_POINT('Ctrl Pts',(-0.230879562273037,5.76043399031358,
131.572103831187));
#201377=CARTESIAN_POINT('Ctrl Pts',(-0.509327186085944,3.75957938742415,
126.37292831768));
#201378=CARTESIAN_POINT('Ctrl Pts',(-0.787774809898847,-1.69614500684454,
125.246022600264));
#201379=CARTESIAN_POINT('Ctrl Pts',(-1.06622243371171,-5.59319500111311,
129.226957980841));
#201380=CARTESIAN_POINT('Ctrl Pts',(-1.34467005752462,-4.35037203212501,
134.657449324165));
#201381=CARTESIAN_POINT('Ctrl Pts',(-1.62311768133752,0.890230306896913,
136.547140379971));
#201382=CARTESIAN_POINT('Ctrl Pts',(-1.90156530515039,5.31275448404895,
133.159497384516));
#201383=CARTESIAN_POINT('Ctrl Pts',(-2.18001292896328,4.85311683284533,
127.607598755059));
#201384=CARTESIAN_POINT('Ctrl Pts',(-2.4584605527762,-0.0662980998053887,
124.993368106748));
#201385=CARTESIAN_POINT('Ctrl Pts',(-2.73690817658909,-4.92478831757726,
127.719155693111));
#201386=CARTESIAN_POINT('Ctrl Pts',(-3.01535580040196,-5.25763866077998,
133.280095884409));
#201387=CARTESIAN_POINT('Ctrl Pts',(-3.29380342421486,-0.758975924653704,
136.565956311869));
#201388=CARTESIAN_POINT('Ctrl Pts',(-3.57225104802777,4.43714860819409,
134.557191765862));
#201389=CARTESIAN_POINT('Ctrl Pts',(-3.85069867184063,5.55575033687191,
129.099758730564));
#201390=CARTESIAN_POINT('Ctrl Pts',(-4.12914629565353,1.56888891945708,
125.208771554989));
#201391=CARTESIAN_POINT('Ctrl Pts',(-4.40759391946644,-3.85970477045413,
126.459857368199));
#201392=CARTESIAN_POINT('Ctrl Pts',(-4.68604154327934,-5.74141833337845,
131.703329426794));
#201393=CARTESIAN_POINT('Ctrl Pts',(-4.96448916709218,-2.34704893180687,
136.120693066776));
#201394=CARTESIAN_POINT('Ctrl Pts',(-5.24293679090511,3.20414377838073,
135.652606903212));
#201395=CARTESIAN_POINT('Ctrl Pts',(-5.52138441471801,5.81088488736209,
130.729219253137));
#201396=CARTESIAN_POINT('Ctrl Pts',(-5.79983203853088,3.07770666236606,
125.874882846113));
#201397=CARTESIAN_POINT('Ctrl Pts',(-6.07827966234377,-2.48373363101511,
125.550495692676));
#201398=CARTESIAN_POINT('Ctrl Pts',(-6.35672728615668,-5.7627440546269,
130.054153739642));
#201399=CARTESIAN_POINT('Ctrl Pts',(-6.63517490996957,-3.74607421773465,
135.247215257776));
#201400=CARTESIAN_POINT('Ctrl Pts',(-6.91362253378244,1.71305481935644,
136.357510407073));
#201401=CARTESIAN_POINT('Ctrl Pts',(-7.19207015759534,5.59797016483923,
132.36473218626));
#201402=CARTESIAN_POINT('Ctrl Pts',(-7.47051778140826,4.33862440488076,
126.938048722207));
#201403=CARTESIAN_POINT('Ctrl Pts',(-7.74896540522111,-0.907705229577551,
125.064317010151));
#201404=CARTESIAN_POINT('Ctrl Pts',(-8.027413029034,-5.31989810191992,128.46540495659));
#201405=CARTESIAN_POINT('Ctrl Pts',(-8.30586065284694,-4.84336451006833,
134.015878891129));
#201406=CARTESIAN_POINT('Ctrl Pts',(-8.58430827665978,0.0839844550257475,
136.615124423653));
#201407=CARTESIAN_POINT('Ctrl Pts',(-8.86275590047269,4.93415580881975,
133.874561889976));
#201408=CARTESIAN_POINT('Ctrl Pts',(-9.14120352428557,5.25007902122049,
128.312634374625));
#201409=CARTESIAN_POINT('Ctrl Pts',(-9.4196511480985,0.741436093738357,
125.040481548942));
#201410=CARTESIAN_POINT('Ctrl Pts',(-9.69809877191133,-4.44855038272257,
127.065052006178));
#201411=CARTESIAN_POINT('Ctrl Pts',(-9.97654639572428,-5.5505363812293,
132.525864401898));
#201412=CARTESIAN_POINT('Ctrl Pts',(-10.2549940195371,-1.55185060416301,
136.404698919952));
#201413=CARTESIAN_POINT('Ctrl Pts',(-10.53344164335,3.87291006601234,135.137096129849));
#201414=CARTESIAN_POINT('Ctrl Pts',(-10.8118892671629,5.7386555876974,129.887921069854));
#201415=CARTESIAN_POINT('Ctrl Pts',(-11.0903368909758,2.33085697319978,
125.480909183646));
#201416=CARTESIAN_POINT('Ctrl Pts',(-11.3687845147887,-3.21888533097506,
125.965889100148));
#201417=CARTESIAN_POINT('Ctrl Pts',(-11.6472321386015,-5.81062926727439,
130.897187968684));
#201418=CARTESIAN_POINT('Ctrl Pts',(-11.9256797624145,-3.06268877196916,
135.743183036409));
#201419=CARTESIAN_POINT('Ctrl Pts',(-12.2041273862274,2.49971308411117,
136.050641576106));
#201420=CARTESIAN_POINT('Ctrl Pts',(-12.4825750100403,5.76500073366654,
131.537024209977));
#201421=CARTESIAN_POINT('Ctrl Pts',(-12.7610226338531,3.73253434492532,
126.350124795028));
#201422=CARTESIAN_POINT('Ctrl Pts',(-13.039470257666,-1.7299487623625,125.256450499474));
#201423=CARTESIAN_POINT('Ctrl Pts',(-13.3179178814789,-5.60269346973446,
129.261034571969));
#201424=CARTESIAN_POINT('Ctrl Pts',(-13.5963655052918,-4.32683658521273,
134.683859884699));
#201425=CARTESIAN_POINT('Ctrl Pts',(-13.8748131291047,0.925171743400955,
136.541614895008));
#201426=CARTESIAN_POINT('Ctrl Pts',(-14.1532607529176,5.3269924369816,133.127113504801));
#201427=CARTESIAN_POINT('Ctrl Pts',(-14.4317083767304,4.83356731902416,
127.578115684011));
#201428=CARTESIAN_POINT('Ctrl Pts',(-14.7101560005434,-0.101670032225581,
124.99387934633));
#201429=CARTESIAN_POINT('Ctrl Pts',(-14.9886036243562,-4.94347759071707,
127.749191439124));
#201430=CARTESIAN_POINT('Ctrl Pts',(-15.2670512481692,-5.24247074564602,
133.312054753593));
#201431=CARTESIAN_POINT('Ctrl Pts',(-15.545498871982,-0.723889394260118,
136.570469664722));
#201432=CARTESIAN_POINT('Ctrl Pts',(-15.823946495795,4.45991094648802,134.530112051601));
#201433=CARTESIAN_POINT('Ctrl Pts',(-16.1023941196078,5.54527100617588,
129.065970883678));
#201434=CARTESIAN_POINT('Ctrl Pts',(-16.3808417434207,1.53479791273714,
125.199324956138));
#201435=CARTESIAN_POINT('Ctrl Pts',(-16.6592893672336,-3.88607948346057,
126.483432980235));
#201436=CARTESIAN_POINT('Ctrl Pts',(-16.9377369910465,-5.73583967989507,
131.738262413989));
#201437=CARTESIAN_POINT('Ctrl Pts',(-17.2161846148594,-2.31464342185212,
136.134881720468));
#201438=CARTESIAN_POINT('Ctrl Pts',(-17.4946322386723,3.23359706425542,
135.633012543814));
#201439=CARTESIAN_POINT('Ctrl Pts',(-17.7730798624852,5.81031981831091,
130.693848139697));
#201440=CARTESIAN_POINT('Ctrl Pts',(-18.0515274862981,3.04764250924188,
125.856239303907));
#201441=CARTESIAN_POINT('Ctrl Pts',(-18.3299751101109,-2.51566938020671,
125.565712226204));
#201442=CARTESIAN_POINT('Ctrl Pts',(-18.6084227339239,-5.76720400652691,
130.089247097961));
#201443=CARTESIAN_POINT('Ctrl Pts',(-18.8868703577367,-3.71895989442774,
135.269936358996));
#201444=CARTESIAN_POINT('Ctrl Pts',(-19.1653179815497,1.74682667935956,
136.346979669161));
#201445=CARTESIAN_POINT('Ctrl Pts',(-19.4437656053625,5.60736487204277,
132.330626842902));
#201446=CARTESIAN_POINT('Ctrl Pts',(-19.7222132291754,4.31500868232164,
126.91170991781));
#201447=CARTESIAN_POINT('Ctrl Pts',(-20.0006608529883,-0.942629686559699,
125.069948819234));
#201448=CARTESIAN_POINT('Ctrl Pts',(-20.2791084768012,-5.33403742351306,
128.497832021735));
#201449=CARTESIAN_POINT('Ctrl Pts',(-20.5575561006141,-4.82372535047263,
134.045302323618));
#201450=CARTESIAN_POINT('Ctrl Pts',(-20.836003724427,0.119354667568119,
136.614505526443));
#201451=CARTESIAN_POINT('Ctrl Pts',(-21.1144513482399,4.95275357691331,
133.844469399368));
#201452=CARTESIAN_POINT('Ctrl Pts',(-21.3928989720528,5.23481390453873,
128.280721819388));
#201453=CARTESIAN_POINT('Ctrl Pts',(-21.6713465958657,0.706335988769417,
125.036075008324));
#201454=CARTESIAN_POINT('Ctrl Pts',(-21.9497942196786,-4.47123019424771,
127.092200875735));
#201455=CARTESIAN_POINT('Ctrl Pts',(-22.2282418434914,-5.53995426048939,
132.559620196804));
#201456=CARTESIAN_POINT('Ctrl Pts',(-22.5066894673044,-1.5177310031529,
136.41404171375));
#201457=CARTESIAN_POINT('Ctrl Pts',(-22.7851370911172,3.89921290079955,
135.11344035146));
#201458=CARTESIAN_POINT('Ctrl Pts',(-23.0635847149301,5.73297063605735,
129.853005223969));
#201459=CARTESIAN_POINT('Ctrl Pts',(-23.342032338743,2.298408427964,125.466819226899));
#201460=CARTESIAN_POINT('Ctrl Pts',(-23.6204799625559,-3.24827884193431,
125.985573014458));
#201461=CARTESIAN_POINT('Ctrl Pts',(-23.8989275863688,-5.80995654333829,
130.932557198412));
#201462=CARTESIAN_POINT('Ctrl Pts',(-24.1773752101816,-3.03256801357094,
135.761734987319));
#201463=CARTESIAN_POINT('Ctrl Pts',(-24.4558228339946,2.53160237148462,
136.035327911625));
#201464=CARTESIAN_POINT('Ctrl Pts',(-24.7342704578075,5.76935385279724,
131.501917439649));
#201465=CARTESIAN_POINT('Ctrl Pts',(-25.0127180816204,3.70535099199371,
126.327486325724));
#201466=CARTESIAN_POINT('Ctrl Pts',(-25.2911657054332,-1.76368841399288,
125.267083978533));
#201467=CARTESIAN_POINT('Ctrl Pts',(-25.5696133292462,-5.61198432848891,
129.295168351611));
#201468=CARTESIAN_POINT('Ctrl Pts',(-25.8480609530591,-4.30314080577957,
134.71012668896));
#201469=CARTESIAN_POINT('Ctrl Pts',(-26.1265085768719,0.960078897325804,
136.535876813977));
#201470=CARTESIAN_POINT('Ctrl Pts',(-26.4049562006848,5.3410329962505,133.094643554625));
#201471=CARTESIAN_POINT('Ctrl Pts',(-26.6834038244978,4.81383869558843,
127.548752162656));
#201472=CARTESIAN_POINT('Ctrl Pts',(-26.9618514483106,-0.137038197225328,
124.994605895435));
#201473=CARTESIAN_POINT('Ctrl Pts',(-27.2402990721235,-4.96198368147699,
127.779340395554));
#201474=CARTESIAN_POINT('Ctrl Pts',(-27.5187466959364,-5.22710856883054,
133.343920699249));
#201475=CARTESIAN_POINT('Ctrl Pts',(-27.7971943197493,-0.688776039878604,
136.574769352283));
#201476=CARTESIAN_POINT('Ctrl Pts',(-28.0756419435621,4.48250802114168,
134.502894278251));
#201477=CARTESIAN_POINT('Ctrl Pts',(-28.3540895673751,5.53458619342344,
129.032247453463));
#201478=CARTESIAN_POINT('Ctrl Pts',(-28.632537191188,1.50065003351598,125.190086053944));
#201479=CARTESIAN_POINT('Ctrl Pts',(-28.9109848150008,-3.91231019636288,
126.507168705834));
#201480=CARTESIAN_POINT('Ctrl Pts',(-29.1894324388138,-5.73004848276283,
131.773160795109));
#201481=CARTESIAN_POINT('Ctrl Pts',(-29.4678800626266,-2.28215214193419,
136.148872849742));
#201482=CARTESIAN_POINT('Ctrl Pts',(-29.7463276864396,3.26293052800175,
135.613239256942));
#201483=CARTESIAN_POINT('Ctrl Pts',(-30.0247753102524,5.80953944572202,
130.658481121338));
#201484=CARTESIAN_POINT('Ctrl Pts',(-30.3032229340653,3.01746542460398,
125.837779116156));
#201485=CARTESIAN_POINT('Ctrl Pts',(-30.5816705578782,-2.54751191034413,
125.581122879776));
#201486=CARTESIAN_POINT('Ctrl Pts',(-30.8601181816911,-5.77145025256159,
130.124366955075));
#201487=CARTESIAN_POINT('Ctrl Pts',(-31.138565805504,-3.69170776369427,
135.292491986665));
#201488=CARTESIAN_POINT('Ctrl Pts',(-31.4170134293169,1.78053381005746,
136.336243547461));
#201489=CARTESIAN_POINT('Ctrl Pts',(-31.6954610531298,5.6165517962788,132.296464943187));
#201490=CARTESIAN_POINT('Ctrl Pts',(-31.9739086769427,4.29123306552915,
126.885515357016));
#201491=CARTESIAN_POINT('Ctrl Pts',(-32.2523563007555,-0.977519214052166,
125.075793119056));
#201492=CARTESIAN_POINT('Ctrl Pts',(-32.5308039245685,-5.34797909038788,
128.530344556146));
#201493=CARTESIAN_POINT('Ctrl Pts',(-32.8092515483813,-4.80390744596015,
134.07460566182));
#201494=CARTESIAN_POINT('Ctrl Pts',(-33.0876991721943,0.154720457379397,
136.613671332177));
#201495=CARTESIAN_POINT('Ctrl Pts',(-33.3661467960071,4.9711678189017,133.814264256411));
#201496=CARTESIAN_POINT('Ctrl Pts',(-33.64459441982,5.21935480990263,128.248902778514));
#201497=CARTESIAN_POINT('Ctrl Pts',(-33.9230420436329,0.671209710260644,
125.031882213649));
#201498=CARTESIAN_POINT('Ctrl Pts',(-34.2014896674458,-4.49374432269368,
127.119487300736));
#201499=CARTESIAN_POINT('Ctrl Pts',(-34.4799372912587,-5.52916685470707,
132.59331094992));
#201500=CARTESIAN_POINT('Ctrl Pts',(-34.7583849150716,-1.48355516206214,
136.423176638752));
#201501=CARTESIAN_POINT('Ctrl Pts',(-35.0368325388844,3.92537124881898,
135.089624898536));
#201502=CARTESIAN_POINT('Ctrl Pts',(-35.3152801626974,5.72707324708195,
129.818124630907));
#201503=CARTESIAN_POINT('Ctrl Pts',(-35.5937277865103,2.26587471435868,
125.45292705471));
#201504=CARTESIAN_POINT('Ctrl Pts',(-35.8721754103231,-3.27755198672651,
126.005435490714));
#201505=CARTESIAN_POINT('Ctrl Pts',(-36.1506230341361,-5.80906852932597,
130.967921677768));
#201506=CARTESIAN_POINT('Ctrl Pts',(-36.4290706579489,-3.00233488224952,
135.780103240898));
#201507=CARTESIAN_POINT('Ctrl Pts',(-36.7075182817618,2.56339784940132,
136.019820411726));
#201508=CARTESIAN_POINT('Ctrl Pts',(-36.9859659055747,5.77349318639923,
131.466784821096));
#201509=CARTESIAN_POINT('Ctrl Pts',(-37.2644135293876,3.67803033591843,
126.305013748643));
#201510=CARTESIAN_POINT('Ctrl Pts',(-37.5428611532005,-1.79736271150026,
125.277922643415));
#201511=CARTESIAN_POINT('Ctrl Pts',(-37.8213087770133,-5.62106723310019,
129.329358054928));
#201512=CARTESIAN_POINT('Ctrl Pts',(-38.0997564008263,-4.27928557188161,
134.736248763623));
#201513=CARTESIAN_POINT('Ctrl Pts',(-38.3782040246392,0.994950475174061,
136.529926349506));
#201514=CARTESIAN_POINT('Ctrl Pts',(-38.656651648452,5.35487564157755,133.062088737171));
#201515=CARTESIAN_POINT('Ctrl Pts',(-38.9350992722649,4.79393169358958,
127.51950927907));
#201516=CARTESIAN_POINT('Ctrl Pts',(-39.2135468960779,-0.172401284224016,
124.995547727136));
#201517=CARTESIAN_POINT('Ctrl Pts',(-39.4919945198907,-4.98030590410683,
127.809601445221));
#201518=CARTESIAN_POINT('Ctrl Pts',(-39.7704421437036,-5.21155269958477,
133.375692540572));
#201519=CARTESIAN_POINT('Ctrl Pts',(-40.0488897675166,-0.65363716264763,
136.578855215227));
#201520=CARTESIAN_POINT('Ctrl Pts',(-40.3273373913294,4.50493899481217,
134.475539454375));
#201521=CARTESIAN_POINT('Ctrl Pts',(-40.6057850151423,5.52369629454426,
128.998589689552));
#201522=CARTESIAN_POINT('Ctrl Pts',(-40.8842326389552,1.46644654715595,
125.181055190758));
#201523=CARTESIAN_POINT('Ctrl Pts',(-41.1626802627681,-3.93839593717207,
126.531063665459));
#201524=CARTESIAN_POINT('Ctrl Pts',(-41.441127886581,-5.72404495657686,
131.808023276983));
#201525=CARTESIAN_POINT('Ctrl Pts',(-41.7195755103939,-2.24957629602936,
136.162665936149));
#201526=CARTESIAN_POINT('Ctrl Pts',(-41.9980231342068,3.29214308265742,
135.593287775304));
#201527=CARTESIAN_POINT('Ctrl Pts',(-42.2764707580197,5.80854379851262,
130.623119508596));
#201528=CARTESIAN_POINT('Ctrl Pts',(-42.5549183818325,2.98717652667487,
125.81950296691));
#201529=CARTESIAN_POINT('Ctrl Pts',(-42.8333660056454,-2.57926004149102,
125.596727082342));
#201530=CARTESIAN_POINT('Ctrl Pts',(-43.1118136294584,-5.7754826353847,
130.159512009603));
#201531=CARTESIAN_POINT('Ctrl Pts',(-43.3902612532712,-3.66431883537201,
135.314881304976));
#201532=CARTESIAN_POINT('Ctrl Pts',(-43.6687088770841,1.81417496242045,
136.325302439805));
#201533=CARTESIAN_POINT('Ctrl Pts',(-43.947156500897,5.62553059712261,132.262247752997));
#201534=CARTESIAN_POINT('Ctrl Pts',(-44.2256041247099,4.26729843551711,
126.859466010475));
#201535=CARTESIAN_POINT('Ctrl Pts',(-44.5040517485228,-1.01237251921066,
125.081849693053));
#201536=CARTESIAN_POINT('Ctrl Pts',(-44.7824993723357,-5.3617225859308,
128.562941355057));
#201537=CARTESIAN_POINT('Ctrl Pts',(-45.0609469961486,-4.78391153089065,
134.103787819889));
#201538=CARTESIAN_POINT('Ctrl Pts',(-45.3393946199614,0.190080513966956,
136.612621871764));
#201539=CARTESIAN_POINT('Ctrl Pts',(-45.6178422437743,4.98939785243841,
133.783947580368));
#201540=CARTESIAN_POINT('Ctrl Pts',(-45.8962898675873,5.20370231015464,
128.217178431071));
#201541=CARTESIAN_POINT('Ctrl Pts',(-46.1747374914001,0.636058559829223,
125.027903320286));
#201542=CARTESIAN_POINT('Ctrl Pts',(-46.453185115213,-4.51609193379101,
127.146910270074));
#201543=CARTESIAN_POINT('Ctrl Pts',(-46.7316327390259,-5.51817456361365,
132.626935412823));
#201544=CARTESIAN_POINT('Ctrl Pts',(-47.0100803628388,-1.4493243472895,
136.43210335646));
#201545=CARTESIAN_POINT('Ctrl Pts',(-47.2885279866517,3.95138414076325,
135.06565065357));
#201546=CARTESIAN_POINT('Ctrl Pts',(-47.5669756104645,5.72096363930122,
129.783280583183));
#201547=CARTESIAN_POINT('Ctrl Pts',(-47.8454232342775,2.23325703793269,
125.439233181862));
#201548=CARTESIAN_POINT('Ctrl Pts',(-48.1238708580903,-3.30670368062431,
126.025475792906));
#201549=CARTESIAN_POINT('Ctrl Pts',(-48.4023184819033,-5.80796525814313,
131.00328009631));
#201550=CARTESIAN_POINT('Ctrl Pts',(-48.6807661057162,-2.97199049830493,
135.798287116504));
#201551=CARTESIAN_POINT('Ctrl Pts',(-48.9592137295291,2.59509833966803,
136.004119651047));
#201552=CARTESIAN_POINT('Ctrl Pts',(-49.2376613533419,5.77741858108801,
131.431627656171));
#201553=CARTESIAN_POINT('Ctrl Pts',(-49.5161089771548,3.65057338907646,
126.282707896514));
#201554=CARTESIAN_POINT('Ctrl Pts',(-49.7945566009678,-1.8309704070716,
125.288966092489));
#201555=CARTESIAN_POINT('Ctrl Pts',(-50.0730042247805,-5.62994184699806,
129.363602415007));
#201556=CARTESIAN_POINT('Ctrl Pts',(-50.3514518485936,-4.25527176748286,
134.762225140725));
#201557=CARTESIAN_POINT('Ctrl Pts',(-50.6298994724063,1.02978518476655,
136.52376372209));
#201558=CARTESIAN_POINT('Ctrl Pts',(-50.9083470962193,5.36851986001845,
133.029450258773));
#201559=CARTESIAN_POINT('Ctrl Pts',(-51.1867947200322,4.77384705068883,
127.490388116857));
#201560=CARTESIAN_POINT('Ctrl Pts',(-51.465242343845,-0.207757982829986,
124.996704806535));
#201561=CARTESIAN_POINT('Ctrl Pts',(-51.743689967658,-4.99844357966987,
127.839973466791));
#201562=CARTESIAN_POINT('Ctrl Pts',(-52.0221375914708,-5.19580371433717,
133.407369100245));
#201563=CARTESIAN_POINT('Ctrl Pts',(-52.3005852152837,-0.618474064651215,
136.58272710215));
#201564=CARTESIAN_POINT('Ctrl Pts',(-52.5790328390967,4.52720303631132,
134.448048593619));
#201565=CARTESIAN_POINT('Ctrl Pts',(-52.8574804629095,5.51260171306762,
128.964998839148));
#201566=CARTESIAN_POINT('Ctrl Pts',(-53.1359280867224,1.43218872108006,
125.172232701224));
#201567=CARTESIAN_POINT('Ctrl Pts',(-53.4143757105353,-3.96433573927151,
126.555116973674));
#201568=CARTESIAN_POINT('Ctrl Pts',(-53.6928233343482,-5.71782932379997,
131.842848567767));
#201569=CARTESIAN_POINT('Ctrl Pts',(-53.9712709581611,-2.21691709124776,
136.176260468582));
#201570=CARTESIAN_POINT('Ctrl Pts',(-54.249718581974,3.32123364574025,135.573158838211));
#201571=CARTESIAN_POINT('Ctrl Pts',(-54.5281662057869,5.80733291357678,
130.58776461181));
#201572=CARTESIAN_POINT('Ctrl Pts',(-54.8066138295998,2.95677693782102,
125.801411533396));
#201573=CARTESIAN_POINT('Ctrl Pts',(-55.0850614534126,-2.61091259720856,
125.612524255684));
#201574=CARTESIAN_POINT('Ctrl Pts',(-55.3635090772256,-5.77930100557468,
130.194680959234));
#201575=CARTESIAN_POINT('Ctrl Pts',(-55.6419567010384,-3.63679412436797,
135.337103484283));
#201576=CARTESIAN_POINT('Ctrl Pts',(-55.9204043248514,1.8477488898629,136.314156751619));
#201577=CARTESIAN_POINT('Ctrl Pts',(-56.1988519486642,5.63430094186134,
132.227976540264));
#201578=CARTESIAN_POINT('Ctrl Pts',(-56.4772995724772,4.24320567919224,
126.833562843453));
#201579=CARTESIAN_POINT('Ctrl Pts',(-56.7557471962901,-1.04718831053316,
125.088118316796));
#201580=CARTESIAN_POINT('Ctrl Pts',(-57.0341948201028,-5.3752674008715,
128.595621210585));
#201581=CARTESIAN_POINT('Ctrl Pts',(-57.3126424439159,-4.76373834622006,
134.13284771647));
#201582=CARTESIAN_POINT('Ctrl Pts',(-57.5910900677287,0.225433527051438,
136.611357184097));
#201583=CARTESIAN_POINT('Ctrl Pts',(-57.8695376915416,5.00744300200284,
133.753520494635));
#201584=CARTESIAN_POINT('Ctrl Pts',(-58.1479853153544,5.18785698530388,
128.185549952615));
#201585=CARTESIAN_POINT('Ctrl Pts',(-58.4264329391674,0.600883840013963,
125.024138475672));
#201586=CARTESIAN_POINT('Ctrl Pts',(-58.7048805629802,-4.53827219944114,
127.174468767579));
#201587=CARTESIAN_POINT('Ctrl Pts',(-58.9833281867932,-5.5069777945324,
132.660492339548));
#201588=CARTESIAN_POINT('Ctrl Pts',(-59.261775810606,-1.41503982726995,
136.440821536091));
#201589=CARTESIAN_POINT('Ctrl Pts',(-59.540223434419,3.97725061271504,135.041518504932));
#201590=CARTESIAN_POINT('Ctrl Pts',(-59.8186710582318,5.71464203910897,
129.748474371954));
#201591=CARTESIAN_POINT('Ctrl Pts',(-60.0971186820448,2.20055660734573,
125.425738115783));
#201592=CARTESIAN_POINT('Ctrl Pts',(-60.3755663058576,-3.3357328434014,
126.045693178431));
#201593=CARTESIAN_POINT('Ctrl Pts',(-60.6540139296705,-5.80664677067165,
131.038631143817));
#201594=CARTESIAN_POINT('Ctrl Pts',(-60.9324615534834,-2.94153598615947,
135.816285940328));
#201595=CARTESIAN_POINT('Ctrl Pts',(-61.2109091772963,2.62670266761142,
135.988226211385));
#201596=CARTESIAN_POINT('Ctrl Pts',(-61.4893568011092,5.78112989140647,
131.396447247635));
#201597=CARTESIAN_POINT('Ctrl Pts',(-61.767804424922,3.62298116889529,126.260569595891));
#201598=CARTESIAN_POINT('Ctrl Pts',(-62.046252048735,-1.86451025536104,
125.300213916535));
#201599=CARTESIAN_POINT('Ctrl Pts',(-62.3246996725479,-5.63860784133039,
129.39790016291));
#201600=CARTESIAN_POINT('Ctrl Pts',(-62.6031472963608,-4.23110028242386,
134.788054857702));
#201601=CARTESIAN_POINT('Ctrl Pts',(-62.8815949201736,1.0645817352901,136.517389160091));
#201602=CARTESIAN_POINT('Ctrl Pts',(-63.1600425439866,5.38196514598156,
132.99672932886));
#201603=CARTESIAN_POINT('Ctrl Pts',(-63.4384901677994,4.75358551113023,
127.461389755115));
#201604=CARTESIAN_POINT('Ctrl Pts',(-63.7169377916123,-0.243106982887504,
124.998077090756));
#201605=CARTESIAN_POINT('Ctrl Pts',(-63.9953854154252,-5.0163960360679,
127.870455334816));
#201606=CARTESIAN_POINT('Ctrl Pts',(-64.2738330392381,-5.17986219667218,
133.438949204482));
#201607=CARTESIAN_POINT('Ctrl Pts',(-64.552280663051,-0.583288048870894,
136.586384869579));
#201608=CARTESIAN_POINT('Ctrl Pts',(-64.8307282868638,4.54929932063727,
134.420422714664));
#201609=CARTESIAN_POINT('Ctrl Pts',(-65.1091759106768,5.50130286010717,
128.93147614697));
#201610=CARTESIAN_POINT('Ctrl Pts',(-65.3876235344896,1.39787782472419,
125.16361891226));
#201611=CARTESIAN_POINT('Ctrl Pts',(-65.6660711583025,-3.99012864145221,
126.579327739175));
#201612=CARTESIAN_POINT('Ctrl Pts',(-65.9445187821156,-5.71140181475477,
131.877635376998));
#201613=CARTESIAN_POINT('Ctrl Pts',(-66.2229664059283,-2.18417573778792,
136.189655943291));
#201614=CARTESIAN_POINT('Ctrl Pts',(-66.5014140297413,3.35020113928917,
135.552853191544));
#201615=CARTESIAN_POINT('Ctrl Pts',(-66.7798616535541,5.80590683578406,
130.552417741069));
#201616=CARTESIAN_POINT('Ctrl Pts',(-67.0583092773671,2.92626778451039,
125.783505486001));
#201617=CARTESIAN_POINT('Ctrl Pts',(-67.3367569011799,-2.64246840459962,
125.628513814431));
#201618=CARTESIAN_POINT('Ctrl Pts',(-67.6152045249929,-5.78290522164069,
130.229872500769));
#201619=CARTESIAN_POINT('Ctrl Pts',(-67.8936521488056,-3.60913465062,135.359157701137));
#201620=CARTESIAN_POINT('Ctrl Pts',(-68.1720997726187,1.88125434829088,
136.302806895912));
#201621=CARTESIAN_POINT('Ctrl Pts',(-68.4505473964314,5.64286250550667,
132.193652574919));
#201622=CARTESIAN_POINT('Ctrl Pts',(-68.7289950202444,4.21895568932047,
126.807806815805));
#201623=CARTESIAN_POINT('Ctrl Pts',(-69.0074426440573,-1.08196529790749,
125.094598758));
#201624=CARTESIAN_POINT('Ctrl Pts',(-69.2858902678701,-5.38861303330182,
128.628382911763));
#201625=CARTESIAN_POINT('Ctrl Pts',(-69.564337891683,-4.74338863947339,
134.161784274737));
#201626=CARTESIAN_POINT('Ctrl Pts',(-69.8427855154959,0.260778186613682,
136.609877316035));
#201627=CARTESIAN_POINT('Ctrl Pts',(-70.1212331393089,5.02530259892534,
133.722984126697));
#201628=CARTESIAN_POINT('Ctrl Pts',(-70.3996807631217,5.17181942250469,
128.154018515153));
#201629=CARTESIAN_POINT('Ctrl Pts',(-70.6781283869345,0.5656868542273,125.020587819316));
#201630=CARTESIAN_POINT('Ctrl Pts',(-70.9565760107477,-4.56028429774593,
127.202161772061));
#201631=CARTESIAN_POINT('Ctrl Pts',(-71.2350236345604,-5.49557696236377,
132.693980486629));
#201632=CARTESIAN_POINT('Ctrl Pts',(-71.5134712583732,-1.38070287242923,
136.449330854589));
#201633=CARTESIAN_POINT('Ctrl Pts',(-71.7919188821862,4.00296970618273,
135.017229346852));
#201634=CARTESIAN_POINT('Ctrl Pts',(-72.0703665059991,5.70810868075446,
129.71370728698));
#201635=CARTESIAN_POINT('Ctrl Pts',(-72.348814129812,2.16777463432419,125.412442356538));
#201636=CARTESIAN_POINT('Ctrl Pts',(-72.6272617536249,-3.36463839937136,
126.06608689813));
#201637=CARTESIAN_POINT('Ctrl Pts',(-72.9057093774378,-5.80511311576878,
131.073973510343));
#201638=CARTESIAN_POINT('Ctrl Pts',(-73.1841570012506,-2.91097247431594,
135.834099045416));
#201639=CARTESIAN_POINT('Ctrl Pts',(-73.4626046250635,2.65820966212185,
135.972140681676));
#201640=CARTESIAN_POINT('Ctrl Pts',(-73.7410522488765,5.78462697983096,
131.361244899111));
#201641=CARTESIAN_POINT('Ctrl Pts',(-74.0194998726893,3.59525469781404,
126.238599667113));
#201642=CARTESIAN_POINT('Ctrl Pts',(-74.2979474965022,-1.89798101353784,
125.31166569876));
#201643=CARTESIAN_POINT('Ctrl Pts',(-74.5763951203151,-5.64706489497548,
129.432250027724));
#201644=CARTESIAN_POINT('Ctrl Pts',(-74.854842744128,-4.20677201238788,
134.813736957424));
#201645=CARTESIAN_POINT('Ctrl Pts',(-75.1332903679409,1.09933883734644,
136.510802899716));
#201646=CARTESIAN_POINT('Ctrl Pts',(-75.4117379917539,5.39521100124704,
132.963927159917));
#201647=CARTESIAN_POINT('Ctrl Pts',(-75.6901856155667,4.73314782571214,
127.432515268386));
#201648=CARTESIAN_POINT('Ctrl Pts',(-75.9686332393795,-0.278446974526432,
124.99966452895));
#201649=CARTESIAN_POINT('Ctrl Pts',(-76.2470808631926,-5.03416260806588,
127.901045919781));
#201650=CARTESIAN_POINT('Ctrl Pts',(-76.5255284870053,-5.16372873730878,
133.470431683069));
#201651=CARTESIAN_POINT('Ctrl Pts',(-76.8039761108183,-0.548080419137594,
136.589828381972));
#201652=CARTESIAN_POINT('Ctrl Pts',(-77.0824237346311,4.57122702900371,
134.392662841198));
#201653=CARTESIAN_POINT('Ctrl Pts',(-77.360871358444,5.48980015434633,128.898022855216));
#201654=CARTESIAN_POINT('Ctrl Pts',(-77.639318982257,1.36351512949127,125.155214143056));
#201655=CARTESIAN_POINT('Ctrl Pts',(-77.9177666060698,-4.0157736879487,
126.603695064822));
#201656=CARTESIAN_POINT('Ctrl Pts',(-78.1962142298826,-5.70476266761487,
131.91238241564));
#201657=CARTESIAN_POINT('Ctrl Pts',(-78.4746618536957,-2.15135344889296,
136.202851863901));
#201658=CARTESIAN_POINT('Ctrl Pts',(-78.7531094775085,3.37904448990285,
135.532371587738));
#201659=CARTESIAN_POINT('Ctrl Pts',(-79.0315571013213,5.8042656179783,130.517080206165));
#201660=CARTESIAN_POINT('Ctrl Pts',(-79.3100047251342,2.8956501972711,125.765785488239));
#201661=CARTESIAN_POINT('Ctrl Pts',(-79.5884523489472,-2.67392629435197,
125.644695166086));
#201662=CARTESIAN_POINT('Ctrl Pts',(-79.8668999727601,-5.78629515002701,
130.265085330171));
#201663=CARTESIAN_POINT('Ctrl Pts',(-80.1453475965729,-3.58134143906054,
135.38104313831));
#201664=CARTESIAN_POINT('Ctrl Pts',(-80.4237952203859,1.91469009614739,
136.291253293255));
#201665=CARTESIAN_POINT('Ctrl Pts',(-80.7022428441988,5.65121497080658,
132.15927712885));
#201666=CARTESIAN_POINT('Ctrl Pts',(-80.9806904680116,4.19454936449412,
126.782198881926));
#201667=CARTESIAN_POINT('Ctrl Pts',(-81.2591380918246,-1.11670219266007,
125.10129077653));
#201668=CARTESIAN_POINT('Ctrl Pts',(-81.5375857156372,-5.40175898869456,
128.661225244595));
#201669=CARTESIAN_POINT('Ctrl Pts',(-81.8160333394505,-4.72286316471603,
134.190596422436));
#201670=CARTESIAN_POINT('Ctrl Pts',(-82.0944809632629,0.296113182944105,
136.608182322418));
#201671=CARTESIAN_POINT('Ctrl Pts',(-82.3729285870762,5.04297598141181,
133.692339608092));
#201672=CARTESIAN_POINT('Ctrl Pts',(-82.6513762108889,5.15559021603496,
128.122585287091));
#201673=CARTESIAN_POINT('Ctrl Pts',(-82.9298238347018,0.530468906706182,
125.017251482786));
#201674=CARTESIAN_POINT('Ctrl Pts',(-83.2082714585147,-4.58212741303929,
127.229988257347));
#201675=CARTESIAN_POINT('Ctrl Pts',(-83.4867190823277,-5.48397248956967,
132.72739861315));
#201676=CARTESIAN_POINT('Ctrl Pts',(-83.7651667061405,-1.34631475513585,
136.45763099664));
#201677=CARTESIAN_POINT('Ctrl Pts',(-84.0436143299535,4.02854046813582,
134.992784079373));
#201678=CARTESIAN_POINT('Ctrl Pts',(-84.3220619537663,5.70136380633342,
129.678980616565));
#201679=CARTESIAN_POINT('Ctrl Pts',(-84.6005095775792,2.13491233361711,
125.399346396808));
#201680=CARTESIAN_POINT('Ctrl Pts',(-84.8789572013921,-3.39341927742779,
126.086656196302));
#201681=CARTESIAN_POINT('Ctrl Pts',(-85.1574048252049,-5.80336435026449,
131.109305886265));
#201682=CARTESIAN_POINT('Ctrl Pts',(-85.4358524490179,-2.88030109531746,
135.851725771696));
#201683=CARTESIAN_POINT('Ctrl Pts',(-85.7143000728307,2.68961815569484,
135.955863657977));
#201684=CARTESIAN_POINT('Ctrl Pts',(-85.9927476966438,5.78790971677558,
131.326021915035));
#201685=CARTESIAN_POINT('Ctrl Pts',(-86.2711953204564,3.56739500324825,
126.216798924288));
#201686=CARTESIAN_POINT('Ctrl Pts',(-86.5496429442695,-1.93138144132926,
125.323321014816));
#201687=CARTESIAN_POINT('Ctrl Pts',(-86.8280905680822,-5.65531269455438,
129.466650736599));
#201688=CARTESIAN_POINT('Ctrl Pts',(-87.1065381918953,-4.18228785886808,
134.83927048823));
#201689=CARTESIAN_POINT('Ctrl Pts',(-87.3849858157081,1.13405520299706,
136.504005185026));
#201690=CARTESIAN_POINT('Ctrl Pts',(-87.663433439521,5.40825693498488,132.931044967442));
#201691=CARTESIAN_POINT('Ctrl Pts',(-87.9418810633338,4.71253475176078,
127.403765726628));
#201692=CARTESIAN_POINT('Ctrl Pts',(-88.2203286871468,-0.313776648210234,
125.00146706229));
#201693=CARTESIAN_POINT('Ctrl Pts',(-88.4987763109598,-5.05174263731727,
127.931744088139));
#201694=CARTESIAN_POINT('Ctrl Pts',(-88.7772239347726,-5.14740393407785,
133.501815369412));
#201695=CARTESIAN_POINT('Ctrl Pts',(-89.0556715585855,-0.512852480082647,
136.593057511728));
#201696=CARTESIAN_POINT('Ctrl Pts',(-89.3341191823985,4.59298534887173,
134.364770001874));
#201697=CARTESIAN_POINT('Ctrl Pts',(-89.6125668062112,5.47809402202166,
128.864640203508));
#201698=CARTESIAN_POINT('Ctrl Pts',(-89.8910144300243,1.32910190870433,
125.147018705051));
#201699=CARTESIAN_POINT('Ctrl Pts',(-90.169462053837,-4.04126992847403,
126.628218047677));
#201700=CARTESIAN_POINT('Ctrl Pts',(-90.44790967765,-5.69791212839678,131.947088396125));
#201701=CARTESIAN_POINT('Ctrl Pts',(-90.7263573014627,-2.1184514408047,
136.215847741432));
#201702=CARTESIAN_POINT('Ctrl Pts',(-91.0048049252757,3.40776262878029,
135.511714785749));
#201703=CARTESIAN_POINT('Ctrl Pts',(-91.2832525490887,5.80240932097568,
130.48175331654));
#201704=CARTESIAN_POINT('Ctrl Pts',(-91.5617001729014,2.86492531064864,
125.748252196732));
#201705=CARTESIAN_POINT('Ctrl Pts',(-91.8401477967144,-2.70528510078237,
125.661067711041));
#201706=CARTESIAN_POINT('Ctrl Pts',(-92.1185954205271,-5.78947066511866,
130.30031814262));
#201707=CARTESIAN_POINT('Ctrl Pts',(-92.3970430443404,-3.55341551957677,
135.402758984829));
#201708=CARTESIAN_POINT('Ctrl Pts',(-92.6754906681528,1.94805489445803,
136.279496371773));
#201709=CARTESIAN_POINT('Ctrl Pts',(-92.9539382919661,5.6593580282576,132.124851475851));
#201710=CARTESIAN_POINT('Ctrl Pts',(-93.2323859157787,4.16998760909852,
126.75673999073));
#201711=CARTESIAN_POINT('Ctrl Pts',(-93.5108335395918,-1.15139770760221,
125.10819412441));
#201712=CARTESIAN_POINT('Ctrl Pts',(-93.7892811634045,-5.41470477992152,
128.694146992097));
#201713=CARTESIAN_POINT('Ctrl Pts',(-94.0677287872175,-4.70216268252734,
134.219283091922));
#201714=CARTESIAN_POINT('Ctrl Pts',(-94.3461764110305,0.331437206691851,
136.606272266052));
#201715=CARTESIAN_POINT('Ctrl Pts',(-94.6246240348431,5.0604624945689,133.661588074364));
#201716=CARTESIAN_POINT('Ctrl Pts',(-94.9030716586564,5.13916996727372,
128.0912514332));
#201717=CARTESIAN_POINT('Ctrl Pts',(-95.1815192824688,0.495231302464415,
125.014129589715));
#201718=CARTESIAN_POINT('Ctrl Pts',(-95.459966906282,-4.60380073591605,
127.257947192314));
#201719=CARTESIAN_POINT('Ctrl Pts',(-95.7384145300948,-5.47216480615837,
132.760745480792));
#201720=CARTESIAN_POINT('Ctrl Pts',(-96.0168621539077,-1.31187674965409,
136.465721654678));
#201721=CARTESIAN_POINT('Ctrl Pts',(-96.2953097777207,4.05396195104042,
134.96818360832));
#201722=CARTESIAN_POINT('Ctrl Pts',(-96.5737574015334,5.69440766577999,
129.64429564752));
#201723=CARTESIAN_POINT('Ctrl Pts',(-96.8522050253465,2.10197092294792,
125.386450721867));
#201724=CARTESIAN_POINT('Ctrl Pts',(-97.1306526491593,-3.42207441108517,
126.107400310748));
#201725=CARTESIAN_POINT('Ctrl Pts',(-97.4091002729722,-5.80140053895979,
131.144626962327));
#201726=CARTESIAN_POINT('Ctrl Pts',(-97.6875478967851,-2.8495229857029,
135.869165466005));
#201727=CARTESIAN_POINT('Ctrl Pts',(-97.965995520598,2.72092698447821,135.93939574344));
#201728=CARTESIAN_POINT('Ctrl Pts',(-98.2444431444108,5.79097798059694,
131.290779600608));
#201729=CARTESIAN_POINT('Ctrl Pts',(-98.5228907682237,3.53940311754856,
126.195168175249));
#201730=CARTESIAN_POINT('Ctrl Pts',(-98.8013383920368,-1.96471030107164,
125.33517943281));
#201731=CARTESIAN_POINT('Ctrl Pts',(-99.0797860158496,-5.6633509344415,
129.501101014807));
#201732=CARTESIAN_POINT('Ctrl Pts',(-99.3582336396624,-4.15764872913354,
134.864654503967));
#201733=CARTESIAN_POINT('Ctrl Pts',(-99.6366812634755,1.16872954581563,
136.496996267908));
#201734=CARTESIAN_POINT('Ctrl Pts',(-99.9151288872883,5.42110246377302,
132.898083969897));
#201735=CARTESIAN_POINT('Ctrl Pts',(-100.193576511101,4.69174705310118,
127.375142195163));
#201736=CARTESIAN_POINT('Ctrl Pts',(-100.472024134914,-0.34909469478497,
125.003484623986));
#201737=CARTESIAN_POINT('Ctrl Pts',(-100.750471758727,-5.06913547238742,
127.96254870236));
#201738=CARTESIAN_POINT('Ctrl Pts',(-101.02891938254,-5.13088839190121,
133.533099100579));
#201739=CARTESIAN_POINT('Ctrl Pts',(-101.307367006353,-0.47760553709043,
136.596072139193));
#201740=CARTESIAN_POINT('Ctrl Pts',(-101.585814630166,4.61457347397855,
134.33674523027));
#201741=CARTESIAN_POINT('Ctrl Pts',(-101.864262253979,5.46618489690847,
128.831329428852));
#201742=CARTESIAN_POINT('Ctrl Pts',(-102.142709877791,1.29463943755703,
125.139032901931));
#201743=CARTESIAN_POINT('Ctrl Pts',(-102.421157501604,-4.06661641825637,
126.652895779031));
#201744=CARTESIAN_POINT('Ctrl Pts',(-102.699605125417,-5.69085045094906,
131.981752032413));
#201745=CARTESIAN_POINT('Ctrl Pts',(-102.97805274923,-2.08547093271925,
136.228643094318));
#201746=CARTESIAN_POINT('Ctrl Pts',(-103.256500373043,3.43635449176034,
135.490883551018));
#201747=CARTESIAN_POINT('Ctrl Pts',(-103.534947996856,5.80033801356182,
130.446438381249));
#201748=CARTESIAN_POINT('Ctrl Pts',(-103.813395620669,2.83409426316523,
125.730906261181));
#201749=CARTESIAN_POINT('Ctrl Pts',(-104.091843244482,-2.73654366187847,
125.677630842606));
#201750=CARTESIAN_POINT('Ctrl Pts',(-104.370290868295,-5.79243164924577,
130.335569632546));
#201751=CARTESIAN_POINT('Ctrl Pts',(-104.648738492108,-3.52535792697413,
135.424304436005));
#201752=CARTESIAN_POINT('Ctrl Pts',(-104.92718611592,1.98134750687769,136.267536567122));
#201753=CARTESIAN_POINT('Ctrl Pts',(-105.205633739733,5.66729137611554,
132.090376891579));
#201754=CARTESIAN_POINT('Ctrl Pts',(-105.484081363546,4.14527133327901,
126.731431085605));
#201755=CARTESIAN_POINT('Ctrl Pts',(-105.762528987359,-1.18605055707886,
125.115308545834));
#201756=CARTESIAN_POINT('Ctrl Pts',(-106.040976611172,-5.42744992727162,
128.72714693434));
#201757=CARTESIAN_POINT('Ctrl Pts',(-106.319424234985,-4.68128795997122,
134.247843220201));
#201758=CARTESIAN_POINT('Ctrl Pts',(-106.597871858798,0.366748948912009,
136.604147217717));
#201759=CARTESIAN_POINT('Ctrl Pts',(-106.876319482611,5.07776149042729,
133.630730665021));
#201760=CARTESIAN_POINT('Ctrl Pts',(-107.154767106424,5.12255928467941,
128.060018114567));
#201761=CARTESIAN_POINT('Ctrl Pts',(-107.433214730236,0.45997534724462,
125.011222255784));
#201762=CARTESIAN_POINT('Ctrl Pts',(-107.711662354049,-4.62530346326349,
127.286037540936));
#201763=CARTESIAN_POINT('Ctrl Pts',(-107.990109977862,-5.46015434966779,
132.794019853873));
#201764=CARTESIAN_POINT('Ctrl Pts',(-108.268557601675,-1.2773901320969,
136.473602528901));
#201765=CARTESIAN_POINT('Ctrl Pts',(-108.547005225488,4.07923321289408,
134.943428845277));
#201766=CARTESIAN_POINT('Ctrl Pts',(-108.825452849301,5.6872405168564,129.609653665109));
#201767=CARTESIAN_POINT('Ctrl Pts',(-109.103900473114,2.06895162297316,
125.373755809571));
#201768=CARTESIAN_POINT('Ctrl Pts',(-109.382348096927,-3.45060273851677,
126.128318472786));
#201769=CARTESIAN_POINT('Ctrl Pts',(-109.66079572074,-5.79922175462486,
131.179935429694));
#201770=CARTESIAN_POINT('Ctrl Pts',(-109.939243344552,-2.81863928596571,
135.886417482107));
#201771=CARTESIAN_POINT('Ctrl Pts',(-110.217690968365,2.7521349883118,135.922737548286));
#201772=CARTESIAN_POINT('Ctrl Pts',(-110.496138592178,5.79383165759959,
131.255519261747));
#201773=CARTESIAN_POINT('Ctrl Pts',(-110.774586215991,3.51128007796473,
126.17370822153));
#201774=CARTESIAN_POINT('Ctrl Pts',(-111.053033839804,-1.99796635775128,
125.347240513325));
#201775=CARTESIAN_POINT('Ctrl Pts',(-111.331481463617,-5.67117931677705,
129.535599585778));
#201776=CARTESIAN_POINT('Ctrl Pts',(-111.60992908743,-4.13285553619637,
134.889888064022));
#201777=CARTESIAN_POINT('Ctrl Pts',(-111.888376711243,1.20336058093108,
136.489776408084));
#201778=CARTESIAN_POINT('Ctrl Pts',(-112.166824335056,5.43374711161577,
132.865045388662));
#201779=CARTESIAN_POINT('Ctrl Pts',(-112.445271958868,4.67078550002918,
127.34664573465));
#201780=CARTESIAN_POINT('Ctrl Pts',(-112.723719582681,-0.384399805526852,
125.005717139274));
#201781=CARTESIAN_POINT('Ctrl Pts',(-113.002167206494,-5.08634046877848,
127.993458620965));
#201782=CARTESIAN_POINT('Ctrl Pts',(-113.280614830307,-5.11418272276831,
133.564281717336));
#201783=CARTESIAN_POINT('Ctrl Pts',(-113.55906245412,-0.442340896249408,
136.598872152659));
#201784=CARTESIAN_POINT('Ctrl Pts',(-113.837510077933,4.63599060436829,
134.308589564856));
#201785=CARTESIAN_POINT('Ctrl Pts',(-114.115957701746,5.45407322030374,
128.798091765594));
#201786=CARTESIAN_POINT('Ctrl Pts',(-114.394405325558,1.26012899306928,
125.131257029612));
#201787=CARTESIAN_POINT('Ctrl Pts',(-114.672852949372,-4.09181221807183,
126.677727344441));
#201788=CARTESIAN_POINT('Ctrl Pts',(-114.951300573184,-5.68357789694507,
132.016372040028));
#201789=CARTESIAN_POINT('Ctrl Pts',(-115.229748196997,-2.05241314674147,
136.241237448422));
#201790=CARTESIAN_POINT('Ctrl Pts',(-115.50819582081,3.46481901936097,135.469878655457));
#201791=CARTESIAN_POINT('Ctrl Pts',(-115.786643444623,5.79805177248978,
130.411136708898));
#201792=CARTESIAN_POINT('Ctrl Pts',(-116.065091068436,2.80315819727665,
125.713748324348));
#201793=CARTESIAN_POINT('Ctrl Pts',(-116.343538692249,-2.76770081934284,
125.694383947029));
#201794=CARTESIAN_POINT('Ctrl Pts',(-116.621986316062,-5.79517799268792,
130.370838493694));
#201795=CARTESIAN_POINT('Ctrl Pts',(-116.900433939875,-3.49716970093708,
135.445678693465));
#201796=CARTESIAN_POINT('Ctrl Pts',(-117.178881563688,2.0145666997373,136.255374322477));
#201797=CARTESIAN_POINT('Ctrl Pts',(-117.4573291875,5.67501472040751,132.055854653499));
#201798=CARTESIAN_POINT('Ctrl Pts',(-117.735776811314,4.12040145290537,
126.706273104381));
#201799=CARTESIAN_POINT('Ctrl Pts',(-118.014224435126,-1.22065945701595,
125.122633777175));
#201800=CARTESIAN_POINT('Ctrl Pts',(-118.29267205894,-5.43999395846872,
128.760223848501));
#201801=CARTESIAN_POINT('Ctrl Pts',(-118.571119682752,-4.6602397705682,
134.276275748964));
#201802=CARTESIAN_POINT('Ctrl Pts',(-118.849567306565,0.402047101114997,
136.601807256156));
#201803=CARTESIAN_POINT('Ctrl Pts',(-119.128014930377,5.09487232796628,
133.599768523497));
#201804=CARTESIAN_POINT('Ctrl Pts',(-119.406462554191,5.10575878376697,
128.028886488555));
#201805=CARTESIAN_POINT('Ctrl Pts',(-119.684910178003,0.424702347469154,
125.008529588725));
#201806=CARTESIAN_POINT('Ctrl Pts',(-119.963357801817,-4.64663479828973,
127.314258262312));
#201807=CARTESIAN_POINT('Ctrl Pts',(-120.241805425629,-5.44794156515001,
132.827220499399));
#201808=CARTESIAN_POINT('Ctrl Pts',(-120.520253049442,-1.24285618037906,
136.48127332728));
#201809=CARTESIAN_POINT('Ctrl Pts',(-120.798700673255,4.10435331726091,
134.918520707537));
#201810=CARTESIAN_POINT('Ctrl Pts',(-121.077148297068,5.67986262514396,
129.575055953004));
#201811=CARTESIAN_POINT('Ctrl Pts',(-121.355595920881,2.03585565723516,
125.361262130332));
#201812=CARTESIAN_POINT('Ctrl Pts',(-121.634043544694,-3.47900320259493,
126.149409907283));
#201813=CARTESIAN_POINT('Ctrl Pts',(-121.912491168507,-5.79682807799514,
131.215229979999));
#201814=CARTESIAN_POINT('Ctrl Pts',(-122.19093879232,-2.78765114051323,
135.903481180724));
#201815=CARTESIAN_POINT('Ctrl Pts',(-122.469386416133,2.78324101077128,
135.905889689793));
#201816=CARTESIAN_POINT('Ctrl Pts',(-122.747834039945,5.79647064203949,
131.220242205036));
#201817=CARTESIAN_POINT('Ctrl Pts',(-123.026281663758,3.48302692660634,
126.152419858339));
#201818=CARTESIAN_POINT('Ctrl Pts',(-123.304729287571,-2.03114837905279,
125.359503809431));
#201819=CARTESIAN_POINT('Ctrl Pts',(-123.583176911384,-5.67879755147744,
129.570145171156));
#201820=CARTESIAN_POINT('Ctrl Pts',(-123.861624535197,-4.10790919877744,
134.914970233354));
#201821=CARTESIAN_POINT('Ctrl Pts',(-124.14007215901,1.23794702507767,136.482345873087));
#201822=CARTESIAN_POINT('Ctrl Pts',(-124.418519782823,5.44619040996103,
132.831930447996));
#201823=CARTESIAN_POINT('Ctrl Pts',(-124.696967406636,4.64965086928273,
127.318277401031));
#201824=CARTESIAN_POINT('Ctrl Pts',(-124.975415030448,-0.419690672193134,
125.00816452543));
#201825=CARTESIAN_POINT('Ctrl Pts',(-125.253862654262,-5.10335698895296,
128.024472698579));
#201826=CARTESIAN_POINT('Ctrl Pts',(-125.532310278074,-5.09728754571388,
133.595362064203));
#201827=CARTESIAN_POINT('Ctrl Pts',(-125.810757901887,-0.407059864303788,
136.601457448367));
#201828=CARTESIAN_POINT('Ctrl Pts',(-126.0892055257,4.65723594642128,134.280304048949));
#201829=CARTESIAN_POINT('Ctrl Pts',(-126.367653149513,5.44175944101008,
128.764928445366));
#201830=CARTESIAN_POINT('Ctrl Pts',(-126.646100773326,1.22557185403828,
125.123691376234));
#201831=CARTESIAN_POINT('Ctrl Pts',(-126.924548397139,-4.11685639428078,
126.702711823764));
#201832=CARTESIAN_POINT('Ctrl Pts',(-127.202996020952,-5.67609473587197,
132.050947136115));
#201833=CARTESIAN_POINT('Ctrl Pts',(-127.481443644765,-2.01927930784003,
136.253630337055));
#201834=CARTESIAN_POINT('Ctrl Pts',(-127.759891268577,3.4931551568182,135.44870087741));
#201835=CARTESIAN_POINT('Ctrl Pts',(-128.038338892391,5.79555068247735,
130.375849607603));
#201836=CARTESIAN_POINT('Ctrl Pts',(-128.316786516203,2.77211825933019,
125.696779022025));
#201837=CARTESIAN_POINT('Ctrl Pts',(-128.595234140016,-2.7987554186355,
125.711326403516));
#201838=CARTESIAN_POINT('Ctrl Pts',(-128.873681763829,-5.79770959367839,
130.406123419165));
#201839=CARTESIAN_POINT('Ctrl Pts',(-129.152129387642,-3.46885188599067,
135.466880965177));
#201840=CARTESIAN_POINT('Ctrl Pts',(-129.430577011455,2.04771124208698,
136.243010088514));
#201841=CARTESIAN_POINT('Ctrl Pts',(-129.709024635268,5.68252777494204,
132.021286040849));
#201842=CARTESIAN_POINT('Ctrl Pts',(-129.98747225908,4.09537888954061,126.681266979298));
#201843=CARTESIAN_POINT('Ctrl Pts',(-130.265919882893,-1.25522312496795,
125.130169546993));
#201844=CARTESIAN_POINT('Ctrl Pts',(-130.544367506706,-5.45233640868912,
128.793376508901));
#201845=CARTESIAN_POINT('Ctrl Pts',(-130.822815130519,-4.63901889426667,
134.304579624636));
#201846=CARTESIAN_POINT('Ctrl Pts',(-131.101262754332,0.437330355314798,
136.599252468079));
#201847=CARTESIAN_POINT('Ctrl Pts',(-131.379710378145,5.11179437313754,
133.568702797104));
#201848=CARTESIAN_POINT('Ctrl Pts',(-131.658158001958,5.08876908708517,
127.997857708758));
#201849=CARTESIAN_POINT('Ctrl Pts',(-131.936605625771,0.389413610192037,
125.006051688315));
#201850=CARTESIAN_POINT('Ctrl Pts',(-132.215053249584,-4.66779395055513,
127.342608310716));
#201851=CARTESIAN_POINT('Ctrl Pts',(-132.493500873397,-5.43552690515385,
132.860346187109));
#201852=CARTESIAN_POINT('Ctrl Pts',(-132.77194849721,-1.20827617416795,
136.488733765571));
#201853=CARTESIAN_POINT('Ctrl Pts',(-133.050396121022,4.12932133330617,
134.893460118082));
#201854=CARTESIAN_POINT('Ctrl Pts',(-133.328843744835,5.67227426403318,
129.540503793235));
#201855=CARTESIAN_POINT('Ctrl Pts',(-133.607291368648,2.00268425211708,
125.348970147109));
#201856=CARTESIAN_POINT('Ctrl Pts',(-133.885738992461,-3.50727475093002,
126.170673832692));
#201857=CARTESIAN_POINT('Ctrl Pts',(-134.164186616274,-5.79421959776922,
131.25050930539));
#201858=CARTESIAN_POINT('Ctrl Pts',(-134.442634240087,-2.75655969762259,
135.920355929551));
#201859=CARTESIAN_POINT('Ctrl Pts',(-134.7210818639,2.81424389921159,135.888852792264));
#201860=CARTESIAN_POINT('Ctrl Pts',(-134.999529487713,5.79889483612785,
131.18494973768));
#201861=CARTESIAN_POINT('Ctrl Pts',(-135.277977111526,3.45464471040472,
126.131303874523));
#201862=CARTESIAN_POINT('Ctrl Pts',(-135.556424735338,-2.06425513540386,
125.371968866708));
#201863=CARTESIAN_POINT('Ctrl Pts',(-135.834872359151,-5.68620535624619,
129.604736490841));
#201864=CARTESIAN_POINT('Ctrl Pts',(-136.113319982964,-4.08281064127246,
134.939900082537));
#201865=CARTESIAN_POINT('Ctrl Pts',(-136.391767606777,1.27248759664198,
136.474704938258));
#201866=CARTESIAN_POINT('Ctrl Pts',(-136.67021523059,5.45843189771781,132.798740374984));
#201867=CARTESIAN_POINT('Ctrl Pts',(-136.948662854403,4.62834394401342,
127.290038245509));
#201868=CARTESIAN_POINT('Ctrl Pts',(-137.227110478216,-0.454965987067202,
125.010826691762));
#201869=CARTESIAN_POINT('Ctrl Pts',(-137.505558102029,-5.12018440235748,
128.055589785961));
#201870=CARTESIAN_POINT('Ctrl Pts',(-137.784005725841,-5.0802034867949,
133.626338989485));
#201871=CARTESIAN_POINT('Ctrl Pts',(-138.062453349655,-0.371763748605222,
136.603827930521));
#201872=CARTESIAN_POINT('Ctrl Pts',(-138.340900973467,4.67830871288359,
134.251889730681));
#201873=CARTESIAN_POINT('Ctrl Pts',(-138.61934859728,5.42924401531914,128.731840697047));
#201874=CARTESIAN_POINT('Ctrl Pts',(-138.897796221093,1.19096930099152,
125.116336222143));
#201875=CARTESIAN_POINT('Ctrl Pts',(-139.176243844906,-4.14174801886209,
126.727848291193));
#201876=CARTESIAN_POINT('Ctrl Pts',(-139.454691468719,-5.66840124502105,
132.085476039479));
#201877=CARTESIAN_POINT('Ctrl Pts',(-139.733139092532,-1.98607064380098,
136.265821300996));
#201878=CARTESIAN_POINT('Ctrl Pts',(-140.011586716345,3.52136185412693,
135.427351001626));
#201879=CARTESIAN_POINT('Ctrl Pts',(-140.290034340158,5.79283483620279,
130.340578384942));
#201880=CARTESIAN_POINT('Ctrl Pts',(-140.56848196397,2.7409755995222,125.679998983016));
#201881=CARTESIAN_POINT('Ctrl Pts',(-140.846929587784,-2.82970630901691,
125.72845758426));
#201882=CARTESIAN_POINT('Ctrl Pts',(-141.125377211596,-5.80002635840773,
130.441423101462));
#201883=CARTESIAN_POINT('Ctrl Pts',(-141.403824835409,-3.44040553146196,
135.487910465481));
#201884=CARTESIAN_POINT('Ctrl Pts',(-141.682272459222,2.08077990574355,
136.230444323395));
#201885=CARTESIAN_POINT('Ctrl Pts',(-141.960720083035,5.68983026132012,
131.986672334579));
#201886=CARTESIAN_POINT('Ctrl Pts',(-142.239167706848,4.07020457040501,
126.656413636965));
#201887=CARTESIAN_POINT('Ctrl Pts',(-142.517615330661,-1.289740280165,125.137915576048));
#201888=CARTESIAN_POINT('Ctrl Pts',(-142.796062954474,-5.46447682057862,
128.826603687055));
#201889=CARTESIAN_POINT('Ctrl Pts',(-143.074510578287,-4.61762611741445,
134.332753798405));
#201890=CARTESIAN_POINT('Ctrl Pts',(-143.352958202099,0.472597404077474,
136.596482948152));
#201891=CARTESIAN_POINT('Ctrl Pts',(-143.631405825913,5.12852699888841,
133.537534636997));
#201892=CARTESIAN_POINT('Ctrl Pts',(-143.909853449725,5.07159082419343,
127.966932924958));
#201893=CARTESIAN_POINT('Ctrl Pts',(-144.188301073538,0.354110443050382,
125.003788646376));
#201894=CARTESIAN_POINT('Ctrl Pts',(-144.466748697351,-4.6887801359991,
127.371086635623));
#201895=CARTESIAN_POINT('Ctrl Pts',(-144.745196321164,-5.4229108297093,
132.893395689516));
#201896=CARTESIAN_POINT('Ctrl Pts',(-145.023643944977,-1.17365139483885,
136.495983567324));
#201897=CARTESIAN_POINT('Ctrl Pts',(-145.30209156879,4.15413633583088,134.868248005541));
#201898=CARTESIAN_POINT('Ctrl Pts',(-145.580539192603,5.66447571471356,
129.505998466145));
#201899=CARTESIAN_POINT('Ctrl Pts',(-145.858986816416,1.96943863679757,
125.336880315387));
#201900=CARTESIAN_POINT('Ctrl Pts',(-146.137434440228,-3.53541633590941,
126.192109461069));
#201901=CARTESIAN_POINT('Ctrl Pts',(-146.415882064041,-5.79139641060527,
131.285772098575));
#201902=CARTESIAN_POINT('Ctrl Pts',(-146.694329687854,-2.72536610939861,
135.937041103293));
#201903=CARTESIAN_POINT('Ctrl Pts',(-146.972777311667,2.84514250480927,
135.871627487008));
#201904=CARTESIAN_POINT('Ctrl Pts',(-147.25122493548,5.80110415003576,131.149643167454));
#201905=CARTESIAN_POINT('Ctrl Pts',(-147.529672559293,3.42613448107249,
126.110361052543));
#201906=CARTESIAN_POINT('Ctrl Pts',(-147.808120183106,-2.09728540002206,
125.38463522326));
#201907=CARTESIAN_POINT('Ctrl Pts',(-148.086567806919,-5.69340245658434,
129.639372263039));
#201908=CARTESIAN_POINT('Ctrl Pts',(-148.365015430732,-4.05756079371773,
134.964676687782));
#201909=CARTESIAN_POINT('Ctrl Pts',(-148.643463054544,1.30698101571045,
136.466853886735));
#201910=CARTESIAN_POINT('Ctrl Pts',(-148.921910678358,5.47047112127328,
132.765476399497));
#201911=CARTESIAN_POINT('Ctrl Pts',(-149.20035830217,4.60686551375719,127.261929314495));
#201912=CARTESIAN_POINT('Ctrl Pts',(-149.478805925983,-0.49022444300932,
125.013703539625));
#201913=CARTESIAN_POINT('Ctrl Pts',(-149.757253549796,-5.13682208544599,
128.086808730058));
#201914=CARTESIAN_POINT('Ctrl Pts',(-150.035701173609,-5.06293117906749,
133.657211345319));
#201915=CARTESIAN_POINT('Ctrl Pts',(-150.314148797422,-0.336453857064764,
136.605983511281));
#201916=CARTESIAN_POINT('Ctrl Pts',(-150.592596421235,4.69920812289605,
134.223347662954));
#201917=CARTESIAN_POINT('Ctrl Pts',(-150.871044045047,5.41652740699458,
128.698829746717));
#201918=CARTESIAN_POINT('Ctrl Pts',(-151.14949166886,1.15632261613933,125.109191839888));
#201919=CARTESIAN_POINT('Ctrl Pts',(-151.427939292673,-4.1664861694474,
126.753135815284));
#201920=CARTESIAN_POINT('Ctrl Pts',(-151.706386916486,-5.66049770947745,
132.119957470642));
#201921=CARTESIAN_POINT('Ctrl Pts',(-151.984834540299,-1.95278838518384,
136.277809888502));
#201922=CARTESIAN_POINT('Ctrl Pts',(-152.263282164112,3.54943806607717,
135.405829819234));
#201923=CARTESIAN_POINT('Ctrl Pts',(-152.541729787925,5.78990433430307,
130.3053243479));
#201924=CARTESIAN_POINT('Ctrl Pts',(-152.820177411738,2.70973137185537,
125.663408829112));
#201925=CARTESIAN_POINT('Ctrl Pts',(-153.09862503555,-2.86055234359039,
125.745776854456));
#201926=CARTESIAN_POINT('Ctrl Pts',(-153.377072659364,-5.80212820102742,
130.476736232542));
#201927=CARTESIAN_POINT('Ctrl Pts',(-153.655520283176,-3.41183169144105,
135.508766415124));
#201928=CARTESIAN_POINT('Ctrl Pts',(-153.933967906989,2.1137714653355,136.21767749275));
#201929=CARTESIAN_POINT('Ctrl Pts',(-154.212415530802,5.69692190894542,
131.952014817313));
#201930=CARTESIAN_POINT('Ctrl Pts',(-154.490863154615,4.04487942834225,
126.631713998332));
#201931=CARTESIAN_POINT('Ctrl Pts',(-154.769310778428,-1.32420964356211,
125.145871577308));
#201932=CARTESIAN_POINT('Ctrl Pts',(-155.047758402241,-5.47641474427016,
128.859904151722));
#201933=CARTESIAN_POINT('Ctrl Pts',(-155.326206026054,-4.59606223272787,
134.360797226267));
#201934=CARTESIAN_POINT('Ctrl Pts',(-155.604653649866,0.507846940569522,
136.593498799002));
#201935=CARTESIAN_POINT('Ctrl Pts',(-155.88310127368,5.14506958518534,133.50626519812));
#201936=CARTESIAN_POINT('Ctrl Pts',(-156.161548897493,5.05422463163864,
127.936113283085));
#201937=CARTESIAN_POINT('Ctrl Pts',(-156.439996521305,0.318794154216047,
125.001740546765));
#201938=CARTESIAN_POINT('Ctrl Pts',(-156.718444145118,-4.70959257697085,
127.399692181761));
#201939=CARTESIAN_POINT('Ctrl Pts',(-156.996891768931,-5.41009380630968,
132.926367781962));
#201940=CARTESIAN_POINT('Ctrl Pts',(-157.275339392744,-1.1389831254257,
136.503022463895));
#201941=CARTESIAN_POINT('Ctrl Pts',(-157.553787016557,4.17879740530553,
134.84288530416));
#201942=CARTESIAN_POINT('Ctrl Pts',(-157.83223464037,5.65646726616335,129.471541250343));
#201943=CARTESIAN_POINT('Ctrl Pts',(-158.110682264183,1.93612004320555,
125.324993083158));
#201944=CARTESIAN_POINT('Ctrl Pts',(-158.389129887996,-3.56342691473634,
126.213715998108));
#201945=CARTESIAN_POINT('Ctrl Pts',(-158.667577511808,-5.78835862111754,
131.321017052882));
#201946=CARTESIAN_POINT('Ctrl Pts',(-158.946025135621,-2.69407153173119,
135.95353608367));
#201947=CARTESIAN_POINT('Ctrl Pts',(-159.224472759434,2.87593568260513,
135.854214412314));
#201948=CARTESIAN_POINT('Ctrl Pts',(-159.502920383247,5.80309850189603,
131.114323802656));
#201949=CARTESIAN_POINT('Ctrl Pts',(-159.78136800706,3.39749729506709,126.089592168444));
#201950=CARTESIAN_POINT('Ctrl Pts',(-160.059815630873,-2.13023794895846,
125.39750240973));
#201951=CARTESIAN_POINT('Ctrl Pts',(-160.338263254686,-5.70038858580074,
129.674051204309));
#201952=CARTESIAN_POINT('Ctrl Pts',(-160.616710878499,-4.03216059175559,
134.989299130986));
#201953=CARTESIAN_POINT('Ctrl Pts',(-160.895158502312,1.34142600411673,
136.458793009441));
#201954=CARTESIAN_POINT('Ctrl Pts',(-161.173606126125,5.48230763450959,
132.732139754142));
#201955=CARTESIAN_POINT('Ctrl Pts',(-161.452053749937,4.58521637440516,
127.233951649575));
#201956=CARTESIAN_POINT('Ctrl Pts',(-161.730501373751,-0.525464733504406,
125.016794962416));
#201957=CARTESIAN_POINT('Ctrl Pts',(-162.008948997563,-5.15326942170307,
128.118128374039));
#201958=CARTESIAN_POINT('Ctrl Pts',(-162.287396621376,-5.04547126256333,
133.687977987722));
#201959=CARTESIAN_POINT('Ctrl Pts',(-162.565844245189,-0.301131498102361,
136.607924110772));
#201960=CARTESIAN_POINT('Ctrl Pts',(-162.844291869002,4.71993340202341,
134.194678903404));
#201961=CARTESIAN_POINT('Ctrl Pts',(-163.122739492814,5.40361008725504,
128.665896817606));
#201962=CARTESIAN_POINT('Ctrl Pts',(-163.401187116628,1.12163308332736,
125.102258494207));
#201963=CARTESIAN_POINT('Ctrl Pts',(-163.67963474044,-4.19106992935549,
126.778573459));
#201964=CARTESIAN_POINT('Ctrl Pts',(-163.958082364253,-5.65238442210956,
132.154390151878));
#201965=CARTESIAN_POINT('Ctrl Pts',(-164.236529988066,-1.91943376527495,
136.289595655332));
#201966=CARTESIAN_POINT('Ctrl Pts',(-164.514977611879,3.57738275229458,
135.384138127707));
#201967=CARTESIAN_POINT('Ctrl Pts',(-164.793425235692,5.78675928536899,
130.270088802833));
#201968=CARTESIAN_POINT('Ctrl Pts',(-165.071872859505,2.67838673409632,
125.647009175068));
#201969=CARTESIAN_POINT('Ctrl Pts',(-165.350320483318,-2.89129237934434,
125.763283572333));
#201970=CARTESIAN_POINT('Ctrl Pts',(-165.628768107131,-5.80401504365309,
130.512061503863));
#201971=CARTESIAN_POINT('Ctrl Pts',(-165.907215730944,-3.38313142474212,
135.52944804128));
#201972=CARTESIAN_POINT('Ctrl Pts',(-166.185663354757,2.14668469834846,
136.204710069657));
#201973=CARTESIAN_POINT('Ctrl Pts',(-166.464110978569,5.70380245503433,
131.917314773299));
#201974=CARTESIAN_POINT('Ctrl Pts',(-166.742558602383,4.01940440178476,
126.607168978656));
#201975=CARTESIAN_POINT('Ctrl Pts',(-167.021006226195,-1.3586299378839,
125.15403725596));
#201976=CARTESIAN_POINT('Ctrl Pts',(-167.299453850008,-5.48814973739939,
128.893276668938));
#201977=CARTESIAN_POINT('Ctrl Pts',(-167.577901473821,-4.57432803926507,
134.388708869063));
#201978=CARTESIAN_POINT('Ctrl Pts',(-167.856349097634,0.543077658606429,
136.590300131209));
#201979=CARTESIAN_POINT('Ctrl Pts',(-168.134796721447,5.16142151903669,
133.474895639175));
#201980=CARTESIAN_POINT('Ctrl Pts',(-168.413244345259,5.03667115293141,
127.905399925171));
#201981=CARTESIAN_POINT('Ctrl Pts',(-168.691691969073,0.283466052347084,
124.999907465374));
#201982=CARTESIAN_POINT('Ctrl Pts',(-168.970139592885,-4.7302305022577,
127.42842388914));
#201983=CARTESIAN_POINT('Ctrl Pts',(-169.248587216698,-5.39707630989451,
132.959261242652));
#201984=CARTESIAN_POINT('Ctrl Pts',(-169.527034840511,-1.10427265057399,
136.509850194457));
#201985=CARTESIAN_POINT('Ctrl Pts',(-169.805482464324,4.20330362790601,
134.81737295376));
#201986=CARTESIAN_POINT('Ctrl Pts',(-170.083930088137,5.6482492151383,129.437133422652));
#201987=CARTESIAN_POINT('Ctrl Pts',(-170.36237771195,1.90272970597286,125.313308890908));
#201988=CARTESIAN_POINT('Ctrl Pts',(-170.640825335763,-3.59130544946847,
126.235492643171));
#201989=CARTESIAN_POINT('Ctrl Pts',(-170.919272959575,-5.78510634187241,
131.356242862295));
#201990=CARTESIAN_POINT('Ctrl Pts',(-171.197720583389,-2.66267712425244,
135.969840259458));
#201991=CARTESIAN_POINT('Ctrl Pts',(-171.476168207202,2.90662229154664,
135.836614213432));
#201992=CARTESIAN_POINT('Ctrl Pts',(-171.754615831014,5.80487781780722,
131.07899295206));
#201993=CARTESIAN_POINT('Ctrl Pts',(-172.033063454828,3.36873421355001,
126.068997991823));
#201994=CARTESIAN_POINT('Ctrl Pts',(-172.31151107864,-2.16311156114431,
125.410569949319));
#201995=CARTESIAN_POINT('Ctrl Pts',(-172.589958702453,-5.70716348502144,
129.70877202961));
#201996=CARTESIAN_POINT('Ctrl Pts',(-172.868406326266,-4.00661097660031,
135.013766499754));
#201997=CARTESIAN_POINT('Ctrl Pts',(-173.146853950079,1.3758212854888,136.450522605077));
#201998=CARTESIAN_POINT('Ctrl Pts',(-173.425301573892,5.49394099882038,
132.698731674224));
#201999=CARTESIAN_POINT('Ctrl Pts',(-173.703749197705,4.56339732817417,
127.206106287473));
#202000=CARTESIAN_POINT('Ctrl Pts',(-173.982196821517,-0.560685552710569,
125.02010084558));
#202001=CARTESIAN_POINT('Ctrl Pts',(-174.260644445331,-5.1695258016666,
128.149547557344));
#202002=CARTESIAN_POINT('Ctrl Pts',(-174.539092069143,-5.02782438426607,
133.718637776622));
#202003=CARTESIAN_POINT('Ctrl Pts',(-174.817539692956,-0.265797980601551,
136.609649657082));
#202004=CARTESIAN_POINT('Ctrl Pts',(-175.095987316769,4.74048378228282,
134.165884514362));
#202005=CARTESIAN_POINT('Ctrl Pts',(-175.374434940582,5.39049253475655,
128.633043130058));
#202006=CARTESIAN_POINT('Ctrl Pts',(-175.652882564395,1.08690198798901,
125.095536442018));
#202007=CARTESIAN_POINT('Ctrl Pts',(-175.931330188208,-4.21549838762608,
126.80416027974));
#202008=CARTESIAN_POINT('Ctrl Pts',(-176.209777812021,-5.64406168355824,
132.188772807274));
#202009=CARTESIAN_POINT('Ctrl Pts',(-176.488225435833,-1.886008020042,136.301178164761));
#202010=CARTESIAN_POINT('Ctrl Pts',(-176.766673059646,3.60519487727851,
135.362276730843));
#202011=CARTESIAN_POINT('Ctrl Pts',(-177.045120683459,5.78339980594152,
130.234873055403));
#202012=CARTESIAN_POINT('Ctrl Pts',(-177.323568307272,2.64694284773159,
125.630800628577));
#202013=CARTESIAN_POINT('Ctrl Pts',(-177.602015931085,-2.92192527719638,
125.780977089175));
#202014=CARTESIAN_POINT('Ctrl Pts',(-177.880463554898,-5.80568681636668,
130.547397606436));
#202015=CARTESIAN_POINT('Ctrl Pts',(-178.158911178711,-3.35430579486411,
135.549954577584));
#202016=CARTESIAN_POINT('Ctrl Pts',(-178.437358802524,2.17951838517049,
136.191542534628));
#202017=CARTESIAN_POINT('Ctrl Pts',(-178.715806426336,5.71047164462571,
131.88257348836));
#202018=CARTESIAN_POINT('Ctrl Pts',(-178.99425405015,3.99378043471903,126.582779487459));
#202019=CARTESIAN_POINT('Ctrl Pts',(-179.272701673962,-1.39299988767372,
125.162412309422));
#202020=CARTESIAN_POINT('Ctrl Pts',(-179.551149297775,-5.49968136512185,
128.926720002072));
#202021=CARTESIAN_POINT('Ctrl Pts',(-179.829596921588,-4.55242434239454,
134.416487692516));
#202022=CARTESIAN_POINT('Ctrl Pts',(-180.108044545401,0.578288252700551,
136.5868870633));
#202023=CARTESIAN_POINT('Ctrl Pts',(-180.386492169214,5.17758219451528,
133.443427122574));
#202024=CARTESIAN_POINT('Ctrl Pts',(-180.664939793027,5.01893103852278,
127.874793989312));
#202025=CARTESIAN_POINT('Ctrl Pts',(-180.94338741684,0.248127446539293,
124.998289470128));
#202026=CARTESIAN_POINT('Ctrl Pts',(-181.221835040653,-4.75069314711374,
127.457280693096));
#202027=CARTESIAN_POINT('Ctrl Pts',(-181.500282664465,-5.38385882283189,
132.992074852706));
#202028=CARTESIAN_POINT('Ctrl Pts',(-181.778730288279,-1.06952125649312,
136.516466506004));
#202029=CARTESIAN_POINT('Ctrl Pts',(-182.057177912091,4.22765409554481,
134.791711899713));
#202030=CARTESIAN_POINT('Ctrl Pts',(-182.335625535904,5.63982186616143,
129.402776258069));
#202031=CARTESIAN_POINT('Ctrl Pts',(-182.614073159717,1.86926886239121,
125.301828171599));
#202032=CARTESIAN_POINT('Ctrl Pts',(-182.89252078353,-3.61905090705647,
126.257438589318));
#202033=CARTESIAN_POINT('Ctrl Pts',(-183.170968407343,-5.78163969338434,
131.391448221508));
#202034=CARTESIAN_POINT('Ctrl Pts',(-183.449416031155,-2.63118405029363,
135.985953026497));
#202035=CARTESIAN_POINT('Ctrl Pts',(-183.727863654969,2.93720119453022,
135.818827542541));
#202036=CARTESIAN_POINT('Ctrl Pts',(-184.006311278781,5.80644203183612,
131.04365192486));
#202037=CARTESIAN_POINT('Ctrl Pts',(-184.284758902595,3.33984630234777,
126.048579285806));
#202038=CARTESIAN_POINT('Ctrl Pts',(-184.563206526407,-2.19590501843575,
125.423837357804));
#202039=CARTESIAN_POINT('Ctrl Pts',(-184.84165415022,-5.71372690320071,
129.743533452349));
#202040=CARTESIAN_POINT('Ctrl Pts',(-185.120101774033,-3.98091289500146,
135.03807788744));
#202041=CARTESIAN_POINT('Ctrl Pts',(-185.398549397846,1.41016558529749,
136.442042980103));
#202042=CARTESIAN_POINT('Ctrl Pts',(-185.676997021659,5.50537078312707,
132.665253397689));
#202043=CARTESIAN_POINT('Ctrl Pts',(-185.955444645472,4.54140918357699,
127.178394260007));
#202044=CARTESIAN_POINT('Ctrl Pts',(-186.233892269285,-0.595885595507362,
125.023621066618));
#202045=CARTESIAN_POINT('Ctrl Pts',(-186.512339893098,-5.18559062295048,
128.181065115723));
#202046=CARTESIAN_POINT('Ctrl Pts',(-186.79078751691,-5.00999119808726,
133.749189575911));
#202047=CARTESIAN_POINT('Ctrl Pts',(-187.069235140724,-0.230454613858838,
136.611160086272));
#202048=CARTESIAN_POINT('Ctrl Pts',(-187.347682764536,4.76085850217237,
134.136965562817));
#202049=CARTESIAN_POINT('Ctrl Pts',(-187.626130388349,5.37717523557474,
128.600269901479));
#202050=CARTESIAN_POINT('Ctrl Pts',(-187.904578012162,1.05213061709833,
125.089025932407));
#202051=CARTESIAN_POINT('Ctrl Pts',(-188.183025635975,-4.23977063905356,
126.829895329374));
#202052=CARTESIAN_POINT('Ctrl Pts',(-188.461473259788,-5.63552980222562,
132.223104162766));
#202053=CARTESIAN_POINT('Ctrl Pts',(-188.739920883601,-1.85251238808831,
136.312556987595));
#202054=CARTESIAN_POINT('Ctrl Pts',(-189.018368507414,3.63287341044046,
135.340246438718));
#202055=CARTESIAN_POINT('Ctrl Pts',(-189.296816131227,5.77982602050738,
130.199678410544));
#202056=CARTESIAN_POINT('Ctrl Pts',(-189.575263755039,2.61540087792624,
125.614783790254));
#202057=CARTESIAN_POINT('Ctrl Pts',(-189.853711378852,-2.95244990203274,
125.798856749341));
#202058=CARTESIAN_POINT('Ctrl Pts',(-190.132159002665,-5.80714345722022,
130.582743230867));
#202059=CARTESIAN_POINT('Ctrl Pts',(-190.410606626478,-3.32535586995153,
135.570285264159));
#202060=CARTESIAN_POINT('Ctrl Pts',(-190.689054250291,2.21227130913674,
136.178175375592));
#202061=CARTESIAN_POINT('Ctrl Pts',(-190.967501874104,5.7169292305904,131.847792249846));
#202062=CARTESIAN_POINT('Ctrl Pts',(-191.245949497917,3.96800847665057,
126.558546428502));
#202063=CARTESIAN_POINT('Ctrl Pts',(-191.52439712173,-1.4273182193404,125.170996427354));
#202064=CARTESIAN_POINT('Ctrl Pts',(-191.802844745543,-5.51100920012879,
128.960232911869));
#202065=CARTESIAN_POINT('Ctrl Pts',(-192.081292369355,-4.53035195376586,
134.444132667273));
#202066=CARTESIAN_POINT('Ctrl Pts',(-192.359739993168,0.613477418111232,
136.583259721745));
#202067=CARTESIAN_POINT('Ctrl Pts',(-192.638187616981,5.19355101278185,
133.411860814392));
#202068=CARTESIAN_POINT('Ctrl Pts',(-192.916635240794,5.00100494577841,
127.844296609621));
#202069=CARTESIAN_POINT('Ctrl Pts',(-193.195082864607,0.21277964627773,
124.996886620986));
#202070=CARTESIAN_POINT('Ctrl Pts',(-193.47353048842,-4.77097975328813,
127.486261524329));
#202071=CARTESIAN_POINT('Ctrl Pts',(-193.751978112233,-5.3704418349007,
133.024807396204));
#202072=CARTESIAN_POINT('Ctrl Pts',(-194.030425736046,-1.03473023090876,
136.522871153366));
#202073=CARTESIAN_POINT('Ctrl Pts',(-194.308873359859,4.25184790590635,
134.765903092897));
#202074=CARTESIAN_POINT('Ctrl Pts',(-194.587320983671,5.63118553151129,
129.368471029708));
#202075=CARTESIAN_POINT('Ctrl Pts',(-194.865768607484,1.83573875236439,
125.290551350653));
#202076=CARTESIAN_POINT('Ctrl Pts',(-195.144216231297,-3.64666225938173,
126.279553023333));
#202077=CARTESIAN_POINT('Ctrl Pts',(-195.42266385511,-5.77795880411129,
131.426631825972));
#202078=CARTESIAN_POINT('Ctrl Pts',(-195.701111478923,-2.59959347684268,
136.001873787725));
#202079=CARTESIAN_POINT('Ctrl Pts',(-195.979559102736,2.96767125844341,
135.800855058734));
#202080=CARTESIAN_POINT('Ctrl Pts',(-196.258006726549,5.80779108602021,
131.008302030633));
#202081=CARTESIAN_POINT('Ctrl Pts',(-196.536454350362,3.31083463191258,
126.028336807015));
#202082=CARTESIAN_POINT('Ctrl Pts',(-196.814901974175,-2.22861710565919,
125.437304143558));
#202083=CARTESIAN_POINT('Ctrl Pts',(-197.093349597988,-5.72007859712835,
129.778334184429));
#202084=CARTESIAN_POINT('Ctrl Pts',(-197.3717972218,-3.95506729921131,135.062232393175));
#202085=CARTESIAN_POINT('Ctrl Pts',(-197.650244845613,1.44445763090186,
136.433354448736));
#202086=CARTESIAN_POINT('Ctrl Pts',(-197.928692469426,5.51659656389443,
132.631706165088));
#202087=CARTESIAN_POINT('Ctrl Pts',(-198.207140093239,4.51925275539276,
127.150816594059));
#202088=CARTESIAN_POINT('Ctrl Pts',(-198.485587717052,-0.631063557543924,
125.027355495085));
#202089=CARTESIAN_POINT('Ctrl Pts',(-198.764035340865,-5.2014632902668,
128.212679881281));
#202090=CARTESIAN_POINT('Ctrl Pts',(-199.042482964678,-4.99197236484219,
133.779632253479));
#202091=CARTESIAN_POINT('Ctrl Pts',(-199.320930588491,-0.19510270753564,
136.612455342372));
#202092=CARTESIAN_POINT('Ctrl Pts',(-199.599378212304,4.7810568066993,134.10792312037));
#202093=CARTESIAN_POINT('Ctrl Pts',(-199.877825836116,5.36365868318719,
128.56757834629));
#202094=CARTESIAN_POINT('Ctrl Pts',(-200.156273459929,1.01732025912016,
125.082727206624));
#202095=CARTESIAN_POINT('Ctrl Pts',(-200.434721083742,-4.26388578422093,
126.855777654281));
#202096=CARTESIAN_POINT('Ctrl Pts',(-200.713168707555,-5.62678909426374,
132.257382946195));
#202097=CARTESIAN_POINT('Ctrl Pts',(-200.991616331368,-1.8189481106068,
136.323731702186));
#202098=CARTESIAN_POINT('Ctrl Pts',(-201.270063955181,3.66041732614217,
135.318048067677));
#202099=CARTESIAN_POINT('Ctrl Pts',(-201.548511578994,5.77603806149454,
130.164506172408));
#202100=CARTESIAN_POINT('Ctrl Pts',(-201.826959202806,2.58376199347953,
125.59895925361));
#202101=CARTESIAN_POINT('Ctrl Pts',(-202.10540682662,-2.9828651227522,125.816921890294));
#202102=CARTESIAN_POINT('Ctrl Pts',(-202.383854450432,-5.80838491223743,
130.618097067413));
#202103=CARTESIAN_POINT('Ctrl Pts',(-202.662302074245,-3.29628272275406,
135.590439347642));
#202104=CARTESIAN_POINT('Ctrl Pts',(-202.940749698058,2.24494225657654,
136.164609087875));
#202105=CARTESIAN_POINT('Ctrl Pts',(-203.219197321871,5.72317497363993,
131.812972346589));
#202106=CARTESIAN_POINT('Ctrl Pts',(-203.497644945684,3.94208948256877,
126.534470699752));
#202107=CARTESIAN_POINT('Ctrl Pts',(-203.776092569497,-1.46158366120557,
125.179789291667));
#202108=CARTESIAN_POINT('Ctrl Pts',(-204.05454019331,-5.52213282266317,
128.993814156497));
#202109=CARTESIAN_POINT('Ctrl Pts',(-204.332987817123,-4.5081116912795,
134.471642768938));
#202110=CARTESIAN_POINT('Ctrl Pts',(-204.611435440935,0.648643850890564,
136.579418240959));
#202111=CARTESIAN_POINT('Ctrl Pts',(-204.889883064748,5.20932738210573,
133.380197884332));
#202112=CARTESIAN_POINT('Ctrl Pts',(-205.168330688562,4.98289353895661,
127.813908916192));
#202113=CARTESIAN_POINT('Ctrl Pts',(-205.446778312374,0.177423961388546,
124.995698969927));
#202114=CARTESIAN_POINT('Ctrl Pts',(-205.725225936187,-4.79108956905296,
127.515365308944));
#202115=CARTESIAN_POINT('Ctrl Pts',(-206.00367356,-5.35682584327266,133.057457660231));
#202116=CARTESIAN_POINT('Ctrl Pts',(-206.282121183813,-0.999900863015179,
136.529063899218));
#202117=CARTESIAN_POINT('Ctrl Pts',(-206.560568807626,4.27588416248015,
134.739947489669));
#202118=CARTESIAN_POINT('Ctrl Pts',(-206.839016431439,5.62234053121038,
129.334219008764));
#202119=CARTESIAN_POINT('Ctrl Pts',(-207.117464055252,1.80214061836306,
125.279478845937));
#202120=CARTESIAN_POINT('Ctrl Pts',(-207.395911679064,-3.67413848329639,
126.301835125757));
#202121=CARTESIAN_POINT('Ctrl Pts',(-207.674359302878,-5.77406381044983,
131.461792371951));
#202122=CARTESIAN_POINT('Ctrl Pts',(-207.95280692669,-2.56790657449899,
136.01760195319));
#202123=CARTESIAN_POINT('Ctrl Pts',(-208.231254550503,2.99803135420673,
135.782697427989));
#202124=CARTESIAN_POINT('Ctrl Pts',(-208.509702174316,5.8089249303698,130.972944579282));
#202125=CARTESIAN_POINT('Ctrl Pts',(-208.788149798129,3.28170027728254,
126.008271305542));
#202126=CARTESIAN_POINT('Ctrl Pts',(-209.066597421942,-2.2612466106562,
125.450969807563));
#202127=CARTESIAN_POINT('Ctrl Pts',(-209.345045045754,-5.72621833144002,
129.813172936296));
#202128=CARTESIAN_POINT('Ctrl Pts',(-209.623492669568,-3.92907514694791,
135.086229121905));
#202129=CARTESIAN_POINT('Ctrl Pts',(-209.90194029338,1.4786961515975,136.424457332932));
#202130=CARTESIAN_POINT('Ctrl Pts',(-210.180387917194,5.52761792514773,
132.598091219525));
#202131=CARTESIAN_POINT('Ctrl Pts',(-210.458835541006,4.49692886463537,
127.123374311529));
#202132=CARTESIAN_POINT('Ctrl Pts',(-210.73728316482,-0.666218135288655,
125.031303992602));
#202133=CARTESIAN_POINT('Ctrl Pts',(-211.015730788632,-5.21714321544808,
128.244390682522));
#202134=CARTESIAN_POINT('Ctrl Pts',(-211.294178412445,-4.97376855222533,
133.809964681263));
#202135=CARTESIAN_POINT('Ctrl Pts',(-211.572626036258,-0.159743571609885,
136.613535377387));
#202136=CARTESIAN_POINT('Ctrl Pts',(-211.851073660071,4.80107794740803,
134.0787582632));
#202137=CARTESIAN_POINT('Ctrl Pts',(-212.129521283884,5.34994337845465,
128.534969675892));
#202138=CARTESIAN_POINT('Ctrl Pts',(-212.407968907697,0.982472203965689,
125.076640498072));
#202139=CARTESIAN_POINT('Ctrl Pts',(-212.686416531509,-4.28784292953254,
126.881806295382));
#202140=CARTESIAN_POINT('Ctrl Pts',(-212.964864155322,-5.61783988356258,
132.291607887347));
#202141=CARTESIAN_POINT('Ctrl Pts',(-213.243311779135,-1.78531643133465,
136.334701894451));
#202142=CARTESIAN_POINT('Ctrl Pts',(-213.521759402948,3.68782560373359,
135.295682440288));
#202143=CARTESIAN_POINT('Ctrl Pts',(-213.800207026761,5.77203606926717,
130.129357644311));
#202144=CARTESIAN_POINT('Ctrl Pts',(-214.078654650574,2.55202736678199,
125.583327605028));
#202145=CARTESIAN_POINT('Ctrl Pts',(-214.357102274386,-3.0131698123076,
125.835171842623));
#202146=CARTESIAN_POINT('Ctrl Pts',(-214.6355498982,-5.80941113541564,130.653457806023));
#202147=CARTESIAN_POINT('Ctrl Pts',(-214.913997522012,-3.26708743058812,
135.610416081219));
#202148=CARTESIAN_POINT('Ctrl Pts',(-215.192445145826,2.27753001685547,
136.15084417418));
#202149=CARTESIAN_POINT('Ctrl Pts',(-215.470892769638,5.72920864233609,
131.778115068854));
#202150=CARTESIAN_POINT('Ctrl Pts',(-215.749340393451,3.9160244129115,126.510553193344));
#202151=CARTESIAN_POINT('Ctrl Pts',(-216.027788017264,-1.49579494355069,
125.18879057654));
#202152=CARTESIAN_POINT('Ctrl Pts',(-216.306235641077,-5.53305182053502,
129.02746249159));
#202153=CARTESIAN_POINT('Ctrl Pts',(-216.58468326489,-4.48570437905656,
134.499016978113));
#202154=CARTESIAN_POINT('Ctrl Pts',(-216.863130888703,0.683786247933482,
136.57536276329));
#202155=CARTESIAN_POINT('Ctrl Pts',(-217.141578512516,5.2249107178877,133.348439505674));
#202156=CARTESIAN_POINT('Ctrl Pts',(-217.420026136328,4.96459748918233,
127.78363203505));
#202157=CARTESIAN_POINT('Ctrl Pts',(-217.698473760142,0.142061701988793,
124.994726560962));
#202158=CARTESIAN_POINT('Ctrl Pts',(-217.976921383954,-4.81102184923216,
127.544590968491));
#202159=CARTESIAN_POINT('Ctrl Pts',(-218.255369007768,-5.34301135249269,
133.090024434919));
#202160=CARTESIAN_POINT('Ctrl Pts',(-218.53381663158,-0.965034443427401,
136.535044514085));
#202161=CARTESIAN_POINT('Ctrl Pts',(-218.812264255394,4.29976197459382,
134.713846051821));
#202162=CARTESIAN_POINT('Ctrl Pts',(-219.090711879206,5.61328719301349,
129.300021464458));
#202163=CARTESIAN_POINT('Ctrl Pts',(-219.369159503019,1.76847570537835,
125.268611067748));
#202164=CARTESIAN_POINT('Ctrl Pts',(-219.647607126831,-3.70147856065836,
126.324284070919));
#202165=CARTESIAN_POINT('Ctrl Pts',(-219.926054750645,-5.76995485673049,
131.496928556552));
#202166=CARTESIAN_POINT('Ctrl Pts',(-220.204502374457,-2.5361245174328,
136.033136940081));
#202167=CARTESIAN_POINT('Ctrl Pts',(-220.48294999827,3.02828035681523,135.764355323142));
#202168=CARTESIAN_POINT('Ctrl Pts',(-220.761397622083,5.80984352286985,
130.937580880991));
#202169=CARTESIAN_POINT('Ctrl Pts',(-221.039845245896,3.25244431804234,
125.988383524923));
#202170=CARTESIAN_POINT('Ctrl Pts',(-221.318292869709,-2.29379232432851,
125.464833843433));
#202171=CARTESIAN_POINT('Ctrl Pts',(-221.596740493522,-5.73214587862558,
129.848048416986));
#202172=CARTESIAN_POINT('Ctrl Pts',(-221.875188117335,-3.90293740136003,
135.110067184424));
#202173=CARTESIAN_POINT('Ctrl Pts',(-222.153635741148,1.51287987866345,
136.415351962378));
#202174=CARTESIAN_POINT('Ctrl Pts',(-222.432083364961,5.53843445848603,
132.564409806615));
#202175=CARTESIAN_POINT('Ctrl Pts',(-222.710530988774,4.47443833852516,
127.0960684293));
#202176=CARTESIAN_POINT('Ctrl Pts',(-222.988978612586,-0.701348026075381,
125.035466412855));
#202177=CARTESIAN_POINT('Ctrl Pts',(-223.267426236399,-5.23262981746888,
128.27619634439));
#202178=CARTESIAN_POINT('Ctrl Pts',(-223.545873860212,-4.95538043478568,
133.840185735283));
#202179=CARTESIAN_POINT('Ctrl Pts',(-223.824321484025,-0.124378516327312,
136.614400151295));
#202180=CARTESIAN_POINT('Ctrl Pts',(-224.102769107838,4.82092118240782,
134.049472072021));
#202181=CARTESIAN_POINT('Ctrl Pts',(-224.381216731651,5.33602982960279,
128.502445098609));
#202182=CARTESIAN_POINT('Ctrl Pts',(-224.659664355464,0.947587742942381,
125.070766032295));
#202183=CARTESIAN_POINT('Ctrl Pts',(-224.938111979277,-4.31164118724753,
126.907980288176));
#202184=CARTESIAN_POINT('Ctrl Pts',(-225.216559603089,-5.60868250173869,
132.325777718005));
#202185=CARTESIAN_POINT('Ctrl Pts',(-225.495007226903,-1.75161859650508,
136.345467157888));
#202186=CARTESIAN_POINT('Ctrl Pts',(-225.773454850715,3.71509722759125,
135.273150385318));
#202187=CARTESIAN_POINT('Ctrl Pts',(-226.051902474528,5.7678201921206,130.0942341287));
#202188=CARTESIAN_POINT('Ctrl Pts',(-226.330350098341,2.52019817377184,
125.567889423742));
#202189=CARTESIAN_POINT('Ctrl Pts',(-226.608797722154,-3.04336284774751,
125.853605930069));
#202190=CARTESIAN_POINT('Ctrl Pts',(-226.887245345967,-5.81022208872781,
130.688824136393));
#202191=CARTESIAN_POINT('Ctrl Pts',(-227.16569296978,-3.23777107529596,
135.630214724643));
#202192=CARTESIAN_POINT('Ctrl Pts',(-227.444140593593,2.31003338242206,
136.13688114457));
#202193=CARTESIAN_POINT('Ctrl Pts',(-227.722588217406,5.73503001309909,
131.74322170829));
#202194=CARTESIAN_POINT('Ctrl Pts',(-228.001035841218,3.88981423352964,
126.486794795549));
#202195=CARTESIAN_POINT('Ctrl Pts',(-228.279483465031,-1.52995079866356,
125.197999948425));
#202196=CARTESIAN_POINT('Ctrl Pts',(-228.557931088844,-5.54376578913698,
129.061176670297));
#202197=CARTESIAN_POINT('Ctrl Pts',(-228.836378712657,-4.46313084740822,
134.526254280438));
#202198=CARTESIAN_POINT('Ctrl Pts',(-229.11482633647,0.718903307025501,
136.571093439014));
#202199=CARTESIAN_POINT('Ctrl Pts',(-229.393273960283,5.24030044268158,
133.316586855238));
#202200=CARTESIAN_POINT('Ctrl Pts',(-229.671721584096,4.94611747442232,
127.753467088116));
#202201=CARTESIAN_POINT('Ctrl Pts',(-229.950169207909,0.106694178440453,
124.993969430123));
#202202=CARTESIAN_POINT('Ctrl Pts',(-230.228616831722,-4.83077585522751,
127.57393742));
#202203=CARTESIAN_POINT('Ctrl Pts',(-230.507064455534,-5.32899887446215,
133.122506513493));
#202204=CARTESIAN_POINT('Ctrl Pts',(-230.785512079348,-0.930132264133436,
136.540812776352));
#202205=CARTESIAN_POINT('Ctrl Pts',(-231.06395970316,4.3234804574463,134.687599746553));
#202206=CARTESIAN_POINT('Ctrl Pts',(-231.342407326973,5.60402585239536,
129.265879663993));
#202207=CARTESIAN_POINT('Ctrl Pts',(-231.620854950786,1.73474526087603,
125.257948418793));
#202208=CARTESIAN_POINT('Ctrl Pts',(-231.899302574599,-3.72868147837107,
126.346899026965));
#202209=CARTESIAN_POINT('Ctrl Pts',(-232.177750198412,-5.76563209521201,
131.532039077795));
#202210=CARTESIAN_POINT('Ctrl Pts',(-232.456197822225,-2.50424848333998,
136.048478172742));
#202211=CARTESIAN_POINT('Ctrl Pts',(-232.734645446038,3.05841714538193,
135.745829423867));
#202212=CARTESIAN_POINT('Ctrl Pts',(-233.01309306985,5.81054682948159,130.902212246173));
#202213=CARTESIAN_POINT('Ctrl Pts',(-233.291540693664,3.22306783828139,
125.968674202107));
#202214=CARTESIAN_POINT('Ctrl Pts',(-233.569988317476,-2.32625304068266,
125.478895737432));
#202215=CARTESIAN_POINT('Ctrl Pts',(-233.84843594129,-5.73786101903762,
129.882959334177));
#202216=CARTESIAN_POINT('Ctrl Pts',(-234.126883565102,-3.87665503099142,
135.133745697402));
#202217=CARTESIAN_POINT('Ctrl Pts',(-234.405331188915,1.54700754540913,
136.406038674476));
#202218=CARTESIAN_POINT('Ctrl Pts',(-234.683778812728,5.54904576309872,
132.530663174436));
#202219=CARTESIAN_POINT('Ctrl Pts',(-234.962226436541,4.45178201045685,
127.0688999592));
#202220=CARTESIAN_POINT('Ctrl Pts',(-235.240674060353,-0.736451928153096,
125.039842601604));
#202221=CARTESIAN_POINT('Ctrl Pts',(-235.519121684167,-5.24792252246713,
128.308095688315));
#202222=CARTESIAN_POINT('Ctrl Pts',(-235.797569307979,-4.93680869390195,
133.870294295687));
#202223=CARTESIAN_POINT('Ctrl Pts',(-236.076016931792,-0.0890088521534987,
136.61504963205));
#202224=CARTESIAN_POINT('Ctrl Pts',(-236.354464555605,4.8405857764003,134.020065632043));
#202225=CARTESIAN_POINT('Ctrl Pts',(-236.632912179418,5.32191855220324,
128.470005819654));
#202226=CARTESIAN_POINT('Ctrl Pts',(-236.911359803231,0.912668168706789,
125.065104026974));
#202227=CARTESIAN_POINT('Ctrl Pts',(-237.189807427044,-4.33527967551271,
126.934298662776));
#202228=CARTESIAN_POINT('Ctrl Pts',(-237.468255050857,-5.59931728812211,
132.359891171993));
#202229=CARTESIAN_POINT('Ctrl Pts',(-237.74670267467,-1.71785585480426,
136.356027093583));
#202230=CARTESIAN_POINT('Ctrl Pts',(-238.025150298482,3.7422311871549,135.250452737698));
#202231=CARTESIAN_POINT('Ctrl Pts',(-238.303597922296,5.76339058627568,
130.059136927086));
#202232=CARTESIAN_POINT('Ctrl Pts',(-238.582045546108,2.48827559389159,
125.552645281824));
#202233=CARTESIAN_POINT('Ctrl Pts',(-238.860493169922,-3.07344311025789,
125.87222346955));
#202234=CARTESIAN_POINT('Ctrl Pts',(-239.138940793734,-5.81081774212379,
130.724194748009));
#202235=CARTESIAN_POINT('Ctrl Pts',(-239.417388417547,-3.20833474320591,
135.649834544268));
#202236=CARTESIAN_POINT('Ctrl Pts',(-239.69583604136,2.34245114885216,136.12272051645));
#202237=CARTESIAN_POINT('Ctrl Pts',(-239.974283665173,5.7406388702159,131.708293557882));
#202238=CARTESIAN_POINT('Ctrl Pts',(-240.252731288985,3.86345991565072,
126.463196386742));
#202239=CARTESIAN_POINT('Ctrl Pts',(-240.531178912799,-1.56404996088748,
125.207417066067));
#202240=CARTESIAN_POINT('Ctrl Pts',(-240.809626536611,-5.5542743314588,
129.094955443325));
#202241=CARTESIAN_POINT('Ctrl Pts',(-241.088074160425,-4.44039193280503,
134.553353666625));
#202242=CARTESIAN_POINT('Ctrl Pts',(-241.366521784237,0.753993726891117,
136.566610426332));
#202243=CARTESIAN_POINT('Ctrl Pts',(-241.64496940805,5.25549598621542,133.284641113335));
#202244=CARTESIAN_POINT('Ctrl Pts',(-241.923417031863,4.92745417946037,
127.723415193164));
#202245=CARTESIAN_POINT('Ctrl Pts',(-242.201864655676,0.071322701300089,
124.993427605467));
#202246=CARTESIAN_POINT('Ctrl Pts',(-242.480312279489,-4.85035085504701,
127.603403576029));
#202247=CARTESIAN_POINT('Ctrl Pts',(-242.758759903302,-5.31478892841856,
133.154902692318));
#202248=CARTESIAN_POINT('Ctrl Pts',(-243.037207527115,-0.895195618446729,
136.546368472274));
#202249=CARTESIAN_POINT('Ctrl Pts',(-243.315655150928,4.34703873214009,
134.661209546432));
#202250=CARTESIAN_POINT('Ctrl Pts',(-243.59410277474,5.59455685253872,129.231794872506));
#202251=CARTESIAN_POINT('Ctrl Pts',(-243.872550398553,1.7009505347501,125.247491294183));
#202252=CARTESIAN_POINT('Ctrl Pts',(-244.150998022366,-3.75574622842035,
126.36967915589));
#202253=CARTESIAN_POINT('Ctrl Pts',(-244.429445646179,-5.76109568607594,
131.567122634643));
#202254=CARTESIAN_POINT('Ctrl Pts',(-244.707893269992,-2.47227965339868,
136.063625082699));
#202255=CARTESIAN_POINT('Ctrl Pts',(-244.986340893805,3.08844060317656,
135.727120416648));
#202256=CARTESIAN_POINT('Ctrl Pts',(-245.264788517618,5.81103482414375,
130.866839985428));
#202257=CARTESIAN_POINT('Ctrl Pts',(-245.543236141431,3.1935719265564,125.949144067427));
#202258=CARTESIAN_POINT('Ctrl Pts',(-245.821683765243,-2.35862755687492,
125.49315496849));
#202259=CARTESIAN_POINT('Ctrl Pts',(-246.100131389057,-5.74336354089951,
129.917904394232));
#202260=CARTESIAN_POINT('Ctrl Pts',(-246.378579012869,-3.85022900974501,
135.157263783424));
#202261=CARTESIAN_POINT('Ctrl Pts',(-246.657026636682,1.58107788722132,
136.396517814333));
#202262=CARTESIAN_POINT('Ctrl Pts',(-246.935474260495,5.55945144577998,
132.496852573479));
#202263=CARTESIAN_POINT('Ctrl Pts',(-247.213921884308,4.42896071996899,
127.04186990797));
#202264=CARTESIAN_POINT('Ctrl Pts',(-247.492369508121,-0.77152854073377,
125.044432396689));
#202265=CARTESIAN_POINT('Ctrl Pts',(-247.770817131934,-5.26302076376676,
128.340087532256));
#202266=CARTESIAN_POINT('Ctrl Pts',(-248.049264755747,-4.91805401775627,
133.90028924679));
#202267=CARTESIAN_POINT('Ctrl Pts',(-248.32771237956,-0.0536358897235281,
136.615483795589));
#202268=CARTESIAN_POINT('Ctrl Pts',(-248.606160003372,4.86007100070672,
133.990540032933));
#202269=CARTESIAN_POINT('Ctrl Pts',(-248.884607627186,5.30761006915461,
128.437653041073));
#202270=CARTESIAN_POINT('Ctrl Pts',(-249.163055250998,0.877714775216597,
125.059654691916));
#202271=CARTESIAN_POINT('Ctrl Pts',(-249.441502874812,-4.35875751839529,
126.960760443945));
#202272=CARTESIAN_POINT('Ctrl Pts',(-249.719950498624,-5.58974458974414,
132.393946985223));
#202273=CARTESIAN_POINT('Ctrl Pts',(-249.998398122437,-1.68402945732324,
136.366381310236));
#202274=CARTESIAN_POINT('Ctrl Pts',(-250.27684574625,3.76922647696617,135.227590338499));
#202275=CARTESIAN_POINT('Ctrl Pts',(-250.555293370063,5.75874741587205,
130.024067340013));
#202276=CARTESIAN_POINT('Ctrl Pts',(-250.833740993876,2.45626081004631,
125.537595744144));
#202277=CARTESIAN_POINT('Ctrl Pts',(-251.112188617689,-3.10340948520656,
125.891023771197));
#202278=CARTESIAN_POINT('Ctrl Pts',(-251.390636241501,-5.81119807352532,
130.759568330183));
#202279=CARTESIAN_POINT('Ctrl Pts',(-251.669083865314,-3.17877952510356,
135.669274813107));
#202280=CARTESIAN_POINT('Ctrl Pts',(-251.947531489127,2.37478211491517,
136.10836281449));
#202281=CARTESIAN_POINT('Ctrl Pts',(-252.22597911294,5.74603500580729,131.673331912019));
#202282=CARTESIAN_POINT('Ctrl Pts',(-252.504426736753,3.83696243592119,
126.439758841162));
#202283=CARTESIAN_POINT('Ctrl Pts',(-252.782874360566,-1.59809116681098,
125.217041580908));
#202284=CARTESIAN_POINT('Ctrl Pts',(-253.061321984379,-5.5645770578269,
129.128797558239));
#202285=CARTESIAN_POINT('Ctrl Pts',(-253.339769608192,-4.41748847836656,
134.580314133917));
#202286=CARTESIAN_POINT('Ctrl Pts',(-253.618217232004,0.789056208225191,
136.561913888683));
#202287=CARTESIAN_POINT('Ctrl Pts',(-253.896664855818,5.27049678355612,
133.252603468789));
#202288=CARTESIAN_POINT('Ctrl Pts',(-254.17511247963,4.90860829937749,127.693477454216));
#202289=CARTESIAN_POINT('Ctrl Pts',(-254.453560103444,0.0359485746511809,
124.993101125124));
#202290=CARTESIAN_POINT('Ctrl Pts',(-254.732007727256,-4.86974611083267,
127.632988310607));
#202291=CARTESIAN_POINT('Ctrl Pts',(-255.010455351069,-5.30038206451776,
133.187211835313));
#202292=CARTESIAN_POINT('Ctrl Pts',(-255.288902974882,-0.860225756393269,
136.55171127444));
#202293=CARTESIAN_POINT('Ctrl Pts',(-255.567350598695,4.37043584157037,
134.634676658854));
#202294=CARTESIAN_POINT('Ctrl Pts',(-255.845798222508,5.58488070320316,
129.197767919676));
#202295=CARTESIAN_POINT('Ctrl Pts',(-256.12424584632,1.66709247927321,125.23724089965));
#202296=CARTESIAN_POINT('Ctrl Pts',(-256.402693470134,-3.78267124144458,
126.39262206856));
#202297=CARTESIAN_POINT('Ctrl Pts',(-256.681141093946,-5.75634686702621,
131.602180844355));
#202298=CARTESIAN_POINT('Ctrl Pts',(-256.95958871776,-2.44021719259262,
136.078571600242));
#202299=CARTESIAN_POINT('Ctrl Pts',(-257.238036341572,3.118345804191,135.708239395799));
#202300=CARTESIAN_POINT('Ctrl Pts',(-257.516483965385,5.81131468939531,
130.8314457702));
#202301=CARTESIAN_POINT('Ctrl Pts',(-257.794931589198,3.16394407961038,
125.929830927563));
#202302=CARTESIAN_POINT('Ctrl Pts',(-258.073379213011,-2.39088900078744,
125.507540987923));
#202303=CARTESIAN_POINT('Ctrl Pts',(-258.351826836824,-5.74870171518396,
129.953014515613));
#202304=CARTESIAN_POINT('Ctrl Pts',(-258.630274460636,-3.82356878618261,
135.180370918811));
#202305=CARTESIAN_POINT('Ctrl Pts',(-258.908722084449,1.61491681105698,
136.387261181902));
#202306=CARTESIAN_POINT('Ctrl Pts',(-259.187169708263,5.56997747689423,
132.462088635074));
#202307=CARTESIAN_POINT('Ctrl Pts',(-259.465617332075,4.40535894966821,
127.016664495574));
#202308=CARTESIAN_POINT('Ctrl Pts',(-259.744064955888,-0.805411631290512,
125.046024618449));
#202309=CARTESIAN_POINT('Ctrl Pts',(-260.022512579701,-5.28013240410161,
128.378470706602));
#202310=CARTESIAN_POINT('Ctrl Pts',(-260.254552266212,-4.95911089365773,
132.993351965875));
#202311=CARTESIAN_POINT('Ctrl Pts',(-260.440213228287,-2.45877638613931,
135.28779596926));
#202312=CARTESIAN_POINT('Ctrl Pts',(-260.53305831576,-0.833059752290926,
135.715219187214));
#202313=CARTESIAN_POINT('Ctrl Pts',(-260.579495465929,-0.013892627260139,
135.717527172907));
#202314=CARTESIAN_POINT('Ctrl Pts',(-260.,-4.31895139421945,128.437223181));
#202315=CARTESIAN_POINT('Ctrl Pts',(-260.,-4.38498592260266,128.532528358389));
#202316=CARTESIAN_POINT('Ctrl Pts',(-260.,-4.44726778822742,128.630071853281));
#202317=CARTESIAN_POINT('Ctrl Pts',(-260.,-4.50561806400233,128.729703648768));
#202318=CARTESIAN_POINT('Ctrl Pts',(-260.,-4.57674440789476,128.851150295837));
#202319=CARTESIAN_POINT('Ctrl Pts',(-260.,-4.64203105700707,128.975698709901));
#202320=CARTESIAN_POINT('Ctrl Pts',(-260.,-4.70159679832533,129.102914350821));
#202321=CARTESIAN_POINT('Ctrl Pts',(-260.,-4.76218361828822,129.232310728038));
#202322=CARTESIAN_POINT('Ctrl Pts',(-260.,-4.81685192576391,129.364467086494));
#202323=CARTESIAN_POINT('Ctrl Pts',(-260.,-4.86568579910616,129.49896261564));
#202324=CARTESIAN_POINT('Ctrl Pts',(-260.,-4.91551630739491,129.636203021146));
#202325=CARTESIAN_POINT('Ctrl Pts',(-260.,-4.95927207158199,129.775879658827));
#202326=CARTESIAN_POINT('Ctrl Pts',(-260.,-4.99699647319888,129.917574401433));
#202327=CARTESIAN_POINT('Ctrl Pts',(-260.,-5.01778238392898,129.995647323587));
#202328=CARTESIAN_POINT('Ctrl Pts',(-260.,-5.03673638081373,130.074333384798));
#202329=CARTESIAN_POINT('Ctrl Pts',(-260.,-5.053859498905,130.15356521114));
#202330=CARTESIAN_POINT('Ctrl Pts',(-260.,-5.05814608601775,130.173400040516));
#202331=CARTESIAN_POINT('Ctrl Pts',(-260.,-5.06231835353811,130.193271261708));
#202332=CARTESIAN_POINT('Ctrl Pts',(-260.,-5.06637485462738,130.213170843715));
#202333=CARTESIAN_POINT('Ctrl Pts',(-260.,-5.09672834375308,130.362072996763));
#202334=CARTESIAN_POINT('Ctrl Pts',(-260.,-5.12052632024444,130.512171985573));
#202335=CARTESIAN_POINT('Ctrl Pts',(-260.,-5.13789473816522,130.662975483895));
#202336=CARTESIAN_POINT('Ctrl Pts',(-260.,-5.15519305516581,130.813170322059));
#202337=CARTESIAN_POINT('Ctrl Pts',(-260.,-5.16611366644811,130.964064788806));
#202338=CARTESIAN_POINT('Ctrl Pts',(-260.,-5.17073417372998,131.11520219772));
#202339=CARTESIAN_POINT('Ctrl Pts',(-260.,-5.17540412114875,131.2679568001));
#202340=CARTESIAN_POINT('Ctrl Pts',(-260.,-5.17363860431495,131.420960346613));
#202341=CARTESIAN_POINT('Ctrl Pts',(-260.,-5.16546781393087,131.573760002852));
#202342=CARTESIAN_POINT('Ctrl Pts',(-260.,-5.15737174576717,131.725162299834));
#202343=CARTESIAN_POINT('Ctrl Pts',(-260.,-5.14298704854922,131.876365240673));
#202344=CARTESIAN_POINT('Ctrl Pts',(-260.,-5.12229299840987,132.026934500077));
#202345=CARTESIAN_POINT('Ctrl Pts',(-260.,-5.11634124929555,132.070239239858));
#202346=CARTESIAN_POINT('Ctrl Pts',(-260.,-5.10986728447182,132.113491559525));
#202347=CARTESIAN_POINT('Ctrl Pts',(-260.,-5.10286982789351,132.156681074128));
#202348=CARTESIAN_POINT('Ctrl Pts',(-260.,-5.09953420587344,132.177269111271));
#202349=CARTESIAN_POINT('Ctrl Pts',(-260.,-5.0960793138402,132.197844652096));
#202350=CARTESIAN_POINT('Ctrl Pts',(-260.,-5.09250595955024,132.218400979179));
#202351=CARTESIAN_POINT('Ctrl Pts',(-260.,-5.06560675391027,132.37314322541));
#202352=CARTESIAN_POINT('Ctrl Pts',(-260.,-5.03208029934396,132.526333519448));
#202353=CARTESIAN_POINT('Ctrl Pts',(-260.,-4.99200835226872,132.677496527965));
#202354=CARTESIAN_POINT('Ctrl Pts',(-260.,-4.95190447601151,132.828779982617));
#202355=CARTESIAN_POINT('Ctrl Pts',(-260.,-4.90524475131742,132.97803376827));
#202356=CARTESIAN_POINT('Ctrl Pts',(-260.,-4.85206024555845,133.124791279933));
#202357=CARTESIAN_POINT('Ctrl Pts',(-260.,-4.79923677150287,133.270552559447));
#202358=CARTESIAN_POINT('Ctrl Pts',(-260.,-4.73997682017671,133.413852179291));
#202359=CARTESIAN_POINT('Ctrl Pts',(-260.,-4.67426001308823,133.554230102829));
#202360=CARTESIAN_POINT('Ctrl Pts',(-260.,-4.64640462459469,133.61373210497));
#202361=CARTESIAN_POINT('Ctrl Pts',(-260.,-4.61738853077812,133.672709069641));
#202362=CARTESIAN_POINT('Ctrl Pts',(-260.,-4.58720737938296,133.731125241234));
#202363=CARTESIAN_POINT('Ctrl Pts',(-260.,-4.53403293595749,133.834045350902));
#202364=CARTESIAN_POINT('Ctrl Pts',(-260.,-4.477242909968,133.935225161206));
#202365=CARTESIAN_POINT('Ctrl Pts',(-260.,-4.41699723107283,134.034557632499));
#202366=CARTESIAN_POINT('Ctrl Pts',(-260.,-4.40019967051461,134.062253281922));
#202367=CARTESIAN_POINT('Ctrl Pts',(-260.,-4.38313337868994,134.089805274928));
#202368=CARTESIAN_POINT('Ctrl Pts',(-260.,-4.36580161636001,134.117211179373));
#202369=CARTESIAN_POINT('Ctrl Pts',(-260.,-4.35192553122814,134.139152783231));
#202370=CARTESIAN_POINT('Ctrl Pts',(-260.,-4.33787717656154,134.161003821598));
#202371=CARTESIAN_POINT('Ctrl Pts',(-260.,-4.32367327517883,134.182740366414));
#202372=CARTESIAN_POINT('Ctrl Pts',(-260.,-4.24013902539044,134.310574678643));
#202373=CARTESIAN_POINT('Ctrl Pts',(-260.,-4.15113473789727,134.434602661712));
#202374=CARTESIAN_POINT('Ctrl Pts',(-260.,-4.05711762681074,134.554623908161));
#202375=CARTESIAN_POINT('Ctrl Pts',(-260.,-3.95953065717921,134.67920239815));
#202376=CARTESIAN_POINT('Ctrl Pts',(-260.,-3.85654276687757,134.799464700792));
#202377=CARTESIAN_POINT('Ctrl Pts',(-260.,-3.74861015630072,134.91517188258));
#202378=CARTESIAN_POINT('Ctrl Pts',(-260.,-3.64067754572386,135.030879064368));
#202379=CARTESIAN_POINT('Ctrl Pts',(-260.,-3.52779965481179,135.142031672907));
#202380=CARTESIAN_POINT('Ctrl Pts',(-260.,-3.41038485629795,135.248367627085));
#202381=CARTESIAN_POINT('Ctrl Pts',(-260.,-3.30440767937894,135.344345173113));
#202382=CARTESIAN_POINT('Ctrl Pts',(-260.,-3.19473354753115,135.436398761565));
#202383=CARTESIAN_POINT('Ctrl Pts',(-260.,-3.08163501453677,135.524313841136));
#202384=CARTESIAN_POINT('Ctrl Pts',(-260.,-3.02508574804119,135.56827138092));
#202385=CARTESIAN_POINT('Ctrl Pts',(-260.,-2.96768000449005,135.611193935658));
#202386=CARTESIAN_POINT('Ctrl Pts',(-260.,-2.90944981012801,135.653052319656));
#202387=CARTESIAN_POINT('Ctrl Pts',(-260.,-2.89195167916156,135.665630733541));
#202388=CARTESIAN_POINT('Ctrl Pts',(-260.,-2.87437909205552,135.678113041256));
#202389=CARTESIAN_POINT('Ctrl Pts',(-260.,-2.85673289693263,135.690498419844));
#202390=CARTESIAN_POINT('Ctrl Pts',(-260.,-2.83758770402918,135.703935903709));
#202391=CARTESIAN_POINT('Ctrl Pts',(-260.,-2.81836309546151,135.717254192549));
#202392=CARTESIAN_POINT('Ctrl Pts',(-260.,-2.79906452111251,135.730449689892));
#202393=CARTESIAN_POINT('Ctrl Pts',(-260.,-2.77695728342425,135.745565624929));
#202394=CARTESIAN_POINT('Ctrl Pts',(-260.,-2.75475127711875,135.76052162606));
#202395=CARTESIAN_POINT('Ctrl Pts',(-260.,-2.73244855505852,135.775316560448));
#202396=CARTESIAN_POINT('Ctrl Pts',(-260.,-2.59643078163644,135.86554653453));
#202397=CARTESIAN_POINT('Ctrl Pts',(-260.,-2.45681907361406,135.949788593943));
#202398=CARTESIAN_POINT('Ctrl Pts',(-260.,-2.31402220930489,136.027954478872));
#202399=CARTESIAN_POINT('Ctrl Pts',(-260.,-2.17122534499573,136.106120363801));
#202400=CARTESIAN_POINT('Ctrl Pts',(-260.,-2.02524274150512,136.178210426187));
#202401=CARTESIAN_POINT('Ctrl Pts',(-260.,-1.8764471723442,136.244098466396));
#202402=CARTESIAN_POINT('Ctrl Pts',(-260.,-1.80305579306763,136.276596841018));
#202403=CARTESIAN_POINT('Ctrl Pts',(-260.,-1.7289795719389,136.307585759908));
#202404=CARTESIAN_POINT('Ctrl Pts',(-260.,-1.65426068122485,136.337046274096));
#202405=CARTESIAN_POINT('Ctrl Pts',(-260.,-1.61863281016888,136.351093797964));
#202406=CARTESIAN_POINT('Ctrl Pts',(-260.,-1.5828587981496,136.364793781341));
#202407=CARTESIAN_POINT('Ctrl Pts',(-260.,-1.5469431056621,136.378143953878));
#202408=CARTESIAN_POINT('Ctrl Pts',(-260.,-1.52194835513068,136.387434718138));
#202409=CARTESIAN_POINT('Ctrl Pts',(-260.,-1.4968838979741,136.396556379419));
#202410=CARTESIAN_POINT('Ctrl Pts',(-260.,-1.47176771023595,136.405502461703));
#202411=CARTESIAN_POINT('Ctrl Pts',(-260.,-1.31515450873548,136.461286189794));
#202412=CARTESIAN_POINT('Ctrl Pts',(-260.,-1.15638749404024,136.510301323187));
#202413=CARTESIAN_POINT('Ctrl Pts',(-260.,-0.995868207088328,136.55243688218));
#202414=CARTESIAN_POINT('Ctrl Pts',(-260.,-0.835850940924087,136.594440663073));
#202415=CARTESIAN_POINT('Ctrl Pts',(-260.,-0.674091715028761,136.629608166435));
#202416=CARTESIAN_POINT('Ctrl Pts',(-260.,-0.510961125684827,136.657785834748));
#202417=CARTESIAN_POINT('Ctrl Pts',(-260.,-0.348088738648444,136.685918903584));
#202418=CARTESIAN_POINT('Ctrl Pts',(-260.,-0.183848703485478,136.707084599764));
#202419=CARTESIAN_POINT('Ctrl Pts',(-260.,-0.0185920708335254,136.72108140677));
#202420=CARTESIAN_POINT('Origin',(-260.,0.,130.804360617566));
#202421=CARTESIAN_POINT('',(0.,0.,0.));
#202422=CARTESIAN_POINT('Origin',(-19.9792411332937,17.,231.631408332131));
#202423=CARTESIAN_POINT('',(-13.4123053085775,17.,235.37258862514));
#202424=CARTESIAN_POINT('',(-12.4213924902778,17.,231.631408332131));
#202425=CARTESIAN_POINT('Origin',(-19.9792411332937,17.,231.631408332131));
#202426=CARTESIAN_POINT('',(-12.4213924902778,-17.,231.631408332131));
#202427=CARTESIAN_POINT('',(-12.4213924902778,17.,231.631408332131));
#202428=CARTESIAN_POINT('',(-13.4123053085775,-17.,235.37258862514));
#202429=CARTESIAN_POINT('Origin',(-19.9792411332937,-17.,231.631408332131));
#202430=CARTESIAN_POINT('',(-13.4123053085775,-12.,235.37258862514));
#202431=CARTESIAN_POINT('',(-13.4123053085775,17.,235.37258862514));
#202432=CARTESIAN_POINT('',(-26.4691126286313,-12.,227.758083651093));
#202433=CARTESIAN_POINT('Origin',(-19.9792411332937,-12.,231.631408332131));
#202434=CARTESIAN_POINT('',(-26.4691126286313,-17.,227.758083651093));
#202435=CARTESIAN_POINT('',(-26.4691126286313,17.,227.758083651093));
#202436=CARTESIAN_POINT('Origin',(-19.9792411332937,-17.,231.631408332131));
#202437=CARTESIAN_POINT('',(-26.4691126286313,17.,227.758083651093));
#202438=CARTESIAN_POINT('Origin',(-19.9792411332937,17.,231.631408332131));
#202439=CARTESIAN_POINT('',(-26.4691126286313,12.,227.758083651093));
#202440=CARTESIAN_POINT('',(-26.4691126286313,17.,227.758083651093));
#202441=CARTESIAN_POINT('',(-13.4123053085775,12.,235.37258862514));
#202442=CARTESIAN_POINT('Origin',(-19.9792411332937,12.,231.631408332131));
#202443=CARTESIAN_POINT('',(-13.4123053085775,17.,235.37258862514));
#202444=CARTESIAN_POINT('Origin',(-19.9792411332937,17.,231.631408332131));
#202445=CARTESIAN_POINT('',(-29.4368821049519,-12.,243.584349198005));
#202446=CARTESIAN_POINT('',(-4.7372016342019,-12.,231.631408332131));
#202447=CARTESIAN_POINT('Origin',(-19.9792411332937,-12.,231.631408332131));
#202448=CARTESIAN_POINT('',(-29.4368821049519,-17.,243.584349198005));
#202449=CARTESIAN_POINT('',(-29.4368821049519,17.,243.584349198005));
#202450=CARTESIAN_POINT('',(-6.77425985905829,-17.,239.243782313943));
#202451=CARTESIAN_POINT('Origin',(-19.9792411332937,-17.,231.631408332131));
#202452=CARTESIAN_POINT('',(-6.77425985905829,-12.,239.243782313943));
#202453=CARTESIAN_POINT('',(-6.77425985905829,17.,239.243782313943));
#202454=CARTESIAN_POINT('Origin',(-19.9792411332937,-12.,231.631408332131));
#202455=CARTESIAN_POINT('',(-4.7372016342019,12.,231.631408332131));
#202456=CARTESIAN_POINT('',(-4.7372016342019,17.,231.631408332131));
#202457=CARTESIAN_POINT('',(-6.77425985905829,12.,239.243782313943));
#202458=CARTESIAN_POINT('Origin',(-19.9792411332937,12.,231.631408332131));
#202459=CARTESIAN_POINT('',(-6.77425985905829,17.,239.243782313943));
#202460=CARTESIAN_POINT('',(-6.77425985905829,17.,239.243782313943));
#202461=CARTESIAN_POINT('',(-29.4368821049519,17.,243.584349198005));
#202462=CARTESIAN_POINT('Origin',(-19.9792411332937,17.,231.631408332131));
#202463=CARTESIAN_POINT('',(-29.4368821049519,12.,243.584349198005));
#202464=CARTESIAN_POINT('',(-29.4368821049519,17.,243.584349198005));
#202465=CARTESIAN_POINT('Origin',(-19.9792411332937,12.,231.631408332131));
#202466=CARTESIAN_POINT('Origin',(-19.9021768039151,17.,231.499263944101));
#202467=CARTESIAN_POINT('Origin',(-19.9021768039151,17.,231.499263944101));
#202468=CARTESIAN_POINT('Origin',(-19.9021768039151,12.,231.499263944101));
#202469=CARTESIAN_POINT('Origin',(-106.310292012757,17.,181.151812280833));
#202470=CARTESIAN_POINT('',(-12.2286695743674,17.,218.329713652237));
#202471=CARTESIAN_POINT('Origin',(-19.9021768039151,17.,231.499263944101));
#202472=CARTESIAN_POINT('',(-185.044899992051,17.,117.634810325701));
#202473=CARTESIAN_POINT('',(-185.044899992051,17.,117.634810325701));
#202474=CARTESIAN_POINT('',(-200.391914451146,17.,143.97391090943));
#202475=CARTESIAN_POINT('Origin',(-192.718407221598,17.,130.804360617566));
#202476=CARTESIAN_POINT('',(-27.5756840334628,17.,244.668814235966));
#202477=CARTESIAN_POINT('',(-189.517108648379,17.,136.462636689939));
#202478=CARTESIAN_POINT('Origin',(-192.718407221598,17.,130.804360617566));
#202479=CARTESIAN_POINT('Origin',(-106.310292012757,12.,181.151812280833));
#202480=CARTESIAN_POINT('',(-200.391914451146,12.,143.97391090943));
#202481=CARTESIAN_POINT('',(-27.5756840334628,12.,244.668814235966));
#202482=CARTESIAN_POINT('',(-185.044899992051,12.,117.634810325701));
#202483=CARTESIAN_POINT('Origin',(-192.718407221598,12.,130.804360617566));
#202484=CARTESIAN_POINT('',(-12.2286695743674,12.,218.329713652237));
#202485=CARTESIAN_POINT('',(-185.044899992051,12.,117.634810325701));
#202486=CARTESIAN_POINT('Origin',(-19.9021768039151,12.,231.499263944101));
#202487=CARTESIAN_POINT('',(-189.517108648379,12.,136.462636689939));
#202488=CARTESIAN_POINT('Origin',(-192.718407221598,12.,130.804360617566));
#202489=CARTESIAN_POINT('Origin',(-192.718407221598,17.,130.804360617566));
#202490=CARTESIAN_POINT('',(-189.517108648378,17.,136.462636689939));
#202491=CARTESIAN_POINT('Origin',(-185.044899992051,17.,117.634810325701));
#202492=CARTESIAN_POINT('',(-12.2286695743674,17.,218.329713652237));
#202493=CARTESIAN_POINT('',(-185.044899992051,17.,117.634810325701));
#202494=CARTESIAN_POINT('Origin',(-192.718407221598,17.,130.804360617566));
#202495=CARTESIAN_POINT('',(-200.391914451146,17.,143.97391090943));
#202496=CARTESIAN_POINT('Origin',(-27.5756840334628,17.,244.668814235966));
#202497=CARTESIAN_POINT('Origin',(-19.9021768039151,17.,231.499263944101));
#202498=CARTESIAN_POINT('Origin',(-106.310292012757,12.,181.151812280833));
#202499=CARTESIAN_POINT('Origin',(-19.9021768039151,-17.,231.499263944101));
#202500=CARTESIAN_POINT('Origin',(-19.9021768039151,-12.,231.499263944101));
#202501=CARTESIAN_POINT('Origin',(-19.9021768039151,-17.,231.499263944101));
#202502=CARTESIAN_POINT('Origin',(-27.5756840334628,-17.,244.668814235966));
#202503=CARTESIAN_POINT('',(-200.391914451146,-12.,143.97391090943));
#202504=CARTESIAN_POINT('',(-27.5756840334628,-12.,244.668814235966));
#202505=CARTESIAN_POINT('',(-200.391914451146,-17.,143.97391090943));
#202506=CARTESIAN_POINT('',(-200.391914451146,-17.,143.97391090943));
#202507=CARTESIAN_POINT('',(-27.5756840334628,-17.,244.668814235966));
#202508=CARTESIAN_POINT('Origin',(-106.310292012757,-12.,181.151812280833));
#202509=CARTESIAN_POINT('',(-12.2286695743674,-12.,218.329713652237));
#202510=CARTESIAN_POINT('Origin',(-19.9021768039151,-12.,231.499263944101));
#202511=CARTESIAN_POINT('',(-185.044899992051,-12.,117.634810325701));
#202512=CARTESIAN_POINT('',(-185.044899992051,-12.,117.634810325701));
#202513=CARTESIAN_POINT('Origin',(-192.718407221598,-12.,130.804360617566));
#202514=CARTESIAN_POINT('',(-189.517108648379,-12.,136.462636689939));
#202515=CARTESIAN_POINT('Origin',(-192.718407221598,-12.,130.804360617566));
#202516=CARTESIAN_POINT('Origin',(-106.310292012757,-12.,181.151812280833));
#202517=CARTESIAN_POINT('Origin',(-192.718407221598,-17.,130.804360617566));
#202518=CARTESIAN_POINT('',(-189.517108648379,-17.,136.462636689939));
#202519=CARTESIAN_POINT('',(-189.517108648378,-17.,136.462636689939));
#202520=CARTESIAN_POINT('Origin',(-192.718407221598,-17.,130.804360617566));
#202521=CARTESIAN_POINT('Origin',(-185.044899992051,-17.,117.634810325701));
#202522=CARTESIAN_POINT('',(-185.044899992051,-17.,117.634810325701));
#202523=CARTESIAN_POINT('',(-12.2286695743674,-17.,218.329713652237));
#202524=CARTESIAN_POINT('',(-185.044899992051,-17.,117.634810325701));
#202525=CARTESIAN_POINT('',(-185.044899992051,-17.,117.634810325701));
#202526=CARTESIAN_POINT('',(-12.2286695743674,-17.,218.329713652237));
#202527=CARTESIAN_POINT('Origin',(-192.718407221598,-17.,130.804360617566));
#202528=CARTESIAN_POINT('Origin',(-192.718407221598,-17.,130.804360617566));
#202529=CARTESIAN_POINT('Origin',(-19.9021768039151,-17.,231.499263944101));
#202530=CARTESIAN_POINT('Origin',(-19.9021768039151,-17.,231.499263944101));
#202531=CARTESIAN_POINT('Origin',(-106.310292012757,-17.,181.151812280833));
#202532=CARTESIAN_POINT('',(0.,0.,0.));
#202533=CARTESIAN_POINT('Origin',(213.235140564004,0.,130.804360617566));
#202534=CARTESIAN_POINT('',(179.180279212536,-4.76405452823405,129.582490119308));
#202535=CARTESIAN_POINT('',(178.834794689177,-4.76405452823405,129.582490119308));
#202536=CARTESIAN_POINT('',(213.235140564004,-4.76405452823405,129.582490119308));
#202537=CARTESIAN_POINT('',(178.764859436029,-4.91824789753406,130.799812991619));
#202538=CARTESIAN_POINT('Ctrl Pts',(178.834794689177,-4.76405452823405,
129.582490119308));
#202539=CARTESIAN_POINT('Ctrl Pts',(178.834348169157,-4.76600152135323,
129.59008141593));
#202540=CARTESIAN_POINT('Ctrl Pts',(178.833901649136,-4.76793019492675,
129.597676684138));
#202541=CARTESIAN_POINT('Ctrl Pts',(178.833455129116,-4.76984053507245,
129.605275828037));
#202542=CARTESIAN_POINT('Ctrl Pts',(178.823192962182,-4.81374501544364,
129.779923502642));
#202543=CARTESIAN_POINT('Ctrl Pts',(178.812930795248,-4.84807446073973,
129.95706774057));
#202544=CARTESIAN_POINT('Ctrl Pts',(178.802668628314,-4.87259841686327,
130.13580416484));
#202545=CARTESIAN_POINT('Ctrl Pts',(178.792640946099,-4.89656201443736,
130.310456562743));
#202546=CARTESIAN_POINT('Ctrl Pts',(178.782613263885,-4.91116315740482,
130.486629512172));
#202547=CARTESIAN_POINT('Ctrl Pts',(178.772585581671,-4.9162311945412,130.663456734298));
#202548=CARTESIAN_POINT('Ctrl Pts',(178.77001019979,-4.91753280449775,130.708870780548));
#202549=CARTESIAN_POINT('Ctrl Pts',(178.76743481791,-4.91820583999571,130.754327852339));
#202550=CARTESIAN_POINT('Ctrl Pts',(178.764859436029,-4.91824789753406,
130.799812991619));
#202551=CARTESIAN_POINT('',(177.723712521315,4.07640974993461,128.054215600239));
#202552=CARTESIAN_POINT('Ctrl Pts',(178.764859435991,-4.91824789753469,
130.799812992297));
#202553=CARTESIAN_POINT('Ctrl Pts',(178.757196290994,-4.9183730412926,130.935155723463));
#202554=CARTESIAN_POINT('Ctrl Pts',(178.749533145997,-4.91290734326878,
131.070645942394));
#202555=CARTESIAN_POINT('Ctrl Pts',(178.741870001,-4.90184112669081,131.205778892166));
#202556=CARTESIAN_POINT('Ctrl Pts',(178.734084063679,-4.89059758781915,
131.343077178612));
#202557=CARTESIAN_POINT('Ctrl Pts',(178.726298126358,-4.87357245610437,
131.480006229492));
#202558=CARTESIAN_POINT('Ctrl Pts',(178.718512189038,-4.85081073812513,
131.61603681248));
#202559=CARTESIAN_POINT('Ctrl Pts',(178.710856306159,-4.82842922645917,
131.749795173024));
#202560=CARTESIAN_POINT('Ctrl Pts',(178.70320042328,-4.80050136400255,131.882684439534));
#202561=CARTESIAN_POINT('Ctrl Pts',(178.695544540401,-4.76712209381898,
132.01420771746));
#202562=CARTESIAN_POINT('Ctrl Pts',(178.687889375061,-4.73374595206982,
132.145718668516));
#202563=CARTESIAN_POINT('Ctrl Pts',(178.680234209721,-4.69491951717209,
132.27586349683));
#202564=CARTESIAN_POINT('Ctrl Pts',(178.672579044381,-4.65078839204757,
132.404157603091));
#202565=CARTESIAN_POINT('Ctrl Pts',(178.664922844915,-4.60665130530803,
132.532469040433));
#202566=CARTESIAN_POINT('Ctrl Pts',(178.657266645449,-4.55720823398827,
132.65892887934));
#202567=CARTESIAN_POINT('Ctrl Pts',(178.649610445982,-4.50265380566106,
132.783070239735));
#202568=CARTESIAN_POINT('Ctrl Pts',(178.641726867593,-4.44647918349511,
132.910898433141));
#202569=CARTESIAN_POINT('Ctrl Pts',(178.633843289203,-4.3848850536798,133.036267873534));
#202570=CARTESIAN_POINT('Ctrl Pts',(178.625959710813,-4.31813542196403,
133.158694820707));
#202571=CARTESIAN_POINT('Ctrl Pts',(178.618292097771,-4.25321435168799,
133.277767963686));
#202572=CARTESIAN_POINT('Ctrl Pts',(178.610624484729,-4.18341682154212,
133.394057413434));
#202573=CARTESIAN_POINT('Ctrl Pts',(178.602956871687,-4.10902994539855,
133.507147322121));
#202574=CARTESIAN_POINT('Ctrl Pts',(178.594965310623,-4.03150030744991,
133.625015152183));
#202575=CARTESIAN_POINT('Ctrl Pts',(178.586973749559,-3.94898534362607,
133.739406770363));
#202576=CARTESIAN_POINT('Ctrl Pts',(178.578982188495,-3.861856090724,133.849890226195));
#202577=CARTESIAN_POINT('Ctrl Pts',(178.570990627431,-3.77472683782194,
133.960373682027));
#202578=CARTESIAN_POINT('Ctrl Pts',(178.562999066367,-3.68298366963375,
134.066948657916));
#202579=CARTESIAN_POINT('Ctrl Pts',(178.555007505303,-3.58703931231371,
134.169227930614));
#202580=CARTESIAN_POINT('Ctrl Pts',(178.547233171184,-3.493702918501,134.268727043871));
#202581=CARTESIAN_POINT('Ctrl Pts',(178.539458837065,-3.39607561388428,
134.364497295231));
#202582=CARTESIAN_POINT('Ctrl Pts',(178.531684502946,-3.2944872852368,134.456146015137));
#202583=CARTESIAN_POINT('Ctrl Pts',(178.523919749999,-3.19302415512523,
134.547681786186));
#202584=CARTESIAN_POINT('Ctrl Pts',(178.516154997052,-3.08761000143176,
134.635105872937));
#202585=CARTESIAN_POINT('Ctrl Pts',(178.508390244105,-2.97861348023738,
134.718060248075));
#202586=CARTESIAN_POINT('Ctrl Pts',(178.50063320322,-2.86972521592481,134.800932231759));
#202587=CARTESIAN_POINT('Ctrl Pts',(178.492876162335,-2.75726197390471,
134.879343103152));
#202588=CARTESIAN_POINT('Ctrl Pts',(178.48511912145,-2.64162734560113,134.952973401313));
#202589=CARTESIAN_POINT('Ctrl Pts',(178.47736793021,-2.52607991827016,135.026548174295));
#202590=CARTESIAN_POINT('Ctrl Pts',(178.46961673897,-2.40736619337517,135.095349340572));
#202591=CARTESIAN_POINT('Ctrl Pts',(178.46186554773,-2.28592046387358,135.159099495541));
#202592=CARTESIAN_POINT('Ctrl Pts',(178.454117650953,-2.16452635204637,
135.222822554993));
#202593=CARTESIAN_POINT('Ctrl Pts',(178.446369754175,-2.04040289054619,
135.281498691652));
#202594=CARTESIAN_POINT('Ctrl Pts',(178.438621857398,-1.91401061513348,
135.334895511776));
#202595=CARTESIAN_POINT('Ctrl Pts',(178.430875581314,-1.78764477826022,
135.388281162436));
#202596=CARTESIAN_POINT('Ctrl Pts',(178.42312930523,-1.6590114313704,135.436389541058));
#202597=CARTESIAN_POINT('Ctrl Pts',(178.415383029146,-1.52859245082243,
135.479035812891));
#202598=CARTESIAN_POINT('Ctrl Pts',(178.407636695881,-1.39817250755127,
135.521682399529));
#202599=CARTESIAN_POINT('Ctrl Pts',(178.399890362615,-1.26596727592271,
135.55886667741));
#202600=CARTESIAN_POINT('Ctrl Pts',(178.39214402935,-1.1324748224956,135.590453370419));
#202601=CARTESIAN_POINT('Ctrl Pts',(178.384395961347,-0.998952474358899,
135.62204713705));
#202602=CARTESIAN_POINT('Ctrl Pts',(178.376647893344,-0.864142711197707,
135.648040734402));
#202603=CARTESIAN_POINT('Ctrl Pts',(178.368899825341,-0.728554452264122,
135.668349872549));
#202604=CARTESIAN_POINT('Ctrl Pts',(178.361143522599,-0.592822088515468,
135.688680595488));
#202605=CARTESIAN_POINT('Ctrl Pts',(178.353387219857,-0.456309963453038,
135.703314732646));
#202606=CARTESIAN_POINT('Ctrl Pts',(178.345630917115,-0.319533349451039,
135.712219774173));
#202607=CARTESIAN_POINT('Ctrl Pts',(178.337870474601,-0.182683733651767,
135.721129568589));
#202608=CARTESIAN_POINT('Ctrl Pts',(178.330110032087,-0.045569738297517,
135.724304165422));
#202609=CARTESIAN_POINT('Ctrl Pts',(178.322349589573,0.0912936838562829,
135.721763237424));
#202610=CARTESIAN_POINT('Ctrl Pts',(178.314576689307,0.228376811325325,
135.719218230503));
#202611=CARTESIAN_POINT('Ctrl Pts',(178.306803789042,0.365208171309374,
135.710939387667));
#202612=CARTESIAN_POINT('Ctrl Pts',(178.299030888776,0.501277348038855,
135.696998360424));
#202613=CARTESIAN_POINT('Ctrl Pts',(178.291540553014,0.632400067457702,
135.683564124637));
#202614=CARTESIAN_POINT('Ctrl Pts',(178.284050217252,0.762814751203412,
135.664872270292));
#202615=CARTESIAN_POINT('Ctrl Pts',(178.27655988149,0.89207580184942,135.641031355404));
#202616=CARTESIAN_POINT('Ctrl Pts',(178.268785547371,1.02623782451768,135.616286504981));
#202617=CARTESIAN_POINT('Ctrl Pts',(178.261011213252,1.15958199216667,135.585916048837));
#202618=CARTESIAN_POINT('Ctrl Pts',(178.253236879133,1.29159962891666,135.549985282569));
#202619=CARTESIAN_POINT('Ctrl Pts',(178.245472126186,1.4234545657279,135.514098797758));
#202620=CARTESIAN_POINT('Ctrl Pts',(178.237707373239,1.55398585084488,135.472665739113));
#202621=CARTESIAN_POINT('Ctrl Pts',(178.229942620292,1.68269299813225,135.425802744926));
#202622=CARTESIAN_POINT('Ctrl Pts',(178.222185579407,1.8112723116667,135.378986295725));
#202623=CARTESIAN_POINT('Ctrl Pts',(178.214428538522,1.93803072786065,135.326750776369));
#202624=CARTESIAN_POINT('Ctrl Pts',(178.206671497637,2.0624813241539,135.269263063311));
#202625=CARTESIAN_POINT('Ctrl Pts',(178.198920306396,2.18683807128473,135.211818702184));
#202626=CARTESIAN_POINT('Ctrl Pts',(178.191169115156,2.30889010907467,135.149130194217));
#202627=CARTESIAN_POINT('Ctrl Pts',(178.183417923916,2.42816930322083,135.081412978409));
#202628=CARTESIAN_POINT('Ctrl Pts',(178.175670027139,2.54739780052724,135.013724544225));
#202629=CARTESIAN_POINT('Ctrl Pts',(178.167922130362,2.66385545891838,134.941011845815));
#202630=CARTESIAN_POINT('Ctrl Pts',(178.160174233585,2.77709782812851,134.863536730462));
#202631=CARTESIAN_POINT('Ctrl Pts',(178.152427957501,2.89031650947627,134.786077821233));
#202632=CARTESIAN_POINT('Ctrl Pts',(178.144681681417,3.00032091694935,134.703858697166));
#202633=CARTESIAN_POINT('Ctrl Pts',(178.136935405333,3.10669507789434,134.617184866792));
#202634=CARTESIAN_POINT('Ctrl Pts',(178.129189072067,3.21307002406919,134.530510396612));
#202635=CARTESIAN_POINT('Ctrl Pts',(178.121442738802,3.3158143671513,134.439381401467));
#202636=CARTESIAN_POINT('Ctrl Pts',(178.113696405536,3.41454507837369,134.344143798815));
#202637=CARTESIAN_POINT('Ctrl Pts',(178.105948337533,3.51329789965441,134.248884868363));
#202638=CARTESIAN_POINT('Ctrl Pts',(178.098200269531,3.60803501918443,134.149515770902));
#202639=CARTESIAN_POINT('Ctrl Pts',(178.090452201528,3.69841043817239,134.046419113848));
#202640=CARTESIAN_POINT('Ctrl Pts',(178.082695898786,3.78888190923111,133.943212884441));
#202641=CARTESIAN_POINT('Ctrl Pts',(178.074939596044,3.87498216137204,133.836271475994));
#202642=CARTESIAN_POINT('Ctrl Pts',(178.067183293302,3.95640532583523,133.726010829382));
#202643=CARTESIAN_POINT('Ctrl Pts',(178.059422850788,4.03787194829287,133.615691333343));
#202644=CARTESIAN_POINT('Ctrl Pts',(178.051662408274,4.11465629020245,133.502049392914));
#202645=CARTESIAN_POINT('Ctrl Pts',(178.04390196576,4.18649655826397,133.385528886034));
#202646=CARTESIAN_POINT('Ctrl Pts',(178.036129065494,4.2584521507015,133.268821330092));
#202647=CARTESIAN_POINT('Ctrl Pts',(178.028356165229,4.32544761811758,133.149226314897));
#202648=CARTESIAN_POINT('Ctrl Pts',(178.020583264963,4.38726735076475,133.027211997081));
#202649=CARTESIAN_POINT('Ctrl Pts',(178.013092929201,4.44683978041561,132.909633207055));
#202650=CARTESIAN_POINT('Ctrl Pts',(178.005602593439,4.50160611609358,132.789808236237));
#202651=CARTESIAN_POINT('Ctrl Pts',(177.998112257677,4.5514168344388,132.668170656622));
#202652=CARTESIAN_POINT('Ctrl Pts',(177.990337833928,4.6031167373512,132.541919695675));
#202653=CARTESIAN_POINT('Ctrl Pts',(177.982563410178,4.64964146881412,132.413315987716));
#202654=CARTESIAN_POINT('Ctrl Pts',(177.974788986429,4.69077100477924,132.282822806201));
#202655=CARTESIAN_POINT('Ctrl Pts',(177.967024164819,4.73184974192762,132.152490795947));
#202656=CARTESIAN_POINT('Ctrl Pts',(177.959259343209,4.76754642582505,132.020274324827));
#202657=CARTESIAN_POINT('Ctrl Pts',(177.951494521598,4.79768865878615,131.886657525006));
#202658=CARTESIAN_POINT('Ctrl Pts',(177.943737432929,4.82780087327161,131.753173793384));
#202659=CARTESIAN_POINT('Ctrl Pts',(177.93598034426,4.85236955970395,131.618292887302));
#202660=CARTESIAN_POINT('Ctrl Pts',(177.928223255591,4.87127192133961,131.482514678874));
#202661=CARTESIAN_POINT('Ctrl Pts',(177.920472037378,4.89015997793087,131.346839225505));
#202662=CARTESIAN_POINT('Ctrl Pts',(177.912720819166,4.90339019157259,131.210268207127));
#202663=CARTESIAN_POINT('Ctrl Pts',(177.904969600953,4.91089077987771,131.073311934001));
#202664=CARTESIAN_POINT('Ctrl Pts',(177.897221785057,4.91838807587815,130.936415776397));
#202665=CARTESIAN_POINT('Ctrl Pts',(177.88947396916,4.92016072820489,130.799135089998));
#202666=CARTESIAN_POINT('Ctrl Pts',(177.881726153264,4.91618880208696,130.661985322185));
#202667=CARTESIAN_POINT('Ctrl Pts',(177.873979987703,4.91221772201521,130.524864768168));
#202668=CARTESIAN_POINT('Ctrl Pts',(177.866233822142,4.90250450894667,130.387875467793));
#202669=CARTESIAN_POINT('Ctrl Pts',(177.858487656581,4.88708135175385,130.251532503375));
#202670=CARTESIAN_POINT('Ctrl Pts',(177.850741463501,4.87165813976965,130.115189054594));
#202671=CARTESIAN_POINT('Ctrl Pts',(177.842995270422,4.85052498725969,129.979492334791));
#202672=CARTESIAN_POINT('Ctrl Pts',(177.835249077342,4.82376588322583,129.844951546144));
#202673=CARTESIAN_POINT('Ctrl Pts',(177.827501179234,4.79700088919644,129.710381143477));
#202674=CARTESIAN_POINT('Ctrl Pts',(177.819753281125,4.76460755599529,129.576967561547));
#202675=CARTESIAN_POINT('Ctrl Pts',(177.812005383017,4.72672075122141,129.445208675187));
#202676=CARTESIAN_POINT('Ctrl Pts',(177.804249662856,4.68879569703309,129.313316768893));
#202677=CARTESIAN_POINT('Ctrl Pts',(177.796493942696,4.64536620236076,129.183083270921));
#202678=CARTESIAN_POINT('Ctrl Pts',(177.788738222535,4.59661683543853,129.054990236354));
#202679=CARTESIAN_POINT('Ctrl Pts',(177.780978374852,4.54784152455826,128.926829031869));
#202680=CARTESIAN_POINT('Ctrl Pts',(177.77321852717,4.49374085422359,128.800810919526));
#202681=CARTESIAN_POINT('Ctrl Pts',(177.765458679487,4.43454670577277,128.677395978269));
#202682=CARTESIAN_POINT('Ctrl Pts',(177.757687345308,4.37526493531858,128.553798352327));
#202683=CARTESIAN_POINT('Ctrl Pts',(177.749916011129,4.31087480777823,128.432811940594));
#202684=CARTESIAN_POINT('Ctrl Pts',(177.742144676949,4.24165347448646,128.314870937958));
#202685=CARTESIAN_POINT('Ctrl Pts',(177.73624105985,4.18906839225497,128.225275187238));
#202686=CARTESIAN_POINT('Ctrl Pts',(177.73033744275,4.13369619242487,128.137436378276));
#202687=CARTESIAN_POINT('Ctrl Pts',(177.724433825651,4.07567416841541,128.051532410901));
#202688=CARTESIAN_POINT('',(177.982416834316,3.01851762861496,126.922258965043));
#202689=CARTESIAN_POINT('Ctrl Pts',(177.981069942749,3.00973836756106,126.914545966284));
#202690=CARTESIAN_POINT('Ctrl Pts',(177.946908021577,3.17701395531151,127.043975206374));
#202691=CARTESIAN_POINT('Ctrl Pts',(177.912210265842,3.33354615464498,127.18245091907));
#202692=CARTESIAN_POINT('Ctrl Pts',(177.827217622719,3.69622248758502,127.54512725201));
#202693=CARTESIAN_POINT('Ctrl Pts',(177.774439956054,3.90152846520454,127.792270849974));
#202694=CARTESIAN_POINT('Ctrl Pts',(177.725138528175,4.08258754759718,128.06179576351));
#202695=CARTESIAN_POINT('',(179.11014056404,-4.9182496345238,130.80625666781));
#202696=CARTESIAN_POINT('Ctrl Pts',(179.110140564008,-4.91824963452358,
130.806256668381));
#202697=CARTESIAN_POINT('Ctrl Pts',(179.104198294929,-4.9182094084543,130.910600839437));
#202698=CARTESIAN_POINT('Ctrl Pts',(179.09825602585,-4.91484884784317,131.014877292883));
#202699=CARTESIAN_POINT('Ctrl Pts',(179.09231375677,-4.90817921990328,131.11893939595));
#202700=CARTESIAN_POINT('Ctrl Pts',(179.084539422651,-4.89945327441634,
131.255084957113));
#202701=CARTESIAN_POINT('Ctrl Pts',(179.076765088532,-4.88504450286705,
131.391082820901));
#202702=CARTESIAN_POINT('Ctrl Pts',(179.068990754413,-4.86495766475957,
131.526420159846));
#202703=CARTESIAN_POINT('Ctrl Pts',(179.061226001466,-4.84489558188487,
131.661590707615));
#202704=CARTESIAN_POINT('Ctrl Pts',(179.053461248519,-4.81916941265581,
131.796101967218));
#202705=CARTESIAN_POINT('Ctrl Pts',(179.045696495572,-4.78783586718883,
131.929443179585));
#202706=CARTESIAN_POINT('Ctrl Pts',(179.037939454687,-4.75653344264092,
132.062651955581));
#202707=CARTESIAN_POINT('Ctrl Pts',(179.030182413802,-4.71963481392058,
132.194692618852));
#202708=CARTESIAN_POINT('Ctrl Pts',(179.022425372917,-4.67724817964733,
132.325061945403));
#202709=CARTESIAN_POINT('Ctrl Pts',(179.014674181676,-4.63489350946472,
132.455332959431));
#202710=CARTESIAN_POINT('Ctrl Pts',(179.006922990436,-4.58705919165299,
132.583934775123));
#202711=CARTESIAN_POINT('Ctrl Pts',(178.999171799196,-4.53390386652968,
132.710377089574));
#202712=CARTESIAN_POINT('Ctrl Pts',(178.991423902419,-4.48077113383746,
132.836765662669));
#202713=CARTESIAN_POINT('Ctrl Pts',(178.983676005642,-4.42232204312134,
132.960996200391));
#202714=CARTESIAN_POINT('Ctrl Pts',(178.975928108865,-4.35876411544756,
133.082596436876));
#202715=CARTESIAN_POINT('Ctrl Pts',(178.968181832781,-4.29521948272209,
133.204171237213));
#202716=CARTESIAN_POINT('Ctrl Pts',(178.960435556697,-4.22656831964791,
133.323116484425));
#202717=CARTESIAN_POINT('Ctrl Pts',(178.952689280612,-4.15306486639283,
133.438983034163));
#202718=CARTESIAN_POINT('Ctrl Pts',(178.944942947347,-4.07956087055197,
133.554850439201));
#202719=CARTESIAN_POINT('Ctrl Pts',(178.937196614082,-4.00120472249036,
133.667638771277));
#202720=CARTESIAN_POINT('Ctrl Pts',(178.929450280816,-3.91829467942949,
133.776926826695));
#202721=CARTESIAN_POINT('Ctrl Pts',(178.921702212813,-3.83536606923948,
133.886239356415));
#202722=CARTESIAN_POINT('Ctrl Pts',(178.91395414481,-3.74788177099222,133.992049738264));
#202723=CARTESIAN_POINT('Ctrl Pts',(178.906206076807,-3.65618084862433,
134.093969205932));
#202724=CARTESIAN_POINT('Ctrl Pts',(178.898449774065,-3.56438246542475,
134.195996994824));
#202725=CARTESIAN_POINT('Ctrl Pts',(178.890693471324,-3.4683587677859,134.294125317703));
#202726=CARTESIAN_POINT('Ctrl Pts',(178.882937168582,-3.3684866595003,134.388001320436));
#202727=CARTESIAN_POINT('Ctrl Pts',(178.875176726068,-3.2685612464633,134.481927427618));
#202728=CARTESIAN_POINT('Ctrl Pts',(178.867416283553,-3.1647836256717,134.571596436813));
#202729=CARTESIAN_POINT('Ctrl Pts',(178.859655841039,-3.0575636481392,134.656695961235));
#202730=CARTESIAN_POINT('Ctrl Pts',(178.851882940774,-2.95017155158026,
134.741932094967));
#202731=CARTESIAN_POINT('Ctrl Pts',(178.844110040508,-2.83932637193757,
134.822583855418));
#202732=CARTESIAN_POINT('Ctrl Pts',(178.836337140243,-2.7254675236648,134.898381848575));
#202733=CARTESIAN_POINT('Ctrl Pts',(178.828846804481,-2.61574773132176,
134.971424393755));
#202734=CARTESIAN_POINT('Ctrl Pts',(178.821356468719,-2.50322983824925,
135.039959777996));
#202735=CARTESIAN_POINT('Ctrl Pts',(178.813866132957,-2.38832672171129,
135.10378831586));
#202736=CARTESIAN_POINT('Ctrl Pts',(178.806091798838,-2.26906701858384,
135.170036932139));
#202737=CARTESIAN_POINT('Ctrl Pts',(178.798317464719,-2.1468598711432,135.231424591867));
#202738=CARTESIAN_POINT('Ctrl Pts',(178.7905431306,-2.02213930829118,135.287678103576));
#202739=CARTESIAN_POINT('Ctrl Pts',(178.782778377653,-1.8975724523863,135.34386228786));
#202740=CARTESIAN_POINT('Ctrl Pts',(178.775013624706,-1.77049869726083,
135.39492475452));
#202741=CARTESIAN_POINT('Ctrl Pts',(178.767248871759,-1.64137841218754,
135.440637137631));
#202742=CARTESIAN_POINT('Ctrl Pts',(178.759491830874,-1.51238637120182,
135.486304118559));
#202743=CARTESIAN_POINT('Ctrl Pts',(178.751734789989,-1.38135221148386,
135.526631460963));
#202744=CARTESIAN_POINT('Ctrl Pts',(178.743977749104,-1.24875779362943,
135.561438190546));
#202745=CARTESIAN_POINT('Ctrl Pts',(178.736226557863,-1.11626336625679,
135.596218672103));
#202746=CARTESIAN_POINT('Ctrl Pts',(178.728475366623,-0.982211399327259,
135.625486728446));
#202747=CARTESIAN_POINT('Ctrl Pts',(178.720724175383,-0.847100147526754,
135.649110807468));
#202748=CARTESIAN_POINT('Ctrl Pts',(178.712976278606,-0.712046321612475,
135.672724845628));
#202749=CARTESIAN_POINT('Ctrl Pts',(178.705228381829,-0.575934490605304,
135.690699610382));
#202750=CARTESIAN_POINT('Ctrl Pts',(178.697480485052,-0.439274155356607,
135.702954423847));
#202751=CARTESIAN_POINT('Ctrl Pts',(178.689734208968,-0.302642406504035,
135.715206673869));
#202752=CARTESIAN_POINT('Ctrl Pts',(178.681987932884,-0.165462770780643,
135.721741317591));
#202753=CARTESIAN_POINT('Ctrl Pts',(178.6742416568,-0.0282505490694401,
135.722529480972));
#202754=CARTESIAN_POINT('Ctrl Pts',(178.666495323534,0.10896268551119,135.723317650172));
#202755=CARTESIAN_POINT('Ctrl Pts',(178.658748990269,0.246208115600862,
135.718359252141));
#202756=CARTESIAN_POINT('Ctrl Pts',(178.651002657004,0.382970155287087,
135.707677548243));
#202757=CARTESIAN_POINT('Ctrl Pts',(178.643254589001,0.519762821883836,
135.69699345225));
#202758=CARTESIAN_POINT('Ctrl Pts',(178.635506520998,0.6560714929648,135.680583530403));
#202759=CARTESIAN_POINT('Ctrl Pts',(178.627758452995,0.791385816082687,
135.658522909105));
#202760=CARTESIAN_POINT('Ctrl Pts',(178.620002150253,0.926843952873513,
135.636438841517));
#202761=CARTESIAN_POINT('Ctrl Pts',(178.612245847511,1.06130524413376,135.608692140596));
#202762=CARTESIAN_POINT('Ctrl Pts',(178.604489544769,1.19426909797958,135.575409179896));
#202763=CARTESIAN_POINT('Ctrl Pts',(178.596729102255,1.32730391863779,135.542108455078));
#202764=CARTESIAN_POINT('Ctrl Pts',(178.588968659741,1.45883933457868,135.503265693328));
#202765=CARTESIAN_POINT('Ctrl Pts',(178.581208217227,1.58839099146788,135.459056861224));
#202766=CARTESIAN_POINT('Ctrl Pts',(178.573435316961,1.71815061617768,135.414777061178));
#202767=CARTESIAN_POINT('Ctrl Pts',(178.565662416696,1.84591975356253,135.365114118798));
#202768=CARTESIAN_POINT('Ctrl Pts',(178.55788951643,1.97123424056386,135.310292111866));
#202769=CARTESIAN_POINT('Ctrl Pts',(178.550399180668,2.09199323031518,135.257463022974));
#202770=CARTESIAN_POINT('Ctrl Pts',(178.542908844906,2.21047265971088,135.199843582111));
#202771=CARTESIAN_POINT('Ctrl Pts',(178.535418509144,2.32628135749008,135.137673219755));
#202772=CARTESIAN_POINT('Ctrl Pts',(178.527644175025,2.44648097724423,135.073145649215));
#202773=CARTESIAN_POINT('Ctrl Pts',(178.519869840906,2.56418410222925,135.003510844547));
#202774=CARTESIAN_POINT('Ctrl Pts',(178.512095506787,2.67892628550298,134.928986299897));
#202775=CARTESIAN_POINT('Ctrl Pts',(178.50433075384,2.7935270592906,134.854553600087));
#202776=CARTESIAN_POINT('Ctrl Pts',(178.496566000893,2.90517382725016,134.775243361484));
#202777=CARTESIAN_POINT('Ctrl Pts',(178.488801247946,3.01342561782393,134.691319468434));
#202778=CARTESIAN_POINT('Ctrl Pts',(178.481044207061,3.12156989119321,134.607478929778));
#202779=CARTESIAN_POINT('Ctrl Pts',(178.473287166176,3.22632559050266,134.519034093746));
#202780=CARTESIAN_POINT('Ctrl Pts',(178.465530125291,3.32727999952759,134.426292542277));
#202781=CARTESIAN_POINT('Ctrl Pts',(178.457778934051,3.42815827804732,134.333620927934));
#202782=CARTESIAN_POINT('Ctrl Pts',(178.45002774281,3.52524068528896,134.236659310972));
#202783=CARTESIAN_POINT('Ctrl Pts',(178.44227655157,3.61814722391349,134.135755780045));
#202784=CARTESIAN_POINT('Ctrl Pts',(178.434528654793,3.7110142747808,134.03489513581));
#202785=CARTESIAN_POINT('Ctrl Pts',(178.426780758016,3.79970872281605,133.930096196904));
#202786=CARTESIAN_POINT('Ctrl Pts',(178.419032861239,3.88388729377466,133.821744012456));
#202787=CARTESIAN_POINT('Ctrl Pts',(178.411286585155,3.9680482563909,133.713414492949));
#202788=CARTESIAN_POINT('Ctrl Pts',(178.403540309071,4.04769498113156,133.601533514834));
#202789=CARTESIAN_POINT('Ctrl Pts',(178.395794032987,4.12252464273607,133.486519008216));
#202790=CARTESIAN_POINT('Ctrl Pts',(178.388047699721,4.19735485671612,133.371503652587));
#202791=CARTESIAN_POINT('Ctrl Pts',(178.380301366456,4.26736772339354,133.253355050009));
#202792=CARTESIAN_POINT('Ctrl Pts',(178.372555033191,4.33230412643066,133.132519550846));
#202793=CARTESIAN_POINT('Ctrl Pts',(178.364806965188,4.39725507152499,133.011656991411));
#202794=CARTESIAN_POINT('Ctrl Pts',(178.357058897185,4.45712710576501,132.888106682375));
#202795=CARTESIAN_POINT('Ctrl Pts',(178.349310829182,4.5117075771597,132.762338605364));
#202796=CARTESIAN_POINT('Ctrl Pts',(178.34155452644,4.56634605732893,132.636436860543));
#202797=CARTESIAN_POINT('Ctrl Pts',(178.333798223698,4.61568158434171,132.508312998465));
#202798=CARTESIAN_POINT('Ctrl Pts',(178.326041920956,4.65954989770888,132.378456489253));
#202799=CARTESIAN_POINT('Ctrl Pts',(178.318281478442,4.70344162491577,132.248530671712));
#202800=CARTESIAN_POINT('Ctrl Pts',(178.310521035928,4.74186021461865,132.116870739491));
#202801=CARTESIAN_POINT('Ctrl Pts',(178.302760593414,4.77469190713373,131.983979307843));
#202802=CARTESIAN_POINT('Ctrl Pts',(178.294987693148,4.80757630399628,131.850874547072));
#202803=CARTESIAN_POINT('Ctrl Pts',(178.287214792883,4.83485580373609,131.716534719739));
#202804=CARTESIAN_POINT('Ctrl Pts',(178.279441892618,4.85646803786489,131.581471458886));
#202805=CARTESIAN_POINT('Ctrl Pts',(178.271951556856,4.87729461284501,131.451318087769));
#202806=CARTESIAN_POINT('Ctrl Pts',(178.264461221094,4.89285877098853,131.320493273089));
#202807=CARTESIAN_POINT('Ctrl Pts',(178.256970885332,4.90315051431672,131.189455536327));
#202808=CARTESIAN_POINT('Ctrl Pts',(178.249196486275,4.91383256144549,131.053448327918));
#202809=CARTESIAN_POINT('Ctrl Pts',(178.241422087219,4.91886823705911,130.916780895422));
#202810=CARTESIAN_POINT('Ctrl Pts',(178.233647688162,4.91818947873383,130.779961564882));
#202811=CARTESIAN_POINT('Ctrl Pts',(178.225882885497,4.91751155823925,130.643311118365));
#202812=CARTESIAN_POINT('Ctrl Pts',(178.218118082831,4.91113324050394,130.50650953409));
#202813=CARTESIAN_POINT('Ctrl Pts',(178.210353280166,4.89903818329087,130.37007045977));
#202814=CARTESIAN_POINT('Ctrl Pts',(178.202596204717,4.88695516258868,130.233767164089));
#202815=CARTESIAN_POINT('Ctrl Pts',(178.194839129269,4.86916675831516,130.097826047365));
#202816=CARTESIAN_POINT('Ctrl Pts',(178.18708205382,4.84570866602806,129.962760601834));
#202817=CARTESIAN_POINT('Ctrl Pts',(178.179330843123,4.822268309275,129.827797272782));
#202818=CARTESIAN_POINT('Ctrl Pts',(178.171579632426,4.79316686341908,129.693708680778));
#202819=CARTESIAN_POINT('Ctrl Pts',(178.163828421728,4.75849178917548,129.561002682436));
#202820=CARTESIAN_POINT('Ctrl Pts',(178.156080584143,4.72383180456287,129.428354434066));
#202821=CARTESIAN_POINT('Ctrl Pts',(178.148332746558,4.68360311496809,129.297087959994));
#202822=CARTESIAN_POINT('Ctrl Pts',(178.140584908972,4.63794412274852,129.167700183401));
#202823=CARTESIAN_POINT('Ctrl Pts',(178.132838713596,4.59229480827461,129.038339831459));
#202824=CARTESIAN_POINT('Ctrl Pts',(178.125092518219,4.54121761075637,128.910857753318));
#202825=CARTESIAN_POINT('Ctrl Pts',(178.117346322843,4.48490045673777,128.785734610686));
#202826=CARTESIAN_POINT('Ctrl Pts',(178.109600091816,4.42858304352998,128.660610892198));
#202827=CARTESIAN_POINT('Ctrl Pts',(178.101853860789,4.36702578624526,128.537846487337));
#202828=CARTESIAN_POINT('Ctrl Pts',(178.094107629763,4.30046414392161,128.41790064318));
#202829=CARTESIAN_POINT('Ctrl Pts',(178.086359685563,4.23388778068198,128.297928271543));
#202830=CARTESIAN_POINT('Ctrl Pts',(178.078611741363,4.16230501986083,128.180776042692));
#202831=CARTESIAN_POINT('Ctrl Pts',(178.070863797163,4.08599631251719,128.066876883076));
#202832=CARTESIAN_POINT('Ctrl Pts',(178.063107919224,4.00960946659292,127.952861093014));
#202833=CARTESIAN_POINT('Ctrl Pts',(178.055352041285,3.92848722617181,127.842105350861));
#202834=CARTESIAN_POINT('Ctrl Pts',(178.047596163346,3.84295255436162,127.735012359804));
#202835=CARTESIAN_POINT('Ctrl Pts',(178.039836154527,3.75737232568789,127.627862329646));
#202836=CARTESIAN_POINT('Ctrl Pts',(178.032076145708,3.6673752392277,127.524379232517));
#202837=CARTESIAN_POINT('Ctrl Pts',(178.024316136889,3.57332260510824,127.424930396016));
#202838=CARTESIAN_POINT('Ctrl Pts',(178.016544381083,3.47912759550359,127.325331015339));
#202839=CARTESIAN_POINT('Ctrl Pts',(178.008772625278,3.38086505267233,127.229778369216));
#202840=CARTESIAN_POINT('Ctrl Pts',(178.001000869473,3.27893153455889,127.138601343667));
#202841=CARTESIAN_POINT('Ctrl Pts',(177.994662241379,3.19579476627145,127.064237548652));
#202842=CARTESIAN_POINT('Ctrl Pts',(177.988323613286,3.11021677117177,126.992783713995));
#202843=CARTESIAN_POINT('Ctrl Pts',(177.981984985192,3.02242700330697,126.924396948641));
#202844=CARTESIAN_POINT('Ctrl Pts',(179.180279212536,-4.76405452823405,
129.582490119308));
#202845=CARTESIAN_POINT('Ctrl Pts',(179.172592770908,-4.79783235438911,
129.714189350837));
#202846=CARTESIAN_POINT('Ctrl Pts',(179.16490632928,-4.82611955095255,129.847191517955));
#202847=CARTESIAN_POINT('Ctrl Pts',(179.157219887652,-4.84884024883698,
129.980994779218));
#202848=CARTESIAN_POINT('Ctrl Pts',(179.149373333716,-4.87203422987842,
130.117585227311));
#202849=CARTESIAN_POINT('Ctrl Pts',(179.141526779781,-4.88942719215613,
130.255010073371));
#202850=CARTESIAN_POINT('Ctrl Pts',(179.133680225846,-4.90099431101235,
130.392732355751));
#202851=CARTESIAN_POINT('Ctrl Pts',(179.125833671911,-4.91256142986858,
130.530454638131));
#202852=CARTESIAN_POINT('Ctrl Pts',(179.117987117976,-4.91830275159455,
130.668473919319));
#202853=CARTESIAN_POINT('Ctrl Pts',(179.11014056404,-4.9182496345238,130.80625666781));
#202854=CARTESIAN_POINT('Origin',(213.235140564004,0.,130.804360617566));
#202855=CARTESIAN_POINT('',(180.930009319727,-4.76405452823406,129.582490119308));
#202856=CARTESIAN_POINT('',(180.584985772263,-4.76405452823404,129.582490119308));
#202857=CARTESIAN_POINT('',(213.235140564004,-4.76405452823405,129.582490119308));
#202858=CARTESIAN_POINT('',(180.514859436037,-4.91824986164052,130.805527225028));
#202859=CARTESIAN_POINT('Ctrl Pts',(180.584985772263,-4.76405452823404,
129.582490119308));
#202860=CARTESIAN_POINT('Ctrl Pts',(180.57727395094,-4.79793105739994,129.714574192378));
#202861=CARTESIAN_POINT('Ctrl Pts',(180.569562129616,-4.82628395215226,
129.847965328554));
#202862=CARTESIAN_POINT('Ctrl Pts',(180.561850308293,-4.84903779404517,
129.982158979024));
#202863=CARTESIAN_POINT('Ctrl Pts',(180.55401849625,-4.8721456703155,130.118440591857));
#202864=CARTESIAN_POINT('Ctrl Pts',(180.546186684208,-4.889478756331,130.255549475578));
#202865=CARTESIAN_POINT('Ctrl Pts',(180.538354872165,-4.90101294444811,
130.392954272389));
#202866=CARTESIAN_POINT('Ctrl Pts',(180.530523060122,-4.91254713256523,
130.5303590692));
#202867=CARTESIAN_POINT('Ctrl Pts',(180.522691248079,-4.91828246897984,
130.668059355764));
#202868=CARTESIAN_POINT('Ctrl Pts',(180.514859436037,-4.91824986164052,
130.805527225028));
#202869=CARTESIAN_POINT('Ctrl Pts',(180.514859435991,-4.91824986164033,
130.805527225829));
#202870=CARTESIAN_POINT('Ctrl Pts',(180.511286581325,-4.91823498623681,
130.86823975205));
#202871=CARTESIAN_POINT('Ctrl Pts',(180.507713726659,-4.91702069103772,
130.930936615505));
#202872=CARTESIAN_POINT('Ctrl Pts',(180.504140871993,-4.9146084703115,130.993587058748));
#202873=CARTESIAN_POINT('Ctrl Pts',(180.496366537874,-4.90935961144405,
131.129910957714));
#202874=CARTESIAN_POINT('Ctrl Pts',(180.488592203755,-4.89842600811054,
131.266232225206));
#202875=CARTESIAN_POINT('Ctrl Pts',(180.480817869636,-4.88179933162287,
131.402038079301));
#202876=CARTESIAN_POINT('Ctrl Pts',(180.473053116689,-4.86519314602801,
131.537676564819));
#202877=CARTESIAN_POINT('Ctrl Pts',(180.465288363742,-4.84290789448837,
131.672800516459));
#202878=CARTESIAN_POINT('Ctrl Pts',(180.457523610795,-4.81498723479294,
131.80689789432));
#202879=CARTESIAN_POINT('Ctrl Pts',(180.44976656991,-4.78709430629035,131.940862084775));
#202880=CARTESIAN_POINT('Ctrl Pts',(180.442009529025,-4.75357718742527,
132.073801350235));
#202881=CARTESIAN_POINT('Ctrl Pts',(180.43425248814,-4.714531200007,132.205209869506));
#202882=CARTESIAN_POINT('Ctrl Pts',(180.4265012969,-4.67551465747153,132.33651929259));
#202883=CARTESIAN_POINT('Ctrl Pts',(180.41875010566,-4.63097765615341,132.466299893888));
#202884=CARTESIAN_POINT('Ctrl Pts',(180.41099891442,-4.58106627286169,132.594057481884));
#202885=CARTESIAN_POINT('Ctrl Pts',(180.403251017643,-4.53117610323931,
132.721760769497));
#202886=CARTESIAN_POINT('Ctrl Pts',(180.395503120866,-4.47591623682387,
132.847442390555));
#202887=CARTESIAN_POINT('Ctrl Pts',(180.387755224089,-4.41548207553511,
132.970624937341));
#202888=CARTESIAN_POINT('Ctrl Pts',(180.380008948005,-4.35506055577006,
133.093781716993));
#202889=CARTESIAN_POINT('Ctrl Pts',(180.37226267192,-4.28946706608026,133.21444011138));
#202890=CARTESIAN_POINT('Ctrl Pts',(180.364516395836,-4.21894430230164,
133.332144634561));
#202891=CARTESIAN_POINT('Ctrl Pts',(180.356770062571,-4.14842101794008,
133.449850026611));
#202892=CARTESIAN_POINT('Ctrl Pts',(180.349023729306,-4.07296858782303,
133.56460116857));
#202893=CARTESIAN_POINT('Ctrl Pts',(180.34127739604,-3.99287442351235,133.675969382799));
#202894=CARTESIAN_POINT('Ctrl Pts',(180.333529328037,-3.91276232266898,
133.787362537167));
#202895=CARTESIAN_POINT('Ctrl Pts',(180.325781260035,-3.82800664740718,
133.895370938959));
#202896=CARTESIAN_POINT('Ctrl Pts',(180.318033192032,-3.73893643047199,
133.999597296028));
#202897=CARTESIAN_POINT('Ctrl Pts',(180.31027688929,-3.64977154865013,134.10393442611));
#202898=CARTESIAN_POINT('Ctrl Pts',(180.302520586548,-3.55628321943548,
134.204481184188));
#202899=CARTESIAN_POINT('Ctrl Pts',(180.294764283806,-3.45883921953503,
134.300875212975));
#202900=CARTESIAN_POINT('Ctrl Pts',(180.287003841292,-3.36134321083779,
134.397320690157));
#202901=CARTESIAN_POINT('Ctrl Pts',(180.279243398778,-3.25988761365962,
134.489608758661));
#202902=CARTESIAN_POINT('Ctrl Pts',(180.271482956264,-3.15487417386967,
134.577416674604));
#202903=CARTESIAN_POINT('Ctrl Pts',(180.263710055998,-3.04969215718354,
134.665365547608));
#202904=CARTESIAN_POINT('Ctrl Pts',(180.255937155733,-2.94094119510187,
134.748819658113));
#202905=CARTESIAN_POINT('Ctrl Pts',(180.248164255467,-2.82905368442206,
134.827498486588));
#202906=CARTESIAN_POINT('Ctrl Pts',(180.240673919705,-2.72123356658074,
134.90331714147));
#202907=CARTESIAN_POINT('Ctrl Pts',(180.233183583943,-2.61050124275258,
134.974701506813));
#202908=CARTESIAN_POINT('Ctrl Pts',(180.225693248181,-2.49726436005296,
135.041441426155));
#202909=CARTESIAN_POINT('Ctrl Pts',(180.217918914062,-2.37973406653057,
135.110711809822));
#202910=CARTESIAN_POINT('Ctrl Pts',(180.210144579943,-2.259133243701,135.175198034593));
#202911=CARTESIAN_POINT('Ctrl Pts',(180.202370245824,-2.13588880765785,
135.234615922153));
#202912=CARTESIAN_POINT('Ctrl Pts',(180.194605492877,-2.01279625936746,
135.293960582477));
#202913=CARTESIAN_POINT('Ctrl Pts',(180.186840739929,-1.88706692913862,
135.348249165653));
#202914=CARTESIAN_POINT('Ctrl Pts',(180.179075986982,-1.75915520874346,
135.397241632142));
#202915=CARTESIAN_POINT('Ctrl Pts',(180.171318946097,-1.63137053207232,
135.446185438622));
#202916=CARTESIAN_POINT('Ctrl Pts',(180.163561905212,-1.5014081415564,135.48984345747));
#202917=CARTESIAN_POINT('Ctrl Pts',(180.155804864327,-1.36974512266039,
135.528022476913));
#202918=CARTESIAN_POINT('Ctrl Pts',(180.148053673087,-1.23818139187112,
135.56617270526));
#202919=CARTESIAN_POINT('Ctrl Pts',(180.140302481847,-1.10491995933232,
135.598852049766));
#202920=CARTESIAN_POINT('Ctrl Pts',(180.132551290607,-0.970455560445589,
135.625916286404));
#202921=CARTESIAN_POINT('Ctrl Pts',(180.12480339383,-0.836048312515253,
135.652969020018));
#202922=CARTESIAN_POINT('Ctrl Pts',(180.117055497053,-0.700439497635642,
135.674411315488));
#202923=CARTESIAN_POINT('Ctrl Pts',(180.109307600276,-0.564136391950636,
135.69014951945));
#202924=CARTESIAN_POINT('Ctrl Pts',(180.101561324192,-0.427861797936961,
135.705884431319));
#202925=CARTESIAN_POINT('Ctrl Pts',(180.093815048108,-0.290893590128375,
135.71591758015));
#202926=CARTESIAN_POINT('Ctrl Pts',(180.086068772024,-0.153746164773559,
135.720206951547));
#202927=CARTESIAN_POINT('Ctrl Pts',(180.078322438758,-0.0165977270276053,
135.724496354607));
#202928=CARTESIAN_POINT('Ctrl Pts',(180.070576105493,0.120729540130282,
135.723041883407));
#202929=CARTESIAN_POINT('Ctrl Pts',(180.062829772227,0.257719625092028,
135.715853634699));
#202930=CARTESIAN_POINT('Ctrl Pts',(180.055081704225,0.394740388033409,
135.708663776232));
#202931=CARTESIAN_POINT('Ctrl Pts',(180.047333636222,0.531423428169907,
135.695737605649));
#202932=CARTESIAN_POINT('Ctrl Pts',(180.039585568219,0.667256642130682,
135.677137201407));
#202933=CARTESIAN_POINT('Ctrl Pts',(180.031829265477,0.803234221247715,
135.658517028435));
#202934=CARTESIAN_POINT('Ctrl Pts',(180.024072962735,0.93835978197096,135.634210628072));
#202935=CARTESIAN_POINT('Ctrl Pts',(180.016316659993,1.07212967055861,135.604331558312));
#202936=CARTESIAN_POINT('Ctrl Pts',(180.008556217479,1.20597095616365,135.574436541194));
#202937=CARTESIAN_POINT('Ctrl Pts',(180.000795774965,1.33845475039577,135.538963029203));
#202938=CARTESIAN_POINT('Ctrl Pts',(179.99303533245,1.46909236623006,135.498074571567));
#202939=CARTESIAN_POINT('Ctrl Pts',(179.985262432185,1.59993969316269,135.457120476149));
#202940=CARTESIAN_POINT('Ctrl Pts',(179.97748953192,1.72893455126841,135.41073419697));
#202941=CARTESIAN_POINT('Ctrl Pts',(179.969716631654,1.85560721049188,135.359127894044));
#202942=CARTESIAN_POINT('Ctrl Pts',(179.962226295892,1.97767499948376,135.309397610217));
#202943=CARTESIAN_POINT('Ctrl Pts',(179.95473596013,2.09758621357152,135.254820363207));
#202944=CARTESIAN_POINT('Ctrl Pts',(179.947245624368,2.21494369894812,135.195625523375));
#202945=CARTESIAN_POINT('Ctrl Pts',(179.939471290249,2.33675082905244,135.134186293199));
#202946=CARTESIAN_POINT('Ctrl Pts',(179.93169695613,2.45619260687545,135.067577785012));
#202947=CARTESIAN_POINT('Ctrl Pts',(179.923922622011,2.57279918657586,134.996005570094));
#202948=CARTESIAN_POINT('Ctrl Pts',(179.916157869064,2.68926205908817,134.924521561534));
#202949=CARTESIAN_POINT('Ctrl Pts',(179.908393116117,2.8028963557451,134.848086220452));
#202950=CARTESIAN_POINT('Ctrl Pts',(179.900628363169,2.9132545146317,134.76695209228));
#202951=CARTESIAN_POINT('Ctrl Pts',(179.892871322284,3.02350306423898,134.685898547668));
#202952=CARTESIAN_POINT('Ctrl Pts',(179.8851142814,3.1304816385372,134.600155733395));
#202953=CARTESIAN_POINT('Ctrl Pts',(179.877357240515,3.2337698066414,134.51002059929));
#202954=CARTESIAN_POINT('Ctrl Pts',(179.869606049274,3.33698008433468,134.419953436792));
#202955=CARTESIAN_POINT('Ctrl Pts',(179.861854858034,3.43650520177386,134.32550080338));
#202956=CARTESIAN_POINT('Ctrl Pts',(179.854103666794,3.53195640262972,134.22700097735));
#202957=CARTESIAN_POINT('Ctrl Pts',(179.846355770017,3.627367034179,134.128543016374));
#202958=CARTESIAN_POINT('Ctrl Pts',(179.83860787324,3.71870692150715,134.026041564233));
#202959=CARTESIAN_POINT('Ctrl Pts',(179.830859976463,3.8056230762406,133.919872784784));
#202960=CARTESIAN_POINT('Ctrl Pts',(179.823113700379,3.89252104998818,133.813726213555));
#202961=CARTESIAN_POINT('Ctrl Pts',(179.815367424295,3.97499688420821,133.703914143201));
#202962=CARTESIAN_POINT('Ctrl Pts',(179.807621148211,4.05273718726214,133.590846640047));
#202963=CARTESIAN_POINT('Ctrl Pts',(179.799874814945,4.13047806417734,133.477778302254));
#202964=CARTESIAN_POINT('Ctrl Pts',(179.79212848168,4.20348311866762,133.361454805873));
#202965=CARTESIAN_POINT('Ctrl Pts',(179.784382148415,4.27148192853796,133.242315743624));
#202966=CARTESIAN_POINT('Ctrl Pts',(179.776634080412,4.33949596627027,133.123150001009));
#202967=CARTESIAN_POINT('Ctrl Pts',(179.768886012409,4.40250133473337,133.001167777338));
#202968=CARTESIAN_POINT('Ctrl Pts',(179.761137944406,4.4602734579108,132.876833474603));
#202969=CARTESIAN_POINT('Ctrl Pts',(179.753381641664,4.51810698198826,132.752367027892));
#202970=CARTESIAN_POINT('Ctrl Pts',(179.745625338922,4.57069598516582,132.625543863588));
#202971=CARTESIAN_POINT('Ctrl Pts',(179.73786903618,4.61786376985074,132.496849100717));
#202972=CARTESIAN_POINT('Ctrl Pts',(179.730108593666,4.66505672940257,132.368085649577));
#202973=CARTESIAN_POINT('Ctrl Pts',(179.722348151152,4.7068225859822,132.237448981634));
#202974=CARTESIAN_POINT('Ctrl Pts',(179.714587708638,4.74303479091117,132.105438645474));
#202975=CARTESIAN_POINT('Ctrl Pts',(179.706814808372,4.77930512688626,131.973216394604));
#202976=CARTESIAN_POINT('Ctrl Pts',(179.699041908107,4.81000390816578,131.839616450211));
#202977=CARTESIAN_POINT('Ctrl Pts',(179.691269007841,4.83505573040974,131.705148687165));
#202978=CARTESIAN_POINT('Ctrl Pts',(179.683778672079,4.85919685581355,131.575569166008));
#202979=CARTESIAN_POINT('Ctrl Pts',(179.676288336317,4.8780944124047,131.445184130401));
#202980=CARTESIAN_POINT('Ctrl Pts',(179.668798000555,4.89172670463108,131.314451697373));
#202981=CARTESIAN_POINT('Ctrl Pts',(179.661023666436,4.90587586936059,131.178762504413));
#202982=CARTESIAN_POINT('Ctrl Pts',(179.653249332317,4.91439744341293,131.042269228285));
#202983=CARTESIAN_POINT('Ctrl Pts',(179.645474998198,4.917210416574,130.905478279901));
#202984=CARTESIAN_POINT('Ctrl Pts',(179.637710245251,4.92001992299706,130.768855914136));
#202985=CARTESIAN_POINT('Ctrl Pts',(179.629945492304,4.91713481879837,130.631936993176));
#202986=CARTESIAN_POINT('Ctrl Pts',(179.622180739356,4.9085256594554,130.495234570511));
#202987=CARTESIAN_POINT('Ctrl Pts',(179.614423698471,4.89992505085085,130.358667922619));
#202988=CARTESIAN_POINT('Ctrl Pts',(179.606666657586,4.88561172534523,130.222317732772));
#202989=CARTESIAN_POINT('Ctrl Pts',(179.598909616701,4.86560826207741,130.086698230016));
#202990=CARTESIAN_POINT('Ctrl Pts',(179.591158425461,4.84561988357684,129.951180998982));
#202991=CARTESIAN_POINT('Ctrl Pts',(179.583407234221,4.81994996506197,129.81639374349));
#202992=CARTESIAN_POINT('Ctrl Pts',(179.575656042981,4.78867297735071,129.68284638293));
#202993=CARTESIAN_POINT('Ctrl Pts',(179.567908146204,4.75740928319356,129.549355783561));
#202994=CARTESIAN_POINT('Ctrl Pts',(179.560160249427,4.7205433487172,129.417104410853));
#202995=CARTESIAN_POINT('Ctrl Pts',(179.55241235265,4.67820085238921,129.286592569673));
#202996=CARTESIAN_POINT('Ctrl Pts',(179.544666076566,4.63586721319865,129.156108028757));
#202997=CARTESIAN_POINT('Ctrl Pts',(179.536919800482,4.58805941135035,129.027362667255));
#202998=CARTESIAN_POINT('Ctrl Pts',(179.529173524397,4.53495305142171,128.900841801294));
#202999=CARTESIAN_POINT('Ctrl Pts',(179.521427191132,4.48184629947401,128.774320001385));
#203000=CARTESIAN_POINT('Ctrl Pts',(179.513680857867,4.42344106271525,128.650023090278));
#203001=CARTESIAN_POINT('Ctrl Pts',(179.505934524601,4.35996101314982,128.528416192429));
#203002=CARTESIAN_POINT('Ctrl Pts',(179.498186456598,4.29646674766747,128.406782061558));
#203003=CARTESIAN_POINT('Ctrl Pts',(179.490438388595,4.22789558882288,128.28783948919));
#203004=CARTESIAN_POINT('Ctrl Pts',(179.482690320592,4.15451686234194,128.172028438107));
#203005=CARTESIAN_POINT('Ctrl Pts',(179.474934017851,4.08106014807724,128.056094301661));
#203006=CARTESIAN_POINT('Ctrl Pts',(179.467177715109,4.00278586890444,127.943298665755));
#203007=CARTESIAN_POINT('Ctrl Pts',(179.459421412367,3.92000665983544,127.834052409762));
#203008=CARTESIAN_POINT('Ctrl Pts',(179.451660969853,3.83718326901008,127.724747845754));
#203009=CARTESIAN_POINT('Ctrl Pts',(179.443900527339,3.74985040611597,127.618996737741));
#203010=CARTESIAN_POINT('Ctrl Pts',(179.436140084824,3.65835995287435,127.517175572926));
#203011=CARTESIAN_POINT('Ctrl Pts',(179.428367184559,3.56672263103505,127.415190955737));
#203012=CARTESIAN_POINT('Ctrl Pts',(179.420594284294,3.47091465521116,127.317149168308));
#203013=CARTESIAN_POINT('Ctrl Pts',(179.412821384028,3.37132423968277,127.223389250265));
#203014=CARTESIAN_POINT('Ctrl Pts',(179.405331048266,3.27535418661257,127.133037741411));
#203015=CARTESIAN_POINT('Ctrl Pts',(179.397840712504,3.17587215439751,127.046662395268));
#203016=CARTESIAN_POINT('Ctrl Pts',(179.390350376742,3.07325184289293,126.964529088364));
#203017=CARTESIAN_POINT('Ctrl Pts',(179.382576042623,2.96674065108638,126.879281672164));
#203018=CARTESIAN_POINT('Ctrl Pts',(179.374801708504,2.85651111111605,126.798334280789));
#203019=CARTESIAN_POINT('Ctrl Pts',(179.367027374385,2.74294549282422,126.722028797895));
#203020=CARTESIAN_POINT('Ctrl Pts',(179.359262621438,2.62951983400729,126.645817354689));
#203021=CARTESIAN_POINT('Ctrl Pts',(179.351497868491,2.51276659876644,126.574236653353));
#203022=CARTESIAN_POINT('Ctrl Pts',(179.343733115544,2.39310151804933,126.507588784339));
#203023=CARTESIAN_POINT('Ctrl Pts',(179.335976074659,2.27355529037732,126.441007110929));
#203024=CARTESIAN_POINT('Ctrl Pts',(179.328219033774,2.15110331196261,126.3793487089));
#203025=CARTESIAN_POINT('Ctrl Pts',(179.320461992889,2.0261904228423,126.322872535145));
#203026=CARTESIAN_POINT('Ctrl Pts',(179.312710801649,1.90137173150333,126.266438950512));
#203027=CARTESIAN_POINT('Ctrl Pts',(179.304959610409,1.77409617810434,126.215179976013));
#203028=CARTESIAN_POINT('Ctrl Pts',(179.297208419168,1.64483302556683,126.169308581126));
#203029=CARTESIAN_POINT('Ctrl Pts',(179.289460522391,1.51562481331742,126.123456682806));
#203030=CARTESIAN_POINT('Ctrl Pts',(179.281712625614,1.3844310498194,126.08298794021));
#203031=CARTESIAN_POINT('Ctrl Pts',(179.273964728837,1.25174058800957,126.048067043487));
#203032=CARTESIAN_POINT('Ctrl Pts',(179.266218452753,1.11907788218387,126.013153451461));
#203033=CARTESIAN_POINT('Ctrl Pts',(179.258472176669,0.984919478625015,
125.983785496472));
#203034=CARTESIAN_POINT('Ctrl Pts',(179.250725900585,0.849768606098465,
125.960077762634));
#203035=CARTESIAN_POINT('Ctrl Pts',(179.24297956732,0.714616735918967,125.936369853791));
#203036=CARTESIAN_POINT('Ctrl Pts',(179.235233234054,0.578472767238265,
125.918322317024));
#203037=CARTESIAN_POINT('Ctrl Pts',(179.227486900789,0.441848922615117,
125.905998381871));
#203038=CARTESIAN_POINT('Ctrl Pts',(179.219738832786,0.305194482029227,
125.893671686858));
#203039=CARTESIAN_POINT('Ctrl Pts',(179.211990764783,0.168060340967948,
125.887071179131));
#203040=CARTESIAN_POINT('Ctrl Pts',(179.20424269678,0.0309622297147287,
125.88620807796));
#203041=CARTESIAN_POINT('Ctrl Pts',(179.196486394038,-0.10628159104269,
125.885344059475));
#203042=CARTESIAN_POINT('Ctrl Pts',(179.188730091296,-0.243488913916986,
125.890229630992));
#203043=CARTESIAN_POINT('Ctrl Pts',(179.180973788555,-0.38014506759449,
125.900823854159));
#203044=CARTESIAN_POINT('Ctrl Pts',(179.17321334604,-0.51687415877599,125.911423731781));
#203045=CARTESIAN_POINT('Ctrl Pts',(179.165452903526,-0.653051106591565,
125.927738285734));
#203046=CARTESIAN_POINT('Ctrl Pts',(179.157692461012,-0.788168961031706,
125.949674968488));
#203047=CARTESIAN_POINT('Ctrl Pts',(179.149919560747,-0.923503718646903,
125.971646865952));
#203048=CARTESIAN_POINT('Ctrl Pts',(179.142146660481,-1.05777560227164,
125.999258848526));
#203049=CARTESIAN_POINT('Ctrl Pts',(179.134373760216,-1.19048952896382,
126.032367559741));
#203050=CARTESIAN_POINT('Ctrl Pts',(179.126883424454,-1.3183789701352,126.064272685909));
#203051=CARTESIAN_POINT('Ctrl Pts',(179.119393088692,-1.44482146351932,
126.101281752664));
#203052=CARTESIAN_POINT('Ctrl Pts',(179.11190275293,-1.56939132576419,126.143224068492));
#203053=CARTESIAN_POINT('Ctrl Pts',(179.104128393758,-1.69868470883825,
126.186756780254));
#203054=CARTESIAN_POINT('Ctrl Pts',(179.096354034586,-1.82637020688291,
126.235742147257));
#203055=CARTESIAN_POINT('Ctrl Pts',(179.088579675415,-1.95195355254964,
126.290043350117));
#203056=CARTESIAN_POINT('Ctrl Pts',(179.080814903304,-2.07738203333556,
126.34427759068));
#203057=CARTESIAN_POINT('Ctrl Pts',(179.073050131194,-2.2007131642445,126.403814470295));
#203058=CARTESIAN_POINT('Ctrl Pts',(179.065285359084,-2.32146807181828,
126.46846750841));
#203059=CARTESIAN_POINT('Ctrl Pts',(179.0575283049,-2.44210295301114,126.533056283545));
#203060=CARTESIAN_POINT('Ctrl Pts',(179.049771250716,-2.56016636431176,
126.602750913835));
#203061=CARTESIAN_POINT('Ctrl Pts',(179.042014196532,-2.6751999888338,126.677317113768));
#203062=CARTESIAN_POINT('Ctrl Pts',(179.034262997838,-2.79014677906578,
126.751827026654));
#203063=CARTESIAN_POINT('Ctrl Pts',(179.026511799144,-2.9020680080604,126.831200977799));
#203064=CARTESIAN_POINT('Ctrl Pts',(179.018760600451,-3.01053084945795,
126.915159277064));
#203065=CARTESIAN_POINT('Ctrl Pts',(179.011012726883,-3.11894716223425,
126.999081559718));
#203066=CARTESIAN_POINT('Ctrl Pts',(179.003264853315,-3.22390772980016,
127.087584040042));
#203067=CARTESIAN_POINT('Ctrl Pts',(178.995516979748,-3.32500976055551,
127.180344453873));
#203068=CARTESIAN_POINT('Ctrl Pts',(178.987770735199,-3.42609053423857,
127.273085364487));
#203069=CARTESIAN_POINT('Ctrl Pts',(178.98002449065,-3.5233140969294,127.370082163717));
#203070=CARTESIAN_POINT('Ctrl Pts',(178.972278246101,-3.61631204294623,
127.470973410753));
#203071=CARTESIAN_POINT('Ctrl Pts',(178.964531952702,-3.70931057542868,
127.571865294032));
#203072=CARTESIAN_POINT('Ctrl Pts',(178.956785659304,-3.79808317311763,
127.676651386634));
#203073=CARTESIAN_POINT('Ctrl Pts',(178.949039365905,-3.8822997754526,127.784934924488));
#203074=CARTESIAN_POINT('Ctrl Pts',(178.941291346114,-3.96653514688435,
127.893242595163));
#203075=CARTESIAN_POINT('Ctrl Pts',(178.933543326323,-4.04621226256158,
128.005048953545));
#203076=CARTESIAN_POINT('Ctrl Pts',(178.925795306531,-4.12104292365446,
128.11992617361));
#203077=CARTESIAN_POINT('Ctrl Pts',(178.918039169389,-4.19595198242991,
128.234923746853));
#203078=CARTESIAN_POINT('Ctrl Pts',(178.910283032246,-4.26600423054555,
128.352998280208));
#203079=CARTESIAN_POINT('Ctrl Pts',(178.902526895103,-4.33095593282109,
128.473694667572));
#203080=CARTESIAN_POINT('Ctrl Pts',(178.894766621628,-4.39594227369947,
128.594455422059));
#203081=CARTESIAN_POINT('Ctrl Pts',(178.887006348154,-4.4558224781109,128.717840465114));
#203082=CARTESIAN_POINT('Ctrl Pts',(178.87924607468,-4.51040040079451,128.843373293024));
#203083=CARTESIAN_POINT('Ctrl Pts',(178.871473622124,-4.56506397883664,
128.969103133919));
#203084=CARTESIAN_POINT('Ctrl Pts',(178.863701169567,-4.61440850661788,
129.096987130188));
#203085=CARTESIAN_POINT('Ctrl Pts',(178.855928717011,-4.658287010806,129.226531353211));
#203086=CARTESIAN_POINT('Ctrl Pts',(178.848884041066,-4.69805693422395,
129.343945652631));
#203087=CARTESIAN_POINT('Ctrl Pts',(178.841839365122,-4.73333712484633,
129.462723429701));
#203088=CARTESIAN_POINT('Ctrl Pts',(178.834794689177,-4.76405452823405,
129.582490119308));
#203089=CARTESIAN_POINT('',(180.860140563953,-4.91824868670176,130.80795481517));
#203090=CARTESIAN_POINT('Ctrl Pts',(180.860140563953,-4.91824868670176,
130.80795481517));
#203091=CARTESIAN_POINT('Ctrl Pts',(180.851235208711,-4.91813337062327,
130.96575169062));
#203092=CARTESIAN_POINT('Ctrl Pts',(180.842329853469,-4.91041999025756,
131.123241678084));
#203093=CARTESIAN_POINT('Ctrl Pts',(180.833424498227,-4.89522072462637,
131.279752161126));
#203094=CARTESIAN_POINT('Ctrl Pts',(180.824474260165,-4.87994485498848,
131.437051453996));
#203095=CARTESIAN_POINT('Ctrl Pts',(180.815524022103,-4.85710756303225,
131.593361207987));
#203096=CARTESIAN_POINT('Ctrl Pts',(180.806573784042,-4.82687215032326,
131.74801749744));
#203097=CARTESIAN_POINT('Ctrl Pts',(180.79756682713,-4.79644513177894,131.903653864388));
#203098=CARTESIAN_POINT('Ctrl Pts',(180.788559870219,-4.75852601683665,
132.057615609648));
#203099=CARTESIAN_POINT('Ctrl Pts',(180.779552913307,-4.71332967202739,
132.209247255443));
#203100=CARTESIAN_POINT('Ctrl Pts',(180.774035108754,-4.68564167489048,
132.302139204833));
#203101=CARTESIAN_POINT('Ctrl Pts',(180.768517304201,-4.65522348627133,
132.394157094063));
#203102=CARTESIAN_POINT('Ctrl Pts',(180.762999499647,-4.6221331923805,132.485154422408));
#203103=CARTESIAN_POINT('Ctrl Pts',(180.755225165528,-4.57551048251068,
132.613365493978));
#203104=CARTESIAN_POINT('Ctrl Pts',(180.747450831409,-4.52347530734763,
132.739838306069));
#203105=CARTESIAN_POINT('Ctrl Pts',(180.73967649729,-4.46617630640889,132.864082021682));
#203106=CARTESIAN_POINT('Ctrl Pts',(180.731911744343,-4.4089479213679,132.988172618018));
#203107=CARTESIAN_POINT('Ctrl Pts',(180.724146991396,-4.34646878029648,
133.11003923229));
#203108=CARTESIAN_POINT('Ctrl Pts',(180.716382238449,-4.27893680000363,
133.229207607393));
#203109=CARTESIAN_POINT('Ctrl Pts',(180.708625197564,-4.21147189342562,
133.348257622787));
#203110=CARTESIAN_POINT('Ctrl Pts',(180.700868156679,-4.13896432627984,
133.464614394248));
#203111=CARTESIAN_POINT('Ctrl Pts',(180.693111115794,-4.06165931338313,
133.577825361259));
#203112=CARTESIAN_POINT('Ctrl Pts',(180.685359924554,-3.9844125967981,133.690950954998));
#203113=CARTESIAN_POINT('Ctrl Pts',(180.677608733314,-3.90237585503431,
133.800935144591));
#203114=CARTESIAN_POINT('Ctrl Pts',(180.669857542074,-3.81583908314369,
133.90735194112));
#203115=CARTESIAN_POINT('Ctrl Pts',(180.662109645297,-3.72933909168942,
134.013723507672));
#203116=CARTESIAN_POINT('Ctrl Pts',(180.65436174852,-3.6383431203381,134.116530394143));
#203117=CARTESIAN_POINT('Ctrl Pts',(180.646613851742,-3.54318300903784,
134.215377654604));
#203118=CARTESIAN_POINT('Ctrl Pts',(180.638867575658,-3.44804280318141,
134.314204238349));
#203119=CARTESIAN_POINT('Ctrl Pts',(180.631121299574,-3.34874046091821,
134.409072562077));
#203120=CARTESIAN_POINT('Ctrl Pts',(180.62337502349,-3.24564616409112,134.499622995263));
#203121=CARTESIAN_POINT('Ctrl Pts',(180.615628690225,-3.14255110624534,
134.590174096871));
#203122=CARTESIAN_POINT('Ctrl Pts',(180.60788235696,-3.03566433172752,134.676406986332));
#203123=CARTESIAN_POINT('Ctrl Pts',(180.600136023694,-2.92539041717838,
134.758001214482));
#203124=CARTESIAN_POINT('Ctrl Pts',(180.592387955691,-2.81509180755061,
134.839613715093));
#203125=CARTESIAN_POINT('Ctrl Pts',(180.584639887688,-2.70140486273715,
134.916585254807));
#203126=CARTESIAN_POINT('Ctrl Pts',(180.576891819685,-2.58476420983551,
134.988637979555));
#203127=CARTESIAN_POINT('Ctrl Pts',(180.569135516943,-2.46799958986003,
135.060767282796));
#203128=CARTESIAN_POINT('Ctrl Pts',(180.561379214202,-2.34827532398418,
135.12796712223));
#203129=CARTESIAN_POINT('Ctrl Pts',(180.55362291146,-2.22605226619562,135.190004740231));
#203130=CARTESIAN_POINT('Ctrl Pts',(180.545862468946,-2.10376397428102,
135.252075469577));
#203131=CARTESIAN_POINT('Ctrl Pts',(180.538102026431,-1.97897458853601,
135.308978325326));
#203132=CARTESIAN_POINT('Ctrl Pts',(180.530341583917,-1.85216521453456,
135.360528643503));
#203133=CARTESIAN_POINT('Ctrl Pts',(180.522568683652,-1.72515227486836,
135.412161714826));
#203134=CARTESIAN_POINT('Ctrl Pts',(180.514795783386,-1.59611323530802,
135.458424946265));
#203135=CARTESIAN_POINT('Ctrl Pts',(180.507022883121,-1.46554549602716,
135.499183240581));
#203136=CARTESIAN_POINT('Ctrl Pts',(180.499532547359,-1.33972422294845,
135.538459868235));
#203137=CARTESIAN_POINT('Ctrl Pts',(180.492042211597,-1.21248376217569,
135.572624766855));
#203138=CARTESIAN_POINT('Ctrl Pts',(180.484551875835,-1.08427646179028,
135.601602285119));
#203139=CARTESIAN_POINT('Ctrl Pts',(180.476777541716,-0.951208142644003,
135.631678494795));
#203140=CARTESIAN_POINT('Ctrl Pts',(180.469003207597,-0.81667670073027,
135.656261472423));
#203141=CARTESIAN_POINT('Ctrl Pts',(180.461228873478,-0.68117543440742,
135.675210963251));
#203142=CARTESIAN_POINT('Ctrl Pts',(180.45346412053,-0.545841161285354,
135.694137100525));
#203143=CARTESIAN_POINT('Ctrl Pts',(180.445699367583,-0.409539825369746,
135.707443511412));
#203144=CARTESIAN_POINT('Ctrl Pts',(180.437934614636,-0.272777411462797,
135.715040361379));
#203145=CARTESIAN_POINT('Ctrl Pts',(180.430177573751,-0.13615083191333,
135.722629666048));
#203146=CARTESIAN_POINT('Ctrl Pts',(180.422420532866,0.000935526450582369,
135.724520673434));
#203147=CARTESIAN_POINT('Ctrl Pts',(180.414663491981,0.137968367048358,
135.720675069693));
#203148=CARTESIAN_POINT('Ctrl Pts',(180.406912300741,0.274897870115078,
135.716832365952));
#203149=CARTESIAN_POINT('Ctrl Pts',(180.399161109501,0.411773546516112,
135.707261672693));
#203150=CARTESIAN_POINT('Ctrl Pts',(180.391409918261,0.548080250301332,
135.691976713551));
#203151=CARTESIAN_POINT('Ctrl Pts',(180.383662021484,0.684329020101435,
135.676698250924));
#203152=CARTESIAN_POINT('Ctrl Pts',(180.375914124707,0.820008910547644,
135.655710396422));
#203153=CARTESIAN_POINT('Ctrl Pts',(180.36816622793,0.9546082748462,135.629078858468));
#203154=CARTESIAN_POINT('Ctrl Pts',(180.360419951846,1.08917948385937,135.602452891258));
#203155=CARTESIAN_POINT('Ctrl Pts',(180.352673675761,1.22267023300946,135.570185664586));
#203156=CARTESIAN_POINT('Ctrl Pts',(180.344927399677,1.35457786262363,135.532394233837));
#203157=CARTESIAN_POINT('Ctrl Pts',(180.337181066412,1.4864864659498,135.494602524121));
#203158=CARTESIAN_POINT('Ctrl Pts',(180.329434733147,1.61681155057666,135.451286636637));
#203159=CARTESIAN_POINT('Ctrl Pts',(180.321688399881,1.74506482999139,135.402613742572));
#203160=CARTESIAN_POINT('Ctrl Pts',(180.313940331878,1.87334683083893,135.35392994855));
#203161=CARTESIAN_POINT('Ctrl Pts',(180.306192263875,1.99955573777708,135.299886899446));
#203162=CARTESIAN_POINT('Ctrl Pts',(180.298444195872,2.12322285774621,135.240700072437));
#203163=CARTESIAN_POINT('Ctrl Pts',(180.29068789313,2.24702141260209,135.181450340963));
#203164=CARTESIAN_POINT('Ctrl Pts',(180.282931590389,2.36827243084956,135.117046079976));
#203165=CARTESIAN_POINT('Ctrl Pts',(180.275175287647,2.48653098406956,135.047749207804));
#203166=CARTESIAN_POINT('Ctrl Pts',(180.267414845133,2.60485265544017,134.978415349805));
#203167=CARTESIAN_POINT('Ctrl Pts',(180.259654402618,2.72017835070013,134.904183888821));
#203168=CARTESIAN_POINT('Ctrl Pts',(180.251893960104,2.83209265750178,134.825359777206));
#203169=CARTESIAN_POINT('Ctrl Pts',(180.244121059839,2.94418661908395,134.746409130129));
#203170=CARTESIAN_POINT('Ctrl Pts',(180.236348159573,3.05285793877241,134.662851338207));
#203171=CARTESIAN_POINT('Ctrl Pts',(180.228575259308,3.15772409849079,134.575031854934));
#203172=CARTESIAN_POINT('Ctrl Pts',(180.221084923546,3.25877810916079,134.490404831082));
#203173=CARTESIAN_POINT('Ctrl Pts',(180.213594587784,3.35629858303754,134.401820790026));
#203174=CARTESIAN_POINT('Ctrl Pts',(180.206104252022,3.44997736733326,134.309619413631));
#203175=CARTESIAN_POINT('Ctrl Pts',(180.198329917903,3.54720801120912,134.213922194025));
#203176=CARTESIAN_POINT('Ctrl Pts',(180.190555583784,3.6406078969809,134.114024781695));
#203177=CARTESIAN_POINT('Ctrl Pts',(180.182781249665,3.72979238454181,134.010266391402));
#203178=CARTESIAN_POINT('Ctrl Pts',(180.175016496718,3.81886696019247,133.906635874052));
#203179=CARTESIAN_POINT('Ctrl Pts',(180.167251743771,3.90373622193616,133.799154140003));
#203180=CARTESIAN_POINT('Ctrl Pts',(180.159486990823,3.98405109229198,133.688198330841));
#203181=CARTESIAN_POINT('Ctrl Pts',(180.151729949938,4.06428619278623,133.577352724553));
#203182=CARTESIAN_POINT('Ctrl Pts',(180.143972909054,4.1399756760726,133.463040224457));
#203183=CARTESIAN_POINT('Ctrl Pts',(180.136215868169,4.21080985828836,133.345671971934));
#203184=CARTESIAN_POINT('Ctrl Pts',(180.128464676928,4.28159062389636,133.228392227724));
#203185=CARTESIAN_POINT('Ctrl Pts',(180.120713485688,4.3475231750704,133.108061651164));
#203186=CARTESIAN_POINT('Ctrl Pts',(180.112962294448,4.40834060892407,132.985121067091));
#203187=CARTESIAN_POINT('Ctrl Pts',(180.105214397671,4.46913219374597,132.862232736046));
#203188=CARTESIAN_POINT('Ctrl Pts',(180.097466500894,4.52481281229799,132.736736953544));
#203189=CARTESIAN_POINT('Ctrl Pts',(180.089718604117,4.57516118934884,132.609099699532));
#203190=CARTESIAN_POINT('Ctrl Pts',(180.081972328033,4.62549903460459,132.481489144482));
#203191=CARTESIAN_POINT('Ctrl Pts',(180.074226051949,4.6705067135582,132.351738372381));
#203192=CARTESIAN_POINT('Ctrl Pts',(180.066479775865,4.71001100838992,132.220333556342));
#203193=CARTESIAN_POINT('Ctrl Pts',(180.058733442599,4.74951559483336,132.088927770302));
#203194=CARTESIAN_POINT('Ctrl Pts',(180.050987109334,4.78351660353165,131.955868290373));
#203195=CARTESIAN_POINT('Ctrl Pts',(180.043240776069,4.811890749551,131.821656285937));
#203196=CARTESIAN_POINT('Ctrl Pts',(180.035492708066,4.84027124976361,131.687414225652));
#203197=CARTESIAN_POINT('Ctrl Pts',(180.027744640063,4.86302229899824,131.552019509708));
#203198=CARTESIAN_POINT('Ctrl Pts',(180.01999657206,4.880071844258,131.415982933526));
#203199=CARTESIAN_POINT('Ctrl Pts',(180.012240269318,4.89713950997736,131.279801776052));
#203200=CARTESIAN_POINT('Ctrl Pts',(180.004483966576,4.90849351826859,131.142977784168));
#203201=CARTESIAN_POINT('Ctrl Pts',(179.996727663834,4.9141137337624,131.006026862009));
#203202=CARTESIAN_POINT('Ctrl Pts',(179.98896722132,4.91973694893445,130.869002845019));
#203203=CARTESIAN_POINT('Ctrl Pts',(179.981206778806,4.91962027373891,130.731852153537));
#203204=CARTESIAN_POINT('Ctrl Pts',(179.973446336292,4.91379573270794,130.595089119934));
#203205=CARTESIAN_POINT('Ctrl Pts',(179.965673436026,4.90796184160662,130.458106542167));
#203206=CARTESIAN_POINT('Ctrl Pts',(179.957900535761,4.89640180751873,130.321513255635));
#203207=CARTESIAN_POINT('Ctrl Pts',(179.950127635495,4.87919950989027,130.185817809681));
#203208=CARTESIAN_POINT('Ctrl Pts',(179.942637299733,4.8626225591104,130.055055234982));
#203209=CARTESIAN_POINT('Ctrl Pts',(179.935146963971,4.84080649473996,129.925126660408));
#203210=CARTESIAN_POINT('Ctrl Pts',(179.927656628209,4.81387053664267,129.796474949971));
#203211=CARTESIAN_POINT('Ctrl Pts',(179.91988229409,4.7859132935074,129.662945370831));
#203212=CARTESIAN_POINT('Ctrl Pts',(179.912107959971,4.75235169095122,129.530368410215));
#203213=CARTESIAN_POINT('Ctrl Pts',(179.904333625852,4.71326321258631,129.399251030601));
#203214=CARTESIAN_POINT('Ctrl Pts',(179.896568872905,4.67422290727756,129.268295241439));
#203215=CARTESIAN_POINT('Ctrl Pts',(179.888804119958,4.62966938940084,129.138795825271));
#203216=CARTESIAN_POINT('Ctrl Pts',(179.88103936701,4.57973127394808,129.011250325107));
#203217=CARTESIAN_POINT('Ctrl Pts',(179.873282326125,4.52984275773558,128.883831504932));
#203218=CARTESIAN_POINT('Ctrl Pts',(179.86552528524,4.47458042844114,128.758363100465));
#203219=CARTESIAN_POINT('Ctrl Pts',(179.857768244355,4.41412279926086,128.635327889471));
#203220=CARTESIAN_POINT('Ctrl Pts',(179.850017053115,4.35371076164904,128.512385460287));
#203221=CARTESIAN_POINT('Ctrl Pts',(179.842265861875,4.28811139405136,128.391872921809));
#203222=CARTESIAN_POINT('Ctrl Pts',(179.834514670635,4.21755130735877,128.274253103586));
#203223=CARTESIAN_POINT('Ctrl Pts',(179.826766773858,4.14702121058527,128.156683276924));
#203224=CARTESIAN_POINT('Ctrl Pts',(179.819018877081,4.07153478894331,128.042004059732));
#203225=CARTESIAN_POINT('Ctrl Pts',(179.811270980304,3.99136447989174,127.930653490672));
#203226=CARTESIAN_POINT('Ctrl Pts',(179.80352470422,3.91121094074054,127.819326213751));
#203227=CARTESIAN_POINT('Ctrl Pts',(179.795778428136,3.82637569128667,127.711326517104));
#203228=CARTESIAN_POINT('Ctrl Pts',(179.788032152051,3.7371741342777,127.607062922232));
#203229=CARTESIAN_POINT('Ctrl Pts',(179.780285818786,3.64797191880316,127.50279855771));
#203230=CARTESIAN_POINT('Ctrl Pts',(179.772539485521,3.5544035856207,127.402270647074));
#203231=CARTESIAN_POINT('Ctrl Pts',(179.764793152255,3.4568241442069,127.305853807722));
#203232=CARTESIAN_POINT('Ctrl Pts',(179.757045084252,3.35922285055371,127.209415376487));
#203233=CARTESIAN_POINT('Ctrl Pts',(179.749297016249,3.25760893928871,127.117090123255));
#203234=CARTESIAN_POINT('Ctrl Pts',(179.741548948246,3.15237321066194,127.029214765655));
#203235=CARTESIAN_POINT('Ctrl Pts',(179.733792645505,3.04702563625045,126.94124601308));
#203236=CARTESIAN_POINT('Ctrl Pts',(179.726036342763,2.93804885563987,126.857736854617));
#203237=CARTESIAN_POINT('Ctrl Pts',(179.718280040021,2.82586602993138,126.77898308951));
#203238=CARTESIAN_POINT('Ctrl Pts',(179.710519597507,2.71362332887097,126.700187291147));
#203239=CARTESIAN_POINT('Ctrl Pts',(179.702759154993,2.59817150202462,126.626152154456));
#203240=CARTESIAN_POINT('Ctrl Pts',(179.694998712478,2.4799605818237,126.557128745499));
#203241=CARTESIAN_POINT('Ctrl Pts',(179.687225812213,2.36155989895946,126.487994534039));
#203242=CARTESIAN_POINT('Ctrl Pts',(179.679452911947,2.2403916176828,126.423888310267));
#203243=CARTESIAN_POINT('Ctrl Pts',(179.671680011682,2.11692893384896,126.365014387373));
#203244=CARTESIAN_POINT('Ctrl Pts',(179.66418967592,1.99795442955653,126.30828067987));
#203245=CARTESIAN_POINT('Ctrl Pts',(179.656699340158,1.87684972432121,126.256405584449));
#203246=CARTESIAN_POINT('Ctrl Pts',(179.649209004396,1.75405185342764,126.209528176879));
#203247=CARTESIAN_POINT('Ctrl Pts',(179.641434670277,1.6265980639352,126.160873398153));
#203248=CARTESIAN_POINT('Ctrl Pts',(179.633660336158,1.49691644622467,126.117448639312));
#203249=CARTESIAN_POINT('Ctrl Pts',(179.625886002039,1.36547540397288,126.079462736802));
#203250=CARTESIAN_POINT('Ctrl Pts',(179.618121249092,1.23419635105852,126.041523648523));
#203251=CARTESIAN_POINT('Ctrl Pts',(179.610356496145,1.10116255992973,126.009010187295));
#203252=CARTESIAN_POINT('Ctrl Pts',(179.602591743197,0.966862147156906,
125.982083079836));
#203253=CARTESIAN_POINT('Ctrl Pts',(179.594834702312,0.832695123447448,
125.955182716759));
#203254=CARTESIAN_POINT('Ctrl Pts',(179.587077661427,0.697264362478954,
125.933857742155));
#203255=CARTESIAN_POINT('Ctrl Pts',(179.579320620542,0.561072529599974,
125.918218920989));
#203256=CARTESIAN_POINT('Ctrl Pts',(179.571569429302,0.424983400041494,
125.90259189318));
#203257=CARTESIAN_POINT('Ctrl Pts',(179.563818238062,0.288134727787094,
125.89264252828));
#203258=CARTESIAN_POINT('Ctrl Pts',(179.556067046822,0.151038393166892,
125.888430342807));
#203259=CARTESIAN_POINT('Ctrl Pts',(179.548319150045,0.0140003281460682,
125.884219947625));
#203260=CARTESIAN_POINT('Ctrl Pts',(179.540571253268,-0.123284799917584,
125.885741893951));
#203261=CARTESIAN_POINT('Ctrl Pts',(179.532823356491,-0.260301197590463,
125.893003743032));
#203262=CARTESIAN_POINT('Ctrl Pts',(179.525077080407,-0.39728893438668,
125.90026407309));
#203263=CARTESIAN_POINT('Ctrl Pts',(179.517330804322,-0.534007662432173,
125.913261897038));
#203264=CARTESIAN_POINT('Ctrl Pts',(179.509584528238,-0.669943198128833,
125.931952673461));
#203265=CARTESIAN_POINT('Ctrl Pts',(179.501838194973,-0.805879737270736,
125.950643587855));
#203266=CARTESIAN_POINT('Ctrl Pts',(179.494091861708,-0.941032685206453,
125.975027485324));
#203267=CARTESIAN_POINT('Ctrl Pts',(179.486345528442,-1.07489497441483,
126.005008176197));
#203268=CARTESIAN_POINT('Ctrl Pts',(179.478597460439,-1.20878724115488,
126.034995581037));
#203269=CARTESIAN_POINT('Ctrl Pts',(179.470849392436,-1.34138789258256,
126.070582187898));
#203270=CARTESIAN_POINT('Ctrl Pts',(179.463101324433,-1.47220240153905,
126.111621209565));
#203271=CARTESIAN_POINT('Ctrl Pts',(179.455345021691,-1.60315594171228,
126.152703847993));
#203272=CARTESIAN_POINT('Ctrl Pts',(179.44758871895,-1.73231917365516,126.199250359929));
#203273=CARTESIAN_POINT('Ctrl Pts',(179.439832416208,-1.85921450417547,
126.251064614673));
#203274=CARTESIAN_POINT('Ctrl Pts',(179.432071973694,-1.98617756255448,
126.302906524244));
#203275=CARTESIAN_POINT('Ctrl Pts',(179.424311531179,-2.11086995231502,
126.360021616145));
#203276=CARTESIAN_POINT('Ctrl Pts',(179.416551088665,-2.23283719094561,
126.422166972686));
#203277=CARTESIAN_POINT('Ctrl Pts',(179.4087781884,-2.35500022221536,126.48441209047));
#203278=CARTESIAN_POINT('Ctrl Pts',(179.401005288134,-2.47442901958706,
126.551703417341));
#203279=CARTESIAN_POINT('Ctrl Pts',(179.393232387869,-2.59069591467029,
126.623753276496));
#203280=CARTESIAN_POINT('Ctrl Pts',(179.385742052107,-2.70273621525825,
126.693183941787));
#203281=CARTESIAN_POINT('Ctrl Pts',(179.378251716345,-2.81184025354116,
126.76703300397));
#203282=CARTESIAN_POINT('Ctrl Pts',(179.370761380583,-2.91765479288965,
126.845007946734));
#203283=CARTESIAN_POINT('Ctrl Pts',(179.362824623581,-3.02977583963157,
126.927630167234));
#203284=CARTESIAN_POINT('Ctrl Pts',(179.354887866579,-3.13858421238573,
127.015166053473));
#203285=CARTESIAN_POINT('Ctrl Pts',(179.346951109577,-3.24361582879236,
127.107315930562));
#203286=CARTESIAN_POINT('Ctrl Pts',(179.339259878588,-3.34539825992441,
127.196615122934));
#203287=CARTESIAN_POINT('Ctrl Pts',(179.331568647598,-3.44363378017725,
127.290246806879));
#203288=CARTESIAN_POINT('Ctrl Pts',(179.323877416609,-3.53792844756241,
127.387893822406));
#203289=CARTESIAN_POINT('Ctrl Pts',(179.316193156561,-3.63213765104985,
127.485452335638));
#203290=CARTESIAN_POINT('Ctrl Pts',(179.308508896513,-3.72241282922045,
127.587018658588));
#203291=CARTESIAN_POINT('Ctrl Pts',(179.300824636464,-3.80839397804645,
127.692236203202));
#203292=CARTESIAN_POINT('Ctrl Pts',(179.293145599922,-3.89431667973043,
127.797382224409));
#203293=CARTESIAN_POINT('Ctrl Pts',(179.28546656338,-3.97595090671817,127.906174222729));
#203294=CARTESIAN_POINT('Ctrl Pts',(179.277787526838,-4.05297468425983,
128.018220048383));
#203295=CARTESIAN_POINT('Ctrl Pts',(179.270111970762,-4.12996355134694,
128.130215090099));
#203296=CARTESIAN_POINT('Ctrl Pts',(179.262436414686,-4.20234590173357,
128.245460696354));
#203297=CARTESIAN_POINT('Ctrl Pts',(179.25476085861,-4.26984142786074,128.363533453791));
#203298=CARTESIAN_POINT('Ctrl Pts',(179.247085795211,-4.33733262159974,
128.481598632399));
#203299=CARTESIAN_POINT('Ctrl Pts',(179.239410731811,-4.39993741066976,
128.60249025877));
#203300=CARTESIAN_POINT('Ctrl Pts',(179.231735668412,-4.45742018209201,
128.725758110404));
#203301=CARTESIAN_POINT('Ctrl Pts',(179.224060790413,-4.51490156495416,
128.849022984367));
#203302=CARTESIAN_POINT('Ctrl Pts',(179.216385912414,-4.56726101346593,
128.974663605236));
#203303=CARTESIAN_POINT('Ctrl Pts',(179.208711034414,-4.61431036413111,
129.102208178455));
#203304=CARTESIAN_POINT('Ctrl Pts',(179.201032838487,-4.66138005470733,
129.229807890485));
#203305=CARTESIAN_POINT('Ctrl Pts',(179.19335464256,-4.70313493368093,129.359312821299));
#203306=CARTESIAN_POINT('Ctrl Pts',(179.185676446633,-4.73943621873225,
129.490234523514));
#203307=CARTESIAN_POINT('Ctrl Pts',(179.183877368601,-4.74794197257219,
129.520910786621));
#203308=CARTESIAN_POINT('Ctrl Pts',(179.182078290568,-4.75614853636364,
129.551664776996));
#203309=CARTESIAN_POINT('Ctrl Pts',(179.180279212536,-4.76405452823405,
129.582490119308));
#203310=CARTESIAN_POINT('Ctrl Pts',(180.930009319727,-4.76405452823405,
129.582490119308));
#203311=CARTESIAN_POINT('Ctrl Pts',(180.922246799312,-4.79822091605315,
129.715704346868));
#203312=CARTESIAN_POINT('Ctrl Pts',(180.914484278898,-4.82680923366528,
129.850405798733));
#203313=CARTESIAN_POINT('Ctrl Pts',(180.906721758483,-4.84970257641179,
129.986089279412));
#203314=CARTESIAN_POINT('Ctrl Pts',(180.89895822607,-4.87259890375656,130.121790449105));
#203315=CARTESIAN_POINT('Ctrl Pts',(180.891194693658,-4.88979869697442,
130.258473522519));
#203316=CARTESIAN_POINT('Ctrl Pts',(180.883431161245,-4.9012362819718,130.395623574));
#203317=CARTESIAN_POINT('Ctrl Pts',(180.875667628833,-4.91267386696918,
130.532773625481));
#203318=CARTESIAN_POINT('Ctrl Pts',(180.86790409642,-4.9183492172088,130.670390267495));
#203319=CARTESIAN_POINT('Ctrl Pts',(180.860140564008,-4.91824868670247,
130.8079548142));
#203320=CARTESIAN_POINT('Origin',(213.235140564004,0.,130.804360617566));
#203321=CARTESIAN_POINT('',(182.679902359578,-4.76405452823405,129.582490119308));
#203322=CARTESIAN_POINT('',(182.334764431275,-4.76405452823405,129.582490119308));
#203323=CARTESIAN_POINT('',(213.235140564004,-4.76405452823405,129.582490119308));
#203324=CARTESIAN_POINT('',(182.264859435942,-4.91824838731473,130.808343477848));
#203325=CARTESIAN_POINT('Ctrl Pts',(182.334764431275,-4.76405452823405,
129.582490119308));
#203326=CARTESIAN_POINT('Ctrl Pts',(182.327037589112,-4.79807206386625,
129.71512397445));
#203327=CARTESIAN_POINT('Ctrl Pts',(182.319310746949,-4.82655566072364,
129.849215252561));
#203328=CARTESIAN_POINT('Ctrl Pts',(182.311583904787,-4.84939387740225,
129.984261791623));
#203329=CARTESIAN_POINT('Ctrl Pts',(182.303796493321,-4.87241111868681,
130.120366935819));
#203330=CARTESIAN_POINT('Ctrl Pts',(182.296009081855,-4.88969399094239,
130.257441989725));
#203331=CARTESIAN_POINT('Ctrl Pts',(182.288221670389,-4.90118122870282,
130.394963956721));
#203332=CARTESIAN_POINT('Ctrl Pts',(182.280434258923,-4.91266846646326,
130.532485923717));
#203333=CARTESIAN_POINT('Ctrl Pts',(182.272646847457,-4.91836005162741,
130.670454396298));
#203334=CARTESIAN_POINT('Ctrl Pts',(182.264859435991,-4.91824838731544,
130.808343476974));
#203335=CARTESIAN_POINT('Ctrl Pts',(182.264859435942,-4.91824838731473,
130.808343477848));
#203336=CARTESIAN_POINT('Ctrl Pts',(182.255745689485,-4.91811770455124,
130.969717526973));
#203337=CARTESIAN_POINT('Ctrl Pts',(182.246631943028,-4.91004084791699,
131.130754613443));
#203338=CARTESIAN_POINT('Ctrl Pts',(182.237518196571,-4.89414028983605,
131.290749233699));
#203339=CARTESIAN_POINT('Ctrl Pts',(182.228343751195,-4.87813383165355,
131.451809442121));
#203340=CARTESIAN_POINT('Ctrl Pts',(182.21916930582,-4.85419921674639,131.611813182237));
#203341=CARTESIAN_POINT('Ctrl Pts',(182.209994860445,-4.82251028849471,
131.770061181852));
#203342=CARTESIAN_POINT('Ctrl Pts',(182.200752520834,-4.79058685063821,
131.929480274271));
#203343=CARTESIAN_POINT('Ctrl Pts',(182.191510181223,-4.75079397460461,
132.087117477438));
#203344=CARTESIAN_POINT('Ctrl Pts',(182.182267841612,-4.70335754186608,
132.242279563777));
#203345=CARTESIAN_POINT('Ctrl Pts',(182.179787432699,-4.69062680965446,
132.28392112189));
#203346=CARTESIAN_POINT('Ctrl Pts',(182.177307023785,-4.67734581439877,
132.325384532998));
#203347=CARTESIAN_POINT('Ctrl Pts',(182.174826614871,-4.66351949799474,
132.366656669639));
#203348=CARTESIAN_POINT('Ctrl Pts',(182.167052280752,-4.62018373880961,
132.496015735516));
#203349=CARTESIAN_POINT('Ctrl Pts',(182.159277946633,-4.57139291895546,
132.623775226555));
#203350=CARTESIAN_POINT('Ctrl Pts',(182.151503612514,-4.51728310406877,
132.749440672524));
#203351=CARTESIAN_POINT('Ctrl Pts',(182.143738859567,-4.46323997469291,
132.874951247062));
#203352=CARTESIAN_POINT('Ctrl Pts',(182.13597410662,-4.40389104628627,132.998372555757));
#203353=CARTESIAN_POINT('Ctrl Pts',(182.128209353673,-4.33942206882534,
133.119225445389));
#203354=CARTESIAN_POINT('Ctrl Pts',(182.120452312788,-4.27501712286173,
133.239958302227));
#203355=CARTESIAN_POINT('Ctrl Pts',(182.112695271903,-4.20550243065429,
133.358127473865));
#203356=CARTESIAN_POINT('Ctrl Pts',(182.104938231018,-4.13111157845121,
133.473274289622));
#203357=CARTESIAN_POINT('Ctrl Pts',(182.097187039777,-4.05677682496856,
133.588334272269));
#203358=CARTESIAN_POINT('Ctrl Pts',(182.089435848537,-3.97757344193555,
133.700376108544));
#203359=CARTESIAN_POINT('Ctrl Pts',(182.081684657297,-3.89378045932293,
133.808966547983));
#203360=CARTESIAN_POINT('Ctrl Pts',(182.07393676052,-3.81002309096304,133.917510833588));
#203361=CARTESIAN_POINT('Ctrl Pts',(182.066188863743,-3.72168024116592,
134.022606331103));
#203362=CARTESIAN_POINT('Ctrl Pts',(182.058440966966,-3.62907356334536,
134.123849755118));
#203363=CARTESIAN_POINT('Ctrl Pts',(182.050694690882,-3.53648625684542,
134.225072001192));
#203364=CARTESIAN_POINT('Ctrl Pts',(182.042948414798,-3.43963716006998,
134.322443488187));
#203365=CARTESIAN_POINT('Ctrl Pts',(182.035202138714,-3.33888715704143,
134.415595256169));
#203366=CARTESIAN_POINT('Ctrl Pts',(182.027455805448,-3.23813641029925,
134.508747711776));
#203367=CARTESIAN_POINT('Ctrl Pts',(182.019709472183,-3.1334849869114,134.597680120798));
#203368=CARTESIAN_POINT('Ctrl Pts',(182.011963138918,-3.02532915435104,
134.682061814194));
#203369=CARTESIAN_POINT('Ctrl Pts',(182.004215070915,-2.91714910104202,
134.766462404286));
#203370=CARTESIAN_POINT('Ctrl Pts',(181.996467002912,-2.8054633851131,134.846310010414));
#203371=CARTESIAN_POINT('Ctrl Pts',(181.988718934909,-2.69069940167571,
134.921315777915));
#203372=CARTESIAN_POINT('Ctrl Pts',(181.980962632167,-2.5758134457109,134.996401262438));
#203373=CARTESIAN_POINT('Ctrl Pts',(181.973206329425,-2.45784301461549,
135.066634414486));
#203374=CARTESIAN_POINT('Ctrl Pts',(181.965450026683,-2.33724287264859,
135.13177079188));
#203375=CARTESIAN_POINT('Ctrl Pts',(181.957689584169,-2.21657836275474,
135.196941934519));
#203376=CARTESIAN_POINT('Ctrl Pts',(181.949929141655,-2.09328169658598,
135.257010710924));
#203377=CARTESIAN_POINT('Ctrl Pts',(181.942168699141,-1.96782911067562,
135.311780240108));
#203378=CARTESIAN_POINT('Ctrl Pts',(181.934395798875,-1.8421751371371,135.366637690203));
#203379=CARTESIAN_POINT('Ctrl Pts',(181.92662289861,-1.71435869267866,135.416178752362));
#203380=CARTESIAN_POINT('Ctrl Pts',(181.918849998344,-1.58487356800099,
135.460255680382));
#203381=CARTESIAN_POINT('Ctrl Pts',(181.911359662582,-1.46009555375806,
135.502730301045));
#203382=CARTESIAN_POINT('Ctrl Pts',(181.90386932682,-1.33376836978196,135.540131073015));
#203383=CARTESIAN_POINT('Ctrl Pts',(181.896378991058,-1.20634228632941,
135.572370826313));
#203384=CARTESIAN_POINT('Ctrl Pts',(181.888604656939,-1.07408480419308,
135.605832959655));
#203385=CARTESIAN_POINT('Ctrl Pts',(181.88083032282,-0.940224496132468,
135.63384098669));
#203386=CARTESIAN_POINT('Ctrl Pts',(181.873055988701,-0.805250920756176,
135.656242110051));
#203387=CARTESIAN_POINT('Ctrl Pts',(181.865291235754,-0.670443688248645,
135.67861562603));
#203388=CARTESIAN_POINT('Ctrl Pts',(181.857526482807,-0.534526300288229,
135.695395923796));
#203389=CARTESIAN_POINT('Ctrl Pts',(181.849761729859,-0.398002284449767,
135.706480286043));
#203390=CARTESIAN_POINT('Ctrl Pts',(181.842004688974,-0.261613866188487,
135.717553639146));
#203391=CARTESIAN_POINT('Ctrl Pts',(181.834247648089,-0.124620406235299,
135.722942283547));
#203392=CARTESIAN_POINT('Ctrl Pts',(181.826490607204,0.0124659437015487,
135.722594819264));
#203393=CARTESIAN_POINT('Ctrl Pts',(181.818739415964,0.149448915755369,
135.722247617006));
#203394=CARTESIAN_POINT('Ctrl Pts',(181.810988224724,0.286524248982427,
135.716172916984));
#203395=CARTESIAN_POINT('Ctrl Pts',(181.803237033484,0.423176614983207,
135.704371292558));
#203396=CARTESIAN_POINT('Ctrl Pts',(181.795489136707,0.559770900083301,
135.692574684136));
#203397=CARTESIAN_POINT('Ctrl Pts',(181.78774123993,0.695942186810799,135.675056026109));
#203398=CARTESIAN_POINT('Ctrl Pts',(181.779993343153,0.831177318203662,
135.651867948989));
#203399=CARTESIAN_POINT('Ctrl Pts',(181.772247067069,0.966384161322348,
135.628684722316));
#203400=CARTESIAN_POINT('Ctrl Pts',(181.764500790985,1.10065485351256,135.599834501441));
#203401=CARTESIAN_POINT('Ctrl Pts',(181.756754514901,1.2334839117036,135.565421476457));
#203402=CARTESIAN_POINT('Ctrl Pts',(181.749008181635,1.36631395040857,135.531008197445));
#203403=CARTESIAN_POINT('Ctrl Pts',(181.74126184837,1.49770195540958,135.491032130437));
#203404=CARTESIAN_POINT('Ctrl Pts',(181.733515515104,1.62715553322994,135.44564793179));
#203405=CARTESIAN_POINT('Ctrl Pts',(181.725767447101,1.75663810128136,135.400253569667));
#203406=CARTESIAN_POINT('Ctrl Pts',(181.718019379098,1.88418501125313,135.34944879525));
#203407=CARTESIAN_POINT('Ctrl Pts',(181.710271311096,2.00932222403949,135.293437055151));
#203408=CARTESIAN_POINT('Ctrl Pts',(181.702515008354,2.13459243414487,135.237365785108));
#203409=CARTESIAN_POINT('Ctrl Pts',(181.694758705612,2.2574474736639,135.176076654553));
#203410=CARTESIAN_POINT('Ctrl Pts',(181.68700240287,2.37743587527888,135.109820142569));
#203411=CARTESIAN_POINT('Ctrl Pts',(181.679241960356,2.49748831831668,135.043528267489));
#203412=CARTESIAN_POINT('Ctrl Pts',(181.671481517842,2.61467074089446,134.972263931206));
#203413=CARTESIAN_POINT('Ctrl Pts',(181.663721075327,2.72856008398556,134.896321386022));
#203414=CARTESIAN_POINT('Ctrl Pts',(181.655948175062,2.84263225236077,134.820256931122));
#203415=CARTESIAN_POINT('Ctrl Pts',(181.648175274797,2.9534004613508,134.739499490654));
#203416=CARTESIAN_POINT('Ctrl Pts',(181.640402374531,3.06047350195551,134.654384644287));
#203417=CARTESIAN_POINT('Ctrl Pts',(181.632912038769,3.16365416783352,134.572363936976));
#203418=CARTESIAN_POINT('Ctrl Pts',(181.625421703007,3.26340342518855,134.486297330141));
#203419=CARTESIAN_POINT('Ctrl Pts',(181.617931367245,3.35940455337579,134.396516531395));
#203420=CARTESIAN_POINT('Ctrl Pts',(181.610157033126,3.45904559351708,134.303331666377));
#203421=CARTESIAN_POINT('Ctrl Pts',(181.602382699007,3.5549643061159,134.205850220831));
#203422=CARTESIAN_POINT('Ctrl Pts',(181.594608364888,3.64676752003656,134.104401483572));
#203423=CARTESIAN_POINT('Ctrl Pts',(181.586843611941,3.73845759470076,134.003077772814));
#203424=CARTESIAN_POINT('Ctrl Pts',(181.579078858994,3.82604200261285,133.897796785766));
#203425=CARTESIAN_POINT('Ctrl Pts',(181.571314106046,3.90916215584225,133.788926633226));
#203426=CARTESIAN_POINT('Ctrl Pts',(181.563557065161,3.99219975296364,133.680164612056));
#203427=CARTESIAN_POINT('Ctrl Pts',(181.555800024276,4.07078168346808,133.567820828264));
#203428=CARTESIAN_POINT('Ctrl Pts',(181.548042983391,4.14458787258715,133.452298386643));
#203429=CARTESIAN_POINT('Ctrl Pts',(181.540291792151,4.21833840388486,133.336863061394));
#203430=CARTESIAN_POINT('Ctrl Pts',(181.532540600911,4.28732015257257,133.21825417763));
#203431=CARTESIAN_POINT('Ctrl Pts',(181.524789409671,4.35125505344596,133.096905605644));
#203432=CARTESIAN_POINT('Ctrl Pts',(181.517041512894,4.41516278028099,132.975608610038));
#203433=CARTESIAN_POINT('Ctrl Pts',(181.509293616117,4.47402774377339,132.851574587362));
#203434=CARTESIAN_POINT('Ctrl Pts',(181.50154571934,4.52761684959189,132.72526371918));
#203435=CARTESIAN_POINT('Ctrl Pts',(181.493799443256,4.5811947457247,132.598979272509));
#203436=CARTESIAN_POINT('Ctrl Pts',(181.486053167172,4.62949882669481,132.470419287337));
#203437=CARTESIAN_POINT('Ctrl Pts',(181.478306891088,4.67234352463098,132.340065358178));
#203438=CARTESIAN_POINT('Ctrl Pts',(181.470560557822,4.71518853883696,132.209710466776));
#203439=CARTESIAN_POINT('Ctrl Pts',(181.462814224557,4.75257396751604,132.07756197638));
#203440=CARTESIAN_POINT('Ctrl Pts',(181.455067891292,4.78436377673831,131.944117747105));
#203441=CARTESIAN_POINT('Ctrl Pts',(181.447319823289,4.81616070506794,131.810643633919));
#203442=CARTESIAN_POINT('Ctrl Pts',(181.439571755286,4.84235942983139,131.675873584696));
#203443=CARTESIAN_POINT('Ctrl Pts',(181.431823687283,4.86287488670871,131.540316389823));
#203444=CARTESIAN_POINT('Ctrl Pts',(181.424067384541,4.88341214765773,131.404615123149));
#203445=CARTESIAN_POINT('Ctrl Pts',(181.416311081799,4.89825401608467,131.268125426831));
#203446=CARTESIAN_POINT('Ctrl Pts',(181.408554779057,4.90736719802281,131.131362523172));
#203447=CARTESIAN_POINT('Ctrl Pts',(181.400794336543,4.91648524394055,130.994526625032));
#203448=CARTESIAN_POINT('Ctrl Pts',(181.393033894029,4.91986850125779,130.85741761965));
#203449=CARTESIAN_POINT('Ctrl Pts',(181.385273451515,4.91753585903247,130.720550489122));
#203450=CARTESIAN_POINT('Ctrl Pts',(181.377500551249,4.91519947224276,130.583463647326));
#203451=CARTESIAN_POINT('Ctrl Pts',(181.369727650984,4.90712887303039,130.4466198468));
#203452=CARTESIAN_POINT('Ctrl Pts',(181.361954750718,4.89339493605524,130.310529611767));
#203453=CARTESIAN_POINT('Ctrl Pts',(181.354464414956,4.88016026228275,130.179386599566));
#203454=CARTESIAN_POINT('Ctrl Pts',(181.346974079194,4.86166689853009,130.048943621018));
#203455=CARTESIAN_POINT('Ctrl Pts',(181.339483743432,4.83802272456425,129.91964643824));
#203456=CARTESIAN_POINT('Ctrl Pts',(181.331709409313,4.81348207455615,129.785446913479));
#203457=CARTESIAN_POINT('Ctrl Pts',(181.323935075194,4.78331458070452,129.652056681576));
#203458=CARTESIAN_POINT('Ctrl Pts',(181.316160741075,4.74758476441283,129.519984517191));
#203459=CARTESIAN_POINT('Ctrl Pts',(181.308395988128,4.71189898192648,129.388075119944));
#203460=CARTESIAN_POINT('Ctrl Pts',(181.300631235181,4.67066461765525,129.257480931918));
#203461=CARTESIAN_POINT('Ctrl Pts',(181.292866482234,4.62399754810301,129.128702616172));
#203462=CARTESIAN_POINT('Ctrl Pts',(181.285109441349,4.57737682894217,129.000052204864));
#203463=CARTESIAN_POINT('Ctrl Pts',(181.277352400464,4.52533427480508,128.873214441886));
#203464=CARTESIAN_POINT('Ctrl Pts',(181.269595359579,4.46803602093881,128.748676503191));
#203465=CARTESIAN_POINT('Ctrl Pts',(181.261844168339,4.41078097613147,128.624232479525));
#203466=CARTESIAN_POINT('Ctrl Pts',(181.254092977099,4.3482782831815,128.502085181832));
#203467=CARTESIAN_POINT('Ctrl Pts',(181.246341785858,4.28074266841829,128.382703071734));
#203468=CARTESIAN_POINT('Ctrl Pts',(181.238593889081,4.2132357580929,128.263371702218));
#203469=CARTESIAN_POINT('Ctrl Pts',(181.230845992304,4.14070037261404,128.146803522334));
#203470=CARTESIAN_POINT('Ctrl Pts',(181.223098095527,4.06339768258434,128.03344338032));
#203471=CARTESIAN_POINT('Ctrl Pts',(181.215351819443,3.98611116261093,127.920106950803));
#203472=CARTESIAN_POINT('Ctrl Pts',(181.207605543359,3.90405954173491,127.809977547203));
#203473=CARTESIAN_POINT('Ctrl Pts',(181.199859267275,3.81754769509268,127.703471606622));
#203474=CARTESIAN_POINT('Ctrl Pts',(181.19211293401,3.7310352098397,127.596964879839));
#203475=CARTESIAN_POINT('Ctrl Pts',(181.184366600744,3.64006267962051,127.494081972915));
#203476=CARTESIAN_POINT('Ctrl Pts',(181.176620267479,3.54497543858795,127.395206440602));
#203477=CARTESIAN_POINT('Ctrl Pts',(181.168872199476,3.44986690342704,127.2963087658));
#203478=CARTESIAN_POINT('Ctrl Pts',(181.161124131473,3.35064209480331,127.201420533123));
#203479=CARTESIAN_POINT('Ctrl Pts',(181.15337606347,3.24768309313699,127.110888323227));
#203480=CARTESIAN_POINT('Ctrl Pts',(181.145619760728,3.14461466541844,127.02025989462));
#203481=CARTESIAN_POINT('Ctrl Pts',(181.137863457986,3.03780441073446,126.933996995563));
#203482=CARTESIAN_POINT('Ctrl Pts',(181.130107155245,2.92766780399824,126.852406127452));
#203483=CARTESIAN_POINT('Ctrl Pts',(181.12234671273,2.81747241403878,126.770771711838));
#203484=CARTESIAN_POINT('Ctrl Pts',(181.114586270216,2.7039474579022,126.693814515155));
#203485=CARTESIAN_POINT('Ctrl Pts',(181.106825827702,2.58753641460957,126.621797005908));
#203486=CARTESIAN_POINT('Ctrl Pts',(181.099052927437,2.4709384979758,126.54966388776));
#203487=CARTESIAN_POINT('Ctrl Pts',(181.091280027171,2.35144557696644,126.48248649467));
#203488=CARTESIAN_POINT('Ctrl Pts',(181.083507126906,2.22952547955141,126.420481148588));
#203489=CARTESIAN_POINT('Ctrl Pts',(181.076016791144,2.11203748477606,126.360729853018));
#203490=CARTESIAN_POINT('Ctrl Pts',(181.068526455382,1.99229599775392,126.305781227551));
#203491=CARTESIAN_POINT('Ctrl Pts',(181.06103611962,1.87073436242814,126.255785455196));
#203492=CARTESIAN_POINT('Ctrl Pts',(181.053261785501,1.74456368075061,126.203894077936));
#203493=CARTESIAN_POINT('Ctrl Pts',(181.045487451382,1.61603243353411,126.15717416632));
#203494=CARTESIAN_POINT('Ctrl Pts',(181.037713117262,1.48560354270351,126.115846441795));
#203495=CARTESIAN_POINT('Ctrl Pts',(181.029948364315,1.35533539382416,126.074569649997));
#203496=CARTESIAN_POINT('Ctrl Pts',(181.022183611368,1.22317462372418,126.038671939907));
#203497=CARTESIAN_POINT('Ctrl Pts',(181.014418858421,1.08960508849571,126.008326441955));
#203498=CARTESIAN_POINT('Ctrl Pts',(181.006661817536,0.956168216412676,
125.97801108358));
#203499=CARTESIAN_POINT('Ctrl Pts',(180.998904776651,0.821325742465903,
125.953237049223));
#203500=CARTESIAN_POINT('Ctrl Pts',(180.991147735766,0.685577341742052,
125.934127895099));
#203501=CARTESIAN_POINT('Ctrl Pts',(180.983396544526,0.549931309943087,
125.915033151336));
#203502=CARTESIAN_POINT('Ctrl Pts',(180.975645353286,0.413381096750075,
125.901594839067));
#203503=CARTESIAN_POINT('Ctrl Pts',(180.967894162046,0.276436897019386,
125.893885517897));
#203504=CARTESIAN_POINT('Ctrl Pts',(180.960146265269,0.139550902226688,
125.886179473395));
#203505=CARTESIAN_POINT('Ctrl Pts',(180.952398368492,0.00227164348105247,
125.884197598944));
#203506=CARTESIAN_POINT('Ctrl Pts',(180.944650471714,-0.134885446705906,
125.887960615657));
#203507=CARTESIAN_POINT('Ctrl Pts',(180.93690419563,-0.272013846586339,
125.891722845229));
#203508=CARTESIAN_POINT('Ctrl Pts',(180.929157919546,-0.409019738167906,
125.901227564989));
#203509=CARTESIAN_POINT('Ctrl Pts',(180.921411643462,-0.545387968662936,
125.916443369275));
#203510=CARTESIAN_POINT('Ctrl Pts',(180.913665310197,-0.681757205797242,
125.931659285882));
#203511=CARTESIAN_POINT('Ctrl Pts',(180.905918976931,-0.817488383898427,
125.952586327784));
#203512=CARTESIAN_POINT('Ctrl Pts',(180.898172643666,-0.95207214594684,
125.979141276291));
#203513=CARTESIAN_POINT('Ctrl Pts',(180.890424575663,-1.08668604709579,
126.005702171595));
#203514=CARTESIAN_POINT('Ctrl Pts',(180.88267650766,-1.22015163738299,126.037893405747));
#203515=CARTESIAN_POINT('Ctrl Pts',(180.874928439657,-1.35197080488857,
126.075580858978));
#203516=CARTESIAN_POINT('Ctrl Pts',(180.867172136915,-1.48393007137391,
126.113308366883));
#203517=CARTESIAN_POINT('Ctrl Pts',(180.859415834173,-1.61423904308519,
126.156543655144));
#203518=CARTESIAN_POINT('Ctrl Pts',(180.851659531431,-1.74241527737747,
126.20510284444));
#203519=CARTESIAN_POINT('Ctrl Pts',(180.843899088917,-1.87065992318532,
126.253687951238));
#203520=CARTESIAN_POINT('Ctrl Pts',(180.836138646403,-1.99676920408849,
126.307602467438));
#203521=CARTESIAN_POINT('Ctrl Pts',(180.828378203889,-2.12028258665798,
126.366615152218));
#203522=CARTESIAN_POINT('Ctrl Pts',(180.820605303623,-2.24399424387421,
126.425722569399));
#203523=CARTESIAN_POINT('Ctrl Pts',(180.812832403358,-2.3651013298266,126.489944326195));
#203524=CARTESIAN_POINT('Ctrl Pts',(180.805059503092,-2.48316897428491,
126.559003752985));
#203525=CARTESIAN_POINT('Ctrl Pts',(180.79756916733,-2.59694456247199,126.62555269566));
#203526=CARTESIAN_POINT('Ctrl Pts',(180.790078831568,-2.707897595887,126.696593525687));
#203527=CARTESIAN_POINT('Ctrl Pts',(180.782588495806,-2.81566748832438,
126.771842836118));
#203528=CARTESIAN_POINT('Ctrl Pts',(180.774860431703,-2.92685778253992,
126.849480409815));
#203529=CARTESIAN_POINT('Ctrl Pts',(180.7671323676,-3.03502137085671,126.931850825884));
#203530=CARTESIAN_POINT('Ctrl Pts',(180.759404303497,-3.13972510257354,
127.018689033452));
#203531=CARTESIAN_POINT('Ctrl Pts',(180.751688447729,-3.24426342957341,
127.105390059193));
#203532=CARTESIAN_POINT('Ctrl Pts',(180.743972591961,-3.3453524815515,127.196544571404));
#203533=CARTESIAN_POINT('Ctrl Pts',(180.736256736193,-3.44258800822052,
127.291844301852));
#203534=CARTESIAN_POINT('Ctrl Pts',(180.728547930298,-3.53973469210992,
127.387056958232));
#203535=CARTESIAN_POINT('Ctrl Pts',(180.720839124402,-3.63303457198762,
127.486407025166));
#203536=CARTESIAN_POINT('Ctrl Pts',(180.713130318507,-3.72211626851405,
127.589545918993));
#203537=CARTESIAN_POINT('Ctrl Pts',(180.705426833656,-3.81113647592418,
127.692613620647));
#203538=CARTESIAN_POINT('Ctrl Pts',(180.697723348805,-3.89594403403888,
127.799464648121));
#203539=CARTESIAN_POINT('Ctrl Pts',(180.690019863954,-3.97620460244335,
127.909713830476));
#203540=CARTESIAN_POINT('Ctrl Pts',(180.682319975564,-4.05642770026874,
128.01991154172));
#203541=CARTESIAN_POINT('Ctrl Pts',(180.674620087175,-4.13210780008793,
128.133503931074));
#203542=CARTESIAN_POINT('Ctrl Pts',(180.666920198785,-4.20295133298381,
128.250073406803));
#203543=CARTESIAN_POINT('Ctrl Pts',(180.659220735343,-4.27379095611665,
128.366636449212));
#203544=CARTESIAN_POINT('Ctrl Pts',(180.6515212719,-4.33979432957215,128.486175917609));
#203545=CARTESIAN_POINT('Ctrl Pts',(180.643821808457,-4.40071176989382,
128.608246098508));
#203546=CARTESIAN_POINT('Ctrl Pts',(180.636122680545,-4.46162655553023,
128.730310959782));
#203547=CARTESIAN_POINT('Ctrl Pts',(180.628423552633,-4.51745567719539,
128.854905956993));
#203548=CARTESIAN_POINT('Ctrl Pts',(180.620724424721,-4.56799625155725,
128.981562409245));
#203549=CARTESIAN_POINT('Ctrl Pts',(180.61302142386,-4.61856224971331,129.108282574417));
#203550=CARTESIAN_POINT('Ctrl Pts',(180.605318422999,-4.66383424513525,
129.237065895624));
#203551=CARTESIAN_POINT('Ctrl Pts',(180.597615422138,-4.70365818002023,
129.367425410944));
#203552=CARTESIAN_POINT('Ctrl Pts',(180.593405538846,-4.72542295989178,
129.438670157685));
#203553=CARTESIAN_POINT('Ctrl Pts',(180.589195655555,-4.74556133082426,
129.510385423281));
#203554=CARTESIAN_POINT('Ctrl Pts',(180.584985772263,-4.76405452823404,
129.582490119308));
#203555=CARTESIAN_POINT('',(182.610140564063,-4.91824890646276,130.801080895348));
#203556=CARTESIAN_POINT('Ctrl Pts',(182.610140564008,-4.91824890646341,
130.80108089632));
#203557=CARTESIAN_POINT('Ctrl Pts',(182.602350736543,-4.91834099197833,
130.939171742779));
#203558=CARTESIAN_POINT('Ctrl Pts',(182.594560909078,-4.91261293631802,
131.077296116385));
#203559=CARTESIAN_POINT('Ctrl Pts',(182.586771081613,-4.90108295938559,
131.214932033668));
#203560=CARTESIAN_POINT('Ctrl Pts',(182.578981013679,-4.88955262652708,
131.352572199721));
#203561=CARTESIAN_POINT('Ctrl Pts',(182.571190945745,-4.87222004712722,
131.48972349604));
#203562=CARTESIAN_POINT('Ctrl Pts',(182.563400877811,-4.84915540080159,
131.625868354217));
#203563=CARTESIAN_POINT('Ctrl Pts',(182.555608953444,-4.82608525799307,
131.762045656762));
#203564=CARTESIAN_POINT('Ctrl Pts',(182.547817029077,-4.79728039275426,
131.897215664416));
#203565=CARTESIAN_POINT('Ctrl Pts',(182.54002510471,-4.76286219548405,132.030870613175));
#203566=CARTESIAN_POINT('Ctrl Pts',(182.532229707094,-4.72842865631017,
132.164585138597));
#203567=CARTESIAN_POINT('Ctrl Pts',(182.524434309478,-4.68837689938111,
132.296782888428));
#203568=CARTESIAN_POINT('Ctrl Pts',(182.516638911862,-4.64287820456094,
132.42697118086));
#203569=CARTESIAN_POINT('Ctrl Pts',(182.508833566481,-4.59732144851264,
132.557325607555));
#203570=CARTESIAN_POINT('Ctrl Pts',(182.501028221099,-4.54630400030386,
132.685665092519));
#203571=CARTESIAN_POINT('Ctrl Pts',(182.493222875718,-4.49004557517999,
132.811516265568));
#203572=CARTESIAN_POINT('Ctrl Pts',(182.48541197276,-4.43374709282834,132.937457047402));
#203573=CARTESIAN_POINT('Ctrl Pts',(182.477601069802,-4.37220036926214,
133.060905643736));
#203574=CARTESIAN_POINT('Ctrl Pts',(182.469790166844,-4.30567070775944,
133.181414007552));
#203575=CARTESIAN_POINT('Ctrl Pts',(182.461966709995,-4.23903411801708,
133.302116055611));
#203576=CARTESIAN_POINT('Ctrl Pts',(182.454143253146,-4.16739879386563,
133.419868104856));
#203577=CARTESIAN_POINT('Ctrl Pts',(182.446319796298,-4.09107330250262,
133.534251145783));
#203578=CARTESIAN_POINT('Ctrl Pts',(182.442108278373,-4.04998581634815,
133.595825745913));
#203579=CARTESIAN_POINT('Ctrl Pts',(182.437896760449,-4.00753987680767,
133.656424612155));
#203580=CARTESIAN_POINT('Ctrl Pts',(182.433685242525,-3.96378825988816,
133.715986571097));
#203581=CARTESIAN_POINT('Ctrl Pts',(182.425910908406,-3.88302410446949,
133.825936137482));
#203582=CARTESIAN_POINT('Ctrl Pts',(182.418136574287,-3.7975538023016,133.932696893848));
#203583=CARTESIAN_POINT('Ctrl Pts',(182.410362240168,-3.70765790045001,
134.035839529106));
#203584=CARTESIAN_POINT('Ctrl Pts',(182.402597487221,-3.61787278726326,
134.138855050285));
#203585=CARTESIAN_POINT('Ctrl Pts',(182.394832734273,-3.52367318095091,
134.238261030556));
#203586=CARTESIAN_POINT('Ctrl Pts',(182.387067981326,-3.42538226341174,
134.333657914763));
#203587=CARTESIAN_POINT('Ctrl Pts',(182.379310940441,-3.32718896979766,
134.42896004944));
#203588=CARTESIAN_POINT('Ctrl Pts',(182.371553899556,-3.22491273033872,
134.520260741664));
#203589=CARTESIAN_POINT('Ctrl Pts',(182.363796858671,-3.11891602473428,
134.607194546777));
#203590=CARTESIAN_POINT('Ctrl Pts',(182.356045667431,-3.01299925206974,
134.694062794431));
#203591=CARTESIAN_POINT('Ctrl Pts',(182.348294476191,-2.90336789877549,
134.77657046277));
#203592=CARTESIAN_POINT('Ctrl Pts',(182.340543284951,-2.79041995640996,
134.854390188985));
#203593=CARTESIAN_POINT('Ctrl Pts',(182.332795388174,-2.67752001993321,
134.932176839741));
#203594=CARTESIAN_POINT('Ctrl Pts',(182.325047491397,-2.56130661932331,
135.005279289951));
#203595=CARTESIAN_POINT('Ctrl Pts',(182.31729959462,-2.44220918470204,135.073411725325));
#203596=CARTESIAN_POINT('Ctrl Pts',(182.309553318536,-2.32313666269663,
135.141529908862));
#203597=CARTESIAN_POINT('Ctrl Pts',(182.301807042451,-2.20118164577595,
135.204679951408));
#203598=CARTESIAN_POINT('Ctrl Pts',(182.294060766367,-2.07680044042566,
135.262620703423));
#203599=CARTESIAN_POINT('Ctrl Pts',(182.286314433102,-1.95241831692144,
135.320561883144));
#203600=CARTESIAN_POINT('Ctrl Pts',(182.278568099837,-1.82561032364971,
135.37329353051));
#203601=CARTESIAN_POINT('Ctrl Pts',(182.270821766571,-1.6968547692407,135.420621762108));
#203602=CARTESIAN_POINT('Ctrl Pts',(182.263073698568,-1.56807038091839,
135.467960592535));
#203603=CARTESIAN_POINT('Ctrl Pts',(182.255325630565,-1.43733793047416,
135.509893464457));
#203604=CARTESIAN_POINT('Ctrl Pts',(182.247577562562,-1.30515260026303,
135.546275816357));
#203605=CARTESIAN_POINT('Ctrl Pts',(182.239821259821,-1.17282678190962,
135.582696835854));
#203606=CARTESIAN_POINT('Ctrl Pts',(182.232064957079,-1.03904537675643,
135.613555447207));
#203607=CARTESIAN_POINT('Ctrl Pts',(182.224308654337,-0.904316068585796,
135.638757737228));
#203608=CARTESIAN_POINT('Ctrl Pts',(182.216548211823,-0.769514851326632,
135.663973478471));
#203609=CARTESIAN_POINT('Ctrl Pts',(182.208787769308,-0.633765109735002,
135.683526827158));
#203610=CARTESIAN_POINT('Ctrl Pts',(182.201027326794,-0.497580452340472,
135.69737571625));
#203611=CARTESIAN_POINT('Ctrl Pts',(182.193254426529,-0.361177179244034,
135.711246836808));
#203612=CARTESIAN_POINT('Ctrl Pts',(182.185481526263,-0.224337985686155,
135.719395175306));
#203613=CARTESIAN_POINT('Ctrl Pts',(182.177708625998,-0.0875781934747493,
135.721830812954));
#203614=CARTESIAN_POINT('Ctrl Pts',(182.170218290236,0.0442100358122264,
135.724177909039));
#203615=CARTESIAN_POINT('Ctrl Pts',(182.162727954474,0.175924228464083,
135.72122044237));
#203616=CARTESIAN_POINT('Ctrl Pts',(182.155237618712,0.307109000857396,
135.713012889228));
#203617=CARTESIAN_POINT('Ctrl Pts',(182.147463284593,0.443267683768998,
135.704494144214));
#203618=CARTESIAN_POINT('Ctrl Pts',(182.139688950474,0.579287317770908,
135.690292354947));
#203619=CARTESIAN_POINT('Ctrl Pts',(182.131914616355,0.714655068745021,
135.670411500491));
#203620=CARTESIAN_POINT('Ctrl Pts',(182.124149863408,0.849855991064199,
135.650555147412));
#203621=CARTESIAN_POINT('Ctrl Pts',(182.116385110461,0.984406245755034,
135.625033711212));
#203622=CARTESIAN_POINT('Ctrl Pts',(182.108620357513,1.11779498803749,135.593903124656));
#203623=CARTESIAN_POINT('Ctrl Pts',(182.100863316628,1.25105124674114,135.562803457436));
#203624=CARTESIAN_POINT('Ctrl Pts',(182.093106275743,1.38314791054298,135.526105814856));
#203625=CARTESIAN_POINT('Ctrl Pts',(182.085349234858,1.5135815913709,135.483917629588));
#203626=CARTESIAN_POINT('Ctrl Pts',(182.077598043618,1.64391691114509,135.441761258759));
#203627=CARTESIAN_POINT('Ctrl Pts',(182.069846852378,1.77259137360677,135.39412270641));
#203628=CARTESIAN_POINT('Ctrl Pts',(182.062095661138,1.8991144349961,135.341159866518));
#203629=CARTESIAN_POINT('Ctrl Pts',(182.054347764361,2.02558372070912,135.288219537246));
#203630=CARTESIAN_POINT('Ctrl Pts',(182.046599867584,2.14990306413975,135.229959571943));
#203631=CARTESIAN_POINT('Ctrl Pts',(182.038851970807,2.27159988415978,135.166586772729));
#203632=CARTESIAN_POINT('Ctrl Pts',(182.031105694723,2.39327124782866,135.103227229737));
#203633=CARTESIAN_POINT('Ctrl Pts',(182.023359418639,2.51232083268777,135.034757160578));
#203634=CARTESIAN_POINT('Ctrl Pts',(182.015613142554,2.62829910799688,134.961430121604));
#203635=CARTESIAN_POINT('Ctrl Pts',(182.007866809289,2.74427823943102,134.888102541346));
#203636=CARTESIAN_POINT('Ctrl Pts',(182.000120476024,2.85718568561855,134.809918128662));
#203637=CARTESIAN_POINT('Ctrl Pts',(181.992374142758,2.96659978945404,134.727174499426));
#203638=CARTESIAN_POINT('Ctrl Pts',(181.984626074756,3.07603839581934,134.644412340328));
#203639=CARTESIAN_POINT('Ctrl Pts',(181.976878006753,3.18198179135113,134.557089168775));
#203640=CARTESIAN_POINT('Ctrl Pts',(181.96912993875,3.28404069419147,134.465543456676));
#203641=CARTESIAN_POINT('Ctrl Pts',(181.961373636008,3.3862080664486,134.373900448704));
#203642=CARTESIAN_POINT('Ctrl Pts',(181.953617333266,3.48448240741909,134.278026196862));
#203643=CARTESIAN_POINT('Ctrl Pts',(181.945861030524,3.57851028979258,134.178297067523));
#203644=CARTESIAN_POINT('Ctrl Pts',(181.93810058801,3.67258835767799,134.078514709744));
#203645=CARTESIAN_POINT('Ctrl Pts',(181.930340145496,3.76241519491009,133.974873670094));
#203646=CARTESIAN_POINT('Ctrl Pts',(181.922579702982,3.84767779134117,133.86778332371));
#203647=CARTESIAN_POINT('Ctrl Pts',(181.914806802716,3.93307725886131,133.760521066396));
#203648=CARTESIAN_POINT('Ctrl Pts',(181.907033902451,4.01389761341318,133.64979875336));
#203649=CARTESIAN_POINT('Ctrl Pts',(181.899261002185,4.08986879258137,133.536055388577));
#203650=CARTESIAN_POINT('Ctrl Pts',(181.891770666423,4.16307822802756,133.426446881605));
#203651=CARTESIAN_POINT('Ctrl Pts',(181.884280330661,4.23178476598698,133.314033418012));
#203652=CARTESIAN_POINT('Ctrl Pts',(181.876789994899,4.29578809292371,133.199227570696));
#203653=CARTESIAN_POINT('Ctrl Pts',(181.86901566078,4.36221812545415,133.080068824786));
#203654=CARTESIAN_POINT('Ctrl Pts',(181.861241326661,4.42379169257108,132.957955240427));
#203655=CARTESIAN_POINT('Ctrl Pts',(181.853466992542,4.480234942605,132.833320430268));
#203656=CARTESIAN_POINT('Ctrl Pts',(181.845702239595,4.53660863137767,132.708839221374));
#203657=CARTESIAN_POINT('Ctrl Pts',(181.837937486648,4.5878644235316,132.58184332178));
#203658=CARTESIAN_POINT('Ctrl Pts',(181.8301727337,4.63377325280224,132.452792752692));
#203659=CARTESIAN_POINT('Ctrl Pts',(181.822415692815,4.67963648477647,132.323870358447));
#203660=CARTESIAN_POINT('Ctrl Pts',(181.81465865193,4.72016319216763,132.192897721815));
#203661=CARTESIAN_POINT('Ctrl Pts',(181.806901611045,4.75517166757724,132.06035642742));
#203662=CARTESIAN_POINT('Ctrl Pts',(181.799150419805,4.7901537428232,131.927915083446));
#203663=CARTESIAN_POINT('Ctrl Pts',(181.791399228565,4.81962576954726,131.793907812746));
#203664=CARTESIAN_POINT('Ctrl Pts',(181.783648037325,4.84345543753907,131.658832669229));
#203665=CARTESIAN_POINT('Ctrl Pts',(181.775900140548,4.86727497728632,131.523814936251));
#203666=CARTESIAN_POINT('Ctrl Pts',(181.768152243771,4.88545686026262,131.387730617391));
#203667=CARTESIAN_POINT('Ctrl Pts',(181.760404346994,4.8979196333033,131.251089090133));
#203668=CARTESIAN_POINT('Ctrl Pts',(181.75265807091,4.91037979940052,131.114476145337));
#203669=CARTESIAN_POINT('Ctrl Pts',(181.744911794826,4.91712319960808,130.97730661308));
#203670=CARTESIAN_POINT('Ctrl Pts',(181.737165518741,4.91812017572067,130.840095749709));
#203671=CARTESIAN_POINT('Ctrl Pts',(181.729419185476,4.91911715919271,130.702883873479));
#203672=CARTESIAN_POINT('Ctrl Pts',(181.721672852211,4.91436763108547,130.565631056479));
#203673=CARTESIAN_POINT('Ctrl Pts',(181.713926518945,4.90389406809912,130.428852919426));
#203674=CARTESIAN_POINT('Ctrl Pts',(181.706178450942,4.89341815963096,130.292044151858));
#203675=CARTESIAN_POINT('Ctrl Pts',(181.698430382939,4.87721569537927,130.155710665513));
#203676=CARTESIAN_POINT('Ctrl Pts',(181.690682314937,4.85536102499316,130.020362926576));
#203677=CARTESIAN_POINT('Ctrl Pts',(181.682926012195,4.83348312720327,129.884871338452));
#203678=CARTESIAN_POINT('Ctrl Pts',(181.675169709453,4.80594108560759,129.75036797714));
#203679=CARTESIAN_POINT('Ctrl Pts',(181.667413406711,4.77286051180006,129.617353626264));
#203680=CARTESIAN_POINT('Ctrl Pts',(181.659652964197,4.73976228189421,129.484268281624));
#203681=CARTESIAN_POINT('Ctrl Pts',(181.651892521683,4.70111973963549,129.352673905927));
#203682=CARTESIAN_POINT('Ctrl Pts',(181.644132079168,4.65710811429238,129.22305512074));
#203683=CARTESIAN_POINT('Ctrl Pts',(181.636359178903,4.61302583758112,129.093228259972));
#203684=CARTESIAN_POINT('Ctrl Pts',(181.628586278637,4.5635573955876,128.965383691997));
#203685=CARTESIAN_POINT('Ctrl Pts',(181.620813378372,4.5089261594554,128.839985920346));
#203686=CARTESIAN_POINT('Ctrl Pts',(181.61332304261,4.45628090636462,128.719146673552));
#203687=CARTESIAN_POINT('Ctrl Pts',(181.605832706848,4.39884183774708,128.600579694375));
#203688=CARTESIAN_POINT('Ctrl Pts',(181.598342371086,4.33684778850805,128.484676517993));
#203689=CARTESIAN_POINT('Ctrl Pts',(181.590568036967,4.27250321604925,128.36437883745));
#203690=CARTESIAN_POINT('Ctrl Pts',(181.582793702848,4.20304761613661,128.246569876445));
#203691=CARTESIAN_POINT('Ctrl Pts',(181.575019368729,4.12869777585513,128.13171441237));
#203692=CARTESIAN_POINT('Ctrl Pts',(181.567254615782,4.05443956510713,128.01700049739));
#203693=CARTESIAN_POINT('Ctrl Pts',(181.559489862835,3.97529932571951,127.905233162034));
#203694=CARTESIAN_POINT('Ctrl Pts',(181.551725109888,3.89154027064978,127.796853778935));
#203695=CARTESIAN_POINT('Ctrl Pts',(181.543968069003,3.80786440625398,127.688582039767));
#203696=CARTESIAN_POINT('Ctrl Pts',(181.536211028118,3.71957909298195,127.583691863779));
#203697=CARTESIAN_POINT('Ctrl Pts',(181.528453987233,3.62699128433114,127.482596434803));
#203698=CARTESIAN_POINT('Ctrl Pts',(181.520702795992,3.5344732968673,127.381577242677));
#203699=CARTESIAN_POINT('Ctrl Pts',(181.512951604752,3.43765953508295,127.28434738878));
#203700=CARTESIAN_POINT('Ctrl Pts',(181.505200413512,3.33689750893684,127.191287399743));
#203701=CARTESIAN_POINT('Ctrl Pts',(181.497452516735,3.23617830933978,127.098266963683));
#203702=CARTESIAN_POINT('Ctrl Pts',(181.489704619958,3.13151446964089,127.00941313221));
#203703=CARTESIAN_POINT('Ctrl Pts',(181.481956723181,3.02329051611814,126.925069765149));
#203704=CARTESIAN_POINT('Ctrl Pts',(181.474210447097,2.91508920071343,126.840744040902));
#203705=CARTESIAN_POINT('Ctrl Pts',(181.466464171013,2.80332956091226,126.760927144587));
#203706=CARTESIAN_POINT('Ctrl Pts',(181.458717894929,2.688429065486,126.685922537134));
#203707=CARTESIAN_POINT('Ctrl Pts',(181.450971561663,2.57352772189059,126.610917376014));
#203708=CARTESIAN_POINT('Ctrl Pts',(181.443225228398,2.45548580379192,126.54072478835));
#203709=CARTESIAN_POINT('Ctrl Pts',(181.435478895133,2.33474926670635,126.475604569448));
#203710=CARTESIAN_POINT('Ctrl Pts',(181.42773082713,2.21398569151045,126.410469767325));
#203711=CARTESIAN_POINT('Ctrl Pts',(181.419982759127,2.0905266405883,126.350409779878));
#203712=CARTESIAN_POINT('Ctrl Pts',(181.412234691124,1.96484177140072,126.295637974083));
#203713=CARTESIAN_POINT('Ctrl Pts',(181.404478388382,1.83902332283823,126.240807956161));
#203714=CARTESIAN_POINT('Ctrl Pts',(181.39672208564,1.71097468939951,126.19127750357));
#203715=CARTESIAN_POINT('Ctrl Pts',(181.388965782898,1.58118509066446,126.1472116215));
#203716=CARTESIAN_POINT('Ctrl Pts',(181.381205340384,1.45132621931234,126.103122220142));
#203717=CARTESIAN_POINT('Ctrl Pts',(181.37344489787,1.31972490610537,126.064503310922));
#203718=CARTESIAN_POINT('Ctrl Pts',(181.365684455356,1.18688359259093,126.031469418289));
#203719=CARTESIAN_POINT('Ctrl Pts',(181.35791155509,1.05382903040709,125.998382496718));
#203720=CARTESIAN_POINT('Ctrl Pts',(181.350138654825,0.919530873392618,
125.970898586219));
#203721=CARTESIAN_POINT('Ctrl Pts',(181.342365754559,0.784500659081397,
125.949080833825));
#203722=CARTESIAN_POINT('Ctrl Pts',(181.334875418797,0.65437913317976,125.928056211687));
#203723=CARTESIAN_POINT('Ctrl Pts',(181.327385083035,0.523578155989451,
125.912292978468));
#203724=CARTESIAN_POINT('Ctrl Pts',(181.319894747273,0.39255623324671,125.901801829929));
#203725=CARTESIAN_POINT('Ctrl Pts',(181.312120413154,0.256566574481517,
125.890912906304));
#203726=CARTESIAN_POINT('Ctrl Pts',(181.304346079035,0.119908110764656,
125.885669248528));
#203727=CARTESIAN_POINT('Ctrl Pts',(181.296571744916,-0.0169109488048534,
125.88613969102));
#203728=CARTESIAN_POINT('Ctrl Pts',(181.288806991969,-0.153561391111778,
125.886609553735));
#203729=CARTESIAN_POINT('Ctrl Pts',(181.281042239022,-0.290371648259795,
125.892779503671));
#203730=CARTESIAN_POINT('Ctrl Pts',(181.273277486075,-0.426828107918584,
125.904666665002));
#203731=CARTESIAN_POINT('Ctrl Pts',(181.26552044519,-0.563149037097825,
125.916542019838));
#203732=CARTESIAN_POINT('Ctrl Pts',(181.257763404305,-0.699116481113278,
125.934123252056));
#203733=CARTESIAN_POINT('Ctrl Pts',(181.25000636342,-0.834216900840216,
125.957375448943));
#203734=CARTESIAN_POINT('Ctrl Pts',(181.242255172179,-0.969215440289043,
125.980610111167));
#203735=CARTESIAN_POINT('Ctrl Pts',(181.234503980939,-1.1033478731167,126.009507159861));
#203736=CARTESIAN_POINT('Ctrl Pts',(181.226752789699,-1.23610621387061,
126.043979908995));
#203737=CARTESIAN_POINT('Ctrl Pts',(181.219004892922,-1.36880812878891,
126.078438006292));
#203738=CARTESIAN_POINT('Ctrl Pts',(181.211256996145,-1.50013673559273,
126.118466992577));
#203739=CARTESIAN_POINT('Ctrl Pts',(181.203509099368,-1.62959488942576,
126.16392921964));
#203740=CARTESIAN_POINT('Ctrl Pts',(181.195762823284,-1.75902596340384,
126.209381936985));
#203741=CARTESIAN_POINT('Ctrl Pts',(181.1880165472,-1.88658699399867,126.260265505053));
#203742=CARTESIAN_POINT('Ctrl Pts',(181.180270271116,-2.01179701886858,
126.316392723589));
#203743=CARTESIAN_POINT('Ctrl Pts',(181.17252393785,-2.13700796800998,126.372520356442));
#203744=CARTESIAN_POINT('Ctrl Pts',(181.164777604585,-2.25986752003577,
126.433891557078));
#203745=CARTESIAN_POINT('Ctrl Pts',(181.15703127132,-2.37991605194676,126.500271556198));
#203746=CARTESIAN_POINT('Ctrl Pts',(181.149283203317,-2.49999146789432,
126.566666420659));
#203747=CARTESIAN_POINT('Ctrl Pts',(181.141535135314,-2.61725426899975,
126.63807212648));
#203748=CARTESIAN_POINT('Ctrl Pts',(181.133787067311,-2.73127108225299,
126.7142088676));
#203749=CARTESIAN_POINT('Ctrl Pts',(181.126030764569,-2.8454090739322,126.790426527755));
#203750=CARTESIAN_POINT('Ctrl Pts',(181.118274461827,-2.95629386060742,
126.871385050119));
#203751=CARTESIAN_POINT('Ctrl Pts',(181.110518159085,-3.06352218360704,
126.956762029739));
#203752=CARTESIAN_POINT('Ctrl Pts',(181.102757716571,-3.17080773759117,
127.042184577624));
#203753=CARTESIAN_POINT('Ctrl Pts',(181.094997274057,-3.27443264399057,
127.132030025815));
#203754=CARTESIAN_POINT('Ctrl Pts',(181.087236831543,-3.37402896821536,
127.22593755927));
#203755=CARTESIAN_POINT('Ctrl Pts',(181.079463931278,-3.4737851733016,127.319995841434));
#203756=CARTESIAN_POINT('Ctrl Pts',(181.071691031012,-3.56949959987051,
127.418128959495));
#203757=CARTESIAN_POINT('Ctrl Pts',(181.063918130747,-3.66084262200152,
127.519940674953));
#203758=CARTESIAN_POINT('Ctrl Pts',(181.056427794985,-3.7488650952,127.618051278106));
#203759=CARTESIAN_POINT('Ctrl Pts',(181.048937459222,-3.83282827290767,
127.7195774321));
#203760=CARTESIAN_POINT('Ctrl Pts',(181.04144712346,-3.9124753229297,127.824139164391));
#203761=CARTESIAN_POINT('Ctrl Pts',(181.033651562904,-3.99536792231622,
127.932961698101));
#203762=CARTESIAN_POINT('Ctrl Pts',(181.025856002347,-4.07385081342254,
128.045421065337));
#203763=CARTESIAN_POINT('Ctrl Pts',(181.018060441791,-4.14758872176929,
128.161125694682));
#203764=CARTESIAN_POINT('Ctrl Pts',(181.01027762814,-4.22120605762,128.276641129674));
#203765=CARTESIAN_POINT('Ctrl Pts',(181.00249481449,-4.29009365664689,128.395390934063));
#203766=CARTESIAN_POINT('Ctrl Pts',(180.994712000839,-4.35395702277294,
128.516951317431));
#203767=CARTESIAN_POINT('Ctrl Pts',(180.986936519403,-4.41776022301778,
128.638397178372));
#203768=CARTESIAN_POINT('Ctrl Pts',(180.979161037966,-4.47654842553653,
128.762648010892));
#203769=CARTESIAN_POINT('Ctrl Pts',(180.971385556529,-4.53007071000093,
128.889251632445));
#203770=CARTESIAN_POINT('Ctrl Pts',(180.963616832862,-4.58354647756522,
129.015745221175));
#203771=CARTESIAN_POINT('Ctrl Pts',(180.955848109195,-4.63176528846851,
129.144587172));
#203772=CARTESIAN_POINT('Ctrl Pts',(180.948079385529,-4.67452267920003,
129.275301827282));
#203773=CARTESIAN_POINT('Ctrl Pts',(180.942056030262,-4.70767393617805,
129.376649338295));
#203774=CARTESIAN_POINT('Ctrl Pts',(180.936032674994,-4.73754299834085,
129.479122066623));
#203775=CARTESIAN_POINT('Ctrl Pts',(180.930009319727,-4.76405452823405,
129.582490119308));
#203776=CARTESIAN_POINT('Ctrl Pts',(182.679902359578,-4.76405452823405,
129.582490119308));
#203777=CARTESIAN_POINT('Ctrl Pts',(182.671073039678,-4.80263856972609,
129.732928711491));
#203778=CARTESIAN_POINT('Ctrl Pts',(182.662243719779,-4.83413672793406,
129.885367666505));
#203779=CARTESIAN_POINT('Ctrl Pts',(182.65341439988,-4.85836093134102,130.039172978278));
#203780=CARTESIAN_POINT('Ctrl Pts',(182.644641758985,-4.88242962971196,
130.19199095106));
#203781=CARTESIAN_POINT('Ctrl Pts',(182.635869118089,-4.89931737459966,
130.346157623678));
#203782=CARTESIAN_POINT('Ctrl Pts',(182.627096477193,-4.90888732968651,
130.501032005425));
#203783=CARTESIAN_POINT('Ctrl Pts',(182.62144450615,-4.91505298831555,130.600813306337));
#203784=CARTESIAN_POINT('Ctrl Pts',(182.615792535106,-4.91818209306794,
130.700887987475));
#203785=CARTESIAN_POINT('Ctrl Pts',(182.610140564063,-4.91824890646276,
130.801080895348));
#203786=CARTESIAN_POINT('Origin',(213.235140564004,0.,130.804360617566));
#203787=CARTESIAN_POINT('',(184.430229652623,-4.76405452823406,129.582490119308));
#203788=CARTESIAN_POINT('',(184.084599308536,-4.76405452823405,129.582490119308));
#203789=CARTESIAN_POINT('',(213.235140564004,-4.76405452823405,129.582490119308));
#203790=CARTESIAN_POINT('',(184.014859436043,-4.9182492280365,130.801605001777));
#203791=CARTESIAN_POINT('Ctrl Pts',(184.084599308536,-4.76405452823405,
129.582490119308));
#203792=CARTESIAN_POINT('Ctrl Pts',(184.075945911235,-4.8018983817438,129.730042729782));
#203793=CARTESIAN_POINT('Ctrl Pts',(184.067292513934,-4.83292755031847,
129.879527941908));
#203794=CARTESIAN_POINT('Ctrl Pts',(184.058639116632,-4.85696110866322,
130.030337458072));
#203795=CARTESIAN_POINT('Ctrl Pts',(184.050029728944,-4.88087243667851,
130.180379984322));
#203796=CARTESIAN_POINT('Ctrl Pts',(184.041420341256,-4.89785903432467,
130.331733166547));
#203797=CARTESIAN_POINT('Ctrl Pts',(184.032810953568,-4.90779083573385,
130.483779621269));
#203798=CARTESIAN_POINT('Ctrl Pts',(184.026827114393,-4.91469380078797,
130.589457465631));
#203799=CARTESIAN_POINT('Ctrl Pts',(184.020843275218,-4.91818976220946,
130.69546982899));
#203800=CARTESIAN_POINT('Ctrl Pts',(184.014859436043,-4.9182492280365,130.801605001777));
#203801=CARTESIAN_POINT('Ctrl Pts',(184.014859435991,-4.91824922803702,
130.801605002707));
#203802=CARTESIAN_POINT('Ctrl Pts',(184.0070245266,-4.91832708928895,130.94057255142));
#203803=CARTESIAN_POINT('Ctrl Pts',(183.999189617208,-4.91251071226177,
131.079545490942));
#203804=CARTESIAN_POINT('Ctrl Pts',(183.991354707817,-4.90082530395939,
131.217996209085));
#203805=CARTESIAN_POINT('Ctrl Pts',(183.983518210813,-4.88913752780615,
131.356474981931));
#203806=CARTESIAN_POINT('Ctrl Pts',(183.97568171381,-4.87157838318562,131.494430945472));
#203807=CARTESIAN_POINT('Ctrl Pts',(183.967845216806,-4.84822496807564,
131.631341706484));
#203808=CARTESIAN_POINT('Ctrl Pts',(183.960005585196,-4.82486221157711,
131.768307231932));
#203809=CARTESIAN_POINT('Ctrl Pts',(183.952165953587,-4.79570063209204,
131.904226349297));
#203810=CARTESIAN_POINT('Ctrl Pts',(183.944326321977,-4.76086839271114,
132.038587180959));
#203811=CARTESIAN_POINT('Ctrl Pts',(183.936091824958,-4.72428172823233,
132.179715479181));
#203812=CARTESIAN_POINT('Ctrl Pts',(183.927857327939,-4.68143846664776,
132.319123983606));
#203813=CARTESIAN_POINT('Ctrl Pts',(183.91962283092,-4.63254572439523,132.456239297702));
#203814=CARTESIAN_POINT('Ctrl Pts',(183.911767314248,-4.58590319711227,
132.58704408557));
#203815=CARTESIAN_POINT('Ctrl Pts',(183.903911797577,-4.53375578798978,
132.71576172528));
#203816=CARTESIAN_POINT('Ctrl Pts',(183.896056280906,-4.47633184758892,
132.84191705918));
#203817=CARTESIAN_POINT('Ctrl Pts',(183.888194193542,-4.41885987532938,
132.968177914837));
#203818=CARTESIAN_POINT('Ctrl Pts',(183.880332106178,-4.35610274681267,
133.09187185747));
#203819=CARTESIAN_POINT('Ctrl Pts',(183.872470018814,-4.28833398097888,
133.212549715225));
#203820=CARTESIAN_POINT('Ctrl Pts',(183.864595817316,-4.2204607950577,133.333413516936));
#203821=CARTESIAN_POINT('Ctrl Pts',(183.856721615819,-4.14756075301982,
133.451251635519));
#203822=CARTESIAN_POINT('Ctrl Pts',(183.848847414322,-4.06995003088787,
133.565644704468));
#203823=CARTESIAN_POINT('Ctrl Pts',(183.847735728798,-4.05899289239229,
133.58179480158));
#203824=CARTESIAN_POINT('Ctrl Pts',(183.846624043273,-4.04794192437879,
133.597876287981));
#203825=CARTESIAN_POINT('Ctrl Pts',(183.845512357748,-4.03679807846351,
133.613888039787));
#203826=CARTESIAN_POINT('Ctrl Pts',(183.837738023629,-3.95886598381865,
133.7258627895));
#203827=CARTESIAN_POINT('Ctrl Pts',(183.82996368951,-3.87614790100592,133.834769861943));
#203828=CARTESIAN_POINT('Ctrl Pts',(183.822189355391,-3.78891333030926,
133.940172926666));
#203829=CARTESIAN_POINT('Ctrl Pts',(183.814424602444,-3.70178626842471,
134.045446091532));
#203830=CARTESIAN_POINT('Ctrl Pts',(183.806659849497,-3.61015404055219,
134.147223542661));
#203831=CARTESIAN_POINT('Ctrl Pts',(183.79889509655,-3.51432952725466,134.245097607858));
#203832=CARTESIAN_POINT('Ctrl Pts',(183.791138055665,-3.41860018821441,
134.342874463155));
#203833=CARTESIAN_POINT('Ctrl Pts',(183.78338101478,-3.31868712171636,134.436755370167));
#203834=CARTESIAN_POINT('Ctrl Pts',(183.775623973895,-3.21494336377899,
134.526365753268));
#203835=CARTESIAN_POINT('Ctrl Pts',(183.767872782655,-3.11127783981671,
134.615908560482));
#203836=CARTESIAN_POINT('Ctrl Pts',(183.760121591415,-3.00378766898042,
134.701186999335));
#203837=CARTESIAN_POINT('Ctrl Pts',(183.752370400174,-2.89286235937896,
134.781863657438));
#203838=CARTESIAN_POINT('Ctrl Pts',(183.744622503397,-2.7819841959931,134.862506025808));
#203839=CARTESIAN_POINT('Ctrl Pts',(183.73687460662,-2.66767411324236,134.938550274043));
#203840=CARTESIAN_POINT('Ctrl Pts',(183.729126709843,-2.55035410782106,
135.009699722468));
#203841=CARTESIAN_POINT('Ctrl Pts',(183.721380433759,-2.43305864321574,
135.080834287963));
#203842=CARTESIAN_POINT('Ctrl Pts',(183.713634157675,-2.31275484235268,
135.147075887609));
#203843=CARTESIAN_POINT('Ctrl Pts',(183.705887881591,-2.18989270931988,
135.20817180609));
#203844=CARTESIAN_POINT('Ctrl Pts',(183.698141548325,-2.06702966934689,
135.269268175567));
#203845=CARTESIAN_POINT('Ctrl Pts',(183.69039521506,-1.94160860959151,135.325218614004));
#203846=CARTESIAN_POINT('Ctrl Pts',(183.682648881795,-1.81410273528698,
135.375817095356));
#203847=CARTESIAN_POINT('Ctrl Pts',(183.674900813792,-1.68656830692579,
135.426426907886));
#203848=CARTESIAN_POINT('Ctrl Pts',(183.667152745789,-1.55694849830684,
135.471682234208));
#203849=CARTESIAN_POINT('Ctrl Pts',(183.659404677786,-1.4257346415192,135.511425923515));
#203850=CARTESIAN_POINT('Ctrl Pts',(183.651648375044,-1.29438132908304,
135.551211852889));
#203851=CARTESIAN_POINT('Ctrl Pts',(183.643892072302,-1.1614309589586,135.585474330078));
#203852=CARTESIAN_POINT('Ctrl Pts',(183.63613576956,-1.02738865306596,135.614106517097));
#203853=CARTESIAN_POINT('Ctrl Pts',(183.628375327046,-0.893274804758753,
135.642753985975));
#203854=CARTESIAN_POINT('Ctrl Pts',(183.620614884532,-0.758068244641496,
135.665765111291));
#203855=CARTESIAN_POINT('Ctrl Pts',(183.612854442018,-0.622281340493539,
135.683084733129));
#203856=CARTESIAN_POINT('Ctrl Pts',(183.605081541752,-0.486276459152402,
135.700432157962));
#203857=CARTESIAN_POINT('Ctrl Pts',(183.597308641487,-0.349689761885385,
135.712069788455));
#203858=CARTESIAN_POINT('Ctrl Pts',(183.589535741221,-0.213036659942975,
135.717994552244));
#203859=CARTESIAN_POINT('Ctrl Pts',(183.582045405459,-0.0813512424637309,
135.723703935946));
#203860=CARTESIAN_POINT('Ctrl Pts',(183.574555069697,0.0503955275397817,
135.724108595028));
#203861=CARTESIAN_POINT('Ctrl Pts',(183.567064733935,0.181747024582314,
135.719251367273));
#203862=CARTESIAN_POINT('Ctrl Pts',(183.559290399816,0.318078753557754,
135.714209976251));
#203863=CARTESIAN_POINT('Ctrl Pts',(183.551516065697,0.45441650227473,135.703483843342));
#203864=CARTESIAN_POINT('Ctrl Pts',(183.543741731578,0.590247502080792,
135.687063859499));
#203865=CARTESIAN_POINT('Ctrl Pts',(183.535976978631,0.725911102318697,
135.67066411182));
#203866=CARTESIAN_POINT('Ctrl Pts',(183.528212225684,0.861068811846414,
135.648584521738));
#203867=CARTESIAN_POINT('Ctrl Pts',(183.520447472737,0.995208524915738,
135.620867967756));
#203868=CARTESIAN_POINT('Ctrl Pts',(183.512690431852,1.12921500853146,135.593178942246));
#203869=CARTESIAN_POINT('Ctrl Pts',(183.504933390967,1.26220512740057,135.559864173125));
#203870=CARTESIAN_POINT('Ctrl Pts',(183.497176350082,1.39367291584853,135.521018212318));
#203871=CARTESIAN_POINT('Ctrl Pts',(183.489425158842,1.52504156341419,135.482201545552));
#203872=CARTESIAN_POINT('Ctrl Pts',(183.481673967602,1.65488979216254,135.43786209979));
#203873=CARTESIAN_POINT('Ctrl Pts',(183.473922776362,1.78272318884635,135.388145199595));
#203874=CARTESIAN_POINT('Ctrl Pts',(183.466174879585,1.91050225292687,135.33844943041));
#203875=CARTESIAN_POINT('Ctrl Pts',(183.458426982807,2.0362678245576,135.283380894017));
#203876=CARTESIAN_POINT('Ctrl Pts',(183.45067908603,2.15954219920582,135.223134265576));
#203877=CARTESIAN_POINT('Ctrl Pts',(183.442932809946,2.28279078751236,135.162900239432));
#203878=CARTESIAN_POINT('Ctrl Pts',(183.435186533862,2.40354886430429,135.097490447235));
#203879=CARTESIAN_POINT('Ctrl Pts',(183.427440257778,2.52136057482751,135.027146891367));
#203880=CARTESIAN_POINT('Ctrl Pts',(183.419693924513,2.63917315501009,134.95680281624));
#203881=CARTESIAN_POINT('Ctrl Pts',(183.411947591247,2.7540389898437,134.881525105199));
#203882=CARTESIAN_POINT('Ctrl Pts',(183.404201257982,2.86552896479428,134.8016005171));
#203883=CARTESIAN_POINT('Ctrl Pts',(183.396453189979,2.97704390715139,134.721658030443));
#203884=CARTESIAN_POINT('Ctrl Pts',(183.388705121976,3.08518116758142,134.637066823728));
#203885=CARTESIAN_POINT('Ctrl Pts',(183.380957053973,3.18954295366573,134.548155324708));
#203886=CARTESIAN_POINT('Ctrl Pts',(183.373200751231,3.29401565669837,134.459149329488));
#203887=CARTESIAN_POINT('Ctrl Pts',(183.36544444849,3.3947045716674,134.36581412358));
#203888=CARTESIAN_POINT('Ctrl Pts',(183.357688145748,3.49124678201167,134.268516931821));
#203889=CARTESIAN_POINT('Ctrl Pts',(183.349927703234,3.58784051984049,134.171167809621));
#203890=CARTESIAN_POINT('Ctrl Pts',(183.342167260719,3.68028287962462,134.069852776656));
#203891=CARTESIAN_POINT('Ctrl Pts',(183.334406818205,3.76825050646584,133.964973087171));
#203892=CARTESIAN_POINT('Ctrl Pts',(183.32663391794,3.85635934675105,133.859925035496));
#203893=CARTESIAN_POINT('Ctrl Pts',(183.318861017674,3.93997886106847,133.751301202296));
#203894=CARTESIAN_POINT('Ctrl Pts',(183.311088117409,4.01882787217965,133.639533556964));
#203895=CARTESIAN_POINT('Ctrl Pts',(183.303597781647,4.094810523129,133.531828947063));
#203896=CARTESIAN_POINT('Ctrl Pts',(183.296107445885,4.16636332155617,133.421205386315));
#203897=CARTESIAN_POINT('Ctrl Pts',(183.288617110123,4.23327549087247,133.308070201539));
#203898=CARTESIAN_POINT('Ctrl Pts',(183.280842776004,4.3027246554253,133.190645461847));
#203899=CARTESIAN_POINT('Ctrl Pts',(183.273068441885,4.36739433944492,133.070142915728));
#203900=CARTESIAN_POINT('Ctrl Pts',(183.265294107765,4.42699971525186,132.94698904631));
#203901=CARTESIAN_POINT('Ctrl Pts',(183.257529354818,4.48653163276008,132.823986953029));
#203902=CARTESIAN_POINT('Ctrl Pts',(183.249764601871,4.5410114917085,132.698340386375));
#203903=CARTESIAN_POINT('Ctrl Pts',(183.241999848924,4.59019856132849,132.570503372294));
#203904=CARTESIAN_POINT('Ctrl Pts',(183.234242808039,4.63933677765773,132.442793327737));
#203905=CARTESIAN_POINT('Ctrl Pts',(183.226485767154,4.6831925265859,132.312897527787));
#203906=CARTESIAN_POINT('Ctrl Pts',(183.218728726269,4.72157187051949,132.181292763323));
#203907=CARTESIAN_POINT('Ctrl Pts',(183.210977535029,4.75992227229126,132.049787243035));
#203908=CARTESIAN_POINT('Ctrl Pts',(183.203226343789,4.79280438017088,131.91657569721));
#203909=CARTESIAN_POINT('Ctrl Pts',(183.195475152549,4.82007321739351,131.782152641192));
#203910=CARTESIAN_POINT('Ctrl Pts',(183.187727255772,4.84733046463286,131.647786718558));
#203911=CARTESIAN_POINT('Ctrl Pts',(183.179979358994,4.86897910880454,131.512210692235));
#203912=CARTESIAN_POINT('Ctrl Pts',(183.172231462217,4.88492472466578,131.375931695254));
#203913=CARTESIAN_POINT('Ctrl Pts',(183.164485186133,4.90086700504792,131.239681204901));
#203914=CARTESIAN_POINT('Ctrl Pts',(183.156738910049,4.91110858455677,131.102728424444));
#203915=CARTESIAN_POINT('Ctrl Pts',(183.148992633965,4.91560666602142,130.965587685597));
#203916=CARTESIAN_POINT('Ctrl Pts',(183.1412463007,4.92010478068989,130.828445934408));
#203917=CARTESIAN_POINT('Ctrl Pts',(183.133499967434,4.91885929989721,130.691116612814));
#203918=CARTESIAN_POINT('Ctrl Pts',(183.125753634169,4.91187953510186,130.554115747194));
#203919=CARTESIAN_POINT('Ctrl Pts',(183.118005566166,4.90489820723658,130.417084201179));
#203920=CARTESIAN_POINT('Ctrl Pts',(183.110257498163,4.89218005994142,130.280381647888));
#203921=CARTESIAN_POINT('Ctrl Pts',(183.10250943016,4.87378639226766,130.144520284571));
#203922=CARTESIAN_POINT('Ctrl Pts',(183.094753127418,4.85537317558499,130.00851452618));
#203923=CARTESIAN_POINT('Ctrl Pts',(183.086996824676,4.83127244146896,129.873352131727));
#203924=CARTESIAN_POINT('Ctrl Pts',(183.079240521934,4.80159698130756,129.739536927184));
#203925=CARTESIAN_POINT('Ctrl Pts',(183.07148007942,4.77190568245958,129.605650301438));
#203926=CARTESIAN_POINT('Ctrl Pts',(183.063719636906,4.73663382932912,129.473112675974));
#203927=CARTESIAN_POINT('Ctrl Pts',(183.055959194392,4.69594422725383,129.342412986144));
#203928=CARTESIAN_POINT('Ctrl Pts',(183.048186294126,4.65518930661703,129.211503485568));
#203929=CARTESIAN_POINT('Ctrl Pts',(183.040413393861,4.6089993893674,129.082438184816));
#203930=CARTESIAN_POINT('Ctrl Pts',(183.032640493595,4.55758592042437,128.955687136269));
#203931=CARTESIAN_POINT('Ctrl Pts',(183.025150157833,4.50804146058063,128.833543807605));
#203932=CARTESIAN_POINT('Ctrl Pts',(183.017659822071,4.453646761226,128.713549675095));
#203933=CARTESIAN_POINT('Ctrl Pts',(183.010169486309,4.39463058805635,128.596102241148));
#203934=CARTESIAN_POINT('Ctrl Pts',(183.00239515219,4.33337679874275,128.474201752045));
#203935=CARTESIAN_POINT('Ctrl Pts',(182.994620818071,4.26695013774061,128.354658745723));
#203936=CARTESIAN_POINT('Ctrl Pts',(182.986846483952,4.19555546106626,128.237943380323));
#203937=CARTESIAN_POINT('Ctrl Pts',(182.979081731005,4.1242487719503,128.121371856181));
#203938=CARTESIAN_POINT('Ctrl Pts',(182.971316978058,4.0479864514346,128.007621369533));
#203939=CARTESIAN_POINT('Ctrl Pts',(182.963552225111,3.96702036354612,127.897139866108));
#203940=CARTESIAN_POINT('Ctrl Pts',(182.955795184226,3.88613469231738,127.786768094469));
#203941=CARTESIAN_POINT('Ctrl Pts',(182.948038143341,3.80055478051184,127.679659158082));
#203942=CARTESIAN_POINT('Ctrl Pts',(182.940281102456,3.71057693779105,127.576233939253));
#203943=CARTESIAN_POINT('Ctrl Pts',(182.932529911216,3.62066694806208,127.472886714187));
#203944=CARTESIAN_POINT('Ctrl Pts',(182.924778719976,3.52636588431209,127.373217971168));
#203945=CARTESIAN_POINT('Ctrl Pts',(182.917027528736,3.42801143282299,127.277616980876));
#203946=CARTESIAN_POINT('Ctrl Pts',(182.909279631959,3.3296987845988,127.182056623554));
#203947=CARTESIAN_POINT('Ctrl Pts',(182.901531735182,3.22733645491275,127.090560852235));
#203948=CARTESIAN_POINT('Ctrl Pts',(182.893783838404,3.12130006999723,127.003483227339));
#203949=CARTESIAN_POINT('Ctrl Pts',(182.88603756232,3.01528586560767,126.916423817206));
#203950=CARTESIAN_POINT('Ctrl Pts',(182.878291286236,2.90559943659399,126.833780963214));
#203951=CARTESIAN_POINT('Ctrl Pts',(182.870545010152,2.79265037187774,126.75586868069));
#203952=CARTESIAN_POINT('Ctrl Pts',(182.862798676887,2.67970047339745,126.677955823035));
#203953=CARTESIAN_POINT('Ctrl Pts',(182.855052343622,2.5634882129824,126.604773828524));
#203954=CARTESIAN_POINT('Ctrl Pts',(182.847306010356,2.4444527713082,126.536593788023));
#203955=CARTESIAN_POINT('Ctrl Pts',(182.839557942353,2.32539067247181,126.468398479076));
#203956=CARTESIAN_POINT('Ctrl Pts',(182.83180987435,2.2035044734996,126.405207547392));
#203957=CARTESIAN_POINT('Ctrl Pts',(182.824061806347,2.07925823407926,126.34724627547));
#203958=CARTESIAN_POINT('Ctrl Pts',(182.816305503605,1.9548799442771,126.289223401619));
#203959=CARTESIAN_POINT('Ctrl Pts',(182.808549200864,1.82813695834241,126.236441456072));
#203960=CARTESIAN_POINT('Ctrl Pts',(182.800792898122,1.69951412583694,126.189077874485));
#203961=CARTESIAN_POINT('Ctrl Pts',(182.793032455608,1.57082264345299,126.141689013529));
#203962=CARTESIAN_POINT('Ctrl Pts',(182.785272013093,1.44024968730915,126.099724398543));
#203963=CARTESIAN_POINT('Ctrl Pts',(182.777511570579,1.3082946128271,126.063311338287));
#203964=CARTESIAN_POINT('Ctrl Pts',(182.769738670314,1.17612771234498,126.026839824555));
#203965=CARTESIAN_POINT('Ctrl Pts',(182.761965770048,1.04257464097785,125.995937762452));
#203966=CARTESIAN_POINT('Ctrl Pts',(182.754192869783,0.908145158251714,
125.970681332172));
#203967=CARTESIAN_POINT('Ctrl Pts',(182.746702534021,0.778602525828482,
125.94634303675));
#203968=CARTESIAN_POINT('Ctrl Pts',(182.739212198259,0.64824640006857,125.927247078214));
#203969=CARTESIAN_POINT('Ctrl Pts',(182.731721862497,0.517534864453755,
125.913415849265));
#203970=CARTESIAN_POINT('Ctrl Pts',(182.723947528378,0.381867361238935,
125.899060205066));
#203971=CARTESIAN_POINT('Ctrl Pts',(182.716173194259,0.245387211553195,
125.890330921351));
#203972=CARTESIAN_POINT('Ctrl Pts',(182.708398860139,0.108600702437423,
125.88730977891));
#203973=CARTESIAN_POINT('Ctrl Pts',(182.700634107192,-0.0280172295310573,
125.884292359757));
#203974=CARTESIAN_POINT('Ctrl Pts',(182.692869354245,-0.164940382578901,
125.886969093325));
#203975=CARTESIAN_POINT('Ctrl Pts',(182.685104601298,-0.301655748620083,
125.895370204882));
#203976=CARTESIAN_POINT('Ctrl Pts',(182.677347560413,-0.438235327031179,
125.903762972337));
#203977=CARTESIAN_POINT('Ctrl Pts',(182.669590519528,-0.57460714143116,
125.91786877949));
#203978=CARTESIAN_POINT('Ctrl Pts',(182.661833478643,-0.710256929006805,
125.937665829797));
#203979=CARTESIAN_POINT('Ctrl Pts',(182.654082287403,-0.845804422024122,
125.957447950995));
#203980=CARTESIAN_POINT('Ctrl Pts',(182.646331096163,-0.980630586681961,
125.982912716527));
#203981=CARTESIAN_POINT('Ctrl Pts',(182.638579904923,-1.11422539084784,
126.013986431671));
#203982=CARTESIAN_POINT('Ctrl Pts',(182.630832008146,-1.24776341365743,
126.045046939657));
#203983=CARTESIAN_POINT('Ctrl Pts',(182.623084111369,-1.38007073689753,
126.081711567367));
#203984=CARTESIAN_POINT('Ctrl Pts',(182.615336214591,-1.51064686501784,
126.123855397858));
#203985=CARTESIAN_POINT('Ctrl Pts',(182.607589938507,-1.64119567942685,
126.165990412768));
#203986=CARTESIAN_POINT('Ctrl Pts',(182.599843662423,-1.7700136471794,126.213602230732));
#203987=CARTESIAN_POINT('Ctrl Pts',(182.592097386339,-1.89661518547082,
126.266515985944));
#203988=CARTESIAN_POINT('Ctrl Pts',(182.584351053074,-2.02321765830595,
126.319430131753));
#203989=CARTESIAN_POINT('Ctrl Pts',(182.576604719809,-2.14760330830669,
126.37764614214));
#203990=CARTESIAN_POINT('Ctrl Pts',(182.568858386543,-2.26930667116602,
126.440941053199));
#203991=CARTESIAN_POINT('Ctrl Pts',(182.56111031854,-2.39103728865015,126.504250138715));
#203992=CARTESIAN_POINT('Ctrl Pts',(182.553362250537,-2.51008407691616,
126.572640207808));
#203993=CARTESIAN_POINT('Ctrl Pts',(182.545614182534,-2.62600666382235,
126.645842604612));
#203994=CARTESIAN_POINT('Ctrl Pts',(182.537857879792,-2.74205245463323,
126.719122801795));
#203995=CARTESIAN_POINT('Ctrl Pts',(182.53010157705,-2.85496708005182,126.797225334571));
#203996=CARTESIAN_POINT('Ctrl Pts',(182.522345274309,-2.96433918540366,
126.879838193579));
#203997=CARTESIAN_POINT('Ctrl Pts',(182.514584831794,-3.07376966594129,
126.962495145556));
#203998=CARTESIAN_POINT('Ctrl Pts',(182.50682438928,-3.17965355724597,127.049666972136));
#203999=CARTESIAN_POINT('Ctrl Pts',(182.499063946766,-3.28161383704965,
127.141002364953));
#204000=CARTESIAN_POINT('Ctrl Pts',(182.491291046501,-3.38373779254603,
127.232484377452));
#204001=CARTESIAN_POINT('Ctrl Pts',(182.483518146235,-3.4819252698745,127.328143039421));
#204002=CARTESIAN_POINT('Ctrl Pts',(182.47574524597,-3.57583663900372,127.427590652991));
#204003=CARTESIAN_POINT('Ctrl Pts',(182.468254910208,-3.66633409331571,
127.523423095313));
#204004=CARTESIAN_POINT('Ctrl Pts',(182.460764574446,-3.75286073415508,
127.622773563756));
#204005=CARTESIAN_POINT('Ctrl Pts',(182.453274238684,-3.83515011659531,
127.725268763516));
#204006=CARTESIAN_POINT('Ctrl Pts',(182.445516365561,-3.92037868426403,
127.831424853274));
#204007=CARTESIAN_POINT('Ctrl Pts',(182.437758492438,-4.00133819468862,
127.941298988973));
#204008=CARTESIAN_POINT('Ctrl Pts',(182.430000619315,-4.07768537362654,
128.054512429718));
#204009=CARTESIAN_POINT('Ctrl Pts',(182.422064270311,-4.15578897855251,
128.170330433359));
#204010=CARTESIAN_POINT('Ctrl Pts',(182.414127921308,-4.22906513008165,
128.289642999518));
#204011=CARTESIAN_POINT('Ctrl Pts',(182.406191572305,-4.29718794017761,
128.4120063651));
#204012=CARTESIAN_POINT('Ctrl Pts',(182.398453166183,-4.36361167865667,
128.53131782896));
#204013=CARTESIAN_POINT('Ctrl Pts',(182.390714760061,-4.42513586114829,
128.653529356966));
#204014=CARTESIAN_POINT('Ctrl Pts',(182.382976353939,-4.48150092218885,
128.778198593709));
#204015=CARTESIAN_POINT('Ctrl Pts',(182.374941033495,-4.54002865001674,
128.907651255019));
#204016=CARTESIAN_POINT('Ctrl Pts',(182.366905713051,-4.5929932099943,129.039753638606));
#204017=CARTESIAN_POINT('Ctrl Pts',(182.358870392607,-4.64015582391395,
129.173981216231));
#204018=CARTESIAN_POINT('Ctrl Pts',(182.350835072163,-4.68731843783359,
129.308208793856));
#204019=CARTESIAN_POINT('Ctrl Pts',(182.342799751719,-4.72867891245574,
129.444561130289));
#204020=CARTESIAN_POINT('Ctrl Pts',(182.334764431275,-4.76405452823405,
129.582490119308));
#204021=CARTESIAN_POINT('',(184.360140563971,-4.91824943376093,130.802000573005));
#204022=CARTESIAN_POINT('Ctrl Pts',(184.360140563971,-4.91824943376093,
130.802000573005));
#204023=CARTESIAN_POINT('Ctrl Pts',(184.352455145915,-4.9183142156431,130.937003725306));
#204024=CARTESIAN_POINT('Ctrl Pts',(184.344769727858,-4.9128161630471,131.072233610613));
#204025=CARTESIAN_POINT('Ctrl Pts',(184.337084309801,-4.90172557734377,
131.207187412745));
#204026=CARTESIAN_POINT('Ctrl Pts',(184.329407784764,-4.89064782487823,
131.341985055925));
#204027=CARTESIAN_POINT('Ctrl Pts',(184.321731259727,-4.87399044269163,
131.476506855924));
#204028=CARTESIAN_POINT('Ctrl Pts',(184.314054734689,-4.85177572413915,
131.610248565828));
#204029=CARTESIAN_POINT('Ctrl Pts',(184.306385156566,-4.82958110892026,
131.743869245425));
#204030=CARTESIAN_POINT('Ctrl Pts',(184.298715578444,-4.80183922716559,
131.876710846574));
#204031=CARTESIAN_POINT('Ctrl Pts',(184.291046000321,-4.76862425691908,
132.008273304941));
#204032=CARTESIAN_POINT('Ctrl Pts',(184.283267874699,-4.73493919537421,
132.141697766086));
#204033=CARTESIAN_POINT('Ctrl Pts',(184.275489749077,-4.69562496363401,
132.273806182506));
#204034=CARTESIAN_POINT('Ctrl Pts',(184.267711623456,-4.65081294627124,
132.404086219441));
#204035=CARTESIAN_POINT('Ctrl Pts',(184.260049224998,-4.606667666365,132.532427879451));
#204036=CARTESIAN_POINT('Ctrl Pts',(184.252386826541,-4.55718721851533,
132.658994805512));
#204037=CARTESIAN_POINT('Ctrl Pts',(184.244724428084,-4.50254756195381,
132.783311985044));
#204038=CARTESIAN_POINT('Ctrl Pts',(184.237062723623,-4.44791285419833,
132.90761790496));
#204039=CARTESIAN_POINT('Ctrl Pts',(184.229401019162,-4.38812002801154,
133.029674116977));
#204040=CARTESIAN_POINT('Ctrl Pts',(184.221739314701,-4.32339297491415,
133.149026104787));
#204041=CARTESIAN_POINT('Ctrl Pts',(184.214076556531,-4.25865701995485,
133.268394506983));
#204042=CARTESIAN_POINT('Ctrl Pts',(184.206413798362,-4.18898567966582,
133.385057593469));
#204043=CARTESIAN_POINT('Ctrl Pts',(184.198751040193,-4.11464827331411,
133.498586415344));
#204044=CARTESIAN_POINT('Ctrl Pts',(184.190886035627,-4.0383488485568,133.615111651125));
#204045=CARTESIAN_POINT('Ctrl Pts',(184.183021031061,-3.95713386805491,
133.728334497134));
#204046=CARTESIAN_POINT('Ctrl Pts',(184.175156026495,-3.87134055205237,
133.837824873583));
#204047=CARTESIAN_POINT('Ctrl Pts',(184.167481864777,-3.78762899462731,
133.944658486767));
#204048=CARTESIAN_POINT('Ctrl Pts',(184.159807703058,-3.69955904336469,
134.047938419428));
#204049=CARTESIAN_POINT('Ctrl Pts',(184.15213354134,-3.60748270613891,134.147301177523));
#204050=CARTESIAN_POINT('Ctrl Pts',(184.14417311535,-3.51197170509786,134.25037040006));
#204051=CARTESIAN_POINT('Ctrl Pts',(184.136212689361,-3.41214997576047,
134.34922420526));
#204052=CARTESIAN_POINT('Ctrl Pts',(184.128252263371,-3.30844873692504,
134.443502002239));
#204053=CARTESIAN_POINT('Ctrl Pts',(184.120291837381,-3.2047474980896,134.537779799218));
#204054=CARTESIAN_POINT('Ctrl Pts',(184.112331411392,-3.09716715988707,
134.627481342045));
#204055=CARTESIAN_POINT('Ctrl Pts',(184.104370985402,-2.98617212354664,
134.712296020186));
#204056=CARTESIAN_POINT('Ctrl Pts',(184.096596651283,-2.87777183200501,
134.795127975026));
#204057=CARTESIAN_POINT('Ctrl Pts',(184.088822317164,-2.76575077820207,
134.873577418346));
#204058=CARTESIAN_POINT('Ctrl Pts',(184.081047983045,-2.65049881953031,
134.947311144687));
#204059=CARTESIAN_POINT('Ctrl Pts',(184.073283230098,-2.53538889859732,
135.020954000799));
#204060=CARTESIAN_POINT('Ctrl Pts',(184.065518477151,-2.41705632156664,
135.089892494809));
#204061=CARTESIAN_POINT('Ctrl Pts',(184.057753724204,-2.29592350409848,
135.153833956469));
#204062=CARTESIAN_POINT('Ctrl Pts',(184.049996683319,-2.17491099745172,
135.217711910569));
#204063=CARTESIAN_POINT('Ctrl Pts',(184.042239642434,-2.05110412867136,
135.27660252783));
#204064=CARTESIAN_POINT('Ctrl Pts',(184.034482601549,-1.92495344569139,
135.330256914922));
#204065=CARTESIAN_POINT('Ctrl Pts',(184.026731410308,-1.79889789392326,
135.383870840824));
#204066=CARTESIAN_POINT('Ctrl Pts',(184.018980219068,-1.67050240435444,
135.432256243768));
#204067=CARTESIAN_POINT('Ctrl Pts',(184.011229027828,-1.54024090802878,
135.475210755146));
#204068=CARTESIAN_POINT('Ctrl Pts',(184.003481131051,-1.41003477631391,
135.518147009712));
#204069=CARTESIAN_POINT('Ctrl Pts',(183.995733234274,-1.27796458578426,
135.55565684151));
#204070=CARTESIAN_POINT('Ctrl Pts',(183.987985337497,-1.14452276743259,
135.587586589369));
#204071=CARTESIAN_POINT('Ctrl Pts',(183.980239061413,-1.01110886223263,
135.619509658213));
#204072=CARTESIAN_POINT('Ctrl Pts',(183.972492785329,-0.876324279891128,
135.645854873884));
#204073=CARTESIAN_POINT('Ctrl Pts',(183.964746509245,-0.740674697423658,
135.666518991693));
#204074=CARTESIAN_POINT('Ctrl Pts',(183.957000175979,-0.605024113621508,
135.68718326204));
#204075=CARTESIAN_POINT('Ctrl Pts',(183.949253842714,-0.468508903458449,
135.702166291965));
#204076=CARTESIAN_POINT('Ctrl Pts',(183.941507509448,-0.331642581234947,
135.711416380527));
#204077=CARTESIAN_POINT('Ctrl Pts',(183.933759441445,-0.194745608747665,
135.720668540583));
#204078=CARTESIAN_POINT('Ctrl Pts',(183.926011373442,-0.0574977577378105,
135.724185178199));
#204079=CARTESIAN_POINT('Ctrl Pts',(183.918263305439,0.0795851196291304,
135.721966668403));
#204080=CARTESIAN_POINT('Ctrl Pts',(183.910507002698,0.216813690309234,
135.719745800749));
#204081=CARTESIAN_POINT('Ctrl Pts',(183.902750699956,0.353876545556638,
135.711777615836));
#204082=CARTESIAN_POINT('Ctrl Pts',(183.894994397214,0.490260064193617,
135.698114609335));
#204083=CARTESIAN_POINT('Ctrl Pts',(183.8872339547,0.626716374821129,135.684444310477));
#204084=CARTESIAN_POINT('Ctrl Pts',(183.879473512186,0.762492239505508,
135.665073188767));
#204085=CARTESIAN_POINT('Ctrl Pts',(183.871713069671,0.89708291638147,135.640105162477));
#204086=CARTESIAN_POINT('Ctrl Pts',(183.863940169406,1.03188965016026,135.615097055295));
#204087=CARTESIAN_POINT('Ctrl Pts',(183.856167269141,1.16550701288779,135.58447417673));
#204088=CARTESIAN_POINT('Ctrl Pts',(183.848394368875,1.29744326874112,135.548390974435));
#204089=CARTESIAN_POINT('Ctrl Pts',(183.840904033113,1.42458330936598,135.513619487432));
#204090=CARTESIAN_POINT('Ctrl Pts',(183.833413697351,1.55016205245454,135.473777870507));
#204091=CARTESIAN_POINT('Ctrl Pts',(183.825923361589,1.67375775862039,135.42904633964));
#204092=CARTESIAN_POINT('Ctrl Pts',(183.81814902747,1.80203963355247,135.382618799184));
#204093=CARTESIAN_POINT('Ctrl Pts',(183.810374693351,1.92859148786851,135.330776154368));
#204094=CARTESIAN_POINT('Ctrl Pts',(183.802600359232,2.05292225893399,135.273666297565));
#204095=CARTESIAN_POINT('Ctrl Pts',(183.794835606285,2.17709980343563,135.216626823557));
#204096=CARTESIAN_POINT('Ctrl Pts',(183.787070853338,2.29906135920444,135.154333215077));
#204097=CARTESIAN_POINT('Ctrl Pts',(183.779306100391,2.41833236849072,135.086982666966));
#204098=CARTESIAN_POINT('Ctrl Pts',(183.771549059506,2.53748491612928,135.019699012369));
#204099=CARTESIAN_POINT('Ctrl Pts',(183.763792018621,2.65395189702597,134.947368604385));
#204100=CARTESIAN_POINT('Ctrl Pts',(183.756034977736,2.76728037800997,134.870235968826));
#204101=CARTESIAN_POINT('Ctrl Pts',(183.748283786496,2.88052339710438,134.793161499588));
#204102=CARTESIAN_POINT('Ctrl Pts',(183.740532595256,2.99063230529288,134.711292230035));
#204103=CARTESIAN_POINT('Ctrl Pts',(183.732781404016,3.09718067282804,134.624917506602));
#204104=CARTESIAN_POINT('Ctrl Pts',(183.725033507239,3.20368375446525,134.53857949473));
#204105=CARTESIAN_POINT('Ctrl Pts',(183.717285610461,3.30662900226592,134.447740083331));
#204106=CARTESIAN_POINT('Ctrl Pts',(183.709537713684,3.4056209657537,134.352730510928));
#204107=CARTESIAN_POINT('Ctrl Pts',(183.7017914376,3.50459222225675,134.25774081248));
#204108=CARTESIAN_POINT('Ctrl Pts',(183.694045161516,3.59961155738863,134.158582958646));
#204109=CARTESIAN_POINT('Ctrl Pts',(183.686298885432,3.6903187776887,134.055626583546));
#204110=CARTESIAN_POINT('Ctrl Pts',(183.678552552167,3.78102666756886,133.952669448445));
#204111=CARTESIAN_POINT('Ctrl Pts',(183.670806218901,3.86742212064859,133.845914029478));
#204112=CARTESIAN_POINT('Ctrl Pts',(183.663059885636,3.94918407243948,133.73576441515));
#204113=CARTESIAN_POINT('Ctrl Pts',(183.655311817633,4.03096433425261,133.625590133579));
#204114=CARTESIAN_POINT('Ctrl Pts',(183.64756374963,4.10810879701171,133.512020457994));
#204115=CARTESIAN_POINT('Ctrl Pts',(183.639815681627,4.18033894554159,133.395489592142));
#204116=CARTESIAN_POINT('Ctrl Pts',(183.632059378885,4.25264586113286,133.278834875899));
#204117=CARTESIAN_POINT('Ctrl Pts',(183.624303076144,4.32002782270208,133.159213015378));
#204118=CARTESIAN_POINT('Ctrl Pts',(183.616546773402,4.38225137155276,133.037084509816));
#204119=CARTESIAN_POINT('Ctrl Pts',(183.608786330888,4.444508130985,132.914890820593));
#204120=CARTESIAN_POINT('Ctrl Pts',(183.601025888373,4.50160082904401,132.790188175812));
#204121=CARTESIAN_POINT('Ctrl Pts',(183.593265445859,4.55334406980649,132.663457399463));
#204122=CARTESIAN_POINT('Ctrl Pts',(183.585492545594,4.60517037341259,132.53652318362));
#204123=CARTESIAN_POINT('Ctrl Pts',(183.577719645328,4.65162992673136,132.407554698248));
#204124=CARTESIAN_POINT('Ctrl Pts',(183.569946745063,4.69258687572239,132.277049137348));
#204125=CARTESIAN_POINT('Ctrl Pts',(183.562456409301,4.73205493645361,132.15128778231));
#204126=CARTESIAN_POINT('Ctrl Pts',(183.554966073539,4.7664134338327,132.024099462039));
#204127=CARTESIAN_POINT('Ctrl Pts',(183.547475737777,4.79558602822751,131.895936408965));
#204128=CARTESIAN_POINT('Ctrl Pts',(183.539701403658,4.82586471040535,131.762914014781));
#204129=CARTESIAN_POINT('Ctrl Pts',(183.531927069538,4.85065239351974,131.62842013976));
#204130=CARTESIAN_POINT('Ctrl Pts',(183.524152735419,4.86980807226552,131.492947868245));
#204131=CARTESIAN_POINT('Ctrl Pts',(183.516387982472,4.88894014334924,131.357642554197));
#204132=CARTESIAN_POINT('Ctrl Pts',(183.508623229525,4.90245396625799,131.221361626208));
#204133=CARTESIAN_POINT('Ctrl Pts',(183.500858476578,4.91025893654111,131.084610931782));
#204134=CARTESIAN_POINT('Ctrl Pts',(183.493101435693,4.91805615481771,130.947996060074));
#204135=CARTESIAN_POINT('Ctrl Pts',(183.485344394808,4.92015578211555,130.810912738245));
#204136=CARTESIAN_POINT('Ctrl Pts',(183.477587353923,4.91651872348393,130.673874203975));
#204137=CARTESIAN_POINT('Ctrl Pts',(183.469836162683,4.9128844075865,130.536939011528));
#204138=CARTESIAN_POINT('Ctrl Pts',(183.462084971443,4.90352202688916,130.40004892866));
#204139=CARTESIAN_POINT('Ctrl Pts',(183.454333780202,4.88844452104653,130.263719121609));
#204140=CARTESIAN_POINT('Ctrl Pts',(183.446585883425,4.87337342354616,130.127447258364));
#204141=CARTESIAN_POINT('Ctrl Pts',(183.438837986648,4.85259207504386,129.991735585091));
#204142=CARTESIAN_POINT('Ctrl Pts',(183.431090089871,4.82616540524861,129.857095847989));
#204143=CARTESIAN_POINT('Ctrl Pts',(183.423343813787,4.79974426334297,129.722484274618));
#204144=CARTESIAN_POINT('Ctrl Pts',(183.415597537703,4.76768022423145,129.588944574821));
#204145=CARTESIAN_POINT('Ctrl Pts',(183.407851261619,4.73008957820223,129.45697958583));
#204146=CARTESIAN_POINT('Ctrl Pts',(183.400104928353,4.69249865468751,129.325013622703));
#204147=CARTESIAN_POINT('Ctrl Pts',(183.392358595088,4.64938114995637,129.194622769583));
#204148=CARTESIAN_POINT('Ctrl Pts',(183.384612261823,4.60090349191246,129.066295566825));
#204149=CARTESIAN_POINT('Ctrl Pts',(183.37686419382,4.55241497763291,128.937939626078));
#204150=CARTESIAN_POINT('Ctrl Pts',(183.369116125817,4.49856405958199,128.811648620967));
#204151=CARTESIAN_POINT('Ctrl Pts',(183.361368057814,4.43956550141456,128.687891571927));
#204152=CARTESIAN_POINT('Ctrl Pts',(183.353611755072,4.38050423887763,128.564002992422));
#204153=CARTESIAN_POINT('Ctrl Pts',(183.34585545233,4.31628457587822,128.44265410226));
#204154=CARTESIAN_POINT('Ctrl Pts',(183.338099149588,4.24716775333799,128.324290227939));
#204155=CARTESIAN_POINT('Ctrl Pts',(183.330338707074,4.17801404106853,128.205863179254));
#204156=CARTESIAN_POINT('Ctrl Pts',(183.32257826456,4.10395817211934,128.090424649892));
#204157=CARTESIAN_POINT('Ctrl Pts',(183.314817822046,4.02530446630552,127.978390515806));
#204158=CARTESIAN_POINT('Ctrl Pts',(183.30704492178,3.94652449858048,127.866176534582));
#204159=CARTESIAN_POINT('Ctrl Pts',(183.299272021515,3.86313218266577,127.757378179998));
#204160=CARTESIAN_POINT('Ctrl Pts',(183.291499121249,3.77547238952982,127.652378495409));
#204161=CARTESIAN_POINT('Ctrl Pts',(183.284008785487,3.69099925067666,127.551195813834));
#204162=CARTESIAN_POINT('Ctrl Pts',(183.276518449725,3.60256372176028,127.453540643053));
#204163=CARTESIAN_POINT('Ctrl Pts',(183.269028113963,3.51050501529534,127.359721652437));
#204164=CARTESIAN_POINT('Ctrl Pts',(183.261253779844,3.41495587499346,127.262345486275));
#204165=CARTESIAN_POINT('Ctrl Pts',(183.253479445725,3.31520071706981,127.168793681802));
#204166=CARTESIAN_POINT('Ctrl Pts',(183.245705111606,3.21157817053554,127.079451394908));
#204167=CARTESIAN_POINT('Ctrl Pts',(183.237940358659,3.10808332952903,126.990219214398));
#204168=CARTESIAN_POINT('Ctrl Pts',(183.230175605712,3.00073087651156,126.905186482029));
#204169=CARTESIAN_POINT('Ctrl Pts',(183.222410852765,2.88989742139538,126.824702848824));
#204170=CARTESIAN_POINT('Ctrl Pts',(183.21465381188,2.77917404762878,126.744299153096));
#204171=CARTESIAN_POINT('Ctrl Pts',(183.206896770995,2.66497686641319,126.668435793291));
#204172=CARTESIAN_POINT('Ctrl Pts',(183.19913973011,2.54771654736785,126.597423078599));
#204173=CARTESIAN_POINT('Ctrl Pts',(183.19138853887,2.43054465524129,126.526463915148));
#204174=CARTESIAN_POINT('Ctrl Pts',(183.18363734763,2.31031455614051,126.460348317669));
#204175=CARTESIAN_POINT('Ctrl Pts',(183.175886156389,2.18746666821171,126.3993438596));
#204176=CARTESIAN_POINT('Ctrl Pts',(183.168138259612,2.0646709939127,126.338365330053));
#204177=CARTESIAN_POINT('Ctrl Pts',(183.160390362835,1.93926009315588,126.282493792761));
#204178=CARTESIAN_POINT('Ctrl Pts',(183.152642466058,1.811699608605,126.231951231839));
#204179=CARTESIAN_POINT('Ctrl Pts',(183.144896189974,1.68416580695755,126.181419243332));
#204180=CARTESIAN_POINT('Ctrl Pts',(183.13714991389,1.55448367913088,126.136214157909));
#204181=CARTESIAN_POINT('Ctrl Pts',(183.129403637806,1.42313913406825,126.096509933062));
#204182=CARTESIAN_POINT('Ctrl Pts',(183.121657304541,1.29179361945,126.056805415127));
#204183=CARTESIAN_POINT('Ctrl Pts',(183.113910971275,1.15878603734873,126.022601951924));
#204184=CARTESIAN_POINT('Ctrl Pts',(183.10616463801,1.02461736894711,125.994023590938));
#204185=CARTESIAN_POINT('Ctrl Pts',(183.098416570007,0.890418654402585,
125.965438830026));
#204186=CARTESIAN_POINT('Ctrl Pts',(183.090668502004,0.755058718467256,
125.942481759427));
#204187=CARTESIAN_POINT('Ctrl Pts',(183.082920434001,0.619048246319054,
125.925225209399));
#204188=CARTESIAN_POINT('Ctrl Pts',(183.075164131259,0.482893220622485,
125.907950318904));
#204189=CARTESIAN_POINT('Ctrl Pts',(183.067407828517,0.346086666046123,
125.896388100937));
#204190=CARTESIAN_POINT('Ctrl Pts',(183.059651525776,0.209144455485154,
125.890559475961));
#204191=CARTESIAN_POINT('Ctrl Pts',(183.051891083261,0.0721291547430187,
125.884727740072));
#204192=CARTESIAN_POINT('Ctrl Pts',(183.044130640747,-0.065021555480375,
125.884635695128));
#204193=CARTESIAN_POINT('Ctrl Pts',(183.036370198233,-0.201793294674736,
125.890252099358));
#204194=CARTESIAN_POINT('Ctrl Pts',(183.028597297968,-0.338784592006899,
125.895877519539));
#204195=CARTESIAN_POINT('Ctrl Pts',(183.020824397702,-0.475395312770501,
125.907229668511));
#204196=CARTESIAN_POINT('Ctrl Pts',(183.013051497437,-0.611116780560397,
125.92422544085));
#204197=CARTESIAN_POINT('Ctrl Pts',(183.005561161675,-0.74190443113344,
125.940603374055));
#204198=CARTESIAN_POINT('Ctrl Pts',(182.998070825913,-0.87186605558637,
125.96222168399));
#204199=CARTESIAN_POINT('Ctrl Pts',(182.990580490151,-1.00055860898726,
125.988961824892));
#204200=CARTESIAN_POINT('Ctrl Pts',(182.982806156032,-1.13413057966649,
126.016715826365));
#204201=CARTESIAN_POINT('Ctrl Pts',(182.975031821913,-1.26675846180681,
126.050075630492));
#204202=CARTESIAN_POINT('Ctrl Pts',(182.967257487794,-1.39793517559902,
126.088964525261));
#204203=CARTESIAN_POINT('Ctrl Pts',(182.959492734846,-1.52895022581513,
126.127805492943));
#204204=CARTESIAN_POINT('Ctrl Pts',(182.951727981899,-1.65851729489495,
126.172161883161));
#204205=CARTESIAN_POINT('Ctrl Pts',(182.943963228952,-1.78613864467428,
126.221905838247));
#204206=CARTESIAN_POINT('Ctrl Pts',(182.936206188067,-1.91363323913031,
126.271600386936));
#204207=CARTESIAN_POINT('Ctrl Pts',(182.928449147182,-2.03918559816484,
126.326671710685));
#204208=CARTESIAN_POINT('Ctrl Pts',(182.920692106297,-2.16231267290643,
126.386942031209));
#204209=CARTESIAN_POINT('Ctrl Pts',(182.912940915057,-2.28534689656263,
126.447166901416));
#204210=CARTESIAN_POINT('Ctrl Pts',(182.905189723817,-2.40595912655983,
126.512582793482));
#204211=CARTESIAN_POINT('Ctrl Pts',(182.897438532577,-2.52368618902095,
126.582963801127));
#204212=CARTESIAN_POINT('Ctrl Pts',(182.8896906358,-2.64136321434017,126.653314894965));
#204213=CARTESIAN_POINT('Ctrl Pts',(182.881942739023,-2.75615717621927,
126.728626706948));
#204214=CARTESIAN_POINT('Ctrl Pts',(182.874194842245,-2.86762962189981,
126.808627466553));
#204215=CARTESIAN_POINT('Ctrl Pts',(182.866448566161,-2.97907874994782,
126.888611491724));
#204216=CARTESIAN_POINT('Ctrl Pts',(182.858702290077,-3.08720742634127,
126.973282285786));
#204217=CARTESIAN_POINT('Ctrl Pts',(182.850956013993,-3.1916066500627,127.062325068059));
#204218=CARTESIAN_POINT('Ctrl Pts',(182.843209680728,-3.29600664443559,
127.151368507625));
#204219=CARTESIAN_POINT('Ctrl Pts',(182.835463347462,-3.39667683373769,
127.24478374609));
#204220=CARTESIAN_POINT('Ctrl Pts',(182.827717014197,-3.49324206073987,
127.342216344492));
#204221=CARTESIAN_POINT('Ctrl Pts',(182.819968946194,-3.58982891285543,
127.43967076225));
#204222=CARTESIAN_POINT('Ctrl Pts',(182.812220878191,-3.68230869825185,
127.541144052529));
#204223=CARTESIAN_POINT('Ctrl Pts',(182.804472810188,-3.77034410495834,
127.64624592796));
#204224=CARTESIAN_POINT('Ctrl Pts',(182.796716507446,-3.85847307674226,
127.751459506914));
#204225=CARTESIAN_POINT('Ctrl Pts',(182.788960204704,-3.94214798261169,
127.860309074608));
#204226=CARTESIAN_POINT('Ctrl Pts',(182.781203901962,-4.02107237968682,
127.972371920586));
#204227=CARTESIAN_POINT('Ctrl Pts',(182.773443459448,-4.10003890108901,
128.08449457788));
#204228=CARTESIAN_POINT('Ctrl Pts',(182.765683016934,-4.17424965007582,
128.19983360216));
#204229=CARTESIAN_POINT('Ctrl Pts',(182.75792257442,-4.24345287600184,128.317939343596));
#204230=CARTESIAN_POINT('Ctrl Pts',(182.750149674154,-4.31276719308979,
128.436234678853));
#204231=CARTESIAN_POINT('Ctrl Pts',(182.742376773889,-4.37705774012523,
128.557305261059));
#204232=CARTESIAN_POINT('Ctrl Pts',(182.734603873624,-4.43611948403242,
128.680678205837));
#204233=CARTESIAN_POINT('Ctrl Pts',(182.727113537862,-4.49303418478051,
128.799566233313));
#204234=CARTESIAN_POINT('Ctrl Pts',(182.7196232021,-4.54509352087592,128.920591853246));
#204235=CARTESIAN_POINT('Ctrl Pts',(182.712132866338,-4.59215775161795,
129.043318242507));
#204236=CARTESIAN_POINT('Ctrl Pts',(182.703253522123,-4.64794957700628,
129.188803023033));
#204237=CARTESIAN_POINT('Ctrl Pts',(182.694374177909,-4.69687000701748,
129.337061417581));
#204238=CARTESIAN_POINT('Ctrl Pts',(182.685494833695,-4.73867041310273,
129.487475740865));
#204239=CARTESIAN_POINT('Ctrl Pts',(182.683630675656,-4.74744612459306,
129.519054206932));
#204240=CARTESIAN_POINT('Ctrl Pts',(182.681766517617,-4.75590817585868,
129.550727615035));
#204241=CARTESIAN_POINT('Ctrl Pts',(182.679902359578,-4.76405452823405,
129.582490119308));
#204242=CARTESIAN_POINT('Ctrl Pts',(184.430229652623,-4.76405452823406,
129.582490119308));
#204243=CARTESIAN_POINT('Ctrl Pts',(184.422327812055,-4.7986868585295,129.717521049511));
#204244=CARTESIAN_POINT('Ctrl Pts',(184.414425971487,-4.82753715525285,
129.853882584735));
#204245=CARTESIAN_POINT('Ctrl Pts',(184.406524130919,-4.85053490297993,
129.991037669732));
#204246=CARTESIAN_POINT('Ctrl Pts',(184.398622290351,-4.873532650707,130.128192754729));
#204247=CARTESIAN_POINT('Ctrl Pts',(184.390720449783,-4.89067785997628,
130.266140963835));
#204248=CARTESIAN_POINT('Ctrl Pts',(184.382818609216,-4.90195570679255,
130.404343978982));
#204249=CARTESIAN_POINT('Ctrl Pts',(184.375259260813,-4.91274473405513,
130.536556813798));
#204250=CARTESIAN_POINT('Ctrl Pts',(184.367699912411,-4.91818571452675,
130.669211977639));
#204251=CARTESIAN_POINT('Ctrl Pts',(184.360140564008,-4.91824943376062,
130.802000572364));
#204252=CARTESIAN_POINT('Origin',(213.235140564004,0.,130.804360617566));
#204253=CARTESIAN_POINT('',(186.18020938313,-4.76405452823405,129.582490119308));
#204254=CARTESIAN_POINT('',(185.834939443695,-4.76405452823405,129.582490119308));
#204255=CARTESIAN_POINT('',(213.235140564004,-4.76405452823405,129.582490119308));
#204256=CARTESIAN_POINT('',(185.764859435953,-4.91824909926408,130.801384027568));
#204257=CARTESIAN_POINT('Ctrl Pts',(185.834939443695,-4.76405452823405,
129.582490119308));
#204258=CARTESIAN_POINT('Ctrl Pts',(185.82716587756,-4.79810227029313,129.71524174885));
#204259=CARTESIAN_POINT('Ctrl Pts',(185.819392311426,-4.82655888961819,
129.849268541578));
#204260=CARTESIAN_POINT('Ctrl Pts',(185.811618745292,-4.84935969226982,
129.984059674321));
#204261=CARTESIAN_POINT('Ctrl Pts',(185.805961071674,-4.8659543281669,130.082161912396));
#204262=CARTESIAN_POINT('Ctrl Pts',(185.800303398056,-4.87955412703471,
130.180668865511));
#204263=CARTESIAN_POINT('Ctrl Pts',(185.794645724439,-4.8901515047038,130.279383167057));
#204264=CARTESIAN_POINT('Ctrl Pts',(185.784716961623,-4.90874905140923,
130.45261883826));
#204265=CARTESIAN_POINT('Ctrl Pts',(185.774788198807,-4.91814347496568,
130.626859993452));
#204266=CARTESIAN_POINT('Ctrl Pts',(185.764859435991,-4.91824909926368,
130.801384026903));
#204267=CARTESIAN_POINT('Ctrl Pts',(185.764859435953,-4.91824909926409,
130.801384027568));
#204268=CARTESIAN_POINT('Ctrl Pts',(185.757191235898,-4.9183306751947,130.936172744721));
#204269=CARTESIAN_POINT('Ctrl Pts',(185.749523035843,-4.91286708241096,
131.071183771682));
#204270=CARTESIAN_POINT('Ctrl Pts',(185.741854835789,-4.901829924088,131.205915667111));
#204271=CARTESIAN_POINT('Ctrl Pts',(185.734195115826,-4.89080497151269,
131.340498565537));
#204272=CARTESIAN_POINT('Ctrl Pts',(185.726535395862,-4.87421874451201,
131.474802549089));
#204273=CARTESIAN_POINT('Ctrl Pts',(185.718875675899,-4.85209485286721,
131.608324921052));
#204274=CARTESIAN_POINT('Ctrl Pts',(185.711222480037,-4.82998980505673,
131.741733566484));
#204275=CARTESIAN_POINT('Ctrl Pts',(185.703569284174,-4.80235654064527,
131.874361530089));
#204276=CARTESIAN_POINT('Ctrl Pts',(185.695916088312,-4.76927054522506,
132.00571049539));
#204277=CARTESIAN_POINT('Ctrl Pts',(185.688267001704,-4.73620231477376,
132.136988935073));
#204278=CARTESIAN_POINT('Ctrl Pts',(185.680617915096,-4.69768727340913,
132.266989353296));
#204279=CARTESIAN_POINT('Ctrl Pts',(185.672968828489,-4.65385205465889,
132.395223313039));
#204280=CARTESIAN_POINT('Ctrl Pts',(185.665321809995,-4.61002868781017,
132.523422601658));
#204281=CARTESIAN_POINT('Ctrl Pts',(185.657674791501,-4.56088813315632,
132.649856001177));
#204282=CARTESIAN_POINT('Ctrl Pts',(185.650027773007,-4.50660683515309,
132.774050414425));
#204283=CARTESIAN_POINT('Ctrl Pts',(185.642381064432,-4.4523277370657,132.898239794315));
#204284=CARTESIAN_POINT('Ctrl Pts',(185.634734355857,-4.39290847102935,
133.020189999991));
#204285=CARTESIAN_POINT('Ctrl Pts',(185.627087647282,-4.3285733387234,133.139448606014));
#204286=CARTESIAN_POINT('Ctrl Pts',(185.619439490905,-4.26422602542105,
133.258729792058));
#204287=CARTESIAN_POINT('Ctrl Pts',(185.611791334528,-4.19496118620005,
133.37531801141));
#204288=CARTESIAN_POINT('Ctrl Pts',(185.604143178151,-4.12104844176228,
133.488786590311));
#204289=CARTESIAN_POINT('Ctrl Pts',(185.596487235631,-4.04706045105567,
133.602370684977));
#204290=CARTESIAN_POINT('Ctrl Pts',(185.58883129311,-3.96841532550673,133.71282845947));
#204291=CARTESIAN_POINT('Ctrl Pts',(185.58117535059,-3.88542548694373,133.819763053048));
#204292=CARTESIAN_POINT('Ctrl Pts',(185.573515374056,-3.80239191997511,
133.926753991828));
#204293=CARTESIAN_POINT('Ctrl Pts',(185.565855397521,-3.71500934088863,
134.03021774658));
#204294=CARTESIAN_POINT('Ctrl Pts',(185.558195420987,-3.62362875719401,
134.129792573348));
#204295=CARTESIAN_POINT('Ctrl Pts',(185.550523572136,-3.5321065413066,134.229521732694));
#204296=CARTESIAN_POINT('Ctrl Pts',(185.542851723284,-3.43657422762343,
134.325349640552));
#204297=CARTESIAN_POINT('Ctrl Pts',(185.535179874433,-3.33741822988249,
134.416952847717));
#204298=CARTESIAN_POINT('Ctrl Pts',(185.528852616497,-3.25564060551483,
134.492501405919));
#204299=CARTESIAN_POINT('Ctrl Pts',(185.522525358561,-3.17139888835135,
134.56517703643));
#204300=CARTESIAN_POINT('Ctrl Pts',(185.516198100626,-3.08492473413098,
134.634820439473));
#204301=CARTESIAN_POINT('Ctrl Pts',(185.508423766507,-2.97867349948799,
134.720391644243));
#204302=CARTESIAN_POINT('Ctrl Pts',(185.500649432388,-2.86869084610792,
134.801674161477));
#204303=CARTESIAN_POINT('Ctrl Pts',(185.492875098269,-2.75535800148616,
134.878324945606));
#204304=CARTESIAN_POINT('Ctrl Pts',(185.485110345321,-2.64216482946666,
134.954881264495));
#204305=CARTESIAN_POINT('Ctrl Pts',(185.477345592374,-2.52563000205102,
135.026816990961));
#204306=CARTESIAN_POINT('Ctrl Pts',(185.469580839427,-2.4061683288018,135.093828770609));
#204307=CARTESIAN_POINT('Ctrl Pts',(185.461823798542,-2.28682530657056,
135.160773993213));
#204308=CARTESIAN_POINT('Ctrl Pts',(185.454066757657,-2.16456156231129,
135.222804811345));
#204309=CARTESIAN_POINT('Ctrl Pts',(185.446309716772,-2.03982114582494,
135.279660915372));
#204310=CARTESIAN_POINT('Ctrl Pts',(185.438558525532,-1.91517479705691,
135.33647414377));
#204311=CARTESIAN_POINT('Ctrl Pts',(185.430807334292,-1.78805584787562,
135.388120263844));
#204312=CARTESIAN_POINT('Ctrl Pts',(185.423056143052,-1.65893291082312,
135.434384878829));
#204313=CARTESIAN_POINT('Ctrl Pts',(185.415308246275,-1.52986485446345,
135.480629830119));
#204314=CARTESIAN_POINT('Ctrl Pts',(185.407560349498,-1.39879487157781,
135.521497693954));
#204315=CARTESIAN_POINT('Ctrl Pts',(185.399812452721,-1.2662113115785,135.556822293049));
#204316=CARTESIAN_POINT('Ctrl Pts',(185.392066176637,-1.13365548520171,
135.592139502999));
#204317=CARTESIAN_POINT('Ctrl Pts',(185.384319900553,-0.999587089008202,
135.62191565399));
#204318=CARTESIAN_POINT('Ctrl Pts',(185.376573624468,-0.864509000677892,
135.646034630782));
#204319=CARTESIAN_POINT('Ctrl Pts',(185.368827291203,-0.729429915231751,
135.670153785614));
#204320=CARTESIAN_POINT('Ctrl Pts',(185.361080957938,-0.593341507654216,
135.688615614195));
#204321=CARTESIAN_POINT('Ctrl Pts',(185.353334624672,-0.456755805682509,
135.701355328251));
#204322=CARTESIAN_POINT('Ctrl Pts',(185.345586556669,-0.320139516289562,
135.714097895278));
#204323=CARTESIAN_POINT('Ctrl Pts',(185.337838488666,-0.183026100098795,
135.721115761585));
#204324=CARTESIAN_POINT('Ctrl Pts',(185.330090420663,-0.0459312508572161,
135.722396138248));
#204325=CARTESIAN_POINT('Ctrl Pts',(185.322334117922,0.0913093044211189,
135.723677875712));
#204326=CARTESIAN_POINT('Ctrl Pts',(185.31457781518,0.228530861759579,135.719209938718));
#204327=CARTESIAN_POINT('Ctrl Pts',(185.306821512438,0.365218627626155,
135.709031698947));
#204328=CARTESIAN_POINT('Ctrl Pts',(185.299061069924,0.501979347869056,
135.698848026743));
#204329=CARTESIAN_POINT('Ctrl Pts',(185.29130062741,0.638205320812515,135.682948024144));
#204330=CARTESIAN_POINT('Ctrl Pts',(185.283540184895,0.773389317112324,
135.661422695271));
#204331=CARTESIAN_POINT('Ctrl Pts',(185.27576728463,0.908790322764111,135.639862812028));
#204332=CARTESIAN_POINT('Ctrl Pts',(185.267994384365,1.04314562582757,135.612659634777));
#204333=CARTESIAN_POINT('Ctrl Pts',(185.260221484099,1.175959709326,135.57995501246));
#204334=CARTESIAN_POINT('Ctrl Pts',(185.252731148337,1.30394566635063,135.548439285542));
#204335=CARTESIAN_POINT('Ctrl Pts',(185.245240812575,1.43050021692963,135.511815237666));
#204336=CARTESIAN_POINT('Ctrl Pts',(185.237750476813,1.55519716015653,135.470252263923));
#204337=CARTESIAN_POINT('Ctrl Pts',(185.229976142694,1.68462202588672,135.427113417397));
#204338=CARTESIAN_POINT('Ctrl Pts',(185.222201808575,1.81245562030366,135.378517082239));
#204339=CARTESIAN_POINT('Ctrl Pts',(185.214427474456,1.93820326668134,135.324598571427));
#204340=CARTESIAN_POINT('Ctrl Pts',(185.206662721509,2.06379594032369,135.270746510361));
#204341=CARTESIAN_POINT('Ctrl Pts',(185.198897968562,2.18730742506553,135.211585476901));
#204342=CARTESIAN_POINT('Ctrl Pts',(185.191133215614,2.30825828556062,135.147300491619));
#204343=CARTESIAN_POINT('Ctrl Pts',(185.183376174729,2.42908901595603,135.083079355091));
#204344=CARTESIAN_POINT('Ctrl Pts',(185.175619133844,2.54736384028493,135.013744576743));
#204345=CARTESIAN_POINT('Ctrl Pts',(185.167862092959,2.66262373291742,134.939529044535));
#204346=CARTESIAN_POINT('Ctrl Pts',(185.160110901719,2.77779670716764,134.865369478838));
#204347=CARTESIAN_POINT('Ctrl Pts',(185.152359710479,2.8899589477656,134.786336696123));
#204348=CARTESIAN_POINT('Ctrl Pts',(185.144608519239,2.99867678011411,134.702709066705));
#204349=CARTESIAN_POINT('Ctrl Pts',(185.136860622462,3.107348404484,134.61911698126));
#204350=CARTESIAN_POINT('Ctrl Pts',(185.129112725685,3.21257822307831,134.530934171219));
#204351=CARTESIAN_POINT('Ctrl Pts',(185.121364828908,3.31396246145469,134.438481675892));
#204352=CARTESIAN_POINT('Ctrl Pts',(185.113618552824,3.41532549243393,134.346048519634));
#204353=CARTESIAN_POINT('Ctrl Pts',(185.10587227674,3.51284425451252,134.249347717836));
#204354=CARTESIAN_POINT('Ctrl Pts',(185.098126000655,3.60614923898019,134.148739592608));
#204355=CARTESIAN_POINT('Ctrl Pts',(185.09037966739,3.69945491220408,134.048130724714));
#204356=CARTESIAN_POINT('Ctrl Pts',(185.082633334125,3.78854647989511,133.943614762498));
#204357=CARTESIAN_POINT('Ctrl Pts',(185.074887000859,3.87309267034491,133.835587469753));
#204358=CARTESIAN_POINT('Ctrl Pts',(185.067138932856,3.95765779432756,133.727535985046));
#204359=CARTESIAN_POINT('Ctrl Pts',(185.059390864854,4.03767527464004,133.615971912911));
#204360=CARTESIAN_POINT('Ctrl Pts',(185.051642796851,4.11285560653182,133.501322208379));
#204361=CARTESIAN_POINT('Ctrl Pts',(185.043886494109,4.18811584097532,133.386550652776));
#204362=CARTESIAN_POINT('Ctrl Pts',(185.036130191367,4.2585284426082,133.268687241189));
#204363=CARTESIAN_POINT('Ctrl Pts',(185.028373888625,4.32384827746161,133.148186365354));
#204364=CARTESIAN_POINT('Ctrl Pts',(185.020613446111,4.38920297547765,133.027621174572));
#204365=CARTESIAN_POINT('Ctrl Pts',(185.012853003597,4.44945931886022,132.904416065631));
#204366=CARTESIAN_POINT('Ctrl Pts',(185.005092561082,4.50441970210254,132.779046974892));
#204367=CARTESIAN_POINT('Ctrl Pts',(184.997319660817,4.55946831263118,132.65347663056));
#204368=CARTESIAN_POINT('Ctrl Pts',(184.989546760552,4.6092038322925,132.525735727174));
#204369=CARTESIAN_POINT('Ctrl Pts',(184.981773860286,4.65347776358927,132.396317830019));
#204370=CARTESIAN_POINT('Ctrl Pts',(184.974283524524,4.69614222596426,132.271604599409));
#204371=CARTESIAN_POINT('Ctrl Pts',(184.966793188762,4.7337352030942,132.145334479326));
#204372=CARTESIAN_POINT('Ctrl Pts',(184.959302853,4.7661688398658,132.017957606847));
#204373=CARTESIAN_POINT('Ctrl Pts',(184.951528518881,4.79983220783342,131.885751201534));
#204374=CARTESIAN_POINT('Ctrl Pts',(184.943754184762,4.8280439150364,131.751933671931));
#204375=CARTESIAN_POINT('Ctrl Pts',(184.935979850643,4.85065041926304,131.616994343548));
#204376=CARTESIAN_POINT('Ctrl Pts',(184.928215097696,4.87322906299363,131.482221315828));
#204377=CARTESIAN_POINT('Ctrl Pts',(184.920450344748,4.8902161844549,131.346329622014));
#204378=CARTESIAN_POINT('Ctrl Pts',(184.912685591801,4.90150830017843,131.209822632781));
#204379=CARTESIAN_POINT('Ctrl Pts',(184.904928550916,4.91278920041345,131.073451224213));
#204380=CARTESIAN_POINT('Ctrl Pts',(184.897171510031,4.91838631929962,130.936466123495));
#204381=CARTESIAN_POINT('Ctrl Pts',(184.889414469146,4.91824747750727,130.799379403521));
#204382=CARTESIAN_POINT('Ctrl Pts',(184.881663277906,4.9181087404166,130.662396061707));
#204383=CARTESIAN_POINT('Ctrl Pts',(184.873912086666,4.91224265275202,130.525311642551));
#204384=CARTESIAN_POINT('Ctrl Pts',(184.866160895426,4.9006490036298,130.388641474728));
#204385=CARTESIAN_POINT('Ctrl Pts',(184.858412998649,4.88906028211778,130.252029395372));
#204386=CARTESIAN_POINT('Ctrl Pts',(184.850665101872,4.87174887389483,130.115831605913));
#204387=CARTESIAN_POINT('Ctrl Pts',(184.842917205095,4.84876662847558,129.980561342814));
#204388=CARTESIAN_POINT('Ctrl Pts',(184.835170929011,4.82578919044663,129.845319375338));
#204389=CARTESIAN_POINT('Ctrl Pts',(184.827424652926,4.7971433401164,129.711004933506));
#204390=CARTESIAN_POINT('Ctrl Pts',(184.819678376842,4.76293249819749,129.578123658363));
#204391=CARTESIAN_POINT('Ctrl Pts',(184.811932043577,4.72872140374189,129.445241402321));
#204392=CARTESIAN_POINT('Ctrl Pts',(184.804185710312,4.68894533320337,129.313792712696));
#204393=CARTESIAN_POINT('Ctrl Pts',(184.796439377046,4.64375819341888,129.184270217756));
#204394=CARTESIAN_POINT('Ctrl Pts',(184.788691309043,4.59856093428778,129.054718717152));
#204395=CARTESIAN_POINT('Ctrl Pts',(184.78094324104,4.54795032338664,128.927094638659));
#204396=CARTESIAN_POINT('Ctrl Pts',(184.773195173037,4.49212908568403,128.801872330446));
#204397=CARTESIAN_POINT('Ctrl Pts',(184.765438870295,4.43624852050568,128.676516934474));
#204398=CARTESIAN_POINT('Ctrl Pts',(184.757682567554,4.37514642537891,128.553568765596));
#204399=CARTESIAN_POINT('Ctrl Pts',(184.749926264812,4.30907259203993,128.433479671793));
#204400=CARTESIAN_POINT('Ctrl Pts',(184.742165822298,4.24296349310673,128.313326482825));
#204401=CARTESIAN_POINT('Ctrl Pts',(184.734405379783,4.17187757104574,128.196035743754));
#204402=CARTESIAN_POINT('Ctrl Pts',(184.726644937269,4.09610843399477,128.08203096092));
#204403=CARTESIAN_POINT('Ctrl Pts',(184.718872037004,4.02021766559842,127.967843167486));
#204404=CARTESIAN_POINT('Ctrl Pts',(184.711099136738,3.93962888900392,127.856952187687));
#204405=CARTESIAN_POINT('Ctrl Pts',(184.703326236473,3.85467708813893,127.749749740764));
#204406=CARTESIAN_POINT('Ctrl Pts',(184.695835900711,3.77281349921669,127.646444372814));
#204407=CARTESIAN_POINT('Ctrl Pts',(184.688345564949,3.68689879343445,127.546564252244));
#204408=CARTESIAN_POINT('Ctrl Pts',(184.680855229187,3.59726419602927,127.450426604133));
#204409=CARTESIAN_POINT('Ctrl Pts',(184.673080895068,3.50423107561896,127.350643867872));
#204410=CARTESIAN_POINT('Ctrl Pts',(184.665306560949,3.4068957149069,127.25457691618));
#204411=CARTESIAN_POINT('Ctrl Pts',(184.65753222683,3.30558680398728,127.162619420857));
#204412=CARTESIAN_POINT('Ctrl Pts',(184.649767473883,3.20440274724626,127.070775254929));
#204413=CARTESIAN_POINT('Ctrl Pts',(184.642002720936,3.09925517067157,126.983030728698));
#204414=CARTESIAN_POINT('Ctrl Pts',(184.634237967988,2.99051163892463,126.899744989882));
#204415=CARTESIAN_POINT('Ctrl Pts',(184.626480927103,2.88187611278586,126.816541971634));
#204416=CARTESIAN_POINT('Ctrl Pts',(184.618723886218,2.7696520474073,126.737789164012));
#204417=CARTESIAN_POINT('Ctrl Pts',(184.610966845333,2.65424206001439,126.663807254868));
#204418=CARTESIAN_POINT('Ctrl Pts',(184.603215654093,2.53891910419166,126.589881136058));
#204419=CARTESIAN_POINT('Ctrl Pts',(184.595464462853,2.42041533625422,126.52071896472));
#204420=CARTESIAN_POINT('Ctrl Pts',(184.587713271613,2.29916420282371,126.456599466013));
#204421=CARTESIAN_POINT('Ctrl Pts',(184.579965374836,2.17796460435902,126.392507219803));
#204422=CARTESIAN_POINT('Ctrl Pts',(184.572217478059,2.0540203077666,126.333453565807));
#204423=CARTESIAN_POINT('Ctrl Pts',(184.564469581282,1.92779113934713,126.279672298405));
#204424=CARTESIAN_POINT('Ctrl Pts',(184.556723305198,1.80158837534844,126.225902280884));
#204425=CARTESIAN_POINT('Ctrl Pts',(184.548977029114,1.67310204963539,126.177402609436));
#204426=CARTESIAN_POINT('Ctrl Pts',(184.54123075303,1.54281347376092,126.134359584624));
#204427=CARTESIAN_POINT('Ctrl Pts',(184.533484419764,1.41252393612583,126.091316242077));
#204428=CARTESIAN_POINT('Ctrl Pts',(184.525738086499,1.28043249301377,126.053729749183));
#204429=CARTESIAN_POINT('Ctrl Pts',(184.517991753233,1.14703679694263,126.021736897372));
#204430=CARTESIAN_POINT('Ctrl Pts',(184.51024368523,1.01361122783021,125.989736880984));
#204431=CARTESIAN_POINT('Ctrl Pts',(184.502495617228,0.878881204667642,
125.963333089485));
#204432=CARTESIAN_POINT('Ctrl Pts',(184.494747549225,0.743355387800147,
125.94261136139));
#204433=CARTESIAN_POINT('Ctrl Pts',(184.486991246483,0.607685532481822,
125.921867609995));
#204434=CARTESIAN_POINT('Ctrl Pts',(184.479234943741,0.471218581013933,
125.906818044672));
#204435=CARTESIAN_POINT('Ctrl Pts',(184.471478640999,0.334469704435209,
125.897496743429));
#204436=CARTESIAN_POINT('Ctrl Pts',(184.463718198485,0.197647840863254,
125.888170467126));
#204437=CARTESIAN_POINT('Ctrl Pts',(184.455957755971,0.0605441429922865,
125.88457855716));
#204438=CARTESIAN_POINT('Ctrl Pts',(184.448197313456,-0.0763263789303934,
125.886702908211));
#204439=CARTESIAN_POINT('Ctrl Pts',(184.440424413191,-0.213416617565448,
125.888830669458));
#204440=CARTESIAN_POINT('Ctrl Pts',(184.432651512926,-0.350272541705855,
125.896693006356));
#204441=CARTESIAN_POINT('Ctrl Pts',(184.42487861266,-0.486383519863692,
125.910219821256));
#204442=CARTESIAN_POINT('Ctrl Pts',(184.417388276898,-0.617546521122763,
125.923254902363));
#204443=CARTESIAN_POINT('Ctrl Pts',(184.409897941136,-0.748017492370623,
125.941549732693));
#204444=CARTESIAN_POINT('Ctrl Pts',(184.402407605374,-0.877350507831442,
125.964997110977));
#204445=CARTESIAN_POINT('Ctrl Pts',(184.394633271255,-1.01158722388324,
125.989333503735));
#204446=CARTESIAN_POINT('Ctrl Pts',(184.386858937136,-1.14502321111271,
126.019297965427));
#204447=CARTESIAN_POINT('Ctrl Pts',(184.379084603017,-1.27714959725893,
126.054826748993));
#204448=CARTESIAN_POINT('Ctrl Pts',(184.37131985007,-1.40911314944234,126.090311746508));
#204449=CARTESIAN_POINT('Ctrl Pts',(184.363555097123,-1.53976993792535,
126.131347320907));
#204450=CARTESIAN_POINT('Ctrl Pts',(184.355790344176,-1.66861912388403,
126.177818357745));
#204451=CARTESIAN_POINT('Ctrl Pts',(184.348033303291,-1.79734033501496,
126.224243238894));
#204452=CARTESIAN_POINT('Ctrl Pts',(184.340276262406,-1.92425715102514,
126.276092707283));
#204453=CARTESIAN_POINT('Ctrl Pts',(184.332519221521,-2.04888214369525,
126.333201369256));
#204454=CARTESIAN_POINT('Ctrl Pts',(184.32476803028,-2.17341315568864,126.390266965143));
#204455=CARTESIAN_POINT('Ctrl Pts',(184.31701683904,-2.29565543039551,126.452583698322));
#204456=CARTESIAN_POINT('Ctrl Pts',(184.3092656478,-2.41514017995914,126.51993755563));
#204457=CARTESIAN_POINT('Ctrl Pts',(184.301517751023,-2.5345741453172,126.587262785753));
#204458=CARTESIAN_POINT('Ctrl Pts',(184.293769854246,-2.65125257672636,
126.659620690311));
#204459=CARTESIAN_POINT('Ctrl Pts',(184.286021957469,-2.76473022900649,
126.736750775986));
#204460=CARTESIAN_POINT('Ctrl Pts',(184.278275681385,-2.87818414420808,
126.81386472771));
#204461=CARTESIAN_POINT('Ctrl Pts',(184.270529405301,-2.98843828887982,
126.895748655367));
#204462=CARTESIAN_POINT('Ctrl Pts',(184.262783129217,-3.09507576243218,
126.982098317919));
#204463=CARTESIAN_POINT('Ctrl Pts',(184.255036795951,-3.20171402315806,
127.068448617884));
#204464=CARTESIAN_POINT('Ctrl Pts',(184.247290462686,-3.30473525564962,
127.159264472488));
#204465=CARTESIAN_POINT('Ctrl Pts',(184.239544129421,-3.40375538006029,
127.254201131682));
#204466=CARTESIAN_POINT('Ctrl Pts',(184.231796061418,-3.50279767934135,
127.349159051283));
#204467=CARTESIAN_POINT('Ctrl Pts',(184.224047993415,-3.59783680540671,
127.448239341269));
#204468=CARTESIAN_POINT('Ctrl Pts',(184.216299925412,-3.6885255965423,127.551060449098));
#204469=CARTESIAN_POINT('Ctrl Pts',(184.20854362267,-3.77931077280425,127.653990836424));
#204470=CARTESIAN_POINT('Ctrl Pts',(184.200787319928,-3.86573611899577,
127.760669689976));
#204471=CARTESIAN_POINT('Ctrl Pts',(184.193031017186,-3.94749450179272,
127.870682001764));
#204472=CARTESIAN_POINT('Ctrl Pts',(184.185270574672,-4.02929652150032,
127.980753030435));
#204473=CARTESIAN_POINT('Ctrl Pts',(184.177510132158,-4.10642639472572,
128.094160739358));
#204474=CARTESIAN_POINT('Ctrl Pts',(184.169749689644,-4.17862097836977,
128.210462049459));
#204475=CARTESIAN_POINT('Ctrl Pts',(184.161976789378,-4.25093145516856,
128.326950056747));
#204476=CARTESIAN_POINT('Ctrl Pts',(184.154203889113,-4.31829061835359,
128.446340606829));
#204477=CARTESIAN_POINT('Ctrl Pts',(184.146430988847,-4.38048143426836,
128.568166201481));
#204478=CARTESIAN_POINT('Ctrl Pts',(184.138940653085,-4.44041145737599,
128.685563128908));
#204479=CARTESIAN_POINT('Ctrl Pts',(184.131450317323,-4.49554224537381,
128.805220854819));
#204480=CARTESIAN_POINT('Ctrl Pts',(184.123959981561,-4.54572295595053,
128.926706264325));
#204481=CARTESIAN_POINT('Ctrl Pts',(184.115260747627,-4.60400255170544,
129.067798737404));
#204482=CARTESIAN_POINT('Ctrl Pts',(184.106561513693,-4.65576212734771,
129.211734291794));
#204483=CARTESIAN_POINT('Ctrl Pts',(184.097862279759,-4.70074664434197,
129.357929130005));
#204484=CARTESIAN_POINT('Ctrl Pts',(184.093441289351,-4.72360798128571,
129.432226014336));
#204485=CARTESIAN_POINT('Ctrl Pts',(184.089020298944,-4.74472023587179,
129.507106006827));
#204486=CARTESIAN_POINT('Ctrl Pts',(184.084599308536,-4.76405452823405,
129.582490119308));
#204487=CARTESIAN_POINT('',(186.110140564058,-4.91824801325411,130.808781321355));
#204488=CARTESIAN_POINT('Ctrl Pts',(186.110140564008,-4.91824801325332,
130.808781322232));
#204489=CARTESIAN_POINT('Ctrl Pts',(186.099074116598,-4.91807260824191,
131.003927891408));
#204490=CARTESIAN_POINT('Ctrl Pts',(186.088007669188,-4.90627932088814,
131.198573828951));
#204491=CARTESIAN_POINT('Ctrl Pts',(186.076941221778,-4.88306599966,131.391599500359));
#204492=CARTESIAN_POINT('Ctrl Pts',(186.069128931883,-4.86667869954997,
131.527864775596));
#204493=CARTESIAN_POINT('Ctrl Pts',(186.061316641987,-4.84460109965971,
131.663323468629));
#204494=CARTESIAN_POINT('Ctrl Pts',(186.053504352092,-4.81691589639799,
131.797589850688));
#204495=CARTESIAN_POINT('Ctrl Pts',(186.045730017973,-4.78936520086549,
131.931203903559));
#204496=CARTESIAN_POINT('Ctrl Pts',(186.037955683854,-4.75620727242799,
132.063882400062));
#204497=CARTESIAN_POINT('Ctrl Pts',(186.030181349735,-4.71751805131938,
132.195118144231));
#204498=CARTESIAN_POINT('Ctrl Pts',(186.022416596788,-4.67887651121803,
132.326192152075));
#204499=CARTESIAN_POINT('Ctrl Pts',(186.014651843841,-4.63471735138709,
132.455826573993));
#204500=CARTESIAN_POINT('Ctrl Pts',(186.006887090894,-4.58516767187299,
132.583523477821));
#204501=CARTESIAN_POINT('Ctrl Pts',(185.999130050009,-4.53566720579912,
132.711093551284));
#204502=CARTESIAN_POINT('Ctrl Pts',(185.991373009124,-4.48078701513992,
132.83672957411));
#204503=CARTESIAN_POINT('Ctrl Pts',(185.983615968239,-4.42070414285521,
132.95994822744));
#204504=CARTESIAN_POINT('Ctrl Pts',(185.975864776998,-4.36066657953178,
133.083073960625));
#204505=CARTESIAN_POINT('Ctrl Pts',(185.968113585758,-4.29543431449837,
133.203785602808));
#204506=CARTESIAN_POINT('Ctrl Pts',(185.960362394518,-4.22523254890233,
133.321619636856));
#204507=CARTESIAN_POINT('Ctrl Pts',(185.952614497741,-4.15506062092945,
133.439403588296));
#204508=CARTESIAN_POINT('Ctrl Pts',(185.944866600964,-4.07992359302457,
133.554312029003));
#204509=CARTESIAN_POINT('Ctrl Pts',(185.937118704187,-4.0000925681456,133.665906093138));
#204510=CARTESIAN_POINT('Ctrl Pts',(185.929372428103,-3.92027824219608,
133.7774768142));
#204511=CARTESIAN_POINT('Ctrl Pts',(185.921626152019,-3.83577209961954,
133.885734219918));
#204512=CARTESIAN_POINT('Ctrl Pts',(185.913879875934,-3.74688829830369,
133.990268830703));
#204513=CARTESIAN_POINT('Ctrl Pts',(185.906133542669,-3.65800384086778,
134.09480421314));
#204514=CARTESIAN_POINT('Ctrl Pts',(185.898387209404,-3.56474191346714,
134.195616447958));
#204515=CARTESIAN_POINT('Ctrl Pts',(185.890640876138,-3.4674563837275,134.292329838968));
#204516=CARTESIAN_POINT('Ctrl Pts',(185.882892808135,-3.37014906756808,
134.389064888271));
#204517=CARTESIAN_POINT('Ctrl Pts',(185.875144740132,-3.26881663328405,
134.481698991651));
#204518=CARTESIAN_POINT('Ctrl Pts',(185.867396672129,-3.16384885446265,
134.569894243576));
#204519=CARTESIAN_POINT('Ctrl Pts',(185.859640369388,-3.05876951463674,
134.658183230465));
#204520=CARTESIAN_POINT('Ctrl Pts',(185.851884066646,-2.95004741195152,
134.742023689953));
#204521=CARTESIAN_POINT('Ctrl Pts',(185.844127763904,-2.83810480523698,
134.82111853621));
#204522=CARTESIAN_POINT('Ctrl Pts',(185.83636732139,-2.72610245138265,134.900255597768));
#204523=CARTESIAN_POINT('Ctrl Pts',(185.828606878875,-2.6108764967903,134.974641787181));
#204524=CARTESIAN_POINT('Ctrl Pts',(185.820846436361,-2.49287620764804,
135.044024669804));
#204525=CARTESIAN_POINT('Ctrl Pts',(185.813073536096,-2.3746864939661,135.11351893199));
#204526=CARTESIAN_POINT('Ctrl Pts',(185.80530063583,-2.25371389122609,135.177993653395));
#204527=CARTESIAN_POINT('Ctrl Pts',(185.797527735565,-2.13043097123238,
135.237243081529));
#204528=CARTESIAN_POINT('Ctrl Pts',(185.790037399803,-2.01162969591266,
135.294338643711));
#204529=CARTESIAN_POINT('Ctrl Pts',(185.782547064041,-1.89068344157314,
135.346582099913));
#204530=CARTESIAN_POINT('Ctrl Pts',(185.775056728279,-1.76802881817535,
135.393833044828));
#204531=CARTESIAN_POINT('Ctrl Pts',(185.76728239416,-1.64072370745012,135.442875523682));
#204532=CARTESIAN_POINT('Ctrl Pts',(185.759508060041,-1.51117486044447,
135.486694787618));
#204533=CARTESIAN_POINT('Ctrl Pts',(185.751733725922,-1.37985004303931,
135.525080575499));
#204534=CARTESIAN_POINT('Ctrl Pts',(185.743968972975,-1.24868707173481,
135.563419056326));
#204535=CARTESIAN_POINT('Ctrl Pts',(185.736204220028,-1.11575285660129,
135.596337276052));
#204536=CARTESIAN_POINT('Ctrl Pts',(185.728439467081,-0.981535022751411,
135.623673023046));
#204537=CARTESIAN_POINT('Ctrl Pts',(185.720682426196,-0.847450495946294,
135.650981619791));
#204538=CARTESIAN_POINT('Ctrl Pts',(185.712925385311,-0.712085268171024,
135.672718700269));
#204539=CARTESIAN_POINT('Ctrl Pts',(185.705168344426,-0.575941665315386,
135.688771970089));
#204540=CARTESIAN_POINT('Ctrl Pts',(185.697417153186,-0.439900729409612,
135.704813134013));
#204541=CARTESIAN_POINT('Ctrl Pts',(185.689665961946,-0.303082973473198,
135.715178973112));
#204542=CARTESIAN_POINT('Ctrl Pts',(185.681914770705,-0.166000094317469,
135.719808413158));
#204543=CARTESIAN_POINT('Ctrl Pts',(185.674166873928,-0.0289754790421877,
135.724435885568));
#204544=CARTESIAN_POINT('Ctrl Pts',(185.666418977151,0.108313645407252,
135.723331794998));
#204545=CARTESIAN_POINT('Ctrl Pts',(185.658671080374,0.245351511000205,
135.716487010336));
#204546=CARTESIAN_POINT('Ctrl Pts',(185.65092480429,0.382360711225824,135.709643657456));
#204547=CARTESIAN_POINT('Ctrl Pts',(185.643178528206,0.519118366904536,
135.697062018493));
#204548=CARTESIAN_POINT('Ctrl Pts',(185.635432252122,0.655110161251152,
135.678785069655));
#204549=CARTESIAN_POINT('Ctrl Pts',(185.627685918857,0.791102959458301,
135.660507985901));
#204550=CARTESIAN_POINT('Ctrl Pts',(185.619939585591,0.926329497570983,
135.636535560459));
#204551=CARTESIAN_POINT('Ctrl Pts',(185.612193252326,1.06028241764848,135.606962439217));
#204552=CARTESIAN_POINT('Ctrl Pts',(185.604445184323,1.19426533555364,135.577382695279));
#204553=CARTESIAN_POINT('Ctrl Pts',(185.59669711632,1.32697368617402,135.542199844023));
#204554=CARTESIAN_POINT('Ctrl Pts',(185.588949048317,1.45791249787162,135.501559166813));
#204555=CARTESIAN_POINT('Ctrl Pts',(185.581192745575,1.58899047289653,135.460875296208));
#204556=CARTESIAN_POINT('Ctrl Pts',(185.573436442833,1.71829477813514,135.414722128319));
#204557=CARTESIAN_POINT('Ctrl Pts',(185.565680140092,1.84534722565303,135.363294339312));
#204558=CARTESIAN_POINT('Ctrl Pts',(185.557919697577,1.97246748488773,135.311839101746));
#204559=CARTESIAN_POINT('Ctrl Pts',(185.550159255063,2.09733313577467,135.25510379514));
#204560=CARTESIAN_POINT('Ctrl Pts',(185.542398812549,2.21948895854959,135.193329952772));
#204561=CARTESIAN_POINT('Ctrl Pts',(185.534625912284,2.34184087669565,135.131456945548));
#204562=CARTESIAN_POINT('Ctrl Pts',(185.526853012018,2.46147393253308,135.064529430542));
#204563=CARTESIAN_POINT('Ctrl Pts',(185.519080111753,2.57795958406316,134.992833781553));
#204564=CARTESIAN_POINT('Ctrl Pts',(185.511589775991,2.69021068875094,134.923744449994));
#204565=CARTESIAN_POINT('Ctrl Pts',(185.504099440229,2.79953899281448,134.850227805036));
#204566=CARTESIAN_POINT('Ctrl Pts',(185.496609104467,2.90559037094153,134.772575286506));
#204567=CARTESIAN_POINT('Ctrl Pts',(185.488834770348,3.01566271930338,134.691978549134));
#204568=CARTESIAN_POINT('Ctrl Pts',(185.481060436228,3.12255342329199,134.606670817637));
#204569=CARTESIAN_POINT('Ctrl Pts',(185.473286102109,3.22583274537233,134.516931985417));
#204570=CARTESIAN_POINT('Ctrl Pts',(185.465521349162,3.32898478491854,134.427303748286));
#204571=CARTESIAN_POINT('Ctrl Pts',(185.457756596215,3.42853400584439,134.333255530036));
#204572=CARTESIAN_POINT('Ctrl Pts',(185.449991843268,3.52408036162776,134.235109904134));
#204573=CARTESIAN_POINT('Ctrl Pts',(185.442234802383,3.61953181942352,134.137061757852));
#204574=CARTESIAN_POINT('Ctrl Pts',(185.434477761498,3.71098805294843,134.034924580939));
#204575=CARTESIAN_POINT('Ctrl Pts',(185.426720720613,3.79808306633545,133.92906029653));
#204576=CARTESIAN_POINT('Ctrl Pts',(185.418969529373,3.88511240069542,133.823275845201));
#204577=CARTESIAN_POINT('Ctrl Pts',(185.411218338133,3.96778681374832,133.713770181484));
#204578=CARTESIAN_POINT('Ctrl Pts',(185.403467146893,4.0457783373907,133.600940798287));
#204579=CARTESIAN_POINT('Ctrl Pts',(185.395719250116,4.12373671255506,133.488159370587));
#204580=CARTESIAN_POINT('Ctrl Pts',(185.387971353338,4.19701593512668,133.372057354035));
#204581=CARTESIAN_POINT('Ctrl Pts',(185.380223456561,4.2653295376257,133.253063743296));
#204582=CARTESIAN_POINT('Ctrl Pts',(185.372477180477,4.33362885039174,133.134095023454));
#204583=CARTESIAN_POINT('Ctrl Pts',(185.364730904393,4.39696441458693,133.01223625137));
#204584=CARTESIAN_POINT('Ctrl Pts',(185.356984628309,4.45509438652842,132.887943366012));
#204585=CARTESIAN_POINT('Ctrl Pts',(185.349238295044,4.51322478757213,132.763649563153));
#204586=CARTESIAN_POINT('Ctrl Pts',(185.341491961778,4.56614935405513,132.636921965314));
#204587=CARTESIAN_POINT('Ctrl Pts',(185.333745628513,4.61367347488339,132.508238585514));
#204588=CARTESIAN_POINT('Ctrl Pts',(185.32599756051,4.661208238409,132.379526387963));
#204589=CARTESIAN_POINT('Ctrl Pts',(185.318249492507,4.70334001430907,132.248857903597));
#204590=CARTESIAN_POINT('Ctrl Pts',(185.310501424504,4.73992348764949,132.116728094201));
#204591=CARTESIAN_POINT('Ctrl Pts',(185.302745121762,4.77654584234074,131.98445785567));
#204592=CARTESIAN_POINT('Ctrl Pts',(185.29498881902,4.80760801048513,131.850723566987));
#204593=CARTESIAN_POINT('Ctrl Pts',(185.287232516278,4.83301530639473,131.716032768426));
#204594=CARTESIAN_POINT('Ctrl Pts',(185.279472073764,4.85843616294317,131.581270081331));
#204595=CARTESIAN_POINT('Ctrl Pts',(185.27171163125,4.87819607698591,131.445550253803));
#204596=CARTESIAN_POINT('Ctrl Pts',(185.263951188736,4.8922521999072,131.30938682976));
#204597=CARTESIAN_POINT('Ctrl Pts',(185.25617828847,4.90633088696485,131.173004824101));
#204598=CARTESIAN_POINT('Ctrl Pts',(185.248405388205,4.91468746198499,131.036178189385));
#204599=CARTESIAN_POINT('Ctrl Pts',(185.24063248794,4.91733122193595,130.899422262165));
#204600=CARTESIAN_POINT('Ctrl Pts',(185.233142152178,4.91987887455347,130.767637757367));
#204601=CARTESIAN_POINT('Ctrl Pts',(185.225651816415,4.91712185788959,130.635919216476));
#204602=CARTESIAN_POINT('Ctrl Pts',(185.218161480653,4.90911395514333,130.504722105494));
#204603=CARTESIAN_POINT('Ctrl Pts',(185.210387146534,4.90080243033051,130.368550616171));
#204604=CARTESIAN_POINT('Ctrl Pts',(185.202612812415,4.8868076562378,130.232509526972));
#204605=CARTESIAN_POINT('Ctrl Pts',(185.194838478296,4.86713283147692,130.097111677475));
#204606=CARTESIAN_POINT('Ctrl Pts',(185.187073725349,4.84748225417918,129.961880693727));
#204607=CARTESIAN_POINT('Ctrl Pts',(185.179308972402,4.82216561011635,129.827291755562));
#204608=CARTESIAN_POINT('Ctrl Pts',(185.171544219455,4.79123805456728,129.693855792288));
#204609=CARTESIAN_POINT('Ctrl Pts',(185.16378717857,4.76034121670238,129.560552359494));
#204610=CARTESIAN_POINT('Ctrl Pts',(185.156030137685,4.72384464525298,129.428400001093));
#204611=CARTESIAN_POINT('Ctrl Pts',(185.1482730968,4.68185500669668,129.297902268069));
#204612=CARTESIAN_POINT('Ctrl Pts',(185.14052190556,4.63989703285347,129.167502944401));
#204613=CARTESIAN_POINT('Ctrl Pts',(185.13277071432,4.59245435629693,129.038756133175));
#204614=CARTESIAN_POINT('Ctrl Pts',(185.12501952308,4.53968412429643,128.912152617871));
#204615=CARTESIAN_POINT('Ctrl Pts',(185.117271626302,4.48693632105218,128.785602912438));
#204616=CARTESIAN_POINT('Ctrl Pts',(185.109523729525,4.42886561609171,128.661195051217));
#204617=CARTESIAN_POINT('Ctrl Pts',(185.101775832748,4.36567809210519,128.539401929507));
#204618=CARTESIAN_POINT('Ctrl Pts',(185.094029556664,4.30250378558652,128.417634284293));
#204619=CARTESIAN_POINT('Ctrl Pts',(185.08628328058,4.23421496891706,128.298480637502));
#204620=CARTESIAN_POINT('Ctrl Pts',(185.078537004496,4.16106451404611,128.182390905223));
#204621=CARTESIAN_POINT('Ctrl Pts',(185.070790671231,4.08791351919513,128.066300315995));
#204622=CARTESIAN_POINT('Ctrl Pts',(185.063044337965,4.00990102295931,127.953274017186));
#204623=CARTESIAN_POINT('Ctrl Pts',(185.0552980047,3.92732399917947,127.843734118332));
#204624=CARTESIAN_POINT('Ctrl Pts',(185.047549936697,3.84472848284773,127.734169688777));
#204625=CARTESIAN_POINT('Ctrl Pts',(185.039801868694,3.75756664022695,127.628093524923));
#204626=CARTESIAN_POINT('Ctrl Pts',(185.032053800691,3.66617635041229,127.525895423275));
#204627=CARTESIAN_POINT('Ctrl Pts',(185.024297497949,3.57468892991002,127.423588704268));
#204628=CARTESIAN_POINT('Ctrl Pts',(185.016541195207,3.47896434590667,127.325168572807));
#204629=CARTESIAN_POINT('Ctrl Pts',(185.008784892466,3.37937842648236,127.230989028559));
#204630=CARTESIAN_POINT('Ctrl Pts',(185.001024449951,3.27973935505435,127.136759217851));
#204631=CARTESIAN_POINT('Ctrl Pts',(184.993264007437,3.17623513657302,127.046774760618));
#204632=CARTESIAN_POINT('Ctrl Pts',(184.985503564923,3.06927466935573,126.961349289642));
#204633=CARTESIAN_POINT('Ctrl Pts',(184.977730664658,2.96214249970095,126.875786686117));
#204634=CARTESIAN_POINT('Ctrl Pts',(184.969957764392,2.85154330970152,126.794797924641));
#204635=CARTESIAN_POINT('Ctrl Pts',(184.962184864127,2.73791569183312,126.718653735408));
#204636=CARTESIAN_POINT('Ctrl Pts',(184.954694528365,2.62841872408481,126.645277579249));
#204637=CARTESIAN_POINT('Ctrl Pts',(184.947204192603,2.51610995032003,126.576400046695));
#204638=CARTESIAN_POINT('Ctrl Pts',(184.939713856841,2.40140163811663,126.512222078918));
#204639=CARTESIAN_POINT('Ctrl Pts',(184.931939522722,2.28234412539138,126.445610783985));
#204640=CARTESIAN_POINT('Ctrl Pts',(184.924165188603,2.16032438692566,126.383851452082));
#204641=CARTESIAN_POINT('Ctrl Pts',(184.916390854484,2.03577561811003,126.327218594444));
#204642=CARTESIAN_POINT('Ctrl Pts',(184.908626101536,1.91138034452076,126.270655531741));
#204643=CARTESIAN_POINT('Ctrl Pts',(184.900861348589,1.78446259457604,126.2192065328));
#204644=CARTESIAN_POINT('Ctrl Pts',(184.893096595642,1.65548204034892,126.173101363693));
#204645=CARTESIAN_POINT('Ctrl Pts',(184.885339554757,1.5266295914267,126.12704198689));
#204646=CARTESIAN_POINT('Ctrl Pts',(184.877582513872,1.3957187812083,126.086316008371));
#204647=CARTESIAN_POINT('Ctrl Pts',(184.869825472987,1.26323091723401,126.051105868213));
#204648=CARTESIAN_POINT('Ctrl Pts',(184.862074281747,1.13084296338832,126.015922280296));
#204649=CARTESIAN_POINT('Ctrl Pts',(184.854323090507,0.996880699273993,
125.986246351446));
#204650=CARTESIAN_POINT('Ctrl Pts',(184.846571899267,0.861841976869711,
125.962211149674));
#204651=CARTESIAN_POINT('Ctrl Pts',(184.83882400249,0.726860649524842,125.938186163504));
#204652=CARTESIAN_POINT('Ctrl Pts',(184.831076105713,0.590804157979271,
125.919797204415));
#204653=CARTESIAN_POINT('Ctrl Pts',(184.823328208936,0.454181755168668,
125.907126500662));
#204654=CARTESIAN_POINT('Ctrl Pts',(184.815581932852,0.317587930819519,
125.894458447347));
#204655=CARTESIAN_POINT('Ctrl Pts',(184.807835656767,0.180428819710515,
125.88750630627));
#204656=CARTESIAN_POINT('Ctrl Pts',(184.800089380683,0.0432196324551924,
125.886300519736));
#204657=CARTESIAN_POINT('Ctrl Pts',(184.792343047418,-0.0939905676472747,
125.8850947243));
#204658=CARTESIAN_POINT('Ctrl Pts',(184.784596714153,-0.231250453683563,
125.889635371485));
#204659=CARTESIAN_POINT('Ctrl Pts',(184.776850380887,-0.368044371329767,
125.899900769302));
#204660=CARTESIAN_POINT('Ctrl Pts',(184.769102312884,-0.504868923025204,
125.910168465984));
#204661=CARTESIAN_POINT('Ctrl Pts',(184.761354244881,-0.641226908890993,
125.926163435116));
#204662=CARTESIAN_POINT('Ctrl Pts',(184.753606176878,-0.77660775018482,
125.947812103976));
#204663=CARTESIAN_POINT('Ctrl Pts',(184.745849874136,-0.912132475847942,
125.969483781299));
#204664=CARTESIAN_POINT('Ctrl Pts',(184.738093571395,-1.04667759570581,
125.996821099783));
#204665=CARTESIAN_POINT('Ctrl Pts',(184.730337268653,-1.17974213555564,
126.029699210084));
#204666=CARTESIAN_POINT('Ctrl Pts',(184.722576826139,-1.312877695957,126.062594868424));
#204667=CARTESIAN_POINT('Ctrl Pts',(184.714816383624,-1.44453072664021,
126.101037101697));
#204668=CARTESIAN_POINT('Ctrl Pts',(184.70705594111,-1.57421633993268,126.144851418349));
#204669=CARTESIAN_POINT('Ctrl Pts',(184.699283040845,-1.70411013608448,
126.188736069632));
#204670=CARTESIAN_POINT('Ctrl Pts',(184.691510140579,-1.83202983856468,
126.238009896672));
#204671=CARTESIAN_POINT('Ctrl Pts',(184.683737240314,-1.95751060444897,
126.292450235481));
#204672=CARTESIAN_POINT('Ctrl Pts',(184.676246904552,-2.07842982842536,
126.344911530846));
#204673=CARTESIAN_POINT('Ctrl Pts',(184.66875656879,-2.19708408278854,126.402170094191));
#204674=CARTESIAN_POINT('Ctrl Pts',(184.661266233028,-2.31308146934551,
126.463987686737));
#204675=CARTESIAN_POINT('Ctrl Pts',(184.653490953882,-2.43349156701393,
126.528156911382));
#204676=CARTESIAN_POINT('Ctrl Pts',(184.645715674736,-2.55142012255629,
126.597442189508));
#204677=CARTESIAN_POINT('Ctrl Pts',(184.63794039559,-2.66640186075916,126.671627359849));
#204678=CARTESIAN_POINT('Ctrl Pts',(184.630174906103,-2.78123882835338,
126.745719125512));
#204679=CARTESIAN_POINT('Ctrl Pts',(184.622409416615,-2.89313603609128,
126.824698297011));
#204680=CARTESIAN_POINT('Ctrl Pts',(184.614643927127,-3.00165158969343,
126.908302250884));
#204681=CARTESIAN_POINT('Ctrl Pts',(184.606887744613,-3.11003708692624,
126.99180600505));
#204682=CARTESIAN_POINT('Ctrl Pts',(184.599131562098,-3.21504869422354,
127.079923265202));
#204683=CARTESIAN_POINT('Ctrl Pts',(184.591375379584,-3.31627290310998,
127.172347801702));
#204684=CARTESIAN_POINT('Ctrl Pts',(184.583624474521,-3.41742823714848,
127.264709450816));
#204685=CARTESIAN_POINT('Ctrl Pts',(184.575873569458,-3.51480101205282,
127.361372283403));
#204686=CARTESIAN_POINT('Ctrl Pts',(184.568122664396,-3.60801021796009,
127.461989403952));
#204687=CARTESIAN_POINT('Ctrl Pts',(184.560375354587,-3.70117618882434,
127.562559853301));
#204688=CARTESIAN_POINT('Ctrl Pts',(184.552628044778,-3.79018216867158,
127.66708065461));
#204689=CARTESIAN_POINT('Ctrl Pts',(184.544880734968,-3.87468379235378,
127.77516789148));
#204690=CARTESIAN_POINT('Ctrl Pts',(184.537135340988,-3.9591645196716,127.883228399511));
#204691=CARTESIAN_POINT('Ctrl Pts',(184.529389947007,-4.03914286792834,
127.994853279576));
#204692=CARTESIAN_POINT('Ctrl Pts',(184.521644553026,-4.11431484242556,
128.10962566958));
#204693=CARTESIAN_POINT('Ctrl Pts',(184.513896696704,-4.18951071487447,
128.22443454692));
#204694=CARTESIAN_POINT('Ctrl Pts',(184.506148840382,-4.25989694066962,
128.342392609911));
#204695=CARTESIAN_POINT('Ctrl Pts',(184.49840098406,-4.32521289149947,128.463054036679));
#204696=CARTESIAN_POINT('Ctrl Pts',(184.49065211975,-4.39053733987044,128.583731161379));
#204697=CARTESIAN_POINT('Ctrl Pts',(184.482903255439,-4.45079002018339,
128.707112002701));
#204698=CARTESIAN_POINT('Ctrl Pts',(184.475154391129,-4.50575679107406,
128.832727081082));
#204699=CARTESIAN_POINT('Ctrl Pts',(184.467398393862,-4.56077415977317,
128.958457790189));
#204700=CARTESIAN_POINT('Ctrl Pts',(184.459642396596,-4.61049574662458,
129.086426484169));
#204701=CARTESIAN_POINT('Ctrl Pts',(184.451886399329,-4.65475582965104,
129.216144250433));
#204702=CARTESIAN_POINT('Ctrl Pts',(184.44466748376,-4.6959510224118,129.336879414498));
#204703=CARTESIAN_POINT('Ctrl Pts',(184.437448568192,-4.73241533402233,
129.459129381269));
#204704=CARTESIAN_POINT('Ctrl Pts',(184.430229652623,-4.76405452823406,
129.582490119308));
#204705=CARTESIAN_POINT('Ctrl Pts',(186.18020938313,-4.76405452823405,129.582490119308));
#204706=CARTESIAN_POINT('Ctrl Pts',(186.17256993295,-4.79768574483935,129.713617722427));
#204707=CARTESIAN_POINT('Ctrl Pts',(186.164930482769,-4.82588839263014,
129.846093738758));
#204708=CARTESIAN_POINT('Ctrl Pts',(186.157291032589,-4.84857298836732,
129.979422414441));
#204709=CARTESIAN_POINT('Ctrl Pts',(186.149432621167,-4.87190776796963,
130.116572544767));
#204710=CARTESIAN_POINT('Ctrl Pts',(186.141574209745,-4.88940334476083,
130.254624496003));
#204711=CARTESIAN_POINT('Ctrl Pts',(186.133715798323,-4.90101953991361,
130.393032850591));
#204712=CARTESIAN_POINT('Ctrl Pts',(186.125857386902,-4.9126357350664,130.531441205178));
#204713=CARTESIAN_POINT('Ctrl Pts',(186.11799897548,-4.91837257034282,130.67020550101));
#204714=CARTESIAN_POINT('Ctrl Pts',(186.110140564058,-4.91824801325411,
130.808781321355));
#204715=CARTESIAN_POINT('Origin',(213.235140564004,0.,130.804360617566));
#204716=CARTESIAN_POINT('',(187.929867347344,-4.76405452823404,129.582490119308));
#204717=CARTESIAN_POINT('',(187.584954980304,-4.76405452823404,129.582490119308));
#204718=CARTESIAN_POINT('',(213.235140564004,-4.76405452823405,129.582490119308));
#204719=CARTESIAN_POINT('',(187.514859436036,-4.91824821531416,130.808550493347));
#204720=CARTESIAN_POINT('Ctrl Pts',(187.584954980304,-4.76405452823404,
129.582490119308));
#204721=CARTESIAN_POINT('Ctrl Pts',(187.577318467045,-4.79766509150003,
129.713537195371));
#204722=CARTESIAN_POINT('Ctrl Pts',(187.569681953786,-4.82585013568644,
129.845916938469));
#204723=CARTESIAN_POINT('Ctrl Pts',(187.562045440527,-4.84852382797168,
129.979133526341));
#204724=CARTESIAN_POINT('Ctrl Pts',(187.554181106445,-4.87187394666516,
130.116324377291));
#204725=CARTESIAN_POINT('Ctrl Pts',(187.546316772363,-4.88937865955207,
130.254402327779));
#204726=CARTESIAN_POINT('Ctrl Pts',(187.538452438282,-4.90100172800805,
130.392820674715));
#204727=CARTESIAN_POINT('Ctrl Pts',(187.5305881042,-4.91262479646404,130.53123902165));
#204728=CARTESIAN_POINT('Ctrl Pts',(187.522723770118,-4.91836624934627,
130.669997300341));
#204729=CARTESIAN_POINT('Ctrl Pts',(187.514859436036,-4.91824821531416,
130.808550493347));
#204730=CARTESIAN_POINT('Ctrl Pts',(187.514859435991,-4.91824821531348,
130.808550494141));
#204731=CARTESIAN_POINT('Ctrl Pts',(187.50296817185,-4.91806974195455,131.018049810722));
#204732=CARTESIAN_POINT('Ctrl Pts',(187.49107690771,-4.90450242768287,131.226999653672));
#204733=CARTESIAN_POINT('Ctrl Pts',(187.47918564357,-4.87777335736303,131.434051126228));
#204734=CARTESIAN_POINT('Ctrl Pts',(187.474567584818,-4.86739292886978,
131.514461068646));
#204735=CARTESIAN_POINT('Ctrl Pts',(187.469949526067,-4.85502785952663,
131.594585104556));
#204736=CARTESIAN_POINT('Ctrl Pts',(187.465331467316,-4.84069308080701,
131.674345421989));
#204737=CARTESIAN_POINT('Ctrl Pts',(187.457557133197,-4.8165610016603,131.808619018444));
#204738=CARTESIAN_POINT('Ctrl Pts',(187.449782799078,-4.78679964152417,
131.942100451967));
#204739=CARTESIAN_POINT('Ctrl Pts',(187.442008464958,-4.75147197296815,
132.074280753873));
#204740=CARTESIAN_POINT('Ctrl Pts',(187.434243712011,-4.71618784260629,
132.206298155371));
#204741=CARTESIAN_POINT('Ctrl Pts',(187.426478959064,-4.67535115311574,
132.337017241715));
#204742=CARTESIAN_POINT('Ctrl Pts',(187.418714206117,-4.62907625661752,
132.465936999476));
#204743=CARTESIAN_POINT('Ctrl Pts',(187.410957165232,-4.58284732099878,
132.594728712316));
#204744=CARTESIAN_POINT('Ctrl Pts',(187.403200124347,-4.53119105843935,
132.721724287424));
#204745=CARTESIAN_POINT('Ctrl Pts',(187.395443083462,-4.47427212062073,
132.846436045442));
#204746=CARTESIAN_POINT('Ctrl Pts',(187.387691892222,-4.41739610581604,
132.971053757354));
#204747=CARTESIAN_POINT('Ctrl Pts',(187.379940700982,-4.35526547673165,
133.093390725966));
#204748=CARTESIAN_POINT('Ctrl Pts',(187.372189509742,-4.28809353286631,
133.212977838274));
#204749=CARTESIAN_POINT('Ctrl Pts',(187.364441612965,-4.22095013886891,
133.332514122869));
#204750=CARTESIAN_POINT('Ctrl Pts',(187.356693716188,-4.14876988281084,
133.44930253558));
#204751=CARTESIAN_POINT('Ctrl Pts',(187.348945819411,-4.07181258012,133.562897435315));
#204752=CARTESIAN_POINT('Ctrl Pts',(187.341199543326,-3.99487137523789,
133.676468573446));
#204753=CARTESIAN_POINT('Ctrl Pts',(187.333453267242,-3.91315533044107,
133.786847203844));
#204754=CARTESIAN_POINT('Ctrl Pts',(187.325706991158,-3.82696805196249,
133.893615963399));
#204755=CARTESIAN_POINT('Ctrl Pts',(187.317960657893,-3.74078013726901,
134.000385511097));
#204756=CARTESIAN_POINT('Ctrl Pts',(187.310214324628,-3.65012116860682,
134.103544830563));
#204757=CARTESIAN_POINT('Ctrl Pts',(187.302467991362,-3.55533531112048,
134.202709317744));
#204758=CARTESIAN_POINT('Ctrl Pts',(187.294719923359,-3.46052822699846,
134.301896012124));
#204759=CARTESIAN_POINT('Ctrl Pts',(187.286971855356,-3.36159268511726,
134.397085811471));
#204760=CARTESIAN_POINT('Ctrl Pts',(187.279223787353,-3.25890970925504,
134.487930973813));
#204761=CARTESIAN_POINT('Ctrl Pts',(187.271467484611,-3.15611760070424,
134.578872687475));
#204762=CARTESIAN_POINT('Ctrl Pts',(187.263711181869,-3.04957039534964,
134.665460280642));
#204763=CARTESIAN_POINT('Ctrl Pts',(187.255954879128,-2.93968263329513,
134.747385988776));
#204764=CARTESIAN_POINT('Ctrl Pts',(187.248194436613,-2.82973622083337,
134.829355423126));
#204765=CARTESIAN_POINT('Ctrl Pts',(187.240433994099,-2.71644602177129,
134.906657794264));
#204766=CARTESIAN_POINT('Ctrl Pts',(187.232673551585,-2.60025471421194,
134.979029285103));
#204767=CARTESIAN_POINT('Ctrl Pts',(187.22490065132,-2.48387688605068,135.051516953085));
#204768=CARTESIAN_POINT('Ctrl Pts',(187.217127751054,-2.36458898340092,
135.119057730363));
#204769=CARTESIAN_POINT('Ctrl Pts',(187.209354850789,-2.24285817365602,
135.181433872078));
#204770=CARTESIAN_POINT('Ctrl Pts',(187.201864515027,-2.12555258546736,
135.241542483926));
#204771=CARTESIAN_POINT('Ctrl Pts',(187.194374179265,-2.0059788977942,135.296855306772));
#204772=CARTESIAN_POINT('Ctrl Pts',(187.186883843503,-1.88456999546703,
135.347220839352));
#204773=CARTESIAN_POINT('Ctrl Pts',(187.179109509384,-1.75855783770604,
135.399495996409));
#204774=CARTESIAN_POINT('Ctrl Pts',(187.171335175265,-1.63016938517756,
135.446606896525));
#204775=CARTESIAN_POINT('Ctrl Pts',(187.163560841146,-1.49986688586205,
135.488331410301));
#204776=CARTESIAN_POINT('Ctrl Pts',(187.155796088199,-1.36972497273157,
135.530004502343));
#204777=CARTESIAN_POINT('Ctrl Pts',(187.148031335251,-1.23767407507255,
135.566304298079));
#204778=CARTESIAN_POINT('Ctrl Pts',(187.140266582304,-1.10419751978648,
135.597056195192));
#204779=CARTESIAN_POINT('Ctrl Pts',(187.132509541419,-0.970853535296745,
135.627777549087));
#204780=CARTESIAN_POINT('Ctrl Pts',(187.124752500534,-0.836087089569735,
135.6529618828));
#204781=CARTESIAN_POINT('Ctrl Pts',(187.116995459649,-0.700397479315045,
135.672484119848));
#204782=CARTESIAN_POINT('Ctrl Pts',(187.109244268409,-0.564810193650936,
135.691991635025));
#204783=CARTESIAN_POINT('Ctrl Pts',(187.101493077169,-0.42830151454915,
135.705845496927));
#204784=CARTESIAN_POINT('Ctrl Pts',(187.093741885929,-0.291381413656383,
135.713971593425));
#204785=CARTESIAN_POINT('Ctrl Pts',(187.085993989152,-0.154519507459005,
135.722094236115));
#204786=CARTESIAN_POINT('Ctrl Pts',(187.078246092375,-0.017246916725652,
135.724493932228));
#204787=CARTESIAN_POINT('Ctrl Pts',(187.070498195598,0.119920991487449,
135.721148391947));
#204788=CARTESIAN_POINT('Ctrl Pts',(187.062751919514,0.257060207131151,
135.717803551481));
#204789=CARTESIAN_POINT('Ctrl Pts',(187.05500564343,0.394094393208233,135.708715874552));
#204790=CARTESIAN_POINT('Ctrl Pts',(187.047259367345,0.53050830372916,135.693915198729));
#204791=CARTESIAN_POINT('Ctrl Pts',(187.03951303408,0.66692322122647,135.679114413651));
#204792=CARTESIAN_POINT('Ctrl Pts',(187.031766700815,0.802717465346965,
135.658600587698));
#204793=CARTESIAN_POINT('Ctrl Pts',(187.024020367549,0.937381428141232,
135.632455388868));
#204794=CARTESIAN_POINT('Ctrl Pts',(187.016272299546,1.07207554799625,135.606304335003));
#204795=CARTESIAN_POINT('Ctrl Pts',(187.008524231543,1.20563849912314,135.574519473305));
#204796=CARTESIAN_POINT('Ctrl Pts',(187.000776163541,1.33757176369478,135.537233406842));
#204797=CARTESIAN_POINT('Ctrl Pts',(186.993019860799,1.46964524851015,135.499907712303));
#204798=CARTESIAN_POINT('Ctrl Pts',(186.985263558057,1.60008520998432,135.457069239991));
#204799=CARTESIAN_POINT('Ctrl Pts',(186.977507255315,1.7284086480416,135.408900399985));
#204800=CARTESIAN_POINT('Ctrl Pts',(186.969746812801,1.85680057618161,135.360705850817));
#204801=CARTESIAN_POINT('Ctrl Pts',(186.961986370287,1.98307337019677,135.307175417617));
#204802=CARTESIAN_POINT('Ctrl Pts',(186.954225927772,2.10676579497374,135.248538938429));
#204803=CARTESIAN_POINT('Ctrl Pts',(186.946453027507,2.23065678181183,135.189808330759));
#204804=CARTESIAN_POINT('Ctrl Pts',(186.938680127242,2.3519587757408,135.125955479745));
#204805=CARTESIAN_POINT('Ctrl Pts',(186.930907226976,2.47023606645755,135.05725573013));
#204806=CARTESIAN_POINT('Ctrl Pts',(186.923416891214,2.58421367973449,134.991053389458));
#204807=CARTESIAN_POINT('Ctrl Pts',(186.915926555452,2.69538242307315,134.920350591354));
#204808=CARTESIAN_POINT('Ctrl Pts',(186.90843621969,2.80338084934492,134.845429643953));
#204809=CARTESIAN_POINT('Ctrl Pts',(186.900661885571,2.91547406877391,134.76766804606));
#204810=CARTESIAN_POINT('Ctrl Pts',(186.892887551452,3.02450689794558,134.685115797058));
#204811=CARTESIAN_POINT('Ctrl Pts',(186.885113217333,3.13004259678052,134.5980417329));
#204812=CARTESIAN_POINT('Ctrl Pts',(186.877348464386,3.23544823229863,134.511074979743));
#204813=CARTESIAN_POINT('Ctrl Pts',(186.869583711439,3.3373650142225,134.419597745934));
#204814=CARTESIAN_POINT('Ctrl Pts',(186.861818958491,3.43538479468078,134.323922291266));
#204815=CARTESIAN_POINT('Ctrl Pts',(186.854061917606,3.53330722051126,134.228341862808));
#204816=CARTESIAN_POINT('Ctrl Pts',(186.846304876721,3.62734006948965,134.128571782767));
#204817=CARTESIAN_POINT('Ctrl Pts',(186.838547835836,3.7171082291624,134.024964516712));
#204818=CARTESIAN_POINT('Ctrl Pts',(186.830796644596,3.8068086939677,133.921435381702));
#204819=CARTESIAN_POINT('Ctrl Pts',(186.823045453356,3.89225061581199,133.814075114605));
#204820=CARTESIAN_POINT('Ctrl Pts',(186.815294262116,3.97309598993045,133.703272709593));
#204821=CARTESIAN_POINT('Ctrl Pts',(186.807546365339,4.05390700260826,133.592517398559));
#204822=CARTESIAN_POINT('Ctrl Pts',(186.799798468562,4.13012512327185,133.478323174578));
#204823=CARTESIAN_POINT('Ctrl Pts',(186.792050571785,4.20145303038427,133.36111158236));
#204824=CARTESIAN_POINT('Ctrl Pts',(186.784304295701,4.27276601723617,133.24392450828));
#204825=CARTESIAN_POINT('Ctrl Pts',(186.776558019617,4.33919062208088,133.123721655165));
#204826=CARTESIAN_POINT('Ctrl Pts',(186.768811743533,4.40047344506548,133.000952641992));
#204827=CARTESIAN_POINT('Ctrl Pts',(186.761065410267,4.46175672042594,132.878182722566));
#204828=CARTESIAN_POINT('Ctrl Pts',(186.753319077002,4.51789796357578,132.752846955089));
#204829=CARTESIAN_POINT('Ctrl Pts',(186.745572743736,4.56869042857052,132.62541823071));
#204830=CARTESIAN_POINT('Ctrl Pts',(186.737824675734,4.61949426818561,132.497960969551));
#204831=CARTESIAN_POINT('Ctrl Pts',(186.730076607731,4.66494680138576,132.368410181932));
#204832=CARTESIAN_POINT('Ctrl Pts',(186.722328539728,4.70489012982407,132.237256960218));
#204833=CARTESIAN_POINT('Ctrl Pts',(186.714572236986,4.74487591050721,132.105964347298));
#204834=CARTESIAN_POINT('Ctrl Pts',(186.706815934244,4.77934067585266,131.973066272786));
#204835=CARTESIAN_POINT('Ctrl Pts',(186.699059631502,4.80817681928663,131.839067695427));
#204836=CARTESIAN_POINT('Ctrl Pts',(186.691299188988,4.83702835343861,131.704997598992));
#204837=CARTESIAN_POINT('Ctrl Pts',(186.683538746474,4.86024521347585,131.569826214457));
#204838=CARTESIAN_POINT('Ctrl Pts',(186.675778303959,4.8777714598113,131.434065825064));
#204839=CARTESIAN_POINT('Ctrl Pts',(186.668005403694,4.89532584083327,131.298087501042));
#204840=CARTESIAN_POINT('Ctrl Pts',(186.660232503429,4.90717131955267,131.161518672433));
#204841=CARTESIAN_POINT('Ctrl Pts',(186.652459603163,4.91330403923953,131.024874745214));
#204842=CARTESIAN_POINT('Ctrl Pts',(186.644969267401,4.91921381911843,130.893198168935));
#204843=CARTESIAN_POINT('Ctrl Pts',(186.637478931639,4.91981897388855,130.761452167314));
#204844=CARTESIAN_POINT('Ctrl Pts',(186.629988595877,4.91516164637668,130.630093430501));
#204845=CARTESIAN_POINT('Ctrl Pts',(186.622214261758,4.91032773487667,130.493754187256));
#204846=CARTESIAN_POINT('Ctrl Pts',(186.614439927639,4.89980909723262,130.357400273068));
#204847=CARTESIAN_POINT('Ctrl Pts',(186.60666559352,4.88359584406322,130.221544442131));
#204848=CARTESIAN_POINT('Ctrl Pts',(186.598900840573,4.86740257227934,130.085856041365));
#204849=CARTESIAN_POINT('Ctrl Pts',(186.591136087626,4.84552869479156,129.95066488697));
#204850=CARTESIAN_POINT('Ctrl Pts',(186.583371334678,4.81801631071333,129.816483149354));
#204851=CARTESIAN_POINT('Ctrl Pts',(186.575614293793,4.79053125232284,129.682434682933));
#204852=CARTESIAN_POINT('Ctrl Pts',(186.567857252908,4.75741891010157,129.549394018657));
#204853=CARTESIAN_POINT('Ctrl Pts',(186.560100212023,4.71877306587156,129.417867265507));
#204854=CARTESIAN_POINT('Ctrl Pts',(186.552349020783,4.68015636477332,129.286439697704));
#204855=CARTESIAN_POINT('Ctrl Pts',(186.544597829543,4.63601457725516,129.156524142229));
#204856=CARTESIAN_POINT('Ctrl Pts',(186.536846638303,4.58649227530057,129.028615232915));
#204857=CARTESIAN_POINT('Ctrl Pts',(186.529098741526,4.53699102164532,128.9007606883));
#204858=CARTESIAN_POINT('Ctrl Pts',(186.521350844749,4.48211394281148,128.774911457366));
#204859=CARTESIAN_POINT('Ctrl Pts',(186.513602947972,4.42205498674884,128.651545540354));
#204860=CARTESIAN_POINT('Ctrl Pts',(186.505856671888,4.3620085937251,128.528205428834));
#204861=CARTESIAN_POINT('Ctrl Pts',(186.498110395804,4.29678265050747,128.407347949309));
#204862=CARTESIAN_POINT('Ctrl Pts',(186.490364119719,4.2266184654652,128.289429324292));
#204863=CARTESIAN_POINT('Ctrl Pts',(186.482617786454,4.15645376248687,128.171509828827));
#204864=CARTESIAN_POINT('Ctrl Pts',(186.474871453189,4.08135094486343,128.056529567145));
#204865=CARTESIAN_POINT('Ctrl Pts',(186.467125119923,4.00159611807821,127.94491808968));
#204866=CARTESIAN_POINT('Ctrl Pts',(186.45937705192,3.92182343075255,127.833281617599));
#204867=CARTESIAN_POINT('Ctrl Pts',(186.451628983917,3.83739688849461,127.725015748974));
#204868=CARTESIAN_POINT('Ctrl Pts',(186.443880915914,3.74864431330477,127.620518775573));
#204869=CARTESIAN_POINT('Ctrl Pts',(186.436124613173,3.65979741082176,127.515910741544));
#204870=CARTESIAN_POINT('Ctrl Pts',(186.428368310431,3.56661554438332,127.415079902877));
#204871=CARTESIAN_POINT('Ctrl Pts',(186.420612007689,3.46946538610199,127.318389734564));
#204872=CARTESIAN_POINT('Ctrl Pts',(186.412851565175,3.37226337585601,127.221647959797));
#204873=CARTESIAN_POINT('Ctrl Pts',(186.405091122661,3.2710891417477,127.129051522826));
#204874=CARTESIAN_POINT('Ctrl Pts',(186.397330680146,3.166343445464,127.040924388816));
#204875=CARTESIAN_POINT('Ctrl Pts',(186.389557779881,3.06142960208977,126.952655785307));
#204876=CARTESIAN_POINT('Ctrl Pts',(186.381784879615,2.95293314934019,126.868871060837));
#204877=CARTESIAN_POINT('Ctrl Pts',(186.37401197935,2.84128562820487,126.789852049702));
#204878=CARTESIAN_POINT('Ctrl Pts',(186.366521643588,2.73369677568628,126.713705578658));
#204879=CARTESIAN_POINT('Ctrl Pts',(186.359031307826,2.6231822342181,126.641984512861));
#204880=CARTESIAN_POINT('Ctrl Pts',(186.351540972064,2.51014900938351,126.574900248537));
#204881=CARTESIAN_POINT('Ctrl Pts',(186.343766637945,2.39283009547328,126.50527246394));
#204882=CARTESIAN_POINT('Ctrl Pts',(186.335992303826,2.27242610514435,126.440419470445));
#204883=CARTESIAN_POINT('Ctrl Pts',(186.328217969707,2.14936308757183,126.380626744435));
#204884=CARTESIAN_POINT('Ctrl Pts',(186.32045321676,2.02645173417003,126.320907707617));
#204885=CARTESIAN_POINT('Ctrl Pts',(186.312688463813,1.90088822208354,126.266236699069));
#204886=CARTESIAN_POINT('Ctrl Pts',(186.304923710865,1.773126210382,126.216855140233));
#204887=CARTESIAN_POINT('Ctrl Pts',(186.29716666998,1.64549109371175,126.167522627858));
#204888=CARTESIAN_POINT('Ctrl Pts',(186.289409629095,1.51566218516442,126.123469250419));
#204889=CARTESIAN_POINT('Ctrl Pts',(186.28165258821,1.38411597992469,126.08488967088));
#204890=CARTESIAN_POINT('Ctrl Pts',(186.27390139697,1.25266897470157,126.046339184501));
#204891=CARTESIAN_POINT('Ctrl Pts',(186.26615020573,1.11950762410406,126.013254389403));
#204892=CARTESIAN_POINT('Ctrl Pts',(186.25839901449,0.985126222273834,125.985781014749));
#204893=CARTESIAN_POINT('Ctrl Pts',(186.250651117713,0.850801936124037,
125.958319317012));
#204894=CARTESIAN_POINT('Ctrl Pts',(186.242903220936,0.715259012346737,
125.936464374276));
#204895=CARTESIAN_POINT('Ctrl Pts',(186.235155324159,0.579004439687522,
125.920311383445));
#204896=CARTESIAN_POINT('Ctrl Pts',(186.227409048075,0.442778368547621,
125.904161771471));
#204897=CARTESIAN_POINT('Ctrl Pts',(186.219662771991,0.305841332620214,
125.893711785003));
#204898=CARTESIAN_POINT('Ctrl Pts',(186.211916495907,0.168707597893969,
125.889005003888));
#204899=CARTESIAN_POINT('Ctrl Pts',(186.204170162641,0.0315728508776698,
125.884298188029));
#204900=CARTESIAN_POINT('Ctrl Pts',(186.196423829376,-0.10575820709968,
125.885334675529));
#204901=CARTESIAN_POINT('Ctrl Pts',(186.18867749611,-0.242769536089092,
125.892105940247));
#204902=CARTESIAN_POINT('Ctrl Pts',(186.180929428107,-0.379811547815777,
125.898878721341));
#204903=CARTESIAN_POINT('Ctrl Pts',(186.173181360104,-0.516533297662758,
125.911388815894));
#204904=CARTESIAN_POINT('Ctrl Pts',(186.165433292102,-0.652422495685759,
125.929575704401));
#204905=CARTESIAN_POINT('Ctrl Pts',(186.15767698936,-0.788456118365381,
125.947781922149));
#204906=CARTESIAN_POINT('Ctrl Pts',(186.149920686618,-0.923655033517907,
125.971676934201));
#204907=CARTESIAN_POINT('Ctrl Pts',(186.142164383876,-1.05751524410295,
126.001148716037));
#204908=CARTESIAN_POINT('Ctrl Pts',(186.134403941362,-1.19144689991294,
126.03063622785));
#204909=CARTESIAN_POINT('Ctrl Pts',(186.126643498848,-1.3240380496573,126.065706340432));
#204910=CARTESIAN_POINT('Ctrl Pts',(186.118883056333,-1.45479951078708,
126.106196992711));
#204911=CARTESIAN_POINT('Ctrl Pts',(186.111110156068,-1.5857708818227,126.146752644179));
#204912=CARTESIAN_POINT('Ctrl Pts',(186.103337255803,-1.7149063263107,126.192746092524));
#204913=CARTESIAN_POINT('Ctrl Pts',(186.095564355537,-1.8417354706294,126.243966608412));
#204914=CARTESIAN_POINT('Ctrl Pts',(186.088074019775,-1.96395405608863,
126.293325129531));
#204915=CARTESIAN_POINT('Ctrl Pts',(186.080583684013,-2.08403082912152,
126.347537155255));
#204916=CARTESIAN_POINT('Ctrl Pts',(186.073093348251,-2.20156793963613,
126.406374525084));
#204917=CARTESIAN_POINT('Ctrl Pts',(186.065318218632,-2.32357398828093,
126.467448980412));
#204918=CARTESIAN_POINT('Ctrl Pts',(186.057543089012,-2.44322994792608,
126.533700949362));
#204919=CARTESIAN_POINT('Ctrl Pts',(186.049767959393,-2.56006520571822,
126.604926226488));
#204920=CARTESIAN_POINT('Ctrl Pts',(186.042002588127,-2.67675382676365,
126.67606211071));
#204921=CARTESIAN_POINT('Ctrl Pts',(186.03423721686,-2.79062845967751,126.75215868097));
#204922=CARTESIAN_POINT('Ctrl Pts',(186.026471845594,-2.90124067215559,
126.832964688585));
#204923=CARTESIAN_POINT('Ctrl Pts',(186.018491328848,-3.01491747957512,
126.916009487709));
#204924=CARTESIAN_POINT('Ctrl Pts',(186.010510812103,-3.12514807592882,
127.004028321582));
#204925=CARTESIAN_POINT('Ctrl Pts',(186.002530295357,-3.2314741111118,127.096698533218));
#204926=CARTESIAN_POINT('Ctrl Pts',(185.994779503498,-3.33473947526146,
127.186701166476));
#204927=CARTESIAN_POINT('Ctrl Pts',(185.987028711639,-3.43432165183175,
127.28109080366));
#204928=CARTESIAN_POINT('Ctrl Pts',(185.979277919781,-3.52983187439647,
127.37952923471));
#204929=CARTESIAN_POINT('Ctrl Pts',(185.971530630239,-3.62529893917089,
127.477923184813));
#204930=CARTESIAN_POINT('Ctrl Pts',(185.963783340697,-3.71669743948121,
127.580362008493));
#204931=CARTESIAN_POINT('Ctrl Pts',(185.956036051155,-3.80367440789667,
127.686469653916));
#204932=CARTESIAN_POINT('Ctrl Pts',(185.948290584601,-3.89063091006273,
127.792552331516));
#204933=CARTESIAN_POINT('Ctrl Pts',(185.940545118047,-3.97316770391064,
127.902301810235));
#204934=CARTESIAN_POINT('Ctrl Pts',(185.932799651493,-4.05097143863642,
128.015308186031));
#204935=CARTESIAN_POINT('Ctrl Pts',(185.925054330194,-4.12877371426179,
128.12831244255));
#204936=CARTESIAN_POINT('Ctrl Pts',(185.917309008896,-4.20184288741614,
128.244573151684));
#204937=CARTESIAN_POINT('Ctrl Pts',(185.909563687597,-4.26990858509716,
128.363650938515));
#204938=CARTESIAN_POINT('Ctrl Pts',(185.901814172698,-4.33801113604076,
128.482793198423));
#204939=CARTESIAN_POINT('Ctrl Pts',(185.894064657798,-4.40110460739271,
128.604755242451));
#204940=CARTESIAN_POINT('Ctrl Pts',(185.886315142899,-4.45896424491958,
128.729072462868));
#204941=CARTESIAN_POINT('Ctrl Pts',(185.878563054062,-4.51684310004943,
128.853430974228));
#204942=CARTESIAN_POINT('Ctrl Pts',(185.870810965225,-4.56948450454414,
128.980145861196));
#204943=CARTESIAN_POINT('Ctrl Pts',(185.863058876388,-4.61671198790392,
129.108732862649));
#204944=CARTESIAN_POINT('Ctrl Pts',(185.855299774332,-4.66398219738179,
129.237436195167));
#204945=CARTESIAN_POINT('Ctrl Pts',(185.847540672277,-4.70582858667214,
129.368014652284));
#204946=CARTESIAN_POINT('Ctrl Pts',(185.839781570221,-4.74212459112503,
129.49996902577));
#204947=CARTESIAN_POINT('Ctrl Pts',(185.838167528046,-4.74967485680883,
129.527418068522));
#204948=CARTESIAN_POINT('Ctrl Pts',(185.83655348587,-4.75698512267265,129.554926614318));
#204949=CARTESIAN_POINT('Ctrl Pts',(185.834939443695,-4.76405452823405,
129.582490119308));
#204950=CARTESIAN_POINT('',(187.860140563976,-4.91824998954374,130.80468132454));
#204951=CARTESIAN_POINT('Ctrl Pts',(187.860140563976,-4.91824998954374,
130.80468132454));
#204952=CARTESIAN_POINT('Ctrl Pts',(187.851985238763,-4.91824054696515,
130.949489407629));
#204953=CARTESIAN_POINT('Ctrl Pts',(187.84382991355,-4.91183143561811,131.094160796668));
#204954=CARTESIAN_POINT('Ctrl Pts',(187.835674588336,-4.89908446976143,
131.238128321115));
#204955=CARTESIAN_POINT('Ctrl Pts',(187.827507043422,-4.8863184042239,131.382311562291));
#204956=CARTESIAN_POINT('Ctrl Pts',(187.819339498508,-4.86719555824919,
131.525788509872));
#204957=CARTESIAN_POINT('Ctrl Pts',(187.811171953594,-4.84182909625093,
131.668000626596));
#204958=CARTESIAN_POINT('Ctrl Pts',(187.802983701521,-4.81639832271632,
131.810573293393));
#204959=CARTESIAN_POINT('Ctrl Pts',(187.794795449448,-4.78469233773483,
131.951874395443));
#204960=CARTESIAN_POINT('Ctrl Pts',(187.786607197375,-4.74687508460216,
132.091357118604));
#204961=CARTESIAN_POINT('Ctrl Pts',(187.778407825462,-4.70900647474592,
132.2310292626));
#204962=CARTESIAN_POINT('Ctrl Pts',(187.770208453549,-4.66501012991102,
132.368877788919));
#204963=CARTESIAN_POINT('Ctrl Pts',(187.762009081637,-4.61509878206581,
132.504374233475));
#204964=CARTESIAN_POINT('Ctrl Pts',(187.7537907155,-4.56507181227561,132.640184561809));
#204965=CARTESIAN_POINT('Ctrl Pts',(187.745572349363,-4.5091025670614,132.773631612781));
#204966=CARTESIAN_POINT('Ctrl Pts',(187.737353983226,-4.44745127249184,
132.904208288544));
#204967=CARTESIAN_POINT('Ctrl Pts',(187.732966020474,-4.4145343179928,132.973925989116));
#204968=CARTESIAN_POINT('Ctrl Pts',(187.728578057722,-4.37999833546582,
133.042825876845));
#204969=CARTESIAN_POINT('Ctrl Pts',(187.724190094969,-4.34388802098799,
133.110834099663));
#204970=CARTESIAN_POINT('Ctrl Pts',(187.71641576085,-4.27990989132784,133.23132706574));
#204971=CARTESIAN_POINT('Ctrl Pts',(187.708641426731,-4.21081318308159,
133.349346880017));
#204972=CARTESIAN_POINT('Ctrl Pts',(187.700867092612,-4.13681326770758,
133.464428107428));
#204973=CARTESIAN_POINT('Ctrl Pts',(187.693102339665,-4.06290455061579,
133.57936750751));
#204974=CARTESIAN_POINT('Ctrl Pts',(187.685337586718,-3.98410485912279,
133.691375200834));
#204975=CARTESIAN_POINT('Ctrl Pts',(187.677572833771,-3.90067606158043,
133.800009015678));
#204976=CARTESIAN_POINT('Ctrl Pts',(187.669815792886,-3.81733012669587,
133.908534933887));
#204977=CARTESIAN_POINT('Ctrl Pts',(187.662058752001,-3.72936447197065,
134.013693334156));
#204978=CARTESIAN_POINT('Ctrl Pts',(187.654301711116,-3.63708479189096,
134.115070100305));
#204979=CARTESIAN_POINT('Ctrl Pts',(187.646550519876,-3.54487470063586,
134.216370417446));
#204980=CARTESIAN_POINT('Ctrl Pts',(187.638799328636,-3.44835732151588,
134.313894488769));
#204981=CARTESIAN_POINT('Ctrl Pts',(187.631048137396,-3.34787900468798,
134.407260731706));
#204982=CARTESIAN_POINT('Ctrl Pts',(187.623300240619,-3.24744339382506,
134.500587291499));
#204983=CARTESIAN_POINT('Ctrl Pts',(187.615552343842,-3.14305047942049,
134.589759272133));
#204984=CARTESIAN_POINT('Ctrl Pts',(187.607804447065,-3.03508373938013,
134.674431645009));
#204985=CARTESIAN_POINT('Ctrl Pts',(187.60005817098,-2.92713958365424,134.759086306249));
#204986=CARTESIAN_POINT('Ctrl Pts',(187.592311894896,-2.81562339669253,
134.839242990757));
#204987=CARTESIAN_POINT('Ctrl Pts',(187.584565618812,-2.70095172170201,
134.914596968378));
#204988=CARTESIAN_POINT('Ctrl Pts',(187.576819285547,-2.58627920023135,
134.989951502245));
#204989=CARTESIAN_POINT('Ctrl Pts',(187.569072952282,-2.4684514709862,135.060503043776));
#204990=CARTESIAN_POINT('Ctrl Pts',(187.561326619016,-2.34791369668973,
135.125990441533));
#204991=CARTESIAN_POINT('Ctrl Pts',(187.553578551013,-2.22734892879446,
135.191492504738));
#204992=CARTESIAN_POINT('Ctrl Pts',(187.54583048301,-2.10407325166797,135.251927980875));
#204993=CARTESIAN_POINT('Ctrl Pts',(187.538082415007,-1.97855567117998,
135.307082074479));
#204994=CARTESIAN_POINT('Ctrl Pts',(187.530326112265,-1.8529046891137,135.36229478651));
#204995=CARTESIAN_POINT('Ctrl Pts',(187.522569809524,-1.72500740244735,
135.412214745672));
#204996=CARTESIAN_POINT('Ctrl Pts',(187.514813506782,-1.59535252627577,
135.456675458525));
#204997=CARTESIAN_POINT('Ctrl Pts',(187.507053064268,-1.46562844939287,
135.501159901399));
#204998=CARTESIAN_POINT('Ctrl Pts',(187.499292621754,-1.33414528842969,
135.540179180866));
#204999=CARTESIAN_POINT('Ctrl Pts',(187.491532179239,-1.20140513403331,
135.573617243752));
#205000=CARTESIAN_POINT('Ctrl Pts',(187.483759278974,-1.06845189335697,
135.607108984385));
#205001=CARTESIAN_POINT('Ctrl Pts',(187.475986378709,-0.934238009971892,
135.635001524974));
#205002=CARTESIAN_POINT('Ctrl Pts',(187.468213478443,-0.799274826844706,
135.657230161833));
#205003=CARTESIAN_POINT('Ctrl Pts',(187.460723142681,-0.669217895375251,
135.678650731752));
#205004=CARTESIAN_POINT('Ctrl Pts',(187.453232806919,-0.538465501906267,
135.694812005137));
#205005=CARTESIAN_POINT('Ctrl Pts',(187.445742471157,-0.40747611749601,
135.705701890745));
#205006=CARTESIAN_POINT('Ctrl Pts',(187.437968137038,-0.271520230763168,
135.717004669676));
#205007=CARTESIAN_POINT('Ctrl Pts',(187.430193802919,-0.134878359929164,
135.722664244519));
#205008=CARTESIAN_POINT('Ctrl Pts',(187.4224194688,0.0019414977692763,135.722610234359));
#205009=CARTESIAN_POINT('Ctrl Pts',(187.414654715853,0.138592737221022,
135.722556290762));
#205010=CARTESIAN_POINT('Ctrl Pts',(187.406889962905,0.275421139878357,
135.716802772767));
#205011=CARTESIAN_POINT('Ctrl Pts',(187.399125209958,0.411913147910088,
135.70533099302));
#205012=CARTESIAN_POINT('Ctrl Pts',(187.391368169073,0.548269590155265,
135.693870607207));
#205013=CARTESIAN_POINT('Ctrl Pts',(187.383611128188,0.684289915601994,
135.676703294552));
#205014=CARTESIAN_POINT('Ctrl Pts',(187.375854087303,0.819460481241922,
135.653862404573));
#205015=CARTESIAN_POINT('Ctrl Pts',(187.368102896063,0.954529113706643,
135.631038739087));
#205016=CARTESIAN_POINT('Ctrl Pts',(187.360351704823,1.08874887791857,135.602550077227));
#205017=CARTESIAN_POINT('Ctrl Pts',(187.352600513583,1.22161152693562,135.568481558491));
#205018=CARTESIAN_POINT('Ctrl Pts',(187.344852616806,1.35441770578278,135.534427519784));
#205019=CARTESIAN_POINT('Ctrl Pts',(187.337104720029,1.4858675387463,135.494798438013));
#205020=CARTESIAN_POINT('Ctrl Pts',(187.329356823252,1.6154634643188,135.449730447617));
#205021=CARTESIAN_POINT('Ctrl Pts',(187.321610547168,1.74503228121749,135.404671884473));
#205022=CARTESIAN_POINT('Ctrl Pts',(187.313864271084,1.87274759303631,135.354176803992));
#205023=CARTESIAN_POINT('Ctrl Pts',(187.306117994999,1.99812786988819,135.298430941679));
#205024=CARTESIAN_POINT('Ctrl Pts',(187.298371661734,2.12350907226879,135.242684667863));
#205025=CARTESIAN_POINT('Ctrl Pts',(187.290625328469,2.24655484804188,135.181687693709));
#205026=CARTESIAN_POINT('Ctrl Pts',(187.282878995203,2.36680486178025,135.115673388492));
#205027=CARTESIAN_POINT('Ctrl Pts',(187.2751309272,2.48708180467538,135.04964429983));
#205028=CARTESIAN_POINT('Ctrl Pts',(187.267382859197,2.60456139703364,134.978595832385));
#205029=CARTESIAN_POINT('Ctrl Pts',(187.259634791194,2.71880941621897,134.902806471884));
#205030=CARTESIAN_POINT('Ctrl Pts',(187.251878488453,2.83317885955863,134.826936561549));
#205031=CARTESIAN_POINT('Ctrl Pts',(187.244122185711,2.9443095425167,134.746315909328));
#205032=CARTESIAN_POINT('Ctrl Pts',(187.236365882969,3.05179722699965,134.661265691298));
#205033=CARTESIAN_POINT('Ctrl Pts',(187.228605440455,3.15934228089629,134.576170079406));
#205034=CARTESIAN_POINT('Ctrl Pts',(187.220844997941,3.26324016595116,134.486640445942));
#205035=CARTESIAN_POINT('Ctrl Pts',(187.213084555426,3.36312185108178,134.393036484411));
#205036=CARTESIAN_POINT('Ctrl Pts',(187.205311655161,3.46316387516043,134.299282261492));
#205037=CARTESIAN_POINT('Ctrl Pts',(187.197538754896,3.55917654184175,134.201440919767));
#205038=CARTESIAN_POINT('Ctrl Pts',(187.18976585463,3.65082902071832,134.099907692633));
#205039=CARTESIAN_POINT('Ctrl Pts',(187.182275518868,3.73914970112908,134.002065454052));
#205040=CARTESIAN_POINT('Ctrl Pts',(187.174785183106,3.82342150061338,133.900795325352));
#205041=CARTESIAN_POINT('Ctrl Pts',(187.167294847344,3.90338643166027,133.796476495608));
#205042=CARTESIAN_POINT('Ctrl Pts',(187.159520513225,3.98638325737254,133.688202385727));
#205043=CARTESIAN_POINT('Ctrl Pts',(187.151746179106,4.06500308682427,133.576300848341));
#205044=CARTESIAN_POINT('Ctrl Pts',(187.143971844987,4.13891212164383,133.461161233309));
#205045=CARTESIAN_POINT('Ctrl Pts',(187.13620709204,4.2127300701834,133.346163517562));
#205046=CARTESIAN_POINT('Ctrl Pts',(187.128442339093,4.28184856640189,133.227935990211));
#205047=CARTESIAN_POINT('Ctrl Pts',(187.120677586145,4.34597429754696,133.106900621032));
#205048=CARTESIAN_POINT('Ctrl Pts',(187.11292054526,4.41003633811182,132.985985465888));
#205049=CARTESIAN_POINT('Ctrl Pts',(187.105163504375,4.46911530015668,132.862268361969));
#205050=CARTESIAN_POINT('Ctrl Pts',(187.09740646349,4.52296160498285,132.736199477914));
#205051=CARTESIAN_POINT('Ctrl Pts',(187.08965527225,4.5767673038917,132.610225663385));
#205052=CARTESIAN_POINT('Ctrl Pts',(187.08190408101,4.62534804688488,132.481903956843));
#205053=CARTESIAN_POINT('Ctrl Pts',(187.07415288977,4.6685007443457,132.351707980812));
#205054=CARTESIAN_POINT('Ctrl Pts',(187.066404992993,4.71163510075898,132.221567341544));
#205055=CARTESIAN_POINT('Ctrl Pts',(187.058657096216,4.74934587746924,132.089554387528));
#205056=CARTESIAN_POINT('Ctrl Pts',(187.050909199439,4.7814786640856,131.956161315341));
#205057=CARTESIAN_POINT('Ctrl Pts',(187.043162923355,4.8136047292157,131.822796146108));
#205058=CARTESIAN_POINT('Ctrl Pts',(187.035416647271,4.84015503356989,131.688051812779));
#205059=CARTESIAN_POINT('Ctrl Pts',(187.027670371187,4.86102556302323,131.552433834661));
#205060=CARTESIAN_POINT('Ctrl Pts',(187.019924037921,4.88189624653807,131.416814855442));
#205061=CARTESIAN_POINT('Ctrl Pts',(187.012177704656,4.89708701202375,131.280322604983));
#205062=CARTESIAN_POINT('Ctrl Pts',(187.00443137139,4.90654537711804,131.143470518309));
#205063=CARTESIAN_POINT('Ctrl Pts',(186.996683303387,4.9160058603476,131.006587784559));
#205064=CARTESIAN_POINT('Ctrl Pts',(186.988935235385,4.91973136175744,130.869345444204));
#205065=CARTESIAN_POINT('Ctrl Pts',(186.981187167382,4.9177214713347,130.732259349382));
#205066=CARTESIAN_POINT('Ctrl Pts',(186.97343086464,4.91570944477649,130.595027557828));
#205067=CARTESIAN_POINT('Ctrl Pts',(186.965674561898,4.90794985542348,130.457952735076));
#205068=CARTESIAN_POINT('Ctrl Pts',(186.957918259156,4.89449441724326,130.321548581599));
#205069=CARTESIAN_POINT('Ctrl Pts',(186.950157816642,4.88103179749054,130.185071625118));
#205070=CARTESIAN_POINT('Ctrl Pts',(186.942397374128,4.8618673259655,130.04926643811));
#205071=CARTESIAN_POINT('Ctrl Pts',(186.934636931613,4.83710415268687,129.914637920003));
#205072=CARTESIAN_POINT('Ctrl Pts',(186.926864031348,4.81230122736411,129.779793284246));
#205073=CARTESIAN_POINT('Ctrl Pts',(186.919091131083,4.78188172714106,129.646129473437));
#205074=CARTESIAN_POINT('Ctrl Pts',(186.911318230817,4.74599935115195,129.514138457872));
#205075=CARTESIAN_POINT('Ctrl Pts',(186.903827895055,4.71142138991215,129.386945648188));
#205076=CARTESIAN_POINT('Ctrl Pts',(186.896337559293,4.67177092859245,129.261306418357));
#205077=CARTESIAN_POINT('Ctrl Pts',(186.888847223531,4.62722754114839,129.137642781537));
#205078=CARTESIAN_POINT('Ctrl Pts',(186.881072889412,4.58099527763089,129.00929040034));
#205079=CARTESIAN_POINT('Ctrl Pts',(186.873298555293,4.52934528322642,128.882659796889));
#205080=CARTESIAN_POINT('Ctrl Pts',(186.865524221174,4.47242470282503,128.758242258316));
#205081=CARTESIAN_POINT('Ctrl Pts',(186.857759468227,4.41557427195186,128.63397805324));
#205082=CARTESIAN_POINT('Ctrl Pts',(186.84999471528,4.35346634033301,128.511921838433));
#205083=CARTESIAN_POINT('Ctrl Pts',(186.842229962332,4.28629738038526,128.392548471191));
#205084=CARTESIAN_POINT('Ctrl Pts',(186.834472921447,4.21919513359548,128.27329366726));
#205085=CARTESIAN_POINT('Ctrl Pts',(186.826715880562,4.14704205228711,128.156716746663));
#205086=CARTESIAN_POINT('Ctrl Pts',(186.818958839677,4.07008197270261,128.04327101417));
#205087=CARTESIAN_POINT('Ctrl Pts',(186.811207648437,3.99317992931273,127.929910831987));
#205088=CARTESIAN_POINT('Ctrl Pts',(186.803456457197,3.91147832157752,127.81967746021));
#205089=CARTESIAN_POINT('Ctrl Pts',(186.795705265957,3.82526584664194,127.712997768431));
#205090=CARTESIAN_POINT('Ctrl Pts',(186.78795736918,3.739090014308,127.606363418365));
#205091=CARTESIAN_POINT('Ctrl Pts',(186.780209472403,3.64840737324212,127.503280047653));
#205092=CARTESIAN_POINT('Ctrl Pts',(186.772461575626,3.55354855977579,127.404143610401));
#205093=CARTESIAN_POINT('Ctrl Pts',(186.764715299542,3.45870958872832,127.305027910354));
#205094=CARTESIAN_POINT('Ctrl Pts',(186.756969023458,3.35969645297088,127.209857783879));
#205095=CARTESIAN_POINT('Ctrl Pts',(186.749222747373,3.25687823804013,127.11899398654));
#205096=CARTESIAN_POINT('Ctrl Pts',(186.741476414108,3.15405926412871,127.028129518465));
#205097=CARTESIAN_POINT('Ctrl Pts',(186.733730080843,3.04743544795587,126.941571701855));
#205098=CARTESIAN_POINT('Ctrl Pts',(186.725983747577,2.9374103889513,126.859642215781));
#205099=CARTESIAN_POINT('Ctrl Pts',(186.718235679574,2.82736069059759,126.777694382167));
#205100=CARTESIAN_POINT('Ctrl Pts',(186.710487611571,2.71390854726417,126.700377175026));
#205101=CARTESIAN_POINT('Ctrl Pts',(186.702739543568,2.5974877383432,126.627969769997));
#205102=CARTESIAN_POINT('Ctrl Pts',(186.694983240827,2.48094319600109,126.555485409516));
#205103=CARTESIAN_POINT('Ctrl Pts',(186.687226938085,2.36142401787533,126.487921481866));
#205104=CARTESIAN_POINT('Ctrl Pts',(186.679470635343,2.23939034738478,126.425512146274));
#205105=CARTESIAN_POINT('Ctrl Pts',(186.671710192829,2.11729154384987,126.36306950094));
#205106=CARTESIAN_POINT('Ctrl Pts',(186.663949750315,1.99267592883989,126.305787092796));
#205107=CARTESIAN_POINT('Ctrl Pts',(186.6561893078,1.86602404364675,126.253851049283));
#205108=CARTESIAN_POINT('Ctrl Pts',(186.648416407535,1.73916884560389,126.201831633423));
#205109=CARTESIAN_POINT('Ctrl Pts',(186.64064350727,1.6102712131062,126.155175865823));
#205110=CARTESIAN_POINT('Ctrl Pts',(186.632870607004,1.47982813283383,126.114020357012));
#205111=CARTESIAN_POINT('Ctrl Pts',(186.625380271242,1.35412698709598,126.074360954611));
#205112=CARTESIAN_POINT('Ctrl Pts',(186.61788993548,1.22699110189288,126.039808938046));
#205113=CARTESIAN_POINT('Ctrl Pts',(186.610399599718,1.09887259295406,126.010441335084));
#205114=CARTESIAN_POINT('Ctrl Pts',(186.602625265599,0.965896431807742,
125.979960250529));
#205115=CARTESIAN_POINT('Ctrl Pts',(186.59485093148,0.831440435162286,125.954967919335));
#205116=CARTESIAN_POINT('Ctrl Pts',(186.587076597361,0.695997472203889,
125.935606097036));
#205117=CARTESIAN_POINT('Ctrl Pts',(186.579311844414,0.560721430592498,
125.916268136452));
#205118=CARTESIAN_POINT('Ctrl Pts',(186.571547091467,0.424461226152909,
125.902546932818));
#205119=CARTESIAN_POINT('Ctrl Pts',(186.56378233852,0.287722567918223,125.894533860295));
#205120=CARTESIAN_POINT('Ctrl Pts',(186.556025297635,0.151119720446433,
125.886528746469));
#205121=CARTESIAN_POINT('Ctrl Pts',(186.54826825675,0.014039752633058,125.884220504122));
#205122=CARTESIAN_POINT('Ctrl Pts',(186.540511215865,-0.123004157933034,
125.887649009221));
#205123=CARTESIAN_POINT('Ctrl Pts',(186.532760024625,-0.259944722620193,
125.891074928858));
#205124=CARTESIAN_POINT('Ctrl Pts',(186.525008833384,-0.396848894920734,
125.90022897531));
#205125=CARTESIAN_POINT('Ctrl Pts',(186.517257642144,-0.533201489500632,
125.915098992935));
#205126=CARTESIAN_POINT('Ctrl Pts',(186.509509745367,-0.669496130590324,
125.929962690404));
#205127=CARTESIAN_POINT('Ctrl Pts',(186.50176184859,-0.805239272386058,
125.950537484778));
#205128=CARTESIAN_POINT('Ctrl Pts',(186.494013951813,-0.939919070470149,
125.976759225211));
#205129=CARTESIAN_POINT('Ctrl Pts',(186.486267675729,-1.07457069644382,
126.002975480622));
#205130=CARTESIAN_POINT('Ctrl Pts',(186.478521399645,-1.20815903761232,
126.034836257913));
#205131=CARTESIAN_POINT('Ctrl Pts',(186.470775123561,-1.34018108035477,
126.072226032164));
#205132=CARTESIAN_POINT('Ctrl Pts',(186.463028790295,-1.47220409765393,
126.109616082418));
#205133=CARTESIAN_POINT('Ctrl Pts',(186.45528245703,-1.60266041728542,126.152535104537));
#205134=CARTESIAN_POINT('Ctrl Pts',(186.447536123765,-1.73106124618654,
126.200817414288));
#205135=CARTESIAN_POINT('Ctrl Pts',(186.439788055762,-1.85949082956307,
126.249110536526));
#205136=CARTESIAN_POINT('Ctrl Pts',(186.432039987759,-1.98586364036161,
126.302769198807));
#205137=CARTESIAN_POINT('Ctrl Pts',(186.424291919756,-2.10971033185508,
126.361579351494));
#205138=CARTESIAN_POINT('Ctrl Pts',(186.416535617014,-2.23368864908604,
126.42045200831));
#205139=CARTESIAN_POINT('Ctrl Pts',(186.408779314272,-2.35513513012335,
126.484486924591));
#205140=CARTESIAN_POINT('Ctrl Pts',(186.40102301153,-2.47360405141956,126.553423537427));
#205141=CARTESIAN_POINT('Ctrl Pts',(186.393262569016,-2.59213620314615,
126.622396943809));
#205142=CARTESIAN_POINT('Ctrl Pts',(186.385502126502,-2.70768729925805,
126.696277049213));
#205143=CARTESIAN_POINT('Ctrl Pts',(186.377741683988,-2.81984100116167,
126.774760167066));
#205144=CARTESIAN_POINT('Ctrl Pts',(186.369968783722,-2.93217474214415,
126.853369272988));
#205145=CARTESIAN_POINT('Ctrl Pts',(186.362195883457,-3.04109987965048,
126.936595919761));
#205146=CARTESIAN_POINT('Ctrl Pts',(186.354422983192,-3.14623284593448,
127.024095819743));
#205147=CARTESIAN_POINT('Ctrl Pts',(186.346932647429,-3.24754396407987,
127.108414877961));
#205148=CARTESIAN_POINT('Ctrl Pts',(186.339442311667,-3.34533360559828,
127.196701689925));
#205149=CARTESIAN_POINT('Ctrl Pts',(186.331951975905,-3.43929258525454,
127.288617513255));
#205150=CARTESIAN_POINT('Ctrl Pts',(186.324290294265,-3.53540093236302,
127.382635965623));
#205151=CARTESIAN_POINT('Ctrl Pts',(186.316628612625,-3.62782449528663,
127.480768053431));
#205152=CARTESIAN_POINT('Ctrl Pts',(186.308966930984,-3.7161827594279,127.582688883663));
#205153=CARTESIAN_POINT('Ctrl Pts',(186.301314183386,-3.80443799181967,
127.68449086727));
#205154=CARTESIAN_POINT('Ctrl Pts',(186.293661435788,-3.88863708801042,
127.790072509402));
#205155=CARTESIAN_POINT('Ctrl Pts',(186.28600868819,-3.96843439155349,127.899070349377));
#205156=CARTESIAN_POINT('Ctrl Pts',(186.278363092695,-4.04815711815039,
128.007966322175));
#205157=CARTESIAN_POINT('Ctrl Pts',(186.2707174972,-4.12348599584845,128.120271821147));
#205158=CARTESIAN_POINT('Ctrl Pts',(186.263071901705,-4.19411426884116,
128.235588817191));
#205159=CARTESIAN_POINT('Ctrl Pts',(186.255431906839,-4.26469080449765,
128.350821340064));
#205160=CARTESIAN_POINT('Ctrl Pts',(186.247791911973,-4.33057337660585,
128.469060628456));
#205161=CARTESIAN_POINT('Ctrl Pts',(186.240151917107,-4.39149772261774,
128.589878552896));
#205162=CARTESIAN_POINT('Ctrl Pts',(186.232515226792,-4.45239571683195,
128.710644219582));
#205163=CARTESIAN_POINT('Ctrl Pts',(186.224878536477,-4.50833957015994,
128.833985944203));
#205164=CARTESIAN_POINT('Ctrl Pts',(186.217241846161,-4.5591105114303,128.959450211322));
#205165=CARTESIAN_POINT('Ctrl Pts',(186.209605532488,-4.60987894867488,
129.084908290537));
#205166=CARTESIAN_POINT('Ctrl Pts',(186.201969218815,-4.65547482316395,
129.212488333294));
#205167=CARTESIAN_POINT('Ctrl Pts',(186.194332905142,-4.695727286753,129.341716330344));
#205168=CARTESIAN_POINT('Ctrl Pts',(186.189625064471,-4.72054321146236,
129.421386292359));
#205169=CARTESIAN_POINT('Ctrl Pts',(186.184917223801,-4.74332916114695,
129.501682227587));
#205170=CARTESIAN_POINT('Ctrl Pts',(186.18020938313,-4.76405452823405,129.582490119308));
#205171=CARTESIAN_POINT('Ctrl Pts',(187.929867347344,-4.76405452823405,
129.582490119308));
#205172=CARTESIAN_POINT('Ctrl Pts',(187.921775086847,-4.79957275528882,
129.72097514753));
#205173=CARTESIAN_POINT('Ctrl Pts',(187.913682826349,-4.82908397265096,
129.861148571076));
#205174=CARTESIAN_POINT('Ctrl Pts',(187.905590565851,-4.85243842824599,
130.00247261879));
#205175=CARTESIAN_POINT('Ctrl Pts',(187.897511509163,-4.87575477733303,
130.143566073847));
#205176=CARTESIAN_POINT('Ctrl Pts',(187.889432452475,-4.8929343404035,130.285806076163));
#205177=CARTESIAN_POINT('Ctrl Pts',(187.881353395787,-4.90387800511191,
130.428643205833));
#205178=CARTESIAN_POINT('Ctrl Pts',(187.87428245186,-4.91345610840887,130.553656975815));
#205179=CARTESIAN_POINT('Ctrl Pts',(187.867211507934,-4.91825817656564,
130.679127798048));
#205180=CARTESIAN_POINT('Ctrl Pts',(187.860140564008,-4.91824998954378,
130.804681323973));
#205181=CARTESIAN_POINT('Origin',(213.235140564004,0.,130.804360617566));
#205182=CARTESIAN_POINT('',(189.680106903305,-4.76405452823404,129.582490119308));
#205183=CARTESIAN_POINT('',(189.334601801321,-4.76405452823404,129.582490119308));
#205184=CARTESIAN_POINT('',(213.235140564004,-4.76405452823405,129.582490119308));
#205185=CARTESIAN_POINT('',(189.264859435947,-4.91824989634823,130.805370355446));
#205186=CARTESIAN_POINT('Ctrl Pts',(189.334601801321,-4.76405452823404,
129.582490119308));
#205187=CARTESIAN_POINT('Ctrl Pts',(189.326589951379,-4.79924357938049,
129.71969169566));
#205188=CARTESIAN_POINT('Ctrl Pts',(189.318578101437,-4.82853357011572,
129.858539643826));
#205189=CARTESIAN_POINT('Ctrl Pts',(189.310566251495,-4.85178106031378,
129.99850479592));
#205190=CARTESIAN_POINT('Ctrl Pts',(189.302564129565,-4.8750003233392,130.138300001905));
#205191=CARTESIAN_POINT('Ctrl Pts',(189.294562007635,-4.89219165463957,
130.279209361064));
#205192=CARTESIAN_POINT('Ctrl Pts',(189.286559885705,-4.90326234654455,
130.420692240633));
#205193=CARTESIAN_POINT('Ctrl Pts',(189.279326402467,-4.91326965023596,
130.548585072909));
#205194=CARTESIAN_POINT('Ctrl Pts',(189.272092919229,-4.91827626236202,
130.676946189752));
#205195=CARTESIAN_POINT('Ctrl Pts',(189.264859435991,-4.91824989634839,
130.805370354665));
#205196=CARTESIAN_POINT('Ctrl Pts',(189.264859435947,-4.91824989634823,
130.805370355446));
#205197=CARTESIAN_POINT('Ctrl Pts',(189.256607171556,-4.91821981685867,
130.951882088204));
#205198=CARTESIAN_POINT('Ctrl Pts',(189.248354907165,-4.91163874752937,
131.098225889341));
#205199=CARTESIAN_POINT('Ctrl Pts',(189.240102642774,-4.89857698727829,
131.243822290761));
#205200=CARTESIAN_POINT('Ctrl Pts',(189.231428856725,-4.88484803865739,
131.396855685653));
#205201=CARTESIAN_POINT('Ctrl Pts',(189.222755070677,-4.86395906746465,
131.549062909309));
#205202=CARTESIAN_POINT('Ctrl Pts',(189.214081284629,-4.83605175230801,
131.699785941922));
#205203=CARTESIAN_POINT('Ctrl Pts',(189.205787676123,-4.80936763247221,
131.843902688434));
#205204=CARTESIAN_POINT('Ctrl Pts',(189.197494067618,-4.77626745182874,
131.986662328151));
#205205=CARTESIAN_POINT('Ctrl Pts',(189.189200459113,-4.73692581437122,
132.127507204926));
#205206=CARTESIAN_POINT('Ctrl Pts',(189.180893279678,-4.69751980172804,
132.268582547836));
#205207=CARTESIAN_POINT('Ctrl Pts',(189.172586100243,-4.65185203318383,
132.407736580464));
#205208=CARTESIAN_POINT('Ctrl Pts',(189.164278920808,-4.60014566525104,
132.544430421043));
#205209=CARTESIAN_POINT('Ctrl Pts',(189.155952232729,-4.54831786968213,
132.681445274498));
#205210=CARTESIAN_POINT('Ctrl Pts',(189.147625544649,-4.49042324122083,
132.815988102357));
#205211=CARTESIAN_POINT('Ctrl Pts',(189.139298856569,-4.42673210121107,
132.947541890022));
#205212=CARTESIAN_POINT('Ctrl Pts',(189.138204974444,-4.41836495704328,
132.964824191878));
#205213=CARTESIAN_POINT('Ctrl Pts',(189.137111092319,-4.40989783749088,
132.982054947649));
#205214=CARTESIAN_POINT('Ctrl Pts',(189.136017210193,-4.40133141131699,
132.99923302166));
#205215=CARTESIAN_POINT('Ctrl Pts',(189.128242876074,-4.34044892888366,
133.121319381593));
#205216=CARTESIAN_POINT('Ctrl Pts',(189.120468541955,-4.27438642335554,
133.241064014106));
#205217=CARTESIAN_POINT('Ctrl Pts',(189.112694207836,-4.20334731880043,
133.357996139725));
#205218=CARTESIAN_POINT('Ctrl Pts',(189.104929454889,-4.13239576359281,
133.47478415695));
#205219=CARTESIAN_POINT('Ctrl Pts',(189.097164701942,-4.05648001367186,
133.588766232983));
#205220=CARTESIAN_POINT('Ctrl Pts',(189.089399948995,-3.97585056850522,
133.699493657586));
#205221=CARTESIAN_POINT('Ctrl Pts',(189.08164290811,-3.8953012056402,133.81011110615));
#205222=CARTESIAN_POINT('Ctrl Pts',(189.073885867225,-3.81004769299365,
133.917480022228));
#205223=CARTESIAN_POINT('Ctrl Pts',(189.06612882634,-3.7203850578337,134.0211786236));
#205224=CARTESIAN_POINT('Ctrl Pts',(189.0583776351,-3.63079003796426,134.124799025051));
#205225=CARTESIAN_POINT('Ctrl Pts',(189.050626443859,-3.53679276837891,
134.224754326412));
#205226=CARTESIAN_POINT('Ctrl Pts',(189.042875252619,-3.43872974898933,
134.320654231006));
#205227=CARTESIAN_POINT('Ctrl Pts',(189.035127355842,-3.34070840899898,
134.416513375581));
#205228=CARTESIAN_POINT('Ctrl Pts',(189.027379459065,-3.23862503510299,
134.508320278819));
#205229=CARTESIAN_POINT('Ctrl Pts',(189.019631562288,-3.13285417567755,
134.595720238657));
#205230=CARTESIAN_POINT('Ctrl Pts',(189.011885286204,-3.02710544123581,
134.683101916308));
#205231=CARTESIAN_POINT('Ctrl Pts',(189.00413901012,-2.91767105670176,134.766078235263));
#205232=CARTESIAN_POINT('Ctrl Pts',(188.996392734036,-2.80495965334516,
134.844333935003));
#205233=CARTESIAN_POINT('Ctrl Pts',(188.98864640077,-2.69224741797864,134.922590212409));
#205234=CARTESIAN_POINT('Ctrl Pts',(188.980900067505,-2.57625843666835,
134.996125578092));
#205235=CARTESIAN_POINT('Ctrl Pts',(188.97315373424,-2.45743106294825,135.064667605725));
#205236=CARTESIAN_POINT('Ctrl Pts',(188.965405666237,-2.33857707866192,
135.13322498287));
#205237=CARTESIAN_POINT('Ctrl Pts',(188.957657598234,-2.21688377571787,
135.19678660152));
#205238=CARTESIAN_POINT('Ctrl Pts',(188.949909530231,-2.09281452597186,
135.255125767782));
#205239=CARTESIAN_POINT('Ctrl Pts',(188.942153227489,-1.96861341395046,
135.313526937605));
#205240=CARTESIAN_POINT('Ctrl Pts',(188.934396924747,-1.84203166516669,
135.366694400722));
#205241=CARTESIAN_POINT('Ctrl Pts',(188.926640622005,-1.71355358688341,
135.414449246582));
#205242=CARTESIAN_POINT('Ctrl Pts',(188.918880179491,-1.5850069359812,135.46222958064));
#205243=CARTESIAN_POINT('Ctrl Pts',(188.911119736977,-1.45456231049509,
135.504591420412));
#205244=CARTESIAN_POINT('Ctrl Pts',(188.903359294463,-1.3227186760497,135.541405937861));
#205245=CARTESIAN_POINT('Ctrl Pts',(188.895586394197,-1.19066339449785,
135.578279553241));
#205246=CARTESIAN_POINT('Ctrl Pts',(188.887813493932,-1.05720499698669,
135.609587961818));
#205247=CARTESIAN_POINT('Ctrl Pts',(188.880040593666,-0.922853008814749,
135.635253432214));
#205248=CARTESIAN_POINT('Ctrl Pts',(188.872550257904,-0.793385053824595,
135.659985898115));
#205249=CARTESIAN_POINT('Ctrl Pts',(188.865059922142,-0.663087653395633,
135.679478527407));
#205250=CARTESIAN_POINT('Ctrl Pts',(188.85756958638,-0.532418820732127,
135.693707533242));
#205251=CARTESIAN_POINT('Ctrl Pts',(188.849795252261,-0.396795639562776,
135.708476036158));
#205252=CARTESIAN_POINT('Ctrl Pts',(188.842020918142,-0.260342690980689,
135.717620678069));
#205253=CARTESIAN_POINT('Ctrl Pts',(188.834246584023,-0.123566010769087,
135.721058137597));
#205254=CARTESIAN_POINT('Ctrl Pts',(188.826481831076,0.0130421044082147,
135.724491360764));
#205255=CARTESIAN_POINT('Ctrl Pts',(188.818717078129,0.149972770293301,
135.722231386573));
#205256=CARTESIAN_POINT('Ctrl Pts',(188.810952325181,0.28671307317168,135.714246428476));
#205257=CARTESIAN_POINT('Ctrl Pts',(188.803195284296,0.423317563653494,
135.706269401151));
#205258=CARTESIAN_POINT('Ctrl Pts',(188.795438243411,0.559731679614168,
135.692578728228));
#205259=CARTESIAN_POINT('Ctrl Pts',(188.787681202526,0.695441094281352,
135.673194640911));
#205260=CARTESIAN_POINT('Ctrl Pts',(188.779930011286,0.8310481694232,135.653825171285));
#205261=CARTESIAN_POINT('Ctrl Pts',(188.772178820046,0.965951215561337,
135.628770888172));
#205262=CARTESIAN_POINT('Ctrl Pts',(188.764427628806,1.09963997862434,135.598103933589));
#205263=CARTESIAN_POINT('Ctrl Pts',(188.756679732029,1.23327192039691,135.567450013279));
#205264=CARTESIAN_POINT('Ctrl Pts',(188.748931835252,1.36569022531323,135.531188253377));
#205265=CARTESIAN_POINT('Ctrl Pts',(188.741183938475,1.49639401993704,135.489442046911));
#205266=CARTESIAN_POINT('Ctrl Pts',(188.733437662391,1.62707047414466,135.447704572852));
#205267=CARTESIAN_POINT('Ctrl Pts',(188.725691386307,1.75603275921754,135.400485053005));
#205268=CARTESIAN_POINT('Ctrl Pts',(188.717945110223,1.88279476236884,135.34795687442));
#205269=CARTESIAN_POINT('Ctrl Pts',(188.710198776957,2.00955770124844,135.295428308083));
#205270=CARTESIAN_POINT('Ctrl Pts',(188.702452443692,2.13411996461381,135.237591154481));
#205271=CARTESIAN_POINT('Ctrl Pts',(188.694706110426,2.25601541168853,135.174666959772));
#205272=CARTESIAN_POINT('Ctrl Pts',(188.686958042423,2.3779381564034,135.111728673626));
#205273=CARTESIAN_POINT('Ctrl Pts',(188.679209974421,2.4971925490977,135.043701258784));
#205274=CARTESIAN_POINT('Ctrl Pts',(188.671461906418,2.61333740197348,134.970852029527));
#205275=CARTESIAN_POINT('Ctrl Pts',(188.663705603676,2.72960569498105,134.897925375242));
#205276=CARTESIAN_POINT('Ctrl Pts',(188.655949300934,2.84275751463042,134.820166877511));
#205277=CARTESIAN_POINT('Ctrl Pts',(188.648192998192,2.95238055850332,134.737887292227));
#205278=CARTESIAN_POINT('Ctrl Pts',(188.640432555678,3.06206211149548,134.655563791851));
#205279=CARTESIAN_POINT('Ctrl Pts',(188.632672113164,3.1682108334075,134.568714643188));
#205280=CARTESIAN_POINT('Ctrl Pts',(188.62491167065,3.27044863445584,134.477690005449));
#205281=CARTESIAN_POINT('Ctrl Pts',(188.617138770384,3.37285055669868,134.386519246881));
#205282=CARTESIAN_POINT('Ctrl Pts',(188.609365870119,3.47132873129138,134.291159876902));
#205283=CARTESIAN_POINT('Ctrl Pts',(188.601592969853,3.5655423497568,134.191998557871));
#205284=CARTESIAN_POINT('Ctrl Pts',(188.594102634091,3.65633106588129,134.096442002558));
#205285=CARTESIAN_POINT('Ctrl Pts',(188.586612298329,3.74315969458697,133.997355351629));
#205286=CARTESIAN_POINT('Ctrl Pts',(188.579121962567,3.82576065600049,133.895111087193));
#205287=CARTESIAN_POINT('Ctrl Pts',(188.571347628448,3.91149345797192,133.788990200394));
#205288=CARTESIAN_POINT('Ctrl Pts',(188.563573294329,3.99294325595813,133.679131372527));
#205289=CARTESIAN_POINT('Ctrl Pts',(188.55579896021,4.06976642462402,133.565915308588));
#205290=CARTESIAN_POINT('Ctrl Pts',(188.548034207263,4.14649491560041,133.452838773329));
#205291=CARTESIAN_POINT('Ctrl Pts',(188.540269454316,4.21860790493604,133.336413554789));
#205292=CARTESIAN_POINT('Ctrl Pts',(188.532504701369,4.28580140731598,133.217054000395));
#205293=CARTESIAN_POINT('Ctrl Pts',(188.524747660484,4.35292817216208,133.097812995594));
#205294=CARTESIAN_POINT('Ctrl Pts',(188.516990619599,4.41514498306898,132.97564379326));
#205295=CARTESIAN_POINT('Ctrl Pts',(188.509233578714,4.47219085493765,132.850990046533));
#205296=CARTESIAN_POINT('Ctrl Pts',(188.501482387474,4.52919370807062,132.726430302165));
#205297=CARTESIAN_POINT('Ctrl Pts',(188.493731196234,4.58103322174094,132.599390096789));
#205298=CARTESIAN_POINT('Ctrl Pts',(188.485980004993,4.6274942862818,132.470337716127));
#205299=CARTESIAN_POINT('Ctrl Pts',(188.478232108216,4.67393560363083,132.341340186169));
#205300=CARTESIAN_POINT('Ctrl Pts',(188.470484211439,4.71500288634316,132.210332548992));
#205301=CARTESIAN_POINT('Ctrl Pts',(188.462736314662,4.75052921414137,132.077802900549));
#205302=CARTESIAN_POINT('Ctrl Pts',(188.454990038578,4.78604811059766,131.945300974451));
#205303=CARTESIAN_POINT('Ctrl Pts',(188.447243762494,4.81602825638518,131.81127804774));
#205304=CARTESIAN_POINT('Ctrl Pts',(188.43949748641,4.84035277110316,131.676236820805));
#205305=CARTESIAN_POINT('Ctrl Pts',(188.431751153145,4.86467746537918,131.541194597026));
#205306=CARTESIAN_POINT('Ctrl Pts',(188.424004819879,4.88334637597157,131.405134442797));
#205307=CARTESIAN_POINT('Ctrl Pts',(188.416258486614,4.89629393546274,131.268568286666));
#205308=CARTESIAN_POINT('Ctrl Pts',(188.408510418611,4.90924439447009,131.13197154749));
#205309=CARTESIAN_POINT('Ctrl Pts',(188.400762350608,4.91647091592922,130.994868970073));
#205310=CARTESIAN_POINT('Ctrl Pts',(188.393014282605,4.91795992613311,130.857776228101));
#205311=CARTESIAN_POINT('Ctrl Pts',(188.385257979863,4.91945051887476,130.720537782331));
#205312=CARTESIAN_POINT('Ctrl Pts',(188.377501677121,4.91519141490565,130.583309584453));
#205313=CARTESIAN_POINT('Ctrl Pts',(188.36974537438,4.90522120243238,130.44660648732));
#205314=CARTESIAN_POINT('Ctrl Pts',(188.361984931865,4.89524566855652,130.309830427629));
#205315=CARTESIAN_POINT('Ctrl Pts',(188.354224489351,4.87955299711073,130.173580415335));
#205316=CARTESIAN_POINT('Ctrl Pts',(188.346464046837,4.85823342019293,130.03836381769));
#205317=CARTESIAN_POINT('Ctrl Pts',(188.338691146572,4.8368796191976,129.902930158358));
#205318=CARTESIAN_POINT('Ctrl Pts',(188.330918246306,4.80988093934744,129.768533612271));
#205319=CARTESIAN_POINT('Ctrl Pts',(188.323145346041,4.77737847532777,129.635669911701));
#205320=CARTESIAN_POINT('Ctrl Pts',(188.315655010279,4.74605755774389,129.50763614131));
#205321=CARTESIAN_POINT('Ctrl Pts',(188.308164674517,4.70962614676043,129.381026001712));
#205322=CARTESIAN_POINT('Ctrl Pts',(188.300674338755,4.66825298866656,129.256265951111));
#205323=CARTESIAN_POINT('Ctrl Pts',(188.292900004636,4.62531115470858,129.126775585272));
#205324=CARTESIAN_POINT('Ctrl Pts',(188.285125670517,4.57690941679345,128.998868183534));
#205325=CARTESIAN_POINT('Ctrl Pts',(188.277351336398,4.52318233493014,128.873038627975));
#205326=CARTESIAN_POINT('Ctrl Pts',(188.269586583451,4.46952146689349,128.747364146098));
#205327=CARTESIAN_POINT('Ctrl Pts',(188.261821830503,4.41054846539562,128.623762771359));
#205328=CARTESIAN_POINT('Ctrl Pts',(188.254057077556,4.34644762117504,128.502714220119));
#205329=CARTESIAN_POINT('Ctrl Pts',(188.246300036671,4.28241044281667,128.381785896006));
#205330=CARTESIAN_POINT('Ctrl Pts',(188.238542995786,4.21325573890659,128.263405692909));
#205331=CARTESIAN_POINT('Ctrl Pts',(188.230785954901,4.13921569857526,128.148032990339));
#205332=CARTESIAN_POINT('Ctrl Pts',(188.223034763661,4.06523149241429,128.032747291222));
#205333=CARTESIAN_POINT('Ctrl Pts',(188.215283572421,3.98636949305475,127.920464906065));
#205334=CARTESIAN_POINT('Ctrl Pts',(188.207532381181,3.90290741050956,127.811619932594));
#205335=CARTESIAN_POINT('Ctrl Pts',(188.199784484404,3.81948080157582,127.702821221139));
#205336=CARTESIAN_POINT('Ctrl Pts',(188.192036587627,3.73145823551986,127.597457325174));
#205337=CARTESIAN_POINT('Ctrl Pts',(188.18428869085,3.63916013680356,127.495932507239));
#205338=CARTESIAN_POINT('Ctrl Pts',(188.176542414766,3.54688134485975,127.394428926108));
#205339=CARTESIAN_POINT('Ctrl Pts',(188.168796138682,3.45032906199472,127.296763114795));
#205340=CARTESIAN_POINT('Ctrl Pts',(188.161049862597,3.34986304757216,127.203305129933));
#205341=CARTESIAN_POINT('Ctrl Pts',(188.153303529332,3.24939629153235,127.109846455185));
#205342=CARTESIAN_POINT('Ctrl Pts',(188.145557196067,3.14501603254435,127.020595935158));
#205343=CARTESIAN_POINT('Ctrl Pts',(188.137810862801,3.03711752980305,126.935885443461));
#205344=CARTESIAN_POINT('Ctrl Pts',(188.130062794798,2.92919486394014,126.851155981437));
#205345=CARTESIAN_POINT('Ctrl Pts',(188.122314726795,2.81775269397828,126.770968812257));
#205346=CARTESIAN_POINT('Ctrl Pts',(188.114566658792,2.703217533875,126.695614090089));
#205347=CARTESIAN_POINT('Ctrl Pts',(188.106810356051,2.58856064444062,126.620179280026));
#205348=CARTESIAN_POINT('Ctrl Pts',(188.099054053309,2.47080452533179,126.549587391881));
#205349=CARTESIAN_POINT('Ctrl Pts',(188.091297750567,2.35040319470329,126.484084250847));
#205350=CARTESIAN_POINT('Ctrl Pts',(188.083537308053,2.22993760225931,126.418546148814));
#205351=CARTESIAN_POINT('Ctrl Pts',(188.075776865539,2.10682433588469,126.358102378005));
#205352=CARTESIAN_POINT('Ctrl Pts',(188.068016423024,1.98153903066888,126.302951267992));
#205353=CARTESIAN_POINT('Ctrl Pts',(188.060243522759,1.85605260635887,126.24771162452));
#205354=CARTESIAN_POINT('Ctrl Pts',(188.052470622493,1.72838753988925,126.197781762542));
#205355=CARTESIAN_POINT('Ctrl Pts',(188.044697722228,1.59903716998487,126.153310930505));
#205356=CARTESIAN_POINT('Ctrl Pts',(188.037207386466,1.47438901184074,126.110456725228));
#205357=CARTESIAN_POINT('Ctrl Pts',(188.029717050704,1.34817624808902,126.072671630003));
#205358=CARTESIAN_POINT('Ctrl Pts',(188.022226714942,1.22084888158536,126.040044184873));
#205359=CARTESIAN_POINT('Ctrl Pts',(188.014452380823,1.08869385928014,126.006179660243));
#205360=CARTESIAN_POINT('Ctrl Pts',(188.006678046704,0.954919418051348,
125.977764338209));
#205361=CARTESIAN_POINT('Ctrl Pts',(187.998903712585,0.820014649177363,
125.954952505473));
#205362=CARTESIAN_POINT('Ctrl Pts',(187.991138959638,0.685276138374253,
125.932168786282));
#205363=CARTESIAN_POINT('Ctrl Pts',(187.98337420669,0.54941045342816,125.914974880467));
#205364=CARTESIAN_POINT('Ctrl Pts',(187.975609453743,0.412920806945482,
125.903475037419));
#205365=CARTESIAN_POINT('Ctrl Pts',(187.967852412858,0.276566723903787,
125.891986616178));
#205366=CARTESIAN_POINT('Ctrl Pts',(187.960095371973,0.139590299674858,
125.886181035769));
#205367=CARTESIAN_POINT('Ctrl Pts',(187.952338331088,0.00250352715083474,
125.886111254749));
#205368=CARTESIAN_POINT('Ctrl Pts',(187.944587139848,-0.134479867171555,
125.886041526351));
#205369=CARTESIAN_POINT('Ctrl Pts',(187.936835948608,-0.271573054772387,
125.891698988073));
#205370=CARTESIAN_POINT('Ctrl Pts',(187.929084757368,-0.408260707894014,
125.90308463504));
#205371=CARTESIAN_POINT('Ctrl Pts',(187.921336860591,-0.544890265116803,
125.914465442803));
#205372=CARTESIAN_POINT('Ctrl Pts',(187.913588963814,-0.681114241876996,
125.931569561129));
#205373=CARTESIAN_POINT('Ctrl Pts',(187.905841067037,-0.816419323400283,
125.954345921621));
#205374=CARTESIAN_POINT('Ctrl Pts',(187.898094790952,-0.951696102017355,
125.977117517791));
#205375=CARTESIAN_POINT('Ctrl Pts',(187.890348514868,-1.08605398242313,
126.005558931233));
#205376=CARTESIAN_POINT('Ctrl Pts',(187.882602238784,-1.21898716676947,
126.039567510856));
#205377=CARTESIAN_POINT('Ctrl Pts',(187.874855905519,-1.35192133239828,
126.073576341522));
#205378=CARTESIAN_POINT('Ctrl Pts',(187.867109572253,-1.48343040221569,
126.113152323472));
#205379=CARTESIAN_POINT('Ctrl Pts',(187.859363238988,-1.61302151430496,
126.158142299741));
#205380=CARTESIAN_POINT('Ctrl Pts',(187.851615170985,-1.74264164742518,
126.203142351204));
#205381=CARTESIAN_POINT('Ctrl Pts',(187.843867102982,-1.87034259886549,
126.253558681377));
#205382=CARTESIAN_POINT('Ctrl Pts',(187.836119034979,-1.99564971249439,
126.309189287403));
#205383=CARTESIAN_POINT('Ctrl Pts',(187.828362732237,-2.12109000401499,
126.364879018299));
#205384=CARTESIAN_POINT('Ctrl Pts',(187.820606429495,-2.24413101750869,
126.425793936487));
#205385=CARTESIAN_POINT('Ctrl Pts',(187.812850126754,-2.36432052537678,
126.491684938155));
#205386=CARTESIAN_POINT('Ctrl Pts',(187.805089684239,-2.48457418200409,
126.557611107835));
#205387=CARTESIAN_POINT('Ctrl Pts',(187.797329241725,-2.60197296592657,
126.628518451041));
#205388=CARTESIAN_POINT('Ctrl Pts',(187.789568799211,-2.71609292447437,
126.70411400448));
#205389=CARTESIAN_POINT('Ctrl Pts',(187.781795898946,-2.83039607851072,
126.779830910613));
#205390=CARTESIAN_POINT('Ctrl Pts',(187.77402299868,-2.94140957229936,126.860250836692));
#205391=CARTESIAN_POINT('Ctrl Pts',(187.766250098415,-3.04874117726313,
126.945039395309));
#205392=CARTESIAN_POINT('Ctrl Pts',(187.758759762653,-3.15217100803496,
127.026745676251));
#205393=CARTESIAN_POINT('Ctrl Pts',(187.751269426891,-3.25218176050425,
127.112508282006));
#205394=CARTESIAN_POINT('Ctrl Pts',(187.743779091128,-3.34845570588935,
127.201996470482));
#205395=CARTESIAN_POINT('Ctrl Pts',(187.736122099101,-3.44687169893981,
127.293475726888));
#205396=CARTESIAN_POINT('Ctrl Pts',(187.728465107073,-3.54171430929935,
127.389156956171));
#205397=CARTESIAN_POINT('Ctrl Pts',(187.720808115045,-3.63259513007057,
127.488725582842));
#205398=CARTESIAN_POINT('Ctrl Pts',(187.713159991201,-3.72337069438334,
127.588178891002));
#205399=CARTESIAN_POINT('Ctrl Pts',(187.705511867358,-3.81019332122524,
127.691510351903));
#205400=CARTESIAN_POINT('Ctrl Pts',(187.697863743514,-3.8927084393723,127.798365928858));
#205401=CARTESIAN_POINT('Ctrl Pts',(187.690222703422,-3.97514713137943,
127.905122535353));
#205402=CARTESIAN_POINT('Ctrl Pts',(187.68258166333,-4.05328600255709,128.015396450587));
#205403=CARTESIAN_POINT('Ctrl Pts',(187.674940623237,-4.12680846773921,
128.1287980724));
#205404=CARTESIAN_POINT('Ctrl Pts',(187.667304890307,-4.2002798671441,128.242120929961));
#205405=CARTESIAN_POINT('Ctrl Pts',(187.659669157377,-4.26914101941565,
128.358566835824));
#205406=CARTESIAN_POINT('Ctrl Pts',(187.652033424447,-4.33311701410075,
128.47771496242));
#205407=CARTESIAN_POINT('Ctrl Pts',(187.6444009553,-4.39706566317769,128.596812160883));
#205408=CARTESIAN_POINT('Ctrl Pts',(187.636768486153,-4.45613311784616,
128.718608927462));
#205409=CARTESIAN_POINT('Ctrl Pts',(187.629136017006,-4.5100892971886,128.842657889351));
#205410=CARTESIAN_POINT('Ctrl Pts',(187.621503159863,-4.56404821939219,
128.966713157266));
#205411=CARTESIAN_POINT('Ctrl Pts',(187.613870302719,-4.61289517533641,
129.093020483825));
#205412=CARTESIAN_POINT('Ctrl Pts',(187.606237445576,-4.65644742360532,
129.221110651926));
#205413=CARTESIAN_POINT('Ctrl Pts',(187.599143290485,-4.69692589686468,
129.340160635574));
#205414=CARTESIAN_POINT('Ctrl Pts',(187.592049135395,-4.73283104437265,
129.460750229615));
#205415=CARTESIAN_POINT('Ctrl Pts',(187.584954980304,-4.76405452823404,
129.582490119308));
#205416=CARTESIAN_POINT('',(189.610140563969,-4.91824791299378,130.799829742121));
#205417=CARTESIAN_POINT('Ctrl Pts',(189.610140563969,-4.91824791299378,
130.799829742121));
#205418=CARTESIAN_POINT('Ctrl Pts',(189.602485915437,-4.91837237034752,
130.934927722133));
#205419=CARTESIAN_POINT('Ctrl Pts',(189.594831266904,-4.91292619023357,
131.070187999666));
#205420=CARTESIAN_POINT('Ctrl Pts',(189.587176618372,-4.90189607666226,
131.205107315747));
#205421=CARTESIAN_POINT('Ctrl Pts',(189.57916408585,-4.89035026324752,131.346334624011));
#205422=CARTESIAN_POINT('Ctrl Pts',(189.571151553328,-4.87268569848204,
131.487187873076));
#205423=CARTESIAN_POINT('Ctrl Pts',(189.563139020806,-4.84894837207892,
131.627089459538));
#205424=CARTESIAN_POINT('Ctrl Pts',(189.555493068658,-4.82629704912697,
131.760590426017));
#205425=CARTESIAN_POINT('Ctrl Pts',(189.547847116509,-4.79811638583712,
131.893224434576));
#205426=CARTESIAN_POINT('Ctrl Pts',(189.54020116436,-4.76449933419752,132.02449551049));
#205427=CARTESIAN_POINT('Ctrl Pts',(189.532556401308,-4.73088751067271,
132.155746171162));
#205428=CARTESIAN_POINT('Ctrl Pts',(189.524911638256,-4.69184107950793,
132.285633931062));
#205429=CARTESIAN_POINT('Ctrl Pts',(189.517266875204,-4.64750370934258,
132.413674861009));
#205430=CARTESIAN_POINT('Ctrl Pts',(189.509621542448,-4.60316303506545,
132.541725332827));
#205431=CARTESIAN_POINT('Ctrl Pts',(189.501976209692,-4.55353076963928,
132.667928320977));
#205432=CARTESIAN_POINT('Ctrl Pts',(189.494330876936,-4.49879968865441,
132.791817390395));
#205433=CARTESIAN_POINT('Ctrl Pts',(189.486683215447,-4.44405193682891,
132.915744195865));
#205434=CARTESIAN_POINT('Ctrl Pts',(189.479035553957,-4.38420244384357,
133.037355313473));
#205435=CARTESIAN_POINT('Ctrl Pts',(189.471387892468,-4.31949088284538,
133.156207035918));
#205436=CARTESIAN_POINT('Ctrl Pts',(189.46373199972,-4.25470967211568,133.275186679718));
#205437=CARTESIAN_POINT('Ctrl Pts',(189.456076106972,-4.18505614095032,
133.39140064717));
#205438=CARTESIAN_POINT('Ctrl Pts',(189.448420214224,-4.11081455193053,
133.504432242937));
#205439=CARTESIAN_POINT('Ctrl Pts',(189.440759493914,-4.0365261485234,133.617535112838));
#205440=CARTESIAN_POINT('Ctrl Pts',(189.433098773603,-3.95764416228724,
133.727451290957));
#205441=CARTESIAN_POINT('Ctrl Pts',(189.425438053292,-3.87449360985302,
133.833796593075));
#205442=CARTESIAN_POINT('Ctrl Pts',(189.417766480026,-3.79122525788974,
133.940292554763));
#205443=CARTESIAN_POINT('Ctrl Pts',(189.41009490676,-3.70367653135893,134.043207240323));
#205444=CARTESIAN_POINT('Ctrl Pts',(189.402423333494,-3.61220996172295,
134.142192586813));
#205445=CARTESIAN_POINT('Ctrl Pts',(189.399907501612,-3.58221422237703,
134.174654049665));
#205446=CARTESIAN_POINT('Ctrl Pts',(189.397391669729,-3.55179740394281,
134.206693246693));
#205447=CARTESIAN_POINT('Ctrl Pts',(189.394875837847,-3.52097305098158,
134.238298857657));
#205448=CARTESIAN_POINT('Ctrl Pts',(189.387101503728,-3.42572073281059,
134.335965391495));
#205449=CARTESIAN_POINT('Ctrl Pts',(189.379327169609,-3.32625077645834,
134.429820383029));
#205450=CARTESIAN_POINT('Ctrl Pts',(189.37155283549,-3.22290063708545,134.519477647482));
#205451=CARTESIAN_POINT('Ctrl Pts',(189.363788082543,-3.11967786752259,
134.609024417371));
#205452=CARTESIAN_POINT('Ctrl Pts',(189.356023329596,-3.01258472214135,
134.694383499813));
#205453=CARTESIAN_POINT('Ctrl Pts',(189.348258576648,-2.90199674489212,
134.775204099137));
#205454=CARTESIAN_POINT('Ctrl Pts',(189.340501535763,-2.79151860518099,
134.855944426302));
#205455=CARTESIAN_POINT('Ctrl Pts',(189.332744494878,-2.67755285489058,
134.932155011651));
#205456=CARTESIAN_POINT('Ctrl Pts',(189.324987453993,-2.56050921726351,
135.003524297492));
#205457=CARTESIAN_POINT('Ctrl Pts',(189.317236262753,-2.44355384315431,
135.074839763199));
#205458=CARTESIAN_POINT('Ctrl Pts',(189.309485071513,-2.32352553408762,
135.141320993499));
#205459=CARTESIAN_POINT('Ctrl Pts',(189.301733880273,-2.20086389176815,
135.202699075713));
#205460=CARTESIAN_POINT('Ctrl Pts',(189.293985983496,-2.07825438391844,
135.264051070604));
#205461=CARTESIAN_POINT('Ctrl Pts',(189.286238086719,-1.95301411779677,
135.320304056746));
#205462=CARTESIAN_POINT('Ctrl Pts',(189.278490189942,-1.82560805826677,
135.371234633793));
#205463=CARTESIAN_POINT('Ctrl Pts',(189.270743913858,-1.69822864933794,
135.422154557262));
#205464=CARTESIAN_POINT('Ctrl Pts',(189.262997637774,-1.56868471092015,
135.467754141087));
#205465=CARTESIAN_POINT('Ctrl Pts',(189.255251361689,-1.43746162023923,
135.507857949641));
#205466=CARTESIAN_POINT('Ctrl Pts',(189.247505028424,-1.3062375608992,135.547962054233));
#205467=CARTESIAN_POINT('Ctrl Pts',(189.239758695159,-1.1733346984564,135.582570188336));
#205468=CARTESIAN_POINT('Ctrl Pts',(189.232012361893,-1.03925363421513,
135.611556780224));
#205469=CARTESIAN_POINT('Ctrl Pts',(189.22426429389,-0.905142543449059,
135.640549863458));
#205470=CARTESIAN_POINT('Ctrl Pts',(189.216516225887,-0.76985310791742,
135.663918816804));
#205471=CARTESIAN_POINT('Ctrl Pts',(189.208768157884,-0.633895788762408,
135.681589255993));
#205472=CARTESIAN_POINT('Ctrl Pts',(189.201011855143,-0.497793972550918,
135.699278475534));
#205473=CARTESIAN_POINT('Ctrl Pts',(189.193255552401,-0.361023243067375,
135.711257032039));
#205474=CARTESIAN_POINT('Ctrl Pts',(189.185499249659,-0.224099407142775,
135.717502435));
#205475=CARTESIAN_POINT('Ctrl Pts',(189.177738807145,-0.0871024908441983,
135.723751171321));
#205476=CARTESIAN_POINT('Ctrl Pts',(189.16997836463,0.0500473039532961,
135.724260655423));
#205477=CARTESIAN_POINT('Ctrl Pts',(189.162217922116,0.186835504032796,
135.719060563334));
#205478=CARTESIAN_POINT('Ctrl Pts',(189.154445021851,0.323843288674548,
135.713852123596));
#205479=CARTESIAN_POINT('Ctrl Pts',(189.146672121585,0.46048792870308,135.702915823248));
#205480=CARTESIAN_POINT('Ctrl Pts',(189.13889922132,0.596260497125072,135.686333219094));
#205481=CARTESIAN_POINT('Ctrl Pts',(189.131408885558,0.727097390693978,
135.67035343437));
#205482=CARTESIAN_POINT('Ctrl Pts',(189.123918549796,0.857124211873021,
135.649130783049));
#205483=CARTESIAN_POINT('Ctrl Pts',(189.116428214034,0.985897556969896,
135.622782461869));
#205484=CARTESIAN_POINT('Ctrl Pts',(189.108653879915,1.11955338258629,135.595435136084));
#205485=CARTESIAN_POINT('Ctrl Pts',(189.100879545796,1.25228218617169,135.562479160128));
#205486=CARTESIAN_POINT('Ctrl Pts',(189.093105211677,1.38357665678069,135.523989702284));
#205487=CARTESIAN_POINT('Ctrl Pts',(189.08534045873,1.51470931868909,135.485547679256));
#205488=CARTESIAN_POINT('Ctrl Pts',(189.077575705783,1.64441079321712,135.441585852083));
#205489=CARTESIAN_POINT('Ctrl Pts',(189.069810952835,1.7721829553513,135.392230562896));
#205490=CARTESIAN_POINT('Ctrl Pts',(189.06205391195,1.89982821237275,135.342924294078));
#205491=CARTESIAN_POINT('Ctrl Pts',(189.054296871065,2.02554760802274,135.288235363609));
#205492=CARTESIAN_POINT('Ctrl Pts',(189.04653983018,2.14885755457138,135.228340078714));
#205493=CARTESIAN_POINT('Ctrl Pts',(189.03878863894,2.2720745121302,135.16848996132));
#205494=CARTESIAN_POINT('Ctrl Pts',(189.0310374477,2.39288528693343,135.103441474395));
#205495=CARTESIAN_POINT('Ctrl Pts',(189.02328625646,2.51082601966835,135.033419113432));
#205496=CARTESIAN_POINT('Ctrl Pts',(189.015538359683,2.62871662444556,134.963426513841));
#205497=CARTESIAN_POINT('Ctrl Pts',(189.007790462906,2.7437392778564,134.888464444029));
#205498=CARTESIAN_POINT('Ctrl Pts',(189.000042566129,2.85545470199736,134.808803338762));
#205499=CARTESIAN_POINT('Ctrl Pts',(188.992296290045,2.96714675767976,134.729158896881));
#205500=CARTESIAN_POINT('Ctrl Pts',(188.984550013961,3.07553264200004,134.644817601504));
#205501=CARTESIAN_POINT('Ctrl Pts',(188.976803737876,3.18020239775109,134.556092986997));
#205502=CARTESIAN_POINT('Ctrl Pts',(188.969057404611,3.28487292615045,134.467367717545));
#205503=CARTESIAN_POINT('Ctrl Pts',(188.961311071346,3.38582697300727,134.374259317201));
#205504=CARTESIAN_POINT('Ctrl Pts',(188.95356473808,3.48268830403982,134.277121081434));
#205505=CARTESIAN_POINT('Ctrl Pts',(188.945816670077,3.57957132649582,134.179961092233));
#205506=CARTESIAN_POINT('Ctrl Pts',(188.938068602074,3.67235953332192,134.078769748627));
#205507=CARTESIAN_POINT('Ctrl Pts',(188.930320534071,3.76071442620922,133.973936309516));
#205508=CARTESIAN_POINT('Ctrl Pts',(188.92256423133,3.8491632237282,133.868991452179));
#205509=CARTESIAN_POINT('Ctrl Pts',(188.914807928588,3.93316904266262,133.7603970663));
#205510=CARTESIAN_POINT('Ctrl Pts',(188.907051625846,4.01243415492057,133.648574958105));
#205511=CARTESIAN_POINT('Ctrl Pts',(188.899291183332,4.09174157335567,133.536693167084));
#205512=CARTESIAN_POINT('Ctrl Pts',(188.891530740818,4.16630303091852,133.421580549039));
#205513=CARTESIAN_POINT('Ctrl Pts',(188.883770298303,4.23586540955038,133.303685985475));
#205514=CARTESIAN_POINT('Ctrl Pts',(188.875997398038,4.30553945588784,133.185602167092));
#205515=CARTESIAN_POINT('Ctrl Pts',(188.868224497773,4.37019820233963,133.064727823987));
#205516=CARTESIAN_POINT('Ctrl Pts',(188.860451597507,4.42963517748233,132.941535214297));
#205517=CARTESIAN_POINT('Ctrl Pts',(188.852961261745,4.48691146886592,132.822820966272));
#205518=CARTESIAN_POINT('Ctrl Pts',(188.845470925983,4.53933892418261,132.701954357632));
#205519=CARTESIAN_POINT('Ctrl Pts',(188.837980590221,4.58677647383961,132.579371784159));
#205520=CARTESIAN_POINT('Ctrl Pts',(188.830206256102,4.63601263261018,132.452141455156));
#205521=CARTESIAN_POINT('Ctrl Pts',(188.822431921983,4.68002899709644,132.322659443626));
#205522=CARTESIAN_POINT('Ctrl Pts',(188.814657587864,4.7186145945435,132.191393194927));
#205523=CARTESIAN_POINT('Ctrl Pts',(188.806892834917,4.75715263869014,132.060288720149));
#205524=CARTESIAN_POINT('Ctrl Pts',(188.79912808197,4.79027312354286,131.927404754878));
#205525=CARTESIAN_POINT('Ctrl Pts',(188.791363329022,4.8178130955777,131.793228676803));
#205526=CARTESIAN_POINT('Ctrl Pts',(188.783606288137,4.84532571452407,131.659185864302));
#205527=CARTESIAN_POINT('Ctrl Pts',(188.775849247252,4.86726877266508,131.523853873413));
#205528=CARTESIAN_POINT('Ctrl Pts',(188.768092206367,4.88352921128275,131.387734858554));
#205529=CARTESIAN_POINT('Ctrl Pts',(188.760341015127,4.89977738777712,131.251718492103));
#205530=CARTESIAN_POINT('Ctrl Pts',(188.752589823887,4.91035142820668,131.114916669642));
#205531=CARTESIAN_POINT('Ctrl Pts',(188.744838632647,4.91518947969835,130.977840994447));
#205532=CARTESIAN_POINT('Ctrl Pts',(188.73709073587,4.9200254748891,130.840823580069));
#205533=CARTESIAN_POINT('Ctrl Pts',(188.729342839093,4.91913031627366,130.70353293436));
#205534=CARTESIAN_POINT('Ctrl Pts',(188.721594942316,4.91249408784202,130.566484810858));
#205535=CARTESIAN_POINT('Ctrl Pts',(188.713848666232,4.90585924756631,130.429465354868));
#205536=CARTESIAN_POINT('Ctrl Pts',(188.706102390148,4.89348574504375,130.29268871044));
#205537=CARTESIAN_POINT('Ctrl Pts',(188.698356114064,4.87541577373173,130.156669259165));
#205538=CARTESIAN_POINT('Ctrl Pts',(188.690609780798,4.85734566903134,130.020648803825));
#205539=CARTESIAN_POINT('Ctrl Pts',(188.682863447533,4.8335790631205,129.885385940352));
#205540=CARTESIAN_POINT('Ctrl Pts',(188.675117114268,4.8042098296649,129.751388170134));
#205541=CARTESIAN_POINT('Ctrl Pts',(188.667369046265,4.77483401917306,129.617360392044));
#205542=CARTESIAN_POINT('Ctrl Pts',(188.659620978262,4.73985316817686,129.484598652787));
#205543=CARTESIAN_POINT('Ctrl Pts',(188.651872910259,4.69941180461004,129.353598144522));
#205544=CARTESIAN_POINT('Ctrl Pts',(188.644116607517,4.65892745948071,129.222458407358));
#205545=CARTESIAN_POINT('Ctrl Pts',(188.636360304775,4.61297112417784,129.093084014587));
#205546=CARTESIAN_POINT('Ctrl Pts',(188.628604002033,4.56173674692024,128.965953449853));
#205547=CARTESIAN_POINT('Ctrl Pts',(188.620843559519,4.51047502433273,128.838755031709));
#205548=CARTESIAN_POINT('Ctrl Pts',(188.613083117005,4.4539298076903,128.713803183936));
#205549=CARTESIAN_POINT('Ctrl Pts',(188.605322674491,4.39234193722288,128.591553493343));
#205550=CARTESIAN_POINT('Ctrl Pts',(188.597549774225,4.33065520043842,128.469107556694));
#205551=CARTESIAN_POINT('Ctrl Pts',(188.58977687396,4.26390982407976,128.349372787105));
#205552=CARTESIAN_POINT('Ctrl Pts',(188.582003973694,4.1923915294448,128.23277816189));
#205553=CARTESIAN_POINT('Ctrl Pts',(188.574513637932,4.12347310496294,128.120422044985));
#205554=CARTESIAN_POINT('Ctrl Pts',(188.56702330217,4.05012292420374,128.010981987703));
#205555=CARTESIAN_POINT('Ctrl Pts',(188.559532966408,3.9726318877381,127.904812558467));
#205556=CARTESIAN_POINT('Ctrl Pts',(188.551758632289,3.89220275507264,127.794617683053));
#205557=CARTESIAN_POINT('Ctrl Pts',(188.54398429817,3.80705779181573,127.687597278996));
#205558=CARTESIAN_POINT('Ctrl Pts',(188.536209964051,3.71747623705813,127.584181509285));
#205559=CARTESIAN_POINT('Ctrl Pts',(188.528445211104,3.62800508356063,127.480893190268));
#205560=CARTESIAN_POINT('Ctrl Pts',(188.520680458157,3.53410847118426,127.38120095924));
#205561=CARTESIAN_POINT('Ctrl Pts',(188.512915705209,3.4361083642224,127.285505353162));
#205562=CARTESIAN_POINT('Ctrl Pts',(188.505158664324,3.33820559234877,127.18990479331));
#205563=CARTESIAN_POINT('Ctrl Pts',(188.49740162344,3.23620771452785,127.098293230294));
#205564=CARTESIAN_POINT('Ctrl Pts',(188.489644582555,3.13047609649216,127.011037210342));
#205565=CARTESIAN_POINT('Ctrl Pts',(188.481893391314,3.02482421149156,126.923846990833));
#205566=CARTESIAN_POINT('Ctrl Pts',(188.474142200074,2.91544449096346,126.841006024537));
#205567=CARTESIAN_POINT('Ctrl Pts',(188.466391008834,2.80273392824307,126.762842884093));
#205568=CARTESIAN_POINT('Ctrl Pts',(188.458643112057,2.69007127051854,126.684712965069));
#205569=CARTESIAN_POINT('Ctrl Pts',(188.45089521528,2.57408090691345,126.611257139848));
#205570=CARTESIAN_POINT('Ctrl Pts',(188.443147318503,2.45519139564007,126.542762528436));
#205571=CARTESIAN_POINT('Ctrl Pts',(188.435401042419,2.33632675348964,126.47428224462));
#205572=CARTESIAN_POINT('Ctrl Pts',(188.427654766335,2.21456450846326,126.410761305459));
#205573=CARTESIAN_POINT('Ctrl Pts',(188.419908490251,2.09036023095675,126.352442248218));
#205574=CARTESIAN_POINT('Ctrl Pts',(188.412162156985,1.96615503660239,126.294122760479));
#205575=CARTESIAN_POINT('Ctrl Pts',(188.40441582372,1.83950812769249,126.241005397451));
#205576=CARTESIAN_POINT('Ctrl Pts',(188.396669490455,1.71089722052739,126.193285497457));
#205577=CARTESIAN_POINT('Ctrl Pts',(188.388921422452,1.58225751184136,126.145554910922));
#205578=CARTESIAN_POINT('Ctrl Pts',(188.381173354449,1.45165329617858,126.10322432862));
#205579=CARTESIAN_POINT('Ctrl Pts',(188.373425286446,1.31957931360486,126.066439818565));
#205580=CARTESIAN_POINT('Ctrl Pts',(188.365668983704,1.18736496123061,126.029616213495));
#205581=CARTESIAN_POINT('Ctrl Pts',(188.357912680962,1.05367809874174,125.998350560498));
#205582=CARTESIAN_POINT('Ctrl Pts',(188.35015637822,0.919026121729599,125.972738317543));
#205583=CARTESIAN_POINT('Ctrl Pts',(188.342395935706,0.78430227690315,125.947112404563));
#205584=CARTESIAN_POINT('Ctrl Pts',(188.334635493192,0.648612677762575,
125.927145970928));
#205585=CARTESIAN_POINT('Ctrl Pts',(188.326875050678,0.512470802420838,
125.912882646731));
#205586=CARTESIAN_POINT('Ctrl Pts',(188.319102150412,0.376110380054625,
125.89859642578));
#205587=CARTESIAN_POINT('Ctrl Pts',(188.311329250147,0.239296621066078,
125.89003163359));
#205588=CARTESIAN_POINT('Ctrl Pts',(188.303556349881,0.102544875559919,
125.88717975746));
#205589=CARTESIAN_POINT('Ctrl Pts',(188.296066014119,-0.0292355995406955,
125.88443155421));
#205590=CARTESIAN_POINT('Ctrl Pts',(188.288575678357,-0.160958183613458,
125.886988114484));
#205591=CARTESIAN_POINT('Ctrl Pts',(188.281085342595,-0.292167329337183,
125.894796348288));
#205592=CARTESIAN_POINT('Ctrl Pts',(188.273311008476,-0.428351309700771,
125.90290063365));
#205593=CARTESIAN_POINT('Ctrl Pts',(188.265536674357,-0.564413539030559,
125.916688360158));
#205594=CARTESIAN_POINT('Ctrl Pts',(188.257762340238,-0.699841173472941,
125.936157109658));
#205595=CARTESIAN_POINT('Ctrl Pts',(188.249997587291,-0.835101905459319,
125.955601865663));
#205596=CARTESIAN_POINT('Ctrl Pts',(188.242232834344,-0.9697292153955,125.980713658957));
#205597=CARTESIAN_POINT('Ctrl Pts',(188.234468081397,-1.10321209062758,
126.011438111871));
#205598=CARTESIAN_POINT('Ctrl Pts',(188.226711040512,-1.23656238878648,
126.042132048826));
#205599=CARTESIAN_POINT('Ctrl Pts',(188.218953999627,-1.36877013572612,
126.07842746462));
#205600=CARTESIAN_POINT('Ctrl Pts',(188.211196958742,-1.49933161871793,
126.120218459218));
#205601=CARTESIAN_POINT('Ctrl Pts',(188.203445767502,-1.62979464427913,
126.161977938902));
#205602=CARTESIAN_POINT('Ctrl Pts',(188.195694576262,-1.75861350609556,
126.20922462979));
#205603=CARTESIAN_POINT('Ctrl Pts',(188.187943385022,-1.88529718210462,
126.261802131685));
#205604=CARTESIAN_POINT('Ctrl Pts',(188.180195488244,-2.01192701417225,
126.314357286739));
#205605=CARTESIAN_POINT('Ctrl Pts',(188.172447591467,-2.13642310505805,
126.372238596868));
#205606=CARTESIAN_POINT('Ctrl Pts',(188.16469969469,-2.25831224638831,126.435240699286));
#205607=CARTESIAN_POINT('Ctrl Pts',(188.156953418606,-2.38017589113758,
126.498229623022));
#205608=CARTESIAN_POINT('Ctrl Pts',(188.149207142522,-2.49943332390471,
126.566337029047));
#205609=CARTESIAN_POINT('Ctrl Pts',(188.141460866438,-2.61563424429333,
126.6393107304));
#205610=CARTESIAN_POINT('Ctrl Pts',(188.133714533173,-2.73183602245093,
126.712284970429));
#205611=CARTESIAN_POINT('Ctrl Pts',(188.125968199908,-2.84498091211698,
126.790125369541));
#205612=CARTESIAN_POINT('Ctrl Pts',(188.118221866642,-2.95464635229878,
126.872535596619));
#205613=CARTESIAN_POINT('Ctrl Pts',(188.110473798639,-3.06433635129529,
126.954964278895));
#205614=CARTESIAN_POINT('Ctrl Pts',(188.102725730636,-3.17054503780084,
127.04196459072));
#205615=CARTESIAN_POINT('Ctrl Pts',(188.094977662633,-3.27288210156859,
127.133199246592));
#205616=CARTESIAN_POINT('Ctrl Pts',(188.087221359892,-3.37532793038579,
127.224530867742));
#205617=CARTESIAN_POINT('Ctrl Pts',(188.07946505715,-3.47389362439947,127.320105562212));
#205618=CARTESIAN_POINT('Ctrl Pts',(188.071708754408,-3.56822461240654,
127.419548041083));
#205619=CARTESIAN_POINT('Ctrl Pts',(188.063948311894,-3.66260594770211,
127.519043595399));
#205620=CARTESIAN_POINT('Ctrl Pts',(188.05618786938,-3.75274781653608,127.622410752998));
#205621=CARTESIAN_POINT('Ctrl Pts',(188.048427426866,-3.83833596421348,
127.729241093332));
#205622=CARTESIAN_POINT('Ctrl Pts',(188.0406545266,-3.92406150558378,127.836242927212));
#205623=CARTESIAN_POINT('Ctrl Pts',(188.032881626335,-4.00521848641537,
127.946718738031));
#205624=CARTESIAN_POINT('Ctrl Pts',(188.025108726069,-4.08153550936666,
128.060230345826));
#205625=CARTESIAN_POINT('Ctrl Pts',(188.017618390307,-4.15507821630353,
128.169615520761));
#205626=CARTESIAN_POINT('Ctrl Pts',(188.010128054545,-4.22412658393381,
128.281819344595));
#205627=CARTESIAN_POINT('Ctrl Pts',(188.002637718783,-4.28847904391944,
128.396429856027));
#205628=CARTESIAN_POINT('Ctrl Pts',(187.994504561361,-4.35835424099316,
128.52087625753));
#205629=CARTESIAN_POINT('Ctrl Pts',(187.98637140394,-4.42289737344505,128.648524117943));
#205630=CARTESIAN_POINT('Ctrl Pts',(187.978238246518,-4.48181742515692,
128.778898786264));
#205631=CARTESIAN_POINT('Ctrl Pts',(187.970122616113,-4.54061050370865,
128.908992496183));
#205632=CARTESIAN_POINT('Ctrl Pts',(187.962006985708,-4.59380452073732,
129.041800991969));
#205633=CARTESIAN_POINT('Ctrl Pts',(187.953891355302,-4.6411539136234,129.176824623322));
#205634=CARTESIAN_POINT('Ctrl Pts',(187.94588335265,-4.68787536899956,129.310057600188));
#205635=CARTESIAN_POINT('Ctrl Pts',(187.937875349997,-4.72890612235297,
129.445447018229));
#205636=CARTESIAN_POINT('Ctrl Pts',(187.929867347344,-4.76405452823405,
129.582490119308));
#205637=CARTESIAN_POINT('Ctrl Pts',(189.680106903305,-4.76405452823404,
129.582490119308));
#205638=CARTESIAN_POINT('Ctrl Pts',(189.67784575609,-4.77392102796961,129.620959452032));
#205639=CARTESIAN_POINT('Ctrl Pts',(189.675584608875,-4.78331723303707,
129.659531493429));
#205640=CARTESIAN_POINT('Ctrl Pts',(189.67332346166,-4.79224143417708,129.69819376801));
#205641=CARTESIAN_POINT('Ctrl Pts',(189.662792978718,-4.83380270327263,
129.87824945843));
#205642=CARTESIAN_POINT('Ctrl Pts',(189.652262495776,-4.86523011335524,
130.060725185327));
#205643=CARTESIAN_POINT('Ctrl Pts',(189.641732012834,-4.88629864809003,
130.244656602775));
#205644=CARTESIAN_POINT('Ctrl Pts',(189.631201529892,-4.90736718282481,
130.428588020222));
#205645=CARTESIAN_POINT('Ctrl Pts',(189.62067104695,-4.91807669726267,130.613975751142));
#205646=CARTESIAN_POINT('Ctrl Pts',(189.610140564008,-4.91824791299315,
130.799829741432));
#205647=CARTESIAN_POINT('Origin',(213.235140564004,0.,130.804360617566));
#205648=CARTESIAN_POINT('',(191.430300680169,-4.76051597898721,129.583432241588));
#205649=CARTESIAN_POINT('',(191.084784152919,-4.76405452823405,129.582490119308));
#205650=CARTESIAN_POINT('',(213.235140564004,-4.76405452823405,129.582490119308));
#205651=CARTESIAN_POINT('',(191.014859436046,-4.91824790535574,130.799821458629));
#205652=CARTESIAN_POINT('Ctrl Pts',(191.084784152919,-4.76405452823405,
129.582490119308));
#205653=CARTESIAN_POINT('Ctrl Pts',(191.074632403862,-4.8083124628535,129.755051134682));
#205654=CARTESIAN_POINT('Ctrl Pts',(191.064480654806,-4.84321315731302,
129.930105519379));
#205655=CARTESIAN_POINT('Ctrl Pts',(191.054328905749,-4.86852710622365,
130.106774150907));
#205656=CARTESIAN_POINT('Ctrl Pts',(191.04439137085,-4.89330690026231,130.279714861098));
#205657=CARTESIAN_POINT('Ctrl Pts',(191.03445383595,-4.90890030782398,130.45420266127));
#205658=CARTESIAN_POINT('Ctrl Pts',(191.02451630105,-4.91513668305779,130.629390764849));
#205659=CARTESIAN_POINT('Ctrl Pts',(191.021297346049,-4.91715676263013,
130.686137496098));
#205660=CARTESIAN_POINT('Ctrl Pts',(191.018078391047,-4.91819542437289,
130.74295751366));
#205661=CARTESIAN_POINT('Ctrl Pts',(191.014859436046,-4.91824790535574,
130.799821458629));
#205662=CARTESIAN_POINT('Ctrl Pts',(191.014859435991,-4.91824790535664,
130.799821459599));
#205663=CARTESIAN_POINT('Ctrl Pts',(191.007192991401,-4.9183728969955,130.93525183469));
#205664=CARTESIAN_POINT('Ctrl Pts',(190.999526546812,-4.91289980315623,
131.070824814365));
#205665=CARTESIAN_POINT('Ctrl Pts',(190.991860102222,-4.90182013838234,
131.206035104495));
#205666=CARTESIAN_POINT('Ctrl Pts',(190.984145221007,-4.8906704722459,131.342099653731));
#205667=CARTESIAN_POINT('Ctrl Pts',(190.976430339793,-4.87384310420628,
131.477796505531));
#205668=CARTESIAN_POINT('Ctrl Pts',(190.968715458578,-4.85138271638349,
131.612611074835));
#205669=CARTESIAN_POINT('Ctrl Pts',(190.961055815356,-4.82908314331645,
131.746460381553));
#205670=CARTESIAN_POINT('Ctrl Pts',(190.953396172134,-4.80123103213926,
131.879439600074));
#205671=CARTESIAN_POINT('Ctrl Pts',(190.945736528912,-4.76792200125562,
132.011051486199));
#205672=CARTESIAN_POINT('Ctrl Pts',(190.938077448338,-4.7346154171254,132.142653704621));
#205673=CARTESIAN_POINT('Ctrl Pts',(190.930418367764,-4.69585280864405,
132.27288840198));
#205674=CARTESIAN_POINT('Ctrl Pts',(190.92275928719,-4.65178043486449,132.401270711564));
#205675=CARTESIAN_POINT('Ctrl Pts',(190.91509902035,-4.60770123499393,132.529672905471));
#205676=CARTESIAN_POINT('Ctrl Pts',(190.907438753509,-4.55831076464351,
132.65622176218));
#205677=CARTESIAN_POINT('Ctrl Pts',(190.899778486669,-4.50380428023245,
132.780450207605));
#205678=CARTESIAN_POINT('Ctrl Pts',(190.892022192202,-4.44861451305745,
132.906235956834));
#205679=CARTESIAN_POINT('Ctrl Pts',(190.884265897736,-4.38817975595761,
133.029642333155));
#205680=CARTESIAN_POINT('Ctrl Pts',(190.876509603269,-4.32275123572271,
133.150209039045));
#205681=CARTESIAN_POINT('Ctrl Pts',(190.868837761032,-4.25803511551729,
133.269462988289));
#205682=CARTESIAN_POINT('Ctrl Pts',(190.861165918795,-4.18843370140229,
133.385938486624));
#205683=CARTESIAN_POINT('Ctrl Pts',(190.853494076558,-4.11423393107197,
133.499219096766));
#205684=CARTESIAN_POINT('Ctrl Pts',(190.845695555977,-4.03880896557229,
133.614370209414));
#205685=CARTESIAN_POINT('Ctrl Pts',(190.837897035395,-3.95863270394605,
133.726219643716));
#205686=CARTESIAN_POINT('Ctrl Pts',(190.830098514814,-3.87404868695243,
133.834365540602));
#205687=CARTESIAN_POINT('Ctrl Pts',(190.822299994233,-3.78946466995879,
133.942511437488));
#205688=CARTESIAN_POINT('Ctrl Pts',(190.814501473652,-3.70047322628425,
134.046953515992));
#205689=CARTESIAN_POINT('Ctrl Pts',(190.80670295307,-3.60745575518182,134.147330260998));
#205690=CARTESIAN_POINT('Ctrl Pts',(190.798928618951,-3.51472677001999,
134.247395695888));
#205691=CARTESIAN_POINT('Ctrl Pts',(190.791154284832,-3.41768425491403,
134.343758457961));
#205692=CARTESIAN_POINT('Ctrl Pts',(190.783379950713,-3.31665570023412,
134.436023876818));
#205693=CARTESIAN_POINT('Ctrl Pts',(190.775615197766,-3.21575165421878,
134.528175586793));
#205694=CARTESIAN_POINT('Ctrl Pts',(190.767850444819,-3.11087162883549,
134.616239739652));
#205695=CARTESIAN_POINT('Ctrl Pts',(190.760085691872,-3.00238209392103,
134.699856070599));
#205696=CARTESIAN_POINT('Ctrl Pts',(190.752328650987,-2.89400031234197,
134.783389352628));
#205697=CARTESIAN_POINT('Ctrl Pts',(190.744571610102,-2.78201646323467,
134.862483366925));
#205698=CARTESIAN_POINT('Ctrl Pts',(190.736814569217,-2.66683218589617,
134.936816201691));
#205699=CARTESIAN_POINT('Ctrl Pts',(190.729063377977,-2.55173476991692,
135.011092981489));
#205700=CARTESIAN_POINT('Ctrl Pts',(190.721312186737,-2.43344205673886,
135.080615517179));
#205701=CARTESIAN_POINT('Ctrl Pts',(190.713560995496,-2.3123866426324,135.145103765631));
#205702=CARTESIAN_POINT('Ctrl Pts',(190.705813098719,-2.19138268030653,
135.209564604857));
#205703=CARTESIAN_POINT('Ctrl Pts',(190.698065201942,-2.06761869682469,
135.268995229124));
#205704=CARTESIAN_POINT('Ctrl Pts',(190.690317305165,-1.94155380476799,
135.323160445584));
#205705=CARTESIAN_POINT('Ctrl Pts',(190.682571029081,-1.81551528276903,
135.377314331847));
#205706=CARTESIAN_POINT('Ctrl Pts',(190.674824752997,-1.68717716851246,
135.426204846825));
#205707=CARTESIAN_POINT('Ctrl Pts',(190.667078476913,-1.55702020428703,
135.469644225873));
#205708=CARTESIAN_POINT('Ctrl Pts',(190.659332143647,-1.42686227927271,
135.513083925581));
#205709=CARTESIAN_POINT('Ctrl Pts',(190.651585810382,-1.29488584835446,
135.551072285292));
#205710=CARTESIAN_POINT('Ctrl Pts',(190.643839477117,-1.16158814539901,
135.583470999527));
#205711=CARTESIAN_POINT('Ctrl Pts',(190.636091409114,-1.02826059134723,
135.615876969229));
#205712=CARTESIAN_POINT('Ctrl Pts',(190.628343341111,-0.893611556303883,
135.642690710273));
#205713=CARTESIAN_POINT('Ctrl Pts',(190.620595273108,-0.758149436995237,
135.663824836354));
#205714=CARTESIAN_POINT('Ctrl Pts',(190.612838970366,-0.622543346934008,
135.684981424036));
#205715=CARTESIAN_POINT('Ctrl Pts',(190.605082667624,-0.486122833271634,
135.700446278109));
#205716=CARTESIAN_POINT('Ctrl Pts',(190.597326364882,-0.349402960938852,
135.710183752717));
#205717=CARTESIAN_POINT('Ctrl Pts',(190.589565922368,-0.21261011709358,
135.719926424509));
#205718=CARTESIAN_POINT('Ctrl Pts',(190.581805479854,-0.0755179868161497,
135.723935614332));
#205719=CARTESIAN_POINT('Ctrl Pts',(190.57404503734,0.0613583669252786,
135.722227859909));
#205720=CARTESIAN_POINT('Ctrl Pts',(190.566272137074,0.198454446740975,
135.720517364047));
#205721=CARTESIAN_POINT('Ctrl Pts',(190.558499236809,0.335333667223026,
135.713071605924));
#205722=CARTESIAN_POINT('Ctrl Pts',(190.550726336543,0.471485185895587,
135.699959128676));
#205723=CARTESIAN_POINT('Ctrl Pts',(190.543236000781,0.602687253919808,
135.687323323004));
#205724=CARTESIAN_POINT('Ctrl Pts',(190.535745665019,0.7332133040056,135.669425686172));
#205725=CARTESIAN_POINT('Ctrl Pts',(190.528255329257,0.862617086158864,
135.646372061704));
#205726=CARTESIAN_POINT('Ctrl Pts',(190.520480995138,0.996927252043568,
135.622444352059));
#205727=CARTESIAN_POINT('Ctrl Pts',(190.512706661019,1.13045382272073,135.592886162405));
#205728=CARTESIAN_POINT('Ctrl Pts',(190.5049323269,1.26268773426236,135.557759690676));
#205729=CARTESIAN_POINT('Ctrl Pts',(190.497167573953,1.3947586793262,135.522676509184));
#205730=CARTESIAN_POINT('Ctrl Pts',(190.489402821006,1.5255397607892,135.482038799179));
#205731=CARTESIAN_POINT('Ctrl Pts',(190.481638068059,1.65452979177848,135.435960150192));
#205732=CARTESIAN_POINT('Ctrl Pts',(190.473881027174,1.78339170804989,135.389927267168));
#205733=CARTESIAN_POINT('Ctrl Pts',(190.466123986289,1.91046574813598,135.338464330073));
#205734=CARTESIAN_POINT('Ctrl Pts',(190.458366945404,2.03526398267376,135.281735248232));
#205735=CARTESIAN_POINT('Ctrl Pts',(190.450615754164,2.15996810589255,135.225048946233));
#205736=CARTESIAN_POINT('Ctrl Pts',(190.442864562924,2.28239948508168,135.163104565135));
#205737=CARTESIAN_POINT('Ctrl Pts',(190.435113371684,2.40208868317336,135.096114690282));
#205738=CARTESIAN_POINT('Ctrl Pts',(190.427365474906,2.52172701016312,135.029153287912));
#205739=CARTESIAN_POINT('Ctrl Pts',(190.419617578129,2.63862513369723,134.95715084752));
#205740=CARTESIAN_POINT('Ctrl Pts',(190.411869681352,2.75233701780585,134.880366506045));
#205741=CARTESIAN_POINT('Ctrl Pts',(190.404123405268,2.86602511583959,134.803598226199));
#205742=CARTESIAN_POINT('Ctrl Pts',(190.396377129184,2.97652797633052,134.722050253513));
#205743=CARTESIAN_POINT('Ctrl Pts',(190.3886308531,3.08342777461511,134.636025558715));
#205744=CARTESIAN_POINT('Ctrl Pts',(190.380884519835,3.1903283620097,134.550000228902));
#205745=CARTESIAN_POINT('Ctrl Pts',(190.373138186569,3.29362552953602,134.459498356145));
#205746=CARTESIAN_POINT('Ctrl Pts',(190.365391853304,3.39293414982598,134.364863519888));
#205747=CARTESIAN_POINT('Ctrl Pts',(190.357643785301,3.49226500959297,134.270207490816));
#205748=CARTESIAN_POINT('Ctrl Pts',(190.349895717298,3.58760526176411,134.171416926171));
#205749=CARTESIAN_POINT('Ctrl Pts',(190.342147649295,3.67860658491866,134.068872320086));
#205750=CARTESIAN_POINT('Ctrl Pts',(190.334391346553,3.76970462536241,133.966218728374));
#205751=CARTESIAN_POINT('Ctrl Pts',(190.326635043811,3.85645426497193,133.859803417977));
#205752=CARTESIAN_POINT('Ctrl Pts',(190.31887874107,3.93854710870415,133.750040460152));
#205753=CARTESIAN_POINT('Ctrl Pts',(190.311118298555,4.02068376785884,133.640218918532));
#205754=CARTESIAN_POINT('Ctrl Pts',(190.303357856041,4.09815845787932,133.527046491708));
#205755=CARTESIAN_POINT('Ctrl Pts',(190.295597413527,4.17070668830499,133.410965455785));
#205756=CARTESIAN_POINT('Ctrl Pts',(190.287824513262,4.24337137959067,133.294698076279));
#205757=CARTESIAN_POINT('Ctrl Pts',(190.280051612996,4.31109361453856,133.175513097328));
#205758=CARTESIAN_POINT('Ctrl Pts',(190.272278712731,4.37365493759366,133.053877354415));
#205759=CARTESIAN_POINT('Ctrl Pts',(190.264788376969,4.43394199897344,132.936663377138));
#205760=CARTESIAN_POINT('Ctrl Pts',(190.257298041207,4.4894367285661,132.817174004629));
#205761=CARTESIAN_POINT('Ctrl Pts',(190.249807705445,4.53998696650629,132.695841890657));
#205762=CARTESIAN_POINT('Ctrl Pts',(190.242033371326,4.59245383208216,132.569909432706));
#205763=CARTESIAN_POINT('Ctrl Pts',(190.234259037206,4.63976006301382,132.44159282362));
#205764=CARTESIAN_POINT('Ctrl Pts',(190.226484703087,4.68168282669612,132.3113539728));
#205765=CARTESIAN_POINT('Ctrl Pts',(190.21871995014,4.72355392431904,132.181275629723));
#205766=CARTESIAN_POINT('Ctrl Pts',(190.210955197193,4.76005463700814,132.049280127086));
#205767=CARTESIAN_POINT('Ctrl Pts',(190.203190444246,4.79100962710627,131.915850525516));
#205768=CARTESIAN_POINT('Ctrl Pts',(190.195433403361,4.82193387227178,131.782553448108));
#205769=CARTESIAN_POINT('Ctrl Pts',(190.187676362476,4.84732326841009,131.647825484707));
#205770=CARTESIAN_POINT('Ctrl Pts',(190.179919321591,4.8670519793402,131.5121657411));
#205771=CARTESIAN_POINT('Ctrl Pts',(190.172168130351,4.8867658126959,131.376608299561));
#205772=CARTESIAN_POINT('Ctrl Pts',(190.164416939111,4.90082740152704,131.240120861754));
#205773=CARTESIAN_POINT('Ctrl Pts',(190.156665747871,4.90916185770046,131.103213285948));
#205774=CARTESIAN_POINT('Ctrl Pts',(190.148917851094,4.91749277150769,130.966363899514));
#205775=CARTESIAN_POINT('Ctrl Pts',(190.141169954316,4.92010137035702,130.829095119669));
#205776=CARTESIAN_POINT('Ctrl Pts',(190.133422057539,4.91696458015609,130.691922278951));
#205777=CARTESIAN_POINT('Ctrl Pts',(190.125675781455,4.91382844610404,130.554778131835));
#205778=CARTESIAN_POINT('Ctrl Pts',(190.117929505371,4.90494932240312,130.417730274544));
#205779=CARTESIAN_POINT('Ctrl Pts',(190.110183229287,4.8903562624689,130.281293997879));
#205780=CARTESIAN_POINT('Ctrl Pts',(190.102436896022,4.87576309481204,130.144856714072));
#205781=CARTESIAN_POINT('Ctrl Pts',(190.094690562756,4.85545594833678,130.009031408648));
#205782=CARTESIAN_POINT('Ctrl Pts',(190.086944229491,4.82951571541046,129.87432781325));
#205783=CARTESIAN_POINT('Ctrl Pts',(190.079196161488,4.80356967334887,129.739594051917));
#205784=CARTESIAN_POINT('Ctrl Pts',(190.071448093485,4.77198810853258,129.605982884305));
#205785=CARTESIAN_POINT('Ctrl Pts',(190.063700025482,4.73490286521561,129.473993029464));
#205786=CARTESIAN_POINT('Ctrl Pts',(190.05594372274,4.69777820726065,129.341862894234));
#205787=CARTESIAN_POINT('Ctrl Pts',(190.048187419998,4.65513829197155,129.211357890945));
#205788=CARTESIAN_POINT('Ctrl Pts',(190.040431117256,4.60716479417153,129.082961296709));
#205789=CARTESIAN_POINT('Ctrl Pts',(190.032670674742,4.55916569147128,128.954496173345));
#205790=CARTESIAN_POINT('Ctrl Pts',(190.024910232228,4.50582748595494,128.828142061345));
#205791=CARTESIAN_POINT('Ctrl Pts',(190.017149789714,4.44737931348167,128.704360545062));
#205792=CARTESIAN_POINT('Ctrl Pts',(190.009376889448,4.38883731481318,128.580380323701));
#205793=CARTESIAN_POINT('Ctrl Pts',(190.001603989183,4.32516913872479,128.458981297068));
#205794=CARTESIAN_POINT('Ctrl Pts',(189.993831088917,4.25664946656522,128.34059959399));
#205795=CARTESIAN_POINT('Ctrl Pts',(189.986340753155,4.19062065707926,128.226521364005));
#205796=CARTESIAN_POINT('Ctrl Pts',(189.978850417393,4.12008712075145,128.115245151775));
#205797=CARTESIAN_POINT('Ctrl Pts',(189.971360081631,4.04533061532805,128.007132833636));
#205798=CARTESIAN_POINT('Ctrl Pts',(189.963585747512,3.96773969427981,127.894921404095));
#205799=CARTESIAN_POINT('Ctrl Pts',(189.955811413393,3.88535347027769,127.785763070711));
#205800=CARTESIAN_POINT('Ctrl Pts',(189.948037079274,3.79844011431754,127.680094982182));
#205801=CARTESIAN_POINT('Ctrl Pts',(189.940272326327,3.71163387130119,127.574557120128));
#205802=CARTESIAN_POINT('Ctrl Pts',(189.93250757338,3.62031184341438,127.472501243445));
#205803=CARTESIAN_POINT('Ctrl Pts',(189.924742820433,3.52478566895689,127.374335974737));
#205804=CARTESIAN_POINT('Ctrl Pts',(189.916985779548,3.42935437244241,127.276268205157));
#205805=CARTESIAN_POINT('Ctrl Pts',(189.909228738663,3.32972750992248,127.18208363199));
#205806=CARTESIAN_POINT('Ctrl Pts',(189.901471697778,3.22625697570096,127.092157903645));
#205807=CARTESIAN_POINT('Ctrl Pts',(189.893720506538,3.12286446941407,127.002299988992));
#205808=CARTESIAN_POINT('Ctrl Pts',(189.885969315298,3.01563435469827,126.916694782037));
#205809=CARTESIAN_POINT('Ctrl Pts',(189.878218124058,2.90495511089095,126.835680879138));
#205810=CARTESIAN_POINT('Ctrl Pts',(189.87047022728,2.79432290871461,126.754701409308));
#205811=CARTESIAN_POINT('Ctrl Pts',(189.862722330503,2.68024480797378,126.678309592735));
#205812=CARTESIAN_POINT('Ctrl Pts',(189.854974433726,2.56314190041725,126.606803392128));
#205813=CARTESIAN_POINT('Ctrl Pts',(189.847228157642,2.44606348826436,126.535312149077));
#205814=CARTESIAN_POINT('Ctrl Pts',(189.839481881558,2.32596186128318,126.468704692871));
#205815=CARTESIAN_POINT('Ctrl Pts',(189.831735605474,2.20328625229884,126.407235107311));
#205816=CARTESIAN_POINT('Ctrl Pts',(189.823989272209,2.0806097377515,126.345765067998));
#205817=CARTESIAN_POINT('Ctrl Pts',(189.816242938943,1.9553595528264,126.289433150157));
#205818=CARTESIAN_POINT('Ctrl Pts',(189.808496605678,1.82800827349247,126.238446819152));
#205819=CARTESIAN_POINT('Ctrl Pts',(189.800748537675,1.70062847472297,126.187449070113));
#205820=CARTESIAN_POINT('Ctrl Pts',(189.793000469672,1.57114700814089,126.141799435301));
#205821=CARTESIAN_POINT('Ctrl Pts',(189.785252401669,1.44005472524652,126.10165656024));
#205822=CARTESIAN_POINT('Ctrl Pts',(189.777496098927,1.30882311591319,126.061471020852));
#205823=CARTESIAN_POINT('Ctrl Pts',(189.769739796186,1.17597764480057,126.02680404717));
#205824=CARTESIAN_POINT('Ctrl Pts',(189.761983493444,1.04202310631098,125.997764014104));
#205825=CARTESIAN_POINT('Ctrl Pts',(189.75422305093,0.907997072250902,125.968708481497));
#205826=CARTESIAN_POINT('Ctrl Pts',(189.746462608415,0.772861176351149,
125.945285940508));
#205827=CARTESIAN_POINT('Ctrl Pts',(189.738702165901,0.637127616130016,
125.927553110265));
#205828=CARTESIAN_POINT('Ctrl Pts',(189.730929265636,0.501176164348156,
125.909791813709));
#205829=CARTESIAN_POINT('Ctrl Pts',(189.723156365371,0.36462552068547,125.897738514198));
#205830=CARTESIAN_POINT('Ctrl Pts',(189.715383465105,0.227991084653854,
125.891397852816));
#205831=CARTESIAN_POINT('Ctrl Pts',(189.707893129343,0.0963236545319259,
125.885287690447));
#205832=CARTESIAN_POINT('Ctrl Pts',(189.700402793581,-0.035421273587108,
125.88448204139));
#205833=CARTESIAN_POINT('Ctrl Pts',(189.692912457819,-0.166786945949541,
125.888939457873));
#205834=CARTESIAN_POINT('Ctrl Pts',(189.6851381237,-0.303133387705632,125.893565878656));
#205835=CARTESIAN_POINT('Ctrl Pts',(189.677363789581,-0.439503151574217,
125.903876996674));
#205836=CARTESIAN_POINT('Ctrl Pts',(189.669589455462,-0.575383499002755,
125.91988348162));
#205837=CARTESIAN_POINT('Ctrl Pts',(189.661824702515,-0.711096386047016,
125.935870240005));
#205838=CARTESIAN_POINT('Ctrl Pts',(189.654059949567,-0.846320672210825,
125.95753835424));
#205839=CARTESIAN_POINT('Ctrl Pts',(189.64629519662,-0.980544123610611,
125.984846504696));
#205840=CARTESIAN_POINT('Ctrl Pts',(189.638538155735,-1.11463426238657,
126.012127532312));
#205841=CARTESIAN_POINT('Ctrl Pts',(189.63078111485,-1.24772516395203,126.045037370947));
#205842=CARTESIAN_POINT('Ctrl Pts',(189.623024073965,-1.37931057719251,
126.083483009097));
#205843=CARTESIAN_POINT('Ctrl Pts',(189.615272882725,-1.51079676084857,
126.121899655092));
#205844=CARTESIAN_POINT('Ctrl Pts',(189.607521691485,-1.64077934216929,
126.165843682135));
#205845=CARTESIAN_POINT('Ctrl Pts',(189.599770500245,-1.76876346787959,
126.215171271157));
#205846=CARTESIAN_POINT('Ctrl Pts',(189.592022603468,-1.89669319692298,
126.264477894638));
#205847=CARTESIAN_POINT('Ctrl Pts',(189.584274706691,-2.02262579569819,
126.319163388819));
#205848=CARTESIAN_POINT('Ctrl Pts',(189.576526809914,-2.14608296936092,
126.379034533409));
#205849=CARTESIAN_POINT('Ctrl Pts',(189.56878053383,-2.26951431844442,126.438893154247));
#205850=CARTESIAN_POINT('Ctrl Pts',(189.561034257746,-2.39047092080065,
126.503935097423));
#205851=CARTESIAN_POINT('Ctrl Pts',(189.553287981662,-2.50849618721501,
126.573919749143));
#205852=CARTESIAN_POINT('Ctrl Pts',(189.545541648396,-2.62652232486488,
126.643904917472));
#205853=CARTESIAN_POINT('Ctrl Pts',(189.537795315131,-2.74161674710555,
126.718832667743));
#205854=CARTESIAN_POINT('Ctrl Pts',(189.530048981866,-2.85334946859526,
126.798417548504));
#205855=CARTESIAN_POINT('Ctrl Pts',(189.522300913863,-2.96510721185335,
126.878020251747));
#205856=CARTESIAN_POINT('Ctrl Pts',(189.51455284586,-3.0735014379343,126.962281934019));
#205857=CARTESIAN_POINT('Ctrl Pts',(189.506804777857,-3.17813335664093,
127.050875379829));
#205858=CARTESIAN_POINT('Ctrl Pts',(189.499048475115,-3.28287647939589,
127.139562983809));
#205859=CARTESIAN_POINT('Ctrl Pts',(189.491292172373,-3.38384900824164,
127.232591294972));
#205860=CARTESIAN_POINT('Ctrl Pts',(189.483535869631,-3.48068691059195,
127.329594194778));
#205861=CARTESIAN_POINT('Ctrl Pts',(189.475775427117,-3.5775764982465,127.426648867953));
#205862=CARTESIAN_POINT('Ctrl Pts',(189.468014984603,-3.67032679795341,
127.527682068888));
#205863=CARTESIAN_POINT('Ctrl Pts',(189.460254542089,-3.75861323503234,
127.632293529382));
#205864=CARTESIAN_POINT('Ctrl Pts',(189.452481641823,-3.84704139733793,
127.737072921479));
#205865=CARTESIAN_POINT('Ctrl Pts',(189.444708741558,-3.93099113791891,
127.845441742504));
#205866=CARTESIAN_POINT('Ctrl Pts',(189.436935841292,-4.01017996607299,
127.95696888087));
#205867=CARTESIAN_POINT('Ctrl Pts',(189.42944550553,-4.08649008085959,128.064441726837));
#205868=CARTESIAN_POINT('Ctrl Pts',(189.421955169768,-4.15837924792512,
128.174846993079));
#205869=CARTESIAN_POINT('Ctrl Pts',(189.414464834006,-4.22563545189443,
128.287777996194));
#205870=CARTESIAN_POINT('Ctrl Pts',(189.406414631678,-4.29791873357895,
128.409150048544));
#205871=CARTESIAN_POINT('Ctrl Pts',(189.398364429349,-4.36506593948658,
128.533801166826));
#205872=CARTESIAN_POINT('Ctrl Pts',(189.39031422702,-4.42677811181953,128.661274382433));
#205873=CARTESIAN_POINT('Ctrl Pts',(189.382275040237,-4.48840583991566,
128.788573169269));
#205874=CARTESIAN_POINT('Ctrl Pts',(189.374235853453,-4.54461318938345,
128.918686050171));
#205875=CARTESIAN_POINT('Ctrl Pts',(189.366196666669,-4.59514535868655,
129.051128689086));
#205876=CARTESIAN_POINT('Ctrl Pts',(189.358170521655,-4.64559555092435,
129.183356469644));
#205877=CARTESIAN_POINT('Ctrl Pts',(189.350144376642,-4.69038878678416,
129.317906148175));
#205878=CARTESIAN_POINT('Ctrl Pts',(189.342118231628,-4.72931719504994,
129.454271016427));
#205879=CARTESIAN_POINT('Ctrl Pts',(189.339612754859,-4.74146925838755,
129.496839274155));
#205880=CARTESIAN_POINT('Ctrl Pts',(189.33710727809,-4.7530501596044,129.539584253036));
#205881=CARTESIAN_POINT('Ctrl Pts',(189.334601801321,-4.76405452823404,
129.582490119308));
#205882=CARTESIAN_POINT('',(191.360141504983,-4.9217530988948,130.806072159341));
#205883=CARTESIAN_POINT('Ctrl Pts',(191.360140564008,-4.9182496968395,130.806087475454));
#205884=CARTESIAN_POINT('Ctrl Pts',(191.354763444185,-4.91821654842555,
130.90049719961));
#205885=CARTESIAN_POINT('Ctrl Pts',(191.349386324361,-4.91546519350092,
130.994855987655));
#205886=CARTESIAN_POINT('Ctrl Pts',(191.344009204538,-4.91000321302235,
131.089056087516));
#205887=CARTESIAN_POINT('Ctrl Pts',(191.336234870419,-4.90210618588047,
131.225252243524));
#205888=CARTESIAN_POINT('Ctrl Pts',(191.3284605363,-4.88852553889003,131.361335297868));
#205889=CARTESIAN_POINT('Ctrl Pts',(191.32068620218,-4.86926290974064,131.49679240361));
#205890=CARTESIAN_POINT('Ctrl Pts',(191.312921449233,-4.85002402006014,
131.632082570575));
#205891=CARTESIAN_POINT('Ctrl Pts',(191.305156696286,-4.82511713569348,
131.76674794049));
#205892=CARTESIAN_POINT('Ctrl Pts',(191.297391943339,-4.79459585657098,
131.900277418538));
#205893=CARTESIAN_POINT('Ctrl Pts',(191.289634902454,-4.76410489161315,
132.033674273226));
#205894=CARTESIAN_POINT('Ctrl Pts',(191.281877861569,-4.72801071553388,
132.165937102515));
#205895=CARTESIAN_POINT('Ctrl Pts',(191.274120820684,-4.68641846168075,
132.296562033099));
#205896=CARTESIAN_POINT('Ctrl Pts',(191.266369629444,-4.64485757286983,
132.427088458406));
#205897=CARTESIAN_POINT('Ctrl Pts',(191.258618438204,-4.59780697707092,
132.555979072473));
#205898=CARTESIAN_POINT('Ctrl Pts',(191.250867246964,-4.5454223270494,132.682742615792));
#205899=CARTESIAN_POINT('Ctrl Pts',(191.243119350187,-4.49305994190156,
132.809452281224));
#205900=CARTESIAN_POINT('Ctrl Pts',(191.235371453409,-4.4353681606558,132.934036313446));
#205901=CARTESIAN_POINT('Ctrl Pts',(191.227623556632,-4.37255162571712,
133.056021192106));
#205902=CARTESIAN_POINT('Ctrl Pts',(191.219877280548,-4.3097482306434,133.177980554159));
#205903=CARTESIAN_POINT('Ctrl Pts',(191.212131004464,-4.24182239299693,
133.297341496706));
#205904=CARTESIAN_POINT('Ctrl Pts',(191.20438472838,-4.16902561416592,133.413653336087));
#205905=CARTESIAN_POINT('Ctrl Pts',(191.196638395115,-4.09622829796563,
133.529966034056));
#205906=CARTESIAN_POINT('Ctrl Pts',(191.188892061849,-4.01856017625269,
133.643229252539));
#205907=CARTESIAN_POINT('Ctrl Pts',(191.181145728584,-3.93631693673612,
133.753019980067));
#205908=CARTESIAN_POINT('Ctrl Pts',(191.173397660581,-3.85405527941647,
133.862835294467));
#205909=CARTESIAN_POINT('Ctrl Pts',(191.165649592578,-3.76721669987783,
133.969176257649));
#205910=CARTESIAN_POINT('Ctrl Pts',(191.157901524575,-3.67613788924386,
134.071652046528));
#205911=CARTESIAN_POINT('Ctrl Pts',(191.150145221833,-3.58496227896587,
134.174236747894));
#205912=CARTESIAN_POINT('Ctrl Pts',(191.142388919091,-3.48953769537748,
134.272947776186));
#205913=CARTESIAN_POINT('Ctrl Pts',(191.134632616349,-3.3902388873648,134.367429989484));
#205914=CARTESIAN_POINT('Ctrl Pts',(191.126872173835,-3.29088708058837,
134.461962630784));
#205915=CARTESIAN_POINT('Ctrl Pts',(191.119111731321,-3.18765722326609,
134.552261702453));
#205916=CARTESIAN_POINT('Ctrl Pts',(191.111351288807,-3.08095725723101,
134.638012328613));
#205917=CARTESIAN_POINT('Ctrl Pts',(191.103578388541,-2.97408600693812,
134.723900609291));
#205918=CARTESIAN_POINT('Ctrl Pts',(191.095805488276,-2.86373383115774,
134.805225621522));
#205919=CARTESIAN_POINT('Ctrl Pts',(191.088032588011,-2.7503384963244,134.881715301443));
#205920=CARTESIAN_POINT('Ctrl Pts',(191.080542252248,-2.64106536753748,
134.955424388834));
#205921=CARTESIAN_POINT('Ctrl Pts',(191.073051916486,-2.52896675349539,
135.024643431626));
#205922=CARTESIAN_POINT('Ctrl Pts',(191.065561580724,-2.41445430827056,
135.08917023478));
#205923=CARTESIAN_POINT('Ctrl Pts',(191.057787246605,-2.29560008888017,
135.156143591289));
#205924=CARTESIAN_POINT('Ctrl Pts',(191.050012912486,-2.17376888976368,
135.218274023238));
#205925=CARTESIAN_POINT('Ctrl Pts',(191.042238578367,-2.04939306878735,
135.275285702166));
#205926=CARTESIAN_POINT('Ctrl Pts',(191.03447382542,-1.92517052989461,135.332227119295));
#205927=CARTESIAN_POINT('Ctrl Pts',(191.026709072473,-1.79840996087941,
135.384062173901));
#205928=CARTESIAN_POINT('Ctrl Pts',(191.018944319526,-1.66957033235678,
135.430559701891));
#205929=CARTESIAN_POINT('Ctrl Pts',(191.011187278641,-1.54085866916962,
135.477011047882));
#205930=CARTESIAN_POINT('Ctrl Pts',(191.003430237756,-1.41007242119069,
135.518135285236));
#205931=CARTESIAN_POINT('Ctrl Pts',(190.995673196871,-1.27769233844608,
135.553748509787));
#205932=CARTESIAN_POINT('Ctrl Pts',(190.987922005631,-1.14541208455148,
135.589334878129));
#205933=CARTESIAN_POINT('Ctrl Pts',(190.980170814391,-1.01154076426068,
135.619418404572));
#205934=CARTESIAN_POINT('Ctrl Pts',(190.972419623151,-0.876575822233106,
135.643864506435));
#205935=CARTESIAN_POINT('Ctrl Pts',(190.964671726373,-0.741668243906204,
135.668300218052));
#205936=CARTESIAN_POINT('Ctrl Pts',(190.956923829596,-0.605668352230964,
135.687103201124));
#205937=CARTESIAN_POINT('Ctrl Pts',(190.949175932819,-0.469085147509697,
135.700189677785));
#205938=CARTESIAN_POINT('Ctrl Pts',(190.941429656735,-0.332530513050464,
135.713273417038));
#205939=CARTESIAN_POINT('Ctrl Pts',(190.933683380651,-0.195393197179081,
135.720642991066));
#205940=CARTESIAN_POINT('Ctrl Pts',(190.925937104567,-0.0581883154667574,
135.722266389584));
#205941=CARTESIAN_POINT('Ctrl Pts',(190.918190771302,0.0790175790607411,
135.723889800085));
#205942=CARTESIAN_POINT('Ctrl Pts',(190.910444438036,0.216290649486569,
135.71976694581));
#205943=CARTESIAN_POINT('Ctrl Pts',(190.902698104771,0.353115177852348,
135.709917949172));
#205944=CARTESIAN_POINT('Ctrl Pts',(190.894950036768,0.489970347122603,
135.700066746919));
#205945=CARTESIAN_POINT('Ctrl Pts',(190.887201968765,0.626376384571554,
135.684486878679));
#205946=CARTESIAN_POINT('Ctrl Pts',(190.879453900762,0.7618224898918,135.663250362806));
#205947=CARTESIAN_POINT('Ctrl Pts',(190.87169759802,0.897412548944634,135.641991276511));
#205948=CARTESIAN_POINT('Ctrl Pts',(190.863941295278,1.03204025099248,135.615063593716));
#205949=CARTESIAN_POINT('Ctrl Pts',(190.856184992537,1.16520424415458,135.58259063839));
#205950=CARTESIAN_POINT('Ctrl Pts',(190.848424550022,1.29843931094942,135.550100351271));
#205951=CARTESIAN_POINT('Ctrl Pts',(190.840664107508,1.43020873675926,135.512059002598));
#205952=CARTESIAN_POINT('Ctrl Pts',(190.832903664994,1.56002710506518,135.468639607288));
#205953=CARTESIAN_POINT('Ctrl Pts',(190.825130764729,1.69005386934062,135.42515051131));
#205954=CARTESIAN_POINT('Ctrl Pts',(190.817357864463,1.81812295188554,135.376266256074));
#205955=CARTESIAN_POINT('Ctrl Pts',(190.809584964198,1.94376883421616,135.322208089718));
#205956=CARTESIAN_POINT('Ctrl Pts',(190.802094628436,2.06484717224159,135.270115073873));
#205957=CARTESIAN_POINT('Ctrl Pts',(190.794604292674,2.1836751523785,135.21321791848));
#205958=CARTESIAN_POINT('Ctrl Pts',(190.787113956912,2.29986015313222,135.151753668411));
#205959=CARTESIAN_POINT('Ctrl Pts',(190.779339622793,2.42045034350282,135.087958982619));
#205960=CARTESIAN_POINT('Ctrl Pts',(190.771565288673,2.5385751745423,135.019041960452));
#205961=CARTESIAN_POINT('Ctrl Pts',(190.763790954554,2.65376888396502,134.945217264807));
#205962=CARTESIAN_POINT('Ctrl Pts',(190.756026201607,2.768820627436,134.871483551501));
#205963=CARTESIAN_POINT('Ctrl Pts',(190.74826144866,2.88094811077286,134.792854407899));
#205964=CARTESIAN_POINT('Ctrl Pts',(190.740496695713,2.98970876424912,134.709591029139));
#205965=CARTESIAN_POINT('Ctrl Pts',(190.732739654828,3.09836139511106,134.62641034874));
#205966=CARTESIAN_POINT('Ctrl Pts',(190.724982613943,3.20365354236057,134.538604829062));
#205967=CARTESIAN_POINT('Ctrl Pts',(190.717225573058,3.3051706250811,134.446479534021));
#205968=CARTESIAN_POINT('Ctrl Pts',(190.709474381818,3.40661115297993,134.354423711382));
#205969=CARTESIAN_POINT('Ctrl Pts',(190.701723190578,3.50428199439297,134.258054859062));
#205970=CARTESIAN_POINT('Ctrl Pts',(190.693971999338,3.59780104010722,134.157718746115));
#205971=CARTESIAN_POINT('Ctrl Pts',(190.68622410256,3.69128033773231,134.057425278691));
#205972=CARTESIAN_POINT('Ctrl Pts',(190.678476205783,3.78061108335151,133.953168189747));
#205973=CARTESIAN_POINT('Ctrl Pts',(190.670728309006,3.86544766517695,133.845330431668));
#205974=CARTESIAN_POINT('Ctrl Pts',(190.662982032922,3.95026650101836,133.737515230923));
#205975=CARTESIAN_POINT('Ctrl Pts',(190.655235756838,4.03059280135912,133.626121157924));
#205976=CARTESIAN_POINT('Ctrl Pts',(190.647489480754,4.10612120249017,133.511564291648));
#205977=CARTESIAN_POINT('Ctrl Pts',(190.639743147489,4.18165016115467,133.397006579739));
#205978=CARTESIAN_POINT('Ctrl Pts',(190.631996814223,4.25238093473435,133.279286354372));
#205979=CARTESIAN_POINT('Ctrl Pts',(190.624250480958,4.31805169463097,133.158848380328));
#205980=CARTESIAN_POINT('Ctrl Pts',(190.616502412955,4.38373716103891,133.038383435034));
#205981=CARTESIAN_POINT('Ctrl Pts',(190.608754344952,4.44436017178771,132.915199873166));
#205982=CARTESIAN_POINT('Ctrl Pts',(190.601006276949,4.49970521791473,132.789766373166));
#205983=CARTESIAN_POINT('Ctrl Pts',(190.593249974207,4.55510908541542,132.664199560951));
#205984=CARTESIAN_POINT('Ctrl Pts',(190.585493671465,4.60522362466958,132.536378392067));
#205985=CARTESIAN_POINT('Ctrl Pts',(190.577737368723,4.64988159868781,132.40679132767));
#205986=CARTESIAN_POINT('Ctrl Pts',(190.569976926209,4.69456340801143,132.277135098755));
#205987=CARTESIAN_POINT('Ctrl Pts',(190.562216483695,4.73378273728387,132.145711470748));
#205988=CARTESIAN_POINT('Ctrl Pts',(190.554456041181,4.76742276936732,132.013022357102));
#205989=CARTESIAN_POINT('Ctrl Pts',(190.546683140915,4.80111680341668,131.880120239111));
#205990=CARTESIAN_POINT('Ctrl Pts',(190.53891024065,4.82921356238978,131.745948958842));
#205991=CARTESIAN_POINT('Ctrl Pts',(190.531137340384,4.85164756449836,131.611019760201));
#205992=CARTESIAN_POINT('Ctrl Pts',(190.523647004622,4.8732660341224,131.480995577798));
#205993=CARTESIAN_POINT('Ctrl Pts',(190.51615666886,4.88962627167772,131.350267930446));
#205994=CARTESIAN_POINT('Ctrl Pts',(190.508666333098,4.90071548822044,131.219295270272));
#205995=CARTESIAN_POINT('Ctrl Pts',(190.500891998979,4.91222515577889,131.083356741879));
#205996=CARTESIAN_POINT('Ctrl Pts',(190.49311766486,4.91809266973481,130.946723642184));
#205997=CARTESIAN_POINT('Ctrl Pts',(190.485343330741,4.91824687616993,130.809903860727));
#205998=CARTESIAN_POINT('Ctrl Pts',(190.477578577794,4.91840089255939,130.673252697422));
#205999=CARTESIAN_POINT('Ctrl Pts',(190.469813824847,4.91285561076338,130.536415697335));
#206000=CARTESIAN_POINT('Ctrl Pts',(190.4620490719,4.90159156190185,130.399906389262));
#206001=CARTESIAN_POINT('Ctrl Pts',(190.454292031015,4.89033870065244,130.26353266416));
#206002=CARTESIAN_POINT('Ctrl Pts',(190.44653499013,4.8733784076575,130.127486370495));
#206003=CARTESIAN_POINT('Ctrl Pts',(190.438777949245,4.85074325071888,129.992281201434));
#206004=CARTESIAN_POINT('Ctrl Pts',(190.431026758005,4.82812516312819,129.857177991643));
#206005=CARTESIAN_POINT('Ctrl Pts',(190.423275566765,4.79984079389075,129.722915027962));
#206006=CARTESIAN_POINT('Ctrl Pts',(190.415524375525,4.76597450893968,129.590000686311));
#206007=CARTESIAN_POINT('Ctrl Pts',(190.407776478747,4.73212261806311,129.457142836802));
#206008=CARTESIAN_POINT('Ctrl Pts',(190.40002858197,4.6926936264518,129.325632847339));
#206009=CARTESIAN_POINT('Ctrl Pts',(190.392280685193,4.64782291118133,129.195968486027));
#206010=CARTESIAN_POINT('Ctrl Pts',(190.384534409109,4.60296158189719,129.066331247704));
#206011=CARTESIAN_POINT('Ctrl Pts',(190.376788133025,4.55266092085215,128.938539238861));
#206012=CARTESIAN_POINT('Ctrl Pts',(190.369041856941,4.49710593053007,128.813074271484));
#206013=CARTESIAN_POINT('Ctrl Pts',(190.361295523676,4.44155053011368,128.687608377954));
#206014=CARTESIAN_POINT('Ctrl Pts',(190.35354919041,4.38074088131789,128.564469917655));
#206015=CARTESIAN_POINT('Ctrl Pts',(190.345802857145,4.31490965259537,128.444119580629));
#206016=CARTESIAN_POINT('Ctrl Pts',(190.338054789142,4.24906368142562,128.32374229198));
#206017=CARTESIAN_POINT('Ctrl Pts',(190.330306721139,4.17819408019494,128.206154711989));
#206018=CARTESIAN_POINT('Ctrl Pts',(190.322558653136,4.10257867349393,128.091791486596));
#206019=CARTESIAN_POINT('Ctrl Pts',(190.314802350394,4.02688290183881,127.977306714606));
#206020=CARTESIAN_POINT('Ctrl Pts',(190.307046047653,3.94643146495612,127.866053469427));
#206021=CARTESIAN_POINT('Ctrl Pts',(190.299289744911,3.86154492337111,127.758436477459));
#206022=CARTESIAN_POINT('Ctrl Pts',(190.291529302397,3.77661307528294,127.650762047062));
#206023=CARTESIAN_POINT('Ctrl Pts',(190.283768859882,3.68724166038745,127.546728033458));
#206024=CARTESIAN_POINT('Ctrl Pts',(190.276008417368,3.59378981017076,127.446704014694));
#206025=CARTESIAN_POINT('Ctrl Pts',(190.268235517103,3.50018794274785,127.346519428494));
#206026=CARTESIAN_POINT('Ctrl Pts',(190.260462616837,3.40249282925593,127.250357975128));
#206027=CARTESIAN_POINT('Ctrl Pts',(190.252689716572,3.30109919916671,127.158551086096));
#206028=CARTESIAN_POINT('Ctrl Pts',(190.24519938081,3.2033914829259,127.070081608727));
#206029=CARTESIAN_POINT('Ctrl Pts',(190.237709045048,3.10224971882835,126.985655790931));
#206030=CARTESIAN_POINT('Ctrl Pts',(190.230218709286,2.99805270289559,126.905532196981));
#206031=CARTESIAN_POINT('Ctrl Pts',(190.222444375167,2.88990502543422,126.822370692614));
#206032=CARTESIAN_POINT('Ctrl Pts',(190.214670041048,2.7781232636251,126.743580659112));
#206033=CARTESIAN_POINT('Ctrl Pts',(190.206895706929,2.66309625889214,126.669496486984));
#206034=CARTESIAN_POINT('Ctrl Pts',(190.199130953982,2.54821101466232,126.595503616977));
#206035=CARTESIAN_POINT('Ctrl Pts',(190.191366201034,2.43008881080192,126.526205278626));
#206036=CARTESIAN_POINT('Ctrl Pts',(190.183601448087,2.30915117022697,126.461895426509));
#206037=CARTESIAN_POINT('Ctrl Pts',(190.175844407202,2.18833364662157,126.397649447844));
#206038=CARTESIAN_POINT('Ctrl Pts',(190.168087366317,2.06470659408811,126.33838227784));
#206039=CARTESIAN_POINT('Ctrl Pts',(190.160330325432,1.938719800928,126.284344179986));
#206040=CARTESIAN_POINT('Ctrl Pts',(190.152579134192,1.81282801538859,126.230346832682));
#206041=CARTESIAN_POINT('Ctrl Pts',(190.144827942952,1.68458038906157,126.181570862152));
#206042=CARTESIAN_POINT('Ctrl Pts',(190.137076751712,1.55445023485514,126.138220078549));
#206043=CARTESIAN_POINT('Ctrl Pts',(190.129328854935,1.42437538943564,126.094887720185));
#206044=CARTESIAN_POINT('Ctrl Pts',(190.121580958158,1.29241997767127,126.0569760859));
#206045=CARTESIAN_POINT('Ctrl Pts',(190.113833061381,1.1590759605821,126.024640334945));
#206046=CARTESIAN_POINT('Ctrl Pts',(190.106086785297,1.02575983618676,125.992311347931));
#206047=CARTESIAN_POINT('Ctrl Pts',(190.098340509213,0.891056063932395,
125.965556016384));
#206048=CARTESIAN_POINT('Ctrl Pts',(190.090594233128,0.755470004251004,
125.944479123622));
#206049=CARTESIAN_POINT('Ctrl Pts',(190.082847899863,0.619882943704145,
125.923402075275));
#206050=CARTESIAN_POINT('Ctrl Pts',(190.075101566598,0.483413969059678,
125.90800360941));
#206051=CARTESIAN_POINT('Ctrl Pts',(190.067355233332,0.346576434879642,
125.898336989689));
#206052=CARTESIAN_POINT('Ctrl Pts',(190.059607165329,0.20970825688259,125.888668205195));
#206053=CARTESIAN_POINT('Ctrl Pts',(190.051859097326,0.0724717450308378,
125.884733848621));
#206054=CARTESIAN_POINT('Ctrl Pts',(190.044111029323,-0.0646172497580651,
125.886535115016));
#206055=CARTESIAN_POINT('Ctrl Pts',(190.036354726582,-0.201851944362056,
125.888338295818));
#206056=CARTESIAN_POINT('Ctrl Pts',(190.02859842384,-0.33893841715767,125.89588927164));
#206057=CARTESIAN_POINT('Ctrl Pts',(190.020842121098,-0.475362889567487,
125.909137110338));
#206058=CARTESIAN_POINT('Ctrl Pts',(190.013081678584,-0.611860175825985,
125.922392019806));
#206059=CARTESIAN_POINT('Ctrl Pts',(190.00532123607,-0.747694370636893,
125.941349796762));
#206060=CARTESIAN_POINT('Ctrl Pts',(189.997560793555,-0.882360418181386,
125.965908059679));
#206061=CARTESIAN_POINT('Ctrl Pts',(189.98978789329,-1.01724264362044,125.990505745699));
#206062=CARTESIAN_POINT('Ctrl Pts',(189.982014993024,-1.15095259295001,
126.02072179713));
#206063=CARTESIAN_POINT('Ctrl Pts',(189.974242092759,-1.28299806253933,
126.056403263712));
#206064=CARTESIAN_POINT('Ctrl Pts',(189.966751756997,-1.4102433467065,126.090787619106));
#206065=CARTESIAN_POINT('Ctrl Pts',(189.959261421235,-1.53594277230061,
126.130246832991));
#206066=CARTESIAN_POINT('Ctrl Pts',(189.951771085473,-1.65967405337326,
126.17460197385));
#206067=CARTESIAN_POINT('Ctrl Pts',(189.943996623503,-1.78809875550871,
126.220639610442));
#206068=CARTESIAN_POINT('Ctrl Pts',(189.936222161534,-1.91480987036354,
126.272097770317));
#206069=CARTESIAN_POINT('Ctrl Pts',(189.928447699565,-2.03931586329617,
126.328830048772));
#206070=CARTESIAN_POINT('Ctrl Pts',(189.92068284859,-2.16366793863765,126.385492193289));
#206071=CARTESIAN_POINT('Ctrl Pts',(189.912917997615,-2.28581996373698,
126.447415322767));
#206072=CARTESIAN_POINT('Ctrl Pts',(189.905153146641,-2.40529676525213,
126.514403679138));
#206073=CARTESIAN_POINT('Ctrl Pts',(189.897396037425,-2.5246544452745,126.581325246367));
#206074=CARTESIAN_POINT('Ctrl Pts',(189.88963892821,-2.6413418709589,126.653301800276));
#206075=CARTESIAN_POINT('Ctrl Pts',(189.881881818995,-2.75490535575686,
126.730090186762));
#206076=CARTESIAN_POINT('Ctrl Pts',(189.874130589026,-2.86838276883409,
126.806820374008));
#206077=CARTESIAN_POINT('Ctrl Pts',(189.866379359057,-2.97874063130287,
126.888354916463));
#206078=CARTESIAN_POINT('Ctrl Pts',(189.858628129089,-3.08555162944487,
126.974405760844));
#206079=CARTESIAN_POINT('Ctrl Pts',(189.850880345889,-3.19231513152848,
127.060418340663));
#206080=CARTESIAN_POINT('Ctrl Pts',(189.84313256269,-3.29553460322023,127.150942982288));
#206081=CARTESIAN_POINT('Ctrl Pts',(189.835384779491,-3.39481360629566,
127.245649665408));
#206082=CARTESIAN_POINT('Ctrl Pts',(189.827638659146,-3.49407130178288,
127.340336022266));
#206083=CARTESIAN_POINT('Ctrl Pts',(189.819892538802,-3.58938992840192,
127.439202365372));
#206084=CARTESIAN_POINT('Ctrl Pts',(189.812146418457,-3.68040819178631,
127.541880180179));
#206085=CARTESIAN_POINT('Ctrl Pts',(189.804400283122,-3.77142663131764,
127.644558193698));
#206086=CARTESIAN_POINT('Ctrl Pts',(189.796654147786,-3.85814443183768,
127.751047400979));
#206087=CARTESIAN_POINT('Ctrl Pts',(189.788908012451,-3.94023932495192,
127.860944723642));
#206088=CARTESIAN_POINT('Ctrl Pts',(189.781160184633,-4.02235215528922,
127.970866058186));
#206089=CARTESIAN_POINT('Ctrl Pts',(189.773412356815,-4.0998398346877,128.084196676547));
#206090=CARTESIAN_POINT('Ctrl Pts',(189.765664528998,-4.17242255225989,
128.200503265887));
#206091=CARTESIAN_POINT('Ctrl Pts',(189.757909049044,-4.24507695609062,
128.31692472533));
#206092=CARTESIAN_POINT('Ctrl Pts',(189.750153569091,-4.31281651589305,
128.436327693783));
#206093=CARTESIAN_POINT('Ctrl Pts',(189.742398089138,-4.37540644239081,
128.55825253326));
#206094=CARTESIAN_POINT('Ctrl Pts',(189.734638486836,-4.43802963794533,
128.68024218068));
#206095=CARTESIAN_POINT('Ctrl Pts',(189.726878884534,-4.49549758245539,
128.804756015469));
#206096=CARTESIAN_POINT('Ctrl Pts',(189.719119282232,-4.54762346778534,
128.931313939624));
#206097=CARTESIAN_POINT('Ctrl Pts',(189.711348586192,-4.59982387637704,
129.058052800933));
#206098=CARTESIAN_POINT('Ctrl Pts',(189.703577890153,-4.64666683607839,
129.186841222174));
#206099=CARTESIAN_POINT('Ctrl Pts',(189.695807194114,-4.68801507639694,
129.317182852141));
#206100=CARTESIAN_POINT('Ctrl Pts',(189.690573763844,-4.71586240582347,
129.404965700449));
#206101=CARTESIAN_POINT('Ctrl Pts',(189.685340333575,-4.74121849260404,
129.493452762972));
#206102=CARTESIAN_POINT('Ctrl Pts',(189.680106903305,-4.76405452823404,
129.582490119308));
#206103=CARTESIAN_POINT('Ctrl Pts',(191.430300680169,-4.76051597898714,
129.583432241587));
#206104=CARTESIAN_POINT('Ctrl Pts',(191.406914637273,-4.86678982625872,
129.983174630901));
#206105=CARTESIAN_POINT('Ctrl Pts',(191.383528594377,-4.92378206388031,
130.394832064542));
#206106=CARTESIAN_POINT('Ctrl Pts',(191.360142551482,-4.9256493795537,130.806055125649));
#206107=CARTESIAN_POINT('Origin',(213.235140564004,0.,130.804360617566));
#206108=CARTESIAN_POINT('',(193.179932595466,-4.75726252818781,129.584191622251));
#206109=CARTESIAN_POINT('',(192.834981455508,-4.76405452823404,129.582490119308));
#206110=CARTESIAN_POINT('',(213.235140564004,-4.76405452823405,129.582490119308));
#206111=CARTESIAN_POINT('',(192.764859436031,-4.9182499011834,130.805346522958));
#206112=CARTESIAN_POINT('Ctrl Pts',(192.834981455508,-4.76405452823404,
129.582490119308));
#206113=CARTESIAN_POINT('Ctrl Pts',(192.827262795634,-4.79795815032377,
129.714679827277));
#206114=CARTESIAN_POINT('Ctrl Pts',(192.819544135761,-4.82632919785479,
129.848178265195));
#206115=CARTESIAN_POINT('Ctrl Pts',(192.811825475887,-4.84909224210237,
129.982480157838));
#206116=CARTESIAN_POINT('Ctrl Pts',(192.803997802578,-4.87217677708874,
130.118678844873));
#206117=CARTESIAN_POINT('Ctrl Pts',(192.796170129268,-4.88949364919261,
130.255703433094));
#206118=CARTESIAN_POINT('Ctrl Pts',(192.788342455959,-4.90101880375934,
130.393024079319));
#206119=CARTESIAN_POINT('Ctrl Pts',(192.78051478265,-4.91254395832607,130.530344725543));
#206120=CARTESIAN_POINT('Ctrl Pts',(192.77268710934,-4.91827744128822,130.667961010208));
#206121=CARTESIAN_POINT('Ctrl Pts',(192.764859436031,-4.9182499011834,130.805346522958));
#206122=CARTESIAN_POINT('Ctrl Pts',(192.764859435991,-4.91824990118326,
130.805346523653));
#206123=CARTESIAN_POINT('Ctrl Pts',(192.761851730581,-4.91823931916517,
130.85813553689));
#206124=CARTESIAN_POINT('Ctrl Pts',(192.758844025171,-4.91737886410589,
130.910915070119));
#206125=CARTESIAN_POINT('Ctrl Pts',(192.755836319761,-4.91566928905583,
130.963666936127));
#206126=CARTESIAN_POINT('Ctrl Pts',(192.748061985642,-4.91125036970399,
131.100020260621));
#206127=CARTESIAN_POINT('Ctrl Pts',(192.740287651523,-4.90114679519269,
131.236405558342));
#206128=CARTESIAN_POINT('Ctrl Pts',(192.732513317404,-4.88534711553905,
131.372310107569));
#206129=CARTESIAN_POINT('Ctrl Pts',(192.724748564456,-4.86956690757853,
131.508047166585));
#206130=CARTESIAN_POINT('Ctrl Pts',(192.716983811509,-4.84810460677939,
131.643304271342));
#206131=CARTESIAN_POINT('Ctrl Pts',(192.709219058562,-4.82100075318953,
131.77756912567));
#206132=CARTESIAN_POINT('Ctrl Pts',(192.701462017677,-4.79392381952918,
131.911700626251));
#206133=CARTESIAN_POINT('Ctrl Pts',(192.693704976792,-4.76121656070021,
132.044841456872));
#206134=CARTESIAN_POINT('Ctrl Pts',(192.685947935907,-4.72297121766863,
132.176485225455));
#206135=CARTESIAN_POINT('Ctrl Pts',(192.678196744667,-4.68475471574775,
132.308029720448));
#206136=CARTESIAN_POINT('Ctrl Pts',(192.670445553427,-4.6410085509534,132.43807902658));
#206137=CARTESIAN_POINT('Ctrl Pts',(192.662694362187,-4.59187578910414,
132.56613807228));
#206138=CARTESIAN_POINT('Ctrl Pts',(192.65494646541,-4.54276390998926,132.69414268947));
#206139=CARTESIAN_POINT('Ctrl Pts',(192.647198568633,-4.48827012711119,
132.820158364431));
#206140=CARTESIAN_POINT('Ctrl Pts',(192.639450671856,-4.42858693265309,
132.943706508822));
#206141=CARTESIAN_POINT('Ctrl Pts',(192.631704395771,-4.36891622263265,
133.067228809605));
#206142=CARTESIAN_POINT('Ctrl Pts',(192.623958119687,-4.30405843013184,
133.188284254661));
#206143=CARTESIAN_POINT('Ctrl Pts',(192.616211843603,-4.23425347381781,
133.30641588913));
#206144=CARTESIAN_POINT('Ctrl Pts',(192.608465510338,-4.16444800221951,
133.42454839562));
#206145=CARTESIAN_POINT('Ctrl Pts',(192.600719177073,-4.08969549283255,
133.539756711864));
#206146=CARTESIAN_POINT('Ctrl Pts',(192.592972843807,-4.01028074241126,
133.65161041861));
#206147=CARTESIAN_POINT('Ctrl Pts',(192.585224775804,-3.93084820760729,
133.763489174218));
#206148=CARTESIAN_POINT('Ctrl Pts',(192.577476707801,-3.84675158046991,
133.872011506716));
#206149=CARTESIAN_POINT('Ctrl Pts',(192.569728639798,-3.7583174692179,133.976778128404));
#206150=CARTESIAN_POINT('Ctrl Pts',(192.561972337057,-3.66978936913993,
134.081656097304));
#206151=CARTESIAN_POINT('Ctrl Pts',(192.554216034315,-3.57691482870239,
134.182770082479));
#206152=CARTESIAN_POINT('Ctrl Pts',(192.546459731573,-3.4800594120266,134.279755494593));
#206153=CARTESIAN_POINT('Ctrl Pts',(192.538699289059,-3.38315230069857,
134.376792670742));
#206154=CARTESIAN_POINT('Ctrl Pts',(192.530938846545,-3.28226036692496,
134.469696618379));
#206155=CARTESIAN_POINT('Ctrl Pts',(192.523178404031,-3.17778338449789,
134.558142154058));
#206156=CARTESIAN_POINT('Ctrl Pts',(192.515405503765,-3.07313868634362,
134.646729670363));
#206157=CARTESIAN_POINT('Ctrl Pts',(192.5076326035,-2.96489774802298,134.73084423263));
#206158=CARTESIAN_POINT('Ctrl Pts',(192.499859703234,-2.85349125072007,
134.810202694404));
#206159=CARTESIAN_POINT('Ctrl Pts',(192.492369367472,-2.74613466020842,
134.886676276202));
#206160=CARTESIAN_POINT('Ctrl Pts',(192.48487903171,-2.63583892488735,134.958733378042));
#206161=CARTESIAN_POINT('Ctrl Pts',(192.477388695948,-2.52301040503746,
135.026161365893));
#206162=CARTESIAN_POINT('Ctrl Pts',(192.469614361829,-2.40590395756583,
135.096145906396));
#206163=CARTESIAN_POINT('Ctrl Pts',(192.46184002771,-2.28569791514371,135.161365067826));
#206164=CARTESIAN_POINT('Ctrl Pts',(192.454065693591,-2.16281745608086,
135.221532078373));
#206165=CARTESIAN_POINT('Ctrl Pts',(192.446300940644,-2.04008843620172,
135.281624938458));
#206166=CARTESIAN_POINT('Ctrl Pts',(192.438536187696,-1.91469190546091,
135.336677865911));
#206167=CARTESIAN_POINT('Ctrl Pts',(192.430771434749,-1.78708078602292,
135.386448059631));
#206168=CARTESIAN_POINT('Ctrl Pts',(192.423014393864,-1.65959641174775,
135.436168820892));
#206169=CARTESIAN_POINT('Ctrl Pts',(192.415257352979,-1.52990218788621,
135.480617148817));
#206170=CARTESIAN_POINT('Ctrl Pts',(192.407500312094,-1.39847401492876,
135.519596931058));
#206171=CARTESIAN_POINT('Ctrl Pts',(192.399749120854,-1.26714495297885,
135.558547318341));
#206172=CARTESIAN_POINT('Ctrl Pts',(192.391997929614,-1.13408491791114,
135.592037257539));
#206173=CARTESIAN_POINT('Ctrl Pts',(192.384246738374,-0.999787758028332,
135.6199195157));
#206174=CARTESIAN_POINT('Ctrl Pts',(192.376498841597,-0.865547678020963,
135.647789923158));
#206175=CARTESIAN_POINT('Ctrl Pts',(192.36875094482,-0.730071900997154,
135.670057310698));
#206176=CARTESIAN_POINT('Ctrl Pts',(192.361003048043,-0.593867123607528,
135.686624938759));
#206177=CARTESIAN_POINT('Ctrl Pts',(192.353256771959,-0.457690837321097,
135.70318910123));
#206178=CARTESIAN_POINT('Ctrl Pts',(192.345510495875,-0.320786241840849,
135.714055828527));
#206179=CARTESIAN_POINT('Ctrl Pts',(192.337764219791,-0.18366746813134,
135.719179975757));
#206180=CARTESIAN_POINT('Ctrl Pts',(192.330017886525,-0.0465476822422854,
135.724304160812));
#206181=CARTESIAN_POINT('Ctrl Pts',(192.32227155326,0.0907858943383346,
135.723685666614));
#206182=CARTESIAN_POINT('Ctrl Pts',(192.314525219994,0.227817198101151,
135.717331448616));
#206183=CARTESIAN_POINT('Ctrl Pts',(192.306777151991,0.364879189074196,
135.710975807636));
#206184=CARTESIAN_POINT('Ctrl Pts',(192.299029083989,0.501638382059588,
135.698881905005));
#206185=CARTESIAN_POINT('Ctrl Pts',(192.291281015986,0.637582305285388,
135.681108700714));
#206186=CARTESIAN_POINT('Ctrl Pts',(192.283524713244,0.773670711330755,
135.663316606849));
#206187=CARTESIAN_POINT('Ctrl Pts',(192.275768410502,0.908941728448333,
135.639833204469));
#206188=CARTESIAN_POINT('Ctrl Pts',(192.26801210776,1.04289102096811,135.610768983579));
#206189=CARTESIAN_POINT('Ctrl Pts',(192.260251665246,1.17691180625858,135.58168925024));
#206190=CARTESIAN_POINT('Ctrl Pts',(192.252491222732,1.30960908320894,135.547022861951));
#206191=CARTESIAN_POINT('Ctrl Pts',(192.244730780217,1.44049317827798,135.50693039013));
#206192=CARTESIAN_POINT('Ctrl Pts',(192.236957879952,1.5715873801157,135.466773558314));
#206193=CARTESIAN_POINT('Ctrl Pts',(192.229184979687,1.70086221469286,135.42117336688));
#206194=CARTESIAN_POINT('Ctrl Pts',(192.221412079421,1.82784666917891,135.37033911253));
#206195=CARTESIAN_POINT('Ctrl Pts',(192.213921743659,1.95021491889024,135.321352811369));
#206196=CARTESIAN_POINT('Ctrl Pts',(192.206431407897,2.07045613849443,135.267506509144));
#206197=CARTESIAN_POINT('Ctrl Pts',(192.198941072135,2.18817178530026,135.209027154379));
#206198=CARTESIAN_POINT('Ctrl Pts',(192.191166738016,2.31035065663324,135.148330537103));
#206199=CARTESIAN_POINT('Ctrl Pts',(192.183392403897,2.43019568637188,135.082450339021));
#206200=CARTESIAN_POINT('Ctrl Pts',(192.175618069778,2.5472357860093,135.011589267518));
#206201=CARTESIAN_POINT('Ctrl Pts',(192.167853316831,2.66413164418405,134.940815525952));
#206202=CARTESIAN_POINT('Ctrl Pts',(192.160088563884,2.7782291190768,134.865073325257));
#206203=CARTESIAN_POINT('Ctrl Pts',(192.152323810936,2.88907911974915,134.784612481749));
#206204=CARTESIAN_POINT('Ctrl Pts',(192.144566770051,2.99981902263817,134.704231553085));
#206205=CARTESIAN_POINT('Ctrl Pts',(192.136809729166,3.10731755571858,134.619141536373));
#206206=CARTESIAN_POINT('Ctrl Pts',(192.129052688281,3.21115248827715,134.529636816659));
#206207=CARTESIAN_POINT('Ctrl Pts',(192.121301497041,3.3149091181053,134.440199593151));
#206208=CARTESIAN_POINT('Ctrl Pts',(192.113550305801,3.41500735156303,134.346354547366));
#206209=CARTESIAN_POINT('Ctrl Pts',(192.105799114561,3.51105638032787,134.248437584862));
#206210=CARTESIAN_POINT('Ctrl Pts',(192.098051217784,3.60706458569329,134.150562239679));
#206211=CARTESIAN_POINT('Ctrl Pts',(192.090303321007,3.69902673613745,134.048618698472));
#206212=CARTESIAN_POINT('Ctrl Pts',(192.08255542423,3.78658756001065,133.942980969388));
#206213=CARTESIAN_POINT('Ctrl Pts',(192.074809148146,3.87413006804709,133.83736533744));
#206214=CARTESIAN_POINT('Ctrl Pts',(192.067062872062,3.95727283142153,133.728057355462));
#206215=CARTESIAN_POINT('Ctrl Pts',(192.059316595977,4.03569996811177,133.615465174476));
#206216=CARTESIAN_POINT('Ctrl Pts',(192.051570262712,4.1141276837333,133.502872162361));
#206217=CARTESIAN_POINT('Ctrl Pts',(192.043823929447,4.18783947974799,133.386995223673));
#206218=CARTESIAN_POINT('Ctrl Pts',(192.036077596181,4.25656226304545,133.268272296851));
#206219=CARTESIAN_POINT('Ctrl Pts',(192.028329528178,4.32530043633368,133.149522782853));
#206220=CARTESIAN_POINT('Ctrl Pts',(192.020581460175,4.38904717787134,133.027926350791));
#206221=CARTESIAN_POINT('Ctrl Pts',(192.012833392173,4.4475750888561,132.903946026995));
#206222=CARTESIAN_POINT('Ctrl Pts',(192.005077089431,4.50616520400119,132.779833935435));
#206223=CARTESIAN_POINT('Ctrl Pts',(191.997320786689,4.55952524142413,132.653333245059));
#206224=CARTESIAN_POINT('Ctrl Pts',(191.989564483947,4.60747555374874,132.524927990297));
#206225=CARTESIAN_POINT('Ctrl Pts',(191.981804041433,4.65545145859881,132.396454201785));
#206226=CARTESIAN_POINT('Ctrl Pts',(191.974043598919,4.69801176383069,132.266074194861));
#206227=CARTESIAN_POINT('Ctrl Pts',(191.966283156404,4.73502688221655,132.134286738517));
#206228=CARTESIAN_POINT('Ctrl Pts',(191.958510256139,4.77210142055647,132.002287725248));
#206229=CARTESIAN_POINT('Ctrl Pts',(191.950737355874,4.80361289384034,131.868877128348));
#206230=CARTESIAN_POINT('Ctrl Pts',(191.942964455608,4.82948279537217,131.73456435423));
#206231=CARTESIAN_POINT('Ctrl Pts',(191.935474119846,4.85441226082101,131.605134187765));
#206232=CARTESIAN_POINT('Ctrl Pts',(191.927983784084,4.87410315800352,131.474866602682));
#206233=CARTESIAN_POINT('Ctrl Pts',(191.920493448322,4.88853100308117,131.344219575456));
#206234=CARTESIAN_POINT('Ctrl Pts',(191.912719114203,4.90350588429017,131.208619026484));
#206235=CARTESIAN_POINT('Ctrl Pts',(191.904944780084,4.91285817377069,131.0721801525));
#206236=CARTESIAN_POINT('Ctrl Pts',(191.897170445965,4.9165037801426,130.935408861902));
#206237=CARTESIAN_POINT('Ctrl Pts',(191.889405693018,4.92014489363048,130.798806129696));
#206238=CARTESIAN_POINT('Ctrl Pts',(191.881640940071,4.91809330722021,130.661872183078));
#206239=CARTESIAN_POINT('Ctrl Pts',(191.873876187123,4.91031645383257,130.525119886796));
#206240=CARTESIAN_POINT('Ctrl Pts',(191.866119146238,4.90254732452534,130.388503414822));
#206241=CARTESIAN_POINT('Ctrl Pts',(191.858362105353,4.88906426651891,130.252068621953));
#206242=CARTESIAN_POINT('Ctrl Pts',(191.850605064468,4.86988672827563,130.116329865154));
#206243=CARTESIAN_POINT('Ctrl Pts',(191.842853873228,4.85072365196311,129.980693470007));
#206244=CARTESIAN_POINT('Ctrl Pts',(191.835102681988,4.82587469733376,129.84575245173));
#206245=CARTESIAN_POINT('Ctrl Pts',(191.827351490748,4.79541122980165,129.712017173592));
#206246=CARTESIAN_POINT('Ctrl Pts',(191.819603593971,4.76496071005587,129.578338736515));
#206247=CARTESIAN_POINT('Ctrl Pts',(191.811855697194,4.72890051026299,129.445865400711));
#206248=CARTESIAN_POINT('Ctrl Pts',(191.804107800417,4.68735326106434,129.31509822682));
#206249=CARTESIAN_POINT('Ctrl Pts',(191.796361524333,4.64581470265456,129.184358406603));
#206250=CARTESIAN_POINT('Ctrl Pts',(191.788615248249,4.59879149613188,129.055324410796));
#206251=CARTESIAN_POINT('Ctrl Pts',(191.780868972164,4.54645628856314,128.928482615487));
#206252=CARTESIAN_POINT('Ctrl Pts',(191.773122638899,4.49412069466779,128.801639883861));
#206253=CARTESIAN_POINT('Ctrl Pts',(191.765376305634,4.43647317060039,128.676989746434));
#206254=CARTESIAN_POINT('Ctrl Pts',(191.757629972368,4.37373455287664,128.5549986806));
#206255=CARTESIAN_POINT('Ctrl Pts',(191.749881904365,4.31098188527447,128.432980295712));
#206256=CARTESIAN_POINT('Ctrl Pts',(191.742133836362,4.24313603409257,128.313622514967));
#206257=CARTESIAN_POINT('Ctrl Pts',(191.734385768359,4.17046364188854,128.197366932459));
#206258=CARTESIAN_POINT('Ctrl Pts',(191.726629465618,4.09771401260122,128.080987792135));
#206259=CARTESIAN_POINT('Ctrl Pts',(191.718873162876,4.02012780272054,127.967717768317));
#206260=CARTESIAN_POINT('Ctrl Pts',(191.711116860134,3.93801514032661,127.857969635863));
#206261=CARTESIAN_POINT('Ctrl Pts',(191.70335641762,3.85585865193233,127.748162927527));
#206262=CARTESIAN_POINT('Ctrl Pts',(191.695595975106,3.76917114412413,127.641882158914));
#206263=CARTESIAN_POINT('Ctrl Pts',(191.687835532591,3.67830220031926,127.539505952251));
#206264=CARTESIAN_POINT('Ctrl Pts',(191.680062632326,3.58728738561886,127.436965402214));
#206265=CARTESIAN_POINT('Ctrl Pts',(191.67228973206,3.49207799308258,127.338342220929));
#206266=CARTESIAN_POINT('Ctrl Pts',(191.664516831795,3.39306016596735,127.243977804914));
#206267=CARTESIAN_POINT('Ctrl Pts',(191.657026496033,3.29764188627902,127.153043773112));
#206268=CARTESIAN_POINT('Ctrl Pts',(191.649536160271,3.19868748848367,127.066064451937));
#206269=CARTESIAN_POINT('Ctrl Pts',(191.642045824509,3.09656904704697,126.983307987809));
#206270=CARTESIAN_POINT('Ctrl Pts',(191.63427149039,2.99057875386455,126.89741378719));
#206271=CARTESIAN_POINT('Ctrl Pts',(191.626497156271,2.88084400593911,126.815796897087));
#206272=CARTESIAN_POINT('Ctrl Pts',(191.618722822152,2.76774498488753,126.738801521804));
#206273=CARTESIAN_POINT('Ctrl Pts',(191.610958069205,2.65478534827152,126.661901036441));
#206274=CARTESIAN_POINT('Ctrl Pts',(191.603193316258,2.53847000824377,126.589610951247));
#206275=CARTESIAN_POINT('Ctrl Pts',(191.59542856331,2.41921284913904,126.522235881753));
#206276=CARTESIAN_POINT('Ctrl Pts',(191.587671522425,2.30007413792603,126.454927730128));
#206277=CARTESIAN_POINT('Ctrl Pts',(191.57991448154,2.17799976045686,126.392525070538));
#206278=CARTESIAN_POINT('Ctrl Pts',(191.572157440656,2.05343297218267,126.335289562945));
#206279=CARTESIAN_POINT('Ctrl Pts',(191.564406249415,1.92896012069234,126.278097217093));
#206280=CARTESIAN_POINT('Ctrl Pts',(191.556655058175,1.80199895334133,126.226064429886));
#206281=CARTESIAN_POINT('Ctrl Pts',(191.548903866935,1.67301742795112,126.179407023391));
#206282=CARTESIAN_POINT('Ctrl Pts',(191.541155970158,1.54409072314994,126.132769447539));
#206283=CARTESIAN_POINT('Ctrl Pts',(191.533408073381,1.41314573509101,126.09150284106));
#206284=CARTESIAN_POINT('Ctrl Pts',(191.525660176604,1.28067030513812,126.055774866836));
#206285=CARTESIAN_POINT('Ctrl Pts',(191.51791390052,1.14822258618934,126.020054366134));
#206286=CARTESIAN_POINT('Ctrl Pts',(191.510167624436,1.01424543935255,125.989870294983));
#206287=CARTESIAN_POINT('Ctrl Pts',(191.502421348352,0.879241386563487,
125.965340298674));
#206288=CARTESIAN_POINT('Ctrl Pts',(191.494675015086,0.744236337205225,
125.940810121289));
#206289=CARTESIAN_POINT('Ctrl Pts',(191.486928681821,0.608204751435609,
125.921934171922));
#206290=CARTESIAN_POINT('Ctrl Pts',(191.479182348555,0.471658457426965,
125.908778796981));
#206291=CARTESIAN_POINT('Ctrl Pts',(191.471434280553,0.335081584822615,
125.895620475986));
#206292=CARTESIAN_POINT('Ctrl Pts',(191.46368621255,0.197990163703318,125.888185316112));
#206293=CARTESIAN_POINT('Ctrl Pts',(191.455938144547,0.0608998465023526,
125.886487675816));
#206294=CARTESIAN_POINT('Ctrl Pts',(191.448181841805,-0.0763361719192702,
125.884788231248));
#206295=CARTESIAN_POINT('Ctrl Pts',(191.440425539063,-0.21357069252026,
125.888838492329));
#206296=CARTESIAN_POINT('Ctrl Pts',(191.432669236321,-0.350288804319249,
125.898600654414));
#206297=CARTESIAN_POINT('Ctrl Pts',(191.424908793807,-0.487079886691054,
125.908368026859));
#206298=CARTESIAN_POINT('Ctrl Pts',(191.417148351293,-0.623353622783719,
125.923853330808));
#206299=CARTESIAN_POINT('Ctrl Pts',(191.409387908778,-0.758602508617255,
125.944967106394));
#206300=CARTESIAN_POINT('Ctrl Pts',(191.401615008513,-0.894068507969185,
125.966114775688));
#206301=CARTESIAN_POINT('Ctrl Pts',(191.393842108248,-1.02850598582216,
125.992908895609));
#206302=CARTESIAN_POINT('Ctrl Pts',(191.386069207982,-1.16141899575531,
126.025209126056));
#206303=CARTESIAN_POINT('Ctrl Pts',(191.37857887222,-1.28950028298996,126.056335161768));
#206304=CARTESIAN_POINT('Ctrl Pts',(191.371088536458,-1.41616571838099,
126.092573851485));
#206305=CARTESIAN_POINT('Ctrl Pts',(191.363598200696,-1.54098858741563,
126.13375709811));
#206306=CARTESIAN_POINT('Ctrl Pts',(191.355823866577,-1.67054415346853,
126.176501820048));
#206307=CARTESIAN_POINT('Ctrl Pts',(191.348049532458,-1.79852506629693,
126.224708848623));
#206308=CARTESIAN_POINT('Ctrl Pts',(191.340275198339,-1.92443623961998,
126.278244377108));
#206309=CARTESIAN_POINT('Ctrl Pts',(191.332510445392,-2.05019223867488,
126.331713927838));
#206310=CARTESIAN_POINT('Ctrl Pts',(191.324745692445,-2.17388321715495,
126.390498760795));
#206311=CARTESIAN_POINT('Ctrl Pts',(191.316980939498,-2.29502917879571,
126.454415315499));
#206312=CARTESIAN_POINT('Ctrl Pts',(191.309223898613,-2.41605481655935,
126.51826838738));
#206313=CARTESIAN_POINT('Ctrl Pts',(191.301466857728,-2.53454012426197,
126.587242856692));
#206314=CARTESIAN_POINT('Ctrl Pts',(191.293709816843,-2.65002536956902,
126.661107233673));
#206315=CARTESIAN_POINT('Ctrl Pts',(191.285958625602,-2.76542352655441,
126.734915908953));
#206316=CARTESIAN_POINT('Ctrl Pts',(191.278207434362,-2.87782579622934,
126.813606942315));
#206317=CARTESIAN_POINT('Ctrl Pts',(191.270456243122,-2.98679765874186,
126.896903284692));
#206318=CARTESIAN_POINT('Ctrl Pts',(191.262708346345,-3.09572320530585,
126.980164223901));
#206319=CARTESIAN_POINT('Ctrl Pts',(191.254960449568,-3.20122093462301,
127.068026342114));
#206320=CARTESIAN_POINT('Ctrl Pts',(191.247212552791,-3.302886096988,127.160169830461));
#206321=CARTESIAN_POINT('Ctrl Pts',(191.239466276707,-3.40452999319271,
127.252294044376));
#206322=CARTESIAN_POINT('Ctrl Pts',(191.231720000623,-3.50234262754816,
127.348697584696));
#206323=CARTESIAN_POINT('Ctrl Pts',(191.223973724539,-3.59595339635909,
127.449021255636));
#206324=CARTESIAN_POINT('Ctrl Pts',(191.216227391273,-3.68956485618348,
127.549345667144));
#206325=CARTESIAN_POINT('Ctrl Pts',(191.208481058008,-3.77897412184559,
127.653589981163));
#206326=CARTESIAN_POINT('Ctrl Pts',(191.200734724743,-3.86384871860262,
127.761359444012));
#206327=CARTESIAN_POINT('Ctrl Pts',(191.19298665674,-3.94874232243708,127.869153041084));
#206328=CARTESIAN_POINT('Ctrl Pts',(191.185238588737,-4.02909899477355,
127.980473050777));
#206329=CARTESIAN_POINT('Ctrl Pts',(191.177490520734,-4.10462793269824,
128.094893401191));
#206330=CARTESIAN_POINT('Ctrl Pts',(191.169734217992,-4.18023714367694,
128.209435358914));
#206331=CARTESIAN_POINT('Ctrl Pts',(191.16197791525,-4.251008154845,128.327083912827));
#206332=CARTESIAN_POINT('Ctrl Pts',(191.154221612508,-4.31669445035687,
128.447385419402));
#206333=CARTESIAN_POINT('Ctrl Pts',(191.146461169994,-4.38241580462248,
128.567751134514));
#206334=CARTESIAN_POINT('Ctrl Pts',(191.13870072748,-4.44304686287264,128.690772273196));
#206335=CARTESIAN_POINT('Ctrl Pts',(191.130940284966,-4.49838857192929,
128.815973502732));
#206336=CARTESIAN_POINT('Ctrl Pts',(191.1231673847,-4.5538191204103,128.941375716397));
#206337=CARTESIAN_POINT('Ctrl Pts',(191.115394484435,-4.603943209069,129.068964650282));
#206338=CARTESIAN_POINT('Ctrl Pts',(191.107621584169,-4.64861083885302,
129.198247193365));
#206339=CARTESIAN_POINT('Ctrl Pts',(191.100131248407,-4.69165468778338,
129.322829990364));
#206340=CARTESIAN_POINT('Ctrl Pts',(191.092640912645,-4.72963181359555,
129.44898510548));
#206341=CARTESIAN_POINT('Ctrl Pts',(191.085150576883,-4.76245299152071,
129.576262671124));
#206342=CARTESIAN_POINT('Ctrl Pts',(191.085028435562,-4.76298819076576,
129.578338125491));
#206343=CARTESIAN_POINT('Ctrl Pts',(191.08490629424,-4.76352203648398,129.580413942056));
#206344=CARTESIAN_POINT('Ctrl Pts',(191.084784152919,-4.76405452823405,
129.582490119308));
#206345=CARTESIAN_POINT('',(193.110140564008,-4.91324924050575,130.80805185308));
#206346=CARTESIAN_POINT('Ctrl Pts',(193.110140564008,-4.91324924050575,
130.80805185308));
#206347=CARTESIAN_POINT('Ctrl Pts',(193.078325358477,-4.91715556795767,
131.371134307201));
#206348=CARTESIAN_POINT('Ctrl Pts',(192.953694278342,-4.56730227853154,
133.572215041493));
#206349=CARTESIAN_POINT('Ctrl Pts',(192.736247323602,-1.31701101669081,
136.470678805982));
#206350=CARTESIAN_POINT('Ctrl Pts',(192.457799699789,4.05535734608101,134.975182673953));
#206351=CARTESIAN_POINT('Ctrl Pts',(192.179352075976,5.70105042302464,129.646904828089));
#206352=CARTESIAN_POINT('Ctrl Pts',(191.900904452163,2.10775667300519,125.382272307895));
#206353=CARTESIAN_POINT('Ctrl Pts',(191.651220653561,-2.85118716275981,
126.026104000732));
#206354=CARTESIAN_POINT('Ctrl Pts',(191.494352729563,-4.4694424636812,128.488577529337));
#206355=CARTESIAN_POINT('Ctrl Pts',(191.430300680169,-4.76051597898714,
129.583432241587));
#206356=CARTESIAN_POINT('Ctrl Pts',(193.179932595466,-4.75726252818781,
129.584191622251));
#206357=CARTESIAN_POINT('Ctrl Pts',(193.15666858498,-4.85769551258501,129.983931752434));
#206358=CARTESIAN_POINT('Ctrl Pts',(193.133404574494,-4.9103928439719,130.396313003733));
#206359=CARTESIAN_POINT('Ctrl Pts',(193.110140564008,-4.91324924050575,
130.80805185308));
#206360=CARTESIAN_POINT('Origin',(213.235140564004,0.,130.804360617566));
#206361=CARTESIAN_POINT('',(194.92989654745,-4.76405452823404,129.582490119308));
#206362=CARTESIAN_POINT('',(194.584773235637,-4.76405452823404,129.582490119308));
#206363=CARTESIAN_POINT('',(213.235140564004,-4.76405452823405,129.582490119308));
#206364=CARTESIAN_POINT('',(194.514859435944,-4.91824832267119,130.808422518846));
#206365=CARTESIAN_POINT('Ctrl Pts',(194.584773235637,-4.76405452823405,
129.582490119308));
#206366=CARTESIAN_POINT('Ctrl Pts',(194.577053952228,-4.79804027850044,
129.715000043791));
#206367=CARTESIAN_POINT('Ctrl Pts',(194.569334668819,-4.82650137584579,
129.848960603857));
#206368=CARTESIAN_POINT('Ctrl Pts',(194.56161538541,-4.84932764823365,129.983870262609));
#206369=CARTESIAN_POINT('Ctrl Pts',(194.553822727173,-4.87237089332568,
130.120062290773));
#206370=CARTESIAN_POINT('Ctrl Pts',(194.546030068937,-4.88967153265256,
130.257221158943));
#206371=CARTESIAN_POINT('Ctrl Pts',(194.5382374107,-4.90116937806975,130.394822109033));
#206372=CARTESIAN_POINT('Ctrl Pts',(194.530444752464,-4.91266722348695,
130.532423059123));
#206373=CARTESIAN_POINT('Ctrl Pts',(194.522652094227,-4.91836225895716,
130.670465679262));
#206374=CARTESIAN_POINT('Ctrl Pts',(194.514859435991,-4.91824832267189,
130.808422518005));
#206375=CARTESIAN_POINT('Ctrl Pts',(194.514859435944,-4.91824832267119,
130.808422518846));
#206376=CARTESIAN_POINT('Ctrl Pts',(194.505690899192,-4.91811426966856,
130.970737137015));
#206377=CARTESIAN_POINT('Ctrl Pts',(194.49652236244,-4.90994121534633,131.132707678005));
#206378=CARTESIAN_POINT('Ctrl Pts',(194.487353825688,-4.89385416878415,
131.293619687154));
#206379=CARTESIAN_POINT('Ctrl Pts',(194.478119857513,-4.87765231673291,
131.45568004767));
#206380=CARTESIAN_POINT('Ctrl Pts',(194.468885889339,-4.85342321642564,
131.616666662758));
#206381=CARTESIAN_POINT('Ctrl Pts',(194.459651921164,-4.82134334935995,
131.775870458012));
#206382=CARTESIAN_POINT('Ctrl Pts',(194.450346899683,-4.78901663493732,
131.936299290638));
#206383=CARTESIAN_POINT('Ctrl Pts',(194.441041878201,-4.74871793267665,
132.094917714119));
#206384=CARTESIAN_POINT('Ctrl Pts',(194.43173685672,-4.70067592055807,132.251021929825));
#206385=CARTESIAN_POINT('Ctrl Pts',(194.429998592026,-4.69170122515761,
132.280183651511));
#206386=CARTESIAN_POINT('Ctrl Pts',(194.428260327332,-4.68245643851761,
132.309257694875));
#206387=CARTESIAN_POINT('Ctrl Pts',(194.426522062638,-4.67294323328106,
132.338239557063));
#206388=CARTESIAN_POINT('Ctrl Pts',(194.418747728519,-4.63039572235757,
132.467860023283));
#206389=CARTESIAN_POINT('Ctrl Pts',(194.4109733944,-4.58238351476863,132.595914150803));
#206390=CARTESIAN_POINT('Ctrl Pts',(194.403199060281,-4.5290396636491,132.721906650284));
#206391=CARTESIAN_POINT('Ctrl Pts',(194.395434307334,-4.47576155405861,
132.84774387527));
#206392=CARTESIAN_POINT('Ctrl Pts',(194.387669554386,-4.41716502578731,
132.971524171027));
#206393=CARTESIAN_POINT('Ctrl Pts',(194.379904801439,-4.35343290862853,
133.092767262498));
#206394=CARTESIAN_POINT('Ctrl Pts',(194.372147760554,-4.28976409110701,
133.213889933622));
#206395=CARTESIAN_POINT('Ctrl Pts',(194.364390719669,-4.22097001613394,
133.332480071522));
#206396=CARTESIAN_POINT('Ctrl Pts',(194.356633678784,-4.14728147357108,
133.448077592107));
#206397=CARTESIAN_POINT('Ctrl Pts',(194.348882487544,-4.07364850011134,
133.563587939702));
#206398=CARTESIAN_POINT('Ctrl Pts',(194.341131296304,-3.99512861499202,
133.676109833574));
#206399=CARTESIAN_POINT('Ctrl Pts',(194.333380105064,-3.91199820569556,
133.785208332753));
#206400=CARTESIAN_POINT('Ctrl Pts',(194.325632208287,-3.82890312904064,
133.894260462159));
#206401=CARTESIAN_POINT('Ctrl Pts',(194.31788431151,-3.74120166215483,133.999891780499));
#206402=CARTESIAN_POINT('Ctrl Pts',(194.310136414733,-3.64921299757971,
134.101697051841));
#206403=CARTESIAN_POINT('Ctrl Pts',(194.302390138649,-3.55724357505019,
134.203481027715));
#206404=CARTESIAN_POINT('Ctrl Pts',(194.294643862565,-3.46098900054278,
134.301440258582));
#206405=CARTESIAN_POINT('Ctrl Pts',(194.286897586481,-3.3608079054297,134.395203594542));
#206406=CARTESIAN_POINT('Ctrl Pts',(194.279151253215,-3.26062607080245,
134.488967622642));
#206407=CARTESIAN_POINT('Ctrl Pts',(194.27140491995,-3.15651794317866,134.578535426871));
#206408=CARTESIAN_POINT('Ctrl Pts',(194.263658586685,-3.04887776981329,
134.663573932121));
#206409=CARTESIAN_POINT('Ctrl Pts',(194.255910518682,-2.94121349117735,
134.748631481155));
#206410=CARTESIAN_POINT('Ctrl Pts',(194.248162450679,-2.83001589956761,
134.829157470545));
#206411=CARTESIAN_POINT('Ctrl Pts',(194.240414382676,-2.71571062383656,
134.904860449304));
#206412=CARTESIAN_POINT('Ctrl Pts',(194.232658079934,-2.60128386309834,
134.980643886089));
#206413=CARTESIAN_POINT('Ctrl Pts',(194.224901777192,-2.48374314685267,
135.051593856377));
#206414=CARTESIAN_POINT('Ctrl Pts',(194.21714547445,-2.36354174294401,135.11746315424));
#206415=CARTESIAN_POINT('Ctrl Pts',(194.209385031936,-2.24327618392683,
135.18336760853));
#206416=CARTESIAN_POINT('Ctrl Pts',(194.201624589422,-2.12034745785099,
135.244185813801));
#206417=CARTESIAN_POINT('Ctrl Pts',(194.193864146908,-1.99523059395582,
135.299717993731));
#206418=CARTESIAN_POINT('Ctrl Pts',(194.186091246642,-1.86991288136339,
135.355339318846));
#206419=CARTESIAN_POINT('Ctrl Pts',(194.178318346377,-1.74240037555429,
135.4056575181));
#206420=CARTESIAN_POINT('Ctrl Pts',(194.170545446111,-1.61318595870733,
135.450521842182));
#206421=CARTESIAN_POINT('Ctrl Pts',(194.16305511035,-1.48866881138538,135.493755235078));
#206422=CARTESIAN_POINT('Ctrl Pts',(194.155564774588,-1.36257163707573,
135.531924303522));
#206423=CARTESIAN_POINT('Ctrl Pts',(194.148074438826,-1.23534416706417,
135.564939138229));
#206424=CARTESIAN_POINT('Ctrl Pts',(194.140300104707,-1.10329282885606,
135.599205740429));
#206425=CARTESIAN_POINT('Ctrl Pts',(194.132525770587,-0.969605493727146,
135.628028094229));
#206426=CARTESIAN_POINT('Ctrl Pts',(194.124751436468,-0.834770781094737,
135.651250425013));
#206427=CARTESIAN_POINT('Ctrl Pts',(194.116986683521,-0.700102240195215,
135.67444413635));
#206428=CARTESIAN_POINT('Ctrl Pts',(194.109221930574,-0.564289516904608,
135.692051490933));
#206429=CARTESIAN_POINT('Ctrl Pts',(194.101457177627,-0.427835504199164,
135.703966708248));
#206430=CARTESIAN_POINT('Ctrl Pts',(194.093700136742,-0.29151701954285,
135.715870091201));
#206431=CARTESIAN_POINT('Ctrl Pts',(194.085943095857,-0.154558899969262,
135.722092553836));
#206432=CARTESIAN_POINT('Ctrl Pts',(194.078186054972,-0.0174729748113956,
135.722579579513));
#206433=CARTESIAN_POINT('Ctrl Pts',(194.070434863732,0.119509572784076,
135.723066237919));
#206434=CARTESIAN_POINT('Ctrl Pts',(194.062683672492,0.256619344746097,
135.717826066908));
#206435=CARTESIAN_POINT('Ctrl Pts',(194.054932481252,0.393341018732792,
135.706856502876));
#206436=CARTESIAN_POINT('Ctrl Pts',(194.047184584475,0.530004582360826,
135.695891601202));
#206437=CARTESIAN_POINT('Ctrl Pts',(194.039436687697,0.666279987193505,
135.679202181027));
#206438=CARTESIAN_POINT('Ctrl Pts',(194.03168879092,0.801653765399529,135.656837748158));
#206439=CARTESIAN_POINT('Ctrl Pts',(194.023942514836,0.936999226329496,
135.634477993447));
#206440=CARTESIAN_POINT('Ctrl Pts',(194.016196238752,1.07144305027789,135.606445650913));
#206441=CARTESIAN_POINT('Ctrl Pts',(194.008449962668,1.20447912930477,135.572841831702));
#206442=CARTESIAN_POINT('Ctrl Pts',(194.000703629403,1.33751619037367,135.539237764435));
#206443=CARTESIAN_POINT('Ctrl Pts',(193.992957296137,1.46914510672559,135.50006223417));
#206444=CARTESIAN_POINT('Ctrl Pts',(193.985210962872,1.59887255256962,135.455466897059));
#206445=CARTESIAN_POINT('Ctrl Pts',(193.977462894869,1.72862904997563,135.410861573131));
#206446=CARTESIAN_POINT('Ctrl Pts',(193.969714826866,1.85648285988052,135.360834154252));
#206447=CARTESIAN_POINT('Ctrl Pts',(193.961966758863,1.98195871352415,135.305585197654));
#206448=CARTESIAN_POINT('Ctrl Pts',(193.954210456121,2.10756792439832,135.250277521806));
#206449=CARTESIAN_POINT('Ctrl Pts',(193.946454153379,2.2307937720316,135.189737380293));
#206450=CARTESIAN_POINT('Ctrl Pts',(193.938697850637,2.35118327273367,135.124212499346));
#206451=CARTESIAN_POINT('Ctrl Pts',(193.930937408123,2.47163702893723,135.058652645797));
#206452=CARTESIAN_POINT('Ctrl Pts',(193.923176965609,2.58925108663829,134.988102952543));
#206453=CARTESIAN_POINT('Ctrl Pts',(193.915416523095,2.70360060345122,134.912855091156));
#206454=CARTESIAN_POINT('Ctrl Pts',(193.907643622829,2.81813368425998,134.837486435221));
#206455=CARTESIAN_POINT('Ctrl Pts',(193.899870722564,2.92939143443346,134.757404768529));
#206456=CARTESIAN_POINT('Ctrl Pts',(193.892097822299,3.03698060945102,134.672943283132));
#206457=CARTESIAN_POINT('Ctrl Pts',(193.884607486536,3.14065864695626,134.591552185475));
#206458=CARTESIAN_POINT('Ctrl Pts',(193.877117150774,3.24092996805332,134.506094375295));
#206459=CARTESIAN_POINT('Ctrl Pts',(193.869626815012,3.33747583876709,134.416899626095));
#206460=CARTESIAN_POINT('Ctrl Pts',(193.861852480893,3.43768227551313,134.32432303087));
#206461=CARTESIAN_POINT('Ctrl Pts',(193.854078146774,3.53419260818798,134.227427275858));
#206462=CARTESIAN_POINT('Ctrl Pts',(193.846303812655,3.62661166846604,134.126539250428));
#206463=CARTESIAN_POINT('Ctrl Pts',(193.838539059708,3.71891683051201,134.025775560474));
#206464=CARTESIAN_POINT('Ctrl Pts',(193.830774306761,3.80714049093836,133.921029675189));
#206465=CARTESIAN_POINT('Ctrl Pts',(193.823009553814,3.8909218276634,133.812667515725));
#206466=CARTESIAN_POINT('Ctrl Pts',(193.815252512929,3.97461995158371,133.704412983086));
#206467=CARTESIAN_POINT('Ctrl Pts',(193.807495472044,4.05388429464595,133.59254963128));
#206468=CARTESIAN_POINT('Ctrl Pts',(193.799738431159,4.12839233419866,133.477478609243));
#206469=CARTESIAN_POINT('Ctrl Pts',(193.791987239919,4.20284418665918,133.36249436316));
#206470=CARTESIAN_POINT('Ctrl Pts',(193.784236048679,4.27254666321562,133.244307588428));
#206471=CARTESIAN_POINT('Ctrl Pts',(193.776484857438,4.33721906272395,133.123350454638));
#206472=CARTESIAN_POINT('Ctrl Pts',(193.768736960661,4.40186397473727,133.002444730857));
#206473=CARTESIAN_POINT('Ctrl Pts',(193.760989063884,4.46148287789932,132.878771333985));
#206474=CARTESIAN_POINT('Ctrl Pts',(193.753241167107,4.51583988094174,132.752789018148));
#206475=CARTESIAN_POINT('Ctrl Pts',(193.745494891023,4.57018551367091,132.626833055096));
#206476=CARTESIAN_POINT('Ctrl Pts',(193.737748614939,4.61927128079769,132.498569492494));
#206477=CARTESIAN_POINT('Ctrl Pts',(193.730002338855,4.66290868628648,132.368478786329));
#206478=CARTESIAN_POINT('Ctrl Pts',(193.72225600559,4.70654641389667,132.238387119863));
#206479=CARTESIAN_POINT('Ctrl Pts',(193.714509672324,4.74473557527959,132.106468653588));
#206480=CARTESIAN_POINT('Ctrl Pts',(193.706763339059,4.77733710840989,131.973220410317));
#206481=CARTESIAN_POINT('Ctrl Pts',(193.699015271056,4.80994594242749,131.839942327026));
#206482=CARTESIAN_POINT('Ctrl Pts',(193.691267203053,4.83696456533113,131.705334253853));
#206483=CARTESIAN_POINT('Ctrl Pts',(193.68351913505,4.85830481722543,131.569904453949));
#206484=CARTESIAN_POINT('Ctrl Pts',(193.675762832308,4.87966774979339,131.434330717642));
#206485=CARTESIAN_POINT('Ctrl Pts',(193.668006529566,4.89534019475674,131.297933896828));
#206486=CARTESIAN_POINT('Ctrl Pts',(193.660250226825,4.9052857224612,131.161229001593));
#206487=CARTESIAN_POINT('Ctrl Pts',(193.65248978431,4.91523655839326,131.02445114284));
#206488=CARTESIAN_POINT('Ctrl Pts',(193.644729341796,4.91945437445847,130.887365272617));
#206489=CARTESIAN_POINT('Ctrl Pts',(193.636968899282,4.9179549245226,130.750486478465));
#206490=CARTESIAN_POINT('Ctrl Pts',(193.629195999017,4.91645306753658,130.613387954321));
#206491=CARTESIAN_POINT('Ctrl Pts',(193.621423098751,4.90921562490836,130.476497561166));
#206492=CARTESIAN_POINT('Ctrl Pts',(193.613650198486,4.89631036227887,130.340326245196));
#206493=CARTESIAN_POINT('Ctrl Pts',(193.606159862724,4.88387423845236,130.209105099557));
#206494=CARTESIAN_POINT('Ctrl Pts',(193.598669526962,4.86617526077355,130.078551963462));
#206495=CARTESIAN_POINT('Ctrl Pts',(193.5911791912,4.84331859353017,129.949113247465));
#206496=CARTESIAN_POINT('Ctrl Pts',(193.583404857081,4.81959530880109,129.814766823208));
#206497=CARTESIAN_POINT('Ctrl Pts',(193.575630522962,4.79024035808555,129.68119542462));
#206498=CARTESIAN_POINT('Ctrl Pts',(193.567856188842,4.75531516453582,129.548908209692));
#206499=CARTESIAN_POINT('Ctrl Pts',(193.560091435895,4.7204330131658,129.416784026935));
#206500=CARTESIAN_POINT('Ctrl Pts',(193.552326682948,4.67999437676145,129.285941253237));
#206501=CARTESIAN_POINT('Ctrl Pts',(193.544561930001,4.63411208200157,129.156881247757));
#206502=CARTESIAN_POINT('Ctrl Pts',(193.536804889116,4.5882753581837,129.027949426493));
#206503=CARTESIAN_POINT('Ctrl Pts',(193.529047848231,4.53700586573875,128.900797215727));
#206504=CARTESIAN_POINT('Ctrl Pts',(193.521290807346,4.48046677125739,128.775912793697));
#206505=CARTESIAN_POINT('Ctrl Pts',(193.513539616106,4.42397031334695,128.651122547982));
#206506=CARTESIAN_POINT('Ctrl Pts',(193.505788424866,4.36221232369776,128.528597041763));
#206507=CARTESIAN_POINT('Ctrl Pts',(193.498037233626,4.29540467300197,128.408806035084));
#206508=CARTESIAN_POINT('Ctrl Pts',(193.490289336849,4.22862541733986,128.289065942777));
#206509=CARTESIAN_POINT('Ctrl Pts',(193.482541440072,4.1568009593707,128.172058379152));
#206510=CARTESIAN_POINT('Ctrl Pts',(193.474793543294,4.08018975694076,128.058229774023));
#206511=CARTESIAN_POINT('Ctrl Pts',(193.46704726721,4.00359457992282,127.944424979385));
#206512=CARTESIAN_POINT('Ctrl Pts',(193.459300991126,3.92221486821154,127.833798144722));
#206513=CARTESIAN_POINT('Ctrl Pts',(193.451554715042,3.83635295632385,127.726767555284));
#206514=CARTESIAN_POINT('Ctrl Pts',(193.443808381777,3.75049041062306,127.619736175771));
#206515=CARTESIAN_POINT('Ctrl Pts',(193.436062048511,3.66014584337031,127.516301399417));
#206516=CARTESIAN_POINT('Ctrl Pts',(193.428315715246,3.56566224751357,127.416848876013));
#206517=CARTESIAN_POINT('Ctrl Pts',(193.420567647243,3.47115749271066,127.317374080907));
#206518=CARTESIAN_POINT('Ctrl Pts',(193.41281957924,3.3725121340977,127.221883596716));
#206519=CARTESIAN_POINT('Ctrl Pts',(193.405071511237,3.27010613528105,127.130726323506));
#206520=CARTESIAN_POINT('Ctrl Pts',(193.397315208495,3.16759129815017,127.03947216726));
#206521=CARTESIAN_POINT('Ctrl Pts',(193.389558905753,3.06130812916382,126.952560682118));
#206522=CARTESIAN_POINT('Ctrl Pts',(193.381802603011,2.95167022977636,126.870300892911));
#206523=CARTESIAN_POINT('Ctrl Pts',(193.374042160497,2.8419738133408,126.787997199178));
#206524=CARTESIAN_POINT('Ctrl Pts',(193.366281717983,2.72891942085808,126.710350369704));
#206525=CARTESIAN_POINT('Ctrl Pts',(193.358521275469,2.61294892541234,126.637625567711));
#206526=CARTESIAN_POINT('Ctrl Pts',(193.350748375203,2.49679226383197,126.564784021411));
#206527=CARTESIAN_POINT('Ctrl Pts',(193.342975474938,2.37771048460871,126.496880485635));
#206528=CARTESIAN_POINT('Ctrl Pts',(193.335202574673,2.25617009023159,126.434134126131));
#206529=CARTESIAN_POINT('Ctrl Pts',(193.32771223891,2.13904799533144,126.373668754842));
#206530=CARTESIAN_POINT('Ctrl Pts',(193.320221903148,2.01964321472039,126.317992247027));
#206531=CARTESIAN_POINT('Ctrl Pts',(193.312731567386,1.89838817010611,126.2672574208));
#206532=CARTESIAN_POINT('Ctrl Pts',(193.304957233267,1.77253570362098,126.214598968217));
#206533=CARTESIAN_POINT('Ctrl Pts',(193.297182899148,1.64429123515347,126.167097516029));
#206534=CARTESIAN_POINT('Ctrl Pts',(193.289408565029,1.51411633445749,126.124976599532));
#206535=CARTESIAN_POINT('Ctrl Pts',(193.281643812082,1.38410186269265,126.082907593301));
#206536=CARTESIAN_POINT('Ctrl Pts',(193.273879059135,1.25216206077593,126.046206048193));
#206537=CARTESIAN_POINT('Ctrl Pts',(193.266114306188,1.11877972194069,126.015048036801));
#206538=CARTESIAN_POINT('Ctrl Pts',(193.258357265303,0.985529860324888,
125.983920971985));
#206539=CARTESIAN_POINT('Ctrl Pts',(193.250600224418,0.850840691275775,
125.958326572221));
#206540=CARTESIAN_POINT('Ctrl Pts',(193.242843183533,0.715211128500449,
125.9383914331));
#206541=CARTESIAN_POINT('Ctrl Pts',(193.235091992293,0.579683845033364,
125.918471327223));
#206542=CARTESIAN_POINT('Ctrl Pts',(193.227340801053,0.443217964620638,
125.904202044029));
#206543=CARTESIAN_POINT('Ctrl Pts',(193.219589609812,0.306323230974984,
125.895659247482));
#206544=CARTESIAN_POINT('Ctrl Pts',(193.211841713035,0.169486681242845,
125.887120081852));
#206545=CARTESIAN_POINT('Ctrl Pts',(193.204093816258,0.0322220301962203,
125.884302586307));
#206546=CARTESIAN_POINT('Ctrl Pts',(193.196345919481,-0.10495542533834,
125.887230619163));
#206547=CARTESIAN_POINT('Ctrl Pts',(193.188599643397,-0.24210418630643,
125.890158039538));
#206548=CARTESIAN_POINT('Ctrl Pts',(193.180853367313,-0.379165397413132,
125.898828589448));
#206549=CARTESIAN_POINT('Ctrl Pts',(193.173107091229,-0.515623724240199,
125.913213999696));
#206550=CARTESIAN_POINT('Ctrl Pts',(193.165360757964,-0.65208305837159,
125.927599516134));
#206551=CARTESIAN_POINT('Ctrl Pts',(193.157614424698,-0.787939110532302,
125.947699936101));
#206552=CARTESIAN_POINT('Ctrl Pts',(193.149868091433,-0.922682026564098,
125.973435143047));
#206553=CARTESIAN_POINT('Ctrl Pts',(193.14212002343,-1.05745511733767,125.999176113215));
#206554=CARTESIAN_POINT('Ctrl Pts',(193.134371955427,-1.19111419199571,
126.030554308008));
#206555=CARTESIAN_POINT('Ctrl Pts',(193.126623887424,-1.32316033142207,
126.06743864229));
#206556=CARTESIAN_POINT('Ctrl Pts',(193.118867584682,-1.45534681105682,
126.104362177682));
#206557=CARTESIAN_POINT('Ctrl Pts',(193.11111128194,-1.58591655391597,126.146803437196));
#206558=CARTESIAN_POINT('Ctrl Pts',(193.103354979199,-1.71438600696752,
126.194581481684));
#206559=CARTESIAN_POINT('Ctrl Pts',(193.095594536684,-1.84292402803436,
126.242385026753));
#206560=CARTESIAN_POINT('Ctrl Pts',(193.08783409417,-1.96935916538758,126.295530881055));
#206561=CARTESIAN_POINT('Ctrl Pts',(193.080073651656,-2.09322948650229,
126.35379061145));
#206562=CARTESIAN_POINT('Ctrl Pts',(193.072300751391,-2.21729865525309,
126.412143865536));
#206563=CARTESIAN_POINT('Ctrl Pts',(193.064527851125,-2.33879443343359,
126.475627219245));
#206564=CARTESIAN_POINT('Ctrl Pts',(193.05675495086,-2.45728027470416,126.54396665526));
#206565=CARTESIAN_POINT('Ctrl Pts',(193.049264615098,-2.57145885719628,
126.609821780639));
#206566=CARTESIAN_POINT('Ctrl Pts',(193.041774279336,-2.68284228060499,
126.680185891838));
#206567=CARTESIAN_POINT('Ctrl Pts',(193.034283943574,-2.791068240227,126.75477778215));
#206568=CARTESIAN_POINT('Ctrl Pts',(193.026549215124,-2.90282536774334,
126.831803436867));
#206569=CARTESIAN_POINT('Ctrl Pts',(193.018814486674,-3.01157783489076,
126.913587324279));
#206570=CARTESIAN_POINT('Ctrl Pts',(193.011079758224,-3.11689046048007,
126.99986631216));
#206571=CARTESIAN_POINT('Ctrl Pts',(193.003357254067,-3.22203664554232,
127.086008941079));
#206572=CARTESIAN_POINT('Ctrl Pts',(192.995634749909,-3.32375351182408,
127.176632275114));
#206573=CARTESIAN_POINT('Ctrl Pts',(192.987912245751,-3.42163455168092,
127.271429814784));
#206574=CARTESIAN_POINT('Ctrl Pts',(192.980196799127,-3.51942613885007,
127.366140719753));
#206575=CARTESIAN_POINT('Ctrl Pts',(192.972481352503,-3.613388589409,127.465017970231));
#206576=CARTESIAN_POINT('Ctrl Pts',(192.964765905879,-3.70314804461637,
127.567714572328));
#206577=CARTESIAN_POINT('Ctrl Pts',(192.957055793399,-3.79284544381304,
127.670340174201));
#206578=CARTESIAN_POINT('Ctrl Pts',(192.949345680918,-3.87834536897914,
127.776779578253));
#206579=CARTESIAN_POINT('Ctrl Pts',(192.941635568438,-3.95931079161108,
127.886648994062));
#206580=CARTESIAN_POINT('Ctrl Pts',(192.933929070916,-4.04023825284938,
127.99646689657));
#206581=CARTESIAN_POINT('Ctrl Pts',(192.926222573394,-4.11663520834471,
128.109711292731));
#206582=CARTESIAN_POINT('Ctrl Pts',(192.918516075872,-4.18820520986374,
128.225965732648));
#206583=CARTESIAN_POINT('Ctrl Pts',(192.910809982444,-4.25977145856918,
128.342214076698));
#206584=CARTESIAN_POINT('Ctrl Pts',(192.903103889017,-4.32651104118669,
128.461471819057));
#206585=CARTESIAN_POINT('Ctrl Pts',(192.895397795589,-4.3881712193687,128.583294114283));
#206586=CARTESIAN_POINT('Ctrl Pts',(192.887692066741,-4.44982848037876,
128.705110646039));
#206587=CARTESIAN_POINT('Ctrl Pts',(192.879986337892,-4.50640664147058,
128.829491133795));
#206588=CARTESIAN_POINT('Ctrl Pts',(192.872280609043,-4.55769962141508,
128.955967471222));
#206589=CARTESIAN_POINT('Ctrl Pts',(192.864570878078,-4.60901924134692,
129.082509496546));
#206590=CARTESIAN_POINT('Ctrl Pts',(192.856861147112,-4.65504805292081,
129.211149177261));
#206591=CARTESIAN_POINT('Ctrl Pts',(192.849151416146,-4.69562867427047,
129.341399778764));
#206592=CARTESIAN_POINT('Ctrl Pts',(192.844428095933,-4.72049014737659,
129.421197024804));
#206593=CARTESIAN_POINT('Ctrl Pts',(192.839704775721,-4.74330770610149,
129.50159857469));
#206594=CARTESIAN_POINT('Ctrl Pts',(192.834981455508,-4.76405452823404,
129.582490119308));
#206595=CARTESIAN_POINT('',(194.860140564008,-4.91266023721352,130.801203006916));
#206596=CARTESIAN_POINT('Ctrl Pts',(194.860140564008,-4.91221266644762,
130.801203294592));
#206597=CARTESIAN_POINT('Ctrl Pts',(194.80188727277,-4.90617542648731,131.832747380102));
#206598=CARTESIAN_POINT('Ctrl Pts',(194.650818106927,-4.08404315233992,
134.516670434198));
#206599=CARTESIAN_POINT('Ctrl Pts',(194.406933066479,0.327902356760881,
136.612472175972));
#206600=CARTESIAN_POINT('Ctrl Pts',(194.128485442666,5.06376798164403,133.667913246476));
#206601=CARTESIAN_POINT('Ctrl Pts',(193.850037818853,5.14627821021483,128.091889343334));
#206602=CARTESIAN_POINT('Ctrl Pts',(193.57159019504,0.499610173265479,125.008494029623));
#206603=CARTESIAN_POINT('Ctrl Pts',(193.348221787245,-3.59620912304385,
126.807588037525));
#206604=CARTESIAN_POINT('Ctrl Pts',(193.217669254053,-4.59434972149962,
128.935771315469));
#206605=CARTESIAN_POINT('Ctrl Pts',(193.179932595466,-4.75726252818781,
129.584191622251));
#206606=CARTESIAN_POINT('Ctrl Pts',(194.92989654745,-4.76405452823406,129.582490119308));
#206607=CARTESIAN_POINT('Ctrl Pts',(194.921111692065,-4.80245103303602,
129.732197508783));
#206608=CARTESIAN_POINT('Ctrl Pts',(194.912326836681,-4.83383095715299,
129.883888334153));
#206609=CARTESIAN_POINT('Ctrl Pts',(194.903541981296,-4.85800796205853,
130.036935244597));
#206610=CARTESIAN_POINT('Ctrl Pts',(194.894810448159,-4.88203821756628,
130.189053192086));
#206611=CARTESIAN_POINT('Ctrl Pts',(194.886078915021,-4.89895263873311,
130.342510630792));
#206612=CARTESIAN_POINT('Ctrl Pts',(194.877347381884,-4.90861601348531,
130.496672634935));
#206613=CARTESIAN_POINT('Ctrl Pts',(194.871611775925,-4.9149637314563,130.597939216148));
#206614=CARTESIAN_POINT('Ctrl Pts',(194.865876169967,-4.91818362286876,
130.699509432803));
#206615=CARTESIAN_POINT('Ctrl Pts',(194.860140564008,-4.9182489840691,130.801199414751));
#206616=CARTESIAN_POINT('Origin',(213.235140564004,0.,130.804360617566));
#206617=CARTESIAN_POINT('',(196.680227908624,-4.76405452823405,129.582490119308));
#206618=CARTESIAN_POINT('',(196.33459504632,-4.76405452823405,129.582490119308));
#206619=CARTESIAN_POINT('',(213.235140564004,-4.76405452823405,129.582490119308));
#206620=CARTESIAN_POINT('',(196.264859436042,-4.91824930178245,130.801739927489));
#206621=CARTESIAN_POINT('Ctrl Pts',(196.33459504632,-4.76405452823405,129.582490119308));
#206622=CARTESIAN_POINT('Ctrl Pts',(196.325979820702,-4.80173843363128,
129.729419094519));
#206623=CARTESIAN_POINT('Ctrl Pts',(196.317364595083,-4.83266542359164,
129.878265641535));
#206624=CARTESIAN_POINT('Ctrl Pts',(196.308749369464,-4.85665623691895,
130.028426819555));
#206625=CARTESIAN_POINT('Ctrl Pts',(196.300175614881,-4.88053156587922,
130.177865168033));
#206626=CARTESIAN_POINT('Ctrl Pts',(196.291601860298,-4.89753723731489,
130.328605301003));
#206627=CARTESIAN_POINT('Ctrl Pts',(196.283028105715,-4.90754478717536,
130.48003481784));
#206628=CARTESIAN_POINT('Ctrl Pts',(196.276971882491,-4.91461379705869,
130.586999735934));
#206629=CARTESIAN_POINT('Ctrl Pts',(196.270915659266,-4.91819205678833,
130.694308241907));
#206630=CARTESIAN_POINT('Ctrl Pts',(196.264859436042,-4.91824930178245,
130.801739927489));
#206631=CARTESIAN_POINT('Ctrl Pts',(196.264859435991,-4.91824930178293,
130.801739928394));
#206632=CARTESIAN_POINT('Ctrl Pts',(196.257012721372,-4.9183234709409,130.940933241881));
#206633=CARTESIAN_POINT('Ctrl Pts',(196.249166006753,-4.91248424618416,
131.080125087051));
#206634=CARTESIAN_POINT('Ctrl Pts',(196.241319292134,-4.90075854751751,
131.218786390696));
#206635=CARTESIAN_POINT('Ctrl Pts',(196.233470637992,-4.88902995053467,
131.357481968145));
#206636=CARTESIAN_POINT('Ctrl Pts',(196.22562198385,-4.87141201293207,131.495646367384));
#206637=CARTESIAN_POINT('Ctrl Pts',(196.217773329708,-4.84798352666506,
131.632755926392));
#206638=CARTESIAN_POINT('Ctrl Pts',(196.209921209237,-4.82454469329633,
131.769926039314));
#206639=CARTESIAN_POINT('Ctrl Pts',(196.202069088767,-4.79529026322915,
131.906040012911));
#206640=CARTESIAN_POINT('Ctrl Pts',(196.194216968297,-4.76035005680923,
132.040584868718));
#206641=CARTESIAN_POINT('Ctrl Pts',(196.186132871399,-4.72437760638351,
132.179104604331));
#206642=CARTESIAN_POINT('Ctrl Pts',(196.1780487745,-4.68237835041523,132.315960659695));
#206643=CARTESIAN_POINT('Ctrl Pts',(196.169964677602,-4.63454850944733,
132.450611866944));
#206644=CARTESIAN_POINT('Ctrl Pts',(196.162096228248,-4.58799455469389,
132.581671182278));
#206645=CARTESIAN_POINT('Ctrl Pts',(196.154227778895,-4.53591733384053,
132.710641463661));
#206646=CARTESIAN_POINT('Ctrl Pts',(196.146359329542,-4.47854577483177,
132.837046231535));
#206647=CARTESIAN_POINT('Ctrl Pts',(196.138167408871,-4.41881567566367,
132.968647489212));
#206648=CARTESIAN_POINT('Ctrl Pts',(196.1299754882,-4.35334689846171,133.097467395895));
#206649=CARTESIAN_POINT('Ctrl Pts',(196.121783567529,-4.2824489092148,133.222999574183));
#206650=CARTESIAN_POINT('Ctrl Pts',(196.113591646858,-4.21155091996789,
133.348531752471));
#206651=CARTESIAN_POINT('Ctrl Pts',(196.105399726187,-4.13522401973526,
133.470775856601));
#206652=CARTESIAN_POINT('Ctrl Pts',(196.097207805515,-4.05382567680301,
133.589262850068));
#206653=CARTESIAN_POINT('Ctrl Pts',(196.089433471396,-3.97657664814305,
133.701709919927));
#206654=CARTESIAN_POINT('Ctrl Pts',(196.081659137277,-3.89452304616624,
133.811118503023));
#206655=CARTESIAN_POINT('Ctrl Pts',(196.073884803158,-3.80793171009603,
133.917050636464));
#206656=CARTESIAN_POINT('Ctrl Pts',(196.066120050211,-3.72144709010858,
134.022852218017));
#206657=CARTESIAN_POINT('Ctrl Pts',(196.058355297264,-3.63043610820173,
134.125185574825));
#206658=CARTESIAN_POINT('Ctrl Pts',(196.050590544317,-3.53520915752512,
134.223641137654));
#206659=CARTESIAN_POINT('Ctrl Pts',(196.042833503432,-3.44007678759841,
134.32199891303));
#206660=CARTESIAN_POINT('Ctrl Pts',(196.035076462547,-3.34073705198568,
134.41648627984));
#206661=CARTESIAN_POINT('Ctrl Pts',(196.027319421662,-3.2375407000163,134.506726520369));
#206662=CARTESIAN_POINT('Ctrl Pts',(196.019568230422,-3.13442216921906,
134.59689871003));
#206663=CARTESIAN_POINT('Ctrl Pts',(196.011817039182,-3.02745310398911,
134.68282989205));
#206664=CARTESIAN_POINT('Ctrl Pts',(196.004065847942,-2.91702095129357,
134.764180289245));
#206665=CARTESIAN_POINT('Ctrl Pts',(195.996317951164,-2.8066357352085,134.845496110351));
#206666=CARTESIAN_POINT('Ctrl Pts',(195.988570054387,-2.69279067328169,
134.92223478758));
#206667=CARTESIAN_POINT('Ctrl Pts',(195.98082215761,-2.57590594841546,134.994097077944));
#206668=CARTESIAN_POINT('Ctrl Pts',(195.973075881526,-2.45904567331386,
135.065944336265));
#206669=CARTESIAN_POINT('Ctrl Pts',(195.965329605442,-2.3391473328201,135.13291703199));
#206670=CARTESIAN_POINT('Ctrl Pts',(195.957583329358,-2.2166593843348,135.194759715181));
#206671=CARTESIAN_POINT('Ctrl Pts',(195.949836996093,-2.09417053167117,
135.256602854881));
#206672=CARTESIAN_POINT('Ctrl Pts',(195.942090662827,-1.96909238187651,
135.313315730276));
#206673=CARTESIAN_POINT('Ctrl Pts',(195.934344329562,-1.84189687727761,
135.364689438602));
#206674=CARTESIAN_POINT('Ctrl Pts',(195.926596261559,-1.7146728881277,135.416074651714));
#206675=CARTESIAN_POINT('Ctrl Pts',(195.918848193556,-1.58533096307996,
135.462118172125));
#206676=CARTESIAN_POINT('Ctrl Pts',(195.911100125553,-1.45436146849866,
135.502659861063));
#206677=CARTESIAN_POINT('Ctrl Pts',(195.903343822811,-1.32325277797986,
135.543244638191));
#206678=CARTESIAN_POINT('Ctrl Pts',(195.895587520069,-1.19051343654138,
135.578315787215));
#206679=CARTESIAN_POINT('Ctrl Pts',(195.887831217328,-1.0566479063914,135.607763397306));
#206680=CARTESIAN_POINT('Ctrl Pts',(195.880070774813,-0.922710928177224,
135.637226724474));
#206681=CARTESIAN_POINT('Ctrl Pts',(195.872310332299,-0.787646948375374,
135.661060464155));
#206682=CARTESIAN_POINT('Ctrl Pts',(195.864549889785,-0.651967989498143,
135.679206338527));
#206683=CARTESIAN_POINT('Ctrl Pts',(195.85677698952,-0.516071226711214,
135.697381342267));
#206684=CARTESIAN_POINT('Ctrl Pts',(195.849004089254,-0.379557901639337,
135.709850199137));
#206685=CARTESIAN_POINT('Ctrl Pts',(195.841231188989,-0.242943397281255,
135.716606699372));
#206686=CARTESIAN_POINT('Ctrl Pts',(195.833740853227,-0.111295174267542,
135.723117583805));
#206687=CARTESIAN_POINT('Ctrl Pts',(195.826250517465,0.0204466914981448,
135.724324215373));
#206688=CARTESIAN_POINT('Ctrl Pts',(195.818760181703,0.151825322225019,
135.720266651456));
#206689=CARTESIAN_POINT('Ctrl Pts',(195.810985847584,0.288185213667395,
135.716055243769));
#206690=CARTESIAN_POINT('Ctrl Pts',(195.803211513465,0.424585729377166,
135.706159236164));
#206691=CARTESIAN_POINT('Ctrl Pts',(195.795437179345,0.560514165651644,
135.690566398395));
#206692=CARTESIAN_POINT('Ctrl Pts',(195.787672426398,0.69627508227663,135.674992777405));
#206693=CARTESIAN_POINT('Ctrl Pts',(195.779907673451,0.831564692377237,
135.653736339747));
#206694=CARTESIAN_POINT('Ctrl Pts',(195.772142920504,0.96587063867978,135.626836845795));
#206695=CARTESIAN_POINT('Ctrl Pts',(195.764385879619,1.10004319042296,135.5999640688));
#206696=CARTESIAN_POINT('Ctrl Pts',(195.756628838734,1.23323364174855,135.567459465525));
#206697=CARTESIAN_POINT('Ctrl Pts',(195.748871797849,1.36493546079199,135.529414506187));
#206698=CARTESIAN_POINT('Ctrl Pts',(195.741120606609,1.496537962469,135.491398236849));
#206699=CARTESIAN_POINT('Ctrl Pts',(195.733369415369,1.62665369222182,135.447850035617));
#206700=CARTESIAN_POINT('Ctrl Pts',(195.725618224129,1.75478736133172,135.398912214731));
#206701=CARTESIAN_POINT('Ctrl Pts',(195.717870327352,1.88286657021454,135.349995193724));
#206702=CARTESIAN_POINT('Ctrl Pts',(195.710122430575,2.00896502951187,135.295693248354));
#206703=CARTESIAN_POINT('Ctrl Pts',(195.702374533797,2.13260385849881,135.236198142252));
#206704=CARTESIAN_POINT('Ctrl Pts',(195.694628257713,2.25621682490795,135.176715481244));
#206705=CARTESIAN_POINT('Ctrl Pts',(195.686881981629,2.37737083230292,135.112041989627));
#206706=CARTESIAN_POINT('Ctrl Pts',(195.679135705545,2.49560856123834,135.042416890384));
#206707=CARTESIAN_POINT('Ctrl Pts',(195.67138937228,2.61384716297782,134.972791277185));
#206708=CARTESIAN_POINT('Ctrl Pts',(195.663643039014,2.72916910640684,134.898214181805));
#206709=CARTESIAN_POINT('Ctrl Pts',(195.655896705749,2.84114353935931,134.818969745645));
#206710=CARTESIAN_POINT('Ctrl Pts',(195.648148637746,2.95314304820954,134.739707563244));
#206711=CARTESIAN_POINT('Ctrl Pts',(195.640400569743,3.06179323579177,134.655776186005));
#206712=CARTESIAN_POINT('Ctrl Pts',(195.63265250174,3.16669431782458,134.567501614122));
#206713=CARTESIAN_POINT('Ctrl Pts',(195.624896198998,3.27170688997588,134.479133222973));
#206714=CARTESIAN_POINT('Ctrl Pts',(195.617139896256,3.37296209730263,134.386412668355));
#206715=CARTESIAN_POINT('Ctrl Pts',(195.609383593514,3.47009479456587,134.289704959123));
#206716=CARTESIAN_POINT('Ctrl Pts',(195.601623151,3.56727933447434,134.192945634076));
#206717=CARTESIAN_POINT('Ctrl Pts',(195.593862708486,3.660336714878,134.092195201126));
#206718=CARTESIAN_POINT('Ctrl Pts',(195.586102265972,3.74894114432121,133.987852938731));
#206719=CARTESIAN_POINT('Ctrl Pts',(195.578329365706,3.83768780946045,133.883343176873));
#206720=CARTESIAN_POINT('Ctrl Pts',(195.570556465441,3.92196699860579,133.775230371938));
#206721=CARTESIAN_POINT('Ctrl Pts',(195.562783565176,4.00149491020802,133.663944773712));
#206722=CARTESIAN_POINT('Ctrl Pts',(195.555293229414,4.07813178190516,133.556704687292));
#206723=CARTESIAN_POINT('Ctrl Pts',(195.547802893651,4.15035665163739,133.446518738335));
#206724=CARTESIAN_POINT('Ctrl Pts',(195.540312557889,4.21795626720724,133.333792963059));
#206725=CARTESIAN_POINT('Ctrl Pts',(195.53253822377,4.28811894274751,133.216793155752));
#206726=CARTESIAN_POINT('Ctrl Pts',(195.524763889651,4.35352096178859,133.096686504988));
#206727=CARTESIAN_POINT('Ctrl Pts',(195.516989555532,4.41387490580435,132.973897752167));
#206728=CARTESIAN_POINT('Ctrl Pts',(195.509224802585,4.47415446897807,132.851260325509));
#206729=CARTESIAN_POINT('Ctrl Pts',(195.501460049638,4.52939816485493,132.725947721159));
#206730=CARTESIAN_POINT('Ctrl Pts',(195.493695296691,4.57936250334169,132.598412491255));
#206731=CARTESIAN_POINT('Ctrl Pts',(195.485938255806,4.62927721654309,132.47100393114));
#206732=CARTESIAN_POINT('Ctrl Pts',(195.478181214921,4.67392286552881,132.341377500251));
#206733=CARTESIAN_POINT('Ctrl Pts',(195.470424174036,4.71310261393714,132.210008800078));
#206734=CARTESIAN_POINT('Ctrl Pts',(195.462672982796,4.75225281659245,132.078739166064));
#206735=CARTESIAN_POINT('Ctrl Pts',(195.454921791556,4.78594521173213,131.945730251064));
#206736=CARTESIAN_POINT('Ctrl Pts',(195.447170600316,4.81403181502214,131.811475678746));
#206737=CARTESIAN_POINT('Ctrl Pts',(195.439422703538,4.84210648075651,131.677278168202));
#206738=CARTESIAN_POINT('Ctrl Pts',(195.431674806761,4.86458001358226,131.54183643523));
#206739=CARTESIAN_POINT('Ctrl Pts',(195.423926909984,4.88135490294342,131.405657028673));
#206740=CARTESIAN_POINT('Ctrl Pts',(195.4161806339,4.89812628335934,131.269506107912));
#206741=CARTESIAN_POINT('Ctrl Pts',(195.408434357816,4.90920134356196,131.132618208275));
#206742=CARTESIAN_POINT('Ctrl Pts',(195.400688081732,4.91453415629017,130.995507391426));
#206743=CARTESIAN_POINT('Ctrl Pts',(195.392941748467,4.919867008384,130.858395562457));
#206744=CARTESIAN_POINT('Ctrl Pts',(195.385195415201,4.91945751322652,130.721061203664));
#206745=CARTESIAN_POINT('Ctrl Pts',(195.377449081936,4.91331184090468,130.584020388543));
#206746=CARTESIAN_POINT('Ctrl Pts',(195.369701013933,4.90716479230216,130.446948884082));
#206747=CARTESIAN_POINT('Ctrl Pts',(195.36195294593,4.8952790278877,130.310171444601));
#206748=CARTESIAN_POINT('Ctrl Pts',(195.354204877927,4.8777127276868,130.174200631005));
#206749=CARTESIAN_POINT('Ctrl Pts',(195.346448575185,4.86012775781292,130.03808530601));
#206750=CARTESIAN_POINT('Ctrl Pts',(195.338692272444,4.83685024208653,129.902778707793));
#206751=CARTESIAN_POINT('Ctrl Pts',(195.330935969702,4.80798990287418,129.768785339588));
#206752=CARTESIAN_POINT('Ctrl Pts',(195.323175527188,4.77911416002987,129.634720455087));
#206753=CARTESIAN_POINT('Ctrl Pts',(195.315415084674,4.74464975455025,129.501970575457));
#206754=CARTESIAN_POINT('Ctrl Pts',(195.307654642159,4.70475651246827,129.371025618033));
#206755=CARTESIAN_POINT('Ctrl Pts',(195.299881741894,4.66479923021246,129.239870456138));
#206756=CARTESIAN_POINT('Ctrl Pts',(195.292108841629,4.61939582587396,129.11052637553));
#206757=CARTESIAN_POINT('Ctrl Pts',(195.284335941363,4.56875487911233,128.983464707008));
#206758=CARTESIAN_POINT('Ctrl Pts',(195.276845605601,4.5199548583218,128.861022050185));
#206759=CARTESIAN_POINT('Ctrl Pts',(195.269355269839,4.46629160511688,128.740699024911));
#206760=CARTESIAN_POINT('Ctrl Pts',(195.261864934077,4.40799146124495,128.622894518794));
#206761=CARTESIAN_POINT('Ctrl Pts',(195.254090599958,4.3474808496989,128.500623419023));
#206762=CARTESIAN_POINT('Ctrl Pts',(195.246316265839,4.28178311163883,128.380678269616));
#206763=CARTESIAN_POINT('Ctrl Pts',(195.23854193172,4.21110023729952,128.263530467021));
#206764=CARTESIAN_POINT('Ctrl Pts',(195.230777178773,4.14050447328558,128.146527038623));
#206765=CARTESIAN_POINT('Ctrl Pts',(195.223012425825,4.06493599723231,128.032314429117));
#206766=CARTESIAN_POINT('Ctrl Pts',(195.215247672878,3.98464394172745,127.9213421091));
#206767=CARTESIAN_POINT('Ctrl Pts',(195.207490631993,3.90443163342391,127.810480008356));
#206768=CARTESIAN_POINT('Ctrl Pts',(195.199733591108,3.81950530971266,127.702852107236));
#206769=CARTESIAN_POINT('Ctrl Pts',(195.191976550223,3.73015871273531,127.59888108397));
#206770=CARTESIAN_POINT('Ctrl Pts',(195.184225358983,3.64087949272173,127.49498846606));
#206771=CARTESIAN_POINT('Ctrl Pts',(195.176474167743,3.5471868880792,127.39474753233));
#206772=CARTESIAN_POINT('Ctrl Pts',(195.168722976503,3.44941620923195,127.29854960184));
#206773=CARTESIAN_POINT('Ctrl Pts',(195.160975079726,3.35168708553179,127.202392558036));
#206774=CARTESIAN_POINT('Ctrl Pts',(195.153227182949,3.24988361311233,127.110275373367));
#206775=CARTESIAN_POINT('Ctrl Pts',(195.145479286172,3.14437925902386,127.022553888247));
#206776=CARTESIAN_POINT('Ctrl Pts',(195.137733010088,3.03889697417174,126.934850752571));
#206777=CARTESIAN_POINT('Ctrl Pts',(195.129986734003,2.92971564790252,126.851541737333));
#206778=CARTESIAN_POINT('Ctrl Pts',(195.122240457919,2.8172429500486,126.772943345328));
#206779=CARTESIAN_POINT('Ctrl Pts',(195.114494124654,2.70476942194696,126.694344373127));
#206780=CARTESIAN_POINT('Ctrl Pts',(195.106747791389,2.58900479424786,126.620456317494));
#206781=CARTESIAN_POINT('Ctrl Pts',(195.099001458123,2.47038658928282,126.551552937692));
#206782=CARTESIAN_POINT('Ctrl Pts',(195.09125339012,2.35174182059327,126.482634127456));
#206783=CARTESIAN_POINT('Ctrl Pts',(195.083505322117,2.23024254102713,126.418702410666));
#206784=CARTESIAN_POINT('Ctrl Pts',(195.075757254114,2.10635143031566,126.359985890509));
#206785=CARTESIAN_POINT('Ctrl Pts',(195.068000951373,1.98232864665704,126.301206965734));
#206786=CARTESIAN_POINT('Ctrl Pts',(195.060244648631,1.8559093076601,126.247654477585));
#206787=CARTESIAN_POINT('Ctrl Pts',(195.052488345889,1.72757717380225,126.199508809847));
#206788=CARTESIAN_POINT('Ctrl Pts',(195.044727903375,1.59917654522038,126.151337445316));
#206789=CARTESIAN_POINT('Ctrl Pts',(195.036967460861,1.46886145881318,126.108578773192));
#206790=CARTESIAN_POINT('Ctrl Pts',(195.029207018346,1.33713048578585,126.071363139595));
#206791=CARTESIAN_POINT('Ctrl Pts',(195.021434118081,1.2051880465063,126.034087764159));
#206792=CARTESIAN_POINT('Ctrl Pts',(195.013661217816,1.0718255591914,126.002373299147));
#206793=CARTESIAN_POINT('Ctrl Pts',(195.00588831755,0.937552310192054,125.976299026394));
#206794=CARTESIAN_POINT('Ctrl Pts',(194.998397981788,0.808160232008243,
125.951172619133));
#206795=CARTESIAN_POINT('Ctrl Pts',(194.990907646026,0.677922763967373,
125.931283499663));
#206796=CARTESIAN_POINT('Ctrl Pts',(194.983417310264,0.547297844753216,
125.916656848757));
#206797=CARTESIAN_POINT('Ctrl Pts',(194.975642976145,0.411720242024034,
125.901475623937));
#206798=CARTESIAN_POINT('Ctrl Pts',(194.967868642026,0.27529575862716,125.891915708546));
#206799=CARTESIAN_POINT('Ctrl Pts',(194.960094307907,0.138530174400293,
125.888061963774));
#206800=CARTESIAN_POINT('Ctrl Pts',(194.95232955496,0.00193314153252316,
125.884212968398));
#206801=CARTESIAN_POINT('Ctrl Pts',(194.944564802013,-0.135003768683377,
125.886056162276));
#206802=CARTESIAN_POINT('Ctrl Pts',(194.936800049066,-0.271767741656031,
125.893624892942));
#206803=CARTESIAN_POINT('Ctrl Pts',(194.929043008181,-0.408395878722369,
125.901186106239));
#206804=CARTESIAN_POINT('Ctrl Pts',(194.921285967296,-0.544851032521165,
125.914461518103));
#206805=CARTESIAN_POINT('Ctrl Pts',(194.913528926411,-0.680618817085562,
125.933432462858));
#206806=CARTESIAN_POINT('Ctrl Pts',(194.90577773517,-0.816284218107408,
125.952389101476));
#206807=CARTESIAN_POINT('Ctrl Pts',(194.89802654393,-0.951262896003321,
125.977032670072));
#206808=CARTESIAN_POINT('Ctrl Pts',(194.89027535269,-1.08504437948985,126.00729258));
#206809=CARTESIAN_POINT('Ctrl Pts',(194.882527455913,-1.21876900227714,
126.037539628659));
#206810=CARTESIAN_POINT('Ctrl Pts',(194.874779559136,-1.35129706216439,
126.073398184829));
#206811=CARTESIAN_POINT('Ctrl Pts',(194.867031662359,-1.48212731246938,
126.114746380538));
#206812=CARTESIAN_POINT('Ctrl Pts',(194.859285386275,-1.61293019590674,
126.156085927097));
#206813=CARTESIAN_POINT('Ctrl Pts',(194.851539110191,-1.74203560361091,
126.202912711391));
#206814=CARTESIAN_POINT('Ctrl Pts',(194.843792834107,-1.86895689731614,
126.255054826737));
#206815=CARTESIAN_POINT('Ctrl Pts',(194.836046500841,-1.9958791279254,126.307197326983));
#206816=CARTESIAN_POINT('Ctrl Pts',(194.828300167576,-2.12061685072737,
126.364655088006));
#206817=CARTESIAN_POINT('Ctrl Pts',(194.820553834311,-2.24270325279445,
126.427207983444));
#206818=CARTESIAN_POINT('Ctrl Pts',(194.812805766308,-2.3648169952645,126.489774887168));
#206819=CARTESIAN_POINT('Ctrl Pts',(194.805057698305,-2.48427788763078,
126.557439017562));
#206820=CARTESIAN_POINT('Ctrl Pts',(194.797309630302,-2.60064393052617,
126.629934404406));
#206821=CARTESIAN_POINT('Ctrl Pts',(194.78955332756,-2.71713364863695,126.70250684021));
#206822=CARTESIAN_POINT('Ctrl Pts',(194.781797024818,-2.83052161429419,
126.779920582553));
#206823=CARTESIAN_POINT('Ctrl Pts',(194.774040722076,-2.94039458115534,
126.861866131887));
#206824=CARTESIAN_POINT('Ctrl Pts',(194.766280279562,-3.050326190527,126.943855418027));
#206825=CARTESIAN_POINT('Ctrl Pts',(194.758519837048,-3.15673875969899,
127.030381084215));
#206826=CARTESIAN_POINT('Ctrl Pts',(194.750759394534,-3.25925313487488,
127.121094123636));
#206827=CARTESIAN_POINT('Ctrl Pts',(194.742986494268,-3.36193207522668,
127.211952783681));
#206828=CARTESIAN_POINT('Ctrl Pts',(194.735213594003,-3.46070003479519,
127.307011978273));
#206829=CARTESIAN_POINT('Ctrl Pts',(194.727440693737,-3.55521502981467,
127.40588608415));
#206830=CARTESIAN_POINT('Ctrl Pts',(194.719950357975,-3.6462941666962,127.501165867229));
#206831=CARTESIAN_POINT('Ctrl Pts',(194.712460022213,-3.73342397889856,
127.599987782716));
#206832=CARTESIAN_POINT('Ctrl Pts',(194.704969686451,-3.81633575408038,
127.701980164651));
#206833=CARTESIAN_POINT('Ctrl Pts',(194.697219842191,-3.90212007209462,
127.807506151856));
#206834=CARTESIAN_POINT('Ctrl Pts',(194.68946999793,-3.98366789287206,127.916769679002));
#206835=CARTESIAN_POINT('Ctrl Pts',(194.681720153669,-4.06063403806943,
128.029394983297));
#206836=CARTESIAN_POINT('Ctrl Pts',(194.673641243833,-4.14086823717748,
128.146802462472));
#206837=CARTESIAN_POINT('Ctrl Pts',(194.665562333997,-4.21612278806056,
128.26786322798));
#206838=CARTESIAN_POINT('Ctrl Pts',(194.657483424161,-4.28605088173785,
128.39211044363));
#206839=CARTESIAN_POINT('Ctrl Pts',(194.649752999485,-4.35296261511464,
128.510998234348));
#206840=CARTESIAN_POINT('Ctrl Pts',(194.642022574809,-4.41499755592588,
128.632802943297));
#206841=CARTESIAN_POINT('Ctrl Pts',(194.634292150133,-4.47189467077365,
128.757084105708));
#206842=CARTESIAN_POINT('Ctrl Pts',(194.626567138405,-4.52875194548538,
128.881278244753));
#206843=CARTESIAN_POINT('Ctrl Pts',(194.618842126678,-4.58047838715712,
129.007945031798));
#206844=CARTESIAN_POINT('Ctrl Pts',(194.61111711495,-4.62685868724639,129.136619105595));
#206845=CARTESIAN_POINT('Ctrl Pts',(194.603396293483,-4.67321382938121,
129.265223383023));
#206846=CARTESIAN_POINT('Ctrl Pts',(194.595675472015,-4.71422847016418,
129.395832410166));
#206847=CARTESIAN_POINT('Ctrl Pts',(194.587954650547,-4.74973548014277,
129.527961020585));
#206848=CARTESIAN_POINT('Ctrl Pts',(194.58689417891,-4.75461244526093,129.546109172866));
#206849=CARTESIAN_POINT('Ctrl Pts',(194.585833707274,-4.75938558135185,
129.564285966276));
#206850=CARTESIAN_POINT('Ctrl Pts',(194.584773235637,-4.76405452823405,
129.582490119308));
#206851=CARTESIAN_POINT('',(196.610140563971,-4.91824935727201,130.801846220335));
#206852=CARTESIAN_POINT('Ctrl Pts',(196.610140563971,-4.91824935727201,
130.801846220335));
#206853=CARTESIAN_POINT('Ctrl Pts',(196.602459708905,-4.91831834504391,
130.936788726876));
#206854=CARTESIAN_POINT('Ctrl Pts',(196.59477885384,-4.91282949710972,131.071957218089));
#206855=CARTESIAN_POINT('Ctrl Pts',(196.587097998774,-4.90175335462761,
131.206849266967));
#206856=CARTESIAN_POINT('Ctrl Pts',(196.579425945198,-4.89068990429389,
131.341586743087));
#206857=CARTESIAN_POINT('Ctrl Pts',(196.571753891622,-4.87405192579336,
131.476048011019));
#206858=CARTESIAN_POINT('Ctrl Pts',(196.564081838046,-4.85186195546942,
131.60972924594));
#206859=CARTESIAN_POINT('Ctrl Pts',(196.556416637028,-4.82969180487755,
131.743291078887));
#206860=CARTESIAN_POINT('Ctrl Pts',(196.548751436009,-4.80197959258732,
131.8760738716));
#206861=CARTESIAN_POINT('Ctrl Pts',(196.541086234991,-4.76879973819775,
132.007578020808));
#206862=CARTESIAN_POINT('Ctrl Pts',(196.533377076582,-4.73542960832549,
132.139836302786));
#206863=CARTESIAN_POINT('Ctrl Pts',(196.525667918172,-4.69652895673484,
132.270800820309));
#206864=CARTESIAN_POINT('Ctrl Pts',(196.517958759763,-4.65222593936672,
132.399972372218));
#206865=CARTESIAN_POINT('Ctrl Pts',(196.51030050335,-4.60821544575988,132.528291030792));
#206866=CARTESIAN_POINT('Ctrl Pts',(196.502642246937,-4.55887385694772,
132.654839949545));
#206867=CARTESIAN_POINT('Ctrl Pts',(196.494983990524,-4.50437694002413,
132.779144515788));
#206868=CARTESIAN_POINT('Ctrl Pts',(196.487326349773,-4.44988440421434,
132.903439088945));
#206869=CARTESIAN_POINT('Ctrl Pts',(196.479668709022,-4.39023752537237,
133.025489301258));
#206870=CARTESIAN_POINT('Ctrl Pts',(196.472011068271,-4.32565999840557,
133.144841047028));
#206871=CARTESIAN_POINT('Ctrl Pts',(196.464352292712,-4.26107290151344,
133.264210479868));
#206872=CARTESIAN_POINT('Ctrl Pts',(196.456693517154,-4.19155389441899,
133.380880298477));
#206873=CARTESIAN_POINT('Ctrl Pts',(196.449034741596,-4.11737209033022,
133.494421979742));
#206874=CARTESIAN_POINT('Ctrl Pts',(196.44128738256,-4.04233227935724,133.609276914914));
#206875=CARTESIAN_POINT('Ctrl Pts',(196.433540023525,-3.96252135406451,
133.720930539313));
#206876=CARTESIAN_POINT('Ctrl Pts',(196.425792664489,-3.87826158539609,
133.82897135909));
#206877=CARTESIAN_POINT('Ctrl Pts',(196.418122442924,-3.79484075880011,
133.935936458026));
#206878=CARTESIAN_POINT('Ctrl Pts',(196.41045222136,-3.70705958893727,134.03936010492));
#206879=CARTESIAN_POINT('Ctrl Pts',(196.402781999795,-3.61526928634412,
134.138878731135));
#206880=CARTESIAN_POINT('Ctrl Pts',(196.394996072024,-3.52209431609966,
134.239898607683));
#206881=CARTESIAN_POINT('Ctrl Pts',(196.387210144253,-3.4247885873534,134.336894393959));
#206882=CARTESIAN_POINT('Ctrl Pts',(196.379424216482,-3.32375503379505,
134.429527584455));
#206883=CARTESIAN_POINT('Ctrl Pts',(196.371638288711,-3.2227214802367,134.52216077495));
#206884=CARTESIAN_POINT('Ctrl Pts',(196.36385236094,-3.1179604696731,134.610431147627));
#206885=CARTESIAN_POINT('Ctrl Pts',(196.356066433169,-3.00990550869428,
134.694045937901));
#206886=CARTESIAN_POINT('Ctrl Pts',(196.34829209905,-2.90201144717865,134.777536221399));
#206887=CARTESIAN_POINT('Ctrl Pts',(196.340517764931,-2.79047001289452,
134.856666115183));
#206888=CARTESIAN_POINT('Ctrl Pts',(196.332743430812,-2.67566902769502,
134.931100046793));
#206889=CARTESIAN_POINT('Ctrl Pts',(196.324978677865,-2.56100952444973,
135.005442245234));
#206890=CARTESIAN_POINT('Ctrl Pts',(196.317213924918,-2.44309878802772,
135.075099785956));
#206891=CARTESIAN_POINT('Ctrl Pts',(196.309449171971,-2.32235744469594,
135.139777432771));
#206892=CARTESIAN_POINT('Ctrl Pts',(196.301692131086,-2.20173602336822,
135.204390840836));
#206893=CARTESIAN_POINT('Ctrl Pts',(196.293935090201,-2.07828993234506,
135.264034014541));
#206894=CARTESIAN_POINT('Ctrl Pts',(196.286178049316,-1.95246819612849,
135.318455322555));
#206895=CARTESIAN_POINT('Ctrl Pts',(196.278426858075,-1.82674134306254,
135.372835591037));
#206896=CARTESIAN_POINT('Ctrl Pts',(196.270675666835,-1.69864276804628,
135.4220016773));
#206897=CARTESIAN_POINT('Ctrl Pts',(196.262924475595,-1.56864516146753,
135.465748331531));
#206898=CARTESIAN_POINT('Ctrl Pts',(196.255176578818,-1.43870280733915,
135.509476392268));
#206899=CARTESIAN_POINT('Ctrl Pts',(196.247428682041,-1.30686339675709,
135.547789477832));
#206900=CARTESIAN_POINT('Ctrl Pts',(196.239680785264,-1.17361841621132,
135.58053093233));
#206901=CARTESIAN_POINT('Ctrl Pts',(196.23193450918,-1.04040130764291,135.613265538021));
#206902=CARTESIAN_POINT('Ctrl Pts',(196.224188233096,-0.90577959335298,
135.640430737586));
#206903=CARTESIAN_POINT('Ctrl Pts',(196.216441957012,-0.770258312508345,
135.661920210048));
#206904=CARTESIAN_POINT('Ctrl Pts',(196.208695623746,-0.634736031276551,
135.68340984114));
#206905=CARTESIAN_POINT('Ctrl Pts',(196.200949290481,-0.49831455638039,
135.699223600296));
#206906=CARTESIAN_POINT('Ctrl Pts',(196.193202957216,-0.361507077887804,
135.709306661626));
#206907=CARTESIAN_POINT('Ctrl Pts',(196.185454889213,-0.224668962309024,
135.719391980987));
#206908=CARTESIAN_POINT('Ctrl Pts',(196.17770682121,-0.0874450609556074,
135.723744020074));
#206909=CARTESIAN_POINT('Ctrl Pts',(196.169958753207,0.0496487812816021,
135.722360013765));
#206910=CARTESIAN_POINT('Ctrl Pts',(196.162202450465,0.186888328485989,
135.720974536519));
#206911=CARTESIAN_POINT('Ctrl Pts',(196.154446147723,0.323997148879435,
135.71384083974));
#206912=CARTESIAN_POINT('Ctrl Pts',(196.146689844981,0.460461311244389,
135.701008291572));
#206913=CARTESIAN_POINT('Ctrl Pts',(196.138929402467,0.596998308641748,
135.688168894286));
#206914=CARTESIAN_POINT('Ctrl Pts',(196.131168959953,0.732889575229854,
135.669624637705));
#206915=CARTESIAN_POINT('Ctrl Pts',(196.123408517439,0.8676297459151,135.645476365666));
#206916=CARTESIAN_POINT('Ctrl Pts',(196.115635617173,1.00258621348393,135.621289328677));
#206917=CARTESIAN_POINT('Ctrl Pts',(196.107862716908,1.13638751074486,135.591480384296));
#206918=CARTESIAN_POINT('Ctrl Pts',(196.100089816642,1.268540970819,135.556200983977));
#206919=CARTESIAN_POINT('Ctrl Pts',(196.09259948088,1.39589031974556,135.522204078723));
#206920=CARTESIAN_POINT('Ctrl Pts',(196.085109145118,1.52170926338293,135.483127633423));
#206921=CARTESIAN_POINT('Ctrl Pts',(196.077618809356,1.64557497313272,135.439149293471));
#206922=CARTESIAN_POINT('Ctrl Pts',(196.069844475237,1.77413708891525,135.393503501393));
#206923=CARTESIAN_POINT('Ctrl Pts',(196.062070141118,1.90100217941226,135.342432174158));
#206924=CARTESIAN_POINT('Ctrl Pts',(196.054295806999,2.02567829082461,135.286080212162));
#206925=CARTESIAN_POINT('Ctrl Pts',(196.046531054052,2.15020075007207,135.229797698922));
#206926=CARTESIAN_POINT('Ctrl Pts',(196.038766301105,2.27253924505167,135.168247659205));
#206927=CARTESIAN_POINT('Ctrl Pts',(196.031001548158,2.3922180264252,135.101624395431));
#206928=CARTESIAN_POINT('Ctrl Pts',(196.023244507273,2.51177794114601,135.03506730282));
#206929=CARTESIAN_POINT('Ctrl Pts',(196.015487466388,2.62868305990259,134.963447202521));
#206930=CARTESIAN_POINT('Ctrl Pts',(196.007730425503,2.7424789694179,134.887005858681));
#206931=CARTESIAN_POINT('Ctrl Pts',(195.999979234263,2.85618906455235,134.810622159854));
#206932=CARTESIAN_POINT('Ctrl Pts',(195.992228043023,2.96679429415914,134.729424671326));
#206933=CARTESIAN_POINT('Ctrl Pts',(195.984476851783,3.0738664750577,134.643700138371));
#206934=CARTESIAN_POINT('Ctrl Pts',(195.976728955005,3.18089314742335,134.55801204063));
#206935=CARTESIAN_POINT('Ctrl Pts',(195.968981058228,3.28438945316746,134.467800969217));
#206936=CARTESIAN_POINT('Ctrl Pts',(195.961233161451,3.38395793279755,134.373395749301));
#206937=CARTESIAN_POINT('Ctrl Pts',(195.953486885367,3.4835055848481,134.279010276921));
#206938=CARTESIAN_POINT('Ctrl Pts',(195.945740609283,3.57912676149234,134.180432669916));
#206939=CARTESIAN_POINT('Ctrl Pts',(195.937994333199,3.67045902587537,134.078030362954));
#206940=CARTESIAN_POINT('Ctrl Pts',(195.930247999934,3.76179196445257,133.975627300082));
#206941=CARTESIAN_POINT('Ctrl Pts',(195.922501666668,3.84883566736076,133.869399772691));
#206942=CARTESIAN_POINT('Ctrl Pts',(195.914755333403,3.93126661625871,133.759749907387));
#206943=CARTESIAN_POINT('Ctrl Pts',(195.9070072654,4.01371602499605,133.650075486756));
#206944=CARTESIAN_POINT('Ctrl Pts',(195.899259197397,4.09155038929708,133.536977515595));
#206945=CARTESIAN_POINT('Ctrl Pts',(195.891511129394,4.16448855602539,133.420888494206));
#206946=CARTESIAN_POINT('Ctrl Pts',(195.883754826652,4.23750424230527,133.304676092023));
#206947=CARTESIAN_POINT('Ctrl Pts',(195.875998523911,4.3056131276605,133.185466620943));
#206948=CARTESIAN_POINT('Ctrl Pts',(195.868242221169,4.36857895453045,133.063719150542));
#206949=CARTESIAN_POINT('Ctrl Pts',(195.860481778655,4.43157838815802,132.941906699851));
#206950=CARTESIAN_POINT('Ctrl Pts',(195.85272133614,4.48942912881509,132.817553904979));
#206951=CARTESIAN_POINT('Ctrl Pts',(195.844960893626,4.5419428571012,132.691140452451));
#206952=CARTESIAN_POINT('Ctrl Pts',(195.837187993361,4.59454088508596,132.564524069826));
#206953=CARTESIAN_POINT('Ctrl Pts',(195.829415093095,4.64178464539287,132.435840786428));
#206954=CARTESIAN_POINT('Ctrl Pts',(195.82164219283,4.68353525993757,132.305586960068));
#206955=CARTESIAN_POINT('Ctrl Pts',(195.814151857068,4.72376813448038,132.180068188384));
#206956=CARTESIAN_POINT('Ctrl Pts',(195.806661521306,4.75890022668183,132.053091374545));
#206957=CARTESIAN_POINT('Ctrl Pts',(195.799171185544,4.78885244545705,131.925108277898));
#206958=CARTESIAN_POINT('Ctrl Pts',(195.791396851425,4.81994031171073,131.792272663244));
#206959=CARTESIAN_POINT('Ctrl Pts',(195.783622517306,4.84554623795796,131.657932169745));
#206960=CARTESIAN_POINT('Ctrl Pts',(195.775848183187,4.86552621996172,131.522579014271));
#206961=CARTESIAN_POINT('Ctrl Pts',(195.76808343024,4.88548157842337,131.387392669463));
#206962=CARTESIAN_POINT('Ctrl Pts',(195.760318677292,4.89982473164211,131.25119652892));
#206963=CARTESIAN_POINT('Ctrl Pts',(195.752553924345,4.90846199760866,131.114495879237));
#206964=CARTESIAN_POINT('Ctrl Pts',(195.74479688346,4.91709068492086,130.977931002566));
#206965=CARTESIAN_POINT('Ctrl Pts',(195.737039842575,4.92002473840631,130.840863001602));
#206966=CARTESIAN_POINT('Ctrl Pts',(195.72928280169,4.91722193961525,130.70380486653));
#206967=CARTESIAN_POINT('Ctrl Pts',(195.72153161045,4.91442125443657,130.566850088065));
#206968=CARTESIAN_POINT('Ctrl Pts',(195.71378041921,4.90589233599108,130.429905549986));
#206969=CARTESIAN_POINT('Ctrl Pts',(195.70602922797,4.89164498773053,130.293486487754));
#206970=CARTESIAN_POINT('Ctrl Pts',(195.698281331193,4.87740369497295,130.157125407263));
#206971=CARTESIAN_POINT('Ctrl Pts',(195.690533434416,4.85744884697578,130.021289746446));
#206972=CARTESIAN_POINT('Ctrl Pts',(195.682785537639,4.83184225710067,129.886491637266));
#206973=CARTESIAN_POINT('Ctrl Pts',(195.675039261555,4.80624102357217,129.751721724946));
#206974=CARTESIAN_POINT('Ctrl Pts',(195.667292985471,4.77499047258891,129.617989316424));
#206975=CARTESIAN_POINT('Ctrl Pts',(195.659546709387,4.73820383137157,129.485797947506));
#206976=CARTESIAN_POINT('Ctrl Pts',(195.651800376121,4.70141691860354,129.353605602781));
#206977=CARTESIAN_POINT('Ctrl Pts',(195.644054042856,4.65909393887212,129.222954697012));
#206978=CARTESIAN_POINT('Ctrl Pts',(195.63630770959,4.61139834311363,129.094334774595));
#206979=CARTESIAN_POINT('Ctrl Pts',(195.628559641587,4.5636920662572,128.965686048638));
#206980=CARTESIAN_POINT('Ctrl Pts',(195.620811573584,4.51061091513302,128.839069577583));
#206981=CARTESIAN_POINT('Ctrl Pts',(195.613063505581,4.45236679435636,128.714955680505));
#206982=CARTESIAN_POINT('Ctrl Pts',(195.60530720284,4.3940607710351,128.590709873701));
#206983=CARTESIAN_POINT('Ctrl Pts',(195.597550900098,4.33058098301466,128.468972308536));
#206984=CARTESIAN_POINT('Ctrl Pts',(195.589794597356,4.26218595554776,128.350189893506));
#206985=CARTESIAN_POINT('Ctrl Pts',(195.582034154842,4.19375442359537,128.231344080725));
#206986=CARTESIAN_POINT('Ctrl Pts',(195.574273712328,4.12040263382347,128.115456891078));
#206987=CARTESIAN_POINT('Ctrl Pts',(195.566513269813,4.04243236885387,128.002946045293));
#206988=CARTESIAN_POINT('Ctrl Pts',(195.558740369548,3.96433693909305,127.89025458711));
#206989=CARTESIAN_POINT('Ctrl Pts',(195.550967469282,3.88160845470985,127.780950615611));
#206990=CARTESIAN_POINT('Ctrl Pts',(195.543194569017,3.79458944858941,127.675419266381));
#206991=CARTESIAN_POINT('Ctrl Pts',(195.535704233255,3.71073380252928,127.573724247514));
#206992=CARTESIAN_POINT('Ctrl Pts',(195.528213897493,3.62289436686037,127.475532553891));
#206993=CARTESIAN_POINT('Ctrl Pts',(195.520723561731,3.53140846885445,127.381154914047));
#206994=CARTESIAN_POINT('Ctrl Pts',(195.512949227612,3.43645385521897,127.283198917303));
#206995=CARTESIAN_POINT('Ctrl Pts',(195.505174893493,3.33727002191439,127.189041608169));
#206996=CARTESIAN_POINT('Ctrl Pts',(195.497400559374,3.23419324712464,127.099070196728));
#206997=CARTESIAN_POINT('Ctrl Pts',(195.489635806427,3.1312435052475,127.009209667011));
#206998=CARTESIAN_POINT('Ctrl Pts',(195.48187105348,3.02441065959921,126.92352502525));
#206999=CARTESIAN_POINT('Ctrl Pts',(195.474106300532,2.91406918468932,126.842368208519));
#207000=CARTESIAN_POINT('Ctrl Pts',(195.466349259647,2.80383730248746,126.761291997883));
#207001=CARTESIAN_POINT('Ctrl Pts',(195.458592218762,2.69010403888476,126.684734892995));
#207002=CARTESIAN_POINT('Ctrl Pts',(195.450835177877,2.57327816695157,126.61300969716));
#207003=CARTESIAN_POINT('Ctrl Pts',(195.443083986637,2.45654039431791,126.541338589853));
#207004=CARTESIAN_POINT('Ctrl Pts',(195.435332795397,2.33671498721072,126.474492342605));
#207005=CARTESIAN_POINT('Ctrl Pts',(195.427581604157,2.2142407268208,126.412741204845));
#207006=CARTESIAN_POINT('Ctrl Pts',(195.41983370738,2.09181852125829,126.351016312966));
#207007=CARTESIAN_POINT('Ctrl Pts',(195.412085810603,1.96675004998067,126.294382399095));
#207008=CARTESIAN_POINT('Ctrl Pts',(195.404337913826,1.83949959574408,126.243064277735));
#207009=CARTESIAN_POINT('Ctrl Pts',(195.396591637742,1.71227575955951,126.19175689102));
#207010=CARTESIAN_POINT('Ctrl Pts',(195.388845361658,1.5828712106282,126.145763231222));
#207011=CARTESIAN_POINT('Ctrl Pts',(195.381099085574,1.45177078996202,126.105260210476));
#207012=CARTESIAN_POINT('Ctrl Pts',(195.373352752308,1.32066940154283,126.064756890746));
#207013=CARTESIAN_POINT('Ctrl Pts',(195.365606419043,1.18787248995334,126.02974440635));
#207014=CARTESIAN_POINT('Ctrl Pts',(195.357860085778,1.05388027198198,126.000349852088));
#207015=CARTESIAN_POINT('Ctrl Pts',(195.350112017775,0.919858047382009,
125.97094871512));
#207016=CARTESIAN_POINT('Ctrl Pts',(195.342363949772,0.784640365557708,
125.947168095513));
#207017=CARTESIAN_POINT('Ctrl Pts',(195.334615881769,0.648737458886747,
125.92908393086));
#207018=CARTESIAN_POINT('Ctrl Pts',(195.326859579027,0.512690112989033,
125.910980546142));
#207019=CARTESIAN_POINT('Ctrl Pts',(195.319103276285,0.375956475623729,
125.898585762068));
#207020=CARTESIAN_POINT('Ctrl Pts',(195.311346973543,0.239052282779265,
125.891923638978));
#207021=CARTESIAN_POINT('Ctrl Pts',(195.303586531029,0.102075020045067,
125.885257960113));
#207022=CARTESIAN_POINT('Ctrl Pts',(195.295826088515,-0.0350725887894774,
125.884331041572));
#207023=CARTESIAN_POINT('Ctrl Pts',(195.288065646001,-0.17187598256682,
125.889114773347));
#207024=CARTESIAN_POINT('Ctrl Pts',(195.280292745735,-0.308898985296921,
125.893906184392));
#207025=CARTESIAN_POINT('Ctrl Pts',(195.27251984547,-0.445576278733256,
125.904426534803));
#207026=CARTESIAN_POINT('Ctrl Pts',(195.264746945204,-0.58139869000898,
125.920595817153));
#207027=CARTESIAN_POINT('Ctrl Pts',(195.257256609442,-0.712283614519818,
125.936177305362));
#207028=CARTESIAN_POINT('Ctrl Pts',(195.24976627368,-0.842374427875423,
125.957004101464));
#207029=CARTESIAN_POINT('Ctrl Pts',(195.242275937918,-0.971227371730748,
125.982960358834));
#207030=CARTESIAN_POINT('Ctrl Pts',(195.234501603799,-1.10496581411534,
126.009900755591));
#207031=CARTESIAN_POINT('Ctrl Pts',(195.22672726968,-1.23779430956464,126.042452598076));
#207032=CARTESIAN_POINT('Ctrl Pts',(195.218952935561,-1.36920532069673,
126.080542262435));
#207033=CARTESIAN_POINT('Ctrl Pts',(195.211188182614,-1.50045437950196,
126.118584984687));
#207034=CARTESIAN_POINT('Ctrl Pts',(195.203423429667,-1.63028905794107,
126.162151841558));
#207035=CARTESIAN_POINT('Ctrl Pts',(195.19565867672,-1.7582108487659,126.211118007625));
#207036=CARTESIAN_POINT('Ctrl Pts',(195.187901635835,-1.88600558586439,
126.260035539804));
#207037=CARTESIAN_POINT('Ctrl Pts',(195.18014459495,-2.01189085348242,126.314341570363));
#207038=CARTESIAN_POINT('Ctrl Pts',(195.172387554065,-2.13538252951149,
126.373861264766));
#207039=CARTESIAN_POINT('Ctrl Pts',(195.164636362824,-2.25878107950726,
126.433336074905));
#207040=CARTESIAN_POINT('Ctrl Pts',(195.156885171584,-2.37978927994142,
126.498016554088));
#207041=CARTESIAN_POINT('Ctrl Pts',(195.149133980344,-2.49794259036277,
126.567679619691));
#207042=CARTESIAN_POINT('Ctrl Pts',(195.141386083567,-2.61604568247549,
126.637313076633));
#207043=CARTESIAN_POINT('Ctrl Pts',(195.13363818679,-2.73129596186393,126.711924709835));
#207044=CARTESIAN_POINT('Ctrl Pts',(195.125890290013,-2.84325332954889,
126.791245422794));
#207045=CARTESIAN_POINT('Ctrl Pts',(195.118144013929,-2.95518727816587,
126.87054954357));
#207046=CARTESIAN_POINT('Ctrl Pts',(195.110397737845,-3.06382936634111,
126.954560558935));
#207047=CARTESIAN_POINT('Ctrl Pts',(195.102651461761,-3.16876868447561,
127.042966183744));
#207048=CARTESIAN_POINT('Ctrl Pts',(195.094905128495,-3.27370877724855,
127.131372461143));
#207049=CARTESIAN_POINT('Ctrl Pts',(195.08715879523,-3.37494574643612,127.224173160824));
#207050=CARTESIAN_POINT('Ctrl Pts',(195.079412461965,-3.47210228418942,
127.321016134081));
#207051=CARTESIAN_POINT('Ctrl Pts',(195.071664393962,-3.56928057947593,
127.41788079465));
#207052=CARTESIAN_POINT('Ctrl Pts',(195.063916325959,-3.6623763481555,127.518789254161));
#207053=CARTESIAN_POINT('Ctrl Pts',(195.056168257956,-3.75104990871693,
127.62335328579));
#207054=CARTESIAN_POINT('Ctrl Pts',(195.048411955214,-3.83981771259343,
127.728028449315));
#207055=CARTESIAN_POINT('Ctrl Pts',(195.040655652472,-3.92415366637445,
127.836366647376));
#207056=CARTESIAN_POINT('Ctrl Pts',(195.03289934973,-4.00375875951405,127.947946981883));
#207057=CARTESIAN_POINT('Ctrl Pts',(195.025138907216,-4.08340634028877,
128.059586870174));
#207058=CARTESIAN_POINT('Ctrl Pts',(195.017378464702,-4.15831781570031,
128.174472015597));
#207059=CARTESIAN_POINT('Ctrl Pts',(195.009618022188,-4.22823870262148,
128.292154309128));
#207060=CARTESIAN_POINT('Ctrl Pts',(195.001845121922,-4.29827183275764,
128.410025516725));
#207061=CARTESIAN_POINT('Ctrl Pts',(194.994072221657,-4.36329817963602,
128.530702500966));
#207062=CARTESIAN_POINT('Ctrl Pts',(194.986299321391,-4.42310983539823,
128.65371363433));
#207063=CARTESIAN_POINT('Ctrl Pts',(194.978808985629,-4.48074718681689,
128.772253003149));
#207064=CARTESIAN_POINT('Ctrl Pts',(194.971318649867,-4.53354227567348,
128.892959480803));
#207065=CARTESIAN_POINT('Ctrl Pts',(194.963828314105,-4.58135270478999,
129.015397102898));
#207066=CARTESIAN_POINT('Ctrl Pts',(194.954994481147,-4.63773860762726,
129.159795636662));
#207067=CARTESIAN_POINT('Ctrl Pts',(194.946160648188,-4.68734145347547,
129.306984074171));
#207068=CARTESIAN_POINT('Ctrl Pts',(194.937326815229,-4.72991114124837,
129.456353325896));
#207069=CARTESIAN_POINT('Ctrl Pts',(194.934850059303,-4.74184647294076,
129.498232222765));
#207070=CARTESIAN_POINT('Ctrl Pts',(194.932373303377,-4.75322921960265,
129.540282405251));
#207071=CARTESIAN_POINT('Ctrl Pts',(194.92989654745,-4.76405452823406,129.582490119308));
#207072=CARTESIAN_POINT('Ctrl Pts',(196.680227908624,-4.76405452823405,
129.582490119308));
#207073=CARTESIAN_POINT('Ctrl Pts',(196.672454999871,-4.79811658810201,
129.71529757377));
#207074=CARTESIAN_POINT('Ctrl Pts',(196.664682091119,-4.82658494688575,
129.849389568182));
#207075=CARTESIAN_POINT('Ctrl Pts',(196.656909182367,-4.84939273648973,
129.984255045228));
#207076=CARTESIAN_POINT('Ctrl Pts',(196.649444140572,-4.87129716224193,
130.113778812316));
#207077=CARTESIAN_POINT('Ctrl Pts',(196.641979098777,-4.88798086211456,
130.244015655847));
#207078=CARTESIAN_POINT('Ctrl Pts',(196.634514056982,-4.89942987008945,
130.374511794635));
#207079=CARTESIAN_POINT('Ctrl Pts',(196.626389559324,-4.91189027433556,
130.516535858678));
#207080=CARTESIAN_POINT('Ctrl Pts',(196.618265061666,-4.91817638477932,
130.659109497139));
#207081=CARTESIAN_POINT('Ctrl Pts',(196.610140564008,-4.91824935727168,
130.801846219679));
#207082=CARTESIAN_POINT('Origin',(213.235140564004,0.,130.804360617566));
#207083=CARTESIAN_POINT('',(198.430216174721,-4.76405452823404,129.582490119308));
#207084=CARTESIAN_POINT('',(198.084936573762,-4.76405452823404,129.582490119308));
#207085=CARTESIAN_POINT('',(213.235140564004,-4.76405452823405,129.582490119308));
#207086=CARTESIAN_POINT('',(198.014859435953,-4.91824901604543,130.801249561772));
#207087=CARTESIAN_POINT('Ctrl Pts',(198.084936573762,-4.76405452823404,
129.582490119308));
#207088=CARTESIAN_POINT('Ctrl Pts',(198.077162780964,-4.79809767465422,
129.715223830524));
#207089=CARTESIAN_POINT('Ctrl Pts',(198.069388988166,-4.82655054116148,
129.849229756449));
#207090=CARTESIAN_POINT('Ctrl Pts',(198.061615195367,-4.84934911569474,
129.983997151406));
#207091=CARTESIAN_POINT('Ctrl Pts',(198.056523854313,-4.8642807354981,130.072261244428));
#207092=CARTESIAN_POINT('Ctrl Pts',(198.051432513259,-4.87678805849738,
130.160851841391));
#207093=CARTESIAN_POINT('Ctrl Pts',(198.046341172205,-4.88686521477497,
130.249625153473));
#207094=CARTESIAN_POINT('Ctrl Pts',(198.035847260134,-4.90763553654045,
130.43259842543));
#207095=CARTESIAN_POINT('Ctrl Pts',(198.025353348062,-4.91813231630581,
130.616759698695));
#207096=CARTESIAN_POINT('Ctrl Pts',(198.014859435991,-4.91824901604501,
130.80124956111));
#207097=CARTESIAN_POINT('Ctrl Pts',(198.014859435953,-4.91824901604543,
130.801249561772));
#207098=CARTESIAN_POINT('Ctrl Pts',(198.007194602125,-4.91833425441149,
130.936002371663));
#207099=CARTESIAN_POINT('Ctrl Pts',(197.999529768297,-4.9128772797748,131.070975950461));
#207100=CARTESIAN_POINT('Ctrl Pts',(197.991864934469,-4.90185011753594,
131.205669087091));
#207101=CARTESIAN_POINT('Ctrl Pts',(197.984208471378,-4.89083499802213,
131.340215125821));
#207102=CARTESIAN_POINT('Ctrl Pts',(197.976552008288,-4.87426182187178,
131.47448093386));
#207103=CARTESIAN_POINT('Ctrl Pts',(197.968895545198,-4.85215462495801,
131.607964100634));
#207104=CARTESIAN_POINT('Ctrl Pts',(197.961245495214,-4.83006594518477,
131.741335460987));
#207105=CARTESIAN_POINT('Ctrl Pts',(197.95359544523,-4.80245253092967,131.873925089211));
#207106=CARTESIAN_POINT('Ctrl Pts',(197.945945395246,-4.76939029060855,
132.005235014974));
#207107=CARTESIAN_POINT('Ctrl Pts',(197.938299305357,-4.73634516515454,
132.136476967365));
#207108=CARTESIAN_POINT('Ctrl Pts',(197.930653215467,-4.69785692034788,
132.266440145392));
#207109=CARTESIAN_POINT('Ctrl Pts',(197.923007125577,-4.65405260327977,
132.394636514511));
#207110=CARTESIAN_POINT('Ctrl Pts',(197.915363000358,-4.61025954177498,
132.522799943444));
#207111=CARTESIAN_POINT('Ctrl Pts',(197.907718875139,-4.56115325357192,
132.649197085549));
#207112=CARTESIAN_POINT('Ctrl Pts',(197.90007474992,-4.50691057686776,132.773355314008));
#207113=CARTESIAN_POINT('Ctrl Pts',(197.892430829445,-4.45266935302643,
132.897510216952));
#207114=CARTESIAN_POINT('Ctrl Pts',(197.88478690897,-4.3932921754651,133.019425956816));
#207115=CARTESIAN_POINT('Ctrl Pts',(197.877142988494,-4.32900370978916,
133.138650647346));
#207116=CARTESIAN_POINT('Ctrl Pts',(197.869497513223,-4.26470216764921,
133.257899588531));
#207117=CARTESIAN_POINT('Ctrl Pts',(197.861852037952,-4.19548754221391,
133.374456038018));
#207118=CARTESIAN_POINT('Ctrl Pts',(197.854206562681,-4.12162977785966,
133.487893929593));
#207119=CARTESIAN_POINT('Ctrl Pts',(197.846553256078,-4.04769636030815,
133.60144801666));
#207120=CARTESIAN_POINT('Ctrl Pts',(197.838899949475,-3.9691105266443,133.711876829538));
#207121=CARTESIAN_POINT('Ctrl Pts',(197.831246642873,-3.8861849641364,133.818784192152));
#207122=CARTESIAN_POINT('Ctrl Pts',(197.823589202619,-3.80321461244542,
133.925749296834));
#207123=CARTESIAN_POINT('Ctrl Pts',(197.815931762365,-3.71590012432521,
134.029188857436));
#207124=CARTESIAN_POINT('Ctrl Pts',(197.808274322111,-3.62459270805556,
134.128741877772));
#207125=CARTESIAN_POINT('Ctrl Pts',(197.800605170645,-3.53314564714557,
134.228447153492));
#207126=CARTESIAN_POINT('Ctrl Pts',(197.792936019179,-3.43769374582733,
134.324253733522));
#207127=CARTESIAN_POINT('Ctrl Pts',(197.785266867713,-3.33862350365245,
134.415839007832));
#207128=CARTESIAN_POINT('Ctrl Pts',(197.779475761273,-3.26381388226844,
134.484996602939));
#207129=CARTESIAN_POINT('Ctrl Pts',(197.773684654833,-3.18694180385115,
134.55174800559));
#207130=CARTESIAN_POINT('Ctrl Pts',(197.767893548393,-3.10818467377065,
134.615970657462));
#207131=CARTESIAN_POINT('Ctrl Pts',(197.760119214274,-3.00245630392844,
134.702187058218));
#207132=CARTESIAN_POINT('Ctrl Pts',(197.752344880155,-2.89297047802538,
134.784137565104));
#207133=CARTESIAN_POINT('Ctrl Pts',(197.744570546035,-2.78010632827789,
134.861476818264));
#207134=CARTESIAN_POINT('Ctrl Pts',(197.736805793088,-2.66738127350782,
134.938720757708));
#207135=CARTESIAN_POINT('Ctrl Pts',(197.729041040141,-2.55128649839717,
135.011364531943));
#207136=CARTESIAN_POINT('Ctrl Pts',(197.721276287194,-2.43223495821874,
135.07910226713));
#207137=CARTESIAN_POINT('Ctrl Pts',(197.713519246309,-2.31330166170844,
135.146772724244));
#207138=CARTESIAN_POINT('Ctrl Pts',(197.705762205424,-2.19141778190944,
135.209546647202));
#207139=CARTESIAN_POINT('Ctrl Pts',(197.698005164539,-2.06702577581684,
135.267161028139));
#207140=CARTESIAN_POINT('Ctrl Pts',(197.690253973299,-1.94272757470384,
135.324731961623));
#207141=CARTESIAN_POINT('Ctrl Pts',(197.682502782059,-1.8159253653342,135.377150933938));
#207142=CARTESIAN_POINT('Ctrl Pts',(197.674751590819,-1.68708644647367,
135.424200699714));
#207143=CARTESIAN_POINT('Ctrl Pts',(197.667003694042,-1.55830228759047,
135.471230468085));
#207144=CARTESIAN_POINT('Ctrl Pts',(197.659255797265,-1.42748350741483,
135.512895434921));
#207145=CARTESIAN_POINT('Ctrl Pts',(197.651507900488,-1.29511743474276,
135.549026453294));
#207146=CARTESIAN_POINT('Ctrl Pts',(197.643761624403,-1.16277905019961,
135.585149913837));
#207147=CARTESIAN_POINT('Ctrl Pts',(197.636015348319,-1.02889439386554,
135.615741625526));
#207148=CARTESIAN_POINT('Ctrl Pts',(197.628269072235,-0.89396562727687,
135.640682414112));
#207149=CARTESIAN_POINT('Ctrl Pts',(197.62052273897,-0.759035864674597,
135.665623386805));
#207150=CARTESIAN_POINT('Ctrl Pts',(197.612776405705,-0.623062360890706,
135.684913282095));
#207151=CARTESIAN_POINT('Ctrl Pts',(197.605030072439,-0.486556739791109,
135.698484196049));
#207152=CARTESIAN_POINT('Ctrl Pts',(197.597282004436,-0.350020549204351,
135.712058149115));
#207153=CARTESIAN_POINT('Ctrl Pts',(197.589533936433,-0.212952393152231,
135.71991053368));
#207154=CARTESIAN_POINT('Ctrl Pts',(197.58178586843,-0.0758678779773515,
135.72202542188));
#207155=CARTESIAN_POINT('Ctrl Pts',(197.574029565689,0.061362332251699,
135.724142557809));
#207156=CARTESIAN_POINT('Ctrl Pts',(197.566273262947,0.198608544793241,
135.720510010164));
#207157=CARTESIAN_POINT('Ctrl Pts',(197.558516960205,0.335355735986595,
135.711164016199));
#207158=CARTESIAN_POINT('Ctrl Pts',(197.550756517691,0.472175913273558,
135.701813033997));
#207159=CARTESIAN_POINT('Ctrl Pts',(197.542996075176,0.608496150094301,
135.686742572151));
#207160=CARTESIAN_POINT('Ctrl Pts',(197.535235632662,0.743808672534506,
135.666040545447));
#207161=CARTESIAN_POINT('Ctrl Pts',(197.527462732397,0.879338410648007,
135.645305286012));
#207162=CARTESIAN_POINT('Ctrl Pts',(197.519689832131,1.01385681788001,135.618920471637));
#207163=CARTESIAN_POINT('Ctrl Pts',(197.511916931866,1.14686752295984,135.587024932284));
#207164=CARTESIAN_POINT('Ctrl Pts',(197.504426596104,1.27504295387604,135.556288876127));
#207165=CARTESIAN_POINT('Ctrl Pts',(197.496936260342,1.40181810066686,135.52043588028));
#207166=CARTESIAN_POINT('Ctrl Pts',(197.48944592458,1.52676573916633,135.479632742289));
#207167=CARTESIAN_POINT('Ctrl Pts',(197.481671590461,1.65645080535675,135.437282540919));
#207168=CARTESIAN_POINT('Ctrl Pts',(197.473897256342,1.78457785099881,135.38946526551));
#207169=CARTESIAN_POINT('Ctrl Pts',(197.466122922223,1.91065138484321,135.336313215299));
#207170=CARTESIAN_POINT('Ctrl Pts',(197.458358169276,2.03656954432468,135.283226670239));
#207171=CARTESIAN_POINT('Ctrl Pts',(197.450593416329,2.16043887068706,135.22481858236));
#207172=CARTESIAN_POINT('Ctrl Pts',(197.442828663381,2.28177881119425,135.161271050348));
#207173=CARTESIAN_POINT('Ctrl Pts',(197.435071622496,2.40299823516199,135.097786634641));
#207174=CARTESIAN_POINT('Ctrl Pts',(197.427314581611,2.52169292860744,135.029173113332));
#207175=CARTESIAN_POINT('Ctrl Pts',(197.419557540726,2.63740245675027,134.955660575847));
#207176=CARTESIAN_POINT('Ctrl Pts',(197.411806349486,2.7530247274378,134.882203474739));
#207177=CARTESIAN_POINT('Ctrl Pts',(197.404055158246,2.86566598491015,134.803854919712));
#207178=CARTESIAN_POINT('Ctrl Pts',(197.396303967006,2.97489086808598,134.720890636023));
#207179=CARTESIAN_POINT('Ctrl Pts',(197.388556070229,3.08406932777271,134.637961614368));
#207180=CARTESIAN_POINT('Ctrl Pts',(197.380808173452,3.18983399049617,134.550421001924));
#207181=CARTESIAN_POINT('Ctrl Pts',(197.373060276675,3.2917791350376,134.458587374163));
#207182=CARTESIAN_POINT('Ctrl Pts',(197.365314000591,3.39370295485246,134.366772956017));
#207183=CARTESIAN_POINT('Ctrl Pts',(197.357567724507,3.49180855536177,134.270667570245));
#207184=CARTESIAN_POINT('Ctrl Pts',(197.349821448422,3.58572424131846,134.170629282976));
#207185=CARTESIAN_POINT('Ctrl Pts',(197.342075115157,3.67964062053938,134.070590257247));
#207186=CARTESIAN_POINT('Ctrl Pts',(197.334328781892,3.76936675589715,133.96661855713));
#207187=CARTESIAN_POINT('Ctrl Pts',(197.326582448626,3.85456897269458,133.859107922539));
#207188=CARTESIAN_POINT('Ctrl Pts',(197.318834380623,3.93979026993763,133.751573211687));
#207189=CARTESIAN_POINT('Ctrl Pts',(197.31108631262,4.02048538988445,133.640498295691));
#207190=CARTESIAN_POINT('Ctrl Pts',(197.303338244617,4.09636223415192,133.52630835937));
#207191=CARTESIAN_POINT('Ctrl Pts',(197.295581941876,4.17231972123249,133.411997060627));
#207192=CARTESIAN_POINT('Ctrl Pts',(197.287825639134,4.24344848632279,133.294564454268));
#207193=CARTESIAN_POINT('Ctrl Pts',(197.280069336392,4.3095006339843,133.17446343141));
#207194=CARTESIAN_POINT('Ctrl Pts',(197.272308893878,4.37558803566593,133.054298307018));
#207195=CARTESIAN_POINT('Ctrl Pts',(197.264548451364,4.43659324710592,132.931462278247));
#207196=CARTESIAN_POINT('Ctrl Pts',(197.256788008849,4.49231576929894,132.80643006976));
#207197=CARTESIAN_POINT('Ctrl Pts',(197.249015108584,4.54812774223136,132.681197148472));
#207198=CARTESIAN_POINT('Ctrl Pts',(197.241242208318,4.59863993554477,132.553761366054));
#207199=CARTESIAN_POINT('Ctrl Pts',(197.233469308053,4.64370085002127,132.424615374699));
#207200=CARTESIAN_POINT('Ctrl Pts',(197.225978972291,4.68712368675483,132.300164165429));
#207201=CARTESIAN_POINT('Ctrl Pts',(197.218488636529,4.72548460943441,132.174125223962));
#207202=CARTESIAN_POINT('Ctrl Pts',(197.210998300767,4.75869302446231,132.046948144235));
#207203=CARTESIAN_POINT('Ctrl Pts',(197.203223966648,4.79316054663953,131.914949106876));
#207204=CARTESIAN_POINT('Ctrl Pts',(197.195449632529,4.82218631642961,131.781305789271));
#207205=CARTESIAN_POINT('Ctrl Pts',(197.18767529841,4.84561381580234,131.646506573209));
#207206=CARTESIAN_POINT('Ctrl Pts',(197.179910545463,4.86901244287585,131.511873485134));
#207207=CARTESIAN_POINT('Ctrl Pts',(197.172145792516,4.88682646091603,131.376087714508));
#207208=CARTESIAN_POINT('Ctrl Pts',(197.164381039568,4.8989493242116,131.239651992747));
#207209=CARTESIAN_POINT('Ctrl Pts',(197.156623998683,4.91106014690847,131.103351780867));
#207210=CARTESIAN_POINT('Ctrl Pts',(197.148866957798,4.91749102928209,130.966403289417));
#207211=CARTESIAN_POINT('Ctrl Pts',(197.141109916913,4.91818667583652,130.829318264172));
#207212=CARTESIAN_POINT('Ctrl Pts',(197.133358725673,4.91888179779847,130.692336615812));
#207213=CARTESIAN_POINT('Ctrl Pts',(197.125607534433,4.91385029058759,130.555219027973));
#207214=CARTESIAN_POINT('Ctrl Pts',(197.117856343193,4.90308880637215,130.418480818499));
#207215=CARTESIAN_POINT('Ctrl Pts',(197.110108446416,4.89233189607456,130.281800726411));
#207216=CARTESIAN_POINT('Ctrl Pts',(197.102360549639,4.87584988319397,130.145500080927));
#207217=CARTESIAN_POINT('Ctrl Pts',(197.094612652862,4.85369149206835,130.010092424621));
#207218=CARTESIAN_POINT('Ctrl Pts',(197.086866376778,4.83153773600045,129.874713092679));
#207219=CARTESIAN_POINT('Ctrl Pts',(197.079120100694,4.80371002654195,129.740226763961));
#207220=CARTESIAN_POINT('Ctrl Pts',(197.071373824609,4.77030870450874,129.607139699695));
#207221=CARTESIAN_POINT('Ctrl Pts',(197.063627491344,4.7369071359146,129.474051653011));
#207222=CARTESIAN_POINT('Ctrl Pts',(197.055881158079,4.69793196781799,129.342363270595));
#207223=CARTESIAN_POINT('Ctrl Pts',(197.048134824813,4.65353410543624,129.212568108461));
#207224=CARTESIAN_POINT('Ctrl Pts',(197.04038675681,4.60912630046099,129.082743879601));
#207225=CARTESIAN_POINT('Ctrl Pts',(197.032638688807,4.55929351124709,128.954814084533));
#207226=CARTESIAN_POINT('Ctrl Pts',(197.024890620804,4.50423557151517,128.829254296682));
#207227=CARTESIAN_POINT('Ctrl Pts',(197.017134318063,4.44911911554975,128.703561062393));
#207228=CARTESIAN_POINT('Ctrl Pts',(197.009378015321,4.3887665729042,128.580243225664));
#207229=CARTESIAN_POINT('Ctrl Pts',(197.001621712579,4.32342498015975,128.459754146657));
#207230=CARTESIAN_POINT('Ctrl Pts',(196.993861270065,4.25804851263973,128.339200759));
#207231=CARTESIAN_POINT('Ctrl Pts',(196.986100827551,4.18767788965592,128.22147947287));
#207232=CARTESIAN_POINT('Ctrl Pts',(196.978340385036,4.11260413590295,128.107015574036));
#207233=CARTESIAN_POINT('Ctrl Pts',(196.970567484771,4.03740986709589,127.992367927591));
#207234=CARTESIAN_POINT('Ctrl Pts',(196.962794584506,3.95749760849355,127.880988435588));
#207235=CARTESIAN_POINT('Ctrl Pts',(196.95502168424,3.87319995331092,127.773270849154));
#207236=CARTESIAN_POINT('Ctrl Pts',(196.947531348478,3.79196673022726,127.669469068311));
#207237=CARTESIAN_POINT('Ctrl Pts',(196.940041012716,3.70666161488837,127.569067811088));
#207238=CARTESIAN_POINT('Ctrl Pts',(196.932550676954,3.61761389535537,127.472386312948));
#207239=CARTESIAN_POINT('Ctrl Pts',(196.924776342835,3.52518990447059,127.372039106421));
#207240=CARTESIAN_POINT('Ctrl Pts',(196.917002008716,3.42844113395928,127.275381426659));
#207241=CARTESIAN_POINT('Ctrl Pts',(196.909227674597,3.32769387143375,127.182808939));
#207242=CARTESIAN_POINT('Ctrl Pts',(196.90146292165,3.22707077090526,127.090350538659));
#207243=CARTESIAN_POINT('Ctrl Pts',(196.893698168703,3.12245926830746,127.001967574988));
#207244=CARTESIAN_POINT('Ctrl Pts',(196.885933415755,3.01422473525758,126.91802142652));
#207245=CARTESIAN_POINT('Ctrl Pts',(196.87817637487,2.90609770227194,126.83415865455));
#207246=CARTESIAN_POINT('Ctrl Pts',(196.870419333985,2.79435510683866,126.754724166296));
#207247=CARTESIAN_POINT('Ctrl Pts',(196.8626622931,2.67939760660565,126.680041094515));
#207248=CARTESIAN_POINT('Ctrl Pts',(196.85491110186,2.56452679671837,126.605414341821));
#207249=CARTESIAN_POINT('Ctrl Pts',(196.84715991062,2.44644623414905,126.535532085827));
#207250=CARTESIAN_POINT('Ctrl Pts',(196.83940871938,2.32558766080939,126.470675685041));
#207251=CARTESIAN_POINT('Ctrl Pts',(196.831660822603,2.20478045558657,126.405846849956));
#207252=CARTESIAN_POINT('Ctrl Pts',(196.823912925826,2.08119793174799,126.346039805974));
#207253=CARTESIAN_POINT('Ctrl Pts',(196.816165029049,1.95529848390204,126.291491142238));
#207254=CARTESIAN_POINT('Ctrl Pts',(196.808418752965,1.82942537150677,126.236953888906));
#207255=CARTESIAN_POINT('Ctrl Pts',(196.800672476881,1.70123665761377,126.187672983311));
#207256=CARTESIAN_POINT('Ctrl Pts',(196.792926200797,1.57121251079405,126.143837652445));
#207257=CARTESIAN_POINT('Ctrl Pts',(196.785179867531,1.44118740416556,126.100001997995));
#207258=CARTESIAN_POINT('Ctrl Pts',(196.777433534266,1.30932720805258,126.061612123386));
#207259=CARTESIAN_POINT('Ctrl Pts',(196.769687201001,1.17612873306436,126.028807846864));
#207260=CARTESIAN_POINT('Ctrl Pts',(196.761939132998,1.04290042920136,125.995996224052));
#207261=CARTESIAN_POINT('Ctrl Pts',(196.754191064995,0.908333629647398,
125.968772781862));
#207262=CARTESIAN_POINT('Ctrl Pts',(196.746442996992,0.772936462800047,
125.947226453579));
#207263=CARTESIAN_POINT('Ctrl Pts',(196.73868669425,0.63739539423235,125.925657225601));
#207264=CARTESIAN_POINT('Ctrl Pts',(196.730930391508,0.501022582156627,
125.909777226043));
#207265=CARTESIAN_POINT('Ctrl Pts',(196.723174088766,0.364332980624142,
125.899623668276));
#207266=CARTESIAN_POINT('Ctrl Pts',(196.715413646252,0.227570423735663,
125.88946469125));
#207267=CARTESIAN_POINT('Ctrl Pts',(196.707653203738,0.0904911310544043,
125.88503825871));
#207268=CARTESIAN_POINT('Ctrl Pts',(196.699892761224,-0.0463897865020519,
125.886329400686));
#207269=CARTESIAN_POINT('Ctrl Pts',(196.692119860958,-0.183490437459122,
125.887622615317));
#207270=CARTESIAN_POINT('Ctrl Pts',(196.684346960693,-0.320391686252509,
125.894651725689));
#207271=CARTESIAN_POINT('Ctrl Pts',(196.676574060427,-0.456582484150821,
125.907349743812));
#207272=CARTESIAN_POINT('Ctrl Pts',(196.669083724665,-0.587822403502649,
125.919586156992));
#207273=CARTESIAN_POINT('Ctrl Pts',(196.661593388903,-0.718402323251377,
125.937086434526));
#207274=CARTESIAN_POINT('Ctrl Pts',(196.654103053141,-0.847875673318612,
125.959746091611));
#207275=CARTESIAN_POINT('Ctrl Pts',(196.646328719022,-0.982258044805317,
125.983264896481));
#207276=CARTESIAN_POINT('Ctrl Pts',(196.638554384903,-1.11587396195838,
126.012416540273));
#207277=CARTESIAN_POINT('Ctrl Pts',(196.630780050784,-1.24821417389864,
126.047140374758));
#207278=CARTESIAN_POINT('Ctrl Pts',(196.623015297837,-1.38039128835494,
126.081821415221));
#207279=CARTESIAN_POINT('Ctrl Pts',(196.61525054489,-1.51129545125909,126.12206088437));
#207280=CARTESIAN_POINT('Ctrl Pts',(196.607485791943,-1.64042513233221,
126.16774671864));
#207281=CARTESIAN_POINT('Ctrl Pts',(196.599728751058,-1.76942655998645,
126.213387177096));
#207282=CARTESIAN_POINT('Ctrl Pts',(196.591971710173,-1.89665664695338,
126.264463106153));
#207283=CARTESIAN_POINT('Ctrl Pts',(196.584214669288,-2.02162696724649,
126.320812082332));
#207284=CARTESIAN_POINT('Ctrl Pts',(196.576463478048,-2.14650304644767,
126.377118565309));
#207285=CARTESIAN_POINT('Ctrl Pts',(196.568712286808,-2.26912239593048,
126.43869002048));
#207286=CARTESIAN_POINT('Ctrl Pts',(196.560961095568,-2.38901493376489,
126.505315292293));
#207287=CARTESIAN_POINT('Ctrl Pts',(196.55321319879,-2.50885651407307,126.571912246589));
#207288=CARTESIAN_POINT('Ctrl Pts',(196.545465302013,-2.62597324680375,
126.643558555793));
#207289=CARTESIAN_POINT('Ctrl Pts',(196.537717405236,-2.73991830932937,
126.719996441748));
#207290=CARTESIAN_POINT('Ctrl Pts',(196.529971129152,-2.85383953700426,
126.796418338546));
#207291=CARTESIAN_POINT('Ctrl Pts',(196.522224853068,-2.96459008963101,
126.87762960081));
#207292=CARTESIAN_POINT('Ctrl Pts',(196.514478576984,-3.07175122234275,
126.963328530934));
#207293=CARTESIAN_POINT('Ctrl Pts',(196.506732243719,-3.17891314609344,
127.049028093668));
#207294=CARTESIAN_POINT('Ctrl Pts',(196.498985910453,-3.28248529172354,
127.139215146181));
#207295=CARTESIAN_POINT('Ctrl Pts',(196.491239577188,-3.38208148791119,
127.233547282816));
#207296=CARTESIAN_POINT('Ctrl Pts',(196.483491509185,-3.48169998797647,
127.327900544479));
#207297=CARTESIAN_POINT('Ctrl Pts',(196.475743441182,-3.57734048303421,
127.426400468601));
#207298=CARTESIAN_POINT('Ctrl Pts',(196.467995373179,-3.6686534951838,127.528667622981));
#207299=CARTESIAN_POINT('Ctrl Pts',(196.460239070437,-3.76006355588962,
127.631043468109));
#207300=CARTESIAN_POINT('Ctrl Pts',(196.452482767696,-3.8471366852804,127.737194249536));
#207301=CARTESIAN_POINT('Ctrl Pts',(196.444726464954,-3.92956322945105,
127.846706836569));
#207302=CARTESIAN_POINT('Ctrl Pts',(196.43696602244,-4.01203376715042,127.956277873767));
#207303=CARTESIAN_POINT('Ctrl Pts',(196.429205579925,-4.08985255625137,
128.069213970078));
#207304=CARTESIAN_POINT('Ctrl Pts',(196.421445137411,-4.16275376138207,
128.185073656464));
#207305=CARTESIAN_POINT('Ctrl Pts',(196.413672237146,-4.23577199399886,
128.301119331103));
#207306=CARTESIAN_POINT('Ctrl Pts',(196.40589933688,-4.30385667334007,128.42009763481));
#207307=CARTESIAN_POINT('Ctrl Pts',(196.398126436615,-4.36678792397595,
128.541542399167));
#207308=CARTESIAN_POINT('Ctrl Pts',(196.390636100853,-4.42743146513705,
128.65857234044));
#207309=CARTESIAN_POINT('Ctrl Pts',(196.383145765091,-4.48328962222919,
128.777892252615));
#207310=CARTESIAN_POINT('Ctrl Pts',(196.375655429329,-4.53420891924256,
128.899069947048));
#207311=CARTESIAN_POINT('Ctrl Pts',(196.366995286457,-4.59308056412885,
129.03917263136));
#207312=CARTESIAN_POINT('Ctrl Pts',(196.358335143585,-4.64550922581911,
129.182135375472));
#207313=CARTESIAN_POINT('Ctrl Pts',(196.349675000714,-4.69123825435021,
129.327381706606));
#207314=CARTESIAN_POINT('Ctrl Pts',(196.344648349249,-4.71778099061184,
129.411687784913));
#207315=CARTESIAN_POINT('Ctrl Pts',(196.339621697785,-4.74206742463025,
129.496762736058));
#207316=CARTESIAN_POINT('Ctrl Pts',(196.33459504632,-4.76405452823405,129.582490119308));
#207317=CARTESIAN_POINT('',(198.360140564038,-4.91824805313947,130.80873672198));
#207318=CARTESIAN_POINT('Ctrl Pts',(198.360140564008,-4.918248053139,130.808736722507));
#207319=CARTESIAN_POINT('Ctrl Pts',(198.348902089221,-4.91807175747449,
131.006873152139));
#207320=CARTESIAN_POINT('Ctrl Pts',(198.337663614434,-4.90591901972274,
131.20449843287));
#207321=CARTESIAN_POINT('Ctrl Pts',(198.326425139647,-4.8819937463978,131.400447962368));
#207322=CARTESIAN_POINT('Ctrl Pts',(198.319350026384,-4.86693173648915,
131.523806793625));
#207323=CARTESIAN_POINT('Ctrl Pts',(198.312274913122,-4.84720485499847,
131.646502289585));
#207324=CARTESIAN_POINT('Ctrl Pts',(198.30519979986,-4.82287271835716,131.768249514185));
#207325=CARTESIAN_POINT('Ctrl Pts',(198.297425465741,-4.79613587993932,
131.902028800401));
#207326=CARTESIAN_POINT('Ctrl Pts',(198.289651131622,-4.76378621750837,
132.0349066804));
#207327=CARTESIAN_POINT('Ctrl Pts',(198.281876797503,-4.7258965824454,132.166375505345));
#207328=CARTESIAN_POINT('Ctrl Pts',(198.274112044556,-4.68805364297136,
132.297682306713));
#207329=CARTESIAN_POINT('Ctrl Pts',(198.266347291608,-4.64468442282832,
132.427583136145));
#207330=CARTESIAN_POINT('Ctrl Pts',(198.258582538661,-4.59591298865343,
132.555579297008));
#207331=CARTESIAN_POINT('Ctrl Pts',(198.250825497776,-4.54718999495454,
132.683448330279));
#207332=CARTESIAN_POINT('Ctrl Pts',(198.243068456891,-4.49307560322901,
132.809416096658));
#207333=CARTESIAN_POINT('Ctrl Pts',(198.235311416006,-4.43374391105737,
132.932998208529));
#207334=CARTESIAN_POINT('Ctrl Pts',(198.227560224766,-4.37445696137642,
133.056487126168));
#207335=CARTESIAN_POINT('Ctrl Pts',(198.219809033526,-4.30996071097418,
133.177593619155));
#207336=CARTESIAN_POINT('Ctrl Pts',(198.212057842286,-4.24047753526522,
133.295852808084));
#207337=CARTESIAN_POINT('Ctrl Pts',(198.204309945509,-4.17102389175934,
133.414061733703));
#207338=CARTESIAN_POINT('Ctrl Pts',(198.196562048732,-4.09658773626326,
133.529425425838));
#207339=CARTESIAN_POINT('Ctrl Pts',(198.188814151955,-4.01743749521107,
133.6415033765));
#207340=CARTESIAN_POINT('Ctrl Pts',(198.181067875871,-3.93830381068304,
133.753557882871));
#207341=CARTESIAN_POINT('Ctrl Pts',(198.173321599787,-3.85445822736556,
133.862327695705));
#207342=CARTESIAN_POINT('Ctrl Pts',(198.165575323702,-3.76621240470724,
133.967401430633));
#207343=CARTESIAN_POINT('Ctrl Pts',(198.157828990437,-3.67796593063832,
134.072475941192));
#207344=CARTESIAN_POINT('Ctrl Pts',(198.150082657172,-3.58531940385276,
134.173854020016));
#207345=CARTESIAN_POINT('Ctrl Pts',(198.142336323906,-3.48862439845058,
134.271157823783));
#207346=CARTESIAN_POINT('Ctrl Pts',(198.134588255903,-3.3919077388725,134.368483418062));
#207347=CARTESIAN_POINT('Ctrl Pts',(198.126840187901,-3.29114107212411,
134.461732644436));
#207348=CARTESIAN_POINT('Ctrl Pts',(198.119092119898,-3.18671210764418,
134.550565230971));
#207349=CARTESIAN_POINT('Ctrl Pts',(198.111335817156,-3.08217215481793,
134.639492229836));
#207350=CARTESIAN_POINT('Ctrl Pts',(198.103579514414,-2.97396242717541,
134.723992958252));
#207351=CARTESIAN_POINT('Ctrl Pts',(198.095823211672,-2.86250336727734,
134.803767765485));
#207352=CARTESIAN_POINT('Ctrl Pts',(198.088062769158,-2.75098481832297,
134.883585150935));
#207353=CARTESIAN_POINT('Ctrl Pts',(198.080302326644,-2.63621380844923,
134.958671375235));
#207354=CARTESIAN_POINT('Ctrl Pts',(198.07254188413,-2.51863805887903,135.028771273606));
#207355=CARTESIAN_POINT('Ctrl Pts',(198.064768983864,-2.40087356627779,
135.098983702558));
#207356=CARTESIAN_POINT('Ctrl Pts',(198.056996083599,-2.2802956808095,135.164193623964));
#207357=CARTESIAN_POINT('Ctrl Pts',(198.049223183333,-2.15737571304909,
135.22419241247));
#207358=CARTESIAN_POINT('Ctrl Pts',(198.041732847571,-2.03892419573207,
135.282010093887));
#207359=CARTESIAN_POINT('Ctrl Pts',(198.034242511809,-1.91829820299034,
135.33498881632));
#207360=CARTESIAN_POINT('Ctrl Pts',(198.026752176047,-1.79593348200914,
135.382985519291));
#207361=CARTESIAN_POINT('Ctrl Pts',(198.018977841928,-1.66892926544145,
135.432802031844));
#207362=CARTESIAN_POINT('Ctrl Pts',(198.011203507809,-1.53964955897284,
135.477409084513));
#207363=CARTESIAN_POINT('Ctrl Pts',(198.00342917369,-1.40856083989839,135.516593572631));
#207364=CARTESIAN_POINT('Ctrl Pts',(197.995664420743,-1.27763367595456,
135.555729769371));
#207365=CARTESIAN_POINT('Ctrl Pts',(197.987899667796,-1.14490230633097,
135.589456587496));
#207366=CARTESIAN_POINT('Ctrl Pts',(197.980134914848,-1.01085335967749,
135.617608850073));
#207367=CARTESIAN_POINT('Ctrl Pts',(197.972377873963,-0.876937552327542,
135.645733151425));
#207368=CARTESIAN_POINT('Ctrl Pts',(197.964620833078,-0.741707152334974,
135.668293835729));
#207369=CARTESIAN_POINT('Ctrl Pts',(197.956863792193,-0.605663792714778,
135.685175552871));
#207370=CARTESIAN_POINT('Ctrl Pts',(197.949112600953,-0.469723024450324,
135.702044539379));
#207371=CARTESIAN_POINT('Ctrl Pts',(197.941361409713,-0.332970903234851,
135.713243034937));
#207372=CARTESIAN_POINT('Ctrl Pts',(197.933610218473,-0.195918744622959,
135.718706851604));
#207373=CARTESIAN_POINT('Ctrl Pts',(197.925862321696,-0.0589248368344638,
135.724168346004));
#207374=CARTESIAN_POINT('Ctrl Pts',(197.918114424919,0.0783684648781298,
135.723899993757));
#207375=CARTESIAN_POINT('Ctrl Pts',(197.910366528142,0.215445457623812,
135.717889524298));
#207376=CARTESIAN_POINT('Ctrl Pts',(197.902620252058,0.352493776817673,
135.711880312099));
#207377=CARTESIAN_POINT('Ctrl Pts',(197.894873975974,0.489325486701273,
135.700131388911));
#207378=CARTESIAN_POINT('Ctrl Pts',(197.88712769989,0.625426018410143,135.682682599354));
#207379=CARTESIAN_POINT('Ctrl Pts',(197.879381366624,0.761527554782069,
135.665233680994));
#207380=CARTESIAN_POINT('Ctrl Pts',(197.871635033359,0.896897514417944,
135.642084862025));
#207381=CARTESIAN_POINT('Ctrl Pts',(197.863888700093,1.03102797264083,135.613327698149));
#207382=CARTESIAN_POINT('Ctrl Pts',(197.856140632091,1.16518846844996,135.584564094306));
#207383=CARTESIAN_POINT('Ctrl Pts',(197.848392564088,1.29810852829368,135.550189728304));
#207384=CARTESIAN_POINT('Ctrl Pts',(197.840644496085,1.42929230533578,135.510346865783));
#207385=CARTESIAN_POINT('Ctrl Pts',(197.832888193343,1.56061550605723,135.470461657794));
#207386=CARTESIAN_POINT('Ctrl Pts',(197.825131890601,1.69019836301931,135.425096457024));
#207387=CARTESIAN_POINT('Ctrl Pts',(197.817375587859,1.81756151209824,135.374443025164));
#207388=CARTESIAN_POINT('Ctrl Pts',(197.809615145345,1.94499263872476,135.323762558043));
#207389=CARTESIAN_POINT('Ctrl Pts',(197.801854702831,2.0702013400551,135.267788395269));
#207390=CARTESIAN_POINT('Ctrl Pts',(197.794094260316,2.19273093447755,135.206759294593));
#207391=CARTESIAN_POINT('Ctrl Pts',(197.786321360051,2.3154572242826,135.145632224586));
#207392=CARTESIAN_POINT('Ctrl Pts',(197.778548459786,2.43549547037675,135.079434189959));
#207393=CARTESIAN_POINT('Ctrl Pts',(197.77077555952,2.55241539546258,135.008448950547));
#207394=CARTESIAN_POINT('Ctrl Pts',(197.763285223758,2.66508498676848,134.940044203388));
#207395=CARTESIAN_POINT('Ctrl Pts',(197.755794887996,2.77485878191613,134.867194432942));
#207396=CARTESIAN_POINT('Ctrl Pts',(197.748304552234,2.88138088807747,134.790188917973));
#207397=CARTESIAN_POINT('Ctrl Pts',(197.740530218115,2.99194181227019,134.710263715498));
#207398=CARTESIAN_POINT('Ctrl Pts',(197.732755883996,3.09934982819655,134.62560823861));
#207399=CARTESIAN_POINT('Ctrl Pts',(197.724981549877,3.20317350249298,134.53649975959));
#207400=CARTESIAN_POINT('Ctrl Pts',(197.71721679693,3.3068692233898,134.447501098806));
#207401=CARTESIAN_POINT('Ctrl Pts',(197.709452043983,3.40698909809778,134.354060607414));
#207402=CARTESIAN_POINT('Ctrl Pts',(197.701687291035,3.50313112391044,134.256498417711));
#207403=CARTESIAN_POINT('Ctrl Pts',(197.69393025015,3.5991776601077,134.15903312815));
#207404=CARTESIAN_POINT('Ctrl Pts',(197.686173209265,3.6912539371464,134.057454563654));
#207405=CARTESIAN_POINT('Ctrl Pts',(197.67841616838,3.77899176281173,133.952122412731));
#207406=CARTESIAN_POINT('Ctrl Pts',(197.67066497714,3.86666342470019,133.846869693603));
#207407=CARTESIAN_POINT('Ctrl Pts',(197.6629137859,3.95000289804419,133.737869321391));
#207408=CARTESIAN_POINT('Ctrl Pts',(197.65516259466,4.02867980116461,133.625516785202));
#207409=CARTESIAN_POINT('Ctrl Pts',(197.647414697883,4.10732326450247,133.513212001837));
#207410=CARTESIAN_POINT('Ctrl Pts',(197.639666801106,4.18130787530829,133.397558207814));
#207411=CARTESIAN_POINT('Ctrl Pts',(197.631918904329,4.25034455999749,133.278982646038));
#207412=CARTESIAN_POINT('Ctrl Pts',(197.624172628245,4.31936680370051,133.160431887714));
#207413=CARTESIAN_POINT('Ctrl Pts',(197.616426352161,4.38344298336774,133.038960914946));
#207414=CARTESIAN_POINT('Ctrl Pts',(197.608680076076,4.4423284843672,132.915024186087));
#207415=CARTESIAN_POINT('Ctrl Pts',(197.600933742811,4.50121442004603,132.791086542354));
#207416=CARTESIAN_POINT('Ctrl Pts',(197.593187409546,4.55490943281703,132.664683459342));
#207417=CARTESIAN_POINT('Ctrl Pts',(197.58544107628,4.60321600539095,132.536291756559));
#207418=CARTESIAN_POINT('Ctrl Pts',(197.577693008277,4.65153339588684,132.407871301344));
#207419=CARTESIAN_POINT('Ctrl Pts',(197.569944940274,4.69445980733516,132.277461706041));
#207420=CARTESIAN_POINT('Ctrl Pts',(197.562196872271,4.73184691452124,132.14555703869));
#207421=CARTESIAN_POINT('Ctrl Pts',(197.55444056953,4.76927375716978,132.013512181488));
#207422=CARTESIAN_POINT('Ctrl Pts',(197.546684266788,4.80114942837765,131.879969454826));
#207423=CARTESIAN_POINT('Ctrl Pts',(197.538927964046,4.82737615466953,131.745435813195));
#207424=CARTESIAN_POINT('Ctrl Pts',(197.531167521532,4.85361687895492,131.610830366909));
#207425=CARTESIAN_POINT('Ctrl Pts',(197.523407079018,4.87420259200423,131.475233338161));
#207426=CARTESIAN_POINT('Ctrl Pts',(197.515646636503,4.88908731990802,131.33915800052));
#207427=CARTESIAN_POINT('Ctrl Pts',(197.507873736238,4.90399594209845,131.202864222668));
#207428=CARTESIAN_POINT('Ctrl Pts',(197.500100835973,4.91318526485212,131.066090991876));
#207429=CARTESIAN_POINT('Ctrl Pts',(197.492327935707,4.91666144796523,130.929353691744));
#207430=CARTESIAN_POINT('Ctrl Pts',(197.484837599945,4.9200112630662,130.797587136892));
#207431=CARTESIAN_POINT('Ctrl Pts',(197.477347264183,4.91805610562799,130.665854253699));
#207432=CARTESIAN_POINT('Ctrl Pts',(197.469856928421,4.91084698530234,130.534610827118));
#207433=CARTESIAN_POINT('Ctrl Pts',(197.462082594302,4.90336452898838,130.398391266127));
#207434=CARTESIAN_POINT('Ctrl Pts',(197.454308260183,4.89019813490943,130.262267507292));
#207435=CARTESIAN_POINT('Ctrl Pts',(197.446533926064,4.87134787981786,130.126752400162));
#207436=CARTESIAN_POINT('Ctrl Pts',(197.438769173117,4.852520855981,129.991404303289));
#207437=CARTESIAN_POINT('Ctrl Pts',(197.43100442017,4.82802396204446,129.856663749147));
#207438=CARTESIAN_POINT('Ctrl Pts',(197.423239667222,4.79790924209346,129.723041993323));
#207439=CARTESIAN_POINT('Ctrl Pts',(197.415482626337,4.76782443250686,129.589552952511));
#207440=CARTESIAN_POINT('Ctrl Pts',(197.407725585452,4.73213298616931,129.457180877599));
#207441=CARTESIAN_POINT('Ctrl Pts',(197.399968544567,4.69093850232438,129.326429959548));
#207442=CARTESIAN_POINT('Ctrl Pts',(197.392217353327,4.64977508356018,129.195777641781));
#207443=CARTESIAN_POINT('Ctrl Pts',(197.384466162087,4.60311700438922,129.066744418897));
#207444=CARTESIAN_POINT('Ctrl Pts',(197.376714970847,4.55111842163095,128.939822021883));
#207445=CARTESIAN_POINT('Ctrl Pts',(197.36896707407,4.49914193965744,128.812953570273));
#207446=CARTESIAN_POINT('Ctrl Pts',(197.361219177293,4.44182961657508,128.688194521179));
#207447=CARTESIAN_POINT('Ctrl Pts',(197.353471280516,4.37938465260795,128.56601901562));
#207448=CARTESIAN_POINT('Ctrl Pts',(197.345725004432,4.3169527507811,128.443869066543));
#207449=CARTESIAN_POINT('Ctrl Pts',(197.337978728348,4.24939052141315,128.324301933984));
#207450=CARTESIAN_POINT('Ctrl Pts',(197.330232452263,4.17694809300133,128.207769064997));
#207451=CARTESIAN_POINT('Ctrl Pts',(197.322486118998,4.10450512983598,128.091235335791));
#207452=CARTESIAN_POINT('Ctrl Pts',(197.314739785733,4.02718210215263,127.97773624689));
#207453=CARTESIAN_POINT('Ctrl Pts',(197.306993452467,3.9452734087893,127.867695707775));
#207454=CARTESIAN_POINT('Ctrl Pts',(197.299245384464,3.86334637254203,127.757630525843));
#207455=CARTESIAN_POINT('Ctrl Pts',(197.291497316461,3.77683186054576,127.65102574846));
#207456=CARTESIAN_POINT('Ctrl Pts',(197.283749248458,3.68606537283357,127.548273221672));
#207457=CARTESIAN_POINT('Ctrl Pts',(197.275992945717,3.59520241741809,127.445411488276));
#207458=CARTESIAN_POINT('Ctrl Pts',(197.268236642975,3.50007871824481,127.3464104776));
#207459=CARTESIAN_POINT('Ctrl Pts',(197.260480340233,3.4010679415342,127.251626470523));
#207460=CARTESIAN_POINT('Ctrl Pts',(197.252719897719,3.30200431979083,127.156791874367));
#207461=CARTESIAN_POINT('Ctrl Pts',(197.244959455205,3.19904977993481,127.066179024781));
#207462=CARTESIAN_POINT('Ctrl Pts',(197.23719901269,3.09261130353576,126.980104037818));
#207463=CARTESIAN_POINT('Ctrl Pts',(197.229426112425,2.98600196264525,126.893890875646));
#207464=CARTESIAN_POINT('Ctrl Pts',(197.22165321216,2.87589782337121,126.812230366043));
#207465=CARTESIAN_POINT('Ctrl Pts',(197.213880311894,2.76273582205164,126.735395904024));
#207466=CARTESIAN_POINT('Ctrl Pts',(197.206389976132,2.65368754451797,126.661354568233));
#207467=CARTESIAN_POINT('Ctrl Pts',(197.19889964037,2.54180012866534,126.591794656438));
#207468=CARTESIAN_POINT('Ctrl Pts',(197.191409304608,2.4274846112473,126.526919615675));
#207469=CARTESIAN_POINT('Ctrl Pts',(197.183634970489,2.30883478624092,126.459584818023));
#207470=CARTESIAN_POINT('Ctrl Pts',(197.17586063637,2.18719325510115,126.397083861596));
#207471=CARTESIAN_POINT('Ctrl Pts',(197.168086302251,2.06299153416462,126.339693889526));
#207472=CARTESIAN_POINT('Ctrl Pts',(197.160321549304,1.93894288074894,126.282374645468));
#207473=CARTESIAN_POINT('Ctrl Pts',(197.152556796357,1.81234066695579,126.230154015391));
#207474=CARTESIAN_POINT('Ctrl Pts',(197.144792043409,1.68364315769026,126.183264559263));
#207475=CARTESIAN_POINT('Ctrl Pts',(197.137035002524,1.55507347260519,126.136421674404));
#207476=CARTESIAN_POINT('Ctrl Pts',(197.129277961639,1.42441299845145,126.094899559184));
#207477=CARTESIAN_POINT('Ctrl Pts',(197.121520920754,1.29214192328729,126.058883580156));
#207478=CARTESIAN_POINT('Ctrl Pts',(197.113769729514,1.15997059476984,126.022894761058));
#207479=CARTESIAN_POINT('Ctrl Pts',(197.106018538274,1.02619145846807,125.99240391571));
#207480=CARTESIAN_POINT('Ctrl Pts',(197.098267347034,0.891301547113867,
125.967547140222));
#207481=CARTESIAN_POINT('Ctrl Pts',(197.090519450257,0.756468967570347,
125.942700929528));
#207482=CARTESIAN_POINT('Ctrl Pts',(197.08277155348,0.620526935649892,125.923484096662));
#207483=CARTESIAN_POINT('Ctrl Pts',(197.075023656703,0.483984194306158,
125.909981968323));
#207484=CARTESIAN_POINT('Ctrl Pts',(197.067277380619,0.347470014760427,
125.896482664339));
#207485=CARTESIAN_POINT('Ctrl Pts',(197.059531104535,0.210355764548132,
125.88869572563));
#207486=CARTESIAN_POINT('Ctrl Pts',(197.051784828451,0.0731564594262019,
125.886654730168));
#207487=CARTESIAN_POINT('Ctrl Pts',(197.044038495185,-0.0640438584697734,
125.884613719641));
#207488=CARTESIAN_POINT('Ctrl Pts',(197.03629216192,-0.201328841606274,
125.888318742812));
#207489=CARTESIAN_POINT('Ctrl Pts',(197.028545828654,-0.338182713167988,
125.897751247032));
#207490=CARTESIAN_POINT('Ctrl Pts',(197.020797760651,-0.475067232205337,
125.907185863595));
#207491=CARTESIAN_POINT('Ctrl Pts',(197.013049692649,-0.611520057590418,
125.922350486614));
#207492=CARTESIAN_POINT('Ctrl Pts',(197.005301624646,-0.747030172182732,
125.943174652768));
#207493=CARTESIAN_POINT('Ctrl Pts',(196.997545321904,-0.882684308537553,
125.964020951094));
#207494=CARTESIAN_POINT('Ctrl Pts',(196.989789019162,-1.01739334560279,
125.990538748746));
#207495=CARTESIAN_POINT('Ctrl Pts',(196.98203271642,-1.15065555846418,126.022606248271));
#207496=CARTESIAN_POINT('Ctrl Pts',(196.974272273906,-1.28398889738112,
126.054690863185));
#207497=CARTESIAN_POINT('Ctrl Pts',(196.966511831392,-1.41587349762368,
126.092330974847));
#207498=CARTESIAN_POINT('Ctrl Pts',(196.958751388877,-1.5458234183235,126.135355046584));
#207499=CARTESIAN_POINT('Ctrl Pts',(196.950978488612,-1.67598194617242,
126.17844818438));
#207500=CARTESIAN_POINT('Ctrl Pts',(196.943205588347,-1.80419922236758,
126.226942414954));
#207501=CARTESIAN_POINT('Ctrl Pts',(196.935432688081,-1.93000905717825,
126.280617908071));
#207502=CARTESIAN_POINT('Ctrl Pts',(196.927942352319,-2.05124538759802,
126.332342161813));
#207503=CARTESIAN_POINT('Ctrl Pts',(196.920452016557,-2.17024599270099,
126.388877382166));
#207504=CARTESIAN_POINT('Ctrl Pts',(196.912961680795,-2.28661753132807,
126.44998772036));
#207505=CARTESIAN_POINT('Ctrl Pts',(196.905186437551,-2.40741545658494,
126.513422492751));
#207506=CARTESIAN_POINT('Ctrl Pts',(196.897411194306,-2.52576305120591,
126.581988282265));
#207507=CARTESIAN_POINT('Ctrl Pts',(196.889635951062,-2.6411937391818,126.655471766969));
#207508=CARTESIAN_POINT('Ctrl Pts',(196.881870490011,-2.75647920144334,
126.728862800595));
#207509=CARTESIAN_POINT('Ctrl Pts',(196.874105028959,-2.86885473277439,
126.807159009799));
#207510=CARTESIAN_POINT('Ctrl Pts',(196.866339567908,-2.97787685313513,
126.890100469075));
#207511=CARTESIAN_POINT('Ctrl Pts',(196.858583393819,-3.08676859046736,
126.972942736017));
#207512=CARTESIAN_POINT('Ctrl Pts',(196.85082721973,-3.19231459493436,127.060418953556));
#207513=CARTESIAN_POINT('Ctrl Pts',(196.843071045641,-3.294099502712,127.152225416244));
#207514=CARTESIAN_POINT('Ctrl Pts',(196.835320138421,-3.39581529293819,
127.243969537295));
#207515=CARTESIAN_POINT('Ctrl Pts',(196.827569231201,-3.49377477829833,
127.340037793094));
#207516=CARTESIAN_POINT('Ctrl Pts',(196.819818323981,-3.58759484370538,
127.440085613955));
#207517=CARTESIAN_POINT('Ctrl Pts',(196.812071001449,-3.6813715186174,127.54008716407));
#207518=CARTESIAN_POINT('Ctrl Pts',(196.804323678917,-3.77101231623895,
127.644064332384));
#207519=CARTESIAN_POINT('Ctrl Pts',(196.796576356385,-3.85617053877141,
127.751635304274));
#207520=CARTESIAN_POINT('Ctrl Pts',(196.788830939126,-3.94130781864133,
127.859179821613));
#207521=CARTESIAN_POINT('Ctrl Pts',(196.781085521866,-4.02196447570508,
127.970316076795));
#207522=CARTESIAN_POINT('Ctrl Pts',(196.773340104606,-4.09783398032599,
128.084629062396));
#207523=CARTESIAN_POINT('Ctrl Pts',(196.765580754941,-4.17383995850953,
128.19914767344));
#207524=CARTESIAN_POINT('Ctrl Pts',(196.757821405275,-4.24504131628586,
128.316854134644));
#207525=CARTESIAN_POINT('Ctrl Pts',(196.75006205561,-4.31117357625514,128.437302219913));
#207526=CARTESIAN_POINT('Ctrl Pts',(196.742313049751,-4.37721767686617,
128.557589738676));
#207527=CARTESIAN_POINT('Ctrl Pts',(196.734564043892,-4.43820602078034,
128.680611220613));
#207528=CARTESIAN_POINT('Ctrl Pts',(196.726815038034,-4.49392167184312,
128.805898441332));
#207529=CARTESIAN_POINT('Ctrl Pts',(196.719050516465,-4.54974888145534,
128.931436522632));
#207530=CARTESIAN_POINT('Ctrl Pts',(196.711285994897,-4.60028211429378,
129.059249060427));
#207531=CARTESIAN_POINT('Ctrl Pts',(196.703521473329,-4.64535222085451,
129.188846517751));
#207532=CARTESIAN_POINT('Ctrl Pts',(196.69575695176,-4.69042232741525,129.318443975074));
#207533=CARTESIAN_POINT('Ctrl Pts',(196.687992430192,-4.73002922227267,
129.449825967771));
#207534=CARTESIAN_POINT('Ctrl Pts',(196.680227908624,-4.76405452823405,
129.582490119308));
#207535=CARTESIAN_POINT('Ctrl Pts',(198.430216174721,-4.76405452823404,
129.582490119308));
#207536=CARTESIAN_POINT('Ctrl Pts',(198.422577902284,-4.7976789144689,129.713591090917));
#207537=CARTESIAN_POINT('Ctrl Pts',(198.414939629846,-4.82587604532326,
129.846036456349));
#207538=CARTESIAN_POINT('Ctrl Pts',(198.407301357409,-4.84855734705283,
129.97933048791));
#207539=CARTESIAN_POINT('Ctrl Pts',(198.399441225181,-4.87189744550764,
130.116496152261));
#207540=CARTESIAN_POINT('Ctrl Pts',(198.391581092952,-4.88939633379473,
130.254560081246));
#207541=CARTESIAN_POINT('Ctrl Pts',(198.383720960724,-4.90101480488931,
130.392976436106));
#207542=CARTESIAN_POINT('Ctrl Pts',(198.375860828495,-4.91263327598389,
130.531392790965));
#207543=CARTESIAN_POINT('Ctrl Pts',(198.368000696266,-4.91837135341764,
130.670161108681));
#207544=CARTESIAN_POINT('Ctrl Pts',(198.360140564038,-4.91824805313947,
130.80873672198));
#207545=CARTESIAN_POINT('Origin',(213.235140564004,0.,130.804360617566));
#207546=CARTESIAN_POINT('',(200.179870531952,-4.76405452823405,129.582490119308));
#207547=CARTESIAN_POINT('',(199.834960626423,-4.76405452823405,129.582490119308));
#207548=CARTESIAN_POINT('',(213.235140564004,-4.76405452823405,129.582490119308));
#207549=CARTESIAN_POINT('',(199.76485943604,-4.91824827604694,130.808478585671));
#207550=CARTESIAN_POINT('Ctrl Pts',(199.834960626423,-4.76405452823405,
129.582490119308));
#207551=CARTESIAN_POINT('Ctrl Pts',(199.827324041593,-4.79766326068053,
129.713530057033));
#207552=CARTESIAN_POINT('Ctrl Pts',(199.819687456764,-4.82584625215587,
129.845899345302));
#207553=CARTESIAN_POINT('Ctrl Pts',(199.812050871934,-4.84851847510395,
129.979102076819));
#207554=CARTESIAN_POINT('Ctrl Pts',(199.804185632618,-4.87186954934494,
130.116293162135));
#207555=CARTESIAN_POINT('Ctrl Pts',(199.796320393303,-4.88937460082088,
130.254367925497));
#207556=CARTESIAN_POINT('Ctrl Pts',(199.788455153987,-4.90099827408403,
130.392779544234));
#207557=CARTESIAN_POINT('Ctrl Pts',(199.780589914672,-4.91262194734719,
130.53119116297));
#207558=CARTESIAN_POINT('Ctrl Pts',(199.772724675356,-4.91836427281118,
130.669939172252));
#207559=CARTESIAN_POINT('Ctrl Pts',(199.76485943604,-4.91824827604694,130.808478585671));
#207560=CARTESIAN_POINT('Ctrl Pts',(199.764859435991,-4.91824827604621,
130.808478586542));
#207561=CARTESIAN_POINT('Ctrl Pts',(199.752723897668,-4.91806930075772,
131.022235637443));
#207562=CARTESIAN_POINT('Ctrl Pts',(199.740588359346,-4.90395198746022,
131.235429274479));
#207563=CARTESIAN_POINT('Ctrl Pts',(199.728452821023,-4.87613221702235,
131.446635998237));
#207564=CARTESIAN_POINT('Ctrl Pts',(199.72464418571,-4.86740121908247,131.512921429102));
#207565=CARTESIAN_POINT('Ctrl Pts',(199.720835550396,-4.85732086664738,
131.57901143828));
#207566=CARTESIAN_POINT('Ctrl Pts',(199.717026915083,-4.84589923841166,
131.64486263045));
#207567=CARTESIAN_POINT('Ctrl Pts',(199.709252580964,-4.82258496786947,
131.779280637941));
#207568=CARTESIAN_POINT('Ctrl Pts',(199.701478246845,-4.79363669851475,
131.912940764209));
#207569=CARTESIAN_POINT('Ctrl Pts',(199.693703912726,-4.75911430351347,
132.045333666666));
#207570=CARTESIAN_POINT('Ctrl Pts',(199.685939159779,-4.7246344542787,132.177563406704));
#207571=CARTESIAN_POINT('Ctrl Pts',(199.678174406832,-4.68459424557846,
132.308528655646));
#207572=CARTESIAN_POINT('Ctrl Pts',(199.670409653885,-4.63910497760412,
132.437727713252));
#207573=CARTESIAN_POINT('Ctrl Pts',(199.662652613,-4.59366089021201,132.566798448532));
#207574=CARTESIAN_POINT('Ctrl Pts',(199.654895572115,-4.54277864283484,
132.694106117038));
#207575=CARTESIAN_POINT('Ctrl Pts',(199.64713853123,-4.48661991546082,132.819162046166));
#207576=CARTESIAN_POINT('Ctrl Pts',(199.63938733999,-4.43050353782002,132.944123669646));
#207577=CARTESIAN_POINT('Ctrl Pts',(199.631636148749,-4.36911875972351,
133.066836578412));
#207578=CARTESIAN_POINT('Ctrl Pts',(199.623884957509,-4.30267602109411,
133.186830369735));
#207579=CARTESIAN_POINT('Ctrl Pts',(199.616137060732,-4.23626152240097,
133.306773160497));
#207580=CARTESIAN_POINT('Ctrl Pts',(199.608389163955,-4.16479352789244,
133.423998791095));
#207581=CARTESIAN_POINT('Ctrl Pts',(199.600641267178,-4.08852913543883,
133.538060047124));
#207582=CARTESIAN_POINT('Ctrl Pts',(199.592894991094,-4.01228069585204,
133.652097443998));
#207583=CARTESIAN_POINT('Ctrl Pts',(199.58514871501,-3.93123807111655,133.762971458094));
#207584=CARTESIAN_POINT('Ctrl Pts',(199.577402438926,-3.84570232123248,
133.870262885899));
#207585=CARTESIAN_POINT('Ctrl Pts',(199.56965610566,-3.76016593994299,133.977555105704));
#207586=CARTESIAN_POINT('Ctrl Pts',(199.561909772395,-3.67013661103911,
134.081264380741));
#207587=CARTESIAN_POINT('Ctrl Pts',(199.554163439129,-3.57595615209479,
134.181004019051));
#207588=CARTESIAN_POINT('Ctrl Pts',(199.546415371126,-3.48175460208978,
134.280765993363));
#207589=CARTESIAN_POINT('Ctrl Pts',(199.538667303124,-3.38340034058184,
134.376556277787));
#207590=CARTESIAN_POINT('Ctrl Pts',(199.530919235121,-3.28127226748557,
134.468024817398));
#207591=CARTESIAN_POINT('Ctrl Pts',(199.523162932379,-3.17903565145775,
134.559590570861));
#207592=CARTESIAN_POINT('Ctrl Pts',(199.515406629637,-3.07301750343207,
134.646825142842));
#207593=CARTESIAN_POINT('Ctrl Pts',(199.507650326895,-2.96363048238186,
134.729418251079));
#207594=CARTESIAN_POINT('Ctrl Pts',(199.499889884381,-2.85418507818486,
134.812055441745));
#207595=CARTESIAN_POINT('Ctrl Pts',(199.492129441867,-2.7413675396017,134.890046010246));
#207596=CARTESIAN_POINT('Ctrl Pts',(199.484368999352,-2.62561893060417,
134.963123449678));
#207597=CARTESIAN_POINT('Ctrl Pts',(199.476596099087,-2.50968451166382,
135.036318199503));
#207598=CARTESIAN_POINT('Ctrl Pts',(199.468823198821,-2.3908099590241,135.104583864727));
#207599=CARTESIAN_POINT('Ctrl Pts',(199.461050298556,-2.26946110594807,
135.167699860748));
#207600=CARTESIAN_POINT('Ctrl Pts',(199.453559962794,-2.15252358934225,
135.228521431332));
#207601=CARTESIAN_POINT('Ctrl Pts',(199.446069627032,-2.03328882194573,
135.284561108335));
#207602=CARTESIAN_POINT('Ctrl Pts',(199.43857929127,-1.91218875833745,135.335664758207));
#207603=CARTESIAN_POINT('Ctrl Pts',(199.430804957151,-1.78649714900839,
135.388706018497));
#207604=CARTESIAN_POINT('Ctrl Pts',(199.423030623032,-1.65839785264128,
135.436597582708));
#207605=CARTESIAN_POINT('Ctrl Pts',(199.415256288913,-1.52835175648752,
135.479114511724));
#207606=CARTESIAN_POINT('Ctrl Pts',(199.407491535966,-1.39846593052474,
135.521579042424));
#207607=CARTESIAN_POINT('Ctrl Pts',(199.399726783019,-1.26663844662274,
135.558681996903));
#207608=CARTESIAN_POINT('Ctrl Pts',(199.391962030072,-1.13335155987423,
135.590245833932));
#207609=CARTESIAN_POINT('Ctrl Pts',(199.384204989187,-1.00019705554075,
135.621778321313));
#207610=CARTESIAN_POINT('Ctrl Pts',(199.376447948302,-0.865586410911478,
135.647782550024));
#207611=CARTESIAN_POINT('Ctrl Pts',(199.368690907417,-0.730018152069129,
135.668130406541));
#207612=CARTESIAN_POINT('Ctrl Pts',(199.360939716176,-0.594552126305398,
135.688462918582));
#207613=CARTESIAN_POINT('Ctrl Pts',(199.353188524936,-0.458130308783093,
135.703147490879));
#207614=CARTESIAN_POINT('Ctrl Pts',(199.345437333696,-0.321262210558749,
135.712106908336));
#207615=CARTESIAN_POINT('Ctrl Pts',(199.337689436919,-0.184452284927075,
135.721062517801));
#207616=CARTESIAN_POINT('Ctrl Pts',(199.329941540142,-0.0471968451682756,
135.724297786676));
#207617=CARTESIAN_POINT('Ctrl Pts',(199.322193643365,0.0899888868944208,
135.72178728837));
#207618=CARTESIAN_POINT('Ctrl Pts',(199.314447367281,0.227145922659364,
135.719277315206));
#207619=CARTESIAN_POINT('Ctrl Pts',(199.306701091197,0.3642328890792,135.711023972638));
#207620=CARTESIAN_POINT('Ctrl Pts',(199.298954815113,0.500734368080969,
135.697053961229));
#207621=CARTESIAN_POINT('Ctrl Pts',(199.291208481847,0.637236854705554,
135.683083846697));
#207622=CARTESIAN_POINT('Ctrl Pts',(199.283462148582,0.773153456354327,
135.663397018924));
#207623=CARTESIAN_POINT('Ctrl Pts',(199.275715815317,0.907974077383442,
135.638072042269));
#207624=CARTESIAN_POINT('Ctrl Pts',(199.267967747314,1.04282489055591,135.61274139426));
#207625=CARTESIAN_POINT('Ctrl Pts',(199.260219679311,1.17657885054553,135.581770157055));
#207626=CARTESIAN_POINT('Ctrl Pts',(199.252471611308,1.30873664156906,135.545287896645));
#207627=CARTESIAN_POINT('Ctrl Pts',(199.244715308566,1.4410348914656,135.508766862454));
#207628=CARTESIAN_POINT('Ctrl Pts',(199.236959005824,1.57173320612938,135.466723208909));
#207629=CARTESIAN_POINT('Ctrl Pts',(199.229202703082,1.70034748405164,135.419336402549));
#207630=CARTESIAN_POINT('Ctrl Pts',(199.221442260568,1.82903040728659,135.371924304424));
#207631=CARTESIAN_POINT('Ctrl Pts',(199.213681818054,1.95562671669996,135.319163521356));
#207632=CARTESIAN_POINT('Ctrl Pts',(199.20592137554,2.0796737866346,135.261281079464));
#207633=CARTESIAN_POINT('Ctrl Pts',(199.198148475274,2.2039199879383,135.203305719538));
#207634=CARTESIAN_POINT('Ctrl Pts',(199.190375575009,2.32560842485003,135.140192451236));
#207635=CARTESIAN_POINT('Ctrl Pts',(199.182602674743,2.44430171903778,135.072213961908));
#207636=CARTESIAN_POINT('Ctrl Pts',(199.175112338981,2.55868021301209,135.006706661894));
#207637=CARTESIAN_POINT('Ctrl Pts',(199.167622003219,2.67027728465172,134.936681889443));
#207638=CARTESIAN_POINT('Ctrl Pts',(199.160131667457,2.7787297750351,134.862419747228));
#207639=CARTESIAN_POINT('Ctrl Pts',(199.152357333338,2.89129427455412,134.78534193332));
#207640=CARTESIAN_POINT('Ctrl Pts',(199.144582999219,3.00082760257082,134.703454927598));
#207641=CARTESIAN_POINT('Ctrl Pts',(199.1368086651,3.10689139061681,134.617024902474));
#207642=CARTESIAN_POINT('Ctrl Pts',(199.129043912153,3.21282446452324,134.530701394631));
#207643=CARTESIAN_POINT('Ctrl Pts',(199.121279159206,3.31529620605177,134.439846252062));
#207644=CARTESIAN_POINT('Ctrl Pts',(199.113514406258,3.41389657407908,134.344769244263));
#207645=CARTESIAN_POINT('Ctrl Pts',(199.105757365373,3.51239901083084,134.249786668289));
#207646=CARTESIAN_POINT('Ctrl Pts',(199.098000324488,3.60703744639372,134.150590841398));
#207647=CARTESIAN_POINT('Ctrl Pts',(199.090243283603,3.69743462970616,134.047531939212));
#207648=CARTESIAN_POINT('Ctrl Pts',(199.082492092363,3.78776364379947,133.944550754547));
#207649=CARTESIAN_POINT('Ctrl Pts',(199.074740901123,3.87385751502113,133.837712585816));
#207650=CARTESIAN_POINT('Ctrl Pts',(199.066989709883,3.95537587695083,133.727404362455));
#207651=CARTESIAN_POINT('Ctrl Pts',(199.059241813106,4.03685959140212,133.617143023032));
#207652=CARTESIAN_POINT('Ctrl Pts',(199.051493916329,4.11377143257403,133.503414876139));
#207653=CARTESIAN_POINT('Ctrl Pts',(199.043746019552,4.18581151837598,133.386639648796));
#207654=CARTESIAN_POINT('Ctrl Pts',(199.035999743468,4.25783653494499,133.269888848313));
#207655=CARTESIAN_POINT('Ctrl Pts',(199.028253467384,4.32499161798016,133.150092567702));
#207656=CARTESIAN_POINT('Ctrl Pts',(199.020507191299,4.38702063536518,133.027698875092));
#207657=CARTESIAN_POINT('Ctrl Pts',(199.012760858034,4.44905011063427,132.905304279));
#207658=CARTESIAN_POINT('Ctrl Pts',(199.005014524769,4.50595326800805,132.780312581386));
#207659=CARTESIAN_POINT('Ctrl Pts',(198.997268191503,4.55752048674992,132.653195406117));
#207660=CARTESIAN_POINT('Ctrl Pts',(198.9895201235,4.60909925361287,132.526049763837));
#207661=CARTESIAN_POINT('Ctrl Pts',(198.981772055497,4.65533955709796,132.396778058965));
#207662=CARTESIAN_POINT('Ctrl Pts',(198.974023987494,4.6960805123652,132.265870413593));
#207663=CARTESIAN_POINT('Ctrl Pts',(198.966267684753,4.73686476760453,132.134823638018));
#207664=CARTESIAN_POINT('Ctrl Pts',(198.958511382011,4.77213788269821,132.002137822608));
#207665=CARTESIAN_POINT('Ctrl Pts',(198.950755079269,4.80178917923892,131.868317261722));
#207666=CARTESIAN_POINT('Ctrl Pts',(198.942994636755,4.8314563015694,131.734425276773));
#207667=CARTESIAN_POINT('Ctrl Pts',(198.935234194241,4.85549555803585,131.599397724268));
#207668=CARTESIAN_POINT('Ctrl Pts',(198.927473751726,4.87384789167415,131.463746537436));
#207669=CARTESIAN_POINT('Ctrl Pts',(198.919700851461,4.89222968610765,131.327877591277));
#207670=CARTESIAN_POINT('Ctrl Pts',(198.911927951196,4.90490627858033,131.191383399763));
#207671=CARTESIAN_POINT('Ctrl Pts',(198.90415505093,4.91187067501122,131.054779335846));
#207672=CARTESIAN_POINT('Ctrl Pts',(198.896664715168,4.91858189808959,130.923141173736));
#207673=CARTESIAN_POINT('Ctrl Pts',(198.889174379406,4.91998901695341,130.791401296814));
#207674=CARTESIAN_POINT('Ctrl Pts',(198.881684043644,4.91613139364612,130.660016643299));
#207675=CARTESIAN_POINT('Ctrl Pts',(198.873909709525,4.91212750737863,130.523650500714));
#207676=CARTESIAN_POINT('Ctrl Pts',(198.866135375406,4.90243908959812,130.387235082915));
#207677=CARTESIAN_POINT('Ctrl Pts',(198.858361041287,4.88705312982617,130.251283074398));
#207678=CARTESIAN_POINT('Ctrl Pts',(198.85059628834,4.87168613187456,130.115498614582));
#207679=CARTESIAN_POINT('Ctrl Pts',(198.842831535393,4.85063560658772,129.980176812465));
#207680=CARTESIAN_POINT('Ctrl Pts',(198.835066782445,4.82394053457245,129.845830085236));
#207681=CARTESIAN_POINT('Ctrl Pts',(198.82730974156,4.79727197647905,129.71161679307));
#207682=CARTESIAN_POINT('Ctrl Pts',(198.819552700675,4.7649701040377,129.578377029504));
#207683=CARTESIAN_POINT('Ctrl Pts',(198.81179565979,4.72712561650387,129.446617465017));
#207684=CARTESIAN_POINT('Ctrl Pts',(198.80404446855,4.68930966779249,129.314957261443));
#207685=CARTESIAN_POINT('Ctrl Pts',(198.79629327731,4.64595953098006,129.184775409413));
#207686=CARTESIAN_POINT('Ctrl Pts',(198.78854208607,4.59721676439492,129.056567413647));
#207687=CARTESIAN_POINT('Ctrl Pts',(198.780794189293,4.54849471478581,128.928413909699));
#207688=CARTESIAN_POINT('Ctrl Pts',(198.773046292516,4.49438473268614,128.802232958104));
#207689=CARTESIAN_POINT('Ctrl Pts',(198.765298395739,4.43507785272916,128.678503730866));
#207690=CARTESIAN_POINT('Ctrl Pts',(198.757552119655,4.37578337849294,128.554800385114));
#207691=CARTESIAN_POINT('Ctrl Pts',(198.749805843571,4.31129433754229,128.433548095968));
#207692=CARTESIAN_POINT('Ctrl Pts',(198.742059567486,4.24184925661964,128.315204546401));
#207693=CARTESIAN_POINT('Ctrl Pts',(198.734313234221,4.1724036630692,128.196860123249));
#207694=CARTESIAN_POINT('Ctrl Pts',(198.726566900956,4.0980021544152,128.081424819717));
#207695=CARTESIAN_POINT('Ctrl Pts',(198.71882056769,4.01892821604465,127.969329919887));
#207696=CARTESIAN_POINT('Ctrl Pts',(198.711072499687,3.93983656961388,127.857209917182));
#207697=CARTESIAN_POINT('Ctrl Pts',(198.703324431684,3.85607063665606,127.748432126146));
#207698=CARTESIAN_POINT('Ctrl Pts',(198.695576363682,3.76795580858273,127.643396826716));
#207699=CARTESIAN_POINT('Ctrl Pts',(198.68782006094,3.67974733102151,127.538249894519));
#207700=CARTESIAN_POINT('Ctrl Pts',(198.680063758198,3.58718097696145,127.436853699544));
#207701=CARTESIAN_POINT('Ctrl Pts',(198.672307455456,3.49062119914604,127.339573942088));
#207702=CARTESIAN_POINT('Ctrl Pts',(198.664547012942,3.39400988446978,127.242242263496));
#207703=CARTESIAN_POINT('Ctrl Pts',(198.656786570428,3.29340118567955,127.149031665843));
#207704=CARTESIAN_POINT('Ctrl Pts',(198.649026127913,3.1891938849692,127.060268547841));
#207705=CARTESIAN_POINT('Ctrl Pts',(198.641253227648,3.08481930144869,126.971362939403));
#207706=CARTESIAN_POINT('Ctrl Pts',(198.633480327383,2.97683488028589,126.886919318566));
#207707=CARTESIAN_POINT('Ctrl Pts',(198.625707427117,2.86567043886961,126.80722214132));
#207708=CARTESIAN_POINT('Ctrl Pts',(198.618217091355,2.7585471049054,126.730422157211));
#207709=CARTESIAN_POINT('Ctrl Pts',(198.610726755593,2.64847119750003,126.658029686858));
#207710=CARTESIAN_POINT('Ctrl Pts',(198.603236419831,2.53584842786697,126.590258600127));
#207711=CARTESIAN_POINT('Ctrl Pts',(198.595462085712,2.4189555316921,126.519917952044));
#207712=CARTESIAN_POINT('Ctrl Pts',(198.587687751593,2.29894855074917,126.454333226861));
#207713=CARTESIAN_POINT('Ctrl Pts',(198.579913417474,2.1762517885438,126.393792489154));
#207714=CARTESIAN_POINT('Ctrl Pts',(198.572148664527,2.05370623913212,126.333326362497));
#207715=CARTESIAN_POINT('Ctrl Pts',(198.56438391158,1.92847785139323,126.277892026139));
#207716=CARTESIAN_POINT('Ctrl Pts',(198.556619158633,1.80101880639067,126.227733658601));
#207717=CARTESIAN_POINT('Ctrl Pts',(198.548862117748,1.6736863555085,126.17762510906));
#207718=CARTESIAN_POINT('Ctrl Pts',(198.541105076863,1.54412801780239,126.132782242412));
#207719=CARTESIAN_POINT('Ctrl Pts',(198.533348035978,1.41281909465994,126.093402618574));
#207720=CARTESIAN_POINT('Ctrl Pts',(198.525596844738,1.2816091925979,126.054052691217));
#207721=CARTESIAN_POINT('Ctrl Pts',(198.517845653498,1.14865170571014,126.020157918166));
#207722=CARTESIAN_POINT('Ctrl Pts',(198.510094462257,1.01444003188544,125.991867034795));
#207723=CARTESIAN_POINT('Ctrl Pts',(198.50234656548,0.880285401602321,125.963588175804));
#207724=CARTESIAN_POINT('Ctrl Pts',(198.494598668703,0.744878026361152,
125.940908549741));
#207725=CARTESIAN_POINT('Ctrl Pts',(198.486850771926,0.608724306023622,
125.92392643793));
#207726=CARTESIAN_POINT('Ctrl Pts',(198.479104495842,0.472599066109263,
125.906947878411));
#207727=CARTESIAN_POINT('Ctrl Pts',(198.471358219758,0.335728179341729,
125.895664510952));
#207728=CARTESIAN_POINT('Ctrl Pts',(198.463611943674,0.198625636898631,
125.890123045077));
#207729=CARTESIAN_POINT('Ctrl Pts',(198.455865610409,0.061522082395698,
125.884581538295));
#207730=CARTESIAN_POINT('Ctrl Pts',(198.448119277143,-0.0758127405487922,
125.884782033463));
#207731=CARTESIAN_POINT('Ctrl Pts',(198.440372943878,-0.212862749645825,
125.890719145876));
#207732=CARTESIAN_POINT('Ctrl Pts',(198.432624875875,-0.349943450142099,
125.896657587864));
#207733=CARTESIAN_POINT('Ctrl Pts',(198.424876807872,-0.486738819347844,
125.908335186536));
#207734=CARTESIAN_POINT('Ctrl Pts',(198.417128739869,-0.622736208410933,
125.925694541964));
#207735=CARTESIAN_POINT('Ctrl Pts',(198.409372437127,-0.75887813711759,
125.943072347121));
#207736=CARTESIAN_POINT('Ctrl Pts',(198.401616134385,-0.894220003067948,
125.966143922283));
#207737=CARTESIAN_POINT('Ctrl Pts',(198.393859831644,-1.02825713663446,
125.994800312979));
#207738=CARTESIAN_POINT('Ctrl Pts',(198.386099389129,-1.16236580985501,
126.023471998453));
#207739=CARTESIAN_POINT('Ctrl Pts',(198.378338946615,-1.2951679847218,126.057734341305));
#207740=CARTESIAN_POINT('Ctrl Pts',(198.370578504101,-1.42617350123758,
126.097428261257));
#207741=CARTESIAN_POINT('Ctrl Pts',(198.362805603836,-1.55738931943859,
126.137185901413));
#207742=CARTESIAN_POINT('Ctrl Pts',(198.35503270357,-1.68680234652046,126.182392413503));
#207743=CARTESIAN_POINT('Ctrl Pts',(198.347259803305,-1.81394093480719,
126.232839935394));
#207744=CARTESIAN_POINT('Ctrl Pts',(198.339769467543,-1.93645771516747,
126.281453562794));
#207745=CARTESIAN_POINT('Ctrl Pts',(198.332279131781,-2.05686226744433,
126.334933642695));
#207746=CARTESIAN_POINT('Ctrl Pts',(198.324788796019,-2.17475536003933,
126.393054440652));
#207747=CARTESIAN_POINT('Ctrl Pts',(198.317013701679,-2.29713037045767,
126.453384805213));
#207748=CARTESIAN_POINT('Ctrl Pts',(198.309238607339,-2.41718687346733,
126.518906845975));
#207749=CARTESIAN_POINT('Ctrl Pts',(198.301463513,-2.53445302826001,126.589419228882));
#207750=CARTESIAN_POINT('Ctrl Pts',(198.293698169544,-2.65157211748876,
126.659843180958));
#207751=CARTESIAN_POINT('Ctrl Pts',(198.285932826088,-2.76590748987507,
126.735244822049));
#207752=CARTESIAN_POINT('Ctrl Pts',(198.278167482632,-2.87700919668973,
126.815375640825));
#207753=CARTESIAN_POINT('Ctrl Pts',(198.270116194762,-2.99220201841537,
126.89845712883));
#207754=CARTESIAN_POINT('Ctrl Pts',(198.262064906893,-3.10391807437486,
126.986622596305));
#207755=CARTESIAN_POINT('Ctrl Pts',(198.254013619023,-3.21168484940525,
127.079543374989));
#207756=CARTESIAN_POINT('Ctrl Pts',(198.246262861591,-3.31542901381586,
127.168995699587));
#207757=CARTESIAN_POINT('Ctrl Pts',(198.23851210416,-3.4155130831933,127.262854447875));
#207758=CARTESIAN_POINT('Ctrl Pts',(198.230761346728,-3.51154654453313,
127.360783418188));
#207759=CARTESIAN_POINT('Ctrl Pts',(198.223014065701,-3.60753693251182,
127.458668464957));
#207760=CARTESIAN_POINT('Ctrl Pts',(198.215266784674,-3.69948005432967,
127.560619822749));
#207761=CARTESIAN_POINT('Ctrl Pts',(198.207519503647,-3.78702100058199,
127.666263263491));
#207762=CARTESIAN_POINT('Ctrl Pts',(198.199774019722,-3.8745416403494,127.771882198593));
#207763=CARTESIAN_POINT('Ctrl Pts',(198.192028535798,-3.95766188812499,
127.881191211036));
#207764=CARTESIAN_POINT('Ctrl Pts',(198.184283051873,-4.036066276408,127.993782016114));
#207765=CARTESIAN_POINT('Ctrl Pts',(198.176537687326,-4.1144694562842,128.106371085887));
#207766=CARTESIAN_POINT('Ctrl Pts',(198.168792322778,-4.18815669953273,
128.222241525939));
#207767=CARTESIAN_POINT('Ctrl Pts',(198.161046958231,-4.25685536445191,
128.340955358857));
#207768=CARTESIAN_POINT('Ctrl Pts',(198.153297277113,-4.32559231583465,
128.459735352199));
#207769=CARTESIAN_POINT('Ctrl Pts',(198.145547595995,-4.38933494059853,
128.581361564616));
#207770=CARTESIAN_POINT('Ctrl Pts',(198.137797914878,-4.44785607756905,
128.705370532851));
#207771=CARTESIAN_POINT('Ctrl Pts',(198.130045641782,-4.50639678766299,
128.82942097743));
#207772=CARTESIAN_POINT('Ctrl Pts',(198.122293368687,-4.55971237526599,
128.955855407105));
#207773=CARTESIAN_POINT('Ctrl Pts',(198.114541095592,-4.60762386482984,
129.084190456579));
#207774=CARTESIAN_POINT('Ctrl Pts',(198.106781573825,-4.65558015346834,
129.212645504231));
#207775=CARTESIAN_POINT('Ctrl Pts',(198.099022052058,-4.69812213230576,
129.343004349367));
#207776=CARTESIAN_POINT('Ctrl Pts',(198.091262530291,-4.73512064756484,
129.474768381012));
#207777=CARTESIAN_POINT('Ctrl Pts',(198.089153878115,-4.74517500427239,
129.510575292887));
#207778=CARTESIAN_POINT('Ctrl Pts',(198.087045225939,-4.75482027712228,
129.546485914373));
#207779=CARTESIAN_POINT('Ctrl Pts',(198.084936573762,-4.76405452823404,
129.582490119308));
#207780=CARTESIAN_POINT('',(200.110140563961,-4.91824997595732,130.804846925942));
#207781=CARTESIAN_POINT('Ctrl Pts',(200.110140563961,-4.91824997595732,
130.804846925942));
#207782=CARTESIAN_POINT('Ctrl Pts',(200.101963209632,-4.91823561914748,
130.95004364306));
#207783=CARTESIAN_POINT('Ctrl Pts',(200.093785855304,-4.91178722962492,
131.095096221673));
#207784=CARTESIAN_POINT('Ctrl Pts',(200.085608500975,-4.8989686251045,131.239434717854));
#207785=CARTESIAN_POINT('Ctrl Pts',(200.077418065999,-4.88612951570811,
131.384004100554));
#207786=CARTESIAN_POINT('Ctrl Pts',(200.069227631024,-4.86689987818642,
131.527856800843));
#207787=CARTESIAN_POINT('Ctrl Pts',(200.061037196048,-4.84139484664338,
131.670431631626));
#207788=CARTESIAN_POINT('Ctrl Pts',(200.052825216095,-4.81582272399528,
131.81338150617));
#207789=CARTESIAN_POINT('Ctrl Pts',(200.044613236142,-4.78394225338721,
131.955046471638));
#207790=CARTESIAN_POINT('Ctrl Pts',(200.036401256189,-4.74591932059585,
132.094877128462));
#207791=CARTESIAN_POINT('Ctrl Pts',(200.028177613076,-4.70784238529188,
132.234906381402));
#207792=CARTESIAN_POINT('Ctrl Pts',(200.019953969963,-4.66360567060591,
132.373095819458));
#207793=CARTESIAN_POINT('Ctrl Pts',(200.01173032685,-4.61342381118858,132.508914459737));
#207794=CARTESIAN_POINT('Ctrl Pts',(200.003487519808,-4.56312501070649,
132.645049604358));
#207795=CARTESIAN_POINT('Ctrl Pts',(199.995244712766,-4.50685348823889,
132.778802607651));
#207796=CARTESIAN_POINT('Ctrl Pts',(199.987001905724,-4.4448713186341,132.90966392666));
#207797=CARTESIAN_POINT('Ctrl Pts',(199.983296451395,-4.41700798305935,
132.96849105176));
#207798=CARTESIAN_POINT('Ctrl Pts',(199.979590997066,-4.38799121645204,
133.026734176052));
#207799=CARTESIAN_POINT('Ctrl Pts',(199.975885542737,-4.35784769754507,
133.084348886725));
#207800=CARTESIAN_POINT('Ctrl Pts',(199.968111208618,-4.29460422813576,
133.205229073381));
#207801=CARTESIAN_POINT('Ctrl Pts',(199.960336874499,-4.22622722019875,
133.3236673123));
#207802=CARTESIAN_POINT('Ctrl Pts',(199.95256254038,-4.15292920796671,133.43919686601));
#207803=CARTESIAN_POINT('Ctrl Pts',(199.944797787433,-4.07972152898389,
133.554584039872));
#207804=CARTESIAN_POINT('Ctrl Pts',(199.937033034486,-4.00160512008709,
133.667069334041));
#207805=CARTESIAN_POINT('Ctrl Pts',(199.929268281538,-3.91883915315159,
133.776208990923));
#207806=CARTESIAN_POINT('Ctrl Pts',(199.921511240653,-3.83615539054131,
133.88524024876));
#207807=CARTESIAN_POINT('Ctrl Pts',(199.913754199768,-3.74883149464554,
133.990932172596));
#207808=CARTESIAN_POINT('Ctrl Pts',(199.905997158883,-3.65717063344393,
134.092868793073));
#207809=CARTESIAN_POINT('Ctrl Pts',(199.898245967643,-3.56557889441098,
134.194728542351));
#207810=CARTESIAN_POINT('Ctrl Pts',(199.890494776403,-3.46965696023711,
134.292838335461));
#207811=CARTESIAN_POINT('Ctrl Pts',(199.882743585163,-3.36974885186079,
134.386814488572));
#207812=CARTESIAN_POINT('Ctrl Pts',(199.874995688386,-3.26988320709536,
134.48075069931));
#207813=CARTESIAN_POINT('Ctrl Pts',(199.867247791609,-3.16603504200538,
134.570556497095));
#207814=CARTESIAN_POINT('Ctrl Pts',(199.859499894832,-3.05858572710474,
134.655884525378));
#207815=CARTESIAN_POINT('Ctrl Pts',(199.851753618747,-2.95115888828444,
134.741194704878));
#207816=CARTESIAN_POINT('Ctrl Pts',(199.844007342663,-2.84013270394872,
134.822028734951));
#207817=CARTESIAN_POINT('Ctrl Pts',(199.836261066579,-2.72592185460808,
134.89807935547));
#207818=CARTESIAN_POINT('Ctrl Pts',(199.828514733314,-2.61171016218902,
134.974130537379));
#207819=CARTESIAN_POINT('Ctrl Pts',(199.820768400049,-2.49431408327654,
135.045398022584));
#207820=CARTESIAN_POINT('Ctrl Pts',(199.813022066783,-2.37417718264307,
135.111617954656));
#207821=CARTESIAN_POINT('Ctrl Pts',(199.80527399878,-2.25401337818375,135.177852716222));
#207822=CARTESIAN_POINT('Ctrl Pts',(199.797525930777,-2.13110787296654,
135.239037486666));
#207823=CARTESIAN_POINT('Ctrl Pts',(199.789777862774,-2.00592835665058,
135.294954619531));
#207824=CARTESIAN_POINT('Ctrl Pts',(199.782021560032,-1.88061579805486,
135.35093118179));
#207825=CARTESIAN_POINT('Ctrl Pts',(199.77426525729,-1.75302475798892,135.401628763137));
#207826=CARTESIAN_POINT('Ctrl Pts',(199.766508954549,-1.623642929,135.446877898267));
#207827=CARTESIAN_POINT('Ctrl Pts',(199.758748512034,-1.49419204503319,
135.492151184223));
#207828=CARTESIAN_POINT('Ctrl Pts',(199.75098806952,-1.362948841577,135.531970116074));
#207829=CARTESIAN_POINT('Ctrl Pts',(199.743227627006,-1.23041469352731,
135.566215586426));
#207830=CARTESIAN_POINT('Ctrl Pts',(199.73545472674,-1.09766778989741,135.600516030646));
#207831=CARTESIAN_POINT('Ctrl Pts',(199.727681826475,-0.96362618299564,
135.629225052453));
#207832=CARTESIAN_POINT('Ctrl Pts',(199.71990892621,-0.828800812444949,
135.65227483667));
#207833=CARTESIAN_POINT('Ctrl Pts',(199.712418590448,-0.698876683722678,
135.674486703171));
#207834=CARTESIAN_POINT('Ctrl Pts',(199.704928254686,-0.568225091055471,
135.691443604055));
#207835=CARTESIAN_POINT('Ctrl Pts',(199.697437918924,-0.437304423404299,
135.703130657461));
#207836=CARTESIAN_POINT('Ctrl Pts',(199.689663584805,-0.301419858842875,
135.715260829049));
#207837=CARTESIAN_POINT('Ctrl Pts',(199.681889250686,-0.164814971104963,
135.721752076884));
#207838=CARTESIAN_POINT('Ctrl Pts',(199.674114916567,-0.0279973195866715,
135.722530929033));
#207839=CARTESIAN_POINT('Ctrl Pts',(199.66635016362,0.10865171640381,135.723308821316));
#207840=CARTESIAN_POINT('Ctrl Pts',(199.658585410673,0.245512607244556,
135.718388323244));
#207841=CARTESIAN_POINT('Ctrl Pts',(199.650820657726,0.382071918374638,
135.707747621637));
#207842=CARTESIAN_POINT('Ctrl Pts',(199.643063616841,0.518495596871722,
135.697117488524));
#207843=CARTESIAN_POINT('Ctrl Pts',(199.635306575956,0.654617904481336,
135.680778488268));
#207844=CARTESIAN_POINT('Ctrl Pts',(199.627549535071,0.789925004703764,
135.658760843077));
#207845=CARTESIAN_POINT('Ctrl Pts',(199.619798343831,0.925130068789412,
135.636759801564));
#207846=CARTESIAN_POINT('Ctrl Pts',(199.612047152591,1.05952076479068,135.609088701334));
#207847=CARTESIAN_POINT('Ctrl Pts',(199.604295961351,1.19258833691385,135.575829586464));
#207848=CARTESIAN_POINT('Ctrl Pts',(199.596548064574,1.32559935176917,135.542584607605));
#207849=CARTESIAN_POINT('Ctrl Pts',(199.588800167797,1.45728798274033,135.503756432513));
#207850=CARTESIAN_POINT('Ctrl Pts',(199.581052271019,1.58715584884965,135.459478164306));
#207851=CARTESIAN_POINT('Ctrl Pts',(199.573305994935,1.71699654940101,135.415209158157));
#207852=CARTESIAN_POINT('Ctrl Pts',(199.565559718851,1.84501687283777,135.365492452586));
#207853=CARTESIAN_POINT('Ctrl Pts',(199.557813442767,1.97073416756975,135.310510848447));
#207854=CARTESIAN_POINT('Ctrl Pts',(199.550067109502,2.09645239031821,135.255528838447));
#207855=CARTESIAN_POINT('Ctrl Pts',(199.542320776237,2.21986719223249,135.195282008988));
#207856=CARTESIAN_POINT('Ctrl Pts',(199.534574442971,2.34051682582934,135.130000922828));
#207857=CARTESIAN_POINT('Ctrl Pts',(199.526826374968,2.46119347807506,135.064705217422));
#207858=CARTESIAN_POINT('Ctrl Pts',(199.519078306965,2.57910338599568,134.994373197965));
#207859=CARTESIAN_POINT('Ctrl Pts',(199.511330238962,2.6938106397786,134.919280701786));
#207860=CARTESIAN_POINT('Ctrl Pts',(199.503573936221,2.80863980579594,134.844108396408));
#207861=CARTESIAN_POINT('Ctrl Pts',(199.495817633479,2.92025919055272,134.764165721911));
#207862=CARTESIAN_POINT('Ctrl Pts',(199.488061330737,3.02826260835506,134.679771387709));
#207863=CARTESIAN_POINT('Ctrl Pts',(199.480300888223,3.13632367083349,134.595332009709));
#207864=CARTESIAN_POINT('Ctrl Pts',(199.472540445709,3.24076462319159,134.506436490939));
#207865=CARTESIAN_POINT('Ctrl Pts',(199.464780003195,3.34121425162771,134.41344227184));
#207866=CARTESIAN_POINT('Ctrl Pts',(199.457007102929,3.44182513072487,134.320298770166));
#207867=CARTESIAN_POINT('Ctrl Pts',(199.449234202664,3.53843160653162,134.223043697568));
#207868=CARTESIAN_POINT('Ctrl Pts',(199.441461302398,3.63070044887218,134.122070266263));
#207869=CARTESIAN_POINT('Ctrl Pts',(199.433970966636,3.71961508638472,134.024767473521));
#207870=CARTESIAN_POINT('Ctrl Pts',(199.426480630874,3.8045017845271,133.924012207482));
#207871=CARTESIAN_POINT('Ctrl Pts',(199.418990295112,3.88510025233675,133.820182079754));
#207872=CARTESIAN_POINT('Ctrl Pts',(199.411215960993,3.96875463554883,133.712415201177));
#207873=CARTESIAN_POINT('Ctrl Pts',(199.403441626874,4.04805418477677,133.600994318284));
#207874=CARTESIAN_POINT('Ctrl Pts',(199.395667292754,4.12266273775037,133.486306741795));
#207875=CARTESIAN_POINT('Ctrl Pts',(199.387902539807,4.19717934235037,133.371760507494));
#207876=CARTESIAN_POINT('Ctrl Pts',(199.38013778686,4.26701624247923,133.253955914529));
#207877=CARTESIAN_POINT('Ctrl Pts',(199.372373033913,4.33187756216918,133.133313139382));
#207878=CARTESIAN_POINT('Ctrl Pts',(199.364615993028,4.39667446068206,133.01279018834));
#207879=CARTESIAN_POINT('Ctrl Pts',(199.356858952143,4.45650542925731,132.889435007023));
#207880=CARTESIAN_POINT('Ctrl Pts',(199.349101911258,4.51111815351607,132.763696236473));
#207881=CARTESIAN_POINT('Ctrl Pts',(199.341350720018,4.56568969389464,132.638052286508));
#207882=CARTESIAN_POINT('Ctrl Pts',(199.333599528778,4.61505066744896,132.510028682241));
#207883=CARTESIAN_POINT('Ctrl Pts',(199.325848337538,4.65899510525039,132.380097801158));
#207884=CARTESIAN_POINT('Ctrl Pts',(199.318100440761,4.7029208654935,132.250222144165));
#207885=CARTESIAN_POINT('Ctrl Pts',(199.310352543983,4.74143454383123,132.118441192244));
#207886=CARTESIAN_POINT('Ctrl Pts',(199.302604647206,4.77437873659335,131.985246192914));
#207887=CARTESIAN_POINT('Ctrl Pts',(199.294858371122,4.80731603814052,131.852079055106));
#207888=CARTESIAN_POINT('Ctrl Pts',(199.287112095038,4.83468607758103,131.717498837516));
#207889=CARTESIAN_POINT('Ctrl Pts',(199.279365818954,4.85638176547755,131.582010416921));
#207890=CARTESIAN_POINT('Ctrl Pts',(199.271619485689,4.8780776135267,131.446520996182));
#207891=CARTESIAN_POINT('Ctrl Pts',(199.263873152423,4.89409896463232,131.310123745109));
#207892=CARTESIAN_POINT('Ctrl Pts',(199.256126819158,4.9043902119798,131.17333176974));
#207893=CARTESIAN_POINT('Ctrl Pts',(199.248378751155,4.91468376398078,131.036509160757));
#207894=CARTESIAN_POINT('Ctrl Pts',(199.240630683152,4.91924462944542,130.899292041369));
#207895=CARTESIAN_POINT('Ctrl Pts',(199.232882615149,4.91806925823009,130.762196251662));
#207896=CARTESIAN_POINT('Ctrl Pts',(199.225126312407,4.91689263781624,130.624954754918));
#207897=CARTESIAN_POINT('Ctrl Pts',(199.217370009665,4.90996760558296,130.487835237022));
#207898=CARTESIAN_POINT('Ctrl Pts',(199.209613706923,4.8973427474991,130.351351703727));
#207899=CARTESIAN_POINT('Ctrl Pts',(199.201853264409,4.88471115114836,130.21479532506));
#207900=CARTESIAN_POINT('Ctrl Pts',(199.194092821895,4.86637371941593,130.07887599463));
#207901=CARTESIAN_POINT('Ctrl Pts',(199.186332379381,4.8424305269433,129.944099230412));
#207902=CARTESIAN_POINT('Ctrl Pts',(199.178559479115,4.81844889873255,129.809106110568));
#207903=CARTESIAN_POINT('Ctrl Pts',(199.17078657885,4.788843611667,129.675259604108));
#207904=CARTESIAN_POINT('Ctrl Pts',(199.163013678584,4.75376536727037,129.543052607823));
#207905=CARTESIAN_POINT('Ctrl Pts',(199.155523342822,4.71996230541452,129.415651668864));
#207906=CARTESIAN_POINT('Ctrl Pts',(199.14803300706,4.68107738037903,129.289773403227));
#207907=CARTESIAN_POINT('Ctrl Pts',(199.140542671298,4.63728759387846,129.165840909366));
#207908=CARTESIAN_POINT('Ctrl Pts',(199.132768337179,4.59183750431285,129.037209477331));
#207909=CARTESIAN_POINT('Ctrl Pts',(199.12499400306,4.54095930328843,128.910266811875));
#207910=CARTESIAN_POINT('Ctrl Pts',(199.117219668941,4.48479714236479,128.785505086742));
#207911=CARTESIAN_POINT('Ctrl Pts',(199.109454915994,4.42870419628514,128.660897119286));
#207912=CARTESIAN_POINT('Ctrl Pts',(199.101690163047,4.36734040620565,128.538465097289));
#207913=CARTESIAN_POINT('Ctrl Pts',(199.0939254101,4.30089935031177,128.418685065235));
#207914=CARTESIAN_POINT('Ctrl Pts',(199.086168369215,4.23452428461125,128.299024000398));
#207915=CARTESIAN_POINT('Ctrl Pts',(199.07841132833,4.16308217693648,128.182010023415));
#207916=CARTESIAN_POINT('Ctrl Pts',(199.070654287445,4.08681409961739,128.068097914961));
#207917=CARTESIAN_POINT('Ctrl Pts',(199.062903096205,4.01060353664873,127.954271708514));
#207918=CARTESIAN_POINT('Ctrl Pts',(199.055151904965,3.92957446447712,127.84354303823));
#207919=CARTESIAN_POINT('Ctrl Pts',(199.047400713724,3.84401297642226,127.736340523173));
#207920=CARTESIAN_POINT('Ctrl Pts',(199.039652816947,3.75848785428223,127.629183572045));
#207921=CARTESIAN_POINT('Ctrl Pts',(199.03190492017,3.66843439109177,127.525550100254));
#207922=CARTESIAN_POINT('Ctrl Pts',(199.024157023393,3.57418080677142,127.425838067248));
#207923=CARTESIAN_POINT('Ctrl Pts',(199.016410747309,3.47994693826904,127.32614689185));
#207924=CARTESIAN_POINT('Ctrl Pts',(199.008664471225,3.38151496456809,127.230375807597));
#207925=CARTESIAN_POINT('Ctrl Pts',(199.000918195141,3.27925176834539,127.138887810096));
#207926=CARTESIAN_POINT('Ctrl Pts',(198.993171861876,3.17698781723904,127.047399137251));
#207927=CARTESIAN_POINT('Ctrl Pts',(198.98542552861,3.07089287855635,126.960193874925));
#207928=CARTESIAN_POINT('Ctrl Pts',(198.977679195345,2.96136858609743,126.877596153051));
#207929=CARTESIAN_POINT('Ctrl Pts',(198.969931127342,2.85181976643257,126.794979933991));
#207930=CARTESIAN_POINT('Ctrl Pts',(198.962183059339,2.73884037688976,126.716973543961));
#207931=CARTESIAN_POINT('Ctrl Pts',(198.954434991336,2.62286248940288,126.643858793965));
#207932=CARTESIAN_POINT('Ctrl Pts',(198.946678688594,2.50676133923701,126.570666336743));
#207933=CARTESIAN_POINT('Ctrl Pts',(198.938922385852,2.38765565632938,126.502376113735));
#207934=CARTESIAN_POINT('Ctrl Pts',(198.931166083111,2.26600415017978,126.439225080854));
#207935=CARTESIAN_POINT('Ctrl Pts',(198.923405640596,2.14428771495838,126.376040342365));
#207936=CARTESIAN_POINT('Ctrl Pts',(198.915645198082,2.02002310306419,126.318000424913));
#207937=CARTESIAN_POINT('Ctrl Pts',(198.907884755568,1.8936897138752,126.265294377681));
#207938=CARTESIAN_POINT('Ctrl Pts',(198.900111855303,1.76715352311459,126.212503722024));
#207939=CARTESIAN_POINT('Ctrl Pts',(198.892338955037,1.63854228569136,126.165064182373));
#207940=CARTESIAN_POINT('Ctrl Pts',(198.884566054772,1.50835214749063,126.123115392024));
#207941=CARTESIAN_POINT('Ctrl Pts',(198.87707571901,1.38289474874265,126.082691545867));
#207942=CARTESIAN_POINT('Ctrl Pts',(198.869585383248,1.25597154700458,126.047366257253));
#207943=CARTESIAN_POINT('Ctrl Pts',(198.862095047486,1.12803418073941,126.017219304675));
#207944=CARTESIAN_POINT('Ctrl Pts',(198.854320713367,0.995246030346574,
125.985929321228));
#207945=CARTESIAN_POINT('Ctrl Pts',(198.846546379248,0.860944660272916,
125.96011898127));
#207946=CARTESIAN_POINT('Ctrl Pts',(198.838772045129,0.72562206766675,125.939933037941));
#207947=CARTESIAN_POINT('Ctrl Pts',(198.831007292181,0.590466248061855,
125.919771971984));
#207948=CARTESIAN_POINT('Ctrl Pts',(198.823242539234,0.454292093069238,
125.905221568033));
#207949=CARTESIAN_POINT('Ctrl Pts',(198.815477786287,0.317604746131932,
125.89637627695));
#207950=CARTESIAN_POINT('Ctrl Pts',(198.807720745402,0.181053158994685,
125.887539771135));
#207951=CARTESIAN_POINT('Ctrl Pts',(198.799963704517,0.0439897818821281,
125.884397126882));
#207952=CARTESIAN_POINT('Ctrl Pts',(198.792206663632,-0.0930724598611862,
125.886991343278));
#207953=CARTESIAN_POINT('Ctrl Pts',(198.784455472392,-0.230031341901755,
125.889583603354));
#207954=CARTESIAN_POINT('Ctrl Pts',(198.776704281152,-0.366988700963738,
125.897904105649));
#207955=CARTESIAN_POINT('Ctrl Pts',(198.768953089912,-0.503429287263447,
125.911943830821));
#207956=CARTESIAN_POINT('Ctrl Pts',(198.761205193135,-0.639811882674504,
125.925977588736));
#207957=CARTESIAN_POINT('Ctrl Pts',(198.753457296358,-0.775677754077462,
125.945725694873));
#207958=CARTESIAN_POINT('Ctrl Pts',(198.745709399581,-0.910514676033535,
125.971127115321));
#207959=CARTESIAN_POINT('Ctrl Pts',(198.737963123496,-1.04532339301227,
125.996523222339));
#207960=CARTESIAN_POINT('Ctrl Pts',(198.730216847412,-1.17910320469284,
126.027570219174));
#207961=CARTESIAN_POINT('Ctrl Pts',(198.722470571328,-1.31135040354105,
126.064155645032));
#207962=CARTESIAN_POINT('Ctrl Pts',(198.714724238063,-1.44359857860805,
126.100741340956));
#207963=CARTESIAN_POINT('Ctrl Pts',(198.706977904797,-1.57431374145571,
126.14286544324));
#207964=CARTESIAN_POINT('Ctrl Pts',(198.699231571532,-1.70300609951057,
126.190365246141));
#207965=CARTESIAN_POINT('Ctrl Pts',(198.691483503529,-1.83172727732661,
126.237875686293));
#207966=CARTESIAN_POINT('Ctrl Pts',(198.683735435526,-1.95842438223704,
126.290764087235));
#207967=CARTESIAN_POINT('Ctrl Pts',(198.675987367523,-2.08262677322981,
126.348819260343));
#207968=CARTESIAN_POINT('Ctrl Pts',(198.668231064781,-2.20696116800184,
126.406936135179));
#207969=CARTESIAN_POINT('Ctrl Pts',(198.660474762039,-2.32879519762787,
126.47023058584));
#207970=CARTESIAN_POINT('Ctrl Pts',(198.652718459298,-2.44768156069828,
126.538444767491));
#207971=CARTESIAN_POINT('Ctrl Pts',(198.644958016783,-2.56663137700036,
126.606695357105));
#207972=CARTESIAN_POINT('Ctrl Pts',(198.637197574269,-2.68263006138942,
126.679870701362));
#207973=CARTESIAN_POINT('Ctrl Pts',(198.629437131755,-2.79525943435933,
126.757669653689));
#207974=CARTESIAN_POINT('Ctrl Pts',(198.62166423149,-2.90806960999747,126.835593495801));
#207975=CARTESIAN_POINT('Ctrl Pts',(198.613891331224,-3.01749935359477,
126.918155542348));
#207976=CARTESIAN_POINT('Ctrl Pts',(198.606118430959,-3.12316300873507,
127.005013846953));
#207977=CARTESIAN_POINT('Ctrl Pts',(198.598628095197,-3.22498552385993,
127.088714633402));
#207978=CARTESIAN_POINT('Ctrl Pts',(198.591137759435,-3.32331078044587,
127.176404536312));
#207979=CARTESIAN_POINT('Ctrl Pts',(198.583647423673,-3.41782753696518,
127.267746701677));
#207980=CARTESIAN_POINT('Ctrl Pts',(198.575987342496,-3.51448622497807,
127.361158856193));
#207981=CARTESIAN_POINT('Ctrl Pts',(198.568327261318,-3.60748705227816,
127.458705550652));
#207982=CARTESIAN_POINT('Ctrl Pts',(198.560667180141,-3.69644762254403,
127.560064386287));
#207983=CARTESIAN_POINT('Ctrl Pts',(198.553016015211,-3.78530464372584,
127.6613052414));
#207984=CARTESIAN_POINT('Ctrl Pts',(198.545364850281,-3.87013049362145,
127.766349116946));
#207985=CARTESIAN_POINT('Ctrl Pts',(198.53771368535,-3.95057739062617,127.874834829461));
#207986=CARTESIAN_POINT('Ctrl Pts',(198.530069653823,-4.03094928465215,
127.983219397595));
#207987=CARTESIAN_POINT('Ctrl Pts',(198.522425622296,-4.10695010528644,
128.095039100229));
#207988=CARTESIAN_POINT('Ctrl Pts',(198.514781590769,-4.17827075473654,
128.209897944369));
#207989=CARTESIAN_POINT('Ctrl Pts',(198.507143088631,-4.24953981365601,
128.324673704173));
#207990=CARTESIAN_POINT('Ctrl Pts',(198.499504586494,-4.31613522474468,
128.442483890537));
#207991=CARTESIAN_POINT('Ctrl Pts',(198.491866084356,-4.37779019060595,
128.562902139357));
#207992=CARTESIAN_POINT('Ctrl Pts',(198.484230874548,-4.43941858208351,
128.683268485777));
#207993=CARTESIAN_POINT('Ctrl Pts',(198.47659566474,-4.49611058101027,128.806240300078));
#207994=CARTESIAN_POINT('Ctrl Pts',(198.468960454932,-4.54764472612785,
128.931365554192));
#207995=CARTESIAN_POINT('Ctrl Pts',(198.461325447542,-4.5991775050181,129.056487491098));
#207996=CARTESIAN_POINT('Ctrl Pts',(198.453690440153,-4.64555254017037,
129.183762384902));
#207997=CARTESIAN_POINT('Ctrl Pts',(198.446055432763,-4.68659615849717,
129.312717392911));
#207998=CARTESIAN_POINT('Ctrl Pts',(198.440775680082,-4.71497860042732,
129.401892231183));
#207999=CARTESIAN_POINT('Ctrl Pts',(198.435495927401,-4.74081256549775,
129.491870059345));
#208000=CARTESIAN_POINT('Ctrl Pts',(198.430216174721,-4.76405452823404,
129.582490119308));
#208001=CARTESIAN_POINT('Ctrl Pts',(200.179870531952,-4.76405452823405,
129.582490119308));
#208002=CARTESIAN_POINT('Ctrl Pts',(200.171798423708,-4.79949019568666,
129.720653248895));
#208003=CARTESIAN_POINT('Ctrl Pts',(200.163726315465,-4.8289461026174,129.860494510444));
#208004=CARTESIAN_POINT('Ctrl Pts',(200.155654207222,-4.85227401211597,
130.001478326166));
#208005=CARTESIAN_POINT('Ctrl Pts',(200.147594415967,-4.87556632625476,
130.142247018897));
#208006=CARTESIAN_POINT('Ctrl Pts',(200.139534624712,-4.89274923115088,
130.284154452949));
#208007=CARTESIAN_POINT('Ctrl Pts',(200.131474833457,-4.90372514985256,
130.426653433092));
#208008=CARTESIAN_POINT('Ctrl Pts',(200.124363410307,-4.91340956969396,
130.552385045013));
#208009=CARTESIAN_POINT('Ctrl Pts',(200.117251987158,-4.91826246131281,
130.678576831645));
#208010=CARTESIAN_POINT('Ctrl Pts',(200.110140564008,-4.9182499759574,130.804846925109));
#208011=CARTESIAN_POINT('Origin',(213.235140564004,0.,130.804360617566));
#208012=CARTESIAN_POINT('',(201.930097584127,-4.76405452823404,129.582490119308));
#208013=CARTESIAN_POINT('',(201.584606355351,-4.76405452823405,129.582490119308));
#208014=CARTESIAN_POINT('',(213.235140564004,-4.76405452823405,129.582490119308));
#208015=CARTESIAN_POINT('',(201.51485943594,-4.91824986053202,130.805531888988));
#208016=CARTESIAN_POINT('Ctrl Pts',(201.584606355351,-4.76405452823405,
129.582490119308));
#208017=CARTESIAN_POINT('Ctrl Pts',(201.576612163084,-4.79917136563237,
129.719410135352));
#208018=CARTESIAN_POINT('Ctrl Pts',(201.568617970816,-4.82841256673479,
129.857966876512));
#208019=CARTESIAN_POINT('Ctrl Pts',(201.560623778548,-4.85163618075089,
129.997633010422));
#208020=CARTESIAN_POINT('Ctrl Pts',(201.55263857145,-4.87483369230245,130.137142164875));
#208021=CARTESIAN_POINT('Ctrl Pts',(201.544653364352,-4.89202704125614,
130.277757877198));
#208022=CARTESIAN_POINT('Ctrl Pts',(201.536668157254,-4.90312503397178,
130.418941412363));
#208023=CARTESIAN_POINT('Ctrl Pts',(201.5293985835,-4.91322842585438,130.547472095315));
#208024=CARTESIAN_POINT('Ctrl Pts',(201.522129009746,-4.9182805956174,130.676473036305));
#208025=CARTESIAN_POINT('Ctrl Pts',(201.514859435991,-4.91824986053224,
130.805531888085));
#208026=CARTESIAN_POINT('Ctrl Pts',(201.51485943594,-4.91824986053202,130.805531888988));
#208027=CARTESIAN_POINT('Ctrl Pts',(201.506582193965,-4.9182148650919,130.952480167015));
#208028=CARTESIAN_POINT('Ctrl Pts',(201.49830495199,-4.91158982122124,131.099253060515));
#208029=CARTESIAN_POINT('Ctrl Pts',(201.490027710014,-4.89844708438231,
131.245267891272));
#208030=CARTESIAN_POINT('Ctrl Pts',(201.481501455677,-4.88490896174189,
131.395675428935));
#208031=CARTESIAN_POINT('Ctrl Pts',(201.472975201339,-4.86445493793769,
131.545278220582));
#208032=CARTESIAN_POINT('Ctrl Pts',(201.464448947001,-4.83721994611014,
131.693453557283));
#208033=CARTESIAN_POINT('Ctrl Pts',(201.456128501245,-4.81064235843921,
131.838052205476));
#208034=CARTESIAN_POINT('Ctrl Pts',(201.447808055489,-4.77760755788874,
131.981291262248));
#208035=CARTESIAN_POINT('Ctrl Pts',(201.439487609733,-4.73829111258486,
132.122609605769));
#208036=CARTESIAN_POINT('Ctrl Pts',(201.430858451104,-4.69751591217013,
132.269171273154));
#208037=CARTESIAN_POINT('Ctrl Pts',(201.422229292475,-4.6499841405859,132.413666610456));
#208038=CARTESIAN_POINT('Ctrl Pts',(201.413600133847,-4.59594544262833,
132.555494122152));
#208039=CARTESIAN_POINT('Ctrl Pts',(201.404970975218,-4.54190674467076,
132.697321633848));
#208040=CARTESIAN_POINT('Ctrl Pts',(201.396341816589,-4.48136133127772,
132.836481025787));
#208041=CARTESIAN_POINT('Ctrl Pts',(201.38771265796,-4.41461067614117,132.972400202214));
#208042=CARTESIAN_POINT('Ctrl Pts',(201.379938323841,-4.3544724960429,133.094854909123));
#208043=CARTESIAN_POINT('Ctrl Pts',(201.372163989722,-4.28914013406402,
133.21499946427));
#208044=CARTESIAN_POINT('Ctrl Pts',(201.364389655603,-4.21881414473507,
133.332361858603));
#208045=CARTESIAN_POINT('Ctrl Pts',(201.356624902656,-4.14857482590277,
133.449579614273));
#208046=CARTESIAN_POINT('Ctrl Pts',(201.348860149708,-4.07335432377154,
133.564021699203));
#208047=CARTESIAN_POINT('Ctrl Pts',(201.341095396761,-3.9934004017413,133.675237886603));
#208048=CARTESIAN_POINT('Ctrl Pts',(201.333338355876,-3.91352589107348,
133.786343612518));
#208049=CARTESIAN_POINT('Ctrl Pts',(201.325581314991,-3.8289275430417,133.89422950163));
#208050=CARTESIAN_POINT('Ctrl Pts',(201.317824274106,-3.73989781193985,
133.998471983619));
#208051=CARTESIAN_POINT('Ctrl Pts',(201.310073082865,-3.65093521885079,
134.102635855541));
#208052=CARTESIAN_POINT('Ctrl Pts',(201.302321891625,-3.55754814710466,
134.203161493023));
#208053=CARTESIAN_POINT('Ctrl Pts',(201.294570700385,-3.46007071453197,
134.299656558247));
#208054=CARTESIAN_POINT('Ctrl Pts',(201.286822803607,-3.36263471246837,
134.396110610494));
#208055=CARTESIAN_POINT('Ctrl Pts',(201.27907490683,-3.26111208461592,134.488537223235));
#208056=CARTESIAN_POINT('Ctrl Pts',(201.271327010053,-3.15587521323921,
134.576579420998));
#208057=CARTESIAN_POINT('Ctrl Pts',(201.263580733969,-3.05066035514734,
134.664603202231));
#208058=CARTESIAN_POINT('Ctrl Pts',(201.255834457884,-2.94173309858087,
134.748244141987));
#208059=CARTESIAN_POINT('Ctrl Pts',(201.2480881818,-2.82950014815832,134.827184498134));
#208060=CARTESIAN_POINT('Ctrl Pts',(201.240341848535,-2.71726636925778,
134.906125437001));
#208061=CARTESIAN_POINT('Ctrl Pts',(201.232595515269,-2.60172716759431,
134.980365498095));
#208062=CARTESIAN_POINT('Ctrl Pts',(201.224849182004,-2.48331923024386,
135.049629591754));
#208063=CARTESIAN_POINT('Ctrl Pts',(201.217101114,-2.36488477625662,135.118909196626));
#208064=CARTESIAN_POINT('Ctrl Pts',(201.209353045997,-2.24358064561767,
135.183210419302));
#208065=CARTESIAN_POINT('Ctrl Pts',(201.201604977994,-2.11986882164754,
135.242303749413));
#208066=CARTESIAN_POINT('Ctrl Pts',(201.193848675252,-1.99602551527869,
135.301459884618));
#208067=CARTESIAN_POINT('Ctrl Pts',(201.18609237251,-1.8697697571969,135.355396901697));
#208068=CARTESIAN_POINT('Ctrl Pts',(201.178336069768,-1.74158475661268,
135.403932945298));
#208069=CARTESIAN_POINT('Ctrl Pts',(201.170575627254,-1.61333133983404,
135.452494894046));
#208070=CARTESIAN_POINT('Ctrl Pts',(201.162815184739,-1.4831469997239,135.49565000241));
#208071=CARTESIAN_POINT('Ctrl Pts',(201.155054742225,-1.35152990844939,
135.533266407394));
#208072=CARTESIAN_POINT('Ctrl Pts',(201.147281841959,-1.21970153373557,
135.57094319757));
#208073=CARTESIAN_POINT('Ctrl Pts',(201.139508941694,-1.08643619206553,
135.603063425218));
#208074=CARTESIAN_POINT('Ctrl Pts',(201.131736041428,-0.952242926124562,
135.629546258777));
#208075=CARTESIAN_POINT('Ctrl Pts',(201.124245705668,-0.822927923447469,
135.655066374622));
#208076=CARTESIAN_POINT('Ctrl Pts',(201.116755369908,-0.692751594327094,
135.675351800014));
#208077=CARTESIAN_POINT('Ctrl Pts',(201.109265034147,-0.562171798684125,
135.690375960488));
#208078=CARTESIAN_POINT('Ctrl Pts',(201.101490700028,-0.426641030368497,
135.705969766576));
#208079=CARTESIAN_POINT('Ctrl Pts',(201.093716365909,-0.290246275975597,
135.715944866885));
#208080=CARTESIAN_POINT('Ctrl Pts',(201.08594203179,-0.153493054712102,
135.7202148612));
#208081=CARTESIAN_POINT('Ctrl Pts',(201.078177278843,-0.0169083695718419,
135.724479593129));
#208082=CARTESIAN_POINT('Ctrl Pts',(201.070412525896,0.12003351640835,135.723053196639));
#208083=CARTESIAN_POINT('Ctrl Pts',(201.062647772949,0.256819892510846,
135.715900763519));
#208084=CARTESIAN_POINT('Ctrl Pts',(201.054890732064,0.39347041045627,135.708755434297));
#208085=CARTESIAN_POINT('Ctrl Pts',(201.047133691179,0.52996533799027,135.695895406474));
#208086=CARTESIAN_POINT('Ctrl Pts',(201.039376650294,0.665790234716704,
135.677337780026));
#208087=CARTESIAN_POINT('Ctrl Pts',(201.031625459054,0.801512704831837,
135.658794148028));
#208088=CARTESIAN_POINT('Ctrl Pts',(201.023874267814,0.936565764060569,
135.634561522245));
#208089=CARTESIAN_POINT('Ctrl Pts',(201.016123076574,1.07043872863637,135.604708937296));
#208090=CARTESIAN_POINT('Ctrl Pts',(201.008375179797,1.20425479363109,135.574869040492));
#208091=CARTESIAN_POINT('Ctrl Pts',(201.00062728302,1.33689138076679,135.539414020244));
#208092=CARTESIAN_POINT('Ctrl Pts',(200.992879386243,1.46784687475884,135.498464218336));
#208093=CARTESIAN_POINT('Ctrl Pts',(200.985133110159,1.59877497568463,135.457522982243));
#208094=CARTESIAN_POINT('Ctrl Pts',(200.977386834075,1.72802231000401,135.411089367299));
#208095=CARTESIAN_POINT('Ctrl Pts',(200.969640557991,1.85510171848053,135.359333798232));
#208096=CARTESIAN_POINT('Ctrl Pts',(200.961894224726,1.98218206502826,135.307577847118));
#208097=CARTESIAN_POINT('Ctrl Pts',(200.954147891461,2.10709409171268,135.250500010957));
#208098=CARTESIAN_POINT('Ctrl Pts',(200.946401558195,2.22937031777955,135.188318994273));
#208099=CARTESIAN_POINT('Ctrl Pts',(200.938653490193,2.35167392675948,135.126124052582));
#208100=CARTESIAN_POINT('Ctrl Pts',(200.93090542219,2.47134021212813,135.058823833469));
#208101=CARTESIAN_POINT('Ctrl Pts',(200.923157354187,2.58792636704384,134.986682960626));
#208102=CARTESIAN_POINT('Ctrl Pts',(200.915401051445,2.70463643111238,134.914465415605));
#208103=CARTESIAN_POINT('Ctrl Pts',(200.907644748703,2.81825949236634,134.837397145802));
#208104=CARTESIAN_POINT('Ctrl Pts',(200.899888445961,2.92838136436711,134.755786391553));
#208105=CARTESIAN_POINT('Ctrl Pts',(200.892128003447,3.03856201172679,134.674132079186));
#208106=CARTESIAN_POINT('Ctrl Pts',(200.884367560933,3.14523744236723,134.587930697037));
#208107=CARTESIAN_POINT('Ctrl Pts',(200.876607118419,3.24802744199153,134.497530096289));
#208108=CARTESIAN_POINT('Ctrl Pts',(200.868834218154,3.35098244924848,134.406984376471));
#208109=CARTESIAN_POINT('Ctrl Pts',(200.861061317888,3.45003927881987,134.312226237882));
#208110=CARTESIAN_POINT('Ctrl Pts',(200.853288417623,3.54485477481942,134.213640261118));
#208111=CARTESIAN_POINT('Ctrl Pts',(200.84579808186,3.63622348872338,134.118638132923));
#208112=CARTESIAN_POINT('Ctrl Pts',(200.838307746098,3.723653677273,134.020081868339));
#208113=CARTESIAN_POINT('Ctrl Pts',(200.830817410335,3.80687549814816,133.918342313739));
#208114=CARTESIAN_POINT('Ctrl Pts',(200.823043076216,3.8932526996479,133.812745273014));
#208115=CARTESIAN_POINT('Ctrl Pts',(200.815268742097,3.97536973042481,133.703384288615));
#208116=CARTESIAN_POINT('Ctrl Pts',(200.807494407978,4.052880654051,133.59063796674));
#208117=CARTESIAN_POINT('Ctrl Pts',(200.799729655031,4.13029605239111,133.47803059463));
#208118=CARTESIAN_POINT('Ctrl Pts',(200.791964902084,4.20311641899065,133.362046505414));
#208119=CARTESIAN_POINT('Ctrl Pts',(200.784200149136,4.27103525191642,133.243098188398));
#208120=CARTESIAN_POINT('Ctrl Pts',(200.776443108251,4.33888662689985,133.124268012527));
#208121=CARTESIAN_POINT('Ctrl Pts',(200.768686067366,4.40184596368367,133.002479805092));
#208122=CARTESIAN_POINT('Ctrl Pts',(200.760929026481,4.45964958136172,132.878175622324));
#208123=CARTESIAN_POINT('Ctrl Pts',(200.753177835241,4.51740960888204,132.753965178307));
#208124=CARTESIAN_POINT('Ctrl Pts',(200.745426644001,4.57002149187464,132.627242888525));
#208125=CARTESIAN_POINT('Ctrl Pts',(200.737675452761,4.61726727407009,132.498475720592));
#208126=CARTESIAN_POINT('Ctrl Pts',(200.729927555984,4.66449297554781,132.369763282141));
#208127=CARTESIAN_POINT('Ctrl Pts',(200.722179659207,4.70635697805043,132.239008060438));
#208128=CARTESIAN_POINT('Ctrl Pts',(200.71443176243,4.74268939321458,132.106697126303));
#208129=CARTESIAN_POINT('Ctrl Pts',(200.706685486346,4.77901420842072,131.974413868764));
#208130=CARTESIAN_POINT('Ctrl Pts',(200.698939210262,4.80980963434076,131.840575922843));
#208131=CARTESIAN_POINT('Ctrl Pts',(200.691192934178,4.83495573265951,131.705685268135));
#208132=CARTESIAN_POINT('Ctrl Pts',(200.683446600912,4.86010201660105,131.570793617694));
#208133=CARTESIAN_POINT('Ctrl Pts',(200.675700267647,4.8795988180791,131.434849627302));
#208134=CARTESIAN_POINT('Ctrl Pts',(200.667953934382,4.89337745463654,131.298364816895));
#208135=CARTESIAN_POINT('Ctrl Pts',(200.660205866379,4.90715917682409,131.161849441661));
#208136=CARTESIAN_POINT('Ctrl Pts',(200.652457798376,4.91522014669572,131.024793394324));
#208137=CARTESIAN_POINT('Ctrl Pts',(200.644709730373,4.91754365174374,130.887712256391));
#208138=CARTESIAN_POINT('Ctrl Pts',(200.636953427631,4.91986962624059,130.750485426993));
#208139=CARTESIAN_POINT('Ctrl Pts',(200.629197124889,4.91644594817341,130.613233845261));
#208140=CARTESIAN_POINT('Ctrl Pts',(200.621440822147,4.90730807097843,130.476472589407));
#208141=CARTESIAN_POINT('Ctrl Pts',(200.613680379633,4.89816531662325,130.339638339953));
#208142=CARTESIAN_POINT('Ctrl Pts',(200.605919937119,4.88330232842366,130.203295326312));
#208143=CARTESIAN_POINT('Ctrl Pts',(200.598159494605,4.86280624831729,130.067951455601));
#208144=CARTESIAN_POINT('Ctrl Pts',(200.590386594339,4.84227726608359,129.932390318894));
#208145=CARTESIAN_POINT('Ctrl Pts',(200.582613694074,4.81609719637891,129.797831914236));
#208146=CARTESIAN_POINT('Ctrl Pts',(200.574840793809,4.78440411361137,129.664772823599));
#208147=CARTESIAN_POINT('Ctrl Pts',(200.567350458046,4.75386315423193,129.53655076606));
#208148=CARTESIAN_POINT('Ctrl Pts',(200.559860122284,4.71820313009367,129.409721203914));
#208149=CARTESIAN_POINT('Ctrl Pts',(200.552369786522,4.67759018838714,129.284711614669));
#208150=CARTESIAN_POINT('Ctrl Pts',(200.544595452403,4.63543739465235,129.154962248855));
#208151=CARTESIAN_POINT('Ctrl Pts',(200.536821118284,4.58781516216797,129.026762581828));
#208152=CARTESIAN_POINT('Ctrl Pts',(200.529046784165,4.53485503596222,128.900608305602));
#208153=CARTESIAN_POINT('Ctrl Pts',(200.521282031218,4.48196017837884,128.774609503247));
#208154=CARTESIAN_POINT('Ctrl Pts',(200.51351727827,4.42374066616417,128.650651433156));
#208155=CARTESIAN_POINT('Ctrl Pts',(200.505752525323,4.36037786647262,128.529214924632));
#208156=CARTESIAN_POINT('Ctrl Pts',(200.497995484438,4.29707799960699,128.407899028561));
#208157=CARTESIAN_POINT('Ctrl Pts',(200.490238443553,4.22864519086966,128.289100054462));
#208158=CARTESIAN_POINT('Ctrl Pts',(200.482481402668,4.15530882871568,128.173278786741));
#208159=CARTESIAN_POINT('Ctrl Pts',(200.474730211428,4.08202777008282,128.057544860739));
#208160=CARTESIAN_POINT('Ctrl Pts',(200.466979020188,4.00385072660107,127.944784500539));
#208161=CARTESIAN_POINT('Ctrl Pts',(200.459227828948,3.92105276066194,127.835433486327));
#208162=CARTESIAN_POINT('Ctrl Pts',(200.451479932171,3.83828998606706,127.726128949213));
#208163=CARTESIAN_POINT('Ctrl Pts',(200.443732035394,3.75091043080558,127.620231187053));
#208164=CARTESIAN_POINT('Ctrl Pts',(200.435984138616,3.65923205254183,127.518146405414));
#208165=CARTESIAN_POINT('Ctrl Pts',(200.428237862532,3.56757285141844,127.41608297771));
#208166=CARTESIAN_POINT('Ctrl Pts',(200.420491586448,3.47161687695752,127.317831234768));
#208167=CARTESIAN_POINT('Ctrl Pts',(200.412745310364,3.37172162921752,127.223763416321));
#208168=CARTESIAN_POINT('Ctrl Pts',(200.404998977099,3.27182564407353,127.129694903486));
#208169=CARTESIAN_POINT('Ctrl Pts',(200.397252643833,3.16799061225729,127.039810644801));
#208170=CARTESIAN_POINT('Ctrl Pts',(200.389506310568,3.06060976543159,126.954444913782));
#208171=CARTESIAN_POINT('Ctrl Pts',(200.381758242565,2.95320487140979,126.869060065699));
#208172=CARTESIAN_POINT('Ctrl Pts',(200.374010174562,2.84225288827149,126.788196002082));
#208173=CARTESIAN_POINT('Ctrl Pts',(200.366262106559,2.72817855582115,126.712145468034));
#208174=CARTESIAN_POINT('Ctrl Pts',(200.358505803817,2.61398298381271,126.636014106574));
#208175=CARTESIAN_POINT('Ctrl Pts',(200.350749501075,2.49665875931106,126.564706711413));
#208176=CARTESIAN_POINT('Ctrl Pts',(200.342993198333,2.37665839565136,126.498471866927));
#208177=CARTESIAN_POINT('Ctrl Pts',(200.335232755819,2.25659398418439,126.43220167091));
#208178=CARTESIAN_POINT('Ctrl Pts',(200.327472313305,2.13385093720195,126.371009594588));
#208179=CARTESIAN_POINT('Ctrl Pts',(200.319711870791,2.00890367369267,126.315096859184));
#208180=CARTESIAN_POINT('Ctrl Pts',(200.311938970525,1.8837558337437,126.259094367693));
#208181=CARTESIAN_POINT('Ctrl Pts',(200.30416607026,1.75639706985327,126.208388297305));
#208182=CARTESIAN_POINT('Ctrl Pts',(200.296393169994,1.62731980308813,126.163130896794));
#208183=CARTESIAN_POINT('Ctrl Pts',(200.288902834233,1.50293482010056,126.11951871679));
#208184=CARTESIAN_POINT('Ctrl Pts',(200.281412498471,1.37695440338238,126.08096602872));
#208185=CARTESIAN_POINT('Ctrl Pts',(200.273922162709,1.24982800848328,126.047564110282));
#208186=CARTESIAN_POINT('Ctrl Pts',(200.26614782859,1.11788157767805,126.012895747953));
#208187=CARTESIAN_POINT('Ctrl Pts',(200.258373494471,0.984282587110447,
125.983666629395));
#208188=CARTESIAN_POINT('Ctrl Pts',(200.250599160352,0.849519179810192,
125.960034015691));
#208189=CARTESIAN_POINT('Ctrl Pts',(200.242834407405,0.714921856365283,
125.936430527071));
#208190=CARTESIAN_POINT('Ctrl Pts',(200.235069654458,0.579163352880725,
125.918409886831));
#208191=CARTESIAN_POINT('Ctrl Pts',(200.227304901511,0.442746238043899,
125.906079405631));
#208192=CARTESIAN_POINT('Ctrl Pts',(200.219547860626,0.306464614608663,
125.893761171238));
#208193=CARTESIAN_POINT('Ctrl Pts',(200.211790819741,0.1695260684516,125.88712188402));
#208194=CARTESIAN_POINT('Ctrl Pts',(200.204033778856,0.0324422606050424,
125.886217618199));
#208195=CARTESIAN_POINT('Ctrl Pts',(200.196282587615,-0.104538171275545,
125.885314034291));
#208196=CARTESIAN_POINT('Ctrl Pts',(200.188531396375,-0.241663257432193,
125.890136866048));
#208197=CARTESIAN_POINT('Ctrl Pts',(200.180780205135,-0.378417685712695,
125.900690245524));
#208198=CARTESIAN_POINT('Ctrl Pts',(200.173032308358,-0.515113989713261,
125.911239139532));
#208199=CARTESIAN_POINT('Ctrl Pts',(200.165284411581,-0.651439560181567,
125.927513706947));
#208200=CARTESIAN_POINT('Ctrl Pts',(200.157536514804,-0.78688078098602,
125.949466005011));
#208201=CARTESIAN_POINT('Ctrl Pts',(200.14979023872,-0.922293670406798,
125.971413711128));
#208202=CARTESIAN_POINT('Ctrl Pts',(200.142043962636,-1.05682219242837,
125.999036723063));
#208203=CARTESIAN_POINT('Ctrl Pts',(200.134297686552,-1.18995993370752,
126.032235470562));
#208204=CARTESIAN_POINT('Ctrl Pts',(200.126551353286,-1.3230986577791,126.065434463126));
#208205=CARTESIAN_POINT('Ctrl Pts',(200.118805020021,-1.454846201273,126.104209178789));
#208206=CARTESIAN_POINT('Ctrl Pts',(200.111058686756,-1.58470877909421,
126.148409463617));
#208207=CARTESIAN_POINT('Ctrl Pts',(200.103310618753,-1.71460043873933,
126.192619646792));
#208208=CARTESIAN_POINT('Ctrl Pts',(200.09556255075,-1.84260592268838,126.242257690929));
#208209=CARTESIAN_POINT('Ctrl Pts',(200.087814482747,-1.96824935395539,
126.297124486282));
#208210=CARTESIAN_POINT('Ctrl Pts',(200.080058180005,-2.09402632055645,
126.352049594717));
#208211=CARTESIAN_POINT('Ctrl Pts',(200.072301877263,-2.21743586078181,
126.41221439872));
#208212=CARTESIAN_POINT('Ctrl Pts',(200.064545574521,-2.33802423904589,
126.477372551933));
#208213=CARTESIAN_POINT('Ctrl Pts',(200.056785132007,-2.45867697895829,
126.542565482013));
#208214=CARTESIAN_POINT('Ctrl Pts',(200.049024689493,-2.57650522087711,
126.612756871751));
#208215=CARTESIAN_POINT('Ctrl Pts',(200.041264246979,-2.69108323663666,
126.687656344));
#208216=CARTESIAN_POINT('Ctrl Pts',(200.033491346713,-2.80584518319893,
126.762676051532));
#208217=CARTESIAN_POINT('Ctrl Pts',(200.025718446448,-2.91734615908058,
126.842418716971));
#208218=CARTESIAN_POINT('Ctrl Pts',(200.017945546182,-3.02519190746045,
126.926552346708));
#208219=CARTESIAN_POINT('Ctrl Pts',(200.01045521042,-3.12911719124147,127.007627507086));
#208220=CARTESIAN_POINT('Ctrl Pts',(200.002964874658,-3.22964815206794,
127.092779730022));
#208221=CARTESIAN_POINT('Ctrl Pts',(199.995474538896,-3.32646505372397,
127.181680213659));
#208222=CARTESIAN_POINT('Ctrl Pts',(199.987817885007,-3.42543171291799,
127.272554675822));
#208223=CARTESIAN_POINT('Ctrl Pts',(199.980161231117,-3.52085100355156,
127.367652463917));
#208224=CARTESIAN_POINT('Ctrl Pts',(199.972504577228,-3.61233263415092,
127.466661409616));
#208225=CARTESIAN_POINT('Ctrl Pts',(199.964856779005,-3.7037084573244,127.565555841815));
#208226=CARTESIAN_POINT('Ctrl Pts',(199.957208980783,-3.79115540274886,
127.668352146295));
#208227=CARTESIAN_POINT('Ctrl Pts',(199.94956118256,-3.87431677020004,127.774698486792));
#208228=CARTESIAN_POINT('Ctrl Pts',(199.941920455469,-3.95740124690412,
127.880946499786));
#208229=CARTESIAN_POINT('Ctrl Pts',(199.934279728377,-4.03620777736056,
127.990737706671));
#208230=CARTESIAN_POINT('Ctrl Pts',(199.926639001285,-4.11041742727574,
128.10368447333));
#208231=CARTESIAN_POINT('Ctrl Pts',(199.918999136713,-4.18461870007081,
128.216618490047));
#208232=CARTESIAN_POINT('Ctrl Pts',(199.911359272141,-4.2542238720399,128.332707043142));
#208233=CARTESIAN_POINT('Ctrl Pts',(199.90371940757,-4.31895501961334,128.451530279217));
#208234=CARTESIAN_POINT('Ctrl Pts',(199.896087179009,-4.38362146868872,
128.570234751988));
#208235=CARTESIAN_POINT('Ctrl Pts',(199.888454950448,-4.44342342148269,
128.69166809915));
#208236=CARTESIAN_POINT('Ctrl Pts',(199.880822721887,-4.49812811338532,
128.815384363793));
#208237=CARTESIAN_POINT('Ctrl Pts',(199.87317903931,-4.55291490299365,128.939286294805));
#208238=CARTESIAN_POINT('Ctrl Pts',(199.865535356733,-4.60258893508908,
129.065477639417));
#208239=CARTESIAN_POINT('Ctrl Pts',(199.857891674155,-4.64696388063631,
129.19348825932));
#208240=CARTESIAN_POINT('Ctrl Pts',(199.850247991578,-4.69133882618354,
129.321498879223));
#208241=CARTESIAN_POINT('Ctrl Pts',(199.842604309,-4.73041455848543,129.451328387816));
#208242=CARTESIAN_POINT('Ctrl Pts',(199.834960626423,-4.76405452823405,
129.582490119308));
#208243=CARTESIAN_POINT('',(201.860140564039,-4.91824790150174,130.799817284683));
#208244=CARTESIAN_POINT('Ctrl Pts',(201.860140564008,-4.91824790150225,
130.799817285234));
#208245=CARTESIAN_POINT('Ctrl Pts',(201.852483585455,-4.91837276654937,
130.934986190149));
#208246=CARTESIAN_POINT('Ctrl Pts',(201.844826606902,-4.91292114291673,
131.07031288466));
#208247=CARTESIAN_POINT('Ctrl Pts',(201.83716962835,-4.90188083750575,131.205293676061));
#208248=CARTESIAN_POINT('Ctrl Pts',(201.829228030736,-4.89043015072319,
131.345291865101));
#208249=CARTESIAN_POINT('Ctrl Pts',(201.821286433122,-4.8729672167622,131.484917501621));
#208250=CARTESIAN_POINT('Ctrl Pts',(201.813344835508,-4.84953772420023,
131.62360839697));
#208251=CARTESIAN_POINT('Ctrl Pts',(201.80569610997,-4.82697226989009,131.757184617366));
#208252=CARTESIAN_POINT('Ctrl Pts',(201.798047384431,-4.79887259272399,
131.889893384014));
#208253=CARTESIAN_POINT('Ctrl Pts',(201.790398658893,-4.76533224076631,
132.021238465837));
#208254=CARTESIAN_POINT('Ctrl Pts',(201.782750978392,-4.73179647139039,
132.152565602125));
#208255=CARTESIAN_POINT('Ctrl Pts',(201.775103297891,-4.69282160461944,
132.282529034708));
#208256=CARTESIAN_POINT('Ctrl Pts',(201.767455617389,-4.64855188812975,
132.410644654051));
#208257=CARTESIAN_POINT('Ctrl Pts',(201.759807225106,-4.60427805138161,
132.538772197334));
#208258=CARTESIAN_POINT('Ctrl Pts',(201.752158832822,-4.5547085165048,132.665051205577));
#208259=CARTESIAN_POINT('Ctrl Pts',(201.744510440538,-4.50003661315956,
132.789015132267));
#208260=CARTESIAN_POINT('Ctrl Pts',(201.736859579318,-4.44534706147838,
132.913019075069));
#208261=CARTESIAN_POINT('Ctrl Pts',(201.729208718099,-4.38555202834284,
133.034706082836));
#208262=CARTESIAN_POINT('Ctrl Pts',(201.72155785688,-4.32089170944105,133.153632397881));
#208263=CARTESIAN_POINT('Ctrl Pts',(201.713898683524,-4.25616114153522,
133.272687918215));
#208264=CARTESIAN_POINT('Ctrl Pts',(201.706239510168,-4.18655493051007,
133.388976406699));
#208265=CARTESIAN_POINT('Ctrl Pts',(201.698580336813,-4.11235781880762,
133.502081179928));
#208266=CARTESIAN_POINT('Ctrl Pts',(201.690916213761,-4.03811275765906,
133.615259046451));
#208267=CARTESIAN_POINT('Ctrl Pts',(201.68325209071,-3.95927112365503,133.725248776863));
#208268=CARTESIAN_POINT('Ctrl Pts',(201.675587967659,-3.87615836955861,
133.831666244126));
#208269=CARTESIAN_POINT('Ctrl Pts',(201.667913108811,-3.79292919227884,
133.938232779488));
#208270=CARTESIAN_POINT('Ctrl Pts',(201.660238249964,-3.70541721587963,
134.041216762563));
#208271=CARTESIAN_POINT('Ctrl Pts',(201.652563391116,-3.61398532778852,
134.140270255585));
#208272=CARTESIAN_POINT('Ctrl Pts',(201.650566022616,-3.59019033991468,
134.166048752722));
#208273=CARTESIAN_POINT('Ctrl Pts',(201.648568654115,-3.56613003589684,
134.191561251679));
#208274=CARTESIAN_POINT('Ctrl Pts',(201.646571285615,-3.54181117222063,
134.216802072424));
#208275=CARTESIAN_POINT('Ctrl Pts',(201.638796951494,-3.44715514275093,
134.315046624639));
#208276=CARTESIAN_POINT('Ctrl Pts',(201.631022617374,-3.34825835130227,
134.409505379128));
#208277=CARTESIAN_POINT('Ctrl Pts',(201.623248283254,-3.24545589596689,
134.499790104085));
#208278=CARTESIAN_POINT('Ctrl Pts',(201.615483530306,-3.14278013546986,
134.589963561187));
#208279=CARTESIAN_POINT('Ctrl Pts',(201.607718777357,-3.03620857922076,
134.675972968507));
#208280=CARTESIAN_POINT('Ctrl Pts',(201.599954024409,-2.92611462881938,
134.757465250827));
#208281=CARTESIAN_POINT('Ctrl Pts',(201.592196983523,-2.8161300252812,134.838876593864));
#208282=CARTESIAN_POINT('Ctrl Pts',(201.584439942637,-2.70263030195642,
134.915779509083));
#208283=CARTESIAN_POINT('Ctrl Pts',(201.576682901751,-2.58602327795652,
134.987859950465));
#208284=CARTESIAN_POINT('Ctrl Pts',(201.568931710509,-2.46950418822028,
135.059886035426));
#208285=CARTESIAN_POINT('Ctrl Pts',(201.561180519268,-2.3498827930975,135.127096680372));
#208286=CARTESIAN_POINT('Ctrl Pts',(201.553429328027,-2.22759704920044,
135.189220301626));
#208287=CARTESIAN_POINT('Ctrl Pts',(201.545681431248,-2.10536328000659,
135.251317518684));
#208288=CARTESIAN_POINT('Ctrl Pts',(201.53793353447,-1.98046776216892,135.308331835635));
#208289=CARTESIAN_POINT('Ctrl Pts',(201.530185637692,-1.85337409203519,
135.360037025902));
#208290=CARTESIAN_POINT('Ctrl Pts',(201.522439361606,-1.72630700715721,
135.411731400558));
#208291=CARTESIAN_POINT('Ctrl Pts',(201.514693085521,-1.59704304647646,
135.458118710247));
#208292=CARTESIAN_POINT('Ctrl Pts',(201.506946809436,-1.46606651029953,
135.499020567965));
#208293=CARTESIAN_POINT('Ctrl Pts',(201.499200476169,-1.33508900728361,
135.539922727611));
#208294=CARTESIAN_POINT('Ctrl Pts',(201.491454142903,-1.20239927673706,
135.575339237944));
#208295=CARTESIAN_POINT('Ctrl Pts',(201.483707809636,-1.0684971462986,135.605141482264));
#208296=CARTESIAN_POINT('Ctrl Pts',(201.475959741632,-0.934565029406161,
135.63495040059));
#208297=CARTESIAN_POINT('Ctrl Pts',(201.468211673628,-0.799420353905459,
135.659142466148));
#208298=CARTESIAN_POINT('Ctrl Pts',(201.460463605623,-0.663573118682993,
135.677640188724));
#208299=CARTESIAN_POINT('Ctrl Pts',(201.45270730288,-0.527581503402445,
135.696157570899));
#208300=CARTESIAN_POINT('Ctrl Pts',(201.444951000137,-0.390886224816852,
135.708968467706));
#208301=CARTESIAN_POINT('Ctrl Pts',(201.437194697394,-0.254002943294543,
135.716047249192));
#208302=CARTESIAN_POINT('Ctrl Pts',(201.429434254879,-0.117046603043397,
135.723129808838));
#208303=CARTESIAN_POINT('Ctrl Pts',(201.421673812363,0.0200975493309183,
135.724474153213));
#208304=CARTESIAN_POINT('Ctrl Pts',(201.413913369848,0.156914869496959,
135.720106826051));
#208305=CARTESIAN_POINT('Ctrl Pts',(201.406140469581,0.293951820971461,
135.715732488067));
#208306=CARTESIAN_POINT('Ctrl Pts',(201.398367569315,0.430660501673616,
135.705628185033));
#208307=CARTESIAN_POINT('Ctrl Pts',(201.390594669048,0.566531497579824,
135.689872374255));
#208308=CARTESIAN_POINT('Ctrl Pts',(201.383104333299,0.697463240297336,
135.674689326915));
#208309=CARTESIAN_POINT('Ctrl Pts',(201.37561399755,0.827616840453072,135.654258578995));
#208310=CARTESIAN_POINT('Ctrl Pts',(201.368123661801,0.956548189162586,
135.628694625935));
#208311=CARTESIAN_POINT('Ctrl Pts',(201.360349327683,1.09036800937337,135.60216140778));
#208312=CARTESIAN_POINT('Ctrl Pts',(201.352574993564,1.22329496617451,135.570014000326));
#208313=CARTESIAN_POINT('Ctrl Pts',(201.344800659445,1.35482130044931,135.532324482313));
#208314=CARTESIAN_POINT('Ctrl Pts',(201.337035906498,1.48618554027203,135.494681413262));
#208315=CARTESIAN_POINT('Ctrl Pts',(201.329271153552,1.61615221984584,135.451509930292));
#208316=CARTESIAN_POINT('Ctrl Pts',(201.321506400605,1.74422245430599,135.402933340966));
#208317=CARTESIAN_POINT('Ctrl Pts',(201.31374935972,1.87216548760419,135.354404998592));
#208318=CARTESIAN_POINT('Ctrl Pts',(201.305992318836,1.99821546100229,135.300482371031));
#208319=CARTESIAN_POINT('Ctrl Pts',(201.298235277951,2.12188772249806,135.241338818505));
#208320=CARTESIAN_POINT('Ctrl Pts',(201.290484086711,2.24546672177877,135.182239866593));
#208321=CARTESIAN_POINT('Ctrl Pts',(201.282732895472,2.36667122683608,135.117927994348));
#208322=CARTESIAN_POINT('Ctrl Pts',(201.274981704232,2.48503602038379,135.048624869459));
#208323=CARTESIAN_POINT('Ctrl Pts',(201.267233807455,2.60335050573666,134.979351200247));
#208324=CARTESIAN_POINT('Ctrl Pts',(201.259485910679,2.71882734343585,134.905090694853));
#208325=CARTESIAN_POINT('Ctrl Pts',(201.251738013902,2.83102561750346,134.826111109024));
#208326=CARTESIAN_POINT('Ctrl Pts',(201.243991737818,2.94320042211094,134.747148044021));
#208327=CARTESIAN_POINT('Ctrl Pts',(201.236245461735,3.0520977076928,134.663468086941));
#208328=CARTESIAN_POINT('Ctrl Pts',(201.228499185651,3.15730561606483,134.575382270814));
#208329=CARTESIAN_POINT('Ctrl Pts',(201.220752852386,3.26251430105758,134.487295804458));
#208330=CARTESIAN_POINT('Ctrl Pts',(201.213006519121,3.36403325472788,134.394803665141));
#208331=CARTESIAN_POINT('Ctrl Pts',(201.205260185856,3.46148409915498,134.298256851543));
#208332=CARTESIAN_POINT('Ctrl Pts',(201.197512117854,3.55895676702291,134.201688416955));
#208333=CARTESIAN_POINT('Ctrl Pts',(201.189764049851,3.6523592351274,134.101063776349));
#208334=CARTESIAN_POINT('Ctrl Pts',(201.182015981848,3.74135064190172,133.996770120879));
#208335=CARTESIAN_POINT('Ctrl Pts',(201.174259679107,3.8304366298024,133.89236562087));
#208336=CARTESIAN_POINT('Ctrl Pts',(201.166503376366,3.91510193715322,133.784284614265));
#208337=CARTESIAN_POINT('Ctrl Pts',(201.158747073624,3.99504627372427,133.672947087119));
#208338=CARTESIAN_POINT('Ctrl Pts',(201.15098663111,4.07503327899471,133.561550135783));
#208339=CARTESIAN_POINT('Ctrl Pts',(201.143226188597,4.1502940782862,133.446893527272));
#208340=CARTESIAN_POINT('Ctrl Pts',(201.135465746083,4.22057282576062,133.329424593974));
#208341=CARTESIAN_POINT('Ctrl Pts',(201.127692845818,4.2909643909197,133.211767089115));
#208342=CARTESIAN_POINT('Ctrl Pts',(201.119919945553,4.35635773583158,133.091288581682));
#208343=CARTESIAN_POINT('Ctrl Pts',(201.112147045288,4.41654351812895,132.968460064212));
#208344=CARTESIAN_POINT('Ctrl Pts',(201.104656709521,4.47454139567703,132.850096672665));
#208345=CARTESIAN_POINT('Ctrl Pts',(201.097166373755,4.5277036290204,132.729551444137));
#208346=CARTESIAN_POINT('Ctrl Pts',(201.089676037989,4.57588649471474,132.607259907595));
#208347=CARTESIAN_POINT('Ctrl Pts',(201.08190170387,4.62589622837748,132.48033165035));
#208348=CARTESIAN_POINT('Ctrl Pts',(201.074127369751,4.67069997109745,132.351119977928));
#208349=CARTESIAN_POINT('Ctrl Pts',(201.066353035632,4.71008390855603,132.220091042775));
#208350=CARTESIAN_POINT('Ctrl Pts',(201.058588282685,4.74941930883149,132.089223589074));
#208351=CARTESIAN_POINT('Ctrl Pts',(201.050823529738,4.78334808245175,131.956543699629));
#208352=CARTESIAN_POINT('Ctrl Pts',(201.043058776791,4.81170431210567,131.822537751155));
#208353=CARTESIAN_POINT('Ctrl Pts',(201.035301735906,4.84003237795253,131.688664899279));
#208354=CARTESIAN_POINT('Ctrl Pts',(201.027544695021,4.86279883378002,131.553468989404));
#208355=CARTESIAN_POINT('Ctrl Pts',(201.019787654136,4.87988756620843,131.417451478421));
#208356=CARTESIAN_POINT('Ctrl Pts',(201.012036462896,4.89696341189084,131.281536539302));
#208357=CARTESIAN_POINT('Ctrl Pts',(201.004285271656,4.90837000793079,131.144801618648));
#208358=CARTESIAN_POINT('Ctrl Pts',(200.996534080416,4.91404238832683,131.007757933741));
#208359=CARTESIAN_POINT('Ctrl Pts',(200.988786183639,4.91971235780988,130.870772496056));
#208360=CARTESIAN_POINT('Ctrl Pts',(200.981038286862,4.91965294290856,130.733478944942));
#208361=CARTESIAN_POINT('Ctrl Pts',(200.973290390085,4.91385108825839,130.596392964019));
#208362=CARTESIAN_POINT('Ctrl Pts',(200.965544114001,4.90805044723114,130.459335658529));
#208363=CARTESIAN_POINT('Ctrl Pts',(200.957797837917,4.89650977221841,130.322486227234));
#208364=CARTESIAN_POINT('Ctrl Pts',(200.950051561833,4.87926812470907,130.186359299041));
#208365=CARTESIAN_POINT('Ctrl Pts',(200.942305228568,4.86202634992579,130.050231365991));
#208366=CARTESIAN_POINT('Ctrl Pts',(200.934558895303,4.83908356779839,129.91482633455));
#208367=CARTESIAN_POINT('Ctrl Pts',(200.926812562038,4.81053056094829,129.780652268141));
#208368=CARTESIAN_POINT('Ctrl Pts',(200.919064494035,4.78197115985042,129.646448154381));
#208369=CARTESIAN_POINT('Ctrl Pts',(200.911316426032,4.74779911535903,129.513475936524));
#208370=CARTESIAN_POINT('Ctrl Pts',(200.903568358029,4.70815593835484,129.382231677338));
#208371=CARTESIAN_POINT('Ctrl Pts',(200.895812055287,4.66847062811032,129.250847930191));
#208372=CARTESIAN_POINT('Ctrl Pts',(200.888055752546,4.62330268292331,129.121196185172));
#208373=CARTESIAN_POINT('Ctrl Pts',(200.880299449804,4.57284313475343,128.993756097678));
#208374=CARTESIAN_POINT('Ctrl Pts',(200.87253900729,4.52235665480324,128.866247991572));
#208375=CARTESIAN_POINT('Ctrl Pts',(200.864778564776,4.46657310317764,128.740954252085));
#208376=CARTESIAN_POINT('Ctrl Pts',(200.857018122262,4.40573054235811,128.618331923648));
#208377=CARTESIAN_POINT('Ctrl Pts',(200.849245221996,4.34479031165874,128.495512750964));
#208378=CARTESIAN_POINT('Ctrl Pts',(200.841472321731,4.27877503146672,128.375373901733));
#208379=CARTESIAN_POINT('Ctrl Pts',(200.833699421466,4.20796780647951,128.258346084589));
#208380=CARTESIAN_POINT('Ctrl Pts',(200.826209085702,4.13973460246116,128.145572523353));
#208381=CARTESIAN_POINT('Ctrl Pts',(200.818718749939,4.06705197339164,128.035687990354));
#208382=CARTESIAN_POINT('Ctrl Pts',(200.811228414176,3.99020865609362,127.929048818241));
#208383=CARTESIAN_POINT('Ctrl Pts',(200.803454080057,3.91045180107535,127.818366389521));
#208384=CARTESIAN_POINT('Ctrl Pts',(200.795679745938,3.82595987893068,127.710829666744));
#208385=CARTESIAN_POINT('Ctrl Pts',(200.787905411818,3.73700950505258,127.606870504736));
#208386=CARTESIAN_POINT('Ctrl Pts',(200.780140658871,3.64816875456051,127.503039463103));
#208387=CARTESIAN_POINT('Ctrl Pts',(200.772375905924,3.55488073677464,127.402777503809));
#208388=CARTESIAN_POINT('Ctrl Pts',(200.764611152976,3.45746497184096,127.306487116281));
#208389=CARTESIAN_POINT('Ctrl Pts',(200.756854112091,3.36014596161846,127.210292365723));
#208390=CARTESIAN_POINT('Ctrl Pts',(200.749097071206,3.25870763916541,127.118061610023));
#208391=CARTESIAN_POINT('Ctrl Pts',(200.741340030321,3.15350913224816,127.030163588352));
#208392=CARTESIAN_POINT('Ctrl Pts',(200.733588839081,3.04838995634344,126.942331851264));
#208393=CARTESIAN_POINT('Ctrl Pts',(200.72583764784,2.93951653884054,126.858826594413));
#208394=CARTESIAN_POINT('Ctrl Pts',(200.7180864566,2.82728386560443,126.779978800964));
#208395=CARTESIAN_POINT('Ctrl Pts',(200.710338559823,2.71509889424786,126.701164519931));
#208396=CARTESIAN_POINT('Ctrl Pts',(200.702590663046,2.59955782612968,126.627003989411));
#208397=CARTESIAN_POINT('Ctrl Pts',(200.694842766268,2.48108746374105,126.557786932845));
#208398=CARTESIAN_POINT('Ctrl Pts',(200.687096490184,2.36264188279868,126.488584354995));
#208399=CARTESIAN_POINT('Ctrl Pts',(200.6793502141,2.24126856372764,126.424323391385));
#208400=CARTESIAN_POINT('Ctrl Pts',(200.671603938015,2.11742159208994,126.36524934797));
#208401=CARTESIAN_POINT('Ctrl Pts',(200.66385760475,1.99357370624226,126.306174868485));
#208402=CARTESIAN_POINT('Ctrl Pts',(200.656111271484,1.86725248426869,126.252287553918));
#208403=CARTESIAN_POINT('Ctrl Pts',(200.648364938219,1.7389344445388,126.203785646968));
#208404=CARTESIAN_POINT('Ctrl Pts',(200.640616870216,1.61058766887319,126.155272878351));
#208405=CARTESIAN_POINT('Ctrl Pts',(200.632868802213,1.48024355127012,126.112148055408));
#208406=CARTESIAN_POINT('Ctrl Pts',(200.625120734209,1.34839593347158,126.074560255067));
#208407=CARTESIAN_POINT('Ctrl Pts',(200.617364431467,1.21640818645573,126.036932505965));
#208408=CARTESIAN_POINT('Ctrl Pts',(200.609608128725,1.08291412377568,126.004853642373));
#208409=CARTESIAN_POINT('Ctrl Pts',(200.601851825983,0.948420550542189,
125.978422209152));
#208410=CARTESIAN_POINT('Ctrl Pts',(200.594091383469,0.813855194038882,
125.951976668679));
#208411=CARTESIAN_POINT('Ctrl Pts',(200.586330940955,0.678289650257551,
125.931184623874));
#208412=CARTESIAN_POINT('Ctrl Pts',(200.57857049844,0.54223712220886,125.916092829709));
#208413=CARTESIAN_POINT('Ctrl Pts',(200.570797598175,0.405966190564276,
125.900976808856));
#208414=CARTESIAN_POINT('Ctrl Pts',(200.563024697909,0.269207102735885,
125.891579351172));
#208415=CARTESIAN_POINT('Ctrl Pts',(200.555251797643,0.132475251099434,
125.887895081193));
#208416=CARTESIAN_POINT('Ctrl Pts',(200.547761461883,0.000713946712914748,
125.884344743708));
#208417=CARTESIAN_POINT('Ctrl Pts',(200.540271126123,-0.131021759319523,
125.88609942386));
#208418=CARTESIAN_POINT('Ctrl Pts',(200.532780790363,-0.262276004943429,
125.893108805682));
#208419=CARTESIAN_POINT('Ctrl Pts',(200.525006456244,-0.398506795217166,
125.900383950348));
#208420=CARTESIAN_POINT('Ctrl Pts',(200.517232122125,-0.534650433432306,
125.913343171992));
#208421=CARTESIAN_POINT('Ctrl Pts',(200.509457788006,-0.670194070517084,
125.931987174331));
#208422=CARTESIAN_POINT('Ctrl Pts',(200.501693035059,-0.805570662182922,
125.950608199603));
#208423=CARTESIAN_POINT('Ctrl Pts',(200.493928282112,-0.940348340398937,
125.974900012985));
#208424=CARTESIAN_POINT('Ctrl Pts',(200.486163529165,-1.07401577096679,
126.004811348498));
#208425=CARTESIAN_POINT('Ctrl Pts',(200.47840648828,-1.20755044115865,126.03469297565));
#208426=CARTESIAN_POINT('Ctrl Pts',(200.470649447395,-1.33997667909172,
126.070182932893));
#208427=CARTESIAN_POINT('Ctrl Pts',(200.46289240651,-1.47079013672649,126.111178388395));
#208428=CARTESIAN_POINT('Ctrl Pts',(200.45514121527,-1.60150494691511,126.152142928905));
#208429=CARTESIAN_POINT('Ctrl Pts',(200.44739002403,-1.73060902603362,126.198604587446));
#208430=CARTESIAN_POINT('Ctrl Pts',(200.43963883279,-1.85761040906449,126.250409955708));
#208431=CARTESIAN_POINT('Ctrl Pts',(200.431890936013,-1.9845578131194,126.302193305306));
#208432=CARTESIAN_POINT('Ctrl Pts',(200.424143039236,-2.10940393734354,
126.359315699986));
#208433=CARTESIAN_POINT('Ctrl Pts',(200.416395142459,-2.23167433202904,
126.421574661321));
#208434=CARTESIAN_POINT('Ctrl Pts',(200.408648866375,-2.35391915038416,
126.483820599422));
#208435=CARTESIAN_POINT('Ctrl Pts',(200.400902590291,-2.47358896269875,
126.551200789732));
#208436=CARTESIAN_POINT('Ctrl Pts',(200.393156314207,-2.59023194178586,
126.623465791066));
#208437=CARTESIAN_POINT('Ctrl Pts',(200.385409980941,-2.70687578190523,
126.695731325845));
#208438=CARTESIAN_POINT('Ctrl Pts',(200.377663647676,-2.82049241186166,
126.772881537696));
#208439=CARTESIAN_POINT('Ctrl Pts',(200.369917314411,-2.93065747463995,
126.854622673241));
#208440=CARTESIAN_POINT('Ctrl Pts',(200.362169246408,-3.04084720811968,
126.936382114147));
#208441=CARTESIAN_POINT('Ctrl Pts',(200.354421178405,-3.14758352241582,
127.022734291636));
#208442=CARTESIAN_POINT('Ctrl Pts',(200.346673110402,-3.25047406136048,
127.113344302386));
#208443=CARTESIAN_POINT('Ctrl Pts',(200.33891680766,-3.3534739535945,127.204050614535));
#208444=CARTESIAN_POINT('Ctrl Pts',(200.331160504918,-3.45261961170661,
127.29902354087));
#208445=CARTESIAN_POINT('Ctrl Pts',(200.323404202176,-3.54755418657293,
127.397889957803));
#208446=CARTESIAN_POINT('Ctrl Pts',(200.315643759662,-3.64253943088031,
127.496809142719));
#208447=CARTESIAN_POINT('Ctrl Pts',(200.307883317148,-3.73330885482172,
127.599625666022));
#208448=CARTESIAN_POINT('Ctrl Pts',(200.300122874634,-3.8195457233528,127.705933027688));
#208449=CARTESIAN_POINT('Ctrl Pts',(200.292349974369,-3.90592102696098,
127.812411043368));
#208450=CARTESIAN_POINT('Ctrl Pts',(200.284577074103,-3.98774900175901,
127.922390781748));
#208451=CARTESIAN_POINT('Ctrl Pts',(200.276804173838,-4.06475558810789,
128.035435723054));
#208452=CARTESIAN_POINT('Ctrl Pts',(200.269313838075,-4.13896279108229,
128.144371196012));
#208453=CARTESIAN_POINT('Ctrl Pts',(200.261823502312,-4.20869289593499,
128.256152623966));
#208454=CARTESIAN_POINT('Ctrl Pts',(200.25433316655,-4.27374183033709,128.37036928025));
#208455=CARTESIAN_POINT('Ctrl Pts',(200.246220788594,-4.34419281654029,
128.494071169452));
#208456=CARTESIAN_POINT('Ctrl Pts',(200.238108410639,-4.40935986504164,
128.620992964794));
#208457=CARTESIAN_POINT('Ctrl Pts',(200.229996032683,-4.46895007272139,
128.750664362025));
#208458=CARTESIAN_POINT('Ctrl Pts',(200.221641782561,-4.53031697432501,
128.88420193782));
#208459=CARTESIAN_POINT('Ctrl Pts',(200.213287532439,-4.58576906133034,
129.02065536604));
#208460=CARTESIAN_POINT('Ctrl Pts',(200.204933282317,-4.6350349423211,129.159479422475));
#208461=CARTESIAN_POINT('Ctrl Pts',(200.196579032196,-4.68430082331187,
129.298303478911));
#208462=CARTESIAN_POINT('Ctrl Pts',(200.188224782074,-4.7273802889641,129.439497817004));
#208463=CARTESIAN_POINT('Ctrl Pts',(200.179870531952,-4.76405452823405,
129.582490119308));
#208464=CARTESIAN_POINT('Ctrl Pts',(201.930097584127,-4.76405452823404,
129.582490119308));
#208465=CARTESIAN_POINT('Ctrl Pts',(201.928404692561,-4.77143981658942,
129.611285246518));
#208466=CARTESIAN_POINT('Ctrl Pts',(201.926711800994,-4.77856158153426,
129.640137793894));
#208467=CARTESIAN_POINT('Ctrl Pts',(201.925018909427,-4.78541909345683,
129.669042528888));
#208468=CARTESIAN_POINT('Ctrl Pts',(201.914205851863,-4.82922028700719,
129.853666617963));
#208469=CARTESIAN_POINT('Ctrl Pts',(201.903392794298,-4.86235268751459,
130.040911499407));
#208470=CARTESIAN_POINT('Ctrl Pts',(201.892579736733,-4.88456555156559,
130.22972818291));
#208471=CARTESIAN_POINT('Ctrl Pts',(201.882347687665,-4.90558487136082,
130.408399345895));
#208472=CARTESIAN_POINT('Ctrl Pts',(201.872115638597,-4.91682686629452,
130.58847825068));
#208473=CARTESIAN_POINT('Ctrl Pts',(201.861883589529,-4.91812325643309,
130.769052020427));
#208474=CARTESIAN_POINT('Ctrl Pts',(201.861302581032,-4.91819686961459,
130.779305577046));
#208475=CARTESIAN_POINT('Ctrl Pts',(201.860721572536,-4.91823842679033,
130.789560721775));
#208476=CARTESIAN_POINT('Ctrl Pts',(201.860140564039,-4.91824790150174,
130.799817284683));
#208477=CARTESIAN_POINT('Origin',(213.235140564004,0.,130.804360617566));
#208478=CARTESIAN_POINT('',(203.680274487341,-4.76405452823405,129.582490119308));
#208479=CARTESIAN_POINT('',(203.334773566427,-4.76405452823405,129.582490119308));
#208480=CARTESIAN_POINT('',(213.235140564004,-4.76405452823405,129.582490119308));
#208481=CARTESIAN_POINT('',(203.264859436027,-4.91824791911963,130.799836396593));
#208482=CARTESIAN_POINT('Ctrl Pts',(203.334773566427,-4.76405452823405,
129.582490119308));
#208483=CARTESIAN_POINT('Ctrl Pts',(203.32473014209,-4.80784291725373,129.753220383514));
#208484=CARTESIAN_POINT('Ctrl Pts',(203.314686717754,-4.84247434312161,
129.926402595191));
#208485=CARTESIAN_POINT('Ctrl Pts',(203.304643293417,-4.86772242676584,
130.101181096774));
#208486=CARTESIAN_POINT('Ctrl Pts',(203.294796401501,-4.89247644913987,
130.272539485777));
#208487=CARTESIAN_POINT('Ctrl Pts',(203.284949509584,-4.90821079695266,
130.445432509572));
#208488=CARTESIAN_POINT('Ctrl Pts',(203.275102617668,-4.91475699054651,
130.619031757498));
#208489=CARTESIAN_POINT('Ctrl Pts',(203.271688223788,-4.9170268726106,130.679227016553));
#208490=CARTESIAN_POINT('Ctrl Pts',(203.268273829907,-4.91819242300989,
130.739506976807));
#208491=CARTESIAN_POINT('Ctrl Pts',(203.264859436027,-4.91824791911963,
130.799836396593));
#208492=CARTESIAN_POINT('Ctrl Pts',(203.264859435991,-4.91824791912021,
130.799836397221));
#208493=CARTESIAN_POINT('Ctrl Pts',(203.257189383465,-4.91837258488303,
130.935359665711));
#208494=CARTESIAN_POINT('Ctrl Pts',(203.249519330939,-4.91289148263668,
131.071020543707));
#208495=CARTESIAN_POINT('Ctrl Pts',(203.241849278414,-4.90179734488421,
131.206313167236));
#208496=CARTESIAN_POINT('Ctrl Pts',(203.234183418891,-4.89070927198605,
131.341531830077));
#208497=CARTESIAN_POINT('Ctrl Pts',(203.226517559368,-4.8740142988451,131.476382241115));
#208498=CARTESIAN_POINT('Ctrl Pts',(203.218851699845,-4.85175723294996,
131.610359882465));
#208499=CARTESIAN_POINT('Ctrl Pts',(203.211187985896,-4.82950639651798,
131.744300025216));
#208500=CARTESIAN_POINT('Ctrl Pts',(203.203524271947,-4.80169662793145,
131.877367489554));
#208501=CARTESIAN_POINT('Ctrl Pts',(203.195860557999,-4.76842439234139,
132.009064679576));
#208502=CARTESIAN_POINT('Ctrl Pts',(203.18819724317,-4.73515388954357,132.140755010911));
#208503=CARTESIAN_POINT('Ctrl Pts',(203.180533928342,-4.69642158345535,
132.271074821851));
#208504=CARTESIAN_POINT('Ctrl Pts',(203.172870613514,-4.6523745561182,132.399538993825));
#208505=CARTESIAN_POINT('Ctrl Pts',(203.165205951912,-4.60831978783102,
132.528025742458));
#208506=CARTESIAN_POINT('Ctrl Pts',(203.157541290311,-4.55894857073882,
132.654655825109));
#208507=CARTESIAN_POINT('Ctrl Pts',(203.14987662871,-4.50445695066178,132.778962005729));
#208508=CARTESIAN_POINT('Ctrl Pts',(203.142204113634,-4.44990949660173,
132.903395554725));
#208509=CARTESIAN_POINT('Ctrl Pts',(203.134531598558,-4.39023132120439,
133.025500078541));
#208510=CARTESIAN_POINT('Ctrl Pts',(203.126859083481,-4.32566565593964,
133.144830590782));
#208511=CARTESIAN_POINT('Ctrl Pts',(203.119182649825,-4.26106701508398,
133.264222048637));
#208512=CARTESIAN_POINT('Ctrl Pts',(203.111506216169,-4.19157611789148,
133.380836329876));
#208513=CARTESIAN_POINT('Ctrl Pts',(203.103829782513,-4.11748010840755,
133.494256641461));
#208514=CARTESIAN_POINT('Ctrl Pts',(203.096141011026,-4.04326500925227,
133.607859246098));
#208515=CARTESIAN_POINT('Ctrl Pts',(203.08845223954,-3.9644302428689,133.718257299233));
#208516=CARTESIAN_POINT('Ctrl Pts',(203.080763468054,-3.88130435803297,
133.825065757565));
#208517=CARTESIAN_POINT('Ctrl Pts',(203.073308445649,-3.80070561283009,
133.928627093911));
#208518=CARTESIAN_POINT('Ctrl Pts',(203.065853423243,-3.71607313595503,
134.028813718384));
#208519=CARTESIAN_POINT('Ctrl Pts',(203.058398400838,-3.62773852230693,
134.125308716569));
#208520=CARTESIAN_POINT('Ctrl Pts',(203.050624066711,-3.53562038179653,
134.225936765238));
#208521=CARTESIAN_POINT('Ctrl Pts',(203.042849732584,-3.43916625203493,
134.322888467361));
#208522=CARTESIAN_POINT('Ctrl Pts',(203.035075398457,-3.33870121485528,
134.415767166326));
#208523=CARTESIAN_POINT('Ctrl Pts',(203.027310645502,-3.23835999185389,
134.508531400596));
#208524=CARTESIAN_POINT('Ctrl Pts',(203.019545892547,-3.13401798102474,
134.597232356386));
#208525=CARTESIAN_POINT('Ctrl Pts',(203.011781139593,-3.026039452382,134.68150754477));
#208526=CARTESIAN_POINT('Ctrl Pts',(203.0040240987,-2.91816816953492,134.76569902985));
#208527=CARTESIAN_POINT('Ctrl Pts',(202.996267057807,-2.80666786281095,
134.845473256243));
#208528=CARTESIAN_POINT('Ctrl Pts',(202.988510016914,-2.69193820449843,
134.920505873222));
#208529=CARTESIAN_POINT('Ctrl Pts',(202.980758825666,-2.57729506471272,
134.995481907523));
#208530=CARTESIAN_POINT('Ctrl Pts',(202.973007634418,-2.45942774649362,
135.065723236469));
#208531=CARTESIAN_POINT('Ctrl Pts',(202.96525644317,-2.33876713339567,135.130947188784));
#208532=CARTESIAN_POINT('Ctrl Pts',(202.957508546385,-2.21815780427522,
135.196143419181));
#208533=CARTESIAN_POINT('Ctrl Pts',(202.949760649599,-2.09475788478772,
135.256326328838));
#208534=CARTESIAN_POINT('Ctrl Pts',(202.942012752814,-1.96902504732344,
135.311257934514));
#208535=CARTESIAN_POINT('Ctrl Pts',(202.934266476722,-1.84331851045724,
135.366178049683));
#208536=CARTESIAN_POINT('Ctrl Pts',(202.92652020063,-1.71528038430399,135.415848889344));
#208537=CARTESIAN_POINT('Ctrl Pts',(202.918773924538,-1.58539025926972,
135.460079765916));
#208538=CARTESIAN_POINT('Ctrl Pts',(202.911027591264,-1.45549917541524,
135.504310968991));
#208539=CARTESIAN_POINT('Ctrl Pts',(202.903281257991,-1.32375643549607,
135.54310200282));
#208540=CARTESIAN_POINT('Ctrl Pts',(202.895534924717,-1.19065842226258,
135.576311537682));
#208541=CARTESIAN_POINT('Ctrl Pts',(202.887786856706,-1.05753060265117,
135.609528509589));
#208542=CARTESIAN_POINT('Ctrl Pts',(202.880038788695,-0.923047285050385,
135.637161400668));
#208543=CARTESIAN_POINT('Ctrl Pts',(202.872290720684,-0.787716324822747,
135.659119731478));
#208544=CARTESIAN_POINT('Ctrl Pts',(202.864534417934,-0.65224153324019,
135.681101399863));
#208545=CARTESIAN_POINT('Ctrl Pts',(202.856778115184,-0.515917685950118,
135.697396397709));
#208546=CARTESIAN_POINT('Ctrl Pts',(202.849021812434,-0.379259621354758,
135.707965944477));
#208547=CARTESIAN_POINT('Ctrl Pts',(202.841261369911,-0.242528618235135,
135.71854113253));
#208548=CARTESIAN_POINT('Ctrl Pts',(202.833500927389,-0.105463432899442,
135.723384766673));
#208549=CARTESIAN_POINT('Ctrl Pts',(202.825740484867,0.0314207805563875,
135.722510248987));
#208550=CARTESIAN_POINT('Ctrl Pts',(202.817967584593,0.168524732702548,
135.721634327448));
#208551=CARTESIAN_POINT('Ctrl Pts',(202.810194684319,0.305446741698207,
135.715021929815));
#208552=CARTESIAN_POINT('Ctrl Pts',(202.802421784046,0.441675557289912,
135.70273848831));
#208553=CARTESIAN_POINT('Ctrl Pts',(202.794931448372,0.572952110607848,
135.690901580996));
#208554=CARTESIAN_POINT('Ctrl Pts',(202.787441112698,0.703584688784279,
135.673798825022));
#208555=CARTESIAN_POINT('Ctrl Pts',(202.779950777025,0.833126405809881,
135.651533345502));
#208556=CARTESIAN_POINT('Ctrl Pts',(202.772176442908,0.96757973795983,135.628423663291));
#208557=CARTESIAN_POINT('Ctrl Pts',(202.764402108791,1.10128376375181,135.599678835429));
#208558=CARTESIAN_POINT('Ctrl Pts',(202.756627774674,1.23372905007338,135.565357959878));
#208559=CARTESIAN_POINT('Ctrl Pts',(202.748863021729,1.36601110941638,135.53107938174));
#208560=CARTESIAN_POINT('Ctrl Pts',(202.741098268784,1.49703714105001,135.491238526238));
#208561=CARTESIAN_POINT('Ctrl Pts',(202.733333515839,1.62630527593573,135.445945929931));
#208562=CARTESIAN_POINT('Ctrl Pts',(202.725576474956,1.75544501988741,135.40069831887));
#208563=CARTESIAN_POINT('Ctrl Pts',(202.717819434073,1.88282997506119,135.350009871036));
#208564=CARTESIAN_POINT('Ctrl Pts',(202.710062393191,2.00797122337188,135.294041522554));
#208565=CARTESIAN_POINT('Ctrl Pts',(202.702311201953,2.13301810169324,135.238115380238));
#208566=CARTESIAN_POINT('Ctrl Pts',(202.694560010715,2.25582428551557,135.17691742141));
#208567=CARTESIAN_POINT('Ctrl Pts',(202.686808819477,2.37591905240151,135.110657369874));
#208568=CARTESIAN_POINT('Ctrl Pts',(202.679060922702,2.49596277580801,135.044425480627));
#208569=CARTESIAN_POINT('Ctrl Pts',(202.671313025927,2.61329703275995,134.973135966364));
#208570=CARTESIAN_POINT('Ctrl Pts',(202.663565129152,2.72747421811156,134.897045244072));
#208571=CARTESIAN_POINT('Ctrl Pts',(202.65581885307,2.84162752005722,134.820970438319));
#208572=CARTESIAN_POINT('Ctrl Pts',(202.648072576988,2.95262473882447,134.740096638841));
#208573=CARTESIAN_POINT('Ctrl Pts',(202.640326300906,3.06004621322242,134.654724267332));
#208574=CARTESIAN_POINT('Ctrl Pts',(202.632579967643,3.1674684805811,134.569351265625));
#208575=CARTESIAN_POINT('Ctrl Pts',(202.62483363438,3.27131464482454,134.479479868875));
#208576=CARTESIAN_POINT('Ctrl Pts',(202.617087301116,3.37119749425472,134.385451305782));
#208577=CARTESIAN_POINT('Ctrl Pts',(202.609339233116,3.47110271175664,134.291401685645));
#208578=CARTESIAN_POINT('Ctrl Pts',(202.601591165115,3.56704256369362,134.193193314579));
#208579=CARTESIAN_POINT('Ctrl Pts',(202.593843097114,3.65866641892285,134.091204559335));
#208580=CARTESIAN_POINT('Ctrl Pts',(202.586086794374,3.75038765307602,133.989107409229));
#208581=CARTESIAN_POINT('Ctrl Pts',(202.578330491635,3.83778346561284,133.883222140185));
#208582=CARTESIAN_POINT('Ctrl Pts',(202.570574188895,3.92054294663494,133.7739609385));
#208583=CARTESIAN_POINT('Ctrl Pts',(202.562813746383,4.00334659888406,133.664641420822));
#208584=CARTESIAN_POINT('Ctrl Pts',(202.555053303871,4.08150876616667,133.551942701296));
#208585=CARTESIAN_POINT('Ctrl Pts',(202.547292861359,4.15476227066247,133.436305437804));
#208586=CARTESIAN_POINT('Ctrl Pts',(202.539519961095,4.22813336818707,133.320482543111));
#208587=CARTESIAN_POINT('Ctrl Pts',(202.531747060832,4.29657986120505,133.201712016897));
#208588=CARTESIAN_POINT('Ctrl Pts',(202.523974160569,4.35988045644892,133.080459356192));
#208589=CARTESIAN_POINT('Ctrl Pts',(202.516483824783,4.42087991581972,132.963614534721));
#208590=CARTESIAN_POINT('Ctrl Pts',(202.508993488998,4.47710098314102,132.844465187877));
#208591=CARTESIAN_POINT('Ctrl Pts',(202.501503153212,4.52838886767896,132.723443035176));
#208592=CARTESIAN_POINT('Ctrl Pts',(202.493728819094,4.58162134777368,132.597832291183));
#208593=CARTESIAN_POINT('Ctrl Pts',(202.485954484976,4.62970780184522,132.46980602598));
#208594=CARTESIAN_POINT('Ctrl Pts',(202.478180150858,4.67242258964327,132.339824783964));
#208595=CARTESIAN_POINT('Ctrl Pts',(202.470415397911,4.7150847352829,132.210003732212));
#208596=CARTESIAN_POINT('Ctrl Pts',(202.462650644965,4.75238826578558,132.078232865362));
#208597=CARTESIAN_POINT('Ctrl Pts',(202.454885892019,4.78415490621555,131.944994167762));
#208598=CARTESIAN_POINT('Ctrl Pts',(202.447128851135,4.81588999557021,131.811887804716));
#208599=CARTESIAN_POINT('Ctrl Pts',(202.439371810251,4.8420990486564,131.677316889991));
#208600=CARTESIAN_POINT('Ctrl Pts',(202.431614769367,4.86265319342588,131.541779754126));
#208601=CARTESIAN_POINT('Ctrl Pts',(202.423863578128,4.88319183815493,131.406344827869));
#208602=CARTESIAN_POINT('Ctrl Pts',(202.416112386889,4.89808400423516,131.269945515757));
#208603=CARTESIAN_POINT('Ctrl Pts',(202.40836119565,4.90725170126882,131.133091210749));
#208604=CARTESIAN_POINT('Ctrl Pts',(202.400613298874,4.91641550178662,130.996295072471));
#208605=CARTESIAN_POINT('Ctrl Pts',(202.392865402097,4.91985964633597,130.859044715197));
#208606=CARTESIAN_POINT('Ctrl Pts',(202.385117505321,4.91755792427646,130.721855321458));
#208607=CARTESIAN_POINT('Ctrl Pts',(202.377371229238,4.91525668368759,130.584694624784));
#208608=CARTESIAN_POINT('Ctrl Pts',(202.369624953155,4.907211973712,130.447595256941));
#208609=CARTESIAN_POINT('Ctrl Pts',(202.361878677072,4.89344971050554,130.311072676042));
#208610=CARTESIAN_POINT('Ctrl Pts',(202.354132343808,4.8796873457092,130.174549087364));
#208611=CARTESIAN_POINT('Ctrl Pts',(202.346386010544,4.86020738267642,130.038602683118));
#208612=CARTESIAN_POINT('Ctrl Pts',(202.338639677279,4.83508760939448,129.903743677918));
#208613=CARTESIAN_POINT('Ctrl Pts',(202.330891609277,4.80996221071351,129.76885447198));
#208614=CARTESIAN_POINT('Ctrl Pts',(202.323143541275,4.77919456014558,129.635053533938));
#208615=CARTESIAN_POINT('Ctrl Pts',(202.315395473273,4.74291346365742,129.502840376172));
#208616=CARTESIAN_POINT('Ctrl Pts',(202.307639170533,4.70659380718827,129.37048670069));
#208617=CARTESIAN_POINT('Ctrl Pts',(202.299882867792,4.66474910293164,129.239724554101));
#208618=CARTESIAN_POINT('Ctrl Pts',(202.292126565051,4.6175580804997,129.111038310469));
#208619=CARTESIAN_POINT('Ctrl Pts',(202.284366122538,4.57034187079823,128.982283383115));
#208620=CARTESIAN_POINT('Ctrl Pts',(202.276605680025,4.51777380687754,128.855606927377));
#208621=CARTESIAN_POINT('Ctrl Pts',(202.268845237512,4.46008021055639,128.731471913872));
#208622=CARTESIAN_POINT('Ctrl Pts',(202.261072337248,4.40229399935262,128.607137627823));
#208623=CARTESIAN_POINT('Ctrl Pts',(202.253299436983,4.33936599324112,128.485353284181));
#208624=CARTESIAN_POINT('Ctrl Pts',(202.245526536719,4.27156821364134,128.366556675755));
#208625=CARTESIAN_POINT('Ctrl Pts',(202.238036200946,4.20623505399508,128.252078623088));
#208626=CARTESIAN_POINT('Ctrl Pts',(202.230545865172,4.13638019427766,128.140375114719));
#208627=CARTESIAN_POINT('Ctrl Pts',(202.223055529399,4.06228318417237,128.03180973542));
#208628=CARTESIAN_POINT('Ctrl Pts',(202.215281195279,3.98537676351187,127.919128066919));
#208629=CARTESIAN_POINT('Ctrl Pts',(202.207506861159,3.90365654367928,127.80947024764));
#208630=CARTESIAN_POINT('Ctrl Pts',(202.199732527038,3.81738802965387,127.703275050614));
#208631=CARTESIAN_POINT('Ctrl Pts',(202.19196777409,3.73122583386185,127.597210729678));
#208632=CARTESIAN_POINT('Ctrl Pts',(202.184203021142,3.64052674103213,127.494600840736));
#208633=CARTESIAN_POINT('Ctrl Pts',(202.176438268194,3.54559989628898,127.395855895854));
#208634=CARTESIAN_POINT('Ctrl Pts',(202.168681227307,3.45076733422572,127.297209025842));
#208635=CARTESIAN_POINT('Ctrl Pts',(202.160924186421,3.35171564577153,127.202419740696));
#208636=CARTESIAN_POINT('Ctrl Pts',(202.153167145535,3.24879443203218,127.111865823948));
#208637=CARTESIAN_POINT('Ctrl Pts',(202.145415954294,3.14595083198053,127.021380194613));
#208638=CARTESIAN_POINT('Ctrl Pts',(202.137664763052,3.03924380716249,126.935123833573));
#208639=CARTESIAN_POINT('Ctrl Pts',(202.129913571811,2.92905976858584,126.853437695697));
#208640=CARTESIAN_POINT('Ctrl Pts',(202.122165675033,2.818922561165,126.771786276608));
#208641=CARTESIAN_POINT('Ctrl Pts',(202.114417778254,2.70531159267622,126.694701449615));
#208642=CARTESIAN_POINT('Ctrl Pts',(202.106669881476,2.58864613328299,126.622483735215));
#208643=CARTESIAN_POINT('Ctrl Pts',(202.098923605391,2.47200507778859,126.550281127204));
#208644=CARTESIAN_POINT('Ctrl Pts',(202.091177329306,2.35231113448206,126.482943812387));
#208645=CARTESIAN_POINT('Ctrl Pts',(202.08343105322,2.23001198118519,126.420728604467));
#208646=CARTESIAN_POINT('Ctrl Pts',(202.075684719954,2.10771192510372,126.358512937288));
#208647=CARTESIAN_POINT('Ctrl Pts',(202.067938386687,1.98280696912467,126.301419629723));
#208648=CARTESIAN_POINT('Ctrl Pts',(202.060192053421,1.85576841756085,126.249659019999));
#208649=CARTESIAN_POINT('Ctrl Pts',(202.052443985416,1.7287014165942,126.197886818844));
#208650=CARTESIAN_POINT('Ctrl Pts',(202.044695917412,1.5995002312647,126.151449839382));
#208651=CARTESIAN_POINT('Ctrl Pts',(202.036947849408,1.46865473825808,126.110509712148));
#208652=CARTESIAN_POINT('Ctrl Pts',(202.029191546665,1.33767018110433,126.06952607326));
#208653=CARTESIAN_POINT('Ctrl Pts',(202.021435243922,1.20503819899675,126.034051073798));
#208654=CARTESIAN_POINT('Ctrl Pts',(202.013678941179,1.07126291727623,126.004196159491));
#208655=CARTESIAN_POINT('Ctrl Pts',(202.005918498663,0.937416235660115,
125.974325310717));
#208656=CARTESIAN_POINT('Ctrl Pts',(201.998158056148,0.802425423148925,
125.950080593152));
#208657=CARTESIAN_POINT('Ctrl Pts',(201.990397613633,0.666802322505834,
125.931521842765));
#208658=CARTESIAN_POINT('Ctrl Pts',(201.982624713366,0.530961507621308,
125.912933300225));
#208659=CARTESIAN_POINT('Ctrl Pts',(201.974851813099,0.394486765759838,
125.900049001524));
#208660=CARTESIAN_POINT('Ctrl Pts',(201.967078912833,0.257893458632686,
125.892876725045));
#208661=CARTESIAN_POINT('Ctrl Pts',(201.959588577084,0.126265662529295,
125.885965178895));
#208662=CARTESIAN_POINT('Ctrl Pts',(201.952098241335,-0.00547192021256673,
125.884357576005));
#208663=CARTESIAN_POINT('Ctrl Pts',(201.944607905586,-0.136862291999976,
125.888015249762));
#208664=CARTESIAN_POINT('Ctrl Pts',(201.936833571467,-0.273234369901628,
125.891811605337));
#208665=CARTESIAN_POINT('Ctrl Pts',(201.929059237349,-0.409664373849437,
125.901292410854));
#208666=CARTESIAN_POINT('Ctrl Pts',(201.92128490323,-0.545639639740232,
125.916471456993));
#208667=CARTESIAN_POINT('Ctrl Pts',(201.913520150283,-0.681447328268266,
125.931631796315));
#208668=CARTESIAN_POINT('Ctrl Pts',(201.905755397337,-0.816801008994345,
125.952476360477));
#208669=CARTESIAN_POINT('Ctrl Pts',(201.89799064439,-0.951188206001152,
125.978966948728));
#208670=CARTESIAN_POINT('Ctrl Pts',(201.890233603505,-1.08544192774853,
126.005431226153));
#208671=CARTESIAN_POINT('Ctrl Pts',(201.882476562621,-1.21873069496959,
126.037530292947));
#208672=CARTESIAN_POINT('Ctrl Pts',(201.874719521736,-1.35054769974211,
126.075174221026));
#208673=CARTESIAN_POINT('Ctrl Pts',(201.866968330497,-1.48226530028765,
126.112789761526));
#208674=CARTESIAN_POINT('Ctrl Pts',(201.859217139257,-1.6125129730937,126.155941733518));
#208675=CARTESIAN_POINT('Ctrl Pts',(201.851465948017,-1.74079499858619,
126.204489332911));
#208676=CARTESIAN_POINT('Ctrl Pts',(201.84371805124,-1.86902250079471,126.253016298278));
#208677=CARTESIAN_POINT('Ctrl Pts',(201.835970154464,-1.99528565245025,
126.306934191786));
#208678=CARTESIAN_POINT('Ctrl Pts',(201.828222257687,-2.11910499138351,
126.366052708239));
#208679=CARTESIAN_POINT('Ctrl Pts',(201.820475981603,-2.24289842998043,
126.425158858373));
#208680=CARTESIAN_POINT('Ctrl Pts',(201.81272970552,-2.36424872005608,126.489463299298));
#208681=CARTESIAN_POINT('Ctrl Pts',(201.804983429436,-2.48269781617095,
126.558728201061));
#208682=CARTESIAN_POINT('Ctrl Pts',(201.797237096171,-2.60114778665004,
126.627993614122));
#208683=CARTESIAN_POINT('Ctrl Pts',(201.789490762906,-2.71669618293738,
126.702219363732));
#208684=CARTESIAN_POINT('Ctrl Pts',(201.781744429641,-2.82891129003388,
126.781122621173));
#208685=CARTESIAN_POINT('Ctrl Pts',(201.773996361638,-2.94115152692565,
126.860043548452));
#208686=CARTESIAN_POINT('Ctrl Pts',(201.766248293636,-3.05005666948663,
126.943643843122));
#208687=CARTESIAN_POINT('Ctrl Pts',(201.758500225633,-3.15522594305475,
127.031598723307));
#208688=CARTESIAN_POINT('Ctrl Pts',(201.750743922892,-3.26050699177834,
127.119647082985));
#208689=CARTESIAN_POINT('Ctrl Pts',(201.74298762015,-3.36204393957021,127.212059022098));
#208690=CARTESIAN_POINT('Ctrl Pts',(201.735231317409,-3.45947053192138,
127.30847064486));
#208691=CARTESIAN_POINT('Ctrl Pts',(201.727470874895,-3.55694912377835,
127.404933725407));
#208692=CARTESIAN_POINT('Ctrl Pts',(201.719710432381,-3.65031272280732,
127.505400457023));
#208693=CARTESIAN_POINT('Ctrl Pts',(201.711949989868,-3.73923432379541,
127.609472554699));
#208694=CARTESIAN_POINT('Ctrl Pts',(201.704177089603,-3.82829866963167,
127.713711718145));
#208695=CARTESIAN_POINT('Ctrl Pts',(201.696404189338,-3.9129065265913,127.821567505439));
#208696=CARTESIAN_POINT('Ctrl Pts',(201.688631289073,-3.99277278490735,
127.932610532582));
#208697=CARTESIAN_POINT('Ctrl Pts',(201.681140953306,-4.06973570361064,
128.039616866056));
#208698=CARTESIAN_POINT('Ctrl Pts',(201.67365061754,-4.14229560697238,128.14958247704));
#208699=CARTESIAN_POINT('Ctrl Pts',(201.666160281774,-4.21023800794793,
128.262101980265));
#208700=CARTESIAN_POINT('Ctrl Pts',(201.658128312424,-4.28309339110042,
128.382757879996));
#208701=CARTESIAN_POINT('Ctrl Pts',(201.650096343074,-4.35085732043947,
128.506711456361));
#208702=CARTESIAN_POINT('Ctrl Pts',(201.642064373724,-4.41322893384724,
128.633509761345));
#208703=CARTESIAN_POINT('Ctrl Pts',(201.634043232433,-4.47551646283025,
128.760137126988));
#208704=CARTESIAN_POINT('Ctrl Pts',(201.626022091142,-4.53242599296163,
128.889601270105));
#208705=CARTESIAN_POINT('Ctrl Pts',(201.618000949852,-4.58370062266684,
129.021421565253));
#208706=CARTESIAN_POINT('Ctrl Pts',(201.609992618133,-4.63489336800769,
129.153031346524));
#208707=CARTESIAN_POINT('Ctrl Pts',(201.601984286414,-4.68046901878164,
129.286989451782));
#208708=CARTESIAN_POINT('Ctrl Pts',(201.593975954695,-4.72021745497381,
129.422792580783));
#208709=CARTESIAN_POINT('Ctrl Pts',(201.590852754914,-4.73571909895888,
129.475754960174));
#208710=CARTESIAN_POINT('Ctrl Pts',(201.587729555133,-4.75033495592387,
129.528997715094));
#208711=CARTESIAN_POINT('Ctrl Pts',(201.584606355351,-4.76405452823405,
129.582490119308));
#208712=CARTESIAN_POINT('',(203.610140564065,-4.91824975435206,130.805915067923));
#208713=CARTESIAN_POINT('Ctrl Pts',(203.610140564008,-4.91824975435174,
130.80591506892));
#208714=CARTESIAN_POINT('Ctrl Pts',(203.60532859344,-4.91822305432427,130.890393366163));
#208715=CARTESIAN_POINT('Ctrl Pts',(203.600516622872,-4.91601993127815,
130.974834611061));
#208716=CARTESIAN_POINT('Ctrl Pts',(203.595704652304,-4.91164526425146,
131.059162227954));
#208717=CARTESIAN_POINT('Ctrl Pts',(203.587930318251,-4.90457744819619,
131.195403930679));
#208718=CARTESIAN_POINT('Ctrl Pts',(203.580155984198,-4.89182542922343,
131.331567131691));
#208719=CARTESIAN_POINT('Ctrl Pts',(203.572381650145,-4.87338772313762,
131.467138983592));
#208720=CARTESIAN_POINT('Ctrl Pts',(203.564616897265,-4.85497273987956,
131.60254375528));
#208721=CARTESIAN_POINT('Ctrl Pts',(203.556852144384,-4.83088606373339,
131.737358244241));
#208722=CARTESIAN_POINT('Ctrl Pts',(203.549087391504,-4.80117818244719,
131.871071038858));
#208723=CARTESIAN_POINT('Ctrl Pts',(203.541330350687,-4.77149980745165,
132.004651028024));
#208724=CARTESIAN_POINT('Ctrl Pts',(203.53357330987,-4.73621142210639,132.1371311212));
#208725=CARTESIAN_POINT('Ctrl Pts',(203.525816269053,-4.69541509058143,
132.268006814446));
#208726=CARTESIAN_POINT('Ctrl Pts',(203.518065077882,-4.65464952389258,
132.398783813296));
#208727=CARTESIAN_POINT('Ctrl Pts',(203.510313886711,-4.60838439436307,
132.527958448688));
#208728=CARTESIAN_POINT('Ctrl Pts',(203.50256269554,-4.55677236142872,132.655038522718));
#208729=CARTESIAN_POINT('Ctrl Pts',(203.494814798833,-4.50518226499348,
132.782064584306));
#208730=CARTESIAN_POINT('Ctrl Pts',(203.487066902126,-4.44824993194415,
132.906997493689));
#208731=CARTESIAN_POINT('Ctrl Pts',(203.479319005419,-4.38617711843204,
133.029362493575));
#208732=CARTESIAN_POINT('Ctrl Pts',(203.471572729406,-4.32411728922029,
133.151701897329));
#208733=CARTESIAN_POINT('Ctrl Pts',(203.463826453393,-4.25691929509247,
133.271474111561));
#208734=CARTESIAN_POINT('Ctrl Pts',(203.456080177379,-4.18483188932866,
133.388226930005));
#208735=CARTESIAN_POINT('Ctrl Pts',(203.448333844186,-4.11274395143813,
133.504980610282));
#208736=CARTESIAN_POINT('Ctrl Pts',(203.440587510992,-4.03576673529106,
133.618714517632));
#208737=CARTESIAN_POINT('Ctrl Pts',(203.432841177798,-3.95419334811849,
133.729003848491));
#208738=CARTESIAN_POINT('Ctrl Pts',(203.425093109867,-3.87260169315755,
133.839317877873));
#208739=CARTESIAN_POINT('Ctrl Pts',(203.417345041936,-3.78641205146594,
133.946185481521));
#208740=CARTESIAN_POINT('Ctrl Pts',(203.409596974005,-3.69595872886982,
134.049213794058));
#208741=CARTESIAN_POINT('Ctrl Pts',(203.401840671336,-3.60540927141139,
134.152351606306));
#208742=CARTESIAN_POINT('Ctrl Pts',(203.394084368667,-3.51058733926155,
134.251641682045));
#208743=CARTESIAN_POINT('Ctrl Pts',(203.386328065998,-3.41186551250551,
134.346726604738));
#208744=CARTESIAN_POINT('Ctrl Pts',(203.378567623557,-3.3130909949427,134.441862277113));
#208745=CARTESIAN_POINT('Ctrl Pts',(203.370807181116,-3.21041272778059,
134.532788065183));
#208746=CARTESIAN_POINT('Ctrl Pts',(203.363046738675,-3.10423672854745,
134.619186615647));
#208747=CARTESIAN_POINT('Ctrl Pts',(203.355273838482,-2.99789028617232,
134.705723860737));
#208748=CARTESIAN_POINT('Ctrl Pts',(203.34750093829,-2.8880352049204,134.787719111404));
#208749=CARTESIAN_POINT('Ctrl Pts',(203.339728038097,-2.77510758697802,
134.864897644019));
#208750=CARTESIAN_POINT('Ctrl Pts',(203.332237701562,-2.66628516014054,
134.939270550948));
#208751=CARTESIAN_POINT('Ctrl Pts',(203.324747365027,-2.55460996759745,
135.009170695082));
#208752=CARTESIAN_POINT('Ctrl Pts',(203.317257028492,-2.44049242510876,
135.074393379207));
#208753=CARTESIAN_POINT('Ctrl Pts',(203.309482694322,-2.32204809275828,
135.142088994682));
#208754=CARTESIAN_POINT('Ctrl Pts',(203.301708360151,-2.20059735556435,
135.204959896962));
#208755=CARTESIAN_POINT('Ctrl Pts',(203.293934025981,-2.0765708843453,135.262727630811));
#208756=CARTESIAN_POINT('Ctrl Pts',(203.286169272982,-1.95269726465683,
135.320424171095));
#208757=CARTESIAN_POINT('Ctrl Pts',(203.278404519984,-1.82625457798257,
135.373029893092));
#208758=CARTESIAN_POINT('Ctrl Pts',(203.270639766985,-1.69770037928056,
135.420310843109));
#208759=CARTESIAN_POINT('Ctrl Pts',(203.262882726048,-1.56927386241116,
135.467544833023));
#208760=CARTESIAN_POINT('Ctrl Pts',(203.25512568511,-1.43874037156367,135.509464441505));
#208761=CARTESIAN_POINT('Ctrl Pts',(203.247368644173,-1.30657952838765,
135.545882841335));
#208762=CARTESIAN_POINT('Ctrl Pts',(203.23961745288,-1.1745183487227,135.582273777769));
#208763=CARTESIAN_POINT('Ctrl Pts',(203.231866261587,-1.04083263478582,
135.613171659453));
#208764=CARTESIAN_POINT('Ctrl Pts',(203.224115070294,-0.906019002783906,
135.638438878113));
#208765=CARTESIAN_POINT('Ctrl Pts',(203.216367173464,-0.771262670161606,
135.663695357533));
#208766=CARTESIAN_POINT('Ctrl Pts',(203.208619276634,-0.635379756424377,
135.683325861913));
#208767=CARTESIAN_POINT('Ctrl Pts',(203.200871379803,-0.498878742470774,
135.697243516513));
#208768=CARTESIAN_POINT('Ctrl Pts',(203.193125103666,-0.362406281580614,
135.711158259841));
#208769=CARTESIAN_POINT('Ctrl Pts',(203.185378827528,-0.22531636634765,
135.719362490687));
#208770=CARTESIAN_POINT('Ctrl Pts',(203.17763255139,-0.0881239079495214,
135.721821063706));
#208771=CARTESIAN_POINT('Ctrl Pts',(203.169886218071,0.0490695631770811,
135.724279654873));
#208772=CARTESIAN_POINT('Ctrl Pts',(203.162139884752,0.186365188076857,
135.720992496577));
#208773=CARTESIAN_POINT('Ctrl Pts',(203.154393551432,0.323247135849997,
135.711976571536));
#208774=CARTESIAN_POINT('Ctrl Pts',(203.146645483375,0.4601597373901,135.702958627442));
#208775=CARTESIAN_POINT('Ctrl Pts',(203.138897415318,0.596658087415218,
135.688209389437));
#208776=CARTESIAN_POINT('Ctrl Pts',(203.131149347261,0.73223095668038,135.667797765158));
#208777=CARTESIAN_POINT('Ctrl Pts',(203.123393044465,0.867947914404447,
135.647364447162));
#208778=CARTESIAN_POINT('Ctrl Pts',(203.115636741669,1.00273703927327,135.621256779485));
#208779=CARTESIAN_POINT('Ctrl Pts',(203.107880438873,1.13609623798184,135.589595031944));
#208780=CARTESIAN_POINT('Ctrl Pts',(203.100119996304,1.26952661451173,135.557916385574));
#208781=CARTESIAN_POINT('Ctrl Pts',(203.092359553736,1.40152516805726,135.520677858664));
#208782=CARTESIAN_POINT('Ctrl Pts',(203.084599111167,1.53160543789726,135.478049508057));
#208783=CARTESIAN_POINT('Ctrl Pts',(203.076826210848,1.66189452412713,135.435352726641));
#208784=CARTESIAN_POINT('Ctrl Pts',(203.069053310528,1.79025880671704,135.387248968902));
#208785=CARTESIAN_POINT('Ctrl Pts',(203.061280410209,1.9162314290031,135.333956645139));
#208786=CARTESIAN_POINT('Ctrl Pts',(203.053790075032,2.03762461883292,135.282601635949));
#208787=CARTESIAN_POINT('Ctrl Pts',(203.046299739856,2.15679673695984,135.226428878422));
#208788=CARTESIAN_POINT('Ctrl Pts',(203.038809404679,2.27335372629928,135.16567302298));
#208789=CARTESIAN_POINT('Ctrl Pts',(203.031035070571,2.39433001860291,135.102613585972));
#208790=CARTESIAN_POINT('Ctrl Pts',(203.023260736462,2.51287217837938,135.034416900165));
#208791=CARTESIAN_POINT('Ctrl Pts',(203.015486402354,2.62851314525934,134.961294789248));
#208792=CARTESIAN_POINT('Ctrl Pts',(203.007721649418,2.74401159498189,134.888262794799));
#208793=CARTESIAN_POINT('Ctrl Pts',(202.999956896482,2.85661563863572,134.810317659964));
#208794=CARTESIAN_POINT('Ctrl Pts',(202.992192143545,2.96588112472585,134.727717880994));
#208795=CARTESIAN_POINT('Ctrl Pts',(202.984435102671,3.07503808679438,134.64520014129));
#208796=CARTESIAN_POINT('Ctrl Pts',(202.976678061797,3.18086278023441,134.558037191785));
#208797=CARTESIAN_POINT('Ctrl Pts',(202.968921020923,3.28293877480054,134.466531567073));
#208798=CARTESIAN_POINT('Ctrl Pts',(202.961169829694,3.38493779306489,134.375094947464));
#208799=CARTESIAN_POINT('Ctrl Pts',(202.953418638464,3.483193449336,134.279322430943));
#208800=CARTESIAN_POINT('Ctrl Pts',(202.945667447235,3.57732153668663,134.179557454146));
#208801=CARTESIAN_POINT('Ctrl Pts',(202.937919550469,3.67140961708933,134.079834880125));
#208802=CARTESIAN_POINT('Ctrl Pts',(202.930171653703,3.76137335005203,133.976123504614));
#208803=CARTESIAN_POINT('Ctrl Pts',(202.922423756936,3.84686479905085,133.868804169065));
#208804=CARTESIAN_POINT('Ctrl Pts',(202.914677480863,3.93233836508166,133.761507282408));
#208805=CARTESIAN_POINT('Ctrl Pts',(202.90693120479,4.01334126447339,133.650604242471));
#208806=CARTESIAN_POINT('Ctrl Pts',(202.899184928717,4.08956560638427,133.536509261688));
#208807=CARTESIAN_POINT('Ctrl Pts',(202.891438595462,4.16579051096613,133.422413438681));
#208808=CARTESIAN_POINT('Ctrl Pts',(202.883692262207,4.23723657049395,133.305125952902));
#208809=CARTESIAN_POINT('Ctrl Pts',(202.875945928953,4.30363925381155,133.185089967062));
#208810=CARTESIAN_POINT('Ctrl Pts',(202.868197860961,4.37005680754998,133.065027099995));
#208811=CARTESIAN_POINT('Ctrl Pts',(202.860449792968,4.43142854843043,132.942214850122));
#208812=CARTESIAN_POINT('Ctrl Pts',(202.852701724976,4.48753611850486,132.817120575339));
#208813=CARTESIAN_POINT('Ctrl Pts',(202.844945422245,4.54370332037339,132.69189334887));
#208814=CARTESIAN_POINT('Ctrl Pts',(202.837189119514,4.59459501491842,132.564379609861));
#208815=CARTESIAN_POINT('Ctrl Pts',(202.829432816783,4.64004099484783,132.435066792397));
#208816=CARTESIAN_POINT('Ctrl Pts',(202.821672374279,4.68551123066541,132.305684956788));
#208817=CARTESIAN_POINT('Ctrl Pts',(202.813911931776,4.72552984631434,132.174502503168));
#208818=CARTESIAN_POINT('Ctrl Pts',(202.806151489272,4.75997697153195,132.04202062459));
#208819=CARTESIAN_POINT('Ctrl Pts',(202.798378589017,4.79447939433392,131.909326074335));
#208820=CARTESIAN_POINT('Ctrl Pts',(202.790605688762,4.82339237153089,131.775328313116));
#208821=CARTESIAN_POINT('Ctrl Pts',(202.782832788507,4.84664731046149,131.640538176758));
#208822=CARTESIAN_POINT('Ctrl Pts',(202.775342452627,4.86905687417027,131.510647999147));
#208823=CARTESIAN_POINT('Ctrl Pts',(202.767852116746,4.8862125852588,131.380022361244));
#208824=CARTESIAN_POINT('Ctrl Pts',(202.760361780866,4.89809886429187,131.249119628855));
#208825=CARTESIAN_POINT('Ctrl Pts',(202.752587446755,4.91043581499945,131.113253681868));
#208826=CARTESIAN_POINT('Ctrl Pts',(202.744813112644,4.91713494470752,130.976658831053));
#208827=CARTESIAN_POINT('Ctrl Pts',(202.737038778533,4.91812200914719,130.839842523405));
#208828=CARTESIAN_POINT('Ctrl Pts',(202.729274025594,4.91910785711814,130.703194829631));
#208829=CARTESIAN_POINT('Ctrl Pts',(202.721509272656,4.91439564375304,130.566326609267));
#208830=CARTESIAN_POINT('Ctrl Pts',(202.713744519717,4.90396277453586,130.429751263082));
#208831=CARTESIAN_POINT('Ctrl Pts',(202.70598747884,4.89354026739166,130.293311565459));
#208832=CARTESIAN_POINT('Ctrl Pts',(202.698230437964,4.87740844109174,130.157164550445));
#208833=CARTESIAN_POINT('Ctrl Pts',(202.690473397087,4.8555967358373,130.021824099935));
#208834=CARTESIAN_POINT('Ctrl Pts',(202.682722205856,4.83380147895985,129.886585710714));
#208835=CARTESIAN_POINT('Ctrl Pts',(202.674971014624,4.80633493061361,129.752153059763));
#208836=CARTESIAN_POINT('Ctrl Pts',(202.667219823393,4.77327836053893,129.619035027143));
#208837=CARTESIAN_POINT('Ctrl Pts',(202.659471926624,4.74023584038906,129.485973573241));
#208838=CARTESIAN_POINT('Ctrl Pts',(202.651724029856,4.70160811803909,129.35422600501));
#208839=CARTESIAN_POINT('Ctrl Pts',(202.643976133088,4.6575275379995,129.224290905409));
#208840=CARTESIAN_POINT('Ctrl Pts',(202.636229857012,4.61345617866757,129.094382985432));
#208841=CARTESIAN_POINT('Ctrl Pts',(202.628483580937,4.56393435592693,128.966287149981));
#208842=CARTESIAN_POINT('Ctrl Pts',(202.620737304862,4.50914413590637,128.840486328279));
#208843=CARTESIAN_POINT('Ctrl Pts',(202.612990971605,4.45435351143753,128.714684577946));
#208844=CARTESIAN_POINT('Ctrl Pts',(202.605244638349,4.39429456820026,128.591178233612));
#208845=CARTESIAN_POINT('Ctrl Pts',(202.597498305092,4.3291971659843,128.470429393101));
#208846=CARTESIAN_POINT('Ctrl Pts',(202.589750237099,4.26408518565718,128.349653511726));
#208847=CARTESIAN_POINT('Ctrl Pts',(202.582002169105,4.19393268660458,128.231636707049));
#208848=CARTESIAN_POINT('Ctrl Pts',(202.574254101111,4.11901484245543,128.116815308156));
#208849=CARTESIAN_POINT('Ctrl Pts',(202.566497798378,4.04401737473066,128.001871875715));
#208850=CARTESIAN_POINT('Ctrl Pts',(202.558741495645,3.9642446586756,127.890130961117));
#208851=CARTESIAN_POINT('Ctrl Pts',(202.550985192912,3.88001478519079,127.781999234607));
#208852=CARTESIAN_POINT('Ctrl Pts',(202.543224750407,3.79573995568691,127.67380979494));
#208853=CARTESIAN_POINT('Ctrl Pts',(202.535464307902,3.70700348138614,127.569233679702));
#208854=CARTESIAN_POINT('Ctrl Pts',(202.527703865397,3.61416223739328,127.468642646229));
#208855=CARTESIAN_POINT('Ctrl Pts',(202.519930965141,3.52117195639349,127.367890135099));
#208856=CARTESIAN_POINT('Ctrl Pts',(202.512158064885,3.42406401521649,127.2711357655));
#208857=CARTESIAN_POINT('Ctrl Pts',(202.504385164629,3.32323111850202,127.178713365623));
#208858=CARTESIAN_POINT('Ctrl Pts',(202.49689482877,3.22606375019959,127.089650751528));
#208859=CARTESIAN_POINT('Ctrl Pts',(202.489404492912,3.12543778266822,127.004610818164));
#208860=CARTESIAN_POINT('Ctrl Pts',(202.481914157053,3.02173043097238,126.923854430864));
#208861=CARTESIAN_POINT('Ctrl Pts',(202.474139822926,2.91409098479571,126.84003614159));
#208862=CARTESIAN_POINT('Ctrl Pts',(202.466365488799,2.80279091121412,126.760567120498));
#208863=CARTESIAN_POINT('Ctrl Pts',(202.458591154673,2.68821700891863,126.685784118888));
#208864=CARTESIAN_POINT('Ctrl Pts',(202.450826401718,2.57378430871652,126.611093280644));
#208865=CARTESIAN_POINT('Ctrl Pts',(202.443061648763,2.45608613190742,126.541077182797));
#208866=CARTESIAN_POINT('Ctrl Pts',(202.435296895808,2.33554220421387,126.476032340409));
#208867=CARTESIAN_POINT('Ctrl Pts',(202.427539854915,2.21511800244725,126.411052101475));
#208868=CARTESIAN_POINT('Ctrl Pts',(202.419782814022,2.09185401638329,126.351033476568));
#208869=CARTESIAN_POINT('Ctrl Pts',(202.412025773129,1.96619850256614,126.29622946253));
#208870=CARTESIAN_POINT('Ctrl Pts',(202.404274581881,1.8406377465481,126.241466776625));
#208871=CARTESIAN_POINT('Ctrl Pts',(202.396523390633,1.71268940938756,126.191911030093));
#208872=CARTESIAN_POINT('Ctrl Pts',(202.388772199385,1.58282555457417,126.147768910503));
#208873=CARTESIAN_POINT('Ctrl Pts',(202.3810243026,1.45301689536158,126.103645552491));
#208874=CARTESIAN_POINT('Ctrl Pts',(202.373276405815,1.3212947071609,126.064931370595));
#208875=CARTESIAN_POINT('Ctrl Pts',(202.36552850903,1.18814999737997,126.031784515897));
#208876=CARTESIAN_POINT('Ctrl Pts',(202.357782232937,1.05503313860108,125.998644594806));
#208877=CARTESIAN_POINT('Ctrl Pts',(202.350035956845,0.92049472925159,125.97106977892));
#208878=CARTESIAN_POINT('Ctrl Pts',(202.342289680753,0.785039482555496,
125.949167925887));
#208879=CARTESIAN_POINT('Ctrl Pts',(202.33454334748,0.649583235958816,125.927265911181));
#208880=CARTESIAN_POINT('Ctrl Pts',(202.326797014206,0.513210524463309,
125.911037005295));
#208881=CARTESIAN_POINT('Ctrl Pts',(202.319050680933,0.376434368889621,
125.900537595839));
#208882=CARTESIAN_POINT('Ctrl Pts',(202.311302612921,0.239627583243728,
125.890035835114));
#208883=CARTESIAN_POINT('Ctrl Pts',(202.30355454491,0.102417563480344,125.885266153919));
#208884=CARTESIAN_POINT('Ctrl Pts',(202.295806476899,-0.0346798563142518,
125.886232887416));
#208885=CARTESIAN_POINT('Ctrl Pts',(202.288050174149,-0.17192298487841,
125.887200648369));
#208886=CARTESIAN_POINT('Ctrl Pts',(202.280293871399,-0.309052882836018,
125.893917000127));
#208887=CARTESIAN_POINT('Ctrl Pts',(202.272537568649,-0.445555471089543,
125.906334139005));
#208888=CARTESIAN_POINT('Ctrl Pts',(202.264777126127,-0.58213091488482,
125.918757905285));
#208889=CARTESIAN_POINT('Ctrl Pts',(202.257016683604,-0.718077994486212,
125.936888469828));
#208890=CARTESIAN_POINT('Ctrl Pts',(202.249256241082,-0.852891040206172,
125.960626527421));
#208891=CARTESIAN_POINT('Ctrl Pts',(202.241483340808,-0.987920499794184,
125.984402691451));
#208892=CARTESIAN_POINT('Ctrl Pts',(202.233710440535,-1.12181190557149,
126.013804252784));
#208893=CARTESIAN_POINT('Ctrl Pts',(202.225937540261,-1.25407213197427,
126.048681260176));
#208894=CARTESIAN_POINT('Ctrl Pts',(202.218447204587,-1.38152436436558,
126.082290400067));
#208895=CARTESIAN_POINT('Ctrl Pts',(202.210956868914,-1.50746165896199,
126.120983714381));
#208896=CARTESIAN_POINT('Ctrl Pts',(202.20346653324,-1.63146064844767,126.164584845498));
#208897=CARTESIAN_POINT('Ctrl Pts',(202.195692103635,-1.76016267956143,
126.209839683114));
#208898=CARTESIAN_POINT('Ctrl Pts',(202.187917674029,-1.88718416540828,
126.260525329425));
#208899=CARTESIAN_POINT('Ctrl Pts',(202.180143244423,-2.01203269537097,
126.316498376447));
#208900=CARTESIAN_POINT('Ctrl Pts',(202.172378418318,-2.1367270040091,126.372402281787));
#208901=CARTESIAN_POINT('Ctrl Pts',(202.164613592212,-2.2592533441934,126.433580433836));
#208902=CARTESIAN_POINT('Ctrl Pts',(202.156848766106,-2.37913536422814,
126.499839972804));
#208903=CARTESIAN_POINT('Ctrl Pts',(202.149091674296,-2.49889797360211,
126.566033512757));
#208904=CARTESIAN_POINT('Ctrl Pts',(202.141334582486,-2.61602116454483,
126.637298179153));
#208905=CARTESIAN_POINT('Ctrl Pts',(202.133577490676,-2.73004978163739,
126.713393586132));
#208906=CARTESIAN_POINT('Ctrl Pts',(202.125826270674,-2.84399208364077,
126.78943139194));
#208907=CARTESIAN_POINT('Ctrl Pts',(202.118075050671,-2.95484415052419,
126.870292443658));
#208908=CARTESIAN_POINT('Ctrl Pts',(202.110323830669,-3.06217692439492,
126.955691296073));
#208909=CARTESIAN_POINT('Ctrl Pts',(202.102576019855,-3.16946249051467,
127.041052587846));
#208910=CARTESIAN_POINT('Ctrl Pts',(202.094828209041,-3.27323153754679,
127.130947467042));
#208911=CARTESIAN_POINT('Ctrl Pts',(202.087080398227,-3.37308562112851,
127.225048329565));
#208912=CARTESIAN_POINT('Ctrl Pts',(202.079334239672,-3.47291841033375,
127.319129124614));
#208913=CARTESIAN_POINT('Ctrl Pts',(202.071588081117,-3.568837612584,127.417413850761));
#208914=CARTESIAN_POINT('Ctrl Pts',(202.063841922562,-3.66047969139515,
127.519536194346));
#208915=CARTESIAN_POINT('Ctrl Pts',(202.056095738413,-3.75212207299657,
127.621658875349));
#208916=CARTESIAN_POINT('Ctrl Pts',(202.048349554264,-3.83948704196994,
127.727618908041));
#208917=CARTESIAN_POINT('Ctrl Pts',(202.040603370115,-3.92224987613099,
127.837015175645));
#208918=CARTESIAN_POINT('Ctrl Pts',(202.032855482865,-4.0050309067957,127.946435495465));
#208919=CARTESIAN_POINT('Ctrl Pts',(202.025107595616,-4.08320755361812,
128.059293241692));
#208920=CARTESIAN_POINT('Ctrl Pts',(202.017359708366,-4.1564973670384,128.175156802663));
#208921=CARTESIAN_POINT('Ctrl Pts',(202.00960402534,-4.22986092326722,128.291136943332));
#208922=CARTESIAN_POINT('Ctrl Pts',(202.001848342314,-4.29832761616902,
128.410128608468));
#208923=CARTESIAN_POINT('Ctrl Pts',(201.994092659288,-4.36165984536912,
128.531673561283));
#208924=CARTESIAN_POINT('Ctrl Pts',(201.986332849536,-4.42502577306113,
128.653283187041));
#208925=CARTESIAN_POINT('Ctrl Pts',(201.978573039783,-4.48325162754233,
128.777448453866));
#208926=CARTESIAN_POINT('Ctrl Pts',(201.97081323003,-4.5361476689452,128.903690370516));
#208927=CARTESIAN_POINT('Ctrl Pts',(201.9630419948,-4.58912159402284,129.030118164673));
#208928=CARTESIAN_POINT('Ctrl Pts',(201.955270759571,-4.63674989270561,
129.158628350682));
#208929=CARTESIAN_POINT('Ctrl Pts',(201.947499524341,-4.67889225145815,
129.28872531785));
#208930=CARTESIAN_POINT('Ctrl Pts',(201.941698877603,-4.71034837504711,
129.385832988111));
#208931=CARTESIAN_POINT('Ctrl Pts',(201.935898230865,-4.73874903929908,
129.483824402015));
#208932=CARTESIAN_POINT('Ctrl Pts',(201.930097584127,-4.76405452823404,
129.582490119308));
#208933=CARTESIAN_POINT('Ctrl Pts',(203.680274487341,-4.76405452823405,
129.582490119308));
#208934=CARTESIAN_POINT('Ctrl Pts',(203.672576598541,-4.7978764752882,129.714361377553));
#208935=CARTESIAN_POINT('Ctrl Pts',(203.664878709741,-4.82619293906168,
129.847536976704));
#208936=CARTESIAN_POINT('Ctrl Pts',(203.65718082094,-4.84892836211919,129.981513850825));
#208937=CARTESIAN_POINT('Ctrl Pts',(203.649340778128,-4.87208363166798,
130.1179648254));
#208938=CARTESIAN_POINT('Ctrl Pts',(203.641500735315,-4.88944965601479,
130.255246526921));
#208939=CARTESIAN_POINT('Ctrl Pts',(203.633660692502,-4.90100205051574,
130.392824515455));
#208940=CARTESIAN_POINT('Ctrl Pts',(203.62582064969,-4.9125544450167,130.530402503989));
#208941=CARTESIAN_POINT('Ctrl Pts',(203.617980606877,-4.91829325611943,
130.668276348449));
#208942=CARTESIAN_POINT('Ctrl Pts',(203.610140564065,-4.91824975435206,
130.805915067923));
#208943=CARTESIAN_POINT('Origin',(213.235140564004,0.,130.804360617566));
#208944=CARTESIAN_POINT('',(205.430026442963,-4.76405452823405,129.582490119308));
#208945=CARTESIAN_POINT('',(205.084976592678,-4.76405452823405,129.582490119308));
#208946=CARTESIAN_POINT('',(213.235140564004,-4.76405452823405,129.582490119308));
#208947=CARTESIAN_POINT('',(205.014859436024,-4.91824993440617,130.805163869501));
#208948=CARTESIAN_POINT('Ctrl Pts',(205.084976592678,-4.76405452823405,
129.582490119308));
#208949=CARTESIAN_POINT('Ctrl Pts',(205.077250789112,-4.79798664166829,
129.714790914597));
#208950=CARTESIAN_POINT('Ctrl Pts',(205.069524985546,-4.82637681902747,
129.848402380795));
#208951=CARTESIAN_POINT('Ctrl Pts',(205.06179918198,-4.84914957344003,129.982818484193));
#208952=CARTESIAN_POINT('Ctrl Pts',(205.053975890988,-4.87220968401055,
130.118930706311));
#208953=CARTESIAN_POINT('Ctrl Pts',(205.046152599995,-4.88950959216643,
130.255867593678));
#208954=CARTESIAN_POINT('Ctrl Pts',(205.038329309002,-4.90102524937068,
130.393100885121));
#208955=CARTESIAN_POINT('Ctrl Pts',(205.030506018009,-4.91254090657492,
130.530334176563));
#208956=CARTESIAN_POINT('Ctrl Pts',(205.022682727017,-4.9182723584033,130.667863456436));
#208957=CARTESIAN_POINT('Ctrl Pts',(205.014859436024,-4.91824993440617,
130.805163869501));
#208958=CARTESIAN_POINT('Ctrl Pts',(205.014859435991,-4.91824993440608,
130.80516387008));
#208959=CARTESIAN_POINT('Ctrl Pts',(205.012416879836,-4.91824293327168,
130.848031247661));
#208960=CARTESIAN_POINT('Ctrl Pts',(205.009974323682,-4.91767549764493,
130.890893474637));
#208961=CARTESIAN_POINT('Ctrl Pts',(205.007531767528,-4.91654795620673,
130.933740897437));
#208962=CARTESIAN_POINT('Ctrl Pts',(204.999757433917,-4.91295914074164,
131.070118584653));
#208963=CARTESIAN_POINT('Ctrl Pts',(204.991983100306,-4.9036859709115,131.206562848942));
#208964=CARTESIAN_POINT('Ctrl Pts',(204.984208766695,-4.88871387579036,
131.342561047847));
#208965=CARTESIAN_POINT('Ctrl Pts',(204.976444014264,-4.87376023245488,
131.478391640977));
#208966=CARTESIAN_POINT('Ctrl Pts',(204.968679261833,-4.85312168071783,
131.613776877648));
#208967=CARTESIAN_POINT('Ctrl Pts',(204.960914509402,-4.82683564131106,
131.748204224457));
#208968=CARTESIAN_POINT('Ctrl Pts',(204.95315746904,-4.80057570959591,131.882498055994));
#208969=CARTESIAN_POINT('Ctrl Pts',(204.945400428679,-4.76867952725585,
132.015835509765));
#208970=CARTESIAN_POINT('Ctrl Pts',(204.937643388317,-4.73123625092355,
132.147709641627));
#208971=CARTESIAN_POINT('Ctrl Pts',(204.929892197607,-4.69382121089179,
132.27948432606));
#208972=CARTESIAN_POINT('Ctrl Pts',(204.922141006897,-4.65086750945265,
132.409797510464));
#208973=CARTESIAN_POINT('Ctrl Pts',(204.914389816187,-4.60251519606229,
132.538153261603));
#208974=CARTESIAN_POINT('Ctrl Pts',(204.906641919949,-4.55418343374924,
132.666454457979));
#208975=CARTESIAN_POINT('Ctrl Pts',(204.898894023711,-4.50045776072558,
132.792799510701));
#208976=CARTESIAN_POINT('Ctrl Pts',(204.891146127472,-4.44152775223612,
132.916708668579));
#208977=CARTESIAN_POINT('Ctrl Pts',(204.883399851932,-4.38261007067356,
133.040591907248));
#208978=CARTESIAN_POINT('Ctrl Pts',(204.875653576392,-4.31849038681639,
133.162039911728));
#208979=CARTESIAN_POINT('Ctrl Pts',(204.867907300851,-4.2494058332061,133.280594275203));
#208980=CARTESIAN_POINT('Ctrl Pts',(204.860160968134,-4.18032076967024,
133.399149513749));
#208981=CARTESIAN_POINT('Ctrl Pts',(204.852414635417,-4.10627096009826,
133.514810730874));
#208982=CARTESIAN_POINT('Ctrl Pts',(204.8446683027,-4.02753857581953,133.627145781688));
#208983=CARTESIAN_POINT('Ctrl Pts',(204.83692023525,-3.94878856000942,133.7395059891));
#208984=CARTESIAN_POINT('Ctrl Pts',(204.829172167799,-3.86535410719281,
133.848538227898));
#208985=CARTESIAN_POINT('Ctrl Pts',(204.821424100349,-3.77755938889782,
133.953841229643));
#208986=CARTESIAN_POINT('Ctrl Pts',(204.813667798163,-3.68967136136312,
134.059256148634));
#208987=CARTESIAN_POINT('Ctrl Pts',(204.805911495977,-3.5974140619154,134.160933612335));
#208988=CARTESIAN_POINT('Ctrl Pts',(204.798155193791,-3.50115082848458,
134.258506812894));
#208989=CARTESIAN_POINT('Ctrl Pts',(204.790394751835,-3.40483621649768,
134.356132091179));
#208990=CARTESIAN_POINT('Ctrl Pts',(204.782634309879,-3.30451169605726,
134.449648474981));
#208991=CARTESIAN_POINT('Ctrl Pts',(204.774873867924,-3.20057505400699,
134.538728353364));
#208992=CARTESIAN_POINT('Ctrl Pts',(204.767100968216,-3.09647156360682,
134.627951230698));
#208993=CARTESIAN_POINT('Ctrl Pts',(204.759328068508,-2.98874467176853,
134.712723128926));
#208994=CARTESIAN_POINT('Ctrl Pts',(204.7515551688,-2.87782332804817,134.792758285182));
#208995=CARTESIAN_POINT('Ctrl Pts',(204.744064827105,-2.77093416223283,
134.869884028534));
#208996=CARTESIAN_POINT('Ctrl Pts',(204.73657448541,-2.66107901674024,134.942611258251));
#208997=CARTESIAN_POINT('Ctrl Pts',(204.729084143715,-2.54866295096712,
135.010724870085));
#208998=CARTESIAN_POINT('Ctrl Pts',(204.721309809264,-2.43198468332284,
135.08142097724));
#208999=CARTESIAN_POINT('Ctrl Pts',(204.713535474812,-2.31217786981156,
135.147370661178));
#209000=CARTESIAN_POINT('Ctrl Pts',(204.70576114036,-2.18966593526101,135.208284567234));
#209001=CARTESIAN_POINT('Ctrl Pts',(204.697996387077,-2.0673049856553,135.269123402377));
#209002=CARTESIAN_POINT('Ctrl Pts',(204.690231633794,-1.94224589503469,
135.324938635623));
#209003=CARTESIAN_POINT('Ctrl Pts',(204.682466880511,-1.8149400992257,135.375484713313));
#209004=CARTESIAN_POINT('Ctrl Pts',(204.674709839286,-1.68776074526766,
135.425980587951));
#209005=CARTESIAN_POINT('Ctrl Pts',(204.666952798062,-1.55833948784361,
135.471217578389));
#209006=CARTESIAN_POINT('Ctrl Pts',(204.659195756837,-1.42715102488418,
135.510996678987));
#209007=CARTESIAN_POINT('Ctrl Pts',(204.651444565255,-1.29606149211033,
135.550745781873));
#209008=CARTESIAN_POINT('Ctrl Pts',(204.643693373672,-1.16320777901492,
135.585045074249));
#209009=CARTESIAN_POINT('Ctrl Pts',(204.635942182089,-1.02908282854748,
135.613744319714));
#209010=CARTESIAN_POINT('Ctrl Pts',(204.628194284967,-0.895014884701764,
135.642431367248));
#209011=CARTESIAN_POINT('Ctrl Pts',(204.620446387844,-0.759677159628549,
135.665523020208));
#209012=CARTESIAN_POINT('Ctrl Pts',(204.612698490721,-0.623575751751765,
135.682919456437));
#209013=CARTESIAN_POINT('Ctrl Pts',(204.604952214289,-0.487502813319543,
135.700312253712));
#209014=CARTESIAN_POINT('Ctrl Pts',(204.597205937857,-0.350666897391173,
135.712012154308));
#209015=CARTESIAN_POINT('Ctrl Pts',(204.589459661425,-0.213581850635355,
135.717970884526));
#209016=CARTESIAN_POINT('Ctrl Pts',(204.58171332781,-0.0764957919198511,
135.723929658732));
#209017=CARTESIAN_POINT('Ctrl Pts',(204.573966994196,0.0608390106965075,
135.724147161014));
#209018=CARTESIAN_POINT('Ctrl Pts',(204.566220660581,0.197906460888714,
135.718627205292));
#209019=CARTESIAN_POINT('Ctrl Pts',(204.558472592227,0.335004606408075,
135.713106013413));
#209020=CARTESIAN_POINT('Ctrl Pts',(204.550724523873,0.471834889791658,
135.701844822528));
#209021=CARTESIAN_POINT('Ctrl Pts',(204.54297645552,0.607884489820787,135.684899471989));
#209022=CARTESIAN_POINT('Ctrl Pts',(204.535220152427,0.744078684979407,
135.667936111731));
#209023=CARTESIAN_POINT('Ctrl Pts',(204.527463849334,0.879490150743396,
135.645276572288));
#209024=CARTESIAN_POINT('Ctrl Pts',(204.519707546241,1.01361388816882,135.617028271603));
#209025=CARTESIAN_POINT('Ctrl Pts',(204.511947103376,1.14780921147885,135.588764893948));
#209026=CARTESIAN_POINT('Ctrl Pts',(204.50418666051,1.28071505826876,135.554906907859));
#209027=CARTESIAN_POINT('Ctrl Pts',(204.496426217644,1.41184078659271,135.515611901016));
#209028=CARTESIAN_POINT('Ctrl Pts',(204.48865331703,1.54317700952478,135.476253814356));
#209029=CARTESIAN_POINT('Ctrl Pts',(204.480880416416,1.67272703389122,135.431441393526));
#209030=CARTESIAN_POINT('Ctrl Pts',(204.473107515801,1.80001858150718,135.381381064181));
#209031=CARTESIAN_POINT('Ctrl Pts',(204.465617183835,1.9226826930735,135.333140580513));
#209032=CARTESIAN_POINT('Ctrl Pts',(204.458126851868,2.04324940016541,135.280027243014));
#209033=CARTESIAN_POINT('Ctrl Pts',(204.450636519902,2.16131878660124,135.222265569598));
#209034=CARTESIAN_POINT('Ctrl Pts',(204.442862185831,2.28386487105517,135.162313814766));
#209035=CARTESIAN_POINT('Ctrl Pts',(204.435087851759,2.40410871112534,135.097164368467));
#209036=CARTESIAN_POINT('Ctrl Pts',(204.427313517688,2.52157799309945,135.027017066677));
#209037=CARTESIAN_POINT('Ctrl Pts',(204.419548764789,2.63890250468257,134.956956215167));
#209038=CARTESIAN_POINT('Ctrl Pts',(204.411784011889,2.75345892929808,134.881909962079));
#209039=CARTESIAN_POINT('Ctrl Pts',(204.40401925899,2.86479666362884,134.802125385353));
#209040=CARTESIAN_POINT('Ctrl Pts',(204.396262218153,2.9760238157537,134.722420051793));
#209041=CARTESIAN_POINT('Ctrl Pts',(204.388505177315,3.08403832372975,134.637985986342));
#209042=CARTESIAN_POINT('Ctrl Pts',(204.380748136478,3.18841617266462,134.549114998349));
#209043=CARTESIAN_POINT('Ctrl Pts',(204.372996945285,3.29271530945384,134.460311028657));
#209044=CARTESIAN_POINT('Ctrl Pts',(204.365245754092,3.39338294937173,134.3670770487));
#209045=CARTESIAN_POINT('Ctrl Pts',(204.357494562899,3.49002624658722,134.269746578845));
#209046=CARTESIAN_POINT('Ctrl Pts',(204.349746666169,3.58662846782897,134.172457477031));
#209047=CARTESIAN_POINT('Ctrl Pts',(204.341998769439,3.67920947343216,134.07107562512));
#209048=CARTESIAN_POINT('Ctrl Pts',(204.334250872709,3.76741172163867,133.965972861684));
#209049=CARTESIAN_POINT('Ctrl Pts',(204.326504596671,3.85559551983956,133.860892083477));
#209050=CARTESIAN_POINT('Ctrl Pts',(204.318758320634,3.9394021313356,133.752092241188));
#209051=CARTESIAN_POINT('Ctrl Pts',(204.311012044596,4.01851319542896,133.639979555411));
#209052=CARTESIAN_POINT('Ctrl Pts',(204.303265711377,4.09762484350567,133.527866042038));
#209053=CARTESIAN_POINT('Ctrl Pts',(204.295519378158,4.17204064960371,133.412439955821));
#209054=CARTESIAN_POINT('Ctrl Pts',(204.287773044939,4.24148485981986,133.294137564688));
#209055=CARTESIAN_POINT('Ctrl Pts',(204.280024976982,4.31094462158894,133.175808680548));
#209056=CARTESIAN_POINT('Ctrl Pts',(204.272276909025,4.37543037414788,133.054602546852));
#209057=CARTESIAN_POINT('Ctrl Pts',(204.264528841068,4.43471190433788,132.930980797105));
#209058=CARTESIAN_POINT('Ctrl Pts',(204.256772538371,4.49405643965077,132.807227660677));
#209059=CARTESIAN_POINT('Ctrl Pts',(204.249016235674,4.54818553428607,132.681054132738));
#209060=CARTESIAN_POINT('Ctrl Pts',(204.241259932977,4.59691659774419,132.552943145182));
#209061=CARTESIAN_POINT('Ctrl Pts',(204.233499490508,4.64567367044088,132.424763780927));
#209062=CARTESIAN_POINT('Ctrl Pts',(204.225739048038,4.68902684761736,132.2946452673));
#209063=CARTESIAN_POINT('Ctrl Pts',(204.217978605568,4.72684350830149,132.163085575211));
#209064=CARTESIAN_POINT('Ctrl Pts',(204.210205705346,4.76472087565255,132.031314691805));
#209065=CARTESIAN_POINT('Ctrl Pts',(204.202432805124,4.79704387379708,131.898098386972));
#209066=CARTESIAN_POINT('Ctrl Pts',(204.194659904902,4.82373089659542,131.763945579792));
#209067=CARTESIAN_POINT('Ctrl Pts',(204.187169568631,4.849447780786,131.634669555555));
#209068=CARTESIAN_POINT('Ctrl Pts',(204.17967923236,4.86993129066992,131.504524239439));
#209069=CARTESIAN_POINT('Ctrl Pts',(204.172188896089,4.88515415502804,131.373967450489));
#209070=CARTESIAN_POINT('Ctrl Pts',(204.164414562036,4.90095419770749,131.238460571561));
#209071=CARTESIAN_POINT('Ctrl Pts',(204.156640227983,4.91113685606931,131.102081156815));
#209072=CARTESIAN_POINT('Ctrl Pts',(204.14886589393,4.915614960675,130.965334593376));
#209073=CARTESIAN_POINT('Ctrl Pts',(204.141101141049,4.9200875464163,130.828756557876));
#209074=CARTESIAN_POINT('Ctrl Pts',(204.133336388169,4.91886955403614,130.691812660983));
#209075=CARTESIAN_POINT('Ctrl Pts',(204.125571635289,4.9119252950968,130.555015559688));
#209076=CARTESIAN_POINT('Ctrl Pts',(204.117814594472,4.90498793329431,130.418354327222));
#209077=CARTESIAN_POINT('Ctrl Pts',(204.110057553655,4.892335642827,130.281839988143));
#209078=CARTESIAN_POINT('Ctrl Pts',(204.102300512838,4.87398474075138,130.145987008266));
#209079=CARTESIAN_POINT('Ctrl Pts',(204.094549321667,4.85564767723613,130.010236476196));
#209080=CARTESIAN_POINT('Ctrl Pts',(204.086798130496,4.83162060788727,129.875146696503));
#209081=CARTESIAN_POINT('Ctrl Pts',(204.079046939325,4.80197179006196,129.741228457414));
#209082=CARTESIAN_POINT('Ctrl Pts',(204.071299042618,4.77233557377983,129.607367137171));
#209083=CARTESIAN_POINT('Ctrl Pts',(204.063551145911,4.73708244567803,129.474676748098));
#209084=CARTESIAN_POINT('Ctrl Pts',(204.055803249204,4.69633198401899,129.343659088033));
#209085=CARTESIAN_POINT('Ctrl Pts',(204.048056973191,4.65559004648194,129.21266883405));
#209086=CARTESIAN_POINT('Ctrl Pts',(204.040310697177,4.60935317869152,129.083350986195));
#209087=CARTESIAN_POINT('Ctrl Pts',(204.032564421164,4.55779106379823,128.956192962492));
#209088=CARTESIAN_POINT('Ctrl Pts',(204.02481808797,4.50622856828952,128.829034000148));
#209089=CARTESIAN_POINT('Ctrl Pts',(204.017071754777,4.44934089415499,128.704035256081));
#209090=CARTESIAN_POINT('Ctrl Pts',(204.009325421583,4.3873460342304,128.58166454333));
#209091=CARTESIAN_POINT('Ctrl Pts',(204.001577353652,4.3253372909914,128.459266426516));
#209092=CARTESIAN_POINT('Ctrl Pts',(203.993829285721,4.25821926274942,128.339497860818));
#209093=CARTESIAN_POINT('Ctrl Pts',(203.98608121779,4.18625589900541,128.222802055274));
#209094=CARTESIAN_POINT('Ctrl Pts',(203.978324915121,4.1142160517463,128.105982224046));
#209095=CARTESIAN_POINT('Ctrl Pts',(203.970568612452,4.03732078748716,127.992242009999));
#209096=CARTESIAN_POINT('Ctrl Pts',(203.962812309783,3.95587771587694,127.881996068177));
#209097=CARTESIAN_POINT('Ctrl Pts',(203.955051867342,3.87439117565101,127.771691284781));
#209098=CARTESIAN_POINT('Ctrl Pts',(203.9472914249,3.78835223661492,127.664884794093));
#209099=CARTESIAN_POINT('Ctrl Pts',(203.939530982459,3.6981081709207,127.561957339337));
#209100=CARTESIAN_POINT('Ctrl Pts',(203.931758082267,3.60771923743896,127.458864656291));
#209101=CARTESIAN_POINT('Ctrl Pts',(203.923985182075,3.51311195774471,127.359663735743));
#209102=CARTESIAN_POINT('Ctrl Pts',(203.916212281882,3.41467038975604,127.264698318444));
#209103=CARTESIAN_POINT('Ctrl Pts',(203.908721945347,3.3198074100404,127.173185122963));
#209104=CARTESIAN_POINT('Ctrl Pts',(203.901231608812,3.22138430351891,127.085605040283));
#209105=CARTESIAN_POINT('Ctrl Pts',(203.893741272277,3.11977150560056,127.002228476866));
#209106=CARTESIAN_POINT('Ctrl Pts',(203.885966938106,3.01430603775704,126.915690674068));
#209107=CARTESIAN_POINT('Ctrl Pts',(203.878192603936,2.90507014731187,126.83340730906));
#209108=CARTESIAN_POINT('Ctrl Pts',(203.870418269766,2.79244191357776,126.755724894042));
#209109=CARTESIAN_POINT('Ctrl Pts',(203.862653516767,2.67995248406615,126.678138215651));
#209110=CARTESIAN_POINT('Ctrl Pts',(203.854888763768,2.56407934847872,126.605141424973));
#209111=CARTESIAN_POINT('Ctrl Pts',(203.84712401077,2.44523452920922,126.537041651322));
#209112=CARTESIAN_POINT('Ctrl Pts',(203.839366969832,2.32650774828062,126.469009515322));
#209113=CARTESIAN_POINT('Ctrl Pts',(203.831609928895,2.20481549434958,126.405864910317));
#209114=CARTESIAN_POINT('Ctrl Pts',(203.823852887958,2.08059942186419,126.34787218964));
#209115=CARTESIAN_POINT('Ctrl Pts',(203.816101696665,1.95647702167689,126.289923201721));
#209116=CARTESIAN_POINT('Ctrl Pts',(203.808350505372,1.82983494402628,126.237118529847));
#209117=CARTESIAN_POINT('Ctrl Pts',(203.800599314079,1.70113982430083,126.189676840678));
#209118=CARTESIAN_POINT('Ctrl Pts',(203.792851417249,1.57249940342463,126.142255315488));
#209119=CARTESIAN_POINT('Ctrl Pts',(203.785103520418,1.44180804206936,126.100192374375));
#209120=CARTESIAN_POINT('Ctrl Pts',(203.777355623588,1.30955255195562,126.063658646743));
#209121=CARTESIAN_POINT('Ctrl Pts',(203.76960934745,1.17732472683343,126.027132561177));
#209122=CARTESIAN_POINT('Ctrl Pts',(203.761863071312,1.04353380034826,125.996133492601));
#209123=CARTESIAN_POINT('Ctrl Pts',(203.754116795175,0.908681568991501,
125.970782143115));
#209124=CARTESIAN_POINT('Ctrl Pts',(203.746370461855,0.77382834218146,125.945430606491));
#209125=CARTESIAN_POINT('Ctrl Pts',(203.738624128536,0.637914179101389,
125.925726944381));
#209126=CARTESIAN_POINT('Ctrl Pts',(203.730877795217,0.501450494577304,
125.911740617608));
#209127=CARTESIAN_POINT('Ctrl Pts',(203.72312972716,0.364956249953434,125.897751158694));
#209128=CARTESIAN_POINT('Ctrl Pts',(203.715381659102,0.227912627860709,
125.889481622733));
#209129=CARTESIAN_POINT('Ctrl Pts',(203.707633591045,0.0908351837803655,
125.88694950684));
#209130=CARTESIAN_POINT('Ctrl Pts',(203.699877288249,-0.0463879478389493,
125.884414699785));
#209131=CARTESIAN_POINT('Ctrl Pts',(203.692120985453,-0.183644581730893,
125.887629501038));
#209132=CARTESIAN_POINT('Ctrl Pts',(203.684364682657,-0.320419586321026,
125.896559241063));
#209133=CARTESIAN_POINT('Ctrl Pts',(203.676604240088,-0.457267591850978,
125.90549374716));
#209134=CARTESIAN_POINT('Ctrl Pts',(203.66884379752,-0.593633067328671,
125.920149228124));
#209135=CARTESIAN_POINT('Ctrl Pts',(203.661083354951,-0.729007973603942,
125.940439315065));
#209136=CARTESIAN_POINT('Ctrl Pts',(203.653310454632,-0.864600195689189,
125.960761973454));
#209137=CARTESIAN_POINT('Ctrl Pts',(203.645537554313,-0.999198286843428,
125.986737238823));
#209138=CARTESIAN_POINT('Ctrl Pts',(203.637764653993,-1.13230545553917,
126.018227792638));
#209139=CARTESIAN_POINT('Ctrl Pts',(203.630274318817,-1.26057383246008,
126.048573582918));
#209140=CARTESIAN_POINT('Ctrl Pts',(203.62278398364,-1.38745750614367,126.084040550359));
#209141=CARTESIAN_POINT('Ctrl Pts',(203.615293648463,-1.51252874683208,
126.124463198551));
#209142=CARTESIAN_POINT('Ctrl Pts',(203.607519314355,-1.64234211159146,
126.166418486956));
#209143=CARTESIAN_POINT('Ctrl Pts',(203.599744980247,-1.77061410292081,
126.213845566141));
#209144=CARTESIAN_POINT('Ctrl Pts',(203.591970646139,-1.89684882919352,
126.266613645589));
#209145=CARTESIAN_POINT('Ctrl Pts',(203.584205893202,-2.02292798244727,
126.319316693095));
#209146=CARTESIAN_POINT('Ctrl Pts',(203.576441140266,-2.14697450902767,
126.377347494701));
#209147=CARTESIAN_POINT('Ctrl Pts',(203.56867638733,-2.2685073041796,126.440525415203));
#209148=CARTESIAN_POINT('Ctrl Pts',(203.560919346456,-2.38991939124546,
126.503640586503));
#209149=CARTESIAN_POINT('Ctrl Pts',(203.553162305581,-2.50882237072727,
126.571892524047));
#209150=CARTESIAN_POINT('Ctrl Pts',(203.545405264707,-2.62475510966509,
126.64505254088));
#209151=CARTESIAN_POINT('Ctrl Pts',(203.537654073478,-2.74060042282238,
126.718157387175));
#209152=CARTESIAN_POINT('Ctrl Pts',(203.529902882249,-2.853479624487,126.7961627379));
#209153=CARTESIAN_POINT('Ctrl Pts',(203.52215169102,-2.96295651638203,126.878794194166));
#209154=CARTESIAN_POINT('Ctrl Pts',(203.514403794253,-3.07238687767773,
126.961390529858));
#209155=CARTESIAN_POINT('Ctrl Pts',(203.506655897487,-3.17841749393087,
127.048608825393));
#209156=CARTESIAN_POINT('Ctrl Pts',(203.498908000721,-3.28064167616848,
127.140131741651));
#209157=CARTESIAN_POINT('Ctrl Pts',(203.491161724648,-3.38284447531104,
127.231635513289));
#209158=CARTESIAN_POINT('Ctrl Pts',(203.483415448574,-3.48124213307604,
127.327441854015));
#209159=CARTESIAN_POINT('Ctrl Pts',(203.475669172501,-3.57546186610856,
127.427193830671));
#209160=CARTESIAN_POINT('Ctrl Pts',(203.467922839247,-3.66968229464993,
127.526946543675));
#209161=CARTESIAN_POINT('Ctrl Pts',(203.460176505992,-3.75972446845858,
127.630644666505));
#209162=CARTESIAN_POINT('Ctrl Pts',(203.452430172738,-3.8452535159746,127.737895476661));
#209163=CARTESIAN_POINT('Ctrl Pts',(203.444682104745,-3.93080171712827,
127.845170304894));
#209164=CARTESIAN_POINT('Ctrl Pts',(203.436934036753,-4.01183453713135,
127.955999097993));
#209165=CARTESIAN_POINT('Ctrl Pts',(203.429185968761,-4.08805858483793,
128.069957562156));
#209166=CARTESIAN_POINT('Ctrl Pts',(203.42142966603,-4.16436364437073,128.184037142734));
#209167=CARTESIAN_POINT('Ctrl Pts',(203.413673363299,-4.23584950448076,
128.301252713431));
#209168=CARTESIAN_POINT('Ctrl Pts',(203.405917060567,-4.30226689243356,
128.421152139742));
#209169=CARTESIAN_POINT('Ctrl Pts',(203.398156618064,-4.3687197293466,128.541115559989));
#209170=CARTESIAN_POINT('Ctrl Pts',(203.39039617556,-4.4300985288876,128.663765340678));
#209171=CARTESIAN_POINT('Ctrl Pts',(203.382635733057,-4.48620134808193,
128.788627369597));
#209172=CARTESIAN_POINT('Ctrl Pts',(203.374862832802,-4.54239422850365,
128.913689838133));
#209173=CARTESIAN_POINT('Ctrl Pts',(203.367089932547,-4.59329405862153,
129.040971288298));
#209174=CARTESIAN_POINT('Ctrl Pts',(203.359317032292,-4.63874784045621,
129.169979531294));
#209175=CARTESIAN_POINT('Ctrl Pts',(203.351826696411,-4.68254926358041,
129.294298001835));
#209176=CARTESIAN_POINT('Ctrl Pts',(203.344336360531,-4.72129362844921,
129.420219603998));
#209177=CARTESIAN_POINT('Ctrl Pts',(203.336846024651,-4.75488897347145,
129.54729502164));
#209178=CARTESIAN_POINT('Ctrl Pts',(203.336155205243,-4.75798740813817,
129.55901494531));
#209179=CARTESIAN_POINT('Ctrl Pts',(203.335464385835,-4.76104262034663,
129.570746736167));
#209180=CARTESIAN_POINT('Ctrl Pts',(203.334773566427,-4.76405452823405,
129.582490119308));
#209181=CARTESIAN_POINT('',(205.360140563955,-4.91824853905311,130.808151475242));
#209182=CARTESIAN_POINT('Ctrl Pts',(205.360140563955,-4.91824853905311,
130.808151475242));
#209183=CARTESIAN_POINT('Ctrl Pts',(205.351139825899,-4.91812565127672,
130.967585745387));
#209184=CARTESIAN_POINT('Ctrl Pts',(205.342139087842,-4.91024632687204,
131.126698725876));
#209185=CARTESIAN_POINT('Ctrl Pts',(205.333138349785,-4.89472759256679,
131.284802973177));
#209186=CARTESIAN_POINT('Ctrl Pts',(205.324085898924,-4.87911969698644,
131.443815592));
#209187=CARTESIAN_POINT('Ctrl Pts',(205.315033448062,-4.85578446545969,
131.601807746443));
#209188=CARTESIAN_POINT('Ctrl Pts',(205.3059809972,-4.82489013514455,131.758099704678));
#209189=CARTESIAN_POINT('Ctrl Pts',(205.296866878366,-4.79378534351451,
131.915456369954));
#209190=CARTESIAN_POINT('Ctrl Pts',(205.287752759532,-4.75501819248919,
132.071089491341));
#209191=CARTESIAN_POINT('Ctrl Pts',(205.278638640698,-4.70880867544122,
132.224326786385));
#209192=CARTESIAN_POINT('Ctrl Pts',(205.274555892192,-4.68810872187624,
132.292970760494));
#209193=CARTESIAN_POINT('Ctrl Pts',(205.270473143687,-4.6659159667685,132.361134266192));
#209194=CARTESIAN_POINT('Ctrl Pts',(205.266390395182,-4.64225323707004,
132.42875833531));
#209195=CARTESIAN_POINT('Ctrl Pts',(205.25861606485,-4.59719489536611,132.557527435603));
#209196=CARTESIAN_POINT('Ctrl Pts',(205.250841734518,-4.54670333252088,
132.684624302624));
#209197=CARTESIAN_POINT('Ctrl Pts',(205.243067404185,-4.49092120076951,
132.809556326463));
#209198=CARTESIAN_POINT('Ctrl Pts',(205.235302655081,-4.43520781594627,
132.934334381772));
#209199=CARTESIAN_POINT('Ctrl Pts',(205.227537905977,-4.3742169933291,133.05695254884));
#209200=CARTESIAN_POINT('Ctrl Pts',(205.219773156873,-4.30814086066012,
133.176934196448));
#209201=CARTESIAN_POINT('Ctrl Pts',(205.212016119882,-4.24213035621027,
133.296796675734));
#209202=CARTESIAN_POINT('Ctrl Pts',(205.204259082892,-4.17104478048607,
133.414027506535));
#209203=CARTESIAN_POINT('Ctrl Pts',(205.196502045902,-4.0951238198962,133.528171176731));
#209204=CARTESIAN_POINT('Ctrl Pts',(205.188750858604,-4.0192601123862,133.642228769556));
#209205=CARTESIAN_POINT('Ctrl Pts',(205.180999671306,-3.93856849366088,
133.753203511446));
#209206=CARTESIAN_POINT('Ctrl Pts',(205.173248484008,-3.85333375056227,
133.860665914698));
#209207=CARTESIAN_POINT('Ctrl Pts',(205.165500591231,-3.76813523516348,
133.96808264273));
#209208=CARTESIAN_POINT('Ctrl Pts',(205.157752698454,-3.67839767841762,
134.071989695647));
#209209=CARTESIAN_POINT('Ctrl Pts',(205.150004805678,-3.58444808691414,
134.171988116966));
#209210=CARTESIAN_POINT('Ctrl Pts',(205.142258533629,-3.49051814807432,
134.271965620309));
#209211=CARTESIAN_POINT('Ctrl Pts',(205.134512261581,-3.39237819453857,
134.368035833586));
#209212=CARTESIAN_POINT('Ctrl Pts',(205.126765989532,-3.29039400191811,
134.459834646285));
#209213=CARTESIAN_POINT('Ctrl Pts',(205.119019660333,-3.18840905688475,
134.551634136252));
#209214=CARTESIAN_POINT('Ctrl Pts',(205.111273331135,-3.0825801067567,134.639161901196));
#209215=CARTESIAN_POINT('Ctrl Pts',(205.103527001936,-2.97330779642674,
134.722092590303));
#209216=CARTESIAN_POINT('Ctrl Pts',(205.095778938027,-2.86401101569629,
134.805041850878));
#209217=CARTESIAN_POINT('Ctrl Pts',(205.088030874119,-2.75126965172672,
134.883391750785));
#209218=CARTESIAN_POINT('Ctrl Pts',(205.08028281021,-2.63551491623087,134.956859165287));
#209219=CARTESIAN_POINT('Ctrl Pts',(205.072526511583,-2.51963715546859,
135.030404661676));
#209220=CARTESIAN_POINT('Ctrl Pts',(205.064770212956,-2.40073995618037,
135.09905709693));
#209221=CARTESIAN_POINT('Ctrl Pts',(205.057013914329,-2.27928130406476,
135.162578120105));
#209222=CARTESIAN_POINT('Ctrl Pts',(205.049253475948,-2.15775782605347,
135.226133046236));
#209223=CARTESIAN_POINT('Ctrl Pts',(205.041493037566,-2.03367052466753,
135.284550936595));
#209224=CARTESIAN_POINT('Ctrl Pts',(205.033732599185,-1.90749822121525,
135.337641283768));
#209225=CARTESIAN_POINT('Ctrl Pts',(205.025959703041,-1.78112337448988,
135.390816856402));
#209226=CARTESIAN_POINT('Ctrl Pts',(205.018186806897,-1.65265720386027,
135.438647659219));
#209227=CARTESIAN_POINT('Ctrl Pts',(205.010413910753,-1.52259542748432,
135.480992549491));
#209228=CARTESIAN_POINT('Ctrl Pts',(205.002923530958,-1.39726092104092,
135.521798357858));
#209229=CARTESIAN_POINT('Ctrl Pts',(204.995433151164,-1.27044508084342,
135.557510033643));
#209230=CARTESIAN_POINT('Ctrl Pts',(204.987942771369,-1.14259930875746,
135.588046422688));
#209231=CARTESIAN_POINT('Ctrl Pts',(204.980168435136,-1.00990696933439,
135.619740430505));
#209232=CARTESIAN_POINT('Ctrl Pts',(204.972394098903,-0.875684739349071,
135.645959422382));
#209233=CARTESIAN_POINT('Ctrl Pts',(204.964619762671,-0.740424173411585,
135.666557148552));
#209234=CARTESIAN_POINT('Ctrl Pts',(204.956855007588,-0.605330303598526,
135.687129489931));
#209235=CARTESIAN_POINT('Ctrl Pts',(204.949090252504,-0.469201026759951,
135.702094291348));
#209236=CARTESIAN_POINT('Ctrl Pts',(204.941325497421,-0.332541196813679,
135.711355565079));
#209237=CARTESIAN_POINT('Ctrl Pts',(204.93356845438,-0.196017098948459,
135.720607640409));
#209238=CARTESIAN_POINT('Ctrl Pts',(204.925811411339,-0.0589638841786129,
135.724167435013));
#209239=CARTESIAN_POINT('Ctrl Pts',(204.918054368298,0.0781056551375337,
135.721990389025));
#209240=CARTESIAN_POINT('Ctrl Pts',(204.910303174885,0.215071829587541,
135.719814984758));
#209241=CARTESIAN_POINT('Ctrl Pts',(204.902551981471,0.35205391474676,135.711911357085));
#209242=CARTESIAN_POINT('Ctrl Pts',(204.894800788057,0.488536635525835,
135.69828695725));
#209243=CARTESIAN_POINT('Ctrl Pts',(204.887052889087,0.624961347859993,
135.684668348112));
#209244=CARTESIAN_POINT('Ctrl Pts',(204.879304990118,0.760886729730015,
135.665333841567));
#209245=CARTESIAN_POINT('Ctrl Pts',(204.871557091148,0.895800372082467,
135.640342912393));
#209246=CARTESIAN_POINT('Ctrl Pts',(204.86381081286,1.03068579361427,135.615357210744));
#209247=CARTESIAN_POINT('Ctrl Pts',(204.856064534572,1.16455951239554,135.584717511067));
#209248=CARTESIAN_POINT('Ctrl Pts',(204.848318256284,1.29691748072938,135.548534740707));
#209249=CARTESIAN_POINT('Ctrl Pts',(204.840571920805,1.42927642625718,135.512351703211));
#209250=CARTESIAN_POINT('Ctrl Pts',(204.832825585326,1.56011922188006,135.470625616466));
#209251=CARTESIAN_POINT('Ctrl Pts',(204.825079249848,1.68895558188255,135.423517694883));
#209252=CARTESIAN_POINT('Ctrl Pts',(204.817331179624,1.81782079400553,135.376399223767));
#209253=CARTESIAN_POINT('Ctrl Pts',(204.809583109401,1.9446783092763,135.323896653782));
#209254=CARTESIAN_POINT('Ctrl Pts',(204.801835039178,2.06905684589674,135.26621974028));
#209255=CARTESIAN_POINT('Ctrl Pts',(204.794078734217,2.19356757344921,135.208481527095));
#209256=CARTESIAN_POINT('Ctrl Pts',(204.786322429256,2.31559370402974,135.145558149584));
#209257=CARTESIAN_POINT('Ctrl Pts',(204.778566124295,2.43468715333658,135.077706090129));
#209258=CARTESIAN_POINT('Ctrl Pts',(204.770805679558,2.55384416642928,135.009817815973));
#209259=CARTESIAN_POINT('Ctrl Pts',(204.763045234822,2.67006504819365,134.936995825692));
#209260=CARTESIAN_POINT('Ctrl Pts',(204.755284790086,2.78293070430418,134.85953999184));
#209261=CARTESIAN_POINT('Ctrl Pts',(204.747511887616,2.89597754207783,134.78195981922));
#209262=CARTESIAN_POINT('Ctrl Pts',(204.739738985146,3.00565807806422,134.699731172902));
#209263=CARTESIAN_POINT('Ctrl Pts',(204.731966082676,3.11158561669959,134.613194824045));
#209264=CARTESIAN_POINT('Ctrl Pts',(204.724475770969,3.21366206571824,134.529804580902));
#209265=CARTESIAN_POINT('Ctrl Pts',(204.716985459263,3.31225343579821,134.442414621717));
#209266=CARTESIAN_POINT('Ctrl Pts',(204.709495147556,3.40704746464756,134.351360848203));
#209267=CARTESIAN_POINT('Ctrl Pts',(204.701720813585,3.50543595201642,134.256854441481));
#209268=CARTESIAN_POINT('Ctrl Pts',(204.693946479614,3.60004509988113,134.158101516487));
#209269=CARTESIAN_POINT('Ctrl Pts',(204.686172145643,3.69048616693734,134.055436580097));
#209270=CARTESIAN_POINT('Ctrl Pts',(204.678407392841,3.78081577349329,133.952898169028));
#209271=CARTESIAN_POINT('Ctrl Pts',(204.670642640039,3.86698726395705,133.846457629871));
#209272=CARTESIAN_POINT('Ctrl Pts',(204.662877887237,3.94864699528088,133.736487826464));
#209273=CARTESIAN_POINT('Ctrl Pts',(204.655120846494,4.03022562103922,133.626627246574));
#209274=CARTESIAN_POINT('Ctrl Pts',(204.647363805751,4.107301173756,133.513244690025));
#209275=CARTESIAN_POINT('Ctrl Pts',(204.639606765008,4.17955898715758,133.396747497522));
#209276=CARTESIAN_POINT('Ctrl Pts',(204.631855573906,4.25176231040909,133.280338156412));
#209277=CARTESIAN_POINT('Ctrl Pts',(204.624104382805,4.31915492055407,133.160819185333));
#209278=CARTESIAN_POINT('Ctrl Pts',(204.616353191703,4.38146456774871,133.038628127078));
#209279=CARTESIAN_POINT('Ctrl Pts',(204.60860529506,4.44374773172442,132.916489003198));
#209280=CARTESIAN_POINT('Ctrl Pts',(204.600857398416,4.50095205236715,132.79168039854));
#209281=CARTESIAN_POINT('Ctrl Pts',(204.593109501772,4.55285059786026,132.664665564628));
#209282=CARTESIAN_POINT('Ctrl Pts',(204.585363225818,4.60473828731866,132.537677299427));
#209283=CARTESIAN_POINT('Ctrl Pts',(204.577616949864,4.65132226139587,132.4084840846));
#209284=CARTESIAN_POINT('Ctrl Pts',(204.56987067391,4.6924233962874,132.277569948406));
#209285=CARTESIAN_POINT('Ctrl Pts',(204.562124340771,4.73352483459662,132.146654845776));
#209286=CARTESIAN_POINT('Ctrl Pts',(204.554378007632,4.7691432358447,132.014019169442));
#209287=CARTESIAN_POINT('Ctrl Pts',(204.546631674493,4.7991492228434,131.880162550722));
#209288=CARTESIAN_POINT('Ctrl Pts',(204.538883606613,4.82916192948898,131.746275955676));
#209289=CARTESIAN_POINT('Ctrl Pts',(204.531135538733,4.85355963536943,131.611168255589));
#209290=CARTESIAN_POINT('Ctrl Pts',(204.523387470853,4.87226407424628,131.475349330816));
#209291=CARTESIAN_POINT('Ctrl Pts',(204.515631168227,4.89098839243932,131.339386055957));
#209292=CARTESIAN_POINT('Ctrl Pts',(204.507874865602,4.90400730292682,131.202710434351));
#209293=CARTESIAN_POINT('Ctrl Pts',(204.500118562976,4.91129439105524,131.065838086747));
#209294=CARTESIAN_POINT('Ctrl Pts',(204.492358120575,4.91858536852522,130.92889268619));
#209295=CARTESIAN_POINT('Ctrl Pts',(204.484597678174,4.92013842339908,130.791750741167));
#209296=CARTESIAN_POINT('Ctrl Pts',(204.476837235773,4.91597931619433,130.654926935789));
#209297=CARTESIAN_POINT('Ctrl Pts',(204.469064335614,4.91181353241767,130.517883488567));
#209298=CARTESIAN_POINT('Ctrl Pts',(204.461291435454,4.90191729087102,130.381159591714));
#209299=CARTESIAN_POINT('Ctrl Pts',(204.453518535295,4.88636827354715,130.245264778043));
#209300=CARTESIAN_POINT('Ctrl Pts',(204.446028198111,4.87138449911938,130.114310056498));
#209301=CARTESIAN_POINT('Ctrl Pts',(204.438537860927,4.85115184404818,129.984125490812));
#209302=CARTESIAN_POINT('Ctrl Pts',(204.431047523743,4.8257841278719,129.855155363851));
#209303=CARTESIAN_POINT('Ctrl Pts',(204.423273190132,4.79945459374589,129.721295329489));
#209304=CARTESIAN_POINT('Ctrl Pts',(204.415498856521,4.7675095188085,129.588319613196));
#209305=CARTESIAN_POINT('Ctrl Pts',(204.40772452291,4.73002020891244,129.456736083143));
#209306=CARTESIAN_POINT('Ctrl Pts',(204.399959770479,4.69257710128169,129.325314718175));
#209307=CARTESIAN_POINT('Ctrl Pts',(204.392195018048,4.64960345998627,129.195282498014));
#209308=CARTESIAN_POINT('Ctrl Pts',(204.384430265617,4.60122183314642,129.067138494556));
#209309=CARTESIAN_POINT('Ctrl Pts',(204.376673225255,4.55288825966949,128.939121765658));
#209310=CARTESIAN_POINT('Ctrl Pts',(204.368916184894,4.49915752696644,128.812989884719));
#209311=CARTESIAN_POINT('Ctrl Pts',(204.361159144532,4.44020225742291,128.689227766969));
#209312=CARTESIAN_POINT('Ctrl Pts',(204.353407953822,4.38129144656131,128.565558979308));
#209313=CARTESIAN_POINT('Ctrl Pts',(204.345656763112,4.31716410838634,128.444256749339));
#209314=CARTESIAN_POINT('Ctrl Pts',(204.337905572402,4.24804120227294,128.325786631119));
#209315=CARTESIAN_POINT('Ctrl Pts',(204.330157676164,4.17894767531605,128.207366865993));
#209316=CARTESIAN_POINT('Ctrl Pts',(204.322409779926,4.10486300002969,128.091777155478));
#209317=CARTESIAN_POINT('Ctrl Pts',(204.314661883687,4.02605426077588,127.979458822496));
#209318=CARTESIAN_POINT('Ctrl Pts',(204.306915608147,3.94726200666425,127.867163984164));
#209319=CARTESIAN_POINT('Ctrl Pts',(204.299169332607,3.86374787853738,127.758139482086));
#209320=CARTESIAN_POINT('Ctrl Pts',(204.291423057066,3.77582228221695,127.65279764729));
#209321=CARTESIAN_POINT('Ctrl Pts',(204.283676724349,3.68789603690174,127.547455034947));
#209322=CARTESIAN_POINT('Ctrl Pts',(204.275930391632,3.59555850894457,127.445795444277));
#209323=CARTESIAN_POINT('Ctrl Pts',(204.268184058915,3.49916012072415,127.348197786906));
#209324=CARTESIAN_POINT('Ctrl Pts',(204.260435991465,3.40274014480243,127.250578273267));
#209325=CARTESIAN_POINT('Ctrl Pts',(204.252687924014,3.30225777370524,127.15702278111));
#209326=CARTESIAN_POINT('Ctrl Pts',(204.244939856564,3.19809967933992,127.067872760834));
#209327=CARTESIAN_POINT('Ctrl Pts',(204.237183554378,3.09383088454986,126.978627990887));
#209328=CARTESIAN_POINT('Ctrl Pts',(204.229427252191,2.9858788601325,126.893798300623));
#209329=CARTESIAN_POINT('Ctrl Pts',(204.221670950005,2.87466313460505,126.813684619061));
#209330=CARTESIAN_POINT('Ctrl Pts',(204.21391050805,2.76338804993092,126.73352817844));
#209331=CARTESIAN_POINT('Ctrl Pts',(204.206150066094,2.64884611955096,126.658092976936));
#209332=CARTESIAN_POINT('Ctrl Pts',(204.198389624139,2.53148428592039,126.587635540846));
#209333=CARTESIAN_POINT('Ctrl Pts',(204.190616724431,2.41393405262733,126.517065000208));
#209334=CARTESIAN_POINT('Ctrl Pts',(204.182843824723,2.29355521370091,126.451488380188));
#209335=CARTESIAN_POINT('Ctrl Pts',(204.175070925015,2.17081844249119,126.391115739674));
#209336=CARTESIAN_POINT('Ctrl Pts',(204.16758058332,2.05254335990331,126.332937746457));
#209337=CARTESIAN_POINT('Ctrl Pts',(204.160090241625,1.932079080105,126.279592079101));
#209338=CARTESIAN_POINT('Ctrl Pts',(204.15259989993,1.80986091391834,126.231223124032));
#209339=CARTESIAN_POINT('Ctrl Pts',(204.144825565478,1.68300890386598,126.181020282947));
#209340=CARTESIAN_POINT('Ctrl Pts',(204.137051231027,1.55386555861245,126.136019952371));
#209341=CARTESIAN_POINT('Ctrl Pts',(204.129276896576,1.42289670472903,126.096436655757));
#209342=CARTESIAN_POINT('Ctrl Pts',(204.121512143292,1.2920892581833,126.056902141999));
#209343=CARTESIAN_POINT('Ctrl Pts',(204.113747390009,1.15946115004296,126.022771490962));
#209344=CARTESIAN_POINT('Ctrl Pts',(204.105982636726,1.02549850401181,125.994211359927));
#209345=CARTESIAN_POINT('Ctrl Pts',(204.098225595501,0.891668911505565,
125.965679595202));
#209346=CARTESIAN_POINT('Ctrl Pts',(204.090468554277,0.756507798773581,
125.942707421116));
#209347=CARTESIAN_POINT('Ctrl Pts',(204.082711513052,0.620516445466882,
125.925411714021));
#209348=CARTESIAN_POINT('Ctrl Pts',(204.07496032147,0.484627644240924,125.908129049746));
#209349=CARTESIAN_POINT('Ctrl Pts',(204.067209129887,0.347910234907202,
125.896514381183));
#209350=CARTESIAN_POINT('Ctrl Pts',(204.059457938304,0.210875335327797,
125.890633452221));
#209351=CARTESIAN_POINT('Ctrl Pts',(204.051710041182,0.0738986791749443,
125.884755022807));
#209352=CARTESIAN_POINT('Ctrl Pts',(204.043962144059,-0.0633948090470082,
125.884605502735));
#209353=CARTESIAN_POINT('Ctrl Pts',(204.036214246936,-0.200489466144424,
125.89019873211));
#209354=CARTESIAN_POINT('Ctrl Pts',(204.028467970504,-0.337555446031198,
125.895790791504));
#209355=CARTESIAN_POINT('Ctrl Pts',(204.020721694072,-0.474422287127775,
125.907123195051));
#209356=CARTESIAN_POINT('Ctrl Pts',(204.01297541764,-0.61057530164394,125.924157664458));
#209357=CARTESIAN_POINT('Ctrl Pts',(204.005229084025,-0.746729321239624,
125.941192259614));
#209358=CARTESIAN_POINT('Ctrl Pts',(203.997482750411,-0.882169115799372,
125.963928956088));
#209359=CARTESIAN_POINT('Ctrl Pts',(203.989736416796,-1.0163864843013,125.992277744523));
#209360=CARTESIAN_POINT('Ctrl Pts',(203.981988348442,-1.15063390987372,
126.020632881478));
#209361=CARTESIAN_POINT('Ctrl Pts',(203.974240280088,-1.28365798219704,
126.054602530483));
#209362=CARTESIAN_POINT('Ctrl Pts',(203.966492211735,-1.41496242369231,
126.094045935717));
#209363=CARTESIAN_POINT('Ctrl Pts',(203.958735908642,-1.54640641710633,
126.133531261871));
#209364=CARTESIAN_POINT('Ctrl Pts',(203.950979605549,-1.67612675374356,
126.178501852826));
#209365=CARTESIAN_POINT('Ctrl Pts',(203.943223302457,-1.80364348801349,
126.228767406774));
#209366=CARTESIAN_POINT('Ctrl Pts',(203.935462859591,-1.93122828181124,
126.279059788964));
#209367=CARTESIAN_POINT('Ctrl Pts',(203.927702416725,-2.05660677247295,
126.334652606956));
#209368=CARTESIAN_POINT('Ctrl Pts',(203.91994197386,-2.17932155377599,126.395308494065));
#209369=CARTESIAN_POINT('Ctrl Pts',(203.912169073245,-2.30223332769157,
126.456061751365));
#209370=CARTESIAN_POINT('Ctrl Pts',(203.904396172631,-2.42247250426769,
126.521894131622));
#209371=CARTESIAN_POINT('Ctrl Pts',(203.896623272017,-2.53960794450345,
126.592523185908));
#209372=CARTESIAN_POINT('Ctrl Pts',(203.88913294005,-2.65248515417354,126.660584658622));
#209373=CARTESIAN_POINT('Ctrl Pts',(203.881642608084,-2.76248011304978,
126.733099943225));
#209374=CARTESIAN_POINT('Ctrl Pts',(203.874152276117,-2.86923605004317,
126.809780845971));
#209375=CARTESIAN_POINT('Ctrl Pts',(203.866074034918,-2.98437116185463,
126.892480361897));
#209376=CARTESIAN_POINT('Ctrl Pts',(203.857995793719,-3.09613368668095,
126.980309741443));
#209377=CARTESIAN_POINT('Ctrl Pts',(203.84991755252,-3.20403203740082,127.07295849962));
#209378=CARTESIAN_POINT('Ctrl Pts',(203.842215517175,-3.30690553306662,
127.161292580348));
#209379=CARTESIAN_POINT('Ctrl Pts',(203.834513481829,-3.40626624325742,
127.25400703648));
#209380=CARTESIAN_POINT('Ctrl Pts',(203.826811446484,-3.50171630356533,
127.350787686261));
#209381=CARTESIAN_POINT('Ctrl Pts',(203.819116363939,-3.59708019895571,
127.447480969971));
#209382=CARTESIAN_POINT('Ctrl Pts',(203.811421281394,-3.68854018756952,
127.548232866472));
#209383=CARTESIAN_POINT('Ctrl Pts',(203.803726198849,-3.77573196917681,
127.65268944826));
#209384=CARTESIAN_POINT('Ctrl Pts',(203.796036329942,-3.8628646758669,127.757075257736));
#209385=CARTESIAN_POINT('Ctrl Pts',(203.788346461035,-3.94573467410029,
127.86516045547));
#209386=CARTESIAN_POINT('Ctrl Pts',(203.780656592127,-4.02401534417658,
127.976555183606));
#209387=CARTESIAN_POINT('Ctrl Pts',(203.772970201974,-4.10226060153588,
128.087899518843));
#209388=CARTESIAN_POINT('Ctrl Pts',(203.76528381182,-4.17592043400376,128.202550080349));
#209389=CARTESIAN_POINT('Ctrl Pts',(203.757597421666,-4.24470957225871,
128.320085328941));
#209390=CARTESIAN_POINT('Ctrl Pts',(203.749911435145,-4.31349509821327,
128.437614405444));
#209391=CARTESIAN_POINT('Ctrl Pts',(203.742225448624,-4.37741023070302,
128.558027528844));
#209392=CARTESIAN_POINT('Ctrl Pts',(203.734539462103,-4.4362141058302,128.680875870803));
#209393=CARTESIAN_POINT('Ctrl Pts',(203.726853680479,-4.49501641333659,
128.803720937816));
#209394=CARTESIAN_POINT('Ctrl Pts',(203.719167898855,-4.54870756838372,
128.929000732856));
#209395=CARTESIAN_POINT('Ctrl Pts',(203.71148211723,-4.59709392678213,129.056244348308));
#209396=CARTESIAN_POINT('Ctrl Pts',(203.703792765134,-4.64550276332794,
129.183547075479));
#209397=CARTESIAN_POINT('Ctrl Pts',(203.696103413038,-4.68860174757454,
129.312815070517));
#209398=CARTESIAN_POINT('Ctrl Pts',(203.688414060942,-4.72624641962959,
129.443560175386));
#209399=CARTESIAN_POINT('Ctrl Pts',(203.685700869741,-4.73952935838289,
129.489693641968));
#209400=CARTESIAN_POINT('Ctrl Pts',(203.682987678541,-4.752133674154,129.536010890174));
#209401=CARTESIAN_POINT('Ctrl Pts',(203.680274487341,-4.76405452823405,
129.582490119308));
#209402=CARTESIAN_POINT('Ctrl Pts',(205.430026442963,-4.76405452823405,
129.582490119308));
#209403=CARTESIAN_POINT('Ctrl Pts',(205.422281762578,-4.79814669522109,
129.71541496097));
#209404=CARTESIAN_POINT('Ctrl Pts',(205.414537082193,-4.82668292020064,
129.849812538585));
#209405=CARTESIAN_POINT('Ctrl Pts',(205.406792401809,-4.8495489326977,129.985179189633));
#209406=CARTESIAN_POINT('Ctrl Pts',(205.399017095509,-4.87250536759203,
130.121081140708));
#209407=CARTESIAN_POINT('Ctrl Pts',(205.391241789208,-4.88974655166597,
130.257959461279));
#209408=CARTESIAN_POINT('Ctrl Pts',(205.383466482908,-4.90120888938085,
130.395295237518));
#209409=CARTESIAN_POINT('Ctrl Pts',(205.375691176608,-4.91267122709574,
130.532631013756));
#209410=CARTESIAN_POINT('Ctrl Pts',(205.367915870308,-4.91835469588896,
130.670423848268));
#209411=CARTESIAN_POINT('Ctrl Pts',(205.360140564008,-4.91824853905384,
130.808151474305));
#209412=CARTESIAN_POINT('Origin',(213.235140564004,0.,130.804360617566));
#209413=CARTESIAN_POINT('',(207.179891338435,-4.76405452823405,129.582490119308));
#209414=CARTESIAN_POINT('',(206.834782106149,-4.76405452823405,129.582490119308));
#209415=CARTESIAN_POINT('',(213.235140564004,-4.76405452823405,129.582490119308));
#209416=CARTESIAN_POINT('',(207.388365636076,-2.6602809725928,126.667684632024));
#209417=CARTESIAN_POINT('Ctrl Pts',(207.388365636076,-2.66028097259279,
126.667684632024));
#209418=CARTESIAN_POINT('Ctrl Pts',(207.380618347121,-2.7756419670554,126.741872859388));
#209419=CARTESIAN_POINT('Ctrl Pts',(207.372871058166,-2.88794064863019,
126.820918329725));
#209420=CARTESIAN_POINT('Ctrl Pts',(207.365123769211,-2.99675018972373,
126.904530959377));
#209421=CARTESIAN_POINT('Ctrl Pts',(207.357377200615,-3.10554961348789,
126.988135814559));
#209422=CARTESIAN_POINT('Ctrl Pts',(207.349630632018,-3.21086023212209,
127.076306746294));
#209423=CARTESIAN_POINT('Ctrl Pts',(207.341884063422,-3.31228656623825,
127.168712014412));
#209424=CARTESIAN_POINT('Ctrl Pts',(207.334136538062,-3.41372542731635,
127.261128695318));
#209425=CARTESIAN_POINT('Ctrl Pts',(207.326389012703,-3.51127876024814,
127.357780490032));
#209426=CARTESIAN_POINT('Ctrl Pts',(207.318641487343,-3.60458666572251,
127.458297553038));
#209427=CARTESIAN_POINT('Ctrl Pts',(207.31089132783,-3.69792629581925,127.558848791775));
#209428=CARTESIAN_POINT('Ctrl Pts',(207.303141168318,-3.78701736032166,
127.663267627633));
#209429=CARTESIAN_POINT('Ctrl Pts',(207.295391008805,-3.8715393602353,127.771150099872));
#209430=CARTESIAN_POINT('Ctrl Pts',(207.287632207676,-3.95615560423753,
127.879152863696));
#209431=CARTESIAN_POINT('Ctrl Pts',(207.279873406546,-4.03619237033408,
127.990626667092));
#209432=CARTESIAN_POINT('Ctrl Pts',(207.272114605417,-4.11137146976527,
128.105137081047));
#209433=CARTESIAN_POINT('Ctrl Pts',(207.264350856575,-4.18659851018636,
128.219720517193));
#209434=CARTESIAN_POINT('Ctrl Pts',(207.256587107732,-4.25696151306608,
128.33734408662));
#209435=CARTESIAN_POINT('Ctrl Pts',(207.24882335889,-4.3222281122226,128.457548480131));
#209436=CARTESIAN_POINT('Ctrl Pts',(207.24104833483,-4.38758949743189,128.577927445323));
#209437=CARTESIAN_POINT('Ctrl Pts',(207.23327331077,-4.44783952903662,128.700894368445));
#209438=CARTESIAN_POINT('Ctrl Pts',(207.22549828671,-4.5027936406439,128.825969227503));
#209439=CARTESIAN_POINT('Ctrl Pts',(207.222173445098,-4.52629372445711,
128.879455119364));
#209440=CARTESIAN_POINT('Ctrl Pts',(207.218848603485,-4.54882597142772,
128.93332628573));
#209441=CARTESIAN_POINT('Ctrl Pts',(207.215523761872,-4.57037874948208,
128.987544405402));
#209442=CARTESIAN_POINT('Ctrl Pts',(207.206734347059,-4.6273547888774,129.130873201093));
#209443=CARTESIAN_POINT('Ctrl Pts',(207.197944932245,-4.67763395894565,
129.2770080242));
#209444=CARTESIAN_POINT('Ctrl Pts',(207.189155517432,-4.72096468861576,
129.425348118949));
#209445=CARTESIAN_POINT('Ctrl Pts',(207.186067457766,-4.73618844143788,
129.47746570278));
#209446=CARTESIAN_POINT('Ctrl Pts',(207.1829793981,-4.75055490266602,129.529855284104));
#209447=CARTESIAN_POINT('Ctrl Pts',(207.179891338435,-4.76405452823404,
129.582490119308));
#209448=CARTESIAN_POINT('',(207.162232148078,-0.703339529199327,125.936661307916));
#209449=CARTESIAN_POINT('Ctrl Pts',(207.162254451653,-0.702949340845361,
125.936604945112));
#209450=CARTESIAN_POINT('Ctrl Pts',(207.181804583648,-1.10465555699531,
125.994615071104));
#209451=CARTESIAN_POINT('Ctrl Pts',(207.218751347755,-1.507343617162,126.104644931362));
#209452=CARTESIAN_POINT('Ctrl Pts',(207.303215754353,-2.15815824480352,
126.375258708658));
#209453=CARTESIAN_POINT('Ctrl Pts',(207.344364632467,-2.41764010127658,
126.511643188268));
#209454=CARTESIAN_POINT('Ctrl Pts',(207.388365636076,-2.66028097259279,
126.667684632024));
#209455=CARTESIAN_POINT('Ctrl Pts',(207.162232148078,-0.703339529199318,
125.936661307916));
#209456=CARTESIAN_POINT('Ctrl Pts',(207.154481493481,-0.838932135396659,
125.956253241135));
#209457=CARTESIAN_POINT('Ctrl Pts',(207.146730838883,-0.973806675997351,
125.981529605001));
#209458=CARTESIAN_POINT('Ctrl Pts',(207.138980184285,-1.10745311122064,
126.012416265954));
#209459=CARTESIAN_POINT('Ctrl Pts',(207.131232508695,-1.24104817869023,
126.043291055446));
#209460=CARTESIAN_POINT('Ctrl Pts',(207.123484833105,-1.37341569924148,
126.079771766144));
#209461=CARTESIAN_POINT('Ctrl Pts',(207.115737157515,-1.5040552264814,126.121733049822));
#209462=CARTESIAN_POINT('Ctrl Pts',(207.10799088649,-1.63467107025817,126.163686726396));
#209463=CARTESIAN_POINT('Ctrl Pts',(207.100244615465,-1.7635591717869,126.211118880199));
#209464=CARTESIAN_POINT('Ctrl Pts',(207.092498344441,-1.89023407151358,
126.2638542342));
#209465=CARTESIAN_POINT('Ctrl Pts',(207.084751800286,-2.01691343773256,
126.316591447622));
#209466=CARTESIAN_POINT('Ctrl Pts',(207.077005256132,-2.14137908586176,
126.374632083229));
#209467=CARTESIAN_POINT('Ctrl Pts',(207.069258711978,-2.2631657454553,126.437752795572));
#209468=CARTESIAN_POINT('Ctrl Pts',(207.061510217176,-2.38498307199125,
126.50088940226));
#209469=CARTESIAN_POINT('Ctrl Pts',(207.053761722375,-2.50411972061654,
126.569108451315));
#209470=CARTESIAN_POINT('Ctrl Pts',(207.046013227573,-2.6201355790416,126.64214094413));
#209471=CARTESIAN_POINT('Ctrl Pts',(207.038256395599,-2.73627626742322,
126.715252017951));
#209472=CARTESIAN_POINT('Ctrl Pts',(207.030499563624,-2.84928912735338,
126.793186671612));
#209473=CARTESIAN_POINT('Ctrl Pts',(207.02274273165,-2.95876314281126,126.875632613842));
#209474=CARTESIAN_POINT('Ctrl Pts',(207.014981565943,-3.06829832127006,
126.958124618521));
#209475=CARTESIAN_POINT('Ctrl Pts',(207.007220400236,-3.17429041402738,
127.045132685755));
#209476=CARTESIAN_POINT('Ctrl Pts',(206.999459234529,-3.27636279218891,
127.13630528586));
#209477=CARTESIAN_POINT('Ctrl Pts',(206.991685903546,-3.37859516417064,
127.227620794877));
#209478=CARTESIAN_POINT('Ctrl Pts',(206.983912572564,-3.47689526586364,
127.323113606467));
#209479=CARTESIAN_POINT('Ctrl Pts',(206.976139241582,-3.57092397027851,
127.422395942855));
#209480=CARTESIAN_POINT('Ctrl Pts',(206.969647872461,-3.64944565290829,
127.50530483921));
#209481=CARTESIAN_POINT('Ctrl Pts',(206.963156503339,-3.72498926082491,
127.59085569901));
#209482=CARTESIAN_POINT('Ctrl Pts',(206.956665134218,-3.79738005623955,
127.678806623316));
#209483=CARTESIAN_POINT('Ctrl Pts',(206.94892298064,-3.88371941628531,127.783704303698));
#209484=CARTESIAN_POINT('Ctrl Pts',(206.941180827061,-3.96585449861086,
127.892359049907));
#209485=CARTESIAN_POINT('Ctrl Pts',(206.933438673483,-4.04343822436111,
128.004398048481));
#209486=CARTESIAN_POINT('Ctrl Pts',(206.925706075313,-4.12092619585383,
128.116298767913));
#209487=CARTESIAN_POINT('Ctrl Pts',(206.917973477143,-4.19387376171754,
128.231575110577));
#209488=CARTESIAN_POINT('Ctrl Pts',(206.910240878973,-4.26197290981029,
128.349819931706));
#209489=CARTESIAN_POINT('Ctrl Pts',(206.902517710807,-4.32998901010194,
128.46792055173));
#209490=CARTESIAN_POINT('Ctrl Pts',(206.894794542642,-4.39316827069869,
128.588982102231));
#209491=CARTESIAN_POINT('Ctrl Pts',(206.887071374476,-4.45124539391761,
128.712567724943));
#209492=CARTESIAN_POINT('Ctrl Pts',(206.879353629328,-4.50928173682043,
128.836066568895));
#209493=CARTESIAN_POINT('Ctrl Pts',(206.871635884179,-4.56222290117221,
128.962085604512));
#209494=CARTESIAN_POINT('Ctrl Pts',(206.863918139031,-4.60984903857043,
129.090162582305));
#209495=CARTESIAN_POINT('Ctrl Pts',(206.85620451266,-4.65744975902884,129.218171208454));
#209496=CARTESIAN_POINT('Ctrl Pts',(206.848490886289,-4.69974096176777,
129.348235221747));
#209497=CARTESIAN_POINT('Ctrl Pts',(206.840777259918,-4.73655075729556,
129.47987204228));
#209498=CARTESIAN_POINT('Ctrl Pts',(206.838778875329,-4.74608714453973,
129.513975456282));
#209499=CARTESIAN_POINT('Ctrl Pts',(206.836780490739,-4.75525588437593,
129.548184340444));
#209500=CARTESIAN_POINT('Ctrl Pts',(206.834782106149,-4.76405452823405,
129.582490119308));
#209501=CARTESIAN_POINT('Ctrl Pts',(210.578629502474,3.43871735229388,135.623751273273));
#209502=CARTESIAN_POINT('Ctrl Pts',(210.532211638871,4.24191310225744,135.050661598608));
#209503=CARTESIAN_POINT('Ctrl Pts',(210.439385837966,5.5417116830592,133.497735776206));
#209504=CARTESIAN_POINT('Ctrl Pts',(210.253744162458,6.40049231640402,129.500124813146));
#209505=CARTESIAN_POINT('Ctrl Pts',(210.021704475947,3.49988613106459,124.739836436729));
#209506=CARTESIAN_POINT('Ctrl Pts',(209.743256852134,-3.22132718841443,
124.582443963435));
#209507=CARTESIAN_POINT('Ctrl Pts',(209.464809228321,-6.97029916743427,
130.151104711613));
#209508=CARTESIAN_POINT('Ctrl Pts',(209.186361604508,-4.320155850937,136.315756482887));
#209509=CARTESIAN_POINT('Ctrl Pts',(208.907913980696,2.30329626696544,137.417975354914));
#209510=CARTESIAN_POINT('Ctrl Pts',(208.629466356883,6.80838731381026,132.441404887444));
#209511=CARTESIAN_POINT('Ctrl Pts',(208.35101873307,5.05782663488002,125.961106241921));
#209512=CARTESIAN_POINT('Ctrl Pts',(208.072571109257,-1.34111875541754,
123.931185212061));
#209513=CARTESIAN_POINT('Ctrl Pts',(207.794123485444,-6.50738248846785,
128.217554840719));
#209514=CARTESIAN_POINT('Ctrl Pts',(207.515675861631,-5.69381680528821,
134.880978212762));
#209515=CARTESIAN_POINT('Ctrl Pts',(207.237228237818,0.352161018465804,
137.798239159538));
#209516=CARTESIAN_POINT('Ctrl Pts',(206.958780614005,6.07448159193836,134.288440920842));
#209517=CARTESIAN_POINT('Ctrl Pts',(206.680332990192,6.21467071562046,127.576957111676));
#209518=CARTESIAN_POINT('Ctrl Pts',(206.40188536638,0.643870262773591,123.831292031177));
#209519=CARTESIAN_POINT('Ctrl Pts',(206.123437742567,-5.51860979104455,
126.493540260974));
#209520=CARTESIAN_POINT('Ctrl Pts',(205.844990118754,-6.60976007302988,
133.117219720399));
#209521=CARTESIAN_POINT('Ctrl Pts',(205.566542494941,-1.62686214948821,
137.615495756827));
#209522=CARTESIAN_POINT('Ctrl Pts',(205.288094871128,4.8510417637676,135.85467075854));
#209523=CARTESIAN_POINT('Ctrl Pts',(205.009647247315,6.87107573233629,129.452857771449));
#209524=CARTESIAN_POINT('Ctrl Pts',(204.731199623502,2.57692653546199,124.293009711503));
#209525=CARTESIAN_POINT('Ctrl Pts',(204.452751999689,-4.08529213152394,
125.116775123829));
#209526=CARTESIAN_POINT('Ctrl Pts',(204.174304375876,-6.9933269740478,131.167153704944));
#209527=CARTESIAN_POINT('Ctrl Pts',(203.895856752063,-3.47483593506387,
136.884143186524));
#209528=CARTESIAN_POINT('Ctrl Pts',(203.617409128251,3.23685955433703,137.014109488232));
#209529=CARTESIAN_POINT('Ctrl Pts',(203.338961504438,6.97403925260401,131.437619947721));
#209530=CARTESIAN_POINT('Ctrl Pts',(203.060513880625,4.30241757323156,125.27919601562));
#209531=CARTESIAN_POINT('Ctrl Pts',(202.782066256812,-2.32291566837452,
124.198128435325));
#209532=CARTESIAN_POINT('Ctrl Pts',(202.503618632999,-6.81360289295739,
129.18786549711));
#209533=CARTESIAN_POINT('Ctrl Pts',(202.225171009186,-5.0429219211382,135.663082604955));
#209534=CARTESIAN_POINT('Ctrl Pts',(201.946723385373,1.36195793536179,137.673371567868));
#209535=CARTESIAN_POINT('Ctrl Pts',(201.66827576156,6.51526498482727,133.371375037445));
#209536=CARTESIAN_POINT('Ctrl Pts',(201.389828137747,5.6813618015098,126.710417660699));
#209537=CARTESIAN_POINT('Ctrl Pts',(201.111380513935,-0.373435327379839,
123.811593861123));
#209538=CARTESIAN_POINT('Ctrl Pts',(200.832932890122,-6.08506363376988,
127.338781095048));
#209539=CARTESIAN_POINT('Ctrl Pts',(200.554485266309,-6.20481573259303,
134.050666607207));
#209540=CARTESIAN_POINT('Ctrl Pts',(200.276037642496,-0.622645295272457,
137.779355505743));
#209541=CARTESIAN_POINT('Ctrl Pts',(199.997590018683,5.53170575049466,135.098364849491));
#209542=CARTESIAN_POINT('Ctrl Pts',(199.71914239487,6.60268945040398,128.471394077867));
#209543=CARTESIAN_POINT('Ctrl Pts',(199.440694771057,1.60612410470526,123.988305584475));
#209544=CARTESIAN_POINT('Ctrl Pts',(199.162247147244,-4.86639082969376,
125.768838683693));
#209545=CARTESIAN_POINT('Ctrl Pts',(198.883799523432,-6.86693032801245,
132.176770441218));
#209546=CARTESIAN_POINT('Ctrl Pts',(198.605351899619,-2.5570963230842,137.323524616753));
#209547=CARTESIAN_POINT('Ctrl Pts',(198.326904275806,4.10258428165832,136.479485555902));
#209548=CARTESIAN_POINT('Ctrl Pts',(198.048456651993,6.99219035394115,130.420283921986));
#209549=CARTESIAN_POINT('Ctrl Pts',(197.77000902818,3.45631507844086,124.714030008118));
#209550=CARTESIAN_POINT('Ctrl Pts',(197.491561404367,-3.25574490376804,
124.604492395141));
#209551=CARTESIAN_POINT('Ctrl Pts',(197.213113780554,-6.97593437139489,
130.192330798173));
#209552=CARTESIAN_POINT('Ctrl Pts',(196.934666156741,-4.28558094504976,
136.342594705906));
#209553=CARTESIAN_POINT('Ctrl Pts',(196.656218532928,2.3430120075278,137.403492044232));
#209554=CARTESIAN_POINT('Ctrl Pts',(196.377770909115,6.81849138768721,132.400109986944));
#209555=CARTESIAN_POINT('Ctrl Pts',(196.099323285303,5.02811028438465,125.930312215887));
#209556=CARTESIAN_POINT('Ctrl Pts',(195.82087566149,-1.38285853342424,123.939526815472));
#209557=CARTESIAN_POINT('Ctrl Pts',(195.542428037677,-6.5230479154113,128.257188313404));
#209558=CARTESIAN_POINT('Ctrl Pts',(195.263980413864,-5.66887493174189,
134.915576722577));
#209559=CARTESIAN_POINT('Ctrl Pts',(194.985532790051,0.394717174261835,
137.795958375315));
#209560=CARTESIAN_POINT('Ctrl Pts',(194.707085166238,6.09558348012494,134.251403247221));
#209561=CARTESIAN_POINT('Ctrl Pts',(194.428637542425,6.19490635356113,127.539184339867));
#209562=CARTESIAN_POINT('Ctrl Pts',(194.150189918612,0.601412926074683,
123.827502918989));
#209563=CARTESIAN_POINT('Ctrl Pts',(193.871742294799,-5.54474959981957,
126.527212884656));
#209564=CARTESIAN_POINT('Ctrl Pts',(193.593294670987,-6.59555811955654,
133.157412666584));
#209565=CARTESIAN_POINT('Ctrl Pts',(193.314847047174,-1.58537093834796,
137.625272568447));
#209566=CARTESIAN_POINT('Ctrl Pts',(193.036399423361,4.88169468552635,135.825047607524));
#209567=CARTESIAN_POINT('Ctrl Pts',(192.757951799548,6.86272137744547,129.411056577024));
#209568=CARTESIAN_POINT('Ctrl Pts',(192.479504175735,2.53724238606986,124.277443893095));
#209569=CARTESIAN_POINT('Ctrl Pts',(192.201056551922,-4.11983840692253,
125.141748821346));
#209570=CARTESIAN_POINT('Ctrl Pts',(191.922608928109,-6.99098896924831,
131.209717356357));
#209571=CARTESIAN_POINT('Ctrl Pts',(191.644161304296,-3.43776219763276,
136.905182851196));
#209572=CARTESIAN_POINT('Ctrl Pts',(191.365713680483,3.27460008958736,136.994290755064));
#209573=CARTESIAN_POINT('Ctrl Pts',(191.08726605667,6.9777648675845,131.395155257469));
#209574=CARTESIAN_POINT('Ctrl Pts',(190.808818432858,4.26870461503614,125.253108347726));
#209575=CARTESIAN_POINT('Ctrl Pts',(190.530370809044,-2.36308664091672,
124.212391080215));
#209576=CARTESIAN_POINT('Ctrl Pts',(190.251923185232,-6.82331671706736,
129.229371781915));
#209577=CARTESIAN_POINT('Ctrl Pts',(189.973475561419,-5.01325206778612,
135.693690281095));
#209578=CARTESIAN_POINT('Ctrl Pts',(189.695027937606,1.40374632081163,137.664953676525));
#209579=CARTESIAN_POINT('Ctrl Pts',(189.416580313793,6.53077041740369,133.331667209374));
#209580=CARTESIAN_POINT('Ctrl Pts',(189.13813268998,5.65633554627347,126.675909450142));
#209581=CARTESIAN_POINT('Ctrl Pts',(188.859685066167,-0.41599536452862,
123.81399662772));
#209582=CARTESIAN_POINT('Ctrl Pts',(188.581237442354,-6.10604685783229,
127.375886813701));
#209583=CARTESIAN_POINT('Ctrl Pts',(188.302789818542,-6.18493958576042,
134.088376935175));
#209584=CARTESIAN_POINT('Ctrl Pts',(188.024342194729,-0.580174985471077,
137.783016493883));
#209585=CARTESIAN_POINT('Ctrl Pts',(187.745894570916,5.55774208334242,135.064612228548));
#209586=CARTESIAN_POINT('Ctrl Pts',(187.467446947103,6.58836568835925,128.431244857581));
#209587=CARTESIAN_POINT('Ctrl Pts',(187.18899932329,1.56460308533104,123.97865493689));
#209588=CARTESIAN_POINT('Ctrl Pts',(186.910551699478,-4.89695331800637,
125.798555082479));
#209589=CARTESIAN_POINT('Ctrl Pts',(186.632104075664,-6.85844885156509,
132.218545967617));
#209590=CARTESIAN_POINT('Ctrl Pts',(186.353656451852,-2.51736494438869,
137.338969602853));
#209591=CARTESIAN_POINT('Ctrl Pts',(186.075208828038,4.13705436656654,136.454406814005));
#209592=CARTESIAN_POINT('Ctrl Pts',(185.796761204226,6.98972282098866,130.377727590732));
#209593=CARTESIAN_POINT('Ctrl Pts',(185.518313580413,3.41917746986535,124.693103276936));
#209594=CARTESIAN_POINT('Ctrl Pts',(185.2398659566,-3.29342493995873,124.62442590766));
#209595=CARTESIAN_POINT('Ctrl Pts',(184.961418332787,-6.97953072271363,
130.234806630193));
#209596=CARTESIAN_POINT('Ctrl Pts',(184.682970708974,-4.25178874032612,
136.368579642862));
#209597=CARTESIAN_POINT('Ctrl Pts',(184.404523085161,2.38313938299372,137.389107198495));
#209598=CARTESIAN_POINT('Ctrl Pts',(184.126075461348,6.82807883617355,132.358574329007));
#209599=CARTESIAN_POINT('Ctrl Pts',(183.847627837535,4.99834740910532,125.899794986266));
#209600=CARTESIAN_POINT('Ctrl Pts',(183.569180213722,-1.42462110408482,
123.948071857337));
#209601=CARTESIAN_POINT('Ctrl Pts',(183.290732589909,-6.53843241923107,
128.296943150732));
#209602=CARTESIAN_POINT('Ctrl Pts',(183.012284966097,-5.64374376128527,
134.950008601993));
#209603=CARTESIAN_POINT('Ctrl Pts',(182.733837342284,0.437269701071178,
137.793426081729));
#209604=CARTESIAN_POINT('Ctrl Pts',(182.455389718471,6.11645366995566,134.214233834728));
#209605=CARTESIAN_POINT('Ctrl Pts',(182.176942094658,6.17491552152431,127.501534682722));
#209606=CARTESIAN_POINT('Ctrl Pts',(181.898494470845,0.558931670205695,
123.82397121282));
#209607=CARTESIAN_POINT('Ctrl Pts',(181.620046847032,-5.57068308070185,
126.561044594899));
#209608=CARTESIAN_POINT('Ctrl Pts',(181.341599223219,-6.58111222344223,
133.197518104296));
#209609=CARTESIAN_POINT('Ctrl Pts',(181.063151599407,-1.54382073804491,
137.634796795631));
#209610=CARTESIAN_POINT('Ctrl Pts',(180.784703975594,4.91216658577983,135.795238324681));
#209611=CARTESIAN_POINT('Ctrl Pts',(180.506256351781,6.85411278995147,129.369307058824));
#209612=CARTESIAN_POINT('Ctrl Pts',(180.227808727968,2.49746418218255,124.262119907186));
#209613=CARTESIAN_POINT('Ctrl Pts',(179.949361104155,-4.15423200110403,
125.16693236216));
#209614=CARTESIAN_POINT('Ctrl Pts',(179.670913480342,-6.98839192089168,
131.252265980172));
#209615=CARTESIAN_POINT('Ctrl Pts',(179.392465856529,-3.40056106730489,
136.925996451342));
#209616=CARTESIAN_POINT('Ctrl Pts',(179.114018232716,3.31221928049139,136.974242649806));
#209617=CARTESIAN_POINT('Ctrl Pts',(178.835570608904,6.98123192042358,131.352668676138));
#209618=CARTESIAN_POINT('Ctrl Pts',(178.55712298509,4.23483347762603,125.227226382977));
#209619=CARTESIAN_POINT('Ctrl Pts',(178.278675361277,-2.40317004799311,
124.22689799325));
#209620=CARTESIAN_POINT('Ctrl Pts',(178.000227737465,-6.83277770089014,
129.270936428355));
#209621=CARTESIAN_POINT('Ctrl Pts',(177.721780113652,-4.98339644641697,
135.724116781409));
#209622=CARTESIAN_POINT('Ctrl Pts',(177.443332489839,1.44548268986267,137.65628156334));
#209623=CARTESIAN_POINT('Ctrl Pts',(177.164884866026,6.54603384991367,133.291865731052));
#209624=CARTESIAN_POINT('Ctrl Pts',(176.886437242213,5.63109969342586,126.64155422085));
#209625=CARTESIAN_POINT('Ctrl Pts',(176.6079896184,-0.458539986806858,123.816658424832));
#209626=CARTESIAN_POINT('Ctrl Pts',(176.329541994587,-6.12680382008778,
127.413119575705));
#209627=CARTESIAN_POINT('Ctrl Pts',(176.051094370774,-6.16483425371434,
134.125965572714));
#209628=CARTESIAN_POINT('Ctrl Pts',(175.772646746962,-0.537683177073775,
137.786418885364));
#209629=CARTESIAN_POINT('Ctrl Pts',(175.494199123148,5.58357247201413,135.030701742416));
#209630=CARTESIAN_POINT('Ctrl Pts',(175.215751499336,6.57379779200069,128.391183573973));
#209631=CARTESIAN_POINT('Ctrl Pts',(174.937303875523,1.5230240890144,123.969257218339));
#209632=CARTESIAN_POINT('Ctrl Pts',(174.65885625171,-4.92733434791298,125.82845697323));
#209633=CARTESIAN_POINT('Ctrl Pts',(174.380408627897,-6.84971323277332,
132.260269090858));
#209634=CARTESIAN_POINT('Ctrl Pts',(174.101961004084,-2.4775402838095,137.354172446613));
#209635=CARTESIAN_POINT('Ctrl Pts',(173.823513380271,4.1713711514037,136.429118707571));
#209636=CARTESIAN_POINT('Ctrl Pts',(173.545065756458,6.98699628128659,130.335187068521));
#209637=CARTESIAN_POINT('Ctrl Pts',(173.266618132645,3.38191316241135,124.672403000642));
#209638=CARTESIAN_POINT('Ctrl Pts',(172.988170508833,-3.33098293707706,
124.644588419932));
#209639=CARTESIAN_POINT('Ctrl Pts',(172.709722885019,-6.98286844495469,
130.277303567246));
#209640=CARTESIAN_POINT('Ctrl Pts',(172.431275261207,-4.21783898400718,
136.394358395635));
#209641=CARTESIAN_POINT('Ctrl Pts',(172.152827637394,2.42317845035331,137.374478352552));
#209642=CARTESIAN_POINT('Ctrl Pts',(171.874380013581,6.83741326768756,132.316981079111));
#209643=CARTESIAN_POINT('Ctrl Pts',(171.595932389768,4.96839931822471,125.869459497128));
#209644=CARTESIAN_POINT('Ctrl Pts',(171.317484765955,-1.46633088488636,
123.956870961504));
#209645=CARTESIAN_POINT('Ctrl Pts',(171.039037142142,-6.55357463903296,
128.336790901335));
#209646=CARTESIAN_POINT('Ctrl Pts',(170.760589518329,-5.61840345982816,
134.984286862899));
#209647=CARTESIAN_POINT('Ctrl Pts',(170.482141894517,0.479806024690783,
137.79063480575));
#209648=CARTESIAN_POINT('Ctrl Pts',(170.203694270703,6.13709721234627,134.176938068128));
#209649=CARTESIAN_POINT('Ctrl Pts',(169.925246646891,6.15469587572206,127.464007413007));
#209650=CARTESIAN_POINT('Ctrl Pts',(169.646799023078,0.51642970291829,123.820698167548));
#209651=CARTESIAN_POINT('Ctrl Pts',(169.368351399265,-5.59641013787386,
126.595033542778));
#209652=CARTESIAN_POINT('Ctrl Pts',(169.089903775452,-6.56642246179436,
133.237534862678));
#209653=CARTESIAN_POINT('Ctrl Pts',(168.811456151639,-1.50221333089678,
137.644067918489));
#209654=CARTESIAN_POINT('Ctrl Pts',(168.533008527826,4.94245646389391,135.76524410303));
#209655=CARTESIAN_POINT('Ctrl Pts',(168.254560904013,6.84525022078748,129.32761071706));
#209656=CARTESIAN_POINT('Ctrl Pts',(167.976113280201,2.45759343384159,124.247038346411));
#209657=CARTESIAN_POINT('Ctrl Pts',(167.697665656387,-4.1884716586909,125.192324799951));
#209658=CARTESIAN_POINT('Ctrl Pts',(167.419218032575,-6.98553591510243,
131.294798006688));
#209659=CARTESIAN_POINT('Ctrl Pts',(167.140770408762,-3.36323392793624,
136.946583212019));
#209660=CARTESIAN_POINT('Ctrl Pts',(166.862322784949,3.34971573589186,136.953965917302));
#209661=CARTESIAN_POINT('Ctrl Pts',(166.583875161136,6.98444028114645,131.310161777048));
#209662=CARTESIAN_POINT('Ctrl Pts',(166.305427537323,4.20080541690416,125.20155108099));
#209663=CARTESIAN_POINT('Ctrl Pts',(166.02697991351,-2.44316440471955,124.241648636582));
#209664=CARTESIAN_POINT('Ctrl Pts',(165.748532289697,-6.84198549362249,
129.312557896394));
#209665=CARTESIAN_POINT('Ctrl Pts',(165.470084665885,-4.95335616345982,
135.754360978348));
#209666=CARTESIAN_POINT('Ctrl Pts',(165.191637042072,1.48716549602113,137.647355549705));
#209667=CARTESIAN_POINT('Ctrl Pts',(164.913189418259,6.56105471673207,133.251972077313));
#209668=CARTESIAN_POINT('Ctrl Pts',(164.634741794446,5.60565517810829,126.60735324588));
#209669=CARTESIAN_POINT('Ctrl Pts',(164.356294170633,-0.501067617717217,
123.819579153818));
#209670=CARTESIAN_POINT('Ctrl Pts',(164.07784654682,-6.1473337513746,127.450478001396));
#209671=CARTESIAN_POINT('Ctrl Pts',(163.799398923007,-6.14450048146789,
134.163431126959));
#209672=CARTESIAN_POINT('Ctrl Pts',(163.520951299194,-0.495171444628521,
137.789562554107));
#209673=CARTESIAN_POINT('Ctrl Pts',(163.242503675381,5.60919595935461,134.996634647659));
#209674=CARTESIAN_POINT('Ctrl Pts',(162.964056051569,6.55898630114736,128.351211711527));
#209675=CARTESIAN_POINT('Ctrl Pts',(162.685608427755,1.48138865648,123.960112777059));
#209676=CARTESIAN_POINT('Ctrl Pts',(162.407160803943,-4.95753279363329,
125.85854324792));
#209677=CARTESIAN_POINT('Ctrl Pts',(162.12871318013,-6.84072379533872,132.301938264875));
#209678=CARTESIAN_POINT('Ctrl Pts',(161.850265556317,-2.4376238170639,137.369132584688));
#209679=CARTESIAN_POINT('Ctrl Pts',(161.571817932504,4.20553336454888,136.403622173655));
#209680=CARTESIAN_POINT('Ctrl Pts',(161.293370308691,6.98401083586784,130.292663931709));
#209681=CARTESIAN_POINT('Ctrl Pts',(161.014922684878,3.34452353692138,124.651929946293));
#209682=CARTESIAN_POINT('Ctrl Pts',(160.736475061065,-3.36841750339773,
124.664979184829));
#209683=CARTESIAN_POINT('Ctrl Pts',(160.458027437253,-6.98594741443756,
130.319820034592));
#209684=CARTESIAN_POINT('Ctrl Pts',(160.179579813439,-4.18373293411359,
136.419930008985));
#209685=CARTESIAN_POINT('Ctrl Pts',(159.901132189627,2.46312772594441,137.35960604848));
#209686=CARTESIAN_POINT('Ctrl Pts',(159.622684565814,6.84649433633851,132.275331778507));
#209687=CARTESIAN_POINT('Ctrl Pts',(159.344236942001,4.93826712148011,125.839306872565));
#209688=CARTESIAN_POINT('Ctrl Pts',(159.065789318188,-1.50798633025781,
123.965923801919));
#209689=CARTESIAN_POINT('Ctrl Pts',(158.787341694375,-6.56847401371661,
128.376730088641));
#209690=CARTESIAN_POINT('Ctrl Pts',(158.508894070562,-5.59285496636459,
135.018410235101));
#209691=CARTESIAN_POINT('Ctrl Pts',(158.230446446749,0.522324568921774,
137.787584650814));
#209692=CARTESIAN_POINT('Ctrl Pts',(157.951998822937,6.15751334234277,134.139517329431));
#209693=CARTESIAN_POINT('Ctrl Pts',(157.673551199123,6.13424816540071,127.426603921307));
#209694=CARTESIAN_POINT('Ctrl Pts',(157.395103575311,0.473908599138188,
123.817683904457));
#209695=CARTESIAN_POINT('Ctrl Pts',(157.116655951498,-5.62192981801017,
126.62917846882));
#209696=CARTESIAN_POINT('Ctrl Pts',(156.838208327685,-6.55148937894732,
133.277461458893));
#209697=CARTESIAN_POINT('Ctrl Pts',(156.559760703872,-1.46055025868114,
137.653085593479));
#209698=CARTESIAN_POINT('Ctrl Pts',(156.281313080059,4.97256319746619,135.735066054016));
#209699=CARTESIAN_POINT('Ctrl Pts',(156.002865456246,6.83613399835919,129.285969096806));
#209700=CARTESIAN_POINT('Ctrl Pts',(155.724417832433,2.4176316184721,124.232199769625));
#209701=CARTESIAN_POINT('Ctrl Pts',(155.44597020862,-4.2225561109203,125.217925193794));
#209702=CARTESIAN_POINT('Ctrl Pts',(155.167522584808,-6.98242105771092,
131.337311859867));
#209703=CARTESIAN_POINT('Ctrl Pts',(154.889074960995,-3.3257821626974,136.96694237038));
#209704=CARTESIAN_POINT('Ctrl Pts',(154.610627337182,3.38708806634394,136.933461308912));
#209705=CARTESIAN_POINT('Ctrl Pts',(154.332179713369,6.98738983086623,131.267636135312));
#209706=CARTESIAN_POINT('Ctrl Pts',(154.053732089556,4.1666216937926,125.17608339317));
#209707=CARTESIAN_POINT('Ctrl Pts',(153.775284465743,-2.48306822909056,
124.256642463619));
#209708=CARTESIAN_POINT('Ctrl Pts',(153.49683684193,-6.85093975406627,129.354234643731));
#209709=CARTESIAN_POINT('Ctrl Pts',(153.218389218117,-4.92313233206838,
135.784421751204));
#209710=CARTESIAN_POINT('Ctrl Pts',(152.939941594304,1.52879319471521,137.638175966376));
#209711=CARTESIAN_POINT('Ctrl Pts',(152.661493970491,6.57583246125511,133.21198772643));
#209712=CARTESIAN_POINT('Ctrl Pts',(152.383046346679,5.58000294317656,126.573307792561));
#209713=CARTESIAN_POINT('Ctrl Pts',(152.104598722866,-0.543576681382813,
123.822758706449));
#209714=CARTESIAN_POINT('Ctrl Pts',(151.826151099053,-6.16763589094857,
127.487960706439));
#209715=CARTESIAN_POINT('Ctrl Pts',(151.54770347524,-6.12393902249645,134.200772209611));
#209716=CARTESIAN_POINT('Ctrl Pts',(151.269255851427,-0.452641363423277,
137.792447383624));
#209717=CARTESIAN_POINT('Ctrl Pts',(150.990808227614,5.63461159587598,134.962412206646));
#209718=CARTESIAN_POINT('Ctrl Pts',(150.712360603801,6.54393176464461,128.311330751416));
#209719=CARTESIAN_POINT('Ctrl Pts',(150.433912979988,1.4396983305442,123.951221951899));
#209720=CARTESIAN_POINT('Ctrl Pts',(150.155465356176,-4.98754753615285,
125.888812791691));
#209721=CARTESIAN_POINT('Ctrl Pts',(149.877017732362,-6.83148087236823,
132.343551945603));
#209722=CARTESIAN_POINT('Ctrl Pts',(149.59857010855,-2.39761702327129,137.383849462723));
#209723=CARTESIAN_POINT('Ctrl Pts',(149.320122484737,4.23953974010866,136.377918157044));
#209724=CARTESIAN_POINT('Ctrl Pts',(149.041674860924,6.98076659535922,130.250159756006));
#209725=CARTESIAN_POINT('Ctrl Pts',(148.763227237111,3.30700997888175,124.631684872525));
#209726=CARTESIAN_POINT('Ctrl Pts',(148.484779613298,-3.40572725176907,
124.685597446761));
#209727=CARTESIAN_POINT('Ctrl Pts',(148.206331989485,-6.98876751706998,
130.362354456768));
#209728=CARTESIAN_POINT('Ctrl Pts',(147.927884365672,-4.14947185445744,
136.445293535346));
#209729=CARTESIAN_POINT('Ctrl Pts',(147.649436741859,2.50298572943186,137.344490837378));
#209730=CARTESIAN_POINT('Ctrl Pts',(147.370989118047,6.85532170562399,132.233627970525));
#209731=CARTESIAN_POINT('Ctrl Pts',(147.092541494233,4.90795193543132,125.809338229895));
#209732=CARTESIAN_POINT('Ctrl Pts',(146.814093870421,-1.54958589664124,
123.975230043125));
#209733=CARTESIAN_POINT('Ctrl Pts',(146.535646246608,-6.58312999118006,
128.41675923269));
#209734=CARTESIAN_POINT('Ctrl Pts',(146.257198622795,-5.56709922760349,
135.052377454143));
#209735=CARTESIAN_POINT('Ctrl Pts',(145.978750998982,0.564823758223794,
137.784275729942));
#209736=CARTESIAN_POINT('Ctrl Pts',(145.700303375169,6.17770130341801,134.101973005276));
#209737=CARTESIAN_POINT('Ctrl Pts',(145.421855751356,6.11357314825767,127.389325593625));
#209738=CARTESIAN_POINT('Ctrl Pts',(145.143408127543,0.431369934500661,
123.81492853524));
#209739=CARTESIAN_POINT('Ctrl Pts',(144.864960503731,-5.64724117546963,
126.663478107772));
#209740=CARTESIAN_POINT('Ctrl Pts',(144.586512879918,-6.53631352825206,
133.317296413447));
#209741=CARTESIAN_POINT('Ctrl Pts',(144.308065256105,-1.41883306523854,
137.661849486446));
#209742=CARTESIAN_POINT('Ctrl Pts',(144.029617632292,5.00248567088053,135.704705295899));
#209743=CARTESIAN_POINT('Ctrl Pts',(143.751170008479,6.82676446047164,129.244383741109));
#209744=CARTESIAN_POINT('Ctrl Pts',(143.472722384666,2.37758021687388,124.217604726676));
#209745=CARTESIAN_POINT('Ctrl Pts',(143.194274760853,-4.25648409478009,
125.243732595056));
#209746=CARTESIAN_POINT('Ctrl Pts',(142.91582713704,-6.97904746413934,131.379805964341));
#209747=CARTESIAN_POINT('Ctrl Pts',(142.637379513228,-3.28820715937746,
136.987073172008));
#209748=CARTESIAN_POINT('Ctrl Pts',(142.358931889414,3.42433488700229,136.912729584442));
#209749=CARTESIAN_POINT('Ctrl Pts',(142.080484265602,6.99008046028611,131.225093326731));
#209750=CARTESIAN_POINT('Ctrl Pts',(141.802036641788,4.13228357498186,125.150824263232));
#209751=CARTESIAN_POINT('Ctrl Pts',(141.523589017976,-2.52288004245522,
124.271878918761));
#209752=CARTESIAN_POINT('Ctrl Pts',(141.245141394163,-6.859640150418,129.395965126019));
#209753=CARTESIAN_POINT('Ctrl Pts',(140.96669377035,-4.89272607219785,135.814297986063));
#209754=CARTESIAN_POINT('Ctrl Pts',(140.688246146537,1.57036424341533,137.628743153505));
#209755=CARTESIAN_POINT('Ctrl Pts',(140.409798522724,6.59036653588803,133.17191416004));
#209756=CARTESIAN_POINT('Ctrl Pts',(140.131350898911,5.55414393918375,126.539419122461));
#209757=CARTESIAN_POINT('Ctrl Pts',(139.852903275098,-0.586065602614643,
123.826196964908));
#209758=CARTESIAN_POINT('Ctrl Pts',(139.574455651286,-6.18770948650656,
127.525566301902));
#209759=CARTESIAN_POINT('Ctrl Pts',(139.296008027473,-6.10315063871238,
134.237987436982));
#209760=CARTESIAN_POINT('Ctrl Pts',(139.01756040366,-0.410094509425858,
137.795073267016));
#209761=CARTESIAN_POINT('Ctrl Pts',(138.739112779847,5.65981843979252,134.928035687503));
#209762=CARTESIAN_POINT('Ctrl Pts',(138.460665156034,6.52863474034383,128.271542171445));
#209763=CARTESIAN_POINT('Ctrl Pts',(138.182217532221,1.39795465605713,123.942585072312));
#209764=CARTESIAN_POINT('Ctrl Pts',(137.903769908408,-5.01737746326431,
125.919264482896));
#209765=CARTESIAN_POINT('Ctrl Pts',(137.625322284595,-6.82198480636163,
132.385108591028));
#209766=CARTESIAN_POINT('Ctrl Pts',(137.346874660782,-2.35752138489827,
137.39832253538));
#209767=CARTESIAN_POINT('Ctrl Pts',(137.06842703697,4.27338901796432,136.352007610208));
#209768=CARTESIAN_POINT('Ctrl Pts',(136.789979413157,6.9772636799772,130.20767611642));
#209769=CARTESIAN_POINT('Ctrl Pts',(136.511531789344,3.26937387837121,124.611668529527));
#209770=CARTESIAN_POINT('Ctrl Pts',(136.233084165531,-3.44291079966457,
124.706442441713));
#209771=CARTESIAN_POINT('Ctrl Pts',(135.954636541718,-6.99132864835187,
130.404905257644));
#209772=CARTESIAN_POINT('Ctrl Pts',(135.676188917905,-4.1150570145959,136.470448034864));
#209773=CARTESIAN_POINT('Ctrl Pts',(135.397741294092,2.54275098386259,137.329133279345));
#209774=CARTESIAN_POINT('Ctrl Pts',(135.11929367028,6.8638950484427,132.191871200516));
#209775=CARTESIAN_POINT('Ctrl Pts',(134.840846046466,4.87745488341857,125.779554679616));
#209776=CARTESIAN_POINT('Ctrl Pts',(134.562398422654,-1.59112804254939,
123.984789340275));
#209777=CARTESIAN_POINT('Ctrl Pts',(134.283950798841,-6.59754202834077,
128.456876850186));
#209778=CARTESIAN_POINT('Ctrl Pts',(134.005503175028,-5.54113719793324,
135.086187261361));
#209779=CARTESIAN_POINT('Ctrl Pts',(133.727055551215,0.607302017773813,
137.780708165749));
#209780=CARTESIAN_POINT('Ctrl Pts',(133.448607927402,6.19766034749954,134.064306486881));
#209781=CARTESIAN_POINT('Ctrl Pts',(133.170160303589,6.09267159041341,127.352173811322));
#209782=CARTESIAN_POINT('Ctrl Pts',(132.891712679776,0.388815285291658,
123.812432161999));
#209783=CARTESIAN_POINT('Ctrl Pts',(132.613265055963,-5.67234327233058,
126.697931188648));
#209784=CARTESIAN_POINT('Ctrl Pts',(132.334817432151,-6.52089547205522,
133.357038250242));
#209785=CARTESIAN_POINT('Ctrl Pts',(132.056369808337,-1.37706329641493,
137.670359272641));
#209786=CARTESIAN_POINT('Ctrl Pts',(131.777922184525,5.0322227753486,135.674162953708));
#209787=CARTESIAN_POINT('Ctrl Pts',(131.499474560712,6.81714195431646,129.20285619093));
#209788=CARTESIAN_POINT('Ctrl Pts',(131.221026936899,2.33744071316646,124.203253758389));
#209789=CARTESIAN_POINT('Ctrl Pts',(130.942579313086,-4.29025435305649,
125.269746047434));
#209790=CARTESIAN_POINT('Ctrl Pts',(130.664131689273,-6.97541525939744,
131.422278745477));
#209791=CARTESIAN_POINT('Ctrl Pts',(130.38568406546,-3.25051031033198,137.006974870947));
#209792=CARTESIAN_POINT('Ctrl Pts',(130.107236441647,3.46145481767177,136.891771512113));
#209793=CARTESIAN_POINT('Ctrl Pts',(129.828788817834,6.99251206970404,131.182534927744));
#209794=CARTESIAN_POINT('Ctrl Pts',(129.550341194022,4.09779233288376,125.125774627163));
#209795=CARTESIAN_POINT('Ctrl Pts',(129.271893570209,-2.5625983695722,124.287357437414));
#209796=CARTESIAN_POINT('Ctrl Pts',(128.993445946396,-6.86808636028122,
129.43774779692));
#209797=CARTESIAN_POINT('Ctrl Pts',(128.714998322583,-4.86213851056362,
135.84398857585));
#209798=CARTESIAN_POINT('Ctrl Pts',(128.43655069877,1.61187710169066,137.61905746063));
#209799=CARTESIAN_POINT('Ctrl Pts',(128.158103074957,6.60465640206541,133.131752863082));
#209800=CARTESIAN_POINT('Ctrl Pts',(127.879655451144,5.52807912434469,126.505688491336));
#209801=CARTESIAN_POINT('Ctrl Pts',(127.601207827331,-0.628532806970051,
123.829893801787));
#209802=CARTESIAN_POINT('Ctrl Pts',(127.322760203518,-6.20755379421381,
127.563293394292));
#209803=CARTESIAN_POINT('Ctrl Pts',(127.044312579706,-6.08213610043705,
134.275075430049));
#209804=CARTESIAN_POINT('Ctrl Pts',(126.765864955893,-0.367532459225645,
137.797440106979));
#209805=CARTESIAN_POINT('Ctrl Pts',(126.48741733208,5.68481555705546,134.893506364063));
#209806=CARTESIAN_POINT('Ctrl Pts',(126.208969708267,6.51309579508176,128.231847445991));
#209807=CARTESIAN_POINT('Ctrl Pts',(125.930522084454,1.35615917984635,123.934202458341));
#209808=CARTESIAN_POINT('Ctrl Pts',(125.652074460641,-5.04702146960864,
125.949897193134));
#209809=CARTESIAN_POINT('Ctrl Pts',(125.373626836828,-6.81223594919939,
132.426606661257));
#209810=CARTESIAN_POINT('Ctrl Pts',(125.095179213015,-2.3173383877032,137.412551266352));
#209811=CARTESIAN_POINT('Ctrl Pts',(124.816731589202,4.3070799438184,136.325891493273));
#209812=CARTESIAN_POINT('Ctrl Pts',(124.538283965389,6.97350221952356,130.165214587198));
#209813=CARTESIAN_POINT('Ctrl Pts',(124.259836341577,3.2316166300094,124.591881659011));
#209814=CARTESIAN_POINT('Ctrl Pts',(123.981388717764,-3.47996676923432,
124.727513397266));
#209815=CARTESIAN_POINT('Ctrl Pts',(123.702941093951,-6.99363071337966,
130.447470860486));
#209816=CARTESIAN_POINT('Ctrl Pts',(123.424493470138,-4.08048968978323,
136.495392575427));
#209817=CARTESIAN_POINT('Ctrl Pts',(123.146045846325,2.58242201572056,137.313533943462));
#209818=CARTESIAN_POINT('Ctrl Pts',(122.867598222512,6.87221404710605,132.150063015792));
#209819=CARTESIAN_POINT('Ctrl Pts',(122.589150598699,4.84677709552158,125.749957325369));
#209820=CARTESIAN_POINT('Ctrl Pts',(122.310702974886,-1.63261122862275,
123.994601339147));
#209821=CARTESIAN_POINT('Ctrl Pts',(122.032255351073,-6.6117095911554,128.497081454556));
#209822=CARTESIAN_POINT('Ctrl Pts',(121.753807727261,-5.51496983938628,
135.119838403918));
#209823=CARTESIAN_POINT('Ctrl Pts',(121.475360103447,0.649757773524084,
137.776882090432));
#209824=CARTESIAN_POINT('Ctrl Pts',(121.196912479635,6.21738973499768,134.026519169992));
#209825=CARTESIAN_POINT('Ctrl Pts',(120.918464855822,6.07154426638285,127.315149951069));
#209826=CARTESIAN_POINT('Ctrl Pts',(120.640017232009,0.346246228389124,
123.810194877238));
#209827=CARTESIAN_POINT('Ctrl Pts',(120.361569608196,-5.69723517842559,
126.732536434776));
#209828=CARTESIAN_POINT('Ctrl Pts',(120.083121984383,-6.50523578167861,
133.396685496627));
#209829=CARTESIAN_POINT('Ctrl Pts',(119.80467436057,-1.3352425000044,137.678614636731));
#209830=CARTESIAN_POINT('Ctrl Pts',(119.526226736757,5.06177340895125,135.6434401592));
#209831=CARTESIAN_POINT('Ctrl Pts',(119.247779112945,6.8072668364591,129.161387985085));
#209832=CARTESIAN_POINT('Ctrl Pts',(118.969331489131,2.29721459473369,124.189147396544));
#209833=CARTESIAN_POINT('Ctrl Pts',(118.690883865319,-4.32386563438011,
125.29596458699));
#209834=CARTESIAN_POINT('Ctrl Pts',(118.412436241506,-6.97152457807781,
131.464728629428));
#209835=CARTESIAN_POINT('Ctrl Pts',(118.133988617693,-3.21269301243169,
137.026646729736));
#209836=CARTESIAN_POINT('Ctrl Pts',(117.85554099388,3.49844648286018,136.870587868534));
#209837=CARTESIAN_POINT('Ctrl Pts',(117.577093370067,6.99468456901571,131.139962515369));
#209838=CARTESIAN_POINT('Ctrl Pts',(117.298645746254,4.06314924558364,125.100935413187));
#209839=CARTESIAN_POINT('Ctrl Pts',(117.020198122441,-2.60222173866402,
124.303077446017));
#209840=CARTESIAN_POINT('Ctrl Pts',(116.741750498628,-6.8762780706787,129.479581108162));
#209841=CARTESIAN_POINT('Ctrl Pts',(116.463302874816,-4.83137078059878,
135.873492420371));
#209842=CARTESIAN_POINT('Ctrl Pts',(116.184855251003,1.65333023126747,137.609119246659));
#209843=CARTESIAN_POINT('Ctrl Pts',(115.90640762719,6.61870153027093,133.09150532375));
#209844=CARTESIAN_POINT('Ctrl Pts',(115.627960003377,5.5018094645007,126.472117149089));
#209845=CARTESIAN_POINT('Ctrl Pts',(115.349512379564,-0.670976720811003,
123.833849080098));
#209846=CARTESIAN_POINT('Ctrl Pts',(115.071064755751,-6.22716807873245,
127.601140585621));
#209847=CARTESIAN_POINT('Ctrl Pts',(114.792617131938,-6.06089618637186,
134.312034814502));
#209848=CARTESIAN_POINT('Ctrl Pts',(114.514169508125,-0.324956789974863,
137.79954781581));
#209849=CARTESIAN_POINT('Ctrl Pts',(114.235721884312,5.70960202138734,134.858825515823));
#209850=CARTESIAN_POINT('Ctrl Pts',(113.957274260499,6.4973155046598,128.192248045959));
#209851=CARTESIAN_POINT('Ctrl Pts',(113.678826636687,1.31431345065849,123.926074420608));
#209852=CARTESIAN_POINT('Ctrl Pts',(113.400379012874,-5.07647845671644,
125.980709787299));
#209853=CARTESIAN_POINT('Ctrl Pts',(113.121931389061,-6.80223466212876,
132.468044618562));
#209854=CARTESIAN_POINT('Ctrl Pts',(112.843483765248,-2.27706952068197,
137.42653512839));
#209855=CARTESIAN_POINT('Ctrl Pts',(112.565036141435,4.34061126924124,136.299570773982));
#209856=CARTESIAN_POINT('Ctrl Pts',(112.286588517622,6.96948235338073,130.122776741767));
#209857=CARTESIAN_POINT('Ctrl Pts',(112.008140893809,3.1937396329048,124.572324994188));
#209858=CARTESIAN_POINT('Ctrl Pts',(111.729693269996,-3.51689378735575,
124.748809532627));
#209859=CARTESIAN_POINT('Ctrl Pts',(111.451245646184,-6.99567362684944,
130.490049688009));
#209860=CARTESIAN_POINT('Ctrl Pts',(111.172798022371,-4.0457711609245,136.52012623271));
#209861=CARTESIAN_POINT('Ctrl Pts',(110.894350398558,2.62199735498092,137.297693407768));
#209862=CARTESIAN_POINT('Ctrl Pts',(110.615902774745,6.88027839335069,132.108204965571));
#209863=CARTESIAN_POINT('Ctrl Pts',(110.337455150932,4.81591970851693,125.720547263895));
#209864=CARTESIAN_POINT('Ctrl Pts',(110.059007527119,-1.67403391768677,
124.004665676154));
#209865=CARTESIAN_POINT('Ctrl Pts',(109.780559903306,-6.62563215463966,
128.537371556004));
#209866=CARTESIAN_POINT('Ctrl Pts',(109.502112279493,-5.48859812160383,
135.153329634858));
#209867=CARTESIAN_POINT('Ctrl Pts',(109.22366465568,0.692189452261082,137.772797645767));
#209868=CARTESIAN_POINT('Ctrl Pts',(108.945217031867,6.23688873483282,133.988612454835));
#209869=CARTESIAN_POINT('Ctrl Pts',(108.666769408055,6.05019195904657,127.278255384801));
#209870=CARTESIAN_POINT('Ctrl Pts',(108.388321784241,0.303664341205276,
123.808216763862));
#209871=CARTESIAN_POINT('Ctrl Pts',(108.109874160429,-5.72191597137591,
126.767292563848));
#209872=CARTESIAN_POINT('Ctrl Pts',(107.831426536616,-6.48933503739778,
133.436236683461));
#209873=CARTESIAN_POINT('Ctrl Pts',(107.552978912803,-1.29337222569216,
137.68661527281));
#209874=CARTESIAN_POINT('Ctrl Pts',(107.27453128899,5.09113647667873,135.612538050821));
#209875=CARTESIAN_POINT('Ctrl Pts',(106.996083665177,6.79713947282576,129.119980660195));
#209876=CARTESIAN_POINT('Ctrl Pts',(106.717636041364,2.25690335216928,124.175286163858));
#209877=CARTESIAN_POINT('Ctrl Pts',(106.439188417551,-4.35731669327239,
125.322387242187));
#209878=CARTESIAN_POINT('Ctrl Pts',(106.160740793739,-6.96737556435125,
131.5071540432));
#209879=CARTESIAN_POINT('Ctrl Pts',(105.882293169926,-3.17475666701035,
137.046088019424));
#209880=CARTESIAN_POINT('Ctrl Pts',(105.603845546113,3.53530851182771,136.849179438675));
#209881=CARTESIAN_POINT('Ctrl Pts',(105.3253979223,6.99659787771835,131.097377667143));
#209882=CARTESIAN_POINT('Ctrl Pts',(105.046950298487,4.02835559679407,125.076307541727));
#209883=CARTESIAN_POINT('Ctrl Pts',(104.768502674674,-2.64174868147234,
124.319038362058));
#209884=CARTESIAN_POINT('Ctrl Pts',(104.490055050861,-6.88421497806359,
129.521463509594));
#209885=CARTESIAN_POINT('Ctrl Pts',(104.211607427049,-4.80042402241278,
135.902808426348));
#209886=CARTESIAN_POINT('Ctrl Pts',(103.933159803235,1.69472209608453,137.598928879852));
#209887=CARTESIAN_POINT('Ctrl Pts',(103.654712179423,6.63250140005722,133.051173033428));
#209888=CARTESIAN_POINT('Ctrl Pts',(103.37626455561,5.47533593308374,126.438706339714));
#209889=CARTESIAN_POINT('Ctrl Pts',(103.097816931797,-0.713395771362793,
123.838062653278));
#209890=CARTESIAN_POINT('Ctrl Pts',(102.819369307984,-6.24655161324796,
127.639106473447));
#209891=CARTESIAN_POINT('Ctrl Pts',(102.540921684171,-6.03943168356949,
134.348864220799));
#209892=CARTESIAN_POINT('Ctrl Pts',(102.262474060358,-0.282369079330704,
137.801396315408));
#209893=CARTESIAN_POINT('Ctrl Pts',(101.984026436545,5.73417691431645,134.823994427897));
#209894=CARTESIAN_POINT('Ctrl Pts',(101.705578812732,6.48129445382252,128.15274543872));
#209895=CARTESIAN_POINT('Ctrl Pts',(101.427131188919,1.27241901910234,123.9182012603));
#209896=CARTESIAN_POINT('Ctrl Pts',(101.148683565106,-5.1057473330482,126.01170112362));
#209897=CARTESIAN_POINT('Ctrl Pts',(100.870235941294,-6.7919813157512,132.509420927444));
#209898=CARTESIAN_POINT('Ctrl Pts',(100.591788317481,-2.23671627601227,
137.440273603317));
#209899=CARTESIAN_POINT('Ctrl Pts',(100.313340693668,4.37398175171709,136.273046427655));
#209900=CARTESIAN_POINT('Ctrl Pts',(100.034893069855,6.96520423050629,130.080364152676));
#209901=CARTESIAN_POINT('Ctrl Pts',(99.7564454460421,3.15574429060373,124.552999259737));
#209902=CARTESIAN_POINT('Ctrl Pts',(99.4779978222292,-3.55369048568456,
124.770330058661));
#209903=CARTESIAN_POINT('Ctrl Pts',(99.1995501984162,-6.99745731306031,
130.532640162439));
#209904=CARTESIAN_POINT('Ctrl Pts',(98.9211025746034,-4.01090271452764,
136.544648090195));
#209905=CARTESIAN_POINT('Ctrl Pts',(98.6426549507905,2.66147553516503,137.281612259238));
#209906=CARTESIAN_POINT('Ctrl Pts',(98.3642073269776,6.88808778834931,132.066298600918));
#209907=CARTESIAN_POINT('Ctrl Pts',(98.0857597031646,4.78488386583629,125.691325584995));
#209908=CARTESIAN_POINT('Ctrl Pts',(97.8073120793519,-1.71539457480834,
124.014981978356));
#209909=CARTESIAN_POINT('Ctrl Pts',(97.5288644555388,-6.63930920288774,
128.577745661565));
#209910=CARTESIAN_POINT('Ctrl Pts',(97.2504168317261,-5.46202302179963,
135.186659713151));
#209911=CARTESIAN_POINT('Ctrl Pts',(96.9719692079131,0.734595481663425,
137.768454983106));
#209912=CARTESIAN_POINT('Ctrl Pts',(96.6935215841003,6.25615662446226,133.950587746053));
#209913=CARTESIAN_POINT('Ctrl Pts',(96.4150739602873,6.0286154596223,127.24149147966));
#209914=CARTESIAN_POINT('Ctrl Pts',(96.1366263364746,0.26107120162757,123.806497895168));
#209915=CARTESIAN_POINT('Ctrl Pts',(95.8581787126614,-5.74638473662552,
126.80219828796));
#209916=CARTESIAN_POINT('Ctrl Pts',(95.5797310888487,-6.47319382842077,
133.47569034516));
#209917=CARTESIAN_POINT('Ctrl Pts',(95.3012834650358,-1.25145402499642,
137.694360884412));
#209918=CARTESIAN_POINT('Ctrl Pts',(95.0228358412229,5.12031089047184,135.581457773658));
#209919=CARTESIAN_POINT('Ctrl Pts',(94.7443882174101,6.78676023868958,129.078635750625));
#209920=CARTESIAN_POINT('Ctrl Pts',(94.465940593597,2.21650847922131,124.161670573963));
#209921=CARTESIAN_POINT('Ctrl Pts',(94.1874929697842,-4.39060629019222,
125.349013033923));
#209922=CARTESIAN_POINT('Ctrl Pts',(93.9090453459715,-6.96296837196094,
131.549553414704));
#209923=CARTESIAN_POINT('Ctrl Pts',(93.6305977221583,-3.13670267981308,
137.065298019608));
#209924=CARTESIAN_POINT('Ctrl Pts',(93.3521500983456,3.5720395386382,136.82754701583));
#209925=CARTESIAN_POINT('Ctrl Pts',(93.0737024745325,6.99825192491364,131.054781961061));
#209926=CARTESIAN_POINT('Ctrl Pts',(92.7952548507199,3.99341267580637,125.051891925383));
#209927=CARTESIAN_POINT('Ctrl Pts',(92.5168072269068,-2.68117773331193,
124.335239594101));
#209928=CARTESIAN_POINT('Ctrl Pts',(92.238359603094,-6.89189678833074,129.563393449252));
#209929=CARTESIAN_POINT('Ctrl Pts',(91.959911979281,-4.7692993827493,135.931935507467));
#209930=CARTESIAN_POINT('Ctrl Pts',(91.6814643554683,1.73605116235111,137.588486737821));
#209931=CARTESIAN_POINT('Ctrl Pts',(91.4030167316553,6.6460555000649,133.010757486647));
#209932=CARTESIAN_POINT('Ctrl Pts',(91.1245691078424,5.44865951108031,126.405457301267));
#209933=CARTESIAN_POINT('Ctrl Pts',(90.8461214840295,-0.755788386771977,
123.84253436519));
#209934=CARTESIAN_POINT('Ctrl Pts',(90.5676738602166,-6.26570367949625,
127.677189650927));
#209935=CARTESIAN_POINT('Ctrl Pts',(90.2892262364038,-6.01774338740505,
134.38556228421));
#209936=CARTESIAN_POINT('Ctrl Pts',(90.0107786125907,-0.239770905396614,
137.802985537273));
#209937=CARTESIAN_POINT('Ctrl Pts',(89.7323309887781,5.75853932521132,134.78901439096));
#209938=CARTESIAN_POINT('Ctrl Pts',(89.453883364965,6.46503323623579,128.113341088056));
#209939=CARTESIAN_POINT('Ctrl Pts',(89.1754357411521,1.23047743759138,123.910583269158));
#209940=CARTESIAN_POINT('Ctrl Pts',(88.8969881173393,-5.13482701403487,
126.042870053701));
#209941=CARTESIAN_POINT('Ctrl Pts',(88.6185404935264,-6.78147629000823,
132.550734054689));
#209942=CARTESIAN_POINT('Ctrl Pts',(88.3400928697134,-2.19628014899849,
137.453766182047));
#209943=CARTESIAN_POINT('Ctrl Pts',(88.0616452459006,4.4071901546906,136.246319437167));
#209944=CARTESIAN_POINT('Ctrl Pts',(87.7831976220877,6.96066800942769,130.037978391542));
#209945=CARTESIAN_POINT('Ctrl Pts',(87.5047499982748,3.1176320110373,124.533905171779));
#209946=CARTESIAN_POINT('Ctrl Pts',(87.2263023744621,-3.59035550070555,
124.792074177916));
#209947=CARTESIAN_POINT('Ctrl Pts',(86.9478547506488,-6.99898170591706,
130.57524070557));
#209948=CARTESIAN_POINT('Ctrl Pts',(86.6694071268362,-3.97588564265574,
136.568957239218));
#209949=CARTESIAN_POINT('Ctrl Pts',(86.3909595030232,2.70085509339449,137.265291093768));
#209950=CARTESIAN_POINT('Ctrl Pts',(86.1125118792103,6.89564194272181,132.024345474689));
#209951=CARTESIAN_POINT('Ctrl Pts',(85.8340642553976,4.75367071752436,125.662293371487));
#209952=CARTESIAN_POINT('Ctrl Pts',(85.5556166315845,-1.75669166735309,
124.025549863481));
#209953=CARTESIAN_POINT('Ctrl Pts',(85.2771690077717,-6.65274022909182,
128.618202275162));
#209954=CARTESIAN_POINT('Ctrl Pts',(84.9987213839588,-5.4352455247236,135.21982740374));
#209955=CARTESIAN_POINT('Ctrl Pts',(84.7202737601459,0.776974290360158,
137.763854263368));
#209956=CARTESIAN_POINT('Ctrl Pts',(84.4418261363329,6.27519268990729,133.912446452669));
#209957=CARTESIAN_POINT('Ctrl Pts',(84.1633785125202,6.00681556763514,127.204859597945));
#209958=CARTESIAN_POINT('Ctrl Pts',(83.8849308887072,0.218468387960617,
123.805038334852));
#209959=CARTESIAN_POINT('Ctrl Pts',(83.6064832648944,-5.77064056747553,
126.837252313669));
#209960=CARTESIAN_POINT('Ctrl Pts',(83.3280356410814,-6.45681275286598,
133.515045019753));
#209961=CARTESIAN_POINT('Ctrl Pts',(83.0495880172686,-1.20948945121144,
137.701851184522));
#209962=CARTESIAN_POINT('Ctrl Pts',(82.7711403934555,5.14929556926191,135.550200479404));
#209963=CARTESIAN_POINT('Ctrl Pts',(82.4926927696429,6.77612951865689,129.037354788424));
#209964=CARTESIAN_POINT('Ctrl Pts',(82.2142451458298,2.17603147273656,124.148301131391));
#209965=CARTESIAN_POINT('Ctrl Pts',(81.9357975220171,-4.42373319158141,
125.375840975569));
#209966=CARTESIAN_POINT('Ctrl Pts',(81.6573498982041,-6.95830316421689,
131.591925172815));
#209967=CARTESIAN_POINT('Ctrl Pts',(81.3789022743912,-3.09853246094448,
137.084276018453));
#209968=CARTESIAN_POINT('Ctrl Pts',(81.1004546505783,3.60863820220999,136.805691401599));
#209969=CARTESIAN_POINT('Ctrl Pts',(80.8220070267654,6.99964664931016,131.012176975526));
#209970=CARTESIAN_POINT('Ctrl Pts',(80.5435594029525,3.95832177744353,125.02768946888));
#209971=CARTESIAN_POINT('Ctrl Pts',(80.2651117791397,-2.72050743312451,
124.351680541802));
#209972=CARTESIAN_POINT('Ctrl Pts',(79.9866641553267,-6.89932321682792,
129.605369373404));
#209973=CARTESIAN_POINT('Ctrl Pts',(79.7082165315139,-4.73799801494326,
135.960872584412));
#209974=CARTESIAN_POINT('Ctrl Pts',(79.4297689077009,1.77731589860328,137.577793207502));
#209975=CARTESIAN_POINT('Ctrl Pts',(79.1513212838881,6.65936332804202,132.970260181018));
#209976=CARTESIAN_POINT('Ctrl Pts',(78.8728736600752,5.42178118699497,126.372371265798));
#209977=CARTESIAN_POINT('Ctrl Pts',(78.5944260362623,-0.798152996164653,
123.847264050135));
#209978=CARTESIAN_POINT('Ctrl Pts',(78.3159784124494,-6.28462356779051,
127.715388706879));
#209979=CARTESIAN_POINT('Ctrl Pts',(78.0375307886365,-5.99583210154638,
134.422127644877));
#209980=CARTESIAN_POINT('Ctrl Pts',(77.7590831648237,-0.197163846663491,
137.804315422519));
#209981=CARTESIAN_POINT('Ctrl Pts',(77.4806355410107,5.78268835131386,134.753886701214));
#209982=CARTESIAN_POINT('Ctrl Pts',(77.2021879171979,6.44853245446487,128.07403645411));
#209983=CARTESIAN_POINT('Ctrl Pts',(76.9237402933849,1.18849026028645,123.903220729472));
#209984=CARTESIAN_POINT('Ctrl Pts',(76.6452926695721,-5.16371642211823,
126.074215422566));
#209985=CARTESIAN_POINT('Ctrl Pts',(76.3668450457591,-6.77071997416741,
132.591982469425));
#209986=CARTESIAN_POINT('Ctrl Pts',(76.0883974219463,-2.15576263801617,
137.467012364608));
#209987=CARTESIAN_POINT('Ctrl Pts',(75.8099497981334,4.44023524761227,136.219390792892));
#209988=CARTESIAN_POINT('Ctrl Pts',(75.5315021743204,6.95587385823614,129.995621028982));
#209989=CARTESIAN_POINT('Ctrl Pts',(75.2530545505077,3.0794042064702,124.515043437855));
#209990=CARTESIAN_POINT('Ctrl Pts',(74.9746069266946,-3.62688747378295,
124.814041084656));
#209991=CARTESIAN_POINT('Ctrl Pts',(74.6961593028819,-7.0002467489329,130.617849738824));
#209992=CARTESIAN_POINT('Ctrl Pts',(74.4177116790688,-3.94072124287924,
136.593052778991));
#209993=CARTESIAN_POINT('Ctrl Pts',(74.1392640552561,2.74013457044532,137.248730516143));
#209994=CARTESIAN_POINT('Ctrl Pts',(73.860816431443,6.90294057654623,131.982347141473));
#209995=CARTESIAN_POINT('Ctrl Pts',(73.5823688076304,4.72228142019582,125.633451699173));
#209996=CARTESIAN_POINT('Ctrl Pts',(73.3039211838172,-1.79792366504193,
124.036368939932));
#209997=CARTESIAN_POINT('Ctrl Pts',(73.0254735600045,-6.66592473556012,
128.658739897661));
#209998=CARTESIAN_POINT('Ctrl Pts',(72.7470259361915,-5.40826662262595,
135.252831477583));
#209999=CARTESIAN_POINT('Ctrl Pts',(72.4685783123786,0.819324307988826,
137.758995657032));
#210000=CARTESIAN_POINT('Ctrl Pts',(72.1901306885658,6.2939962257795,133.87418998802));
#210001=CARTESIAN_POINT('Ctrl Pts',(71.9116830647529,5.98479309088811,127.168361097063));
#210002=CARTESIAN_POINT('Ctrl Pts',(71.63323544094,0.17585747886725,123.803838136996));
#210003=CARTESIAN_POINT('Ctrl Pts',(71.3547878171271,-5.79468256511725,
126.872453342036));
#210004=CARTESIAN_POINT('Ctrl Pts',(71.0763401933142,-6.44019241774003,
133.554299248939));
#210005=CARTESIAN_POINT('Ctrl Pts',(70.7978925695013,-1.16748005934989,
137.709085895581));
#210006=CARTESIAN_POINT('Ctrl Pts',(70.5194449456884,5.17808943901089,135.518767326308));
#210007=CARTESIAN_POINT('Ctrl Pts',(70.2409973218756,6.76524770665308,128.996139303274));
#210008=CARTESIAN_POINT('Ctrl Pts',(69.9625496980626,2.1354738326052,124.135178331551));
#210009=CARTESIAN_POINT('Ctrl Pts',(69.6841020742497,-4.45669616991057,
125.402870073008));
#210010=CARTESIAN_POINT('Ctrl Pts',(69.4056544504369,-6.95338011399016,
131.634267747431));
#210011=CARTESIAN_POINT('Ctrl Pts',(69.1272068266238,-3.06024742481583,
137.103021312725));
#210012=CARTESIAN_POINT('Ctrl Pts',(68.8487592028112,3.64510314636624,136.783613405848));
#210013=CARTESIAN_POINT('Ctrl Pts',(68.5703115789981,7.00078199922599,130.969564289278));
#210014=CARTESIAN_POINT('Ctrl Pts',(68.2918639551854,3.92308420201135,125.003701069051));
#210015=CARTESIAN_POINT('Ctrl Pts',(68.0134163313723,-2.75973632353393,
124.368360595937));
#210016=CARTESIAN_POINT('Ctrl Pts',(67.7349687075595,-6.90649398836592,
129.647389726619));
#210017=CARTESIAN_POINT('Ctrl Pts',(67.4565210837467,-4.70652107887851,
135.98961858491));
#210018=CARTESIAN_POINT('Ctrl Pts',(67.1780734599337,1.81851477576126,137.566848685147));
#210019=CARTESIAN_POINT('Ctrl Pts',(66.8996258361208,6.67242439086218,132.929682617185));
#210020=CARTESIAN_POINT('Ctrl Pts',(66.6211782123079,5.39470195681365,126.339449459324));
#210021=CARTESIAN_POINT('Ctrl Pts',(66.3427305884951,-0.840488029704522,
123.852251532852));
#210022=CARTESIAN_POINT('Ctrl Pts',(66.0642829646821,-6.30331057704718,
127.753702225821));
#210023=CARTESIAN_POINT('Ctrl Pts',(65.7858353408693,-5.97369863792435,
134.458558947856));
#210024=CARTESIAN_POINT('Ctrl Pts',(65.5073877170563,-0.154549481951222,
137.805385921867));
#210025=CARTESIAN_POINT('Ctrl Pts',(65.2289400932435,5.80662309777304,134.718612660325));
#210026=CARTESIAN_POINT('Ctrl Pts',(64.9504924694306,6.43179271995227,128.03483299333));
#210027=CARTESIAN_POINT('Ctrl Pts',(64.6720448456177,1.14645904303803,123.896113914062));
#210028=CARTESIAN_POINT('Ctrl Pts',(64.3935972218049,-5.19241448679041,
126.1057360687));
#210029=CARTESIAN_POINT('Ctrl Pts',(64.1151495979918,-6.75971276680813,
132.633164643176));
#210030=CARTESIAN_POINT('Ctrl Pts',(63.8367019741791,-2.11516524445634,
137.480011660159));
#210031=CARTESIAN_POINT('Ctrl Pts',(63.5582543503661,4.47311580598391,136.192261492683));
#210032=CARTESIAN_POINT('Ctrl Pts',(63.2798067265533,6.95082195458075,129.953293634565));
#210033=CARTESIAN_POINT('Ctrl Pts',(63.0013591027403,3.041062293448,124.496414756892));
#210034=CARTESIAN_POINT('Ctrl Pts',(62.7229114789275,-3.66328505121137,
124.836229964889));
#210035=CARTESIAN_POINT('Ctrl Pts',(62.4444638551145,-7.00125239523119,
130.660465683307));
#210036=CARTESIAN_POINT('Ctrl Pts',(62.1660162313017,-3.90541081822766,
136.616933816649));
#210037=CARTESIAN_POINT('Ctrl Pts',(61.8875686074887,2.77931251080179,137.231931140021));
#210038=CARTESIAN_POINT('Ctrl Pts',(61.609120983676,6.909983419369,131.940305157533));
#210039=CARTESIAN_POINT('Ctrl Pts',(61.3306733598629,4.69071713699276,125.604801636791));
#210040=CARTESIAN_POINT('Ctrl Pts',(61.0522257360502,-1.83908904000824,
124.047438806804));
#210041=CARTESIAN_POINT('Ctrl Pts',(60.7737781122372,-6.67886223373588,
128.699357026925));
#210042=CARTESIAN_POINT('Ctrl Pts',(60.4953304884244,-5.38108731521968,
135.285670711703));
#210043=CARTESIAN_POINT('Ctrl Pts',(60.2168828646114,0.861643965253713,
137.753879344138));
#210044=CARTESIAN_POINT('Ctrl Pts',(59.9384352407986,6.31256653530686,133.835819769716));
#210045=CARTESIAN_POINT('Ctrl Pts',(59.6599876169856,5.96254884543232,127.131997329482));
#210046=CARTESIAN_POINT('Ctrl Pts',(59.3815399931728,0.133240053310041,
123.802897346075));
#210047=CARTESIAN_POINT('Ctrl Pts',(59.1030923693598,-5.81850983866561,
126.907800068673));
#210048=CARTESIAN_POINT('Ctrl Pts',(58.824644745547,-6.42333343891552,133.593451578138));
#210049=CARTESIAN_POINT('Ctrl Pts',(58.5461971217341,-1.12542740608588,
137.716064749505));
#210050=CARTESIAN_POINT('Ctrl Pts',(58.2677494979212,5.20669143275151,135.487159479138));
#210051=CARTESIAN_POINT('Ctrl Pts',(57.9893018741083,6.75411520590753,128.954990822428));
#210052=CARTESIAN_POINT('Ctrl Pts',(57.7108542502954,2.09483706170563,124.122302660713));
#210053=CARTESIAN_POINT('Ctrl Pts',(57.4324066264825,-4.48949400372376,
125.430099324666));
#210054=CARTESIAN_POINT('Ctrl Pts',(57.1539590026696,-6.94819940370625,
131.676579569534));
#210055=CARTESIAN_POINT('Ctrl Pts',(56.8755113788568,-3.02184899009409,
137.121533207807));
#210056=CARTESIAN_POINT('Ctrl Pts',(56.5970637550437,3.68143301988451,136.761313846687));
#210057=CARTESIAN_POINT('Ctrl Pts',(56.318616131231,7.00165793259049,130.926945481348));
#210058=CARTESIAN_POINT('Ctrl Pts',(56.040168507418,3.88770125525153,124.979927614796));
#210059=CARTESIAN_POINT('Ctrl Pts',(55.7617208836052,-2.79886295089852,
124.385279138419));
#210060=CARTESIAN_POINT('Ctrl Pts',(55.4832732597923,-6.91340883722955,
129.689452951814));
#210061=CARTESIAN_POINT('Ctrl Pts',(55.2048256359794,-4.67486974094423,
136.018172443767));
#210062=CARTESIAN_POINT('Ctrl Pts',(54.9263780121665,1.85964626718557,137.555653576309));
#210063=CARTESIAN_POINT('Ctrl Pts',(54.6479303883536,6.68523820454244,132.889026298762));
#210064=CARTESIAN_POINT('Ctrl Pts',(54.3694827645407,5.36742282396772,126.306693101776));
#210065=CARTESIAN_POINT('Ctrl Pts',(54.0910351407278,-0.882791918651148,
123.857496628527));
#210066=CARTESIAN_POINT('Ctrl Pts',(53.8125875169149,-6.32176401481248,
127.792128788032));
#210067=CARTESIAN_POINT('Ctrl Pts',(53.534139893102,-5.95134381670231,134.494854843172));
#210068=CARTESIAN_POINT('Ctrl Pts',(53.2556922692892,-0.111929390351441,
137.806196995646));
#210069=CARTESIAN_POINT('Ctrl Pts',(52.9772446454762,5.83034267767769,134.683193575387));
#210070=CARTESIAN_POINT('Ctrl Pts',(52.6987970216634,6.41481465299549,127.995732158415));
#210071=CARTESIAN_POINT('Ctrl Pts',(52.4203493978505,1.10438534332797,123.889263086274));
#210072=CARTESIAN_POINT('Ctrl Pts',(52.1419017740376,-5.22092014463445,
126.137430824095));
#210073=CARTESIAN_POINT('Ctrl Pts',(51.8634541502246,-6.74845507580631,
132.674279049921));
#210074=CARTESIAN_POINT('Ctrl Pts',(51.5850065264118,-2.07448947267055,
137.492763587005));
#210075=CARTESIAN_POINT('Ctrl Pts',(51.3065589025989,4.50583061140446,136.164932541826));
#210076=CARTESIAN_POINT('Ctrl Pts',(51.028111278786,6.94551248566166,129.910997776748));
#210077=CARTESIAN_POINT('Ctrl Pts',(50.7496636549731,3.00260769274395,124.478019819181));
#210078=CARTESIAN_POINT('Ctrl Pts',(50.4712160311602,-3.69954688426507,
124.858639996399));
#210079=CARTESIAN_POINT('Ctrl Pts',(50.1927684073473,-7.00199860754717,
130.70308695987));
#210080=CARTESIAN_POINT('Ctrl Pts',(49.9143207835345,-3.86995567714208,
136.640599467269));
#210081=CARTESIAN_POINT('Ctrl Pts',(49.6358731597215,2.81838746271124,137.214893587909));
#210082=CARTESIAN_POINT('Ctrl Pts',(49.3574255359087,6.91677021021505,131.89822108075));
#210083=CARTESIAN_POINT('Ctrl Pts',(49.0789779120958,4.65897903754105,125.576344245977));
#210084=CARTESIAN_POINT('Ctrl Pts',(48.8005302882828,-1.88018626685394,
124.058759053897));
#210085=CARTESIAN_POINT('Ctrl Pts',(48.5220826644701,-6.69155224421552,
128.740052157871));
#210086=CARTESIAN_POINT('Ctrl Pts',(48.243635040657,-5.35370860964396,135.318343889229));
#210087=CARTESIAN_POINT('Ctrl Pts',(47.9651874168443,0.903931693984841,
137.748505514272));
#210088=CARTESIAN_POINT('Ctrl Pts',(47.6867397930313,6.33090293035988,133.797337219578));
#210089=CARTESIAN_POINT('Ctrl Pts',(47.4082921692184,5.94008365553619,127.095769642671));
#210090=CARTESIAN_POINT('Ctrl Pts',(47.1298445454056,0.0906176904940206,
123.80221599695));
#210091=CARTESIAN_POINT('Ctrl Pts',(46.8513969215926,-5.84212150519187,
126.943291183793));
#210092=CARTESIAN_POINT('Ctrl Pts',(46.5729492977799,-6.40623644110861,
133.632500556544));
#210093=CARTESIAN_POINT('Ctrl Pts',(46.2945016739667,-1.08333304969514,
137.722787487691));
#210094=CARTESIAN_POINT('Ctrl Pts',(46.016054050154,5.23510049062639,135.455378109134));
#210095=CARTESIAN_POINT('Ctrl Pts',(45.737606426341,6.7427324289391,128.913910870662));
#210096=CARTESIAN_POINT('Ctrl Pts',(45.4591588025282,2.0541226658487,124.10967459599));
#210097=CARTESIAN_POINT('Ctrl Pts',(45.1807111787153,-4.5221254776858,125.457527721552));
#210098=CARTESIAN_POINT('Ctrl Pts',(44.9022635549024,-6.94276122533821,
131.718859071242));
#210099=CARTESIAN_POINT('Ctrl Pts',(44.6238159310895,-2.98333857964632,
137.139811017737));
#210100=CARTESIAN_POINT('Ctrl Pts',(44.3453683072766,3.71762647654865,136.738793550433));
#210101=CARTESIAN_POINT('Ctrl Pts',(44.0669206834637,7.00227441694529,130.88432213099));
#210102=CARTESIAN_POINT('Ctrl Pts',(43.7884730596509,3.85217424829189,124.956369987047));
#210103=CARTESIAN_POINT('Ctrl Pts',(43.5100254358379,-2.8378858653675,124.402435542326));
#210104=CARTESIAN_POINT('Ctrl Pts',(43.2315778120251,-6.92006750718621,
129.731557490323));
#210105=CARTESIAN_POINT('Ctrl Pts',(42.9531301882121,-4.64304517399252,
136.04653310291));
#210106=CARTESIAN_POINT('Ctrl Pts',(42.6746825643993,1.90070884873357,137.544208295828));
#210107=CARTESIAN_POINT('Ctrl Pts',(42.3962349405864,6.69780429426274,132.848292732287));
#210108=CARTESIAN_POINT('Ctrl Pts',(42.1177873167735,5.33994479929498,126.274103406951));
#210109=CARTESIAN_POINT('Ctrl Pts',(41.8393396929606,-0.925063095418803,
123.862999142802));
#210110=CARTESIAN_POINT('Ctrl Pts',(41.5608920691476,-6.33998319728738,
127.8306669696));
#210111=CARTESIAN_POINT('Ctrl Pts',(41.2824444453348,-5.92876846624656,
134.531013985867));
#210112=CARTESIAN_POINT('Ctrl Pts',(41.0039968215219,-0.069305151166692,
137.806748613804));
#210113=CARTESIAN_POINT('Ctrl Pts',(40.725549197709,5.85384621209049,134.647630758868));
#210114=CARTESIAN_POINT('Ctrl Pts',(40.4471015738961,6.39759888272248,127.956735398261));
#210115=CARTESIAN_POINT('Ctrl Pts',(40.1686539500832,1.06227072021291,123.882668499967));
#210116=CARTESIAN_POINT('Ctrl Pts',(39.8902063262704,-5.24923233936253,
126.169298514289));
#210117=CARTESIAN_POINT('Ctrl Pts',(39.6117587024575,-6.73694731831984,
132.715324166149));
#210118=CARTESIAN_POINT('Ctrl Pts',(39.3333110786445,-2.03373682991476,
137.505267672621));
#210119=CARTESIAN_POINT('Ctrl Pts',(39.0548634548317,4.53837845161457,136.137404953004));
#210120=CARTESIAN_POINT('Ctrl Pts',(38.7764158310188,6.9399456482232,129.86873502282));
#210121=CARTESIAN_POINT('Ctrl Pts',(38.4979682072059,2.96404182930761,124.459859306355));
#210122=CARTESIAN_POINT('Ctrl Pts',(38.219520583393,-3.73567162924815,124.881270348773));
#210123=CARTESIAN_POINT('Ctrl Pts',(37.9410729595801,-7.00248535822977,
130.745711989165));
#210124=CARTESIAN_POINT('Ctrl Pts',(37.6626253357672,-3.83435713342598,
136.664048853912));
#210125=CARTESIAN_POINT('Ctrl Pts',(37.3841777119543,2.8573579782368,137.197618491141));
#210126=CARTESIAN_POINT('Ctrl Pts',(37.1057300881414,6.92330069759731,131.856096470565));
#210127=CARTESIAN_POINT('Ctrl Pts',(36.8272824643285,4.62706829790778,125.548080581235));
#210128=CARTESIAN_POINT('Ctrl Pts',(36.5488348405156,-1.92121382270608,
124.070329261737));
#210129=CARTESIAN_POINT('Ctrl Pts',(36.2703872167028,-6.70399429676593,
128.780823782526));
#210130=CARTESIAN_POINT('Ctrl Pts',(35.9919395928899,-5.32613152042688,
135.350849799446));
#210131=CARTESIAN_POINT('Ctrl Pts',(35.7134919690769,0.946185927194629,
137.742874366562));
#210132=CARTESIAN_POINT('Ctrl Pts',(35.4350443452641,6.34900473147662,133.758743763591));
#210133=CARTESIAN_POINT('Ctrl Pts',(35.1565967214512,5.91739835365575,127.059679379064));
#210134=CARTESIAN_POINT('Ctrl Pts',(34.8781490976383,0.0479919698059151,
123.80179411487));
#210135=CARTESIAN_POINT('Ctrl Pts',(34.5997014738253,-5.8655166897575,126.978925372262));
#210136=CARTESIAN_POINT('Ctrl Pts',(34.3212538500126,-6.38890205785425,
133.671444737187));
#210137=CARTESIAN_POINT('Ctrl Pts',(34.0428062261996,-1.04119854999986,
137.729253861025));
#210138=CARTESIAN_POINT('Ctrl Pts',(33.7643586023867,5.26331555992738,135.423424393967));
#210139=CARTESIAN_POINT('Ctrl Pts',(33.4859109785738,6.73109979754094,128.872900970206));
#210140=CARTESIAN_POINT('Ctrl Pts',(33.207463354761,2.01333215372067,124.097294605319));
#210141=CARTESIAN_POINT('Ctrl Pts',(32.9290157309481,-4.55458938262534,
125.485154247296));
#210142=CARTESIAN_POINT('Ctrl Pts',(32.6505681071352,-6.93706578039975,
131.761104685873));
#210143=CARTESIAN_POINT('Ctrl Pts',(32.3721204833222,-2.94471762049033,
137.157854065221));
#210144=CARTESIAN_POINT('Ctrl Pts',(32.0936728595094,3.75368217519627,136.716053351584));
#210145=CARTESIAN_POINT('Ctrl Pts',(31.8152252356965,7.00263142944649,130.84169581763));
#210146=CARTESIAN_POINT('Ctrl Pts',(31.5367776118836,3.8165044975991,124.933029058741));
#210147=CARTESIAN_POINT('Ctrl Pts',(31.2583299880707,-2.87680362093211,
124.41982917192));
#210148=CARTESIAN_POINT('Ctrl Pts',(30.9798823642578,-6.92646975149653,
129.773701781947));
#210149=CARTESIAN_POINT('Ctrl Pts',(30.7014347404449,-4.6110485572945,136.074699511423));
#210150=CARTESIAN_POINT('Ctrl Pts',(30.422987116632,1.94170099881587,137.532513267813));
#210151=CARTESIAN_POINT('Ctrl Pts',(30.1445394928192,6.71012219438185,132.807483427156));
#210152=CARTESIAN_POINT('Ctrl Pts',(29.8660918690062,5.31226890100394,126.241681582474));
#210153=CARTESIAN_POINT('Ctrl Pts',(29.5876442451933,-0.967299993633269,
123.868758871779));
#210154=CARTESIAN_POINT('Ctrl Pts',(29.3091966213805,-6.35796744935336,
127.869315342481));
#210155=CARTESIAN_POINT('Ctrl Pts',(29.0307489975676,-5.90597342309497,
134.567035036052));
#210156=CARTESIAN_POINT('Ctrl Pts',(28.7523013737546,-0.026678343854083,
137.807040755898));
#210157=CARTESIAN_POINT('Ctrl Pts',(28.4738537499418,5.87713283007914,134.611925528561));
#210158=CARTESIAN_POINT('Ctrl Pts',(28.1954061261289,6.38014604707014,127.917844157905));
#210159=CARTESIAN_POINT('Ctrl Pts',(27.916958502316,1.02011673426565,123.876330399509));
#210160=CARTESIAN_POINT('Ctrl Pts',(27.6385108785031,-5.27735002185588,
126.201337958415));
#210161=CARTESIAN_POINT('Ctrl Pts',(27.3600632546902,-6.72518992077305,
132.756298470923));
#210162=CARTESIAN_POINT('Ctrl Pts',(27.0816156308773,-1.99290882629253,
137.51752345366));
#210163=CARTESIAN_POINT('Ctrl Pts',(26.8031680070644,4.57075812054227,136.109679746264));
#210164=CARTESIAN_POINT('Ctrl Pts',(26.5247203832516,6.93412164854658,129.826506938842));
#210165=CARTESIAN_POINT('Ctrl Pts',(26.2462727594386,2.92536613221128,124.441933891359));
#210166=CARTESIAN_POINT('Ctrl Pts',(25.9678251356258,-3.7716579475455,124.904120183435));
#210167=CARTESIAN_POINT('Ctrl Pts',(25.6893775118128,-7.00271262924226,
130.788339191706));
#210168=CARTESIAN_POINT('Ctrl Pts',(25.410929888,-3.79861650619593,136.687281107654));
#210169=CARTESIAN_POINT('Ctrl Pts',(25.1324822641871,2.89622261331168,137.180106489852));
#210170=CARTESIAN_POINT('Ctrl Pts',(24.8540346403742,6.92957463952618,131.813932887921));
#210171=CARTESIAN_POINT('Ctrl Pts',(24.5755870165613,4.59498610055721,125.520011689881));
#210172=CARTESIAN_POINT('Ctrl Pts',(24.2971393927484,-1.96217018727317,
124.082149001586));
#210173=CARTESIAN_POINT('Ctrl Pts',(24.0186917689355,-6.71618793034234,
128.821670390082));
#210174=CARTESIAN_POINT('Ctrl Pts',(23.7402441451226,-5.29835706944761,
135.383187237832));
#210175=CARTESIAN_POINT('Ctrl Pts',(23.4617965213097,0.988405099136929,
137.736986109674));
#210176=CARTESIAN_POINT('Ctrl Pts',(23.1833488974968,6.36687126788796,133.720040831851));
#210177=CARTESIAN_POINT('Ctrl Pts',(22.9049012736839,5.89449378040337,127.023727875996));
#210178=CARTESIAN_POINT('Ctrl Pts',(22.6264536498711,0.00536447075796404,
123.801631715467));
#210179=CARTESIAN_POINT('Ctrl Pts',(22.3480060260581,-5.88869452544514,
127.01470131364));
#210180=CARTESIAN_POINT('Ctrl Pts',(22.0695584022453,-6.3713309314846,133.710282676972));
#210181=CARTESIAN_POINT('Ctrl Pts',(21.7911107784324,-0.999025468309402,
137.735463629893));
#210182=CARTESIAN_POINT('Ctrl Pts',(21.5126631546195,5.29133559513472,135.391299517692));
#210183=CARTESIAN_POINT('Ctrl Pts',(21.2342155308066,6.71921774276442,128.831962640697));
#210184=CARTESIAN_POINT('Ctrl Pts',(20.9557679069937,1.97246703682929,124.085163147446));
#210185=CARTESIAN_POINT('Ctrl Pts',(20.6773202831809,-4.58688451558038,
125.51297787819));
#210186=CARTESIAN_POINT('Ctrl Pts',(20.3988726593679,-6.93111327993769,
131.803314848003));
#210187=CARTESIAN_POINT('Ctrl Pts',(20.120425035555,-2.90598754374001,137.175661681671));
#210188=CARTESIAN_POINT('Ctrl Pts',(19.8419774117421,3.78959877977074,136.693094092787));
#210189=CARTESIAN_POINT('Ctrl Pts',(19.5635297879293,7.00272895686486,130.799068120799));
#210190=CARTESIAN_POINT('Ctrl Pts',(19.2850821641163,3.78069332492835,124.909905694786));
#210191=CARTESIAN_POINT('Ctrl Pts',(19.0066345403035,-2.91561477548059,
124.437459382677));
#210192=CARTESIAN_POINT('Ctrl Pts',(18.7281869164906,-6.932615332923,129.815884265012));
#210193=CARTESIAN_POINT('Ctrl Pts',(18.4497392926777,-4.57888107649638,
136.102670625591));
#210194=CARTESIAN_POINT('Ctrl Pts',(18.1712916688647,1.98262119845391,137.520568925627));
#210195=CARTESIAN_POINT('Ctrl Pts',(17.892844045052,6.72219144845534,132.766599895572));
#210196=CARTESIAN_POINT('Ctrl Pts',(17.614396421239,5.28439615463518,126.209428829746));
#210197=CARTESIAN_POINT('Ctrl Pts',(17.3359487974261,-1.00950104819076,
123.87477560203));
#210198=CARTESIAN_POINT('Ctrl Pts',(17.0575011736132,-6.37571610459714,
127.908072474542));
#210199=CARTESIAN_POINT('Ctrl Pts',(16.7790535498004,-5.88295953192644,
134.602916658952));
#210200=CARTESIAN_POINT('Ctrl Pts',(16.5006059259874,0.0159494520341194,
137.807073411106));
#210201=CARTESIAN_POINT('Ctrl Pts',(16.2221583021745,5.90020166874948,134.576079207535));
#210202=CARTESIAN_POINT('Ctrl Pts',(15.9437106783617,6.3624567927597,127.879059878479));
#210203=CARTESIAN_POINT('Ctrl Pts',(15.6652630545488,0.977924947517885,
123.870249019757));
#210204=CARTESIAN_POINT('Ctrl Pts',(15.3868154307359,-5.3052721502032,126.233547969238));
#210205=CARTESIAN_POINT('Ctrl Pts',(15.108367806923,-6.71318331884074,132.797200445919));
#210206=CARTESIAN_POINT('Ctrl Pts',(14.8299201831101,-1.95200697470083,
137.529530475982));
#210207=CARTESIAN_POINT('Ctrl Pts',(14.5514725592972,4.6029684183469,136.081757948972));
#210208=CARTESIAN_POINT('Ctrl Pts',(14.2730249354843,6.92804070244224,129.784315089592));
#210209=CARTESIAN_POINT('Ctrl Pts',(13.9945773116714,2.88658203459712,124.424244238425));
#210210=CARTESIAN_POINT('Ctrl Pts',(13.7161296878585,-3.80750450567058,
124.927188653676));
#210211=CARTESIAN_POINT('Ctrl Pts',(13.4376820640456,-7.00268041216303,
130.830966987928));
#210212=CARTESIAN_POINT('Ctrl Pts',(13.1592344402328,-3.7627351198343,136.710295367612));
#210213=CARTESIAN_POINT('Ctrl Pts',(12.8807868164199,2.93497992779253,137.162358232954));
#210214=CARTESIAN_POINT('Ctrl Pts',(12.602339192607,6.93559180351842,131.771731895206));
#210215=CARTESIAN_POINT('Ctrl Pts',(12.323891568794,4.56273363430679,125.49213861202));
#210216=CARTESIAN_POINT('Ctrl Pts',(12.0454439449812,-2.00305384290271,
124.094217835458));
#210217=CARTESIAN_POINT('Ctrl Pts',(11.7669963211683,-6.72813269310505,
128.862590466954));
#210218=CARTESIAN_POINT('Ctrl Pts',(11.4885486973554,-5.27038628589867,
135.415355006116));
#210219=CARTESIAN_POINT('Ctrl Pts',(11.2101010735425,1.03058764536478,137.730840961799));
#210220=CARTESIAN_POINT('Ctrl Pts',(10.9316534497296,6.38450187754329,133.681229858508));
#210221=CARTESIAN_POINT('Ctrl Pts',(10.6532058259167,5.87137078451608,126.987916465666));
#210222=CARTESIAN_POINT('Ctrl Pts',(10.3747582021038,-0.0372632270726686,
123.801728804758));
#210223=CARTESIAN_POINT('Ctrl Pts',(10.0963105782909,-5.91165415339157,
127.050617682238));
#210224=CARTESIAN_POINT('Ctrl Pts',(9.81786295447806,-6.35352371310424,
133.749012936746));
#210225=CARTESIAN_POINT('Ctrl Pts',(9.53941533066515,-0.956815367363035,
137.741416564191));
#210226=CARTESIAN_POINT('Ctrl Pts',(9.26096770685226,5.31915955795546,135.35900467071));
#210227=CARTESIAN_POINT('Ctrl Pts',(8.98252008303941,6.70708670490366,128.791097399121));
#210228=CARTESIAN_POINT('Ctrl Pts',(8.70407245922646,1.93152882944647,124.073280671906));
#210229=CARTESIAN_POINT('Ctrl Pts',(8.42562483541358,-4.61900967984285,
125.540997583217));
#210230=CARTESIAN_POINT('Ctrl Pts',(8.14717721160073,-6.92490394452403,
131.845487993513));
#210231=CARTESIAN_POINT('Ctrl Pts',(7.86872958778781,-2.86714978455288,
137.193233207215));
#210232=CARTESIAN_POINT('Ctrl Pts',(7.59028196397491,3.82537495936868,136.669916624805));
#210233=CARTESIAN_POINT('Ctrl Pts',(7.31183434016203,7.00256699558648,130.756440620084));
#210234=CARTESIAN_POINT('Ctrl Pts',(7.03338671634916,3.7447420572761,124.887000752025));
#210235=CARTESIAN_POINT('Ctrl Pts',(6.75493909253623,-2.95431789085107,
124.455325521299));
#210236=CARTESIAN_POINT('Ctrl Pts',(6.47649146872337,-6.9385040237388,129.858103376433));
#210237=CARTESIAN_POINT('Ctrl Pts',(6.19804384491048,-4.54654392357636,
136.130445408932));
#210238=CARTESIAN_POINT('Ctrl Pts',(5.91959622109758,2.02346793133434,137.508375711873));
#210239=CARTESIAN_POINT('Ctrl Pts',(5.64114859728465,6.73401160925262,132.725643652489));
#210240=CARTESIAN_POINT('Ctrl Pts',(5.36270097347181,5.25632759302358,126.177346343905));
#210241=CARTESIAN_POINT('Ctrl Pts',(5.08425334965889,-1.05166469531565,
123.881049110601));
#210242=CARTESIAN_POINT('Ctrl Pts',(4.80580572584599,-6.39322850533622,
127.946936929627));
#210243=CARTESIAN_POINT('Ctrl Pts',(4.5273581020331,-5.85972764552883,134.638657524961));
#210244=CARTESIAN_POINT('Ctrl Pts',(4.24891047822024,0.0585766569097649,
137.806846578216));
#210245=CARTESIAN_POINT('Ctrl Pts',(3.97046285440732,5.92305187327717,134.54009312409));
#210246=CARTESIAN_POINT('Ctrl Pts',(3.69201523059441,6.34453177527304,127.840383997147));
#210247=CARTESIAN_POINT('Ctrl Pts',(3.41356760678156,0.935696923401329,
123.864424586062));
#210248=CARTESIAN_POINT('Ctrl Pts',(3.13511998296867,-5.33299768974021,
126.265927353204));
#210249=CARTESIAN_POINT('Ctrl Pts',(2.85667235915575,-6.70092795743158,
132.838028575505));
#210250=CARTESIAN_POINT('Ctrl Pts',(2.57822473534285,-1.91103279077285,
137.541288294661));
#210251=CARTESIAN_POINT('Ctrl Pts',(2.29977711153,4.63500815146407,136.053640595781));
#210252=CARTESIAN_POINT('Ctrl Pts',(2.02132948771708,6.92170303524179,129.742161038504));
#210253=CARTESIAN_POINT('Ctrl Pts',(1.74288186390418,2.84769097362441,124.40679100305));
#210254=CARTESIAN_POINT('Ctrl Pts',(1.46443424009131,-3.84320997531586,
124.950474904685));
#210255=CARTESIAN_POINT('Ctrl Pts',(1.18598661627842,-7.00238870818588,
130.873593798241));
#210256=CARTESIAN_POINT('Ctrl Pts',(0.907538992465495,-3.72671430393905,
136.733090780986));
#210257=CARTESIAN_POINT('Ctrl Pts',(0.629091368652655,2.97362848551254,
137.144374378117));
#210258=CARTESIAN_POINT('Ctrl Pts',(0.350643744839755,6.94135196660579,
131.729495056193));
#210259=CARTESIAN_POINT('Ctrl Pts',(0.0721961210268491,4.53031209428387,
125.4644623805));
#210260=CARTESIAN_POINT('Ctrl Pts',(-0.206251502786054,-2.04386327463549,
124.106535316138));
#210261=CARTESIAN_POINT('Ctrl Pts',(-0.484699126598912,-6.73982814243653,
128.903582496833));
#210262=CARTESIAN_POINT('Ctrl Pts',(-0.763146750411823,-5.24222020624778,
135.447351912307));
#210263=CARTESIAN_POINT('Ctrl Pts',(-1.04159437422473,1.07273200278813,
137.724439150648));
#210264=CARTESIAN_POINT('Ctrl Pts',(-1.32004199803759,6.40189590713365,
133.642312281717));
#210265=CARTESIAN_POINT('Ctrl Pts',(-1.59848962185049,5.84803022282516,
126.952246475077));
#210266=CARTESIAN_POINT('Ctrl Pts',(-1.87693724566341,-0.0798895441007186,
123.802085379146));
#210267=CARTESIAN_POINT('Ctrl Pts',(-2.1553848694763,-5.93439472281934,
127.08667314716));
#210268=CARTESIAN_POINT('Ctrl Pts',(-2.43383249328916,-6.33548106256618,
133.787634081347));
#210269=CARTESIAN_POINT('Ctrl Pts',(-2.71228011710207,-0.914569811271147,
137.747112443329));
#210270=CARTESIAN_POINT('Ctrl Pts',(-2.99072774091498,5.34678641736288,
135.326541049718));
#210271=CARTESIAN_POINT('Ctrl Pts',(-3.26917536472784,6.6947071334783,128.750306759754));
#210272=CARTESIAN_POINT('Ctrl Pts',(-3.54762298854074,1.89051904855254,
124.061647619009));
#210273=CARTESIAN_POINT('Ctrl Pts',(-3.82607061235365,-4.65096368500298,
125.569212324096));
#210274=CARTESIAN_POINT('Ctrl Pts',(-4.10451823616654,-6.91843800424817,
131.887622559669));
#210275=CARTESIAN_POINT('Ctrl Pts',(-4.38296585997939,-2.82820578207579,
137.210567990736));
#210276=CARTESIAN_POINT('Ctrl Pts',(-4.66141348379231,3.86100938829084,
136.646521806489));
#210277=CARTESIAN_POINT('Ctrl Pts',(-4.93986110760522,7.00214555161287,
130.713814895061));
#210278=CARTESIAN_POINT('Ctrl Pts',(-5.21830873141809,3.70865202682979,
124.864315079211));
#210279=CARTESIAN_POINT('Ctrl Pts',(-5.49675635523098,-2.99291153288594,
124.473426925751));
#210280=CARTESIAN_POINT('Ctrl Pts',(-5.77520397904388,-6.9441356057364,
129.900357551763));
#210281=CARTESIAN_POINT('Ctrl Pts',(-6.05365160285679,-4.51403829679898,
136.158022832244));
#210282=CARTESIAN_POINT('Ctrl Pts',(-6.33209922666964,2.06423968386644,
137.495934078373));
#210283=CARTESIAN_POINT('Ctrl Pts',(-6.61054685048256,6.74558223877327,
132.684616215558));
#210284=CARTESIAN_POINT('Ctrl Pts',(-6.88899447429547,5.22806425626005,
126.145435313781));
#210285=CARTESIAN_POINT('Ctrl Pts',(-7.16744209810832,-1.09378937261818,
123.887579165027));
#210286=CARTESIAN_POINT('Ctrl Pts',(-7.44588972192122,-6.41050400264194,
127.985907267597));
#210287=CARTESIAN_POINT('Ctrl Pts',(-7.72433734573414,-5.8362786247684,
134.674256309687));
#210288=CARTESIAN_POINT('Ctrl Pts',(-8.002784969547,0.101201691205851,137.806360265633));
#210289=CARTESIAN_POINT('Ctrl Pts',(-8.28123259335988,5.94568259693924,
134.503968611703));
#210290=CARTESIAN_POINT('Ctrl Pts',(-8.55968021717279,6.32637165882838,
127.80181794706));
#210291=CARTESIAN_POINT('Ctrl Pts',(-8.8381278409857,0.893434226691435,
123.858857314246));
#210292=CARTESIAN_POINT('Ctrl Pts',(-9.11657546479855,-5.3605256130866,
126.298474910485));
#210293=CARTESIAN_POINT('Ctrl Pts',(-9.39502308861147,-6.68842429067269,
132.878781346775));
#210294=CARTESIAN_POINT('Ctrl Pts',(-9.67347071242438,-1.86998779282204,
137.552796474009));
#210295=CARTESIAN_POINT('Ctrl Pts',(-9.95191833623725,4.66687613264966,
136.025328728591));
#210296=CARTESIAN_POINT('Ctrl Pts',(-10.2303659600501,6.91510888178999,
129.700046347612));
#210297=CARTESIAN_POINT('Ctrl Pts',(-10.508813583863,2.80869439041515,124.389574831969));
#210298=CARTESIAN_POINT('Ctrl Pts',(-10.787261207676,-3.87877303340228,
124.973978073582));
#210299=CARTESIAN_POINT('Ctrl Pts',(-11.0657088314888,-7.00183752812002,
130.916218043094));
#210300=CARTESIAN_POINT('Ctrl Pts',(-11.3441564553017,-3.69055539327479,
136.755666503084));
#210301=CARTESIAN_POINT('Ctrl Pts',(-11.6226040791146,3.01216685433575,
137.126155591738));
#210302=CARTESIAN_POINT('Ctrl Pts',(-11.9010517029275,6.94685491534338,
131.687223935982));
#210303=CARTESIAN_POINT('Ctrl Pts',(-12.1794993267404,4.49772268187999,
125.436984020872));
#210304=CARTESIAN_POINT('Ctrl Pts',(-12.4579469505533,-2.08459697026297,
124.119100987199));
#210305=CARTESIAN_POINT('Ctrl Pts',(-12.7363945743662,-6.75127384495765,
128.944644960744));
#210306=CARTESIAN_POINT('Ctrl Pts',(-13.0148421981791,-5.21385987419926,
135.479176770748));
#210307=CARTESIAN_POINT('Ctrl Pts',(-13.2932898219919,1.11483660973293,
137.717780913442));
#210308=CARTESIAN_POINT('Ctrl Pts',(-13.5717374458049,6.41905271211686,
133.603289543584));
#210309=CARTESIAN_POINT('Ctrl Pts',(-13.8501850696177,5.82447296022373,
126.916719225995));
#210310=CARTESIAN_POINT('Ctrl Pts',(-14.1286326934306,-0.122512900792341,
123.802701425419));
#210311=CARTESIAN_POINT('Ctrl Pts',(-14.4070803172435,-5.95691539106803,
127.122866372359));
#210312=CARTESIAN_POINT('Ctrl Pts',(-14.6855279410564,-6.31720364844761,
133.826144679651));
#210313=CARTESIAN_POINT('Ctrl Pts',(-14.9639755648693,-0.872290365458834,
137.752551056246));
#210314=CARTESIAN_POINT('Ctrl Pts',(-15.2424231886822,5.37421514963333,
135.293909857666));
#210315=CARTESIAN_POINT('Ctrl Pts',(-15.5208708124951,6.68207948721813,
128.709592234107));
#210316=CARTESIAN_POINT('Ctrl Pts',(-15.799318436308,1.84943921378025,124.050264419823));
#210317=CARTESIAN_POINT('Ctrl Pts',(-16.0777660601209,-4.68274534699314,
125.59762105532));
#210318=CARTESIAN_POINT('Ctrl Pts',(-16.3562136839338,-6.91171569870797,
131.929716985153));
#210319=CARTESIAN_POINT('Ctrl Pts',(-16.6346613077467,-2.78915697939336,
137.227665389888));
#210320=CARTESIAN_POINT('Ctrl Pts',(-16.9131089315595,3.89650074609022,
136.622910504741));
#210321=CARTESIAN_POINT('Ctrl Pts',(-17.1915565553724,7.00146464056082,
130.671192525245));
#210322=CARTESIAN_POINT('Ctrl Pts',(-17.4700041791854,3.67242457091876,
124.841849516969));
#210323=CARTESIAN_POINT('Ctrl Pts',(-17.7484518029982,-3.0313942714833,
124.491762925279));
#210324=CARTESIAN_POINT('Ctrl Pts',(-18.0268994268111,-6.94950987023543,
129.942645225261));
#210325=CARTESIAN_POINT('Ctrl Pts',(-18.305347050624,-4.48136540067248,
136.185401873632));
#210326=CARTESIAN_POINT('Ctrl Pts',(-18.5837946744369,2.10493494523792,
137.483244486159));
#210327=CARTESIAN_POINT('Ctrl Pts',(-18.8622422982498,6.75690290826339,
132.643519105064));
#210328=CARTESIAN_POINT('Ctrl Pts',(-19.1406899220627,5.19960719165284,
126.113696921846));
#210329=CARTESIAN_POINT('Ctrl Pts',(-19.4191375458756,-1.1358735191536,
123.894365523333));
#210330=CARTESIAN_POINT('Ctrl Pts',(-19.6975851696885,-6.42754195636435,
128.024982044393));
#210331=CARTESIAN_POINT('Ctrl Pts',(-19.9760327935014,-5.81261333855723,
134.709711694007));
#210332=CARTESIAN_POINT('Ctrl Pts',(-20.2544804173143,0.143822975436045,
137.805614491377));
#210333=CARTESIAN_POINT('Ctrl Pts',(-20.5329280411272,5.96809300114641,
134.467707008981));
#210334=CARTESIAN_POINT('Ctrl Pts',(-20.81137566494,6.30797711635522,127.763363157294));
#210335=CARTESIAN_POINT('Ctrl Pts',(-21.089823288753,0.851138423447451,
123.853547410611));
#210336=CARTESIAN_POINT('Ctrl Pts',(-21.3682709125658,-5.38785490018508,
126.331189435016));
#210337=CARTESIAN_POINT('Ctrl Pts',(-21.6467185363787,-6.67567278189203,
132.919457249623));
#210338=CARTESIAN_POINT('Ctrl Pts',(-21.9251661601916,-1.82887350178604,
137.564054587584));
#210339=CARTESIAN_POINT('Ctrl Pts',(-22.2036137840045,4.69857118102365,
135.996823396506));
#210340=CARTESIAN_POINT('Ctrl Pts',(-22.4820614078173,6.90825848643574,
129.657972577492));
#210341=CARTESIAN_POINT('Ctrl Pts',(-22.7605090316303,2.76959373000234,
124.372596363135));
#210342=CARTESIAN_POINT('Ctrl Pts',(-23.0389566554432,-3.91419236212754,
124.997697289448));
#210343=CARTESIAN_POINT('Ctrl Pts',(-23.3174042792561,-7.0010268923895,
130.958838143028));
#210344=CARTESIAN_POINT('Ctrl Pts',(-23.5958519030689,-3.65425972772349,
136.778021697354));
#210345=CARTESIAN_POINT('Ctrl Pts',(-23.8742995268818,3.05059360620828,
137.107702548922));
#210346=CARTESIAN_POINT('Ctrl Pts',(-24.1527471506948,6.95210044581739,
131.644920100946));
#210347=CARTESIAN_POINT('Ctrl Pts',(-24.4311947745076,4.4649666047081,125.409704551357));
#210348=CARTESIAN_POINT('Ctrl Pts',(-24.7096423983205,-2.12525342038311,
124.131914383013));
#210349=CARTESIAN_POINT('Ctrl Pts',(-24.9880900221334,-6.76246937654364,
128.985776337104));
#210350=CARTESIAN_POINT('Ctrl Pts',(-25.2665376459463,-5.18530634065569,
135.510828402156));
#210351=CARTESIAN_POINT('Ctrl Pts',(-25.5449852697592,1.15689990599717,
137.710866496904));
#210352=CARTESIAN_POINT('Ctrl Pts',(-25.8234328935721,6.43597165674122,
133.564163090109));
#210353=CARTESIAN_POINT('Ctrl Pts',(-26.101880517385,5.8006998696348,126.881336034893));
#210354=CARTESIAN_POINT('Ctrl Pts',(-26.3803281411979,-0.165131717723356,
123.803576920747));
#210355=CARTESIAN_POINT('Ctrl Pts',(-26.6587757650107,-5.9792153236265,
127.15919601668));
#210356=CARTESIAN_POINT('Ctrl Pts',(-26.9372233888237,-6.29869214802456,
133.864543304637));
#210357=CARTESIAN_POINT('Ctrl Pts',(-27.2156710126366,-0.829978596605981,
137.75773220141));
#210358=CARTESIAN_POINT('Ctrl Pts',(-27.4941186364494,5.40144473838504,
135.261112303716));
#210359=CARTESIAN_POINT('Ctrl Pts',(-27.7725662602623,6.66920423404522,
128.668955330874));
#210360=CARTESIAN_POINT('Ctrl Pts',(-28.0510138840753,1.80829084735756,
124.039131496154));
#210361=CARTESIAN_POINT('Ctrl Pts',(-28.3294615078881,-4.71435348813263,
125.626222724194));
#210362=CARTESIAN_POINT('Ctrl Pts',(-28.607909131701,-6.9047372770006,131.971769710144));
#210363=CARTESIAN_POINT('Ctrl Pts',(-28.8863567555139,-2.75000482347336,
137.244524771118));
#210364=CARTESIAN_POINT('Ctrl Pts',(-29.1648043793268,3.93184771762154,
136.599083594488));
#210365=CARTESIAN_POINT('Ctrl Pts',(-29.4432520031397,7.00052428766157,
130.628575090021));
#210366=CARTESIAN_POINT('Ctrl Pts',(-29.7216996269525,3.63606103196502,
124.819604897767));
#210367=CARTESIAN_POINT('Ctrl Pts',(-30.0001472507655,-3.06976468065099,
124.510332840438));
#210368=CARTESIAN_POINT('Ctrl Pts',(-30.2785948745783,-6.95462661809053,
129.984964829937));
#210369=CARTESIAN_POINT('Ctrl Pts',(-30.5570424983912,-4.44852644590303,
136.212581518559));
#210370=CARTESIAN_POINT('Ctrl Pts',(-30.8354901222041,2.14555220747066,
137.470307405446));
#210371=CARTESIAN_POINT('Ctrl Pts',(-31.113937746017,6.7679731982313,132.602353843876));
#210372=CARTESIAN_POINT('Ctrl Pts',(-31.3923853698299,5.17095745368924,
126.082132344179));
#210373=CARTESIAN_POINT('Ctrl Pts',(-31.6708329936428,-1.17791557547805,
123.901407934047));
#210374=CARTESIAN_POINT('Ctrl Pts',(-31.9492806174558,-6.44434173515584,
128.064159812084));
#210375=CARTESIAN_POINT('Ctrl Pts',(-32.2277282412685,-5.78873266382121,
134.745022364106));
#210376=CARTESIAN_POINT('Ctrl Pts',(-32.5061758650815,0.186438930252996,
137.804609283086));
#210377=CARTESIAN_POINT('Ctrl Pts',(-32.7846234888944,5.99028225547263,
134.431309659613));
#210378=CARTESIAN_POINT('Ctrl Pts',(-33.0630711127073,6.28934882947028,
127.725021052809));
#210379=CARTESIAN_POINT('Ctrl Pts',(-33.3415187365202,0.808811080956172,
123.848495071916));
#210380=CARTESIAN_POINT('Ctrl Pts',(-33.619966360333,-5.41498453833882,
126.364069714552));
#210381=CARTESIAN_POINT('Ctrl Pts',(-33.898413984146,-6.66267390360147,
132.960054776787));
#210382=CARTESIAN_POINT('Ctrl Pts',(-34.1768616079588,-1.78769144116968,
137.575062218212));
#210383=CARTESIAN_POINT('Ctrl Pts',(-34.4553092317717,4.73009212211488,
135.968125655805));
#210384=CARTESIAN_POINT('Ctrl Pts',(-34.7337568555846,6.90115210302259,
129.615941287202));
#210385=CARTESIAN_POINT('Ctrl Pts',(-35.0122044793975,2.73039044127535,
124.355856225691));
#210386=CARTESIAN_POINT('Ctrl Pts',(-35.2906521032104,-3.94946664901538,
125.02163167336));
#210387=CARTESIAN_POINT('Ctrl Pts',(-35.5690997270233,-6.99995683103299,
131.00145251874));
#210388=CARTESIAN_POINT('Ctrl Pts',(-35.8475473508362,-3.61782865223385,
136.800155535415));
#210389=CARTESIAN_POINT('Ctrl Pts',(-36.125994974649,3.08890731721304,137.089015933453));
#210390=CARTESIAN_POINT('Ctrl Pts',(-36.404442598462,6.95708836365274,131.60258511867));
#210391=CARTESIAN_POINT('Ctrl Pts',(-36.6828902222748,4.43204507655667,
125.382624982808));
#210392=CARTESIAN_POINT('Ctrl Pts',(-36.9613378460878,-2.16583111845593,
124.144975028777));
#210393=CARTESIAN_POINT('Ctrl Pts',(-37.2397854699006,-6.7734143223399,
129.026975101771));
#210394=CARTESIAN_POINT('Ctrl Pts',(-37.5182330937135,-5.15656066367905,
135.54230563367));
#210395=CARTESIAN_POINT('Ctrl Pts',(-37.7966807175264,1.19892033290996,
137.703696157251));
#210396=CARTESIAN_POINT('Ctrl Pts',(-38.0751283413393,6.45265211406898,
133.524934371139));
#210397=CARTESIAN_POINT('Ctrl Pts',(-38.3535759651522,5.77671183197903,
126.846098212911));
#210398=CARTESIAN_POINT('Ctrl Pts',(-38.6320235889651,-0.207744415637528,
123.80471183269));
#210399=CARTESIAN_POINT('Ctrl Pts',(-38.910471212778,-6.00129369416227,
127.195660733917));
#210400=CARTESIAN_POINT('Ctrl Pts',(-39.1889188365908,-6.27994724724761,
133.902828533427));
#210401=CARTESIAN_POINT('Ctrl Pts',(-39.4673664604039,-0.787636072591,137.762655686833));
#210402=CARTESIAN_POINT('Ctrl Pts',(-39.7458140842166,5.42847417461558,
135.228149603194));
#210403=CARTESIAN_POINT('Ctrl Pts',(-40.0242617080296,6.65608185105682,
128.628397555869));
#210404=CARTESIAN_POINT('Ctrl Pts',(-40.3027093318424,1.76707547405252,
124.028249260538));
#210405=CARTESIAN_POINT('Ctrl Pts',(-40.5811569556554,-4.7457869371699,
125.655016270872));
#210406=CARTESIAN_POINT('Ctrl Pts',(-40.8596045794682,-6.89750299771422,
132.013779176361));
#210407=CARTESIAN_POINT('Ctrl Pts',(-41.1380522032811,-2.7107507651133,
137.261145509698));
#210408=CARTESIAN_POINT('Ctrl Pts',(-41.416499827094,3.96704899308973,136.575041958643));
#210409=CARTESIAN_POINT('Ctrl Pts',(-41.694947450907,6.99932452776054,130.585964168594));
#210410=CARTESIAN_POINT('Ctrl Pts',(-41.9733950747197,3.59956275743227,
124.79758204589));
#210411=CARTESIAN_POINT('Ctrl Pts',(-42.2518426985328,-3.10802133855968,
124.529135983109));
#210412=CARTESIAN_POINT('Ctrl Pts',(-42.5302903223456,-6.95948565969872,
130.027314797628));
#210413=CARTESIAN_POINT('Ctrl Pts',(-42.8087379461585,-4.41552264935019,
136.23956075987));
#210414=CARTESIAN_POINT('Ctrl Pts',(-43.0871855699714,2.18608996547759,
137.457123315624));
#210415=CARTESIAN_POINT('Ctrl Pts',(-43.3656331937842,6.77879269846351,
132.561121957388));
#210416=CARTESIAN_POINT('Ctrl Pts',(-43.6440808175972,5.14211610399531,
126.050742750417));
#210417=CARTESIAN_POINT('Ctrl Pts',(-43.92252844141,-1.21991398370768,123.908706136214));
#210418=CARTESIAN_POINT('Ctrl Pts',(-44.200976065223,-6.46090271649442,
128.103439118922));
#210419=CARTESIAN_POINT('Ctrl Pts',(-44.4794236890358,-5.76463748546755,
134.780187011534));
#210420=CARTESIAN_POINT('Ctrl Pts',(-44.7578713128487,0.229047976506494,
137.803344678006));
#210421=CARTESIAN_POINT('Ctrl Pts',(-45.0363189366615,6.01224953768695,
134.394777912313));
#210422=CARTESIAN_POINT('Ctrl Pts',(-45.3147665604746,6.27048748845154,
127.686793054383));
#210423=CARTESIAN_POINT('Ctrl Pts',(-45.5932141842873,0.766453767672844,
123.843700485376));
#210424=CARTESIAN_POINT('Ctrl Pts',(-45.8716618081003,-5.44191352224889,
126.397114530699));
#210425=CARTESIAN_POINT('Ctrl Pts',(-46.1501094319132,-6.6494281374793,
133.000572423912));
#210426=CARTESIAN_POINT('Ctrl Pts',(-46.4285570557261,-1.74644313698983,
137.585818958004));
#210427=CARTESIAN_POINT('Ctrl Pts',(-46.7070046795389,4.76143778790304,
135.93923656989));
#210428=CARTESIAN_POINT('Ctrl Pts',(-46.9854523033519,6.89378999488032,
129.573954034227));
#210429=CARTESIAN_POINT('Ctrl Pts',(-47.2638999271647,2.69108597692664,
124.339355039948));
#210430=CARTESIAN_POINT('Ctrl Pts',(-47.5423475509777,-3.98459458696386,
125.045780338419));
#210431=CARTESIAN_POINT('Ctrl Pts',(-47.8207951747905,-6.998627383702,131.044059591139));
#210432=CARTESIAN_POINT('Ctrl Pts',(-48.0992427986034,-3.58126351677304,
136.822067197091));
#210433=CARTESIAN_POINT('Ctrl Pts',(-48.3776904224163,3.1271065676212,137.070096437769));
#210434=CARTESIAN_POINT('Ctrl Pts',(-48.6561380462292,6.9618184840203,131.560220557891));
#210435=CARTESIAN_POINT('Ctrl Pts',(-48.9345856700421,4.39895931734504,
125.355746318666));
#210436=CARTESIAN_POINT('Ctrl Pts',(-49.213033293855,-2.20632856086043,
124.158282440523));
#210437=CARTESIAN_POINT('Ctrl Pts',(-49.4914809176678,-6.78410827677761,
129.068239728113));
#210438=CARTESIAN_POINT('Ctrl Pts',(-49.7699285414808,-5.12762390845042,
135.573607298891));
#210439=CARTESIAN_POINT('Ctrl Pts',(-50.0483761652936,1.2408963333889,137.696270160183));
#210440=CARTESIAN_POINT('Ctrl Pts',(-50.3268237891066,6.46909346599971,
133.485604840309));
#210441=CARTESIAN_POINT('Ctrl Pts',(-50.6052714129194,5.7525097361419,126.811007065796));
#210442=CARTESIAN_POINT('Ctrl Pts',(-50.8837190367324,-0.250349415506305,
123.806106119193));
#210443=CARTESIAN_POINT('Ctrl Pts',(-51.1621666605453,-6.02314968455324,
127.232259172855));
#210444=CARTESIAN_POINT('Ctrl Pts',(-51.4406142843581,-6.26096964071598,
133.94099894735));
#210445=CARTESIAN_POINT('Ctrl Pts',(-51.719061908171,-0.745264362431691,
137.767321330073));
#210446=CARTESIAN_POINT('Ctrl Pts',(-51.997509531984,5.45530245673899,135.195022977544));
#210447=CARTESIAN_POINT('Ctrl Pts',(-52.2759571557968,6.64271282450778,
128.587920411975));
#210448=CARTESIAN_POINT('Ctrl Pts',(-52.5544047796097,1.72579462111621,
124.01761811622));
#210449=CARTESIAN_POINT('Ctrl Pts',(-52.8328524034226,-4.77704452932697,
125.684000628399));
#210450=CARTESIAN_POINT('Ctrl Pts',(-53.1113000272355,-6.89001312891767,
132.05574382713));
#210451=CARTESIAN_POINT('Ctrl Pts',(-53.3897476510484,-2.67139625888694,
137.277526989739));
#210452=CARTESIAN_POINT('Ctrl Pts',(-53.6681952748612,4.00210326809833,
136.550786488079));
#210453=CARTESIAN_POINT('Ctrl Pts',(-53.9466428986742,6.99786540531528,
130.543361339928));
#210454=CARTESIAN_POINT('Ctrl Pts',(-54.225090522487,3.56293109977782,124.775781777402));
#210455=CARTESIAN_POINT('Ctrl Pts',(-54.5035381462999,-3.14616282759469,
124.548171656537));
#210456=CARTESIAN_POINT('Ctrl Pts',(-54.7819857701128,-6.9640868150063,
130.069693559035));
#210457=CARTESIAN_POINT('Ctrl Pts',(-55.0604333939257,-4.382355233982,136.266338597842));
#210458=CARTESIAN_POINT('Ctrl Pts',(-55.3388810177386,2.22654671711671,
137.443692705233));
#210459=CARTESIAN_POINT('Ctrl Pts',(-55.6173286415515,6.78936100803939,
132.519824973462));
#210460=CARTESIAN_POINT('Ctrl Pts',(-55.8957762653644,5.11308421129812,
126.019529303714));
#210461=CARTESIAN_POINT('Ctrl Pts',(-56.1742238891773,-1.26186718757599,
123.916259859391));
#210462=CARTESIAN_POINT('Ctrl Pts',(-56.4526715129901,-6.47722428670686,
128.142818509401));
#210463=CARTESIAN_POINT('Ctrl Pts',(-56.7311191368031,-5.74032869635189,
134.815204333253));
#210464=CARTESIAN_POINT('Ctrl Pts',(-57.0095667606159,0.271648535303317,
137.801820722997));
#210465=CARTESIAN_POINT('Ctrl Pts',(-57.2880143844289,6.03399403378365,
134.358113120779));
#210466=CARTESIAN_POINT('Ctrl Pts',(-57.5664620082417,6.25139379221294,
127.64868057857));
#210467=CARTESIAN_POINT('Ctrl Pts',(-57.8449096320546,0.724068053163303,
123.839163828657));
#210468=CARTESIAN_POINT('Ctrl Pts',(-58.1233572558676,-5.46864085405239,
126.430322658971));
#210469=CARTESIAN_POINT('Ctrl Pts',(-58.4018048796803,-6.63593597435208,
133.0410086896));
#210470=CARTESIAN_POINT('Ctrl Pts',(-58.6802525034934,-1.705130117717,137.596324408362));
#210471=CARTESIAN_POINT('Ctrl Pts',(-58.9587001273061,4.79260701686295,
135.910157209259));
#210472=CARTESIAN_POINT('Ctrl Pts',(-59.2371477511191,6.88617243481463,
129.532012374421));
#210473=CARTESIAN_POINT('Ctrl Pts',(-59.515595374932,2.65168179339722,124.323093417365));
#210474=CARTESIAN_POINT('Ctrl Pts',(-59.7940429987449,-4.01957487429483,
125.070142389788));
#210475=CARTESIAN_POINT('Ctrl Pts',(-60.0724906225578,-6.99703859965941,
131.086657781405));
#210476=CARTESIAN_POINT('Ctrl Pts',(-60.3509382463707,-3.5445656762756,
136.843755870437));
#210477=CARTESIAN_POINT('Ctrl Pts',(-60.6293858701835,3.16518994194552,
137.050944762941));
#210478=CARTESIAN_POINT('Ctrl Pts',(-60.9078334939965,6.96629063164357,
131.517827988445));
#210479=CARTESIAN_POINT('Ctrl Pts',(-61.1862811178092,4.36571055307847,
125.32906955493));
#210480=CARTESIAN_POINT('Ctrl Pts',(-61.4647287416223,-2.24674424694855,
124.171836125139));
#210481=CARTESIAN_POINT('Ctrl Pts',(-61.743176365435,-6.79455084358828,
129.109568687053));
#210482=CARTESIAN_POINT('Ctrl Pts',(-62.0216239892481,-5.09849714723216,
135.60473223792));
#210483=CARTESIAN_POINT('Ctrl Pts',(-62.3000716130609,1.2828263519976,137.688588780872));
#210484=CARTESIAN_POINT('Ctrl Pts',(-62.5785192368738,6.48529510329292,
133.446175954988));
#210485=CARTESIAN_POINT('Ctrl Pts',(-62.8569668606868,5.72809447894126,
126.776063893867));
#210486=CARTESIAN_POINT('Ctrl Pts',(-63.1354144844995,-0.292945138585431,
123.80775972859));
#210487=CARTESIAN_POINT('Ctrl Pts',(-63.4138621083125,-6.04478248491762,
127.268989977326));
#210488=CARTESIAN_POINT('Ctrl Pts',(-63.6923097321254,-6.24176003165182,
133.979053131985));
#210489=CARTESIAN_POINT('Ctrl Pts',(-63.9707573559382,-0.702865036227365,
137.771728958244));
#210490=CARTESIAN_POINT('Ctrl Pts',(-64.2492049797512,5.48192859062395,
135.161733654286));
#210491=CARTESIAN_POINT('Ctrl Pts',(-64.527652603564,6.62909764979204,128.547525399088));
#210492=CARTESIAN_POINT('Ctrl Pts',(-64.806100227377,1.68444981822529,124.007238457143));
#210493=CARTESIAN_POINT('Ctrl Pts',(-65.0845478511898,-4.80812510634223,
125.713174722747));
#210494=CARTESIAN_POINT('Ctrl Pts',(-65.3629954750027,-6.88226794815085,
132.097662107432));
#210495=CARTESIAN_POINT('Ctrl Pts',(-65.6414430988157,-2.63194276308962,
137.29366860422));
#210496=CARTESIAN_POINT('Ctrl Pts',(-65.9198907226284,4.03700924369883,
136.526318081592));
#210497=CARTESIAN_POINT('Ctrl Pts',(-66.1983383464414,6.99614697439381,
130.500768182686));
#210498=CARTESIAN_POINT('Ctrl Pts',(-66.4767859702543,3.5261674164012,124.75420490012));
#210499=CARTESIAN_POINT('Ctrl Pts',(-66.7552335940671,-3.18418773440913,
124.567439155348));
#210500=CARTESIAN_POINT('Ctrl Pts',(-67.0336812178801,-6.96842991351606,
130.112099543802));
#210501=CARTESIAN_POINT('Ctrl Pts',(-67.3121288416929,-4.34902542882876,
136.292914040211));
#210502=CARTESIAN_POINT('Ctrl Pts',(-67.5905764655059,2.26692096324861,
137.43001607195));
#210503=CARTESIAN_POINT('Ctrl Pts',(-67.8690240893187,6.79967773534632,
132.478464422373));
#210504=CARTESIAN_POINT('Ctrl Pts',(-68.1474717131316,5.08386285138514,
125.988493160695));
#210505=CARTESIAN_POINT('Ctrl Pts',(-68.4259193369445,-1.30377363249137,
123.924068823677));
#210506=CARTESIAN_POINT('Ctrl Pts',(-68.7043669607574,-6.49330584099122,
128.182296524302));
#210507=CARTESIAN_POINT('Ctrl Pts',(-68.9828145845703,-5.71580719724563,
134.850073031684));
#210508=CARTESIAN_POINT('Ctrl Pts',(-69.2612622083832,0.314239028063776,
137.800037474531));
#210509=CARTESIAN_POINT('Ctrl Pts',(-69.5397098321961,6.05551493801243,
134.32131664364));
#210510=CARTESIAN_POINT('Ctrl Pts',(-69.818157456009,6.23206844827842,127.610685037641));
#210511=CARTESIAN_POINT('Ctrl Pts',(-70.0966050798218,0.681655508046095,
123.834885269867));
#210512=CARTESIAN_POINT('Ctrl Pts',(-70.3750527036349,-5.49516554335789,
126.463692868828));
#210513=CARTESIAN_POINT('Ctrl Pts',(-70.6535003274475,-6.62219791417695,
133.081362075471));
#210514=CARTESIAN_POINT('Ctrl Pts',(-70.9319479512606,-1.66375391422059,
137.606578180005));
#210515=CARTESIAN_POINT('Ctrl Pts',(-71.2103955750734,4.82359865400735,
135.880888651457));
#210516=CARTESIAN_POINT('Ctrl Pts',(-71.4888431988863,6.87829970509706,
129.490117861946));
#210517=CARTESIAN_POINT('Ctrl Pts',(-71.7672908226993,2.6121793508235,124.307071960521));
#210518=CARTESIAN_POINT('Ctrl Pts',(-72.045738446512,-4.05440621480077,
125.094716924722));
#210519=CARTESIAN_POINT('Ctrl Pts',(-72.3241860703251,-6.99519053777849,
131.129245511046));
#210520=CARTESIAN_POINT('Ctrl Pts',(-72.6026336941378,-3.5077364905931,
136.865220751771));
#210521=CARTESIAN_POINT('Ctrl Pts',(-72.8810813179508,3.20315602899298,
137.031561618638));
#210522=CARTESIAN_POINT('Ctrl Pts',(-73.1595289417638,6.97050464080582,
131.475408981201));
#210523=CARTESIAN_POINT('Ctrl Pts',(-73.4379765655765,4.33230001580124,
125.302595680118));
#210524=CARTESIAN_POINT('Ctrl Pts',(-73.7164241893894,-2.28707667910305,
124.18563558039));
#210525=CARTESIAN_POINT('Ctrl Pts',(-73.9948718132024,-6.80474163581863,
129.150960447132));
#210526=CARTESIAN_POINT('Ctrl Pts',(-74.2733194370152,-5.0691814593271,
135.635679297414));
#210527=CARTESIAN_POINT('Ctrl Pts',(-74.5517670608282,1.32470883500465,
137.680652303954));
#210528=CARTESIAN_POINT('Ctrl Pts',(-74.830214684641,6.5012564255912,133.406649176227));
#210529=CARTESIAN_POINT('Ctrl Pts',(-75.108662308454,5.70346696509291,126.741269991954));
#210530=CARTESIAN_POINT('Ctrl Pts',(-75.3871099322667,-0.335530006474783,
123.809672599606));
#210531=CARTESIAN_POINT('Ctrl Pts',(-75.6655575560798,-6.06619129364391,
127.305851786256));
#210532=CARTESIAN_POINT('Ctrl Pts',(-75.9440051798925,-6.22231913187452,
134.016989677222));
#210533=CARTESIAN_POINT('Ctrl Pts',(-76.2224528037055,-0.66043966510086,
137.775878408018));
#210534=CARTESIAN_POINT('Ctrl Pts',(-76.5009004275184,5.50835158962877,
135.128282866967));
#210535=CARTESIAN_POINT('Ctrl Pts',(-76.7793480513312,6.61523683142527,
128.507214014061));
#210536=CARTESIAN_POINT('Ctrl Pts',(-77.0577956751442,1.64304259742666,
123.997110667925));
#210537=CARTESIAN_POINT('Ctrl Pts',(-77.336243298957,-4.83902751651344,
125.742537472861));
#210538=CARTESIAN_POINT('Ctrl Pts',(-77.6146909227699,-6.87426774241415,
132.139532463972));
#210539=CARTESIAN_POINT('Ctrl Pts',(-77.8931385465828,-2.59239173968542,
137.309569755007));
#210540=CARTESIAN_POINT('Ctrl Pts',(-78.1715861703958,4.07176562643718,
136.501637645866));
#210541=CARTESIAN_POINT('Ctrl Pts',(-78.4500337942086,6.99416929867323,
130.458186275174));
#210542=CARTESIAN_POINT('Ctrl Pts',(-78.7284814180215,3.48927306959449,
124.732852213582));
#210543=CARTESIAN_POINT('Ctrl Pts',(-79.0069290418344,-3.22209464997582,
124.586937765577));
#210544=CARTESIAN_POINT('Ctrl Pts',(-79.2853766656473,-6.97251479429268,
130.154531180556));
#210545=CARTESIAN_POINT('Ctrl Pts',(-79.5638242894601,-4.3155344689392,
136.319286102215));
#210546=CARTESIAN_POINT('Ctrl Pts',(-79.8422719132732,2.30721120779087,
137.416093922569));
#210547=CARTESIAN_POINT('Ctrl Pts',(-80.1207195370859,6.80974249809405,
132.437041836753));
#210548=CARTESIAN_POINT('Ctrl Pts',(-80.3991671608989,5.0544531070646,125.957635471416));
#210549=CARTESIAN_POINT('Ctrl Pts',(-80.6776147847117,-1.34563176559565,
123.932132739704));
#210550=CARTESIAN_POINT('Ctrl Pts',(-80.9560624085247,-6.50914678343976,
128.221871700751));
#210551=CARTESIAN_POINT('Ctrl Pts',(-81.2345100323374,-5.69107389680138,
134.884791814753));
#210552=CARTESIAN_POINT('Ctrl Pts',(-81.5129576561506,0.356817876581242,
137.797994998686));
#210553=CARTESIAN_POINT('Ctrl Pts',(-81.7914052799631,6.07681145290804,
134.284389844403));
#210554=CARTESIAN_POINT('Ctrl Pts',(-82.0698529037763,6.21251217275584,
127.572807839535));
#210555=CARTESIAN_POINT('Ctrl Pts',(-82.348300527589,0.639217703933302,
123.830864967548));
#210556=CARTESIAN_POINT('Ctrl Pts',(-82.626748151402,-5.52148660728364,
126.497223923725));
#210557=CARTESIAN_POINT('Ctrl Pts',(-82.9051957752149,-6.60821446602265,
133.121631086217));
#210558=CARTESIAN_POINT('Ctrl Pts',(-83.1836433990278,-1.62231605971109,
137.616579892973));
#210559=CARTESIAN_POINT('Ctrl Pts',(-83.4620910228406,4.85441155092967,
135.851431981043));
#210560=CARTESIAN_POINT('Ctrl Pts',(-83.7405386466535,6.87017209745416,
129.448272049221));
#210561=CARTESIAN_POINT('Ctrl Pts',(-84.0189862704665,2.57258011298421,
124.291291263097));
#210562=CARTESIAN_POINT('Ctrl Pts',(-84.2974338942792,-4.08908731779306,
125.119503032603));
#210563=CARTESIAN_POINT('Ctrl Pts',(-84.5758815180923,-6.99308326653956,
131.171821201958));
#210564=CARTESIAN_POINT('Ctrl Pts',(-84.8543291419051,-3.47077732444568,
136.886461045702));
#210565=CARTESIAN_POINT('Ctrl Pts',(-85.132776765718,3.2410034219148,137.011947723114));
#210566=CARTESIAN_POINT('Ctrl Pts',(-85.4112243895309,6.97446035535538,
131.432965108015));
#210567=CARTESIAN_POINT('Ctrl Pts',(-85.6896720133437,4.29872894355427,
125.27632567523));
#210568=CARTESIAN_POINT('Ctrl Pts',(-85.9681196371569,-2.327324362789,124.19968029493));
#210569=CARTESIAN_POINT('Ctrl Pts',(-86.2465672609694,-6.81468027584547,
129.192413474561));
#210570=CARTESIAN_POINT('Ctrl Pts',(-86.5250148847825,-5.03967793103904,
135.666447330617));
#210571=CARTESIAN_POINT('Ctrl Pts',(-86.8034625085954,1.36654223043768,
137.672461023519));
#210572=CARTESIAN_POINT('Ctrl Pts',(-87.0819101324082,6.51697684144191,
133.367025968708));
#210573=CARTESIAN_POINT('Ctrl Pts',(-87.3603577562212,5.67862810717874,
126.706626649358));
#210574=CARTESIAN_POINT('Ctrl Pts',(-87.638805380034,-0.378102441176264,
123.811844661359));
#210575=CARTESIAN_POINT('Ctrl Pts',(-87.917253003847,-6.08737531742114,
127.342843233717));
#210576=CARTESIAN_POINT('Ctrl Pts',(-88.1957006276599,-6.20264766177327,
134.054807177307));
#210577=CARTESIAN_POINT('Ctrl Pts',(-88.4741482514726,-0.617989821139493,
137.779769525637));
#210578=CARTESIAN_POINT('Ctrl Pts',(-88.7525958752857,5.53457047463998,
135.094671855119));
#210579=CARTESIAN_POINT('Ctrl Pts',(-89.0310434990984,6.6011308830247,128.466987750645));
#210580=CARTESIAN_POINT('Ctrl Pts',(-89.3094911229114,1.60157449308101,
123.987235123859));
#210581=CARTESIAN_POINT('Ctrl Pts',(-89.5879387467241,-4.86975061474005,
125.772087790693));
#210582=CARTESIAN_POINT('Ctrl Pts',(-89.8663863705374,-6.8660128081587,
132.181353345229));
#210583=CARTESIAN_POINT('Ctrl Pts',(-90.1448339943499,-2.55274465425183,
137.325229852876));
#210584=CARTESIAN_POINT('Ctrl Pts',(-90.4232816181632,4.10637112840284,
136.476746095445));
#210585=CARTESIAN_POINT('Ctrl Pts',(-90.7017292419757,6.99193245143733,
130.415617195278));
#210586=CARTESIAN_POINT('Ctrl Pts',(-90.9801768657889,3.45224942649073,
124.711724509022));
#210587=CARTESIAN_POINT('Ctrl Pts',(-91.2586244896016,-3.2598821696406,
124.606666764696));
#210588=CARTESIAN_POINT('Ctrl Pts',(-91.5370721134145,-6.97634130596949,
130.196986896981));
#210589=CARTESIAN_POINT('Ctrl Pts',(-91.8155197372274,-4.28188359533257,
136.345453806627));
#210590=CARTESIAN_POINT('Ctrl Pts',(-92.0939673610402,2.34741595777304,
137.401926772977));
#210591=CARTESIAN_POINT('Ctrl Pts',(-92.3724149848533,6.81955492332935,
132.395558751529));
#210592=CARTESIAN_POINT('Ctrl Pts',(-92.650862608666,5.02485606812542,125.926957379319));
#210593=CARTESIAN_POINT('Ctrl Pts',(-92.929310232479,-1.38744003581995,
123.940451308663));
#210594=CARTESIAN_POINT('Ctrl Pts',(-93.2077578562919,-6.52474652706058,
128.261542572277));
#210595=CARTESIAN_POINT('Ctrl Pts',(-93.4862054801047,-5.66612971152105,
134.919359395943));
#210596=CARTESIAN_POINT('Ctrl Pts',(-93.7646531039176,0.39938350308132,
137.795693371147));
#210597=CARTESIAN_POINT('Ctrl Pts',(-94.0431007277306,6.09788278932073,
134.247334091402));
#210598=CARTESIAN_POINT('Ctrl Pts',(-94.3215483515434,6.19272569030992,
127.535050387806));
#210599=CARTESIAN_POINT('Ctrl Pts',(-94.5999959753563,0.596756213373149,
123.827103070676));
#210600=CARTESIAN_POINT('Ctrl Pts',(-94.8784435991693,-5.54760307049237,
126.530914581157));
#210601=CARTESIAN_POINT('Ctrl Pts',(-95.1568912229821,-6.59398614805128,
133.161814229653));
#210602=CARTESIAN_POINT('Ctrl Pts',(-95.4353388467949,-1.58081808968337,
137.626329176652));
#210603=CARTESIAN_POINT('Ctrl Pts',(-95.7137864706081,4.88504456584684,
135.821788289543));
#210604=CARTESIAN_POINT('Ctrl Pts',(-95.9922340944205,6.86178991305786,
129.406476486855));
#210605=CARTESIAN_POINT('Ctrl Pts',(-96.2706817182339,2.53288554724217,
124.275751909854));
#210606=CARTESIAN_POINT('Ctrl Pts',(-96.5491293420464,-4.12361689815126,
125.144499794972));
#210607=CARTESIAN_POINT('Ctrl Pts',(-96.8275769658595,-6.99071686402826,
131.214383276482));
#210608=CARTESIAN_POINT('Ctrl Pts',(-97.1060245896722,-3.4336895473684,
136.907475965166));
#210609=CARTESIAN_POINT('Ctrl Pts',(-97.3844722134854,3.27873071826322,
136.992103803166));
#210610=CARTESIAN_POINT('Ctrl Pts',(-97.6629198372979,6.9781576287114,131.390497941658));
#210611=CARTESIAN_POINT('Ctrl Pts',(-97.9413674611112,4.26499858032525,
125.250260513709));
#210612=CARTESIAN_POINT('Ctrl Pts',(-98.2198150849237,-2.36748580661544,
124.21396974833));
#210613=CARTESIAN_POINT('Ctrl Pts',(-98.498262708737,-6.82436639538843,
129.233926233285));
#210614=CARTESIAN_POINT('Ctrl Pts',(-98.7767103325495,-5.00998765563179,
135.69703519741));
#210615=CARTESIAN_POINT('Ctrl Pts',(-99.0551579563628,1.40832498814648,
137.664015243098));
#210616=CARTESIAN_POINT('Ctrl Pts',(-99.3336055801754,6.53245576831905,
133.327307800681));
#210617=CARTESIAN_POINT('Ctrl Pts',(-99.6120532039884,5.65357882561176,
126.672135149802));
#210618=CARTESIAN_POINT('Ctrl Pts',(-99.8905008278013,-0.420660865152761,
123.814275833361));
#210619=CARTESIAN_POINT('Ctrl Pts',(-100.168948451614,-6.10833377126732,
127.379962948978));
#210620=CARTESIAN_POINT('Ctrl Pts',(-100.447396075427,-6.18274635028192,
134.092504230901));
#210621=CARTESIAN_POINT('Ctrl Pts',(-100.72584369924,-0.575517077338011,
137.783402166914));
#210622=CARTESIAN_POINT('Ctrl Pts',(-101.004291323053,5.56058427410689,
135.060901864211));
#210623=CARTESIAN_POINT('Ctrl Pts',(-101.282738946866,6.58678032729173,
128.426848099441));
#210624=CARTESIAN_POINT('Ctrl Pts',(-101.561186570679,1.56004704180311,
123.977612190885));
#210625=CARTESIAN_POINT('Ctrl Pts',(-101.839634194492,-4.90029326256724,
125.801824581246));
#210626=CARTESIAN_POINT('Ctrl Pts',(-102.118081818304,-6.85750345127332,
132.223123201514));
#210627=CARTESIAN_POINT('Ctrl Pts',(-102.396529442117,-2.51300297592632,
137.340648317539));
#210628=CARTESIAN_POINT('Ctrl Pts',(-102.67497706593,4.14082446727623,136.451644352694));
#210629=CARTESIAN_POINT('Ctrl Pts',(-102.953424689743,6.98943651557314,
130.373062520413));
#210630=CARTESIAN_POINT('Ctrl Pts',(-103.231872313556,3.41509785901489,
124.690822569333));
#210631=CARTESIAN_POINT('Ctrl Pts',(-103.510319937369,-3.29754889317273,
124.626625421641));
#210632=CARTESIAN_POINT('Ctrl Pts',(-103.788767561182,-6.97990930675369,
130.239465119861));
#210633=CARTESIAN_POINT('Ctrl Pts',(-104.067215184995,-4.24807405495459,
136.371416183792));
#210634=CARTESIAN_POINT('Ctrl Pts',(-104.345662808808,2.38753372339306,
137.387515148146));
#210635=CARTESIAN_POINT('Ctrl Pts',(-104.62411043262,6.82911464744894,132.354016703874));
#210636=CARTESIAN_POINT('Ctrl Pts',(-104.902558056433,4.99507283129728,
125.896460021193));
#210637=CARTESIAN_POINT('Ctrl Pts',(-105.181005680246,-1.42919689394351,
123.949024222305));
#210638=CARTESIAN_POINT('Ctrl Pts',(-105.459453304059,-6.54010449379936,
128.301307668861));
#210639=CARTESIAN_POINT('Ctrl Pts',(-105.737900927872,-5.64097556572054,
134.953774494342));
#210640=CARTESIAN_POINT('Ctrl Pts',(-106.016348551685,0.441934330278796,
137.793132677202));
#210641=CARTESIAN_POINT('Ctrl Pts',(-106.294796175498,6.11872816644418,
134.210150757753));
#210642=CARTESIAN_POINT('Ctrl Pts',(-106.573243799311,6.17270973413615,
127.49741408157));
#210643=CARTESIAN_POINT('Ctrl Pts',(-106.851691423124,0.554272609792058,
123.823599718647));
#210644=CARTESIAN_POINT('Ctrl Pts',(-107.130139046936,-5.57351396522919,
126.564763592701));
#210645=CARTESIAN_POINT('Ctrl Pts',(-107.40858667075,-6.57951348749827,
133.201910016778));
#210646=CARTESIAN_POINT('Ctrl Pts',(-107.687034294562,-1.53926154185996,
137.635825669776));
#210647=CARTESIAN_POINT('Ctrl Pts',(-107.965481918375,4.91549656364115,
135.791958675416));
#210648=CARTESIAN_POINT('Ctrl Pts',(-108.243929542188,6.85315346251289,
129.364732723601));
#210649=CARTESIAN_POINT('Ctrl Pts',(-108.522377166001,2.49309712449469,
124.260454476607));
#210650=CARTESIAN_POINT('Ctrl Pts',(-108.800824789814,-4.15799367636883,
125.169706285567));
#210651=CARTESIAN_POINT('Ctrl Pts',(-109.079272413627,-6.98809141793296,
131.256930157466));
#210652=CARTESIAN_POINT('Ctrl Pts',(-109.35772003744,-3.39647453366164,
136.928264731447));
#210653=CARTESIAN_POINT('Ctrl Pts',(-109.636167661252,3.31633652003941,
136.97203059412));
#210654=CARTESIAN_POINT('Ctrl Pts',(-109.914615285065,6.98159632387027,
131.348009055767));
#210655=CARTESIAN_POINT('Ctrl Pts',(-110.193062908878,4.23111017600536,
125.22440116141));
#210656=CARTESIAN_POINT('Ctrl Pts',(-110.471510532691,-2.40755952238467,
124.228503411086));
#210657=CARTESIAN_POINT('Ctrl Pts',(-110.749958156504,-6.83379963552497,
129.275497185033));
#210658=CARTESIAN_POINT('Ctrl Pts',(-111.028405780317,-4.98011173328953,
135.727441764346));
#210659=CARTESIAN_POINT('Ctrl Pts',(-111.30685340413,1.45005555985492,137.655315275653));
#210660=CARTESIAN_POINT('Ctrl Pts',(-111.585301027943,6.54769263264538,
133.287496143919));
#210661=CARTESIAN_POINT('Ctrl Pts',(-111.863748651756,5.62832004860235,
126.63779677138));
#210662=CARTESIAN_POINT('Ctrl Pts',(-112.142196275568,-0.463203701385527,
123.816966025527));
#210663=CARTESIAN_POINT('Ctrl Pts',(-112.420643899382,-6.12906587855929,
127.417209556553));
#210664=CARTESIAN_POINT('Ctrl Pts',(-112.699091523194,-6.16261593485082,
134.130079441122));
#210665=CARTESIAN_POINT('Ctrl Pts',(-112.977539147007,-0.533023007539609,
137.786776197239));
#210666=CARTESIAN_POINT('Ctrl Pts',(-113.25598677082,5.58639202407863,135.026974145601));
#210667=CARTESIAN_POINT('Ctrl Pts',(-113.534434394633,6.57218569599142,
128.386796547837));
#210668=CARTESIAN_POINT('Ctrl Pts',(-113.812882018446,1.5184617824084,123.968242225583));
#210669=CARTESIAN_POINT('Ctrl Pts',(-114.091329642259,-4.93065432822552,
125.831746742611));
#210670=CARTESIAN_POINT('Ctrl Pts',(-114.369777266072,-6.84873998707567,
132.26484048503));
#210671=CARTESIAN_POINT('Ctrl Pts',(-114.648224889884,-2.4731681773514,
137.355824577657));
#210672=CARTESIAN_POINT('Ctrl Pts',(-114.926672513697,4.17512436637621,
136.426333347767));
#210673=CARTESIAN_POINT('Ctrl Pts',(-115.20512013751,6.98668158356849,130.330523827459));
#210674=CARTESIAN_POINT('Ctrl Pts',(-115.483567761323,3.377819743832,124.670147169045));
#210675=CARTESIAN_POINT('Ctrl Pts',(-115.762015385136,-3.33509342481799,
124.646812996834));
#210676=CARTESIAN_POINT('Ctrl Pts',(-116.040463008949,-6.98321866443162,
130.281964275151));
#210677=CARTESIAN_POINT('Ctrl Pts',(-116.318910632762,-4.21410710063033,
136.397172271667));
#210678=CARTESIAN_POINT('Ctrl Pts',(-116.597358256575,2.42756301807353,
137.372859582102));
#210679=CARTESIAN_POINT('Ctrl Pts',(-116.875805880388,6.83842131621399,
132.312417233142));
#210680=CARTESIAN_POINT('Ctrl Pts',(-117.154253504201,4.96510450020791,
125.866144527128));
#210681=CARTESIAN_POINT('Ctrl Pts',(-117.432701128013,-1.47090079265054,
123.957851162959));
#210682=CARTESIAN_POINT('Ctrl Pts',(-117.711148751826,-6.55522011456102,
128.341165516992));
#210683=CARTESIAN_POINT('Ctrl Pts',(-117.989596375639,-5.61561239149597,
134.988035834682));
#210684=CARTESIAN_POINT('Ctrl Pts',(-118.268043999452,0.484468781437156,
137.790313011739));
#210685=CARTESIAN_POINT('Ctrl Pts',(-118.546491623265,6.13934681184524,
134.172841221298));
#210686=CARTESIAN_POINT('Ctrl Pts',(-118.824939247078,6.15246504593319,
127.459900315453));
#210687=CARTESIAN_POINT('Ctrl Pts',(-119.103386870891,0.511768467435545,
123.820355041281));
#210688=CARTESIAN_POINT('Ctrl Pts',(-119.381834494704,-5.59921833135585,
126.598769704074));
#210689=CARTESIAN_POINT('Ctrl Pts',(-119.660282118516,-6.56479702065358,
133.241916961827));
#210690=CARTESIAN_POINT('Ctrl Pts',(-119.93872974233,-1.49764795613459,
137.645069020452));
#210691=CARTESIAN_POINT('Ctrl Pts',(-120.217177366142,4.94576641590264,
135.761944244007));
#210692=CARTESIAN_POINT('Ctrl Pts',(-120.495624989955,6.84426306584611,
129.323042306287));
#210693=CARTESIAN_POINT('Ctrl Pts',(-120.774072613768,2.45321631911644,
124.245399530209));
#210694=CARTESIAN_POINT('Ctrl Pts',(-121.052520237581,-4.19221637860163,
125.195121570349));
#210695=CARTESIAN_POINT('Ctrl Pts',(-121.330967861394,-6.98520702554029,
131.299460268319));
#210696=CARTESIAN_POINT('Ctrl Pts',(-121.609415485207,-3.35913366234199,
136.948826574209));
#210697=CARTESIAN_POINT('Ctrl Pts',(-121.88786310902,3.3538194337463,136.951728839794));
#210698=CARTESIAN_POINT('Ctrl Pts',(-122.166310732833,6.98477631340985,
131.305500024783));
#210699=CARTESIAN_POINT('Ctrl Pts',(-122.444758356646,4.19706498634193,
125.198748576561));
#210700=CARTESIAN_POINT('Ctrl Pts',(-122.723205980458,-2.44754402515043,
124.24328074465));
#210701=CARTESIAN_POINT('Ctrl Pts',(-123.001653604271,-6.84297964670285,
129.317124789377));
#210702=CARTESIAN_POINT('Ctrl Pts',(-123.280101228084,-4.95005127107555,
135.7576659047));
#210703=CARTESIAN_POINT('Ctrl Pts',(-123.558548851897,1.49173239922134,
137.646361443563));
#210704=CARTESIAN_POINT('Ctrl Pts',(-123.83699647571,6.5626868698133,133.247592473656));
#210705=CARTESIAN_POINT('Ctrl Pts',(-124.115444099523,5.60285271212367,
126.603612786514));
#210706=CARTESIAN_POINT('Ctrl Pts',(-124.393891723336,-0.505729373435472,
123.819915138168));
#210707=CARTESIAN_POINT('Ctrl Pts',(-124.672339347149,-6.14957087106115,
127.454581676257));
#210708=CARTESIAN_POINT('Ctrl Pts',(-124.950786970961,-6.14225716141998,
134.167531415611));
#210709=CARTESIAN_POINT('Ctrl Pts',(-125.229234594775,-0.490509186377616,
137.789891491587));
#210710=CARTESIAN_POINT('Ctrl Pts',(-125.507682218587,5.6119927682395,134.992889956494));
#210711=CARTESIAN_POINT('Ctrl Pts',(-125.786129842401,6.55734752993325,
128.346834579959));
#210712=CARTESIAN_POINT('Ctrl Pts',(-126.064577466213,1.47682025585389,
123.959125575163));
#210713=CARTESIAN_POINT('Ctrl Pts',(-126.343025090026,-4.9608326866744,
125.861853166013));
#210714=CARTESIAN_POINT('Ctrl Pts',(-126.621472713839,-6.8397227402992,
132.306503649927));
#210715=CARTESIAN_POINT('Ctrl Pts',(-126.899920337652,-2.43324173462049,
137.370758070868));
#210716=CARTESIAN_POINT('Ctrl Pts',(-127.178367961465,4.20926955470684,
136.400814018573));
#210717=CARTESIAN_POINT('Ctrl Pts',(-127.456815585278,6.98366775750873,
130.288002692701));
#210718=CARTESIAN_POINT('Ctrl Pts',(-127.73526320909,3.34041646229627,124.649699074291));
#210719=CARTESIAN_POINT('Ctrl Pts',(-128.013710832904,-3.37251437334987,
124.66722874222));
#210720=CARTESIAN_POINT('Ctrl Pts',(-128.292158456716,-6.9862692563739,
130.324482788031));
#210721=CARTESIAN_POINT('Ctrl Pts',(-128.570606080529,-4.17998399101771,
136.422721115849));
#210722=CARTESIAN_POINT('Ctrl Pts',(-128.849053704342,2.46750235851359,
137.357960617914));
#210723=CARTESIAN_POINT('Ctrl Pts',(-129.127501328155,6.84747458476236,
132.270761880817));
#210724=CARTESIAN_POINT('Ctrl Pts',(-129.405948951968,4.93495218534535,
125.836012020477));
#210725=CARTESIAN_POINT('Ctrl Pts',(-129.684396575781,-1.51255018658779,
123.966931803538));
#210726=CARTESIAN_POINT('Ctrl Pts',(-129.962844199593,-6.57009282923063,
128.381114639724));
#210727=CARTESIAN_POINT('Ctrl Pts',(-130.241291823406,-5.59004112868908,
135.022142147398));
#210728=CARTESIAN_POINT('Ctrl Pts',(-130.519739447219,0.52698528042665,
137.78723447924));
#210729=CARTESIAN_POINT('Ctrl Pts',(-130.798187071032,6.15973796149245,
134.135406864555));
#210730=CARTESIAN_POINT('Ctrl Pts',(-131.076634694845,6.13199237587537,
127.422510479544));
#210731=CARTESIAN_POINT('Ctrl Pts',(-131.355082318658,0.4692453613103,123.81736915881));
#210732=CARTESIAN_POINT('Ctrl Pts',(-131.633529942471,-5.62471521638866,
126.632931655165));
#210733=CARTESIAN_POINT('Ctrl Pts',(-131.911977566284,-6.54983729284086,
133.281833582332));
#210734=CARTESIAN_POINT('Ctrl Pts',(-132.190425190097,-1.45597887451291,
137.654058886162));
#210735=CARTESIAN_POINT('Ctrl Pts',(-132.46887281391,4.97585300097076,135.731746107516));
#210736=CARTESIAN_POINT('Ctrl Pts',(-132.747320437723,6.83511905249447,
129.281406779768));
#210737=CARTESIAN_POINT('Ctrl Pts',(-133.025768061535,2.4132446089053,124.230587628526));
#210738=CARTESIAN_POINT('Ctrl Pts',(-133.304215685348,-4.22628373671482,
125.220744707546));
#210739=CARTESIAN_POINT('Ctrl Pts',(-133.582663309161,-6.98206379373247,
131.341972033073));
#210740=CARTESIAN_POINT('Ctrl Pts',(-133.861110932974,-3.32166831708915,
136.969160731525));
#210741=CARTESIAN_POINT('Ctrl Pts',(-134.139558556787,3.39117807044069,
136.931199292478));
#210742=CARTESIAN_POINT('Ctrl Pts',(-134.4180061806,6.98769747949419,131.262972423894));
#210743=CARTESIAN_POINT('Ctrl Pts',(-134.696453804413,4.16286427289247,
125.173303709728));
#210744=CARTESIAN_POINT('Ctrl Pts',(-134.974901428226,-2.48743783327188,
124.25830120144));
#210745=CARTESIAN_POINT('Ctrl Pts',(-135.253349052039,-6.85190608875344,
129.358807503792));
#210746=CARTESIAN_POINT('Ctrl Pts',(-135.531796675851,-4.91980738289134,
135.787706498505));
#210747=CARTESIAN_POINT('Ctrl Pts',(-135.810244299665,1.53335396189511,
137.637154078616));
#210748=CARTESIAN_POINT('Ctrl Pts',(-136.088691923477,6.57743792420584,
133.207598268539));
#210749=CARTESIAN_POINT('Ctrl Pts',(-136.36713954729,5.57717775987727,126.569584461903));
#210750=CARTESIAN_POINT('Ctrl Pts',(-136.645587171103,-0.548236305497475,
123.823123062006));
#210751=CARTESIAN_POINT('Ctrl Pts',(-136.924034794916,-6.1698479889529,
127.492077923251));
#210752=CARTESIAN_POINT('Ctrl Pts',(-137.202482418729,-6.12167078439119,
134.204858766568));
#210753=CARTESIAN_POINT('Ctrl Pts',(-137.480930042542,-0.447977189217358,
137.792747934521));
#210754=CARTESIAN_POINT('Ctrl Pts',(-137.759377666354,5.63738555794455,
134.958650559891));
#210755=CARTESIAN_POINT('Ctrl Pts',(-138.037825290167,6.54226637895086,
128.306963676612));
#210756=CARTESIAN_POINT('Ctrl Pts',(-138.31627291398,1.43512400518173,123.950262577445));
#210757=CARTESIAN_POINT('Ctrl Pts',(-138.594720537793,-4.99082721964375,
125.892142735845));
#210758=CARTESIAN_POINT('Ctrl Pts',(-138.873168161606,-6.83045204508126,
132.348111152362));
#210759=CARTESIAN_POINT('Ctrl Pts',(-139.151615785419,-2.39322512722196,
137.385448243807));
#210760=CARTESIAN_POINT('Ctrl Pts',(-139.430063409232,4.24325876700673,
136.375087310741));
#210761=CARTESIAN_POINT('Ctrl Pts',(-139.708511033045,6.98039514907165,
130.245500691775));
#210762=CARTESIAN_POINT('Ctrl Pts',(-139.986958656858,3.30288940040013,
124.629479042785));
#210763=CARTESIAN_POINT('Ctrl Pts',(-140.26540628067,-3.40981035212143,
124.687871901284));
#210764=CARTESIAN_POINT('Ctrl Pts',(-140.543853904484,-6.98906096953965,
130.36701908296));
#210765=CARTESIAN_POINT('Ctrl Pts',(-140.822301528296,-4.1457059905611,
136.448061769617));
#210766=CARTESIAN_POINT('Ctrl Pts',(-141.100749152109,2.50735026474636,
137.342818807668));
#210767=CARTESIAN_POINT('Ctrl Pts',(-141.379196775922,6.85627411762182,
132.229052190456));
#210768=CARTESIAN_POINT('Ctrl Pts',(-141.657644399735,4.90461700401472,
125.80606361781));
#210769=CARTESIAN_POINT('Ctrl Pts',(-141.936092023548,-1.5541435324211,
123.976265807557));
#210770=CARTESIAN_POINT('Ctrl Pts',(-142.214539647361,-6.58472208669408,
128.421153556726));
#210771=CARTESIAN_POINT('Ctrl Pts',(-142.492987271174,-5.56426272485295,
135.056092168669));
#210772=CARTESIAN_POINT('Ctrl Pts',(-142.771434894987,0.569482251782813,
137.783897193782));
#210773=CARTESIAN_POINT('Ctrl Pts',(-143.0498825188,6.17990085978423,134.097849074668));
#210774=CARTESIAN_POINT('Ctrl Pts',(-143.328330142612,6.11129248258502,
127.385245959334));
#210775=CARTESIAN_POINT('Ctrl Pts',(-143.606777766425,0.426704867125613,
123.814642181877));
#210776=CARTESIAN_POINT('Ctrl Pts',(-143.885225390238,-5.65000367553061,
126.667248180088));
#210777=CARTESIAN_POINT('Ctrl Pts',(-144.163673014051,-6.53463485839856,
133.321658399163));
#210778=CARTESIAN_POINT('Ctrl Pts',(-144.442120637864,-1.4142558410586,
137.662794933783));
#210779=CARTESIAN_POINT('Ctrl Pts',(-144.720568261677,5.00575520397605,
135.701365384942));
#210780=CARTESIAN_POINT('Ctrl Pts',(-144.99901588549,6.82572176129271,129.239827686864));
#210781=CARTESIAN_POINT('Ctrl Pts',(-145.277463509303,2.37318347502772,
124.216019320419));
#210782=CARTESIAN_POINT('Ctrl Pts',(-145.555911133116,-4.26019448832994,
125.246574747685));
#210783=CARTESIAN_POINT('Ctrl Pts',(-145.834358756928,-6.97866183898313,
131.384463876438));
#210784=CARTESIAN_POINT('Ctrl Pts',(-146.112806380741,-3.28407988619528,
136.989266449907));
#210785=CARTESIAN_POINT('Ctrl Pts',(-146.391254004554,3.42841104578457,
136.910442712901));
#210786=CARTESIAN_POINT('Ctrl Pts',(-146.669701628367,6.99035971387901,
131.220427828976));
#210787=CARTESIAN_POINT('Ctrl Pts',(-146.94814925218,4.12850930297597,125.148067503779));
#210788=CARTESIAN_POINT('Ctrl Pts',(-147.226596875993,-2.52723946847004,
124.27356422487));
#210789=CARTESIAN_POINT('Ctrl Pts',(-147.505044499806,-6.86057863090408,
129.400543783708));
#210790=CARTESIAN_POINT('Ctrl Pts',(-147.783492123619,-4.88938118943532,
135.817562432597));
#210791=CARTESIAN_POINT('Ctrl Pts',(-148.061939747432,1.57491870557395,
137.627693521995));
#210792=CARTESIAN_POINT('Ctrl Pts',(-148.340387371245,6.5919452492172,133.167515010566));
#210793=CARTESIAN_POINT('Ctrl Pts',(-148.618834995057,5.55129614325799,
126.535713058481));
#210794=CARTESIAN_POINT('Ctrl Pts',(-148.89728261887,-0.590722922461593,
123.826589678167));
#210795=CARTESIAN_POINT('Ctrl Pts',(-149.175730242683,-6.18989648085842,
127.529696908099));
#210796=CARTESIAN_POINT('Ctrl Pts',(-149.454177866496,-6.10085756660025,
134.242060110815));
#210797=CARTESIAN_POINT('Ctrl Pts',(-149.732625490309,-0.405428592098244,
137.795345420191));
#210798=CARTESIAN_POINT('Ctrl Pts',(-150.011073114122,5.66256945225453,
134.924257224548));
#210799=CARTESIAN_POINT('Ctrl Pts',(-150.289520737935,6.52694280188189,
128.267185315226));
#210800=CARTESIAN_POINT('Ctrl Pts',(-150.567968361748,1.39337457546175,
123.94165356085));
#210801=CARTESIAN_POINT('Ctrl Pts',(-150.84641598556,-5.02063681567507,
125.922614329717));
#210802=CARTESIAN_POINT('Ctrl Pts',(-151.124863609373,-6.8209282449509,
132.389661450552));
#210803=CARTESIAN_POINT('Ctrl Pts',(-151.403311233186,-2.35311983798619,
137.399894552124));
#210804=CARTESIAN_POINT('Ctrl Pts',(-151.681758856999,4.2770907437925,136.349154177582));
#210805=CARTESIAN_POINT('Ctrl Pts',(-151.960206480812,6.97686387952531,
130.20301939961));
#210806=CARTESIAN_POINT('Ctrl Pts',(-152.238654104625,3.26523994872261,
124.609487823786));
#210807=CARTESIAN_POINT('Ctrl Pts',(-152.517101728438,-3.44697997911642,
124.708741709087));
#210808=CARTESIAN_POINT('Ctrl Pts',(-152.795549352251,-6.99159370048095,
130.40957158374));
#210809=CARTESIAN_POINT('Ctrl Pts',(-153.073996976064,-4.11127436944443,
136.473193293963));
#210810=CARTESIAN_POINT('Ctrl Pts',(-153.352444599876,2.54710526019297,
137.327434712448));
#210811=CARTESIAN_POINT('Ctrl Pts',(-153.63089222369,6.86481958872245,132.187289707623));
#210812=CARTESIAN_POINT('Ctrl Pts',(-153.909339847502,4.87410008029735,
125.776300428876));
#210813=CARTESIAN_POINT('Ctrl Pts',(-154.187787471315,-1.5956792888948,
123.98585282914));
#210814=CARTESIAN_POINT('Ctrl Pts',(-154.466235095128,-6.5991073448593,
128.461280784342));
#210815=CARTESIAN_POINT('Ctrl Pts',(-154.744682718941,-5.53827813521478,
135.089884640464));
#210816=CARTESIAN_POINT('Ctrl Pts',(-155.023130342754,0.611958120764675,
137.78030127903));
#210817=CARTESIAN_POINT('Ctrl Pts',(-155.301577966567,6.19983475957701,
134.060169243357));
#210818=CARTESIAN_POINT('Ctrl Pts',(-155.58002559038,6.0903661331043,127.348108135675));
#210819=CARTESIAN_POINT('Ctrl Pts',(-155.858473214192,0.38414856123516,
123.812174211531));
#210820=CARTESIAN_POINT('Ctrl Pts',(-156.136920838005,-5.67508277170857,
126.701718007236));
#210821=CARTESIAN_POINT('Ctrl Pts',(-156.415368461818,-6.51919028065846,
133.3613899366));
#210822=CARTESIAN_POINT('Ctrl Pts',(-156.693816085631,-1.37248040183399,
137.671276839599));
#210823=CARTESIAN_POINT('Ctrl Pts',(-156.972263709444,5.03547191688086,
135.670803202055));
#210824=CARTESIAN_POINT('Ctrl Pts',(-157.250711333257,6.81607154046107,
129.198306568304));
#210825=CARTESIAN_POINT('Ctrl Pts',(-157.52915895707,2.33303440196427,124.201695145721));
#210826=CARTESIAN_POINT('Ctrl Pts',(-157.807606580883,-4.29394737687161,
125.272610733624));
#210827=CARTESIAN_POINT('Ctrl Pts',(-158.086054204696,-6.97500128735293,
131.426934223863));
#210828=CARTESIAN_POINT('Ctrl Pts',(-158.364501828508,-3.2463697625135,
137.009142984327));
#210829=CARTESIAN_POINT('Ctrl Pts',(-158.642949452322,3.46551698009634,
136.889459870208));
#210830=CARTESIAN_POINT('Ctrl Pts',(-158.921397076134,6.99276291791392,
131.177867816534));
#210831=CARTESIAN_POINT('Ctrl Pts',(-159.199844699947,4.09400134962899,
125.123040893851));
#210832=CARTESIAN_POINT('Ctrl Pts',(-159.47829232376,-2.56694745588028,
124.289069249361));
#210833=CARTESIAN_POINT('Ctrl Pts',(-159.756739947573,-6.86899695179061,
129.442332082575));
#210834=CARTESIAN_POINT('Ctrl Pts',(-160.035187571386,-4.85877381816122,
135.84723260065));
#210835=CARTESIAN_POINT('Ctrl Pts',(-160.313635195198,1.61642509006095,
137.617980124263));
#210836=CARTESIAN_POINT('Ctrl Pts',(-160.592082819012,6.60620830727321,
133.12734418504));
#210837=CARTESIAN_POINT('Ctrl Pts',(-160.870530442824,5.52520882131862,
126.501999831362));
#210838=CARTESIAN_POINT('Ctrl Pts',(-161.148978066638,-0.633187649970563,
123.830314858198));
#210839=CARTESIAN_POINT('Ctrl Pts',(-161.42742569045,-6.20971560387352,
127.567437236815));
#210840=CARTESIAN_POINT('Ctrl Pts',(-161.705873314263,-6.07981827928859,
134.279134069845));
#210841=CARTESIAN_POINT('Ctrl Pts',(-161.984320938076,-0.362864971672915,
137.79768385235));
#210842=CARTESIAN_POINT('Ctrl Pts',(-162.262768561889,5.68754351797111,
134.889711224922));
#210843=CARTESIAN_POINT('Ctrl Pts',(-162.541216185702,6.5113773665471,128.227500969805));
#210844=CARTESIAN_POINT('Ctrl Pts',(-162.819663809515,1.35157351373451,
123.93329884439));
#210845=CARTESIAN_POINT('Ctrl Pts',(-163.098111433328,-5.05026037016286,
125.953266818493));
#210846=CARTESIAN_POINT('Ctrl Pts',(-163.376559057141,-6.81115169281603,
132.431153004838));
#210847=CARTESIAN_POINT('Ctrl Pts',(-163.655006680953,-2.31292735302948,
137.414096460505));
#210848=CARTESIAN_POINT('Ctrl Pts',(-163.933454304766,4.31076423140788,
136.323015580059));
#210849=CARTESIAN_POINT('Ctrl Pts',(-164.211901928579,6.97307407972212,
130.160560390364));
#210850=CARTESIAN_POINT('Ctrl Pts',(-164.490349552392,3.2274695023783,124.589726158078));
#210851=CARTESIAN_POINT('Ctrl Pts',(-164.768797176205,-3.4840218770001,
124.729837392289));
#210852=CARTESIAN_POINT('Ctrl Pts',(-165.047244800018,-6.99386735534677,
130.452138713572));
#210853=CARTESIAN_POINT('Ctrl Pts',(-165.325692423831,-4.07669040354407,
136.498114757629));
#210854=CARTESIAN_POINT('Ctrl Pts',(-165.604140047644,2.58676587171747,
137.31180890232));
#210855=CARTESIAN_POINT('Ctrl Pts',(-165.882587671457,6.87311068140868,
132.145475979844));
#210856=CARTESIAN_POINT('Ctrl Pts',(-166.161035295269,4.84340254500906,
125.746723556562));
#210857=CARTESIAN_POINT('Ctrl Pts',(-166.439482919082,-1.63715591688565,
123.995692513036));
#210858=CARTESIAN_POINT('Ctrl Pts',(-166.717930542895,-6.61324807067504,
128.501494835643));
#210859=CARTESIAN_POINT('Ctrl Pts',(-166.996378166708,-5.5120883226436,
135.12351831059));
#210860=CARTESIAN_POINT('Ctrl Pts',(-167.274825790521,0.654411313413328,
137.776446868231));
#210861=CARTESIAN_POINT('Ctrl Pts',(-167.553273414334,6.21953892221278,
134.022368766858));
#210862=CARTESIAN_POINT('Ctrl Pts',(-167.831721038147,6.06921410286677,
127.311098384725));
#210863=CARTESIAN_POINT('Ctrl Pts',(-168.11016866196,0.3415780205785,123.809965339223));
#210864=CARTESIAN_POINT('Ctrl Pts',(-168.388616285773,-5.69995157560742,
126.736339859314));
#210865=CARTESIAN_POINT('Ctrl Pts',(-168.667063909585,-6.50350413192509,
133.401026722375));
#210866=CARTESIAN_POINT('Ctrl Pts',(-168.945511533399,-1.33065410484337,
137.679504289309));
#210867=CARTESIAN_POINT('Ctrl Pts',(-169.223959157211,5.06500203852252,
135.640060691349));
#210868=CARTESIAN_POINT('Ctrl Pts',(-169.502406781024,6.80616874759175,
129.156844962666));
#210869=CARTESIAN_POINT('Ctrl Pts',(-169.780854404837,2.29279887745254,
124.18761563522));
#210870=CARTESIAN_POINT('Ctrl Pts',(-170.05930202865,-4.32754115161411,
125.298851700587));
#210871=CARTESIAN_POINT('Ctrl Pts',(-170.337749652463,-6.97108227448498,
131.469381501595));
#210872=CARTESIAN_POINT('Ctrl Pts',(-170.616197276276,-3.20853934340632,
137.028789598255));
#210873=CARTESIAN_POINT('Ctrl Pts',(-170.894644900089,3.50249449840198,
136.868251541923));
#210874=CARTESIAN_POINT('Ctrl Pts',(-171.173092523901,6.99490700254731,
131.135293963646));
#210875=CARTESIAN_POINT('Ctrl Pts',(-171.451540147715,4.05934169155642,
125.098224807315));
#210876=CARTESIAN_POINT('Ctrl Pts',(-171.729987771527,-2.60656032410858,
124.304815700371));
#210877=CARTESIAN_POINT('Ctrl Pts',(-172.00843539534,-6.87716073946864,
129.484170851909));
#210878=CARTESIAN_POINT('Ctrl Pts',(-172.286883019153,-4.82798640323697,
135.876715903229));
#210879=CARTESIAN_POINT('Ctrl Pts',(-172.565330642966,1.65787157732142,
137.608014245356));
#210880=CARTESIAN_POINT('Ctrl Pts',(-172.843778266779,6.62022656985093,
133.087087280501));
#210881=CARTESIAN_POINT('Ctrl Pts',(-173.122225890592,5.49891676073447,
126.468446029806));
#210882=CARTESIAN_POINT('Ctrl Pts',(-173.400673514405,-0.675628914478315,
123.834298464058));
#210883=CARTESIAN_POINT('Ctrl Pts',(-173.679121138218,-6.22930462359329,
127.605297510917));
#210884=CARTESIAN_POINT('Ctrl Pts',(-173.95756876203,-6.05855370207473,
134.316079269865));
#210885=CARTESIAN_POINT('Ctrl Pts',(-174.236016385844,-0.320287905152608,
137.799763144343));
#210886=CARTESIAN_POINT('Ctrl Pts',(-174.514464009656,5.71230682967103,
134.855013841124));
#210887=CARTESIAN_POINT('Ctrl Pts',(-174.792911633469,6.49557064972945,
128.187912110866));
#210888=CARTESIAN_POINT('Ctrl Pts',(-175.071359257282,1.30972236895365,
123.925198737649));
#210889=CARTESIAN_POINT('Ctrl Pts',(-175.349806881095,-5.07969678539539,
125.984099066334));
#210890=CARTESIAN_POINT('Ctrl Pts',(-175.628254504908,-6.80112275095037,
132.472584277733));
#210891=CARTESIAN_POINT('Ctrl Pts',(-175.906702128721,-2.27264916169912,
137.428053442694));
#210892=CARTESIAN_POINT('Ctrl Pts',(-176.185149752534,4.34427798206938,
136.296672486746));
#210893=CARTESIAN_POINT('Ctrl Pts',(-176.463597376347,6.96902589009458,
130.118125237372));
#210894=CARTESIAN_POINT('Ctrl Pts',(-176.742045000159,3.18957946096438,
124.570194777934));
#210895=CARTESIAN_POINT('Ctrl Pts',(-177.020492623972,-3.52093467317244,
124.751158169184));
#210896=CARTESIAN_POINT('Ctrl Pts',(-177.298940247785,-6.99588184988549,
130.494718895118));
#210897=CARTESIAN_POINT('Ctrl Pts',(-177.577387871598,-4.04195537438161,
136.522825237142));
#210898=CARTESIAN_POINT('Ctrl Pts',(-177.855835495411,2.62633062968132,
137.295941956302));
#210899=CARTESIAN_POINT('Ctrl Pts',(-178.134283119224,6.88114708845103,
132.103612556543));
#210900=CARTESIAN_POINT('Ctrl Pts',(-178.412730743037,4.81252553565828,
125.717334096849));
#210901=CARTESIAN_POINT('Ctrl Pts',(-178.69117836685,-1.67857187946192,
124.005784494632));
#210902=CARTESIAN_POINT('Ctrl Pts',(-178.969625990663,-6.62714374015151,
128.541794220484));
#210903=CARTESIAN_POINT('Ctrl Pts',(-179.248073614475,-5.48569425761253,
135.15699193274));
#210904=CARTESIAN_POINT('Ctrl Pts',(-179.526521238288,0.696840256609583,
137.772334104211));
#210905=CARTESIAN_POINT('Ctrl Pts',(-179.804968862101,6.23901261754625,
133.984449045885));
#210906=CARTESIAN_POINT('Ctrl Pts',(-180.083416485914,6.0478371756692,127.27421807789));
#210907=CARTESIAN_POINT('Ctrl Pts',(-180.361864109727,0.298994822622653,
123.808015646805));
#210908=CARTESIAN_POINT('Ctrl Pts',(-180.64031173354,-5.72460916570447,
126.771112453397));
#210909=CARTESIAN_POINT('Ctrl Pts',(-180.918759357353,-6.48757699345442,
133.440567287733));
#210910=CARTESIAN_POINT('Ctrl Pts',(-181.197206981166,-1.28877849997557,
137.687476978041));
#210911=CARTESIAN_POINT('Ctrl Pts',(-181.475654604978,5.094344474651,135.609138992));
#210912=CARTESIAN_POINT('Ctrl Pts',(-181.754102228792,6.79601374963652,
129.115444406326));
#210913=CARTESIAN_POINT('Ctrl Pts',(-182.032549852604,2.25247839243521,
124.173781310638));
#210914=CARTESIAN_POINT('Ctrl Pts',(-182.310997476417,-4.36097456772779,
125.32529667621));
#210915=CARTESIAN_POINT('Ctrl Pts',(-182.58944510023,-6.96690494559973,
131.511804136733));
#210916=CARTESIAN_POINT('Ctrl Pts',(-182.867892724043,-3.17059003069381,
137.048205563678));
#210917=CARTESIAN_POINT('Ctrl Pts',(-183.146340347856,3.53934223048593,
136.84681851393));
#210918=CARTESIAN_POINT('Ctrl Pts',(-183.424787971669,6.99679188832936,
131.092707847901));
#210919=CARTESIAN_POINT('Ctrl Pts',(-183.703235595482,4.02453161308464,
125.07362016374));
#210920=CARTESIAN_POINT('Ctrl Pts',(-183.981683219295,-2.64607660528548,
124.320802994409));
#210921=CARTESIAN_POINT('Ctrl Pts',(-184.260130843107,-6.88506969142675,
129.52605854136));
#210922=CARTESIAN_POINT('Ctrl Pts',(-184.53857846692,-4.79702008550057,
135.906011247817));
#210923=CARTESIAN_POINT('Ctrl Pts',(-184.817026090733,1.6992566315413,137.597796254561));
#210924=CARTESIAN_POINT('Ctrl Pts',(-185.095473714546,6.63399951749853,
133.046745788687));
#210925=CARTESIAN_POINT('Ctrl Pts',(-185.373921338359,5.47242093576752,
126.435052897159));
#210926=CARTESIAN_POINT('Ctrl Pts',(-185.652368962172,-0.718045143308166,
123.838540348135));
#210927=CARTESIAN_POINT('Ctrl Pts',(-185.930816585985,-6.24866281413942,
127.64327632748));
#210928=CARTESIAN_POINT('Ctrl Pts',(-186.209264209798,-6.03706462292539,
134.35289434186));
#210929=CARTESIAN_POINT('Ctrl Pts',(-186.487711833611,-0.277698970246197,
137.801583219124));
#210930=CARTESIAN_POINT('Ctrl Pts',(-186.766159457423,5.73685846974069,
134.820166358884));
#210931=CARTESIAN_POINT('Ctrl Pts',(-187.044607081237,6.47952323715255,
128.148420205389));
#210932=CARTESIAN_POINT('Ctrl Pts',(-187.323054705049,1.2678226919294,123.917353540782));
#210933=CARTESIAN_POINT('Ctrl Pts',(-187.601502328862,-5.10894497059535,
126.01510993074));
#210934=CARTESIAN_POINT('Ctrl Pts',(-187.879949952675,-6.79084179098006,
132.513953733987));
#210935=CARTESIAN_POINT('Ctrl Pts',(-188.158397576488,-2.23228675651833,
137.44176498151));
#210936=CARTESIAN_POINT('Ctrl Pts',(-188.436845200301,4.37763075391265,
136.270125873797));
#210937=CARTESIAN_POINT('Ctrl Pts',(-188.715292824114,6.96471946064982,
130.075715513085));
#210938=CARTESIAN_POINT('Ctrl Pts',(-188.993740447926,3.15157122851057,
124.550894407098));
#210939=CARTESIAN_POINT('Ctrl Pts',(-189.27218807174,-3.55771699981564,
124.772703249722));
#210940=CARTESIAN_POINT('Ctrl Pts',(-189.550635695553,-6.99763710944952,
130.53731055055));
#210941=CARTESIAN_POINT('Ctrl Pts',(-189.829083319365,-4.00707056907658,
136.547323816845));
#210942=CARTESIAN_POINT('Ctrl Pts',(-190.107530943179,2.66579806799723,
137.279834462351));
#210943=CARTESIAN_POINT('Ctrl Pts',(-190.385978566991,6.88892851205765,
132.061700988983));
#210944=CARTESIAN_POINT('Ctrl Pts',(-190.664426190804,4.78147019640398,
125.688133138775));
#210945=CARTESIAN_POINT('Ctrl Pts',(-190.942873814617,-1.71992564193992,
124.016128399968));
#210946=CARTESIAN_POINT('Ctrl Pts',(-191.22132143843,-6.64079383837953,
128.582177445553));
#210947=CARTESIAN_POINT('Ctrl Pts',(-191.499769062243,-5.45909691816341,
135.190304266535));
#210948=CARTESIAN_POINT('Ctrl Pts',(-191.778216686055,0.739243378134395,
137.767963139373));
#210949=CARTESIAN_POINT('Ctrl Pts',(-192.056664309869,6.25825512397307,
133.946411485565));
#210950=CARTESIAN_POINT('Ctrl Pts',(-192.335111933681,6.0262361436405,127.237468581785));
#210951=CARTESIAN_POINT('Ctrl Pts',(-192.613559557494,0.256400545303713,
123.806325206523));
#210952=CARTESIAN_POINT('Ctrl Pts',(-192.892007181307,-5.74905462830365,
126.806034500975));
#210953=CARTESIAN_POINT('Ctrl Pts',(-193.17045480512,-6.47140945543246,
133.480010167483));
#210954=CARTESIAN_POINT('Ctrl Pts',(-193.448902428933,-1.24685513894648,
137.695194610365));
#210955=CARTESIAN_POINT('Ctrl Pts',(-193.727350052746,5.12349813797151,
135.578039249819));
#210956=CARTESIAN_POINT('Ctrl Pts',(-194.005797676559,6.78560692289256,
129.074106433399));
#210957=CARTESIAN_POINT('Ctrl Pts',(-194.284245300372,2.2120744410027,124.160192684611));
#210958=CARTESIAN_POINT('Ctrl Pts',(-194.562692924184,-4.39424638632456,
125.35194468056));
#210959=CARTESIAN_POINT('Ctrl Pts',(-194.841140547997,-6.9624694554897,
131.554200557291));
#210960=CARTESIAN_POINT('Ctrl Pts',(-195.11958817181,-3.13252323060231,
137.067390161131));
#210961=CARTESIAN_POINT('Ctrl Pts',(-195.398035795623,3.57605881094196,
136.825161580438));
#210962=CARTESIAN_POINT('Ctrl Pts',(-195.676483419436,6.99841750541489,
131.050111047343));
#210963=CARTESIAN_POINT('Ctrl Pts',(-195.954931043249,3.98957240411393,
125.04922787486));
#210964=CARTESIAN_POINT('Ctrl Pts',(-196.233378667062,-2.68549483512068,
124.337030539057));
#210965=CARTESIAN_POINT('Ctrl Pts',(-196.511826290875,-6.89272351459547,
129.567993598765));
#210966=CARTESIAN_POINT('Ctrl Pts',(-196.790273914688,-4.76587601242081,
135.935117548864));
#210967=CARTESIAN_POINT('Ctrl Pts',(-197.0687215385,1.74057871918182,137.58732653051));
#210968=CARTESIAN_POINT('Ctrl Pts',(-197.347169162313,6.64752663985393,
133.006321204467));
#210969=CARTESIAN_POINT('Ctrl Pts',(-197.625616786126,5.44572232823074,
126.401821670817));
#210970=CARTESIAN_POINT('Ctrl Pts',(-197.904064409939,-0.760434764710735,
123.843040353244));
#210971=CARTESIAN_POINT('Ctrl Pts',(-198.182512033752,-6.26778945818702,
127.681372279183));
#210972=CARTESIAN_POINT('Ctrl Pts',(-198.460959657565,-6.01535183812634,
134.389577921633));
#210973=CARTESIAN_POINT('Ctrl Pts',(-198.739407281378,-0.235099745102313,
137.803144009248));
#210974=CARTESIAN_POINT('Ctrl Pts',(-199.017854905191,5.76119752841001,
134.785170069484));
#210975=CARTESIAN_POINT('Ctrl Pts',(-199.296302529004,6.46323572345932,
128.10902671676));
#210976=CARTESIAN_POINT('Ctrl Pts',(-199.574750152817,1.22587603526843,
123.909763544495));
#210977=CARTESIAN_POINT('Ctrl Pts',(-199.853197776629,-5.13800384196074,
126.04629826259));
#210978=CARTESIAN_POINT('Ctrl Pts',(-200.131645400443,-6.78030919386985,
132.555259840639));
#210979=CARTESIAN_POINT('Ctrl Pts',(-200.410093024255,-2.19184163313082,
137.455230568865));
#210980=CARTESIAN_POINT('Ctrl Pts',(-200.688540648069,4.41082131103843,
136.243376724908));
#210981=CARTESIAN_POINT('Ctrl Pts',(-200.96698827188,6.96015495096418,130.03333278901));
#210982=CARTESIAN_POINT('Ctrl Pts',(-201.245435895694,3.11344621342587,
124.531825760752));
#210983=CARTESIAN_POINT('Ctrl Pts',(-201.523883519507,-3.59436749394705,
124.794471835542));
#210984=CARTESIAN_POINT('Ctrl Pts',(-201.80233114332,-6.99913306899709,
130.579912101622));
#210985=CARTESIAN_POINT('Ctrl Pts',(-202.080778767133,-3.97203728029775,
136.571609588935));
#210986=CARTESIAN_POINT('Ctrl Pts',(-202.359226390945,2.705166724186,137.263487017335));
#210987=CARTESIAN_POINT('Ctrl Pts',(-202.637674014758,6.89645466388467,
132.019742830214));
#210988=CARTESIAN_POINT('Ctrl Pts',(-202.916121638571,4.75023767801316,
125.659121764391));
#210989=CARTESIAN_POINT('Ctrl Pts',(-203.194569262384,-1.76121567194074,
124.026723845744));
#210990=CARTESIAN_POINT('Ctrl Pts',(-203.473016886197,-6.65419785954973,
128.622643014438));
#210991=CARTESIAN_POINT('Ctrl Pts',(-203.75146451001,-5.43229728987039,
135.223454077576));
#210992=CARTESIAN_POINT('Ctrl Pts',(-204.029912133822,0.781619106723946,
137.763334135682));
#210993=CARTESIAN_POINT('Ctrl Pts',(-204.308359757636,6.27726572845484,
133.908257495395));
#210994=CARTESIAN_POINT('Ctrl Pts',(-204.586807381448,6.00441180721532,
127.200851258176));
#210995=CARTESIAN_POINT('Ctrl Pts',(-204.865255005262,0.213796766968775,
123.804894081017));
#210996=CARTESIAN_POINT('Ctrl Pts',(-205.143702629074,-5.77328705756903,
126.841104707996));
#210997=CARTESIAN_POINT('Ctrl Pts',(-205.422150252887,-6.4550021169537,
133.519353900054));
#210998=CARTESIAN_POINT('Ctrl Pts',(-205.7005978767,-1.20488557524167,137.702656900301));
#210999=CARTESIAN_POINT('Ctrl Pts',(-205.979045500513,5.15246194818434,
135.546762617222));
#211000=CARTESIAN_POINT('Ctrl Pts',(-206.257493124326,6.77494865298866,
129.032832575676));
#211001=CARTESIAN_POINT('Ctrl Pts',(-206.535940748139,2.17158852033829,
124.14685026067));
#211002=CARTESIAN_POINT('Ctrl Pts',(-206.814388371952,-4.42735537450605,
125.378794726189));
#211003=CARTESIAN_POINT('Ctrl Pts',(-207.092835995765,-6.9577759685135,
131.596569192254));
#211004=CARTESIAN_POINT('Ctrl Pts',(-207.371283619578,-3.09434035370993,
137.086342679721));
#211005=CARTESIAN_POINT('Ctrl Pts',(-207.64973124339,3.61264287922363,136.803281543952));
#211006=CARTESIAN_POINT('Ctrl Pts',(-207.928178867203,6.99978379356611,
131.007505140413));
#211007=CARTESIAN_POINT('Ctrl Pts',(-208.206626491016,3.95446536007061,
125.025048844539));
#211008=CARTESIAN_POINT('Ctrl Pts',(-208.485074114829,-2.72481355295718,
124.353497733001));
#211009=CARTESIAN_POINT('Ctrl Pts',(-208.763521738642,-6.90012192535954,
129.609974470206));
#211010=CARTESIAN_POINT('Ctrl Pts',(-209.041969362455,-4.73455533805275,
135.964033727826));
#211011=CARTESIAN_POINT('Ctrl Pts',(-209.320416986268,1.78183630903778,
137.576605461163));
#211012=CARTESIAN_POINT('Ctrl Pts',(-209.598864610081,6.66080743566547,
132.965815025787));
#211013=CARTESIAN_POINT('Ctrl Pts',(-209.877312233893,5.41882192745001,
126.368753582173));
#211014=CARTESIAN_POINT('Ctrl Pts',(-210.155759857706,-0.802796207923886,
123.847798312635));
#211015=CARTESIAN_POINT('Ctrl Pts',(-210.434207481519,-6.28668384699127,
127.719583954367));
#211016=CARTESIAN_POINT('Ctrl Pts',(-210.712655105332,-5.99341615225276,
134.42612864986));
#211017=CARTESIAN_POINT('Ctrl Pts',(-210.991102729145,-0.19249180825093,
137.804445456879));
#211018=CARTESIAN_POINT('Ctrl Pts',(-211.269550352958,5.78532310378624,
134.750026269725));
#211019=CARTESIAN_POINT('Ctrl Pts',(-211.547997976771,6.44670871218949,
128.069733104719));
#211020=CARTESIAN_POINT('Ctrl Pts',(-211.826445600584,1.18388395332015,
123.902429030038));
#211021=CARTESIAN_POINT('Ctrl Pts',(-212.104893224396,-5.16687232270428,
126.077662906191));
#211022=CARTESIAN_POINT('Ctrl Pts',(-212.38334084821,-6.76952534990887,
132.596501067076));
#211023=CARTESIAN_POINT('Ctrl Pts',(-212.661788472022,-2.15131529024619,
137.468449705789));
#211024=CARTESIAN_POINT('Ctrl Pts',(-212.940236095835,4.44384842355829,
136.216426031276));
#211025=CARTESIAN_POINT('Ctrl Pts',(-213.218683719648,6.95533253017721,
129.990978635656));
#211026=CARTESIAN_POINT('Ctrl Pts',(-213.497131343461,3.0752058284468,124.512989545492));
#211027=CARTESIAN_POINT('Ctrl Pts',(-213.775578967274,-3.63088479746918,
124.81646312));
#211028=CARTESIAN_POINT('Ctrl Pts',(-214.054026591087,-7.00036967309483,
130.622521969716));
#211029=CARTESIAN_POINT('Ctrl Pts',(-214.3324742149,-3.93685680621679,136.595681653493));
#211030=CARTESIAN_POINT('Ctrl Pts',(-214.610921838713,2.74443513942699,
137.246900227015));
#211031=CARTESIAN_POINT('Ctrl Pts',(-214.889369462525,6.90372526504794,
131.977739635008));
#211032=CARTESIAN_POINT('Ctrl Pts',(-215.167817086339,4.71882913781829,
125.630301048724));
#211033=CARTESIAN_POINT('Ctrl Pts',(-215.446264710151,-1.80244043944716,
124.037570439344));
#211034=CARTESIAN_POINT('Ctrl Pts',(-215.724712333964,-6.66735530697114,
128.66318942767));
#211035=CARTESIAN_POINT('Ctrl Pts',(-216.003159957777,-5.40529636580357,
135.256440137483));
#211036=CARTESIAN_POINT('Ctrl Pts',(-216.28160758159,0.823965872130078,
137.758447264668));
#211037=CARTESIAN_POINT('Ctrl Pts',(-216.560055205403,6.29604372654653,
133.869988489185));
#211038=CARTESIAN_POINT('Ctrl Pts',(-216.838502829216,5.98236497510254,
127.164367463932));
#211039=CARTESIAN_POINT('Ctrl Pts',(-217.116950453029,0.171185066315507,
123.803722323317));
#211040=CARTESIAN_POINT('Ctrl Pts',(-217.395398076842,-5.79730555555969,
126.876321774922));
#211041=CARTESIAN_POINT('Ctrl Pts',(-217.673845700654,-6.43835558599724,
133.558597027552));
#211042=CARTESIAN_POINT('Ctrl Pts',(-217.952293324468,-1.16287136405879,
137.709863571333));
#211043=CARTESIAN_POINT('Ctrl Pts',(-218.23074094828,5.18123483202488,135.515310253174));
#211044=CARTESIAN_POINT('Ctrl Pts',(-218.509188572093,6.76403933487094,
128.991624362576));
#211045=CARTESIAN_POINT('Ctrl Pts',(-218.787636195906,2.13102213066266,
124.133754533223));
#211046=CARTESIAN_POINT('Ctrl Pts',(-219.066083819719,-4.46030030540597,
125.405845818157));
#211047=CARTESIAN_POINT('Ctrl Pts',(-219.344531443532,-6.95282465859006,
131.638908471637));
#211048=CARTESIAN_POINT('Ctrl Pts',(-219.622979067345,-3.0560428148978,
137.105062417155));
#211049=CARTESIAN_POINT('Ctrl Pts',(-219.901426691158,3.6490930796943,136.781179215245));
#211050=CARTESIAN_POINT('Ctrl Pts',(-220.179874314971,7.00089070215466,
130.964891705888));
#211051=CARTESIAN_POINT('Ctrl Pts',(-220.458321938783,3.91921178185968,
125.001083968743));
#211052=CARTESIAN_POINT('Ctrl Pts',(-220.736769562596,-2.76403130182543,
124.370203966041));
#211053=CARTESIAN_POINT('Ctrl Pts',(-221.015217186409,-6.90726464956813,
129.651999600063));
#211054=CARTESIAN_POINT('Ctrl Pts',(-221.293664810222,-4.7030592229955,
135.992758713204));
#211055=CARTESIAN_POINT('Ctrl Pts',(-221.572112434035,1.82302787229404,
137.565633443793));
#211056=CARTESIAN_POINT('Ctrl Pts',(-221.850560057848,6.67384141280798,
132.925228753618));
#211057=CARTESIAN_POINT('Ctrl Pts',(-222.129007681661,5.39172073022998,
126.33584985658));
#211058=CARTESIAN_POINT('Ctrl Pts',(-222.407455305474,-0.845127903228338,
123.85281405));
#211059=CARTESIAN_POINT('Ctrl Pts',(-222.685902929286,-6.30534528041361,
127.757909937084));
#211060=CARTESIAN_POINT('Ctrl Pts',(-222.964350553099,-5.9712583781396,
134.462545172141));
#211061=CARTESIAN_POINT('Ctrl Pts',(-223.242798176912,-0.14987673854478,
137.805487513793));
#211062=CARTESIAN_POINT('Ctrl Pts',(-223.521245800725,5.80923430188729,
134.714736261875));
#211063=CARTESIAN_POINT('Ctrl Pts',(-223.799693424538,6.42994281575757,
128.030540825308));
#211064=CARTESIAN_POINT('Ctrl Pts',(-224.078141048351,1.1418480021166,123.895350269195));
#211065=CARTESIAN_POINT('Ctrl Pts',(-224.356588672164,-5.19554934309376,
126.109202699315));
#211066=CARTESIAN_POINT('Ctrl Pts',(-224.635036295977,-6.75849065869668,
132.637675885092));
#211067=CARTESIAN_POINT('Ctrl Pts',(-224.913483919789,-2.11070922958169,
137.481421902441));
#211068=CARTESIAN_POINT('Ctrl Pts',(-225.191931543603,4.47671086764076,
136.189274791569));
#211069=CARTESIAN_POINT('Ctrl Pts',(-225.470379167415,6.95025237698553,
129.948654622468));
#211070=CARTESIAN_POINT('Ctrl Pts',(-225.748826791228,3.03685149058481,
124.494386459301));
#211071=CARTESIAN_POINT('Ctrl Pts',(-226.027274415041,-3.66726755721984,
124.838676288203));
#211072=CARTESIAN_POINT('Ctrl Pts',(-226.305722038854,-7.00134687591997,
130.665138575908));
#211073=CARTESIAN_POINT('Ctrl Pts',(-226.584169662667,-3.9015304504591,
136.619539118521));
#211074=CARTESIAN_POINT('Ctrl Pts',(-226.86261728648,2.78360185861461,137.230074706019));
#211075=CARTESIAN_POINT('Ctrl Pts',(-227.141064910293,6.91074004613266,
131.935692959814));
#211076=CARTESIAN_POINT('Ctrl Pts',(-227.419512534106,4.68724573967455,
125.601672059739));
#211077=CARTESIAN_POINT('Ctrl Pts',(-227.697960157918,-1.8435984168596,
124.048667778841));
#211078=CARTESIAN_POINT('Ctrl Pts',(-227.976407781732,-6.68026569308986,
128.703815182788));
#211079=CARTESIAN_POINT('Ctrl Pts',(-228.254855405544,-5.37809514649209,
135.289261223946));
#211080=CARTESIAN_POINT('Ctrl Pts',(-228.533303029357,0.86628210517778,
137.753302707416));
#211081=CARTESIAN_POINT('Ctrl Pts',(-228.81175065317,6.31458842242258,133.831605885006));
#211082=CARTESIAN_POINT('Ctrl Pts',(-229.090198276983,5.96009646425557,
127.128018550972));
#211083=CARTESIAN_POINT('Ctrl Pts',(-229.368645900796,0.128567022336676,
123.802809976843));
#211084=CARTESIAN_POINT('Ctrl Pts',(-229.647093524609,-5.82110923226107,
126.911684396774));
#211085=CARTESIAN_POINT('Ctrl Pts',(-229.925541148421,-6.42147047940683,
133.597738095807));
#211086=CARTESIAN_POINT('Ctrl Pts',(-230.203988772235,-1.12081406224988,
137.716814356412));
#211087=CARTESIAN_POINT('Ctrl Pts',(-230.482436396047,5.20981572330331,
135.483683323156));
#211088=CARTESIAN_POINT('Ctrl Pts',(-230.76088401986,6.75287937278817,128.950483321085));
#211089=CARTESIAN_POINT('Ctrl Pts',(-231.039331643673,2.0903767751783,124.120905987538));
#211090=CARTESIAN_POINT('Ctrl Pts',(-231.317779267486,-4.49307995823781,
125.433096954076));
#211091=CARTESIAN_POINT('Ctrl Pts',(-231.596226891299,-6.94761570919197,
131.681216826544));
#211092=CARTESIAN_POINT('Ctrl Pts',(-231.874674515112,-3.01763203329532,
137.123548679767));
#211093=CARTESIAN_POINT('Ctrl Pts',(-232.153122138925,3.68540806167951,
136.758855413326));
#211094=CARTESIAN_POINT('Ctrl Pts',(-232.431569762738,7.00173819016367,
130.922272322824));
#211095=CARTESIAN_POINT('Ctrl Pts',(-232.71001738655,3.88381297581431,124.977334135496));
#211096=CARTESIAN_POINT('Ctrl Pts',(-232.988465010364,-2.80314662849731,
124.38714861912));
#211097=CARTESIAN_POINT('Ctrl Pts',(-233.266912634176,-6.914151422545,129.694067431082));
#211098=CARTESIAN_POINT('Ctrl Pts',(-233.545360257989,-4.67138883434919,
136.021291440583));
#211099=CARTESIAN_POINT('Ctrl Pts',(-233.823807881803,1.86415188258208,
137.554410884971));
#211100=CARTESIAN_POINT('Ctrl Pts',(-234.102255505615,6.68662808830262,
132.884563891901));
#211101=CARTESIAN_POINT('Ctrl Pts',(-234.380703129428,5.36441974081549,
126.303111713297));
#211102=CARTESIAN_POINT('Ctrl Pts',(-234.659150753241,-0.887428282007554,
123.858087379481));
#211103=CARTESIAN_POINT('Ctrl Pts',(-234.937598377053,-6.32377306694735,
127.796348807152));
#211104=CARTESIAN_POINT('Ctrl Pts',(-235.216046000867,-5.94887933685163,
134.498826139047));
#211105=CARTESIAN_POINT('Ctrl Pts',(-235.494493624679,-0.107256115101469,
137.806270141374));
#211106=CARTESIAN_POINT('Ctrl Pts',(-235.772941248493,5.83293023667497,
134.679301353618));
#211107=CARTESIAN_POINT('Ctrl Pts',(-236.051388872305,6.41293865542997,
127.991451330808));
#211108=CARTESIAN_POINT('Ctrl Pts',(-236.329836496118,1.09976973931543,
123.88852752427));
#211109=CARTESIAN_POINT('Ctrl Pts',(-236.608284119931,-5.22403384049169,
126.140916473241));
#211110=CARTESIAN_POINT('Ctrl Pts',(-236.886731743744,-6.7472055291277,
132.678782768935));
#211111=CARTESIAN_POINT('Ctrl Pts',(-237.165179367557,-2.07002495581049,
137.494146678133));
#211112=CARTESIAN_POINT('Ctrl Pts',(-237.44362699137,4.50940742555574,136.161924011888));
#211113=CARTESIAN_POINT('Ctrl Pts',(-237.722074615182,6.94491467963605,
129.906362317783));
#211114=CARTESIAN_POINT('Ctrl Pts',(-238.000522238996,2.99838462107406,
124.476017191522));
#211115=CARTESIAN_POINT('Ctrl Pts',(-238.278969862808,-3.70351442502255,
124.861110517033));
#211116=CARTESIAN_POINT('Ctrl Pts',(-238.557417486622,-7.00206464126185,
130.707760341024));
#211117=CARTESIAN_POINT('Ctrl Pts',(-238.835865110434,-3.86605952205578,
136.64318109997));
#211118=CARTESIAN_POINT('Ctrl Pts',(-239.114312734247,2.82266543041169,
137.213011077826));
#211119=CARTESIAN_POINT('Ctrl Pts',(-239.39276035806,6.91749874720356,131.893604362681));
#211120=CARTESIAN_POINT('Ctrl Pts',(-239.671207981873,4.655488653916,125.573235858291));
#211121=CARTESIAN_POINT('Ctrl Pts',(-239.949655605686,-1.88468807905538,
124.060015453022));
#211122=CARTESIAN_POINT('Ctrl Pts',(-240.228103229498,-6.69292853950653,
128.74451877439));
#211123=CARTESIAN_POINT('Ctrl Pts',(-240.506550853312,-5.35069463988719,
135.321916120768));
#211124=CARTESIAN_POINT('Ctrl Pts',(-240.784998477124,0.908566237823527,
137.747900654559));
#211125=CARTESIAN_POINT('Ctrl Pts',(-241.063446100938,6.33289912890243,
133.79311110514));
#211126=CARTESIAN_POINT('Ctrl Pts',(-241.34189372475,5.9376070998423,127.091805866219));
#211127=CARTESIAN_POINT('Ctrl Pts',(-241.620341348563,0.0859442142595387,
123.802157075403));
#211128=CARTESIAN_POINT('Ctrl Pts',(-241.898788972376,-5.84469720561911,
126.947191263173));
#211129=CARTESIAN_POINT('Ctrl Pts',(-242.177236596189,-6.40434742286629,
133.636775654432));
#211130=CARTESIAN_POINT('Ctrl Pts',(-242.455684220002,-1.07871522826414,
137.723508997977));
#211131=CARTESIAN_POINT('Ctrl Pts',(-242.734131843815,5.23820356294377,
135.451882999115));
#211132=CARTESIAN_POINT('Ctrl Pts',(-243.012579467628,6.74146918027728,
128.909410975699));
#211133=CARTESIAN_POINT('Ctrl Pts',(-243.29102709144,2.04965396001378,124.108305099723));
#211134=CARTESIAN_POINT('Ctrl Pts',(-243.569474715254,-4.52569311833944,
125.460547124147));
#211135=CARTESIAN_POINT('Ctrl Pts',(-243.847922339066,-6.94214931333881,
131.72349268922));
#211136=CARTESIAN_POINT('Ctrl Pts',(-244.12636996288,-2.9791094322281,137.141800782542));
#211137=CARTESIAN_POINT('Ctrl Pts',(-244.404817586691,3.72158647951367,
136.736310965414));
#211138=CARTESIAN_POINT('Ctrl Pts',(-244.683265210505,7.00232622618917,
130.879648570499));
#211139=CARTESIAN_POINT('Ctrl Pts',(-244.961712834317,3.84827025365086,
124.953800224859));
#211140=CARTESIAN_POINT('Ctrl Pts',(-245.240160458131,-2.84215808354001,
124.404331064352));
#211141=CARTESIAN_POINT('Ctrl Pts',(-245.518608081943,-6.92078198909823,
129.736176404423));
#211142=CARTESIAN_POINT('Ctrl Pts',(-245.797055705757,-4.63954534567172,
136.049630852671));
#211143=CARTESIAN_POINT('Ctrl Pts',(-246.075503329569,1.90520681603656,
137.542938200555));
#211144=CARTESIAN_POINT('Ctrl Pts',(-246.353950953382,6.69916698833444,
132.843821947487));
#211145=CARTESIAN_POINT('Ctrl Pts',(-246.632398577195,5.33691997085474,
126.270540365447));
#211146=CARTESIAN_POINT('Ctrl Pts',(-246.910846201008,-0.929695776805409,
123.86361810567));
#211147=CARTESIAN_POINT('Ctrl Pts',(-247.189293824821,-6.34196652374499,
127.834899140205));
#211148=CARTESIAN_POINT('Ctrl Pts',(-247.467741448634,-5.9262798576518,
134.534970206175));
#211149=CARTESIAN_POINT('Ctrl Pts',(-247.746189072447,-0.0646315172428821,
137.806793310625));
#211150=CARTESIAN_POINT('Ctrl Pts',(-248.024636696259,5.85641003008765,
134.643722858007));
#211151=CARTESIAN_POINT('Ctrl Pts',(-248.303084320073,6.39569686130214,
127.952466069697));
#211152=CARTESIAN_POINT('Ctrl Pts',(-248.581531943885,1.05765072414216,
123.881961048084));
#211153=CARTESIAN_POINT('Ctrl Pts',(-248.859979567699,-5.25232475939459,
126.172803052805));
#211154=CARTESIAN_POINT('Ctrl Pts',(-249.138427191511,-6.73567037937639,
132.719820195375));
#211155=CARTESIAN_POINT('Ctrl Pts',(-249.416874815324,-2.02926397650361,
137.506623561341));
#211156=CARTESIAN_POINT('Ctrl Pts',(-249.695322439137,4.54193688572079,
136.134374705723));
#211157=CARTESIAN_POINT('Ctrl Pts',(-249.97377006295,6.93931963591783,129.864103288757));
#211158=CARTESIAN_POINT('Ctrl Pts',(-250.252217686763,2.95980664532115,
124.457882422832));
#211159=CARTESIAN_POINT('Ctrl Pts',(-250.530665310576,-3.73962405773988,
124.883764975191));
#211160=CARTESIAN_POINT('Ctrl Pts',(-250.809112934388,-7.00252294251614,
130.750385685678));
#211161=CARTESIAN_POINT('Ctrl Pts',(-251.087560558202,-3.83044533540895,
136.666606721818));
#211162=CARTESIAN_POINT('Ctrl Pts',(-251.366008182014,2.86162440732935,
137.195709974661));
#211163=CARTESIAN_POINT('Ctrl Pts',(-251.644455805827,6.9240011177651,131.851475403357));
#211164=CARTESIAN_POINT('Ctrl Pts',(-251.92290342964,4.62355905740654,125.54499349784));
#211165=CARTESIAN_POINT('Ctrl Pts',(-252.201351053453,-1.92570790361727,
124.071613041873));
#211166=CARTESIAN_POINT('Ctrl Pts',(-252.479798677266,-6.70534337666252,
128.785298693283));
#211167=CARTESIAN_POINT('Ctrl Pts',(-252.758246301079,-5.3230958619522,
135.354403619622));
#211168=CARTESIAN_POINT('Ctrl Pts',(-253.036693924892,0.950816704398073,
137.74224130304));
#211169=CARTESIAN_POINT('Ctrl Pts',(-253.315141548704,6.35097516523885,
133.754505582129));
#211170=CARTESIAN_POINT('Ctrl Pts',(-253.593589172518,5.91489771943887,
127.055730740027));
#211171=CARTESIAN_POINT('Ctrl Pts',(-253.87203679633,0.0433182135112656,
123.801763664947));
#211172=CARTESIAN_POINT('Ctrl Pts',(-254.150484420143,-5.86806858651122,
126.982841017323));
#211173=CARTESIAN_POINT('Ctrl Pts',(-254.428932043956,-6.38698707931617,
133.675708334441));
#211174=CARTESIAN_POINT('Ctrl Pts',(-254.707379667769,-1.03657636838919,
137.729947101491));
#211175=CARTESIAN_POINT('Ctrl Pts',(-254.985827291582,5.26639719763008,
135.41991073597));
#211176=CARTESIAN_POINT('Ctrl Pts',(-255.264274915395,6.72980937160111,
128.868408326187));
#211177=CARTESIAN_POINT('Ctrl Pts',(-255.542722539208,2.00885483266244,
124.095953322692));
#211178=CARTESIAN_POINT('Ctrl Pts',(-255.821170163021,-4.5581378946222,
125.488193449449));
#211179=CARTESIAN_POINT('Ctrl Pts',(-256.099617786833,-6.93642696247006,
131.765738008466));
#211180=CARTESIAN_POINT('Ctrl Pts',(-256.378065410647,-2.94047400549736,
137.159811411449));
#211181=CARTESIAN_POINT('Ctrl Pts',(-256.656513034459,3.7576223973322,136.713559240208));
#211182=CARTESIAN_POINT('Ctrl Pts',(-256.934960658272,7.0026634652268,130.836998362911));
#211183=CARTESIAN_POINT('Ctrl Pts',(-257.213408282085,3.81256854888166,
124.930527794066));
#211184=CARTESIAN_POINT('Ctrl Pts',(-257.491855905898,-2.88103328591622,
124.421666290213));
#211185=CARTESIAN_POINT('Ctrl Pts',(-257.770303529711,-6.92721451599304,
129.778484277494));
#211186=CARTESIAN_POINT('Ctrl Pts',(-258.048751153524,-4.60741964202412,
136.077475067175));
#211187=CARTESIAN_POINT('Ctrl Pts',(-258.327198777336,1.94598288966397,
137.53178391186));
#211188=CARTESIAN_POINT('Ctrl Pts',(-258.60564640115,6.71185090883407,132.801931226644));
#211189=CARTESIAN_POINT('Ctrl Pts',(-258.884094024962,5.30847971878909,
126.240167716581));
#211190=CARTESIAN_POINT('Ctrl Pts',(-259.162541648776,-0.970525071554103,
123.86553674091));
#211191=CARTESIAN_POINT('Ctrl Pts',(-259.440989272588,-6.36258613651914,
127.881151058581));
#211192=CARTESIAN_POINT('Ctrl Pts',(-259.673028959099,-5.97575359986218,
133.442106215535));
#211193=CARTESIAN_POINT('Ctrl Pts',(-259.858689921174,-2.9628379271774,
136.206922793942));
#211194=CARTESIAN_POINT('Ctrl Pts',(-259.951535008647,-1.00384119663989,
136.721969923993));
#211195=CARTESIAN_POINT('Ctrl Pts',(-259.997972158816,-0.016740685831905,
136.724751058381));
#211196=CARTESIAN_POINT('Ctrl Pts',(210.384788400103,3.2437100417032,135.350446923363));
#211197=CARTESIAN_POINT('Ctrl Pts',(210.338370536501,4.00135710969089,134.809856772425));
#211198=CARTESIAN_POINT('Ctrl Pts',(210.245544735596,5.2274450014198,133.344996311945));
#211199=CARTESIAN_POINT('Ctrl Pts',(210.059903060087,6.03752477204218,129.574087134129));
#211200=CARTESIAN_POINT('Ctrl Pts',(209.827863373576,3.30140998082846,125.08375145776));
#211201=CARTESIAN_POINT('Ctrl Pts',(209.549415749763,-3.03864792542705,
124.935284604053));
#211202=CARTESIAN_POINT('Ctrl Pts',(209.27096812595,-6.57501826603042,130.18815040753));
#211203=CARTESIAN_POINT('Ctrl Pts',(208.992520502138,-4.0751627655632,136.003208990552));
#211204=CARTESIAN_POINT('Ctrl Pts',(208.714072878324,2.17267791003586,137.042921783734));
#211205=CARTESIAN_POINT('Ctrl Pts',(208.435625254512,6.42228832295553,132.348569225854));
#211206=CARTESIAN_POINT('Ctrl Pts',(208.157177630698,4.77100074356668,126.235763887068));
#211207=CARTESIAN_POINT('Ctrl Pts',(207.878730006886,-1.26506482749479,
124.320958291314));
#211208=CARTESIAN_POINT('Ctrl Pts',(207.600282383073,-6.13835327551471,
128.364250828182));
#211209=CARTESIAN_POINT('Ctrl Pts',(207.32183475926,-5.37092434612766,134.649796015418));
#211210=CARTESIAN_POINT('Ctrl Pts',(207.043387135447,0.332190207827403,
137.40162108792));
#211211=CARTESIAN_POINT('Ctrl Pts',(206.764939511634,5.73000189292936,134.090861108297));
#211212=CARTESIAN_POINT('Ctrl Pts',(206.486491887821,5.86224098722307,127.759980958474));
#211213=CARTESIAN_POINT('Ctrl Pts',(206.208044264008,0.607356820266201,
124.226729984437));
#211214=CARTESIAN_POINT('Ctrl Pts',(205.929596640195,-5.20565320191231,
126.738003936844));
#211215=CARTESIAN_POINT('Ctrl Pts',(205.651149016382,-6.23492509722864,
132.986059061584));
#211216=CARTESIAN_POINT('Ctrl Pts',(205.37270139257,-1.53460390898592,137.229240938669));
#211217=CARTESIAN_POINT('Ctrl Pts',(205.094253768756,4.57594250116295,135.568271122458));
#211218=CARTESIAN_POINT('Ctrl Pts',(204.815806144944,6.48142172411287,129.529500574057));
#211219=CARTESIAN_POINT('Ctrl Pts',(204.537358521131,2.43079079302514,124.662263970705));
#211220=CARTESIAN_POINT('Ctrl Pts',(204.258910897318,-3.85361800715474,
125.439314209572));
#211221=CARTESIAN_POINT('Ctrl Pts',(203.980463273505,-6.5967401814699,131.146579956944));
#211222=CARTESIAN_POINT('Ctrl Pts',(203.702015649692,-3.27778036432047,
136.539362872731));
#211223=CARTESIAN_POINT('Ctrl Pts',(203.42356802588,3.05329946149495,136.661958874297));
#211224=CARTESIAN_POINT('Ctrl Pts',(203.145120402066,6.5785462535266,131.40170824395));
#211225=CARTESIAN_POINT('Ctrl Pts',(202.866672778254,4.05843041346184,125.592524323598));
#211226=CARTESIAN_POINT('Ctrl Pts',(202.58822515444,-2.19118470860141,124.572763346851));
#211227=CARTESIAN_POINT('Ctrl Pts',(202.309777530628,-6.42720813017419,
129.279535830482));
#211228=CARTESIAN_POINT('Ctrl Pts',(202.031329906815,-4.75694126595338,
135.387547802118));
#211229=CARTESIAN_POINT('Ctrl Pts',(201.752882283002,1.28472223178851,137.283834652022));
#211230=CARTESIAN_POINT('Ctrl Pts',(201.474434659189,6.14578876089344,133.225801404307));
#211231=CARTESIAN_POINT('Ctrl Pts',(201.195987035376,5.35917565710019,126.94258236746));
#211232=CARTESIAN_POINT('Ctrl Pts',(200.917539411563,-0.352258065224466,
124.208148884143));
#211233=CARTESIAN_POINT('Ctrl Pts',(200.63909178775,-5.73998383440169,127.535311740963));
#211234=CARTESIAN_POINT('Ctrl Pts',(200.360644163938,-5.85294487354697,
133.866570813476));
#211235=CARTESIAN_POINT('Ctrl Pts',(200.082196540124,-0.587335506164227,
137.383808313225));
#211236=CARTESIAN_POINT('Ctrl Pts',(199.803748916312,5.2180064984534,134.854854804556));
#211237=CARTESIAN_POINT('Ctrl Pts',(199.525301292498,6.22825544477889,128.603695015683));
#211238=CARTESIAN_POINT('Ctrl Pts',(199.246853668687,1.51504190454761,124.374839406449));
#211239=CARTESIAN_POINT('Ctrl Pts',(198.968406044873,-4.5904211320519,126.054399690658));
#211240=CARTESIAN_POINT('Ctrl Pts',(198.689958421061,-6.47751140283473,
132.098942018204));
#211241=CARTESIAN_POINT('Ctrl Pts',(198.411510797247,-2.41208513843682,
136.95382728238));
#211242=CARTESIAN_POINT('Ctrl Pts',(198.133063173434,3.86992953127461,136.15765309974));
#211243=CARTESIAN_POINT('Ctrl Pts',(197.854615549622,6.59566801831256,130.442064648858));
#211244=CARTESIAN_POINT('Ctrl Pts',(197.576167925809,3.26030981281707,125.059408494076));
#211245=CARTESIAN_POINT('Ctrl Pts',(197.297720301996,-3.07111383566833,
124.956082684267));
#211246=CARTESIAN_POINT('Ctrl Pts',(197.019272678183,-6.58033390142619,
130.227038590899));
#211247=CARTESIAN_POINT('Ctrl Pts',(196.74082505437,-4.04254857895594,136.028525236289));
#211248=CARTESIAN_POINT('Ctrl Pts',(196.462377430557,2.21014139809766,137.029259811701));
#211249=CARTESIAN_POINT('Ctrl Pts',(196.183929806745,6.43181940170927,132.309616130935));
#211250=CARTESIAN_POINT('Ctrl Pts',(195.905482182931,4.74296958699597,126.206716169203));
#211251=CARTESIAN_POINT('Ctrl Pts',(195.627034559119,-1.30443757122094,
124.328826848098));
#211252=CARTESIAN_POINT('Ctrl Pts',(195.348586935305,-6.15313032680387,
128.401636713722));
#211253=CARTESIAN_POINT('Ctrl Pts',(195.070139311493,-5.34739690918169,
134.682432467391));
#211254=CARTESIAN_POINT('Ctrl Pts',(194.791691687679,0.372333033116476,
137.399469645412));
#211255=CARTESIAN_POINT('Ctrl Pts',(194.513244063867,5.74990710746052,134.055923815831));
#211256=CARTESIAN_POINT('Ctrl Pts',(194.234796440054,5.84359744862664,127.724350254736));
#211257=CARTESIAN_POINT('Ctrl Pts',(193.956348816241,0.567307210110782,
124.223155750211));
#211258=CARTESIAN_POINT('Ctrl Pts',(193.677901192428,-5.23031063999889,
126.769767009054));
#211259=CARTESIAN_POINT('Ctrl Pts',(193.399453568615,-6.22152852682933,
133.023972693263));
#211260=CARTESIAN_POINT('Ctrl Pts',(193.121005944802,-1.49546563606909,
137.238463313985));
#211261=CARTESIAN_POINT('Ctrl Pts',(192.84255832099,4.60485711668079,135.540327880088));
#211262=CARTESIAN_POINT('Ctrl Pts',(192.564110697177,6.47354113897745,129.490069896797));
#211263=CARTESIAN_POINT('Ctrl Pts',(192.285663073364,2.39335710461987,124.64758087922));
#211264=CARTESIAN_POINT('Ctrl Pts',(192.007215449551,-3.88620518688872,
125.462871665772));
#211265=CARTESIAN_POINT('Ctrl Pts',(191.728767825738,-6.59453476332446,
131.18672985278));
#211266=CARTESIAN_POINT('Ctrl Pts',(191.450320201925,-3.24280905319821,
136.559209392401));
#211267=CARTESIAN_POINT('Ctrl Pts',(191.171872578112,3.08889975678785,136.643264047941));
#211268=CARTESIAN_POINT('Ctrl Pts',(190.893424954299,6.58206059142805,131.361651697256));
#211269=CARTESIAN_POINT('Ctrl Pts',(190.614977330486,4.02662929408197,125.567916069518));
#211270=CARTESIAN_POINT('Ctrl Pts',(190.336529706674,-2.22907761274862,
124.586217166899));
#211271=CARTESIAN_POINT('Ctrl Pts',(190.05808208286,-6.43637108995848,129.318688322246));
#211272=CARTESIAN_POINT('Ctrl Pts',(189.779634459048,-4.72895396970476,
135.416419737866));
#211273=CARTESIAN_POINT('Ctrl Pts',(189.501186835235,1.32414082646293,137.275894133543));
#211274=CARTESIAN_POINT('Ctrl Pts',(189.222739211422,6.16041489098677,133.188345380025));
#211275=CARTESIAN_POINT('Ctrl Pts',(188.944291587609,5.33556862369218,126.910031093937));
#211276=CARTESIAN_POINT('Ctrl Pts',(188.665843963796,-0.392404551757433,
124.210415391489));
#211277=CARTESIAN_POINT('Ctrl Pts',(188.387396339983,-5.75977711417006,
127.570313219673));
#211278=CARTESIAN_POINT('Ctrl Pts',(188.10894871617,-5.83419588941534,133.902142614521));
#211279=CARTESIAN_POINT('Ctrl Pts',(187.830501092358,-0.547273658602122,
137.387261689231));
#211280=CARTESIAN_POINT('Ctrl Pts',(187.552053468544,5.24256632866185,134.823016271676));
#211281=CARTESIAN_POINT('Ctrl Pts',(187.273605844732,6.214743973489,128.565822630237));
#211282=CARTESIAN_POINT('Ctrl Pts',(186.995158220918,1.47587551380139,124.365736040492));
#211283=CARTESIAN_POINT('Ctrl Pts',(186.716710597106,-4.61925044254253,
126.082430892781));
#211284=CARTESIAN_POINT('Ctrl Pts',(186.438262973293,-6.46951090511933,
132.138348483055));
#211285=CARTESIAN_POINT('Ctrl Pts',(186.15981534948,-2.37460689906969,136.968396393875));
#211286=CARTESIAN_POINT('Ctrl Pts',(185.881367725667,3.90244484122886,136.133996556155));
#211287=CARTESIAN_POINT('Ctrl Pts',(185.602920101854,6.59334041746713,130.401921658061));
#211288=CARTESIAN_POINT('Ctrl Pts',(185.324472478041,3.22527825263932,125.039668503516));
#211289=CARTESIAN_POINT('Ctrl Pts',(185.046024854228,-3.10665706276191,
124.974885780916));
#211290=CARTESIAN_POINT('Ctrl Pts',(184.767577230416,-6.5837263061198,130.26710564752));
#211291=CARTESIAN_POINT('Ctrl Pts',(184.489129606603,-4.01067270706429,
136.05303658523));
#211292=CARTESIAN_POINT('Ctrl Pts',(184.21068198279,2.247993177529,137.015690720733));
#211293=CARTESIAN_POINT('Ctrl Pts',(183.932234358977,6.44086315254518,132.270435931769));
#211294=CARTESIAN_POINT('Ctrl Pts',(183.653786735164,4.71489454403,126.177929550814));
#211295=CARTESIAN_POINT('Ctrl Pts',(183.375339111351,-1.34383181504516,
124.33688730648));
#211296=CARTESIAN_POINT('Ctrl Pts',(183.096891487538,-6.16764238592767,
128.439137081397));
#211297=CARTESIAN_POINT('Ctrl Pts',(182.818443863726,-5.32369091022383,
134.71491173846));
#211298=CARTESIAN_POINT('Ctrl Pts',(182.539996239912,0.412472435216218,
137.397080956463));
#211299=CARTESIAN_POINT('Ctrl Pts',(182.2615486161,5.76959376309122,134.020862255314));
#211300=CARTESIAN_POINT('Ctrl Pts',(181.983100992287,5.82474028301032,127.688835683913));
#211301=CARTESIAN_POINT('Ctrl Pts',(181.704653368474,0.527235037225083,
124.219824324685));
#211302=CARTESIAN_POINT('Ctrl Pts',(181.426205744661,-5.25477345090652,
126.801680146133));
#211303=CARTESIAN_POINT('Ctrl Pts',(181.147758120848,-6.20790184760947,
133.061803779016));
#211304=CARTESIAN_POINT('Ctrl Pts',(180.869310497035,-1.45627171922457,
137.247447428754));
#211305=CARTESIAN_POINT('Ctrl Pts',(180.590862873222,4.63360097629919,135.5122090613));
#211306=CARTESIAN_POINT('Ctrl Pts',(180.31241524941,6.46542073859599,129.450687965235));
#211307=CARTESIAN_POINT('Ctrl Pts',(180.033967625596,2.35583469548556,124.633125906077));
#211308=CARTESIAN_POINT('Ctrl Pts',(179.755520001784,-3.91864834385308,
125.4866270652));
#211309=CARTESIAN_POINT('Ctrl Pts',(179.477072377971,-6.59208499180493,
131.226865573221));
#211310=CARTESIAN_POINT('Ctrl Pts',(179.198624754158,-3.20771757354326,
136.578842667508));
#211311=CARTESIAN_POINT('Ctrl Pts',(178.920177130345,3.12438558908937,136.62435285703));
#211312=CARTESIAN_POINT('Ctrl Pts',(178.641729506532,6.58533103007041,131.32157450091));
#211313=CARTESIAN_POINT('Ctrl Pts',(178.363281882719,3.99467896572256,125.5435018533));
#211314=CARTESIAN_POINT('Ctrl Pts',(178.084834258906,-2.26688791720775,
124.599901402811));
#211315=CARTESIAN_POINT('Ctrl Pts',(177.806386635093,-6.44529554785546,
129.357895865998));
#211316=CARTESIAN_POINT('Ctrl Pts',(177.527939011281,-4.70079144021631,
135.445120772143));
#211317=CARTESIAN_POINT('Ctrl Pts',(177.249491387467,1.36351035455298,137.26771380997));
#211318=CARTESIAN_POINT('Ctrl Pts',(176.971043763655,6.17481274467203,133.150801016333));
#211319=CARTESIAN_POINT('Ctrl Pts',(176.692596139842,5.31176387881016,126.877624126216));
#211320=CARTESIAN_POINT('Ctrl Pts',(176.414148516029,-0.432536497586617,
124.212926239906));
#211321=CARTESIAN_POINT('Ctrl Pts',(176.135700892216,-5.77935696328393,
127.605434537195));
#211322=CARTESIAN_POINT('Ctrl Pts',(175.857253268403,-5.81523071700703,
133.937599626117));
#211323=CARTESIAN_POINT('Ctrl Pts',(175.57880564459,-0.50719153161477,137.390471133416));
#211324=CARTESIAN_POINT('Ctrl Pts',(175.300358020777,5.2669318936477,134.791028826034));
#211325=CARTESIAN_POINT('Ctrl Pts',(175.021910396965,6.20100221257536,128.528033194638));
#211326=CARTESIAN_POINT('Ctrl Pts',(174.743462773151,1.43665443394553,124.356871260137));
#211327=CARTESIAN_POINT('Ctrl Pts',(174.465015149339,-4.64790858500931,
126.110637067746));
#211328=CARTESIAN_POINT('Ctrl Pts',(174.186567525525,-6.46127067729819,
132.177705516496));
#211329=CARTESIAN_POINT('Ctrl Pts',(173.908119901713,-2.33704066777073,
136.982737094758));
#211330=CARTESIAN_POINT('Ctrl Pts',(173.6296722779,3.93481554465429,136.11014252095));
#211331=CARTESIAN_POINT('Ctrl Pts',(173.351224654087,6.59076849796787,130.361793579788));
#211332=CARTESIAN_POINT('Ctrl Pts',(173.072777030274,3.1901271785899,125.020142125741));
#211333=CARTESIAN_POINT('Ctrl Pts',(172.794329406461,-3.14208517153551,
124.993904890899));
#211334=CARTESIAN_POINT('Ctrl Pts',(172.515881782648,-6.58687474841394,
130.30719261232));
#211335=CARTESIAN_POINT('Ctrl Pts',(172.237434158836,-3.97864821822065,
136.077353442554));
#211336=CARTESIAN_POINT('Ctrl Pts',(171.958986535022,2.28576165674636,137.001891466644));
#211337=CARTESIAN_POINT('Ctrl Pts',(171.68053891121,6.44966823482829,132.231201406644));
#211338=CARTESIAN_POINT('Ctrl Pts',(171.402091287397,4.68664478891289,126.149314366529));
#211339=CARTESIAN_POINT('Ctrl Pts',(171.123643663584,-1.38317626268716,
124.345187419464));
#211340=CARTESIAN_POINT('Ctrl Pts',(170.845196039771,-6.18192590079466,
128.476725093301));
#211341=CARTESIAN_POINT('Ctrl Pts',(170.566748415958,-5.29978763994156,
134.747246102621));
#211342=CARTESIAN_POINT('Ctrl Pts',(170.288300792145,0.452596552998033,
137.394447971839));
#211343=CARTESIAN_POINT('Ctrl Pts',(170.009853168332,5.78906662430322,133.985681506144));
#211344=CARTESIAN_POINT('Ctrl Pts',(169.73140554452,5.80566727950083,127.653436560012));
#211345=CARTESIAN_POINT('Ctrl Pts',(169.452957920706,0.487143327451347,
124.216736891574));
#211346=CARTESIAN_POINT('Ctrl Pts',(169.174510296894,-5.27904154425138,
126.833741604011));
#211347=CARTESIAN_POINT('Ctrl Pts',(168.896062673081,-6.19404513230377,
133.099551214382));
#211348=CARTESIAN_POINT('Ctrl Pts',(168.617615049268,-1.41702383969606,
137.256192792574));
#211349=CARTESIAN_POINT('Ctrl Pts',(168.339167425455,4.66217313612931,135.483915791456));
#211350=CARTESIAN_POINT('Ctrl Pts',(168.060719801642,6.45706075967145,129.411356194513));
#211351=CARTESIAN_POINT('Ctrl Pts',(167.782272177829,2.3182249900303,124.618899610305));
#211352=CARTESIAN_POINT('Ctrl Pts',(167.503824554016,-3.95094629386185,
125.510579515201));
#211353=CARTESIAN_POINT('Ctrl Pts',(167.225376930203,-6.58939094815179,
131.266985637585));
#211354=CARTESIAN_POINT('Ctrl Pts',(166.946929306391,-3.1725072307341,136.59826196706));
#211355=CARTESIAN_POINT('Ctrl Pts',(166.668481682578,3.15975564613386,136.605226004165));
#211356=CARTESIAN_POINT('Ctrl Pts',(166.390034058765,6.58835744684964,131.281478139015));
#211357=CARTESIAN_POINT('Ctrl Pts',(166.111586434952,3.96258061306513,125.519282580138));
#211358=CARTESIAN_POINT('Ctrl Pts',(165.833138811139,-2.30461422130139,
124.613815547242));
#211359=CARTESIAN_POINT('Ctrl Pts',(165.554691187326,-6.45398117295568,
129.397157009033));
#211360=CARTESIAN_POINT('Ctrl Pts',(165.276243563513,-4.67245472117232,
135.473649841348));
#211361=CARTESIAN_POINT('Ctrl Pts',(164.9977959397,1.40282935726546,137.259293984466));
#211362=CARTESIAN_POINT('Ctrl Pts',(164.719348315888,6.18898178840028,133.11316970443));
#211363=CARTESIAN_POINT('Ctrl Pts',(164.440900692075,5.2877623045642,126.845362665158));
#211364=CARTESIAN_POINT('Ctrl Pts',(164.162453068262,-0.472652415616787,
124.215681336348));
#211365=CARTESIAN_POINT('Ctrl Pts',(163.884005444449,-5.79872265620017,
127.640674392099));
#211366=CARTESIAN_POINT('Ctrl Pts',(163.605557820636,-5.79605005908598,
133.97294053439));
#211367=CARTESIAN_POINT('Ctrl Pts',(163.327110196823,-0.467090610458611,
137.393436526853));
#211368=CARTESIAN_POINT('Ctrl Pts',(163.04866257301,5.29110229053537,134.758893652935));
#211369=CARTESIAN_POINT('Ctrl Pts',(162.770214949197,6.18703067124424,128.49032810919));
#211370=CARTESIAN_POINT('Ctrl Pts',(162.491767325384,1.39738011833125,124.34824539387));
#211371=CARTESIAN_POINT('Ctrl Pts',(162.213319701571,-4.67639449751423,
126.139017170363));
#211372=CARTESIAN_POINT('Ctrl Pts',(161.934872077759,-6.45279102471594,
132.217011660137));
#211373=CARTESIAN_POINT('Ctrl Pts',(161.656424453946,-2.29938783657033,
136.996848853628));
#211374=CARTESIAN_POINT('Ctrl Pts',(161.377976830133,3.96704044204275,136.086091878046));
#211375=CARTESIAN_POINT('Ctrl Pts',(161.09952920632,6.58795235511813,130.321681900999));
#211376=CARTESIAN_POINT('Ctrl Pts',(160.821081582507,3.15485789320466,125.000830084311));
#211377=CARTESIAN_POINT('Ctrl Pts',(160.542633958694,-3.17739684918762,
125.013139309456));
#211378=CARTESIAN_POINT('Ctrl Pts',(160.264186334881,-6.58977911164196,
130.347297999864));
#211379=CARTESIAN_POINT('Ctrl Pts',(159.985738711068,-3.94647629910411,
136.10147490719));
#211380=CARTESIAN_POINT('Ctrl Pts',(159.707291087255,2.32344543622502,136.98786256077));
#211381=CARTESIAN_POINT('Ctrl Pts',(159.428843463442,6.45823432228318,132.191914009409));
#211382=CARTESIAN_POINT('Ctrl Pts',(159.15039583963,4.65822136844951,126.120871676696));
#211383=CARTESIAN_POINT('Ctrl Pts',(158.871948215817,-1.42246945622416,
124.353726879487));
#211384=CARTESIAN_POINT('Ctrl Pts',(158.593500592004,-6.19598034212407,
128.514399356595));
#211385=CARTESIAN_POINT('Ctrl Pts',(158.315052968191,-5.2756879840792,134.779434361708));
#211386=CARTESIAN_POINT('Ctrl Pts',(158.036605344378,0.49270389964821,137.391570789103));
#211387=CARTESIAN_POINT('Ctrl Pts',(157.758157720565,5.80832496952254,133.950382871961));
#211388=CARTESIAN_POINT('Ctrl Pts',(157.479710096752,5.78637914485521,127.618154194761));
#211389=CARTESIAN_POINT('Ctrl Pts',(157.201262472939,0.447033566402335,
124.213893565282));
#211390=CARTESIAN_POINT('Ctrl Pts',(156.922814849126,-5.3031140207705,126.865950194636));
#211391=CARTESIAN_POINT('Ctrl Pts',(156.644367225313,-6.17995889437779,
133.137213600617));
#211392=CARTESIAN_POINT('Ctrl Pts',(156.365919601501,-1.37772345182797,
137.264699081378));
#211393=CARTESIAN_POINT('Ctrl Pts',(156.087471977688,4.69057253741941,135.455449118975));
#211394=CARTESIAN_POINT('Ctrl Pts',(155.809024353875,6.44846151198586,129.372076042081));
#211395=CARTESIAN_POINT('Ctrl Pts',(155.530576730062,2.28052938189546,124.604902519066));
#211396=CARTESIAN_POINT('Ctrl Pts',(155.252129106249,-3.98309784010292,
125.534728128207));
#211397=CARTESIAN_POINT('Ctrl Pts',(154.973681482436,-6.58645273219382,
131.307088559209));
#211398=CARTESIAN_POINT('Ctrl Pts',(154.695233858623,-3.13717932950269,
136.617466571466));
#211399=CARTESIAN_POINT('Ctrl Pts',(154.41678623481,3.19500861727094,136.585884198101));
#211400=CARTESIAN_POINT('Ctrl Pts',(154.138338610998,6.59113972962085,131.241364097354));
#211401=CARTESIAN_POINT('Ctrl Pts',(153.859890987185,3.93033542552574,125.495259147487));
#211402=CARTESIAN_POINT('Ctrl Pts',(153.581443363372,-2.3422551270676,124.627959084596));
#211403=CARTESIAN_POINT('Ctrl Pts',(153.302995739559,-6.46242764341012,
129.436470296516));
#211404=CARTESIAN_POINT('Ctrl Pts',(153.024548115746,-4.64394486260028,
135.502005888322));
#211405=CARTESIAN_POINT('Ctrl Pts',(152.746100491933,1.44209637762021,137.250634969033));
#211406=CARTESIAN_POINT('Ctrl Pts',(152.46765286812,6.20292149713234,133.075452838754));
#211407=CARTESIAN_POINT('Ctrl Pts',(152.189205244307,5.26356479034146,126.813247906226));
#211408=CARTESIAN_POINT('Ctrl Pts',(151.910757620494,-0.512750819337957,
124.218680578724));
#211409=CARTESIAN_POINT('Ctrl Pts',(151.632309996682,-5.8178734753159,127.676031478561));
#211410=CARTESIAN_POINT('Ctrl Pts',(151.353862372869,-5.77665462639848,
134.008164029768));
#211411=CARTESIAN_POINT('Ctrl Pts',(151.075414749056,-0.4269723810881,137.39615775966));
#211412=CARTESIAN_POINT('Ctrl Pts',(150.796967125243,5.31507662368183,134.72661194316));
#211413=CARTESIAN_POINT('Ctrl Pts',(150.51851950143,6.17282986721635,128.452708771068));
#211414=CARTESIAN_POINT('Ctrl Pts',(150.240071877617,1.35805402228283,124.339858761329));
#211415=CARTESIAN_POINT('Ctrl Pts',(149.961624253804,-4.70470712450132,
126.167570148998));
#211416=CARTESIAN_POINT('Ctrl Pts',(149.683176629991,-6.44407226158927,
132.256265457474));
#211417=CARTESIAN_POINT('Ctrl Pts',(149.404729006178,-2.26164980070799,
137.010731147569));
#211418=CARTESIAN_POINT('Ctrl Pts',(149.126281382365,3.99911833928874,136.061845518646));
#211419=CARTESIAN_POINT('Ctrl Pts',(148.847833758553,6.58489209327119,130.281588108047));
#211420=CARTESIAN_POINT('Ctrl Pts',(148.56938613474,3.11947170339994,124.981733094838));
#211421=CARTESIAN_POINT('Ctrl Pts',(148.290938510927,-3.21259078723097,
125.032588323847));
#211422=CARTESIAN_POINT('Ctrl Pts',(148.012490887114,-6.59243928818165,
130.387420324031));
#211423=CARTESIAN_POINT('Ctrl Pts',(147.734043263301,-3.91415814185689,
136.125400085308));
#211424=CARTESIAN_POINT('Ctrl Pts',(147.455595639488,2.36104311957866,136.973604522958));
#211425=CARTESIAN_POINT('Ctrl Pts',(147.177148015675,6.46656109749016,132.152575195872));
#211426=CARTESIAN_POINT('Ctrl Pts',(146.898700391862,4.6296253358803,126.092602535266));
#211427=CARTESIAN_POINT('Ctrl Pts',(146.62025276805,-1.46170993963237,124.362505370115));
#211428=CARTESIAN_POINT('Ctrl Pts',(146.341805144237,-6.20980518912327,
128.552158475246));
#211429=CARTESIAN_POINT('Ctrl Pts',(146.063357520424,-5.2513928356585,134.811475322978));
#211430=CARTESIAN_POINT('Ctrl Pts',(145.784909896611,0.532792988974217,
137.388449514872));
#211431=CARTESIAN_POINT('Ctrl Pts',(145.506462272798,5.82736808512415,133.914967660766));
#211432=CARTESIAN_POINT('Ctrl Pts',(145.228014648985,5.76687659380242,127.582989895561));
#211433=CARTESIAN_POINT('Ctrl Pts',(144.949567025172,0.406907240360106,
124.211294451169));
#211434=CARTESIAN_POINT('Ctrl Pts',(144.671119401359,-5.32698998844935,
126.898304724507));
#211435=CARTESIAN_POINT('Ctrl Pts',(144.392671777546,-6.16564365580234,
133.174789542127));
#211436=CARTESIAN_POINT('Ctrl Pts',(144.114224153734,-1.33837201191069,
137.272965979966));
#211437=CARTESIAN_POINT('Ctrl Pts',(143.83577652992,4.71879812781917,135.426810098699));
#211438=CARTESIAN_POINT('Ctrl Pts',(143.557328906108,6.43962331418753,129.332848963481));
#211439=CARTESIAN_POINT('Ctrl Pts',(143.278881282295,2.24274926790569,124.591135151027));
#211440=CARTESIAN_POINT('Ctrl Pts',(143.000433658482,-4.01510179118866,
125.559072009383));
#211441=CARTESIAN_POINT('Ctrl Pts',(142.721986034669,-6.58327045280769,
131.347172852065));
#211442=CARTESIAN_POINT('Ctrl Pts',(142.443538410856,-3.10173517893752,
136.636455769093));
#211443=CARTESIAN_POINT('Ctrl Pts',(142.165090787043,3.23014319618891,136.566328155556));
#211444=CARTESIAN_POINT('Ctrl Pts',(141.886643163231,6.5936777752854,131.201233862367));
#211445=CARTESIAN_POINT('Ctrl Pts',(141.608195539417,3.89794459796173,125.471432445543));
#211446=CARTESIAN_POINT('Ctrl Pts',(141.329747915605,-2.37980923970876,
124.642331490782));
#211447=CARTESIAN_POINT('Ctrl Pts',(141.051300291792,-6.47063464623165,
129.475834271677));
#211448=CARTESIAN_POINT('Ctrl Pts',(140.772852667979,-4.61526292094352,
135.530187862324));
#211449=CARTESIAN_POINT('Ctrl Pts',(140.494405044166,1.48130996056343,137.241737084533));
#211450=CARTESIAN_POINT('Ctrl Pts',(140.215957420353,6.21663135432719,133.037651816923));
#211451=CARTESIAN_POINT('Ctrl Pts',(139.93750979654,5.23917223278974,126.781281039444));
#211452=CARTESIAN_POINT('Ctrl Pts',(139.659062172727,-0.552830222889001,
124.221923855894));
#211453=CARTESIAN_POINT('Ctrl Pts',(139.380614548914,-5.83680871099059,
127.711504486408));
#211454=CARTESIAN_POINT('Ctrl Pts',(139.102166925101,-5.75704513764935,
134.043268807033));
#211455=CARTESIAN_POINT('Ctrl Pts',(138.823719301288,-0.386838330098996,
137.398634730999));
#211456=CARTESIAN_POINT('Ctrl Pts',(138.545271677476,5.33885400470937,134.694184892919));
#211457=CARTESIAN_POINT('Ctrl Pts',(138.266824053663,6.15840032670771,128.41517657427));
#211458=CARTESIAN_POINT('Ctrl Pts',(137.98837642985,1.31867760304303,124.331711673279));
#211459=CARTESIAN_POINT('Ctrl Pts',(137.709928806037,-4.7328454168358,126.196294945608));
#211460=CARTESIAN_POINT('Ctrl Pts',(137.431481182224,-6.43511471099507,
132.295465453942));
#211461=CARTESIAN_POINT('Ctrl Pts',(137.153033558411,-2.22382795858067,
137.024383462168));
#211462=CARTESIAN_POINT('Ctrl Pts',(136.874585934598,4.03104804773404,136.037404341212));
#211463=CARTESIAN_POINT('Ctrl Pts',(136.596138310785,6.5815878258261,130.241513686623));
#211464=CARTESIAN_POINT('Ctrl Pts',(136.317690686972,3.08396992042408,124.96285186497));
#211465=CARTESIAN_POINT('Ctrl Pts',(136.03924306316,-3.24766568154122,125.052251213384));
#211466=CARTESIAN_POINT('Ctrl Pts',(135.760795439346,-6.5948551794591,130.427558098075));
#211467=CARTESIAN_POINT('Ctrl Pts',(135.482347815534,-3.88169494404043,
136.149128090351));
#211468=CARTESIAN_POINT('Ctrl Pts',(135.203900191721,2.3985533136112,136.959117881544));
#211469=CARTESIAN_POINT('Ctrl Pts',(134.925452567908,6.47464825189767,132.113186423748));
#211470=CARTESIAN_POINT('Ctrl Pts',(134.647004944095,4.60085775084163,126.064507989766));
#211471=CARTESIAN_POINT('Ctrl Pts',(134.368557320282,-1.50089625884118,
124.371522566057));
#211472=CARTESIAN_POINT('Ctrl Pts',(134.090109696469,-6.22339992950755,
128.590001050074));
#211473=CARTESIAN_POINT('Ctrl Pts',(133.811662072656,-5.22690309494509,
134.843367799137));
#211474=CARTESIAN_POINT('Ctrl Pts',(133.533214448844,0.572862335460145,
137.385084264805));
#211475=CARTESIAN_POINT('Ctrl Pts',(133.25476682503,5.84619526545829,133.879437184883));
#211476=CARTESIAN_POINT('Ctrl Pts',(132.976319201218,5.7471603490167,127.547944965438));
#211477=CARTESIAN_POINT('Ctrl Pts',(132.697871577405,0.366765836220533,
124.208939645549));
#211478=CARTESIAN_POINT('Ctrl Pts',(132.419423953592,-5.35066856255522,
126.930803994717));
#211479=CARTESIAN_POINT('Ctrl Pts',(132.140976329779,-6.15109994703373,
133.212277646521));
#211480=CARTESIAN_POINT('Ctrl Pts',(131.862528705966,-1.29897097812634,
137.280993182001));
#211481=CARTESIAN_POINT('Ctrl Pts',(131.584081082153,4.74684886141891,135.397999791857));
#211482=CARTESIAN_POINT('Ctrl Pts',(131.30563345834,6.43054649377913,129.293676412286));
#211483=CARTESIAN_POINT('Ctrl Pts',(131.027185834528,2.20488604801711,124.577598016342));
#211484=CARTESIAN_POINT('Ctrl Pts',(130.748738210715,-4.04695696120101,
125.583610256657));
#211485=CARTESIAN_POINT('Ctrl Pts',(130.470290586902,-6.57984422791396,
131.387237030814));
#211486=CARTESIAN_POINT('Ctrl Pts',(130.191842963089,-3.06617609243459,
136.65522885629));
#211487=CARTESIAN_POINT('Ctrl Pts',(129.913395339276,3.26515808096253,136.546558601182));
#211488=CARTESIAN_POINT('Ctrl Pts',(129.634947715463,6.59597148979528,131.161088921098));
#211489=CARTESIAN_POINT('Ctrl Pts',(129.35650009165,3.86540933062731,125.447803357213));
#211490=CARTESIAN_POINT('Ctrl Pts',(129.078052467837,-2.41727516764341,
124.656932233223));
#211491=CARTESIAN_POINT('Ctrl Pts',(128.799604844024,-6.47860187730669,
129.515247475871));
#211492=CARTESIAN_POINT('Ctrl Pts',(128.521157220212,-4.58640995902212,
135.558194719059));
#211493=CARTESIAN_POINT('Ctrl Pts',(128.242709596398,1.52046865302106,137.232600660681));
#211494=CARTESIAN_POINT('Ctrl Pts',(127.964261972586,6.23011085196111,132.999768039666));
#211495=CARTESIAN_POINT('Ctrl Pts',(127.685814348773,5.2145855357842,126.749463249355));
#211496=CARTESIAN_POINT('Ctrl Pts',(127.40736672496,-0.592889141112855,
124.225411047681));
#211497=CARTESIAN_POINT('Ctrl Pts',(127.128919101147,-5.85552766157182,
127.747092101177));
#211498=CARTESIAN_POINT('Ctrl Pts',(126.850471477334,-5.7372223194756,134.078253565364));
#211499=CARTESIAN_POINT('Ctrl Pts',(126.572023853521,-0.346689944673359,
137.400867349086));
#211500=CARTESIAN_POINT('Ctrl Pts',(126.293576229708,5.36243355253846,134.66161370381));
#211501=CARTESIAN_POINT('Ctrl Pts',(126.015128605896,6.14374258441013,128.377732909565));
#211502=CARTESIAN_POINT('Ctrl Pts',(125.736680982083,1.27925231971985,124.323804431618));
#211503=CARTESIAN_POINT('Ctrl Pts',(125.45823335827,-4.76080833184274,126.225190495787));
#211504=CARTESIAN_POINT('Ctrl Pts',(125.179785734457,-6.42591870485886,
132.334610196974));
#211505=CARTESIAN_POINT('Ctrl Pts',(124.901338110644,-2.1859237116904,137.037805291532));
#211506=CARTESIAN_POINT('Ctrl Pts',(124.622890486831,4.06282838421153,136.012769251418));
#211507=CARTESIAN_POINT('Ctrl Pts',(124.344442863018,6.5780396752237,130.201460121699));
#211508=CARTESIAN_POINT('Ctrl Pts',(124.065995239205,3.04835385980878,124.944187094356));
#211509=CARTESIAN_POINT('Ctrl Pts',(123.787547615392,-3.28262023240536,
125.07212724945));
#211510=CARTESIAN_POINT('Ctrl Pts',(123.509099991579,-6.59702669595264,
130.467709834674));
#211511=CARTESIAN_POINT('Ctrl Pts',(123.230652367767,-3.84908790859021,
136.17265804307));
#211512=CARTESIAN_POINT('Ctrl Pts',(122.952204743954,2.43597462836867,136.944403173336));
#211513=CARTESIAN_POINT('Ctrl Pts',(122.673757120141,6.48249548583303,132.073749152604));
#211514=CARTESIAN_POINT('Ctrl Pts',(122.395309496328,4.57191967932717,126.036589081248));
#211515=CARTESIAN_POINT('Ctrl Pts',(122.116861872515,-1.54002696178715,
124.380778133181));
#211516=CARTESIAN_POINT('Ctrl Pts',(121.838414248702,-6.23676405951882,
128.627925678811));
#211517=CARTESIAN_POINT('Ctrl Pts',(121.559966624889,-5.20221966941523,
134.8751106084));
#211518=CARTESIAN_POINT('Ctrl Pts',(121.281519001076,0.612910454321425,
137.381475163605));
#211519=CARTESIAN_POINT('Ctrl Pts',(121.003071377263,5.86480581287692,133.843792760907));
#211520=CARTESIAN_POINT('Ctrl Pts',(120.724623753451,5.72723114109079,127.513020702994));
#211521=CARTESIAN_POINT('Ctrl Pts',(120.446176129638,0.326610841437887,
124.206829235678));
#211522=CARTESIAN_POINT('Ctrl Pts',(120.167728505825,-5.3741488656698,126.963446800991));
#211523=CARTESIAN_POINT('Ctrl Pts',(119.889280882012,-6.13632830699453,
133.249676524665));
#211524=CARTESIAN_POINT('Ctrl Pts',(119.610833258199,-1.25952181049465,
137.288780390037));
#211525=CARTESIAN_POINT('Ctrl Pts',(119.332385634386,4.77472369878856,135.369019266025));
#211526=CARTESIAN_POINT('Ctrl Pts',(119.053938010573,6.42123138710552,129.254559840052));
#211527=CARTESIAN_POINT('Ctrl Pts',(118.77549038676,2.16694112526505,124.564291616636));
#211528=CARTESIAN_POINT('Ctrl Pts',(118.497042762948,-4.07866216973492,
125.608341960757));
#211529=CARTESIAN_POINT('Ctrl Pts',(118.218595139134,-6.57617418447253,
131.427279610862));
#211530=CARTESIAN_POINT('Ctrl Pts',(117.940147515322,-3.03050338764912,
136.673785137412));
#211531=CARTESIAN_POINT('Ctrl Pts',(117.661699891509,3.30005197410286,136.526576267552));
#211532=CARTESIAN_POINT('Ctrl Pts',(117.383252267696,6.59802078815589,131.120930761129));
#211533=CARTESIAN_POINT('Ctrl Pts',(117.104804643883,3.83273082912851,125.424372758082));
#211534=CARTESIAN_POINT('Ctrl Pts',(116.82635702007,-2.45465152255762,124.671760770883));
#211535=CARTESIAN_POINT('Ctrl Pts',(116.547909396257,-6.48632904140672,
129.554708448625));
#211536=CARTESIAN_POINT('Ctrl Pts',(116.269461772444,-4.55738704599302,
135.586025420722));
#211537=CARTESIAN_POINT('Ctrl Pts',(115.991014148631,1.55957100395386,137.223226036031));
#211538=CARTESIAN_POINT('Ctrl Pts',(115.712566524818,6.24335949054626,132.961802910777));
#211539=CARTESIAN_POINT('Ctrl Pts',(115.434118901006,5.18980561039392,126.717795714978));
#211540=CARTESIAN_POINT('Ctrl Pts',(115.155671277193,-0.632926089611396,
124.229142024863));
#211541=CARTESIAN_POINT('Ctrl Pts',(114.87722365338,-5.87402963342224,127.782793004156));
#211542=CARTESIAN_POINT('Ctrl Pts',(114.598776029567,-5.71718690641897,
134.113117008387));
#211543=CARTESIAN_POINT('Ctrl Pts',(114.320328405754,-0.306528712524212,
137.40285553119));
#211544=CARTESIAN_POINT('Ctrl Pts',(114.041880781941,5.38581439342023,134.628899582769));
#211545=CARTESIAN_POINT('Ctrl Pts',(113.763433158128,6.12885718347172,128.340379164441));
#211546=CARTESIAN_POINT('Ctrl Pts',(113.484985534315,1.23977963323159,124.316137329349));
#211547=CARTESIAN_POINT('Ctrl Pts',(113.206537910502,-4.78859483334625,
126.254255728798));
#211548=CARTESIAN_POINT('Ctrl Pts',(112.92809028669,-6.41648458394181,132.373698236044));
#211549=CARTESIAN_POINT('Ctrl Pts',(112.649642662877,-2.14793846459313,
137.050996138312));
#211550=CARTESIAN_POINT('Ctrl Pts',(112.371195039064,4.09445817108915,135.987941162125));
#211551=CARTESIAN_POINT('Ctrl Pts',(112.092747415251,6.57424777294209,130.161428897475));
#211552=CARTESIAN_POINT('Ctrl Pts',(111.814299791438,3.01262484132005,124.925739474628));
#211553=CARTESIAN_POINT('Ctrl Pts',(111.535852167625,-3.31745314456969,
125.092215695531));
#211554=CARTESIAN_POINT('Ctrl Pts',(111.257404543812,-6.59895375719588,
130.507874045991));
#211555=CARTESIAN_POINT('Ctrl Pts',(110.978956919999,-3.816338243772,136.195989071554));
#211556=CARTESIAN_POINT('Ctrl Pts',(110.700509296186,2.47330567719032,136.929460943594));
#211557=CARTESIAN_POINT('Ctrl Pts',(110.422061672374,6.49010250851429,132.0342648438));
#211558=CARTESIAN_POINT('Ctrl Pts',(110.143614048561,4.54281219364771,126.008846844259));
#211559=CARTESIAN_POINT('Ctrl Pts',(109.865166424748,-1.57910059846782,
124.390271728514));
#211560=CARTESIAN_POINT('Ctrl Pts',(109.586718800935,-6.24989708394428,
128.665930956147));
#211561=CARTESIAN_POINT('Ctrl Pts',(109.308271177122,-5.17734347372243,
134.906702574525));
#211562=CARTESIAN_POINT('Ctrl Pts',(109.029823553309,0.652935861560398,
137.377622345005));
#211563=CARTESIAN_POINT('Ctrl Pts',(108.751375929496,5.88319903775945,133.808035709655));
#211564=CARTESIAN_POINT('Ctrl Pts',(108.472928305683,5.70708970850866,127.478218402361));
#211565=CARTESIAN_POINT('Ctrl Pts',(108.19448068187,0.286443743970404,124.204963299759));
#211566=CARTESIAN_POINT('Ctrl Pts',(107.916033058058,-5.39743002772183,
126.996231933739));
#211567=CARTESIAN_POINT('Ctrl Pts',(107.637585434244,-6.12132928305326,
133.286984790727));
#211568=CARTESIAN_POINT('Ctrl Pts',(107.359137810432,-1.22002597081922,
137.296327315513));
#211569=CARTESIAN_POINT('Ctrl Pts',(107.080690186619,4.80242160701559,135.339869595089));
#211570=CARTESIAN_POINT('Ctrl Pts',(106.802242562806,6.41167833934146,129.215500696253));
#211571=CARTESIAN_POINT('Ctrl Pts',(106.523794938993,2.12891590571267,124.551216444981));
#211572=CARTESIAN_POINT('Ctrl Pts',(106.24534731518,-4.11021624194206,125.633266205238));
#211573=CARTESIAN_POINT('Ctrl Pts',(105.966899691367,-6.57226045847839,
131.467299108419));
#211574=CARTESIAN_POINT('Ctrl Pts',(105.688452067554,-2.99471838644612,
136.692123924851));
#211575=CARTESIAN_POINT('Ctrl Pts',(105.410004443742,3.33482358260376,136.506381895117));
#211576=CARTESIAN_POINT('Ctrl Pts',(105.131556819929,6.59982559442975,131.080760870538));
#211577=CARTESIAN_POINT('Ctrl Pts',(104.853109196116,3.79991030437941,125.401141516381));
#211578=CARTESIAN_POINT('Ctrl Pts',(104.574661572303,-2.49193691945696,
124.686816554284));
#211579=CARTESIAN_POINT('Ctrl Pts',(104.29621394849,-6.49381585219884,129.594215727701));
#211580=CARTESIAN_POINT('Ctrl Pts',(104.017766324677,-4.52819525731082,
135.613678936038));
#211581=CARTESIAN_POINT('Ctrl Pts',(103.739318700864,1.59861556440955,137.213613557961));
#211582=CARTESIAN_POINT('Ctrl Pts',(103.460871077051,6.25637677914949,132.923757837073));
#211583=CARTESIAN_POINT('Ctrl Pts',(103.182423453238,5.16483337484823,126.686279609768));
#211584=CARTESIAN_POINT('Ctrl Pts',(102.903975829425,-0.672939584800916,
124.233116649188));
#211585=CARTESIAN_POINT('Ctrl Pts',(102.625528205613,-5.89231394094447,
127.818605872432));
#211586=CARTESIAN_POINT('Ctrl Pts',(102.347080581799,-5.69693964089892,
134.147857844226));
#211587=CARTESIAN_POINT('Ctrl Pts',(102.068632957987,-0.266356121840884,
137.40459920364));
#211588=CARTESIAN_POINT('Ctrl Pts',(101.790185334174,5.40899566096888,134.59604374203));
#211589=CARTESIAN_POINT('Ctrl Pts',(101.511737710361,6.11374467547657,128.303116723058));
#211590=CARTESIAN_POINT('Ctrl Pts',(101.233290086548,1.20026100625305,124.308710650579));
#211591=CARTESIAN_POINT('Ctrl Pts',(100.954842462735,-4.81620389170723,
126.28348956762));
#211592=CARTESIAN_POINT('Ctrl Pts',(100.676394838922,-6.40681269782886,
132.412728122731));
#211593=CARTESIAN_POINT('Ctrl Pts',(100.397947215109,-2.10987362484612,
137.063955513716));
#211594=CARTESIAN_POINT('Ctrl Pts',(100.119499591297,4.12593623631335,135.962920993349));
#211595=CARTESIAN_POINT('Ctrl Pts',(99.8410519674839,6.5702122594916,130.121421497322));
#211596=CARTESIAN_POINT('Ctrl Pts',(99.5626043436712,2.97678418891005,124.907509689368));
#211597=CARTESIAN_POINT('Ctrl Pts',(99.2841567198582,-3.35216312728773,
125.112515807244));
#211598=CARTESIAN_POINT('Ctrl Pts',(99.0057090960455,-6.6006362917809,130.548049243728));
#211599=CARTESIAN_POINT('Ctrl Pts',(98.7272614722323,-3.78344716313679,
136.219120311263));
#211600=CARTESIAN_POINT('Ctrl Pts',(98.4488138484198,2.51054507676055,136.914291746006));
#211601=CARTESIAN_POINT('Ctrl Pts',(98.1703662246066,6.49746903806041,131.994734960442));
#211602=CARTESIAN_POINT('Ctrl Pts',(97.8919186007939,4.51353637239165,125.981282306795));
#211603=CARTESIAN_POINT('Ctrl Pts',(97.6134709769809,-1.61811572099509,
124.400003000271));
#211604=CARTESIAN_POINT('Ctrl Pts',(97.335023353168,-6.26279851613479,128.704015473778));
#211605=CARTESIAN_POINT('Ctrl Pts',(97.0565757293552,-5.15227542966332,
134.938142526861));
#211606=CARTESIAN_POINT('Ctrl Pts',(96.7781281055422,0.692937074020952,
137.373525951775));
#211607=CARTESIAN_POINT('Ctrl Pts',(96.4996804817294,5.90137425853808,133.772167356118));
#211608=CARTESIAN_POINT('Ctrl Pts',(96.2212328579164,5.6867367976186,127.443539353151));
#211609=CARTESIAN_POINT('Ctrl Pts',(95.9427852341037,0.246266032224636,
124.203341906934));
#211610=CARTESIAN_POINT('Ctrl Pts',(95.6643376102905,-5.42051118601915,
127.029158178097));
#211611=CARTESIAN_POINT('Ctrl Pts',(95.3858899864779,-6.10610343100435,
133.324201062238));
#211612=CARTESIAN_POINT('Ctrl Pts',(95.1074423626648,-1.18048492263276,
137.303633678775));
#211613=CARTESIAN_POINT('Ctrl Pts',(94.828994738852,4.82994155974394,135.3105518592));
#211614=CARTESIAN_POINT('Ctrl Pts',(94.5505471150391,6.40188770447863,129.176500428244));
#211615=CARTESIAN_POINT('Ctrl Pts',(94.2720994912261,2.09081179839861,124.538372985881));
#211616=CARTESIAN_POINT('Ctrl Pts',(93.9936518674133,-4.14161800857485,
125.658382066524));
#211617=CARTESIAN_POINT('Ctrl Pts',(93.7152042436005,-6.56810319495607,
131.507294040545));
#211618=CARTESIAN_POINT('Ctrl Pts',(93.4367566197874,-2.95882241485189,
136.710244539055));
#211619=CARTESIAN_POINT('Ctrl Pts',(93.1583089959747,3.36947161799043,136.485976232185));
#211620=CARTESIAN_POINT('Ctrl Pts',(92.8798613721617,6.60138584173913,131.040580737834));
#211621=CARTESIAN_POINT('Ctrl Pts',(92.6014137483489,3.76694897255651,125.37811049295));
#211622=CARTESIAN_POINT('Ctrl Pts',(92.3229661245359,-2.5291299767175,124.702099025532));
#211623=CARTESIAN_POINT('Ctrl Pts',(92.044518500723,-6.50106203225643,129.633767849141));
#211624=CARTESIAN_POINT('Ctrl Pts',(91.7660708769102,-4.49883567468812,
135.641154240296));
#211625=CARTESIAN_POINT('Ctrl Pts',(91.4876232530973,1.63760088757763,137.203763582666));
#211626=CARTESIAN_POINT('Ctrl Pts',(91.2091756292845,6.26916223541028,132.885634228324));
#211627=CARTESIAN_POINT('Ctrl Pts',(90.9307280054714,5.13966975450256,126.654916101563));
#211628=CARTESIAN_POINT('Ctrl Pts',(90.6522803816587,-0.71292814396669,
124.237334773374));
#211629=CARTESIAN_POINT('Ctrl Pts',(90.3738327578456,-5.91037990660673,
127.85452937895));
#211630=CARTESIAN_POINT('Ctrl Pts',(90.0953851340328,-5.67648127318543,
134.182474785545));
#211631=CARTESIAN_POINT('Ctrl Pts',(89.8169375102199,-0.226173661233629,
137.406098301819));
#211632=CARTESIAN_POINT('Ctrl Pts',(89.5384898864071,5.43197649619419,134.563047399079));
#211633=CARTESIAN_POINT('Ctrl Pts',(89.260042262594,6.09840562042418,128.265946966186));
#211634=CARTESIAN_POINT('Ctrl Pts',(88.9815946387814,1.1606979031614,124.301524670509));
#211635=CARTESIAN_POINT('Ctrl Pts',(88.7031470149683,-4.84363448386183,
126.312890928981));
#211636=CARTESIAN_POINT('Ctrl Pts',(88.4246993911556,-6.39690340491527,
132.45169841077));
#211637=CARTESIAN_POINT('Ctrl Pts',(88.1462517673426,-2.07173060295614,
137.076682937528));
#211638=CARTESIAN_POINT('Ctrl Pts',(87.8678041435297,4.15726141345302,135.937709672222));
#211639=CARTESIAN_POINT('Ctrl Pts',(87.5893565197169,6.5659332844097,130.081439403729));
#211640=CARTESIAN_POINT('Ctrl Pts',(87.3109088959039,2.94083323066708,124.889498414087));
#211641=CARTESIAN_POINT('Ctrl Pts',(87.032461272091,-3.38674889436835,125.133026832359));
#211642=CARTESIAN_POINT('Ctrl Pts',(86.7540136482781,-6.60207423736065,
130.588233939178));
#211643=CARTESIAN_POINT('Ctrl Pts',(86.4755660244652,-3.75041588547566,
136.242050905059));
#211644=CARTESIAN_POINT('Ctrl Pts',(86.1971184006524,2.54769144715974,136.898896142674));
#211645=CARTESIAN_POINT('Ctrl Pts',(85.9186707768394,6.50459480150186,131.955160967326));
#211646=CARTESIAN_POINT('Ctrl Pts',(85.6402231530266,4.48409330038545,125.953896490271));
#211647=CARTESIAN_POINT('Ctrl Pts',(85.3617755292137,-1.65707088364924,
124.409971587854));
#211648=CARTESIAN_POINT('Ctrl Pts',(85.0833279054008,-6.27546787802325,
128.742177820471));
#211649=CARTESIAN_POINT('Ctrl Pts',(84.8048802815879,-5.12701646614329,
134.969429300388));
#211650=CARTESIAN_POINT('Ctrl Pts',(84.526432657775,0.732912609443495,137.369186135708));
#211651=CARTESIAN_POINT('Ctrl Pts',(84.2479850339622,5.91933080172332,133.73618902941));
#211652=CARTESIAN_POINT('Ctrl Pts',(83.9695374101491,5.6661731626052,127.408984840408));
#211653=CARTESIAN_POINT('Ctrl Pts',(83.6910897863363,0.206079195000604,
124.201965117285));
#211654=CARTESIAN_POINT('Ctrl Pts',(83.4126421625234,-5.44339148528112,
127.062224313968));
#211655=CARTESIAN_POINT('Ctrl Pts',(83.1341945387106,-6.09065131504733,
133.361323960135));
#211656=CARTESIAN_POINT('Ctrl Pts',(82.8557469148977,-1.14090013114324,
137.310699209084));
#211657=CARTESIAN_POINT('Ctrl Pts',(82.5772992910847,4.85728253721157,135.281067144739));
#211658=CARTESIAN_POINT('Ctrl Pts',(82.2988516672719,6.39185984531258,129.137560481192));
#211659=CARTESIAN_POINT('Ctrl Pts',(82.0204040434589,2.05263021528453,124.52576171526));
#211660=CARTESIAN_POINT('Ctrl Pts',(81.7419564196462,-4.17286630602932,
125.683688613938));
#211661=CARTESIAN_POINT('Ctrl Pts',(81.4635087958331,-6.56370254795435,
131.547262925216));
#211662=CARTESIAN_POINT('Ctrl Pts',(81.1850611720204,-2.92281680300497,
136.728146308557));
#211663=CARTESIAN_POINT('Ctrl Pts',(80.9066135482074,3.40399479636718,136.465360034899));
#211664=CARTESIAN_POINT('Ctrl Pts',(80.6281659243945,6.60270147226842,131.000391851905));
#211665=CARTESIAN_POINT('Ctrl Pts',(80.3497183005816,3.73384805505426,125.355280541214));
#211666=CARTESIAN_POINT('Ctrl Pts',(80.0712706767688,-2.56622931613655,
124.717607618327));
#211667=CARTESIAN_POINT('Ctrl Pts',(79.7928230529558,-6.50806731306963,
129.673363347327));
#211668=CARTESIAN_POINT('Ctrl Pts',(79.514375429143,-4.46930938605503,135.668450315387));
#211669=CARTESIAN_POINT('Ctrl Pts',(79.23592780533,1.67652552884245,137.193676475141));
#211670=CARTESIAN_POINT('Ctrl Pts',(78.9574801815173,6.28171538555901,132.847433497217));
#211671=CARTESIAN_POINT('Ctrl Pts',(78.6790325577042,5.11431568180404,126.62370635255));
#211672=CARTESIAN_POINT('Ctrl Pts',(78.4005849338915,-0.752890285318027,
124.241796241119));
#211673=CARTESIAN_POINT('Ctrl Pts',(78.1221373100785,-5.92822686096799,
127.890562192549));
#211674=CARTESIAN_POINT('Ctrl Pts',(77.8436896862655,-5.65581256137084,
134.216966549603));
#211675=CARTESIAN_POINT('Ctrl Pts',(77.5652420624528,-0.185982819678218,
137.407352770183));
#211676=CARTESIAN_POINT('Ctrl Pts',(77.2867944386398,5.45475604753291,134.529911776607));
#211677=CARTESIAN_POINT('Ctrl Pts',(77.008346814827,6.08284058670873,128.228871271165));
#211678=CARTESIAN_POINT('Ctrl Pts',(76.729899191014,1.12109178998211,124.294579655415));
#211679=CARTESIAN_POINT('Ctrl Pts',(76.4514515672013,-4.8708855933594,126.342458723402));
#211680=CARTESIAN_POINT('Ctrl Pts',(76.1730039433881,-6.38675707239351,
132.4906076561));
#211681=CARTESIAN_POINT('Ctrl Pts',(75.8945563195755,-2.03351081232684,
137.089177938131));
#211682=CARTESIAN_POINT('Ctrl Pts',(75.6161086957625,4.18843254174224,135.912308132958));
#211683=CARTESIAN_POINT('Ctrl Pts',(75.3376610719495,6.56141100625526,130.041484098248));
#211684=CARTESIAN_POINT('Ctrl Pts',(75.0592134481368,2.90477329876725,124.871706316201));
#211685=CARTESIAN_POINT('Ctrl Pts',(74.7807658243238,-3.42120916422307,
125.153748010832));
#211686=CARTESIAN_POINT('Ctrl Pts',(74.5023182005109,-6.60326754065171,
130.628426643279));
#211687=CARTESIAN_POINT('Ctrl Pts',(74.223870576698,-3.71724563477466,136.264780003243));
#211688=CARTESIAN_POINT('Ctrl Pts',(73.9454229528852,2.58474341191554,136.883274704086));
#211689=CARTESIAN_POINT('Ctrl Pts',(73.6669753290721,6.51147953479087,131.915544330879));
#211690=CARTESIAN_POINT('Ctrl Pts',(73.3885277052595,4.45448406865298,125.926690409479));
#211691=CARTESIAN_POINT('Ctrl Pts',(73.1100800814464,-1.6959646429323,124.420177121874));
#211692=CARTESIAN_POINT('Ctrl Pts',(72.8316324576336,-6.28790470014163,
128.780416582107));
#211693=CARTESIAN_POINT('Ctrl Pts',(72.5531848338207,-5.1015675191428,135.000561735763));
#211694=CARTESIAN_POINT('Ctrl Pts',(72.2747372100078,0.772860986519783,
137.364603057617));
#211695=CARTESIAN_POINT('Ctrl Pts',(71.996289586195,5.93706800192887,133.700102062723));
#211696=CARTESIAN_POINT('Ctrl Pts',(71.7178419623819,5.64539956546153,127.374556144564));
#211697=CARTESIAN_POINT('Ctrl Pts',(71.4393943385692,0.165884721436248,
124.20083298183));
#211698=CARTESIAN_POINT('Ctrl Pts',(71.1609467147562,-5.46607007766984,
127.095429116077));
#211699=CARTESIAN_POINT('Ctrl Pts',(70.8824990909434,-6.07497350776591,
133.398352108815));
#211700=CARTESIAN_POINT('Ctrl Pts',(70.6040514671303,-1.10127306317963,
137.317523644624));
#211701=CARTESIAN_POINT('Ctrl Pts',(70.3256038433176,4.88444352628841,135.251416544269));
#211702=CARTESIAN_POINT('Ctrl Pts',(70.0471562195047,6.38159513342946,129.098682298033));
#211703=CARTESIAN_POINT('Ctrl Pts',(69.7687085956917,2.01437257120279,124.513383100429));
#211704=CARTESIAN_POINT('Ctrl Pts',(69.4902609718789,-4.20395997638847,
125.709184909736));
#211705=CARTESIAN_POINT('Ctrl Pts',(69.211813348066,-6.5590586805409,131.587204281367));
#211706=CARTESIAN_POINT('Ctrl Pts',(68.9333657242531,-2.88670288510633,
136.745828570004));
#211707=CARTESIAN_POINT('Ctrl Pts',(68.6549181004402,3.43839183846502,136.444534067195));
#211708=CARTESIAN_POINT('Ctrl Pts',(68.3764704766273,6.60377243726651,130.960195701968));
#211709=CARTESIAN_POINT('Ctrl Pts',(68.0980228528144,3.70060877843901,125.332652507142));
#211710=CARTESIAN_POINT('Ctrl Pts',(67.8195752290015,-2.6032335629848,124.733341757993));
#211711=CARTESIAN_POINT('Ctrl Pts',(67.5411276051886,-6.51483143505509,
129.713000755032));
#211712=CARTESIAN_POINT('Ctrl Pts',(67.2626799813758,-4.43961748551916,
135.695566149845));
#211713=CARTESIAN_POINT('Ctrl Pts',(66.9842323575627,1.71538804583728,137.183352609169));
#211714=CARTESIAN_POINT('Ctrl Pts',(66.7057847337499,6.29403576443417,132.809157059292));
#211715=CARTESIAN_POINT('Ctrl Pts',(66.4273371099371,5.08877209625689,126.592651519219));
#211716=CARTESIAN_POINT('Ctrl Pts',(66.1488894861241,-0.792824528042931,
124.246500887099));
#211717=CARTESIAN_POINT('Ctrl Pts',(65.8704418623113,-5.94585414270274,
127.92670297802));
#211718=CARTESIAN_POINT('Ctrl Pts',(65.5919942384984,-5.63493427134196,
134.251331858291));
#211719=CARTESIAN_POINT('Ctrl Pts',(65.3135466146855,-0.145785086460763,
137.408362562243));
#211720=CARTESIAN_POINT('Ctrl Pts',(65.0350989908726,5.47733347088038,134.496638102466));
#211721=CARTESIAN_POINT('Ctrl Pts',(64.7566513670597,6.06705015109826,128.191891011849));
#211722=CARTESIAN_POINT('Ctrl Pts',(64.4782037432468,1.0814441343344,124.28787586265));
#211723=CARTESIAN_POINT('Ctrl Pts',(64.199756119434,-4.89795621039988,126.37219185524));
#211724=CARTESIAN_POINT('Ctrl Pts',(63.921308495621,-6.37637407623982,132.529454416925));
#211725=CARTESIAN_POINT('Ctrl Pts',(63.6428608718081,-1.99521566920641,
137.101440052517));
#211726=CARTESIAN_POINT('Ctrl Pts',(63.3644132479953,4.21944846612332,135.886717316821));
#211727=CARTESIAN_POINT('Ctrl Pts',(63.0859656241823,6.556645592603,130.001557061437));
#211728=CARTESIAN_POINT('Ctrl Pts',(62.8075180003696,2.86860572942485,124.854134055001));
#211729=CARTESIAN_POINT('Ctrl Pts',(62.5290703765565,-3.4555426599142,125.174678574835));
#211730=CARTESIAN_POINT('Ctrl Pts',(62.2506227527437,-6.60421615743575,
130.66862586668));
#211731=CARTESIAN_POINT('Ctrl Pts',(61.9721751289308,-3.68393764016947,
136.287306763578));
#211732=CARTESIAN_POINT('Ctrl Pts',(61.6937275051179,2.62169959805353,136.867428009101));
#211733=CARTESIAN_POINT('Ctrl Pts',(61.415279881305,6.51812298281107,131.875886519111));
#211734=CARTESIAN_POINT('Ctrl Pts',(61.1368322574921,4.42470977437533,125.899665072552));
#211735=CARTESIAN_POINT('Ctrl Pts',(60.8583846336791,-1.73479555762186,
124.430619224162));
#211736=CARTESIAN_POINT('Ctrl Pts',(60.5799370098664,-6.30010852163892,
128.818730341733));
#211737=CARTESIAN_POINT('Ctrl Pts',(60.3014893860534,-5.07592953168175,
135.031538679362));
#211738=CARTESIAN_POINT('Ctrl Pts',(60.0230417622406,0.81278072494776,137.35977688733));
#211739=CARTESIAN_POINT('Ctrl Pts',(59.7445941384276,5.95458520189618,133.663907793273));
#211740=CARTESIAN_POINT('Ctrl Pts',(59.4661465146148,5.62441677596096,127.340254541386));
#211741=CARTESIAN_POINT('Ctrl Pts',(59.1876988908018,0.125684100952275,
124.199945542519));
#211742=CARTESIAN_POINT('Ctrl Pts',(58.909251266989,-5.48854612282181,127.128771354006));
#211743=CARTESIAN_POINT('Ctrl Pts',(58.6308036431761,-6.05907059010694,
133.435284136186));
#211744=CARTESIAN_POINT('Ctrl Pts',(58.3523560193632,-1.06160518713815,
137.324106732513));
#211745=CARTESIAN_POINT('Ctrl Pts',(58.0739083955504,4.91142352051418,135.221601156507));
#211746=CARTESIAN_POINT('Ctrl Pts',(57.7954607717374,6.37109394919177,129.059867319411));
#211747=CARTESIAN_POINT('Ctrl Pts',(57.5170131479246,1.97604028380464,124.501237600083));
#211748=CARTESIAN_POINT('Ctrl Pts',(57.2385655241116,-4.23489786746425,
125.734870009144));
#211749=CARTESIAN_POINT('Ctrl Pts',(56.9601179002987,-6.554171764796,131.627116628959));
#211750=CARTESIAN_POINT('Ctrl Pts',(56.6816702764859,-2.85048199937133,
136.76329066817));
#211751=CARTESIAN_POINT('Ctrl Pts',(56.4032226526729,3.47266146968847,136.423499100792));
#211752=CARTESIAN_POINT('Ctrl Pts',(56.1247750288601,6.60459869704857,130.919993777505));
#211753=CARTESIAN_POINT('Ctrl Pts',(55.8463274050471,3.66723237440476,125.310227229228));
#211754=CARTESIAN_POINT('Ctrl Pts',(55.5678797812343,-2.6401413460556,124.749300861495));
#211755=CARTESIAN_POINT('Ctrl Pts',(55.2894321574214,-6.5213541475661,129.752678603477));
#211756=CARTESIAN_POINT('Ctrl Pts',(55.0109845336085,-4.40976107332459,
135.722500738884));
#211757=CARTESIAN_POINT('Ctrl Pts',(54.7325369097956,1.75418699849736,137.172792367301));
#211758=CARTESIAN_POINT('Ctrl Pts',(54.4540892859827,6.30612291549916,132.770806332897));
#211759=CARTESIAN_POINT('Ctrl Pts',(54.1756416621698,5.06303994438864,126.561752752318));
#211760=CARTESIAN_POINT('Ctrl Pts',(53.897194038357,-0.832729392363195,
124.251448536985));
#211761=CARTESIAN_POINT('Ctrl Pts',(53.618746414544,-5.96326109862574,127.962950396153));
#211762=CARTESIAN_POINT('Ctrl Pts',(53.3402987907312,-5.61384717675129,
134.285569438194));
#211763=CARTESIAN_POINT('Ctrl Pts',(53.0618511669183,-0.105581951123662,
137.409127640582));
#211764=CARTESIAN_POINT('Ctrl Pts',(52.7834035431054,5.49970792962155,134.463227609627));
#211765=CARTESIAN_POINT('Ctrl Pts',(52.5049559192925,6.05103489871361,128.155007558556));
#211766=CARTESIAN_POINT('Ctrl Pts',(52.2265082954796,1.04175640537643,124.281413540623));
#211767=CARTESIAN_POINT('Ctrl Pts',(51.9480606716666,-4.9248453318719,126.402089222721));
#211768=CARTESIAN_POINT('Ctrl Pts',(51.6696130478539,-6.36575480119974,
132.568237253767));
#211769=CARTESIAN_POINT('Ctrl Pts',(51.3911654240409,-1.95684659263562,
137.113468826308));
#211770=CARTESIAN_POINT('Ctrl Pts',(51.112717800228,4.25030803728985,135.860938172086));
#211771=CARTESIAN_POINT('Ctrl Pts',(50.8342701764151,6.55163722003711,129.961659772806));
#211772=CARTESIAN_POINT('Ctrl Pts',(50.5558225526023,2.83233186284197,124.836782281636));
#211773=CARTESIAN_POINT('Ctrl Pts',(50.2773749287893,-3.48974810920128,
125.195817748775));
#211774=CARTESIAN_POINT('Ctrl Pts',(49.9989273049765,-6.60492005256131,
130.708830119782));
#211775=CARTESIAN_POINT('Ctrl Pts',(49.7204796811635,-3.65049313590031,
136.309630351328));
#211776=CARTESIAN_POINT('Ctrl Pts',(49.4420320573507,2.65855863614892,136.851356644924));
#211777=CARTESIAN_POINT('Ctrl Pts',(49.1635844335378,6.52452489938715,131.836189001557));
#211778=CARTESIAN_POINT('Ctrl Pts',(48.8851368097249,4.39477152084969,125.87282148092));
#211779=CARTESIAN_POINT('Ctrl Pts',(48.606689185912,-1.77356218882415,124.441297507781));
#211780=CARTESIAN_POINT('Ctrl Pts',(48.3282415620992,-6.31207889029818,
128.857117679619));
#211781=CARTESIAN_POINT('Ctrl Pts',(48.0497939382862,-5.05010345378512,
135.062358983324));
#211782=CARTESIAN_POINT('Ctrl Pts',(47.7713463144734,0.852670345487299,
137.354707803682));
#211783=CARTESIAN_POINT('Ctrl Pts',(47.4928986906604,5.97188175251911,133.627607562248));
#211784=CARTESIAN_POINT('Ctrl Pts',(47.2144510668476,5.60322557162828,127.306081301933));
#211785=CARTESIAN_POINT('Ctrl Pts',(46.9360034430346,0.0854788231980546,
124.199302832238));
#211786=CARTESIAN_POINT('Ctrl Pts',(46.6575558192218,-5.5108187878785,127.162249792247));
#211787=CARTESIAN_POINT('Ctrl Pts',(46.3791081954089,-6.04294315135938,
133.47211867372));
#211788=CARTESIAN_POINT('Ctrl Pts',(46.100660571596,-1.02189797292572,137.330448228811));
#211789=CARTESIAN_POINT('Ctrl Pts',(45.822212947783,4.93822152013526,135.191622086273));
#211790=CARTESIAN_POINT('Ctrl Pts',(45.5437653239702,6.36035668172477,129.02111698363));
#211791=CARTESIAN_POINT('Ctrl Pts',(45.2653177001572,1.9376347735074,124.489325664279));
#211792=CARTESIAN_POINT('Ctrl Pts',(44.9868700763445,-4.26567883284234,
125.76074296039));
#211793=CARTESIAN_POINT('Ctrl Pts',(44.7084224525315,-6.54904198180601,
131.666998489025));
#211794=CARTESIAN_POINT('Ctrl Pts',(44.4299748287186,-2.81415548797717,
136.780531955991));
#211795=CARTESIAN_POINT('Ctrl Pts',(44.1515272049057,3.50680242016433,136.402255915145));
#211796=CARTESIAN_POINT('Ctrl Pts',(43.8730795810928,6.60518022099696,130.879787568212));
#211797=CARTESIAN_POINT('Ctrl Pts',(43.59463195728,3.63372007972613,125.288005538446));
#211798=CARTESIAN_POINT('Ctrl Pts',(43.316184333467,-2.6769512977182,124.765484337463));
#211799=CARTESIAN_POINT('Ctrl Pts',(43.0377367096542,-6.52763520890084,
129.792395422388));
#211800=CARTESIAN_POINT('Ctrl Pts',(42.7592890858413,-4.37974125581177,
135.749253084432));
#211801=CARTESIAN_POINT('Ctrl Pts',(42.4808414620283,1.79292094911309,137.161996140853));
#211802=CARTESIAN_POINT('Ctrl Pts',(42.2023938382155,6.31797639086063,132.732382739134));
#211803=CARTESIAN_POINT('Ctrl Pts',(41.9239462144025,5.0371201797131,126.531011196811));
#211804=CARTESIAN_POINT('Ctrl Pts',(41.6454985905898,-0.872603399589798,
124.256639007436));
#211805=CARTESIAN_POINT('Ctrl Pts',(41.3670509667768,-5.98044708371573,
127.999303103786));
#211806=CARTESIAN_POINT('Ctrl Pts',(41.0886033429639,-5.592552058989,134.319678020622));
#211807=CARTESIAN_POINT('Ctrl Pts',(40.810155719151,-0.0653749034083074,
137.409647976851));
#211808=CARTESIAN_POINT('Ctrl Pts',(40.5317080953382,5.52187859466303,134.429681536124));
#211809=CARTESIAN_POINT('Ctrl Pts',(40.2532604715252,6.03479542300531,128.118222278014));
#211810=CARTESIAN_POINT('Ctrl Pts',(39.9748128477124,1.00203007375177,124.275192928799));
#211811=CARTESIAN_POINT('Ctrl Pts',(39.6963652238994,-4.95155196138904,
126.432149717987));
#211812=CARTESIAN_POINT('Ctrl Pts',(39.4179176000866,-6.35489964077443,
132.60695472951));
#211813=CARTESIAN_POINT('Ctrl Pts',(39.1394699762736,-1.91840500439501,
137.125263813774));
#211814=CARTESIAN_POINT('Ctrl Pts',(38.8610223524608,4.28101011172891,135.834971654011));
#211815=CARTESIAN_POINT('Ctrl Pts',(38.5825747286478,6.54638607414467,129.921793710766));
#211816=CARTESIAN_POINT('Ctrl Pts',(38.304127104835,2.79595304316033,124.819651639079));
#211817=CARTESIAN_POINT('Ctrl Pts',(38.0256794810221,-3.52382424458856,
125.217164749334));
#211818=CARTESIAN_POINT('Ctrl Pts',(37.7472318572093,-6.60537919994535,
130.749037912801));
#211819=CARTESIAN_POINT('Ctrl Pts',(37.4687842333963,-3.61691336126579,
136.331749939282));
#211820=CARTESIAN_POINT('Ctrl Pts',(37.1903366095834,2.69531916037638,136.835061207086));
#211821=CARTESIAN_POINT('Ctrl Pts',(36.9118889857706,6.53068504729366,131.796453249222));
#211822=CARTESIAN_POINT('Ctrl Pts',(36.6334413619576,4.36467041744916,125.846160629286));
#211823=CARTESIAN_POINT('Ctrl Pts',(36.3549937381448,-1.8122631000273,124.452211577043));
#211824=CARTESIAN_POINT('Ctrl Pts',(36.0765461143319,-6.32381536255287,
128.895577173308));
#211825=CARTESIAN_POINT('Ctrl Pts',(35.798098490519,-5.02409024244786,135.093021505591));
#211826=CARTESIAN_POINT('Ctrl Pts',(35.5196508667061,0.892528370013623,
137.34939599451));
#211827=CARTESIAN_POINT('Ctrl Pts',(35.2412032428932,5.98895701286753,133.591202714771));
#211828=CARTESIAN_POINT('Ctrl Pts',(34.9627556190803,5.58182673771145,127.272037692505));
#211829=CARTESIAN_POINT('Ctrl Pts',(34.6843079952674,0.0452703779943793,
124.198904874802));
#211830=CARTESIAN_POINT('Ctrl Pts',(34.4058603714545,-5.53288724751859,
127.195863190245));
#211831=CARTESIAN_POINT('Ctrl Pts',(34.1274127476417,-6.02659178913083,
133.508854356496));
#211832=CARTESIAN_POINT('Ctrl Pts',(33.8489651238287,-0.982152891908117,
137.336547898535));
#211833=CARTESIAN_POINT('Ctrl Pts',(33.5705175000158,4.96483653214189,135.161480444452));
#211834=CARTESIAN_POINT('Ctrl Pts',(33.292069876203,6.34938372890195,128.982432726597));
#211835=CARTESIAN_POINT('Ctrl Pts',(33.0136222523901,1.89915746344075,124.477647734417));
#211836=CARTESIAN_POINT('Ctrl Pts',(32.7351746285772,-4.29630173192265,
125.786802804744));
#211837=CARTESIAN_POINT('Ctrl Pts',(32.4567270047643,-6.543669521657,131.706848383727));
#211838=CARTESIAN_POINT('Ctrl Pts',(32.1782793809514,-2.77772469701646,
136.797551794587));
#211839=CARTESIAN_POINT('Ctrl Pts',(31.8998317571386,3.54081342478663,136.380805297429));
#211840=CARTESIAN_POINT('Ctrl Pts',(31.6213841333256,6.60551698756319,130.839578563946));
#211841=CARTESIAN_POINT('Ctrl Pts',(31.3429365095127,3.6000731362139,125.26598825823));
#211842=CARTESIAN_POINT('Ctrl Pts',(31.0644888856998,-2.71366205396602,
124.781891586214));
#211843=CARTESIAN_POINT('Ctrl Pts',(30.7860412618869,-6.53367438631237,
129.83214974004));
#211844=CARTESIAN_POINT('Ctrl Pts',(30.507593638074,-4.34955914537615,135.775822195171));
#211845=CARTESIAN_POINT('Ctrl Pts',(30.2291460142612,1.83158846238341,137.150964329883));
#211846=CARTESIAN_POINT('Ctrl Pts',(29.9506983904483,6.32959575128355,132.693887701803));
#211847=CARTESIAN_POINT('Ctrl Pts',(29.6722507666353,5.01101376269691,126.500427991838));
#211848=CARTESIAN_POINT('Ctrl Pts',(29.3938031428225,-0.912445072176531,
124.26207210612));
#211849=CARTESIAN_POINT('Ctrl Pts',(29.1153555190096,-5.99741146113971,
128.035759753857));
#211850=CARTESIAN_POINT('Ctrl Pts',(28.8369078951967,-5.57104970715349,
134.353656341672));
#211851=CARTESIAN_POINT('Ctrl Pts',(28.5584602713837,-0.0251654332018655,
137.409923551768));
#211852=CARTESIAN_POINT('Ctrl Pts',(28.280012647571,5.54384464446253,134.396001125022));
#211853=CARTESIAN_POINT('Ctrl Pts',(28.001565023758,6.0183323257333,128.081536533317));
#211854=CARTESIAN_POINT('Ctrl Pts',(27.7231173999451,0.962266611534229,
124.269214257685));
#211855=CARTESIAN_POINT('Ctrl Pts',(27.4446697761322,-4.97807510932732,
126.462372227135));
#211856=CARTESIAN_POINT('Ctrl Pts',(27.1662221523194,-6.34380899720599,
132.645605409466));
#211857=CARTESIAN_POINT('Ctrl Pts',(26.8877745285064,-1.87989232895117,
137.136824577849));
#211858=CARTESIAN_POINT('Ctrl Pts',(26.6093269046936,4.31155355176403,135.808818724794));
#211859=CARTESIAN_POINT('Ctrl Pts',(26.3308792808807,6.5408923495088,129.881960352566));
#211860=CARTESIAN_POINT('Ctrl Pts',(26.0524316570678,2.75947061841045,124.802742762115));
#211861=CARTESIAN_POINT('Ctrl Pts',(25.7739840332549,-3.55776980337282,
125.238718785491));
#211862=CARTESIAN_POINT('Ctrl Pts',(25.4955364094419,-6.60559358257403,
130.789247755823));
#211863=CARTESIAN_POINT('Ctrl Pts',(25.2170887856292,-3.58319956057628,
136.353664707793));
#211864=CARTESIAN_POINT('Ctrl Pts',(24.9386411618162,2.73197980856112,136.81854229942));
#211865=CARTESIAN_POINT('Ctrl Pts',(24.6601935380033,6.5366031982641,131.756680734531));
#211866=CARTESIAN_POINT('Ctrl Pts',(24.3817459141905,4.3344075795813,125.819683505575));
#211867=CARTESIAN_POINT('Ctrl Pts',(24.1032982903775,-1.85089685715453,
124.463361027524));
#211868=CARTESIAN_POINT('Ctrl Pts',(23.8248506665647,-6.33531750350378,
128.934107397669));
#211869=CARTESIAN_POINT('Ctrl Pts',(23.5464030427517,-4.99789086159903,
135.123525109951));
#211870=CARTESIAN_POINT('Ctrl Pts',(23.2679554189389,0.932353321572971,
137.343841656646));
#211871=CARTESIAN_POINT('Ctrl Pts',(22.9895077951259,6.00581035021119,133.554694599836));
#211872=CARTESIAN_POINT('Ctrl Pts',(22.7110601713131,5.56022106715229,127.238124974604));
#211873=CARTESIAN_POINT('Ctrl Pts',(22.4326125475002,0.00506025528043594,
124.198751684957));
#211874=CARTESIAN_POINT('Ctrl Pts',(22.1541649236873,-5.554750683987,127.229610302442));
#211875=CARTESIAN_POINT('Ctrl Pts',(21.8757172998744,-6.01001710932725,
133.545489823263));
#211876=CARTESIAN_POINT('Ctrl Pts',(21.5972696760615,-0.942371416853923,
137.342405515655));
#211877=CARTESIAN_POINT('Ctrl Pts',(21.3188220522486,4.99126757030501,135.131177347952));
#211878=CARTESIAN_POINT('Ctrl Pts',(21.0403744284357,6.33817549733007,128.943815981773));
#211879=CARTESIAN_POINT('Ctrl Pts',(20.7619268046228,1.86060977939589,124.466204243228));
#211880=CARTESIAN_POINT('Ctrl Pts',(20.48347918081,-4.32676542996233,125.813048576547));
#211881=CARTESIAN_POINT('Ctrl Pts',(20.205031556997,-6.5380545834274,131.746664836412));
#211882=CARTESIAN_POINT('Ctrl Pts',(19.9265839331841,-2.74119097644563,
136.814349553278));
#211883=CARTESIAN_POINT('Ctrl Pts',(19.6481363093713,3.57469322326559,136.359148042506));
#211884=CARTESIAN_POINT('Ctrl Pts',(19.3696886855584,6.60560898426828,130.799368254665));
#211885=CARTESIAN_POINT('Ctrl Pts',(19.0912410617455,3.56629279066743,125.244176204439));
#211886=CARTESIAN_POINT('Ctrl Pts',(18.8127934379326,-2.75027225446848,
124.798521999768));
#211887=CARTESIAN_POINT('Ctrl Pts',(18.5343458141197,-6.53947145601676,
129.871940083324));
#211888=CARTESIAN_POINT('Ctrl Pts',(18.2558981903068,-4.31921586042675,
135.802207086573));
#211889=CARTESIAN_POINT('Ctrl Pts',(17.9774505664939,1.87018810546999,137.139697343177));
#211890=CARTESIAN_POINT('Ctrl Pts',(17.6990029426811,6.34098056620813,132.65532264735));
#211891=CARTESIAN_POINT('Ctrl Pts',(17.4205553188681,4.98472166072295,126.470004270672));
#211892=CARTESIAN_POINT('Ctrl Pts',(17.1421076950552,-0.95225293377558,
124.26774763171));
#211893=CARTESIAN_POINT('Ctrl Pts',(16.8636600712423,-6.01415360227624,
128.072318995452));
#211894=CARTESIAN_POINT('Ctrl Pts',(16.5852124474295,-5.54934091802252,
134.387503142263));
#211895=CARTESIAN_POINT('Ctrl Pts',(16.3067648236166,0.0150449695187284,
137.409954355121));
#211896=CARTESIAN_POINT('Ctrl Pts',(16.0283171998036,5.56560526505998,134.362187624359));
#211897=CARTESIAN_POINT('Ctrl Pts',(15.7498695759908,6.00164621694371,128.044951683866));
#211898=CARTESIAN_POINT('Ctrl Pts',(15.4714219521779,0.922467492173741,
124.263477748823));
#211899=CARTESIAN_POINT('Ctrl Pts',(15.192974328365,-5.00441379286154,126.492755630261));
#211900=CARTESIAN_POINT('Ctrl Pts',(14.9145267045521,-6.33248328146239,
132.684187861418));
#211901=CARTESIAN_POINT('Ctrl Pts',(14.6360790807393,-1.84130999340576,
137.148150690142));
#211902=CARTESIAN_POINT('Ctrl Pts',(14.3576314569263,4.34193722559672,135.782480353541));
#211903=CARTESIAN_POINT('Ctrl Pts',(14.0791838331134,6.53515624970152,129.842161174248));
#211904=CARTESIAN_POINT('Ctrl Pts',(13.8007362093005,2.72288594046203,124.786056277307));
#211905=CARTESIAN_POINT('Ctrl Pts',(13.5222885854877,-3.59158352768866,
125.260479058552));
#211906=CARTESIAN_POINT('Ctrl Pts',(13.2438409616747,-6.60556319250329,
130.829458158858));
#211907=CARTESIAN_POINT('Ctrl Pts',(12.9653933378619,-3.54935298310934,
136.375373844801));
#211908=CARTESIAN_POINT('Ctrl Pts',(12.686945714049,2.76853922222938,136.801800534039));
#211909=CARTESIAN_POINT('Ctrl Pts',(12.4084980902361,6.5422791329992,131.716872931266));
#211910=CARTESIAN_POINT('Ctrl Pts',(12.1300504664232,4.30398412864651,125.793391090908));
#211911=CARTESIAN_POINT('Ctrl Pts',(11.8516028426103,-1.88946202861834,
124.474745446076));
#211912=CARTESIAN_POINT('Ctrl Pts',(11.5731552187974,-6.34658488693473,
128.972706924952));
#211913=CARTESIAN_POINT('Ctrl Pts',(11.2947075949845,-4.97150628206636,
135.153868666082));
#211914=CARTESIAN_POINT('Ctrl Pts',(11.0162599711716,0.972143724437105,
137.338044995907));
#211915=CARTESIAN_POINT('Ctrl Pts',(10.7378123473587,6.0224411400439,133.518084570262));
#211916=CARTESIAN_POINT('Ctrl Pts',(10.4593647235458,5.53840936055655,127.204344404875));
#211917=CARTESIAN_POINT('Ctrl Pts',(10.1809170997329,-0.0351500549433496,
124.198843268382));
#211918=CARTESIAN_POINT('Ctrl Pts',(9.90246947592002,-5.57640828712608,
127.263489878326));
#211919=CARTESIAN_POINT('Ctrl Pts',(9.62402185210712,-5.99321972612948,
133.582023716479));
#211920=CARTESIAN_POINT('Ctrl Pts',(9.34557422829421,-0.902555021880531,
137.348020863117));
#211921=CARTESIAN_POINT('Ctrl Pts',(9.06712660448133,5.01751365521256,135.100713919668));
#211922=CARTESIAN_POINT('Ctrl Pts',(8.78867898066847,6.32673240233446,128.905268180115));
#211923=CARTESIAN_POINT('Ctrl Pts',(8.51023135685555,1.82199314977141,124.454995614755));
#211924=CARTESIAN_POINT('Ctrl Pts',(8.23178373304265,-4.35706879811783,
125.839479303254));
#211925=CARTESIAN_POINT('Ctrl Pts',(7.9533361092298,-6.53219737518076,131.786446371669));
#211926=CARTESIAN_POINT('Ctrl Pts',(7.67488848541689,-2.70455568003535,
136.83092460962));
#211927=CARTESIAN_POINT('Ctrl Pts',(7.39644086160398,3.60844056017245,136.337284952891));
#211928=CARTESIAN_POINT('Ctrl Pts',(7.1179932377911,6.60545620770325,130.759158130379));
#211929=CARTESIAN_POINT('Ctrl Pts',(6.83954561397822,3.53238029483008,125.222570185327));
#211930=CARTESIAN_POINT('Ctrl Pts',(6.5610979901653,-2.78678054262086,124.815374961881));
#211931=CARTESIAN_POINT('Ctrl Pts',(6.28265036635242,-6.54502620320144,
129.911764977794));
#211932=CARTESIAN_POINT('Ctrl Pts',(6.00420274253956,-4.28871252534551,
135.828406780936));
#211933=CARTESIAN_POINT('Ctrl Pts',(5.72575511872663,1.90871844804856,137.128195598241));
#211934=CARTESIAN_POINT('Ctrl Pts',(5.44730749491374,6.35213041376593,132.616689004818));
#211935=CARTESIAN_POINT('Ctrl Pts',(5.16885987110085,4.95824484805471,126.439741160674));
#211936=CARTESIAN_POINT('Ctrl Pts',(4.89041224728798,-0.992025509291961,
124.273665373899));
#211937=CARTESIAN_POINT('Ctrl Pts',(4.61196462347505,-6.03067288673954,
128.108979473854));
#211938=CARTESIAN_POINT('Ctrl Pts',(4.33351699966218,-5.52742649602286,
134.421217168191));
#211939=CARTESIAN_POINT('Ctrl Pts',(4.05506937584931,0.0552548147426717,
137.409740385768));
#211940=CARTESIAN_POINT('Ctrl Pts',(3.77662175203639,5.58715965010757,134.328242287108));
#211941=CARTESIAN_POINT('Ctrl Pts',(3.49817412822347,5.98473771494644,128.008469085329));
#211942=CARTESIAN_POINT('Ctrl Pts',(3.21972650441063,0.882634190440881,
124.25798361478));
#211943=CARTESIAN_POINT('Ctrl Pts',(2.94127888059773,-5.03056703600248,
126.523298801495));
#211944=CARTESIAN_POINT('Ctrl Pts',(2.66283125678483,-6.32092291322184,
132.722700655682));
#211945=CARTESIAN_POINT('Ctrl Pts',(2.38438363297192,-1.80265942744139,
137.159241730961));
#211946=CARTESIAN_POINT('Ctrl Pts',(2.10593600915906,4.37216000734877,135.755957516231));
#211947=CARTESIAN_POINT('Ctrl Pts',(1.82748838534615,6.529177987276,129.802397650584));
#211948=CARTESIAN_POINT('Ctrl Pts',(1.54904076153325,2.68620036497402,124.769592802981));
#211949=CARTESIAN_POINT('Ctrl Pts',(1.27059313772038,-3.62526416455594,
125.282444762183));
#211950=CARTESIAN_POINT('Ctrl Pts',(0.992145513907496,-6.60528803085927,
130.869667631896));
#211951=CARTESIAN_POINT('Ctrl Pts',(0.713697890094564,-3.51537488306232,
136.396876545864));
#211952=CARTESIAN_POINT('Ctrl Pts',(0.435250266281723,2.80499604665836,
136.784836531317));
#211953=CARTESIAN_POINT('Ctrl Pts',(0.156802642468823,6.54771264117505,
131.677031314524));
#211954=CARTESIAN_POINT('Ctrl Pts',(-0.121644981344083,4.27340119199728,
125.767284359559));
#211955=CARTESIAN_POINT('Ctrl Pts',(-0.400092605156985,-1.92795718537184,
124.486364410847));
#211956=CARTESIAN_POINT('Ctrl Pts',(-0.678540228969845,-6.35761709532873,
129.011374324836));
#211957=CARTESIAN_POINT('Ctrl Pts',(-0.956987852782752,-4.94493748154019,
135.184051049593));
#211958=CARTESIAN_POINT('Ctrl Pts',(-1.23543547659566,1.01189810415772,
137.332006227089));
#211959=CARTESIAN_POINT('Ctrl Pts',(-1.51388310040852,6.03884876610542,
133.48137398265));
#211960=CARTESIAN_POINT('Ctrl Pts',(-1.79233072422142,5.51639242616521,
127.170697235071));
#211961=CARTESIAN_POINT('Ctrl Pts',(-2.07077834803434,-0.0753590626689394,
124.19917962168));
#211962=CARTESIAN_POINT('Ctrl Pts',(-2.34922597184723,-5.59785925440532,
127.297500662476));
#211963=CARTESIAN_POINT('Ctrl Pts',(-2.6276735956601,-5.97620026197078,
133.618454682368));
#211964=CARTESIAN_POINT('Ctrl Pts',(-2.906121219473,-0.862705182398668,
137.353393732843));
#211965=CARTESIAN_POINT('Ctrl Pts',(-3.18456884328591,5.04357381430661,
135.070091288433));
#211966=CARTESIAN_POINT('Ctrl Pts',(-3.46301646709877,6.31505486794284,
128.866790750024));
#211967=CARTESIAN_POINT('Ctrl Pts',(-3.74146409091167,1.78330900552073,
124.444022264336));
#211968=CARTESIAN_POINT('Ctrl Pts',(-4.01991171472458,-4.38721071348669,
125.866094005463));
#211969=CARTESIAN_POINT('Ctrl Pts',(-4.29835933853748,-6.52609811395827,
131.826191515377));
#211970=CARTESIAN_POINT('Ctrl Pts',(-4.57680696235032,-2.66782016531947,
136.847276349416));
#211971=CARTESIAN_POINT('Ctrl Pts',(-4.85525458616324,3.64205418498746,
136.31521683873));
#211972=CARTESIAN_POINT('Ctrl Pts',(-5.13370220997616,6.60505866352928,
130.718949681087));
#211973=CARTESIAN_POINT('Ctrl Pts',(-5.41214983378902,3.49833690534187,
125.201171001511));
#211974=CARTESIAN_POINT('Ctrl Pts',(-5.69059745760191,-2.82318556559566,
124.832449848059));
#211975=CARTESIAN_POINT('Ctrl Pts',(-5.96904508141481,-6.55033842203324,
129.951622947723));
#211976=CARTESIAN_POINT('Ctrl Pts',(-6.24749270522772,-4.2580502704442,
135.854420307421));
#211977=CARTESIAN_POINT('Ctrl Pts',(-6.52594032904057,1.9471780623631,137.116459521273));
#211978=CARTESIAN_POINT('Ctrl Pts',(-6.80438795285348,6.36304488079526,
132.577988205793));
#211979=CARTESIAN_POINT('Ctrl Pts',(-7.0828355766664,4.93158430580029,126.409639783256));
#211980=CARTESIAN_POINT('Ctrl Pts',(-7.36128320047925,-1.03176132493798,
124.279825113401));
#211981=CARTESIAN_POINT('Ctrl Pts',(-7.63973082429214,-6.04696870240127,
128.145739830595));
#211982=CARTESIAN_POINT('Ctrl Pts',(-7.91817844810507,-5.50530725320171,
134.454797170168));
#211983=CARTESIAN_POINT('Ctrl Pts',(-8.19662607191793,0.09546261247915,
137.40928165164));
#211984=CARTESIAN_POINT('Ctrl Pts',(-8.47507369573082,5.60850700089942,
134.294166371127));
#211985=CARTESIAN_POINT('Ctrl Pts',(-8.75352131954372,5.96760744629241,
127.972090089581));
#211986=CARTESIAN_POINT('Ctrl Pts',(-9.03196894335663,0.842768182373745,
124.252732059145));
#211987=CARTESIAN_POINT('Ctrl Pts',(-9.31041656716948,-5.05653386963193,
126.554000609049));
#211988=CARTESIAN_POINT('Ctrl Pts',(-9.5888641909824,-6.30912832085822,
132.76114236515));
#211989=CARTESIAN_POINT('Ctrl Pts',(-9.86731181479532,-1.76394206326903,
137.170097289323));
#211990=CARTESIAN_POINT('Ctrl Pts',(-10.1457594386081,4.40222077710389,
135.729251195677));
#211991=CARTESIAN_POINT('Ctrl Pts',(-10.424207062421,6.52295778375913,129.762671255026));
#211992=CARTESIAN_POINT('Ctrl Pts',(-10.7026546862339,2.64941525134336,
124.753352949195));
#211993=CARTESIAN_POINT('Ctrl Pts',(-10.9811023100469,-3.65881046592654,
125.304615082438));
#211994=CARTESIAN_POINT('Ctrl Pts',(-11.2595499338597,-6.60476810783814,
130.909874684957));
#211995=CARTESIAN_POINT('Ctrl Pts',(-11.5379975576726,-3.48126651950624,
136.418172014193));
#211996=CARTESIAN_POINT('Ctrl Pts',(-11.8164451814855,2.84134893092756,
136.767650919861));
#211997=CARTESIAN_POINT('Ctrl Pts',(-12.0948928052984,6.5529035214511,131.637157360647));
#211998=CARTESIAN_POINT('Ctrl Pts',(-12.3733404291112,4.2426599028951,125.741364278924));
#211999=CARTESIAN_POINT('Ctrl Pts',(-12.6517880529242,-1.96638090096281,
124.498217491291));
#212000=CARTESIAN_POINT('Ctrl Pts',(-12.9302356767371,-6.36841371988325,
129.050108164486));
#212001=CARTESIAN_POINT('Ctrl Pts',(-13.2086833005499,-4.91818544453708,
135.214071142064));
#212002=CARTESIAN_POINT('Ctrl Pts',(-13.4871309243628,1.05161498762227,
137.325725573964));
#212003=CARTESIAN_POINT('Ctrl Pts',(-13.7655785481758,6.05503262040511,
133.444564197323));
#212004=CARTESIAN_POINT('Ctrl Pts',(-14.0440261719886,5.49417107982388,
127.137184712));
#212005=CARTESIAN_POINT('Ctrl Pts',(-14.3224737958015,-0.115565277936756,
124.199760732389));
#212006=CARTESIAN_POINT('Ctrl Pts',(-14.6009214196144,-5.61910279095105,
127.331641394614));
#212007=CARTESIAN_POINT('Ctrl Pts',(-14.8793690434273,-5.95895934751375,
133.654781370965));
#212008=CARTESIAN_POINT('Ctrl Pts',(-15.1578166672402,-0.822823375059262,
137.358523925738));
#212009=CARTESIAN_POINT('Ctrl Pts',(-15.4362642910531,5.06944708191823,
135.039310588977));
#212010=CARTESIAN_POINT('Ctrl Pts',(-15.714711914866,6.3031433268707,128.828385117298));
#212011=CARTESIAN_POINT('Ctrl Pts',(-15.9931595386788,1.74455878009922,
124.433284598595));
#212012=CARTESIAN_POINT('Ctrl Pts',(-16.2716071624918,-4.41719005914895,
125.892891696959));
#212013=CARTESIAN_POINT('Ctrl Pts',(-16.5500547863046,-6.51975702577033,
131.865898794765));
#212014=CARTESIAN_POINT('Ctrl Pts',(-16.8285024101176,-2.63098579354628,
136.863404166748));
#212015=CARTESIAN_POINT('Ctrl Pts',(-17.1069500339304,3.67553285214529,
136.292944517765));
#212016=CARTESIAN_POINT('Ctrl Pts',(-17.3853976577434,6.60441636647752,
130.678744396729));
#212017=CARTESIAN_POINT('Ctrl Pts',(-17.6638452815562,3.46416388369313,
125.179979445948));
#212018=CARTESIAN_POINT('Ctrl Pts',(-17.9422929053691,-2.8594859743911,
124.849746025587));
#212019=CARTESIAN_POINT('Ctrl Pts',(-18.220740529182,-6.55540791566593,
129.991512516161));
#212020=CARTESIAN_POINT('Ctrl Pts',(-18.4991881529949,-4.22723023192423,
135.880246702087));
#212021=CARTESIAN_POINT('Ctrl Pts',(-18.7776357768078,1.98556552327847,
137.104489547159));
#212022=CARTESIAN_POINT('Ctrl Pts',(-19.0560834006207,6.37372356285652,
132.539221684343));
#212023=CARTESIAN_POINT('Ctrl Pts',(-19.3345310244336,4.90474102187576,
126.379701253833));
#212024=CARTESIAN_POINT('Ctrl Pts',(-19.6129786482465,-1.07145890828896,
124.286226621967));
#212025=CARTESIAN_POINT('Ctrl Pts',(-19.8914262720594,-6.06304044541393,
128.182598703507));
#212026=CARTESIAN_POINT('Ctrl Pts',(-20.1698738958722,-5.48298400919569,
134.488241903877));
#212027=CARTESIAN_POINT('Ctrl Pts',(-20.4483215196851,0.135666872813404,
137.408578169733));
#212028=CARTESIAN_POINT('Ctrl Pts',(-20.7267691434981,5.62964652640204,
134.25996113911));
#212029=CARTESIAN_POINT('Ctrl Pts',(-21.0052167673109,5.95025604574973,
127.935816044659));
#212030=CARTESIAN_POINT('Ctrl Pts',(-21.2836643911238,0.802870945221437,
124.247723276515));
#212031=CARTESIAN_POINT('Ctrl Pts',(-21.5621120149367,-5.08231333153929,
126.584859915257));
#212032=CARTESIAN_POINT('Ctrl Pts',(-21.8405596387496,-6.29709994142449,
132.79951156535));
#212033=CARTESIAN_POINT('Ctrl Pts',(-22.1190072625625,-1.725159335575,137.180716962973));
#212034=CARTESIAN_POINT('Ctrl Pts',(-22.3974548863754,4.43211842094896,
135.702362381491));
#212035=CARTESIAN_POINT('Ctrl Pts',(-22.6759025101882,6.51649586964294,
129.722983459651));
#212036=CARTESIAN_POINT('Ctrl Pts',(-22.9543501340012,2.61253196265622,
124.737337317723));
#212037=CARTESIAN_POINT('Ctrl Pts',(-23.232797757814,-3.6922211887298,125.326989197785));
#212038=CARTESIAN_POINT('Ctrl Pts',(-23.511245381627,-6.60400344270576,
130.950077828156));
#212039=CARTESIAN_POINT('Ctrl Pts',(-23.7896930054398,-3.4470291563393,
136.439259460675));
#212040=CARTESIAN_POINT('Ctrl Pts',(-24.0681406292527,2.87759652796706,
136.75024433649));
#212041=CARTESIAN_POINT('Ctrl Pts',(-24.3465882530656,6.55785158147733,
131.597252547181));
#212042=CARTESIAN_POINT('Ctrl Pts',(-24.6250358768785,4.21176140046998,
125.715631809479));
#212043=CARTESIAN_POINT('Ctrl Pts',(-24.9034835006914,-2.00473175158637,
124.510304248187));
#212044=CARTESIAN_POINT('Ctrl Pts',(-25.1819311245043,-6.3789743605254,
129.088907008606));
#212045=CARTESIAN_POINT('Ctrl Pts',(-25.4603787483172,-4.89125116236366,
135.24392783109));
#212046=CARTESIAN_POINT('Ctrl Pts',(-25.73882637213,1.09129290310671,137.319203269261));
#212047=CARTESIAN_POINT('Ctrl Pts',(-26.017273995943,6.07099210324431,133.407656578282));
#212048=CARTESIAN_POINT('Ctrl Pts',(-26.2957216197559,5.47174614495268,
127.103808077481));
#212049=CARTESIAN_POINT('Ctrl Pts',(-26.5741692435687,-0.155767210890682,
124.200586578976));
#212050=CARTESIAN_POINT('Ctrl Pts',(-26.8526168673816,-5.64013810957666,
127.365910809639));
#212051=CARTESIAN_POINT('Ctrl Pts',(-27.1310644911945,-5.94149762162655,
133.691002436174));
#212052=CARTESIAN_POINT('Ctrl Pts',(-27.4095121150075,-0.782911077696857,
137.363411251701));
#212053=CARTESIAN_POINT('Ctrl Pts',(-27.6879597388203,5.09513249930392,
135.008372961895));
#212054=CARTESIAN_POINT('Ctrl Pts',(-27.9664073626332,6.29099822050462,
128.79005270507));
#212055=CARTESIAN_POINT('Ctrl Pts',(-28.2448549864461,1.70574390941038,
124.422783015417));
#212056=CARTESIAN_POINT('Ctrl Pts',(-28.523302610259,-4.44700572420938,
125.919871384741));
#212057=CARTESIAN_POINT('Ctrl Pts',(-28.8017502340719,-6.51317434558802,
131.905566738465));
#212058=CARTESIAN_POINT('Ctrl Pts',(-29.0801978578848,-2.59405392962697,
136.879307463993));
#212059=CARTESIAN_POINT('Ctrl Pts',(-29.3586454816977,3.7088753210816,136.270468815306));
#212060=CARTESIAN_POINT('Ctrl Pts',(-29.6370931055106,6.6035293403484,130.638543767126));
#212061=CARTESIAN_POINT('Ctrl Pts',(-29.9155407293234,3.42986249617799,
125.158996303897));
#212062=CARTESIAN_POINT('Ctrl Pts',(-30.1939883531365,-2.89568042388203,
124.86726285355));
#212063=CARTESIAN_POINT('Ctrl Pts',(-30.4724359769491,-6.56023449624756,
130.031432204983));
#212064=CARTESIAN_POINT('Ctrl Pts',(-30.7508836007622,-4.19625355183344,
135.905885007927));
#212065=CARTESIAN_POINT('Ctrl Pts',(-31.029331224575,2.02387940833292,137.092286119451));
#212066=CARTESIAN_POINT('Ctrl Pts',(-31.3077788483879,6.38416606424714,
132.50039087698));
#212067=CARTESIAN_POINT('Ctrl Pts',(-31.5862264722008,4.8777159909692,126.349926681791));
#212068=CARTESIAN_POINT('Ctrl Pts',(-31.8646740960137,-1.11111678833609,
124.292869662384));
#212069=CARTESIAN_POINT('Ctrl Pts',(-32.1431217198266,-6.07888752023319,
128.219554726771));
#212070=CARTESIAN_POINT('Ctrl Pts',(-32.4215693436394,-5.46045759120085,
134.52155013001));
#212071=CARTESIAN_POINT('Ctrl Pts',(-32.7000169674524,0.175866105961793,
137.407629966116));
#212072=CARTESIAN_POINT('Ctrl Pts',(-32.9784645912652,5.65057744328232,
134.225627858545));
#212073=CARTESIAN_POINT('Ctrl Pts',(-33.2569122150782,5.93268415628106,
127.89964829471));
#212074=CARTESIAN_POINT('Ctrl Pts',(-33.535359838891,0.762943957391,124.242957452493));
#212075=CARTESIAN_POINT('Ctrl Pts',(-33.813807462704,-5.10790446645711,
126.615875576613));
#212076=CARTESIAN_POINT('Ctrl Pts',(-34.0922550865168,-6.28483822063666,
132.837806834499));
#212077=CARTESIAN_POINT('Ctrl Pts',(-34.3707027103298,-1.68631268146717,
137.191100358392));
#212078=CARTESIAN_POINT('Ctrl Pts',(-34.6491503341426,4.46185183101625,
135.675292070049));
#212079=CARTESIAN_POINT('Ctrl Pts',(-34.9275979579556,6.5097924843757,129.683335735103));
#212080=CARTESIAN_POINT('Ctrl Pts',(-35.2060455817684,2.57555186563646,
124.721546502031));
#212081=CARTESIAN_POINT('Ctrl Pts',(-35.4844932055813,-3.72549509491909,
125.349566279145));
#212082=CARTESIAN_POINT('Ctrl Pts',(-35.7629408293942,-6.60299406379731,
130.990275571749));
#212083=CARTESIAN_POINT('Ctrl Pts',(-36.0413884532071,-3.41266406223907,
136.460138103909));
#212084=CARTESIAN_POINT('Ctrl Pts',(-36.3198360770199,2.91373749460914,
136.73261742621));
#212085=CARTESIAN_POINT('Ctrl Pts',(-36.5982837008328,6.56255663790157,
131.557318352812));
#212086=CARTESIAN_POINT('Ctrl Pts',(-36.8767313246458,4.18070682967726,
125.690087904753));
#212087=CARTESIAN_POINT('Ctrl Pts',(-37.1551789484586,-2.04300831613737,
124.522624233657));
#212088=CARTESIAN_POINT('Ctrl Pts',(-37.4336265722715,-6.38929862592666,
129.12776941949));
#212089=CARTESIAN_POINT('Ctrl Pts',(-37.7120741960844,-4.86413563307991,
135.273620010322));
#212090=CARTESIAN_POINT('Ctrl Pts',(-37.9905218198973,1.13093038033133,
137.312439554669));
#212091=CARTESIAN_POINT('Ctrl Pts',(-38.2689694437102,6.0867266232385,133.370652493151));
#212092=CARTESIAN_POINT('Ctrl Pts',(-38.5474170675231,5.44911845251588,
127.070568568297));
#212093=CARTESIAN_POINT('Ctrl Pts',(-38.825864691336,-0.195963371833029,
124.201657130839));
#212094=CARTESIAN_POINT('Ctrl Pts',(-39.1043123151489,-5.66096443081045,
127.400307637685));
#212095=CARTESIAN_POINT('Ctrl Pts',(-39.3827599389617,-5.92381573136,133.727116535809));
#212096=CARTESIAN_POINT('Ctrl Pts',(-39.6612075627747,-0.742969769276543,
137.368055529631));
#212097=CARTESIAN_POINT('Ctrl Pts',(-39.9396551865875,5.12062911468111,
134.977279553588));
#212098=CARTESIAN_POINT('Ctrl Pts',(-40.2181028104005,6.27861999888597,
128.751794933764));
#212099=CARTESIAN_POINT('Ctrl Pts',(-40.4965504342133,1.66686583175366,
124.412517903944));
#212100=CARTESIAN_POINT('Ctrl Pts',(-40.7749980580263,-4.47665660383728,
125.947032069068));
#212101=CARTESIAN_POINT('Ctrl Pts',(-41.0534456818391,-6.5063503173351,
131.945193876568));
#212102=CARTESIAN_POINT('Ctrl Pts',(-41.3318933056519,-2.55702594208532,
136.894985651848));
#212103=CARTESIAN_POINT('Ctrl Pts',(-41.6103409294649,3.74208035627896,
136.247790564197));
#212104=CARTESIAN_POINT('Ctrl Pts',(-41.8887885532778,6.60239761801125,
130.598349281928));
#212105=CARTESIAN_POINT('Ctrl Pts',(-42.1672361770906,3.39543401384647,
125.138222352896));
#212106=CARTESIAN_POINT('Ctrl Pts',(-42.4456838009036,-2.93176757287012,
124.884999682853));
#212107=CARTESIAN_POINT('Ctrl Pts',(-42.7241314247165,-6.56481798492739,
130.071380534953));
#212108=CARTESIAN_POINT('Ctrl Pts',(-43.0025790485293,-4.16512137802412,
135.931334274905));
#212109=CARTESIAN_POINT('Ctrl Pts',(-43.2810266723423,2.06211829779186,
137.079849690351));
#212110=CARTESIAN_POINT('Ctrl Pts',(-43.5594742961552,6.39437199801655,
132.461497222591));
#212111=CARTESIAN_POINT('Ctrl Pts',(-43.837921919968,4.85051021450257,126.320317170437));
#212112=CARTESIAN_POINT('Ctrl Pts',(-44.116369543781,-1.150733495542,124.299753988494));
#212113=CARTESIAN_POINT('Ctrl Pts',(-44.3948171675938,-6.09450933963988,
128.256606530968));
#212114=CARTESIAN_POINT('Ctrl Pts',(-44.6732647914067,-5.43772883394191,
134.554720614319));
#212115=CARTESIAN_POINT('Ctrl Pts',(-44.9517124152196,0.216058822326645,
137.406437075925));
#212116=CARTESIAN_POINT('Ctrl Pts',(-45.2301600390324,5.67129897593744,
134.191167801664));
#212117=CARTESIAN_POINT('Ctrl Pts',(-45.5086076628454,5.91489242901924,
127.863588179946));
#212118=CARTESIAN_POINT('Ctrl Pts',(-45.7870552866582,0.722988698391639,
124.238434763679));
#212119=CARTESIAN_POINT('Ctrl Pts',(-46.0655029104712,-5.13330632609627,
126.647046443824));
#212120=CARTESIAN_POINT('Ctrl Pts',(-46.343950534284,-6.27234361285742,
132.876026753548));
#212121=CARTESIAN_POINT('Ctrl Pts',(-46.622398158097,-1.64740354042306,
137.201247090823));
#212122=CARTESIAN_POINT('Ctrl Pts',(-46.9008457819097,4.49141990552312,
135.64804126445));
#212123=CARTESIAN_POINT('Ctrl Pts',(-47.1792934057228,6.50284787635396,
129.643729550545));
#212124=CARTESIAN_POINT('Ctrl Pts',(-47.4577410295356,2.53847633059532,
124.705981087252));
#212125=CARTESIAN_POINT('Ctrl Pts',(-47.7361886533485,-3.75863095151733,
125.372345489915));
#212126=CARTESIAN_POINT('Ctrl Pts',(-48.0146362771614,-6.60174000851572,
131.030466426196));
#212127=CARTESIAN_POINT('Ctrl Pts',(-48.2930839009743,-3.37817251061699,
136.480807170229));
#212128=CARTESIAN_POINT('Ctrl Pts',(-48.5715315247872,2.94977049163681,
136.714770842195));
#212129=CARTESIAN_POINT('Ctrl Pts',(-48.8499791486,6.56701851637621,131.517356257317));
#212130=CARTESIAN_POINT('Ctrl Pts',(-49.128426772413,4.14949734125552,125.664733511282));
#212131=CARTESIAN_POINT('Ctrl Pts',(-49.4068743962258,-2.08120917626415,
124.535176991179));
#212132=CARTESIAN_POINT('Ctrl Pts',(-49.6853220200388,-6.39938613351776,
129.166693957078));
#212133=CARTESIAN_POINT('Ctrl Pts',(-49.9637696438516,-4.83683986146123,
135.303146579501));
#212134=CARTESIAN_POINT('Ctrl Pts',(-50.2422172676646,1.17052595051479,
137.305434680818));
#212135=CARTESIAN_POINT('Ctrl Pts',(-50.5206648914774,6.10223559733929,
133.333553313131));
#212136=CARTESIAN_POINT('Ctrl Pts',(-50.7991125152903,5.42628884099088,
127.03746741615));
#212137=CARTESIAN_POINT('Ctrl Pts',(-51.0775601391032,-0.236152271280866,
124.202972348307));
#212138=CARTESIAN_POINT('Ctrl Pts',(-51.3560077629162,-5.68158098292544,
127.434830604167));
#212139=CARTESIAN_POINT('Ctrl Pts',(-51.634455386729,-5.90591433192304,
133.763122331648));
#212140=CARTESIAN_POINT('Ctrl Pts',(-51.9129030105419,-0.703000929838195,
137.372456587432));
#212141=CARTESIAN_POINT('Ctrl Pts',(-52.1913506343548,5.14593598326309,
134.946031516236));
#212142=CARTESIAN_POINT('Ctrl Pts',(-52.4697982581677,6.26600912069438,
128.713613221033));
#212143=CARTESIAN_POINT('Ctrl Pts',(-52.7482458819806,1.62792598777083,
124.402489644555));
#212144=CARTESIAN_POINT('Ctrl Pts',(-53.0266935057934,-4.50614159930848,
125.97437274349));
#212145=CARTESIAN_POINT('Ctrl Pts',(-53.3051411296064,-6.49928519387843,
131.984778740675));
#212146=CARTESIAN_POINT('Ctrl Pts',(-53.5835887534191,-2.51990320300721,
136.910438149353));
#212147=CARTESIAN_POINT('Ctrl Pts',(-53.8620363772322,3.7751467273123,136.22491060479));
#212148=CARTESIAN_POINT('Ctrl Pts',(-54.140484001045,6.60102124140245,130.558162430556));
#212149=CARTESIAN_POINT('Ctrl Pts',(-54.418931624858,3.36087971245889,125.117658362733));
#212150=CARTESIAN_POINT('Ctrl Pts',(-54.6973792486707,-2.96774608413265,
124.902955856252));
#212151=CARTESIAN_POINT('Ctrl Pts',(-54.9758268724838,-6.56915821186243,
130.111356025769));
#212152=CARTESIAN_POINT('Ctrl Pts',(-55.2542744962966,-4.13383486411065,
135.956593559989));
#212153=CARTESIAN_POINT('Ctrl Pts',(-55.5327221201095,2.10028077469877,
137.067180720695));
#212154=CARTESIAN_POINT('Ctrl Pts',(-55.8111697439224,6.40434098598004,
132.422542162396));
#212155=CARTESIAN_POINT('Ctrl Pts',(-56.0896173677353,4.82312470059616,
126.29087381696));
#212156=CARTESIAN_POINT('Ctrl Pts',(-56.3680649915482,-1.19030756189505,
124.306879345194));
#212157=CARTESIAN_POINT('Ctrl Pts',(-56.646512615361,-6.10990532476174,
128.293752743129));
#212158=CARTESIAN_POINT('Ctrl Pts',(-56.924960239174,-5.41479857964128,
134.587752127659));
#212159=CARTESIAN_POINT('Ctrl Pts',(-57.2034078629868,0.256243532552689,
137.404999543363));
#212160=CARTESIAN_POINT('Ctrl Pts',(-57.4818554867998,5.69181035652338,
134.156582245398));
#212161=CARTESIAN_POINT('Ctrl Pts',(-57.7603031106126,5.89688152324325,
127.827637036585));
#212162=CARTESIAN_POINT('Ctrl Pts',(-58.0387507344255,0.683006648780185,
124.234155377662));
#212163=CARTESIAN_POINT('Ctrl Pts',(-58.3171983582384,-5.15851796918197,
126.67837136184));
#212164=CARTESIAN_POINT('Ctrl Pts',(-58.5956459820513,-6.25961658107885,
132.91416990625));
#212165=CARTESIAN_POINT('Ctrl Pts',(-58.8740936058642,-1.60843335423465,
137.211156784272));
#212166=CARTESIAN_POINT('Ctrl Pts',(-59.1525412296771,4.52082154881365,
135.620610974484));
#212167=CARTESIAN_POINT('Ctrl Pts',(-59.4309888534899,6.49566230291273,
129.604166373598));
#212168=CARTESIAN_POINT('Ctrl Pts',(-59.7094364773029,2.50130673138007,
124.69064165017));
#212169=CARTESIAN_POINT('Ctrl Pts',(-59.9878841011157,-3.79162753066369,
125.395325986002));
#212170=CARTESIAN_POINT('Ctrl Pts',(-60.2663317249287,-6.60024132333016,
131.070648902209));
#212171=CARTESIAN_POINT('Ctrl Pts',(-60.5447793487415,-3.34355577957023,
136.501265893734));
#212172=CARTESIAN_POINT('Ctrl Pts',(-60.8232269725544,2.98569418383416,
136.696705245755));
#212173=CARTESIAN_POINT('Ctrl Pts',(-61.1016745963673,6.57123705156454,
131.477367741508));
#212174=CARTESIAN_POINT('Ctrl Pts',(-61.3801222201802,4.11813409168408,
125.639569568584));
#212175=CARTESIAN_POINT('Ctrl Pts',(-61.6585698439931,-2.11933291641938,
124.547962055604));
#212176=CARTESIAN_POINT('Ctrl Pts',(-61.937017467806,-6.40923650950231,
129.205679179005));
#212177=CARTESIAN_POINT('Ctrl Pts',(-62.2154650916189,-4.80936485896274,
135.332506444514));
#212178=CARTESIAN_POINT('Ctrl Pts',(-62.4939127154318,1.21007814642843,
137.298188907278));
#212179=CARTESIAN_POINT('Ctrl Pts',(-62.7723603392447,6.1175184508558,133.296360412945));
#212180=CARTESIAN_POINT('Ctrl Pts',(-63.0508079630576,5.40325815633759,
127.004505847616));
#212181=CARTESIAN_POINT('Ctrl Pts',(-63.3292555868704,-0.276332420019459,
124.204532182646));
#212182=CARTESIAN_POINT('Ctrl Pts',(-63.6077032106833,-5.70198700196771,
127.469478429822));
#212183=CARTESIAN_POINT('Ctrl Pts',(-63.8861508344962,-5.8877940866586,
133.799018489484));
#212184=CARTESIAN_POINT('Ctrl Pts',(-64.1645984583092,-0.663006040441876,
137.376614262022));
#212185=CARTESIAN_POINT('Ctrl Pts',(-64.4430460821219,5.17105216729505,
134.914630007745));
#212186=CARTESIAN_POINT('Ctrl Pts',(-64.721493705935,6.25316605323042,128.675508981716));
#212187=CARTESIAN_POINT('Ctrl Pts',(-64.9999413297477,1.58892582039159,
124.392698608848));
#212188=CARTESIAN_POINT('Ctrl Pts',(-65.2783889535607,-4.53545961804555,
126.00189239489));
#212189=CARTESIAN_POINT('Ctrl Pts',(-65.5568365773735,-6.49197923701883,
132.024319863954));
#212190=CARTESIAN_POINT('Ctrl Pts',(-65.8352842011867,-2.48268708798906,
136.92566438391));
#212191=CARTESIAN_POINT('Ctrl Pts',(-66.1137318249993,3.80807320889562,
136.201829784909));
#212192=CARTESIAN_POINT('Ctrl Pts',(-66.3921794488124,6.59940026152389,
130.517984702147));
#212193=CARTESIAN_POINT('Ctrl Pts',(-66.6706270726251,3.3262008724376,125.097305095413));
#212194=CARTESIAN_POINT('Ctrl Pts',(-66.9490746964381,-3.00361462447264,
124.921130708376));
#212195=CARTESIAN_POINT('Ctrl Pts',(-67.227522320251,-6.57325501622426,
130.151357196124));
#212196=CARTESIAN_POINT('Ctrl Pts',(-67.5059699440638,-4.10239516942585,
135.981661927186));
#212197=CARTESIAN_POINT('Ctrl Pts',(-67.7844175678767,2.13836542492937,
137.054279679937));
#212198=CARTESIAN_POINT('Ctrl Pts',(-68.0628651916897,6.41407265873309,
132.383527139888));
#212199=CARTESIAN_POINT('Ctrl Pts',(-68.3413128155024,4.79556046403026,
126.261597712398));
#212200=CARTESIAN_POINT('Ctrl Pts',(-68.6197604393155,-1.22983752096341,
124.314245468451));
#212201=CARTESIAN_POINT('Ctrl Pts',(-68.8982080631282,-6.12507490509475,
128.330991986789));
#212202=CARTESIAN_POINT('Ctrl Pts',(-69.1766556869413,-5.39166767798822,
134.620643446035));
#212203=CARTESIAN_POINT('Ctrl Pts',(-69.455103310754,0.296418747580413,
137.403317421698));
#212204=CARTESIAN_POINT('Ctrl Pts',(-69.733550934567,5.7121108249834,134.121872471326));
#212205=CARTESIAN_POINT('Ctrl Pts',(-70.0119985583799,5.87865210635384,
127.791796196812));
#212206=CARTESIAN_POINT('Ctrl Pts',(-70.2904461821926,0.642999290106501,
124.230119453016));
#212207=CARTESIAN_POINT('Ctrl Pts',(-70.5688938060058,-5.18353846148724,
126.709849169906));
#212208=CARTESIAN_POINT('Ctrl Pts',(-70.8473414298183,-6.24665759690589,
132.95223487919));
#212209=CARTESIAN_POINT('Ctrl Pts',(-71.1257890536316,-1.56940356695681,
137.220829071533));
#212210=CARTESIAN_POINT('Ctrl Pts',(-71.4042366774442,4.55005567139915,
135.593002216589));
#212211=CARTESIAN_POINT('Ctrl Pts',(-71.6826843012574,6.48823603031619,
129.56464767029));
#212212=CARTESIAN_POINT('Ctrl Pts',(-71.9611319250699,2.46404444532374,
124.675528759193));
#212213=CARTESIAN_POINT('Ctrl Pts',(-72.2395795488831,-3.82448360965763,
125.418506915858));
#212214=CARTESIAN_POINT('Ctrl Pts',(-72.518027172696,-6.59849806377525,
131.110821510811));
#212215=CARTESIAN_POINT('Ctrl Pts',(-72.7964747965087,-3.30881515183405,
136.52151351632));
#212216=CARTESIAN_POINT('Ctrl Pts',(-73.0749224203217,3.02150724003593,
136.678421306317));
#212217=CARTESIAN_POINT('Ctrl Pts',(-73.3533700441346,6.57521208714753,
131.437354287172));
#212218=CARTESIAN_POINT('Ctrl Pts',(-73.6318176679474,4.08661824313884,
125.614597009117));
#212219=CARTESIAN_POINT('Ctrl Pts',(-73.9102652917603,-2.15737812391465,
124.56097895318));
#212220=CARTESIAN_POINT('Ctrl Pts',(-74.1887129155733,-6.41884938887091,
129.244723640663));
#212221=CARTESIAN_POINT('Ctrl Pts',(-74.4671605393861,-4.78171164368069,
135.361698517417));
#212222=CARTESIAN_POINT('Ctrl Pts',(-74.745608163199,1.24958550245192,137.290702502541));
#212223=CARTESIAN_POINT('Ctrl Pts',(-75.0240557870119,6.13257461747648,
133.25907517079));
#212224=CARTESIAN_POINT('Ctrl Pts',(-75.3025034108249,5.380027251966,126.971685084098));
#212225=CARTESIAN_POINT('Ctrl Pts',(-75.5809510346376,-0.31650232915867,
124.206336576053));
#212226=CARTESIAN_POINT('Ctrl Pts',(-75.8593986584506,-5.72218173178456,
127.504249830764));
#212227=CARTESIAN_POINT('Ctrl Pts',(-76.1378462822634,-5.86945566701928,
133.83480367917));
#212228=CARTESIAN_POINT('Ctrl Pts',(-76.4162939060764,-0.622986583113102,
137.380528399336));
#212229=CARTESIAN_POINT('Ctrl Pts',(-76.6947415298893,5.19597673608708,
134.88307619171));
#212230=CARTESIAN_POINT('Ctrl Pts',(-76.9731891537022,6.24009127239896,
128.637483627779));
#212231=CARTESIAN_POINT('Ctrl Pts',(-77.2516367775151,1.54986677478153,
124.383145159635));
#212232=CARTESIAN_POINT('Ctrl Pts',(-77.5300844013279,-4.56460957365852,
126.029590003516));
#212233=CARTESIAN_POINT('Ctrl Pts',(-77.8085320251407,-6.48443271748106,
132.063815781194));
#212234=CARTESIAN_POINT('Ctrl Pts',(-78.0869796489538,-2.44537897608793,
136.940663791305));
#212235=CARTESIAN_POINT('Ctrl Pts',(-78.3654272727665,3.84085858092573,
136.178548959823));
#212236=CARTESIAN_POINT('Ctrl Pts',(-78.6438748965796,6.5975347384416,130.477817585504));
#212237=CARTESIAN_POINT('Ctrl Pts',(-78.9223225203923,3.29139877882003,
125.077163305135));
#212238=CARTESIAN_POINT('Ctrl Pts',(-79.2007701442053,-3.03937186476788,
124.939523565746));
#212239=CARTESIAN_POINT('Ctrl Pts',(-79.4792177680182,-6.57710824620412,
130.191382563762));
#212240=CARTESIAN_POINT('Ctrl Pts',(-79.7576653918309,-4.07080345897965,
136.00653844758));
#212241=CARTESIAN_POINT('Ctrl Pts',(-80.036113015644,2.17637083724304,137.041147046131));
#212242=CARTESIAN_POINT('Ctrl Pts',(-80.314560639457,6.42356665566488,132.344453600785));
#212243=CARTESIAN_POINT('Ctrl Pts',(-80.5930082632696,4.76781852620778,
126.232489941585));
#212244=CARTESIAN_POINT('Ctrl Pts',(-80.8714558870828,-1.26932190795047,
124.321852085313));
#212245=CARTESIAN_POINT('Ctrl Pts',(-81.1499035108954,-6.14001751852468,
128.368322882032));
#212246=CARTESIAN_POINT('Ctrl Pts',(-81.4283511347085,-5.36833698610627,
134.653393350648));
#212247=CARTESIAN_POINT('Ctrl Pts',(-81.7067987585213,0.336582978702201,
137.401390773263));
#212248=CARTESIAN_POINT('Ctrl Pts',(-81.9852463823341,5.73219962907597,
134.087039765632));
#212249=CARTESIAN_POINT('Ctrl Pts',(-82.2636940061471,5.86020485384888,
127.756066988721));
#212250=CARTESIAN_POINT('Ctrl Pts',(-82.54214162996,0.602968104857597,124.226327139294));
#212251=CARTESIAN_POINT('Ctrl Pts',(-82.8205892537728,-5.20836687586887,
126.741478701599));
#212252=CARTESIAN_POINT('Ctrl Pts',(-83.0990368775859,-6.23346714053832,
132.990220261861));
#212253=CARTESIAN_POINT('Ctrl Pts',(-83.3774845013985,-1.53031562485268,
137.230263594196));
#212254=CARTESIAN_POINT('Ctrl Pts',(-83.6559321252116,4.57912118999838,
135.56521601382));
#212255=CARTESIAN_POINT('Ctrl Pts',(-83.9343797490243,6.48056933374724,
129.525174905002));
#212256=CARTESIAN_POINT('Ctrl Pts',(-84.2128273728376,2.42669085319518,
124.660642974335));
#212257=CARTESIAN_POINT('Ctrl Pts',(-84.4912749966499,-3.85719797100462,
125.441887420503));
#212258=CARTESIAN_POINT('Ctrl Pts',(-84.7697226204634,-6.59651029444787,
131.150982763393));
#212259=CARTESIAN_POINT('Ctrl Pts',(-85.0481702442759,-3.27395191473627,
136.541549287701));
#212260=CARTESIAN_POINT('Ctrl Pts',(-85.326617868089,3.05720833317481,136.659919701402));
#212261=CARTESIAN_POINT('Ctrl Pts',(-85.6050654919017,6.57894347582879,
131.397317377022));
#212262=CARTESIAN_POINT('Ctrl Pts',(-85.8835131157147,4.05495096345227,
125.58981675825));
#212263=CARTESIAN_POINT('Ctrl Pts',(-86.1619607395276,-2.19534338896908,
124.574227201559));
#212264=CARTESIAN_POINT('Ctrl Pts',(-86.4404083633404,-6.42822441541511,
129.283825895241));
#212265=CARTESIAN_POINT('Ctrl Pts',(-86.7188559871533,-4.75388124031539,
135.390721716488));
#212266=CARTESIAN_POINT('Ctrl Pts',(-86.9973036109663,1.28904655462414,
137.282975744021));
#212267=CARTESIAN_POINT('Ctrl Pts',(-87.2757512347791,6.14740353928957,
133.221698968287));
#212268=CARTESIAN_POINT('Ctrl Pts',(-87.554198858592,5.35659698870609,126.939006341782));
#212269=CARTESIAN_POINT('Ctrl Pts',(-87.8326464824051,-0.356660510187587,
124.208385461669));
#212270=CARTESIAN_POINT('Ctrl Pts',(-88.1110941062178,-5.74216442405318,
127.539143518524));
#212271=CARTESIAN_POINT('Ctrl Pts',(-88.3895417300309,-5.85089975254147,
133.870476574676));
#212272=CARTESIAN_POINT('Ctrl Pts',(-88.6679893538435,-0.582944040787213,
137.384198854334));
#212273=CARTESIAN_POINT('Ctrl Pts',(-88.9464369776566,5.22070876605056,
134.851371237371));
#212274=CARTESIAN_POINT('Ctrl Pts',(-89.2248846014694,6.22678526269035,
128.599538568266));
#212275=CARTESIAN_POINT('Ctrl Pts',(-89.5033322252823,1.51075029828878,
124.373829650922));
#212276=CARTESIAN_POINT('Ctrl Pts',(-89.7817798490951,-4.59359038598471,
126.057464543021));
#212277=CARTESIAN_POINT('Ctrl Pts',(-90.0602274729082,-6.47664591490472,
132.103265028861));
#212278=CARTESIAN_POINT('Ctrl Pts',(-90.338675096721,-2.40798024976945,
136.955435815729));
#212279=CARTESIAN_POINT('Ctrl Pts',(-90.6171227205338,3.87350162852866,
136.155068992212));
#212280=CARTESIAN_POINT('Ctrl Pts',(-90.8955703443469,6.59542474128344,
130.437662569033));
#212281=CARTESIAN_POINT('Ctrl Pts',(-91.1740179681596,3.25647472121003,
125.057233738258));
#212282=CARTESIAN_POINT('Ctrl Pts',(-91.4524655919725,-3.07501648002118,
124.958133746811));
#212283=CARTESIAN_POINT('Ctrl Pts',(-91.7309132157855,-6.58071775901922,
130.231430645527));
#212284=CARTESIAN_POINT('Ctrl Pts',(-92.0093608395982,-4.03906090341396,
136.031222199361));
#212285=CARTESIAN_POINT('Ctrl Pts',(-92.2878084634112,2.21429560333469,
137.027783305909));
#212286=CARTESIAN_POINT('Ctrl Pts',(-92.5662560872241,6.4328226249721,132.305322992969));
#212287=CARTESIAN_POINT('Ctrl Pts',(-92.844703711037,4.73989991511645,126.203551583122));
#212288=CARTESIAN_POINT('Ctrl Pts',(-93.1231513348499,-1.30875925974737,
124.329698913911));
#212289=CARTESIAN_POINT('Ctrl Pts',(-93.4015989586628,-6.15473261134757,
128.40574404555));
#212290=CARTESIAN_POINT('Ctrl Pts',(-93.6800465824757,-5.34480736852315,
134.686000627937));
#212291=CARTESIAN_POINT('Ctrl Pts',(-93.9584942062885,0.37673473761816,
137.399219669449));
#212292=CARTESIAN_POINT('Ctrl Pts',(-94.2369418301014,5.75207602440345,
134.052085419056));
#212293=CARTESIAN_POINT('Ctrl Pts',(-94.5153894539144,5.84154044929785,
127.720450736271));
#212294=CARTESIAN_POINT('Ctrl Pts',(-94.7938370777271,0.56291457640357,
124.222778577022));
#212295=CARTESIAN_POINT('Ctrl Pts',(-95.0722847015402,-5.23300229230026,
126.773258784876));
#212296=CARTESIAN_POINT('Ctrl Pts',(-95.350732325353,-6.22004570075364,
133.028124646699));
#212297=CARTESIAN_POINT('Ctrl Pts',(-95.6291799491659,-1.49117097634027,
137.239460002661));
#212298=CARTESIAN_POINT('Ctrl Pts',(-95.9076275729788,4.60801702757804,
135.537253395802));
#212299=CARTESIAN_POINT('Ctrl Pts',(-96.1860751967916,6.47266249729856,
129.48574954041));
#212300=CARTESIAN_POINT('Ctrl Pts',(-96.4645228206046,2.38924733914408,
124.645984847192));
#212301=CARTESIAN_POINT('Ctrl Pts',(-96.7429704444176,-3.88976940246256,
125.465466633565));
#212302=CARTESIAN_POINT('Ctrl Pts',(-97.0214180682302,-6.59427808900543,
131.191131171763));
#212303=CARTESIAN_POINT('Ctrl Pts',(-97.2998656920433,-3.23896736014657,
136.561372465446));
#212304=CARTESIAN_POINT('Ctrl Pts',(-97.5783133158561,3.09279614033489,
136.641201116591));
#212305=CARTESIAN_POINT('Ctrl Pts',(-97.856760939669,6.58243107933991,131.357258494642));
#212306=CARTESIAN_POINT('Ctrl Pts',(-98.135208563482,4.02313342606635,125.565229734223));
#212307=CARTESIAN_POINT('Ctrl Pts',(-98.4136561872948,-2.2332273047675,
124.587706309824));
#212308=CARTESIAN_POINT('Ctrl Pts',(-98.6921038111079,-6.43736124173946,
129.322984493793));
#212309=CARTESIAN_POINT('Ctrl Pts',(-98.9705514349205,-4.72587468013238,
135.419574966262));
#212310=CARTESIAN_POINT('Ctrl Pts',(-99.2489990587337,1.32845984070286,
137.275008918035));
#212311=CARTESIAN_POINT('Ctrl Pts',(-99.5274466825463,6.16200466680371,
133.184233190419));
#212312=CARTESIAN_POINT('Ctrl Pts',(-99.8058943063594,5.3329682347749,126.906470831589));
#212313=CARTESIAN_POINT('Ctrl Pts',(-100.084341930172,-0.396805475030165,
124.210678763569));
#212314=CARTESIAN_POINT('Ctrl Pts',(-100.362789553985,-5.76193433830736,
127.574158200105));
#212315=CARTESIAN_POINT('Ctrl Pts',(-100.641237177798,-5.83212703082168,
133.906035854126));
#212316=CARTESIAN_POINT('Ctrl Pts',(-100.919684801611,-0.542879897255484,
137.387625491007));
#212317=CARTESIAN_POINT('Ctrl Pts',(-101.198132425424,5.24524734073077,
134.819516319564));
#212318=CARTESIAN_POINT('Ctrl Pts',(-101.476580049237,6.21324851716398,
128.561675209245));
#212319=CARTESIAN_POINT('Ctrl Pts',(-101.75502767305,1.47157784038775,124.3647524279));
#212320=CARTESIAN_POINT('Ctrl Pts',(-102.033475296863,-4.62240098113028,
126.085514980508));
#212321=CARTESIAN_POINT('Ctrl Pts',(-102.311922920676,-6.4686191178319,
132.142666145147));
#212322=CARTESIAN_POINT('Ctrl Pts',(-102.590370544489,-2.3704922948573,
136.969979909799));
#212323=CARTESIAN_POINT('Ctrl Pts',(-102.868818168302,3.90600114210426,
136.131390752135));
#212324=CARTESIAN_POINT('Ctrl Pts',(-103.147265792114,6.59307034823604,
130.397521140692));
#212325=CARTESIAN_POINT('Ctrl Pts',(-103.425713415927,3.22142999373166,
125.037517133282));
#212326=CARTESIAN_POINT('Ctrl Pts',(-103.70416103974,-3.11054714940797,
124.976960561963));
#212327=CARTESIAN_POINT('Ctrl Pts',(-103.982608663553,-6.58408342091771,
130.271499957422));
#212328=CARTESIAN_POINT('Ctrl Pts',(-104.261056287366,-4.00716867896111,
136.055712267864));
#212329=CARTESIAN_POINT('Ctrl Pts',(-104.539503911179,2.25213831788793,
137.014188954471));
#212330=CARTESIAN_POINT('Ctrl Pts',(-104.817951534992,6.44184022367115,
132.266136766442));
#212331=CARTESIAN_POINT('Ctrl Pts',(-105.096399158805,4.71180566529118,
126.17478370933));
#212332=CARTESIAN_POINT('Ctrl Pts',(-105.374846782618,-1.34814811498862,
124.337785663482));
#212333=CARTESIAN_POINT('Ctrl Pts',(-105.65329440643,-6.16921963829011,
128.443254090687));
#212334=CARTESIAN_POINT('Ctrl Pts',(-105.931742030243,-5.32107969713743,
134.718464069627));
#212335=CARTESIAN_POINT('Ctrl Pts',(-106.210189654056,0.416872536489867,
137.396804190707));
#212336=CARTESIAN_POINT('Ctrl Pts',(-106.488637277869,5.77173927443855,
134.017010726842));
#212337=CARTESIAN_POINT('Ctrl Pts',(-106.767084901682,5.82265958431723,
127.684948759235));
#212338=CARTESIAN_POINT('Ctrl Pts',(-107.045532525495,0.52284018894291,
124.219473897692));
#212339=CARTESIAN_POINT('Ctrl Pts',(-107.323980149308,-5.25744379790729,
126.805188242113));
#212340=CARTESIAN_POINT('Ctrl Pts',(-107.602427773121,-6.20639377488812,
133.065946629143));
#212341=CARTESIAN_POINT('Ctrl Pts',(-107.880875396933,-1.45197107193893,
137.248417956151));
#212342=CARTESIAN_POINT('Ctrl Pts',(-108.159323020746,4.63674211339212,
135.509115398702));
#212343=CARTESIAN_POINT('Ctrl Pts',(-108.437770644559,6.46451581396073,
129.446373037437));
#212344=CARTESIAN_POINT('Ctrl Pts',(-108.716218268372,2.35171529065418,
124.631554920928));
#212345=CARTESIAN_POINT('Ctrl Pts',(-108.994665892185,-3.92219669708481,
125.489243681306));
#212346=CARTESIAN_POINT('Ctrl Pts',(-109.273113515998,-6.59180153016358,
131.231265248209));
#212347=CARTESIAN_POINT('Ctrl Pts',(-109.551561139811,-3.20386278442967,
136.580982315001));
#212348=CARTESIAN_POINT('Ctrl Pts',(-109.830008763624,3.12826934279688,
136.622266245509));
#212349=CARTESIAN_POINT('Ctrl Pts',(-110.108456387437,6.5856747684467,131.317179124427));
#212350=CARTESIAN_POINT('Ctrl Pts',(-110.38690401125,3.99116680999183,125.540836848117));
#212351=CARTESIAN_POINT('Ctrl Pts',(-110.665351635062,-2.27102846750687,
124.601415778499));
#212352=CARTESIAN_POINT('Ctrl Pts',(-110.943799258875,-6.44625952927566,
129.362197985281));
#212353=CARTESIAN_POINT('Ctrl Pts',(-111.222246882688,-4.69769300092514,
135.448257197571));
#212354=CARTESIAN_POINT('Ctrl Pts',(-111.500694506501,1.36782390021364,
137.266802319797));
#212355=CARTESIAN_POINT('Ctrl Pts',(-111.779142130314,6.17637745896884,
133.1466792255));
#212356=CARTESIAN_POINT('Ctrl Pts',(-112.057589754127,5.30914186574463,
126.874079759138));
#212357=CARTESIAN_POINT('Ctrl Pts',(-112.33603737794,-0.436935736099303,
124.213216396775));
#212358=CARTESIAN_POINT('Ctrl Pts',(-112.614485001753,-5.78149074196569,
127.609292578024));
#212359=CARTESIAN_POINT('Ctrl Pts',(-112.892932625565,-5.81313819748998,
133.94148019986));
#212360=CARTESIAN_POINT('Ctrl Pts',(-113.171380249379,-0.502795637109545,
137.390808182378));
#212361=CARTESIAN_POINT('Ctrl Pts',(-113.449827873191,5.26959155084185,
134.787512618686));
#212362=CARTESIAN_POINT('Ctrl Pts',(-113.728275497004,6.19948153742887,
128.523894953756));
#212363=CARTESIAN_POINT('Ctrl Pts',(-114.006723120817,1.43235085262869,
124.355913826926));
#212364=CARTESIAN_POINT('Ctrl Pts',(-114.28517074463,-4.65104029150761,
126.113740276555));
#212365=CARTESIAN_POINT('Ctrl Pts',(-114.563618368443,-6.46035262369882,
132.182017670029));
#212366=CARTESIAN_POINT('Ctrl Pts',(-114.842065992256,-2.33291650048142,
136.984295534578));
#212367=CARTESIAN_POINT('Ctrl Pts',(-115.120513616069,3.93835591737112,
136.107515116997));
#212368=CARTESIAN_POINT('Ctrl Pts',(-115.398961239881,6.59047164654225,
130.357394787938));
#212369=CARTESIAN_POINT('Ctrl Pts',(-115.677408863695,3.18626589498021,
125.018014220813));
#212370=CARTESIAN_POINT('Ctrl Pts',(-115.955856487507,-3.14596255632626,
124.996003313566));
#212371=CARTESIAN_POINT('Ctrl Pts',(-116.23430411132,-6.58720510718372,
130.311589014666));
#212372=CARTESIAN_POINT('Ctrl Pts',(-116.512751735133,-3.97512796739924,
136.0800077456));
#212373=CARTESIAN_POINT('Ctrl Pts',(-116.791199358946,2.28989757862811,
137.00036449556));
#212374=CARTESIAN_POINT('Ctrl Pts',(-117.069646982759,6.45061911761184,
132.226896373261));
#212375=CARTESIAN_POINT('Ctrl Pts',(-117.348094606572,4.68353681777373,
126.146187386213));
#212376=CARTESIAN_POINT('Ctrl Pts',(-117.626542230384,-1.38748701410568,
124.346112034364));
#212377=CARTESIAN_POINT('Ctrl Pts',(-117.904989854198,-6.18347806253024,
128.480851627495));
#212378=CARTESIAN_POINT('Ctrl Pts',(-118.18343747801,-5.29715485118671,
134.750782472776));
#212379=CARTESIAN_POINT('Ctrl Pts',(-118.461885101824,0.45699488799644,
137.394144426544));
#212380=CARTESIAN_POINT('Ctrl Pts',(-118.740332725636,5.79118865055225,
133.981816988697));
#212381=CARTESIAN_POINT('Ctrl Pts',(-119.018780349449,5.80356295854445,
127.649562373154));
#212382=CARTESIAN_POINT('Ctrl Pts',(-119.297227973262,0.482746427446748,
124.216413223762));
#212383=CARTESIAN_POINT('Ctrl Pts',(-119.575675597075,-5.28169048700048,
126.837265890154));
#212384=CARTESIAN_POINT('Ctrl Pts',(-119.854123220888,-6.19251186881905,
133.103684807684));
#212385=CARTESIAN_POINT('Ctrl Pts',(-120.132570844701,-1.41271736421608,
137.257137122728));
#212386=CARTESIAN_POINT('Ctrl Pts',(-120.411018468513,4.66529538302207,
135.480803065184));
#212387=CARTESIAN_POINT('Ctrl Pts',(-120.689466092327,6.45612958561205,
129.407046855192));
#212388=CARTESIAN_POINT('Ctrl Pts',(-120.967913716139,2.31409609848935,
124.61735373025));
#212389=CARTESIAN_POINT('Ctrl Pts',(-121.246361339953,-3.95447865326606,
125.51321768266));
#212390=CARTESIAN_POINT('Ctrl Pts',(-121.524808963765,-6.5890807096919,
131.271383505546));
#212391=CARTESIAN_POINT('Ctrl Pts',(-121.803256587578,-3.16863948839908,
136.600378109714));
#212392=CARTESIAN_POINT('Ctrl Pts',(-122.081704211391,3.16362662608795,
136.603115789794));
#212393=CARTESIAN_POINT('Ctrl Pts',(-122.360151835204,6.58867442295306,
131.277080751534));
#212394=CARTESIAN_POINT('Ctrl Pts',(-122.638599459017,3.9590522997634,125.51663900382));
#212395=CARTESIAN_POINT('Ctrl Pts',(-122.91704708283,-2.30874547645122,
124.615355099576));
#212396=CARTESIAN_POINT('Ctrl Pts',(-123.195494706643,-6.45491894829438,
129.401464916637));
#212397=CARTESIAN_POINT('Ctrl Pts',(-123.473942330455,-4.66933724697619,
135.476767347585));
#212398=CARTESIAN_POINT('Ctrl Pts',(-123.752389954268,1.40713727450679,
137.258356253404));
#212399=CARTESIAN_POINT('Ctrl Pts',(-124.030837578081,6.19052138319586,
133.109038465103));
#212400=CARTESIAN_POINT('Ctrl Pts',(-124.309285201894,5.28511876451003,
126.841834324687));
#212401=CARTESIAN_POINT('Ctrl Pts',(-124.587732825707,-0.477049806354697,
124.215998267256));
#212402=CARTESIAN_POINT('Ctrl Pts',(-124.86618044952,-5.80083291035842,
127.644545350364));
#212403=CARTESIAN_POINT('Ctrl Pts',(-125.144628073333,-5.79393395618462,
133.976808298475));
#212404=CARTESIAN_POINT('Ctrl Pts',(-125.423075697146,-0.462692745686338,
137.393746810514));
#212405=CARTESIAN_POINT('Ctrl Pts',(-125.701523320958,5.2937404943001,134.755361320645));
#212406=CARTESIAN_POINT('Ctrl Pts',(-125.979970944772,6.18548483362552,
128.486199201761));
#212407=CARTESIAN_POINT('Ctrl Pts',(-126.258418568584,1.39307078858202,
124.34731417552));
#212408=CARTESIAN_POINT('Ctrl Pts',(-126.536866192397,-4.67950725587653,
126.142139385264));
#212409=CARTESIAN_POINT('Ctrl Pts',(-126.81531381621,-6.45184673882346,
132.221318145323));
#212410=CARTESIAN_POINT('Ctrl Pts',(-127.093761440023,-2.29525425902701,
136.998382159598));
#212411=CARTESIAN_POINT('Ctrl Pts',(-127.372209063836,3.97056475541062,
136.083442971518));
#212412=CARTESIAN_POINT('Ctrl Pts',(-127.650656687649,6.58762873249828,
130.317284997668));
#212413=CARTESIAN_POINT('Ctrl Pts',(-127.929104311462,3.15098372797424,
124.998725723536));
#212414=CARTESIAN_POINT('Ctrl Pts',(-128.207551935275,-3.18126138844507,
125.015261295985));
#212415=CARTESIAN_POINT('Ctrl Pts',(-128.485999559087,-6.59008270214206,
130.351696331743));
#212416=CARTESIAN_POINT('Ctrl Pts',(-128.764447182901,-3.94293995600869,
136.104107732291));
#212417=CARTESIAN_POINT('Ctrl Pts',(-129.042894806713,2.32757198637139,
136.986310441447));
#212418=CARTESIAN_POINT('Ctrl Pts',(-129.321342430526,6.45915898148892,
132.187603267495));
#212419=CARTESIAN_POINT('Ctrl Pts',(-129.599790054339,4.6550944200771,126.117763673416));
#212420=CARTESIAN_POINT('Ctrl Pts',(-129.878237678152,-1.42677449938118,
124.354677718024));
#212421=CARTESIAN_POINT('Ctrl Pts',(-130.156685301965,-6.19750735571679,
128.518535262782));
#212422=CARTESIAN_POINT('Ctrl Pts',(-130.435132925778,-5.27303371721495,
134.782954639811));
#212423=CARTESIAN_POINT('Ctrl Pts',(-130.713580549591,0.497100305389368,
137.391240475519));
#212424=CARTESIAN_POINT('Ctrl Pts',(-130.992028173403,5.81042343204081,
133.946505508738));
#212425=CARTESIAN_POINT('Ctrl Pts',(-131.270475797217,5.78425127961196,
127.614292889281));
#212426=CARTESIAN_POINT('Ctrl Pts',(-131.548923421029,0.442634777604211,
124.213596668645));
#212427=CARTESIAN_POINT('Ctrl Pts',(-131.827371044842,-5.30574146111081,
126.869490540348));
#212428=CARTESIAN_POINT('Ctrl Pts',(-132.105818668655,-6.17840049694519,
133.141337783923));
#212429=CARTESIAN_POINT('Ctrl Pts',(-132.384266292468,-1.37341130773126,
137.265617179298));
#212430=CARTESIAN_POINT('Ctrl Pts',(-132.662713916281,4.69367577841589,
135.45231744437));
#212431=CARTESIAN_POINT('Ctrl Pts',(-132.941161540094,6.44750412300737,
129.367772450924));
#212432=CARTESIAN_POINT('Ctrl Pts',(-133.219609163907,2.27639115664257,
124.603381801387));
#212433=CARTESIAN_POINT('Ctrl Pts',(-133.49805678772,-3.98661407478655,
125.537387749261));
#212434=CARTESIAN_POINT('Ctrl Pts',(-133.776504411532,-6.58611572841139,
131.311484457178));
#212435=CARTESIAN_POINT('Ctrl Pts',(-134.054952035345,-3.13329877726696,
136.619559130867));
#212436=CARTESIAN_POINT('Ctrl Pts',(-134.333399659158,3.19886668003099,
136.583750459073));
#212437=CARTESIAN_POINT('Ctrl Pts',(-134.611847282971,6.59142993170542,
131.236964861823));
#212438=CARTESIAN_POINT('Ctrl Pts',(-134.890294906784,3.92679108539655,
125.492637097993));
#212439=CARTESIAN_POINT('Ctrl Pts',(-135.168742530597,-2.34637693398254,
124.629523756529));
#212440=CARTESIAN_POINT('Ctrl Pts',(-135.44719015441,-6.46333917791768,
129.440783832808));
#212441=CARTESIAN_POINT('Ctrl Pts',(-135.725637778223,-4.64080846901838,
135.505104359849));
#212442=CARTESIAN_POINT('Ctrl Pts',(-136.004085402036,1.44639850681073,
137.24967103183));
#212443=CARTESIAN_POINT('Ctrl Pts',(-136.282533025848,6.20443591537649,
133.07131230402));
#212444=CARTESIAN_POINT('Ctrl Pts',(-136.560980649661,5.26089982125598,
126.809735723105));
#212445=CARTESIAN_POINT('Ctrl Pts',(-136.839428273474,-0.517146199354053,
124.219024271924));
#212446=CARTESIAN_POINT('Ctrl Pts',(-137.117875897287,-5.81996012675442,
127.679915210822));
#212447=CARTESIAN_POINT('Ctrl Pts',(-137.3963235211,-5.77451501852576,134.012018840873));
#212448=CARTESIAN_POINT('Ctrl Pts',(-137.674771144913,-0.422572709013315,
137.396441266521));
#212449=CARTESIAN_POINT('Ctrl Pts',(-137.953218768726,5.31769327625758,
134.723063616821));
#212450=CARTESIAN_POINT('Ctrl Pts',(-138.231666392539,6.17125892440694,
128.448589350091));
#212451=CARTESIAN_POINT('Ctrl Pts',(-138.510114016352,1.35373910378499,
124.338953792345));
#212452=CARTESIAN_POINT('Ctrl Pts',(-138.788561640165,-4.70780081938319,
126.170711254294));
#212453=CARTESIAN_POINT('Ctrl Pts',(-139.067009263977,-6.44310177839452,
132.260566114734));
#212454=CARTESIAN_POINT('Ctrl Pts',(-139.34545688779,-2.25750696608163,
137.012239262869));
#212455=CARTESIAN_POINT('Ctrl Pts',(-139.623904511603,4.00262646271346,
136.059175207703));
#212456=CARTESIAN_POINT('Ctrl Pts',(-139.902352135416,6.5845417114487,130.277193256163));
#212457=CARTESIAN_POINT('Ctrl Pts',(-140.180799759229,3.11558480010749,
124.979652356196));
#212458=CARTESIAN_POINT('Ctrl Pts',(-140.459247383042,-3.21644233775325,
125.034733795609));
#212459=CARTESIAN_POINT('Ctrl Pts',(-140.737695006855,-6.59271609916233,
130.391820422461));
#212460=CARTESIAN_POINT('Ctrl Pts',(-141.016142630668,-3.91060583752806,
136.128011334905));
#212461=CARTESIAN_POINT('Ctrl Pts',(-141.294590254481,2.36516014507876,
136.97202731291));
#212462=CARTESIAN_POINT('Ctrl Pts',(-141.573037878293,6.46745949885459,
132.148258905163));
#212463=CARTESIAN_POINT('Ctrl Pts',(-141.851485502106,4.62647952614482,
126.089513624195));
#212464=CARTESIAN_POINT('Ctrl Pts',(-142.129933125919,-1.4660091150024,
124.363482397054));
#212465=CARTESIAN_POINT('Ctrl Pts',(-142.408380749732,-6.21130699798892,
128.556303600169));
#212466=CARTESIAN_POINT('Ctrl Pts',(-142.686828373545,-5.24871718904012,
134.814979378581));
#212467=CARTESIAN_POINT('Ctrl Pts',(-142.965275997358,0.537187302547703,
137.388092445238));
#212468=CARTESIAN_POINT('Ctrl Pts',(-143.243723621171,5.82944290615228,
133.911077595444));
#212469=CARTESIAN_POINT('Ctrl Pts',(-143.522171244983,5.76472526312116,
127.579141614542));
#212470=CARTESIAN_POINT('Ctrl Pts',(-143.800618868797,0.402506725767204,
124.21102433671));
#212471=CARTESIAN_POINT('Ctrl Pts',(-144.079066492609,-5.32959582902011,
126.901860998601));
#212472=CARTESIAN_POINT('Ctrl Pts',(-144.357514116423,-6.1640601821688,
133.178904162615));
#212473=CARTESIAN_POINT('Ctrl Pts',(-144.635961740235,-1.33405435898536,
137.27385781163));
#212474=CARTESIAN_POINT('Ctrl Pts',(-144.914409364048,4.72188224792766,
135.423659591808));
#212475=CARTESIAN_POINT('Ctrl Pts',(-145.192856987861,6.43863974576633,
129.328551279958));
#212476=CARTESIAN_POINT('Ctrl Pts',(-145.471304611674,2.23860186228433,
124.589639652074));
#212477=CARTESIAN_POINT('Ctrl Pts',(-145.749752235487,-4.01860177085642,
125.56175298548));
#212478=CARTESIAN_POINT('Ctrl Pts',(-146.0281998593,-6.58290669619051,131.35156661715));
#212479=CARTESIAN_POINT('Ctrl Pts',(-146.306647483113,-3.09784196059638,
136.638524667701));
#212480=CARTESIAN_POINT('Ctrl Pts',(-146.585095106925,3.2339881987928,136.564170970937));
#212481=CARTESIAN_POINT('Ctrl Pts',(-146.863542730738,6.59394119259793,
131.196832941802));
#212482=CARTESIAN_POINT('Ctrl Pts',(-147.141990354551,3.89438436234147,
125.468832020033));
#212483=CARTESIAN_POINT('Ctrl Pts',(-147.420437978364,-2.38392144565404,
124.643921224334));
#212484=CARTESIAN_POINT('Ctrl Pts',(-147.698885602177,-6.47151990613084,
129.480153276819));
#212485=CARTESIAN_POINT('Ctrl Pts',(-147.97733322599,-4.61210772419611,
135.533267184325));
#212486=CARTESIAN_POINT('Ctrl Pts',(-148.255780849803,1.48560614228611,
137.240746976909));
#212487=CARTESIAN_POINT('Ctrl Pts',(-148.534228473616,6.21812053990256,
133.033502140209));
#212488=CARTESIAN_POINT('Ctrl Pts',(-148.812676097428,5.23648593342438,
126.777785143819));
#212489=CARTESIAN_POINT('Ctrl Pts',(-149.091123721242,-0.557223429310831,
124.222294298654));
#212490=CARTESIAN_POINT('Ctrl Pts',(-149.369571345054,-5.83887168238761,
127.715400848752));
#212491=CARTESIAN_POINT('Ctrl Pts',(-149.648018968867,-5.75488210408933,
134.047110522317));
#212492=CARTESIAN_POINT('Ctrl Pts',(-149.92646659268,-0.382437013753756,
137.398891450554));
#212493=CARTESIAN_POINT('Ctrl Pts',(-150.204914216493,5.34144900913504,
134.690620704017));
#212494=CARTESIAN_POINT('Ctrl Pts',(-150.483361840306,6.15680433691945,
128.411066792389));
#212495=CARTESIAN_POINT('Ctrl Pts',(-150.761809464119,1.31435725568762,
124.330832987197));
#212496=CARTESIAN_POINT('Ctrl Pts',(-151.040257087932,-4.73591993359918,
126.199454824906));
#212497=CARTESIAN_POINT('Ctrl Pts',(-151.318704711745,-6.43411806645975,
132.299760123916));
#212498=CARTESIAN_POINT('Ctrl Pts',(-151.597152335558,-2.21967602038541,
137.025866330917));
#212499=CARTESIAN_POINT('Ctrl Pts',(-151.87559995937,4.03453985122072,136.034712724799));
#212500=CARTESIAN_POINT('Ctrl Pts',(-152.154047583183,6.58121069778455,
130.237121049039));
#212501=CARTESIAN_POINT('Ctrl Pts',(-152.432495206996,3.08007042310019,
124.960794825562));
#212502=CARTESIAN_POINT('Ctrl Pts',(-152.710942830809,-3.25150410060774,
125.054420090877));
#212503=CARTESIAN_POINT('Ctrl Pts',(-152.989390454622,-6.59510520066311,
130.431959800007));
#212504=CARTESIAN_POINT('Ctrl Pts',(-153.267838078435,-3.87812681010997,
136.151717667683));
#212505=CARTESIAN_POINT('Ctrl Pts',(-153.546285702248,2.40266066190714,
136.957515639215));
#212506=CARTESIAN_POINT('Ctrl Pts',(-153.824733326061,6.47552036213011,
132.108864744186));
#212507=CARTESIAN_POINT('Ctrl Pts',(-154.103180949873,4.59769319631231,
126.061438285362));
#212508=CARTESIAN_POINT('Ctrl Pts',(-154.381628573686,-1.50518940711724,
124.372525745196));
#212509=CARTESIAN_POINT('Ctrl Pts',(-154.660076197499,-6.22487647799626,
128.594155240135));
#212510=CARTESIAN_POINT('Ctrl Pts',(-154.938523821312,-5.22420616771914,
134.846855502398));
#212511=CARTESIAN_POINT('Ctrl Pts',(-155.216971445125,0.577254394032953,
137.384700452354));
#212512=CARTESIAN_POINT('Ctrl Pts',(-155.495419068938,5.84824636811312,
133.87553456161));
#212513=CARTESIAN_POINT('Ctrl Pts',(-155.773866692751,5.74498563261573,
127.544109851479));
#212514=CARTESIAN_POINT('Ctrl Pts',(-156.052314316564,0.362363758895462,
124.208696323275));
#212515=CARTESIAN_POINT('Ctrl Pts',(-156.330761940377,-5.353252706796,126.934376065411));
#212516=CARTESIAN_POINT('Ctrl Pts',(-156.60920956419,-6.14949145587554,
133.216382551721));
#212517=CARTESIAN_POINT('Ctrl Pts',(-156.887657188002,-1.29464797636456,
137.281858714364));
#212518=CARTESIAN_POINT('Ctrl Pts',(-157.166104811815,4.74991374635575,
135.394830569423));
#212519=CARTESIAN_POINT('Ctrl Pts',(-157.444552435628,6.42953678236183,
129.28938479565));
#212520=CARTESIAN_POINT('Ctrl Pts',(-157.723000059441,2.20072961571137,
124.576127791533));
#212521=CARTESIAN_POINT('Ctrl Pts',(-158.001447683254,-4.05044055615985,
125.586312488451));
#212522=CARTESIAN_POINT('Ctrl Pts',(-158.279895307067,-6.57945373194114,
131.391628500203));
#212523=CARTESIAN_POINT('Ctrl Pts',(-158.55834293088,-3.06227035225273,
136.657274017441));
#212524=CARTESIAN_POINT('Ctrl Pts',(-158.836790554693,3.2689898809326,136.54437805091));
#212525=CARTESIAN_POINT('Ctrl Pts',(-159.115238178505,6.59620811257463,
131.156686478575));
#212526=CARTESIAN_POINT('Ctrl Pts',(-159.393685802319,3.86183333144169,
125.445224652049));
#212527=CARTESIAN_POINT('Ctrl Pts',(-159.672133426131,-2.42137762023968,
124.658546969484));
#212528=CARTESIAN_POINT('Ctrl Pts',(-159.950581049944,-6.47946082979399,
129.519571789819));
#212529=CARTESIAN_POINT('Ctrl Pts',(-160.229028673757,-4.58323607602601,
135.56125477743));
#212530=CARTESIAN_POINT('Ctrl Pts',(-160.50747629757,1.52475872807955,137.231584419323));
#212531=CARTESIAN_POINT('Ctrl Pts',(-160.785923921383,6.23157474968534,
132.99560937474));
#212532=CARTESIAN_POINT('Ctrl Pts',(-161.064371545196,5.2118780056808,126.745983770767));
#212533=CARTESIAN_POINT('Ctrl Pts',(-161.342819169009,-0.597280011148509,
124.225808226271));
#212534=CARTESIAN_POINT('Ctrl Pts',(-161.621266792821,-5.85756687648338,
127.751000949223));
#212535=CARTESIAN_POINT('Ctrl Pts',(-161.899714416635,-5.73503594038016,
134.08208204247));
#212536=CARTESIAN_POINT('Ctrl Pts',(-162.178162040447,-0.342287147149402,
137.401097271823));
#212537=CARTESIAN_POINT('Ctrl Pts',(-162.45660966426,5.36500681265522,134.658033784415));
#212538=CARTESIAN_POINT('Ctrl Pts',(-162.735057288073,6.14212160678308,
128.373632919072));
#212539=CARTESIAN_POINT('Ctrl Pts',(-163.013504911886,1.27492670359879,
124.322952060995));
#212540=CARTESIAN_POINT('Ctrl Pts',(-163.291952535699,-4.76386355656041,
126.228369031995));
#212541=CARTESIAN_POINT('Ctrl Pts',(-163.570400159512,-6.42489593591386,
132.338898720518));
#212542=CARTESIAN_POINT('Ctrl Pts',(-163.848847783325,-2.18176282377798,
137.039262858781));
#212543=CARTESIAN_POINT('Ctrl Pts',(-164.127295407138,4.06630373837012,
136.010056429275));
#212544=CARTESIAN_POINT('Ctrl Pts',(-164.405743030951,6.57763581493773,
130.197069861187));
#212545=CARTESIAN_POINT('Ctrl Pts',(-164.684190654763,3.04444191295097,
124.942153830408));
#212546=CARTESIAN_POINT('Ctrl Pts',(-164.962638278576,-3.28644537778151,
125.074319452304));
#212547=CARTESIAN_POINT('Ctrl Pts',(-165.241085902389,-6.59724991811553,
130.472112977002));
#212548=CARTESIAN_POINT('Ctrl Pts',(-165.519533526202,-3.84550407727676,
136.175225852179));
#212549=CARTESIAN_POINT('Ctrl Pts',(-165.797981150015,2.44007214726114,
136.942775958099));
#212550=CARTESIAN_POINT('Ctrl Pts',(-166.076428773828,6.48334127261722,
132.069422244329));
#212551=CARTESIAN_POINT('Ctrl Pts',(-166.354876397641,4.56873649726763,
126.03353869726));
#212552=CARTESIAN_POINT('Ctrl Pts',(-166.633324021454,-1.54431392388507,
124.381807427344));
#212553=CARTESIAN_POINT('Ctrl Pts',(-166.911771645267,-6.23821529291649,
128.632088780075));
#212554=CARTESIAN_POINT('Ctrl Pts',(-167.19021926908,-5.19950156151742,
134.878581830081));
#212555=CARTESIAN_POINT('Ctrl Pts',(-167.468666892892,0.617300095144361,
137.381064622557));
#212556=CARTESIAN_POINT('Ctrl Pts',(-167.747114516705,5.86683312115408,
133.839877724298));
#212557=CARTESIAN_POINT('Ctrl Pts',(-168.025562140518,5.72503311955499,
127.509198898206));
#212558=CARTESIAN_POINT('Ctrl Pts',(-168.304009764331,0.32220736450136,
124.206612714607));
#212559=CARTESIAN_POINT('Ctrl Pts',(-168.582457388144,-5.37671121782417,
126.967034535923));
#212560=CARTESIAN_POINT('Ctrl Pts',(-168.860905011957,-6.1346948579149,
133.253771562468));
#212561=CARTESIAN_POINT('Ctrl Pts',(-169.13935263577,-1.25519362008691,
137.289619591024));
#212562=CARTESIAN_POINT('Ctrl Pts',(-169.417800259582,4.77776923498369,
135.365831445486));
#212563=CARTESIAN_POINT('Ctrl Pts',(-169.696247883396,6.42019557010726,
129.250274449328));
#212564=CARTESIAN_POINT('Ctrl Pts',(-169.974695507208,2.16277582029264,
124.562846720449));
#212565=CARTESIAN_POINT('Ctrl Pts',(-170.253143131021,-4.08212925089891,
125.611065348116));
#212566=CARTESIAN_POINT('Ctrl Pts',(-170.531590754834,-6.57575696361412,
131.431668621828));
#212567=CARTESIAN_POINT('Ctrl Pts',(-170.810038378647,-3.02658527035502,
136.675806485322));
#212568=CARTESIAN_POINT('Ctrl Pts',(-171.08848600246,3.30387042945021,136.524372432426));
#212569=CARTESIAN_POINT('Ctrl Pts',(-171.366933626273,6.59823060763395,
131.116526959784));
#212570=CARTESIAN_POINT('Ctrl Pts',(-171.645381250086,3.82913919888762,
125.421815868818));
#212571=CARTESIAN_POINT('Ctrl Pts',(-171.923828873899,-2.45874406978715,
124.673400450021));
#212572=CARTESIAN_POINT('Ctrl Pts',(-172.202276497711,-6.48716165465291,
129.559037911142));
#212573=CARTESIAN_POINT('Ctrl Pts',(-172.480724121525,-4.55419459435809,
135.589066102071));
#212574=CARTESIAN_POINT('Ctrl Pts',(-172.759171745337,1.5638548133772,137.222183698596));
#212575=CARTESIAN_POINT('Ctrl Pts',(-173.03761936915,6.24479804617409,132.957635411742));
#212576=CARTESIAN_POINT('Ctrl Pts',(-173.316066992963,5.18707694988104,
126.714332782362));
#212577=CARTESIAN_POINT('Ctrl Pts',(-173.594514616776,-0.637314460555731,
124.229565924566));
#212578=CARTESIAN_POINT('Ctrl Pts',(-173.872962240589,-5.8760450162844,
127.786714193059));
#212579=CARTESIAN_POINT('Ctrl Pts',(-174.151409864401,-5.71497726280517,
134.11693210545));
#212580=CARTESIAN_POINT('Ctrl Pts',(-174.429857488215,-0.302124596968923,
137.403058648589));
#212581=CARTESIAN_POINT('Ctrl Pts',(-174.708305112027,5.38836581387496,
134.625304065538));
#212582=CARTESIAN_POINT('Ctrl Pts',(-174.98675273584,6.1272112780718,128.336289117263));
#212583=CARTESIAN_POINT('Ctrl Pts',(-175.265200359654,1.2354489086321,124.315311305772));
#212584=CARTESIAN_POINT('Ctrl Pts',(-175.543647983466,-4.79163065280562,
126.257452804136));
#212585=CARTESIAN_POINT('Ctrl Pts',(-175.822095607279,-6.41543572848632,
132.377980454247));
#212586=CARTESIAN_POINT('Ctrl Pts',(-176.100543231092,-2.14376878114676,
137.05242835005));
#212587=CARTESIAN_POINT('Ctrl Pts',(-176.378990854905,4.09791694713909,
135.985207234778));
#212588=CARTESIAN_POINT('Ctrl Pts',(-176.657438478718,6.57381719537689,
130.157041176716));
#212589=CARTESIAN_POINT('Ctrl Pts',(-176.93588610253,3.00870058988678,124.923730061481));
#212590=CARTESIAN_POINT('Ctrl Pts',(-177.214333726344,-3.32126487451375,
125.094431142515));
#212591=CARTESIAN_POINT('Ctrl Pts',(-177.492781350156,-6.59915017204588,
130.512278465557));
#212592=CARTESIAN_POINT('Ctrl Pts',(-177.771228973969,-3.81273884787578,
136.198535017289));
#212593=CARTESIAN_POINT('Ctrl Pts',(-178.049676597782,2.47739321484437,
136.927808815745));
#212594=CARTESIAN_POINT('Ctrl Pts',(-178.328124221595,6.49092194050925,
132.029932867148));
#212595=CARTESIAN_POINT('Ctrl Pts',(-178.606571845408,4.53961050201187,
126.005815893719));
#212596=CARTESIAN_POINT('Ctrl Pts',(-178.885019469221,-1.58338121553252,
124.391327099562));
#212597=CARTESIAN_POINT('Ctrl Pts',(-179.163467093034,-6.25132294847495,
128.670102814346));
#212598=CARTESIAN_POINT('Ctrl Pts',(-179.441914716847,-5.1746042858732,
134.910157185999));
#212599=CARTESIAN_POINT('Ctrl Pts',(-179.72036234066,0.657322921973241,
137.377185090575));
#212600=CARTESIAN_POINT('Ctrl Pts',(-179.998809964472,5.88520247653593,
133.804108404782));
#212601=CARTESIAN_POINT('Ctrl Pts',(-180.277257588285,5.70486846328706,
127.474410048364));
#212602=CARTESIAN_POINT('Ctrl Pts',(-180.555705212098,0.282039030594865,
124.204773587913));
#212603=CARTESIAN_POINT('Ctrl Pts',(-180.834152835911,-5.39997049284089,
126.999835199963));
#212604=CARTESIAN_POINT('Ctrl Pts',(-181.112600459724,-6.11967093658025,
133.291069809391));
#212605=CARTESIAN_POINT('Ctrl Pts',(-181.391048083537,-1.21569275214809,
137.297140154028));
#212606=CARTESIAN_POINT('Ctrl Pts',(-181.669495707349,4.8054476816156,135.336663294571));
#212607=CARTESIAN_POINT('Ctrl Pts',(-181.947943331163,6.41061645514481,
129.21122169024));
#212608=CARTESIAN_POINT('Ctrl Pts',(-182.226390954976,2.12474188242055,
124.549796930959));
#212609=CARTESIAN_POINT('Ctrl Pts',(-182.504838578788,-4.11366668083735,
125.636010647245));
#212610=CARTESIAN_POINT('Ctrl Pts',(-182.783286202602,-6.5718165281946,
131.471685498325));
#212611=CARTESIAN_POINT('Ctrl Pts',(-183.061733826414,-2.99078803722709,
136.694121384618));
#212612=CARTESIAN_POINT('Ctrl Pts',(-183.340181450227,3.33862855183402,
136.5041548568));
#212613=CARTESIAN_POINT('Ctrl Pts',(-183.61862907404,6.60000860283161,131.076355873553));
#212614=CARTESIAN_POINT('Ctrl Pts',(-183.897076697853,3.79630317617236,
125.398606537762));
#212615=CARTESIAN_POINT('Ctrl Pts',(-184.175524321666,-2.49601940966891,
124.68848111554));
#212616=CARTESIAN_POINT('Ctrl Pts',(-184.453971945479,-6.49462209535141,
129.598550178357));
#212617=CARTESIAN_POINT('Ctrl Pts',(-184.732419569291,-4.52498435533419,
135.616700127691));
#212618=CARTESIAN_POINT('Ctrl Pts',(-185.010867193105,1.60289294946002,
137.212545163075));
#212619=CARTESIAN_POINT('Ctrl Pts',(-185.289314816917,6.25778993937471,
132.919581658354));
#212620=CARTESIAN_POINT('Ctrl Pts',(-185.56776244073,5.16208368503734,126.682833351442));
#212621=CARTESIAN_POINT('Ctrl Pts',(-185.846210064543,-0.677325294041226,
124.233567254297));
#212622=CARTESIAN_POINT('Ctrl Pts',(-186.124657688356,-5.89430541707644,
127.822539256894));
#212623=CARTESIAN_POINT('Ctrl Pts',(-186.403105312169,-5.69470681464601,
134.151659419877));
#212624=CARTESIAN_POINT('Ctrl Pts',(-186.681552935982,-0.261950851450417,
137.404775508174));
#212625=CARTESIAN_POINT('Ctrl Pts',(-186.960000559794,5.41152514721792,
134.592432760195));
#212626=CARTESIAN_POINT('Ctrl Pts',(-187.238448183608,6.11207390329327,
128.299036770752));
#212627=CARTESIAN_POINT('Ctrl Pts',(-187.51689580742,1.19592533365239,124.307911004657));
#212628=CARTESIAN_POINT('Ctrl Pts',(-187.795343431234,-4.81922019341476,
126.286705063617));
#212629=CARTESIAN_POINT('Ctrl Pts',(-188.073791055046,-6.40573779472858,
132.417003876913));
#212630=CARTESIAN_POINT('Ctrl Pts',(-188.352238678859,-2.10569530037498,
137.065362316871));
#212631=CARTESIAN_POINT('Ctrl Pts',(-188.630686302672,4.12937830608858,
135.960166062105));
#212632=CARTESIAN_POINT('Ctrl Pts',(-188.909133926485,6.56975498060235,
130.117036478904));
#212633=CARTESIAN_POINT('Ctrl Pts',(-189.187581550298,2.97284777831579,
124.905524201484));
#212634=CARTESIAN_POINT('Ctrl Pts',(-189.466029174111,-3.35596130055467,
125.114754416262));
#212635=CARTESIAN_POINT('Ctrl Pts',(-189.744476797923,-6.60080589203976,
130.552454777323));
#212636=CARTESIAN_POINT('Ctrl Pts',(-190.022924421737,-3.77983233603489,
136.221644299282));
#212637=CARTESIAN_POINT('Ctrl Pts',(-190.301372045549,2.5146224817104,136.912614766765));
#212638=CARTESIAN_POINT('Ctrl Pts',(-190.579819669362,6.49826208490189,
131.990398075938));
#212639=CARTESIAN_POINT('Ctrl Pts',(-190.858267293175,4.51031628981952,
125.978270902017));
#212640=CARTESIAN_POINT('Ctrl Pts',(-191.136714916988,-1.62238983440674,
124.401084409096));
#212641=CARTESIAN_POINT('Ctrl Pts',(-191.415162540801,-6.26419895896261,
128.708195934325));
#212642=CARTESIAN_POINT('Ctrl Pts',(-191.693610164614,-5.14951526336424,
134.941580400114));
#212643=CARTESIAN_POINT('Ctrl Pts',(-191.972057788427,0.697321391460013,
137.373062000163));
#212644=CARTESIAN_POINT('Ctrl Pts',(-192.25050541224,5.90335375357599,133.768227928508));
#212645=CARTESIAN_POINT('Ctrl Pts',(-192.528953036052,5.68449241101982,
127.439744591064));
#212646=CARTESIAN_POINT('Ctrl Pts',(-192.807400659866,0.241860245628379,
124.203179011344));
#212647=CARTESIAN_POINT('Ctrl Pts',(-193.085848283678,-5.42302966996514,
127.032776842093));
#212648=CARTESIAN_POINT('Ctrl Pts',(-193.364295907491,-6.10442024858855,
133.32827591039));
#212649=CARTESIAN_POINT('Ctrl Pts',(-193.642743531304,-1.17614683626724,
137.304420124699));
#212650=CARTESIAN_POINT('Ctrl Pts',(-193.921191155117,4.83294806061645,
135.307327197512));
#212651=CARTESIAN_POINT('Ctrl Pts',(-194.19963877893,6.40079979243214,129.172227965502));
#212652=CARTESIAN_POINT('Ctrl Pts',(-194.478086402743,2.08662921145659,
124.536978906625));
#212653=CARTESIAN_POINT('Ctrl Pts',(-194.756534026555,-4.14505167734362,
125.661147461485));
#212654=CARTESIAN_POINT('Ctrl Pts',(-195.034981650369,-6.5676325716969,
131.511677646851));
#212655=CARTESIAN_POINT('Ctrl Pts',(-195.313429274181,-2.95487997934909,
136.712218036662));
#212656=CARTESIAN_POINT('Ctrl Pts',(-195.591876897994,3.3732629601091,136.483726073203));
#212657=CARTESIAN_POINT('Ctrl Pts',(-195.870324521807,6.60154203228333,
131.03617470844));
#212658=CARTESIAN_POINT('Ctrl Pts',(-196.14877214562,3.76332648004682,125.375597518911));
#212659=CARTESIAN_POINT('Ctrl Pts',(-196.427219769433,-2.53320225863353,
124.703788407225));
#212660=CARTESIAN_POINT('Ctrl Pts',(-196.705667393246,-6.50184187543975,
129.63810712732));
#212661=CARTESIAN_POINT('Ctrl Pts',(-196.984115017059,-4.49560644135098,
135.644155830301));
#212662=CARTESIAN_POINT('Ctrl Pts',(-197.262562640871,1.64187168975517,
137.202669169918));
#212663=CARTESIAN_POINT('Ctrl Pts',(-197.541010264685,6.27054994786743,
132.881449524674));
#212664=CARTESIAN_POINT('Ctrl Pts',(-197.819457888497,5.13689913728475,
126.651486645231));
#212665=CARTESIAN_POINT('Ctrl Pts',(-198.097905512311,-0.717311028988463,
124.237812067191));
#212666=CARTESIAN_POINT('Ctrl Pts',(-198.376353136123,-5.91234740221361,
127.858474813215));
#212667=CARTESIAN_POINT('Ctrl Pts',(-198.654800759936,-5.67422534703162,
134.186262698915));
#212668=CARTESIAN_POINT('Ctrl Pts',(-198.933248383749,-0.221767399246752,
137.406247786956));
#212669=CARTESIAN_POINT('Ctrl Pts',(-199.211696007562,5.43448395450644,
134.559421086446));
#212670=CARTESIAN_POINT('Ctrl Pts',(-199.490143631375,6.09671004336861,
128.261877259937));
#212671=CARTESIAN_POINT('Ctrl Pts',(-199.768591255188,1.15635744321901,
124.300751431872));
#212672=CARTESIAN_POINT('Ctrl Pts',(-200.047038879001,-4.84663115604747,
126.316124726487));
#212673=CARTESIAN_POINT('Ctrl Pts',(-200.325486502814,-6.39580249400115,
132.455967542492));
#212674=CARTESIAN_POINT('Ctrl Pts',(-200.603934126626,-2.06754379228947,
137.078064279972));
#212675=CARTESIAN_POINT('Ctrl Pts',(-200.882381750439,4.16068664940635,
135.934933839164));
#212676=CARTESIAN_POINT('Ctrl Pts',(-201.160829374253,6.56544932114097,
130.077057250143));
#212677=CARTESIAN_POINT('Ctrl Pts',(-201.439276998065,2.9368848067771,124.887536925038));
#212678=CARTESIAN_POINT('Ctrl Pts',(-201.717724621878,-3.39053337021544,
125.13528852046));
#212679=CARTESIAN_POINT('Ctrl Pts',(-201.996172245691,-6.60221701674386,
130.592640423553));
#212680=CARTESIAN_POINT('Ctrl Pts',(-202.274619869504,-3.74678576111652,
136.244552841837));
#212681=CARTESIAN_POINT('Ctrl Pts',(-202.553067493317,2.55175856831618,
136.897194374181));
#212682=CARTESIAN_POINT('Ctrl Pts',(-202.83151511713,6.50536143380309,131.950819335672));
#212683=CARTESIAN_POINT('Ctrl Pts',(-203.109962740942,4.48085494619837,
125.950904742844));
#212684=CARTESIAN_POINT('Ctrl Pts',(-203.388410364755,-1.66133833502902,
124.411078994385));
#212685=CARTESIAN_POINT('Ctrl Pts',(-203.666857988568,-6.27684284725421,
128.746366728457));
#212686=CARTESIAN_POINT('Ctrl Pts',(-203.945305612381,-5.12423542367342,
134.97285030803));
#212687=CARTESIAN_POINT('Ctrl Pts',(-204.223753236194,0.737294021446153,
137.368695504108));
#212688=CARTESIAN_POINT('Ctrl Pts',(-204.502200860007,5.9212862796718,133.732237625041));
#212689=CARTESIAN_POINT('Ctrl Pts',(-204.78064848382,5.66390571779574,127.405203810847));
#212690=CARTESIAN_POINT('Ctrl Pts',(-205.059096107633,0.20167249844203,
124.201829043986));
#212691=CARTESIAN_POINT('Ctrl Pts',(-205.337543731446,-5.44588789473034,
127.065858241646));
#212692=CARTESIAN_POINT('Ctrl Pts',(-205.615991355258,-6.08894335906002,
133.36538848678));
#212693=CARTESIAN_POINT('Ctrl Pts',(-205.894438979071,-1.13655733783284,
137.311459233274));
#212694=CARTESIAN_POINT('Ctrl Pts',(-206.172886602884,4.86026935294961,
135.277824241371));
#212695=CARTESIAN_POINT('Ctrl Pts',(-206.451334226697,6.39074594572923,
129.133294720038));
#212696=CARTESIAN_POINT('Ctrl Pts',(-206.72978185051,2.04843921967989,124.524393122426));
#212697=CARTESIAN_POINT('Ctrl Pts',(-207.008229474323,-4.17628307743617,
125.686474859378));
#212698=CARTESIAN_POINT('Ctrl Pts',(-207.286677098136,-6.56320524915893,
131.551643585487));
#212699=CARTESIAN_POINT('Ctrl Pts',(-207.565124721949,-2.9188624273063,
136.730095770877));
#212700=CARTESIAN_POINT('Ctrl Pts',(-207.843572345762,3.40777237088467,
136.463086838631));
#212701=CARTESIAN_POINT('Ctrl Pts',(-208.122019969575,6.60283083916734,
130.995984953369));
#212702=CARTESIAN_POINT('Ctrl Pts',(-208.400467593387,3.73021033247459,
125.352789664874));
#212703=CARTESIAN_POINT('Ctrl Pts',(-208.678915217201,-2.57029123885685,
124.719321757855));
#212704=CARTESIAN_POINT('Ctrl Pts',(-208.957362841013,-6.50882072738636,
129.677707292235));
#212705=CARTESIAN_POINT('Ctrl Pts',(-209.235810464827,-4.4660619410178,
135.671432192519));
#212706=CARTESIAN_POINT('Ctrl Pts',(-209.514258088639,1.68078958989102,
137.192556085085));
#212707=CARTESIAN_POINT('Ctrl Pts',(-209.792705712452,6.28307759882623,
132.8432404237));
#212708=CARTESIAN_POINT('Ctrl Pts',(-210.071153336265,5.11152423984512,
126.620293825292));
#212709=CARTESIAN_POINT('Ctrl Pts',(-210.349600960078,-0.757270183712145,
124.242300205957));
#212710=CARTESIAN_POINT('Ctrl Pts',(-210.62804858389,-5.93017030314353,
127.894519530418));
#212711=CARTESIAN_POINT('Ctrl Pts',(-210.906496207704,-5.65353361891029,
134.220740660327));
#212712=CARTESIAN_POINT('Ctrl Pts',(-211.184943831516,-0.181575729370575,
137.407475430382));
#212713=CARTESIAN_POINT('Ctrl Pts',(-211.463391455329,5.4572413849935,134.52627026755));
#212714=CARTESIAN_POINT('Ctrl Pts',(-211.741839079142,6.08112026761121,
128.224811961777));
#212715=CARTESIAN_POINT('Ctrl Pts',(-212.020286702955,1.11674670353533,
124.293832852717));
#212716=CARTESIAN_POINT('Ctrl Pts',(-212.298734326768,-4.87386252498038,
126.345710702588));
#212717=CARTESIAN_POINT('Ctrl Pts',(-212.577181950581,-6.38563019446009,
132.494870007167));
#212718=CARTESIAN_POINT('Ctrl Pts',(-212.855629574394,-2.02931567060901,
137.090533768676));
#212719=CARTESIAN_POINT('Ctrl Pts',(-213.134077198207,4.19184081695006,
135.909511500946));
#212720=CARTESIAN_POINT('Ctrl Pts',(-213.412524822019,6.56090037654053,
130.037104971874));
#212721=CARTESIAN_POINT('Ctrl Pts',(-213.690972445832,2.90081300789186,
124.869768898671));
#212722=CARTESIAN_POINT('Ctrl Pts',(-213.969420069645,-3.42497980241531,
125.156032694208));
#212723=CARTESIAN_POINT('Ctrl Pts',(-214.247867693459,-6.60338349386843,
130.632833915152));
#212724=CARTESIAN_POINT('Ctrl Pts',(-214.52631531727,-3.71360034767391,
136.267259796069));
#212725=CARTESIAN_POINT('Ctrl Pts',(-214.804762941084,2.58880009856982,
136.881548209402));
#212726=CARTESIAN_POINT('Ctrl Pts',(-215.083210564897,6.51221972414398,
131.911198112957));
#212727=CARTESIAN_POINT('Ctrl Pts',(-215.36165818871,4.45122756284936,125.923718430264));
#212728=CARTESIAN_POINT('Ctrl Pts',(-215.640105812523,-1.70022527414834,
124.421310485075));
#212729=CARTESIAN_POINT('Ctrl Pts',(-215.918553436335,-6.28925414482577,
128.784613782311));
#212730=CARTESIAN_POINT('Ctrl Pts',(-216.197001060149,-5.09876570355457,
135.003965751026));
#212731=CARTESIAN_POINT('Ctrl Pts',(-216.475448683961,0.77723933073121,
137.364085764208));
#212732=CARTESIAN_POINT('Ctrl Pts',(-216.753896307774,5.93899939032692,
133.696138828015));
#212733=CARTESIAN_POINT('Ctrl Pts',(-217.032343931587,5.64310914646246,
127.370788987637));
#212734=CARTESIAN_POINT('Ctrl Pts',(-217.3107915554,0.161477278206604,124.200723735865));
#212735=CARTESIAN_POINT('Ctrl Pts',(-217.589239179213,-5.46854432011718,
127.099078172778));
#212736=CARTESIAN_POINT('Ctrl Pts',(-217.867686803026,-6.07324084149572,
133.402406163341));
#212737=CARTESIAN_POINT('Ctrl Pts',(-218.146134426838,-1.09692572384833,
137.318257218917));
#212738=CARTESIAN_POINT('Ctrl Pts',(-218.424582050652,4.88741054621452,
135.24815551939));
#212739=CARTESIAN_POINT('Ctrl Pts',(-218.703029674464,6.38045528758512,
129.094423396537));
#212740=CARTESIAN_POINT('Ctrl Pts',(-218.981477298277,2.01017332223456,
124.512040044732));
#212741=CARTESIAN_POINT('Ctrl Pts',(-219.25992492209,-4.20735972382344,
125.711991902411));
#212742=CARTESIAN_POINT('Ctrl Pts',(-219.538372545903,-6.55853472463687,
131.591581833275));
#212743=CARTESIAN_POINT('Ctrl Pts',(-219.816820169716,-2.8827367157428,
136.747753924796));
#212744=CARTESIAN_POINT('Ctrl Pts',(-220.095267793529,3.44215550540127,
136.442237917877));
#212745=CARTESIAN_POINT('Ctrl Pts',(-220.373715417342,6.60387497572639,
130.955788097589));
#212746=CARTESIAN_POINT('Ctrl Pts',(-220.652163041155,3.69695596058723,
125.330183820803));
#212747=CARTESIAN_POINT('Ctrl Pts',(-220.930610664968,-2.60728497599312,
124.735080591838));
#212748=CARTESIAN_POINT('Ctrl Pts',(-221.20905828878,-6.51555839258729,
129.717349205704));
#212749=CARTESIAN_POINT('Ctrl Pts',(-221.487505912593,-4.43635194911701,
135.698528203611));
#212750=CARTESIAN_POINT('Ctrl Pts',(-221.765953536406,1.71964520775051,
137.182206283321));
#212751=CARTESIAN_POINT('Ctrl Pts',(-222.044401160219,6.295372428034,132.804955771283));
#212752=CARTESIAN_POINT('Ctrl Pts',(-222.322848784032,5.08595993299503,
126.589256047487));
#212753=CARTESIAN_POINT('Ctrl Pts',(-222.601296407845,-0.797201277510683,
124.247031504286));
#212754=CARTESIAN_POINT('Ctrl Pts',(-222.879744031658,-5.94777345943203,
127.930672072853));
#212755=CARTESIAN_POINT('Ctrl Pts',(-223.158191655471,-5.63263239702162,
134.255092026522));
#212756=CARTESIAN_POINT('Ctrl Pts',(-223.436639279283,-0.141377331138957,
137.40845839296));
#212757=CARTESIAN_POINT('Ctrl Pts',(-223.715086903097,5.47979659539413,
134.492981531924));
#212758=CARTESIAN_POINT('Ctrl Pts',(-223.993534526909,6.06530515370598,
128.187842249741));
#212759=CARTESIAN_POINT('Ctrl Pts',(-224.271982150722,1.07709458239186,
124.287155523561));
#212760=CARTESIAN_POINT('Ctrl Pts',(-224.550429774535,-4.90091329114502,
126.375461895601));
#212761=CARTESIAN_POINT('Ctrl Pts',(-224.828877398348,-6.37522127304402,
132.533709829396));
#212762=CARTESIAN_POINT('Ctrl Pts',(-225.107325022161,-1.99101235188949,
137.102770320923));
#212763=CARTESIAN_POINT('Ctrl Pts',(-225.385772645974,4.22283965429091,
135.883899989486));
#212764=CARTESIAN_POINT('Ctrl Pts',(-225.664220269787,6.55610831536389,
129.997181124546));
#212765=CARTESIAN_POINT('Ctrl Pts',(-225.9426678936,2.86463371831382,124.852220780782));
#212766=CARTESIAN_POINT('Ctrl Pts',(-226.221115517412,-3.45929932072906,
125.176986168825));
#212767=CARTESIAN_POINT('Ctrl Pts',(-226.499563141226,-6.60430528018926,
130.673033762736));
#212768=CARTESIAN_POINT('Ctrl Pts',(-226.778010765038,-3.68027732540471,
136.289764320562));
#212769=CARTESIAN_POINT('Ctrl Pts',(-227.056458388851,2.62574569988376,
136.865676852203));
#212770=CARTESIAN_POINT('Ctrl Pts',(-227.334906012664,6.51883670178814,
131.871535875972));
#212771=CARTESIAN_POINT('Ctrl Pts',(-227.613353636477,4.42143523762624,
125.896712971676));
#212772=CARTESIAN_POINT('Ctrl Pts',(-227.89180126029,-1.73904921079426,
124.431778502036));
#212773=CARTESIAN_POINT('Ctrl Pts',(-228.170248884103,-6.30143239177224,
128.822935678624));
#212774=CARTESIAN_POINT('Ctrl Pts',(-228.448696507916,-5.07310704679746,
135.034925576111));
#212775=CARTESIAN_POINT('Ctrl Pts',(-228.727144131728,0.81715583912702,
137.359232951281));
#212776=CARTESIAN_POINT('Ctrl Pts',(-229.005591755541,5.95649242917557,
133.659932875084));
#212777=CARTESIAN_POINT('Ctrl Pts',(-229.284039379354,5.62210346764449,
127.336501396687));
#212778=CARTESIAN_POINT('Ctrl Pts',(-229.562487003167,0.121276074371264,
124.199863127936));
#212779=CARTESIAN_POINT('Ctrl Pts',(-229.84093462698,-5.4909981065832,127.132435404515));
#212780=CARTESIAN_POINT('Ctrl Pts',(-230.119382250793,-6.0573132777586,
133.439327568368));
#212781=CARTESIAN_POINT('Ctrl Pts',(-230.397829874606,-1.05725346287773,
137.324813829725));
#212782=CARTESIAN_POINT('Ctrl Pts',(-230.676277498418,4.91437063468431,
135.218322130955));
#212783=CARTESIAN_POINT('Ctrl Pts',(-230.954725122232,6.3699281993239,129.055615435388));
#212784=CARTESIAN_POINT('Ctrl Pts',(-231.233172746044,1.97183293707754,
124.49992013129));
#212785=CARTESIAN_POINT('Ctrl Pts',(-231.511620369858,-4.23828046494889,
125.73769764504));
#212786=CARTESIAN_POINT('Ctrl Pts',(-231.79006799367,-6.55362117119865,
131.631490910294));
#212787=CARTESIAN_POINT('Ctrl Pts',(-232.068515617483,-2.84650418331021,
136.765191844092));
#212788=CARTESIAN_POINT('Ctrl Pts',(-232.346963241296,3.47641108958031,
136.421180083507));
#212789=CARTESIAN_POINT('Ctrl Pts',(-232.625410865109,6.60467440326965,
130.915585630608));
#212790=CARTESIAN_POINT('Ctrl Pts',(-232.903858488922,3.66356459663667,
125.307780824367));
#212791=CARTESIAN_POINT('Ctrl Pts',(-233.182306112735,-2.64418209922576,
124.751064325225));
#212792=CARTESIAN_POINT('Ctrl Pts',(-233.460753736548,-6.52205462137589,
129.75703139878));
#212793=CARTESIAN_POINT('Ctrl Pts',(-233.73920136036,-4.40647756656326,
135.725442859523));
#212794=CARTESIAN_POINT('Ctrl Pts',(-234.017648984174,1.75843710352442,
137.17162014814));
#212795=CARTESIAN_POINT('Ctrl Pts',(-234.296096607986,6.30743397990132,
132.766596986079));
#212796=CARTESIAN_POINT('Ctrl Pts',(-234.574544231799,5.06020716402928,
126.558374461932));
#212797=CARTESIAN_POINT('Ctrl Pts',(-234.852991855612,-0.837102830722735,
124.252005786856));
#212798=CARTESIAN_POINT('Ctrl Pts',(-235.131439479425,-5.96515621878728,
127.966931100874));
#212799=CARTESIAN_POINT('Ctrl Pts',(-235.409887103238,-5.6115224558684,
134.289315524594));
#212800=CARTESIAN_POINT('Ctrl Pts',(-235.688334727051,-0.101173694118813,
137.409196638266));
#212801=CARTESIAN_POINT('Ctrl Pts',(-235.966782350864,5.50214874991674,
134.459556113093));
#212802=CARTESIAN_POINT('Ctrl Pts',(-236.245229974676,6.04926528768773,
128.150969493757));
#212803=CARTESIAN_POINT('Ctrl Pts',(-236.52367759849,1.03740254911254,124.280719691838));
#212804=CARTESIAN_POINT('Ctrl Pts',(-236.802125222302,-4.92778245216537,
126.405377203086));
#212805=CARTESIAN_POINT('Ctrl Pts',(-237.080572846115,-6.36457611545918,
132.572485569954));
#212806=CARTESIAN_POINT('Ctrl Pts',(-237.359020469928,-1.95263525547508,
137.114773483282));
#212807=CARTESIAN_POINT('Ctrl Pts',(-237.637468093741,4.25368201275546,
135.858100253825));
#212808=CARTESIAN_POINT('Ctrl Pts',(-237.915915717553,6.55107331518259,
129.957287187551));
#212809=CARTESIAN_POINT('Ctrl Pts',(-238.194363341367,2.8283482786799,124.834893221623));
#212810=CARTESIAN_POINT('Ctrl Pts',(-238.47281096518,-3.49349065343433,
125.198148167872));
#212811=CARTESIAN_POINT('Ctrl Pts',(-238.751258588993,-6.60498234154917,
130.713238476685));
#212812=CARTESIAN_POINT('Ctrl Pts',(-239.029706212805,-3.64681792910581,
136.312065581403));
#212813=CARTESIAN_POINT('Ctrl Pts',(-239.308153836619,2.66259400322518,
136.8495808907));
#212814=CARTESIAN_POINT('Ctrl Pts',(-239.586601460431,6.52521212154101,
131.831834094415));
#212815=CARTESIAN_POINT('Ctrl Pts',(-239.865049084244,4.39147907449425,
125.869889367774));
#212816=CARTESIAN_POINT('Ctrl Pts',(-240.143496708057,-1.77780870633274,
124.44248265737));
#212817=CARTESIAN_POINT('Ctrl Pts',(-240.42194433187,-6.31337713682396,
128.861330997368));
#212818=CARTESIAN_POINT('Ctrl Pts',(-240.700391955683,-5.04726040419313,
135.065728636055));
#212819=CARTESIAN_POINT('Ctrl Pts',(-240.978839579496,0.857042067512721,
137.354137245149));
#212820=CARTESIAN_POINT('Ctrl Pts',(-241.257287203309,5.97376474800676,
133.623621107872));
#212821=CARTESIAN_POINT('Ctrl Pts',(-241.535734827122,5.60088945971499,
127.302342308534));
#212822=CARTESIAN_POINT('Ctrl Pts',(-241.814182450934,0.0810703766063902,
124.199247252091));
#212823=CARTESIAN_POINT('Ctrl Pts',(-242.092630074747,-5.51324842209508,
127.165928700792));
#212824=CARTESIAN_POINT('Ctrl Pts',(-242.37107769856,-6.04116125805038,
133.476151333726));
#212825=CARTESIAN_POINT('Ctrl Pts',(-242.649525322373,-1.01754202499167,
137.331128822742));
#212826=CARTESIAN_POINT('Ctrl Pts',(-242.927972946186,4.94114861934255,
135.188325181553));
#212827=CARTESIAN_POINT('Ctrl Pts',(-243.206420569999,6.35916507103108,
129.016872274634));
#212828=CARTESIAN_POINT('Ctrl Pts',(-243.484868193812,1.93341948492588,
124.488033831209));
#212829=CARTESIAN_POINT('Ctrl Pts',(-243.763315817625,-4.26904415503308,
125.763591134728));
#212830=CARTESIAN_POINT('Ctrl Pts',(-244.041763441437,-6.54846477091785,
131.671369337695));
#212831=CARTESIAN_POINT('Ctrl Pts',(-244.320211065251,-2.8101661726183,
136.782408882594));
#212832=CARTESIAN_POINT('Ctrl Pts',(-244.598658689063,3.51053785406796,
136.399914115825));
#212833=CARTESIAN_POINT('Ctrl Pts',(-244.877106312876,6.60522909217403,
130.875379042142));
#212834=CARTESIAN_POINT('Ctrl Pts',(-245.155553936689,3.6300374779527,125.285581505715));
#212835=CARTESIAN_POINT('Ctrl Pts',(-245.434001560502,-2.68098124131831,
124.767272365732));
#212836=CARTESIAN_POINT('Ctrl Pts',(-245.712449184315,-6.528309173032,129.796752401026));
#212837=CARTESIAN_POINT('Ctrl Pts',(-245.990896808128,-4.37643990036281,
135.752175162922));
#212838=CARTESIAN_POINT('Ctrl Pts',(-246.269344431941,1.79716383976481,
137.160798071814));
#212839=CARTESIAN_POINT('Ctrl Pts',(-246.547792055753,6.31926180748295,
132.728165489484));
#212840=CARTESIAN_POINT('Ctrl Pts',(-246.826239679567,5.03426688722615,
126.527650212955));
#212841=CARTESIAN_POINT('Ctrl Pts',(-247.104687303379,-0.876973364781528,
124.257222869343));
#212842=CARTESIAN_POINT('Ctrl Pts',(-247.383134927193,-5.98231793708558,
128.003295270889));
#212843=CARTESIAN_POINT('Ctrl Pts',(-247.661582551005,-5.59020457768662,
134.32340988638));
#212844=CARTESIAN_POINT('Ctrl Pts',(-247.940030174818,-0.0609663080697638,
137.409690138946));
#212845=CARTESIAN_POINT('Ctrl Pts',(-248.218477798631,5.524297020294,134.425995249648));
#212846=CARTESIAN_POINT('Ctrl Pts',(-248.496925422444,6.03300126391963,
128.114195060156));
#212847=CARTESIAN_POINT('Ctrl Pts',(-248.775373046256,0.997672074500306,
124.274525596028));
#212848=CARTESIAN_POINT('Ctrl Pts',(-249.05382067007,-4.95446901239483,
126.435455516518));
#212849=CARTESIAN_POINT('Ctrl Pts',(-249.332268293882,-6.35369511616563,
132.611195791991));
#212850=CARTESIAN_POINT('Ctrl Pts',(-249.610715917695,-1.91418580344349,
137.126542810973));
#212851=CARTESIAN_POINT('Ctrl Pts',(-249.889163541508,4.28436674946925,
135.832113249982));
#212852=CARTESIAN_POINT('Ctrl Pts',(-250.167611165321,6.54579556256923,
129.917424639176));
#212853=CARTESIAN_POINT('Ctrl Pts',(-250.446058789134,2.79195803356287,
124.817786863269));
#212854=CARTESIAN_POINT('Ctrl Pts',(-250.724506412947,-3.52755253356211,
125.219517907192));
#212855=CARTESIAN_POINT('Ctrl Pts',(-251.00295403676,-6.60541465285253,
130.75344656718));
#212856=CARTESIAN_POINT('Ctrl Pts',(-251.281401660573,-3.61322339864049,
136.334162752248));
#212857=CARTESIAN_POINT('Ctrl Pts',(-251.559849284386,2.6993436431913,136.83326092127));
#212858=CARTESIAN_POINT('Ctrl Pts',(-251.838296908198,6.53134574711249,
131.792094239578));
#212859=CARTESIAN_POINT('Ctrl Pts',(-252.116744532012,4.3613601835781,125.843248612281));
#212860=CARTESIAN_POINT('Ctrl Pts',(-252.395192155824,-1.81650232468185,
124.453422554885));
#212861=CARTESIAN_POINT('Ctrl Pts',(-252.673639779637,-6.32508793705065,
128.899798314935));
#212862=CARTESIAN_POINT('Ctrl Pts',(-252.95208740345,-5.02122673409033,
135.096373791053));
#212863=CARTESIAN_POINT('Ctrl Pts',(-253.230535027263,0.896896539007115,
137.348798831588));
#212864=CARTESIAN_POINT('Ctrl Pts',(-253.508982651076,5.99081570467794,
133.587204877683));
#212865=CARTESIAN_POINT('Ctrl Pts',(-253.787430274889,5.57946791275175,
127.26831297809));
#212866=CARTESIAN_POINT('Ctrl Pts',(-254.065877898701,0.0408616672245685,
124.198876151673));
#212867=CARTESIAN_POINT('Ctrl Pts',(-254.344325522515,-5.53529442795169,
127.199556781751));
#212868=CARTESIAN_POINT('Ctrl Pts',(-254.622773146327,-6.0247854077167,
133.512876168065));
#212869=CARTESIAN_POINT('Ctrl Pts',(-254.90122077014,-0.977792831057213,
137.337201825807));
#212870=CARTESIAN_POINT('Ctrl Pts',(-255.179668393953,4.96774341227684,
135.158166043599));
#212871=CARTESIAN_POINT('Ctrl Pts',(-255.458116017766,6.34816648213513,
128.97819485735));
#212872=CARTESIAN_POINT('Ctrl Pts',(-255.736563641579,1.89493404819936,
124.476382515012));
#212873=CARTESIAN_POINT('Ctrl Pts',(-256.015011265392,-4.29964901022966,
125.789669655819));
#212874=CARTESIAN_POINT('Ctrl Pts',(-256.293458889205,-6.54306693065544,
131.711218953762));
#212875=CARTESIAN_POINT('Ctrl Pts',(-256.571906513018,-2.77372173452912,
136.799398141047));
#212876=CARTESIAN_POINT('Ctrl Pts',(-256.85035413683,3.54453019961847,136.378452625405));
#212877=CARTESIAN_POINT('Ctrl Pts',(-257.128801760644,6.60554720661629,
130.835147498674));
#212878=CARTESIAN_POINT('Ctrl Pts',(-257.407249384456,3.5963603924579,125.263628838565));
#212879=CARTESIAN_POINT('Ctrl Pts',(-257.685697008269,-2.71765185753996,
124.783624522784));
#212880=CARTESIAN_POINT('Ctrl Pts',(-257.964144632082,-6.53437691572335,
129.836661023534));
#212881=CARTESIAN_POINT('Ctrl Pts',(-258.242592255895,-4.34613602341029,
135.778440351053));
#212882=CARTESIAN_POINT('Ctrl Pts',(-258.521039879708,1.83562753012831,
137.150276335207));
#212883=CARTESIAN_POINT('Ctrl Pts',(-258.799487503521,6.33122643152078,
132.688650362788));
#212884=CARTESIAN_POINT('Ctrl Pts',(-259.077935127334,5.00743946241547,
126.498999976245));
#212885=CARTESIAN_POINT('Ctrl Pts',(-259.356382751147,-0.915487258132909,
124.259032700089));
#212886=CARTESIAN_POINT('Ctrl Pts',(-259.634830374959,-6.00176822571329,
128.046924274587));
#212887=CARTESIAN_POINT('Ctrl Pts',(-259.86687006147,-5.63687269779404,
133.292521465648));
#212888=CARTESIAN_POINT('Ctrl Pts',(-260.052531023546,-2.79481741349804,
135.900547185714));
#212889=CARTESIAN_POINT('Ctrl Pts',(-260.145376111017,-0.946914048523564,
136.386386345067));
#212890=CARTESIAN_POINT('Ctrl Pts',(-260.191813261187,-0.0157913329746497,
136.389009763222));
#212891=CARTESIAN_POINT('Ctrl Pts',(210.190947297731,3.04870273111253,135.077142573452));
#212892=CARTESIAN_POINT('Ctrl Pts',(210.144529434129,3.76080111712433,134.569051946243));
#212893=CARTESIAN_POINT('Ctrl Pts',(210.051703633225,4.91317831978039,133.192256847685));
#212894=CARTESIAN_POINT('Ctrl Pts',(209.866061957716,5.67455722768035,129.648049455111));
#212895=CARTESIAN_POINT('Ctrl Pts',(209.634022271206,3.10293383059235,125.427666478792));
#212896=CARTESIAN_POINT('Ctrl Pts',(209.355574647392,-2.85596866243967,
125.28812524467));
#212897=CARTESIAN_POINT('Ctrl Pts',(209.07712702358,-6.17973736462657,130.225196103446));
#212898=CARTESIAN_POINT('Ctrl Pts',(208.798679399767,-3.83016968018938,
135.690661498217));
#212899=CARTESIAN_POINT('Ctrl Pts',(208.520231775954,2.04205955310628,136.667868212554));
#212900=CARTESIAN_POINT('Ctrl Pts',(208.241784152142,6.03618933210081,132.255733564264));
#212901=CARTESIAN_POINT('Ctrl Pts',(207.963336528328,4.48417485225333,126.510421532214));
#212902=CARTESIAN_POINT('Ctrl Pts',(207.684888904515,-1.18901089957204,
124.710731370568));
#212903=CARTESIAN_POINT('Ctrl Pts',(207.406441280703,-5.76932406256156,
128.510946815645));
#212904=CARTESIAN_POINT('Ctrl Pts',(207.12799365689,-5.04803188696711,134.418613818075));
#212905=CARTESIAN_POINT('Ctrl Pts',(206.849546033077,0.312219397189005,
137.005003016302));
#212906=CARTESIAN_POINT('Ctrl Pts',(206.571098409264,5.38552219392035,133.893281295751));
#212907=CARTESIAN_POINT('Ctrl Pts',(206.292650785451,5.50981125882569,127.943004805273));
#212908=CARTESIAN_POINT('Ctrl Pts',(206.014203161638,0.570843377758803,
124.622167937696));
#212909=CARTESIAN_POINT('Ctrl Pts',(205.735755537825,-4.89269661278007,
126.982467612715));
#212910=CARTESIAN_POINT('Ctrl Pts',(205.457307914013,-5.86009012142741,
132.854898402769));
#212911=CARTESIAN_POINT('Ctrl Pts',(205.178860290199,-1.44234566848361,
136.842986120511));
#212912=CARTESIAN_POINT('Ctrl Pts',(204.900412666387,4.30084323855829,135.281871486376));
#212913=CARTESIAN_POINT('Ctrl Pts',(204.621965042573,6.09176771588946,129.606143376667));
#212914=CARTESIAN_POINT('Ctrl Pts',(204.343517418761,2.28465505058828,125.031518229909));
#212915=CARTESIAN_POINT('Ctrl Pts',(204.065069794948,-3.62194388278553,
125.761853295313));
#212916=CARTESIAN_POINT('Ctrl Pts',(203.786622171135,-6.20015338889199,
131.126006208945));
#212917=CARTESIAN_POINT('Ctrl Pts',(203.508174547322,-3.08072479357708,
136.194582558939));
#212918=CARTESIAN_POINT('Ctrl Pts',(203.229726923509,2.86973936865286,136.309808260363));
#212919=CARTESIAN_POINT('Ctrl Pts',(202.951279299696,6.1830532544492,131.365796540178));
#212920=CARTESIAN_POINT('Ctrl Pts',(202.672831675884,3.81444325369211,125.905852631576));
#212921=CARTESIAN_POINT('Ctrl Pts',(202.39438405207,-2.05945374882828,124.947398258377));
#212922=CARTESIAN_POINT('Ctrl Pts',(202.115936428258,-6.04081336739099,
129.371206163854));
#212923=CARTESIAN_POINT('Ctrl Pts',(201.837488804444,-4.47096061076856,
135.112012999282));
#212924=CARTESIAN_POINT('Ctrl Pts',(201.559041180632,1.20748652821524,136.894297736177));
#212925=CARTESIAN_POINT('Ctrl Pts',(201.280593556819,5.77631253695961,133.08022777117));
#212926=CARTESIAN_POINT('Ctrl Pts',(201.002145933006,5.03698951269057,127.174747074221));
#212927=CARTESIAN_POINT('Ctrl Pts',(200.723698309193,-0.331080803069094,
124.604703907164));
#212928=CARTESIAN_POINT('Ctrl Pts',(200.44525068538,-5.39490403503349,127.731842386878));
#212929=CARTESIAN_POINT('Ctrl Pts',(200.166803061567,-5.50107401450091,
133.682475019745));
#212930=CARTESIAN_POINT('Ctrl Pts',(199.888355437754,-0.552025717056,136.988261120707));
#212931=CARTESIAN_POINT('Ctrl Pts',(199.609907813942,4.90430724641216,134.611344759621));
#212932=CARTESIAN_POINT('Ctrl Pts',(199.331460190128,5.85382143915379,128.735995953499));
#212933=CARTESIAN_POINT('Ctrl Pts',(199.053012566316,1.42395970438994,124.761373228423));
#212934=CARTESIAN_POINT('Ctrl Pts',(198.774564942502,-4.31445143441004,
126.339960697623));
#212935=CARTESIAN_POINT('Ctrl Pts',(198.49611731869,-6.088092477657,132.02111359519));
#212936=CARTESIAN_POINT('Ctrl Pts',(198.217669694877,-2.26707395378944,
136.584129948007));
#212937=CARTESIAN_POINT('Ctrl Pts',(197.939222071064,3.6372747808909,135.835820643578));
#212938=CARTESIAN_POINT('Ctrl Pts',(197.660774447251,6.19914568268399,130.46384537573));
#212939=CARTESIAN_POINT('Ctrl Pts',(197.382326823438,3.06430454719326,125.404786980035));
#212940=CARTESIAN_POINT('Ctrl Pts',(197.103879199626,-2.88648276756863,
125.307672973393));
#212941=CARTESIAN_POINT('Ctrl Pts',(196.825431575812,-6.1847334314575,130.261746383626));
#212942=CARTESIAN_POINT('Ctrl Pts',(196.546983952,-3.79951621286212,135.71445576667));
#212943=CARTESIAN_POINT('Ctrl Pts',(196.268536328187,2.07727078866752,136.65502757917));
#212944=CARTESIAN_POINT('Ctrl Pts',(195.990088704374,6.04514741573133,132.219122274927));
#212945=CARTESIAN_POINT('Ctrl Pts',(195.711641080561,4.45782888960729,126.483120122517));
#212946=CARTESIAN_POINT('Ctrl Pts',(195.433193456748,-1.22601660901765,
124.718126880723));
#212947=CARTESIAN_POINT('Ctrl Pts',(195.154745832935,-5.78321273819644,
128.54608511404));
#212948=CARTESIAN_POINT('Ctrl Pts',(194.876298209123,-5.02591888662151,
134.449288212205));
#212949=CARTESIAN_POINT('Ctrl Pts',(194.597850585309,0.349948891971121,
137.002980915508));
#212950=CARTESIAN_POINT('Ctrl Pts',(194.319402961497,5.40423073479611,133.860444384439));
#212951=CARTESIAN_POINT('Ctrl Pts',(194.040955337684,5.49228854369214,127.909516169605));
#212952=CARTESIAN_POINT('Ctrl Pts',(193.762507713871,0.533201494146887,
124.618808581434));
#212953=CARTESIAN_POINT('Ctrl Pts',(193.484060090058,-4.91587168017823,
127.012321133451));
#212954=CARTESIAN_POINT('Ctrl Pts',(193.205612466245,-5.84749893410212,
132.890532719942));
#212955=CARTESIAN_POINT('Ctrl Pts',(192.927164842432,-1.40556033379022,
136.851654059523));
#212956=CARTESIAN_POINT('Ctrl Pts',(192.648717218619,4.32801954783523,135.255608152653));
#212957=CARTESIAN_POINT('Ctrl Pts',(192.370269594806,6.08436090050943,129.569083216569));
#212958=CARTESIAN_POINT('Ctrl Pts',(192.091821970994,2.24947182316989,125.017717865345));
#212959=CARTESIAN_POINT('Ctrl Pts',(191.81337434718,-3.65257196685492,125.783994510198));
#212960=CARTESIAN_POINT('Ctrl Pts',(191.534926723368,-6.19808055740059,
131.163742349203));
#212961=CARTESIAN_POINT('Ctrl Pts',(191.256479099555,-3.04785590876364,
136.213235933607));
#212962=CARTESIAN_POINT('Ctrl Pts',(190.978031475742,2.90319942398833,136.292237340818));
#212963=CARTESIAN_POINT('Ctrl Pts',(190.699583851929,6.18635631527163,131.328148137043));
#212964=CARTESIAN_POINT('Ctrl Pts',(190.421136228116,3.7845539731278,125.882723791311));
#212965=CARTESIAN_POINT('Ctrl Pts',(190.142688604304,-2.09506858458051,
124.960043253581));
#212966=CARTESIAN_POINT('Ctrl Pts',(189.86424098049,-6.04942546284962,129.408004862578));
#212967=CARTESIAN_POINT('Ctrl Pts',(189.585793356678,-4.44465587162338,
135.139149194637));
#212968=CARTESIAN_POINT('Ctrl Pts',(189.307345732864,1.24453533211424,136.886834590562));
#212969=CARTESIAN_POINT('Ctrl Pts',(189.028898109051,5.79005936456987,133.045023550676));
#212970=CARTESIAN_POINT('Ctrl Pts',(188.750450485239,5.01480170111087,127.144152737732));
#212971=CARTESIAN_POINT('Ctrl Pts',(188.472002861426,-0.368813738986236,
124.606834155258));
#212972=CARTESIAN_POINT('Ctrl Pts',(188.193555237613,-5.41350737050784,
127.764739625646));
#212973=CARTESIAN_POINT('Ctrl Pts',(187.9151076138,-5.48345219307025,133.715908293866));
#212974=CARTESIAN_POINT('Ctrl Pts',(187.636659989987,-0.51437233173317,
136.991506884579));
#212975=CARTESIAN_POINT('Ctrl Pts',(187.358212366174,4.92739057398128,134.581420314804));
#212976=CARTESIAN_POINT('Ctrl Pts',(187.079764742362,5.84112225861874,128.700400402891));
#212977=CARTESIAN_POINT('Ctrl Pts',(186.801317118548,1.38714794227173,124.752817144095));
#212978=CARTESIAN_POINT('Ctrl Pts',(186.522869494736,-4.34154756707868,
126.366306703083));
#212979=CARTESIAN_POINT('Ctrl Pts',(186.244421870923,-6.08057295867359,
132.058150998494));
#212980=CARTESIAN_POINT('Ctrl Pts',(185.96597424711,-2.23184885375068,136.597823184897));
#212981=CARTESIAN_POINT('Ctrl Pts',(185.687526623297,3.66783531589119,135.813586298303));
#212982=CARTESIAN_POINT('Ctrl Pts',(185.409078999484,6.19695801394562,130.42611572539));
#212983=CARTESIAN_POINT('Ctrl Pts',(185.130631375671,3.03137903541329,125.386233730096));
#212984=CARTESIAN_POINT('Ctrl Pts',(184.852183751858,-2.9198891855651,125.325345654173));
#212985=CARTESIAN_POINT('Ctrl Pts',(184.573736128045,-6.18792188952598,
130.299404664846));
#212986=CARTESIAN_POINT('Ctrl Pts',(184.295288504232,-3.76955667380246,
135.737493527599));
#212987=CARTESIAN_POINT('Ctrl Pts',(184.01684088042,2.11284697206427,136.642274242971));
#212988=CARTESIAN_POINT('Ctrl Pts',(183.738393256607,6.05364746891681,132.182297534532));
#212989=CARTESIAN_POINT('Ctrl Pts',(183.459945632794,4.43144167895468,126.456064115361));
#212990=CARTESIAN_POINT('Ctrl Pts',(183.181498008981,-1.2630425260055,124.725702755623));
#212991=CARTESIAN_POINT('Ctrl Pts',(182.903050385168,-5.79685235262429,
128.581331012064));
#212992=CARTESIAN_POINT('Ctrl Pts',(182.624602761355,-5.00363805916239,
134.479814874928));
#212993=CARTESIAN_POINT('Ctrl Pts',(182.346155137542,0.387675169361259,
137.000735831198));
#212994=CARTESIAN_POINT('Ctrl Pts',(182.06770751373,5.42273385622678,133.827490675898));
#212995=CARTESIAN_POINT('Ctrl Pts',(181.789259889916,5.47456504449634,127.876136685104));
#212996=CARTESIAN_POINT('Ctrl Pts',(181.510812266103,0.495538404244469,
124.615677436551));
#212997=CARTESIAN_POINT('Ctrl Pts',(181.232364642291,-4.93886382111119,
127.042315697369));
#212998=CARTESIAN_POINT('Ctrl Pts',(180.953917018477,-5.83469147177671,
132.926089453735));
#212999=CARTESIAN_POINT('Ctrl Pts',(180.675469394665,-1.36872270040423,
136.860098061879));
#213000=CARTESIAN_POINT('Ctrl Pts',(180.397021770852,4.35503536681857,135.229179797918));
#213001=CARTESIAN_POINT('Ctrl Pts',(180.118574147039,6.07672868724052,129.532068871648));
#213002=CARTESIAN_POINT('Ctrl Pts',(179.840126523226,2.21420520878857,125.004131904969));
#213003=CARTESIAN_POINT('Ctrl Pts',(179.561678899413,-3.68306468660213,
125.80632176824));
#213004=CARTESIAN_POINT('Ctrl Pts',(179.2832312756,-6.19577806271818,131.20146516627));
#213005=CARTESIAN_POINT('Ctrl Pts',(179.004783651788,-3.01487407978163,
136.231688883676));
#213006=CARTESIAN_POINT('Ctrl Pts',(178.726336027974,2.93655189768736,136.274463064253));
#213007=CARTESIAN_POINT('Ctrl Pts',(178.447888404162,6.18943013971724,131.290480325685));
#213008=CARTESIAN_POINT('Ctrl Pts',(178.169440780348,3.75452445381909,125.859777323623));
#213009=CARTESIAN_POINT('Ctrl Pts',(177.890993156536,-2.13060578642238,
124.972904812372));
#213010=CARTESIAN_POINT('Ctrl Pts',(177.612545532723,-6.05781339482078,
129.44485530364));
#213011=CARTESIAN_POINT('Ctrl Pts',(177.33409790891,-4.41818643401566,135.166124762878));
#213012=CARTESIAN_POINT('Ctrl Pts',(177.055650285097,1.28153801924328,136.879146056599));
#213013=CARTESIAN_POINT('Ctrl Pts',(176.777202661284,5.80359163943039,133.009736301615));
#213014=CARTESIAN_POINT('Ctrl Pts',(176.498755037472,4.99242806419446,127.113694031581));
#213015=CARTESIAN_POINT('Ctrl Pts',(176.220307413658,-0.406533008366379,
124.60919405498));
#213016=CARTESIAN_POINT('Ctrl Pts',(175.941859789846,-5.43191010648008,
127.797749498684));
#213017=CARTESIAN_POINT('Ctrl Pts',(175.663412166033,-5.46562718029972,
133.749233679521));
#213018=CARTESIAN_POINT('Ctrl Pts',(175.38496454222,-0.476699886155768,
136.994523381468));
#213019=CARTESIAN_POINT('Ctrl Pts',(175.106516918407,4.95029131528126,134.551355909651));
#213020=CARTESIAN_POINT('Ctrl Pts',(174.828069294595,5.82820663315002,128.664882815304));
#213021=CARTESIAN_POINT('Ctrl Pts',(174.549621670781,1.35028477887665,124.744485301934));
#213022=CARTESIAN_POINT('Ctrl Pts',(174.271174046969,-4.36848282210566,
126.392817162263));
#213023=CARTESIAN_POINT('Ctrl Pts',(173.992726423155,-6.07282812182305,
132.095141942134));
#213024=CARTESIAN_POINT('Ctrl Pts',(173.714278799343,-2.19654105173196,
136.611301742902));
#213025=CARTESIAN_POINT('Ctrl Pts',(173.435831175529,3.69825993790488,135.791166334329));
#213026=CARTESIAN_POINT('Ctrl Pts',(173.157383551717,6.19454071464915,130.388400091055));
#213027=CARTESIAN_POINT('Ctrl Pts',(172.878935927904,2.99834119476844,125.367881250842));
#213028=CARTESIAN_POINT('Ctrl Pts',(172.600488304091,-2.95318740599396,
125.343221361866));
#213029=CARTESIAN_POINT('Ctrl Pts',(172.322040680278,-6.1908810518732,130.337081657394));
#213030=CARTESIAN_POINT('Ctrl Pts',(172.043593056465,-3.7394574524341,135.760348489473));
#213031=CARTESIAN_POINT('Ctrl Pts',(171.765145432652,2.14834486313941,136.629304580736));
#213032=CARTESIAN_POINT('Ctrl Pts',(171.486697808839,6.06192320196904,132.145421734178));
#213033=CARTESIAN_POINT('Ctrl Pts',(171.208250185027,4.40489025960108,126.42916923593));
#213034=CARTESIAN_POINT('Ctrl Pts',(170.929802561213,-1.30002164048796,
124.733503877423));
#213035=CARTESIAN_POINT('Ctrl Pts',(170.651354937401,-5.81027716255637,
128.616659285268));
#213036=CARTESIAN_POINT('Ctrl Pts',(170.372907313588,-4.98117182005496,
134.510205342342));
#213037=CARTESIAN_POINT('Ctrl Pts',(170.094459689775,0.42538708130529,136.998261137926));
#213038=CARTESIAN_POINT('Ctrl Pts',(169.816012065962,5.44103603626017,133.794424944161));
#213039=CARTESIAN_POINT('Ctrl Pts',(169.537564442149,5.45663868327959,127.842865707018));
#213040=CARTESIAN_POINT('Ctrl Pts',(169.259116818336,0.457856951984399,
124.612775615598));
#213041=CARTESIAN_POINT('Ctrl Pts',(168.980669194523,-4.9616729506289,127.072449665244));
#213042=CARTESIAN_POINT('Ctrl Pts',(168.702221570711,-5.82166780281318,
132.961567566087));
#213043=CARTESIAN_POINT('Ctrl Pts',(168.423773946897,-1.33183434849535,
136.868317666657));
#213044=CARTESIAN_POINT('Ctrl Pts',(168.145326323085,4.38188980836473,135.202587479883));
#213045=CARTESIAN_POINT('Ctrl Pts',(167.866878699272,6.06887129855542,129.495101671966));
#213046=CARTESIAN_POINT('Ctrl Pts',(167.588431075459,2.17885654621902,124.9907608742));
#213047=CARTESIAN_POINT('Ctrl Pts',(167.309983451646,-3.71342092903282,
125.82883423045));
#213048=CARTESIAN_POINT('Ctrl Pts',(167.031535827833,-6.19324598120115,
131.239173268482));
#213049=CARTESIAN_POINT('Ctrl Pts',(166.75308820402,-2.98178053353198,136.249940722101));
#213050=CARTESIAN_POINT('Ctrl Pts',(166.474640580207,2.96979555637586,136.25648609103));
#213051=CARTESIAN_POINT('Ctrl Pts',(166.196192956395,6.19227461255283,131.252794500981));
#213052=CARTESIAN_POINT('Ctrl Pts',(165.917745332582,3.7243558092261,125.837014079288));
#213053=CARTESIAN_POINT('Ctrl Pts',(165.639297708769,-2.16606403788322,
124.985982457902));
#213054=CARTESIAN_POINT('Ctrl Pts',(165.360850084956,-6.06597685228888,
129.481756121673));
#213055=CARTESIAN_POINT('Ctrl Pts',(165.082402461143,-4.39155327888481,
135.192938704347));
#213056=CARTESIAN_POINT('Ctrl Pts',(164.80395483733,1.31849321850979,136.871232419228));
#213057=CARTESIAN_POINT('Ctrl Pts',(164.525507213517,5.81690886006848,132.974367331546));
#213058=CARTESIAN_POINT('Ctrl Pts',(164.247059589704,4.96986943102014,127.083372084437));
#213059=CARTESIAN_POINT('Ctrl Pts',(163.968611965891,-0.444237213516358,
124.611783518878));
#213060=CARTESIAN_POINT('Ctrl Pts',(163.690164342078,-5.45011156102575,
127.830870782803));
#213061=CARTESIAN_POINT('Ctrl Pts',(163.411716718265,-5.44759963670407,
133.782449941821));
#213062=CARTESIAN_POINT('Ctrl Pts',(163.133269094453,-0.439009776288703,
136.9973104996));
#213063=CARTESIAN_POINT('Ctrl Pts',(162.85482147064,4.97300862171615,134.52115265821));
#213064=CARTESIAN_POINT('Ctrl Pts',(162.576373846827,5.81507504134112,128.629444506854));
#213065=CARTESIAN_POINT('Ctrl Pts',(162.297926223014,1.31337158018249,124.736378010682));
#213066=CARTESIAN_POINT('Ctrl Pts',(162.019478599201,-4.39525620139515,
126.419491092807));
#213067=CARTESIAN_POINT('Ctrl Pts',(161.741030975388,-6.06485825409316,
132.132085055398));
#213068=CARTESIAN_POINT('Ctrl Pts',(161.462583351575,-2.16115185607673,
136.624565122567));
#213069=CARTESIAN_POINT('Ctrl Pts',(161.184135727762,3.72854751953661,135.768561582436));
#213070=CARTESIAN_POINT('Ctrl Pts',(160.905688103949,6.19189387436843,130.350699870288));
#213071=CARTESIAN_POINT('Ctrl Pts',(160.627240480137,2.96519224948793,125.349730222329));
#213072=CARTESIAN_POINT('Ctrl Pts',(160.348792856324,-2.9863761949775,125.361299434083));
#213073=CARTESIAN_POINT('Ctrl Pts',(160.070345232511,-6.19361080884636,
130.374775965136));
#213074=CARTESIAN_POINT('Ctrl Pts',(159.791897608698,-3.70921966409463,
135.783019805394));
#213075=CARTESIAN_POINT('Ctrl Pts',(159.513449984885,2.18376314650564,136.616119073061));
#213076=CARTESIAN_POINT('Ctrl Pts',(159.235002361072,6.06997430822783,132.108496240312));
#213077=CARTESIAN_POINT('Ctrl Pts',(158.956554737259,4.37817561541891,126.402436480826));
#213078=CARTESIAN_POINT('Ctrl Pts',(158.678107113446,-1.3369525821905,124.741529957054));
#213079=CARTESIAN_POINT('Ctrl Pts',(158.399659489633,-5.82348667053154,
128.652068624549));
#213080=CARTESIAN_POINT('Ctrl Pts',(158.121211865821,-4.95852100179383,
134.540458488317));
#213081=CARTESIAN_POINT('Ctrl Pts',(157.842764242008,0.463083230374652,
136.995556927392));
#213082=CARTESIAN_POINT('Ctrl Pts',(157.564316618195,5.45913659670229,133.761248414491));
#213083=CARTESIAN_POINT('Ctrl Pts',(157.285868994382,5.43851012430973,127.809704468215));
#213084=CARTESIAN_POINT('Ctrl Pts',(157.007421370569,0.420158533666468,
124.610103226106));
#213085=CARTESIAN_POINT('Ctrl Pts',(156.728973746756,-4.98429822353081,
127.102721920452));
#213086=CARTESIAN_POINT('Ctrl Pts',(156.450526122943,-5.80842840980828,
132.996965742341));
#213087=CARTESIAN_POINT('Ctrl Pts',(156.172078499131,-1.2948966449748,136.876312569277));
#213088=CARTESIAN_POINT('Ctrl Pts',(155.893630875317,4.40858187737264,135.175832183934));
#213089=CARTESIAN_POINT('Ctrl Pts',(155.615183251505,6.06078902561252,129.458182987356));
#213090=CARTESIAN_POINT('Ctrl Pts',(155.336735627692,2.14342714531882,124.977605268507));
#213091=CARTESIAN_POINT('Ctrl Pts',(155.058288003879,-3.74363956928552,
125.85153106262));
#213092=CARTESIAN_POINT('Ctrl Pts',(154.779840380066,-6.19048440667673,
131.276865258552));
#213093=CARTESIAN_POINT('Ctrl Pts',(154.501392756253,-2.94857649630798,
136.267990772552));
#213094=CARTESIAN_POINT('Ctrl Pts',(154.22294513244,3.00292916819795,136.238307087292));
#213095=CARTESIAN_POINT('Ctrl Pts',(153.944497508627,6.19488962837548,131.215092059396));
#213096=CARTESIAN_POINT('Ctrl Pts',(153.666049884815,3.69404915725887,125.814434901805));
#213097=CARTESIAN_POINT('Ctrl Pts',(153.387602261001,-2.20144202504465,
124.999275705575));
#213098=CARTESIAN_POINT('Ctrl Pts',(153.109154637189,-6.07391553275397,
129.518705949301));
#213099=CARTESIAN_POINT('Ctrl Pts',(152.830707013376,-4.36475739313218,
135.219590025439));
#213100=CARTESIAN_POINT('Ctrl Pts',(152.552259389563,1.3553995605252,136.863093971691));
#213101=CARTESIAN_POINT('Ctrl Pts',(152.27381176575,5.83001053300956,132.93891795108));
#213102=CARTESIAN_POINT('Ctrl Pts',(151.995364141937,4.94712663750637,127.053188019893));
#213103=CARTESIAN_POINT('Ctrl Pts',(151.716916518124,-0.481924957293099,
124.614602450997));
#213104=CARTESIAN_POINT('Ctrl Pts',(151.438468894311,-5.46811105968323,
127.864102250682));
#213105=CARTESIAN_POINT('Ctrl Pts',(151.160021270498,-5.4293702303005,133.815555849925));
#213106=CARTESIAN_POINT('Ctrl Pts',(150.881573646685,-0.40130339875292,
136.999868135696));
#213107=CARTESIAN_POINT('Ctrl Pts',(150.603126022873,4.99554165148768,134.490811679673));
#213108=CARTESIAN_POINT('Ctrl Pts',(150.324678399059,5.80172796978809,128.59408679072));
#213109=CARTESIAN_POINT('Ctrl Pts',(150.046230775247,1.27640971402146,124.728495570759));
#213110=CARTESIAN_POINT('Ctrl Pts',(149.767783151434,-4.42186671284978,
126.446327506304));
#213111=CARTESIAN_POINT('Ctrl Pts',(149.489335527621,-6.05666365081033,
132.168978969345));
#213112=CARTESIAN_POINT('Ctrl Pts',(149.210887903808,-2.12568257814469,
136.637612832414));
#213113=CARTESIAN_POINT('Ctrl Pts',(148.932440279995,3.75869693846883,135.74577288025));
#213114=CARTESIAN_POINT('Ctrl Pts',(148.653992656183,6.18901759118317,130.313016460088));
#213115=CARTESIAN_POINT('Ctrl Pts',(148.375545032369,2.93193342791814,125.331781317152));
#213116=CARTESIAN_POINT('Ctrl Pts',(148.097097408557,-3.01945432269288,
125.379579200934));
#213117=CARTESIAN_POINT('Ctrl Pts',(147.818649784743,-6.19611105929333,
130.412486191295));
#213118=CARTESIAN_POINT('Ctrl Pts',(147.540202160931,-3.67884442925635,
135.805506635269));
#213119=CARTESIAN_POINT('Ctrl Pts',(147.261754537118,2.21910050972548,136.602718208539));
#213120=CARTESIAN_POINT('Ctrl Pts',(146.983306913305,6.07780048935632,132.071522421221));
#213121=CARTESIAN_POINT('Ctrl Pts',(146.704859289492,4.35129873632927,126.375866840638));
#213122=CARTESIAN_POINT('Ctrl Pts',(146.426411665679,-1.37383398262348,
124.749780697104));
#213123=CARTESIAN_POINT('Ctrl Pts',(146.147964041867,-5.83648038706648,
128.687557717801));
#213124=CARTESIAN_POINT('Ctrl Pts',(145.869516418053,-4.93568644371351,
134.570573191811));
#213125=CARTESIAN_POINT('Ctrl Pts',(145.591068794241,0.500762219724632,
136.992623299802));
#213126=CARTESIAN_POINT('Ctrl Pts',(145.312621170428,5.47703486683029,133.727962316256));
#213127=CARTESIAN_POINT('Ctrl Pts',(145.034173546615,5.42018003934715,127.776654197497));
#213128=CARTESIAN_POINT('Ctrl Pts',(144.755725922802,0.382444546219556,
124.607660367099));
#213129=CARTESIAN_POINT('Ctrl Pts',(144.477278298989,-5.00673880142907,
127.133131341243));
#213130=CARTESIAN_POINT('Ctrl Pts',(144.198830675176,-5.79497378335261,
133.032282670807));
#213131=CARTESIAN_POINT('Ctrl Pts',(143.920383051363,-1.25791095858285,
136.884082473484));
#213132=CARTESIAN_POINT('Ctrl Pts',(143.64193542755,4.43511058475782,135.148914901497));
#213133=CARTESIAN_POINT('Ctrl Pts',(143.363487803737,6.05248216790344,129.421314185853));
#213134=CARTESIAN_POINT('Ctrl Pts',(143.085040179924,2.10791831893749,124.964665575378));
#213135=CARTESIAN_POINT('Ctrl Pts',(142.806592556112,-3.77371948759721,
125.87441142371));
#213136=CARTESIAN_POINT('Ctrl Pts',(142.528144932299,-6.18749344147606,
131.314539739788));
#213137=CARTESIAN_POINT('Ctrl Pts',(142.249697308486,-2.91526319849757,
136.285838366179));
#213138=CARTESIAN_POINT('Ctrl Pts',(141.971249684673,3.03595150537554,136.219926726669));
#213139=CARTESIAN_POINT('Ctrl Pts',(141.69280206086,6.19727509028471,131.177374398005));
#213140=CARTESIAN_POINT('Ctrl Pts',(141.414354437047,3.6636056209416,125.792040627854));
#213141=CARTESIAN_POINT('Ctrl Pts',(141.135906813234,-2.23673843696229,
125.012784062803));
#213142=CARTESIAN_POINT('Ctrl Pts',(140.857459189421,-6.0816291420453,129.555703417335));
#213143=CARTESIAN_POINT('Ctrl Pts',(140.579011565609,-4.33779976968917,
135.246077738584));
#213144=CARTESIAN_POINT('Ctrl Pts',(140.300563941795,1.39225567771152,136.854731015561));
#213145=CARTESIAN_POINT('Ctrl Pts',(140.022116317983,5.84289617276637,132.903389473806));
#213146=CARTESIAN_POINT('Ctrl Pts',(139.74366869417,4.92420052639575,127.023142956427));
#213147=CARTESIAN_POINT('Ctrl Pts',(139.465221070357,-0.519594843163371,
124.617650746882));
#213148=CARTESIAN_POINT('Ctrl Pts',(139.186773446544,-5.48590793547459,
127.897442670915));
#213149=CARTESIAN_POINT('Ctrl Pts',(138.908325822731,-5.41093963658633,
133.848550177083));
#213150=CARTESIAN_POINT('Ctrl Pts',(138.629878198918,-0.363582150772119,
137.002196194983));
#213151=CARTESIAN_POINT('Ctrl Pts',(138.351430575105,5.0178895696262,134.460334098336));
#213152=CARTESIAN_POINT('Ctrl Pts',(138.072982951292,5.78816591307159,128.558810977095));
#213153=CARTESIAN_POINT('Ctrl Pts',(137.79453532748,1.23940055002892,124.720838274248));
#213154=CARTESIAN_POINT('Ctrl Pts',(137.516087703667,-4.44831337040726,
126.473325408321));
#213155=CARTESIAN_POINT('Ctrl Pts',(137.237640079854,-6.0482446156285,132.205822316857));
#213156=CARTESIAN_POINT('Ctrl Pts',(136.959192456041,-2.09013453226308,
136.650444388955));
#213157=CARTESIAN_POINT('Ctrl Pts',(136.680744832228,3.78870707750376,135.722801072215));
#213158=CARTESIAN_POINT('Ctrl Pts',(136.402297208415,6.18591197167502,130.275351256826));
#213159=CARTESIAN_POINT('Ctrl Pts',(136.123849584602,2.89856596247695,125.314035200413));
#213160=CARTESIAN_POINT('Ctrl Pts',(135.845401960789,-3.05242056341787,
125.398059985055));
#213161=CARTESIAN_POINT('Ctrl Pts',(135.566954336976,-6.19838171056633,
130.450210938505));
#213162=CARTESIAN_POINT('Ctrl Pts',(135.288506713164,-3.64833287348497,
135.827808145838));
#213163=CARTESIAN_POINT('Ctrl Pts',(135.01005908935,2.25435564335981,136.589102483743));
#213164=CARTESIAN_POINT('Ctrl Pts',(134.731611465538,6.08540145535266,132.034501646982));
#213165=CARTESIAN_POINT('Ctrl Pts',(134.453163841725,4.32426061826468,126.349461299917));
#213166=CARTESIAN_POINT('Ctrl Pts',(134.174716217912,-1.41066447513297,
124.75825579184));
#213167=CARTESIAN_POINT('Ctrl Pts',(133.896268594099,-5.84925783067434,
128.723125249964));
#213168=CARTESIAN_POINT('Ctrl Pts',(133.617820970286,-4.91266899195694,
134.600548336913));
#213169=CARTESIAN_POINT('Ctrl Pts',(133.339373346473,0.538422653146471,
136.989460363863));
#213170=CARTESIAN_POINT('Ctrl Pts',(133.06092572266,5.49473018341705,133.694567882885));
#213171=CARTESIAN_POINT('Ctrl Pts',(132.782478098847,5.40164910761999,127.743716119554));
#213172=CARTESIAN_POINT('Ctrl Pts',(132.504030475035,0.344716387149417,
124.605447129098));
#213173=CARTESIAN_POINT('Ctrl Pts',(132.225582851222,-5.02899385277987,
127.163676800786));
#213174=CARTESIAN_POINT('Ctrl Pts',(131.947135227409,-5.78130442201224,
133.067517042801));
#213175=CARTESIAN_POINT('Ctrl Pts',(131.668687603596,-1.22087865983776,
136.891627091362));
#213176=CARTESIAN_POINT('Ctrl Pts',(131.390239979783,4.46147494748924,135.121836630005));
#213177=CARTESIAN_POINT('Ctrl Pts',(131.11179235597,6.04395103324181,129.384496633644));
#213178=CARTESIAN_POINT('Ctrl Pts',(130.833344732157,2.07233138286776,124.951942274296));
#213179=CARTESIAN_POINT('Ctrl Pts',(130.554897108344,-3.80365956934553,
125.897474465882));
#213180=CARTESIAN_POINT('Ctrl Pts',(130.276449484532,-6.18427319643048,
131.35219531615));
#213181=CARTESIAN_POINT('Ctrl Pts',(129.998001860718,-2.88184187453723,
136.303482841632));
#213182=CARTESIAN_POINT('Ctrl Pts',(129.719554236906,3.0688613442533,136.201345690253));
#213183=CARTESIAN_POINT('Ctrl Pts',(129.441106613093,6.1994309098865,131.139642914452));
#213184=CARTESIAN_POINT('Ctrl Pts',(129.16265898928,3.63302632837089,125.769832087263));
#213185=CARTESIAN_POINT('Ctrl Pts',(128.884211365467,-2.27195196571463,
125.026507029031));
#213186=CARTESIAN_POINT('Ctrl Pts',(128.605763741654,-6.08911739433215,
129.592747154821));
#213187=CARTESIAN_POINT('Ctrl Pts',(128.327316117841,-4.31068140748063,
135.272400862266));
#213188=CARTESIAN_POINT('Ctrl Pts',(128.048868494028,1.42906020435147,136.846143860731));
#213189=CARTESIAN_POINT('Ctrl Pts',(127.770420870216,5.85556530185681,132.867783216248));
#213190=CARTESIAN_POINT('Ctrl Pts',(127.491973246402,4.9010919472237,126.993238007373));
#213191=CARTESIAN_POINT('Ctrl Pts',(127.21352562259,-0.557245475255655,
124.620928293575));
#213192=CARTESIAN_POINT('Ctrl Pts',(126.935077998777,-5.50350152892981,
127.930890808061));
#213193=CARTESIAN_POINT('Ctrl Pts',(126.656630374964,-5.39230853851415,
133.881431700678));
#213194=CARTESIAN_POINT('Ctrl Pts',(126.378182751151,-0.325847430121078,
137.004294591193));
#213195=CARTESIAN_POINT('Ctrl Pts',(126.099735127338,5.04005154802147,134.429721043558));
#213196=CARTESIAN_POINT('Ctrl Pts',(125.821287503525,5.77438937373851,128.523618373138));
#213197=CARTESIAN_POINT('Ctrl Pts',(125.542839879712,1.20234545959337,124.713406404895));
#213198=CARTESIAN_POINT('Ctrl Pts',(125.264392255899,-4.47459519407686,
126.50048379844));
#213199=CARTESIAN_POINT('Ctrl Pts',(124.985944632086,-6.03960146051831,
132.24261373269));
#213200=CARTESIAN_POINT('Ctrl Pts',(124.707497008274,-2.05450903567761,
136.663059316712));
#213201=CARTESIAN_POINT('Ctrl Pts',(124.429049384461,3.81857682460466,135.69964700956));
#213202=CARTESIAN_POINT('Ctrl Pts',(124.150601760648,6.18257713092382,130.237705656202));
#213203=CARTESIAN_POINT('Ctrl Pts',(123.872154136835,2.86509108960817,125.296492529702));
#213204=CARTESIAN_POINT('Ctrl Pts',(123.593706513022,-3.08527369557641,
125.416741101634));
#213205=CARTESIAN_POINT('Ctrl Pts',(123.315258889209,-6.20042267852561,
130.487948808862));
#213206=CARTESIAN_POINT('Ctrl Pts',(123.036811265396,-3.61768612739718,
135.849923510712));
#213207=CARTESIAN_POINT('Ctrl Pts',(122.758363641583,2.28952724101679,136.575272403211));
#213208=CARTESIAN_POINT('Ctrl Pts',(122.47991601777,6.09277692456002,131.997435289415));
#213209=CARTESIAN_POINT('Ctrl Pts',(122.201468393958,4.29706226313277,126.323220837128));
#213210=CARTESIAN_POINT('Ctrl Pts',(121.923020770144,-1.44744269495155,
124.766954927214));
#213211=CARTESIAN_POINT('Ctrl Pts',(121.644573146332,-5.86181852788225,
128.758769903068));
#213212=CARTESIAN_POINT('Ctrl Pts',(121.366125522519,-4.88946949944416,
134.630382812884));
#213213=CARTESIAN_POINT('Ctrl Pts',(121.087677898706,0.576063135118759,
136.986068236777));
#213214=CARTESIAN_POINT('Ctrl Pts',(120.809230274893,5.51222189075617,133.661066351821));
#213215=CARTESIAN_POINT('Ctrl Pts',(120.53078265108,5.38291801579874,127.710891454918));
#213216=CARTESIAN_POINT('Ctrl Pts',(120.252335027267,0.306975454486648,
124.603463594118));
#213217=CARTESIAN_POINT('Ctrl Pts',(119.973887403454,-5.05106255291402,
127.194357167205));
#213218=CARTESIAN_POINT('Ctrl Pts',(119.695439779642,-5.76742083231046,
133.102667552701));
#213219=CARTESIAN_POINT('Ctrl Pts',(119.416992155829,-1.18380112098488,
136.898946143343));
#213220=CARTESIAN_POINT('Ctrl Pts',(119.138544532016,4.48767398862585,135.09459837285));
#213221=CARTESIAN_POINT('Ctrl Pts',(118.860096908203,6.03519593775195,129.347731695017));
#213222=CARTESIAN_POINT('Ctrl Pts',(118.58164928439,2.0366676557964,124.939435836727));
#213223=CARTESIAN_POINT('Ctrl Pts',(118.303201660577,-3.83345870508974,
125.920719334523));
#213224=CARTESIAN_POINT('Ctrl Pts',(118.024754036764,-6.18082379086727,
131.389830592295));
#213225=CARTESIAN_POINT('Ctrl Pts',(117.746306412951,-2.84831376286653,
136.320923545089));
#213226=CARTESIAN_POINT('Ctrl Pts',(117.467858789138,3.10165746534553,136.18256466657));
#213227=CARTESIAN_POINT('Ctrl Pts',(117.189411165326,6.20135700729606,131.101899006891));
#213228=CARTESIAN_POINT('Ctrl Pts',(116.910963541513,3.60231241267338,125.747810102979));
#213229=CARTESIAN_POINT('Ctrl Pts',(116.6325159177,-2.30708130645123,125.040444095748));
#213230=CARTESIAN_POINT('Ctrl Pts',(116.354068293887,-6.09638001213474,
129.62983578909));
#213231=CARTESIAN_POINT('Ctrl Pts',(116.075620670074,-4.28340331138726,
135.298558421074));
#213232=CARTESIAN_POINT('Ctrl Pts',(115.797173046261,1.46581177664024,136.837332825402));
#213233=CARTESIAN_POINT('Ctrl Pts',(115.518725422448,5.86801745082159,132.832100497806));
#213234=CARTESIAN_POINT('Ctrl Pts',(115.240277798635,4.87780175628715,126.963474280869));
#213235=CARTESIAN_POINT('Ctrl Pts',(114.961830174822,-0.594875458411799,
124.624434969628));
#213236=CARTESIAN_POINT('Ctrl Pts',(114.68338255101,-5.52089118811201,127.964445422689));
#213237=CARTESIAN_POINT('Ctrl Pts',(114.404934927196,-5.37347762646609,
133.914199202272));
#213238=CARTESIAN_POINT('Ctrl Pts',(114.126487303384,-0.288100635073559,
137.006163246571));
#213239=CARTESIAN_POINT('Ctrl Pts',(113.848039679571,5.06202676545313,134.398973649715));
#213240=CARTESIAN_POINT('Ctrl Pts',(113.569592055758,5.76039886228364,128.488510282924));
#213241=CARTESIAN_POINT('Ctrl Pts',(113.291144431945,1.16524581580469,124.706200238089));
#213242=CARTESIAN_POINT('Ctrl Pts',(113.012696808132,-4.50071120997606,
126.527801670297));
#213243=CARTESIAN_POINT('Ctrl Pts',(112.734249184319,-6.03073450575487,
132.279351853526));
#213244=CARTESIAN_POINT('Ctrl Pts',(112.455801560506,-2.01880740850426,
136.675457148234));
#213245=CARTESIAN_POINT('Ctrl Pts',(112.177353936694,3.84830507293705,135.676311550269));
#213246=CARTESIAN_POINT('Ctrl Pts',(111.898906312881,6.17901319250346,130.200081053184));
#213247=CARTESIAN_POINT('Ctrl Pts',(111.620458689068,2.8315100497353,125.279153955068));
#213248=CARTESIAN_POINT('Ctrl Pts',(111.342011065255,-3.11801250178361,
125.435621858436));
#213249=CARTESIAN_POINT('Ctrl Pts',(111.063563441442,-6.20223388754234,
130.525698403974));
#213250=CARTESIAN_POINT('Ctrl Pts',(110.785115817629,-3.58690532661952,
135.871851910398));
#213251=CARTESIAN_POINT('Ctrl Pts',(110.506668193816,2.32461399939974,136.56122847942));
#213252=CARTESIAN_POINT('Ctrl Pts',(110.228220570003,6.09992662367788,131.960324722029));
#213253=CARTESIAN_POINT('Ctrl Pts',(109.94977294619,4.26970467877848,126.297146424621));
#213254=CARTESIAN_POINT('Ctrl Pts',(109.671325322378,-1.48416727924886,
124.775877780875));
#213255=CARTESIAN_POINT('Ctrl Pts',(109.392877698565,-5.8741620132489,128.794490356288));
#213256=CARTESIAN_POINT('Ctrl Pts',(109.114430074752,-4.86608882584101,
134.660075514194));
#213257=CARTESIAN_POINT('Ctrl Pts',(108.835982450939,0.61368227085971,136.982447044243));
#213258=CARTESIAN_POINT('Ctrl Pts',(108.557534827126,5.52950934068608,133.627458964475));
#213259=CARTESIAN_POINT('Ctrl Pts',(108.279087203313,5.36398745797076,127.67818141992));
#213260=CARTESIAN_POINT('Ctrl Pts',(108.0006395795,0.269223146735527,124.601709835656));
#213261=CARTESIAN_POINT('Ctrl Pts',(107.722191955687,-5.07294408406776,
127.225171303631));
#213262=CARTESIAN_POINT('Ctrl Pts',(107.443744331874,-5.75332352870873,
133.137732897993));
#213263=CARTESIAN_POINT('Ctrl Pts',(107.165296708062,-1.14667971594628,
136.906039358215));
#213264=CARTESIAN_POINT('Ctrl Pts',(106.886849084249,4.51370673735246,135.067201139359));
#213265=CARTESIAN_POINT('Ctrl Pts',(106.608401460436,6.02621720585718,129.31102073231));
#213266=CARTESIAN_POINT('Ctrl Pts',(106.329953836623,2.00092845925606,124.927146726103));
#213267=CARTESIAN_POINT('Ctrl Pts',(106.05150621281,-3.86311579061174,125.944145168289));
#213268=CARTESIAN_POINT('Ctrl Pts',(105.773058588997,-6.17714535260555,
131.427444173636));
#213269=CARTESIAN_POINT('Ctrl Pts',(105.494610965184,-2.81468010588189,
136.338159830278));
#213270=CARTESIAN_POINT('Ctrl Pts',(105.216163341371,3.13433865337982,136.163584351558));
#213271=CARTESIAN_POINT('Ctrl Pts',(104.937715717558,6.20305331114115,131.064144073934));
#213272=CARTESIAN_POINT('Ctrl Pts',(104.659268093745,3.57146501196475,125.725975491034));
#213273=CARTESIAN_POINT('Ctrl Pts',(104.380820469933,-2.34212515744159,
125.054594746511));
#213274=CARTESIAN_POINT('Ctrl Pts',(104.10237284612,-6.10341672633411,129.666967945808));
#213275=CARTESIAN_POINT('Ctrl Pts',(103.823925222307,-4.25596649220884,
135.324549445729));
#213276=CARTESIAN_POINT('Ctrl Pts',(103.545477598494,1.50250903273456,136.828298236068));
#213277=CARTESIAN_POINT('Ctrl Pts',(103.267029974681,5.88025215824177,132.796342640716));
#213278=CARTESIAN_POINT('Ctrl Pts',(102.988582350868,4.85433081661274,126.933852879821));
#213279=CARTESIAN_POINT('Ctrl Pts',(102.710134727055,-0.63248339823904,
124.628170645098));
#213280=CARTESIAN_POINT('Ctrl Pts',(102.431687103242,-5.53807626864099,
127.998105271418));
#213281=CARTESIAN_POINT('Ctrl Pts',(102.153239479429,-5.35444759822839,
133.946851467654));
#213282=CARTESIAN_POINT('Ctrl Pts',(101.874791855617,-0.250343164351048,
137.00780209187));
#213283=CARTESIAN_POINT('Ctrl Pts',(101.596344231803,5.0838144076213,134.368093056165));
#213284=CARTESIAN_POINT('Ctrl Pts',(101.317896607991,5.74619489713063,128.453488007394));
#213285=CARTESIAN_POINT('Ctrl Pts',(101.039448984178,1.12810299340375,124.69922004086));
#213286=CARTESIAN_POINT('Ctrl Pts',(100.761001360365,-4.52666045036627,
126.55527801162));
#213287=CARTESIAN_POINT('Ctrl Pts',(100.482553736552,-6.0216440799065,132.316035318018));
#213288=CARTESIAN_POINT('Ctrl Pts',(100.204106112739,-1.98303097367997,
136.687637424115));
#213289=CARTESIAN_POINT('Ctrl Pts',(99.9256584889259,3.87789072090961,135.652795559044));
#213290=CARTESIAN_POINT('Ctrl Pts',(99.6472108651132,6.17522028847693,130.162478841968));
#213291=CARTESIAN_POINT('Ctrl Pts',(99.3687632413001,2.79782408721636,125.262020118999));
#213292=CARTESIAN_POINT('Ctrl Pts',(99.0903156174874,-3.15063576889091,
125.454701555827));
#213293=CARTESIAN_POINT('Ctrl Pts',(98.8118679936743,-6.20381527050148,
130.563458325018));
#213294=CARTESIAN_POINT('Ctrl Pts',(98.5334203698616,-3.55599161174595,
135.89359253233));
#213295=CARTESIAN_POINT('Ctrl Pts',(98.2549727460486,2.35961461835606,136.546971232774));
#213296=CARTESIAN_POINT('Ctrl Pts',(97.9765251222358,6.10685028777152,131.923171319966));
#213297=CARTESIAN_POINT('Ctrl Pts',(97.6980774984228,4.24218887894701,126.271239028595));
#213298=CARTESIAN_POINT('Ctrl Pts',(97.4196298746099,-1.52083686718185,
124.785024022185));
#213299=CARTESIAN_POINT('Ctrl Pts',(97.141182250797,-5.88628782938184,128.830285285991));
#213300=CARTESIAN_POINT('Ctrl Pts',(96.8627346269842,-4.842527837527,134.689625340572));
#213301=CARTESIAN_POINT('Ctrl Pts',(96.5842870031713,0.651278666378471,
136.978596920444));
#213302=CARTESIAN_POINT('Ctrl Pts',(96.3058393793584,5.54659189261388,133.593746966183));
#213303=CARTESIAN_POINT('Ctrl Pts',(96.0273917555454,5.34485813561491,127.645587226641));
#213304=CARTESIAN_POINT('Ctrl Pts',(95.7489441317327,0.231460862821695,
124.6001859187));
#213305=CARTESIAN_POINT('Ctrl Pts',(95.4704965079195,-5.09463763541278,
127.256118068232));
#213306=CARTESIAN_POINT('Ctrl Pts',(95.192048884107,-5.73901303358793,133.172711779316));
#213307=CARTESIAN_POINT('Ctrl Pts',(94.9136012602939,-1.10951582026908,
136.912906473138));
#213308=CARTESIAN_POINT('Ctrl Pts',(94.635153636481,4.53957222901603,135.039645944743));
#213309=CARTESIAN_POINT('Ctrl Pts',(94.3567060126683,6.01701517026768,129.274365105863));
#213310=CARTESIAN_POINT('Ctrl Pts',(94.0782583888551,1.96511511757592,124.915075397801));
#213311=CARTESIAN_POINT('Ctrl Pts',(93.7998107650425,-3.89262972695748,
125.967751099126));
#213312=CARTESIAN_POINT('Ctrl Pts',(93.5213631412293,-6.17323801795121,
131.465034666385));
#213313=CARTESIAN_POINT('Ctrl Pts',(93.2429155174167,-2.7809421498907,136.355191058501));
#213314=CARTESIAN_POINT('Ctrl Pts',(92.9644678936037,3.16690369734264,136.14440544854));
#213315=CARTESIAN_POINT('Ctrl Pts',(92.6860202697908,6.20451975856463,131.026379514606));
#213316=CARTESIAN_POINT('Ctrl Pts',(92.4075726459779,3.54048526930663,125.704329060518));
#213317=CARTESIAN_POINT('Ctrl Pts',(92.129125022165,-2.37708222012305,125.068958456964));
#213318=CARTESIAN_POINT('Ctrl Pts',(91.850677398352,-6.1102272761821,129.70414224903));
#213319=CARTESIAN_POINT('Ctrl Pts',(91.5722297745392,-4.22837196662692,
135.350372973126));
#213320=CARTESIAN_POINT('Ctrl Pts',(91.2937821507264,1.53915061280415,136.819040427511));
#213321=CARTESIAN_POINT('Ctrl Pts',(91.0153345269133,5.89226897075567,132.76051097));
#213322=CARTESIAN_POINT('Ctrl Pts',(90.7368869031008,4.8306799979248,126.90437490186));
#213323=CARTESIAN_POINT('Ctrl Pts',(90.4584392792875,-0.670067901161403,
124.632135181558));
#213324=CARTESIAN_POINT('Ctrl Pts',(90.1799916554748,-5.5550561337172,128.031869106972));
#213325=CARTESIAN_POINT('Ctrl Pts',(89.9015440316619,-5.3352191589658,133.979387286881));
#213326=CARTESIAN_POINT('Ctrl Pts',(89.6230964078489,-0.212576417070642,
137.009211066365));
#213327=CARTESIAN_POINT('Ctrl Pts',(89.3446487840362,5.10541366717708,134.337080407198));
#213328=CARTESIAN_POINT('Ctrl Pts',(89.0662011602232,5.73177800461257,128.418552844315));
#213329=CARTESIAN_POINT('Ctrl Pts',(88.7877535364103,1.09091836873142,124.69246607186));
#213330=CARTESIAN_POINT('Ctrl Pts',(88.5093059125973,-4.5524419536888,126.58291180426));
#213331=CARTESIAN_POINT('Ctrl Pts',(88.2308582887847,-6.0123305198223,132.352662766849));
#213332=CARTESIAN_POINT('Ctrl Pts',(87.9524106649715,-1.94718105691378,
136.69959969301));
#213333=CARTESIAN_POINT('Ctrl Pts',(87.6739630411587,3.90733267221543,135.629099907278));
#213334=CARTESIAN_POINT('Ctrl Pts',(87.395515417346,6.17119855939173,130.124900415918));
#213335=CARTESIAN_POINT('Ctrl Pts',(87.1170677935327,2.76403445029686,125.245091656395));
#213336=CARTESIAN_POINT('Ctrl Pts',(86.8386201697203,-3.18314228803115,
125.473979486801));
#213337=CARTESIAN_POINT('Ctrl Pts',(86.5601725459069,-6.20516676880425,
130.601227172784));
#213338=CARTESIAN_POINT('Ctrl Pts',(86.2817249220945,-3.52494612829556,
135.915144570902));
#213339=CARTESIAN_POINT('Ctrl Pts',(86.0032772982812,2.394527800925,136.532501191579));
#213340=CARTESIAN_POINT('Ctrl Pts',(85.7248296744686,6.11354766028192,131.885976459962));
#213341=CARTESIAN_POINT('Ctrl Pts',(85.4463820506556,4.21451588324655,126.245499609054));
#213342=CARTESIAN_POINT('Ctrl Pts',(85.1679344268427,-1.55745009994542,
124.794393312227));
#213343=CARTESIAN_POINT('Ctrl Pts',(84.8894868030298,-5.89819552695468,
128.86615336578));
#213344=CARTESIAN_POINT('Ctrl Pts',(84.611039179217,-4.81878740756302,134.719031197036));
#213345=CARTESIAN_POINT('Ctrl Pts',(84.332591555404,0.68885092852684,136.974518008049));
#213346=CARTESIAN_POINT('Ctrl Pts',(84.0541439315912,5.56346891353935,133.559931606153));
#213347=CARTESIAN_POINT('Ctrl Pts',(83.7756963077782,5.32553075757526,127.613110082872));
#213348=CARTESIAN_POINT('Ctrl Pts',(83.4972486839655,0.193690002040587,
124.598891899719));
#213349=CARTESIAN_POINT('Ctrl Pts',(83.2188010601524,-5.11614240308669,
127.287196314267));
#213350=CARTESIAN_POINT('Ctrl Pts',(82.9403534363397,-5.72448987722869,
133.207602900518));
#213351=CARTESIAN_POINT('Ctrl Pts',(82.6619058125266,-1.07231081107503,
136.919547233648));
#213352=CARTESIAN_POINT('Ctrl Pts',(82.3834581887138,4.56526950516122,135.011933810073));
#213353=CARTESIAN_POINT('Ctrl Pts',(82.1050105649009,6.00759017196827,129.237766173961));
#213354=CARTESIAN_POINT('Ctrl Pts',(81.826562941088,1.92922895783247,124.903222299129));
#213355=CARTESIAN_POINT('Ctrl Pts',(81.5481153172751,-3.92199942047723,
125.991536252305));
#213356=CARTESIAN_POINT('Ctrl Pts',(81.2696676934623,-6.16910193169181,
131.502600677615));
#213357=CARTESIAN_POINT('Ctrl Pts',(80.9912200696492,-2.74710114506546,
136.372016598662));
#213358=CARTESIAN_POINT('Ctrl Pts',(80.7127724458365,3.19935139052435,136.125028668197));
#213359=CARTESIAN_POINT('Ctrl Pts',(80.4343248220235,6.20575629522666,130.988606728286));
#213360=CARTESIAN_POINT('Ctrl Pts',(80.1558771982107,3.50937433266497,125.682871613546));
#213361=CARTESIAN_POINT('Ctrl Pts',(79.8774295743978,-2.41195119914859,
125.083534694853));
#213362=CARTESIAN_POINT('Ctrl Pts',(79.5989819505849,-6.11681140931136,
129.741357321249));
#213363=CARTESIAN_POINT('Ctrl Pts',(79.320534326772,-4.20062075716678,135.376028046362));
#213364=CARTESIAN_POINT('Ctrl Pts',(79.0420867029591,1.57573515908161,136.809559742781));
#213365=CARTESIAN_POINT('Ctrl Pts',(78.7636390791462,5.90406744307602,132.724606813414));
#213366=CARTESIAN_POINT('Ctrl Pts',(78.4851914553333,4.80685017661309,126.875041439303));
#213367=CARTESIAN_POINT('Ctrl Pts',(78.2067438315204,-0.707627574471386,
124.636328432103));
#213368=CARTESIAN_POINT('Ctrl Pts',(77.9282962077074,-5.57183015414549,
128.065735678218));
#213369=CARTESIAN_POINT('Ctrl Pts',(77.6498485838947,-5.31579302119528,
134.011805454327));
#213370=CARTESIAN_POINT('Ctrl Pts',(77.3714009600817,-0.174801792692954,
137.010390117845));
#213371=CARTESIAN_POINT('Ctrl Pts',(77.0929533362689,5.12682374375196,134.305936852001));
#213372=CARTESIAN_POINT('Ctrl Pts',(76.814505712456,5.7171487189526,128.38370608822));
#213373=CARTESIAN_POINT('Ctrl Pts',(76.536058088643,1.05369331967776,124.68593858136));
#213374=CARTESIAN_POINT('Ctrl Pts',(76.2576104648302,-4.57805476460059,
126.610702024239));
#213375=CARTESIAN_POINT('Ctrl Pts',(75.9791628410172,-6.00279417061961,
132.389232842773));
#213376=CARTESIAN_POINT('Ctrl Pts',(75.7007152172044,-1.91125898663751,
136.711343511654));
#213377=CARTESIAN_POINT('Ctrl Pts',(75.4222675933915,3.93662983587222,135.605225473025));
#213378=CARTESIAN_POINT('Ctrl Pts',(75.1438199695785,6.16694815427437,130.087347167514));
#213379=CARTESIAN_POINT('Ctrl Pts',(74.8653723457658,2.73014239106432,125.228369194547));
#213380=CARTESIAN_POINT('Ctrl Pts',(74.5869247219528,-3.21553085466319,
125.493454937009));
#213381=CARTESIAN_POINT('Ctrl Pts',(74.3084770981399,-6.20628833237051,
130.639003547736));
#213382=CARTESIAN_POINT('Ctrl Pts',(74.0300294743271,-3.49377002667009,
135.936507227495));
#213383=CARTESIAN_POINT('Ctrl Pts',(73.7515818505141,2.42935225338577,136.517818892029));
#213384=CARTESIAN_POINT('Ctrl Pts',(73.4731342267013,6.1200184930355,131.848741520285));
#213385=CARTESIAN_POINT('Ctrl Pts',(73.1946866028884,4.18668671711015,126.219929119786));
#213386=CARTESIAN_POINT('Ctrl Pts',(72.9162389790755,-1.59400562082267,
124.803985303816));
#213387=CARTESIAN_POINT('Ctrl Pts',(72.6377913552626,-5.90988466472314,
128.902093266552));
#213388=CARTESIAN_POINT('Ctrl Pts',(72.3593437314497,-4.79486841565966,
134.748291993943));
#213389=CARTESIAN_POINT('Ctrl Pts',(72.0808961076369,0.726397665050741,
136.970210458201));
#213390=CARTESIAN_POINT('Ctrl Pts',(71.8024484838239,5.58013977807825,133.526014137426));
#213391=CARTESIAN_POINT('Ctrl Pts',(71.524000860011,5.30600604003494,127.580751192065));
#213392=CARTESIAN_POINT('Ctrl Pts',(71.2455532361981,0.155911964005252,
124.597827826664));
#213393=CARTESIAN_POINT('Ctrl Pts',(70.9671056123853,-5.13745759022245,
127.318404890117));
#213394=CARTESIAN_POINT('Ctrl Pts',(70.6886579885723,-5.70975459779179,
133.242404968692));
#213395=CARTESIAN_POINT('Ctrl Pts',(70.4102103647595,-1.03506606700937,
136.925961393668));
#213396=CARTESIAN_POINT('Ctrl Pts',(70.1317627409465,4.59079761356593,134.98406576223));
#213397=CARTESIAN_POINT('Ctrl Pts',(69.8533151171337,5.99794256020584,129.201225292793));
#213398=CARTESIAN_POINT('Ctrl Pts',(69.5748674933208,1.89327130980037,124.891587869307));
#213399=CARTESIAN_POINT('Ctrl Pts',(69.2964198695077,-3.95122378286636,
126.015499746463));
#213400=CARTESIAN_POINT('Ctrl Pts',(69.0179722456952,-6.16473724709165,
131.540140815303));
#213401=CARTESIAN_POINT('Ctrl Pts',(68.7395246218819,-2.71315834539685,
136.388635827283));
#213402=CARTESIAN_POINT('Ctrl Pts',(68.4610769980694,3.23168053056381,136.105454728543));
#213403=CARTESIAN_POINT('Ctrl Pts',(68.1826293742561,6.20676287530703,130.950827114659));
#213404=CARTESIAN_POINT('Ctrl Pts',(67.9041817504435,3.47813335486666,125.661603945233));
#213405=CARTESIAN_POINT('Ctrl Pts',(67.6257341266304,-2.44673080243567,
125.09832292005));
#213406=CARTESIAN_POINT('Ctrl Pts',(67.3472865028177,-6.12316888174425,
129.778611783445));
#213407=CARTESIAN_POINT('Ctrl Pts',(67.0688388790048,-4.17271389215982,
135.401513714782));
#213408=CARTESIAN_POINT('Ctrl Pts',(66.7903912551918,1.61226131591331,136.799856533191));
#213409=CARTESIAN_POINT('Ctrl Pts',(66.511943631379,5.91564713800617,132.688631501398));
#213410=CARTESIAN_POINT('Ctrl Pts',(66.233496007566,4.78284223570014,126.845853579115));
#213411=CARTESIAN_POINT('Ctrl Pts',(65.9550483837533,-0.745161026381345,
124.640750241348));
#213412=CARTESIAN_POINT('Ctrl Pts',(65.6766007599402,-5.58839770835831,
128.099703730218));
#213413=CARTESIAN_POINT('Ctrl Pts',(65.3981531361275,-5.2961699047596,134.044104768727));
#213414=CARTESIAN_POINT('Ctrl Pts',(65.1197055123145,-0.137020690970298,
137.011339202618));
#213415=CARTESIAN_POINT('Ctrl Pts',(64.8412578885016,5.14804384398771,134.274663544608));
#213416=CARTESIAN_POINT('Ctrl Pts',(64.5628102646887,5.70230758224426,128.348949030369));
#213417=CARTESIAN_POINT('Ctrl Pts',(64.2843626408759,1.01642922563077,124.679637811238));
#213418=CARTESIAN_POINT('Ctrl Pts',(64.0059150170629,-4.60349793400934,
126.638647641779));
#213419=CARTESIAN_POINT('Ctrl Pts',(63.72746739325,-5.9930353856715,132.425744190676));
#213420=CARTESIAN_POINT('Ctrl Pts',(63.4490197694371,-1.87526609395646,
136.722868444874));
#213421=CARTESIAN_POINT('Ctrl Pts',(63.1705721456243,3.96578112626272,135.581173140958));
#213422=CARTESIAN_POINT('Ctrl Pts',(62.8921245218114,6.16246923062527,130.049820488308));
#213423=CARTESIAN_POINT('Ctrl Pts',(62.6136768979985,2.69614916540168,125.211853353112));
#213424=CARTESIAN_POINT('Ctrl Pts',(62.3352292741856,-3.24780026861702,
125.513127184779));
#213425=CARTESIAN_POINT('Ctrl Pts',(62.0567816503727,-6.20717991964031,
130.676786050054));
#213426=CARTESIAN_POINT('Ctrl Pts',(61.7783340265599,-3.46246446211126,
135.957679710507));
#213427=CARTESIAN_POINT('Ctrl Pts',(61.4998864027468,2.46408668530527,136.502924878181));
#213428=CARTESIAN_POINT('Ctrl Pts',(61.2214387789342,6.12626254625314,131.81146788069));
#213429=CARTESIAN_POINT('Ctrl Pts',(60.942991155121,4.15870241175792,126.194528508313));
#213430=CARTESIAN_POINT('Ctrl Pts',(60.6645435313083,-1.63050207523548,
124.813799641521));
#213431=CARTESIAN_POINT('Ctrl Pts',(60.3860959074953,-5.92135480954196,
128.938103656541));
#213432=CARTESIAN_POINT('Ctrl Pts',(60.1076482836825,-4.77077174814381,
134.777406647022));
#213433=CARTESIAN_POINT('Ctrl Pts',(59.8292006598696,0.763917484641806,
136.965674430521));
#213434=CARTESIAN_POINT('Ctrl Pts',(59.5507530360567,5.59660386848551,133.491995816827));
#213435=CARTESIAN_POINT('Ctrl Pts',(59.2723054122438,5.28628470648961,127.548511753291));
#213436=CARTESIAN_POINT('Ctrl Pts',(58.9938577884309,0.11812814859451,124.596993738963));
#213437=CARTESIAN_POINT('Ctrl Pts',(58.715410164618,-5.15858240697801,127.34974263934));
#213438=CARTESIAN_POINT('Ctrl Pts',(58.4369625408051,-5.69480774129836,
133.277116694236));
#213439=CARTESIAN_POINT('Ctrl Pts',(58.1585149169922,-0.997782968190397,
136.932148715521));
#213440=CARTESIAN_POINT('Ctrl Pts',(57.8800672931793,4.61615560827684,134.956042833877));
#213441=CARTESIAN_POINT('Ctrl Pts',(57.6016196693665,5.98807269247603,129.164743816393));
#213442=CARTESIAN_POINT('Ctrl Pts',(57.3231720455535,1.85724350590365,124.880172539454));
#213443=CARTESIAN_POINT('Ctrl Pts',(57.0447244217407,-3.98030173120474,
126.039640693622));
#213444=CARTESIAN_POINT('Ctrl Pts',(56.7662767979277,-6.16014412588574,
131.577653688385));
#213445=CARTESIAN_POINT('Ctrl Pts',(56.4878291741149,-2.67911500864857,
136.405048128532));
#213446=CARTESIAN_POINT('Ctrl Pts',(56.209381550302,3.26388991949243,136.085684354897));
#213447=CARTESIAN_POINT('Ctrl Pts',(55.9309339264891,6.20753946150667,130.913042073662));
#213448=CARTESIAN_POINT('Ctrl Pts',(55.6524863026762,3.44676349355797,125.640526843659));
#213449=CARTESIAN_POINT('Ctrl Pts',(55.3740386788633,-2.48141974121268,
125.113322584571));
#213450=CARTESIAN_POINT('Ctrl Pts',(55.0955910550504,-6.12929945790263,
129.815904255142));
#213451=CARTESIAN_POINT('Ctrl Pts',(54.8171434312375,-4.14465240570495,
135.426829034002));
#213452=CARTESIAN_POINT('Ctrl Pts',(54.5386958074246,1.64872772980914,136.789931158292));
#213453=CARTESIAN_POINT('Ctrl Pts',(54.2602481836117,5.92700762645589,132.652586367033));
#213454=CARTESIAN_POINT('Ctrl Pts',(53.9818005597989,4.75865706480954,126.81681240286));
#213455=CARTESIAN_POINT('Ctrl Pts',(53.703352935986,-0.78266686607524,124.645400445441));
#213456=CARTESIAN_POINT('Ctrl Pts',(53.4249053121731,-5.604758182439,128.133772004274));
#213457=CARTESIAN_POINT('Ctrl Pts',(53.1464576883601,-5.27635053680027,
134.076284033214));
#213458=CARTESIAN_POINT('Ctrl Pts',(52.8680100645473,-0.0992345118958833,
137.012058285519));
#213459=CARTESIAN_POINT('Ctrl Pts',(52.5895624407343,5.1690731815654,134.243261643865));
#213460=CARTESIAN_POINT('Ctrl Pts',(52.3111148169216,5.68725514443172,128.314282958697));
#213461=CARTESIAN_POINT('Ctrl Pts',(52.0326671931086,0.979127467424884,
124.673563994973));
#213462=CARTESIAN_POINT('Ctrl Pts',(51.7542195692957,-4.62877051910935,
126.666747621346));
#213463=CARTESIAN_POINT('Ctrl Pts',(51.4757719454828,-5.98305452659317,
132.462195457613));
#213464=CARTESIAN_POINT('Ctrl Pts',(51.1973243216699,-1.83920371260068,
136.734174065611));
#213465=CARTESIAN_POINT('Ctrl Pts',(50.9188766978571,3.99478546317524,135.556943802347));
#213466=CARTESIAN_POINT('Ctrl Pts',(50.6404290740441,6.15776195441257,130.012321768865));
#213467=CARTESIAN_POINT('Ctrl Pts',(50.3619814502312,2.66205603294,125.195544744091));
#213468=CARTESIAN_POINT('Ctrl Pts',(50.0835338264184,-3.27994933413751,
125.532995501151));
#213469=CARTESIAN_POINT('Ctrl Pts',(49.8050862026055,-6.20784149757545,
130.714573279694));
#213470=CARTESIAN_POINT('Ctrl Pts',(49.5266385787925,-3.43103059465853,
135.978661235386));
#213471=CARTESIAN_POINT('Ctrl Pts',(49.2481909549797,2.4987298095866,136.487819701939));
#213472=CARTESIAN_POINT('Ctrl Pts',(48.9697433311668,6.13227958855924,131.774156922365));
#213473=CARTESIAN_POINT('Ctrl Pts',(48.6912957073539,4.13056400415832,126.169298715863));
#213474=CARTESIAN_POINT('Ctrl Pts',(48.412848083541,-1.66693811079436,124.823835961664));
#213475=CARTESIAN_POINT('Ctrl Pts',(48.1344004597282,-5.93260553638082,
128.974183201367));
#213476=CARTESIAN_POINT('Ctrl Pts',(47.8559528359152,-4.7464982979263,134.806374077418));
#213477=CARTESIAN_POINT('Ctrl Pts',(47.5775052121024,0.801408996989757,
136.960910093092));
#213478=CARTESIAN_POINT('Ctrl Pts',(47.2990575882894,5.61286057467834,133.457877904919));
#213479=CARTESIAN_POINT('Ctrl Pts',(47.0206099644766,5.26636748772036,127.516392961194));
#213480=CARTESIAN_POINT('Ctrl Pts',(46.7421623406636,0.0803399559020909,
124.596389667526));
#213481=CARTESIAN_POINT('Ctrl Pts',(46.4637147168508,-5.17951607056515,
127.381208400702));
#213482=CARTESIAN_POINT('Ctrl Pts',(46.1852670930379,-5.67964986161014,
133.311736790894));
#213483=CARTESIAN_POINT('Ctrl Pts',(45.9068194692249,-0.960462896156299,
136.938108969933));
#213484=CARTESIAN_POINT('Ctrl Pts',(45.6283718454121,4.64134254964412,134.927866063412));
#213485=CARTESIAN_POINT('Ctrl Pts',(45.3499242215992,5.97798093451044,129.128323096598));
#213486=CARTESIAN_POINT('Ctrl Pts',(45.0714765977863,1.82114688116607,124.868976732569));
#213487=CARTESIAN_POINT('Ctrl Pts',(44.7930289739735,-4.00923218799886,
126.063958199228));
#213488=CARTESIAN_POINT('Ctrl Pts',(44.5145813501605,-6.15532273827383,
131.615137906808));
#213489=CARTESIAN_POINT('Ctrl Pts',(44.2361337263477,-2.644972396308,136.421252894246));
#213490=CARTESIAN_POINT('Ctrl Pts',(43.9576861025347,3.29597836378001,136.065718279858));
#213491=CARTESIAN_POINT('Ctrl Pts',(43.6792384787219,6.20808602504863,130.875253005433));
#213492=CARTESIAN_POINT('Ctrl Pts',(43.4007908549089,3.41526591116036,125.619641089845));
#213493=CARTESIAN_POINT('Ctrl Pts',(43.1223432310961,-2.5160167300689,125.128533132602));
#213494=CARTESIAN_POINT('Ctrl Pts',(42.8438956072832,-6.13520291061547,
129.853233354452));
#213495=CARTESIAN_POINT('Ctrl Pts',(42.5654479834703,-4.11643733763101,
135.451973065955));
#213496=CARTESIAN_POINT('Ctrl Pts',(42.2870003596574,1.68513304949262,136.779783985877));
#213497=CARTESIAN_POINT('Ctrl Pts',(42.0085527358444,5.93814848745852,132.616472745983));
#213498=CARTESIAN_POINT('Ctrl Pts',(41.7301051120316,4.73429556013123,126.787918986671));
#213499=CARTESIAN_POINT('Ctrl Pts',(41.4516574882187,-0.820143703760798,
124.65027887207));
#213500=CARTESIAN_POINT('Ctrl Pts',(41.1732098644058,-5.62091097014408,
128.167939237972));
#213501=CARTESIAN_POINT('Ctrl Pts',(40.8947622405929,-5.25633565173145,
134.108342055376));
#213502=CARTESIAN_POINT('Ctrl Pts',(40.61631461678,-0.0614446556499193,
137.012547339898));
#213503=CARTESIAN_POINT('Ctrl Pts',(40.3378669929672,5.18991097723558,134.211732313379));
#213504=CARTESIAN_POINT('Ctrl Pts',(40.0594193691542,5.67199196328813,128.279709157768));
#213505=CARTESIAN_POINT('Ctrl Pts',(39.7809717453414,0.941789427290636,
124.66771735763));
#213506=CARTESIAN_POINT('Ctrl Pts',(39.5025241215285,-4.65387158341555,
126.695000921683));
#213507=CARTESIAN_POINT('Ctrl Pts',(39.2240764977156,-5.97285196322902,
132.49858529287));
#213508=CARTESIAN_POINT('Ctrl Pts',(38.9456288739027,-1.80307317887526,
136.745259954929));
#213509=CARTESIAN_POINT('Ctrl Pts',(38.6671812500898,4.02364177184326,135.532538355018));
#213510=CARTESIAN_POINT('Ctrl Pts',(38.3887336262769,6.15282650006613,129.974852398711));
#213511=CARTESIAN_POINT('Ctrl Pts',(38.110286002464,2.62786425701304,125.179443971804));
#213512=CARTESIAN_POINT('Ctrl Pts',(37.8318383786511,-3.31197685992897,
125.553059149895));
#213513=CARTESIAN_POINT('Ctrl Pts',(37.5533907548383,-6.20827304166094,
130.752363836438));
#213514=CARTESIAN_POINT('Ctrl Pts',(37.2749431310254,-3.3994695891056,135.999451024653));
#213515=CARTESIAN_POINT('Ctrl Pts',(36.9964955072125,2.53328034251594,136.47250392303));
#213516=CARTESIAN_POINT('Ctrl Pts',(36.7180478833995,6.13806939699002,131.73681002788));
#213517=CARTESIAN_POINT('Ctrl Pts',(36.4396002595867,4.10227253699055,126.144240677337));
#213518=CARTESIAN_POINT('Ctrl Pts',(36.1611526357737,-1.70331237734853,
124.834093892349));
#213519=CARTESIAN_POINT('Ctrl Pts',(35.8827050119609,-5.94363642833981,
129.01033056409));
#213520=CARTESIAN_POINT('Ctrl Pts',(35.604257388148,-4.72204896446884,134.835193211735));
#213521=CARTESIAN_POINT('Ctrl Pts',(35.3258097643351,0.838870812832614,
136.955917622458));
#213522=CARTESIAN_POINT('Ctrl Pts',(35.0473621405222,5.62890929425843,133.423661665951));
#213523=CARTESIAN_POINT('Ctrl Pts',(34.7689145167094,5.24625512176713,127.484396005948));
#213524=CARTESIAN_POINT('Ctrl Pts',(34.4904668928964,0.0425487861828518,
124.596015634733));
#213525=CARTESIAN_POINT('Ctrl Pts',(34.2120192690835,-5.20025780527969,
127.412801008228));
#213526=CARTESIAN_POINT('Ctrl Pts',(33.9335716452707,-5.66428152040741,
133.346263975806));
#213527=CARTESIAN_POINT('Ctrl Pts',(33.6551240214578,-0.923107233816384,
136.943841936043));
#213528=CARTESIAN_POINT('Ctrl Pts',(33.3766763976448,4.66635750435639,134.899536494936));
#213529=CARTESIAN_POINT('Ctrl Pts',(33.098228773832,5.96766766026296,129.091964482989));
#213530=CARTESIAN_POINT('Ctrl Pts',(32.8197811500191,1.78498277316083,124.858000863516));
#213531=CARTESIAN_POINT('Ctrl Pts',(32.5413335262063,-4.03801408121996,
126.08845136219));
#213532=CARTESIAN_POINT('Ctrl Pts',(32.2628859023933,-6.15027326291425,
131.65259208158));
#213533=CARTESIAN_POINT('Ctrl Pts',(31.9844382785804,-2.6107317735426,136.437249523951));
#213534=CARTESIAN_POINT('Ctrl Pts',(31.7059906547675,3.32794467437699,136.045557243275));
#213535=CARTESIAN_POINT('Ctrl Pts',(31.4275430309546,6.20840254567991,130.837461310262));
#213536=CARTESIAN_POINT('Ctrl Pts',(31.1490954071417,3.3836417748287,125.598947457719));
#213537=CARTESIAN_POINT('Ctrl Pts',(30.8706477833288,-2.55052048699994,
125.143954000505));
#213538=CARTESIAN_POINT('Ctrl Pts',(30.5922001595159,-6.14087902112821,
129.890597698133));
#213539=CARTESIAN_POINT('Ctrl Pts',(30.3137525357031,-4.08806973345779,
135.476944878919));
#213540=CARTESIAN_POINT('Ctrl Pts',(30.0353049118902,1.72147592595096,136.769415391952));
#213541=CARTESIAN_POINT('Ctrl Pts',(29.7568572880773,5.94906930818524,132.58029197645));
#213542=CARTESIAN_POINT('Ctrl Pts',(29.4784096642643,4.70975862438989,126.759174401203));
#213543=CARTESIAN_POINT('Ctrl Pts',(29.1999620404515,-0.857590150719802,
124.65538534046));
#213544=CARTESIAN_POINT('Ctrl Pts',(28.9215144166386,-5.63685547292606,
128.202204165235));
#213545=CARTESIAN_POINT('Ctrl Pts',(28.6430667928257,-5.23612599121204,
134.140277647291));
#213546=CARTESIAN_POINT('Ctrl Pts',(28.3646191690128,-0.0236525225496446,
137.012806347637));
#213547=CARTESIAN_POINT('Ctrl Pts',(28.0861715451999,5.2105564588459,134.180076721482));
#213548=CARTESIAN_POINT('Ctrl Pts',(27.807723921387,5.65651860439647,128.245228908728));
#213549=CARTESIAN_POINT('Ctrl Pts',(27.5292762975741,0.904416488802812,
124.662098115861));
#213550=CARTESIAN_POINT('Ctrl Pts',(27.2508286737613,-4.67880019679877,
126.723406495856));
#213551=CARTESIAN_POINT('Ctrl Pts',(26.9723810499484,-5.96242807363892,
132.53491234801));
#213552=CARTESIAN_POINT('Ctrl Pts',(26.6939334261354,-1.76687583160983,
136.756125702037));
#213553=CARTESIAN_POINT('Ctrl Pts',(26.4154858023226,4.05234898298581,135.507957703324));
#213554=CARTESIAN_POINT('Ctrl Pts',(26.1370381785097,6.14766305047102,129.937413766291));
#213555=CARTESIAN_POINT('Ctrl Pts',(25.8585905546968,2.59357510460964,125.163551632871));
#213556=CARTESIAN_POINT('Ctrl Pts',(25.5801429308839,-3.34388165920016,
125.573317387547));
#213557=CARTESIAN_POINT('Ctrl Pts',(25.301695307071,-6.2084745359058,130.790156319941));
#213558=CARTESIAN_POINT('Ctrl Pts',(25.0232476832582,-3.36778261495664,
136.020048307934));
#213559=CARTESIAN_POINT('Ctrl Pts',(24.7448000594452,2.56773700381057,136.456978108987));
#213560=CARTESIAN_POINT('Ctrl Pts',(24.4663524356323,6.14363175700203,131.69942858114));
#213561=CARTESIAN_POINT('Ctrl Pts',(24.1879048118195,4.07382905860539,126.11935532127));
#213562=CARTESIAN_POINT('Ctrl Pts',(23.9094571880065,-1.73962352703587,
124.844573053462));
#213563=CARTESIAN_POINT('Ctrl Pts',(23.6310095641937,-5.95444707666522,
129.046544405257));
#213564=CARTESIAN_POINT('Ctrl Pts',(23.3525619403807,-4.69742465375045,
134.863862982068));
#213565=CARTESIAN_POINT('Ctrl Pts',(23.0741143165679,0.876301544009003,
136.950697203617));
#213566=CARTESIAN_POINT('Ctrl Pts',(22.795666692755,5.64474943253441,133.389348367819));
#213567=CARTESIAN_POINT('Ctrl Pts',(22.5172190689421,5.22594835390121,127.452522073212));
#213568=CARTESIAN_POINT('Ctrl Pts',(22.2387714451292,0.0047560398029127,
124.595871654449));
#213569=CARTESIAN_POINT('Ctrl Pts',(21.9603238213163,-5.22080684252888,
127.444519291243));
#213570=CARTESIAN_POINT('Ctrl Pts',(21.6818761975034,-5.64870328716988,
133.380696969555));
#213571=CARTESIAN_POINT('Ctrl Pts',(21.4034285736905,-0.885717365398449,
136.949347401415));
#213572=CARTESIAN_POINT('Ctrl Pts',(21.1249809498776,4.69119954547528,134.871055178212));
#213573=CARTESIAN_POINT('Ctrl Pts',(20.8465333260648,5.95713325189572,129.055669322849));
#213574=CARTESIAN_POINT('Ctrl Pts',(20.5680857022518,1.74875252196249,124.847245339011));
#213575=CARTESIAN_POINT('Ctrl Pts',(20.289638078439,-4.06664634434428,126.113119274905));
#213576=CARTESIAN_POINT('Ctrl Pts',(20.011190454626,-6.14499588691713,131.690014824823));
#213577=CARTESIAN_POINT('Ctrl Pts',(19.7327428308132,-2.57639440915122,
136.453037424885));
#213578=CARTESIAN_POINT('Ctrl Pts',(19.4542952070003,3.35978766676044,136.025201992224));
#213579=CARTESIAN_POINT('Ctrl Pts',(19.1758475831874,6.20848901167171,130.799668388532));
#213580=CARTESIAN_POINT('Ctrl Pts',(18.8973999593745,3.3518922564065,125.578446714094));
#213581=CARTESIAN_POINT('Ctrl Pts',(18.6189523355616,-2.58492973345636,
125.159584616859));
#213582=CARTESIAN_POINT('Ctrl Pts',(18.3405047117487,-6.14632757911053,
129.927995901635));
#213583=CARTESIAN_POINT('Ctrl Pts',(18.0620570879358,-4.05955064435711,
135.501743547556));
#213584=CARTESIAN_POINT('Ctrl Pts',(17.7836094641229,1.75775501248606,136.758825760728));
#213585=CARTESIAN_POINT('Ctrl Pts',(17.5051618403101,5.95976968396092,132.544045399129));
#213586=CARTESIAN_POINT('Ctrl Pts',(17.2267142164972,4.68504716681072,126.730579711598));
#213587=CARTESIAN_POINT('Ctrl Pts',(16.9482665926842,-0.8950048193604,124.660719661391));
#213588=CARTESIAN_POINT('Ctrl Pts',(16.6698189688713,-5.65259109995534,
128.236565516362));
#213589=CARTESIAN_POINT('Ctrl Pts',(16.3913713450585,-5.21572230411858,
134.172089625574));
#213590=CARTESIAN_POINT('Ctrl Pts',(16.1129237212456,0.0141404870033325,
137.012835299135));
#213591=CARTESIAN_POINT('Ctrl Pts',(15.8344760974327,5.23100886137047,134.148296041183));
#213592=CARTESIAN_POINT('Ctrl Pts',(15.5560284736198,5.64083564112771,128.210843489254));
#213593=CARTESIAN_POINT('Ctrl Pts',(15.2775808498069,0.8670100368296,124.656706477888));
#213594=CARTESIAN_POINT('Ctrl Pts',(14.999133225994,-4.70355543551987,126.751963291284));
#213595=CARTESIAN_POINT('Ctrl Pts',(14.7206856021811,-5.95178324408404,
132.571175276918));
#213596=CARTESIAN_POINT('Ctrl Pts',(14.4422379783683,-1.73061301211068,
136.766770904302));
#213597=CARTESIAN_POINT('Ctrl Pts',(14.1637903545553,4.08090603284655,135.48320275811));
#213598=CARTESIAN_POINT('Ctrl Pts',(13.8853427307424,6.14227179696077,129.900007258904));
#213599=CARTESIAN_POINT('Ctrl Pts',(13.6068951069296,2.55918984632695,125.147868316191));
#213600=CARTESIAN_POINT('Ctrl Pts',(13.3284474831167,-3.37566254970675,
125.593769463429));
#213601=CARTESIAN_POINT('Ctrl Pts',(13.0499998593037,-6.20844597284355,
130.827949329789));
#213602=CARTESIAN_POINT('Ctrl Pts',(12.7715522354909,-3.33597084638438,
136.04045232199));
#213603=CARTESIAN_POINT('Ctrl Pts',(12.493104611678,2.60209851666622,136.441242835124));
#213604=CARTESIAN_POINT('Ctrl Pts',(12.2146569878651,6.14896646247997,131.662013967328));
#213605=CARTESIAN_POINT('Ctrl Pts',(11.9362093640522,4.04523462298623,126.094643569795));
#213606=CARTESIAN_POINT('Ctrl Pts',(11.6577617402393,-1.77587021433397,
124.855273056695));
#213607=CARTESIAN_POINT('Ctrl Pts',(11.3793141164265,-5.96503708076441,
129.08282338295));
#213608=CARTESIAN_POINT('Ctrl Pts',(11.1008664926135,-4.67262627823404,
134.892382326048));
#213609=CARTESIAN_POINT('Ctrl Pts',(10.8224188688007,0.913699803509421,
136.945249030013));
#213610=CARTESIAN_POINT('Ctrl Pts',(10.5439712449878,5.6603804025445,133.354939282016));
#213611=CARTESIAN_POINT('Ctrl Pts',(10.2655236211749,5.20544793659703,127.420772344084));
#213612=CARTESIAN_POINT('Ctrl Pts',(9.98707599736195,-0.0330368828140487,
124.595957732005));
#213613=CARTESIAN_POINT('Ctrl Pts',(9.70862837354909,-5.24116242086055,
127.476362074414));
#213614=CARTESIAN_POINT('Ctrl Pts',(9.43018074973619,-5.63291573915475,
133.415034496211));
#213615=CARTESIAN_POINT('Ctrl Pts',(9.15173312592329,-0.848294676398009,
136.954625162043));
#213616=CARTESIAN_POINT('Ctrl Pts',(8.87328550211039,4.71586775246963,134.842423168626));
#213617=CARTESIAN_POINT('Ctrl Pts',(8.59483787829755,5.94637809976527,129.019438961107));
#213618=CARTESIAN_POINT('Ctrl Pts',(8.3163902544846,1.71245747009635,124.836710557603));
#213619=CARTESIAN_POINT('Ctrl Pts',(8.03794263067172,-4.09512791639282,
126.137961023291));
#213620=CARTESIAN_POINT('Ctrl Pts',(7.75949500685887,-6.1394908058375,131.727404749824));
#213621=CARTESIAN_POINT('Ctrl Pts',(7.48104738304595,-2.54196157551782,
136.468616012024));
#213622=CARTESIAN_POINT('Ctrl Pts',(7.20259975923305,3.39150616097622,136.004653280976));
#213623=CARTESIAN_POINT('Ctrl Pts',(6.92415213542018,6.20834541982004,130.761875640674));
#213624=CARTESIAN_POINT('Ctrl Pts',(6.64570451160728,3.32001853238404,125.558139618628));
#213625=CARTESIAN_POINT('Ctrl Pts',(6.36725688779438,-2.61924319439064,
125.175424402463));
#213626=CARTESIAN_POINT('Ctrl Pts',(6.08880926398148,-6.15154838266407,
129.965426579154));
#213627=CARTESIAN_POINT('Ctrl Pts',(5.81036164016863,-4.03088112711464,
135.52636815294));
#213628=CARTESIAN_POINT('Ctrl Pts',(5.53191401635571,1.79396896476278,136.748015484609));
#213629=CARTESIAN_POINT('Ctrl Pts',(5.2534663925428,5.97024921827925,132.507734357147));
#213630=CARTESIAN_POINT('Ctrl Pts',(4.97501876872993,4.66016210308585,126.702135977443));
#213631=CARTESIAN_POINT('Ctrl Pts',(4.69657114491704,-0.932386323268277,
124.666281637197));
#213632=CARTESIAN_POINT('Ctrl Pts',(4.41812352110413,-5.66811726814286,
128.27102201808));
#213633=CARTESIAN_POINT('Ctrl Pts',(4.13967589729124,-5.19512534651691,
134.203776811419));
#213634=CARTESIAN_POINT('Ctrl Pts',(3.86122827347838,0.051932972575587,
137.012634193321));
#213635=CARTESIAN_POINT('Ctrl Pts',(3.58278064966546,5.25126742693796,134.116391450127));
#213636=CARTESIAN_POINT('Ctrl Pts',(3.30433302585255,5.62494365461986,128.176554173511));
#213637=CARTESIAN_POINT('Ctrl Pts',(3.02588540203969,0.829571457480427,
124.651542643499));
#213638=CARTESIAN_POINT('Ctrl Pts',(2.74743777822681,-4.72813638226476,
126.780670249786));
#213639=CARTESIAN_POINT('Ctrl Pts',(2.46899015441389,-5.9409178690121,132.607372735859));
#213640=CARTESIAN_POINT('Ctrl Pts',(2.19054253060099,-1.69428606410994,
136.77719516726));
#213641=CARTESIAN_POINT('Ctrl Pts',(1.91209490678813,4.10931186323347,135.458274436681));
#213642=CARTESIAN_POINT('Ctrl Pts',(1.63364728297522,6.13665293931019,129.862634262664));
#213643=CARTESIAN_POINT('Ctrl Pts',(1.35519965916232,2.52470975632363,125.132394602912));
#213644=CARTESIAN_POINT('Ctrl Pts',(1.07675203534945,-3.40731835379603,
125.614414619682));
#213645=CARTESIAN_POINT('Ctrl Pts',(0.798304411536565,-6.20818735353264,
130.86574146555));
#213646=CARTESIAN_POINT('Ctrl Pts',(0.519856787723634,-3.30403546218559,
136.060662310741));
#213647=CARTESIAN_POINT('Ctrl Pts',(0.241409163910791,2.63636360780418,
136.425298684517));
#213648=CARTESIAN_POINT('Ctrl Pts',(-0.0370384599021062,6.15407331574431,
131.624567572855));
#213649=CARTESIAN_POINT('Ctrl Pts',(-0.315486083715014,4.01649028971072,
126.070106338619));
#213650=CARTESIAN_POINT('Ctrl Pts',(-0.593933707527915,-1.81205109610819,
124.866193505555));
#213651=CARTESIAN_POINT('Ctrl Pts',(-0.872381331340776,-5.97540604822092,
129.119166152838));
#213652=CARTESIAN_POINT('Ctrl Pts',(-1.15082895515369,-4.6476547568326,
134.920750186879));
#213653=CARTESIAN_POINT('Ctrl Pts',(-1.42927657896659,0.951064205527318,
136.939573303531));
#213654=CARTESIAN_POINT('Ctrl Pts',(-1.70772420277945,5.67580162507719,
133.320435683583));
#213655=CARTESIAN_POINT('Ctrl Pts',(-1.98617182659235,5.18475462950527,
127.389147995065));
#213656=CARTESIAN_POINT('Ctrl Pts',(-2.26461945040527,-0.0708285812371651,
124.596273864213));
#213657=CARTESIAN_POINT('Ctrl Pts',(-2.54306707421816,-5.26132378599129,
127.508328177794));
#213658=CARTESIAN_POINT('Ctrl Pts',(-2.82151469803103,-5.61691946137538,
133.449275283389));
#213659=CARTESIAN_POINT('Ctrl Pts',(-3.09996232184393,-0.810840553526189,
136.959675022356));
#213660=CARTESIAN_POINT('Ctrl Pts',(-3.37840994565684,4.74036121125036,
134.813641527147));
#213661=CARTESIAN_POINT('Ctrl Pts',(-3.6568575694697,5.93540260240737,128.983274740293));
#213662=CARTESIAN_POINT('Ctrl Pts',(-3.9353051932826,1.6760989624889,124.826396909662));
#213663=CARTESIAN_POINT('Ctrl Pts',(-4.21375281709551,-4.12345774197041,
126.162975686831));
#213664=CARTESIAN_POINT('Ctrl Pts',(-4.49220044090841,-6.13375822366836,
131.764760471086));
#213665=CARTESIAN_POINT('Ctrl Pts',(-4.77064806472125,-2.50743454856317,
136.483984708096));
#213666=CARTESIAN_POINT('Ctrl Pts',(-5.04909568853418,3.4230989816841,135.983911870971));
#213667=CARTESIAN_POINT('Ctrl Pts',(-5.32754331234708,6.20797177544568,
130.724084467112));
#213668=CARTESIAN_POINT('Ctrl Pts',(-5.60599093615995,3.28802178385396,
125.538026923812));
#213669=CARTESIAN_POINT('Ctrl Pts',(-5.88443855997284,-2.65345959830539,
125.191472770368));
#213670=CARTESIAN_POINT('Ctrl Pts',(-6.16288618378574,-6.15654123833006,
130.002888343683));
#213671=CARTESIAN_POINT('Ctrl Pts',(-6.44133380759864,-4.00206224408943,
135.550817782599));
#213672=CARTESIAN_POINT('Ctrl Pts',(-6.71978143141151,1.83011644085978,
136.736984964173));
#213673=CARTESIAN_POINT('Ctrl Pts',(-6.9982290552244,5.98050752281724,132.471360196026));
#213674=CARTESIAN_POINT('Ctrl Pts',(-7.27667667903734,4.63510435534053,
126.673844252731));
#213675=CARTESIAN_POINT('Ctrl Pts',(-7.55512430285017,-0.969733277257762,
124.672071061776));
#213676=CARTESIAN_POINT('Ctrl Pts',(-7.83357192666308,-5.68343340216059,
128.305572393592));
#213677=CARTESIAN_POINT('Ctrl Pts',(-8.112019550476,-5.17433588163501,134.235338030648));
#213678=CARTESIAN_POINT('Ctrl Pts',(-8.39046717428886,0.0897235337524442,
137.012203037646));
#213679=CARTESIAN_POINT('Ctrl Pts',(-8.66891479810176,5.27133140485959,
134.084364130551));
#213680=CARTESIAN_POINT('Ctrl Pts',(-8.94736242191464,5.60884323375645,
128.142362232103));
#213681=CARTESIAN_POINT('Ctrl Pts',(-9.22581004572757,0.792102138056052,
124.646606804043));
#213682=CARTESIAN_POINT('Ctrl Pts',(-9.50425766954039,-4.75254212617725,
126.809526307613));
#213683=CARTESIAN_POINT('Ctrl Pts',(-9.78270529335335,-5.92983235104376,
132.643503383524));
#213684=CARTESIAN_POINT('Ctrl Pts',(-10.0611529171662,-1.65789633371603,
136.787398104638));
#213685=CARTESIAN_POINT('Ctrl Pts',(-10.3396005409791,4.13756542155812,
135.433173662763));
#213686=CARTESIAN_POINT('Ctrl Pts',(-10.618048164792,6.13080668572826,129.82529616244));
#213687=CARTESIAN_POINT('Ctrl Pts',(-10.8964957886049,2.49013611227157,
125.11713106642));
#213688=CARTESIAN_POINT('Ctrl Pts',(-11.1749434124178,-3.4388478984508,
125.635252091294));
#213689=CARTESIAN_POINT('Ctrl Pts',(-11.4533910362307,-6.20769868755626,
130.90353132682));
#213690=CARTESIAN_POINT('Ctrl Pts',(-11.7318386600436,-3.2719776457377,
136.080677525301));
#213691=CARTESIAN_POINT('Ctrl Pts',(-12.0102862838565,2.67053100751937,
136.409146247984));
#213692=CARTESIAN_POINT('Ctrl Pts',(-12.2887339076694,6.15895212755882,
131.587090785312));
#213693=CARTESIAN_POINT('Ctrl Pts',(-12.5671815314823,3.98759712391021,
126.045744536976));
#213694=CARTESIAN_POINT('Ctrl Pts',(-12.8456291552951,-1.84816483166266,
124.877333995382));
#213695=CARTESIAN_POINT('Ctrl Pts',(-13.1240767791081,-5.98555359480885,
129.155571368227));
#213696=CARTESIAN_POINT('Ctrl Pts',(-13.4025244029209,-4.62251101487491,
134.948965513381));
#213697=CARTESIAN_POINT('Ctrl Pts',(-13.6809720267338,0.988393365511613,
136.933670234486));
#213698=CARTESIAN_POINT('Ctrl Pts',(-13.9594196505467,5.69101252869335,
133.285838851062));
#213699=CARTESIAN_POINT('Ctrl Pts',(-14.2378672743596,5.16386919942402,
127.357650198006));
#213700=CARTESIAN_POINT('Ctrl Pts',(-14.5163148981725,-0.108617655081171,
124.59682003936));
#213701=CARTESIAN_POINT('Ctrl Pts',(-14.7947625219854,-5.28129019083405,
127.540416416869));
#213702=CARTESIAN_POINT('Ctrl Pts',(-15.0732101457983,-5.60071504657988,
133.483418062279));
#213703=CARTESIAN_POINT('Ctrl Pts',(-15.3516577696111,-0.77335638465969,
136.96449679523));
#213704=CARTESIAN_POINT('Ctrl Pts',(-15.6301053934241,4.76467901420313,
134.784711320289));
#213705=CARTESIAN_POINT('Ctrl Pts',(-15.908553017237,5.92420716652329,128.947178000488));
#213706=CARTESIAN_POINT('Ctrl Pts',(-16.1870006410499,1.63967834641818,
124.816304777366));
#213707=CARTESIAN_POINT('Ctrl Pts',(-16.4654482648627,-4.15163477130477,
126.188162338596));
#213708=CARTESIAN_POINT('Ctrl Pts',(-16.7438958886757,-6.12779835283271,
131.802080604377));
#213709=CARTESIAN_POINT('Ctrl Pts',(-17.0223435124885,-2.4728146076992,
136.499142943608));
#213710=CARTESIAN_POINT('Ctrl Pts',(-17.3007911363014,3.45456495820035,
135.96297853079));
#213711=CARTESIAN_POINT('Ctrl Pts',(-17.5792387601143,6.20736809239421,
130.686296268213));
#213712=CARTESIAN_POINT('Ctrl Pts',(-17.8576863839272,3.25590319646751,
125.518109374927));
#213713=CARTESIAN_POINT('Ctrl Pts',(-18.13613400774,-2.6875776772989,125.207729125896));
#213714=CARTESIAN_POINT('Ctrl Pts',(-18.414581631553,-6.16130596109642,
130.040379807061));
#213715=CARTESIAN_POINT('Ctrl Pts',(-18.6930292553659,-3.97309506317598,
135.575091530542));
#213716=CARTESIAN_POINT('Ctrl Pts',(-18.9714768791788,1.86619610131902,
136.72573460816));
#213717=CARTESIAN_POINT('Ctrl Pts',(-19.2499245029916,5.99054421744964,
132.434924263623));
#213718=CARTESIAN_POINT('Ctrl Pts',(-19.5283721268046,4.6098748520987,126.645705585822));
#213719=CARTESIAN_POINT('Ctrl Pts',(-19.8068197506174,-1.00704429742433,
124.678087720601));
#213720=CARTESIAN_POINT('Ctrl Pts',(-20.0852673744304,-5.6985389344635,
128.340215362621));
#213721=CARTESIAN_POINT('Ctrl Pts',(-20.3637149982432,-5.15335467983417,
134.266772113748));
#213722=CARTESIAN_POINT('Ctrl Pts',(-20.6421626220562,0.127510770190762,
137.011541848088));
#213723=CARTESIAN_POINT('Ctrl Pts',(-20.920610245869,5.29120005165768,134.05221526924));
#213724=CARTESIAN_POINT('Ctrl Pts',(-21.1990578696819,5.59253497514422,
128.108268932023));
#213725=CARTESIAN_POINT('Ctrl Pts',(-21.4775054934948,0.754603466995427,
124.64189914242));
#213726=CARTESIAN_POINT('Ctrl Pts',(-21.7559531173077,-4.77677176289349,
126.838530395495));
#213727=CARTESIAN_POINT('Ctrl Pts',(-22.0344007411205,-5.91852710095694,
132.679565881077));
#213728=CARTESIAN_POINT('Ctrl Pts',(-22.3128483649335,-1.62144516936395,
136.797379338361));
#213729=CARTESIAN_POINT('Ctrl Pts',(-22.5912959887463,4.16566566087426,
135.407901366475));
#213730=CARTESIAN_POINT('Ctrl Pts',(-22.8697436125593,6.12473325285015,
129.787994341809));
#213731=CARTESIAN_POINT('Ctrl Pts',(-23.1481912363721,2.45547019531011,
125.102078272311));
#213732=CARTESIAN_POINT('Ctrl Pts',(-23.426638860185,-3.47025001533206,
125.656281106122));
#213733=CARTESIAN_POINT('Ctrl Pts',(-23.7050864839979,-6.20697999302203,
130.941317513284));
#213734=CARTESIAN_POINT('Ctrl Pts',(-23.9835341078108,-3.23979858495512,
136.100497223997));
#213735=CARTESIAN_POINT('Ctrl Pts',(-24.2619817316237,2.70459944972584,
136.392786124057));
#213736=CARTESIAN_POINT('Ctrl Pts',(-24.5404293554366,6.16360271713728,
131.549584993415));
#213737=CARTESIAN_POINT('Ctrl Pts',(-24.8188769792495,3.95855619623184,
126.021559067602));
#213738=CARTESIAN_POINT('Ctrl Pts',(-25.0973246030624,-1.88421008278963,
124.88869411336));
#213739=CARTESIAN_POINT('Ctrl Pts',(-25.3757722268753,-5.99547934450715,
129.192037680109));
#213740=CARTESIAN_POINT('Ctrl Pts',(-25.6542198506882,-4.59719598407162,
134.977027260026));
#213741=CARTESIAN_POINT('Ctrl Pts',(-25.932667474501,1.02568590021626,136.92754004162));
#213742=CARTESIAN_POINT('Ctrl Pts',(-26.211115098314,5.7060125497474,133.251150066453));
#213743=CARTESIAN_POINT('Ctrl Pts',(-26.4895627221268,5.14279242027056,
127.326280120068));
#213744=CARTESIAN_POINT('Ctrl Pts',(-26.7680103459397,-0.146402704058008,
124.597596237205));
#213745=CARTESIAN_POINT('Ctrl Pts',(-27.0464579697526,-5.30106089552683,
127.572625602596));
#213746=CARTESIAN_POINT('Ctrl Pts',(-27.3249055935655,-5.58430309522854,
133.517461567711));
#213747=CARTESIAN_POINT('Ctrl Pts',(-27.6033532173784,-0.735843558787732,
136.969090301993));
#213748=CARTESIAN_POINT('Ctrl Pts',(-27.8818008411913,4.78882026022281,
134.755633620073));
#213749=CARTESIAN_POINT('Ctrl Pts',(-28.1602484650042,5.91279220696403,
128.911150079267));
#213750=CARTESIAN_POINT('Ctrl Pts',(-28.4386960888171,1.60319697146318,
124.806434534681));
#213751=CARTESIAN_POINT('Ctrl Pts',(-28.7171437126299,-4.17965796028613,
126.213520045287));
#213752=CARTESIAN_POINT('Ctrl Pts',(-28.9955913364429,-6.12161141417542,
131.839363766787));
#213753=CARTESIAN_POINT('Ctrl Pts',(-29.2740389602557,-2.43810303578058,
136.514090156867));
#213754=CARTESIAN_POINT('Ctrl Pts',(-29.5524865840687,3.48590292454168,
135.941854036124));
#213755=CARTESIAN_POINT('Ctrl Pts',(-29.8309342078815,6.20653439303521,
130.648512444231));
#213756=CARTESIAN_POINT('Ctrl Pts',(-30.1093818316944,3.22366396039099,
125.498387710026));
#213757=CARTESIAN_POINT('Ctrl Pts',(-30.3878294555073,-2.72159616711309,
125.224192866663));
#213758=CARTESIAN_POINT('Ctrl Pts',(-30.6662770793202,-6.16584237440457,
130.077899580028));
#213759=CARTESIAN_POINT('Ctrl Pts',(-30.9447247031331,-3.94398065776386,
135.599188497297));
#213760=CARTESIAN_POINT('Ctrl Pts',(-31.2231723269461,1.90220660919519,
136.714264833456));
#213761=CARTESIAN_POINT('Ctrl Pts',(-31.5016199507588,6.00035893026297,
132.398427910084));
#213762=CARTESIAN_POINT('Ctrl Pts',(-31.7800675745718,4.58447452824918,
126.617721019404));
#213763=CARTESIAN_POINT('Ctrl Pts',(-32.0585151983846,-1.04431800119413,
124.68433139072));
#213764=CARTESIAN_POINT('Ctrl Pts',(-32.3369628221976,-5.71343330531054,
128.374949641459));
#213765=CARTESIAN_POINT('Ctrl Pts',(-32.6154104460104,-5.1321825185805,
134.298077895915));
#213766=CARTESIAN_POINT('Ctrl Pts',(-32.8938580698234,0.165293281670594,
137.010650649146));
#213767=CARTESIAN_POINT('Ctrl Pts',(-33.1723056936362,5.31087263109202,
134.019946057479));
#213768=CARTESIAN_POINT('Ctrl Pts',(-33.4507533174492,5.57601948309184,
128.074275536613));
#213769=CARTESIAN_POINT('Ctrl Pts',(-33.729200941262,0.717076833825826,
124.637419833072));
#213770=CARTESIAN_POINT('Ctrl Pts',(-34.0076485650749,-4.80082439457541,
126.867681438675));
#213771=CARTESIAN_POINT('Ctrl Pts',(-34.2860961888878,-5.90700253767186,
132.715558892209));
#213772=CARTESIAN_POINT('Ctrl Pts',(-34.5645438127007,-1.58493392176466,
136.807138498572));
#213773=CARTESIAN_POINT('Ctrl Pts',(-34.8429914365135,4.19361153991761,
135.382458484293));
#213774=CARTESIAN_POINT('Ctrl Pts',(-35.1214390603265,6.11843286572883,
129.750730183006));
#213775=CARTESIAN_POINT('Ctrl Pts',(-35.3998866841394,2.42071328999757,
125.087236778371));
#213776=CARTESIAN_POINT('Ctrl Pts',(-35.6783343079523,-3.50152354082281,
125.677500884929));
#213777=CARTESIAN_POINT('Ctrl Pts',(-35.9567819317651,-6.20603129656164,
130.979098624759));
#213778=CARTESIAN_POINT('Ctrl Pts',(-36.2352295555781,-3.2074994722443,
136.120120672404));
#213779=CARTESIAN_POINT('Ctrl Pts',(-36.5136771793909,2.73856767200523,
136.376218918968));
#213780=CARTESIAN_POINT('Ctrl Pts',(-36.7921248032039,6.1680249121504,131.512051586954));
#213781=CARTESIAN_POINT('Ctrl Pts',(-37.0705724270167,3.92936858279784,
125.997550826698));
#213782=CARTESIAN_POINT('Ctrl Pts',(-37.3490200508296,-1.92018551381882,
124.900273438536));
#213783=CARTESIAN_POINT('Ctrl Pts',(-37.6274676746425,-6.00518292951342,
129.228563737208));
#213784=CARTESIAN_POINT('Ctrl Pts',(-37.9059152984554,-4.57171060248077,
135.004934386972));
#213785=CARTESIAN_POINT('Ctrl Pts',(-38.1843629222683,1.0629404277527,136.921182952087));
#213786=CARTESIAN_POINT('Ctrl Pts',(-38.4628105460811,5.72080113240803,
133.216370615161));
#213787=CARTESIAN_POINT('Ctrl Pts',(-38.7412581698941,5.12152507305273,
127.295038923683));
#213788=CARTESIAN_POINT('Ctrl Pts',(-39.0197057937069,-0.184182328028525,
124.598602428988));
#213789=CARTESIAN_POINT('Ctrl Pts',(-39.2981534175199,-5.32063516745863,
127.604954541453));
#213790=CARTESIAN_POINT('Ctrl Pts',(-39.5766010413327,-5.56768421547239,
133.55140453819));
#213791=CARTESIAN_POINT('Ctrl Pts',(-39.8550486651457,-0.698303465962086,
136.973455372429));
#213792=CARTESIAN_POINT('Ctrl Pts',(-40.1334962889585,4.81278405474664,
134.726409503982));
#213793=CARTESIAN_POINT('Ctrl Pts',(-40.4119439127715,5.90115814671511,
128.875192311658));
#213794=CARTESIAN_POINT('Ctrl Pts',(-40.6903915365843,1.56665618945481,
124.796786547352));
#213795=CARTESIAN_POINT('Ctrl Pts',(-40.9688391603973,-4.20752627050468,
126.239047867263));
#213796=CARTESIAN_POINT('Ctrl Pts',(-41.2472867842101,-6.11519763695597,
131.876608576776));
#213797=CARTESIAN_POINT('Ctrl Pts',(-41.5257344080229,-2.40330111905734,
136.528825793999));
#213798=CARTESIAN_POINT('Ctrl Pts',(-41.8041820318359,3.51711171946819,
135.920539169751));
#213799=CARTESIAN_POINT('Ctrl Pts',(-42.0826296556488,6.20547070826194,
130.610734395262));
#213800=CARTESIAN_POINT('Ctrl Pts',(-42.3610772794617,3.19130527026066,
125.478862659902));
#213801=CARTESIAN_POINT('Ctrl Pts',(-42.6395249032745,-2.75551380718057,
125.240863382598));
#213802=CARTESIAN_POINT('Ctrl Pts',(-42.9179725270875,-6.17015031015604,
130.115446272278));
#213803=CARTESIAN_POINT('Ctrl Pts',(-43.1964201509003,-3.91472010669807,
135.623107789941));
#213804=CARTESIAN_POINT('Ctrl Pts',(-43.4748677747133,1.93814663010615,
136.702576065077));
#213805=CARTESIAN_POINT('Ctrl Pts',(-43.7533153985261,6.00995129756958,
132.361872487794));
#213806=CARTESIAN_POINT('Ctrl Pts',(-44.031763022339,4.55890432500984,126.589891590455));
#213807=CARTESIAN_POINT('Ctrl Pts',(-44.3102106461518,-1.08155300737633,
124.690801840773));
#213808=CARTESIAN_POINT('Ctrl Pts',(-44.5886582699649,-5.72811596278534,
128.409773943013));
#213809=CARTESIAN_POINT('Ctrl Pts',(-44.8671058937777,-5.11082018241628,
134.329254217104));
#213810=CARTESIAN_POINT('Ctrl Pts',(-45.1455535175906,0.2030696681468,137.009529473845));
#213811=CARTESIAN_POINT('Ctrl Pts',(-45.4240011414034,5.33034841418793,
133.987557691017));
#213812=CARTESIAN_POINT('Ctrl Pts',(-45.7024487652165,5.55929736958694,
128.040383305508));
#213813=CARTESIAN_POINT('Ctrl Pts',(-45.9808963890292,0.679523629110432,
124.633169041983));
#213814=CARTESIAN_POINT('Ctrl Pts',(-46.2593440128422,-4.82469912994364,
126.896978356949));
#213815=CARTESIAN_POINT('Ctrl Pts',(-46.537791636655,-5.89525908823553,
132.751481083186));
#213816=CARTESIAN_POINT('Ctrl Pts',(-46.816239260468,-1.54836394385628,
136.816675223641));
#213817=CARTESIAN_POINT('Ctrl Pts',(-47.0946868842807,4.22140202314317,
135.35684595901));
#213818=CARTESIAN_POINT('Ctrl Pts',(-47.3731345080937,6.11190575782758,
129.713505066864));
#213819=CARTESIAN_POINT('Ctrl Pts',(-47.6515821319066,2.38586668426401,
125.072607134557));
#213820=CARTESIAN_POINT('Ctrl Pts',(-47.9300297557195,-3.53266731607082,
125.69891064141));
#213821=CARTESIAN_POINT('Ctrl Pts',(-48.2084773795324,-6.20485263332943,
131.016873261253));
#213822=CARTESIAN_POINT('Ctrl Pts',(-48.4869250033452,-3.17508150446096,
136.139547143367));
#213823=CARTESIAN_POINT('Ctrl Pts',(-48.7653726271582,2.77243441565242,
136.359445246621));
#213824=CARTESIAN_POINT('Ctrl Pts',(-49.043820250971,6.1722185487321,131.474491956744));
#213825=CARTESIAN_POINT('Ctrl Pts',(-49.322267874784,3.900035365166,125.973720703898));
#213826=CARTESIAN_POINT('Ctrl Pts',(-49.6007154985968,-1.95608979166789,
124.912071541833));
#213827=CARTESIAN_POINT('Ctrl Pts',(-49.8791631224098,-6.0146639902579,
129.265148186042));
#213828=CARTESIAN_POINT('Ctrl Pts',(-50.1576107462225,-4.54605581447205,
135.032685860113));
#213829=CARTESIAN_POINT('Ctrl Pts',(-50.4360583700356,1.10015556764067,
136.914599201455));
#213830=CARTESIAN_POINT('Ctrl Pts',(-50.7145059938484,5.73537772867887,
133.181501785951));
#213831=CARTESIAN_POINT('Ctrl Pts',(-50.9929536176612,5.10006794583985,
127.263927766504));
#213832=CARTESIAN_POINT('Ctrl Pts',(-51.2714012414742,-0.221955127055423,
124.599838577421));
#213833=CARTESIAN_POINT('Ctrl Pts',(-51.5498488652871,-5.34001228129766,
127.637402035479));
#213834=CARTESIAN_POINT('Ctrl Pts',(-51.8282964891,-5.5508590231301,133.585245715947));
#213835=CARTESIAN_POINT('Ctrl Pts',(-52.1067441129128,-0.660737497244709,
136.977591844792));
#213836=CARTESIAN_POINT('Ctrl Pts',(-52.3851917367258,4.8365695097872,134.697040054928));
#213837=CARTESIAN_POINT('Ctrl Pts',(-52.6636393605386,5.889305416881,128.83930603009));
#213838=CARTESIAN_POINT('Ctrl Pts',(-52.9420869843516,1.53005735442545,
124.78736117289));
#213839=CARTESIAN_POINT('Ctrl Pts',(-53.2205346081644,-4.23523866929,126.264744858582));
#213840=CARTESIAN_POINT('Ctrl Pts',(-53.4989822319774,-6.1085572588392,
131.913813654221));
#213841=CARTESIAN_POINT('Ctrl Pts',(-53.7774298557902,-2.36841014712749,
136.543349308967));
#213842=CARTESIAN_POINT('Ctrl Pts',(-54.0558774796031,3.54819018652628,
135.8990347215));
#213843=CARTESIAN_POINT('Ctrl Pts',(-54.334325103416,6.20417707748961,130.572963521183));
#213844=CARTESIAN_POINT('Ctrl Pts',(-54.6127727272289,3.15882832513996,
125.459534948064));
#213845=CARTESIAN_POINT('Ctrl Pts',(-54.8912203510417,-2.7893293406706,
125.257740055968));
#213846=CARTESIAN_POINT('Ctrl Pts',(-55.1696679748547,-6.17422960871856,
130.153018492501));
#213847=CARTESIAN_POINT('Ctrl Pts',(-55.4481155986676,-3.88531449423931,
135.646848522136));
#213848=CARTESIAN_POINT('Ctrl Pts',(-55.7265632224805,1.97401483228084,
136.690668736158));
#213849=CARTESIAN_POINT('Ctrl Pts',(-56.0050108462934,6.01932096392068,
132.32525935133));
#213850=CARTESIAN_POINT('Ctrl Pts',(-56.2834584701062,4.53316518989421,
126.562218330207));
#213851=CARTESIAN_POINT('Ctrl Pts',(-56.5619060939192,-1.11874793621411,
124.697498830995));
#213852=CARTESIAN_POINT('Ctrl Pts',(-56.840353717732,-5.74258636281662,
128.444686976857));
#213853=CARTESIAN_POINT('Ctrl Pts',(-57.118801341545,-5.08926846293066,
134.360299922064));
#213854=CARTESIAN_POINT('Ctrl Pts',(-57.3972489653578,0.240838529802063,
137.00817836373));
#213855=CARTESIAN_POINT('Ctrl Pts',(-57.6756965891708,5.34962667926312,
133.955051370017));
#213856=CARTESIAN_POINT('Ctrl Pts',(-57.9541442129836,5.54236925427356,
128.0065934946));
#213857=CARTESIAN_POINT('Ctrl Pts',(-58.2325918367966,0.641945244397073,
124.629146926667));
#213858=CARTESIAN_POINT('Ctrl Pts',(-58.5110394606094,-4.84839508431156,
126.92642006471));
#213859=CARTESIAN_POINT('Ctrl Pts',(-58.7894870844223,-5.88329718780563,
132.787331122898));
#213860=CARTESIAN_POINT('Ctrl Pts',(-59.0679347082352,-1.5117365907523,
136.825989160181));
#213861=CARTESIAN_POINT('Ctrl Pts',(-59.3463823320481,4.24903608076433,
135.331064739709));
#213862=CARTESIAN_POINT('Ctrl Pts',(-59.624829955861,6.10515217101086,129.676320372777));
#213863=CARTESIAN_POINT('Ctrl Pts',(-59.9032775796738,2.3509316693629,125.058189882977));
#213864=CARTESIAN_POINT('Ctrl Pts',(-60.1817252034868,-3.56368018703254,
125.720509582217));
#213865=CARTESIAN_POINT('Ctrl Pts',(-60.4601728272995,-6.20344404700091,
131.054640023013));
#213866=CARTESIAN_POINT('Ctrl Pts',(-60.7386204511126,-3.14254588286485,
136.158775917031));
#213867=CARTESIAN_POINT('Ctrl Pts',(-61.0170680749254,2.80619842572279,
136.342465728569));
#213868=CARTESIAN_POINT('Ctrl Pts',(-61.2955156987383,6.17618347148551,
131.436907494571));
#213869=CARTESIAN_POINT('Ctrl Pts',(-61.5739633225512,3.87055763028967,
125.950069582238));
#213870=CARTESIAN_POINT('Ctrl Pts',(-61.8524109463641,-1.9919215858902,
124.924087986069));
#213871=CARTESIAN_POINT('Ctrl Pts',(-62.130858570177,-6.02392217541635,
129.301789670958));
#213872=CARTESIAN_POINT('Ctrl Pts',(-62.4093061939898,-4.5202325706933,
135.060280651108));
#213873=CARTESIAN_POINT('Ctrl Pts',(-62.6877538178028,1.13732994085927,
136.907789033684));
#213874=CARTESIAN_POINT('Ctrl Pts',(-62.9662014416156,5.74974179841868,
133.146544870902));
#213875=CARTESIAN_POINT('Ctrl Pts',(-63.2446490654287,5.0784218337339,127.232947801366));
#213876=CARTESIAN_POINT('Ctrl Pts',(-63.5230966892413,-0.25971970145348,
124.601304636701));
#213877=CARTESIAN_POINT('Ctrl Pts',(-63.8015443130544,-5.3591915190178,
127.669966882319));
#213878=CARTESIAN_POINT('Ctrl Pts',(-64.0799919368672,-5.53382814166538,
133.618983846983));
#213879=CARTESIAN_POINT('Ctrl Pts',(-64.3584395606801,-0.623147044656387,
136.9814995658));
#213880=CARTESIAN_POINT('Ctrl Pts',(-64.636887184493,4.86017574396616,134.667526361205));
#213881=CARTESIAN_POINT('Ctrl Pts',(-64.9153348083059,5.8772344566688,128.803492564343));
#213882=CARTESIAN_POINT('Ctrl Pts',(-65.1937824321189,1.4934018225579,124.778158760555));
#213883=CARTESIAN_POINT('Ctrl Pts',(-65.4722300559316,-4.26279412974889,
126.290610067033));
#213884=CARTESIAN_POINT('Ctrl Pts',(-65.7506776797446,-6.10169052588679,
131.950977620477));
#213885=CARTESIAN_POINT('Ctrl Pts',(-66.0291253035574,-2.33343141288849,
136.5576601636));
#213886=CARTESIAN_POINT('Ctrl Pts',(-66.3075729273703,3.57913717409239,
135.877341488227));
#213887=CARTESIAN_POINT('Ctrl Pts',(-66.5860205511832,6.20265354865397,
130.535201221608));
#213888=CARTESIAN_POINT('Ctrl Pts',(-66.8644681749961,3.126234328474,125.440405290707));
#213889=CARTESIAN_POINT('Ctrl Pts',(-67.142915798809,-2.82304151453613,
125.274822261403));
#213890=CARTESIAN_POINT('Ctrl Pts',(-67.421363422622,-6.17808011893247,
130.190614848446));
#213891=CARTESIAN_POINT('Ctrl Pts',(-67.6998110464348,-3.85576491002292,
135.670409814162));
#213892=CARTESIAN_POINT('Ctrl Pts',(-67.9782586702478,2.00980988661012,
136.678543287925));
#213893=CARTESIAN_POINT('Ctrl Pts',(-68.2567062940606,6.02846758211988,
132.288589857404));
#213894=CARTESIAN_POINT('Ctrl Pts',(-68.5351539178734,4.50725807667536,
126.534702264101));
#213895=CARTESIAN_POINT('Ctrl Pts',(-68.8136015416864,-1.15590140943545,
124.704422113226));
#213896=CARTESIAN_POINT('Ctrl Pts',(-69.0920491654993,-5.75684396919829,
128.479687449276));
#213897=CARTESIAN_POINT('Ctrl Pts',(-69.3704967893121,-5.0675281587308,
134.391213860386));
#213898=CARTESIAN_POINT('Ctrl Pts',(-69.648944413125,0.278598467097045,
137.006597368867));
#213899=CARTESIAN_POINT('Ctrl Pts',(-69.9273920369379,5.36870671195437,
133.922428299012));
#213900=CARTESIAN_POINT('Ctrl Pts',(-70.2058396607509,5.52523576442926,
127.972907355982));
#213901=CARTESIAN_POINT('Ctrl Pts',(-70.4842872845636,0.604343072166899,
124.625353636165));
#213902=CARTESIAN_POINT('Ctrl Pts',(-70.7627349083767,-4.87191137961658,
126.956005470983));
#213903=CARTESIAN_POINT('Ctrl Pts',(-71.0411825321895,-5.87111727963483,
132.823107682909));
#213904=CARTESIAN_POINT('Ctrl Pts',(-71.3196301560023,-1.47505321969301,
136.835079963061));
#213905=CARTESIAN_POINT('Ctrl Pts',(-71.5980777798154,4.27651268879093,
135.305115781721));
#213906=CARTESIAN_POINT('Ctrl Pts',(-71.8765254036282,6.09817235553532,
129.639177478635));
#213907=CARTESIAN_POINT('Ctrl Pts',(-72.1549730274411,2.31590953982396,
125.043985557866));
#213908=CARTESIAN_POINT('Ctrl Pts',(-72.433420651254,-3.5945610045145,125.742296906994));
#213909=CARTESIAN_POINT('Ctrl Pts',(-72.7118682750669,-6.20180558977201,
131.092397510578));
#213910=CARTESIAN_POINT('Ctrl Pts',(-72.9903158988798,-3.109893813075,136.177806280867));
#213911=CARTESIAN_POINT('Ctrl Pts',(-73.2687635226926,2.8398584510789,136.325280993997));
#213912=CARTESIAN_POINT('Ctrl Pts',(-73.5472111465057,6.17991953348924,
131.399299593141));
#213913=CARTESIAN_POINT('Ctrl Pts',(-73.8256587703184,3.84093647047644,
125.926598338115));
#213914=CARTESIAN_POINT('Ctrl Pts',(-74.1041063941314,-2.02767956872624,
124.93632232597));
#213915=CARTESIAN_POINT('Ctrl Pts',(-74.3825540179442,-6.0329571419232,
129.338486834193));
#213916=CARTESIAN_POINT('Ctrl Pts',(-74.6610016417573,-4.49424182803428,
135.08771773742));
#213917=CARTESIAN_POINT('Ctrl Pts',(-74.9394492655699,1.17446216989917,
136.900752701129));
#213918=CARTESIAN_POINT('Ctrl Pts',(-75.217896889383,5.76389280936176,133.111501165354));
#213919=CARTESIAN_POINT('Ctrl Pts',(-75.4963445131958,5.05658753883907,
127.202100176243));
#213920=CARTESIAN_POINT('Ctrl Pts',(-75.7747921370087,-0.297474651842549,
124.603000552501));
#213921=CARTESIAN_POINT('Ctrl Pts',(-76.0532397608216,-5.37817216992523,
127.702647875272));
#213922=CARTESIAN_POINT('Ctrl Pts',(-76.3316873846344,-5.51659220216403,
133.65261768112));
#213923=CARTESIAN_POINT('Ctrl Pts',(-76.6101350084474,-0.585533501125347,
136.985178390654));
#213924=CARTESIAN_POINT('Ctrl Pts',(-76.8885826322602,4.8836018825454,134.637869516455));
#213925=CARTESIAN_POINT('Ctrl Pts',(-77.1670302560731,5.86494571337264,
128.767753241497));
#213926=CARTESIAN_POINT('Ctrl Pts',(-77.4454778798861,1.4566909521364,124.769179651345));
#213927=CARTESIAN_POINT('Ctrl Pts',(-77.7239255036988,-4.29019163080361,
126.316642534169));
#213928=CARTESIAN_POINT('Ctrl Pts',(-78.0023731275119,-6.09459769254796,
131.988099098418));
#213929=CARTESIAN_POINT('Ctrl Pts',(-78.2808207513247,-2.29836621249045,
136.571757827603));
#213930=CARTESIAN_POINT('Ctrl Pts',(-78.5592683751376,3.60995153541429,
135.855460273781));
#213931=CARTESIAN_POINT('Ctrl Pts',(-78.8377159989505,6.20090017820995,
130.497448895834));
#213932=CARTESIAN_POINT('Ctrl Pts',(-79.1161636227633,3.09352448804556,
125.421474396687));
#213933=CARTESIAN_POINT('Ctrl Pts',(-79.3946112465763,-2.85664907955992,
125.292109365916));
#213934=CARTESIAN_POINT('Ctrl Pts',(-79.6730588703891,-6.18170169811556,
130.228233946967));
#213935=CARTESIAN_POINT('Ctrl Pts',(-79.9515064942021,-3.8260724490201,
135.693790792945));
#213936=CARTESIAN_POINT('Ctrl Pts',(-80.2299541180149,2.04553046669522,
136.666200169693));
#213937=CARTESIAN_POINT('Ctrl Pts',(-80.5084017418279,6.03739081323573,
132.251865364817));
#213938=CARTESIAN_POINT('Ctrl Pts',(-80.7868493656406,4.48118394535095,
126.507344411756));
#213939=CARTESIAN_POINT('Ctrl Pts',(-81.0652969894537,-1.19301205030527,
124.711571430921));
#213940=CARTESIAN_POINT('Ctrl Pts',(-81.3437446132665,-5.77088825360962,
128.514774063314));
#213941=CARTESIAN_POINT('Ctrl Pts',(-81.6221922370794,-5.04560007541116,
134.421994886542));
#213942=CARTESIAN_POINT('Ctrl Pts',(-81.9006398608923,0.316348080823153,
137.00478654784));
#213943=CARTESIAN_POINT('Ctrl Pts',(-82.179087484705,5.38758780524389,133.889689686862));
#213944=CARTESIAN_POINT('Ctrl Pts',(-82.4575351085182,5.50789753494193,
127.939326137905));
#213945=CARTESIAN_POINT('Ctrl Pts',(-82.7359827323308,0.566718505781886,
124.621789311041));
#213946=CARTESIAN_POINT('Ctrl Pts',(-83.0144303561439,-4.89524714445407,
126.985733479472));
#213947=CARTESIAN_POINT('Ctrl Pts',(-83.2928779799568,-5.858719815054,132.858809437506));
#213948=CARTESIAN_POINT('Ctrl Pts',(-83.5713256037696,-1.43831518999427,
136.843947295418));
#213949=CARTESIAN_POINT('Ctrl Pts',(-83.8497732275826,4.30383082906709,
135.279000046597));
#213950=CARTESIAN_POINT('Ctrl Pts',(-84.1282208513953,6.09096657004034,
129.602077760783));
#213951=CARTESIAN_POINT('Ctrl Pts',(-84.4066684752085,2.28080159340614,
125.029994685571));
#213952=CARTESIAN_POINT('Ctrl Pts',(-84.685116099021,-3.6253086242162,125.764271808403));
#213953=CARTESIAN_POINT('Ctrl Pts',(-84.9635637228342,-6.19993732235617,
131.130144324829));
#213954=CARTESIAN_POINT('Ctrl Pts',(-85.242011346647,-3.07712650502686,
136.196637529698));
#213955=CARTESIAN_POINT('Ctrl Pts',(-85.5204589704598,2.87341324443482,
136.307891679689));
#213956=CARTESIAN_POINT('Ctrl Pts',(-85.7989065942728,6.18342659630218,
131.361669646028));
#213957=CARTESIAN_POINT('Ctrl Pts',(-86.0773542180856,3.81117298335027,
125.903307841269));
#213958=CARTESIAN_POINT('Ctrl Pts',(-86.3558018418987,-2.06336241514917,
124.948774108188));
#213959=CARTESIAN_POINT('Ctrl Pts',(-86.6342494657113,-6.04176855498474,
129.375238315919));
#213960=CARTESIAN_POINT('Ctrl Pts',(-86.9126970895244,-4.46808454959173,
135.114996102359));
#213961=CARTESIAN_POINT('Ctrl Pts',(-87.1911447133372,1.2115508788106,136.893490464523));
#213962=CARTESIAN_POINT('Ctrl Pts',(-87.4695923371502,5.77783023713722,
133.076371967865));
#213963=CARTESIAN_POINT('Ctrl Pts',(-87.7480399609628,5.03456587023344,
127.171386034204));
#213964=CARTESIAN_POINT('Ctrl Pts',(-88.026487584776,-0.33521857919891,
124.60492626198));
#213965=CARTESIAN_POINT('Ctrl Pts',(-88.3049352085887,-5.39695353068522,
127.735443803332));
#213966=CARTESIAN_POINT('Ctrl Pts',(-88.5833828324018,-5.49915184330967,
133.686145972045));
#213967=CARTESIAN_POINT('Ctrl Pts',(-88.8618304562145,-0.547898260434929,
136.988628183031));
#213968=CARTESIAN_POINT('Ctrl Pts',(-89.1402780800275,4.90684705746115,
134.608070619623));
#213969=CARTESIAN_POINT('Ctrl Pts',(-89.4187257038403,5.85243964235601,
128.732089385887));
#213970=CARTESIAN_POINT('Ctrl Pts',(-89.6971733276532,1.41992610349655,
124.760424177987));
#213971=CARTESIAN_POINT('Ctrl Pts',(-89.9756209514662,-4.31743015722937,
126.342841295349));
#213972=CARTESIAN_POINT('Ctrl Pts',(-90.254068575279,-6.08727902165076,
132.025176712493));
#213973=CARTESIAN_POINT('Ctrl Pts',(-90.5325161990919,-2.26321584528708,
136.585641778581));
#213974=CARTESIAN_POINT('Ctrl Pts',(-90.8109638229048,3.64063212865448,
135.833391888981));
#213975=CARTESIAN_POINT('Ctrl Pts',(-91.0894114467178,6.19891703112955,
130.459707942787));
#213976=CARTESIAN_POINT('Ctrl Pts',(-91.3678590705306,3.06070001592934,
125.402742967496));
#213977=CARTESIAN_POINT('Ctrl Pts',(-91.6463066943433,-2.89015079040179,
125.309600728926));
#213978=CARTESIAN_POINT('Ctrl Pts',(-91.9247543181566,-6.18509421206894,
130.265874394073));
#213979=CARTESIAN_POINT('Ctrl Pts',(-92.2032019419691,-3.79623821149537,
135.716990592095));
#213980=CARTESIAN_POINT('Ctrl Pts',(-92.4816495657822,2.08117524889636,
136.653639838841));
#213981=CARTESIAN_POINT('Ctrl Pts',(-92.7600971895951,6.04609032661485,
132.21508723441));
#213982=CARTESIAN_POINT('Ctrl Pts',(-93.0385448134079,4.45494376210749,
126.480145786926));
#213983=CARTESIAN_POINT('Ctrl Pts',(-93.3169924372209,-1.23007848367479,
124.718946519161));
#213984=CARTESIAN_POINT('Ctrl Pts',(-93.5954400610337,-5.78471869563455,
128.549945518824));
#213985=CARTESIAN_POINT('Ctrl Pts',(-93.8738876848466,-5.02348502552524,
134.45264185993));
#213986=CARTESIAN_POINT('Ctrl Pts',(-94.1523353086595,0.354085972155003,
137.002745967751));
#213987=CARTESIAN_POINT('Ctrl Pts',(-94.4307829324724,5.40626925948619,
133.85683674671));
#213988=CARTESIAN_POINT('Ctrl Pts',(-94.7092305562852,5.49035520828578,
127.905851084735));
#213989=CARTESIAN_POINT('Ctrl Pts',(-94.9876781800983,0.529072939433998,
124.618454083368));
#213990=CARTESIAN_POINT('Ctrl Pts',(-95.2661258039109,-4.91840151410816,
127.015602988595));
#213991=CARTESIAN_POINT('Ctrl Pts',(-95.5445734277241,-5.84610525345601,
132.894435063746));
#213992=CARTESIAN_POINT('Ctrl Pts',(-95.8230210515366,-1.40152386299717,
136.85259082867));
#213993=CARTESIAN_POINT('Ctrl Pts',(-96.10146867535,4.33098948930923,135.252718502061));
#213994=CARTESIAN_POINT('Ctrl Pts',(-96.3799162991623,6.08353508153927,
129.565022593965));
#213995=CARTESIAN_POINT('Ctrl Pts',(-96.6583639229758,2.245609131046,125.01621778453));
#213996=CARTESIAN_POINT('Ctrl Pts',(-96.9368115467883,-3.65592190677386,
125.786433472156));
#213997=CARTESIAN_POINT('Ctrl Pts',(-97.2152591706015,-6.19783931398261,
131.167879067045));
#213998=CARTESIAN_POINT('Ctrl Pts',(-97.493706794414,-3.04424517292474,
136.215268965725));
#213999=CARTESIAN_POINT('Ctrl Pts',(-97.7721544182274,2.90686156240656,
136.290298430015));
#214000=CARTESIAN_POINT('Ctrl Pts',(-98.0506020420397,6.18670452996842,
131.324019047625));
#214001=CARTESIAN_POINT('Ctrl Pts',(-98.3290496658531,3.78126827180747,
125.880198954735));
#214002=CARTESIAN_POINT('Ctrl Pts',(-98.6074972896656,-2.09896880291958,
124.961442871316));
#214003=CARTESIAN_POINT('Ctrl Pts',(-98.8859449134787,-6.05035608809047,
129.412042754299));
#214004=CARTESIAN_POINT('Ctrl Pts',(-99.1643925372916,-4.44176170463296,
135.142114735114));
#214005=CARTESIAN_POINT('Ctrl Pts',(-99.4428401611044,1.24859469325925,
136.886002592972));
#214006=CARTESIAN_POINT('Ctrl Pts',(-99.7212877849174,5.79155356528836,
133.041158580159));
#214007=CARTESIAN_POINT('Ctrl Pts',(-99.9997354087301,5.01235764393804,
127.140806513377));
#214008=CARTESIAN_POINT('Ctrl Pts',(-100.278183032543,-0.37295008490757,
124.607081693777));
#214009=CARTESIAN_POINT('Ctrl Pts',(-100.556630656356,-5.41553490534739,
127.768353451233));
#214010=CARTESIAN_POINT('Ctrl Pts',(-100.835078280169,-5.48150771136145,
133.719567477352));
#214011=CARTESIAN_POINT('Ctrl Pts',(-101.113525903981,-0.510242717172956,
136.9918488151));
#214012=CARTESIAN_POINT('Ctrl Pts',(-101.391973527794,4.92991040735466,
134.578130774917));
#214013=CARTESIAN_POINT('Ctrl Pts',(-101.670421151607,5.83971670703623,
128.696502319049));
#214014=CARTESIAN_POINT('Ctrl Pts',(-101.94886877542,1.38310863897239,124.751892664915));
#214015=CARTESIAN_POINT('Ctrl Pts',(-102.227316399233,-4.34450869969331,
126.36920537977));
#214016=CARTESIAN_POINT('Ctrl Pts',(-102.505764023046,-6.07973478439049,
132.062209088779));
#214017=CARTESIAN_POINT('Ctrl Pts',(-102.784211646859,-2.22798161378826,
136.599311502058));
#214018=CARTESIAN_POINT('Ctrl Pts',(-103.062659270672,3.6711778169323,135.811137151577));
#214019=CARTESIAN_POINT('Ctrl Pts',(-103.341106894485,6.19670418089893,
130.42197976097));
#214020=CARTESIAN_POINT('Ctrl Pts',(-103.619554518298,3.02776212844844,
125.384211697232));
#214021=CARTESIAN_POINT('Ctrl Pts',(-103.89800214211,-2.92354540564323,
125.327295702285));
#214022=CARTESIAN_POINT('Ctrl Pts',(-104.176449765923,-6.18825753508174,
130.303534794984));
#214023=CARTESIAN_POINT('Ctrl Pts',(-104.454897389736,-3.76626330296762,
135.740008351935));
#214024=CARTESIAN_POINT('Ctrl Pts',(-104.733345013549,2.1167429123828,136.640862760796));
#214025=CARTESIAN_POINT('Ctrl Pts',(-105.011792637362,6.05456579989334,
132.17825682901));
#214026=CARTESIAN_POINT('Ctrl Pts',(-105.290240261175,4.42853849928509,
126.453107397468));
#214027=CARTESIAN_POINT('Ctrl Pts',(-105.568687884988,-1.26709933603374,
124.726547104658));
#214028=CARTESIAN_POINT('Ctrl Pts',(-105.847135508801,-5.79833478278087,
128.585200512514));
#214029=CARTESIAN_POINT('Ctrl Pts',(-106.125583132613,-5.00118382855433,
134.483153644914));
#214030=CARTESIAN_POINT('Ctrl Pts',(-106.404030756427,0.391810742700936,
137.000475704212));
#214031=CARTESIAN_POINT('Ctrl Pts',(-106.682478380239,5.42475038243292,
133.823870695931));
#214032=CARTESIAN_POINT('Ctrl Pts',(-106.960926004052,5.47260943449832,
127.872483436902));
#214033=CARTESIAN_POINT('Ctrl Pts',(-107.239373627865,0.491407768093767,
124.615348076738));
#214034=CARTESIAN_POINT('Ctrl Pts',(-107.517821251678,-4.94137363058539,
127.045612891524));
#214035=CARTESIAN_POINT('Ctrl Pts',(-107.796268875491,-5.83327406227795,
132.929983241508));
#214036=CARTESIAN_POINT('Ctrl Pts',(-108.074716499304,-1.36468060201792,
136.861010242526));
#214037=CARTESIAN_POINT('Ctrl Pts',(-108.353164123117,4.3579876631431,135.22627212199));
#214038=CARTESIAN_POINT('Ctrl Pts',(-108.631611746929,6.07587816540856,
129.528013351273));
#214039=CARTESIAN_POINT('Ctrl Pts',(-108.910059370743,2.21033345681367,
125.00265536525));
#214040=CARTESIAN_POINT('Ctrl Pts',(-109.188506994555,-3.68639971780079,
125.808781077045));
#214041=CARTESIAN_POINT('Ctrl Pts',(-109.466954618368,-6.19551164239422,
131.205600338952));
#214042=CARTESIAN_POINT('Ctrl Pts',(-109.745402242181,-3.01125103519769,
136.233699898554));
#214043=CARTESIAN_POINT('Ctrl Pts',(-110.023849865994,2.94020216555433,
136.272501896897));
#214044=CARTESIAN_POINT('Ctrl Pts',(-110.302297489807,6.18975321302316,
131.286349193086));
#214045=CARTESIAN_POINT('Ctrl Pts',(-110.58074511362,3.75122344397827,125.857272534824));
#214046=CARTESIAN_POINT('Ctrl Pts',(-110.859192737433,-2.13449741262907,
124.974328145912));
#214047=CARTESIAN_POINT('Ctrl Pts',(-111.137640361246,-6.05871942302636,
129.44889878553));
#214048=CARTESIAN_POINT('Ctrl Pts',(-111.416087985058,-4.41527426856075,
135.169072630797));
#214049=CARTESIAN_POINT('Ctrl Pts',(-111.694535608871,1.28559224057236,
136.878289363941));
#214050=CARTESIAN_POINT('Ctrl Pts',(-111.972983232684,5.8050622852923,133.005862307081));
#214051=CARTESIAN_POINT('Ctrl Pts',(-112.251430856497,4.9899636828869,127.110362746893));
#214052=CARTESIAN_POINT('Ctrl Pts',(-112.52987848031,-0.410667770813077,
124.609466768025));
#214053=CARTESIAN_POINT('Ctrl Pts',(-112.808326104123,-5.43391560537209,
127.801375599495));
#214054=CARTESIAN_POINT('Ctrl Pts',(-113.086773727936,-5.46366046012913,
133.752880958598));
#214055=CARTESIAN_POINT('Ctrl Pts',(-113.365221351749,-0.472568266679477,
136.994840167519));
#214056=CARTESIAN_POINT('Ctrl Pts',(-113.643668975562,4.95279107760506,
134.548051091771));
#214057=CARTESIAN_POINT('Ctrl Pts',(-113.922116599375,5.8267773788663,128.660993359675));
#214058=CARTESIAN_POINT('Ctrl Pts',(-114.200564223187,1.34623992284899,
124.74358542827));
#214059=CARTESIAN_POINT('Ctrl Pts',(-114.479011847001,-4.37142625478972,
126.395733810498));
#214060=CARTESIAN_POINT('Ctrl Pts',(-114.757459470813,-6.07196526032194,
132.099194855029));
#214061=CARTESIAN_POINT('Ctrl Pts',(-115.035907094626,-2.19266482361144,
136.612766491501));
#214062=CARTESIAN_POINT('Ctrl Pts',(-115.314354718439,3.70158746836604,
135.788696886227));
#214063=CARTESIAN_POINT('Ctrl Pts',(-115.592802342252,6.19426170951602,
130.384265748418));
#214064=CARTESIAN_POINT('Ctrl Pts',(-115.871249966065,2.99471204612843,
125.36588127258));
#214065=CARTESIAN_POINT('Ctrl Pts',(-116.149697589878,-2.95683168783455,
125.345193630298));
#214066=CARTESIAN_POINT('Ctrl Pts',(-116.428145213691,-6.19119154993583,
130.34121375418));
#214067=CARTESIAN_POINT('Ctrl Pts',(-116.706592837503,-3.73614883416816,
135.762843219532));
#214068=CARTESIAN_POINT('Ctrl Pts',(-116.985040461316,2.1522321391827,136.627869409019));
#214069=CARTESIAN_POINT('Ctrl Pts',(-117.263488085129,6.06281691900968,
132.14137551338));
#214070=CARTESIAN_POINT('Ctrl Pts',(-117.541935708942,4.40196913533955,
126.426230245297));
#214071=CARTESIAN_POINT('Ctrl Pts',(-117.820383332755,-1.30407323556081,
124.73437290577));
#214072=CARTESIAN_POINT('Ctrl Pts',(-118.098830956568,-5.81173601049948,
128.620537737998));
#214073=CARTESIAN_POINT('Ctrl Pts',(-118.377278580381,-4.97869731087745,
134.51352911087));
#214074=CARTESIAN_POINT('Ctrl Pts',(-118.655726204194,0.429520994555717,
136.997975841351));
#214075=CARTESIAN_POINT('Ctrl Pts',(-118.934173828006,5.44303048925927,
133.790792756097));
#214076=CARTESIAN_POINT('Ctrl Pts',(-119.21262145182,5.45466087115571,127.839224430854));
#214077=CARTESIAN_POINT('Ctrl Pts',(-119.491069075632,0.453724387457947,
124.612471406243));
#214078=CARTESIAN_POINT('Ctrl Pts',(-119.769516699445,-4.96416264264509,
127.075762076232));
#214079=CARTESIAN_POINT('Ctrl Pts',(-120.047964323258,-5.82022671698453,
132.965452653541));
#214080=CARTESIAN_POINT('Ctrl Pts',(-120.326411947071,-1.32778677229758,
136.869205225004));
#214081=CARTESIAN_POINT('Ctrl Pts',(-120.604859570884,4.38482435014149,
135.199661886361));
#214082=CARTESIAN_POINT('Ctrl Pts',(-120.883307194697,6.06799610537801,
129.491051404098));
#214083=CARTESIAN_POINT('Ctrl Pts',(-121.16175481851,2.17497587786225,124.989307930291));
#214084=CARTESIAN_POINT('Ctrl Pts',(-121.440202442323,-3.71674092793051,
125.831313794972));
#214085=CARTESIAN_POINT('Ctrl Pts',(-121.718650066136,-6.19295439384353,
131.243306742772));
#214086=CARTESIAN_POINT('Ctrl Pts',(-121.997097689948,-2.97814531445616,
136.251929645219));
#214087=CARTESIAN_POINT('Ctrl Pts',(-122.275545313761,2.97343381842962,
136.254502739794));
#214088=CARTESIAN_POINT('Ctrl Pts',(-122.553992937574,6.19257253249627,
131.248661478285));
#214089=CARTESIAN_POINT('Ctrl Pts',(-122.832440561387,3.72103961318487,
125.83452943108));
#214090=CARTESIAN_POINT('Ctrl Pts',(-123.1108881852,-2.16994692775201,124.987429454503));
#214091=CARTESIAN_POINT('Ctrl Pts',(-123.389335809013,-6.06685824988591,
129.485805043896));
#214092=CARTESIAN_POINT('Ctrl Pts',(-123.667783432826,-4.38862322287681,
135.19586879047));
#214093=CARTESIAN_POINT('Ctrl Pts',(-123.946231056639,1.32254214979223,
136.870351063246));
#214094=CARTESIAN_POINT('Ctrl Pts',(-124.224678680451,5.81835589657845,
132.97048445655));
#214095=CARTESIAN_POINT('Ctrl Pts',(-124.503126304264,4.96738481689638,
127.080055862859));
#214096=CARTESIAN_POINT('Ctrl Pts',(-124.781573928077,-0.448370239273912,
124.612081396343));
#214097=CARTESIAN_POINT('Ctrl Pts',(-125.06002155189,-5.4520949496557,127.834509024472));
#214098=CARTESIAN_POINT('Ctrl Pts',(-125.338469175703,-5.44561075094924,
133.786085181339));
#214099=CARTESIAN_POINT('Ctrl Pts',(-125.616916799516,-0.434876304995071,
136.997602129441));
#214100=CARTESIAN_POINT('Ctrl Pts',(-125.895364423329,4.97548822036069,
134.517832684797));
#214101=CARTESIAN_POINT('Ctrl Pts',(-126.173812047142,5.8136221373178,128.625563823564));
#214102=CARTESIAN_POINT('Ctrl Pts',(-126.452259670955,1.30932132131015,
124.735502775877));
#214103=CARTESIAN_POINT('Ctrl Pts',(-126.730707294768,-4.39818182507867,
126.422425604514));
#214104=CARTESIAN_POINT('Ctrl Pts',(-127.00915491858,-6.0639707373477,132.136132640718));
#214105=CARTESIAN_POINT('Ctrl Pts',(-127.287602542393,-2.15726678343353,
136.626006248326));
#214106=CARTESIAN_POINT('Ctrl Pts',(-127.566050166206,3.73185995611441,
135.766071924465));
#214107=CARTESIAN_POINT('Ctrl Pts',(-127.844497790019,6.19158970748781,
130.346567302635));
#214108=CARTESIAN_POINT('Ctrl Pts',(-128.122945413832,2.96155099365221,
125.34775237278));
#214109=CARTESIAN_POINT('Ctrl Pts',(-128.401393037645,-2.99000840354028,
125.363293849751));
#214110=CARTESIAN_POINT('Ctrl Pts',(-128.679840661458,-6.19389614791022,
130.378909875453));
#214111=CARTESIAN_POINT('Ctrl Pts',(-128.958288285271,-3.70589592099968,
135.785494348734));
#214112=CARTESIAN_POINT('Ctrl Pts',(-129.236735909083,2.18764161422919,
136.614660264981));
#214113=CARTESIAN_POINT('Ctrl Pts',(-129.515183532897,6.07084337821547,
132.104444654172));
#214114=CARTESIAN_POINT('Ctrl Pts',(-129.793631156709,4.37523665480886,
126.399515326358));
#214115=CARTESIAN_POINT('Ctrl Pts',(-130.072078780522,-1.34099881217456,
124.742423632508));
#214116=CARTESIAN_POINT('Ctrl Pts',(-130.350526404335,-5.82492188220296,
128.655955885842));
#214117=CARTESIAN_POINT('Ctrl Pts',(-130.628974028148,-4.95602630574081,
134.543767132223));
#214118=CARTESIAN_POINT('Ctrl Pts',(-130.907421651961,0.467215330352083,
136.995246471799));
#214119=CARTESIAN_POINT('Ctrl Pts',(-131.185869275774,5.46110890258918,
133.757604152921));
#214120=CARTESIAN_POINT('Ctrl Pts',(-131.464316899587,5.43651018334856,
127.80607529902));
#214121=CARTESIAN_POINT('Ctrl Pts',(-131.742764523399,0.416024193898128,
124.60982417848));
#214122=CARTESIAN_POINT('Ctrl Pts',(-132.021212147213,-4.98676770583297,
127.106049425532));
#214123=CARTESIAN_POINT('Ctrl Pts',(-132.299659771025,-5.80696370104951,
133.000841985516));
#214124=CARTESIAN_POINT('Ctrl Pts',(-132.578107394838,-1.2908437409496,
136.877175472434));
#214125=CARTESIAN_POINT('Ctrl Pts',(-132.856555018651,4.41149855586104,
135.172888781227));
#214126=CARTESIAN_POINT('Ctrl Pts',(-133.135002642464,6.05988919352027,
129.454138122079));
#214127=CARTESIAN_POINT('Ctrl Pts',(-133.413450266277,2.13953770437982,
124.976175974248));
#214128=CARTESIAN_POINT('Ctrl Pts',(-133.69189789009,-3.74694441285829,
125.854030790976));
#214129=CARTESIAN_POINT('Ctrl Pts',(-133.970345513903,-6.19016766309031,
131.280996881284));
#214130=CARTESIAN_POINT('Ctrl Pts',(-134.248793137716,-2.94492923744478,
136.269957530209));
#214131=CARTESIAN_POINT('Ctrl Pts',(-134.527240761528,3.00655528962129,
136.236301625668));
#214132=CARTESIAN_POINT('Ctrl Pts',(-134.805688385342,6.19516238391663,
131.210957299752));
#214133=CARTESIAN_POINT('Ctrl Pts',(-135.084136009154,3.69071789790064,
125.811970486258));
#214134=CARTESIAN_POINT('Ctrl Pts',(-135.362583632967,-2.2053160346932,
125.000746311619));
#214135=CARTESIAN_POINT('Ctrl Pts',(-135.64103125678,-6.07477226708194,
129.522760161825));
#214136=CARTESIAN_POINT('Ctrl Pts',(-135.919478880593,-4.36180955514542,
135.222502221193));
#214137=CARTESIAN_POINT('Ctrl Pts',(-136.197926504406,1.35944305172635,
136.862187985044));
#214138=CARTESIAN_POINT('Ctrl Pts',(-136.476374128219,5.83143390654715,
132.935026339502));
#214139=CARTESIAN_POINT('Ctrl Pts',(-136.754821752032,4.9446218826347,127.049886984307));
#214140=CARTESIAN_POINT('Ctrl Pts',(-137.033269375845,-0.486056093210629,
124.614925481843));
#214141=CARTESIAN_POINT('Ctrl Pts',(-137.311716999657,-5.47007226455594,
127.867752498391));
#214142=CARTESIAN_POINT('Ctrl Pts',(-137.59016462347,-5.42735925266033,
133.819178915179));
#214143=CARTESIAN_POINT('Ctrl Pts',(-137.868612247283,-0.397168228809268,
137.000134598521));
#214144=CARTESIAN_POINT('Ctrl Pts',(-138.147059871096,4.99800099457058,
134.487476673751));
#214145=CARTESIAN_POINT('Ctrl Pts',(-138.425507494909,5.80025146986304,
128.590215023569));
#214146=CARTESIAN_POINT('Ctrl Pts',(-138.703955118722,1.27235420238826,
124.727645007244));
#214147=CARTESIAN_POINT('Ctrl Pts',(-138.982402742535,-4.42477441912264,
126.449279772744));
#214148=CARTESIAN_POINT('Ctrl Pts',(-139.260850366348,-6.05575151170779,
132.173021077107));
#214149=CARTESIAN_POINT('Ctrl Pts',(-139.539297990161,-2.12178880494131,
136.639030281933));
#214150=CARTESIAN_POINT('Ctrl Pts',(-139.817745613973,3.76199415842019,
135.743263104665));
#214151=CARTESIAN_POINT('Ctrl Pts',(-140.096193237787,6.18868827382574,
130.308885820552));
#214152=CARTESIAN_POINT('Ctrl Pts',(-140.374640861599,2.92828019981485,
125.329825669606));
#214153=CARTESIAN_POINT('Ctrl Pts',(-140.653088485412,-3.02307432338508,
125.381595689934));
#214154=CARTESIAN_POINT('Ctrl Pts',(-140.931536109225,-6.19637122878504,
130.416621761961));
#214155=CARTESIAN_POINT('Ctrl Pts',(-141.209983733038,-3.675505684495,135.807960900193));
#214156=CARTESIAN_POINT('Ctrl Pts',(-141.488431356851,2.22297002541115,
136.601235818153));
#214157=CARTESIAN_POINT('Ctrl Pts',(-141.766878980664,6.07864488008735,
132.06746561987));
#214158=CARTESIAN_POINT('Ctrl Pts',(-142.045326604476,4.34834204827492,
126.372963630579));
#214159=CARTESIAN_POINT('Ctrl Pts',(-142.32377422829,-1.3778746975837,124.750698986551));
#214160=CARTESIAN_POINT('Ctrl Pts',(-142.602221852102,-5.83789190928377,
128.691453643612));
#214161=CARTESIAN_POINT('Ctrl Pts',(-142.880669475915,-4.93317165322728,
134.573866588494));
#214162=CARTESIAN_POINT('Ctrl Pts',(-143.159117099728,0.504892353312588,
136.992287696695));
#214163=CARTESIAN_POINT('Ctrl Pts',(-143.437564723541,5.47898495252035,
133.72430611622));
#214164=CARTESIAN_POINT('Ctrl Pts',(-143.716012347354,5.4181580436573,127.77303726975));
#214165=CARTESIAN_POINT('Ctrl Pts',(-143.994459971167,0.378308584408798,
124.607406491544));
#214166=CARTESIAN_POINT('Ctrl Pts',(-144.27290759498,-5.00918798250961,
127.136473817112));
#214167=CARTESIAN_POINT('Ctrl Pts',(-144.551355218793,-5.79348550593904,
133.036149926065));
#214168=CARTESIAN_POINT('Ctrl Pts',(-144.829802842605,-1.2538528769121,
136.884920689477));
#214169=CARTESIAN_POINT('Ctrl Pts',(-145.108250466418,4.43800929187927,
135.145953798675));
#214170=CARTESIAN_POINT('Ctrl Pts',(-145.386698090231,6.05155773023994,
129.417274873051));
#214171=CARTESIAN_POINT('Ctrl Pts',(-145.665145714044,2.10402024954095,
124.963259983731));
#214172=CARTESIAN_POINT('Ctrl Pts',(-145.943593337857,-3.77700905338292,
125.876931223274));
#214173=CARTESIAN_POINT('Ctrl Pts',(-146.22204096167,-6.18715155339789,
131.318669357863));
#214174=CARTESIAN_POINT('Ctrl Pts',(-146.500488585483,-2.9116040349975,
136.287782885497));
#214175=CARTESIAN_POINT('Ctrl Pts',(-146.778936209295,3.03956535180104,
136.217899228972));
#214176=CARTESIAN_POINT('Ctrl Pts',(-147.057383833109,6.19752267131684,
131.173238054629));
#214177=CARTESIAN_POINT('Ctrl Pts',(-147.335831456921,3.66025942170698,
125.789596536289));
#214178=CARTESIAN_POINT('Ctrl Pts',(-147.614279080735,-2.24060342283806,
125.014278223797));
#214179=CARTESIAN_POINT('Ctrl Pts',(-147.892726704547,-6.08246118135759,
129.559762769929));
#214180=CARTESIAN_POINT('Ctrl Pts',(-148.17117432836,-4.33483425895693,
135.248971936054));
#214181=CARTESIAN_POINT('Ctrl Pts',(-148.449621952173,1.39629357899829,
136.853800431821));
#214182=CARTESIAN_POINT('Ctrl Pts',(-148.728069575986,5.84429583058792,
132.899489269852));
#214183=CARTESIAN_POINT('Ctrl Pts',(-149.006517199799,4.9216757235908,127.019857229157));
#214184=CARTESIAN_POINT('Ctrl Pts',(-149.284964823612,-0.52372393616008,
124.617998919139));
#214185=CARTESIAN_POINT('Ctrl Pts',(-149.563412447425,-5.48784688391679,
127.901104789406));
#214186=CARTESIAN_POINT('Ctrl Pts',(-149.841860071237,-5.40890664157841,
133.852160933818));
#214187=CARTESIAN_POINT('Ctrl Pts',(-150.12030769505,-0.359445435409253,
137.002437480918));
#214188=CARTESIAN_POINT('Ctrl Pts',(-150.398755318863,5.02032856601553,
134.456984183485));
#214189=CARTESIAN_POINT('Ctrl Pts',(-150.677202942676,5.78666587195703,
128.554948269553));
#214190=CARTESIAN_POINT('Ctrl Pts',(-150.955650566489,1.23533993591347,
124.720012413542));
#214191=CARTESIAN_POINT('Ctrl Pts',(-151.234098190302,-4.45120305152329,
126.476295320094));
#214192=CARTESIAN_POINT('Ctrl Pts',(-151.512545814115,-6.0473078879686,
132.209858797279));
#214193=CARTESIAN_POINT('Ctrl Pts',(-151.790993437928,-2.08623220278462,
136.651838109709));
#214194=CARTESIAN_POINT('Ctrl Pts',(-152.069441061741,3.79198895864895,
135.720271272016));
#214195=CARTESIAN_POINT('Ctrl Pts',(-152.347888685554,6.18555751604382,
130.27122269847));
#214196=CARTESIAN_POINT('Ctrl Pts',(-152.626336309366,2.89490089747778,
125.312101827337));
#214197=CARTESIAN_POINT('Ctrl Pts',(-152.904783933179,-3.05602822209906,
125.400098472666));
#214198=CARTESIAN_POINT('Ctrl Pts',(-153.183231556992,-6.19861670084527,
130.454348016274));
#214199=CARTESIAN_POINT('Ctrl Pts',(-153.461679180805,-3.64497925077551,
135.830242041403));
#214200=CARTESIAN_POINT('Ctrl Pts',(-153.740126804618,2.25821606362131,
136.587596565983));
#214201=CARTESIAN_POINT('Ctrl Pts',(-154.018574428431,6.08622113553776,
132.030439780749));
#214202=CARTESIAN_POINT('Ctrl Pts',(-154.297022052244,4.32128631232727,
126.346576141847));
#214203=CARTESIAN_POINT('Ctrl Pts',(-154.575469676057,-1.41469952533967,
124.759198661251));
#214204=CARTESIAN_POINT('Ctrl Pts',(-154.85391729987,-5.85064561113321,
128.727029695929));
#214205=CARTESIAN_POINT('Ctrl Pts',(-155.132364923682,-4.9101342002235,
134.603826364333));
#214206=CARTESIAN_POINT('Ctrl Pts',(-155.410812547495,0.542550667301237,
136.989099625678));
#214207=CARTESIAN_POINT('Ctrl Pts',(-155.689260171308,5.49665797664923,
133.690899879866));
#214208=CARTESIAN_POINT('Ctrl Pts',(-155.967707795121,5.39960513212718,
127.740111567281));
#214209=CARTESIAN_POINT('Ctrl Pts',(-156.246155418934,0.340578956555753,
124.605218435021));
#214210=CARTESIAN_POINT('Ctrl Pts',(-156.524603042747,-5.03142264188343,
127.167034123586));
#214211=CARTESIAN_POINT('Ctrl Pts',(-156.80305066656,-5.77979263109261,
133.071375166841));
#214212=CARTESIAN_POINT('Ctrl Pts',(-157.081498290373,-1.21681555089514,
136.89244058913));
#214213=CARTESIAN_POINT('Ctrl Pts',(-157.359945914186,4.46435557583064,
135.118857936792));
#214214=CARTESIAN_POINT('Ctrl Pts',(-157.638393537999,6.04300202426259,
129.380463022997));
#214215=CARTESIAN_POINT('Ctrl Pts',(-157.916841161811,2.06842482945845,
124.950560437346));
#214216=CARTESIAN_POINT('Ctrl Pts',(-158.195288785624,-3.80693373544809,
125.900014243279));
#214217=CARTESIAN_POINT('Ctrl Pts',(-158.473736409437,-6.18390617652933,
131.356322776543));
#214218=CARTESIAN_POINT('Ctrl Pts',(-158.75218403325,-2.87817094199197,
136.305405050556));
#214219=CARTESIAN_POINT('Ctrl Pts',(-159.030631657063,3.07246278176887,
136.199296231612));
#214220=CARTESIAN_POINT('Ctrl Pts',(-159.309079280876,6.19965330723533,
131.135505140616));
#214221=CARTESIAN_POINT('Ctrl Pts',(-159.587526904689,3.62966531325439,
125.767408410247));
#214222=CARTESIAN_POINT('Ctrl Pts',(-159.865974528502,-2.27580778459908,
125.028024689608));
#214223=CARTESIAN_POINT('Ctrl Pts',(-160.144422152314,-6.08992470779737,
129.596811497064));
#214224=CARTESIAN_POINT('Ctrl Pts',(-160.422869776128,-4.3076983338908,
135.275276954208));
#214225=CARTESIAN_POINT('Ctrl Pts',(-160.70131739994,1.43309236609815,136.845188714382));
#214226=CARTESIAN_POINT('Ctrl Pts',(-160.979765023753,5.85694119209746,
132.863874564441));
#214227=CARTESIAN_POINT('Ctrl Pts',(-161.258212647566,4.89854719004298,
126.989967710171));
#214228=CARTESIAN_POINT('Ctrl Pts',(-161.536660271379,-0.561372372326459,
124.621301594343));
#214229=CARTESIAN_POINT('Ctrl Pts',(-161.815107895192,-5.50541814909322,
127.934564661631));
#214230=CARTESIAN_POINT('Ctrl Pts',(-162.093555519005,-5.39025360147175,
133.885030015096));
#214231=CARTESIAN_POINT('Ctrl Pts',(-162.372003142818,-0.32170932262588,
137.004510691297));
#214232=CARTESIAN_POINT('Ctrl Pts',(-162.650450766631,5.04247010733932,
134.426356343909));
#214233=CARTESIAN_POINT('Ctrl Pts',(-162.928898390443,5.77286584701905,
128.519764868338));
#214234=CARTESIAN_POINT('Ctrl Pts',(-163.207346014257,1.19827989346308,
124.712605277602));
#214235=CARTESIAN_POINT('Ctrl Pts',(-163.485793638069,-4.47746674295796,
126.503471245498));
#214236=CARTESIAN_POINT('Ctrl Pts',(-163.764241261882,-6.03864017901171,
132.246644436198));
#214237=CARTESIAN_POINT('Ctrl Pts',(-164.042688885695,-2.05059829452646,
136.664429257056));
#214238=CARTESIAN_POINT('Ctrl Pts',(-164.321136509508,3.82184324533235,
135.697097278492));
#214239=CARTESIAN_POINT('Ctrl Pts',(-164.599584133321,6.18219755015336,
130.23357933201));
#214240=CARTESIAN_POINT('Ctrl Pts',(-164.878031757134,2.86141432352365,
125.294581502737));
#214241=CARTESIAN_POINT('Ctrl Pts',(-165.156479380946,-3.08886887856293,
125.418801512319));
#214242=CARTESIAN_POINT('Ctrl Pts',(-165.43492700476,-6.20063248088431,
130.492087240433));
#214243=CARTESIAN_POINT('Ctrl Pts',(-165.713374628572,-3.61431775100944,
135.85233694673));
#214244=CARTESIAN_POINT('Ctrl Pts',(-165.991822252385,2.2933784228048,136.573743013877));
#214245=CARTESIAN_POINT('Ctrl Pts',(-166.270269876198,6.09357186382579,
131.993368508814));
#214246=CARTESIAN_POINT('Ctrl Pts',(-166.548717500011,4.2940704495262,126.320353837957));
#214247=CARTESIAN_POINT('Ctrl Pts',(-166.827165123824,-1.45147193088449,
124.767922341652));
#214248=CARTESIAN_POINT('Ctrl Pts',(-167.105612747637,-5.86318251515793,
128.762682724506));
#214249=CARTESIAN_POINT('Ctrl Pts',(-167.38406037145,-4.88691480039125,
134.633645349573));
#214250=CARTESIAN_POINT('Ctrl Pts',(-167.662507995262,0.580188876875391,
136.985682376883));
#214251=CARTESIAN_POINT('Ctrl Pts',(-167.940955619076,5.51412732009539,
133.657386681736));
#214252=CARTESIAN_POINT('Ctrl Pts',(-168.219403242888,5.38085213624319,
127.707299411689));
#214253=CARTESIAN_POINT('Ctrl Pts',(-168.497850866701,0.302836708424229,
124.60326008999));
#214254=CARTESIAN_POINT('Ctrl Pts',(-168.776298490514,-5.05347086004094,
127.197729212531));
#214255=CARTESIAN_POINT('Ctrl Pts',(-169.054746114327,-5.7658855839047,
133.106516402559));
#214256=CARTESIAN_POINT('Ctrl Pts',(-169.33319373814,-1.17973313533045,
136.899734892741));
#214257=CARTESIAN_POINT('Ctrl Pts',(-169.611641361953,4.49053643144484,
135.091602199623));
#214258=CARTESIAN_POINT('Ctrl Pts',(-169.890088985766,6.03422239262278,
129.34370393599));
#214259=CARTESIAN_POINT('Ctrl Pts',(-170.168536609579,2.03275276313275,
124.938077805679));
#214260=CARTESIAN_POINT('Ctrl Pts',(-170.446984233392,-3.83671735018369,
125.923278995643));
#214261=CARTESIAN_POINT('Ctrl Pts',(-170.725431857205,-6.18043165274327,
131.393955742061));
#214262=CARTESIAN_POINT('Ctrl Pts',(-171.003879481017,-2.84463119730373,
136.32282337239));
#214263=CARTESIAN_POINT('Ctrl Pts',(-171.282327104831,3.10524636049842,
136.180493322929));
#214264=CARTESIAN_POINT('Ctrl Pts',(-171.560774728643,6.20155421272058,
131.097759955922));
#214265=CARTESIAN_POINT('Ctrl Pts',(-171.839222352457,3.59893670621881,
125.745406930321));
#214266=CARTESIAN_POINT('Ctrl Pts',(-172.117669976268,-2.31092781546573,
125.04198519967));
#214267=CARTESIAN_POINT('Ctrl Pts',(-172.396117600082,-6.09716256983718,
129.633904970377));
#214268=CARTESIAN_POINT('Ctrl Pts',(-172.674565223895,-4.2804027854792,
135.301416300912));
#214269=CARTESIAN_POINT('Ctrl Pts',(-172.953012847708,1.469838049433,136.836353151837));
#214270=CARTESIAN_POINT('Ctrl Pts',(-173.23146047152,5.86936952249723,132.828183542982));
#214271=CARTESIAN_POINT('Ctrl Pts',(-173.509908095334,4.8752371390276,126.960219534917));
#214272=CARTESIAN_POINT('Ctrl Pts',(-173.788355719146,-0.599000006633149,
124.624833385073));
#214273=CARTESIAN_POINT('Ctrl Pts',(-174.06680334296,-5.5227854089755,127.968130875202));
#214274=CARTESIAN_POINT('Ctrl Pts',(-174.345250966772,-5.37140082353563,
133.917784941036));
#214275=CARTESIAN_POINT('Ctrl Pts',(-174.623698590585,-0.283961288785237,
137.006354152836));
#214276=CARTESIAN_POINT('Ctrl Pts',(-174.902146214398,5.06442479807889,
134.39559428995));
#214277=CARTESIAN_POINT('Ctrl Pts',(-175.18059383821,5.75885190641417,128.484666123661));
#214278=CARTESIAN_POINT('Ctrl Pts',(-175.459041462024,1.16117544831056,
124.705423873895));
#214279=CARTESIAN_POINT('Ctrl Pts',(-175.737489085836,-4.50356452021585,
126.530806541938));
#214280=CARTESIAN_POINT('Ctrl Pts',(-176.01593670965,-6.02974870602229,
132.28337663076));
#214281=CARTESIAN_POINT('Ctrl Pts',(-176.294384333462,-2.01488840059438,
136.676803257405));
#214282=CARTESIAN_POINT('Ctrl Pts',(-176.572831957276,3.85155591220881,
135.67374198281));
#214283=CARTESIAN_POINT('Ctrl Pts',(-176.851279581088,6.17860850065921,
130.195957116059));
#214284=CARTESIAN_POINT('Ctrl Pts',(-177.129727204901,2.82782171880919,
125.277265345029));
#214285=CARTESIAN_POINT('Ctrl Pts',(-177.408174828714,-3.12159507585506,
125.437704115845));
#214286=CARTESIAN_POINT('Ctrl Pts',(-177.686622452527,-6.20241849420629,
130.529838035997));
#214287=CARTESIAN_POINT('Ctrl Pts',(-177.965070076339,-3.58352232136993,
135.874244797437));
#214288=CARTESIAN_POINT('Ctrl Pts',(-178.243517700153,2.32845580000743,
136.559675675186));
#214289=CARTESIAN_POINT('Ctrl Pts',(-178.521965323965,6.10069679256748,
131.956253177754));
#214290=CARTESIAN_POINT('Ctrl Pts',(-178.800412947778,4.26669546836545,
126.294297690589));
#214291=CARTESIAN_POINT('Ctrl Pts',(-179.078860571591,-1.48819055160311,
124.776869704492));
#214292=CARTESIAN_POINT('Ctrl Pts',(-179.357308195404,-5.8755021567984,
128.798411408209));
#214293=CARTESIAN_POINT('Ctrl Pts',(-179.635755819217,-4.86351431413387,
134.663322439258));
#214294=CARTESIAN_POINT('Ctrl Pts',(-179.91420344303,0.617805587336893,
136.982036076937));
#214295=CARTESIAN_POINT('Ctrl Pts',(-180.192651066843,5.53139233552561,
133.623767763677));
#214296=CARTESIAN_POINT('Ctrl Pts',(-180.471098690656,5.36189975090491,
127.674602018838));
#214297=CARTESIAN_POINT('Ctrl Pts',(-180.749546314469,0.265083238567079,
124.601531529021));
#214298=CARTESIAN_POINT('Ctrl Pts',(-181.027993938281,-5.07533181997731,
127.22855794653));
#214299=CARTESIAN_POINT('Ctrl Pts',(-181.306441562095,-5.75176487970607,
133.141572331048));
#214300=CARTESIAN_POINT('Ctrl Pts',(-181.584889185907,-1.14260700432061,
136.906803330016));
#214301=CARTESIAN_POINT('Ctrl Pts',(-181.86333680972,4.5165508885802,135.064187597142));
#214302=CARTESIAN_POINT('Ctrl Pts',(-182.141784433533,6.02521916065313,
129.306998974155));
#214303=CARTESIAN_POINT('Ctrl Pts',(-182.420232057346,1.99700537240587,
124.925812551278));
#214304=CARTESIAN_POINT('Ctrl Pts',(-182.698679681159,-3.86635879394691,
125.946724618282));
#214305=CARTESIAN_POINT('Ctrl Pts',(-182.977127304972,-6.17672811078948,
131.431566859916));
#214306=CARTESIAN_POINT('Ctrl Pts',(-183.255574928785,-2.81098604376035,
136.340037205557));
#214307=CARTESIAN_POINT('Ctrl Pts',(-183.534022552597,3.13791487318212,
136.161491199671));
#214308=CARTESIAN_POINT('Ctrl Pts',(-183.81247017641,6.20322531733387,131.060003899207));
#214309=CARTESIAN_POINT('Ctrl Pts',(-184.090917800223,3.56807473926006,
125.723592911784));
#214310=CARTESIAN_POINT('Ctrl Pts',(-184.369365424036,-2.34596221405232,
125.056159236672));
#214311=CARTESIAN_POINT('Ctrl Pts',(-184.647813047849,-6.10417449927606,
129.671041815353));
#214312=CARTESIAN_POINT('Ctrl Pts',(-184.926260671662,-4.25294862516783,
135.327389007565));
#214313=CARTESIAN_POINT('Ctrl Pts',(-185.204708295475,1.50652926737877,
136.827294071589));
#214314=CARTESIAN_POINT('Ctrl Pts',(-185.483155919288,5.88158036125089,
132.792417528021));
#214315=CARTESIAN_POINT('Ctrl Pts',(-185.761603543101,4.85174643430717,
126.930613805724));
#214316=CARTESIAN_POINT('Ctrl Pts',(-186.040051166913,-0.6366054447743,
124.628594160457));
#214317=CARTESIAN_POINT('Ctrl Pts',(-186.318498790727,-5.53994802001346,
128.001802186308));
#214318=CARTESIAN_POINT('Ctrl Pts',(-186.596946414539,-5.35234900636664,
133.950424497894));
#214319=CARTESIAN_POINT('Ctrl Pts',(-186.875394038353,-0.246202732654624,
137.007967797222));
#214320=CARTESIAN_POINT('Ctrl Pts',(-187.153841662165,5.08619182469514,
134.364699161505));
#214321=CARTESIAN_POINT('Ctrl Pts',(-187.432289285978,5.744624569434,128.449653336115));
#214322=CARTESIAN_POINT('Ctrl Pts',(-187.71073690979,1.12402797537536,124.698468468532));
#214323=CARTESIAN_POINT('Ctrl Pts',(-187.989184533604,-4.52949541623416,
126.558300196495));
#214324=CARTESIAN_POINT('Ctrl Pts',(-188.267632157416,-6.0206337984771,
132.32005401984));
#214325=CARTESIAN_POINT('Ctrl Pts',(-188.54607978123,-1.97910384423165,
136.688959652232));
#214326=CARTESIAN_POINT('Ctrl Pts',(-188.824527405043,3.88112585826452,
135.650206250412));
#214327=CARTESIAN_POINT('Ctrl Pts',(-189.102975028855,6.17479050055486,
130.158357444724));
#214328=CARTESIAN_POINT('Ctrl Pts',(-189.381422652668,2.79412432812102,
125.260153995869));
#214329=CARTESIAN_POINT('Ctrl Pts',(-189.659870276481,-3.15420560129371,
125.456805582802));
#214330=CARTESIAN_POINT('Ctrl Pts',(-189.938317900294,-6.20397467462999,
130.567599004095));
#214331=CARTESIAN_POINT('Ctrl Pts',(-190.216765524107,-3.55259410299321,
135.89596478172));
#214332=CARTESIAN_POINT('Ctrl Pts',(-190.49521314792,2.36344689542356,136.545395071179));
#214333=CARTESIAN_POINT('Ctrl Pts',(-190.773660771733,6.10759565774615,
131.919095162891));
#214334=CARTESIAN_POINT('Ctrl Pts',(-191.052108395545,4.23916238323504,
126.26840866526));
#214335=CARTESIAN_POINT('Ctrl Pts',(-191.330556019359,-1.52485402687357,
124.786040418225));
#214336=CARTESIAN_POINT('Ctrl Pts',(-191.609003643171,-5.88760407954571,
128.834214423098));
#214337=CARTESIAN_POINT('Ctrl Pts',(-191.887451266984,-4.83993360856504,
134.692856533694));
#214338=CARTESIAN_POINT('Ctrl Pts',(-192.165898890797,0.655399404785621,
136.978160860955));
#214339=CARTESIAN_POINT('Ctrl Pts',(-192.44434651461,5.54845238317892,133.59004437145));
#214340=CARTESIAN_POINT('Ctrl Pts',(-192.722794138423,5.34274867839911,
127.642020600343));
#214341=CARTESIAN_POINT('Ctrl Pts',(-193.001241762236,0.227319945953055,
124.600032816164));
#214342=CARTESIAN_POINT('Ctrl Pts',(-193.279689386049,-5.09700471162664,
127.259519183211));
#214343=CARTESIAN_POINT('Ctrl Pts',(-193.558137009861,-5.73743104174462,
133.176541653297));
#214344=CARTESIAN_POINT('Ctrl Pts',(-193.836584633675,-1.105438533588,136.913645639033));
#214345=CARTESIAN_POINT('Ctrl Pts',(-194.115032257487,4.5423979832614,135.036615145204));
#214346=CARTESIAN_POINT('Ctrl Pts',(-194.3934798813,6.01599266197172,129.270349497605));
#214347=CARTESIAN_POINT('Ctrl Pts',(-194.671927505113,1.96118398191049,
124.913765128639));
#214348=CARTESIAN_POINT('Ctrl Pts',(-194.950375128926,-3.89585696836267,
125.970350242409));
#214349=CARTESIAN_POINT('Ctrl Pts',(-195.228822752739,-6.17279568790409,
131.469154736412));
#214350=CARTESIAN_POINT('Ctrl Pts',(-195.507270376552,-2.77723672809589,
136.357045912194));
#214351=CARTESIAN_POINT('Ctrl Pts',(-195.785718000365,3.17046710927626,
136.142290565968));
#214352=CARTESIAN_POINT('Ctrl Pts',(-196.064165624178,6.20466655915177,
131.022238369536));
#214353=CARTESIAN_POINT('Ctrl Pts',(-196.342613247991,3.5370805559797,125.701967162963));
#214354=CARTESIAN_POINT('Ctrl Pts',(-196.621060871803,-2.38090968214636,
125.070546275391));
#214355=CARTESIAN_POINT('Ctrl Pts',(-196.899508495616,-6.11096023628406,
129.708220655875));
#214356=CARTESIAN_POINT('Ctrl Pts',(-197.177956119429,-4.22533687028115,
135.353194111738));
#214357=CARTESIAN_POINT('Ctrl Pts',(-197.456403743242,1.54316466032852,
136.818011809327));
#214358=CARTESIAN_POINT('Ctrl Pts',(-197.734851367055,5.89357325588093,
132.75657784488));
#214359=CARTESIAN_POINT('Ctrl Pts',(-198.013298990868,4.82807594633875,
126.901151619645));
#214360=CARTESIAN_POINT('Ctrl Pts',(-198.291746614681,-0.674187293266194,
124.632583781138));
#214361=CARTESIAN_POINT('Ctrl Pts',(-198.570194238494,-5.55690534624021,
128.035577347248));
#214362=CARTESIAN_POINT('Ctrl Pts',(-198.848641862306,-5.33309885593691,
133.982947476197));
#214363=CARTESIAN_POINT('Ctrl Pts',(-199.12708948612,-0.2084350533912,137.009351564664));
#214364=CARTESIAN_POINT('Ctrl Pts',(-199.405537109932,5.10777038060287,
134.333672103408));
#214365=CARTESIAN_POINT('Ctrl Pts',(-199.683984733745,5.7301843632779,128.414727803113));
#214366=CARTESIAN_POINT('Ctrl Pts',(-199.962432357558,1.08683885116959,
124.691739319248));
#214367=CARTESIAN_POINT('Ctrl Pts',(-200.240879981371,-4.5552584701342,
126.585951190383));
#214368=CARTESIAN_POINT('Ctrl Pts',(-200.519327605184,-6.01129579413245,
132.356675244344));
#214369=CARTESIAN_POINT('Ctrl Pts',(-200.797775228997,-1.94324595144814,
136.700897991079));
#214370=CARTESIAN_POINT('Ctrl Pts',(-201.076222852809,3.91055198777426,
135.626490953421));
#214371=CARTESIAN_POINT('Ctrl Pts',(-201.354670476623,6.17074369131775,
130.120781711275));
#214372=CARTESIAN_POINT('Ctrl Pts',(-201.633118100435,2.76032340012831,
125.243248089324));
#214373=CARTESIAN_POINT('Ctrl Pts',(-201.911565724248,-3.18669924648382,
125.476105205376));
#214374=CARTESIAN_POINT('Ctrl Pts',(-202.190013348061,-6.20530096449064,
130.605368745483));
#214375=CARTESIAN_POINT('Ctrl Pts',(-202.468460971874,-3.52153424193529,
135.91749609474));
#214376=CARTESIAN_POINT('Ctrl Pts',(-202.746908595687,2.39835041244635,
136.530901731028));
#214377=CARTESIAN_POINT('Ctrl Pts',(-203.0253562195,6.11426820372151,131.881895841131));
#214378=CARTESIAN_POINT('Ctrl Pts',(-203.303803843313,4.21147221438356,
126.242687721299));
#214379=CARTESIAN_POINT('Ctrl Pts',(-203.582251467125,-1.56146099811728,
124.795434143027));
#214380=CARTESIAN_POINT('Ctrl Pts',(-203.860699090939,-5.89948783495869,
128.870090442477));
#214381=CARTESIAN_POINT('Ctrl Pts',(-204.139146714752,-4.81617355747646,
134.722246538484));
#214382=CARTESIAN_POINT('Ctrl Pts',(-204.417594338564,0.69296893616836,
136.974056872534));
#214383=CARTESIAN_POINT('Ctrl Pts',(-204.696041962377,5.56530683088876,
133.556217754686));
#214384=CARTESIAN_POINT('Ctrl Pts',(-204.97448958619,5.32339962837619,127.60955636352));
#214385=CARTESIAN_POINT('Ctrl Pts',(-205.252937210003,0.18954822991528,
124.598764006957));
#214386=CARTESIAN_POINT('Ctrl Pts',(-205.531384833816,-5.11848873189165,
127.290611775294));
#214387=CARTESIAN_POINT('Ctrl Pts',(-205.809832457629,-5.72288460116635,
133.211423073505));
#214388=CARTESIAN_POINT('Ctrl Pts',(-206.088280081441,-1.06822910042401,
136.920261566246));
#214389=CARTESIAN_POINT('Ctrl Pts',(-206.366727705255,4.56807675771487,
135.00888586552));
#214390=CARTESIAN_POINT('Ctrl Pts',(-206.645175329067,6.00654323846982,
129.233756864401));
#214391=CARTESIAN_POINT('Ctrl Pts',(-206.92362295288,1.92528991902147,124.901935984182));
#214392=CARTESIAN_POINT('Ctrl Pts',(-207.202070576693,-3.92521078036628,
125.994154992568));
#214393=CARTESIAN_POINT('Ctrl Pts',(-207.480518200506,-6.16863452980439,
131.506717978718));
#214394=CARTESIAN_POINT('Ctrl Pts',(-207.758965824319,-2.74338450090264,
136.373848862034));
#214395=CARTESIAN_POINT('Ctrl Pts',(-208.037413448132,3.20290186254569,
136.12289213331));
#214396=CARTESIAN_POINT('Ctrl Pts',(-208.315861071945,6.20587788476857,
130.984464766326));
#214397=CARTESIAN_POINT('Ctrl Pts',(-208.594308695758,3.50595530487857,
125.680530485208));
#214398=CARTESIAN_POINT('Ctrl Pts',(-208.872756319571,-2.41576892475653,
125.085145782709));
#214399=CARTESIAN_POINT('Ctrl Pts',(-209.151203943383,-6.11751952941318,
129.745440114266));
#214400=CARTESIAN_POINT('Ctrl Pts',(-209.429651567197,-4.19756854398286,
135.378830657213));
#214401=CARTESIAN_POINT('Ctrl Pts',(-209.708099191009,1.57974287074426,
136.808506709009));
#214402=CARTESIAN_POINT('Ctrl Pts',(-209.986546814822,5.90534776198698,
132.720665821612));
#214403=CARTESIAN_POINT('Ctrl Pts',(-210.264994438635,4.80422655224024,
126.87183406841));
#214404=CARTESIAN_POINT('Ctrl Pts',(-210.543442062448,-0.711744159500396,
124.63680209928));
#214405=CARTESIAN_POINT('Ctrl Pts',(-210.821889686261,-5.57365675929581,
128.06945510647));
#214406=CARTESIAN_POINT('Ctrl Pts',(-211.100337310074,-5.31365108556781,
134.015352670796));
#214407=CARTESIAN_POINT('Ctrl Pts',(-211.378784933887,-0.170659650490228,
137.010505403884));
#214408=CARTESIAN_POINT('Ctrl Pts',(-211.657232557699,5.12915966620077,
134.302514265376));
#214409=CARTESIAN_POINT('Ctrl Pts',(-211.935680181513,5.71553182303293,
128.379890818834));
#214410=CARTESIAN_POINT('Ctrl Pts',(-212.214127805325,1.04960945375051,
124.685236675394));
#214411=CARTESIAN_POINT('Ctrl Pts',(-212.492575429138,-4.58085272725645,
126.613758498985));
#214412=CARTESIAN_POINT('Ctrl Pts',(-212.771023052951,-6.00173503901134,
132.393238947258));
#214413=CARTESIAN_POINT('Ctrl Pts',(-213.049470676764,-1.90731605097184,
136.712617831564));
#214414=CARTESIAN_POINT('Ctrl Pts',(-213.327918300577,3.93983321034183,
135.602596970618));
#214415=CARTESIAN_POINT('Ctrl Pts',(-213.60636592439,6.16646822290386,130.083231308093));
#214416=CARTESIAN_POINT('Ctrl Pts',(-213.884813548203,2.72642018733693,
125.226548251849));
#214417=CARTESIAN_POINT('Ctrl Pts',(-214.163261172015,-3.21907480736146,
125.495602268416));
#214418=CARTESIAN_POINT('Ctrl Pts',(-214.441708795829,-6.20639731464204,
130.643145860587));
#214419=CARTESIAN_POINT('Ctrl Pts',(-214.720156419641,-3.49034388913101,
135.938837938644));
#214420=CARTESIAN_POINT('Ctrl Pts',(-214.998604043455,2.43316505771265,
136.516196191791));
#214421=CARTESIAN_POINT('Ctrl Pts',(-215.277051667267,6.12071418324004,
131.844656590906));
#214422=CARTESIAN_POINT('Ctrl Pts',(-215.55549929108,4.18362598788043,126.217135811804));
#214423=CARTESIAN_POINT('Ctrl Pts',(-215.833946914893,-1.59801010884951,
124.805050530808));
#214424=CARTESIAN_POINT('Ctrl Pts',(-216.112394538706,-5.91115298268039,
128.90603813695));
#214425=CARTESIAN_POINT('Ctrl Pts',(-216.390842162519,-4.79223504130557,
134.75149136457));
#214426=CARTESIAN_POINT('Ctrl Pts',(-216.669289786332,0.730512789332353,
136.969724263749));
#214427=CARTESIAN_POINT('Ctrl Pts',(-216.947737410145,5.5819550541073,133.522289166845));
#214428=CARTESIAN_POINT('Ctrl Pts',(-217.226185033957,5.3038533178224,127.577210511344));
#214429=CARTESIAN_POINT('Ctrl Pts',(-217.50463265777,0.151769490097695,
124.597725148413));
#214430=CARTESIAN_POINT('Ctrl Pts',(-217.783080281583,-5.13978308467467,
127.321834570635));
#214431=CARTESIAN_POINT('Ctrl Pts',(-218.061527905396,-5.70812609699421,
133.24621529913));
#214432=CARTESIAN_POINT('Ctrl Pts',(-218.339975529209,-1.03098008363786,
136.9266508665));
#214433=CARTESIAN_POINT('Ctrl Pts',(-218.618423153022,4.59358626040416,
134.981000785606));
#214434=CARTESIAN_POINT('Ctrl Pts',(-218.896870776835,5.99687124029931,
129.197222430498));
#214435=CARTESIAN_POINT('Ctrl Pts',(-219.175318400648,1.88932451380644,
124.890325556239));
#214436=CARTESIAN_POINT('Ctrl Pts',(-219.45376602446,-3.95441914224089,
126.018137986666));
#214437=CARTESIAN_POINT('Ctrl Pts',(-219.732213648274,-6.16424479068368,
131.544255194914));
#214438=CARTESIAN_POINT('Ctrl Pts',(-220.010661272086,-2.70943061658779,
136.390445432439));
#214439=CARTESIAN_POINT('Ctrl Pts',(-220.289108895899,3.23521793110825,
136.103296620509));
#214440=CARTESIAN_POINT('Ctrl Pts',(-220.567556519712,6.20685924929812,
130.94668448929));
#214441=CARTESIAN_POINT('Ctrl Pts',(-220.846004143525,3.47470013931478,
125.659283672863));
#214442=CARTESIAN_POINT('Ctrl Pts',(-221.124451767337,-2.45053865016082,
125.099957217636));
#214443=CARTESIAN_POINT('Ctrl Pts',(-221.402899391151,-6.12385213560643,
129.782698811345));
#214444=CARTESIAN_POINT('Ctrl Pts',(-221.681347014963,-4.16964467523852,
135.404297694017));
#214445=CARTESIAN_POINT('Ctrl Pts',(-221.959794638777,1.61626254320698,
136.79877912285));
#214446=CARTESIAN_POINT('Ctrl Pts',(-222.238242262589,5.91690344326002,
132.684682788949));
#214447=CARTESIAN_POINT('Ctrl Pts',(-222.516689886402,4.7801991357601,126.842662238393));
#214448=CARTESIAN_POINT('Ctrl Pts',(-222.795137510215,-0.749274651793031,
124.64124895857));
#214449=CARTESIAN_POINT('Ctrl Pts',(-223.073585134028,-5.59020163845046,
128.103434208622));
#214450=CARTESIAN_POINT('Ctrl Pts',(-223.352032757841,-5.29400641590365,
134.047638880903));
#214451=CARTESIAN_POINT('Ctrl Pts',(-223.630480381654,-0.132877923733138,
137.011429272127));
#214452=CARTESIAN_POINT('Ctrl Pts',(-223.908928005467,5.15035888890098,
134.271226801972));
#214453=CARTESIAN_POINT('Ctrl Pts',(-224.187375629279,5.70066749165438,
128.345143674176));
#214454=CARTESIAN_POINT('Ctrl Pts',(-224.465823253093,1.01234116266713,
124.678960777928));
#214455=CARTESIAN_POINT('Ctrl Pts',(-224.744270876905,-4.60627723919628,
126.641721091889));
#214456=CARTESIAN_POINT('Ctrl Pts',(-225.022718500718,-5.99195188739136,
132.4297437737));
#214457=CARTESIAN_POINT('Ctrl Pts',(-225.301166124531,-1.87131547419729,
136.724118739406));
#214458=CARTESIAN_POINT('Ctrl Pts',(-225.579613748344,3.96896844094108,
135.578525187401));
#214459=CARTESIAN_POINT('Ctrl Pts',(-225.858061372157,6.16196425374224,
130.045707626623));
#214460=CARTESIAN_POINT('Ctrl Pts',(-226.13650899597,2.69241594604283,125.210055102262));
#214461=CARTESIAN_POINT('Ctrl Pts',(-226.414956619783,-3.25133108423828,
125.515296049447));
#214462=CARTESIAN_POINT('Ctrl Pts',(-226.693404243596,-6.20726368445854,
130.680928949564));
#214463=CARTESIAN_POINT('Ctrl Pts',(-226.971851867408,-3.45902420035033,
135.959989522602));
#214464=CARTESIAN_POINT('Ctrl Pts',(-227.250299491222,2.46788954115291,
136.501278998386));
#214465=CARTESIAN_POINT('Ctrl Pts',(-227.528747115034,6.12693335744362,
131.80737879213));
#214466=CARTESIAN_POINT('Ctrl Pts',(-227.807194738847,4.15562473557794,
126.191753883612));
#214467=CARTESIAN_POINT('Ctrl Pts',(-228.08564236266,-1.63450000472891,
124.81488922523));
#214468=CARTESIAN_POINT('Ctrl Pts',(-228.364089986473,-5.9225990904546,
128.942056174461));
#214469=CARTESIAN_POINT('Ctrl Pts',(-228.642537610286,-4.76811894710285,
134.780589928275));
#214470=CARTESIAN_POINT('Ctrl Pts',(-228.920985234099,0.768029573076269,
136.965163195147));
#214471=CARTESIAN_POINT('Ctrl Pts',(-229.199432857912,5.59839643592858,
133.48825986516));
#214472=CARTESIAN_POINT('Ctrl Pts',(-229.477880481725,5.28411047103341,
127.544984242401));
#214473=CARTESIAN_POINT('Ctrl Pts',(-229.756328105537,0.11398512640586,
124.59691627903));
#214474=CARTESIAN_POINT('Ctrl Pts',(-230.03477572935,-5.16088698090536,
127.353186412258));
#214475=CARTESIAN_POINT('Ctrl Pts',(-230.313223353163,-5.69315607611037,
133.280917040931));
#214476=CARTESIAN_POINT('Ctrl Pts',(-230.591670976976,-0.993692863505588,
136.932813303039));
#214477=CARTESIAN_POINT('Ctrl Pts',(-230.870118600789,4.6189255460653,134.952960938754));
#214478=CARTESIAN_POINT('Ctrl Pts',(-231.148566224602,5.98697702585963,
129.160747549691));
#214479=CARTESIAN_POINT('Ctrl Pts',(-231.427013848415,1.85328909897679,
124.878934275042));
#214480=CARTESIAN_POINT('Ctrl Pts',(-231.705461472227,-3.98348097165998,
126.042298336002));
#214481=CARTESIAN_POINT('Ctrl Pts',(-231.983909096041,-6.15962663320533,
131.581764994044));
#214482=CARTESIAN_POINT('Ctrl Pts',(-232.262356719853,-2.6753763333251,
136.406835008417));
#214483=CARTESIAN_POINT('Ctrl Pts',(-232.540804343666,3.26741411748112,
136.083504753687));
#214484=CARTESIAN_POINT('Ctrl Pts',(-232.819251967479,6.20761061637562,
130.90889893839));
#214485=CARTESIAN_POINT('Ctrl Pts',(-233.097699591292,3.44331621745904,
125.638227513236));
#214486=CARTESIAN_POINT('Ctrl Pts',(-233.376147215105,-2.48521756995422,
125.114980031328));
#214487=CARTESIAN_POINT('Ctrl Pts',(-233.654594838918,-6.12995782020675,
129.819995366479));
#214488=CARTESIAN_POINT('Ctrl Pts',(-233.933042462731,-4.14156629877734,
135.429594278462));
#214489=CARTESIAN_POINT('Ctrl Pts',(-234.211490086544,1.65272232446679,
136.788829411307));
#214490=CARTESIAN_POINT('Ctrl Pts',(-234.489937710357,5.92823987150001,
132.648630080257));
#214491=CARTESIAN_POINT('Ctrl Pts',(-234.768385334169,4.75599458724306,
126.813637210565));
#214492=CARTESIAN_POINT('Ctrl Pts',(-235.046832957982,-0.786777379437916,
124.64592419423));
#214493=CARTESIAN_POINT('Ctrl Pts',(-235.325280581795,-5.6065393706272,
128.137513394595));
#214494=CARTESIAN_POINT('Ctrl Pts',(-235.603728205608,-5.27416557488518,
134.079804910139));
#214495=CARTESIAN_POINT('Ctrl Pts',(-235.882175829421,-0.0950912731361558,
137.012123135159));
#214496=CARTESIAN_POINT('Ctrl Pts',(-236.160623453234,5.17136726315852,
134.239810872567));
#214497=CARTESIAN_POINT('Ctrl Pts',(-236.439071077047,5.68559191994549,
128.310487656705));
#214498=CARTESIAN_POINT('Ctrl Pts',(-236.71751870086,0.975035358909668,
124.672911859406));
#214499=CARTESIAN_POINT('Ctrl Pts',(-236.995966324673,-4.63153106383903,
126.669837932931));
#214500=CARTESIAN_POINT('Ctrl Pts',(-237.274413948486,-5.98194670179065,
132.466188370973));
#214501=CARTESIAN_POINT('Ctrl Pts',(-237.552861572298,-1.83524555513966,
136.735400288432));
#214502=CARTESIAN_POINT('Ctrl Pts',(-237.831309196112,3.99795659995517,
135.554276495761));
#214503=CARTESIAN_POINT('Ctrl Pts',(-238.109756819924,6.15723195072914,
130.008212057319));
#214504=CARTESIAN_POINT('Ctrl Pts',(-238.388204443737,2.65831193628575,
125.193769251723));
#214505=CARTESIAN_POINT('Ctrl Pts',(-238.66665206755,-3.28346688184612,
125.535185818711));
#214506=CARTESIAN_POINT('Ctrl Pts',(-238.945099691363,-6.20790004183648,
130.718716612347));
#214507=CARTESIAN_POINT('Ctrl Pts',(-239.223547315176,-3.42757633615586,
135.980950062836));
#214508=CARTESIAN_POINT('Ctrl Pts',(-239.501994938989,2.50252257603867,
136.486150703575));
#214509=CARTESIAN_POINT('Ctrl Pts',(-239.780442562802,6.13292549587844,
131.770063826148));
#214510=CARTESIAN_POINT('Ctrl Pts',(-240.058890186614,4.12746949507249,
126.166542877259));
#214511=CARTESIAN_POINT('Ctrl Pts',(-240.337337810428,-1.67092933361012,
124.824949861719));
#214512=CARTESIAN_POINT('Ctrl Pts',(-240.61578543424,-5.93382573414137,
128.978143220346));
#214513=CARTESIAN_POINT('Ctrl Pts',(-240.894233058053,-4.74382616849909,
134.80954115134));
#214514=CARTESIAN_POINT('Ctrl Pts',(-241.172680681866,0.805517897201924,
136.960373835741));
#214515=CARTESIAN_POINT('Ctrl Pts',(-241.451128305679,5.6146303671111,133.454131110603));
#214516=CARTESIAN_POINT('Ctrl Pts',(-241.729575929492,5.26417181958768,
127.512878750849));
#214517=CARTESIAN_POINT('Ctrl Pts',(-242.008023553305,0.0761965389532375,
124.596337428779));
#214518=CARTESIAN_POINT('Ctrl Pts',(-242.286471177117,-5.18179963857104,
127.384666138411));
#214519=CARTESIAN_POINT('Ctrl Pts',(-242.564918800931,-5.67797509323448,
133.315527013022));
#214520=CARTESIAN_POINT('Ctrl Pts',(-242.843366424743,-0.956368821719198,
136.938748647509));
#214521=CARTESIAN_POINT('Ctrl Pts',(-243.121814048556,4.64409367574132,
134.924767363992));
#214522=CARTESIAN_POINT('Ctrl Pts',(-243.400261672369,5.9768609617849,129.124333573571));
#214523=CARTESIAN_POINT('Ctrl Pts',(-243.678709296182,1.81718500983798,
124.867762562695));
#214524=CARTESIAN_POINT('Ctrl Pts',(-243.957156919995,-4.01239519172672,
126.066635145309));
#214525=CARTESIAN_POINT('Ctrl Pts',(-244.235604543808,-6.15478022849689,
131.619245986169));
#214526=CARTESIAN_POINT('Ctrl Pts',(-244.514052167621,-2.64122291300849,
136.423016982646));
#214527=CARTESIAN_POINT('Ctrl Pts',(-244.792499791433,3.29948922862226,
136.063517266237));
#214528=CARTESIAN_POINT('Ctrl Pts',(-245.070947415247,6.20813195815889,
130.871109513785));
#214529=CARTESIAN_POINT('Ctrl Pts',(-245.349395039059,3.41180470225455,
125.617362786572));
#214530=CARTESIAN_POINT('Ctrl Pts',(-245.627842662872,-2.51980439909662,
125.13021366711));
#214531=CARTESIAN_POINT('Ctrl Pts',(-245.906290286685,-6.13583635696575,
129.857328397629));
#214532=CARTESIAN_POINT('Ctrl Pts',(-246.184737910498,-4.1133344550539,
135.454719473173));
#214533=CARTESIAN_POINT('Ctrl Pts',(-246.463185534311,1.68912086349306,
136.778657943074));
#214534=CARTESIAN_POINT('Ctrl Pts',(-246.741633158124,5.93935662663147,
132.612509031482));
#214535=CARTESIAN_POINT('Ctrl Pts',(-247.020080781937,4.73161380359756,
126.784760060463));
#214536=CARTESIAN_POINT('Ctrl Pts',(-247.29852840575,-0.824250952757648,
124.650827633015));
#214537=CARTESIAN_POINT('Ctrl Pts',(-247.576976029562,-5.62266935042617,
128.171691401572));
#214538=CARTESIAN_POINT('Ctrl Pts',(-247.855423653376,-5.25412929772145,
134.111849566585));
#214539=CARTESIAN_POINT('Ctrl Pts',(-248.133871277188,-0.0573010988966442,
137.012586967267));
#214540=CARTESIAN_POINT('Ctrl Pts',(-248.412318901001,5.19218401050035,
134.208267641291));
#214541=CARTESIAN_POINT('Ctrl Pts',(-248.690766524814,5.67030566653712,
128.275924050614));
#214542=CARTESIAN_POINT('Ctrl Pts',(-248.969214148627,0.937693424858449,
124.667090143972));
#214543=CARTESIAN_POINT('Ctrl Pts',(-249.24766177244,-4.65661326539506,
126.698107980232));
#214544=CARTESIAN_POINT('Ctrl Pts',(-249.526109396252,-5.97171985295489,
132.502571388608));
#214545=CARTESIAN_POINT('Ctrl Pts',(-249.804557020066,-1.79910763038337,
136.746462060605));
#214546=CARTESIAN_POINT('Ctrl Pts',(-250.083004643878,4.02679661321771,
135.52985179424));
#214547=CARTESIAN_POINT('Ctrl Pts',(-250.361452267692,6.15227148922063,
129.970745989595));
#214548=CARTESIAN_POINT('Ctrl Pts',(-250.639899891504,2.62410942180459,
125.177691303707));
#214549=CARTESIAN_POINT('Ctrl Pts',(-250.918347515317,-3.31548100938434,
125.555270839195));
#214550=CARTESIAN_POINT('Ctrl Pts',(-251.19679513913,-6.20830636318893,
130.756507448682));
#214551=CARTESIAN_POINT('Ctrl Pts',(-251.475242762943,-3.39600146187203,
136.001718782677));
#214552=CARTESIAN_POINT('Ctrl Pts',(-251.753690386756,2.53706287905323,
136.47081186788));
#214553=CARTESIAN_POINT('Ctrl Pts',(-252.032138010569,6.13869037645988,
131.732713075798));
#214554=CARTESIAN_POINT('Ctrl Pts',(-252.310585634382,4.09916130974965,
126.141503726722));
#214555=CARTESIAN_POINT('Ctrl Pts',(-252.589033258195,-1.70729674574642,
124.835232067896));
#214556=CARTESIAN_POINT('Ctrl Pts',(-252.867480882007,-5.94483249743877,
129.014297936587));
#214557=CARTESIAN_POINT('Ctrl Pts',(-253.14592850582,-4.71935760622846,
134.838343962485));
#214558=CARTESIAN_POINT('Ctrl Pts',(-253.424376129633,0.842976373616159,
136.955356360136));
#214559=CARTESIAN_POINT('Ctrl Pts',(-253.702823753446,5.63065624411703,
133.419904173236));
#214560=CARTESIAN_POINT('Ctrl Pts',(-253.981271377259,5.24403810606461,
127.480895216153));
#214561=CARTESIAN_POINT('Ctrl Pts',(-254.259719001072,0.0384051209378723,
124.595988638398));
#214562=CARTESIAN_POINT('Ctrl Pts',(-254.538166624885,-5.20252026939218,
127.416272546179));
#214563=CARTESIAN_POINT('Ctrl Pts',(-254.816614248698,-5.66258373611722,
133.350044001689));
#214564=CARTESIAN_POINT('Ctrl Pts',(-255.095061872511,-0.919009293725241,
136.944456550123));
#214565=CARTESIAN_POINT('Ctrl Pts',(-255.373509496324,4.6690896269236,134.896421351226));
#214566=CARTESIAN_POINT('Ctrl Pts',(-255.651957120136,5.96652359266914,
129.087981388513));
#214567=CARTESIAN_POINT('Ctrl Pts',(-255.93040474395,1.78101326373629,124.856811707331));
#214568=CARTESIAN_POINT('Ctrl Pts',(-256.208852367762,-4.04116012583712,
126.091145862189));
#214569=CARTESIAN_POINT('Ctrl Pts',(-256.487299991575,-6.14970689884083,
131.656699899059));
#214570=CARTESIAN_POINT('Ctrl Pts',(-256.765747615388,-2.60696946356087,
136.438984870644));
#214571=CARTESIAN_POINT('Ctrl Pts',(-257.044195239201,3.33143800190474,
136.043346010603));
#214572=CARTESIAN_POINT('Ctrl Pts',(-257.322642863014,6.2084309480058,130.833296634437));
#214573=CARTESIAN_POINT('Ctrl Pts',(-257.601090486826,3.38015223603414,
125.596729883064));
#214574=CARTESIAN_POINT('Ctrl Pts',(-257.87953811064,-2.5542704291637,125.145582755354));
#214575=CARTESIAN_POINT('Ctrl Pts',(-258.157985734452,-6.14153931545366,
129.894837769574));
#214576=CARTESIAN_POINT('Ctrl Pts',(-258.436433358265,-4.08485240479644,
135.479405634932));
#214577=CARTESIAN_POINT('Ctrl Pts',(-258.714880982078,1.72527217059264,
136.768768758555));
#214578=CARTESIAN_POINT('Ctrl Pts',(-258.993328605892,5.95060195420752,
132.575369498931));
#214579=CARTESIAN_POINT('Ctrl Pts',(-259.271776229703,4.70639920604184,
126.75783223591));
#214580=CARTESIAN_POINT('Ctrl Pts',(-259.550223853517,-0.860449444711704,
124.652528659269));
#214581=CARTESIAN_POINT('Ctrl Pts',(-259.82867147733,-5.64095031490746,
128.212697490595));
#214582=CARTESIAN_POINT('Ctrl Pts',(-260.060711163841,-5.29799179572588,
133.142936715762));
#214583=CARTESIAN_POINT('Ctrl Pts',(-260.246372125917,-2.62679689981868,
135.594171577488));
#214584=CARTESIAN_POINT('Ctrl Pts',(-260.339217213388,-0.889986900407246,
136.05080276614));
#214585=CARTESIAN_POINT('Ctrl Pts',(-260.385654363559,-0.0148419801173944,
136.053268468065));
#214586=CARTESIAN_POINT('Ctrl Pts',(209.997106195361,2.85369542052185,134.803838223542));
#214587=CARTESIAN_POINT('Ctrl Pts',(209.950688331758,3.52024512455777,134.328247120061));
#214588=CARTESIAN_POINT('Ctrl Pts',(209.857862530854,4.598911638141,133.039517383424));
#214589=CARTESIAN_POINT('Ctrl Pts',(209.672220855345,5.31158968331849,129.722011776094));
#214590=CARTESIAN_POINT('Ctrl Pts',(209.440181168834,2.90445768035623,125.771581499823));
#214591=CARTESIAN_POINT('Ctrl Pts',(209.161733545021,-2.67328939945229,
125.640965885288));
#214592=CARTESIAN_POINT('Ctrl Pts',(208.883285921209,-5.78445646322271,
130.262241799363));
#214593=CARTESIAN_POINT('Ctrl Pts',(208.604838297395,-3.58517659481558,
135.378114005881));
#214594=CARTESIAN_POINT('Ctrl Pts',(208.326390673583,1.91144119617671,136.292814641374));
#214595=CARTESIAN_POINT('Ctrl Pts',(208.04794304977,5.65009034124608,132.162897902674));
#214596=CARTESIAN_POINT('Ctrl Pts',(207.769495425957,4.19734896093999,126.785079177362));
#214597=CARTESIAN_POINT('Ctrl Pts',(207.491047802144,-1.1129569716493,125.100504449821));
#214598=CARTESIAN_POINT('Ctrl Pts',(207.212600178331,-5.4002948496084,128.657642803108));
#214599=CARTESIAN_POINT('Ctrl Pts',(206.934152554519,-4.72513942780656,
134.187431620732));
#214600=CARTESIAN_POINT('Ctrl Pts',(206.655704930705,0.292248586550605,
136.608384944684));
#214601=CARTESIAN_POINT('Ctrl Pts',(206.377257306892,5.04104249491135,133.695701483205));
#214602=CARTESIAN_POINT('Ctrl Pts',(206.09880968308,5.15738153042831,128.12602865207));
#214603=CARTESIAN_POINT('Ctrl Pts',(205.820362059267,0.534329935251406,
125.017605890956));
#214604=CARTESIAN_POINT('Ctrl Pts',(205.541914435454,-4.57974002364783,
127.226931288585));
#214605=CARTESIAN_POINT('Ctrl Pts',(205.263466811641,-5.48525514562618,
132.723737743954));
#214606=CARTESIAN_POINT('Ctrl Pts',(204.985019187828,-1.35008742798131,
136.456731302353));
#214607=CARTESIAN_POINT('Ctrl Pts',(204.706571564015,4.02574397595362,134.995471850294));
#214608=CARTESIAN_POINT('Ctrl Pts',(204.428123940202,5.70211370766606,129.682786179275));
#214609=CARTESIAN_POINT('Ctrl Pts',(204.149676316389,2.13851930815143,125.40077248911));
#214610=CARTESIAN_POINT('Ctrl Pts',(203.871228692576,-3.39026975841633,
126.084392381055));
#214611=CARTESIAN_POINT('Ctrl Pts',(203.592781068764,-5.8035665963141,131.105432460946));
#214612=CARTESIAN_POINT('Ctrl Pts',(203.314333444951,-2.88366922283368,
135.849802245147));
#214613=CARTESIAN_POINT('Ctrl Pts',(203.035885821138,2.68617927581077,135.957657646429));
#214614=CARTESIAN_POINT('Ctrl Pts',(202.757438197325,5.78756025537181,131.329884836407));
#214615=CARTESIAN_POINT('Ctrl Pts',(202.478990573512,3.57045609392238,126.219180939555));
#214616=CARTESIAN_POINT('Ctrl Pts',(202.200542949699,-1.92772278905516,
125.322033169903));
#214617=CARTESIAN_POINT('Ctrl Pts',(201.922095325886,-5.6544186046078,129.462876497226));
#214618=CARTESIAN_POINT('Ctrl Pts',(201.643647702073,-4.18497995558374,
134.836478196445));
#214619=CARTESIAN_POINT('Ctrl Pts',(201.36520007826,1.13025082464198,136.504760820331));
#214620=CARTESIAN_POINT('Ctrl Pts',(201.086752454448,5.4068363130258,132.934654138033));
#214621=CARTESIAN_POINT('Ctrl Pts',(200.808304830635,4.71480336828096,127.406911780982));
#214622=CARTESIAN_POINT('Ctrl Pts',(200.529857206822,-0.309903540913717,
125.001258930184));
#214623=CARTESIAN_POINT('Ctrl Pts',(200.251409583008,-5.04982423566531,
127.928373032793));
#214624=CARTESIAN_POINT('Ctrl Pts',(199.972961959197,-5.14920315545485,
133.498379226012));
#214625=CARTESIAN_POINT('Ctrl Pts',(199.694514335383,-0.516715927947778,
136.59271392819));
#214626=CARTESIAN_POINT('Ctrl Pts',(199.416066711571,4.59060799437092,134.367834714685));
#214627=CARTESIAN_POINT('Ctrl Pts',(199.137619087757,5.47938743352869,128.868296891315));
#214628=CARTESIAN_POINT('Ctrl Pts',(198.859171463945,1.33287750423228,125.147907050397));
#214629=CARTESIAN_POINT('Ctrl Pts',(198.580723840131,-4.03848173676817,
126.625521704588));
#214630=CARTESIAN_POINT('Ctrl Pts',(198.302276216319,-5.69867355247927,
131.943285172176));
#214631=CARTESIAN_POINT('Ctrl Pts',(198.023828592506,-2.12206276914206,
136.214432613634));
#214632=CARTESIAN_POINT('Ctrl Pts',(197.745380968693,3.4046200305072,135.513988187415));
#214633=CARTESIAN_POINT('Ctrl Pts',(197.46693334488,5.80262334705539,130.485626102603));
#214634=CARTESIAN_POINT('Ctrl Pts',(197.188485721067,2.86829928156946,125.750165465994));
#214635=CARTESIAN_POINT('Ctrl Pts',(196.910038097254,-2.70185169946893,
125.65926326252));
#214636=CARTESIAN_POINT('Ctrl Pts',(196.631590473441,-5.78913296148881,
130.296454176353));
#214637=CARTESIAN_POINT('Ctrl Pts',(196.353142849628,-3.5564838467683,135.400386297052));
#214638=CARTESIAN_POINT('Ctrl Pts',(196.074695225815,1.94440017923737,136.280795346639));
#214639=CARTESIAN_POINT('Ctrl Pts',(195.796247602003,5.6584754297534,132.128628418917));
#214640=CARTESIAN_POINT('Ctrl Pts',(195.51779997819,4.17268819221861,126.759524075833));
#214641=CARTESIAN_POINT('Ctrl Pts',(195.239352354377,-1.14759564681435,
125.107426913349));
#214642=CARTESIAN_POINT('Ctrl Pts',(194.960904730564,-5.41329514958902,
128.690533514357));
#214643=CARTESIAN_POINT('Ctrl Pts',(194.682457106751,-4.70444086406131,
134.216143957018));
#214644=CARTESIAN_POINT('Ctrl Pts',(194.404009482938,0.327564750825761,
136.606492185605));
#214645=CARTESIAN_POINT('Ctrl Pts',(194.125561859125,5.0585543621317,133.664964953048));
#214646=CARTESIAN_POINT('Ctrl Pts',(193.847114235312,5.14097963875765,128.094682084473));
#214647=CARTESIAN_POINT('Ctrl Pts',(193.568666611499,0.499095778182989,
125.014461412655));
#214648=CARTESIAN_POINT('Ctrl Pts',(193.290218987687,-4.60143272035756,
127.254875257849));
#214649=CARTESIAN_POINT('Ctrl Pts',(193.011771363874,-5.4734693413749,132.757092746623));
#214650=CARTESIAN_POINT('Ctrl Pts',(192.733323740061,-1.31565503151135,
136.464844805061));
#214651=CARTESIAN_POINT('Ctrl Pts',(192.454876116248,4.05118197898966,134.970888425217));
#214652=CARTESIAN_POINT('Ctrl Pts',(192.176428492435,5.69518066204141,129.648096536341));
#214653=CARTESIAN_POINT('Ctrl Pts',(191.897980868622,2.1055865417199,125.38785485147));
#214654=CARTESIAN_POINT('Ctrl Pts',(191.619533244809,-3.4189387468211,126.105117354624));
#214655=CARTESIAN_POINT('Ctrl Pts',(191.341085620997,-5.80162635147675,
131.140754845624));
#214656=CARTESIAN_POINT('Ctrl Pts',(191.062637997183,-2.85290276432908,
135.867262474811));
#214657=CARTESIAN_POINT('Ctrl Pts',(190.784190373371,2.71749909118881,135.941210633695));
#214658=CARTESIAN_POINT('Ctrl Pts',(190.505742749557,5.79065203911519,131.29464457683));
#214659=CARTESIAN_POINT('Ctrl Pts',(190.227295125745,3.54247865217362,126.197531513104));
#214660=CARTESIAN_POINT('Ctrl Pts',(189.948847501932,-1.96105955641241,
125.333869340265));
#214661=CARTESIAN_POINT('Ctrl Pts',(189.670399878119,-5.66247983574075,
129.497321402909));
#214662=CARTESIAN_POINT('Ctrl Pts',(189.391952254306,-4.160357773542,134.861878651407));
#214663=CARTESIAN_POINT('Ctrl Pts',(189.113504630493,1.16492983776554,136.497775047581));
#214664=CARTESIAN_POINT('Ctrl Pts',(188.83505700668,5.41970383815296,132.901701721328));
#214665=CARTESIAN_POINT('Ctrl Pts',(188.556609382867,4.69403477852959,127.378274381527));
#214666=CARTESIAN_POINT('Ctrl Pts',(188.278161759054,-0.345222926215044,
125.003252919028));
#214667=CARTESIAN_POINT('Ctrl Pts',(187.999714135242,-5.0672376268456,127.959166031618));
#214668=CARTESIAN_POINT('Ctrl Pts',(187.721266511429,-5.13270849672517,
133.529673973213));
#214669=CARTESIAN_POINT('Ctrl Pts',(187.442818887616,-0.48147100486422,
136.595752079925));
#214670=CARTESIAN_POINT('Ctrl Pts',(187.164371263803,4.61221481930072,134.339824357932));
#214671=CARTESIAN_POINT('Ctrl Pts',(186.88592363999,5.4675005437485,128.834978175547));
#214672=CARTESIAN_POINT('Ctrl Pts',(186.607476016177,1.29842037074208,125.139898247696));
#214673=CARTESIAN_POINT('Ctrl Pts',(186.329028392364,-4.06384469161484,
126.650182513385));
#214674=CARTESIAN_POINT('Ctrl Pts',(186.050580768551,-5.69163501222784,
131.977953513933));
#214675=CARTESIAN_POINT('Ctrl Pts',(185.772133144738,-2.08909080843167,
136.227249975919));
#214676=CARTESIAN_POINT('Ctrl Pts',(185.493685520926,3.4332257905535,135.493176040453));
#214677=CARTESIAN_POINT('Ctrl Pts',(185.215237897112,5.80057561042411,130.450309792719));
#214678=CARTESIAN_POINT('Ctrl Pts',(184.9367902733,2.83747981818726,125.732798956676));
#214679=CARTESIAN_POINT('Ctrl Pts',(184.658342649487,-2.73312130836828,
125.675805527429));
#214680=CARTESIAN_POINT('Ctrl Pts',(184.379895025674,-5.79211747293216,
130.331703682172));
#214681=CARTESIAN_POINT('Ctrl Pts',(184.101447401861,-3.52844064054064,
135.421950469967));
#214682=CARTESIAN_POINT('Ctrl Pts',(183.822999778048,1.97770076659953,136.26885776521));
#214683=CARTESIAN_POINT('Ctrl Pts',(183.544552154236,5.66643178528845,132.094159137294));
#214684=CARTESIAN_POINT('Ctrl Pts',(183.266104530422,4.14798881387936,126.734198679909));
#214685=CARTESIAN_POINT('Ctrl Pts',(182.98765690661,-1.18225323696583,125.114518204765));
#214686=CARTESIAN_POINT('Ctrl Pts',(182.709209282797,-5.42606231932092,
128.72352494273));
#214687=CARTESIAN_POINT('Ctrl Pts',(182.430761658984,-4.68358520810093,
134.244718011395));
#214688=CARTESIAN_POINT('Ctrl Pts',(182.152314035171,0.362877903506298,
136.604390705933));
#214689=CARTESIAN_POINT('Ctrl Pts',(181.873866411358,5.07587394936235,133.634119096483));
#214690=CARTESIAN_POINT('Ctrl Pts',(181.595418787545,5.12438980598236,128.063437686296));
#214691=CARTESIAN_POINT('Ctrl Pts',(181.316971163732,0.463841771263853,
125.011530548415));
#214692=CARTESIAN_POINT('Ctrl Pts',(181.038523539919,-4.62295419131585,
127.282951248603));
#214693=CARTESIAN_POINT('Ctrl Pts',(180.760075916106,-5.46148109594396,
132.790375128456));
#214694=CARTESIAN_POINT('Ctrl Pts',(180.481628292294,-1.2811736815839,136.472748695004));
#214695=CARTESIAN_POINT('Ctrl Pts',(180.203180668481,4.07646975733793,134.946150534538));
#214696=CARTESIAN_POINT('Ctrl Pts',(179.924733044668,5.68803663588505,129.61344977806));
#214697=CARTESIAN_POINT('Ctrl Pts',(179.646285420855,2.07257572209157,125.37513790386));
#214698=CARTESIAN_POINT('Ctrl Pts',(179.367837797042,-3.44748102935117,
126.12601647128));
#214699=CARTESIAN_POINT('Ctrl Pts',(179.089390173229,-5.79947113363144,
131.176064759319));
#214700=CARTESIAN_POINT('Ctrl Pts',(178.810942549416,-2.82203058602,135.884535099843));
#214701=CARTESIAN_POINT('Ctrl Pts',(178.532494925603,2.74871820628535,135.924573271475));
#214702=CARTESIAN_POINT('Ctrl Pts',(178.254047301791,5.79352924936408,131.259386150458));
#214703=CARTESIAN_POINT('Ctrl Pts',(177.975599677977,3.51436994191561,126.176052793945));
#214704=CARTESIAN_POINT('Ctrl Pts',(177.697152054165,-1.99432365563702,
125.345908221933));
#214705=CARTESIAN_POINT('Ctrl Pts',(177.418704430351,-5.6703312417861,129.531814741282));
#214706=CARTESIAN_POINT('Ctrl Pts',(177.140256806539,-4.135581427815,134.887128753614));
#214707=CARTESIAN_POINT('Ctrl Pts',(176.861809182726,1.19956568393359,136.490578303229));
#214708=CARTESIAN_POINT('Ctrl Pts',(176.583361558913,5.43237053418876,132.868671586896));
#214709=CARTESIAN_POINT('Ctrl Pts',(176.3049139351,4.67309224957875,127.349763936946));
#214710=CARTESIAN_POINT('Ctrl Pts',(176.026466311287,-0.380529519146142,
125.005461870054));
#214711=CARTESIAN_POINT('Ctrl Pts',(175.748018687475,-5.08446324967622,
127.990064460173));
#214712=CARTESIAN_POINT('Ctrl Pts',(175.469571063661,-5.11602364359241,
133.560867732924));
#214713=CARTESIAN_POINT('Ctrl Pts',(175.191123439849,-0.446208240696769,
136.59857562952));
#214714=CARTESIAN_POINT('Ctrl Pts',(174.912675816035,4.63365073691483,134.311682993269));
#214715=CARTESIAN_POINT('Ctrl Pts',(174.634228192223,5.45541105372469,128.801732435971));
#214716=CARTESIAN_POINT('Ctrl Pts',(174.35578056841,1.26391512380778,125.132099343732));
#214717=CARTESIAN_POINT('Ctrl Pts',(174.077332944597,-4.089057059202,126.674997256779));
#214718=CARTESIAN_POINT('Ctrl Pts',(173.798885320784,-5.68438556634791,
132.012578367773));
#214719=CARTESIAN_POINT('Ctrl Pts',(173.520437696972,-2.0560414356932,136.239866391045));
#214720=CARTESIAN_POINT('Ctrl Pts',(173.241990073158,3.46170433115548,135.472190147709));
#214721=CARTESIAN_POINT('Ctrl Pts',(172.963542449346,5.79831293133042,130.41500660232));
#214722=CARTESIAN_POINT('Ctrl Pts',(172.685094825533,2.80655521094699,125.715620375941));
#214723=CARTESIAN_POINT('Ctrl Pts',(172.40664720172,-2.76428964045241,125.692537832834));
#214724=CARTESIAN_POINT('Ctrl Pts',(172.128199577907,-5.79488735533246,
130.366970702468));
#214725=CARTESIAN_POINT('Ctrl Pts',(171.849751954094,-3.50026668664755,
135.443343536393));
#214726=CARTESIAN_POINT('Ctrl Pts',(171.571304330281,2.01092806953244,136.256717694829));
#214727=CARTESIAN_POINT('Ctrl Pts',(171.292856706468,5.6741781691098,132.059642061713));
#214728=CARTESIAN_POINT('Ctrl Pts',(171.014409082656,4.12313573028927,126.709024105332));
#214729=CARTESIAN_POINT('Ctrl Pts',(170.735961458842,-1.21686701828875,
125.121820335384));
#214730=CARTESIAN_POINT('Ctrl Pts',(170.45751383503,-5.43862842431808,128.756593477234));
#214731=CARTESIAN_POINT('Ctrl Pts',(170.179066211217,-4.66255600016836,
134.273164582064));
#214732=CARTESIAN_POINT('Ctrl Pts',(169.900618587404,0.398177609612544,
136.602074304013));
#214733=CARTESIAN_POINT('Ctrl Pts',(169.62217096359,5.09300544821711,133.603168382178));
#214734=CARTESIAN_POINT('Ctrl Pts',(169.343723339778,5.10761008705837,128.032294854024));
#214735=CARTESIAN_POINT('Ctrl Pts',(169.065275715965,0.428570576517446,
125.008814339624));
#214736=CARTESIAN_POINT('Ctrl Pts',(168.786828092152,-4.64430435700642,
127.311157726477));
#214737=CARTESIAN_POINT('Ctrl Pts',(168.508380468339,-5.4492904733226,132.823583917792));
#214738=CARTESIAN_POINT('Ctrl Pts',(168.229932844526,-1.24664485729461,
136.480442540741));
#214739=CARTESIAN_POINT('Ctrl Pts',(167.951485220714,4.10160648060013,134.92125916831));
#214740=CARTESIAN_POINT('Ctrl Pts',(167.673037596901,5.6806818374394,129.578847149419));
#214741=CARTESIAN_POINT('Ctrl Pts',(167.394589973088,2.03948810240773,125.362622138095));
#214742=CARTESIAN_POINT('Ctrl Pts',(167.116142349275,-3.47589556420378,
126.147088945699));
#214743=CARTESIAN_POINT('Ctrl Pts',(166.837694725462,-5.79710101425052,
131.21136089938));
#214744=CARTESIAN_POINT('Ctrl Pts',(166.559247101649,-2.79105383632985,
135.901619477142));
#214745=CARTESIAN_POINT('Ctrl Pts',(166.280799477836,2.77983546661788,135.907746177893));
#214746=CARTESIAN_POINT('Ctrl Pts',(166.002351854023,5.79619177825601,131.224110862948));
#214747=CARTESIAN_POINT('Ctrl Pts',(165.72390423021,3.48613100538707,126.154745578436));
#214748=CARTESIAN_POINT('Ctrl Pts',(165.445456606397,-2.02751385446508,
125.358149368562));
#214749=CARTESIAN_POINT('Ctrl Pts',(165.167008982585,-5.67797253162207,
129.566355234311));
#214750=CARTESIAN_POINT('Ctrl Pts',(164.888561358772,-4.11065183659732,
134.912227567346));
#214751=CARTESIAN_POINT('Ctrl Pts',(164.610113734959,1.23415707975413,136.483170853989));
#214752=CARTESIAN_POINT('Ctrl Pts',(164.331666111146,5.44483593173667,132.835564958663));
#214753=CARTESIAN_POINT('Ctrl Pts',(164.053218487333,4.65197655747607,127.321381503715));
#214754=CARTESIAN_POINT('Ctrl Pts',(163.77477086352,-0.415822011415935,
125.007885701408));
#214755=CARTESIAN_POINT('Ctrl Pts',(163.496323239708,-5.10150046585131,
128.021067173507));
#214756=CARTESIAN_POINT('Ctrl Pts',(163.217875615894,-5.09914921432216,
133.591959349252));
#214757=CARTESIAN_POINT('Ctrl Pts',(162.939427992082,-0.41092894211879,
136.601184472346));
#214758=CARTESIAN_POINT('Ctrl Pts',(162.660980368268,4.65491495289691,134.283411663486));
#214759=CARTESIAN_POINT('Ctrl Pts',(162.382532744456,5.443119411438,128.768560904517));
#214760=CARTESIAN_POINT('Ctrl Pts',(162.104085120643,1.22936304203373,125.124510627495));
#214761=CARTESIAN_POINT('Ctrl Pts',(161.82563749683,-4.11411790527609,126.69996501525));
#214762=CARTESIAN_POINT('Ctrl Pts',(161.547189873017,-5.67692548347038,
132.04715845066));
#214763=CARTESIAN_POINT('Ctrl Pts',(161.268742249204,-2.02291587558315,
136.252281391507));
#214764=CARTESIAN_POINT('Ctrl Pts',(160.990294625391,3.49005459703047,135.451031286826));
#214765=CARTESIAN_POINT('Ctrl Pts',(160.711847001578,5.79583539361873,130.379717839577));
#214766=CARTESIAN_POINT('Ctrl Pts',(160.433399377766,2.77552660577121,125.698630360346));
#214767=CARTESIAN_POINT('Ctrl Pts',(160.154951753952,-2.79535554076737,
125.70945955871));
#214768=CARTESIAN_POINT('Ctrl Pts',(159.87650413014,-5.79744250605075,130.402253930408));
#214769=CARTESIAN_POINT('Ctrl Pts',(159.598056506327,-3.47196302908515,
135.4645647036));
#214770=CARTESIAN_POINT('Ctrl Pts',(159.319608882514,2.04408085678626,136.244375585352));
#214771=CARTESIAN_POINT('Ctrl Pts',(159.041161258701,5.68171429417248,132.025078471215));
#214772=CARTESIAN_POINT('Ctrl Pts',(158.762713634888,4.09812986238831,126.684001284956));
#214773=CARTESIAN_POINT('Ctrl Pts',(158.484266011075,-1.25143570815684,
125.129333034622));
#214774=CARTESIAN_POINT('Ctrl Pts',(158.205818387262,-5.450992998939,128.789737892503));
#214775=CARTESIAN_POINT('Ctrl Pts',(157.927370763449,-4.64135401950845,
134.301482614925));
#214776=CARTESIAN_POINT('Ctrl Pts',(157.648923139637,0.43346256110109,136.59954306568));
#214777=CARTESIAN_POINT('Ctrl Pts',(157.370475515823,5.10994822388206,133.572113957021));
#214778=CARTESIAN_POINT('Ctrl Pts',(157.092027892011,5.09064110376424,128.001254741669));
#214779=CARTESIAN_POINT('Ctrl Pts',(156.813580268198,0.39328350093061,125.006312886931));
#214780=CARTESIAN_POINT('Ctrl Pts',(156.535132644385,-4.66548242629113,
127.339493646268));
#214781=CARTESIAN_POINT('Ctrl Pts',(156.256685020572,-5.43689792523874,
132.856717884066));
#214782=CARTESIAN_POINT('Ctrl Pts',(155.978237396759,-1.21206983812162,
136.487926057176));
#214783=CARTESIAN_POINT('Ctrl Pts',(155.699789772946,4.12659121732586,134.896215248893));
#214784=CARTESIAN_POINT('Ctrl Pts',(155.421342149133,5.67311653923917,129.544289932631));
#214785=CARTESIAN_POINT('Ctrl Pts',(155.142894525321,2.0063249087422,125.350308017949));
#214786=CARTESIAN_POINT('Ctrl Pts',(154.864446901507,-3.50418129846815,
126.168333997033));
#214787=CARTESIAN_POINT('Ctrl Pts',(154.585999277695,-5.79451608115961,
131.246641957895));
#214788=CARTESIAN_POINT('Ctrl Pts',(154.307551653882,-2.75997366311328,
135.918514973638));
#214789=CARTESIAN_POINT('Ctrl Pts',(154.029104030069,2.81084971912495,135.890729976482));
#214790=CARTESIAN_POINT('Ctrl Pts',(153.750656406256,5.79863952713012,131.188820021437));
#214791=CARTESIAN_POINT('Ctrl Pts',(153.472208782443,3.457762888992,126.133610656121));
#214792=CARTESIAN_POINT('Ctrl Pts',(153.19376115863,-2.0606289230217,125.370592326552));
#214793=CARTESIAN_POINT('Ctrl Pts',(152.915313534817,-5.68540342209783,
129.600941602086));
#214794=CARTESIAN_POINT('Ctrl Pts',(152.636865911004,-4.08556992366409,
134.937174162558));
#214795=CARTESIAN_POINT('Ctrl Pts',(152.358418287191,1.26870274343019,136.475552974349));
#214796=CARTESIAN_POINT('Ctrl Pts',(152.079970663379,5.45709956888678,132.802383063404));
#214797=CARTESIAN_POINT('Ctrl Pts',(151.801523039566,4.63068848467127,127.293128133558));
#214798=CARTESIAN_POINT('Ctrl Pts',(151.523075415753,-0.451099095248245,
125.010524323271));
#214799=CARTESIAN_POINT('Ctrl Pts',(151.24462779194,-5.11834864405056,128.052173022803));
#214800=CARTESIAN_POINT('Ctrl Pts',(150.966180168127,-5.08208583420252,
133.622947670083));
#214801=CARTESIAN_POINT('Ctrl Pts',(150.687732544314,-0.375634416417742,
136.603578511732));
#214802=CARTESIAN_POINT('Ctrl Pts',(150.409284920501,4.67600667929353,134.255011416186));
#214803=CARTESIAN_POINT('Ctrl Pts',(150.130837296688,5.43062607235983,128.735464810371));
#214804=CARTESIAN_POINT('Ctrl Pts',(149.852389672876,1.19476540576009,125.117132380189));
#214805=CARTESIAN_POINT('Ctrl Pts',(149.573942049063,-4.13902630119825,
126.725084863609));
#214806=CARTESIAN_POINT('Ctrl Pts',(149.29549442525,-5.66925504003138,132.081692481218));
#214807=CARTESIAN_POINT('Ctrl Pts',(149.017046801437,-1.98971535558138,
136.264494517259));
#214808=CARTESIAN_POINT('Ctrl Pts',(148.738599177624,3.5182755376489,135.429700241853));
#214809=CARTESIAN_POINT('Ctrl Pts',(148.460151553811,5.79314308909515,130.344444812129));
#214810=CARTESIAN_POINT('Ctrl Pts',(148.181703929998,2.74439515243632,125.681829539465));
#214811=CARTESIAN_POINT('Ctrl Pts',(147.903256306185,-2.82631785815477,
125.726570078021));
#214812=CARTESIAN_POINT('Ctrl Pts',(147.624808682372,-5.79978283040501,
130.437552058559));
#214813=CARTESIAN_POINT('Ctrl Pts',(147.346361058559,-3.4435307166558,135.48561318523));
#214814=CARTESIAN_POINT('Ctrl Pts',(147.067913434747,2.07715789987228,136.23183189412));
#214815=CARTESIAN_POINT('Ctrl Pts',(146.789465810933,5.68903988122249,131.990469646568));
#214816=CARTESIAN_POINT('Ctrl Pts',(146.511018187121,4.07297213677825,126.65913114601));
#214817=CARTESIAN_POINT('Ctrl Pts',(146.232570563308,-1.2859580256146,125.137056024094));
#214818=CARTESIAN_POINT('Ctrl Pts',(145.954122939495,-5.46315558500969,
128.822956960357));
#214819=CARTESIAN_POINT('Ctrl Pts',(145.675675315682,-4.61998005176852,
134.329671060644));
#214820=CARTESIAN_POINT('Ctrl Pts',(145.397227691869,0.468731450475054,
136.596797084732));
#214821=CARTESIAN_POINT('Ctrl Pts',(145.118780068056,5.12670164853643,133.540956971746));
#214822=CARTESIAN_POINT('Ctrl Pts',(144.840332444244,5.07348348489189,127.970318499433));
#214823=CARTESIAN_POINT('Ctrl Pts',(144.56188482043,0.357981852079004,125.004026283029));
#214824=CARTESIAN_POINT('Ctrl Pts',(144.283437196618,-4.6864876144088,127.367957957979));
#214825=CARTESIAN_POINT('Ctrl Pts',(144.004989572805,-5.42430391090288,
132.889775799486));
#214826=CARTESIAN_POINT('Ctrl Pts',(143.726541948992,-1.17744990525502,
136.495198967004));
#214827=CARTESIAN_POINT('Ctrl Pts',(143.448094325179,4.15142304169647,134.871019704297));
#214828=CARTESIAN_POINT('Ctrl Pts',(143.169646701366,5.66534102161933,129.509779408224));
#214829=CARTESIAN_POINT('Ctrl Pts',(142.891199077553,1.9730873699693,125.338195999729));
#214830=CARTESIAN_POINT('Ctrl Pts',(142.61275145374,-3.53233718400576,126.189750838038));
#214831=CARTESIAN_POINT('Ctrl Pts',(142.334303829928,-5.79171643014443,
131.281906627513));
#214832=CARTESIAN_POINT('Ctrl Pts',(142.055856206114,-2.72879121805762,
135.935220963265));
#214833=CARTESIAN_POINT('Ctrl Pts',(141.777408582302,2.84175981456215,135.873525297782));
#214834=CARTESIAN_POINT('Ctrl Pts',(141.498960958489,5.80087240528401,131.153514933643));
#214835=CARTESIAN_POINT('Ctrl Pts',(141.220513334676,3.42926664392146,126.112648810165));
#214836=CARTESIAN_POINT('Ctrl Pts',(140.942065710863,-2.09366763421581,
125.383236634823));
#214837=CARTESIAN_POINT('Ctrl Pts',(140.66361808705,-5.69262363785895,129.635572562993));
#214838=CARTESIAN_POINT('Ctrl Pts',(140.385170463237,-4.06033661843482,
134.961967614844));
#214839=CARTESIAN_POINT('Ctrl Pts',(140.106722839424,1.30320139485961,136.467724946589));
#214840=CARTESIAN_POINT('Ctrl Pts',(139.828275215611,5.46916099120554,132.769127130691));
#214841=CARTESIAN_POINT('Ctrl Pts',(139.549827591798,4.60922882000175,127.26500487341));
#214842=CARTESIAN_POINT('Ctrl Pts',(139.271379967986,-0.486359463437733,
125.013377637868));
#214843=CARTESIAN_POINT('Ctrl Pts',(138.992932344173,-5.13500715995863,
128.083380855422));
#214844=CARTESIAN_POINT('Ctrl Pts',(138.71448472036,-5.06483413552331,133.653831547135));
#214845=CARTESIAN_POINT('Ctrl Pts',(138.436037096547,-0.340325971445257,
136.605757658967));
#214846=CARTESIAN_POINT('Ctrl Pts',(138.157589472734,4.69692513454305,134.226483303753));
#214847=CARTESIAN_POINT('Ctrl Pts',(137.879141848921,5.41793149943546,128.70244537992));
#214848=CARTESIAN_POINT('Ctrl Pts',(137.600694225109,1.16012349701482,125.109964875215));
#214849=CARTESIAN_POINT('Ctrl Pts',(137.322246601295,-4.16378132397874,
126.750355871033));
#214850=CARTESIAN_POINT('Ctrl Pts',(137.043798977483,-5.66137452026194,
132.116179179772));
#214851=CARTESIAN_POINT('Ctrl Pts',(136.765351353669,-1.95644110594549,
136.276505315742));
#214852=CARTESIAN_POINT('Ctrl Pts',(136.486903729857,3.54636610727348,135.408197803219));
#214853=CARTESIAN_POINT('Ctrl Pts',(136.208456106044,5.79023611752392,130.309188827029));
#214854=CARTESIAN_POINT('Ctrl Pts',(135.930008482231,2.71316200452982,125.665218535856));
#214855=CARTESIAN_POINT('Ctrl Pts',(135.651560858418,-2.85717544529452,
125.743868756725));
#214856=CARTESIAN_POINT('Ctrl Pts',(135.373113234605,-5.80190824167357,
130.472863778936));
#214857=CARTESIAN_POINT('Ctrl Pts',(135.094665610792,-3.41497080292952,
135.506488201326));
#214858=CARTESIAN_POINT('Ctrl Pts',(134.816217986979,2.11015797310843,136.219087085943));
#214859=CARTESIAN_POINT('Ctrl Pts',(134.537770363167,5.69615465880763,131.955816870215));
#214860=CARTESIAN_POINT('Ctrl Pts',(134.259322739353,4.04766348568775,126.634414610068));
#214861=CARTESIAN_POINT('Ctrl Pts',(133.980875115541,-1.32043269142476,
125.144989017623));
#214862=CARTESIAN_POINT('Ctrl Pts',(133.702427491728,-5.47511573184112,
128.856249449853));
#214863=CARTESIAN_POINT('Ctrl Pts',(133.423979867915,-4.59843488896879,
134.357728874689));
#214864=CARTESIAN_POINT('Ctrl Pts',(133.145532244102,0.503982970832797,
136.59383646292));
#214865=CARTESIAN_POINT('Ctrl Pts',(132.867084620289,5.14326510137581,133.509698580887));
#214866=CARTESIAN_POINT('Ctrl Pts',(132.588636996476,5.05613786622328,127.93948727367));
#214867=CARTESIAN_POINT('Ctrl Pts',(132.310189372663,0.322666938078297,
125.001954612649));
#214868=CARTESIAN_POINT('Ctrl Pts',(132.03174174885,-4.70731914300451,127.396549606854));
#214869=CARTESIAN_POINT('Ctrl Pts',(131.753294125038,-5.41150889699075,
132.92275643908));
#214870=CARTESIAN_POINT('Ctrl Pts',(131.474846501225,-1.14278634154918,
136.502261000723));
#214871=CARTESIAN_POINT('Ctrl Pts',(131.196398877412,4.17610103355955,134.845673468154));
#214872=CARTESIAN_POINT('Ctrl Pts',(130.917951253599,5.65735557270449,129.475316855001));
#214873=CARTESIAN_POINT('Ctrl Pts',(130.639503629786,1.93977671771839,125.326286532249));
#214874=CARTESIAN_POINT('Ctrl Pts',(130.361056005973,-3.56036217749005,
126.211338675105));
#214875=CARTESIAN_POINT('Ctrl Pts',(130.08260838216,-5.788702164947,131.317153601487));
#214876=CARTESIAN_POINT('Ctrl Pts',(129.804160758347,-2.69750765663984,
135.951736826975));
#214877=CARTESIAN_POINT('Ctrl Pts',(129.525713134534,2.87256460754407,135.856132779323));
#214878=CARTESIAN_POINT('Ctrl Pts',(129.247265510721,5.80289032997773,131.118196907806));
#214879=CARTESIAN_POINT('Ctrl Pts',(128.968817886909,3.40064332611445,126.091860817314));
#214880=CARTESIAN_POINT('Ctrl Pts',(128.690370263096,-2.12662876378584,
125.396081824838));
#214881=CARTESIAN_POINT('Ctrl Pts',(128.411922639283,-5.69963291135762,
129.670246833772));
#214882=CARTESIAN_POINT('Ctrl Pts',(128.13347501547,-4.03495285593914,134.986607005474));
#214883=CARTESIAN_POINT('Ctrl Pts',(127.855027391657,1.33765175568188,136.459687060782));
#214884=CARTESIAN_POINT('Ctrl Pts',(127.576579767844,5.48101975175251,132.73579839283));
#214885=CARTESIAN_POINT('Ctrl Pts',(127.298132144031,4.5875983586632,127.237012765392));
#214886=CARTESIAN_POINT('Ctrl Pts',(127.019684520218,-0.521601809398458,
125.016445539469));
#214887=CARTESIAN_POINT('Ctrl Pts',(126.741236896406,-5.15147539628782,
128.114689514947));
#214888=CARTESIAN_POINT('Ctrl Pts',(126.462789272592,-5.0473947575527,133.684609835992));
#214889=CARTESIAN_POINT('Ctrl Pts',(126.18434164878,-0.305004915568794,
136.607721833301));
#214890=CARTESIAN_POINT('Ctrl Pts',(125.905894024967,4.71766954350447,134.197828383304));
#214891=CARTESIAN_POINT('Ctrl Pts',(125.627446401154,5.40503616306688,128.669503836711));
#214892=CARTESIAN_POINT('Ctrl Pts',(125.348998777341,1.12543859946687,125.10300837817));
#214893=CARTESIAN_POINT('Ctrl Pts',(125.070551153528,-4.18838205631096,
126.775777101093));
#214894=CARTESIAN_POINT('Ctrl Pts',(124.792103529715,-5.65328421617778,
132.150617268407));
#214895=CARTESIAN_POINT('Ctrl Pts',(124.513655905902,-1.9230943596648,136.288313341892));
#214896=CARTESIAN_POINT('Ctrl Pts',(124.23520828209,3.57432526499779,135.386524767704));
#214897=CARTESIAN_POINT('Ctrl Pts',(123.956760658277,5.78711458662396,130.273951190703));
#214898=CARTESIAN_POINT('Ctrl Pts',(123.678313034464,2.68182831940755,125.648797965047));
#214899=CARTESIAN_POINT('Ctrl Pts',(123.399865410651,-2.88792715874745,
125.761354953818));
#214900=CARTESIAN_POINT('Ctrl Pts',(123.121417786838,-5.8038186610986,130.50818778305));
#214901=CARTESIAN_POINT('Ctrl Pts',(122.842970163025,-3.38628434620416,
135.527188978355));
#214902=CARTESIAN_POINT('Ctrl Pts',(122.564522539212,2.1430798536649,136.206141633086));
#214903=CARTESIAN_POINT('Ctrl Pts',(122.286074915399,5.703058363287,131.921121426228));
#214904=CARTESIAN_POINT('Ctrl Pts',(122.007627291586,4.02220484693838,126.609852593007));
#214905=CARTESIAN_POINT('Ctrl Pts',(121.729179667773,-1.35485842811595,
125.153131721247));
#214906=CARTESIAN_POINT('Ctrl Pts',(121.450732043961,-5.48687299624567,
128.889614127324));
#214907=CARTESIAN_POINT('Ctrl Pts',(121.172284420148,-4.57671932947311,
134.385655017367));
#214908=CARTESIAN_POINT('Ctrl Pts',(120.893836796335,0.539215815916097,
136.59066130995));
#214909=CARTESIAN_POINT('Ctrl Pts',(120.615389172522,5.15963796863542,133.478339942736));
#214910=CARTESIAN_POINT('Ctrl Pts',(120.336941548709,5.0386048905067,127.908762206842));
#214911=CARTESIAN_POINT('Ctrl Pts',(120.058493924896,0.287340067535411,
125.000097952557));
#214912=CARTESIAN_POINT('Ctrl Pts',(119.780046301083,-4.72797624015824,
127.42526753342));
#214913=CARTESIAN_POINT('Ctrl Pts',(119.50159867727,-5.39851335762638,132.955658580739));
#214914=CARTESIAN_POINT('Ctrl Pts',(119.223151053457,-1.10808043147514,
136.509111896649));
#214915=CARTESIAN_POINT('Ctrl Pts',(118.944703429644,4.20062427846316,134.820177479675));
#214916=CARTESIAN_POINT('Ctrl Pts',(118.666255805832,5.64916048839838,129.440903549983));
#214917=CARTESIAN_POINT('Ctrl Pts',(118.387808182019,1.90639418632776,125.314580056818));
#214918=CARTESIAN_POINT('Ctrl Pts',(118.109360558206,-3.58825524044456,
126.23309670829));
#214919=CARTESIAN_POINT('Ctrl Pts',(117.830912934393,-5.785473397262,131.352381573729));
#214920=CARTESIAN_POINT('Ctrl Pts',(117.55246531058,-2.66612413808396,135.968061952766));
#214921=CARTESIAN_POINT('Ctrl Pts',(117.274017686767,2.9032629565882,135.838553065588));
#214922=CARTESIAN_POINT('Ctrl Pts',(116.995570062954,5.80469322643624,131.082867252651));
#214923=CARTESIAN_POINT('Ctrl Pts',(116.717122439142,3.37189399621826,126.071247447876));
#214924=CARTESIAN_POINT('Ctrl Pts',(116.438674815328,-2.15951109034483,
125.409127420613));
#214925=CARTESIAN_POINT('Ctrl Pts',(116.160227191516,-5.70643098286277,
129.704963129555));
#214926=CARTESIAN_POINT('Ctrl Pts',(115.881779567703,-4.00941957678149,
135.011091421425));
#214927=CARTESIAN_POINT('Ctrl Pts',(115.60333194389,1.37205254932662,136.451439614773));
#214928=CARTESIAN_POINT('Ctrl Pts',(115.324884320077,5.49267541109693,132.702398084833));
#214929=CARTESIAN_POINT('Ctrl Pts',(115.046436696264,4.56579790218037,127.20915284676));
#214930=CARTESIAN_POINT('Ctrl Pts',(114.767989072451,-0.556824827212187,
125.019727914392));
#214931=CARTESIAN_POINT('Ctrl Pts',(114.489541448638,-5.1677527428018,128.146097841224));
#214932=CARTESIAN_POINT('Ctrl Pts',(114.211093824825,-5.02976834651319,
133.715281396157));
#214933=CARTESIAN_POINT('Ctrl Pts',(113.932646201012,-0.269672557622912,
136.60947096195));
#214934=CARTESIAN_POINT('Ctrl Pts',(113.6541985772,4.73823913748602,134.169047716661));
#214935=CARTESIAN_POINT('Ctrl Pts',(113.375750953387,5.39194054109557,128.636641401405));
#214936=CARTESIAN_POINT('Ctrl Pts',(113.097303329574,1.09071199837779,125.09626314683));
#214937=CARTESIAN_POINT('Ctrl Pts',(112.818855705761,-4.21282758660586,
126.801347611796));
#214938=CARTESIAN_POINT('Ctrl Pts',(112.540408081948,-5.64498442756793,
132.185005471008));
#214939=CARTESIAN_POINT('Ctrl Pts',(112.261960458135,-1.8896763524154,136.299918158156));
#214940=CARTESIAN_POINT('Ctrl Pts',(111.983512834322,3.60215197478495,135.364681938413));
#214941=CARTESIAN_POINT('Ctrl Pts',(111.705065210509,5.78377861206482,130.238733208892));
#214942=CARTESIAN_POINT('Ctrl Pts',(111.426617586696,2.65039525815055,125.632568435507));
#214943=CARTESIAN_POINT('Ctrl Pts',(111.148169962883,-2.91857185899754,
125.77902802134));
#214944=CARTESIAN_POINT('Ctrl Pts',(110.869722339071,-5.80551401788879,
130.543522761958));
#214945=CARTESIAN_POINT('Ctrl Pts',(110.591274715258,-3.35747240946702,
135.547714749242));
#214946=CARTESIAN_POINT('Ctrl Pts',(110.312827091445,2.17592232160915,136.192996015246));
#214947=CARTESIAN_POINT('Ctrl Pts',(110.034379467632,5.70975073884148,131.886384600257));
#214948=CARTESIAN_POINT('Ctrl Pts',(109.755931843819,3.99659716390926,126.585446004984));
#214949=CARTESIAN_POINT('Ctrl Pts',(109.477484220006,-1.38923396002991,
125.161483833236));
#214950=CARTESIAN_POINT('Ctrl Pts',(109.199036596193,-5.49842694255352,
128.923049756431));
#214951=CARTESIAN_POINT('Ctrl Pts',(108.92058897238,-4.55483417795961,134.413448453863));
#214952=CARTESIAN_POINT('Ctrl Pts',(108.642141348568,0.57442868015902,136.58727174348));
#214953=CARTESIAN_POINT('Ctrl Pts',(108.363693724754,5.17581964361271,133.446882219296));
#214954=CARTESIAN_POINT('Ctrl Pts',(108.085246100942,5.02088520743284,127.878144437479));
#214955=CARTESIAN_POINT('Ctrl Pts',(107.806798477129,0.252002549500665,
124.998456371553));
#214956=CARTESIAN_POINT('Ctrl Pts',(107.528350853316,-4.74845814041369,
127.454110673523));
#214957=CARTESIAN_POINT('Ctrl Pts',(107.249903229503,-5.38531777436419,
132.988481005259));
#214958=CARTESIAN_POINT('Ctrl Pts',(106.97145560569,-1.07333346107335,136.515751400918));
#214959=CARTESIAN_POINT('Ctrl Pts',(106.693007981877,4.22499186768932,134.794532683627));
#214960=CARTESIAN_POINT('Ctrl Pts',(106.414560358064,5.64075607237289,129.406540768369));
#214961=CARTESIAN_POINT('Ctrl Pts',(106.136112734251,1.87294101279944,125.303077007226));
#214962=CARTESIAN_POINT('Ctrl Pts',(105.857665110439,-3.61601533928142,
126.25502413134));
#214963=CARTESIAN_POINT('Ctrl Pts',(105.579217486626,-5.78203024673271,
131.387589238853));
#214964=CARTESIAN_POINT('Ctrl Pts',(105.300769862813,-2.63464182531766,
135.984195735705));
#214965=CARTESIAN_POINT('Ctrl Pts',(105.022322239,2.93385372415587,135.820786808));
#214966=CARTESIAN_POINT('Ctrl Pts',(104.743874615187,5.80628102785255,131.047527277329));
#214967=CARTESIAN_POINT('Ctrl Pts',(104.465426991374,3.34301971955009,126.050809465687));
#214968=CARTESIAN_POINT('Ctrl Pts',(104.186979367561,-2.19231339542621,
125.422372938737));
#214969=CARTESIAN_POINT('Ctrl Pts',(103.908531743748,-5.71301760046937,
129.739720163916));
#214970=CARTESIAN_POINT('Ctrl Pts',(103.630084119935,-3.98373772710686,
135.03541995542));
#214971=CARTESIAN_POINT('Ctrl Pts',(103.351636496123,1.40640250105958,136.442982914176));
#214972=CARTESIAN_POINT('Ctrl Pts',(103.07318887231,5.50412753733405,132.66892744436));
#214973=CARTESIAN_POINT('Ctrl Pts',(102.794741248497,4.54382825837723,127.181426149873));
#214974=CARTESIAN_POINT('Ctrl Pts',(102.516293624684,-0.592027211677165,
125.023224641008));
#214975=CARTESIAN_POINT('Ctrl Pts',(102.237846000871,-5.18383859633749,
128.177604670405));
#214976=CARTESIAN_POINT('Ctrl Pts',(101.959398377058,-5.01195555555783,
133.745845091081));
#214977=CARTESIAN_POINT('Ctrl Pts',(101.680950753245,-0.234330206861215,
136.611004980102));
#214978=CARTESIAN_POINT('Ctrl Pts',(101.402503129432,4.75863315427373,134.140142370299));
#214979=CARTESIAN_POINT('Ctrl Pts',(101.124055505619,5.37864511878468,128.603859291732));
#214980=CARTESIAN_POINT('Ctrl Pts',(100.845607881807,1.05594498055446,125.089729431141));
#214981=CARTESIAN_POINT('Ctrl Pts',(100.567160257994,-4.23711700902531,
126.827066455619));
#214982=CARTESIAN_POINT('Ctrl Pts',(100.288712634181,-5.63647546198416,
132.219342513305));
#214983=CARTESIAN_POINT('Ctrl Pts',(100.010265010368,-1.85618832251382,
136.311319334515));
#214984=CARTESIAN_POINT('Ctrl Pts',(99.731817386555,3.62984520550588,135.342670124737));
#214985=CARTESIAN_POINT('Ctrl Pts',(99.4533697627421,5.78022831746224,130.203536186614));
#214986=CARTESIAN_POINT('Ctrl Pts',(99.1749221389292,2.61886398552269,125.616530548629));
#214987=CARTESIAN_POINT('Ctrl Pts',(98.8964745151164,-2.9491084104941,125.796887304409));
#214988=CARTESIAN_POINT('Ctrl Pts',(98.6180268913035,-5.80699424922206,
130.578867406308));
#214989=CARTESIAN_POINT('Ctrl Pts',(98.3395792674906,-3.32853606035512,
135.568064753397));
#214990=CARTESIAN_POINT('Ctrl Pts',(98.0611316436778,2.20868415995158,136.179650719541));
#214991=CARTESIAN_POINT('Ctrl Pts',(97.7826840198649,5.71623153748262,131.851607679491));
#214992=CARTESIAN_POINT('Ctrl Pts',(97.5042363960519,3.97084138550236,126.561195750394));
#214993=CARTESIAN_POINT('Ctrl Pts',(97.2257887722391,-1.42355801336861,
125.170045044101));
#214994=CARTESIAN_POINT('Ctrl Pts',(96.9473411484261,-5.50977714262889,
128.956555098203));
#214995=CARTESIAN_POINT('Ctrl Pts',(96.6688935246133,-4.53278024539068,
134.441108154283));
#214996=CARTESIAN_POINT('Ctrl Pts',(96.3904459008004,0.609620258735999,
136.583667889112));
#214997=CARTESIAN_POINT('Ctrl Pts',(96.1119982769875,5.19180952668969,133.415326576248));
#214998=CARTESIAN_POINT('Ctrl Pts',(95.8335506531746,5.00297947361121,127.847635100131));
#214999=CARTESIAN_POINT('Ctrl Pts',(95.5551030293618,0.216655693418756,
124.997029930466));
#215000=CARTESIAN_POINT('Ctrl Pts',(95.2766554055487,-4.7687640848064,127.483077958369));
#215001=CARTESIAN_POINT('Ctrl Pts',(94.9982077817361,-5.37192263617151,
133.021222496396));
#215002=CARTESIAN_POINT('Ctrl Pts',(94.7197601579228,-1.03854671790542,
136.522179267501));
#215003=CARTESIAN_POINT('Ctrl Pts',(94.4413125341102,4.24920289828813,134.768740030285));
#215004=CARTESIAN_POINT('Ctrl Pts',(94.1628649102971,5.63214263605674,129.372229783482));
#215005=CARTESIAN_POINT('Ctrl Pts',(93.8844172864844,1.83941843675322,125.29177780972));
#215006=CARTESIAN_POINT('Ctrl Pts',(93.6059696626714,-3.6436414453401,126.277120131727));
#215007=CARTESIAN_POINT('Ctrl Pts',(93.3275220388585,-5.77837284094635,
131.422775292226));
#215008=CARTESIAN_POINT('Ctrl Pts',(93.0490744150458,-2.60306188492951,
136.000137577949));
#215009=CARTESIAN_POINT('Ctrl Pts',(92.7706267912327,2.96433577669487,135.802834664895));
#215010=CARTESIAN_POINT('Ctrl Pts',(92.49217916742,5.80765367539012,131.012178291378));
#215011=CARTESIAN_POINT('Ctrl Pts',(92.213731543607,3.31402156605677,126.030547628085));
#215012=CARTESIAN_POINT('Ctrl Pts',(91.9352839197941,-2.22503446352861,
125.435817888395));
#215013=CARTESIAN_POINT('Ctrl Pts',(91.6568362959812,-5.71939252010779,
129.77451664892));
#215014=CARTESIAN_POINT('Ctrl Pts',(91.3783886721684,-3.95790825856573,
135.059591705955));
#215015=CARTESIAN_POINT('Ctrl Pts',(91.0999410483554,1.44070033803066,136.434317272356));
#215016=CARTESIAN_POINT('Ctrl Pts',(90.8214934245425,5.51537570610103,132.635387711677));
#215017=CARTESIAN_POINT('Ctrl Pts',(90.5430458007297,4.52169024134706,127.153833702157));
#215018=CARTESIAN_POINT('Ctrl Pts',(90.2645981769166,-0.627207658356129,
125.026935589742));
#215019=CARTESIAN_POINT('Ctrl Pts',(89.9861505531037,-5.19973236082766,
128.209208834995));
#215020=CARTESIAN_POINT('Ctrl Pts',(89.707702929291,-4.99395704474619,133.776299788217));
#215021=CARTESIAN_POINT('Ctrl Pts',(89.4292553054779,-0.198979172907652,
136.61232383091));
#215022=CARTESIAN_POINT('Ctrl Pts',(89.1508076816652,4.77885083815996,134.111113415317));
#215023=CARTESIAN_POINT('Ctrl Pts',(88.8723600578521,5.36515038880097,128.571158722445));
#215024=CARTESIAN_POINT('Ctrl Pts',(88.5939124340396,1.02113883430145,125.08340747321));
#215025=CARTESIAN_POINT('Ctrl Pts',(88.3154648102263,-4.26124942351577,
126.85293267954));
#215026=CARTESIAN_POINT('Ctrl Pts',(88.0370171864138,-5.62775763472933,
132.253627122929));
#215027=CARTESIAN_POINT('Ctrl Pts',(87.7585695626006,-1.82263151087143,
136.322516448493));
#215028=CARTESIAN_POINT('Ctrl Pts',(87.480121938788,3.65740393097785,135.320490142334));
#215029=CARTESIAN_POINT('Ctrl Pts',(87.2016743149749,5.77646383437373,130.168361428106));
#215030=CARTESIAN_POINT('Ctrl Pts',(86.9232266911622,2.58723566992664,125.600684898703));
#215031=CARTESIAN_POINT('Ctrl Pts',(86.6447790673492,-2.97953568169397,
125.814932141244));
#215032=CARTESIAN_POINT('Ctrl Pts',(86.3663314435363,-5.80825930024783,
130.614220406392));
#215033=CARTESIAN_POINT('Ctrl Pts',(86.0878838197235,-3.29947637111547,
135.588238236744));
#215034=CARTESIAN_POINT('Ctrl Pts',(85.8094361959104,2.24136415469026,136.166106240484));
#215035=CARTESIAN_POINT('Ctrl Pts',(85.5309885720977,5.72250051906197,131.816791952599));
#215036=CARTESIAN_POINT('Ctrl Pts',(85.2525409482847,3.94493846610766,126.537102727838));
#215037=CARTESIAN_POINT('Ctrl Pts',(84.9740933244718,-1.45782931624159,
125.178815036599));
#215038=CARTESIAN_POINT('Ctrl Pts',(84.6956457006588,-5.52092317588609,
128.990128911089));
#215039=CARTESIAN_POINT('Ctrl Pts',(84.417198076846,-4.51055834898274,134.468633093685));
#215040=CARTESIAN_POINT('Ctrl Pts',(84.138750453033,0.644789247610192,136.579849880389));
#215041=CARTESIAN_POINT('Ctrl Pts',(83.8603028292202,5.20760702535536,133.383674182895));
#215042=CARTESIAN_POINT('Ctrl Pts',(83.5818552054073,4.98488835254533,127.817235325336));
#215043=CARTESIAN_POINT('Ctrl Pts',(83.3034075815944,0.181300809080568,
124.995818682153));
#215044=CARTESIAN_POINT('Ctrl Pts',(83.0249599577814,-4.78889332089225,
127.512168314565));
#215045=CARTESIAN_POINT('Ctrl Pts',(82.7465123339688,-5.35832843941005,
133.053881840899));
#215046=CARTESIAN_POINT('Ctrl Pts',(82.4680647101557,-1.00372149100682,
136.528395258211));
#215047=CARTESIAN_POINT('Ctrl Pts',(82.1896170863428,4.27325647311088,134.742800475408));
#215048=CARTESIAN_POINT('Ctrl Pts',(81.91116946253,5.62332049862395,129.337971866731));
#215049=CARTESIAN_POINT('Ctrl Pts',(81.632721838717,1.80582770038043,125.280682882997));
#215050=CARTESIAN_POINT('Ctrl Pts',(81.3542742149043,-3.67113253492515,
126.299383890674));
#215051=CARTESIAN_POINT('Ctrl Pts',(81.0758265910913,-5.77450131542928,
131.457938430015));
#215052=CARTESIAN_POINT('Ctrl Pts',(80.7973789672785,-2.57138548712596,
136.015886888767));
#215053=CARTESIAN_POINT('Ctrl Pts',(80.5189313434656,2.99470798468153,135.784697301496));
#215054=CARTESIAN_POINT('Ctrl Pts',(80.2404837196526,5.80881111818491,130.976821604667));
#215055=CARTESIAN_POINT('Ctrl Pts',(79.9620360958398,3.2849006102757,126.010462685879));
#215056=CARTESIAN_POINT('Ctrl Pts',(79.6835884720269,-2.25767308216064,
125.449461771377));
#215057=CARTESIAN_POINT('Ctrl Pts',(79.4051408482139,-5.72555550555307,
129.809351295171));
#215058=CARTESIAN_POINT('Ctrl Pts',(79.1266932244012,-3.93193212827854,
135.083605777338));
#215059=CARTESIAN_POINT('Ctrl Pts',(78.8482456005881,1.47494478932078,136.425443010422));
#215060=CARTESIAN_POINT('Ctrl Pts',(78.5697979767754,5.526419500593,132.601780129612));
#215061=CARTESIAN_POINT('Ctrl Pts',(78.2913503529625,4.49938467142216,127.126376526057));
#215062=CARTESIAN_POINT('Ctrl Pts',(78.0129027291494,-0.662364863624755,
125.030860623086));
#215063=CARTESIAN_POINT('Ctrl Pts',(77.7344551053368,-5.21543344732299,
128.240909163888));
#215064=CARTESIAN_POINT('Ctrl Pts',(77.4560074815235,-4.97577348101974,
133.806644359053));
#215065=CARTESIAN_POINT('Ctrl Pts',(77.1775598577108,-0.163620765707691,
136.613427465507));
#215066=CARTESIAN_POINT('Ctrl Pts',(76.8991122338979,4.79889143997102,134.081961927395));
#215067=CARTESIAN_POINT('Ctrl Pts',(76.620664610085,5.35145685119646,128.538540905275));
#215068=CARTESIAN_POINT('Ctrl Pts',(76.3422169862721,0.986294849373407,
125.077297507303));
#215069=CARTESIAN_POINT('Ctrl Pts',(76.0637693624593,-4.28522393584178,
126.878945325076));
#215070=CARTESIAN_POINT('Ctrl Pts',(75.7853217386464,-5.61883126884571,
132.287858029448));
#215071=CARTESIAN_POINT('Ctrl Pts',(75.5068741148335,-1.78900716094817,
136.333509085178));
#215072=CARTESIAN_POINT('Ctrl Pts',(75.2284264910206,3.68482713000219,135.298142813091));
#215073=CARTESIAN_POINT('Ctrl Pts',(74.9499788672077,5.77248530229349,130.133210236781));
#215074=CARTESIAN_POINT('Ctrl Pts',(74.6715312433948,2.55551148336137,125.585032072894));
#215075=CARTESIAN_POINT('Ctrl Pts',(74.3930836195819,-3.0098525451033,125.833161863185));
#215076=CARTESIAN_POINT('Ctrl Pts',(74.1146359957691,-5.80930912408932,
130.649580452192));
#215077=CARTESIAN_POINT('Ctrl Pts',(73.8361883719562,-3.27029441856551,
135.608234451746));
#215078=CARTESIAN_POINT('Ctrl Pts',(73.5577407481433,2.273961094856,136.152363079971));
#215079=CARTESIAN_POINT('Ctrl Pts',(73.2792931243304,5.72855745128013,131.781938709691));
#215080=CARTESIAN_POINT('Ctrl Pts',(73.0008455005175,3.91888936556733,126.513167830092));
#215081=CARTESIAN_POINT('Ctrl Pts',(72.7223978767045,-1.49204659871303,
125.187793485758));
#215082=CARTESIAN_POINT('Ctrl Pts',(72.4439502528918,-5.53186462930466,
129.023769950998));
#215083=CARTESIAN_POINT('Ctrl Pts',(72.1655026290786,-4.48816931217651,
134.496022252122));
#215084=CARTESIAN_POINT('Ctrl Pts',(71.8870550052659,0.679934343581693,
136.575817858786));
#215085=CARTESIAN_POINT('Ctrl Pts',(71.6086073814528,5.22321155422762,133.351926212129));
#215086=CARTESIAN_POINT('Ctrl Pts',(71.3301597576401,4.96661251460835,127.786946239566));
#215087=CARTESIAN_POINT('Ctrl Pts',(71.0517121338272,0.145939206574258,
124.994822671498));
#215088=CARTESIAN_POINT('Ctrl Pts',(70.7732645100143,-4.80884510277506,
127.541380664158));
#215089=CARTESIAN_POINT('Ctrl Pts',(70.4948168862015,-5.34453568781766,
133.086457828568));
#215090=CARTESIAN_POINT('Ctrl Pts',(70.2163692623885,-0.968859070839113,
136.534399142713));
#215091=CARTESIAN_POINT('Ctrl Pts',(69.9379216385757,4.29715170084345,134.716714980192));
#215092=CARTESIAN_POINT('Ctrl Pts',(69.6594740147628,5.61428998698222,129.303768287553));
#215093=CARTESIAN_POINT('Ctrl Pts',(69.3810263909498,1.77217004839796,125.269792638185));
#215094=CARTESIAN_POINT('Ctrl Pts',(69.102578767137,-3.69848758934425,126.321814583191));
#215095=CARTESIAN_POINT('Ctrl Pts',(68.8241311433241,-5.77041581364239,
131.493077349239));
#215096=CARTESIAN_POINT('Ctrl Pts',(68.5456835195112,-2.53961380568736,
136.031443084562));
#215097=CARTESIAN_POINT('Ctrl Pts',(68.2672358956983,3.02496922266262,135.76637538989));
#215098=CARTESIAN_POINT('Ctrl Pts',(67.9887882718854,5.80975331334755,130.94145852735));
#215099=CARTESIAN_POINT('Ctrl Pts',(67.7103406480725,3.25565793129432,125.990555383323));
#215100=CARTESIAN_POINT('Ctrl Pts',(67.4318930242597,-2.29022804188655,
125.463304082106));
#215101=CARTESIAN_POINT('Ctrl Pts',(67.1534454004468,-5.73150632843341,
129.844222811859));
#215102=CARTESIAN_POINT('Ctrl Pts',(66.8749977766338,-3.90581029880048,
135.107461279717));
#215103=CARTESIAN_POINT('Ctrl Pts',(66.5965501528209,1.50913458598933,136.416360457212));
#215104=CARTESIAN_POINT('Ctrl Pts',(66.3181025290079,5.53725851157817,132.568105943505));
#215105=CARTESIAN_POINT('Ctrl Pts',(66.0396549051952,4.47691237514338,127.09905563901));
#215106=CARTESIAN_POINT('Ctrl Pts',(65.7612072813823,-0.69749752471975,
125.034999595595));
#215107=CARTESIAN_POINT('Ctrl Pts',(65.4827596575694,-5.23094127401388,
128.272704482416));
#215108=CARTESIAN_POINT('Ctrl Pts',(65.2043120337565,-4.95740553817722,
133.836877679162));
#215109=CARTESIAN_POINT('Ctrl Pts',(64.9258644099437,-0.128256295479839,
136.614315842995));
#215110=CARTESIAN_POINT('Ctrl Pts',(64.6474167861306,4.81875421709505,134.05268898675));
#215111=CARTESIAN_POINT('Ctrl Pts',(64.3689691623179,5.33756501339024,128.506007048888));
#215112=CARTESIAN_POINT('Ctrl Pts',(64.0905215385049,0.951414316927145,
125.071399759827));
#215113=CARTESIAN_POINT('Ctrl Pts',(63.8120739146922,-4.30903965761881,
126.905103428319));
#215114=CARTESIAN_POINT('Ctrl Pts',(63.5336262908791,-5.60969669510319,
132.322033964426));
#215115=CARTESIAN_POINT('Ctrl Pts',(63.2551786670663,-1.75531651870651,
136.344296837232));
#215116=CARTESIAN_POINT('Ctrl Pts',(62.9767310432534,3.71211378640213,135.275628965096));
#215117=CARTESIAN_POINT('Ctrl Pts',(62.6982834194405,5.76829286864752,130.098083915181));
#215118=CARTESIAN_POINT('Ctrl Pts',(62.4198357956276,2.52369260137852,125.569572651222));
#215119=CARTESIAN_POINT('Ctrl Pts',(62.1413881718147,-3.04005787731984,
125.851575794724));
#215120=CARTESIAN_POINT('Ctrl Pts',(61.8629405480017,-5.81014368184488,
130.684946233427));
#215121=CARTESIAN_POINT('Ctrl Pts',(61.5844929241889,-3.24099128405306,
135.628052657436));
#215122=CARTESIAN_POINT('Ctrl Pts',(61.3060453003759,2.306473772557,136.138421747261));
#215123=CARTESIAN_POINT('Ctrl Pts',(61.0275976765631,5.73440210969521,131.747049242268));
#215124=CARTESIAN_POINT('Ctrl Pts',(60.7491500527502,3.89269504914048,126.489391944074));
#215125=CARTESIAN_POINT('Ctrl Pts',(60.4707024289374,-1.5262085928491,125.196980058879));
#215126=CARTESIAN_POINT('Ctrl Pts',(60.1922548051244,-5.54260109744501,
129.057476971348));
#215127=CARTESIAN_POINT('Ctrl Pts',(59.9138071813117,-4.46561396460588,
134.52327461468));
#215128=CARTESIAN_POINT('Ctrl Pts',(59.6353595574987,0.715054244335847,
136.571571973714));
#215129=CARTESIAN_POINT('Ctrl Pts',(59.3569119336859,5.23862253507484,133.320083840384));
#215130=CARTESIAN_POINT('Ctrl Pts',(59.0784643098728,4.94815263701827,127.756768965196));
#215131=CARTESIAN_POINT('Ctrl Pts',(58.80001668606,0.110572196236736,124.994041935407));
#215132=CARTESIAN_POINT('Ctrl Pts',(58.5215690622471,-4.82861869113419,
127.570713924673));
#215133=CARTESIAN_POINT('Ctrl Pts',(58.2431214384343,-5.3305448924898,133.118949252284));
#215134=CARTESIAN_POINT('Ctrl Pts',(57.9646738146213,-0.933960749242644,
136.54019069853));
#215135=CARTESIAN_POINT('Ctrl Pts',(57.6862261908085,4.32088769603949,134.690484511247));
#215136=CARTESIAN_POINT('Ctrl Pts',(57.4077785669955,5.6050514357603,129.269620313377));
#215137=CARTESIAN_POINT('Ctrl Pts',(57.1293309431827,1.73844672800264,125.259107478825));
#215138=CARTESIAN_POINT('Ctrl Pts',(56.8508833193697,-3.72570559494523,
126.3444113781));
#215139=CARTESIAN_POINT('Ctrl Pts',(56.5724356955568,-5.76611648697549,
131.528190747811));
#215140=CARTESIAN_POINT('Ctrl Pts',(56.293988071744,-2.50774801792579,136.046805588895));
#215141=CARTESIAN_POINT('Ctrl Pts',(56.0155404479311,3.05511836929639,135.747869609001));
#215142=CARTESIAN_POINT('Ctrl Pts',(55.7370928241181,5.81048022596477,130.906090369819));
#215143=CARTESIAN_POINT('Ctrl Pts',(55.4586452003054,3.22629461271119,125.97082645809));
#215144=CARTESIAN_POINT('Ctrl Pts',(55.1801975764924,-2.32269813636975,
125.477344307648));
#215145=CARTESIAN_POINT('Ctrl Pts',(54.9017499526795,-5.73724476823917,
129.879129906805));
#215146=CARTESIAN_POINT('Ctrl Pts',(54.6233023288666,-3.87954373808533,
135.131157329118));
#215147=CARTESIAN_POINT('Ctrl Pts',(54.3448547050537,1.54326846112093,136.407069949284));
#215148=CARTESIAN_POINT('Ctrl Pts',(54.0664070812409,5.54789233741261,132.534366401168));
#215149=CARTESIAN_POINT('Ctrl Pts',(53.7879594574279,4.45427418523046,127.071872053402));
#215150=CARTESIAN_POINT('Ctrl Pts',(53.5095118336151,-0.732604339787292,
125.039352353899));
#215151=CARTESIAN_POINT('Ctrl Pts',(53.2310642098022,-5.24625526625226,
128.304593612394));
#215152=CARTESIAN_POINT('Ctrl Pts',(52.9526165859893,-4.93885389684926,
133.866998628235));
#215153=CARTESIAN_POINT('Ctrl Pts',(52.6741689621764,-0.0928870726681018,
136.614988930455));
#215154=CARTESIAN_POINT('Ctrl Pts',(52.3957213383635,4.83843843350925,134.023295678104));
#215155=CARTESIAN_POINT('Ctrl Pts',(52.1172737145507,5.32347539014984,128.473558358838));
#215156=CARTESIAN_POINT('Ctrl Pts',(51.8388260907377,0.91649852947334,125.065714449322));
#215157=CARTESIAN_POINT('Ctrl Pts',(51.5603784669247,-4.33269570634681,
126.931406019971));
#215158=CARTESIAN_POINT('Ctrl Pts',(51.2819308431118,-5.6003542519866,132.356153661459));
#215159=CARTESIAN_POINT('Ctrl Pts',(51.0034832192991,-1.72156083256576,
136.354879304913));
#215160=CARTESIAN_POINT('Ctrl Pts',(50.7250355954861,3.73926288906064,135.252949432607));
#215161=CARTESIAN_POINT('Ctrl Pts',(50.4465879716733,5.76388668878802,130.062983764924));
#215162=CARTESIAN_POINT('Ctrl Pts',(50.1681403478604,2.49178020303801,125.554307206545));
#215163=CARTESIAN_POINT('Ctrl Pts',(49.8896927240475,-3.07015055907373,
125.870173253527));
#215164=CARTESIAN_POINT('Ctrl Pts',(49.6112451002346,-5.81076294258959,
130.720316439607));
#215165=CARTESIAN_POINT('Ctrl Pts',(49.3327974764216,-3.21156805341676,
135.647692119444));
#215166=CARTESIAN_POINT('Ctrl Pts',(49.0543498526089,2.33890098302428,136.124282758954));
#215167=CARTESIAN_POINT('Ctrl Pts',(48.7759022287959,5.74003427773134,131.712124843171));
#215168=CARTESIAN_POINT('Ctrl Pts',(48.497454604983,3.86635648746696,126.465775950806));
#215169=CARTESIAN_POINT('Ctrl Pts',(48.2190069811701,-1.56031403276457,
125.206374415548));
#215170=CARTESIAN_POINT('Ctrl Pts',(47.9405593573573,-5.55313218246346,
129.091248723115));
#215171=CARTESIAN_POINT('Ctrl Pts',(47.6621117335443,-4.44289314206747,
134.550389171513));
#215172=CARTESIAN_POINT('Ctrl Pts',(47.3836641097315,0.750147648492217,
136.567112382502));
#215173=CARTESIAN_POINT('Ctrl Pts',(47.1052164859186,5.25383939683757,133.288148247589));
#215174=CARTESIAN_POINT('Ctrl Pts',(46.8267688621057,4.92950940381243,127.726704620456));
#215175=CARTESIAN_POINT('Ctrl Pts',(46.5483212382927,0.0752010886061242,
124.993476502813));
#215176=CARTESIAN_POINT('Ctrl Pts',(46.2698736144798,-4.84821335325179,
127.600167009156));
#215177=CARTESIAN_POINT('Ctrl Pts',(45.991425990667,-5.31635657186091,133.151354908068));
#215178=CARTESIAN_POINT('Ctrl Pts',(45.7129783668541,-0.899027819386881,
136.545769711054));
#215179=CARTESIAN_POINT('Ctrl Pts',(45.4345307430412,4.344463579153,134.664110040551));
#215180=CARTESIAN_POINT('Ctrl Pts',(45.1560831192283,5.5956051872961,129.235529209567));
#215181=CARTESIAN_POINT('Ctrl Pts',(44.8776354954154,1.70465898882477,125.248627800858));
#215182=CARTESIAN_POINT('Ctrl Pts',(44.5991878716026,-3.7527855431554,126.367173438067));
#215183=CARTESIAN_POINT('Ctrl Pts',(44.3207402477896,-5.76160349474165,
131.563277324591));
#215184=CARTESIAN_POINT('Ctrl Pts',(44.0422926239769,-2.47578930463884,
136.0619738325));
#215185=CARTESIAN_POINT('Ctrl Pts',(43.7638450001637,3.08515430739569,135.72918064457));
#215186=CARTESIAN_POINT('Ctrl Pts',(43.485397376351,5.8109918291003,130.870718442656));
#215187=CARTESIAN_POINT('Ctrl Pts',(43.206949752538,3.19681174259461,125.951276641244));
#215188=CARTESIAN_POINT('Ctrl Pts',(42.9285021287252,-2.3550821624196,125.491581927739));
#215189=CARTESIAN_POINT('Ctrl Pts',(42.6500545049123,-5.74277061233009,
129.914071286517));
#215190=CARTESIAN_POINT('Ctrl Pts',(42.3716068810994,-3.85313341945026,
135.154693047476));
#215191=CARTESIAN_POINT('Ctrl Pts',(42.0931592572865,1.57734514987214,136.397571830902));
#215192=CARTESIAN_POINT('Ctrl Pts',(41.8147116334736,5.5583205840564,132.50056275283));
#215193=CARTESIAN_POINT('Ctrl Pts',(41.5362640096606,4.43147094054935,127.04482677653));
#215194=CARTESIAN_POINT('Ctrl Pts',(41.2578163858478,-0.767684007931795,
125.043918736703));
#215195=CARTESIAN_POINT('Ctrl Pts',(40.9793687620349,-5.26137485657243,
128.336575372158));
#215196=CARTESIAN_POINT('Ctrl Pts',(40.700921138222,-4.9201192444739,133.897006090131));
#215197=CARTESIAN_POINT('Ctrl Pts',(40.4224735144091,-0.0575144078915333,
136.615446702946));
#215198=CARTESIAN_POINT('Ctrl Pts',(40.1440258905964,4.85794335980812,133.993783090635));
#215199=CARTESIAN_POINT('Ctrl Pts',(39.8655782667833,5.30918850357096,128.441196037522));
#215200=CARTESIAN_POINT('Ctrl Pts',(39.5871306429705,0.8815487808295,125.060241786462));
#215201=CARTESIAN_POINT('Ctrl Pts',(39.3086830191576,-4.35619120544207,
126.957852125381));
#215202=CARTESIAN_POINT('Ctrl Pts',(39.0302353953447,-5.59080428568363,
132.39021585623));
#215203=CARTESIAN_POINT('Ctrl Pts',(38.7517877715318,-1.6877413533555,136.365256096082));
#215204=CARTESIAN_POINT('Ctrl Pts',(38.4733401477189,3.76627343195761,135.230105056025));
#215205=CARTESIAN_POINT('Ctrl Pts',(38.194892523906,5.7592669259876,130.027911086658));
#215206=CARTESIAN_POINT('Ctrl Pts',(37.9164449000932,2.45977547086574,125.539236304527));
#215207=CARTESIAN_POINT('Ctrl Pts',(37.6379972762802,-3.10012947526937,
125.888953550457));
#215208=CARTESIAN_POINT('Ctrl Pts',(37.3595496524674,-5.81116688337655,
130.755689760074));
#215209=CARTESIAN_POINT('Ctrl Pts',(37.0811020286545,-3.18202581694541,
135.667152110023));
#215210=CARTESIAN_POINT('Ctrl Pts',(36.8026544048415,2.3712415246555,136.109946638975));
#215211=CARTESIAN_POINT('Ctrl Pts',(36.5242067810287,5.74545374668639,131.677166806538));
#215212=CARTESIAN_POINT('Ctrl Pts',(36.2457591572158,3.83987465653194,126.442320725389));
#215213=CARTESIAN_POINT('Ctrl Pts',(35.9673115334029,-1.59436165466975,
125.215976207654));
#215214=CARTESIAN_POINT('Ctrl Pts',(35.6888639095901,-5.56345749412674,
129.125083954872));
#215215=CARTESIAN_POINT('Ctrl Pts',(35.4104162857771,-4.42000768648982,
134.57736491788));
#215216=CARTESIAN_POINT('Ctrl Pts',(35.1319686619643,0.785213255651605,
136.562439250406));
#215217=CARTESIAN_POINT('Ctrl Pts',(34.8535210381513,5.26886157564935,133.25612061713));
#215218=CARTESIAN_POINT('Ctrl Pts',(34.5750734143385,4.91068350582282,127.69675431939));
#215219=CARTESIAN_POINT('Ctrl Pts',(34.2966257905255,0.0398271943713243,
124.993126394665));
#215220=CARTESIAN_POINT('Ctrl Pts',(34.0181781667127,-4.86762836304081,
127.629738826211));
#215221=CARTESIAN_POINT('Ctrl Pts',(33.7397305428998,-5.30197125168398,
133.183673595116));
#215222=CARTESIAN_POINT('Ctrl Pts',(33.4612829190869,-0.864061575724654,
136.551135973552));
#215223=CARTESIAN_POINT('Ctrl Pts',(33.182835295274,4.36787847657091,134.637592545421));
#215224=CARTESIAN_POINT('Ctrl Pts',(32.9043876714611,5.58595159162396,129.201496239381));
#215225=CARTESIAN_POINT('Ctrl Pts',(32.6259400476482,1.67080808288091,125.238353992614));
#215226=CARTESIAN_POINT('Ctrl Pts',(32.3474924238352,-3.77972643051725,
126.390099919638));
#215227=CARTESIAN_POINT('Ctrl Pts',(32.0690448000224,-5.75687700417149,
131.598335779433));
#215228=CARTESIAN_POINT('Ctrl Pts',(31.7905971762095,-2.44373885006871,
136.076947253315));
#215229=CARTESIAN_POINT('Ctrl Pts',(31.5121495523967,3.11507592396733,135.71030918912));
#215230=CARTESIAN_POINT('Ctrl Pts',(31.2337019285837,5.81128810379662,130.835344056578));
#215231=CARTESIAN_POINT('Ctrl Pts',(30.9552543047708,3.16721041344351,125.931906657209));
#215232=CARTESIAN_POINT('Ctrl Pts',(30.676806680958,-2.38737892003384,125.506016414799));
#215233=CARTESIAN_POINT('Ctrl Pts',(30.398359057145,-5.74808365594406,129.949045656226));
#215234=CARTESIAN_POINT('Ctrl Pts',(30.1199114333322,-3.82658032153943,
135.178067562667));
#215235=CARTESIAN_POINT('Ctrl Pts',(29.8414638095193,1.61136338951851,136.387866454021));
#215236=CARTESIAN_POINT('Ctrl Pts',(29.5630161857064,5.56854286508694,132.466696251098));
#215237=CARTESIAN_POINT('Ctrl Pts',(29.2845685618935,4.40850348608286,127.017920810568));
#215238=CARTESIAN_POINT('Ctrl Pts',(29.0061209380806,-0.802735229263066,
125.048698574801));
#215239=CARTESIAN_POINT('Ctrl Pts',(28.7276733142678,-5.27629948471241,
128.368648576612));
#215240=CARTESIAN_POINT('Ctrl Pts',(28.4492256904548,-4.90120227527057,
133.926898952911));
#215241=CARTESIAN_POINT('Ctrl Pts',(28.170778066642,-0.0221396118974229,
136.615689143506));
#215242=CARTESIAN_POINT('Ctrl Pts',(27.892330442829,4.87726827322928,133.964152317942));
#215243=CARTESIAN_POINT('Ctrl Pts',(27.6138828190162,5.29470488305963,128.408921284139));
#215244=CARTESIAN_POINT('Ctrl Pts',(27.3354351952032,0.846566366071392,
125.054981974037));
#215245=CARTESIAN_POINT('Ctrl Pts',(27.0569875713904,-4.37952528427021,
126.984440764576));
#215246=CARTESIAN_POINT('Ctrl Pts',(26.7785399475775,-5.58104715007188,
132.424219286554));
#215247=CARTESIAN_POINT('Ctrl Pts',(26.5000923237646,-1.65385933426847,
136.375426826225));
#215248=CARTESIAN_POINT('Ctrl Pts',(26.2216446999517,3.79314441420758,135.207096681855));
#215249=CARTESIAN_POINT('Ctrl Pts',(25.9431970761388,5.75443375143326,129.992867180015));
#215250=CARTESIAN_POINT('Ctrl Pts',(25.6647494523259,2.42767959080881,125.524360503627));
#215251=CARTESIAN_POINT('Ctrl Pts',(25.3863018285131,-3.12999351502748,
125.907915989602));
#215252=CARTESIAN_POINT('Ctrl Pts',(25.1078542047001,-5.81135548923757,
130.791064884058));
#215253=CARTESIAN_POINT('Ctrl Pts',(24.8294065808873,-3.152365669337,135.686431908074));
#215254=CARTESIAN_POINT('Ctrl Pts',(24.5509589570743,2.40349419906,136.095413918554));
#215255=CARTESIAN_POINT('Ctrl Pts',(24.2725113332615,5.75066031573997,131.64217642775));
#215256=CARTESIAN_POINT('Ctrl Pts',(23.9940637094486,3.81325053762949,126.419027136963));
#215257=CARTESIAN_POINT('Ctrl Pts',(23.7156160856357,-1.62835019691723,
125.2257850794));
#215258=CARTESIAN_POINT('Ctrl Pts',(23.4371684618228,-5.57357664982666,
129.158981412844));
#215259=CARTESIAN_POINT('Ctrl Pts',(23.1587208380098,-4.39695844590187,
134.604200854185));
#215260=CARTESIAN_POINT('Ctrl Pts',(22.880273214197,0.820249766445046,136.557552750588));
#215261=CARTESIAN_POINT('Ctrl Pts',(22.6018255903841,5.28368851485763,133.224002135804));
#215262=CARTESIAN_POINT('Ctrl Pts',(22.3233779665712,4.89167564065013,127.666919171818));
#215263=CARTESIAN_POINT('Ctrl Pts',(22.0449303427584,0.00445182432539013,
124.992991623939));
#215264=CARTESIAN_POINT('Ctrl Pts',(21.7664827189454,-4.88686300107076,
127.659428280044));
#215265=CARTESIAN_POINT('Ctrl Pts',(21.4880350951325,-5.28738946501251,
133.215904115845));
#215266=CARTESIAN_POINT('Ctrl Pts',(21.2095874713197,-0.829063313942982,
136.556289287176));
#215267=CARTESIAN_POINT('Ctrl Pts',(20.9311398475068,4.39113152064558,134.610933008472));
#215268=CARTESIAN_POINT('Ctrl Pts',(20.6526922236938,5.57609100646137,129.167522663925));
#215269=CARTESIAN_POINT('Ctrl Pts',(20.374244599881,1.6368952645291,125.228286434793));
#215270=CARTESIAN_POINT('Ctrl Pts',(20.0957969760681,-3.80652725872624,
126.413189973261));
#215271=CARTESIAN_POINT('Ctrl Pts',(19.8173493522552,-5.75193719040684,
131.633364813234));
#215272=CARTESIAN_POINT('Ctrl Pts',(19.5389017284423,-2.41159784185683,
136.091725296493));
#215273=CARTESIAN_POINT('Ctrl Pts',(19.2604541046294,3.14488211025528,135.691255941942));
#215274=CARTESIAN_POINT('Ctrl Pts',(18.9820064808165,5.81136903907515,130.799968522399));
#215275=CARTESIAN_POINT('Ctrl Pts',(18.7035588570036,3.13749172214556,125.912717223747));
#215276=CARTESIAN_POINT('Ctrl Pts',(18.4251112331907,-2.41958721244422,
125.52064723395));
#215277=CARTESIAN_POINT('Ctrl Pts',(18.1466636093778,-5.75318370220431,
129.984051719947));
#215278=CARTESIAN_POINT('Ctrl Pts',(17.868215985565,-3.79988542828747,135.201280008538));
#215279=CARTESIAN_POINT('Ctrl Pts',(17.589768361752,1.64532191950215,136.377954178279));
#215280=CARTESIAN_POINT('Ctrl Pts',(17.3113207379392,5.57855880171371,132.432768150908));
#215281=CARTESIAN_POINT('Ctrl Pts',(17.0328731141263,4.38537267289848,126.991155152525));
#215282=CARTESIAN_POINT('Ctrl Pts',(16.7544254903134,-0.83775670494522,
125.053691691071));
#215283=CARTESIAN_POINT('Ctrl Pts',(16.4759778665005,-5.29102859763445,
128.400812037271));
#215284=CARTESIAN_POINT('Ctrl Pts',(16.1975302426876,-4.88210369021464,
133.956676108886));
#215285=CARTESIAN_POINT('Ctrl Pts',(15.9190826188747,0.013236004487936,
136.61571624315));
#215286=CARTESIAN_POINT('Ctrl Pts',(15.6406349950618,4.89641245768097,133.934404458007));
#215287=CARTESIAN_POINT('Ctrl Pts',(15.3621873712489,5.2800250653117,128.376735294641));
#215288=CARTESIAN_POINT('Ctrl Pts',(15.0837397474361,0.811552581485459,
125.049935206953));
#215289=CARTESIAN_POINT('Ctrl Pts',(14.8052921236231,-4.40269707817821,
127.011170952307));
#215290=CARTESIAN_POINT('Ctrl Pts',(14.5268444998103,-5.57108320670569,
132.458162692417));
#215291=CARTESIAN_POINT('Ctrl Pts',(14.2483968759974,-1.6199160308156,136.385391118461));
#215292=CARTESIAN_POINT('Ctrl Pts',(13.9699492521845,3.81987484009636,135.18392516268));
#215293=CARTESIAN_POINT('Ctrl Pts',(13.6915016283715,5.74938734422005,129.95785334356));
#215294=CARTESIAN_POINT('Ctrl Pts',(13.4130540045587,2.39549375219187,125.509680355073));
#215295=CARTESIAN_POINT('Ctrl Pts',(13.1346063807458,-3.15974157172482,
125.927059868305));
#215296=CARTESIAN_POINT('Ctrl Pts',(12.8561587569329,-5.81132875318382,
130.82644050072));
#215297=CARTESIAN_POINT('Ctrl Pts',(12.57771113312,-3.12258870965941,135.705530799178));
#215298=CARTESIAN_POINT('Ctrl Pts',(12.2992635093071,2.43565781110307,136.080685136208));
#215299=CARTESIAN_POINT('Ctrl Pts',(12.0208158854942,5.75565379196074,131.607155003388));
#215300=CARTESIAN_POINT('Ctrl Pts',(11.7423682616813,3.78648511732596,126.395896048684));
#215301=CARTESIAN_POINT('Ctrl Pts',(11.4639206378685,-1.66227840004959,
125.235800667314));
#215302=CARTESIAN_POINT('Ctrl Pts',(11.1854730140555,-5.58348927459409,
129.192939840948));
#215303=CARTESIAN_POINT('Ctrl Pts',(10.9070253902426,-4.37374627440173,
134.630895986013));
#215304=CARTESIAN_POINT('Ctrl Pts',(10.6285777664298,0.855255882581734,
136.552453064119));
#215305=CARTESIAN_POINT('Ctrl Pts',(10.3501301426169,5.29831966504511,133.19179399377));
#215306=CARTESIAN_POINT('Ctrl Pts',(10.071682518804,4.87248651263752,127.637200283293));
#215307=CARTESIAN_POINT('Ctrl Pts',(9.79323489499104,-0.0309237106847325,
124.993072195629));
#215308=CARTESIAN_POINT('Ctrl Pts',(9.51478727117816,-4.90591655459505,
127.689234270502));
#215309=CARTESIAN_POINT('Ctrl Pts',(9.23633964736526,-5.27261175218,133.248045275945));
#215310=CARTESIAN_POINT('Ctrl Pts',(8.95789202355236,-0.794034330915497,
136.561229460968));
#215311=CARTESIAN_POINT('Ctrl Pts',(8.67944439973947,4.41422184972672,134.584132417584));
#215312=CARTESIAN_POINT('Ctrl Pts',(8.40099677592661,5.56602379719609,129.1336097421));
#215313=CARTESIAN_POINT('Ctrl Pts',(8.12254915211368,1.60292179042129,125.218425500451));
#215314=CARTESIAN_POINT('Ctrl Pts',(7.84410152830078,-3.83318703466779,
126.436442743329));
#215315=CARTESIAN_POINT('Ctrl Pts',(7.56565390448795,-5.74678423649425,
131.668363127979));
#215316=CARTESIAN_POINT('Ctrl Pts',(7.28720628067502,-2.37936747100029,
136.106307414428));
#215317=CARTESIAN_POINT('Ctrl Pts',(7.00875865686212,3.17457176177998,135.672021609062));
#215318=CARTESIAN_POINT('Ctrl Pts',(6.73031103304925,5.81123463193681,130.764593150968));
#215319=CARTESIAN_POINT('Ctrl Pts',(6.45186340923634,3.10765676993803,125.89370905193));
#215320=CARTESIAN_POINT('Ctrl Pts',(6.17341578542346,-2.45170584616043,
125.535473843045));
#215321=CARTESIAN_POINT('Ctrl Pts',(5.89496816161054,-5.75807056212669,
130.019088180515));
#215322=CARTESIAN_POINT('Ctrl Pts',(5.61652053779771,-3.77304972888379,
135.224329524944));
#215323=CARTESIAN_POINT('Ctrl Pts',(5.33807291398477,1.67921948147701,136.367835370977));
#215324=CARTESIAN_POINT('Ctrl Pts',(5.05962529017187,5.58836802279258,132.398779709476));
#215325=CARTESIAN_POINT('Ctrl Pts',(4.781177666359,4.36207935811697,126.964530794212));
#215326=CARTESIAN_POINT('Ctrl Pts',(4.50273004254611,-0.872747137244579,
125.058897900495));
#215327=CARTESIAN_POINT('Ctrl Pts',(4.2242824187332,-5.30556164954619,128.433064562307));
#215328=CARTESIAN_POINT('Ctrl Pts',(3.94583479492031,-4.86282419701095,
133.986336454649));
#215329=CARTESIAN_POINT('Ctrl Pts',(3.66738717110745,0.0486111304084952,
136.615528000873));
#215330=CARTESIAN_POINT('Ctrl Pts',(3.38893954729453,4.91537520376836,133.904540613147));
#215331=CARTESIAN_POINT('Ctrl Pts',(3.11049192348162,5.26514959429328,128.344639261694));
#215332=CARTESIAN_POINT('Ctrl Pts',(2.83204429966877,0.776508724519974,
125.045101672218));
#215333=CARTESIAN_POINT('Ctrl Pts',(2.55359667585587,-4.42570572852705,
127.038041698076));
#215334=CARTESIAN_POINT('Ctrl Pts',(2.27514905204296,-5.56091282480238,
132.492044816037));
#215335=CARTESIAN_POINT('Ctrl Pts',(1.99670142823006,-1.58591270077849,
136.395148603559));
#215336=CARTESIAN_POINT('Ctrl Pts',(1.7182538044172,3.84646371911817,135.160591357131));
#215337=CARTESIAN_POINT('Ctrl Pts',(1.43980618060429,5.7441278913444,129.922870874744));
#215338=CARTESIAN_POINT('Ctrl Pts',(1.16135855679139,2.36321914767325,125.495196402842));
#215339=CARTESIAN_POINT('Ctrl Pts',(0.882910932978526,-3.18937254303613,
125.946384477181));
#215340=CARTESIAN_POINT('Ctrl Pts',(0.604463309165634,-5.81108667620601,
130.861815299204));
#215341=CARTESIAN_POINT('Ctrl Pts',(0.326015685352703,-3.09269604130886,
135.724448075619));
#215342=CARTESIAN_POINT('Ctrl Pts',(0.0475680615398608,2.46773116894999,
136.065760837718));
#215343=CARTESIAN_POINT('Ctrl Pts',(-0.230879562273037,5.76043399031358,
131.572103831187));
#215344=CARTESIAN_POINT('Ctrl Pts',(-0.509327186085944,3.75957938742415,
126.37292831768));
#215345=CARTESIAN_POINT('Ctrl Pts',(-0.787774809898847,-1.69614500684454,
125.246022600264));
#215346=CARTESIAN_POINT('Ctrl Pts',(-1.06622243371171,-5.59319500111311,
129.226957980841));
#215347=CARTESIAN_POINT('Ctrl Pts',(-1.34467005752462,-4.35037203212501,
134.657449324165));
#215348=CARTESIAN_POINT('Ctrl Pts',(-1.62311768133752,0.890230306896913,
136.547140379971));
#215349=CARTESIAN_POINT('Ctrl Pts',(-1.90156530515039,5.31275448404895,
133.159497384516));
#215350=CARTESIAN_POINT('Ctrl Pts',(-2.18001292896328,4.85311683284533,
127.607598755059));
#215351=CARTESIAN_POINT('Ctrl Pts',(-2.4584605527762,-0.0662980998053887,
124.993368106748));
#215352=CARTESIAN_POINT('Ctrl Pts',(-2.73690817658909,-4.92478831757726,
127.719155693111));
#215353=CARTESIAN_POINT('Ctrl Pts',(-3.01535580040196,-5.25763866077998,
133.280095884409));
#215354=CARTESIAN_POINT('Ctrl Pts',(-3.29380342421486,-0.758975924653704,
136.565956311869));
#215355=CARTESIAN_POINT('Ctrl Pts',(-3.57225104802777,4.43714860819409,
134.557191765862));
#215356=CARTESIAN_POINT('Ctrl Pts',(-3.85069867184063,5.55575033687191,
129.099758730564));
#215357=CARTESIAN_POINT('Ctrl Pts',(-4.12914629565353,1.56888891945708,
125.208771554989));
#215358=CARTESIAN_POINT('Ctrl Pts',(-4.40759391946644,-3.85970477045413,
126.459857368199));
#215359=CARTESIAN_POINT('Ctrl Pts',(-4.68604154327934,-5.74141833337845,
131.703329426794));
#215360=CARTESIAN_POINT('Ctrl Pts',(-4.96448916709218,-2.34704893180687,
136.120693066776));
#215361=CARTESIAN_POINT('Ctrl Pts',(-5.24293679090511,3.20414377838073,
135.652606903212));
#215362=CARTESIAN_POINT('Ctrl Pts',(-5.52138441471801,5.81088488736209,
130.729219253137));
#215363=CARTESIAN_POINT('Ctrl Pts',(-5.79983203853088,3.07770666236606,
125.874882846113));
#215364=CARTESIAN_POINT('Ctrl Pts',(-6.07827966234377,-2.48373363101511,
125.550495692676));
#215365=CARTESIAN_POINT('Ctrl Pts',(-6.35672728615668,-5.7627440546269,
130.054153739642));
#215366=CARTESIAN_POINT('Ctrl Pts',(-6.63517490996957,-3.74607421773465,
135.247215257776));
#215367=CARTESIAN_POINT('Ctrl Pts',(-6.91362253378244,1.71305481935644,
136.357510407073));
#215368=CARTESIAN_POINT('Ctrl Pts',(-7.19207015759534,5.59797016483923,
132.36473218626));
#215369=CARTESIAN_POINT('Ctrl Pts',(-7.47051778140826,4.33862440488076,
126.938048722207));
#215370=CARTESIAN_POINT('Ctrl Pts',(-7.74896540522111,-0.907705229577551,
125.064317010151));
#215371=CARTESIAN_POINT('Ctrl Pts',(-8.027413029034,-5.31989810191992,128.46540495659));
#215372=CARTESIAN_POINT('Ctrl Pts',(-8.30586065284694,-4.84336451006833,
134.015878891129));
#215373=CARTESIAN_POINT('Ctrl Pts',(-8.58430827665978,0.0839844550257475,
136.615124423653));
#215374=CARTESIAN_POINT('Ctrl Pts',(-8.86275590047269,4.93415580881975,
133.874561889976));
#215375=CARTESIAN_POINT('Ctrl Pts',(-9.14120352428557,5.25007902122049,
128.312634374625));
#215376=CARTESIAN_POINT('Ctrl Pts',(-9.4196511480985,0.741436093738357,
125.040481548942));
#215377=CARTESIAN_POINT('Ctrl Pts',(-9.69809877191133,-4.44855038272257,
127.065052006178));
#215378=CARTESIAN_POINT('Ctrl Pts',(-9.97654639572428,-5.5505363812293,
132.525864401898));
#215379=CARTESIAN_POINT('Ctrl Pts',(-10.2549940195371,-1.55185060416301,
136.404698919952));
#215380=CARTESIAN_POINT('Ctrl Pts',(-10.53344164335,3.87291006601234,135.137096129849));
#215381=CARTESIAN_POINT('Ctrl Pts',(-10.8118892671629,5.7386555876974,129.887921069854));
#215382=CARTESIAN_POINT('Ctrl Pts',(-11.0903368909758,2.33085697319978,
125.480909183646));
#215383=CARTESIAN_POINT('Ctrl Pts',(-11.3687845147887,-3.21888533097506,
125.965889100148));
#215384=CARTESIAN_POINT('Ctrl Pts',(-11.6472321386015,-5.81062926727439,
130.897187968684));
#215385=CARTESIAN_POINT('Ctrl Pts',(-11.9256797624145,-3.06268877196916,
135.743183036409));
#215386=CARTESIAN_POINT('Ctrl Pts',(-12.2041273862274,2.49971308411117,
136.050641576106));
#215387=CARTESIAN_POINT('Ctrl Pts',(-12.4825750100403,5.76500073366654,
131.537024209977));
#215388=CARTESIAN_POINT('Ctrl Pts',(-12.7610226338531,3.73253434492532,
126.350124795028));
#215389=CARTESIAN_POINT('Ctrl Pts',(-13.039470257666,-1.7299487623625,125.256450499474));
#215390=CARTESIAN_POINT('Ctrl Pts',(-13.3179178814789,-5.60269346973446,
129.261034571969));
#215391=CARTESIAN_POINT('Ctrl Pts',(-13.5963655052918,-4.32683658521273,
134.683859884699));
#215392=CARTESIAN_POINT('Ctrl Pts',(-13.8748131291047,0.925171743400955,
136.541614895008));
#215393=CARTESIAN_POINT('Ctrl Pts',(-14.1532607529176,5.3269924369816,133.127113504801));
#215394=CARTESIAN_POINT('Ctrl Pts',(-14.4317083767304,4.83356731902416,
127.578115684011));
#215395=CARTESIAN_POINT('Ctrl Pts',(-14.7101560005434,-0.101670032225581,
124.99387934633));
#215396=CARTESIAN_POINT('Ctrl Pts',(-14.9886036243562,-4.94347759071707,
127.749191439124));
#215397=CARTESIAN_POINT('Ctrl Pts',(-15.2670512481692,-5.24247074564602,
133.312054753593));
#215398=CARTESIAN_POINT('Ctrl Pts',(-15.545498871982,-0.723889394260118,
136.570469664722));
#215399=CARTESIAN_POINT('Ctrl Pts',(-15.823946495795,4.45991094648802,134.530112051601));
#215400=CARTESIAN_POINT('Ctrl Pts',(-16.1023941196078,5.54527100617588,
129.065970883678));
#215401=CARTESIAN_POINT('Ctrl Pts',(-16.3808417434207,1.53479791273714,
125.199324956138));
#215402=CARTESIAN_POINT('Ctrl Pts',(-16.6592893672336,-3.88607948346057,
126.483432980235));
#215403=CARTESIAN_POINT('Ctrl Pts',(-16.9377369910465,-5.73583967989507,
131.738262413989));
#215404=CARTESIAN_POINT('Ctrl Pts',(-17.2161846148594,-2.31464342185212,
136.134881720468));
#215405=CARTESIAN_POINT('Ctrl Pts',(-17.4946322386723,3.23359706425542,
135.633012543814));
#215406=CARTESIAN_POINT('Ctrl Pts',(-17.7730798624852,5.81031981831091,
130.693848139697));
#215407=CARTESIAN_POINT('Ctrl Pts',(-18.0515274862981,3.04764250924188,
125.856239303907));
#215408=CARTESIAN_POINT('Ctrl Pts',(-18.3299751101109,-2.51566938020671,
125.565712226204));
#215409=CARTESIAN_POINT('Ctrl Pts',(-18.6084227339239,-5.76720400652691,
130.089247097961));
#215410=CARTESIAN_POINT('Ctrl Pts',(-18.8868703577367,-3.71895989442774,
135.269936358996));
#215411=CARTESIAN_POINT('Ctrl Pts',(-19.1653179815497,1.74682667935956,
136.346979669161));
#215412=CARTESIAN_POINT('Ctrl Pts',(-19.4437656053625,5.60736487204277,
132.330626842902));
#215413=CARTESIAN_POINT('Ctrl Pts',(-19.7222132291754,4.31500868232164,
126.91170991781));
#215414=CARTESIAN_POINT('Ctrl Pts',(-20.0006608529883,-0.942629686559699,
125.069948819234));
#215415=CARTESIAN_POINT('Ctrl Pts',(-20.2791084768012,-5.33403742351306,
128.497832021735));
#215416=CARTESIAN_POINT('Ctrl Pts',(-20.5575561006141,-4.82372535047263,
134.045302323618));
#215417=CARTESIAN_POINT('Ctrl Pts',(-20.836003724427,0.119354667568119,
136.614505526443));
#215418=CARTESIAN_POINT('Ctrl Pts',(-21.1144513482399,4.95275357691331,
133.844469399368));
#215419=CARTESIAN_POINT('Ctrl Pts',(-21.3928989720528,5.23481390453873,
128.280721819388));
#215420=CARTESIAN_POINT('Ctrl Pts',(-21.6713465958657,0.706335988769417,
125.036075008324));
#215421=CARTESIAN_POINT('Ctrl Pts',(-21.9497942196786,-4.47123019424771,
127.092200875735));
#215422=CARTESIAN_POINT('Ctrl Pts',(-22.2282418434914,-5.53995426048939,
132.559620196804));
#215423=CARTESIAN_POINT('Ctrl Pts',(-22.5066894673044,-1.5177310031529,
136.41404171375));
#215424=CARTESIAN_POINT('Ctrl Pts',(-22.7851370911172,3.89921290079955,
135.11344035146));
#215425=CARTESIAN_POINT('Ctrl Pts',(-23.0635847149301,5.73297063605735,
129.853005223969));
#215426=CARTESIAN_POINT('Ctrl Pts',(-23.342032338743,2.298408427964,125.466819226899));
#215427=CARTESIAN_POINT('Ctrl Pts',(-23.6204799625559,-3.24827884193431,
125.985573014458));
#215428=CARTESIAN_POINT('Ctrl Pts',(-23.8989275863688,-5.80995654333829,
130.932557198412));
#215429=CARTESIAN_POINT('Ctrl Pts',(-24.1773752101816,-3.03256801357094,
135.761734987319));
#215430=CARTESIAN_POINT('Ctrl Pts',(-24.4558228339946,2.53160237148462,
136.035327911625));
#215431=CARTESIAN_POINT('Ctrl Pts',(-24.7342704578075,5.76935385279724,
131.501917439649));
#215432=CARTESIAN_POINT('Ctrl Pts',(-25.0127180816204,3.70535099199371,
126.327486325724));
#215433=CARTESIAN_POINT('Ctrl Pts',(-25.2911657054332,-1.76368841399288,
125.267083978533));
#215434=CARTESIAN_POINT('Ctrl Pts',(-25.5696133292462,-5.61198432848891,
129.295168351611));
#215435=CARTESIAN_POINT('Ctrl Pts',(-25.8480609530591,-4.30314080577957,
134.71012668896));
#215436=CARTESIAN_POINT('Ctrl Pts',(-26.1265085768719,0.960078897325804,
136.535876813977));
#215437=CARTESIAN_POINT('Ctrl Pts',(-26.4049562006848,5.3410329962505,133.094643554625));
#215438=CARTESIAN_POINT('Ctrl Pts',(-26.6834038244978,4.81383869558843,
127.548752162656));
#215439=CARTESIAN_POINT('Ctrl Pts',(-26.9618514483106,-0.137038197225328,
124.994605895435));
#215440=CARTESIAN_POINT('Ctrl Pts',(-27.2402990721235,-4.96198368147699,
127.779340395554));
#215441=CARTESIAN_POINT('Ctrl Pts',(-27.5187466959364,-5.22710856883054,
133.343920699249));
#215442=CARTESIAN_POINT('Ctrl Pts',(-27.7971943197493,-0.688776039878604,
136.574769352283));
#215443=CARTESIAN_POINT('Ctrl Pts',(-28.0756419435621,4.48250802114168,
134.502894278251));
#215444=CARTESIAN_POINT('Ctrl Pts',(-28.3540895673751,5.53458619342344,
129.032247453463));
#215445=CARTESIAN_POINT('Ctrl Pts',(-28.632537191188,1.50065003351598,125.190086053944));
#215446=CARTESIAN_POINT('Ctrl Pts',(-28.9109848150008,-3.91231019636288,
126.507168705834));
#215447=CARTESIAN_POINT('Ctrl Pts',(-29.1894324388138,-5.73004848276283,
131.773160795109));
#215448=CARTESIAN_POINT('Ctrl Pts',(-29.4678800626266,-2.28215214193419,
136.148872849742));
#215449=CARTESIAN_POINT('Ctrl Pts',(-29.7463276864396,3.26293052800175,
135.613239256942));
#215450=CARTESIAN_POINT('Ctrl Pts',(-30.0247753102524,5.80953944572202,
130.658481121338));
#215451=CARTESIAN_POINT('Ctrl Pts',(-30.3032229340653,3.01746542460398,
125.837779116156));
#215452=CARTESIAN_POINT('Ctrl Pts',(-30.5816705578782,-2.54751191034413,
125.581122879776));
#215453=CARTESIAN_POINT('Ctrl Pts',(-30.8601181816911,-5.77145025256159,
130.124366955075));
#215454=CARTESIAN_POINT('Ctrl Pts',(-31.138565805504,-3.69170776369427,
135.292491986665));
#215455=CARTESIAN_POINT('Ctrl Pts',(-31.4170134293169,1.78053381005746,
136.336243547461));
#215456=CARTESIAN_POINT('Ctrl Pts',(-31.6954610531298,5.6165517962788,132.296464943187));
#215457=CARTESIAN_POINT('Ctrl Pts',(-31.9739086769427,4.29123306552915,
126.885515357016));
#215458=CARTESIAN_POINT('Ctrl Pts',(-32.2523563007555,-0.977519214052166,
125.075793119056));
#215459=CARTESIAN_POINT('Ctrl Pts',(-32.5308039245685,-5.34797909038788,
128.530344556146));
#215460=CARTESIAN_POINT('Ctrl Pts',(-32.8092515483813,-4.80390744596015,
134.07460566182));
#215461=CARTESIAN_POINT('Ctrl Pts',(-33.0876991721943,0.154720457379397,
136.613671332177));
#215462=CARTESIAN_POINT('Ctrl Pts',(-33.3661467960071,4.9711678189017,133.814264256411));
#215463=CARTESIAN_POINT('Ctrl Pts',(-33.64459441982,5.21935480990263,128.248902778514));
#215464=CARTESIAN_POINT('Ctrl Pts',(-33.9230420436329,0.671209710260644,
125.031882213649));
#215465=CARTESIAN_POINT('Ctrl Pts',(-34.2014896674458,-4.49374432269368,
127.119487300736));
#215466=CARTESIAN_POINT('Ctrl Pts',(-34.4799372912587,-5.52916685470707,
132.59331094992));
#215467=CARTESIAN_POINT('Ctrl Pts',(-34.7583849150716,-1.48355516206214,
136.423176638752));
#215468=CARTESIAN_POINT('Ctrl Pts',(-35.0368325388844,3.92537124881898,
135.089624898536));
#215469=CARTESIAN_POINT('Ctrl Pts',(-35.3152801626974,5.72707324708195,
129.818124630907));
#215470=CARTESIAN_POINT('Ctrl Pts',(-35.5937277865103,2.26587471435868,
125.45292705471));
#215471=CARTESIAN_POINT('Ctrl Pts',(-35.8721754103231,-3.27755198672651,
126.005435490714));
#215472=CARTESIAN_POINT('Ctrl Pts',(-36.1506230341361,-5.80906852932597,
130.967921677768));
#215473=CARTESIAN_POINT('Ctrl Pts',(-36.4290706579489,-3.00233488224952,
135.780103240898));
#215474=CARTESIAN_POINT('Ctrl Pts',(-36.7075182817618,2.56339784940132,
136.019820411726));
#215475=CARTESIAN_POINT('Ctrl Pts',(-36.9859659055747,5.77349318639923,
131.466784821096));
#215476=CARTESIAN_POINT('Ctrl Pts',(-37.2644135293876,3.67803033591843,
126.305013748643));
#215477=CARTESIAN_POINT('Ctrl Pts',(-37.5428611532005,-1.79736271150026,
125.277922643415));
#215478=CARTESIAN_POINT('Ctrl Pts',(-37.8213087770133,-5.62106723310019,
129.329358054928));
#215479=CARTESIAN_POINT('Ctrl Pts',(-38.0997564008263,-4.27928557188161,
134.736248763623));
#215480=CARTESIAN_POINT('Ctrl Pts',(-38.3782040246392,0.994950475174061,
136.529926349506));
#215481=CARTESIAN_POINT('Ctrl Pts',(-38.656651648452,5.35487564157755,133.062088737171));
#215482=CARTESIAN_POINT('Ctrl Pts',(-38.9350992722649,4.79393169358958,
127.51950927907));
#215483=CARTESIAN_POINT('Ctrl Pts',(-39.2135468960779,-0.172401284224016,
124.995547727136));
#215484=CARTESIAN_POINT('Ctrl Pts',(-39.4919945198907,-4.98030590410683,
127.809601445221));
#215485=CARTESIAN_POINT('Ctrl Pts',(-39.7704421437036,-5.21155269958477,
133.375692540572));
#215486=CARTESIAN_POINT('Ctrl Pts',(-40.0488897675166,-0.65363716264763,
136.578855215227));
#215487=CARTESIAN_POINT('Ctrl Pts',(-40.3273373913294,4.50493899481217,
134.475539454375));
#215488=CARTESIAN_POINT('Ctrl Pts',(-40.6057850151423,5.52369629454426,
128.998589689552));
#215489=CARTESIAN_POINT('Ctrl Pts',(-40.8842326389552,1.46644654715595,
125.181055190758));
#215490=CARTESIAN_POINT('Ctrl Pts',(-41.1626802627681,-3.93839593717207,
126.531063665459));
#215491=CARTESIAN_POINT('Ctrl Pts',(-41.441127886581,-5.72404495657686,
131.808023276983));
#215492=CARTESIAN_POINT('Ctrl Pts',(-41.7195755103939,-2.24957629602936,
136.162665936149));
#215493=CARTESIAN_POINT('Ctrl Pts',(-41.9980231342068,3.29214308265742,
135.593287775304));
#215494=CARTESIAN_POINT('Ctrl Pts',(-42.2764707580197,5.80854379851262,
130.623119508596));
#215495=CARTESIAN_POINT('Ctrl Pts',(-42.5549183818325,2.98717652667487,
125.81950296691));
#215496=CARTESIAN_POINT('Ctrl Pts',(-42.8333660056454,-2.57926004149102,
125.596727082342));
#215497=CARTESIAN_POINT('Ctrl Pts',(-43.1118136294584,-5.7754826353847,
130.159512009603));
#215498=CARTESIAN_POINT('Ctrl Pts',(-43.3902612532712,-3.66431883537201,
135.314881304976));
#215499=CARTESIAN_POINT('Ctrl Pts',(-43.6687088770841,1.81417496242045,
136.325302439805));
#215500=CARTESIAN_POINT('Ctrl Pts',(-43.947156500897,5.62553059712261,132.262247752997));
#215501=CARTESIAN_POINT('Ctrl Pts',(-44.2256041247099,4.26729843551711,
126.859466010475));
#215502=CARTESIAN_POINT('Ctrl Pts',(-44.5040517485228,-1.01237251921066,
125.081849693053));
#215503=CARTESIAN_POINT('Ctrl Pts',(-44.7824993723357,-5.3617225859308,
128.562941355057));
#215504=CARTESIAN_POINT('Ctrl Pts',(-45.0609469961486,-4.78391153089065,
134.103787819889));
#215505=CARTESIAN_POINT('Ctrl Pts',(-45.3393946199614,0.190080513966956,
136.612621871764));
#215506=CARTESIAN_POINT('Ctrl Pts',(-45.6178422437743,4.98939785243841,
133.783947580368));
#215507=CARTESIAN_POINT('Ctrl Pts',(-45.8962898675873,5.20370231015464,
128.217178431071));
#215508=CARTESIAN_POINT('Ctrl Pts',(-46.1747374914001,0.636058559829223,
125.027903320286));
#215509=CARTESIAN_POINT('Ctrl Pts',(-46.453185115213,-4.51609193379101,
127.146910270074));
#215510=CARTESIAN_POINT('Ctrl Pts',(-46.7316327390259,-5.51817456361365,
132.626935412823));
#215511=CARTESIAN_POINT('Ctrl Pts',(-47.0100803628388,-1.4493243472895,
136.43210335646));
#215512=CARTESIAN_POINT('Ctrl Pts',(-47.2885279866517,3.95138414076325,
135.06565065357));
#215513=CARTESIAN_POINT('Ctrl Pts',(-47.5669756104645,5.72096363930122,
129.783280583183));
#215514=CARTESIAN_POINT('Ctrl Pts',(-47.8454232342775,2.23325703793269,
125.439233181862));
#215515=CARTESIAN_POINT('Ctrl Pts',(-48.1238708580903,-3.30670368062431,
126.025475792906));
#215516=CARTESIAN_POINT('Ctrl Pts',(-48.4023184819033,-5.80796525814313,
131.00328009631));
#215517=CARTESIAN_POINT('Ctrl Pts',(-48.6807661057162,-2.97199049830493,
135.798287116504));
#215518=CARTESIAN_POINT('Ctrl Pts',(-48.9592137295291,2.59509833966803,
136.004119651047));
#215519=CARTESIAN_POINT('Ctrl Pts',(-49.2376613533419,5.77741858108801,
131.431627656171));
#215520=CARTESIAN_POINT('Ctrl Pts',(-49.5161089771548,3.65057338907646,
126.282707896514));
#215521=CARTESIAN_POINT('Ctrl Pts',(-49.7945566009678,-1.8309704070716,
125.288966092489));
#215522=CARTESIAN_POINT('Ctrl Pts',(-50.0730042247805,-5.62994184699806,
129.363602415007));
#215523=CARTESIAN_POINT('Ctrl Pts',(-50.3514518485936,-4.25527176748286,
134.762225140725));
#215524=CARTESIAN_POINT('Ctrl Pts',(-50.6298994724063,1.02978518476655,
136.52376372209));
#215525=CARTESIAN_POINT('Ctrl Pts',(-50.9083470962193,5.36851986001845,
133.029450258773));
#215526=CARTESIAN_POINT('Ctrl Pts',(-51.1867947200322,4.77384705068883,
127.490388116857));
#215527=CARTESIAN_POINT('Ctrl Pts',(-51.465242343845,-0.207757982829986,
124.996704806535));
#215528=CARTESIAN_POINT('Ctrl Pts',(-51.743689967658,-4.99844357966987,
127.839973466791));
#215529=CARTESIAN_POINT('Ctrl Pts',(-52.0221375914708,-5.19580371433717,
133.407369100245));
#215530=CARTESIAN_POINT('Ctrl Pts',(-52.3005852152837,-0.618474064651215,
136.58272710215));
#215531=CARTESIAN_POINT('Ctrl Pts',(-52.5790328390967,4.52720303631132,
134.448048593619));
#215532=CARTESIAN_POINT('Ctrl Pts',(-52.8574804629095,5.51260171306762,
128.964998839148));
#215533=CARTESIAN_POINT('Ctrl Pts',(-53.1359280867224,1.43218872108006,
125.172232701224));
#215534=CARTESIAN_POINT('Ctrl Pts',(-53.4143757105353,-3.96433573927151,
126.555116973674));
#215535=CARTESIAN_POINT('Ctrl Pts',(-53.6928233343482,-5.71782932379997,
131.842848567767));
#215536=CARTESIAN_POINT('Ctrl Pts',(-53.9712709581611,-2.21691709124776,
136.176260468582));
#215537=CARTESIAN_POINT('Ctrl Pts',(-54.249718581974,3.32123364574025,135.573158838211));
#215538=CARTESIAN_POINT('Ctrl Pts',(-54.5281662057869,5.80733291357678,
130.58776461181));
#215539=CARTESIAN_POINT('Ctrl Pts',(-54.8066138295998,2.95677693782102,
125.801411533396));
#215540=CARTESIAN_POINT('Ctrl Pts',(-55.0850614534126,-2.61091259720856,
125.612524255684));
#215541=CARTESIAN_POINT('Ctrl Pts',(-55.3635090772256,-5.77930100557468,
130.194680959234));
#215542=CARTESIAN_POINT('Ctrl Pts',(-55.6419567010384,-3.63679412436797,
135.337103484283));
#215543=CARTESIAN_POINT('Ctrl Pts',(-55.9204043248514,1.8477488898629,136.314156751619));
#215544=CARTESIAN_POINT('Ctrl Pts',(-56.1988519486642,5.63430094186134,
132.227976540264));
#215545=CARTESIAN_POINT('Ctrl Pts',(-56.4772995724772,4.24320567919224,
126.833562843453));
#215546=CARTESIAN_POINT('Ctrl Pts',(-56.7557471962901,-1.04718831053316,
125.088118316796));
#215547=CARTESIAN_POINT('Ctrl Pts',(-57.0341948201028,-5.3752674008715,
128.595621210585));
#215548=CARTESIAN_POINT('Ctrl Pts',(-57.3126424439159,-4.76373834622006,
134.13284771647));
#215549=CARTESIAN_POINT('Ctrl Pts',(-57.5910900677287,0.225433527051438,
136.611357184097));
#215550=CARTESIAN_POINT('Ctrl Pts',(-57.8695376915416,5.00744300200284,
133.753520494635));
#215551=CARTESIAN_POINT('Ctrl Pts',(-58.1479853153544,5.18785698530388,
128.185549952615));
#215552=CARTESIAN_POINT('Ctrl Pts',(-58.4264329391674,0.600883840013963,
125.024138475672));
#215553=CARTESIAN_POINT('Ctrl Pts',(-58.7048805629802,-4.53827219944114,
127.174468767579));
#215554=CARTESIAN_POINT('Ctrl Pts',(-58.9833281867932,-5.5069777945324,
132.660492339548));
#215555=CARTESIAN_POINT('Ctrl Pts',(-59.261775810606,-1.41503982726995,
136.440821536091));
#215556=CARTESIAN_POINT('Ctrl Pts',(-59.540223434419,3.97725061271504,135.041518504932));
#215557=CARTESIAN_POINT('Ctrl Pts',(-59.8186710582318,5.71464203910897,
129.748474371954));
#215558=CARTESIAN_POINT('Ctrl Pts',(-60.0971186820448,2.20055660734573,
125.425738115783));
#215559=CARTESIAN_POINT('Ctrl Pts',(-60.3755663058576,-3.3357328434014,
126.045693178431));
#215560=CARTESIAN_POINT('Ctrl Pts',(-60.6540139296705,-5.80664677067165,
131.038631143817));
#215561=CARTESIAN_POINT('Ctrl Pts',(-60.9324615534834,-2.94153598615947,
135.816285940328));
#215562=CARTESIAN_POINT('Ctrl Pts',(-61.2109091772963,2.62670266761142,
135.988226211385));
#215563=CARTESIAN_POINT('Ctrl Pts',(-61.4893568011092,5.78112989140647,
131.396447247635));
#215564=CARTESIAN_POINT('Ctrl Pts',(-61.767804424922,3.62298116889529,126.260569595891));
#215565=CARTESIAN_POINT('Ctrl Pts',(-62.046252048735,-1.86451025536104,
125.300213916535));
#215566=CARTESIAN_POINT('Ctrl Pts',(-62.3246996725479,-5.63860784133039,
129.39790016291));
#215567=CARTESIAN_POINT('Ctrl Pts',(-62.6031472963608,-4.23110028242386,
134.788054857702));
#215568=CARTESIAN_POINT('Ctrl Pts',(-62.8815949201736,1.0645817352901,136.517389160091));
#215569=CARTESIAN_POINT('Ctrl Pts',(-63.1600425439866,5.38196514598156,
132.99672932886));
#215570=CARTESIAN_POINT('Ctrl Pts',(-63.4384901677994,4.75358551113023,
127.461389755115));
#215571=CARTESIAN_POINT('Ctrl Pts',(-63.7169377916123,-0.243106982887504,
124.998077090756));
#215572=CARTESIAN_POINT('Ctrl Pts',(-63.9953854154252,-5.0163960360679,
127.870455334816));
#215573=CARTESIAN_POINT('Ctrl Pts',(-64.2738330392381,-5.17986219667218,
133.438949204482));
#215574=CARTESIAN_POINT('Ctrl Pts',(-64.552280663051,-0.583288048870894,
136.586384869579));
#215575=CARTESIAN_POINT('Ctrl Pts',(-64.8307282868638,4.54929932063727,
134.420422714664));
#215576=CARTESIAN_POINT('Ctrl Pts',(-65.1091759106768,5.50130286010717,
128.93147614697));
#215577=CARTESIAN_POINT('Ctrl Pts',(-65.3876235344896,1.39787782472419,
125.16361891226));
#215578=CARTESIAN_POINT('Ctrl Pts',(-65.6660711583025,-3.99012864145221,
126.579327739175));
#215579=CARTESIAN_POINT('Ctrl Pts',(-65.9445187821156,-5.71140181475477,
131.877635376998));
#215580=CARTESIAN_POINT('Ctrl Pts',(-66.2229664059283,-2.18417573778792,
136.189655943291));
#215581=CARTESIAN_POINT('Ctrl Pts',(-66.5014140297413,3.35020113928917,
135.552853191544));
#215582=CARTESIAN_POINT('Ctrl Pts',(-66.7798616535541,5.80590683578406,
130.552417741069));
#215583=CARTESIAN_POINT('Ctrl Pts',(-67.0583092773671,2.92626778451039,
125.783505486001));
#215584=CARTESIAN_POINT('Ctrl Pts',(-67.3367569011799,-2.64246840459962,
125.628513814431));
#215585=CARTESIAN_POINT('Ctrl Pts',(-67.6152045249929,-5.78290522164069,
130.229872500769));
#215586=CARTESIAN_POINT('Ctrl Pts',(-67.8936521488056,-3.60913465062,135.359157701137));
#215587=CARTESIAN_POINT('Ctrl Pts',(-68.1720997726187,1.88125434829088,
136.302806895912));
#215588=CARTESIAN_POINT('Ctrl Pts',(-68.4505473964314,5.64286250550667,
132.193652574919));
#215589=CARTESIAN_POINT('Ctrl Pts',(-68.7289950202444,4.21895568932047,
126.807806815805));
#215590=CARTESIAN_POINT('Ctrl Pts',(-69.0074426440573,-1.08196529790749,
125.094598758));
#215591=CARTESIAN_POINT('Ctrl Pts',(-69.2858902678701,-5.38861303330182,
128.628382911763));
#215592=CARTESIAN_POINT('Ctrl Pts',(-69.564337891683,-4.74338863947339,
134.161784274737));
#215593=CARTESIAN_POINT('Ctrl Pts',(-69.8427855154959,0.260778186613682,
136.609877316035));
#215594=CARTESIAN_POINT('Ctrl Pts',(-70.1212331393089,5.02530259892534,
133.722984126697));
#215595=CARTESIAN_POINT('Ctrl Pts',(-70.3996807631217,5.17181942250469,
128.154018515153));
#215596=CARTESIAN_POINT('Ctrl Pts',(-70.6781283869345,0.5656868542273,125.020587819316));
#215597=CARTESIAN_POINT('Ctrl Pts',(-70.9565760107477,-4.56028429774593,
127.202161772061));
#215598=CARTESIAN_POINT('Ctrl Pts',(-71.2350236345604,-5.49557696236377,
132.693980486629));
#215599=CARTESIAN_POINT('Ctrl Pts',(-71.5134712583732,-1.38070287242923,
136.449330854589));
#215600=CARTESIAN_POINT('Ctrl Pts',(-71.7919188821862,4.00296970618273,
135.017229346852));
#215601=CARTESIAN_POINT('Ctrl Pts',(-72.0703665059991,5.70810868075446,
129.71370728698));
#215602=CARTESIAN_POINT('Ctrl Pts',(-72.348814129812,2.16777463432419,125.412442356538));
#215603=CARTESIAN_POINT('Ctrl Pts',(-72.6272617536249,-3.36463839937136,
126.06608689813));
#215604=CARTESIAN_POINT('Ctrl Pts',(-72.9057093774378,-5.80511311576878,
131.073973510343));
#215605=CARTESIAN_POINT('Ctrl Pts',(-73.1841570012506,-2.91097247431594,
135.834099045416));
#215606=CARTESIAN_POINT('Ctrl Pts',(-73.4626046250635,2.65820966212185,
135.972140681676));
#215607=CARTESIAN_POINT('Ctrl Pts',(-73.7410522488765,5.78462697983096,
131.361244899111));
#215608=CARTESIAN_POINT('Ctrl Pts',(-74.0194998726893,3.59525469781404,
126.238599667113));
#215609=CARTESIAN_POINT('Ctrl Pts',(-74.2979474965022,-1.89798101353784,
125.31166569876));
#215610=CARTESIAN_POINT('Ctrl Pts',(-74.5763951203151,-5.64706489497548,
129.432250027724));
#215611=CARTESIAN_POINT('Ctrl Pts',(-74.854842744128,-4.20677201238788,
134.813736957424));
#215612=CARTESIAN_POINT('Ctrl Pts',(-75.1332903679409,1.09933883734644,
136.510802899716));
#215613=CARTESIAN_POINT('Ctrl Pts',(-75.4117379917539,5.39521100124704,
132.963927159917));
#215614=CARTESIAN_POINT('Ctrl Pts',(-75.6901856155667,4.73314782571214,
127.432515268386));
#215615=CARTESIAN_POINT('Ctrl Pts',(-75.9686332393795,-0.278446974526432,
124.99966452895));
#215616=CARTESIAN_POINT('Ctrl Pts',(-76.2470808631926,-5.03416260806588,
127.901045919781));
#215617=CARTESIAN_POINT('Ctrl Pts',(-76.5255284870053,-5.16372873730878,
133.470431683069));
#215618=CARTESIAN_POINT('Ctrl Pts',(-76.8039761108183,-0.548080419137594,
136.589828381972));
#215619=CARTESIAN_POINT('Ctrl Pts',(-77.0824237346311,4.57122702900371,
134.392662841198));
#215620=CARTESIAN_POINT('Ctrl Pts',(-77.360871358444,5.48980015434633,128.898022855216));
#215621=CARTESIAN_POINT('Ctrl Pts',(-77.639318982257,1.36351512949127,125.155214143056));
#215622=CARTESIAN_POINT('Ctrl Pts',(-77.9177666060698,-4.0157736879487,
126.603695064822));
#215623=CARTESIAN_POINT('Ctrl Pts',(-78.1962142298826,-5.70476266761487,
131.91238241564));
#215624=CARTESIAN_POINT('Ctrl Pts',(-78.4746618536957,-2.15135344889296,
136.202851863901));
#215625=CARTESIAN_POINT('Ctrl Pts',(-78.7531094775085,3.37904448990285,
135.532371587738));
#215626=CARTESIAN_POINT('Ctrl Pts',(-79.0315571013213,5.8042656179783,130.517080206165));
#215627=CARTESIAN_POINT('Ctrl Pts',(-79.3100047251342,2.8956501972711,125.765785488239));
#215628=CARTESIAN_POINT('Ctrl Pts',(-79.5884523489472,-2.67392629435197,
125.644695166086));
#215629=CARTESIAN_POINT('Ctrl Pts',(-79.8668999727601,-5.78629515002701,
130.265085330171));
#215630=CARTESIAN_POINT('Ctrl Pts',(-80.1453475965729,-3.58134143906054,
135.38104313831));
#215631=CARTESIAN_POINT('Ctrl Pts',(-80.4237952203859,1.91469009614739,
136.291253293255));
#215632=CARTESIAN_POINT('Ctrl Pts',(-80.7022428441988,5.65121497080658,
132.15927712885));
#215633=CARTESIAN_POINT('Ctrl Pts',(-80.9806904680116,4.19454936449412,
126.782198881926));
#215634=CARTESIAN_POINT('Ctrl Pts',(-81.2591380918246,-1.11670219266007,
125.10129077653));
#215635=CARTESIAN_POINT('Ctrl Pts',(-81.5375857156372,-5.40175898869456,
128.661225244595));
#215636=CARTESIAN_POINT('Ctrl Pts',(-81.8160333394505,-4.72286316471603,
134.190596422436));
#215637=CARTESIAN_POINT('Ctrl Pts',(-82.0944809632629,0.296113182944105,
136.608182322418));
#215638=CARTESIAN_POINT('Ctrl Pts',(-82.3729285870762,5.04297598141181,
133.692339608092));
#215639=CARTESIAN_POINT('Ctrl Pts',(-82.6513762108889,5.15559021603496,
128.122585287091));
#215640=CARTESIAN_POINT('Ctrl Pts',(-82.9298238347018,0.530468906706182,
125.017251482786));
#215641=CARTESIAN_POINT('Ctrl Pts',(-83.2082714585147,-4.58212741303929,
127.229988257347));
#215642=CARTESIAN_POINT('Ctrl Pts',(-83.4867190823277,-5.48397248956967,
132.72739861315));
#215643=CARTESIAN_POINT('Ctrl Pts',(-83.7651667061405,-1.34631475513585,
136.45763099664));
#215644=CARTESIAN_POINT('Ctrl Pts',(-84.0436143299535,4.02854046813582,
134.992784079373));
#215645=CARTESIAN_POINT('Ctrl Pts',(-84.3220619537663,5.70136380633342,
129.678980616565));
#215646=CARTESIAN_POINT('Ctrl Pts',(-84.6005095775792,2.13491233361711,
125.399346396808));
#215647=CARTESIAN_POINT('Ctrl Pts',(-84.8789572013921,-3.39341927742779,
126.086656196302));
#215648=CARTESIAN_POINT('Ctrl Pts',(-85.1574048252049,-5.80336435026449,
131.109305886265));
#215649=CARTESIAN_POINT('Ctrl Pts',(-85.4358524490179,-2.88030109531746,
135.851725771696));
#215650=CARTESIAN_POINT('Ctrl Pts',(-85.7143000728307,2.68961815569484,
135.955863657977));
#215651=CARTESIAN_POINT('Ctrl Pts',(-85.9927476966438,5.78790971677558,
131.326021915035));
#215652=CARTESIAN_POINT('Ctrl Pts',(-86.2711953204564,3.56739500324825,
126.216798924288));
#215653=CARTESIAN_POINT('Ctrl Pts',(-86.5496429442695,-1.93138144132926,
125.323321014816));
#215654=CARTESIAN_POINT('Ctrl Pts',(-86.8280905680822,-5.65531269455438,
129.466650736599));
#215655=CARTESIAN_POINT('Ctrl Pts',(-87.1065381918953,-4.18228785886808,
134.83927048823));
#215656=CARTESIAN_POINT('Ctrl Pts',(-87.3849858157081,1.13405520299706,
136.504005185026));
#215657=CARTESIAN_POINT('Ctrl Pts',(-87.663433439521,5.40825693498488,132.931044967442));
#215658=CARTESIAN_POINT('Ctrl Pts',(-87.9418810633338,4.71253475176078,
127.403765726628));
#215659=CARTESIAN_POINT('Ctrl Pts',(-88.2203286871468,-0.313776648210234,
125.00146706229));
#215660=CARTESIAN_POINT('Ctrl Pts',(-88.4987763109598,-5.05174263731727,
127.931744088139));
#215661=CARTESIAN_POINT('Ctrl Pts',(-88.7772239347726,-5.14740393407785,
133.501815369412));
#215662=CARTESIAN_POINT('Ctrl Pts',(-89.0556715585855,-0.512852480082647,
136.593057511728));
#215663=CARTESIAN_POINT('Ctrl Pts',(-89.3341191823985,4.59298534887173,
134.364770001874));
#215664=CARTESIAN_POINT('Ctrl Pts',(-89.6125668062112,5.47809402202166,
128.864640203508));
#215665=CARTESIAN_POINT('Ctrl Pts',(-89.8910144300243,1.32910190870433,
125.147018705051));
#215666=CARTESIAN_POINT('Ctrl Pts',(-90.169462053837,-4.04126992847403,
126.628218047677));
#215667=CARTESIAN_POINT('Ctrl Pts',(-90.44790967765,-5.69791212839678,131.947088396125));
#215668=CARTESIAN_POINT('Ctrl Pts',(-90.7263573014627,-2.1184514408047,
136.215847741432));
#215669=CARTESIAN_POINT('Ctrl Pts',(-91.0048049252757,3.40776262878029,
135.511714785749));
#215670=CARTESIAN_POINT('Ctrl Pts',(-91.2832525490887,5.80240932097568,
130.48175331654));
#215671=CARTESIAN_POINT('Ctrl Pts',(-91.5617001729014,2.86492531064864,
125.748252196732));
#215672=CARTESIAN_POINT('Ctrl Pts',(-91.8401477967144,-2.70528510078237,
125.661067711041));
#215673=CARTESIAN_POINT('Ctrl Pts',(-92.1185954205271,-5.78947066511866,
130.30031814262));
#215674=CARTESIAN_POINT('Ctrl Pts',(-92.3970430443404,-3.55341551957677,
135.402758984829));
#215675=CARTESIAN_POINT('Ctrl Pts',(-92.6754906681528,1.94805489445803,
136.279496371773));
#215676=CARTESIAN_POINT('Ctrl Pts',(-92.9539382919661,5.6593580282576,132.124851475851));
#215677=CARTESIAN_POINT('Ctrl Pts',(-93.2323859157787,4.16998760909852,
126.75673999073));
#215678=CARTESIAN_POINT('Ctrl Pts',(-93.5108335395918,-1.15139770760221,
125.10819412441));
#215679=CARTESIAN_POINT('Ctrl Pts',(-93.7892811634045,-5.41470477992152,
128.694146992097));
#215680=CARTESIAN_POINT('Ctrl Pts',(-94.0677287872175,-4.70216268252734,
134.219283091922));
#215681=CARTESIAN_POINT('Ctrl Pts',(-94.3461764110305,0.331437206691851,
136.606272266052));
#215682=CARTESIAN_POINT('Ctrl Pts',(-94.6246240348431,5.0604624945689,133.661588074364));
#215683=CARTESIAN_POINT('Ctrl Pts',(-94.9030716586564,5.13916996727372,
128.0912514332));
#215684=CARTESIAN_POINT('Ctrl Pts',(-95.1815192824688,0.495231302464415,
125.014129589715));
#215685=CARTESIAN_POINT('Ctrl Pts',(-95.459966906282,-4.60380073591605,
127.257947192314));
#215686=CARTESIAN_POINT('Ctrl Pts',(-95.7384145300948,-5.47216480615837,
132.760745480792));
#215687=CARTESIAN_POINT('Ctrl Pts',(-96.0168621539077,-1.31187674965409,
136.465721654678));
#215688=CARTESIAN_POINT('Ctrl Pts',(-96.2953097777207,4.05396195104042,
134.96818360832));
#215689=CARTESIAN_POINT('Ctrl Pts',(-96.5737574015334,5.69440766577999,
129.64429564752));
#215690=CARTESIAN_POINT('Ctrl Pts',(-96.8522050253465,2.10197092294792,
125.386450721867));
#215691=CARTESIAN_POINT('Ctrl Pts',(-97.1306526491593,-3.42207441108517,
126.107400310748));
#215692=CARTESIAN_POINT('Ctrl Pts',(-97.4091002729722,-5.80140053895979,
131.144626962327));
#215693=CARTESIAN_POINT('Ctrl Pts',(-97.6875478967851,-2.8495229857029,
135.869165466005));
#215694=CARTESIAN_POINT('Ctrl Pts',(-97.965995520598,2.72092698447821,135.93939574344));
#215695=CARTESIAN_POINT('Ctrl Pts',(-98.2444431444108,5.79097798059694,
131.290779600608));
#215696=CARTESIAN_POINT('Ctrl Pts',(-98.5228907682237,3.53940311754856,
126.195168175249));
#215697=CARTESIAN_POINT('Ctrl Pts',(-98.8013383920368,-1.96471030107164,
125.33517943281));
#215698=CARTESIAN_POINT('Ctrl Pts',(-99.0797860158496,-5.6633509344415,
129.501101014807));
#215699=CARTESIAN_POINT('Ctrl Pts',(-99.3582336396624,-4.15764872913354,
134.864654503967));
#215700=CARTESIAN_POINT('Ctrl Pts',(-99.6366812634755,1.16872954581563,
136.496996267908));
#215701=CARTESIAN_POINT('Ctrl Pts',(-99.9151288872883,5.42110246377302,
132.898083969897));
#215702=CARTESIAN_POINT('Ctrl Pts',(-100.193576511101,4.69174705310118,
127.375142195163));
#215703=CARTESIAN_POINT('Ctrl Pts',(-100.472024134914,-0.34909469478497,
125.003484623986));
#215704=CARTESIAN_POINT('Ctrl Pts',(-100.750471758727,-5.06913547238742,
127.96254870236));
#215705=CARTESIAN_POINT('Ctrl Pts',(-101.02891938254,-5.13088839190121,
133.533099100579));
#215706=CARTESIAN_POINT('Ctrl Pts',(-101.307367006353,-0.47760553709043,
136.596072139193));
#215707=CARTESIAN_POINT('Ctrl Pts',(-101.585814630166,4.61457347397855,
134.33674523027));
#215708=CARTESIAN_POINT('Ctrl Pts',(-101.864262253979,5.46618489690847,
128.831329428852));
#215709=CARTESIAN_POINT('Ctrl Pts',(-102.142709877791,1.29463943755703,
125.139032901931));
#215710=CARTESIAN_POINT('Ctrl Pts',(-102.421157501604,-4.06661641825637,
126.652895779031));
#215711=CARTESIAN_POINT('Ctrl Pts',(-102.699605125417,-5.69085045094906,
131.981752032413));
#215712=CARTESIAN_POINT('Ctrl Pts',(-102.97805274923,-2.08547093271925,
136.228643094318));
#215713=CARTESIAN_POINT('Ctrl Pts',(-103.256500373043,3.43635449176034,
135.490883551018));
#215714=CARTESIAN_POINT('Ctrl Pts',(-103.534947996856,5.80033801356182,
130.446438381249));
#215715=CARTESIAN_POINT('Ctrl Pts',(-103.813395620669,2.83409426316523,
125.730906261181));
#215716=CARTESIAN_POINT('Ctrl Pts',(-104.091843244482,-2.73654366187847,
125.677630842606));
#215717=CARTESIAN_POINT('Ctrl Pts',(-104.370290868295,-5.79243164924577,
130.335569632546));
#215718=CARTESIAN_POINT('Ctrl Pts',(-104.648738492108,-3.52535792697413,
135.424304436005));
#215719=CARTESIAN_POINT('Ctrl Pts',(-104.92718611592,1.98134750687769,136.267536567122));
#215720=CARTESIAN_POINT('Ctrl Pts',(-105.205633739733,5.66729137611554,
132.090376891579));
#215721=CARTESIAN_POINT('Ctrl Pts',(-105.484081363546,4.14527133327901,
126.731431085605));
#215722=CARTESIAN_POINT('Ctrl Pts',(-105.762528987359,-1.18605055707886,
125.115308545834));
#215723=CARTESIAN_POINT('Ctrl Pts',(-106.040976611172,-5.42744992727162,
128.72714693434));
#215724=CARTESIAN_POINT('Ctrl Pts',(-106.319424234985,-4.68128795997122,
134.247843220201));
#215725=CARTESIAN_POINT('Ctrl Pts',(-106.597871858798,0.366748948912009,
136.604147217717));
#215726=CARTESIAN_POINT('Ctrl Pts',(-106.876319482611,5.07776149042729,
133.630730665021));
#215727=CARTESIAN_POINT('Ctrl Pts',(-107.154767106424,5.12255928467941,
128.060018114567));
#215728=CARTESIAN_POINT('Ctrl Pts',(-107.433214730236,0.45997534724462,
125.011222255784));
#215729=CARTESIAN_POINT('Ctrl Pts',(-107.711662354049,-4.62530346326349,
127.286037540936));
#215730=CARTESIAN_POINT('Ctrl Pts',(-107.990109977862,-5.46015434966779,
132.794019853873));
#215731=CARTESIAN_POINT('Ctrl Pts',(-108.268557601675,-1.2773901320969,
136.473602528901));
#215732=CARTESIAN_POINT('Ctrl Pts',(-108.547005225488,4.07923321289408,
134.943428845277));
#215733=CARTESIAN_POINT('Ctrl Pts',(-108.825452849301,5.6872405168564,129.609653665109));
#215734=CARTESIAN_POINT('Ctrl Pts',(-109.103900473114,2.06895162297316,
125.373755809571));
#215735=CARTESIAN_POINT('Ctrl Pts',(-109.382348096927,-3.45060273851677,
126.128318472786));
#215736=CARTESIAN_POINT('Ctrl Pts',(-109.66079572074,-5.79922175462486,
131.179935429694));
#215737=CARTESIAN_POINT('Ctrl Pts',(-109.939243344552,-2.81863928596571,
135.886417482107));
#215738=CARTESIAN_POINT('Ctrl Pts',(-110.217690968365,2.7521349883118,135.922737548286));
#215739=CARTESIAN_POINT('Ctrl Pts',(-110.496138592178,5.79383165759959,
131.255519261747));
#215740=CARTESIAN_POINT('Ctrl Pts',(-110.774586215991,3.51128007796473,
126.17370822153));
#215741=CARTESIAN_POINT('Ctrl Pts',(-111.053033839804,-1.99796635775128,
125.347240513325));
#215742=CARTESIAN_POINT('Ctrl Pts',(-111.331481463617,-5.67117931677705,
129.535599585778));
#215743=CARTESIAN_POINT('Ctrl Pts',(-111.60992908743,-4.13285553619637,
134.889888064022));
#215744=CARTESIAN_POINT('Ctrl Pts',(-111.888376711243,1.20336058093108,
136.489776408084));
#215745=CARTESIAN_POINT('Ctrl Pts',(-112.166824335056,5.43374711161577,
132.865045388662));
#215746=CARTESIAN_POINT('Ctrl Pts',(-112.445271958868,4.67078550002918,
127.34664573465));
#215747=CARTESIAN_POINT('Ctrl Pts',(-112.723719582681,-0.384399805526852,
125.005717139274));
#215748=CARTESIAN_POINT('Ctrl Pts',(-113.002167206494,-5.08634046877848,
127.993458620965));
#215749=CARTESIAN_POINT('Ctrl Pts',(-113.280614830307,-5.11418272276831,
133.564281717336));
#215750=CARTESIAN_POINT('Ctrl Pts',(-113.55906245412,-0.442340896249408,
136.598872152659));
#215751=CARTESIAN_POINT('Ctrl Pts',(-113.837510077933,4.63599060436829,
134.308589564856));
#215752=CARTESIAN_POINT('Ctrl Pts',(-114.115957701746,5.45407322030374,
128.798091765594));
#215753=CARTESIAN_POINT('Ctrl Pts',(-114.394405325558,1.26012899306928,
125.131257029612));
#215754=CARTESIAN_POINT('Ctrl Pts',(-114.672852949372,-4.09181221807183,
126.677727344441));
#215755=CARTESIAN_POINT('Ctrl Pts',(-114.951300573184,-5.68357789694507,
132.016372040028));
#215756=CARTESIAN_POINT('Ctrl Pts',(-115.229748196997,-2.05241314674147,
136.241237448422));
#215757=CARTESIAN_POINT('Ctrl Pts',(-115.50819582081,3.46481901936097,135.469878655457));
#215758=CARTESIAN_POINT('Ctrl Pts',(-115.786643444623,5.79805177248978,
130.411136708898));
#215759=CARTESIAN_POINT('Ctrl Pts',(-116.065091068436,2.80315819727665,
125.713748324348));
#215760=CARTESIAN_POINT('Ctrl Pts',(-116.343538692249,-2.76770081934284,
125.694383947029));
#215761=CARTESIAN_POINT('Ctrl Pts',(-116.621986316062,-5.79517799268792,
130.370838493694));
#215762=CARTESIAN_POINT('Ctrl Pts',(-116.900433939875,-3.49716970093708,
135.445678693465));
#215763=CARTESIAN_POINT('Ctrl Pts',(-117.178881563688,2.0145666997373,136.255374322477));
#215764=CARTESIAN_POINT('Ctrl Pts',(-117.4573291875,5.67501472040751,132.055854653499));
#215765=CARTESIAN_POINT('Ctrl Pts',(-117.735776811314,4.12040145290537,
126.706273104381));
#215766=CARTESIAN_POINT('Ctrl Pts',(-118.014224435126,-1.22065945701595,
125.122633777175));
#215767=CARTESIAN_POINT('Ctrl Pts',(-118.29267205894,-5.43999395846872,
128.760223848501));
#215768=CARTESIAN_POINT('Ctrl Pts',(-118.571119682752,-4.6602397705682,
134.276275748964));
#215769=CARTESIAN_POINT('Ctrl Pts',(-118.849567306565,0.402047101114997,
136.601807256156));
#215770=CARTESIAN_POINT('Ctrl Pts',(-119.128014930377,5.09487232796628,
133.599768523497));
#215771=CARTESIAN_POINT('Ctrl Pts',(-119.406462554191,5.10575878376697,
128.028886488555));
#215772=CARTESIAN_POINT('Ctrl Pts',(-119.684910178003,0.424702347469154,
125.008529588725));
#215773=CARTESIAN_POINT('Ctrl Pts',(-119.963357801817,-4.64663479828973,
127.314258262312));
#215774=CARTESIAN_POINT('Ctrl Pts',(-120.241805425629,-5.44794156515001,
132.827220499399));
#215775=CARTESIAN_POINT('Ctrl Pts',(-120.520253049442,-1.24285618037906,
136.48127332728));
#215776=CARTESIAN_POINT('Ctrl Pts',(-120.798700673255,4.10435331726091,
134.918520707537));
#215777=CARTESIAN_POINT('Ctrl Pts',(-121.077148297068,5.67986262514396,
129.575055953004));
#215778=CARTESIAN_POINT('Ctrl Pts',(-121.355595920881,2.03585565723516,
125.361262130332));
#215779=CARTESIAN_POINT('Ctrl Pts',(-121.634043544694,-3.47900320259493,
126.149409907283));
#215780=CARTESIAN_POINT('Ctrl Pts',(-121.912491168507,-5.79682807799514,
131.215229979999));
#215781=CARTESIAN_POINT('Ctrl Pts',(-122.19093879232,-2.78765114051323,
135.903481180724));
#215782=CARTESIAN_POINT('Ctrl Pts',(-122.469386416133,2.78324101077128,
135.905889689793));
#215783=CARTESIAN_POINT('Ctrl Pts',(-122.747834039945,5.79647064203949,
131.220242205036));
#215784=CARTESIAN_POINT('Ctrl Pts',(-123.026281663758,3.48302692660634,
126.152419858339));
#215785=CARTESIAN_POINT('Ctrl Pts',(-123.304729287571,-2.03114837905279,
125.359503809431));
#215786=CARTESIAN_POINT('Ctrl Pts',(-123.583176911384,-5.67879755147744,
129.570145171156));
#215787=CARTESIAN_POINT('Ctrl Pts',(-123.861624535197,-4.10790919877744,
134.914970233354));
#215788=CARTESIAN_POINT('Ctrl Pts',(-124.14007215901,1.23794702507767,136.482345873087));
#215789=CARTESIAN_POINT('Ctrl Pts',(-124.418519782823,5.44619040996103,
132.831930447996));
#215790=CARTESIAN_POINT('Ctrl Pts',(-124.696967406636,4.64965086928273,
127.318277401031));
#215791=CARTESIAN_POINT('Ctrl Pts',(-124.975415030448,-0.419690672193134,
125.00816452543));
#215792=CARTESIAN_POINT('Ctrl Pts',(-125.253862654262,-5.10335698895296,
128.024472698579));
#215793=CARTESIAN_POINT('Ctrl Pts',(-125.532310278074,-5.09728754571388,
133.595362064203));
#215794=CARTESIAN_POINT('Ctrl Pts',(-125.810757901887,-0.407059864303788,
136.601457448367));
#215795=CARTESIAN_POINT('Ctrl Pts',(-126.0892055257,4.65723594642128,134.280304048949));
#215796=CARTESIAN_POINT('Ctrl Pts',(-126.367653149513,5.44175944101008,
128.764928445366));
#215797=CARTESIAN_POINT('Ctrl Pts',(-126.646100773326,1.22557185403828,
125.123691376234));
#215798=CARTESIAN_POINT('Ctrl Pts',(-126.924548397139,-4.11685639428078,
126.702711823764));
#215799=CARTESIAN_POINT('Ctrl Pts',(-127.202996020952,-5.67609473587197,
132.050947136115));
#215800=CARTESIAN_POINT('Ctrl Pts',(-127.481443644765,-2.01927930784003,
136.253630337055));
#215801=CARTESIAN_POINT('Ctrl Pts',(-127.759891268577,3.4931551568182,135.44870087741));
#215802=CARTESIAN_POINT('Ctrl Pts',(-128.038338892391,5.79555068247735,
130.375849607603));
#215803=CARTESIAN_POINT('Ctrl Pts',(-128.316786516203,2.77211825933019,
125.696779022025));
#215804=CARTESIAN_POINT('Ctrl Pts',(-128.595234140016,-2.7987554186355,
125.711326403516));
#215805=CARTESIAN_POINT('Ctrl Pts',(-128.873681763829,-5.79770959367839,
130.406123419165));
#215806=CARTESIAN_POINT('Ctrl Pts',(-129.152129387642,-3.46885188599067,
135.466880965177));
#215807=CARTESIAN_POINT('Ctrl Pts',(-129.430577011455,2.04771124208698,
136.243010088514));
#215808=CARTESIAN_POINT('Ctrl Pts',(-129.709024635268,5.68252777494204,
132.021286040849));
#215809=CARTESIAN_POINT('Ctrl Pts',(-129.98747225908,4.09537888954061,126.681266979298));
#215810=CARTESIAN_POINT('Ctrl Pts',(-130.265919882893,-1.25522312496795,
125.130169546993));
#215811=CARTESIAN_POINT('Ctrl Pts',(-130.544367506706,-5.45233640868912,
128.793376508901));
#215812=CARTESIAN_POINT('Ctrl Pts',(-130.822815130519,-4.63901889426667,
134.304579624636));
#215813=CARTESIAN_POINT('Ctrl Pts',(-131.101262754332,0.437330355314798,
136.599252468079));
#215814=CARTESIAN_POINT('Ctrl Pts',(-131.379710378145,5.11179437313754,
133.568702797104));
#215815=CARTESIAN_POINT('Ctrl Pts',(-131.658158001958,5.08876908708517,
127.997857708758));
#215816=CARTESIAN_POINT('Ctrl Pts',(-131.936605625771,0.389413610192037,
125.006051688315));
#215817=CARTESIAN_POINT('Ctrl Pts',(-132.215053249584,-4.66779395055513,
127.342608310716));
#215818=CARTESIAN_POINT('Ctrl Pts',(-132.493500873397,-5.43552690515385,
132.860346187109));
#215819=CARTESIAN_POINT('Ctrl Pts',(-132.77194849721,-1.20827617416795,
136.488733765571));
#215820=CARTESIAN_POINT('Ctrl Pts',(-133.050396121022,4.12932133330617,
134.893460118082));
#215821=CARTESIAN_POINT('Ctrl Pts',(-133.328843744835,5.67227426403318,
129.540503793235));
#215822=CARTESIAN_POINT('Ctrl Pts',(-133.607291368648,2.00268425211708,
125.348970147109));
#215823=CARTESIAN_POINT('Ctrl Pts',(-133.885738992461,-3.50727475093002,
126.170673832692));
#215824=CARTESIAN_POINT('Ctrl Pts',(-134.164186616274,-5.79421959776922,
131.25050930539));
#215825=CARTESIAN_POINT('Ctrl Pts',(-134.442634240087,-2.75655969762259,
135.920355929551));
#215826=CARTESIAN_POINT('Ctrl Pts',(-134.7210818639,2.81424389921159,135.888852792264));
#215827=CARTESIAN_POINT('Ctrl Pts',(-134.999529487713,5.79889483612785,
131.18494973768));
#215828=CARTESIAN_POINT('Ctrl Pts',(-135.277977111526,3.45464471040472,
126.131303874523));
#215829=CARTESIAN_POINT('Ctrl Pts',(-135.556424735338,-2.06425513540386,
125.371968866708));
#215830=CARTESIAN_POINT('Ctrl Pts',(-135.834872359151,-5.68620535624619,
129.604736490841));
#215831=CARTESIAN_POINT('Ctrl Pts',(-136.113319982964,-4.08281064127246,
134.939900082537));
#215832=CARTESIAN_POINT('Ctrl Pts',(-136.391767606777,1.27248759664198,
136.474704938258));
#215833=CARTESIAN_POINT('Ctrl Pts',(-136.67021523059,5.45843189771781,132.798740374984));
#215834=CARTESIAN_POINT('Ctrl Pts',(-136.948662854403,4.62834394401342,
127.290038245509));
#215835=CARTESIAN_POINT('Ctrl Pts',(-137.227110478216,-0.454965987067202,
125.010826691762));
#215836=CARTESIAN_POINT('Ctrl Pts',(-137.505558102029,-5.12018440235748,
128.055589785961));
#215837=CARTESIAN_POINT('Ctrl Pts',(-137.784005725841,-5.0802034867949,
133.626338989485));
#215838=CARTESIAN_POINT('Ctrl Pts',(-138.062453349655,-0.371763748605222,
136.603827930521));
#215839=CARTESIAN_POINT('Ctrl Pts',(-138.340900973467,4.67830871288359,
134.251889730681));
#215840=CARTESIAN_POINT('Ctrl Pts',(-138.61934859728,5.42924401531914,128.731840697047));
#215841=CARTESIAN_POINT('Ctrl Pts',(-138.897796221093,1.19096930099152,
125.116336222143));
#215842=CARTESIAN_POINT('Ctrl Pts',(-139.176243844906,-4.14174801886209,
126.727848291193));
#215843=CARTESIAN_POINT('Ctrl Pts',(-139.454691468719,-5.66840124502105,
132.085476039479));
#215844=CARTESIAN_POINT('Ctrl Pts',(-139.733139092532,-1.98607064380098,
136.265821300996));
#215845=CARTESIAN_POINT('Ctrl Pts',(-140.011586716345,3.52136185412693,
135.427351001626));
#215846=CARTESIAN_POINT('Ctrl Pts',(-140.290034340158,5.79283483620279,
130.340578384942));
#215847=CARTESIAN_POINT('Ctrl Pts',(-140.56848196397,2.7409755995222,125.679998983016));
#215848=CARTESIAN_POINT('Ctrl Pts',(-140.846929587784,-2.82970630901691,
125.72845758426));
#215849=CARTESIAN_POINT('Ctrl Pts',(-141.125377211596,-5.80002635840773,
130.441423101462));
#215850=CARTESIAN_POINT('Ctrl Pts',(-141.403824835409,-3.44040553146196,
135.487910465481));
#215851=CARTESIAN_POINT('Ctrl Pts',(-141.682272459222,2.08077990574355,
136.230444323395));
#215852=CARTESIAN_POINT('Ctrl Pts',(-141.960720083035,5.68983026132012,
131.986672334579));
#215853=CARTESIAN_POINT('Ctrl Pts',(-142.239167706848,4.07020457040501,
126.656413636965));
#215854=CARTESIAN_POINT('Ctrl Pts',(-142.517615330661,-1.289740280165,125.137915576048));
#215855=CARTESIAN_POINT('Ctrl Pts',(-142.796062954474,-5.46447682057862,
128.826603687055));
#215856=CARTESIAN_POINT('Ctrl Pts',(-143.074510578287,-4.61762611741445,
134.332753798405));
#215857=CARTESIAN_POINT('Ctrl Pts',(-143.352958202099,0.472597404077474,
136.596482948152));
#215858=CARTESIAN_POINT('Ctrl Pts',(-143.631405825913,5.12852699888841,
133.537534636997));
#215859=CARTESIAN_POINT('Ctrl Pts',(-143.909853449725,5.07159082419343,
127.966932924958));
#215860=CARTESIAN_POINT('Ctrl Pts',(-144.188301073538,0.354110443050382,
125.003788646376));
#215861=CARTESIAN_POINT('Ctrl Pts',(-144.466748697351,-4.6887801359991,
127.371086635623));
#215862=CARTESIAN_POINT('Ctrl Pts',(-144.745196321164,-5.4229108297093,
132.893395689516));
#215863=CARTESIAN_POINT('Ctrl Pts',(-145.023643944977,-1.17365139483885,
136.495983567324));
#215864=CARTESIAN_POINT('Ctrl Pts',(-145.30209156879,4.15413633583088,134.868248005541));
#215865=CARTESIAN_POINT('Ctrl Pts',(-145.580539192603,5.66447571471356,
129.505998466145));
#215866=CARTESIAN_POINT('Ctrl Pts',(-145.858986816416,1.96943863679757,
125.336880315387));
#215867=CARTESIAN_POINT('Ctrl Pts',(-146.137434440228,-3.53541633590941,
126.192109461069));
#215868=CARTESIAN_POINT('Ctrl Pts',(-146.415882064041,-5.79139641060527,
131.285772098575));
#215869=CARTESIAN_POINT('Ctrl Pts',(-146.694329687854,-2.72536610939861,
135.937041103293));
#215870=CARTESIAN_POINT('Ctrl Pts',(-146.972777311667,2.84514250480927,
135.871627487008));
#215871=CARTESIAN_POINT('Ctrl Pts',(-147.25122493548,5.80110415003576,131.149643167454));
#215872=CARTESIAN_POINT('Ctrl Pts',(-147.529672559293,3.42613448107249,
126.110361052543));
#215873=CARTESIAN_POINT('Ctrl Pts',(-147.808120183106,-2.09728540002206,
125.38463522326));
#215874=CARTESIAN_POINT('Ctrl Pts',(-148.086567806919,-5.69340245658434,
129.639372263039));
#215875=CARTESIAN_POINT('Ctrl Pts',(-148.365015430732,-4.05756079371773,
134.964676687782));
#215876=CARTESIAN_POINT('Ctrl Pts',(-148.643463054544,1.30698101571045,
136.466853886735));
#215877=CARTESIAN_POINT('Ctrl Pts',(-148.921910678358,5.47047112127328,
132.765476399497));
#215878=CARTESIAN_POINT('Ctrl Pts',(-149.20035830217,4.60686551375719,127.261929314495));
#215879=CARTESIAN_POINT('Ctrl Pts',(-149.478805925983,-0.49022444300932,
125.013703539625));
#215880=CARTESIAN_POINT('Ctrl Pts',(-149.757253549796,-5.13682208544599,
128.086808730058));
#215881=CARTESIAN_POINT('Ctrl Pts',(-150.035701173609,-5.06293117906749,
133.657211345319));
#215882=CARTESIAN_POINT('Ctrl Pts',(-150.314148797422,-0.336453857064764,
136.605983511281));
#215883=CARTESIAN_POINT('Ctrl Pts',(-150.592596421235,4.69920812289605,
134.223347662954));
#215884=CARTESIAN_POINT('Ctrl Pts',(-150.871044045047,5.41652740699458,
128.698829746717));
#215885=CARTESIAN_POINT('Ctrl Pts',(-151.14949166886,1.15632261613933,125.109191839888));
#215886=CARTESIAN_POINT('Ctrl Pts',(-151.427939292673,-4.1664861694474,
126.753135815284));
#215887=CARTESIAN_POINT('Ctrl Pts',(-151.706386916486,-5.66049770947745,
132.119957470642));
#215888=CARTESIAN_POINT('Ctrl Pts',(-151.984834540299,-1.95278838518384,
136.277809888502));
#215889=CARTESIAN_POINT('Ctrl Pts',(-152.263282164112,3.54943806607717,
135.405829819234));
#215890=CARTESIAN_POINT('Ctrl Pts',(-152.541729787925,5.78990433430307,
130.3053243479));
#215891=CARTESIAN_POINT('Ctrl Pts',(-152.820177411738,2.70973137185537,
125.663408829112));
#215892=CARTESIAN_POINT('Ctrl Pts',(-153.09862503555,-2.86055234359039,
125.745776854456));
#215893=CARTESIAN_POINT('Ctrl Pts',(-153.377072659364,-5.80212820102742,
130.476736232542));
#215894=CARTESIAN_POINT('Ctrl Pts',(-153.655520283176,-3.41183169144105,
135.508766415124));
#215895=CARTESIAN_POINT('Ctrl Pts',(-153.933967906989,2.1137714653355,136.21767749275));
#215896=CARTESIAN_POINT('Ctrl Pts',(-154.212415530802,5.69692190894542,
131.952014817313));
#215897=CARTESIAN_POINT('Ctrl Pts',(-154.490863154615,4.04487942834225,
126.631713998332));
#215898=CARTESIAN_POINT('Ctrl Pts',(-154.769310778428,-1.32420964356211,
125.145871577308));
#215899=CARTESIAN_POINT('Ctrl Pts',(-155.047758402241,-5.47641474427016,
128.859904151722));
#215900=CARTESIAN_POINT('Ctrl Pts',(-155.326206026054,-4.59606223272787,
134.360797226267));
#215901=CARTESIAN_POINT('Ctrl Pts',(-155.604653649866,0.507846940569522,
136.593498799002));
#215902=CARTESIAN_POINT('Ctrl Pts',(-155.88310127368,5.14506958518534,133.50626519812));
#215903=CARTESIAN_POINT('Ctrl Pts',(-156.161548897493,5.05422463163864,
127.936113283085));
#215904=CARTESIAN_POINT('Ctrl Pts',(-156.439996521305,0.318794154216047,
125.001740546765));
#215905=CARTESIAN_POINT('Ctrl Pts',(-156.718444145118,-4.70959257697085,
127.399692181761));
#215906=CARTESIAN_POINT('Ctrl Pts',(-156.996891768931,-5.41009380630968,
132.926367781962));
#215907=CARTESIAN_POINT('Ctrl Pts',(-157.275339392744,-1.1389831254257,
136.503022463895));
#215908=CARTESIAN_POINT('Ctrl Pts',(-157.553787016557,4.17879740530553,
134.84288530416));
#215909=CARTESIAN_POINT('Ctrl Pts',(-157.83223464037,5.65646726616335,129.471541250343));
#215910=CARTESIAN_POINT('Ctrl Pts',(-158.110682264183,1.93612004320555,
125.324993083158));
#215911=CARTESIAN_POINT('Ctrl Pts',(-158.389129887996,-3.56342691473634,
126.213715998108));
#215912=CARTESIAN_POINT('Ctrl Pts',(-158.667577511808,-5.78835862111754,
131.321017052882));
#215913=CARTESIAN_POINT('Ctrl Pts',(-158.946025135621,-2.69407153173119,
135.95353608367));
#215914=CARTESIAN_POINT('Ctrl Pts',(-159.224472759434,2.87593568260513,
135.854214412314));
#215915=CARTESIAN_POINT('Ctrl Pts',(-159.502920383247,5.80309850189603,
131.114323802656));
#215916=CARTESIAN_POINT('Ctrl Pts',(-159.78136800706,3.39749729506709,126.089592168444));
#215917=CARTESIAN_POINT('Ctrl Pts',(-160.059815630873,-2.13023794895846,
125.39750240973));
#215918=CARTESIAN_POINT('Ctrl Pts',(-160.338263254686,-5.70038858580074,
129.674051204309));
#215919=CARTESIAN_POINT('Ctrl Pts',(-160.616710878499,-4.03216059175559,
134.989299130986));
#215920=CARTESIAN_POINT('Ctrl Pts',(-160.895158502312,1.34142600411673,
136.458793009441));
#215921=CARTESIAN_POINT('Ctrl Pts',(-161.173606126125,5.48230763450959,
132.732139754142));
#215922=CARTESIAN_POINT('Ctrl Pts',(-161.452053749937,4.58521637440516,
127.233951649575));
#215923=CARTESIAN_POINT('Ctrl Pts',(-161.730501373751,-0.525464733504406,
125.016794962416));
#215924=CARTESIAN_POINT('Ctrl Pts',(-162.008948997563,-5.15326942170307,
128.118128374039));
#215925=CARTESIAN_POINT('Ctrl Pts',(-162.287396621376,-5.04547126256333,
133.687977987722));
#215926=CARTESIAN_POINT('Ctrl Pts',(-162.565844245189,-0.301131498102361,
136.607924110772));
#215927=CARTESIAN_POINT('Ctrl Pts',(-162.844291869002,4.71993340202341,
134.194678903404));
#215928=CARTESIAN_POINT('Ctrl Pts',(-163.122739492814,5.40361008725504,
128.665896817606));
#215929=CARTESIAN_POINT('Ctrl Pts',(-163.401187116628,1.12163308332736,
125.102258494207));
#215930=CARTESIAN_POINT('Ctrl Pts',(-163.67963474044,-4.19106992935549,
126.778573459));
#215931=CARTESIAN_POINT('Ctrl Pts',(-163.958082364253,-5.65238442210956,
132.154390151878));
#215932=CARTESIAN_POINT('Ctrl Pts',(-164.236529988066,-1.91943376527495,
136.289595655332));
#215933=CARTESIAN_POINT('Ctrl Pts',(-164.514977611879,3.57738275229458,
135.384138127707));
#215934=CARTESIAN_POINT('Ctrl Pts',(-164.793425235692,5.78675928536899,
130.270088802833));
#215935=CARTESIAN_POINT('Ctrl Pts',(-165.071872859505,2.67838673409632,
125.647009175068));
#215936=CARTESIAN_POINT('Ctrl Pts',(-165.350320483318,-2.89129237934434,
125.763283572333));
#215937=CARTESIAN_POINT('Ctrl Pts',(-165.628768107131,-5.80401504365309,
130.512061503863));
#215938=CARTESIAN_POINT('Ctrl Pts',(-165.907215730944,-3.38313142474212,
135.52944804128));
#215939=CARTESIAN_POINT('Ctrl Pts',(-166.185663354757,2.14668469834846,
136.204710069657));
#215940=CARTESIAN_POINT('Ctrl Pts',(-166.464110978569,5.70380245503433,
131.917314773299));
#215941=CARTESIAN_POINT('Ctrl Pts',(-166.742558602383,4.01940440178476,
126.607168978656));
#215942=CARTESIAN_POINT('Ctrl Pts',(-167.021006226195,-1.3586299378839,
125.15403725596));
#215943=CARTESIAN_POINT('Ctrl Pts',(-167.299453850008,-5.48814973739939,
128.893276668938));
#215944=CARTESIAN_POINT('Ctrl Pts',(-167.577901473821,-4.57432803926507,
134.388708869063));
#215945=CARTESIAN_POINT('Ctrl Pts',(-167.856349097634,0.543077658606429,
136.590300131209));
#215946=CARTESIAN_POINT('Ctrl Pts',(-168.134796721447,5.16142151903669,
133.474895639175));
#215947=CARTESIAN_POINT('Ctrl Pts',(-168.413244345259,5.03667115293141,
127.905399925171));
#215948=CARTESIAN_POINT('Ctrl Pts',(-168.691691969073,0.283466052347084,
124.999907465374));
#215949=CARTESIAN_POINT('Ctrl Pts',(-168.970139592885,-4.7302305022577,
127.42842388914));
#215950=CARTESIAN_POINT('Ctrl Pts',(-169.248587216698,-5.39707630989451,
132.959261242652));
#215951=CARTESIAN_POINT('Ctrl Pts',(-169.527034840511,-1.10427265057399,
136.509850194457));
#215952=CARTESIAN_POINT('Ctrl Pts',(-169.805482464324,4.20330362790601,
134.81737295376));
#215953=CARTESIAN_POINT('Ctrl Pts',(-170.083930088137,5.6482492151383,129.437133422652));
#215954=CARTESIAN_POINT('Ctrl Pts',(-170.36237771195,1.90272970597286,125.313308890908));
#215955=CARTESIAN_POINT('Ctrl Pts',(-170.640825335763,-3.59130544946847,
126.235492643171));
#215956=CARTESIAN_POINT('Ctrl Pts',(-170.919272959575,-5.78510634187241,
131.356242862295));
#215957=CARTESIAN_POINT('Ctrl Pts',(-171.197720583389,-2.66267712425244,
135.969840259458));
#215958=CARTESIAN_POINT('Ctrl Pts',(-171.476168207202,2.90662229154664,
135.836614213432));
#215959=CARTESIAN_POINT('Ctrl Pts',(-171.754615831014,5.80487781780722,
131.07899295206));
#215960=CARTESIAN_POINT('Ctrl Pts',(-172.033063454828,3.36873421355001,
126.068997991823));
#215961=CARTESIAN_POINT('Ctrl Pts',(-172.31151107864,-2.16311156114431,
125.410569949319));
#215962=CARTESIAN_POINT('Ctrl Pts',(-172.589958702453,-5.70716348502144,
129.70877202961));
#215963=CARTESIAN_POINT('Ctrl Pts',(-172.868406326266,-4.00661097660031,
135.013766499754));
#215964=CARTESIAN_POINT('Ctrl Pts',(-173.146853950079,1.3758212854888,136.450522605077));
#215965=CARTESIAN_POINT('Ctrl Pts',(-173.425301573892,5.49394099882038,
132.698731674224));
#215966=CARTESIAN_POINT('Ctrl Pts',(-173.703749197705,4.56339732817417,
127.206106287473));
#215967=CARTESIAN_POINT('Ctrl Pts',(-173.982196821517,-0.560685552710569,
125.02010084558));
#215968=CARTESIAN_POINT('Ctrl Pts',(-174.260644445331,-5.1695258016666,
128.149547557344));
#215969=CARTESIAN_POINT('Ctrl Pts',(-174.539092069143,-5.02782438426607,
133.718637776622));
#215970=CARTESIAN_POINT('Ctrl Pts',(-174.817539692956,-0.265797980601551,
136.609649657082));
#215971=CARTESIAN_POINT('Ctrl Pts',(-175.095987316769,4.74048378228282,
134.165884514362));
#215972=CARTESIAN_POINT('Ctrl Pts',(-175.374434940582,5.39049253475655,
128.633043130058));
#215973=CARTESIAN_POINT('Ctrl Pts',(-175.652882564395,1.08690198798901,
125.095536442018));
#215974=CARTESIAN_POINT('Ctrl Pts',(-175.931330188208,-4.21549838762608,
126.80416027974));
#215975=CARTESIAN_POINT('Ctrl Pts',(-176.209777812021,-5.64406168355824,
132.188772807274));
#215976=CARTESIAN_POINT('Ctrl Pts',(-176.488225435833,-1.886008020042,136.301178164761));
#215977=CARTESIAN_POINT('Ctrl Pts',(-176.766673059646,3.60519487727851,
135.362276730843));
#215978=CARTESIAN_POINT('Ctrl Pts',(-177.045120683459,5.78339980594152,
130.234873055403));
#215979=CARTESIAN_POINT('Ctrl Pts',(-177.323568307272,2.64694284773159,
125.630800628577));
#215980=CARTESIAN_POINT('Ctrl Pts',(-177.602015931085,-2.92192527719638,
125.780977089175));
#215981=CARTESIAN_POINT('Ctrl Pts',(-177.880463554898,-5.80568681636668,
130.547397606436));
#215982=CARTESIAN_POINT('Ctrl Pts',(-178.158911178711,-3.35430579486411,
135.549954577584));
#215983=CARTESIAN_POINT('Ctrl Pts',(-178.437358802524,2.17951838517049,
136.191542534628));
#215984=CARTESIAN_POINT('Ctrl Pts',(-178.715806426336,5.71047164462571,
131.88257348836));
#215985=CARTESIAN_POINT('Ctrl Pts',(-178.99425405015,3.99378043471903,126.582779487459));
#215986=CARTESIAN_POINT('Ctrl Pts',(-179.272701673962,-1.39299988767372,
125.162412309422));
#215987=CARTESIAN_POINT('Ctrl Pts',(-179.551149297775,-5.49968136512185,
128.926720002072));
#215988=CARTESIAN_POINT('Ctrl Pts',(-179.829596921588,-4.55242434239454,
134.416487692516));
#215989=CARTESIAN_POINT('Ctrl Pts',(-180.108044545401,0.578288252700551,
136.5868870633));
#215990=CARTESIAN_POINT('Ctrl Pts',(-180.386492169214,5.17758219451528,
133.443427122574));
#215991=CARTESIAN_POINT('Ctrl Pts',(-180.664939793027,5.01893103852278,
127.874793989312));
#215992=CARTESIAN_POINT('Ctrl Pts',(-180.94338741684,0.248127446539293,
124.998289470128));
#215993=CARTESIAN_POINT('Ctrl Pts',(-181.221835040653,-4.75069314711374,
127.457280693096));
#215994=CARTESIAN_POINT('Ctrl Pts',(-181.500282664465,-5.38385882283189,
132.992074852706));
#215995=CARTESIAN_POINT('Ctrl Pts',(-181.778730288279,-1.06952125649312,
136.516466506004));
#215996=CARTESIAN_POINT('Ctrl Pts',(-182.057177912091,4.22765409554481,
134.791711899713));
#215997=CARTESIAN_POINT('Ctrl Pts',(-182.335625535904,5.63982186616143,
129.402776258069));
#215998=CARTESIAN_POINT('Ctrl Pts',(-182.614073159717,1.86926886239121,
125.301828171599));
#215999=CARTESIAN_POINT('Ctrl Pts',(-182.89252078353,-3.61905090705647,
126.257438589318));
#216000=CARTESIAN_POINT('Ctrl Pts',(-183.170968407343,-5.78163969338434,
131.391448221508));
#216001=CARTESIAN_POINT('Ctrl Pts',(-183.449416031155,-2.63118405029363,
135.985953026497));
#216002=CARTESIAN_POINT('Ctrl Pts',(-183.727863654969,2.93720119453022,
135.818827542541));
#216003=CARTESIAN_POINT('Ctrl Pts',(-184.006311278781,5.80644203183612,
131.04365192486));
#216004=CARTESIAN_POINT('Ctrl Pts',(-184.284758902595,3.33984630234777,
126.048579285806));
#216005=CARTESIAN_POINT('Ctrl Pts',(-184.563206526407,-2.19590501843575,
125.423837357804));
#216006=CARTESIAN_POINT('Ctrl Pts',(-184.84165415022,-5.71372690320071,
129.743533452349));
#216007=CARTESIAN_POINT('Ctrl Pts',(-185.120101774033,-3.98091289500146,
135.03807788744));
#216008=CARTESIAN_POINT('Ctrl Pts',(-185.398549397846,1.41016558529749,
136.442042980103));
#216009=CARTESIAN_POINT('Ctrl Pts',(-185.676997021659,5.50537078312707,
132.665253397689));
#216010=CARTESIAN_POINT('Ctrl Pts',(-185.955444645472,4.54140918357699,
127.178394260007));
#216011=CARTESIAN_POINT('Ctrl Pts',(-186.233892269285,-0.595885595507362,
125.023621066618));
#216012=CARTESIAN_POINT('Ctrl Pts',(-186.512339893098,-5.18559062295048,
128.181065115723));
#216013=CARTESIAN_POINT('Ctrl Pts',(-186.79078751691,-5.00999119808726,
133.749189575911));
#216014=CARTESIAN_POINT('Ctrl Pts',(-187.069235140724,-0.230454613858838,
136.611160086272));
#216015=CARTESIAN_POINT('Ctrl Pts',(-187.347682764536,4.76085850217237,
134.136965562817));
#216016=CARTESIAN_POINT('Ctrl Pts',(-187.626130388349,5.37717523557474,
128.600269901479));
#216017=CARTESIAN_POINT('Ctrl Pts',(-187.904578012162,1.05213061709833,
125.089025932407));
#216018=CARTESIAN_POINT('Ctrl Pts',(-188.183025635975,-4.23977063905356,
126.829895329374));
#216019=CARTESIAN_POINT('Ctrl Pts',(-188.461473259788,-5.63552980222562,
132.223104162766));
#216020=CARTESIAN_POINT('Ctrl Pts',(-188.739920883601,-1.85251238808831,
136.312556987595));
#216021=CARTESIAN_POINT('Ctrl Pts',(-189.018368507414,3.63287341044046,
135.340246438718));
#216022=CARTESIAN_POINT('Ctrl Pts',(-189.296816131227,5.77982602050738,
130.199678410544));
#216023=CARTESIAN_POINT('Ctrl Pts',(-189.575263755039,2.61540087792624,
125.614783790254));
#216024=CARTESIAN_POINT('Ctrl Pts',(-189.853711378852,-2.95244990203274,
125.798856749341));
#216025=CARTESIAN_POINT('Ctrl Pts',(-190.132159002665,-5.80714345722022,
130.582743230867));
#216026=CARTESIAN_POINT('Ctrl Pts',(-190.410606626478,-3.32535586995153,
135.570285264159));
#216027=CARTESIAN_POINT('Ctrl Pts',(-190.689054250291,2.21227130913674,
136.178175375592));
#216028=CARTESIAN_POINT('Ctrl Pts',(-190.967501874104,5.7169292305904,131.847792249846));
#216029=CARTESIAN_POINT('Ctrl Pts',(-191.245949497917,3.96800847665057,
126.558546428502));
#216030=CARTESIAN_POINT('Ctrl Pts',(-191.52439712173,-1.4273182193404,125.170996427354));
#216031=CARTESIAN_POINT('Ctrl Pts',(-191.802844745543,-5.51100920012879,
128.960232911869));
#216032=CARTESIAN_POINT('Ctrl Pts',(-192.081292369355,-4.53035195376586,
134.444132667273));
#216033=CARTESIAN_POINT('Ctrl Pts',(-192.359739993168,0.613477418111232,
136.583259721745));
#216034=CARTESIAN_POINT('Ctrl Pts',(-192.638187616981,5.19355101278185,
133.411860814392));
#216035=CARTESIAN_POINT('Ctrl Pts',(-192.916635240794,5.00100494577841,
127.844296609621));
#216036=CARTESIAN_POINT('Ctrl Pts',(-193.195082864607,0.21277964627773,
124.996886620986));
#216037=CARTESIAN_POINT('Ctrl Pts',(-193.47353048842,-4.77097975328813,
127.486261524329));
#216038=CARTESIAN_POINT('Ctrl Pts',(-193.751978112233,-5.3704418349007,
133.024807396204));
#216039=CARTESIAN_POINT('Ctrl Pts',(-194.030425736046,-1.03473023090876,
136.522871153366));
#216040=CARTESIAN_POINT('Ctrl Pts',(-194.308873359859,4.25184790590635,
134.765903092897));
#216041=CARTESIAN_POINT('Ctrl Pts',(-194.587320983671,5.63118553151129,
129.368471029708));
#216042=CARTESIAN_POINT('Ctrl Pts',(-194.865768607484,1.83573875236439,
125.290551350653));
#216043=CARTESIAN_POINT('Ctrl Pts',(-195.144216231297,-3.64666225938173,
126.279553023333));
#216044=CARTESIAN_POINT('Ctrl Pts',(-195.42266385511,-5.77795880411129,
131.426631825972));
#216045=CARTESIAN_POINT('Ctrl Pts',(-195.701111478923,-2.59959347684268,
136.001873787725));
#216046=CARTESIAN_POINT('Ctrl Pts',(-195.979559102736,2.96767125844341,
135.800855058734));
#216047=CARTESIAN_POINT('Ctrl Pts',(-196.258006726549,5.80779108602021,
131.008302030633));
#216048=CARTESIAN_POINT('Ctrl Pts',(-196.536454350362,3.31083463191258,
126.028336807015));
#216049=CARTESIAN_POINT('Ctrl Pts',(-196.814901974175,-2.22861710565919,
125.437304143558));
#216050=CARTESIAN_POINT('Ctrl Pts',(-197.093349597988,-5.72007859712835,
129.778334184429));
#216051=CARTESIAN_POINT('Ctrl Pts',(-197.3717972218,-3.95506729921131,135.062232393175));
#216052=CARTESIAN_POINT('Ctrl Pts',(-197.650244845613,1.44445763090186,
136.433354448736));
#216053=CARTESIAN_POINT('Ctrl Pts',(-197.928692469426,5.51659656389443,
132.631706165088));
#216054=CARTESIAN_POINT('Ctrl Pts',(-198.207140093239,4.51925275539276,
127.150816594059));
#216055=CARTESIAN_POINT('Ctrl Pts',(-198.485587717052,-0.631063557543924,
125.027355495085));
#216056=CARTESIAN_POINT('Ctrl Pts',(-198.764035340865,-5.2014632902668,
128.212679881281));
#216057=CARTESIAN_POINT('Ctrl Pts',(-199.042482964678,-4.99197236484219,
133.779632253479));
#216058=CARTESIAN_POINT('Ctrl Pts',(-199.320930588491,-0.19510270753564,
136.612455342372));
#216059=CARTESIAN_POINT('Ctrl Pts',(-199.599378212304,4.7810568066993,134.10792312037));
#216060=CARTESIAN_POINT('Ctrl Pts',(-199.877825836116,5.36365868318719,
128.56757834629));
#216061=CARTESIAN_POINT('Ctrl Pts',(-200.156273459929,1.01732025912016,
125.082727206624));
#216062=CARTESIAN_POINT('Ctrl Pts',(-200.434721083742,-4.26388578422093,
126.855777654281));
#216063=CARTESIAN_POINT('Ctrl Pts',(-200.713168707555,-5.62678909426374,
132.257382946195));
#216064=CARTESIAN_POINT('Ctrl Pts',(-200.991616331368,-1.8189481106068,
136.323731702186));
#216065=CARTESIAN_POINT('Ctrl Pts',(-201.270063955181,3.66041732614217,
135.318048067677));
#216066=CARTESIAN_POINT('Ctrl Pts',(-201.548511578994,5.77603806149454,
130.164506172408));
#216067=CARTESIAN_POINT('Ctrl Pts',(-201.826959202806,2.58376199347953,
125.59895925361));
#216068=CARTESIAN_POINT('Ctrl Pts',(-202.10540682662,-2.9828651227522,125.816921890294));
#216069=CARTESIAN_POINT('Ctrl Pts',(-202.383854450432,-5.80838491223743,
130.618097067413));
#216070=CARTESIAN_POINT('Ctrl Pts',(-202.662302074245,-3.29628272275406,
135.590439347642));
#216071=CARTESIAN_POINT('Ctrl Pts',(-202.940749698058,2.24494225657654,
136.164609087875));
#216072=CARTESIAN_POINT('Ctrl Pts',(-203.219197321871,5.72317497363993,
131.812972346589));
#216073=CARTESIAN_POINT('Ctrl Pts',(-203.497644945684,3.94208948256877,
126.534470699752));
#216074=CARTESIAN_POINT('Ctrl Pts',(-203.776092569497,-1.46158366120557,
125.179789291667));
#216075=CARTESIAN_POINT('Ctrl Pts',(-204.05454019331,-5.52213282266317,
128.993814156497));
#216076=CARTESIAN_POINT('Ctrl Pts',(-204.332987817123,-4.5081116912795,
134.471642768938));
#216077=CARTESIAN_POINT('Ctrl Pts',(-204.611435440935,0.648643850890564,
136.579418240959));
#216078=CARTESIAN_POINT('Ctrl Pts',(-204.889883064748,5.20932738210573,
133.380197884332));
#216079=CARTESIAN_POINT('Ctrl Pts',(-205.168330688562,4.98289353895661,
127.813908916192));
#216080=CARTESIAN_POINT('Ctrl Pts',(-205.446778312374,0.177423961388546,
124.995698969927));
#216081=CARTESIAN_POINT('Ctrl Pts',(-205.725225936187,-4.79108956905296,
127.515365308944));
#216082=CARTESIAN_POINT('Ctrl Pts',(-206.00367356,-5.35682584327266,133.057457660231));
#216083=CARTESIAN_POINT('Ctrl Pts',(-206.282121183813,-0.999900863015179,
136.529063899218));
#216084=CARTESIAN_POINT('Ctrl Pts',(-206.560568807626,4.27588416248015,
134.739947489669));
#216085=CARTESIAN_POINT('Ctrl Pts',(-206.839016431439,5.62234053121038,
129.334219008764));
#216086=CARTESIAN_POINT('Ctrl Pts',(-207.117464055252,1.80214061836306,
125.279478845937));
#216087=CARTESIAN_POINT('Ctrl Pts',(-207.395911679064,-3.67413848329639,
126.301835125757));
#216088=CARTESIAN_POINT('Ctrl Pts',(-207.674359302878,-5.77406381044983,
131.461792371951));
#216089=CARTESIAN_POINT('Ctrl Pts',(-207.95280692669,-2.56790657449899,
136.01760195319));
#216090=CARTESIAN_POINT('Ctrl Pts',(-208.231254550503,2.99803135420673,
135.782697427989));
#216091=CARTESIAN_POINT('Ctrl Pts',(-208.509702174316,5.8089249303698,130.972944579282));
#216092=CARTESIAN_POINT('Ctrl Pts',(-208.788149798129,3.28170027728254,
126.008271305542));
#216093=CARTESIAN_POINT('Ctrl Pts',(-209.066597421942,-2.2612466106562,
125.450969807563));
#216094=CARTESIAN_POINT('Ctrl Pts',(-209.345045045754,-5.72621833144002,
129.813172936296));
#216095=CARTESIAN_POINT('Ctrl Pts',(-209.623492669568,-3.92907514694791,
135.086229121905));
#216096=CARTESIAN_POINT('Ctrl Pts',(-209.90194029338,1.4786961515975,136.424457332932));
#216097=CARTESIAN_POINT('Ctrl Pts',(-210.180387917194,5.52761792514773,
132.598091219525));
#216098=CARTESIAN_POINT('Ctrl Pts',(-210.458835541006,4.49692886463537,
127.123374311529));
#216099=CARTESIAN_POINT('Ctrl Pts',(-210.73728316482,-0.666218135288655,
125.031303992602));
#216100=CARTESIAN_POINT('Ctrl Pts',(-211.015730788632,-5.21714321544808,
128.244390682522));
#216101=CARTESIAN_POINT('Ctrl Pts',(-211.294178412445,-4.97376855222533,
133.809964681263));
#216102=CARTESIAN_POINT('Ctrl Pts',(-211.572626036258,-0.159743571609885,
136.613535377387));
#216103=CARTESIAN_POINT('Ctrl Pts',(-211.851073660071,4.80107794740803,
134.0787582632));
#216104=CARTESIAN_POINT('Ctrl Pts',(-212.129521283884,5.34994337845465,
128.534969675892));
#216105=CARTESIAN_POINT('Ctrl Pts',(-212.407968907697,0.982472203965689,
125.076640498072));
#216106=CARTESIAN_POINT('Ctrl Pts',(-212.686416531509,-4.28784292953254,
126.881806295382));
#216107=CARTESIAN_POINT('Ctrl Pts',(-212.964864155322,-5.61783988356258,
132.291607887347));
#216108=CARTESIAN_POINT('Ctrl Pts',(-213.243311779135,-1.78531643133465,
136.334701894451));
#216109=CARTESIAN_POINT('Ctrl Pts',(-213.521759402948,3.68782560373359,
135.295682440288));
#216110=CARTESIAN_POINT('Ctrl Pts',(-213.800207026761,5.77203606926717,
130.129357644311));
#216111=CARTESIAN_POINT('Ctrl Pts',(-214.078654650574,2.55202736678199,
125.583327605028));
#216112=CARTESIAN_POINT('Ctrl Pts',(-214.357102274386,-3.0131698123076,
125.835171842623));
#216113=CARTESIAN_POINT('Ctrl Pts',(-214.6355498982,-5.80941113541564,130.653457806023));
#216114=CARTESIAN_POINT('Ctrl Pts',(-214.913997522012,-3.26708743058812,
135.610416081219));
#216115=CARTESIAN_POINT('Ctrl Pts',(-215.192445145826,2.27753001685547,
136.15084417418));
#216116=CARTESIAN_POINT('Ctrl Pts',(-215.470892769638,5.72920864233609,
131.778115068854));
#216117=CARTESIAN_POINT('Ctrl Pts',(-215.749340393451,3.9160244129115,126.510553193344));
#216118=CARTESIAN_POINT('Ctrl Pts',(-216.027788017264,-1.49579494355069,
125.18879057654));
#216119=CARTESIAN_POINT('Ctrl Pts',(-216.306235641077,-5.53305182053502,
129.02746249159));
#216120=CARTESIAN_POINT('Ctrl Pts',(-216.58468326489,-4.48570437905656,
134.499016978113));
#216121=CARTESIAN_POINT('Ctrl Pts',(-216.863130888703,0.683786247933482,
136.57536276329));
#216122=CARTESIAN_POINT('Ctrl Pts',(-217.141578512516,5.2249107178877,133.348439505674));
#216123=CARTESIAN_POINT('Ctrl Pts',(-217.420026136328,4.96459748918233,
127.78363203505));
#216124=CARTESIAN_POINT('Ctrl Pts',(-217.698473760142,0.142061701988793,
124.994726560962));
#216125=CARTESIAN_POINT('Ctrl Pts',(-217.976921383954,-4.81102184923216,
127.544590968491));
#216126=CARTESIAN_POINT('Ctrl Pts',(-218.255369007768,-5.34301135249269,
133.090024434919));
#216127=CARTESIAN_POINT('Ctrl Pts',(-218.53381663158,-0.965034443427401,
136.535044514085));
#216128=CARTESIAN_POINT('Ctrl Pts',(-218.812264255394,4.29976197459382,
134.713846051821));
#216129=CARTESIAN_POINT('Ctrl Pts',(-219.090711879206,5.61328719301349,
129.300021464458));
#216130=CARTESIAN_POINT('Ctrl Pts',(-219.369159503019,1.76847570537835,
125.268611067748));
#216131=CARTESIAN_POINT('Ctrl Pts',(-219.647607126831,-3.70147856065836,
126.324284070919));
#216132=CARTESIAN_POINT('Ctrl Pts',(-219.926054750645,-5.76995485673049,
131.496928556552));
#216133=CARTESIAN_POINT('Ctrl Pts',(-220.204502374457,-2.5361245174328,
136.033136940081));
#216134=CARTESIAN_POINT('Ctrl Pts',(-220.48294999827,3.02828035681523,135.764355323142));
#216135=CARTESIAN_POINT('Ctrl Pts',(-220.761397622083,5.80984352286985,
130.937580880991));
#216136=CARTESIAN_POINT('Ctrl Pts',(-221.039845245896,3.25244431804234,
125.988383524923));
#216137=CARTESIAN_POINT('Ctrl Pts',(-221.318292869709,-2.29379232432851,
125.464833843433));
#216138=CARTESIAN_POINT('Ctrl Pts',(-221.596740493522,-5.73214587862558,
129.848048416986));
#216139=CARTESIAN_POINT('Ctrl Pts',(-221.875188117335,-3.90293740136003,
135.110067184424));
#216140=CARTESIAN_POINT('Ctrl Pts',(-222.153635741148,1.51287987866345,
136.415351962378));
#216141=CARTESIAN_POINT('Ctrl Pts',(-222.432083364961,5.53843445848603,
132.564409806615));
#216142=CARTESIAN_POINT('Ctrl Pts',(-222.710530988774,4.47443833852516,
127.0960684293));
#216143=CARTESIAN_POINT('Ctrl Pts',(-222.988978612586,-0.701348026075381,
125.035466412855));
#216144=CARTESIAN_POINT('Ctrl Pts',(-223.267426236399,-5.23262981746888,
128.27619634439));
#216145=CARTESIAN_POINT('Ctrl Pts',(-223.545873860212,-4.95538043478568,
133.840185735283));
#216146=CARTESIAN_POINT('Ctrl Pts',(-223.824321484025,-0.124378516327312,
136.614400151295));
#216147=CARTESIAN_POINT('Ctrl Pts',(-224.102769107838,4.82092118240782,
134.049472072021));
#216148=CARTESIAN_POINT('Ctrl Pts',(-224.381216731651,5.33602982960279,
128.502445098609));
#216149=CARTESIAN_POINT('Ctrl Pts',(-224.659664355464,0.947587742942381,
125.070766032295));
#216150=CARTESIAN_POINT('Ctrl Pts',(-224.938111979277,-4.31164118724753,
126.907980288176));
#216151=CARTESIAN_POINT('Ctrl Pts',(-225.216559603089,-5.60868250173869,
132.325777718005));
#216152=CARTESIAN_POINT('Ctrl Pts',(-225.495007226903,-1.75161859650508,
136.345467157888));
#216153=CARTESIAN_POINT('Ctrl Pts',(-225.773454850715,3.71509722759125,
135.273150385318));
#216154=CARTESIAN_POINT('Ctrl Pts',(-226.051902474528,5.7678201921206,130.0942341287));
#216155=CARTESIAN_POINT('Ctrl Pts',(-226.330350098341,2.52019817377184,
125.567889423742));
#216156=CARTESIAN_POINT('Ctrl Pts',(-226.608797722154,-3.04336284774751,
125.853605930069));
#216157=CARTESIAN_POINT('Ctrl Pts',(-226.887245345967,-5.81022208872781,
130.688824136393));
#216158=CARTESIAN_POINT('Ctrl Pts',(-227.16569296978,-3.23777107529596,
135.630214724643));
#216159=CARTESIAN_POINT('Ctrl Pts',(-227.444140593593,2.31003338242206,
136.13688114457));
#216160=CARTESIAN_POINT('Ctrl Pts',(-227.722588217406,5.73503001309909,
131.74322170829));
#216161=CARTESIAN_POINT('Ctrl Pts',(-228.001035841218,3.88981423352964,
126.486794795549));
#216162=CARTESIAN_POINT('Ctrl Pts',(-228.279483465031,-1.52995079866356,
125.197999948425));
#216163=CARTESIAN_POINT('Ctrl Pts',(-228.557931088844,-5.54376578913698,
129.061176670297));
#216164=CARTESIAN_POINT('Ctrl Pts',(-228.836378712657,-4.46313084740822,
134.526254280438));
#216165=CARTESIAN_POINT('Ctrl Pts',(-229.11482633647,0.718903307025501,
136.571093439014));
#216166=CARTESIAN_POINT('Ctrl Pts',(-229.393273960283,5.24030044268158,
133.316586855238));
#216167=CARTESIAN_POINT('Ctrl Pts',(-229.671721584096,4.94611747442232,
127.753467088116));
#216168=CARTESIAN_POINT('Ctrl Pts',(-229.950169207909,0.106694178440453,
124.993969430123));
#216169=CARTESIAN_POINT('Ctrl Pts',(-230.228616831722,-4.83077585522751,
127.57393742));
#216170=CARTESIAN_POINT('Ctrl Pts',(-230.507064455534,-5.32899887446215,
133.122506513493));
#216171=CARTESIAN_POINT('Ctrl Pts',(-230.785512079348,-0.930132264133436,
136.540812776352));
#216172=CARTESIAN_POINT('Ctrl Pts',(-231.06395970316,4.3234804574463,134.687599746553));
#216173=CARTESIAN_POINT('Ctrl Pts',(-231.342407326973,5.60402585239536,
129.265879663993));
#216174=CARTESIAN_POINT('Ctrl Pts',(-231.620854950786,1.73474526087603,
125.257948418793));
#216175=CARTESIAN_POINT('Ctrl Pts',(-231.899302574599,-3.72868147837107,
126.346899026965));
#216176=CARTESIAN_POINT('Ctrl Pts',(-232.177750198412,-5.76563209521201,
131.532039077795));
#216177=CARTESIAN_POINT('Ctrl Pts',(-232.456197822225,-2.50424848333998,
136.048478172742));
#216178=CARTESIAN_POINT('Ctrl Pts',(-232.734645446038,3.05841714538193,
135.745829423867));
#216179=CARTESIAN_POINT('Ctrl Pts',(-233.01309306985,5.81054682948159,130.902212246173));
#216180=CARTESIAN_POINT('Ctrl Pts',(-233.291540693664,3.22306783828139,
125.968674202107));
#216181=CARTESIAN_POINT('Ctrl Pts',(-233.569988317476,-2.32625304068266,
125.478895737432));
#216182=CARTESIAN_POINT('Ctrl Pts',(-233.84843594129,-5.73786101903762,
129.882959334177));
#216183=CARTESIAN_POINT('Ctrl Pts',(-234.126883565102,-3.87665503099142,
135.133745697402));
#216184=CARTESIAN_POINT('Ctrl Pts',(-234.405331188915,1.54700754540913,
136.406038674476));
#216185=CARTESIAN_POINT('Ctrl Pts',(-234.683778812728,5.54904576309872,
132.530663174436));
#216186=CARTESIAN_POINT('Ctrl Pts',(-234.962226436541,4.45178201045685,
127.0688999592));
#216187=CARTESIAN_POINT('Ctrl Pts',(-235.240674060353,-0.736451928153096,
125.039842601604));
#216188=CARTESIAN_POINT('Ctrl Pts',(-235.519121684167,-5.24792252246713,
128.308095688315));
#216189=CARTESIAN_POINT('Ctrl Pts',(-235.797569307979,-4.93680869390195,
133.870294295687));
#216190=CARTESIAN_POINT('Ctrl Pts',(-236.076016931792,-0.0890088521534987,
136.61504963205));
#216191=CARTESIAN_POINT('Ctrl Pts',(-236.354464555605,4.8405857764003,134.020065632043));
#216192=CARTESIAN_POINT('Ctrl Pts',(-236.632912179418,5.32191855220324,
128.470005819654));
#216193=CARTESIAN_POINT('Ctrl Pts',(-236.911359803231,0.912668168706789,
125.065104026974));
#216194=CARTESIAN_POINT('Ctrl Pts',(-237.189807427044,-4.33527967551271,
126.934298662776));
#216195=CARTESIAN_POINT('Ctrl Pts',(-237.468255050857,-5.59931728812211,
132.359891171993));
#216196=CARTESIAN_POINT('Ctrl Pts',(-237.74670267467,-1.71785585480426,
136.356027093583));
#216197=CARTESIAN_POINT('Ctrl Pts',(-238.025150298482,3.7422311871549,135.250452737698));
#216198=CARTESIAN_POINT('Ctrl Pts',(-238.303597922296,5.76339058627568,
130.059136927086));
#216199=CARTESIAN_POINT('Ctrl Pts',(-238.582045546108,2.48827559389159,
125.552645281824));
#216200=CARTESIAN_POINT('Ctrl Pts',(-238.860493169922,-3.07344311025789,
125.87222346955));
#216201=CARTESIAN_POINT('Ctrl Pts',(-239.138940793734,-5.81081774212379,
130.724194748009));
#216202=CARTESIAN_POINT('Ctrl Pts',(-239.417388417547,-3.20833474320591,
135.649834544268));
#216203=CARTESIAN_POINT('Ctrl Pts',(-239.69583604136,2.34245114885216,136.12272051645));
#216204=CARTESIAN_POINT('Ctrl Pts',(-239.974283665173,5.7406388702159,131.708293557882));
#216205=CARTESIAN_POINT('Ctrl Pts',(-240.252731288985,3.86345991565072,
126.463196386742));
#216206=CARTESIAN_POINT('Ctrl Pts',(-240.531178912799,-1.56404996088748,
125.207417066067));
#216207=CARTESIAN_POINT('Ctrl Pts',(-240.809626536611,-5.5542743314588,
129.094955443325));
#216208=CARTESIAN_POINT('Ctrl Pts',(-241.088074160425,-4.44039193280503,
134.553353666625));
#216209=CARTESIAN_POINT('Ctrl Pts',(-241.366521784237,0.753993726891117,
136.566610426332));
#216210=CARTESIAN_POINT('Ctrl Pts',(-241.64496940805,5.25549598621542,133.284641113335));
#216211=CARTESIAN_POINT('Ctrl Pts',(-241.923417031863,4.92745417946037,
127.723415193164));
#216212=CARTESIAN_POINT('Ctrl Pts',(-242.201864655676,0.071322701300089,
124.993427605467));
#216213=CARTESIAN_POINT('Ctrl Pts',(-242.480312279489,-4.85035085504701,
127.603403576029));
#216214=CARTESIAN_POINT('Ctrl Pts',(-242.758759903302,-5.31478892841856,
133.154902692318));
#216215=CARTESIAN_POINT('Ctrl Pts',(-243.037207527115,-0.895195618446729,
136.546368472274));
#216216=CARTESIAN_POINT('Ctrl Pts',(-243.315655150928,4.34703873214009,
134.661209546432));
#216217=CARTESIAN_POINT('Ctrl Pts',(-243.59410277474,5.59455685253872,129.231794872506));
#216218=CARTESIAN_POINT('Ctrl Pts',(-243.872550398553,1.7009505347501,125.247491294183));
#216219=CARTESIAN_POINT('Ctrl Pts',(-244.150998022366,-3.75574622842035,
126.36967915589));
#216220=CARTESIAN_POINT('Ctrl Pts',(-244.429445646179,-5.76109568607594,
131.567122634643));
#216221=CARTESIAN_POINT('Ctrl Pts',(-244.707893269992,-2.47227965339868,
136.063625082699));
#216222=CARTESIAN_POINT('Ctrl Pts',(-244.986340893805,3.08844060317656,
135.727120416648));
#216223=CARTESIAN_POINT('Ctrl Pts',(-245.264788517618,5.81103482414375,
130.866839985428));
#216224=CARTESIAN_POINT('Ctrl Pts',(-245.543236141431,3.1935719265564,125.949144067427));
#216225=CARTESIAN_POINT('Ctrl Pts',(-245.821683765243,-2.35862755687492,
125.49315496849));
#216226=CARTESIAN_POINT('Ctrl Pts',(-246.100131389057,-5.74336354089951,
129.917904394232));
#216227=CARTESIAN_POINT('Ctrl Pts',(-246.378579012869,-3.85022900974501,
135.157263783424));
#216228=CARTESIAN_POINT('Ctrl Pts',(-246.657026636682,1.58107788722132,
136.396517814333));
#216229=CARTESIAN_POINT('Ctrl Pts',(-246.935474260495,5.55945144577998,
132.496852573479));
#216230=CARTESIAN_POINT('Ctrl Pts',(-247.213921884308,4.42896071996899,
127.04186990797));
#216231=CARTESIAN_POINT('Ctrl Pts',(-247.492369508121,-0.77152854073377,
125.044432396689));
#216232=CARTESIAN_POINT('Ctrl Pts',(-247.770817131934,-5.26302076376676,
128.340087532256));
#216233=CARTESIAN_POINT('Ctrl Pts',(-248.049264755747,-4.91805401775627,
133.90028924679));
#216234=CARTESIAN_POINT('Ctrl Pts',(-248.32771237956,-0.0536358897235281,
136.615483795589));
#216235=CARTESIAN_POINT('Ctrl Pts',(-248.606160003372,4.86007100070672,
133.990540032933));
#216236=CARTESIAN_POINT('Ctrl Pts',(-248.884607627186,5.30761006915461,
128.437653041073));
#216237=CARTESIAN_POINT('Ctrl Pts',(-249.163055250998,0.877714775216597,
125.059654691916));
#216238=CARTESIAN_POINT('Ctrl Pts',(-249.441502874812,-4.35875751839529,
126.960760443945));
#216239=CARTESIAN_POINT('Ctrl Pts',(-249.719950498624,-5.58974458974414,
132.393946985223));
#216240=CARTESIAN_POINT('Ctrl Pts',(-249.998398122437,-1.68402945732324,
136.366381310236));
#216241=CARTESIAN_POINT('Ctrl Pts',(-250.27684574625,3.76922647696617,135.227590338499));
#216242=CARTESIAN_POINT('Ctrl Pts',(-250.555293370063,5.75874741587205,
130.024067340013));
#216243=CARTESIAN_POINT('Ctrl Pts',(-250.833740993876,2.45626081004631,
125.537595744144));
#216244=CARTESIAN_POINT('Ctrl Pts',(-251.112188617689,-3.10340948520656,
125.891023771197));
#216245=CARTESIAN_POINT('Ctrl Pts',(-251.390636241501,-5.81119807352532,
130.759568330183));
#216246=CARTESIAN_POINT('Ctrl Pts',(-251.669083865314,-3.17877952510356,
135.669274813107));
#216247=CARTESIAN_POINT('Ctrl Pts',(-251.947531489127,2.37478211491517,
136.10836281449));
#216248=CARTESIAN_POINT('Ctrl Pts',(-252.22597911294,5.74603500580729,131.673331912019));
#216249=CARTESIAN_POINT('Ctrl Pts',(-252.504426736753,3.83696243592119,
126.439758841162));
#216250=CARTESIAN_POINT('Ctrl Pts',(-252.782874360566,-1.59809116681098,
125.217041580908));
#216251=CARTESIAN_POINT('Ctrl Pts',(-253.061321984379,-5.5645770578269,
129.128797558239));
#216252=CARTESIAN_POINT('Ctrl Pts',(-253.339769608192,-4.41748847836656,
134.580314133917));
#216253=CARTESIAN_POINT('Ctrl Pts',(-253.618217232004,0.789056208225191,
136.561913888683));
#216254=CARTESIAN_POINT('Ctrl Pts',(-253.896664855818,5.27049678355612,
133.252603468789));
#216255=CARTESIAN_POINT('Ctrl Pts',(-254.17511247963,4.90860829937749,127.693477454216));
#216256=CARTESIAN_POINT('Ctrl Pts',(-254.453560103444,0.0359485746511809,
124.993101125124));
#216257=CARTESIAN_POINT('Ctrl Pts',(-254.732007727256,-4.86974611083267,
127.632988310607));
#216258=CARTESIAN_POINT('Ctrl Pts',(-255.010455351069,-5.30038206451776,
133.187211835313));
#216259=CARTESIAN_POINT('Ctrl Pts',(-255.288902974882,-0.860225756393269,
136.55171127444));
#216260=CARTESIAN_POINT('Ctrl Pts',(-255.567350598695,4.37043584157037,
134.634676658854));
#216261=CARTESIAN_POINT('Ctrl Pts',(-255.845798222508,5.58488070320316,
129.197767919676));
#216262=CARTESIAN_POINT('Ctrl Pts',(-256.12424584632,1.66709247927321,125.23724089965));
#216263=CARTESIAN_POINT('Ctrl Pts',(-256.402693470134,-3.78267124144458,
126.39262206856));
#216264=CARTESIAN_POINT('Ctrl Pts',(-256.681141093946,-5.75634686702621,
131.602180844355));
#216265=CARTESIAN_POINT('Ctrl Pts',(-256.95958871776,-2.44021719259262,
136.078571600242));
#216266=CARTESIAN_POINT('Ctrl Pts',(-257.238036341572,3.118345804191,135.708239395799));
#216267=CARTESIAN_POINT('Ctrl Pts',(-257.516483965385,5.81131468939531,
130.8314457702));
#216268=CARTESIAN_POINT('Ctrl Pts',(-257.794931589198,3.16394407961038,
125.929830927563));
#216269=CARTESIAN_POINT('Ctrl Pts',(-258.073379213011,-2.39088900078744,
125.507540987923));
#216270=CARTESIAN_POINT('Ctrl Pts',(-258.351826836824,-5.74870171518396,
129.953014515613));
#216271=CARTESIAN_POINT('Ctrl Pts',(-258.630274460636,-3.82356878618261,
135.180370918811));
#216272=CARTESIAN_POINT('Ctrl Pts',(-258.908722084449,1.61491681105698,
136.387261181902));
#216273=CARTESIAN_POINT('Ctrl Pts',(-259.187169708263,5.56997747689423,
132.462088635074));
#216274=CARTESIAN_POINT('Ctrl Pts',(-259.465617332075,4.40535894966821,
127.016664495574));
#216275=CARTESIAN_POINT('Ctrl Pts',(-259.744064955888,-0.805411631290512,
125.046024618449));
#216276=CARTESIAN_POINT('Ctrl Pts',(-260.022512579701,-5.28013240410161,
128.378470706602));
#216277=CARTESIAN_POINT('Ctrl Pts',(-260.254552266212,-4.95911089365773,
132.993351965875));
#216278=CARTESIAN_POINT('Ctrl Pts',(-260.440213228287,-2.45877638613931,
135.28779596926));
#216279=CARTESIAN_POINT('Ctrl Pts',(-260.53305831576,-0.833059752290926,
135.715219187214));
#216280=CARTESIAN_POINT('Ctrl Pts',(-260.579495465929,-0.013892627260139,
135.717527172907));
#216281=CARTESIAN_POINT('',(178.484852205224,2.29534567378642,125.352234455441));
#216282=CARTESIAN_POINT('Ctrl Pts',(178.484852205224,2.2953456737888,125.352234455442));
#216283=CARTESIAN_POINT('Ctrl Pts',(178.474769645589,2.30871694763094,125.378556419204));
#216284=CARTESIAN_POINT('Ctrl Pts',(178.464760721661,2.32210067769615,125.404904734779));
#216285=CARTESIAN_POINT('Ctrl Pts',(178.410116963477,2.39571594247993,125.549964067863));
#216286=CARTESIAN_POINT('Ctrl Pts',(178.366752083918,2.45614810993821,125.669573427325));
#216287=CARTESIAN_POINT('Ctrl Pts',(178.280651552913,2.57861371139863,125.916725903007));
#216288=CARTESIAN_POINT('Ctrl Pts',(178.23809773572,2.6405199714625,126.044243888829));
#216289=CARTESIAN_POINT('Ctrl Pts',(178.119236076123,2.81530092068313,126.41694099985));
#216290=CARTESIAN_POINT('Ctrl Pts',(178.04659616344,2.92444065582699,126.665761747735));
#216291=CARTESIAN_POINT('Ctrl Pts',(177.979076132606,3.02442025815032,126.922107774054));
#216292=CARTESIAN_POINT('',(179.686624807795,-5.92158244890185,130.806643466513));
#216293=CARTESIAN_POINT('Ctrl Pts',(178.484852205224,2.29534567378572,125.35223445544));
#216294=CARTESIAN_POINT('Ctrl Pts',(178.508237305251,2.75521539300514,125.540445630445));
#216295=CARTESIAN_POINT('Ctrl Pts',(178.624438279882,4.91660179655204,126.757108707475));
#216296=CARTESIAN_POINT('Ctrl Pts',(178.833455129117,6.97691126644166,131.352329330672));
#216297=CARTESIAN_POINT('Ctrl Pts',(179.11190275293,3.31016936242742,136.970424136732));
#216298=CARTESIAN_POINT('Ctrl Pts',(179.390350376743,-3.39845647489431,
136.922207797627));
#216299=CARTESIAN_POINT('Ctrl Pts',(179.581924395032,-5.86538284120287,
133.021055300245));
#216300=CARTESIAN_POINT('Ctrl Pts',(179.680682538715,-5.92608698495012,
130.932358269279));
#216301=CARTESIAN_POINT('Ctrl Pts',(179.686624807795,-5.92546899106887,
130.806644964827));
#216302=CARTESIAN_POINT('',(181.436624793272,-5.91313131605275,130.808682171932));
#216303=CARTESIAN_POINT('Ctrl Pts',(179.686624807795,-5.9167495603248,130.80664160337));
#216304=CARTESIAN_POINT('Ctrl Pts',(179.693977154138,-5.91680943647244,
130.651326226339));
#216305=CARTESIAN_POINT('Ctrl Pts',(179.701329500482,-5.91074953815374,
130.495761078002));
#216306=CARTESIAN_POINT('Ctrl Pts',(179.708681846825,-5.89853708827506,
130.340474014242));
#216307=CARTESIAN_POINT('Ctrl Pts',(179.716025830516,-5.88633852899205,
130.185363575961));
#216308=CARTESIAN_POINT('Ctrl Pts',(179.723369814208,-5.86800137290794,
130.030530968938));
#216309=CARTESIAN_POINT('Ctrl Pts',(179.730713797899,-5.84354481501677,
129.876505802743));
#216310=CARTESIAN_POINT('Ctrl Pts',(179.738051104691,-5.81911049219403,
129.722620670976));
#216311=CARTESIAN_POINT('Ctrl Pts',(179.745388411482,-5.78856789958858,
129.569541892852));
#216312=CARTESIAN_POINT('Ctrl Pts',(179.752725718274,-5.75198815284064,
129.417795490325));
#216313=CARTESIAN_POINT('Ctrl Pts',(179.760058027822,-5.71543331957921,
129.266152438212));
#216314=CARTESIAN_POINT('Ctrl Pts',(179.767390337371,-5.6728496059675,129.11584032425));
#216315=CARTESIAN_POINT('Ctrl Pts',(179.774722646919,-5.62435943793095,
128.96737627483));
#216316=CARTESIAN_POINT('Ctrl Pts',(179.782052360326,-5.57588643874756,
128.818964791891));
#216317=CARTESIAN_POINT('Ctrl Pts',(179.789382073733,-5.52151126173289,
128.672400433808));
#216318=CARTESIAN_POINT('Ctrl Pts',(179.796711787139,-5.46140653421223,
128.528186364447));
#216319=CARTESIAN_POINT('Ctrl Pts',(179.804040294966,-5.40131169262705,
128.383996015199));
#216320=CARTESIAN_POINT('Ctrl Pts',(179.811368802792,-5.33548932152652,
128.24215553726));
#216321=CARTESIAN_POINT('Ctrl Pts',(179.818697310619,-5.26416055459471,
128.103148997209));
#216322=CARTESIAN_POINT('Ctrl Pts',(179.826026126248,-5.19282879179809,
127.964136618774));
#216323=CARTESIAN_POINT('Ctrl Pts',(179.833354941878,-5.11599034668846,
127.827958754184));
#216324=CARTESIAN_POINT('Ctrl Pts',(179.840683757508,-5.03391263741617,
127.695075471208));
#216325=CARTESIAN_POINT('Ctrl Pts',(179.848014394317,-4.95181453217909,
127.562159167297));
#216326=CARTESIAN_POINT('Ctrl Pts',(179.855345031126,-4.86447477205808,
127.432539398244));
#216327=CARTESIAN_POINT('Ctrl Pts',(179.862675667936,-4.77220433056239,
127.306647594766));
#216328=CARTESIAN_POINT('Ctrl Pts',(179.870013917591,-4.67983806647012,
127.180625053001));
#216329=CARTESIAN_POINT('Ctrl Pts',(179.877352167246,-4.58253111937658,
127.058338516905));
#216330=CARTESIAN_POINT('Ctrl Pts',(179.884690416902,-4.48063543929967,
126.940187145452));
#216331=CARTESIAN_POINT('Ctrl Pts',(179.892032632595,-4.37868468856922,
126.821971917776));
#216332=CARTESIAN_POINT('Ctrl Pts',(179.899374848289,-4.27214052426441,
126.707896584654));
#216333=CARTESIAN_POINT('Ctrl Pts',(179.906717063983,-4.16139154293925,
126.598323172553));
#216334=CARTESIAN_POINT('Ctrl Pts',(179.914070345708,-4.05047564310977,
126.48858461374));
#216335=CARTESIAN_POINT('Ctrl Pts',(179.921423627433,-3.93534254692211,
126.383361787399));
#216336=CARTESIAN_POINT('Ctrl Pts',(179.928776909158,-3.81641438967868,
126.282976784186));
#216337=CARTESIAN_POINT('Ctrl Pts',(179.934933147562,-3.71684658903447,
126.198933490997));
#216338=CARTESIAN_POINT('Ctrl Pts',(179.941089385965,-3.61461941093371,
126.118280447087));
#216339=CARTESIAN_POINT('Ctrl Pts',(179.947245624368,-3.50999522101216,
126.041182675165));
#216340=CARTESIAN_POINT('Ctrl Pts',(179.954668890774,-3.38383811283284,
125.948217253306));
#216341=CARTESIAN_POINT('Ctrl Pts',(179.962092157179,-3.25379427861745,
125.860126797838));
#216342=CARTESIAN_POINT('Ctrl Pts',(179.969515423585,-3.12027719627839,
125.777254016261));
#216343=CARTESIAN_POINT('Ctrl Pts',(179.976929916306,-2.98691792004263,
125.694479183429));
#216344=CARTESIAN_POINT('Ctrl Pts',(179.984344409027,-2.85009388096072,
125.616909944266));
#216345=CARTESIAN_POINT('Ctrl Pts',(179.991758901748,-2.71025060387357,
125.544848071074));
#216346=CARTESIAN_POINT('Ctrl Pts',(179.999166248101,-2.5705421130023,125.47285565383));
#216347=CARTESIAN_POINT('Ctrl Pts',(180.006573594455,-2.42782050707694,
125.406360204809));
#216348=CARTESIAN_POINT('Ctrl Pts',(180.013980940809,-2.28255910179349,
125.345619507262));
#216349=CARTESIAN_POINT('Ctrl Pts',(180.021382762484,-2.13740603794629,
125.284924112419));
#216350=CARTESIAN_POINT('Ctrl Pts',(180.02878458416,-1.98971728942356,125.229975066268));
#216351=CARTESIAN_POINT('Ctrl Pts',(180.036186405835,-1.83998941521192,
125.180983561525));
#216352=CARTESIAN_POINT('Ctrl Pts',(180.043584320146,-1.69034058117979,
125.132017919016));
#216353=CARTESIAN_POINT('Ctrl Pts',(180.050982234458,-1.53865511912818,
125.089003670412));
#216354=CARTESIAN_POINT('Ctrl Pts',(180.058380148769,-1.38544804064297,
125.052103296376));
#216355=CARTESIAN_POINT('Ctrl Pts',(180.065776833681,-1.23226642239424,
125.015209054514));
#216356=CARTESIAN_POINT('Ctrl Pts',(180.073173518594,-1.07756405213862,
124.984426758055));
#216357=CARTESIAN_POINT('Ctrl Pts',(180.080570203506,-0.921869639997064,
124.959868601201));
#216358=CARTESIAN_POINT('Ctrl Pts',(180.087966560441,-0.76618213150912,
124.935311533282));
#216359=CARTESIAN_POINT('Ctrl Pts',(180.095362917377,-0.609503037337292,
124.916978114377));
#216360=CARTESIAN_POINT('Ctrl Pts',(180.102759274312,-0.452369496104509,
124.904929085503));
#216361=CARTESIAN_POINT('Ctrl Pts',(180.110156763649,-0.295211897325392,
124.892878211893));
#216362=CARTESIAN_POINT('Ctrl Pts',(180.117554252985,-0.137600085177405,
124.887113672636));
#216363=CARTESIAN_POINT('Ctrl Pts',(180.124951742322,0.0199256168518951,
124.887644169037));
#216364=CARTESIAN_POINT('Ctrl Pts',(180.132351824837,0.177506539271902,
124.888174851403));
#216365=CARTESIAN_POINT('Ctrl Pts',(180.139751907352,0.335000918410661,
124.895004961724));
#216366=CARTESIAN_POINT('Ctrl Pts',(180.147151989867,0.491870521751642,
124.908091123018));
#216367=CARTESIAN_POINT('Ctrl Pts',(180.154560209533,0.648912619348167,
124.921191673893));
#216368=CARTESIAN_POINT('Ctrl Pts',(180.1619684292,0.805328196918372,124.940561982845));
#216369=CARTESIAN_POINT('Ctrl Pts',(180.169376648866,0.960585487624677,
124.966106933161));
#216370=CARTESIAN_POINT('Ctrl Pts',(180.176789428168,1.115938336603,124.991667605968));
#216371=CARTESIAN_POINT('Ctrl Pts',(180.184202207471,1.27013111337955,125.023410417793));
#216372=CARTESIAN_POINT('Ctrl Pts',(180.191614986773,1.42264479111333,125.061189684987));
#216373=CARTESIAN_POINT('Ctrl Pts',(180.199038357801,1.57537638754186,125.09902293297));
#216374=CARTESIAN_POINT('Ctrl Pts',(180.20646172883,1.72642373571236,125.142909758842));
#216375=CARTESIAN_POINT('Ctrl Pts',(180.213885099859,1.87528465261602,125.192655169651));
#216376=CARTESIAN_POINT('Ctrl Pts',(180.2178211493,1.95421428262784,125.219031380086));
#216377=CARTESIAN_POINT('Ctrl Pts',(180.221757198741,2.03252957801731,125.247053850963));
#216378=CARTESIAN_POINT('Ctrl Pts',(180.225693248181,2.11015834979351,125.276688204941));
#216379=CARTESIAN_POINT('Ctrl Pts',(180.233116514587,2.25656379065098,125.332577671686));
#216380=CARTESIAN_POINT('Ctrl Pts',(180.240539780992,2.40096865457811,125.394372189534));
#216381=CARTESIAN_POINT('Ctrl Pts',(180.247963047398,2.5428611171387,125.461909129584));
#216382=CARTESIAN_POINT('Ctrl Pts',(180.255377540119,2.68458587459203,125.529366246579));
#216383=CARTESIAN_POINT('Ctrl Pts',(180.26279203284,2.82380380761203,125.602552117214));
#216384=CARTESIAN_POINT('Ctrl Pts',(180.270206525561,2.9600202095537,125.681255024126));
#216385=CARTESIAN_POINT('Ctrl Pts',(180.277613871915,3.09610532099887,125.759882074213));
#216386=CARTESIAN_POINT('Ctrl Pts',(180.285021218268,3.22919433968091,125.844015388928));
#216387=CARTESIAN_POINT('Ctrl Pts',(180.292428564622,3.35881454655656,125.933396092511));
#216388=CARTESIAN_POINT('Ctrl Pts',(180.299830386298,3.48833807779142,126.022710132594));
#216389=CARTESIAN_POINT('Ctrl Pts',(180.307232207973,3.61439764263109,126.11726355784));
#216390=CARTESIAN_POINT('Ctrl Pts',(180.314634029648,3.73654715640086,126.21675275393));
#216391=CARTESIAN_POINT('Ctrl Pts',(180.32203194396,3.8586321883935,126.316189430449));
#216392=CARTESIAN_POINT('Ctrl Pts',(180.329429858271,3.97681099133407,126.420556453577));
#216393=CARTESIAN_POINT('Ctrl Pts',(180.336827772583,4.09066848929571,126.529508354249));
#216394=CARTESIAN_POINT('Ctrl Pts',(180.344224457495,4.20450706620659,126.638442149092));
#216395=CARTESIAN_POINT('Ctrl Pts',(180.351621142407,4.31402549395549,126.751959051452));
#216396=CARTESIAN_POINT('Ctrl Pts',(180.359017827319,4.4188435996499,126.869674886236));
#216397=CARTESIAN_POINT('Ctrl Pts',(180.366414184255,4.52365705759943,126.987385501376));
#216398=CARTESIAN_POINT('Ctrl Pts',(180.37381054119,4.62377035965245,127.109294399949));
#216399=CARTESIAN_POINT('Ctrl Pts',(180.381206898125,4.71884206612648,127.234982504021));
#216400=CARTESIAN_POINT('Ctrl Pts',(180.388604387462,4.81392832832141,127.360689851263));
#216401=CARTESIAN_POINT('Ctrl Pts',(180.396001876799,4.90397123280667,127.490177258346));
#216402=CARTESIAN_POINT('Ctrl Pts',(180.403399366135,4.98867140088571,127.622994839086));
#216403=CARTESIAN_POINT('Ctrl Pts',(180.41079944865,5.07340126047743,127.755858978823));
#216404=CARTESIAN_POINT('Ctrl Pts',(180.418199531165,5.15278445416412,127.892055301928));
#216405=CARTESIAN_POINT('Ctrl Pts',(180.42559961368,5.22656654840633,128.031107531824));
#216406=CARTESIAN_POINT('Ctrl Pts',(180.433007833347,5.30042977364622,128.170312663941));
#216407=CARTESIAN_POINT('Ctrl Pts',(180.440416053013,5.36867942446826,128.312379644405));
#216408=CARTESIAN_POINT('Ctrl Pts',(180.44782427268,5.43110809229362,128.456809669807));
#216409=CARTESIAN_POINT('Ctrl Pts',(180.455237051982,5.49357518392232,128.60132858948));
#216410=CARTESIAN_POINT('Ctrl Pts',(180.462649831284,5.55021401954599,128.748213104701));
#216411=CARTESIAN_POINT('Ctrl Pts',(180.470062610586,5.60086662026004,128.896947797918));
#216412=CARTESIAN_POINT('Ctrl Pts',(180.477485981615,5.65159159578549,129.04589501024));
#216413=CARTESIAN_POINT('Ctrl Pts',(180.484909352643,5.69631314746229,129.196697323519));
#216414=CARTESIAN_POINT('Ctrl Pts',(180.492332723672,5.73492388620217,129.348826838512));
#216415=CARTESIAN_POINT('Ctrl Pts',(180.496268773113,5.75539622633393,129.429489557658));
#216416=CARTESIAN_POINT('Ctrl Pts',(180.500204822554,5.77415145806278,129.510525263669));
#216417=CARTESIAN_POINT('Ctrl Pts',(180.504140871994,5.79117948410592,129.591854640108));
#216418=CARTESIAN_POINT('Ctrl Pts',(180.5115641384,5.82329380979685,129.745239305871));
#216419=CARTESIAN_POINT('Ctrl Pts',(180.518987404805,5.84935868805641,129.900132653963));
#216420=CARTESIAN_POINT('Ctrl Pts',(180.526410671211,5.86923428957744,130.056016167097));
#216421=CARTESIAN_POINT('Ctrl Pts',(180.533825163932,5.88908639978802,130.211715438863));
#216422=CARTESIAN_POINT('Ctrl Pts',(180.541239656653,5.90276374747488,130.368402179512));
#216423=CARTESIAN_POINT('Ctrl Pts',(180.548654149374,5.91017705542789,130.525545739925));
#216424=CARTESIAN_POINT('Ctrl Pts',(180.556061495727,5.91758321815559,130.682537839459));
#216425=CARTESIAN_POINT('Ctrl Pts',(180.563468842081,5.91873734318499,130.839985511826));
#216426=CARTESIAN_POINT('Ctrl Pts',(180.570876188435,5.91360171383272,130.997351116438));
#216427=CARTESIAN_POINT('Ctrl Pts',(180.57827801011,5.90846991482658,131.154599351844));
#216428=CARTESIAN_POINT('Ctrl Pts',(180.585679831786,5.89705771424754,131.311765269877));
#216429=CARTESIAN_POINT('Ctrl Pts',(180.593081653461,5.87937943175644,131.468309455911));
#216430=CARTESIAN_POINT('Ctrl Pts',(180.600479567773,5.86171048149293,131.624771003489));
#216431=CARTESIAN_POINT('Ctrl Pts',(180.607877482084,5.83778207877467,131.780611102708));
#216432=CARTESIAN_POINT('Ctrl Pts',(180.615275396395,5.80766051783306,131.935293803967));
#216433=CARTESIAN_POINT('Ctrl Pts',(180.622672081308,5.77754396254863,132.089950799766));
#216434=CARTESIAN_POINT('Ctrl Pts',(180.63006876622,5.74123636296223,132.243450413284));
#216435=CARTESIAN_POINT('Ctrl Pts',(180.637465451132,5.69885544372551,132.395265138277));
#216436=CARTESIAN_POINT('Ctrl Pts',(180.644861808067,5.65647640370319,132.547073131647));
#216437=CARTESIAN_POINT('Ctrl Pts',(180.652258165003,5.60802467985748,132.697196025489));
#216438=CARTESIAN_POINT('Ctrl Pts',(180.659654521938,5.55366829783429,132.84512003507));
#216439=CARTESIAN_POINT('Ctrl Pts',(180.667052011275,5.49930359371009,132.993066692195));
#216440=CARTESIAN_POINT('Ctrl Pts',(180.674449500611,5.4390325601511,133.138813444321));
#216441=CARTESIAN_POINT('Ctrl Pts',(180.681846989948,5.37307187764845,133.281865241199));
#216442=CARTESIAN_POINT('Ctrl Pts',(180.689247072463,5.30708807273077,133.424967184663));
#216443=CARTESIAN_POINT('Ctrl Pts',(180.696647154978,5.23541080405183,133.56537195318));
#216444=CARTESIAN_POINT('Ctrl Pts',(180.704047237493,5.15830324904222,133.702608045482));
#216445=CARTESIAN_POINT('Ctrl Pts',(180.71145545716,5.08111090634927,133.839995042975));
#216446=CARTESIAN_POINT('Ctrl Pts',(180.718863676826,4.99847653549861,133.974206080262));
#216447=CARTESIAN_POINT('Ctrl Pts',(180.726271896493,4.91070768452162,134.104797043204));
#216448=CARTESIAN_POINT('Ctrl Pts',(180.733684675795,4.82288481328128,134.235468382706));
#216449=CARTESIAN_POINT('Ctrl Pts',(180.741097455097,4.72992138477512,134.362514907542));
#216450=CARTESIAN_POINT('Ctrl Pts',(180.748510234399,4.6321656429306,134.485525109809));
#216451=CARTESIAN_POINT('Ctrl Pts',(180.755933605427,4.53427022309773,134.608711074823));
#216452=CARTESIAN_POINT('Ctrl Pts',(180.763356976456,4.43156905705897,134.727848916707));
#216453=CARTESIAN_POINT('Ctrl Pts',(180.770780347485,4.32444823497244,134.842562943545));
#216454=CARTESIAN_POINT('Ctrl Pts',(180.774716396926,4.26765020477355,134.9033870731));
#216455=CARTESIAN_POINT('Ctrl Pts',(180.778652446367,4.20961023112803,134.962968159235));
#216456=CARTESIAN_POINT('Ctrl Pts',(180.782588495807,4.15038958737084,135.02125483435));
#216457=CARTESIAN_POINT('Ctrl Pts',(180.790011762213,4.03870130145738,135.131181684552));
#216458=CARTESIAN_POINT('Ctrl Pts',(180.797435028618,3.92247384426901,135.236834442952));
#216459=CARTESIAN_POINT('Ctrl Pts',(180.804858295024,3.80206787792984,135.337815195933));
#216460=CARTESIAN_POINT('Ctrl Pts',(180.812272787745,3.68180422144385,135.43867659805));
#216461=CARTESIAN_POINT('Ctrl Pts',(180.819687280466,3.5573721694491,135.534876748629));
#216462=CARTESIAN_POINT('Ctrl Pts',(180.827101773187,3.42916991556503,135.626053707414));
#216463=CARTESIAN_POINT('Ctrl Pts',(180.83450911954,3.30109122784012,135.717142786413));
#216464=CARTESIAN_POINT('Ctrl Pts',(180.841916465894,3.16924987469744,135.803218097274));
#216465=CARTESIAN_POINT('Ctrl Pts',(180.849323812248,3.03407780160299,135.883957300012));
#216466=CARTESIAN_POINT('Ctrl Pts',(180.856725633923,2.89900654493989,135.964636284407));
#216467=CARTESIAN_POINT('Ctrl Pts',(180.864127455599,2.76060983375698,136.039986894538));
#216468=CARTESIAN_POINT('Ctrl Pts',(180.871529277274,2.61934923298189,136.109729611159));
#216469=CARTESIAN_POINT('Ctrl Pts',(180.878927191586,2.47816320257805,136.179435511143));
#216470=CARTESIAN_POINT('Ctrl Pts',(180.886325105897,2.33411662733151,136.243539248482));
#216471=CARTESIAN_POINT('Ctrl Pts',(180.893723020208,2.18769625047188,136.301806904541));
#216472=CARTESIAN_POINT('Ctrl Pts',(180.901119705121,2.04130020602305,136.360064877571));
#216473=CARTESIAN_POINT('Ctrl Pts',(180.908516390033,1.8925314893964,136.412488556298));
#216474=CARTESIAN_POINT('Ctrl Pts',(180.915913074945,1.74189753958409,136.458891855794));
#216475=CARTESIAN_POINT('Ctrl Pts',(180.92330943188,1.59127026903901,136.505293097718));
#216476=CARTESIAN_POINT('Ctrl Pts',(180.930705788816,1.43877828651029,136.5456743813));
#216477=CARTESIAN_POINT('Ctrl Pts',(180.938102145751,1.28494467561209,136.579899358075));
#216478=CARTESIAN_POINT('Ctrl Pts',(180.945499635088,1.13108751239619,136.61412957478));
#216479=CARTESIAN_POINT('Ctrl Pts',(180.952897124424,0.97588867623078,136.642201526869));
#216480=CARTESIAN_POINT('Ctrl Pts',(180.960294613761,0.819881788008743,
136.664029927023));
#216481=CARTESIAN_POINT('Ctrl Pts',(180.967694696276,0.663820211813073,
136.685865979089));
#216482=CARTESIAN_POINT('Ctrl Pts',(180.975094778791,0.50695038905536,136.701454069904));
#216483=CARTESIAN_POINT('Ctrl Pts',(180.982494861306,0.34981126093449,136.710760760142));
#216484=CARTESIAN_POINT('Ctrl Pts',(180.989903080972,0.192499342187787,
136.720077684043));
#216485=CARTESIAN_POINT('Ctrl Pts',(180.997311300639,0.0349178995625732,
136.72309939146));
#216486=CARTESIAN_POINT('Ctrl Pts',(181.004719520305,-0.122393183915837,
136.719844576722));
#216487=CARTESIAN_POINT('Ctrl Pts',(181.012132299607,-0.279801089741335,
136.7165877587));
#216488=CARTESIAN_POINT('Ctrl Pts',(181.01954507891,-0.436937933096332,
136.707046743394));
#216489=CARTESIAN_POINT('Ctrl Pts',(181.026957858212,-0.593269266378005,
136.691292088211));
#216490=CARTESIAN_POINT('Ctrl Pts',(181.03438122924,-0.749823973199911,
136.675514922038));
#216491=CARTESIAN_POINT('Ctrl Pts',(181.041804600269,-0.905570502595506,
136.653506436043));
#216492=CARTESIAN_POINT('Ctrl Pts',(181.049227971298,-1.05998408315404,
136.625388388154));
#216493=CARTESIAN_POINT('Ctrl Pts',(181.053164020739,-1.14185786866959,
136.61047952448));
#216494=CARTESIAN_POINT('Ctrl Pts',(181.05710007018,-1.22335714732034,136.59385388328));
#216495=CARTESIAN_POINT('Ctrl Pts',(181.06103611962,-1.30440558235503,136.575535250101));
#216496=CARTESIAN_POINT('Ctrl Pts',(181.068459386026,-1.45726040139478,
136.540986879633));
#216497=CARTESIAN_POINT('Ctrl Pts',(181.075882652431,-1.60897283890215,
136.500309324795));
#216498=CARTESIAN_POINT('Ctrl Pts',(181.083305918837,-1.75901317219453,
136.453590938817));
#216499=CARTESIAN_POINT('Ctrl Pts',(181.090720411558,-1.90887617027225,
136.406927770093));
#216500=CARTESIAN_POINT('Ctrl Pts',(181.098134904279,-2.05707064500866,
136.354238091858));
#216501=CARTESIAN_POINT('Ctrl Pts',(181.105549397,-2.20307685243817,136.295661278134));
#216502=CARTESIAN_POINT('Ctrl Pts',(181.112956743353,-2.34894233358859,
136.237140922947));
#216503=CARTESIAN_POINT('Ctrl Pts',(181.120364089707,-2.49262340217373,
136.172744866634));
#216504=CARTESIAN_POINT('Ctrl Pts',(181.127771436061,-2.6336153873598,136.102662284512));
#216505=CARTESIAN_POINT('Ctrl Pts',(181.135173257736,-2.77450221540357,
136.032631972624));
#216506=CARTESIAN_POINT('Ctrl Pts',(181.142575079412,-2.91270362066783,
135.956923745224));
#216507=CARTESIAN_POINT('Ctrl Pts',(181.149976901087,-3.04773494857795,
135.875774842979));
#216508=CARTESIAN_POINT('Ctrl Pts',(181.157374815399,-3.1826949945026,135.794668778606));
#216509=CARTESIAN_POINT('Ctrl Pts',(181.16477272971,-3.31448797669285,135.708127951092));
#216510=CARTESIAN_POINT('Ctrl Pts',(181.172170644021,-3.44265399617015,
135.616435432566));
#216511=CARTESIAN_POINT('Ctrl Pts',(181.179567328934,-3.57079871677919,
135.524758151673));
#216512=CARTESIAN_POINT('Ctrl Pts',(181.186964013846,-3.69531736762194,
135.427931095897));
#216513=CARTESIAN_POINT('Ctrl Pts',(181.194360698758,-3.81577910700978,
135.326280604586));
#216514=CARTESIAN_POINT('Ctrl Pts',(181.201757055694,-3.93623550499821,
135.224634620564));
#216515=CARTESIAN_POINT('Ctrl Pts',(181.209153412629,-4.0526350639138,135.118165867008));
#216516=CARTESIAN_POINT('Ctrl Pts',(181.216549769564,-4.16458033046145,
135.007240729303));
#216517=CARTESIAN_POINT('Ctrl Pts',(181.223947258901,-4.27654273611478,
134.896298608676));
#216518=CARTESIAN_POINT('Ctrl Pts',(181.231344748238,-4.38404922633616,
134.78089900815));
#216519=CARTESIAN_POINT('Ctrl Pts',(181.238742237574,-4.48673961136266,
134.661444778215));
#216520=CARTESIAN_POINT('Ctrl Pts',(181.246142320089,-4.58946599434432,
134.541948673785));
#216521=CARTESIAN_POINT('Ctrl Pts',(181.253542402604,-4.68737266758336,
134.418395392961));
#216522=CARTESIAN_POINT('Ctrl Pts',(181.260942485119,-4.78014018674565,
134.291220287464));
#216523=CARTESIAN_POINT('Ctrl Pts',(181.268350704786,-4.87300971333234,
134.163905339864));
#216524=CARTESIAN_POINT('Ctrl Pts',(181.275758924452,-4.96072858024092,
134.032960915913));
#216525=CARTESIAN_POINT('Ctrl Pts',(181.283167144119,-5.04302069557768,
133.898851339232));
#216526=CARTESIAN_POINT('Ctrl Pts',(181.290579923421,-5.12536346033855,
133.764659220344));
#216527=CARTESIAN_POINT('Ctrl Pts',(181.297992702723,-5.20227263606082,
133.627298391857));
#216528=CARTESIAN_POINT('Ctrl Pts',(181.305405482025,-5.27351870270403,
133.487256637678));
#216529=CARTESIAN_POINT('Ctrl Pts',(181.312828853054,-5.34486656906833,
133.347014785273));
#216530=CARTESIAN_POINT('Ctrl Pts',(181.320252224083,-5.4105350099472,133.204084694854));
#216531=CARTESIAN_POINT('Ctrl Pts',(181.327675595111,-5.47034281196722,
133.058973684604));
#216532=CARTESIAN_POINT('Ctrl Pts',(181.331611644552,-5.50205434366603,
132.982032345081));
#216533=CARTESIAN_POINT('Ctrl Pts',(181.335547693993,-5.53211907170173,
132.904478128601));
#216534=CARTESIAN_POINT('Ctrl Pts',(181.339483743433,-5.56051574565194,
132.826388116107));
#216535=CARTESIAN_POINT('Ctrl Pts',(181.348080014218,-5.622533640077,132.655840742883));
#216536=CARTESIAN_POINT('Ctrl Pts',(181.356676285003,-5.67674712583689,
132.482312359138));
#216537=CARTESIAN_POINT('Ctrl Pts',(181.365272555788,-5.7229002646624,132.306473503879));
#216538=CARTESIAN_POINT('Ctrl Pts',(181.373836240798,-5.76887845136683,
132.13130119875));
#216539=CARTESIAN_POINT('Ctrl Pts',(181.382399925807,-5.8068571937891,131.953836020863));
#216540=CARTESIAN_POINT('Ctrl Pts',(181.390963610817,-5.83663002103799,
131.774762884679));
#216541=CARTESIAN_POINT('Ctrl Pts',(181.399463586485,-5.86618135400975,
131.597021959055));
#216542=CARTESIAN_POINT('Ctrl Pts',(181.407963562153,-5.88764834009424,
131.417697041437));
#216543=CARTESIAN_POINT('Ctrl Pts',(181.416463537821,-5.90087621830845,
131.237477713398));
#216544=CARTESIAN_POINT('Ctrl Pts',(181.423183949748,-5.91133469418984,
131.094989291209));
#216545=CARTESIAN_POINT('Ctrl Pts',(181.429904361675,-5.91664371146173,
130.95194217167));
#216546=CARTESIAN_POINT('Ctrl Pts',(181.436624773602,-5.91674841954496,
130.808685234569));
#216547=CARTESIAN_POINT('',(183.186624807795,-5.9097261727316,130.800419732287));
#216548=CARTESIAN_POINT('Ctrl Pts',(181.436624807795,-5.91046065331948,
130.808679910655));
#216549=CARTESIAN_POINT('Ctrl Pts',(181.497060327612,-5.90180348691877,
129.521756724088));
#216550=CARTESIAN_POINT('Ctrl Pts',(181.650311722033,-4.85487069311502,
126.24557662955));
#216551=CARTESIAN_POINT('Ctrl Pts',(181.89637899106,0.558585749835051,123.828291345372));
#216552=CARTESIAN_POINT('Ctrl Pts',(182.174826614872,6.17109389324245,127.503578787286));
#216553=CARTESIAN_POINT('Ctrl Pts',(182.453274238685,6.11266822346165,134.212123479067));
#216554=CARTESIAN_POINT('Ctrl Pts',(182.731721862497,0.436999076760051,
137.789100579601));
#216555=CARTESIAN_POINT('Ctrl Pts',(182.976172052201,-4.89824093256168,
135.294398866638));
#216556=CARTESIAN_POINT('Ctrl Pts',(183.1278063673,-5.90209859011289,132.053299422131));
#216557=CARTESIAN_POINT('Ctrl Pts',(183.186624807795,-5.9097261727316,130.800419732287));
#216558=CARTESIAN_POINT('',(184.936624807795,-5.92486718842363,130.801517542038));
#216559=CARTESIAN_POINT('Ctrl Pts',(183.186624807795,-5.9097261727316,130.800419732287));
#216560=CARTESIAN_POINT('Ctrl Pts',(183.220622241905,-5.91413496418055,
130.076247273033));
#216561=CARTESIAN_POINT('Ctrl Pts',(183.347435550617,-5.4548282023846,127.380421002293));
#216562=CARTESIAN_POINT('Ctrl Pts',(183.567064733937,-1.42373941229825,
123.952315184543));
#216563=CARTESIAN_POINT('Ctrl Pts',(183.845512357749,4.99525395369783,125.90283040054));
#216564=CARTESIAN_POINT('Ctrl Pts',(184.123959981563,6.82385296796736,132.357612432922));
#216565=CARTESIAN_POINT('Ctrl Pts',(184.402407605375,2.38166446842562,137.385031927559));
#216566=CARTESIAN_POINT('Ctrl Pts',(184.673295880787,-4.06914253102304,
136.392824298985));
#216567=CARTESIAN_POINT('Ctrl Pts',(184.851368281593,-5.91419482002716,
132.605670887374));
#216568=CARTESIAN_POINT('Ctrl Pts',(184.936624807795,-5.92486718842363,
130.801517542038));
#216569=CARTESIAN_POINT('',(186.686624807795,-5.91810304431807,130.809680029163));
#216570=CARTESIAN_POINT('Ctrl Pts',(184.936624807795,-5.92486718842363,
130.801517542038));
#216571=CARTESIAN_POINT('Ctrl Pts',(184.944184156197,-5.92581346379487,
130.641550624367));
#216572=CARTESIAN_POINT('Ctrl Pts',(185.044559379204,-5.84727879099301,
128.518407035367));
#216573=CARTESIAN_POINT('Ctrl Pts',(185.237750476814,-3.29138665363019,
124.628250642296));
#216574=CARTESIAN_POINT('Ctrl Pts',(185.516198100626,3.4170613558443,124.696885507443));
#216575=CARTESIAN_POINT('Ctrl Pts',(185.794645724439,6.98539691202545,130.377991632052));
#216576=CARTESIAN_POINT('Ctrl Pts',(186.073093348252,4.13449396166582,136.450910025061));
#216577=CARTESIAN_POINT('Ctrl Pts',(186.351540972065,-2.5158069582057,137.334925361857));
#216578=CARTESIAN_POINT('Ctrl Pts',(186.55605145858,-5.7022149293107,133.576472626177));
#216579=CARTESIAN_POINT('Ctrl Pts',(186.667746070489,-5.92222955506447,
131.210299569289));
#216580=CARTESIAN_POINT('Ctrl Pts',(186.686624807795,-5.91851213263273,
130.809680396867));
#216581=CARTESIAN_POINT('',(188.436624807759,-5.91674998742092,130.804746434304));
#216582=CARTESIAN_POINT('Ctrl Pts',(186.686624807795,-5.91674760990531,
130.809678810848));
#216583=CARTESIAN_POINT('Ctrl Pts',(186.693927872074,-5.91688686513407,
130.654750624113));
#216584=CARTESIAN_POINT('Ctrl Pts',(186.701230936354,-5.91093684901184,
130.499626658566));
#216585=CARTESIAN_POINT('Ctrl Pts',(186.708534000633,-5.89887823475046,
130.344832452937));
#216586=CARTESIAN_POINT('Ctrl Pts',(186.71583126983,-5.88682918916652,130.190161078655));
#216587=CARTESIAN_POINT('Ctrl Pts',(186.723128539027,-5.86868122137412,
130.035819325382));
#216588=CARTESIAN_POINT('Ctrl Pts',(186.730425808224,-5.84446706708341,
129.882332817401));
#216589=CARTESIAN_POINT('Ctrl Pts',(186.737842908702,-5.81985528279573,
129.726325848082));
#216590=CARTESIAN_POINT('Ctrl Pts',(186.745260009179,-5.78897632400346,
129.57120286325));
#216591=CARTESIAN_POINT('Ctrl Pts',(186.752677109657,-5.75191958714079,
129.417511085149));
#216592=CARTESIAN_POINT('Ctrl Pts',(186.759968840886,-5.71548921030546,
129.266417117715));
#216593=CARTESIAN_POINT('Ctrl Pts',(186.767260572116,-5.67308835349849,
129.116706741788));
#216594=CARTESIAN_POINT('Ctrl Pts',(186.774552303345,-5.62485348468246,
128.968889604895));
#216595=CARTESIAN_POINT('Ctrl Pts',(186.781843715033,-5.57662072963386,
128.821078945703));
#216596=CARTESIAN_POINT('Ctrl Pts',(186.789135126721,-5.52255459037707,
128.675161726577));
#216597=CARTESIAN_POINT('Ctrl Pts',(186.796426538409,-5.46284118724312,
128.531631701602));
#216598=CARTESIAN_POINT('Ctrl Pts',(186.803719166403,-5.40311782310642,
128.388077733878));
#216599=CARTESIAN_POINT('Ctrl Pts',(186.811011794397,-5.33774546886925,
128.246912107963));
#216600=CARTESIAN_POINT('Ctrl Pts',(186.818304422391,-5.26695796755661,
128.108607600227));
#216601=CARTESIAN_POINT('Ctrl Pts',(186.8258154055,-5.19405095418979,127.966161993203));
#216602=CARTESIAN_POINT('Ctrl Pts',(186.833326388608,-5.11539964036747,
127.826751909787));
#216603=CARTESIAN_POINT('Ctrl Pts',(186.840837371716,-5.03130930734334,
127.690864637748));
#216604=CARTESIAN_POINT('Ctrl Pts',(186.84814077682,-4.949542944875,127.558732827339));
#216605=CARTESIAN_POINT('Ctrl Pts',(186.855444181923,-4.86263449198645,
127.429931967507));
#216606=CARTESIAN_POINT('Ctrl Pts',(186.862747587026,-4.77090702822886,
127.30487827149));
#216607=CARTESIAN_POINT('Ctrl Pts',(186.870362359137,-4.6752689357269,127.174493145188));
#216608=CARTESIAN_POINT('Ctrl Pts',(186.877977131248,-4.57439219292684,
127.048182094909));
#216609=CARTESIAN_POINT('Ctrl Pts',(186.885591903359,-4.46868683856503,
126.926375509119));
#216610=CARTESIAN_POINT('Ctrl Pts',(186.89320667547,-4.3629814842032,126.80456892333));
#216611=CARTESIAN_POINT('Ctrl Pts',(186.900821447581,-4.25244789244555,
126.687267089292));
#216612=CARTESIAN_POINT('Ctrl Pts',(186.908436219692,-4.13753558760197,
126.574853574916));
#216613=CARTESIAN_POINT('Ctrl Pts',(186.915859486097,-4.02551323950221,
126.465267174611));
#216614=CARTESIAN_POINT('Ctrl Pts',(186.923282752503,-3.9089647500179,126.359968661986));
#216615=CARTESIAN_POINT('Ctrl Pts',(186.930706018908,-3.78825199071475,
126.259354851085));
#216616=CARTESIAN_POINT('Ctrl Pts',(186.938120511629,-3.66768190386831,
126.158859957352));
#216617=CARTESIAN_POINT('Ctrl Pts',(186.94553500435,-3.54295762806711,126.063038980729));
#216618=CARTESIAN_POINT('Ctrl Pts',(186.952949497071,-3.4144784567078,125.972252647831));
#216619=CARTESIAN_POINT('Ctrl Pts',(186.960356843425,-3.28612311841112,
125.881553818218));
#216620=CARTESIAN_POINT('Ctrl Pts',(186.967764189779,-3.15402039231062,
125.795880185779));
#216621=CARTESIAN_POINT('Ctrl Pts',(186.975171536132,-3.01860320296358,
125.715552774313));
#216622=CARTESIAN_POINT('Ctrl Pts',(186.982573357808,-2.88328701286552,
125.63528527406));
#216623=CARTESIAN_POINT('Ctrl Pts',(186.989975179483,-2.74466160138934,
125.560356244931));
#216624=CARTESIAN_POINT('Ctrl Pts',(186.997377001159,-2.60318938208514,
125.491043800031));
#216625=CARTESIAN_POINT('Ctrl Pts',(187.00477491547,-2.46179184486368,125.421767944631));
#216626=CARTESIAN_POINT('Ctrl Pts',(187.012172829781,-2.3175508271054,125.358102932441));
#216627=CARTESIAN_POINT('Ctrl Pts',(187.019570744093,-2.17095378175324,
125.300281199535));
#216628=CARTESIAN_POINT('Ctrl Pts',(187.026967429005,-2.02438109817091,
125.242469075553));
#216629=CARTESIAN_POINT('Ctrl Pts',(187.034364113917,-1.87545351098578,
125.190498440448));
#216630=CARTESIAN_POINT('Ctrl Pts',(187.041760798829,-1.72467902321808,
125.144553833817));
#216631=CARTESIAN_POINT('Ctrl Pts',(187.049157155765,-1.573911220949,125.098611264417));
#216632=CARTESIAN_POINT('Ctrl Pts',(187.0565535127,-1.42129703801589,125.058694301019));
#216633=CARTESIAN_POINT('Ctrl Pts',(187.063949869636,-1.2673599706079,125.024937699367));
#216634=CARTESIAN_POINT('Ctrl Pts',(187.071347358972,-1.11339933504184,
124.991175929494));
#216635=CARTESIAN_POINT('Ctrl Pts',(187.078744848309,-0.958115776379954,
124.963576479304));
#216636=CARTESIAN_POINT('Ctrl Pts',(187.086142337645,-0.802043172628662,
124.942223011561));
#216637=CARTESIAN_POINT('Ctrl Pts',(187.09354242016,-0.645915857868791,
124.920862058393));
#216638=CARTESIAN_POINT('Ctrl Pts',(187.100942502675,-0.488999316935465,
124.905751497561));
#216639=CARTESIAN_POINT('Ctrl Pts',(187.10834258519,-0.331832590309043,
124.896923127883));
#216640=CARTESIAN_POINT('Ctrl Pts',(187.115750804857,-0.174493042708975,
124.888085050506));
#216641=CARTESIAN_POINT('Ctrl Pts',(187.123159024523,-0.016903132952331,
124.885542980791));
#216642=CARTESIAN_POINT('Ctrl Pts',(187.13056724419,0.140397315335382,124.889276581278));
#216643=CARTESIAN_POINT('Ctrl Pts',(187.137980023492,0.297794579424681,
124.893012479734));
#216644=CARTESIAN_POINT('Ctrl Pts',(187.145392802794,0.454901655364147,
124.903031721345));
#216645=CARTESIAN_POINT('Ctrl Pts',(187.152805582096,0.611184312778971,
124.919262122357));
#216646=CARTESIAN_POINT('Ctrl Pts',(187.160228953124,0.767690274183362,
124.935515714127));
#216647=CARTESIAN_POINT('Ctrl Pts',(187.167652324153,0.923369095910833,
124.957998137041));
#216648=CARTESIAN_POINT('Ctrl Pts',(187.175075695182,1.07769637957054,124.986586036512));
#216649=CARTESIAN_POINT('Ctrl Pts',(187.179011744623,1.15952440839869,125.001744026769));
#216650=CARTESIAN_POINT('Ctrl Pts',(187.182947794064,1.24097270681647,125.01861764673));
#216651=CARTESIAN_POINT('Ctrl Pts',(187.186883843504,1.32196501082129,125.037182878614));
#216652=CARTESIAN_POINT('Ctrl Pts',(187.19430710991,1.47471396849223,125.072196326546));
#216653=CARTESIAN_POINT('Ctrl Pts',(187.201730376315,1.62630189479336,125.113335453442));
#216654=CARTESIAN_POINT('Ctrl Pts',(187.209153642721,1.77619933841254,125.160510294185));
#216655=CARTESIAN_POINT('Ctrl Pts',(187.216568135442,1.92591961570148,125.207629378185));
#216656=CARTESIAN_POINT('Ctrl Pts',(187.223982628163,2.07395303475566,125.260769865369));
#216657=CARTESIAN_POINT('Ctrl Pts',(187.231397120884,2.21978027822349,125.319790800442));
#216658=CARTESIAN_POINT('Ctrl Pts',(187.238804467237,2.36546696790406,125.378754848915));
#216659=CARTESIAN_POINT('Ctrl Pts',(187.246211813591,2.50895137152433,125.443587922699));
#216660=CARTESIAN_POINT('Ctrl Pts',(187.253619159945,2.64972939637269,125.514099311307));
#216661=CARTESIAN_POINT('Ctrl Pts',(187.26102098162,2.79040242365833,125.584558109861));
#216662=CARTESIAN_POINT('Ctrl Pts',(187.268422803296,2.92837275898145,125.660686624124));
#216663=CARTESIAN_POINT('Ctrl Pts',(187.275824624971,3.0631564720913,125.742246139407));
#216664=CARTESIAN_POINT('Ctrl Pts',(187.283222539282,3.19786903392806,125.823762600057));
#216665=CARTESIAN_POINT('Ctrl Pts',(187.290620453594,3.3293980051506,125.910704159221));
#216666=CARTESIAN_POINT('Ctrl Pts',(187.298018367905,3.45728435048477,126.002786346309));
#216667=CARTESIAN_POINT('Ctrl Pts',(187.305415052817,3.58514944342875,126.094853231009));
#216668=CARTESIAN_POINT('Ctrl Pts',(187.31281173773,3.70937280925888,126.192058830229));
#216669=CARTESIAN_POINT('Ctrl Pts',(187.320208422642,3.82952460154685,126.2940754948));
#216670=CARTESIAN_POINT('Ctrl Pts',(187.327604779577,3.94967106617857,126.396087635844));
#216671=CARTESIAN_POINT('Ctrl Pts',(187.335001136513,4.06574603167699,126.502910176461));
#216672=CARTESIAN_POINT('Ctrl Pts',(187.342397493448,4.17735316173905,126.614175523252));
#216673=CARTESIAN_POINT('Ctrl Pts',(187.349794982785,4.28897737913757,126.725457905052));
#216674=CARTESIAN_POINT('Ctrl Pts',(187.357192472121,4.39613213470813,126.841184183831));
#216675=CARTESIAN_POINT('Ctrl Pts',(187.364589961458,4.4984584664945,126.96095041467));
#216676=CARTESIAN_POINT('Ctrl Pts',(187.371990043973,4.6008206686173,127.080758629375));
#216677=CARTESIAN_POINT('Ctrl Pts',(187.379390126488,4.69835083467273,127.204609332144));
#216678=CARTESIAN_POINT('Ctrl Pts',(187.386790209003,4.79073084686722,127.332066200991));
#216679=CARTESIAN_POINT('Ctrl Pts',(187.394198428669,4.88321244038255,127.45966322177));
#216680=CARTESIAN_POINT('Ctrl Pts',(187.401606648336,4.97053235119977,127.590874025252));
#216681=CARTESIAN_POINT('Ctrl Pts',(187.409014868002,5.05241590194538,127.725233449638));
#216682=CARTESIAN_POINT('Ctrl Pts',(187.416427647304,5.13434985065019,127.859675570009));
#216683=CARTESIAN_POINT('Ctrl Pts',(187.423840426606,5.21084059102242,127.997269847324));
#216684=CARTESIAN_POINT('Ctrl Pts',(187.431253205909,5.28166008873117,128.137527801358));
#216685=CARTESIAN_POINT('Ctrl Pts',(187.438676576937,5.35258077665936,128.277986162534));
#216686=CARTESIAN_POINT('Ctrl Pts',(187.446099947966,5.41781388333707,128.421115463055));
#216687=CARTESIAN_POINT('Ctrl Pts',(187.453523318995,5.47717974033229,128.566407835537));
#216688=CARTESIAN_POINT('Ctrl Pts',(187.457459368436,5.50865694217581,128.64344533767));
#216689=CARTESIAN_POINT('Ctrl Pts',(187.461395417877,5.53848548259736,128.721090701616));
#216690=CARTESIAN_POINT('Ctrl Pts',(187.465331467317,5.56664434588085,128.799266782113));
#216691=CARTESIAN_POINT('Ctrl Pts',(187.472754733723,5.61975108322465,128.946704430135));
#216692=CARTESIAN_POINT('Ctrl Pts',(187.480178000128,5.66707654755361,129.096476348691));
#216693=CARTESIAN_POINT('Ctrl Pts',(187.487601266534,5.70841024769987,129.248088467055));
#216694=CARTESIAN_POINT('Ctrl Pts',(187.495015759255,5.74969509484514,129.399521392486));
#216695=CARTESIAN_POINT('Ctrl Pts',(187.502430251976,5.78500217687627,129.552789831813));
#216696=CARTESIAN_POINT('Ctrl Pts',(187.509844744697,5.81416937976279,129.707380678858));
#216697=CARTESIAN_POINT('Ctrl Pts',(187.517252091051,5.84330847020106,129.861822525424));
#216698=CARTESIAN_POINT('Ctrl Pts',(187.524659437404,5.86631939401667,130.017583877895));
#216699=CARTESIAN_POINT('Ctrl Pts',(187.532066783758,5.88309012691937,130.17413754512));
#216700=CARTESIAN_POINT('Ctrl Pts',(187.539468605433,5.89984835157674,130.330574448713));
#216701=CARTESIAN_POINT('Ctrl Pts',(187.546870427109,5.91037561281063,130.487802120845));
#216702=CARTESIAN_POINT('Ctrl Pts',(187.554272248784,5.91461117192879,130.64528438617));
#216703=CARTESIAN_POINT('Ctrl Pts',(187.561670163096,5.91884449512825,130.802683517833));
#216704=CARTESIAN_POINT('Ctrl Pts',(187.569068077407,5.91679272080989,130.960336602811));
#216705=CARTESIAN_POINT('Ctrl Pts',(187.576465991718,5.90844706236015,131.117703678424));
#216706=CARTESIAN_POINT('Ctrl Pts',(187.583862676631,5.90010279080743,131.275044602484));
#216707=CARTESIAN_POINT('Ctrl Pts',(187.591259361543,5.88546673073356,131.432099239102));
#216708=CARTESIAN_POINT('Ctrl Pts',(187.598656046455,5.86458220017064,131.588328843926));
#216709=CARTESIAN_POINT('Ctrl Pts',(187.60605240339,5.84369859564966,131.744551521365));
#216710=CARTESIAN_POINT('Ctrl Pts',(187.613448760326,5.81656712099775,131.899948869742));
#216711=CARTESIAN_POINT('Ctrl Pts',(187.620845117261,5.78328281349836,132.053988746889));
#216712=CARTESIAN_POINT('Ctrl Pts',(187.628242606598,5.74999341008647,132.208052207934));
#216713=CARTESIAN_POINT('Ctrl Pts',(187.635640095934,5.71054937699733,132.360757419028));
#216714=CARTESIAN_POINT('Ctrl Pts',(187.643037585271,5.66509653682644,132.511584033214));
#216715=CARTESIAN_POINT('Ctrl Pts',(187.650437667786,5.61962776323287,132.662463519436));
#216716=CARTESIAN_POINT('Ctrl Pts',(187.657837750301,5.56814609641887,132.811462740405));
#216717=CARTESIAN_POINT('Ctrl Pts',(187.665237832816,5.51084667598898,132.958078211923));
#216718=CARTESIAN_POINT('Ctrl Pts',(187.672646052482,5.45348424895594,133.104854902223));
#216719=CARTESIAN_POINT('Ctrl Pts',(187.680054272149,5.39029142860743,133.249242260506));
#216720=CARTESIAN_POINT('Ctrl Pts',(187.687462491815,5.3215110989095,133.390757761603));
#216721=CARTESIAN_POINT('Ctrl Pts',(187.694875271117,5.2526884360661,133.53236036313));
#216722=CARTESIAN_POINT('Ctrl Pts',(187.702288050419,5.17827158724947,133.671087257152));
#216723=CARTESIAN_POINT('Ctrl Pts',(187.709700829722,5.09854826658263,133.806482556433));
#216724=CARTESIAN_POINT('Ctrl Pts',(187.71712420075,5.01871103349667,133.942071314867));
#216725=CARTESIAN_POINT('Ctrl Pts',(187.724547571779,4.93355238690208,134.074318658072));
#216726=CARTESIAN_POINT('Ctrl Pts',(187.731970942808,4.84340249483737,134.20279891118));
#216727=CARTESIAN_POINT('Ctrl Pts',(187.735906992249,4.79560285894802,134.270922224219));
#216728=CARTESIAN_POINT('Ctrl Pts',(187.739843041689,4.74640066993037,134.337987035869));
#216729=CARTESIAN_POINT('Ctrl Pts',(187.74377909113,4.69584947277127,134.403933966114));
#216730=CARTESIAN_POINT('Ctrl Pts',(187.751202357536,4.6005114925774,134.528307818423));
#216731=CARTESIAN_POINT('Ctrl Pts',(187.758625623941,4.50008470519337,134.649079452252));
#216732=CARTESIAN_POINT('Ctrl Pts',(187.766048890346,4.39487101069584,134.765804718124));
#216733=CARTESIAN_POINT('Ctrl Pts',(187.773463383067,4.28978167004782,134.882392024425));
#216734=CARTESIAN_POINT('Ctrl Pts',(187.780877875788,4.17991693151612,134.994942207732));
#216735=CARTESIAN_POINT('Ctrl Pts',(187.788292368509,4.06562085926568,135.103041530498));
#216736=CARTESIAN_POINT('Ctrl Pts',(187.795699714863,3.95143494987295,135.211036663066));
#216737=CARTESIAN_POINT('Ctrl Pts',(187.803107061217,3.83282647904385,135.314589220668));
#216738=CARTESIAN_POINT('Ctrl Pts',(187.810514407571,3.71017843575953,135.413319994402));
#216739=CARTESIAN_POINT('Ctrl Pts',(187.817916229246,3.58762186801298,135.511977131));
#216740=CARTESIAN_POINT('Ctrl Pts',(187.825318050921,3.4610320163687,135.60581941131));
#216741=CARTESIAN_POINT('Ctrl Pts',(187.832719872597,3.33082714958386,135.69450591828));
#216742=CARTESIAN_POINT('Ctrl Pts',(187.840117786908,3.20069101693379,135.783145608334));
#216743=CARTESIAN_POINT('Ctrl Pts',(187.847515701219,3.06694397743706,135.866634735812));
#216744=CARTESIAN_POINT('Ctrl Pts',(187.854913615531,2.93003556760929,135.944674045271));
#216745=CARTESIAN_POINT('Ctrl Pts',(187.862310300443,2.79314990947657,136.022700386012));
#216746=CARTESIAN_POINT('Ctrl Pts',(187.869706985355,2.65310424769539,136.095278521522));
#216747=CARTESIAN_POINT('Ctrl Pts',(187.877103670267,2.51037525760295,136.162153692006));
#216748=CARTESIAN_POINT('Ctrl Pts',(187.884500027203,2.36765259626331,136.229025897175));
#216749=CARTESIAN_POINT('Ctrl Pts',(187.891896384138,2.22224718122004,136.290195481735));
#216750=CARTESIAN_POINT('Ctrl Pts',(187.899292741074,2.0746580887224,136.345454767407));
#216751=CARTESIAN_POINT('Ctrl Pts',(187.90669023041,1.92704639995784,136.400722513416));
#216752=CARTESIAN_POINT('Ctrl Pts',(187.914087719747,1.77725071766979,136.450078027893));
#216753=CARTESIAN_POINT('Ctrl Pts',(187.921485209083,1.62578764516406,136.493362735278));
#216754=CARTESIAN_POINT('Ctrl Pts',(187.928885291598,1.47427147751353,136.53666261605));
#216755=CARTESIAN_POINT('Ctrl Pts',(187.936285374113,1.32108711461301,136.573887350165));
#216756=CARTESIAN_POINT('Ctrl Pts',(187.943685456628,1.16676362970169,136.60492896859));
#216757=CARTESIAN_POINT('Ctrl Pts',(187.951093676295,1.01227045025355,136.636004720467));
#216758=CARTESIAN_POINT('Ctrl Pts',(187.958501895961,0.856636013498965,
136.660883705003));
#216759=CARTESIAN_POINT('Ctrl Pts',(187.965910115627,0.700397566244245,
136.679509450719));
#216760=CARTESIAN_POINT('Ctrl Pts',(187.973322894929,0.544062956832329,
136.698146660271));
#216761=CARTESIAN_POINT('Ctrl Pts',(187.980735674231,0.387123967424787,
136.710522932578));
#216762=CARTESIAN_POINT('Ctrl Pts',(187.988148453534,0.23011966537511,136.716633911495));
#216763=CARTESIAN_POINT('Ctrl Pts',(187.995571824562,0.072891028215697,
136.722753622065));
#216764=CARTESIAN_POINT('Ctrl Pts',(188.002995195591,-0.0844027356615752,
136.72259016019));
#216765=CARTESIAN_POINT('Ctrl Pts',(188.01041856662,-0.241225030045429,
136.716191217928));
#216766=CARTESIAN_POINT('Ctrl Pts',(188.014354616061,-0.324375973428068,
136.7127983452));
#216767=CARTESIAN_POINT('Ctrl Pts',(188.018290665501,-0.407394483839031,
136.707653318947));
#216768=CARTESIAN_POINT('Ctrl Pts',(188.022226714942,-0.490201660815617,
136.700769091733));
#216769=CARTESIAN_POINT('Ctrl Pts',(188.029649981348,-0.646373412268205,
136.687785654058));
#216770=CARTESIAN_POINT('Ctrl Pts',(188.037073247753,-0.80226513988054,
136.668573771693));
#216771=CARTESIAN_POINT('Ctrl Pts',(188.044496514159,-0.957339983753277,
136.643147368083));
#216772=CARTESIAN_POINT('Ctrl Pts',(188.051911006879,-1.11223154203839,
136.61775101637));
#216773=CARTESIAN_POINT('Ctrl Pts',(188.0593254996,-1.26630777361279,136.58615482358));
#216774=CARTESIAN_POINT('Ctrl Pts',(188.066739992321,-1.41903461427524,
136.548424625391));
#216775=CARTESIAN_POINT('Ctrl Pts',(188.074147338675,-1.57161425105952,
136.510730792987));
#216776=CARTESIAN_POINT('Ctrl Pts',(188.081554685029,-1.72284672618799,
136.466914814107));
#216777=CARTESIAN_POINT('Ctrl Pts',(188.088962031383,-1.87220598557174,
136.417093936555));
#216778=CARTESIAN_POINT('Ctrl Pts',(188.096363853058,-2.02145384718316,
136.367310217293));
#216779=CARTESIAN_POINT('Ctrl Pts',(188.103765674734,-2.16883092230147,
136.311530634628));
#216780=CARTESIAN_POINT('Ctrl Pts',(188.111167496409,-2.31382430327432,
136.249922815914));
#216781=CARTESIAN_POINT('Ctrl Pts',(188.11856541072,-2.45874114337115,136.188347519488));
#216782=CARTESIAN_POINT('Ctrl Pts',(188.125963325032,-2.60127645265397,
136.120950259984));
#216783=CARTESIAN_POINT('Ctrl Pts',(188.133361239343,-2.7409354735747,136.047947490328));
#216784=CARTESIAN_POINT('Ctrl Pts',(188.140757924255,-2.88057128569987,
135.974956852407));
#216785=CARTESIAN_POINT('Ctrl Pts',(188.148154609167,-3.01733142762264,
135.896362725914));
#216786=CARTESIAN_POINT('Ctrl Pts',(188.15555129408,-3.1507439080487,135.812428447418));
#216787=CARTESIAN_POINT('Ctrl Pts',(188.162947651015,-3.28415047282601,
135.728497890655));
#216788=CARTESIAN_POINT('Ctrl Pts',(188.170344007951,-3.41420935528581,
135.639227851488));
#216789=CARTESIAN_POINT('Ctrl Pts',(188.177740364886,-3.54047606690486,
135.544925961718));
#216790=CARTESIAN_POINT('Ctrl Pts',(188.185137854223,-3.66676211027926,
135.450609634088));
#216791=CARTESIAN_POINT('Ctrl Pts',(188.192535343559,-3.78925452766934,
135.351260145295));
#216792=CARTESIAN_POINT('Ctrl Pts',(188.199932832896,-3.90754066825958,
135.247226414368));
#216793=CARTESIAN_POINT('Ctrl Pts',(188.207332915411,-4.02586827387267,
135.143156214579));
#216794=CARTESIAN_POINT('Ctrl Pts',(188.214732997926,-4.13998638682651,
135.034398749718));
#216795=CARTESIAN_POINT('Ctrl Pts',(188.222133080441,-4.24951819270741,
134.921340784187));
#216796=CARTESIAN_POINT('Ctrl Pts',(188.229541300107,-4.35917044006939,
134.808158499799));
#216797=CARTESIAN_POINT('Ctrl Pts',(188.236949519774,-4.4642260490177,134.690666539206));
#216798=CARTESIAN_POINT('Ctrl Pts',(188.24435773944,-4.56434711347478,134.569286379147));
#216799=CARTESIAN_POINT('Ctrl Pts',(188.251770518742,-4.66452980077634,
134.447831511624));
#216800=CARTESIAN_POINT('Ctrl Pts',(188.259183298044,-4.75977166640558,
134.322483972582));
#216801=CARTESIAN_POINT('Ctrl Pts',(188.266596077347,-4.84977766634151,
134.193694940048));
#216802=CARTESIAN_POINT('Ctrl Pts',(188.274019448375,-4.93991227107106,
134.064721887705));
#216803=CARTESIAN_POINT('Ctrl Pts',(188.281442819404,-5.02479586745561,
133.932297834228));
#216804=CARTESIAN_POINT('Ctrl Pts',(188.288866190433,-5.10417853681512,
133.796900011929));
#216805=CARTESIAN_POINT('Ctrl Pts',(188.292802239874,-5.14626913287155,
133.725108837719));
#216806=CARTESIAN_POINT('Ctrl Pts',(188.296738289315,-5.18681400928749,
133.652482001339));
#216807=CARTESIAN_POINT('Ctrl Pts',(188.300674338755,-5.22578141579513,
133.579092885161));
#216808=CARTESIAN_POINT('Ctrl Pts',(188.308522635262,-5.30348058216972,
133.432758457005));
#216809=CARTESIAN_POINT('Ctrl Pts',(188.316370931769,-5.37511838685106,
133.282990724991));
#216810=CARTESIAN_POINT('Ctrl Pts',(188.324219228275,-5.44039662476336,
133.130304539453));
#216811=CARTESIAN_POINT('Ctrl Pts',(188.332053990155,-5.50556228836188,
132.977881665902));
#216812=CARTESIAN_POINT('Ctrl Pts',(188.339888752035,-5.56439012663925,
132.822550655319));
#216813=CARTESIAN_POINT('Ctrl Pts',(188.347723513915,-5.61662765213832,
132.664850977588));
#216814=CARTESIAN_POINT('Ctrl Pts',(188.355539641514,-5.6687409353559,132.507526374433));
#216815=CARTESIAN_POINT('Ctrl Pts',(188.363355769114,-5.71429507358988,
132.347844634376));
#216816=CARTESIAN_POINT('Ctrl Pts',(188.371171896713,-5.75308575484795,
132.1863645466));
#216817=CARTESIAN_POINT('Ctrl Pts',(188.378976980979,-5.7918216291147,132.025112612533));
#216818=CARTESIAN_POINT('Ctrl Pts',(188.386782065244,-5.82381301965768,
131.862067694374));
#216819=CARTESIAN_POINT('Ctrl Pts',(188.39458714951,-5.8489048080885,131.697805136503));
#216820=CARTESIAN_POINT('Ctrl Pts',(188.402376866656,-5.87394719429565,
131.533865988645));
#216821=CARTESIAN_POINT('Ctrl Pts',(188.410166583802,-5.89211702687552,
131.368714288067));
#216822=CARTESIAN_POINT('Ctrl Pts',(188.417956300948,-5.90330990566078,
131.20293648265));
#216823=CARTESIAN_POINT('Ctrl Pts',(188.424179136552,-5.91225136570458,
131.070504455847));
#216824=CARTESIAN_POINT('Ctrl Pts',(188.430401972156,-5.91674131959235,
130.937673208914));
#216825=CARTESIAN_POINT('Ctrl Pts',(188.436624807759,-5.91674998742092,
130.804746434304));
#216826=CARTESIAN_POINT('',(190.186624807795,-5.9167474892903,130.798909885783));
#216827=CARTESIAN_POINT('Ctrl Pts',(188.436624807795,-5.91674998742097,
130.80474643354));
#216828=CARTESIAN_POINT('Ctrl Pts',(188.444336312247,-5.91676072880488,
130.640020016287));
#216829=CARTESIAN_POINT('Ctrl Pts',(188.452047816698,-5.9098880006331,130.475412038668));
#216830=CARTESIAN_POINT('Ctrl Pts',(188.45975932115,-5.89618734660479,130.311506342716));
#216831=CARTESIAN_POINT('Ctrl Pts',(188.467479281045,-5.88247167020258,
130.147420928874));
#216832=CARTESIAN_POINT('Ctrl Pts',(188.47519924094,-5.86191315565751,129.984039656638));
#216833=CARTESIAN_POINT('Ctrl Pts',(188.482919200835,-5.83461887000143,
129.821938506494));
#216834=CARTESIAN_POINT('Ctrl Pts',(188.490936097646,-5.80627474974523,
129.65360237375));
#216835=CARTESIAN_POINT('Ctrl Pts',(188.498952994457,-5.77066650315088,
129.486647185334));
#216836=CARTESIAN_POINT('Ctrl Pts',(188.506969891268,-5.72797103557548,
129.321701392353));
#216837=CARTESIAN_POINT('Ctrl Pts',(188.514715160958,-5.6867221685032,129.162344264416));
#216838=CARTESIAN_POINT('Ctrl Pts',(188.522460430647,-5.63885863849107,
129.004862872487));
#216839=CARTESIAN_POINT('Ctrl Pts',(188.530205700337,-5.5845895056426,128.849804244379));
#216840=CARTESIAN_POINT('Ctrl Pts',(188.538358410709,-5.52746553966337,
128.686588741718));
#216841=CARTESIAN_POINT('Ctrl Pts',(188.546511121081,-5.46324405110737,
128.526058178221));
#216842=CARTESIAN_POINT('Ctrl Pts',(188.554663831453,-5.39222426567471,
128.368822067026));
#216843=CARTESIAN_POINT('Ctrl Pts',(188.562816541824,-5.32120448024206,
128.21158595583));
#216844=CARTESIAN_POINT('Ctrl Pts',(188.570969252196,-5.24338665044448,
128.057644630733));
#216845=CARTESIAN_POINT('Ctrl Pts',(188.579121962568,-5.15912334327355,
127.907573277876));
#216846=CARTESIAN_POINT('Ctrl Pts',(188.586545228974,-5.08239929092767,
127.770929194955));
#216847=CARTESIAN_POINT('Ctrl Pts',(188.593968495379,-5.00012675873199,
127.637128755464));
#216848=CARTESIAN_POINT('Ctrl Pts',(188.601391761784,-4.91254156507233,
127.506654455104));
#216849=CARTESIAN_POINT('Ctrl Pts',(188.608806254505,-4.82505988983811,
127.376334364533));
#216850=CARTESIAN_POINT('Ctrl Pts',(188.616220747226,-4.73227825779838,
127.249332894892));
#216851=CARTESIAN_POINT('Ctrl Pts',(188.623635239947,-4.6344785403192,127.126108420962));
#216852=CARTESIAN_POINT('Ctrl Pts',(188.631042586301,-4.53677308588965,
127.00300271542));
#216853=CARTESIAN_POINT('Ctrl Pts',(188.638449932655,-4.43405940528752,
126.883667048682));
#216854=CARTESIAN_POINT('Ctrl Pts',(188.645857279009,-4.32666280054533,
126.76853113989));
#216855=CARTESIAN_POINT('Ctrl Pts',(188.653259100684,-4.21934629624284,
126.653481103803));
#216856=CARTESIAN_POINT('Ctrl Pts',(188.66066092236,-4.10735407577181,126.542624860554));
#216857=CARTESIAN_POINT('Ctrl Pts',(188.668062744035,-3.99105179769123,
126.436359231274));
#216858=CARTESIAN_POINT('Ctrl Pts',(188.675460658346,-3.87481091467824,
126.330149698793));
#216859=CARTESIAN_POINT('Ctrl Pts',(188.682858572658,-3.75426478020397,
126.22852620523));
#216860=CARTESIAN_POINT('Ctrl Pts',(188.690256486969,-3.62981591611858,
126.131848768722));
#216861=CARTESIAN_POINT('Ctrl Pts',(188.697653171881,-3.50538773317637,
126.035187398249));
#216862=CARTESIAN_POINT('Ctrl Pts',(188.705049856793,-3.3770584023365,125.943470682302));
#216863=CARTESIAN_POINT('Ctrl Pts',(188.712446541706,-3.24526362374814,
125.857018444755));
#216864=CARTESIAN_POINT('Ctrl Pts',(188.719842898641,-3.11347468907845,
125.77057004059));
#216865=CARTESIAN_POINT('Ctrl Pts',(188.727239255577,-2.97822092432744,
125.689385855431));
#216866=CARTESIAN_POINT('Ctrl Pts',(188.734635612512,-2.83996688492409,
125.613742286863));
#216867=CARTESIAN_POINT('Ctrl Pts',(188.742033101849,-2.70169167847449,
125.53808713707));
#216868=CARTESIAN_POINT('Ctrl Pts',(188.749430591185,-2.56041561025224,
125.467974472102));
#216869=CARTESIAN_POINT('Ctrl Pts',(188.756828080522,-2.41662755324927,
125.403634570878));
#216870=CARTESIAN_POINT('Ctrl Pts',(188.764228163037,-2.27278909156605,
125.339272115401));
#216871=CARTESIAN_POINT('Ctrl Pts',(188.771628245552,-2.1264372284147,125.280686605083));
#216872=CARTESIAN_POINT('Ctrl Pts',(188.779028328067,-1.97808036179923,
125.228059993966));
#216873=CARTESIAN_POINT('Ctrl Pts',(188.786436547733,-1.82956036155703,
125.175375514479));
#216874=CARTESIAN_POINT('Ctrl Pts',(188.7938447674,-1.67903130693944,125.128663144689));
#216875=CARTESIAN_POINT('Ctrl Pts',(188.801252987066,-1.52701699451342,
125.088055022082));
#216876=CARTESIAN_POINT('Ctrl Pts',(188.808665766368,-1.37490911981405,
125.047421905852));
#216877=CARTESIAN_POINT('Ctrl Pts',(188.81607854567,-1.22131452911263,125.012900604892));
#216878=CARTESIAN_POINT('Ctrl Pts',(188.823491324972,-1.06676621647483,
124.984571927082));
#216879=CARTESIAN_POINT('Ctrl Pts',(188.830914696001,-0.911997077960795,
124.956202771929));
#216880=CARTESIAN_POINT('Ctrl Pts',(188.83833806703,-0.75627186444372,124.934043964435));
#216881=CARTESIAN_POINT('Ctrl Pts',(188.845761438059,-0.600128509702636,
124.918124440318));
#216882=CARTESIAN_POINT('Ctrl Pts',(188.8496974875,-0.517337556408728,124.909683526647));
#216883=CARTESIAN_POINT('Ctrl Pts',(188.853633536941,-0.434429058316661,
124.90299582822));
#216884=CARTESIAN_POINT('Ctrl Pts',(188.857569586381,-0.3514829554707,124.898059719837));
#216885=CARTESIAN_POINT('Ctrl Pts',(188.864992852787,-0.195049194165717,
124.888750373478));
#216886=CARTESIAN_POINT('Ctrl Pts',(188.872416119192,-0.0380087817261698,
124.885646179091));
#216887=CARTESIAN_POINT('Ctrl Pts',(188.879839385598,0.1191048789509,124.888809536702));
#216888=CARTESIAN_POINT('Ctrl Pts',(188.887253878319,0.276032844328527,
124.891969155487));
#216889=CARTESIAN_POINT('Ctrl Pts',(188.89466837104,0.433033516041292,124.90138157371));
#216890=CARTESIAN_POINT('Ctrl Pts',(188.902082863761,0.589568892045253,
124.917057407774));
#216891=CARTESIAN_POINT('Ctrl Pts',(188.909490210115,0.745953393360701,
124.932718132878));
#216892=CARTESIAN_POINT('Ctrl Pts',(188.916897556468,0.901873122835364,
124.954630218564));
#216893=CARTESIAN_POINT('Ctrl Pts',(188.924304902822,1.05679071189202,124.98275225271));
#216894=CARTESIAN_POINT('Ctrl Pts',(188.931706724498,1.21159275756575,125.010853312383));
#216895=CARTESIAN_POINT('Ctrl Pts',(188.939108546173,1.36539378534926,125.045155031959));
#216896=CARTESIAN_POINT('Ctrl Pts',(188.946510367848,1.51766229100495,125.085564264052));
#216897=CARTESIAN_POINT('Ctrl Pts',(188.95390828216,1.66985041530155,125.125952164426));
#216898=CARTESIAN_POINT('Ctrl Pts',(188.961306196471,1.8205072687502,125.17244106084));
#216899=CARTESIAN_POINT('Ctrl Pts',(188.968704110782,1.96911238500255,125.22488689886));
#216900=CARTESIAN_POINT('Ctrl Pts',(188.976100795695,2.11769280578066,125.277324021333));
#216901=CARTESIAN_POINT('Ctrl Pts',(188.983497480607,2.26422181439622,125.33571599657));
#216902=CARTESIAN_POINT('Ctrl Pts',(188.990894165519,2.40819482739287,125.39986913031));
#216903=CARTESIAN_POINT('Ctrl Pts',(188.998290522454,2.55216145647515,125.464019419434));
#216904=CARTESIAN_POINT('Ctrl Pts',(189.00568687939,2.69357197430951,125.533930207192));
#216905=CARTESIAN_POINT('Ctrl Pts',(189.013083236325,2.83194273622357,125.609360049592));
#216906=CARTESIAN_POINT('Ctrl Pts',(189.020480725662,2.97033468305507,125.684801440493));
#216907=CARTESIAN_POINT('Ctrl Pts',(189.027878214998,3.10568561952156,125.765763389823));
#216908=CARTESIAN_POINT('Ctrl Pts',(189.035275704335,3.23753755765109,125.851959066268));
#216909=CARTESIAN_POINT('Ctrl Pts',(189.04267578685,3.36943571627262,125.938184958474));
#216910=CARTESIAN_POINT('Ctrl Pts',(189.050075869365,3.49783212220785,126.029648026486));
#216911=CARTESIAN_POINT('Ctrl Pts',(189.05747595188,3.62229889082746,126.126018891269));
#216912=CARTESIAN_POINT('Ctrl Pts',(189.064884171547,3.74690252345494,126.222495725726));
#216913=CARTESIAN_POINT('Ctrl Pts',(189.072292391213,3.86756759402008,126.323890905695));
#216914=CARTESIAN_POINT('Ctrl Pts',(189.079700610879,3.98389980667395,126.429835169831));
#216915=CARTESIAN_POINT('Ctrl Pts',(189.087113390182,4.10030361986379,126.535844640893));
#216916=CARTESIAN_POINT('Ctrl Pts',(189.094526169484,4.21236899608596,126.646408513676));
#216917=CARTESIAN_POINT('Ctrl Pts',(189.101938948786,4.31973985307035,126.761122043812));
#216918=CARTESIAN_POINT('Ctrl Pts',(189.109362319814,4.42726412657015,126.875999482018));
#216919=CARTESIAN_POINT('Ctrl Pts',(189.116785690843,4.53008024059027,126.995038137808));
#216920=CARTESIAN_POINT('Ctrl Pts',(189.124209061872,4.627873084345,127.11780107272));
#216921=CARTESIAN_POINT('Ctrl Pts',(189.128145111313,4.6797251966109,127.182892926467));
#216922=CARTESIAN_POINT('Ctrl Pts',(189.132081160754,4.73016581507376,127.249031329645));
#216923=CARTESIAN_POINT('Ctrl Pts',(189.136017210194,4.77915309751256,127.316148147971));
#216924=CARTESIAN_POINT('Ctrl Pts',(189.1434404766,4.87154158335144,127.442728372691));
#216925=CARTESIAN_POINT('Ctrl Pts',(189.150863743005,4.95903740885353,127.573173026402));
#216926=CARTESIAN_POINT('Ctrl Pts',(189.158287009411,5.04129975781475,127.707067070878));
#216927=CARTESIAN_POINT('Ctrl Pts',(189.165701502132,5.12346487951111,127.840802863713));
#216928=CARTESIAN_POINT('Ctrl Pts',(189.173115994853,5.20040864350211,127.977979617276));
#216929=CARTESIAN_POINT('Ctrl Pts',(189.180530487574,5.27183131466145,128.118150433635));
#216930=CARTESIAN_POINT('Ctrl Pts',(189.187937833927,5.34318514596105,128.258186148084));
#216931=CARTESIAN_POINT('Ctrl Pts',(189.195345180281,5.40902831002284,128.401209849912));
#216932=CARTESIAN_POINT('Ctrl Pts',(189.202752526635,5.46910518719545,128.546747051454));
#216933=CARTESIAN_POINT('Ctrl Pts',(189.21015434831,5.52913725676648,128.692175705861));
#216934=CARTESIAN_POINT('Ctrl Pts',(189.217556169986,5.58341146092722,128.840113783703));
#216935=CARTESIAN_POINT('Ctrl Pts',(189.224957991661,5.6317188761904,128.990063766976));
#216936=CARTESIAN_POINT('Ctrl Pts',(189.232355905972,5.68000079034474,129.139934592819));
#216937=CARTESIAN_POINT('Ctrl Pts',(189.239753820284,5.72232207444452,129.291814854514));
#216938=CARTESIAN_POINT('Ctrl Pts',(189.247151734595,5.75852260079111,129.445188804042));
#216939=CARTESIAN_POINT('Ctrl Pts',(189.254548419507,5.79471711126733,129.598537265604));
#216940=CARTESIAN_POINT('Ctrl Pts',(189.26194510442,5.82479279708112,129.753378559388));
#216941=CARTESIAN_POINT('Ctrl Pts',(189.269341789332,5.84863987901503,129.909183468564));
#216942=CARTESIAN_POINT('Ctrl Pts',(189.276738146267,5.8724859035443,130.064981469187));
#216943=CARTESIAN_POINT('Ctrl Pts',(189.284134503203,5.89010381686027,130.221742631245));
#216944=CARTESIAN_POINT('Ctrl Pts',(189.291530860138,5.90143533087373,130.3789295444));
#216945=CARTESIAN_POINT('Ctrl Pts',(189.298928349475,5.91276857977092,130.536140523273));
#216946=CARTESIAN_POINT('Ctrl Pts',(189.306325838811,5.9178134861293,130.693777010678));
#216947=CARTESIAN_POINT('Ctrl Pts',(189.313723328148,5.91656381556915,130.851298649032));
#216948=CARTESIAN_POINT('Ctrl Pts',(189.321123410663,5.91531370693891,131.008875506353));
#216949=CARTESIAN_POINT('Ctrl Pts',(189.328523493178,5.90776463111646,131.166337061412));
#216950=CARTESIAN_POINT('Ctrl Pts',(189.335923575693,5.89396242191814,131.323145285339));
#216951=CARTESIAN_POINT('Ctrl Pts',(189.343331795359,5.88014503577195,131.480125936029));
#216952=CARTESIAN_POINT('Ctrl Pts',(189.350740015026,5.86006081725151,131.636451448796));
#216953=CARTESIAN_POINT('Ctrl Pts',(189.358148234692,5.83380730984865,131.791590496599));
#216954=CARTESIAN_POINT('Ctrl Pts',(189.365561013994,5.80753764385015,131.946825029897));
#216955=CARTESIAN_POINT('Ctrl Pts',(189.372973793296,5.77509119954317,132.100871278681));
#216956=CARTESIAN_POINT('Ctrl Pts',(189.380386572599,5.7366160286638,132.253210886634));
#216957=CARTESIAN_POINT('Ctrl Pts',(189.387809943627,5.69808588265588,132.405768164563));
#216958=CARTESIAN_POINT('Ctrl Pts',(189.395233314656,5.65350991124101,132.556613574327));
#216959=CARTESIAN_POINT('Ctrl Pts',(189.402656685685,5.60308539804483,132.705245828387));
#216960=CARTESIAN_POINT('Ctrl Pts',(189.406592735126,5.57634911122828,132.784054215872));
#216961=CARTESIAN_POINT('Ctrl Pts',(189.410528784567,5.54796938585717,132.862240759177));
#216962=CARTESIAN_POINT('Ctrl Pts',(189.414464834007,5.51798092849068,132.93973342701));
#216963=CARTESIAN_POINT('Ctrl Pts',(189.421888100413,5.46142363380593,133.085882180079));
#216964=CARTESIAN_POINT('Ctrl Pts',(189.429311366818,5.39897048314281,133.230003417703));
#216965=CARTESIAN_POINT('Ctrl Pts',(189.436734633224,5.33078644043194,133.371586063258));
#216966=CARTESIAN_POINT('Ctrl Pts',(189.444149125945,5.26268298559709,133.513001369884));
#216967=CARTESIAN_POINT('Ctrl Pts',(189.451563618666,5.18886228167012,133.651883723719));
#216968=CARTESIAN_POINT('Ctrl Pts',(189.458978111387,5.10953830238054,133.787739389865));
#216969=CARTESIAN_POINT('Ctrl Pts',(189.466385457741,5.03029077852894,133.923464113205));
#216970=CARTESIAN_POINT('Ctrl Pts',(189.473792804094,4.94555072602297,134.056167636292));
#216971=CARTESIAN_POINT('Ctrl Pts',(189.481200150448,4.85557917610903,134.1853784269));
#216972=CARTESIAN_POINT('Ctrl Pts',(189.488601972123,4.76567473037149,134.314492847226));
#216973=CARTESIAN_POINT('Ctrl Pts',(189.496003793799,4.67054676872829,134.440119416974));
#216974=CARTESIAN_POINT('Ctrl Pts',(189.503405615474,4.57050093892078,134.561813442263));
#216975=CARTESIAN_POINT('Ctrl Pts',(189.510803529786,4.470507922528,134.683443226223));
#216976=CARTESIAN_POINT('Ctrl Pts',(189.518201444097,4.36560244470111,134.801144312466));
#216977=CARTESIAN_POINT('Ctrl Pts',(189.525599358408,4.25613186592361,134.914503206622));
#216978=CARTESIAN_POINT('Ctrl Pts',(189.53299604332,4.1466794791702,135.027843262585));
#216979=CARTESIAN_POINT('Ctrl Pts',(189.540392728233,4.03266375619807,135.136842290347));
#216980=CARTESIAN_POINT('Ctrl Pts',(189.547789413145,3.9144706037665,135.241121874919));
#216981=CARTESIAN_POINT('Ctrl Pts',(189.55518577008,3.79628269214324,135.345396835624));
#216982=CARTESIAN_POINT('Ctrl Pts',(189.562582127016,3.67391799928616,135.444952522259));
#216983=CARTESIAN_POINT('Ctrl Pts',(189.569978483951,3.5477971575957,135.539449411987));
#216984=CARTESIAN_POINT('Ctrl Pts',(189.577375973288,3.42165700648274,135.633960769431));
#216985=CARTESIAN_POINT('Ctrl Pts',(189.584773462624,3.2917598602477,135.723411563957));
#216986=CARTESIAN_POINT('Ctrl Pts',(189.592170951961,3.15855696719353,135.807504473932));
#216987=CARTESIAN_POINT('Ctrl Pts',(189.599571034476,3.02530738007121,135.891626862547));
#216988=CARTESIAN_POINT('Ctrl Pts',(189.606971116991,2.88875005437881,135.970387427978));
#216989=CARTESIAN_POINT('Ctrl Pts',(189.614371199506,2.74936242334025,136.043533913767));
#216990=CARTESIAN_POINT('Ctrl Pts',(189.621779419172,2.6098215212719,136.116760831637));
#216991=CARTESIAN_POINT('Ctrl Pts',(189.629187638839,2.46744442931756,136.184361167894));
#216992=CARTESIAN_POINT('Ctrl Pts',(189.636595858505,2.3227308926061,136.246129793398));
#216993=CARTESIAN_POINT('Ctrl Pts',(189.644008637807,2.17792828712777,136.307936436459));
#216994=CARTESIAN_POINT('Ctrl Pts',(189.651421417109,2.03078671951321,136.363904084189));
#216995=CARTESIAN_POINT('Ctrl Pts',(189.658834196411,1.88182232319197,136.413877112455));
#216996=CARTESIAN_POINT('Ctrl Pts',(189.66625756744,1.73264507955527,136.463921544528));
#216997=CARTESIAN_POINT('Ctrl Pts',(189.673680938469,1.58164016277834,136.507954145901));
#216998=CARTESIAN_POINT('Ctrl Pts',(189.681104309498,1.42933595688406,136.545869938717));
#216999=CARTESIAN_POINT('Ctrl Pts',(189.685040358939,1.3485806124279,136.565973801845));
#217000=CARTESIAN_POINT('Ctrl Pts',(189.688976408379,1.26746012441086,136.584358871603));
#217001=CARTESIAN_POINT('Ctrl Pts',(189.69291245782,1.18605385454001,136.601015412931));
#217002=CARTESIAN_POINT('Ctrl Pts',(189.700335724226,1.03252417016951,136.632429130043));
#217003=CARTESIAN_POINT('Ctrl Pts',(189.707758990631,0.877513437794605,
136.657786574917));
#217004=CARTESIAN_POINT('Ctrl Pts',(189.715182257037,0.721540807687306,
136.676950286983));
#217005=CARTESIAN_POINT('Ctrl Pts',(189.722596749758,0.56575252427599,136.696091349132));
#217006=CARTESIAN_POINT('Ctrl Pts',(189.730011242479,0.409004972998288,
136.709053204846));
#217007=CARTESIAN_POINT('Ctrl Pts',(189.7374257352,0.251829205035335,136.715749000509));
#217008=CARTESIAN_POINT('Ctrl Pts',(189.744833081553,0.0948049289951359,
136.722438342512));
#217009=CARTESIAN_POINT('Ctrl Pts',(189.752240427907,-0.0626463716075346,
136.722873632068));
#217010=CARTESIAN_POINT('Ctrl Pts',(189.759647774261,-0.219986889591926,
136.717019607471));
#217011=CARTESIAN_POINT('Ctrl Pts',(189.767049595936,-0.377210057081186,
136.711169949027));
#217012=CARTESIAN_POINT('Ctrl Pts',(189.774451417612,-0.534322235037135,
136.699040330281));
#217013=CARTESIAN_POINT('Ctrl Pts',(189.781853239287,-0.690784079832339,
136.68064753343));
#217014=CARTESIAN_POINT('Ctrl Pts',(189.789251153599,-0.847163329639719,
136.662264445992));
#217015=CARTESIAN_POINT('Ctrl Pts',(189.79664906791,-1.00289256018978,136.637624808542));
#217016=CARTESIAN_POINT('Ctrl Pts',(189.804046982221,-1.15743613013174,
136.606797361484));
#217017=CARTESIAN_POINT('Ctrl Pts',(189.811443667134,-1.31195401773457,
136.575975037388));
#217018=CARTESIAN_POINT('Ctrl Pts',(189.818840352046,-1.4652862700588,136.538967017513));
#217019=CARTESIAN_POINT('Ctrl Pts',(189.826237036958,-1.61690592382758,
136.4958934336));
#217020=CARTESIAN_POINT('Ctrl Pts',(189.833633393893,-1.76851885462208,
136.452821759614));
#217021=CARTESIAN_POINT('Ctrl Pts',(189.841029750829,-1.91841897876412,
136.403685158374));
#217022=CARTESIAN_POINT('Ctrl Pts',(189.848426107764,-2.0660932839906,136.348653999445));
#217023=CARTESIAN_POINT('Ctrl Pts',(189.855823597101,-2.21379019853027,
136.293614415105));
#217024=CARTESIAN_POINT('Ctrl Pts',(189.863221086437,-2.35926026579751,
136.232678606497));
#217025=CARTESIAN_POINT('Ctrl Pts',(189.870618575774,-2.50200942995244,
136.166065511994));
#217026=CARTESIAN_POINT('Ctrl Pts',(189.878018658289,-2.64480863460694,
136.099429066372));
#217027=CARTESIAN_POINT('Ctrl Pts',(189.885418740804,-2.78488469905547,
136.027111530211));
#217028=CARTESIAN_POINT('Ctrl Pts',(189.892818823319,-2.92176732847544,
135.949378230826));
#217029=CARTESIAN_POINT('Ctrl Pts',(189.900227042986,-3.05880047441704,
135.871559455687));
#217030=CARTESIAN_POINT('Ctrl Pts',(189.907635262652,-3.19263284780672,
135.788313208874));
#217031=CARTESIAN_POINT('Ctrl Pts',(189.915043482319,-3.32282174323811,
135.699949062806));
#217032=CARTESIAN_POINT('Ctrl Pts',(189.922456261621,-3.45309076776235,
135.611530530079));
#217033=CARTESIAN_POINT('Ctrl Pts',(189.929869040923,-3.579711546312,135.517988042663));
#217034=CARTESIAN_POINT('Ctrl Pts',(189.937281820225,-3.70227416517129,
135.419671719583));
#217035=CARTESIAN_POINT('Ctrl Pts',(189.944705191254,-3.82501190724813,
135.321214917531));
#217036=CARTESIAN_POINT('Ctrl Pts',(189.952128562282,-3.94367962786938,
135.217970900963));
#217037=CARTESIAN_POINT('Ctrl Pts',(189.959551933311,-4.05790340171897,
135.110327471226));
#217038=CARTESIAN_POINT('Ctrl Pts',(189.963487982752,-4.1184675873743,135.053252341912));
#217039=CARTESIAN_POINT('Ctrl Pts',(189.967424032192,-4.17778307250271,
134.994940957179));
#217040=CARTESIAN_POINT('Ctrl Pts',(189.971360081633,-4.23579876978104,
134.935454824241));
#217041=CARTESIAN_POINT('Ctrl Pts',(189.97868580183,-4.34377677455446,134.824740065172));
#217042=CARTESIAN_POINT('Ctrl Pts',(189.986011522027,-4.44759549208393,
134.709599597571));
#217043=CARTESIAN_POINT('Ctrl Pts',(189.993337242224,-4.54686303201109,
134.590383217952));
#217044=CARTESIAN_POINT('Ctrl Pts',(190.000654105557,-4.6460105565541,134.471310972051));
#217045=CARTESIAN_POINT('Ctrl Pts',(190.00797096889,-4.74061760854022,134.348172911224));
#217046=CARTESIAN_POINT('Ctrl Pts',(190.015287832222,-4.83032801012746,
134.221356648743));
#217047=CARTESIAN_POINT('Ctrl Pts',(190.022596306275,-4.91993555265535,
134.094685789707));
#217048=CARTESIAN_POINT('Ctrl Pts',(190.029904780328,-5.00465740532908,
133.964345439033));
#217049=CARTESIAN_POINT('Ctrl Pts',(190.037213254381,-5.08417700870137,
133.830756941033));
#217050=CARTESIAN_POINT('Ctrl Pts',(190.044516984866,-5.16364499985177,
133.697255148686));
#217051=CARTESIAN_POINT('Ctrl Pts',(190.051820715352,-5.23791726272298,
133.560509731128));
#217052=CARTESIAN_POINT('Ctrl Pts',(190.059124445837,-5.30671991172705,
133.420971849862));
#217053=CARTESIAN_POINT('Ctrl Pts',(190.06642496806,-5.3754923382356,133.281495262502));
#217054=CARTESIAN_POINT('Ctrl Pts',(190.073725490283,-5.43879976191837,
133.139228995741));
#217055=CARTESIAN_POINT('Ctrl Pts',(190.081026012506,-5.49641386784294,
132.994649446895));
#217056=CARTESIAN_POINT('Ctrl Pts',(190.088324859137,-5.55401475037018,
132.850103081465));
#217057=CARTESIAN_POINT('Ctrl Pts',(190.095623705769,-5.60592477449524,
132.703244847386));
#217058=CARTESIAN_POINT('Ctrl Pts',(190.1029225524,-5.65196358703582,132.554571511522));
#217059=CARTESIAN_POINT('Ctrl Pts',(190.110223624323,-5.69801643600718,
132.405852847751));
#217060=CARTESIAN_POINT('Ctrl Pts',(190.117524696245,-5.73819437761977,
132.255318341899));
#217061=CARTESIAN_POINT('Ctrl Pts',(190.124825768168,-5.77236675875697,
132.103480536934));
#217062=CARTESIAN_POINT('Ctrl Pts',(190.132127831751,-5.80654378132449,
131.951622108746));
#217063=CARTESIAN_POINT('Ctrl Pts',(190.139429895335,-5.83471354286302,
131.79846040554));
#217064=CARTESIAN_POINT('Ctrl Pts',(190.146731958918,-5.85679658929349,
131.644517908875));
#217065=CARTESIAN_POINT('Ctrl Pts',(190.154040273153,-5.87889853906686,
131.490443635655));
#217066=CARTESIAN_POINT('Ctrl Pts',(190.161348587387,-5.89490331910291,
131.33558761541));
#217067=CARTESIAN_POINT('Ctrl Pts',(190.168656901621,-5.90478335808391,
131.180477695875));
#217068=CARTESIAN_POINT('Ctrl Pts',(190.174646203679,-5.91288023732375,
131.053362176412));
#217069=CARTESIAN_POINT('Ctrl Pts',(190.180635505737,-5.91686463980822,
130.926076303123));
#217070=CARTESIAN_POINT('Ctrl Pts',(190.186624807795,-5.9167474892903,130.798909885783));
#217071=CARTESIAN_POINT('',(191.936624807795,-5.92167388468568,130.806439789968));
#217072=CARTESIAN_POINT('Ctrl Pts',(190.186624807795,-5.91709367293974,
130.798909566865));
#217073=CARTESIAN_POINT('Ctrl Pts',(190.207685773679,-5.92124324054971,
130.351707301601));
#217074=CARTESIAN_POINT('Ctrl Pts',(190.321562614164,-5.67042057656234,
127.938289561738));
#217075=CARTESIAN_POINT('Ctrl Pts',(190.52825532926,-2.36162413690314,124.216470821409));
#217076=CARTESIAN_POINT('Ctrl Pts',(190.80670295307,4.26606273237082,125.256543993538));
#217077=CARTESIAN_POINT('Ctrl Pts',(191.085150576885,6.97344635934664,131.394789617243));
#217078=CARTESIAN_POINT('Ctrl Pts',(191.363598200697,3.27257345387652,136.990459834304));
#217079=CARTESIAN_POINT('Ctrl Pts',(191.64204582451,-3.43563458160472,136.901407078928));
#217080=CARTESIAN_POINT('Ctrl Pts',(191.833054693543,-5.87156050063434,
132.996862586964));
#217081=CARTESIAN_POINT('Ctrl Pts',(191.931247687971,-5.92616743922034,
130.920188992212));
#217082=CARTESIAN_POINT('Ctrl Pts',(191.936624807795,-5.92565178765728,
130.806441186659));
#217083=CARTESIAN_POINT('',(193.686624807763,-5.91674833022066,130.808805764476));
#217084=CARTESIAN_POINT('Ctrl Pts',(191.936624807795,-5.91674963529206,
130.806438061004));
#217085=CARTESIAN_POINT('Ctrl Pts',(191.943982571507,-5.91680420246894,
130.651025731606));
#217086=CARTESIAN_POINT('Ctrl Pts',(191.95134033522,-5.91073134974623,130.495363673782));
#217087=CARTESIAN_POINT('Ctrl Pts',(191.958698098932,-5.89849824070525,
130.3399803134));
#217088=CARTESIAN_POINT('Ctrl Pts',(191.966047433817,-5.88627914553708,
130.184774955408));
#217089=CARTESIAN_POINT('Ctrl Pts',(191.973396768702,-5.86791386650228,
130.029848035039));
#217090=CARTESIAN_POINT('Ctrl Pts',(191.980746103587,-5.84342153691622,
129.875729741274));
#217091=CARTESIAN_POINT('Ctrl Pts',(191.988088691781,-5.81895169129261,
129.721752928126));
#217092=CARTESIAN_POINT('Ctrl Pts',(191.995431279975,-5.7883660488743,129.568583637425));
#217093=CARTESIAN_POINT('Ctrl Pts',(192.00277386817,-5.7517356631725,129.416748487506));
#217094=CARTESIAN_POINT('Ctrl Pts',(192.010111385737,-5.71513057359504,
129.265018191543));
#217095=CARTESIAN_POINT('Ctrl Pts',(192.017448903304,-5.67248913923677,
129.114620570674));
#217096=CARTESIAN_POINT('Ctrl Pts',(192.024786420871,-5.62393372693014,
128.966073371895));
#217097=CARTESIAN_POINT('Ctrl Pts',(192.032121243465,-5.57539614838435,
128.817580732537));
#217098=CARTESIAN_POINT('Ctrl Pts',(192.03945606606,-5.52094902955856,128.670937524576));
#217099=CARTESIAN_POINT('Ctrl Pts',(192.046790888654,-5.46076494507694,
128.52664755901));
#217100=CARTESIAN_POINT('Ctrl Pts',(192.054124432835,-5.40059135029389,
128.382382742256));
#217101=CARTESIAN_POINT('Ctrl Pts',(192.061457977017,-5.33468292520694,
128.240470702987));
#217102=CARTESIAN_POINT('Ctrl Pts',(192.068791521199,-5.2632607654466,128.101396193566));
#217103=CARTESIAN_POINT('Ctrl Pts',(192.076125297015,-5.19183634977695,
127.962317291398));
#217104=CARTESIAN_POINT('Ctrl Pts',(192.083459072831,-5.11489802642811,
127.826076435999));
#217105=CARTESIAN_POINT('Ctrl Pts',(192.090792848647,-5.03271319836429,
127.693134424325));
#217106=CARTESIAN_POINT('Ctrl Pts',(192.098128366077,-4.95050885317121,
127.560160841782));
#217107=CARTESIAN_POINT('Ctrl Pts',(192.105463883507,-4.86305572373874,
127.43048798552));
#217108=CARTESIAN_POINT('Ctrl Pts',(192.112799400937,-4.77066480062535,
127.304548062218));
#217109=CARTESIAN_POINT('Ctrl Pts',(192.120142509709,-4.67817826447584,
127.178477806865));
#217110=CARTESIAN_POINT('Ctrl Pts',(192.12748561848,-4.58074395310877,127.056148507902));
#217111=CARTESIAN_POINT('Ctrl Pts',(192.134828727252,-4.47871388483845,
126.937960159743));
#217112=CARTESIAN_POINT('Ctrl Pts',(192.142175724157,-4.37662979224858,
126.81970923155));
#217113=CARTESIAN_POINT('Ctrl Pts',(192.149522721062,-4.26994535451669,
126.705603899663));
#217114=CARTESIAN_POINT('Ctrl Pts',(192.156869717967,-4.15904929270293,
126.596007074508));
#217115=CARTESIAN_POINT('Ctrl Pts',(192.164227936362,-4.04798385296286,
126.486242855825));
#217116=CARTESIAN_POINT('Ctrl Pts',(192.171586154757,-3.93269421798494,
126.381001158029));
#217117=CARTESIAN_POINT('Ctrl Pts',(192.178944373152,-3.81360275633488,
126.280605034052));
#217118=CARTESIAN_POINT('Ctrl Pts',(192.18560993948,-3.70572174572714,126.189659510622));
#217119=CARTESIAN_POINT('Ctrl Pts',(192.192275505808,-3.59472154676677,
126.102689823874));
#217120=CARTESIAN_POINT('Ctrl Pts',(192.198941072137,-3.48093537284348,
126.019904588655));
#217121=CARTESIAN_POINT('Ctrl Pts',(192.206364338542,-3.35421469515357,
125.927708843354));
#217122=CARTESIAN_POINT('Ctrl Pts',(192.213787604947,-3.22363703874374,
125.840411633728));
#217123=CARTESIAN_POINT('Ctrl Pts',(192.221210871353,-3.08961796002339,
125.758353143969));
#217124=CARTESIAN_POINT('Ctrl Pts',(192.228625364074,-2.95575728072412,
125.676391640529));
#217125=CARTESIAN_POINT('Ctrl Pts',(192.236039856795,-2.8184635906989,125.599656725305));
#217126=CARTESIAN_POINT('Ctrl Pts',(192.243454349516,-2.67818424350777,
125.528447452973));
#217127=CARTESIAN_POINT('Ctrl Pts',(192.25086169587,-2.53804010283326,125.457306814819));
#217128=CARTESIAN_POINT('Ctrl Pts',(192.258269042224,-2.39491636453648,
125.39168138473));
#217129=CARTESIAN_POINT('Ctrl Pts',(192.265676388577,-2.24928790474382,
125.331826059971));
#217130=CARTESIAN_POINT('Ctrl Pts',(192.273078210253,-2.10376806015,125.272015377571));
#217131=CARTESIAN_POINT('Ctrl Pts',(192.280480031928,-1.95574755751648,
125.21796637283));
#217132=CARTESIAN_POINT('Ctrl Pts',(192.287881853604,-1.80572423221982,
125.169887211854));
#217133=CARTESIAN_POINT('Ctrl Pts',(192.295279767915,-1.65578010306985,
125.121833431494));
#217134=CARTESIAN_POINT('Ctrl Pts',(192.302677682226,-1.5038356114583,125.079743332305));
#217135=CARTESIAN_POINT('Ctrl Pts',(192.310075596538,-1.35040674849502,
125.04377625692));
#217136=CARTESIAN_POINT('Ctrl Pts',(192.31747228145,-1.19700338262484,125.007815158611));
#217137=CARTESIAN_POINT('Ctrl Pts',(192.324868966362,-1.04211649807024,
124.977975149715));
#217138=CARTESIAN_POINT('Ctrl Pts',(192.332265651274,-0.886275478114352,
124.954365203944));
#217139=CARTESIAN_POINT('Ctrl Pts',(192.33966200821,-0.73044136831249,124.930756305064));
#217140=CARTESIAN_POINT('Ctrl Pts',(192.347058365145,-0.573653576316578,
124.913376975953));
#217141=CARTESIAN_POINT('Ctrl Pts',(192.354454722081,-0.416449600545396,
124.902284686785));
#217142=CARTESIAN_POINT('Ctrl Pts',(192.361852211417,-0.259221556444396,
124.891190699359));
#217143=CARTESIAN_POINT('Ctrl Pts',(192.369249700754,-0.10157757409154,
124.886385694742));
#217144=CARTESIAN_POINT('Ctrl Pts',(192.37664719009,0.0559419800692496,
124.887875084974));
#217145=CARTESIAN_POINT('Ctrl Pts',(192.384047272605,0.213516752465648,
124.88936499731));
#217146=CARTESIAN_POINT('Ctrl Pts',(192.39144735512,0.370966636778287,124.897153694073));
#217147=CARTESIAN_POINT('Ctrl Pts',(192.398847437635,0.527753674510833,
124.911194522712));
#217148=CARTESIAN_POINT('Ctrl Pts',(192.406255657302,0.684713115709465,
124.925250790685));
#217149=CARTESIAN_POINT('Ctrl Pts',(192.413663876968,0.841007882692738,
124.945572886768));
#217150=CARTESIAN_POINT('Ctrl Pts',(192.421072096635,0.996106797477932,
124.972062458991));
#217151=CARTESIAN_POINT('Ctrl Pts',(192.428484875937,1.15130117305738,124.998568335104));
#217152=CARTESIAN_POINT('Ctrl Pts',(192.435897655239,1.30529786549359,125.031249174006));
#217153=CARTESIAN_POINT('Ctrl Pts',(192.443310434541,1.45757874437968,125.069956135283));
#217154=CARTESIAN_POINT('Ctrl Pts',(192.45073380557,1.61007720932673,125.108718402881));
#217155=CARTESIAN_POINT('Ctrl Pts',(192.458157176598,1.76085460737413,125.153523883713));
#217156=CARTESIAN_POINT('Ctrl Pts',(192.465580547627,1.90940995179483,125.204174531507));
#217157=CARTESIAN_POINT('Ctrl Pts',(192.469516597068,1.9881775599421,125.231030720313));
#217158=CARTESIAN_POINT('Ctrl Pts',(192.473452646509,2.06632082359468,125.259529399429));
#217159=CARTESIAN_POINT('Ctrl Pts',(192.477388695949,2.14376776436376,125.289635752718));
#217160=CARTESIAN_POINT('Ctrl Pts',(192.484811962355,2.28983027762013,125.346415395433));
#217161=CARTESIAN_POINT('Ctrl Pts',(192.49223522876,2.43385630529008,125.409087801767));
#217162=CARTESIAN_POINT('Ctrl Pts',(192.499658495166,2.57533502238865,125.477487230207));
#217163=CARTESIAN_POINT('Ctrl Pts',(192.507072987887,2.71664652339273,125.545805816202));
#217164=CARTESIAN_POINT('Ctrl Pts',(192.514487480608,2.85541637385971,125.619837789946));
#217165=CARTESIAN_POINT('Ctrl Pts',(192.521901973329,2.99115116509402,125.699368426577));
#217166=CARTESIAN_POINT('Ctrl Pts',(192.529309319682,3.1267551300262,125.778822408586));
#217167=CARTESIAN_POINT('Ctrl Pts',(192.536716666036,3.25932953951027,125.863764315137));
#217168=CARTESIAN_POINT('Ctrl Pts',(192.54412401239,3.38840325911156,125.953932397693));
#217169=CARTESIAN_POINT('Ctrl Pts',(192.551525834065,3.51738071066331,126.044033229491));
#217170=CARTESIAN_POINT('Ctrl Pts',(192.558927655741,3.64286236637453,126.139352263232));
#217171=CARTESIAN_POINT('Ctrl Pts',(192.566329477416,3.76440399802195,126.239583174779));
#217172=CARTESIAN_POINT('Ctrl Pts',(192.573727391728,3.88588146878789,126.339761175208));
#217173=CARTESIAN_POINT('Ctrl Pts',(192.581125306039,4.00342277045593,126.444845652573));
#217174=CARTESIAN_POINT('Ctrl Pts',(192.58852322035,4.11661493775789,126.554488617525));
#217175=CARTESIAN_POINT('Ctrl Pts',(192.595919905262,4.22978829457512,126.664113361806));
#217176=CARTESIAN_POINT('Ctrl Pts',(192.603316590175,4.33861368359645,126.778294830715));
#217177=CARTESIAN_POINT('Ctrl Pts',(192.610713275087,4.44271327755592,126.896646542057));
#217178=CARTESIAN_POINT('Ctrl Pts',(192.618109632022,4.54680825563025,127.01499300556));
#217179=CARTESIAN_POINT('Ctrl Pts',(192.625505988958,4.64617760874819,127.137509063529));
#217180=CARTESIAN_POINT('Ctrl Pts',(192.632902345893,4.74048245459971,127.263773567354));
#217181=CARTESIAN_POINT('Ctrl Pts',(192.64029983523,4.83480173876412,127.390057402596));
#217182=CARTESIAN_POINT('Ctrl Pts',(192.647697324566,4.92405474836339,127.520090527295));
#217183=CARTESIAN_POINT('Ctrl Pts',(192.655094813903,5.00794484883268,127.653421241197));
#217184=CARTESIAN_POINT('Ctrl Pts',(192.662494896418,5.09186435684631,127.786798693974));
#217185=CARTESIAN_POINT('Ctrl Pts',(192.669894978933,5.1704170140703,127.923475721708));
#217186=CARTESIAN_POINT('Ctrl Pts',(192.677295061448,5.24335129090999,128.062974507837));
#217187=CARTESIAN_POINT('Ctrl Pts',(192.684703281114,5.31636576648502,128.202626687223));
#217188=CARTESIAN_POINT('Ctrl Pts',(192.692111500781,5.38374935076555,128.345106490511));
#217189=CARTESIAN_POINT('Ctrl Pts',(192.699519720447,5.4452976753735,128.48991386098));
#217190=CARTESIAN_POINT('Ctrl Pts',(192.706932499749,5.50688388194844,128.634810357969));
#217191=CARTESIAN_POINT('Ctrl Pts',(192.714345279052,5.56262754045087,128.782036928429));
#217192=CARTESIAN_POINT('Ctrl Pts',(192.721758058354,5.61237381239609,128.931077202695));
#217193=CARTESIAN_POINT('Ctrl Pts',(192.729181429382,5.66219116414747,129.080330432694));
#217194=CARTESIAN_POINT('Ctrl Pts',(192.736604800411,5.70599391075369,129.231402184733));
#217195=CARTESIAN_POINT('Ctrl Pts',(192.74402817144,5.74367787858866,129.383763915644));
#217196=CARTESIAN_POINT('Ctrl Pts',(192.747964220881,5.76365882254902,129.464549761242));
#217197=CARTESIAN_POINT('Ctrl Pts',(192.751900270321,5.7819204194436,129.545698134267));
#217198=CARTESIAN_POINT('Ctrl Pts',(192.755836319762,5.79845305499836,129.627129658289));
#217199=CARTESIAN_POINT('Ctrl Pts',(192.763259586168,5.82963308968896,129.780706971204));
#217200=CARTESIAN_POINT('Ctrl Pts',(192.770682852573,5.85475460525286,129.935756113794));
#217201=CARTESIAN_POINT('Ctrl Pts',(192.778106118978,5.87368093133555,130.091757727195));
#217202=CARTESIAN_POINT('Ctrl Pts',(192.785520611699,5.89258488807253,130.247574959644));
#217203=CARTESIAN_POINT('Ctrl Pts',(192.79293510442,5.90530818568646,130.404342055148));
#217204=CARTESIAN_POINT('Ctrl Pts',(192.800349597141,5.91176477883311,130.561527830965));
#217205=CARTESIAN_POINT('Ctrl Pts',(192.807756943495,5.91821514887222,130.718562105214));
#217206=CARTESIAN_POINT('Ctrl Pts',(192.815164289849,5.91841082384763,130.876013885927));
#217207=CARTESIAN_POINT('Ctrl Pts',(192.822571636203,5.91231736054565,131.033345312885));
#217208=CARTESIAN_POINT('Ctrl Pts',(192.829973457878,5.90622844197851,131.190559396129));
#217209=CARTESIAN_POINT('Ctrl Pts',(192.837375279553,5.89385973928897,131.347652932937));
#217210=CARTESIAN_POINT('Ctrl Pts',(192.844777101229,5.8752288554425,131.504086605847));
#217211=CARTESIAN_POINT('Ctrl Pts',(192.85217501554,5.8566078066946,131.660437698638));
#217212=CARTESIAN_POINT('Ctrl Pts',(192.859572929851,5.83173120439777,131.816129251521));
#217213=CARTESIAN_POINT('Ctrl Pts',(192.866970844163,5.80066860403245,131.970625728376));
#217214=CARTESIAN_POINT('Ctrl Pts',(192.874367529075,5.76961116570776,132.125096530719));
#217215=CARTESIAN_POINT('Ctrl Pts',(192.881764213987,5.73236984310127,132.278372285581));
#217216=CARTESIAN_POINT('Ctrl Pts',(192.889160898899,5.6890655697637,132.429926213114));
#217217=CARTESIAN_POINT('Ctrl Pts',(192.896557255835,5.64576321658296,132.581473420587));
#217218=CARTESIAN_POINT('Ctrl Pts',(192.90395361277,5.5963985497707,132.731298593605));
#217219=CARTESIAN_POINT('Ctrl Pts',(192.911349969705,5.54114271941322,132.878888979771));
#217220=CARTESIAN_POINT('Ctrl Pts',(192.918747459042,5.48587842924699,133.026501962402));
#217221=CARTESIAN_POINT('Ctrl Pts',(192.926144948379,5.42472131052274,133.17187912729));
#217222=CARTESIAN_POINT('Ctrl Pts',(192.933542437715,5.35789105322837,133.314526752354));
#217223=CARTESIAN_POINT('Ctrl Pts',(192.94094252023,5.29103736869093,133.457224382321));
#217224=CARTESIAN_POINT('Ctrl Pts',(192.948342602745,5.21850674434839,133.597190229583));
#217225=CARTESIAN_POINT('Ctrl Pts',(192.95574268526,5.14056522291733,133.733954403645));
#217226=CARTESIAN_POINT('Ctrl Pts',(192.963150904926,5.06253799677085,133.870868963976));
#217227=CARTESIAN_POINT('Ctrl Pts',(192.970559124593,4.97908817626604,134.004574495774));
#217228=CARTESIAN_POINT('Ctrl Pts',(192.977967344259,4.89052600718495,134.13462876526));
#217229=CARTESIAN_POINT('Ctrl Pts',(192.985380123561,4.80190932956638,134.26476308098));
#217230=CARTESIAN_POINT('Ctrl Pts',(192.992792902864,4.70817425520031,134.391241357163));
#217231=CARTESIAN_POINT('Ctrl Pts',(193.000205682166,4.60967152652743,134.51365421339));
#217232=CARTESIAN_POINT('Ctrl Pts',(193.007629053194,4.51102805253667,134.636241978846));
#217233=CARTESIAN_POINT('Ctrl Pts',(193.015052424223,4.40760356345385,134.754752442234));
#217234=CARTESIAN_POINT('Ctrl Pts',(193.022475795252,4.29978642922707,134.868812268839));
#217235=CARTESIAN_POINT('Ctrl Pts',(193.026411844693,4.24261919762311,134.929289525733));
#217236=CARTESIAN_POINT('Ctrl Pts',(193.030347894133,4.18421761234096,134.988516202176));
#217237=CARTESIAN_POINT('Ctrl Pts',(193.034283943574,4.12464325826948,135.046441304506));
#217238=CARTESIAN_POINT('Ctrl Pts',(193.04170720998,4.01228788574312,135.155686239721));
#217239=CARTESIAN_POINT('Ctrl Pts',(193.049130476385,3.89541944365211,135.260629531099));
#217240=CARTESIAN_POINT('Ctrl Pts',(193.05655374279,3.77440100965145,135.360875467848));
#217241=CARTESIAN_POINT('Ctrl Pts',(193.063968235512,3.65352560938941,135.461002922225));
#217242=CARTESIAN_POINT('Ctrl Pts',(193.071382728233,3.52851026521044,135.55644383722));
#217243=CARTESIAN_POINT('Ctrl Pts',(193.078797220954,3.39975536658942,135.6468387032));
#217244=CARTESIAN_POINT('Ctrl Pts',(193.086204567307,3.27112456678774,135.737146443204));
#217245=CARTESIAN_POINT('Ctrl Pts',(193.093611913661,3.13876169151149,135.822417603552));
#217246=CARTESIAN_POINT('Ctrl Pts',(193.101019260015,3.0031006403987,135.902332479605));
#217247=CARTESIAN_POINT('Ctrl Pts',(193.10842108169,2.86754077041626,135.982187752127));
#217248=CARTESIAN_POINT('Ctrl Pts',(193.115822903366,2.72868794285352,136.056694506122));
#217249=CARTESIAN_POINT('Ctrl Pts',(193.123224725041,2.58700541559937,136.125576037201));
#217250=CARTESIAN_POINT('Ctrl Pts',(193.130622639352,2.44539768144717,136.194421206256));
#217251=CARTESIAN_POINT('Ctrl Pts',(193.138020553664,2.30096355740562,136.257646903513));
#217252=CARTESIAN_POINT('Ctrl Pts',(193.145418467975,2.15419120161526,136.315022177613));
#217253=CARTESIAN_POINT('Ctrl Pts',(193.152815152887,2.00744323672871,136.372387916984));
#217254=CARTESIAN_POINT('Ctrl Pts',(193.1602118378,1.85835815862988,136.423905027017));
#217255=CARTESIAN_POINT('Ctrl Pts',(193.167608522712,1.70744452966099,136.46939051516));
#217256=CARTESIAN_POINT('Ctrl Pts',(193.175004879647,1.55653759236051,136.514873986428));
#217257=CARTESIAN_POINT('Ctrl Pts',(193.182401236583,1.40380262282025,136.554326259858));
#217258=CARTESIAN_POINT('Ctrl Pts',(193.189797593518,1.24976352495471,136.58761417367));
#217259=CARTESIAN_POINT('Ctrl Pts',(193.197195082855,1.09570084331009,136.620907183947));
#217260=CARTESIAN_POINT('Ctrl Pts',(193.204592572191,0.94033400067869,136.648033876561));
#217261=CARTESIAN_POINT('Ctrl Pts',(193.211990061528,0.78419712723474,136.668912214077));
#217262=CARTESIAN_POINT('Ctrl Pts',(193.219390144043,0.628005520252473,
136.689797870461));
#217263=CARTESIAN_POINT('Ctrl Pts',(193.226790226558,0.471043714796622,
136.704430761329));
#217264=CARTESIAN_POINT('Ctrl Pts',(193.234190309073,0.313850845635412,
136.712780728661));
#217265=CARTESIAN_POINT('Ctrl Pts',(193.241598528739,0.156485126754066,
136.721139877641));
#217266=CARTESIAN_POINT('Ctrl Pts',(193.249006748406,-0.00111179024260466,
136.723202286104));
#217267=CARTESIAN_POINT('Ctrl Pts',(193.256414968072,-0.15840014612975,
136.718989934455));
#217268=CARTESIAN_POINT('Ctrl Pts',(193.263827747375,-0.315785310375573,
136.714774990174));
#217269=CARTESIAN_POINT('Ctrl Pts',(193.271240526677,-0.472861163480505,
136.704277615075));
#217270=CARTESIAN_POINT('Ctrl Pts',(193.278653305979,-0.629093697246785,
136.687571618591));
#217271=CARTESIAN_POINT('Ctrl Pts',(193.286076677007,-0.785549463383723,
136.670841751796));
#217272=CARTESIAN_POINT('Ctrl Pts',(193.293500048036,-0.941159135255626,
136.647885600237));
#217273=CARTESIAN_POINT('Ctrl Pts',(193.300923419065,-1.09539869234955,
136.618828114018));
#217274=CARTESIAN_POINT('Ctrl Pts',(193.304859468506,-1.17718020644852,
136.6034211376));
#217275=CARTESIAN_POINT('Ctrl Pts',(193.308795517947,-1.25857677010934,
136.586299695192));
#217276=CARTESIAN_POINT('Ctrl Pts',(193.312731567387,-1.33951219278451,
136.567488036588));
#217277=CARTESIAN_POINT('Ctrl Pts',(193.320154833793,-1.49215387404138,
136.532009835551));
#217278=CARTESIAN_POINT('Ctrl Pts',(193.327578100198,-1.64361588484665,
136.490409517706));
#217279=CARTESIAN_POINT('Ctrl Pts',(193.335001366604,-1.79336905016339,
136.442778659217));
#217280=CARTESIAN_POINT('Ctrl Pts',(193.342415859325,-1.94294521967514,
136.395204096447));
#217281=CARTESIAN_POINT('Ctrl Pts',(193.349830352046,-2.0908162116855,136.3416132926));
#217282=CARTESIAN_POINT('Ctrl Pts',(193.357244844767,-2.23646314026778,
136.282148782941));
#217283=CARTESIAN_POINT('Ctrl Pts',(193.364652191121,-2.38196968885627,
136.222741587416));
#217284=CARTESIAN_POINT('Ctrl Pts',(193.372059537474,-2.52525609829113,
136.157472096766));
#217285=CARTESIAN_POINT('Ctrl Pts',(193.379466883828,-2.66581885865279,
136.08653255488));
#217286=CARTESIAN_POINT('Ctrl Pts',(193.386868705504,-2.80627678200372,
136.015645922381));
#217287=CARTESIAN_POINT('Ctrl Pts',(193.394270527179,-2.94401476924652,
135.9390978265));
#217288=CARTESIAN_POINT('Ctrl Pts',(193.401672348854,-3.07854961893739,
135.857128453737));
#217289=CARTESIAN_POINT('Ctrl Pts',(193.409070263166,-3.21301344872921,
135.775202351967));
#217290=CARTESIAN_POINT('Ctrl Pts',(193.416468177477,-3.34427719051927,
135.687860866565));
#217291=CARTESIAN_POINT('Ctrl Pts',(193.423866091788,-3.47188267699022,
135.595389863951));
#217292=CARTESIAN_POINT('Ctrl Pts',(193.4312627767,-3.59946695774474,135.502934228339));
#217293=CARTESIAN_POINT('Ctrl Pts',(193.438659461613,-3.72339388777422,
135.405350986174));
#217294=CARTESIAN_POINT('Ctrl Pts',(193.446056146525,-3.84323461989282,
135.302969093412));
#217295=CARTESIAN_POINT('Ctrl Pts',(193.45345250346,-3.96307003814781,135.200591740371));
#217296=CARTESIAN_POINT('Ctrl Pts',(193.460848860396,-4.07881933492679,
135.093416402282));
#217297=CARTESIAN_POINT('Ctrl Pts',(193.468245217331,-4.19008729459038,
134.981811877151));
#217298=CARTESIAN_POINT('Ctrl Pts',(193.475642706668,-4.30137228966243,
134.870190265084));
#217299=CARTESIAN_POINT('Ctrl Pts',(193.483040196004,-4.40817431791499,
134.754138380124));
#217300=CARTESIAN_POINT('Ctrl Pts',(193.490437685341,-4.51013564852389,
134.634061257879));
#217301=CARTESIAN_POINT('Ctrl Pts',(193.497837767856,-4.61213272151835,
134.513942042786));
#217302=CARTESIAN_POINT('Ctrl Pts',(193.505237850371,-4.70928547688403,
134.389795065409));
#217303=CARTESIAN_POINT('Ctrl Pts',(193.512637932886,-4.80127712631488,
134.262057613953));
#217304=CARTESIAN_POINT('Ctrl Pts',(193.520046152552,-4.89336993002218,
134.134179702037));
#217305=CARTESIAN_POINT('Ctrl Pts',(193.527454372219,-4.98029007582845,
134.002703734542));
#217306=CARTESIAN_POINT('Ctrl Pts',(193.534862591885,-5.06176430342499,
133.868095707138));
#217307=CARTESIAN_POINT('Ctrl Pts',(193.542275371188,-5.14328867704949,
133.733404830738));
#217308=CARTESIAN_POINT('Ctrl Pts',(193.54968815049,-5.21936027347246,133.595578379247));
#217309=CARTESIAN_POINT('Ctrl Pts',(193.557100929792,-5.28975254618504,
133.455105524687));
#217310=CARTESIAN_POINT('Ctrl Pts',(193.564524300821,-5.36024539867765,
133.314431955926));
#217311=CARTESIAN_POINT('Ctrl Pts',(193.571947671849,-5.42504256684365,
133.171104771232));
#217312=CARTESIAN_POINT('Ctrl Pts',(193.579371042878,-5.48396592885686,
133.025632382487));
#217313=CARTESIAN_POINT('Ctrl Pts',(193.583307092319,-5.51520850924322,
132.948499431412));
#217314=CARTESIAN_POINT('Ctrl Pts',(193.58724314176,-5.54480058572185,132.870763639298));
#217315=CARTESIAN_POINT('Ctrl Pts',(193.591179191201,-5.57272137747765,
132.792502215014));
#217316=CARTESIAN_POINT('Ctrl Pts',(193.59982438893,-5.63404702115283,132.62060765482));
#217317=CARTESIAN_POINT('Ctrl Pts',(193.60846958666,-5.6874596691831,132.445749915596));
#217318=CARTESIAN_POINT('Ctrl Pts',(193.61711478439,-5.7327048543804,132.268609781835));
#217319=CARTESIAN_POINT('Ctrl Pts',(193.625725250551,-5.77776826973561,
132.092181298032));
#217320=CARTESIAN_POINT('Ctrl Pts',(193.634335716713,-5.81472962923724,
131.913488824043));
#217321=CARTESIAN_POINT('Ctrl Pts',(193.642946182875,-5.84338413695381,
131.733226803029));
#217322=CARTESIAN_POINT('Ctrl Pts',(193.651489290023,-5.87181448266578,
131.554374957907));
#217323=CARTESIAN_POINT('Ctrl Pts',(193.660032397172,-5.89206736515099,
131.373978144609));
#217324=CARTESIAN_POINT('Ctrl Pts',(193.668575504321,-5.90398986112245,
131.192734512496));
#217325=CARTESIAN_POINT('Ctrl Pts',(193.674591938801,-5.91238621090631,
131.065094718366));
#217326=CARTESIAN_POINT('Ctrl Pts',(193.680608373282,-5.91665199363111,
130.937035352127));
#217327=CARTESIAN_POINT('Ctrl Pts',(193.686624807763,-5.91674833022066,
130.808805764476));
#217328=CARTESIAN_POINT('',(195.436626015881,-5.91264468443637,130.800534531502));
#217329=CARTESIAN_POINT('Ctrl Pts',(193.686624807795,-5.91674833022117,
130.808805763797));
#217330=CARTESIAN_POINT('Ctrl Pts',(193.694249891429,-5.91687042486749,
130.646290683926));
#217331=CARTESIAN_POINT('Ctrl Pts',(193.701874975063,-5.91029198571113,
130.483707620702));
#217332=CARTESIAN_POINT('Ctrl Pts',(193.709500058697,-5.89702633263468,
130.321648493507));
#217333=CARTESIAN_POINT('Ctrl Pts',(193.716903394445,-5.8841464629385,130.164302267934));
#217334=CARTESIAN_POINT('Ctrl Pts',(193.724306730192,-5.86496295699468,
130.007450318832));
#217335=CARTESIAN_POINT('Ctrl Pts',(193.731710065939,-5.839540805705,129.851630991173));
#217336=CARTESIAN_POINT('Ctrl Pts',(193.739114086533,-5.81411630273351,
129.695797249413));
#217337=CARTESIAN_POINT('Ctrl Pts',(193.746518107128,-5.78245206455313,
129.540996686389));
#217338=CARTESIAN_POINT('Ctrl Pts',(193.753922127722,-5.74466447835844,
129.387758840923));
#217339=CARTESIAN_POINT('Ctrl Pts',(193.761328280158,-5.70686601197486,
129.234476873648));
#217340=CARTESIAN_POINT('Ctrl Pts',(193.768734432594,-5.66294077563007,
129.082758880831));
#217341=CARTESIAN_POINT('Ctrl Pts',(193.776140585029,-5.61305539489754,
128.933120468277));
#217342=CARTESIAN_POINT('Ctrl Pts',(193.783931104195,-5.56058104765214,
128.775716076322));
#217343=CARTESIAN_POINT('Ctrl Pts',(193.79172162336,-5.50151156375219,128.620613319595));
#217344=CARTESIAN_POINT('Ctrl Pts',(193.799512142525,-5.43609843388967,
128.468388789919));
#217345=CARTESIAN_POINT('Ctrl Pts',(193.806931140232,-5.37380478565584,
128.32342368392));
#217346=CARTESIAN_POINT('Ctrl Pts',(193.814350137939,-5.3057587036248,128.181068965662));
#217347=CARTESIAN_POINT('Ctrl Pts',(193.821769135646,-5.23222448513309,
128.041797043696));
#217348=CARTESIAN_POINT('Ctrl Pts',(193.829193605055,-5.15863603325452,
127.902422405087));
#217349=CARTESIAN_POINT('Ctrl Pts',(193.836618074465,-5.07955156595895,
127.766135413061));
#217350=CARTESIAN_POINT('Ctrl Pts',(193.844042543874,-4.99527888296432,
127.633379784462));
#217351=CARTESIAN_POINT('Ctrl Pts',(193.851477405336,-4.91088824323663,
127.500438337403));
#217352=CARTESIAN_POINT('Ctrl Pts',(193.858912266798,-4.82129510231583,
127.371038424274));
#217353=CARTESIAN_POINT('Ctrl Pts',(193.86634712826,-4.72684806539047,127.245591458262));
#217354=CARTESIAN_POINT('Ctrl Pts',(193.867440357178,-4.71296048557474,
127.227145620151));
#217355=CARTESIAN_POINT('Ctrl Pts',(193.868533586096,-4.69896802508309,
127.20878518446));
#217356=CARTESIAN_POINT('Ctrl Pts',(193.869626815014,-4.68487185884326,
127.190511391503));
#217357=CARTESIAN_POINT('Ctrl Pts',(193.877050081419,-4.58915576902482,
127.066428291302));
#217358=CARTESIAN_POINT('Ctrl Pts',(193.884473347825,-4.48836185950119,
126.945962881474));
#217359=CARTESIAN_POINT('Ctrl Pts',(193.89189661423,-4.38279338078887,126.82955839056));
#217360=CARTESIAN_POINT('Ctrl Pts',(193.899311106951,-4.27734967525132,
126.713291480087));
#217361=CARTESIAN_POINT('Ctrl Pts',(193.906725599672,-4.16714288156309,
126.601076208577));
#217362=CARTESIAN_POINT('Ctrl Pts',(193.914140092393,-4.0525183215702,126.493325264447));
#217363=CARTESIAN_POINT('Ctrl Pts',(193.921547438747,-3.93800424104399,
126.385678174735));
#217364=CARTESIAN_POINT('Ctrl Pts',(193.928954785101,-3.81908114123644,
126.282487100167));
#217365=CARTESIAN_POINT('Ctrl Pts',(193.936362131454,-3.69613316353616,
126.184130082202));
#217366=CARTESIAN_POINT('Ctrl Pts',(193.94376395313,-3.57327688507596,126.085846422612));
#217367=CARTESIAN_POINT('Ctrl Pts',(193.951165774805,-3.44640199616621,
125.992389872936));
#217368=CARTESIAN_POINT('Ctrl Pts',(193.958567596481,-3.31592780126095,
125.904100075582));
#217369=CARTESIAN_POINT('Ctrl Pts',(193.965965510792,-3.18552248266734,
125.815856885725));
#217370=CARTESIAN_POINT('Ctrl Pts',(193.973363425103,-3.05152195049331,
125.732775224944));
#217371=CARTESIAN_POINT('Ctrl Pts',(193.980761339415,-2.91437665000294,
125.655152979063));
#217372=CARTESIAN_POINT('Ctrl Pts',(193.988158024327,-2.77725414057385,
125.577543632592));
#217373=CARTESIAN_POINT('Ctrl Pts',(193.995554709239,-2.63698822459584,
125.505392084079));
#217374=CARTESIAN_POINT('Ctrl Pts',(194.002951394151,-2.49405635059935,
125.438951641306));
#217375=CARTESIAN_POINT('Ctrl Pts',(194.010347751087,-2.35113081435208,
125.372514144571));
#217376=CARTESIAN_POINT('Ctrl Pts',(194.017744108022,-2.20553989364301,
125.31178740741));
#217377=CARTESIAN_POINT('Ctrl Pts',(194.025140464957,-2.057783294511,125.256977588125));
#217378=CARTESIAN_POINT('Ctrl Pts',(194.032537954294,-1.9100040734663,125.202159377317));
#217379=CARTESIAN_POINT('Ctrl Pts',(194.039935443631,-1.76005886381328,
125.15326001798));
#217380=CARTESIAN_POINT('Ctrl Pts',(194.047332932967,-1.60846474911433,
125.110436512579));
#217381=CARTESIAN_POINT('Ctrl Pts',(194.054733015482,-1.45681749333343,
125.067597995464));
#217382=CARTESIAN_POINT('Ctrl Pts',(194.062133097997,-1.30352054068615,
125.030839674279));
#217383=CARTESIAN_POINT('Ctrl Pts',(194.069533180512,-1.14910329058166,
125.000267907239));
#217384=CARTESIAN_POINT('Ctrl Pts',(194.076941400178,-0.994516242836139,
124.969662523398));
#217385=CARTESIAN_POINT('Ctrl Pts',(194.084349619845,-0.838806803898584,
124.945257351789));
#217386=CARTESIAN_POINT('Ctrl Pts',(194.091757839511,-0.68251238996658,
124.927107228436));
#217387=CARTESIAN_POINT('Ctrl Pts',(194.099170618813,-0.526121779430448,
124.908945933984));
#217388=CARTESIAN_POINT('Ctrl Pts',(194.106583398116,-0.369145847837443,
124.897047387302));
#217389=CARTESIAN_POINT('Ctrl Pts',(194.113996177418,-0.212123673302736,
124.891414303779));
#217390=CARTESIAN_POINT('Ctrl Pts',(194.121419548446,-0.0548771381217091,
124.885773171442));
#217391=CARTESIAN_POINT('Ctrl Pts',(194.128842919475,0.102415399659899,
124.886415380671));
#217392=CARTESIAN_POINT('Ctrl Pts',(194.136266290504,0.259217491474521,
124.893291606413));
#217393=CARTESIAN_POINT('Ctrl Pts',(194.140202339945,0.342357722969995,
124.896937546294));
#217394=CARTESIAN_POINT('Ctrl Pts',(194.144138389385,0.425360189154594,
124.902335228505));
#217395=CARTESIAN_POINT('Ctrl Pts',(194.148074438826,0.508146029354237,
124.909471460393));
#217396=CARTESIAN_POINT('Ctrl Pts',(194.155497705232,0.664277540311929,
124.922930171021));
#217397=CARTESIAN_POINT('Ctrl Pts',(194.162920971637,0.820110071483281,
124.942616445193));
#217398=CARTESIAN_POINT('Ctrl Pts',(194.170344238043,0.975106807833801,
124.968514725511));
#217399=CARTESIAN_POINT('Ctrl Pts',(194.177758730764,1.12992035091363,124.994382396213));
#217400=CARTESIAN_POINT('Ctrl Pts',(194.185173223485,1.28389970087569,125.0264473977));
#217401=CARTESIAN_POINT('Ctrl Pts',(194.192587716206,1.43651099637365,125.064642269093));
#217402=CARTESIAN_POINT('Ctrl Pts',(194.199995062559,1.58897519935966,125.102800326831));
#217403=CARTESIAN_POINT('Ctrl Pts',(194.207402408913,1.74007361322188,125.147076402391));
#217404=CARTESIAN_POINT('Ctrl Pts',(194.214809755267,1.88928054317001,125.197351647384));
#217405=CARTESIAN_POINT('Ctrl Pts',(194.222211576942,2.03837618896044,125.247589395203));
#217406=CARTESIAN_POINT('Ctrl Pts',(194.229613398618,2.18558280757734,125.303817284624));
#217407=CARTESIAN_POINT('Ctrl Pts',(194.237015220293,2.33038800394414,125.365866127951));
#217408=CARTESIAN_POINT('Ctrl Pts',(194.244413134605,2.47511675877508,125.427882216177));
#217409=CARTESIAN_POINT('Ctrl Pts',(194.251811048916,2.61744627377012,125.495712991953));
#217410=CARTESIAN_POINT('Ctrl Pts',(194.259208963227,2.75688245248113,125.569140497485));
#217411=CARTESIAN_POINT('Ctrl Pts',(194.26660564814,2.89629545942845,125.642555800698));
#217412=CARTESIAN_POINT('Ctrl Pts',(194.274002333052,3.03281575440156,125.721565813977));
#217413=CARTESIAN_POINT('Ctrl Pts',(194.281399017964,3.16597214979834,125.805905765394));
#217414=CARTESIAN_POINT('Ctrl Pts',(194.2887953749,3.29912264090107,125.89024197709));
#217415=CARTESIAN_POINT('Ctrl Pts',(194.296191731835,3.42890921364481,125.979907457263));
#217416=CARTESIAN_POINT('Ctrl Pts',(194.30358808877,3.55488831789053,126.07459322267));
#217417=CARTESIAN_POINT('Ctrl Pts',(194.310985578107,3.68088670985897,126.169293484709));
#217418=CARTESIAN_POINT('Ctrl Pts',(194.318383067444,3.80307617420363,126.269015338105));
#217419=CARTESIAN_POINT('Ctrl Pts',(194.32578055678,3.92104512400985,126.373408609478));
#217420=CARTESIAN_POINT('Ctrl Pts',(194.333180639295,4.03905542764841,126.477838475751));
#217421=CARTESIAN_POINT('Ctrl Pts',(194.34058072181,4.15284199170322,126.586942773136));
#217422=CARTESIAN_POINT('Ctrl Pts',(194.347980804325,4.26202918068377,126.700333592131));
#217423=CARTESIAN_POINT('Ctrl Pts',(194.355389023992,4.37133643220337,126.813849095989));
#217424=CARTESIAN_POINT('Ctrl Pts',(194.362797243658,4.47603394942869,126.931660265503));
#217425=CARTESIAN_POINT('Ctrl Pts',(194.370205463325,4.57578511067753,127.053344597419));
#217426=CARTESIAN_POINT('Ctrl Pts',(194.377618242627,4.67559766710175,127.17510382401));
#217427=CARTESIAN_POINT('Ctrl Pts',(194.385031021929,4.77045757678608,127.300740665929));
#217428=CARTESIAN_POINT('Ctrl Pts',(194.392443801231,4.86007117030686,127.429803049224));
#217429=CARTESIAN_POINT('Ctrl Pts',(194.39986717226,4.94981280793254,127.559049842905));
#217430=CARTESIAN_POINT('Ctrl Pts',(194.407290543289,5.03429295787514,127.691731639473));
#217431=CARTESIAN_POINT('Ctrl Pts',(194.414713914317,5.11326315514323,127.827370448158));
#217432=CARTESIAN_POINT('Ctrl Pts',(194.418649963758,5.15513504859709,127.899289399128));
#217433=CARTESIAN_POINT('Ctrl Pts',(194.422586013199,5.19545868610213,127.972039303758));
#217434=CARTESIAN_POINT('Ctrl Pts',(194.426522062639,5.23420254088829,128.04554668338));
#217435=CARTESIAN_POINT('Ctrl Pts',(194.433945329045,5.30727224186316,128.184179307264));
#217436=CARTESIAN_POINT('Ctrl Pts',(194.44136859545,5.37494091137785,128.325926541199));
#217437=CARTESIAN_POINT('Ctrl Pts',(194.448791861856,5.4369314766717,128.470328338338));
#217438=CARTESIAN_POINT('Ctrl Pts',(194.456206354577,5.49884877426541,128.614559464546));
#217439=CARTESIAN_POINT('Ctrl Pts',(194.463620847298,5.55510118019554,128.761438569126));
#217440=CARTESIAN_POINT('Ctrl Pts',(194.471035340019,5.60545688611216,128.910480035154));
#217441=CARTESIAN_POINT('Ctrl Pts',(194.478442686372,5.6557640573036,129.059377849406));
#217442=CARTESIAN_POINT('Ctrl Pts',(194.485850032726,5.70018572444837,129.21043352466));
#217443=CARTESIAN_POINT('Ctrl Pts',(194.49325737908,5.73853772718516,129.363140538545));
#217444=CARTESIAN_POINT('Ctrl Pts',(194.500659200755,5.77686112555123,129.515733657777));
#217445=CARTESIAN_POINT('Ctrl Pts',(194.508061022431,5.80912378280913,129.669975302801));
#217446=CARTESIAN_POINT('Ctrl Pts',(194.515462844106,5.83519107930323,129.825342931045));
#217447=CARTESIAN_POINT('Ctrl Pts',(194.522860758417,5.86124461507446,129.980628541928));
#217448=CARTESIAN_POINT('Ctrl Pts',(194.530258672729,5.88110924179336,130.13703858504));
#217449=CARTESIAN_POINT('Ctrl Pts',(194.53765658704,5.8947012623256,130.294039551533));
#217450=CARTESIAN_POINT('Ctrl Pts',(194.545053271952,5.90829102411064,130.451014427314));
#217451=CARTESIAN_POINT('Ctrl Pts',(194.552449956865,5.91561021638582,130.608579660035));
#217452=CARTESIAN_POINT('Ctrl Pts',(194.559846641777,5.91662691086489,130.766195710526));
#217453=CARTESIAN_POINT('Ctrl Pts',(194.567242998712,5.91764356026267,130.923804772156));
#217454=CARTESIAN_POINT('Ctrl Pts',(194.574639355648,5.91235826511605,131.081464273787));
#217455=CARTESIAN_POINT('Ctrl Pts',(194.582035712583,5.90079123209493,131.238634031134));
#217456=CARTESIAN_POINT('Ctrl Pts',(194.58943320192,5.88922242813151,131.395827851571));
#217457=CARTESIAN_POINT('Ctrl Pts',(194.596830691256,5.87136999872203,131.552531406112));
#217458=CARTESIAN_POINT('Ctrl Pts',(194.604228180593,5.84730608186697,131.708209137763));
#217459=CARTESIAN_POINT('Ctrl Pts',(194.611628263108,5.82323372944323,131.863941442));
#217460=CARTESIAN_POINT('Ctrl Pts',(194.619028345623,5.79294561132196,132.0186468387));
#217461=CARTESIAN_POINT('Ctrl Pts',(194.626428428138,5.75656504659628,132.171799620522));
#217462=CARTESIAN_POINT('Ctrl Pts',(194.633836647804,5.72014447769965,132.325120809573));
#217463=CARTESIAN_POINT('Ctrl Pts',(194.641244867471,5.67761816964086,132.476885610823));
#217464=CARTESIAN_POINT('Ctrl Pts',(194.648653087137,5.62915963413416,132.626582441586));
#217465=CARTESIAN_POINT('Ctrl Pts',(194.656065866439,5.58067127320736,132.776371408251));
#217466=CARTESIAN_POINT('Ctrl Pts',(194.663478645741,5.52624353814764,132.924089518748));
#217467=CARTESIAN_POINT('Ctrl Pts',(194.670891425043,5.46609803607665,133.069245343661));
#217468=CARTESIAN_POINT('Ctrl Pts',(194.678314796072,5.4058665952918,133.214608574024));
#217469=CARTESIAN_POINT('Ctrl Pts',(194.685738167101,5.33990122668302,133.35740186875));
#217470=CARTESIAN_POINT('Ctrl Pts',(194.69316153813,5.26846977602395,133.49715782152));
#217471=CARTESIAN_POINT('Ctrl Pts',(194.697097587571,5.23059510690934,133.571259781079));
#217472=CARTESIAN_POINT('Ctrl Pts',(194.701033637011,5.19118446278821,133.644508299809));
#217473=CARTESIAN_POINT('Ctrl Pts',(194.704969686452,5.15028262235604,133.716837136331));
#217474=CARTESIAN_POINT('Ctrl Pts',(194.712392952858,5.07314302780579,133.853247064702));
#217475=CARTESIAN_POINT('Ctrl Pts',(194.719816219263,4.99046363417835,133.986796475152));
#217476=CARTESIAN_POINT('Ctrl Pts',(194.727239485669,4.90248172731818,134.117003591961));
#217477=CARTESIAN_POINT('Ctrl Pts',(194.73465397839,4.81460380776549,134.247056814772));
#217478=CARTESIAN_POINT('Ctrl Pts',(194.742068471111,4.7214360566969,134.373775300779));
#217479=CARTESIAN_POINT('Ctrl Pts',(194.749482963832,4.62326173930799,134.496701535243));
#217480=CARTESIAN_POINT('Ctrl Pts',(194.756890310185,4.52518204602216,134.619509288774));
#217481=CARTESIAN_POINT('Ctrl Pts',(194.764297656539,4.4221056244628,134.738531777645));
#217482=CARTESIAN_POINT('Ctrl Pts',(194.771705002893,4.31435908307288,134.853340274814));
#217483=CARTESIAN_POINT('Ctrl Pts',(194.779106824568,4.2066929031187,134.968063143474));
#217484=CARTESIAN_POINT('Ctrl Pts',(194.786508646244,4.0943637931164,135.078578007448));
#217485=CARTESIAN_POINT('Ctrl Pts',(194.793910467919,3.97773861771825,135.184489160384));
#217486=CARTESIAN_POINT('Ctrl Pts',(194.801308382231,3.86117500784292,135.290344403647));
#217487=CARTESIAN_POINT('Ctrl Pts',(194.808706296542,3.74032012477287,135.39160052553));
#217488=CARTESIAN_POINT('Ctrl Pts',(194.816104210853,3.61557758426522,135.487898734701));
#217489=CARTESIAN_POINT('Ctrl Pts',(194.823500895765,3.49085577370419,135.584180940857));
#217490=CARTESIAN_POINT('Ctrl Pts',(194.830897580678,3.36224788314285,135.675506641639));
#217491=CARTESIAN_POINT('Ctrl Pts',(194.83829426559,3.23019058414608,135.761557340775));
#217492=CARTESIAN_POINT('Ctrl Pts',(194.845690622525,3.09813914070806,135.847604224333));
#217493=CARTESIAN_POINT('Ctrl Pts',(194.853086979461,2.96263890570939,135.928376367518));
#217494=CARTESIAN_POINT('Ctrl Pts',(194.860483336396,2.82415527368646,136.003598787972));
#217495=CARTESIAN_POINT('Ctrl Pts',(194.867880825733,2.68565043946621,136.078832725171));
#217496=CARTESIAN_POINT('Ctrl Pts',(194.875278315069,2.54416162679036,136.148515069628));
#217497=CARTESIAN_POINT('Ctrl Pts',(194.882675804406,2.40017840727624,136.212417031449));
#217498=CARTESIAN_POINT('Ctrl Pts',(194.890075886921,2.25614471466828,136.276341394004));
#217499=CARTESIAN_POINT('Ctrl Pts',(194.897475969436,2.10961521526799,136.33448118823));
#217500=CARTESIAN_POINT('Ctrl Pts',(194.904876051951,1.96109885853,136.386656008315));
#217501=CARTESIAN_POINT('Ctrl Pts',(194.912284271617,1.81241919278925,136.438888199978));
#217502=CARTESIAN_POINT('Ctrl Pts',(194.919692491284,1.66174865902651,136.485142194737));
#217503=CARTESIAN_POINT('Ctrl Pts',(194.92710071095,1.50961145356359,136.525287449974));
#217504=CARTESIAN_POINT('Ctrl Pts',(194.934513490252,1.35738061018877,136.565457413946));
#217505=CARTESIAN_POINT('Ctrl Pts',(194.941926269555,1.20368165996157,136.599511065906));
#217506=CARTESIAN_POINT('Ctrl Pts',(194.949339048857,1.04904784043026,136.627369220598));
#217507=CARTESIAN_POINT('Ctrl Pts',(194.956762419885,0.894193072846361,
136.655267180328));
#217508=CARTESIAN_POINT('Ctrl Pts',(194.964185790914,0.738401136849904,
136.676951911201));
#217509=CARTESIAN_POINT('Ctrl Pts',(194.971609161943,0.582210051798615,
136.692396114919));
#217510=CARTESIAN_POINT('Ctrl Pts',(194.975545211384,0.499393790750225,
136.700585002308));
#217511=CARTESIAN_POINT('Ctrl Pts',(194.979481260825,0.416465321632257,
136.70702032481));
#217512=CARTESIAN_POINT('Ctrl Pts',(194.983417310265,0.333504579172153,
136.711703950924));
#217513=CARTESIAN_POINT('Ctrl Pts',(194.990840576671,0.177043208009956,
136.720537123605));
#217514=CARTESIAN_POINT('Ctrl Pts',(194.998263843076,0.0199940748712888,
136.723163326617));
#217515=CARTESIAN_POINT('Ctrl Pts',(195.005687109482,-0.137109229893286,
136.71952178372));
#217516=CARTESIAN_POINT('Ctrl Pts',(195.013101602203,-0.294026851598554,
136.715884544824));
#217517=CARTESIAN_POINT('Ctrl Pts',(195.020516094924,-0.450998147931574,
136.70599431416));
#217518=CARTESIAN_POINT('Ctrl Pts',(195.027930587645,-0.607485087027711,
136.689842112868));
#217519=CARTESIAN_POINT('Ctrl Pts',(195.035337933998,-0.763821198120527,
136.673705479675));
#217520=CARTESIAN_POINT('Ctrl Pts',(195.042745280352,-0.919673512534122,
136.651318929462));
#217521=CARTESIAN_POINT('Ctrl Pts',(195.050152626706,-1.07450479022457,
136.622725509723));
#217522=CARTESIAN_POINT('Ctrl Pts',(195.057554448381,-1.22922058890767,
136.594153416035));
#217523=CARTESIAN_POINT('Ctrl Pts',(195.064956270057,-1.38291650166136,
136.559383737918));
#217524=CARTESIAN_POINT('Ctrl Pts',(195.072358091732,-1.53506131021855,
136.518511240044));
#217525=CARTESIAN_POINT('Ctrl Pts',(195.079756006044,-1.68712580271452,
136.477660318445));
#217526=CARTESIAN_POINT('Ctrl Pts',(195.087153920355,-1.83764046212198,
136.430713089725));
#217527=CARTESIAN_POINT('Ctrl Pts',(195.094551834666,-1.98608526295548,
136.377815191775));
#217528=CARTESIAN_POINT('Ctrl Pts',(195.101948519579,-2.13450539495601,
136.324926084496));
#217529=CARTESIAN_POINT('Ctrl Pts',(195.109345204491,-2.28085599977257,
136.266088395828));
#217530=CARTESIAN_POINT('Ctrl Pts',(195.116741889403,-2.42463308582467,
136.201497354913));
#217531=CARTESIAN_POINT('Ctrl Pts',(195.124138246339,-2.56840379665031,
136.136909178033));
#217532=CARTESIAN_POINT('Ctrl Pts',(195.131534603274,-2.70960087509142,
136.066568309123));
#217533=CARTESIAN_POINT('Ctrl Pts',(195.138930960209,-2.84774141358831,
135.990717663107));
#217534=CARTESIAN_POINT('Ctrl Pts',(195.146328449546,-2.98590310175456,
135.914855404164));
#217535=CARTESIAN_POINT('Ctrl Pts',(195.153725938883,-3.1210069909607,135.833481868153));
#217536=CARTESIAN_POINT('Ctrl Pts',(195.161123428219,-3.25259596837197,
135.746885279015));
#217537=CARTESIAN_POINT('Ctrl Pts',(195.168523510734,-3.38423107409569,
135.660258333577));
#217538=CARTESIAN_POINT('Ctrl Pts',(195.175923593249,-3.51234850319129,
135.568404894722));
#217539=CARTESIAN_POINT('Ctrl Pts',(195.183323675764,-3.63652137552785,
135.471655642292));
#217540=CARTESIAN_POINT('Ctrl Pts',(195.190731895431,-3.76083078870214,
135.374800004113));
#217541=CARTESIAN_POINT('Ctrl Pts',(195.198140115097,-3.88118668830531,
135.273038030831));
#217542=CARTESIAN_POINT('Ctrl Pts',(195.205548334764,-3.99719590421933,
135.166740182184));
#217543=CARTESIAN_POINT('Ctrl Pts',(195.212961114066,-4.11327652186949,
135.060376908984));
#217544=CARTESIAN_POINT('Ctrl Pts',(195.220373893368,-4.2250048606152,134.949472459869));
#217545=CARTESIAN_POINT('Ctrl Pts',(195.22778667267,-4.33202607173832,134.834432661125));
#217546=CARTESIAN_POINT('Ctrl Pts',(195.235210043698,-4.43920019978721,
134.719228488122));
#217547=CARTESIAN_POINT('Ctrl Pts',(195.242633414727,-4.54165352484936,
134.599877446827));
#217548=CARTESIAN_POINT('Ctrl Pts',(195.250056785756,-4.63907226748901,
134.476817432767));
#217549=CARTESIAN_POINT('Ctrl Pts',(195.253992835197,-4.6907260223665,134.411568060529));
#217550=CARTESIAN_POINT('Ctrl Pts',(195.257928884637,-4.7409651046425,134.345276439808));
#217551=CARTESIAN_POINT('Ctrl Pts',(195.261864934078,-4.78974787966705,
134.278010831926));
#217552=CARTESIAN_POINT('Ctrl Pts',(195.269344497194,-4.88244840344199,
134.150187905093));
#217553=CARTESIAN_POINT('Ctrl Pts',(195.27682406031,-4.97016722581075,134.018460598548));
#217554=CARTESIAN_POINT('Ctrl Pts',(195.284303623426,-5.05256043017122,
133.883250622416));
#217555=CARTESIAN_POINT('Ctrl Pts',(195.291774119838,-5.13485375774175,
133.748204547404));
#217556=CARTESIAN_POINT('Ctrl Pts',(195.29924461625,-5.21183412944589,133.609684515291));
#217557=CARTESIAN_POINT('Ctrl Pts',(195.306715112662,-5.28319868593022,
133.468144056114));
#217558=CARTESIAN_POINT('Ctrl Pts',(195.314177953125,-5.35449010624771,
133.326748651109));
#217559=CARTESIAN_POINT('Ctrl Pts',(195.321640793587,-5.42017700590164,
133.182339305798));
#217560=CARTESIAN_POINT('Ctrl Pts',(195.329103634049,-5.48000059220959,
133.03539716408));
#217561=CARTESIAN_POINT('Ctrl Pts',(195.336560224284,-5.53977407546993,
132.888578088357));
#217562=CARTESIAN_POINT('Ctrl Pts',(195.344016814518,-5.59369388645601,
132.739230777314));
#217563=CARTESIAN_POINT('Ctrl Pts',(195.351473404753,-5.64154786489769,
132.587859496334));
#217564=CARTESIAN_POINT('Ctrl Pts',(195.358924751708,-5.68936819367592,
132.436594655673));
#217565=CARTESIAN_POINT('Ctrl Pts',(195.366376098664,-5.73113107811833,
132.28330902832));
#217566=CARTESIAN_POINT('Ctrl Pts',(195.373827445619,-5.76667310995969,
132.128525186405));
#217567=CARTESIAN_POINT('Ctrl Pts',(195.381275645374,-5.80220013002815,
131.97380672004));
#217568=CARTESIAN_POINT('Ctrl Pts',(195.388723845128,-5.83151144890194,
131.817591655312));
#217569=CARTESIAN_POINT('Ctrl Pts',(195.396172044882,-5.85449396429676,
131.660416097376));
#217570=CARTESIAN_POINT('Ctrl Pts',(195.403619442704,-5.87747400521164,
131.503257462208));
#217571=CARTESIAN_POINT('Ctrl Pts',(195.411066840526,-5.89412654082032,
131.345138900639));
#217572=CARTESIAN_POINT('Ctrl Pts',(195.418514238348,-5.90438986155658,
131.186605205818));
#217573=CARTESIAN_POINT('Ctrl Pts',(195.424551094831,-5.91270930356792,
131.058097882038));
#217574=CARTESIAN_POINT('Ctrl Pts',(195.430587951313,-5.91683153852153,
130.929318034017));
#217575=CARTESIAN_POINT('Ctrl Pts',(195.436624807795,-5.91674877781543,
130.800557629312));
#217576=CARTESIAN_POINT('',(197.186623444831,-5.92116344383671,130.801362336707));
#217577=CARTESIAN_POINT('Ctrl Pts',(195.436626945312,-5.90948723714756,
130.800516761409));
#217578=CARTESIAN_POINT('Ctrl Pts',(195.471188816171,-5.9137909198465,130.064246680543));
#217579=CARTESIAN_POINT('Ctrl Pts',(195.598566561638,-5.44429779229546,
127.356026198653));
#217580=CARTESIAN_POINT('Ctrl Pts',(195.818760181701,-1.38200268831043,
123.943775431166));
#217581=CARTESIAN_POINT('Ctrl Pts',(196.097207805517,5.0249984088633,125.933328743181));
#217582=CARTESIAN_POINT('Ctrl Pts',(196.375655429329,6.81427145311116,132.39912238462));
#217583=CARTESIAN_POINT('Ctrl Pts',(196.654103053143,2.34156192761705,137.399407870579));
#217584=CARTESIAN_POINT('Ctrl Pts',(196.924425368086,-4.08962105397609,
136.370105731155));
#217585=CARTESIAN_POINT('Ctrl Pts',(197.101931808425,-5.91344458449586,
132.593748677927));
#217586=CARTESIAN_POINT('Ctrl Pts',(197.18662237416,-5.92463101698242,130.801383223244));
#217587=CARTESIAN_POINT('',(198.936625519421,-5.91828595945227,130.809611426597));
#217588=CARTESIAN_POINT('Ctrl Pts',(197.186624807795,-5.91674922678536,
130.801335748166));
#217589=CARTESIAN_POINT('Ctrl Pts',(197.194749305453,-5.91666143946249,
130.629620706627));
#217590=CARTESIAN_POINT('Ctrl Pts',(197.20287380311,-5.90909912685711,130.458101858393));
#217591=CARTESIAN_POINT('Ctrl Pts',(197.210998300767,-5.89410901923282,
130.287244158827));
#217592=CARTESIAN_POINT('Ctrl Pts',(197.218421567172,-5.88041271860844,
130.131133310534));
#217593=CARTESIAN_POINT('Ctrl Pts',(197.225844833577,-5.86048931664855,
129.975330918972));
#217594=CARTESIAN_POINT('Ctrl Pts',(197.233268099982,-5.83435518767231,
129.820373774879));
#217595=CARTESIAN_POINT('Ctrl Pts',(197.240682592703,-5.80825194706619,
129.665599777262));
#217596=CARTESIAN_POINT('Ctrl Pts',(197.248097085424,-5.77595265235115,
129.511669403079));
#217597=CARTESIAN_POINT('Ctrl Pts',(197.255511578145,-5.73752557677412,
129.359116410395));
#217598=CARTESIAN_POINT('Ctrl Pts',(197.262918924498,-5.69913553865926,
129.206710454028));
#217599=CARTESIAN_POINT('Ctrl Pts',(197.270326270852,-5.65462956830657,
129.055679595785));
#217600=CARTESIAN_POINT('Ctrl Pts',(197.277733617205,-5.60412731398305,
128.906549348981));
#217601=CARTESIAN_POINT('Ctrl Pts',(197.285135438881,-5.55366272614622,
128.757530329141));
#217602=CARTESIAN_POINT('Ctrl Pts',(197.292537260556,-5.49721087842226,
128.610409450263));
#217603=CARTESIAN_POINT('Ctrl Pts',(197.299939082232,-5.43494173808804,
128.465698849356));
#217604=CARTESIAN_POINT('Ctrl Pts',(197.307336996543,-5.37270546914825,
128.321064640048));
#217605=CARTESIAN_POINT('Ctrl Pts',(197.314734910855,-5.3046581706263,128.178838516762));
#217606=CARTESIAN_POINT('Ctrl Pts',(197.322132825166,-5.23101855199436,
128.03951424368));
#217607=CARTESIAN_POINT('Ctrl Pts',(197.329529510078,-5.15739117093109,
127.900213123764));
#217608=CARTESIAN_POINT('Ctrl Pts',(197.336926194991,-5.07817348849507,
127.76381322667));
#217609=CARTESIAN_POINT('Ctrl Pts',(197.344322879903,-4.9936309933754,127.630785336515));
#217610=CARTESIAN_POINT('Ctrl Pts',(197.351719236839,-4.90909224695859,
127.497763344956));
#217611=CARTESIAN_POINT('Ctrl Pts',(197.359115593775,-4.81922935754628,
127.368113378099));
#217612=CARTESIAN_POINT('Ctrl Pts',(197.36651195071,-4.72435198303289,127.242278515352));
#217613=CARTESIAN_POINT('Ctrl Pts',(197.373909440047,-4.62946008255125,
127.116424386966));
#217614=CARTESIAN_POINT('Ctrl Pts',(197.381306929384,-4.52955239306734,
126.9943868238));
#217615=CARTESIAN_POINT('Ctrl Pts',(197.388704418721,-4.42497971392021,
126.876576879388));
#217616=CARTESIAN_POINT('Ctrl Pts',(197.396104501236,-4.32037037698219,
126.758725636883));
#217617=CARTESIAN_POINT('Ctrl Pts',(197.403504583751,-4.21109304215689,
126.645105242758));
#217618=CARTESIAN_POINT('Ctrl Pts',(197.410904666267,-4.09753619015153,
126.536090741738));
#217619=CARTESIAN_POINT('Ctrl Pts',(197.418312885934,-3.9838544707137,126.426956368068));
#217620=CARTESIAN_POINT('Ctrl Pts',(197.4257211056,-3.86588410582371,126.322438260625));
#217621=CARTESIAN_POINT('Ctrl Pts',(197.433129325267,-3.74404811053006,
126.222872397726));
#217622=CARTESIAN_POINT('Ctrl Pts',(197.440542104569,-3.62213712721409,
126.123245253698));
#217623=CARTESIAN_POINT('Ctrl Pts',(197.447954883872,-3.49635607014594,
126.028576651746));
#217624=CARTESIAN_POINT('Ctrl Pts',(197.455367663174,-3.36715745966806,
125.939159572974));
#217625=CARTESIAN_POINT('Ctrl Pts',(197.462791034203,-3.23777424415678,
125.849614730886));
#217626=CARTESIAN_POINT('Ctrl Pts',(197.470214405232,-3.10496403682583,
125.765336597878));
#217627=CARTESIAN_POINT('Ctrl Pts',(197.477637776261,-2.96920520601125,
125.686572911233));
#217628=CARTESIAN_POINT('Ctrl Pts',(197.481573825702,-2.89722261642787,
125.644810514667));
#217629=CARTESIAN_POINT('Ctrl Pts',(197.485509875143,-2.82441143032903,
125.604597636826));
#217630=CARTESIAN_POINT('Ctrl Pts',(197.489445924583,-2.75084517427645,
125.565965692624));
#217631=CARTESIAN_POINT('Ctrl Pts',(197.496869190989,-2.61210151128014,
125.493107051516));
#217632=CARTESIAN_POINT('Ctrl Pts',(197.504292457394,-2.47025146129094,
125.425654175521));
#217633=CARTESIAN_POINT('Ctrl Pts',(197.5117157238,-2.32575549227818,125.363883436965));
#217634=CARTESIAN_POINT('Ctrl Pts',(197.519130216521,-2.18143030550119,
125.302185706292));
#217635=CARTESIAN_POINT('Ctrl Pts',(197.526544709242,-2.03446576441921,
125.246156890495));
#217636=CARTESIAN_POINT('Ctrl Pts',(197.533959201963,-1.88534783816607,
125.19602805863));
#217637=CARTESIAN_POINT('Ctrl Pts',(197.541366548317,-1.73637363738422,
125.14594754282));
#217638=CARTESIAN_POINT('Ctrl Pts',(197.548773894671,-1.58525053483429,
125.101755808138));
#217639=CARTESIAN_POINT('Ctrl Pts',(197.556181241024,-1.432485332562,125.063636243892));
#217640=CARTESIAN_POINT('Ctrl Pts',(197.5635830627,-1.27983406834118,125.025545110655));
#217641=CARTESIAN_POINT('Ctrl Pts',(197.570984884375,-1.12554350365379,
124.993517220284));
#217642=CARTESIAN_POINT('Ctrl Pts',(197.57838670605,-0.970136385334234,
124.967686397057));
#217643=CARTESIAN_POINT('Ctrl Pts',(197.585784620362,-0.814811305222937,
124.941869209721));
#217644=CARTESIAN_POINT('Ctrl Pts',(197.593182534673,-0.658371212651233,
124.922242635465));
#217645=CARTESIAN_POINT('Ctrl Pts',(197.600580448984,-0.501349743220964,
124.908889559417));
#217646=CARTESIAN_POINT('Ctrl Pts',(197.607977133896,-0.3443543679101,124.895538702408));
#217647=CARTESIAN_POINT('Ctrl Pts',(197.615373818808,-0.186778179082625,
124.88845930607));
#217648=CARTESIAN_POINT('Ctrl Pts',(197.622770503721,-0.0291607638722707,
124.887682477566));
#217649=CARTESIAN_POINT('Ctrl Pts',(197.630166860656,0.128449662416806,
124.886905683508));
#217650=CARTESIAN_POINT('Ctrl Pts',(197.637563217591,0.286100938161007,
124.892430903457));
#217651=CARTESIAN_POINT('Ctrl Pts',(197.644959574526,0.443252910452061,
124.9042371087));
#217652=CARTESIAN_POINT('Ctrl Pts',(197.652357063863,0.600428943111264,
124.916045121502));
#217653=CARTESIAN_POINT('Ctrl Pts',(197.659754553199,0.757105147833064,
124.934136006373));
#217654=CARTESIAN_POINT('Ctrl Pts',(197.667152042536,0.912746078026357,
124.958436810369));
#217655=CARTESIAN_POINT('Ctrl Pts',(197.674552125051,1.06844156790636,124.982746132975));
#217656=CARTESIAN_POINT('Ctrl Pts',(197.681952207565,1.2231006920997,125.013269651301));
#217657=CARTESIAN_POINT('Ctrl Pts',(197.68935229008,1.37619793154745,125.049883246362));
#217658=CARTESIAN_POINT('Ctrl Pts',(197.696760509747,1.52946351714884,125.086537101834));
#217659=CARTESIAN_POINT('Ctrl Pts',(197.704168729413,1.68116342485591,125.12929432084));
#217660=CARTESIAN_POINT('Ctrl Pts',(197.711576949079,1.83078633663098,125.177980613327));
#217661=CARTESIAN_POINT('Ctrl Pts',(197.718989728381,1.98050133881175,125.226696871413));
#217662=CARTESIAN_POINT('Ctrl Pts',(197.726402507683,2.12813644850627,125.281349345265));
#217663=CARTESIAN_POINT('Ctrl Pts',(197.733815286985,2.27320057411559,125.341715680144));
#217664=CARTESIAN_POINT('Ctrl Pts',(197.741238658014,2.41847197415036,125.402168269274));
#217665=CARTESIAN_POINT('Ctrl Pts',(197.748662029042,2.56116471546263,125.468350868582));
#217666=CARTESIAN_POINT('Ctrl Pts',(197.756085400071,2.7008117998894,125.539994921295));
#217667=CARTESIAN_POINT('Ctrl Pts',(197.760021449512,2.77485603483877,125.577982317118));
#217668=CARTESIAN_POINT('Ctrl Pts',(197.763957498952,2.84804449245546,125.617504387378));
#217669=CARTESIAN_POINT('Ctrl Pts',(197.767893548393,2.92031099958208,125.658516252623));
#217670=CARTESIAN_POINT('Ctrl Pts',(197.775316814799,3.05660337666153,125.735863350536));
#217671=CARTESIAN_POINT('Ctrl Pts',(197.782740081204,3.19002680850025,125.818745887891));
#217672=CARTESIAN_POINT('Ctrl Pts',(197.790163347609,3.32009988104743,125.906925845936));
#217673=CARTESIAN_POINT('Ctrl Pts',(197.79757784033,3.4500192180248,125.995001582594));
#217674=CARTESIAN_POINT('Ctrl Pts',(197.804992333051,3.57659577183659,126.08836206974));
#217675=CARTESIAN_POINT('Ctrl Pts',(197.812406825772,3.69937245935516,126.186723346248));
#217676=CARTESIAN_POINT('Ctrl Pts',(197.819814172126,3.82203081007992,126.284989818454));
#217677=CARTESIAN_POINT('Ctrl Pts',(197.82722151848,3.94089629635784,126.38824725262));
#217678=CARTESIAN_POINT('Ctrl Pts',(197.834628864833,4.05554068868584,126.49616838823));
#217679=CARTESIAN_POINT('Ctrl Pts',(197.842030686509,4.17009957490073,126.604009032185));
#217680=CARTESIAN_POINT('Ctrl Pts',(197.849432508184,4.28044336511714,126.716506196922));
#217681=CARTESIAN_POINT('Ctrl Pts',(197.85683432986,4.38617691174633,126.833292416016));
#217682=CARTESIAN_POINT('Ctrl Pts',(197.864232244171,4.49185464245934,126.950016984573));
#217683=CARTESIAN_POINT('Ctrl Pts',(197.871630158482,4.59292672653128,127.071025822277));
#217684=CARTESIAN_POINT('Ctrl Pts',(197.879028072794,4.68903498727919,127.195914767817));
#217685=CARTESIAN_POINT('Ctrl Pts',(197.886424757706,4.78512727657764,127.32078295908));
#217686=CARTESIAN_POINT('Ctrl Pts',(197.893821442618,4.87625715228911,127.449529682885));
#217687=CARTESIAN_POINT('Ctrl Pts',(197.90121812753,4.96210678305087,127.581717783478));
#217688=CARTESIAN_POINT('Ctrl Pts',(197.908614484466,5.04795260715005,127.713900022711));
#217689=CARTESIAN_POINT('Ctrl Pts',(197.916010841401,5.12851844851035,127.849523022255));
#217690=CARTESIAN_POINT('Ctrl Pts',(197.923407198337,5.20353003334438,127.988120969634));
#217691=CARTESIAN_POINT('Ctrl Pts',(197.930804687674,5.27855310264355,128.126740136713));
#217692=CARTESIAN_POINT('Ctrl Pts',(197.93820217701,5.34802004452218,128.268334830214));
#217693=CARTESIAN_POINT('Ctrl Pts',(197.945599666347,5.41170281439631,128.412415130906));
#217694=CARTESIAN_POINT('Ctrl Pts',(197.952999748862,5.47540790816671,128.556545938723));
#217695=CARTESIAN_POINT('Ctrl Pts',(197.960399831377,5.5333246421133,128.703163747315));
#217696=CARTESIAN_POINT('Ctrl Pts',(197.967799913892,5.58527338516755,128.851759333269));
#217697=CARTESIAN_POINT('Ctrl Pts',(197.975208133559,5.63727925120526,129.000518315345));
#217698=CARTESIAN_POINT('Ctrl Pts',(197.982616353225,5.68330389749944,129.15125906534));
#217699=CARTESIAN_POINT('Ctrl Pts',(197.990024572892,5.72321757932056,129.303457188875));
#217700=CARTESIAN_POINT('Ctrl Pts',(197.997437352194,5.76315582734688,129.455748987816));
#217701=CARTESIAN_POINT('Ctrl Pts',(198.004850131496,5.79697553623499,129.609499583923));
#217702=CARTESIAN_POINT('Ctrl Pts',(198.012262910798,5.82459833231772,129.76417561976));
#217703=CARTESIAN_POINT('Ctrl Pts',(198.019686281827,5.85226059714686,129.91907266397));
#217704=CARTESIAN_POINT('Ctrl Pts',(198.027109652855,5.87370821410285,130.074897420031));
#217705=CARTESIAN_POINT('Ctrl Pts',(198.034533023884,5.88891470369336,130.231111827664));
#217706=CARTESIAN_POINT('Ctrl Pts',(198.038469073325,5.89697754934896,130.313940454904));
#217707=CARTESIAN_POINT('Ctrl Pts',(198.042405122766,5.90328666138535,130.396878621457));
#217708=CARTESIAN_POINT('Ctrl Pts',(198.046341172207,5.90784402994841,130.479846395531));
#217709=CARTESIAN_POINT('Ctrl Pts',(198.053764438612,5.91643908482775,130.636321028099));
#217710=CARTESIAN_POINT('Ctrl Pts',(198.061187705018,5.9188262827532,130.793373976012));
#217711=CARTESIAN_POINT('Ctrl Pts',(198.068610971423,5.91494565958679,130.950471557045));
#217712=CARTESIAN_POINT('Ctrl Pts',(198.076025464144,5.91106962299469,131.107383461784));
#217713=CARTESIAN_POINT('Ctrl Pts',(198.083439956865,5.90094052019157,131.264339525099));
#217714=CARTESIAN_POINT('Ctrl Pts',(198.090854449586,5.88455019112052,131.420801702085));
#217715=CARTESIAN_POINT('Ctrl Pts',(198.09826179594,5.86817565966571,131.577113074935));
#217716=CARTESIAN_POINT('Ctrl Pts',(198.105669142294,5.84555195468406,131.732931140355));
#217717=CARTESIAN_POINT('Ctrl Pts',(198.113076488647,5.81672294120831,131.887718724436));
#217718=CARTESIAN_POINT('Ctrl Pts',(198.120478310323,5.78791542949845,132.042390862097));
#217719=CARTESIAN_POINT('Ctrl Pts',(198.127880131998,5.75291189262878,132.196033683341));
#217720=CARTESIAN_POINT('Ctrl Pts',(198.135281953674,5.71180790358625,132.348116114732));
#217721=CARTESIAN_POINT('Ctrl Pts',(198.142679867985,5.67072561301959,132.500118262991));
#217722=CARTESIAN_POINT('Ctrl Pts',(198.150077782296,5.6235493809752,132.650561302415));
#217723=CARTESIAN_POINT('Ctrl Pts',(198.157475696608,5.57042563656271,132.798925429756));
#217724=CARTESIAN_POINT('Ctrl Pts',(198.16487238152,5.5173107203528,132.94726490167));
#217725=CARTESIAN_POINT('Ctrl Pts',(198.172269066432,5.45825037911139,133.093525796069));
#217726=CARTESIAN_POINT('Ctrl Pts',(198.179665751344,5.39344060874215,133.237204419061));
#217727=CARTESIAN_POINT('Ctrl Pts',(198.18706210828,5.32863371210605,133.380876671192));
#217728=CARTESIAN_POINT('Ctrl Pts',(198.194458465215,5.25807804673258,133.5219665393));
#217729=CARTESIAN_POINT('Ctrl Pts',(198.20185482215,5.18201726216687,133.659991486062));
#217730=CARTESIAN_POINT('Ctrl Pts',(198.209252311487,5.1059448325008,133.798037564794));
#217731=CARTESIAN_POINT('Ctrl Pts',(198.216649800824,5.02436578559861,133.933017460883));
#217732=CARTESIAN_POINT('Ctrl Pts',(198.22404729016,4.93756904071554,134.064474500649));
#217733=CARTESIAN_POINT('Ctrl Pts',(198.231447372675,4.85074186936809,134.195977622476));
#217734=CARTESIAN_POINT('Ctrl Pts',(198.23884745519,4.75869356396067,134.323955117915));
#217735=CARTESIAN_POINT('Ctrl Pts',(198.246247537705,4.66175545359166,134.447980610569));
#217736=CARTESIAN_POINT('Ctrl Pts',(198.253655757372,4.56471074980486,134.572142482001));
#217737=CARTESIAN_POINT('Ctrl Pts',(198.261063977038,4.4627657331708,134.692343377834));
#217738=CARTESIAN_POINT('Ctrl Pts',(198.268472196704,4.35629146133617,134.808190692181));
#217739=CARTESIAN_POINT('Ctrl Pts',(198.275884976006,4.24975165636372,134.924109308617));
#217740=CARTESIAN_POINT('Ctrl Pts',(198.283297755308,4.13867730416189,135.035668740291));
#217741=CARTESIAN_POINT('Ctrl Pts',(198.290710534611,4.0234747705666,135.142514756496));
#217742=CARTESIAN_POINT('Ctrl Pts',(198.298133905639,3.9081076301889,135.249513439299));
#217743=CARTESIAN_POINT('Ctrl Pts',(198.305557276668,3.7886008105804,135.351785013754));
#217744=CARTESIAN_POINT('Ctrl Pts',(198.312980647697,3.6653926842793,135.449016367192));
#217745=CARTESIAN_POINT('Ctrl Pts',(198.316916697138,3.60006477937584,135.500570763819));
#217746=CARTESIAN_POINT('Ctrl Pts',(198.320852746578,3.53369678008804,135.550708903358));
#217747=CARTESIAN_POINT('Ctrl Pts',(198.324788796019,3.4663570110182,135.599389255089));
#217748=CARTESIAN_POINT('Ctrl Pts',(198.332212062425,3.33935630815509,135.691198879192));
#217749=CARTESIAN_POINT('Ctrl Pts',(198.33963532883,3.2085135538949,135.778098250994));
#217750=CARTESIAN_POINT('Ctrl Pts',(198.347058595235,3.07424533812585,135.859748452689));
#217751=CARTESIAN_POINT('Ctrl Pts',(198.354473087956,2.94013581623739,135.941302150627));
#217752=CARTESIAN_POINT('Ctrl Pts',(198.361887580677,2.80260920746114,136.017618835655));
#217753=CARTESIAN_POINT('Ctrl Pts',(198.369302073398,2.66211377350456,136.088400816071));
#217754=CARTESIAN_POINT('Ctrl Pts',(198.376709419752,2.52175375433678,136.15911457415));
#217755=CARTESIAN_POINT('Ctrl Pts',(198.384116766106,2.37843093774423,136.22430408084));
#217756=CARTESIAN_POINT('Ctrl Pts',(198.39152411246,2.23262097347329,136.283715885415));
#217757=CARTESIAN_POINT('Ctrl Pts',(198.398925934135,2.08691975977482,136.343083378425));
#217758=CARTESIAN_POINT('Ctrl Pts',(198.406327755811,1.93873543618441,136.396681609322));
#217759=CARTESIAN_POINT('Ctrl Pts',(198.413729577486,1.7885664693587,136.444303928202));
#217760=CARTESIAN_POINT('Ctrl Pts',(198.421127491797,1.63847677556185,136.49190110763));
#217761=CARTESIAN_POINT('Ctrl Pts',(198.428525406109,1.48640487996303,136.533528545095));
#217762=CARTESIAN_POINT('Ctrl Pts',(198.43592332042,1.33286725626621,136.569028469201));
#217763=CARTESIAN_POINT('Ctrl Pts',(198.443320005332,1.17935514773689,136.604522493864));
#217764=CARTESIAN_POINT('Ctrl Pts',(198.450716690245,1.02437815788533,136.633890942145));
#217765=CARTESIAN_POINT('Ctrl Pts',(198.458113375157,0.868465999221073,
136.657026452098));
#217766=CARTESIAN_POINT('Ctrl Pts',(198.465509732092,0.712560753865369,
136.680160936198));
#217767=CARTESIAN_POINT('Ctrl Pts',(198.472906089028,0.555720791400502,
136.697062976703));
#217768=CARTESIAN_POINT('Ctrl Pts',(198.480302445963,0.398483782675044,
136.707676739666));
#217769=CARTESIAN_POINT('Ctrl Pts',(198.4876999353,0.241222700562017,136.718292127623));
#217770=CARTESIAN_POINT('Ctrl Pts',(198.495097424636,0.0835648236240816,
136.722617295928));
#217771=CARTESIAN_POINT('Ctrl Pts',(198.502494913973,-0.0739494677253907,
136.720648477257));
#217772=CARTESIAN_POINT('Ctrl Pts',(198.509894996488,-0.231518975465559,
136.718678968419));
#217773=CARTESIAN_POINT('Ctrl Pts',(198.517295079003,-0.388944424367331,
136.710411084445));
#217774=CARTESIAN_POINT('Ctrl Pts',(198.524695161518,-0.545688000420484,
136.695893115032));
#217775=CARTESIAN_POINT('Ctrl Pts',(198.532103381184,-0.702603932149111,
136.681359181619));
#217776=CARTESIAN_POINT('Ctrl Pts',(198.539511600851,-0.858836121715699,
136.660561472159));
#217777=CARTESIAN_POINT('Ctrl Pts',(198.546919820517,-1.01385369294746,
136.633599954889));
#217778=CARTESIAN_POINT('Ctrl Pts',(198.55433259982,-1.16896667490789,136.606621843255));
#217779=CARTESIAN_POINT('Ctrl Pts',(198.561745379122,-1.32286318481004,
136.573472442769));
#217780=CARTESIAN_POINT('Ctrl Pts',(198.569158158424,-1.47502554766598,
136.534302170168));
#217781=CARTESIAN_POINT('Ctrl Pts',(198.576581529452,-1.62740532724162,
136.495075929244));
#217782=CARTESIAN_POINT('Ctrl Pts',(198.584004900481,-1.77804565442718,
136.449811741413));
#217783=CARTESIAN_POINT('Ctrl Pts',(198.59142827151,-1.92644614760085,136.398709176862));
#217784=CARTESIAN_POINT('Ctrl Pts',(198.595364320951,-2.00513164990258,
136.371613370947));
#217785=CARTESIAN_POINT('Ctrl Pts',(198.599300370392,-2.083187811426,136.34287698262));
#217786=CARTESIAN_POINT('Ctrl Pts',(198.603236419832,-2.16054276008407,
136.312535046934));
#217787=CARTESIAN_POINT('Ctrl Pts',(198.610659686238,-2.30643177908773,
136.255311103171));
#217788=CARTESIAN_POINT('Ctrl Pts',(198.618082952643,-2.4502663863924,136.192200621447));
#217789=CARTESIAN_POINT('Ctrl Pts',(198.625506219049,-2.59153626383937,
136.12337089728));
#217790=CARTESIAN_POINT('Ctrl Pts',(198.63292071177,-2.73263917202303,136.054622524132));
#217791=CARTESIAN_POINT('Ctrl Pts',(198.640335204491,-2.87118305185535,
135.980168525608));
#217792=CARTESIAN_POINT('Ctrl Pts',(198.647749697212,-3.00667515047484,
135.900225127344));
#217793=CARTESIAN_POINT('Ctrl Pts',(198.655157043566,-3.14203665670858,
135.820358781537));
#217794=CARTESIAN_POINT('Ctrl Pts',(198.662564389919,-3.27435191817235,
135.735013757533));
#217795=CARTESIAN_POINT('Ctrl Pts',(198.669971736273,-3.40315059928627,
135.644453236626));
#217796=CARTESIAN_POINT('Ctrl Pts',(198.677373557949,-3.53185321748438,
135.553960259172));
#217797=CARTESIAN_POINT('Ctrl Pts',(198.684775379624,-3.65704417362253,
135.458259743947));
#217798=CARTESIAN_POINT('Ctrl Pts',(198.692177201299,-3.77828017388039,
135.357659365744));
#217799=CARTESIAN_POINT('Ctrl Pts',(198.699575115611,-3.89945217459736,
135.257112093699));
#217800=CARTESIAN_POINT('Ctrl Pts',(198.706973029922,-4.01667309082048,
135.151670347788));
#217801=CARTESIAN_POINT('Ctrl Pts',(198.714370944233,-4.12953101835425,
135.041683372673));
#217802=CARTESIAN_POINT('Ctrl Pts',(198.721767629146,-4.24237019094798,
134.931714675399));
#217803=CARTESIAN_POINT('Ctrl Pts',(198.729164314058,-4.35084754678297,
134.81720250832));
#217804=CARTESIAN_POINT('Ctrl Pts',(198.73656099897,-4.45458643666219,134.69853450182));
#217805=CARTESIAN_POINT('Ctrl Pts',(198.743957355906,-4.55832072665023,
134.579871757183));
#217806=CARTESIAN_POINT('Ctrl Pts',(198.751353712841,-4.65731672275938,
134.457053820572));
#217807=CARTESIAN_POINT('Ctrl Pts',(198.758750069776,-4.75123682608077,
134.330502870084));
#217808=CARTESIAN_POINT('Ctrl Pts',(198.766147559113,-4.84517130880985,
134.203932544323));
#217809=CARTESIAN_POINT('Ctrl Pts',(198.77354504845,-4.93402812889303,134.073628366469));
#217810=CARTESIAN_POINT('Ctrl Pts',(198.780942537786,-5.01751202795966,
133.940042937537));
#217811=CARTESIAN_POINT('Ctrl Pts',(198.788342620301,-5.10102519217775,
133.80641068044));
#217812=CARTESIAN_POINT('Ctrl Pts',(198.795742702816,-5.17916148769389,
133.669495198516));
#217813=CARTESIAN_POINT('Ctrl Pts',(198.803142785331,-5.25167084038773,
133.529775071685));
#217814=CARTESIAN_POINT('Ctrl Pts',(198.810551004998,-5.32425992456896,
133.389901308211));
#217815=CARTESIAN_POINT('Ctrl Pts',(198.817959224664,-5.39120953722308,
133.247217072428));
#217816=CARTESIAN_POINT('Ctrl Pts',(198.825367444331,-5.45231683291927,
133.102223040768));
#217817=CARTESIAN_POINT('Ctrl Pts',(198.832780223633,-5.51346173913636,
132.957139767702));
#217818=CARTESIAN_POINT('Ctrl Pts',(198.840193002935,-5.56875703240109,
132.809744214664));
#217819=CARTESIAN_POINT('Ctrl Pts',(198.847605782237,-5.61804944659764,
132.660553220203));
#217820=CARTESIAN_POINT('Ctrl Pts',(198.855029153265,-5.66741229210717,
132.511149054653));
#217821=CARTESIAN_POINT('Ctrl Pts',(198.862452524294,-5.71075502537524,
132.359944681874));
#217822=CARTESIAN_POINT('Ctrl Pts',(198.869875895323,-5.74797508196189,
132.207468959657));
#217823=CARTESIAN_POINT('Ctrl Pts',(198.873811944764,-5.76771004904698,
132.126622673133));
#217824=CARTESIAN_POINT('Ctrl Pts',(198.877747994205,-5.78572457362142,
132.045419093963));
#217825=CARTESIAN_POINT('Ctrl Pts',(198.881684043645,-5.80200928305024,
131.96393762747));
#217826=CARTESIAN_POINT('Ctrl Pts',(198.892415019576,-5.84640680080297,
131.741792131358));
#217827=CARTESIAN_POINT('Ctrl Pts',(198.903145995507,-5.87805736973165,
131.517021225439));
#217828=CARTESIAN_POINT('Ctrl Pts',(198.913876971438,-5.89671799543621,
131.290824845232));
#217829=CARTESIAN_POINT('Ctrl Pts',(198.921459583557,-5.90990377532492,
131.130992279687));
#217830=CARTESIAN_POINT('Ctrl Pts',(198.929042195676,-5.91660456247561,
130.970448251875));
#217831=CARTESIAN_POINT('Ctrl Pts',(198.936624807795,-5.91674765788855,
130.809625156515));
#217832=CARTESIAN_POINT('',(200.686624807795,-5.90698642445631,130.80494468951));
#217833=CARTESIAN_POINT('Ctrl Pts',(198.936625793059,-5.9188774747153,130.809606147102));
#217834=CARTESIAN_POINT('Ctrl Pts',(199.011127751193,-5.90425259497605,
129.228876773919));
#217835=CARTESIAN_POINT('Ctrl Pts',(199.178445583929,-4.43793552679426,
125.654919300417));
#217836=CARTESIAN_POINT('Ctrl Pts',(199.438579291272,1.60513008150291,123.992524011201));
#217837=CARTESIAN_POINT('Ctrl Pts',(199.717026915084,6.59860307470548,128.472837940681));
#217838=CARTESIAN_POINT('Ctrl Pts',(199.995474538897,5.52828220193623,135.095707309003));
#217839=CARTESIAN_POINT('Ctrl Pts',(200.27392216271,-0.622259942815148,
137.775038711833));
#217840=CARTESIAN_POINT('Ctrl Pts',(200.504305585676,-5.2380063121806,134.691886300211));
#217841=CARTESIAN_POINT('Ctrl Pts',(200.641873134038,-5.90782357734734,
131.759296891607));
#217842=CARTESIAN_POINT('Ctrl Pts',(200.686624807795,-5.90698642445631,
130.80494468951));
#217843=CARTESIAN_POINT('',(202.436624807795,-5.91672686803579,130.798894919773));
#217844=CARTESIAN_POINT('Ctrl Pts',(200.686624807795,-5.90698642445631,
130.80494468951));
#217845=CARTESIAN_POINT('Ctrl Pts',(200.734689008642,-5.90608730535493,
129.77995116259));
#217846=CARTESIAN_POINT('Ctrl Pts',(200.875569084094,-5.16390162333142,
126.774392662908));
#217847=CARTESIAN_POINT('Ctrl Pts',(201.109265034148,-0.373204209884669,
123.815921653964));
#217848=CARTESIAN_POINT('Ctrl Pts',(201.387712657962,5.67784563147399,126.712951384136));
#217849=CARTESIAN_POINT('Ctrl Pts',(201.666160281774,6.5112327157493,133.369786323417));
#217850=CARTESIAN_POINT('Ctrl Pts',(201.944607905587,1.36111502553663,137.669120366955));
#217851=CARTESIAN_POINT('Ctrl Pts',(202.201429414261,-4.54266270085758,
135.816111494225));
#217852=CARTESIAN_POINT('Ctrl Pts',(202.36543504833,-5.90274340491685,132.310756663458));
#217853=CARTESIAN_POINT('Ctrl Pts',(202.436624807795,-5.91672686803579,
130.798894919773));
#217854=CARTESIAN_POINT('',(204.186624807795,-5.92581928566479,130.806233519117));
#217855=CARTESIAN_POINT('Ctrl Pts',(202.436624807795,-5.91672686803579,
130.798894919773));
#217856=CARTESIAN_POINT('Ctrl Pts',(202.458250922934,-5.9209747821421,130.339619647749));
#217857=CARTESIAN_POINT('Ctrl Pts',(202.572692912681,-5.66197777958727,
127.913946320691));
#217858=CARTESIAN_POINT('Ctrl Pts',(202.779950777024,-2.32147802600033,
124.202217003606));
#217859=CARTESIAN_POINT('Ctrl Pts',(203.058398400839,4.2997548257633,125.28261551589));
#217860=CARTESIAN_POINT('Ctrl Pts',(203.336846024651,6.96972305013295,131.437228026285));
#217861=CARTESIAN_POINT('Ctrl Pts',(203.615293648464,3.23485627607878,137.010266301744));
#217862=CARTESIAN_POINT('Ctrl Pts',(203.893741272277,-3.4726853742618,136.880380435614));
#217863=CARTESIAN_POINT('Ctrl Pts',(204.084184992054,-5.87766124044895,
132.972676372107));
#217864=CARTESIAN_POINT('Ctrl Pts',(204.181812837227,-5.92623998325372,
130.908018473525));
#217865=CARTESIAN_POINT('Ctrl Pts',(204.186624807795,-5.92581928566479,
130.806233519117));
#217866=CARTESIAN_POINT('',(205.936623590202,-5.91340924895264,130.808944439334));
#217867=CARTESIAN_POINT('Ctrl Pts',(204.186624807795,-5.92581928566479,
130.806233519117));
#217868=CARTESIAN_POINT('Ctrl Pts',(204.274628711831,-5.91812534204668,
128.944735566654));
#217869=CARTESIAN_POINT('Ctrl Pts',(204.455448490471,-3.96770241261772,
125.106068119418));
#217870=CARTESIAN_POINT('Ctrl Pts',(204.729084143717,2.57533168687046,124.297039558175));
#217871=CARTESIAN_POINT('Ctrl Pts',(205.007531767529,6.86682325353852,129.453694210665));
#217872=CARTESIAN_POINT('Ctrl Pts',(205.285979391342,4.84803947518153,135.851545143624));
#217873=CARTESIAN_POINT('Ctrl Pts',(205.564427015155,-1.62585529160082,
137.611280375001));
#217874=CARTESIAN_POINT('Ctrl Pts',(205.781308123836,-5.50460122239126,
134.109769780245));
#217875=CARTESIAN_POINT('Ctrl Pts',(205.905373357914,-5.91576144076024,
131.474232650613));
#217876=CARTESIAN_POINT('Ctrl Pts',(205.936622717388,-5.911015738934,130.80896117583));
#217877=CARTESIAN_POINT('',(207.097234316256,3.07028764517384,135.860950196139));
#217878=CARTESIAN_POINT('Ctrl Pts',(205.936624807795,-5.91674824245351,
130.808921091594));
#217879=CARTESIAN_POINT('Ctrl Pts',(205.944320535086,-5.91687464410253,
130.644927890423));
#217880=CARTESIAN_POINT('Ctrl Pts',(205.952016262377,-5.91017796225583,
130.480857837863));
#217881=CARTESIAN_POINT('Ctrl Pts',(205.959711989668,-5.89667042808694,
130.31732014181));
#217882=CARTESIAN_POINT('Ctrl Pts',(205.967107144318,-5.8836904587688,130.160169750732));
#217883=CARTESIAN_POINT('Ctrl Pts',(205.974502298968,-5.86442165241146,
130.003511317041));
#217884=CARTESIAN_POINT('Ctrl Pts',(205.981897453618,-5.83892794642443,
129.847882181341));
#217885=CARTESIAN_POINT('Ctrl Pts',(205.989293079306,-5.81343261660182,
129.692243132757));
#217886=CARTESIAN_POINT('Ctrl Pts',(205.996688704995,-5.78171165733105,
129.53763388078));
#217887=CARTESIAN_POINT('Ctrl Pts',(206.004084330683,-5.74388042102671,
129.384583074623));
#217888=CARTESIAN_POINT('Ctrl Pts',(206.011481882822,-5.70603933025007,
129.231492401015));
#217889=CARTESIAN_POINT('Ctrl Pts',(206.01887943496,-5.66208488256809,129.079961343446));
#217890=CARTESIAN_POINT('Ctrl Pts',(206.026276987099,-5.61218269697228,
128.930504716408));
#217891=CARTESIAN_POINT('Ctrl Pts',(206.033677921977,-5.56225769219368,
128.780979746109));
#217892=CARTESIAN_POINT('Ctrl Pts',(206.041078856855,-5.50637965184727,
128.633531448377));
#217893=CARTESIAN_POINT('Ctrl Pts',(206.048479791733,-5.44476278582211,
128.488655807227));
#217894=CARTESIAN_POINT('Ctrl Pts',(206.055889603669,-5.38307201339005,
128.343606394855));
#217895=CARTESIAN_POINT('Ctrl Pts',(206.063299415605,-5.31562881696656,
128.201136143459));
#217896=CARTESIAN_POINT('Ctrl Pts',(206.070709227541,-5.24269425134762,
128.06171817835));
#217897=CARTESIAN_POINT('Ctrl Pts',(206.078124284764,-5.16970805651977,
127.922201521501));
#217898=CARTESIAN_POINT('Ctrl Pts',(206.085539341988,-5.09122293266157,
127.785741777807));
#217899=CARTESIAN_POINT('Ctrl Pts',(206.092954399211,-5.00754363174057,
127.652783656945));
#217900=CARTESIAN_POINT('Ctrl Pts',(206.100380033849,-4.92374496414771,
127.519635874265));
#217901=CARTESIAN_POINT('Ctrl Pts',(206.107805668488,-4.83473753693092,
127.389999992524));
#217902=CARTESIAN_POINT('Ctrl Pts',(206.115231303126,-4.74086717656672,
127.264288728938));
#217903=CARTESIAN_POINT('Ctrl Pts',(206.117261623011,-4.71520110645441,
127.229916706794));
#217904=CARTESIAN_POINT('Ctrl Pts',(206.119291942896,-4.68917170648531,
127.195837875561));
#217905=CARTESIAN_POINT('Ctrl Pts',(206.121322262781,-4.66278652276695,
127.162060189869));
#217906=CARTESIAN_POINT('Ctrl Pts',(206.128745542087,-4.56631670550191,
127.038561820438));
#217907=CARTESIAN_POINT('Ctrl Pts',(206.136168821393,-4.46479117026267,
126.918712002184));
#217908=CARTESIAN_POINT('Ctrl Pts',(206.1435921007,-4.35851586193957,126.802952110088));
#217909=CARTESIAN_POINT('Ctrl Pts',(206.151006606373,-4.25236616125308,
126.687329035533));
#217910=CARTESIAN_POINT('Ctrl Pts',(206.158421112046,-4.14147811176257,
126.575786537499));
#217911=CARTESIAN_POINT('Ctrl Pts',(206.165835617719,-4.02619954292322,
126.4687351952));
#217912=CARTESIAN_POINT('Ctrl Pts',(206.173242977064,-3.9110320831151,126.361787032278));
#217913=CARTESIAN_POINT('Ctrl Pts',(206.180650336408,-3.79148280018012,
126.259321659787));
#217914=CARTESIAN_POINT('Ctrl Pts',(206.188057695753,-3.66793813141363,
126.161714774232));
#217915=CARTESIAN_POINT('Ctrl Pts',(206.195459530445,-3.54448560632645,
126.064180687105));
#217916=CARTESIAN_POINT('Ctrl Pts',(206.202861365137,-3.41704392042245,
125.971498102217));
#217917=CARTESIAN_POINT('Ctrl Pts',(206.210263199829,-3.28603443959317,
125.884004103622));
#217918=CARTESIAN_POINT('Ctrl Pts',(206.217661127171,-3.15509411728722,
125.796556292186));
#217919=CARTESIAN_POINT('Ctrl Pts',(206.225059054513,-3.02059006058692,
125.714291818989));
#217920=CARTESIAN_POINT('Ctrl Pts',(206.232456981854,-2.88297452136991,
125.637505822661));
#217921=CARTESIAN_POINT('Ctrl Pts',(206.239853679775,-2.74538185171612,
125.560732586972));
#217922=CARTESIAN_POINT('Ctrl Pts',(206.247250377697,-2.60467905146201,
125.489436202917));
#217923=CARTESIAN_POINT('Ctrl Pts',(206.254647075618,-2.4613451038374,125.423867067499));
#217924=CARTESIAN_POINT('Ctrl Pts',(206.262043445548,-2.3180175120597,125.358300839608));
#217925=CARTESIAN_POINT('Ctrl Pts',(206.269439815478,-2.1720593443594,125.298461510681));
#217926=CARTESIAN_POINT('Ctrl Pts',(206.276836185407,-2.02397155401354,
125.244552193614));
#217927=CARTESIAN_POINT('Ctrl Pts',(206.284233687713,-1.87586109160203,
125.190634623095));
#217928=CARTESIAN_POINT('Ctrl Pts',(206.291631190018,-1.72562070814953,
125.142648999845));
#217929=CARTESIAN_POINT('Ctrl Pts',(206.299028692324,-1.57376843488975,
125.100749176045));
#217930=CARTESIAN_POINT('Ctrl Pts',(206.306428787771,-1.42186293089913,
125.058834664561));
#217931=CARTESIAN_POINT('Ctrl Pts',(206.313828883218,-1.26834477174244,
125.023010299208));
#217932=CARTESIAN_POINT('Ctrl Pts',(206.321228978665,-1.1137439959854,124.993379213887));
#217933=CARTESIAN_POINT('Ctrl Pts',(206.328637211142,-0.958973223613178,
124.963715546683));
#217934=CARTESIAN_POINT('Ctrl Pts',(206.336045443619,-0.803117824125187,
124.940258829909));
#217935=CARTESIAN_POINT('Ctrl Pts',(206.343453676096,-0.646715539100822,
124.923060627429));
#217936=CARTESIAN_POINT('Ctrl Pts',(206.35086646816,-0.490216992290331,
124.905851839875));
#217937=CARTESIAN_POINT('Ctrl Pts',(206.358279260223,-0.333171260766503,
124.894909268023));
#217938=CARTESIAN_POINT('Ctrl Pts',(206.365692052287,-0.176117430763197,
124.890232345954));
#217939=CARTESIAN_POINT('Ctrl Pts',(206.373115435889,-0.0188391992448544,
124.885548741409));
#217940=CARTESIAN_POINT('Ctrl Pts',(206.380538819491,0.13844678157505,124.887148662973));
#217941=CARTESIAN_POINT('Ctrl Pts',(206.387962203094,0.295204371712296,
124.894979521256));
#217942=CARTESIAN_POINT('Ctrl Pts',(206.391898097594,0.378317594721756,
124.899131459738));
#217943=CARTESIAN_POINT('Ctrl Pts',(206.395833992093,0.461282402246363,
124.905034131635));
#217944=CARTESIAN_POINT('Ctrl Pts',(206.399769886593,0.544020024813092,
124.912673866295));
#217945=CARTESIAN_POINT('Ctrl Pts',(206.407193124759,0.700066147897168,
124.927082679821));
#217946=CARTESIAN_POINT('Ctrl Pts',(206.414616362924,0.855775400938864,
124.947717077111));
#217947=CARTESIAN_POINT('Ctrl Pts',(206.42203960109,1.0106110768226,124.974558235503));
#217948=CARTESIAN_POINT('Ctrl Pts',(206.429454065568,1.1652637490334,125.001367669744));
#217949=CARTESIAN_POINT('Ctrl Pts',(206.436868530046,1.31904453505951,125.034369199787));
#217950=CARTESIAN_POINT('Ctrl Pts',(206.444282994524,1.47141999714576,125.07349211842));
#217951=CARTESIAN_POINT('Ctrl Pts',(206.451690312658,1.62364859393998,125.11257732889));
#217952=CARTESIAN_POINT('Ctrl Pts',(206.459097630792,1.77447420420068,125.157772089943));
#217953=CARTESIAN_POINT('Ctrl Pts',(206.466504948926,1.92337186920565,125.208954357494));
#217954=CARTESIAN_POINT('Ctrl Pts',(206.47390674243,2.07215848127999,125.260098451574));
#217955=CARTESIAN_POINT('Ctrl Pts',(206.481308535935,2.21901965969763,125.317221039542));
#217956=CARTESIAN_POINT('Ctrl Pts',(206.48871032944,2.36344405149433,125.380149819859));
#217957=CARTESIAN_POINT('Ctrl Pts',(206.496108215656,2.50779220395472,125.443045381076));
#217958=CARTESIAN_POINT('Ctrl Pts',(206.503506101871,2.64970579024399,125.511740881817));
#217959=CARTESIAN_POINT('Ctrl Pts',(206.510903988087,2.78869205246822,125.586015362698));
#217960=CARTESIAN_POINT('Ctrl Pts',(206.518300645105,2.92765522138042,125.660277502477));
#217961=CARTESIAN_POINT('Ctrl Pts',(206.525697302122,3.06369170265306,125.740116606851));
#217962=CARTESIAN_POINT('Ctrl Pts',(206.533093959139,3.19633193171053,125.825265042582));
#217963=CARTESIAN_POINT('Ctrl Pts',(206.540490288307,3.32896628161558,125.910409704189));
#217964=CARTESIAN_POINT('Ctrl Pts',(206.547886617474,3.45820436447894,126.000863027573));
#217965=CARTESIAN_POINT('Ctrl Pts',(206.555282946642,3.58360452178626,126.096313337224));
#217966=CARTESIAN_POINT('Ctrl Pts',(206.562680408361,3.70902388080001,126.191778262557));
#217967=CARTESIAN_POINT('Ctrl Pts',(206.57007787008,3.83060384705553,126.292241471571));
#217968=CARTESIAN_POINT('Ctrl Pts',(206.577475331799,3.94793497542389,126.397350293965));
#217969=CARTESIAN_POINT('Ctrl Pts',(206.584875386871,4.06530723695059,126.502495964703));
#217970=CARTESIAN_POINT('Ctrl Pts',(206.592275441942,4.17842741707443,126.612290242479));
#217971=CARTESIAN_POINT('Ctrl Pts',(206.599675497014,4.28692225118017,126.726342940454));
#217972=CARTESIAN_POINT('Ctrl Pts',(206.607083689639,4.39553639284793,126.840521057759));
#217973=CARTESIAN_POINT('Ctrl Pts',(206.614491882264,4.49951477334651,126.958966676524));
#217974=CARTESIAN_POINT('Ctrl Pts',(206.621900074889,4.59852335176967,127.081255254334));
#217975=CARTESIAN_POINT('Ctrl Pts',(206.629312827337,4.69759287104336,127.203619102085));
#217976=CARTESIAN_POINT('Ctrl Pts',(206.636725579785,4.79168627026316,127.329830323613));
#217977=CARTESIAN_POINT('Ctrl Pts',(206.644138332232,4.88051264007905,127.459435067942));
#217978=CARTESIAN_POINT('Ctrl Pts',(206.651561676931,4.96946593591552,127.589225007439));
#217979=CARTESIAN_POINT('Ctrl Pts',(206.658985021629,5.05313697283413,127.722417839174));
#217980=CARTESIAN_POINT('Ctrl Pts',(206.666408366327,5.13128020290801,127.85853407112));
#217981=CARTESIAN_POINT('Ctrl Pts',(206.670344747687,5.17271725948344,127.930712505499));
#217982=CARTESIAN_POINT('Ctrl Pts',(206.674281129047,5.21260076983565,128.003712593246));
#217983=CARTESIAN_POINT('Ctrl Pts',(206.678217510406,5.25089964747057,128.077460646043));
#217984=CARTESIAN_POINT('Ctrl Pts',(206.685640788461,5.32312415823055,128.21653566238));
#217985=CARTESIAN_POINT('Ctrl Pts',(206.693064066516,5.38992876580883,128.358692359875));
#217986=CARTESIAN_POINT('Ctrl Pts',(206.70048734457,5.45103920233567,128.503469012753));
#217987=CARTESIAN_POINT('Ctrl Pts',(206.707901848764,5.51207741006405,128.648074548482));
#217988=CARTESIAN_POINT('Ctrl Pts',(206.715316352958,5.56743469941679,128.795293535183));
#217989=CARTESIAN_POINT('Ctrl Pts',(206.722730857152,5.6168822217327,128.944638952993));
#217990=CARTESIAN_POINT('Ctrl Pts',(206.730138214794,5.66628208350716,129.093840422569));
#217991=CARTESIAN_POINT('Ctrl Pts',(206.737545572437,5.70978340170174,129.245163890935));
#217992=CARTESIAN_POINT('Ctrl Pts',(206.744952930079,5.7472051019998,129.398101723177));
#217993=CARTESIAN_POINT('Ctrl Pts',(206.752354762849,5.78459889084891,129.550925484801));
#217994=CARTESIAN_POINT('Ctrl Pts',(206.75975659562,5.81592200238151,129.705360851746));
#217995=CARTESIAN_POINT('Ctrl Pts',(206.767158428391,5.84104299956971,129.860884470715));
#217996=CARTESIAN_POINT('Ctrl Pts',(206.774556353595,5.86615073491423,130.016325985859));
#217997=CARTESIAN_POINT('Ctrl Pts',(206.7819542788,5.88506281728999,130.172854241276));
#217998=CARTESIAN_POINT('Ctrl Pts',(206.789352204005,5.89769879798622,130.329935227508));
#217999=CARTESIAN_POINT('Ctrl Pts',(206.796748899477,5.91033267824491,130.486990102683));
#218000=CARTESIAN_POINT('Ctrl Pts',(206.804145594949,5.9166924974782,130.644597154589));
#218001=CARTESIAN_POINT('Ctrl Pts',(206.811542290421,5.91674961156378,130.802216658633));
#218002=CARTESIAN_POINT('Ctrl Pts',(206.818938657709,5.91680672311526,130.959829169251));
#218003=CARTESIAN_POINT('Ctrl Pts',(206.826335024997,5.91056168541304,131.117453757611));
#218004=CARTESIAN_POINT('Ctrl Pts',(206.833731392284,5.89803799224837,131.274550371277));
#218005=CARTESIAN_POINT('Ctrl Pts',(206.841128891758,5.88551238204215,131.431671032222));
#218006=CARTESIAN_POINT('Ctrl Pts',(206.848526391231,5.86670623237485,131.588263185411));
#218007=CARTESIAN_POINT('Ctrl Pts',(206.855923890704,5.84169493924775,131.743791721622));
#218008=CARTESIAN_POINT('Ctrl Pts',(206.863323983132,5.81667487921999,131.899374773335));
#218009=CARTESIAN_POINT('Ctrl Pts',(206.870724075559,5.78544540453156,132.053893097464));
#218010=CARTESIAN_POINT('Ctrl Pts',(206.878124167987,5.74813303139562,132.206821745683));
#218011=CARTESIAN_POINT('Ctrl Pts',(206.885532397178,5.71077963148349,132.359918546418));
#218012=CARTESIAN_POINT('Ctrl Pts',(206.892940626368,5.66733006439983,132.511421817639));
#218013=CARTESIAN_POINT('Ctrl Pts',(206.900348855559,5.61796095209888,132.660821040843));
#218014=CARTESIAN_POINT('Ctrl Pts',(206.907761644179,5.56856145534191,132.810312212512));
#218015=CARTESIAN_POINT('Ctrl Pts',(206.9151744328,5.5132352846973,132.957696407148));
#218016=CARTESIAN_POINT('Ctrl Pts',(206.922587221421,5.45220703402161,133.102483551759));
#218017=CARTESIAN_POINT('Ctrl Pts',(206.930010601368,5.3910915867254,133.247477566952));
#218018=CARTESIAN_POINT('Ctrl Pts',(206.937433981315,5.32425794604157,133.389866784108));
#218019=CARTESIAN_POINT('Ctrl Pts',(206.944857361262,5.2519767974538,133.52918543423));
#218020=CARTESIAN_POINT('Ctrl Pts',(206.948793285581,5.21365286245629,133.60305308846));
#218021=CARTESIAN_POINT('Ctrl Pts',(206.9527292099,5.17379827248436,133.676058022512));
#218022=CARTESIAN_POINT('Ctrl Pts',(206.956665134219,5.13245820404137,133.748134275011));
#218023=CARTESIAN_POINT('Ctrl Pts',(206.964088434769,5.05448928799419,133.884072784351));
#218024=CARTESIAN_POINT('Ctrl Pts',(206.97151173532,4.9709980519811,134.01711704531));
#218025=CARTESIAN_POINT('Ctrl Pts',(206.97893503587,4.88222471713909,134.146786738493));
#218026=CARTESIAN_POINT('Ctrl Pts',(206.986349890745,4.79355238193565,134.27630890323));
#218027=CARTESIAN_POINT('Ctrl Pts',(206.993764745621,4.6996101168209,134.40246383611));
#218028=CARTESIAN_POINT('Ctrl Pts',(207.001179600497,4.60068401122566,134.524795698488));
#218029=CARTESIAN_POINT('Ctrl Pts',(207.008587484203,4.50185091226226,134.647012549015));
#218030=CARTESIAN_POINT('Ctrl Pts',(207.015995367909,4.39804353314303,134.76541319544));
#218031=CARTESIAN_POINT('Ctrl Pts',(207.023403251615,4.28959116052852,134.879570825398));
#218032=CARTESIAN_POINT('Ctrl Pts',(207.030804839437,4.18123096047179,134.993631433958));
#218033=CARTESIAN_POINT('Ctrl Pts',(207.038206427259,4.06823388760403,135.103455940601));
#218034=CARTESIAN_POINT('Ctrl Pts',(207.04560801508,3.95096917488711,135.208650928342));
#218035=CARTESIAN_POINT('Ctrl Pts',(207.053005982973,3.83376181337625,135.313794467873));
#218036=CARTESIAN_POINT('Ctrl Pts',(207.060403950865,3.71229124444,135.414312747539));
#218037=CARTESIAN_POINT('Ctrl Pts',(207.067801918757,3.58696326793364,135.509849442013));
#218038=CARTESIAN_POINT('Ctrl Pts',(207.075197872091,3.46166941979266,135.605360120658));
#218039=CARTESIAN_POINT('Ctrl Pts',(207.082593825425,3.33252055199012,135.695891689038));
#218040=CARTESIAN_POINT('Ctrl Pts',(207.089989778758,3.19995513205736,135.781128415577));
#218041=CARTESIAN_POINT('Ctrl Pts',(207.092357450587,3.15751686939226,135.808415309787));
#218042=CARTESIAN_POINT('Ctrl Pts',(207.094725122416,3.11472870081105,135.835159892579));
#218043=CARTESIAN_POINT('Ctrl Pts',(207.097092794244,3.07160564976242,135.861352736884));
#218044=CARTESIAN_POINT('',(207.496354727754,-4.58101859761927,134.548389190118));
#218045=CARTESIAN_POINT('Ctrl Pts',(207.491512994556,-4.5779532771514,134.556042095633));
#218046=CARTESIAN_POINT('Ctrl Pts',(207.421356448526,-4.23683712701248,
134.83229957677));
#218047=CARTESIAN_POINT('Ctrl Pts',(207.352125680575,-3.86351417701888,
135.072882748138));
#218048=CARTESIAN_POINT('Ctrl Pts',(207.181195423578,-2.80904512107275,
135.629548817307));
#218049=CARTESIAN_POINT('Ctrl Pts',(207.088686747424,-2.07976512179529,
135.888075083137));
#218050=CARTESIAN_POINT('Ctrl Pts',(207.01614411327,-1.16577810051545,136.0860323564));
#218051=CARTESIAN_POINT('Ctrl Pts',(207.004225116839,-0.992744253302746,
136.118115831311));
#218052=CARTESIAN_POINT('Ctrl Pts',(206.992042736604,-0.781551616182621,
136.150680383293));
#218053=CARTESIAN_POINT('Ctrl Pts',(206.989976350538,-0.744182570385334,
136.156193421598));
#218054=CARTESIAN_POINT('Ctrl Pts',(206.987814094324,-0.703290708056184,
136.161952974892));
#218055=CARTESIAN_POINT('Ctrl Pts',(206.987630613907,-0.699805954358256,
136.162441630612));
#218056=CARTESIAN_POINT('Ctrl Pts',(206.987412352986,-0.695642812310952,
136.163022825853));
#218057=CARTESIAN_POINT('Ctrl Pts',(206.987376833818,-0.694964747275408,
136.163117405068));
#218058=CARTESIAN_POINT('Ctrl Pts',(206.987297040828,-0.693440213561303,
136.163329868685));
#218059=CARTESIAN_POINT('Ctrl Pts',(206.987252783207,-0.692593737269296,
136.163447708353));
#218060=CARTESIAN_POINT('Ctrl Pts',(206.9871907909,-0.691406822344562,136.163612761929));
#218061=CARTESIAN_POINT('Ctrl Pts',(206.987173018248,-0.691066400707796,
136.163660080629));
#218062=CARTESIAN_POINT('Ctrl Pts',(206.987143756372,-0.690505675199503,
136.163737987573));
#218063=CARTESIAN_POINT('Ctrl Pts',(206.987132262873,-0.690285372904867,
136.163768587615));
#218064=CARTESIAN_POINT('Ctrl Pts',(206.987110033778,-0.689859179030206,
136.163827769298));
#218065=CARTESIAN_POINT('Ctrl Pts',(206.987099297795,-0.689653287658265,
136.163856352005));
#218066=CARTESIAN_POINT('Ctrl Pts',(206.987074311334,-0.689173982563819,
136.163922873553));
#218067=CARTESIAN_POINT('Ctrl Pts',(206.987060062896,-0.688900567806784,
136.163960806763));
#218068=CARTESIAN_POINT('Ctrl Pts',(206.987015178065,-0.688038975675799,
136.164080300919));
#218069=CARTESIAN_POINT('Ctrl Pts',(206.986984558832,-0.687450790881196,
136.164161814515));
#218070=CARTESIAN_POINT('Ctrl Pts',(206.986555882125,-0.6792100354052,136.165302995029));
#218071=CARTESIAN_POINT('Ctrl Pts',(206.986161508294,-0.671555860542454,
136.16635249923));
#218072=CARTESIAN_POINT('Ctrl Pts',(206.980492339162,-0.560455784136554,
136.181434286989));
#218073=CARTESIAN_POINT('Ctrl Pts',(206.975892611292,-0.456712139527467,
136.193609075703));
#218074=CARTESIAN_POINT('Ctrl Pts',(206.962946640849,-0.110636466825927,
136.227783756113));
#218075=CARTESIAN_POINT('Ctrl Pts',(206.957730504988,0.133311986351349,
136.241404694132));
#218076=CARTESIAN_POINT('Ctrl Pts',(206.955350122412,0.720758476191309,
136.247635367825));
#218077=CARTESIAN_POINT('Ctrl Pts',(206.962101132817,1.06313123841359,136.230086185341));
#218078=CARTESIAN_POINT('Ctrl Pts',(206.998981742942,1.96417607662476,136.132510665149));
#218079=CARTESIAN_POINT('Ctrl Pts',(207.041779761648,2.52223568288148,136.018742195627));
#218080=CARTESIAN_POINT('Ctrl Pts',(207.098250784982,3.06082119940109,135.858058984553));
#218081=CARTESIAN_POINT('',(207.686626030528,-5.91241378256136,130.800689035563));
#218082=CARTESIAN_POINT('Ctrl Pts',(207.495311715924,-4.57621626203826,
134.554850623626));
#218083=CARTESIAN_POINT('Ctrl Pts',(207.501394604565,-4.65780291324943,
134.455301455535));
#218084=CARTESIAN_POINT('Ctrl Pts',(207.507477493205,-4.73605204032821,
134.353195881539));
#218085=CARTESIAN_POINT('Ctrl Pts',(207.513560381845,-4.81080786236673,
134.248784847229));
#218086=CARTESIAN_POINT('Ctrl Pts',(207.521051269147,-4.90286732147391,
134.120205920782));
#218087=CARTESIAN_POINT('Ctrl Pts',(207.528542156449,-4.98990483109698,
133.987743324545));
#218088=CARTESIAN_POINT('Ctrl Pts',(207.53603304375,-5.07157846591905,133.851822254162));
#218089=CARTESIAN_POINT('Ctrl Pts',(207.54351476451,-5.15315215733168,133.716067509366));
#218090=CARTESIAN_POINT('Ctrl Pts',(207.55099648527,-5.22937485457296,133.57686302416));
#218091=CARTESIAN_POINT('Ctrl Pts',(207.558478206029,-5.29994590927886,
133.434665527879));
#218092=CARTESIAN_POINT('Ctrl Pts',(207.565952157474,-5.37044368021461,
133.292615695094));
#218093=CARTESIAN_POINT('Ctrl Pts',(207.57342610892,-5.43530133283305,133.14757936331));
#218094=CARTESIAN_POINT('Ctrl Pts',(207.580900060365,-5.49426246614912,
133.000040584129));
#218095=CARTESIAN_POINT('Ctrl Pts',(207.588367634612,-5.55317329048892,
132.852627693385));
#218096=CARTESIAN_POINT('Ctrl Pts',(207.595835208858,-5.6061974800907,132.702716943952));
#218097=CARTESIAN_POINT('Ctrl Pts',(207.603302783105,-5.6531254094204,132.550815216995));
#218098=CARTESIAN_POINT('Ctrl Pts',(207.610764849886,-5.70001872858451,
132.399025520208));
#218099=CARTESIAN_POINT('Ctrl Pts',(207.618226916667,-5.74082463923541,
132.24524811883));
#218100=CARTESIAN_POINT('Ctrl Pts',(207.625688983447,-5.77538238228886,
132.090007886784));
#218101=CARTESIAN_POINT('Ctrl Pts',(207.633147775048,-5.80992495758262,
131.934835791321));
#218102=CARTESIAN_POINT('Ctrl Pts',(207.640606566648,-5.83822474834345,
131.778202498953));
#218103=CARTESIAN_POINT('Ctrl Pts',(207.648065358249,-5.86017137152897,
131.620646142865));
#218104=CARTESIAN_POINT('Ctrl Pts',(207.655522975005,-5.88211453787224,
131.463114603691));
#218105=CARTESIAN_POINT('Ctrl Pts',(207.662980591761,-5.89770647524243,
131.304660650395));
#218106=CARTESIAN_POINT('Ctrl Pts',(207.670438208517,-5.90688824017458,
131.145830792819));
#218107=CARTESIAN_POINT('Ctrl Pts',(207.67583374161,-5.91353118230476,131.030918511769));
#218108=CARTESIAN_POINT('Ctrl Pts',(207.681229274702,-5.91681984302548,
130.915809664487));
#218109=CARTESIAN_POINT('Ctrl Pts',(207.686624807795,-5.91674887527788,
130.800712412811));
#218110=CARTESIAN_POINT('',(207.794693732013,-5.48556781411874,128.562630683018));
#218111=CARTESIAN_POINT('Ctrl Pts',(207.686626923708,-5.90924709096476,
130.800671958988));
#218112=CARTESIAN_POINT('Ctrl Pts',(207.721753951025,-5.91343857842015,
130.052291188706));
#218113=CARTESIAN_POINT('Ctrl Pts',(207.757773583639,-5.77836975406095,
129.286353104056));
#218114=CARTESIAN_POINT('Ctrl Pts',(207.793793216252,-5.49329697336549,
128.580043386892));
#218115=CARTESIAN_POINT('Ctrl Pts',(207.79468582155,-5.48614114834957,128.562577472722));
#218116=CARTESIAN_POINT('Ctrl Pts',(207.389091944887,-2.65474895531873,
126.670261218454));
#218117=CARTESIAN_POINT('Ctrl Pts',(207.41658252432,-2.94491541138629,126.767817078822));
#218118=CARTESIAN_POINT('Ctrl Pts',(207.448404209708,-3.22924395023264,
126.88438600989));
#218119=CARTESIAN_POINT('Ctrl Pts',(207.51505243423,-3.7596051150903,127.144324967448));
#218120=CARTESIAN_POINT('Ctrl Pts',(207.549736377932,-4.0084503222057,127.286186718169));
#218121=CARTESIAN_POINT('Ctrl Pts',(207.620038152494,-4.47672081944709,
127.597196151352));
#218122=CARTESIAN_POINT('Ctrl Pts',(207.655802877471,-4.69804475485952,
127.766387134892));
#218123=CARTESIAN_POINT('Ctrl Pts',(207.726681002879,-5.11470254565544,
128.138303711736));
#218124=CARTESIAN_POINT('Ctrl Pts',(207.761943960977,-5.31058055330982,
128.342384269375));
#218125=CARTESIAN_POINT('Ctrl Pts',(207.79468582155,-5.48614114834947,128.56257747272));
#218126=CARTESIAN_POINT('',(207.110140564062,-4.91824906508338,130.801328076312));
#218127=CARTESIAN_POINT('Ctrl Pts',(207.179891338435,-4.76405452823404,
129.582490119308));
#218128=CARTESIAN_POINT('Ctrl Pts',(207.171149836886,-4.80226849123941,
129.731485781088));
#218129=CARTESIAN_POINT('Ctrl Pts',(207.162408335336,-4.83353292882372,
129.882448181632));
#218130=CARTESIAN_POINT('Ctrl Pts',(207.153666833787,-4.85766325863286,
130.034756350278));
#218131=CARTESIAN_POINT('Ctrl Pts',(207.14497546476,-4.88165520097116,130.186191031391));
#218132=CARTESIAN_POINT('Ctrl Pts',(207.136284095732,-4.89859453685566,
130.338955897152));
#218133=CARTESIAN_POINT('Ctrl Pts',(207.127592726705,-4.90834771356455,
130.492421865171));
#218134=CARTESIAN_POINT('Ctrl Pts',(207.121775339157,-4.91487580005554,
130.595141127065));
#218135=CARTESIAN_POINT('Ctrl Pts',(207.11595795161,-4.91818546141412,130.698174100575));
#218136=CARTESIAN_POINT('Ctrl Pts',(207.110140564062,-4.91824906508338,
130.801328076312));
#218137=CARTESIAN_POINT('Ctrl Pts',(207.110140564008,-4.91824906508397,
130.801328077268));
#218138=CARTESIAN_POINT('Ctrl Pts',(207.10232974179,-4.91833446369157,130.939829657053));
#218139=CARTESIAN_POINT('Ctrl Pts',(207.094518919572,-4.91256506400957,
131.078351340995));
#218140=CARTESIAN_POINT('Ctrl Pts',(207.086708097354,-4.90096241100966,
131.216368515998));
#218141=CARTESIAN_POINT('Ctrl Pts',(207.078896410447,-4.88935847354873,
131.354400970065));
#218142=CARTESIAN_POINT('Ctrl Pts',(207.071084723539,-4.87192002824314,
131.491928423436));
#218143=CARTESIAN_POINT('Ctrl Pts',(207.063273036631,-4.84872054892325,
131.62843106416));
#218144=CARTESIAN_POINT('Ctrl Pts',(207.055458899586,-4.82551379308231,
131.764976518963));
#218145=CARTESIAN_POINT('Ctrl Pts',(207.047644762541,-4.79654246897585,
131.90049614474));
#218146=CARTESIAN_POINT('Ctrl Pts',(207.039830625497,-4.76193119291241,
132.034480276976));
#218147=CARTESIAN_POINT('Ctrl Pts',(207.032012451602,-4.72730203636823,
132.168533626559));
#218148=CARTESIAN_POINT('Ctrl Pts',(207.024194277707,-4.68702722138493,
132.301049533832));
#218149=CARTESIAN_POINT('Ctrl Pts',(207.016376103812,-4.64128115697165,
132.431533713595));
#218150=CARTESIAN_POINT('Ctrl Pts',(207.008547530707,-4.59547424421175,
132.562191454661));
#218151=CARTESIAN_POINT('Ctrl Pts',(207.000718957602,-4.54418167570927,
132.690811711221));
#218152=CARTESIAN_POINT('Ctrl Pts',(206.992890384497,-4.48762617673331,
132.816919774559));
#218153=CARTESIAN_POINT('Ctrl Pts',(206.985055811211,-4.43102733100928,
132.943124492946));
#218154=CARTESIAN_POINT('Ctrl Pts',(206.977221237926,-4.36915768710697,
133.066812840935));
#218155=CARTESIAN_POINT('Ctrl Pts',(206.96938666464,-4.30228542176686,133.187535645161));
#218156=CARTESIAN_POINT('Ctrl Pts',(206.961539696176,-4.23530735696238,
133.308449446476));
#218157=CARTESIAN_POINT('Ctrl Pts',(206.953692727712,-4.16331106348637,
133.426388009929));
#218158=CARTESIAN_POINT('Ctrl Pts',(206.945845759248,-4.08660777588555,
133.540931455051));
#218159=CARTESIAN_POINT('Ctrl Pts',(206.942922552185,-4.05803373571842,
133.583601972889));
#218160=CARTESIAN_POINT('Ctrl Pts',(206.939999345122,-4.02880687363292,
133.625801664281));
#218161=CARTESIAN_POINT('Ctrl Pts',(206.937076138059,-3.99894465188146,
133.667510060695));
#218162=CARTESIAN_POINT('Ctrl Pts',(206.929301998061,-3.91952739284056,
133.77843169773));
#218163=CARTESIAN_POINT('Ctrl Pts',(206.921527858062,-3.83536570986394,
133.886222330092));
#218164=CARTESIAN_POINT('Ctrl Pts',(206.913753718064,-3.74673486748187,
133.990449269078));
#218165=CARTESIAN_POINT('Ctrl Pts',(206.905989161858,-3.658213287293,134.09454771934));
#218166=CARTESIAN_POINT('Ctrl Pts',(206.898224605652,-3.56523376076694,
134.195090922469));
#218167=CARTESIAN_POINT('Ctrl Pts',(206.890460049446,-3.46811454805166,
134.291675421838));
#218168=CARTESIAN_POINT('Ctrl Pts',(206.882703207698,-3.37109182792838,
134.388163959878));
#218169=CARTESIAN_POINT('Ctrl Pts',(206.874946365951,-3.26993788205166,
134.480701347399));
#218170=CARTESIAN_POINT('Ctrl Pts',(206.867189524203,-3.16501068250007,
134.568917755153));
#218171=CARTESIAN_POINT('Ctrl Pts',(206.859438534277,-3.0601626408413,134.657067611766));
#218172=CARTESIAN_POINT('Ctrl Pts',(206.851687544352,-2.9515473094897,134.74090272641));
#218173=CARTESIAN_POINT('Ctrl Pts',(206.843936554426,-2.83955863515276,
134.820090914788));
#218174=CARTESIAN_POINT('Ctrl Pts',(206.836188861569,-2.72761759787636,
134.899245418577));
#218175=CARTESIAN_POINT('Ctrl Pts',(206.828441168712,-2.61230639015696,
134.973756702305));
#218176=CARTESIAN_POINT('Ctrl Pts',(206.820693475855,-2.49405090237109,
135.043333743086));
#218177=CARTESIAN_POINT('Ctrl Pts',(206.812947405249,-2.37582017552251,
135.112896215471));
#218178=CARTESIAN_POINT('Ctrl Pts',(206.805201334644,-2.25464673160865,
135.177526301768));
#218179=CARTESIAN_POINT('Ctrl Pts',(206.797455264038,-2.13098388076607,
135.236977312298));
#218180=CARTESIAN_POINT('Ctrl Pts',(206.789709137619,-2.00732013888212,
135.296428751197));
#218181=CARTESIAN_POINT('Ctrl Pts',(206.7819630112,-1.88116730665591,135.350700870453));
#218182=CARTESIAN_POINT('Ctrl Pts',(206.774216884781,-1.75300127162441,
135.399593974446));
#218183=CARTESIAN_POINT('Ctrl Pts',(206.766469024802,-1.62480655341618,
135.44849802057));
#218184=CARTESIAN_POINT('Ctrl Pts',(206.758721164823,-1.49459810110302,
135.492020516664));
#218185=CARTESIAN_POINT('Ctrl Pts',(206.750973304844,-1.36286927639058,
135.530010879485));
#218186=CARTESIAN_POINT('Ctrl Pts',(206.743217210822,-1.23100045680149,
135.568041616583));
#218187=CARTESIAN_POINT('Ctrl Pts',(206.735461116801,-1.09760841340135,
135.600528367403));
#218188=CARTESIAN_POINT('Ctrl Pts',(206.72770502278,-0.963199626022195,
135.627371040832));
#218189=CARTESIAN_POINT('Ctrl Pts',(206.719944789696,-0.828719111006118,
135.654228038931));
#218190=CARTESIAN_POINT('Ctrl Pts',(206.712184556613,-0.693221156955318,
135.675434897598));
#218191=CARTESIAN_POINT('Ctrl Pts',(206.70442432353,-0.557218799917317,
135.690943295831));
#218192=CARTESIAN_POINT('Ctrl Pts',(206.696651631796,-0.420998098163723,
135.706476591992));
#218193=CARTESIAN_POINT('Ctrl Pts',(206.688878940061,-0.284271765407574,
135.716293117923));
#218194=CARTESIAN_POINT('Ctrl Pts',(206.681106248327,-0.147555186392696,
135.720396676167));
#218195=CARTESIAN_POINT('Ctrl Pts',(206.6736136703,-0.015765624822631,135.724352349619));
#218196=CARTESIAN_POINT('Ctrl Pts',(206.666121092273,0.11601456527462,135.722999745079));
#218197=CARTESIAN_POINT('Ctrl Pts',(206.658628514246,0.247328944919121,
135.716387842196));
#218198=CARTESIAN_POINT('Ctrl Pts',(206.650854101252,0.383582743781857,
135.709527231134));
#218199=CARTESIAN_POINT('Ctrl Pts',(206.643079688257,0.519766647294013,
135.696982181141));
#218200=CARTESIAN_POINT('Ctrl Pts',(206.635305275263,0.655367801387527,
135.678750436549));
#218201=CARTESIAN_POINT('Ctrl Pts',(206.627540442734,0.790801853192383,
135.660541159068));
#218202=CARTESIAN_POINT('Ctrl Pts',(206.619775610205,0.925654200685813,
135.636659181934));
#218203=CARTESIAN_POINT('Ctrl Pts',(206.612010777677,1.05941334753652,135.607154223538));
#218204=CARTESIAN_POINT('Ctrl Pts',(206.604253656593,1.19303965490963,135.577678567237));
#218205=CARTESIAN_POINT('Ctrl Pts',(206.596496535509,1.32557454289324,135.542591126398));
#218206=CARTESIAN_POINT('Ctrl Pts',(206.588739414425,1.45651334525474,135.501993206179));
#218207=CARTESIAN_POINT('Ctrl Pts',(206.580988142457,1.5873534156012,135.461425898081));
#218208=CARTESIAN_POINT('Ctrl Pts',(206.573236870489,1.71659942391051,135.415356496345));
#218209=CARTESIAN_POINT('Ctrl Pts',(206.565485598521,1.84375893376221,135.363936919885));
#218210=CARTESIAN_POINT('Ctrl Pts',(206.557737620497,1.97086440649336,135.312539194452));
#218211=CARTESIAN_POINT('Ctrl Pts',(206.549989642474,2.09588478259786,135.255795962539));
#218212=CARTESIAN_POINT('Ctrl Pts',(206.542241664451,2.21834499216241,135.193908266043));
#218213=CARTESIAN_POINT('Ctrl Pts',(206.534495306817,2.34077959076295,135.132033512555));
#218214=CARTESIAN_POINT('Ctrl Pts',(206.526748949182,2.46065473910694,135.065016610731));
#218215=CARTESIAN_POINT('Ctrl Pts',(206.519002591548,2.57751784727511,134.993105633615));
#218216=CARTESIAN_POINT('Ctrl Pts',(206.511256176506,2.69438182151258,134.92119412357));
#218217=CARTESIAN_POINT('Ctrl Pts',(206.503509761464,2.80823337806547,134.844388670749));
#218218=CARTESIAN_POINT('Ctrl Pts',(206.495763346422,2.9186472625684,134.762981743565));
#218219=CARTESIAN_POINT('Ctrl Pts',(206.488015196492,3.0290858753689,134.681556584482));
#218220=CARTESIAN_POINT('Ctrl Pts',(206.480267046562,3.13608496949048,134.595528132329));
#218221=CARTESIAN_POINT('Ctrl Pts',(206.472518896633,3.23925116627507,134.505230102469));
#218222=CARTESIAN_POINT('Ctrl Pts',(206.464762512191,3.34252700513922,134.414836106449));
#218223=CARTESIAN_POINT('Ctrl Pts',(206.45700612775,3.44196151476943,134.320163726309));
#218224=CARTESIAN_POINT('Ctrl Pts',(206.449249743308,3.53719670723884,134.221585005399));
#218225=CARTESIAN_POINT('Ctrl Pts',(206.441489219088,3.63248272913906,134.122953670532));
#218226=CARTESIAN_POINT('Ctrl Pts',(206.433728694868,3.7235647084274,134.020412132682));
#218227=CARTESIAN_POINT('Ctrl Pts',(206.425968170648,3.81012466952417,133.914365933507));
#218228=CARTESIAN_POINT('Ctrl Pts',(206.418195189496,3.89682357375458,133.808149512546));
#218229=CARTESIAN_POINT('Ctrl Pts',(206.410422208344,3.9789857203556,133.698417501723));
#218230=CARTESIAN_POINT('Ctrl Pts',(206.402649227192,4.05633571762412,133.58560559211));
#218231=CARTESIAN_POINT('Ctrl Pts',(206.395159781606,4.13086421374525,133.47690873025));
#218232=CARTESIAN_POINT('Ctrl Pts',(206.387670336019,4.20092534590809,133.365353006456));
#218233=CARTESIAN_POINT('Ctrl Pts',(206.380180890433,4.266313865227,133.251348371085));
#218234=CARTESIAN_POINT('Ctrl Pts',(206.372406547022,4.33418975784089,133.133007009811));
#218235=CARTESIAN_POINT('Ctrl Pts',(206.36463220361,4.39724549814214,133.011651903751));
#218236=CARTESIAN_POINT('Ctrl Pts',(206.356857860199,4.45520197698344,132.887713301771));
#218237=CARTESIAN_POINT('Ctrl Pts',(206.349093097628,4.51308703219629,132.763927437583));
#218238=CARTESIAN_POINT('Ctrl Pts',(206.341328335058,4.56588516553323,132.637564763071));
#218239=CARTESIAN_POINT('Ctrl Pts',(206.333563572488,4.61336172857185,132.509082478706));
#218240=CARTESIAN_POINT('Ctrl Pts',(206.32580652166,4.66079113922843,132.380727799318));
#218241=CARTESIAN_POINT('Ctrl Pts',(206.318049470833,4.70290936280457,132.250258063749));
#218242=CARTESIAN_POINT('Ctrl Pts',(206.310292420006,4.73952884382674,132.118152610628));
#218243=CARTESIAN_POINT('Ctrl Pts',(206.302541218515,4.7761207113015,131.986146773889));
#218244=CARTESIAN_POINT('Ctrl Pts',(206.294790017025,4.80722198540851,131.852508049919));
#218245=CARTESIAN_POINT('Ctrl Pts',(206.287038815535,4.83269430378063,131.717732846565));
#218246=CARTESIAN_POINT('Ctrl Pts',(206.279290908073,4.85815579718011,131.583014918637));
#218247=CARTESIAN_POINT('Ctrl Pts',(206.271543000612,4.87799302016867,131.447161855274));
#218248=CARTESIAN_POINT('Ctrl Pts',(206.26379509315,4.89211832584772,131.310682006019));
#218249=CARTESIAN_POINT('Ctrl Pts',(206.256048806118,4.90624067730134,131.17423070073));
#218250=CARTESIAN_POINT('Ctrl Pts',(206.248302519086,4.9146534473754,131.037153258931));
#218251=CARTESIAN_POINT('Ctrl Pts',(206.240556232054,4.91732070875142,130.899964538952));
#218252=CARTESIAN_POINT('Ctrl Pts',(206.232809887587,4.91998798990394,130.762774801783));
#218253=CARTESIAN_POINT('Ctrl Pts',(206.22506354312,4.91690966975381,130.625474175676));
#218254=CARTESIAN_POINT('Ctrl Pts',(206.217317198653,4.90810194759419,130.488578517817));
#218255=CARTESIAN_POINT('Ctrl Pts',(206.209569119204,4.89929225273097,130.351652198845));
#218256=CARTESIAN_POINT('Ctrl Pts',(206.201821039754,4.88475062745858,130.21513141869));
#218257=CARTESIAN_POINT('Ctrl Pts',(206.194072960305,4.86454520291237,130.079527511726));
#218258=CARTESIAN_POINT('Ctrl Pts',(206.186316645792,4.84431830298384,129.943779477834));
#218259=CARTESIAN_POINT('Ctrl Pts',(206.178560331278,4.81841563632905,129.808950651116));
#218260=CARTESIAN_POINT('Ctrl Pts',(206.170804016765,4.78695671008173,129.675543308032));
#218261=CARTESIAN_POINT('Ctrl Pts',(206.163043562283,4.75548099249017,129.542064758175));
#218262=CARTESIAN_POINT('Ctrl Pts',(206.155283107802,4.71844321146889,129.410009580029));
#218263=CARTESIAN_POINT('Ctrl Pts',(206.14752265332,4.6760126848635,129.279864493105));
#218264=CARTESIAN_POINT('Ctrl Pts',(206.139749740871,4.63351404393066,129.149510482424));
#218265=CARTESIAN_POINT('Ctrl Pts',(206.131976828422,4.5856054945835,129.021073056925));
#218266=CARTESIAN_POINT('Ctrl Pts',(206.124203915972,4.53250473784456,128.895019405546));
#218267=CARTESIAN_POINT('Ctrl Pts',(206.116713699522,4.48133522265336,128.773550247191));
#218268=CARTESIAN_POINT('Ctrl Pts',(206.109223483071,4.42534474547032,128.654294760804));
#218269=CARTESIAN_POINT('Ctrl Pts',(206.101733266621,4.36476734543776,128.537647339999));
#218270=CARTESIAN_POINT('Ctrl Pts',(206.093958959944,4.30189235529015,128.416575695624));
#218271=CARTESIAN_POINT('Ctrl Pts',(206.086184653268,4.23387645089009,128.297930328045));
#218272=CARTESIAN_POINT('Ctrl Pts',(206.078410346591,4.16093074001882,128.18217861792));
#218273=CARTESIAN_POINT('Ctrl Pts',(206.070645621474,4.08807493217016,128.066569567707));
#218274=CARTESIAN_POINT('Ctrl Pts',(206.062880896357,4.01030161335004,127.953847406604));
#218275=CARTESIAN_POINT('Ctrl Pts',(206.05511617124,3.92786859889688,127.844456677858));
#218276=CARTESIAN_POINT('Ctrl Pts',(206.04735915854,3.84551746214591,127.735174602927));
#218277=CARTESIAN_POINT('Ctrl Pts',(206.039602145841,3.7585160740671,127.629217685533));
#218278=CARTESIAN_POINT('Ctrl Pts',(206.031845133142,3.66716633068647,127.52700281507));
#218279=CARTESIAN_POINT('Ctrl Pts',(206.024093970412,3.57588547893075,127.424865030194));
#218280=CARTESIAN_POINT('Ctrl Pts',(206.016342807682,3.48026305863852,127.326463965419));
#218281=CARTESIAN_POINT('Ctrl Pts',(206.008591644952,3.38064191709146,127.232184349392));
#218282=CARTESIAN_POINT('Ctrl Pts',(206.000843777079,3.28106312240745,127.137944809658));
#218283=CARTESIAN_POINT('Ctrl Pts',(205.993095909207,3.17748927055705,127.04782350237));
#218284=CARTESIAN_POINT('Ctrl Pts',(205.985348041334,3.070300668997,126.962168942954));
#218285=CARTESIAN_POINT('Ctrl Pts',(205.97760179439,2.96313449232946,126.876532303301));
#218286=CARTESIAN_POINT('Ctrl Pts',(205.969855547446,2.85235537539139,126.79536079669));
#218287=CARTESIAN_POINT('Ctrl Pts',(205.962109300503,2.73837705773569,126.718962943879));
#218288=CARTESIAN_POINT('Ctrl Pts',(205.954362996587,2.62439790178891,126.642564529175));
#218289=CARTESIAN_POINT('Ctrl Pts',(205.94661669267,2.5072198229346,126.570940056014));
#218290=CARTESIAN_POINT('Ctrl Pts',(205.938870388754,2.38728557715688,126.50435472971));
#218291=CARTESIAN_POINT('Ctrl Pts',(205.931122350283,2.26732447565317,126.437754493592));
#218292=CARTESIAN_POINT('Ctrl Pts',(205.923374311811,2.14460632090196,126.376195839389));
#218293=CARTESIAN_POINT('Ctrl Pts',(205.915626273339,2.01959813448211,126.319897836173));
#218294=CARTESIAN_POINT('Ctrl Pts',(205.907870000251,1.8944570893462,126.263539999433));
#218295=CARTESIAN_POINT('Ctrl Pts',(205.900113727163,1.76702150772587,126.212454143145));
#218296=CARTESIAN_POINT('Ctrl Pts',(205.892357454075,1.63777856078686,126.166811216392));
#218297=CARTESIAN_POINT('Ctrl Pts',(205.884597041329,1.5084666346276,126.121143929212));
#218298=CARTESIAN_POINT('Ctrl Pts',(205.876836628582,1.3773457946557,126.08092547459));
#218299=CARTESIAN_POINT('Ctrl Pts',(205.869076215836,1.24491704770284,126.046276485603));
#218300=CARTESIAN_POINT('Ctrl Pts',(205.861303345232,1.11227571174918,126.011571874297));
#218301=CARTESIAN_POINT('Ctrl Pts',(205.853530474629,0.97832265542302,125.982454678108));
#218302=CARTESIAN_POINT('Ctrl Pts',(205.845757604025,0.843568606457823,
125.958994267258));
#218303=CARTESIAN_POINT('Ctrl Pts',(205.838266950286,0.713707198462261,
125.93638565543));
#218304=CARTESIAN_POINT('Ctrl Pts',(205.830776296547,0.583102259513571,
125.919030219509));
#218305=CARTESIAN_POINT('Ctrl Pts',(205.823285642808,0.452212191984598,
125.90694423789));
#218306=CARTESIAN_POINT('Ctrl Pts',(205.815511295583,0.316364925691163,
125.894400523959));
#218307=CARTESIAN_POINT('Ctrl Pts',(205.807736948359,0.179780181164248,
125.887493536688));
#218308=CARTESIAN_POINT('Ctrl Pts',(205.799962601134,0.0429652936190226,
125.886298291198));
#218309=CARTESIAN_POINT('Ctrl Pts',(205.792197834953,-0.0936809843600888,
125.885104518719));
#218310=CARTESIAN_POINT('Ctrl Pts',(205.784433068771,-0.23055645382959,
125.889608485683));
#218311=CARTESIAN_POINT('Ctrl Pts',(205.77666830259,-0.367147747384615,
125.899833566556));
#218312=CARTESIAN_POINT('Ctrl Pts',(205.768911248356,-0.503603378781414,
125.910048491902));
#218313=CARTESIAN_POINT('Ctrl Pts',(205.761154194123,-0.639775008589745,
125.925973194331));
#218314=CARTESIAN_POINT('Ctrl Pts',(205.753397139889,-0.775148709250783,
125.94757901438));
#218315=CARTESIAN_POINT('Ctrl Pts',(205.745645935201,-0.910420325464687,
125.969168541617));
#218316=CARTESIAN_POINT('Ctrl Pts',(205.737894730512,-1.04489482568991,
125.996430597873));
#218317=CARTESIAN_POINT('Ctrl Pts',(205.730143525824,-1.17806320546229,
126.029284686606));
#218318=CARTESIAN_POINT('Ctrl Pts',(205.722395615495,-1.31117498700093,
126.062124811938));
#218319=CARTESIAN_POINT('Ctrl Pts',(205.714647705166,-1.44298137338557,
126.100552149252));
#218320=CARTESIAN_POINT('Ctrl Pts',(205.706899794837,-1.57298357962825,
126.144435111646));
#218321=CARTESIAN_POINT('Ctrl Pts',(205.699153505139,-1.70295859328728,
126.188308895034));
#218322=CARTESIAN_POINT('Ctrl Pts',(205.691407215442,-1.83112980724108,
126.237635908722));
#218323=CARTESIAN_POINT('Ctrl Pts',(205.683660925745,-1.9570140146508,126.292234820454));
#218324=CARTESIAN_POINT('Ctrl Pts',(205.675914578818,-2.08289915209403,
126.346834135564));
#218325=CARTESIAN_POINT('Ctrl Pts',(205.668168231891,-2.2064968905978,126.406705270871));
#218326=CARTESIAN_POINT('Ctrl Pts',(205.660421884964,-2.32734478203693,
126.471619068844));
#218327=CARTESIAN_POINT('Ctrl Pts',(205.652673803264,-2.44821973703175,
126.536547404084));
#218328=CARTESIAN_POINT('Ctrl Pts',(205.644925721563,-2.56634327519558,
126.606520464177));
#218329=CARTESIAN_POINT('Ctrl Pts',(205.637177639863,-2.6812786482065,126.68126373862));
#218330=CARTESIAN_POINT('Ctrl Pts',(205.629421323445,-2.79633617537112,
126.756086450761));
#218331=CARTESIAN_POINT('Ctrl Pts',(205.621665007027,-2.90819844040077,
126.835689291279));
#218332=CARTESIAN_POINT('Ctrl Pts',(205.613908690609,-3.01645828850523,
126.919754787342));
#218333=CARTESIAN_POINT('Ctrl Pts',(205.606148234409,-3.12477591819194,
127.003865151724));
#218334=CARTESIAN_POINT('Ctrl Pts',(205.598387778208,-3.22948700142695,
127.092442665323));
#218335=CARTESIAN_POINT('Ctrl Pts',(205.590627322007,-3.3302192372797,127.185131018031));
#218336=CARTESIAN_POINT('Ctrl Pts',(205.582854408177,-3.43111317560035,
127.277968160599));
#218337=CARTESIAN_POINT('Ctrl Pts',(205.575081494346,-3.52801522649826,
127.374929052501));
#218338=CARTESIAN_POINT('Ctrl Pts',(205.567308580516,-3.62059096362825,
127.475621496428));
#218339=CARTESIAN_POINT('Ctrl Pts',(205.559818393342,-3.70979941414655,
127.572651422196));
#218340=CARTESIAN_POINT('Ctrl Pts',(205.552328206168,-3.79499060911529,
127.673145922983));
#218341=CARTESIAN_POINT('Ctrl Pts',(205.544838018995,-3.87590312513928,
127.776728204766));
#218342=CARTESIAN_POINT('Ctrl Pts',(205.53706126549,-3.95991126511941,127.884273430835));
#218343=CARTESIAN_POINT('Ctrl Pts',(205.529284511985,-4.03957765797006,
127.995494127098));
#218344=CARTESIAN_POINT('Ctrl Pts',(205.521507758481,-4.11456321009359,
128.110004914871));
#218345=CARTESIAN_POINT('Ctrl Pts',(205.513743508267,-4.18942820212018,
128.224331594755));
#218346=CARTESIAN_POINT('Ctrl Pts',(205.505979258053,-4.25962712878069,
128.341937508539));
#218347=CARTESIAN_POINT('Ctrl Pts',(205.498215007839,-4.32486122114154,
128.462404494927));
#218348=CARTESIAN_POINT('Ctrl Pts',(205.490457952857,-4.39003486021618,
128.582759842984));
#218349=CARTESIAN_POINT('Ctrl Pts',(205.482700897876,-4.45025263063646,
128.705970650087));
#218350=CARTESIAN_POINT('Ctrl Pts',(205.474943842894,-4.50525896992651,
128.831589805638));
#218351=CARTESIAN_POINT('Ctrl Pts',(205.467193142368,-4.5602202488983,128.957106055974));
#218352=CARTESIAN_POINT('Ctrl Pts',(205.459442441842,-4.60997843839768,
129.085026371888));
#218353=CARTESIAN_POINT('Ctrl Pts',(205.451691741317,-4.65432411968393,
129.214879554002));
#218354=CARTESIAN_POINT('Ctrl Pts',(205.444469975199,-4.69564349946542,
129.335871109256));
#218355=CARTESIAN_POINT('Ctrl Pts',(205.437248209081,-4.73226423551571,
129.458540250484));
#218356=CARTESIAN_POINT('Ctrl Pts',(205.430026442963,-4.76405452823405,
129.582490119308));
#218357=CARTESIAN_POINT('Ctrl Pts',(210.578629502474,3.43871735229388,135.623751273273));
#218358=CARTESIAN_POINT('Ctrl Pts',(210.532211638871,4.24191310225744,135.050661598608));
#218359=CARTESIAN_POINT('Ctrl Pts',(210.439385837966,5.5417116830592,133.497735776206));
#218360=CARTESIAN_POINT('Ctrl Pts',(210.253744162458,6.40049231640402,129.500124813146));
#218361=CARTESIAN_POINT('Ctrl Pts',(210.021704475947,3.49988613106459,124.739836436729));
#218362=CARTESIAN_POINT('Ctrl Pts',(209.743256852134,-3.22132718841443,
124.582443963435));
#218363=CARTESIAN_POINT('Ctrl Pts',(209.464809228321,-6.97029916743427,
130.151104711613));
#218364=CARTESIAN_POINT('Ctrl Pts',(209.186361604508,-4.320155850937,136.315756482887));
#218365=CARTESIAN_POINT('Ctrl Pts',(208.907913980696,2.30329626696544,137.417975354914));
#218366=CARTESIAN_POINT('Ctrl Pts',(208.629466356883,6.80838731381026,132.441404887444));
#218367=CARTESIAN_POINT('Ctrl Pts',(208.35101873307,5.05782663488002,125.961106241921));
#218368=CARTESIAN_POINT('Ctrl Pts',(208.072571109257,-1.34111875541754,
123.931185212061));
#218369=CARTESIAN_POINT('Ctrl Pts',(207.794123485444,-6.50738248846785,
128.217554840719));
#218370=CARTESIAN_POINT('Ctrl Pts',(207.515675861631,-5.69381680528821,
134.880978212762));
#218371=CARTESIAN_POINT('Ctrl Pts',(207.237228237818,0.352161018465804,
137.798239159538));
#218372=CARTESIAN_POINT('Ctrl Pts',(206.958780614005,6.07448159193836,134.288440920842));
#218373=CARTESIAN_POINT('Ctrl Pts',(206.680332990192,6.21467071562046,127.576957111676));
#218374=CARTESIAN_POINT('Ctrl Pts',(206.40188536638,0.643870262773591,123.831292031177));
#218375=CARTESIAN_POINT('Ctrl Pts',(206.123437742567,-5.51860979104455,
126.493540260974));
#218376=CARTESIAN_POINT('Ctrl Pts',(205.844990118754,-6.60976007302988,
133.117219720399));
#218377=CARTESIAN_POINT('Ctrl Pts',(205.566542494941,-1.62686214948821,
137.615495756827));
#218378=CARTESIAN_POINT('Ctrl Pts',(205.288094871128,4.8510417637676,135.85467075854));
#218379=CARTESIAN_POINT('Ctrl Pts',(205.009647247315,6.87107573233629,129.452857771449));
#218380=CARTESIAN_POINT('Ctrl Pts',(204.731199623502,2.57692653546199,124.293009711503));
#218381=CARTESIAN_POINT('Ctrl Pts',(204.452751999689,-4.08529213152394,
125.116775123829));
#218382=CARTESIAN_POINT('Ctrl Pts',(204.174304375876,-6.9933269740478,131.167153704944));
#218383=CARTESIAN_POINT('Ctrl Pts',(203.895856752063,-3.47483593506387,
136.884143186524));
#218384=CARTESIAN_POINT('Ctrl Pts',(203.617409128251,3.23685955433703,137.014109488232));
#218385=CARTESIAN_POINT('Ctrl Pts',(203.338961504438,6.97403925260401,131.437619947721));
#218386=CARTESIAN_POINT('Ctrl Pts',(203.060513880625,4.30241757323156,125.27919601562));
#218387=CARTESIAN_POINT('Ctrl Pts',(202.782066256812,-2.32291566837452,
124.198128435325));
#218388=CARTESIAN_POINT('Ctrl Pts',(202.503618632999,-6.81360289295739,
129.18786549711));
#218389=CARTESIAN_POINT('Ctrl Pts',(202.225171009186,-5.0429219211382,135.663082604955));
#218390=CARTESIAN_POINT('Ctrl Pts',(201.946723385373,1.36195793536179,137.673371567868));
#218391=CARTESIAN_POINT('Ctrl Pts',(201.66827576156,6.51526498482727,133.371375037445));
#218392=CARTESIAN_POINT('Ctrl Pts',(201.389828137747,5.6813618015098,126.710417660699));
#218393=CARTESIAN_POINT('Ctrl Pts',(201.111380513935,-0.373435327379839,
123.811593861123));
#218394=CARTESIAN_POINT('Ctrl Pts',(200.832932890122,-6.08506363376988,
127.338781095048));
#218395=CARTESIAN_POINT('Ctrl Pts',(200.554485266309,-6.20481573259303,
134.050666607207));
#218396=CARTESIAN_POINT('Ctrl Pts',(200.276037642496,-0.622645295272457,
137.779355505743));
#218397=CARTESIAN_POINT('Ctrl Pts',(199.997590018683,5.53170575049466,135.098364849491));
#218398=CARTESIAN_POINT('Ctrl Pts',(199.71914239487,6.60268945040398,128.471394077867));
#218399=CARTESIAN_POINT('Ctrl Pts',(199.440694771057,1.60612410470526,123.988305584475));
#218400=CARTESIAN_POINT('Ctrl Pts',(199.162247147244,-4.86639082969376,
125.768838683693));
#218401=CARTESIAN_POINT('Ctrl Pts',(198.883799523432,-6.86693032801245,
132.176770441218));
#218402=CARTESIAN_POINT('Ctrl Pts',(198.605351899619,-2.5570963230842,137.323524616753));
#218403=CARTESIAN_POINT('Ctrl Pts',(198.326904275806,4.10258428165832,136.479485555902));
#218404=CARTESIAN_POINT('Ctrl Pts',(198.048456651993,6.99219035394115,130.420283921986));
#218405=CARTESIAN_POINT('Ctrl Pts',(197.77000902818,3.45631507844086,124.714030008118));
#218406=CARTESIAN_POINT('Ctrl Pts',(197.491561404367,-3.25574490376804,
124.604492395141));
#218407=CARTESIAN_POINT('Ctrl Pts',(197.213113780554,-6.97593437139489,
130.192330798173));
#218408=CARTESIAN_POINT('Ctrl Pts',(196.934666156741,-4.28558094504976,
136.342594705906));
#218409=CARTESIAN_POINT('Ctrl Pts',(196.656218532928,2.3430120075278,137.403492044232));
#218410=CARTESIAN_POINT('Ctrl Pts',(196.377770909115,6.81849138768721,132.400109986944));
#218411=CARTESIAN_POINT('Ctrl Pts',(196.099323285303,5.02811028438465,125.930312215887));
#218412=CARTESIAN_POINT('Ctrl Pts',(195.82087566149,-1.38285853342424,123.939526815472));
#218413=CARTESIAN_POINT('Ctrl Pts',(195.542428037677,-6.5230479154113,128.257188313404));
#218414=CARTESIAN_POINT('Ctrl Pts',(195.263980413864,-5.66887493174189,
134.915576722577));
#218415=CARTESIAN_POINT('Ctrl Pts',(194.985532790051,0.394717174261835,
137.795958375315));
#218416=CARTESIAN_POINT('Ctrl Pts',(194.707085166238,6.09558348012494,134.251403247221));
#218417=CARTESIAN_POINT('Ctrl Pts',(194.428637542425,6.19490635356113,127.539184339867));
#218418=CARTESIAN_POINT('Ctrl Pts',(194.150189918612,0.601412926074683,
123.827502918989));
#218419=CARTESIAN_POINT('Ctrl Pts',(193.871742294799,-5.54474959981957,
126.527212884656));
#218420=CARTESIAN_POINT('Ctrl Pts',(193.593294670987,-6.59555811955654,
133.157412666584));
#218421=CARTESIAN_POINT('Ctrl Pts',(193.314847047174,-1.58537093834796,
137.625272568447));
#218422=CARTESIAN_POINT('Ctrl Pts',(193.036399423361,4.88169468552635,135.825047607524));
#218423=CARTESIAN_POINT('Ctrl Pts',(192.757951799548,6.86272137744547,129.411056577024));
#218424=CARTESIAN_POINT('Ctrl Pts',(192.479504175735,2.53724238606986,124.277443893095));
#218425=CARTESIAN_POINT('Ctrl Pts',(192.201056551922,-4.11983840692253,
125.141748821346));
#218426=CARTESIAN_POINT('Ctrl Pts',(191.922608928109,-6.99098896924831,
131.209717356357));
#218427=CARTESIAN_POINT('Ctrl Pts',(191.644161304296,-3.43776219763276,
136.905182851196));
#218428=CARTESIAN_POINT('Ctrl Pts',(191.365713680483,3.27460008958736,136.994290755064));
#218429=CARTESIAN_POINT('Ctrl Pts',(191.08726605667,6.9777648675845,131.395155257469));
#218430=CARTESIAN_POINT('Ctrl Pts',(190.808818432858,4.26870461503614,125.253108347726));
#218431=CARTESIAN_POINT('Ctrl Pts',(190.530370809044,-2.36308664091672,
124.212391080215));
#218432=CARTESIAN_POINT('Ctrl Pts',(190.251923185232,-6.82331671706736,
129.229371781915));
#218433=CARTESIAN_POINT('Ctrl Pts',(189.973475561419,-5.01325206778612,
135.693690281095));
#218434=CARTESIAN_POINT('Ctrl Pts',(189.695027937606,1.40374632081163,137.664953676525));
#218435=CARTESIAN_POINT('Ctrl Pts',(189.416580313793,6.53077041740369,133.331667209374));
#218436=CARTESIAN_POINT('Ctrl Pts',(189.13813268998,5.65633554627347,126.675909450142));
#218437=CARTESIAN_POINT('Ctrl Pts',(188.859685066167,-0.41599536452862,
123.81399662772));
#218438=CARTESIAN_POINT('Ctrl Pts',(188.581237442354,-6.10604685783229,
127.375886813701));
#218439=CARTESIAN_POINT('Ctrl Pts',(188.302789818542,-6.18493958576042,
134.088376935175));
#218440=CARTESIAN_POINT('Ctrl Pts',(188.024342194729,-0.580174985471077,
137.783016493883));
#218441=CARTESIAN_POINT('Ctrl Pts',(187.745894570916,5.55774208334242,135.064612228548));
#218442=CARTESIAN_POINT('Ctrl Pts',(187.467446947103,6.58836568835925,128.431244857581));
#218443=CARTESIAN_POINT('Ctrl Pts',(187.18899932329,1.56460308533104,123.97865493689));
#218444=CARTESIAN_POINT('Ctrl Pts',(186.910551699478,-4.89695331800637,
125.798555082479));
#218445=CARTESIAN_POINT('Ctrl Pts',(186.632104075664,-6.85844885156509,
132.218545967617));
#218446=CARTESIAN_POINT('Ctrl Pts',(186.353656451852,-2.51736494438869,
137.338969602853));
#218447=CARTESIAN_POINT('Ctrl Pts',(186.075208828038,4.13705436656654,136.454406814005));
#218448=CARTESIAN_POINT('Ctrl Pts',(185.796761204226,6.98972282098866,130.377727590732));
#218449=CARTESIAN_POINT('Ctrl Pts',(185.518313580413,3.41917746986535,124.693103276936));
#218450=CARTESIAN_POINT('Ctrl Pts',(185.2398659566,-3.29342493995873,124.62442590766));
#218451=CARTESIAN_POINT('Ctrl Pts',(184.961418332787,-6.97953072271363,
130.234806630193));
#218452=CARTESIAN_POINT('Ctrl Pts',(184.682970708974,-4.25178874032612,
136.368579642862));
#218453=CARTESIAN_POINT('Ctrl Pts',(184.404523085161,2.38313938299372,137.389107198495));
#218454=CARTESIAN_POINT('Ctrl Pts',(184.126075461348,6.82807883617355,132.358574329007));
#218455=CARTESIAN_POINT('Ctrl Pts',(183.847627837535,4.99834740910532,125.899794986266));
#218456=CARTESIAN_POINT('Ctrl Pts',(183.569180213722,-1.42462110408482,
123.948071857337));
#218457=CARTESIAN_POINT('Ctrl Pts',(183.290732589909,-6.53843241923107,
128.296943150732));
#218458=CARTESIAN_POINT('Ctrl Pts',(183.012284966097,-5.64374376128527,
134.950008601993));
#218459=CARTESIAN_POINT('Ctrl Pts',(182.733837342284,0.437269701071178,
137.793426081729));
#218460=CARTESIAN_POINT('Ctrl Pts',(182.455389718471,6.11645366995566,134.214233834728));
#218461=CARTESIAN_POINT('Ctrl Pts',(182.176942094658,6.17491552152431,127.501534682722));
#218462=CARTESIAN_POINT('Ctrl Pts',(181.898494470845,0.558931670205695,
123.82397121282));
#218463=CARTESIAN_POINT('Ctrl Pts',(181.620046847032,-5.57068308070185,
126.561044594899));
#218464=CARTESIAN_POINT('Ctrl Pts',(181.341599223219,-6.58111222344223,
133.197518104296));
#218465=CARTESIAN_POINT('Ctrl Pts',(181.063151599407,-1.54382073804491,
137.634796795631));
#218466=CARTESIAN_POINT('Ctrl Pts',(180.784703975594,4.91216658577983,135.795238324681));
#218467=CARTESIAN_POINT('Ctrl Pts',(180.506256351781,6.85411278995147,129.369307058824));
#218468=CARTESIAN_POINT('Ctrl Pts',(180.227808727968,2.49746418218255,124.262119907186));
#218469=CARTESIAN_POINT('Ctrl Pts',(179.949361104155,-4.15423200110403,
125.16693236216));
#218470=CARTESIAN_POINT('Ctrl Pts',(179.670913480342,-6.98839192089168,
131.252265980172));
#218471=CARTESIAN_POINT('Ctrl Pts',(179.392465856529,-3.40056106730489,
136.925996451342));
#218472=CARTESIAN_POINT('Ctrl Pts',(179.114018232716,3.31221928049139,136.974242649806));
#218473=CARTESIAN_POINT('Ctrl Pts',(178.835570608904,6.98123192042358,131.352668676138));
#218474=CARTESIAN_POINT('Ctrl Pts',(178.55712298509,4.23483347762603,125.227226382977));
#218475=CARTESIAN_POINT('Ctrl Pts',(178.278675361277,-2.40317004799311,
124.22689799325));
#218476=CARTESIAN_POINT('Ctrl Pts',(178.000227737465,-6.83277770089014,
129.270936428355));
#218477=CARTESIAN_POINT('Ctrl Pts',(177.721780113652,-4.98339644641697,
135.724116781409));
#218478=CARTESIAN_POINT('Ctrl Pts',(177.443332489839,1.44548268986267,137.65628156334));
#218479=CARTESIAN_POINT('Ctrl Pts',(177.164884866026,6.54603384991367,133.291865731052));
#218480=CARTESIAN_POINT('Ctrl Pts',(176.886437242213,5.63109969342586,126.64155422085));
#218481=CARTESIAN_POINT('Ctrl Pts',(176.6079896184,-0.458539986806858,123.816658424832));
#218482=CARTESIAN_POINT('Ctrl Pts',(176.329541994587,-6.12680382008778,
127.413119575705));
#218483=CARTESIAN_POINT('Ctrl Pts',(176.051094370774,-6.16483425371434,
134.125965572714));
#218484=CARTESIAN_POINT('Ctrl Pts',(175.772646746962,-0.537683177073775,
137.786418885364));
#218485=CARTESIAN_POINT('Ctrl Pts',(175.494199123148,5.58357247201413,135.030701742416));
#218486=CARTESIAN_POINT('Ctrl Pts',(175.215751499336,6.57379779200069,128.391183573973));
#218487=CARTESIAN_POINT('Ctrl Pts',(174.937303875523,1.5230240890144,123.969257218339));
#218488=CARTESIAN_POINT('Ctrl Pts',(174.65885625171,-4.92733434791298,125.82845697323));
#218489=CARTESIAN_POINT('Ctrl Pts',(174.380408627897,-6.84971323277332,
132.260269090858));
#218490=CARTESIAN_POINT('Ctrl Pts',(174.101961004084,-2.4775402838095,137.354172446613));
#218491=CARTESIAN_POINT('Ctrl Pts',(173.823513380271,4.1713711514037,136.429118707571));
#218492=CARTESIAN_POINT('Ctrl Pts',(173.545065756458,6.98699628128659,130.335187068521));
#218493=CARTESIAN_POINT('Ctrl Pts',(173.266618132645,3.38191316241135,124.672403000642));
#218494=CARTESIAN_POINT('Ctrl Pts',(172.988170508833,-3.33098293707706,
124.644588419932));
#218495=CARTESIAN_POINT('Ctrl Pts',(172.709722885019,-6.98286844495469,
130.277303567246));
#218496=CARTESIAN_POINT('Ctrl Pts',(172.431275261207,-4.21783898400718,
136.394358395635));
#218497=CARTESIAN_POINT('Ctrl Pts',(172.152827637394,2.42317845035331,137.374478352552));
#218498=CARTESIAN_POINT('Ctrl Pts',(171.874380013581,6.83741326768756,132.316981079111));
#218499=CARTESIAN_POINT('Ctrl Pts',(171.595932389768,4.96839931822471,125.869459497128));
#218500=CARTESIAN_POINT('Ctrl Pts',(171.317484765955,-1.46633088488636,
123.956870961504));
#218501=CARTESIAN_POINT('Ctrl Pts',(171.039037142142,-6.55357463903296,
128.336790901335));
#218502=CARTESIAN_POINT('Ctrl Pts',(170.760589518329,-5.61840345982816,
134.984286862899));
#218503=CARTESIAN_POINT('Ctrl Pts',(170.482141894517,0.479806024690783,
137.79063480575));
#218504=CARTESIAN_POINT('Ctrl Pts',(170.203694270703,6.13709721234627,134.176938068128));
#218505=CARTESIAN_POINT('Ctrl Pts',(169.925246646891,6.15469587572206,127.464007413007));
#218506=CARTESIAN_POINT('Ctrl Pts',(169.646799023078,0.51642970291829,123.820698167548));
#218507=CARTESIAN_POINT('Ctrl Pts',(169.368351399265,-5.59641013787386,
126.595033542778));
#218508=CARTESIAN_POINT('Ctrl Pts',(169.089903775452,-6.56642246179436,
133.237534862678));
#218509=CARTESIAN_POINT('Ctrl Pts',(168.811456151639,-1.50221333089678,
137.644067918489));
#218510=CARTESIAN_POINT('Ctrl Pts',(168.533008527826,4.94245646389391,135.76524410303));
#218511=CARTESIAN_POINT('Ctrl Pts',(168.254560904013,6.84525022078748,129.32761071706));
#218512=CARTESIAN_POINT('Ctrl Pts',(167.976113280201,2.45759343384159,124.247038346411));
#218513=CARTESIAN_POINT('Ctrl Pts',(167.697665656387,-4.1884716586909,125.192324799951));
#218514=CARTESIAN_POINT('Ctrl Pts',(167.419218032575,-6.98553591510243,
131.294798006688));
#218515=CARTESIAN_POINT('Ctrl Pts',(167.140770408762,-3.36323392793624,
136.946583212019));
#218516=CARTESIAN_POINT('Ctrl Pts',(166.862322784949,3.34971573589186,136.953965917302));
#218517=CARTESIAN_POINT('Ctrl Pts',(166.583875161136,6.98444028114645,131.310161777048));
#218518=CARTESIAN_POINT('Ctrl Pts',(166.305427537323,4.20080541690416,125.20155108099));
#218519=CARTESIAN_POINT('Ctrl Pts',(166.02697991351,-2.44316440471955,124.241648636582));
#218520=CARTESIAN_POINT('Ctrl Pts',(165.748532289697,-6.84198549362249,
129.312557896394));
#218521=CARTESIAN_POINT('Ctrl Pts',(165.470084665885,-4.95335616345982,
135.754360978348));
#218522=CARTESIAN_POINT('Ctrl Pts',(165.191637042072,1.48716549602113,137.647355549705));
#218523=CARTESIAN_POINT('Ctrl Pts',(164.913189418259,6.56105471673207,133.251972077313));
#218524=CARTESIAN_POINT('Ctrl Pts',(164.634741794446,5.60565517810829,126.60735324588));
#218525=CARTESIAN_POINT('Ctrl Pts',(164.356294170633,-0.501067617717217,
123.819579153818));
#218526=CARTESIAN_POINT('Ctrl Pts',(164.07784654682,-6.1473337513746,127.450478001396));
#218527=CARTESIAN_POINT('Ctrl Pts',(163.799398923007,-6.14450048146789,
134.163431126959));
#218528=CARTESIAN_POINT('Ctrl Pts',(163.520951299194,-0.495171444628521,
137.789562554107));
#218529=CARTESIAN_POINT('Ctrl Pts',(163.242503675381,5.60919595935461,134.996634647659));
#218530=CARTESIAN_POINT('Ctrl Pts',(162.964056051569,6.55898630114736,128.351211711527));
#218531=CARTESIAN_POINT('Ctrl Pts',(162.685608427755,1.48138865648,123.960112777059));
#218532=CARTESIAN_POINT('Ctrl Pts',(162.407160803943,-4.95753279363329,
125.85854324792));
#218533=CARTESIAN_POINT('Ctrl Pts',(162.12871318013,-6.84072379533872,132.301938264875));
#218534=CARTESIAN_POINT('Ctrl Pts',(161.850265556317,-2.4376238170639,137.369132584688));
#218535=CARTESIAN_POINT('Ctrl Pts',(161.571817932504,4.20553336454888,136.403622173655));
#218536=CARTESIAN_POINT('Ctrl Pts',(161.293370308691,6.98401083586784,130.292663931709));
#218537=CARTESIAN_POINT('Ctrl Pts',(161.014922684878,3.34452353692138,124.651929946293));
#218538=CARTESIAN_POINT('Ctrl Pts',(160.736475061065,-3.36841750339773,
124.664979184829));
#218539=CARTESIAN_POINT('Ctrl Pts',(160.458027437253,-6.98594741443756,
130.319820034592));
#218540=CARTESIAN_POINT('Ctrl Pts',(160.179579813439,-4.18373293411359,
136.419930008985));
#218541=CARTESIAN_POINT('Ctrl Pts',(159.901132189627,2.46312772594441,137.35960604848));
#218542=CARTESIAN_POINT('Ctrl Pts',(159.622684565814,6.84649433633851,132.275331778507));
#218543=CARTESIAN_POINT('Ctrl Pts',(159.344236942001,4.93826712148011,125.839306872565));
#218544=CARTESIAN_POINT('Ctrl Pts',(159.065789318188,-1.50798633025781,
123.965923801919));
#218545=CARTESIAN_POINT('Ctrl Pts',(158.787341694375,-6.56847401371661,
128.376730088641));
#218546=CARTESIAN_POINT('Ctrl Pts',(158.508894070562,-5.59285496636459,
135.018410235101));
#218547=CARTESIAN_POINT('Ctrl Pts',(158.230446446749,0.522324568921774,
137.787584650814));
#218548=CARTESIAN_POINT('Ctrl Pts',(157.951998822937,6.15751334234277,134.139517329431));
#218549=CARTESIAN_POINT('Ctrl Pts',(157.673551199123,6.13424816540071,127.426603921307));
#218550=CARTESIAN_POINT('Ctrl Pts',(157.395103575311,0.473908599138188,
123.817683904457));
#218551=CARTESIAN_POINT('Ctrl Pts',(157.116655951498,-5.62192981801017,
126.62917846882));
#218552=CARTESIAN_POINT('Ctrl Pts',(156.838208327685,-6.55148937894732,
133.277461458893));
#218553=CARTESIAN_POINT('Ctrl Pts',(156.559760703872,-1.46055025868114,
137.653085593479));
#218554=CARTESIAN_POINT('Ctrl Pts',(156.281313080059,4.97256319746619,135.735066054016));
#218555=CARTESIAN_POINT('Ctrl Pts',(156.002865456246,6.83613399835919,129.285969096806));
#218556=CARTESIAN_POINT('Ctrl Pts',(155.724417832433,2.4176316184721,124.232199769625));
#218557=CARTESIAN_POINT('Ctrl Pts',(155.44597020862,-4.2225561109203,125.217925193794));
#218558=CARTESIAN_POINT('Ctrl Pts',(155.167522584808,-6.98242105771092,
131.337311859867));
#218559=CARTESIAN_POINT('Ctrl Pts',(154.889074960995,-3.3257821626974,136.96694237038));
#218560=CARTESIAN_POINT('Ctrl Pts',(154.610627337182,3.38708806634394,136.933461308912));
#218561=CARTESIAN_POINT('Ctrl Pts',(154.332179713369,6.98738983086623,131.267636135312));
#218562=CARTESIAN_POINT('Ctrl Pts',(154.053732089556,4.1666216937926,125.17608339317));
#218563=CARTESIAN_POINT('Ctrl Pts',(153.775284465743,-2.48306822909056,
124.256642463619));
#218564=CARTESIAN_POINT('Ctrl Pts',(153.49683684193,-6.85093975406627,129.354234643731));
#218565=CARTESIAN_POINT('Ctrl Pts',(153.218389218117,-4.92313233206838,
135.784421751204));
#218566=CARTESIAN_POINT('Ctrl Pts',(152.939941594304,1.52879319471521,137.638175966376));
#218567=CARTESIAN_POINT('Ctrl Pts',(152.661493970491,6.57583246125511,133.21198772643));
#218568=CARTESIAN_POINT('Ctrl Pts',(152.383046346679,5.58000294317656,126.573307792561));
#218569=CARTESIAN_POINT('Ctrl Pts',(152.104598722866,-0.543576681382813,
123.822758706449));
#218570=CARTESIAN_POINT('Ctrl Pts',(151.826151099053,-6.16763589094857,
127.487960706439));
#218571=CARTESIAN_POINT('Ctrl Pts',(151.54770347524,-6.12393902249645,134.200772209611));
#218572=CARTESIAN_POINT('Ctrl Pts',(151.269255851427,-0.452641363423277,
137.792447383624));
#218573=CARTESIAN_POINT('Ctrl Pts',(150.990808227614,5.63461159587598,134.962412206646));
#218574=CARTESIAN_POINT('Ctrl Pts',(150.712360603801,6.54393176464461,128.311330751416));
#218575=CARTESIAN_POINT('Ctrl Pts',(150.433912979988,1.4396983305442,123.951221951899));
#218576=CARTESIAN_POINT('Ctrl Pts',(150.155465356176,-4.98754753615285,
125.888812791691));
#218577=CARTESIAN_POINT('Ctrl Pts',(149.877017732362,-6.83148087236823,
132.343551945603));
#218578=CARTESIAN_POINT('Ctrl Pts',(149.59857010855,-2.39761702327129,137.383849462723));
#218579=CARTESIAN_POINT('Ctrl Pts',(149.320122484737,4.23953974010866,136.377918157044));
#218580=CARTESIAN_POINT('Ctrl Pts',(149.041674860924,6.98076659535922,130.250159756006));
#218581=CARTESIAN_POINT('Ctrl Pts',(148.763227237111,3.30700997888175,124.631684872525));
#218582=CARTESIAN_POINT('Ctrl Pts',(148.484779613298,-3.40572725176907,
124.685597446761));
#218583=CARTESIAN_POINT('Ctrl Pts',(148.206331989485,-6.98876751706998,
130.362354456768));
#218584=CARTESIAN_POINT('Ctrl Pts',(147.927884365672,-4.14947185445744,
136.445293535346));
#218585=CARTESIAN_POINT('Ctrl Pts',(147.649436741859,2.50298572943186,137.344490837378));
#218586=CARTESIAN_POINT('Ctrl Pts',(147.370989118047,6.85532170562399,132.233627970525));
#218587=CARTESIAN_POINT('Ctrl Pts',(147.092541494233,4.90795193543132,125.809338229895));
#218588=CARTESIAN_POINT('Ctrl Pts',(146.814093870421,-1.54958589664124,
123.975230043125));
#218589=CARTESIAN_POINT('Ctrl Pts',(146.535646246608,-6.58312999118006,
128.41675923269));
#218590=CARTESIAN_POINT('Ctrl Pts',(146.257198622795,-5.56709922760349,
135.052377454143));
#218591=CARTESIAN_POINT('Ctrl Pts',(145.978750998982,0.564823758223794,
137.784275729942));
#218592=CARTESIAN_POINT('Ctrl Pts',(145.700303375169,6.17770130341801,134.101973005276));
#218593=CARTESIAN_POINT('Ctrl Pts',(145.421855751356,6.11357314825767,127.389325593625));
#218594=CARTESIAN_POINT('Ctrl Pts',(145.143408127543,0.431369934500661,
123.81492853524));
#218595=CARTESIAN_POINT('Ctrl Pts',(144.864960503731,-5.64724117546963,
126.663478107772));
#218596=CARTESIAN_POINT('Ctrl Pts',(144.586512879918,-6.53631352825206,
133.317296413447));
#218597=CARTESIAN_POINT('Ctrl Pts',(144.308065256105,-1.41883306523854,
137.661849486446));
#218598=CARTESIAN_POINT('Ctrl Pts',(144.029617632292,5.00248567088053,135.704705295899));
#218599=CARTESIAN_POINT('Ctrl Pts',(143.751170008479,6.82676446047164,129.244383741109));
#218600=CARTESIAN_POINT('Ctrl Pts',(143.472722384666,2.37758021687388,124.217604726676));
#218601=CARTESIAN_POINT('Ctrl Pts',(143.194274760853,-4.25648409478009,
125.243732595056));
#218602=CARTESIAN_POINT('Ctrl Pts',(142.91582713704,-6.97904746413934,131.379805964341));
#218603=CARTESIAN_POINT('Ctrl Pts',(142.637379513228,-3.28820715937746,
136.987073172008));
#218604=CARTESIAN_POINT('Ctrl Pts',(142.358931889414,3.42433488700229,136.912729584442));
#218605=CARTESIAN_POINT('Ctrl Pts',(142.080484265602,6.99008046028611,131.225093326731));
#218606=CARTESIAN_POINT('Ctrl Pts',(141.802036641788,4.13228357498186,125.150824263232));
#218607=CARTESIAN_POINT('Ctrl Pts',(141.523589017976,-2.52288004245522,
124.271878918761));
#218608=CARTESIAN_POINT('Ctrl Pts',(141.245141394163,-6.859640150418,129.395965126019));
#218609=CARTESIAN_POINT('Ctrl Pts',(140.96669377035,-4.89272607219785,135.814297986063));
#218610=CARTESIAN_POINT('Ctrl Pts',(140.688246146537,1.57036424341533,137.628743153505));
#218611=CARTESIAN_POINT('Ctrl Pts',(140.409798522724,6.59036653588803,133.17191416004));
#218612=CARTESIAN_POINT('Ctrl Pts',(140.131350898911,5.55414393918375,126.539419122461));
#218613=CARTESIAN_POINT('Ctrl Pts',(139.852903275098,-0.586065602614643,
123.826196964908));
#218614=CARTESIAN_POINT('Ctrl Pts',(139.574455651286,-6.18770948650656,
127.525566301902));
#218615=CARTESIAN_POINT('Ctrl Pts',(139.296008027473,-6.10315063871238,
134.237987436982));
#218616=CARTESIAN_POINT('Ctrl Pts',(139.01756040366,-0.410094509425858,
137.795073267016));
#218617=CARTESIAN_POINT('Ctrl Pts',(138.739112779847,5.65981843979252,134.928035687503));
#218618=CARTESIAN_POINT('Ctrl Pts',(138.460665156034,6.52863474034383,128.271542171445));
#218619=CARTESIAN_POINT('Ctrl Pts',(138.182217532221,1.39795465605713,123.942585072312));
#218620=CARTESIAN_POINT('Ctrl Pts',(137.903769908408,-5.01737746326431,
125.919264482896));
#218621=CARTESIAN_POINT('Ctrl Pts',(137.625322284595,-6.82198480636163,
132.385108591028));
#218622=CARTESIAN_POINT('Ctrl Pts',(137.346874660782,-2.35752138489827,
137.39832253538));
#218623=CARTESIAN_POINT('Ctrl Pts',(137.06842703697,4.27338901796432,136.352007610208));
#218624=CARTESIAN_POINT('Ctrl Pts',(136.789979413157,6.9772636799772,130.20767611642));
#218625=CARTESIAN_POINT('Ctrl Pts',(136.511531789344,3.26937387837121,124.611668529527));
#218626=CARTESIAN_POINT('Ctrl Pts',(136.233084165531,-3.44291079966457,
124.706442441713));
#218627=CARTESIAN_POINT('Ctrl Pts',(135.954636541718,-6.99132864835187,
130.404905257644));
#218628=CARTESIAN_POINT('Ctrl Pts',(135.676188917905,-4.1150570145959,136.470448034864));
#218629=CARTESIAN_POINT('Ctrl Pts',(135.397741294092,2.54275098386259,137.329133279345));
#218630=CARTESIAN_POINT('Ctrl Pts',(135.11929367028,6.8638950484427,132.191871200516));
#218631=CARTESIAN_POINT('Ctrl Pts',(134.840846046466,4.87745488341857,125.779554679616));
#218632=CARTESIAN_POINT('Ctrl Pts',(134.562398422654,-1.59112804254939,
123.984789340275));
#218633=CARTESIAN_POINT('Ctrl Pts',(134.283950798841,-6.59754202834077,
128.456876850186));
#218634=CARTESIAN_POINT('Ctrl Pts',(134.005503175028,-5.54113719793324,
135.086187261361));
#218635=CARTESIAN_POINT('Ctrl Pts',(133.727055551215,0.607302017773813,
137.780708165749));
#218636=CARTESIAN_POINT('Ctrl Pts',(133.448607927402,6.19766034749954,134.064306486881));
#218637=CARTESIAN_POINT('Ctrl Pts',(133.170160303589,6.09267159041341,127.352173811322));
#218638=CARTESIAN_POINT('Ctrl Pts',(132.891712679776,0.388815285291658,
123.812432161999));
#218639=CARTESIAN_POINT('Ctrl Pts',(132.613265055963,-5.67234327233058,
126.697931188648));
#218640=CARTESIAN_POINT('Ctrl Pts',(132.334817432151,-6.52089547205522,
133.357038250242));
#218641=CARTESIAN_POINT('Ctrl Pts',(132.056369808337,-1.37706329641493,
137.670359272641));
#218642=CARTESIAN_POINT('Ctrl Pts',(131.777922184525,5.0322227753486,135.674162953708));
#218643=CARTESIAN_POINT('Ctrl Pts',(131.499474560712,6.81714195431646,129.20285619093));
#218644=CARTESIAN_POINT('Ctrl Pts',(131.221026936899,2.33744071316646,124.203253758389));
#218645=CARTESIAN_POINT('Ctrl Pts',(130.942579313086,-4.29025435305649,
125.269746047434));
#218646=CARTESIAN_POINT('Ctrl Pts',(130.664131689273,-6.97541525939744,
131.422278745477));
#218647=CARTESIAN_POINT('Ctrl Pts',(130.38568406546,-3.25051031033198,137.006974870947));
#218648=CARTESIAN_POINT('Ctrl Pts',(130.107236441647,3.46145481767177,136.891771512113));
#218649=CARTESIAN_POINT('Ctrl Pts',(129.828788817834,6.99251206970404,131.182534927744));
#218650=CARTESIAN_POINT('Ctrl Pts',(129.550341194022,4.09779233288376,125.125774627163));
#218651=CARTESIAN_POINT('Ctrl Pts',(129.271893570209,-2.5625983695722,124.287357437414));
#218652=CARTESIAN_POINT('Ctrl Pts',(128.993445946396,-6.86808636028122,
129.43774779692));
#218653=CARTESIAN_POINT('Ctrl Pts',(128.714998322583,-4.86213851056362,
135.84398857585));
#218654=CARTESIAN_POINT('Ctrl Pts',(128.43655069877,1.61187710169066,137.61905746063));
#218655=CARTESIAN_POINT('Ctrl Pts',(128.158103074957,6.60465640206541,133.131752863082));
#218656=CARTESIAN_POINT('Ctrl Pts',(127.879655451144,5.52807912434469,126.505688491336));
#218657=CARTESIAN_POINT('Ctrl Pts',(127.601207827331,-0.628532806970051,
123.829893801787));
#218658=CARTESIAN_POINT('Ctrl Pts',(127.322760203518,-6.20755379421381,
127.563293394292));
#218659=CARTESIAN_POINT('Ctrl Pts',(127.044312579706,-6.08213610043705,
134.275075430049));
#218660=CARTESIAN_POINT('Ctrl Pts',(126.765864955893,-0.367532459225645,
137.797440106979));
#218661=CARTESIAN_POINT('Ctrl Pts',(126.48741733208,5.68481555705546,134.893506364063));
#218662=CARTESIAN_POINT('Ctrl Pts',(126.208969708267,6.51309579508176,128.231847445991));
#218663=CARTESIAN_POINT('Ctrl Pts',(125.930522084454,1.35615917984635,123.934202458341));
#218664=CARTESIAN_POINT('Ctrl Pts',(125.652074460641,-5.04702146960864,
125.949897193134));
#218665=CARTESIAN_POINT('Ctrl Pts',(125.373626836828,-6.81223594919939,
132.426606661257));
#218666=CARTESIAN_POINT('Ctrl Pts',(125.095179213015,-2.3173383877032,137.412551266352));
#218667=CARTESIAN_POINT('Ctrl Pts',(124.816731589202,4.3070799438184,136.325891493273));
#218668=CARTESIAN_POINT('Ctrl Pts',(124.538283965389,6.97350221952356,130.165214587198));
#218669=CARTESIAN_POINT('Ctrl Pts',(124.259836341577,3.2316166300094,124.591881659011));
#218670=CARTESIAN_POINT('Ctrl Pts',(123.981388717764,-3.47996676923432,
124.727513397266));
#218671=CARTESIAN_POINT('Ctrl Pts',(123.702941093951,-6.99363071337966,
130.447470860486));
#218672=CARTESIAN_POINT('Ctrl Pts',(123.424493470138,-4.08048968978323,
136.495392575427));
#218673=CARTESIAN_POINT('Ctrl Pts',(123.146045846325,2.58242201572056,137.313533943462));
#218674=CARTESIAN_POINT('Ctrl Pts',(122.867598222512,6.87221404710605,132.150063015792));
#218675=CARTESIAN_POINT('Ctrl Pts',(122.589150598699,4.84677709552158,125.749957325369));
#218676=CARTESIAN_POINT('Ctrl Pts',(122.310702974886,-1.63261122862275,
123.994601339147));
#218677=CARTESIAN_POINT('Ctrl Pts',(122.032255351073,-6.6117095911554,128.497081454556));
#218678=CARTESIAN_POINT('Ctrl Pts',(121.753807727261,-5.51496983938628,
135.119838403918));
#218679=CARTESIAN_POINT('Ctrl Pts',(121.475360103447,0.649757773524084,
137.776882090432));
#218680=CARTESIAN_POINT('Ctrl Pts',(121.196912479635,6.21738973499768,134.026519169992));
#218681=CARTESIAN_POINT('Ctrl Pts',(120.918464855822,6.07154426638285,127.315149951069));
#218682=CARTESIAN_POINT('Ctrl Pts',(120.640017232009,0.346246228389124,
123.810194877238));
#218683=CARTESIAN_POINT('Ctrl Pts',(120.361569608196,-5.69723517842559,
126.732536434776));
#218684=CARTESIAN_POINT('Ctrl Pts',(120.083121984383,-6.50523578167861,
133.396685496627));
#218685=CARTESIAN_POINT('Ctrl Pts',(119.80467436057,-1.3352425000044,137.678614636731));
#218686=CARTESIAN_POINT('Ctrl Pts',(119.526226736757,5.06177340895125,135.6434401592));
#218687=CARTESIAN_POINT('Ctrl Pts',(119.247779112945,6.8072668364591,129.161387985085));
#218688=CARTESIAN_POINT('Ctrl Pts',(118.969331489131,2.29721459473369,124.189147396544));
#218689=CARTESIAN_POINT('Ctrl Pts',(118.690883865319,-4.32386563438011,
125.29596458699));
#218690=CARTESIAN_POINT('Ctrl Pts',(118.412436241506,-6.97152457807781,
131.464728629428));
#218691=CARTESIAN_POINT('Ctrl Pts',(118.133988617693,-3.21269301243169,
137.026646729736));
#218692=CARTESIAN_POINT('Ctrl Pts',(117.85554099388,3.49844648286018,136.870587868534));
#218693=CARTESIAN_POINT('Ctrl Pts',(117.577093370067,6.99468456901571,131.139962515369));
#218694=CARTESIAN_POINT('Ctrl Pts',(117.298645746254,4.06314924558364,125.100935413187));
#218695=CARTESIAN_POINT('Ctrl Pts',(117.020198122441,-2.60222173866402,
124.303077446017));
#218696=CARTESIAN_POINT('Ctrl Pts',(116.741750498628,-6.8762780706787,129.479581108162));
#218697=CARTESIAN_POINT('Ctrl Pts',(116.463302874816,-4.83137078059878,
135.873492420371));
#218698=CARTESIAN_POINT('Ctrl Pts',(116.184855251003,1.65333023126747,137.609119246659));
#218699=CARTESIAN_POINT('Ctrl Pts',(115.90640762719,6.61870153027093,133.09150532375));
#218700=CARTESIAN_POINT('Ctrl Pts',(115.627960003377,5.5018094645007,126.472117149089));
#218701=CARTESIAN_POINT('Ctrl Pts',(115.349512379564,-0.670976720811003,
123.833849080098));
#218702=CARTESIAN_POINT('Ctrl Pts',(115.071064755751,-6.22716807873245,
127.601140585621));
#218703=CARTESIAN_POINT('Ctrl Pts',(114.792617131938,-6.06089618637186,
134.312034814502));
#218704=CARTESIAN_POINT('Ctrl Pts',(114.514169508125,-0.324956789974863,
137.79954781581));
#218705=CARTESIAN_POINT('Ctrl Pts',(114.235721884312,5.70960202138734,134.858825515823));
#218706=CARTESIAN_POINT('Ctrl Pts',(113.957274260499,6.4973155046598,128.192248045959));
#218707=CARTESIAN_POINT('Ctrl Pts',(113.678826636687,1.31431345065849,123.926074420608));
#218708=CARTESIAN_POINT('Ctrl Pts',(113.400379012874,-5.07647845671644,
125.980709787299));
#218709=CARTESIAN_POINT('Ctrl Pts',(113.121931389061,-6.80223466212876,
132.468044618562));
#218710=CARTESIAN_POINT('Ctrl Pts',(112.843483765248,-2.27706952068197,
137.42653512839));
#218711=CARTESIAN_POINT('Ctrl Pts',(112.565036141435,4.34061126924124,136.299570773982));
#218712=CARTESIAN_POINT('Ctrl Pts',(112.286588517622,6.96948235338073,130.122776741767));
#218713=CARTESIAN_POINT('Ctrl Pts',(112.008140893809,3.1937396329048,124.572324994188));
#218714=CARTESIAN_POINT('Ctrl Pts',(111.729693269996,-3.51689378735575,
124.748809532627));
#218715=CARTESIAN_POINT('Ctrl Pts',(111.451245646184,-6.99567362684944,
130.490049688009));
#218716=CARTESIAN_POINT('Ctrl Pts',(111.172798022371,-4.0457711609245,136.52012623271));
#218717=CARTESIAN_POINT('Ctrl Pts',(110.894350398558,2.62199735498092,137.297693407768));
#218718=CARTESIAN_POINT('Ctrl Pts',(110.615902774745,6.88027839335069,132.108204965571));
#218719=CARTESIAN_POINT('Ctrl Pts',(110.337455150932,4.81591970851693,125.720547263895));
#218720=CARTESIAN_POINT('Ctrl Pts',(110.059007527119,-1.67403391768677,
124.004665676154));
#218721=CARTESIAN_POINT('Ctrl Pts',(109.780559903306,-6.62563215463966,
128.537371556004));
#218722=CARTESIAN_POINT('Ctrl Pts',(109.502112279493,-5.48859812160383,
135.153329634858));
#218723=CARTESIAN_POINT('Ctrl Pts',(109.22366465568,0.692189452261082,137.772797645767));
#218724=CARTESIAN_POINT('Ctrl Pts',(108.945217031867,6.23688873483282,133.988612454835));
#218725=CARTESIAN_POINT('Ctrl Pts',(108.666769408055,6.05019195904657,127.278255384801));
#218726=CARTESIAN_POINT('Ctrl Pts',(108.388321784241,0.303664341205276,
123.808216763862));
#218727=CARTESIAN_POINT('Ctrl Pts',(108.109874160429,-5.72191597137591,
126.767292563848));
#218728=CARTESIAN_POINT('Ctrl Pts',(107.831426536616,-6.48933503739778,
133.436236683461));
#218729=CARTESIAN_POINT('Ctrl Pts',(107.552978912803,-1.29337222569216,
137.68661527281));
#218730=CARTESIAN_POINT('Ctrl Pts',(107.27453128899,5.09113647667873,135.612538050821));
#218731=CARTESIAN_POINT('Ctrl Pts',(106.996083665177,6.79713947282576,129.119980660195));
#218732=CARTESIAN_POINT('Ctrl Pts',(106.717636041364,2.25690335216928,124.175286163858));
#218733=CARTESIAN_POINT('Ctrl Pts',(106.439188417551,-4.35731669327239,
125.322387242187));
#218734=CARTESIAN_POINT('Ctrl Pts',(106.160740793739,-6.96737556435125,
131.5071540432));
#218735=CARTESIAN_POINT('Ctrl Pts',(105.882293169926,-3.17475666701035,
137.046088019424));
#218736=CARTESIAN_POINT('Ctrl Pts',(105.603845546113,3.53530851182771,136.849179438675));
#218737=CARTESIAN_POINT('Ctrl Pts',(105.3253979223,6.99659787771835,131.097377667143));
#218738=CARTESIAN_POINT('Ctrl Pts',(105.046950298487,4.02835559679407,125.076307541727));
#218739=CARTESIAN_POINT('Ctrl Pts',(104.768502674674,-2.64174868147234,
124.319038362058));
#218740=CARTESIAN_POINT('Ctrl Pts',(104.490055050861,-6.88421497806359,
129.521463509594));
#218741=CARTESIAN_POINT('Ctrl Pts',(104.211607427049,-4.80042402241278,
135.902808426348));
#218742=CARTESIAN_POINT('Ctrl Pts',(103.933159803235,1.69472209608453,137.598928879852));
#218743=CARTESIAN_POINT('Ctrl Pts',(103.654712179423,6.63250140005722,133.051173033428));
#218744=CARTESIAN_POINT('Ctrl Pts',(103.37626455561,5.47533593308374,126.438706339714));
#218745=CARTESIAN_POINT('Ctrl Pts',(103.097816931797,-0.713395771362793,
123.838062653278));
#218746=CARTESIAN_POINT('Ctrl Pts',(102.819369307984,-6.24655161324796,
127.639106473447));
#218747=CARTESIAN_POINT('Ctrl Pts',(102.540921684171,-6.03943168356949,
134.348864220799));
#218748=CARTESIAN_POINT('Ctrl Pts',(102.262474060358,-0.282369079330704,
137.801396315408));
#218749=CARTESIAN_POINT('Ctrl Pts',(101.984026436545,5.73417691431645,134.823994427897));
#218750=CARTESIAN_POINT('Ctrl Pts',(101.705578812732,6.48129445382252,128.15274543872));
#218751=CARTESIAN_POINT('Ctrl Pts',(101.427131188919,1.27241901910234,123.9182012603));
#218752=CARTESIAN_POINT('Ctrl Pts',(101.148683565106,-5.1057473330482,126.01170112362));
#218753=CARTESIAN_POINT('Ctrl Pts',(100.870235941294,-6.7919813157512,132.509420927444));
#218754=CARTESIAN_POINT('Ctrl Pts',(100.591788317481,-2.23671627601227,
137.440273603317));
#218755=CARTESIAN_POINT('Ctrl Pts',(100.313340693668,4.37398175171709,136.273046427655));
#218756=CARTESIAN_POINT('Ctrl Pts',(100.034893069855,6.96520423050629,130.080364152676));
#218757=CARTESIAN_POINT('Ctrl Pts',(99.7564454460421,3.15574429060373,124.552999259737));
#218758=CARTESIAN_POINT('Ctrl Pts',(99.4779978222292,-3.55369048568456,
124.770330058661));
#218759=CARTESIAN_POINT('Ctrl Pts',(99.1995501984162,-6.99745731306031,
130.532640162439));
#218760=CARTESIAN_POINT('Ctrl Pts',(98.9211025746034,-4.01090271452764,
136.544648090195));
#218761=CARTESIAN_POINT('Ctrl Pts',(98.6426549507905,2.66147553516503,137.281612259238));
#218762=CARTESIAN_POINT('Ctrl Pts',(98.3642073269776,6.88808778834931,132.066298600918));
#218763=CARTESIAN_POINT('Ctrl Pts',(98.0857597031646,4.78488386583629,125.691325584995));
#218764=CARTESIAN_POINT('Ctrl Pts',(97.8073120793519,-1.71539457480834,
124.014981978356));
#218765=CARTESIAN_POINT('Ctrl Pts',(97.5288644555388,-6.63930920288774,
128.577745661565));
#218766=CARTESIAN_POINT('Ctrl Pts',(97.2504168317261,-5.46202302179963,
135.186659713151));
#218767=CARTESIAN_POINT('Ctrl Pts',(96.9719692079131,0.734595481663425,
137.768454983106));
#218768=CARTESIAN_POINT('Ctrl Pts',(96.6935215841003,6.25615662446226,133.950587746053));
#218769=CARTESIAN_POINT('Ctrl Pts',(96.4150739602873,6.0286154596223,127.24149147966));
#218770=CARTESIAN_POINT('Ctrl Pts',(96.1366263364746,0.26107120162757,123.806497895168));
#218771=CARTESIAN_POINT('Ctrl Pts',(95.8581787126614,-5.74638473662552,
126.80219828796));
#218772=CARTESIAN_POINT('Ctrl Pts',(95.5797310888487,-6.47319382842077,
133.47569034516));
#218773=CARTESIAN_POINT('Ctrl Pts',(95.3012834650358,-1.25145402499642,
137.694360884412));
#218774=CARTESIAN_POINT('Ctrl Pts',(95.0228358412229,5.12031089047184,135.581457773658));
#218775=CARTESIAN_POINT('Ctrl Pts',(94.7443882174101,6.78676023868958,129.078635750625));
#218776=CARTESIAN_POINT('Ctrl Pts',(94.465940593597,2.21650847922131,124.161670573963));
#218777=CARTESIAN_POINT('Ctrl Pts',(94.1874929697842,-4.39060629019222,
125.349013033923));
#218778=CARTESIAN_POINT('Ctrl Pts',(93.9090453459715,-6.96296837196094,
131.549553414704));
#218779=CARTESIAN_POINT('Ctrl Pts',(93.6305977221583,-3.13670267981308,
137.065298019608));
#218780=CARTESIAN_POINT('Ctrl Pts',(93.3521500983456,3.5720395386382,136.82754701583));
#218781=CARTESIAN_POINT('Ctrl Pts',(93.0737024745325,6.99825192491364,131.054781961061));
#218782=CARTESIAN_POINT('Ctrl Pts',(92.7952548507199,3.99341267580637,125.051891925383));
#218783=CARTESIAN_POINT('Ctrl Pts',(92.5168072269068,-2.68117773331193,
124.335239594101));
#218784=CARTESIAN_POINT('Ctrl Pts',(92.238359603094,-6.89189678833074,129.563393449252));
#218785=CARTESIAN_POINT('Ctrl Pts',(91.959911979281,-4.7692993827493,135.931935507467));
#218786=CARTESIAN_POINT('Ctrl Pts',(91.6814643554683,1.73605116235111,137.588486737821));
#218787=CARTESIAN_POINT('Ctrl Pts',(91.4030167316553,6.6460555000649,133.010757486647));
#218788=CARTESIAN_POINT('Ctrl Pts',(91.1245691078424,5.44865951108031,126.405457301267));
#218789=CARTESIAN_POINT('Ctrl Pts',(90.8461214840295,-0.755788386771977,
123.84253436519));
#218790=CARTESIAN_POINT('Ctrl Pts',(90.5676738602166,-6.26570367949625,
127.677189650927));
#218791=CARTESIAN_POINT('Ctrl Pts',(90.2892262364038,-6.01774338740505,
134.38556228421));
#218792=CARTESIAN_POINT('Ctrl Pts',(90.0107786125907,-0.239770905396614,
137.802985537273));
#218793=CARTESIAN_POINT('Ctrl Pts',(89.7323309887781,5.75853932521132,134.78901439096));
#218794=CARTESIAN_POINT('Ctrl Pts',(89.453883364965,6.46503323623579,128.113341088056));
#218795=CARTESIAN_POINT('Ctrl Pts',(89.1754357411521,1.23047743759138,123.910583269158));
#218796=CARTESIAN_POINT('Ctrl Pts',(88.8969881173393,-5.13482701403487,
126.042870053701));
#218797=CARTESIAN_POINT('Ctrl Pts',(88.6185404935264,-6.78147629000823,
132.550734054689));
#218798=CARTESIAN_POINT('Ctrl Pts',(88.3400928697134,-2.19628014899849,
137.453766182047));
#218799=CARTESIAN_POINT('Ctrl Pts',(88.0616452459006,4.4071901546906,136.246319437167));
#218800=CARTESIAN_POINT('Ctrl Pts',(87.7831976220877,6.96066800942769,130.037978391542));
#218801=CARTESIAN_POINT('Ctrl Pts',(87.5047499982748,3.1176320110373,124.533905171779));
#218802=CARTESIAN_POINT('Ctrl Pts',(87.2263023744621,-3.59035550070555,
124.792074177916));
#218803=CARTESIAN_POINT('Ctrl Pts',(86.9478547506488,-6.99898170591706,
130.57524070557));
#218804=CARTESIAN_POINT('Ctrl Pts',(86.6694071268362,-3.97588564265574,
136.568957239218));
#218805=CARTESIAN_POINT('Ctrl Pts',(86.3909595030232,2.70085509339449,137.265291093768));
#218806=CARTESIAN_POINT('Ctrl Pts',(86.1125118792103,6.89564194272181,132.024345474689));
#218807=CARTESIAN_POINT('Ctrl Pts',(85.8340642553976,4.75367071752436,125.662293371487));
#218808=CARTESIAN_POINT('Ctrl Pts',(85.5556166315845,-1.75669166735309,
124.025549863481));
#218809=CARTESIAN_POINT('Ctrl Pts',(85.2771690077717,-6.65274022909182,
128.618202275162));
#218810=CARTESIAN_POINT('Ctrl Pts',(84.9987213839588,-5.4352455247236,135.21982740374));
#218811=CARTESIAN_POINT('Ctrl Pts',(84.7202737601459,0.776974290360158,
137.763854263368));
#218812=CARTESIAN_POINT('Ctrl Pts',(84.4418261363329,6.27519268990729,133.912446452669));
#218813=CARTESIAN_POINT('Ctrl Pts',(84.1633785125202,6.00681556763514,127.204859597945));
#218814=CARTESIAN_POINT('Ctrl Pts',(83.8849308887072,0.218468387960617,
123.805038334852));
#218815=CARTESIAN_POINT('Ctrl Pts',(83.6064832648944,-5.77064056747553,
126.837252313669));
#218816=CARTESIAN_POINT('Ctrl Pts',(83.3280356410814,-6.45681275286598,
133.515045019753));
#218817=CARTESIAN_POINT('Ctrl Pts',(83.0495880172686,-1.20948945121144,
137.701851184522));
#218818=CARTESIAN_POINT('Ctrl Pts',(82.7711403934555,5.14929556926191,135.550200479404));
#218819=CARTESIAN_POINT('Ctrl Pts',(82.4926927696429,6.77612951865689,129.037354788424));
#218820=CARTESIAN_POINT('Ctrl Pts',(82.2142451458298,2.17603147273656,124.148301131391));
#218821=CARTESIAN_POINT('Ctrl Pts',(81.9357975220171,-4.42373319158141,
125.375840975569));
#218822=CARTESIAN_POINT('Ctrl Pts',(81.6573498982041,-6.95830316421689,
131.591925172815));
#218823=CARTESIAN_POINT('Ctrl Pts',(81.3789022743912,-3.09853246094448,
137.084276018453));
#218824=CARTESIAN_POINT('Ctrl Pts',(81.1004546505783,3.60863820220999,136.805691401599));
#218825=CARTESIAN_POINT('Ctrl Pts',(80.8220070267654,6.99964664931016,131.012176975526));
#218826=CARTESIAN_POINT('Ctrl Pts',(80.5435594029525,3.95832177744353,125.02768946888));
#218827=CARTESIAN_POINT('Ctrl Pts',(80.2651117791397,-2.72050743312451,
124.351680541802));
#218828=CARTESIAN_POINT('Ctrl Pts',(79.9866641553267,-6.89932321682792,
129.605369373404));
#218829=CARTESIAN_POINT('Ctrl Pts',(79.7082165315139,-4.73799801494326,
135.960872584412));
#218830=CARTESIAN_POINT('Ctrl Pts',(79.4297689077009,1.77731589860328,137.577793207502));
#218831=CARTESIAN_POINT('Ctrl Pts',(79.1513212838881,6.65936332804202,132.970260181018));
#218832=CARTESIAN_POINT('Ctrl Pts',(78.8728736600752,5.42178118699497,126.372371265798));
#218833=CARTESIAN_POINT('Ctrl Pts',(78.5944260362623,-0.798152996164653,
123.847264050135));
#218834=CARTESIAN_POINT('Ctrl Pts',(78.3159784124494,-6.28462356779051,
127.715388706879));
#218835=CARTESIAN_POINT('Ctrl Pts',(78.0375307886365,-5.99583210154638,
134.422127644877));
#218836=CARTESIAN_POINT('Ctrl Pts',(77.7590831648237,-0.197163846663491,
137.804315422519));
#218837=CARTESIAN_POINT('Ctrl Pts',(77.4806355410107,5.78268835131386,134.753886701214));
#218838=CARTESIAN_POINT('Ctrl Pts',(77.2021879171979,6.44853245446487,128.07403645411));
#218839=CARTESIAN_POINT('Ctrl Pts',(76.9237402933849,1.18849026028645,123.903220729472));
#218840=CARTESIAN_POINT('Ctrl Pts',(76.6452926695721,-5.16371642211823,
126.074215422566));
#218841=CARTESIAN_POINT('Ctrl Pts',(76.3668450457591,-6.77071997416741,
132.591982469425));
#218842=CARTESIAN_POINT('Ctrl Pts',(76.0883974219463,-2.15576263801617,
137.467012364608));
#218843=CARTESIAN_POINT('Ctrl Pts',(75.8099497981334,4.44023524761227,136.219390792892));
#218844=CARTESIAN_POINT('Ctrl Pts',(75.5315021743204,6.95587385823614,129.995621028982));
#218845=CARTESIAN_POINT('Ctrl Pts',(75.2530545505077,3.0794042064702,124.515043437855));
#218846=CARTESIAN_POINT('Ctrl Pts',(74.9746069266946,-3.62688747378295,
124.814041084656));
#218847=CARTESIAN_POINT('Ctrl Pts',(74.6961593028819,-7.0002467489329,130.617849738824));
#218848=CARTESIAN_POINT('Ctrl Pts',(74.4177116790688,-3.94072124287924,
136.593052778991));
#218849=CARTESIAN_POINT('Ctrl Pts',(74.1392640552561,2.74013457044532,137.248730516143));
#218850=CARTESIAN_POINT('Ctrl Pts',(73.860816431443,6.90294057654623,131.982347141473));
#218851=CARTESIAN_POINT('Ctrl Pts',(73.5823688076304,4.72228142019582,125.633451699173));
#218852=CARTESIAN_POINT('Ctrl Pts',(73.3039211838172,-1.79792366504193,
124.036368939932));
#218853=CARTESIAN_POINT('Ctrl Pts',(73.0254735600045,-6.66592473556012,
128.658739897661));
#218854=CARTESIAN_POINT('Ctrl Pts',(72.7470259361915,-5.40826662262595,
135.252831477583));
#218855=CARTESIAN_POINT('Ctrl Pts',(72.4685783123786,0.819324307988826,
137.758995657032));
#218856=CARTESIAN_POINT('Ctrl Pts',(72.1901306885658,6.2939962257795,133.87418998802));
#218857=CARTESIAN_POINT('Ctrl Pts',(71.9116830647529,5.98479309088811,127.168361097063));
#218858=CARTESIAN_POINT('Ctrl Pts',(71.63323544094,0.17585747886725,123.803838136996));
#218859=CARTESIAN_POINT('Ctrl Pts',(71.3547878171271,-5.79468256511725,
126.872453342036));
#218860=CARTESIAN_POINT('Ctrl Pts',(71.0763401933142,-6.44019241774003,
133.554299248939));
#218861=CARTESIAN_POINT('Ctrl Pts',(70.7978925695013,-1.16748005934989,
137.709085895581));
#218862=CARTESIAN_POINT('Ctrl Pts',(70.5194449456884,5.17808943901089,135.518767326308));
#218863=CARTESIAN_POINT('Ctrl Pts',(70.2409973218756,6.76524770665308,128.996139303274));
#218864=CARTESIAN_POINT('Ctrl Pts',(69.9625496980626,2.1354738326052,124.135178331551));
#218865=CARTESIAN_POINT('Ctrl Pts',(69.6841020742497,-4.45669616991057,
125.402870073008));
#218866=CARTESIAN_POINT('Ctrl Pts',(69.4056544504369,-6.95338011399016,
131.634267747431));
#218867=CARTESIAN_POINT('Ctrl Pts',(69.1272068266238,-3.06024742481583,
137.103021312725));
#218868=CARTESIAN_POINT('Ctrl Pts',(68.8487592028112,3.64510314636624,136.783613405848));
#218869=CARTESIAN_POINT('Ctrl Pts',(68.5703115789981,7.00078199922599,130.969564289278));
#218870=CARTESIAN_POINT('Ctrl Pts',(68.2918639551854,3.92308420201135,125.003701069051));
#218871=CARTESIAN_POINT('Ctrl Pts',(68.0134163313723,-2.75973632353393,
124.368360595937));
#218872=CARTESIAN_POINT('Ctrl Pts',(67.7349687075595,-6.90649398836592,
129.647389726619));
#218873=CARTESIAN_POINT('Ctrl Pts',(67.4565210837467,-4.70652107887851,
135.98961858491));
#218874=CARTESIAN_POINT('Ctrl Pts',(67.1780734599337,1.81851477576126,137.566848685147));
#218875=CARTESIAN_POINT('Ctrl Pts',(66.8996258361208,6.67242439086218,132.929682617185));
#218876=CARTESIAN_POINT('Ctrl Pts',(66.6211782123079,5.39470195681365,126.339449459324));
#218877=CARTESIAN_POINT('Ctrl Pts',(66.3427305884951,-0.840488029704522,
123.852251532852));
#218878=CARTESIAN_POINT('Ctrl Pts',(66.0642829646821,-6.30331057704718,
127.753702225821));
#218879=CARTESIAN_POINT('Ctrl Pts',(65.7858353408693,-5.97369863792435,
134.458558947856));
#218880=CARTESIAN_POINT('Ctrl Pts',(65.5073877170563,-0.154549481951222,
137.805385921867));
#218881=CARTESIAN_POINT('Ctrl Pts',(65.2289400932435,5.80662309777304,134.718612660325));
#218882=CARTESIAN_POINT('Ctrl Pts',(64.9504924694306,6.43179271995227,128.03483299333));
#218883=CARTESIAN_POINT('Ctrl Pts',(64.6720448456177,1.14645904303803,123.896113914062));
#218884=CARTESIAN_POINT('Ctrl Pts',(64.3935972218049,-5.19241448679041,
126.1057360687));
#218885=CARTESIAN_POINT('Ctrl Pts',(64.1151495979918,-6.75971276680813,
132.633164643176));
#218886=CARTESIAN_POINT('Ctrl Pts',(63.8367019741791,-2.11516524445634,
137.480011660159));
#218887=CARTESIAN_POINT('Ctrl Pts',(63.5582543503661,4.47311580598391,136.192261492683));
#218888=CARTESIAN_POINT('Ctrl Pts',(63.2798067265533,6.95082195458075,129.953293634565));
#218889=CARTESIAN_POINT('Ctrl Pts',(63.0013591027403,3.041062293448,124.496414756892));
#218890=CARTESIAN_POINT('Ctrl Pts',(62.7229114789275,-3.66328505121137,
124.836229964889));
#218891=CARTESIAN_POINT('Ctrl Pts',(62.4444638551145,-7.00125239523119,
130.660465683307));
#218892=CARTESIAN_POINT('Ctrl Pts',(62.1660162313017,-3.90541081822766,
136.616933816649));
#218893=CARTESIAN_POINT('Ctrl Pts',(61.8875686074887,2.77931251080179,137.231931140021));
#218894=CARTESIAN_POINT('Ctrl Pts',(61.609120983676,6.909983419369,131.940305157533));
#218895=CARTESIAN_POINT('Ctrl Pts',(61.3306733598629,4.69071713699276,125.604801636791));
#218896=CARTESIAN_POINT('Ctrl Pts',(61.0522257360502,-1.83908904000824,
124.047438806804));
#218897=CARTESIAN_POINT('Ctrl Pts',(60.7737781122372,-6.67886223373588,
128.699357026925));
#218898=CARTESIAN_POINT('Ctrl Pts',(60.4953304884244,-5.38108731521968,
135.285670711703));
#218899=CARTESIAN_POINT('Ctrl Pts',(60.2168828646114,0.861643965253713,
137.753879344138));
#218900=CARTESIAN_POINT('Ctrl Pts',(59.9384352407986,6.31256653530686,133.835819769716));
#218901=CARTESIAN_POINT('Ctrl Pts',(59.6599876169856,5.96254884543232,127.131997329482));
#218902=CARTESIAN_POINT('Ctrl Pts',(59.3815399931728,0.133240053310041,
123.802897346075));
#218903=CARTESIAN_POINT('Ctrl Pts',(59.1030923693598,-5.81850983866561,
126.907800068673));
#218904=CARTESIAN_POINT('Ctrl Pts',(58.824644745547,-6.42333343891552,133.593451578138));
#218905=CARTESIAN_POINT('Ctrl Pts',(58.5461971217341,-1.12542740608588,
137.716064749505));
#218906=CARTESIAN_POINT('Ctrl Pts',(58.2677494979212,5.20669143275151,135.487159479138));
#218907=CARTESIAN_POINT('Ctrl Pts',(57.9893018741083,6.75411520590753,128.954990822428));
#218908=CARTESIAN_POINT('Ctrl Pts',(57.7108542502954,2.09483706170563,124.122302660713));
#218909=CARTESIAN_POINT('Ctrl Pts',(57.4324066264825,-4.48949400372376,
125.430099324666));
#218910=CARTESIAN_POINT('Ctrl Pts',(57.1539590026696,-6.94819940370625,
131.676579569534));
#218911=CARTESIAN_POINT('Ctrl Pts',(56.8755113788568,-3.02184899009409,
137.121533207807));
#218912=CARTESIAN_POINT('Ctrl Pts',(56.5970637550437,3.68143301988451,136.761313846687));
#218913=CARTESIAN_POINT('Ctrl Pts',(56.318616131231,7.00165793259049,130.926945481348));
#218914=CARTESIAN_POINT('Ctrl Pts',(56.040168507418,3.88770125525153,124.979927614796));
#218915=CARTESIAN_POINT('Ctrl Pts',(55.7617208836052,-2.79886295089852,
124.385279138419));
#218916=CARTESIAN_POINT('Ctrl Pts',(55.4832732597923,-6.91340883722955,
129.689452951814));
#218917=CARTESIAN_POINT('Ctrl Pts',(55.2048256359794,-4.67486974094423,
136.018172443767));
#218918=CARTESIAN_POINT('Ctrl Pts',(54.9263780121665,1.85964626718557,137.555653576309));
#218919=CARTESIAN_POINT('Ctrl Pts',(54.6479303883536,6.68523820454244,132.889026298762));
#218920=CARTESIAN_POINT('Ctrl Pts',(54.3694827645407,5.36742282396772,126.306693101776));
#218921=CARTESIAN_POINT('Ctrl Pts',(54.0910351407278,-0.882791918651148,
123.857496628527));
#218922=CARTESIAN_POINT('Ctrl Pts',(53.8125875169149,-6.32176401481248,
127.792128788032));
#218923=CARTESIAN_POINT('Ctrl Pts',(53.534139893102,-5.95134381670231,134.494854843172));
#218924=CARTESIAN_POINT('Ctrl Pts',(53.2556922692892,-0.111929390351441,
137.806196995646));
#218925=CARTESIAN_POINT('Ctrl Pts',(52.9772446454762,5.83034267767769,134.683193575387));
#218926=CARTESIAN_POINT('Ctrl Pts',(52.6987970216634,6.41481465299549,127.995732158415));
#218927=CARTESIAN_POINT('Ctrl Pts',(52.4203493978505,1.10438534332797,123.889263086274));
#218928=CARTESIAN_POINT('Ctrl Pts',(52.1419017740376,-5.22092014463445,
126.137430824095));
#218929=CARTESIAN_POINT('Ctrl Pts',(51.8634541502246,-6.74845507580631,
132.674279049921));
#218930=CARTESIAN_POINT('Ctrl Pts',(51.5850065264118,-2.07448947267055,
137.492763587005));
#218931=CARTESIAN_POINT('Ctrl Pts',(51.3065589025989,4.50583061140446,136.164932541826));
#218932=CARTESIAN_POINT('Ctrl Pts',(51.028111278786,6.94551248566166,129.910997776748));
#218933=CARTESIAN_POINT('Ctrl Pts',(50.7496636549731,3.00260769274395,124.478019819181));
#218934=CARTESIAN_POINT('Ctrl Pts',(50.4712160311602,-3.69954688426507,
124.858639996399));
#218935=CARTESIAN_POINT('Ctrl Pts',(50.1927684073473,-7.00199860754717,
130.70308695987));
#218936=CARTESIAN_POINT('Ctrl Pts',(49.9143207835345,-3.86995567714208,
136.640599467269));
#218937=CARTESIAN_POINT('Ctrl Pts',(49.6358731597215,2.81838746271124,137.214893587909));
#218938=CARTESIAN_POINT('Ctrl Pts',(49.3574255359087,6.91677021021505,131.89822108075));
#218939=CARTESIAN_POINT('Ctrl Pts',(49.0789779120958,4.65897903754105,125.576344245977));
#218940=CARTESIAN_POINT('Ctrl Pts',(48.8005302882828,-1.88018626685394,
124.058759053897));
#218941=CARTESIAN_POINT('Ctrl Pts',(48.5220826644701,-6.69155224421552,
128.740052157871));
#218942=CARTESIAN_POINT('Ctrl Pts',(48.243635040657,-5.35370860964396,135.318343889229));
#218943=CARTESIAN_POINT('Ctrl Pts',(47.9651874168443,0.903931693984841,
137.748505514272));
#218944=CARTESIAN_POINT('Ctrl Pts',(47.6867397930313,6.33090293035988,133.797337219578));
#218945=CARTESIAN_POINT('Ctrl Pts',(47.4082921692184,5.94008365553619,127.095769642671));
#218946=CARTESIAN_POINT('Ctrl Pts',(47.1298445454056,0.0906176904940206,
123.80221599695));
#218947=CARTESIAN_POINT('Ctrl Pts',(46.8513969215926,-5.84212150519187,
126.943291183793));
#218948=CARTESIAN_POINT('Ctrl Pts',(46.5729492977799,-6.40623644110861,
133.632500556544));
#218949=CARTESIAN_POINT('Ctrl Pts',(46.2945016739667,-1.08333304969514,
137.722787487691));
#218950=CARTESIAN_POINT('Ctrl Pts',(46.016054050154,5.23510049062639,135.455378109134));
#218951=CARTESIAN_POINT('Ctrl Pts',(45.737606426341,6.7427324289391,128.913910870662));
#218952=CARTESIAN_POINT('Ctrl Pts',(45.4591588025282,2.0541226658487,124.10967459599));
#218953=CARTESIAN_POINT('Ctrl Pts',(45.1807111787153,-4.5221254776858,125.457527721552));
#218954=CARTESIAN_POINT('Ctrl Pts',(44.9022635549024,-6.94276122533821,
131.718859071242));
#218955=CARTESIAN_POINT('Ctrl Pts',(44.6238159310895,-2.98333857964632,
137.139811017737));
#218956=CARTESIAN_POINT('Ctrl Pts',(44.3453683072766,3.71762647654865,136.738793550433));
#218957=CARTESIAN_POINT('Ctrl Pts',(44.0669206834637,7.00227441694529,130.88432213099));
#218958=CARTESIAN_POINT('Ctrl Pts',(43.7884730596509,3.85217424829189,124.956369987047));
#218959=CARTESIAN_POINT('Ctrl Pts',(43.5100254358379,-2.8378858653675,124.402435542326));
#218960=CARTESIAN_POINT('Ctrl Pts',(43.2315778120251,-6.92006750718621,
129.731557490323));
#218961=CARTESIAN_POINT('Ctrl Pts',(42.9531301882121,-4.64304517399252,
136.04653310291));
#218962=CARTESIAN_POINT('Ctrl Pts',(42.6746825643993,1.90070884873357,137.544208295828));
#218963=CARTESIAN_POINT('Ctrl Pts',(42.3962349405864,6.69780429426274,132.848292732287));
#218964=CARTESIAN_POINT('Ctrl Pts',(42.1177873167735,5.33994479929498,126.274103406951));
#218965=CARTESIAN_POINT('Ctrl Pts',(41.8393396929606,-0.925063095418803,
123.862999142802));
#218966=CARTESIAN_POINT('Ctrl Pts',(41.5608920691476,-6.33998319728738,
127.8306669696));
#218967=CARTESIAN_POINT('Ctrl Pts',(41.2824444453348,-5.92876846624656,
134.531013985867));
#218968=CARTESIAN_POINT('Ctrl Pts',(41.0039968215219,-0.069305151166692,
137.806748613804));
#218969=CARTESIAN_POINT('Ctrl Pts',(40.725549197709,5.85384621209049,134.647630758868));
#218970=CARTESIAN_POINT('Ctrl Pts',(40.4471015738961,6.39759888272248,127.956735398261));
#218971=CARTESIAN_POINT('Ctrl Pts',(40.1686539500832,1.06227072021291,123.882668499967));
#218972=CARTESIAN_POINT('Ctrl Pts',(39.8902063262704,-5.24923233936253,
126.169298514289));
#218973=CARTESIAN_POINT('Ctrl Pts',(39.6117587024575,-6.73694731831984,
132.715324166149));
#218974=CARTESIAN_POINT('Ctrl Pts',(39.3333110786445,-2.03373682991476,
137.505267672621));
#218975=CARTESIAN_POINT('Ctrl Pts',(39.0548634548317,4.53837845161457,136.137404953004));
#218976=CARTESIAN_POINT('Ctrl Pts',(38.7764158310188,6.9399456482232,129.86873502282));
#218977=CARTESIAN_POINT('Ctrl Pts',(38.4979682072059,2.96404182930761,124.459859306355));
#218978=CARTESIAN_POINT('Ctrl Pts',(38.219520583393,-3.73567162924815,124.881270348773));
#218979=CARTESIAN_POINT('Ctrl Pts',(37.9410729595801,-7.00248535822977,
130.745711989165));
#218980=CARTESIAN_POINT('Ctrl Pts',(37.6626253357672,-3.83435713342598,
136.664048853912));
#218981=CARTESIAN_POINT('Ctrl Pts',(37.3841777119543,2.8573579782368,137.197618491141));
#218982=CARTESIAN_POINT('Ctrl Pts',(37.1057300881414,6.92330069759731,131.856096470565));
#218983=CARTESIAN_POINT('Ctrl Pts',(36.8272824643285,4.62706829790778,125.548080581235));
#218984=CARTESIAN_POINT('Ctrl Pts',(36.5488348405156,-1.92121382270608,
124.070329261737));
#218985=CARTESIAN_POINT('Ctrl Pts',(36.2703872167028,-6.70399429676593,
128.780823782526));
#218986=CARTESIAN_POINT('Ctrl Pts',(35.9919395928899,-5.32613152042688,
135.350849799446));
#218987=CARTESIAN_POINT('Ctrl Pts',(35.7134919690769,0.946185927194629,
137.742874366562));
#218988=CARTESIAN_POINT('Ctrl Pts',(35.4350443452641,6.34900473147662,133.758743763591));
#218989=CARTESIAN_POINT('Ctrl Pts',(35.1565967214512,5.91739835365575,127.059679379064));
#218990=CARTESIAN_POINT('Ctrl Pts',(34.8781490976383,0.0479919698059151,
123.80179411487));
#218991=CARTESIAN_POINT('Ctrl Pts',(34.5997014738253,-5.8655166897575,126.978925372262));
#218992=CARTESIAN_POINT('Ctrl Pts',(34.3212538500126,-6.38890205785425,
133.671444737187));
#218993=CARTESIAN_POINT('Ctrl Pts',(34.0428062261996,-1.04119854999986,
137.729253861025));
#218994=CARTESIAN_POINT('Ctrl Pts',(33.7643586023867,5.26331555992738,135.423424393967));
#218995=CARTESIAN_POINT('Ctrl Pts',(33.4859109785738,6.73109979754094,128.872900970206));
#218996=CARTESIAN_POINT('Ctrl Pts',(33.207463354761,2.01333215372067,124.097294605319));
#218997=CARTESIAN_POINT('Ctrl Pts',(32.9290157309481,-4.55458938262534,
125.485154247296));
#218998=CARTESIAN_POINT('Ctrl Pts',(32.6505681071352,-6.93706578039975,
131.761104685873));
#218999=CARTESIAN_POINT('Ctrl Pts',(32.3721204833222,-2.94471762049033,
137.157854065221));
#219000=CARTESIAN_POINT('Ctrl Pts',(32.0936728595094,3.75368217519627,136.716053351584));
#219001=CARTESIAN_POINT('Ctrl Pts',(31.8152252356965,7.00263142944649,130.84169581763));
#219002=CARTESIAN_POINT('Ctrl Pts',(31.5367776118836,3.8165044975991,124.933029058741));
#219003=CARTESIAN_POINT('Ctrl Pts',(31.2583299880707,-2.87680362093211,
124.41982917192));
#219004=CARTESIAN_POINT('Ctrl Pts',(30.9798823642578,-6.92646975149653,
129.773701781947));
#219005=CARTESIAN_POINT('Ctrl Pts',(30.7014347404449,-4.6110485572945,136.074699511423));
#219006=CARTESIAN_POINT('Ctrl Pts',(30.422987116632,1.94170099881587,137.532513267813));
#219007=CARTESIAN_POINT('Ctrl Pts',(30.1445394928192,6.71012219438185,132.807483427156));
#219008=CARTESIAN_POINT('Ctrl Pts',(29.8660918690062,5.31226890100394,126.241681582474));
#219009=CARTESIAN_POINT('Ctrl Pts',(29.5876442451933,-0.967299993633269,
123.868758871779));
#219010=CARTESIAN_POINT('Ctrl Pts',(29.3091966213805,-6.35796744935336,
127.869315342481));
#219011=CARTESIAN_POINT('Ctrl Pts',(29.0307489975676,-5.90597342309497,
134.567035036052));
#219012=CARTESIAN_POINT('Ctrl Pts',(28.7523013737546,-0.026678343854083,
137.807040755898));
#219013=CARTESIAN_POINT('Ctrl Pts',(28.4738537499418,5.87713283007914,134.611925528561));
#219014=CARTESIAN_POINT('Ctrl Pts',(28.1954061261289,6.38014604707014,127.917844157905));
#219015=CARTESIAN_POINT('Ctrl Pts',(27.916958502316,1.02011673426565,123.876330399509));
#219016=CARTESIAN_POINT('Ctrl Pts',(27.6385108785031,-5.27735002185588,
126.201337958415));
#219017=CARTESIAN_POINT('Ctrl Pts',(27.3600632546902,-6.72518992077305,
132.756298470923));
#219018=CARTESIAN_POINT('Ctrl Pts',(27.0816156308773,-1.99290882629253,
137.51752345366));
#219019=CARTESIAN_POINT('Ctrl Pts',(26.8031680070644,4.57075812054227,136.109679746264));
#219020=CARTESIAN_POINT('Ctrl Pts',(26.5247203832516,6.93412164854658,129.826506938842));
#219021=CARTESIAN_POINT('Ctrl Pts',(26.2462727594386,2.92536613221128,124.441933891359));
#219022=CARTESIAN_POINT('Ctrl Pts',(25.9678251356258,-3.7716579475455,124.904120183435));
#219023=CARTESIAN_POINT('Ctrl Pts',(25.6893775118128,-7.00271262924226,
130.788339191706));
#219024=CARTESIAN_POINT('Ctrl Pts',(25.410929888,-3.79861650619593,136.687281107654));
#219025=CARTESIAN_POINT('Ctrl Pts',(25.1324822641871,2.89622261331168,137.180106489852));
#219026=CARTESIAN_POINT('Ctrl Pts',(24.8540346403742,6.92957463952618,131.813932887921));
#219027=CARTESIAN_POINT('Ctrl Pts',(24.5755870165613,4.59498610055721,125.520011689881));
#219028=CARTESIAN_POINT('Ctrl Pts',(24.2971393927484,-1.96217018727317,
124.082149001586));
#219029=CARTESIAN_POINT('Ctrl Pts',(24.0186917689355,-6.71618793034234,
128.821670390082));
#219030=CARTESIAN_POINT('Ctrl Pts',(23.7402441451226,-5.29835706944761,
135.383187237832));
#219031=CARTESIAN_POINT('Ctrl Pts',(23.4617965213097,0.988405099136929,
137.736986109674));
#219032=CARTESIAN_POINT('Ctrl Pts',(23.1833488974968,6.36687126788796,133.720040831851));
#219033=CARTESIAN_POINT('Ctrl Pts',(22.9049012736839,5.89449378040337,127.023727875996));
#219034=CARTESIAN_POINT('Ctrl Pts',(22.6264536498711,0.00536447075796404,
123.801631715467));
#219035=CARTESIAN_POINT('Ctrl Pts',(22.3480060260581,-5.88869452544514,
127.01470131364));
#219036=CARTESIAN_POINT('Ctrl Pts',(22.0695584022453,-6.3713309314846,133.710282676972));
#219037=CARTESIAN_POINT('Ctrl Pts',(21.7911107784324,-0.999025468309402,
137.735463629893));
#219038=CARTESIAN_POINT('Ctrl Pts',(21.5126631546195,5.29133559513472,135.391299517692));
#219039=CARTESIAN_POINT('Ctrl Pts',(21.2342155308066,6.71921774276442,128.831962640697));
#219040=CARTESIAN_POINT('Ctrl Pts',(20.9557679069937,1.97246703682929,124.085163147446));
#219041=CARTESIAN_POINT('Ctrl Pts',(20.6773202831809,-4.58688451558038,
125.51297787819));
#219042=CARTESIAN_POINT('Ctrl Pts',(20.3988726593679,-6.93111327993769,
131.803314848003));
#219043=CARTESIAN_POINT('Ctrl Pts',(20.120425035555,-2.90598754374001,137.175661681671));
#219044=CARTESIAN_POINT('Ctrl Pts',(19.8419774117421,3.78959877977074,136.693094092787));
#219045=CARTESIAN_POINT('Ctrl Pts',(19.5635297879293,7.00272895686486,130.799068120799));
#219046=CARTESIAN_POINT('Ctrl Pts',(19.2850821641163,3.78069332492835,124.909905694786));
#219047=CARTESIAN_POINT('Ctrl Pts',(19.0066345403035,-2.91561477548059,
124.437459382677));
#219048=CARTESIAN_POINT('Ctrl Pts',(18.7281869164906,-6.932615332923,129.815884265012));
#219049=CARTESIAN_POINT('Ctrl Pts',(18.4497392926777,-4.57888107649638,
136.102670625591));
#219050=CARTESIAN_POINT('Ctrl Pts',(18.1712916688647,1.98262119845391,137.520568925627));
#219051=CARTESIAN_POINT('Ctrl Pts',(17.892844045052,6.72219144845534,132.766599895572));
#219052=CARTESIAN_POINT('Ctrl Pts',(17.614396421239,5.28439615463518,126.209428829746));
#219053=CARTESIAN_POINT('Ctrl Pts',(17.3359487974261,-1.00950104819076,
123.87477560203));
#219054=CARTESIAN_POINT('Ctrl Pts',(17.0575011736132,-6.37571610459714,
127.908072474542));
#219055=CARTESIAN_POINT('Ctrl Pts',(16.7790535498004,-5.88295953192644,
134.602916658952));
#219056=CARTESIAN_POINT('Ctrl Pts',(16.5006059259874,0.0159494520341194,
137.807073411106));
#219057=CARTESIAN_POINT('Ctrl Pts',(16.2221583021745,5.90020166874948,134.576079207535));
#219058=CARTESIAN_POINT('Ctrl Pts',(15.9437106783617,6.3624567927597,127.879059878479));
#219059=CARTESIAN_POINT('Ctrl Pts',(15.6652630545488,0.977924947517885,
123.870249019757));
#219060=CARTESIAN_POINT('Ctrl Pts',(15.3868154307359,-5.3052721502032,126.233547969238));
#219061=CARTESIAN_POINT('Ctrl Pts',(15.108367806923,-6.71318331884074,132.797200445919));
#219062=CARTESIAN_POINT('Ctrl Pts',(14.8299201831101,-1.95200697470083,
137.529530475982));
#219063=CARTESIAN_POINT('Ctrl Pts',(14.5514725592972,4.6029684183469,136.081757948972));
#219064=CARTESIAN_POINT('Ctrl Pts',(14.2730249354843,6.92804070244224,129.784315089592));
#219065=CARTESIAN_POINT('Ctrl Pts',(13.9945773116714,2.88658203459712,124.424244238425));
#219066=CARTESIAN_POINT('Ctrl Pts',(13.7161296878585,-3.80750450567058,
124.927188653676));
#219067=CARTESIAN_POINT('Ctrl Pts',(13.4376820640456,-7.00268041216303,
130.830966987928));
#219068=CARTESIAN_POINT('Ctrl Pts',(13.1592344402328,-3.7627351198343,136.710295367612));
#219069=CARTESIAN_POINT('Ctrl Pts',(12.8807868164199,2.93497992779253,137.162358232954));
#219070=CARTESIAN_POINT('Ctrl Pts',(12.602339192607,6.93559180351842,131.771731895206));
#219071=CARTESIAN_POINT('Ctrl Pts',(12.323891568794,4.56273363430679,125.49213861202));
#219072=CARTESIAN_POINT('Ctrl Pts',(12.0454439449812,-2.00305384290271,
124.094217835458));
#219073=CARTESIAN_POINT('Ctrl Pts',(11.7669963211683,-6.72813269310505,
128.862590466954));
#219074=CARTESIAN_POINT('Ctrl Pts',(11.4885486973554,-5.27038628589867,
135.415355006116));
#219075=CARTESIAN_POINT('Ctrl Pts',(11.2101010735425,1.03058764536478,137.730840961799));
#219076=CARTESIAN_POINT('Ctrl Pts',(10.9316534497296,6.38450187754329,133.681229858508));
#219077=CARTESIAN_POINT('Ctrl Pts',(10.6532058259167,5.87137078451608,126.987916465666));
#219078=CARTESIAN_POINT('Ctrl Pts',(10.3747582021038,-0.0372632270726686,
123.801728804758));
#219079=CARTESIAN_POINT('Ctrl Pts',(10.0963105782909,-5.91165415339157,
127.050617682238));
#219080=CARTESIAN_POINT('Ctrl Pts',(9.81786295447806,-6.35352371310424,
133.749012936746));
#219081=CARTESIAN_POINT('Ctrl Pts',(9.53941533066515,-0.956815367363035,
137.741416564191));
#219082=CARTESIAN_POINT('Ctrl Pts',(9.26096770685226,5.31915955795546,135.35900467071));
#219083=CARTESIAN_POINT('Ctrl Pts',(8.98252008303941,6.70708670490366,128.791097399121));
#219084=CARTESIAN_POINT('Ctrl Pts',(8.70407245922646,1.93152882944647,124.073280671906));
#219085=CARTESIAN_POINT('Ctrl Pts',(8.42562483541358,-4.61900967984285,
125.540997583217));
#219086=CARTESIAN_POINT('Ctrl Pts',(8.14717721160073,-6.92490394452403,
131.845487993513));
#219087=CARTESIAN_POINT('Ctrl Pts',(7.86872958778781,-2.86714978455288,
137.193233207215));
#219088=CARTESIAN_POINT('Ctrl Pts',(7.59028196397491,3.82537495936868,136.669916624805));
#219089=CARTESIAN_POINT('Ctrl Pts',(7.31183434016203,7.00256699558648,130.756440620084));
#219090=CARTESIAN_POINT('Ctrl Pts',(7.03338671634916,3.7447420572761,124.887000752025));
#219091=CARTESIAN_POINT('Ctrl Pts',(6.75493909253623,-2.95431789085107,
124.455325521299));
#219092=CARTESIAN_POINT('Ctrl Pts',(6.47649146872337,-6.9385040237388,129.858103376433));
#219093=CARTESIAN_POINT('Ctrl Pts',(6.19804384491048,-4.54654392357636,
136.130445408932));
#219094=CARTESIAN_POINT('Ctrl Pts',(5.91959622109758,2.02346793133434,137.508375711873));
#219095=CARTESIAN_POINT('Ctrl Pts',(5.64114859728465,6.73401160925262,132.725643652489));
#219096=CARTESIAN_POINT('Ctrl Pts',(5.36270097347181,5.25632759302358,126.177346343905));
#219097=CARTESIAN_POINT('Ctrl Pts',(5.08425334965889,-1.05166469531565,
123.881049110601));
#219098=CARTESIAN_POINT('Ctrl Pts',(4.80580572584599,-6.39322850533622,
127.946936929627));
#219099=CARTESIAN_POINT('Ctrl Pts',(4.5273581020331,-5.85972764552883,134.638657524961));
#219100=CARTESIAN_POINT('Ctrl Pts',(4.24891047822024,0.0585766569097649,
137.806846578216));
#219101=CARTESIAN_POINT('Ctrl Pts',(3.97046285440732,5.92305187327717,134.54009312409));
#219102=CARTESIAN_POINT('Ctrl Pts',(3.69201523059441,6.34453177527304,127.840383997147));
#219103=CARTESIAN_POINT('Ctrl Pts',(3.41356760678156,0.935696923401329,
123.864424586062));
#219104=CARTESIAN_POINT('Ctrl Pts',(3.13511998296867,-5.33299768974021,
126.265927353204));
#219105=CARTESIAN_POINT('Ctrl Pts',(2.85667235915575,-6.70092795743158,
132.838028575505));
#219106=CARTESIAN_POINT('Ctrl Pts',(2.57822473534285,-1.91103279077285,
137.541288294661));
#219107=CARTESIAN_POINT('Ctrl Pts',(2.29977711153,4.63500815146407,136.053640595781));
#219108=CARTESIAN_POINT('Ctrl Pts',(2.02132948771708,6.92170303524179,129.742161038504));
#219109=CARTESIAN_POINT('Ctrl Pts',(1.74288186390418,2.84769097362441,124.40679100305));
#219110=CARTESIAN_POINT('Ctrl Pts',(1.46443424009131,-3.84320997531586,
124.950474904685));
#219111=CARTESIAN_POINT('Ctrl Pts',(1.18598661627842,-7.00238870818588,
130.873593798241));
#219112=CARTESIAN_POINT('Ctrl Pts',(0.907538992465495,-3.72671430393905,
136.733090780986));
#219113=CARTESIAN_POINT('Ctrl Pts',(0.629091368652655,2.97362848551254,
137.144374378117));
#219114=CARTESIAN_POINT('Ctrl Pts',(0.350643744839755,6.94135196660579,
131.729495056193));
#219115=CARTESIAN_POINT('Ctrl Pts',(0.0721961210268491,4.53031209428387,
125.4644623805));
#219116=CARTESIAN_POINT('Ctrl Pts',(-0.206251502786054,-2.04386327463549,
124.106535316138));
#219117=CARTESIAN_POINT('Ctrl Pts',(-0.484699126598912,-6.73982814243653,
128.903582496833));
#219118=CARTESIAN_POINT('Ctrl Pts',(-0.763146750411823,-5.24222020624778,
135.447351912307));
#219119=CARTESIAN_POINT('Ctrl Pts',(-1.04159437422473,1.07273200278813,
137.724439150648));
#219120=CARTESIAN_POINT('Ctrl Pts',(-1.32004199803759,6.40189590713365,
133.642312281717));
#219121=CARTESIAN_POINT('Ctrl Pts',(-1.59848962185049,5.84803022282516,
126.952246475077));
#219122=CARTESIAN_POINT('Ctrl Pts',(-1.87693724566341,-0.0798895441007186,
123.802085379146));
#219123=CARTESIAN_POINT('Ctrl Pts',(-2.1553848694763,-5.93439472281934,
127.08667314716));
#219124=CARTESIAN_POINT('Ctrl Pts',(-2.43383249328916,-6.33548106256618,
133.787634081347));
#219125=CARTESIAN_POINT('Ctrl Pts',(-2.71228011710207,-0.914569811271147,
137.747112443329));
#219126=CARTESIAN_POINT('Ctrl Pts',(-2.99072774091498,5.34678641736288,
135.326541049718));
#219127=CARTESIAN_POINT('Ctrl Pts',(-3.26917536472784,6.6947071334783,128.750306759754));
#219128=CARTESIAN_POINT('Ctrl Pts',(-3.54762298854074,1.89051904855254,
124.061647619009));
#219129=CARTESIAN_POINT('Ctrl Pts',(-3.82607061235365,-4.65096368500298,
125.569212324096));
#219130=CARTESIAN_POINT('Ctrl Pts',(-4.10451823616654,-6.91843800424817,
131.887622559669));
#219131=CARTESIAN_POINT('Ctrl Pts',(-4.38296585997939,-2.82820578207579,
137.210567990736));
#219132=CARTESIAN_POINT('Ctrl Pts',(-4.66141348379231,3.86100938829084,
136.646521806489));
#219133=CARTESIAN_POINT('Ctrl Pts',(-4.93986110760522,7.00214555161287,
130.713814895061));
#219134=CARTESIAN_POINT('Ctrl Pts',(-5.21830873141809,3.70865202682979,
124.864315079211));
#219135=CARTESIAN_POINT('Ctrl Pts',(-5.49675635523098,-2.99291153288594,
124.473426925751));
#219136=CARTESIAN_POINT('Ctrl Pts',(-5.77520397904388,-6.9441356057364,
129.900357551763));
#219137=CARTESIAN_POINT('Ctrl Pts',(-6.05365160285679,-4.51403829679898,
136.158022832244));
#219138=CARTESIAN_POINT('Ctrl Pts',(-6.33209922666964,2.06423968386644,
137.495934078373));
#219139=CARTESIAN_POINT('Ctrl Pts',(-6.61054685048256,6.74558223877327,
132.684616215558));
#219140=CARTESIAN_POINT('Ctrl Pts',(-6.88899447429547,5.22806425626005,
126.145435313781));
#219141=CARTESIAN_POINT('Ctrl Pts',(-7.16744209810832,-1.09378937261818,
123.887579165027));
#219142=CARTESIAN_POINT('Ctrl Pts',(-7.44588972192122,-6.41050400264194,
127.985907267597));
#219143=CARTESIAN_POINT('Ctrl Pts',(-7.72433734573414,-5.8362786247684,
134.674256309687));
#219144=CARTESIAN_POINT('Ctrl Pts',(-8.002784969547,0.101201691205851,137.806360265633));
#219145=CARTESIAN_POINT('Ctrl Pts',(-8.28123259335988,5.94568259693924,
134.503968611703));
#219146=CARTESIAN_POINT('Ctrl Pts',(-8.55968021717279,6.32637165882838,
127.80181794706));
#219147=CARTESIAN_POINT('Ctrl Pts',(-8.8381278409857,0.893434226691435,
123.858857314246));
#219148=CARTESIAN_POINT('Ctrl Pts',(-9.11657546479855,-5.3605256130866,
126.298474910485));
#219149=CARTESIAN_POINT('Ctrl Pts',(-9.39502308861147,-6.68842429067269,
132.878781346775));
#219150=CARTESIAN_POINT('Ctrl Pts',(-9.67347071242438,-1.86998779282204,
137.552796474009));
#219151=CARTESIAN_POINT('Ctrl Pts',(-9.95191833623725,4.66687613264966,
136.025328728591));
#219152=CARTESIAN_POINT('Ctrl Pts',(-10.2303659600501,6.91510888178999,
129.700046347612));
#219153=CARTESIAN_POINT('Ctrl Pts',(-10.508813583863,2.80869439041515,124.389574831969));
#219154=CARTESIAN_POINT('Ctrl Pts',(-10.787261207676,-3.87877303340228,
124.973978073582));
#219155=CARTESIAN_POINT('Ctrl Pts',(-11.0657088314888,-7.00183752812002,
130.916218043094));
#219156=CARTESIAN_POINT('Ctrl Pts',(-11.3441564553017,-3.69055539327479,
136.755666503084));
#219157=CARTESIAN_POINT('Ctrl Pts',(-11.6226040791146,3.01216685433575,
137.126155591738));
#219158=CARTESIAN_POINT('Ctrl Pts',(-11.9010517029275,6.94685491534338,
131.687223935982));
#219159=CARTESIAN_POINT('Ctrl Pts',(-12.1794993267404,4.49772268187999,
125.436984020872));
#219160=CARTESIAN_POINT('Ctrl Pts',(-12.4579469505533,-2.08459697026297,
124.119100987199));
#219161=CARTESIAN_POINT('Ctrl Pts',(-12.7363945743662,-6.75127384495765,
128.944644960744));
#219162=CARTESIAN_POINT('Ctrl Pts',(-13.0148421981791,-5.21385987419926,
135.479176770748));
#219163=CARTESIAN_POINT('Ctrl Pts',(-13.2932898219919,1.11483660973293,
137.717780913442));
#219164=CARTESIAN_POINT('Ctrl Pts',(-13.5717374458049,6.41905271211686,
133.603289543584));
#219165=CARTESIAN_POINT('Ctrl Pts',(-13.8501850696177,5.82447296022373,
126.916719225995));
#219166=CARTESIAN_POINT('Ctrl Pts',(-14.1286326934306,-0.122512900792341,
123.802701425419));
#219167=CARTESIAN_POINT('Ctrl Pts',(-14.4070803172435,-5.95691539106803,
127.122866372359));
#219168=CARTESIAN_POINT('Ctrl Pts',(-14.6855279410564,-6.31720364844761,
133.826144679651));
#219169=CARTESIAN_POINT('Ctrl Pts',(-14.9639755648693,-0.872290365458834,
137.752551056246));
#219170=CARTESIAN_POINT('Ctrl Pts',(-15.2424231886822,5.37421514963333,
135.293909857666));
#219171=CARTESIAN_POINT('Ctrl Pts',(-15.5208708124951,6.68207948721813,
128.709592234107));
#219172=CARTESIAN_POINT('Ctrl Pts',(-15.799318436308,1.84943921378025,124.050264419823));
#219173=CARTESIAN_POINT('Ctrl Pts',(-16.0777660601209,-4.68274534699314,
125.59762105532));
#219174=CARTESIAN_POINT('Ctrl Pts',(-16.3562136839338,-6.91171569870797,
131.929716985153));
#219175=CARTESIAN_POINT('Ctrl Pts',(-16.6346613077467,-2.78915697939336,
137.227665389888));
#219176=CARTESIAN_POINT('Ctrl Pts',(-16.9131089315595,3.89650074609022,
136.622910504741));
#219177=CARTESIAN_POINT('Ctrl Pts',(-17.1915565553724,7.00146464056082,
130.671192525245));
#219178=CARTESIAN_POINT('Ctrl Pts',(-17.4700041791854,3.67242457091876,
124.841849516969));
#219179=CARTESIAN_POINT('Ctrl Pts',(-17.7484518029982,-3.0313942714833,
124.491762925279));
#219180=CARTESIAN_POINT('Ctrl Pts',(-18.0268994268111,-6.94950987023543,
129.942645225261));
#219181=CARTESIAN_POINT('Ctrl Pts',(-18.305347050624,-4.48136540067248,
136.185401873632));
#219182=CARTESIAN_POINT('Ctrl Pts',(-18.5837946744369,2.10493494523792,
137.483244486159));
#219183=CARTESIAN_POINT('Ctrl Pts',(-18.8622422982498,6.75690290826339,
132.643519105064));
#219184=CARTESIAN_POINT('Ctrl Pts',(-19.1406899220627,5.19960719165284,
126.113696921846));
#219185=CARTESIAN_POINT('Ctrl Pts',(-19.4191375458756,-1.1358735191536,
123.894365523333));
#219186=CARTESIAN_POINT('Ctrl Pts',(-19.6975851696885,-6.42754195636435,
128.024982044393));
#219187=CARTESIAN_POINT('Ctrl Pts',(-19.9760327935014,-5.81261333855723,
134.709711694007));
#219188=CARTESIAN_POINT('Ctrl Pts',(-20.2544804173143,0.143822975436045,
137.805614491377));
#219189=CARTESIAN_POINT('Ctrl Pts',(-20.5329280411272,5.96809300114641,
134.467707008981));
#219190=CARTESIAN_POINT('Ctrl Pts',(-20.81137566494,6.30797711635522,127.763363157294));
#219191=CARTESIAN_POINT('Ctrl Pts',(-21.089823288753,0.851138423447451,
123.853547410611));
#219192=CARTESIAN_POINT('Ctrl Pts',(-21.3682709125658,-5.38785490018508,
126.331189435016));
#219193=CARTESIAN_POINT('Ctrl Pts',(-21.6467185363787,-6.67567278189203,
132.919457249623));
#219194=CARTESIAN_POINT('Ctrl Pts',(-21.9251661601916,-1.82887350178604,
137.564054587584));
#219195=CARTESIAN_POINT('Ctrl Pts',(-22.2036137840045,4.69857118102365,
135.996823396506));
#219196=CARTESIAN_POINT('Ctrl Pts',(-22.4820614078173,6.90825848643574,
129.657972577492));
#219197=CARTESIAN_POINT('Ctrl Pts',(-22.7605090316303,2.76959373000234,
124.372596363135));
#219198=CARTESIAN_POINT('Ctrl Pts',(-23.0389566554432,-3.91419236212754,
124.997697289448));
#219199=CARTESIAN_POINT('Ctrl Pts',(-23.3174042792561,-7.0010268923895,
130.958838143028));
#219200=CARTESIAN_POINT('Ctrl Pts',(-23.5958519030689,-3.65425972772349,
136.778021697354));
#219201=CARTESIAN_POINT('Ctrl Pts',(-23.8742995268818,3.05059360620828,
137.107702548922));
#219202=CARTESIAN_POINT('Ctrl Pts',(-24.1527471506948,6.95210044581739,
131.644920100946));
#219203=CARTESIAN_POINT('Ctrl Pts',(-24.4311947745076,4.4649666047081,125.409704551357));
#219204=CARTESIAN_POINT('Ctrl Pts',(-24.7096423983205,-2.12525342038311,
124.131914383013));
#219205=CARTESIAN_POINT('Ctrl Pts',(-24.9880900221334,-6.76246937654364,
128.985776337104));
#219206=CARTESIAN_POINT('Ctrl Pts',(-25.2665376459463,-5.18530634065569,
135.510828402156));
#219207=CARTESIAN_POINT('Ctrl Pts',(-25.5449852697592,1.15689990599717,
137.710866496904));
#219208=CARTESIAN_POINT('Ctrl Pts',(-25.8234328935721,6.43597165674122,
133.564163090109));
#219209=CARTESIAN_POINT('Ctrl Pts',(-26.101880517385,5.8006998696348,126.881336034893));
#219210=CARTESIAN_POINT('Ctrl Pts',(-26.3803281411979,-0.165131717723356,
123.803576920747));
#219211=CARTESIAN_POINT('Ctrl Pts',(-26.6587757650107,-5.9792153236265,
127.15919601668));
#219212=CARTESIAN_POINT('Ctrl Pts',(-26.9372233888237,-6.29869214802456,
133.864543304637));
#219213=CARTESIAN_POINT('Ctrl Pts',(-27.2156710126366,-0.829978596605981,
137.75773220141));
#219214=CARTESIAN_POINT('Ctrl Pts',(-27.4941186364494,5.40144473838504,
135.261112303716));
#219215=CARTESIAN_POINT('Ctrl Pts',(-27.7725662602623,6.66920423404522,
128.668955330874));
#219216=CARTESIAN_POINT('Ctrl Pts',(-28.0510138840753,1.80829084735756,
124.039131496154));
#219217=CARTESIAN_POINT('Ctrl Pts',(-28.3294615078881,-4.71435348813263,
125.626222724194));
#219218=CARTESIAN_POINT('Ctrl Pts',(-28.607909131701,-6.9047372770006,131.971769710144));
#219219=CARTESIAN_POINT('Ctrl Pts',(-28.8863567555139,-2.75000482347336,
137.244524771118));
#219220=CARTESIAN_POINT('Ctrl Pts',(-29.1648043793268,3.93184771762154,
136.599083594488));
#219221=CARTESIAN_POINT('Ctrl Pts',(-29.4432520031397,7.00052428766157,
130.628575090021));
#219222=CARTESIAN_POINT('Ctrl Pts',(-29.7216996269525,3.63606103196502,
124.819604897767));
#219223=CARTESIAN_POINT('Ctrl Pts',(-30.0001472507655,-3.06976468065099,
124.510332840438));
#219224=CARTESIAN_POINT('Ctrl Pts',(-30.2785948745783,-6.95462661809053,
129.984964829937));
#219225=CARTESIAN_POINT('Ctrl Pts',(-30.5570424983912,-4.44852644590303,
136.212581518559));
#219226=CARTESIAN_POINT('Ctrl Pts',(-30.8354901222041,2.14555220747066,
137.470307405446));
#219227=CARTESIAN_POINT('Ctrl Pts',(-31.113937746017,6.7679731982313,132.602353843876));
#219228=CARTESIAN_POINT('Ctrl Pts',(-31.3923853698299,5.17095745368924,
126.082132344179));
#219229=CARTESIAN_POINT('Ctrl Pts',(-31.6708329936428,-1.17791557547805,
123.901407934047));
#219230=CARTESIAN_POINT('Ctrl Pts',(-31.9492806174558,-6.44434173515584,
128.064159812084));
#219231=CARTESIAN_POINT('Ctrl Pts',(-32.2277282412685,-5.78873266382121,
134.745022364106));
#219232=CARTESIAN_POINT('Ctrl Pts',(-32.5061758650815,0.186438930252996,
137.804609283086));
#219233=CARTESIAN_POINT('Ctrl Pts',(-32.7846234888944,5.99028225547263,
134.431309659613));
#219234=CARTESIAN_POINT('Ctrl Pts',(-33.0630711127073,6.28934882947028,
127.725021052809));
#219235=CARTESIAN_POINT('Ctrl Pts',(-33.3415187365202,0.808811080956172,
123.848495071916));
#219236=CARTESIAN_POINT('Ctrl Pts',(-33.619966360333,-5.41498453833882,
126.364069714552));
#219237=CARTESIAN_POINT('Ctrl Pts',(-33.898413984146,-6.66267390360147,
132.960054776787));
#219238=CARTESIAN_POINT('Ctrl Pts',(-34.1768616079588,-1.78769144116968,
137.575062218212));
#219239=CARTESIAN_POINT('Ctrl Pts',(-34.4553092317717,4.73009212211488,
135.968125655805));
#219240=CARTESIAN_POINT('Ctrl Pts',(-34.7337568555846,6.90115210302259,
129.615941287202));
#219241=CARTESIAN_POINT('Ctrl Pts',(-35.0122044793975,2.73039044127535,
124.355856225691));
#219242=CARTESIAN_POINT('Ctrl Pts',(-35.2906521032104,-3.94946664901538,
125.02163167336));
#219243=CARTESIAN_POINT('Ctrl Pts',(-35.5690997270233,-6.99995683103299,
131.00145251874));
#219244=CARTESIAN_POINT('Ctrl Pts',(-35.8475473508362,-3.61782865223385,
136.800155535415));
#219245=CARTESIAN_POINT('Ctrl Pts',(-36.125994974649,3.08890731721304,137.089015933453));
#219246=CARTESIAN_POINT('Ctrl Pts',(-36.404442598462,6.95708836365274,131.60258511867));
#219247=CARTESIAN_POINT('Ctrl Pts',(-36.6828902222748,4.43204507655667,
125.382624982808));
#219248=CARTESIAN_POINT('Ctrl Pts',(-36.9613378460878,-2.16583111845593,
124.144975028777));
#219249=CARTESIAN_POINT('Ctrl Pts',(-37.2397854699006,-6.7734143223399,
129.026975101771));
#219250=CARTESIAN_POINT('Ctrl Pts',(-37.5182330937135,-5.15656066367905,
135.54230563367));
#219251=CARTESIAN_POINT('Ctrl Pts',(-37.7966807175264,1.19892033290996,
137.703696157251));
#219252=CARTESIAN_POINT('Ctrl Pts',(-38.0751283413393,6.45265211406898,
133.524934371139));
#219253=CARTESIAN_POINT('Ctrl Pts',(-38.3535759651522,5.77671183197903,
126.846098212911));
#219254=CARTESIAN_POINT('Ctrl Pts',(-38.6320235889651,-0.207744415637528,
123.80471183269));
#219255=CARTESIAN_POINT('Ctrl Pts',(-38.910471212778,-6.00129369416227,
127.195660733917));
#219256=CARTESIAN_POINT('Ctrl Pts',(-39.1889188365908,-6.27994724724761,
133.902828533427));
#219257=CARTESIAN_POINT('Ctrl Pts',(-39.4673664604039,-0.787636072591,137.762655686833));
#219258=CARTESIAN_POINT('Ctrl Pts',(-39.7458140842166,5.42847417461558,
135.228149603194));
#219259=CARTESIAN_POINT('Ctrl Pts',(-40.0242617080296,6.65608185105682,
128.628397555869));
#219260=CARTESIAN_POINT('Ctrl Pts',(-40.3027093318424,1.76707547405252,
124.028249260538));
#219261=CARTESIAN_POINT('Ctrl Pts',(-40.5811569556554,-4.7457869371699,
125.655016270872));
#219262=CARTESIAN_POINT('Ctrl Pts',(-40.8596045794682,-6.89750299771422,
132.013779176361));
#219263=CARTESIAN_POINT('Ctrl Pts',(-41.1380522032811,-2.7107507651133,
137.261145509698));
#219264=CARTESIAN_POINT('Ctrl Pts',(-41.416499827094,3.96704899308973,136.575041958643));
#219265=CARTESIAN_POINT('Ctrl Pts',(-41.694947450907,6.99932452776054,130.585964168594));
#219266=CARTESIAN_POINT('Ctrl Pts',(-41.9733950747197,3.59956275743227,
124.79758204589));
#219267=CARTESIAN_POINT('Ctrl Pts',(-42.2518426985328,-3.10802133855968,
124.529135983109));
#219268=CARTESIAN_POINT('Ctrl Pts',(-42.5302903223456,-6.95948565969872,
130.027314797628));
#219269=CARTESIAN_POINT('Ctrl Pts',(-42.8087379461585,-4.41552264935019,
136.23956075987));
#219270=CARTESIAN_POINT('Ctrl Pts',(-43.0871855699714,2.18608996547759,
137.457123315624));
#219271=CARTESIAN_POINT('Ctrl Pts',(-43.3656331937842,6.77879269846351,
132.561121957388));
#219272=CARTESIAN_POINT('Ctrl Pts',(-43.6440808175972,5.14211610399531,
126.050742750417));
#219273=CARTESIAN_POINT('Ctrl Pts',(-43.92252844141,-1.21991398370768,123.908706136214));
#219274=CARTESIAN_POINT('Ctrl Pts',(-44.200976065223,-6.46090271649442,
128.103439118922));
#219275=CARTESIAN_POINT('Ctrl Pts',(-44.4794236890358,-5.76463748546755,
134.780187011534));
#219276=CARTESIAN_POINT('Ctrl Pts',(-44.7578713128487,0.229047976506494,
137.803344678006));
#219277=CARTESIAN_POINT('Ctrl Pts',(-45.0363189366615,6.01224953768695,
134.394777912313));
#219278=CARTESIAN_POINT('Ctrl Pts',(-45.3147665604746,6.27048748845154,
127.686793054383));
#219279=CARTESIAN_POINT('Ctrl Pts',(-45.5932141842873,0.766453767672844,
123.843700485376));
#219280=CARTESIAN_POINT('Ctrl Pts',(-45.8716618081003,-5.44191352224889,
126.397114530699));
#219281=CARTESIAN_POINT('Ctrl Pts',(-46.1501094319132,-6.6494281374793,
133.000572423912));
#219282=CARTESIAN_POINT('Ctrl Pts',(-46.4285570557261,-1.74644313698983,
137.585818958004));
#219283=CARTESIAN_POINT('Ctrl Pts',(-46.7070046795389,4.76143778790304,
135.93923656989));
#219284=CARTESIAN_POINT('Ctrl Pts',(-46.9854523033519,6.89378999488032,
129.573954034227));
#219285=CARTESIAN_POINT('Ctrl Pts',(-47.2638999271647,2.69108597692664,
124.339355039948));
#219286=CARTESIAN_POINT('Ctrl Pts',(-47.5423475509777,-3.98459458696386,
125.045780338419));
#219287=CARTESIAN_POINT('Ctrl Pts',(-47.8207951747905,-6.998627383702,131.044059591139));
#219288=CARTESIAN_POINT('Ctrl Pts',(-48.0992427986034,-3.58126351677304,
136.822067197091));
#219289=CARTESIAN_POINT('Ctrl Pts',(-48.3776904224163,3.1271065676212,137.070096437769));
#219290=CARTESIAN_POINT('Ctrl Pts',(-48.6561380462292,6.9618184840203,131.560220557891));
#219291=CARTESIAN_POINT('Ctrl Pts',(-48.9345856700421,4.39895931734504,
125.355746318666));
#219292=CARTESIAN_POINT('Ctrl Pts',(-49.213033293855,-2.20632856086043,
124.158282440523));
#219293=CARTESIAN_POINT('Ctrl Pts',(-49.4914809176678,-6.78410827677761,
129.068239728113));
#219294=CARTESIAN_POINT('Ctrl Pts',(-49.7699285414808,-5.12762390845042,
135.573607298891));
#219295=CARTESIAN_POINT('Ctrl Pts',(-50.0483761652936,1.2408963333889,137.696270160183));
#219296=CARTESIAN_POINT('Ctrl Pts',(-50.3268237891066,6.46909346599971,
133.485604840309));
#219297=CARTESIAN_POINT('Ctrl Pts',(-50.6052714129194,5.7525097361419,126.811007065796));
#219298=CARTESIAN_POINT('Ctrl Pts',(-50.8837190367324,-0.250349415506305,
123.806106119193));
#219299=CARTESIAN_POINT('Ctrl Pts',(-51.1621666605453,-6.02314968455324,
127.232259172855));
#219300=CARTESIAN_POINT('Ctrl Pts',(-51.4406142843581,-6.26096964071598,
133.94099894735));
#219301=CARTESIAN_POINT('Ctrl Pts',(-51.719061908171,-0.745264362431691,
137.767321330073));
#219302=CARTESIAN_POINT('Ctrl Pts',(-51.997509531984,5.45530245673899,135.195022977544));
#219303=CARTESIAN_POINT('Ctrl Pts',(-52.2759571557968,6.64271282450778,
128.587920411975));
#219304=CARTESIAN_POINT('Ctrl Pts',(-52.5544047796097,1.72579462111621,
124.01761811622));
#219305=CARTESIAN_POINT('Ctrl Pts',(-52.8328524034226,-4.77704452932697,
125.684000628399));
#219306=CARTESIAN_POINT('Ctrl Pts',(-53.1113000272355,-6.89001312891767,
132.05574382713));
#219307=CARTESIAN_POINT('Ctrl Pts',(-53.3897476510484,-2.67139625888694,
137.277526989739));
#219308=CARTESIAN_POINT('Ctrl Pts',(-53.6681952748612,4.00210326809833,
136.550786488079));
#219309=CARTESIAN_POINT('Ctrl Pts',(-53.9466428986742,6.99786540531528,
130.543361339928));
#219310=CARTESIAN_POINT('Ctrl Pts',(-54.225090522487,3.56293109977782,124.775781777402));
#219311=CARTESIAN_POINT('Ctrl Pts',(-54.5035381462999,-3.14616282759469,
124.548171656537));
#219312=CARTESIAN_POINT('Ctrl Pts',(-54.7819857701128,-6.9640868150063,
130.069693559035));
#219313=CARTESIAN_POINT('Ctrl Pts',(-55.0604333939257,-4.382355233982,136.266338597842));
#219314=CARTESIAN_POINT('Ctrl Pts',(-55.3388810177386,2.22654671711671,
137.443692705233));
#219315=CARTESIAN_POINT('Ctrl Pts',(-55.6173286415515,6.78936100803939,
132.519824973462));
#219316=CARTESIAN_POINT('Ctrl Pts',(-55.8957762653644,5.11308421129812,
126.019529303714));
#219317=CARTESIAN_POINT('Ctrl Pts',(-56.1742238891773,-1.26186718757599,
123.916259859391));
#219318=CARTESIAN_POINT('Ctrl Pts',(-56.4526715129901,-6.47722428670686,
128.142818509401));
#219319=CARTESIAN_POINT('Ctrl Pts',(-56.7311191368031,-5.74032869635189,
134.815204333253));
#219320=CARTESIAN_POINT('Ctrl Pts',(-57.0095667606159,0.271648535303317,
137.801820722997));
#219321=CARTESIAN_POINT('Ctrl Pts',(-57.2880143844289,6.03399403378365,
134.358113120779));
#219322=CARTESIAN_POINT('Ctrl Pts',(-57.5664620082417,6.25139379221294,
127.64868057857));
#219323=CARTESIAN_POINT('Ctrl Pts',(-57.8449096320546,0.724068053163303,
123.839163828657));
#219324=CARTESIAN_POINT('Ctrl Pts',(-58.1233572558676,-5.46864085405239,
126.430322658971));
#219325=CARTESIAN_POINT('Ctrl Pts',(-58.4018048796803,-6.63593597435208,
133.0410086896));
#219326=CARTESIAN_POINT('Ctrl Pts',(-58.6802525034934,-1.705130117717,137.596324408362));
#219327=CARTESIAN_POINT('Ctrl Pts',(-58.9587001273061,4.79260701686295,
135.910157209259));
#219328=CARTESIAN_POINT('Ctrl Pts',(-59.2371477511191,6.88617243481463,
129.532012374421));
#219329=CARTESIAN_POINT('Ctrl Pts',(-59.515595374932,2.65168179339722,124.323093417365));
#219330=CARTESIAN_POINT('Ctrl Pts',(-59.7940429987449,-4.01957487429483,
125.070142389788));
#219331=CARTESIAN_POINT('Ctrl Pts',(-60.0724906225578,-6.99703859965941,
131.086657781405));
#219332=CARTESIAN_POINT('Ctrl Pts',(-60.3509382463707,-3.5445656762756,
136.843755870437));
#219333=CARTESIAN_POINT('Ctrl Pts',(-60.6293858701835,3.16518994194552,
137.050944762941));
#219334=CARTESIAN_POINT('Ctrl Pts',(-60.9078334939965,6.96629063164357,
131.517827988445));
#219335=CARTESIAN_POINT('Ctrl Pts',(-61.1862811178092,4.36571055307847,
125.32906955493));
#219336=CARTESIAN_POINT('Ctrl Pts',(-61.4647287416223,-2.24674424694855,
124.171836125139));
#219337=CARTESIAN_POINT('Ctrl Pts',(-61.743176365435,-6.79455084358828,
129.109568687053));
#219338=CARTESIAN_POINT('Ctrl Pts',(-62.0216239892481,-5.09849714723216,
135.60473223792));
#219339=CARTESIAN_POINT('Ctrl Pts',(-62.3000716130609,1.2828263519976,137.688588780872));
#219340=CARTESIAN_POINT('Ctrl Pts',(-62.5785192368738,6.48529510329292,
133.446175954988));
#219341=CARTESIAN_POINT('Ctrl Pts',(-62.8569668606868,5.72809447894126,
126.776063893867));
#219342=CARTESIAN_POINT('Ctrl Pts',(-63.1354144844995,-0.292945138585431,
123.80775972859));
#219343=CARTESIAN_POINT('Ctrl Pts',(-63.4138621083125,-6.04478248491762,
127.268989977326));
#219344=CARTESIAN_POINT('Ctrl Pts',(-63.6923097321254,-6.24176003165182,
133.979053131985));
#219345=CARTESIAN_POINT('Ctrl Pts',(-63.9707573559382,-0.702865036227365,
137.771728958244));
#219346=CARTESIAN_POINT('Ctrl Pts',(-64.2492049797512,5.48192859062395,
135.161733654286));
#219347=CARTESIAN_POINT('Ctrl Pts',(-64.527652603564,6.62909764979204,128.547525399088));
#219348=CARTESIAN_POINT('Ctrl Pts',(-64.806100227377,1.68444981822529,124.007238457143));
#219349=CARTESIAN_POINT('Ctrl Pts',(-65.0845478511898,-4.80812510634223,
125.713174722747));
#219350=CARTESIAN_POINT('Ctrl Pts',(-65.3629954750027,-6.88226794815085,
132.097662107432));
#219351=CARTESIAN_POINT('Ctrl Pts',(-65.6414430988157,-2.63194276308962,
137.29366860422));
#219352=CARTESIAN_POINT('Ctrl Pts',(-65.9198907226284,4.03700924369883,
136.526318081592));
#219353=CARTESIAN_POINT('Ctrl Pts',(-66.1983383464414,6.99614697439381,
130.500768182686));
#219354=CARTESIAN_POINT('Ctrl Pts',(-66.4767859702543,3.5261674164012,124.75420490012));
#219355=CARTESIAN_POINT('Ctrl Pts',(-66.7552335940671,-3.18418773440913,
124.567439155348));
#219356=CARTESIAN_POINT('Ctrl Pts',(-67.0336812178801,-6.96842991351606,
130.112099543802));
#219357=CARTESIAN_POINT('Ctrl Pts',(-67.3121288416929,-4.34902542882876,
136.292914040211));
#219358=CARTESIAN_POINT('Ctrl Pts',(-67.5905764655059,2.26692096324861,
137.43001607195));
#219359=CARTESIAN_POINT('Ctrl Pts',(-67.8690240893187,6.79967773534632,
132.478464422373));
#219360=CARTESIAN_POINT('Ctrl Pts',(-68.1474717131316,5.08386285138514,
125.988493160695));
#219361=CARTESIAN_POINT('Ctrl Pts',(-68.4259193369445,-1.30377363249137,
123.924068823677));
#219362=CARTESIAN_POINT('Ctrl Pts',(-68.7043669607574,-6.49330584099122,
128.182296524302));
#219363=CARTESIAN_POINT('Ctrl Pts',(-68.9828145845703,-5.71580719724563,
134.850073031684));
#219364=CARTESIAN_POINT('Ctrl Pts',(-69.2612622083832,0.314239028063776,
137.800037474531));
#219365=CARTESIAN_POINT('Ctrl Pts',(-69.5397098321961,6.05551493801243,
134.32131664364));
#219366=CARTESIAN_POINT('Ctrl Pts',(-69.818157456009,6.23206844827842,127.610685037641));
#219367=CARTESIAN_POINT('Ctrl Pts',(-70.0966050798218,0.681655508046095,
123.834885269867));
#219368=CARTESIAN_POINT('Ctrl Pts',(-70.3750527036349,-5.49516554335789,
126.463692868828));
#219369=CARTESIAN_POINT('Ctrl Pts',(-70.6535003274475,-6.62219791417695,
133.081362075471));
#219370=CARTESIAN_POINT('Ctrl Pts',(-70.9319479512606,-1.66375391422059,
137.606578180005));
#219371=CARTESIAN_POINT('Ctrl Pts',(-71.2103955750734,4.82359865400735,
135.880888651457));
#219372=CARTESIAN_POINT('Ctrl Pts',(-71.4888431988863,6.87829970509706,
129.490117861946));
#219373=CARTESIAN_POINT('Ctrl Pts',(-71.7672908226993,2.6121793508235,124.307071960521));
#219374=CARTESIAN_POINT('Ctrl Pts',(-72.045738446512,-4.05440621480077,
125.094716924722));
#219375=CARTESIAN_POINT('Ctrl Pts',(-72.3241860703251,-6.99519053777849,
131.129245511046));
#219376=CARTESIAN_POINT('Ctrl Pts',(-72.6026336941378,-3.5077364905931,
136.865220751771));
#219377=CARTESIAN_POINT('Ctrl Pts',(-72.8810813179508,3.20315602899298,
137.031561618638));
#219378=CARTESIAN_POINT('Ctrl Pts',(-73.1595289417638,6.97050464080582,
131.475408981201));
#219379=CARTESIAN_POINT('Ctrl Pts',(-73.4379765655765,4.33230001580124,
125.302595680118));
#219380=CARTESIAN_POINT('Ctrl Pts',(-73.7164241893894,-2.28707667910305,
124.18563558039));
#219381=CARTESIAN_POINT('Ctrl Pts',(-73.9948718132024,-6.80474163581863,
129.150960447132));
#219382=CARTESIAN_POINT('Ctrl Pts',(-74.2733194370152,-5.0691814593271,
135.635679297414));
#219383=CARTESIAN_POINT('Ctrl Pts',(-74.5517670608282,1.32470883500465,
137.680652303954));
#219384=CARTESIAN_POINT('Ctrl Pts',(-74.830214684641,6.5012564255912,133.406649176227));
#219385=CARTESIAN_POINT('Ctrl Pts',(-75.108662308454,5.70346696509291,126.741269991954));
#219386=CARTESIAN_POINT('Ctrl Pts',(-75.3871099322667,-0.335530006474783,
123.809672599606));
#219387=CARTESIAN_POINT('Ctrl Pts',(-75.6655575560798,-6.06619129364391,
127.305851786256));
#219388=CARTESIAN_POINT('Ctrl Pts',(-75.9440051798925,-6.22231913187452,
134.016989677222));
#219389=CARTESIAN_POINT('Ctrl Pts',(-76.2224528037055,-0.66043966510086,
137.775878408018));
#219390=CARTESIAN_POINT('Ctrl Pts',(-76.5009004275184,5.50835158962877,
135.128282866967));
#219391=CARTESIAN_POINT('Ctrl Pts',(-76.7793480513312,6.61523683142527,
128.507214014061));
#219392=CARTESIAN_POINT('Ctrl Pts',(-77.0577956751442,1.64304259742666,
123.997110667925));
#219393=CARTESIAN_POINT('Ctrl Pts',(-77.336243298957,-4.83902751651344,
125.742537472861));
#219394=CARTESIAN_POINT('Ctrl Pts',(-77.6146909227699,-6.87426774241415,
132.139532463972));
#219395=CARTESIAN_POINT('Ctrl Pts',(-77.8931385465828,-2.59239173968542,
137.309569755007));
#219396=CARTESIAN_POINT('Ctrl Pts',(-78.1715861703958,4.07176562643718,
136.501637645866));
#219397=CARTESIAN_POINT('Ctrl Pts',(-78.4500337942086,6.99416929867323,
130.458186275174));
#219398=CARTESIAN_POINT('Ctrl Pts',(-78.7284814180215,3.48927306959449,
124.732852213582));
#219399=CARTESIAN_POINT('Ctrl Pts',(-79.0069290418344,-3.22209464997582,
124.586937765577));
#219400=CARTESIAN_POINT('Ctrl Pts',(-79.2853766656473,-6.97251479429268,
130.154531180556));
#219401=CARTESIAN_POINT('Ctrl Pts',(-79.5638242894601,-4.3155344689392,
136.319286102215));
#219402=CARTESIAN_POINT('Ctrl Pts',(-79.8422719132732,2.30721120779087,
137.416093922569));
#219403=CARTESIAN_POINT('Ctrl Pts',(-80.1207195370859,6.80974249809405,
132.437041836753));
#219404=CARTESIAN_POINT('Ctrl Pts',(-80.3991671608989,5.0544531070646,125.957635471416));
#219405=CARTESIAN_POINT('Ctrl Pts',(-80.6776147847117,-1.34563176559565,
123.932132739704));
#219406=CARTESIAN_POINT('Ctrl Pts',(-80.9560624085247,-6.50914678343976,
128.221871700751));
#219407=CARTESIAN_POINT('Ctrl Pts',(-81.2345100323374,-5.69107389680138,
134.884791814753));
#219408=CARTESIAN_POINT('Ctrl Pts',(-81.5129576561506,0.356817876581242,
137.797994998686));
#219409=CARTESIAN_POINT('Ctrl Pts',(-81.7914052799631,6.07681145290804,
134.284389844403));
#219410=CARTESIAN_POINT('Ctrl Pts',(-82.0698529037763,6.21251217275584,
127.572807839535));
#219411=CARTESIAN_POINT('Ctrl Pts',(-82.348300527589,0.639217703933302,
123.830864967548));
#219412=CARTESIAN_POINT('Ctrl Pts',(-82.626748151402,-5.52148660728364,
126.497223923725));
#219413=CARTESIAN_POINT('Ctrl Pts',(-82.9051957752149,-6.60821446602265,
133.121631086217));
#219414=CARTESIAN_POINT('Ctrl Pts',(-83.1836433990278,-1.62231605971109,
137.616579892973));
#219415=CARTESIAN_POINT('Ctrl Pts',(-83.4620910228406,4.85441155092967,
135.851431981043));
#219416=CARTESIAN_POINT('Ctrl Pts',(-83.7405386466535,6.87017209745416,
129.448272049221));
#219417=CARTESIAN_POINT('Ctrl Pts',(-84.0189862704665,2.57258011298421,
124.291291263097));
#219418=CARTESIAN_POINT('Ctrl Pts',(-84.2974338942792,-4.08908731779306,
125.119503032603));
#219419=CARTESIAN_POINT('Ctrl Pts',(-84.5758815180923,-6.99308326653956,
131.171821201958));
#219420=CARTESIAN_POINT('Ctrl Pts',(-84.8543291419051,-3.47077732444568,
136.886461045702));
#219421=CARTESIAN_POINT('Ctrl Pts',(-85.132776765718,3.2410034219148,137.011947723114));
#219422=CARTESIAN_POINT('Ctrl Pts',(-85.4112243895309,6.97446035535538,
131.432965108015));
#219423=CARTESIAN_POINT('Ctrl Pts',(-85.6896720133437,4.29872894355427,
125.27632567523));
#219424=CARTESIAN_POINT('Ctrl Pts',(-85.9681196371569,-2.327324362789,124.19968029493));
#219425=CARTESIAN_POINT('Ctrl Pts',(-86.2465672609694,-6.81468027584547,
129.192413474561));
#219426=CARTESIAN_POINT('Ctrl Pts',(-86.5250148847825,-5.03967793103904,
135.666447330617));
#219427=CARTESIAN_POINT('Ctrl Pts',(-86.8034625085954,1.36654223043768,
137.672461023519));
#219428=CARTESIAN_POINT('Ctrl Pts',(-87.0819101324082,6.51697684144191,
133.367025968708));
#219429=CARTESIAN_POINT('Ctrl Pts',(-87.3603577562212,5.67862810717874,
126.706626649358));
#219430=CARTESIAN_POINT('Ctrl Pts',(-87.638805380034,-0.378102441176264,
123.811844661359));
#219431=CARTESIAN_POINT('Ctrl Pts',(-87.917253003847,-6.08737531742114,
127.342843233717));
#219432=CARTESIAN_POINT('Ctrl Pts',(-88.1957006276599,-6.20264766177327,
134.054807177307));
#219433=CARTESIAN_POINT('Ctrl Pts',(-88.4741482514726,-0.617989821139493,
137.779769525637));
#219434=CARTESIAN_POINT('Ctrl Pts',(-88.7525958752857,5.53457047463998,
135.094671855119));
#219435=CARTESIAN_POINT('Ctrl Pts',(-89.0310434990984,6.6011308830247,128.466987750645));
#219436=CARTESIAN_POINT('Ctrl Pts',(-89.3094911229114,1.60157449308101,
123.987235123859));
#219437=CARTESIAN_POINT('Ctrl Pts',(-89.5879387467241,-4.86975061474005,
125.772087790693));
#219438=CARTESIAN_POINT('Ctrl Pts',(-89.8663863705374,-6.8660128081587,
132.181353345229));
#219439=CARTESIAN_POINT('Ctrl Pts',(-90.1448339943499,-2.55274465425183,
137.325229852876));
#219440=CARTESIAN_POINT('Ctrl Pts',(-90.4232816181632,4.10637112840284,
136.476746095445));
#219441=CARTESIAN_POINT('Ctrl Pts',(-90.7017292419757,6.99193245143733,
130.415617195278));
#219442=CARTESIAN_POINT('Ctrl Pts',(-90.9801768657889,3.45224942649073,
124.711724509022));
#219443=CARTESIAN_POINT('Ctrl Pts',(-91.2586244896016,-3.2598821696406,
124.606666764696));
#219444=CARTESIAN_POINT('Ctrl Pts',(-91.5370721134145,-6.97634130596949,
130.196986896981));
#219445=CARTESIAN_POINT('Ctrl Pts',(-91.8155197372274,-4.28188359533257,
136.345453806627));
#219446=CARTESIAN_POINT('Ctrl Pts',(-92.0939673610402,2.34741595777304,
137.401926772977));
#219447=CARTESIAN_POINT('Ctrl Pts',(-92.3724149848533,6.81955492332935,
132.395558751529));
#219448=CARTESIAN_POINT('Ctrl Pts',(-92.650862608666,5.02485606812542,125.926957379319));
#219449=CARTESIAN_POINT('Ctrl Pts',(-92.929310232479,-1.38744003581995,
123.940451308663));
#219450=CARTESIAN_POINT('Ctrl Pts',(-93.2077578562919,-6.52474652706058,
128.261542572277));
#219451=CARTESIAN_POINT('Ctrl Pts',(-93.4862054801047,-5.66612971152105,
134.919359395943));
#219452=CARTESIAN_POINT('Ctrl Pts',(-93.7646531039176,0.39938350308132,
137.795693371147));
#219453=CARTESIAN_POINT('Ctrl Pts',(-94.0431007277306,6.09788278932073,
134.247334091402));
#219454=CARTESIAN_POINT('Ctrl Pts',(-94.3215483515434,6.19272569030992,
127.535050387806));
#219455=CARTESIAN_POINT('Ctrl Pts',(-94.5999959753563,0.596756213373149,
123.827103070676));
#219456=CARTESIAN_POINT('Ctrl Pts',(-94.8784435991693,-5.54760307049237,
126.530914581157));
#219457=CARTESIAN_POINT('Ctrl Pts',(-95.1568912229821,-6.59398614805128,
133.161814229653));
#219458=CARTESIAN_POINT('Ctrl Pts',(-95.4353388467949,-1.58081808968337,
137.626329176652));
#219459=CARTESIAN_POINT('Ctrl Pts',(-95.7137864706081,4.88504456584684,
135.821788289543));
#219460=CARTESIAN_POINT('Ctrl Pts',(-95.9922340944205,6.86178991305786,
129.406476486855));
#219461=CARTESIAN_POINT('Ctrl Pts',(-96.2706817182339,2.53288554724217,
124.275751909854));
#219462=CARTESIAN_POINT('Ctrl Pts',(-96.5491293420464,-4.12361689815126,
125.144499794972));
#219463=CARTESIAN_POINT('Ctrl Pts',(-96.8275769658595,-6.99071686402826,
131.214383276482));
#219464=CARTESIAN_POINT('Ctrl Pts',(-97.1060245896722,-3.4336895473684,
136.907475965166));
#219465=CARTESIAN_POINT('Ctrl Pts',(-97.3844722134854,3.27873071826322,
136.992103803166));
#219466=CARTESIAN_POINT('Ctrl Pts',(-97.6629198372979,6.9781576287114,131.390497941658));
#219467=CARTESIAN_POINT('Ctrl Pts',(-97.9413674611112,4.26499858032525,
125.250260513709));
#219468=CARTESIAN_POINT('Ctrl Pts',(-98.2198150849237,-2.36748580661544,
124.21396974833));
#219469=CARTESIAN_POINT('Ctrl Pts',(-98.498262708737,-6.82436639538843,
129.233926233285));
#219470=CARTESIAN_POINT('Ctrl Pts',(-98.7767103325495,-5.00998765563179,
135.69703519741));
#219471=CARTESIAN_POINT('Ctrl Pts',(-99.0551579563628,1.40832498814648,
137.664015243098));
#219472=CARTESIAN_POINT('Ctrl Pts',(-99.3336055801754,6.53245576831905,
133.327307800681));
#219473=CARTESIAN_POINT('Ctrl Pts',(-99.6120532039884,5.65357882561176,
126.672135149802));
#219474=CARTESIAN_POINT('Ctrl Pts',(-99.8905008278013,-0.420660865152761,
123.814275833361));
#219475=CARTESIAN_POINT('Ctrl Pts',(-100.168948451614,-6.10833377126732,
127.379962948978));
#219476=CARTESIAN_POINT('Ctrl Pts',(-100.447396075427,-6.18274635028192,
134.092504230901));
#219477=CARTESIAN_POINT('Ctrl Pts',(-100.72584369924,-0.575517077338011,
137.783402166914));
#219478=CARTESIAN_POINT('Ctrl Pts',(-101.004291323053,5.56058427410689,
135.060901864211));
#219479=CARTESIAN_POINT('Ctrl Pts',(-101.282738946866,6.58678032729173,
128.426848099441));
#219480=CARTESIAN_POINT('Ctrl Pts',(-101.561186570679,1.56004704180311,
123.977612190885));
#219481=CARTESIAN_POINT('Ctrl Pts',(-101.839634194492,-4.90029326256724,
125.801824581246));
#219482=CARTESIAN_POINT('Ctrl Pts',(-102.118081818304,-6.85750345127332,
132.223123201514));
#219483=CARTESIAN_POINT('Ctrl Pts',(-102.396529442117,-2.51300297592632,
137.340648317539));
#219484=CARTESIAN_POINT('Ctrl Pts',(-102.67497706593,4.14082446727623,136.451644352694));
#219485=CARTESIAN_POINT('Ctrl Pts',(-102.953424689743,6.98943651557314,
130.373062520413));
#219486=CARTESIAN_POINT('Ctrl Pts',(-103.231872313556,3.41509785901489,
124.690822569333));
#219487=CARTESIAN_POINT('Ctrl Pts',(-103.510319937369,-3.29754889317273,
124.626625421641));
#219488=CARTESIAN_POINT('Ctrl Pts',(-103.788767561182,-6.97990930675369,
130.239465119861));
#219489=CARTESIAN_POINT('Ctrl Pts',(-104.067215184995,-4.24807405495459,
136.371416183792));
#219490=CARTESIAN_POINT('Ctrl Pts',(-104.345662808808,2.38753372339306,
137.387515148146));
#219491=CARTESIAN_POINT('Ctrl Pts',(-104.62411043262,6.82911464744894,132.354016703874));
#219492=CARTESIAN_POINT('Ctrl Pts',(-104.902558056433,4.99507283129728,
125.896460021193));
#219493=CARTESIAN_POINT('Ctrl Pts',(-105.181005680246,-1.42919689394351,
123.949024222305));
#219494=CARTESIAN_POINT('Ctrl Pts',(-105.459453304059,-6.54010449379936,
128.301307668861));
#219495=CARTESIAN_POINT('Ctrl Pts',(-105.737900927872,-5.64097556572054,
134.953774494342));
#219496=CARTESIAN_POINT('Ctrl Pts',(-106.016348551685,0.441934330278796,
137.793132677202));
#219497=CARTESIAN_POINT('Ctrl Pts',(-106.294796175498,6.11872816644418,
134.210150757753));
#219498=CARTESIAN_POINT('Ctrl Pts',(-106.573243799311,6.17270973413615,
127.49741408157));
#219499=CARTESIAN_POINT('Ctrl Pts',(-106.851691423124,0.554272609792058,
123.823599718647));
#219500=CARTESIAN_POINT('Ctrl Pts',(-107.130139046936,-5.57351396522919,
126.564763592701));
#219501=CARTESIAN_POINT('Ctrl Pts',(-107.40858667075,-6.57951348749827,
133.201910016778));
#219502=CARTESIAN_POINT('Ctrl Pts',(-107.687034294562,-1.53926154185996,
137.635825669776));
#219503=CARTESIAN_POINT('Ctrl Pts',(-107.965481918375,4.91549656364115,
135.791958675416));
#219504=CARTESIAN_POINT('Ctrl Pts',(-108.243929542188,6.85315346251289,
129.364732723601));
#219505=CARTESIAN_POINT('Ctrl Pts',(-108.522377166001,2.49309712449469,
124.260454476607));
#219506=CARTESIAN_POINT('Ctrl Pts',(-108.800824789814,-4.15799367636883,
125.169706285567));
#219507=CARTESIAN_POINT('Ctrl Pts',(-109.079272413627,-6.98809141793296,
131.256930157466));
#219508=CARTESIAN_POINT('Ctrl Pts',(-109.35772003744,-3.39647453366164,
136.928264731447));
#219509=CARTESIAN_POINT('Ctrl Pts',(-109.636167661252,3.31633652003941,
136.97203059412));
#219510=CARTESIAN_POINT('Ctrl Pts',(-109.914615285065,6.98159632387027,
131.348009055767));
#219511=CARTESIAN_POINT('Ctrl Pts',(-110.193062908878,4.23111017600536,
125.22440116141));
#219512=CARTESIAN_POINT('Ctrl Pts',(-110.471510532691,-2.40755952238467,
124.228503411086));
#219513=CARTESIAN_POINT('Ctrl Pts',(-110.749958156504,-6.83379963552497,
129.275497185033));
#219514=CARTESIAN_POINT('Ctrl Pts',(-111.028405780317,-4.98011173328953,
135.727441764346));
#219515=CARTESIAN_POINT('Ctrl Pts',(-111.30685340413,1.45005555985492,137.655315275653));
#219516=CARTESIAN_POINT('Ctrl Pts',(-111.585301027943,6.54769263264538,
133.287496143919));
#219517=CARTESIAN_POINT('Ctrl Pts',(-111.863748651756,5.62832004860235,
126.63779677138));
#219518=CARTESIAN_POINT('Ctrl Pts',(-112.142196275568,-0.463203701385527,
123.816966025527));
#219519=CARTESIAN_POINT('Ctrl Pts',(-112.420643899382,-6.12906587855929,
127.417209556553));
#219520=CARTESIAN_POINT('Ctrl Pts',(-112.699091523194,-6.16261593485082,
134.130079441122));
#219521=CARTESIAN_POINT('Ctrl Pts',(-112.977539147007,-0.533023007539609,
137.786776197239));
#219522=CARTESIAN_POINT('Ctrl Pts',(-113.25598677082,5.58639202407863,135.026974145601));
#219523=CARTESIAN_POINT('Ctrl Pts',(-113.534434394633,6.57218569599142,
128.386796547837));
#219524=CARTESIAN_POINT('Ctrl Pts',(-113.812882018446,1.5184617824084,123.968242225583));
#219525=CARTESIAN_POINT('Ctrl Pts',(-114.091329642259,-4.93065432822552,
125.831746742611));
#219526=CARTESIAN_POINT('Ctrl Pts',(-114.369777266072,-6.84873998707567,
132.26484048503));
#219527=CARTESIAN_POINT('Ctrl Pts',(-114.648224889884,-2.4731681773514,
137.355824577657));
#219528=CARTESIAN_POINT('Ctrl Pts',(-114.926672513697,4.17512436637621,
136.426333347767));
#219529=CARTESIAN_POINT('Ctrl Pts',(-115.20512013751,6.98668158356849,130.330523827459));
#219530=CARTESIAN_POINT('Ctrl Pts',(-115.483567761323,3.377819743832,124.670147169045));
#219531=CARTESIAN_POINT('Ctrl Pts',(-115.762015385136,-3.33509342481799,
124.646812996834));
#219532=CARTESIAN_POINT('Ctrl Pts',(-116.040463008949,-6.98321866443162,
130.281964275151));
#219533=CARTESIAN_POINT('Ctrl Pts',(-116.318910632762,-4.21410710063033,
136.397172271667));
#219534=CARTESIAN_POINT('Ctrl Pts',(-116.597358256575,2.42756301807353,
137.372859582102));
#219535=CARTESIAN_POINT('Ctrl Pts',(-116.875805880388,6.83842131621399,
132.312417233142));
#219536=CARTESIAN_POINT('Ctrl Pts',(-117.154253504201,4.96510450020791,
125.866144527128));
#219537=CARTESIAN_POINT('Ctrl Pts',(-117.432701128013,-1.47090079265054,
123.957851162959));
#219538=CARTESIAN_POINT('Ctrl Pts',(-117.711148751826,-6.55522011456102,
128.341165516992));
#219539=CARTESIAN_POINT('Ctrl Pts',(-117.989596375639,-5.61561239149597,
134.988035834682));
#219540=CARTESIAN_POINT('Ctrl Pts',(-118.268043999452,0.484468781437156,
137.790313011739));
#219541=CARTESIAN_POINT('Ctrl Pts',(-118.546491623265,6.13934681184524,
134.172841221298));
#219542=CARTESIAN_POINT('Ctrl Pts',(-118.824939247078,6.15246504593319,
127.459900315453));
#219543=CARTESIAN_POINT('Ctrl Pts',(-119.103386870891,0.511768467435545,
123.820355041281));
#219544=CARTESIAN_POINT('Ctrl Pts',(-119.381834494704,-5.59921833135585,
126.598769704074));
#219545=CARTESIAN_POINT('Ctrl Pts',(-119.660282118516,-6.56479702065358,
133.241916961827));
#219546=CARTESIAN_POINT('Ctrl Pts',(-119.93872974233,-1.49764795613459,
137.645069020452));
#219547=CARTESIAN_POINT('Ctrl Pts',(-120.217177366142,4.94576641590264,
135.761944244007));
#219548=CARTESIAN_POINT('Ctrl Pts',(-120.495624989955,6.84426306584611,
129.323042306287));
#219549=CARTESIAN_POINT('Ctrl Pts',(-120.774072613768,2.45321631911644,
124.245399530209));
#219550=CARTESIAN_POINT('Ctrl Pts',(-121.052520237581,-4.19221637860163,
125.195121570349));
#219551=CARTESIAN_POINT('Ctrl Pts',(-121.330967861394,-6.98520702554029,
131.299460268319));
#219552=CARTESIAN_POINT('Ctrl Pts',(-121.609415485207,-3.35913366234199,
136.948826574209));
#219553=CARTESIAN_POINT('Ctrl Pts',(-121.88786310902,3.3538194337463,136.951728839794));
#219554=CARTESIAN_POINT('Ctrl Pts',(-122.166310732833,6.98477631340985,
131.305500024783));
#219555=CARTESIAN_POINT('Ctrl Pts',(-122.444758356646,4.19706498634193,
125.198748576561));
#219556=CARTESIAN_POINT('Ctrl Pts',(-122.723205980458,-2.44754402515043,
124.24328074465));
#219557=CARTESIAN_POINT('Ctrl Pts',(-123.001653604271,-6.84297964670285,
129.317124789377));
#219558=CARTESIAN_POINT('Ctrl Pts',(-123.280101228084,-4.95005127107555,
135.7576659047));
#219559=CARTESIAN_POINT('Ctrl Pts',(-123.558548851897,1.49173239922134,
137.646361443563));
#219560=CARTESIAN_POINT('Ctrl Pts',(-123.83699647571,6.5626868698133,133.247592473656));
#219561=CARTESIAN_POINT('Ctrl Pts',(-124.115444099523,5.60285271212367,
126.603612786514));
#219562=CARTESIAN_POINT('Ctrl Pts',(-124.393891723336,-0.505729373435472,
123.819915138168));
#219563=CARTESIAN_POINT('Ctrl Pts',(-124.672339347149,-6.14957087106115,
127.454581676257));
#219564=CARTESIAN_POINT('Ctrl Pts',(-124.950786970961,-6.14225716141998,
134.167531415611));
#219565=CARTESIAN_POINT('Ctrl Pts',(-125.229234594775,-0.490509186377616,
137.789891491587));
#219566=CARTESIAN_POINT('Ctrl Pts',(-125.507682218587,5.6119927682395,134.992889956494));
#219567=CARTESIAN_POINT('Ctrl Pts',(-125.786129842401,6.55734752993325,
128.346834579959));
#219568=CARTESIAN_POINT('Ctrl Pts',(-126.064577466213,1.47682025585389,
123.959125575163));
#219569=CARTESIAN_POINT('Ctrl Pts',(-126.343025090026,-4.9608326866744,
125.861853166013));
#219570=CARTESIAN_POINT('Ctrl Pts',(-126.621472713839,-6.8397227402992,
132.306503649927));
#219571=CARTESIAN_POINT('Ctrl Pts',(-126.899920337652,-2.43324173462049,
137.370758070868));
#219572=CARTESIAN_POINT('Ctrl Pts',(-127.178367961465,4.20926955470684,
136.400814018573));
#219573=CARTESIAN_POINT('Ctrl Pts',(-127.456815585278,6.98366775750873,
130.288002692701));
#219574=CARTESIAN_POINT('Ctrl Pts',(-127.73526320909,3.34041646229627,124.649699074291));
#219575=CARTESIAN_POINT('Ctrl Pts',(-128.013710832904,-3.37251437334987,
124.66722874222));
#219576=CARTESIAN_POINT('Ctrl Pts',(-128.292158456716,-6.9862692563739,
130.324482788031));
#219577=CARTESIAN_POINT('Ctrl Pts',(-128.570606080529,-4.17998399101771,
136.422721115849));
#219578=CARTESIAN_POINT('Ctrl Pts',(-128.849053704342,2.46750235851359,
137.357960617914));
#219579=CARTESIAN_POINT('Ctrl Pts',(-129.127501328155,6.84747458476236,
132.270761880817));
#219580=CARTESIAN_POINT('Ctrl Pts',(-129.405948951968,4.93495218534535,
125.836012020477));
#219581=CARTESIAN_POINT('Ctrl Pts',(-129.684396575781,-1.51255018658779,
123.966931803538));
#219582=CARTESIAN_POINT('Ctrl Pts',(-129.962844199593,-6.57009282923063,
128.381114639724));
#219583=CARTESIAN_POINT('Ctrl Pts',(-130.241291823406,-5.59004112868908,
135.022142147398));
#219584=CARTESIAN_POINT('Ctrl Pts',(-130.519739447219,0.52698528042665,
137.78723447924));
#219585=CARTESIAN_POINT('Ctrl Pts',(-130.798187071032,6.15973796149245,
134.135406864555));
#219586=CARTESIAN_POINT('Ctrl Pts',(-131.076634694845,6.13199237587537,
127.422510479544));
#219587=CARTESIAN_POINT('Ctrl Pts',(-131.355082318658,0.4692453613103,123.81736915881));
#219588=CARTESIAN_POINT('Ctrl Pts',(-131.633529942471,-5.62471521638866,
126.632931655165));
#219589=CARTESIAN_POINT('Ctrl Pts',(-131.911977566284,-6.54983729284086,
133.281833582332));
#219590=CARTESIAN_POINT('Ctrl Pts',(-132.190425190097,-1.45597887451291,
137.654058886162));
#219591=CARTESIAN_POINT('Ctrl Pts',(-132.46887281391,4.97585300097076,135.731746107516));
#219592=CARTESIAN_POINT('Ctrl Pts',(-132.747320437723,6.83511905249447,
129.281406779768));
#219593=CARTESIAN_POINT('Ctrl Pts',(-133.025768061535,2.4132446089053,124.230587628526));
#219594=CARTESIAN_POINT('Ctrl Pts',(-133.304215685348,-4.22628373671482,
125.220744707546));
#219595=CARTESIAN_POINT('Ctrl Pts',(-133.582663309161,-6.98206379373247,
131.341972033073));
#219596=CARTESIAN_POINT('Ctrl Pts',(-133.861110932974,-3.32166831708915,
136.969160731525));
#219597=CARTESIAN_POINT('Ctrl Pts',(-134.139558556787,3.39117807044069,
136.931199292478));
#219598=CARTESIAN_POINT('Ctrl Pts',(-134.4180061806,6.98769747949419,131.262972423894));
#219599=CARTESIAN_POINT('Ctrl Pts',(-134.696453804413,4.16286427289247,
125.173303709728));
#219600=CARTESIAN_POINT('Ctrl Pts',(-134.974901428226,-2.48743783327188,
124.25830120144));
#219601=CARTESIAN_POINT('Ctrl Pts',(-135.253349052039,-6.85190608875344,
129.358807503792));
#219602=CARTESIAN_POINT('Ctrl Pts',(-135.531796675851,-4.91980738289134,
135.787706498505));
#219603=CARTESIAN_POINT('Ctrl Pts',(-135.810244299665,1.53335396189511,
137.637154078616));
#219604=CARTESIAN_POINT('Ctrl Pts',(-136.088691923477,6.57743792420584,
133.207598268539));
#219605=CARTESIAN_POINT('Ctrl Pts',(-136.36713954729,5.57717775987727,126.569584461903));
#219606=CARTESIAN_POINT('Ctrl Pts',(-136.645587171103,-0.548236305497475,
123.823123062006));
#219607=CARTESIAN_POINT('Ctrl Pts',(-136.924034794916,-6.1698479889529,
127.492077923251));
#219608=CARTESIAN_POINT('Ctrl Pts',(-137.202482418729,-6.12167078439119,
134.204858766568));
#219609=CARTESIAN_POINT('Ctrl Pts',(-137.480930042542,-0.447977189217358,
137.792747934521));
#219610=CARTESIAN_POINT('Ctrl Pts',(-137.759377666354,5.63738555794455,
134.958650559891));
#219611=CARTESIAN_POINT('Ctrl Pts',(-138.037825290167,6.54226637895086,
128.306963676612));
#219612=CARTESIAN_POINT('Ctrl Pts',(-138.31627291398,1.43512400518173,123.950262577445));
#219613=CARTESIAN_POINT('Ctrl Pts',(-138.594720537793,-4.99082721964375,
125.892142735845));
#219614=CARTESIAN_POINT('Ctrl Pts',(-138.873168161606,-6.83045204508126,
132.348111152362));
#219615=CARTESIAN_POINT('Ctrl Pts',(-139.151615785419,-2.39322512722196,
137.385448243807));
#219616=CARTESIAN_POINT('Ctrl Pts',(-139.430063409232,4.24325876700673,
136.375087310741));
#219617=CARTESIAN_POINT('Ctrl Pts',(-139.708511033045,6.98039514907165,
130.245500691775));
#219618=CARTESIAN_POINT('Ctrl Pts',(-139.986958656858,3.30288940040013,
124.629479042785));
#219619=CARTESIAN_POINT('Ctrl Pts',(-140.26540628067,-3.40981035212143,
124.687871901284));
#219620=CARTESIAN_POINT('Ctrl Pts',(-140.543853904484,-6.98906096953965,
130.36701908296));
#219621=CARTESIAN_POINT('Ctrl Pts',(-140.822301528296,-4.1457059905611,
136.448061769617));
#219622=CARTESIAN_POINT('Ctrl Pts',(-141.100749152109,2.50735026474636,
137.342818807668));
#219623=CARTESIAN_POINT('Ctrl Pts',(-141.379196775922,6.85627411762182,
132.229052190456));
#219624=CARTESIAN_POINT('Ctrl Pts',(-141.657644399735,4.90461700401472,
125.80606361781));
#219625=CARTESIAN_POINT('Ctrl Pts',(-141.936092023548,-1.5541435324211,
123.976265807557));
#219626=CARTESIAN_POINT('Ctrl Pts',(-142.214539647361,-6.58472208669408,
128.421153556726));
#219627=CARTESIAN_POINT('Ctrl Pts',(-142.492987271174,-5.56426272485295,
135.056092168669));
#219628=CARTESIAN_POINT('Ctrl Pts',(-142.771434894987,0.569482251782813,
137.783897193782));
#219629=CARTESIAN_POINT('Ctrl Pts',(-143.0498825188,6.17990085978423,134.097849074668));
#219630=CARTESIAN_POINT('Ctrl Pts',(-143.328330142612,6.11129248258502,
127.385245959334));
#219631=CARTESIAN_POINT('Ctrl Pts',(-143.606777766425,0.426704867125613,
123.814642181877));
#219632=CARTESIAN_POINT('Ctrl Pts',(-143.885225390238,-5.65000367553061,
126.667248180088));
#219633=CARTESIAN_POINT('Ctrl Pts',(-144.163673014051,-6.53463485839856,
133.321658399163));
#219634=CARTESIAN_POINT('Ctrl Pts',(-144.442120637864,-1.4142558410586,
137.662794933783));
#219635=CARTESIAN_POINT('Ctrl Pts',(-144.720568261677,5.00575520397605,
135.701365384942));
#219636=CARTESIAN_POINT('Ctrl Pts',(-144.99901588549,6.82572176129271,129.239827686864));
#219637=CARTESIAN_POINT('Ctrl Pts',(-145.277463509303,2.37318347502772,
124.216019320419));
#219638=CARTESIAN_POINT('Ctrl Pts',(-145.555911133116,-4.26019448832994,
125.246574747685));
#219639=CARTESIAN_POINT('Ctrl Pts',(-145.834358756928,-6.97866183898313,
131.384463876438));
#219640=CARTESIAN_POINT('Ctrl Pts',(-146.112806380741,-3.28407988619528,
136.989266449907));
#219641=CARTESIAN_POINT('Ctrl Pts',(-146.391254004554,3.42841104578457,
136.910442712901));
#219642=CARTESIAN_POINT('Ctrl Pts',(-146.669701628367,6.99035971387901,
131.220427828976));
#219643=CARTESIAN_POINT('Ctrl Pts',(-146.94814925218,4.12850930297597,125.148067503779));
#219644=CARTESIAN_POINT('Ctrl Pts',(-147.226596875993,-2.52723946847004,
124.27356422487));
#219645=CARTESIAN_POINT('Ctrl Pts',(-147.505044499806,-6.86057863090408,
129.400543783708));
#219646=CARTESIAN_POINT('Ctrl Pts',(-147.783492123619,-4.88938118943532,
135.817562432597));
#219647=CARTESIAN_POINT('Ctrl Pts',(-148.061939747432,1.57491870557395,
137.627693521995));
#219648=CARTESIAN_POINT('Ctrl Pts',(-148.340387371245,6.5919452492172,133.167515010566));
#219649=CARTESIAN_POINT('Ctrl Pts',(-148.618834995057,5.55129614325799,
126.535713058481));
#219650=CARTESIAN_POINT('Ctrl Pts',(-148.89728261887,-0.590722922461593,
123.826589678167));
#219651=CARTESIAN_POINT('Ctrl Pts',(-149.175730242683,-6.18989648085842,
127.529696908099));
#219652=CARTESIAN_POINT('Ctrl Pts',(-149.454177866496,-6.10085756660025,
134.242060110815));
#219653=CARTESIAN_POINT('Ctrl Pts',(-149.732625490309,-0.405428592098244,
137.795345420191));
#219654=CARTESIAN_POINT('Ctrl Pts',(-150.011073114122,5.66256945225453,
134.924257224548));
#219655=CARTESIAN_POINT('Ctrl Pts',(-150.289520737935,6.52694280188189,
128.267185315226));
#219656=CARTESIAN_POINT('Ctrl Pts',(-150.567968361748,1.39337457546175,
123.94165356085));
#219657=CARTESIAN_POINT('Ctrl Pts',(-150.84641598556,-5.02063681567507,
125.922614329717));
#219658=CARTESIAN_POINT('Ctrl Pts',(-151.124863609373,-6.8209282449509,
132.389661450552));
#219659=CARTESIAN_POINT('Ctrl Pts',(-151.403311233186,-2.35311983798619,
137.399894552124));
#219660=CARTESIAN_POINT('Ctrl Pts',(-151.681758856999,4.2770907437925,136.349154177582));
#219661=CARTESIAN_POINT('Ctrl Pts',(-151.960206480812,6.97686387952531,
130.20301939961));
#219662=CARTESIAN_POINT('Ctrl Pts',(-152.238654104625,3.26523994872261,
124.609487823786));
#219663=CARTESIAN_POINT('Ctrl Pts',(-152.517101728438,-3.44697997911642,
124.708741709087));
#219664=CARTESIAN_POINT('Ctrl Pts',(-152.795549352251,-6.99159370048095,
130.40957158374));
#219665=CARTESIAN_POINT('Ctrl Pts',(-153.073996976064,-4.11127436944443,
136.473193293963));
#219666=CARTESIAN_POINT('Ctrl Pts',(-153.352444599876,2.54710526019297,
137.327434712448));
#219667=CARTESIAN_POINT('Ctrl Pts',(-153.63089222369,6.86481958872245,132.187289707623));
#219668=CARTESIAN_POINT('Ctrl Pts',(-153.909339847502,4.87410008029735,
125.776300428876));
#219669=CARTESIAN_POINT('Ctrl Pts',(-154.187787471315,-1.5956792888948,
123.98585282914));
#219670=CARTESIAN_POINT('Ctrl Pts',(-154.466235095128,-6.5991073448593,
128.461280784342));
#219671=CARTESIAN_POINT('Ctrl Pts',(-154.744682718941,-5.53827813521478,
135.089884640464));
#219672=CARTESIAN_POINT('Ctrl Pts',(-155.023130342754,0.611958120764675,
137.78030127903));
#219673=CARTESIAN_POINT('Ctrl Pts',(-155.301577966567,6.19983475957701,
134.060169243357));
#219674=CARTESIAN_POINT('Ctrl Pts',(-155.58002559038,6.0903661331043,127.348108135675));
#219675=CARTESIAN_POINT('Ctrl Pts',(-155.858473214192,0.38414856123516,
123.812174211531));
#219676=CARTESIAN_POINT('Ctrl Pts',(-156.136920838005,-5.67508277170857,
126.701718007236));
#219677=CARTESIAN_POINT('Ctrl Pts',(-156.415368461818,-6.51919028065846,
133.3613899366));
#219678=CARTESIAN_POINT('Ctrl Pts',(-156.693816085631,-1.37248040183399,
137.671276839599));
#219679=CARTESIAN_POINT('Ctrl Pts',(-156.972263709444,5.03547191688086,
135.670803202055));
#219680=CARTESIAN_POINT('Ctrl Pts',(-157.250711333257,6.81607154046107,
129.198306568304));
#219681=CARTESIAN_POINT('Ctrl Pts',(-157.52915895707,2.33303440196427,124.201695145721));
#219682=CARTESIAN_POINT('Ctrl Pts',(-157.807606580883,-4.29394737687161,
125.272610733624));
#219683=CARTESIAN_POINT('Ctrl Pts',(-158.086054204696,-6.97500128735293,
131.426934223863));
#219684=CARTESIAN_POINT('Ctrl Pts',(-158.364501828508,-3.2463697625135,
137.009142984327));
#219685=CARTESIAN_POINT('Ctrl Pts',(-158.642949452322,3.46551698009634,
136.889459870208));
#219686=CARTESIAN_POINT('Ctrl Pts',(-158.921397076134,6.99276291791392,
131.177867816534));
#219687=CARTESIAN_POINT('Ctrl Pts',(-159.199844699947,4.09400134962899,
125.123040893851));
#219688=CARTESIAN_POINT('Ctrl Pts',(-159.47829232376,-2.56694745588028,
124.289069249361));
#219689=CARTESIAN_POINT('Ctrl Pts',(-159.756739947573,-6.86899695179061,
129.442332082575));
#219690=CARTESIAN_POINT('Ctrl Pts',(-160.035187571386,-4.85877381816122,
135.84723260065));
#219691=CARTESIAN_POINT('Ctrl Pts',(-160.313635195198,1.61642509006095,
137.617980124263));
#219692=CARTESIAN_POINT('Ctrl Pts',(-160.592082819012,6.60620830727321,
133.12734418504));
#219693=CARTESIAN_POINT('Ctrl Pts',(-160.870530442824,5.52520882131862,
126.501999831362));
#219694=CARTESIAN_POINT('Ctrl Pts',(-161.148978066638,-0.633187649970563,
123.830314858198));
#219695=CARTESIAN_POINT('Ctrl Pts',(-161.42742569045,-6.20971560387352,
127.567437236815));
#219696=CARTESIAN_POINT('Ctrl Pts',(-161.705873314263,-6.07981827928859,
134.279134069845));
#219697=CARTESIAN_POINT('Ctrl Pts',(-161.984320938076,-0.362864971672915,
137.79768385235));
#219698=CARTESIAN_POINT('Ctrl Pts',(-162.262768561889,5.68754351797111,
134.889711224922));
#219699=CARTESIAN_POINT('Ctrl Pts',(-162.541216185702,6.5113773665471,128.227500969805));
#219700=CARTESIAN_POINT('Ctrl Pts',(-162.819663809515,1.35157351373451,
123.93329884439));
#219701=CARTESIAN_POINT('Ctrl Pts',(-163.098111433328,-5.05026037016286,
125.953266818493));
#219702=CARTESIAN_POINT('Ctrl Pts',(-163.376559057141,-6.81115169281603,
132.431153004838));
#219703=CARTESIAN_POINT('Ctrl Pts',(-163.655006680953,-2.31292735302948,
137.414096460505));
#219704=CARTESIAN_POINT('Ctrl Pts',(-163.933454304766,4.31076423140788,
136.323015580059));
#219705=CARTESIAN_POINT('Ctrl Pts',(-164.211901928579,6.97307407972212,
130.160560390364));
#219706=CARTESIAN_POINT('Ctrl Pts',(-164.490349552392,3.2274695023783,124.589726158078));
#219707=CARTESIAN_POINT('Ctrl Pts',(-164.768797176205,-3.4840218770001,
124.729837392289));
#219708=CARTESIAN_POINT('Ctrl Pts',(-165.047244800018,-6.99386735534677,
130.452138713572));
#219709=CARTESIAN_POINT('Ctrl Pts',(-165.325692423831,-4.07669040354407,
136.498114757629));
#219710=CARTESIAN_POINT('Ctrl Pts',(-165.604140047644,2.58676587171747,
137.31180890232));
#219711=CARTESIAN_POINT('Ctrl Pts',(-165.882587671457,6.87311068140868,
132.145475979844));
#219712=CARTESIAN_POINT('Ctrl Pts',(-166.161035295269,4.84340254500906,
125.746723556562));
#219713=CARTESIAN_POINT('Ctrl Pts',(-166.439482919082,-1.63715591688565,
123.995692513036));
#219714=CARTESIAN_POINT('Ctrl Pts',(-166.717930542895,-6.61324807067504,
128.501494835643));
#219715=CARTESIAN_POINT('Ctrl Pts',(-166.996378166708,-5.5120883226436,
135.12351831059));
#219716=CARTESIAN_POINT('Ctrl Pts',(-167.274825790521,0.654411313413328,
137.776446868231));
#219717=CARTESIAN_POINT('Ctrl Pts',(-167.553273414334,6.21953892221278,
134.022368766858));
#219718=CARTESIAN_POINT('Ctrl Pts',(-167.831721038147,6.06921410286677,
127.311098384725));
#219719=CARTESIAN_POINT('Ctrl Pts',(-168.11016866196,0.3415780205785,123.809965339223));
#219720=CARTESIAN_POINT('Ctrl Pts',(-168.388616285773,-5.69995157560742,
126.736339859314));
#219721=CARTESIAN_POINT('Ctrl Pts',(-168.667063909585,-6.50350413192509,
133.401026722375));
#219722=CARTESIAN_POINT('Ctrl Pts',(-168.945511533399,-1.33065410484337,
137.679504289309));
#219723=CARTESIAN_POINT('Ctrl Pts',(-169.223959157211,5.06500203852252,
135.640060691349));
#219724=CARTESIAN_POINT('Ctrl Pts',(-169.502406781024,6.80616874759175,
129.156844962666));
#219725=CARTESIAN_POINT('Ctrl Pts',(-169.780854404837,2.29279887745254,
124.18761563522));
#219726=CARTESIAN_POINT('Ctrl Pts',(-170.05930202865,-4.32754115161411,
125.298851700587));
#219727=CARTESIAN_POINT('Ctrl Pts',(-170.337749652463,-6.97108227448498,
131.469381501595));
#219728=CARTESIAN_POINT('Ctrl Pts',(-170.616197276276,-3.20853934340632,
137.028789598255));
#219729=CARTESIAN_POINT('Ctrl Pts',(-170.894644900089,3.50249449840198,
136.868251541923));
#219730=CARTESIAN_POINT('Ctrl Pts',(-171.173092523901,6.99490700254731,
131.135293963646));
#219731=CARTESIAN_POINT('Ctrl Pts',(-171.451540147715,4.05934169155642,
125.098224807315));
#219732=CARTESIAN_POINT('Ctrl Pts',(-171.729987771527,-2.60656032410858,
124.304815700371));
#219733=CARTESIAN_POINT('Ctrl Pts',(-172.00843539534,-6.87716073946864,
129.484170851909));
#219734=CARTESIAN_POINT('Ctrl Pts',(-172.286883019153,-4.82798640323697,
135.876715903229));
#219735=CARTESIAN_POINT('Ctrl Pts',(-172.565330642966,1.65787157732142,
137.608014245356));
#219736=CARTESIAN_POINT('Ctrl Pts',(-172.843778266779,6.62022656985093,
133.087087280501));
#219737=CARTESIAN_POINT('Ctrl Pts',(-173.122225890592,5.49891676073447,
126.468446029806));
#219738=CARTESIAN_POINT('Ctrl Pts',(-173.400673514405,-0.675628914478315,
123.834298464058));
#219739=CARTESIAN_POINT('Ctrl Pts',(-173.679121138218,-6.22930462359329,
127.605297510917));
#219740=CARTESIAN_POINT('Ctrl Pts',(-173.95756876203,-6.05855370207473,
134.316079269865));
#219741=CARTESIAN_POINT('Ctrl Pts',(-174.236016385844,-0.320287905152608,
137.799763144343));
#219742=CARTESIAN_POINT('Ctrl Pts',(-174.514464009656,5.71230682967103,
134.855013841124));
#219743=CARTESIAN_POINT('Ctrl Pts',(-174.792911633469,6.49557064972945,
128.187912110866));
#219744=CARTESIAN_POINT('Ctrl Pts',(-175.071359257282,1.30972236895365,
123.925198737649));
#219745=CARTESIAN_POINT('Ctrl Pts',(-175.349806881095,-5.07969678539539,
125.984099066334));
#219746=CARTESIAN_POINT('Ctrl Pts',(-175.628254504908,-6.80112275095037,
132.472584277733));
#219747=CARTESIAN_POINT('Ctrl Pts',(-175.906702128721,-2.27264916169912,
137.428053442694));
#219748=CARTESIAN_POINT('Ctrl Pts',(-176.185149752534,4.34427798206938,
136.296672486746));
#219749=CARTESIAN_POINT('Ctrl Pts',(-176.463597376347,6.96902589009458,
130.118125237372));
#219750=CARTESIAN_POINT('Ctrl Pts',(-176.742045000159,3.18957946096438,
124.570194777934));
#219751=CARTESIAN_POINT('Ctrl Pts',(-177.020492623972,-3.52093467317244,
124.751158169184));
#219752=CARTESIAN_POINT('Ctrl Pts',(-177.298940247785,-6.99588184988549,
130.494718895118));
#219753=CARTESIAN_POINT('Ctrl Pts',(-177.577387871598,-4.04195537438161,
136.522825237142));
#219754=CARTESIAN_POINT('Ctrl Pts',(-177.855835495411,2.62633062968132,
137.295941956302));
#219755=CARTESIAN_POINT('Ctrl Pts',(-178.134283119224,6.88114708845103,
132.103612556543));
#219756=CARTESIAN_POINT('Ctrl Pts',(-178.412730743037,4.81252553565828,
125.717334096849));
#219757=CARTESIAN_POINT('Ctrl Pts',(-178.69117836685,-1.67857187946192,
124.005784494632));
#219758=CARTESIAN_POINT('Ctrl Pts',(-178.969625990663,-6.62714374015151,
128.541794220484));
#219759=CARTESIAN_POINT('Ctrl Pts',(-179.248073614475,-5.48569425761253,
135.15699193274));
#219760=CARTESIAN_POINT('Ctrl Pts',(-179.526521238288,0.696840256609583,
137.772334104211));
#219761=CARTESIAN_POINT('Ctrl Pts',(-179.804968862101,6.23901261754625,
133.984449045885));
#219762=CARTESIAN_POINT('Ctrl Pts',(-180.083416485914,6.0478371756692,127.27421807789));
#219763=CARTESIAN_POINT('Ctrl Pts',(-180.361864109727,0.298994822622653,
123.808015646805));
#219764=CARTESIAN_POINT('Ctrl Pts',(-180.64031173354,-5.72460916570447,
126.771112453397));
#219765=CARTESIAN_POINT('Ctrl Pts',(-180.918759357353,-6.48757699345442,
133.440567287733));
#219766=CARTESIAN_POINT('Ctrl Pts',(-181.197206981166,-1.28877849997557,
137.687476978041));
#219767=CARTESIAN_POINT('Ctrl Pts',(-181.475654604978,5.094344474651,135.609138992));
#219768=CARTESIAN_POINT('Ctrl Pts',(-181.754102228792,6.79601374963652,
129.115444406326));
#219769=CARTESIAN_POINT('Ctrl Pts',(-182.032549852604,2.25247839243521,
124.173781310638));
#219770=CARTESIAN_POINT('Ctrl Pts',(-182.310997476417,-4.36097456772779,
125.32529667621));
#219771=CARTESIAN_POINT('Ctrl Pts',(-182.58944510023,-6.96690494559973,
131.511804136733));
#219772=CARTESIAN_POINT('Ctrl Pts',(-182.867892724043,-3.17059003069381,
137.048205563678));
#219773=CARTESIAN_POINT('Ctrl Pts',(-183.146340347856,3.53934223048593,
136.84681851393));
#219774=CARTESIAN_POINT('Ctrl Pts',(-183.424787971669,6.99679188832936,
131.092707847901));
#219775=CARTESIAN_POINT('Ctrl Pts',(-183.703235595482,4.02453161308464,
125.07362016374));
#219776=CARTESIAN_POINT('Ctrl Pts',(-183.981683219295,-2.64607660528548,
124.320802994409));
#219777=CARTESIAN_POINT('Ctrl Pts',(-184.260130843107,-6.88506969142675,
129.52605854136));
#219778=CARTESIAN_POINT('Ctrl Pts',(-184.53857846692,-4.79702008550057,
135.906011247817));
#219779=CARTESIAN_POINT('Ctrl Pts',(-184.817026090733,1.6992566315413,137.597796254561));
#219780=CARTESIAN_POINT('Ctrl Pts',(-185.095473714546,6.63399951749853,
133.046745788687));
#219781=CARTESIAN_POINT('Ctrl Pts',(-185.373921338359,5.47242093576752,
126.435052897159));
#219782=CARTESIAN_POINT('Ctrl Pts',(-185.652368962172,-0.718045143308166,
123.838540348135));
#219783=CARTESIAN_POINT('Ctrl Pts',(-185.930816585985,-6.24866281413942,
127.64327632748));
#219784=CARTESIAN_POINT('Ctrl Pts',(-186.209264209798,-6.03706462292539,
134.35289434186));
#219785=CARTESIAN_POINT('Ctrl Pts',(-186.487711833611,-0.277698970246197,
137.801583219124));
#219786=CARTESIAN_POINT('Ctrl Pts',(-186.766159457423,5.73685846974069,
134.820166358884));
#219787=CARTESIAN_POINT('Ctrl Pts',(-187.044607081237,6.47952323715255,
128.148420205389));
#219788=CARTESIAN_POINT('Ctrl Pts',(-187.323054705049,1.2678226919294,123.917353540782));
#219789=CARTESIAN_POINT('Ctrl Pts',(-187.601502328862,-5.10894497059535,
126.01510993074));
#219790=CARTESIAN_POINT('Ctrl Pts',(-187.879949952675,-6.79084179098006,
132.513953733987));
#219791=CARTESIAN_POINT('Ctrl Pts',(-188.158397576488,-2.23228675651833,
137.44176498151));
#219792=CARTESIAN_POINT('Ctrl Pts',(-188.436845200301,4.37763075391265,
136.270125873797));
#219793=CARTESIAN_POINT('Ctrl Pts',(-188.715292824114,6.96471946064982,
130.075715513085));
#219794=CARTESIAN_POINT('Ctrl Pts',(-188.993740447926,3.15157122851057,
124.550894407098));
#219795=CARTESIAN_POINT('Ctrl Pts',(-189.27218807174,-3.55771699981564,
124.772703249722));
#219796=CARTESIAN_POINT('Ctrl Pts',(-189.550635695553,-6.99763710944952,
130.53731055055));
#219797=CARTESIAN_POINT('Ctrl Pts',(-189.829083319365,-4.00707056907658,
136.547323816845));
#219798=CARTESIAN_POINT('Ctrl Pts',(-190.107530943179,2.66579806799723,
137.279834462351));
#219799=CARTESIAN_POINT('Ctrl Pts',(-190.385978566991,6.88892851205765,
132.061700988983));
#219800=CARTESIAN_POINT('Ctrl Pts',(-190.664426190804,4.78147019640398,
125.688133138775));
#219801=CARTESIAN_POINT('Ctrl Pts',(-190.942873814617,-1.71992564193992,
124.016128399968));
#219802=CARTESIAN_POINT('Ctrl Pts',(-191.22132143843,-6.64079383837953,
128.582177445553));
#219803=CARTESIAN_POINT('Ctrl Pts',(-191.499769062243,-5.45909691816341,
135.190304266535));
#219804=CARTESIAN_POINT('Ctrl Pts',(-191.778216686055,0.739243378134395,
137.767963139373));
#219805=CARTESIAN_POINT('Ctrl Pts',(-192.056664309869,6.25825512397307,
133.946411485565));
#219806=CARTESIAN_POINT('Ctrl Pts',(-192.335111933681,6.0262361436405,127.237468581785));
#219807=CARTESIAN_POINT('Ctrl Pts',(-192.613559557494,0.256400545303713,
123.806325206523));
#219808=CARTESIAN_POINT('Ctrl Pts',(-192.892007181307,-5.74905462830365,
126.806034500975));
#219809=CARTESIAN_POINT('Ctrl Pts',(-193.17045480512,-6.47140945543246,
133.480010167483));
#219810=CARTESIAN_POINT('Ctrl Pts',(-193.448902428933,-1.24685513894648,
137.695194610365));
#219811=CARTESIAN_POINT('Ctrl Pts',(-193.727350052746,5.12349813797151,
135.578039249819));
#219812=CARTESIAN_POINT('Ctrl Pts',(-194.005797676559,6.78560692289256,
129.074106433399));
#219813=CARTESIAN_POINT('Ctrl Pts',(-194.284245300372,2.2120744410027,124.160192684611));
#219814=CARTESIAN_POINT('Ctrl Pts',(-194.562692924184,-4.39424638632456,
125.35194468056));
#219815=CARTESIAN_POINT('Ctrl Pts',(-194.841140547997,-6.9624694554897,
131.554200557291));
#219816=CARTESIAN_POINT('Ctrl Pts',(-195.11958817181,-3.13252323060231,
137.067390161131));
#219817=CARTESIAN_POINT('Ctrl Pts',(-195.398035795623,3.57605881094196,
136.825161580438));
#219818=CARTESIAN_POINT('Ctrl Pts',(-195.676483419436,6.99841750541489,
131.050111047343));
#219819=CARTESIAN_POINT('Ctrl Pts',(-195.954931043249,3.98957240411393,
125.04922787486));
#219820=CARTESIAN_POINT('Ctrl Pts',(-196.233378667062,-2.68549483512068,
124.337030539057));
#219821=CARTESIAN_POINT('Ctrl Pts',(-196.511826290875,-6.89272351459547,
129.567993598765));
#219822=CARTESIAN_POINT('Ctrl Pts',(-196.790273914688,-4.76587601242081,
135.935117548864));
#219823=CARTESIAN_POINT('Ctrl Pts',(-197.0687215385,1.74057871918182,137.58732653051));
#219824=CARTESIAN_POINT('Ctrl Pts',(-197.347169162313,6.64752663985393,
133.006321204467));
#219825=CARTESIAN_POINT('Ctrl Pts',(-197.625616786126,5.44572232823074,
126.401821670817));
#219826=CARTESIAN_POINT('Ctrl Pts',(-197.904064409939,-0.760434764710735,
123.843040353244));
#219827=CARTESIAN_POINT('Ctrl Pts',(-198.182512033752,-6.26778945818702,
127.681372279183));
#219828=CARTESIAN_POINT('Ctrl Pts',(-198.460959657565,-6.01535183812634,
134.389577921633));
#219829=CARTESIAN_POINT('Ctrl Pts',(-198.739407281378,-0.235099745102313,
137.803144009248));
#219830=CARTESIAN_POINT('Ctrl Pts',(-199.017854905191,5.76119752841001,
134.785170069484));
#219831=CARTESIAN_POINT('Ctrl Pts',(-199.296302529004,6.46323572345932,
128.10902671676));
#219832=CARTESIAN_POINT('Ctrl Pts',(-199.574750152817,1.22587603526843,
123.909763544495));
#219833=CARTESIAN_POINT('Ctrl Pts',(-199.853197776629,-5.13800384196074,
126.04629826259));
#219834=CARTESIAN_POINT('Ctrl Pts',(-200.131645400443,-6.78030919386985,
132.555259840639));
#219835=CARTESIAN_POINT('Ctrl Pts',(-200.410093024255,-2.19184163313082,
137.455230568865));
#219836=CARTESIAN_POINT('Ctrl Pts',(-200.688540648069,4.41082131103843,
136.243376724908));
#219837=CARTESIAN_POINT('Ctrl Pts',(-200.96698827188,6.96015495096418,130.03333278901));
#219838=CARTESIAN_POINT('Ctrl Pts',(-201.245435895694,3.11344621342587,
124.531825760752));
#219839=CARTESIAN_POINT('Ctrl Pts',(-201.523883519507,-3.59436749394705,
124.794471835542));
#219840=CARTESIAN_POINT('Ctrl Pts',(-201.80233114332,-6.99913306899709,
130.579912101622));
#219841=CARTESIAN_POINT('Ctrl Pts',(-202.080778767133,-3.97203728029775,
136.571609588935));
#219842=CARTESIAN_POINT('Ctrl Pts',(-202.359226390945,2.705166724186,137.263487017335));
#219843=CARTESIAN_POINT('Ctrl Pts',(-202.637674014758,6.89645466388467,
132.019742830214));
#219844=CARTESIAN_POINT('Ctrl Pts',(-202.916121638571,4.75023767801316,
125.659121764391));
#219845=CARTESIAN_POINT('Ctrl Pts',(-203.194569262384,-1.76121567194074,
124.026723845744));
#219846=CARTESIAN_POINT('Ctrl Pts',(-203.473016886197,-6.65419785954973,
128.622643014438));
#219847=CARTESIAN_POINT('Ctrl Pts',(-203.75146451001,-5.43229728987039,
135.223454077576));
#219848=CARTESIAN_POINT('Ctrl Pts',(-204.029912133822,0.781619106723946,
137.763334135682));
#219849=CARTESIAN_POINT('Ctrl Pts',(-204.308359757636,6.27726572845484,
133.908257495395));
#219850=CARTESIAN_POINT('Ctrl Pts',(-204.586807381448,6.00441180721532,
127.200851258176));
#219851=CARTESIAN_POINT('Ctrl Pts',(-204.865255005262,0.213796766968775,
123.804894081017));
#219852=CARTESIAN_POINT('Ctrl Pts',(-205.143702629074,-5.77328705756903,
126.841104707996));
#219853=CARTESIAN_POINT('Ctrl Pts',(-205.422150252887,-6.4550021169537,
133.519353900054));
#219854=CARTESIAN_POINT('Ctrl Pts',(-205.7005978767,-1.20488557524167,137.702656900301));
#219855=CARTESIAN_POINT('Ctrl Pts',(-205.979045500513,5.15246194818434,
135.546762617222));
#219856=CARTESIAN_POINT('Ctrl Pts',(-206.257493124326,6.77494865298866,
129.032832575676));
#219857=CARTESIAN_POINT('Ctrl Pts',(-206.535940748139,2.17158852033829,
124.14685026067));
#219858=CARTESIAN_POINT('Ctrl Pts',(-206.814388371952,-4.42735537450605,
125.378794726189));
#219859=CARTESIAN_POINT('Ctrl Pts',(-207.092835995765,-6.9577759685135,
131.596569192254));
#219860=CARTESIAN_POINT('Ctrl Pts',(-207.371283619578,-3.09434035370993,
137.086342679721));
#219861=CARTESIAN_POINT('Ctrl Pts',(-207.64973124339,3.61264287922363,136.803281543952));
#219862=CARTESIAN_POINT('Ctrl Pts',(-207.928178867203,6.99978379356611,
131.007505140413));
#219863=CARTESIAN_POINT('Ctrl Pts',(-208.206626491016,3.95446536007061,
125.025048844539));
#219864=CARTESIAN_POINT('Ctrl Pts',(-208.485074114829,-2.72481355295718,
124.353497733001));
#219865=CARTESIAN_POINT('Ctrl Pts',(-208.763521738642,-6.90012192535954,
129.609974470206));
#219866=CARTESIAN_POINT('Ctrl Pts',(-209.041969362455,-4.73455533805275,
135.964033727826));
#219867=CARTESIAN_POINT('Ctrl Pts',(-209.320416986268,1.78183630903778,
137.576605461163));
#219868=CARTESIAN_POINT('Ctrl Pts',(-209.598864610081,6.66080743566547,
132.965815025787));
#219869=CARTESIAN_POINT('Ctrl Pts',(-209.877312233893,5.41882192745001,
126.368753582173));
#219870=CARTESIAN_POINT('Ctrl Pts',(-210.155759857706,-0.802796207923886,
123.847798312635));
#219871=CARTESIAN_POINT('Ctrl Pts',(-210.434207481519,-6.28668384699127,
127.719583954367));
#219872=CARTESIAN_POINT('Ctrl Pts',(-210.712655105332,-5.99341615225276,
134.42612864986));
#219873=CARTESIAN_POINT('Ctrl Pts',(-210.991102729145,-0.19249180825093,
137.804445456879));
#219874=CARTESIAN_POINT('Ctrl Pts',(-211.269550352958,5.78532310378624,
134.750026269725));
#219875=CARTESIAN_POINT('Ctrl Pts',(-211.547997976771,6.44670871218949,
128.069733104719));
#219876=CARTESIAN_POINT('Ctrl Pts',(-211.826445600584,1.18388395332015,
123.902429030038));
#219877=CARTESIAN_POINT('Ctrl Pts',(-212.104893224396,-5.16687232270428,
126.077662906191));
#219878=CARTESIAN_POINT('Ctrl Pts',(-212.38334084821,-6.76952534990887,
132.596501067076));
#219879=CARTESIAN_POINT('Ctrl Pts',(-212.661788472022,-2.15131529024619,
137.468449705789));
#219880=CARTESIAN_POINT('Ctrl Pts',(-212.940236095835,4.44384842355829,
136.216426031276));
#219881=CARTESIAN_POINT('Ctrl Pts',(-213.218683719648,6.95533253017721,
129.990978635656));
#219882=CARTESIAN_POINT('Ctrl Pts',(-213.497131343461,3.0752058284468,124.512989545492));
#219883=CARTESIAN_POINT('Ctrl Pts',(-213.775578967274,-3.63088479746918,
124.81646312));
#219884=CARTESIAN_POINT('Ctrl Pts',(-214.054026591087,-7.00036967309483,
130.622521969716));
#219885=CARTESIAN_POINT('Ctrl Pts',(-214.3324742149,-3.93685680621679,136.595681653493));
#219886=CARTESIAN_POINT('Ctrl Pts',(-214.610921838713,2.74443513942699,
137.246900227015));
#219887=CARTESIAN_POINT('Ctrl Pts',(-214.889369462525,6.90372526504794,
131.977739635008));
#219888=CARTESIAN_POINT('Ctrl Pts',(-215.167817086339,4.71882913781829,
125.630301048724));
#219889=CARTESIAN_POINT('Ctrl Pts',(-215.446264710151,-1.80244043944716,
124.037570439344));
#219890=CARTESIAN_POINT('Ctrl Pts',(-215.724712333964,-6.66735530697114,
128.66318942767));
#219891=CARTESIAN_POINT('Ctrl Pts',(-216.003159957777,-5.40529636580357,
135.256440137483));
#219892=CARTESIAN_POINT('Ctrl Pts',(-216.28160758159,0.823965872130078,
137.758447264668));
#219893=CARTESIAN_POINT('Ctrl Pts',(-216.560055205403,6.29604372654653,
133.869988489185));
#219894=CARTESIAN_POINT('Ctrl Pts',(-216.838502829216,5.98236497510254,
127.164367463932));
#219895=CARTESIAN_POINT('Ctrl Pts',(-217.116950453029,0.171185066315507,
123.803722323317));
#219896=CARTESIAN_POINT('Ctrl Pts',(-217.395398076842,-5.79730555555969,
126.876321774922));
#219897=CARTESIAN_POINT('Ctrl Pts',(-217.673845700654,-6.43835558599724,
133.558597027552));
#219898=CARTESIAN_POINT('Ctrl Pts',(-217.952293324468,-1.16287136405879,
137.709863571333));
#219899=CARTESIAN_POINT('Ctrl Pts',(-218.23074094828,5.18123483202488,135.515310253174));
#219900=CARTESIAN_POINT('Ctrl Pts',(-218.509188572093,6.76403933487094,
128.991624362576));
#219901=CARTESIAN_POINT('Ctrl Pts',(-218.787636195906,2.13102213066266,
124.133754533223));
#219902=CARTESIAN_POINT('Ctrl Pts',(-219.066083819719,-4.46030030540597,
125.405845818157));
#219903=CARTESIAN_POINT('Ctrl Pts',(-219.344531443532,-6.95282465859006,
131.638908471637));
#219904=CARTESIAN_POINT('Ctrl Pts',(-219.622979067345,-3.0560428148978,
137.105062417155));
#219905=CARTESIAN_POINT('Ctrl Pts',(-219.901426691158,3.6490930796943,136.781179215245));
#219906=CARTESIAN_POINT('Ctrl Pts',(-220.179874314971,7.00089070215466,
130.964891705888));
#219907=CARTESIAN_POINT('Ctrl Pts',(-220.458321938783,3.91921178185968,
125.001083968743));
#219908=CARTESIAN_POINT('Ctrl Pts',(-220.736769562596,-2.76403130182543,
124.370203966041));
#219909=CARTESIAN_POINT('Ctrl Pts',(-221.015217186409,-6.90726464956813,
129.651999600063));
#219910=CARTESIAN_POINT('Ctrl Pts',(-221.293664810222,-4.7030592229955,
135.992758713204));
#219911=CARTESIAN_POINT('Ctrl Pts',(-221.572112434035,1.82302787229404,
137.565633443793));
#219912=CARTESIAN_POINT('Ctrl Pts',(-221.850560057848,6.67384141280798,
132.925228753618));
#219913=CARTESIAN_POINT('Ctrl Pts',(-222.129007681661,5.39172073022998,
126.33584985658));
#219914=CARTESIAN_POINT('Ctrl Pts',(-222.407455305474,-0.845127903228338,
123.85281405));
#219915=CARTESIAN_POINT('Ctrl Pts',(-222.685902929286,-6.30534528041361,
127.757909937084));
#219916=CARTESIAN_POINT('Ctrl Pts',(-222.964350553099,-5.9712583781396,
134.462545172141));
#219917=CARTESIAN_POINT('Ctrl Pts',(-223.242798176912,-0.14987673854478,
137.805487513793));
#219918=CARTESIAN_POINT('Ctrl Pts',(-223.521245800725,5.80923430188729,
134.714736261875));
#219919=CARTESIAN_POINT('Ctrl Pts',(-223.799693424538,6.42994281575757,
128.030540825308));
#219920=CARTESIAN_POINT('Ctrl Pts',(-224.078141048351,1.1418480021166,123.895350269195));
#219921=CARTESIAN_POINT('Ctrl Pts',(-224.356588672164,-5.19554934309376,
126.109202699315));
#219922=CARTESIAN_POINT('Ctrl Pts',(-224.635036295977,-6.75849065869668,
132.637675885092));
#219923=CARTESIAN_POINT('Ctrl Pts',(-224.913483919789,-2.11070922958169,
137.481421902441));
#219924=CARTESIAN_POINT('Ctrl Pts',(-225.191931543603,4.47671086764076,
136.189274791569));
#219925=CARTESIAN_POINT('Ctrl Pts',(-225.470379167415,6.95025237698553,
129.948654622468));
#219926=CARTESIAN_POINT('Ctrl Pts',(-225.748826791228,3.03685149058481,
124.494386459301));
#219927=CARTESIAN_POINT('Ctrl Pts',(-226.027274415041,-3.66726755721984,
124.838676288203));
#219928=CARTESIAN_POINT('Ctrl Pts',(-226.305722038854,-7.00134687591997,
130.665138575908));
#219929=CARTESIAN_POINT('Ctrl Pts',(-226.584169662667,-3.9015304504591,
136.619539118521));
#219930=CARTESIAN_POINT('Ctrl Pts',(-226.86261728648,2.78360185861461,137.230074706019));
#219931=CARTESIAN_POINT('Ctrl Pts',(-227.141064910293,6.91074004613266,
131.935692959814));
#219932=CARTESIAN_POINT('Ctrl Pts',(-227.419512534106,4.68724573967455,
125.601672059739));
#219933=CARTESIAN_POINT('Ctrl Pts',(-227.697960157918,-1.8435984168596,
124.048667778841));
#219934=CARTESIAN_POINT('Ctrl Pts',(-227.976407781732,-6.68026569308986,
128.703815182788));
#219935=CARTESIAN_POINT('Ctrl Pts',(-228.254855405544,-5.37809514649209,
135.289261223946));
#219936=CARTESIAN_POINT('Ctrl Pts',(-228.533303029357,0.86628210517778,
137.753302707416));
#219937=CARTESIAN_POINT('Ctrl Pts',(-228.81175065317,6.31458842242258,133.831605885006));
#219938=CARTESIAN_POINT('Ctrl Pts',(-229.090198276983,5.96009646425557,
127.128018550972));
#219939=CARTESIAN_POINT('Ctrl Pts',(-229.368645900796,0.128567022336676,
123.802809976843));
#219940=CARTESIAN_POINT('Ctrl Pts',(-229.647093524609,-5.82110923226107,
126.911684396774));
#219941=CARTESIAN_POINT('Ctrl Pts',(-229.925541148421,-6.42147047940683,
133.597738095807));
#219942=CARTESIAN_POINT('Ctrl Pts',(-230.203988772235,-1.12081406224988,
137.716814356412));
#219943=CARTESIAN_POINT('Ctrl Pts',(-230.482436396047,5.20981572330331,
135.483683323156));
#219944=CARTESIAN_POINT('Ctrl Pts',(-230.76088401986,6.75287937278817,128.950483321085));
#219945=CARTESIAN_POINT('Ctrl Pts',(-231.039331643673,2.0903767751783,124.120905987538));
#219946=CARTESIAN_POINT('Ctrl Pts',(-231.317779267486,-4.49307995823781,
125.433096954076));
#219947=CARTESIAN_POINT('Ctrl Pts',(-231.596226891299,-6.94761570919197,
131.681216826544));
#219948=CARTESIAN_POINT('Ctrl Pts',(-231.874674515112,-3.01763203329532,
137.123548679767));
#219949=CARTESIAN_POINT('Ctrl Pts',(-232.153122138925,3.68540806167951,
136.758855413326));
#219950=CARTESIAN_POINT('Ctrl Pts',(-232.431569762738,7.00173819016367,
130.922272322824));
#219951=CARTESIAN_POINT('Ctrl Pts',(-232.71001738655,3.88381297581431,124.977334135496));
#219952=CARTESIAN_POINT('Ctrl Pts',(-232.988465010364,-2.80314662849731,
124.38714861912));
#219953=CARTESIAN_POINT('Ctrl Pts',(-233.266912634176,-6.914151422545,129.694067431082));
#219954=CARTESIAN_POINT('Ctrl Pts',(-233.545360257989,-4.67138883434919,
136.021291440583));
#219955=CARTESIAN_POINT('Ctrl Pts',(-233.823807881803,1.86415188258208,
137.554410884971));
#219956=CARTESIAN_POINT('Ctrl Pts',(-234.102255505615,6.68662808830262,
132.884563891901));
#219957=CARTESIAN_POINT('Ctrl Pts',(-234.380703129428,5.36441974081549,
126.303111713297));
#219958=CARTESIAN_POINT('Ctrl Pts',(-234.659150753241,-0.887428282007554,
123.858087379481));
#219959=CARTESIAN_POINT('Ctrl Pts',(-234.937598377053,-6.32377306694735,
127.796348807152));
#219960=CARTESIAN_POINT('Ctrl Pts',(-235.216046000867,-5.94887933685163,
134.498826139047));
#219961=CARTESIAN_POINT('Ctrl Pts',(-235.494493624679,-0.107256115101469,
137.806270141374));
#219962=CARTESIAN_POINT('Ctrl Pts',(-235.772941248493,5.83293023667497,
134.679301353618));
#219963=CARTESIAN_POINT('Ctrl Pts',(-236.051388872305,6.41293865542997,
127.991451330808));
#219964=CARTESIAN_POINT('Ctrl Pts',(-236.329836496118,1.09976973931543,
123.88852752427));
#219965=CARTESIAN_POINT('Ctrl Pts',(-236.608284119931,-5.22403384049169,
126.140916473241));
#219966=CARTESIAN_POINT('Ctrl Pts',(-236.886731743744,-6.7472055291277,
132.678782768935));
#219967=CARTESIAN_POINT('Ctrl Pts',(-237.165179367557,-2.07002495581049,
137.494146678133));
#219968=CARTESIAN_POINT('Ctrl Pts',(-237.44362699137,4.50940742555574,136.161924011888));
#219969=CARTESIAN_POINT('Ctrl Pts',(-237.722074615182,6.94491467963605,
129.906362317783));
#219970=CARTESIAN_POINT('Ctrl Pts',(-238.000522238996,2.99838462107406,
124.476017191522));
#219971=CARTESIAN_POINT('Ctrl Pts',(-238.278969862808,-3.70351442502255,
124.861110517033));
#219972=CARTESIAN_POINT('Ctrl Pts',(-238.557417486622,-7.00206464126185,
130.707760341024));
#219973=CARTESIAN_POINT('Ctrl Pts',(-238.835865110434,-3.86605952205578,
136.64318109997));
#219974=CARTESIAN_POINT('Ctrl Pts',(-239.114312734247,2.82266543041169,
137.213011077826));
#219975=CARTESIAN_POINT('Ctrl Pts',(-239.39276035806,6.91749874720356,131.893604362681));
#219976=CARTESIAN_POINT('Ctrl Pts',(-239.671207981873,4.655488653916,125.573235858291));
#219977=CARTESIAN_POINT('Ctrl Pts',(-239.949655605686,-1.88468807905538,
124.060015453022));
#219978=CARTESIAN_POINT('Ctrl Pts',(-240.228103229498,-6.69292853950653,
128.74451877439));
#219979=CARTESIAN_POINT('Ctrl Pts',(-240.506550853312,-5.35069463988719,
135.321916120768));
#219980=CARTESIAN_POINT('Ctrl Pts',(-240.784998477124,0.908566237823527,
137.747900654559));
#219981=CARTESIAN_POINT('Ctrl Pts',(-241.063446100938,6.33289912890243,
133.79311110514));
#219982=CARTESIAN_POINT('Ctrl Pts',(-241.34189372475,5.9376070998423,127.091805866219));
#219983=CARTESIAN_POINT('Ctrl Pts',(-241.620341348563,0.0859442142595387,
123.802157075403));
#219984=CARTESIAN_POINT('Ctrl Pts',(-241.898788972376,-5.84469720561911,
126.947191263173));
#219985=CARTESIAN_POINT('Ctrl Pts',(-242.177236596189,-6.40434742286629,
133.636775654432));
#219986=CARTESIAN_POINT('Ctrl Pts',(-242.455684220002,-1.07871522826414,
137.723508997977));
#219987=CARTESIAN_POINT('Ctrl Pts',(-242.734131843815,5.23820356294377,
135.451882999115));
#219988=CARTESIAN_POINT('Ctrl Pts',(-243.012579467628,6.74146918027728,
128.909410975699));
#219989=CARTESIAN_POINT('Ctrl Pts',(-243.29102709144,2.04965396001378,124.108305099723));
#219990=CARTESIAN_POINT('Ctrl Pts',(-243.569474715254,-4.52569311833944,
125.460547124147));
#219991=CARTESIAN_POINT('Ctrl Pts',(-243.847922339066,-6.94214931333881,
131.72349268922));
#219992=CARTESIAN_POINT('Ctrl Pts',(-244.12636996288,-2.9791094322281,137.141800782542));
#219993=CARTESIAN_POINT('Ctrl Pts',(-244.404817586691,3.72158647951367,
136.736310965414));
#219994=CARTESIAN_POINT('Ctrl Pts',(-244.683265210505,7.00232622618917,
130.879648570499));
#219995=CARTESIAN_POINT('Ctrl Pts',(-244.961712834317,3.84827025365086,
124.953800224859));
#219996=CARTESIAN_POINT('Ctrl Pts',(-245.240160458131,-2.84215808354001,
124.404331064352));
#219997=CARTESIAN_POINT('Ctrl Pts',(-245.518608081943,-6.92078198909823,
129.736176404423));
#219998=CARTESIAN_POINT('Ctrl Pts',(-245.797055705757,-4.63954534567172,
136.049630852671));
#219999=CARTESIAN_POINT('Ctrl Pts',(-246.075503329569,1.90520681603656,
137.542938200555));
#220000=CARTESIAN_POINT('Ctrl Pts',(-246.353950953382,6.69916698833444,
132.843821947487));
#220001=CARTESIAN_POINT('Ctrl Pts',(-246.632398577195,5.33691997085474,
126.270540365447));
#220002=CARTESIAN_POINT('Ctrl Pts',(-246.910846201008,-0.929695776805409,
123.86361810567));
#220003=CARTESIAN_POINT('Ctrl Pts',(-247.189293824821,-6.34196652374499,
127.834899140205));
#220004=CARTESIAN_POINT('Ctrl Pts',(-247.467741448634,-5.9262798576518,
134.534970206175));
#220005=CARTESIAN_POINT('Ctrl Pts',(-247.746189072447,-0.0646315172428821,
137.806793310625));
#220006=CARTESIAN_POINT('Ctrl Pts',(-248.024636696259,5.85641003008765,
134.643722858007));
#220007=CARTESIAN_POINT('Ctrl Pts',(-248.303084320073,6.39569686130214,
127.952466069697));
#220008=CARTESIAN_POINT('Ctrl Pts',(-248.581531943885,1.05765072414216,
123.881961048084));
#220009=CARTESIAN_POINT('Ctrl Pts',(-248.859979567699,-5.25232475939459,
126.172803052805));
#220010=CARTESIAN_POINT('Ctrl Pts',(-249.138427191511,-6.73567037937639,
132.719820195375));
#220011=CARTESIAN_POINT('Ctrl Pts',(-249.416874815324,-2.02926397650361,
137.506623561341));
#220012=CARTESIAN_POINT('Ctrl Pts',(-249.695322439137,4.54193688572079,
136.134374705723));
#220013=CARTESIAN_POINT('Ctrl Pts',(-249.97377006295,6.93931963591783,129.864103288757));
#220014=CARTESIAN_POINT('Ctrl Pts',(-250.252217686763,2.95980664532115,
124.457882422832));
#220015=CARTESIAN_POINT('Ctrl Pts',(-250.530665310576,-3.73962405773988,
124.883764975191));
#220016=CARTESIAN_POINT('Ctrl Pts',(-250.809112934388,-7.00252294251614,
130.750385685678));
#220017=CARTESIAN_POINT('Ctrl Pts',(-251.087560558202,-3.83044533540895,
136.666606721818));
#220018=CARTESIAN_POINT('Ctrl Pts',(-251.366008182014,2.86162440732935,
137.195709974661));
#220019=CARTESIAN_POINT('Ctrl Pts',(-251.644455805827,6.9240011177651,131.851475403357));
#220020=CARTESIAN_POINT('Ctrl Pts',(-251.92290342964,4.62355905740654,125.54499349784));
#220021=CARTESIAN_POINT('Ctrl Pts',(-252.201351053453,-1.92570790361727,
124.071613041873));
#220022=CARTESIAN_POINT('Ctrl Pts',(-252.479798677266,-6.70534337666252,
128.785298693283));
#220023=CARTESIAN_POINT('Ctrl Pts',(-252.758246301079,-5.3230958619522,
135.354403619622));
#220024=CARTESIAN_POINT('Ctrl Pts',(-253.036693924892,0.950816704398073,
137.74224130304));
#220025=CARTESIAN_POINT('Ctrl Pts',(-253.315141548704,6.35097516523885,
133.754505582129));
#220026=CARTESIAN_POINT('Ctrl Pts',(-253.593589172518,5.91489771943887,
127.055730740027));
#220027=CARTESIAN_POINT('Ctrl Pts',(-253.87203679633,0.0433182135112656,
123.801763664947));
#220028=CARTESIAN_POINT('Ctrl Pts',(-254.150484420143,-5.86806858651122,
126.982841017323));
#220029=CARTESIAN_POINT('Ctrl Pts',(-254.428932043956,-6.38698707931617,
133.675708334441));
#220030=CARTESIAN_POINT('Ctrl Pts',(-254.707379667769,-1.03657636838919,
137.729947101491));
#220031=CARTESIAN_POINT('Ctrl Pts',(-254.985827291582,5.26639719763008,
135.41991073597));
#220032=CARTESIAN_POINT('Ctrl Pts',(-255.264274915395,6.72980937160111,
128.868408326187));
#220033=CARTESIAN_POINT('Ctrl Pts',(-255.542722539208,2.00885483266244,
124.095953322692));
#220034=CARTESIAN_POINT('Ctrl Pts',(-255.821170163021,-4.5581378946222,
125.488193449449));
#220035=CARTESIAN_POINT('Ctrl Pts',(-256.099617786833,-6.93642696247006,
131.765738008466));
#220036=CARTESIAN_POINT('Ctrl Pts',(-256.378065410647,-2.94047400549736,
137.159811411449));
#220037=CARTESIAN_POINT('Ctrl Pts',(-256.656513034459,3.7576223973322,136.713559240208));
#220038=CARTESIAN_POINT('Ctrl Pts',(-256.934960658272,7.0026634652268,130.836998362911));
#220039=CARTESIAN_POINT('Ctrl Pts',(-257.213408282085,3.81256854888166,
124.930527794066));
#220040=CARTESIAN_POINT('Ctrl Pts',(-257.491855905898,-2.88103328591622,
124.421666290213));
#220041=CARTESIAN_POINT('Ctrl Pts',(-257.770303529711,-6.92721451599304,
129.778484277494));
#220042=CARTESIAN_POINT('Ctrl Pts',(-258.048751153524,-4.60741964202412,
136.077475067175));
#220043=CARTESIAN_POINT('Ctrl Pts',(-258.327198777336,1.94598288966397,
137.53178391186));
#220044=CARTESIAN_POINT('Ctrl Pts',(-258.60564640115,6.71185090883407,132.801931226644));
#220045=CARTESIAN_POINT('Ctrl Pts',(-258.884094024962,5.30847971878909,
126.240167716581));
#220046=CARTESIAN_POINT('Ctrl Pts',(-259.162541648776,-0.970525071554103,
123.86553674091));
#220047=CARTESIAN_POINT('Ctrl Pts',(-259.440989272588,-6.36258613651914,
127.881151058581));
#220048=CARTESIAN_POINT('Ctrl Pts',(-259.673028959099,-5.97575359986218,
133.442106215535));
#220049=CARTESIAN_POINT('Ctrl Pts',(-259.858689921174,-2.9628379271774,
136.206922793942));
#220050=CARTESIAN_POINT('Ctrl Pts',(-259.951535008647,-1.00384119663989,
136.721969923993));
#220051=CARTESIAN_POINT('Ctrl Pts',(-259.997972158816,-0.016740685831905,
136.724751058381));
#220052=CARTESIAN_POINT('Ctrl Pts',(210.384788400103,3.2437100417032,135.350446923363));
#220053=CARTESIAN_POINT('Ctrl Pts',(210.338370536501,4.00135710969089,134.809856772425));
#220054=CARTESIAN_POINT('Ctrl Pts',(210.245544735596,5.2274450014198,133.344996311945));
#220055=CARTESIAN_POINT('Ctrl Pts',(210.059903060087,6.03752477204218,129.574087134129));
#220056=CARTESIAN_POINT('Ctrl Pts',(209.827863373576,3.30140998082846,125.08375145776));
#220057=CARTESIAN_POINT('Ctrl Pts',(209.549415749763,-3.03864792542705,
124.935284604053));
#220058=CARTESIAN_POINT('Ctrl Pts',(209.27096812595,-6.57501826603042,130.18815040753));
#220059=CARTESIAN_POINT('Ctrl Pts',(208.992520502138,-4.0751627655632,136.003208990552));
#220060=CARTESIAN_POINT('Ctrl Pts',(208.714072878324,2.17267791003586,137.042921783734));
#220061=CARTESIAN_POINT('Ctrl Pts',(208.435625254512,6.42228832295553,132.348569225854));
#220062=CARTESIAN_POINT('Ctrl Pts',(208.157177630698,4.77100074356668,126.235763887068));
#220063=CARTESIAN_POINT('Ctrl Pts',(207.878730006886,-1.26506482749479,
124.320958291314));
#220064=CARTESIAN_POINT('Ctrl Pts',(207.600282383073,-6.13835327551471,
128.364250828182));
#220065=CARTESIAN_POINT('Ctrl Pts',(207.32183475926,-5.37092434612766,134.649796015418));
#220066=CARTESIAN_POINT('Ctrl Pts',(207.043387135447,0.332190207827403,
137.40162108792));
#220067=CARTESIAN_POINT('Ctrl Pts',(206.764939511634,5.73000189292936,134.090861108297));
#220068=CARTESIAN_POINT('Ctrl Pts',(206.486491887821,5.86224098722307,127.759980958474));
#220069=CARTESIAN_POINT('Ctrl Pts',(206.208044264008,0.607356820266201,
124.226729984437));
#220070=CARTESIAN_POINT('Ctrl Pts',(205.929596640195,-5.20565320191231,
126.738003936844));
#220071=CARTESIAN_POINT('Ctrl Pts',(205.651149016382,-6.23492509722864,
132.986059061584));
#220072=CARTESIAN_POINT('Ctrl Pts',(205.37270139257,-1.53460390898592,137.229240938669));
#220073=CARTESIAN_POINT('Ctrl Pts',(205.094253768756,4.57594250116295,135.568271122458));
#220074=CARTESIAN_POINT('Ctrl Pts',(204.815806144944,6.48142172411287,129.529500574057));
#220075=CARTESIAN_POINT('Ctrl Pts',(204.537358521131,2.43079079302514,124.662263970705));
#220076=CARTESIAN_POINT('Ctrl Pts',(204.258910897318,-3.85361800715474,
125.439314209572));
#220077=CARTESIAN_POINT('Ctrl Pts',(203.980463273505,-6.5967401814699,131.146579956944));
#220078=CARTESIAN_POINT('Ctrl Pts',(203.702015649692,-3.27778036432047,
136.539362872731));
#220079=CARTESIAN_POINT('Ctrl Pts',(203.42356802588,3.05329946149495,136.661958874297));
#220080=CARTESIAN_POINT('Ctrl Pts',(203.145120402066,6.5785462535266,131.40170824395));
#220081=CARTESIAN_POINT('Ctrl Pts',(202.866672778254,4.05843041346184,125.592524323598));
#220082=CARTESIAN_POINT('Ctrl Pts',(202.58822515444,-2.19118470860141,124.572763346851));
#220083=CARTESIAN_POINT('Ctrl Pts',(202.309777530628,-6.42720813017419,
129.279535830482));
#220084=CARTESIAN_POINT('Ctrl Pts',(202.031329906815,-4.75694126595338,
135.387547802118));
#220085=CARTESIAN_POINT('Ctrl Pts',(201.752882283002,1.28472223178851,137.283834652022));
#220086=CARTESIAN_POINT('Ctrl Pts',(201.474434659189,6.14578876089344,133.225801404307));
#220087=CARTESIAN_POINT('Ctrl Pts',(201.195987035376,5.35917565710019,126.94258236746));
#220088=CARTESIAN_POINT('Ctrl Pts',(200.917539411563,-0.352258065224466,
124.208148884143));
#220089=CARTESIAN_POINT('Ctrl Pts',(200.63909178775,-5.73998383440169,127.535311740963));
#220090=CARTESIAN_POINT('Ctrl Pts',(200.360644163938,-5.85294487354697,
133.866570813476));
#220091=CARTESIAN_POINT('Ctrl Pts',(200.082196540124,-0.587335506164227,
137.383808313225));
#220092=CARTESIAN_POINT('Ctrl Pts',(199.803748916312,5.2180064984534,134.854854804556));
#220093=CARTESIAN_POINT('Ctrl Pts',(199.525301292498,6.22825544477889,128.603695015683));
#220094=CARTESIAN_POINT('Ctrl Pts',(199.246853668687,1.51504190454761,124.374839406449));
#220095=CARTESIAN_POINT('Ctrl Pts',(198.968406044873,-4.5904211320519,126.054399690658));
#220096=CARTESIAN_POINT('Ctrl Pts',(198.689958421061,-6.47751140283473,
132.098942018204));
#220097=CARTESIAN_POINT('Ctrl Pts',(198.411510797247,-2.41208513843682,
136.95382728238));
#220098=CARTESIAN_POINT('Ctrl Pts',(198.133063173434,3.86992953127461,136.15765309974));
#220099=CARTESIAN_POINT('Ctrl Pts',(197.854615549622,6.59566801831256,130.442064648858));
#220100=CARTESIAN_POINT('Ctrl Pts',(197.576167925809,3.26030981281707,125.059408494076));
#220101=CARTESIAN_POINT('Ctrl Pts',(197.297720301996,-3.07111383566833,
124.956082684267));
#220102=CARTESIAN_POINT('Ctrl Pts',(197.019272678183,-6.58033390142619,
130.227038590899));
#220103=CARTESIAN_POINT('Ctrl Pts',(196.74082505437,-4.04254857895594,136.028525236289));
#220104=CARTESIAN_POINT('Ctrl Pts',(196.462377430557,2.21014139809766,137.029259811701));
#220105=CARTESIAN_POINT('Ctrl Pts',(196.183929806745,6.43181940170927,132.309616130935));
#220106=CARTESIAN_POINT('Ctrl Pts',(195.905482182931,4.74296958699597,126.206716169203));
#220107=CARTESIAN_POINT('Ctrl Pts',(195.627034559119,-1.30443757122094,
124.328826848098));
#220108=CARTESIAN_POINT('Ctrl Pts',(195.348586935305,-6.15313032680387,
128.401636713722));
#220109=CARTESIAN_POINT('Ctrl Pts',(195.070139311493,-5.34739690918169,
134.682432467391));
#220110=CARTESIAN_POINT('Ctrl Pts',(194.791691687679,0.372333033116476,
137.399469645412));
#220111=CARTESIAN_POINT('Ctrl Pts',(194.513244063867,5.74990710746052,134.055923815831));
#220112=CARTESIAN_POINT('Ctrl Pts',(194.234796440054,5.84359744862664,127.724350254736));
#220113=CARTESIAN_POINT('Ctrl Pts',(193.956348816241,0.567307210110782,
124.223155750211));
#220114=CARTESIAN_POINT('Ctrl Pts',(193.677901192428,-5.23031063999889,
126.769767009054));
#220115=CARTESIAN_POINT('Ctrl Pts',(193.399453568615,-6.22152852682933,
133.023972693263));
#220116=CARTESIAN_POINT('Ctrl Pts',(193.121005944802,-1.49546563606909,
137.238463313985));
#220117=CARTESIAN_POINT('Ctrl Pts',(192.84255832099,4.60485711668079,135.540327880088));
#220118=CARTESIAN_POINT('Ctrl Pts',(192.564110697177,6.47354113897745,129.490069896797));
#220119=CARTESIAN_POINT('Ctrl Pts',(192.285663073364,2.39335710461987,124.64758087922));
#220120=CARTESIAN_POINT('Ctrl Pts',(192.007215449551,-3.88620518688872,
125.462871665772));
#220121=CARTESIAN_POINT('Ctrl Pts',(191.728767825738,-6.59453476332446,
131.18672985278));
#220122=CARTESIAN_POINT('Ctrl Pts',(191.450320201925,-3.24280905319821,
136.559209392401));
#220123=CARTESIAN_POINT('Ctrl Pts',(191.171872578112,3.08889975678785,136.643264047941));
#220124=CARTESIAN_POINT('Ctrl Pts',(190.893424954299,6.58206059142805,131.361651697256));
#220125=CARTESIAN_POINT('Ctrl Pts',(190.614977330486,4.02662929408197,125.567916069518));
#220126=CARTESIAN_POINT('Ctrl Pts',(190.336529706674,-2.22907761274862,
124.586217166899));
#220127=CARTESIAN_POINT('Ctrl Pts',(190.05808208286,-6.43637108995848,129.318688322246));
#220128=CARTESIAN_POINT('Ctrl Pts',(189.779634459048,-4.72895396970476,
135.416419737866));
#220129=CARTESIAN_POINT('Ctrl Pts',(189.501186835235,1.32414082646293,137.275894133543));
#220130=CARTESIAN_POINT('Ctrl Pts',(189.222739211422,6.16041489098677,133.188345380025));
#220131=CARTESIAN_POINT('Ctrl Pts',(188.944291587609,5.33556862369218,126.910031093937));
#220132=CARTESIAN_POINT('Ctrl Pts',(188.665843963796,-0.392404551757433,
124.210415391489));
#220133=CARTESIAN_POINT('Ctrl Pts',(188.387396339983,-5.75977711417006,
127.570313219673));
#220134=CARTESIAN_POINT('Ctrl Pts',(188.10894871617,-5.83419588941534,133.902142614521));
#220135=CARTESIAN_POINT('Ctrl Pts',(187.830501092358,-0.547273658602122,
137.387261689231));
#220136=CARTESIAN_POINT('Ctrl Pts',(187.552053468544,5.24256632866185,134.823016271676));
#220137=CARTESIAN_POINT('Ctrl Pts',(187.273605844732,6.214743973489,128.565822630237));
#220138=CARTESIAN_POINT('Ctrl Pts',(186.995158220918,1.47587551380139,124.365736040492));
#220139=CARTESIAN_POINT('Ctrl Pts',(186.716710597106,-4.61925044254253,
126.082430892781));
#220140=CARTESIAN_POINT('Ctrl Pts',(186.438262973293,-6.46951090511933,
132.138348483055));
#220141=CARTESIAN_POINT('Ctrl Pts',(186.15981534948,-2.37460689906969,136.968396393875));
#220142=CARTESIAN_POINT('Ctrl Pts',(185.881367725667,3.90244484122886,136.133996556155));
#220143=CARTESIAN_POINT('Ctrl Pts',(185.602920101854,6.59334041746713,130.401921658061));
#220144=CARTESIAN_POINT('Ctrl Pts',(185.324472478041,3.22527825263932,125.039668503516));
#220145=CARTESIAN_POINT('Ctrl Pts',(185.046024854228,-3.10665706276191,
124.974885780916));
#220146=CARTESIAN_POINT('Ctrl Pts',(184.767577230416,-6.5837263061198,130.26710564752));
#220147=CARTESIAN_POINT('Ctrl Pts',(184.489129606603,-4.01067270706429,
136.05303658523));
#220148=CARTESIAN_POINT('Ctrl Pts',(184.21068198279,2.247993177529,137.015690720733));
#220149=CARTESIAN_POINT('Ctrl Pts',(183.932234358977,6.44086315254518,132.270435931769));
#220150=CARTESIAN_POINT('Ctrl Pts',(183.653786735164,4.71489454403,126.177929550814));
#220151=CARTESIAN_POINT('Ctrl Pts',(183.375339111351,-1.34383181504516,
124.33688730648));
#220152=CARTESIAN_POINT('Ctrl Pts',(183.096891487538,-6.16764238592767,
128.439137081397));
#220153=CARTESIAN_POINT('Ctrl Pts',(182.818443863726,-5.32369091022383,
134.71491173846));
#220154=CARTESIAN_POINT('Ctrl Pts',(182.539996239912,0.412472435216218,
137.397080956463));
#220155=CARTESIAN_POINT('Ctrl Pts',(182.2615486161,5.76959376309122,134.020862255314));
#220156=CARTESIAN_POINT('Ctrl Pts',(181.983100992287,5.82474028301032,127.688835683913));
#220157=CARTESIAN_POINT('Ctrl Pts',(181.704653368474,0.527235037225083,
124.219824324685));
#220158=CARTESIAN_POINT('Ctrl Pts',(181.426205744661,-5.25477345090652,
126.801680146133));
#220159=CARTESIAN_POINT('Ctrl Pts',(181.147758120848,-6.20790184760947,
133.061803779016));
#220160=CARTESIAN_POINT('Ctrl Pts',(180.869310497035,-1.45627171922457,
137.247447428754));
#220161=CARTESIAN_POINT('Ctrl Pts',(180.590862873222,4.63360097629919,135.5122090613));
#220162=CARTESIAN_POINT('Ctrl Pts',(180.31241524941,6.46542073859599,129.450687965235));
#220163=CARTESIAN_POINT('Ctrl Pts',(180.033967625596,2.35583469548556,124.633125906077));
#220164=CARTESIAN_POINT('Ctrl Pts',(179.755520001784,-3.91864834385308,
125.4866270652));
#220165=CARTESIAN_POINT('Ctrl Pts',(179.477072377971,-6.59208499180493,
131.226865573221));
#220166=CARTESIAN_POINT('Ctrl Pts',(179.198624754158,-3.20771757354326,
136.578842667508));
#220167=CARTESIAN_POINT('Ctrl Pts',(178.920177130345,3.12438558908937,136.62435285703));
#220168=CARTESIAN_POINT('Ctrl Pts',(178.641729506532,6.58533103007041,131.32157450091));
#220169=CARTESIAN_POINT('Ctrl Pts',(178.363281882719,3.99467896572256,125.5435018533));
#220170=CARTESIAN_POINT('Ctrl Pts',(178.084834258906,-2.26688791720775,
124.599901402811));
#220171=CARTESIAN_POINT('Ctrl Pts',(177.806386635093,-6.44529554785546,
129.357895865998));
#220172=CARTESIAN_POINT('Ctrl Pts',(177.527939011281,-4.70079144021631,
135.445120772143));
#220173=CARTESIAN_POINT('Ctrl Pts',(177.249491387467,1.36351035455298,137.26771380997));
#220174=CARTESIAN_POINT('Ctrl Pts',(176.971043763655,6.17481274467203,133.150801016333));
#220175=CARTESIAN_POINT('Ctrl Pts',(176.692596139842,5.31176387881016,126.877624126216));
#220176=CARTESIAN_POINT('Ctrl Pts',(176.414148516029,-0.432536497586617,
124.212926239906));
#220177=CARTESIAN_POINT('Ctrl Pts',(176.135700892216,-5.77935696328393,
127.605434537195));
#220178=CARTESIAN_POINT('Ctrl Pts',(175.857253268403,-5.81523071700703,
133.937599626117));
#220179=CARTESIAN_POINT('Ctrl Pts',(175.57880564459,-0.50719153161477,137.390471133416));
#220180=CARTESIAN_POINT('Ctrl Pts',(175.300358020777,5.2669318936477,134.791028826034));
#220181=CARTESIAN_POINT('Ctrl Pts',(175.021910396965,6.20100221257536,128.528033194638));
#220182=CARTESIAN_POINT('Ctrl Pts',(174.743462773151,1.43665443394553,124.356871260137));
#220183=CARTESIAN_POINT('Ctrl Pts',(174.465015149339,-4.64790858500931,
126.110637067746));
#220184=CARTESIAN_POINT('Ctrl Pts',(174.186567525525,-6.46127067729819,
132.177705516496));
#220185=CARTESIAN_POINT('Ctrl Pts',(173.908119901713,-2.33704066777073,
136.982737094758));
#220186=CARTESIAN_POINT('Ctrl Pts',(173.6296722779,3.93481554465429,136.11014252095));
#220187=CARTESIAN_POINT('Ctrl Pts',(173.351224654087,6.59076849796787,130.361793579788));
#220188=CARTESIAN_POINT('Ctrl Pts',(173.072777030274,3.1901271785899,125.020142125741));
#220189=CARTESIAN_POINT('Ctrl Pts',(172.794329406461,-3.14208517153551,
124.993904890899));
#220190=CARTESIAN_POINT('Ctrl Pts',(172.515881782648,-6.58687474841394,
130.30719261232));
#220191=CARTESIAN_POINT('Ctrl Pts',(172.237434158836,-3.97864821822065,
136.077353442554));
#220192=CARTESIAN_POINT('Ctrl Pts',(171.958986535022,2.28576165674636,137.001891466644));
#220193=CARTESIAN_POINT('Ctrl Pts',(171.68053891121,6.44966823482829,132.231201406644));
#220194=CARTESIAN_POINT('Ctrl Pts',(171.402091287397,4.68664478891289,126.149314366529));
#220195=CARTESIAN_POINT('Ctrl Pts',(171.123643663584,-1.38317626268716,
124.345187419464));
#220196=CARTESIAN_POINT('Ctrl Pts',(170.845196039771,-6.18192590079466,
128.476725093301));
#220197=CARTESIAN_POINT('Ctrl Pts',(170.566748415958,-5.29978763994156,
134.747246102621));
#220198=CARTESIAN_POINT('Ctrl Pts',(170.288300792145,0.452596552998033,
137.394447971839));
#220199=CARTESIAN_POINT('Ctrl Pts',(170.009853168332,5.78906662430322,133.985681506144));
#220200=CARTESIAN_POINT('Ctrl Pts',(169.73140554452,5.80566727950083,127.653436560012));
#220201=CARTESIAN_POINT('Ctrl Pts',(169.452957920706,0.487143327451347,
124.216736891574));
#220202=CARTESIAN_POINT('Ctrl Pts',(169.174510296894,-5.27904154425138,
126.833741604011));
#220203=CARTESIAN_POINT('Ctrl Pts',(168.896062673081,-6.19404513230377,
133.099551214382));
#220204=CARTESIAN_POINT('Ctrl Pts',(168.617615049268,-1.41702383969606,
137.256192792574));
#220205=CARTESIAN_POINT('Ctrl Pts',(168.339167425455,4.66217313612931,135.483915791456));
#220206=CARTESIAN_POINT('Ctrl Pts',(168.060719801642,6.45706075967145,129.411356194513));
#220207=CARTESIAN_POINT('Ctrl Pts',(167.782272177829,2.3182249900303,124.618899610305));
#220208=CARTESIAN_POINT('Ctrl Pts',(167.503824554016,-3.95094629386185,
125.510579515201));
#220209=CARTESIAN_POINT('Ctrl Pts',(167.225376930203,-6.58939094815179,
131.266985637585));
#220210=CARTESIAN_POINT('Ctrl Pts',(166.946929306391,-3.1725072307341,136.59826196706));
#220211=CARTESIAN_POINT('Ctrl Pts',(166.668481682578,3.15975564613386,136.605226004165));
#220212=CARTESIAN_POINT('Ctrl Pts',(166.390034058765,6.58835744684964,131.281478139015));
#220213=CARTESIAN_POINT('Ctrl Pts',(166.111586434952,3.96258061306513,125.519282580138));
#220214=CARTESIAN_POINT('Ctrl Pts',(165.833138811139,-2.30461422130139,
124.613815547242));
#220215=CARTESIAN_POINT('Ctrl Pts',(165.554691187326,-6.45398117295568,
129.397157009033));
#220216=CARTESIAN_POINT('Ctrl Pts',(165.276243563513,-4.67245472117232,
135.473649841348));
#220217=CARTESIAN_POINT('Ctrl Pts',(164.9977959397,1.40282935726546,137.259293984466));
#220218=CARTESIAN_POINT('Ctrl Pts',(164.719348315888,6.18898178840028,133.11316970443));
#220219=CARTESIAN_POINT('Ctrl Pts',(164.440900692075,5.2877623045642,126.845362665158));
#220220=CARTESIAN_POINT('Ctrl Pts',(164.162453068262,-0.472652415616787,
124.215681336348));
#220221=CARTESIAN_POINT('Ctrl Pts',(163.884005444449,-5.79872265620017,
127.640674392099));
#220222=CARTESIAN_POINT('Ctrl Pts',(163.605557820636,-5.79605005908598,
133.97294053439));
#220223=CARTESIAN_POINT('Ctrl Pts',(163.327110196823,-0.467090610458611,
137.393436526853));
#220224=CARTESIAN_POINT('Ctrl Pts',(163.04866257301,5.29110229053537,134.758893652935));
#220225=CARTESIAN_POINT('Ctrl Pts',(162.770214949197,6.18703067124424,128.49032810919));
#220226=CARTESIAN_POINT('Ctrl Pts',(162.491767325384,1.39738011833125,124.34824539387));
#220227=CARTESIAN_POINT('Ctrl Pts',(162.213319701571,-4.67639449751423,
126.139017170363));
#220228=CARTESIAN_POINT('Ctrl Pts',(161.934872077759,-6.45279102471594,
132.217011660137));
#220229=CARTESIAN_POINT('Ctrl Pts',(161.656424453946,-2.29938783657033,
136.996848853628));
#220230=CARTESIAN_POINT('Ctrl Pts',(161.377976830133,3.96704044204275,136.086091878046));
#220231=CARTESIAN_POINT('Ctrl Pts',(161.09952920632,6.58795235511813,130.321681900999));
#220232=CARTESIAN_POINT('Ctrl Pts',(160.821081582507,3.15485789320466,125.000830084311));
#220233=CARTESIAN_POINT('Ctrl Pts',(160.542633958694,-3.17739684918762,
125.013139309456));
#220234=CARTESIAN_POINT('Ctrl Pts',(160.264186334881,-6.58977911164196,
130.347297999864));
#220235=CARTESIAN_POINT('Ctrl Pts',(159.985738711068,-3.94647629910411,
136.10147490719));
#220236=CARTESIAN_POINT('Ctrl Pts',(159.707291087255,2.32344543622502,136.98786256077));
#220237=CARTESIAN_POINT('Ctrl Pts',(159.428843463442,6.45823432228318,132.191914009409));
#220238=CARTESIAN_POINT('Ctrl Pts',(159.15039583963,4.65822136844951,126.120871676696));
#220239=CARTESIAN_POINT('Ctrl Pts',(158.871948215817,-1.42246945622416,
124.353726879487));
#220240=CARTESIAN_POINT('Ctrl Pts',(158.593500592004,-6.19598034212407,
128.514399356595));
#220241=CARTESIAN_POINT('Ctrl Pts',(158.315052968191,-5.2756879840792,134.779434361708));
#220242=CARTESIAN_POINT('Ctrl Pts',(158.036605344378,0.49270389964821,137.391570789103));
#220243=CARTESIAN_POINT('Ctrl Pts',(157.758157720565,5.80832496952254,133.950382871961));
#220244=CARTESIAN_POINT('Ctrl Pts',(157.479710096752,5.78637914485521,127.618154194761));
#220245=CARTESIAN_POINT('Ctrl Pts',(157.201262472939,0.447033566402335,
124.213893565282));
#220246=CARTESIAN_POINT('Ctrl Pts',(156.922814849126,-5.3031140207705,126.865950194636));
#220247=CARTESIAN_POINT('Ctrl Pts',(156.644367225313,-6.17995889437779,
133.137213600617));
#220248=CARTESIAN_POINT('Ctrl Pts',(156.365919601501,-1.37772345182797,
137.264699081378));
#220249=CARTESIAN_POINT('Ctrl Pts',(156.087471977688,4.69057253741941,135.455449118975));
#220250=CARTESIAN_POINT('Ctrl Pts',(155.809024353875,6.44846151198586,129.372076042081));
#220251=CARTESIAN_POINT('Ctrl Pts',(155.530576730062,2.28052938189546,124.604902519066));
#220252=CARTESIAN_POINT('Ctrl Pts',(155.252129106249,-3.98309784010292,
125.534728128207));
#220253=CARTESIAN_POINT('Ctrl Pts',(154.973681482436,-6.58645273219382,
131.307088559209));
#220254=CARTESIAN_POINT('Ctrl Pts',(154.695233858623,-3.13717932950269,
136.617466571466));
#220255=CARTESIAN_POINT('Ctrl Pts',(154.41678623481,3.19500861727094,136.585884198101));
#220256=CARTESIAN_POINT('Ctrl Pts',(154.138338610998,6.59113972962085,131.241364097354));
#220257=CARTESIAN_POINT('Ctrl Pts',(153.859890987185,3.93033542552574,125.495259147487));
#220258=CARTESIAN_POINT('Ctrl Pts',(153.581443363372,-2.3422551270676,124.627959084596));
#220259=CARTESIAN_POINT('Ctrl Pts',(153.302995739559,-6.46242764341012,
129.436470296516));
#220260=CARTESIAN_POINT('Ctrl Pts',(153.024548115746,-4.64394486260028,
135.502005888322));
#220261=CARTESIAN_POINT('Ctrl Pts',(152.746100491933,1.44209637762021,137.250634969033));
#220262=CARTESIAN_POINT('Ctrl Pts',(152.46765286812,6.20292149713234,133.075452838754));
#220263=CARTESIAN_POINT('Ctrl Pts',(152.189205244307,5.26356479034146,126.813247906226));
#220264=CARTESIAN_POINT('Ctrl Pts',(151.910757620494,-0.512750819337957,
124.218680578724));
#220265=CARTESIAN_POINT('Ctrl Pts',(151.632309996682,-5.8178734753159,127.676031478561));
#220266=CARTESIAN_POINT('Ctrl Pts',(151.353862372869,-5.77665462639848,
134.008164029768));
#220267=CARTESIAN_POINT('Ctrl Pts',(151.075414749056,-0.4269723810881,137.39615775966));
#220268=CARTESIAN_POINT('Ctrl Pts',(150.796967125243,5.31507662368183,134.72661194316));
#220269=CARTESIAN_POINT('Ctrl Pts',(150.51851950143,6.17282986721635,128.452708771068));
#220270=CARTESIAN_POINT('Ctrl Pts',(150.240071877617,1.35805402228283,124.339858761329));
#220271=CARTESIAN_POINT('Ctrl Pts',(149.961624253804,-4.70470712450132,
126.167570148998));
#220272=CARTESIAN_POINT('Ctrl Pts',(149.683176629991,-6.44407226158927,
132.256265457474));
#220273=CARTESIAN_POINT('Ctrl Pts',(149.404729006178,-2.26164980070799,
137.010731147569));
#220274=CARTESIAN_POINT('Ctrl Pts',(149.126281382365,3.99911833928874,136.061845518646));
#220275=CARTESIAN_POINT('Ctrl Pts',(148.847833758553,6.58489209327119,130.281588108047));
#220276=CARTESIAN_POINT('Ctrl Pts',(148.56938613474,3.11947170339994,124.981733094838));
#220277=CARTESIAN_POINT('Ctrl Pts',(148.290938510927,-3.21259078723097,
125.032588323847));
#220278=CARTESIAN_POINT('Ctrl Pts',(148.012490887114,-6.59243928818165,
130.387420324031));
#220279=CARTESIAN_POINT('Ctrl Pts',(147.734043263301,-3.91415814185689,
136.125400085308));
#220280=CARTESIAN_POINT('Ctrl Pts',(147.455595639488,2.36104311957866,136.973604522958));
#220281=CARTESIAN_POINT('Ctrl Pts',(147.177148015675,6.46656109749016,132.152575195872));
#220282=CARTESIAN_POINT('Ctrl Pts',(146.898700391862,4.6296253358803,126.092602535266));
#220283=CARTESIAN_POINT('Ctrl Pts',(146.62025276805,-1.46170993963237,124.362505370115));
#220284=CARTESIAN_POINT('Ctrl Pts',(146.341805144237,-6.20980518912327,
128.552158475246));
#220285=CARTESIAN_POINT('Ctrl Pts',(146.063357520424,-5.2513928356585,134.811475322978));
#220286=CARTESIAN_POINT('Ctrl Pts',(145.784909896611,0.532792988974217,
137.388449514872));
#220287=CARTESIAN_POINT('Ctrl Pts',(145.506462272798,5.82736808512415,133.914967660766));
#220288=CARTESIAN_POINT('Ctrl Pts',(145.228014648985,5.76687659380242,127.582989895561));
#220289=CARTESIAN_POINT('Ctrl Pts',(144.949567025172,0.406907240360106,
124.211294451169));
#220290=CARTESIAN_POINT('Ctrl Pts',(144.671119401359,-5.32698998844935,
126.898304724507));
#220291=CARTESIAN_POINT('Ctrl Pts',(144.392671777546,-6.16564365580234,
133.174789542127));
#220292=CARTESIAN_POINT('Ctrl Pts',(144.114224153734,-1.33837201191069,
137.272965979966));
#220293=CARTESIAN_POINT('Ctrl Pts',(143.83577652992,4.71879812781917,135.426810098699));
#220294=CARTESIAN_POINT('Ctrl Pts',(143.557328906108,6.43962331418753,129.332848963481));
#220295=CARTESIAN_POINT('Ctrl Pts',(143.278881282295,2.24274926790569,124.591135151027));
#220296=CARTESIAN_POINT('Ctrl Pts',(143.000433658482,-4.01510179118866,
125.559072009383));
#220297=CARTESIAN_POINT('Ctrl Pts',(142.721986034669,-6.58327045280769,
131.347172852065));
#220298=CARTESIAN_POINT('Ctrl Pts',(142.443538410856,-3.10173517893752,
136.636455769093));
#220299=CARTESIAN_POINT('Ctrl Pts',(142.165090787043,3.23014319618891,136.566328155556));
#220300=CARTESIAN_POINT('Ctrl Pts',(141.886643163231,6.5936777752854,131.201233862367));
#220301=CARTESIAN_POINT('Ctrl Pts',(141.608195539417,3.89794459796173,125.471432445543));
#220302=CARTESIAN_POINT('Ctrl Pts',(141.329747915605,-2.37980923970876,
124.642331490782));
#220303=CARTESIAN_POINT('Ctrl Pts',(141.051300291792,-6.47063464623165,
129.475834271677));
#220304=CARTESIAN_POINT('Ctrl Pts',(140.772852667979,-4.61526292094352,
135.530187862324));
#220305=CARTESIAN_POINT('Ctrl Pts',(140.494405044166,1.48130996056343,137.241737084533));
#220306=CARTESIAN_POINT('Ctrl Pts',(140.215957420353,6.21663135432719,133.037651816923));
#220307=CARTESIAN_POINT('Ctrl Pts',(139.93750979654,5.23917223278974,126.781281039444));
#220308=CARTESIAN_POINT('Ctrl Pts',(139.659062172727,-0.552830222889001,
124.221923855894));
#220309=CARTESIAN_POINT('Ctrl Pts',(139.380614548914,-5.83680871099059,
127.711504486408));
#220310=CARTESIAN_POINT('Ctrl Pts',(139.102166925101,-5.75704513764935,
134.043268807033));
#220311=CARTESIAN_POINT('Ctrl Pts',(138.823719301288,-0.386838330098996,
137.398634730999));
#220312=CARTESIAN_POINT('Ctrl Pts',(138.545271677476,5.33885400470937,134.694184892919));
#220313=CARTESIAN_POINT('Ctrl Pts',(138.266824053663,6.15840032670771,128.41517657427));
#220314=CARTESIAN_POINT('Ctrl Pts',(137.98837642985,1.31867760304303,124.331711673279));
#220315=CARTESIAN_POINT('Ctrl Pts',(137.709928806037,-4.7328454168358,126.196294945608));
#220316=CARTESIAN_POINT('Ctrl Pts',(137.431481182224,-6.43511471099507,
132.295465453942));
#220317=CARTESIAN_POINT('Ctrl Pts',(137.153033558411,-2.22382795858067,
137.024383462168));
#220318=CARTESIAN_POINT('Ctrl Pts',(136.874585934598,4.03104804773404,136.037404341212));
#220319=CARTESIAN_POINT('Ctrl Pts',(136.596138310785,6.5815878258261,130.241513686623));
#220320=CARTESIAN_POINT('Ctrl Pts',(136.317690686972,3.08396992042408,124.96285186497));
#220321=CARTESIAN_POINT('Ctrl Pts',(136.03924306316,-3.24766568154122,125.052251213384));
#220322=CARTESIAN_POINT('Ctrl Pts',(135.760795439346,-6.5948551794591,130.427558098075));
#220323=CARTESIAN_POINT('Ctrl Pts',(135.482347815534,-3.88169494404043,
136.149128090351));
#220324=CARTESIAN_POINT('Ctrl Pts',(135.203900191721,2.3985533136112,136.959117881544));
#220325=CARTESIAN_POINT('Ctrl Pts',(134.925452567908,6.47464825189767,132.113186423748));
#220326=CARTESIAN_POINT('Ctrl Pts',(134.647004944095,4.60085775084163,126.064507989766));
#220327=CARTESIAN_POINT('Ctrl Pts',(134.368557320282,-1.50089625884118,
124.371522566057));
#220328=CARTESIAN_POINT('Ctrl Pts',(134.090109696469,-6.22339992950755,
128.590001050074));
#220329=CARTESIAN_POINT('Ctrl Pts',(133.811662072656,-5.22690309494509,
134.843367799137));
#220330=CARTESIAN_POINT('Ctrl Pts',(133.533214448844,0.572862335460145,
137.385084264805));
#220331=CARTESIAN_POINT('Ctrl Pts',(133.25476682503,5.84619526545829,133.879437184883));
#220332=CARTESIAN_POINT('Ctrl Pts',(132.976319201218,5.7471603490167,127.547944965438));
#220333=CARTESIAN_POINT('Ctrl Pts',(132.697871577405,0.366765836220533,
124.208939645549));
#220334=CARTESIAN_POINT('Ctrl Pts',(132.419423953592,-5.35066856255522,
126.930803994717));
#220335=CARTESIAN_POINT('Ctrl Pts',(132.140976329779,-6.15109994703373,
133.212277646521));
#220336=CARTESIAN_POINT('Ctrl Pts',(131.862528705966,-1.29897097812634,
137.280993182001));
#220337=CARTESIAN_POINT('Ctrl Pts',(131.584081082153,4.74684886141891,135.397999791857));
#220338=CARTESIAN_POINT('Ctrl Pts',(131.30563345834,6.43054649377913,129.293676412286));
#220339=CARTESIAN_POINT('Ctrl Pts',(131.027185834528,2.20488604801711,124.577598016342));
#220340=CARTESIAN_POINT('Ctrl Pts',(130.748738210715,-4.04695696120101,
125.583610256657));
#220341=CARTESIAN_POINT('Ctrl Pts',(130.470290586902,-6.57984422791396,
131.387237030814));
#220342=CARTESIAN_POINT('Ctrl Pts',(130.191842963089,-3.06617609243459,
136.65522885629));
#220343=CARTESIAN_POINT('Ctrl Pts',(129.913395339276,3.26515808096253,136.546558601182));
#220344=CARTESIAN_POINT('Ctrl Pts',(129.634947715463,6.59597148979528,131.161088921098));
#220345=CARTESIAN_POINT('Ctrl Pts',(129.35650009165,3.86540933062731,125.447803357213));
#220346=CARTESIAN_POINT('Ctrl Pts',(129.078052467837,-2.41727516764341,
124.656932233223));
#220347=CARTESIAN_POINT('Ctrl Pts',(128.799604844024,-6.47860187730669,
129.515247475871));
#220348=CARTESIAN_POINT('Ctrl Pts',(128.521157220212,-4.58640995902212,
135.558194719059));
#220349=CARTESIAN_POINT('Ctrl Pts',(128.242709596398,1.52046865302106,137.232600660681));
#220350=CARTESIAN_POINT('Ctrl Pts',(127.964261972586,6.23011085196111,132.999768039666));
#220351=CARTESIAN_POINT('Ctrl Pts',(127.685814348773,5.2145855357842,126.749463249355));
#220352=CARTESIAN_POINT('Ctrl Pts',(127.40736672496,-0.592889141112855,
124.225411047681));
#220353=CARTESIAN_POINT('Ctrl Pts',(127.128919101147,-5.85552766157182,
127.747092101177));
#220354=CARTESIAN_POINT('Ctrl Pts',(126.850471477334,-5.7372223194756,134.078253565364));
#220355=CARTESIAN_POINT('Ctrl Pts',(126.572023853521,-0.346689944673359,
137.400867349086));
#220356=CARTESIAN_POINT('Ctrl Pts',(126.293576229708,5.36243355253846,134.66161370381));
#220357=CARTESIAN_POINT('Ctrl Pts',(126.015128605896,6.14374258441013,128.377732909565));
#220358=CARTESIAN_POINT('Ctrl Pts',(125.736680982083,1.27925231971985,124.323804431618));
#220359=CARTESIAN_POINT('Ctrl Pts',(125.45823335827,-4.76080833184274,126.225190495787));
#220360=CARTESIAN_POINT('Ctrl Pts',(125.179785734457,-6.42591870485886,
132.334610196974));
#220361=CARTESIAN_POINT('Ctrl Pts',(124.901338110644,-2.1859237116904,137.037805291532));
#220362=CARTESIAN_POINT('Ctrl Pts',(124.622890486831,4.06282838421153,136.012769251418));
#220363=CARTESIAN_POINT('Ctrl Pts',(124.344442863018,6.5780396752237,130.201460121699));
#220364=CARTESIAN_POINT('Ctrl Pts',(124.065995239205,3.04835385980878,124.944187094356));
#220365=CARTESIAN_POINT('Ctrl Pts',(123.787547615392,-3.28262023240536,
125.07212724945));
#220366=CARTESIAN_POINT('Ctrl Pts',(123.509099991579,-6.59702669595264,
130.467709834674));
#220367=CARTESIAN_POINT('Ctrl Pts',(123.230652367767,-3.84908790859021,
136.17265804307));
#220368=CARTESIAN_POINT('Ctrl Pts',(122.952204743954,2.43597462836867,136.944403173336));
#220369=CARTESIAN_POINT('Ctrl Pts',(122.673757120141,6.48249548583303,132.073749152604));
#220370=CARTESIAN_POINT('Ctrl Pts',(122.395309496328,4.57191967932717,126.036589081248));
#220371=CARTESIAN_POINT('Ctrl Pts',(122.116861872515,-1.54002696178715,
124.380778133181));
#220372=CARTESIAN_POINT('Ctrl Pts',(121.838414248702,-6.23676405951882,
128.627925678811));
#220373=CARTESIAN_POINT('Ctrl Pts',(121.559966624889,-5.20221966941523,
134.8751106084));
#220374=CARTESIAN_POINT('Ctrl Pts',(121.281519001076,0.612910454321425,
137.381475163605));
#220375=CARTESIAN_POINT('Ctrl Pts',(121.003071377263,5.86480581287692,133.843792760907));
#220376=CARTESIAN_POINT('Ctrl Pts',(120.724623753451,5.72723114109079,127.513020702994));
#220377=CARTESIAN_POINT('Ctrl Pts',(120.446176129638,0.326610841437887,
124.206829235678));
#220378=CARTESIAN_POINT('Ctrl Pts',(120.167728505825,-5.3741488656698,126.963446800991));
#220379=CARTESIAN_POINT('Ctrl Pts',(119.889280882012,-6.13632830699453,
133.249676524665));
#220380=CARTESIAN_POINT('Ctrl Pts',(119.610833258199,-1.25952181049465,
137.288780390037));
#220381=CARTESIAN_POINT('Ctrl Pts',(119.332385634386,4.77472369878856,135.369019266025));
#220382=CARTESIAN_POINT('Ctrl Pts',(119.053938010573,6.42123138710552,129.254559840052));
#220383=CARTESIAN_POINT('Ctrl Pts',(118.77549038676,2.16694112526505,124.564291616636));
#220384=CARTESIAN_POINT('Ctrl Pts',(118.497042762948,-4.07866216973492,
125.608341960757));
#220385=CARTESIAN_POINT('Ctrl Pts',(118.218595139134,-6.57617418447253,
131.427279610862));
#220386=CARTESIAN_POINT('Ctrl Pts',(117.940147515322,-3.03050338764912,
136.673785137412));
#220387=CARTESIAN_POINT('Ctrl Pts',(117.661699891509,3.30005197410286,136.526576267552));
#220388=CARTESIAN_POINT('Ctrl Pts',(117.383252267696,6.59802078815589,131.120930761129));
#220389=CARTESIAN_POINT('Ctrl Pts',(117.104804643883,3.83273082912851,125.424372758082));
#220390=CARTESIAN_POINT('Ctrl Pts',(116.82635702007,-2.45465152255762,124.671760770883));
#220391=CARTESIAN_POINT('Ctrl Pts',(116.547909396257,-6.48632904140672,
129.554708448625));
#220392=CARTESIAN_POINT('Ctrl Pts',(116.269461772444,-4.55738704599302,
135.586025420722));
#220393=CARTESIAN_POINT('Ctrl Pts',(115.991014148631,1.55957100395386,137.223226036031));
#220394=CARTESIAN_POINT('Ctrl Pts',(115.712566524818,6.24335949054626,132.961802910777));
#220395=CARTESIAN_POINT('Ctrl Pts',(115.434118901006,5.18980561039392,126.717795714978));
#220396=CARTESIAN_POINT('Ctrl Pts',(115.155671277193,-0.632926089611396,
124.229142024863));
#220397=CARTESIAN_POINT('Ctrl Pts',(114.87722365338,-5.87402963342224,127.782793004156));
#220398=CARTESIAN_POINT('Ctrl Pts',(114.598776029567,-5.71718690641897,
134.113117008387));
#220399=CARTESIAN_POINT('Ctrl Pts',(114.320328405754,-0.306528712524212,
137.40285553119));
#220400=CARTESIAN_POINT('Ctrl Pts',(114.041880781941,5.38581439342023,134.628899582769));
#220401=CARTESIAN_POINT('Ctrl Pts',(113.763433158128,6.12885718347172,128.340379164441));
#220402=CARTESIAN_POINT('Ctrl Pts',(113.484985534315,1.23977963323159,124.316137329349));
#220403=CARTESIAN_POINT('Ctrl Pts',(113.206537910502,-4.78859483334625,
126.254255728798));
#220404=CARTESIAN_POINT('Ctrl Pts',(112.92809028669,-6.41648458394181,132.373698236044));
#220405=CARTESIAN_POINT('Ctrl Pts',(112.649642662877,-2.14793846459313,
137.050996138312));
#220406=CARTESIAN_POINT('Ctrl Pts',(112.371195039064,4.09445817108915,135.987941162125));
#220407=CARTESIAN_POINT('Ctrl Pts',(112.092747415251,6.57424777294209,130.161428897475));
#220408=CARTESIAN_POINT('Ctrl Pts',(111.814299791438,3.01262484132005,124.925739474628));
#220409=CARTESIAN_POINT('Ctrl Pts',(111.535852167625,-3.31745314456969,
125.092215695531));
#220410=CARTESIAN_POINT('Ctrl Pts',(111.257404543812,-6.59895375719588,
130.507874045991));
#220411=CARTESIAN_POINT('Ctrl Pts',(110.978956919999,-3.816338243772,136.195989071554));
#220412=CARTESIAN_POINT('Ctrl Pts',(110.700509296186,2.47330567719032,136.929460943594));
#220413=CARTESIAN_POINT('Ctrl Pts',(110.422061672374,6.49010250851429,132.0342648438));
#220414=CARTESIAN_POINT('Ctrl Pts',(110.143614048561,4.54281219364771,126.008846844259));
#220415=CARTESIAN_POINT('Ctrl Pts',(109.865166424748,-1.57910059846782,
124.390271728514));
#220416=CARTESIAN_POINT('Ctrl Pts',(109.586718800935,-6.24989708394428,
128.665930956147));
#220417=CARTESIAN_POINT('Ctrl Pts',(109.308271177122,-5.17734347372243,
134.906702574525));
#220418=CARTESIAN_POINT('Ctrl Pts',(109.029823553309,0.652935861560398,
137.377622345005));
#220419=CARTESIAN_POINT('Ctrl Pts',(108.751375929496,5.88319903775945,133.808035709655));
#220420=CARTESIAN_POINT('Ctrl Pts',(108.472928305683,5.70708970850866,127.478218402361));
#220421=CARTESIAN_POINT('Ctrl Pts',(108.19448068187,0.286443743970404,124.204963299759));
#220422=CARTESIAN_POINT('Ctrl Pts',(107.916033058058,-5.39743002772183,
126.996231933739));
#220423=CARTESIAN_POINT('Ctrl Pts',(107.637585434244,-6.12132928305326,
133.286984790727));
#220424=CARTESIAN_POINT('Ctrl Pts',(107.359137810432,-1.22002597081922,
137.296327315513));
#220425=CARTESIAN_POINT('Ctrl Pts',(107.080690186619,4.80242160701559,135.339869595089));
#220426=CARTESIAN_POINT('Ctrl Pts',(106.802242562806,6.41167833934146,129.215500696253));
#220427=CARTESIAN_POINT('Ctrl Pts',(106.523794938993,2.12891590571267,124.551216444981));
#220428=CARTESIAN_POINT('Ctrl Pts',(106.24534731518,-4.11021624194206,125.633266205238));
#220429=CARTESIAN_POINT('Ctrl Pts',(105.966899691367,-6.57226045847839,
131.467299108419));
#220430=CARTESIAN_POINT('Ctrl Pts',(105.688452067554,-2.99471838644612,
136.692123924851));
#220431=CARTESIAN_POINT('Ctrl Pts',(105.410004443742,3.33482358260376,136.506381895117));
#220432=CARTESIAN_POINT('Ctrl Pts',(105.131556819929,6.59982559442975,131.080760870538));
#220433=CARTESIAN_POINT('Ctrl Pts',(104.853109196116,3.79991030437941,125.401141516381));
#220434=CARTESIAN_POINT('Ctrl Pts',(104.574661572303,-2.49193691945696,
124.686816554284));
#220435=CARTESIAN_POINT('Ctrl Pts',(104.29621394849,-6.49381585219884,129.594215727701));
#220436=CARTESIAN_POINT('Ctrl Pts',(104.017766324677,-4.52819525731082,
135.613678936038));
#220437=CARTESIAN_POINT('Ctrl Pts',(103.739318700864,1.59861556440955,137.213613557961));
#220438=CARTESIAN_POINT('Ctrl Pts',(103.460871077051,6.25637677914949,132.923757837073));
#220439=CARTESIAN_POINT('Ctrl Pts',(103.182423453238,5.16483337484823,126.686279609768));
#220440=CARTESIAN_POINT('Ctrl Pts',(102.903975829425,-0.672939584800916,
124.233116649188));
#220441=CARTESIAN_POINT('Ctrl Pts',(102.625528205613,-5.89231394094447,
127.818605872432));
#220442=CARTESIAN_POINT('Ctrl Pts',(102.347080581799,-5.69693964089892,
134.147857844226));
#220443=CARTESIAN_POINT('Ctrl Pts',(102.068632957987,-0.266356121840884,
137.40459920364));
#220444=CARTESIAN_POINT('Ctrl Pts',(101.790185334174,5.40899566096888,134.59604374203));
#220445=CARTESIAN_POINT('Ctrl Pts',(101.511737710361,6.11374467547657,128.303116723058));
#220446=CARTESIAN_POINT('Ctrl Pts',(101.233290086548,1.20026100625305,124.308710650579));
#220447=CARTESIAN_POINT('Ctrl Pts',(100.954842462735,-4.81620389170723,
126.28348956762));
#220448=CARTESIAN_POINT('Ctrl Pts',(100.676394838922,-6.40681269782886,
132.412728122731));
#220449=CARTESIAN_POINT('Ctrl Pts',(100.397947215109,-2.10987362484612,
137.063955513716));
#220450=CARTESIAN_POINT('Ctrl Pts',(100.119499591297,4.12593623631335,135.962920993349));
#220451=CARTESIAN_POINT('Ctrl Pts',(99.8410519674839,6.5702122594916,130.121421497322));
#220452=CARTESIAN_POINT('Ctrl Pts',(99.5626043436712,2.97678418891005,124.907509689368));
#220453=CARTESIAN_POINT('Ctrl Pts',(99.2841567198582,-3.35216312728773,
125.112515807244));
#220454=CARTESIAN_POINT('Ctrl Pts',(99.0057090960455,-6.6006362917809,130.548049243728));
#220455=CARTESIAN_POINT('Ctrl Pts',(98.7272614722323,-3.78344716313679,
136.219120311263));
#220456=CARTESIAN_POINT('Ctrl Pts',(98.4488138484198,2.51054507676055,136.914291746006));
#220457=CARTESIAN_POINT('Ctrl Pts',(98.1703662246066,6.49746903806041,131.994734960442));
#220458=CARTESIAN_POINT('Ctrl Pts',(97.8919186007939,4.51353637239165,125.981282306795));
#220459=CARTESIAN_POINT('Ctrl Pts',(97.6134709769809,-1.61811572099509,
124.400003000271));
#220460=CARTESIAN_POINT('Ctrl Pts',(97.335023353168,-6.26279851613479,128.704015473778));
#220461=CARTESIAN_POINT('Ctrl Pts',(97.0565757293552,-5.15227542966332,
134.938142526861));
#220462=CARTESIAN_POINT('Ctrl Pts',(96.7781281055422,0.692937074020952,
137.373525951775));
#220463=CARTESIAN_POINT('Ctrl Pts',(96.4996804817294,5.90137425853808,133.772167356118));
#220464=CARTESIAN_POINT('Ctrl Pts',(96.2212328579164,5.6867367976186,127.443539353151));
#220465=CARTESIAN_POINT('Ctrl Pts',(95.9427852341037,0.246266032224636,
124.203341906934));
#220466=CARTESIAN_POINT('Ctrl Pts',(95.6643376102905,-5.42051118601915,
127.029158178097));
#220467=CARTESIAN_POINT('Ctrl Pts',(95.3858899864779,-6.10610343100435,
133.324201062238));
#220468=CARTESIAN_POINT('Ctrl Pts',(95.1074423626648,-1.18048492263276,
137.303633678775));
#220469=CARTESIAN_POINT('Ctrl Pts',(94.828994738852,4.82994155974394,135.3105518592));
#220470=CARTESIAN_POINT('Ctrl Pts',(94.5505471150391,6.40188770447863,129.176500428244));
#220471=CARTESIAN_POINT('Ctrl Pts',(94.2720994912261,2.09081179839861,124.538372985881));
#220472=CARTESIAN_POINT('Ctrl Pts',(93.9936518674133,-4.14161800857485,
125.658382066524));
#220473=CARTESIAN_POINT('Ctrl Pts',(93.7152042436005,-6.56810319495607,
131.507294040545));
#220474=CARTESIAN_POINT('Ctrl Pts',(93.4367566197874,-2.95882241485189,
136.710244539055));
#220475=CARTESIAN_POINT('Ctrl Pts',(93.1583089959747,3.36947161799043,136.485976232185));
#220476=CARTESIAN_POINT('Ctrl Pts',(92.8798613721617,6.60138584173913,131.040580737834));
#220477=CARTESIAN_POINT('Ctrl Pts',(92.6014137483489,3.76694897255651,125.37811049295));
#220478=CARTESIAN_POINT('Ctrl Pts',(92.3229661245359,-2.5291299767175,124.702099025532));
#220479=CARTESIAN_POINT('Ctrl Pts',(92.044518500723,-6.50106203225643,129.633767849141));
#220480=CARTESIAN_POINT('Ctrl Pts',(91.7660708769102,-4.49883567468812,
135.641154240296));
#220481=CARTESIAN_POINT('Ctrl Pts',(91.4876232530973,1.63760088757763,137.203763582666));
#220482=CARTESIAN_POINT('Ctrl Pts',(91.2091756292845,6.26916223541028,132.885634228324));
#220483=CARTESIAN_POINT('Ctrl Pts',(90.9307280054714,5.13966975450256,126.654916101563));
#220484=CARTESIAN_POINT('Ctrl Pts',(90.6522803816587,-0.71292814396669,
124.237334773374));
#220485=CARTESIAN_POINT('Ctrl Pts',(90.3738327578456,-5.91037990660673,
127.85452937895));
#220486=CARTESIAN_POINT('Ctrl Pts',(90.0953851340328,-5.67648127318543,
134.182474785545));
#220487=CARTESIAN_POINT('Ctrl Pts',(89.8169375102199,-0.226173661233629,
137.406098301819));
#220488=CARTESIAN_POINT('Ctrl Pts',(89.5384898864071,5.43197649619419,134.563047399079));
#220489=CARTESIAN_POINT('Ctrl Pts',(89.260042262594,6.09840562042418,128.265946966186));
#220490=CARTESIAN_POINT('Ctrl Pts',(88.9815946387814,1.1606979031614,124.301524670509));
#220491=CARTESIAN_POINT('Ctrl Pts',(88.7031470149683,-4.84363448386183,
126.312890928981));
#220492=CARTESIAN_POINT('Ctrl Pts',(88.4246993911556,-6.39690340491527,
132.45169841077));
#220493=CARTESIAN_POINT('Ctrl Pts',(88.1462517673426,-2.07173060295614,
137.076682937528));
#220494=CARTESIAN_POINT('Ctrl Pts',(87.8678041435297,4.15726141345302,135.937709672222));
#220495=CARTESIAN_POINT('Ctrl Pts',(87.5893565197169,6.5659332844097,130.081439403729));
#220496=CARTESIAN_POINT('Ctrl Pts',(87.3109088959039,2.94083323066708,124.889498414087));
#220497=CARTESIAN_POINT('Ctrl Pts',(87.032461272091,-3.38674889436835,125.133026832359));
#220498=CARTESIAN_POINT('Ctrl Pts',(86.7540136482781,-6.60207423736065,
130.588233939178));
#220499=CARTESIAN_POINT('Ctrl Pts',(86.4755660244652,-3.75041588547566,
136.242050905059));
#220500=CARTESIAN_POINT('Ctrl Pts',(86.1971184006524,2.54769144715974,136.898896142674));
#220501=CARTESIAN_POINT('Ctrl Pts',(85.9186707768394,6.50459480150186,131.955160967326));
#220502=CARTESIAN_POINT('Ctrl Pts',(85.6402231530266,4.48409330038545,125.953896490271));
#220503=CARTESIAN_POINT('Ctrl Pts',(85.3617755292137,-1.65707088364924,
124.409971587854));
#220504=CARTESIAN_POINT('Ctrl Pts',(85.0833279054008,-6.27546787802325,
128.742177820471));
#220505=CARTESIAN_POINT('Ctrl Pts',(84.8048802815879,-5.12701646614329,
134.969429300388));
#220506=CARTESIAN_POINT('Ctrl Pts',(84.526432657775,0.732912609443495,137.369186135708));
#220507=CARTESIAN_POINT('Ctrl Pts',(84.2479850339622,5.91933080172332,133.73618902941));
#220508=CARTESIAN_POINT('Ctrl Pts',(83.9695374101491,5.6661731626052,127.408984840408));
#220509=CARTESIAN_POINT('Ctrl Pts',(83.6910897863363,0.206079195000604,
124.201965117285));
#220510=CARTESIAN_POINT('Ctrl Pts',(83.4126421625234,-5.44339148528112,
127.062224313968));
#220511=CARTESIAN_POINT('Ctrl Pts',(83.1341945387106,-6.09065131504733,
133.361323960135));
#220512=CARTESIAN_POINT('Ctrl Pts',(82.8557469148977,-1.14090013114324,
137.310699209084));
#220513=CARTESIAN_POINT('Ctrl Pts',(82.5772992910847,4.85728253721157,135.281067144739));
#220514=CARTESIAN_POINT('Ctrl Pts',(82.2988516672719,6.39185984531258,129.137560481192));
#220515=CARTESIAN_POINT('Ctrl Pts',(82.0204040434589,2.05263021528453,124.52576171526));
#220516=CARTESIAN_POINT('Ctrl Pts',(81.7419564196462,-4.17286630602932,
125.683688613938));
#220517=CARTESIAN_POINT('Ctrl Pts',(81.4635087958331,-6.56370254795435,
131.547262925216));
#220518=CARTESIAN_POINT('Ctrl Pts',(81.1850611720204,-2.92281680300497,
136.728146308557));
#220519=CARTESIAN_POINT('Ctrl Pts',(80.9066135482074,3.40399479636718,136.465360034899));
#220520=CARTESIAN_POINT('Ctrl Pts',(80.6281659243945,6.60270147226842,131.000391851905));
#220521=CARTESIAN_POINT('Ctrl Pts',(80.3497183005816,3.73384805505426,125.355280541214));
#220522=CARTESIAN_POINT('Ctrl Pts',(80.0712706767688,-2.56622931613655,
124.717607618327));
#220523=CARTESIAN_POINT('Ctrl Pts',(79.7928230529558,-6.50806731306963,
129.673363347327));
#220524=CARTESIAN_POINT('Ctrl Pts',(79.514375429143,-4.46930938605503,135.668450315387));
#220525=CARTESIAN_POINT('Ctrl Pts',(79.23592780533,1.67652552884245,137.193676475141));
#220526=CARTESIAN_POINT('Ctrl Pts',(78.9574801815173,6.28171538555901,132.847433497217));
#220527=CARTESIAN_POINT('Ctrl Pts',(78.6790325577042,5.11431568180404,126.62370635255));
#220528=CARTESIAN_POINT('Ctrl Pts',(78.4005849338915,-0.752890285318027,
124.241796241119));
#220529=CARTESIAN_POINT('Ctrl Pts',(78.1221373100785,-5.92822686096799,
127.890562192549));
#220530=CARTESIAN_POINT('Ctrl Pts',(77.8436896862655,-5.65581256137084,
134.216966549603));
#220531=CARTESIAN_POINT('Ctrl Pts',(77.5652420624528,-0.185982819678218,
137.407352770183));
#220532=CARTESIAN_POINT('Ctrl Pts',(77.2867944386398,5.45475604753291,134.529911776607));
#220533=CARTESIAN_POINT('Ctrl Pts',(77.008346814827,6.08284058670873,128.228871271165));
#220534=CARTESIAN_POINT('Ctrl Pts',(76.729899191014,1.12109178998211,124.294579655415));
#220535=CARTESIAN_POINT('Ctrl Pts',(76.4514515672013,-4.8708855933594,126.342458723402));
#220536=CARTESIAN_POINT('Ctrl Pts',(76.1730039433881,-6.38675707239351,
132.4906076561));
#220537=CARTESIAN_POINT('Ctrl Pts',(75.8945563195755,-2.03351081232684,
137.089177938131));
#220538=CARTESIAN_POINT('Ctrl Pts',(75.6161086957625,4.18843254174224,135.912308132958));
#220539=CARTESIAN_POINT('Ctrl Pts',(75.3376610719495,6.56141100625526,130.041484098248));
#220540=CARTESIAN_POINT('Ctrl Pts',(75.0592134481368,2.90477329876725,124.871706316201));
#220541=CARTESIAN_POINT('Ctrl Pts',(74.7807658243238,-3.42120916422307,
125.153748010832));
#220542=CARTESIAN_POINT('Ctrl Pts',(74.5023182005109,-6.60326754065171,
130.628426643279));
#220543=CARTESIAN_POINT('Ctrl Pts',(74.223870576698,-3.71724563477466,136.264780003243));
#220544=CARTESIAN_POINT('Ctrl Pts',(73.9454229528852,2.58474341191554,136.883274704086));
#220545=CARTESIAN_POINT('Ctrl Pts',(73.6669753290721,6.51147953479087,131.915544330879));
#220546=CARTESIAN_POINT('Ctrl Pts',(73.3885277052595,4.45448406865298,125.926690409479));
#220547=CARTESIAN_POINT('Ctrl Pts',(73.1100800814464,-1.6959646429323,124.420177121874));
#220548=CARTESIAN_POINT('Ctrl Pts',(72.8316324576336,-6.28790470014163,
128.780416582107));
#220549=CARTESIAN_POINT('Ctrl Pts',(72.5531848338207,-5.1015675191428,135.000561735763));
#220550=CARTESIAN_POINT('Ctrl Pts',(72.2747372100078,0.772860986519783,
137.364603057617));
#220551=CARTESIAN_POINT('Ctrl Pts',(71.996289586195,5.93706800192887,133.700102062723));
#220552=CARTESIAN_POINT('Ctrl Pts',(71.7178419623819,5.64539956546153,127.374556144564));
#220553=CARTESIAN_POINT('Ctrl Pts',(71.4393943385692,0.165884721436248,
124.20083298183));
#220554=CARTESIAN_POINT('Ctrl Pts',(71.1609467147562,-5.46607007766984,
127.095429116077));
#220555=CARTESIAN_POINT('Ctrl Pts',(70.8824990909434,-6.07497350776591,
133.398352108815));
#220556=CARTESIAN_POINT('Ctrl Pts',(70.6040514671303,-1.10127306317963,
137.317523644624));
#220557=CARTESIAN_POINT('Ctrl Pts',(70.3256038433176,4.88444352628841,135.251416544269));
#220558=CARTESIAN_POINT('Ctrl Pts',(70.0471562195047,6.38159513342946,129.098682298033));
#220559=CARTESIAN_POINT('Ctrl Pts',(69.7687085956917,2.01437257120279,124.513383100429));
#220560=CARTESIAN_POINT('Ctrl Pts',(69.4902609718789,-4.20395997638847,
125.709184909736));
#220561=CARTESIAN_POINT('Ctrl Pts',(69.211813348066,-6.5590586805409,131.587204281367));
#220562=CARTESIAN_POINT('Ctrl Pts',(68.9333657242531,-2.88670288510633,
136.745828570004));
#220563=CARTESIAN_POINT('Ctrl Pts',(68.6549181004402,3.43839183846502,136.444534067195));
#220564=CARTESIAN_POINT('Ctrl Pts',(68.3764704766273,6.60377243726651,130.960195701968));
#220565=CARTESIAN_POINT('Ctrl Pts',(68.0980228528144,3.70060877843901,125.332652507142));
#220566=CARTESIAN_POINT('Ctrl Pts',(67.8195752290015,-2.6032335629848,124.733341757993));
#220567=CARTESIAN_POINT('Ctrl Pts',(67.5411276051886,-6.51483143505509,
129.713000755032));
#220568=CARTESIAN_POINT('Ctrl Pts',(67.2626799813758,-4.43961748551916,
135.695566149845));
#220569=CARTESIAN_POINT('Ctrl Pts',(66.9842323575627,1.71538804583728,137.183352609169));
#220570=CARTESIAN_POINT('Ctrl Pts',(66.7057847337499,6.29403576443417,132.809157059292));
#220571=CARTESIAN_POINT('Ctrl Pts',(66.4273371099371,5.08877209625689,126.592651519219));
#220572=CARTESIAN_POINT('Ctrl Pts',(66.1488894861241,-0.792824528042931,
124.246500887099));
#220573=CARTESIAN_POINT('Ctrl Pts',(65.8704418623113,-5.94585414270274,
127.92670297802));
#220574=CARTESIAN_POINT('Ctrl Pts',(65.5919942384984,-5.63493427134196,
134.251331858291));
#220575=CARTESIAN_POINT('Ctrl Pts',(65.3135466146855,-0.145785086460763,
137.408362562243));
#220576=CARTESIAN_POINT('Ctrl Pts',(65.0350989908726,5.47733347088038,134.496638102466));
#220577=CARTESIAN_POINT('Ctrl Pts',(64.7566513670597,6.06705015109826,128.191891011849));
#220578=CARTESIAN_POINT('Ctrl Pts',(64.4782037432468,1.0814441343344,124.28787586265));
#220579=CARTESIAN_POINT('Ctrl Pts',(64.199756119434,-4.89795621039988,126.37219185524));
#220580=CARTESIAN_POINT('Ctrl Pts',(63.921308495621,-6.37637407623982,132.529454416925));
#220581=CARTESIAN_POINT('Ctrl Pts',(63.6428608718081,-1.99521566920641,
137.101440052517));
#220582=CARTESIAN_POINT('Ctrl Pts',(63.3644132479953,4.21944846612332,135.886717316821));
#220583=CARTESIAN_POINT('Ctrl Pts',(63.0859656241823,6.556645592603,130.001557061437));
#220584=CARTESIAN_POINT('Ctrl Pts',(62.8075180003696,2.86860572942485,124.854134055001));
#220585=CARTESIAN_POINT('Ctrl Pts',(62.5290703765565,-3.4555426599142,125.174678574835));
#220586=CARTESIAN_POINT('Ctrl Pts',(62.2506227527437,-6.60421615743575,
130.66862586668));
#220587=CARTESIAN_POINT('Ctrl Pts',(61.9721751289308,-3.68393764016947,
136.287306763578));
#220588=CARTESIAN_POINT('Ctrl Pts',(61.6937275051179,2.62169959805353,136.867428009101));
#220589=CARTESIAN_POINT('Ctrl Pts',(61.415279881305,6.51812298281107,131.875886519111));
#220590=CARTESIAN_POINT('Ctrl Pts',(61.1368322574921,4.42470977437533,125.899665072552));
#220591=CARTESIAN_POINT('Ctrl Pts',(60.8583846336791,-1.73479555762186,
124.430619224162));
#220592=CARTESIAN_POINT('Ctrl Pts',(60.5799370098664,-6.30010852163892,
128.818730341733));
#220593=CARTESIAN_POINT('Ctrl Pts',(60.3014893860534,-5.07592953168175,
135.031538679362));
#220594=CARTESIAN_POINT('Ctrl Pts',(60.0230417622406,0.81278072494776,137.35977688733));
#220595=CARTESIAN_POINT('Ctrl Pts',(59.7445941384276,5.95458520189618,133.663907793273));
#220596=CARTESIAN_POINT('Ctrl Pts',(59.4661465146148,5.62441677596096,127.340254541386));
#220597=CARTESIAN_POINT('Ctrl Pts',(59.1876988908018,0.125684100952275,
124.199945542519));
#220598=CARTESIAN_POINT('Ctrl Pts',(58.909251266989,-5.48854612282181,127.128771354006));
#220599=CARTESIAN_POINT('Ctrl Pts',(58.6308036431761,-6.05907059010694,
133.435284136186));
#220600=CARTESIAN_POINT('Ctrl Pts',(58.3523560193632,-1.06160518713815,
137.324106732513));
#220601=CARTESIAN_POINT('Ctrl Pts',(58.0739083955504,4.91142352051418,135.221601156507));
#220602=CARTESIAN_POINT('Ctrl Pts',(57.7954607717374,6.37109394919177,129.059867319411));
#220603=CARTESIAN_POINT('Ctrl Pts',(57.5170131479246,1.97604028380464,124.501237600083));
#220604=CARTESIAN_POINT('Ctrl Pts',(57.2385655241116,-4.23489786746425,
125.734870009144));
#220605=CARTESIAN_POINT('Ctrl Pts',(56.9601179002987,-6.554171764796,131.627116628959));
#220606=CARTESIAN_POINT('Ctrl Pts',(56.6816702764859,-2.85048199937133,
136.76329066817));
#220607=CARTESIAN_POINT('Ctrl Pts',(56.4032226526729,3.47266146968847,136.423499100792));
#220608=CARTESIAN_POINT('Ctrl Pts',(56.1247750288601,6.60459869704857,130.919993777505));
#220609=CARTESIAN_POINT('Ctrl Pts',(55.8463274050471,3.66723237440476,125.310227229228));
#220610=CARTESIAN_POINT('Ctrl Pts',(55.5678797812343,-2.6401413460556,124.749300861495));
#220611=CARTESIAN_POINT('Ctrl Pts',(55.2894321574214,-6.5213541475661,129.752678603477));
#220612=CARTESIAN_POINT('Ctrl Pts',(55.0109845336085,-4.40976107332459,
135.722500738884));
#220613=CARTESIAN_POINT('Ctrl Pts',(54.7325369097956,1.75418699849736,137.172792367301));
#220614=CARTESIAN_POINT('Ctrl Pts',(54.4540892859827,6.30612291549916,132.770806332897));
#220615=CARTESIAN_POINT('Ctrl Pts',(54.1756416621698,5.06303994438864,126.561752752318));
#220616=CARTESIAN_POINT('Ctrl Pts',(53.897194038357,-0.832729392363195,
124.251448536985));
#220617=CARTESIAN_POINT('Ctrl Pts',(53.618746414544,-5.96326109862574,127.962950396153));
#220618=CARTESIAN_POINT('Ctrl Pts',(53.3402987907312,-5.61384717675129,
134.285569438194));
#220619=CARTESIAN_POINT('Ctrl Pts',(53.0618511669183,-0.105581951123662,
137.409127640582));
#220620=CARTESIAN_POINT('Ctrl Pts',(52.7834035431054,5.49970792962155,134.463227609627));
#220621=CARTESIAN_POINT('Ctrl Pts',(52.5049559192925,6.05103489871361,128.155007558556));
#220622=CARTESIAN_POINT('Ctrl Pts',(52.2265082954796,1.04175640537643,124.281413540623));
#220623=CARTESIAN_POINT('Ctrl Pts',(51.9480606716666,-4.9248453318719,126.402089222721));
#220624=CARTESIAN_POINT('Ctrl Pts',(51.6696130478539,-6.36575480119974,
132.568237253767));
#220625=CARTESIAN_POINT('Ctrl Pts',(51.3911654240409,-1.95684659263562,
137.113468826308));
#220626=CARTESIAN_POINT('Ctrl Pts',(51.112717800228,4.25030803728985,135.860938172086));
#220627=CARTESIAN_POINT('Ctrl Pts',(50.8342701764151,6.55163722003711,129.961659772806));
#220628=CARTESIAN_POINT('Ctrl Pts',(50.5558225526023,2.83233186284197,124.836782281636));
#220629=CARTESIAN_POINT('Ctrl Pts',(50.2773749287893,-3.48974810920128,
125.195817748775));
#220630=CARTESIAN_POINT('Ctrl Pts',(49.9989273049765,-6.60492005256131,
130.708830119782));
#220631=CARTESIAN_POINT('Ctrl Pts',(49.7204796811635,-3.65049313590031,
136.309630351328));
#220632=CARTESIAN_POINT('Ctrl Pts',(49.4420320573507,2.65855863614892,136.851356644924));
#220633=CARTESIAN_POINT('Ctrl Pts',(49.1635844335378,6.52452489938715,131.836189001557));
#220634=CARTESIAN_POINT('Ctrl Pts',(48.8851368097249,4.39477152084969,125.87282148092));
#220635=CARTESIAN_POINT('Ctrl Pts',(48.606689185912,-1.77356218882415,124.441297507781));
#220636=CARTESIAN_POINT('Ctrl Pts',(48.3282415620992,-6.31207889029818,
128.857117679619));
#220637=CARTESIAN_POINT('Ctrl Pts',(48.0497939382862,-5.05010345378512,
135.062358983324));
#220638=CARTESIAN_POINT('Ctrl Pts',(47.7713463144734,0.852670345487299,
137.354707803682));
#220639=CARTESIAN_POINT('Ctrl Pts',(47.4928986906604,5.97188175251911,133.627607562248));
#220640=CARTESIAN_POINT('Ctrl Pts',(47.2144510668476,5.60322557162828,127.306081301933));
#220641=CARTESIAN_POINT('Ctrl Pts',(46.9360034430346,0.0854788231980546,
124.199302832238));
#220642=CARTESIAN_POINT('Ctrl Pts',(46.6575558192218,-5.5108187878785,127.162249792247));
#220643=CARTESIAN_POINT('Ctrl Pts',(46.3791081954089,-6.04294315135938,
133.47211867372));
#220644=CARTESIAN_POINT('Ctrl Pts',(46.100660571596,-1.02189797292572,137.330448228811));
#220645=CARTESIAN_POINT('Ctrl Pts',(45.822212947783,4.93822152013526,135.191622086273));
#220646=CARTESIAN_POINT('Ctrl Pts',(45.5437653239702,6.36035668172477,129.02111698363));
#220647=CARTESIAN_POINT('Ctrl Pts',(45.2653177001572,1.9376347735074,124.489325664279));
#220648=CARTESIAN_POINT('Ctrl Pts',(44.9868700763445,-4.26567883284234,
125.76074296039));
#220649=CARTESIAN_POINT('Ctrl Pts',(44.7084224525315,-6.54904198180601,
131.666998489025));
#220650=CARTESIAN_POINT('Ctrl Pts',(44.4299748287186,-2.81415548797717,
136.780531955991));
#220651=CARTESIAN_POINT('Ctrl Pts',(44.1515272049057,3.50680242016433,136.402255915145));
#220652=CARTESIAN_POINT('Ctrl Pts',(43.8730795810928,6.60518022099696,130.879787568212));
#220653=CARTESIAN_POINT('Ctrl Pts',(43.59463195728,3.63372007972613,125.288005538446));
#220654=CARTESIAN_POINT('Ctrl Pts',(43.316184333467,-2.6769512977182,124.765484337463));
#220655=CARTESIAN_POINT('Ctrl Pts',(43.0377367096542,-6.52763520890084,
129.792395422388));
#220656=CARTESIAN_POINT('Ctrl Pts',(42.7592890858413,-4.37974125581177,
135.749253084432));
#220657=CARTESIAN_POINT('Ctrl Pts',(42.4808414620283,1.79292094911309,137.161996140853));
#220658=CARTESIAN_POINT('Ctrl Pts',(42.2023938382155,6.31797639086063,132.732382739134));
#220659=CARTESIAN_POINT('Ctrl Pts',(41.9239462144025,5.0371201797131,126.531011196811));
#220660=CARTESIAN_POINT('Ctrl Pts',(41.6454985905898,-0.872603399589798,
124.256639007436));
#220661=CARTESIAN_POINT('Ctrl Pts',(41.3670509667768,-5.98044708371573,
127.999303103786));
#220662=CARTESIAN_POINT('Ctrl Pts',(41.0886033429639,-5.592552058989,134.319678020622));
#220663=CARTESIAN_POINT('Ctrl Pts',(40.810155719151,-0.0653749034083074,
137.409647976851));
#220664=CARTESIAN_POINT('Ctrl Pts',(40.5317080953382,5.52187859466303,134.429681536124));
#220665=CARTESIAN_POINT('Ctrl Pts',(40.2532604715252,6.03479542300531,128.118222278014));
#220666=CARTESIAN_POINT('Ctrl Pts',(39.9748128477124,1.00203007375177,124.275192928799));
#220667=CARTESIAN_POINT('Ctrl Pts',(39.6963652238994,-4.95155196138904,
126.432149717987));
#220668=CARTESIAN_POINT('Ctrl Pts',(39.4179176000866,-6.35489964077443,
132.60695472951));
#220669=CARTESIAN_POINT('Ctrl Pts',(39.1394699762736,-1.91840500439501,
137.125263813774));
#220670=CARTESIAN_POINT('Ctrl Pts',(38.8610223524608,4.28101011172891,135.834971654011));
#220671=CARTESIAN_POINT('Ctrl Pts',(38.5825747286478,6.54638607414467,129.921793710766));
#220672=CARTESIAN_POINT('Ctrl Pts',(38.304127104835,2.79595304316033,124.819651639079));
#220673=CARTESIAN_POINT('Ctrl Pts',(38.0256794810221,-3.52382424458856,
125.217164749334));
#220674=CARTESIAN_POINT('Ctrl Pts',(37.7472318572093,-6.60537919994535,
130.749037912801));
#220675=CARTESIAN_POINT('Ctrl Pts',(37.4687842333963,-3.61691336126579,
136.331749939282));
#220676=CARTESIAN_POINT('Ctrl Pts',(37.1903366095834,2.69531916037638,136.835061207086));
#220677=CARTESIAN_POINT('Ctrl Pts',(36.9118889857706,6.53068504729366,131.796453249222));
#220678=CARTESIAN_POINT('Ctrl Pts',(36.6334413619576,4.36467041744916,125.846160629286));
#220679=CARTESIAN_POINT('Ctrl Pts',(36.3549937381448,-1.8122631000273,124.452211577043));
#220680=CARTESIAN_POINT('Ctrl Pts',(36.0765461143319,-6.32381536255287,
128.895577173308));
#220681=CARTESIAN_POINT('Ctrl Pts',(35.798098490519,-5.02409024244786,135.093021505591));
#220682=CARTESIAN_POINT('Ctrl Pts',(35.5196508667061,0.892528370013623,
137.34939599451));
#220683=CARTESIAN_POINT('Ctrl Pts',(35.2412032428932,5.98895701286753,133.591202714771));
#220684=CARTESIAN_POINT('Ctrl Pts',(34.9627556190803,5.58182673771145,127.272037692505));
#220685=CARTESIAN_POINT('Ctrl Pts',(34.6843079952674,0.0452703779943793,
124.198904874802));
#220686=CARTESIAN_POINT('Ctrl Pts',(34.4058603714545,-5.53288724751859,
127.195863190245));
#220687=CARTESIAN_POINT('Ctrl Pts',(34.1274127476417,-6.02659178913083,
133.508854356496));
#220688=CARTESIAN_POINT('Ctrl Pts',(33.8489651238287,-0.982152891908117,
137.336547898535));
#220689=CARTESIAN_POINT('Ctrl Pts',(33.5705175000158,4.96483653214189,135.161480444452));
#220690=CARTESIAN_POINT('Ctrl Pts',(33.292069876203,6.34938372890195,128.982432726597));
#220691=CARTESIAN_POINT('Ctrl Pts',(33.0136222523901,1.89915746344075,124.477647734417));
#220692=CARTESIAN_POINT('Ctrl Pts',(32.7351746285772,-4.29630173192265,
125.786802804744));
#220693=CARTESIAN_POINT('Ctrl Pts',(32.4567270047643,-6.543669521657,131.706848383727));
#220694=CARTESIAN_POINT('Ctrl Pts',(32.1782793809514,-2.77772469701646,
136.797551794587));
#220695=CARTESIAN_POINT('Ctrl Pts',(31.8998317571386,3.54081342478663,136.380805297429));
#220696=CARTESIAN_POINT('Ctrl Pts',(31.6213841333256,6.60551698756319,130.839578563946));
#220697=CARTESIAN_POINT('Ctrl Pts',(31.3429365095127,3.6000731362139,125.26598825823));
#220698=CARTESIAN_POINT('Ctrl Pts',(31.0644888856998,-2.71366205396602,
124.781891586214));
#220699=CARTESIAN_POINT('Ctrl Pts',(30.7860412618869,-6.53367438631237,
129.83214974004));
#220700=CARTESIAN_POINT('Ctrl Pts',(30.507593638074,-4.34955914537615,135.775822195171));
#220701=CARTESIAN_POINT('Ctrl Pts',(30.2291460142612,1.83158846238341,137.150964329883));
#220702=CARTESIAN_POINT('Ctrl Pts',(29.9506983904483,6.32959575128355,132.693887701803));
#220703=CARTESIAN_POINT('Ctrl Pts',(29.6722507666353,5.01101376269691,126.500427991838));
#220704=CARTESIAN_POINT('Ctrl Pts',(29.3938031428225,-0.912445072176531,
124.26207210612));
#220705=CARTESIAN_POINT('Ctrl Pts',(29.1153555190096,-5.99741146113971,
128.035759753857));
#220706=CARTESIAN_POINT('Ctrl Pts',(28.8369078951967,-5.57104970715349,
134.353656341672));
#220707=CARTESIAN_POINT('Ctrl Pts',(28.5584602713837,-0.0251654332018655,
137.409923551768));
#220708=CARTESIAN_POINT('Ctrl Pts',(28.280012647571,5.54384464446253,134.396001125022));
#220709=CARTESIAN_POINT('Ctrl Pts',(28.001565023758,6.0183323257333,128.081536533317));
#220710=CARTESIAN_POINT('Ctrl Pts',(27.7231173999451,0.962266611534229,
124.269214257685));
#220711=CARTESIAN_POINT('Ctrl Pts',(27.4446697761322,-4.97807510932732,
126.462372227135));
#220712=CARTESIAN_POINT('Ctrl Pts',(27.1662221523194,-6.34380899720599,
132.645605409466));
#220713=CARTESIAN_POINT('Ctrl Pts',(26.8877745285064,-1.87989232895117,
137.136824577849));
#220714=CARTESIAN_POINT('Ctrl Pts',(26.6093269046936,4.31155355176403,135.808818724794));
#220715=CARTESIAN_POINT('Ctrl Pts',(26.3308792808807,6.5408923495088,129.881960352566));
#220716=CARTESIAN_POINT('Ctrl Pts',(26.0524316570678,2.75947061841045,124.802742762115));
#220717=CARTESIAN_POINT('Ctrl Pts',(25.7739840332549,-3.55776980337282,
125.238718785491));
#220718=CARTESIAN_POINT('Ctrl Pts',(25.4955364094419,-6.60559358257403,
130.789247755823));
#220719=CARTESIAN_POINT('Ctrl Pts',(25.2170887856292,-3.58319956057628,
136.353664707793));
#220720=CARTESIAN_POINT('Ctrl Pts',(24.9386411618162,2.73197980856112,136.81854229942));
#220721=CARTESIAN_POINT('Ctrl Pts',(24.6601935380033,6.5366031982641,131.756680734531));
#220722=CARTESIAN_POINT('Ctrl Pts',(24.3817459141905,4.3344075795813,125.819683505575));
#220723=CARTESIAN_POINT('Ctrl Pts',(24.1032982903775,-1.85089685715453,
124.463361027524));
#220724=CARTESIAN_POINT('Ctrl Pts',(23.8248506665647,-6.33531750350378,
128.934107397669));
#220725=CARTESIAN_POINT('Ctrl Pts',(23.5464030427517,-4.99789086159903,
135.123525109951));
#220726=CARTESIAN_POINT('Ctrl Pts',(23.2679554189389,0.932353321572971,
137.343841656646));
#220727=CARTESIAN_POINT('Ctrl Pts',(22.9895077951259,6.00581035021119,133.554694599836));
#220728=CARTESIAN_POINT('Ctrl Pts',(22.7110601713131,5.56022106715229,127.238124974604));
#220729=CARTESIAN_POINT('Ctrl Pts',(22.4326125475002,0.00506025528043594,
124.198751684957));
#220730=CARTESIAN_POINT('Ctrl Pts',(22.1541649236873,-5.554750683987,127.229610302442));
#220731=CARTESIAN_POINT('Ctrl Pts',(21.8757172998744,-6.01001710932725,
133.545489823263));
#220732=CARTESIAN_POINT('Ctrl Pts',(21.5972696760615,-0.942371416853923,
137.342405515655));
#220733=CARTESIAN_POINT('Ctrl Pts',(21.3188220522486,4.99126757030501,135.131177347952));
#220734=CARTESIAN_POINT('Ctrl Pts',(21.0403744284357,6.33817549733007,128.943815981773));
#220735=CARTESIAN_POINT('Ctrl Pts',(20.7619268046228,1.86060977939589,124.466204243228));
#220736=CARTESIAN_POINT('Ctrl Pts',(20.48347918081,-4.32676542996233,125.813048576547));
#220737=CARTESIAN_POINT('Ctrl Pts',(20.205031556997,-6.5380545834274,131.746664836412));
#220738=CARTESIAN_POINT('Ctrl Pts',(19.9265839331841,-2.74119097644563,
136.814349553278));
#220739=CARTESIAN_POINT('Ctrl Pts',(19.6481363093713,3.57469322326559,136.359148042506));
#220740=CARTESIAN_POINT('Ctrl Pts',(19.3696886855584,6.60560898426828,130.799368254665));
#220741=CARTESIAN_POINT('Ctrl Pts',(19.0912410617455,3.56629279066743,125.244176204439));
#220742=CARTESIAN_POINT('Ctrl Pts',(18.8127934379326,-2.75027225446848,
124.798521999768));
#220743=CARTESIAN_POINT('Ctrl Pts',(18.5343458141197,-6.53947145601676,
129.871940083324));
#220744=CARTESIAN_POINT('Ctrl Pts',(18.2558981903068,-4.31921586042675,
135.802207086573));
#220745=CARTESIAN_POINT('Ctrl Pts',(17.9774505664939,1.87018810546999,137.139697343177));
#220746=CARTESIAN_POINT('Ctrl Pts',(17.6990029426811,6.34098056620813,132.65532264735));
#220747=CARTESIAN_POINT('Ctrl Pts',(17.4205553188681,4.98472166072295,126.470004270672));
#220748=CARTESIAN_POINT('Ctrl Pts',(17.1421076950552,-0.95225293377558,
124.26774763171));
#220749=CARTESIAN_POINT('Ctrl Pts',(16.8636600712423,-6.01415360227624,
128.072318995452));
#220750=CARTESIAN_POINT('Ctrl Pts',(16.5852124474295,-5.54934091802252,
134.387503142263));
#220751=CARTESIAN_POINT('Ctrl Pts',(16.3067648236166,0.0150449695187284,
137.409954355121));
#220752=CARTESIAN_POINT('Ctrl Pts',(16.0283171998036,5.56560526505998,134.362187624359));
#220753=CARTESIAN_POINT('Ctrl Pts',(15.7498695759908,6.00164621694371,128.044951683866));
#220754=CARTESIAN_POINT('Ctrl Pts',(15.4714219521779,0.922467492173741,
124.263477748823));
#220755=CARTESIAN_POINT('Ctrl Pts',(15.192974328365,-5.00441379286154,126.492755630261));
#220756=CARTESIAN_POINT('Ctrl Pts',(14.9145267045521,-6.33248328146239,
132.684187861418));
#220757=CARTESIAN_POINT('Ctrl Pts',(14.6360790807393,-1.84130999340576,
137.148150690142));
#220758=CARTESIAN_POINT('Ctrl Pts',(14.3576314569263,4.34193722559672,135.782480353541));
#220759=CARTESIAN_POINT('Ctrl Pts',(14.0791838331134,6.53515624970152,129.842161174248));
#220760=CARTESIAN_POINT('Ctrl Pts',(13.8007362093005,2.72288594046203,124.786056277307));
#220761=CARTESIAN_POINT('Ctrl Pts',(13.5222885854877,-3.59158352768866,
125.260479058552));
#220762=CARTESIAN_POINT('Ctrl Pts',(13.2438409616747,-6.60556319250329,
130.829458158858));
#220763=CARTESIAN_POINT('Ctrl Pts',(12.9653933378619,-3.54935298310934,
136.375373844801));
#220764=CARTESIAN_POINT('Ctrl Pts',(12.686945714049,2.76853922222938,136.801800534039));
#220765=CARTESIAN_POINT('Ctrl Pts',(12.4084980902361,6.5422791329992,131.716872931266));
#220766=CARTESIAN_POINT('Ctrl Pts',(12.1300504664232,4.30398412864651,125.793391090908));
#220767=CARTESIAN_POINT('Ctrl Pts',(11.8516028426103,-1.88946202861834,
124.474745446076));
#220768=CARTESIAN_POINT('Ctrl Pts',(11.5731552187974,-6.34658488693473,
128.972706924952));
#220769=CARTESIAN_POINT('Ctrl Pts',(11.2947075949845,-4.97150628206636,
135.153868666082));
#220770=CARTESIAN_POINT('Ctrl Pts',(11.0162599711716,0.972143724437105,
137.338044995907));
#220771=CARTESIAN_POINT('Ctrl Pts',(10.7378123473587,6.0224411400439,133.518084570262));
#220772=CARTESIAN_POINT('Ctrl Pts',(10.4593647235458,5.53840936055655,127.204344404875));
#220773=CARTESIAN_POINT('Ctrl Pts',(10.1809170997329,-0.0351500549433496,
124.198843268382));
#220774=CARTESIAN_POINT('Ctrl Pts',(9.90246947592002,-5.57640828712608,
127.263489878326));
#220775=CARTESIAN_POINT('Ctrl Pts',(9.62402185210712,-5.99321972612948,
133.582023716479));
#220776=CARTESIAN_POINT('Ctrl Pts',(9.34557422829421,-0.902555021880531,
137.348020863117));
#220777=CARTESIAN_POINT('Ctrl Pts',(9.06712660448133,5.01751365521256,135.100713919668));
#220778=CARTESIAN_POINT('Ctrl Pts',(8.78867898066847,6.32673240233446,128.905268180115));
#220779=CARTESIAN_POINT('Ctrl Pts',(8.51023135685555,1.82199314977141,124.454995614755));
#220780=CARTESIAN_POINT('Ctrl Pts',(8.23178373304265,-4.35706879811783,
125.839479303254));
#220781=CARTESIAN_POINT('Ctrl Pts',(7.9533361092298,-6.53219737518076,131.786446371669));
#220782=CARTESIAN_POINT('Ctrl Pts',(7.67488848541689,-2.70455568003535,
136.83092460962));
#220783=CARTESIAN_POINT('Ctrl Pts',(7.39644086160398,3.60844056017245,136.337284952891));
#220784=CARTESIAN_POINT('Ctrl Pts',(7.1179932377911,6.60545620770325,130.759158130379));
#220785=CARTESIAN_POINT('Ctrl Pts',(6.83954561397822,3.53238029483008,125.222570185327));
#220786=CARTESIAN_POINT('Ctrl Pts',(6.5610979901653,-2.78678054262086,124.815374961881));
#220787=CARTESIAN_POINT('Ctrl Pts',(6.28265036635242,-6.54502620320144,
129.911764977794));
#220788=CARTESIAN_POINT('Ctrl Pts',(6.00420274253956,-4.28871252534551,
135.828406780936));
#220789=CARTESIAN_POINT('Ctrl Pts',(5.72575511872663,1.90871844804856,137.128195598241));
#220790=CARTESIAN_POINT('Ctrl Pts',(5.44730749491374,6.35213041376593,132.616689004818));
#220791=CARTESIAN_POINT('Ctrl Pts',(5.16885987110085,4.95824484805471,126.439741160674));
#220792=CARTESIAN_POINT('Ctrl Pts',(4.89041224728798,-0.992025509291961,
124.273665373899));
#220793=CARTESIAN_POINT('Ctrl Pts',(4.61196462347505,-6.03067288673954,
128.108979473854));
#220794=CARTESIAN_POINT('Ctrl Pts',(4.33351699966218,-5.52742649602286,
134.421217168191));
#220795=CARTESIAN_POINT('Ctrl Pts',(4.05506937584931,0.0552548147426717,
137.409740385768));
#220796=CARTESIAN_POINT('Ctrl Pts',(3.77662175203639,5.58715965010757,134.328242287108));
#220797=CARTESIAN_POINT('Ctrl Pts',(3.49817412822347,5.98473771494644,128.008469085329));
#220798=CARTESIAN_POINT('Ctrl Pts',(3.21972650441063,0.882634190440881,
124.25798361478));
#220799=CARTESIAN_POINT('Ctrl Pts',(2.94127888059773,-5.03056703600248,
126.523298801495));
#220800=CARTESIAN_POINT('Ctrl Pts',(2.66283125678483,-6.32092291322184,
132.722700655682));
#220801=CARTESIAN_POINT('Ctrl Pts',(2.38438363297192,-1.80265942744139,
137.159241730961));
#220802=CARTESIAN_POINT('Ctrl Pts',(2.10593600915906,4.37216000734877,135.755957516231));
#220803=CARTESIAN_POINT('Ctrl Pts',(1.82748838534615,6.529177987276,129.802397650584));
#220804=CARTESIAN_POINT('Ctrl Pts',(1.54904076153325,2.68620036497402,124.769592802981));
#220805=CARTESIAN_POINT('Ctrl Pts',(1.27059313772038,-3.62526416455594,
125.282444762183));
#220806=CARTESIAN_POINT('Ctrl Pts',(0.992145513907496,-6.60528803085927,
130.869667631896));
#220807=CARTESIAN_POINT('Ctrl Pts',(0.713697890094564,-3.51537488306232,
136.396876545864));
#220808=CARTESIAN_POINT('Ctrl Pts',(0.435250266281723,2.80499604665836,
136.784836531317));
#220809=CARTESIAN_POINT('Ctrl Pts',(0.156802642468823,6.54771264117505,
131.677031314524));
#220810=CARTESIAN_POINT('Ctrl Pts',(-0.121644981344083,4.27340119199728,
125.767284359559));
#220811=CARTESIAN_POINT('Ctrl Pts',(-0.400092605156985,-1.92795718537184,
124.486364410847));
#220812=CARTESIAN_POINT('Ctrl Pts',(-0.678540228969845,-6.35761709532873,
129.011374324836));
#220813=CARTESIAN_POINT('Ctrl Pts',(-0.956987852782752,-4.94493748154019,
135.184051049593));
#220814=CARTESIAN_POINT('Ctrl Pts',(-1.23543547659566,1.01189810415772,
137.332006227089));
#220815=CARTESIAN_POINT('Ctrl Pts',(-1.51388310040852,6.03884876610542,
133.48137398265));
#220816=CARTESIAN_POINT('Ctrl Pts',(-1.79233072422142,5.51639242616521,
127.170697235071));
#220817=CARTESIAN_POINT('Ctrl Pts',(-2.07077834803434,-0.0753590626689394,
124.19917962168));
#220818=CARTESIAN_POINT('Ctrl Pts',(-2.34922597184723,-5.59785925440532,
127.297500662476));
#220819=CARTESIAN_POINT('Ctrl Pts',(-2.6276735956601,-5.97620026197078,
133.618454682368));
#220820=CARTESIAN_POINT('Ctrl Pts',(-2.906121219473,-0.862705182398668,
137.353393732843));
#220821=CARTESIAN_POINT('Ctrl Pts',(-3.18456884328591,5.04357381430661,
135.070091288433));
#220822=CARTESIAN_POINT('Ctrl Pts',(-3.46301646709877,6.31505486794284,
128.866790750024));
#220823=CARTESIAN_POINT('Ctrl Pts',(-3.74146409091167,1.78330900552073,
124.444022264336));
#220824=CARTESIAN_POINT('Ctrl Pts',(-4.01991171472458,-4.38721071348669,
125.866094005463));
#220825=CARTESIAN_POINT('Ctrl Pts',(-4.29835933853748,-6.52609811395827,
131.826191515377));
#220826=CARTESIAN_POINT('Ctrl Pts',(-4.57680696235032,-2.66782016531947,
136.847276349416));
#220827=CARTESIAN_POINT('Ctrl Pts',(-4.85525458616324,3.64205418498746,
136.31521683873));
#220828=CARTESIAN_POINT('Ctrl Pts',(-5.13370220997616,6.60505866352928,
130.718949681087));
#220829=CARTESIAN_POINT('Ctrl Pts',(-5.41214983378902,3.49833690534187,
125.201171001511));
#220830=CARTESIAN_POINT('Ctrl Pts',(-5.69059745760191,-2.82318556559566,
124.832449848059));
#220831=CARTESIAN_POINT('Ctrl Pts',(-5.96904508141481,-6.55033842203324,
129.951622947723));
#220832=CARTESIAN_POINT('Ctrl Pts',(-6.24749270522772,-4.2580502704442,
135.854420307421));
#220833=CARTESIAN_POINT('Ctrl Pts',(-6.52594032904057,1.9471780623631,137.116459521273));
#220834=CARTESIAN_POINT('Ctrl Pts',(-6.80438795285348,6.36304488079526,
132.577988205793));
#220835=CARTESIAN_POINT('Ctrl Pts',(-7.0828355766664,4.93158430580029,126.409639783256));
#220836=CARTESIAN_POINT('Ctrl Pts',(-7.36128320047925,-1.03176132493798,
124.279825113401));
#220837=CARTESIAN_POINT('Ctrl Pts',(-7.63973082429214,-6.04696870240127,
128.145739830595));
#220838=CARTESIAN_POINT('Ctrl Pts',(-7.91817844810507,-5.50530725320171,
134.454797170168));
#220839=CARTESIAN_POINT('Ctrl Pts',(-8.19662607191793,0.09546261247915,
137.40928165164));
#220840=CARTESIAN_POINT('Ctrl Pts',(-8.47507369573082,5.60850700089942,
134.294166371127));
#220841=CARTESIAN_POINT('Ctrl Pts',(-8.75352131954372,5.96760744629241,
127.972090089581));
#220842=CARTESIAN_POINT('Ctrl Pts',(-9.03196894335663,0.842768182373745,
124.252732059145));
#220843=CARTESIAN_POINT('Ctrl Pts',(-9.31041656716948,-5.05653386963193,
126.554000609049));
#220844=CARTESIAN_POINT('Ctrl Pts',(-9.5888641909824,-6.30912832085822,
132.76114236515));
#220845=CARTESIAN_POINT('Ctrl Pts',(-9.86731181479532,-1.76394206326903,
137.170097289323));
#220846=CARTESIAN_POINT('Ctrl Pts',(-10.1457594386081,4.40222077710389,
135.729251195677));
#220847=CARTESIAN_POINT('Ctrl Pts',(-10.424207062421,6.52295778375913,129.762671255026));
#220848=CARTESIAN_POINT('Ctrl Pts',(-10.7026546862339,2.64941525134336,
124.753352949195));
#220849=CARTESIAN_POINT('Ctrl Pts',(-10.9811023100469,-3.65881046592654,
125.304615082438));
#220850=CARTESIAN_POINT('Ctrl Pts',(-11.2595499338597,-6.60476810783814,
130.909874684957));
#220851=CARTESIAN_POINT('Ctrl Pts',(-11.5379975576726,-3.48126651950624,
136.418172014193));
#220852=CARTESIAN_POINT('Ctrl Pts',(-11.8164451814855,2.84134893092756,
136.767650919861));
#220853=CARTESIAN_POINT('Ctrl Pts',(-12.0948928052984,6.5529035214511,131.637157360647));
#220854=CARTESIAN_POINT('Ctrl Pts',(-12.3733404291112,4.2426599028951,125.741364278924));
#220855=CARTESIAN_POINT('Ctrl Pts',(-12.6517880529242,-1.96638090096281,
124.498217491291));
#220856=CARTESIAN_POINT('Ctrl Pts',(-12.9302356767371,-6.36841371988325,
129.050108164486));
#220857=CARTESIAN_POINT('Ctrl Pts',(-13.2086833005499,-4.91818544453708,
135.214071142064));
#220858=CARTESIAN_POINT('Ctrl Pts',(-13.4871309243628,1.05161498762227,
137.325725573964));
#220859=CARTESIAN_POINT('Ctrl Pts',(-13.7655785481758,6.05503262040511,
133.444564197323));
#220860=CARTESIAN_POINT('Ctrl Pts',(-14.0440261719886,5.49417107982388,
127.137184712));
#220861=CARTESIAN_POINT('Ctrl Pts',(-14.3224737958015,-0.115565277936756,
124.199760732389));
#220862=CARTESIAN_POINT('Ctrl Pts',(-14.6009214196144,-5.61910279095105,
127.331641394614));
#220863=CARTESIAN_POINT('Ctrl Pts',(-14.8793690434273,-5.95895934751375,
133.654781370965));
#220864=CARTESIAN_POINT('Ctrl Pts',(-15.1578166672402,-0.822823375059262,
137.358523925738));
#220865=CARTESIAN_POINT('Ctrl Pts',(-15.4362642910531,5.06944708191823,
135.039310588977));
#220866=CARTESIAN_POINT('Ctrl Pts',(-15.714711914866,6.3031433268707,128.828385117298));
#220867=CARTESIAN_POINT('Ctrl Pts',(-15.9931595386788,1.74455878009922,
124.433284598595));
#220868=CARTESIAN_POINT('Ctrl Pts',(-16.2716071624918,-4.41719005914895,
125.892891696959));
#220869=CARTESIAN_POINT('Ctrl Pts',(-16.5500547863046,-6.51975702577033,
131.865898794765));
#220870=CARTESIAN_POINT('Ctrl Pts',(-16.8285024101176,-2.63098579354628,
136.863404166748));
#220871=CARTESIAN_POINT('Ctrl Pts',(-17.1069500339304,3.67553285214529,
136.292944517765));
#220872=CARTESIAN_POINT('Ctrl Pts',(-17.3853976577434,6.60441636647752,
130.678744396729));
#220873=CARTESIAN_POINT('Ctrl Pts',(-17.6638452815562,3.46416388369313,
125.179979445948));
#220874=CARTESIAN_POINT('Ctrl Pts',(-17.9422929053691,-2.8594859743911,
124.849746025587));
#220875=CARTESIAN_POINT('Ctrl Pts',(-18.220740529182,-6.55540791566593,
129.991512516161));
#220876=CARTESIAN_POINT('Ctrl Pts',(-18.4991881529949,-4.22723023192423,
135.880246702087));
#220877=CARTESIAN_POINT('Ctrl Pts',(-18.7776357768078,1.98556552327847,
137.104489547159));
#220878=CARTESIAN_POINT('Ctrl Pts',(-19.0560834006207,6.37372356285652,
132.539221684343));
#220879=CARTESIAN_POINT('Ctrl Pts',(-19.3345310244336,4.90474102187576,
126.379701253833));
#220880=CARTESIAN_POINT('Ctrl Pts',(-19.6129786482465,-1.07145890828896,
124.286226621967));
#220881=CARTESIAN_POINT('Ctrl Pts',(-19.8914262720594,-6.06304044541393,
128.182598703507));
#220882=CARTESIAN_POINT('Ctrl Pts',(-20.1698738958722,-5.48298400919569,
134.488241903877));
#220883=CARTESIAN_POINT('Ctrl Pts',(-20.4483215196851,0.135666872813404,
137.408578169733));
#220884=CARTESIAN_POINT('Ctrl Pts',(-20.7267691434981,5.62964652640204,
134.25996113911));
#220885=CARTESIAN_POINT('Ctrl Pts',(-21.0052167673109,5.95025604574973,
127.935816044659));
#220886=CARTESIAN_POINT('Ctrl Pts',(-21.2836643911238,0.802870945221437,
124.247723276515));
#220887=CARTESIAN_POINT('Ctrl Pts',(-21.5621120149367,-5.08231333153929,
126.584859915257));
#220888=CARTESIAN_POINT('Ctrl Pts',(-21.8405596387496,-6.29709994142449,
132.79951156535));
#220889=CARTESIAN_POINT('Ctrl Pts',(-22.1190072625625,-1.725159335575,137.180716962973));
#220890=CARTESIAN_POINT('Ctrl Pts',(-22.3974548863754,4.43211842094896,
135.702362381491));
#220891=CARTESIAN_POINT('Ctrl Pts',(-22.6759025101882,6.51649586964294,
129.722983459651));
#220892=CARTESIAN_POINT('Ctrl Pts',(-22.9543501340012,2.61253196265622,
124.737337317723));
#220893=CARTESIAN_POINT('Ctrl Pts',(-23.232797757814,-3.6922211887298,125.326989197785));
#220894=CARTESIAN_POINT('Ctrl Pts',(-23.511245381627,-6.60400344270576,
130.950077828156));
#220895=CARTESIAN_POINT('Ctrl Pts',(-23.7896930054398,-3.4470291563393,
136.439259460675));
#220896=CARTESIAN_POINT('Ctrl Pts',(-24.0681406292527,2.87759652796706,
136.75024433649));
#220897=CARTESIAN_POINT('Ctrl Pts',(-24.3465882530656,6.55785158147733,
131.597252547181));
#220898=CARTESIAN_POINT('Ctrl Pts',(-24.6250358768785,4.21176140046998,
125.715631809479));
#220899=CARTESIAN_POINT('Ctrl Pts',(-24.9034835006914,-2.00473175158637,
124.510304248187));
#220900=CARTESIAN_POINT('Ctrl Pts',(-25.1819311245043,-6.3789743605254,
129.088907008606));
#220901=CARTESIAN_POINT('Ctrl Pts',(-25.4603787483172,-4.89125116236366,
135.24392783109));
#220902=CARTESIAN_POINT('Ctrl Pts',(-25.73882637213,1.09129290310671,137.319203269261));
#220903=CARTESIAN_POINT('Ctrl Pts',(-26.017273995943,6.07099210324431,133.407656578282));
#220904=CARTESIAN_POINT('Ctrl Pts',(-26.2957216197559,5.47174614495268,
127.103808077481));
#220905=CARTESIAN_POINT('Ctrl Pts',(-26.5741692435687,-0.155767210890682,
124.200586578976));
#220906=CARTESIAN_POINT('Ctrl Pts',(-26.8526168673816,-5.64013810957666,
127.365910809639));
#220907=CARTESIAN_POINT('Ctrl Pts',(-27.1310644911945,-5.94149762162655,
133.691002436174));
#220908=CARTESIAN_POINT('Ctrl Pts',(-27.4095121150075,-0.782911077696857,
137.363411251701));
#220909=CARTESIAN_POINT('Ctrl Pts',(-27.6879597388203,5.09513249930392,
135.008372961895));
#220910=CARTESIAN_POINT('Ctrl Pts',(-27.9664073626332,6.29099822050462,
128.79005270507));
#220911=CARTESIAN_POINT('Ctrl Pts',(-28.2448549864461,1.70574390941038,
124.422783015417));
#220912=CARTESIAN_POINT('Ctrl Pts',(-28.523302610259,-4.44700572420938,
125.919871384741));
#220913=CARTESIAN_POINT('Ctrl Pts',(-28.8017502340719,-6.51317434558802,
131.905566738465));
#220914=CARTESIAN_POINT('Ctrl Pts',(-29.0801978578848,-2.59405392962697,
136.879307463993));
#220915=CARTESIAN_POINT('Ctrl Pts',(-29.3586454816977,3.7088753210816,136.270468815306));
#220916=CARTESIAN_POINT('Ctrl Pts',(-29.6370931055106,6.6035293403484,130.638543767126));
#220917=CARTESIAN_POINT('Ctrl Pts',(-29.9155407293234,3.42986249617799,
125.158996303897));
#220918=CARTESIAN_POINT('Ctrl Pts',(-30.1939883531365,-2.89568042388203,
124.86726285355));
#220919=CARTESIAN_POINT('Ctrl Pts',(-30.4724359769491,-6.56023449624756,
130.031432204983));
#220920=CARTESIAN_POINT('Ctrl Pts',(-30.7508836007622,-4.19625355183344,
135.905885007927));
#220921=CARTESIAN_POINT('Ctrl Pts',(-31.029331224575,2.02387940833292,137.092286119451));
#220922=CARTESIAN_POINT('Ctrl Pts',(-31.3077788483879,6.38416606424714,
132.50039087698));
#220923=CARTESIAN_POINT('Ctrl Pts',(-31.5862264722008,4.8777159909692,126.349926681791));
#220924=CARTESIAN_POINT('Ctrl Pts',(-31.8646740960137,-1.11111678833609,
124.292869662384));
#220925=CARTESIAN_POINT('Ctrl Pts',(-32.1431217198266,-6.07888752023319,
128.219554726771));
#220926=CARTESIAN_POINT('Ctrl Pts',(-32.4215693436394,-5.46045759120085,
134.52155013001));
#220927=CARTESIAN_POINT('Ctrl Pts',(-32.7000169674524,0.175866105961793,
137.407629966116));
#220928=CARTESIAN_POINT('Ctrl Pts',(-32.9784645912652,5.65057744328232,
134.225627858545));
#220929=CARTESIAN_POINT('Ctrl Pts',(-33.2569122150782,5.93268415628106,
127.89964829471));
#220930=CARTESIAN_POINT('Ctrl Pts',(-33.535359838891,0.762943957391,124.242957452493));
#220931=CARTESIAN_POINT('Ctrl Pts',(-33.813807462704,-5.10790446645711,
126.615875576613));
#220932=CARTESIAN_POINT('Ctrl Pts',(-34.0922550865168,-6.28483822063666,
132.837806834499));
#220933=CARTESIAN_POINT('Ctrl Pts',(-34.3707027103298,-1.68631268146717,
137.191100358392));
#220934=CARTESIAN_POINT('Ctrl Pts',(-34.6491503341426,4.46185183101625,
135.675292070049));
#220935=CARTESIAN_POINT('Ctrl Pts',(-34.9275979579556,6.5097924843757,129.683335735103));
#220936=CARTESIAN_POINT('Ctrl Pts',(-35.2060455817684,2.57555186563646,
124.721546502031));
#220937=CARTESIAN_POINT('Ctrl Pts',(-35.4844932055813,-3.72549509491909,
125.349566279145));
#220938=CARTESIAN_POINT('Ctrl Pts',(-35.7629408293942,-6.60299406379731,
130.990275571749));
#220939=CARTESIAN_POINT('Ctrl Pts',(-36.0413884532071,-3.41266406223907,
136.460138103909));
#220940=CARTESIAN_POINT('Ctrl Pts',(-36.3198360770199,2.91373749460914,
136.73261742621));
#220941=CARTESIAN_POINT('Ctrl Pts',(-36.5982837008328,6.56255663790157,
131.557318352812));
#220942=CARTESIAN_POINT('Ctrl Pts',(-36.8767313246458,4.18070682967726,
125.690087904753));
#220943=CARTESIAN_POINT('Ctrl Pts',(-37.1551789484586,-2.04300831613737,
124.522624233657));
#220944=CARTESIAN_POINT('Ctrl Pts',(-37.4336265722715,-6.38929862592666,
129.12776941949));
#220945=CARTESIAN_POINT('Ctrl Pts',(-37.7120741960844,-4.86413563307991,
135.273620010322));
#220946=CARTESIAN_POINT('Ctrl Pts',(-37.9905218198973,1.13093038033133,
137.312439554669));
#220947=CARTESIAN_POINT('Ctrl Pts',(-38.2689694437102,6.0867266232385,133.370652493151));
#220948=CARTESIAN_POINT('Ctrl Pts',(-38.5474170675231,5.44911845251588,
127.070568568297));
#220949=CARTESIAN_POINT('Ctrl Pts',(-38.825864691336,-0.195963371833029,
124.201657130839));
#220950=CARTESIAN_POINT('Ctrl Pts',(-39.1043123151489,-5.66096443081045,
127.400307637685));
#220951=CARTESIAN_POINT('Ctrl Pts',(-39.3827599389617,-5.92381573136,133.727116535809));
#220952=CARTESIAN_POINT('Ctrl Pts',(-39.6612075627747,-0.742969769276543,
137.368055529631));
#220953=CARTESIAN_POINT('Ctrl Pts',(-39.9396551865875,5.12062911468111,
134.977279553588));
#220954=CARTESIAN_POINT('Ctrl Pts',(-40.2181028104005,6.27861999888597,
128.751794933764));
#220955=CARTESIAN_POINT('Ctrl Pts',(-40.4965504342133,1.66686583175366,
124.412517903944));
#220956=CARTESIAN_POINT('Ctrl Pts',(-40.7749980580263,-4.47665660383728,
125.947032069068));
#220957=CARTESIAN_POINT('Ctrl Pts',(-41.0534456818391,-6.5063503173351,
131.945193876568));
#220958=CARTESIAN_POINT('Ctrl Pts',(-41.3318933056519,-2.55702594208532,
136.894985651848));
#220959=CARTESIAN_POINT('Ctrl Pts',(-41.6103409294649,3.74208035627896,
136.247790564197));
#220960=CARTESIAN_POINT('Ctrl Pts',(-41.8887885532778,6.60239761801125,
130.598349281928));
#220961=CARTESIAN_POINT('Ctrl Pts',(-42.1672361770906,3.39543401384647,
125.138222352896));
#220962=CARTESIAN_POINT('Ctrl Pts',(-42.4456838009036,-2.93176757287012,
124.884999682853));
#220963=CARTESIAN_POINT('Ctrl Pts',(-42.7241314247165,-6.56481798492739,
130.071380534953));
#220964=CARTESIAN_POINT('Ctrl Pts',(-43.0025790485293,-4.16512137802412,
135.931334274905));
#220965=CARTESIAN_POINT('Ctrl Pts',(-43.2810266723423,2.06211829779186,
137.079849690351));
#220966=CARTESIAN_POINT('Ctrl Pts',(-43.5594742961552,6.39437199801655,
132.461497222591));
#220967=CARTESIAN_POINT('Ctrl Pts',(-43.837921919968,4.85051021450257,126.320317170437));
#220968=CARTESIAN_POINT('Ctrl Pts',(-44.116369543781,-1.150733495542,124.299753988494));
#220969=CARTESIAN_POINT('Ctrl Pts',(-44.3948171675938,-6.09450933963988,
128.256606530968));
#220970=CARTESIAN_POINT('Ctrl Pts',(-44.6732647914067,-5.43772883394191,
134.554720614319));
#220971=CARTESIAN_POINT('Ctrl Pts',(-44.9517124152196,0.216058822326645,
137.406437075925));
#220972=CARTESIAN_POINT('Ctrl Pts',(-45.2301600390324,5.67129897593744,
134.191167801664));
#220973=CARTESIAN_POINT('Ctrl Pts',(-45.5086076628454,5.91489242901924,
127.863588179946));
#220974=CARTESIAN_POINT('Ctrl Pts',(-45.7870552866582,0.722988698391639,
124.238434763679));
#220975=CARTESIAN_POINT('Ctrl Pts',(-46.0655029104712,-5.13330632609627,
126.647046443824));
#220976=CARTESIAN_POINT('Ctrl Pts',(-46.343950534284,-6.27234361285742,
132.876026753548));
#220977=CARTESIAN_POINT('Ctrl Pts',(-46.622398158097,-1.64740354042306,
137.201247090823));
#220978=CARTESIAN_POINT('Ctrl Pts',(-46.9008457819097,4.49141990552312,
135.64804126445));
#220979=CARTESIAN_POINT('Ctrl Pts',(-47.1792934057228,6.50284787635396,
129.643729550545));
#220980=CARTESIAN_POINT('Ctrl Pts',(-47.4577410295356,2.53847633059532,
124.705981087252));
#220981=CARTESIAN_POINT('Ctrl Pts',(-47.7361886533485,-3.75863095151733,
125.372345489915));
#220982=CARTESIAN_POINT('Ctrl Pts',(-48.0146362771614,-6.60174000851572,
131.030466426196));
#220983=CARTESIAN_POINT('Ctrl Pts',(-48.2930839009743,-3.37817251061699,
136.480807170229));
#220984=CARTESIAN_POINT('Ctrl Pts',(-48.5715315247872,2.94977049163681,
136.714770842195));
#220985=CARTESIAN_POINT('Ctrl Pts',(-48.8499791486,6.56701851637621,131.517356257317));
#220986=CARTESIAN_POINT('Ctrl Pts',(-49.128426772413,4.14949734125552,125.664733511282));
#220987=CARTESIAN_POINT('Ctrl Pts',(-49.4068743962258,-2.08120917626415,
124.535176991179));
#220988=CARTESIAN_POINT('Ctrl Pts',(-49.6853220200388,-6.39938613351776,
129.166693957078));
#220989=CARTESIAN_POINT('Ctrl Pts',(-49.9637696438516,-4.83683986146123,
135.303146579501));
#220990=CARTESIAN_POINT('Ctrl Pts',(-50.2422172676646,1.17052595051479,
137.305434680818));
#220991=CARTESIAN_POINT('Ctrl Pts',(-50.5206648914774,6.10223559733929,
133.333553313131));
#220992=CARTESIAN_POINT('Ctrl Pts',(-50.7991125152903,5.42628884099088,
127.03746741615));
#220993=CARTESIAN_POINT('Ctrl Pts',(-51.0775601391032,-0.236152271280866,
124.202972348307));
#220994=CARTESIAN_POINT('Ctrl Pts',(-51.3560077629162,-5.68158098292544,
127.434830604167));
#220995=CARTESIAN_POINT('Ctrl Pts',(-51.634455386729,-5.90591433192304,
133.763122331648));
#220996=CARTESIAN_POINT('Ctrl Pts',(-51.9129030105419,-0.703000929838195,
137.372456587432));
#220997=CARTESIAN_POINT('Ctrl Pts',(-52.1913506343548,5.14593598326309,
134.946031516236));
#220998=CARTESIAN_POINT('Ctrl Pts',(-52.4697982581677,6.26600912069438,
128.713613221033));
#220999=CARTESIAN_POINT('Ctrl Pts',(-52.7482458819806,1.62792598777083,
124.402489644555));
#221000=CARTESIAN_POINT('Ctrl Pts',(-53.0266935057934,-4.50614159930848,
125.97437274349));
#221001=CARTESIAN_POINT('Ctrl Pts',(-53.3051411296064,-6.49928519387843,
131.984778740675));
#221002=CARTESIAN_POINT('Ctrl Pts',(-53.5835887534191,-2.51990320300721,
136.910438149353));
#221003=CARTESIAN_POINT('Ctrl Pts',(-53.8620363772322,3.7751467273123,136.22491060479));
#221004=CARTESIAN_POINT('Ctrl Pts',(-54.140484001045,6.60102124140245,130.558162430556));
#221005=CARTESIAN_POINT('Ctrl Pts',(-54.418931624858,3.36087971245889,125.117658362733));
#221006=CARTESIAN_POINT('Ctrl Pts',(-54.6973792486707,-2.96774608413265,
124.902955856252));
#221007=CARTESIAN_POINT('Ctrl Pts',(-54.9758268724838,-6.56915821186243,
130.111356025769));
#221008=CARTESIAN_POINT('Ctrl Pts',(-55.2542744962966,-4.13383486411065,
135.956593559989));
#221009=CARTESIAN_POINT('Ctrl Pts',(-55.5327221201095,2.10028077469877,
137.067180720695));
#221010=CARTESIAN_POINT('Ctrl Pts',(-55.8111697439224,6.40434098598004,
132.422542162396));
#221011=CARTESIAN_POINT('Ctrl Pts',(-56.0896173677353,4.82312470059616,
126.29087381696));
#221012=CARTESIAN_POINT('Ctrl Pts',(-56.3680649915482,-1.19030756189505,
124.306879345194));
#221013=CARTESIAN_POINT('Ctrl Pts',(-56.646512615361,-6.10990532476174,
128.293752743129));
#221014=CARTESIAN_POINT('Ctrl Pts',(-56.924960239174,-5.41479857964128,
134.587752127659));
#221015=CARTESIAN_POINT('Ctrl Pts',(-57.2034078629868,0.256243532552689,
137.404999543363));
#221016=CARTESIAN_POINT('Ctrl Pts',(-57.4818554867998,5.69181035652338,
134.156582245398));
#221017=CARTESIAN_POINT('Ctrl Pts',(-57.7603031106126,5.89688152324325,
127.827637036585));
#221018=CARTESIAN_POINT('Ctrl Pts',(-58.0387507344255,0.683006648780185,
124.234155377662));
#221019=CARTESIAN_POINT('Ctrl Pts',(-58.3171983582384,-5.15851796918197,
126.67837136184));
#221020=CARTESIAN_POINT('Ctrl Pts',(-58.5956459820513,-6.25961658107885,
132.91416990625));
#221021=CARTESIAN_POINT('Ctrl Pts',(-58.8740936058642,-1.60843335423465,
137.211156784272));
#221022=CARTESIAN_POINT('Ctrl Pts',(-59.1525412296771,4.52082154881365,
135.620610974484));
#221023=CARTESIAN_POINT('Ctrl Pts',(-59.4309888534899,6.49566230291273,
129.604166373598));
#221024=CARTESIAN_POINT('Ctrl Pts',(-59.7094364773029,2.50130673138007,
124.69064165017));
#221025=CARTESIAN_POINT('Ctrl Pts',(-59.9878841011157,-3.79162753066369,
125.395325986002));
#221026=CARTESIAN_POINT('Ctrl Pts',(-60.2663317249287,-6.60024132333016,
131.070648902209));
#221027=CARTESIAN_POINT('Ctrl Pts',(-60.5447793487415,-3.34355577957023,
136.501265893734));
#221028=CARTESIAN_POINT('Ctrl Pts',(-60.8232269725544,2.98569418383416,
136.696705245755));
#221029=CARTESIAN_POINT('Ctrl Pts',(-61.1016745963673,6.57123705156454,
131.477367741508));
#221030=CARTESIAN_POINT('Ctrl Pts',(-61.3801222201802,4.11813409168408,
125.639569568584));
#221031=CARTESIAN_POINT('Ctrl Pts',(-61.6585698439931,-2.11933291641938,
124.547962055604));
#221032=CARTESIAN_POINT('Ctrl Pts',(-61.937017467806,-6.40923650950231,
129.205679179005));
#221033=CARTESIAN_POINT('Ctrl Pts',(-62.2154650916189,-4.80936485896274,
135.332506444514));
#221034=CARTESIAN_POINT('Ctrl Pts',(-62.4939127154318,1.21007814642843,
137.298188907278));
#221035=CARTESIAN_POINT('Ctrl Pts',(-62.7723603392447,6.1175184508558,133.296360412945));
#221036=CARTESIAN_POINT('Ctrl Pts',(-63.0508079630576,5.40325815633759,
127.004505847616));
#221037=CARTESIAN_POINT('Ctrl Pts',(-63.3292555868704,-0.276332420019459,
124.204532182646));
#221038=CARTESIAN_POINT('Ctrl Pts',(-63.6077032106833,-5.70198700196771,
127.469478429822));
#221039=CARTESIAN_POINT('Ctrl Pts',(-63.8861508344962,-5.8877940866586,
133.799018489484));
#221040=CARTESIAN_POINT('Ctrl Pts',(-64.1645984583092,-0.663006040441876,
137.376614262022));
#221041=CARTESIAN_POINT('Ctrl Pts',(-64.4430460821219,5.17105216729505,
134.914630007745));
#221042=CARTESIAN_POINT('Ctrl Pts',(-64.721493705935,6.25316605323042,128.675508981716));
#221043=CARTESIAN_POINT('Ctrl Pts',(-64.9999413297477,1.58892582039159,
124.392698608848));
#221044=CARTESIAN_POINT('Ctrl Pts',(-65.2783889535607,-4.53545961804555,
126.00189239489));
#221045=CARTESIAN_POINT('Ctrl Pts',(-65.5568365773735,-6.49197923701883,
132.024319863954));
#221046=CARTESIAN_POINT('Ctrl Pts',(-65.8352842011867,-2.48268708798906,
136.92566438391));
#221047=CARTESIAN_POINT('Ctrl Pts',(-66.1137318249993,3.80807320889562,
136.201829784909));
#221048=CARTESIAN_POINT('Ctrl Pts',(-66.3921794488124,6.59940026152389,
130.517984702147));
#221049=CARTESIAN_POINT('Ctrl Pts',(-66.6706270726251,3.3262008724376,125.097305095413));
#221050=CARTESIAN_POINT('Ctrl Pts',(-66.9490746964381,-3.00361462447264,
124.921130708376));
#221051=CARTESIAN_POINT('Ctrl Pts',(-67.227522320251,-6.57325501622426,
130.151357196124));
#221052=CARTESIAN_POINT('Ctrl Pts',(-67.5059699440638,-4.10239516942585,
135.981661927186));
#221053=CARTESIAN_POINT('Ctrl Pts',(-67.7844175678767,2.13836542492937,
137.054279679937));
#221054=CARTESIAN_POINT('Ctrl Pts',(-68.0628651916897,6.41407265873309,
132.383527139888));
#221055=CARTESIAN_POINT('Ctrl Pts',(-68.3413128155024,4.79556046403026,
126.261597712398));
#221056=CARTESIAN_POINT('Ctrl Pts',(-68.6197604393155,-1.22983752096341,
124.314245468451));
#221057=CARTESIAN_POINT('Ctrl Pts',(-68.8982080631282,-6.12507490509475,
128.330991986789));
#221058=CARTESIAN_POINT('Ctrl Pts',(-69.1766556869413,-5.39166767798822,
134.620643446035));
#221059=CARTESIAN_POINT('Ctrl Pts',(-69.455103310754,0.296418747580413,
137.403317421698));
#221060=CARTESIAN_POINT('Ctrl Pts',(-69.733550934567,5.7121108249834,134.121872471326));
#221061=CARTESIAN_POINT('Ctrl Pts',(-70.0119985583799,5.87865210635384,
127.791796196812));
#221062=CARTESIAN_POINT('Ctrl Pts',(-70.2904461821926,0.642999290106501,
124.230119453016));
#221063=CARTESIAN_POINT('Ctrl Pts',(-70.5688938060058,-5.18353846148724,
126.709849169906));
#221064=CARTESIAN_POINT('Ctrl Pts',(-70.8473414298183,-6.24665759690589,
132.95223487919));
#221065=CARTESIAN_POINT('Ctrl Pts',(-71.1257890536316,-1.56940356695681,
137.220829071533));
#221066=CARTESIAN_POINT('Ctrl Pts',(-71.4042366774442,4.55005567139915,
135.593002216589));
#221067=CARTESIAN_POINT('Ctrl Pts',(-71.6826843012574,6.48823603031619,
129.56464767029));
#221068=CARTESIAN_POINT('Ctrl Pts',(-71.9611319250699,2.46404444532374,
124.675528759193));
#221069=CARTESIAN_POINT('Ctrl Pts',(-72.2395795488831,-3.82448360965763,
125.418506915858));
#221070=CARTESIAN_POINT('Ctrl Pts',(-72.518027172696,-6.59849806377525,
131.110821510811));
#221071=CARTESIAN_POINT('Ctrl Pts',(-72.7964747965087,-3.30881515183405,
136.52151351632));
#221072=CARTESIAN_POINT('Ctrl Pts',(-73.0749224203217,3.02150724003593,
136.678421306317));
#221073=CARTESIAN_POINT('Ctrl Pts',(-73.3533700441346,6.57521208714753,
131.437354287172));
#221074=CARTESIAN_POINT('Ctrl Pts',(-73.6318176679474,4.08661824313884,
125.614597009117));
#221075=CARTESIAN_POINT('Ctrl Pts',(-73.9102652917603,-2.15737812391465,
124.56097895318));
#221076=CARTESIAN_POINT('Ctrl Pts',(-74.1887129155733,-6.41884938887091,
129.244723640663));
#221077=CARTESIAN_POINT('Ctrl Pts',(-74.4671605393861,-4.78171164368069,
135.361698517417));
#221078=CARTESIAN_POINT('Ctrl Pts',(-74.745608163199,1.24958550245192,137.290702502541));
#221079=CARTESIAN_POINT('Ctrl Pts',(-75.0240557870119,6.13257461747648,
133.25907517079));
#221080=CARTESIAN_POINT('Ctrl Pts',(-75.3025034108249,5.380027251966,126.971685084098));
#221081=CARTESIAN_POINT('Ctrl Pts',(-75.5809510346376,-0.31650232915867,
124.206336576053));
#221082=CARTESIAN_POINT('Ctrl Pts',(-75.8593986584506,-5.72218173178456,
127.504249830764));
#221083=CARTESIAN_POINT('Ctrl Pts',(-76.1378462822634,-5.86945566701928,
133.83480367917));
#221084=CARTESIAN_POINT('Ctrl Pts',(-76.4162939060764,-0.622986583113102,
137.380528399336));
#221085=CARTESIAN_POINT('Ctrl Pts',(-76.6947415298893,5.19597673608708,
134.88307619171));
#221086=CARTESIAN_POINT('Ctrl Pts',(-76.9731891537022,6.24009127239896,
128.637483627779));
#221087=CARTESIAN_POINT('Ctrl Pts',(-77.2516367775151,1.54986677478153,
124.383145159635));
#221088=CARTESIAN_POINT('Ctrl Pts',(-77.5300844013279,-4.56460957365852,
126.029590003516));
#221089=CARTESIAN_POINT('Ctrl Pts',(-77.8085320251407,-6.48443271748106,
132.063815781194));
#221090=CARTESIAN_POINT('Ctrl Pts',(-78.0869796489538,-2.44537897608793,
136.940663791305));
#221091=CARTESIAN_POINT('Ctrl Pts',(-78.3654272727665,3.84085858092573,
136.178548959823));
#221092=CARTESIAN_POINT('Ctrl Pts',(-78.6438748965796,6.5975347384416,130.477817585504));
#221093=CARTESIAN_POINT('Ctrl Pts',(-78.9223225203923,3.29139877882003,
125.077163305135));
#221094=CARTESIAN_POINT('Ctrl Pts',(-79.2007701442053,-3.03937186476788,
124.939523565746));
#221095=CARTESIAN_POINT('Ctrl Pts',(-79.4792177680182,-6.57710824620412,
130.191382563762));
#221096=CARTESIAN_POINT('Ctrl Pts',(-79.7576653918309,-4.07080345897965,
136.00653844758));
#221097=CARTESIAN_POINT('Ctrl Pts',(-80.036113015644,2.17637083724304,137.041147046131));
#221098=CARTESIAN_POINT('Ctrl Pts',(-80.314560639457,6.42356665566488,132.344453600785));
#221099=CARTESIAN_POINT('Ctrl Pts',(-80.5930082632696,4.76781852620778,
126.232489941585));
#221100=CARTESIAN_POINT('Ctrl Pts',(-80.8714558870828,-1.26932190795047,
124.321852085313));
#221101=CARTESIAN_POINT('Ctrl Pts',(-81.1499035108954,-6.14001751852468,
128.368322882032));
#221102=CARTESIAN_POINT('Ctrl Pts',(-81.4283511347085,-5.36833698610627,
134.653393350648));
#221103=CARTESIAN_POINT('Ctrl Pts',(-81.7067987585213,0.336582978702201,
137.401390773263));
#221104=CARTESIAN_POINT('Ctrl Pts',(-81.9852463823341,5.73219962907597,
134.087039765632));
#221105=CARTESIAN_POINT('Ctrl Pts',(-82.2636940061471,5.86020485384888,
127.756066988721));
#221106=CARTESIAN_POINT('Ctrl Pts',(-82.54214162996,0.602968104857597,124.226327139294));
#221107=CARTESIAN_POINT('Ctrl Pts',(-82.8205892537728,-5.20836687586887,
126.741478701599));
#221108=CARTESIAN_POINT('Ctrl Pts',(-83.0990368775859,-6.23346714053832,
132.990220261861));
#221109=CARTESIAN_POINT('Ctrl Pts',(-83.3774845013985,-1.53031562485268,
137.230263594196));
#221110=CARTESIAN_POINT('Ctrl Pts',(-83.6559321252116,4.57912118999838,
135.56521601382));
#221111=CARTESIAN_POINT('Ctrl Pts',(-83.9343797490243,6.48056933374724,
129.525174905002));
#221112=CARTESIAN_POINT('Ctrl Pts',(-84.2128273728376,2.42669085319518,
124.660642974335));
#221113=CARTESIAN_POINT('Ctrl Pts',(-84.4912749966499,-3.85719797100462,
125.441887420503));
#221114=CARTESIAN_POINT('Ctrl Pts',(-84.7697226204634,-6.59651029444787,
131.150982763393));
#221115=CARTESIAN_POINT('Ctrl Pts',(-85.0481702442759,-3.27395191473627,
136.541549287701));
#221116=CARTESIAN_POINT('Ctrl Pts',(-85.326617868089,3.05720833317481,136.659919701402));
#221117=CARTESIAN_POINT('Ctrl Pts',(-85.6050654919017,6.57894347582879,
131.397317377022));
#221118=CARTESIAN_POINT('Ctrl Pts',(-85.8835131157147,4.05495096345227,
125.58981675825));
#221119=CARTESIAN_POINT('Ctrl Pts',(-86.1619607395276,-2.19534338896908,
124.574227201559));
#221120=CARTESIAN_POINT('Ctrl Pts',(-86.4404083633404,-6.42822441541511,
129.283825895241));
#221121=CARTESIAN_POINT('Ctrl Pts',(-86.7188559871533,-4.75388124031539,
135.390721716488));
#221122=CARTESIAN_POINT('Ctrl Pts',(-86.9973036109663,1.28904655462414,
137.282975744021));
#221123=CARTESIAN_POINT('Ctrl Pts',(-87.2757512347791,6.14740353928957,
133.221698968287));
#221124=CARTESIAN_POINT('Ctrl Pts',(-87.554198858592,5.35659698870609,126.939006341782));
#221125=CARTESIAN_POINT('Ctrl Pts',(-87.8326464824051,-0.356660510187587,
124.208385461669));
#221126=CARTESIAN_POINT('Ctrl Pts',(-88.1110941062178,-5.74216442405318,
127.539143518524));
#221127=CARTESIAN_POINT('Ctrl Pts',(-88.3895417300309,-5.85089975254147,
133.870476574676));
#221128=CARTESIAN_POINT('Ctrl Pts',(-88.6679893538435,-0.582944040787213,
137.384198854334));
#221129=CARTESIAN_POINT('Ctrl Pts',(-88.9464369776566,5.22070876605056,
134.851371237371));
#221130=CARTESIAN_POINT('Ctrl Pts',(-89.2248846014694,6.22678526269035,
128.599538568266));
#221131=CARTESIAN_POINT('Ctrl Pts',(-89.5033322252823,1.51075029828878,
124.373829650922));
#221132=CARTESIAN_POINT('Ctrl Pts',(-89.7817798490951,-4.59359038598471,
126.057464543021));
#221133=CARTESIAN_POINT('Ctrl Pts',(-90.0602274729082,-6.47664591490472,
132.103265028861));
#221134=CARTESIAN_POINT('Ctrl Pts',(-90.338675096721,-2.40798024976945,
136.955435815729));
#221135=CARTESIAN_POINT('Ctrl Pts',(-90.6171227205338,3.87350162852866,
136.155068992212));
#221136=CARTESIAN_POINT('Ctrl Pts',(-90.8955703443469,6.59542474128344,
130.437662569033));
#221137=CARTESIAN_POINT('Ctrl Pts',(-91.1740179681596,3.25647472121003,
125.057233738258));
#221138=CARTESIAN_POINT('Ctrl Pts',(-91.4524655919725,-3.07501648002118,
124.958133746811));
#221139=CARTESIAN_POINT('Ctrl Pts',(-91.7309132157855,-6.58071775901922,
130.231430645527));
#221140=CARTESIAN_POINT('Ctrl Pts',(-92.0093608395982,-4.03906090341396,
136.031222199361));
#221141=CARTESIAN_POINT('Ctrl Pts',(-92.2878084634112,2.21429560333469,
137.027783305909));
#221142=CARTESIAN_POINT('Ctrl Pts',(-92.5662560872241,6.4328226249721,132.305322992969));
#221143=CARTESIAN_POINT('Ctrl Pts',(-92.844703711037,4.73989991511645,126.203551583122));
#221144=CARTESIAN_POINT('Ctrl Pts',(-93.1231513348499,-1.30875925974737,
124.329698913911));
#221145=CARTESIAN_POINT('Ctrl Pts',(-93.4015989586628,-6.15473261134757,
128.40574404555));
#221146=CARTESIAN_POINT('Ctrl Pts',(-93.6800465824757,-5.34480736852315,
134.686000627937));
#221147=CARTESIAN_POINT('Ctrl Pts',(-93.9584942062885,0.37673473761816,
137.399219669449));
#221148=CARTESIAN_POINT('Ctrl Pts',(-94.2369418301014,5.75207602440345,
134.052085419056));
#221149=CARTESIAN_POINT('Ctrl Pts',(-94.5153894539144,5.84154044929785,
127.720450736271));
#221150=CARTESIAN_POINT('Ctrl Pts',(-94.7938370777271,0.56291457640357,
124.222778577022));
#221151=CARTESIAN_POINT('Ctrl Pts',(-95.0722847015402,-5.23300229230026,
126.773258784876));
#221152=CARTESIAN_POINT('Ctrl Pts',(-95.350732325353,-6.22004570075364,
133.028124646699));
#221153=CARTESIAN_POINT('Ctrl Pts',(-95.6291799491659,-1.49117097634027,
137.239460002661));
#221154=CARTESIAN_POINT('Ctrl Pts',(-95.9076275729788,4.60801702757804,
135.537253395802));
#221155=CARTESIAN_POINT('Ctrl Pts',(-96.1860751967916,6.47266249729856,
129.48574954041));
#221156=CARTESIAN_POINT('Ctrl Pts',(-96.4645228206046,2.38924733914408,
124.645984847192));
#221157=CARTESIAN_POINT('Ctrl Pts',(-96.7429704444176,-3.88976940246256,
125.465466633565));
#221158=CARTESIAN_POINT('Ctrl Pts',(-97.0214180682302,-6.59427808900543,
131.191131171763));
#221159=CARTESIAN_POINT('Ctrl Pts',(-97.2998656920433,-3.23896736014657,
136.561372465446));
#221160=CARTESIAN_POINT('Ctrl Pts',(-97.5783133158561,3.09279614033489,
136.641201116591));
#221161=CARTESIAN_POINT('Ctrl Pts',(-97.856760939669,6.58243107933991,131.357258494642));
#221162=CARTESIAN_POINT('Ctrl Pts',(-98.135208563482,4.02313342606635,125.565229734223));
#221163=CARTESIAN_POINT('Ctrl Pts',(-98.4136561872948,-2.2332273047675,
124.587706309824));
#221164=CARTESIAN_POINT('Ctrl Pts',(-98.6921038111079,-6.43736124173946,
129.322984493793));
#221165=CARTESIAN_POINT('Ctrl Pts',(-98.9705514349205,-4.72587468013238,
135.419574966262));
#221166=CARTESIAN_POINT('Ctrl Pts',(-99.2489990587337,1.32845984070286,
137.275008918035));
#221167=CARTESIAN_POINT('Ctrl Pts',(-99.5274466825463,6.16200466680371,
133.184233190419));
#221168=CARTESIAN_POINT('Ctrl Pts',(-99.8058943063594,5.3329682347749,126.906470831589));
#221169=CARTESIAN_POINT('Ctrl Pts',(-100.084341930172,-0.396805475030165,
124.210678763569));
#221170=CARTESIAN_POINT('Ctrl Pts',(-100.362789553985,-5.76193433830736,
127.574158200105));
#221171=CARTESIAN_POINT('Ctrl Pts',(-100.641237177798,-5.83212703082168,
133.906035854126));
#221172=CARTESIAN_POINT('Ctrl Pts',(-100.919684801611,-0.542879897255484,
137.387625491007));
#221173=CARTESIAN_POINT('Ctrl Pts',(-101.198132425424,5.24524734073077,
134.819516319564));
#221174=CARTESIAN_POINT('Ctrl Pts',(-101.476580049237,6.21324851716398,
128.561675209245));
#221175=CARTESIAN_POINT('Ctrl Pts',(-101.75502767305,1.47157784038775,124.3647524279));
#221176=CARTESIAN_POINT('Ctrl Pts',(-102.033475296863,-4.62240098113028,
126.085514980508));
#221177=CARTESIAN_POINT('Ctrl Pts',(-102.311922920676,-6.4686191178319,
132.142666145147));
#221178=CARTESIAN_POINT('Ctrl Pts',(-102.590370544489,-2.3704922948573,
136.969979909799));
#221179=CARTESIAN_POINT('Ctrl Pts',(-102.868818168302,3.90600114210426,
136.131390752135));
#221180=CARTESIAN_POINT('Ctrl Pts',(-103.147265792114,6.59307034823604,
130.397521140692));
#221181=CARTESIAN_POINT('Ctrl Pts',(-103.425713415927,3.22142999373166,
125.037517133282));
#221182=CARTESIAN_POINT('Ctrl Pts',(-103.70416103974,-3.11054714940797,
124.976960561963));
#221183=CARTESIAN_POINT('Ctrl Pts',(-103.982608663553,-6.58408342091771,
130.271499957422));
#221184=CARTESIAN_POINT('Ctrl Pts',(-104.261056287366,-4.00716867896111,
136.055712267864));
#221185=CARTESIAN_POINT('Ctrl Pts',(-104.539503911179,2.25213831788793,
137.014188954471));
#221186=CARTESIAN_POINT('Ctrl Pts',(-104.817951534992,6.44184022367115,
132.266136766442));
#221187=CARTESIAN_POINT('Ctrl Pts',(-105.096399158805,4.71180566529118,
126.17478370933));
#221188=CARTESIAN_POINT('Ctrl Pts',(-105.374846782618,-1.34814811498862,
124.337785663482));
#221189=CARTESIAN_POINT('Ctrl Pts',(-105.65329440643,-6.16921963829011,
128.443254090687));
#221190=CARTESIAN_POINT('Ctrl Pts',(-105.931742030243,-5.32107969713743,
134.718464069627));
#221191=CARTESIAN_POINT('Ctrl Pts',(-106.210189654056,0.416872536489867,
137.396804190707));
#221192=CARTESIAN_POINT('Ctrl Pts',(-106.488637277869,5.77173927443855,
134.017010726842));
#221193=CARTESIAN_POINT('Ctrl Pts',(-106.767084901682,5.82265958431723,
127.684948759235));
#221194=CARTESIAN_POINT('Ctrl Pts',(-107.045532525495,0.52284018894291,
124.219473897692));
#221195=CARTESIAN_POINT('Ctrl Pts',(-107.323980149308,-5.25744379790729,
126.805188242113));
#221196=CARTESIAN_POINT('Ctrl Pts',(-107.602427773121,-6.20639377488812,
133.065946629143));
#221197=CARTESIAN_POINT('Ctrl Pts',(-107.880875396933,-1.45197107193893,
137.248417956151));
#221198=CARTESIAN_POINT('Ctrl Pts',(-108.159323020746,4.63674211339212,
135.509115398702));
#221199=CARTESIAN_POINT('Ctrl Pts',(-108.437770644559,6.46451581396073,
129.446373037437));
#221200=CARTESIAN_POINT('Ctrl Pts',(-108.716218268372,2.35171529065418,
124.631554920928));
#221201=CARTESIAN_POINT('Ctrl Pts',(-108.994665892185,-3.92219669708481,
125.489243681306));
#221202=CARTESIAN_POINT('Ctrl Pts',(-109.273113515998,-6.59180153016358,
131.231265248209));
#221203=CARTESIAN_POINT('Ctrl Pts',(-109.551561139811,-3.20386278442967,
136.580982315001));
#221204=CARTESIAN_POINT('Ctrl Pts',(-109.830008763624,3.12826934279688,
136.622266245509));
#221205=CARTESIAN_POINT('Ctrl Pts',(-110.108456387437,6.5856747684467,131.317179124427));
#221206=CARTESIAN_POINT('Ctrl Pts',(-110.38690401125,3.99116680999183,125.540836848117));
#221207=CARTESIAN_POINT('Ctrl Pts',(-110.665351635062,-2.27102846750687,
124.601415778499));
#221208=CARTESIAN_POINT('Ctrl Pts',(-110.943799258875,-6.44625952927566,
129.362197985281));
#221209=CARTESIAN_POINT('Ctrl Pts',(-111.222246882688,-4.69769300092514,
135.448257197571));
#221210=CARTESIAN_POINT('Ctrl Pts',(-111.500694506501,1.36782390021364,
137.266802319797));
#221211=CARTESIAN_POINT('Ctrl Pts',(-111.779142130314,6.17637745896884,
133.1466792255));
#221212=CARTESIAN_POINT('Ctrl Pts',(-112.057589754127,5.30914186574463,
126.874079759138));
#221213=CARTESIAN_POINT('Ctrl Pts',(-112.33603737794,-0.436935736099303,
124.213216396775));
#221214=CARTESIAN_POINT('Ctrl Pts',(-112.614485001753,-5.78149074196569,
127.609292578024));
#221215=CARTESIAN_POINT('Ctrl Pts',(-112.892932625565,-5.81313819748998,
133.94148019986));
#221216=CARTESIAN_POINT('Ctrl Pts',(-113.171380249379,-0.502795637109545,
137.390808182378));
#221217=CARTESIAN_POINT('Ctrl Pts',(-113.449827873191,5.26959155084185,
134.787512618686));
#221218=CARTESIAN_POINT('Ctrl Pts',(-113.728275497004,6.19948153742887,
128.523894953756));
#221219=CARTESIAN_POINT('Ctrl Pts',(-114.006723120817,1.43235085262869,
124.355913826926));
#221220=CARTESIAN_POINT('Ctrl Pts',(-114.28517074463,-4.65104029150761,
126.113740276555));
#221221=CARTESIAN_POINT('Ctrl Pts',(-114.563618368443,-6.46035262369882,
132.182017670029));
#221222=CARTESIAN_POINT('Ctrl Pts',(-114.842065992256,-2.33291650048142,
136.984295534578));
#221223=CARTESIAN_POINT('Ctrl Pts',(-115.120513616069,3.93835591737112,
136.107515116997));
#221224=CARTESIAN_POINT('Ctrl Pts',(-115.398961239881,6.59047164654225,
130.357394787938));
#221225=CARTESIAN_POINT('Ctrl Pts',(-115.677408863695,3.18626589498021,
125.018014220813));
#221226=CARTESIAN_POINT('Ctrl Pts',(-115.955856487507,-3.14596255632626,
124.996003313566));
#221227=CARTESIAN_POINT('Ctrl Pts',(-116.23430411132,-6.58720510718372,
130.311589014666));
#221228=CARTESIAN_POINT('Ctrl Pts',(-116.512751735133,-3.97512796739924,
136.0800077456));
#221229=CARTESIAN_POINT('Ctrl Pts',(-116.791199358946,2.28989757862811,
137.00036449556));
#221230=CARTESIAN_POINT('Ctrl Pts',(-117.069646982759,6.45061911761184,
132.226896373261));
#221231=CARTESIAN_POINT('Ctrl Pts',(-117.348094606572,4.68353681777373,
126.146187386213));
#221232=CARTESIAN_POINT('Ctrl Pts',(-117.626542230384,-1.38748701410568,
124.346112034364));
#221233=CARTESIAN_POINT('Ctrl Pts',(-117.904989854198,-6.18347806253024,
128.480851627495));
#221234=CARTESIAN_POINT('Ctrl Pts',(-118.18343747801,-5.29715485118671,
134.750782472776));
#221235=CARTESIAN_POINT('Ctrl Pts',(-118.461885101824,0.45699488799644,
137.394144426544));
#221236=CARTESIAN_POINT('Ctrl Pts',(-118.740332725636,5.79118865055225,
133.981816988697));
#221237=CARTESIAN_POINT('Ctrl Pts',(-119.018780349449,5.80356295854445,
127.649562373154));
#221238=CARTESIAN_POINT('Ctrl Pts',(-119.297227973262,0.482746427446748,
124.216413223762));
#221239=CARTESIAN_POINT('Ctrl Pts',(-119.575675597075,-5.28169048700048,
126.837265890154));
#221240=CARTESIAN_POINT('Ctrl Pts',(-119.854123220888,-6.19251186881905,
133.103684807684));
#221241=CARTESIAN_POINT('Ctrl Pts',(-120.132570844701,-1.41271736421608,
137.257137122728));
#221242=CARTESIAN_POINT('Ctrl Pts',(-120.411018468513,4.66529538302207,
135.480803065184));
#221243=CARTESIAN_POINT('Ctrl Pts',(-120.689466092327,6.45612958561205,
129.407046855192));
#221244=CARTESIAN_POINT('Ctrl Pts',(-120.967913716139,2.31409609848935,
124.61735373025));
#221245=CARTESIAN_POINT('Ctrl Pts',(-121.246361339953,-3.95447865326606,
125.51321768266));
#221246=CARTESIAN_POINT('Ctrl Pts',(-121.524808963765,-6.5890807096919,
131.271383505546));
#221247=CARTESIAN_POINT('Ctrl Pts',(-121.803256587578,-3.16863948839908,
136.600378109714));
#221248=CARTESIAN_POINT('Ctrl Pts',(-122.081704211391,3.16362662608795,
136.603115789794));
#221249=CARTESIAN_POINT('Ctrl Pts',(-122.360151835204,6.58867442295306,
131.277080751534));
#221250=CARTESIAN_POINT('Ctrl Pts',(-122.638599459017,3.9590522997634,125.51663900382));
#221251=CARTESIAN_POINT('Ctrl Pts',(-122.91704708283,-2.30874547645122,
124.615355099576));
#221252=CARTESIAN_POINT('Ctrl Pts',(-123.195494706643,-6.45491894829438,
129.401464916637));
#221253=CARTESIAN_POINT('Ctrl Pts',(-123.473942330455,-4.66933724697619,
135.476767347585));
#221254=CARTESIAN_POINT('Ctrl Pts',(-123.752389954268,1.40713727450679,
137.258356253404));
#221255=CARTESIAN_POINT('Ctrl Pts',(-124.030837578081,6.19052138319586,
133.109038465103));
#221256=CARTESIAN_POINT('Ctrl Pts',(-124.309285201894,5.28511876451003,
126.841834324687));
#221257=CARTESIAN_POINT('Ctrl Pts',(-124.587732825707,-0.477049806354697,
124.215998267256));
#221258=CARTESIAN_POINT('Ctrl Pts',(-124.86618044952,-5.80083291035842,
127.644545350364));
#221259=CARTESIAN_POINT('Ctrl Pts',(-125.144628073333,-5.79393395618462,
133.976808298475));
#221260=CARTESIAN_POINT('Ctrl Pts',(-125.423075697146,-0.462692745686338,
137.393746810514));
#221261=CARTESIAN_POINT('Ctrl Pts',(-125.701523320958,5.2937404943001,134.755361320645));
#221262=CARTESIAN_POINT('Ctrl Pts',(-125.979970944772,6.18548483362552,
128.486199201761));
#221263=CARTESIAN_POINT('Ctrl Pts',(-126.258418568584,1.39307078858202,
124.34731417552));
#221264=CARTESIAN_POINT('Ctrl Pts',(-126.536866192397,-4.67950725587653,
126.142139385264));
#221265=CARTESIAN_POINT('Ctrl Pts',(-126.81531381621,-6.45184673882346,
132.221318145323));
#221266=CARTESIAN_POINT('Ctrl Pts',(-127.093761440023,-2.29525425902701,
136.998382159598));
#221267=CARTESIAN_POINT('Ctrl Pts',(-127.372209063836,3.97056475541062,
136.083442971518));
#221268=CARTESIAN_POINT('Ctrl Pts',(-127.650656687649,6.58762873249828,
130.317284997668));
#221269=CARTESIAN_POINT('Ctrl Pts',(-127.929104311462,3.15098372797424,
124.998725723536));
#221270=CARTESIAN_POINT('Ctrl Pts',(-128.207551935275,-3.18126138844507,
125.015261295985));
#221271=CARTESIAN_POINT('Ctrl Pts',(-128.485999559087,-6.59008270214206,
130.351696331743));
#221272=CARTESIAN_POINT('Ctrl Pts',(-128.764447182901,-3.94293995600869,
136.104107732291));
#221273=CARTESIAN_POINT('Ctrl Pts',(-129.042894806713,2.32757198637139,
136.986310441447));
#221274=CARTESIAN_POINT('Ctrl Pts',(-129.321342430526,6.45915898148892,
132.187603267495));
#221275=CARTESIAN_POINT('Ctrl Pts',(-129.599790054339,4.6550944200771,126.117763673416));
#221276=CARTESIAN_POINT('Ctrl Pts',(-129.878237678152,-1.42677449938118,
124.354677718024));
#221277=CARTESIAN_POINT('Ctrl Pts',(-130.156685301965,-6.19750735571679,
128.518535262782));
#221278=CARTESIAN_POINT('Ctrl Pts',(-130.435132925778,-5.27303371721495,
134.782954639811));
#221279=CARTESIAN_POINT('Ctrl Pts',(-130.713580549591,0.497100305389368,
137.391240475519));
#221280=CARTESIAN_POINT('Ctrl Pts',(-130.992028173403,5.81042343204081,
133.946505508738));
#221281=CARTESIAN_POINT('Ctrl Pts',(-131.270475797217,5.78425127961196,
127.614292889281));
#221282=CARTESIAN_POINT('Ctrl Pts',(-131.548923421029,0.442634777604211,
124.213596668645));
#221283=CARTESIAN_POINT('Ctrl Pts',(-131.827371044842,-5.30574146111081,
126.869490540348));
#221284=CARTESIAN_POINT('Ctrl Pts',(-132.105818668655,-6.17840049694519,
133.141337783923));
#221285=CARTESIAN_POINT('Ctrl Pts',(-132.384266292468,-1.37341130773126,
137.265617179298));
#221286=CARTESIAN_POINT('Ctrl Pts',(-132.662713916281,4.69367577841589,
135.45231744437));
#221287=CARTESIAN_POINT('Ctrl Pts',(-132.941161540094,6.44750412300737,
129.367772450924));
#221288=CARTESIAN_POINT('Ctrl Pts',(-133.219609163907,2.27639115664257,
124.603381801387));
#221289=CARTESIAN_POINT('Ctrl Pts',(-133.49805678772,-3.98661407478655,
125.537387749261));
#221290=CARTESIAN_POINT('Ctrl Pts',(-133.776504411532,-6.58611572841139,
131.311484457178));
#221291=CARTESIAN_POINT('Ctrl Pts',(-134.054952035345,-3.13329877726696,
136.619559130867));
#221292=CARTESIAN_POINT('Ctrl Pts',(-134.333399659158,3.19886668003099,
136.583750459073));
#221293=CARTESIAN_POINT('Ctrl Pts',(-134.611847282971,6.59142993170542,
131.236964861823));
#221294=CARTESIAN_POINT('Ctrl Pts',(-134.890294906784,3.92679108539655,
125.492637097993));
#221295=CARTESIAN_POINT('Ctrl Pts',(-135.168742530597,-2.34637693398254,
124.629523756529));
#221296=CARTESIAN_POINT('Ctrl Pts',(-135.44719015441,-6.46333917791768,
129.440783832808));
#221297=CARTESIAN_POINT('Ctrl Pts',(-135.725637778223,-4.64080846901838,
135.505104359849));
#221298=CARTESIAN_POINT('Ctrl Pts',(-136.004085402036,1.44639850681073,
137.24967103183));
#221299=CARTESIAN_POINT('Ctrl Pts',(-136.282533025848,6.20443591537649,
133.07131230402));
#221300=CARTESIAN_POINT('Ctrl Pts',(-136.560980649661,5.26089982125598,
126.809735723105));
#221301=CARTESIAN_POINT('Ctrl Pts',(-136.839428273474,-0.517146199354053,
124.219024271924));
#221302=CARTESIAN_POINT('Ctrl Pts',(-137.117875897287,-5.81996012675442,
127.679915210822));
#221303=CARTESIAN_POINT('Ctrl Pts',(-137.3963235211,-5.77451501852576,134.012018840873));
#221304=CARTESIAN_POINT('Ctrl Pts',(-137.674771144913,-0.422572709013315,
137.396441266521));
#221305=CARTESIAN_POINT('Ctrl Pts',(-137.953218768726,5.31769327625758,
134.723063616821));
#221306=CARTESIAN_POINT('Ctrl Pts',(-138.231666392539,6.17125892440694,
128.448589350091));
#221307=CARTESIAN_POINT('Ctrl Pts',(-138.510114016352,1.35373910378499,
124.338953792345));
#221308=CARTESIAN_POINT('Ctrl Pts',(-138.788561640165,-4.70780081938319,
126.170711254294));
#221309=CARTESIAN_POINT('Ctrl Pts',(-139.067009263977,-6.44310177839452,
132.260566114734));
#221310=CARTESIAN_POINT('Ctrl Pts',(-139.34545688779,-2.25750696608163,
137.012239262869));
#221311=CARTESIAN_POINT('Ctrl Pts',(-139.623904511603,4.00262646271346,
136.059175207703));
#221312=CARTESIAN_POINT('Ctrl Pts',(-139.902352135416,6.5845417114487,130.277193256163));
#221313=CARTESIAN_POINT('Ctrl Pts',(-140.180799759229,3.11558480010749,
124.979652356196));
#221314=CARTESIAN_POINT('Ctrl Pts',(-140.459247383042,-3.21644233775325,
125.034733795609));
#221315=CARTESIAN_POINT('Ctrl Pts',(-140.737695006855,-6.59271609916233,
130.391820422461));
#221316=CARTESIAN_POINT('Ctrl Pts',(-141.016142630668,-3.91060583752806,
136.128011334905));
#221317=CARTESIAN_POINT('Ctrl Pts',(-141.294590254481,2.36516014507876,
136.97202731291));
#221318=CARTESIAN_POINT('Ctrl Pts',(-141.573037878293,6.46745949885459,
132.148258905163));
#221319=CARTESIAN_POINT('Ctrl Pts',(-141.851485502106,4.62647952614482,
126.089513624195));
#221320=CARTESIAN_POINT('Ctrl Pts',(-142.129933125919,-1.4660091150024,
124.363482397054));
#221321=CARTESIAN_POINT('Ctrl Pts',(-142.408380749732,-6.21130699798892,
128.556303600169));
#221322=CARTESIAN_POINT('Ctrl Pts',(-142.686828373545,-5.24871718904012,
134.814979378581));
#221323=CARTESIAN_POINT('Ctrl Pts',(-142.965275997358,0.537187302547703,
137.388092445238));
#221324=CARTESIAN_POINT('Ctrl Pts',(-143.243723621171,5.82944290615228,
133.911077595444));
#221325=CARTESIAN_POINT('Ctrl Pts',(-143.522171244983,5.76472526312116,
127.579141614542));
#221326=CARTESIAN_POINT('Ctrl Pts',(-143.800618868797,0.402506725767204,
124.21102433671));
#221327=CARTESIAN_POINT('Ctrl Pts',(-144.079066492609,-5.32959582902011,
126.901860998601));
#221328=CARTESIAN_POINT('Ctrl Pts',(-144.357514116423,-6.1640601821688,
133.178904162615));
#221329=CARTESIAN_POINT('Ctrl Pts',(-144.635961740235,-1.33405435898536,
137.27385781163));
#221330=CARTESIAN_POINT('Ctrl Pts',(-144.914409364048,4.72188224792766,
135.423659591808));
#221331=CARTESIAN_POINT('Ctrl Pts',(-145.192856987861,6.43863974576633,
129.328551279958));
#221332=CARTESIAN_POINT('Ctrl Pts',(-145.471304611674,2.23860186228433,
124.589639652074));
#221333=CARTESIAN_POINT('Ctrl Pts',(-145.749752235487,-4.01860177085642,
125.56175298548));
#221334=CARTESIAN_POINT('Ctrl Pts',(-146.0281998593,-6.58290669619051,131.35156661715));
#221335=CARTESIAN_POINT('Ctrl Pts',(-146.306647483113,-3.09784196059638,
136.638524667701));
#221336=CARTESIAN_POINT('Ctrl Pts',(-146.585095106925,3.2339881987928,136.564170970937));
#221337=CARTESIAN_POINT('Ctrl Pts',(-146.863542730738,6.59394119259793,
131.196832941802));
#221338=CARTESIAN_POINT('Ctrl Pts',(-147.141990354551,3.89438436234147,
125.468832020033));
#221339=CARTESIAN_POINT('Ctrl Pts',(-147.420437978364,-2.38392144565404,
124.643921224334));
#221340=CARTESIAN_POINT('Ctrl Pts',(-147.698885602177,-6.47151990613084,
129.480153276819));
#221341=CARTESIAN_POINT('Ctrl Pts',(-147.97733322599,-4.61210772419611,
135.533267184325));
#221342=CARTESIAN_POINT('Ctrl Pts',(-148.255780849803,1.48560614228611,
137.240746976909));
#221343=CARTESIAN_POINT('Ctrl Pts',(-148.534228473616,6.21812053990256,
133.033502140209));
#221344=CARTESIAN_POINT('Ctrl Pts',(-148.812676097428,5.23648593342438,
126.777785143819));
#221345=CARTESIAN_POINT('Ctrl Pts',(-149.091123721242,-0.557223429310831,
124.222294298654));
#221346=CARTESIAN_POINT('Ctrl Pts',(-149.369571345054,-5.83887168238761,
127.715400848752));
#221347=CARTESIAN_POINT('Ctrl Pts',(-149.648018968867,-5.75488210408933,
134.047110522317));
#221348=CARTESIAN_POINT('Ctrl Pts',(-149.92646659268,-0.382437013753756,
137.398891450554));
#221349=CARTESIAN_POINT('Ctrl Pts',(-150.204914216493,5.34144900913504,
134.690620704017));
#221350=CARTESIAN_POINT('Ctrl Pts',(-150.483361840306,6.15680433691945,
128.411066792389));
#221351=CARTESIAN_POINT('Ctrl Pts',(-150.761809464119,1.31435725568762,
124.330832987197));
#221352=CARTESIAN_POINT('Ctrl Pts',(-151.040257087932,-4.73591993359918,
126.199454824906));
#221353=CARTESIAN_POINT('Ctrl Pts',(-151.318704711745,-6.43411806645975,
132.299760123916));
#221354=CARTESIAN_POINT('Ctrl Pts',(-151.597152335558,-2.21967602038541,
137.025866330917));
#221355=CARTESIAN_POINT('Ctrl Pts',(-151.87559995937,4.03453985122072,136.034712724799));
#221356=CARTESIAN_POINT('Ctrl Pts',(-152.154047583183,6.58121069778455,
130.237121049039));
#221357=CARTESIAN_POINT('Ctrl Pts',(-152.432495206996,3.08007042310019,
124.960794825562));
#221358=CARTESIAN_POINT('Ctrl Pts',(-152.710942830809,-3.25150410060774,
125.054420090877));
#221359=CARTESIAN_POINT('Ctrl Pts',(-152.989390454622,-6.59510520066311,
130.431959800007));
#221360=CARTESIAN_POINT('Ctrl Pts',(-153.267838078435,-3.87812681010997,
136.151717667683));
#221361=CARTESIAN_POINT('Ctrl Pts',(-153.546285702248,2.40266066190714,
136.957515639215));
#221362=CARTESIAN_POINT('Ctrl Pts',(-153.824733326061,6.47552036213011,
132.108864744186));
#221363=CARTESIAN_POINT('Ctrl Pts',(-154.103180949873,4.59769319631231,
126.061438285362));
#221364=CARTESIAN_POINT('Ctrl Pts',(-154.381628573686,-1.50518940711724,
124.372525745196));
#221365=CARTESIAN_POINT('Ctrl Pts',(-154.660076197499,-6.22487647799626,
128.594155240135));
#221366=CARTESIAN_POINT('Ctrl Pts',(-154.938523821312,-5.22420616771914,
134.846855502398));
#221367=CARTESIAN_POINT('Ctrl Pts',(-155.216971445125,0.577254394032953,
137.384700452354));
#221368=CARTESIAN_POINT('Ctrl Pts',(-155.495419068938,5.84824636811312,
133.87553456161));
#221369=CARTESIAN_POINT('Ctrl Pts',(-155.773866692751,5.74498563261573,
127.544109851479));
#221370=CARTESIAN_POINT('Ctrl Pts',(-156.052314316564,0.362363758895462,
124.208696323275));
#221371=CARTESIAN_POINT('Ctrl Pts',(-156.330761940377,-5.353252706796,126.934376065411));
#221372=CARTESIAN_POINT('Ctrl Pts',(-156.60920956419,-6.14949145587554,
133.216382551721));
#221373=CARTESIAN_POINT('Ctrl Pts',(-156.887657188002,-1.29464797636456,
137.281858714364));
#221374=CARTESIAN_POINT('Ctrl Pts',(-157.166104811815,4.74991374635575,
135.394830569423));
#221375=CARTESIAN_POINT('Ctrl Pts',(-157.444552435628,6.42953678236183,
129.28938479565));
#221376=CARTESIAN_POINT('Ctrl Pts',(-157.723000059441,2.20072961571137,
124.576127791533));
#221377=CARTESIAN_POINT('Ctrl Pts',(-158.001447683254,-4.05044055615985,
125.586312488451));
#221378=CARTESIAN_POINT('Ctrl Pts',(-158.279895307067,-6.57945373194114,
131.391628500203));
#221379=CARTESIAN_POINT('Ctrl Pts',(-158.55834293088,-3.06227035225273,
136.657274017441));
#221380=CARTESIAN_POINT('Ctrl Pts',(-158.836790554693,3.2689898809326,136.54437805091));
#221381=CARTESIAN_POINT('Ctrl Pts',(-159.115238178505,6.59620811257463,
131.156686478575));
#221382=CARTESIAN_POINT('Ctrl Pts',(-159.393685802319,3.86183333144169,
125.445224652049));
#221383=CARTESIAN_POINT('Ctrl Pts',(-159.672133426131,-2.42137762023968,
124.658546969484));
#221384=CARTESIAN_POINT('Ctrl Pts',(-159.950581049944,-6.47946082979399,
129.519571789819));
#221385=CARTESIAN_POINT('Ctrl Pts',(-160.229028673757,-4.58323607602601,
135.56125477743));
#221386=CARTESIAN_POINT('Ctrl Pts',(-160.50747629757,1.52475872807955,137.231584419323));
#221387=CARTESIAN_POINT('Ctrl Pts',(-160.785923921383,6.23157474968534,
132.99560937474));
#221388=CARTESIAN_POINT('Ctrl Pts',(-161.064371545196,5.2118780056808,126.745983770767));
#221389=CARTESIAN_POINT('Ctrl Pts',(-161.342819169009,-0.597280011148509,
124.225808226271));
#221390=CARTESIAN_POINT('Ctrl Pts',(-161.621266792821,-5.85756687648338,
127.751000949223));
#221391=CARTESIAN_POINT('Ctrl Pts',(-161.899714416635,-5.73503594038016,
134.08208204247));
#221392=CARTESIAN_POINT('Ctrl Pts',(-162.178162040447,-0.342287147149402,
137.401097271823));
#221393=CARTESIAN_POINT('Ctrl Pts',(-162.45660966426,5.36500681265522,134.658033784415));
#221394=CARTESIAN_POINT('Ctrl Pts',(-162.735057288073,6.14212160678308,
128.373632919072));
#221395=CARTESIAN_POINT('Ctrl Pts',(-163.013504911886,1.27492670359879,
124.322952060995));
#221396=CARTESIAN_POINT('Ctrl Pts',(-163.291952535699,-4.76386355656041,
126.228369031995));
#221397=CARTESIAN_POINT('Ctrl Pts',(-163.570400159512,-6.42489593591386,
132.338898720518));
#221398=CARTESIAN_POINT('Ctrl Pts',(-163.848847783325,-2.18176282377798,
137.039262858781));
#221399=CARTESIAN_POINT('Ctrl Pts',(-164.127295407138,4.06630373837012,
136.010056429275));
#221400=CARTESIAN_POINT('Ctrl Pts',(-164.405743030951,6.57763581493773,
130.197069861187));
#221401=CARTESIAN_POINT('Ctrl Pts',(-164.684190654763,3.04444191295097,
124.942153830408));
#221402=CARTESIAN_POINT('Ctrl Pts',(-164.962638278576,-3.28644537778151,
125.074319452304));
#221403=CARTESIAN_POINT('Ctrl Pts',(-165.241085902389,-6.59724991811553,
130.472112977002));
#221404=CARTESIAN_POINT('Ctrl Pts',(-165.519533526202,-3.84550407727676,
136.175225852179));
#221405=CARTESIAN_POINT('Ctrl Pts',(-165.797981150015,2.44007214726114,
136.942775958099));
#221406=CARTESIAN_POINT('Ctrl Pts',(-166.076428773828,6.48334127261722,
132.069422244329));
#221407=CARTESIAN_POINT('Ctrl Pts',(-166.354876397641,4.56873649726763,
126.03353869726));
#221408=CARTESIAN_POINT('Ctrl Pts',(-166.633324021454,-1.54431392388507,
124.381807427344));
#221409=CARTESIAN_POINT('Ctrl Pts',(-166.911771645267,-6.23821529291649,
128.632088780075));
#221410=CARTESIAN_POINT('Ctrl Pts',(-167.19021926908,-5.19950156151742,
134.878581830081));
#221411=CARTESIAN_POINT('Ctrl Pts',(-167.468666892892,0.617300095144361,
137.381064622557));
#221412=CARTESIAN_POINT('Ctrl Pts',(-167.747114516705,5.86683312115408,
133.839877724298));
#221413=CARTESIAN_POINT('Ctrl Pts',(-168.025562140518,5.72503311955499,
127.509198898206));
#221414=CARTESIAN_POINT('Ctrl Pts',(-168.304009764331,0.32220736450136,
124.206612714607));
#221415=CARTESIAN_POINT('Ctrl Pts',(-168.582457388144,-5.37671121782417,
126.967034535923));
#221416=CARTESIAN_POINT('Ctrl Pts',(-168.860905011957,-6.1346948579149,
133.253771562468));
#221417=CARTESIAN_POINT('Ctrl Pts',(-169.13935263577,-1.25519362008691,
137.289619591024));
#221418=CARTESIAN_POINT('Ctrl Pts',(-169.417800259582,4.77776923498369,
135.365831445486));
#221419=CARTESIAN_POINT('Ctrl Pts',(-169.696247883396,6.42019557010726,
129.250274449328));
#221420=CARTESIAN_POINT('Ctrl Pts',(-169.974695507208,2.16277582029264,
124.562846720449));
#221421=CARTESIAN_POINT('Ctrl Pts',(-170.253143131021,-4.08212925089891,
125.611065348116));
#221422=CARTESIAN_POINT('Ctrl Pts',(-170.531590754834,-6.57575696361412,
131.431668621828));
#221423=CARTESIAN_POINT('Ctrl Pts',(-170.810038378647,-3.02658527035502,
136.675806485322));
#221424=CARTESIAN_POINT('Ctrl Pts',(-171.08848600246,3.30387042945021,136.524372432426));
#221425=CARTESIAN_POINT('Ctrl Pts',(-171.366933626273,6.59823060763395,
131.116526959784));
#221426=CARTESIAN_POINT('Ctrl Pts',(-171.645381250086,3.82913919888762,
125.421815868818));
#221427=CARTESIAN_POINT('Ctrl Pts',(-171.923828873899,-2.45874406978715,
124.673400450021));
#221428=CARTESIAN_POINT('Ctrl Pts',(-172.202276497711,-6.48716165465291,
129.559037911142));
#221429=CARTESIAN_POINT('Ctrl Pts',(-172.480724121525,-4.55419459435809,
135.589066102071));
#221430=CARTESIAN_POINT('Ctrl Pts',(-172.759171745337,1.5638548133772,137.222183698596));
#221431=CARTESIAN_POINT('Ctrl Pts',(-173.03761936915,6.24479804617409,132.957635411742));
#221432=CARTESIAN_POINT('Ctrl Pts',(-173.316066992963,5.18707694988104,
126.714332782362));
#221433=CARTESIAN_POINT('Ctrl Pts',(-173.594514616776,-0.637314460555731,
124.229565924566));
#221434=CARTESIAN_POINT('Ctrl Pts',(-173.872962240589,-5.8760450162844,
127.786714193059));
#221435=CARTESIAN_POINT('Ctrl Pts',(-174.151409864401,-5.71497726280517,
134.11693210545));
#221436=CARTESIAN_POINT('Ctrl Pts',(-174.429857488215,-0.302124596968923,
137.403058648589));
#221437=CARTESIAN_POINT('Ctrl Pts',(-174.708305112027,5.38836581387496,
134.625304065538));
#221438=CARTESIAN_POINT('Ctrl Pts',(-174.98675273584,6.1272112780718,128.336289117263));
#221439=CARTESIAN_POINT('Ctrl Pts',(-175.265200359654,1.2354489086321,124.315311305772));
#221440=CARTESIAN_POINT('Ctrl Pts',(-175.543647983466,-4.79163065280562,
126.257452804136));
#221441=CARTESIAN_POINT('Ctrl Pts',(-175.822095607279,-6.41543572848632,
132.377980454247));
#221442=CARTESIAN_POINT('Ctrl Pts',(-176.100543231092,-2.14376878114676,
137.05242835005));
#221443=CARTESIAN_POINT('Ctrl Pts',(-176.378990854905,4.09791694713909,
135.985207234778));
#221444=CARTESIAN_POINT('Ctrl Pts',(-176.657438478718,6.57381719537689,
130.157041176716));
#221445=CARTESIAN_POINT('Ctrl Pts',(-176.93588610253,3.00870058988678,124.923730061481));
#221446=CARTESIAN_POINT('Ctrl Pts',(-177.214333726344,-3.32126487451375,
125.094431142515));
#221447=CARTESIAN_POINT('Ctrl Pts',(-177.492781350156,-6.59915017204588,
130.512278465557));
#221448=CARTESIAN_POINT('Ctrl Pts',(-177.771228973969,-3.81273884787578,
136.198535017289));
#221449=CARTESIAN_POINT('Ctrl Pts',(-178.049676597782,2.47739321484437,
136.927808815745));
#221450=CARTESIAN_POINT('Ctrl Pts',(-178.328124221595,6.49092194050925,
132.029932867148));
#221451=CARTESIAN_POINT('Ctrl Pts',(-178.606571845408,4.53961050201187,
126.005815893719));
#221452=CARTESIAN_POINT('Ctrl Pts',(-178.885019469221,-1.58338121553252,
124.391327099562));
#221453=CARTESIAN_POINT('Ctrl Pts',(-179.163467093034,-6.25132294847495,
128.670102814346));
#221454=CARTESIAN_POINT('Ctrl Pts',(-179.441914716847,-5.1746042858732,
134.910157185999));
#221455=CARTESIAN_POINT('Ctrl Pts',(-179.72036234066,0.657322921973241,
137.377185090575));
#221456=CARTESIAN_POINT('Ctrl Pts',(-179.998809964472,5.88520247653593,
133.804108404782));
#221457=CARTESIAN_POINT('Ctrl Pts',(-180.277257588285,5.70486846328706,
127.474410048364));
#221458=CARTESIAN_POINT('Ctrl Pts',(-180.555705212098,0.282039030594865,
124.204773587913));
#221459=CARTESIAN_POINT('Ctrl Pts',(-180.834152835911,-5.39997049284089,
126.999835199963));
#221460=CARTESIAN_POINT('Ctrl Pts',(-181.112600459724,-6.11967093658025,
133.291069809391));
#221461=CARTESIAN_POINT('Ctrl Pts',(-181.391048083537,-1.21569275214809,
137.297140154028));
#221462=CARTESIAN_POINT('Ctrl Pts',(-181.669495707349,4.8054476816156,135.336663294571));
#221463=CARTESIAN_POINT('Ctrl Pts',(-181.947943331163,6.41061645514481,
129.21122169024));
#221464=CARTESIAN_POINT('Ctrl Pts',(-182.226390954976,2.12474188242055,
124.549796930959));
#221465=CARTESIAN_POINT('Ctrl Pts',(-182.504838578788,-4.11366668083735,
125.636010647245));
#221466=CARTESIAN_POINT('Ctrl Pts',(-182.783286202602,-6.5718165281946,
131.471685498325));
#221467=CARTESIAN_POINT('Ctrl Pts',(-183.061733826414,-2.99078803722709,
136.694121384618));
#221468=CARTESIAN_POINT('Ctrl Pts',(-183.340181450227,3.33862855183402,
136.5041548568));
#221469=CARTESIAN_POINT('Ctrl Pts',(-183.61862907404,6.60000860283161,131.076355873553));
#221470=CARTESIAN_POINT('Ctrl Pts',(-183.897076697853,3.79630317617236,
125.398606537762));
#221471=CARTESIAN_POINT('Ctrl Pts',(-184.175524321666,-2.49601940966891,
124.68848111554));
#221472=CARTESIAN_POINT('Ctrl Pts',(-184.453971945479,-6.49462209535141,
129.598550178357));
#221473=CARTESIAN_POINT('Ctrl Pts',(-184.732419569291,-4.52498435533419,
135.616700127691));
#221474=CARTESIAN_POINT('Ctrl Pts',(-185.010867193105,1.60289294946002,
137.212545163075));
#221475=CARTESIAN_POINT('Ctrl Pts',(-185.289314816917,6.25778993937471,
132.919581658354));
#221476=CARTESIAN_POINT('Ctrl Pts',(-185.56776244073,5.16208368503734,126.682833351442));
#221477=CARTESIAN_POINT('Ctrl Pts',(-185.846210064543,-0.677325294041226,
124.233567254297));
#221478=CARTESIAN_POINT('Ctrl Pts',(-186.124657688356,-5.89430541707644,
127.822539256894));
#221479=CARTESIAN_POINT('Ctrl Pts',(-186.403105312169,-5.69470681464601,
134.151659419877));
#221480=CARTESIAN_POINT('Ctrl Pts',(-186.681552935982,-0.261950851450417,
137.404775508174));
#221481=CARTESIAN_POINT('Ctrl Pts',(-186.960000559794,5.41152514721792,
134.592432760195));
#221482=CARTESIAN_POINT('Ctrl Pts',(-187.238448183608,6.11207390329327,
128.299036770752));
#221483=CARTESIAN_POINT('Ctrl Pts',(-187.51689580742,1.19592533365239,124.307911004657));
#221484=CARTESIAN_POINT('Ctrl Pts',(-187.795343431234,-4.81922019341476,
126.286705063617));
#221485=CARTESIAN_POINT('Ctrl Pts',(-188.073791055046,-6.40573779472858,
132.417003876913));
#221486=CARTESIAN_POINT('Ctrl Pts',(-188.352238678859,-2.10569530037498,
137.065362316871));
#221487=CARTESIAN_POINT('Ctrl Pts',(-188.630686302672,4.12937830608858,
135.960166062105));
#221488=CARTESIAN_POINT('Ctrl Pts',(-188.909133926485,6.56975498060235,
130.117036478904));
#221489=CARTESIAN_POINT('Ctrl Pts',(-189.187581550298,2.97284777831579,
124.905524201484));
#221490=CARTESIAN_POINT('Ctrl Pts',(-189.466029174111,-3.35596130055467,
125.114754416262));
#221491=CARTESIAN_POINT('Ctrl Pts',(-189.744476797923,-6.60080589203976,
130.552454777323));
#221492=CARTESIAN_POINT('Ctrl Pts',(-190.022924421737,-3.77983233603489,
136.221644299282));
#221493=CARTESIAN_POINT('Ctrl Pts',(-190.301372045549,2.5146224817104,136.912614766765));
#221494=CARTESIAN_POINT('Ctrl Pts',(-190.579819669362,6.49826208490189,
131.990398075938));
#221495=CARTESIAN_POINT('Ctrl Pts',(-190.858267293175,4.51031628981952,
125.978270902017));
#221496=CARTESIAN_POINT('Ctrl Pts',(-191.136714916988,-1.62238983440674,
124.401084409096));
#221497=CARTESIAN_POINT('Ctrl Pts',(-191.415162540801,-6.26419895896261,
128.708195934325));
#221498=CARTESIAN_POINT('Ctrl Pts',(-191.693610164614,-5.14951526336424,
134.941580400114));
#221499=CARTESIAN_POINT('Ctrl Pts',(-191.972057788427,0.697321391460013,
137.373062000163));
#221500=CARTESIAN_POINT('Ctrl Pts',(-192.25050541224,5.90335375357599,133.768227928508));
#221501=CARTESIAN_POINT('Ctrl Pts',(-192.528953036052,5.68449241101982,
127.439744591064));
#221502=CARTESIAN_POINT('Ctrl Pts',(-192.807400659866,0.241860245628379,
124.203179011344));
#221503=CARTESIAN_POINT('Ctrl Pts',(-193.085848283678,-5.42302966996514,
127.032776842093));
#221504=CARTESIAN_POINT('Ctrl Pts',(-193.364295907491,-6.10442024858855,
133.32827591039));
#221505=CARTESIAN_POINT('Ctrl Pts',(-193.642743531304,-1.17614683626724,
137.304420124699));
#221506=CARTESIAN_POINT('Ctrl Pts',(-193.921191155117,4.83294806061645,
135.307327197512));
#221507=CARTESIAN_POINT('Ctrl Pts',(-194.19963877893,6.40079979243214,129.172227965502));
#221508=CARTESIAN_POINT('Ctrl Pts',(-194.478086402743,2.08662921145659,
124.536978906625));
#221509=CARTESIAN_POINT('Ctrl Pts',(-194.756534026555,-4.14505167734362,
125.661147461485));
#221510=CARTESIAN_POINT('Ctrl Pts',(-195.034981650369,-6.5676325716969,
131.511677646851));
#221511=CARTESIAN_POINT('Ctrl Pts',(-195.313429274181,-2.95487997934909,
136.712218036662));
#221512=CARTESIAN_POINT('Ctrl Pts',(-195.591876897994,3.3732629601091,136.483726073203));
#221513=CARTESIAN_POINT('Ctrl Pts',(-195.870324521807,6.60154203228333,
131.03617470844));
#221514=CARTESIAN_POINT('Ctrl Pts',(-196.14877214562,3.76332648004682,125.375597518911));
#221515=CARTESIAN_POINT('Ctrl Pts',(-196.427219769433,-2.53320225863353,
124.703788407225));
#221516=CARTESIAN_POINT('Ctrl Pts',(-196.705667393246,-6.50184187543975,
129.63810712732));
#221517=CARTESIAN_POINT('Ctrl Pts',(-196.984115017059,-4.49560644135098,
135.644155830301));
#221518=CARTESIAN_POINT('Ctrl Pts',(-197.262562640871,1.64187168975517,
137.202669169918));
#221519=CARTESIAN_POINT('Ctrl Pts',(-197.541010264685,6.27054994786743,
132.881449524674));
#221520=CARTESIAN_POINT('Ctrl Pts',(-197.819457888497,5.13689913728475,
126.651486645231));
#221521=CARTESIAN_POINT('Ctrl Pts',(-198.097905512311,-0.717311028988463,
124.237812067191));
#221522=CARTESIAN_POINT('Ctrl Pts',(-198.376353136123,-5.91234740221361,
127.858474813215));
#221523=CARTESIAN_POINT('Ctrl Pts',(-198.654800759936,-5.67422534703162,
134.186262698915));
#221524=CARTESIAN_POINT('Ctrl Pts',(-198.933248383749,-0.221767399246752,
137.406247786956));
#221525=CARTESIAN_POINT('Ctrl Pts',(-199.211696007562,5.43448395450644,
134.559421086446));
#221526=CARTESIAN_POINT('Ctrl Pts',(-199.490143631375,6.09671004336861,
128.261877259937));
#221527=CARTESIAN_POINT('Ctrl Pts',(-199.768591255188,1.15635744321901,
124.300751431872));
#221528=CARTESIAN_POINT('Ctrl Pts',(-200.047038879001,-4.84663115604747,
126.316124726487));
#221529=CARTESIAN_POINT('Ctrl Pts',(-200.325486502814,-6.39580249400115,
132.455967542492));
#221530=CARTESIAN_POINT('Ctrl Pts',(-200.603934126626,-2.06754379228947,
137.078064279972));
#221531=CARTESIAN_POINT('Ctrl Pts',(-200.882381750439,4.16068664940635,
135.934933839164));
#221532=CARTESIAN_POINT('Ctrl Pts',(-201.160829374253,6.56544932114097,
130.077057250143));
#221533=CARTESIAN_POINT('Ctrl Pts',(-201.439276998065,2.9368848067771,124.887536925038));
#221534=CARTESIAN_POINT('Ctrl Pts',(-201.717724621878,-3.39053337021544,
125.13528852046));
#221535=CARTESIAN_POINT('Ctrl Pts',(-201.996172245691,-6.60221701674386,
130.592640423553));
#221536=CARTESIAN_POINT('Ctrl Pts',(-202.274619869504,-3.74678576111652,
136.244552841837));
#221537=CARTESIAN_POINT('Ctrl Pts',(-202.553067493317,2.55175856831618,
136.897194374181));
#221538=CARTESIAN_POINT('Ctrl Pts',(-202.83151511713,6.50536143380309,131.950819335672));
#221539=CARTESIAN_POINT('Ctrl Pts',(-203.109962740942,4.48085494619837,
125.950904742844));
#221540=CARTESIAN_POINT('Ctrl Pts',(-203.388410364755,-1.66133833502902,
124.411078994385));
#221541=CARTESIAN_POINT('Ctrl Pts',(-203.666857988568,-6.27684284725421,
128.746366728457));
#221542=CARTESIAN_POINT('Ctrl Pts',(-203.945305612381,-5.12423542367342,
134.97285030803));
#221543=CARTESIAN_POINT('Ctrl Pts',(-204.223753236194,0.737294021446153,
137.368695504108));
#221544=CARTESIAN_POINT('Ctrl Pts',(-204.502200860007,5.9212862796718,133.732237625041));
#221545=CARTESIAN_POINT('Ctrl Pts',(-204.78064848382,5.66390571779574,127.405203810847));
#221546=CARTESIAN_POINT('Ctrl Pts',(-205.059096107633,0.20167249844203,
124.201829043986));
#221547=CARTESIAN_POINT('Ctrl Pts',(-205.337543731446,-5.44588789473034,
127.065858241646));
#221548=CARTESIAN_POINT('Ctrl Pts',(-205.615991355258,-6.08894335906002,
133.36538848678));
#221549=CARTESIAN_POINT('Ctrl Pts',(-205.894438979071,-1.13655733783284,
137.311459233274));
#221550=CARTESIAN_POINT('Ctrl Pts',(-206.172886602884,4.86026935294961,
135.277824241371));
#221551=CARTESIAN_POINT('Ctrl Pts',(-206.451334226697,6.39074594572923,
129.133294720038));
#221552=CARTESIAN_POINT('Ctrl Pts',(-206.72978185051,2.04843921967989,124.524393122426));
#221553=CARTESIAN_POINT('Ctrl Pts',(-207.008229474323,-4.17628307743617,
125.686474859378));
#221554=CARTESIAN_POINT('Ctrl Pts',(-207.286677098136,-6.56320524915893,
131.551643585487));
#221555=CARTESIAN_POINT('Ctrl Pts',(-207.565124721949,-2.9188624273063,
136.730095770877));
#221556=CARTESIAN_POINT('Ctrl Pts',(-207.843572345762,3.40777237088467,
136.463086838631));
#221557=CARTESIAN_POINT('Ctrl Pts',(-208.122019969575,6.60283083916734,
130.995984953369));
#221558=CARTESIAN_POINT('Ctrl Pts',(-208.400467593387,3.73021033247459,
125.352789664874));
#221559=CARTESIAN_POINT('Ctrl Pts',(-208.678915217201,-2.57029123885685,
124.719321757855));
#221560=CARTESIAN_POINT('Ctrl Pts',(-208.957362841013,-6.50882072738636,
129.677707292235));
#221561=CARTESIAN_POINT('Ctrl Pts',(-209.235810464827,-4.4660619410178,
135.671432192519));
#221562=CARTESIAN_POINT('Ctrl Pts',(-209.514258088639,1.68078958989102,
137.192556085085));
#221563=CARTESIAN_POINT('Ctrl Pts',(-209.792705712452,6.28307759882623,
132.8432404237));
#221564=CARTESIAN_POINT('Ctrl Pts',(-210.071153336265,5.11152423984512,
126.620293825292));
#221565=CARTESIAN_POINT('Ctrl Pts',(-210.349600960078,-0.757270183712145,
124.242300205957));
#221566=CARTESIAN_POINT('Ctrl Pts',(-210.62804858389,-5.93017030314353,
127.894519530418));
#221567=CARTESIAN_POINT('Ctrl Pts',(-210.906496207704,-5.65353361891029,
134.220740660327));
#221568=CARTESIAN_POINT('Ctrl Pts',(-211.184943831516,-0.181575729370575,
137.407475430382));
#221569=CARTESIAN_POINT('Ctrl Pts',(-211.463391455329,5.4572413849935,134.52627026755));
#221570=CARTESIAN_POINT('Ctrl Pts',(-211.741839079142,6.08112026761121,
128.224811961777));
#221571=CARTESIAN_POINT('Ctrl Pts',(-212.020286702955,1.11674670353533,
124.293832852717));
#221572=CARTESIAN_POINT('Ctrl Pts',(-212.298734326768,-4.87386252498038,
126.345710702588));
#221573=CARTESIAN_POINT('Ctrl Pts',(-212.577181950581,-6.38563019446009,
132.494870007167));
#221574=CARTESIAN_POINT('Ctrl Pts',(-212.855629574394,-2.02931567060901,
137.090533768676));
#221575=CARTESIAN_POINT('Ctrl Pts',(-213.134077198207,4.19184081695006,
135.909511500946));
#221576=CARTESIAN_POINT('Ctrl Pts',(-213.412524822019,6.56090037654053,
130.037104971874));
#221577=CARTESIAN_POINT('Ctrl Pts',(-213.690972445832,2.90081300789186,
124.869768898671));
#221578=CARTESIAN_POINT('Ctrl Pts',(-213.969420069645,-3.42497980241531,
125.156032694208));
#221579=CARTESIAN_POINT('Ctrl Pts',(-214.247867693459,-6.60338349386843,
130.632833915152));
#221580=CARTESIAN_POINT('Ctrl Pts',(-214.52631531727,-3.71360034767391,
136.267259796069));
#221581=CARTESIAN_POINT('Ctrl Pts',(-214.804762941084,2.58880009856982,
136.881548209402));
#221582=CARTESIAN_POINT('Ctrl Pts',(-215.083210564897,6.51221972414398,
131.911198112957));
#221583=CARTESIAN_POINT('Ctrl Pts',(-215.36165818871,4.45122756284936,125.923718430264));
#221584=CARTESIAN_POINT('Ctrl Pts',(-215.640105812523,-1.70022527414834,
124.421310485075));
#221585=CARTESIAN_POINT('Ctrl Pts',(-215.918553436335,-6.28925414482577,
128.784613782311));
#221586=CARTESIAN_POINT('Ctrl Pts',(-216.197001060149,-5.09876570355457,
135.003965751026));
#221587=CARTESIAN_POINT('Ctrl Pts',(-216.475448683961,0.77723933073121,
137.364085764208));
#221588=CARTESIAN_POINT('Ctrl Pts',(-216.753896307774,5.93899939032692,
133.696138828015));
#221589=CARTESIAN_POINT('Ctrl Pts',(-217.032343931587,5.64310914646246,
127.370788987637));
#221590=CARTESIAN_POINT('Ctrl Pts',(-217.3107915554,0.161477278206604,124.200723735865));
#221591=CARTESIAN_POINT('Ctrl Pts',(-217.589239179213,-5.46854432011718,
127.099078172778));
#221592=CARTESIAN_POINT('Ctrl Pts',(-217.867686803026,-6.07324084149572,
133.402406163341));
#221593=CARTESIAN_POINT('Ctrl Pts',(-218.146134426838,-1.09692572384833,
137.318257218917));
#221594=CARTESIAN_POINT('Ctrl Pts',(-218.424582050652,4.88741054621452,
135.24815551939));
#221595=CARTESIAN_POINT('Ctrl Pts',(-218.703029674464,6.38045528758512,
129.094423396537));
#221596=CARTESIAN_POINT('Ctrl Pts',(-218.981477298277,2.01017332223456,
124.512040044732));
#221597=CARTESIAN_POINT('Ctrl Pts',(-219.25992492209,-4.20735972382344,
125.711991902411));
#221598=CARTESIAN_POINT('Ctrl Pts',(-219.538372545903,-6.55853472463687,
131.591581833275));
#221599=CARTESIAN_POINT('Ctrl Pts',(-219.816820169716,-2.8827367157428,
136.747753924796));
#221600=CARTESIAN_POINT('Ctrl Pts',(-220.095267793529,3.44215550540127,
136.442237917877));
#221601=CARTESIAN_POINT('Ctrl Pts',(-220.373715417342,6.60387497572639,
130.955788097589));
#221602=CARTESIAN_POINT('Ctrl Pts',(-220.652163041155,3.69695596058723,
125.330183820803));
#221603=CARTESIAN_POINT('Ctrl Pts',(-220.930610664968,-2.60728497599312,
124.735080591838));
#221604=CARTESIAN_POINT('Ctrl Pts',(-221.20905828878,-6.51555839258729,
129.717349205704));
#221605=CARTESIAN_POINT('Ctrl Pts',(-221.487505912593,-4.43635194911701,
135.698528203611));
#221606=CARTESIAN_POINT('Ctrl Pts',(-221.765953536406,1.71964520775051,
137.182206283321));
#221607=CARTESIAN_POINT('Ctrl Pts',(-222.044401160219,6.295372428034,132.804955771283));
#221608=CARTESIAN_POINT('Ctrl Pts',(-222.322848784032,5.08595993299503,
126.589256047487));
#221609=CARTESIAN_POINT('Ctrl Pts',(-222.601296407845,-0.797201277510683,
124.247031504286));
#221610=CARTESIAN_POINT('Ctrl Pts',(-222.879744031658,-5.94777345943203,
127.930672072853));
#221611=CARTESIAN_POINT('Ctrl Pts',(-223.158191655471,-5.63263239702162,
134.255092026522));
#221612=CARTESIAN_POINT('Ctrl Pts',(-223.436639279283,-0.141377331138957,
137.40845839296));
#221613=CARTESIAN_POINT('Ctrl Pts',(-223.715086903097,5.47979659539413,
134.492981531924));
#221614=CARTESIAN_POINT('Ctrl Pts',(-223.993534526909,6.06530515370598,
128.187842249741));
#221615=CARTESIAN_POINT('Ctrl Pts',(-224.271982150722,1.07709458239186,
124.287155523561));
#221616=CARTESIAN_POINT('Ctrl Pts',(-224.550429774535,-4.90091329114502,
126.375461895601));
#221617=CARTESIAN_POINT('Ctrl Pts',(-224.828877398348,-6.37522127304402,
132.533709829396));
#221618=CARTESIAN_POINT('Ctrl Pts',(-225.107325022161,-1.99101235188949,
137.102770320923));
#221619=CARTESIAN_POINT('Ctrl Pts',(-225.385772645974,4.22283965429091,
135.883899989486));
#221620=CARTESIAN_POINT('Ctrl Pts',(-225.664220269787,6.55610831536389,
129.997181124546));
#221621=CARTESIAN_POINT('Ctrl Pts',(-225.9426678936,2.86463371831382,124.852220780782));
#221622=CARTESIAN_POINT('Ctrl Pts',(-226.221115517412,-3.45929932072906,
125.176986168825));
#221623=CARTESIAN_POINT('Ctrl Pts',(-226.499563141226,-6.60430528018926,
130.673033762736));
#221624=CARTESIAN_POINT('Ctrl Pts',(-226.778010765038,-3.68027732540471,
136.289764320562));
#221625=CARTESIAN_POINT('Ctrl Pts',(-227.056458388851,2.62574569988376,
136.865676852203));
#221626=CARTESIAN_POINT('Ctrl Pts',(-227.334906012664,6.51883670178814,
131.871535875972));
#221627=CARTESIAN_POINT('Ctrl Pts',(-227.613353636477,4.42143523762624,
125.896712971676));
#221628=CARTESIAN_POINT('Ctrl Pts',(-227.89180126029,-1.73904921079426,
124.431778502036));
#221629=CARTESIAN_POINT('Ctrl Pts',(-228.170248884103,-6.30143239177224,
128.822935678624));
#221630=CARTESIAN_POINT('Ctrl Pts',(-228.448696507916,-5.07310704679746,
135.034925576111));
#221631=CARTESIAN_POINT('Ctrl Pts',(-228.727144131728,0.81715583912702,
137.359232951281));
#221632=CARTESIAN_POINT('Ctrl Pts',(-229.005591755541,5.95649242917557,
133.659932875084));
#221633=CARTESIAN_POINT('Ctrl Pts',(-229.284039379354,5.62210346764449,
127.336501396687));
#221634=CARTESIAN_POINT('Ctrl Pts',(-229.562487003167,0.121276074371264,
124.199863127936));
#221635=CARTESIAN_POINT('Ctrl Pts',(-229.84093462698,-5.4909981065832,127.132435404515));
#221636=CARTESIAN_POINT('Ctrl Pts',(-230.119382250793,-6.0573132777586,
133.439327568368));
#221637=CARTESIAN_POINT('Ctrl Pts',(-230.397829874606,-1.05725346287773,
137.324813829725));
#221638=CARTESIAN_POINT('Ctrl Pts',(-230.676277498418,4.91437063468431,
135.218322130955));
#221639=CARTESIAN_POINT('Ctrl Pts',(-230.954725122232,6.3699281993239,129.055615435388));
#221640=CARTESIAN_POINT('Ctrl Pts',(-231.233172746044,1.97183293707754,
124.49992013129));
#221641=CARTESIAN_POINT('Ctrl Pts',(-231.511620369858,-4.23828046494889,
125.73769764504));
#221642=CARTESIAN_POINT('Ctrl Pts',(-231.79006799367,-6.55362117119865,
131.631490910294));
#221643=CARTESIAN_POINT('Ctrl Pts',(-232.068515617483,-2.84650418331021,
136.765191844092));
#221644=CARTESIAN_POINT('Ctrl Pts',(-232.346963241296,3.47641108958031,
136.421180083507));
#221645=CARTESIAN_POINT('Ctrl Pts',(-232.625410865109,6.60467440326965,
130.915585630608));
#221646=CARTESIAN_POINT('Ctrl Pts',(-232.903858488922,3.66356459663667,
125.307780824367));
#221647=CARTESIAN_POINT('Ctrl Pts',(-233.182306112735,-2.64418209922576,
124.751064325225));
#221648=CARTESIAN_POINT('Ctrl Pts',(-233.460753736548,-6.52205462137589,
129.75703139878));
#221649=CARTESIAN_POINT('Ctrl Pts',(-233.73920136036,-4.40647756656326,
135.725442859523));
#221650=CARTESIAN_POINT('Ctrl Pts',(-234.017648984174,1.75843710352442,
137.17162014814));
#221651=CARTESIAN_POINT('Ctrl Pts',(-234.296096607986,6.30743397990132,
132.766596986079));
#221652=CARTESIAN_POINT('Ctrl Pts',(-234.574544231799,5.06020716402928,
126.558374461932));
#221653=CARTESIAN_POINT('Ctrl Pts',(-234.852991855612,-0.837102830722735,
124.252005786856));
#221654=CARTESIAN_POINT('Ctrl Pts',(-235.131439479425,-5.96515621878728,
127.966931100874));
#221655=CARTESIAN_POINT('Ctrl Pts',(-235.409887103238,-5.6115224558684,
134.289315524594));
#221656=CARTESIAN_POINT('Ctrl Pts',(-235.688334727051,-0.101173694118813,
137.409196638266));
#221657=CARTESIAN_POINT('Ctrl Pts',(-235.966782350864,5.50214874991674,
134.459556113093));
#221658=CARTESIAN_POINT('Ctrl Pts',(-236.245229974676,6.04926528768773,
128.150969493757));
#221659=CARTESIAN_POINT('Ctrl Pts',(-236.52367759849,1.03740254911254,124.280719691838));
#221660=CARTESIAN_POINT('Ctrl Pts',(-236.802125222302,-4.92778245216537,
126.405377203086));
#221661=CARTESIAN_POINT('Ctrl Pts',(-237.080572846115,-6.36457611545918,
132.572485569954));
#221662=CARTESIAN_POINT('Ctrl Pts',(-237.359020469928,-1.95263525547508,
137.114773483282));
#221663=CARTESIAN_POINT('Ctrl Pts',(-237.637468093741,4.25368201275546,
135.858100253825));
#221664=CARTESIAN_POINT('Ctrl Pts',(-237.915915717553,6.55107331518259,
129.957287187551));
#221665=CARTESIAN_POINT('Ctrl Pts',(-238.194363341367,2.8283482786799,124.834893221623));
#221666=CARTESIAN_POINT('Ctrl Pts',(-238.47281096518,-3.49349065343433,
125.198148167872));
#221667=CARTESIAN_POINT('Ctrl Pts',(-238.751258588993,-6.60498234154917,
130.713238476685));
#221668=CARTESIAN_POINT('Ctrl Pts',(-239.029706212805,-3.64681792910581,
136.312065581403));
#221669=CARTESIAN_POINT('Ctrl Pts',(-239.308153836619,2.66259400322518,
136.8495808907));
#221670=CARTESIAN_POINT('Ctrl Pts',(-239.586601460431,6.52521212154101,
131.831834094415));
#221671=CARTESIAN_POINT('Ctrl Pts',(-239.865049084244,4.39147907449425,
125.869889367774));
#221672=CARTESIAN_POINT('Ctrl Pts',(-240.143496708057,-1.77780870633274,
124.44248265737));
#221673=CARTESIAN_POINT('Ctrl Pts',(-240.42194433187,-6.31337713682396,
128.861330997368));
#221674=CARTESIAN_POINT('Ctrl Pts',(-240.700391955683,-5.04726040419313,
135.065728636055));
#221675=CARTESIAN_POINT('Ctrl Pts',(-240.978839579496,0.857042067512721,
137.354137245149));
#221676=CARTESIAN_POINT('Ctrl Pts',(-241.257287203309,5.97376474800676,
133.623621107872));
#221677=CARTESIAN_POINT('Ctrl Pts',(-241.535734827122,5.60088945971499,
127.302342308534));
#221678=CARTESIAN_POINT('Ctrl Pts',(-241.814182450934,0.0810703766063902,
124.199247252091));
#221679=CARTESIAN_POINT('Ctrl Pts',(-242.092630074747,-5.51324842209508,
127.165928700792));
#221680=CARTESIAN_POINT('Ctrl Pts',(-242.37107769856,-6.04116125805038,
133.476151333726));
#221681=CARTESIAN_POINT('Ctrl Pts',(-242.649525322373,-1.01754202499167,
137.331128822742));
#221682=CARTESIAN_POINT('Ctrl Pts',(-242.927972946186,4.94114861934255,
135.188325181553));
#221683=CARTESIAN_POINT('Ctrl Pts',(-243.206420569999,6.35916507103108,
129.016872274634));
#221684=CARTESIAN_POINT('Ctrl Pts',(-243.484868193812,1.93341948492588,
124.488033831209));
#221685=CARTESIAN_POINT('Ctrl Pts',(-243.763315817625,-4.26904415503308,
125.763591134728));
#221686=CARTESIAN_POINT('Ctrl Pts',(-244.041763441437,-6.54846477091785,
131.671369337695));
#221687=CARTESIAN_POINT('Ctrl Pts',(-244.320211065251,-2.8101661726183,
136.782408882594));
#221688=CARTESIAN_POINT('Ctrl Pts',(-244.598658689063,3.51053785406796,
136.399914115825));
#221689=CARTESIAN_POINT('Ctrl Pts',(-244.877106312876,6.60522909217403,
130.875379042142));
#221690=CARTESIAN_POINT('Ctrl Pts',(-245.155553936689,3.6300374779527,125.285581505715));
#221691=CARTESIAN_POINT('Ctrl Pts',(-245.434001560502,-2.68098124131831,
124.767272365732));
#221692=CARTESIAN_POINT('Ctrl Pts',(-245.712449184315,-6.528309173032,129.796752401026));
#221693=CARTESIAN_POINT('Ctrl Pts',(-245.990896808128,-4.37643990036281,
135.752175162922));
#221694=CARTESIAN_POINT('Ctrl Pts',(-246.269344431941,1.79716383976481,
137.160798071814));
#221695=CARTESIAN_POINT('Ctrl Pts',(-246.547792055753,6.31926180748295,
132.728165489484));
#221696=CARTESIAN_POINT('Ctrl Pts',(-246.826239679567,5.03426688722615,
126.527650212955));
#221697=CARTESIAN_POINT('Ctrl Pts',(-247.104687303379,-0.876973364781528,
124.257222869343));
#221698=CARTESIAN_POINT('Ctrl Pts',(-247.383134927193,-5.98231793708558,
128.003295270889));
#221699=CARTESIAN_POINT('Ctrl Pts',(-247.661582551005,-5.59020457768662,
134.32340988638));
#221700=CARTESIAN_POINT('Ctrl Pts',(-247.940030174818,-0.0609663080697638,
137.409690138946));
#221701=CARTESIAN_POINT('Ctrl Pts',(-248.218477798631,5.524297020294,134.425995249648));
#221702=CARTESIAN_POINT('Ctrl Pts',(-248.496925422444,6.03300126391963,
128.114195060156));
#221703=CARTESIAN_POINT('Ctrl Pts',(-248.775373046256,0.997672074500306,
124.274525596028));
#221704=CARTESIAN_POINT('Ctrl Pts',(-249.05382067007,-4.95446901239483,
126.435455516518));
#221705=CARTESIAN_POINT('Ctrl Pts',(-249.332268293882,-6.35369511616563,
132.611195791991));
#221706=CARTESIAN_POINT('Ctrl Pts',(-249.610715917695,-1.91418580344349,
137.126542810973));
#221707=CARTESIAN_POINT('Ctrl Pts',(-249.889163541508,4.28436674946925,
135.832113249982));
#221708=CARTESIAN_POINT('Ctrl Pts',(-250.167611165321,6.54579556256923,
129.917424639176));
#221709=CARTESIAN_POINT('Ctrl Pts',(-250.446058789134,2.79195803356287,
124.817786863269));
#221710=CARTESIAN_POINT('Ctrl Pts',(-250.724506412947,-3.52755253356211,
125.219517907192));
#221711=CARTESIAN_POINT('Ctrl Pts',(-251.00295403676,-6.60541465285253,
130.75344656718));
#221712=CARTESIAN_POINT('Ctrl Pts',(-251.281401660573,-3.61322339864049,
136.334162752248));
#221713=CARTESIAN_POINT('Ctrl Pts',(-251.559849284386,2.6993436431913,136.83326092127));
#221714=CARTESIAN_POINT('Ctrl Pts',(-251.838296908198,6.53134574711249,
131.792094239578));
#221715=CARTESIAN_POINT('Ctrl Pts',(-252.116744532012,4.3613601835781,125.843248612281));
#221716=CARTESIAN_POINT('Ctrl Pts',(-252.395192155824,-1.81650232468185,
124.453422554885));
#221717=CARTESIAN_POINT('Ctrl Pts',(-252.673639779637,-6.32508793705065,
128.899798314935));
#221718=CARTESIAN_POINT('Ctrl Pts',(-252.95208740345,-5.02122673409033,
135.096373791053));
#221719=CARTESIAN_POINT('Ctrl Pts',(-253.230535027263,0.896896539007115,
137.348798831588));
#221720=CARTESIAN_POINT('Ctrl Pts',(-253.508982651076,5.99081570467794,
133.587204877683));
#221721=CARTESIAN_POINT('Ctrl Pts',(-253.787430274889,5.57946791275175,
127.26831297809));
#221722=CARTESIAN_POINT('Ctrl Pts',(-254.065877898701,0.0408616672245685,
124.198876151673));
#221723=CARTESIAN_POINT('Ctrl Pts',(-254.344325522515,-5.53529442795169,
127.199556781751));
#221724=CARTESIAN_POINT('Ctrl Pts',(-254.622773146327,-6.0247854077167,
133.512876168065));
#221725=CARTESIAN_POINT('Ctrl Pts',(-254.90122077014,-0.977792831057213,
137.337201825807));
#221726=CARTESIAN_POINT('Ctrl Pts',(-255.179668393953,4.96774341227684,
135.158166043599));
#221727=CARTESIAN_POINT('Ctrl Pts',(-255.458116017766,6.34816648213513,
128.97819485735));
#221728=CARTESIAN_POINT('Ctrl Pts',(-255.736563641579,1.89493404819936,
124.476382515012));
#221729=CARTESIAN_POINT('Ctrl Pts',(-256.015011265392,-4.29964901022966,
125.789669655819));
#221730=CARTESIAN_POINT('Ctrl Pts',(-256.293458889205,-6.54306693065544,
131.711218953762));
#221731=CARTESIAN_POINT('Ctrl Pts',(-256.571906513018,-2.77372173452912,
136.799398141047));
#221732=CARTESIAN_POINT('Ctrl Pts',(-256.85035413683,3.54453019961847,136.378452625405));
#221733=CARTESIAN_POINT('Ctrl Pts',(-257.128801760644,6.60554720661629,
130.835147498674));
#221734=CARTESIAN_POINT('Ctrl Pts',(-257.407249384456,3.5963603924579,125.263628838565));
#221735=CARTESIAN_POINT('Ctrl Pts',(-257.685697008269,-2.71765185753996,
124.783624522784));
#221736=CARTESIAN_POINT('Ctrl Pts',(-257.964144632082,-6.53437691572335,
129.836661023534));
#221737=CARTESIAN_POINT('Ctrl Pts',(-258.242592255895,-4.34613602341029,
135.778440351053));
#221738=CARTESIAN_POINT('Ctrl Pts',(-258.521039879708,1.83562753012831,
137.150276335207));
#221739=CARTESIAN_POINT('Ctrl Pts',(-258.799487503521,6.33122643152078,
132.688650362788));
#221740=CARTESIAN_POINT('Ctrl Pts',(-259.077935127334,5.00743946241547,
126.498999976245));
#221741=CARTESIAN_POINT('Ctrl Pts',(-259.356382751147,-0.915487258132909,
124.259032700089));
#221742=CARTESIAN_POINT('Ctrl Pts',(-259.634830374959,-6.00176822571329,
128.046924274587));
#221743=CARTESIAN_POINT('Ctrl Pts',(-259.86687006147,-5.63687269779404,
133.292521465648));
#221744=CARTESIAN_POINT('Ctrl Pts',(-260.052531023546,-2.79481741349804,
135.900547185714));
#221745=CARTESIAN_POINT('Ctrl Pts',(-260.145376111017,-0.946914048523564,
136.386386345067));
#221746=CARTESIAN_POINT('Ctrl Pts',(-260.191813261187,-0.0157913329746497,
136.389009763222));
#221747=CARTESIAN_POINT('Ctrl Pts',(210.190947297731,3.04870273111253,135.077142573452));
#221748=CARTESIAN_POINT('Ctrl Pts',(210.144529434129,3.76080111712433,134.569051946243));
#221749=CARTESIAN_POINT('Ctrl Pts',(210.051703633225,4.91317831978039,133.192256847685));
#221750=CARTESIAN_POINT('Ctrl Pts',(209.866061957716,5.67455722768035,129.648049455111));
#221751=CARTESIAN_POINT('Ctrl Pts',(209.634022271206,3.10293383059235,125.427666478792));
#221752=CARTESIAN_POINT('Ctrl Pts',(209.355574647392,-2.85596866243967,
125.28812524467));
#221753=CARTESIAN_POINT('Ctrl Pts',(209.07712702358,-6.17973736462657,130.225196103446));
#221754=CARTESIAN_POINT('Ctrl Pts',(208.798679399767,-3.83016968018938,
135.690661498217));
#221755=CARTESIAN_POINT('Ctrl Pts',(208.520231775954,2.04205955310628,136.667868212554));
#221756=CARTESIAN_POINT('Ctrl Pts',(208.241784152142,6.03618933210081,132.255733564264));
#221757=CARTESIAN_POINT('Ctrl Pts',(207.963336528328,4.48417485225333,126.510421532214));
#221758=CARTESIAN_POINT('Ctrl Pts',(207.684888904515,-1.18901089957204,
124.710731370568));
#221759=CARTESIAN_POINT('Ctrl Pts',(207.406441280703,-5.76932406256156,
128.510946815645));
#221760=CARTESIAN_POINT('Ctrl Pts',(207.12799365689,-5.04803188696711,134.418613818075));
#221761=CARTESIAN_POINT('Ctrl Pts',(206.849546033077,0.312219397189005,
137.005003016302));
#221762=CARTESIAN_POINT('Ctrl Pts',(206.571098409264,5.38552219392035,133.893281295751));
#221763=CARTESIAN_POINT('Ctrl Pts',(206.292650785451,5.50981125882569,127.943004805273));
#221764=CARTESIAN_POINT('Ctrl Pts',(206.014203161638,0.570843377758803,
124.622167937696));
#221765=CARTESIAN_POINT('Ctrl Pts',(205.735755537825,-4.89269661278007,
126.982467612715));
#221766=CARTESIAN_POINT('Ctrl Pts',(205.457307914013,-5.86009012142741,
132.854898402769));
#221767=CARTESIAN_POINT('Ctrl Pts',(205.178860290199,-1.44234566848361,
136.842986120511));
#221768=CARTESIAN_POINT('Ctrl Pts',(204.900412666387,4.30084323855829,135.281871486376));
#221769=CARTESIAN_POINT('Ctrl Pts',(204.621965042573,6.09176771588946,129.606143376667));
#221770=CARTESIAN_POINT('Ctrl Pts',(204.343517418761,2.28465505058828,125.031518229909));
#221771=CARTESIAN_POINT('Ctrl Pts',(204.065069794948,-3.62194388278553,
125.761853295313));
#221772=CARTESIAN_POINT('Ctrl Pts',(203.786622171135,-6.20015338889199,
131.126006208945));
#221773=CARTESIAN_POINT('Ctrl Pts',(203.508174547322,-3.08072479357708,
136.194582558939));
#221774=CARTESIAN_POINT('Ctrl Pts',(203.229726923509,2.86973936865286,136.309808260363));
#221775=CARTESIAN_POINT('Ctrl Pts',(202.951279299696,6.1830532544492,131.365796540178));
#221776=CARTESIAN_POINT('Ctrl Pts',(202.672831675884,3.81444325369211,125.905852631576));
#221777=CARTESIAN_POINT('Ctrl Pts',(202.39438405207,-2.05945374882828,124.947398258377));
#221778=CARTESIAN_POINT('Ctrl Pts',(202.115936428258,-6.04081336739099,
129.371206163854));
#221779=CARTESIAN_POINT('Ctrl Pts',(201.837488804444,-4.47096061076856,
135.112012999282));
#221780=CARTESIAN_POINT('Ctrl Pts',(201.559041180632,1.20748652821524,136.894297736177));
#221781=CARTESIAN_POINT('Ctrl Pts',(201.280593556819,5.77631253695961,133.08022777117));
#221782=CARTESIAN_POINT('Ctrl Pts',(201.002145933006,5.03698951269057,127.174747074221));
#221783=CARTESIAN_POINT('Ctrl Pts',(200.723698309193,-0.331080803069094,
124.604703907164));
#221784=CARTESIAN_POINT('Ctrl Pts',(200.44525068538,-5.39490403503349,127.731842386878));
#221785=CARTESIAN_POINT('Ctrl Pts',(200.166803061567,-5.50107401450091,
133.682475019745));
#221786=CARTESIAN_POINT('Ctrl Pts',(199.888355437754,-0.552025717056,136.988261120707));
#221787=CARTESIAN_POINT('Ctrl Pts',(199.609907813942,4.90430724641216,134.611344759621));
#221788=CARTESIAN_POINT('Ctrl Pts',(199.331460190128,5.85382143915379,128.735995953499));
#221789=CARTESIAN_POINT('Ctrl Pts',(199.053012566316,1.42395970438994,124.761373228423));
#221790=CARTESIAN_POINT('Ctrl Pts',(198.774564942502,-4.31445143441004,
126.339960697623));
#221791=CARTESIAN_POINT('Ctrl Pts',(198.49611731869,-6.088092477657,132.02111359519));
#221792=CARTESIAN_POINT('Ctrl Pts',(198.217669694877,-2.26707395378944,
136.584129948007));
#221793=CARTESIAN_POINT('Ctrl Pts',(197.939222071064,3.6372747808909,135.835820643578));
#221794=CARTESIAN_POINT('Ctrl Pts',(197.660774447251,6.19914568268399,130.46384537573));
#221795=CARTESIAN_POINT('Ctrl Pts',(197.382326823438,3.06430454719326,125.404786980035));
#221796=CARTESIAN_POINT('Ctrl Pts',(197.103879199626,-2.88648276756863,
125.307672973393));
#221797=CARTESIAN_POINT('Ctrl Pts',(196.825431575812,-6.1847334314575,130.261746383626));
#221798=CARTESIAN_POINT('Ctrl Pts',(196.546983952,-3.79951621286212,135.71445576667));
#221799=CARTESIAN_POINT('Ctrl Pts',(196.268536328187,2.07727078866752,136.65502757917));
#221800=CARTESIAN_POINT('Ctrl Pts',(195.990088704374,6.04514741573133,132.219122274927));
#221801=CARTESIAN_POINT('Ctrl Pts',(195.711641080561,4.45782888960729,126.483120122517));
#221802=CARTESIAN_POINT('Ctrl Pts',(195.433193456748,-1.22601660901765,
124.718126880723));
#221803=CARTESIAN_POINT('Ctrl Pts',(195.154745832935,-5.78321273819644,
128.54608511404));
#221804=CARTESIAN_POINT('Ctrl Pts',(194.876298209123,-5.02591888662151,
134.449288212205));
#221805=CARTESIAN_POINT('Ctrl Pts',(194.597850585309,0.349948891971121,
137.002980915508));
#221806=CARTESIAN_POINT('Ctrl Pts',(194.319402961497,5.40423073479611,133.860444384439));
#221807=CARTESIAN_POINT('Ctrl Pts',(194.040955337684,5.49228854369214,127.909516169605));
#221808=CARTESIAN_POINT('Ctrl Pts',(193.762507713871,0.533201494146887,
124.618808581434));
#221809=CARTESIAN_POINT('Ctrl Pts',(193.484060090058,-4.91587168017823,
127.012321133451));
#221810=CARTESIAN_POINT('Ctrl Pts',(193.205612466245,-5.84749893410212,
132.890532719942));
#221811=CARTESIAN_POINT('Ctrl Pts',(192.927164842432,-1.40556033379022,
136.851654059523));
#221812=CARTESIAN_POINT('Ctrl Pts',(192.648717218619,4.32801954783523,135.255608152653));
#221813=CARTESIAN_POINT('Ctrl Pts',(192.370269594806,6.08436090050943,129.569083216569));
#221814=CARTESIAN_POINT('Ctrl Pts',(192.091821970994,2.24947182316989,125.017717865345));
#221815=CARTESIAN_POINT('Ctrl Pts',(191.81337434718,-3.65257196685492,125.783994510198));
#221816=CARTESIAN_POINT('Ctrl Pts',(191.534926723368,-6.19808055740059,
131.163742349203));
#221817=CARTESIAN_POINT('Ctrl Pts',(191.256479099555,-3.04785590876364,
136.213235933607));
#221818=CARTESIAN_POINT('Ctrl Pts',(190.978031475742,2.90319942398833,136.292237340818));
#221819=CARTESIAN_POINT('Ctrl Pts',(190.699583851929,6.18635631527163,131.328148137043));
#221820=CARTESIAN_POINT('Ctrl Pts',(190.421136228116,3.7845539731278,125.882723791311));
#221821=CARTESIAN_POINT('Ctrl Pts',(190.142688604304,-2.09506858458051,
124.960043253581));
#221822=CARTESIAN_POINT('Ctrl Pts',(189.86424098049,-6.04942546284962,129.408004862578));
#221823=CARTESIAN_POINT('Ctrl Pts',(189.585793356678,-4.44465587162338,
135.139149194637));
#221824=CARTESIAN_POINT('Ctrl Pts',(189.307345732864,1.24453533211424,136.886834590562));
#221825=CARTESIAN_POINT('Ctrl Pts',(189.028898109051,5.79005936456987,133.045023550676));
#221826=CARTESIAN_POINT('Ctrl Pts',(188.750450485239,5.01480170111087,127.144152737732));
#221827=CARTESIAN_POINT('Ctrl Pts',(188.472002861426,-0.368813738986236,
124.606834155258));
#221828=CARTESIAN_POINT('Ctrl Pts',(188.193555237613,-5.41350737050784,
127.764739625646));
#221829=CARTESIAN_POINT('Ctrl Pts',(187.9151076138,-5.48345219307025,133.715908293866));
#221830=CARTESIAN_POINT('Ctrl Pts',(187.636659989987,-0.51437233173317,
136.991506884579));
#221831=CARTESIAN_POINT('Ctrl Pts',(187.358212366174,4.92739057398128,134.581420314804));
#221832=CARTESIAN_POINT('Ctrl Pts',(187.079764742362,5.84112225861874,128.700400402891));
#221833=CARTESIAN_POINT('Ctrl Pts',(186.801317118548,1.38714794227173,124.752817144095));
#221834=CARTESIAN_POINT('Ctrl Pts',(186.522869494736,-4.34154756707868,
126.366306703083));
#221835=CARTESIAN_POINT('Ctrl Pts',(186.244421870923,-6.08057295867359,
132.058150998494));
#221836=CARTESIAN_POINT('Ctrl Pts',(185.96597424711,-2.23184885375068,136.597823184897));
#221837=CARTESIAN_POINT('Ctrl Pts',(185.687526623297,3.66783531589119,135.813586298303));
#221838=CARTESIAN_POINT('Ctrl Pts',(185.409078999484,6.19695801394562,130.42611572539));
#221839=CARTESIAN_POINT('Ctrl Pts',(185.130631375671,3.03137903541329,125.386233730096));
#221840=CARTESIAN_POINT('Ctrl Pts',(184.852183751858,-2.9198891855651,125.325345654173));
#221841=CARTESIAN_POINT('Ctrl Pts',(184.573736128045,-6.18792188952598,
130.299404664846));
#221842=CARTESIAN_POINT('Ctrl Pts',(184.295288504232,-3.76955667380246,
135.737493527599));
#221843=CARTESIAN_POINT('Ctrl Pts',(184.01684088042,2.11284697206427,136.642274242971));
#221844=CARTESIAN_POINT('Ctrl Pts',(183.738393256607,6.05364746891681,132.182297534532));
#221845=CARTESIAN_POINT('Ctrl Pts',(183.459945632794,4.43144167895468,126.456064115361));
#221846=CARTESIAN_POINT('Ctrl Pts',(183.181498008981,-1.2630425260055,124.725702755623));
#221847=CARTESIAN_POINT('Ctrl Pts',(182.903050385168,-5.79685235262429,
128.581331012064));
#221848=CARTESIAN_POINT('Ctrl Pts',(182.624602761355,-5.00363805916239,
134.479814874928));
#221849=CARTESIAN_POINT('Ctrl Pts',(182.346155137542,0.387675169361259,
137.000735831198));
#221850=CARTESIAN_POINT('Ctrl Pts',(182.06770751373,5.42273385622678,133.827490675898));
#221851=CARTESIAN_POINT('Ctrl Pts',(181.789259889916,5.47456504449634,127.876136685104));
#221852=CARTESIAN_POINT('Ctrl Pts',(181.510812266103,0.495538404244469,
124.615677436551));
#221853=CARTESIAN_POINT('Ctrl Pts',(181.232364642291,-4.93886382111119,
127.042315697369));
#221854=CARTESIAN_POINT('Ctrl Pts',(180.953917018477,-5.83469147177671,
132.926089453735));
#221855=CARTESIAN_POINT('Ctrl Pts',(180.675469394665,-1.36872270040423,
136.860098061879));
#221856=CARTESIAN_POINT('Ctrl Pts',(180.397021770852,4.35503536681857,135.229179797918));
#221857=CARTESIAN_POINT('Ctrl Pts',(180.118574147039,6.07672868724052,129.532068871648));
#221858=CARTESIAN_POINT('Ctrl Pts',(179.840126523226,2.21420520878857,125.004131904969));
#221859=CARTESIAN_POINT('Ctrl Pts',(179.561678899413,-3.68306468660213,
125.80632176824));
#221860=CARTESIAN_POINT('Ctrl Pts',(179.2832312756,-6.19577806271818,131.20146516627));
#221861=CARTESIAN_POINT('Ctrl Pts',(179.004783651788,-3.01487407978163,
136.231688883676));
#221862=CARTESIAN_POINT('Ctrl Pts',(178.726336027974,2.93655189768736,136.274463064253));
#221863=CARTESIAN_POINT('Ctrl Pts',(178.447888404162,6.18943013971724,131.290480325685));
#221864=CARTESIAN_POINT('Ctrl Pts',(178.169440780348,3.75452445381909,125.859777323623));
#221865=CARTESIAN_POINT('Ctrl Pts',(177.890993156536,-2.13060578642238,
124.972904812372));
#221866=CARTESIAN_POINT('Ctrl Pts',(177.612545532723,-6.05781339482078,
129.44485530364));
#221867=CARTESIAN_POINT('Ctrl Pts',(177.33409790891,-4.41818643401566,135.166124762878));
#221868=CARTESIAN_POINT('Ctrl Pts',(177.055650285097,1.28153801924328,136.879146056599));
#221869=CARTESIAN_POINT('Ctrl Pts',(176.777202661284,5.80359163943039,133.009736301615));
#221870=CARTESIAN_POINT('Ctrl Pts',(176.498755037472,4.99242806419446,127.113694031581));
#221871=CARTESIAN_POINT('Ctrl Pts',(176.220307413658,-0.406533008366379,
124.60919405498));
#221872=CARTESIAN_POINT('Ctrl Pts',(175.941859789846,-5.43191010648008,
127.797749498684));
#221873=CARTESIAN_POINT('Ctrl Pts',(175.663412166033,-5.46562718029972,
133.749233679521));
#221874=CARTESIAN_POINT('Ctrl Pts',(175.38496454222,-0.476699886155768,
136.994523381468));
#221875=CARTESIAN_POINT('Ctrl Pts',(175.106516918407,4.95029131528126,134.551355909651));
#221876=CARTESIAN_POINT('Ctrl Pts',(174.828069294595,5.82820663315002,128.664882815304));
#221877=CARTESIAN_POINT('Ctrl Pts',(174.549621670781,1.35028477887665,124.744485301934));
#221878=CARTESIAN_POINT('Ctrl Pts',(174.271174046969,-4.36848282210566,
126.392817162263));
#221879=CARTESIAN_POINT('Ctrl Pts',(173.992726423155,-6.07282812182305,
132.095141942134));
#221880=CARTESIAN_POINT('Ctrl Pts',(173.714278799343,-2.19654105173196,
136.611301742902));
#221881=CARTESIAN_POINT('Ctrl Pts',(173.435831175529,3.69825993790488,135.791166334329));
#221882=CARTESIAN_POINT('Ctrl Pts',(173.157383551717,6.19454071464915,130.388400091055));
#221883=CARTESIAN_POINT('Ctrl Pts',(172.878935927904,2.99834119476844,125.367881250842));
#221884=CARTESIAN_POINT('Ctrl Pts',(172.600488304091,-2.95318740599396,
125.343221361866));
#221885=CARTESIAN_POINT('Ctrl Pts',(172.322040680278,-6.1908810518732,130.337081657394));
#221886=CARTESIAN_POINT('Ctrl Pts',(172.043593056465,-3.7394574524341,135.760348489473));
#221887=CARTESIAN_POINT('Ctrl Pts',(171.765145432652,2.14834486313941,136.629304580736));
#221888=CARTESIAN_POINT('Ctrl Pts',(171.486697808839,6.06192320196904,132.145421734178));
#221889=CARTESIAN_POINT('Ctrl Pts',(171.208250185027,4.40489025960108,126.42916923593));
#221890=CARTESIAN_POINT('Ctrl Pts',(170.929802561213,-1.30002164048796,
124.733503877423));
#221891=CARTESIAN_POINT('Ctrl Pts',(170.651354937401,-5.81027716255637,
128.616659285268));
#221892=CARTESIAN_POINT('Ctrl Pts',(170.372907313588,-4.98117182005496,
134.510205342342));
#221893=CARTESIAN_POINT('Ctrl Pts',(170.094459689775,0.42538708130529,136.998261137926));
#221894=CARTESIAN_POINT('Ctrl Pts',(169.816012065962,5.44103603626017,133.794424944161));
#221895=CARTESIAN_POINT('Ctrl Pts',(169.537564442149,5.45663868327959,127.842865707018));
#221896=CARTESIAN_POINT('Ctrl Pts',(169.259116818336,0.457856951984399,
124.612775615598));
#221897=CARTESIAN_POINT('Ctrl Pts',(168.980669194523,-4.9616729506289,127.072449665244));
#221898=CARTESIAN_POINT('Ctrl Pts',(168.702221570711,-5.82166780281318,
132.961567566087));
#221899=CARTESIAN_POINT('Ctrl Pts',(168.423773946897,-1.33183434849535,
136.868317666657));
#221900=CARTESIAN_POINT('Ctrl Pts',(168.145326323085,4.38188980836473,135.202587479883));
#221901=CARTESIAN_POINT('Ctrl Pts',(167.866878699272,6.06887129855542,129.495101671966));
#221902=CARTESIAN_POINT('Ctrl Pts',(167.588431075459,2.17885654621902,124.9907608742));
#221903=CARTESIAN_POINT('Ctrl Pts',(167.309983451646,-3.71342092903282,
125.82883423045));
#221904=CARTESIAN_POINT('Ctrl Pts',(167.031535827833,-6.19324598120115,
131.239173268482));
#221905=CARTESIAN_POINT('Ctrl Pts',(166.75308820402,-2.98178053353198,136.249940722101));
#221906=CARTESIAN_POINT('Ctrl Pts',(166.474640580207,2.96979555637586,136.25648609103));
#221907=CARTESIAN_POINT('Ctrl Pts',(166.196192956395,6.19227461255283,131.252794500981));
#221908=CARTESIAN_POINT('Ctrl Pts',(165.917745332582,3.7243558092261,125.837014079288));
#221909=CARTESIAN_POINT('Ctrl Pts',(165.639297708769,-2.16606403788322,
124.985982457902));
#221910=CARTESIAN_POINT('Ctrl Pts',(165.360850084956,-6.06597685228888,
129.481756121673));
#221911=CARTESIAN_POINT('Ctrl Pts',(165.082402461143,-4.39155327888481,
135.192938704347));
#221912=CARTESIAN_POINT('Ctrl Pts',(164.80395483733,1.31849321850979,136.871232419228));
#221913=CARTESIAN_POINT('Ctrl Pts',(164.525507213517,5.81690886006848,132.974367331546));
#221914=CARTESIAN_POINT('Ctrl Pts',(164.247059589704,4.96986943102014,127.083372084437));
#221915=CARTESIAN_POINT('Ctrl Pts',(163.968611965891,-0.444237213516358,
124.611783518878));
#221916=CARTESIAN_POINT('Ctrl Pts',(163.690164342078,-5.45011156102575,
127.830870782803));
#221917=CARTESIAN_POINT('Ctrl Pts',(163.411716718265,-5.44759963670407,
133.782449941821));
#221918=CARTESIAN_POINT('Ctrl Pts',(163.133269094453,-0.439009776288703,
136.9973104996));
#221919=CARTESIAN_POINT('Ctrl Pts',(162.85482147064,4.97300862171615,134.52115265821));
#221920=CARTESIAN_POINT('Ctrl Pts',(162.576373846827,5.81507504134112,128.629444506854));
#221921=CARTESIAN_POINT('Ctrl Pts',(162.297926223014,1.31337158018249,124.736378010682));
#221922=CARTESIAN_POINT('Ctrl Pts',(162.019478599201,-4.39525620139515,
126.419491092807));
#221923=CARTESIAN_POINT('Ctrl Pts',(161.741030975388,-6.06485825409316,
132.132085055398));
#221924=CARTESIAN_POINT('Ctrl Pts',(161.462583351575,-2.16115185607673,
136.624565122567));
#221925=CARTESIAN_POINT('Ctrl Pts',(161.184135727762,3.72854751953661,135.768561582436));
#221926=CARTESIAN_POINT('Ctrl Pts',(160.905688103949,6.19189387436843,130.350699870288));
#221927=CARTESIAN_POINT('Ctrl Pts',(160.627240480137,2.96519224948793,125.349730222329));
#221928=CARTESIAN_POINT('Ctrl Pts',(160.348792856324,-2.9863761949775,125.361299434083));
#221929=CARTESIAN_POINT('Ctrl Pts',(160.070345232511,-6.19361080884636,
130.374775965136));
#221930=CARTESIAN_POINT('Ctrl Pts',(159.791897608698,-3.70921966409463,
135.783019805394));
#221931=CARTESIAN_POINT('Ctrl Pts',(159.513449984885,2.18376314650564,136.616119073061));
#221932=CARTESIAN_POINT('Ctrl Pts',(159.235002361072,6.06997430822783,132.108496240312));
#221933=CARTESIAN_POINT('Ctrl Pts',(158.956554737259,4.37817561541891,126.402436480826));
#221934=CARTESIAN_POINT('Ctrl Pts',(158.678107113446,-1.3369525821905,124.741529957054));
#221935=CARTESIAN_POINT('Ctrl Pts',(158.399659489633,-5.82348667053154,
128.652068624549));
#221936=CARTESIAN_POINT('Ctrl Pts',(158.121211865821,-4.95852100179383,
134.540458488317));
#221937=CARTESIAN_POINT('Ctrl Pts',(157.842764242008,0.463083230374652,
136.995556927392));
#221938=CARTESIAN_POINT('Ctrl Pts',(157.564316618195,5.45913659670229,133.761248414491));
#221939=CARTESIAN_POINT('Ctrl Pts',(157.285868994382,5.43851012430973,127.809704468215));
#221940=CARTESIAN_POINT('Ctrl Pts',(157.007421370569,0.420158533666468,
124.610103226106));
#221941=CARTESIAN_POINT('Ctrl Pts',(156.728973746756,-4.98429822353081,
127.102721920452));
#221942=CARTESIAN_POINT('Ctrl Pts',(156.450526122943,-5.80842840980828,
132.996965742341));
#221943=CARTESIAN_POINT('Ctrl Pts',(156.172078499131,-1.2948966449748,136.876312569277));
#221944=CARTESIAN_POINT('Ctrl Pts',(155.893630875317,4.40858187737264,135.175832183934));
#221945=CARTESIAN_POINT('Ctrl Pts',(155.615183251505,6.06078902561252,129.458182987356));
#221946=CARTESIAN_POINT('Ctrl Pts',(155.336735627692,2.14342714531882,124.977605268507));
#221947=CARTESIAN_POINT('Ctrl Pts',(155.058288003879,-3.74363956928552,
125.85153106262));
#221948=CARTESIAN_POINT('Ctrl Pts',(154.779840380066,-6.19048440667673,
131.276865258552));
#221949=CARTESIAN_POINT('Ctrl Pts',(154.501392756253,-2.94857649630798,
136.267990772552));
#221950=CARTESIAN_POINT('Ctrl Pts',(154.22294513244,3.00292916819795,136.238307087292));
#221951=CARTESIAN_POINT('Ctrl Pts',(153.944497508627,6.19488962837548,131.215092059396));
#221952=CARTESIAN_POINT('Ctrl Pts',(153.666049884815,3.69404915725887,125.814434901805));
#221953=CARTESIAN_POINT('Ctrl Pts',(153.387602261001,-2.20144202504465,
124.999275705575));
#221954=CARTESIAN_POINT('Ctrl Pts',(153.109154637189,-6.07391553275397,
129.518705949301));
#221955=CARTESIAN_POINT('Ctrl Pts',(152.830707013376,-4.36475739313218,
135.219590025439));
#221956=CARTESIAN_POINT('Ctrl Pts',(152.552259389563,1.3553995605252,136.863093971691));
#221957=CARTESIAN_POINT('Ctrl Pts',(152.27381176575,5.83001053300956,132.93891795108));
#221958=CARTESIAN_POINT('Ctrl Pts',(151.995364141937,4.94712663750637,127.053188019893));
#221959=CARTESIAN_POINT('Ctrl Pts',(151.716916518124,-0.481924957293099,
124.614602450997));
#221960=CARTESIAN_POINT('Ctrl Pts',(151.438468894311,-5.46811105968323,
127.864102250682));
#221961=CARTESIAN_POINT('Ctrl Pts',(151.160021270498,-5.4293702303005,133.815555849925));
#221962=CARTESIAN_POINT('Ctrl Pts',(150.881573646685,-0.40130339875292,
136.999868135696));
#221963=CARTESIAN_POINT('Ctrl Pts',(150.603126022873,4.99554165148768,134.490811679673));
#221964=CARTESIAN_POINT('Ctrl Pts',(150.324678399059,5.80172796978809,128.59408679072));
#221965=CARTESIAN_POINT('Ctrl Pts',(150.046230775247,1.27640971402146,124.728495570759));
#221966=CARTESIAN_POINT('Ctrl Pts',(149.767783151434,-4.42186671284978,
126.446327506304));
#221967=CARTESIAN_POINT('Ctrl Pts',(149.489335527621,-6.05666365081033,
132.168978969345));
#221968=CARTESIAN_POINT('Ctrl Pts',(149.210887903808,-2.12568257814469,
136.637612832414));
#221969=CARTESIAN_POINT('Ctrl Pts',(148.932440279995,3.75869693846883,135.74577288025));
#221970=CARTESIAN_POINT('Ctrl Pts',(148.653992656183,6.18901759118317,130.313016460088));
#221971=CARTESIAN_POINT('Ctrl Pts',(148.375545032369,2.93193342791814,125.331781317152));
#221972=CARTESIAN_POINT('Ctrl Pts',(148.097097408557,-3.01945432269288,
125.379579200934));
#221973=CARTESIAN_POINT('Ctrl Pts',(147.818649784743,-6.19611105929333,
130.412486191295));
#221974=CARTESIAN_POINT('Ctrl Pts',(147.540202160931,-3.67884442925635,
135.805506635269));
#221975=CARTESIAN_POINT('Ctrl Pts',(147.261754537118,2.21910050972548,136.602718208539));
#221976=CARTESIAN_POINT('Ctrl Pts',(146.983306913305,6.07780048935632,132.071522421221));
#221977=CARTESIAN_POINT('Ctrl Pts',(146.704859289492,4.35129873632927,126.375866840638));
#221978=CARTESIAN_POINT('Ctrl Pts',(146.426411665679,-1.37383398262348,
124.749780697104));
#221979=CARTESIAN_POINT('Ctrl Pts',(146.147964041867,-5.83648038706648,
128.687557717801));
#221980=CARTESIAN_POINT('Ctrl Pts',(145.869516418053,-4.93568644371351,
134.570573191811));
#221981=CARTESIAN_POINT('Ctrl Pts',(145.591068794241,0.500762219724632,
136.992623299802));
#221982=CARTESIAN_POINT('Ctrl Pts',(145.312621170428,5.47703486683029,133.727962316256));
#221983=CARTESIAN_POINT('Ctrl Pts',(145.034173546615,5.42018003934715,127.776654197497));
#221984=CARTESIAN_POINT('Ctrl Pts',(144.755725922802,0.382444546219556,
124.607660367099));
#221985=CARTESIAN_POINT('Ctrl Pts',(144.477278298989,-5.00673880142907,
127.133131341243));
#221986=CARTESIAN_POINT('Ctrl Pts',(144.198830675176,-5.79497378335261,
133.032282670807));
#221987=CARTESIAN_POINT('Ctrl Pts',(143.920383051363,-1.25791095858285,
136.884082473484));
#221988=CARTESIAN_POINT('Ctrl Pts',(143.64193542755,4.43511058475782,135.148914901497));
#221989=CARTESIAN_POINT('Ctrl Pts',(143.363487803737,6.05248216790344,129.421314185853));
#221990=CARTESIAN_POINT('Ctrl Pts',(143.085040179924,2.10791831893749,124.964665575378));
#221991=CARTESIAN_POINT('Ctrl Pts',(142.806592556112,-3.77371948759721,
125.87441142371));
#221992=CARTESIAN_POINT('Ctrl Pts',(142.528144932299,-6.18749344147606,
131.314539739788));
#221993=CARTESIAN_POINT('Ctrl Pts',(142.249697308486,-2.91526319849757,
136.285838366179));
#221994=CARTESIAN_POINT('Ctrl Pts',(141.971249684673,3.03595150537554,136.219926726669));
#221995=CARTESIAN_POINT('Ctrl Pts',(141.69280206086,6.19727509028471,131.177374398005));
#221996=CARTESIAN_POINT('Ctrl Pts',(141.414354437047,3.6636056209416,125.792040627854));
#221997=CARTESIAN_POINT('Ctrl Pts',(141.135906813234,-2.23673843696229,
125.012784062803));
#221998=CARTESIAN_POINT('Ctrl Pts',(140.857459189421,-6.0816291420453,129.555703417335));
#221999=CARTESIAN_POINT('Ctrl Pts',(140.579011565609,-4.33779976968917,
135.246077738584));
#222000=CARTESIAN_POINT('Ctrl Pts',(140.300563941795,1.39225567771152,136.854731015561));
#222001=CARTESIAN_POINT('Ctrl Pts',(140.022116317983,5.84289617276637,132.903389473806));
#222002=CARTESIAN_POINT('Ctrl Pts',(139.74366869417,4.92420052639575,127.023142956427));
#222003=CARTESIAN_POINT('Ctrl Pts',(139.465221070357,-0.519594843163371,
124.617650746882));
#222004=CARTESIAN_POINT('Ctrl Pts',(139.186773446544,-5.48590793547459,
127.897442670915));
#222005=CARTESIAN_POINT('Ctrl Pts',(138.908325822731,-5.41093963658633,
133.848550177083));
#222006=CARTESIAN_POINT('Ctrl Pts',(138.629878198918,-0.363582150772119,
137.002196194983));
#222007=CARTESIAN_POINT('Ctrl Pts',(138.351430575105,5.0178895696262,134.460334098336));
#222008=CARTESIAN_POINT('Ctrl Pts',(138.072982951292,5.78816591307159,128.558810977095));
#222009=CARTESIAN_POINT('Ctrl Pts',(137.79453532748,1.23940055002892,124.720838274248));
#222010=CARTESIAN_POINT('Ctrl Pts',(137.516087703667,-4.44831337040726,
126.473325408321));
#222011=CARTESIAN_POINT('Ctrl Pts',(137.237640079854,-6.0482446156285,132.205822316857));
#222012=CARTESIAN_POINT('Ctrl Pts',(136.959192456041,-2.09013453226308,
136.650444388955));
#222013=CARTESIAN_POINT('Ctrl Pts',(136.680744832228,3.78870707750376,135.722801072215));
#222014=CARTESIAN_POINT('Ctrl Pts',(136.402297208415,6.18591197167502,130.275351256826));
#222015=CARTESIAN_POINT('Ctrl Pts',(136.123849584602,2.89856596247695,125.314035200413));
#222016=CARTESIAN_POINT('Ctrl Pts',(135.845401960789,-3.05242056341787,
125.398059985055));
#222017=CARTESIAN_POINT('Ctrl Pts',(135.566954336976,-6.19838171056633,
130.450210938505));
#222018=CARTESIAN_POINT('Ctrl Pts',(135.288506713164,-3.64833287348497,
135.827808145838));
#222019=CARTESIAN_POINT('Ctrl Pts',(135.01005908935,2.25435564335981,136.589102483743));
#222020=CARTESIAN_POINT('Ctrl Pts',(134.731611465538,6.08540145535266,132.034501646982));
#222021=CARTESIAN_POINT('Ctrl Pts',(134.453163841725,4.32426061826468,126.349461299917));
#222022=CARTESIAN_POINT('Ctrl Pts',(134.174716217912,-1.41066447513297,
124.75825579184));
#222023=CARTESIAN_POINT('Ctrl Pts',(133.896268594099,-5.84925783067434,
128.723125249964));
#222024=CARTESIAN_POINT('Ctrl Pts',(133.617820970286,-4.91266899195694,
134.600548336913));
#222025=CARTESIAN_POINT('Ctrl Pts',(133.339373346473,0.538422653146471,
136.989460363863));
#222026=CARTESIAN_POINT('Ctrl Pts',(133.06092572266,5.49473018341705,133.694567882885));
#222027=CARTESIAN_POINT('Ctrl Pts',(132.782478098847,5.40164910761999,127.743716119554));
#222028=CARTESIAN_POINT('Ctrl Pts',(132.504030475035,0.344716387149417,
124.605447129098));
#222029=CARTESIAN_POINT('Ctrl Pts',(132.225582851222,-5.02899385277987,
127.163676800786));
#222030=CARTESIAN_POINT('Ctrl Pts',(131.947135227409,-5.78130442201224,
133.067517042801));
#222031=CARTESIAN_POINT('Ctrl Pts',(131.668687603596,-1.22087865983776,
136.891627091362));
#222032=CARTESIAN_POINT('Ctrl Pts',(131.390239979783,4.46147494748924,135.121836630005));
#222033=CARTESIAN_POINT('Ctrl Pts',(131.11179235597,6.04395103324181,129.384496633644));
#222034=CARTESIAN_POINT('Ctrl Pts',(130.833344732157,2.07233138286776,124.951942274296));
#222035=CARTESIAN_POINT('Ctrl Pts',(130.554897108344,-3.80365956934553,
125.897474465882));
#222036=CARTESIAN_POINT('Ctrl Pts',(130.276449484532,-6.18427319643048,
131.35219531615));
#222037=CARTESIAN_POINT('Ctrl Pts',(129.998001860718,-2.88184187453723,
136.303482841632));
#222038=CARTESIAN_POINT('Ctrl Pts',(129.719554236906,3.0688613442533,136.201345690253));
#222039=CARTESIAN_POINT('Ctrl Pts',(129.441106613093,6.1994309098865,131.139642914452));
#222040=CARTESIAN_POINT('Ctrl Pts',(129.16265898928,3.63302632837089,125.769832087263));
#222041=CARTESIAN_POINT('Ctrl Pts',(128.884211365467,-2.27195196571463,
125.026507029031));
#222042=CARTESIAN_POINT('Ctrl Pts',(128.605763741654,-6.08911739433215,
129.592747154821));
#222043=CARTESIAN_POINT('Ctrl Pts',(128.327316117841,-4.31068140748063,
135.272400862266));
#222044=CARTESIAN_POINT('Ctrl Pts',(128.048868494028,1.42906020435147,136.846143860731));
#222045=CARTESIAN_POINT('Ctrl Pts',(127.770420870216,5.85556530185681,132.867783216248));
#222046=CARTESIAN_POINT('Ctrl Pts',(127.491973246402,4.9010919472237,126.993238007373));
#222047=CARTESIAN_POINT('Ctrl Pts',(127.21352562259,-0.557245475255655,
124.620928293575));
#222048=CARTESIAN_POINT('Ctrl Pts',(126.935077998777,-5.50350152892981,
127.930890808061));
#222049=CARTESIAN_POINT('Ctrl Pts',(126.656630374964,-5.39230853851415,
133.881431700678));
#222050=CARTESIAN_POINT('Ctrl Pts',(126.378182751151,-0.325847430121078,
137.004294591193));
#222051=CARTESIAN_POINT('Ctrl Pts',(126.099735127338,5.04005154802147,134.429721043558));
#222052=CARTESIAN_POINT('Ctrl Pts',(125.821287503525,5.77438937373851,128.523618373138));
#222053=CARTESIAN_POINT('Ctrl Pts',(125.542839879712,1.20234545959337,124.713406404895));
#222054=CARTESIAN_POINT('Ctrl Pts',(125.264392255899,-4.47459519407686,
126.50048379844));
#222055=CARTESIAN_POINT('Ctrl Pts',(124.985944632086,-6.03960146051831,
132.24261373269));
#222056=CARTESIAN_POINT('Ctrl Pts',(124.707497008274,-2.05450903567761,
136.663059316712));
#222057=CARTESIAN_POINT('Ctrl Pts',(124.429049384461,3.81857682460466,135.69964700956));
#222058=CARTESIAN_POINT('Ctrl Pts',(124.150601760648,6.18257713092382,130.237705656202));
#222059=CARTESIAN_POINT('Ctrl Pts',(123.872154136835,2.86509108960817,125.296492529702));
#222060=CARTESIAN_POINT('Ctrl Pts',(123.593706513022,-3.08527369557641,
125.416741101634));
#222061=CARTESIAN_POINT('Ctrl Pts',(123.315258889209,-6.20042267852561,
130.487948808862));
#222062=CARTESIAN_POINT('Ctrl Pts',(123.036811265396,-3.61768612739718,
135.849923510712));
#222063=CARTESIAN_POINT('Ctrl Pts',(122.758363641583,2.28952724101679,136.575272403211));
#222064=CARTESIAN_POINT('Ctrl Pts',(122.47991601777,6.09277692456002,131.997435289415));
#222065=CARTESIAN_POINT('Ctrl Pts',(122.201468393958,4.29706226313277,126.323220837128));
#222066=CARTESIAN_POINT('Ctrl Pts',(121.923020770144,-1.44744269495155,
124.766954927214));
#222067=CARTESIAN_POINT('Ctrl Pts',(121.644573146332,-5.86181852788225,
128.758769903068));
#222068=CARTESIAN_POINT('Ctrl Pts',(121.366125522519,-4.88946949944416,
134.630382812884));
#222069=CARTESIAN_POINT('Ctrl Pts',(121.087677898706,0.576063135118759,
136.986068236777));
#222070=CARTESIAN_POINT('Ctrl Pts',(120.809230274893,5.51222189075617,133.661066351821));
#222071=CARTESIAN_POINT('Ctrl Pts',(120.53078265108,5.38291801579874,127.710891454918));
#222072=CARTESIAN_POINT('Ctrl Pts',(120.252335027267,0.306975454486648,
124.603463594118));
#222073=CARTESIAN_POINT('Ctrl Pts',(119.973887403454,-5.05106255291402,
127.194357167205));
#222074=CARTESIAN_POINT('Ctrl Pts',(119.695439779642,-5.76742083231046,
133.102667552701));
#222075=CARTESIAN_POINT('Ctrl Pts',(119.416992155829,-1.18380112098488,
136.898946143343));
#222076=CARTESIAN_POINT('Ctrl Pts',(119.138544532016,4.48767398862585,135.09459837285));
#222077=CARTESIAN_POINT('Ctrl Pts',(118.860096908203,6.03519593775195,129.347731695017));
#222078=CARTESIAN_POINT('Ctrl Pts',(118.58164928439,2.0366676557964,124.939435836727));
#222079=CARTESIAN_POINT('Ctrl Pts',(118.303201660577,-3.83345870508974,
125.920719334523));
#222080=CARTESIAN_POINT('Ctrl Pts',(118.024754036764,-6.18082379086727,
131.389830592295));
#222081=CARTESIAN_POINT('Ctrl Pts',(117.746306412951,-2.84831376286653,
136.320923545089));
#222082=CARTESIAN_POINT('Ctrl Pts',(117.467858789138,3.10165746534553,136.18256466657));
#222083=CARTESIAN_POINT('Ctrl Pts',(117.189411165326,6.20135700729606,131.101899006891));
#222084=CARTESIAN_POINT('Ctrl Pts',(116.910963541513,3.60231241267338,125.747810102979));
#222085=CARTESIAN_POINT('Ctrl Pts',(116.6325159177,-2.30708130645123,125.040444095748));
#222086=CARTESIAN_POINT('Ctrl Pts',(116.354068293887,-6.09638001213474,
129.62983578909));
#222087=CARTESIAN_POINT('Ctrl Pts',(116.075620670074,-4.28340331138726,
135.298558421074));
#222088=CARTESIAN_POINT('Ctrl Pts',(115.797173046261,1.46581177664024,136.837332825402));
#222089=CARTESIAN_POINT('Ctrl Pts',(115.518725422448,5.86801745082159,132.832100497806));
#222090=CARTESIAN_POINT('Ctrl Pts',(115.240277798635,4.87780175628715,126.963474280869));
#222091=CARTESIAN_POINT('Ctrl Pts',(114.961830174822,-0.594875458411799,
124.624434969628));
#222092=CARTESIAN_POINT('Ctrl Pts',(114.68338255101,-5.52089118811201,127.964445422689));
#222093=CARTESIAN_POINT('Ctrl Pts',(114.404934927196,-5.37347762646609,
133.914199202272));
#222094=CARTESIAN_POINT('Ctrl Pts',(114.126487303384,-0.288100635073559,
137.006163246571));
#222095=CARTESIAN_POINT('Ctrl Pts',(113.848039679571,5.06202676545313,134.398973649715));
#222096=CARTESIAN_POINT('Ctrl Pts',(113.569592055758,5.76039886228364,128.488510282924));
#222097=CARTESIAN_POINT('Ctrl Pts',(113.291144431945,1.16524581580469,124.706200238089));
#222098=CARTESIAN_POINT('Ctrl Pts',(113.012696808132,-4.50071120997606,
126.527801670297));
#222099=CARTESIAN_POINT('Ctrl Pts',(112.734249184319,-6.03073450575487,
132.279351853526));
#222100=CARTESIAN_POINT('Ctrl Pts',(112.455801560506,-2.01880740850426,
136.675457148234));
#222101=CARTESIAN_POINT('Ctrl Pts',(112.177353936694,3.84830507293705,135.676311550269));
#222102=CARTESIAN_POINT('Ctrl Pts',(111.898906312881,6.17901319250346,130.200081053184));
#222103=CARTESIAN_POINT('Ctrl Pts',(111.620458689068,2.8315100497353,125.279153955068));
#222104=CARTESIAN_POINT('Ctrl Pts',(111.342011065255,-3.11801250178361,
125.435621858436));
#222105=CARTESIAN_POINT('Ctrl Pts',(111.063563441442,-6.20223388754234,
130.525698403974));
#222106=CARTESIAN_POINT('Ctrl Pts',(110.785115817629,-3.58690532661952,
135.871851910398));
#222107=CARTESIAN_POINT('Ctrl Pts',(110.506668193816,2.32461399939974,136.56122847942));
#222108=CARTESIAN_POINT('Ctrl Pts',(110.228220570003,6.09992662367788,131.960324722029));
#222109=CARTESIAN_POINT('Ctrl Pts',(109.94977294619,4.26970467877848,126.297146424621));
#222110=CARTESIAN_POINT('Ctrl Pts',(109.671325322378,-1.48416727924886,
124.775877780875));
#222111=CARTESIAN_POINT('Ctrl Pts',(109.392877698565,-5.8741620132489,128.794490356288));
#222112=CARTESIAN_POINT('Ctrl Pts',(109.114430074752,-4.86608882584101,
134.660075514194));
#222113=CARTESIAN_POINT('Ctrl Pts',(108.835982450939,0.61368227085971,136.982447044243));
#222114=CARTESIAN_POINT('Ctrl Pts',(108.557534827126,5.52950934068608,133.627458964475));
#222115=CARTESIAN_POINT('Ctrl Pts',(108.279087203313,5.36398745797076,127.67818141992));
#222116=CARTESIAN_POINT('Ctrl Pts',(108.0006395795,0.269223146735527,124.601709835656));
#222117=CARTESIAN_POINT('Ctrl Pts',(107.722191955687,-5.07294408406776,
127.225171303631));
#222118=CARTESIAN_POINT('Ctrl Pts',(107.443744331874,-5.75332352870873,
133.137732897993));
#222119=CARTESIAN_POINT('Ctrl Pts',(107.165296708062,-1.14667971594628,
136.906039358215));
#222120=CARTESIAN_POINT('Ctrl Pts',(106.886849084249,4.51370673735246,135.067201139359));
#222121=CARTESIAN_POINT('Ctrl Pts',(106.608401460436,6.02621720585718,129.31102073231));
#222122=CARTESIAN_POINT('Ctrl Pts',(106.329953836623,2.00092845925606,124.927146726103));
#222123=CARTESIAN_POINT('Ctrl Pts',(106.05150621281,-3.86311579061174,125.944145168289));
#222124=CARTESIAN_POINT('Ctrl Pts',(105.773058588997,-6.17714535260555,
131.427444173636));
#222125=CARTESIAN_POINT('Ctrl Pts',(105.494610965184,-2.81468010588189,
136.338159830278));
#222126=CARTESIAN_POINT('Ctrl Pts',(105.216163341371,3.13433865337982,136.163584351558));
#222127=CARTESIAN_POINT('Ctrl Pts',(104.937715717558,6.20305331114115,131.064144073934));
#222128=CARTESIAN_POINT('Ctrl Pts',(104.659268093745,3.57146501196475,125.725975491034));
#222129=CARTESIAN_POINT('Ctrl Pts',(104.380820469933,-2.34212515744159,
125.054594746511));
#222130=CARTESIAN_POINT('Ctrl Pts',(104.10237284612,-6.10341672633411,129.666967945808));
#222131=CARTESIAN_POINT('Ctrl Pts',(103.823925222307,-4.25596649220884,
135.324549445729));
#222132=CARTESIAN_POINT('Ctrl Pts',(103.545477598494,1.50250903273456,136.828298236068));
#222133=CARTESIAN_POINT('Ctrl Pts',(103.267029974681,5.88025215824177,132.796342640716));
#222134=CARTESIAN_POINT('Ctrl Pts',(102.988582350868,4.85433081661274,126.933852879821));
#222135=CARTESIAN_POINT('Ctrl Pts',(102.710134727055,-0.63248339823904,
124.628170645098));
#222136=CARTESIAN_POINT('Ctrl Pts',(102.431687103242,-5.53807626864099,
127.998105271418));
#222137=CARTESIAN_POINT('Ctrl Pts',(102.153239479429,-5.35444759822839,
133.946851467654));
#222138=CARTESIAN_POINT('Ctrl Pts',(101.874791855617,-0.250343164351048,
137.00780209187));
#222139=CARTESIAN_POINT('Ctrl Pts',(101.596344231803,5.0838144076213,134.368093056165));
#222140=CARTESIAN_POINT('Ctrl Pts',(101.317896607991,5.74619489713063,128.453488007394));
#222141=CARTESIAN_POINT('Ctrl Pts',(101.039448984178,1.12810299340375,124.69922004086));
#222142=CARTESIAN_POINT('Ctrl Pts',(100.761001360365,-4.52666045036627,
126.55527801162));
#222143=CARTESIAN_POINT('Ctrl Pts',(100.482553736552,-6.0216440799065,132.316035318018));
#222144=CARTESIAN_POINT('Ctrl Pts',(100.204106112739,-1.98303097367997,
136.687637424115));
#222145=CARTESIAN_POINT('Ctrl Pts',(99.9256584889259,3.87789072090961,135.652795559044));
#222146=CARTESIAN_POINT('Ctrl Pts',(99.6472108651132,6.17522028847693,130.162478841968));
#222147=CARTESIAN_POINT('Ctrl Pts',(99.3687632413001,2.79782408721636,125.262020118999));
#222148=CARTESIAN_POINT('Ctrl Pts',(99.0903156174874,-3.15063576889091,
125.454701555827));
#222149=CARTESIAN_POINT('Ctrl Pts',(98.8118679936743,-6.20381527050148,
130.563458325018));
#222150=CARTESIAN_POINT('Ctrl Pts',(98.5334203698616,-3.55599161174595,
135.89359253233));
#222151=CARTESIAN_POINT('Ctrl Pts',(98.2549727460486,2.35961461835606,136.546971232774));
#222152=CARTESIAN_POINT('Ctrl Pts',(97.9765251222358,6.10685028777152,131.923171319966));
#222153=CARTESIAN_POINT('Ctrl Pts',(97.6980774984228,4.24218887894701,126.271239028595));
#222154=CARTESIAN_POINT('Ctrl Pts',(97.4196298746099,-1.52083686718185,
124.785024022185));
#222155=CARTESIAN_POINT('Ctrl Pts',(97.141182250797,-5.88628782938184,128.830285285991));
#222156=CARTESIAN_POINT('Ctrl Pts',(96.8627346269842,-4.842527837527,134.689625340572));
#222157=CARTESIAN_POINT('Ctrl Pts',(96.5842870031713,0.651278666378471,
136.978596920444));
#222158=CARTESIAN_POINT('Ctrl Pts',(96.3058393793584,5.54659189261388,133.593746966183));
#222159=CARTESIAN_POINT('Ctrl Pts',(96.0273917555454,5.34485813561491,127.645587226641));
#222160=CARTESIAN_POINT('Ctrl Pts',(95.7489441317327,0.231460862821695,
124.6001859187));
#222161=CARTESIAN_POINT('Ctrl Pts',(95.4704965079195,-5.09463763541278,
127.256118068232));
#222162=CARTESIAN_POINT('Ctrl Pts',(95.192048884107,-5.73901303358793,133.172711779316));
#222163=CARTESIAN_POINT('Ctrl Pts',(94.9136012602939,-1.10951582026908,
136.912906473138));
#222164=CARTESIAN_POINT('Ctrl Pts',(94.635153636481,4.53957222901603,135.039645944743));
#222165=CARTESIAN_POINT('Ctrl Pts',(94.3567060126683,6.01701517026768,129.274365105863));
#222166=CARTESIAN_POINT('Ctrl Pts',(94.0782583888551,1.96511511757592,124.915075397801));
#222167=CARTESIAN_POINT('Ctrl Pts',(93.7998107650425,-3.89262972695748,
125.967751099126));
#222168=CARTESIAN_POINT('Ctrl Pts',(93.5213631412293,-6.17323801795121,
131.465034666385));
#222169=CARTESIAN_POINT('Ctrl Pts',(93.2429155174167,-2.7809421498907,136.355191058501));
#222170=CARTESIAN_POINT('Ctrl Pts',(92.9644678936037,3.16690369734264,136.14440544854));
#222171=CARTESIAN_POINT('Ctrl Pts',(92.6860202697908,6.20451975856463,131.026379514606));
#222172=CARTESIAN_POINT('Ctrl Pts',(92.4075726459779,3.54048526930663,125.704329060518));
#222173=CARTESIAN_POINT('Ctrl Pts',(92.129125022165,-2.37708222012305,125.068958456964));
#222174=CARTESIAN_POINT('Ctrl Pts',(91.850677398352,-6.1102272761821,129.70414224903));
#222175=CARTESIAN_POINT('Ctrl Pts',(91.5722297745392,-4.22837196662692,
135.350372973126));
#222176=CARTESIAN_POINT('Ctrl Pts',(91.2937821507264,1.53915061280415,136.819040427511));
#222177=CARTESIAN_POINT('Ctrl Pts',(91.0153345269133,5.89226897075567,132.76051097));
#222178=CARTESIAN_POINT('Ctrl Pts',(90.7368869031008,4.8306799979248,126.90437490186));
#222179=CARTESIAN_POINT('Ctrl Pts',(90.4584392792875,-0.670067901161403,
124.632135181558));
#222180=CARTESIAN_POINT('Ctrl Pts',(90.1799916554748,-5.5550561337172,128.031869106972));
#222181=CARTESIAN_POINT('Ctrl Pts',(89.9015440316619,-5.3352191589658,133.979387286881));
#222182=CARTESIAN_POINT('Ctrl Pts',(89.6230964078489,-0.212576417070642,
137.009211066365));
#222183=CARTESIAN_POINT('Ctrl Pts',(89.3446487840362,5.10541366717708,134.337080407198));
#222184=CARTESIAN_POINT('Ctrl Pts',(89.0662011602232,5.73177800461257,128.418552844315));
#222185=CARTESIAN_POINT('Ctrl Pts',(88.7877535364103,1.09091836873142,124.69246607186));
#222186=CARTESIAN_POINT('Ctrl Pts',(88.5093059125973,-4.5524419536888,126.58291180426));
#222187=CARTESIAN_POINT('Ctrl Pts',(88.2308582887847,-6.0123305198223,132.352662766849));
#222188=CARTESIAN_POINT('Ctrl Pts',(87.9524106649715,-1.94718105691378,
136.69959969301));
#222189=CARTESIAN_POINT('Ctrl Pts',(87.6739630411587,3.90733267221543,135.629099907278));
#222190=CARTESIAN_POINT('Ctrl Pts',(87.395515417346,6.17119855939173,130.124900415918));
#222191=CARTESIAN_POINT('Ctrl Pts',(87.1170677935327,2.76403445029686,125.245091656395));
#222192=CARTESIAN_POINT('Ctrl Pts',(86.8386201697203,-3.18314228803115,
125.473979486801));
#222193=CARTESIAN_POINT('Ctrl Pts',(86.5601725459069,-6.20516676880425,
130.601227172784));
#222194=CARTESIAN_POINT('Ctrl Pts',(86.2817249220945,-3.52494612829556,
135.915144570902));
#222195=CARTESIAN_POINT('Ctrl Pts',(86.0032772982812,2.394527800925,136.532501191579));
#222196=CARTESIAN_POINT('Ctrl Pts',(85.7248296744686,6.11354766028192,131.885976459962));
#222197=CARTESIAN_POINT('Ctrl Pts',(85.4463820506556,4.21451588324655,126.245499609054));
#222198=CARTESIAN_POINT('Ctrl Pts',(85.1679344268427,-1.55745009994542,
124.794393312227));
#222199=CARTESIAN_POINT('Ctrl Pts',(84.8894868030298,-5.89819552695468,
128.86615336578));
#222200=CARTESIAN_POINT('Ctrl Pts',(84.611039179217,-4.81878740756302,134.719031197036));
#222201=CARTESIAN_POINT('Ctrl Pts',(84.332591555404,0.68885092852684,136.974518008049));
#222202=CARTESIAN_POINT('Ctrl Pts',(84.0541439315912,5.56346891353935,133.559931606153));
#222203=CARTESIAN_POINT('Ctrl Pts',(83.7756963077782,5.32553075757526,127.613110082872));
#222204=CARTESIAN_POINT('Ctrl Pts',(83.4972486839655,0.193690002040587,
124.598891899719));
#222205=CARTESIAN_POINT('Ctrl Pts',(83.2188010601524,-5.11614240308669,
127.287196314267));
#222206=CARTESIAN_POINT('Ctrl Pts',(82.9403534363397,-5.72448987722869,
133.207602900518));
#222207=CARTESIAN_POINT('Ctrl Pts',(82.6619058125266,-1.07231081107503,
136.919547233648));
#222208=CARTESIAN_POINT('Ctrl Pts',(82.3834581887138,4.56526950516122,135.011933810073));
#222209=CARTESIAN_POINT('Ctrl Pts',(82.1050105649009,6.00759017196827,129.237766173961));
#222210=CARTESIAN_POINT('Ctrl Pts',(81.826562941088,1.92922895783247,124.903222299129));
#222211=CARTESIAN_POINT('Ctrl Pts',(81.5481153172751,-3.92199942047723,
125.991536252305));
#222212=CARTESIAN_POINT('Ctrl Pts',(81.2696676934623,-6.16910193169181,
131.502600677615));
#222213=CARTESIAN_POINT('Ctrl Pts',(80.9912200696492,-2.74710114506546,
136.372016598662));
#222214=CARTESIAN_POINT('Ctrl Pts',(80.7127724458365,3.19935139052435,136.125028668197));
#222215=CARTESIAN_POINT('Ctrl Pts',(80.4343248220235,6.20575629522666,130.988606728286));
#222216=CARTESIAN_POINT('Ctrl Pts',(80.1558771982107,3.50937433266497,125.682871613546));
#222217=CARTESIAN_POINT('Ctrl Pts',(79.8774295743978,-2.41195119914859,
125.083534694853));
#222218=CARTESIAN_POINT('Ctrl Pts',(79.5989819505849,-6.11681140931136,
129.741357321249));
#222219=CARTESIAN_POINT('Ctrl Pts',(79.320534326772,-4.20062075716678,135.376028046362));
#222220=CARTESIAN_POINT('Ctrl Pts',(79.0420867029591,1.57573515908161,136.809559742781));
#222221=CARTESIAN_POINT('Ctrl Pts',(78.7636390791462,5.90406744307602,132.724606813414));
#222222=CARTESIAN_POINT('Ctrl Pts',(78.4851914553333,4.80685017661309,126.875041439303));
#222223=CARTESIAN_POINT('Ctrl Pts',(78.2067438315204,-0.707627574471386,
124.636328432103));
#222224=CARTESIAN_POINT('Ctrl Pts',(77.9282962077074,-5.57183015414549,
128.065735678218));
#222225=CARTESIAN_POINT('Ctrl Pts',(77.6498485838947,-5.31579302119528,
134.011805454327));
#222226=CARTESIAN_POINT('Ctrl Pts',(77.3714009600817,-0.174801792692954,
137.010390117845));
#222227=CARTESIAN_POINT('Ctrl Pts',(77.0929533362689,5.12682374375196,134.305936852001));
#222228=CARTESIAN_POINT('Ctrl Pts',(76.814505712456,5.7171487189526,128.38370608822));
#222229=CARTESIAN_POINT('Ctrl Pts',(76.536058088643,1.05369331967776,124.68593858136));
#222230=CARTESIAN_POINT('Ctrl Pts',(76.2576104648302,-4.57805476460059,
126.610702024239));
#222231=CARTESIAN_POINT('Ctrl Pts',(75.9791628410172,-6.00279417061961,
132.389232842773));
#222232=CARTESIAN_POINT('Ctrl Pts',(75.7007152172044,-1.91125898663751,
136.711343511654));
#222233=CARTESIAN_POINT('Ctrl Pts',(75.4222675933915,3.93662983587222,135.605225473025));
#222234=CARTESIAN_POINT('Ctrl Pts',(75.1438199695785,6.16694815427437,130.087347167514));
#222235=CARTESIAN_POINT('Ctrl Pts',(74.8653723457658,2.73014239106432,125.228369194547));
#222236=CARTESIAN_POINT('Ctrl Pts',(74.5869247219528,-3.21553085466319,
125.493454937009));
#222237=CARTESIAN_POINT('Ctrl Pts',(74.3084770981399,-6.20628833237051,
130.639003547736));
#222238=CARTESIAN_POINT('Ctrl Pts',(74.0300294743271,-3.49377002667009,
135.936507227495));
#222239=CARTESIAN_POINT('Ctrl Pts',(73.7515818505141,2.42935225338577,136.517818892029));
#222240=CARTESIAN_POINT('Ctrl Pts',(73.4731342267013,6.1200184930355,131.848741520285));
#222241=CARTESIAN_POINT('Ctrl Pts',(73.1946866028884,4.18668671711015,126.219929119786));
#222242=CARTESIAN_POINT('Ctrl Pts',(72.9162389790755,-1.59400562082267,
124.803985303816));
#222243=CARTESIAN_POINT('Ctrl Pts',(72.6377913552626,-5.90988466472314,
128.902093266552));
#222244=CARTESIAN_POINT('Ctrl Pts',(72.3593437314497,-4.79486841565966,
134.748291993943));
#222245=CARTESIAN_POINT('Ctrl Pts',(72.0808961076369,0.726397665050741,
136.970210458201));
#222246=CARTESIAN_POINT('Ctrl Pts',(71.8024484838239,5.58013977807825,133.526014137426));
#222247=CARTESIAN_POINT('Ctrl Pts',(71.524000860011,5.30600604003494,127.580751192065));
#222248=CARTESIAN_POINT('Ctrl Pts',(71.2455532361981,0.155911964005252,
124.597827826664));
#222249=CARTESIAN_POINT('Ctrl Pts',(70.9671056123853,-5.13745759022245,
127.318404890117));
#222250=CARTESIAN_POINT('Ctrl Pts',(70.6886579885723,-5.70975459779179,
133.242404968692));
#222251=CARTESIAN_POINT('Ctrl Pts',(70.4102103647595,-1.03506606700937,
136.925961393668));
#222252=CARTESIAN_POINT('Ctrl Pts',(70.1317627409465,4.59079761356593,134.98406576223));
#222253=CARTESIAN_POINT('Ctrl Pts',(69.8533151171337,5.99794256020584,129.201225292793));
#222254=CARTESIAN_POINT('Ctrl Pts',(69.5748674933208,1.89327130980037,124.891587869307));
#222255=CARTESIAN_POINT('Ctrl Pts',(69.2964198695077,-3.95122378286636,
126.015499746463));
#222256=CARTESIAN_POINT('Ctrl Pts',(69.0179722456952,-6.16473724709165,
131.540140815303));
#222257=CARTESIAN_POINT('Ctrl Pts',(68.7395246218819,-2.71315834539685,
136.388635827283));
#222258=CARTESIAN_POINT('Ctrl Pts',(68.4610769980694,3.23168053056381,136.105454728543));
#222259=CARTESIAN_POINT('Ctrl Pts',(68.1826293742561,6.20676287530703,130.950827114659));
#222260=CARTESIAN_POINT('Ctrl Pts',(67.9041817504435,3.47813335486666,125.661603945233));
#222261=CARTESIAN_POINT('Ctrl Pts',(67.6257341266304,-2.44673080243567,
125.09832292005));
#222262=CARTESIAN_POINT('Ctrl Pts',(67.3472865028177,-6.12316888174425,
129.778611783445));
#222263=CARTESIAN_POINT('Ctrl Pts',(67.0688388790048,-4.17271389215982,
135.401513714782));
#222264=CARTESIAN_POINT('Ctrl Pts',(66.7903912551918,1.61226131591331,136.799856533191));
#222265=CARTESIAN_POINT('Ctrl Pts',(66.511943631379,5.91564713800617,132.688631501398));
#222266=CARTESIAN_POINT('Ctrl Pts',(66.233496007566,4.78284223570014,126.845853579115));
#222267=CARTESIAN_POINT('Ctrl Pts',(65.9550483837533,-0.745161026381345,
124.640750241348));
#222268=CARTESIAN_POINT('Ctrl Pts',(65.6766007599402,-5.58839770835831,
128.099703730218));
#222269=CARTESIAN_POINT('Ctrl Pts',(65.3981531361275,-5.2961699047596,134.044104768727));
#222270=CARTESIAN_POINT('Ctrl Pts',(65.1197055123145,-0.137020690970298,
137.011339202618));
#222271=CARTESIAN_POINT('Ctrl Pts',(64.8412578885016,5.14804384398771,134.274663544608));
#222272=CARTESIAN_POINT('Ctrl Pts',(64.5628102646887,5.70230758224426,128.348949030369));
#222273=CARTESIAN_POINT('Ctrl Pts',(64.2843626408759,1.01642922563077,124.679637811238));
#222274=CARTESIAN_POINT('Ctrl Pts',(64.0059150170629,-4.60349793400934,
126.638647641779));
#222275=CARTESIAN_POINT('Ctrl Pts',(63.72746739325,-5.9930353856715,132.425744190676));
#222276=CARTESIAN_POINT('Ctrl Pts',(63.4490197694371,-1.87526609395646,
136.722868444874));
#222277=CARTESIAN_POINT('Ctrl Pts',(63.1705721456243,3.96578112626272,135.581173140958));
#222278=CARTESIAN_POINT('Ctrl Pts',(62.8921245218114,6.16246923062527,130.049820488308));
#222279=CARTESIAN_POINT('Ctrl Pts',(62.6136768979985,2.69614916540168,125.211853353112));
#222280=CARTESIAN_POINT('Ctrl Pts',(62.3352292741856,-3.24780026861702,
125.513127184779));
#222281=CARTESIAN_POINT('Ctrl Pts',(62.0567816503727,-6.20717991964031,
130.676786050054));
#222282=CARTESIAN_POINT('Ctrl Pts',(61.7783340265599,-3.46246446211126,
135.957679710507));
#222283=CARTESIAN_POINT('Ctrl Pts',(61.4998864027468,2.46408668530527,136.502924878181));
#222284=CARTESIAN_POINT('Ctrl Pts',(61.2214387789342,6.12626254625314,131.81146788069));
#222285=CARTESIAN_POINT('Ctrl Pts',(60.942991155121,4.15870241175792,126.194528508313));
#222286=CARTESIAN_POINT('Ctrl Pts',(60.6645435313083,-1.63050207523548,
124.813799641521));
#222287=CARTESIAN_POINT('Ctrl Pts',(60.3860959074953,-5.92135480954196,
128.938103656541));
#222288=CARTESIAN_POINT('Ctrl Pts',(60.1076482836825,-4.77077174814381,
134.777406647022));
#222289=CARTESIAN_POINT('Ctrl Pts',(59.8292006598696,0.763917484641806,
136.965674430521));
#222290=CARTESIAN_POINT('Ctrl Pts',(59.5507530360567,5.59660386848551,133.491995816827));
#222291=CARTESIAN_POINT('Ctrl Pts',(59.2723054122438,5.28628470648961,127.548511753291));
#222292=CARTESIAN_POINT('Ctrl Pts',(58.9938577884309,0.11812814859451,124.596993738963));
#222293=CARTESIAN_POINT('Ctrl Pts',(58.715410164618,-5.15858240697801,127.34974263934));
#222294=CARTESIAN_POINT('Ctrl Pts',(58.4369625408051,-5.69480774129836,
133.277116694236));
#222295=CARTESIAN_POINT('Ctrl Pts',(58.1585149169922,-0.997782968190397,
136.932148715521));
#222296=CARTESIAN_POINT('Ctrl Pts',(57.8800672931793,4.61615560827684,134.956042833877));
#222297=CARTESIAN_POINT('Ctrl Pts',(57.6016196693665,5.98807269247603,129.164743816393));
#222298=CARTESIAN_POINT('Ctrl Pts',(57.3231720455535,1.85724350590365,124.880172539454));
#222299=CARTESIAN_POINT('Ctrl Pts',(57.0447244217407,-3.98030173120474,
126.039640693622));
#222300=CARTESIAN_POINT('Ctrl Pts',(56.7662767979277,-6.16014412588574,
131.577653688385));
#222301=CARTESIAN_POINT('Ctrl Pts',(56.4878291741149,-2.67911500864857,
136.405048128532));
#222302=CARTESIAN_POINT('Ctrl Pts',(56.209381550302,3.26388991949243,136.085684354897));
#222303=CARTESIAN_POINT('Ctrl Pts',(55.9309339264891,6.20753946150667,130.913042073662));
#222304=CARTESIAN_POINT('Ctrl Pts',(55.6524863026762,3.44676349355797,125.640526843659));
#222305=CARTESIAN_POINT('Ctrl Pts',(55.3740386788633,-2.48141974121268,
125.113322584571));
#222306=CARTESIAN_POINT('Ctrl Pts',(55.0955910550504,-6.12929945790263,
129.815904255142));
#222307=CARTESIAN_POINT('Ctrl Pts',(54.8171434312375,-4.14465240570495,
135.426829034002));
#222308=CARTESIAN_POINT('Ctrl Pts',(54.5386958074246,1.64872772980914,136.789931158292));
#222309=CARTESIAN_POINT('Ctrl Pts',(54.2602481836117,5.92700762645589,132.652586367033));
#222310=CARTESIAN_POINT('Ctrl Pts',(53.9818005597989,4.75865706480954,126.81681240286));
#222311=CARTESIAN_POINT('Ctrl Pts',(53.703352935986,-0.78266686607524,124.645400445441));
#222312=CARTESIAN_POINT('Ctrl Pts',(53.4249053121731,-5.604758182439,128.133772004274));
#222313=CARTESIAN_POINT('Ctrl Pts',(53.1464576883601,-5.27635053680027,
134.076284033214));
#222314=CARTESIAN_POINT('Ctrl Pts',(52.8680100645473,-0.0992345118958833,
137.012058285519));
#222315=CARTESIAN_POINT('Ctrl Pts',(52.5895624407343,5.1690731815654,134.243261643865));
#222316=CARTESIAN_POINT('Ctrl Pts',(52.3111148169216,5.68725514443172,128.314282958697));
#222317=CARTESIAN_POINT('Ctrl Pts',(52.0326671931086,0.979127467424884,
124.673563994973));
#222318=CARTESIAN_POINT('Ctrl Pts',(51.7542195692957,-4.62877051910935,
126.666747621346));
#222319=CARTESIAN_POINT('Ctrl Pts',(51.4757719454828,-5.98305452659317,
132.462195457613));
#222320=CARTESIAN_POINT('Ctrl Pts',(51.1973243216699,-1.83920371260068,
136.734174065611));
#222321=CARTESIAN_POINT('Ctrl Pts',(50.9188766978571,3.99478546317524,135.556943802347));
#222322=CARTESIAN_POINT('Ctrl Pts',(50.6404290740441,6.15776195441257,130.012321768865));
#222323=CARTESIAN_POINT('Ctrl Pts',(50.3619814502312,2.66205603294,125.195544744091));
#222324=CARTESIAN_POINT('Ctrl Pts',(50.0835338264184,-3.27994933413751,
125.532995501151));
#222325=CARTESIAN_POINT('Ctrl Pts',(49.8050862026055,-6.20784149757545,
130.714573279694));
#222326=CARTESIAN_POINT('Ctrl Pts',(49.5266385787925,-3.43103059465853,
135.978661235386));
#222327=CARTESIAN_POINT('Ctrl Pts',(49.2481909549797,2.4987298095866,136.487819701939));
#222328=CARTESIAN_POINT('Ctrl Pts',(48.9697433311668,6.13227958855924,131.774156922365));
#222329=CARTESIAN_POINT('Ctrl Pts',(48.6912957073539,4.13056400415832,126.169298715863));
#222330=CARTESIAN_POINT('Ctrl Pts',(48.412848083541,-1.66693811079436,124.823835961664));
#222331=CARTESIAN_POINT('Ctrl Pts',(48.1344004597282,-5.93260553638082,
128.974183201367));
#222332=CARTESIAN_POINT('Ctrl Pts',(47.8559528359152,-4.7464982979263,134.806374077418));
#222333=CARTESIAN_POINT('Ctrl Pts',(47.5775052121024,0.801408996989757,
136.960910093092));
#222334=CARTESIAN_POINT('Ctrl Pts',(47.2990575882894,5.61286057467834,133.457877904919));
#222335=CARTESIAN_POINT('Ctrl Pts',(47.0206099644766,5.26636748772036,127.516392961194));
#222336=CARTESIAN_POINT('Ctrl Pts',(46.7421623406636,0.0803399559020909,
124.596389667526));
#222337=CARTESIAN_POINT('Ctrl Pts',(46.4637147168508,-5.17951607056515,
127.381208400702));
#222338=CARTESIAN_POINT('Ctrl Pts',(46.1852670930379,-5.67964986161014,
133.311736790894));
#222339=CARTESIAN_POINT('Ctrl Pts',(45.9068194692249,-0.960462896156299,
136.938108969933));
#222340=CARTESIAN_POINT('Ctrl Pts',(45.6283718454121,4.64134254964412,134.927866063412));
#222341=CARTESIAN_POINT('Ctrl Pts',(45.3499242215992,5.97798093451044,129.128323096598));
#222342=CARTESIAN_POINT('Ctrl Pts',(45.0714765977863,1.82114688116607,124.868976732569));
#222343=CARTESIAN_POINT('Ctrl Pts',(44.7930289739735,-4.00923218799886,
126.063958199228));
#222344=CARTESIAN_POINT('Ctrl Pts',(44.5145813501605,-6.15532273827383,
131.615137906808));
#222345=CARTESIAN_POINT('Ctrl Pts',(44.2361337263477,-2.644972396308,136.421252894246));
#222346=CARTESIAN_POINT('Ctrl Pts',(43.9576861025347,3.29597836378001,136.065718279858));
#222347=CARTESIAN_POINT('Ctrl Pts',(43.6792384787219,6.20808602504863,130.875253005433));
#222348=CARTESIAN_POINT('Ctrl Pts',(43.4007908549089,3.41526591116036,125.619641089845));
#222349=CARTESIAN_POINT('Ctrl Pts',(43.1223432310961,-2.5160167300689,125.128533132602));
#222350=CARTESIAN_POINT('Ctrl Pts',(42.8438956072832,-6.13520291061547,
129.853233354452));
#222351=CARTESIAN_POINT('Ctrl Pts',(42.5654479834703,-4.11643733763101,
135.451973065955));
#222352=CARTESIAN_POINT('Ctrl Pts',(42.2870003596574,1.68513304949262,136.779783985877));
#222353=CARTESIAN_POINT('Ctrl Pts',(42.0085527358444,5.93814848745852,132.616472745983));
#222354=CARTESIAN_POINT('Ctrl Pts',(41.7301051120316,4.73429556013123,126.787918986671));
#222355=CARTESIAN_POINT('Ctrl Pts',(41.4516574882187,-0.820143703760798,
124.65027887207));
#222356=CARTESIAN_POINT('Ctrl Pts',(41.1732098644058,-5.62091097014408,
128.167939237972));
#222357=CARTESIAN_POINT('Ctrl Pts',(40.8947622405929,-5.25633565173145,
134.108342055376));
#222358=CARTESIAN_POINT('Ctrl Pts',(40.61631461678,-0.0614446556499193,
137.012547339898));
#222359=CARTESIAN_POINT('Ctrl Pts',(40.3378669929672,5.18991097723558,134.211732313379));
#222360=CARTESIAN_POINT('Ctrl Pts',(40.0594193691542,5.67199196328813,128.279709157768));
#222361=CARTESIAN_POINT('Ctrl Pts',(39.7809717453414,0.941789427290636,
124.66771735763));
#222362=CARTESIAN_POINT('Ctrl Pts',(39.5025241215285,-4.65387158341555,
126.695000921683));
#222363=CARTESIAN_POINT('Ctrl Pts',(39.2240764977156,-5.97285196322902,
132.49858529287));
#222364=CARTESIAN_POINT('Ctrl Pts',(38.9456288739027,-1.80307317887526,
136.745259954929));
#222365=CARTESIAN_POINT('Ctrl Pts',(38.6671812500898,4.02364177184326,135.532538355018));
#222366=CARTESIAN_POINT('Ctrl Pts',(38.3887336262769,6.15282650006613,129.974852398711));
#222367=CARTESIAN_POINT('Ctrl Pts',(38.110286002464,2.62786425701304,125.179443971804));
#222368=CARTESIAN_POINT('Ctrl Pts',(37.8318383786511,-3.31197685992897,
125.553059149895));
#222369=CARTESIAN_POINT('Ctrl Pts',(37.5533907548383,-6.20827304166094,
130.752363836438));
#222370=CARTESIAN_POINT('Ctrl Pts',(37.2749431310254,-3.3994695891056,135.999451024653));
#222371=CARTESIAN_POINT('Ctrl Pts',(36.9964955072125,2.53328034251594,136.47250392303));
#222372=CARTESIAN_POINT('Ctrl Pts',(36.7180478833995,6.13806939699002,131.73681002788));
#222373=CARTESIAN_POINT('Ctrl Pts',(36.4396002595867,4.10227253699055,126.144240677337));
#222374=CARTESIAN_POINT('Ctrl Pts',(36.1611526357737,-1.70331237734853,
124.834093892349));
#222375=CARTESIAN_POINT('Ctrl Pts',(35.8827050119609,-5.94363642833981,
129.01033056409));
#222376=CARTESIAN_POINT('Ctrl Pts',(35.604257388148,-4.72204896446884,134.835193211735));
#222377=CARTESIAN_POINT('Ctrl Pts',(35.3258097643351,0.838870812832614,
136.955917622458));
#222378=CARTESIAN_POINT('Ctrl Pts',(35.0473621405222,5.62890929425843,133.423661665951));
#222379=CARTESIAN_POINT('Ctrl Pts',(34.7689145167094,5.24625512176713,127.484396005948));
#222380=CARTESIAN_POINT('Ctrl Pts',(34.4904668928964,0.0425487861828518,
124.596015634733));
#222381=CARTESIAN_POINT('Ctrl Pts',(34.2120192690835,-5.20025780527969,
127.412801008228));
#222382=CARTESIAN_POINT('Ctrl Pts',(33.9335716452707,-5.66428152040741,
133.346263975806));
#222383=CARTESIAN_POINT('Ctrl Pts',(33.6551240214578,-0.923107233816384,
136.943841936043));
#222384=CARTESIAN_POINT('Ctrl Pts',(33.3766763976448,4.66635750435639,134.899536494936));
#222385=CARTESIAN_POINT('Ctrl Pts',(33.098228773832,5.96766766026296,129.091964482989));
#222386=CARTESIAN_POINT('Ctrl Pts',(32.8197811500191,1.78498277316083,124.858000863516));
#222387=CARTESIAN_POINT('Ctrl Pts',(32.5413335262063,-4.03801408121996,
126.08845136219));
#222388=CARTESIAN_POINT('Ctrl Pts',(32.2628859023933,-6.15027326291425,
131.65259208158));
#222389=CARTESIAN_POINT('Ctrl Pts',(31.9844382785804,-2.6107317735426,136.437249523951));
#222390=CARTESIAN_POINT('Ctrl Pts',(31.7059906547675,3.32794467437699,136.045557243275));
#222391=CARTESIAN_POINT('Ctrl Pts',(31.4275430309546,6.20840254567991,130.837461310262));
#222392=CARTESIAN_POINT('Ctrl Pts',(31.1490954071417,3.3836417748287,125.598947457719));
#222393=CARTESIAN_POINT('Ctrl Pts',(30.8706477833288,-2.55052048699994,
125.143954000505));
#222394=CARTESIAN_POINT('Ctrl Pts',(30.5922001595159,-6.14087902112821,
129.890597698133));
#222395=CARTESIAN_POINT('Ctrl Pts',(30.3137525357031,-4.08806973345779,
135.476944878919));
#222396=CARTESIAN_POINT('Ctrl Pts',(30.0353049118902,1.72147592595096,136.769415391952));
#222397=CARTESIAN_POINT('Ctrl Pts',(29.7568572880773,5.94906930818524,132.58029197645));
#222398=CARTESIAN_POINT('Ctrl Pts',(29.4784096642643,4.70975862438989,126.759174401203));
#222399=CARTESIAN_POINT('Ctrl Pts',(29.1999620404515,-0.857590150719802,
124.65538534046));
#222400=CARTESIAN_POINT('Ctrl Pts',(28.9215144166386,-5.63685547292606,
128.202204165235));
#222401=CARTESIAN_POINT('Ctrl Pts',(28.6430667928257,-5.23612599121204,
134.140277647291));
#222402=CARTESIAN_POINT('Ctrl Pts',(28.3646191690128,-0.0236525225496446,
137.012806347637));
#222403=CARTESIAN_POINT('Ctrl Pts',(28.0861715451999,5.2105564588459,134.180076721482));
#222404=CARTESIAN_POINT('Ctrl Pts',(27.807723921387,5.65651860439647,128.245228908728));
#222405=CARTESIAN_POINT('Ctrl Pts',(27.5292762975741,0.904416488802812,
124.662098115861));
#222406=CARTESIAN_POINT('Ctrl Pts',(27.2508286737613,-4.67880019679877,
126.723406495856));
#222407=CARTESIAN_POINT('Ctrl Pts',(26.9723810499484,-5.96242807363892,
132.53491234801));
#222408=CARTESIAN_POINT('Ctrl Pts',(26.6939334261354,-1.76687583160983,
136.756125702037));
#222409=CARTESIAN_POINT('Ctrl Pts',(26.4154858023226,4.05234898298581,135.507957703324));
#222410=CARTESIAN_POINT('Ctrl Pts',(26.1370381785097,6.14766305047102,129.937413766291));
#222411=CARTESIAN_POINT('Ctrl Pts',(25.8585905546968,2.59357510460964,125.163551632871));
#222412=CARTESIAN_POINT('Ctrl Pts',(25.5801429308839,-3.34388165920016,
125.573317387547));
#222413=CARTESIAN_POINT('Ctrl Pts',(25.301695307071,-6.2084745359058,130.790156319941));
#222414=CARTESIAN_POINT('Ctrl Pts',(25.0232476832582,-3.36778261495664,
136.020048307934));
#222415=CARTESIAN_POINT('Ctrl Pts',(24.7448000594452,2.56773700381057,136.456978108987));
#222416=CARTESIAN_POINT('Ctrl Pts',(24.4663524356323,6.14363175700203,131.69942858114));
#222417=CARTESIAN_POINT('Ctrl Pts',(24.1879048118195,4.07382905860539,126.11935532127));
#222418=CARTESIAN_POINT('Ctrl Pts',(23.9094571880065,-1.73962352703587,
124.844573053462));
#222419=CARTESIAN_POINT('Ctrl Pts',(23.6310095641937,-5.95444707666522,
129.046544405257));
#222420=CARTESIAN_POINT('Ctrl Pts',(23.3525619403807,-4.69742465375045,
134.863862982068));
#222421=CARTESIAN_POINT('Ctrl Pts',(23.0741143165679,0.876301544009003,
136.950697203617));
#222422=CARTESIAN_POINT('Ctrl Pts',(22.795666692755,5.64474943253441,133.389348367819));
#222423=CARTESIAN_POINT('Ctrl Pts',(22.5172190689421,5.22594835390121,127.452522073212));
#222424=CARTESIAN_POINT('Ctrl Pts',(22.2387714451292,0.0047560398029127,
124.595871654449));
#222425=CARTESIAN_POINT('Ctrl Pts',(21.9603238213163,-5.22080684252888,
127.444519291243));
#222426=CARTESIAN_POINT('Ctrl Pts',(21.6818761975034,-5.64870328716988,
133.380696969555));
#222427=CARTESIAN_POINT('Ctrl Pts',(21.4034285736905,-0.885717365398449,
136.949347401415));
#222428=CARTESIAN_POINT('Ctrl Pts',(21.1249809498776,4.69119954547528,134.871055178212));
#222429=CARTESIAN_POINT('Ctrl Pts',(20.8465333260648,5.95713325189572,129.055669322849));
#222430=CARTESIAN_POINT('Ctrl Pts',(20.5680857022518,1.74875252196249,124.847245339011));
#222431=CARTESIAN_POINT('Ctrl Pts',(20.289638078439,-4.06664634434428,126.113119274905));
#222432=CARTESIAN_POINT('Ctrl Pts',(20.011190454626,-6.14499588691713,131.690014824823));
#222433=CARTESIAN_POINT('Ctrl Pts',(19.7327428308132,-2.57639440915122,
136.453037424885));
#222434=CARTESIAN_POINT('Ctrl Pts',(19.4542952070003,3.35978766676044,136.025201992224));
#222435=CARTESIAN_POINT('Ctrl Pts',(19.1758475831874,6.20848901167171,130.799668388532));
#222436=CARTESIAN_POINT('Ctrl Pts',(18.8973999593745,3.3518922564065,125.578446714094));
#222437=CARTESIAN_POINT('Ctrl Pts',(18.6189523355616,-2.58492973345636,
125.159584616859));
#222438=CARTESIAN_POINT('Ctrl Pts',(18.3405047117487,-6.14632757911053,
129.927995901635));
#222439=CARTESIAN_POINT('Ctrl Pts',(18.0620570879358,-4.05955064435711,
135.501743547556));
#222440=CARTESIAN_POINT('Ctrl Pts',(17.7836094641229,1.75775501248606,136.758825760728));
#222441=CARTESIAN_POINT('Ctrl Pts',(17.5051618403101,5.95976968396092,132.544045399129));
#222442=CARTESIAN_POINT('Ctrl Pts',(17.2267142164972,4.68504716681072,126.730579711598));
#222443=CARTESIAN_POINT('Ctrl Pts',(16.9482665926842,-0.8950048193604,124.660719661391));
#222444=CARTESIAN_POINT('Ctrl Pts',(16.6698189688713,-5.65259109995534,
128.236565516362));
#222445=CARTESIAN_POINT('Ctrl Pts',(16.3913713450585,-5.21572230411858,
134.172089625574));
#222446=CARTESIAN_POINT('Ctrl Pts',(16.1129237212456,0.0141404870033325,
137.012835299135));
#222447=CARTESIAN_POINT('Ctrl Pts',(15.8344760974327,5.23100886137047,134.148296041183));
#222448=CARTESIAN_POINT('Ctrl Pts',(15.5560284736198,5.64083564112771,128.210843489254));
#222449=CARTESIAN_POINT('Ctrl Pts',(15.2775808498069,0.8670100368296,124.656706477888));
#222450=CARTESIAN_POINT('Ctrl Pts',(14.999133225994,-4.70355543551987,126.751963291284));
#222451=CARTESIAN_POINT('Ctrl Pts',(14.7206856021811,-5.95178324408404,
132.571175276918));
#222452=CARTESIAN_POINT('Ctrl Pts',(14.4422379783683,-1.73061301211068,
136.766770904302));
#222453=CARTESIAN_POINT('Ctrl Pts',(14.1637903545553,4.08090603284655,135.48320275811));
#222454=CARTESIAN_POINT('Ctrl Pts',(13.8853427307424,6.14227179696077,129.900007258904));
#222455=CARTESIAN_POINT('Ctrl Pts',(13.6068951069296,2.55918984632695,125.147868316191));
#222456=CARTESIAN_POINT('Ctrl Pts',(13.3284474831167,-3.37566254970675,
125.593769463429));
#222457=CARTESIAN_POINT('Ctrl Pts',(13.0499998593037,-6.20844597284355,
130.827949329789));
#222458=CARTESIAN_POINT('Ctrl Pts',(12.7715522354909,-3.33597084638438,
136.04045232199));
#222459=CARTESIAN_POINT('Ctrl Pts',(12.493104611678,2.60209851666622,136.441242835124));
#222460=CARTESIAN_POINT('Ctrl Pts',(12.2146569878651,6.14896646247997,131.662013967328));
#222461=CARTESIAN_POINT('Ctrl Pts',(11.9362093640522,4.04523462298623,126.094643569795));
#222462=CARTESIAN_POINT('Ctrl Pts',(11.6577617402393,-1.77587021433397,
124.855273056695));
#222463=CARTESIAN_POINT('Ctrl Pts',(11.3793141164265,-5.96503708076441,
129.08282338295));
#222464=CARTESIAN_POINT('Ctrl Pts',(11.1008664926135,-4.67262627823404,
134.892382326048));
#222465=CARTESIAN_POINT('Ctrl Pts',(10.8224188688007,0.913699803509421,
136.945249030013));
#222466=CARTESIAN_POINT('Ctrl Pts',(10.5439712449878,5.6603804025445,133.354939282016));
#222467=CARTESIAN_POINT('Ctrl Pts',(10.2655236211749,5.20544793659703,127.420772344084));
#222468=CARTESIAN_POINT('Ctrl Pts',(9.98707599736195,-0.0330368828140487,
124.595957732005));
#222469=CARTESIAN_POINT('Ctrl Pts',(9.70862837354909,-5.24116242086055,
127.476362074414));
#222470=CARTESIAN_POINT('Ctrl Pts',(9.43018074973619,-5.63291573915475,
133.415034496211));
#222471=CARTESIAN_POINT('Ctrl Pts',(9.15173312592329,-0.848294676398009,
136.954625162043));
#222472=CARTESIAN_POINT('Ctrl Pts',(8.87328550211039,4.71586775246963,134.842423168626));
#222473=CARTESIAN_POINT('Ctrl Pts',(8.59483787829755,5.94637809976527,129.019438961107));
#222474=CARTESIAN_POINT('Ctrl Pts',(8.3163902544846,1.71245747009635,124.836710557603));
#222475=CARTESIAN_POINT('Ctrl Pts',(8.03794263067172,-4.09512791639282,
126.137961023291));
#222476=CARTESIAN_POINT('Ctrl Pts',(7.75949500685887,-6.1394908058375,131.727404749824));
#222477=CARTESIAN_POINT('Ctrl Pts',(7.48104738304595,-2.54196157551782,
136.468616012024));
#222478=CARTESIAN_POINT('Ctrl Pts',(7.20259975923305,3.39150616097622,136.004653280976));
#222479=CARTESIAN_POINT('Ctrl Pts',(6.92415213542018,6.20834541982004,130.761875640674));
#222480=CARTESIAN_POINT('Ctrl Pts',(6.64570451160728,3.32001853238404,125.558139618628));
#222481=CARTESIAN_POINT('Ctrl Pts',(6.36725688779438,-2.61924319439064,
125.175424402463));
#222482=CARTESIAN_POINT('Ctrl Pts',(6.08880926398148,-6.15154838266407,
129.965426579154));
#222483=CARTESIAN_POINT('Ctrl Pts',(5.81036164016863,-4.03088112711464,
135.52636815294));
#222484=CARTESIAN_POINT('Ctrl Pts',(5.53191401635571,1.79396896476278,136.748015484609));
#222485=CARTESIAN_POINT('Ctrl Pts',(5.2534663925428,5.97024921827925,132.507734357147));
#222486=CARTESIAN_POINT('Ctrl Pts',(4.97501876872993,4.66016210308585,126.702135977443));
#222487=CARTESIAN_POINT('Ctrl Pts',(4.69657114491704,-0.932386323268277,
124.666281637197));
#222488=CARTESIAN_POINT('Ctrl Pts',(4.41812352110413,-5.66811726814286,
128.27102201808));
#222489=CARTESIAN_POINT('Ctrl Pts',(4.13967589729124,-5.19512534651691,
134.203776811419));
#222490=CARTESIAN_POINT('Ctrl Pts',(3.86122827347838,0.051932972575587,
137.012634193321));
#222491=CARTESIAN_POINT('Ctrl Pts',(3.58278064966546,5.25126742693796,134.116391450127));
#222492=CARTESIAN_POINT('Ctrl Pts',(3.30433302585255,5.62494365461986,128.176554173511));
#222493=CARTESIAN_POINT('Ctrl Pts',(3.02588540203969,0.829571457480427,
124.651542643499));
#222494=CARTESIAN_POINT('Ctrl Pts',(2.74743777822681,-4.72813638226476,
126.780670249786));
#222495=CARTESIAN_POINT('Ctrl Pts',(2.46899015441389,-5.9409178690121,132.607372735859));
#222496=CARTESIAN_POINT('Ctrl Pts',(2.19054253060099,-1.69428606410994,
136.77719516726));
#222497=CARTESIAN_POINT('Ctrl Pts',(1.91209490678813,4.10931186323347,135.458274436681));
#222498=CARTESIAN_POINT('Ctrl Pts',(1.63364728297522,6.13665293931019,129.862634262664));
#222499=CARTESIAN_POINT('Ctrl Pts',(1.35519965916232,2.52470975632363,125.132394602912));
#222500=CARTESIAN_POINT('Ctrl Pts',(1.07675203534945,-3.40731835379603,
125.614414619682));
#222501=CARTESIAN_POINT('Ctrl Pts',(0.798304411536565,-6.20818735353264,
130.86574146555));
#222502=CARTESIAN_POINT('Ctrl Pts',(0.519856787723634,-3.30403546218559,
136.060662310741));
#222503=CARTESIAN_POINT('Ctrl Pts',(0.241409163910791,2.63636360780418,
136.425298684517));
#222504=CARTESIAN_POINT('Ctrl Pts',(-0.0370384599021062,6.15407331574431,
131.624567572855));
#222505=CARTESIAN_POINT('Ctrl Pts',(-0.315486083715014,4.01649028971072,
126.070106338619));
#222506=CARTESIAN_POINT('Ctrl Pts',(-0.593933707527915,-1.81205109610819,
124.866193505555));
#222507=CARTESIAN_POINT('Ctrl Pts',(-0.872381331340776,-5.97540604822092,
129.119166152838));
#222508=CARTESIAN_POINT('Ctrl Pts',(-1.15082895515369,-4.6476547568326,
134.920750186879));
#222509=CARTESIAN_POINT('Ctrl Pts',(-1.42927657896659,0.951064205527318,
136.939573303531));
#222510=CARTESIAN_POINT('Ctrl Pts',(-1.70772420277945,5.67580162507719,
133.320435683583));
#222511=CARTESIAN_POINT('Ctrl Pts',(-1.98617182659235,5.18475462950527,
127.389147995065));
#222512=CARTESIAN_POINT('Ctrl Pts',(-2.26461945040527,-0.0708285812371651,
124.596273864213));
#222513=CARTESIAN_POINT('Ctrl Pts',(-2.54306707421816,-5.26132378599129,
127.508328177794));
#222514=CARTESIAN_POINT('Ctrl Pts',(-2.82151469803103,-5.61691946137538,
133.449275283389));
#222515=CARTESIAN_POINT('Ctrl Pts',(-3.09996232184393,-0.810840553526189,
136.959675022356));
#222516=CARTESIAN_POINT('Ctrl Pts',(-3.37840994565684,4.74036121125036,
134.813641527147));
#222517=CARTESIAN_POINT('Ctrl Pts',(-3.6568575694697,5.93540260240737,128.983274740293));
#222518=CARTESIAN_POINT('Ctrl Pts',(-3.9353051932826,1.6760989624889,124.826396909662));
#222519=CARTESIAN_POINT('Ctrl Pts',(-4.21375281709551,-4.12345774197041,
126.162975686831));
#222520=CARTESIAN_POINT('Ctrl Pts',(-4.49220044090841,-6.13375822366836,
131.764760471086));
#222521=CARTESIAN_POINT('Ctrl Pts',(-4.77064806472125,-2.50743454856317,
136.483984708096));
#222522=CARTESIAN_POINT('Ctrl Pts',(-5.04909568853418,3.4230989816841,135.983911870971));
#222523=CARTESIAN_POINT('Ctrl Pts',(-5.32754331234708,6.20797177544568,
130.724084467112));
#222524=CARTESIAN_POINT('Ctrl Pts',(-5.60599093615995,3.28802178385396,
125.538026923812));
#222525=CARTESIAN_POINT('Ctrl Pts',(-5.88443855997284,-2.65345959830539,
125.191472770368));
#222526=CARTESIAN_POINT('Ctrl Pts',(-6.16288618378574,-6.15654123833006,
130.002888343683));
#222527=CARTESIAN_POINT('Ctrl Pts',(-6.44133380759864,-4.00206224408943,
135.550817782599));
#222528=CARTESIAN_POINT('Ctrl Pts',(-6.71978143141151,1.83011644085978,
136.736984964173));
#222529=CARTESIAN_POINT('Ctrl Pts',(-6.9982290552244,5.98050752281724,132.471360196026));
#222530=CARTESIAN_POINT('Ctrl Pts',(-7.27667667903734,4.63510435534053,
126.673844252731));
#222531=CARTESIAN_POINT('Ctrl Pts',(-7.55512430285017,-0.969733277257762,
124.672071061776));
#222532=CARTESIAN_POINT('Ctrl Pts',(-7.83357192666308,-5.68343340216059,
128.305572393592));
#222533=CARTESIAN_POINT('Ctrl Pts',(-8.112019550476,-5.17433588163501,134.235338030648));
#222534=CARTESIAN_POINT('Ctrl Pts',(-8.39046717428886,0.0897235337524442,
137.012203037646));
#222535=CARTESIAN_POINT('Ctrl Pts',(-8.66891479810176,5.27133140485959,
134.084364130551));
#222536=CARTESIAN_POINT('Ctrl Pts',(-8.94736242191464,5.60884323375645,
128.142362232103));
#222537=CARTESIAN_POINT('Ctrl Pts',(-9.22581004572757,0.792102138056052,
124.646606804043));
#222538=CARTESIAN_POINT('Ctrl Pts',(-9.50425766954039,-4.75254212617725,
126.809526307613));
#222539=CARTESIAN_POINT('Ctrl Pts',(-9.78270529335335,-5.92983235104376,
132.643503383524));
#222540=CARTESIAN_POINT('Ctrl Pts',(-10.0611529171662,-1.65789633371603,
136.787398104638));
#222541=CARTESIAN_POINT('Ctrl Pts',(-10.3396005409791,4.13756542155812,
135.433173662763));
#222542=CARTESIAN_POINT('Ctrl Pts',(-10.618048164792,6.13080668572826,129.82529616244));
#222543=CARTESIAN_POINT('Ctrl Pts',(-10.8964957886049,2.49013611227157,
125.11713106642));
#222544=CARTESIAN_POINT('Ctrl Pts',(-11.1749434124178,-3.4388478984508,
125.635252091294));
#222545=CARTESIAN_POINT('Ctrl Pts',(-11.4533910362307,-6.20769868755626,
130.90353132682));
#222546=CARTESIAN_POINT('Ctrl Pts',(-11.7318386600436,-3.2719776457377,
136.080677525301));
#222547=CARTESIAN_POINT('Ctrl Pts',(-12.0102862838565,2.67053100751937,
136.409146247984));
#222548=CARTESIAN_POINT('Ctrl Pts',(-12.2887339076694,6.15895212755882,
131.587090785312));
#222549=CARTESIAN_POINT('Ctrl Pts',(-12.5671815314823,3.98759712391021,
126.045744536976));
#222550=CARTESIAN_POINT('Ctrl Pts',(-12.8456291552951,-1.84816483166266,
124.877333995382));
#222551=CARTESIAN_POINT('Ctrl Pts',(-13.1240767791081,-5.98555359480885,
129.155571368227));
#222552=CARTESIAN_POINT('Ctrl Pts',(-13.4025244029209,-4.62251101487491,
134.948965513381));
#222553=CARTESIAN_POINT('Ctrl Pts',(-13.6809720267338,0.988393365511613,
136.933670234486));
#222554=CARTESIAN_POINT('Ctrl Pts',(-13.9594196505467,5.69101252869335,
133.285838851062));
#222555=CARTESIAN_POINT('Ctrl Pts',(-14.2378672743596,5.16386919942402,
127.357650198006));
#222556=CARTESIAN_POINT('Ctrl Pts',(-14.5163148981725,-0.108617655081171,
124.59682003936));
#222557=CARTESIAN_POINT('Ctrl Pts',(-14.7947625219854,-5.28129019083405,
127.540416416869));
#222558=CARTESIAN_POINT('Ctrl Pts',(-15.0732101457983,-5.60071504657988,
133.483418062279));
#222559=CARTESIAN_POINT('Ctrl Pts',(-15.3516577696111,-0.77335638465969,
136.96449679523));
#222560=CARTESIAN_POINT('Ctrl Pts',(-15.6301053934241,4.76467901420313,
134.784711320289));
#222561=CARTESIAN_POINT('Ctrl Pts',(-15.908553017237,5.92420716652329,128.947178000488));
#222562=CARTESIAN_POINT('Ctrl Pts',(-16.1870006410499,1.63967834641818,
124.816304777366));
#222563=CARTESIAN_POINT('Ctrl Pts',(-16.4654482648627,-4.15163477130477,
126.188162338596));
#222564=CARTESIAN_POINT('Ctrl Pts',(-16.7438958886757,-6.12779835283271,
131.802080604377));
#222565=CARTESIAN_POINT('Ctrl Pts',(-17.0223435124885,-2.4728146076992,
136.499142943608));
#222566=CARTESIAN_POINT('Ctrl Pts',(-17.3007911363014,3.45456495820035,
135.96297853079));
#222567=CARTESIAN_POINT('Ctrl Pts',(-17.5792387601143,6.20736809239421,
130.686296268213));
#222568=CARTESIAN_POINT('Ctrl Pts',(-17.8576863839272,3.25590319646751,
125.518109374927));
#222569=CARTESIAN_POINT('Ctrl Pts',(-18.13613400774,-2.6875776772989,125.207729125896));
#222570=CARTESIAN_POINT('Ctrl Pts',(-18.414581631553,-6.16130596109642,
130.040379807061));
#222571=CARTESIAN_POINT('Ctrl Pts',(-18.6930292553659,-3.97309506317598,
135.575091530542));
#222572=CARTESIAN_POINT('Ctrl Pts',(-18.9714768791788,1.86619610131902,
136.72573460816));
#222573=CARTESIAN_POINT('Ctrl Pts',(-19.2499245029916,5.99054421744964,
132.434924263623));
#222574=CARTESIAN_POINT('Ctrl Pts',(-19.5283721268046,4.6098748520987,126.645705585822));
#222575=CARTESIAN_POINT('Ctrl Pts',(-19.8068197506174,-1.00704429742433,
124.678087720601));
#222576=CARTESIAN_POINT('Ctrl Pts',(-20.0852673744304,-5.6985389344635,
128.340215362621));
#222577=CARTESIAN_POINT('Ctrl Pts',(-20.3637149982432,-5.15335467983417,
134.266772113748));
#222578=CARTESIAN_POINT('Ctrl Pts',(-20.6421626220562,0.127510770190762,
137.011541848088));
#222579=CARTESIAN_POINT('Ctrl Pts',(-20.920610245869,5.29120005165768,134.05221526924));
#222580=CARTESIAN_POINT('Ctrl Pts',(-21.1990578696819,5.59253497514422,
128.108268932023));
#222581=CARTESIAN_POINT('Ctrl Pts',(-21.4775054934948,0.754603466995427,
124.64189914242));
#222582=CARTESIAN_POINT('Ctrl Pts',(-21.7559531173077,-4.77677176289349,
126.838530395495));
#222583=CARTESIAN_POINT('Ctrl Pts',(-22.0344007411205,-5.91852710095694,
132.679565881077));
#222584=CARTESIAN_POINT('Ctrl Pts',(-22.3128483649335,-1.62144516936395,
136.797379338361));
#222585=CARTESIAN_POINT('Ctrl Pts',(-22.5912959887463,4.16566566087426,
135.407901366475));
#222586=CARTESIAN_POINT('Ctrl Pts',(-22.8697436125593,6.12473325285015,
129.787994341809));
#222587=CARTESIAN_POINT('Ctrl Pts',(-23.1481912363721,2.45547019531011,
125.102078272311));
#222588=CARTESIAN_POINT('Ctrl Pts',(-23.426638860185,-3.47025001533206,
125.656281106122));
#222589=CARTESIAN_POINT('Ctrl Pts',(-23.7050864839979,-6.20697999302203,
130.941317513284));
#222590=CARTESIAN_POINT('Ctrl Pts',(-23.9835341078108,-3.23979858495512,
136.100497223997));
#222591=CARTESIAN_POINT('Ctrl Pts',(-24.2619817316237,2.70459944972584,
136.392786124057));
#222592=CARTESIAN_POINT('Ctrl Pts',(-24.5404293554366,6.16360271713728,
131.549584993415));
#222593=CARTESIAN_POINT('Ctrl Pts',(-24.8188769792495,3.95855619623184,
126.021559067602));
#222594=CARTESIAN_POINT('Ctrl Pts',(-25.0973246030624,-1.88421008278963,
124.88869411336));
#222595=CARTESIAN_POINT('Ctrl Pts',(-25.3757722268753,-5.99547934450715,
129.192037680109));
#222596=CARTESIAN_POINT('Ctrl Pts',(-25.6542198506882,-4.59719598407162,
134.977027260026));
#222597=CARTESIAN_POINT('Ctrl Pts',(-25.932667474501,1.02568590021626,136.92754004162));
#222598=CARTESIAN_POINT('Ctrl Pts',(-26.211115098314,5.7060125497474,133.251150066453));
#222599=CARTESIAN_POINT('Ctrl Pts',(-26.4895627221268,5.14279242027056,
127.326280120068));
#222600=CARTESIAN_POINT('Ctrl Pts',(-26.7680103459397,-0.146402704058008,
124.597596237205));
#222601=CARTESIAN_POINT('Ctrl Pts',(-27.0464579697526,-5.30106089552683,
127.572625602596));
#222602=CARTESIAN_POINT('Ctrl Pts',(-27.3249055935655,-5.58430309522854,
133.517461567711));
#222603=CARTESIAN_POINT('Ctrl Pts',(-27.6033532173784,-0.735843558787732,
136.969090301993));
#222604=CARTESIAN_POINT('Ctrl Pts',(-27.8818008411913,4.78882026022281,
134.755633620073));
#222605=CARTESIAN_POINT('Ctrl Pts',(-28.1602484650042,5.91279220696403,
128.911150079267));
#222606=CARTESIAN_POINT('Ctrl Pts',(-28.4386960888171,1.60319697146318,
124.806434534681));
#222607=CARTESIAN_POINT('Ctrl Pts',(-28.7171437126299,-4.17965796028613,
126.213520045287));
#222608=CARTESIAN_POINT('Ctrl Pts',(-28.9955913364429,-6.12161141417542,
131.839363766787));
#222609=CARTESIAN_POINT('Ctrl Pts',(-29.2740389602557,-2.43810303578058,
136.514090156867));
#222610=CARTESIAN_POINT('Ctrl Pts',(-29.5524865840687,3.48590292454168,
135.941854036124));
#222611=CARTESIAN_POINT('Ctrl Pts',(-29.8309342078815,6.20653439303521,
130.648512444231));
#222612=CARTESIAN_POINT('Ctrl Pts',(-30.1093818316944,3.22366396039099,
125.498387710026));
#222613=CARTESIAN_POINT('Ctrl Pts',(-30.3878294555073,-2.72159616711309,
125.224192866663));
#222614=CARTESIAN_POINT('Ctrl Pts',(-30.6662770793202,-6.16584237440457,
130.077899580028));
#222615=CARTESIAN_POINT('Ctrl Pts',(-30.9447247031331,-3.94398065776386,
135.599188497297));
#222616=CARTESIAN_POINT('Ctrl Pts',(-31.2231723269461,1.90220660919519,
136.714264833456));
#222617=CARTESIAN_POINT('Ctrl Pts',(-31.5016199507588,6.00035893026297,
132.398427910084));
#222618=CARTESIAN_POINT('Ctrl Pts',(-31.7800675745718,4.58447452824918,
126.617721019404));
#222619=CARTESIAN_POINT('Ctrl Pts',(-32.0585151983846,-1.04431800119413,
124.68433139072));
#222620=CARTESIAN_POINT('Ctrl Pts',(-32.3369628221976,-5.71343330531054,
128.374949641459));
#222621=CARTESIAN_POINT('Ctrl Pts',(-32.6154104460104,-5.1321825185805,
134.298077895915));
#222622=CARTESIAN_POINT('Ctrl Pts',(-32.8938580698234,0.165293281670594,
137.010650649146));
#222623=CARTESIAN_POINT('Ctrl Pts',(-33.1723056936362,5.31087263109202,
134.019946057479));
#222624=CARTESIAN_POINT('Ctrl Pts',(-33.4507533174492,5.57601948309184,
128.074275536613));
#222625=CARTESIAN_POINT('Ctrl Pts',(-33.729200941262,0.717076833825826,
124.637419833072));
#222626=CARTESIAN_POINT('Ctrl Pts',(-34.0076485650749,-4.80082439457541,
126.867681438675));
#222627=CARTESIAN_POINT('Ctrl Pts',(-34.2860961888878,-5.90700253767186,
132.715558892209));
#222628=CARTESIAN_POINT('Ctrl Pts',(-34.5645438127007,-1.58493392176466,
136.807138498572));
#222629=CARTESIAN_POINT('Ctrl Pts',(-34.8429914365135,4.19361153991761,
135.382458484293));
#222630=CARTESIAN_POINT('Ctrl Pts',(-35.1214390603265,6.11843286572883,
129.750730183006));
#222631=CARTESIAN_POINT('Ctrl Pts',(-35.3998866841394,2.42071328999757,
125.087236778371));
#222632=CARTESIAN_POINT('Ctrl Pts',(-35.6783343079523,-3.50152354082281,
125.677500884929));
#222633=CARTESIAN_POINT('Ctrl Pts',(-35.9567819317651,-6.20603129656164,
130.979098624759));
#222634=CARTESIAN_POINT('Ctrl Pts',(-36.2352295555781,-3.2074994722443,
136.120120672404));
#222635=CARTESIAN_POINT('Ctrl Pts',(-36.5136771793909,2.73856767200523,
136.376218918968));
#222636=CARTESIAN_POINT('Ctrl Pts',(-36.7921248032039,6.1680249121504,131.512051586954));
#222637=CARTESIAN_POINT('Ctrl Pts',(-37.0705724270167,3.92936858279784,
125.997550826698));
#222638=CARTESIAN_POINT('Ctrl Pts',(-37.3490200508296,-1.92018551381882,
124.900273438536));
#222639=CARTESIAN_POINT('Ctrl Pts',(-37.6274676746425,-6.00518292951342,
129.228563737208));
#222640=CARTESIAN_POINT('Ctrl Pts',(-37.9059152984554,-4.57171060248077,
135.004934386972));
#222641=CARTESIAN_POINT('Ctrl Pts',(-38.1843629222683,1.0629404277527,136.921182952087));
#222642=CARTESIAN_POINT('Ctrl Pts',(-38.4628105460811,5.72080113240803,
133.216370615161));
#222643=CARTESIAN_POINT('Ctrl Pts',(-38.7412581698941,5.12152507305273,
127.295038923683));
#222644=CARTESIAN_POINT('Ctrl Pts',(-39.0197057937069,-0.184182328028525,
124.598602428988));
#222645=CARTESIAN_POINT('Ctrl Pts',(-39.2981534175199,-5.32063516745863,
127.604954541453));
#222646=CARTESIAN_POINT('Ctrl Pts',(-39.5766010413327,-5.56768421547239,
133.55140453819));
#222647=CARTESIAN_POINT('Ctrl Pts',(-39.8550486651457,-0.698303465962086,
136.973455372429));
#222648=CARTESIAN_POINT('Ctrl Pts',(-40.1334962889585,4.81278405474664,
134.726409503982));
#222649=CARTESIAN_POINT('Ctrl Pts',(-40.4119439127715,5.90115814671511,
128.875192311658));
#222650=CARTESIAN_POINT('Ctrl Pts',(-40.6903915365843,1.56665618945481,
124.796786547352));
#222651=CARTESIAN_POINT('Ctrl Pts',(-40.9688391603973,-4.20752627050468,
126.239047867263));
#222652=CARTESIAN_POINT('Ctrl Pts',(-41.2472867842101,-6.11519763695597,
131.876608576776));
#222653=CARTESIAN_POINT('Ctrl Pts',(-41.5257344080229,-2.40330111905734,
136.528825793999));
#222654=CARTESIAN_POINT('Ctrl Pts',(-41.8041820318359,3.51711171946819,
135.920539169751));
#222655=CARTESIAN_POINT('Ctrl Pts',(-42.0826296556488,6.20547070826194,
130.610734395262));
#222656=CARTESIAN_POINT('Ctrl Pts',(-42.3610772794617,3.19130527026066,
125.478862659902));
#222657=CARTESIAN_POINT('Ctrl Pts',(-42.6395249032745,-2.75551380718057,
125.240863382598));
#222658=CARTESIAN_POINT('Ctrl Pts',(-42.9179725270875,-6.17015031015604,
130.115446272278));
#222659=CARTESIAN_POINT('Ctrl Pts',(-43.1964201509003,-3.91472010669807,
135.623107789941));
#222660=CARTESIAN_POINT('Ctrl Pts',(-43.4748677747133,1.93814663010615,
136.702576065077));
#222661=CARTESIAN_POINT('Ctrl Pts',(-43.7533153985261,6.00995129756958,
132.361872487794));
#222662=CARTESIAN_POINT('Ctrl Pts',(-44.031763022339,4.55890432500984,126.589891590455));
#222663=CARTESIAN_POINT('Ctrl Pts',(-44.3102106461518,-1.08155300737633,
124.690801840773));
#222664=CARTESIAN_POINT('Ctrl Pts',(-44.5886582699649,-5.72811596278534,
128.409773943013));
#222665=CARTESIAN_POINT('Ctrl Pts',(-44.8671058937777,-5.11082018241628,
134.329254217104));
#222666=CARTESIAN_POINT('Ctrl Pts',(-45.1455535175906,0.2030696681468,137.009529473845));
#222667=CARTESIAN_POINT('Ctrl Pts',(-45.4240011414034,5.33034841418793,
133.987557691017));
#222668=CARTESIAN_POINT('Ctrl Pts',(-45.7024487652165,5.55929736958694,
128.040383305508));
#222669=CARTESIAN_POINT('Ctrl Pts',(-45.9808963890292,0.679523629110432,
124.633169041983));
#222670=CARTESIAN_POINT('Ctrl Pts',(-46.2593440128422,-4.82469912994364,
126.896978356949));
#222671=CARTESIAN_POINT('Ctrl Pts',(-46.537791636655,-5.89525908823553,
132.751481083186));
#222672=CARTESIAN_POINT('Ctrl Pts',(-46.816239260468,-1.54836394385628,
136.816675223641));
#222673=CARTESIAN_POINT('Ctrl Pts',(-47.0946868842807,4.22140202314317,
135.35684595901));
#222674=CARTESIAN_POINT('Ctrl Pts',(-47.3731345080937,6.11190575782758,
129.713505066864));
#222675=CARTESIAN_POINT('Ctrl Pts',(-47.6515821319066,2.38586668426401,
125.072607134557));
#222676=CARTESIAN_POINT('Ctrl Pts',(-47.9300297557195,-3.53266731607082,
125.69891064141));
#222677=CARTESIAN_POINT('Ctrl Pts',(-48.2084773795324,-6.20485263332943,
131.016873261253));
#222678=CARTESIAN_POINT('Ctrl Pts',(-48.4869250033452,-3.17508150446096,
136.139547143367));
#222679=CARTESIAN_POINT('Ctrl Pts',(-48.7653726271582,2.77243441565242,
136.359445246621));
#222680=CARTESIAN_POINT('Ctrl Pts',(-49.043820250971,6.1722185487321,131.474491956744));
#222681=CARTESIAN_POINT('Ctrl Pts',(-49.322267874784,3.900035365166,125.973720703898));
#222682=CARTESIAN_POINT('Ctrl Pts',(-49.6007154985968,-1.95608979166789,
124.912071541833));
#222683=CARTESIAN_POINT('Ctrl Pts',(-49.8791631224098,-6.0146639902579,
129.265148186042));
#222684=CARTESIAN_POINT('Ctrl Pts',(-50.1576107462225,-4.54605581447205,
135.032685860113));
#222685=CARTESIAN_POINT('Ctrl Pts',(-50.4360583700356,1.10015556764067,
136.914599201455));
#222686=CARTESIAN_POINT('Ctrl Pts',(-50.7145059938484,5.73537772867887,
133.181501785951));
#222687=CARTESIAN_POINT('Ctrl Pts',(-50.9929536176612,5.10006794583985,
127.263927766504));
#222688=CARTESIAN_POINT('Ctrl Pts',(-51.2714012414742,-0.221955127055423,
124.599838577421));
#222689=CARTESIAN_POINT('Ctrl Pts',(-51.5498488652871,-5.34001228129766,
127.637402035479));
#222690=CARTESIAN_POINT('Ctrl Pts',(-51.8282964891,-5.5508590231301,133.585245715947));
#222691=CARTESIAN_POINT('Ctrl Pts',(-52.1067441129128,-0.660737497244709,
136.977591844792));
#222692=CARTESIAN_POINT('Ctrl Pts',(-52.3851917367258,4.8365695097872,134.697040054928));
#222693=CARTESIAN_POINT('Ctrl Pts',(-52.6636393605386,5.889305416881,128.83930603009));
#222694=CARTESIAN_POINT('Ctrl Pts',(-52.9420869843516,1.53005735442545,
124.78736117289));
#222695=CARTESIAN_POINT('Ctrl Pts',(-53.2205346081644,-4.23523866929,126.264744858582));
#222696=CARTESIAN_POINT('Ctrl Pts',(-53.4989822319774,-6.1085572588392,
131.913813654221));
#222697=CARTESIAN_POINT('Ctrl Pts',(-53.7774298557902,-2.36841014712749,
136.543349308967));
#222698=CARTESIAN_POINT('Ctrl Pts',(-54.0558774796031,3.54819018652628,
135.8990347215));
#222699=CARTESIAN_POINT('Ctrl Pts',(-54.334325103416,6.20417707748961,130.572963521183));
#222700=CARTESIAN_POINT('Ctrl Pts',(-54.6127727272289,3.15882832513996,
125.459534948064));
#222701=CARTESIAN_POINT('Ctrl Pts',(-54.8912203510417,-2.7893293406706,
125.257740055968));
#222702=CARTESIAN_POINT('Ctrl Pts',(-55.1696679748547,-6.17422960871856,
130.153018492501));
#222703=CARTESIAN_POINT('Ctrl Pts',(-55.4481155986676,-3.88531449423931,
135.646848522136));
#222704=CARTESIAN_POINT('Ctrl Pts',(-55.7265632224805,1.97401483228084,
136.690668736158));
#222705=CARTESIAN_POINT('Ctrl Pts',(-56.0050108462934,6.01932096392068,
132.32525935133));
#222706=CARTESIAN_POINT('Ctrl Pts',(-56.2834584701062,4.53316518989421,
126.562218330207));
#222707=CARTESIAN_POINT('Ctrl Pts',(-56.5619060939192,-1.11874793621411,
124.697498830995));
#222708=CARTESIAN_POINT('Ctrl Pts',(-56.840353717732,-5.74258636281662,
128.444686976857));
#222709=CARTESIAN_POINT('Ctrl Pts',(-57.118801341545,-5.08926846293066,
134.360299922064));
#222710=CARTESIAN_POINT('Ctrl Pts',(-57.3972489653578,0.240838529802063,
137.00817836373));
#222711=CARTESIAN_POINT('Ctrl Pts',(-57.6756965891708,5.34962667926312,
133.955051370017));
#222712=CARTESIAN_POINT('Ctrl Pts',(-57.9541442129836,5.54236925427356,
128.0065934946));
#222713=CARTESIAN_POINT('Ctrl Pts',(-58.2325918367966,0.641945244397073,
124.629146926667));
#222714=CARTESIAN_POINT('Ctrl Pts',(-58.5110394606094,-4.84839508431156,
126.92642006471));
#222715=CARTESIAN_POINT('Ctrl Pts',(-58.7894870844223,-5.88329718780563,
132.787331122898));
#222716=CARTESIAN_POINT('Ctrl Pts',(-59.0679347082352,-1.5117365907523,
136.825989160181));
#222717=CARTESIAN_POINT('Ctrl Pts',(-59.3463823320481,4.24903608076433,
135.331064739709));
#222718=CARTESIAN_POINT('Ctrl Pts',(-59.624829955861,6.10515217101086,129.676320372777));
#222719=CARTESIAN_POINT('Ctrl Pts',(-59.9032775796738,2.3509316693629,125.058189882977));
#222720=CARTESIAN_POINT('Ctrl Pts',(-60.1817252034868,-3.56368018703254,
125.720509582217));
#222721=CARTESIAN_POINT('Ctrl Pts',(-60.4601728272995,-6.20344404700091,
131.054640023013));
#222722=CARTESIAN_POINT('Ctrl Pts',(-60.7386204511126,-3.14254588286485,
136.158775917031));
#222723=CARTESIAN_POINT('Ctrl Pts',(-61.0170680749254,2.80619842572279,
136.342465728569));
#222724=CARTESIAN_POINT('Ctrl Pts',(-61.2955156987383,6.17618347148551,
131.436907494571));
#222725=CARTESIAN_POINT('Ctrl Pts',(-61.5739633225512,3.87055763028967,
125.950069582238));
#222726=CARTESIAN_POINT('Ctrl Pts',(-61.8524109463641,-1.9919215858902,
124.924087986069));
#222727=CARTESIAN_POINT('Ctrl Pts',(-62.130858570177,-6.02392217541635,
129.301789670958));
#222728=CARTESIAN_POINT('Ctrl Pts',(-62.4093061939898,-4.5202325706933,
135.060280651108));
#222729=CARTESIAN_POINT('Ctrl Pts',(-62.6877538178028,1.13732994085927,
136.907789033684));
#222730=CARTESIAN_POINT('Ctrl Pts',(-62.9662014416156,5.74974179841868,
133.146544870902));
#222731=CARTESIAN_POINT('Ctrl Pts',(-63.2446490654287,5.0784218337339,127.232947801366));
#222732=CARTESIAN_POINT('Ctrl Pts',(-63.5230966892413,-0.25971970145348,
124.601304636701));
#222733=CARTESIAN_POINT('Ctrl Pts',(-63.8015443130544,-5.3591915190178,
127.669966882319));
#222734=CARTESIAN_POINT('Ctrl Pts',(-64.0799919368672,-5.53382814166538,
133.618983846983));
#222735=CARTESIAN_POINT('Ctrl Pts',(-64.3584395606801,-0.623147044656387,
136.9814995658));
#222736=CARTESIAN_POINT('Ctrl Pts',(-64.636887184493,4.86017574396616,134.667526361205));
#222737=CARTESIAN_POINT('Ctrl Pts',(-64.9153348083059,5.8772344566688,128.803492564343));
#222738=CARTESIAN_POINT('Ctrl Pts',(-65.1937824321189,1.4934018225579,124.778158760555));
#222739=CARTESIAN_POINT('Ctrl Pts',(-65.4722300559316,-4.26279412974889,
126.290610067033));
#222740=CARTESIAN_POINT('Ctrl Pts',(-65.7506776797446,-6.10169052588679,
131.950977620477));
#222741=CARTESIAN_POINT('Ctrl Pts',(-66.0291253035574,-2.33343141288849,
136.5576601636));
#222742=CARTESIAN_POINT('Ctrl Pts',(-66.3075729273703,3.57913717409239,
135.877341488227));
#222743=CARTESIAN_POINT('Ctrl Pts',(-66.5860205511832,6.20265354865397,
130.535201221608));
#222744=CARTESIAN_POINT('Ctrl Pts',(-66.8644681749961,3.126234328474,125.440405290707));
#222745=CARTESIAN_POINT('Ctrl Pts',(-67.142915798809,-2.82304151453613,
125.274822261403));
#222746=CARTESIAN_POINT('Ctrl Pts',(-67.421363422622,-6.17808011893247,
130.190614848446));
#222747=CARTESIAN_POINT('Ctrl Pts',(-67.6998110464348,-3.85576491002292,
135.670409814162));
#222748=CARTESIAN_POINT('Ctrl Pts',(-67.9782586702478,2.00980988661012,
136.678543287925));
#222749=CARTESIAN_POINT('Ctrl Pts',(-68.2567062940606,6.02846758211988,
132.288589857404));
#222750=CARTESIAN_POINT('Ctrl Pts',(-68.5351539178734,4.50725807667536,
126.534702264101));
#222751=CARTESIAN_POINT('Ctrl Pts',(-68.8136015416864,-1.15590140943545,
124.704422113226));
#222752=CARTESIAN_POINT('Ctrl Pts',(-69.0920491654993,-5.75684396919829,
128.479687449276));
#222753=CARTESIAN_POINT('Ctrl Pts',(-69.3704967893121,-5.0675281587308,
134.391213860386));
#222754=CARTESIAN_POINT('Ctrl Pts',(-69.648944413125,0.278598467097045,
137.006597368867));
#222755=CARTESIAN_POINT('Ctrl Pts',(-69.9273920369379,5.36870671195437,
133.922428299012));
#222756=CARTESIAN_POINT('Ctrl Pts',(-70.2058396607509,5.52523576442926,
127.972907355982));
#222757=CARTESIAN_POINT('Ctrl Pts',(-70.4842872845636,0.604343072166899,
124.625353636165));
#222758=CARTESIAN_POINT('Ctrl Pts',(-70.7627349083767,-4.87191137961658,
126.956005470983));
#222759=CARTESIAN_POINT('Ctrl Pts',(-71.0411825321895,-5.87111727963483,
132.823107682909));
#222760=CARTESIAN_POINT('Ctrl Pts',(-71.3196301560023,-1.47505321969301,
136.835079963061));
#222761=CARTESIAN_POINT('Ctrl Pts',(-71.5980777798154,4.27651268879093,
135.305115781721));
#222762=CARTESIAN_POINT('Ctrl Pts',(-71.8765254036282,6.09817235553532,
129.639177478635));
#222763=CARTESIAN_POINT('Ctrl Pts',(-72.1549730274411,2.31590953982396,
125.043985557866));
#222764=CARTESIAN_POINT('Ctrl Pts',(-72.433420651254,-3.5945610045145,125.742296906994));
#222765=CARTESIAN_POINT('Ctrl Pts',(-72.7118682750669,-6.20180558977201,
131.092397510578));
#222766=CARTESIAN_POINT('Ctrl Pts',(-72.9903158988798,-3.109893813075,136.177806280867));
#222767=CARTESIAN_POINT('Ctrl Pts',(-73.2687635226926,2.8398584510789,136.325280993997));
#222768=CARTESIAN_POINT('Ctrl Pts',(-73.5472111465057,6.17991953348924,
131.399299593141));
#222769=CARTESIAN_POINT('Ctrl Pts',(-73.8256587703184,3.84093647047644,
125.926598338115));
#222770=CARTESIAN_POINT('Ctrl Pts',(-74.1041063941314,-2.02767956872624,
124.93632232597));
#222771=CARTESIAN_POINT('Ctrl Pts',(-74.3825540179442,-6.0329571419232,
129.338486834193));
#222772=CARTESIAN_POINT('Ctrl Pts',(-74.6610016417573,-4.49424182803428,
135.08771773742));
#222773=CARTESIAN_POINT('Ctrl Pts',(-74.9394492655699,1.17446216989917,
136.900752701129));
#222774=CARTESIAN_POINT('Ctrl Pts',(-75.217896889383,5.76389280936176,133.111501165354));
#222775=CARTESIAN_POINT('Ctrl Pts',(-75.4963445131958,5.05658753883907,
127.202100176243));
#222776=CARTESIAN_POINT('Ctrl Pts',(-75.7747921370087,-0.297474651842549,
124.603000552501));
#222777=CARTESIAN_POINT('Ctrl Pts',(-76.0532397608216,-5.37817216992523,
127.702647875272));
#222778=CARTESIAN_POINT('Ctrl Pts',(-76.3316873846344,-5.51659220216403,
133.65261768112));
#222779=CARTESIAN_POINT('Ctrl Pts',(-76.6101350084474,-0.585533501125347,
136.985178390654));
#222780=CARTESIAN_POINT('Ctrl Pts',(-76.8885826322602,4.8836018825454,134.637869516455));
#222781=CARTESIAN_POINT('Ctrl Pts',(-77.1670302560731,5.86494571337264,
128.767753241497));
#222782=CARTESIAN_POINT('Ctrl Pts',(-77.4454778798861,1.4566909521364,124.769179651345));
#222783=CARTESIAN_POINT('Ctrl Pts',(-77.7239255036988,-4.29019163080361,
126.316642534169));
#222784=CARTESIAN_POINT('Ctrl Pts',(-78.0023731275119,-6.09459769254796,
131.988099098418));
#222785=CARTESIAN_POINT('Ctrl Pts',(-78.2808207513247,-2.29836621249045,
136.571757827603));
#222786=CARTESIAN_POINT('Ctrl Pts',(-78.5592683751376,3.60995153541429,
135.855460273781));
#222787=CARTESIAN_POINT('Ctrl Pts',(-78.8377159989505,6.20090017820995,
130.497448895834));
#222788=CARTESIAN_POINT('Ctrl Pts',(-79.1161636227633,3.09352448804556,
125.421474396687));
#222789=CARTESIAN_POINT('Ctrl Pts',(-79.3946112465763,-2.85664907955992,
125.292109365916));
#222790=CARTESIAN_POINT('Ctrl Pts',(-79.6730588703891,-6.18170169811556,
130.228233946967));
#222791=CARTESIAN_POINT('Ctrl Pts',(-79.9515064942021,-3.8260724490201,
135.693790792945));
#222792=CARTESIAN_POINT('Ctrl Pts',(-80.2299541180149,2.04553046669522,
136.666200169693));
#222793=CARTESIAN_POINT('Ctrl Pts',(-80.5084017418279,6.03739081323573,
132.251865364817));
#222794=CARTESIAN_POINT('Ctrl Pts',(-80.7868493656406,4.48118394535095,
126.507344411756));
#222795=CARTESIAN_POINT('Ctrl Pts',(-81.0652969894537,-1.19301205030527,
124.711571430921));
#222796=CARTESIAN_POINT('Ctrl Pts',(-81.3437446132665,-5.77088825360962,
128.514774063314));
#222797=CARTESIAN_POINT('Ctrl Pts',(-81.6221922370794,-5.04560007541116,
134.421994886542));
#222798=CARTESIAN_POINT('Ctrl Pts',(-81.9006398608923,0.316348080823153,
137.00478654784));
#222799=CARTESIAN_POINT('Ctrl Pts',(-82.179087484705,5.38758780524389,133.889689686862));
#222800=CARTESIAN_POINT('Ctrl Pts',(-82.4575351085182,5.50789753494193,
127.939326137905));
#222801=CARTESIAN_POINT('Ctrl Pts',(-82.7359827323308,0.566718505781886,
124.621789311041));
#222802=CARTESIAN_POINT('Ctrl Pts',(-83.0144303561439,-4.89524714445407,
126.985733479472));
#222803=CARTESIAN_POINT('Ctrl Pts',(-83.2928779799568,-5.858719815054,132.858809437506));
#222804=CARTESIAN_POINT('Ctrl Pts',(-83.5713256037696,-1.43831518999427,
136.843947295418));
#222805=CARTESIAN_POINT('Ctrl Pts',(-83.8497732275826,4.30383082906709,
135.279000046597));
#222806=CARTESIAN_POINT('Ctrl Pts',(-84.1282208513953,6.09096657004034,
129.602077760783));
#222807=CARTESIAN_POINT('Ctrl Pts',(-84.4066684752085,2.28080159340614,
125.029994685571));
#222808=CARTESIAN_POINT('Ctrl Pts',(-84.685116099021,-3.6253086242162,125.764271808403));
#222809=CARTESIAN_POINT('Ctrl Pts',(-84.9635637228342,-6.19993732235617,
131.130144324829));
#222810=CARTESIAN_POINT('Ctrl Pts',(-85.242011346647,-3.07712650502686,
136.196637529698));
#222811=CARTESIAN_POINT('Ctrl Pts',(-85.5204589704598,2.87341324443482,
136.307891679689));
#222812=CARTESIAN_POINT('Ctrl Pts',(-85.7989065942728,6.18342659630218,
131.361669646028));
#222813=CARTESIAN_POINT('Ctrl Pts',(-86.0773542180856,3.81117298335027,
125.903307841269));
#222814=CARTESIAN_POINT('Ctrl Pts',(-86.3558018418987,-2.06336241514917,
124.948774108188));
#222815=CARTESIAN_POINT('Ctrl Pts',(-86.6342494657113,-6.04176855498474,
129.375238315919));
#222816=CARTESIAN_POINT('Ctrl Pts',(-86.9126970895244,-4.46808454959173,
135.114996102359));
#222817=CARTESIAN_POINT('Ctrl Pts',(-87.1911447133372,1.2115508788106,136.893490464523));
#222818=CARTESIAN_POINT('Ctrl Pts',(-87.4695923371502,5.77783023713722,
133.076371967865));
#222819=CARTESIAN_POINT('Ctrl Pts',(-87.7480399609628,5.03456587023344,
127.171386034204));
#222820=CARTESIAN_POINT('Ctrl Pts',(-88.026487584776,-0.33521857919891,
124.60492626198));
#222821=CARTESIAN_POINT('Ctrl Pts',(-88.3049352085887,-5.39695353068522,
127.735443803332));
#222822=CARTESIAN_POINT('Ctrl Pts',(-88.5833828324018,-5.49915184330967,
133.686145972045));
#222823=CARTESIAN_POINT('Ctrl Pts',(-88.8618304562145,-0.547898260434929,
136.988628183031));
#222824=CARTESIAN_POINT('Ctrl Pts',(-89.1402780800275,4.90684705746115,
134.608070619623));
#222825=CARTESIAN_POINT('Ctrl Pts',(-89.4187257038403,5.85243964235601,
128.732089385887));
#222826=CARTESIAN_POINT('Ctrl Pts',(-89.6971733276532,1.41992610349655,
124.760424177987));
#222827=CARTESIAN_POINT('Ctrl Pts',(-89.9756209514662,-4.31743015722937,
126.342841295349));
#222828=CARTESIAN_POINT('Ctrl Pts',(-90.254068575279,-6.08727902165076,
132.025176712493));
#222829=CARTESIAN_POINT('Ctrl Pts',(-90.5325161990919,-2.26321584528708,
136.585641778581));
#222830=CARTESIAN_POINT('Ctrl Pts',(-90.8109638229048,3.64063212865448,
135.833391888981));
#222831=CARTESIAN_POINT('Ctrl Pts',(-91.0894114467178,6.19891703112955,
130.459707942787));
#222832=CARTESIAN_POINT('Ctrl Pts',(-91.3678590705306,3.06070001592934,
125.402742967496));
#222833=CARTESIAN_POINT('Ctrl Pts',(-91.6463066943433,-2.89015079040179,
125.309600728926));
#222834=CARTESIAN_POINT('Ctrl Pts',(-91.9247543181566,-6.18509421206894,
130.265874394073));
#222835=CARTESIAN_POINT('Ctrl Pts',(-92.2032019419691,-3.79623821149537,
135.716990592095));
#222836=CARTESIAN_POINT('Ctrl Pts',(-92.4816495657822,2.08117524889636,
136.653639838841));
#222837=CARTESIAN_POINT('Ctrl Pts',(-92.7600971895951,6.04609032661485,
132.21508723441));
#222838=CARTESIAN_POINT('Ctrl Pts',(-93.0385448134079,4.45494376210749,
126.480145786926));
#222839=CARTESIAN_POINT('Ctrl Pts',(-93.3169924372209,-1.23007848367479,
124.718946519161));
#222840=CARTESIAN_POINT('Ctrl Pts',(-93.5954400610337,-5.78471869563455,
128.549945518824));
#222841=CARTESIAN_POINT('Ctrl Pts',(-93.8738876848466,-5.02348502552524,
134.45264185993));
#222842=CARTESIAN_POINT('Ctrl Pts',(-94.1523353086595,0.354085972155003,
137.002745967751));
#222843=CARTESIAN_POINT('Ctrl Pts',(-94.4307829324724,5.40626925948619,
133.85683674671));
#222844=CARTESIAN_POINT('Ctrl Pts',(-94.7092305562852,5.49035520828578,
127.905851084735));
#222845=CARTESIAN_POINT('Ctrl Pts',(-94.9876781800983,0.529072939433998,
124.618454083368));
#222846=CARTESIAN_POINT('Ctrl Pts',(-95.2661258039109,-4.91840151410816,
127.015602988595));
#222847=CARTESIAN_POINT('Ctrl Pts',(-95.5445734277241,-5.84610525345601,
132.894435063746));
#222848=CARTESIAN_POINT('Ctrl Pts',(-95.8230210515366,-1.40152386299717,
136.85259082867));
#222849=CARTESIAN_POINT('Ctrl Pts',(-96.10146867535,4.33098948930923,135.252718502061));
#222850=CARTESIAN_POINT('Ctrl Pts',(-96.3799162991623,6.08353508153927,
129.565022593965));
#222851=CARTESIAN_POINT('Ctrl Pts',(-96.6583639229758,2.245609131046,125.01621778453));
#222852=CARTESIAN_POINT('Ctrl Pts',(-96.9368115467883,-3.65592190677386,
125.786433472156));
#222853=CARTESIAN_POINT('Ctrl Pts',(-97.2152591706015,-6.19783931398261,
131.167879067045));
#222854=CARTESIAN_POINT('Ctrl Pts',(-97.493706794414,-3.04424517292474,
136.215268965725));
#222855=CARTESIAN_POINT('Ctrl Pts',(-97.7721544182274,2.90686156240656,
136.290298430015));
#222856=CARTESIAN_POINT('Ctrl Pts',(-98.0506020420397,6.18670452996842,
131.324019047625));
#222857=CARTESIAN_POINT('Ctrl Pts',(-98.3290496658531,3.78126827180747,
125.880198954735));
#222858=CARTESIAN_POINT('Ctrl Pts',(-98.6074972896656,-2.09896880291958,
124.961442871316));
#222859=CARTESIAN_POINT('Ctrl Pts',(-98.8859449134787,-6.05035608809047,
129.412042754299));
#222860=CARTESIAN_POINT('Ctrl Pts',(-99.1643925372916,-4.44176170463296,
135.142114735114));
#222861=CARTESIAN_POINT('Ctrl Pts',(-99.4428401611044,1.24859469325925,
136.886002592972));
#222862=CARTESIAN_POINT('Ctrl Pts',(-99.7212877849174,5.79155356528836,
133.041158580159));
#222863=CARTESIAN_POINT('Ctrl Pts',(-99.9997354087301,5.01235764393804,
127.140806513377));
#222864=CARTESIAN_POINT('Ctrl Pts',(-100.278183032543,-0.37295008490757,
124.607081693777));
#222865=CARTESIAN_POINT('Ctrl Pts',(-100.556630656356,-5.41553490534739,
127.768353451233));
#222866=CARTESIAN_POINT('Ctrl Pts',(-100.835078280169,-5.48150771136145,
133.719567477352));
#222867=CARTESIAN_POINT('Ctrl Pts',(-101.113525903981,-0.510242717172956,
136.9918488151));
#222868=CARTESIAN_POINT('Ctrl Pts',(-101.391973527794,4.92991040735466,
134.578130774917));
#222869=CARTESIAN_POINT('Ctrl Pts',(-101.670421151607,5.83971670703623,
128.696502319049));
#222870=CARTESIAN_POINT('Ctrl Pts',(-101.94886877542,1.38310863897239,124.751892664915));
#222871=CARTESIAN_POINT('Ctrl Pts',(-102.227316399233,-4.34450869969331,
126.36920537977));
#222872=CARTESIAN_POINT('Ctrl Pts',(-102.505764023046,-6.07973478439049,
132.062209088779));
#222873=CARTESIAN_POINT('Ctrl Pts',(-102.784211646859,-2.22798161378826,
136.599311502058));
#222874=CARTESIAN_POINT('Ctrl Pts',(-103.062659270672,3.6711778169323,135.811137151577));
#222875=CARTESIAN_POINT('Ctrl Pts',(-103.341106894485,6.19670418089893,
130.42197976097));
#222876=CARTESIAN_POINT('Ctrl Pts',(-103.619554518298,3.02776212844844,
125.384211697232));
#222877=CARTESIAN_POINT('Ctrl Pts',(-103.89800214211,-2.92354540564323,
125.327295702285));
#222878=CARTESIAN_POINT('Ctrl Pts',(-104.176449765923,-6.18825753508174,
130.303534794984));
#222879=CARTESIAN_POINT('Ctrl Pts',(-104.454897389736,-3.76626330296762,
135.740008351935));
#222880=CARTESIAN_POINT('Ctrl Pts',(-104.733345013549,2.1167429123828,136.640862760796));
#222881=CARTESIAN_POINT('Ctrl Pts',(-105.011792637362,6.05456579989334,
132.17825682901));
#222882=CARTESIAN_POINT('Ctrl Pts',(-105.290240261175,4.42853849928509,
126.453107397468));
#222883=CARTESIAN_POINT('Ctrl Pts',(-105.568687884988,-1.26709933603374,
124.726547104658));
#222884=CARTESIAN_POINT('Ctrl Pts',(-105.847135508801,-5.79833478278087,
128.585200512514));
#222885=CARTESIAN_POINT('Ctrl Pts',(-106.125583132613,-5.00118382855433,
134.483153644914));
#222886=CARTESIAN_POINT('Ctrl Pts',(-106.404030756427,0.391810742700936,
137.000475704212));
#222887=CARTESIAN_POINT('Ctrl Pts',(-106.682478380239,5.42475038243292,
133.823870695931));
#222888=CARTESIAN_POINT('Ctrl Pts',(-106.960926004052,5.47260943449832,
127.872483436902));
#222889=CARTESIAN_POINT('Ctrl Pts',(-107.239373627865,0.491407768093767,
124.615348076738));
#222890=CARTESIAN_POINT('Ctrl Pts',(-107.517821251678,-4.94137363058539,
127.045612891524));
#222891=CARTESIAN_POINT('Ctrl Pts',(-107.796268875491,-5.83327406227795,
132.929983241508));
#222892=CARTESIAN_POINT('Ctrl Pts',(-108.074716499304,-1.36468060201792,
136.861010242526));
#222893=CARTESIAN_POINT('Ctrl Pts',(-108.353164123117,4.3579876631431,135.22627212199));
#222894=CARTESIAN_POINT('Ctrl Pts',(-108.631611746929,6.07587816540856,
129.528013351273));
#222895=CARTESIAN_POINT('Ctrl Pts',(-108.910059370743,2.21033345681367,
125.00265536525));
#222896=CARTESIAN_POINT('Ctrl Pts',(-109.188506994555,-3.68639971780079,
125.808781077045));
#222897=CARTESIAN_POINT('Ctrl Pts',(-109.466954618368,-6.19551164239422,
131.205600338952));
#222898=CARTESIAN_POINT('Ctrl Pts',(-109.745402242181,-3.01125103519769,
136.233699898554));
#222899=CARTESIAN_POINT('Ctrl Pts',(-110.023849865994,2.94020216555433,
136.272501896897));
#222900=CARTESIAN_POINT('Ctrl Pts',(-110.302297489807,6.18975321302316,
131.286349193086));
#222901=CARTESIAN_POINT('Ctrl Pts',(-110.58074511362,3.75122344397827,125.857272534824));
#222902=CARTESIAN_POINT('Ctrl Pts',(-110.859192737433,-2.13449741262907,
124.974328145912));
#222903=CARTESIAN_POINT('Ctrl Pts',(-111.137640361246,-6.05871942302636,
129.44889878553));
#222904=CARTESIAN_POINT('Ctrl Pts',(-111.416087985058,-4.41527426856075,
135.169072630797));
#222905=CARTESIAN_POINT('Ctrl Pts',(-111.694535608871,1.28559224057236,
136.878289363941));
#222906=CARTESIAN_POINT('Ctrl Pts',(-111.972983232684,5.8050622852923,133.005862307081));
#222907=CARTESIAN_POINT('Ctrl Pts',(-112.251430856497,4.9899636828869,127.110362746893));
#222908=CARTESIAN_POINT('Ctrl Pts',(-112.52987848031,-0.410667770813077,
124.609466768025));
#222909=CARTESIAN_POINT('Ctrl Pts',(-112.808326104123,-5.43391560537209,
127.801375599495));
#222910=CARTESIAN_POINT('Ctrl Pts',(-113.086773727936,-5.46366046012913,
133.752880958598));
#222911=CARTESIAN_POINT('Ctrl Pts',(-113.365221351749,-0.472568266679477,
136.994840167519));
#222912=CARTESIAN_POINT('Ctrl Pts',(-113.643668975562,4.95279107760506,
134.548051091771));
#222913=CARTESIAN_POINT('Ctrl Pts',(-113.922116599375,5.8267773788663,128.660993359675));
#222914=CARTESIAN_POINT('Ctrl Pts',(-114.200564223187,1.34623992284899,
124.74358542827));
#222915=CARTESIAN_POINT('Ctrl Pts',(-114.479011847001,-4.37142625478972,
126.395733810498));
#222916=CARTESIAN_POINT('Ctrl Pts',(-114.757459470813,-6.07196526032194,
132.099194855029));
#222917=CARTESIAN_POINT('Ctrl Pts',(-115.035907094626,-2.19266482361144,
136.612766491501));
#222918=CARTESIAN_POINT('Ctrl Pts',(-115.314354718439,3.70158746836604,
135.788696886227));
#222919=CARTESIAN_POINT('Ctrl Pts',(-115.592802342252,6.19426170951602,
130.384265748418));
#222920=CARTESIAN_POINT('Ctrl Pts',(-115.871249966065,2.99471204612843,
125.36588127258));
#222921=CARTESIAN_POINT('Ctrl Pts',(-116.149697589878,-2.95683168783455,
125.345193630298));
#222922=CARTESIAN_POINT('Ctrl Pts',(-116.428145213691,-6.19119154993583,
130.34121375418));
#222923=CARTESIAN_POINT('Ctrl Pts',(-116.706592837503,-3.73614883416816,
135.762843219532));
#222924=CARTESIAN_POINT('Ctrl Pts',(-116.985040461316,2.1522321391827,136.627869409019));
#222925=CARTESIAN_POINT('Ctrl Pts',(-117.263488085129,6.06281691900968,
132.14137551338));
#222926=CARTESIAN_POINT('Ctrl Pts',(-117.541935708942,4.40196913533955,
126.426230245297));
#222927=CARTESIAN_POINT('Ctrl Pts',(-117.820383332755,-1.30407323556081,
124.73437290577));
#222928=CARTESIAN_POINT('Ctrl Pts',(-118.098830956568,-5.81173601049948,
128.620537737998));
#222929=CARTESIAN_POINT('Ctrl Pts',(-118.377278580381,-4.97869731087745,
134.51352911087));
#222930=CARTESIAN_POINT('Ctrl Pts',(-118.655726204194,0.429520994555717,
136.997975841351));
#222931=CARTESIAN_POINT('Ctrl Pts',(-118.934173828006,5.44303048925927,
133.790792756097));
#222932=CARTESIAN_POINT('Ctrl Pts',(-119.21262145182,5.45466087115571,127.839224430854));
#222933=CARTESIAN_POINT('Ctrl Pts',(-119.491069075632,0.453724387457947,
124.612471406243));
#222934=CARTESIAN_POINT('Ctrl Pts',(-119.769516699445,-4.96416264264509,
127.075762076232));
#222935=CARTESIAN_POINT('Ctrl Pts',(-120.047964323258,-5.82022671698453,
132.965452653541));
#222936=CARTESIAN_POINT('Ctrl Pts',(-120.326411947071,-1.32778677229758,
136.869205225004));
#222937=CARTESIAN_POINT('Ctrl Pts',(-120.604859570884,4.38482435014149,
135.199661886361));
#222938=CARTESIAN_POINT('Ctrl Pts',(-120.883307194697,6.06799610537801,
129.491051404098));
#222939=CARTESIAN_POINT('Ctrl Pts',(-121.16175481851,2.17497587786225,124.989307930291));
#222940=CARTESIAN_POINT('Ctrl Pts',(-121.440202442323,-3.71674092793051,
125.831313794972));
#222941=CARTESIAN_POINT('Ctrl Pts',(-121.718650066136,-6.19295439384353,
131.243306742772));
#222942=CARTESIAN_POINT('Ctrl Pts',(-121.997097689948,-2.97814531445616,
136.251929645219));
#222943=CARTESIAN_POINT('Ctrl Pts',(-122.275545313761,2.97343381842962,
136.254502739794));
#222944=CARTESIAN_POINT('Ctrl Pts',(-122.553992937574,6.19257253249627,
131.248661478285));
#222945=CARTESIAN_POINT('Ctrl Pts',(-122.832440561387,3.72103961318487,
125.83452943108));
#222946=CARTESIAN_POINT('Ctrl Pts',(-123.1108881852,-2.16994692775201,124.987429454503));
#222947=CARTESIAN_POINT('Ctrl Pts',(-123.389335809013,-6.06685824988591,
129.485805043896));
#222948=CARTESIAN_POINT('Ctrl Pts',(-123.667783432826,-4.38862322287681,
135.19586879047));
#222949=CARTESIAN_POINT('Ctrl Pts',(-123.946231056639,1.32254214979223,
136.870351063246));
#222950=CARTESIAN_POINT('Ctrl Pts',(-124.224678680451,5.81835589657845,
132.97048445655));
#222951=CARTESIAN_POINT('Ctrl Pts',(-124.503126304264,4.96738481689638,
127.080055862859));
#222952=CARTESIAN_POINT('Ctrl Pts',(-124.781573928077,-0.448370239273912,
124.612081396343));
#222953=CARTESIAN_POINT('Ctrl Pts',(-125.06002155189,-5.4520949496557,127.834509024472));
#222954=CARTESIAN_POINT('Ctrl Pts',(-125.338469175703,-5.44561075094924,
133.786085181339));
#222955=CARTESIAN_POINT('Ctrl Pts',(-125.616916799516,-0.434876304995071,
136.997602129441));
#222956=CARTESIAN_POINT('Ctrl Pts',(-125.895364423329,4.97548822036069,
134.517832684797));
#222957=CARTESIAN_POINT('Ctrl Pts',(-126.173812047142,5.8136221373178,128.625563823564));
#222958=CARTESIAN_POINT('Ctrl Pts',(-126.452259670955,1.30932132131015,
124.735502775877));
#222959=CARTESIAN_POINT('Ctrl Pts',(-126.730707294768,-4.39818182507867,
126.422425604514));
#222960=CARTESIAN_POINT('Ctrl Pts',(-127.00915491858,-6.0639707373477,132.136132640718));
#222961=CARTESIAN_POINT('Ctrl Pts',(-127.287602542393,-2.15726678343353,
136.626006248326));
#222962=CARTESIAN_POINT('Ctrl Pts',(-127.566050166206,3.73185995611441,
135.766071924465));
#222963=CARTESIAN_POINT('Ctrl Pts',(-127.844497790019,6.19158970748781,
130.346567302635));
#222964=CARTESIAN_POINT('Ctrl Pts',(-128.122945413832,2.96155099365221,
125.34775237278));
#222965=CARTESIAN_POINT('Ctrl Pts',(-128.401393037645,-2.99000840354028,
125.363293849751));
#222966=CARTESIAN_POINT('Ctrl Pts',(-128.679840661458,-6.19389614791022,
130.378909875453));
#222967=CARTESIAN_POINT('Ctrl Pts',(-128.958288285271,-3.70589592099968,
135.785494348734));
#222968=CARTESIAN_POINT('Ctrl Pts',(-129.236735909083,2.18764161422919,
136.614660264981));
#222969=CARTESIAN_POINT('Ctrl Pts',(-129.515183532897,6.07084337821547,
132.104444654172));
#222970=CARTESIAN_POINT('Ctrl Pts',(-129.793631156709,4.37523665480886,
126.399515326358));
#222971=CARTESIAN_POINT('Ctrl Pts',(-130.072078780522,-1.34099881217456,
124.742423632508));
#222972=CARTESIAN_POINT('Ctrl Pts',(-130.350526404335,-5.82492188220296,
128.655955885842));
#222973=CARTESIAN_POINT('Ctrl Pts',(-130.628974028148,-4.95602630574081,
134.543767132223));
#222974=CARTESIAN_POINT('Ctrl Pts',(-130.907421651961,0.467215330352083,
136.995246471799));
#222975=CARTESIAN_POINT('Ctrl Pts',(-131.185869275774,5.46110890258918,
133.757604152921));
#222976=CARTESIAN_POINT('Ctrl Pts',(-131.464316899587,5.43651018334856,
127.80607529902));
#222977=CARTESIAN_POINT('Ctrl Pts',(-131.742764523399,0.416024193898128,
124.60982417848));
#222978=CARTESIAN_POINT('Ctrl Pts',(-132.021212147213,-4.98676770583297,
127.106049425532));
#222979=CARTESIAN_POINT('Ctrl Pts',(-132.299659771025,-5.80696370104951,
133.000841985516));
#222980=CARTESIAN_POINT('Ctrl Pts',(-132.578107394838,-1.2908437409496,
136.877175472434));
#222981=CARTESIAN_POINT('Ctrl Pts',(-132.856555018651,4.41149855586104,
135.172888781227));
#222982=CARTESIAN_POINT('Ctrl Pts',(-133.135002642464,6.05988919352027,
129.454138122079));
#222983=CARTESIAN_POINT('Ctrl Pts',(-133.413450266277,2.13953770437982,
124.976175974248));
#222984=CARTESIAN_POINT('Ctrl Pts',(-133.69189789009,-3.74694441285829,
125.854030790976));
#222985=CARTESIAN_POINT('Ctrl Pts',(-133.970345513903,-6.19016766309031,
131.280996881284));
#222986=CARTESIAN_POINT('Ctrl Pts',(-134.248793137716,-2.94492923744478,
136.269957530209));
#222987=CARTESIAN_POINT('Ctrl Pts',(-134.527240761528,3.00655528962129,
136.236301625668));
#222988=CARTESIAN_POINT('Ctrl Pts',(-134.805688385342,6.19516238391663,
131.210957299752));
#222989=CARTESIAN_POINT('Ctrl Pts',(-135.084136009154,3.69071789790064,
125.811970486258));
#222990=CARTESIAN_POINT('Ctrl Pts',(-135.362583632967,-2.2053160346932,
125.000746311619));
#222991=CARTESIAN_POINT('Ctrl Pts',(-135.64103125678,-6.07477226708194,
129.522760161825));
#222992=CARTESIAN_POINT('Ctrl Pts',(-135.919478880593,-4.36180955514542,
135.222502221193));
#222993=CARTESIAN_POINT('Ctrl Pts',(-136.197926504406,1.35944305172635,
136.862187985044));
#222994=CARTESIAN_POINT('Ctrl Pts',(-136.476374128219,5.83143390654715,
132.935026339502));
#222995=CARTESIAN_POINT('Ctrl Pts',(-136.754821752032,4.9446218826347,127.049886984307));
#222996=CARTESIAN_POINT('Ctrl Pts',(-137.033269375845,-0.486056093210629,
124.614925481843));
#222997=CARTESIAN_POINT('Ctrl Pts',(-137.311716999657,-5.47007226455594,
127.867752498391));
#222998=CARTESIAN_POINT('Ctrl Pts',(-137.59016462347,-5.42735925266033,
133.819178915179));
#222999=CARTESIAN_POINT('Ctrl Pts',(-137.868612247283,-0.397168228809268,
137.000134598521));
#223000=CARTESIAN_POINT('Ctrl Pts',(-138.147059871096,4.99800099457058,
134.487476673751));
#223001=CARTESIAN_POINT('Ctrl Pts',(-138.425507494909,5.80025146986304,
128.590215023569));
#223002=CARTESIAN_POINT('Ctrl Pts',(-138.703955118722,1.27235420238826,
124.727645007244));
#223003=CARTESIAN_POINT('Ctrl Pts',(-138.982402742535,-4.42477441912264,
126.449279772744));
#223004=CARTESIAN_POINT('Ctrl Pts',(-139.260850366348,-6.05575151170779,
132.173021077107));
#223005=CARTESIAN_POINT('Ctrl Pts',(-139.539297990161,-2.12178880494131,
136.639030281933));
#223006=CARTESIAN_POINT('Ctrl Pts',(-139.817745613973,3.76199415842019,
135.743263104665));
#223007=CARTESIAN_POINT('Ctrl Pts',(-140.096193237787,6.18868827382574,
130.308885820552));
#223008=CARTESIAN_POINT('Ctrl Pts',(-140.374640861599,2.92828019981485,
125.329825669606));
#223009=CARTESIAN_POINT('Ctrl Pts',(-140.653088485412,-3.02307432338508,
125.381595689934));
#223010=CARTESIAN_POINT('Ctrl Pts',(-140.931536109225,-6.19637122878504,
130.416621761961));
#223011=CARTESIAN_POINT('Ctrl Pts',(-141.209983733038,-3.675505684495,135.807960900193));
#223012=CARTESIAN_POINT('Ctrl Pts',(-141.488431356851,2.22297002541115,
136.601235818153));
#223013=CARTESIAN_POINT('Ctrl Pts',(-141.766878980664,6.07864488008735,
132.06746561987));
#223014=CARTESIAN_POINT('Ctrl Pts',(-142.045326604476,4.34834204827492,
126.372963630579));
#223015=CARTESIAN_POINT('Ctrl Pts',(-142.32377422829,-1.3778746975837,124.750698986551));
#223016=CARTESIAN_POINT('Ctrl Pts',(-142.602221852102,-5.83789190928377,
128.691453643612));
#223017=CARTESIAN_POINT('Ctrl Pts',(-142.880669475915,-4.93317165322728,
134.573866588494));
#223018=CARTESIAN_POINT('Ctrl Pts',(-143.159117099728,0.504892353312588,
136.992287696695));
#223019=CARTESIAN_POINT('Ctrl Pts',(-143.437564723541,5.47898495252035,
133.72430611622));
#223020=CARTESIAN_POINT('Ctrl Pts',(-143.716012347354,5.4181580436573,127.77303726975));
#223021=CARTESIAN_POINT('Ctrl Pts',(-143.994459971167,0.378308584408798,
124.607406491544));
#223022=CARTESIAN_POINT('Ctrl Pts',(-144.27290759498,-5.00918798250961,
127.136473817112));
#223023=CARTESIAN_POINT('Ctrl Pts',(-144.551355218793,-5.79348550593904,
133.036149926065));
#223024=CARTESIAN_POINT('Ctrl Pts',(-144.829802842605,-1.2538528769121,
136.884920689477));
#223025=CARTESIAN_POINT('Ctrl Pts',(-145.108250466418,4.43800929187927,
135.145953798675));
#223026=CARTESIAN_POINT('Ctrl Pts',(-145.386698090231,6.05155773023994,
129.417274873051));
#223027=CARTESIAN_POINT('Ctrl Pts',(-145.665145714044,2.10402024954095,
124.963259983731));
#223028=CARTESIAN_POINT('Ctrl Pts',(-145.943593337857,-3.77700905338292,
125.876931223274));
#223029=CARTESIAN_POINT('Ctrl Pts',(-146.22204096167,-6.18715155339789,
131.318669357863));
#223030=CARTESIAN_POINT('Ctrl Pts',(-146.500488585483,-2.9116040349975,
136.287782885497));
#223031=CARTESIAN_POINT('Ctrl Pts',(-146.778936209295,3.03956535180104,
136.217899228972));
#223032=CARTESIAN_POINT('Ctrl Pts',(-147.057383833109,6.19752267131684,
131.173238054629));
#223033=CARTESIAN_POINT('Ctrl Pts',(-147.335831456921,3.66025942170698,
125.789596536289));
#223034=CARTESIAN_POINT('Ctrl Pts',(-147.614279080735,-2.24060342283806,
125.014278223797));
#223035=CARTESIAN_POINT('Ctrl Pts',(-147.892726704547,-6.08246118135759,
129.559762769929));
#223036=CARTESIAN_POINT('Ctrl Pts',(-148.17117432836,-4.33483425895693,
135.248971936054));
#223037=CARTESIAN_POINT('Ctrl Pts',(-148.449621952173,1.39629357899829,
136.853800431821));
#223038=CARTESIAN_POINT('Ctrl Pts',(-148.728069575986,5.84429583058792,
132.899489269852));
#223039=CARTESIAN_POINT('Ctrl Pts',(-149.006517199799,4.9216757235908,127.019857229157));
#223040=CARTESIAN_POINT('Ctrl Pts',(-149.284964823612,-0.52372393616008,
124.617998919139));
#223041=CARTESIAN_POINT('Ctrl Pts',(-149.563412447425,-5.48784688391679,
127.901104789406));
#223042=CARTESIAN_POINT('Ctrl Pts',(-149.841860071237,-5.40890664157841,
133.852160933818));
#223043=CARTESIAN_POINT('Ctrl Pts',(-150.12030769505,-0.359445435409253,
137.002437480918));
#223044=CARTESIAN_POINT('Ctrl Pts',(-150.398755318863,5.02032856601553,
134.456984183485));
#223045=CARTESIAN_POINT('Ctrl Pts',(-150.677202942676,5.78666587195703,
128.554948269553));
#223046=CARTESIAN_POINT('Ctrl Pts',(-150.955650566489,1.23533993591347,
124.720012413542));
#223047=CARTESIAN_POINT('Ctrl Pts',(-151.234098190302,-4.45120305152329,
126.476295320094));
#223048=CARTESIAN_POINT('Ctrl Pts',(-151.512545814115,-6.0473078879686,
132.209858797279));
#223049=CARTESIAN_POINT('Ctrl Pts',(-151.790993437928,-2.08623220278462,
136.651838109709));
#223050=CARTESIAN_POINT('Ctrl Pts',(-152.069441061741,3.79198895864895,
135.720271272016));
#223051=CARTESIAN_POINT('Ctrl Pts',(-152.347888685554,6.18555751604382,
130.27122269847));
#223052=CARTESIAN_POINT('Ctrl Pts',(-152.626336309366,2.89490089747778,
125.312101827337));
#223053=CARTESIAN_POINT('Ctrl Pts',(-152.904783933179,-3.05602822209906,
125.400098472666));
#223054=CARTESIAN_POINT('Ctrl Pts',(-153.183231556992,-6.19861670084527,
130.454348016274));
#223055=CARTESIAN_POINT('Ctrl Pts',(-153.461679180805,-3.64497925077551,
135.830242041403));
#223056=CARTESIAN_POINT('Ctrl Pts',(-153.740126804618,2.25821606362131,
136.587596565983));
#223057=CARTESIAN_POINT('Ctrl Pts',(-154.018574428431,6.08622113553776,
132.030439780749));
#223058=CARTESIAN_POINT('Ctrl Pts',(-154.297022052244,4.32128631232727,
126.346576141847));
#223059=CARTESIAN_POINT('Ctrl Pts',(-154.575469676057,-1.41469952533967,
124.759198661251));
#223060=CARTESIAN_POINT('Ctrl Pts',(-154.85391729987,-5.85064561113321,
128.727029695929));
#223061=CARTESIAN_POINT('Ctrl Pts',(-155.132364923682,-4.9101342002235,
134.603826364333));
#223062=CARTESIAN_POINT('Ctrl Pts',(-155.410812547495,0.542550667301237,
136.989099625678));
#223063=CARTESIAN_POINT('Ctrl Pts',(-155.689260171308,5.49665797664923,
133.690899879866));
#223064=CARTESIAN_POINT('Ctrl Pts',(-155.967707795121,5.39960513212718,
127.740111567281));
#223065=CARTESIAN_POINT('Ctrl Pts',(-156.246155418934,0.340578956555753,
124.605218435021));
#223066=CARTESIAN_POINT('Ctrl Pts',(-156.524603042747,-5.03142264188343,
127.167034123586));
#223067=CARTESIAN_POINT('Ctrl Pts',(-156.80305066656,-5.77979263109261,
133.071375166841));
#223068=CARTESIAN_POINT('Ctrl Pts',(-157.081498290373,-1.21681555089514,
136.89244058913));
#223069=CARTESIAN_POINT('Ctrl Pts',(-157.359945914186,4.46435557583064,
135.118857936792));
#223070=CARTESIAN_POINT('Ctrl Pts',(-157.638393537999,6.04300202426259,
129.380463022997));
#223071=CARTESIAN_POINT('Ctrl Pts',(-157.916841161811,2.06842482945845,
124.950560437346));
#223072=CARTESIAN_POINT('Ctrl Pts',(-158.195288785624,-3.80693373544809,
125.900014243279));
#223073=CARTESIAN_POINT('Ctrl Pts',(-158.473736409437,-6.18390617652933,
131.356322776543));
#223074=CARTESIAN_POINT('Ctrl Pts',(-158.75218403325,-2.87817094199197,
136.305405050556));
#223075=CARTESIAN_POINT('Ctrl Pts',(-159.030631657063,3.07246278176887,
136.199296231612));
#223076=CARTESIAN_POINT('Ctrl Pts',(-159.309079280876,6.19965330723533,
131.135505140616));
#223077=CARTESIAN_POINT('Ctrl Pts',(-159.587526904689,3.62966531325439,
125.767408410247));
#223078=CARTESIAN_POINT('Ctrl Pts',(-159.865974528502,-2.27580778459908,
125.028024689608));
#223079=CARTESIAN_POINT('Ctrl Pts',(-160.144422152314,-6.08992470779737,
129.596811497064));
#223080=CARTESIAN_POINT('Ctrl Pts',(-160.422869776128,-4.3076983338908,
135.275276954208));
#223081=CARTESIAN_POINT('Ctrl Pts',(-160.70131739994,1.43309236609815,136.845188714382));
#223082=CARTESIAN_POINT('Ctrl Pts',(-160.979765023753,5.85694119209746,
132.863874564441));
#223083=CARTESIAN_POINT('Ctrl Pts',(-161.258212647566,4.89854719004298,
126.989967710171));
#223084=CARTESIAN_POINT('Ctrl Pts',(-161.536660271379,-0.561372372326459,
124.621301594343));
#223085=CARTESIAN_POINT('Ctrl Pts',(-161.815107895192,-5.50541814909322,
127.934564661631));
#223086=CARTESIAN_POINT('Ctrl Pts',(-162.093555519005,-5.39025360147175,
133.885030015096));
#223087=CARTESIAN_POINT('Ctrl Pts',(-162.372003142818,-0.32170932262588,
137.004510691297));
#223088=CARTESIAN_POINT('Ctrl Pts',(-162.650450766631,5.04247010733932,
134.426356343909));
#223089=CARTESIAN_POINT('Ctrl Pts',(-162.928898390443,5.77286584701905,
128.519764868338));
#223090=CARTESIAN_POINT('Ctrl Pts',(-163.207346014257,1.19827989346308,
124.712605277602));
#223091=CARTESIAN_POINT('Ctrl Pts',(-163.485793638069,-4.47746674295796,
126.503471245498));
#223092=CARTESIAN_POINT('Ctrl Pts',(-163.764241261882,-6.03864017901171,
132.246644436198));
#223093=CARTESIAN_POINT('Ctrl Pts',(-164.042688885695,-2.05059829452646,
136.664429257056));
#223094=CARTESIAN_POINT('Ctrl Pts',(-164.321136509508,3.82184324533235,
135.697097278492));
#223095=CARTESIAN_POINT('Ctrl Pts',(-164.599584133321,6.18219755015336,
130.23357933201));
#223096=CARTESIAN_POINT('Ctrl Pts',(-164.878031757134,2.86141432352365,
125.294581502737));
#223097=CARTESIAN_POINT('Ctrl Pts',(-165.156479380946,-3.08886887856293,
125.418801512319));
#223098=CARTESIAN_POINT('Ctrl Pts',(-165.43492700476,-6.20063248088431,
130.492087240433));
#223099=CARTESIAN_POINT('Ctrl Pts',(-165.713374628572,-3.61431775100944,
135.85233694673));
#223100=CARTESIAN_POINT('Ctrl Pts',(-165.991822252385,2.2933784228048,136.573743013877));
#223101=CARTESIAN_POINT('Ctrl Pts',(-166.270269876198,6.09357186382579,
131.993368508814));
#223102=CARTESIAN_POINT('Ctrl Pts',(-166.548717500011,4.2940704495262,126.320353837957));
#223103=CARTESIAN_POINT('Ctrl Pts',(-166.827165123824,-1.45147193088449,
124.767922341652));
#223104=CARTESIAN_POINT('Ctrl Pts',(-167.105612747637,-5.86318251515793,
128.762682724506));
#223105=CARTESIAN_POINT('Ctrl Pts',(-167.38406037145,-4.88691480039125,
134.633645349573));
#223106=CARTESIAN_POINT('Ctrl Pts',(-167.662507995262,0.580188876875391,
136.985682376883));
#223107=CARTESIAN_POINT('Ctrl Pts',(-167.940955619076,5.51412732009539,
133.657386681736));
#223108=CARTESIAN_POINT('Ctrl Pts',(-168.219403242888,5.38085213624319,
127.707299411689));
#223109=CARTESIAN_POINT('Ctrl Pts',(-168.497850866701,0.302836708424229,
124.60326008999));
#223110=CARTESIAN_POINT('Ctrl Pts',(-168.776298490514,-5.05347086004094,
127.197729212531));
#223111=CARTESIAN_POINT('Ctrl Pts',(-169.054746114327,-5.7658855839047,
133.106516402559));
#223112=CARTESIAN_POINT('Ctrl Pts',(-169.33319373814,-1.17973313533045,
136.899734892741));
#223113=CARTESIAN_POINT('Ctrl Pts',(-169.611641361953,4.49053643144484,
135.091602199623));
#223114=CARTESIAN_POINT('Ctrl Pts',(-169.890088985766,6.03422239262278,
129.34370393599));
#223115=CARTESIAN_POINT('Ctrl Pts',(-170.168536609579,2.03275276313275,
124.938077805679));
#223116=CARTESIAN_POINT('Ctrl Pts',(-170.446984233392,-3.83671735018369,
125.923278995643));
#223117=CARTESIAN_POINT('Ctrl Pts',(-170.725431857205,-6.18043165274327,
131.393955742061));
#223118=CARTESIAN_POINT('Ctrl Pts',(-171.003879481017,-2.84463119730373,
136.32282337239));
#223119=CARTESIAN_POINT('Ctrl Pts',(-171.282327104831,3.10524636049842,
136.180493322929));
#223120=CARTESIAN_POINT('Ctrl Pts',(-171.560774728643,6.20155421272058,
131.097759955922));
#223121=CARTESIAN_POINT('Ctrl Pts',(-171.839222352457,3.59893670621881,
125.745406930321));
#223122=CARTESIAN_POINT('Ctrl Pts',(-172.117669976268,-2.31092781546573,
125.04198519967));
#223123=CARTESIAN_POINT('Ctrl Pts',(-172.396117600082,-6.09716256983718,
129.633904970377));
#223124=CARTESIAN_POINT('Ctrl Pts',(-172.674565223895,-4.2804027854792,
135.301416300912));
#223125=CARTESIAN_POINT('Ctrl Pts',(-172.953012847708,1.469838049433,136.836353151837));
#223126=CARTESIAN_POINT('Ctrl Pts',(-173.23146047152,5.86936952249723,132.828183542982));
#223127=CARTESIAN_POINT('Ctrl Pts',(-173.509908095334,4.8752371390276,126.960219534917));
#223128=CARTESIAN_POINT('Ctrl Pts',(-173.788355719146,-0.599000006633149,
124.624833385073));
#223129=CARTESIAN_POINT('Ctrl Pts',(-174.06680334296,-5.5227854089755,127.968130875202));
#223130=CARTESIAN_POINT('Ctrl Pts',(-174.345250966772,-5.37140082353563,
133.917784941036));
#223131=CARTESIAN_POINT('Ctrl Pts',(-174.623698590585,-0.283961288785237,
137.006354152836));
#223132=CARTESIAN_POINT('Ctrl Pts',(-174.902146214398,5.06442479807889,
134.39559428995));
#223133=CARTESIAN_POINT('Ctrl Pts',(-175.18059383821,5.75885190641417,128.484666123661));
#223134=CARTESIAN_POINT('Ctrl Pts',(-175.459041462024,1.16117544831056,
124.705423873895));
#223135=CARTESIAN_POINT('Ctrl Pts',(-175.737489085836,-4.50356452021585,
126.530806541938));
#223136=CARTESIAN_POINT('Ctrl Pts',(-176.01593670965,-6.02974870602229,
132.28337663076));
#223137=CARTESIAN_POINT('Ctrl Pts',(-176.294384333462,-2.01488840059438,
136.676803257405));
#223138=CARTESIAN_POINT('Ctrl Pts',(-176.572831957276,3.85155591220881,
135.67374198281));
#223139=CARTESIAN_POINT('Ctrl Pts',(-176.851279581088,6.17860850065921,
130.195957116059));
#223140=CARTESIAN_POINT('Ctrl Pts',(-177.129727204901,2.82782171880919,
125.277265345029));
#223141=CARTESIAN_POINT('Ctrl Pts',(-177.408174828714,-3.12159507585506,
125.437704115845));
#223142=CARTESIAN_POINT('Ctrl Pts',(-177.686622452527,-6.20241849420629,
130.529838035997));
#223143=CARTESIAN_POINT('Ctrl Pts',(-177.965070076339,-3.58352232136993,
135.874244797437));
#223144=CARTESIAN_POINT('Ctrl Pts',(-178.243517700153,2.32845580000743,
136.559675675186));
#223145=CARTESIAN_POINT('Ctrl Pts',(-178.521965323965,6.10069679256748,
131.956253177754));
#223146=CARTESIAN_POINT('Ctrl Pts',(-178.800412947778,4.26669546836545,
126.294297690589));
#223147=CARTESIAN_POINT('Ctrl Pts',(-179.078860571591,-1.48819055160311,
124.776869704492));
#223148=CARTESIAN_POINT('Ctrl Pts',(-179.357308195404,-5.8755021567984,
128.798411408209));
#223149=CARTESIAN_POINT('Ctrl Pts',(-179.635755819217,-4.86351431413387,
134.663322439258));
#223150=CARTESIAN_POINT('Ctrl Pts',(-179.91420344303,0.617805587336893,
136.982036076937));
#223151=CARTESIAN_POINT('Ctrl Pts',(-180.192651066843,5.53139233552561,
133.623767763677));
#223152=CARTESIAN_POINT('Ctrl Pts',(-180.471098690656,5.36189975090491,
127.674602018838));
#223153=CARTESIAN_POINT('Ctrl Pts',(-180.749546314469,0.265083238567079,
124.601531529021));
#223154=CARTESIAN_POINT('Ctrl Pts',(-181.027993938281,-5.07533181997731,
127.22855794653));
#223155=CARTESIAN_POINT('Ctrl Pts',(-181.306441562095,-5.75176487970607,
133.141572331048));
#223156=CARTESIAN_POINT('Ctrl Pts',(-181.584889185907,-1.14260700432061,
136.906803330016));
#223157=CARTESIAN_POINT('Ctrl Pts',(-181.86333680972,4.5165508885802,135.064187597142));
#223158=CARTESIAN_POINT('Ctrl Pts',(-182.141784433533,6.02521916065313,
129.306998974155));
#223159=CARTESIAN_POINT('Ctrl Pts',(-182.420232057346,1.99700537240587,
124.925812551278));
#223160=CARTESIAN_POINT('Ctrl Pts',(-182.698679681159,-3.86635879394691,
125.946724618282));
#223161=CARTESIAN_POINT('Ctrl Pts',(-182.977127304972,-6.17672811078948,
131.431566859916));
#223162=CARTESIAN_POINT('Ctrl Pts',(-183.255574928785,-2.81098604376035,
136.340037205557));
#223163=CARTESIAN_POINT('Ctrl Pts',(-183.534022552597,3.13791487318212,
136.161491199671));
#223164=CARTESIAN_POINT('Ctrl Pts',(-183.81247017641,6.20322531733387,131.060003899207));
#223165=CARTESIAN_POINT('Ctrl Pts',(-184.090917800223,3.56807473926006,
125.723592911784));
#223166=CARTESIAN_POINT('Ctrl Pts',(-184.369365424036,-2.34596221405232,
125.056159236672));
#223167=CARTESIAN_POINT('Ctrl Pts',(-184.647813047849,-6.10417449927606,
129.671041815353));
#223168=CARTESIAN_POINT('Ctrl Pts',(-184.926260671662,-4.25294862516783,
135.327389007565));
#223169=CARTESIAN_POINT('Ctrl Pts',(-185.204708295475,1.50652926737877,
136.827294071589));
#223170=CARTESIAN_POINT('Ctrl Pts',(-185.483155919288,5.88158036125089,
132.792417528021));
#223171=CARTESIAN_POINT('Ctrl Pts',(-185.761603543101,4.85174643430717,
126.930613805724));
#223172=CARTESIAN_POINT('Ctrl Pts',(-186.040051166913,-0.6366054447743,
124.628594160457));
#223173=CARTESIAN_POINT('Ctrl Pts',(-186.318498790727,-5.53994802001346,
128.001802186308));
#223174=CARTESIAN_POINT('Ctrl Pts',(-186.596946414539,-5.35234900636664,
133.950424497894));
#223175=CARTESIAN_POINT('Ctrl Pts',(-186.875394038353,-0.246202732654624,
137.007967797222));
#223176=CARTESIAN_POINT('Ctrl Pts',(-187.153841662165,5.08619182469514,
134.364699161505));
#223177=CARTESIAN_POINT('Ctrl Pts',(-187.432289285978,5.744624569434,128.449653336115));
#223178=CARTESIAN_POINT('Ctrl Pts',(-187.71073690979,1.12402797537536,124.698468468532));
#223179=CARTESIAN_POINT('Ctrl Pts',(-187.989184533604,-4.52949541623416,
126.558300196495));
#223180=CARTESIAN_POINT('Ctrl Pts',(-188.267632157416,-6.0206337984771,
132.32005401984));
#223181=CARTESIAN_POINT('Ctrl Pts',(-188.54607978123,-1.97910384423165,
136.688959652232));
#223182=CARTESIAN_POINT('Ctrl Pts',(-188.824527405043,3.88112585826452,
135.650206250412));
#223183=CARTESIAN_POINT('Ctrl Pts',(-189.102975028855,6.17479050055486,
130.158357444724));
#223184=CARTESIAN_POINT('Ctrl Pts',(-189.381422652668,2.79412432812102,
125.260153995869));
#223185=CARTESIAN_POINT('Ctrl Pts',(-189.659870276481,-3.15420560129371,
125.456805582802));
#223186=CARTESIAN_POINT('Ctrl Pts',(-189.938317900294,-6.20397467462999,
130.567599004095));
#223187=CARTESIAN_POINT('Ctrl Pts',(-190.216765524107,-3.55259410299321,
135.89596478172));
#223188=CARTESIAN_POINT('Ctrl Pts',(-190.49521314792,2.36344689542356,136.545395071179));
#223189=CARTESIAN_POINT('Ctrl Pts',(-190.773660771733,6.10759565774615,
131.919095162891));
#223190=CARTESIAN_POINT('Ctrl Pts',(-191.052108395545,4.23916238323504,
126.26840866526));
#223191=CARTESIAN_POINT('Ctrl Pts',(-191.330556019359,-1.52485402687357,
124.786040418225));
#223192=CARTESIAN_POINT('Ctrl Pts',(-191.609003643171,-5.88760407954571,
128.834214423098));
#223193=CARTESIAN_POINT('Ctrl Pts',(-191.887451266984,-4.83993360856504,
134.692856533694));
#223194=CARTESIAN_POINT('Ctrl Pts',(-192.165898890797,0.655399404785621,
136.978160860955));
#223195=CARTESIAN_POINT('Ctrl Pts',(-192.44434651461,5.54845238317892,133.59004437145));
#223196=CARTESIAN_POINT('Ctrl Pts',(-192.722794138423,5.34274867839911,
127.642020600343));
#223197=CARTESIAN_POINT('Ctrl Pts',(-193.001241762236,0.227319945953055,
124.600032816164));
#223198=CARTESIAN_POINT('Ctrl Pts',(-193.279689386049,-5.09700471162664,
127.259519183211));
#223199=CARTESIAN_POINT('Ctrl Pts',(-193.558137009861,-5.73743104174462,
133.176541653297));
#223200=CARTESIAN_POINT('Ctrl Pts',(-193.836584633675,-1.105438533588,136.913645639033));
#223201=CARTESIAN_POINT('Ctrl Pts',(-194.115032257487,4.5423979832614,135.036615145204));
#223202=CARTESIAN_POINT('Ctrl Pts',(-194.3934798813,6.01599266197172,129.270349497605));
#223203=CARTESIAN_POINT('Ctrl Pts',(-194.671927505113,1.96118398191049,
124.913765128639));
#223204=CARTESIAN_POINT('Ctrl Pts',(-194.950375128926,-3.89585696836267,
125.970350242409));
#223205=CARTESIAN_POINT('Ctrl Pts',(-195.228822752739,-6.17279568790409,
131.469154736412));
#223206=CARTESIAN_POINT('Ctrl Pts',(-195.507270376552,-2.77723672809589,
136.357045912194));
#223207=CARTESIAN_POINT('Ctrl Pts',(-195.785718000365,3.17046710927626,
136.142290565968));
#223208=CARTESIAN_POINT('Ctrl Pts',(-196.064165624178,6.20466655915177,
131.022238369536));
#223209=CARTESIAN_POINT('Ctrl Pts',(-196.342613247991,3.5370805559797,125.701967162963));
#223210=CARTESIAN_POINT('Ctrl Pts',(-196.621060871803,-2.38090968214636,
125.070546275391));
#223211=CARTESIAN_POINT('Ctrl Pts',(-196.899508495616,-6.11096023628406,
129.708220655875));
#223212=CARTESIAN_POINT('Ctrl Pts',(-197.177956119429,-4.22533687028115,
135.353194111738));
#223213=CARTESIAN_POINT('Ctrl Pts',(-197.456403743242,1.54316466032852,
136.818011809327));
#223214=CARTESIAN_POINT('Ctrl Pts',(-197.734851367055,5.89357325588093,
132.75657784488));
#223215=CARTESIAN_POINT('Ctrl Pts',(-198.013298990868,4.82807594633875,
126.901151619645));
#223216=CARTESIAN_POINT('Ctrl Pts',(-198.291746614681,-0.674187293266194,
124.632583781138));
#223217=CARTESIAN_POINT('Ctrl Pts',(-198.570194238494,-5.55690534624021,
128.035577347248));
#223218=CARTESIAN_POINT('Ctrl Pts',(-198.848641862306,-5.33309885593691,
133.982947476197));
#223219=CARTESIAN_POINT('Ctrl Pts',(-199.12708948612,-0.2084350533912,137.009351564664));
#223220=CARTESIAN_POINT('Ctrl Pts',(-199.405537109932,5.10777038060287,
134.333672103408));
#223221=CARTESIAN_POINT('Ctrl Pts',(-199.683984733745,5.7301843632779,128.414727803113));
#223222=CARTESIAN_POINT('Ctrl Pts',(-199.962432357558,1.08683885116959,
124.691739319248));
#223223=CARTESIAN_POINT('Ctrl Pts',(-200.240879981371,-4.5552584701342,
126.585951190383));
#223224=CARTESIAN_POINT('Ctrl Pts',(-200.519327605184,-6.01129579413245,
132.356675244344));
#223225=CARTESIAN_POINT('Ctrl Pts',(-200.797775228997,-1.94324595144814,
136.700897991079));
#223226=CARTESIAN_POINT('Ctrl Pts',(-201.076222852809,3.91055198777426,
135.626490953421));
#223227=CARTESIAN_POINT('Ctrl Pts',(-201.354670476623,6.17074369131775,
130.120781711275));
#223228=CARTESIAN_POINT('Ctrl Pts',(-201.633118100435,2.76032340012831,
125.243248089324));
#223229=CARTESIAN_POINT('Ctrl Pts',(-201.911565724248,-3.18669924648382,
125.476105205376));
#223230=CARTESIAN_POINT('Ctrl Pts',(-202.190013348061,-6.20530096449064,
130.605368745483));
#223231=CARTESIAN_POINT('Ctrl Pts',(-202.468460971874,-3.52153424193529,
135.91749609474));
#223232=CARTESIAN_POINT('Ctrl Pts',(-202.746908595687,2.39835041244635,
136.530901731028));
#223233=CARTESIAN_POINT('Ctrl Pts',(-203.0253562195,6.11426820372151,131.881895841131));
#223234=CARTESIAN_POINT('Ctrl Pts',(-203.303803843313,4.21147221438356,
126.242687721299));
#223235=CARTESIAN_POINT('Ctrl Pts',(-203.582251467125,-1.56146099811728,
124.795434143027));
#223236=CARTESIAN_POINT('Ctrl Pts',(-203.860699090939,-5.89948783495869,
128.870090442477));
#223237=CARTESIAN_POINT('Ctrl Pts',(-204.139146714752,-4.81617355747646,
134.722246538484));
#223238=CARTESIAN_POINT('Ctrl Pts',(-204.417594338564,0.69296893616836,
136.974056872534));
#223239=CARTESIAN_POINT('Ctrl Pts',(-204.696041962377,5.56530683088876,
133.556217754686));
#223240=CARTESIAN_POINT('Ctrl Pts',(-204.97448958619,5.32339962837619,127.60955636352));
#223241=CARTESIAN_POINT('Ctrl Pts',(-205.252937210003,0.18954822991528,
124.598764006957));
#223242=CARTESIAN_POINT('Ctrl Pts',(-205.531384833816,-5.11848873189165,
127.290611775294));
#223243=CARTESIAN_POINT('Ctrl Pts',(-205.809832457629,-5.72288460116635,
133.211423073505));
#223244=CARTESIAN_POINT('Ctrl Pts',(-206.088280081441,-1.06822910042401,
136.920261566246));
#223245=CARTESIAN_POINT('Ctrl Pts',(-206.366727705255,4.56807675771487,
135.00888586552));
#223246=CARTESIAN_POINT('Ctrl Pts',(-206.645175329067,6.00654323846982,
129.233756864401));
#223247=CARTESIAN_POINT('Ctrl Pts',(-206.92362295288,1.92528991902147,124.901935984182));
#223248=CARTESIAN_POINT('Ctrl Pts',(-207.202070576693,-3.92521078036628,
125.994154992568));
#223249=CARTESIAN_POINT('Ctrl Pts',(-207.480518200506,-6.16863452980439,
131.506717978718));
#223250=CARTESIAN_POINT('Ctrl Pts',(-207.758965824319,-2.74338450090264,
136.373848862034));
#223251=CARTESIAN_POINT('Ctrl Pts',(-208.037413448132,3.20290186254569,
136.12289213331));
#223252=CARTESIAN_POINT('Ctrl Pts',(-208.315861071945,6.20587788476857,
130.984464766326));
#223253=CARTESIAN_POINT('Ctrl Pts',(-208.594308695758,3.50595530487857,
125.680530485208));
#223254=CARTESIAN_POINT('Ctrl Pts',(-208.872756319571,-2.41576892475653,
125.085145782709));
#223255=CARTESIAN_POINT('Ctrl Pts',(-209.151203943383,-6.11751952941318,
129.745440114266));
#223256=CARTESIAN_POINT('Ctrl Pts',(-209.429651567197,-4.19756854398286,
135.378830657213));
#223257=CARTESIAN_POINT('Ctrl Pts',(-209.708099191009,1.57974287074426,
136.808506709009));
#223258=CARTESIAN_POINT('Ctrl Pts',(-209.986546814822,5.90534776198698,
132.720665821612));
#223259=CARTESIAN_POINT('Ctrl Pts',(-210.264994438635,4.80422655224024,
126.87183406841));
#223260=CARTESIAN_POINT('Ctrl Pts',(-210.543442062448,-0.711744159500396,
124.63680209928));
#223261=CARTESIAN_POINT('Ctrl Pts',(-210.821889686261,-5.57365675929581,
128.06945510647));
#223262=CARTESIAN_POINT('Ctrl Pts',(-211.100337310074,-5.31365108556781,
134.015352670796));
#223263=CARTESIAN_POINT('Ctrl Pts',(-211.378784933887,-0.170659650490228,
137.010505403884));
#223264=CARTESIAN_POINT('Ctrl Pts',(-211.657232557699,5.12915966620077,
134.302514265376));
#223265=CARTESIAN_POINT('Ctrl Pts',(-211.935680181513,5.71553182303293,
128.379890818834));
#223266=CARTESIAN_POINT('Ctrl Pts',(-212.214127805325,1.04960945375051,
124.685236675394));
#223267=CARTESIAN_POINT('Ctrl Pts',(-212.492575429138,-4.58085272725645,
126.613758498985));
#223268=CARTESIAN_POINT('Ctrl Pts',(-212.771023052951,-6.00173503901134,
132.393238947258));
#223269=CARTESIAN_POINT('Ctrl Pts',(-213.049470676764,-1.90731605097184,
136.712617831564));
#223270=CARTESIAN_POINT('Ctrl Pts',(-213.327918300577,3.93983321034183,
135.602596970618));
#223271=CARTESIAN_POINT('Ctrl Pts',(-213.60636592439,6.16646822290386,130.083231308093));
#223272=CARTESIAN_POINT('Ctrl Pts',(-213.884813548203,2.72642018733693,
125.226548251849));
#223273=CARTESIAN_POINT('Ctrl Pts',(-214.163261172015,-3.21907480736146,
125.495602268416));
#223274=CARTESIAN_POINT('Ctrl Pts',(-214.441708795829,-6.20639731464204,
130.643145860587));
#223275=CARTESIAN_POINT('Ctrl Pts',(-214.720156419641,-3.49034388913101,
135.938837938644));
#223276=CARTESIAN_POINT('Ctrl Pts',(-214.998604043455,2.43316505771265,
136.516196191791));
#223277=CARTESIAN_POINT('Ctrl Pts',(-215.277051667267,6.12071418324004,
131.844656590906));
#223278=CARTESIAN_POINT('Ctrl Pts',(-215.55549929108,4.18362598788043,126.217135811804));
#223279=CARTESIAN_POINT('Ctrl Pts',(-215.833946914893,-1.59801010884951,
124.805050530808));
#223280=CARTESIAN_POINT('Ctrl Pts',(-216.112394538706,-5.91115298268039,
128.90603813695));
#223281=CARTESIAN_POINT('Ctrl Pts',(-216.390842162519,-4.79223504130557,
134.75149136457));
#223282=CARTESIAN_POINT('Ctrl Pts',(-216.669289786332,0.730512789332353,
136.969724263749));
#223283=CARTESIAN_POINT('Ctrl Pts',(-216.947737410145,5.5819550541073,133.522289166845));
#223284=CARTESIAN_POINT('Ctrl Pts',(-217.226185033957,5.3038533178224,127.577210511344));
#223285=CARTESIAN_POINT('Ctrl Pts',(-217.50463265777,0.151769490097695,
124.597725148413));
#223286=CARTESIAN_POINT('Ctrl Pts',(-217.783080281583,-5.13978308467467,
127.321834570635));
#223287=CARTESIAN_POINT('Ctrl Pts',(-218.061527905396,-5.70812609699421,
133.24621529913));
#223288=CARTESIAN_POINT('Ctrl Pts',(-218.339975529209,-1.03098008363786,
136.9266508665));
#223289=CARTESIAN_POINT('Ctrl Pts',(-218.618423153022,4.59358626040416,
134.981000785606));
#223290=CARTESIAN_POINT('Ctrl Pts',(-218.896870776835,5.99687124029931,
129.197222430498));
#223291=CARTESIAN_POINT('Ctrl Pts',(-219.175318400648,1.88932451380644,
124.890325556239));
#223292=CARTESIAN_POINT('Ctrl Pts',(-219.45376602446,-3.95441914224089,
126.018137986666));
#223293=CARTESIAN_POINT('Ctrl Pts',(-219.732213648274,-6.16424479068368,
131.544255194914));
#223294=CARTESIAN_POINT('Ctrl Pts',(-220.010661272086,-2.70943061658779,
136.390445432439));
#223295=CARTESIAN_POINT('Ctrl Pts',(-220.289108895899,3.23521793110825,
136.103296620509));
#223296=CARTESIAN_POINT('Ctrl Pts',(-220.567556519712,6.20685924929812,
130.94668448929));
#223297=CARTESIAN_POINT('Ctrl Pts',(-220.846004143525,3.47470013931478,
125.659283672863));
#223298=CARTESIAN_POINT('Ctrl Pts',(-221.124451767337,-2.45053865016082,
125.099957217636));
#223299=CARTESIAN_POINT('Ctrl Pts',(-221.402899391151,-6.12385213560643,
129.782698811345));
#223300=CARTESIAN_POINT('Ctrl Pts',(-221.681347014963,-4.16964467523852,
135.404297694017));
#223301=CARTESIAN_POINT('Ctrl Pts',(-221.959794638777,1.61626254320698,
136.79877912285));
#223302=CARTESIAN_POINT('Ctrl Pts',(-222.238242262589,5.91690344326002,
132.684682788949));
#223303=CARTESIAN_POINT('Ctrl Pts',(-222.516689886402,4.7801991357601,126.842662238393));
#223304=CARTESIAN_POINT('Ctrl Pts',(-222.795137510215,-0.749274651793031,
124.64124895857));
#223305=CARTESIAN_POINT('Ctrl Pts',(-223.073585134028,-5.59020163845046,
128.103434208622));
#223306=CARTESIAN_POINT('Ctrl Pts',(-223.352032757841,-5.29400641590365,
134.047638880903));
#223307=CARTESIAN_POINT('Ctrl Pts',(-223.630480381654,-0.132877923733138,
137.011429272127));
#223308=CARTESIAN_POINT('Ctrl Pts',(-223.908928005467,5.15035888890098,
134.271226801972));
#223309=CARTESIAN_POINT('Ctrl Pts',(-224.187375629279,5.70066749165438,
128.345143674176));
#223310=CARTESIAN_POINT('Ctrl Pts',(-224.465823253093,1.01234116266713,
124.678960777928));
#223311=CARTESIAN_POINT('Ctrl Pts',(-224.744270876905,-4.60627723919628,
126.641721091889));
#223312=CARTESIAN_POINT('Ctrl Pts',(-225.022718500718,-5.99195188739136,
132.4297437737));
#223313=CARTESIAN_POINT('Ctrl Pts',(-225.301166124531,-1.87131547419729,
136.724118739406));
#223314=CARTESIAN_POINT('Ctrl Pts',(-225.579613748344,3.96896844094108,
135.578525187401));
#223315=CARTESIAN_POINT('Ctrl Pts',(-225.858061372157,6.16196425374224,
130.045707626623));
#223316=CARTESIAN_POINT('Ctrl Pts',(-226.13650899597,2.69241594604283,125.210055102262));
#223317=CARTESIAN_POINT('Ctrl Pts',(-226.414956619783,-3.25133108423828,
125.515296049447));
#223318=CARTESIAN_POINT('Ctrl Pts',(-226.693404243596,-6.20726368445854,
130.680928949564));
#223319=CARTESIAN_POINT('Ctrl Pts',(-226.971851867408,-3.45902420035033,
135.959989522602));
#223320=CARTESIAN_POINT('Ctrl Pts',(-227.250299491222,2.46788954115291,
136.501278998386));
#223321=CARTESIAN_POINT('Ctrl Pts',(-227.528747115034,6.12693335744362,
131.80737879213));
#223322=CARTESIAN_POINT('Ctrl Pts',(-227.807194738847,4.15562473557794,
126.191753883612));
#223323=CARTESIAN_POINT('Ctrl Pts',(-228.08564236266,-1.63450000472891,
124.81488922523));
#223324=CARTESIAN_POINT('Ctrl Pts',(-228.364089986473,-5.9225990904546,
128.942056174461));
#223325=CARTESIAN_POINT('Ctrl Pts',(-228.642537610286,-4.76811894710285,
134.780589928275));
#223326=CARTESIAN_POINT('Ctrl Pts',(-228.920985234099,0.768029573076269,
136.965163195147));
#223327=CARTESIAN_POINT('Ctrl Pts',(-229.199432857912,5.59839643592858,
133.48825986516));
#223328=CARTESIAN_POINT('Ctrl Pts',(-229.477880481725,5.28411047103341,
127.544984242401));
#223329=CARTESIAN_POINT('Ctrl Pts',(-229.756328105537,0.11398512640586,
124.59691627903));
#223330=CARTESIAN_POINT('Ctrl Pts',(-230.03477572935,-5.16088698090536,
127.353186412258));
#223331=CARTESIAN_POINT('Ctrl Pts',(-230.313223353163,-5.69315607611037,
133.280917040931));
#223332=CARTESIAN_POINT('Ctrl Pts',(-230.591670976976,-0.993692863505588,
136.932813303039));
#223333=CARTESIAN_POINT('Ctrl Pts',(-230.870118600789,4.6189255460653,134.952960938754));
#223334=CARTESIAN_POINT('Ctrl Pts',(-231.148566224602,5.98697702585963,
129.160747549691));
#223335=CARTESIAN_POINT('Ctrl Pts',(-231.427013848415,1.85328909897679,
124.878934275042));
#223336=CARTESIAN_POINT('Ctrl Pts',(-231.705461472227,-3.98348097165998,
126.042298336002));
#223337=CARTESIAN_POINT('Ctrl Pts',(-231.983909096041,-6.15962663320533,
131.581764994044));
#223338=CARTESIAN_POINT('Ctrl Pts',(-232.262356719853,-2.6753763333251,
136.406835008417));
#223339=CARTESIAN_POINT('Ctrl Pts',(-232.540804343666,3.26741411748112,
136.083504753687));
#223340=CARTESIAN_POINT('Ctrl Pts',(-232.819251967479,6.20761061637562,
130.90889893839));
#223341=CARTESIAN_POINT('Ctrl Pts',(-233.097699591292,3.44331621745904,
125.638227513236));
#223342=CARTESIAN_POINT('Ctrl Pts',(-233.376147215105,-2.48521756995422,
125.114980031328));
#223343=CARTESIAN_POINT('Ctrl Pts',(-233.654594838918,-6.12995782020675,
129.819995366479));
#223344=CARTESIAN_POINT('Ctrl Pts',(-233.933042462731,-4.14156629877734,
135.429594278462));
#223345=CARTESIAN_POINT('Ctrl Pts',(-234.211490086544,1.65272232446679,
136.788829411307));
#223346=CARTESIAN_POINT('Ctrl Pts',(-234.489937710357,5.92823987150001,
132.648630080257));
#223347=CARTESIAN_POINT('Ctrl Pts',(-234.768385334169,4.75599458724306,
126.813637210565));
#223348=CARTESIAN_POINT('Ctrl Pts',(-235.046832957982,-0.786777379437916,
124.64592419423));
#223349=CARTESIAN_POINT('Ctrl Pts',(-235.325280581795,-5.6065393706272,
128.137513394595));
#223350=CARTESIAN_POINT('Ctrl Pts',(-235.603728205608,-5.27416557488518,
134.079804910139));
#223351=CARTESIAN_POINT('Ctrl Pts',(-235.882175829421,-0.0950912731361558,
137.012123135159));
#223352=CARTESIAN_POINT('Ctrl Pts',(-236.160623453234,5.17136726315852,
134.239810872567));
#223353=CARTESIAN_POINT('Ctrl Pts',(-236.439071077047,5.68559191994549,
128.310487656705));
#223354=CARTESIAN_POINT('Ctrl Pts',(-236.71751870086,0.975035358909668,
124.672911859406));
#223355=CARTESIAN_POINT('Ctrl Pts',(-236.995966324673,-4.63153106383903,
126.669837932931));
#223356=CARTESIAN_POINT('Ctrl Pts',(-237.274413948486,-5.98194670179065,
132.466188370973));
#223357=CARTESIAN_POINT('Ctrl Pts',(-237.552861572298,-1.83524555513966,
136.735400288432));
#223358=CARTESIAN_POINT('Ctrl Pts',(-237.831309196112,3.99795659995517,
135.554276495761));
#223359=CARTESIAN_POINT('Ctrl Pts',(-238.109756819924,6.15723195072914,
130.008212057319));
#223360=CARTESIAN_POINT('Ctrl Pts',(-238.388204443737,2.65831193628575,
125.193769251723));
#223361=CARTESIAN_POINT('Ctrl Pts',(-238.66665206755,-3.28346688184612,
125.535185818711));
#223362=CARTESIAN_POINT('Ctrl Pts',(-238.945099691363,-6.20790004183648,
130.718716612347));
#223363=CARTESIAN_POINT('Ctrl Pts',(-239.223547315176,-3.42757633615586,
135.980950062836));
#223364=CARTESIAN_POINT('Ctrl Pts',(-239.501994938989,2.50252257603867,
136.486150703575));
#223365=CARTESIAN_POINT('Ctrl Pts',(-239.780442562802,6.13292549587844,
131.770063826148));
#223366=CARTESIAN_POINT('Ctrl Pts',(-240.058890186614,4.12746949507249,
126.166542877259));
#223367=CARTESIAN_POINT('Ctrl Pts',(-240.337337810428,-1.67092933361012,
124.824949861719));
#223368=CARTESIAN_POINT('Ctrl Pts',(-240.61578543424,-5.93382573414137,
128.978143220346));
#223369=CARTESIAN_POINT('Ctrl Pts',(-240.894233058053,-4.74382616849909,
134.80954115134));
#223370=CARTESIAN_POINT('Ctrl Pts',(-241.172680681866,0.805517897201924,
136.960373835741));
#223371=CARTESIAN_POINT('Ctrl Pts',(-241.451128305679,5.6146303671111,133.454131110603));
#223372=CARTESIAN_POINT('Ctrl Pts',(-241.729575929492,5.26417181958768,
127.512878750849));
#223373=CARTESIAN_POINT('Ctrl Pts',(-242.008023553305,0.0761965389532375,
124.596337428779));
#223374=CARTESIAN_POINT('Ctrl Pts',(-242.286471177117,-5.18179963857104,
127.384666138411));
#223375=CARTESIAN_POINT('Ctrl Pts',(-242.564918800931,-5.67797509323448,
133.315527013022));
#223376=CARTESIAN_POINT('Ctrl Pts',(-242.843366424743,-0.956368821719198,
136.938748647509));
#223377=CARTESIAN_POINT('Ctrl Pts',(-243.121814048556,4.64409367574132,
134.924767363992));
#223378=CARTESIAN_POINT('Ctrl Pts',(-243.400261672369,5.9768609617849,129.124333573571));
#223379=CARTESIAN_POINT('Ctrl Pts',(-243.678709296182,1.81718500983798,
124.867762562695));
#223380=CARTESIAN_POINT('Ctrl Pts',(-243.957156919995,-4.01239519172672,
126.066635145309));
#223381=CARTESIAN_POINT('Ctrl Pts',(-244.235604543808,-6.15478022849689,
131.619245986169));
#223382=CARTESIAN_POINT('Ctrl Pts',(-244.514052167621,-2.64122291300849,
136.423016982646));
#223383=CARTESIAN_POINT('Ctrl Pts',(-244.792499791433,3.29948922862226,
136.063517266237));
#223384=CARTESIAN_POINT('Ctrl Pts',(-245.070947415247,6.20813195815889,
130.871109513785));
#223385=CARTESIAN_POINT('Ctrl Pts',(-245.349395039059,3.41180470225455,
125.617362786572));
#223386=CARTESIAN_POINT('Ctrl Pts',(-245.627842662872,-2.51980439909662,
125.13021366711));
#223387=CARTESIAN_POINT('Ctrl Pts',(-245.906290286685,-6.13583635696575,
129.857328397629));
#223388=CARTESIAN_POINT('Ctrl Pts',(-246.184737910498,-4.1133344550539,
135.454719473173));
#223389=CARTESIAN_POINT('Ctrl Pts',(-246.463185534311,1.68912086349306,
136.778657943074));
#223390=CARTESIAN_POINT('Ctrl Pts',(-246.741633158124,5.93935662663147,
132.612509031482));
#223391=CARTESIAN_POINT('Ctrl Pts',(-247.020080781937,4.73161380359756,
126.784760060463));
#223392=CARTESIAN_POINT('Ctrl Pts',(-247.29852840575,-0.824250952757648,
124.650827633015));
#223393=CARTESIAN_POINT('Ctrl Pts',(-247.576976029562,-5.62266935042617,
128.171691401572));
#223394=CARTESIAN_POINT('Ctrl Pts',(-247.855423653376,-5.25412929772145,
134.111849566585));
#223395=CARTESIAN_POINT('Ctrl Pts',(-248.133871277188,-0.0573010988966442,
137.012586967267));
#223396=CARTESIAN_POINT('Ctrl Pts',(-248.412318901001,5.19218401050035,
134.208267641291));
#223397=CARTESIAN_POINT('Ctrl Pts',(-248.690766524814,5.67030566653712,
128.275924050614));
#223398=CARTESIAN_POINT('Ctrl Pts',(-248.969214148627,0.937693424858449,
124.667090143972));
#223399=CARTESIAN_POINT('Ctrl Pts',(-249.24766177244,-4.65661326539506,
126.698107980232));
#223400=CARTESIAN_POINT('Ctrl Pts',(-249.526109396252,-5.97171985295489,
132.502571388608));
#223401=CARTESIAN_POINT('Ctrl Pts',(-249.804557020066,-1.79910763038337,
136.746462060605));
#223402=CARTESIAN_POINT('Ctrl Pts',(-250.083004643878,4.02679661321771,
135.52985179424));
#223403=CARTESIAN_POINT('Ctrl Pts',(-250.361452267692,6.15227148922063,
129.970745989595));
#223404=CARTESIAN_POINT('Ctrl Pts',(-250.639899891504,2.62410942180459,
125.177691303707));
#223405=CARTESIAN_POINT('Ctrl Pts',(-250.918347515317,-3.31548100938434,
125.555270839195));
#223406=CARTESIAN_POINT('Ctrl Pts',(-251.19679513913,-6.20830636318893,
130.756507448682));
#223407=CARTESIAN_POINT('Ctrl Pts',(-251.475242762943,-3.39600146187203,
136.001718782677));
#223408=CARTESIAN_POINT('Ctrl Pts',(-251.753690386756,2.53706287905323,
136.47081186788));
#223409=CARTESIAN_POINT('Ctrl Pts',(-252.032138010569,6.13869037645988,
131.732713075798));
#223410=CARTESIAN_POINT('Ctrl Pts',(-252.310585634382,4.09916130974965,
126.141503726722));
#223411=CARTESIAN_POINT('Ctrl Pts',(-252.589033258195,-1.70729674574642,
124.835232067896));
#223412=CARTESIAN_POINT('Ctrl Pts',(-252.867480882007,-5.94483249743877,
129.014297936587));
#223413=CARTESIAN_POINT('Ctrl Pts',(-253.14592850582,-4.71935760622846,
134.838343962485));
#223414=CARTESIAN_POINT('Ctrl Pts',(-253.424376129633,0.842976373616159,
136.955356360136));
#223415=CARTESIAN_POINT('Ctrl Pts',(-253.702823753446,5.63065624411703,
133.419904173236));
#223416=CARTESIAN_POINT('Ctrl Pts',(-253.981271377259,5.24403810606461,
127.480895216153));
#223417=CARTESIAN_POINT('Ctrl Pts',(-254.259719001072,0.0384051209378723,
124.595988638398));
#223418=CARTESIAN_POINT('Ctrl Pts',(-254.538166624885,-5.20252026939218,
127.416272546179));
#223419=CARTESIAN_POINT('Ctrl Pts',(-254.816614248698,-5.66258373611722,
133.350044001689));
#223420=CARTESIAN_POINT('Ctrl Pts',(-255.095061872511,-0.919009293725241,
136.944456550123));
#223421=CARTESIAN_POINT('Ctrl Pts',(-255.373509496324,4.6690896269236,134.896421351226));
#223422=CARTESIAN_POINT('Ctrl Pts',(-255.651957120136,5.96652359266914,
129.087981388513));
#223423=CARTESIAN_POINT('Ctrl Pts',(-255.93040474395,1.78101326373629,124.856811707331));
#223424=CARTESIAN_POINT('Ctrl Pts',(-256.208852367762,-4.04116012583712,
126.091145862189));
#223425=CARTESIAN_POINT('Ctrl Pts',(-256.487299991575,-6.14970689884083,
131.656699899059));
#223426=CARTESIAN_POINT('Ctrl Pts',(-256.765747615388,-2.60696946356087,
136.438984870644));
#223427=CARTESIAN_POINT('Ctrl Pts',(-257.044195239201,3.33143800190474,
136.043346010603));
#223428=CARTESIAN_POINT('Ctrl Pts',(-257.322642863014,6.2084309480058,130.833296634437));
#223429=CARTESIAN_POINT('Ctrl Pts',(-257.601090486826,3.38015223603414,
125.596729883064));
#223430=CARTESIAN_POINT('Ctrl Pts',(-257.87953811064,-2.5542704291637,125.145582755354));
#223431=CARTESIAN_POINT('Ctrl Pts',(-258.157985734452,-6.14153931545366,
129.894837769574));
#223432=CARTESIAN_POINT('Ctrl Pts',(-258.436433358265,-4.08485240479644,
135.479405634932));
#223433=CARTESIAN_POINT('Ctrl Pts',(-258.714880982078,1.72527217059264,
136.768768758555));
#223434=CARTESIAN_POINT('Ctrl Pts',(-258.993328605892,5.95060195420752,
132.575369498931));
#223435=CARTESIAN_POINT('Ctrl Pts',(-259.271776229703,4.70639920604184,
126.75783223591));
#223436=CARTESIAN_POINT('Ctrl Pts',(-259.550223853517,-0.860449444711704,
124.652528659269));
#223437=CARTESIAN_POINT('Ctrl Pts',(-259.82867147733,-5.64095031490746,
128.212697490595));
#223438=CARTESIAN_POINT('Ctrl Pts',(-260.060711163841,-5.29799179572588,
133.142936715762));
#223439=CARTESIAN_POINT('Ctrl Pts',(-260.246372125917,-2.62679689981868,
135.594171577488));
#223440=CARTESIAN_POINT('Ctrl Pts',(-260.339217213388,-0.889986900407246,
136.05080276614));
#223441=CARTESIAN_POINT('Ctrl Pts',(-260.385654363559,-0.0148419801173944,
136.053268468065));
#223442=CARTESIAN_POINT('Ctrl Pts',(209.997106195361,2.85369542052185,134.803838223542));
#223443=CARTESIAN_POINT('Ctrl Pts',(209.950688331758,3.52024512455777,134.328247120061));
#223444=CARTESIAN_POINT('Ctrl Pts',(209.857862530854,4.598911638141,133.039517383424));
#223445=CARTESIAN_POINT('Ctrl Pts',(209.672220855345,5.31158968331849,129.722011776094));
#223446=CARTESIAN_POINT('Ctrl Pts',(209.440181168834,2.90445768035623,125.771581499823));
#223447=CARTESIAN_POINT('Ctrl Pts',(209.161733545021,-2.67328939945229,
125.640965885288));
#223448=CARTESIAN_POINT('Ctrl Pts',(208.883285921209,-5.78445646322271,
130.262241799363));
#223449=CARTESIAN_POINT('Ctrl Pts',(208.604838297395,-3.58517659481558,
135.378114005881));
#223450=CARTESIAN_POINT('Ctrl Pts',(208.326390673583,1.91144119617671,136.292814641374));
#223451=CARTESIAN_POINT('Ctrl Pts',(208.04794304977,5.65009034124608,132.162897902674));
#223452=CARTESIAN_POINT('Ctrl Pts',(207.769495425957,4.19734896093999,126.785079177362));
#223453=CARTESIAN_POINT('Ctrl Pts',(207.491047802144,-1.1129569716493,125.100504449821));
#223454=CARTESIAN_POINT('Ctrl Pts',(207.212600178331,-5.4002948496084,128.657642803108));
#223455=CARTESIAN_POINT('Ctrl Pts',(206.934152554519,-4.72513942780656,
134.187431620732));
#223456=CARTESIAN_POINT('Ctrl Pts',(206.655704930705,0.292248586550605,
136.608384944684));
#223457=CARTESIAN_POINT('Ctrl Pts',(206.377257306892,5.04104249491135,133.695701483205));
#223458=CARTESIAN_POINT('Ctrl Pts',(206.09880968308,5.15738153042831,128.12602865207));
#223459=CARTESIAN_POINT('Ctrl Pts',(205.820362059267,0.534329935251406,
125.017605890956));
#223460=CARTESIAN_POINT('Ctrl Pts',(205.541914435454,-4.57974002364783,
127.226931288585));
#223461=CARTESIAN_POINT('Ctrl Pts',(205.263466811641,-5.48525514562618,
132.723737743954));
#223462=CARTESIAN_POINT('Ctrl Pts',(204.985019187828,-1.35008742798131,
136.456731302353));
#223463=CARTESIAN_POINT('Ctrl Pts',(204.706571564015,4.02574397595362,134.995471850294));
#223464=CARTESIAN_POINT('Ctrl Pts',(204.428123940202,5.70211370766606,129.682786179275));
#223465=CARTESIAN_POINT('Ctrl Pts',(204.149676316389,2.13851930815143,125.40077248911));
#223466=CARTESIAN_POINT('Ctrl Pts',(203.871228692576,-3.39026975841633,
126.084392381055));
#223467=CARTESIAN_POINT('Ctrl Pts',(203.592781068764,-5.8035665963141,131.105432460946));
#223468=CARTESIAN_POINT('Ctrl Pts',(203.314333444951,-2.88366922283368,
135.849802245147));
#223469=CARTESIAN_POINT('Ctrl Pts',(203.035885821138,2.68617927581077,135.957657646429));
#223470=CARTESIAN_POINT('Ctrl Pts',(202.757438197325,5.78756025537181,131.329884836407));
#223471=CARTESIAN_POINT('Ctrl Pts',(202.478990573512,3.57045609392238,126.219180939555));
#223472=CARTESIAN_POINT('Ctrl Pts',(202.200542949699,-1.92772278905516,
125.322033169903));
#223473=CARTESIAN_POINT('Ctrl Pts',(201.922095325886,-5.6544186046078,129.462876497226));
#223474=CARTESIAN_POINT('Ctrl Pts',(201.643647702073,-4.18497995558374,
134.836478196445));
#223475=CARTESIAN_POINT('Ctrl Pts',(201.36520007826,1.13025082464198,136.504760820331));
#223476=CARTESIAN_POINT('Ctrl Pts',(201.086752454448,5.4068363130258,132.934654138033));
#223477=CARTESIAN_POINT('Ctrl Pts',(200.808304830635,4.71480336828096,127.406911780982));
#223478=CARTESIAN_POINT('Ctrl Pts',(200.529857206822,-0.309903540913717,
125.001258930184));
#223479=CARTESIAN_POINT('Ctrl Pts',(200.251409583008,-5.04982423566531,
127.928373032793));
#223480=CARTESIAN_POINT('Ctrl Pts',(199.972961959197,-5.14920315545485,
133.498379226012));
#223481=CARTESIAN_POINT('Ctrl Pts',(199.694514335383,-0.516715927947778,
136.59271392819));
#223482=CARTESIAN_POINT('Ctrl Pts',(199.416066711571,4.59060799437092,134.367834714685));
#223483=CARTESIAN_POINT('Ctrl Pts',(199.137619087757,5.47938743352869,128.868296891315));
#223484=CARTESIAN_POINT('Ctrl Pts',(198.859171463945,1.33287750423228,125.147907050397));
#223485=CARTESIAN_POINT('Ctrl Pts',(198.580723840131,-4.03848173676817,
126.625521704588));
#223486=CARTESIAN_POINT('Ctrl Pts',(198.302276216319,-5.69867355247927,
131.943285172176));
#223487=CARTESIAN_POINT('Ctrl Pts',(198.023828592506,-2.12206276914206,
136.214432613634));
#223488=CARTESIAN_POINT('Ctrl Pts',(197.745380968693,3.4046200305072,135.513988187415));
#223489=CARTESIAN_POINT('Ctrl Pts',(197.46693334488,5.80262334705539,130.485626102603));
#223490=CARTESIAN_POINT('Ctrl Pts',(197.188485721067,2.86829928156946,125.750165465994));
#223491=CARTESIAN_POINT('Ctrl Pts',(196.910038097254,-2.70185169946893,
125.65926326252));
#223492=CARTESIAN_POINT('Ctrl Pts',(196.631590473441,-5.78913296148881,
130.296454176353));
#223493=CARTESIAN_POINT('Ctrl Pts',(196.353142849628,-3.5564838467683,135.400386297052));
#223494=CARTESIAN_POINT('Ctrl Pts',(196.074695225815,1.94440017923737,136.280795346639));
#223495=CARTESIAN_POINT('Ctrl Pts',(195.796247602003,5.6584754297534,132.128628418917));
#223496=CARTESIAN_POINT('Ctrl Pts',(195.51779997819,4.17268819221861,126.759524075833));
#223497=CARTESIAN_POINT('Ctrl Pts',(195.239352354377,-1.14759564681435,
125.107426913349));
#223498=CARTESIAN_POINT('Ctrl Pts',(194.960904730564,-5.41329514958902,
128.690533514357));
#223499=CARTESIAN_POINT('Ctrl Pts',(194.682457106751,-4.70444086406131,
134.216143957018));
#223500=CARTESIAN_POINT('Ctrl Pts',(194.404009482938,0.327564750825761,
136.606492185605));
#223501=CARTESIAN_POINT('Ctrl Pts',(194.125561859125,5.0585543621317,133.664964953048));
#223502=CARTESIAN_POINT('Ctrl Pts',(193.847114235312,5.14097963875765,128.094682084473));
#223503=CARTESIAN_POINT('Ctrl Pts',(193.568666611499,0.499095778182989,
125.014461412655));
#223504=CARTESIAN_POINT('Ctrl Pts',(193.290218987687,-4.60143272035756,
127.254875257849));
#223505=CARTESIAN_POINT('Ctrl Pts',(193.011771363874,-5.4734693413749,132.757092746623));
#223506=CARTESIAN_POINT('Ctrl Pts',(192.733323740061,-1.31565503151135,
136.464844805061));
#223507=CARTESIAN_POINT('Ctrl Pts',(192.454876116248,4.05118197898966,134.970888425217));
#223508=CARTESIAN_POINT('Ctrl Pts',(192.176428492435,5.69518066204141,129.648096536341));
#223509=CARTESIAN_POINT('Ctrl Pts',(191.897980868622,2.1055865417199,125.38785485147));
#223510=CARTESIAN_POINT('Ctrl Pts',(191.619533244809,-3.4189387468211,126.105117354624));
#223511=CARTESIAN_POINT('Ctrl Pts',(191.341085620997,-5.80162635147675,
131.140754845624));
#223512=CARTESIAN_POINT('Ctrl Pts',(191.062637997183,-2.85290276432908,
135.867262474811));
#223513=CARTESIAN_POINT('Ctrl Pts',(190.784190373371,2.71749909118881,135.941210633695));
#223514=CARTESIAN_POINT('Ctrl Pts',(190.505742749557,5.79065203911519,131.29464457683));
#223515=CARTESIAN_POINT('Ctrl Pts',(190.227295125745,3.54247865217362,126.197531513104));
#223516=CARTESIAN_POINT('Ctrl Pts',(189.948847501932,-1.96105955641241,
125.333869340265));
#223517=CARTESIAN_POINT('Ctrl Pts',(189.670399878119,-5.66247983574075,
129.497321402909));
#223518=CARTESIAN_POINT('Ctrl Pts',(189.391952254306,-4.160357773542,134.861878651407));
#223519=CARTESIAN_POINT('Ctrl Pts',(189.113504630493,1.16492983776554,136.497775047581));
#223520=CARTESIAN_POINT('Ctrl Pts',(188.83505700668,5.41970383815296,132.901701721328));
#223521=CARTESIAN_POINT('Ctrl Pts',(188.556609382867,4.69403477852959,127.378274381527));
#223522=CARTESIAN_POINT('Ctrl Pts',(188.278161759054,-0.345222926215044,
125.003252919028));
#223523=CARTESIAN_POINT('Ctrl Pts',(187.999714135242,-5.0672376268456,127.959166031618));
#223524=CARTESIAN_POINT('Ctrl Pts',(187.721266511429,-5.13270849672517,
133.529673973213));
#223525=CARTESIAN_POINT('Ctrl Pts',(187.442818887616,-0.48147100486422,
136.595752079925));
#223526=CARTESIAN_POINT('Ctrl Pts',(187.164371263803,4.61221481930072,134.339824357932));
#223527=CARTESIAN_POINT('Ctrl Pts',(186.88592363999,5.4675005437485,128.834978175547));
#223528=CARTESIAN_POINT('Ctrl Pts',(186.607476016177,1.29842037074208,125.139898247696));
#223529=CARTESIAN_POINT('Ctrl Pts',(186.329028392364,-4.06384469161484,
126.650182513385));
#223530=CARTESIAN_POINT('Ctrl Pts',(186.050580768551,-5.69163501222784,
131.977953513933));
#223531=CARTESIAN_POINT('Ctrl Pts',(185.772133144738,-2.08909080843167,
136.227249975919));
#223532=CARTESIAN_POINT('Ctrl Pts',(185.493685520926,3.4332257905535,135.493176040453));
#223533=CARTESIAN_POINT('Ctrl Pts',(185.215237897112,5.80057561042411,130.450309792719));
#223534=CARTESIAN_POINT('Ctrl Pts',(184.9367902733,2.83747981818726,125.732798956676));
#223535=CARTESIAN_POINT('Ctrl Pts',(184.658342649487,-2.73312130836828,
125.675805527429));
#223536=CARTESIAN_POINT('Ctrl Pts',(184.379895025674,-5.79211747293216,
130.331703682172));
#223537=CARTESIAN_POINT('Ctrl Pts',(184.101447401861,-3.52844064054064,
135.421950469967));
#223538=CARTESIAN_POINT('Ctrl Pts',(183.822999778048,1.97770076659953,136.26885776521));
#223539=CARTESIAN_POINT('Ctrl Pts',(183.544552154236,5.66643178528845,132.094159137294));
#223540=CARTESIAN_POINT('Ctrl Pts',(183.266104530422,4.14798881387936,126.734198679909));
#223541=CARTESIAN_POINT('Ctrl Pts',(182.98765690661,-1.18225323696583,125.114518204765));
#223542=CARTESIAN_POINT('Ctrl Pts',(182.709209282797,-5.42606231932092,
128.72352494273));
#223543=CARTESIAN_POINT('Ctrl Pts',(182.430761658984,-4.68358520810093,
134.244718011395));
#223544=CARTESIAN_POINT('Ctrl Pts',(182.152314035171,0.362877903506298,
136.604390705933));
#223545=CARTESIAN_POINT('Ctrl Pts',(181.873866411358,5.07587394936235,133.634119096483));
#223546=CARTESIAN_POINT('Ctrl Pts',(181.595418787545,5.12438980598236,128.063437686296));
#223547=CARTESIAN_POINT('Ctrl Pts',(181.316971163732,0.463841771263853,
125.011530548415));
#223548=CARTESIAN_POINT('Ctrl Pts',(181.038523539919,-4.62295419131585,
127.282951248603));
#223549=CARTESIAN_POINT('Ctrl Pts',(180.760075916106,-5.46148109594396,
132.790375128456));
#223550=CARTESIAN_POINT('Ctrl Pts',(180.481628292294,-1.2811736815839,136.472748695004));
#223551=CARTESIAN_POINT('Ctrl Pts',(180.203180668481,4.07646975733793,134.946150534538));
#223552=CARTESIAN_POINT('Ctrl Pts',(179.924733044668,5.68803663588505,129.61344977806));
#223553=CARTESIAN_POINT('Ctrl Pts',(179.646285420855,2.07257572209157,125.37513790386));
#223554=CARTESIAN_POINT('Ctrl Pts',(179.367837797042,-3.44748102935117,
126.12601647128));
#223555=CARTESIAN_POINT('Ctrl Pts',(179.089390173229,-5.79947113363144,
131.176064759319));
#223556=CARTESIAN_POINT('Ctrl Pts',(178.810942549416,-2.82203058602,135.884535099843));
#223557=CARTESIAN_POINT('Ctrl Pts',(178.532494925603,2.74871820628535,135.924573271475));
#223558=CARTESIAN_POINT('Ctrl Pts',(178.254047301791,5.79352924936408,131.259386150458));
#223559=CARTESIAN_POINT('Ctrl Pts',(177.975599677977,3.51436994191561,126.176052793945));
#223560=CARTESIAN_POINT('Ctrl Pts',(177.697152054165,-1.99432365563702,
125.345908221933));
#223561=CARTESIAN_POINT('Ctrl Pts',(177.418704430351,-5.6703312417861,129.531814741282));
#223562=CARTESIAN_POINT('Ctrl Pts',(177.140256806539,-4.135581427815,134.887128753614));
#223563=CARTESIAN_POINT('Ctrl Pts',(176.861809182726,1.19956568393359,136.490578303229));
#223564=CARTESIAN_POINT('Ctrl Pts',(176.583361558913,5.43237053418876,132.868671586896));
#223565=CARTESIAN_POINT('Ctrl Pts',(176.3049139351,4.67309224957875,127.349763936946));
#223566=CARTESIAN_POINT('Ctrl Pts',(176.026466311287,-0.380529519146142,
125.005461870054));
#223567=CARTESIAN_POINT('Ctrl Pts',(175.748018687475,-5.08446324967622,
127.990064460173));
#223568=CARTESIAN_POINT('Ctrl Pts',(175.469571063661,-5.11602364359241,
133.560867732924));
#223569=CARTESIAN_POINT('Ctrl Pts',(175.191123439849,-0.446208240696769,
136.59857562952));
#223570=CARTESIAN_POINT('Ctrl Pts',(174.912675816035,4.63365073691483,134.311682993269));
#223571=CARTESIAN_POINT('Ctrl Pts',(174.634228192223,5.45541105372469,128.801732435971));
#223572=CARTESIAN_POINT('Ctrl Pts',(174.35578056841,1.26391512380778,125.132099343732));
#223573=CARTESIAN_POINT('Ctrl Pts',(174.077332944597,-4.089057059202,126.674997256779));
#223574=CARTESIAN_POINT('Ctrl Pts',(173.798885320784,-5.68438556634791,
132.012578367773));
#223575=CARTESIAN_POINT('Ctrl Pts',(173.520437696972,-2.0560414356932,136.239866391045));
#223576=CARTESIAN_POINT('Ctrl Pts',(173.241990073158,3.46170433115548,135.472190147709));
#223577=CARTESIAN_POINT('Ctrl Pts',(172.963542449346,5.79831293133042,130.41500660232));
#223578=CARTESIAN_POINT('Ctrl Pts',(172.685094825533,2.80655521094699,125.715620375941));
#223579=CARTESIAN_POINT('Ctrl Pts',(172.40664720172,-2.76428964045241,125.692537832834));
#223580=CARTESIAN_POINT('Ctrl Pts',(172.128199577907,-5.79488735533246,
130.366970702468));
#223581=CARTESIAN_POINT('Ctrl Pts',(171.849751954094,-3.50026668664755,
135.443343536393));
#223582=CARTESIAN_POINT('Ctrl Pts',(171.571304330281,2.01092806953244,136.256717694829));
#223583=CARTESIAN_POINT('Ctrl Pts',(171.292856706468,5.6741781691098,132.059642061713));
#223584=CARTESIAN_POINT('Ctrl Pts',(171.014409082656,4.12313573028927,126.709024105332));
#223585=CARTESIAN_POINT('Ctrl Pts',(170.735961458842,-1.21686701828875,
125.121820335384));
#223586=CARTESIAN_POINT('Ctrl Pts',(170.45751383503,-5.43862842431808,128.756593477234));
#223587=CARTESIAN_POINT('Ctrl Pts',(170.179066211217,-4.66255600016836,
134.273164582064));
#223588=CARTESIAN_POINT('Ctrl Pts',(169.900618587404,0.398177609612544,
136.602074304013));
#223589=CARTESIAN_POINT('Ctrl Pts',(169.62217096359,5.09300544821711,133.603168382178));
#223590=CARTESIAN_POINT('Ctrl Pts',(169.343723339778,5.10761008705837,128.032294854024));
#223591=CARTESIAN_POINT('Ctrl Pts',(169.065275715965,0.428570576517446,
125.008814339624));
#223592=CARTESIAN_POINT('Ctrl Pts',(168.786828092152,-4.64430435700642,
127.311157726477));
#223593=CARTESIAN_POINT('Ctrl Pts',(168.508380468339,-5.4492904733226,132.823583917792));
#223594=CARTESIAN_POINT('Ctrl Pts',(168.229932844526,-1.24664485729461,
136.480442540741));
#223595=CARTESIAN_POINT('Ctrl Pts',(167.951485220714,4.10160648060013,134.92125916831));
#223596=CARTESIAN_POINT('Ctrl Pts',(167.673037596901,5.6806818374394,129.578847149419));
#223597=CARTESIAN_POINT('Ctrl Pts',(167.394589973088,2.03948810240773,125.362622138095));
#223598=CARTESIAN_POINT('Ctrl Pts',(167.116142349275,-3.47589556420378,
126.147088945699));
#223599=CARTESIAN_POINT('Ctrl Pts',(166.837694725462,-5.79710101425052,
131.21136089938));
#223600=CARTESIAN_POINT('Ctrl Pts',(166.559247101649,-2.79105383632985,
135.901619477142));
#223601=CARTESIAN_POINT('Ctrl Pts',(166.280799477836,2.77983546661788,135.907746177893));
#223602=CARTESIAN_POINT('Ctrl Pts',(166.002351854023,5.79619177825601,131.224110862948));
#223603=CARTESIAN_POINT('Ctrl Pts',(165.72390423021,3.48613100538707,126.154745578436));
#223604=CARTESIAN_POINT('Ctrl Pts',(165.445456606397,-2.02751385446508,
125.358149368562));
#223605=CARTESIAN_POINT('Ctrl Pts',(165.167008982585,-5.67797253162207,
129.566355234311));
#223606=CARTESIAN_POINT('Ctrl Pts',(164.888561358772,-4.11065183659732,
134.912227567346));
#223607=CARTESIAN_POINT('Ctrl Pts',(164.610113734959,1.23415707975413,136.483170853989));
#223608=CARTESIAN_POINT('Ctrl Pts',(164.331666111146,5.44483593173667,132.835564958663));
#223609=CARTESIAN_POINT('Ctrl Pts',(164.053218487333,4.65197655747607,127.321381503715));
#223610=CARTESIAN_POINT('Ctrl Pts',(163.77477086352,-0.415822011415935,
125.007885701408));
#223611=CARTESIAN_POINT('Ctrl Pts',(163.496323239708,-5.10150046585131,
128.021067173507));
#223612=CARTESIAN_POINT('Ctrl Pts',(163.217875615894,-5.09914921432216,
133.591959349252));
#223613=CARTESIAN_POINT('Ctrl Pts',(162.939427992082,-0.41092894211879,
136.601184472346));
#223614=CARTESIAN_POINT('Ctrl Pts',(162.660980368268,4.65491495289691,134.283411663486));
#223615=CARTESIAN_POINT('Ctrl Pts',(162.382532744456,5.443119411438,128.768560904517));
#223616=CARTESIAN_POINT('Ctrl Pts',(162.104085120643,1.22936304203373,125.124510627495));
#223617=CARTESIAN_POINT('Ctrl Pts',(161.82563749683,-4.11411790527609,126.69996501525));
#223618=CARTESIAN_POINT('Ctrl Pts',(161.547189873017,-5.67692548347038,
132.04715845066));
#223619=CARTESIAN_POINT('Ctrl Pts',(161.268742249204,-2.02291587558315,
136.252281391507));
#223620=CARTESIAN_POINT('Ctrl Pts',(160.990294625391,3.49005459703047,135.451031286826));
#223621=CARTESIAN_POINT('Ctrl Pts',(160.711847001578,5.79583539361873,130.379717839577));
#223622=CARTESIAN_POINT('Ctrl Pts',(160.433399377766,2.77552660577121,125.698630360346));
#223623=CARTESIAN_POINT('Ctrl Pts',(160.154951753952,-2.79535554076737,
125.70945955871));
#223624=CARTESIAN_POINT('Ctrl Pts',(159.87650413014,-5.79744250605075,130.402253930408));
#223625=CARTESIAN_POINT('Ctrl Pts',(159.598056506327,-3.47196302908515,
135.4645647036));
#223626=CARTESIAN_POINT('Ctrl Pts',(159.319608882514,2.04408085678626,136.244375585352));
#223627=CARTESIAN_POINT('Ctrl Pts',(159.041161258701,5.68171429417248,132.025078471215));
#223628=CARTESIAN_POINT('Ctrl Pts',(158.762713634888,4.09812986238831,126.684001284956));
#223629=CARTESIAN_POINT('Ctrl Pts',(158.484266011075,-1.25143570815684,
125.129333034622));
#223630=CARTESIAN_POINT('Ctrl Pts',(158.205818387262,-5.450992998939,128.789737892503));
#223631=CARTESIAN_POINT('Ctrl Pts',(157.927370763449,-4.64135401950845,
134.301482614925));
#223632=CARTESIAN_POINT('Ctrl Pts',(157.648923139637,0.43346256110109,136.59954306568));
#223633=CARTESIAN_POINT('Ctrl Pts',(157.370475515823,5.10994822388206,133.572113957021));
#223634=CARTESIAN_POINT('Ctrl Pts',(157.092027892011,5.09064110376424,128.001254741669));
#223635=CARTESIAN_POINT('Ctrl Pts',(156.813580268198,0.39328350093061,125.006312886931));
#223636=CARTESIAN_POINT('Ctrl Pts',(156.535132644385,-4.66548242629113,
127.339493646268));
#223637=CARTESIAN_POINT('Ctrl Pts',(156.256685020572,-5.43689792523874,
132.856717884066));
#223638=CARTESIAN_POINT('Ctrl Pts',(155.978237396759,-1.21206983812162,
136.487926057176));
#223639=CARTESIAN_POINT('Ctrl Pts',(155.699789772946,4.12659121732586,134.896215248893));
#223640=CARTESIAN_POINT('Ctrl Pts',(155.421342149133,5.67311653923917,129.544289932631));
#223641=CARTESIAN_POINT('Ctrl Pts',(155.142894525321,2.0063249087422,125.350308017949));
#223642=CARTESIAN_POINT('Ctrl Pts',(154.864446901507,-3.50418129846815,
126.168333997033));
#223643=CARTESIAN_POINT('Ctrl Pts',(154.585999277695,-5.79451608115961,
131.246641957895));
#223644=CARTESIAN_POINT('Ctrl Pts',(154.307551653882,-2.75997366311328,
135.918514973638));
#223645=CARTESIAN_POINT('Ctrl Pts',(154.029104030069,2.81084971912495,135.890729976482));
#223646=CARTESIAN_POINT('Ctrl Pts',(153.750656406256,5.79863952713012,131.188820021437));
#223647=CARTESIAN_POINT('Ctrl Pts',(153.472208782443,3.457762888992,126.133610656121));
#223648=CARTESIAN_POINT('Ctrl Pts',(153.19376115863,-2.0606289230217,125.370592326552));
#223649=CARTESIAN_POINT('Ctrl Pts',(152.915313534817,-5.68540342209783,
129.600941602086));
#223650=CARTESIAN_POINT('Ctrl Pts',(152.636865911004,-4.08556992366409,
134.937174162558));
#223651=CARTESIAN_POINT('Ctrl Pts',(152.358418287191,1.26870274343019,136.475552974349));
#223652=CARTESIAN_POINT('Ctrl Pts',(152.079970663379,5.45709956888678,132.802383063404));
#223653=CARTESIAN_POINT('Ctrl Pts',(151.801523039566,4.63068848467127,127.293128133558));
#223654=CARTESIAN_POINT('Ctrl Pts',(151.523075415753,-0.451099095248245,
125.010524323271));
#223655=CARTESIAN_POINT('Ctrl Pts',(151.24462779194,-5.11834864405056,128.052173022803));
#223656=CARTESIAN_POINT('Ctrl Pts',(150.966180168127,-5.08208583420252,
133.622947670083));
#223657=CARTESIAN_POINT('Ctrl Pts',(150.687732544314,-0.375634416417742,
136.603578511732));
#223658=CARTESIAN_POINT('Ctrl Pts',(150.409284920501,4.67600667929353,134.255011416186));
#223659=CARTESIAN_POINT('Ctrl Pts',(150.130837296688,5.43062607235983,128.735464810371));
#223660=CARTESIAN_POINT('Ctrl Pts',(149.852389672876,1.19476540576009,125.117132380189));
#223661=CARTESIAN_POINT('Ctrl Pts',(149.573942049063,-4.13902630119825,
126.725084863609));
#223662=CARTESIAN_POINT('Ctrl Pts',(149.29549442525,-5.66925504003138,132.081692481218));
#223663=CARTESIAN_POINT('Ctrl Pts',(149.017046801437,-1.98971535558138,
136.264494517259));
#223664=CARTESIAN_POINT('Ctrl Pts',(148.738599177624,3.5182755376489,135.429700241853));
#223665=CARTESIAN_POINT('Ctrl Pts',(148.460151553811,5.79314308909515,130.344444812129));
#223666=CARTESIAN_POINT('Ctrl Pts',(148.181703929998,2.74439515243632,125.681829539465));
#223667=CARTESIAN_POINT('Ctrl Pts',(147.903256306185,-2.82631785815477,
125.726570078021));
#223668=CARTESIAN_POINT('Ctrl Pts',(147.624808682372,-5.79978283040501,
130.437552058559));
#223669=CARTESIAN_POINT('Ctrl Pts',(147.346361058559,-3.4435307166558,135.48561318523));
#223670=CARTESIAN_POINT('Ctrl Pts',(147.067913434747,2.07715789987228,136.23183189412));
#223671=CARTESIAN_POINT('Ctrl Pts',(146.789465810933,5.68903988122249,131.990469646568));
#223672=CARTESIAN_POINT('Ctrl Pts',(146.511018187121,4.07297213677825,126.65913114601));
#223673=CARTESIAN_POINT('Ctrl Pts',(146.232570563308,-1.2859580256146,125.137056024094));
#223674=CARTESIAN_POINT('Ctrl Pts',(145.954122939495,-5.46315558500969,
128.822956960357));
#223675=CARTESIAN_POINT('Ctrl Pts',(145.675675315682,-4.61998005176852,
134.329671060644));
#223676=CARTESIAN_POINT('Ctrl Pts',(145.397227691869,0.468731450475054,
136.596797084732));
#223677=CARTESIAN_POINT('Ctrl Pts',(145.118780068056,5.12670164853643,133.540956971746));
#223678=CARTESIAN_POINT('Ctrl Pts',(144.840332444244,5.07348348489189,127.970318499433));
#223679=CARTESIAN_POINT('Ctrl Pts',(144.56188482043,0.357981852079004,125.004026283029));
#223680=CARTESIAN_POINT('Ctrl Pts',(144.283437196618,-4.6864876144088,127.367957957979));
#223681=CARTESIAN_POINT('Ctrl Pts',(144.004989572805,-5.42430391090288,
132.889775799486));
#223682=CARTESIAN_POINT('Ctrl Pts',(143.726541948992,-1.17744990525502,
136.495198967004));
#223683=CARTESIAN_POINT('Ctrl Pts',(143.448094325179,4.15142304169647,134.871019704297));
#223684=CARTESIAN_POINT('Ctrl Pts',(143.169646701366,5.66534102161933,129.509779408224));
#223685=CARTESIAN_POINT('Ctrl Pts',(142.891199077553,1.9730873699693,125.338195999729));
#223686=CARTESIAN_POINT('Ctrl Pts',(142.61275145374,-3.53233718400576,126.189750838038));
#223687=CARTESIAN_POINT('Ctrl Pts',(142.334303829928,-5.79171643014443,
131.281906627513));
#223688=CARTESIAN_POINT('Ctrl Pts',(142.055856206114,-2.72879121805762,
135.935220963265));
#223689=CARTESIAN_POINT('Ctrl Pts',(141.777408582302,2.84175981456215,135.873525297782));
#223690=CARTESIAN_POINT('Ctrl Pts',(141.498960958489,5.80087240528401,131.153514933643));
#223691=CARTESIAN_POINT('Ctrl Pts',(141.220513334676,3.42926664392146,126.112648810165));
#223692=CARTESIAN_POINT('Ctrl Pts',(140.942065710863,-2.09366763421581,
125.383236634823));
#223693=CARTESIAN_POINT('Ctrl Pts',(140.66361808705,-5.69262363785895,129.635572562993));
#223694=CARTESIAN_POINT('Ctrl Pts',(140.385170463237,-4.06033661843482,
134.961967614844));
#223695=CARTESIAN_POINT('Ctrl Pts',(140.106722839424,1.30320139485961,136.467724946589));
#223696=CARTESIAN_POINT('Ctrl Pts',(139.828275215611,5.46916099120554,132.769127130691));
#223697=CARTESIAN_POINT('Ctrl Pts',(139.549827591798,4.60922882000175,127.26500487341));
#223698=CARTESIAN_POINT('Ctrl Pts',(139.271379967986,-0.486359463437733,
125.013377637868));
#223699=CARTESIAN_POINT('Ctrl Pts',(138.992932344173,-5.13500715995863,
128.083380855422));
#223700=CARTESIAN_POINT('Ctrl Pts',(138.71448472036,-5.06483413552331,133.653831547135));
#223701=CARTESIAN_POINT('Ctrl Pts',(138.436037096547,-0.340325971445257,
136.605757658967));
#223702=CARTESIAN_POINT('Ctrl Pts',(138.157589472734,4.69692513454305,134.226483303753));
#223703=CARTESIAN_POINT('Ctrl Pts',(137.879141848921,5.41793149943546,128.70244537992));
#223704=CARTESIAN_POINT('Ctrl Pts',(137.600694225109,1.16012349701482,125.109964875215));
#223705=CARTESIAN_POINT('Ctrl Pts',(137.322246601295,-4.16378132397874,
126.750355871033));
#223706=CARTESIAN_POINT('Ctrl Pts',(137.043798977483,-5.66137452026194,
132.116179179772));
#223707=CARTESIAN_POINT('Ctrl Pts',(136.765351353669,-1.95644110594549,
136.276505315742));
#223708=CARTESIAN_POINT('Ctrl Pts',(136.486903729857,3.54636610727348,135.408197803219));
#223709=CARTESIAN_POINT('Ctrl Pts',(136.208456106044,5.79023611752392,130.309188827029));
#223710=CARTESIAN_POINT('Ctrl Pts',(135.930008482231,2.71316200452982,125.665218535856));
#223711=CARTESIAN_POINT('Ctrl Pts',(135.651560858418,-2.85717544529452,
125.743868756725));
#223712=CARTESIAN_POINT('Ctrl Pts',(135.373113234605,-5.80190824167357,
130.472863778936));
#223713=CARTESIAN_POINT('Ctrl Pts',(135.094665610792,-3.41497080292952,
135.506488201326));
#223714=CARTESIAN_POINT('Ctrl Pts',(134.816217986979,2.11015797310843,136.219087085943));
#223715=CARTESIAN_POINT('Ctrl Pts',(134.537770363167,5.69615465880763,131.955816870215));
#223716=CARTESIAN_POINT('Ctrl Pts',(134.259322739353,4.04766348568775,126.634414610068));
#223717=CARTESIAN_POINT('Ctrl Pts',(133.980875115541,-1.32043269142476,
125.144989017623));
#223718=CARTESIAN_POINT('Ctrl Pts',(133.702427491728,-5.47511573184112,
128.856249449853));
#223719=CARTESIAN_POINT('Ctrl Pts',(133.423979867915,-4.59843488896879,
134.357728874689));
#223720=CARTESIAN_POINT('Ctrl Pts',(133.145532244102,0.503982970832797,
136.59383646292));
#223721=CARTESIAN_POINT('Ctrl Pts',(132.867084620289,5.14326510137581,133.509698580887));
#223722=CARTESIAN_POINT('Ctrl Pts',(132.588636996476,5.05613786622328,127.93948727367));
#223723=CARTESIAN_POINT('Ctrl Pts',(132.310189372663,0.322666938078297,
125.001954612649));
#223724=CARTESIAN_POINT('Ctrl Pts',(132.03174174885,-4.70731914300451,127.396549606854));
#223725=CARTESIAN_POINT('Ctrl Pts',(131.753294125038,-5.41150889699075,
132.92275643908));
#223726=CARTESIAN_POINT('Ctrl Pts',(131.474846501225,-1.14278634154918,
136.502261000723));
#223727=CARTESIAN_POINT('Ctrl Pts',(131.196398877412,4.17610103355955,134.845673468154));
#223728=CARTESIAN_POINT('Ctrl Pts',(130.917951253599,5.65735557270449,129.475316855001));
#223729=CARTESIAN_POINT('Ctrl Pts',(130.639503629786,1.93977671771839,125.326286532249));
#223730=CARTESIAN_POINT('Ctrl Pts',(130.361056005973,-3.56036217749005,
126.211338675105));
#223731=CARTESIAN_POINT('Ctrl Pts',(130.08260838216,-5.788702164947,131.317153601487));
#223732=CARTESIAN_POINT('Ctrl Pts',(129.804160758347,-2.69750765663984,
135.951736826975));
#223733=CARTESIAN_POINT('Ctrl Pts',(129.525713134534,2.87256460754407,135.856132779323));
#223734=CARTESIAN_POINT('Ctrl Pts',(129.247265510721,5.80289032997773,131.118196907806));
#223735=CARTESIAN_POINT('Ctrl Pts',(128.968817886909,3.40064332611445,126.091860817314));
#223736=CARTESIAN_POINT('Ctrl Pts',(128.690370263096,-2.12662876378584,
125.396081824838));
#223737=CARTESIAN_POINT('Ctrl Pts',(128.411922639283,-5.69963291135762,
129.670246833772));
#223738=CARTESIAN_POINT('Ctrl Pts',(128.13347501547,-4.03495285593914,134.986607005474));
#223739=CARTESIAN_POINT('Ctrl Pts',(127.855027391657,1.33765175568188,136.459687060782));
#223740=CARTESIAN_POINT('Ctrl Pts',(127.576579767844,5.48101975175251,132.73579839283));
#223741=CARTESIAN_POINT('Ctrl Pts',(127.298132144031,4.5875983586632,127.237012765392));
#223742=CARTESIAN_POINT('Ctrl Pts',(127.019684520218,-0.521601809398458,
125.016445539469));
#223743=CARTESIAN_POINT('Ctrl Pts',(126.741236896406,-5.15147539628782,
128.114689514947));
#223744=CARTESIAN_POINT('Ctrl Pts',(126.462789272592,-5.0473947575527,133.684609835992));
#223745=CARTESIAN_POINT('Ctrl Pts',(126.18434164878,-0.305004915568794,
136.607721833301));
#223746=CARTESIAN_POINT('Ctrl Pts',(125.905894024967,4.71766954350447,134.197828383304));
#223747=CARTESIAN_POINT('Ctrl Pts',(125.627446401154,5.40503616306688,128.669503836711));
#223748=CARTESIAN_POINT('Ctrl Pts',(125.348998777341,1.12543859946687,125.10300837817));
#223749=CARTESIAN_POINT('Ctrl Pts',(125.070551153528,-4.18838205631096,
126.775777101093));
#223750=CARTESIAN_POINT('Ctrl Pts',(124.792103529715,-5.65328421617778,
132.150617268407));
#223751=CARTESIAN_POINT('Ctrl Pts',(124.513655905902,-1.9230943596648,136.288313341892));
#223752=CARTESIAN_POINT('Ctrl Pts',(124.23520828209,3.57432526499779,135.386524767704));
#223753=CARTESIAN_POINT('Ctrl Pts',(123.956760658277,5.78711458662396,130.273951190703));
#223754=CARTESIAN_POINT('Ctrl Pts',(123.678313034464,2.68182831940755,125.648797965047));
#223755=CARTESIAN_POINT('Ctrl Pts',(123.399865410651,-2.88792715874745,
125.761354953818));
#223756=CARTESIAN_POINT('Ctrl Pts',(123.121417786838,-5.8038186610986,130.50818778305));
#223757=CARTESIAN_POINT('Ctrl Pts',(122.842970163025,-3.38628434620416,
135.527188978355));
#223758=CARTESIAN_POINT('Ctrl Pts',(122.564522539212,2.1430798536649,136.206141633086));
#223759=CARTESIAN_POINT('Ctrl Pts',(122.286074915399,5.703058363287,131.921121426228));
#223760=CARTESIAN_POINT('Ctrl Pts',(122.007627291586,4.02220484693838,126.609852593007));
#223761=CARTESIAN_POINT('Ctrl Pts',(121.729179667773,-1.35485842811595,
125.153131721247));
#223762=CARTESIAN_POINT('Ctrl Pts',(121.450732043961,-5.48687299624567,
128.889614127324));
#223763=CARTESIAN_POINT('Ctrl Pts',(121.172284420148,-4.57671932947311,
134.385655017367));
#223764=CARTESIAN_POINT('Ctrl Pts',(120.893836796335,0.539215815916097,
136.59066130995));
#223765=CARTESIAN_POINT('Ctrl Pts',(120.615389172522,5.15963796863542,133.478339942736));
#223766=CARTESIAN_POINT('Ctrl Pts',(120.336941548709,5.0386048905067,127.908762206842));
#223767=CARTESIAN_POINT('Ctrl Pts',(120.058493924896,0.287340067535411,
125.000097952557));
#223768=CARTESIAN_POINT('Ctrl Pts',(119.780046301083,-4.72797624015824,
127.42526753342));
#223769=CARTESIAN_POINT('Ctrl Pts',(119.50159867727,-5.39851335762638,132.955658580739));
#223770=CARTESIAN_POINT('Ctrl Pts',(119.223151053457,-1.10808043147514,
136.509111896649));
#223771=CARTESIAN_POINT('Ctrl Pts',(118.944703429644,4.20062427846316,134.820177479675));
#223772=CARTESIAN_POINT('Ctrl Pts',(118.666255805832,5.64916048839838,129.440903549983));
#223773=CARTESIAN_POINT('Ctrl Pts',(118.387808182019,1.90639418632776,125.314580056818));
#223774=CARTESIAN_POINT('Ctrl Pts',(118.109360558206,-3.58825524044456,
126.23309670829));
#223775=CARTESIAN_POINT('Ctrl Pts',(117.830912934393,-5.785473397262,131.352381573729));
#223776=CARTESIAN_POINT('Ctrl Pts',(117.55246531058,-2.66612413808396,135.968061952766));
#223777=CARTESIAN_POINT('Ctrl Pts',(117.274017686767,2.9032629565882,135.838553065588));
#223778=CARTESIAN_POINT('Ctrl Pts',(116.995570062954,5.80469322643624,131.082867252651));
#223779=CARTESIAN_POINT('Ctrl Pts',(116.717122439142,3.37189399621826,126.071247447876));
#223780=CARTESIAN_POINT('Ctrl Pts',(116.438674815328,-2.15951109034483,
125.409127420613));
#223781=CARTESIAN_POINT('Ctrl Pts',(116.160227191516,-5.70643098286277,
129.704963129555));
#223782=CARTESIAN_POINT('Ctrl Pts',(115.881779567703,-4.00941957678149,
135.011091421425));
#223783=CARTESIAN_POINT('Ctrl Pts',(115.60333194389,1.37205254932662,136.451439614773));
#223784=CARTESIAN_POINT('Ctrl Pts',(115.324884320077,5.49267541109693,132.702398084833));
#223785=CARTESIAN_POINT('Ctrl Pts',(115.046436696264,4.56579790218037,127.20915284676));
#223786=CARTESIAN_POINT('Ctrl Pts',(114.767989072451,-0.556824827212187,
125.019727914392));
#223787=CARTESIAN_POINT('Ctrl Pts',(114.489541448638,-5.1677527428018,128.146097841224));
#223788=CARTESIAN_POINT('Ctrl Pts',(114.211093824825,-5.02976834651319,
133.715281396157));
#223789=CARTESIAN_POINT('Ctrl Pts',(113.932646201012,-0.269672557622912,
136.60947096195));
#223790=CARTESIAN_POINT('Ctrl Pts',(113.6541985772,4.73823913748602,134.169047716661));
#223791=CARTESIAN_POINT('Ctrl Pts',(113.375750953387,5.39194054109557,128.636641401405));
#223792=CARTESIAN_POINT('Ctrl Pts',(113.097303329574,1.09071199837779,125.09626314683));
#223793=CARTESIAN_POINT('Ctrl Pts',(112.818855705761,-4.21282758660586,
126.801347611796));
#223794=CARTESIAN_POINT('Ctrl Pts',(112.540408081948,-5.64498442756793,
132.185005471008));
#223795=CARTESIAN_POINT('Ctrl Pts',(112.261960458135,-1.8896763524154,136.299918158156));
#223796=CARTESIAN_POINT('Ctrl Pts',(111.983512834322,3.60215197478495,135.364681938413));
#223797=CARTESIAN_POINT('Ctrl Pts',(111.705065210509,5.78377861206482,130.238733208892));
#223798=CARTESIAN_POINT('Ctrl Pts',(111.426617586696,2.65039525815055,125.632568435507));
#223799=CARTESIAN_POINT('Ctrl Pts',(111.148169962883,-2.91857185899754,
125.77902802134));
#223800=CARTESIAN_POINT('Ctrl Pts',(110.869722339071,-5.80551401788879,
130.543522761958));
#223801=CARTESIAN_POINT('Ctrl Pts',(110.591274715258,-3.35747240946702,
135.547714749242));
#223802=CARTESIAN_POINT('Ctrl Pts',(110.312827091445,2.17592232160915,136.192996015246));
#223803=CARTESIAN_POINT('Ctrl Pts',(110.034379467632,5.70975073884148,131.886384600257));
#223804=CARTESIAN_POINT('Ctrl Pts',(109.755931843819,3.99659716390926,126.585446004984));
#223805=CARTESIAN_POINT('Ctrl Pts',(109.477484220006,-1.38923396002991,
125.161483833236));
#223806=CARTESIAN_POINT('Ctrl Pts',(109.199036596193,-5.49842694255352,
128.923049756431));
#223807=CARTESIAN_POINT('Ctrl Pts',(108.92058897238,-4.55483417795961,134.413448453863));
#223808=CARTESIAN_POINT('Ctrl Pts',(108.642141348568,0.57442868015902,136.58727174348));
#223809=CARTESIAN_POINT('Ctrl Pts',(108.363693724754,5.17581964361271,133.446882219296));
#223810=CARTESIAN_POINT('Ctrl Pts',(108.085246100942,5.02088520743284,127.878144437479));
#223811=CARTESIAN_POINT('Ctrl Pts',(107.806798477129,0.252002549500665,
124.998456371553));
#223812=CARTESIAN_POINT('Ctrl Pts',(107.528350853316,-4.74845814041369,
127.454110673523));
#223813=CARTESIAN_POINT('Ctrl Pts',(107.249903229503,-5.38531777436419,
132.988481005259));
#223814=CARTESIAN_POINT('Ctrl Pts',(106.97145560569,-1.07333346107335,136.515751400918));
#223815=CARTESIAN_POINT('Ctrl Pts',(106.693007981877,4.22499186768932,134.794532683627));
#223816=CARTESIAN_POINT('Ctrl Pts',(106.414560358064,5.64075607237289,129.406540768369));
#223817=CARTESIAN_POINT('Ctrl Pts',(106.136112734251,1.87294101279944,125.303077007226));
#223818=CARTESIAN_POINT('Ctrl Pts',(105.857665110439,-3.61601533928142,
126.25502413134));
#223819=CARTESIAN_POINT('Ctrl Pts',(105.579217486626,-5.78203024673271,
131.387589238853));
#223820=CARTESIAN_POINT('Ctrl Pts',(105.300769862813,-2.63464182531766,
135.984195735705));
#223821=CARTESIAN_POINT('Ctrl Pts',(105.022322239,2.93385372415587,135.820786808));
#223822=CARTESIAN_POINT('Ctrl Pts',(104.743874615187,5.80628102785255,131.047527277329));
#223823=CARTESIAN_POINT('Ctrl Pts',(104.465426991374,3.34301971955009,126.050809465687));
#223824=CARTESIAN_POINT('Ctrl Pts',(104.186979367561,-2.19231339542621,
125.422372938737));
#223825=CARTESIAN_POINT('Ctrl Pts',(103.908531743748,-5.71301760046937,
129.739720163916));
#223826=CARTESIAN_POINT('Ctrl Pts',(103.630084119935,-3.98373772710686,
135.03541995542));
#223827=CARTESIAN_POINT('Ctrl Pts',(103.351636496123,1.40640250105958,136.442982914176));
#223828=CARTESIAN_POINT('Ctrl Pts',(103.07318887231,5.50412753733405,132.66892744436));
#223829=CARTESIAN_POINT('Ctrl Pts',(102.794741248497,4.54382825837723,127.181426149873));
#223830=CARTESIAN_POINT('Ctrl Pts',(102.516293624684,-0.592027211677165,
125.023224641008));
#223831=CARTESIAN_POINT('Ctrl Pts',(102.237846000871,-5.18383859633749,
128.177604670405));
#223832=CARTESIAN_POINT('Ctrl Pts',(101.959398377058,-5.01195555555783,
133.745845091081));
#223833=CARTESIAN_POINT('Ctrl Pts',(101.680950753245,-0.234330206861215,
136.611004980102));
#223834=CARTESIAN_POINT('Ctrl Pts',(101.402503129432,4.75863315427373,134.140142370299));
#223835=CARTESIAN_POINT('Ctrl Pts',(101.124055505619,5.37864511878468,128.603859291732));
#223836=CARTESIAN_POINT('Ctrl Pts',(100.845607881807,1.05594498055446,125.089729431141));
#223837=CARTESIAN_POINT('Ctrl Pts',(100.567160257994,-4.23711700902531,
126.827066455619));
#223838=CARTESIAN_POINT('Ctrl Pts',(100.288712634181,-5.63647546198416,
132.219342513305));
#223839=CARTESIAN_POINT('Ctrl Pts',(100.010265010368,-1.85618832251382,
136.311319334515));
#223840=CARTESIAN_POINT('Ctrl Pts',(99.731817386555,3.62984520550588,135.342670124737));
#223841=CARTESIAN_POINT('Ctrl Pts',(99.4533697627421,5.78022831746224,130.203536186614));
#223842=CARTESIAN_POINT('Ctrl Pts',(99.1749221389292,2.61886398552269,125.616530548629));
#223843=CARTESIAN_POINT('Ctrl Pts',(98.8964745151164,-2.9491084104941,125.796887304409));
#223844=CARTESIAN_POINT('Ctrl Pts',(98.6180268913035,-5.80699424922206,
130.578867406308));
#223845=CARTESIAN_POINT('Ctrl Pts',(98.3395792674906,-3.32853606035512,
135.568064753397));
#223846=CARTESIAN_POINT('Ctrl Pts',(98.0611316436778,2.20868415995158,136.179650719541));
#223847=CARTESIAN_POINT('Ctrl Pts',(97.7826840198649,5.71623153748262,131.851607679491));
#223848=CARTESIAN_POINT('Ctrl Pts',(97.5042363960519,3.97084138550236,126.561195750394));
#223849=CARTESIAN_POINT('Ctrl Pts',(97.2257887722391,-1.42355801336861,
125.170045044101));
#223850=CARTESIAN_POINT('Ctrl Pts',(96.9473411484261,-5.50977714262889,
128.956555098203));
#223851=CARTESIAN_POINT('Ctrl Pts',(96.6688935246133,-4.53278024539068,
134.441108154283));
#223852=CARTESIAN_POINT('Ctrl Pts',(96.3904459008004,0.609620258735999,
136.583667889112));
#223853=CARTESIAN_POINT('Ctrl Pts',(96.1119982769875,5.19180952668969,133.415326576248));
#223854=CARTESIAN_POINT('Ctrl Pts',(95.8335506531746,5.00297947361121,127.847635100131));
#223855=CARTESIAN_POINT('Ctrl Pts',(95.5551030293618,0.216655693418756,
124.997029930466));
#223856=CARTESIAN_POINT('Ctrl Pts',(95.2766554055487,-4.7687640848064,127.483077958369));
#223857=CARTESIAN_POINT('Ctrl Pts',(94.9982077817361,-5.37192263617151,
133.021222496396));
#223858=CARTESIAN_POINT('Ctrl Pts',(94.7197601579228,-1.03854671790542,
136.522179267501));
#223859=CARTESIAN_POINT('Ctrl Pts',(94.4413125341102,4.24920289828813,134.768740030285));
#223860=CARTESIAN_POINT('Ctrl Pts',(94.1628649102971,5.63214263605674,129.372229783482));
#223861=CARTESIAN_POINT('Ctrl Pts',(93.8844172864844,1.83941843675322,125.29177780972));
#223862=CARTESIAN_POINT('Ctrl Pts',(93.6059696626714,-3.6436414453401,126.277120131727));
#223863=CARTESIAN_POINT('Ctrl Pts',(93.3275220388585,-5.77837284094635,
131.422775292226));
#223864=CARTESIAN_POINT('Ctrl Pts',(93.0490744150458,-2.60306188492951,
136.000137577949));
#223865=CARTESIAN_POINT('Ctrl Pts',(92.7706267912327,2.96433577669487,135.802834664895));
#223866=CARTESIAN_POINT('Ctrl Pts',(92.49217916742,5.80765367539012,131.012178291378));
#223867=CARTESIAN_POINT('Ctrl Pts',(92.213731543607,3.31402156605677,126.030547628085));
#223868=CARTESIAN_POINT('Ctrl Pts',(91.9352839197941,-2.22503446352861,
125.435817888395));
#223869=CARTESIAN_POINT('Ctrl Pts',(91.6568362959812,-5.71939252010779,
129.77451664892));
#223870=CARTESIAN_POINT('Ctrl Pts',(91.3783886721684,-3.95790825856573,
135.059591705955));
#223871=CARTESIAN_POINT('Ctrl Pts',(91.0999410483554,1.44070033803066,136.434317272356));
#223872=CARTESIAN_POINT('Ctrl Pts',(90.8214934245425,5.51537570610103,132.635387711677));
#223873=CARTESIAN_POINT('Ctrl Pts',(90.5430458007297,4.52169024134706,127.153833702157));
#223874=CARTESIAN_POINT('Ctrl Pts',(90.2645981769166,-0.627207658356129,
125.026935589742));
#223875=CARTESIAN_POINT('Ctrl Pts',(89.9861505531037,-5.19973236082766,
128.209208834995));
#223876=CARTESIAN_POINT('Ctrl Pts',(89.707702929291,-4.99395704474619,133.776299788217));
#223877=CARTESIAN_POINT('Ctrl Pts',(89.4292553054779,-0.198979172907652,
136.61232383091));
#223878=CARTESIAN_POINT('Ctrl Pts',(89.1508076816652,4.77885083815996,134.111113415317));
#223879=CARTESIAN_POINT('Ctrl Pts',(88.8723600578521,5.36515038880097,128.571158722445));
#223880=CARTESIAN_POINT('Ctrl Pts',(88.5939124340396,1.02113883430145,125.08340747321));
#223881=CARTESIAN_POINT('Ctrl Pts',(88.3154648102263,-4.26124942351577,
126.85293267954));
#223882=CARTESIAN_POINT('Ctrl Pts',(88.0370171864138,-5.62775763472933,
132.253627122929));
#223883=CARTESIAN_POINT('Ctrl Pts',(87.7585695626006,-1.82263151087143,
136.322516448493));
#223884=CARTESIAN_POINT('Ctrl Pts',(87.480121938788,3.65740393097785,135.320490142334));
#223885=CARTESIAN_POINT('Ctrl Pts',(87.2016743149749,5.77646383437373,130.168361428106));
#223886=CARTESIAN_POINT('Ctrl Pts',(86.9232266911622,2.58723566992664,125.600684898703));
#223887=CARTESIAN_POINT('Ctrl Pts',(86.6447790673492,-2.97953568169397,
125.814932141244));
#223888=CARTESIAN_POINT('Ctrl Pts',(86.3663314435363,-5.80825930024783,
130.614220406392));
#223889=CARTESIAN_POINT('Ctrl Pts',(86.0878838197235,-3.29947637111547,
135.588238236744));
#223890=CARTESIAN_POINT('Ctrl Pts',(85.8094361959104,2.24136415469026,136.166106240484));
#223891=CARTESIAN_POINT('Ctrl Pts',(85.5309885720977,5.72250051906197,131.816791952599));
#223892=CARTESIAN_POINT('Ctrl Pts',(85.2525409482847,3.94493846610766,126.537102727838));
#223893=CARTESIAN_POINT('Ctrl Pts',(84.9740933244718,-1.45782931624159,
125.178815036599));
#223894=CARTESIAN_POINT('Ctrl Pts',(84.6956457006588,-5.52092317588609,
128.990128911089));
#223895=CARTESIAN_POINT('Ctrl Pts',(84.417198076846,-4.51055834898274,134.468633093685));
#223896=CARTESIAN_POINT('Ctrl Pts',(84.138750453033,0.644789247610192,136.579849880389));
#223897=CARTESIAN_POINT('Ctrl Pts',(83.8603028292202,5.20760702535536,133.383674182895));
#223898=CARTESIAN_POINT('Ctrl Pts',(83.5818552054073,4.98488835254533,127.817235325336));
#223899=CARTESIAN_POINT('Ctrl Pts',(83.3034075815944,0.181300809080568,
124.995818682153));
#223900=CARTESIAN_POINT('Ctrl Pts',(83.0249599577814,-4.78889332089225,
127.512168314565));
#223901=CARTESIAN_POINT('Ctrl Pts',(82.7465123339688,-5.35832843941005,
133.053881840899));
#223902=CARTESIAN_POINT('Ctrl Pts',(82.4680647101557,-1.00372149100682,
136.528395258211));
#223903=CARTESIAN_POINT('Ctrl Pts',(82.1896170863428,4.27325647311088,134.742800475408));
#223904=CARTESIAN_POINT('Ctrl Pts',(81.91116946253,5.62332049862395,129.337971866731));
#223905=CARTESIAN_POINT('Ctrl Pts',(81.632721838717,1.80582770038043,125.280682882997));
#223906=CARTESIAN_POINT('Ctrl Pts',(81.3542742149043,-3.67113253492515,
126.299383890674));
#223907=CARTESIAN_POINT('Ctrl Pts',(81.0758265910913,-5.77450131542928,
131.457938430015));
#223908=CARTESIAN_POINT('Ctrl Pts',(80.7973789672785,-2.57138548712596,
136.015886888767));
#223909=CARTESIAN_POINT('Ctrl Pts',(80.5189313434656,2.99470798468153,135.784697301496));
#223910=CARTESIAN_POINT('Ctrl Pts',(80.2404837196526,5.80881111818491,130.976821604667));
#223911=CARTESIAN_POINT('Ctrl Pts',(79.9620360958398,3.2849006102757,126.010462685879));
#223912=CARTESIAN_POINT('Ctrl Pts',(79.6835884720269,-2.25767308216064,
125.449461771377));
#223913=CARTESIAN_POINT('Ctrl Pts',(79.4051408482139,-5.72555550555307,
129.809351295171));
#223914=CARTESIAN_POINT('Ctrl Pts',(79.1266932244012,-3.93193212827854,
135.083605777338));
#223915=CARTESIAN_POINT('Ctrl Pts',(78.8482456005881,1.47494478932078,136.425443010422));
#223916=CARTESIAN_POINT('Ctrl Pts',(78.5697979767754,5.526419500593,132.601780129612));
#223917=CARTESIAN_POINT('Ctrl Pts',(78.2913503529625,4.49938467142216,127.126376526057));
#223918=CARTESIAN_POINT('Ctrl Pts',(78.0129027291494,-0.662364863624755,
125.030860623086));
#223919=CARTESIAN_POINT('Ctrl Pts',(77.7344551053368,-5.21543344732299,
128.240909163888));
#223920=CARTESIAN_POINT('Ctrl Pts',(77.4560074815235,-4.97577348101974,
133.806644359053));
#223921=CARTESIAN_POINT('Ctrl Pts',(77.1775598577108,-0.163620765707691,
136.613427465507));
#223922=CARTESIAN_POINT('Ctrl Pts',(76.8991122338979,4.79889143997102,134.081961927395));
#223923=CARTESIAN_POINT('Ctrl Pts',(76.620664610085,5.35145685119646,128.538540905275));
#223924=CARTESIAN_POINT('Ctrl Pts',(76.3422169862721,0.986294849373407,
125.077297507303));
#223925=CARTESIAN_POINT('Ctrl Pts',(76.0637693624593,-4.28522393584178,
126.878945325076));
#223926=CARTESIAN_POINT('Ctrl Pts',(75.7853217386464,-5.61883126884571,
132.287858029448));
#223927=CARTESIAN_POINT('Ctrl Pts',(75.5068741148335,-1.78900716094817,
136.333509085178));
#223928=CARTESIAN_POINT('Ctrl Pts',(75.2284264910206,3.68482713000219,135.298142813091));
#223929=CARTESIAN_POINT('Ctrl Pts',(74.9499788672077,5.77248530229349,130.133210236781));
#223930=CARTESIAN_POINT('Ctrl Pts',(74.6715312433948,2.55551148336137,125.585032072894));
#223931=CARTESIAN_POINT('Ctrl Pts',(74.3930836195819,-3.0098525451033,125.833161863185));
#223932=CARTESIAN_POINT('Ctrl Pts',(74.1146359957691,-5.80930912408932,
130.649580452192));
#223933=CARTESIAN_POINT('Ctrl Pts',(73.8361883719562,-3.27029441856551,
135.608234451746));
#223934=CARTESIAN_POINT('Ctrl Pts',(73.5577407481433,2.273961094856,136.152363079971));
#223935=CARTESIAN_POINT('Ctrl Pts',(73.2792931243304,5.72855745128013,131.781938709691));
#223936=CARTESIAN_POINT('Ctrl Pts',(73.0008455005175,3.91888936556733,126.513167830092));
#223937=CARTESIAN_POINT('Ctrl Pts',(72.7223978767045,-1.49204659871303,
125.187793485758));
#223938=CARTESIAN_POINT('Ctrl Pts',(72.4439502528918,-5.53186462930466,
129.023769950998));
#223939=CARTESIAN_POINT('Ctrl Pts',(72.1655026290786,-4.48816931217651,
134.496022252122));
#223940=CARTESIAN_POINT('Ctrl Pts',(71.8870550052659,0.679934343581693,
136.575817858786));
#223941=CARTESIAN_POINT('Ctrl Pts',(71.6086073814528,5.22321155422762,133.351926212129));
#223942=CARTESIAN_POINT('Ctrl Pts',(71.3301597576401,4.96661251460835,127.786946239566));
#223943=CARTESIAN_POINT('Ctrl Pts',(71.0517121338272,0.145939206574258,
124.994822671498));
#223944=CARTESIAN_POINT('Ctrl Pts',(70.7732645100143,-4.80884510277506,
127.541380664158));
#223945=CARTESIAN_POINT('Ctrl Pts',(70.4948168862015,-5.34453568781766,
133.086457828568));
#223946=CARTESIAN_POINT('Ctrl Pts',(70.2163692623885,-0.968859070839113,
136.534399142713));
#223947=CARTESIAN_POINT('Ctrl Pts',(69.9379216385757,4.29715170084345,134.716714980192));
#223948=CARTESIAN_POINT('Ctrl Pts',(69.6594740147628,5.61428998698222,129.303768287553));
#223949=CARTESIAN_POINT('Ctrl Pts',(69.3810263909498,1.77217004839796,125.269792638185));
#223950=CARTESIAN_POINT('Ctrl Pts',(69.102578767137,-3.69848758934425,126.321814583191));
#223951=CARTESIAN_POINT('Ctrl Pts',(68.8241311433241,-5.77041581364239,
131.493077349239));
#223952=CARTESIAN_POINT('Ctrl Pts',(68.5456835195112,-2.53961380568736,
136.031443084562));
#223953=CARTESIAN_POINT('Ctrl Pts',(68.2672358956983,3.02496922266262,135.76637538989));
#223954=CARTESIAN_POINT('Ctrl Pts',(67.9887882718854,5.80975331334755,130.94145852735));
#223955=CARTESIAN_POINT('Ctrl Pts',(67.7103406480725,3.25565793129432,125.990555383323));
#223956=CARTESIAN_POINT('Ctrl Pts',(67.4318930242597,-2.29022804188655,
125.463304082106));
#223957=CARTESIAN_POINT('Ctrl Pts',(67.1534454004468,-5.73150632843341,
129.844222811859));
#223958=CARTESIAN_POINT('Ctrl Pts',(66.8749977766338,-3.90581029880048,
135.107461279717));
#223959=CARTESIAN_POINT('Ctrl Pts',(66.5965501528209,1.50913458598933,136.416360457212));
#223960=CARTESIAN_POINT('Ctrl Pts',(66.3181025290079,5.53725851157817,132.568105943505));
#223961=CARTESIAN_POINT('Ctrl Pts',(66.0396549051952,4.47691237514338,127.09905563901));
#223962=CARTESIAN_POINT('Ctrl Pts',(65.7612072813823,-0.69749752471975,
125.034999595595));
#223963=CARTESIAN_POINT('Ctrl Pts',(65.4827596575694,-5.23094127401388,
128.272704482416));
#223964=CARTESIAN_POINT('Ctrl Pts',(65.2043120337565,-4.95740553817722,
133.836877679162));
#223965=CARTESIAN_POINT('Ctrl Pts',(64.9258644099437,-0.128256295479839,
136.614315842995));
#223966=CARTESIAN_POINT('Ctrl Pts',(64.6474167861306,4.81875421709505,134.05268898675));
#223967=CARTESIAN_POINT('Ctrl Pts',(64.3689691623179,5.33756501339024,128.506007048888));
#223968=CARTESIAN_POINT('Ctrl Pts',(64.0905215385049,0.951414316927145,
125.071399759827));
#223969=CARTESIAN_POINT('Ctrl Pts',(63.8120739146922,-4.30903965761881,
126.905103428319));
#223970=CARTESIAN_POINT('Ctrl Pts',(63.5336262908791,-5.60969669510319,
132.322033964426));
#223971=CARTESIAN_POINT('Ctrl Pts',(63.2551786670663,-1.75531651870651,
136.344296837232));
#223972=CARTESIAN_POINT('Ctrl Pts',(62.9767310432534,3.71211378640213,135.275628965096));
#223973=CARTESIAN_POINT('Ctrl Pts',(62.6982834194405,5.76829286864752,130.098083915181));
#223974=CARTESIAN_POINT('Ctrl Pts',(62.4198357956276,2.52369260137852,125.569572651222));
#223975=CARTESIAN_POINT('Ctrl Pts',(62.1413881718147,-3.04005787731984,
125.851575794724));
#223976=CARTESIAN_POINT('Ctrl Pts',(61.8629405480017,-5.81014368184488,
130.684946233427));
#223977=CARTESIAN_POINT('Ctrl Pts',(61.5844929241889,-3.24099128405306,
135.628052657436));
#223978=CARTESIAN_POINT('Ctrl Pts',(61.3060453003759,2.306473772557,136.138421747261));
#223979=CARTESIAN_POINT('Ctrl Pts',(61.0275976765631,5.73440210969521,131.747049242268));
#223980=CARTESIAN_POINT('Ctrl Pts',(60.7491500527502,3.89269504914048,126.489391944074));
#223981=CARTESIAN_POINT('Ctrl Pts',(60.4707024289374,-1.5262085928491,125.196980058879));
#223982=CARTESIAN_POINT('Ctrl Pts',(60.1922548051244,-5.54260109744501,
129.057476971348));
#223983=CARTESIAN_POINT('Ctrl Pts',(59.9138071813117,-4.46561396460588,
134.52327461468));
#223984=CARTESIAN_POINT('Ctrl Pts',(59.6353595574987,0.715054244335847,
136.571571973714));
#223985=CARTESIAN_POINT('Ctrl Pts',(59.3569119336859,5.23862253507484,133.320083840384));
#223986=CARTESIAN_POINT('Ctrl Pts',(59.0784643098728,4.94815263701827,127.756768965196));
#223987=CARTESIAN_POINT('Ctrl Pts',(58.80001668606,0.110572196236736,124.994041935407));
#223988=CARTESIAN_POINT('Ctrl Pts',(58.5215690622471,-4.82861869113419,
127.570713924673));
#223989=CARTESIAN_POINT('Ctrl Pts',(58.2431214384343,-5.3305448924898,133.118949252284));
#223990=CARTESIAN_POINT('Ctrl Pts',(57.9646738146213,-0.933960749242644,
136.54019069853));
#223991=CARTESIAN_POINT('Ctrl Pts',(57.6862261908085,4.32088769603949,134.690484511247));
#223992=CARTESIAN_POINT('Ctrl Pts',(57.4077785669955,5.6050514357603,129.269620313377));
#223993=CARTESIAN_POINT('Ctrl Pts',(57.1293309431827,1.73844672800264,125.259107478825));
#223994=CARTESIAN_POINT('Ctrl Pts',(56.8508833193697,-3.72570559494523,
126.3444113781));
#223995=CARTESIAN_POINT('Ctrl Pts',(56.5724356955568,-5.76611648697549,
131.528190747811));
#223996=CARTESIAN_POINT('Ctrl Pts',(56.293988071744,-2.50774801792579,136.046805588895));
#223997=CARTESIAN_POINT('Ctrl Pts',(56.0155404479311,3.05511836929639,135.747869609001));
#223998=CARTESIAN_POINT('Ctrl Pts',(55.7370928241181,5.81048022596477,130.906090369819));
#223999=CARTESIAN_POINT('Ctrl Pts',(55.4586452003054,3.22629461271119,125.97082645809));
#224000=CARTESIAN_POINT('Ctrl Pts',(55.1801975764924,-2.32269813636975,
125.477344307648));
#224001=CARTESIAN_POINT('Ctrl Pts',(54.9017499526795,-5.73724476823917,
129.879129906805));
#224002=CARTESIAN_POINT('Ctrl Pts',(54.6233023288666,-3.87954373808533,
135.131157329118));
#224003=CARTESIAN_POINT('Ctrl Pts',(54.3448547050537,1.54326846112093,136.407069949284));
#224004=CARTESIAN_POINT('Ctrl Pts',(54.0664070812409,5.54789233741261,132.534366401168));
#224005=CARTESIAN_POINT('Ctrl Pts',(53.7879594574279,4.45427418523046,127.071872053402));
#224006=CARTESIAN_POINT('Ctrl Pts',(53.5095118336151,-0.732604339787292,
125.039352353899));
#224007=CARTESIAN_POINT('Ctrl Pts',(53.2310642098022,-5.24625526625226,
128.304593612394));
#224008=CARTESIAN_POINT('Ctrl Pts',(52.9526165859893,-4.93885389684926,
133.866998628235));
#224009=CARTESIAN_POINT('Ctrl Pts',(52.6741689621764,-0.0928870726681018,
136.614988930455));
#224010=CARTESIAN_POINT('Ctrl Pts',(52.3957213383635,4.83843843350925,134.023295678104));
#224011=CARTESIAN_POINT('Ctrl Pts',(52.1172737145507,5.32347539014984,128.473558358838));
#224012=CARTESIAN_POINT('Ctrl Pts',(51.8388260907377,0.91649852947334,125.065714449322));
#224013=CARTESIAN_POINT('Ctrl Pts',(51.5603784669247,-4.33269570634681,
126.931406019971));
#224014=CARTESIAN_POINT('Ctrl Pts',(51.2819308431118,-5.6003542519866,132.356153661459));
#224015=CARTESIAN_POINT('Ctrl Pts',(51.0034832192991,-1.72156083256576,
136.354879304913));
#224016=CARTESIAN_POINT('Ctrl Pts',(50.7250355954861,3.73926288906064,135.252949432607));
#224017=CARTESIAN_POINT('Ctrl Pts',(50.4465879716733,5.76388668878802,130.062983764924));
#224018=CARTESIAN_POINT('Ctrl Pts',(50.1681403478604,2.49178020303801,125.554307206545));
#224019=CARTESIAN_POINT('Ctrl Pts',(49.8896927240475,-3.07015055907373,
125.870173253527));
#224020=CARTESIAN_POINT('Ctrl Pts',(49.6112451002346,-5.81076294258959,
130.720316439607));
#224021=CARTESIAN_POINT('Ctrl Pts',(49.3327974764216,-3.21156805341676,
135.647692119444));
#224022=CARTESIAN_POINT('Ctrl Pts',(49.0543498526089,2.33890098302428,136.124282758954));
#224023=CARTESIAN_POINT('Ctrl Pts',(48.7759022287959,5.74003427773134,131.712124843171));
#224024=CARTESIAN_POINT('Ctrl Pts',(48.497454604983,3.86635648746696,126.465775950806));
#224025=CARTESIAN_POINT('Ctrl Pts',(48.2190069811701,-1.56031403276457,
125.206374415548));
#224026=CARTESIAN_POINT('Ctrl Pts',(47.9405593573573,-5.55313218246346,
129.091248723115));
#224027=CARTESIAN_POINT('Ctrl Pts',(47.6621117335443,-4.44289314206747,
134.550389171513));
#224028=CARTESIAN_POINT('Ctrl Pts',(47.3836641097315,0.750147648492217,
136.567112382502));
#224029=CARTESIAN_POINT('Ctrl Pts',(47.1052164859186,5.25383939683757,133.288148247589));
#224030=CARTESIAN_POINT('Ctrl Pts',(46.8267688621057,4.92950940381243,127.726704620456));
#224031=CARTESIAN_POINT('Ctrl Pts',(46.5483212382927,0.0752010886061242,
124.993476502813));
#224032=CARTESIAN_POINT('Ctrl Pts',(46.2698736144798,-4.84821335325179,
127.600167009156));
#224033=CARTESIAN_POINT('Ctrl Pts',(45.991425990667,-5.31635657186091,133.151354908068));
#224034=CARTESIAN_POINT('Ctrl Pts',(45.7129783668541,-0.899027819386881,
136.545769711054));
#224035=CARTESIAN_POINT('Ctrl Pts',(45.4345307430412,4.344463579153,134.664110040551));
#224036=CARTESIAN_POINT('Ctrl Pts',(45.1560831192283,5.5956051872961,129.235529209567));
#224037=CARTESIAN_POINT('Ctrl Pts',(44.8776354954154,1.70465898882477,125.248627800858));
#224038=CARTESIAN_POINT('Ctrl Pts',(44.5991878716026,-3.7527855431554,126.367173438067));
#224039=CARTESIAN_POINT('Ctrl Pts',(44.3207402477896,-5.76160349474165,
131.563277324591));
#224040=CARTESIAN_POINT('Ctrl Pts',(44.0422926239769,-2.47578930463884,
136.0619738325));
#224041=CARTESIAN_POINT('Ctrl Pts',(43.7638450001637,3.08515430739569,135.72918064457));
#224042=CARTESIAN_POINT('Ctrl Pts',(43.485397376351,5.8109918291003,130.870718442656));
#224043=CARTESIAN_POINT('Ctrl Pts',(43.206949752538,3.19681174259461,125.951276641244));
#224044=CARTESIAN_POINT('Ctrl Pts',(42.9285021287252,-2.3550821624196,125.491581927739));
#224045=CARTESIAN_POINT('Ctrl Pts',(42.6500545049123,-5.74277061233009,
129.914071286517));
#224046=CARTESIAN_POINT('Ctrl Pts',(42.3716068810994,-3.85313341945026,
135.154693047476));
#224047=CARTESIAN_POINT('Ctrl Pts',(42.0931592572865,1.57734514987214,136.397571830902));
#224048=CARTESIAN_POINT('Ctrl Pts',(41.8147116334736,5.5583205840564,132.50056275283));
#224049=CARTESIAN_POINT('Ctrl Pts',(41.5362640096606,4.43147094054935,127.04482677653));
#224050=CARTESIAN_POINT('Ctrl Pts',(41.2578163858478,-0.767684007931795,
125.043918736703));
#224051=CARTESIAN_POINT('Ctrl Pts',(40.9793687620349,-5.26137485657243,
128.336575372158));
#224052=CARTESIAN_POINT('Ctrl Pts',(40.700921138222,-4.9201192444739,133.897006090131));
#224053=CARTESIAN_POINT('Ctrl Pts',(40.4224735144091,-0.0575144078915333,
136.615446702946));
#224054=CARTESIAN_POINT('Ctrl Pts',(40.1440258905964,4.85794335980812,133.993783090635));
#224055=CARTESIAN_POINT('Ctrl Pts',(39.8655782667833,5.30918850357096,128.441196037522));
#224056=CARTESIAN_POINT('Ctrl Pts',(39.5871306429705,0.8815487808295,125.060241786462));
#224057=CARTESIAN_POINT('Ctrl Pts',(39.3086830191576,-4.35619120544207,
126.957852125381));
#224058=CARTESIAN_POINT('Ctrl Pts',(39.0302353953447,-5.59080428568363,
132.39021585623));
#224059=CARTESIAN_POINT('Ctrl Pts',(38.7517877715318,-1.6877413533555,136.365256096082));
#224060=CARTESIAN_POINT('Ctrl Pts',(38.4733401477189,3.76627343195761,135.230105056025));
#224061=CARTESIAN_POINT('Ctrl Pts',(38.194892523906,5.7592669259876,130.027911086658));
#224062=CARTESIAN_POINT('Ctrl Pts',(37.9164449000932,2.45977547086574,125.539236304527));
#224063=CARTESIAN_POINT('Ctrl Pts',(37.6379972762802,-3.10012947526937,
125.888953550457));
#224064=CARTESIAN_POINT('Ctrl Pts',(37.3595496524674,-5.81116688337655,
130.755689760074));
#224065=CARTESIAN_POINT('Ctrl Pts',(37.0811020286545,-3.18202581694541,
135.667152110023));
#224066=CARTESIAN_POINT('Ctrl Pts',(36.8026544048415,2.3712415246555,136.109946638975));
#224067=CARTESIAN_POINT('Ctrl Pts',(36.5242067810287,5.74545374668639,131.677166806538));
#224068=CARTESIAN_POINT('Ctrl Pts',(36.2457591572158,3.83987465653194,126.442320725389));
#224069=CARTESIAN_POINT('Ctrl Pts',(35.9673115334029,-1.59436165466975,
125.215976207654));
#224070=CARTESIAN_POINT('Ctrl Pts',(35.6888639095901,-5.56345749412674,
129.125083954872));
#224071=CARTESIAN_POINT('Ctrl Pts',(35.4104162857771,-4.42000768648982,
134.57736491788));
#224072=CARTESIAN_POINT('Ctrl Pts',(35.1319686619643,0.785213255651605,
136.562439250406));
#224073=CARTESIAN_POINT('Ctrl Pts',(34.8535210381513,5.26886157564935,133.25612061713));
#224074=CARTESIAN_POINT('Ctrl Pts',(34.5750734143385,4.91068350582282,127.69675431939));
#224075=CARTESIAN_POINT('Ctrl Pts',(34.2966257905255,0.0398271943713243,
124.993126394665));
#224076=CARTESIAN_POINT('Ctrl Pts',(34.0181781667127,-4.86762836304081,
127.629738826211));
#224077=CARTESIAN_POINT('Ctrl Pts',(33.7397305428998,-5.30197125168398,
133.183673595116));
#224078=CARTESIAN_POINT('Ctrl Pts',(33.4612829190869,-0.864061575724654,
136.551135973552));
#224079=CARTESIAN_POINT('Ctrl Pts',(33.182835295274,4.36787847657091,134.637592545421));
#224080=CARTESIAN_POINT('Ctrl Pts',(32.9043876714611,5.58595159162396,129.201496239381));
#224081=CARTESIAN_POINT('Ctrl Pts',(32.6259400476482,1.67080808288091,125.238353992614));
#224082=CARTESIAN_POINT('Ctrl Pts',(32.3474924238352,-3.77972643051725,
126.390099919638));
#224083=CARTESIAN_POINT('Ctrl Pts',(32.0690448000224,-5.75687700417149,
131.598335779433));
#224084=CARTESIAN_POINT('Ctrl Pts',(31.7905971762095,-2.44373885006871,
136.076947253315));
#224085=CARTESIAN_POINT('Ctrl Pts',(31.5121495523967,3.11507592396733,135.71030918912));
#224086=CARTESIAN_POINT('Ctrl Pts',(31.2337019285837,5.81128810379662,130.835344056578));
#224087=CARTESIAN_POINT('Ctrl Pts',(30.9552543047708,3.16721041344351,125.931906657209));
#224088=CARTESIAN_POINT('Ctrl Pts',(30.676806680958,-2.38737892003384,125.506016414799));
#224089=CARTESIAN_POINT('Ctrl Pts',(30.398359057145,-5.74808365594406,129.949045656226));
#224090=CARTESIAN_POINT('Ctrl Pts',(30.1199114333322,-3.82658032153943,
135.178067562667));
#224091=CARTESIAN_POINT('Ctrl Pts',(29.8414638095193,1.61136338951851,136.387866454021));
#224092=CARTESIAN_POINT('Ctrl Pts',(29.5630161857064,5.56854286508694,132.466696251098));
#224093=CARTESIAN_POINT('Ctrl Pts',(29.2845685618935,4.40850348608286,127.017920810568));
#224094=CARTESIAN_POINT('Ctrl Pts',(29.0061209380806,-0.802735229263066,
125.048698574801));
#224095=CARTESIAN_POINT('Ctrl Pts',(28.7276733142678,-5.27629948471241,
128.368648576612));
#224096=CARTESIAN_POINT('Ctrl Pts',(28.4492256904548,-4.90120227527057,
133.926898952911));
#224097=CARTESIAN_POINT('Ctrl Pts',(28.170778066642,-0.0221396118974229,
136.615689143506));
#224098=CARTESIAN_POINT('Ctrl Pts',(27.892330442829,4.87726827322928,133.964152317942));
#224099=CARTESIAN_POINT('Ctrl Pts',(27.6138828190162,5.29470488305963,128.408921284139));
#224100=CARTESIAN_POINT('Ctrl Pts',(27.3354351952032,0.846566366071392,
125.054981974037));
#224101=CARTESIAN_POINT('Ctrl Pts',(27.0569875713904,-4.37952528427021,
126.984440764576));
#224102=CARTESIAN_POINT('Ctrl Pts',(26.7785399475775,-5.58104715007188,
132.424219286554));
#224103=CARTESIAN_POINT('Ctrl Pts',(26.5000923237646,-1.65385933426847,
136.375426826225));
#224104=CARTESIAN_POINT('Ctrl Pts',(26.2216446999517,3.79314441420758,135.207096681855));
#224105=CARTESIAN_POINT('Ctrl Pts',(25.9431970761388,5.75443375143326,129.992867180015));
#224106=CARTESIAN_POINT('Ctrl Pts',(25.6647494523259,2.42767959080881,125.524360503627));
#224107=CARTESIAN_POINT('Ctrl Pts',(25.3863018285131,-3.12999351502748,
125.907915989602));
#224108=CARTESIAN_POINT('Ctrl Pts',(25.1078542047001,-5.81135548923757,
130.791064884058));
#224109=CARTESIAN_POINT('Ctrl Pts',(24.8294065808873,-3.152365669337,135.686431908074));
#224110=CARTESIAN_POINT('Ctrl Pts',(24.5509589570743,2.40349419906,136.095413918554));
#224111=CARTESIAN_POINT('Ctrl Pts',(24.2725113332615,5.75066031573997,131.64217642775));
#224112=CARTESIAN_POINT('Ctrl Pts',(23.9940637094486,3.81325053762949,126.419027136963));
#224113=CARTESIAN_POINT('Ctrl Pts',(23.7156160856357,-1.62835019691723,
125.2257850794));
#224114=CARTESIAN_POINT('Ctrl Pts',(23.4371684618228,-5.57357664982666,
129.158981412844));
#224115=CARTESIAN_POINT('Ctrl Pts',(23.1587208380098,-4.39695844590187,
134.604200854185));
#224116=CARTESIAN_POINT('Ctrl Pts',(22.880273214197,0.820249766445046,136.557552750588));
#224117=CARTESIAN_POINT('Ctrl Pts',(22.6018255903841,5.28368851485763,133.224002135804));
#224118=CARTESIAN_POINT('Ctrl Pts',(22.3233779665712,4.89167564065013,127.666919171818));
#224119=CARTESIAN_POINT('Ctrl Pts',(22.0449303427584,0.00445182432539013,
124.992991623939));
#224120=CARTESIAN_POINT('Ctrl Pts',(21.7664827189454,-4.88686300107076,
127.659428280044));
#224121=CARTESIAN_POINT('Ctrl Pts',(21.4880350951325,-5.28738946501251,
133.215904115845));
#224122=CARTESIAN_POINT('Ctrl Pts',(21.2095874713197,-0.829063313942982,
136.556289287176));
#224123=CARTESIAN_POINT('Ctrl Pts',(20.9311398475068,4.39113152064558,134.610933008472));
#224124=CARTESIAN_POINT('Ctrl Pts',(20.6526922236938,5.57609100646137,129.167522663925));
#224125=CARTESIAN_POINT('Ctrl Pts',(20.374244599881,1.6368952645291,125.228286434793));
#224126=CARTESIAN_POINT('Ctrl Pts',(20.0957969760681,-3.80652725872624,
126.413189973261));
#224127=CARTESIAN_POINT('Ctrl Pts',(19.8173493522552,-5.75193719040684,
131.633364813234));
#224128=CARTESIAN_POINT('Ctrl Pts',(19.5389017284423,-2.41159784185683,
136.091725296493));
#224129=CARTESIAN_POINT('Ctrl Pts',(19.2604541046294,3.14488211025528,135.691255941942));
#224130=CARTESIAN_POINT('Ctrl Pts',(18.9820064808165,5.81136903907515,130.799968522399));
#224131=CARTESIAN_POINT('Ctrl Pts',(18.7035588570036,3.13749172214556,125.912717223747));
#224132=CARTESIAN_POINT('Ctrl Pts',(18.4251112331907,-2.41958721244422,
125.52064723395));
#224133=CARTESIAN_POINT('Ctrl Pts',(18.1466636093778,-5.75318370220431,
129.984051719947));
#224134=CARTESIAN_POINT('Ctrl Pts',(17.868215985565,-3.79988542828747,135.201280008538));
#224135=CARTESIAN_POINT('Ctrl Pts',(17.589768361752,1.64532191950215,136.377954178279));
#224136=CARTESIAN_POINT('Ctrl Pts',(17.3113207379392,5.57855880171371,132.432768150908));
#224137=CARTESIAN_POINT('Ctrl Pts',(17.0328731141263,4.38537267289848,126.991155152525));
#224138=CARTESIAN_POINT('Ctrl Pts',(16.7544254903134,-0.83775670494522,
125.053691691071));
#224139=CARTESIAN_POINT('Ctrl Pts',(16.4759778665005,-5.29102859763445,
128.400812037271));
#224140=CARTESIAN_POINT('Ctrl Pts',(16.1975302426876,-4.88210369021464,
133.956676108886));
#224141=CARTESIAN_POINT('Ctrl Pts',(15.9190826188747,0.013236004487936,
136.61571624315));
#224142=CARTESIAN_POINT('Ctrl Pts',(15.6406349950618,4.89641245768097,133.934404458007));
#224143=CARTESIAN_POINT('Ctrl Pts',(15.3621873712489,5.2800250653117,128.376735294641));
#224144=CARTESIAN_POINT('Ctrl Pts',(15.0837397474361,0.811552581485459,
125.049935206953));
#224145=CARTESIAN_POINT('Ctrl Pts',(14.8052921236231,-4.40269707817821,
127.011170952307));
#224146=CARTESIAN_POINT('Ctrl Pts',(14.5268444998103,-5.57108320670569,
132.458162692417));
#224147=CARTESIAN_POINT('Ctrl Pts',(14.2483968759974,-1.6199160308156,136.385391118461));
#224148=CARTESIAN_POINT('Ctrl Pts',(13.9699492521845,3.81987484009636,135.18392516268));
#224149=CARTESIAN_POINT('Ctrl Pts',(13.6915016283715,5.74938734422005,129.95785334356));
#224150=CARTESIAN_POINT('Ctrl Pts',(13.4130540045587,2.39549375219187,125.509680355073));
#224151=CARTESIAN_POINT('Ctrl Pts',(13.1346063807458,-3.15974157172482,
125.927059868305));
#224152=CARTESIAN_POINT('Ctrl Pts',(12.8561587569329,-5.81132875318382,
130.82644050072));
#224153=CARTESIAN_POINT('Ctrl Pts',(12.57771113312,-3.12258870965941,135.705530799178));
#224154=CARTESIAN_POINT('Ctrl Pts',(12.2992635093071,2.43565781110307,136.080685136208));
#224155=CARTESIAN_POINT('Ctrl Pts',(12.0208158854942,5.75565379196074,131.607155003388));
#224156=CARTESIAN_POINT('Ctrl Pts',(11.7423682616813,3.78648511732596,126.395896048684));
#224157=CARTESIAN_POINT('Ctrl Pts',(11.4639206378685,-1.66227840004959,
125.235800667314));
#224158=CARTESIAN_POINT('Ctrl Pts',(11.1854730140555,-5.58348927459409,
129.192939840948));
#224159=CARTESIAN_POINT('Ctrl Pts',(10.9070253902426,-4.37374627440173,
134.630895986013));
#224160=CARTESIAN_POINT('Ctrl Pts',(10.6285777664298,0.855255882581734,
136.552453064119));
#224161=CARTESIAN_POINT('Ctrl Pts',(10.3501301426169,5.29831966504511,133.19179399377));
#224162=CARTESIAN_POINT('Ctrl Pts',(10.071682518804,4.87248651263752,127.637200283293));
#224163=CARTESIAN_POINT('Ctrl Pts',(9.79323489499104,-0.0309237106847325,
124.993072195629));
#224164=CARTESIAN_POINT('Ctrl Pts',(9.51478727117816,-4.90591655459505,
127.689234270502));
#224165=CARTESIAN_POINT('Ctrl Pts',(9.23633964736526,-5.27261175218,133.248045275945));
#224166=CARTESIAN_POINT('Ctrl Pts',(8.95789202355236,-0.794034330915497,
136.561229460968));
#224167=CARTESIAN_POINT('Ctrl Pts',(8.67944439973947,4.41422184972672,134.584132417584));
#224168=CARTESIAN_POINT('Ctrl Pts',(8.40099677592661,5.56602379719609,129.1336097421));
#224169=CARTESIAN_POINT('Ctrl Pts',(8.12254915211368,1.60292179042129,125.218425500451));
#224170=CARTESIAN_POINT('Ctrl Pts',(7.84410152830078,-3.83318703466779,
126.436442743329));
#224171=CARTESIAN_POINT('Ctrl Pts',(7.56565390448795,-5.74678423649425,
131.668363127979));
#224172=CARTESIAN_POINT('Ctrl Pts',(7.28720628067502,-2.37936747100029,
136.106307414428));
#224173=CARTESIAN_POINT('Ctrl Pts',(7.00875865686212,3.17457176177998,135.672021609062));
#224174=CARTESIAN_POINT('Ctrl Pts',(6.73031103304925,5.81123463193681,130.764593150968));
#224175=CARTESIAN_POINT('Ctrl Pts',(6.45186340923634,3.10765676993803,125.89370905193));
#224176=CARTESIAN_POINT('Ctrl Pts',(6.17341578542346,-2.45170584616043,
125.535473843045));
#224177=CARTESIAN_POINT('Ctrl Pts',(5.89496816161054,-5.75807056212669,
130.019088180515));
#224178=CARTESIAN_POINT('Ctrl Pts',(5.61652053779771,-3.77304972888379,
135.224329524944));
#224179=CARTESIAN_POINT('Ctrl Pts',(5.33807291398477,1.67921948147701,136.367835370977));
#224180=CARTESIAN_POINT('Ctrl Pts',(5.05962529017187,5.58836802279258,132.398779709476));
#224181=CARTESIAN_POINT('Ctrl Pts',(4.781177666359,4.36207935811697,126.964530794212));
#224182=CARTESIAN_POINT('Ctrl Pts',(4.50273004254611,-0.872747137244579,
125.058897900495));
#224183=CARTESIAN_POINT('Ctrl Pts',(4.2242824187332,-5.30556164954619,128.433064562307));
#224184=CARTESIAN_POINT('Ctrl Pts',(3.94583479492031,-4.86282419701095,
133.986336454649));
#224185=CARTESIAN_POINT('Ctrl Pts',(3.66738717110745,0.0486111304084952,
136.615528000873));
#224186=CARTESIAN_POINT('Ctrl Pts',(3.38893954729453,4.91537520376836,133.904540613147));
#224187=CARTESIAN_POINT('Ctrl Pts',(3.11049192348162,5.26514959429328,128.344639261694));
#224188=CARTESIAN_POINT('Ctrl Pts',(2.83204429966877,0.776508724519974,
125.045101672218));
#224189=CARTESIAN_POINT('Ctrl Pts',(2.55359667585587,-4.42570572852705,
127.038041698076));
#224190=CARTESIAN_POINT('Ctrl Pts',(2.27514905204296,-5.56091282480238,
132.492044816037));
#224191=CARTESIAN_POINT('Ctrl Pts',(1.99670142823006,-1.58591270077849,
136.395148603559));
#224192=CARTESIAN_POINT('Ctrl Pts',(1.7182538044172,3.84646371911817,135.160591357131));
#224193=CARTESIAN_POINT('Ctrl Pts',(1.43980618060429,5.7441278913444,129.922870874744));
#224194=CARTESIAN_POINT('Ctrl Pts',(1.16135855679139,2.36321914767325,125.495196402842));
#224195=CARTESIAN_POINT('Ctrl Pts',(0.882910932978526,-3.18937254303613,
125.946384477181));
#224196=CARTESIAN_POINT('Ctrl Pts',(0.604463309165634,-5.81108667620601,
130.861815299204));
#224197=CARTESIAN_POINT('Ctrl Pts',(0.326015685352703,-3.09269604130886,
135.724448075619));
#224198=CARTESIAN_POINT('Ctrl Pts',(0.0475680615398608,2.46773116894999,
136.065760837718));
#224199=CARTESIAN_POINT('Ctrl Pts',(-0.230879562273037,5.76043399031358,
131.572103831187));
#224200=CARTESIAN_POINT('Ctrl Pts',(-0.509327186085944,3.75957938742415,
126.37292831768));
#224201=CARTESIAN_POINT('Ctrl Pts',(-0.787774809898847,-1.69614500684454,
125.246022600264));
#224202=CARTESIAN_POINT('Ctrl Pts',(-1.06622243371171,-5.59319500111311,
129.226957980841));
#224203=CARTESIAN_POINT('Ctrl Pts',(-1.34467005752462,-4.35037203212501,
134.657449324165));
#224204=CARTESIAN_POINT('Ctrl Pts',(-1.62311768133752,0.890230306896913,
136.547140379971));
#224205=CARTESIAN_POINT('Ctrl Pts',(-1.90156530515039,5.31275448404895,
133.159497384516));
#224206=CARTESIAN_POINT('Ctrl Pts',(-2.18001292896328,4.85311683284533,
127.607598755059));
#224207=CARTESIAN_POINT('Ctrl Pts',(-2.4584605527762,-0.0662980998053887,
124.993368106748));
#224208=CARTESIAN_POINT('Ctrl Pts',(-2.73690817658909,-4.92478831757726,
127.719155693111));
#224209=CARTESIAN_POINT('Ctrl Pts',(-3.01535580040196,-5.25763866077998,
133.280095884409));
#224210=CARTESIAN_POINT('Ctrl Pts',(-3.29380342421486,-0.758975924653704,
136.565956311869));
#224211=CARTESIAN_POINT('Ctrl Pts',(-3.57225104802777,4.43714860819409,
134.557191765862));
#224212=CARTESIAN_POINT('Ctrl Pts',(-3.85069867184063,5.55575033687191,
129.099758730564));
#224213=CARTESIAN_POINT('Ctrl Pts',(-4.12914629565353,1.56888891945708,
125.208771554989));
#224214=CARTESIAN_POINT('Ctrl Pts',(-4.40759391946644,-3.85970477045413,
126.459857368199));
#224215=CARTESIAN_POINT('Ctrl Pts',(-4.68604154327934,-5.74141833337845,
131.703329426794));
#224216=CARTESIAN_POINT('Ctrl Pts',(-4.96448916709218,-2.34704893180687,
136.120693066776));
#224217=CARTESIAN_POINT('Ctrl Pts',(-5.24293679090511,3.20414377838073,
135.652606903212));
#224218=CARTESIAN_POINT('Ctrl Pts',(-5.52138441471801,5.81088488736209,
130.729219253137));
#224219=CARTESIAN_POINT('Ctrl Pts',(-5.79983203853088,3.07770666236606,
125.874882846113));
#224220=CARTESIAN_POINT('Ctrl Pts',(-6.07827966234377,-2.48373363101511,
125.550495692676));
#224221=CARTESIAN_POINT('Ctrl Pts',(-6.35672728615668,-5.7627440546269,
130.054153739642));
#224222=CARTESIAN_POINT('Ctrl Pts',(-6.63517490996957,-3.74607421773465,
135.247215257776));
#224223=CARTESIAN_POINT('Ctrl Pts',(-6.91362253378244,1.71305481935644,
136.357510407073));
#224224=CARTESIAN_POINT('Ctrl Pts',(-7.19207015759534,5.59797016483923,
132.36473218626));
#224225=CARTESIAN_POINT('Ctrl Pts',(-7.47051778140826,4.33862440488076,
126.938048722207));
#224226=CARTESIAN_POINT('Ctrl Pts',(-7.74896540522111,-0.907705229577551,
125.064317010151));
#224227=CARTESIAN_POINT('Ctrl Pts',(-8.027413029034,-5.31989810191992,128.46540495659));
#224228=CARTESIAN_POINT('Ctrl Pts',(-8.30586065284694,-4.84336451006833,
134.015878891129));
#224229=CARTESIAN_POINT('Ctrl Pts',(-8.58430827665978,0.0839844550257475,
136.615124423653));
#224230=CARTESIAN_POINT('Ctrl Pts',(-8.86275590047269,4.93415580881975,
133.874561889976));
#224231=CARTESIAN_POINT('Ctrl Pts',(-9.14120352428557,5.25007902122049,
128.312634374625));
#224232=CARTESIAN_POINT('Ctrl Pts',(-9.4196511480985,0.741436093738357,
125.040481548942));
#224233=CARTESIAN_POINT('Ctrl Pts',(-9.69809877191133,-4.44855038272257,
127.065052006178));
#224234=CARTESIAN_POINT('Ctrl Pts',(-9.97654639572428,-5.5505363812293,
132.525864401898));
#224235=CARTESIAN_POINT('Ctrl Pts',(-10.2549940195371,-1.55185060416301,
136.404698919952));
#224236=CARTESIAN_POINT('Ctrl Pts',(-10.53344164335,3.87291006601234,135.137096129849));
#224237=CARTESIAN_POINT('Ctrl Pts',(-10.8118892671629,5.7386555876974,129.887921069854));
#224238=CARTESIAN_POINT('Ctrl Pts',(-11.0903368909758,2.33085697319978,
125.480909183646));
#224239=CARTESIAN_POINT('Ctrl Pts',(-11.3687845147887,-3.21888533097506,
125.965889100148));
#224240=CARTESIAN_POINT('Ctrl Pts',(-11.6472321386015,-5.81062926727439,
130.897187968684));
#224241=CARTESIAN_POINT('Ctrl Pts',(-11.9256797624145,-3.06268877196916,
135.743183036409));
#224242=CARTESIAN_POINT('Ctrl Pts',(-12.2041273862274,2.49971308411117,
136.050641576106));
#224243=CARTESIAN_POINT('Ctrl Pts',(-12.4825750100403,5.76500073366654,
131.537024209977));
#224244=CARTESIAN_POINT('Ctrl Pts',(-12.7610226338531,3.73253434492532,
126.350124795028));
#224245=CARTESIAN_POINT('Ctrl Pts',(-13.039470257666,-1.7299487623625,125.256450499474));
#224246=CARTESIAN_POINT('Ctrl Pts',(-13.3179178814789,-5.60269346973446,
129.261034571969));
#224247=CARTESIAN_POINT('Ctrl Pts',(-13.5963655052918,-4.32683658521273,
134.683859884699));
#224248=CARTESIAN_POINT('Ctrl Pts',(-13.8748131291047,0.925171743400955,
136.541614895008));
#224249=CARTESIAN_POINT('Ctrl Pts',(-14.1532607529176,5.3269924369816,133.127113504801));
#224250=CARTESIAN_POINT('Ctrl Pts',(-14.4317083767304,4.83356731902416,
127.578115684011));
#224251=CARTESIAN_POINT('Ctrl Pts',(-14.7101560005434,-0.101670032225581,
124.99387934633));
#224252=CARTESIAN_POINT('Ctrl Pts',(-14.9886036243562,-4.94347759071707,
127.749191439124));
#224253=CARTESIAN_POINT('Ctrl Pts',(-15.2670512481692,-5.24247074564602,
133.312054753593));
#224254=CARTESIAN_POINT('Ctrl Pts',(-15.545498871982,-0.723889394260118,
136.570469664722));
#224255=CARTESIAN_POINT('Ctrl Pts',(-15.823946495795,4.45991094648802,134.530112051601));
#224256=CARTESIAN_POINT('Ctrl Pts',(-16.1023941196078,5.54527100617588,
129.065970883678));
#224257=CARTESIAN_POINT('Ctrl Pts',(-16.3808417434207,1.53479791273714,
125.199324956138));
#224258=CARTESIAN_POINT('Ctrl Pts',(-16.6592893672336,-3.88607948346057,
126.483432980235));
#224259=CARTESIAN_POINT('Ctrl Pts',(-16.9377369910465,-5.73583967989507,
131.738262413989));
#224260=CARTESIAN_POINT('Ctrl Pts',(-17.2161846148594,-2.31464342185212,
136.134881720468));
#224261=CARTESIAN_POINT('Ctrl Pts',(-17.4946322386723,3.23359706425542,
135.633012543814));
#224262=CARTESIAN_POINT('Ctrl Pts',(-17.7730798624852,5.81031981831091,
130.693848139697));
#224263=CARTESIAN_POINT('Ctrl Pts',(-18.0515274862981,3.04764250924188,
125.856239303907));
#224264=CARTESIAN_POINT('Ctrl Pts',(-18.3299751101109,-2.51566938020671,
125.565712226204));
#224265=CARTESIAN_POINT('Ctrl Pts',(-18.6084227339239,-5.76720400652691,
130.089247097961));
#224266=CARTESIAN_POINT('Ctrl Pts',(-18.8868703577367,-3.71895989442774,
135.269936358996));
#224267=CARTESIAN_POINT('Ctrl Pts',(-19.1653179815497,1.74682667935956,
136.346979669161));
#224268=CARTESIAN_POINT('Ctrl Pts',(-19.4437656053625,5.60736487204277,
132.330626842902));
#224269=CARTESIAN_POINT('Ctrl Pts',(-19.7222132291754,4.31500868232164,
126.91170991781));
#224270=CARTESIAN_POINT('Ctrl Pts',(-20.0006608529883,-0.942629686559699,
125.069948819234));
#224271=CARTESIAN_POINT('Ctrl Pts',(-20.2791084768012,-5.33403742351306,
128.497832021735));
#224272=CARTESIAN_POINT('Ctrl Pts',(-20.5575561006141,-4.82372535047263,
134.045302323618));
#224273=CARTESIAN_POINT('Ctrl Pts',(-20.836003724427,0.119354667568119,
136.614505526443));
#224274=CARTESIAN_POINT('Ctrl Pts',(-21.1144513482399,4.95275357691331,
133.844469399368));
#224275=CARTESIAN_POINT('Ctrl Pts',(-21.3928989720528,5.23481390453873,
128.280721819388));
#224276=CARTESIAN_POINT('Ctrl Pts',(-21.6713465958657,0.706335988769417,
125.036075008324));
#224277=CARTESIAN_POINT('Ctrl Pts',(-21.9497942196786,-4.47123019424771,
127.092200875735));
#224278=CARTESIAN_POINT('Ctrl Pts',(-22.2282418434914,-5.53995426048939,
132.559620196804));
#224279=CARTESIAN_POINT('Ctrl Pts',(-22.5066894673044,-1.5177310031529,
136.41404171375));
#224280=CARTESIAN_POINT('Ctrl Pts',(-22.7851370911172,3.89921290079955,
135.11344035146));
#224281=CARTESIAN_POINT('Ctrl Pts',(-23.0635847149301,5.73297063605735,
129.853005223969));
#224282=CARTESIAN_POINT('Ctrl Pts',(-23.342032338743,2.298408427964,125.466819226899));
#224283=CARTESIAN_POINT('Ctrl Pts',(-23.6204799625559,-3.24827884193431,
125.985573014458));
#224284=CARTESIAN_POINT('Ctrl Pts',(-23.8989275863688,-5.80995654333829,
130.932557198412));
#224285=CARTESIAN_POINT('Ctrl Pts',(-24.1773752101816,-3.03256801357094,
135.761734987319));
#224286=CARTESIAN_POINT('Ctrl Pts',(-24.4558228339946,2.53160237148462,
136.035327911625));
#224287=CARTESIAN_POINT('Ctrl Pts',(-24.7342704578075,5.76935385279724,
131.501917439649));
#224288=CARTESIAN_POINT('Ctrl Pts',(-25.0127180816204,3.70535099199371,
126.327486325724));
#224289=CARTESIAN_POINT('Ctrl Pts',(-25.2911657054332,-1.76368841399288,
125.267083978533));
#224290=CARTESIAN_POINT('Ctrl Pts',(-25.5696133292462,-5.61198432848891,
129.295168351611));
#224291=CARTESIAN_POINT('Ctrl Pts',(-25.8480609530591,-4.30314080577957,
134.71012668896));
#224292=CARTESIAN_POINT('Ctrl Pts',(-26.1265085768719,0.960078897325804,
136.535876813977));
#224293=CARTESIAN_POINT('Ctrl Pts',(-26.4049562006848,5.3410329962505,133.094643554625));
#224294=CARTESIAN_POINT('Ctrl Pts',(-26.6834038244978,4.81383869558843,
127.548752162656));
#224295=CARTESIAN_POINT('Ctrl Pts',(-26.9618514483106,-0.137038197225328,
124.994605895435));
#224296=CARTESIAN_POINT('Ctrl Pts',(-27.2402990721235,-4.96198368147699,
127.779340395554));
#224297=CARTESIAN_POINT('Ctrl Pts',(-27.5187466959364,-5.22710856883054,
133.343920699249));
#224298=CARTESIAN_POINT('Ctrl Pts',(-27.7971943197493,-0.688776039878604,
136.574769352283));
#224299=CARTESIAN_POINT('Ctrl Pts',(-28.0756419435621,4.48250802114168,
134.502894278251));
#224300=CARTESIAN_POINT('Ctrl Pts',(-28.3540895673751,5.53458619342344,
129.032247453463));
#224301=CARTESIAN_POINT('Ctrl Pts',(-28.632537191188,1.50065003351598,125.190086053944));
#224302=CARTESIAN_POINT('Ctrl Pts',(-28.9109848150008,-3.91231019636288,
126.507168705834));
#224303=CARTESIAN_POINT('Ctrl Pts',(-29.1894324388138,-5.73004848276283,
131.773160795109));
#224304=CARTESIAN_POINT('Ctrl Pts',(-29.4678800626266,-2.28215214193419,
136.148872849742));
#224305=CARTESIAN_POINT('Ctrl Pts',(-29.7463276864396,3.26293052800175,
135.613239256942));
#224306=CARTESIAN_POINT('Ctrl Pts',(-30.0247753102524,5.80953944572202,
130.658481121338));
#224307=CARTESIAN_POINT('Ctrl Pts',(-30.3032229340653,3.01746542460398,
125.837779116156));
#224308=CARTESIAN_POINT('Ctrl Pts',(-30.5816705578782,-2.54751191034413,
125.581122879776));
#224309=CARTESIAN_POINT('Ctrl Pts',(-30.8601181816911,-5.77145025256159,
130.124366955075));
#224310=CARTESIAN_POINT('Ctrl Pts',(-31.138565805504,-3.69170776369427,
135.292491986665));
#224311=CARTESIAN_POINT('Ctrl Pts',(-31.4170134293169,1.78053381005746,
136.336243547461));
#224312=CARTESIAN_POINT('Ctrl Pts',(-31.6954610531298,5.6165517962788,132.296464943187));
#224313=CARTESIAN_POINT('Ctrl Pts',(-31.9739086769427,4.29123306552915,
126.885515357016));
#224314=CARTESIAN_POINT('Ctrl Pts',(-32.2523563007555,-0.977519214052166,
125.075793119056));
#224315=CARTESIAN_POINT('Ctrl Pts',(-32.5308039245685,-5.34797909038788,
128.530344556146));
#224316=CARTESIAN_POINT('Ctrl Pts',(-32.8092515483813,-4.80390744596015,
134.07460566182));
#224317=CARTESIAN_POINT('Ctrl Pts',(-33.0876991721943,0.154720457379397,
136.613671332177));
#224318=CARTESIAN_POINT('Ctrl Pts',(-33.3661467960071,4.9711678189017,133.814264256411));
#224319=CARTESIAN_POINT('Ctrl Pts',(-33.64459441982,5.21935480990263,128.248902778514));
#224320=CARTESIAN_POINT('Ctrl Pts',(-33.9230420436329,0.671209710260644,
125.031882213649));
#224321=CARTESIAN_POINT('Ctrl Pts',(-34.2014896674458,-4.49374432269368,
127.119487300736));
#224322=CARTESIAN_POINT('Ctrl Pts',(-34.4799372912587,-5.52916685470707,
132.59331094992));
#224323=CARTESIAN_POINT('Ctrl Pts',(-34.7583849150716,-1.48355516206214,
136.423176638752));
#224324=CARTESIAN_POINT('Ctrl Pts',(-35.0368325388844,3.92537124881898,
135.089624898536));
#224325=CARTESIAN_POINT('Ctrl Pts',(-35.3152801626974,5.72707324708195,
129.818124630907));
#224326=CARTESIAN_POINT('Ctrl Pts',(-35.5937277865103,2.26587471435868,
125.45292705471));
#224327=CARTESIAN_POINT('Ctrl Pts',(-35.8721754103231,-3.27755198672651,
126.005435490714));
#224328=CARTESIAN_POINT('Ctrl Pts',(-36.1506230341361,-5.80906852932597,
130.967921677768));
#224329=CARTESIAN_POINT('Ctrl Pts',(-36.4290706579489,-3.00233488224952,
135.780103240898));
#224330=CARTESIAN_POINT('Ctrl Pts',(-36.7075182817618,2.56339784940132,
136.019820411726));
#224331=CARTESIAN_POINT('Ctrl Pts',(-36.9859659055747,5.77349318639923,
131.466784821096));
#224332=CARTESIAN_POINT('Ctrl Pts',(-37.2644135293876,3.67803033591843,
126.305013748643));
#224333=CARTESIAN_POINT('Ctrl Pts',(-37.5428611532005,-1.79736271150026,
125.277922643415));
#224334=CARTESIAN_POINT('Ctrl Pts',(-37.8213087770133,-5.62106723310019,
129.329358054928));
#224335=CARTESIAN_POINT('Ctrl Pts',(-38.0997564008263,-4.27928557188161,
134.736248763623));
#224336=CARTESIAN_POINT('Ctrl Pts',(-38.3782040246392,0.994950475174061,
136.529926349506));
#224337=CARTESIAN_POINT('Ctrl Pts',(-38.656651648452,5.35487564157755,133.062088737171));
#224338=CARTESIAN_POINT('Ctrl Pts',(-38.9350992722649,4.79393169358958,
127.51950927907));
#224339=CARTESIAN_POINT('Ctrl Pts',(-39.2135468960779,-0.172401284224016,
124.995547727136));
#224340=CARTESIAN_POINT('Ctrl Pts',(-39.4919945198907,-4.98030590410683,
127.809601445221));
#224341=CARTESIAN_POINT('Ctrl Pts',(-39.7704421437036,-5.21155269958477,
133.375692540572));
#224342=CARTESIAN_POINT('Ctrl Pts',(-40.0488897675166,-0.65363716264763,
136.578855215227));
#224343=CARTESIAN_POINT('Ctrl Pts',(-40.3273373913294,4.50493899481217,
134.475539454375));
#224344=CARTESIAN_POINT('Ctrl Pts',(-40.6057850151423,5.52369629454426,
128.998589689552));
#224345=CARTESIAN_POINT('Ctrl Pts',(-40.8842326389552,1.46644654715595,
125.181055190758));
#224346=CARTESIAN_POINT('Ctrl Pts',(-41.1626802627681,-3.93839593717207,
126.531063665459));
#224347=CARTESIAN_POINT('Ctrl Pts',(-41.441127886581,-5.72404495657686,
131.808023276983));
#224348=CARTESIAN_POINT('Ctrl Pts',(-41.7195755103939,-2.24957629602936,
136.162665936149));
#224349=CARTESIAN_POINT('Ctrl Pts',(-41.9980231342068,3.29214308265742,
135.593287775304));
#224350=CARTESIAN_POINT('Ctrl Pts',(-42.2764707580197,5.80854379851262,
130.623119508596));
#224351=CARTESIAN_POINT('Ctrl Pts',(-42.5549183818325,2.98717652667487,
125.81950296691));
#224352=CARTESIAN_POINT('Ctrl Pts',(-42.8333660056454,-2.57926004149102,
125.596727082342));
#224353=CARTESIAN_POINT('Ctrl Pts',(-43.1118136294584,-5.7754826353847,
130.159512009603));
#224354=CARTESIAN_POINT('Ctrl Pts',(-43.3902612532712,-3.66431883537201,
135.314881304976));
#224355=CARTESIAN_POINT('Ctrl Pts',(-43.6687088770841,1.81417496242045,
136.325302439805));
#224356=CARTESIAN_POINT('Ctrl Pts',(-43.947156500897,5.62553059712261,132.262247752997));
#224357=CARTESIAN_POINT('Ctrl Pts',(-44.2256041247099,4.26729843551711,
126.859466010475));
#224358=CARTESIAN_POINT('Ctrl Pts',(-44.5040517485228,-1.01237251921066,
125.081849693053));
#224359=CARTESIAN_POINT('Ctrl Pts',(-44.7824993723357,-5.3617225859308,
128.562941355057));
#224360=CARTESIAN_POINT('Ctrl Pts',(-45.0609469961486,-4.78391153089065,
134.103787819889));
#224361=CARTESIAN_POINT('Ctrl Pts',(-45.3393946199614,0.190080513966956,
136.612621871764));
#224362=CARTESIAN_POINT('Ctrl Pts',(-45.6178422437743,4.98939785243841,
133.783947580368));
#224363=CARTESIAN_POINT('Ctrl Pts',(-45.8962898675873,5.20370231015464,
128.217178431071));
#224364=CARTESIAN_POINT('Ctrl Pts',(-46.1747374914001,0.636058559829223,
125.027903320286));
#224365=CARTESIAN_POINT('Ctrl Pts',(-46.453185115213,-4.51609193379101,
127.146910270074));
#224366=CARTESIAN_POINT('Ctrl Pts',(-46.7316327390259,-5.51817456361365,
132.626935412823));
#224367=CARTESIAN_POINT('Ctrl Pts',(-47.0100803628388,-1.4493243472895,
136.43210335646));
#224368=CARTESIAN_POINT('Ctrl Pts',(-47.2885279866517,3.95138414076325,
135.06565065357));
#224369=CARTESIAN_POINT('Ctrl Pts',(-47.5669756104645,5.72096363930122,
129.783280583183));
#224370=CARTESIAN_POINT('Ctrl Pts',(-47.8454232342775,2.23325703793269,
125.439233181862));
#224371=CARTESIAN_POINT('Ctrl Pts',(-48.1238708580903,-3.30670368062431,
126.025475792906));
#224372=CARTESIAN_POINT('Ctrl Pts',(-48.4023184819033,-5.80796525814313,
131.00328009631));
#224373=CARTESIAN_POINT('Ctrl Pts',(-48.6807661057162,-2.97199049830493,
135.798287116504));
#224374=CARTESIAN_POINT('Ctrl Pts',(-48.9592137295291,2.59509833966803,
136.004119651047));
#224375=CARTESIAN_POINT('Ctrl Pts',(-49.2376613533419,5.77741858108801,
131.431627656171));
#224376=CARTESIAN_POINT('Ctrl Pts',(-49.5161089771548,3.65057338907646,
126.282707896514));
#224377=CARTESIAN_POINT('Ctrl Pts',(-49.7945566009678,-1.8309704070716,
125.288966092489));
#224378=CARTESIAN_POINT('Ctrl Pts',(-50.0730042247805,-5.62994184699806,
129.363602415007));
#224379=CARTESIAN_POINT('Ctrl Pts',(-50.3514518485936,-4.25527176748286,
134.762225140725));
#224380=CARTESIAN_POINT('Ctrl Pts',(-50.6298994724063,1.02978518476655,
136.52376372209));
#224381=CARTESIAN_POINT('Ctrl Pts',(-50.9083470962193,5.36851986001845,
133.029450258773));
#224382=CARTESIAN_POINT('Ctrl Pts',(-51.1867947200322,4.77384705068883,
127.490388116857));
#224383=CARTESIAN_POINT('Ctrl Pts',(-51.465242343845,-0.207757982829986,
124.996704806535));
#224384=CARTESIAN_POINT('Ctrl Pts',(-51.743689967658,-4.99844357966987,
127.839973466791));
#224385=CARTESIAN_POINT('Ctrl Pts',(-52.0221375914708,-5.19580371433717,
133.407369100245));
#224386=CARTESIAN_POINT('Ctrl Pts',(-52.3005852152837,-0.618474064651215,
136.58272710215));
#224387=CARTESIAN_POINT('Ctrl Pts',(-52.5790328390967,4.52720303631132,
134.448048593619));
#224388=CARTESIAN_POINT('Ctrl Pts',(-52.8574804629095,5.51260171306762,
128.964998839148));
#224389=CARTESIAN_POINT('Ctrl Pts',(-53.1359280867224,1.43218872108006,
125.172232701224));
#224390=CARTESIAN_POINT('Ctrl Pts',(-53.4143757105353,-3.96433573927151,
126.555116973674));
#224391=CARTESIAN_POINT('Ctrl Pts',(-53.6928233343482,-5.71782932379997,
131.842848567767));
#224392=CARTESIAN_POINT('Ctrl Pts',(-53.9712709581611,-2.21691709124776,
136.176260468582));
#224393=CARTESIAN_POINT('Ctrl Pts',(-54.249718581974,3.32123364574025,135.573158838211));
#224394=CARTESIAN_POINT('Ctrl Pts',(-54.5281662057869,5.80733291357678,
130.58776461181));
#224395=CARTESIAN_POINT('Ctrl Pts',(-54.8066138295998,2.95677693782102,
125.801411533396));
#224396=CARTESIAN_POINT('Ctrl Pts',(-55.0850614534126,-2.61091259720856,
125.612524255684));
#224397=CARTESIAN_POINT('Ctrl Pts',(-55.3635090772256,-5.77930100557468,
130.194680959234));
#224398=CARTESIAN_POINT('Ctrl Pts',(-55.6419567010384,-3.63679412436797,
135.337103484283));
#224399=CARTESIAN_POINT('Ctrl Pts',(-55.9204043248514,1.8477488898629,136.314156751619));
#224400=CARTESIAN_POINT('Ctrl Pts',(-56.1988519486642,5.63430094186134,
132.227976540264));
#224401=CARTESIAN_POINT('Ctrl Pts',(-56.4772995724772,4.24320567919224,
126.833562843453));
#224402=CARTESIAN_POINT('Ctrl Pts',(-56.7557471962901,-1.04718831053316,
125.088118316796));
#224403=CARTESIAN_POINT('Ctrl Pts',(-57.0341948201028,-5.3752674008715,
128.595621210585));
#224404=CARTESIAN_POINT('Ctrl Pts',(-57.3126424439159,-4.76373834622006,
134.13284771647));
#224405=CARTESIAN_POINT('Ctrl Pts',(-57.5910900677287,0.225433527051438,
136.611357184097));
#224406=CARTESIAN_POINT('Ctrl Pts',(-57.8695376915416,5.00744300200284,
133.753520494635));
#224407=CARTESIAN_POINT('Ctrl Pts',(-58.1479853153544,5.18785698530388,
128.185549952615));
#224408=CARTESIAN_POINT('Ctrl Pts',(-58.4264329391674,0.600883840013963,
125.024138475672));
#224409=CARTESIAN_POINT('Ctrl Pts',(-58.7048805629802,-4.53827219944114,
127.174468767579));
#224410=CARTESIAN_POINT('Ctrl Pts',(-58.9833281867932,-5.5069777945324,
132.660492339548));
#224411=CARTESIAN_POINT('Ctrl Pts',(-59.261775810606,-1.41503982726995,
136.440821536091));
#224412=CARTESIAN_POINT('Ctrl Pts',(-59.540223434419,3.97725061271504,135.041518504932));
#224413=CARTESIAN_POINT('Ctrl Pts',(-59.8186710582318,5.71464203910897,
129.748474371954));
#224414=CARTESIAN_POINT('Ctrl Pts',(-60.0971186820448,2.20055660734573,
125.425738115783));
#224415=CARTESIAN_POINT('Ctrl Pts',(-60.3755663058576,-3.3357328434014,
126.045693178431));
#224416=CARTESIAN_POINT('Ctrl Pts',(-60.6540139296705,-5.80664677067165,
131.038631143817));
#224417=CARTESIAN_POINT('Ctrl Pts',(-60.9324615534834,-2.94153598615947,
135.816285940328));
#224418=CARTESIAN_POINT('Ctrl Pts',(-61.2109091772963,2.62670266761142,
135.988226211385));
#224419=CARTESIAN_POINT('Ctrl Pts',(-61.4893568011092,5.78112989140647,
131.396447247635));
#224420=CARTESIAN_POINT('Ctrl Pts',(-61.767804424922,3.62298116889529,126.260569595891));
#224421=CARTESIAN_POINT('Ctrl Pts',(-62.046252048735,-1.86451025536104,
125.300213916535));
#224422=CARTESIAN_POINT('Ctrl Pts',(-62.3246996725479,-5.63860784133039,
129.39790016291));
#224423=CARTESIAN_POINT('Ctrl Pts',(-62.6031472963608,-4.23110028242386,
134.788054857702));
#224424=CARTESIAN_POINT('Ctrl Pts',(-62.8815949201736,1.0645817352901,136.517389160091));
#224425=CARTESIAN_POINT('Ctrl Pts',(-63.1600425439866,5.38196514598156,
132.99672932886));
#224426=CARTESIAN_POINT('Ctrl Pts',(-63.4384901677994,4.75358551113023,
127.461389755115));
#224427=CARTESIAN_POINT('Ctrl Pts',(-63.7169377916123,-0.243106982887504,
124.998077090756));
#224428=CARTESIAN_POINT('Ctrl Pts',(-63.9953854154252,-5.0163960360679,
127.870455334816));
#224429=CARTESIAN_POINT('Ctrl Pts',(-64.2738330392381,-5.17986219667218,
133.438949204482));
#224430=CARTESIAN_POINT('Ctrl Pts',(-64.552280663051,-0.583288048870894,
136.586384869579));
#224431=CARTESIAN_POINT('Ctrl Pts',(-64.8307282868638,4.54929932063727,
134.420422714664));
#224432=CARTESIAN_POINT('Ctrl Pts',(-65.1091759106768,5.50130286010717,
128.93147614697));
#224433=CARTESIAN_POINT('Ctrl Pts',(-65.3876235344896,1.39787782472419,
125.16361891226));
#224434=CARTESIAN_POINT('Ctrl Pts',(-65.6660711583025,-3.99012864145221,
126.579327739175));
#224435=CARTESIAN_POINT('Ctrl Pts',(-65.9445187821156,-5.71140181475477,
131.877635376998));
#224436=CARTESIAN_POINT('Ctrl Pts',(-66.2229664059283,-2.18417573778792,
136.189655943291));
#224437=CARTESIAN_POINT('Ctrl Pts',(-66.5014140297413,3.35020113928917,
135.552853191544));
#224438=CARTESIAN_POINT('Ctrl Pts',(-66.7798616535541,5.80590683578406,
130.552417741069));
#224439=CARTESIAN_POINT('Ctrl Pts',(-67.0583092773671,2.92626778451039,
125.783505486001));
#224440=CARTESIAN_POINT('Ctrl Pts',(-67.3367569011799,-2.64246840459962,
125.628513814431));
#224441=CARTESIAN_POINT('Ctrl Pts',(-67.6152045249929,-5.78290522164069,
130.229872500769));
#224442=CARTESIAN_POINT('Ctrl Pts',(-67.8936521488056,-3.60913465062,135.359157701137));
#224443=CARTESIAN_POINT('Ctrl Pts',(-68.1720997726187,1.88125434829088,
136.302806895912));
#224444=CARTESIAN_POINT('Ctrl Pts',(-68.4505473964314,5.64286250550667,
132.193652574919));
#224445=CARTESIAN_POINT('Ctrl Pts',(-68.7289950202444,4.21895568932047,
126.807806815805));
#224446=CARTESIAN_POINT('Ctrl Pts',(-69.0074426440573,-1.08196529790749,
125.094598758));
#224447=CARTESIAN_POINT('Ctrl Pts',(-69.2858902678701,-5.38861303330182,
128.628382911763));
#224448=CARTESIAN_POINT('Ctrl Pts',(-69.564337891683,-4.74338863947339,
134.161784274737));
#224449=CARTESIAN_POINT('Ctrl Pts',(-69.8427855154959,0.260778186613682,
136.609877316035));
#224450=CARTESIAN_POINT('Ctrl Pts',(-70.1212331393089,5.02530259892534,
133.722984126697));
#224451=CARTESIAN_POINT('Ctrl Pts',(-70.3996807631217,5.17181942250469,
128.154018515153));
#224452=CARTESIAN_POINT('Ctrl Pts',(-70.6781283869345,0.5656868542273,125.020587819316));
#224453=CARTESIAN_POINT('Ctrl Pts',(-70.9565760107477,-4.56028429774593,
127.202161772061));
#224454=CARTESIAN_POINT('Ctrl Pts',(-71.2350236345604,-5.49557696236377,
132.693980486629));
#224455=CARTESIAN_POINT('Ctrl Pts',(-71.5134712583732,-1.38070287242923,
136.449330854589));
#224456=CARTESIAN_POINT('Ctrl Pts',(-71.7919188821862,4.00296970618273,
135.017229346852));
#224457=CARTESIAN_POINT('Ctrl Pts',(-72.0703665059991,5.70810868075446,
129.71370728698));
#224458=CARTESIAN_POINT('Ctrl Pts',(-72.348814129812,2.16777463432419,125.412442356538));
#224459=CARTESIAN_POINT('Ctrl Pts',(-72.6272617536249,-3.36463839937136,
126.06608689813));
#224460=CARTESIAN_POINT('Ctrl Pts',(-72.9057093774378,-5.80511311576878,
131.073973510343));
#224461=CARTESIAN_POINT('Ctrl Pts',(-73.1841570012506,-2.91097247431594,
135.834099045416));
#224462=CARTESIAN_POINT('Ctrl Pts',(-73.4626046250635,2.65820966212185,
135.972140681676));
#224463=CARTESIAN_POINT('Ctrl Pts',(-73.7410522488765,5.78462697983096,
131.361244899111));
#224464=CARTESIAN_POINT('Ctrl Pts',(-74.0194998726893,3.59525469781404,
126.238599667113));
#224465=CARTESIAN_POINT('Ctrl Pts',(-74.2979474965022,-1.89798101353784,
125.31166569876));
#224466=CARTESIAN_POINT('Ctrl Pts',(-74.5763951203151,-5.64706489497548,
129.432250027724));
#224467=CARTESIAN_POINT('Ctrl Pts',(-74.854842744128,-4.20677201238788,
134.813736957424));
#224468=CARTESIAN_POINT('Ctrl Pts',(-75.1332903679409,1.09933883734644,
136.510802899716));
#224469=CARTESIAN_POINT('Ctrl Pts',(-75.4117379917539,5.39521100124704,
132.963927159917));
#224470=CARTESIAN_POINT('Ctrl Pts',(-75.6901856155667,4.73314782571214,
127.432515268386));
#224471=CARTESIAN_POINT('Ctrl Pts',(-75.9686332393795,-0.278446974526432,
124.99966452895));
#224472=CARTESIAN_POINT('Ctrl Pts',(-76.2470808631926,-5.03416260806588,
127.901045919781));
#224473=CARTESIAN_POINT('Ctrl Pts',(-76.5255284870053,-5.16372873730878,
133.470431683069));
#224474=CARTESIAN_POINT('Ctrl Pts',(-76.8039761108183,-0.548080419137594,
136.589828381972));
#224475=CARTESIAN_POINT('Ctrl Pts',(-77.0824237346311,4.57122702900371,
134.392662841198));
#224476=CARTESIAN_POINT('Ctrl Pts',(-77.360871358444,5.48980015434633,128.898022855216));
#224477=CARTESIAN_POINT('Ctrl Pts',(-77.639318982257,1.36351512949127,125.155214143056));
#224478=CARTESIAN_POINT('Ctrl Pts',(-77.9177666060698,-4.0157736879487,
126.603695064822));
#224479=CARTESIAN_POINT('Ctrl Pts',(-78.1962142298826,-5.70476266761487,
131.91238241564));
#224480=CARTESIAN_POINT('Ctrl Pts',(-78.4746618536957,-2.15135344889296,
136.202851863901));
#224481=CARTESIAN_POINT('Ctrl Pts',(-78.7531094775085,3.37904448990285,
135.532371587738));
#224482=CARTESIAN_POINT('Ctrl Pts',(-79.0315571013213,5.8042656179783,130.517080206165));
#224483=CARTESIAN_POINT('Ctrl Pts',(-79.3100047251342,2.8956501972711,125.765785488239));
#224484=CARTESIAN_POINT('Ctrl Pts',(-79.5884523489472,-2.67392629435197,
125.644695166086));
#224485=CARTESIAN_POINT('Ctrl Pts',(-79.8668999727601,-5.78629515002701,
130.265085330171));
#224486=CARTESIAN_POINT('Ctrl Pts',(-80.1453475965729,-3.58134143906054,
135.38104313831));
#224487=CARTESIAN_POINT('Ctrl Pts',(-80.4237952203859,1.91469009614739,
136.291253293255));
#224488=CARTESIAN_POINT('Ctrl Pts',(-80.7022428441988,5.65121497080658,
132.15927712885));
#224489=CARTESIAN_POINT('Ctrl Pts',(-80.9806904680116,4.19454936449412,
126.782198881926));
#224490=CARTESIAN_POINT('Ctrl Pts',(-81.2591380918246,-1.11670219266007,
125.10129077653));
#224491=CARTESIAN_POINT('Ctrl Pts',(-81.5375857156372,-5.40175898869456,
128.661225244595));
#224492=CARTESIAN_POINT('Ctrl Pts',(-81.8160333394505,-4.72286316471603,
134.190596422436));
#224493=CARTESIAN_POINT('Ctrl Pts',(-82.0944809632629,0.296113182944105,
136.608182322418));
#224494=CARTESIAN_POINT('Ctrl Pts',(-82.3729285870762,5.04297598141181,
133.692339608092));
#224495=CARTESIAN_POINT('Ctrl Pts',(-82.6513762108889,5.15559021603496,
128.122585287091));
#224496=CARTESIAN_POINT('Ctrl Pts',(-82.9298238347018,0.530468906706182,
125.017251482786));
#224497=CARTESIAN_POINT('Ctrl Pts',(-83.2082714585147,-4.58212741303929,
127.229988257347));
#224498=CARTESIAN_POINT('Ctrl Pts',(-83.4867190823277,-5.48397248956967,
132.72739861315));
#224499=CARTESIAN_POINT('Ctrl Pts',(-83.7651667061405,-1.34631475513585,
136.45763099664));
#224500=CARTESIAN_POINT('Ctrl Pts',(-84.0436143299535,4.02854046813582,
134.992784079373));
#224501=CARTESIAN_POINT('Ctrl Pts',(-84.3220619537663,5.70136380633342,
129.678980616565));
#224502=CARTESIAN_POINT('Ctrl Pts',(-84.6005095775792,2.13491233361711,
125.399346396808));
#224503=CARTESIAN_POINT('Ctrl Pts',(-84.8789572013921,-3.39341927742779,
126.086656196302));
#224504=CARTESIAN_POINT('Ctrl Pts',(-85.1574048252049,-5.80336435026449,
131.109305886265));
#224505=CARTESIAN_POINT('Ctrl Pts',(-85.4358524490179,-2.88030109531746,
135.851725771696));
#224506=CARTESIAN_POINT('Ctrl Pts',(-85.7143000728307,2.68961815569484,
135.955863657977));
#224507=CARTESIAN_POINT('Ctrl Pts',(-85.9927476966438,5.78790971677558,
131.326021915035));
#224508=CARTESIAN_POINT('Ctrl Pts',(-86.2711953204564,3.56739500324825,
126.216798924288));
#224509=CARTESIAN_POINT('Ctrl Pts',(-86.5496429442695,-1.93138144132926,
125.323321014816));
#224510=CARTESIAN_POINT('Ctrl Pts',(-86.8280905680822,-5.65531269455438,
129.466650736599));
#224511=CARTESIAN_POINT('Ctrl Pts',(-87.1065381918953,-4.18228785886808,
134.83927048823));
#224512=CARTESIAN_POINT('Ctrl Pts',(-87.3849858157081,1.13405520299706,
136.504005185026));
#224513=CARTESIAN_POINT('Ctrl Pts',(-87.663433439521,5.40825693498488,132.931044967442));
#224514=CARTESIAN_POINT('Ctrl Pts',(-87.9418810633338,4.71253475176078,
127.403765726628));
#224515=CARTESIAN_POINT('Ctrl Pts',(-88.2203286871468,-0.313776648210234,
125.00146706229));
#224516=CARTESIAN_POINT('Ctrl Pts',(-88.4987763109598,-5.05174263731727,
127.931744088139));
#224517=CARTESIAN_POINT('Ctrl Pts',(-88.7772239347726,-5.14740393407785,
133.501815369412));
#224518=CARTESIAN_POINT('Ctrl Pts',(-89.0556715585855,-0.512852480082647,
136.593057511728));
#224519=CARTESIAN_POINT('Ctrl Pts',(-89.3341191823985,4.59298534887173,
134.364770001874));
#224520=CARTESIAN_POINT('Ctrl Pts',(-89.6125668062112,5.47809402202166,
128.864640203508));
#224521=CARTESIAN_POINT('Ctrl Pts',(-89.8910144300243,1.32910190870433,
125.147018705051));
#224522=CARTESIAN_POINT('Ctrl Pts',(-90.169462053837,-4.04126992847403,
126.628218047677));
#224523=CARTESIAN_POINT('Ctrl Pts',(-90.44790967765,-5.69791212839678,131.947088396125));
#224524=CARTESIAN_POINT('Ctrl Pts',(-90.7263573014627,-2.1184514408047,
136.215847741432));
#224525=CARTESIAN_POINT('Ctrl Pts',(-91.0048049252757,3.40776262878029,
135.511714785749));
#224526=CARTESIAN_POINT('Ctrl Pts',(-91.2832525490887,5.80240932097568,
130.48175331654));
#224527=CARTESIAN_POINT('Ctrl Pts',(-91.5617001729014,2.86492531064864,
125.748252196732));
#224528=CARTESIAN_POINT('Ctrl Pts',(-91.8401477967144,-2.70528510078237,
125.661067711041));
#224529=CARTESIAN_POINT('Ctrl Pts',(-92.1185954205271,-5.78947066511866,
130.30031814262));
#224530=CARTESIAN_POINT('Ctrl Pts',(-92.3970430443404,-3.55341551957677,
135.402758984829));
#224531=CARTESIAN_POINT('Ctrl Pts',(-92.6754906681528,1.94805489445803,
136.279496371773));
#224532=CARTESIAN_POINT('Ctrl Pts',(-92.9539382919661,5.6593580282576,132.124851475851));
#224533=CARTESIAN_POINT('Ctrl Pts',(-93.2323859157787,4.16998760909852,
126.75673999073));
#224534=CARTESIAN_POINT('Ctrl Pts',(-93.5108335395918,-1.15139770760221,
125.10819412441));
#224535=CARTESIAN_POINT('Ctrl Pts',(-93.7892811634045,-5.41470477992152,
128.694146992097));
#224536=CARTESIAN_POINT('Ctrl Pts',(-94.0677287872175,-4.70216268252734,
134.219283091922));
#224537=CARTESIAN_POINT('Ctrl Pts',(-94.3461764110305,0.331437206691851,
136.606272266052));
#224538=CARTESIAN_POINT('Ctrl Pts',(-94.6246240348431,5.0604624945689,133.661588074364));
#224539=CARTESIAN_POINT('Ctrl Pts',(-94.9030716586564,5.13916996727372,
128.0912514332));
#224540=CARTESIAN_POINT('Ctrl Pts',(-95.1815192824688,0.495231302464415,
125.014129589715));
#224541=CARTESIAN_POINT('Ctrl Pts',(-95.459966906282,-4.60380073591605,
127.257947192314));
#224542=CARTESIAN_POINT('Ctrl Pts',(-95.7384145300948,-5.47216480615837,
132.760745480792));
#224543=CARTESIAN_POINT('Ctrl Pts',(-96.0168621539077,-1.31187674965409,
136.465721654678));
#224544=CARTESIAN_POINT('Ctrl Pts',(-96.2953097777207,4.05396195104042,
134.96818360832));
#224545=CARTESIAN_POINT('Ctrl Pts',(-96.5737574015334,5.69440766577999,
129.64429564752));
#224546=CARTESIAN_POINT('Ctrl Pts',(-96.8522050253465,2.10197092294792,
125.386450721867));
#224547=CARTESIAN_POINT('Ctrl Pts',(-97.1306526491593,-3.42207441108517,
126.107400310748));
#224548=CARTESIAN_POINT('Ctrl Pts',(-97.4091002729722,-5.80140053895979,
131.144626962327));
#224549=CARTESIAN_POINT('Ctrl Pts',(-97.6875478967851,-2.8495229857029,
135.869165466005));
#224550=CARTESIAN_POINT('Ctrl Pts',(-97.965995520598,2.72092698447821,135.93939574344));
#224551=CARTESIAN_POINT('Ctrl Pts',(-98.2444431444108,5.79097798059694,
131.290779600608));
#224552=CARTESIAN_POINT('Ctrl Pts',(-98.5228907682237,3.53940311754856,
126.195168175249));
#224553=CARTESIAN_POINT('Ctrl Pts',(-98.8013383920368,-1.96471030107164,
125.33517943281));
#224554=CARTESIAN_POINT('Ctrl Pts',(-99.0797860158496,-5.6633509344415,
129.501101014807));
#224555=CARTESIAN_POINT('Ctrl Pts',(-99.3582336396624,-4.15764872913354,
134.864654503967));
#224556=CARTESIAN_POINT('Ctrl Pts',(-99.6366812634755,1.16872954581563,
136.496996267908));
#224557=CARTESIAN_POINT('Ctrl Pts',(-99.9151288872883,5.42110246377302,
132.898083969897));
#224558=CARTESIAN_POINT('Ctrl Pts',(-100.193576511101,4.69174705310118,
127.375142195163));
#224559=CARTESIAN_POINT('Ctrl Pts',(-100.472024134914,-0.34909469478497,
125.003484623986));
#224560=CARTESIAN_POINT('Ctrl Pts',(-100.750471758727,-5.06913547238742,
127.96254870236));
#224561=CARTESIAN_POINT('Ctrl Pts',(-101.02891938254,-5.13088839190121,
133.533099100579));
#224562=CARTESIAN_POINT('Ctrl Pts',(-101.307367006353,-0.47760553709043,
136.596072139193));
#224563=CARTESIAN_POINT('Ctrl Pts',(-101.585814630166,4.61457347397855,
134.33674523027));
#224564=CARTESIAN_POINT('Ctrl Pts',(-101.864262253979,5.46618489690847,
128.831329428852));
#224565=CARTESIAN_POINT('Ctrl Pts',(-102.142709877791,1.29463943755703,
125.139032901931));
#224566=CARTESIAN_POINT('Ctrl Pts',(-102.421157501604,-4.06661641825637,
126.652895779031));
#224567=CARTESIAN_POINT('Ctrl Pts',(-102.699605125417,-5.69085045094906,
131.981752032413));
#224568=CARTESIAN_POINT('Ctrl Pts',(-102.97805274923,-2.08547093271925,
136.228643094318));
#224569=CARTESIAN_POINT('Ctrl Pts',(-103.256500373043,3.43635449176034,
135.490883551018));
#224570=CARTESIAN_POINT('Ctrl Pts',(-103.534947996856,5.80033801356182,
130.446438381249));
#224571=CARTESIAN_POINT('Ctrl Pts',(-103.813395620669,2.83409426316523,
125.730906261181));
#224572=CARTESIAN_POINT('Ctrl Pts',(-104.091843244482,-2.73654366187847,
125.677630842606));
#224573=CARTESIAN_POINT('Ctrl Pts',(-104.370290868295,-5.79243164924577,
130.335569632546));
#224574=CARTESIAN_POINT('Ctrl Pts',(-104.648738492108,-3.52535792697413,
135.424304436005));
#224575=CARTESIAN_POINT('Ctrl Pts',(-104.92718611592,1.98134750687769,136.267536567122));
#224576=CARTESIAN_POINT('Ctrl Pts',(-105.205633739733,5.66729137611554,
132.090376891579));
#224577=CARTESIAN_POINT('Ctrl Pts',(-105.484081363546,4.14527133327901,
126.731431085605));
#224578=CARTESIAN_POINT('Ctrl Pts',(-105.762528987359,-1.18605055707886,
125.115308545834));
#224579=CARTESIAN_POINT('Ctrl Pts',(-106.040976611172,-5.42744992727162,
128.72714693434));
#224580=CARTESIAN_POINT('Ctrl Pts',(-106.319424234985,-4.68128795997122,
134.247843220201));
#224581=CARTESIAN_POINT('Ctrl Pts',(-106.597871858798,0.366748948912009,
136.604147217717));
#224582=CARTESIAN_POINT('Ctrl Pts',(-106.876319482611,5.07776149042729,
133.630730665021));
#224583=CARTESIAN_POINT('Ctrl Pts',(-107.154767106424,5.12255928467941,
128.060018114567));
#224584=CARTESIAN_POINT('Ctrl Pts',(-107.433214730236,0.45997534724462,
125.011222255784));
#224585=CARTESIAN_POINT('Ctrl Pts',(-107.711662354049,-4.62530346326349,
127.286037540936));
#224586=CARTESIAN_POINT('Ctrl Pts',(-107.990109977862,-5.46015434966779,
132.794019853873));
#224587=CARTESIAN_POINT('Ctrl Pts',(-108.268557601675,-1.2773901320969,
136.473602528901));
#224588=CARTESIAN_POINT('Ctrl Pts',(-108.547005225488,4.07923321289408,
134.943428845277));
#224589=CARTESIAN_POINT('Ctrl Pts',(-108.825452849301,5.6872405168564,129.609653665109));
#224590=CARTESIAN_POINT('Ctrl Pts',(-109.103900473114,2.06895162297316,
125.373755809571));
#224591=CARTESIAN_POINT('Ctrl Pts',(-109.382348096927,-3.45060273851677,
126.128318472786));
#224592=CARTESIAN_POINT('Ctrl Pts',(-109.66079572074,-5.79922175462486,
131.179935429694));
#224593=CARTESIAN_POINT('Ctrl Pts',(-109.939243344552,-2.81863928596571,
135.886417482107));
#224594=CARTESIAN_POINT('Ctrl Pts',(-110.217690968365,2.7521349883118,135.922737548286));
#224595=CARTESIAN_POINT('Ctrl Pts',(-110.496138592178,5.79383165759959,
131.255519261747));
#224596=CARTESIAN_POINT('Ctrl Pts',(-110.774586215991,3.51128007796473,
126.17370822153));
#224597=CARTESIAN_POINT('Ctrl Pts',(-111.053033839804,-1.99796635775128,
125.347240513325));
#224598=CARTESIAN_POINT('Ctrl Pts',(-111.331481463617,-5.67117931677705,
129.535599585778));
#224599=CARTESIAN_POINT('Ctrl Pts',(-111.60992908743,-4.13285553619637,
134.889888064022));
#224600=CARTESIAN_POINT('Ctrl Pts',(-111.888376711243,1.20336058093108,
136.489776408084));
#224601=CARTESIAN_POINT('Ctrl Pts',(-112.166824335056,5.43374711161577,
132.865045388662));
#224602=CARTESIAN_POINT('Ctrl Pts',(-112.445271958868,4.67078550002918,
127.34664573465));
#224603=CARTESIAN_POINT('Ctrl Pts',(-112.723719582681,-0.384399805526852,
125.005717139274));
#224604=CARTESIAN_POINT('Ctrl Pts',(-113.002167206494,-5.08634046877848,
127.993458620965));
#224605=CARTESIAN_POINT('Ctrl Pts',(-113.280614830307,-5.11418272276831,
133.564281717336));
#224606=CARTESIAN_POINT('Ctrl Pts',(-113.55906245412,-0.442340896249408,
136.598872152659));
#224607=CARTESIAN_POINT('Ctrl Pts',(-113.837510077933,4.63599060436829,
134.308589564856));
#224608=CARTESIAN_POINT('Ctrl Pts',(-114.115957701746,5.45407322030374,
128.798091765594));
#224609=CARTESIAN_POINT('Ctrl Pts',(-114.394405325558,1.26012899306928,
125.131257029612));
#224610=CARTESIAN_POINT('Ctrl Pts',(-114.672852949372,-4.09181221807183,
126.677727344441));
#224611=CARTESIAN_POINT('Ctrl Pts',(-114.951300573184,-5.68357789694507,
132.016372040028));
#224612=CARTESIAN_POINT('Ctrl Pts',(-115.229748196997,-2.05241314674147,
136.241237448422));
#224613=CARTESIAN_POINT('Ctrl Pts',(-115.50819582081,3.46481901936097,135.469878655457));
#224614=CARTESIAN_POINT('Ctrl Pts',(-115.786643444623,5.79805177248978,
130.411136708898));
#224615=CARTESIAN_POINT('Ctrl Pts',(-116.065091068436,2.80315819727665,
125.713748324348));
#224616=CARTESIAN_POINT('Ctrl Pts',(-116.343538692249,-2.76770081934284,
125.694383947029));
#224617=CARTESIAN_POINT('Ctrl Pts',(-116.621986316062,-5.79517799268792,
130.370838493694));
#224618=CARTESIAN_POINT('Ctrl Pts',(-116.900433939875,-3.49716970093708,
135.445678693465));
#224619=CARTESIAN_POINT('Ctrl Pts',(-117.178881563688,2.0145666997373,136.255374322477));
#224620=CARTESIAN_POINT('Ctrl Pts',(-117.4573291875,5.67501472040751,132.055854653499));
#224621=CARTESIAN_POINT('Ctrl Pts',(-117.735776811314,4.12040145290537,
126.706273104381));
#224622=CARTESIAN_POINT('Ctrl Pts',(-118.014224435126,-1.22065945701595,
125.122633777175));
#224623=CARTESIAN_POINT('Ctrl Pts',(-118.29267205894,-5.43999395846872,
128.760223848501));
#224624=CARTESIAN_POINT('Ctrl Pts',(-118.571119682752,-4.6602397705682,
134.276275748964));
#224625=CARTESIAN_POINT('Ctrl Pts',(-118.849567306565,0.402047101114997,
136.601807256156));
#224626=CARTESIAN_POINT('Ctrl Pts',(-119.128014930377,5.09487232796628,
133.599768523497));
#224627=CARTESIAN_POINT('Ctrl Pts',(-119.406462554191,5.10575878376697,
128.028886488555));
#224628=CARTESIAN_POINT('Ctrl Pts',(-119.684910178003,0.424702347469154,
125.008529588725));
#224629=CARTESIAN_POINT('Ctrl Pts',(-119.963357801817,-4.64663479828973,
127.314258262312));
#224630=CARTESIAN_POINT('Ctrl Pts',(-120.241805425629,-5.44794156515001,
132.827220499399));
#224631=CARTESIAN_POINT('Ctrl Pts',(-120.520253049442,-1.24285618037906,
136.48127332728));
#224632=CARTESIAN_POINT('Ctrl Pts',(-120.798700673255,4.10435331726091,
134.918520707537));
#224633=CARTESIAN_POINT('Ctrl Pts',(-121.077148297068,5.67986262514396,
129.575055953004));
#224634=CARTESIAN_POINT('Ctrl Pts',(-121.355595920881,2.03585565723516,
125.361262130332));
#224635=CARTESIAN_POINT('Ctrl Pts',(-121.634043544694,-3.47900320259493,
126.149409907283));
#224636=CARTESIAN_POINT('Ctrl Pts',(-121.912491168507,-5.79682807799514,
131.215229979999));
#224637=CARTESIAN_POINT('Ctrl Pts',(-122.19093879232,-2.78765114051323,
135.903481180724));
#224638=CARTESIAN_POINT('Ctrl Pts',(-122.469386416133,2.78324101077128,
135.905889689793));
#224639=CARTESIAN_POINT('Ctrl Pts',(-122.747834039945,5.79647064203949,
131.220242205036));
#224640=CARTESIAN_POINT('Ctrl Pts',(-123.026281663758,3.48302692660634,
126.152419858339));
#224641=CARTESIAN_POINT('Ctrl Pts',(-123.304729287571,-2.03114837905279,
125.359503809431));
#224642=CARTESIAN_POINT('Ctrl Pts',(-123.583176911384,-5.67879755147744,
129.570145171156));
#224643=CARTESIAN_POINT('Ctrl Pts',(-123.861624535197,-4.10790919877744,
134.914970233354));
#224644=CARTESIAN_POINT('Ctrl Pts',(-124.14007215901,1.23794702507767,136.482345873087));
#224645=CARTESIAN_POINT('Ctrl Pts',(-124.418519782823,5.44619040996103,
132.831930447996));
#224646=CARTESIAN_POINT('Ctrl Pts',(-124.696967406636,4.64965086928273,
127.318277401031));
#224647=CARTESIAN_POINT('Ctrl Pts',(-124.975415030448,-0.419690672193134,
125.00816452543));
#224648=CARTESIAN_POINT('Ctrl Pts',(-125.253862654262,-5.10335698895296,
128.024472698579));
#224649=CARTESIAN_POINT('Ctrl Pts',(-125.532310278074,-5.09728754571388,
133.595362064203));
#224650=CARTESIAN_POINT('Ctrl Pts',(-125.810757901887,-0.407059864303788,
136.601457448367));
#224651=CARTESIAN_POINT('Ctrl Pts',(-126.0892055257,4.65723594642128,134.280304048949));
#224652=CARTESIAN_POINT('Ctrl Pts',(-126.367653149513,5.44175944101008,
128.764928445366));
#224653=CARTESIAN_POINT('Ctrl Pts',(-126.646100773326,1.22557185403828,
125.123691376234));
#224654=CARTESIAN_POINT('Ctrl Pts',(-126.924548397139,-4.11685639428078,
126.702711823764));
#224655=CARTESIAN_POINT('Ctrl Pts',(-127.202996020952,-5.67609473587197,
132.050947136115));
#224656=CARTESIAN_POINT('Ctrl Pts',(-127.481443644765,-2.01927930784003,
136.253630337055));
#224657=CARTESIAN_POINT('Ctrl Pts',(-127.759891268577,3.4931551568182,135.44870087741));
#224658=CARTESIAN_POINT('Ctrl Pts',(-128.038338892391,5.79555068247735,
130.375849607603));
#224659=CARTESIAN_POINT('Ctrl Pts',(-128.316786516203,2.77211825933019,
125.696779022025));
#224660=CARTESIAN_POINT('Ctrl Pts',(-128.595234140016,-2.7987554186355,
125.711326403516));
#224661=CARTESIAN_POINT('Ctrl Pts',(-128.873681763829,-5.79770959367839,
130.406123419165));
#224662=CARTESIAN_POINT('Ctrl Pts',(-129.152129387642,-3.46885188599067,
135.466880965177));
#224663=CARTESIAN_POINT('Ctrl Pts',(-129.430577011455,2.04771124208698,
136.243010088514));
#224664=CARTESIAN_POINT('Ctrl Pts',(-129.709024635268,5.68252777494204,
132.021286040849));
#224665=CARTESIAN_POINT('Ctrl Pts',(-129.98747225908,4.09537888954061,126.681266979298));
#224666=CARTESIAN_POINT('Ctrl Pts',(-130.265919882893,-1.25522312496795,
125.130169546993));
#224667=CARTESIAN_POINT('Ctrl Pts',(-130.544367506706,-5.45233640868912,
128.793376508901));
#224668=CARTESIAN_POINT('Ctrl Pts',(-130.822815130519,-4.63901889426667,
134.304579624636));
#224669=CARTESIAN_POINT('Ctrl Pts',(-131.101262754332,0.437330355314798,
136.599252468079));
#224670=CARTESIAN_POINT('Ctrl Pts',(-131.379710378145,5.11179437313754,
133.568702797104));
#224671=CARTESIAN_POINT('Ctrl Pts',(-131.658158001958,5.08876908708517,
127.997857708758));
#224672=CARTESIAN_POINT('Ctrl Pts',(-131.936605625771,0.389413610192037,
125.006051688315));
#224673=CARTESIAN_POINT('Ctrl Pts',(-132.215053249584,-4.66779395055513,
127.342608310716));
#224674=CARTESIAN_POINT('Ctrl Pts',(-132.493500873397,-5.43552690515385,
132.860346187109));
#224675=CARTESIAN_POINT('Ctrl Pts',(-132.77194849721,-1.20827617416795,
136.488733765571));
#224676=CARTESIAN_POINT('Ctrl Pts',(-133.050396121022,4.12932133330617,
134.893460118082));
#224677=CARTESIAN_POINT('Ctrl Pts',(-133.328843744835,5.67227426403318,
129.540503793235));
#224678=CARTESIAN_POINT('Ctrl Pts',(-133.607291368648,2.00268425211708,
125.348970147109));
#224679=CARTESIAN_POINT('Ctrl Pts',(-133.885738992461,-3.50727475093002,
126.170673832692));
#224680=CARTESIAN_POINT('Ctrl Pts',(-134.164186616274,-5.79421959776922,
131.25050930539));
#224681=CARTESIAN_POINT('Ctrl Pts',(-134.442634240087,-2.75655969762259,
135.920355929551));
#224682=CARTESIAN_POINT('Ctrl Pts',(-134.7210818639,2.81424389921159,135.888852792264));
#224683=CARTESIAN_POINT('Ctrl Pts',(-134.999529487713,5.79889483612785,
131.18494973768));
#224684=CARTESIAN_POINT('Ctrl Pts',(-135.277977111526,3.45464471040472,
126.131303874523));
#224685=CARTESIAN_POINT('Ctrl Pts',(-135.556424735338,-2.06425513540386,
125.371968866708));
#224686=CARTESIAN_POINT('Ctrl Pts',(-135.834872359151,-5.68620535624619,
129.604736490841));
#224687=CARTESIAN_POINT('Ctrl Pts',(-136.113319982964,-4.08281064127246,
134.939900082537));
#224688=CARTESIAN_POINT('Ctrl Pts',(-136.391767606777,1.27248759664198,
136.474704938258));
#224689=CARTESIAN_POINT('Ctrl Pts',(-136.67021523059,5.45843189771781,132.798740374984));
#224690=CARTESIAN_POINT('Ctrl Pts',(-136.948662854403,4.62834394401342,
127.290038245509));
#224691=CARTESIAN_POINT('Ctrl Pts',(-137.227110478216,-0.454965987067202,
125.010826691762));
#224692=CARTESIAN_POINT('Ctrl Pts',(-137.505558102029,-5.12018440235748,
128.055589785961));
#224693=CARTESIAN_POINT('Ctrl Pts',(-137.784005725841,-5.0802034867949,
133.626338989485));
#224694=CARTESIAN_POINT('Ctrl Pts',(-138.062453349655,-0.371763748605222,
136.603827930521));
#224695=CARTESIAN_POINT('Ctrl Pts',(-138.340900973467,4.67830871288359,
134.251889730681));
#224696=CARTESIAN_POINT('Ctrl Pts',(-138.61934859728,5.42924401531914,128.731840697047));
#224697=CARTESIAN_POINT('Ctrl Pts',(-138.897796221093,1.19096930099152,
125.116336222143));
#224698=CARTESIAN_POINT('Ctrl Pts',(-139.176243844906,-4.14174801886209,
126.727848291193));
#224699=CARTESIAN_POINT('Ctrl Pts',(-139.454691468719,-5.66840124502105,
132.085476039479));
#224700=CARTESIAN_POINT('Ctrl Pts',(-139.733139092532,-1.98607064380098,
136.265821300996));
#224701=CARTESIAN_POINT('Ctrl Pts',(-140.011586716345,3.52136185412693,
135.427351001626));
#224702=CARTESIAN_POINT('Ctrl Pts',(-140.290034340158,5.79283483620279,
130.340578384942));
#224703=CARTESIAN_POINT('Ctrl Pts',(-140.56848196397,2.7409755995222,125.679998983016));
#224704=CARTESIAN_POINT('Ctrl Pts',(-140.846929587784,-2.82970630901691,
125.72845758426));
#224705=CARTESIAN_POINT('Ctrl Pts',(-141.125377211596,-5.80002635840773,
130.441423101462));
#224706=CARTESIAN_POINT('Ctrl Pts',(-141.403824835409,-3.44040553146196,
135.487910465481));
#224707=CARTESIAN_POINT('Ctrl Pts',(-141.682272459222,2.08077990574355,
136.230444323395));
#224708=CARTESIAN_POINT('Ctrl Pts',(-141.960720083035,5.68983026132012,
131.986672334579));
#224709=CARTESIAN_POINT('Ctrl Pts',(-142.239167706848,4.07020457040501,
126.656413636965));
#224710=CARTESIAN_POINT('Ctrl Pts',(-142.517615330661,-1.289740280165,125.137915576048));
#224711=CARTESIAN_POINT('Ctrl Pts',(-142.796062954474,-5.46447682057862,
128.826603687055));
#224712=CARTESIAN_POINT('Ctrl Pts',(-143.074510578287,-4.61762611741445,
134.332753798405));
#224713=CARTESIAN_POINT('Ctrl Pts',(-143.352958202099,0.472597404077474,
136.596482948152));
#224714=CARTESIAN_POINT('Ctrl Pts',(-143.631405825913,5.12852699888841,
133.537534636997));
#224715=CARTESIAN_POINT('Ctrl Pts',(-143.909853449725,5.07159082419343,
127.966932924958));
#224716=CARTESIAN_POINT('Ctrl Pts',(-144.188301073538,0.354110443050382,
125.003788646376));
#224717=CARTESIAN_POINT('Ctrl Pts',(-144.466748697351,-4.6887801359991,
127.371086635623));
#224718=CARTESIAN_POINT('Ctrl Pts',(-144.745196321164,-5.4229108297093,
132.893395689516));
#224719=CARTESIAN_POINT('Ctrl Pts',(-145.023643944977,-1.17365139483885,
136.495983567324));
#224720=CARTESIAN_POINT('Ctrl Pts',(-145.30209156879,4.15413633583088,134.868248005541));
#224721=CARTESIAN_POINT('Ctrl Pts',(-145.580539192603,5.66447571471356,
129.505998466145));
#224722=CARTESIAN_POINT('Ctrl Pts',(-145.858986816416,1.96943863679757,
125.336880315387));
#224723=CARTESIAN_POINT('Ctrl Pts',(-146.137434440228,-3.53541633590941,
126.192109461069));
#224724=CARTESIAN_POINT('Ctrl Pts',(-146.415882064041,-5.79139641060527,
131.285772098575));
#224725=CARTESIAN_POINT('Ctrl Pts',(-146.694329687854,-2.72536610939861,
135.937041103293));
#224726=CARTESIAN_POINT('Ctrl Pts',(-146.972777311667,2.84514250480927,
135.871627487008));
#224727=CARTESIAN_POINT('Ctrl Pts',(-147.25122493548,5.80110415003576,131.149643167454));
#224728=CARTESIAN_POINT('Ctrl Pts',(-147.529672559293,3.42613448107249,
126.110361052543));
#224729=CARTESIAN_POINT('Ctrl Pts',(-147.808120183106,-2.09728540002206,
125.38463522326));
#224730=CARTESIAN_POINT('Ctrl Pts',(-148.086567806919,-5.69340245658434,
129.639372263039));
#224731=CARTESIAN_POINT('Ctrl Pts',(-148.365015430732,-4.05756079371773,
134.964676687782));
#224732=CARTESIAN_POINT('Ctrl Pts',(-148.643463054544,1.30698101571045,
136.466853886735));
#224733=CARTESIAN_POINT('Ctrl Pts',(-148.921910678358,5.47047112127328,
132.765476399497));
#224734=CARTESIAN_POINT('Ctrl Pts',(-149.20035830217,4.60686551375719,127.261929314495));
#224735=CARTESIAN_POINT('Ctrl Pts',(-149.478805925983,-0.49022444300932,
125.013703539625));
#224736=CARTESIAN_POINT('Ctrl Pts',(-149.757253549796,-5.13682208544599,
128.086808730058));
#224737=CARTESIAN_POINT('Ctrl Pts',(-150.035701173609,-5.06293117906749,
133.657211345319));
#224738=CARTESIAN_POINT('Ctrl Pts',(-150.314148797422,-0.336453857064764,
136.605983511281));
#224739=CARTESIAN_POINT('Ctrl Pts',(-150.592596421235,4.69920812289605,
134.223347662954));
#224740=CARTESIAN_POINT('Ctrl Pts',(-150.871044045047,5.41652740699458,
128.698829746717));
#224741=CARTESIAN_POINT('Ctrl Pts',(-151.14949166886,1.15632261613933,125.109191839888));
#224742=CARTESIAN_POINT('Ctrl Pts',(-151.427939292673,-4.1664861694474,
126.753135815284));
#224743=CARTESIAN_POINT('Ctrl Pts',(-151.706386916486,-5.66049770947745,
132.119957470642));
#224744=CARTESIAN_POINT('Ctrl Pts',(-151.984834540299,-1.95278838518384,
136.277809888502));
#224745=CARTESIAN_POINT('Ctrl Pts',(-152.263282164112,3.54943806607717,
135.405829819234));
#224746=CARTESIAN_POINT('Ctrl Pts',(-152.541729787925,5.78990433430307,
130.3053243479));
#224747=CARTESIAN_POINT('Ctrl Pts',(-152.820177411738,2.70973137185537,
125.663408829112));
#224748=CARTESIAN_POINT('Ctrl Pts',(-153.09862503555,-2.86055234359039,
125.745776854456));
#224749=CARTESIAN_POINT('Ctrl Pts',(-153.377072659364,-5.80212820102742,
130.476736232542));
#224750=CARTESIAN_POINT('Ctrl Pts',(-153.655520283176,-3.41183169144105,
135.508766415124));
#224751=CARTESIAN_POINT('Ctrl Pts',(-153.933967906989,2.1137714653355,136.21767749275));
#224752=CARTESIAN_POINT('Ctrl Pts',(-154.212415530802,5.69692190894542,
131.952014817313));
#224753=CARTESIAN_POINT('Ctrl Pts',(-154.490863154615,4.04487942834225,
126.631713998332));
#224754=CARTESIAN_POINT('Ctrl Pts',(-154.769310778428,-1.32420964356211,
125.145871577308));
#224755=CARTESIAN_POINT('Ctrl Pts',(-155.047758402241,-5.47641474427016,
128.859904151722));
#224756=CARTESIAN_POINT('Ctrl Pts',(-155.326206026054,-4.59606223272787,
134.360797226267));
#224757=CARTESIAN_POINT('Ctrl Pts',(-155.604653649866,0.507846940569522,
136.593498799002));
#224758=CARTESIAN_POINT('Ctrl Pts',(-155.88310127368,5.14506958518534,133.50626519812));
#224759=CARTESIAN_POINT('Ctrl Pts',(-156.161548897493,5.05422463163864,
127.936113283085));
#224760=CARTESIAN_POINT('Ctrl Pts',(-156.439996521305,0.318794154216047,
125.001740546765));
#224761=CARTESIAN_POINT('Ctrl Pts',(-156.718444145118,-4.70959257697085,
127.399692181761));
#224762=CARTESIAN_POINT('Ctrl Pts',(-156.996891768931,-5.41009380630968,
132.926367781962));
#224763=CARTESIAN_POINT('Ctrl Pts',(-157.275339392744,-1.1389831254257,
136.503022463895));
#224764=CARTESIAN_POINT('Ctrl Pts',(-157.553787016557,4.17879740530553,
134.84288530416));
#224765=CARTESIAN_POINT('Ctrl Pts',(-157.83223464037,5.65646726616335,129.471541250343));
#224766=CARTESIAN_POINT('Ctrl Pts',(-158.110682264183,1.93612004320555,
125.324993083158));
#224767=CARTESIAN_POINT('Ctrl Pts',(-158.389129887996,-3.56342691473634,
126.213715998108));
#224768=CARTESIAN_POINT('Ctrl Pts',(-158.667577511808,-5.78835862111754,
131.321017052882));
#224769=CARTESIAN_POINT('Ctrl Pts',(-158.946025135621,-2.69407153173119,
135.95353608367));
#224770=CARTESIAN_POINT('Ctrl Pts',(-159.224472759434,2.87593568260513,
135.854214412314));
#224771=CARTESIAN_POINT('Ctrl Pts',(-159.502920383247,5.80309850189603,
131.114323802656));
#224772=CARTESIAN_POINT('Ctrl Pts',(-159.78136800706,3.39749729506709,126.089592168444));
#224773=CARTESIAN_POINT('Ctrl Pts',(-160.059815630873,-2.13023794895846,
125.39750240973));
#224774=CARTESIAN_POINT('Ctrl Pts',(-160.338263254686,-5.70038858580074,
129.674051204309));
#224775=CARTESIAN_POINT('Ctrl Pts',(-160.616710878499,-4.03216059175559,
134.989299130986));
#224776=CARTESIAN_POINT('Ctrl Pts',(-160.895158502312,1.34142600411673,
136.458793009441));
#224777=CARTESIAN_POINT('Ctrl Pts',(-161.173606126125,5.48230763450959,
132.732139754142));
#224778=CARTESIAN_POINT('Ctrl Pts',(-161.452053749937,4.58521637440516,
127.233951649575));
#224779=CARTESIAN_POINT('Ctrl Pts',(-161.730501373751,-0.525464733504406,
125.016794962416));
#224780=CARTESIAN_POINT('Ctrl Pts',(-162.008948997563,-5.15326942170307,
128.118128374039));
#224781=CARTESIAN_POINT('Ctrl Pts',(-162.287396621376,-5.04547126256333,
133.687977987722));
#224782=CARTESIAN_POINT('Ctrl Pts',(-162.565844245189,-0.301131498102361,
136.607924110772));
#224783=CARTESIAN_POINT('Ctrl Pts',(-162.844291869002,4.71993340202341,
134.194678903404));
#224784=CARTESIAN_POINT('Ctrl Pts',(-163.122739492814,5.40361008725504,
128.665896817606));
#224785=CARTESIAN_POINT('Ctrl Pts',(-163.401187116628,1.12163308332736,
125.102258494207));
#224786=CARTESIAN_POINT('Ctrl Pts',(-163.67963474044,-4.19106992935549,
126.778573459));
#224787=CARTESIAN_POINT('Ctrl Pts',(-163.958082364253,-5.65238442210956,
132.154390151878));
#224788=CARTESIAN_POINT('Ctrl Pts',(-164.236529988066,-1.91943376527495,
136.289595655332));
#224789=CARTESIAN_POINT('Ctrl Pts',(-164.514977611879,3.57738275229458,
135.384138127707));
#224790=CARTESIAN_POINT('Ctrl Pts',(-164.793425235692,5.78675928536899,
130.270088802833));
#224791=CARTESIAN_POINT('Ctrl Pts',(-165.071872859505,2.67838673409632,
125.647009175068));
#224792=CARTESIAN_POINT('Ctrl Pts',(-165.350320483318,-2.89129237934434,
125.763283572333));
#224793=CARTESIAN_POINT('Ctrl Pts',(-165.628768107131,-5.80401504365309,
130.512061503863));
#224794=CARTESIAN_POINT('Ctrl Pts',(-165.907215730944,-3.38313142474212,
135.52944804128));
#224795=CARTESIAN_POINT('Ctrl Pts',(-166.185663354757,2.14668469834846,
136.204710069657));
#224796=CARTESIAN_POINT('Ctrl Pts',(-166.464110978569,5.70380245503433,
131.917314773299));
#224797=CARTESIAN_POINT('Ctrl Pts',(-166.742558602383,4.01940440178476,
126.607168978656));
#224798=CARTESIAN_POINT('Ctrl Pts',(-167.021006226195,-1.3586299378839,
125.15403725596));
#224799=CARTESIAN_POINT('Ctrl Pts',(-167.299453850008,-5.48814973739939,
128.893276668938));
#224800=CARTESIAN_POINT('Ctrl Pts',(-167.577901473821,-4.57432803926507,
134.388708869063));
#224801=CARTESIAN_POINT('Ctrl Pts',(-167.856349097634,0.543077658606429,
136.590300131209));
#224802=CARTESIAN_POINT('Ctrl Pts',(-168.134796721447,5.16142151903669,
133.474895639175));
#224803=CARTESIAN_POINT('Ctrl Pts',(-168.413244345259,5.03667115293141,
127.905399925171));
#224804=CARTESIAN_POINT('Ctrl Pts',(-168.691691969073,0.283466052347084,
124.999907465374));
#224805=CARTESIAN_POINT('Ctrl Pts',(-168.970139592885,-4.7302305022577,
127.42842388914));
#224806=CARTESIAN_POINT('Ctrl Pts',(-169.248587216698,-5.39707630989451,
132.959261242652));
#224807=CARTESIAN_POINT('Ctrl Pts',(-169.527034840511,-1.10427265057399,
136.509850194457));
#224808=CARTESIAN_POINT('Ctrl Pts',(-169.805482464324,4.20330362790601,
134.81737295376));
#224809=CARTESIAN_POINT('Ctrl Pts',(-170.083930088137,5.6482492151383,129.437133422652));
#224810=CARTESIAN_POINT('Ctrl Pts',(-170.36237771195,1.90272970597286,125.313308890908));
#224811=CARTESIAN_POINT('Ctrl Pts',(-170.640825335763,-3.59130544946847,
126.235492643171));
#224812=CARTESIAN_POINT('Ctrl Pts',(-170.919272959575,-5.78510634187241,
131.356242862295));
#224813=CARTESIAN_POINT('Ctrl Pts',(-171.197720583389,-2.66267712425244,
135.969840259458));
#224814=CARTESIAN_POINT('Ctrl Pts',(-171.476168207202,2.90662229154664,
135.836614213432));
#224815=CARTESIAN_POINT('Ctrl Pts',(-171.754615831014,5.80487781780722,
131.07899295206));
#224816=CARTESIAN_POINT('Ctrl Pts',(-172.033063454828,3.36873421355001,
126.068997991823));
#224817=CARTESIAN_POINT('Ctrl Pts',(-172.31151107864,-2.16311156114431,
125.410569949319));
#224818=CARTESIAN_POINT('Ctrl Pts',(-172.589958702453,-5.70716348502144,
129.70877202961));
#224819=CARTESIAN_POINT('Ctrl Pts',(-172.868406326266,-4.00661097660031,
135.013766499754));
#224820=CARTESIAN_POINT('Ctrl Pts',(-173.146853950079,1.3758212854888,136.450522605077));
#224821=CARTESIAN_POINT('Ctrl Pts',(-173.425301573892,5.49394099882038,
132.698731674224));
#224822=CARTESIAN_POINT('Ctrl Pts',(-173.703749197705,4.56339732817417,
127.206106287473));
#224823=CARTESIAN_POINT('Ctrl Pts',(-173.982196821517,-0.560685552710569,
125.02010084558));
#224824=CARTESIAN_POINT('Ctrl Pts',(-174.260644445331,-5.1695258016666,
128.149547557344));
#224825=CARTESIAN_POINT('Ctrl Pts',(-174.539092069143,-5.02782438426607,
133.718637776622));
#224826=CARTESIAN_POINT('Ctrl Pts',(-174.817539692956,-0.265797980601551,
136.609649657082));
#224827=CARTESIAN_POINT('Ctrl Pts',(-175.095987316769,4.74048378228282,
134.165884514362));
#224828=CARTESIAN_POINT('Ctrl Pts',(-175.374434940582,5.39049253475655,
128.633043130058));
#224829=CARTESIAN_POINT('Ctrl Pts',(-175.652882564395,1.08690198798901,
125.095536442018));
#224830=CARTESIAN_POINT('Ctrl Pts',(-175.931330188208,-4.21549838762608,
126.80416027974));
#224831=CARTESIAN_POINT('Ctrl Pts',(-176.209777812021,-5.64406168355824,
132.188772807274));
#224832=CARTESIAN_POINT('Ctrl Pts',(-176.488225435833,-1.886008020042,136.301178164761));
#224833=CARTESIAN_POINT('Ctrl Pts',(-176.766673059646,3.60519487727851,
135.362276730843));
#224834=CARTESIAN_POINT('Ctrl Pts',(-177.045120683459,5.78339980594152,
130.234873055403));
#224835=CARTESIAN_POINT('Ctrl Pts',(-177.323568307272,2.64694284773159,
125.630800628577));
#224836=CARTESIAN_POINT('Ctrl Pts',(-177.602015931085,-2.92192527719638,
125.780977089175));
#224837=CARTESIAN_POINT('Ctrl Pts',(-177.880463554898,-5.80568681636668,
130.547397606436));
#224838=CARTESIAN_POINT('Ctrl Pts',(-178.158911178711,-3.35430579486411,
135.549954577584));
#224839=CARTESIAN_POINT('Ctrl Pts',(-178.437358802524,2.17951838517049,
136.191542534628));
#224840=CARTESIAN_POINT('Ctrl Pts',(-178.715806426336,5.71047164462571,
131.88257348836));
#224841=CARTESIAN_POINT('Ctrl Pts',(-178.99425405015,3.99378043471903,126.582779487459));
#224842=CARTESIAN_POINT('Ctrl Pts',(-179.272701673962,-1.39299988767372,
125.162412309422));
#224843=CARTESIAN_POINT('Ctrl Pts',(-179.551149297775,-5.49968136512185,
128.926720002072));
#224844=CARTESIAN_POINT('Ctrl Pts',(-179.829596921588,-4.55242434239454,
134.416487692516));
#224845=CARTESIAN_POINT('Ctrl Pts',(-180.108044545401,0.578288252700551,
136.5868870633));
#224846=CARTESIAN_POINT('Ctrl Pts',(-180.386492169214,5.17758219451528,
133.443427122574));
#224847=CARTESIAN_POINT('Ctrl Pts',(-180.664939793027,5.01893103852278,
127.874793989312));
#224848=CARTESIAN_POINT('Ctrl Pts',(-180.94338741684,0.248127446539293,
124.998289470128));
#224849=CARTESIAN_POINT('Ctrl Pts',(-181.221835040653,-4.75069314711374,
127.457280693096));
#224850=CARTESIAN_POINT('Ctrl Pts',(-181.500282664465,-5.38385882283189,
132.992074852706));
#224851=CARTESIAN_POINT('Ctrl Pts',(-181.778730288279,-1.06952125649312,
136.516466506004));
#224852=CARTESIAN_POINT('Ctrl Pts',(-182.057177912091,4.22765409554481,
134.791711899713));
#224853=CARTESIAN_POINT('Ctrl Pts',(-182.335625535904,5.63982186616143,
129.402776258069));
#224854=CARTESIAN_POINT('Ctrl Pts',(-182.614073159717,1.86926886239121,
125.301828171599));
#224855=CARTESIAN_POINT('Ctrl Pts',(-182.89252078353,-3.61905090705647,
126.257438589318));
#224856=CARTESIAN_POINT('Ctrl Pts',(-183.170968407343,-5.78163969338434,
131.391448221508));
#224857=CARTESIAN_POINT('Ctrl Pts',(-183.449416031155,-2.63118405029363,
135.985953026497));
#224858=CARTESIAN_POINT('Ctrl Pts',(-183.727863654969,2.93720119453022,
135.818827542541));
#224859=CARTESIAN_POINT('Ctrl Pts',(-184.006311278781,5.80644203183612,
131.04365192486));
#224860=CARTESIAN_POINT('Ctrl Pts',(-184.284758902595,3.33984630234777,
126.048579285806));
#224861=CARTESIAN_POINT('Ctrl Pts',(-184.563206526407,-2.19590501843575,
125.423837357804));
#224862=CARTESIAN_POINT('Ctrl Pts',(-184.84165415022,-5.71372690320071,
129.743533452349));
#224863=CARTESIAN_POINT('Ctrl Pts',(-185.120101774033,-3.98091289500146,
135.03807788744));
#224864=CARTESIAN_POINT('Ctrl Pts',(-185.398549397846,1.41016558529749,
136.442042980103));
#224865=CARTESIAN_POINT('Ctrl Pts',(-185.676997021659,5.50537078312707,
132.665253397689));
#224866=CARTESIAN_POINT('Ctrl Pts',(-185.955444645472,4.54140918357699,
127.178394260007));
#224867=CARTESIAN_POINT('Ctrl Pts',(-186.233892269285,-0.595885595507362,
125.023621066618));
#224868=CARTESIAN_POINT('Ctrl Pts',(-186.512339893098,-5.18559062295048,
128.181065115723));
#224869=CARTESIAN_POINT('Ctrl Pts',(-186.79078751691,-5.00999119808726,
133.749189575911));
#224870=CARTESIAN_POINT('Ctrl Pts',(-187.069235140724,-0.230454613858838,
136.611160086272));
#224871=CARTESIAN_POINT('Ctrl Pts',(-187.347682764536,4.76085850217237,
134.136965562817));
#224872=CARTESIAN_POINT('Ctrl Pts',(-187.626130388349,5.37717523557474,
128.600269901479));
#224873=CARTESIAN_POINT('Ctrl Pts',(-187.904578012162,1.05213061709833,
125.089025932407));
#224874=CARTESIAN_POINT('Ctrl Pts',(-188.183025635975,-4.23977063905356,
126.829895329374));
#224875=CARTESIAN_POINT('Ctrl Pts',(-188.461473259788,-5.63552980222562,
132.223104162766));
#224876=CARTESIAN_POINT('Ctrl Pts',(-188.739920883601,-1.85251238808831,
136.312556987595));
#224877=CARTESIAN_POINT('Ctrl Pts',(-189.018368507414,3.63287341044046,
135.340246438718));
#224878=CARTESIAN_POINT('Ctrl Pts',(-189.296816131227,5.77982602050738,
130.199678410544));
#224879=CARTESIAN_POINT('Ctrl Pts',(-189.575263755039,2.61540087792624,
125.614783790254));
#224880=CARTESIAN_POINT('Ctrl Pts',(-189.853711378852,-2.95244990203274,
125.798856749341));
#224881=CARTESIAN_POINT('Ctrl Pts',(-190.132159002665,-5.80714345722022,
130.582743230867));
#224882=CARTESIAN_POINT('Ctrl Pts',(-190.410606626478,-3.32535586995153,
135.570285264159));
#224883=CARTESIAN_POINT('Ctrl Pts',(-190.689054250291,2.21227130913674,
136.178175375592));
#224884=CARTESIAN_POINT('Ctrl Pts',(-190.967501874104,5.7169292305904,131.847792249846));
#224885=CARTESIAN_POINT('Ctrl Pts',(-191.245949497917,3.96800847665057,
126.558546428502));
#224886=CARTESIAN_POINT('Ctrl Pts',(-191.52439712173,-1.4273182193404,125.170996427354));
#224887=CARTESIAN_POINT('Ctrl Pts',(-191.802844745543,-5.51100920012879,
128.960232911869));
#224888=CARTESIAN_POINT('Ctrl Pts',(-192.081292369355,-4.53035195376586,
134.444132667273));
#224889=CARTESIAN_POINT('Ctrl Pts',(-192.359739993168,0.613477418111232,
136.583259721745));
#224890=CARTESIAN_POINT('Ctrl Pts',(-192.638187616981,5.19355101278185,
133.411860814392));
#224891=CARTESIAN_POINT('Ctrl Pts',(-192.916635240794,5.00100494577841,
127.844296609621));
#224892=CARTESIAN_POINT('Ctrl Pts',(-193.195082864607,0.21277964627773,
124.996886620986));
#224893=CARTESIAN_POINT('Ctrl Pts',(-193.47353048842,-4.77097975328813,
127.486261524329));
#224894=CARTESIAN_POINT('Ctrl Pts',(-193.751978112233,-5.3704418349007,
133.024807396204));
#224895=CARTESIAN_POINT('Ctrl Pts',(-194.030425736046,-1.03473023090876,
136.522871153366));
#224896=CARTESIAN_POINT('Ctrl Pts',(-194.308873359859,4.25184790590635,
134.765903092897));
#224897=CARTESIAN_POINT('Ctrl Pts',(-194.587320983671,5.63118553151129,
129.368471029708));
#224898=CARTESIAN_POINT('Ctrl Pts',(-194.865768607484,1.83573875236439,
125.290551350653));
#224899=CARTESIAN_POINT('Ctrl Pts',(-195.144216231297,-3.64666225938173,
126.279553023333));
#224900=CARTESIAN_POINT('Ctrl Pts',(-195.42266385511,-5.77795880411129,
131.426631825972));
#224901=CARTESIAN_POINT('Ctrl Pts',(-195.701111478923,-2.59959347684268,
136.001873787725));
#224902=CARTESIAN_POINT('Ctrl Pts',(-195.979559102736,2.96767125844341,
135.800855058734));
#224903=CARTESIAN_POINT('Ctrl Pts',(-196.258006726549,5.80779108602021,
131.008302030633));
#224904=CARTESIAN_POINT('Ctrl Pts',(-196.536454350362,3.31083463191258,
126.028336807015));
#224905=CARTESIAN_POINT('Ctrl Pts',(-196.814901974175,-2.22861710565919,
125.437304143558));
#224906=CARTESIAN_POINT('Ctrl Pts',(-197.093349597988,-5.72007859712835,
129.778334184429));
#224907=CARTESIAN_POINT('Ctrl Pts',(-197.3717972218,-3.95506729921131,135.062232393175));
#224908=CARTESIAN_POINT('Ctrl Pts',(-197.650244845613,1.44445763090186,
136.433354448736));
#224909=CARTESIAN_POINT('Ctrl Pts',(-197.928692469426,5.51659656389443,
132.631706165088));
#224910=CARTESIAN_POINT('Ctrl Pts',(-198.207140093239,4.51925275539276,
127.150816594059));
#224911=CARTESIAN_POINT('Ctrl Pts',(-198.485587717052,-0.631063557543924,
125.027355495085));
#224912=CARTESIAN_POINT('Ctrl Pts',(-198.764035340865,-5.2014632902668,
128.212679881281));
#224913=CARTESIAN_POINT('Ctrl Pts',(-199.042482964678,-4.99197236484219,
133.779632253479));
#224914=CARTESIAN_POINT('Ctrl Pts',(-199.320930588491,-0.19510270753564,
136.612455342372));
#224915=CARTESIAN_POINT('Ctrl Pts',(-199.599378212304,4.7810568066993,134.10792312037));
#224916=CARTESIAN_POINT('Ctrl Pts',(-199.877825836116,5.36365868318719,
128.56757834629));
#224917=CARTESIAN_POINT('Ctrl Pts',(-200.156273459929,1.01732025912016,
125.082727206624));
#224918=CARTESIAN_POINT('Ctrl Pts',(-200.434721083742,-4.26388578422093,
126.855777654281));
#224919=CARTESIAN_POINT('Ctrl Pts',(-200.713168707555,-5.62678909426374,
132.257382946195));
#224920=CARTESIAN_POINT('Ctrl Pts',(-200.991616331368,-1.8189481106068,
136.323731702186));
#224921=CARTESIAN_POINT('Ctrl Pts',(-201.270063955181,3.66041732614217,
135.318048067677));
#224922=CARTESIAN_POINT('Ctrl Pts',(-201.548511578994,5.77603806149454,
130.164506172408));
#224923=CARTESIAN_POINT('Ctrl Pts',(-201.826959202806,2.58376199347953,
125.59895925361));
#224924=CARTESIAN_POINT('Ctrl Pts',(-202.10540682662,-2.9828651227522,125.816921890294));
#224925=CARTESIAN_POINT('Ctrl Pts',(-202.383854450432,-5.80838491223743,
130.618097067413));
#224926=CARTESIAN_POINT('Ctrl Pts',(-202.662302074245,-3.29628272275406,
135.590439347642));
#224927=CARTESIAN_POINT('Ctrl Pts',(-202.940749698058,2.24494225657654,
136.164609087875));
#224928=CARTESIAN_POINT('Ctrl Pts',(-203.219197321871,5.72317497363993,
131.812972346589));
#224929=CARTESIAN_POINT('Ctrl Pts',(-203.497644945684,3.94208948256877,
126.534470699752));
#224930=CARTESIAN_POINT('Ctrl Pts',(-203.776092569497,-1.46158366120557,
125.179789291667));
#224931=CARTESIAN_POINT('Ctrl Pts',(-204.05454019331,-5.52213282266317,
128.993814156497));
#224932=CARTESIAN_POINT('Ctrl Pts',(-204.332987817123,-4.5081116912795,
134.471642768938));
#224933=CARTESIAN_POINT('Ctrl Pts',(-204.611435440935,0.648643850890564,
136.579418240959));
#224934=CARTESIAN_POINT('Ctrl Pts',(-204.889883064748,5.20932738210573,
133.380197884332));
#224935=CARTESIAN_POINT('Ctrl Pts',(-205.168330688562,4.98289353895661,
127.813908916192));
#224936=CARTESIAN_POINT('Ctrl Pts',(-205.446778312374,0.177423961388546,
124.995698969927));
#224937=CARTESIAN_POINT('Ctrl Pts',(-205.725225936187,-4.79108956905296,
127.515365308944));
#224938=CARTESIAN_POINT('Ctrl Pts',(-206.00367356,-5.35682584327266,133.057457660231));
#224939=CARTESIAN_POINT('Ctrl Pts',(-206.282121183813,-0.999900863015179,
136.529063899218));
#224940=CARTESIAN_POINT('Ctrl Pts',(-206.560568807626,4.27588416248015,
134.739947489669));
#224941=CARTESIAN_POINT('Ctrl Pts',(-206.839016431439,5.62234053121038,
129.334219008764));
#224942=CARTESIAN_POINT('Ctrl Pts',(-207.117464055252,1.80214061836306,
125.279478845937));
#224943=CARTESIAN_POINT('Ctrl Pts',(-207.395911679064,-3.67413848329639,
126.301835125757));
#224944=CARTESIAN_POINT('Ctrl Pts',(-207.674359302878,-5.77406381044983,
131.461792371951));
#224945=CARTESIAN_POINT('Ctrl Pts',(-207.95280692669,-2.56790657449899,
136.01760195319));
#224946=CARTESIAN_POINT('Ctrl Pts',(-208.231254550503,2.99803135420673,
135.782697427989));
#224947=CARTESIAN_POINT('Ctrl Pts',(-208.509702174316,5.8089249303698,130.972944579282));
#224948=CARTESIAN_POINT('Ctrl Pts',(-208.788149798129,3.28170027728254,
126.008271305542));
#224949=CARTESIAN_POINT('Ctrl Pts',(-209.066597421942,-2.2612466106562,
125.450969807563));
#224950=CARTESIAN_POINT('Ctrl Pts',(-209.345045045754,-5.72621833144002,
129.813172936296));
#224951=CARTESIAN_POINT('Ctrl Pts',(-209.623492669568,-3.92907514694791,
135.086229121905));
#224952=CARTESIAN_POINT('Ctrl Pts',(-209.90194029338,1.4786961515975,136.424457332932));
#224953=CARTESIAN_POINT('Ctrl Pts',(-210.180387917194,5.52761792514773,
132.598091219525));
#224954=CARTESIAN_POINT('Ctrl Pts',(-210.458835541006,4.49692886463537,
127.123374311529));
#224955=CARTESIAN_POINT('Ctrl Pts',(-210.73728316482,-0.666218135288655,
125.031303992602));
#224956=CARTESIAN_POINT('Ctrl Pts',(-211.015730788632,-5.21714321544808,
128.244390682522));
#224957=CARTESIAN_POINT('Ctrl Pts',(-211.294178412445,-4.97376855222533,
133.809964681263));
#224958=CARTESIAN_POINT('Ctrl Pts',(-211.572626036258,-0.159743571609885,
136.613535377387));
#224959=CARTESIAN_POINT('Ctrl Pts',(-211.851073660071,4.80107794740803,
134.0787582632));
#224960=CARTESIAN_POINT('Ctrl Pts',(-212.129521283884,5.34994337845465,
128.534969675892));
#224961=CARTESIAN_POINT('Ctrl Pts',(-212.407968907697,0.982472203965689,
125.076640498072));
#224962=CARTESIAN_POINT('Ctrl Pts',(-212.686416531509,-4.28784292953254,
126.881806295382));
#224963=CARTESIAN_POINT('Ctrl Pts',(-212.964864155322,-5.61783988356258,
132.291607887347));
#224964=CARTESIAN_POINT('Ctrl Pts',(-213.243311779135,-1.78531643133465,
136.334701894451));
#224965=CARTESIAN_POINT('Ctrl Pts',(-213.521759402948,3.68782560373359,
135.295682440288));
#224966=CARTESIAN_POINT('Ctrl Pts',(-213.800207026761,5.77203606926717,
130.129357644311));
#224967=CARTESIAN_POINT('Ctrl Pts',(-214.078654650574,2.55202736678199,
125.583327605028));
#224968=CARTESIAN_POINT('Ctrl Pts',(-214.357102274386,-3.0131698123076,
125.835171842623));
#224969=CARTESIAN_POINT('Ctrl Pts',(-214.6355498982,-5.80941113541564,130.653457806023));
#224970=CARTESIAN_POINT('Ctrl Pts',(-214.913997522012,-3.26708743058812,
135.610416081219));
#224971=CARTESIAN_POINT('Ctrl Pts',(-215.192445145826,2.27753001685547,
136.15084417418));
#224972=CARTESIAN_POINT('Ctrl Pts',(-215.470892769638,5.72920864233609,
131.778115068854));
#224973=CARTESIAN_POINT('Ctrl Pts',(-215.749340393451,3.9160244129115,126.510553193344));
#224974=CARTESIAN_POINT('Ctrl Pts',(-216.027788017264,-1.49579494355069,
125.18879057654));
#224975=CARTESIAN_POINT('Ctrl Pts',(-216.306235641077,-5.53305182053502,
129.02746249159));
#224976=CARTESIAN_POINT('Ctrl Pts',(-216.58468326489,-4.48570437905656,
134.499016978113));
#224977=CARTESIAN_POINT('Ctrl Pts',(-216.863130888703,0.683786247933482,
136.57536276329));
#224978=CARTESIAN_POINT('Ctrl Pts',(-217.141578512516,5.2249107178877,133.348439505674));
#224979=CARTESIAN_POINT('Ctrl Pts',(-217.420026136328,4.96459748918233,
127.78363203505));
#224980=CARTESIAN_POINT('Ctrl Pts',(-217.698473760142,0.142061701988793,
124.994726560962));
#224981=CARTESIAN_POINT('Ctrl Pts',(-217.976921383954,-4.81102184923216,
127.544590968491));
#224982=CARTESIAN_POINT('Ctrl Pts',(-218.255369007768,-5.34301135249269,
133.090024434919));
#224983=CARTESIAN_POINT('Ctrl Pts',(-218.53381663158,-0.965034443427401,
136.535044514085));
#224984=CARTESIAN_POINT('Ctrl Pts',(-218.812264255394,4.29976197459382,
134.713846051821));
#224985=CARTESIAN_POINT('Ctrl Pts',(-219.090711879206,5.61328719301349,
129.300021464458));
#224986=CARTESIAN_POINT('Ctrl Pts',(-219.369159503019,1.76847570537835,
125.268611067748));
#224987=CARTESIAN_POINT('Ctrl Pts',(-219.647607126831,-3.70147856065836,
126.324284070919));
#224988=CARTESIAN_POINT('Ctrl Pts',(-219.926054750645,-5.76995485673049,
131.496928556552));
#224989=CARTESIAN_POINT('Ctrl Pts',(-220.204502374457,-2.5361245174328,
136.033136940081));
#224990=CARTESIAN_POINT('Ctrl Pts',(-220.48294999827,3.02828035681523,135.764355323142));
#224991=CARTESIAN_POINT('Ctrl Pts',(-220.761397622083,5.80984352286985,
130.937580880991));
#224992=CARTESIAN_POINT('Ctrl Pts',(-221.039845245896,3.25244431804234,
125.988383524923));
#224993=CARTESIAN_POINT('Ctrl Pts',(-221.318292869709,-2.29379232432851,
125.464833843433));
#224994=CARTESIAN_POINT('Ctrl Pts',(-221.596740493522,-5.73214587862558,
129.848048416986));
#224995=CARTESIAN_POINT('Ctrl Pts',(-221.875188117335,-3.90293740136003,
135.110067184424));
#224996=CARTESIAN_POINT('Ctrl Pts',(-222.153635741148,1.51287987866345,
136.415351962378));
#224997=CARTESIAN_POINT('Ctrl Pts',(-222.432083364961,5.53843445848603,
132.564409806615));
#224998=CARTESIAN_POINT('Ctrl Pts',(-222.710530988774,4.47443833852516,
127.0960684293));
#224999=CARTESIAN_POINT('Ctrl Pts',(-222.988978612586,-0.701348026075381,
125.035466412855));
#225000=CARTESIAN_POINT('Ctrl Pts',(-223.267426236399,-5.23262981746888,
128.27619634439));
#225001=CARTESIAN_POINT('Ctrl Pts',(-223.545873860212,-4.95538043478568,
133.840185735283));
#225002=CARTESIAN_POINT('Ctrl Pts',(-223.824321484025,-0.124378516327312,
136.614400151295));
#225003=CARTESIAN_POINT('Ctrl Pts',(-224.102769107838,4.82092118240782,
134.049472072021));
#225004=CARTESIAN_POINT('Ctrl Pts',(-224.381216731651,5.33602982960279,
128.502445098609));
#225005=CARTESIAN_POINT('Ctrl Pts',(-224.659664355464,0.947587742942381,
125.070766032295));
#225006=CARTESIAN_POINT('Ctrl Pts',(-224.938111979277,-4.31164118724753,
126.907980288176));
#225007=CARTESIAN_POINT('Ctrl Pts',(-225.216559603089,-5.60868250173869,
132.325777718005));
#225008=CARTESIAN_POINT('Ctrl Pts',(-225.495007226903,-1.75161859650508,
136.345467157888));
#225009=CARTESIAN_POINT('Ctrl Pts',(-225.773454850715,3.71509722759125,
135.273150385318));
#225010=CARTESIAN_POINT('Ctrl Pts',(-226.051902474528,5.7678201921206,130.0942341287));
#225011=CARTESIAN_POINT('Ctrl Pts',(-226.330350098341,2.52019817377184,
125.567889423742));
#225012=CARTESIAN_POINT('Ctrl Pts',(-226.608797722154,-3.04336284774751,
125.853605930069));
#225013=CARTESIAN_POINT('Ctrl Pts',(-226.887245345967,-5.81022208872781,
130.688824136393));
#225014=CARTESIAN_POINT('Ctrl Pts',(-227.16569296978,-3.23777107529596,
135.630214724643));
#225015=CARTESIAN_POINT('Ctrl Pts',(-227.444140593593,2.31003338242206,
136.13688114457));
#225016=CARTESIAN_POINT('Ctrl Pts',(-227.722588217406,5.73503001309909,
131.74322170829));
#225017=CARTESIAN_POINT('Ctrl Pts',(-228.001035841218,3.88981423352964,
126.486794795549));
#225018=CARTESIAN_POINT('Ctrl Pts',(-228.279483465031,-1.52995079866356,
125.197999948425));
#225019=CARTESIAN_POINT('Ctrl Pts',(-228.557931088844,-5.54376578913698,
129.061176670297));
#225020=CARTESIAN_POINT('Ctrl Pts',(-228.836378712657,-4.46313084740822,
134.526254280438));
#225021=CARTESIAN_POINT('Ctrl Pts',(-229.11482633647,0.718903307025501,
136.571093439014));
#225022=CARTESIAN_POINT('Ctrl Pts',(-229.393273960283,5.24030044268158,
133.316586855238));
#225023=CARTESIAN_POINT('Ctrl Pts',(-229.671721584096,4.94611747442232,
127.753467088116));
#225024=CARTESIAN_POINT('Ctrl Pts',(-229.950169207909,0.106694178440453,
124.993969430123));
#225025=CARTESIAN_POINT('Ctrl Pts',(-230.228616831722,-4.83077585522751,
127.57393742));
#225026=CARTESIAN_POINT('Ctrl Pts',(-230.507064455534,-5.32899887446215,
133.122506513493));
#225027=CARTESIAN_POINT('Ctrl Pts',(-230.785512079348,-0.930132264133436,
136.540812776352));
#225028=CARTESIAN_POINT('Ctrl Pts',(-231.06395970316,4.3234804574463,134.687599746553));
#225029=CARTESIAN_POINT('Ctrl Pts',(-231.342407326973,5.60402585239536,
129.265879663993));
#225030=CARTESIAN_POINT('Ctrl Pts',(-231.620854950786,1.73474526087603,
125.257948418793));
#225031=CARTESIAN_POINT('Ctrl Pts',(-231.899302574599,-3.72868147837107,
126.346899026965));
#225032=CARTESIAN_POINT('Ctrl Pts',(-232.177750198412,-5.76563209521201,
131.532039077795));
#225033=CARTESIAN_POINT('Ctrl Pts',(-232.456197822225,-2.50424848333998,
136.048478172742));
#225034=CARTESIAN_POINT('Ctrl Pts',(-232.734645446038,3.05841714538193,
135.745829423867));
#225035=CARTESIAN_POINT('Ctrl Pts',(-233.01309306985,5.81054682948159,130.902212246173));
#225036=CARTESIAN_POINT('Ctrl Pts',(-233.291540693664,3.22306783828139,
125.968674202107));
#225037=CARTESIAN_POINT('Ctrl Pts',(-233.569988317476,-2.32625304068266,
125.478895737432));
#225038=CARTESIAN_POINT('Ctrl Pts',(-233.84843594129,-5.73786101903762,
129.882959334177));
#225039=CARTESIAN_POINT('Ctrl Pts',(-234.126883565102,-3.87665503099142,
135.133745697402));
#225040=CARTESIAN_POINT('Ctrl Pts',(-234.405331188915,1.54700754540913,
136.406038674476));
#225041=CARTESIAN_POINT('Ctrl Pts',(-234.683778812728,5.54904576309872,
132.530663174436));
#225042=CARTESIAN_POINT('Ctrl Pts',(-234.962226436541,4.45178201045685,
127.0688999592));
#225043=CARTESIAN_POINT('Ctrl Pts',(-235.240674060353,-0.736451928153096,
125.039842601604));
#225044=CARTESIAN_POINT('Ctrl Pts',(-235.519121684167,-5.24792252246713,
128.308095688315));
#225045=CARTESIAN_POINT('Ctrl Pts',(-235.797569307979,-4.93680869390195,
133.870294295687));
#225046=CARTESIAN_POINT('Ctrl Pts',(-236.076016931792,-0.0890088521534987,
136.61504963205));
#225047=CARTESIAN_POINT('Ctrl Pts',(-236.354464555605,4.8405857764003,134.020065632043));
#225048=CARTESIAN_POINT('Ctrl Pts',(-236.632912179418,5.32191855220324,
128.470005819654));
#225049=CARTESIAN_POINT('Ctrl Pts',(-236.911359803231,0.912668168706789,
125.065104026974));
#225050=CARTESIAN_POINT('Ctrl Pts',(-237.189807427044,-4.33527967551271,
126.934298662776));
#225051=CARTESIAN_POINT('Ctrl Pts',(-237.468255050857,-5.59931728812211,
132.359891171993));
#225052=CARTESIAN_POINT('Ctrl Pts',(-237.74670267467,-1.71785585480426,
136.356027093583));
#225053=CARTESIAN_POINT('Ctrl Pts',(-238.025150298482,3.7422311871549,135.250452737698));
#225054=CARTESIAN_POINT('Ctrl Pts',(-238.303597922296,5.76339058627568,
130.059136927086));
#225055=CARTESIAN_POINT('Ctrl Pts',(-238.582045546108,2.48827559389159,
125.552645281824));
#225056=CARTESIAN_POINT('Ctrl Pts',(-238.860493169922,-3.07344311025789,
125.87222346955));
#225057=CARTESIAN_POINT('Ctrl Pts',(-239.138940793734,-5.81081774212379,
130.724194748009));
#225058=CARTESIAN_POINT('Ctrl Pts',(-239.417388417547,-3.20833474320591,
135.649834544268));
#225059=CARTESIAN_POINT('Ctrl Pts',(-239.69583604136,2.34245114885216,136.12272051645));
#225060=CARTESIAN_POINT('Ctrl Pts',(-239.974283665173,5.7406388702159,131.708293557882));
#225061=CARTESIAN_POINT('Ctrl Pts',(-240.252731288985,3.86345991565072,
126.463196386742));
#225062=CARTESIAN_POINT('Ctrl Pts',(-240.531178912799,-1.56404996088748,
125.207417066067));
#225063=CARTESIAN_POINT('Ctrl Pts',(-240.809626536611,-5.5542743314588,
129.094955443325));
#225064=CARTESIAN_POINT('Ctrl Pts',(-241.088074160425,-4.44039193280503,
134.553353666625));
#225065=CARTESIAN_POINT('Ctrl Pts',(-241.366521784237,0.753993726891117,
136.566610426332));
#225066=CARTESIAN_POINT('Ctrl Pts',(-241.64496940805,5.25549598621542,133.284641113335));
#225067=CARTESIAN_POINT('Ctrl Pts',(-241.923417031863,4.92745417946037,
127.723415193164));
#225068=CARTESIAN_POINT('Ctrl Pts',(-242.201864655676,0.071322701300089,
124.993427605467));
#225069=CARTESIAN_POINT('Ctrl Pts',(-242.480312279489,-4.85035085504701,
127.603403576029));
#225070=CARTESIAN_POINT('Ctrl Pts',(-242.758759903302,-5.31478892841856,
133.154902692318));
#225071=CARTESIAN_POINT('Ctrl Pts',(-243.037207527115,-0.895195618446729,
136.546368472274));
#225072=CARTESIAN_POINT('Ctrl Pts',(-243.315655150928,4.34703873214009,
134.661209546432));
#225073=CARTESIAN_POINT('Ctrl Pts',(-243.59410277474,5.59455685253872,129.231794872506));
#225074=CARTESIAN_POINT('Ctrl Pts',(-243.872550398553,1.7009505347501,125.247491294183));
#225075=CARTESIAN_POINT('Ctrl Pts',(-244.150998022366,-3.75574622842035,
126.36967915589));
#225076=CARTESIAN_POINT('Ctrl Pts',(-244.429445646179,-5.76109568607594,
131.567122634643));
#225077=CARTESIAN_POINT('Ctrl Pts',(-244.707893269992,-2.47227965339868,
136.063625082699));
#225078=CARTESIAN_POINT('Ctrl Pts',(-244.986340893805,3.08844060317656,
135.727120416648));
#225079=CARTESIAN_POINT('Ctrl Pts',(-245.264788517618,5.81103482414375,
130.866839985428));
#225080=CARTESIAN_POINT('Ctrl Pts',(-245.543236141431,3.1935719265564,125.949144067427));
#225081=CARTESIAN_POINT('Ctrl Pts',(-245.821683765243,-2.35862755687492,
125.49315496849));
#225082=CARTESIAN_POINT('Ctrl Pts',(-246.100131389057,-5.74336354089951,
129.917904394232));
#225083=CARTESIAN_POINT('Ctrl Pts',(-246.378579012869,-3.85022900974501,
135.157263783424));
#225084=CARTESIAN_POINT('Ctrl Pts',(-246.657026636682,1.58107788722132,
136.396517814333));
#225085=CARTESIAN_POINT('Ctrl Pts',(-246.935474260495,5.55945144577998,
132.496852573479));
#225086=CARTESIAN_POINT('Ctrl Pts',(-247.213921884308,4.42896071996899,
127.04186990797));
#225087=CARTESIAN_POINT('Ctrl Pts',(-247.492369508121,-0.77152854073377,
125.044432396689));
#225088=CARTESIAN_POINT('Ctrl Pts',(-247.770817131934,-5.26302076376676,
128.340087532256));
#225089=CARTESIAN_POINT('Ctrl Pts',(-248.049264755747,-4.91805401775627,
133.90028924679));
#225090=CARTESIAN_POINT('Ctrl Pts',(-248.32771237956,-0.0536358897235281,
136.615483795589));
#225091=CARTESIAN_POINT('Ctrl Pts',(-248.606160003372,4.86007100070672,
133.990540032933));
#225092=CARTESIAN_POINT('Ctrl Pts',(-248.884607627186,5.30761006915461,
128.437653041073));
#225093=CARTESIAN_POINT('Ctrl Pts',(-249.163055250998,0.877714775216597,
125.059654691916));
#225094=CARTESIAN_POINT('Ctrl Pts',(-249.441502874812,-4.35875751839529,
126.960760443945));
#225095=CARTESIAN_POINT('Ctrl Pts',(-249.719950498624,-5.58974458974414,
132.393946985223));
#225096=CARTESIAN_POINT('Ctrl Pts',(-249.998398122437,-1.68402945732324,
136.366381310236));
#225097=CARTESIAN_POINT('Ctrl Pts',(-250.27684574625,3.76922647696617,135.227590338499));
#225098=CARTESIAN_POINT('Ctrl Pts',(-250.555293370063,5.75874741587205,
130.024067340013));
#225099=CARTESIAN_POINT('Ctrl Pts',(-250.833740993876,2.45626081004631,
125.537595744144));
#225100=CARTESIAN_POINT('Ctrl Pts',(-251.112188617689,-3.10340948520656,
125.891023771197));
#225101=CARTESIAN_POINT('Ctrl Pts',(-251.390636241501,-5.81119807352532,
130.759568330183));
#225102=CARTESIAN_POINT('Ctrl Pts',(-251.669083865314,-3.17877952510356,
135.669274813107));
#225103=CARTESIAN_POINT('Ctrl Pts',(-251.947531489127,2.37478211491517,
136.10836281449));
#225104=CARTESIAN_POINT('Ctrl Pts',(-252.22597911294,5.74603500580729,131.673331912019));
#225105=CARTESIAN_POINT('Ctrl Pts',(-252.504426736753,3.83696243592119,
126.439758841162));
#225106=CARTESIAN_POINT('Ctrl Pts',(-252.782874360566,-1.59809116681098,
125.217041580908));
#225107=CARTESIAN_POINT('Ctrl Pts',(-253.061321984379,-5.5645770578269,
129.128797558239));
#225108=CARTESIAN_POINT('Ctrl Pts',(-253.339769608192,-4.41748847836656,
134.580314133917));
#225109=CARTESIAN_POINT('Ctrl Pts',(-253.618217232004,0.789056208225191,
136.561913888683));
#225110=CARTESIAN_POINT('Ctrl Pts',(-253.896664855818,5.27049678355612,
133.252603468789));
#225111=CARTESIAN_POINT('Ctrl Pts',(-254.17511247963,4.90860829937749,127.693477454216));
#225112=CARTESIAN_POINT('Ctrl Pts',(-254.453560103444,0.0359485746511809,
124.993101125124));
#225113=CARTESIAN_POINT('Ctrl Pts',(-254.732007727256,-4.86974611083267,
127.632988310607));
#225114=CARTESIAN_POINT('Ctrl Pts',(-255.010455351069,-5.30038206451776,
133.187211835313));
#225115=CARTESIAN_POINT('Ctrl Pts',(-255.288902974882,-0.860225756393269,
136.55171127444));
#225116=CARTESIAN_POINT('Ctrl Pts',(-255.567350598695,4.37043584157037,
134.634676658854));
#225117=CARTESIAN_POINT('Ctrl Pts',(-255.845798222508,5.58488070320316,
129.197767919676));
#225118=CARTESIAN_POINT('Ctrl Pts',(-256.12424584632,1.66709247927321,125.23724089965));
#225119=CARTESIAN_POINT('Ctrl Pts',(-256.402693470134,-3.78267124144458,
126.39262206856));
#225120=CARTESIAN_POINT('Ctrl Pts',(-256.681141093946,-5.75634686702621,
131.602180844355));
#225121=CARTESIAN_POINT('Ctrl Pts',(-256.95958871776,-2.44021719259262,
136.078571600242));
#225122=CARTESIAN_POINT('Ctrl Pts',(-257.238036341572,3.118345804191,135.708239395799));
#225123=CARTESIAN_POINT('Ctrl Pts',(-257.516483965385,5.81131468939531,
130.8314457702));
#225124=CARTESIAN_POINT('Ctrl Pts',(-257.794931589198,3.16394407961038,
125.929830927563));
#225125=CARTESIAN_POINT('Ctrl Pts',(-258.073379213011,-2.39088900078744,
125.507540987923));
#225126=CARTESIAN_POINT('Ctrl Pts',(-258.351826836824,-5.74870171518396,
129.953014515613));
#225127=CARTESIAN_POINT('Ctrl Pts',(-258.630274460636,-3.82356878618261,
135.180370918811));
#225128=CARTESIAN_POINT('Ctrl Pts',(-258.908722084449,1.61491681105698,
136.387261181902));
#225129=CARTESIAN_POINT('Ctrl Pts',(-259.187169708263,5.56997747689423,
132.462088635074));
#225130=CARTESIAN_POINT('Ctrl Pts',(-259.465617332075,4.40535894966821,
127.016664495574));
#225131=CARTESIAN_POINT('Ctrl Pts',(-259.744064955888,-0.805411631290512,
125.046024618449));
#225132=CARTESIAN_POINT('Ctrl Pts',(-260.022512579701,-5.28013240410161,
128.378470706602));
#225133=CARTESIAN_POINT('Ctrl Pts',(-260.254552266212,-4.95911089365773,
132.993351965875));
#225134=CARTESIAN_POINT('Ctrl Pts',(-260.440213228287,-2.45877638613931,
135.28779596926));
#225135=CARTESIAN_POINT('Ctrl Pts',(-260.53305831576,-0.833059752290926,
135.715219187214));
#225136=CARTESIAN_POINT('Ctrl Pts',(-260.579495465929,-0.013892627260139,
135.717527172907));
#225137=CARTESIAN_POINT('',(177.785583446829,-5.06713383344665,133.858953737923));
#225138=CARTESIAN_POINT('',(177.476367722506,-5.12057379406247,130.804360617566));
#225139=CARTESIAN_POINT('Ctrl Pts',(177.783358963677,-5.06757454116058,
133.84805929277));
#225140=CARTESIAN_POINT('Ctrl Pts',(177.741301979325,-5.0865756231635,133.64169093706));
#225141=CARTESIAN_POINT('Ctrl Pts',(177.703514081134,-5.10373431764903,
133.434432378098));
#225142=CARTESIAN_POINT('Ctrl Pts',(177.627192311405,-5.13661944562339,
132.960177896229));
#225143=CARTESIAN_POINT('Ctrl Pts',(177.591437451862,-5.1506006863121,132.693106637366));
#225144=CARTESIAN_POINT('Ctrl Pts',(177.518755771383,-5.17068200829881,
132.013332647003));
#225145=CARTESIAN_POINT('Ctrl Pts',(177.491556503003,-5.1685893640333,131.600259531465));
#225146=CARTESIAN_POINT('Ctrl Pts',(177.477967247678,-5.13994992058266,
131.059495215027));
#225147=CARTESIAN_POINT('Ctrl Pts',(177.476367722506,-5.13129070204266,
130.931828234693));
#225148=CARTESIAN_POINT('Ctrl Pts',(177.476367722506,-5.12057379406246,
130.804360617566));
#225149=CARTESIAN_POINT('',(177.936624807795,-5.91674751037323,130.798932819469));
#225150=CARTESIAN_POINT('Ctrl Pts',(177.785647847033,-5.06709630945435,
133.859269053708));
#225151=CARTESIAN_POINT('Ctrl Pts',(177.79294899737,-5.14728668343649,133.72625938859));
#225152=CARTESIAN_POINT('Ctrl Pts',(177.800250147706,-5.22230291617104,
133.589979284485));
#225153=CARTESIAN_POINT('Ctrl Pts',(177.807551298043,-5.29186881662205,
133.450878138793));
#225154=CARTESIAN_POINT('Ctrl Pts',(177.814849277387,-5.36140450361573,
133.311837406702));
#225155=CARTESIAN_POINT('Ctrl Pts',(177.82214725673,-5.42549439663099,133.169978413749));
#225156=CARTESIAN_POINT('Ctrl Pts',(177.829445236074,-5.48390773829624,
133.025776040299));
#225157=CARTESIAN_POINT('Ctrl Pts',(177.836741578552,-5.5423079784222,132.881606010025));
#225158=CARTESIAN_POINT('Ctrl Pts',(177.844037921031,-5.59503405761397,
132.735094001483));
#225159=CARTESIAN_POINT('Ctrl Pts',(177.851334263509,-5.64190307126974,
132.586735521142));
#225160=CARTESIAN_POINT('Ctrl Pts',(177.858632982365,-5.68878734989527,
132.438328721292));
#225161=CARTESIAN_POINT('Ctrl Pts',(177.86593170122,-5.72981062989802,132.288074613004));
#225162=CARTESIAN_POINT('Ctrl Pts',(177.873230420075,-5.76483961792187,
132.136484764235));
#225163=CARTESIAN_POINT('Ctrl Pts',(177.880530161697,-5.79987351453996,
131.984873673257));
#225164=CARTESIAN_POINT('Ctrl Pts',(177.887829903318,-5.82891136813785,
131.831926845543));
#225165=CARTESIAN_POINT('Ctrl Pts',(177.895129644939,-5.85187103627661,
131.678166052023));
#225166=CARTESIAN_POINT('Ctrl Pts',(177.902435936344,-5.87485130526188,
131.524267294728));
#225167=CARTESIAN_POINT('Ctrl Pts',(177.909742227748,-5.89174244466227,
131.369553494223));
#225168=CARTESIAN_POINT('Ctrl Pts',(177.917048519153,-5.90251416797608,
131.21455210863));
#225169=CARTESIAN_POINT('Ctrl Pts',(177.9235739487,-5.91213466046586,131.076116537779));
#225170=CARTESIAN_POINT('Ctrl Pts',(177.930099378248,-5.9168745824033,130.937451810787));
#225171=CARTESIAN_POINT('Ctrl Pts',(177.936624807795,-5.91674751037323,
130.798932819469));
#225172=CARTESIAN_POINT('',(178.183682610571,-3.73058779372404,126.219102738339));
#225173=CARTESIAN_POINT('Ctrl Pts',(177.936624807795,-5.91746116842021,
130.798932164786));
#225174=CARTESIAN_POINT('Ctrl Pts',(177.957120624423,-5.9215064818599,130.363799294495));
#225175=CARTESIAN_POINT('Ctrl Pts',(178.039473225349,-5.74509580593375,
128.618678131439));
#225176=CARTESIAN_POINT('Ctrl Pts',(178.121825826274,-4.74534417957617,
127.058332616678));
#225177=CARTESIAN_POINT('Ctrl Pts',(178.183682610571,-3.73058779372456,
126.219102738339));
#225178=CARTESIAN_POINT('Ctrl Pts',(177.476367722506,-5.12057379406248,
130.804360617566));
#225179=CARTESIAN_POINT('Ctrl Pts',(177.476367722506,-5.10013257136415,
130.561231353665));
#225180=CARTESIAN_POINT('Ctrl Pts',(177.482192124778,-5.07221048657026,
130.318826954245));
#225181=CARTESIAN_POINT('Ctrl Pts',(177.495566578132,-5.02964518562034,
130.038571223779));
#225182=CARTESIAN_POINT('Ctrl Pts',(177.497588701151,-5.0234574971161,129.999383302672));
#225183=CARTESIAN_POINT('Ctrl Pts',(177.499824837013,-5.01684285690672,
129.959067960444));
#225184=CARTESIAN_POINT('Ctrl Pts',(177.499890045632,-5.01665015058729,
129.957894766361));
#225185=CARTESIAN_POINT('Ctrl Pts',(177.499971960186,-5.01640830578995,
129.956424078135));
#225186=CARTESIAN_POINT('Ctrl Pts',(177.499988541006,-5.01635936437147,
129.956126544398));
#225187=CARTESIAN_POINT('Ctrl Pts',(177.500014499698,-5.01628276091504,
129.95566097563));
#225188=CARTESIAN_POINT('Ctrl Pts',(177.500023871669,-5.01625510823518,
129.955492939538));
#225189=CARTESIAN_POINT('Ctrl Pts',(177.500041185287,-5.0162040301161,129.955182604992));
#225190=CARTESIAN_POINT('Ctrl Pts',(177.500049126247,-5.01618060563769,
129.955040304703));
#225191=CARTESIAN_POINT('Ctrl Pts',(177.500066566138,-5.01612916686506,
129.954727864379));
#225192=CARTESIAN_POINT('Ctrl Pts',(177.500076065797,-5.01610115158613,
129.95455772672));
#225193=CARTESIAN_POINT('Ctrl Pts',(177.500102731179,-5.01602252400973,
129.954080297032));
#225194=CARTESIAN_POINT('Ctrl Pts',(177.500119903333,-5.01597190148107,
129.953773005773));
#225195=CARTESIAN_POINT('Ctrl Pts',(177.500219182879,-5.01567930376682,
129.951997389358));
#225196=CARTESIAN_POINT('Ctrl Pts',(177.500301490531,-5.01543701294836,
129.950529128138));
#225197=CARTESIAN_POINT('Ctrl Pts',(177.500536651928,-5.01474557825448,
129.946344990489));
#225198=CARTESIAN_POINT('Ctrl Pts',(177.500690012856,-5.01429563401943,
129.94362927491));
#225199=CARTESIAN_POINT('Ctrl Pts',(177.501483934731,-5.01197134589284,
129.929637033759));
#225200=CARTESIAN_POINT('Ctrl Pts',(177.502136129423,-5.0100786087708,129.918364247601));
#225201=CARTESIAN_POINT('Ctrl Pts',(177.507494427648,-4.99465822545836,
129.82749951209));
#225202=CARTESIAN_POINT('Ctrl Pts',(177.512808699789,-4.98015314808467,
129.748006760148));
#225203=CARTESIAN_POINT('Ctrl Pts',(177.536252366813,-4.91867001249372,
129.434266685906));
#225204=CARTESIAN_POINT('Ctrl Pts',(177.559035115434,-4.86392156822592,
129.202282649367));
#225205=CARTESIAN_POINT('Ctrl Pts',(177.641117942126,-4.68015889981346,
128.524160057609));
#225206=CARTESIAN_POINT('Ctrl Pts',(177.714428393931,-4.53033676743336,
128.085641009048));
#225207=CARTESIAN_POINT('Ctrl Pts',(177.860352889966,-4.2591342270638,127.393966784111));
#225208=CARTESIAN_POINT('Ctrl Pts',(177.922457124534,-4.14884818442793,
127.134214134108));
#225209=CARTESIAN_POINT('Ctrl Pts',(178.050554224604,-3.93347667359594,
126.653734659887));
#225210=CARTESIAN_POINT('Ctrl Pts',(178.114950700917,-3.82966817966767,
126.432690898171));
#225211=CARTESIAN_POINT('Ctrl Pts',(178.184070351179,-3.72422348156493,
126.213846503759));
#225212=CARTESIAN_POINT('Origin',(210.,0.,130.804360617566));
#225213=CARTESIAN_POINT('',(178.655995448006,0.643991232007665,124.924876168436));
#225214=CARTESIAN_POINT('Ctrl Pts',(178.656596669642,0.650137269913459,
124.923437892962));
#225215=CARTESIAN_POINT('Ctrl Pts',(178.631192637209,1.19960075686107,124.98418119942));
#225216=CARTESIAN_POINT('Ctrl Pts',(178.571783995707,1.75472463999775,125.12573841184));
#225217=CARTESIAN_POINT('Ctrl Pts',(178.487391008075,2.2825507450488,125.345610175187));
#225218=CARTESIAN_POINT('Ctrl Pts',(178.486208584818,2.28991117210278,125.34869374146));
#225219=CARTESIAN_POINT('Ctrl Pts',(178.485021693585,2.29726490846875,125.351792002425));
#225220=CARTESIAN_POINT('',(179.938376004444,-5.92191450869858,130.805748116515));
#225221=CARTESIAN_POINT('Ctrl Pts',(179.938375192211,-5.91674983355068,
130.805764069745));
#225222=CARTESIAN_POINT('Ctrl Pts',(179.934802337543,-5.91673193815412,
130.881208453364));
#225223=CARTESIAN_POINT('Ctrl Pts',(179.931229482876,-5.91527111751309,
130.956633994371));
#225224=CARTESIAN_POINT('Ctrl Pts',(179.927656628208,-5.91236916926149,
131.032003690964));
#225225=CARTESIAN_POINT('Ctrl Pts',(179.920233361803,-5.90633983502618,
131.18859817597));
#225226=CARTESIAN_POINT('Ctrl Pts',(179.912810095397,-5.89407576518302,
131.345189745836));
#225227=CARTESIAN_POINT('Ctrl Pts',(179.905386828992,-5.87556700792397,
131.501241452354));
#225228=CARTESIAN_POINT('Ctrl Pts',(179.897972336271,-5.85708012647892,
131.657108718716));
#225229=CARTESIAN_POINT('Ctrl Pts',(179.89055784355,-5.83236329248394,131.81243702474));
#225230=CARTESIAN_POINT('Ctrl Pts',(179.883143350829,-5.80145853932096,
131.966689907845));
#225231=CARTESIAN_POINT('Ctrl Pts',(179.875736004475,-5.77058357332259,
132.120794116214));
#225232=CARTESIAN_POINT('Ctrl Pts',(179.868328658121,-5.73353263444466,
132.27382460163));
#225233=CARTESIAN_POINT('Ctrl Pts',(179.860921311767,-5.69039947340868,
132.425250618624));
#225234=CARTESIAN_POINT('Ctrl Pts',(179.853519490092,-5.64729848271151,
132.576563696382));
#225235=CARTESIAN_POINT('Ctrl Pts',(179.846117668417,-5.59812440416739,
132.726274330983));
#225236=CARTESIAN_POINT('Ctrl Pts',(179.838715846741,-5.54302190257774,
132.873862671212));
#225237=CARTESIAN_POINT('Ctrl Pts',(179.83131793243,-5.48794848916994,133.021373100704));
#225238=CARTESIAN_POINT('Ctrl Pts',(179.823920018118,-5.42695301563993,
133.166763118208));
#225239=CARTESIAN_POINT('Ctrl Pts',(179.816522103807,-5.3602297308131,133.309528834554));
#225240=CARTESIAN_POINT('Ctrl Pts',(179.809125418895,-5.2935175341856,133.452270825829));
#225241=CARTESIAN_POINT('Ctrl Pts',(179.801728733983,-5.22107957331895,
133.592389043643));
#225242=CARTESIAN_POINT('Ctrl Pts',(179.79433204907,-5.1431579462292,133.729400258774));
#225243=CARTESIAN_POINT('Ctrl Pts',(179.786935692135,-5.06523977426604,
133.866405398685));
#225244=CARTESIAN_POINT('Ctrl Pts',(179.779539335199,-4.98183860409271,
134.000303485351));
#225245=CARTESIAN_POINT('Ctrl Pts',(179.772142978264,-4.89324200758084,
134.13063679638));
#225246=CARTESIAN_POINT('Ctrl Pts',(179.764745488927,-4.80463184670375,
134.260990061772));
#225247=CARTESIAN_POINT('Ctrl Pts',(179.757347999591,-4.71082488554907,
134.387777156069));
#225248=CARTESIAN_POINT('Ctrl Pts',(179.749950510254,-4.61215135748797,
134.510570328055));
#225249=CARTESIAN_POINT('Ctrl Pts',(179.742550427739,-4.51344323957483,
134.633406544996));
#225250=CARTESIAN_POINT('Ctrl Pts',(179.735150345224,-4.4098653918718,134.752245761303));
#225251=CARTESIAN_POINT('Ctrl Pts',(179.727750262709,-4.30178744852212,
134.866694344654));
#225252=CARTESIAN_POINT('Ctrl Pts',(179.720342043042,-4.19359066236287,
134.981268775988));
#225253=CARTESIAN_POINT('Ctrl Pts',(179.712933823376,-4.08088415489833,
135.091442661055));
#225254=CARTESIAN_POINT('Ctrl Pts',(179.70552560371,-3.96407396764172,135.19685969458));
#225255=CARTESIAN_POINT('Ctrl Pts',(179.698112824407,-3.84719188566385,
135.30234161053));
#225256=CARTESIAN_POINT('Ctrl Pts',(179.690700045105,-3.72620137726176,
135.403060602727));
#225257=CARTESIAN_POINT('Ctrl Pts',(179.683287265803,-3.60154006095042,
135.49870186548));
#225258=CARTESIAN_POINT('Ctrl Pts',(179.675863894774,-3.47670062270434,
135.594479784955));
#225259=CARTESIAN_POINT('Ctrl Pts',(179.668440523746,-3.34818020526591,
135.685165269879));
#225260=CARTESIAN_POINT('Ctrl Pts',(179.661017152717,-3.21644446134536,
135.77048743729));
#225261=CARTESIAN_POINT('Ctrl Pts',(179.657081103276,-3.14659500896289,
135.815727297728));
#225262=CARTESIAN_POINT('Ctrl Pts',(179.653145053835,-3.07584201855703,
135.859460108231));
#225263=CARTESIAN_POINT('Ctrl Pts',(179.649209004394,-3.00425738879533,
135.901650888324));
#225264=CARTESIAN_POINT('Ctrl Pts',(179.641785737989,-2.86925101114459,
135.981221382851));
#225265=CARTESIAN_POINT('Ctrl Pts',(179.634362471584,-2.73087705919654,
136.05554484203));
#225266=CARTESIAN_POINT('Ctrl Pts',(179.626939205178,-2.58958190348824,
136.124322659501));
#225267=CARTESIAN_POINT('Ctrl Pts',(179.619524712457,-2.44845374692,136.193019187303));
#225268=CARTESIAN_POINT('Ctrl Pts',(179.612110219736,-2.30441159141906,
136.256182958357));
#225269=CARTESIAN_POINT('Ctrl Pts',(179.604695727015,-2.15792949821889,
136.313559365407));
#225270=CARTESIAN_POINT('Ctrl Pts',(179.597288380661,-2.01158858997503,
136.370880470916));
#225271=CARTESIAN_POINT('Ctrl Pts',(179.589881034308,-1.86281277106264,
136.422425182046));
#225272=CARTESIAN_POINT('Ctrl Pts',(179.582473687954,-1.71209924723198,
136.467985493044));
#225273=CARTESIAN_POINT('Ctrl Pts',(179.575071866278,-1.5614981312336,136.513511823442));
#225274=CARTESIAN_POINT('Ctrl Pts',(179.567670044603,-1.40896254372182,
136.553062533368));
#225275=CARTESIAN_POINT('Ctrl Pts',(179.560268222928,-1.25500804510559,
136.586478341136));
#225276=CARTESIAN_POINT('Ctrl Pts',(179.552870308616,-1.10113481787052,
136.619876508959));
#225277=CARTESIAN_POINT('Ctrl Pts',(179.545472394305,-0.945844535144645,
136.647146145406));
#225278=CARTESIAN_POINT('Ctrl Pts',(179.538074479993,-0.789666129390942,
136.668178313112));
#225279=CARTESIAN_POINT('Ctrl Pts',(179.530677795081,-0.633513677655301,
136.689206985652));
#225280=CARTESIAN_POINT('Ctrl Pts',(179.523281110169,-0.476473765410261,
136.704000196932));
#225281=CARTESIAN_POINT('Ctrl Pts',(179.515884425257,-0.319083806977362,
136.712500433669));
#225282=CARTESIAN_POINT('Ctrl Pts',(179.508488068321,-0.161700827380124,
136.721000293498));
#225283=CARTESIAN_POINT('Ctrl Pts',(179.501091711386,-0.0039682052111765,
136.723207713473));
#225284=CARTESIAN_POINT('Ctrl Pts',(179.493695354451,0.153573525095219,
136.71911722582));
#225285=CARTESIAN_POINT('Ctrl Pts',(179.486297865114,0.311139375442765,
136.715026111904));
#225286=CARTESIAN_POINT('Ctrl Pts',(179.478900375777,0.468513902538733,
136.704635180148));
#225287=CARTESIAN_POINT('Ctrl Pts',(179.471502886441,0.625158727965406,
136.687991055259));
#225288=CARTESIAN_POINT('Ctrl Pts',(179.464102803926,0.781858464992578,
136.671341095798));
#225289=CARTESIAN_POINT('Ctrl Pts',(179.456702721411,0.937827620086148,
136.648433618271));
#225290=CARTESIAN_POINT('Ctrl Pts',(179.449302638896,1.09253522294258,136.619366838468));
#225291=CARTESIAN_POINT('Ctrl Pts',(179.44189441923,1.24741294271294,136.590268096752));
#225292=CARTESIAN_POINT('Ctrl Pts',(179.434486199563,1.40102597280012,136.554996596033));
#225293=CARTESIAN_POINT('Ctrl Pts',(179.427077979897,1.55285506812971,136.513701358832));
#225294=CARTESIAN_POINT('Ctrl Pts',(179.419665200595,1.70477761173422,136.472380705102));
#225295=CARTESIAN_POINT('Ctrl Pts',(179.412252421292,1.85491367752859,136.425029039235));
#225296=CARTESIAN_POINT('Ctrl Pts',(179.40483964199,2.0027618670726,136.371844381916));
#225297=CARTESIAN_POINT('Ctrl Pts',(179.397416270962,2.15082130904315,136.318583731865));
#225298=CARTESIAN_POINT('Ctrl Pts',(179.389992899933,2.29658600076753,136.259473584504));
#225299=CARTESIAN_POINT('Ctrl Pts',(179.382569528904,2.43957634407283,136.194759287789));
#225300=CARTESIAN_POINT('Ctrl Pts',(179.378633479463,2.51539325509978,136.160446214872));
#225301=CARTESIAN_POINT('Ctrl Pts',(179.374697430023,2.59043062670582,136.124558372525));
#225302=CARTESIAN_POINT('Ctrl Pts',(179.370761380582,2.66462016584161,136.087137343332));
#225303=CARTESIAN_POINT('Ctrl Pts',(179.363338114176,2.80453932127499,136.016562450144));
#225304=CARTESIAN_POINT('Ctrl Pts',(179.355914847771,2.94186425343108,135.940318170553));
#225305=CARTESIAN_POINT('Ctrl Pts',(179.348491581365,3.07610246214482,135.858618644704));
#225306=CARTESIAN_POINT('Ctrl Pts',(179.341077088644,3.21018201244378,135.777015680909));
#225307=CARTESIAN_POINT('Ctrl Pts',(179.333662595923,3.3411817853958,135.689970497116));
#225308=CARTESIAN_POINT('Ctrl Pts',(179.326248103202,3.46863133103027,135.597744313025));
#225309=CARTESIAN_POINT('Ctrl Pts',(179.318840756849,3.59595803599425,135.505607020003));
#225310=CARTESIAN_POINT('Ctrl Pts',(179.311433410495,3.71974102546335,135.408298885418));
#225311=CARTESIAN_POINT('Ctrl Pts',(179.304026064141,3.83953654645319,135.306125790357));
#225312=CARTESIAN_POINT('Ctrl Pts',(179.296624242466,3.95924271942392,135.204028899845));
#225313=CARTESIAN_POINT('Ctrl Pts',(179.28922242079,4.07496706275787,135.097074514833));
#225314=CARTESIAN_POINT('Ctrl Pts',(179.281820599115,4.18629689526787,134.985610295255));
#225315=CARTESIAN_POINT('Ctrl Pts',(179.274422684804,4.29756795762586,134.87420491677));
#225316=CARTESIAN_POINT('Ctrl Pts',(179.267024770492,4.40444886607418,134.758294708461));
#225317=CARTESIAN_POINT('Ctrl Pts',(179.259626856181,4.50656206760595,134.638265792882));
#225318=CARTESIAN_POINT('Ctrl Pts',(179.252230171269,4.6086582997761,134.518256823932));
#225319=CARTESIAN_POINT('Ctrl Pts',(179.244833486356,4.70598815587262,134.394130790199));
#225320=CARTESIAN_POINT('Ctrl Pts',(179.237436801444,4.79821276277581,134.266308746241));
#225321=CARTESIAN_POINT('Ctrl Pts',(179.230040444509,4.89043328034328,134.138492370046));
#225322=CARTESIAN_POINT('Ctrl Pts',(179.222644087573,4.97754878040159,134.006980612211));
#225323=CARTESIAN_POINT('Ctrl Pts',(179.215247730638,5.05926249069234,133.872225284199));
#225324=CARTESIAN_POINT('Ctrl Pts',(179.207850241301,5.14098871156078,133.737449324802));
#225325=CARTESIAN_POINT('Ctrl Pts',(179.200452751965,5.21731130237002,133.599429125651));
#225326=CARTESIAN_POINT('Ctrl Pts',(179.193055262628,5.28797848312044,133.45864284155));
#225327=CARTESIAN_POINT('Ctrl Pts',(179.185655180113,5.3586704361415,133.317807205035));
#225328=CARTESIAN_POINT('Ctrl Pts',(179.178255097598,5.42370286461153,133.174203886429));
#225329=CARTESIAN_POINT('Ctrl Pts',(179.170855015083,5.4828713978363,133.028332694119));
#225330=CARTESIAN_POINT('Ctrl Pts',(179.163446795416,5.54210499294605,132.882301101438));
#225331=CARTESIAN_POINT('Ctrl Pts',(179.15603857575,5.59546167541947,132.733997000985));
#225332=CARTESIAN_POINT('Ctrl Pts',(179.148630356084,5.64278615747782,132.583937798662));
#225333=CARTESIAN_POINT('Ctrl Pts',(179.141217576781,5.69013976696525,132.433786237403));
#225334=CARTESIAN_POINT('Ctrl Pts',(179.133804797479,5.73145368024142,132.281877781146));
#225335=CARTESIAN_POINT('Ctrl Pts',(179.126392018177,5.76662347961273,132.128741305616));
#225336=CARTESIAN_POINT('Ctrl Pts',(179.118968647149,5.80184353124267,131.975386021508));
#225337=CARTESIAN_POINT('Ctrl Pts',(179.11154527612,5.83090186655938,131.820799579596));
#225338=CARTESIAN_POINT('Ctrl Pts',(179.104121905091,5.85374566921849,131.665518095967));
#225339=CARTESIAN_POINT('Ctrl Pts',(179.10018585565,5.86585800151788,131.583184127419));
#225340=CARTESIAN_POINT('Ctrl Pts',(179.096249806209,5.87622407559727,131.50065480612));
#225341=CARTESIAN_POINT('Ctrl Pts',(179.092313756769,5.88484196200156,131.41801006535));
#225342=CARTESIAN_POINT('Ctrl Pts',(179.084890490363,5.90109502680501,131.262144663512));
#225343=CARTESIAN_POINT('Ctrl Pts',(179.077467223958,5.91117603521354,131.105397413357));
#225344=CARTESIAN_POINT('Ctrl Pts',(179.070043957552,5.91499894102585,130.948298417199));
#225345=CARTESIAN_POINT('Ctrl Pts',(179.062629464831,5.91881732848096,130.791385099008));
#225346=CARTESIAN_POINT('Ctrl Pts',(179.05521497211,5.91639232723587,130.63412123188));
#225347=CARTESIAN_POINT('Ctrl Pts',(179.047800479389,5.90768941912305,130.477043814329));
#225348=CARTESIAN_POINT('Ctrl Pts',(179.040393133036,5.89899489920073,130.320117793906));
#225349=CARTESIAN_POINT('Ctrl Pts',(179.032985786682,5.88403453903981,130.163378235523));
#225350=CARTESIAN_POINT('Ctrl Pts',(179.025578440328,5.8628258257359,130.007363817331));
#225351=CARTESIAN_POINT('Ctrl Pts',(179.018176618653,5.84163293069053,129.851465760579));
#225352=CARTESIAN_POINT('Ctrl Pts',(179.010774796977,5.81420101177123,129.696292135444));
#225353=CARTESIAN_POINT('Ctrl Pts',(179.003372975302,5.78059950086301,129.542378060982));
#225354=CARTESIAN_POINT('Ctrl Pts',(178.99597506099,5.74701572793086,129.388545236562));
#225355=CARTESIAN_POINT('Ctrl Pts',(178.988577146679,5.70726892866063,129.235971002404));
#225356=CARTESIAN_POINT('Ctrl Pts',(178.981179232368,5.66147988227038,129.08518171322));
#225357=CARTESIAN_POINT('Ctrl Pts',(178.973782547456,5.61569844518896,128.93441748248));
#225358=CARTESIAN_POINT('Ctrl Pts',(178.966385862543,5.56387686221214,128.785437964842));
#225359=CARTESIAN_POINT('Ctrl Pts',(178.958989177631,5.5061862092642,128.638755854132));
#225360=CARTESIAN_POINT('Ctrl Pts',(178.951592820696,5.44849811438028,128.49208024746));
#225361=CARTESIAN_POINT('Ctrl Pts',(178.94419646376,5.38494160360329,128.347702192559));
#225362=CARTESIAN_POINT('Ctrl Pts',(178.936800106825,5.31573638605803,128.206115587466));
#225363=CARTESIAN_POINT('Ctrl Pts',(178.929402617488,5.24652057301731,128.064507305103));
#225364=CARTESIAN_POINT('Ctrl Pts',(178.922005128152,5.17165449515218,127.925691658915));
#225365=CARTESIAN_POINT('Ctrl Pts',(178.914607638815,5.09140434440064,127.790138932899));
#225366=CARTESIAN_POINT('Ctrl Pts',(178.9072075563,5.01112606208312,127.654538689084));
#225367=CARTESIAN_POINT('Ctrl Pts',(178.899807473785,4.9254601391764,127.522203963786));
#225368=CARTESIAN_POINT('Ctrl Pts',(178.89240739127,4.8347166112795,127.393576858499));
#225369=CARTESIAN_POINT('Ctrl Pts',(178.884999171604,4.743873301545,127.264808314486));
#225370=CARTESIAN_POINT('Ctrl Pts',(178.877590951937,4.64794145183068,127.139755837558));
#225371=CARTESIAN_POINT('Ctrl Pts',(178.870182732271,4.54727243353588,127.018829746248));
#225372=CARTESIAN_POINT('Ctrl Pts',(178.862769952969,4.44654145513995,126.897829226946));
#225373=CARTESIAN_POINT('Ctrl Pts',(178.855357173667,4.34106774789423,126.780960430458));
#225374=CARTESIAN_POINT('Ctrl Pts',(178.847944394365,4.23123982961107,126.668597076596));
#225375=CARTESIAN_POINT('Ctrl Pts',(178.840521023336,4.12125498404791,126.556073172705));
#225376=CARTESIAN_POINT('Ctrl Pts',(178.833097652307,4.00690377237975,126.448067824391));
#225377=CARTESIAN_POINT('Ctrl Pts',(178.825674281278,3.88860869573101,126.344915251381));
#225378=CARTESIAN_POINT('Ctrl Pts',(178.821738231838,3.82588580763872,126.290221282058));
#225379=CARTESIAN_POINT('Ctrl Pts',(178.817802182397,3.76205466852198,126.236890896299));
#225380=CARTESIAN_POINT('Ctrl Pts',(178.813866132956,3.69718148559496,126.184968923298));
#225381=CARTESIAN_POINT('Ctrl Pts',(178.806443476583,3.57484274165308,126.087053749827));
#225382=CARTESIAN_POINT('Ctrl Pts',(178.79902082021,3.448426597239,125.993853866056));
#225383=CARTESIAN_POINT('Ctrl Pts',(178.791598163837,3.31833243238178,125.905728111376));
#225384=CARTESIAN_POINT('Ctrl Pts',(178.784183856821,3.18838460363009,125.817701484737));
#225385=CARTESIAN_POINT('Ctrl Pts',(178.776769549805,3.05476729371877,125.734737835851));
#225386=CARTESIAN_POINT('Ctrl Pts',(178.769355242789,2.91791360112221,125.657156446476));
#225387=CARTESIAN_POINT('Ctrl Pts',(178.76194781101,2.78118681203899,125.579646997804));
#225388=CARTESIAN_POINT('Ctrl Pts',(178.754540379231,2.641229936335,125.507510057233));
#225389=CARTESIAN_POINT('Ctrl Pts',(178.747132947452,2.49850564450236,125.44102209507));
#225390=CARTESIAN_POINT('Ctrl Pts',(178.739588257635,2.35313670375903,125.373302125976));
#225391=CARTESIAN_POINT('Ctrl Pts',(178.732043567817,2.20489709196751,125.311442779602));
#225392=CARTESIAN_POINT('Ctrl Pts',(178.724498878,2.05430357548496,125.255688039169));
#225393=CARTESIAN_POINT('Ctrl Pts',(178.717100998755,1.90664042737168,125.201018218802));
#225394=CARTESIAN_POINT('Ctrl Pts',(178.70970311951,1.7567145097062,125.152217743023));
#225395=CARTESIAN_POINT('Ctrl Pts',(178.702305240265,1.60503429277867,125.109468565779));
#225396=CARTESIAN_POINT('Ctrl Pts',(178.694687145161,1.44883894547903,125.065446855357));
#225397=CARTESIAN_POINT('Ctrl Pts',(178.687069050057,1.29078361105623,125.027842463903));
#225398=CARTESIAN_POINT('Ctrl Pts',(178.679450954953,1.13144104857084,124.996799019433));
#225399=CARTESIAN_POINT('Ctrl Pts',(178.67183285985,0.972098486085417,124.965755574963));
#225400=CARTESIAN_POINT('Ctrl Pts',(178.664214764746,0.811469119563494,
124.94127316358));
#225401=CARTESIAN_POINT('Ctrl Pts',(178.656596669642,0.650137269913457,
124.923437892962));
#225402=CARTESIAN_POINT('',(181.688375192211,-5.9116597264178,130.809147953816));
#225403=CARTESIAN_POINT('Ctrl Pts',(181.688375192211,-5.9116597264178,130.809147953816));
#225404=CARTESIAN_POINT('Ctrl Pts',(181.658364251836,-5.91648848400863,
131.447879361033));
#225405=CARTESIAN_POINT('Ctrl Pts',(181.535537436858,-5.52634643860716,
134.05629721562));
#225406=CARTESIAN_POINT('Ctrl Pts',(181.31989474727,-1.71655817300176,137.588974723689));
#225407=CARTESIAN_POINT('Ctrl Pts',(181.041447123461,4.78024637596874,135.91579927174));
#225408=CARTESIAN_POINT('Ctrl Pts',(180.762999499646,6.88423803344246,129.54546140426));
#225409=CARTESIAN_POINT('Ctrl Pts',(180.484551875834,2.66195125190711,124.331990413167));
#225410=CARTESIAN_POINT('Ctrl Pts',(180.209677598402,-3.92096128402385,
125.056887831312));
#225411=CARTESIAN_POINT('Ctrl Pts',(180.027619195576,-5.92009025890988,
128.918301208267));
#225412=CARTESIAN_POINT('Ctrl Pts',(179.938376667353,-5.92612969673344,
130.805735096168));
#225413=CARTESIAN_POINT('',(183.438375192211,-5.90878783959383,130.801050019915));
#225414=CARTESIAN_POINT('Ctrl Pts',(183.438375192211,-5.90878783959383,
130.801050019915));
#225415=CARTESIAN_POINT('Ctrl Pts',(183.381926166128,-5.90269714734493,
132.003937776489));
#225416=CARTESIAN_POINT('Ctrl Pts',(183.232661265441,-4.96014564476939,
135.193432897632));
#225417=CARTESIAN_POINT('Ctrl Pts',(182.99058049015,0.258615936756311,137.79797758789));
#225418=CARTESIAN_POINT('Ctrl Pts',(182.712132866336,6.02371625752071,134.36700050664));
#225419=CARTESIAN_POINT('Ctrl Pts',(182.433685242524,6.2533156125226,127.662131411966));
#225420=CARTESIAN_POINT('Ctrl Pts',(182.155237618711,0.736423411067356,
123.844817450807));
#225421=CARTESIAN_POINT('Ctrl Pts',(181.906800935273,-4.78965977321783,
126.145110250613));
#225422=CARTESIAN_POINT('Ctrl Pts',(181.75118012644,-5.90155441818334,129.472452618097));
#225423=CARTESIAN_POINT('Ctrl Pts',(181.688375192211,-5.9116597264178,130.809147953816));
#225424=CARTESIAN_POINT('',(185.188375192211,-5.92379981193959,130.800775453898));
#225425=CARTESIAN_POINT('Ctrl Pts',(185.188375192211,-5.92379981193959,
130.800775453898));
#225426=CARTESIAN_POINT('Ctrl Pts',(185.105488080421,-5.9112852874943,132.555621405934));
#225427=CARTESIAN_POINT('Ctrl Pts',(184.929785094025,-4.15424292220225,
136.29728126716));
#225428=CARTESIAN_POINT('Ctrl Pts',(184.661266233027,2.21295931186131,137.443665672644));
#225429=CARTESIAN_POINT('Ctrl Pts',(184.382818609213,6.78199394032505,132.531241830544));
#225430=CARTESIAN_POINT('Ctrl Pts',(184.104370985402,5.11870745645332,126.031898516554));
#225431=CARTESIAN_POINT('Ctrl Pts',(183.825923361588,-1.24842111713792,
123.918214725658));
#225432=CARTESIAN_POINT('Ctrl Pts',(183.603924763859,-5.41009564609318,
127.278197857111));
#225433=CARTESIAN_POINT('Ctrl Pts',(183.474742040733,-5.91271172097454,
130.026098884935));
#225434=CARTESIAN_POINT('Ctrl Pts',(183.438375192211,-5.90878783959383,
130.801050019915));
#225435=CARTESIAN_POINT('',(186.938375192211,-5.91753456722523,130.809401790279));
#225436=CARTESIAN_POINT('Ctrl Pts',(186.938375192211,-5.9200304115163,130.809403916499));
#225437=CARTESIAN_POINT('Ctrl Pts',(186.921865869317,-5.92320279675294,
131.159511089235));
#225438=CARTESIAN_POINT('Ctrl Pts',(186.812540671824,-5.73530460751272,
133.474529816069));
#225439=CARTESIAN_POINT('Ctrl Pts',(186.610399599713,-2.68163859043372,
137.268598778454));
#225440=CARTESIAN_POINT('Ctrl Pts',(186.331951975907,3.98905548069682,136.554577735401));
#225441=CARTESIAN_POINT('Ctrl Pts',(186.05350435209,6.99400244126163,130.556388074787));
#225442=CARTESIAN_POINT('Ctrl Pts',(185.775056728279,3.57180283432081,124.78607306685));
#225443=CARTESIAN_POINT('Ctrl Pts',(185.496609104465,-3.13270908509169,
124.546270308331));
#225444=CARTESIAN_POINT('Ctrl Pts',(185.301048592443,-5.81959460894973,
128.416832856216));
#225445=CARTESIAN_POINT('Ctrl Pts',(185.198303955025,-5.92529888389735,
130.590568476525));
#225446=CARTESIAN_POINT('Ctrl Pts',(185.188375192211,-5.92379981193959,
130.800775453898));
#225447=CARTESIAN_POINT('',(188.688375158851,-5.91280930184219,130.805575254198));
#225448=CARTESIAN_POINT('Ctrl Pts',(188.688375135582,-5.9167498750567,130.805576560215));
#225449=CARTESIAN_POINT('Ctrl Pts',(188.680495520896,-5.916715288546,130.97387375165));
#225450=CARTESIAN_POINT('Ctrl Pts',(188.67261590621,-5.90949584186738,131.141986835927));
#225451=CARTESIAN_POINT('Ctrl Pts',(188.664736291524,-5.89516395080611,
131.309308689764));
#225452=CARTESIAN_POINT('Ctrl Pts',(188.656841930411,-5.88080523810475,
131.476943680682));
#225453=CARTESIAN_POINT('Ctrl Pts',(188.648947569298,-5.85930751799326,
131.643784192002));
#225454=CARTESIAN_POINT('Ctrl Pts',(188.641053208185,-5.83079446595158,
131.809231981636));
#225455=CARTESIAN_POINT('Ctrl Pts',(188.633135901846,-5.80219853976692,
131.975160650825));
#225456=CARTESIAN_POINT('Ctrl Pts',(188.625218595508,-5.76654654061531,
132.139688210389));
#225457=CARTESIAN_POINT('Ctrl Pts',(188.617301289169,-5.72401296888253,
132.30222779945));
#225458=CARTESIAN_POINT('Ctrl Pts',(188.609371641021,-5.68141309414261,
132.465020761625));
#225459=CARTESIAN_POINT('Ctrl Pts',(188.601441992874,-5.63191030844115,
132.625819284766));
#225460=CARTESIAN_POINT('Ctrl Pts',(188.593512344726,-5.5757279961427,132.784054501865));
#225461=CARTESIAN_POINT('Ctrl Pts',(188.585563505692,-5.51940971458834,
132.94267267089));
#225462=CARTESIAN_POINT('Ctrl Pts',(188.577614666658,-5.45637968482179,
133.098714854591));
#225463=CARTESIAN_POINT('Ctrl Pts',(188.569665827625,-5.38690907388433,
133.251632811704));
#225464=CARTESIAN_POINT('Ctrl Pts',(188.566288207219,-5.35738962430293,
133.316610704718));
#225465=CARTESIAN_POINT('Ctrl Pts',(188.562910586813,-5.32670783786975,
133.381024824207));
#225466=CARTESIAN_POINT('Ctrl Pts',(188.559532966408,-5.29488692684622,
133.444834626984));
#225467=CARTESIAN_POINT('Ctrl Pts',(188.552109700002,-5.22495156661437,
133.585074532128));
#225468=CARTESIAN_POINT('Ctrl Pts',(188.544686433597,-5.14933503520301,
133.722746124474));
#225469=CARTESIAN_POINT('Ctrl Pts',(188.537263167192,-5.06824922202705,
133.857355931339));
#225470=CARTESIAN_POINT('Ctrl Pts',(188.529848674471,-4.98725924554844,
133.991806640591));
#225471=CARTESIAN_POINT('Ctrl Pts',(188.52243418175,-4.90081304514209,134.123202450914));
#225472=CARTESIAN_POINT('Ctrl Pts',(188.515019689029,-4.80916968995939,
134.251071724647));
#225473=CARTESIAN_POINT('Ctrl Pts',(188.507612342675,-4.71761466409284,
134.37881775316));
#225474=CARTESIAN_POINT('Ctrl Pts',(188.500204996321,-4.62087267180682,
134.503043710459));
#225475=CARTESIAN_POINT('Ctrl Pts',(188.492797649967,-4.51924756505893,
134.623304451692));
#225476=CARTESIAN_POINT('Ctrl Pts',(188.485395828292,-4.41769825414966,
134.743475497927));
#225477=CARTESIAN_POINT('Ctrl Pts',(188.477994006617,-4.31127332042061,
134.859686932794));
#225478=CARTESIAN_POINT('Ctrl Pts',(188.470592184941,-4.2003185360947,134.971524492174));
#225479=CARTESIAN_POINT('Ctrl Pts',(188.46319427063,-4.08942232393587,135.083303013377));
#225480=CARTESIAN_POINT('Ctrl Pts',(188.455796356319,-3.97400128576268,
135.190711993113));
#225481=CARTESIAN_POINT('Ctrl Pts',(188.448398442007,-3.85443981639646,
135.293372119476));
#225482=CARTESIAN_POINT('Ctrl Pts',(188.441001757095,-3.73489821597734,
135.396015185588));
#225483=CARTESIAN_POINT('Ctrl Pts',(188.433605072183,-3.61121783291183,
135.493910721659));
#225484=CARTESIAN_POINT('Ctrl Pts',(188.426208387271,-3.483818170251,135.586717935786));
#225485=CARTESIAN_POINT('Ctrl Pts',(188.418812030335,-3.35642415662479,
135.679521034743));
#225486=CARTESIAN_POINT('Ctrl Pts',(188.4114156734,-3.22531149304034,135.767236040568));
#225487=CARTESIAN_POINT('Ctrl Pts',(188.404019316464,-3.09093063134526,
135.849564121362));
#225488=CARTESIAN_POINT('Ctrl Pts',(188.396621827128,-2.95652919559707,
135.931904806795));
#225489=CARTESIAN_POINT('Ctrl Pts',(188.389224337791,-2.81885888376706,
136.00885672998));
#225490=CARTESIAN_POINT('Ctrl Pts',(188.381826848455,-2.67839669617966,
136.080165930539));
#225491=CARTESIAN_POINT('Ctrl Pts',(188.37442676594,-2.53788526979019,136.151500128428));
#225492=CARTESIAN_POINT('Ctrl Pts',(188.367026683425,-2.39458035173523,
136.217187496532));
#225493=CARTESIAN_POINT('Ctrl Pts',(188.35962660091,-2.24898081214349,136.277021384424));
#225494=CARTESIAN_POINT('Ctrl Pts',(188.352218381243,-2.10322117088992,
136.336921065828));
#225495=CARTESIAN_POINT('Ctrl Pts',(188.344810161577,-1.95516221465031,
136.390954270921));
#225496=CARTESIAN_POINT('Ctrl Pts',(188.33740194191,-1.80532063496924,136.43896335134));
#225497=CARTESIAN_POINT('Ctrl Pts',(188.329989162608,-1.65538683029596,
136.487001980547));
#225498=CARTESIAN_POINT('Ctrl Pts',(188.322576383306,-1.50366857485122,
136.529008997548));
#225499=CARTESIAN_POINT('Ctrl Pts',(188.315163604004,-1.35069426213214,
136.564877571169));
#225500=CARTESIAN_POINT('Ctrl Pts',(188.307740232975,-1.19750137254131,
136.600797395489));
#225501=CARTESIAN_POINT('Ctrl Pts',(188.300316861946,-1.04304920681346,
136.630561188534));
#225502=CARTESIAN_POINT('Ctrl Pts',(188.292893490918,-0.887873634317857,
136.654113686883));
#225503=CARTESIAN_POINT('Ctrl Pts',(188.288957441477,-0.805595822389184,
136.666601786643));
#225504=CARTESIAN_POINT('Ctrl Pts',(188.285021392036,-0.72311468724722,
136.67734453826));
#225505=CARTESIAN_POINT('Ctrl Pts',(188.281085342595,-0.640510152529407,
136.686339647366));
#225506=CARTESIAN_POINT('Ctrl Pts',(188.273662076189,-0.484720578059533,
136.703304142411));
#225507=CARTESIAN_POINT('Ctrl Pts',(188.266238809784,-0.328020986091857,
136.714100671442));
#225508=CARTESIAN_POINT('Ctrl Pts',(188.258815543378,-0.170941080575582,
136.718640768985));
#225509=CARTESIAN_POINT('Ctrl Pts',(188.251401050657,-0.014046830462841,
136.72317550051));
#225510=CARTESIAN_POINT('Ctrl Pts',(188.243986557936,0.143226468969914,
136.721468508825));
#225511=CARTESIAN_POINT('Ctrl Pts',(188.236572065215,0.300341982397618,
136.713482824469));
#225512=CARTESIAN_POINT('Ctrl Pts',(188.229164718861,0.457306061978129,
136.705504837015));
#225513=CARTESIAN_POINT('Ctrl Pts',(188.221757372508,0.61411228800125,136.691260223337));
#225514=CARTESIAN_POINT('Ctrl Pts',(188.214350026154,0.770221908090596,
136.670764011026));
#225515=CARTESIAN_POINT('Ctrl Pts',(188.206948204478,0.926215095735712,
136.650283085563));
#225516=CARTESIAN_POINT('Ctrl Pts',(188.199546382803,1.08151234342266,136.623559893873));
#225517=CARTESIAN_POINT('Ctrl Pts',(188.192144561128,1.23557822068304,136.590661424046));
#225518=CARTESIAN_POINT('Ctrl Pts',(188.184746646816,1.38956276776613,136.557780321065));
#225519=CARTESIAN_POINT('Ctrl Pts',(188.177348732505,1.54231687484672,136.518730509913));
#225520=CARTESIAN_POINT('Ctrl Pts',(188.169950818194,1.69331364128615,136.473630365491));
#225521=CARTESIAN_POINT('Ctrl Pts',(188.162554133281,1.84428531480222,136.428537715894));
#225522=CARTESIAN_POINT('Ctrl Pts',(188.155157448369,1.99349986995265,136.377396835288));
#225523=CARTESIAN_POINT('Ctrl Pts',(188.147760763457,2.14044383721241,136.320376457123));
#225524=CARTESIAN_POINT('Ctrl Pts',(188.140364406522,2.28738128882264,136.263358607301));
#225525=CARTESIAN_POINT('Ctrl Pts',(188.132968049586,2.43204800471394,136.20046191333));
#225526=CARTESIAN_POINT('Ctrl Pts',(188.125571692651,2.57394908891939,136.131903827166));
#225527=CARTESIAN_POINT('Ctrl Pts',(188.118174203314,2.71587189854313,136.063335244583));
#225528=CARTESIAN_POINT('Ctrl Pts',(188.110776713978,2.85502789723953,135.989103706352));
#225529=CARTESIAN_POINT('Ctrl Pts',(188.103379224641,2.99094559062203,135.909473254564));
#225530=CARTESIAN_POINT('Ctrl Pts',(188.095979142126,3.12691092974114,135.829814888445));
#225531=CARTESIAN_POINT('Ctrl Pts',(188.088579059611,3.25963538151613,135.744754029243));
#225532=CARTESIAN_POINT('Ctrl Pts',(188.081178977096,3.38867543359986,135.65459869092));
#225533=CARTESIAN_POINT('Ctrl Pts',(188.07377075743,3.51785737848661,135.564344217535));
#225534=CARTESIAN_POINT('Ctrl Pts',(188.066362537763,3.64334652662018,135.46898429159));
#225535=CARTESIAN_POINT('Ctrl Pts',(188.058954318097,3.76473095956622,135.368868407524));
#225536=CARTESIAN_POINT('Ctrl Pts',(188.051541538795,3.88619010260547,135.268690903801));
#225537=CARTESIAN_POINT('Ctrl Pts',(188.044128759492,4.0035392187013,135.163751857378));
#225538=CARTESIAN_POINT('Ctrl Pts',(188.03671598019,4.11640281816916,135.054438075809));
#225539=CARTESIAN_POINT('Ctrl Pts',(188.029292609162,4.22942768244064,134.944968101584));
#225540=CARTESIAN_POINT('Ctrl Pts',(188.021869238133,4.33795397276301,134.831111177405));
#225541=CARTESIAN_POINT('Ctrl Pts',(188.014445867104,4.44164554397361,134.713288274123));
#225542=CARTESIAN_POINT('Ctrl Pts',(188.010509817663,4.49662530307466,134.650815743681));
#225543=CARTESIAN_POINT('Ctrl Pts',(188.006573768223,4.55024655251569,134.587228748358));
#225544=CARTESIAN_POINT('Ctrl Pts',(188.002637718782,4.60246416130131,134.522593290011));
#225545=CARTESIAN_POINT('Ctrl Pts',(187.995214452376,4.70094494181516,134.400692832772));
#225546=CARTESIAN_POINT('Ctrl Pts',(187.987791185971,4.79472832452141,134.274692815747));
#225547=CARTESIAN_POINT('Ctrl Pts',(187.980367919565,4.88345356298841,134.144991076123));
#225548=CARTESIAN_POINT('Ctrl Pts',(187.972953426844,4.9720739355918,134.015442633183));
#225549=CARTESIAN_POINT('Ctrl Pts',(187.965538934123,5.05564785509995,133.882201481457));
#225550=CARTESIAN_POINT('Ctrl Pts',(187.958124441402,5.13385404545199,133.745699292812));
#225551=CARTESIAN_POINT('Ctrl Pts',(187.950717095049,5.21198485773338,133.609328670115));
#225552=CARTESIAN_POINT('Ctrl Pts',(187.943309748695,5.28475805618814,133.469703589541));
#225553=CARTESIAN_POINT('Ctrl Pts',(187.935902402341,5.3518950751355,133.327285441504));
#225554=CARTESIAN_POINT('Ctrl Pts',(187.928500580666,5.41898202076117,133.184973514294));
#225555=CARTESIAN_POINT('Ctrl Pts',(187.92109875899,5.48044099847369,133.03987300371));
#225556=CARTESIAN_POINT('Ctrl Pts',(187.913696937315,5.53603895400241,132.892470591267));
#225557=CARTESIAN_POINT('Ctrl Pts',(187.906299023003,5.59160755980321,132.74514599141));
#225558=CARTESIAN_POINT('Ctrl Pts',(187.898901108692,5.64132117383657,132.595522258129));
#225559=CARTESIAN_POINT('Ctrl Pts',(187.891503194381,5.68499458559291,132.44410667238));
#225560=CARTESIAN_POINT('Ctrl Pts',(187.884106509468,5.72866073962051,132.292716249155));
#225561=CARTESIAN_POINT('Ctrl Pts',(187.876709824556,5.76628858020843,132.139534922778));
#225562=CARTESIAN_POINT('Ctrl Pts',(187.869313139644,5.79774252476681,131.985085894254));
#225563=CARTESIAN_POINT('Ctrl Pts',(187.861916782709,5.82919507462433,131.830643714162));
#225564=CARTESIAN_POINT('Ctrl Pts',(187.854520425773,5.85447419827982,131.67493430948));
#225565=CARTESIAN_POINT('Ctrl Pts',(187.847124068838,5.87349534086361,131.518491588294));
#225566=CARTESIAN_POINT('Ctrl Pts',(187.839726579501,5.8925193956329,131.362024915329));
#225567=CARTESIAN_POINT('Ctrl Pts',(187.832329090164,5.90528351654167,131.204825072902));
#225568=CARTESIAN_POINT('Ctrl Pts',(187.824931600828,5.91175499544869,131.047431463797));
#225569=CARTESIAN_POINT('Ctrl Pts',(187.817531518313,5.9182287429226,130.889982680606));
#225570=CARTESIAN_POINT('Ctrl Pts',(187.810131435798,5.91840544118585,130.73234036825));
#225571=CARTESIAN_POINT('Ctrl Pts',(187.802731353283,5.91230450185313,130.575044155298));
#225572=CARTESIAN_POINT('Ctrl Pts',(187.795323133616,5.90619685391042,130.417574978989));
#225573=CARTESIAN_POINT('Ctrl Pts',(187.78791491395,5.89379779728831,130.260453035358));
#225574=CARTESIAN_POINT('Ctrl Pts',(187.780506694283,5.87517871958054,130.10421379333));
#225575=CARTESIAN_POINT('Ctrl Pts',(187.773093914981,5.8565481821411,129.947878388655));
#225576=CARTESIAN_POINT('Ctrl Pts',(187.765681135679,5.83169005401839,129.792427135914));
#225577=CARTESIAN_POINT('Ctrl Pts',(187.758268356377,5.80072680601682,129.638385024143));
#225578=CARTESIAN_POINT('Ctrl Pts',(187.750844985348,5.76971931627449,129.484122809779));
#225579=CARTESIAN_POINT('Ctrl Pts',(187.74342161432,5.73258937218858,129.331274119478));
#225580=CARTESIAN_POINT('Ctrl Pts',(187.735998243291,5.68950945378594,129.180349306712));
#225581=CARTESIAN_POINT('Ctrl Pts',(187.73206219385,5.66666744736085,129.100325349594));
#225582=CARTESIAN_POINT('Ctrl Pts',(187.728126144409,5.64215350241321,129.020841949638));
#225583=CARTESIAN_POINT('Ctrl Pts',(187.724190094969,5.61599875376964,128.941972752443));
#225584=CARTESIAN_POINT('Ctrl Pts',(187.716766828563,5.56667171408872,128.793227907954));
#225585=CARTESIAN_POINT('Ctrl Pts',(187.709343562158,5.51135654039937,128.646219205077));
#225586=CARTESIAN_POINT('Ctrl Pts',(187.701920295752,5.45019295213473,128.501465190717));
#225587=CARTESIAN_POINT('Ctrl Pts',(187.694505803031,5.38910165415207,128.356882263581));
#225588=CARTESIAN_POINT('Ctrl Pts',(187.68709131031,5.32217584452053,128.214549061059));
#225589=CARTESIAN_POINT('Ctrl Pts',(187.679676817589,5.24960504344817,128.074969210988));
#225590=CARTESIAN_POINT('Ctrl Pts',(187.672269471236,5.17710418884611,127.935523893231));
#225591=CARTESIAN_POINT('Ctrl Pts',(187.664862124882,5.09896934552089,127.798826973745));
#225592=CARTESIAN_POINT('Ctrl Pts',(187.657454778528,5.01543812273929,127.665362210514));
#225593=CARTESIAN_POINT('Ctrl Pts',(187.650052956853,4.9319692006951,127.53199699034));
#225594=CARTESIAN_POINT('Ctrl Pts',(187.642651135177,4.84311211035346,127.401859441534));
#225595=CARTESIAN_POINT('Ctrl Pts',(187.635249313502,4.74915033913089,127.275408702502));
#225596=CARTESIAN_POINT('Ctrl Pts',(187.62785139919,4.65523816959588,127.149024715831));
#225597=CARTESIAN_POINT('Ctrl Pts',(187.620453484879,4.55622690793055,127.026323961781));
#225598=CARTESIAN_POINT('Ctrl Pts',(187.613055570568,4.45244323316465,126.907736460947));
#225599=CARTESIAN_POINT('Ctrl Pts',(187.605658885656,4.34867680536279,126.789168667204));
#225600=CARTESIAN_POINT('Ctrl Pts',(187.598262200743,4.24013978411027,126.674713050673));
#225601=CARTESIAN_POINT('Ctrl Pts',(187.590865515831,4.12719906752894,126.56476648375));
#225602=CARTESIAN_POINT('Ctrl Pts',(187.583469158896,4.01426335885729,126.454824791973));
#225603=CARTESIAN_POINT('Ctrl Pts',(187.57607280196,3.89692461059156,126.349392012655));
#225604=CARTESIAN_POINT('Ctrl Pts',(187.568676445025,3.77558631075384,126.248827874566));
#225605=CARTESIAN_POINT('Ctrl Pts',(187.561278955688,3.65422943371256,126.14824833985));
#225606=CARTESIAN_POINT('Ctrl Pts',(187.553881466352,3.52887207328063,126.05253916878));
#225607=CARTESIAN_POINT('Ctrl Pts',(187.546483977015,3.39995036474609,125.962019440019));
#225608=CARTESIAN_POINT('Ctrl Pts',(187.5390838945,3.27098346290651,125.871467979709));
#225609=CARTESIAN_POINT('Ctrl Pts',(187.531683811985,3.13845003058641,125.786109797999));
#225610=CARTESIAN_POINT('Ctrl Pts',(187.52428372947,3.00281456503668,125.706220245773));
#225611=CARTESIAN_POINT('Ctrl Pts',(187.516875509804,2.86702995434889,125.626242846772));
#225612=CARTESIAN_POINT('Ctrl Pts',(187.509467290137,2.72813682027947,125.551746275818));
#225613=CARTESIAN_POINT('Ctrl Pts',(187.502059070471,2.58662425473907,125.482959906541));
#225614=CARTESIAN_POINT('Ctrl Pts',(187.494646291169,2.44502459057584,125.414131200402));
#225615=CARTESIAN_POINT('Ctrl Pts',(187.487233511867,2.3008026235927,125.351019848396));
#225616=CARTESIAN_POINT('Ctrl Pts',(187.479820732564,2.15446624039682,125.293806581764));
#225617=CARTESIAN_POINT('Ctrl Pts',(187.472397361536,2.00792076491405,125.236511566134));
#225618=CARTESIAN_POINT('Ctrl Pts',(187.464973990507,1.85925519113648,125.185131589024));
#225619=CARTESIAN_POINT('Ctrl Pts',(187.457550619478,1.7089921235619,125.139797396619));
#225620=CARTESIAN_POINT('Ctrl Pts',(187.453614570037,1.62931903962022,125.115760120027));
#225621=CARTESIAN_POINT('Ctrl Pts',(187.449678520597,1.54919701811686,125.093421677015));
#225622=CARTESIAN_POINT('Ctrl Pts',(187.445742471156,1.46870484831581,125.072795680218));
#225623=CARTESIAN_POINT('Ctrl Pts',(187.43831920475,1.31689912814708,125.033895693975));
#225624=CARTESIAN_POINT('Ctrl Pts',(187.430895938345,1.1633173403862,125.000972121415));
#225625=CARTESIAN_POINT('Ctrl Pts',(187.423472671939,1.00847127499773,124.97418769989));
#225626=CARTESIAN_POINT('Ctrl Pts',(187.416058179218,0.853808224799215,
124.947434935327));
#225627=CARTESIAN_POINT('Ctrl Pts',(187.408643686497,0.697884235571734,
124.926806941762));
#225628=CARTESIAN_POINT('Ctrl Pts',(187.401229193776,0.541225463979645,
124.912416493625));
#225629=CARTESIAN_POINT('Ctrl Pts',(187.393821847423,0.384717686009742,
124.898039915544));
#225630=CARTESIAN_POINT('Ctrl Pts',(187.386414501069,0.227476904821062,
124.889888948137));
#225631=CARTESIAN_POINT('Ctrl Pts',(187.379007154715,0.0700385533196246,
124.888025167006));
#225632=CARTESIAN_POINT('Ctrl Pts',(187.37160533304,-0.0872823747195095,
124.886162775954));
#225633=CARTESIAN_POINT('Ctrl Pts',(187.364203511364,-0.244800208001704,
124.890578238706));
#225634=CARTESIAN_POINT('Ctrl Pts',(187.356801689689,-0.401975428509942,
124.901281224794));
#225635=CARTESIAN_POINT('Ctrl Pts',(187.349403775377,-0.559067677442723,
124.911978560858));
#225636=CARTESIAN_POINT('Ctrl Pts',(187.342005861066,-0.715817302305466,
124.928956784745));
#225637=CARTESIAN_POINT('Ctrl Pts',(187.334607946755,-0.871685936598251,
124.952173488771));
#225638=CARTESIAN_POINT('Ctrl Pts',(187.327211261842,-1.02752866835165,
124.975386334601));
#225639=CARTESIAN_POINT('Ctrl Pts',(187.31981457693,-1.18249033124199,125.00483554804));
#225640=CARTESIAN_POINT('Ctrl Pts',(187.312417892018,-1.33603870788574,
125.040426966531));
#225641=CARTESIAN_POINT('Ctrl Pts',(187.305021535083,-1.48958027603362,
125.076016806862));
#225642=CARTESIAN_POINT('Ctrl Pts',(187.297625178147,-1.64170831888113,
125.117748226424));
#225643=CARTESIAN_POINT('Ctrl Pts',(187.290228821212,-1.79190209129523,
125.165476201504));
#225644=CARTESIAN_POINT('Ctrl Pts',(187.282831331875,-1.94211885875933,
125.213211483858));
#225645=CARTESIAN_POINT('Ctrl Pts',(187.275433842538,-2.09040041034268,
125.266945036705));
#225646=CARTESIAN_POINT('Ctrl Pts',(187.268036353202,-2.2362425543513,125.326482396885));
#225647=CARTESIAN_POINT('Ctrl Pts',(187.260636270687,-2.38213582309748,
125.386040627795));
#225648=CARTESIAN_POINT('Ctrl Pts',(187.253236188172,-2.52558763631716,
125.451406575745));
#225649=CARTESIAN_POINT('Ctrl Pts',(187.245836105657,-2.66611526140484,
125.522338279919));
#225650=CARTESIAN_POINT('Ctrl Pts',(187.23842788599,-2.80679741106287,125.593347980794));
#225651=CARTESIAN_POINT('Ctrl Pts',(187.231019666324,-2.94454861767688,
125.669935491864));
#225652=CARTESIAN_POINT('Ctrl Pts',(187.223611446657,-3.07891153659171,
125.751813308303));
#225653=CARTESIAN_POINT('Ctrl Pts',(187.216198667355,-3.2133571536413,125.833741519172));
#225654=CARTESIAN_POINT('Ctrl Pts',(187.208785888053,-3.34441001746257,
125.920966317233));
#225655=CARTESIAN_POINT('Ctrl Pts',(187.201373108751,-3.47164354862595,
126.013158092752));
#225656=CARTESIAN_POINT('Ctrl Pts',(187.193949737723,-3.59905887702523,
126.105481596203));
#225657=CARTESIAN_POINT('Ctrl Pts',(187.186526366694,-3.72264368091018,
126.202786021196));
#225658=CARTESIAN_POINT('Ctrl Pts',(187.179102995665,-3.84200547931489,
126.304702357274));
#225659=CARTESIAN_POINT('Ctrl Pts',(187.175166946224,-3.90529396887533,
126.358740844111));
#225660=CARTESIAN_POINT('Ctrl Pts',(187.171230896784,-3.96739584334917,
126.414075295879));
#225661=CARTESIAN_POINT('Ctrl Pts',(187.167294847343,-4.02825706251959,
126.470646782902));
#225662=CARTESIAN_POINT('Ctrl Pts',(187.159982110724,-4.14133035410826,
126.57575023523));
#225663=CARTESIAN_POINT('Ctrl Pts',(187.152669374104,-4.25048290247324,
126.685464074864));
#225664=CARTESIAN_POINT('Ctrl Pts',(187.145356637485,-4.355306958856,126.799459637936));
#225665=CARTESIAN_POINT('Ctrl Pts',(187.138052644169,-4.4600056848014,126.913318904872));
#225666=CARTESIAN_POINT('Ctrl Pts',(187.130748650852,-4.56038595696257,
127.03144942948));
#225667=CARTESIAN_POINT('Ctrl Pts',(187.123444657536,-4.65607377997443,
127.153482980896));
#225668=CARTESIAN_POINT('Ctrl Pts',(187.11614769061,-4.75166955197894,127.275399136901));
#225669=CARTESIAN_POINT('Ctrl Pts',(187.108850723683,-4.84258162128955,
127.401210547057));
#225670=CARTESIAN_POINT('Ctrl Pts',(187.101553756756,-4.92847369766666,
127.530513099139));
#225671=CARTESIAN_POINT('Ctrl Pts',(187.094262461591,-5.01429901214382,
127.659715147376));
#225672=CARTESIAN_POINT('Ctrl Pts',(187.086971166426,-5.09511188989882,
127.792402615212));
#225673=CARTESIAN_POINT('Ctrl Pts',(187.079679871261,-5.1706173282255,127.92813965812));
#225674=CARTESIAN_POINT('Ctrl Pts',(187.072391625532,-5.24609118793796,
128.063819931771));
#225675=CARTESIAN_POINT('Ctrl Pts',(187.065103379803,-5.31626183691263,
128.202546907271));
#225676=CARTESIAN_POINT('Ctrl Pts',(187.057815134074,-5.38087854125002,
128.343857277431));
#225677=CARTESIAN_POINT('Ctrl Pts',(187.050528398168,-5.44548185967987,
128.48513837393));
#225678=CARTESIAN_POINT('Ctrl Pts',(187.043241662262,-5.50453336306754,
128.629001449778));
#225679=CARTESIAN_POINT('Ctrl Pts',(187.035954926356,-5.55782922554555,
128.774960493842));
#225680=CARTESIAN_POINT('Ctrl Pts',(187.028668162023,-5.61112529593695,
128.920920107308));
#225681=CARTESIAN_POINT('Ctrl Pts',(187.021381397691,-5.65866555016246,
129.068975342758));
#225682=CARTESIAN_POINT('Ctrl Pts',(187.014094633358,-5.7002951840503,129.218622500097));
#225683=CARTESIAN_POINT('Ctrl Pts',(187.006803471584,-5.74194994073617,
129.368359967031));
#225684=CARTESIAN_POINT('Ctrl Pts',(186.999512309809,-5.77768684994215,
129.519690902912));
#225685=CARTESIAN_POINT('Ctrl Pts',(186.992221148034,-5.80740158088912,
129.672098527418));
#225686=CARTESIAN_POINT('Ctrl Pts',(186.984927500083,-5.8371264441105,129.824558120621));
#225687=CARTESIAN_POINT('Ctrl Pts',(186.977633852133,-5.86082497829701,
129.97809475339));
#225688=CARTESIAN_POINT('Ctrl Pts',(186.970340204182,-5.87844452383703,
130.132184641597));
#225689=CARTESIAN_POINT('Ctrl Pts',(186.963039152689,-5.89608195439748,
130.286430941374));
#225690=CARTESIAN_POINT('Ctrl Pts',(186.955738101197,-5.90762804625571,
130.441231234208));
#225691=CARTESIAN_POINT('Ctrl Pts',(186.948437049704,-5.91308220639865,
130.596059434488));
#225692=CARTESIAN_POINT('Ctrl Pts',(186.945083097206,-5.91558773509581,
130.66718431692));
#225693=CARTESIAN_POINT('Ctrl Pts',(186.941729144709,-5.91680841145624,
130.738315114615));
#225694=CARTESIAN_POINT('Ctrl Pts',(186.938375192211,-5.91674785298769,
130.809401120074));
#225695=CARTESIAN_POINT('',(190.438375193894,-5.91568182138061,130.798900870218));
#225696=CARTESIAN_POINT('Ctrl Pts',(190.438375192211,-5.91556591356672,
130.798901012961));
#225697=CARTESIAN_POINT('Ctrl Pts',(190.368989697902,-5.90218450277572,
132.273183331429));
#225698=CARTESIAN_POINT('Ctrl Pts',(190.206788328991,-4.59798200865986,
135.740709904657));
#225699=CARTESIAN_POINT('Ctrl Pts',(189.951771085471,1.22745627517318,137.694274377758));
#225700=CARTESIAN_POINT('Ctrl Pts',(189.673323461659,6.46014967796433,133.495833572777));
#225701=CARTESIAN_POINT('Ctrl Pts',(189.394875837845,5.75628112256356,126.824060607722));
#225702=CARTESIAN_POINT('Ctrl Pts',(189.116428214034,-0.237328574507486,
123.809988903246));
#225703=CARTESIAN_POINT('Ctrl Pts',(188.880927998822,-5.12203658652489,
126.696922428952));
#225704=CARTESIAN_POINT('Ctrl Pts',(188.738243658214,-5.90521979014647,
129.742180863919));
#225705=CARTESIAN_POINT('Ctrl Pts',(188.688375192211,-5.90715995150835,
130.805573381844));
#225706=CARTESIAN_POINT('',(192.188375873533,-5.92197168067619,130.805533319426));
#225707=CARTESIAN_POINT('Ctrl Pts',(192.188375192211,-5.91674988112158,
130.805546681526));
#225708=CARTESIAN_POINT('Ctrl Pts',(192.185367486799,-5.91673715075054,
130.869052886841));
#225709=CARTESIAN_POINT('Ctrl Pts',(192.182359781387,-5.91570200665032,
130.932547687523));
#225710=CARTESIAN_POINT('Ctrl Pts',(192.179352075975,-5.91364535475517,
130.996009204001));
#225711=CARTESIAN_POINT('Ctrl Pts',(192.17192880957,-5.90856936730653,131.152637489943));
#225712=CARTESIAN_POINT('Ctrl Pts',(192.164505543164,-5.89725874201999,
131.309300813403));
#225713=CARTESIAN_POINT('Ctrl Pts',(192.157082276759,-5.87970025871574,
131.465462296703));
#225714=CARTESIAN_POINT('Ctrl Pts',(192.149667784038,-5.86216252808058,
131.621439210099));
#225715=CARTESIAN_POINT('Ctrl Pts',(192.142253291317,-5.83839167951754,
131.776915096634));
#225716=CARTESIAN_POINT('Ctrl Pts',(192.134838798596,-5.80842648002977,
131.931353247794));
#225717=CARTESIAN_POINT('Ctrl Pts',(192.127431452242,-5.77849016212943,
132.08564254565));
#225718=CARTESIAN_POINT('Ctrl Pts',(192.120024105888,-5.74237144971965,
132.238895735347));
#225719=CARTESIAN_POINT('Ctrl Pts',(192.112616759534,-5.70016086098663,
132.390581510562));
#225720=CARTESIAN_POINT('Ctrl Pts',(192.105214937859,-5.65798175450327,
132.542154152802));
#225721=CARTESIAN_POINT('Ctrl Pts',(192.097813116184,-5.60971991816693,
132.692161350184));
#225722=CARTESIAN_POINT('Ctrl Pts',(192.090411294508,-5.55551684961682,
132.84008238051));
#225723=CARTESIAN_POINT('Ctrl Pts',(192.083013380197,-5.5013423944446,132.987925324475));
#225724=CARTESIAN_POINT('Ctrl Pts',(192.075615465886,-5.44123308132258,
133.133683944999));
#225725=CARTESIAN_POINT('Ctrl Pts',(192.068217551574,-5.37538008816079,
133.2768531798));
#225726=CARTESIAN_POINT('Ctrl Pts',(192.060820866662,-5.30953803857184,
133.419998622472));
#225727=CARTESIAN_POINT('Ctrl Pts',(192.05342418175,-5.23795435917514,133.560555194648));
#225728=CARTESIAN_POINT('Ctrl Pts',(192.046027496837,-5.16086820194777,
133.69803820234));
#225729=CARTESIAN_POINT('Ctrl Pts',(192.038631139902,-5.08378546280139,
133.835515113891));
#225730=CARTESIAN_POINT('Ctrl Pts',(192.031234782967,-5.00120091351712,
133.969918406331));
#225731=CARTESIAN_POINT('Ctrl Pts',(192.023838426031,-4.91339933435241,
134.100788615215));
#225732=CARTESIAN_POINT('Ctrl Pts',(192.016440936695,-4.82558431254177,
134.231678860662));
#225733=CARTESIAN_POINT('Ctrl Pts',(192.009043447358,-4.73255087844258,
134.359034635486));
#225734=CARTESIAN_POINT('Ctrl Pts',(192.001645958021,-4.63462665546448,
134.482426186171));
#225735=CARTESIAN_POINT('Ctrl Pts',(191.994245875506,-4.53666810530159,
134.605860991573));
#225736=CARTESIAN_POINT('Ctrl Pts',(191.986845792991,-4.43381558469625,
134.725328513823));
#225737=CARTESIAN_POINT('Ctrl Pts',(191.979445710476,-4.32643632479157,
134.840432877824));
#225738=CARTESIAN_POINT('Ctrl Pts',(191.97203749081,-4.21893899035197,134.955663810906));
#225739=CARTESIAN_POINT('Ctrl Pts',(191.964629271143,-4.10690523078763,
135.066521731207));
#225740=CARTESIAN_POINT('Ctrl Pts',(191.957221051477,-3.99073891115741,
135.172647868363));
#225741=CARTESIAN_POINT('Ctrl Pts',(191.949808272175,-3.8745010930958,135.278839324385));
#225742=CARTESIAN_POINT('Ctrl Pts',(191.942395492873,-3.75412593146085,
135.380292954059));
#225743=CARTESIAN_POINT('Ctrl Pts',(191.934982713571,-3.63004912034786,
135.476691293616));
#225744=CARTESIAN_POINT('Ctrl Pts',(191.927559342542,-3.50579502246853,
135.573227371642));
#225745=CARTESIAN_POINT('Ctrl Pts',(191.920135971513,-3.37782901450236,
135.664693516634));
#225746=CARTESIAN_POINT('Ctrl Pts',(191.912712600484,-3.24661509159063,
135.750816016087));
#225747=CARTESIAN_POINT('Ctrl Pts',(191.908776551044,-3.17704232122627,
135.796480231779));
#225748=CARTESIAN_POINT('Ctrl Pts',(191.904840501603,-3.10655685573822,
135.84064292555));
#225749=CARTESIAN_POINT('Ctrl Pts',(191.900904452162,-3.03523037952588,
135.883268679906));
#225750=CARTESIAN_POINT('Ctrl Pts',(191.893481185756,-2.90071087141565,
135.963659522316));
#225751=CARTESIAN_POINT('Ctrl Pts',(191.886057919351,-2.76279191120802,
136.038823925974));
#225752=CARTESIAN_POINT('Ctrl Pts',(191.878634652946,-2.62191804346816,
136.108460572868));
#225753=CARTESIAN_POINT('Ctrl Pts',(191.871220160225,-2.48121067694097,
136.178014915029));
#225754=CARTESIAN_POINT('Ctrl Pts',(191.863805667504,-2.33755568601003,
136.242054341289));
#225755=CARTESIAN_POINT('Ctrl Pts',(191.856391174783,-2.19142557325891,
136.300321363365));
#225756=CARTESIAN_POINT('Ctrl Pts',(191.848983828429,-2.04543630621208,
136.358532225492));
#225757=CARTESIAN_POINT('Ctrl Pts',(191.841576482075,-1.89697701105787,
136.410981622255));
#225758=CARTESIAN_POINT('Ctrl Pts',(191.834169135721,-1.74654361814439,
136.457458525122));
#225759=CARTESIAN_POINT('Ctrl Pts',(191.826767314046,-1.59622242413098,
136.503900763762));
#225760=CARTESIAN_POINT('Ctrl Pts',(191.819365492371,-1.44393041914754,
136.544379268321));
#225761=CARTESIAN_POINT('Ctrl Pts',(191.811963670695,-1.29018218445807,
136.578731621702));
#225762=CARTESIAN_POINT('Ctrl Pts',(191.804565756384,-1.1365151122651,136.613065840743));
#225763=CARTESIAN_POINT('Ctrl Pts',(191.797167842073,-0.981393704726121,
136.641280267975));
#225764=CARTESIAN_POINT('Ctrl Pts',(191.789769927761,-0.825346221371544,
136.663262748287));
#225765=CARTESIAN_POINT('Ctrl Pts',(191.782373242849,-0.669324670277544,
136.68524157551));
#225766=CARTESIAN_POINT('Ctrl Pts',(191.774976557937,-0.512377718094195,
136.700990459225));
#225767=CARTESIAN_POINT('Ctrl Pts',(191.767579873025,-0.355042419086338,
136.710448615822));
#225768=CARTESIAN_POINT('Ctrl Pts',(191.760183516089,-0.19771409649043,
136.719906353036));
#225769=CARTESIAN_POINT('Ctrl Pts',(191.752787159154,-0.0399978339334864,
136.723073895353));
#225770=CARTESIAN_POINT('Ctrl Pts',(191.745390802218,0.117565877448984,
136.719942484716));
#225771=CARTESIAN_POINT('Ctrl Pts',(191.737993312882,0.275153712237935,
136.716810594653));
#225772=CARTESIAN_POINT('Ctrl Pts',(191.730595823545,0.432588576099383,
136.707377838831));
#225773=CARTESIAN_POINT('Ctrl Pts',(191.723198334209,0.589331816772684,
136.691687563833));
#225774=CARTESIAN_POINT('Ctrl Pts',(191.715798251694,0.746130003545964,
136.675991788633));
#225775=CARTESIAN_POINT('Ctrl Pts',(191.708398169179,0.902235713210191,
136.654034164045));
#225776=CARTESIAN_POINT('Ctrl Pts',(191.700998086664,1.0571173874321,136.625909671872));
#225777=CARTESIAN_POINT('Ctrl Pts',(191.693589866998,1.21216936997707,136.597754253928));
#225778=CARTESIAN_POINT('Ctrl Pts',(191.686181647331,1.36599426160672,136.563418492823));
#225779=CARTESIAN_POINT('Ctrl Pts',(191.678773427665,1.51807191972469,136.523048247525));
#225780=CARTESIAN_POINT('Ctrl Pts',(191.671360648363,1.67024317910383,136.482653155014));
#225781=CARTESIAN_POINT('Ctrl Pts',(191.663947869061,1.82066470625482,136.43621628731));
#225782=CARTESIAN_POINT('Ctrl Pts',(191.656535089759,1.96883390661907,136.383932609274));
#225783=CARTESIAN_POINT('Ctrl Pts',(191.64911171873,2.11721481808522,136.331574225866));
#225784=CARTESIAN_POINT('Ctrl Pts',(191.641688347701,2.26333662937201,136.273352484731));
#225785=CARTESIAN_POINT('Ctrl Pts',(191.634264976672,2.40671825768975,136.209509809827));
#225786=CARTESIAN_POINT('Ctrl Pts',(191.630328927231,2.48274263741927,136.175658891709));
#225787=CARTESIAN_POINT('Ctrl Pts',(191.626392877791,2.55799707823944,136.140228488059));
#225788=CARTESIAN_POINT('Ctrl Pts',(191.62245682835,2.63241303524121,136.103259764973));
#225789=CARTESIAN_POINT('Ctrl Pts',(191.615033561944,2.77275920770318,136.033537906988));
#225790=CARTESIAN_POINT('Ctrl Pts',(191.607610295539,2.91054571611699,135.958130975866));
#225791=CARTESIAN_POINT('Ctrl Pts',(191.600187029134,3.04527876591065,135.877250109798));
#225792=CARTESIAN_POINT('Ctrl Pts',(191.592772536413,3.17985257242841,135.796464838196));
#225793=CARTESIAN_POINT('Ctrl Pts',(191.585358043692,3.31137978699819,135.710218699948));
#225794=CARTESIAN_POINT('Ctrl Pts',(191.577943550971,3.43938837824726,135.618770046154));
#225795=CARTESIAN_POINT('Ctrl Pts',(191.570536204617,3.56727358999668,135.527409534016));
#225796=CARTESIAN_POINT('Ctrl Pts',(191.563128858263,3.69164662828833,135.430856704515));
#225797=CARTESIAN_POINT('Ctrl Pts',(191.555721511909,3.81206188637452,135.329414731823));
#225798=CARTESIAN_POINT('Ctrl Pts',(191.548319690234,3.93238733421826,135.228048418381));
#225799=CARTESIAN_POINT('Ctrl Pts',(191.540917868558,4.04876059514704,135.121800461911));
#225800=CARTESIAN_POINT('Ctrl Pts',(191.533516046883,4.16076687931502,135.011016003796));
#225801=CARTESIAN_POINT('Ctrl Pts',(191.526118132572,4.27271403623751,134.900290027933));
#225802=CARTESIAN_POINT('Ctrl Pts',(191.51872021826,4.38029854276746,134.785032581598));
#225803=CARTESIAN_POINT('Ctrl Pts',(191.511322303949,4.48314050245561,134.665627481918));
#225804=CARTESIAN_POINT('Ctrl Pts',(191.503925619037,4.58596537167568,134.546242225199));
#225805=CARTESIAN_POINT('Ctrl Pts',(191.496528934124,4.68404901487392,134.422710965694));
#225806=CARTESIAN_POINT('Ctrl Pts',(191.489132249212,4.77705000213056,134.295452687341));
#225807=CARTESIAN_POINT('Ctrl Pts',(191.481735892277,4.87004686562598,134.168200051753));
#225808=CARTESIAN_POINT('Ctrl Pts',(191.474339535341,4.95796130103329,134.037221027301));
#225809=CARTESIAN_POINT('Ctrl Pts',(191.466943178406,5.04049379128799,133.902965610541));
#225810=CARTESIAN_POINT('Ctrl Pts',(191.459545689069,5.12303891747765,133.768689638933));
#225811=CARTESIAN_POINT('Ctrl Pts',(191.452148199733,5.20020026233308,133.63113659425));
#225812=CARTESIAN_POINT('Ctrl Pts',(191.444750710396,5.27172313985551,133.490783089779));
#225813=CARTESIAN_POINT('Ctrl Pts',(191.437350627881,5.34327108961184,133.350380384605));
#225814=CARTESIAN_POINT('Ctrl Pts',(191.429950545366,5.40917646734144,133.207175597486));
#225815=CARTESIAN_POINT('Ctrl Pts',(191.422550462851,5.4692318636611,133.061667283488));
#225816=CARTESIAN_POINT('Ctrl Pts',(191.415142243184,5.52935329706284,132.915998968139));
#225817=CARTESIAN_POINT('Ctrl Pts',(191.407734023518,5.58361176011364,132.768022412689));
#225818=CARTESIAN_POINT('Ctrl Pts',(191.400325803851,5.63184881831531,132.618254068169));
#225819=CARTESIAN_POINT('Ctrl Pts',(191.392913024549,5.68011556562145,132.468393543732));
#225820=CARTESIAN_POINT('Ctrl Pts',(191.385500245247,5.72235342333643,132.316739391503));
#225821=CARTESIAN_POINT('Ctrl Pts',(191.378087465945,5.75845475628461,132.163819841788));
#225822=CARTESIAN_POINT('Ctrl Pts',(191.370664094916,5.79460767251027,132.01068179345));
#225823=CARTESIAN_POINT('Ctrl Pts',(191.363240723888,5.82460648099202,131.856275102001));
#225824=CARTESIAN_POINT('Ctrl Pts',(191.355817352859,5.84839510287327,131.701135552089));
#225825=CARTESIAN_POINT('Ctrl Pts',(191.351881303418,5.86100840099461,131.618876840204));
#225826=CARTESIAN_POINT('Ctrl Pts',(191.347945253977,5.87187666241779,131.536412149219));
#225827=CARTESIAN_POINT('Ctrl Pts',(191.344009204537,5.88099747114688,131.453821399187));
#225828=CARTESIAN_POINT('Ctrl Pts',(191.336585938131,5.89819903175955,131.298057822193));
#225829=CARTESIAN_POINT('Ctrl Pts',(191.329162671726,5.90923401839223,131.14137484216));
#225830=CARTESIAN_POINT('Ctrl Pts',(191.32173940532,5.91401315955457,130.984302027795));
#225831=CARTESIAN_POINT('Ctrl Pts',(191.314324912599,5.91878665216895,130.827414860453));
#225832=CARTESIAN_POINT('Ctrl Pts',(191.306910419878,5.91731900564953,130.67013914539));
#225833=CARTESIAN_POINT('Ctrl Pts',(191.299495927157,5.90957243360595,130.513011661047));
#225834=CARTESIAN_POINT('Ctrl Pts',(191.292088580803,5.90183332800017,130.35603562209));
#225835=CARTESIAN_POINT('Ctrl Pts',(191.28468123445,5.88782736319993,130.199207899769));
#225836=CARTESIAN_POINT('Ctrl Pts',(191.277273888096,5.86756874689005,130.043067268706));
#225837=CARTESIAN_POINT('Ctrl Pts',(191.269872066421,5.84732524022051,129.887043093216));
#225838=CARTESIAN_POINT('Ctrl Pts',(191.262470244745,5.82083841545084,129.731705357212));
#225839=CARTESIAN_POINT('Ctrl Pts',(191.25506842307,5.78817444575804,129.577589592487));
#225840=CARTESIAN_POINT('Ctrl Pts',(191.247670508758,5.7555277191206,129.423555184274));
#225841=CARTESIAN_POINT('Ctrl Pts',(191.240272594447,5.71671041893551,129.270741826916));
#225842=CARTESIAN_POINT('Ctrl Pts',(191.232874680136,5.67184011811256,129.119676600586));
#225843=CARTESIAN_POINT('Ctrl Pts',(191.225477995223,5.6269772739196,128.968636478556));
#225844=CARTESIAN_POINT('Ctrl Pts',(191.218081310311,5.57606353168593,128.819344268479));
#225845=CARTESIAN_POINT('Ctrl Pts',(191.210684625399,5.51926684325338,128.672313696069));
#225846=CARTESIAN_POINT('Ctrl Pts',(191.203288268464,5.46247267324549,128.525289643149));
#225847=CARTESIAN_POINT('Ctrl Pts',(191.195891911528,5.39979621022294,128.380527376718));
#225848=CARTESIAN_POINT('Ctrl Pts',(191.188495554593,5.33145415274227,128.238522123095));
#225849=CARTESIAN_POINT('Ctrl Pts',(191.181098065256,5.26310163191814,128.096495128106));
#225850=CARTESIAN_POINT('Ctrl Pts',(191.17370057592,5.18908195138688,127.957226322785));
#225851=CARTESIAN_POINT('Ctrl Pts',(191.166303086583,5.10965843540239,127.821187602801));
#225852=CARTESIAN_POINT('Ctrl Pts',(191.158903004068,5.03020707762741,127.685101194655));
#225853=CARTESIAN_POINT('Ctrl Pts',(191.151502921553,4.94534830094565,127.552247448424));
#225854=CARTESIAN_POINT('Ctrl Pts',(191.144102839038,4.8553894440146,127.423070344689));
#225855=CARTESIAN_POINT('Ctrl Pts',(191.136694619372,4.7653316680724,127.293751197449));
#225856=CARTESIAN_POINT('Ctrl Pts',(191.129286399705,4.67016282567414,127.168117073055));
#225857=CARTESIAN_POINT('Ctrl Pts',(191.121878180039,4.5702317839837,127.046580421338));
#225858=CARTESIAN_POINT('Ctrl Pts',(191.114465400737,4.47023923640445,126.924968965839));
#225859=CARTESIAN_POINT('Ctrl Pts',(191.107052621435,4.3654788968777,126.807460286267));
#225860=CARTESIAN_POINT('Ctrl Pts',(191.099639842133,4.25633700107888,126.694430460526));
#225861=CARTESIAN_POINT('Ctrl Pts',(191.092216471104,4.14703915822113,126.58123913247));
#225862=CARTESIAN_POINT('Ctrl Pts',(191.084793100075,4.03334752442669,126.472539696962));
#225863=CARTESIAN_POINT('Ctrl Pts',(191.077369729046,3.91568255850171,126.368668939423));
#225864=CARTESIAN_POINT('Ctrl Pts',(191.073433679605,3.85329377023497,126.31359417143));
#225865=CARTESIAN_POINT('Ctrl Pts',(191.069497630165,3.78978845095696,126.259876215498));
#225866=CARTESIAN_POINT('Ctrl Pts',(191.065561580724,3.72523253376711,126.207560303014));
#225867=CARTESIAN_POINT('Ctrl Pts',(191.058138314318,3.60348208867042,126.108894124795));
#225868=CARTESIAN_POINT('Ctrl Pts',(191.050715047913,3.47762493989561,126.014919100111));
#225869=CARTESIAN_POINT('Ctrl Pts',(191.043291781507,3.34805837517246,125.925996580418));
#225870=CARTESIAN_POINT('Ctrl Pts',(191.035877288786,3.2186449473689,125.837179159759));
#225871=CARTESIAN_POINT('Ctrl Pts',(191.028462796065,3.08553113521307,125.753402566677));
#225872=CARTESIAN_POINT('Ctrl Pts',(191.021048303344,2.94914812114376,125.674988733792));
#225873=CARTESIAN_POINT('Ctrl Pts',(191.013640956991,2.81289655815807,125.596650479111));
#225874=CARTESIAN_POINT('Ctrl Pts',(191.006233610637,2.67338238768785,125.523664879322));
#225875=CARTESIAN_POINT('Ctrl Pts',(190.998826264283,2.53106657568212,125.456311201941));
#225876=CARTESIAN_POINT('Ctrl Pts',(190.991424442608,2.38885690817838,125.389007759474));
#225877=CARTESIAN_POINT('Ctrl Pts',(190.984022620932,2.24385009572029,125.327328034653));
#225878=CARTESIAN_POINT('Ctrl Pts',(190.976620799257,2.09653246459078,125.271505822127));
#225879=CARTESIAN_POINT('Ctrl Pts',(190.969222884945,1.94929260129213,125.215713077712));
#225880=CARTESIAN_POINT('Ctrl Pts',(190.961824970634,1.79974469693171,125.165771819394));
#225881=CARTESIAN_POINT('Ctrl Pts',(190.954427056323,1.64839575001803,125.121868029465));
#225882=CARTESIAN_POINT('Ctrl Pts',(190.94703037141,1.49707195455342,125.077971535549));
#225883=CARTESIAN_POINT('Ctrl Pts',(190.939633686498,1.34394806872582,125.040110622631));
#225884=CARTESIAN_POINT('Ctrl Pts',(190.932237001586,1.18954708660089,125.008421669366));
#225885=CARTESIAN_POINT('Ctrl Pts',(190.924840644651,1.03515295077734,124.976734121223));
#225886=CARTESIAN_POINT('Ctrl Pts',(190.917444287715,0.879482196927022,
124.951218063633));
#225887=CARTESIAN_POINT('Ctrl Pts',(190.91004793078,0.723068603840397,124.931958863885));
#225888=CARTESIAN_POINT('Ctrl Pts',(190.902650441443,0.566631063433394,
124.912696715504));
#225889=CARTESIAN_POINT('Ctrl Pts',(190.895252952107,0.409450827861063,
124.899693377976));
#225890=CARTESIAN_POINT('Ctrl Pts',(190.88785546277,0.252067249504715,124.892982380283));
#225891=CARTESIAN_POINT('Ctrl Pts',(190.880455380255,0.0946285005788653,
124.88626903006));
#225892=CARTESIAN_POINT('Ctrl Pts',(190.87305529774,-0.0630133603256108,
124.885852427237));
#225893=CARTESIAN_POINT('Ctrl Pts',(190.865655215225,-0.220318675722416,
124.891713981445));
#225894=CARTESIAN_POINT('Ctrl Pts',(190.858246995558,-0.377796964484852,
124.897581981035));
#225895=CARTESIAN_POINT('Ctrl Pts',(190.850838775892,-0.534937595424837,
124.909741910448));
#225896=CARTESIAN_POINT('Ctrl Pts',(190.843430556225,-0.691204991596928,
124.928123197065));
#225897=CARTESIAN_POINT('Ctrl Pts',(190.836017776923,-0.84756856774404,
124.946515797058));
#225898=CARTESIAN_POINT('Ctrl Pts',(190.828604997621,-1.00305747031484,
124.971137326051));
#225899=CARTESIAN_POINT('Ctrl Pts',(190.821192218319,-1.15714652449987,
125.001866112326));
#225900=CARTESIAN_POINT('Ctrl Pts',(190.81376884729,-1.31145574835155,125.032638805332));
#225901=CARTESIAN_POINT('Ctrl Pts',(190.806345476262,-1.46436076711051,
125.069536096735));
#225902=CARTESIAN_POINT('Ctrl Pts',(190.798922105233,-1.61535096541017,
125.112386283379));
#225903=CARTESIAN_POINT('Ctrl Pts',(190.794986055792,-1.69540959150786,
125.135106480513));
#225904=CARTESIAN_POINT('Ctrl Pts',(190.791050006351,-1.77493020547604,
125.15949943687));
#225905=CARTESIAN_POINT('Ctrl Pts',(190.787113956911,-1.85383911441731,
125.185534129735));
#225906=CARTESIAN_POINT('Ctrl Pts',(190.779690690505,-2.0026588540193,125.234634747963));
#225907=CARTESIAN_POINT('Ctrl Pts',(190.7722674241,-2.14975156694095,125.289726135378));
#225908=CARTESIAN_POINT('Ctrl Pts',(190.764844157694,-2.29459849424747,
125.350669361848));
#225909=CARTESIAN_POINT('Ctrl Pts',(190.757429664973,-2.4392742245148,125.411540558485));
#225910=CARTESIAN_POINT('Ctrl Pts',(190.750015172252,-2.58170911190695,
125.478249683713));
#225911=CARTESIAN_POINT('Ctrl Pts',(190.742600679531,-2.72139924075281,
125.550607983978));
#225912=CARTESIAN_POINT('Ctrl Pts',(190.735193333178,-2.86095473099336,
125.62289654259));
#225913=CARTESIAN_POINT('Ctrl Pts',(190.727785986824,-2.99777040011747,
125.700823265995));
#225914=CARTESIAN_POINT('Ctrl Pts',(190.72037864047,-3.13136212909958,125.784151281399));
#225915=CARTESIAN_POINT('Ctrl Pts',(190.712976818795,-3.26485422033005,
125.867417147625));
#225916=CARTESIAN_POINT('Ctrl Pts',(190.705574997119,-3.39512684380415,
125.956076087876));
#225917=CARTESIAN_POINT('Ctrl Pts',(190.698173175444,-3.5217204302287,126.049845313793));
#225918=CARTESIAN_POINT('Ctrl Pts',(190.690775261132,-3.6482471888842,126.143565039666));
#225919=CARTESIAN_POINT('Ctrl Pts',(190.683377346821,-3.77109847913389,
126.242389457018));
#225920=CARTESIAN_POINT('Ctrl Pts',(190.67597943251,-3.88984378373164,126.345992541614));
#225921=CARTESIAN_POINT('Ctrl Pts',(190.668582747597,-4.0085693550141,126.449578409258));
#225922=CARTESIAN_POINT('Ctrl Pts',(190.661186062685,-4.12319001387754,
126.557941122862));
#225923=CARTESIAN_POINT('Ctrl Pts',(190.653789377773,-4.23330833002912,
126.670714388701));
#225924=CARTESIAN_POINT('Ctrl Pts',(190.646393020838,-4.34342176341914,
126.783482654056));
#225925=CARTESIAN_POINT('Ctrl Pts',(190.638996663902,-4.44903299024769,
126.900660815703));
#225926=CARTESIAN_POINT('Ctrl Pts',(190.631600306967,-4.54978166812228,
127.021845933534));
#225927=CARTESIAN_POINT('Ctrl Pts',(190.62420281763,-4.65054577087687,127.143049605116));
#225928=CARTESIAN_POINT('Ctrl Pts',(190.616805328294,-4.7464456036807,127.268261167321));
#225929=CARTESIAN_POINT('Ctrl Pts',(190.609407838957,-4.83716142451464,
127.397044970948));
#225930=CARTESIAN_POINT('Ctrl Pts',(190.602007756442,-4.92790904563891,
127.525873919538));
#225931=CARTESIAN_POINT('Ctrl Pts',(190.594607673927,-5.01346882182785,
127.658277297765));
#225932=CARTESIAN_POINT('Ctrl Pts',(190.587207591412,-5.09356469563254,
127.793791027952));
#225933=CARTESIAN_POINT('Ctrl Pts',(190.579799371746,-5.17374864308446,
127.929453769417));
#225934=CARTESIAN_POINT('Ctrl Pts',(190.572391152079,-5.24845649947873,
128.068233371551));
#225935=CARTESIAN_POINT('Ctrl Pts',(190.564982932413,-5.31745814713684,
128.209641092078));
#225936=CARTESIAN_POINT('Ctrl Pts',(190.557570153111,-5.38650226415769,
128.351135846697));
#225937=CARTESIAN_POINT('Ctrl Pts',(190.550157373809,-5.44983302436487,
128.495261601939));
#225938=CARTESIAN_POINT('Ctrl Pts',(190.542744594507,-5.50726892380859,
128.641510746828));
#225939=CARTESIAN_POINT('Ctrl Pts',(190.535321223478,-5.56478689035895,
128.787968859353));
#225940=CARTESIAN_POINT('Ctrl Pts',(190.527897852449,-5.61639305166817,
128.9365560694));
#225941=CARTESIAN_POINT('Ctrl Pts',(190.52047448142,-5.66195586638615,129.086749972048));
#225942=CARTESIAN_POINT('Ctrl Pts',(190.516538431979,-5.68611436401442,
129.166386383086));
#225943=CARTESIAN_POINT('Ctrl Pts',(190.512602382539,-5.70857471323609,
129.246474316501));
#225944=CARTESIAN_POINT('Ctrl Pts',(190.508666333098,-5.72932318152839,
129.326935003837));
#225945=CARTESIAN_POINT('Ctrl Pts',(190.498971765574,-5.78042706879116,
129.525111266141));
#225946=CARTESIAN_POINT('Ctrl Pts',(190.48927719805,-5.82126881850071,129.726034303134));
#225947=CARTESIAN_POINT('Ctrl Pts',(190.479582630525,-5.85160626396125,
129.928783839625));
#225948=CARTESIAN_POINT('Ctrl Pts',(190.470087632604,-5.88131919141924,
130.127359631965));
#225949=CARTESIAN_POINT('Ctrl Pts',(190.460592634683,-5.90095589270113,
130.327687736164));
#225950=CARTESIAN_POINT('Ctrl Pts',(190.451097636761,-5.91033348368092,
130.528881627115));
#225951=CARTESIAN_POINT('Ctrl Pts',(190.446856827631,-5.91452185462971,
130.618742088053));
#225952=CARTESIAN_POINT('Ctrl Pts',(190.4426160185,-5.9166642962425,130.708774942494));
#225953=CARTESIAN_POINT('Ctrl Pts',(190.438375209369,-5.91674747976679,
130.798899557834));
#225954=CARTESIAN_POINT('',(193.938375192211,-5.91196518873725,130.809243212275));
#225955=CARTESIAN_POINT('Ctrl Pts',(193.938375192211,-5.91196518873725,
130.809243212275));
#225956=CARTESIAN_POINT('Ctrl Pts',(193.908929401091,-5.91681433885312,
131.435864751108));
#225957=CARTESIAN_POINT('Ctrl Pts',(193.78666773537,-5.53611148477146,134.031915457605));
#225958=CARTESIAN_POINT('Ctrl Pts',(193.571590195038,-1.75782624092181,
137.578399843691));
#225959=CARTESIAN_POINT('Ctrl Pts',(193.293142571227,4.74904303118782,135.944803285106));
#225960=CARTESIAN_POINT('Ctrl Pts',(193.014694947413,6.89177376128537,129.587391039638));
#225961=CARTESIAN_POINT('Ctrl Pts',(192.736247323601,2.70130108662762,124.348314384016));
#225962=CARTESIAN_POINT('Ctrl Pts',(192.46080781812,-3.8994475031143,125.034534503354));
#225963=CARTESIAN_POINT('Ctrl Pts',(192.278184187244,-5.92103596021112,
128.906232297951));
#225964=CARTESIAN_POINT('Ctrl Pts',(192.188376430972,-5.92624401559878,
130.805522386918));
#225965=CARTESIAN_POINT('',(195.688375192211,-5.90858988324653,130.801212225252));
#225966=CARTESIAN_POINT('Ctrl Pts',(195.688375192211,-5.90858988324653,
130.801212225252));
#225967=CARTESIAN_POINT('Ctrl Pts',(195.632491315384,-5.90286694115081,
131.992156895353));
#225968=CARTESIAN_POINT('Ctrl Pts',(195.483791563953,-4.97462506172764,
135.169312250667));
#225969=CARTESIAN_POINT('Ctrl Pts',(195.242275937916,0.216039013678407,
137.799422280975));
#225970=CARTESIAN_POINT('Ctrl Pts',(194.963828314104,6.00191785180767,134.403602569768));
#225971=CARTESIAN_POINT('Ctrl Pts',(194.685380690291,6.27232739411319,127.70025533723));
#225972=CARTESIAN_POINT('Ctrl Pts',(194.406933066478,0.778774481457,123.849429213348));
#225973=CARTESIAN_POINT('Ctrl Pts',(194.157931233786,-4.77381132895269,
126.121196694781));
#225974=CARTESIAN_POINT('Ctrl Pts',(194.001745275696,-5.90152936629919,
129.46069533092));
#225975=CARTESIAN_POINT('Ctrl Pts',(193.938375192211,-5.91196518873725,
130.809243212275));
#225976=CARTESIAN_POINT('',(197.438375192211,-5.92351700154912,130.800613675003));
#225977=CARTESIAN_POINT('Ctrl Pts',(197.438375192211,-5.92351700154912,
130.800613675003));
#225978=CARTESIAN_POINT('Ctrl Pts',(197.356053229677,-5.91065473800382,
132.543712972427));
#225979=CARTESIAN_POINT('Ctrl Pts',(197.180915392537,-4.17421686252449,
136.274385756281));
#225980=CARTESIAN_POINT('Ctrl Pts',(196.912961680794,2.17250297652081,137.457013573142));
#225981=CARTESIAN_POINT('Ctrl Pts',(196.634514056981,6.77135626959459,132.57249375751));
#225982=CARTESIAN_POINT('Ctrl Pts',(196.356066433169,5.14766395005485,126.063145964373));
#225983=CARTESIAN_POINT('Ctrl Pts',(196.077618809355,-1.20648006222068,
123.910742816309));
#225984=CARTESIAN_POINT('Ctrl Pts',(195.85505506237,-5.39917704206329,127.253819372125));
#225985=CARTESIAN_POINT('Ctrl Pts',(195.725307189988,-5.91237200604756,
130.014152192806));
#225986=CARTESIAN_POINT('Ctrl Pts',(195.688375192211,-5.90858988324653,
130.801212225252));
#225987=CARTESIAN_POINT('',(199.188375192211,-5.92038509218979,130.80931765918));
#225988=CARTESIAN_POINT('Ctrl Pts',(199.188375192211,-5.92038509218979,
130.80931765918));
#225989=CARTESIAN_POINT('Ctrl Pts',(199.172431018573,-5.92341887942187,
131.147387550494));
#225990=CARTESIAN_POINT('Ctrl Pts',(199.06367097033,-5.7429796640639,133.450227209526));
#225991=CARTESIAN_POINT('Ctrl Pts',(198.862095047485,-2.72093855833704,
137.252155115847));
#225992=CARTESIAN_POINT('Ctrl Pts',(198.583647423671,3.9539783690358,136.578753710139));
#225993=CARTESIAN_POINT('Ctrl Pts',(198.305199799859,6.99538233784591,130.598967147137));
#225994=CARTESIAN_POINT('Ctrl Pts',(198.026752176046,3.60837168160217,124.807927149431));
#225995=CARTESIAN_POINT('Ctrl Pts',(197.748304552233,-3.09455627127803,
124.527316566881));
#225996=CARTESIAN_POINT('Ctrl Pts',(197.552178890954,-5.81278598755467,
128.392589611084));
#225997=CARTESIAN_POINT('Ctrl Pts',(197.448869104281,-5.92515660607875,
130.578413788211));
#225998=CARTESIAN_POINT('Ctrl Pts',(197.438375192211,-5.92351700154912,
130.800613675003));
#225999=CARTESIAN_POINT('',(200.938375192211,-5.90723919874194,130.805767413591));
#226000=CARTESIAN_POINT('Ctrl Pts',(200.938375192211,-5.90723919874194,
130.805767413591));
#226001=CARTESIAN_POINT('Ctrl Pts',(200.895992932866,-5.90915334356233,
131.70949422463));
#226002=CARTESIAN_POINT('Ctrl Pts',(200.760794798915,-5.28885804543136,
134.58986393661));
#226003=CARTESIAN_POINT('Ctrl Pts',(200.532780790362,-0.799939293036777,
137.756889485374));
#226004=CARTESIAN_POINT('Ctrl Pts',(200.254333166548,5.41697271486199,135.235383878266));
#226005=CARTESIAN_POINT('Ctrl Pts',(199.975885542736,6.65595143161651,128.641984362081));
#226006=CARTESIAN_POINT('Ctrl Pts',(199.697437918923,1.77843594402775,124.035702986741));
#226007=CARTESIAN_POINT('Ctrl Pts',(199.434934468748,-4.36050283967217,
125.557080494142));
#226008=CARTESIAN_POINT('Ctrl Pts',(199.265246893177,-5.90575828303711,
129.179380091958));
#226009=CARTESIAN_POINT('Ctrl Pts',(199.188375192211,-5.92038509218979,
130.80931765918));
#226010=CARTESIAN_POINT('',(202.688375192211,-5.91520709160217,130.79891930971));
#226011=CARTESIAN_POINT('Ctrl Pts',(202.688375192211,-5.91520709160217,
130.79891930971));
#226012=CARTESIAN_POINT('Ctrl Pts',(202.619554847158,-5.90204591476485,
132.26141930917));
#226013=CARTESIAN_POINT('Ctrl Pts',(202.457918627501,-4.61506249001968,
135.717037067151));
#226014=CARTESIAN_POINT('Ctrl Pts',(202.203466533238,1.18549267223545,137.701618597998));
#226015=CARTESIAN_POINT('Ctrl Pts',(201.925018909427,6.44364622673833,133.535108470905));
#226016=CARTESIAN_POINT('Ctrl Pts',(201.646571285612,5.78040368780743,126.859174470383));
#226017=CARTESIAN_POINT('Ctrl Pts',(201.368123661802,-0.194747451439191,
123.808673806412));
#226018=CARTESIAN_POINT('Ctrl Pts',(201.132058297333,-5.10870273655874,
126.672675766875));
#226019=CARTESIAN_POINT('Ctrl Pts',(200.98880880747,-5.90496142391559,129.730359660658));
#226020=CARTESIAN_POINT('Ctrl Pts',(200.938375192211,-5.90723919874194,
130.805767413591));
#226021=CARTESIAN_POINT('',(204.438375192211,-5.92105141345348,130.805327648265));
#226022=CARTESIAN_POINT('Ctrl Pts',(204.438375192211,-5.92634035306676,
130.805328512059));
#226023=CARTESIAN_POINT('Ctrl Pts',(204.435932636055,-5.9264572190019,130.856982408026));
#226024=CARTESIAN_POINT('Ctrl Pts',(204.433490079899,-5.92584057372106,
130.908633442257));
#226025=CARTESIAN_POINT('Ctrl Pts',(204.338231649138,-5.87285210044721,
132.922235594029));
#226026=CARTESIAN_POINT('Ctrl Pts',(204.152599899928,-3.62660601729001,
136.789783698913));
#226027=CARTESIAN_POINT('Ctrl Pts',(203.874152276118,3.07543675800755,137.09079434209));
#226028=CARTESIAN_POINT('Ctrl Pts',(203.595704652303,6.95130345427144,131.614879558226));
#226029=CARTESIAN_POINT('Ctrl Pts',(203.317257028491,4.43926183532277,125.394137434058));
#226030=CARTESIAN_POINT('Ctrl Pts',(203.038809404678,-2.1522445239837,124.145126127266));
#226031=CARTESIAN_POINT('Ctrl Pts',(202.829182125918,-5.62563427618384,
127.811846704057));
#226032=CARTESIAN_POINT('Ctrl Pts',(202.712370721762,-5.91979598762536,
130.288990713325));
#226033=CARTESIAN_POINT('Ctrl Pts',(202.688375192211,-5.91520709160217,
130.79891930971));
#226034=CARTESIAN_POINT('',(206.188375157422,-5.91500286463066,130.809335122326));
#226035=CARTESIAN_POINT('Ctrl Pts',(206.188375135149,-5.91674790721062,
130.80933706396));
#226036=CARTESIAN_POINT('Ctrl Pts',(206.179566065341,-5.91659014051484,
130.996913839284));
#226037=CARTESIAN_POINT('Ctrl Pts',(206.170756995534,-5.90750858188079,
131.184105581818));
#226038=CARTESIAN_POINT('Ctrl Pts',(206.161947925727,-5.88963571160845,
131.370153642484));
#226039=CARTESIAN_POINT('Ctrl Pts',(206.153074186251,-5.87163163195439,
131.557567530276));
#226040=CARTESIAN_POINT('Ctrl Pts',(206.144200446775,-5.84470678641371,
131.74382085212));
#226041=CARTESIAN_POINT('Ctrl Pts',(206.135326707299,-5.80904529038186,
131.928159254686));
#226042=CARTESIAN_POINT('Ctrl Pts',(206.126381804847,-5.77309780689119,
132.113975959543));
#226043=CARTESIAN_POINT('Ctrl Pts',(206.117436902394,-5.72827303913071,
132.297846882214));
#226044=CARTESIAN_POINT('Ctrl Pts',(206.108491999942,-5.67480770886274,
132.479021189124));
#226045=CARTESIAN_POINT('Ctrl Pts',(206.106239088835,-5.66134164402378,
132.524652721779));
#226046=CARTESIAN_POINT('Ctrl Pts',(206.103986177728,-5.64732768966758,
132.570113299786));
#226047=CARTESIAN_POINT('Ctrl Pts',(206.101733266621,-5.63277009911369,
132.615391145478));
#226048=CARTESIAN_POINT('Ctrl Pts',(206.094310026419,-5.58480349665586,
132.764579599188));
#226049=CARTESIAN_POINT('Ctrl Pts',(206.086886786216,-5.53083319938669,
132.91208669215));
#226050=CARTESIAN_POINT('Ctrl Pts',(206.079463546014,-5.47099418136574,
133.057392625763));
#226051=CARTESIAN_POINT('Ctrl Pts',(206.072049079851,-5.41122589119732,
133.202526812296));
#226052=CARTESIAN_POINT('Ctrl Pts',(206.064634613687,-5.34560282846522,
133.345464676374));
#226053=CARTESIAN_POINT('Ctrl Pts',(206.057220147523,-5.274309902267,133.485700882685));
#226054=CARTESIAN_POINT('Ctrl Pts',(206.049812828053,-5.20308569425869,
133.625801917405));
#226055=CARTESIAN_POINT('Ctrl Pts',(206.042405508582,-5.12620267075052,
133.763206148049));
#226056=CARTESIAN_POINT('Ctrl Pts',(206.034998189112,-5.04389400946855,
133.897427668851));
#226057=CARTESIAN_POINT('Ctrl Pts',(206.027596394619,-4.96164674063805,
134.031549076396));
#226058=CARTESIAN_POINT('Ctrl Pts',(206.020194600126,-4.87398208622341,
134.162492184038));
#226059=CARTESIAN_POINT('Ctrl Pts',(206.012792805633,-4.78117932515222,
134.289795285328));
#226060=CARTESIAN_POINT('Ctrl Pts',(206.005394918777,-4.68842555753051,
134.417031179371));
#226061=CARTESIAN_POINT('Ctrl Pts',(205.99799703192,-4.59053930480269,134.540630593273));
#226062=CARTESIAN_POINT('Ctrl Pts',(205.990599145064,-4.48784330175735,
134.660160542533));
#226063=CARTESIAN_POINT('Ctrl Pts',(205.983202487927,-4.38516436944237,
134.779670622824));
#226064=CARTESIAN_POINT('Ctrl Pts',(205.975805830791,-4.27767751662466,
134.895112298157));
#226065=CARTESIAN_POINT('Ctrl Pts',(205.968409173654,-4.16574599834706,
135.0060853634));
#226066=CARTESIAN_POINT('Ctrl Pts',(205.961012844691,-4.05381944622384,
135.117053505014));
#226067=CARTESIAN_POINT('Ctrl Pts',(205.953616515728,-3.93744888583708,
135.223553167924));
#226068=CARTESIAN_POINT('Ctrl Pts',(205.946220186765,-3.81703449993298,
135.325220954805));
#226069=CARTESIAN_POINT('Ctrl Pts',(205.938822725573,-3.69660168102824,
135.426904304962));
#226070=CARTESIAN_POINT('Ctrl Pts',(205.931425264382,-3.5721240892894,135.523754065483));
#226071=CARTESIAN_POINT('Ctrl Pts',(205.924027803191,-3.44403492469912,
135.61544718922));
#226072=CARTESIAN_POINT('Ctrl Pts',(205.916627748971,-3.31590086107405,
135.707172454105));
#226073=CARTESIAN_POINT('Ctrl Pts',(205.909227694752,-3.18415300742791,
135.793737266225));
#226074=CARTESIAN_POINT('Ctrl Pts',(205.901827640532,-3.04925332393586,
135.874862045331));
#226075=CARTESIAN_POINT('Ctrl Pts',(205.894419449247,-2.9142053053851,135.956076028864));
#226076=CARTESIAN_POINT('Ctrl Pts',(205.887011257962,-2.77599885578924,
136.031837840764));
#226077=CARTESIAN_POINT('Ctrl Pts',(205.879603066678,-2.63512094888712,
136.10191365149));
#226078=CARTESIAN_POINT('Ctrl Pts',(205.872190315849,-2.49415633539396,
136.172032592006));
#226079=CARTESIAN_POINT('Ctrl Pts',(205.864777565021,-2.35051732811826,
136.236458405575));
#226080=CARTESIAN_POINT('Ctrl Pts',(205.857364814192,-2.20471013894131,
136.295005731371));
#226081=CARTESIAN_POINT('Ctrl Pts',(205.849941471535,-2.05869461081846,
136.353636713455));
#226082=CARTESIAN_POINT('Ctrl Pts',(205.842518128878,-1.91050506407407,
136.406372307113));
#226083=CARTESIAN_POINT('Ctrl Pts',(205.835094786222,-1.76066288435223,
136.453077000087));
#226084=CARTESIAN_POINT('Ctrl Pts',(205.831158405083,-1.68120596618447,
136.477843130523));
#226085=CARTESIAN_POINT('Ctrl Pts',(205.827222023945,-1.60128453480154,
136.500914311524));
#226086=CARTESIAN_POINT('Ctrl Pts',(205.823285642806,-1.5209772722179,136.52227620805));
#226087=CARTESIAN_POINT('Ctrl Pts',(205.815862363887,-1.36953278846232,
136.562560751281));
#226088=CARTESIAN_POINT('Ctrl Pts',(205.808439084968,-1.21625774237482,
136.596885322964));
#226089=CARTESIAN_POINT('Ctrl Pts',(205.801015806049,-1.06166241873887,
136.625082520486));
#226090=CARTESIAN_POINT('Ctrl Pts',(205.793601300696,-0.907249811172222,
136.653246391767));
#226091=CARTESIAN_POINT('Ctrl Pts',(205.786186795344,-0.751520395763363,
136.675297237676));
#226092=CARTESIAN_POINT('Ctrl Pts',(205.778772289991,-0.594999279427515,
136.691117485314));
#226093=CARTESIAN_POINT('Ctrl Pts',(205.771364930901,-0.438629021562489,
136.706922485052));
#226094=CARTESIAN_POINT('Ctrl Pts',(205.76395757181,-0.281468950781068,
136.716508804378));
#226095=CARTESIAN_POINT('Ctrl Pts',(205.75655021272,-0.124053917183144,
136.719809982418));
#226096=CARTESIAN_POINT('Ctrl Pts',(205.749148378216,0.0332437125062621,
136.723108698361));
#226097=CARTESIAN_POINT('Ctrl Pts',(205.741746543712,0.190795554774945,
136.720131598888));
#226098=CARTESIAN_POINT('Ctrl Pts',(205.734344709207,0.348062200778197,
136.710864089747));
#226099=CARTESIAN_POINT('Ctrl Pts',(205.726946781988,0.505245828778614,
136.701601472745));
#226100=CARTESIAN_POINT('Ctrl Pts',(205.719548854768,0.662144188633564,
136.686055081083));
#226101=CARTESIAN_POINT('Ctrl Pts',(205.712150927548,0.818218547581937,
136.664262406068));
#226102=CARTESIAN_POINT('Ctrl Pts',(205.704754229649,0.97426697149117,136.642473352365));
#226103=CARTESIAN_POINT('Ctrl Pts',(205.697357531751,1.12949129690173,136.614440126908));
#226104=CARTESIAN_POINT('Ctrl Pts',(205.689960833853,1.28335846744775,136.580252029853));
#226105=CARTESIAN_POINT('Ctrl Pts',(205.682564463884,1.43721881635304,136.546065448514));
#226106=CARTESIAN_POINT('Ctrl Pts',(205.675168093915,1.5897217656208,136.505724619111));
#226107=CARTESIAN_POINT('Ctrl Pts',(205.667771723946,1.74034526633639,136.459369805573));
#226108=CARTESIAN_POINT('Ctrl Pts',(205.66037422154,1.89099182858503,136.413007894781));
#226109=CARTESIAN_POINT('Ctrl Pts',(205.652976719135,2.03975801251326,136.360630276258));
#226110=CARTESIAN_POINT('Ctrl Pts',(205.645579216729,2.18613787059475,136.30242680244));
#226111=CARTESIAN_POINT('Ctrl Pts',(205.63817912112,2.3325690423081,136.244202925325));
#226112=CARTESIAN_POINT('Ctrl Pts',(205.630779025511,2.47661187598612,136.180149264629));
#226113=CARTESIAN_POINT('Ctrl Pts',(205.623378929902,2.61778144864533,136.110503364386));
#226114=CARTESIAN_POINT('Ctrl Pts',(205.61597069717,2.75910625094721,136.040780881718));
#226115=CARTESIAN_POINT('Ctrl Pts',(205.608562464438,2.89755114766472,135.965454044387));
#226116=CARTESIAN_POINT('Ctrl Pts',(205.601154231705,3.03265618688166,135.884806170337));
#226117=CARTESIAN_POINT('Ctrl Pts',(205.593741439334,3.16784438091394,135.804108658914));
#226118=CARTESIAN_POINT('Ctrl Pts',(205.586328646963,3.29968830944655,135.718083788424));
#226119=CARTESIAN_POINT('Ctrl Pts',(205.578915854592,3.4277584000582,135.627057260869));
#226120=CARTESIAN_POINT('Ctrl Pts',(205.571492470601,3.55601148104427,135.535900671891));
#226121=CARTESIAN_POINT('Ctrl Pts',(205.56406908661,3.68047966012121,135.439728380284));
#226122=CARTESIAN_POINT('Ctrl Pts',(205.55664570262,3.80076710215312,135.338905798473));
#226123=CARTESIAN_POINT('Ctrl Pts',(205.552709808078,3.86454376885181,135.285449443535));
#226124=CARTESIAN_POINT('Ctrl Pts',(205.548773913536,3.92714579463605,135.230686447014));
#226125=CARTESIAN_POINT('Ctrl Pts',(205.544838018994,3.98851860995265,135.174675235595));
#226126=CARTESIAN_POINT('Ctrl Pts',(205.537414752403,4.10427038243128,135.069035678946));
#226127=CARTESIAN_POINT('Ctrl Pts',(205.529991485813,4.21599734533866,134.958634520244));
#226128=CARTESIAN_POINT('Ctrl Pts',(205.522568219222,4.32328283706097,134.843810589193));
#226129=CARTESIAN_POINT('Ctrl Pts',(205.515153726284,4.43044152670348,134.729122369998));
#226130=CARTESIAN_POINT('Ctrl Pts',(205.507739233346,4.53316894181514,134.610022053583));
#226131=CARTESIAN_POINT('Ctrl Pts',(205.500324740408,4.63108233208609,134.486887874212));
#226132=CARTESIAN_POINT('Ctrl Pts',(205.492917393806,4.7289013501625,134.363872375674));
#226133=CARTESIAN_POINT('Ctrl Pts',(205.485510047204,4.82191534978399,134.236831044588));
#226134=CARTESIAN_POINT('Ctrl Pts',(205.478102700602,4.90977931610782,134.106177939833));
#226135=CARTESIAN_POINT('Ctrl Pts',(205.470700878647,4.99757775054161,133.975622280541));
#226136=CARTESIAN_POINT('Ctrl Pts',(205.463299056693,5.08023359234056,133.841460519697));
#226137=CARTESIAN_POINT('Ctrl Pts',(205.455897234738,5.15744299933014,133.704138586853));
#226138=CARTESIAN_POINT('Ctrl Pts',(205.448499320116,5.23461164839757,133.566889144614));
#226139=CARTESIAN_POINT('Ctrl Pts',(205.441101405494,5.30633940608169,133.426483177278));
#226140=CARTESIAN_POINT('Ctrl Pts',(205.433703490873,5.37236661664779,133.283394199192));
#226141=CARTESIAN_POINT('Ctrl Pts',(205.426306805605,5.4383828550952,133.140328999019));
#226142=CARTESIAN_POINT('Ctrl Pts',(205.418910120337,5.49870027026613,132.994582011598));
#226143=CARTESIAN_POINT('Ctrl Pts',(205.411513435069,5.55310586287155,132.846649979591));
#226144=CARTESIAN_POINT('Ctrl Pts',(205.40411707775,5.60750904328352,132.698724506482));
#226145=CARTESIAN_POINT('Ctrl Pts',(205.396720720431,5.6560007934494,132.548614531768));
#226146=CARTESIAN_POINT('Ctrl Pts',(205.389324363111,5.6984169411165,132.396835084456));
#226147=CARTESIAN_POINT('Ctrl Pts',(205.381926873363,5.74083958296442,132.245032398749));
#226148=CARTESIAN_POINT('Ctrl Pts',(205.374529383615,5.77718466965693,132.091560091043));
#226149=CARTESIAN_POINT('Ctrl Pts',(205.367131893866,5.80733845234025,131.936946447634));
#226150=CARTESIAN_POINT('Ctrl Pts',(205.359731810911,5.83750280549823,131.782278604073));
#226151=CARTESIAN_POINT('Ctrl Pts',(205.352331727957,5.8614714620337,131.626468994384));
#226152=CARTESIAN_POINT('Ctrl Pts',(205.344931645002,5.87918216165979,131.470053994821));
#226153=CARTESIAN_POINT('Ctrl Pts',(205.337523424855,5.89691233611661,131.313467000041));
#226154=CARTESIAN_POINT('Ctrl Pts',(205.330115204709,5.90837076922905,131.156273657112));
#226155=CARTESIAN_POINT('Ctrl Pts',(205.322706984562,5.91354720906745,130.999014075358));
#226156=CARTESIAN_POINT('Ctrl Pts',(205.315294204756,5.91872683493454,130.84165770246));
#226157=CARTESIAN_POINT('Ctrl Pts',(205.30788142495,5.91761676570394,130.684235381923));
#226158=CARTESIAN_POINT('Ctrl Pts',(205.300468645144,5.91025882921648,130.527284573548));
#226159=CARTESIAN_POINT('Ctrl Pts',(205.293045273578,5.90289037933228,130.370109505815));
#226160=CARTESIAN_POINT('Ctrl Pts',(205.285621902013,5.88925626469626,130.213407666724));
#226161=CARTESIAN_POINT('Ctrl Pts',(205.278198530447,5.86944995847761,130.057709596387));
#226162=CARTESIAN_POINT('Ctrl Pts',(205.274262485358,5.85894819204549,129.975154840818));
#226163=CARTESIAN_POINT('Ctrl Pts',(205.270326440269,5.84671205599,129.892882092421));
#226164=CARTESIAN_POINT('Ctrl Pts',(205.266390395181,5.8327612125786,129.810968852179));
#226165=CARTESIAN_POINT('Ctrl Pts',(205.258967132391,5.80645034102074,129.656482941948));
#226166=CARTESIAN_POINT('Ctrl Pts',(205.251543869601,5.77395789796265,129.502809451314));
#226167=CARTESIAN_POINT('Ctrl Pts',(205.244120606812,5.73534373383937,129.350482074768));
#226168=CARTESIAN_POINT('Ctrl Pts',(205.236706117758,5.69677520874019,129.198334737669));
#226169=CARTESIAN_POINT('Ctrl Pts',(205.229291628704,5.65209945553443,129.047530706073));
#226170=CARTESIAN_POINT('Ctrl Pts',(205.22187713965,5.60142780672731,128.898596443141));
#226171=CARTESIAN_POINT('Ctrl Pts',(205.214469797011,5.55080499751139,128.749805729682));
#226172=CARTESIAN_POINT('Ctrl Pts',(205.207062454371,5.49419791719723,128.602881548161));
#226173=CARTESIAN_POINT('Ctrl Pts',(205.199655111732,5.43176843551374,128.458337977979));
#226174=CARTESIAN_POINT('Ctrl Pts',(205.192253293815,5.36938551648445,128.313902214751));
#226175=CARTESIAN_POINT('Ctrl Pts',(205.184851475898,5.30118899017215,128.171843868699));
#226176=CARTESIAN_POINT('Ctrl Pts',(205.17744965798,5.22738979486144,128.03265960644));
#226177=CARTESIAN_POINT('Ctrl Pts',(205.170051747467,5.15362955798969,127.893548819258));
#226178=CARTESIAN_POINT('Ctrl Pts',(205.162653836954,5.07427271682429,127.757309423218));
#226179=CARTESIAN_POINT('Ctrl Pts',(205.155255926441,4.98957730139766,127.624415819951));
#226180=CARTESIAN_POINT('Ctrl Pts',(205.147859245375,4.90489596136757,127.491544302061));
#226181=CARTESIAN_POINT('Ctrl Pts',(205.140462564308,4.81487800835612,127.362017787878));
#226182=CARTESIAN_POINT('Ctrl Pts',(205.133065883242,4.7198262340098,127.236283981162));
#226183=CARTESIAN_POINT('Ctrl Pts',(205.125669530182,4.62477867473806,127.110555750117));
#226184=CARTESIAN_POINT('Ctrl Pts',(205.118273177122,4.52469796309431,126.988620189907));
#226185=CARTESIAN_POINT('Ctrl Pts',(205.110876824062,4.41992866778351,126.870893808985));
#226186=CARTESIAN_POINT('Ctrl Pts',(205.103479338627,4.31514333238748,126.753149404261));
#226187=CARTESIAN_POINT('Ctrl Pts',(205.096081853192,4.20566823223877,126.639615740833));
#226188=CARTESIAN_POINT('Ctrl Pts',(205.088684367756,4.0918863448901,126.53067407045));
#226189=CARTESIAN_POINT('Ctrl Pts',(205.081284289166,3.97806457180816,126.42169421105));
#226190=CARTESIAN_POINT('Ctrl Pts',(205.073884210575,3.85993327514114,126.317309807603));
#226191=CARTESIAN_POINT('Ctrl Pts',(205.066484131984,3.73791006961344,126.217863165917));
#226192=CARTESIAN_POINT('Ctrl Pts',(205.059075916258,3.61575268720724,126.118307172572));
#226193=CARTESIAN_POINT('Ctrl Pts',(205.051667700531,3.48969513894966,126.02370002017));
#226194=CARTESIAN_POINT('Ctrl Pts',(205.044259484804,3.36018629211852,125.93434227625));
#226195=CARTESIAN_POINT('Ctrl Pts',(205.036846709456,3.23059773496496,125.844929534275));
#226196=CARTESIAN_POINT('Ctrl Pts',(205.029433934108,3.09755396123104,125.76077283788));
#226197=CARTESIAN_POINT('Ctrl Pts',(205.02202115876,2.9615297594948,125.682127506302));
#226198=CARTESIAN_POINT('Ctrl Pts',(205.014597791674,2.82531119969063,125.603369802408));
#226199=CARTESIAN_POINT('Ctrl Pts',(205.007174424588,2.68610403603951,125.530139364625));
#226200=CARTESIAN_POINT('Ctrl Pts',(204.999751057502,2.5444051509773,125.462644321264));
#226201=CARTESIAN_POINT('Ctrl Pts',(204.995814962124,2.46927208532876,125.42685639307));
#226202=CARTESIAN_POINT('Ctrl Pts',(204.991878866746,2.39343879236606,125.39268011218));
#226203=CARTESIAN_POINT('Ctrl Pts',(204.987942771368,2.31698110677334,125.360140828344));
#226204=CARTESIAN_POINT('Ctrl Pts',(204.980519502944,2.17278594159917,125.298773454077));
#226205=CARTESIAN_POINT('Ctrl Pts',(204.97309623452,2.02593299682858,125.243045954815));
#226206=CARTESIAN_POINT('Ctrl Pts',(204.965672966097,1.87690363642786,125.193196451186));
#226207=CARTESIAN_POINT('Ctrl Pts',(204.958258471337,1.7280504158966,125.143405865378));
#226208=CARTESIAN_POINT('Ctrl Pts',(204.950843976577,1.57702625054469,125.099479563857));
#226209=CARTESIAN_POINT('Ctrl Pts',(204.943429481818,1.42433424764934,125.061608445177));
#226210=CARTESIAN_POINT('Ctrl Pts',(204.936022133407,1.27178941463677,125.023773828004));
#226211=CARTESIAN_POINT('Ctrl Pts',(204.928614784996,1.11758030422428,124.991982864216));
#226212=CARTESIAN_POINT('Ctrl Pts',(204.921207436585,0.962226921405626,
124.966377240215));
#226213=CARTESIAN_POINT('Ctrl Pts',(204.913805612837,0.80698940662729,124.940790713794));
#226214=CARTESIAN_POINT('Ctrl Pts',(204.906403789088,0.650609685497499,
124.921380402016));
#226215=CARTESIAN_POINT('Ctrl Pts',(204.899001965339,0.493619635819424,
124.908237296465));
#226216=CARTESIAN_POINT('Ctrl Pts',(204.89160404894,0.336712459641496,124.89510112903));
#226217=CARTESIAN_POINT('Ctrl Pts',(204.884206132541,0.179195967619653,
124.888225610057));
#226218=CARTESIAN_POINT('Ctrl Pts',(204.876808216143,0.0216087595666902,
124.887650076733));
#226219=CARTESIAN_POINT('Ctrl Pts',(204.869411529128,-0.135952260670864,
124.88707463905));
#226220=CARTESIAN_POINT('Ctrl Pts',(204.862014842114,-0.293583600686453,
124.89279711053));
#226221=CARTESIAN_POINT('Ctrl Pts',(204.854618155099,-0.450744927651624,
124.90480473829));
#226222=CARTESIAN_POINT('Ctrl Pts',(204.847221796053,-0.607899286109743,
124.916811833635));
#226223=CARTESIAN_POINT('Ctrl Pts',(204.839825437006,-0.764583300742472,
124.935103502707));
#226224=CARTESIAN_POINT('Ctrl Pts',(204.83242907796,-0.920260302747,124.95961498258));
#226225=CARTESIAN_POINT('Ctrl Pts',(204.825031586505,-1.07596113944049,
124.984130215246));
#226226=CARTESIAN_POINT('Ctrl Pts',(204.81763409505,-1.23065428774014,125.014867096753));
#226227=CARTESIAN_POINT('Ctrl Pts',(204.810236603595,-1.38381198042967,
125.051709492622));
#226228=CARTESIAN_POINT('Ctrl Pts',(204.802836518957,-1.53702336240519,
125.088564803558));
#226229=CARTESIAN_POINT('Ctrl Pts',(204.795436434318,-1.68869785439576,
125.131529802889));
#226230=CARTESIAN_POINT('Ctrl Pts',(204.78803634968,-1.83832173330245,125.180438163676));
#226231=CARTESIAN_POINT('Ctrl Pts',(204.780628127893,-1.98811013894526,
125.229400304201));
#226232=CARTESIAN_POINT('Ctrl Pts',(204.773219906105,-2.13584307336326,
125.284318741618));
#226233=CARTESIAN_POINT('Ctrl Pts',(204.765811684318,-2.2810250362999,125.344978294787));
#226234=CARTESIAN_POINT('Ctrl Pts',(204.758398902893,-2.42629635631982,
125.405675182902));
#226235=CARTESIAN_POINT('Ctrl Pts',(204.750986121469,-2.56901323864276,
125.47212007064));
#226236=CARTESIAN_POINT('Ctrl Pts',(204.743573340044,-2.70870424060689,
125.544051510734));
#226237=CARTESIAN_POINT('Ctrl Pts',(204.736149966909,-2.84859483927297,
125.616085729662));
#226238=CARTESIAN_POINT('Ctrl Pts',(204.728726593773,-2.98545059862428,
125.693621974519));
#226239=CARTESIAN_POINT('Ctrl Pts',(204.721303220637,-3.11882783680492,
125.77635470201));
#226240=CARTESIAN_POINT('Ctrl Pts',(204.717367196277,-3.18954717814477,
125.820221287307));
#226241=CARTESIAN_POINT('Ctrl Pts',(204.713431171916,-3.25928911964002,
125.865548075032));
#226242=CARTESIAN_POINT('Ctrl Pts',(204.709495147555,-3.3279913467505,125.912284968268));
#226243=CARTESIAN_POINT('Ctrl Pts',(204.702104411593,-3.45699461857756,
126.000043580996));
#226244=CARTESIAN_POINT('Ctrl Pts',(204.694713675631,-3.58272775527118,
126.093046915379));
#226245=CARTESIAN_POINT('Ctrl Pts',(204.68732293967,-3.70473253445668,126.191022627494));
#226246=CARTESIAN_POINT('Ctrl Pts',(204.679940958213,-3.82659279604236,
126.288882285019));
#226247=CARTESIAN_POINT('Ctrl Pts',(204.672558976756,-3.94473319850045,
126.391702364622));
#226248=CARTESIAN_POINT('Ctrl Pts',(204.665176995299,-4.05872330506565,
126.499166580659));
#226249=CARTESIAN_POINT('Ctrl Pts',(204.657802110667,-4.17260382482097,
126.60652748369));
#226250=CARTESIAN_POINT('Ctrl Pts',(204.650427226035,-4.28234171832161,
126.71852337928));
#226251=CARTESIAN_POINT('Ctrl Pts',(204.643052341403,-4.38753867962024,
126.83479705247));
#226252=CARTESIAN_POINT('Ctrl Pts',(204.635682901836,-4.49265797131831,
126.950984877841));
#226253=CARTESIAN_POINT('Ctrl Pts',(204.628313462269,-4.59324275370197,
127.071443914587));
#226254=CARTESIAN_POINT('Ctrl Pts',(204.620944022703,-4.68893086223868,
127.195779465417));
#226255=CARTESIAN_POINT('Ctrl Pts',(204.613336988099,-4.78770401129907,
127.324123667047));
#226256=CARTESIAN_POINT('Ctrl Pts',(204.605729953495,-4.88125914129115,
127.45659826124));
#226257=CARTESIAN_POINT('Ctrl Pts',(204.598122918891,-4.96924186267879,
127.592730833064));
#226258=CARTESIAN_POINT('Ctrl Pts',(204.590758398115,-5.05441967681546,
127.724523470504));
#226259=CARTESIAN_POINT('Ctrl Pts',(204.583393877339,-5.13437472757324,
127.859744080796));
#226260=CARTESIAN_POINT('Ctrl Pts',(204.576029356562,-5.20882895299715,
127.997933796692));
#226261=CARTESIAN_POINT('Ctrl Pts',(204.568664962593,-5.283281896423,128.136121133155));
#226262=CARTESIAN_POINT('Ctrl Pts',(204.561300568623,-5.35223402382612,
128.277277141798));
#226263=CARTESIAN_POINT('Ctrl Pts',(204.553936174654,-5.41545310427121,
128.420918099287));
#226264=CARTESIAN_POINT('Ctrl Pts',(204.54657042013,-5.47868386429348,128.564585594107));
#226265=CARTESIAN_POINT('Ctrl Pts',(204.539204665606,-5.53617931718692,
128.710738606591));
#226266=CARTESIAN_POINT('Ctrl Pts',(204.531838911082,-5.58775535548524,
128.858873365039));
#226267=CARTESIAN_POINT('Ctrl Pts',(204.524470308052,-5.63935133941324,
129.007065410574));
#226268=CARTESIAN_POINT('Ctrl Pts',(204.517101705023,-5.68502322819046,
129.157240371933));
#226269=CARTESIAN_POINT('Ctrl Pts',(204.509733101994,-5.7246368129675,129.308879450143));
#226270=CARTESIAN_POINT('Ctrl Pts',(204.502356410778,-5.76429387980796,
129.460684975799));
#226271=CARTESIAN_POINT('Ctrl Pts',(204.494979719562,-5.79787927133109,
129.613957462062));
#226272=CARTESIAN_POINT('Ctrl Pts',(204.487603028346,-5.82530980176946,
129.768167452221));
#226273=CARTESIAN_POINT('Ctrl Pts',(204.480221494494,-5.85275833974991,
129.922478677858));
#226274=CARTESIAN_POINT('Ctrl Pts',(204.472839960642,-5.87404391676752,
130.077728261269));
#226275=CARTESIAN_POINT('Ctrl Pts',(204.465458426791,-5.88913528604936,
130.233382382334));
#226276=CARTESIAN_POINT('Ctrl Pts',(204.458067024258,-5.90424683161207,
130.389244603885));
#226277=CARTESIAN_POINT('Ctrl Pts',(204.450675621726,-5.91314761819259,
130.545512068223));
#226278=CARTESIAN_POINT('Ctrl Pts',(204.443284219194,-5.91585846087386,
130.701651156428));
#226279=CARTESIAN_POINT('Ctrl Pts',(204.441647876866,-5.91645859956244,
130.736217938293));
#226280=CARTESIAN_POINT('Ctrl Pts',(204.440011534539,-5.91675556357633,
130.770778450004));
#226281=CARTESIAN_POINT('Ctrl Pts',(204.438375192211,-5.91674992108927,
130.805326945742));
#226282=CARTESIAN_POINT('',(207.300060471638,3.90699806772732,135.242283170684));
#226283=CARTESIAN_POINT('Ctrl Pts',(207.300060471638,3.90699806772668,135.242283170685));
#226284=CARTESIAN_POINT('Ctrl Pts',(207.271881568382,4.36049763724443,134.850189658193));
#226285=CARTESIAN_POINT('Ctrl Pts',(207.150886790522,6.05211717572361,132.884390582407));
#226286=CARTESIAN_POINT('Ctrl Pts',(206.937076138059,6.29112482667552,127.7385118325));
#226287=CARTESIAN_POINT('Ctrl Pts',(206.658628514245,0.821087121814331,
123.854289400871));
#226288=CARTESIAN_POINT('Ctrl Pts',(206.409061532297,-4.75784521223805,
126.09730669271));
#226289=CARTESIAN_POINT('Ctrl Pts',(206.252310424952,-5.90151704252715,
129.448939722285));
#226290=CARTESIAN_POINT('Ctrl Pts',(206.188375192211,-5.91227720962736,
130.809332089608));
#226291=CARTESIAN_POINT('Ctrl Pts',(207.097092794244,3.07160564976241,135.861352736884));
#226292=CARTESIAN_POINT('Ctrl Pts',(207.16165438619,3.37382896112027,135.677782976688));
#226293=CARTESIAN_POINT('Ctrl Pts',(207.23109396594,3.65610320797724,135.468837830569));
#226294=CARTESIAN_POINT('Ctrl Pts',(207.299797282174,3.91217312619061,135.243147838555));
#226295=CARTESIAN_POINT('Origin',(210.,0.,130.804360617566));
#226296=CARTESIAN_POINT('',(207.956496781212,-5.9049774143355,130.419651541055));
#226297=CARTESIAN_POINT('Ctrl Pts',(207.794825763995,-5.47599840541864,
128.563518805578));
#226298=CARTESIAN_POINT('Ctrl Pts',(207.883706865838,-5.72070422757077,
129.161512240337));
#226299=CARTESIAN_POINT('Ctrl Pts',(207.940449287037,-5.86515699931026,
129.80416200646));
#226300=CARTESIAN_POINT('Ctrl Pts',(207.955834607772,-5.90485866211524,
130.429427632964));
#226301=CARTESIAN_POINT('',(207.851560096186,-5.62714347058183,132.623000814592));
#226302=CARTESIAN_POINT('Ctrl Pts',(207.851491355655,-5.63013302498849,
132.623572722691));
#226303=CARTESIAN_POINT('Ctrl Pts',(207.832959583949,-5.58032197094584,
132.77772894207));
#226304=CARTESIAN_POINT('Ctrl Pts',(207.812258447827,-5.52411769153045,
132.929986067143));
#226305=CARTESIAN_POINT('Ctrl Pts',(207.709562033561,-5.24073952453561,
133.610284849743));
#226306=CARTESIAN_POINT('Ctrl Pts',(207.605087833971,-4.94084622400808,
134.106396899339));
#226307=CARTESIAN_POINT('Ctrl Pts',(207.49642148088,-4.59106392006869,134.53666053107));
#226308=CARTESIAN_POINT('',(207.938375235231,-5.91423241434992,130.80143089854));
#226309=CARTESIAN_POINT('Ctrl Pts',(207.938375192211,-5.90834445110727,
130.801434732496));
#226310=CARTESIAN_POINT('Ctrl Pts',(207.909436826869,-5.90555594570905,
131.418178106961));
#226311=CARTESIAN_POINT('Ctrl Pts',(207.880498461528,-5.81083010793395,
132.035697025576));
#226312=CARTESIAN_POINT('Ctrl Pts',(207.851560096186,-5.62714347058182,
132.623000814592));
#226313=CARTESIAN_POINT('Ctrl Pts',(207.956549707745,-5.9038746591298,130.414239390529));
#226314=CARTESIAN_POINT('Ctrl Pts',(207.95049155637,-5.91238172765814,130.542980568468));
#226315=CARTESIAN_POINT('Ctrl Pts',(207.944433404995,-5.91668521597131,
130.672132721857));
#226316=CARTESIAN_POINT('Ctrl Pts',(207.938375253621,-5.91674927385308,
130.801429259683));
#226317=CARTESIAN_POINT('Ctrl Pts',(210.579426101437,-2.14555810197798,
126.384433368448));
#226318=CARTESIAN_POINT('Ctrl Pts',(210.533016425084,-2.88204635455982,
126.741945114569));
#226319=CARTESIAN_POINT('Ctrl Pts',(210.440198811428,-4.16073755837059,
127.832228156677));
#226320=CARTESIAN_POINT('Ctrl Pts',(210.254565323169,-5.41774734084591,
130.983824311839));
#226321=CARTESIAN_POINT('Ctrl Pts',(210.022525636658,-3.70466367662459,
135.280954889074));
#226322=CARTESIAN_POINT('Ctrl Pts',(209.744078012845,1.77278938863763,136.341871604603));
#226323=CARTESIAN_POINT('Ctrl Pts',(209.465630389032,5.61248518735455,132.305536381355));
#226324=CARTESIAN_POINT('Ctrl Pts',(209.187182765219,4.2990952821384,126.894094626803));
#226325=CARTESIAN_POINT('Ctrl Pts',(208.908735141406,-0.967335548355457,
125.073681250508));
#226326=CARTESIAN_POINT('Ctrl Pts',(208.630287517594,-5.34357155608916,
128.520706403956));
#226327=CARTESIAN_POINT('Ctrl Pts',(208.351839893781,-4.80999390579215,
134.065650134797));
#226328=CARTESIAN_POINT('Ctrl Pts',(208.073392269968,0.144086686833323,
136.613971320579));
#226329=CARTESIAN_POINT('Ctrl Pts',(207.794944646155,4.96557142732685,133.823362329787));
#226330=CARTESIAN_POINT('Ctrl Pts',(207.516497022342,5.22403776314189,128.258534510045));
#226331=CARTESIAN_POINT('Ctrl Pts',(207.238049398529,0.681816090004523,
125.033145533949));
#226332=CARTESIAN_POINT('Ctrl Pts',(206.959601774716,-4.48693345015888,
127.111248278652));
#226333=CARTESIAN_POINT('Ctrl Pts',(206.681154150904,-5.53242507739068,
132.583126545744));
#226334=CARTESIAN_POINT('Ctrl Pts',(206.40270652709,-1.49388053201802,136.420413394932));
#226335=CARTESIAN_POINT('Ctrl Pts',(206.124258903278,3.91746311099657,135.0968180907));
#226336=CARTESIAN_POINT('Ctrl Pts',(205.845811279465,5.72885172159717,129.828666190814));
#226337=CARTESIAN_POINT('Ctrl Pts',(205.567363655652,2.27570431130586,125.457128678938));
#226338=CARTESIAN_POINT('Ctrl Pts',(205.288916031839,-3.26870357308214,
125.999436687584));
#226339=CARTESIAN_POINT('Ctrl Pts',(205.010468408026,-5.80933288384994,
130.9572347388));
#226340=CARTESIAN_POINT('Ctrl Pts',(204.732020784213,-3.01146890392974,
135.774549108008));
#226341=CARTESIAN_POINT('Ctrl Pts',(204.4535731604,2.5537877891123,136.024502973214));
#226342=CARTESIAN_POINT('Ctrl Pts',(204.175125536587,5.77223831170541,131.477401078575));
#226343=CARTESIAN_POINT('Ctrl Pts',(203.896677912775,3.6862837897924,126.311807855303));
#226344=CARTESIAN_POINT('Ctrl Pts',(203.618230288961,-1.78718543642468,
125.274651160291));
#226345=CARTESIAN_POINT('Ctrl Pts',(203.339782665149,-5.61831856260093,
129.319027308227));
#226346=CARTESIAN_POINT('Ctrl Pts',(203.061335041336,-4.28649139606962,
134.728352208566));
#226347=CARTESIAN_POINT('Ctrl Pts',(202.782887417523,0.984411954691954,
136.531720532469));
#226348=CARTESIAN_POINT('Ctrl Pts',(202.50443979371,5.3506888113544,133.071924892697));
#226349=CARTESIAN_POINT('Ctrl Pts',(202.225992169897,4.79994404549834,127.528348460205));
#226350=CARTESIAN_POINT('Ctrl Pts',(201.947544546084,-0.161714807569177,
124.995267158526));
#226351=CARTESIAN_POINT('Ctrl Pts',(201.669096922271,-4.97476565284641,
127.800458955558));
#226352=CARTESIAN_POINT('Ctrl Pts',(201.390649298458,-5.21624989388704,
133.366089631302));
#226353=CARTESIAN_POINT('Ctrl Pts',(201.112201674645,-0.664255310463968,
136.577616490799));
#226354=CARTESIAN_POINT('Ctrl Pts',(200.833754050833,4.49815745262305,134.483803242045));
#226355=CARTESIAN_POINT('Ctrl Pts',(200.55530642702,5.52698326394509,129.008761972148));
#226356=CARTESIAN_POINT('Ctrl Pts',(200.276858803207,1.47678146385132,125.183788137525));
#226357=CARTESIAN_POINT('Ctrl Pts',(199.998411179394,-3.93051035674001,
126.523845831826));
#226358=CARTESIAN_POINT('Ctrl Pts',(199.719963555581,-5.7258551755912,131.79748749945));
#226359=CARTESIAN_POINT('Ctrl Pts',(199.441515931768,-2.25941881165118,
136.158494079568));
#226360=CARTESIAN_POINT('Ctrl Pts',(199.163068307955,3.28331306145151,135.599313572066));
#226361=CARTESIAN_POINT('Ctrl Pts',(198.884620684142,5.80884062984016,130.633805545853));
#226362=CARTESIAN_POINT('Ctrl Pts',(198.606173060329,2.99632743704681,125.825029298466));
#226363=CARTESIAN_POINT('Ctrl Pts',(198.327725436517,-2.56966429165962,
125.592015279473));
#226364=CARTESIAN_POINT('Ctrl Pts',(198.049277812704,-5.77426007141042,
130.148891988961));
#226365=CARTESIAN_POINT('Ctrl Pts',(197.770830188891,-3.6725929338218,135.308112346714));
#226366=CARTESIAN_POINT('Ctrl Pts',(197.492382565078,1.80400769380988,136.328604885883));
#226367=CARTESIAN_POINT('Ctrl Pts',(197.213934941265,5.62281338150559,132.272586816804));
#226368=CARTESIAN_POINT('Ctrl Pts',(196.935487317452,4.27452826130232,126.867340597462));
#226369=CARTESIAN_POINT('Ctrl Pts',(196.657039693639,-1.00183950872307,
125.080023442474));
#226370=CARTESIAN_POINT('Ctrl Pts',(196.378592069827,-5.35756571281285,
128.553092501978));
#226371=CARTESIAN_POINT('Ctrl Pts',(196.100144446013,-4.78995075846325,
134.094966979145));
#226372=CARTESIAN_POINT('Ctrl Pts',(195.821696822201,0.179394940810534,
136.612934965078));
#226373=CARTESIAN_POINT('Ctrl Pts',(195.543249198387,4.98388545340951,133.79310689028));
#226374=CARTESIAN_POINT('Ctrl Pts',(195.264801574575,5.20842871066526,128.22676699923));
#226375=CARTESIAN_POINT('Ctrl Pts',(194.986353950762,0.64668042870769,125.029109720981));
#226376=CARTESIAN_POINT('Ctrl Pts',(194.70790632695,-4.50933557513701,127.138625880003));
#226377=CARTESIAN_POINT('Ctrl Pts',(194.429458703136,-5.52149247872048,
132.616773181746));
#226378=CARTESIAN_POINT('Ctrl Pts',(194.151011079324,-1.4596675342632,136.429401878284));
#226379=CARTESIAN_POINT('Ctrl Pts',(193.87256345551,3.9435205654586,135.072892454764));
#226380=CARTESIAN_POINT('Ctrl Pts',(193.594115831698,5.72280591721378,129.793810802232));
#226381=CARTESIAN_POINT('Ctrl Pts',(193.315668207884,2.24311220566103,125.443375061888));
#226382=CARTESIAN_POINT('Ctrl Pts',(193.037220584072,-3.29789204077089,
126.019423148508));
#226383=CARTESIAN_POINT('Ctrl Pts',(192.758772960259,-5.80829461271728,
130.992595012001));
#226384=CARTESIAN_POINT('Ctrl Pts',(192.480325336446,-2.98115818654302,
135.792788662769));
#226385=CARTESIAN_POINT('Ctrl Pts',(192.201877712633,2.58551697539033,136.008860638253));
#226386=CARTESIAN_POINT('Ctrl Pts',(191.92343008882,5.77622834646622,131.442251348686));
#226387=CARTESIAN_POINT('Ctrl Pts',(191.644982465007,3.658868051582,126.289451639914));
#226388=CARTESIAN_POINT('Ctrl Pts',(191.366534841194,-1.82081323706467,
125.285632716038));
#226389=CARTESIAN_POINT('Ctrl Pts',(191.088087217381,-5.6272561125207,129.35325512882));
#226390=CARTESIAN_POINT('Ctrl Pts',(190.809639593569,-4.26252552731426,
134.754372595315));
#226391=CARTESIAN_POINT('Ctrl Pts',(190.531191969755,1.01925778154541,136.525622023071));
#226392=CARTESIAN_POINT('Ctrl Pts',(190.252744345943,5.36439298267566,133.039311718326));
#226393=CARTESIAN_POINT('Ctrl Pts',(189.974296722129,4.77991309789331,127.499190535413));
#226394=CARTESIAN_POINT('Ctrl Pts',(189.695849098317,-0.197073412116412,
124.996359191464));
#226395=CARTESIAN_POINT('Ctrl Pts',(189.417401474504,-4.99295908396257,
127.830797421458));
#226396=CARTESIAN_POINT('Ctrl Pts',(189.138953850692,-5.20055927725872,
133.397794962038));
#226397=CARTESIAN_POINT('Ctrl Pts',(188.860506226878,-0.629099556198964,
136.581553036358));
#226398=CARTESIAN_POINT('Ctrl Pts',(188.582058603065,4.52047192378579,134.456353509349));
#226399=CARTESIAN_POINT('Ctrl Pts',(188.303610979253,5.51595054314194,128.975150924561));
#226400=CARTESIAN_POINT('Ctrl Pts',(188.02516335544,1.44254008251539,125.174902685784));
#226401=CARTESIAN_POINT('Ctrl Pts',(187.746715731627,-3.95649424194195,
126.547851272005));
#226402=CARTESIAN_POINT('Ctrl Pts',(187.468268107814,-5.71970364354381,
131.832324004755));
#226403=CARTESIAN_POINT('Ctrl Pts',(187.189820484001,-2.22678481978599,
136.172148603481));
#226404=CARTESIAN_POINT('Ctrl Pts',(186.911372860188,3.312440468869,135.579238274173));
#226405=CARTESIAN_POINT('Ctrl Pts',(186.632925236375,5.80769478834652,130.598448644184));
#226406=CARTESIAN_POINT('Ctrl Pts',(186.354477612562,2.96596131899707,125.806882058373));
#226407=CARTESIAN_POINT('Ctrl Pts',(186.076029988749,-2.60134570724499,
125.607754128061));
#226408=CARTESIAN_POINT('Ctrl Pts',(185.797582364937,-5.7781431113317,130.184053693262));
#226409=CARTESIAN_POINT('Ctrl Pts',(185.519134741124,-3.64510927408837,
135.33038501822));
#226410=CARTESIAN_POINT('Ctrl Pts',(185.240687117311,1.83760191255446,136.317521027561));
#226411=CARTESIAN_POINT('Ctrl Pts',(184.962239493498,5.63164671340385,132.238331952975));
#226412=CARTESIAN_POINT('Ctrl Pts',(184.683791869685,4.25048330587202,126.841393274542));
#226413=CARTESIAN_POINT('Ctrl Pts',(184.405344245872,-1.03666661210287,
125.086227982629));
#226414=CARTESIAN_POINT('Ctrl Pts',(184.126896622059,-5.37117055753467,
128.585747235914));
#226415=CARTESIAN_POINT('Ctrl Pts',(183.848448998247,-4.7698311568614,134.124063801647));
#226416=CARTESIAN_POINT('Ctrl Pts',(183.570001374433,0.214750057761129,
136.611735317726));
#226417=CARTESIAN_POINT('Ctrl Pts',(183.291553750621,5.00198646042476,133.762713190383));
#226418=CARTESIAN_POINT('Ctrl Pts',(183.013106126807,5.19264166658148,128.195109572179));
#226419=CARTESIAN_POINT('Ctrl Pts',(182.734658502995,0.611512855797894,
125.025280195685));
#226420=CARTESIAN_POINT('Ctrl Pts',(182.456210879182,-4.53156639540017,
127.166143403126));
#226421=CARTESIAN_POINT('Ctrl Pts',(182.177763255369,-5.5103575085511,132.650350493844));
#226422=CARTESIAN_POINT('Ctrl Pts',(181.899315631556,-1.42539926727337,
136.438183069882));
#226423=CARTESIAN_POINT('Ctrl Pts',(181.620868007743,3.96943126600311,135.048808039769));
#226424=CARTESIAN_POINT('Ctrl Pts',(181.34242038393,5.71654838332065,129.758993181434));
#226425=CARTESIAN_POINT('Ctrl Pts',(181.063972760118,2.21043680528058,125.429819927867));
#226426=CARTESIAN_POINT('Ctrl Pts',(180.785525136304,-3.32695821097111,
126.039587007222));
#226427=CARTESIAN_POINT('Ctrl Pts',(180.507077512492,-5.80704116228462,
131.027948262352));
#226428=CARTESIAN_POINT('Ctrl Pts',(180.228629888679,-2.95073697519064,
135.810843394787));
#226429=CARTESIAN_POINT('Ctrl Pts',(179.950182264866,2.61715034058839,135.993025435236));
#226430=CARTESIAN_POINT('Ctrl Pts',(179.671734641053,5.78000434826875,131.407077988614));
#226431=CARTESIAN_POINT('Ctrl Pts',(179.39328701724,3.63131672880039,126.26726272238));
#226432=CARTESIAN_POINT('Ctrl Pts',(179.114839393428,-1.8543735647511,125.296818772266));
#226433=CARTESIAN_POINT('Ctrl Pts',(178.836391769614,-5.63598514348121,
129.387536719606));
#226434=CARTESIAN_POINT('Ctrl Pts',(178.557944145802,-4.23840170853308,
134.780246613475));
#226435=CARTESIAN_POINT('Ctrl Pts',(178.279496521988,1.05406583912245,136.519311509933));
#226436=CARTESIAN_POINT('Ctrl Pts',(178.001048898175,5.3778983746034,133.006615727177));
#226437=CARTESIAN_POINT('Ctrl Pts',(177.722601274363,4.75970502876524,127.470155084831));
#226438=CARTESIAN_POINT('Ctrl Pts',(177.44415365055,-0.232424713990654,
124.997666442073));
#226439=CARTESIAN_POINT('Ctrl Pts',(177.165706026737,-5.01096749916768,
127.861246073811));
#226440=CARTESIAN_POINT('Ctrl Pts',(176.887258402924,-5.18467595198119,
133.429404192122));
#226441=CARTESIAN_POINT('Ctrl Pts',(176.608810779111,-0.593920490425269,
136.585275505922));
#226442=CARTESIAN_POINT('Ctrl Pts',(176.330363155298,4.54261888720253,134.428768450716));
#226443=CARTESIAN_POINT('Ctrl Pts',(176.051915531486,5.50471342676105,128.941607659011));
#226444=CARTESIAN_POINT('Ctrl Pts',(175.773467907672,1.40824524732727,125.166225835676));
#226445=CARTESIAN_POINT('Ctrl Pts',(175.49502028386,-3.98233151779528,126.572014438702));
#226446=CARTESIAN_POINT('Ctrl Pts',(175.216572660047,-5.7133401657742,131.867122418498));
#226447=CARTESIAN_POINT('Ctrl Pts',(174.938125036234,-2.19406831359054,
136.185604222037));
#226448=CARTESIAN_POINT('Ctrl Pts',(174.659677412421,3.34144513258691,135.558986041432));
#226449=CARTESIAN_POINT('Ctrl Pts',(174.381229788608,5.80633374058666,130.563099372659));
#226450=CARTESIAN_POINT('Ctrl Pts',(174.102782164795,2.93548529615992,125.788920001687));
#226451=CARTESIAN_POINT('Ctrl Pts',(173.824334540982,-2.63293072900865,
125.623685538813));
#226452=CARTESIAN_POINT('Ctrl Pts',(173.54588691717,-5.7818120400351,130.219238383264));
#226453=CARTESIAN_POINT('Ctrl Pts',(173.267439293356,-3.61749054349026,
135.352489976228));
#226454=CARTESIAN_POINT('Ctrl Pts',(172.988991669544,1.87112803828436,136.306232877052));
#226455=CARTESIAN_POINT('Ctrl Pts',(172.71054404573,5.64027136256211,132.204023952811));
#226456=CARTESIAN_POINT('Ctrl Pts',(172.432096421918,4.22628084721974,126.815592800833));
#226457=CARTESIAN_POINT('Ctrl Pts',(172.153648798105,-1.07145530142008,
125.092644410292));
#226458=CARTESIAN_POINT('Ctrl Pts',(171.875201174292,-5.38457637155629,
128.618484181386));
#226459=CARTESIAN_POINT('Ctrl Pts',(171.596753550479,-4.74953480741189,
134.153037611328));
#226460=CARTESIAN_POINT('Ctrl Pts',(171.318305926666,0.25009721706947,136.610320475968));
#226461=CARTESIAN_POINT('Ctrl Pts',(171.039858302853,5.01990211699227,133.732209867644));
#226462=CARTESIAN_POINT('Ctrl Pts',(170.76141067904,5.1766622072511,128.163548831885));
#226463=CARTESIAN_POINT('Ctrl Pts',(170.482963055228,0.576322623054293,
125.021664816339));
#226464=CARTESIAN_POINT('Ctrl Pts',(170.204515431414,-4.55362929680409,
127.193795741725));
#226465=CARTESIAN_POINT('Ctrl Pts',(169.926067807602,-5.4990183500578,132.683859402108));
#226466=CARTESIAN_POINT('Ctrl Pts',(169.647620183788,-1.39107818158956,
136.446755498118));
#226467=CARTESIAN_POINT('Ctrl Pts',(169.369172559976,3.99519487781229,135.024566345214));
#226468=CARTESIAN_POINT('Ctrl Pts',(169.090724936163,5.71007902062496,129.724214297113));
#226469=CARTESIAN_POINT('Ctrl Pts',(168.81227731235,2.17767949635139,125.416463949427));
#226470=CARTESIAN_POINT('Ctrl Pts',(168.533829688537,-3.35590109951139,
126.059927426375));
#226471=CARTESIAN_POINT('Ctrl Pts',(168.255382064725,-5.80557252980615,
131.063293227581));
#226472=CARTESIAN_POINT('Ctrl Pts',(167.976934440911,-2.92020642319446,
135.828712609743));
#226473=CARTESIAN_POINT('Ctrl Pts',(167.698486817099,2.64868672631821,135.976997964335));
#226474=CARTESIAN_POINT('Ctrl Pts',(167.420039193286,5.78356616988455,131.371882294628));
#226475=CARTESIAN_POINT('Ctrl Pts',(167.141591569473,3.60363084624196,126.245241928676));
#226476=CARTESIAN_POINT('Ctrl Pts',(166.86314394566,-1.88786517794308,125.308208912483));
#226477=CARTESIAN_POINT('Ctrl Pts',(166.584696321847,-5.64450533093961,
129.421870811324));
#226478=CARTESIAN_POINT('Ctrl Pts',(166.306248698034,-4.21412083421794,
134.805973303719));
#226479=CARTESIAN_POINT('Ctrl Pts',(166.027801074221,1.08883483790225,136.512789227187));
#226480=CARTESIAN_POINT('Ctrl Pts',(165.749353450409,5.3912044865292,132.973838130654));
#226481=CARTESIAN_POINT('Ctrl Pts',(165.470905826595,4.73932058701693,127.441243184462));
#226482=CARTESIAN_POINT('Ctrl Pts',(165.192458202783,-0.267767403281747,
124.999188861871));
#226483=CARTESIAN_POINT('Ctrl Pts',(164.914010578969,-5.02879023112935,
127.891803784357));
#226484=CARTESIAN_POINT('Ctrl Pts',(164.635562955157,-5.16860050662956,
133.46091615025));
#226485=CARTESIAN_POINT('Ctrl Pts',(164.357115331344,-0.55871941670932,
136.588783761558));
#226486=CARTESIAN_POINT('Ctrl Pts',(164.078667707531,4.56459752220588,134.401049088318));
#226487=CARTESIAN_POINT('Ctrl Pts',(163.800220083718,5.49327233119978,128.908133418456));
#226488=CARTESIAN_POINT('Ctrl Pts',(163.521772459905,1.37389822909362,125.157757908727));
#226489=CARTESIAN_POINT('Ctrl Pts',(163.243324836092,-4.00802122688977,
126.596334436543));
#226490=CARTESIAN_POINT('Ctrl Pts',(162.964877212279,-5.70676497808368,
131.901881451211));
#226491=CARTESIAN_POINT('Ctrl Pts',(162.686429588467,-2.16127050538683,
136.198860436632));
#226492=CARTESIAN_POINT('Ctrl Pts',(162.407981964654,3.37032597782655,135.538557624299));
#226493=CARTESIAN_POINT('Ctrl Pts',(162.129534340841,5.80475753699479,130.527759041158));
#226494=CARTESIAN_POINT('Ctrl Pts',(161.851086717028,2.90490049783562,125.771143793998));
#226495=CARTESIAN_POINT('Ctrl Pts',(161.572639093215,-2.66441818655578,
125.639808921385));
#226496=CARTESIAN_POINT('Ctrl Pts',(161.294191469402,-5.7852667215671,130.254444755185));
#226497=CARTESIAN_POINT('Ctrl Pts',(161.015743845589,-3.58973776544978,
135.37442640163));
#226498=CARTESIAN_POINT('Ctrl Pts',(160.737296221776,1.90458482867669,136.294740852644));
#226499=CARTESIAN_POINT('Ctrl Pts',(160.458848597964,5.64868700939082,132.169664087608));
#226500=CARTESIAN_POINT('Ctrl Pts',(160.18040097415,4.20192178217643,126.789940132385));
#226501=CARTESIAN_POINT('Ctrl Pts',(159.901953350338,-1.10620428756715,
125.099272487699));
#226502=CARTESIAN_POINT('Ctrl Pts',(159.623505726525,-5.39778265812024,
128.651302125312));
#226503=CARTESIAN_POINT('Ctrl Pts',(159.345058102712,-4.72906246220349,
134.18188733455));
#226504=CARTESIAN_POINT('Ctrl Pts',(159.066610478899,0.285435108933367,
136.608690492233));
#226505=CARTESIAN_POINT('Ctrl Pts',(158.788162855086,5.03763175924073,133.701598052375));
#226506=CARTESIAN_POINT('Ctrl Pts',(158.509715231273,5.16049092479898,128.132085947844));
#226507=CARTESIAN_POINT('Ctrl Pts',(158.23126760746,0.541111034464008,125.018263716911));
#226508=CARTESIAN_POINT('Ctrl Pts',(157.952819983648,-4.57552346179978,
127.221581871133));
#226509=CARTESIAN_POINT('Ctrl Pts',(157.674372359834,-5.48747542341729,
132.717298664853));
#226510=CARTESIAN_POINT('Ctrl Pts',(157.395924736022,-1.35670554899215,
136.455118845335));
#226511=CARTESIAN_POINT('Ctrl Pts',(157.117477112209,4.02081044620608,135.000168269382));
#226512=CARTESIAN_POINT('Ctrl Pts',(156.839029488396,5.70339806885126,129.68947543801));
#226513=CARTESIAN_POINT('Ctrl Pts',(156.560581864583,2.1448414927076,125.403307621479));
#226514=CARTESIAN_POINT('Ctrl Pts',(156.28213424077,-3.38471963390224,126.080443652244));
#226515=CARTESIAN_POINT('Ctrl Pts',(156.003686616957,-5.8038887697026,131.098628597966));
#226516=CARTESIAN_POINT('Ctrl Pts',(155.725238993144,-2.88956766187541,
135.846395645489));
#226517=CARTESIAN_POINT('Ctrl Pts',(155.446791369331,2.68012496398725,135.960778819456));
#226518=CARTESIAN_POINT('Ctrl Pts',(155.168343745519,5.78691367932904,131.336665570917));
#226519=CARTESIAN_POINT('Ctrl Pts',(154.889896121706,3.57581142981733,126.223390074792));
#226520=CARTESIAN_POINT('Ctrl Pts',(154.611448497893,-1.92128683559663,
125.319802714623));
#226521=CARTESIAN_POINT('Ctrl Pts',(154.33300087408,-5.65281635917722,129.456256131708));
#226522=CARTESIAN_POINT('Ctrl Pts',(154.054553250267,-4.18968380410554,
134.831551712731));
#226523=CARTESIAN_POINT('Ctrl Pts',(153.776105626454,1.12356348950664,136.50605541652));
#226524=CARTESIAN_POINT('Ctrl Pts',(153.497658002641,5.40431082539012,132.940980143345));
#226525=CARTESIAN_POINT('Ctrl Pts',(153.219210378828,4.71876052800142,127.412455905645));
#226526=CARTESIAN_POINT('Ctrl Pts',(152.940762755016,-0.303100170353132,
125.000926394444));
#226527=CARTESIAN_POINT('Ctrl Pts',(152.662315131202,-5.04642661941966,
127.922469420767));
#226528=CARTESIAN_POINT('Ctrl Pts',(152.38386750739,-5.15233353688545,133.492329668737));
#226529=CARTESIAN_POINT('Ctrl Pts',(152.105419883576,-0.523497639439988,
136.592077673268));
#226530=CARTESIAN_POINT('Ctrl Pts',(151.826972259764,4.58640701436939,134.373196449306));
#226531=CARTESIAN_POINT('Ctrl Pts',(151.548524635951,5.48162768041213,128.874729443297));
#226532=CARTESIAN_POINT('Ctrl Pts',(151.270077012138,1.33950030055583,125.149499218718));
#226533=CARTESIAN_POINT('Ctrl Pts',(150.991629388325,-4.03356241728369,
126.620810364342));
#226534=CARTESIAN_POINT('Ctrl Pts',(150.713181764512,-5.69997832411825,
131.936599814887));
#226535=CARTESIAN_POINT('Ctrl Pts',(150.434734140699,-2.1283926105098,136.211916756054));
#226536=CARTESIAN_POINT('Ctrl Pts',(150.156286516886,3.39908193439765,135.517953779753));
#226537=CARTESIAN_POINT('Ctrl Pts',(149.877838893074,5.8029662359777,130.49242895923));
#226538=CARTESIAN_POINT('Ctrl Pts',(149.599391269261,2.87420805735513,125.753554094008));
#226539=CARTESIAN_POINT('Ctrl Pts',(149.320943645448,-2.69580691310719,
125.65612367832));
#226540=CARTESIAN_POINT('Ctrl Pts',(149.042496021635,-5.7885070279132,130.289671504441));
#226541=CARTESIAN_POINT('Ctrl Pts',(148.764048397822,-3.56185196835627,
135.396193481562));
#226542=CARTESIAN_POINT('Ctrl Pts',(148.485600774009,1.93797104397778,136.283045380177));
#226543=CARTESIAN_POINT('Ctrl Pts',(148.207153150196,5.6568933420451,132.135253630582));
#226544=CARTESIAN_POINT('Ctrl Pts',(147.928705526383,4.17740701337624,126.764436219762));
#226545=CARTESIAN_POINT('Ctrl Pts',(147.65025790257,-1.14091228290746,125.106111969245));
#226546=CARTESIAN_POINT('Ctrl Pts',(147.371810278758,-5.41078892786276,
128.684199851613));
#226547=CARTESIAN_POINT('Ctrl Pts',(147.093362654945,-4.70841487984645,
134.210611902278));
#226548=CARTESIAN_POINT('Ctrl Pts',(146.814915031132,0.320762423894332,
136.60684542692));
#226549=CARTESIAN_POINT('Ctrl Pts',(146.536467407319,5.05517473019176,133.670878878906));
#226550=CARTESIAN_POINT('Ctrl Pts',(146.258019783506,5.14412841845787,128.100722085923));
#226551=CARTESIAN_POINT('Ctrl Pts',(145.979572159693,0.505879394805349,
125.015077023433));
#226552=CARTESIAN_POINT('Ctrl Pts',(145.70112453588,-4.59724807909095,127.249500761725));
#226553=CARTESIAN_POINT('Ctrl Pts',(145.422676912067,-5.47572915635697,
132.750667042976));
#226554=CARTESIAN_POINT('Ctrl Pts',(145.144229288255,-1.32228264317164,
136.463272801628));
#226555=CARTESIAN_POINT('Ctrl Pts',(144.865781664442,4.0462770219901,134.975614716357));
#226556=CARTESIAN_POINT('Ctrl Pts',(144.587334040629,5.69650577556471,129.654777891387));
#226557=CARTESIAN_POINT('Ctrl Pts',(144.308886416816,2.11192401117359,125.390351431538));
#226558=CARTESIAN_POINT('Ctrl Pts',(144.030438793003,-3.41341274626234,
126.101134924595));
#226559=CARTESIAN_POINT('Ctrl Pts',(143.75199116919,-5.80198994436631,131.133953064144));
#226560=CARTESIAN_POINT('Ctrl Pts',(143.473543545377,-2.85882182656403,
135.863891846773));
#226561=CARTESIAN_POINT('Ctrl Pts',(143.195095921564,2.71146388864014,135.944368601604));
#226562=CARTESIAN_POINT('Ctrl Pts',(142.916648297751,5.790046752559,131.301429122451));
#226563=CARTESIAN_POINT('Ctrl Pts',(142.638200673938,3.54785951038517,126.201707970457));
#226564=CARTESIAN_POINT('Ctrl Pts',(142.359753050125,-1.95463729925998,
125.331599749072));
#226565=CARTESIAN_POINT('Ctrl Pts',(142.081305426313,-5.66091792022584,
129.490691406602));
#226566=CARTESIAN_POINT('Ctrl Pts',(141.8028578025,-4.16509152371897,134.856980892698));
#226567=CARTESIAN_POINT('Ctrl Pts',(141.524410178687,1.15825050705268,136.499110327454));
#226568=CARTESIAN_POINT('Ctrl Pts',(141.245962554874,5.41721690552589,132.908042982814));
#226569=CARTESIAN_POINT('Ctrl Pts',(140.967514931061,4.69802561357932,127.383794315106));
#226570=CARTESIAN_POINT('Ctrl Pts',(140.689067307248,-0.338421705936203,
125.002878975406));
#226571=CARTESIAN_POINT('Ctrl Pts',(140.410619683435,-5.06387601051571,
127.953241846716));
#226572=CARTESIAN_POINT('Ctrl Pts',(140.132172059623,-5.13587564552739,
133.523643583541));
#226573=CARTESIAN_POINT('Ctrl Pts',(139.85372443581,-0.48825646377323,136.595157118993));
#226574=CARTESIAN_POINT('Ctrl Pts',(139.575276811997,4.60804655553434,134.34521156577));
#226575=CARTESIAN_POINT('Ctrl Pts',(139.296829188184,5.46977990589493,128.841396971331));
#226576=CARTESIAN_POINT('Ctrl Pts',(139.018381564371,1.30505273634171,125.141450071677));
#226577=CARTESIAN_POINT('Ctrl Pts',(138.739933940558,-4.05895414253892,
126.645441315135));
#226578=CARTESIAN_POINT('Ctrl Pts',(138.461486316745,-5.69298045535984,
131.971276223022));
#226579=CARTESIAN_POINT('Ctrl Pts',(138.183038692932,-2.09543584726193,
136.224772696493));
#226580=CARTESIAN_POINT('Ctrl Pts',(137.904591069119,3.42771193673771,135.49717527128));
#226581=CARTESIAN_POINT('Ctrl Pts',(137.626143445306,5.80095990391266,130.457110436044));
#226582=CARTESIAN_POINT('Ctrl Pts',(137.347695821494,2.84340911203807,125.736151553513));
#226583=CARTESIAN_POINT('Ctrl Pts',(137.069248197681,-2.727095745542,125.672629205068));
#226584=CARTESIAN_POINT('Ctrl Pts',(136.790800573868,-5.7915328390027,130.324917325691));
#226585=CARTESIAN_POINT('Ctrl Pts',(136.512352950055,-3.53383418552815,
135.417790409441));
#226586=CARTESIAN_POINT('Ctrl Pts',(136.233905326242,1.97128544704926,136.271146893031));
#226587=CARTESIAN_POINT('Ctrl Pts',(135.955457702429,5.66489005643625,132.100793856825));
#226588=CARTESIAN_POINT('Ctrl Pts',(135.677010078616,4.15273744922295,126.739082008025));
#226589=CARTESIAN_POINT('Ctrl Pts',(135.398562454803,-1.17557800132362,
125.113162601491));
#226590=CARTESIAN_POINT('Ctrl Pts',(135.12011483099,-5.42359469883174,128.717176141249));
#226591=CARTESIAN_POINT('Ctrl Pts',(134.841667207177,-4.68759282544451,
134.239210250113));
#226592=CARTESIAN_POINT('Ctrl Pts',(134.563219583365,0.356077852885664,
136.604785348398));
#226593=CARTESIAN_POINT('Ctrl Pts',(134.284771959552,5.0725303797842,133.640053485549));
#226594=CARTESIAN_POINT('Ctrl Pts',(134.006324335739,5.12757529454644,128.069458408322));
#226595=CARTESIAN_POINT('Ctrl Pts',(133.727876711926,0.470629009599695,
125.012104853988));
#226596=CARTESIAN_POINT('Ctrl Pts',(133.449429088113,-4.61880234366392,
127.277551378957));
#226597=CARTESIAN_POINT('Ctrl Pts',(133.1709814643,-5.46377998413907,132.783963299997));
#226598=CARTESIAN_POINT('Ctrl Pts',(132.892533840487,-1.28781073968153,
136.47121706485));
#226599=CARTESIAN_POINT('Ctrl Pts',(132.614086216674,4.07159366149105,134.950906595976));
#226600=CARTESIAN_POINT('Ctrl Pts',(132.335638592862,5.68940239616175,129.620122942976));
#226601=CARTESIAN_POINT('Ctrl Pts',(132.057190969048,2.07892827151876,125.377595859696));
#226602=CARTESIAN_POINT('Ctrl Pts',(131.778743345236,-3.44197937335791,
126.122000476702));
#226603=CARTESIAN_POINT('Ctrl Pts',(131.500295721423,-5.79987612415893,
131.169265317152));
#226604=CARTESIAN_POINT('Ctrl Pts',(131.22184809761,-2.82797005655853,135.881200565267));
#226605=CARTESIAN_POINT('Ctrl Pts',(130.943400473797,2.74270233900145,135.927767918864));
#226606=CARTESIAN_POINT('Ctrl Pts',(130.664952849984,5.79296527347731,131.26617425493));
#226607=CARTESIAN_POINT('Ctrl Pts',(130.386505226171,3.51977612371406,126.180196419108));
#226608=CARTESIAN_POINT('Ctrl Pts',(130.108057602358,-1.98791533311939,
125.343599578688));
#226609=CARTESIAN_POINT('Ctrl Pts',(129.829609978546,-5.66880971387908,
129.52517535999));
#226610=CARTESIAN_POINT('Ctrl Pts',(129.551162354732,-4.14034490433441,
134.882259901329));
#226611=CARTESIAN_POINT('Ctrl Pts',(129.27271473092,1.19289460520041,136.491954217345));
#226612=CARTESIAN_POINT('Ctrl Pts',(128.994267107107,5.42992224869717,132.875027869557));
#226613=CARTESIAN_POINT('Ctrl Pts',(128.715819483294,4.67711661209022,127.355259474909));
#226614=CARTESIAN_POINT('Ctrl Pts',(128.437371859481,-0.373730701178542,
125.005046532403));
#226615=CARTESIAN_POINT('Ctrl Pts',(128.158924235668,-5.0811377578241,127.984119921918));
#226616=CARTESIAN_POINT('Ctrl Pts',(127.880476611855,-5.11922744240848,
133.554856734316));
#226617=CARTESIAN_POINT('Ctrl Pts',(127.602028988042,-0.452997195583419,
136.598021984625));
#226618=CARTESIAN_POINT('Ctrl Pts',(127.323581364229,4.62951534383955,134.3170954747));
#226619=CARTESIAN_POINT('Ctrl Pts',(127.045133740417,5.45772944667181,128.808137237705));
#226620=CARTESIAN_POINT('Ctrl Pts',(126.766686116604,1.2705568129186,125.133610765869));
#226621=CARTESIAN_POINT('Ctrl Pts',(126.488238492791,-4.08419546175569,
126.67022637621));
#226622=CARTESIAN_POINT('Ctrl Pts',(126.209790868978,-5.68577163111709,
132.005909390672));
#226623=CARTESIAN_POINT('Ctrl Pts',(125.931343245165,-2.06240143686808,
136.237427781569));
#226624=CARTESIAN_POINT('Ctrl Pts',(125.652895621352,3.45621492395137,135.476222868834));
#226625=CARTESIAN_POINT('Ctrl Pts',(125.374447997539,5.79873861514512,130.421804780342));
#226626=CARTESIAN_POINT('Ctrl Pts',(125.096000373726,2.8125048031507,125.718936817367));
#226627=CARTESIAN_POINT('Ctrl Pts',(124.817552749914,-2.75828352444112,
125.68932489001));
#226628=CARTESIAN_POINT('Ctrl Pts',(124.5391051261,-5.79434404271298,130.36018091289));
#226629=CARTESIAN_POINT('Ctrl Pts',(124.260657502288,-3.50568545517477,
135.439216384981));
#226630=CARTESIAN_POINT('Ctrl Pts',(123.982209878475,2.00452680341345,136.25904583211));
#226631=CARTESIAN_POINT('Ctrl Pts',(123.703762254662,5.67267685624313,132.066286043259));
#226632=CARTESIAN_POINT('Ctrl Pts',(123.425314630849,4.12791400385628,126.71387843668));
#226633=CARTESIAN_POINT('Ctrl Pts',(123.146867007036,-1.21020015826455,
125.120424123171));
#226634=CARTESIAN_POINT('Ctrl Pts',(122.868419383223,-5.43619949650465,
128.750229772276));
#226635=CARTESIAN_POINT('Ctrl Pts',(122.58997175941,-4.66659707056658,134.267681318331));
#226636=CARTESIAN_POINT('Ctrl Pts',(122.311524135597,0.391380087281262,
136.602510333005));
#226637=CARTESIAN_POINT('Ctrl Pts',(122.033076511785,5.08969806489794,133.609123014551));
#226638=CARTESIAN_POINT('Ctrl Pts',(121.754628887972,5.11083216644683,128.038296073528));
#226639=CARTESIAN_POINT('Ctrl Pts',(121.476181264159,0.435361185062875,
125.00934731871));
#226640=CARTESIAN_POINT('Ctrl Pts',(121.197733640346,-4.64018545681751,
127.305732683402));
#226641=CARTESIAN_POINT('Ctrl Pts',(120.919286016533,-5.45162834954452,
132.817186202114));
#226642=CARTESIAN_POINT('Ctrl Pts',(120.64083839272,-1.25329111589093,136.478951340622));
#226643=CARTESIAN_POINT('Ctrl Pts',(120.362390768907,4.09675942659154,134.92604482381));
#226644=CARTESIAN_POINT('Ctrl Pts',(120.083943145094,5.68208819386074,129.585511876926));
#226645=CARTESIAN_POINT('Ctrl Pts',(119.805495521281,2.04585549641223,125.36504137862));
#226646=CARTESIAN_POINT('Ctrl Pts',(119.527047897469,-3.47041845664194,
126.143039535386));
#226647=CARTESIAN_POINT('Ctrl Pts',(119.248600273655,-5.79754738740892,
131.204564048482));
#226648=CARTESIAN_POINT('Ctrl Pts',(118.970152649843,-2.7970134950826,135.898321159589));
#226649=CARTESIAN_POINT('Ctrl Pts',(118.69170502603,2.77383915751901,135.910977386384));
#226650=CARTESIAN_POINT('Ctrl Pts',(118.413257402217,5.795669133937,131.230902274733));
#226651=CARTESIAN_POINT('Ctrl Pts',(118.134809778404,3.49156231044436,126.158856217863));
#226652=CARTESIAN_POINT('Ctrl Pts',(117.856362154591,-2.02111970404504,
125.355801758813));
#226653=CARTESIAN_POINT('Ctrl Pts',(117.577914530778,-5.67649144770371,
129.559706714059));
#226654=CARTESIAN_POINT('Ctrl Pts',(117.299466906965,-4.11544486294674,
134.907387801903));
#226655=CARTESIAN_POINT('Ctrl Pts',(117.021019283153,1.22749450019975,136.484587351363));
#226656=CARTESIAN_POINT('Ctrl Pts',(116.74257165934,5.44242638410263,132.841936026965));
#226657=CARTESIAN_POINT('Ctrl Pts',(116.464124035527,4.65603429832517,127.326852442422));
#226658=CARTESIAN_POINT('Ctrl Pts',(116.185676411714,-0.409025847692317,
125.007428985116));
#226659=CARTESIAN_POINT('Ctrl Pts',(115.907228787901,-5.09821122170419,
128.015102502178));
#226660=CARTESIAN_POINT('Ctrl Pts',(115.628781164088,-5.10238954443416,
133.585967964446));
#226661=CARTESIAN_POINT('Ctrl Pts',(115.350333540275,-0.417721141415912,
136.600672164005));
#226662=CARTESIAN_POINT('Ctrl Pts',(115.071885916462,4.65081258375125,134.288849217947));
#226663=CARTESIAN_POINT('Ctrl Pts',(114.793438292649,5.44547674927697,128.77495147487));
#226664=CARTESIAN_POINT('Ctrl Pts',(114.514990668836,1.23601380854556,125.125981591782));
#226665=CARTESIAN_POINT('Ctrl Pts',(114.236543045024,-4.10928543960769,
126.695164629152));
#226666=CARTESIAN_POINT('Ctrl Pts',(113.958095421211,-5.67835211851559,
132.040498034489));
#226667=CARTESIAN_POINT('Ctrl Pts',(113.679647797398,-2.02929060343055,
136.249881542344));
#226668=CARTESIAN_POINT('Ctrl Pts',(113.401200173585,3.48458983985001,135.455097348814));
#226669=CARTESIAN_POINT('Ctrl Pts',(113.122752549772,5.79630245198571,130.386513300387));
#226670=CARTESIAN_POINT('Ctrl Pts',(112.844304925959,2.78149627586357,125.701910523471));
#226671=CARTESIAN_POINT('Ctrl Pts',(112.565857302146,-2.78936909412988,
125.706210114483));
#226672=CARTESIAN_POINT('Ctrl Pts',(112.287409678333,-5.7969405348739,130.395460959329));
#226673=CARTESIAN_POINT('Ctrl Pts',(112.008962054521,-3.47740682035766,
135.460470614237));
#226674=CARTESIAN_POINT('Ctrl Pts',(111.730514430707,2.03769388129978,136.246742645822));
#226675=CARTESIAN_POINT('Ctrl Pts',(111.452066806895,5.68025345292297,132.031731468582));
#226676=CARTESIAN_POINT('Ctrl Pts',(111.173619183082,4.10293759711819,126.688826439658));
#226677=CARTESIAN_POINT('Ctrl Pts',(110.895171559269,-1.24477747079359,
125.127896265209));
#226678=CARTESIAN_POINT('Ctrl Pts',(110.616723935456,-5.44860285380605,
128.783359519875));
#226679=CARTESIAN_POINT('Ctrl Pts',(110.338276311643,-4.64542839321807,
134.296024051927));
#226680=CARTESIAN_POINT('Ctrl Pts',(110.05982868783,0.426667818943798,136.600020465042));
#226681=CARTESIAN_POINT('Ctrl Pts',(109.781381064017,5.10667714937814,133.57808861205));
#226682=CARTESIAN_POINT('Ctrl Pts',(109.502933440204,5.0938996545818,128.007236236273));
#226683=CARTESIAN_POINT('Ctrl Pts',(109.224485816392,0.400077228057368,
125.006804519781));
#226684=CARTESIAN_POINT('Ctrl Pts',(108.946038192578,-4.66139662619255,
127.334043630792));
#226685=CARTESIAN_POINT('Ctrl Pts',(108.667590568766,-5.43927470285667,
132.850334518237));
#226686=CARTESIAN_POINT('Ctrl Pts',(108.389142944953,-1.21872505093712,
136.486475342347));
#226687=CARTESIAN_POINT('Ctrl Pts',(108.11069532114,4.1217733847649,134.901030321119));
#226688=CARTESIAN_POINT('Ctrl Pts',(107.832247697327,5.67456343969215,129.550945975765));
#226689=CARTESIAN_POINT('Ctrl Pts',(107.553800073514,2.01270691137792,125.352688453517));
#226690=CARTESIAN_POINT('Ctrl Pts',(107.275352449701,-3.49872894229381,
126.164251321038));
#226691=CARTESIAN_POINT('Ctrl Pts',(106.996904825888,-5.7950038204084,131.239847950126));
#226692=CARTESIAN_POINT('Ctrl Pts',(106.718457202076,-2.76595328924301,
135.91525299533));
#226693=CARTESIAN_POINT('Ctrl Pts',(106.440009578262,2.80487319040651,135.893997626342));
#226694=CARTESIAN_POINT('Ctrl Pts',(106.16156195445,5.7981582337456,131.195614488879));
#226695=CARTESIAN_POINT('Ctrl Pts',(105.883114330637,3.46321911604922,126.137688157493));
#226696=CARTESIAN_POINT('Ctrl Pts',(105.604666706824,-2.05424918163679,
125.36820583729));
#226697=CARTESIAN_POINT('Ctrl Pts',(105.326219083011,-5.68396283705021,
129.594284189235));
#226698=CARTESIAN_POINT('Ctrl Pts',(105.047771459198,-4.09039232223623,
134.932363663296));
#226699=CARTESIAN_POINT('Ctrl Pts',(104.769323835385,1.26204890993897,136.47701000249));
#226700=CARTESIAN_POINT('Ctrl Pts',(104.490876211572,5.45472884839698,132.808768681268));
#226701=CARTESIAN_POINT('Ctrl Pts',(104.21242858776,4.63477945349693,127.29857427028));
#226702=CARTESIAN_POINT('Ctrl Pts',(103.933980963947,-0.444305837602887,
125.010026245263));
#226703=CARTESIAN_POINT('Ctrl Pts',(103.655533340134,-5.1150957694926,128.046188439421));
#226704=CARTESIAN_POINT('Ctrl Pts',(103.377085716321,-5.08536257553889,
133.616976121092));
#226705=CARTESIAN_POINT('Ctrl Pts',(103.098638092508,-0.38242960843803,
136.603107558928));
#226706=CARTESIAN_POINT('Ctrl Pts',(102.820190468695,4.6719374860923,134.260473842188));
#226707=CARTESIAN_POINT('Ctrl Pts',(102.541742844882,5.4330222677386,128.741840912539));
#226708=CARTESIAN_POINT('Ctrl Pts',(102.263295221069,1.2014250032263,125.118562832119));
#226709=CARTESIAN_POINT('Ctrl Pts',(101.984847597256,-4.13422314637653,
126.720255149861));
#226710=CARTESIAN_POINT('Ctrl Pts',(101.706399973443,-5.67072219248816,
132.07504087278));
#226711=CARTESIAN_POINT('Ctrl Pts',(101.427952349631,-1.99610457388343,
136.262133517338));
#226712=CARTESIAN_POINT('Ctrl Pts',(101.149504725818,3.51283563299066,135.433799494034));
#226713=CARTESIAN_POINT('Ctrl Pts',(100.871057102005,5.7936515047074,130.351237303918));
#226714=CARTESIAN_POINT('Ctrl Pts',(100.592609478192,2.75038467920892,125.685073302739));
#226715=CARTESIAN_POINT('Ctrl Pts',(100.314161854379,-2.82035130272114,
125.723284252797));
#226716=CARTESIAN_POINT('Ctrl Pts',(100.035714230566,-5.79932221927147,
130.430756157697));
#226717=CARTESIAN_POINT('Ctrl Pts',(99.7572666067534,-3.44899932895201,
135.481552309624));
#226718=CARTESIAN_POINT('Ctrl Pts',(99.4788189829407,2.07078545168999,136.234237790066));
#226719=CARTESIAN_POINT('Ctrl Pts',(99.2003713591278,5.6876195657222,131.997131413226));
#226720=CARTESIAN_POINT('Ctrl Pts',(98.9219237353147,4.07780915451857,126.663926945268));
#226721=CARTESIAN_POINT('Ctrl Pts',(98.6434761115021,-1.27930865763567,
125.13557875072));
#226722=CARTESIAN_POINT('Ctrl Pts',(98.3650284876889,-5.460804311125,128.816564156414));
#226723=CARTESIAN_POINT('Ctrl Pts',(98.0865808638763,-4.62408757781209,
134.324237400649));
#226724=CARTESIAN_POINT('Ctrl Pts',(97.8081332400632,0.461939740273397,
136.597315836771));
#226725=CARTESIAN_POINT('Ctrl Pts',(97.5296856162504,5.12346700405862,133.546951428038));
#226726=CARTESIAN_POINT('Ctrl Pts',(97.2512379924375,5.07677838639178,127.97628004749));
#226727=CARTESIAN_POINT('Ctrl Pts',(96.9727903686245,0.364778446043045,
125.004476551425));
#226728=CARTESIAN_POINT('Ctrl Pts',(96.6943427448119,-4.68243506580139,
127.362483172053));
#226729=CARTESIAN_POINT('Ctrl Pts',(96.4158951209985,-5.42671950184442,
132.883407020047));
#226730=CARTESIAN_POINT('Ctrl Pts',(96.1374474971861,-1.18411382567837,
136.493788791223));
#226731=CARTESIAN_POINT('Ctrl Pts',(95.8589998733729,4.14663460910971,134.875864014826));
#226732=CARTESIAN_POINT('Ctrl Pts',(95.5805522495601,5.66682841248846,129.516426520346));
#226733=CARTESIAN_POINT('Ctrl Pts',(95.3021046257473,1.97948374474885,125.340537542131));
#226734=CARTESIAN_POINT('Ctrl Pts',(95.0236570019342,-3.52690978125809,
126.185635047646));
#226735=CARTESIAN_POINT('Ctrl Pts',(94.7452093781216,-5.79224551741027,
131.275115714627));
#226736=CARTESIAN_POINT('Ctrl Pts',(94.4667617543085,-2.73479058998699,
135.931995445075));
#226737=CARTESIAN_POINT('Ctrl Pts',(94.1883141304955,2.8358032876865,135.876829267928));
#226738=CARTESIAN_POINT('Ctrl Pts',(93.909866506683,5.80043248066857,131.160312204968));
#226739=CARTESIAN_POINT('Ctrl Pts',(93.6314188828698,3.43474759079615,126.116693022386));
#226740=CARTESIAN_POINT('Ctrl Pts',(93.352971259057,-2.08730253826965,125.380811354481));
#226741=CARTESIAN_POINT('Ctrl Pts',(93.0745236352441,-5.69122360506351,
129.628906504239));
#226742=CARTESIAN_POINT('Ctrl Pts',(92.7960760114314,-4.06518821053398,
134.957186560018));
#226743=CARTESIAN_POINT('Ctrl Pts',(92.5176283876181,1.29655655399172,136.469222451509));
#226744=CARTESIAN_POINT('Ctrl Pts',(92.2391807638055,5.46682918570788,132.775527061492));
#226745=CARTESIAN_POINT('Ctrl Pts',(91.9607331399925,4.61335286521161,127.270426006341));
#226746=CARTESIAN_POINT('Ctrl Pts',(91.6822855161797,-0.479569363597252,
125.012838216602));
#226747=CARTESIAN_POINT('Ctrl Pts',(91.4038378923669,-5.13179077552621,
128.077376581749));
#226748=CARTESIAN_POINT('Ctrl Pts',(91.1253902685539,-5.06814716666323,
133.647880055237));
#226749=CARTESIAN_POINT('Ctrl Pts',(90.846942644741,-0.347123904390365,
136.605328079151));
#226750=CARTESIAN_POINT('Ctrl Pts',(90.5684950209282,4.69288926807169,134.231970398883));
#226751=CARTESIAN_POINT('Ctrl Pts',(90.2900473971151,5.42036646356212,128.708806777632));
#226752=CARTESIAN_POINT('Ctrl Pts',(90.0115997733025,1.16679167866171,125.111354761782));
#226753=CARTESIAN_POINT('Ctrl Pts',(89.7331521494893,-4.15900765798632,
126.7454970086));
#226754=CARTESIAN_POINT('Ctrl Pts',(89.4547045256766,-5.66288213576447,
132.109536625546));
#226755=CARTESIAN_POINT('Ctrl Pts',(89.1762569018636,-1.96284457794726,
136.274183252551));
#226756=CARTESIAN_POINT('Ctrl Pts',(88.8978092780507,3.5409512567151,135.412330093694));
#226757=CARTESIAN_POINT('Ctrl Pts',(88.619361654238,5.79078587154194,130.3159780981));
#226758=CARTESIAN_POINT('Ctrl Pts',(88.3409140304249,2.71917116603865,125.668425779081));
#226759=CARTESIAN_POINT('Ctrl Pts',(88.0624664066122,-2.85122900215762,
125.740546672265));
#226760=CARTESIAN_POINT('Ctrl Pts',(87.7840187827991,-5.80148900765152,
130.466065200115));
#226761=CARTESIAN_POINT('Ctrl Pts',(87.5055711589863,-3.42046403360785,
135.502460689953));
#226762=CARTESIAN_POINT('Ctrl Pts',(87.2271235351733,2.10380028836375,136.221531728214));
#226763=CARTESIAN_POINT('Ctrl Pts',(86.9486759113605,5.69477492168681,131.962487159311));
#226764=CARTESIAN_POINT('Ctrl Pts',(86.6702282875477,4.05252960720113,126.63918087617));
#226765=CARTESIAN_POINT('Ctrl Pts',(86.3917806637346,-1.31379243922498,
125.14347129503));
#226766=CARTESIAN_POINT('Ctrl Pts',(86.113333039922,-5.47280341633199,128.849842451481));
#226767=CARTESIAN_POINT('Ctrl Pts',(85.8348854161089,-4.6025754151404,134.352320319043));
#226768=CARTESIAN_POINT('Ctrl Pts',(85.5564377922961,0.497194544256039,
136.594396548415));
#226769=CARTESIAN_POINT('Ctrl Pts',(85.2779901684829,5.1400670067851,133.515712616316));
#226770=CARTESIAN_POINT('Ctrl Pts',(84.9995425446705,5.05946899631168,127.945428654274));
#226771=CARTESIAN_POINT('Ctrl Pts',(84.7210949208572,0.329466147029263,
125.002363499906));
#226772=CARTESIAN_POINT('Ctrl Pts',(84.4426472970446,-4.70329999605691,
127.391050253351));
#226773=CARTESIAN_POINT('Ctrl Pts',(84.1641996732315,-5.41396321174535,
132.916402482027));
#226774=CARTESIAN_POINT('Ctrl Pts',(83.8857520494189,-1.14945872264635,
136.500891416245));
#226775=CARTESIAN_POINT('Ctrl Pts',(83.6073044256056,4.17134217838416,134.850546837477));
#226776=CARTESIAN_POINT('Ctrl Pts',(83.328856801793,5.65888339887398,129.481954789796));
#226777=CARTESIAN_POINT('Ctrl Pts',(83.05040917798,1.94618722762166,125.328589094719));
#226778=CARTESIAN_POINT('Ctrl Pts',(82.7719615541671,-3.5549599292834,126.207189922827));
#226779=CARTESIAN_POINT('Ctrl Pts',(82.4935139303543,-5.78927258062435,
131.310366035126));
#226780=CARTESIAN_POINT('Ctrl Pts',(82.2150663065413,-2.70352655206008,
135.948547888425));
#226781=CARTESIAN_POINT('Ctrl Pts',(81.9366186827285,2.86662830323276,135.859472947324));
#226782=CARTESIAN_POINT('Ctrl Pts',(81.6581710589156,5.80249179043285,131.124996731141));
#226783=CARTESIAN_POINT('Ctrl Pts',(81.3797234351026,3.40614878970799,126.095871590527));
#226784=CARTESIAN_POINT('Ctrl Pts',(81.1012758112897,-2.12027854913937,
125.393617843285));
#226785=CARTESIAN_POINT('Ctrl Pts',(80.822828187477,-5.6982734826932,129.663572376127));
#226786=CARTESIAN_POINT('Ctrl Pts',(80.5443805636639,-4.03983346178761,
134.981855572247));
#226787=CARTESIAN_POINT('Ctrl Pts',(80.2659329398512,1.33101615366455,136.461224986989));
#226788=CARTESIAN_POINT('Ctrl Pts',(79.9874853160382,5.47872694765296,132.742212399419));
#226789=CARTESIAN_POINT('Ctrl Pts',(79.7090376922254,4.59175532743923,127.242408693648));
#226790=CARTESIAN_POINT('Ctrl Pts',(79.4305900684125,-0.514815118972584,
125.015864794932));
#226791=CARTESIAN_POINT('Ctrl Pts',(79.1521424445996,-5.1482956211654,128.108665773475));
#226792=CARTESIAN_POINT('Ctrl Pts',(78.8736948207867,-5.05074395573051,
133.678678621723));
#226793=CARTESIAN_POINT('Ctrl Pts',(78.5952471969738,-0.31180533753877,
136.607333642391));
#226794=CARTESIAN_POINT('Ctrl Pts',(78.3167995731609,4.71366715331346,134.203339944237));
#226795=CARTESIAN_POINT('Ctrl Pts',(78.0383519493481,5.407509805713,128.675850294243));
#226796=CARTESIAN_POINT('Ctrl Pts',(77.7599043255351,1.1321151182024,125.104357647873));
#226797=CARTESIAN_POINT('Ctrl Pts',(77.4814567017223,-4.18363805603787,
126.770889270024));
#226798=CARTESIAN_POINT('Ctrl Pts',(77.2030090779094,-5.65483223886072,
132.143984014535));
#226799=CARTESIAN_POINT('Ctrl Pts',(76.9245614540965,-1.92951184808342,
136.286030301474));
#226800=CARTESIAN_POINT('Ctrl Pts',(76.6461138302835,3.56893566918854,135.390689943351));
#226801=CARTESIAN_POINT('Ctrl Pts',(76.3676662064707,5.78770565867644,130.280736989476));
#226802=CARTESIAN_POINT('Ctrl Pts',(76.0892185826578,2.68785689298084,125.651968569378));
#226803=CARTESIAN_POINT('Ctrl Pts',(75.8107709588449,-2.8820010482549,125.75799673322));
#226804=CARTESIAN_POINT('Ctrl Pts',(75.532323335032,-5.8034408197229,130.501386778194));
#226805=CARTESIAN_POINT('Ctrl Pts',(75.2538757112192,-3.39180199171105,
135.523194980456));
#226806=CARTESIAN_POINT('Ctrl Pts',(74.9754280874062,2.13673716794415,136.208624931095));
#226807=CARTESIAN_POINT('Ctrl Pts',(74.6969804635933,5.70171925567246,131.92779999059));
#226808=CARTESIAN_POINT('Ctrl Pts',(74.4185328397805,4.02709989190878,126.61458914934));
#226809=CARTESIAN_POINT('Ctrl Pts',(74.1400852159675,-1.34822753775231,
125.151573605674));
#226810=CARTESIAN_POINT('Ctrl Pts',(73.8616375921548,-5.48459972479585,
128.883193171938));
#226811=CARTESIAN_POINT('Ctrl Pts',(73.5831899683417,-4.58089270234404,
134.380271766487));
#226812=CARTESIAN_POINT('Ctrl Pts',(73.3047423445289,0.532430924512096,
136.591262708148));
#226813=CARTESIAN_POINT('Ctrl Pts',(73.026294720716,5.15647654243839,133.484373334449));
#226814=CARTESIAN_POINT('Ctrl Pts',(72.7478470969032,5.04197212574731,127.914683199832));
#226815=CARTESIAN_POINT('Ctrl Pts',(72.46939947309,0.294141639526237,125.000465443524));
#226816=CARTESIAN_POINT('Ctrl Pts',(72.1909518492774,-4.72399064380143,
127.419743816117));
#226817=CARTESIAN_POINT('Ctrl Pts',(71.9125042254643,-5.40100630524849,
132.949319681519));
#226818=CARTESIAN_POINT('Ctrl Pts',(71.6340566016516,-1.11476102599866,
136.507782954223));
#226819=CARTESIAN_POINT('Ctrl Pts',(71.3556089778387,4.19589517704018,134.82507972721));
#226820=CARTESIAN_POINT('Ctrl Pts',(71.0771613540258,5.65072869325411,129.447532061481));
#226821=CARTESIAN_POINT('Ctrl Pts',(70.7987137302128,1.91281859381102,125.316843554035));
#226822=CARTESIAN_POINT('Ctrl Pts',(70.5202661064001,-3.58287834696108,
126.22891514786));
#226823=CARTESIAN_POINT('Ctrl Pts',(70.241818482587,-5.78608512021397,131.345597605407));
#226824=CARTESIAN_POINT('Ctrl Pts',(69.9633708587742,-2.67216233396265,
135.964909712024));
#226825=CARTESIAN_POINT('Ctrl Pts',(69.6849232349613,2.89734709481291,135.841929307673));
#226826=CARTESIAN_POINT('Ctrl Pts',(69.4064756111484,5.80433608672999,131.089669376025));
#226827=CARTESIAN_POINT('Ctrl Pts',(69.1280279873355,3.37742377252397,126.07522463346));
#226828=CARTESIAN_POINT('Ctrl Pts',(68.8495803635227,-2.15317599230747,
125.406624829152));
#226829=CARTESIAN_POINT('Ctrl Pts',(68.5711327397097,-5.70511220870344,
129.698280520343));
#226830=CARTESIAN_POINT('Ctrl Pts',(68.2926851158969,-4.01432901552682,
135.006369785865));
#226831=CARTESIAN_POINT('Ctrl Pts',(68.014237492084,1.36542643204398,136.45301790528));
#226832=CARTESIAN_POINT('Ctrl Pts',(67.735789868271,5.49042169335597,132.708825929535));
#226833=CARTESIAN_POINT('Ctrl Pts',(67.4573422444582,4.56998764048497,127.214523370394));
#226834=CARTESIAN_POINT('Ctrl Pts',(67.1788946206453,-0.550041797684044,
125.019105868103));
#226835=CARTESIAN_POINT('Ctrl Pts',(66.9004469968323,-5.164609694817,128.140054855163));
#226836=CARTESIAN_POINT('Ctrl Pts',(66.6219993730196,-5.03315358762317,
133.709370679297));
#226837=CARTESIAN_POINT('Ctrl Pts',(66.3435517492066,-0.2764752166261,136.609124174332));
#226838=CARTESIAN_POINT('Ctrl Pts',(66.0651041253938,4.73427037188528,134.174583539162));
#226839=CARTESIAN_POINT('Ctrl Pts',(65.7866565015808,5.39445277059944,128.642972683589));
#226840=CARTESIAN_POINT('Ctrl Pts',(65.508208877768,1.0973966068015,125.097571749668));
#226841=CARTESIAN_POINT('Ctrl Pts',(65.2297612539551,-4.20811342784249,
126.796430993211));
#226842=CARTESIAN_POINT('Ctrl Pts',(64.9513136301422,-5.64657280006891,
132.178381763287));
#226843=CARTESIAN_POINT('Ctrl Pts',(64.6728660063292,-1.89610761944867,
136.297674225111));
#226844=CARTESIAN_POINT('Ctrl Pts',(64.3944183825164,3.59678783343796,135.368879844889));
#226845=CARTESIAN_POINT('Ctrl Pts',(64.1159707587035,5.78441098024938,130.245515283918));
#226846=CARTESIAN_POINT('Ctrl Pts',(63.8375231348906,2.65644302039782,125.635702283457));
#226847=CARTESIAN_POINT('Ctrl Pts',(63.5590755110777,-2.91266630074331,
125.775633789045));
#226848=CARTESIAN_POINT('Ctrl Pts',(63.2806278872649,-5.80517758316048,
130.53671958308));
#226849=CARTESIAN_POINT('Ctrl Pts',(63.0021802634519,-3.36301426534433,
135.543754412816));
#226850=CARTESIAN_POINT('Ctrl Pts',(62.723732639639,2.16959486994269,136.195517876976));
#226851=CARTESIAN_POINT('Ctrl Pts',(62.4452850158262,5.70845231035428,131.893071192411));
#226852=CARTESIAN_POINT('Ctrl Pts',(62.1668373920132,4.00152095094907,126.590152676031));
#226853=CARTESIAN_POINT('Ctrl Pts',(61.8883897682004,-1.38261267721222,
125.159885382419));
#226854=CARTESIAN_POINT('Ctrl Pts',(61.6099421443874,-5.49619279939966,
128.916615081961));
#226855=CARTESIAN_POINT('Ctrl Pts',(61.3314945205747,-4.55904024288434,
134.408090707227));
#226856=CARTESIAN_POINT('Ctrl Pts',(61.0530468967616,0.567647575344072,
136.587914432096));
#226857=CARTESIAN_POINT('Ctrl Pts',(60.7745992729488,5.17269500295686,133.452934743723));
#226858=CARTESIAN_POINT('Ctrl Pts',(60.496151649136,5.02428842305186,127.884044823451));
#226859=CARTESIAN_POINT('Ctrl Pts',(60.2177040253229,0.258806232497024,
124.998782452612));
#226860=CARTESIAN_POINT('Ctrl Pts',(59.9392564015102,-4.74450624233532,
127.448562797104));
#226861=CARTESIAN_POINT('Ctrl Pts',(59.6608087776971,-5.38784926247686,
132.982157398764));
#226862=CARTESIAN_POINT('Ctrl Pts',(59.3823611538844,-1.08002202147149,
136.514463149789));
#226863=CARTESIAN_POINT('Ctrl Pts',(59.1039135300714,4.22029269525717,134.799463627718));
#226864=CARTESIAN_POINT('Ctrl Pts',(58.8254659062585,5.64236459780459,129.413159610949));
#226865=CARTESIAN_POINT('Ctrl Pts',(58.5470182824457,1.8793790798041,125.305301355313));
#226866=CARTESIAN_POINT('Ctrl Pts',(58.2685706586328,-3.61066399976409,
126.250809917708));
#226867=CARTESIAN_POINT('Ctrl Pts',(57.9901230348199,-5.78268325429153,
131.380809119953));
#226868=CARTESIAN_POINT('Ctrl Pts',(57.711675411007,-2.64069909790739,135.981080309579));
#226869=CARTESIAN_POINT('Ctrl Pts',(57.4332277871941,2.92795852413098,135.824198999061));
#226870=CARTESIAN_POINT('Ctrl Pts',(57.1547801633813,5.80596530121877,131.054331448687));
#226871=CARTESIAN_POINT('Ctrl Pts',(56.8763325395683,3.34857360366007,126.054752916266));
#226872=CARTESIAN_POINT('Ctrl Pts',(56.5978849157555,-2.18599364874745,
125.419831830104));
#226873=CARTESIAN_POINT('Ctrl Pts',(56.3194372919424,-5.71173952968275,
129.733029650764));
#226874=CARTESIAN_POINT('Ctrl Pts',(56.0409896681298,-3.98867581682796,
135.030728292487));
#226875=CARTESIAN_POINT('Ctrl Pts',(55.7625420443167,1.39978611404518,136.444601510497));
#226876=CARTESIAN_POINT('Ctrl Pts',(55.4840944205039,5.50191298946419,132.675368888989));
#226877=CARTESIAN_POINT('Ctrl Pts',(55.2056467966909,4.54805061095778,127.186771069878));
#226878=CARTESIAN_POINT('Ctrl Pts',(54.9271991728781,-0.585248094394635,
125.022561316018));
#226879=CARTESIAN_POINT('Ctrl Pts',(54.6487515490652,-5.18073239195715,
128.171542663682));
#226880=CARTESIAN_POINT('Ctrl Pts',(54.3703039252523,-5.01537671415865,
133.739955090657));
#226881=CARTESIAN_POINT('Ctrl Pts',(54.0918563014394,-0.241134850822232,
136.610699608625));
#226882=CARTESIAN_POINT('Ctrl Pts',(53.8134086776265,4.75469816032759,134.145702249237));
#226883=CARTESIAN_POINT('Ctrl Pts',(53.5349610538137,5.38119584205463,128.610175163959));
#226884=CARTESIAN_POINT('Ctrl Pts',(53.2565134300007,1.06263743096531,125.090997318624));
#226885=CARTESIAN_POINT('Ctrl Pts',(52.9780658061879,-4.23243286645675,
126.822121231705));
#226886=CARTESIAN_POINT('Ctrl Pts',(52.6996181823749,-5.63810412544538,
132.21272859718));
#226887=CARTESIAN_POINT('Ctrl Pts',(52.4211705585621,-1.86263312984859,
136.309114591992));
#226888=CARTESIAN_POINT('Ctrl Pts',(52.1427229347491,3.62450671739182,135.346900606486));
#226889=CARTESIAN_POINT('Ctrl Pts',(51.8642753109363,5.7809019583462,130.210314286579));
#226890=CARTESIAN_POINT('Ctrl Pts',(51.5858276871234,2.62493071234137,125.619627524071));
#226891=CARTESIAN_POINT('Ctrl Pts',(51.3073800633105,-2.94322362331098,
125.793457186192));
#226892=CARTESIAN_POINT('Ctrl Pts',(51.0289324394976,-5.80669923360788,
130.572062305503));
#226893=CARTESIAN_POINT('Ctrl Pts',(50.7504848156848,-3.33410192124705,
135.564138225197));
#226894=CARTESIAN_POINT('Ctrl Pts',(50.4720371918718,2.20237217680579,136.182211051539));
#226895=CARTESIAN_POINT('Ctrl Pts',(50.193589568059,5.71497383623647,131.858302051661));
#226896=CARTESIAN_POINT('Ctrl Pts',(49.915141944246,3.97579373215887,126.565872361749));
#226897=CARTESIAN_POINT('Ctrl Pts',(49.6366943204332,-1.41694658345112,
125.168406317271));
#226898=CARTESIAN_POINT('Ctrl Pts',(49.3582466966203,-5.50758221055828,
128.950106943089));
#226899=CARTESIAN_POINT('Ctrl Pts',(49.0797990728074,-4.53701884651156,
134.435776110423));
#226900=CARTESIAN_POINT('Ctrl Pts',(48.8013514489945,0.602843191786665,
136.584351844331));
#226901=CARTESIAN_POINT('Ctrl Pts',(48.5229038251815,5.18872178735999,133.421398009111));
#226902=CARTESIAN_POINT('Ctrl Pts',(48.2444562013688,5.006418543501,127.853514660444));
#226903=CARTESIAN_POINT('Ctrl Pts',(47.9660085775558,0.223461235307256,
124.997314589534));
#226904=CARTESIAN_POINT('Ctrl Pts',(47.6875609537429,-4.7648460314457,127.477506128414));
#226905=CARTESIAN_POINT('Ctrl Pts',(47.40911332993,-5.37449257096935,133.014914416948));
#226906=CARTESIAN_POINT('Ctrl Pts',(47.1306657061172,-1.04524299633083,
136.520931755405));
#226907=CARTESIAN_POINT('Ctrl Pts',(46.8522180823042,4.24453382897653,134.773699488214));
#226908=CARTESIAN_POINT('Ctrl Pts',(46.5737704584914,5.6337914224598,129.378838711881));
#226909=CARTESIAN_POINT('Ctrl Pts',(46.2953228346785,1.84586992471411,125.293962926255));
#226910=CARTESIAN_POINT('Ctrl Pts',(46.0168752108656,-3.63831585808481,
126.272873421051));
#226911=CARTESIAN_POINT('Ctrl Pts',(45.7384275870526,-5.77906710891461,
131.415999273987));
#226912=CARTESIAN_POINT('Ctrl Pts',(45.4599799632399,-2.60913800977569,
135.997059081882));
#226913=CARTESIAN_POINT('Ctrl Pts',(45.1815323394269,2.95846145686929,135.806282678493));
#226914=CARTESIAN_POINT('Ctrl Pts',(44.903084715614,5.80737937352832,131.018984258588));
#226915=CARTESIAN_POINT('Ctrl Pts',(44.6246370918012,3.31959935216964,126.034457197533));
#226916=CARTESIAN_POINT('Ctrl Pts',(44.3461894679882,-2.21873030238901,
125.43323835675));
#226917=CARTESIAN_POINT('Ctrl Pts',(44.0677418441753,-5.7181552000533,129.767818479747));
#226918=CARTESIAN_POINT('Ctrl Pts',(43.7892942203624,-3.96287481627985,
135.054930189501));
#226919=CARTESIAN_POINT('Ctrl Pts',(43.5108465965496,1.43409392645716,136.435976114513));
#226920=CARTESIAN_POINT('Ctrl Pts',(43.2323989727367,5.51320041016325,132.641842517543));
#226921=CARTESIAN_POINT('Ctrl Pts',(42.9539513489238,4.52594505174265,127.159152820475));
#226922=CARTESIAN_POINT('Ctrl Pts',(42.6755037251109,-0.620432704521861,
125.026231010632));
#226923=CARTESIAN_POINT('Ctrl Pts',(42.397056101298,-5.19666311515333,128.203128032237));
#226924=CARTESIAN_POINT('Ctrl Pts',(42.1186084774851,-4.99741399406557,
133.770430722483));
#226925=CARTESIAN_POINT('Ctrl Pts',(41.8401608536722,-0.205785549677785,
136.612059886891));
#226926=CARTESIAN_POINT('Ctrl Pts',(41.5617132298594,4.77494976168102,134.11669714467));
#226927=CARTESIAN_POINT('Ctrl Pts',(41.2832656060464,5.36773951131901,128.577458950676));
#226928=CARTESIAN_POINT('Ctrl Pts',(41.0048179822336,1.02783887870806,125.084634598359));
#226929=CARTESIAN_POINT('Ctrl Pts',(40.7263703584206,-4.25659547071474,
126.847959033542));
#226930=CARTESIAN_POINT('Ctrl Pts',(40.4479227346078,-5.62942652880005,
132.24702324348));
#226931=CARTESIAN_POINT('Ctrl Pts',(40.1694751107948,-1.82908961969292,
136.320350978189));
#226932=CARTESIAN_POINT('Ctrl Pts',(39.891027486982,3.65209129391637,135.324753042595));
#226933=CARTESIAN_POINT('Ctrl Pts',(39.6125798631691,5.77717872299504,130.175135301845));
#226934=CARTESIAN_POINT('Ctrl Pts',(39.3341322393562,2.59332113651206,125.603744886877));
#226935=CARTESIAN_POINT('Ctrl Pts',(39.0556846155433,-2.97367188364494,
125.811466264208));
#226936=CARTESIAN_POINT('Ctrl Pts',(38.7772369917304,-5.80800571467979,
130.607413635826));
#226937=CARTESIAN_POINT('Ctrl Pts',(38.4987893679175,-3.30506603077697,
135.584345662267));
#226938=CARTESIAN_POINT('Ctrl Pts',(38.2203417441046,2.23506787395795,136.16870494788));
#226939=CARTESIAN_POINT('Ctrl Pts',(37.9418941202917,5.72128359166147,131.823493856722));
#226940=CARTESIAN_POINT('Ctrl Pts',(37.6634464964789,3.94991918886983,126.541749106207));
#226941=CARTESIAN_POINT('Ctrl Pts',(37.3849988726659,-1.45122798421329,
125.177136094481));
#226942=CARTESIAN_POINT('Ctrl Pts',(37.1065512488531,-5.51876753623267,
128.983667514269));
#226943=CARTESIAN_POINT('Ctrl Pts',(36.8281036250402,-4.51482932923697,
134.463326950183));
#226944=CARTESIAN_POINT('Ctrl Pts',(36.5496560012273,0.6380164696531,136.580575076865));
#226945=CARTESIAN_POINT('Ctrl Pts',(36.2712083774144,5.20455630176915,133.389764299214));
#226946=CARTESIAN_POINT('Ctrl Pts',(35.9927607536015,4.9883631492699,127.82309384212));
#226947=CARTESIAN_POINT('Ctrl Pts',(35.7143131297886,0.188107957679239,
124.996061908681));
#226948=CARTESIAN_POINT('Ctrl Pts',(35.4358655059757,-4.78500925743413,
127.50657273754));
#226949=CARTESIAN_POINT('Ctrl Pts',(35.1574178821628,-5.36093672566315,
133.047589522248));
#226950=CARTESIAN_POINT('Ctrl Pts',(34.87897025835,-1.01042523932657,136.527188531377));
#226951=CARTESIAN_POINT('Ctrl Pts',(34.6005226345371,4.26861767993396,134.747788263399));
#226952=CARTESIAN_POINT('Ctrl Pts',(34.3220750107242,5.62500948490202,129.34457063605));
#226953=CARTESIAN_POINT('Ctrl Pts',(34.0436273869112,1.81229237023524,125.282828687009));
#226954=CARTESIAN_POINT('Ctrl Pts',(33.7651797630984,-3.66583289727342,
126.295104840318));
#226955=CARTESIAN_POINT('Ctrl Pts',(33.4867321392855,-5.77523681808073,
131.451166763527));
#226956=CARTESIAN_POINT('Ctrl Pts',(33.2082845154725,-2.57748023907555,
136.012845436834));
#226957=CARTESIAN_POINT('Ctrl Pts',(32.9298368916598,2.98885476273036,135.788181009863));
#226958=CARTESIAN_POINT('Ctrl Pts',(32.6513892678468,5.80857825125962,130.983629115531));
#226959=CARTESIAN_POINT('Ctrl Pts',(32.3729416440339,3.29050209170421,126.014338229324));
#226960=CARTESIAN_POINT('Ctrl Pts',(32.094494020221,-2.25138474016344,125.446843912307));
#226961=CARTESIAN_POINT('Ctrl Pts',(31.8160463964081,-5.72435898208005,
129.802645718181));
#226962=CARTESIAN_POINT('Ctrl Pts',(31.5375987725953,-3.93692696994811,
135.078974580096));
#226963=CARTESIAN_POINT('Ctrl Pts',(31.2591511487823,1.46834859799131,136.427142036947));
#226964=CARTESIAN_POINT('Ctrl Pts',(30.9807035249695,5.52428353719365,132.608248057529));
#226965=CARTESIAN_POINT('Ctrl Pts',(30.7022559011566,4.50367178196922,127.131669645585));
#226966=CARTESIAN_POINT('Ctrl Pts',(30.4238082773436,-0.655594324287056,
125.030114815962));
#226967=CARTESIAN_POINT('Ctrl Pts',(30.1453606535308,-5.21240127408669,
128.234809790423));
#226968=CARTESIAN_POINT('Ctrl Pts',(29.8669130297179,-4.97926609295916,
133.80079644549));
#226969=CARTESIAN_POINT('Ctrl Pts',(29.588465405905,-0.170428623074124,
136.613204958723));
#226970=CARTESIAN_POINT('Ctrl Pts',(29.3100177820921,4.79502442551506,134.087569300254));
#226971=CARTESIAN_POINT('Ctrl Pts',(29.0315701582792,5.35408427702179,128.544825256054));
#226972=CARTESIAN_POINT('Ctrl Pts',(28.7531225344664,0.99300223950345,125.078483824645));
#226973=CARTESIAN_POINT('Ctrl Pts',(28.4746749106534,-4.28060034526213,
126.873943441297));
#226974=CARTESIAN_POINT('Ctrl Pts',(28.1962272868406,-5.6205403316845,132.281264431386));
#226975=CARTESIAN_POINT('Ctrl Pts',(27.9177796630277,-1.79547833194873,
136.331382967337));
#226976=CARTESIAN_POINT('Ctrl Pts',(27.6393320392148,3.67954054085496,135.3024379739));
#226977=CARTESIAN_POINT('Ctrl Pts',(27.3608844154018,5.77324141216173,130.139979633288));
#226978=CARTESIAN_POINT('Ctrl Pts',(27.082436791589,2.56161546421434,125.58805496041));
#226979=CARTESIAN_POINT('Ctrl Pts',(26.8039891677761,-3.00400995347367,
125.82966035576));
#226980=CARTESIAN_POINT('Ctrl Pts',(26.5255415439632,-5.80909697796402,
130.642772264091));
#226981=CARTESIAN_POINT('Ctrl Pts',(26.2470939201503,-3.27590766986969,
135.604375975235));
#226982=CARTESIAN_POINT('Ctrl Pts',(25.9686462963375,2.2676807498481,136.155000066467));
#226983=CARTESIAN_POINT('Ctrl Pts',(25.6901986725246,5.727381342819,131.788647897428));
#226984=CARTESIAN_POINT('Ctrl Pts',(25.4117510487116,3.92389827987267,126.517783803302));
#226985=CARTESIAN_POINT('Ctrl Pts',(25.1333034248988,-1.48545560918882,
125.186074390566));
#226986=CARTESIAN_POINT('Ctrl Pts',(24.8548558010858,-5.5297483619465,129.017295551901));
#226987=CARTESIAN_POINT('Ctrl Pts',(24.576408177273,-4.49247251330123,134.490742205601));
#226988=CARTESIAN_POINT('Ctrl Pts',(24.2979605534601,0.673166105584617,
136.576584269648));
#226989=CARTESIAN_POINT('Ctrl Pts',(24.0195129296472,5.22019795943058,133.358034786234));
#226990=CARTESIAN_POINT('Ctrl Pts',(23.7410653058343,4.97012290940784,127.792783495733));
#226991=CARTESIAN_POINT('Ctrl Pts',(23.4626176820214,0.152747709641667,
124.995024456474));
#226992=CARTESIAN_POINT('Ctrl Pts',(23.1841700582085,-4.80499517314482,
127.53576154741));
#226993=CARTESIAN_POINT('Ctrl Pts',(22.9057224343956,-5.34718222887511,
133.080181503877));
#226994=CARTESIAN_POINT('Ctrl Pts',(22.6272748105827,-0.975570040643468,
136.533233245855));
#226995=CARTESIAN_POINT('Ctrl Pts',(22.3488271867698,4.29254335569345,134.721730913422));
#226996=CARTESIAN_POINT('Ctrl Pts',(22.070379562957,5.61601911054919,129.310356653276));
#226997=CARTESIAN_POINT('Ctrl Pts',(21.791931939144,1.77864766059611,125.27189905016));
#226998=CARTESIAN_POINT('Ctrl Pts',(21.5134843153312,-3.69321409767591,
126.317503351717));
#226999=CARTESIAN_POINT('Ctrl Pts',(21.2350366915183,-5.77119252372273,
131.486310285425));
#227000=CARTESIAN_POINT('Ctrl Pts',(20.9565890677054,-2.54572695889727,
136.028438789465));
#227001=CARTESIAN_POINT('Ctrl Pts',(20.6781414438925,3.01913731547902,135.769894663934));
#227002=CARTESIAN_POINT('Ctrl Pts',(20.3996938200796,5.80956188998761,130.948267329615));
#227003=CARTESIAN_POINT('Ctrl Pts',(20.1212461962667,3.26128290047392,125.994396757156));
#227004=CARTESIAN_POINT('Ctrl Pts',(19.8427985724538,-2.28395575204823,
125.460647992615));
#227005=CARTESIAN_POINT('Ctrl Pts',(19.5643509486409,-5.7303506458796,129.837510075529));
#227006=CARTESIAN_POINT('Ctrl Pts',(19.285903324828,-3.91083323933969,135.102860573299));
#227007=CARTESIAN_POINT('Ctrl Pts',(19.0074557010152,1.50254885932817,136.418099605148));
#227008=CARTESIAN_POINT('Ctrl Pts',(18.7290080772022,5.53516195986603,132.574586753804));
#227009=CARTESIAN_POINT('Ctrl Pts',(18.4505604533894,4.48123162698169,127.104322563612));
#227010=CARTESIAN_POINT('Ctrl Pts',(18.1721128295765,-0.690731650763477,
125.034212588094));
#227011=CARTESIAN_POINT('Ctrl Pts',(17.8936652057636,-5.22794628557398,
128.26658676426));
#227012=CARTESIAN_POINT('Ctrl Pts',(17.6152175819507,-4.96093368331654,
133.831051134467));
#227013=CARTESIAN_POINT('Ctrl Pts',(17.3367699581378,-0.135065381175154,
136.614134781694));
#227014=CARTESIAN_POINT('Ctrl Pts',(17.0583223343249,4.81492140795562,134.058319795333));
#227015=CARTESIAN_POINT('Ctrl Pts',(16.779874710512,5.34023064516271,128.512275289347));
#227016=CARTESIAN_POINT('Ctrl Pts',(16.5014270866992,0.958128804235671,
125.0725452254));
#227017=CARTESIAN_POINT('Ctrl Pts',(16.2229794628862,-4.30444660058956,
126.900073492105));
#227018=CARTESIAN_POINT('Ctrl Pts',(15.9445318390734,-5.61144586338,132.315450892077));
#227019=CARTESIAN_POINT('Ctrl Pts',(15.6660842152604,-1.76180051209467,
136.342210150638));
#227020=CARTESIAN_POINT('Ctrl Pts',(15.3876365914476,3.70685344106567,135.279956227294));
#227021=CARTESIAN_POINT('Ctrl Pts',(15.1091889676347,5.76909017174479,130.104848583611));
#227022=CARTESIAN_POINT('Ctrl Pts',(14.8307413438218,2.52981487031356,125.572558326068));
#227023=CARTESIAN_POINT('Ctrl Pts',(14.5522937200089,-3.03423670860886,
125.848038786661));
#227024=CARTESIAN_POINT('Ctrl Pts',(14.273846096196,-5.80997298302346,130.678136880072));
#227025=CARTESIAN_POINT('Ctrl Pts',(13.9953984723831,-3.24662791899898,
135.624228421867));
#227026=CARTESIAN_POINT('Ctrl Pts',(13.7169508485702,2.30020959599411,136.141096915141));
#227027=CARTESIAN_POINT('Ctrl Pts',(13.4385032247574,5.73326686375462,131.753765465006));
#227028=CARTESIAN_POINT('Ctrl Pts',(13.1600556009444,3.89773196938174,126.493977341077));
#227029=CARTESIAN_POINT('Ctrl Pts',(12.8816079771316,-1.51962819006047,
125.195220874312));
#227030=CARTESIAN_POINT('Ctrl Pts',(12.6031603533186,-5.54052428080121,
129.050989809886));
#227031=CARTESIAN_POINT('Ctrl Pts',(12.3247127295058,-4.46994922714442,
134.518020860792));
#227032=CARTESIAN_POINT('Ctrl Pts',(12.0462651056929,0.708290797098533,
136.572379570561));
#227033=CARTESIAN_POINT('Ctrl Pts',(11.76781748188,5.23564618073708,133.326210645918));
#227034=CARTESIAN_POINT('Ctrl Pts',(11.4893698580671,4.95169849981347,127.762584744442));
#227035=CARTESIAN_POINT('Ctrl Pts',(11.2109222342542,0.117381801481337,
124.994202271355));
#227036=CARTESIAN_POINT('Ctrl Pts',(10.9324746104413,-4.82480303799234,
127.565071476419));
#227037=CARTESIAN_POINT('Ctrl Pts',(10.6540269866284,-5.33322959028317,
133.112689154126));
#227038=CARTESIAN_POINT('Ctrl Pts',(10.3755793628155,-0.940678691853753,
136.539065674851));
#227039=CARTESIAN_POINT('Ctrl Pts',(10.0971317390026,4.31630996968034,134.695528403849));
#227040=CARTESIAN_POINT('Ctrl Pts',(9.81868411518972,5.60682063254294,129.276198031366));
#227041=CARTESIAN_POINT('Ctrl Pts',(9.54023649137686,1.74493704251384,125.261174420708));
#227042=CARTESIAN_POINT('Ctrl Pts',(9.26178886756394,-3.72045844467185,
126.340068125262));
#227043=CARTESIAN_POINT('Ctrl Pts',(8.98334124375105,-5.76693437570339,
131.52142853743));
#227044=CARTESIAN_POINT('Ctrl Pts',(8.70489361993813,-2.51387934587036,
136.043838561958));
#227045=CARTESIAN_POINT('Ctrl Pts',(8.42644599612531,3.0493079929842,135.751424318317));
#227046=CARTESIAN_POINT('Ctrl Pts',(8.14799837231237,5.81033025326331,130.912900211183));
#227047=CARTESIAN_POINT('Ctrl Pts',(7.86955074849947,3.23194286120641,125.974633519968));
#227048=CARTESIAN_POINT('Ctrl Pts',(7.59110312468663,-2.3164421311127,125.47465008616));
#227049=CARTESIAN_POINT('Ctrl Pts',(7.31265550087371,-5.73612996942864,
129.872410259879));
#227050=CARTESIAN_POINT('Ctrl Pts',(7.0342078770608,-3.88459459136738,135.126587284006));
#227051=CARTESIAN_POINT('Ctrl Pts',(6.75576025324794,1.53669344316449,136.408849154185));
#227052=CARTESIAN_POINT('Ctrl Pts',(6.47731262943506,5.54583527507644,132.540859853697));
#227053=CARTESIAN_POINT('Ctrl Pts',(6.19886500562214,4.45862541830825,127.077112587908));
#227054=CARTESIAN_POINT('Ctrl Pts',(5.92041738180924,-0.725843381924555,
125.038524175185));
#227055=CARTESIAN_POINT('Ctrl Pts',(5.64196975799638,-5.24329757358911,
128.29845777624));
#227056=CARTESIAN_POINT('Ctrl Pts',(5.36352213418349,-4.94241744445191,
133.861193668313));
#227057=CARTESIAN_POINT('Ctrl Pts',(5.08507451037056,-0.0996971343788212,
136.614849321347));
#227058=CARTESIAN_POINT('Ctrl Pts',(4.80662688655771,4.83463997171276,134.028949713759));
#227059=CARTESIAN_POINT('Ctrl Pts',(4.5281792627448,5.32617912909322,128.479810256704));
#227060=CARTESIAN_POINT('Ctrl Pts',(4.24973163893191,0.923219865152705,
125.066819020683));
#227061=CARTESIAN_POINT('Ctrl Pts',(3.97128401511898,-4.32813335306523,
126.926348217707));
#227062=CARTESIAN_POINT('Ctrl Pts',(3.69283639130614,-5.60214346088543,
132.349581358763));
#227063=CARTESIAN_POINT('Ctrl Pts',(3.41438876749324,-1.72805740807474,
136.352832126888));
#227064=CARTESIAN_POINT('Ctrl Pts',(3.13594114368033,3.73402898245891,135.257308635848));
#227065=CARTESIAN_POINT('Ctrl Pts',(2.85749351986744,5.76472515556999,130.06974345461));
#227066=CARTESIAN_POINT('Ctrl Pts',(2.5790458960546,2.49792053319242,125.557255558086));
#227067=CARTESIAN_POINT('Ctrl Pts',(2.30059827224166,-3.06435102898697,
125.866600875889));
#227068=CARTESIAN_POINT('Ctrl Pts',(2.02215064842876,-5.81063369739741,
130.713506173321));
#227069=CARTESIAN_POINT('Ctrl Pts',(1.74370302461591,-3.21722786313679,
135.643902266527));
#227070=CARTESIAN_POINT('Ctrl Pts',(1.46525540080302,2.33265320702766,136.12699600909));
#227071=CARTESIAN_POINT('Ctrl Pts',(1.18680777699008,5.73893993637821,131.718847852038));
#227072=CARTESIAN_POINT('Ctrl Pts',(0.908360153177235,3.87142122699929,
126.47033060169));
#227073=CARTESIAN_POINT('Ctrl Pts',(0.629912529364331,-1.55374446055069,
125.204575206795));
#227074=CARTESIAN_POINT('Ctrl Pts',(0.351464905551429,-5.55109489349118,
129.084749039672));
#227075=CARTESIAN_POINT('Ctrl Pts',(0.0730172817385382,-4.44726030537518,
134.545161904937));
#227076=CARTESIAN_POINT('Ctrl Pts',(-0.205430342074321,0.743389242636492,
136.56796113541));
#227077=CARTESIAN_POINT('Ctrl Pts',(-0.48387796588724,5.25090039324876,
133.294293057522));
#227078=CARTESIAN_POINT('Ctrl Pts',(-0.762325589700153,4.93309060321035,
127.732498707276));
#227079=CARTESIAN_POINT('Ctrl Pts',(-1.040773213513,0.0820115436953976,
124.993595383789));
#227080=CARTESIAN_POINT('Ctrl Pts',(-1.3192208373259,-4.84443211798899,
127.594501438479));
#227081=CARTESIAN_POINT('Ctrl Pts',(-1.5976684611388,-5.31907932690746,
133.145111268411));
#227082=CARTESIAN_POINT('Ctrl Pts',(-1.8761160849517,-0.905752485869179,
136.544685602242));
#227083=CARTESIAN_POINT('Ctrl Pts',(-2.15456370876455,4.33991664121397,
134.669181705622));
#227084=CARTESIAN_POINT('Ctrl Pts',(-2.43301133257747,5.59741439173625,
129.242096036083));
#227085=CARTESIAN_POINT('Ctrl Pts',(-2.71145895639038,1.71116176514775,
125.250655196059));
#227086=CARTESIAN_POINT('Ctrl Pts',(-2.98990658020324,-3.74756492871192,
126.362798324807));
#227087=CARTESIAN_POINT('Ctrl Pts',(-3.26835420401613,-5.76246253181,131.556520218218));
#227088=CARTESIAN_POINT('Ctrl Pts',(-3.54680182782904,-2.48193858011979,
136.059044183669));
#227089=CARTESIAN_POINT('Ctrl Pts',(-3.82524945164193,3.0793656772603,135.732770657435));
#227090=CARTESIAN_POINT('Ctrl Pts',(-4.1036970754548,5.81088331261472,130.877529070775));
#227091=CARTESIAN_POINT('Ctrl Pts',(-4.38214469926771,3.20248306110764,
125.955049250094));
#227092=CARTESIAN_POINT('Ctrl Pts',(-4.66059232308062,-2.34884267356213,
125.488849674089));
#227093=CARTESIAN_POINT('Ctrl Pts',(-4.93903994689347,-5.7416967385722,
129.907344977992));
#227094=CARTESIAN_POINT('Ctrl Pts',(-5.21748757070636,-3.85821199831392,
135.150153833014));
#227095=CARTESIAN_POINT('Ctrl Pts',(-5.49593519451928,1.57078108426016,
136.399391026839));
#227096=CARTESIAN_POINT('Ctrl Pts',(-5.77438281833216,5.55630308732125,
132.507068606974));
#227097=CARTESIAN_POINT('Ctrl Pts',(-6.05283044214503,4.43585399363028,
127.050040726751));
#227098=CARTESIAN_POINT('Ctrl Pts',(-6.33127806595794,-0.76092821669219,
125.043049417465));
#227099=CARTESIAN_POINT('Ctrl Pts',(-6.60972568977086,-5.25845456928442,
128.330421645371));
#227100=CARTESIAN_POINT('Ctrl Pts',(-6.88817331358369,-4.92371806249131,
133.891222930087));
#227101=CARTESIAN_POINT('Ctrl Pts',(-7.16662093739661,-0.0643251932685087,
136.615348551203));
#227102=CARTESIAN_POINT('Ctrl Pts',(-7.44506856120951,4.8541793861078,133.999460143849));
#227103=CARTESIAN_POINT('Ctrl Pts',(-7.72351618502242,5.3119302494974,128.44743136113));
#227104=CARTESIAN_POINT('Ctrl Pts',(-8.00196380883526,0.888276715818123,
125.06130542268));
#227105=CARTESIAN_POINT('Ctrl Pts',(-8.28041143264819,-4.35165972496785,
126.952766644486));
#227106=CARTESIAN_POINT('Ctrl Pts',(-8.55885905646108,-5.59263346890473,
132.383654566726));
#227107=CARTESIAN_POINT('Ctrl Pts',(-8.83730668027396,-1.69425027025207,
136.363248502487));
#227108=CARTESIAN_POINT('Ctrl Pts',(-9.11575430408684,3.76106615803527,
135.234496038775));
#227109=CARTESIAN_POINT('Ctrl Pts',(-9.39420192789976,5.7601465253845,130.034665547118));
#227110=CARTESIAN_POINT('Ctrl Pts',(-9.67264955171265,2.4659336347071,125.542147223509));
#227111=CARTESIAN_POINT('Ctrl Pts',(-9.95109717552551,-3.09435179871079,
125.885345935621));
#227112=CARTESIAN_POINT('Ctrl Pts',(-10.2295447993384,-5.81107909660284,
130.748878833214));
#227113=CARTESIAN_POINT('Ctrl Pts',(-10.5079924231513,-3.18770859171301,
135.663396780189));
#227114=CARTESIAN_POINT('Ctrl Pts',(-10.7864400469642,2.36501038073878,
136.112697870828));
#227115=CARTESIAN_POINT('Ctrl Pts',(-11.0648876707771,5.74440035047196,
131.683896352409));
#227116=CARTESIAN_POINT('Ctrl Pts',(-11.34333529459,3.84496702767957,126.446844461378));
#227117=CARTESIAN_POINT('Ctrl Pts',(-11.6217829184029,-1.58780315646856,
125.214137041385));
#227118=CARTESIAN_POINT('Ctrl Pts',(-11.9002305422157,-5.56145980831845,
129.118571990297));
#227119=CARTESIAN_POINT('Ctrl Pts',(-12.1786781660286,-4.42440658873985,
134.572164332316));
#227120=CARTESIAN_POINT('Ctrl Pts',(-12.4571257898416,0.778460141612691,
136.563329127923));
#227121=CARTESIAN_POINT('Ctrl Pts',(-12.7355734136544,5.26596003171537,
133.262283203764));
#227122=CARTESIAN_POINT('Ctrl Pts',(-13.0140210374673,4.91429990912079,
127.702526499083));
#227123=CARTESIAN_POINT('Ctrl Pts',(-13.2924686612802,0.0466382469415425,
124.993203816266));
#227124=CARTESIAN_POINT('Ctrl Pts',(-13.5709162850931,-4.86388168577195,
127.624050343051));
#227125=CARTESIAN_POINT('Ctrl Pts',(-13.849363908906,-5.30473196309121,
133.177446645321));
#227126=CARTESIAN_POINT('Ctrl Pts',(-14.1278115327188,-0.87079271689315,
136.550092819781));
#227127=CARTESIAN_POINT('Ctrl Pts',(-14.4062591565318,4.36336249554048,
134.642691795028));
#227128=CARTESIAN_POINT('Ctrl Pts',(-14.6847067803446,5.58780073668082,
129.20805193109));
#227129=CARTESIAN_POINT('Ctrl Pts',(-14.9631544041576,1.67732308005318,
125.240341766008));
#227130=CARTESIAN_POINT('Ctrl Pts',(-15.2416020279704,-3.77453254535539,
126.385693108075));
#227131=CARTESIAN_POINT('Ctrl Pts',(-15.5200496517834,-5.75777715774833,
131.591584027456));
#227132=CARTESIAN_POINT('Ctrl Pts',(-15.7984972755962,-2.44990584522241,
136.074055091149));
#227133=CARTESIAN_POINT('Ctrl Pts',(-16.0769448994091,3.1093092545088,135.713934372506));
#227134=CARTESIAN_POINT('Ctrl Pts',(-16.355392523222,5.81122104754806,130.842155219084));
#227135=CARTESIAN_POINT('Ctrl Pts',(-16.6338401470349,3.17290459182133,
125.935644673236));
#227136=CARTESIAN_POINT('Ctrl Pts',(-16.9122877708478,-2.38115617878252,
125.50324623023));
#227137=CARTESIAN_POINT('Ctrl Pts',(-17.1907353946607,-5.74705074703162,
129.94231293535));
#227138=CARTESIAN_POINT('Ctrl Pts',(-17.4691830184736,-3.83168643779603,
135.173559347056));
#227139=CARTESIAN_POINT('Ctrl Pts',(-17.7476306422864,1.6048105194851,136.389725573584));
#227140=CARTESIAN_POINT('Ctrl Pts',(-18.0260782660994,5.56656500871184,
132.473214265779));
#227141=CARTESIAN_POINT('Ctrl Pts',(-18.3045258899123,4.4129181967513,127.023107983299));
#227142=CARTESIAN_POINT('Ctrl Pts',(-18.5829735137251,-0.795984854984928,
125.047788147249));
#227143=CARTESIAN_POINT('Ctrl Pts',(-18.861421137538,-5.27341671101187,
128.362477187221));
#227144=CARTESIAN_POINT('Ctrl Pts',(-19.1398687613509,-4.90483623034722,
133.921137807042));
#227145=CARTESIAN_POINT('Ctrl Pts',(-19.4183163851638,-0.0289508685644962,
136.615632452765));
#227146=CARTESIAN_POINT('Ctrl Pts',(-19.6967640089767,4.87353892710056,
133.969852178351));
#227147=CARTESIAN_POINT('Ctrl Pts',(-19.9752116327896,5.29748453437273,
128.415139802436));
#227148=CARTESIAN_POINT('Ctrl Pts',(-20.2536592566025,0.853300651063172,
125.056004635698));
#227149=CARTESIAN_POINT('Ctrl Pts',(-20.5321068804154,-4.37502484451904,
126.979327793496));
#227150=CARTESIAN_POINT('Ctrl Pts',(-20.8105545042282,-5.58291623983416,
132.417669253371));
#227151=CARTESIAN_POINT('Ctrl Pts',(-21.0890021280412,-1.66038035136256,
136.37345889145));
#227152=CARTESIAN_POINT('Ctrl Pts',(-21.367449751854,3.78796396592178,135.211519281404));
#227153=CARTESIAN_POINT('Ctrl Pts',(-21.6458973756669,5.75535445085128,
129.999616160961));
#227154=CARTESIAN_POINT('Ctrl Pts',(-21.9243449994798,2.43385536014432,
125.527233882186));
#227155=CARTESIAN_POINT('Ctrl Pts',(-22.2027926232928,-3.12423790609075,
125.904273271251));
#227156=CARTESIAN_POINT('Ctrl Pts',(-22.4812402471056,-5.81130916413533,
130.784253549004));
#227157=CARTESIAN_POINT('Ctrl Pts',(-22.7596878709185,-3.15807119857507,
135.682711240481));
#227158=CARTESIAN_POINT('Ctrl Pts',(-23.0381354947314,2.39727991812053,
136.098203030175));
#227159=CARTESIAN_POINT('Ctrl Pts',(-23.3165831185443,5.74964790369824,
131.648912261261));
#227160=CARTESIAN_POINT('Ctrl Pts',(-23.5950307423572,3.81837035169266,
126.423519790431));
#227161=CARTESIAN_POINT('Ctrl Pts',(-23.8734783661701,-1.62180301575654,
125.223906023766));
#227162=CARTESIAN_POINT('Ctrl Pts',(-24.151925989983,-5.57161864120731,
129.15245740844));
#227163=CARTESIAN_POINT('Ctrl Pts',(-24.4303736137958,-4.4013889240913,
134.599027142342));
#227164=CARTESIAN_POINT('Ctrl Pts',(-24.7088212376087,0.813502194462058,
136.558483719739));
#227165=CARTESIAN_POINT('Ctrl Pts',(-24.9872688614217,5.28082453809644,
133.230182270781));
#227166=CARTESIAN_POINT('Ctrl Pts',(-25.2657164852345,4.89532711384086,
127.672669230493));
#227167=CARTESIAN_POINT('Ctrl Pts',(-25.5441641090475,0.0112632219902977,
124.993027583295));
#227168=CARTESIAN_POINT('Ctrl Pts',(-25.8226117328602,-4.88315102063038,
127.65371709519));
#227169=CARTESIAN_POINT('Ctrl Pts',(-26.1010593566733,-5.29018803048126,
133.209694086655));
#227170=CARTESIAN_POINT('Ctrl Pts',(-26.3795069804861,-0.835800680372761,
136.555287127099));
#227171=CARTESIAN_POINT('Ctrl Pts',(-26.6579546042989,4.38664666386508,
134.616059653661));
#227172=CARTESIAN_POINT('Ctrl Pts',(-26.9364022281119,5.57798002361419,
129.174066977901));
#227173=CARTESIAN_POINT('Ctrl Pts',(-27.2148498519247,1.64342224113504,
125.23023451272));
#227174=CARTESIAN_POINT('Ctrl Pts',(-27.4932974757377,-3.80136029530733,
126.408751626694));
#227175=CARTESIAN_POINT('Ctrl Pts',(-27.7717450995505,-5.75287842713667,
131.626618665841));
#227176=CARTESIAN_POINT('Ctrl Pts',(-28.0501927233634,-2.41778232816299,
136.088870728161));
#227177=CARTESIAN_POINT('Ctrl Pts',(-28.3286403471763,3.13913761515943,
135.694916161515));
#227178=CARTESIAN_POINT('Ctrl Pts',(-28.6070879709892,5.8113434455484,130.8067799669));
#227179=CARTESIAN_POINT('Ctrl Pts',(-28.8855355948021,3.14320854938853,
125.916420508438));
#227180=CARTESIAN_POINT('Ctrl Pts',(-29.163983218615,-2.41338144938502,
125.517839221114));
#227181=CARTESIAN_POINT('Ctrl Pts',(-29.4424308424279,-5.75219179641212,
129.977312836202));
#227182=CARTESIAN_POINT('Ctrl Pts',(-29.7208784662408,-3.80501889272807,
135.196802958832));
#227183=CARTESIAN_POINT('Ctrl Pts',(-29.9993260900537,1.6387804878663,136.379853152576));
#227184=CARTESIAN_POINT('Ctrl Pts',(-30.2777737138665,5.576620658989,132.439298084597));
#227185=CARTESIAN_POINT('Ctrl Pts',(-30.5562213376795,4.38981887756547,
126.996315355552));
#227186=CARTESIAN_POINT('Ctrl Pts',(-30.8346689614924,-0.831011997766135,
125.052740188944));
#227187=CARTESIAN_POINT('Ctrl Pts',(-31.1131165853052,-5.2881834443438,
128.394623213959));
#227188=CARTESIAN_POINT('Ctrl Pts',(-31.3915642091181,-4.88577264769286,
133.950937190672));
#227189=CARTESIAN_POINT('Ctrl Pts',(-31.670011832931,0.00642452892459172,
136.615701015511));
#227190=CARTESIAN_POINT('Ctrl Pts',(-31.9484594567439,4.89271787731614,
133.940126914399));
#227191=CARTESIAN_POINT('Ctrl Pts',(-32.2269070805568,5.28284251901049,
128.382936777197));
#227192=CARTESIAN_POINT('Ctrl Pts',(-32.5053547043697,0.818292966938792,
125.050916856162));
#227193=CARTESIAN_POINT('Ctrl Pts',(-32.7838023281826,-4.3982278459157,
127.006030680504));
#227194=CARTESIAN_POINT('Ctrl Pts',(-33.0622499519955,-5.57299213374921,
132.451624158271));
#227195=CARTESIAN_POINT('Ctrl Pts',(-33.3406975758084,-1.62644890646854,
136.383462915428));
#227196=CARTESIAN_POINT('Ctrl Pts',(-33.6191451996212,3.81472140941051,
135.188379215148));
#227197=CARTESIAN_POINT('Ctrl Pts',(-33.8975928234342,5.75034910954236,
129.964596594906));
#227198=CARTESIAN_POINT('Ctrl Pts',(-34.176040447247,2.40168689817613,125.512516086734));
#227199=CARTESIAN_POINT('Ctrl Pts',(-34.4544880710599,-3.15400824368619,
125.923382181419));
#227200=CARTESIAN_POINT('Ctrl Pts',(-34.7329356948729,-5.81132389146964,
130.81962900987));
#227201=CARTESIAN_POINT('Ctrl Pts',(-35.0113833186857,-3.1283167819475,
135.701844931696));
#227202=CARTESIAN_POINT('Ctrl Pts',(-35.2898309424986,2.42946062341331,
136.083512024245));
#227203=CARTESIAN_POINT('Ctrl Pts',(-35.5682785663115,5.75468240160701,
131.613896874941));
#227204=CARTESIAN_POINT('Ctrl Pts',(-35.8467261901244,3.79163218458816,
126.400357453152));
#227205=CARTESIAN_POINT('Ctrl Pts',(-36.1251738139373,-1.65574277853735,
125.233881791944));
#227206=CARTESIAN_POINT('Ctrl Pts',(-36.4036214377501,-5.58157101571846,
129.186404038463));
#227207=CARTESIAN_POINT('Ctrl Pts',(-36.6820690615631,-4.37820816435757,
134.625749339604));
#227208=CARTESIAN_POINT('Ctrl Pts',(-36.960516685376,0.848514102688449,
136.553425090409));
#227209=CARTESIAN_POINT('Ctrl Pts',(-37.2389643091888,5.29549336158222,
133.197991448084));
#227210=CARTESIAN_POINT('Ctrl Pts',(-37.5174119330018,4.87617292041449,
127.64292800788));
#227211=CARTESIAN_POINT('Ctrl Pts',(-37.7958595568146,-0.0241122203237842,
124.993066691407));
#227212=CARTESIAN_POINT('Ctrl Pts',(-38.0743071806275,-4.90223940853195,
127.683500595584));
#227213=CARTESIAN_POINT('Ctrl Pts',(-38.3527548044404,-5.27544806800837,
133.241852397473));
#227214=CARTESIAN_POINT('Ctrl Pts',(-38.6312024282533,-0.800777672950798,
136.560268331721));
#227215=CARTESIAN_POINT('Ctrl Pts',(-38.9096500520661,4.40976828338437,
134.589286268384));
#227216=CARTESIAN_POINT('Ctrl Pts',(-39.1880976758791,5.56795261644649,
129.140142435842));
#227217=CARTESIAN_POINT('Ctrl Pts',(-39.4665452996919,1.6094605046014,125.220333810727));
#227218=CARTESIAN_POINT('Ctrl Pts',(-39.7449929235049,-3.82804718445556,
126.43197302622));
#227219=CARTESIAN_POINT('Ctrl Pts',(-40.0234405473177,-5.74776652149929,
131.661622835152));
#227220=CARTESIAN_POINT('Ctrl Pts',(-40.3018881711306,-2.38556921929025,
136.103490545709));
#227221=CARTESIAN_POINT('Ctrl Pts',(-40.5803357949436,3.16884965391132,
135.675716729192));
#227222=CARTESIAN_POINT('Ctrl Pts',(-40.8587834187564,5.81125050208024,
130.771404625066));
#227223=CARTESIAN_POINT('Ctrl Pts',(-41.1372310425694,3.11339603420704,
125.897377468058));
#227224=CARTESIAN_POINT('Ctrl Pts',(-41.4156786663821,-2.4455172912504,
125.532628105994));
#227225=CARTESIAN_POINT('Ctrl Pts',(-41.6941262901951,-5.75711969621025,
130.012343383614));
#227226=CARTESIAN_POINT('Ctrl Pts',(-41.9725739140079,-3.77821035128576,
135.219883807042));
#227227=CARTESIAN_POINT('Ctrl Pts',(-42.2510215378209,1.67268973063362,
136.369774129642));
#227228=CARTESIAN_POINT('Ctrl Pts',(-42.5294691616338,5.58646966553678,
132.405321320208));
#227229=CARTESIAN_POINT('Ctrl Pts',(-42.8079167854466,4.366556892027,126.969663836325));
#227230=CARTESIAN_POINT('Ctrl Pts',(-43.0863644092596,-0.866008347092154,
125.057905359049));
#227231=CARTESIAN_POINT('Ctrl Pts',(-43.3648120330724,-5.3027542220935,
128.426858534403));
#227232=CARTESIAN_POINT('Ctrl Pts',(-43.6432596568854,-4.86652802093628,
133.98061997675));
#227233=CARTESIAN_POINT('Ctrl Pts',(-43.9217072806982,0.0417996883503892,
136.615554236903));
#227234=CARTESIAN_POINT('Ctrl Pts',(-44.2001549045111,4.9117155260715,133.910285453475));
#227235=CARTESIAN_POINT('Ctrl Pts',(-44.478602528324,5.26800474597596,128.350823478709));
#227236=CARTESIAN_POINT('Ctrl Pts',(-44.7570501521369,0.783254960667603,
125.046042272601));
#227237=CARTESIAN_POINT('Ctrl Pts',(-45.0354977759497,-4.42126786936209,
127.032874316024));
#227238=CARTESIAN_POINT('Ctrl Pts',(-45.3139453997627,-5.56286151839129,
132.485518023215));
#227239=CARTESIAN_POINT('Ctrl Pts',(-45.5923930235756,-1.59245719291215,
136.393260203719));
#227240=CARTESIAN_POINT('Ctrl Pts',(-45.8708406473885,3.84133749699455,
135.165076697471));
#227241=CARTESIAN_POINT('Ctrl Pts',(-46.1492882712014,5.74513068693249,
129.929608146614));
#227242=CARTESIAN_POINT('Ctrl Pts',(-46.4277358950142,2.3694294408167,125.497994382526));
#227243=CARTESIAN_POINT('Ctrl Pts',(-46.7061835188271,-3.18366170834627,
125.942671958037));
#227244=CARTESIAN_POINT('Ctrl Pts',(-46.98463114264,-5.81112327806003,130.85500390496));
#227245=CARTESIAN_POINT('Ctrl Pts',(-47.263078766453,-3.09844644439114,
135.720797144829));
#227246=CARTESIAN_POINT('Ctrl Pts',(-47.5415263902657,2.46155130414924,
136.068625397419));
#227247=CARTESIAN_POINT('Ctrl Pts',(-47.8199740140787,5.75950365764311,
131.578851490957));
#227248=CARTESIAN_POINT('Ctrl Pts',(-48.0984216378915,3.76475351715869,
126.377358307829));
#227249=CARTESIAN_POINT('Ctrl Pts',(-48.3768692617045,-1.6896211871606,
125.244063976264));
#227250=CARTESIAN_POINT('Ctrl Pts',(-48.6553168855173,-5.59131656306301,
129.220410622463));
#227251=CARTESIAN_POINT('Ctrl Pts',(-48.9337645093303,-4.35486516851022,
134.652329933902));
#227252=CARTESIAN_POINT('Ctrl Pts',(-49.2122121331431,0.883494568912716,
136.548153427379));
#227253=CARTESIAN_POINT('Ctrl Pts',(-49.4906597569561,5.3099659586141,133.165711928516));
#227254=CARTESIAN_POINT('Ctrl Pts',(-49.7691073807689,4.85683803860733,
127.613303933314));
#227255=CARTESIAN_POINT('Ctrl Pts',(-50.0475550045819,-0.0594867691506708,
124.993321139153));
#227256=CARTESIAN_POINT('Ctrl Pts',(-50.3260026283946,-4.92114614214944,
127.713399740592));
#227257=CARTESIAN_POINT('Ctrl Pts',(-50.6044502522077,-5.26051262186729,
133.273920386136));
#227258=CARTESIAN_POINT('Ctrl Pts',(-50.8828978760204,-0.765724992417492,
136.565036249065));
#227259=CARTESIAN_POINT('Ctrl Pts',(-51.1613454998334,4.4327264973184,134.562372631296));
#227260=CARTESIAN_POINT('Ctrl Pts',(-51.4397931236463,5.55771888674681,
129.106279562002));
#227261=CARTESIAN_POINT('Ctrl Pts',(-51.7182407474591,1.57543912891688,
125.210640026899));
#227262=CARTESIAN_POINT('Ctrl Pts',(-51.9966883712721,-3.85459222390762,
126.455356446176));
#227263=CARTESIAN_POINT('Ctrl Pts',(-52.2751359950849,-5.7424416302597,
131.696595238295));
#227264=CARTESIAN_POINT('Ctrl Pts',(-52.5535836188979,-2.35326771227282,
136.117914002047));
#227265=CARTESIAN_POINT('Ctrl Pts',(-52.8320312427106,3.19844426977395,
135.656336786975));
#227266=CARTESIAN_POINT('Ctrl Pts',(-53.1104788665238,5.81094222058764,
130.736030504428));
#227267=CARTESIAN_POINT('Ctrl Pts',(-53.3889264903363,3.08346815099054,
125.878516257743));
#227268=CARTESIAN_POINT('Ctrl Pts',(-53.6673741141495,-2.47756251357323,
125.547612336859));
#227269=CARTESIAN_POINT('Ctrl Pts',(-53.9458217379622,-5.76183426382087,
130.047403279515));
#227270=CARTESIAN_POINT('Ctrl Pts',(-54.2242693617753,-3.75126180686946,
135.242801036416));
#227271=CARTESIAN_POINT('Ctrl Pts',(-54.502716985588,1.70653699126786,136.359488878264));
#227272=CARTESIAN_POINT('Ctrl Pts',(-54.7811646094011,5.59611166339667,
132.371285231631));
#227273=CARTESIAN_POINT('Ctrl Pts',(-55.0596122332138,4.3431331021171,126.943154413196));
#227274=CARTESIAN_POINT('Ctrl Pts',(-55.3380598570268,-0.900972606160421,
125.063283466166));
#227275=CARTESIAN_POINT('Ctrl Pts',(-55.6165074808396,-5.31712850433539,
128.459181954061));
#227276=CARTESIAN_POINT('Ctrl Pts',(-55.8949551046525,-4.84710306319425,
134.01018506537));
#227277=CARTESIAN_POINT('Ctrl Pts',(-56.1734027284654,0.0771732988733811,
136.615192122377));
#227278=CARTESIAN_POINT('Ctrl Pts',(-56.4518503522783,4.93053116940174,
133.880328901363));
#227279=CARTESIAN_POINT('Ctrl Pts',(-56.7302979760911,5.25297176508825,
128.318801096944));
#227280=CARTESIAN_POINT('Ctrl Pts',(-57.0087455999042,0.748187930595796,
125.041381065643));
#227281=CARTESIAN_POINT('Ctrl Pts',(-57.2871932237169,-4.44414406110167,
127.059857705357));
#227282=CARTESIAN_POINT('Ctrl Pts',(-57.5656408475299,-5.55252476915405,
132.519349592253));
#227283=CARTESIAN_POINT('Ctrl Pts',(-57.8440884713427,-1.55840647026886,
136.402850393281));
#227284=CARTESIAN_POINT('Ctrl Pts',(-58.1225360951557,3.867811242405,135.141612591857));
#227285=CARTESIAN_POINT('Ctrl Pts',(-58.4009837189685,5.73969937639226,
129.894652112598));
#227286=CARTESIAN_POINT('Ctrl Pts',(-58.6794313427815,2.33708418337799,
125.483669307672));
#227287=CARTESIAN_POINT('Ctrl Pts',(-58.9578789665944,-3.21319720125095,
125.962141886319));
#227288=CARTESIAN_POINT('Ctrl Pts',(-59.2363265904072,-5.81070733134035,
130.890376923444));
#227289=CARTESIAN_POINT('Ctrl Pts',(-59.5147742142201,-3.06846129276222,
135.739567177598));
#227290=CARTESIAN_POINT('Ctrl Pts',(-59.793221838033,2.49355077119662,136.053543701326));
#227291=CARTESIAN_POINT('Ctrl Pts',(-60.071669461846,5.76411149315304,131.543777407928));
#227292=CARTESIAN_POINT('Ctrl Pts',(-60.3501170856587,3.73773534540316,
126.354523206705));
#227293=CARTESIAN_POINT('Ctrl Pts',(-60.6285647094717,-1.72343698624942,
125.254452199421));
#227294=CARTESIAN_POINT('Ctrl Pts',(-60.9070123332846,-5.6008549221161,
129.254475900312));
#227295=CARTESIAN_POINT('Ctrl Pts',(-61.1854599570975,-4.33136080153256,
134.678767940282));
#227296=CARTESIAN_POINT('Ctrl Pts',(-61.4639075809103,0.918442296920838,
136.542668925995));
#227297=CARTESIAN_POINT('Ctrl Pts',(-61.7423552047232,5.32424179290464,
133.133344908207));
#227298=CARTESIAN_POINT('Ctrl Pts',(-62.0208028285362,4.83732318488056,
127.583798104527));
#227299=CARTESIAN_POINT('Ctrl Pts',(-62.299250452349,-0.0948591136734494,
124.993790917104));
#227300=CARTESIAN_POINT('Ctrl Pts',(-62.5776980761619,-4.93987052088691,
127.743413422294));
#227301=CARTESIAN_POINT('Ctrl Pts',(-62.8561456999749,-5.24538224549645,
133.305896864355));
#227302=CARTESIAN_POINT('Ctrl Pts',(-63.1345933237877,-0.730643937663188,
136.569590702456));
#227303=CARTESIAN_POINT('Ctrl Pts',(-63.4130409476006,4.45552045494177,
134.53531973969));
#227304=CARTESIAN_POINT('Ctrl Pts',(-63.6914885714135,5.5472792137301,129.072479611178));
#227305=CARTESIAN_POINT('Ctrl Pts',(-63.9699361952264,1.54135937475606,
125.201153520444));
#227306=CARTESIAN_POINT('Ctrl Pts',(-64.2483838190392,-3.88099443002729,
126.478901020081));
#227307=CARTESIAN_POINT('Ctrl Pts',(-64.5268314428522,-5.73690395073373,
131.731534579357));
#227308=CARTESIAN_POINT('Ctrl Pts',(-64.805279066665,-2.32087900405488,
136.132140562712));
#227309=CARTESIAN_POINT('Ctrl Pts',(-65.083726690478,3.22792036610792,135.636777052998));
#227310=CARTESIAN_POINT('Ctrl Pts',(-65.3621743142908,5.81041861249411,
130.700658915789));
#227311=CARTESIAN_POINT('Ctrl Pts',(-65.6406219381037,3.05342600872776,
125.859837576403));
#227312=CARTESIAN_POINT('Ctrl Pts',(-65.9190695619166,-2.50951592890599,
125.562791358466));
#227313=CARTESIAN_POINT('Ctrl Pts',(-66.1975171857295,-5.76633532454392,
130.082491224748));
#227314=CARTESIAN_POINT('Ctrl Pts',(-66.4759648095424,-3.72417425806736,
135.26555379775));
#227315=CARTESIAN_POINT('Ctrl Pts',(-66.7544124333553,1.74032101554631,
136.348997779564));
#227316=CARTESIAN_POINT('Ctrl Pts',(-67.0328600571681,5.60554629528092,
132.337191080086));
#227317=CARTESIAN_POINT('Ctrl Pts',(-67.3113076809811,4.31954837581292,
126.916788068483));
#227318=CARTESIAN_POINT('Ctrl Pts',(-67.5897553047939,-0.935903479357421,
125.068874311009));
#227319=CARTESIAN_POINT('Ctrl Pts',(-67.8682029286069,-5.33130575842519,
128.491592275178));
#227320=CARTESIAN_POINT('Ctrl Pts',(-68.1466505524197,-4.82749849426569,
134.039631360986));
#227321=CARTESIAN_POINT('Ctrl Pts',(-68.4250981762326,0.112544049711387,
136.614614685353));
#227322=CARTESIAN_POINT('Ctrl Pts',(-68.7035458000455,4.94916411008632,
133.850258368115));
#227323=CARTESIAN_POINT('Ctrl Pts',(-68.9819934238584,5.23774413340002,
128.286870818499));
#227324=CARTESIAN_POINT('Ctrl Pts',(-69.2604410476712,0.713093176145084,
125.036933408012));
#227325=CARTESIAN_POINT('Ctrl Pts',(-69.5388886714842,-4.46685557344872,
127.086979848621));
#227326=CARTESIAN_POINT('Ctrl Pts',(-69.8173362952971,-5.54198226906957,
132.553117611744));
#227327=CARTESIAN_POINT('Ctrl Pts',(-70.09578391911,-1.52429800030071,136.412233128746));
#227328=CARTESIAN_POINT('Ctrl Pts',(-70.3742315429229,3.89414166464747,
135.117987767775));
#227329=CARTESIAN_POINT('Ctrl Pts',(-70.6526791667357,5.73405537918087,
129.859729788164));
#227330=CARTESIAN_POINT('Ctrl Pts',(-70.9311267905487,2.3046523244254,125.469541392991));
#227331=CARTESIAN_POINT('Ctrl Pts',(-71.2095744143614,-3.24261362795168,
125.981791244794));
#227332=CARTESIAN_POINT('Ctrl Pts',(-71.4880220381746,-5.81007606672361,
130.925746754563));
#227333=CARTESIAN_POINT('Ctrl Pts',(-71.7664696619872,-3.03836243817177,
135.758154334473));
#227334=CARTESIAN_POINT('Ctrl Pts',(-72.0449172858002,2.52545783880292,
136.038267494822));
#227335=CARTESIAN_POINT('Ctrl Pts',(-72.3233649096131,5.76850573739207,
131.508675925537));
#227336=CARTESIAN_POINT('Ctrl Pts',(-72.601812533426,3.71057867048956,126.331852995942));
#227337=CARTESIAN_POINT('Ctrl Pts',(-72.8802601572389,-1.75718892274731,
125.265046076474));
#227338=CARTESIAN_POINT('Ctrl Pts',(-73.1587077810518,-5.61018573943046,
129.28859860971));
#227339=CARTESIAN_POINT('Ctrl Pts',(-73.4371554048648,-4.30769593438731,
134.705062379074));
#227340=CARTESIAN_POINT('Ctrl Pts',(-73.7156030286775,0.953355991712339,
136.536971789486));
#227341=CARTESIAN_POINT('Ctrl Pts',(-73.9940506524905,5.33832033545752,
133.100891586529));
#227342=CARTESIAN_POINT('Ctrl Pts',(-74.2724982763033,4.81762908236426,
127.554411614868));
#227343=CARTESIAN_POINT('Ctrl Pts',(-74.5509459001162,-0.130227943157576,
124.994476007852));
#227344=CARTESIAN_POINT('Ctrl Pts',(-74.8293935239292,-4.95841185090586,
127.77354052852));
#227345=CARTESIAN_POINT('Ctrl Pts',(-75.107841147742,-5.23005749955717,
133.337780647228));
#227346=CARTESIAN_POINT('Ctrl Pts',(-75.3862887715549,-0.695535808628632,
136.573931523126));
#227347=CARTESIAN_POINT('Ctrl Pts',(-75.6647363953679,4.4781493116164,134.508128596022));
#227348=CARTESIAN_POINT('Ctrl Pts',(-75.9431840191806,5.53663398424198,
129.038743835842));
#227349=CARTESIAN_POINT('Ctrl Pts',(-76.2216316429937,1.50722250495638,
125.191874642891));
#227350=CARTESIAN_POINT('Ctrl Pts',(-76.5000792668064,-3.90725282447187,
126.502605875483));
#227351=CARTESIAN_POINT('Ctrl Pts',(-76.7785268906195,-5.73115368812196,
131.766439563647));
#227352=CARTESIAN_POINT('Ctrl Pts',(-77.0569745144322,-2.28840429481114,
136.146169700531));
#227353=CARTESIAN_POINT('Ctrl Pts',(-77.3354221382452,3.25727685066645,
135.617038252052));
#227354=CARTESIAN_POINT('Ctrl Pts',(-77.613869762058,5.80967969720196,130.665291169852));
#227355=CARTESIAN_POINT('Ctrl Pts',(-77.8923173858709,3.0232707206408,125.841342116181));
#227356=CARTESIAN_POINT('Ctrl Pts',(-78.1707650096839,-2.54137635320382,
125.57816460835));
#227357=CARTESIAN_POINT('Ctrl Pts',(-78.4492126334967,-5.77062271159095,
130.117605919119));
#227358=CARTESIAN_POINT('Ctrl Pts',(-78.7276602573096,-3.69694870861804,
135.288141247929));
#227359=CARTESIAN_POINT('Ctrl Pts',(-79.0061078811224,1.77404055158998,
136.338301222296));
#227360=CARTESIAN_POINT('Ctrl Pts',(-79.2845555049354,5.61477321158579,
132.303040128944));
#227361=CARTESIAN_POINT('Ctrl Pts',(-79.5630031287483,4.29580358705489,
126.8905657792));
#227362=CARTESIAN_POINT('Ctrl Pts',(-79.8414507525611,-0.970799672307275,
125.074677686406));
#227363=CARTESIAN_POINT('Ctrl Pts',(-80.1198983763742,-5.34528545901998,
128.524088296775));
#227364=CARTESIAN_POINT('Ctrl Pts',(-80.3983460001869,-4.80771504060458,
134.068957772455));
#227365=CARTESIAN_POINT('Ctrl Pts',(-80.6767936239998,0.147910630189091,
136.613821947228));
#227366=CARTESIAN_POINT('Ctrl Pts',(-80.9552412478128,4.96761365767528,
133.820074968005));
#227367=CARTESIAN_POINT('Ctrl Pts',(-81.2336888716256,5.22232241517632,
128.255033826564));
#227368=CARTESIAN_POINT('Ctrl Pts',(-81.5121364954386,0.6779719977639,125.032699464516));
#227369=CARTESIAN_POINT('Ctrl Pts',(-81.7905841192513,-4.48940156482041,
127.114239740797));
#227370=CARTESIAN_POINT('Ctrl Pts',(-82.0690317430644,-5.53123440879372,
132.586820830401));
#227371=CARTESIAN_POINT('Ctrl Pts',(-82.3474793668772,-1.490133046909,136.421408062431));
#227372=CARTESIAN_POINT('Ctrl Pts',(-82.62592699069,3.92032778803891,135.094203100652));
#227373=CARTESIAN_POINT('Ctrl Pts',(-82.9043746145031,5.72819890443852,
129.824842467372));
#227374=CARTESIAN_POINT('Ctrl Pts',(-83.1828222383158,2.27213506573304,
125.455611161998));
#227375=CARTESIAN_POINT('Ctrl Pts',(-83.4612698621288,-3.27190989841242,
126.001619305352));
#227376=CARTESIAN_POINT('Ctrl Pts',(-83.7397174859417,-5.80922950760163,
130.961112087674));
#227377=CARTESIAN_POINT('Ctrl Pts',(-84.0181651097544,-3.00815099594316,
135.776557926701));
#227378=CARTESIAN_POINT('Ctrl Pts',(-84.2966127335676,2.55727132464077,
136.022797343974));
#227379=CARTESIAN_POINT('Ctrl Pts',(-84.5750603573801,5.77268622752965,
131.473548344486));
#227380=CARTESIAN_POINT('Ctrl Pts',(-84.8535079811934,3.68328449871872,
126.309348515594));
#227381=CARTESIAN_POINT('Ctrl Pts',(-85.131955605006,-1.79087574596318,
125.275845214866));
#227382=CARTESIAN_POINT('Ctrl Pts',(-85.4104032288191,-5.61930866924928,
129.322777486226));
#227383=CARTESIAN_POINT('Ctrl Pts',(-85.6888508526319,-4.28387144398495,
134.731212275928));
#227384=CARTESIAN_POINT('Ctrl Pts',(-85.9672984764448,0.98823435954663,
136.531062228962));
#227385=CARTESIAN_POINT('Ctrl Pts',(-86.2457461002577,5.35220106458756,
133.068353166051));
#227386=CARTESIAN_POINT('Ctrl Pts',(-86.5241937240705,4.79775646083024,
127.525145553266));
#227387=CARTESIAN_POINT('Ctrl Pts',(-86.8026413478836,-0.165591946996939,
124.995376386011));
#227388=CARTESIAN_POINT('Ctrl Pts',(-87.0810889716963,-4.97676944515001,
127.803779942897));
#227389=CARTESIAN_POINT('Ctrl Pts',(-87.3595365955093,-5.21453895191432,
133.36957055329));
#227390=CARTESIAN_POINT('Ctrl Pts',(-87.6379842193221,-0.660401906259044,
136.578058550223));
#227391=CARTESIAN_POINT('Ctrl Pts',(-87.916431843135,4.50061222882128,134.480800207869));
#227392=CARTESIAN_POINT('Ctrl Pts',(-88.1948794669479,5.52578359274576,
129.005073486085));
#227393=CARTESIAN_POINT('Ctrl Pts',(-88.4733270907608,1.47302978447255,
125.182803738068));
#227394=CARTESIAN_POINT('Ctrl Pts',(-88.7517747145737,-3.93336643422502,
126.526470133988));
#227395=CARTESIAN_POINT('Ctrl Pts',(-89.0302223383866,-5.7251910555031,
131.801308897747));
#227396=CARTESIAN_POINT('Ctrl Pts',(-89.3086699621995,-2.25584478790559,
136.16000089565));
#227397=CARTESIAN_POINT('Ctrl Pts',(-89.5871175860123,3.28651263563227,
135.597121115567));
#227398=CARTESIAN_POINT('Ctrl Pts',(-89.8655652098253,5.80872550209253,
130.629928577187));
#227399=CARTESIAN_POINT('Ctrl Pts',(-90.1440128336381,2.99300340414587,
125.823030562435));
#227400=CARTESIAN_POINT('Ctrl Pts',(-90.4224604574511,-2.57314260586573,
125.593731516848));
#227401=CARTESIAN_POINT('Ctrl Pts',(-90.7009080812639,-5.77469626609129,
130.152746061436));
#227402=CARTESIAN_POINT('Ctrl Pts',(-90.9793557050769,-3.66958616737523,
135.310562549967));
#227403=CARTESIAN_POINT('Ctrl Pts',(-91.2578033288896,1.80769434990835,
136.327399602824));
#227404=CARTESIAN_POINT('Ctrl Pts',(-91.5362509527026,5.62379207040447,
132.268833643682));
#227405=CARTESIAN_POINT('Ctrl Pts',(-91.8146985765155,4.27189961571542,
126.864488517025));
#227406=CARTESIAN_POINT('Ctrl Pts',(-92.0931462003284,-1.00565989191805,
125.080693377311));
#227407=CARTESIAN_POINT('Ctrl Pts',(-92.3715938241412,-5.3590670880956,
128.556668814702));
#227408=CARTESIAN_POINT('Ctrl Pts',(-92.6500414479542,-4.78775343529548,
134.098163213075));
#227409=CARTESIAN_POINT('Ctrl Pts',(-92.928489071767,0.183271729783054,
136.612813937377));
#227410=CARTESIAN_POINT('Ctrl Pts',(-93.2069366955801,4.98587912851244,
133.789779819492));
#227411=CARTESIAN_POINT('Ctrl Pts',(-93.4853843193926,5.2067071818758,128.223291300872));
#227412=CARTESIAN_POINT('Ctrl Pts',(-93.7638319432059,0.642825696881324,
125.028679392048));
#227413=CARTESIAN_POINT('Ctrl Pts',(-94.0422795670186,-4.51178119976554,
127.14163637176));
#227414=CARTESIAN_POINT('Ctrl Pts',(-94.3207271908314,-5.52028158659305,
132.62045799934));
#227415=CARTESIAN_POINT('Ctrl Pts',(-94.5991748146444,-1.45591287608963,
136.430374854359));
#227416=CARTESIAN_POINT('Ctrl Pts',(-94.8776224384574,3.94636864224209,
135.07025947184));
#227417=CARTESIAN_POINT('Ctrl Pts',(-95.1560700622702,5.7221301691794,129.789991442987));
#227418=CARTESIAN_POINT('Ctrl Pts',(-95.4345176860831,2.23953361224044,
125.441879130882));
#227419=CARTESIAN_POINT('Ctrl Pts',(-95.7129653098959,-3.30108492704829,
126.021625333256));
#227420=CARTESIAN_POINT('Ctrl Pts',(-95.9914129337089,-5.80816768534362,
130.996471612301));
#227421=CARTESIAN_POINT('Ctrl Pts',(-96.2698605575217,-2.97782808557417,
135.794777272329));
#227422=CARTESIAN_POINT('Ctrl Pts',(-96.5483081813347,2.58899004984866,
136.007133822036));
#227423=CARTESIAN_POINT('Ctrl Pts',(-96.8267558051475,5.77665280865574,
131.438395966436));
#227424=CARTESIAN_POINT('Ctrl Pts',(-97.1052034289604,3.65585384148698,
126.287010599573));
#227425=CARTESIAN_POINT('Ctrl Pts',(-97.3836510527732,-1.82449620761995,
125.286849214428));
#227426=CARTESIAN_POINT('Ctrl Pts',(-97.6620986765863,-5.62822337351841,
129.35701126335));
#227427=CARTESIAN_POINT('Ctrl Pts',(-97.9405463003989,-4.25988821315111,
134.757216661848));
#227428=CARTESIAN_POINT('Ctrl Pts',(-98.2189939242121,1.02307610799351,
136.524940463405));
#227429=CARTESIAN_POINT('Ctrl Pts',(-98.4974415480248,5.36588346593846,
133.035730852497));
#227430=CARTESIAN_POINT('Ctrl Pts',(-98.7758891718378,4.77770605666655,
127.496001004183));
#227431=CARTESIAN_POINT('Ctrl Pts',(-99.0543367956506,-0.200949814765295,
124.996492018215));
#227432=CARTESIAN_POINT('Ctrl Pts',(-99.3327844194636,-4.99494262337204,
127.834130544897));
#227433=CARTESIAN_POINT('Ctrl Pts',(-99.6112320432764,-5.19882717761281,
133.401265404553));
#227434=CARTESIAN_POINT('Ctrl Pts',(-99.8896796670892,-0.625243532454567,
136.581971630822));
#227435=CARTESIAN_POINT('Ctrl Pts',(-100.168127290903,4.5229083741848,134.453335587896));
#227436=CARTESIAN_POINT('Ctrl Pts',(-100.446574914715,5.51472844130613,
128.971469809575));
#227437=CARTESIAN_POINT('Ctrl Pts',(-100.725022538528,1.43878248032906,
125.173941142103));
#227438=CARTESIAN_POINT('Ctrl Pts',(-101.003470162341,-3.95933429163924,
126.550492911299));
#227439=CARTESIAN_POINT('Ctrl Pts',(-101.281917786154,-5.71901627382367,
131.836141289563));
#227440=CARTESIAN_POINT('Ctrl Pts',(-101.560365409967,-2.22320168984167,
136.17363363555));
#227441=CARTESIAN_POINT('Ctrl Pts',(-101.83881303378,3.31562663766449,135.577026381578));
#227442=CARTESIAN_POINT('Ctrl Pts',(-102.117260657593,5.80755606252295,
130.594572448163));
#227443=CARTESIAN_POINT('Ctrl Pts',(-102.395708281405,2.96262518080941,
125.804903593708));
#227444=CARTESIAN_POINT('Ctrl Pts',(-102.674155905219,-2.60481350978186,
125.609491507123));
#227445=CARTESIAN_POINT('Ctrl Pts',(-102.952603529031,-5.77855583709781,
130.187910349571));
#227446=CARTESIAN_POINT('Ctrl Pts',(-103.231051152844,-3.64208764826766,
135.332816873036));
#227447=CARTESIAN_POINT('Ctrl Pts',(-103.509498776657,1.84128116344741,
136.316293325111));
#227448=CARTESIAN_POINT('Ctrl Pts',(-103.78794640047,5.63260253753978,132.234572891835));
#227449=CARTESIAN_POINT('Ctrl Pts',(-104.066394024283,4.24783734756473,
126.838557248259));
#227450=CARTESIAN_POINT('Ctrl Pts',(-104.344841648096,-1.04048284643121,
125.086921160811));
#227451=CARTESIAN_POINT('Ctrl Pts',(-104.623289271909,-5.3726501349701,
128.589332621676));
#227452=CARTESIAN_POINT('Ctrl Pts',(-104.901736895722,-4.76761441802147,
134.12724660063));
#227453=CARTESIAN_POINT('Ctrl Pts',(-105.180184519534,0.218626038175886,
136.611590693152));
#227454=CARTESIAN_POINT('Ctrl Pts',(-105.458632143348,5.00395984576562,
133.759374045173));
#227455=CARTESIAN_POINT('Ctrl Pts',(-105.73707976716,5.1908990121252,128.191644417652));
#227456=CARTESIAN_POINT('Ctrl Pts',(-106.015527390973,0.607655575856702,
125.024873339572));
#227457=CARTESIAN_POINT('Ctrl Pts',(-106.293975014786,-4.53399364899913,
127.169168726316));
#227458=CARTESIAN_POINT('Ctrl Pts',(-106.572422638599,-5.50912420832816,
132.654027872123));
#227459=CARTESIAN_POINT('Ctrl Pts',(-106.850870262412,-1.42163875588365,
136.43913317226));
#227460=CARTESIAN_POINT('Ctrl Pts',(-107.129317886225,3.97226326230387,
135.046157768576));
#227461=CARTESIAN_POINT('Ctrl Pts',(-107.407765510038,5.71584939828273,
129.755178006424));
#227462=CARTESIAN_POINT('Ctrl Pts',(-107.686213133851,2.20684917200607,
125.428345808491));
#227463=CARTESIAN_POINT('Ctrl Pts',(-107.964660757664,-3.3301376327682,
126.041808587174));
#227464=CARTESIAN_POINT('Ctrl Pts',(-108.243108381476,-5.80689063929651,
131.031824018185));
#227465=CARTESIAN_POINT('Ctrl Pts',(-108.521556005289,-2.94739483068967,
135.812811696231));
#227466=CARTESIAN_POINT('Ctrl Pts',(-108.800003629102,2.62061283907833,
135.991277509423));
#227467=CARTESIAN_POINT('Ctrl Pts',(-109.078451252915,5.7804053337882,131.403220093974));
#227468=CARTESIAN_POINT('Ctrl Pts',(-109.356898876728,3.62828771524594,
126.264840075618));
#227469=CARTESIAN_POINT('Ctrl Pts',(-109.635346500541,-1.85804906189805,
125.298057667405));
#227470=CARTESIAN_POINT('Ctrl Pts',(-109.913794124354,-5.636929521901,129.391298672536));
#227471=CARTESIAN_POINT('Ctrl Pts',(-110.192241748167,-4.2357471305931,
134.783074573235));
#227472=CARTESIAN_POINT('Ctrl Pts',(-110.470689371979,1.05787994597834,
136.518606719657));
#227473=CARTESIAN_POINT('Ctrl Pts',(-110.749136995792,5.37936703250445,
133.003025854698));
#227474=CARTESIAN_POINT('Ctrl Pts',(-111.027584619605,4.75747861284798,
127.466979047582));
#227475=CARTESIAN_POINT('Ctrl Pts',(-111.306032243418,-0.23630023626489,
124.997822863128));
#227476=CARTESIAN_POINT('Ctrl Pts',(-111.584479867231,-5.01293071215839,
127.864591209862));
#227477=CARTESIAN_POINT('Ctrl Pts',(-111.862927491044,-5.18292275885852,
133.432864026556));
#227478=CARTESIAN_POINT('Ctrl Pts',(-112.141375114857,-0.590061990020461,
136.585670619917));
#227479=CARTESIAN_POINT('Ctrl Pts',(-112.41982273867,4.54503692151536,134.425735753813));
#227480=CARTESIAN_POINT('Ctrl Pts',(-112.698270362483,5.50346893957634,
128.937934051507));
#227481=CARTESIAN_POINT('Ctrl Pts',(-112.976717986295,1.40448186157095,
125.165287183403));
#227482=CARTESIAN_POINT('Ctrl Pts',(-113.255165610108,-3.98515543446448,
126.574673317241));
#227483=CARTESIAN_POINT('Ctrl Pts',(-113.533613233921,-5.71262957189362,
131.870935448366));
#227484=CARTESIAN_POINT('Ctrl Pts',(-113.812060857734,-2.19047621022174,
136.187067415062));
#227485=CARTESIAN_POINT('Ctrl Pts',(-114.090508481547,3.34461777793161,
135.556754794705));
#227486=CARTESIAN_POINT('Ctrl Pts',(-114.36895610536,5.80617142182825,130.559224092919));
#227487=CARTESIAN_POINT('Ctrl Pts',(-114.647403729173,2.9321371763071,125.786961881698));
#227488=CARTESIAN_POINT('Ctrl Pts',(-114.925851352986,-2.63638789137572,
125.625443995184));
#227489=CARTESIAN_POINT('Ctrl Pts',(-115.204298976799,-5.78220128159277,
130.223097480497));
#227490=CARTESIAN_POINT('Ctrl Pts',(-115.482746600612,-3.61445417026275,
135.354903392492));
#227491=CARTESIAN_POINT('Ctrl Pts',(-115.761194224424,1.87479974763623,
136.304982800703));
#227492=CARTESIAN_POINT('Ctrl Pts',(-116.039641848237,5.64120428651674,
132.200259142944));
#227493=CARTESIAN_POINT('Ctrl Pts',(-116.31808947205,4.22361767423897,126.812772933795));
#227494=CARTESIAN_POINT('Ctrl Pts',(-116.596537095863,-1.07526724547036,
125.093360806132));
#227495=CARTESIAN_POINT('Ctrl Pts',(-116.874984719676,-5.38603409631742,
128.622078507325));
#227496=CARTESIAN_POINT('Ctrl Pts',(-117.153432343489,-4.7472987350426,
134.156206857421));
#227497=CARTESIAN_POINT('Ctrl Pts',(-117.431879967302,0.253972245300257,
136.610152259881));
#227498=CARTESIAN_POINT('Ctrl Pts',(-117.710327591115,5.02185513944583,
133.728858771743));
#227499=CARTESIAN_POINT('Ctrl Pts',(-117.988775214928,5.17489849170343,
128.160094349593));
#227500=CARTESIAN_POINT('Ctrl Pts',(-118.26722283874,0.572462937930709,
125.021281448121));
#227501=CARTESIAN_POINT('Ctrl Pts',(-118.545670462553,-4.55603808943068,
127.196835784245));
#227502=CARTESIAN_POINT('Ctrl Pts',(-118.824118086366,-5.49776268743969,
132.687529204804));
#227503=CARTESIAN_POINT('Ctrl Pts',(-119.102565710179,-1.38731195633035,
136.447682691592));
#227504=CARTESIAN_POINT('Ctrl Pts',(-119.381013333992,3.99801068868978,
135.021898883958));
#227505=CARTESIAN_POINT('Ctrl Pts',(-119.659460957805,5.70935682448427,
129.720403447709));
#227506=CARTESIAN_POINT('Ctrl Pts',(-119.937908581618,2.17408295616475,
125.415011696306));
#227507=CARTESIAN_POINT('Ctrl Pts',(-120.216356205431,-3.3590669390133,
126.062168319208));
#227508=CARTESIAN_POINT('Ctrl Pts',(-120.494803829244,-5.80539841678086,
131.067167995328));
#227509=CARTESIAN_POINT('Ctrl Pts',(-120.773251453056,-2.91685235900652,
135.830660530138));
#227510=CARTESIAN_POINT('Ctrl Pts',(-121.051699076869,2.65213852053535,
135.975228993696));
#227511=CARTESIAN_POINT('Ctrl Pts',(-121.330146700682,5.78394366387473,
131.368022030553));
#227512=CARTESIAN_POINT('Ctrl Pts',(-121.608594324495,3.60058714147007,
126.242837765265));
#227513=CARTESIAN_POINT('Ctrl Pts',(-121.887041948308,-1.89153306548558,
125.309470158462));
#227514=CARTESIAN_POINT('Ctrl Pts',(-122.165489572121,-5.64542679178685,
129.425638443252));
#227515=CARTESIAN_POINT('Ctrl Pts',(-122.443937195934,-4.21144909086733,
134.808785051914));
#227516=CARTESIAN_POINT('Ctrl Pts',(-122.722384819747,1.09264458383337,
136.512061232418));
#227517=CARTESIAN_POINT('Ctrl Pts',(-123.00083244356,5.39265126464657,132.97023938455));
#227518=CARTESIAN_POINT('Ctrl Pts',(-123.279280067372,4.73707487890982,
127.438080758883));
#227519=CARTESIAN_POINT('Ctrl Pts',(-123.557727691185,-0.27164190157181,
124.999368871432));
#227520=CARTESIAN_POINT('Ctrl Pts',(-123.836175314998,-5.03073304495359,
127.895160809065));
#227521=CARTESIAN_POINT('Ctrl Pts',(-124.114622938811,-5.16682628499523,
133.464365248398));
#227522=CARTESIAN_POINT('Ctrl Pts',(-124.393070562624,-0.554858582622917,
136.589155380447));
#227523=CARTESIAN_POINT('Ctrl Pts',(-124.671518186437,4.56699705083122,
134.398001728342));
#227524=CARTESIAN_POINT('Ctrl Pts',(-124.94996581025,5.49200550478084,128.904467454562));
#227525=CARTESIAN_POINT('Ctrl Pts',(-125.228413434063,1.37012919922165,
125.156842182641));
#227526=CARTESIAN_POINT('Ctrl Pts',(-125.506861057876,-4.0108289058903,
126.599010455801));
#227527=CARTESIAN_POINT('Ctrl Pts',(-125.785308681688,-5.70603118637341,
131.905690084846));
#227528=CARTESIAN_POINT('Ctrl Pts',(-126.063756305501,-2.1576695617001,
136.200301736396));
#227529=CARTESIAN_POINT('Ctrl Pts',(-126.342203929314,3.37348498215772,
135.536307106118));
#227530=CARTESIAN_POINT('Ctrl Pts',(-126.620651553127,5.8045716313158,130.523884821299));
#227531=CARTESIAN_POINT('Ctrl Pts',(-126.89909917694,2.90154052038371,125.769206091244));
#227532=CARTESIAN_POINT('Ctrl Pts',(-127.177546800753,-2.66786458064647,
125.641588389905));
#227533=CARTESIAN_POINT('Ctrl Pts',(-127.455994424566,-5.7856324644928,
130.258306150342));
#227534=CARTESIAN_POINT('Ctrl Pts',(-127.734442048379,-3.5866867573295,
135.376821289913));
#227535=CARTESIAN_POINT('Ctrl Pts',(-128.012889672192,1.90824886043053,
136.293468448719));
#227536=CARTESIAN_POINT('Ctrl Pts',(-128.291337296005,5.64959699859458,
132.16589366852));
#227537=CARTESIAN_POINT('Ctrl Pts',(-128.569784919818,4.19924149320669,
126.787136529081));
#227538=CARTESIAN_POINT('Ctrl Pts',(-128.84823254363,-1.11001180008614,
125.100012074652));
#227539=CARTESIAN_POINT('Ctrl Pts',(-129.126680167443,-5.39921847619124,
128.654905258242));
#227540=CARTESIAN_POINT('Ctrl Pts',(-129.405127791256,-4.72680713916258,
134.185042910317));
#227541=CARTESIAN_POINT('Ctrl Pts',(-129.683575415069,0.289309041389885,
136.608498690867));
#227542=CARTESIAN_POINT('Ctrl Pts',(-129.962023038882,5.03956434643776,
133.69823512996));
#227543=CARTESIAN_POINT('Ctrl Pts',(-130.240470662695,5.15870621351431,
128.128642265792));
#227544=CARTESIAN_POINT('Ctrl Pts',(-130.518918286508,0.537249087180579,
125.017903850796));
#227545=CARTESIAN_POINT('Ctrl Pts',(-130.79736591032,-4.57791370419536,
127.224636520332));
#227546=CARTESIAN_POINT('Ctrl Pts',(-131.075813534134,-5.4861974449331,
132.720960755981));
#227547=CARTESIAN_POINT('Ctrl Pts',(-131.354261157946,-1.35293374942274,
136.456023095549));
#227548=CARTESIAN_POINT('Ctrl Pts',(-131.632708781759,4.02360996731925,
134.99748371691));
#227549=CARTESIAN_POINT('Ctrl Pts',(-131.911156405572,5.7026526883694,129.685669055425));
#227550=CARTESIAN_POINT('Ctrl Pts',(-132.189604029385,2.1412361788793,125.401877288427));
#227551=CARTESIAN_POINT('Ctrl Pts',(-132.468051653198,-3.38787177379785,
126.082703774923));
#227552=CARTESIAN_POINT('Ctrl Pts',(-132.746499277011,-5.80369107309236,
131.102502234048));
#227553=CARTESIAN_POINT('Ctrl Pts',(-133.024946900823,-2.88620180228584,
135.848323112653));
#227554=CARTESIAN_POINT('Ctrl Pts',(-133.303394524637,2.68356592602436,
135.95898886954));
#227555=CARTESIAN_POINT('Ctrl Pts',(-133.581842148449,5.78726766780228,
131.332803080451));
#227556=CARTESIAN_POINT('Ctrl Pts',(-133.860289772262,3.57275314661281,
126.221004483821));
#227557=CARTESIAN_POINT('Ctrl Pts',(-134.138737396075,-1.92494697761906,
125.321086264707));
#227558=CARTESIAN_POINT('Ctrl Pts',(-134.417185019888,-5.65371486830715,
129.460029303025));
#227559=CARTESIAN_POINT('Ctrl Pts',(-134.695632643701,-4.1869949943469,
134.834347145171));
#227560=CARTESIAN_POINT('Ctrl Pts',(-134.974080267514,1.1273687333409,136.505304244234));
#227561=CARTESIAN_POINT('Ctrl Pts',(-135.252527891327,5.40573567011315,
132.937372656969));
#227562=CARTESIAN_POINT('Ctrl Pts',(-135.53097551514,4.71649561092,127.409307208922));
#227563=CARTESIAN_POINT('Ctrl Pts',(-135.809423138953,-0.306973501088704,
125.001129985841));
#227564=CARTESIAN_POINT('Ctrl Pts',(-136.087870762765,-5.04834896208586,
127.925838209736));
#227565=CARTESIAN_POINT('Ctrl Pts',(-136.366318386578,-5.15053835248403,
133.49576790279));
#227566=CARTESIAN_POINT('Ctrl Pts',(-136.644766010391,-0.519634614735935,
136.592425783278));
#227567=CARTESIAN_POINT('Ctrl Pts',(-136.923213634204,4.58878794839197,
134.37013453918));
#227568=CARTESIAN_POINT('Ctrl Pts',(-137.201661258017,5.48033856170195,
128.871071258858));
#227569=CARTESIAN_POINT('Ctrl Pts',(-137.48010888183,1.33572576623031,125.148606452753));
#227570=CARTESIAN_POINT('Ctrl Pts',(-137.758556505643,-4.03635375457527,
126.623503425159));
#227571=CARTESIAN_POINT('Ctrl Pts',(-138.037004129456,-5.69922136176977,
131.940403911158));
#227572=CARTESIAN_POINT('Ctrl Pts',(-138.315451753269,-2.12478295993955,
136.213336109146));
#227573=CARTESIAN_POINT('Ctrl Pts',(-138.593899377082,3.40222718065648,
135.515684073514));
#227574=CARTESIAN_POINT('Ctrl Pts',(-138.872347000894,5.80275675026745,
130.488555942812));
#227575=CARTESIAN_POINT('Ctrl Pts',(-139.150794624707,2.870836346809,125.751636880291));
#227576=CARTESIAN_POINT('Ctrl Pts',(-139.42924224852,-2.69924241121433,
125.65792409305));
#227577=CARTESIAN_POINT('Ctrl Pts',(-139.707689872333,-5.78884925865424,
130.293535054436));
#227578=CARTESIAN_POINT('Ctrl Pts',(-139.986137496146,-3.55878643839929,
135.398569753122));
#227579=CARTESIAN_POINT('Ctrl Pts',(-140.264585119959,1.94162726236197,
136.281750695826));
#227580=CARTESIAN_POINT('Ctrl Pts',(-140.543032743772,5.65778036277742,
132.131477741989));
#227581=CARTESIAN_POINT('Ctrl Pts',(-140.821480367585,4.17470970773734,
126.761648984083));
#227582=CARTESIAN_POINT('Ctrl Pts',(-141.099927991397,-1.14471522280625,
125.106874719905));
#227583=CARTESIAN_POINT('Ctrl Pts',(-141.37837561521,-5.41220278603824,
128.687811658017));
#227584=CARTESIAN_POINT('Ctrl Pts',(-141.656823239023,-4.70614038970644,
134.213753690789));
#227585=CARTESIAN_POINT('Ctrl Pts',(-141.935270862836,0.324635117026387,
136.60663004738));
#227586=CARTESIAN_POINT('Ctrl Pts',(-142.213718486649,5.05708681051884,
133.667504254592));
#227587=CARTESIAN_POINT('Ctrl Pts',(-142.492166110462,5.14232277757003,
128.097289331719));
#227588=CARTESIAN_POINT('Ctrl Pts',(-142.770613734275,0.502015328467386,
125.014740672754));
#227589=CARTESIAN_POINT('Ctrl Pts',(-143.049061358088,-4.59961968268416,
127.252569904414));
#227590=CARTESIAN_POINT('Ctrl Pts',(-143.327508981901,-5.4744289093626,
132.754321286837));
#227591=CARTESIAN_POINT('Ctrl Pts',(-143.605956605714,-1.31850540905707,
136.464154075075));
#227592=CARTESIAN_POINT('Ctrl Pts',(-143.884404229526,4.04906014960179,
134.972913172143));
#227593=CARTESIAN_POINT('Ctrl Pts',(-144.162851853339,5.69573723836169,
129.650976116669));
#227594=CARTESIAN_POINT('Ctrl Pts',(-144.441299477152,2.10831005730047,
125.388943071553));
#227595=CARTESIAN_POINT('Ctrl Pts',(-144.719747100965,-3.41655106974776,
126.103414193369));
#227596=CARTESIAN_POINT('Ctrl Pts',(-144.998194724778,-5.80176867149642,
131.13782542502));
#227597=CARTESIAN_POINT('Ctrl Pts',(-145.276642348591,-2.85544429629671,
135.865798789283));
#227598=CARTESIAN_POINT('Ctrl Pts',(-145.555089972404,2.71489389099137,
135.942557738738));
#227599=CARTESIAN_POINT('Ctrl Pts',(-145.833537596217,5.79037722239768,
131.29756454872));
#227600=CARTESIAN_POINT('Ctrl Pts',(-146.111985220029,3.54478676207412,
126.199341040322));
#227601=CARTESIAN_POINT('Ctrl Pts',(-146.390432843843,-1.95828956013508,
125.332905555698));
#227602=CARTESIAN_POINT('Ctrl Pts',(-146.668880467655,-5.66179344434354,
129.49446997749));
#227603=CARTESIAN_POINT('Ctrl Pts',(-146.947328091469,-4.16238574718705,
134.859759905796));
#227604=CARTESIAN_POINT('Ctrl Pts',(-147.225775715281,1.16205110778606,
136.498336005488));
#227605=CARTESIAN_POINT('Ctrl Pts',(-147.504223339094,5.41861976405632,
132.904426889841));
#227606=CARTESIAN_POINT('Ctrl Pts',(-147.782670962907,4.6957415714508,127.380659463914));
#227607=CARTESIAN_POINT('Ctrl Pts',(-148.06111858672,-0.342293725589094,
125.003106141093));
#227608=CARTESIAN_POINT('Ctrl Pts',(-148.339566210533,-5.06577781079073,
127.956622275114));
#227609=CARTESIAN_POINT('Ctrl Pts',(-148.618013834346,-5.1340595648799,
133.527070826096));
#227610=CARTESIAN_POINT('Ctrl Pts',(-148.896461458158,-0.48439139159784,
136.595481707227));
#227611=CARTESIAN_POINT('Ctrl Pts',(-149.174909081971,4.61040880672808,
134.342135218952));
#227612=CARTESIAN_POINT('Ctrl Pts',(-149.453356705784,5.4684685426618,128.837746701901));
#227613=CARTESIAN_POINT('Ctrl Pts',(-149.731804329597,1.30127283742975,
125.140580298914));
#227614=CARTESIAN_POINT('Ctrl Pts',(-150.01025195341,-4.06172903468827,
126.648151317718));
#227615=CARTESIAN_POINT('Ctrl Pts',(-150.288699577223,-5.69220035042211,
131.975075640969));
#227616=CARTESIAN_POINT('Ctrl Pts',(-150.567147201036,-2.09181762356486,
136.226170050321));
#227617=CARTESIAN_POINT('Ctrl Pts',(-150.845594824849,3.43084330837664,
135.494886461086));
#227618=CARTESIAN_POINT('Ctrl Pts',(-151.124042448661,5.80072684593324,
130.453238766583));
#227619=CARTESIAN_POINT('Ctrl Pts',(-151.402490072475,2.84002579333802,
125.734254899877));
#227620=CARTESIAN_POINT('Ctrl Pts',(-151.680937696287,-2.73052022036177,
125.674450499292));
#227621=CARTESIAN_POINT('Ctrl Pts',(-151.9593853201,-5.79185154487752,130.32878288736));
#227622=CARTESIAN_POINT('Ctrl Pts',(-152.237832943913,-3.53075424732904,
135.420147976222));
#227623=CARTESIAN_POINT('Ctrl Pts',(-152.516280567726,1.97493371658077,
136.269829976228));
#227624=CARTESIAN_POINT('Ctrl Pts',(-152.794728191539,5.66575407582884,
132.097012638644));
#227625=CARTESIAN_POINT('Ctrl Pts',(-153.073175815352,4.15002322686382,
126.736311243251));
#227626=CARTESIAN_POINT('Ctrl Pts',(-153.351623439165,-1.17937622768304,
125.113948487592));
#227627=CARTESIAN_POINT('Ctrl Pts',(-153.630071062978,-5.42498654472129,
128.720796487292));
#227628=CARTESIAN_POINT('Ctrl Pts',(-153.90851868679,-4.6852992524868,134.242338134946));
#227629=CARTESIAN_POINT('Ctrl Pts',(-154.186966310604,0.359949163189457,
136.604546398667));
#227630=CARTESIAN_POINT('Ctrl Pts',(-154.465413934416,5.0744218823891,133.636667284384));
#227631=CARTESIAN_POINT('Ctrl Pts',(-154.743861558229,5.12574879096345,
128.066036709167));
#227632=CARTESIAN_POINT('Ctrl Pts',(-155.022309182042,0.466762967392146,
125.011792031209));
#227633=CARTESIAN_POINT('Ctrl Pts',(-155.300756805855,-4.62115522057418,
127.280634901405));
#227634=CARTESIAN_POINT('Ctrl Pts',(-155.579204429668,-5.46245751681569,
132.787609561181));
#227635=CARTESIAN_POINT('Ctrl Pts',(-155.857652053481,-1.28402821098903,
136.472075328871));
#227636=CARTESIAN_POINT('Ctrl Pts',(-156.136099677293,4.07436029247137,
134.948188160129));
#227637=CARTESIAN_POINT('Ctrl Pts',(-156.414547301107,5.68861073071636,
129.616325916999));
#227638=CARTESIAN_POINT('Ctrl Pts',(-156.692994924919,2.07530581151645,
125.376209524969));
#227639=CARTESIAN_POINT('Ctrl Pts',(-156.971442548732,-3.44510376414151,
126.124298807112));
#227640=CARTESIAN_POINT('Ctrl Pts',(-157.249890172545,-5.79963128322921,
131.173136259331));
#227641=CARTESIAN_POINT('Ctrl Pts',(-157.528337796358,-2.82458098076833,
135.883086912459));
#227642=CARTESIAN_POINT('Ctrl Pts',(-157.806785420171,2.74612125456611,
135.925936210153));
#227643=CARTESIAN_POINT('Ctrl Pts',(-158.085233043984,5.79327221243612,
131.262307741136));
#227644=CARTESIAN_POINT('Ctrl Pts',(-158.363680667797,3.51668902415852,
126.177848237519));
#227645=CARTESIAN_POINT('Ctrl Pts',(-158.64212829161,-1.9915595775106,125.344927593469));
#227646=CARTESIAN_POINT('Ctrl Pts',(-158.920575915422,-5.66966222054205,
129.528959190434));
#227647=CARTESIAN_POINT('Ctrl Pts',(-159.199023539236,-4.13762226129274,
134.885022392109));
#227648=CARTESIAN_POINT('Ctrl Pts',(-159.477471163048,1.19669042199943,
136.491156774389));
#227649=CARTESIAN_POINT('Ctrl Pts',(-159.755918786861,5.43130306905165,
132.871403303985));
#227650=CARTESIAN_POINT('Ctrl Pts',(-160.034366410674,4.67481352955083,
127.352138585409));
#227651=CARTESIAN_POINT('Ctrl Pts',(-160.312814034487,-0.377601266270116,
125.005297263965));
#227652=CARTESIAN_POINT('Ctrl Pts',(-160.5912616583,-5.08301894523598,127.987511864483));
#227653=CARTESIAN_POINT('Ctrl Pts',(-160.869709282113,-5.1173905328107,
133.558272858373));
#227654=CARTESIAN_POINT('Ctrl Pts',(-161.148156905926,-0.449130219157962,
136.598323039052));
#227655=CARTESIAN_POINT('Ctrl Pts',(-161.426604529739,4.63185882466967,
134.314004805186));
#227656=CARTESIAN_POINT('Ctrl Pts',(-161.705052153551,5.45639588750942,
128.804495018547));
#227657=CARTESIAN_POINT('Ctrl Pts',(-161.983499777364,1.26677168948586,
125.13276401854));
#227658=CARTESIAN_POINT('Ctrl Pts',(-162.261947401177,-4.08695380593746,
126.67295322014));
#227659=CARTESIAN_POINT('Ctrl Pts',(-162.54039502499,-5.68496841249774,
132.009703989503));
#227660=CARTESIAN_POINT('Ctrl Pts',(-162.818842648803,-2.05877477411906,
136.238803084352));
#227661=CARTESIAN_POINT('Ctrl Pts',(-163.097290272616,3.45933230493559,
135.473915039499));
#227662=CARTESIAN_POINT('Ctrl Pts',(-163.375737896429,5.79848199353304,
130.417934601304));
#227663=CARTESIAN_POINT('Ctrl Pts',(-163.654185520242,2.80911000166655,
125.717060794092));
#227664=CARTESIAN_POINT('Ctrl Pts',(-163.932633144055,-2.76169684907854,
125.691166996241));
#227665=CARTESIAN_POINT('Ctrl Pts',(-164.211080767867,-5.79463921191188,
130.36404834299));
#227666=CARTESIAN_POINT('Ctrl Pts',(-164.489528391681,-3.50259122286156,
135.441555159625));
#227667=CARTESIAN_POINT('Ctrl Pts',(-164.767976015493,2.00816698890481,
136.257706731653));
#227668=CARTESIAN_POINT('Ctrl Pts',(-165.046423639306,5.67351784227885,
132.062499635604));
#227669=CARTESIAN_POINT('Ctrl Pts',(-165.324871263119,4.12518296535417,
126.711124245485));
#227670=CARTESIAN_POINT('Ctrl Pts',(-165.603318886932,-1.21399353033979,
125.121233115594));
#227671=CARTESIAN_POINT('Ctrl Pts',(-165.881766510745,-5.43756927853226,
128.753858523801));
#227672=CARTESIAN_POINT('Ctrl Pts',(-166.160214134558,-4.66428449978105,
134.270795183582));
#227673=CARTESIAN_POINT('Ctrl Pts',(-166.438661758371,0.395249871304121,
136.602247821935));
#227674=CARTESIAN_POINT('Ctrl Pts',(-166.717109382183,5.09156891968999,
133.60572536201));
#227675=CARTESIAN_POINT('Ctrl Pts',(-166.995557005996,5.10898486785074,
128.034885556215));
#227676=CARTESIAN_POINT('Ctrl Pts',(-167.274004629809,0.431493310242956,
125.009058035423));
#227677=CARTESIAN_POINT('Ctrl Pts',(-167.552452253622,-4.64251951985801,
127.30883047135));
#227678=CARTESIAN_POINT('Ctrl Pts',(-167.830899877435,-5.45028371089662,
132.820824345507));
#227679=CARTESIAN_POINT('Ctrl Pts',(-168.109347501248,-1.24950343278299,
136.479786563416));
#227680=CARTESIAN_POINT('Ctrl Pts',(-168.387795125061,4.09950945842204,
134.923309597059));
#227681=CARTESIAN_POINT('Ctrl Pts',(-168.666242748874,5.68127342950807,
129.581719740392));
#227682=CARTESIAN_POINT('Ctrl Pts',(-168.944690372687,2.04222466451309,
125.36367712052));
#227683=CARTESIAN_POINT('Ctrl Pts',(-169.223137996499,-3.47352879894819,
126.145356842267));
#227684=CARTESIAN_POINT('Ctrl Pts',(-169.501585620313,-5.79727898749155,
131.208433428525));
#227685=CARTESIAN_POINT('Ctrl Pts',(-169.780033244125,-2.79361299935373,
135.900186841566));
#227686=CARTESIAN_POINT('Ctrl Pts',(-170.058480867939,2.77724685960862,
135.909124899701));
#227687=CARTESIAN_POINT('Ctrl Pts',(-170.336928491751,5.79595253064181,
131.227033964152));
#227688=CARTESIAN_POINT('Ctrl Pts',(-170.615376115564,3.48846097403773,
126.156526871832));
#227689=CARTESIAN_POINT('Ctrl Pts',(-170.893823739377,-2.02475579691427,
125.357151932539));
#227690=CARTESIAN_POINT('Ctrl Pts',(-171.17227136319,-5.67732090532164,
129.563495663847));
#227691=CARTESIAN_POINT('Ctrl Pts',(-171.450718987003,-4.11270545428381,
134.910133667999));
#227692=CARTESIAN_POINT('Ctrl Pts',(-171.729166610815,1.23128539240979,
136.483766816968));
#227693=CARTESIAN_POINT('Ctrl Pts',(-172.007614234629,5.44378511511418,
132.838303123102));
#227694=CARTESIAN_POINT('Ctrl Pts',(-172.286061858441,4.65371226071637,
127.323745630264));
#227695=CARTESIAN_POINT('Ctrl Pts',(-172.564509482254,-0.412894814796852,
125.00770327326));
#227696=CARTESIAN_POINT('Ctrl Pts',(-172.842957106067,-5.10007172654484,
128.018505833219));
#227697=CARTESIAN_POINT('Ctrl Pts',(-173.12140472988,-5.10053187395325,
133.589372843419));
#227698=CARTESIAN_POINT('Ctrl Pts',(-173.399852353693,-0.413852404033268,
136.600949673471));
#227699=CARTESIAN_POINT('Ctrl Pts',(-173.678299977506,4.65313720737985,
134.285744340263));
#227700=CARTESIAN_POINT('Ctrl Pts',(-173.956747601319,5.44412104360021,
128.771317440947));
#227701=CARTESIAN_POINT('Ctrl Pts',(-174.235195225131,1.23222360085094,
125.125157901261));
#227702=CARTESIAN_POINT('Ctrl Pts',(-174.513642848945,-4.11202713361109,
126.697908213384));
#227703=CARTESIAN_POINT('Ctrl Pts',(-174.792090472757,-5.67752581597763,
132.044287673595));
#227704=CARTESIAN_POINT('Ctrl Pts',(-175.070538096571,-2.02565563601667,
136.251234743121));
#227705=CARTESIAN_POINT('Ctrl Pts',(-175.348985720383,3.48769311466452,
135.452770585855));
#227706=CARTESIAN_POINT('Ctrl Pts',(-175.627433344196,5.79602227624969,
130.382644755183));
#227707=CARTESIAN_POINT('Ctrl Pts',(-175.905880968009,2.77809011739122,
125.700055200075));
#227708=CARTESIAN_POINT('Ctrl Pts',(-176.184328591822,-2.79277114210269,
125.708072964459));
#227709=CARTESIAN_POINT('Ctrl Pts',(-176.462776215635,-5.79721215645926,
130.399330114555));
#227710=CARTESIAN_POINT('Ctrl Pts',(-176.741223839448,-3.47429840858841,
135.462790510077));
#227711=CARTESIAN_POINT('Ctrl Pts',(-177.019671463261,2.04132584786218,
136.245381411334));
#227712=CARTESIAN_POINT('Ctrl Pts',(-177.298119087073,5.68107137443935,
132.02794001176));
#227713=CARTESIAN_POINT('Ctrl Pts',(-177.576566710886,4.10018984367198,
126.686088924097));
#227714=CARTESIAN_POINT('Ctrl Pts',(-177.855014334699,-1.24856584802001,
125.128728333976));
#227715=CARTESIAN_POINT('Ctrl Pts',(-178.133461958512,-5.4499505212146,
128.786996542421));
#227716=CARTESIAN_POINT('Ctrl Pts',(-178.411909582325,-4.64309691029714,
134.29912378221));
#227717=CARTESIAN_POINT('Ctrl Pts',(-178.690357206138,0.430535933288815,
136.599734402363));
#227718=CARTESIAN_POINT('Ctrl Pts',(-178.968804829951,5.10852728703229,
133.574679634036));
#227719=CARTESIAN_POINT('Ctrl Pts',(-179.247252453763,5.09203162942501,
128.00383702718));
#227720=CARTESIAN_POINT('Ctrl Pts',(-179.525700077576,0.396207663951002,
125.006538786706));
#227721=CARTESIAN_POINT('Ctrl Pts',(-179.80414770139,-4.66371178887382,
127.337155569449));
#227722=CARTESIAN_POINT('Ctrl Pts',(-180.082595325202,-5.43790794271038,
132.853964409027));
#227723=CARTESIAN_POINT('Ctrl Pts',(-180.361042949015,-1.2149323537682,
136.487287492965));
#227724=CARTESIAN_POINT('Ctrl Pts',(-180.639490572828,4.12450671554208,
134.898278404822));
#227725=CARTESIAN_POINT('Ctrl Pts',(-180.917938196641,5.67372560662389,
129.547158869193));
#227726=CARTESIAN_POINT('Ctrl Pts',(-181.196385820454,2.00906784212309,
125.351346322599));
#227727=CARTESIAN_POINT('Ctrl Pts',(-181.474833444267,-3.50182512086801,
126.166587518521));
#227728=CARTESIAN_POINT('Ctrl Pts',(-181.75328106808,-5.79471187144949,
131.243715624654));
#227729=CARTESIAN_POINT('Ctrl Pts',(-182.031728691892,-2.76254149958135,
135.917097942958));
#227730=CARTESIAN_POINT('Ctrl Pts',(-182.310176315705,2.80826955274668,
135.892124430331));
#227731=CARTESIAN_POINT('Ctrl Pts',(-182.588623939518,5.79841807769547,
131.191744524852));
#227732=CARTESIAN_POINT('Ctrl Pts',(-182.867071563331,3.46010365771282,
126.135377733334));
#227733=CARTESIAN_POINT('Ctrl Pts',(-183.145519187144,-2.05787698824661,
125.369578119929));
#227734=CARTESIAN_POINT('Ctrl Pts',(-183.423966810957,-5.68476921488759,
129.598078117967));
#227735=CARTESIAN_POINT('Ctrl Pts',(-183.70241443477,-4.08763624946197,
134.93509280296));
#227736=CARTESIAN_POINT('Ctrl Pts',(-183.980862058583,1.26583473708647,
136.476166407061));
#227737=CARTESIAN_POINT('Ctrl Pts',(-184.259309682396,5.45606543971754,
132.805127573733));
#227738=CARTESIAN_POINT('Ctrl Pts',(-184.537757306209,4.63243854686269,
127.295481650585));
#227739=CARTESIAN_POINT('Ctrl Pts',(-184.816204930021,-0.448173063354899,
125.010324079826));
#227740=CARTESIAN_POINT('Ctrl Pts',(-185.094652553834,-5.11693552282041,
128.049603032828));
#227741=CARTESIAN_POINT('Ctrl Pts',(-185.373100177647,-5.08348421301165,
133.620369628814));
#227742=CARTESIAN_POINT('Ctrl Pts',(-185.65154780146,-0.378559253454916,
136.60336151315));
#227743=CARTESIAN_POINT('Ctrl Pts',(-185.929995425273,4.67424316637891,
134.257354871388));
#227744=CARTESIAN_POINT('Ctrl Pts',(-186.208443049086,5.4316444657843,128.73821519851));
#227745=CARTESIAN_POINT('Ctrl Pts',(-186.486890672899,1.19762985171755,
125.117762228929));
#227746=CARTESIAN_POINT('Ctrl Pts',(-186.765338296712,-4.13694808860639,
126.72301537273));
#227747=CARTESIAN_POINT('Ctrl Pts',(-187.043785920525,-5.66987283665109,
132.078825411735));
#227748=CARTESIAN_POINT('Ctrl Pts',(-187.322233544337,-1.99246143649967,
136.263464565965));
#227749=CARTESIAN_POINT('Ctrl Pts',(-187.600681168151,3.51592468664221,
135.43145388367));
#227750=CARTESIAN_POINT('Ctrl Pts',(-187.879128791963,5.79334778522967,
130.347370535898));
#227751=CARTESIAN_POINT('Ctrl Pts',(-188.157576415776,2.74696728996466,
125.683238747971));
#227752=CARTESIAN_POINT('Ctrl Pts',(-188.436024039589,-2.82374194796541,
125.72516777749));
#227753=CARTESIAN_POINT('Ctrl Pts',(-188.714471663402,-5.79957028317828,
130.434626894674));
#227754=CARTESIAN_POINT('Ctrl Pts',(-188.992919287215,-3.44587685290989,
135.483853240698));
#227755=CARTESIAN_POINT('Ctrl Pts',(-189.271366911028,2.07440906473995,
136.232854471987));
#227756=CARTESIAN_POINT('Ctrl Pts',(-189.54981453484,5.68841439241029,131.993335047731));
#227757=CARTESIAN_POINT('Ctrl Pts',(-189.828262158654,4.07504478794802,
126.661206206783));
#227758=CARTESIAN_POINT('Ctrl Pts',(-190.106709782466,-1.28309189963338,
125.136433864998));
#227759=CARTESIAN_POINT('Ctrl Pts',(-190.385157406279,-5.46212981397553,
128.820209315208));
#227760=CARTESIAN_POINT('Ctrl Pts',(-190.663605030092,-4.62173726915045,
134.327322881104));
#227761=CARTESIAN_POINT('Ctrl Pts',(-190.942052653905,0.465806041606811,
136.597006233083));
#227762=CARTESIAN_POINT('Ctrl Pts',(-191.220500277718,5.12529635601715,
133.543531250871));
#227763=CARTESIAN_POINT('Ctrl Pts',(-191.49894790153,5.07488970389458,127.972892272577));
#227764=CARTESIAN_POINT('Ctrl Pts',(-191.777395525344,0.360907336037817,
125.004234378408));
#227765=CARTESIAN_POINT('Ctrl Pts',(-192.055843149156,-4.68473124233415,
127.365609146106));
#227766=CARTESIAN_POINT('Ctrl Pts',(-192.33429077297,-5.42533067084548,
132.887028523726));
#227767=CARTESIAN_POINT('Ctrl Pts',(-192.612738396782,-1.1803162549878,
136.494577839569));
#227768=CARTESIAN_POINT('Ctrl Pts',(-192.891186020595,4.14935113754904,
134.873095510955));
#227769=CARTESIAN_POINT('Ctrl Pts',(-193.169633644408,5.66596754175055,
129.512644584067));
#227770=CARTESIAN_POINT('Ctrl Pts',(-193.448081268221,1.97583657298603,
125.339217588127));
#227771=CARTESIAN_POINT('Ctrl Pts',(-193.726528892034,-3.52999168137001,
126.187990049162));
#227772=CARTESIAN_POINT('Ctrl Pts',(-194.004976515847,-5.79193003022761,
131.27898154032));
#227773=CARTESIAN_POINT('Ctrl Pts',(-194.28342413966,-2.73136763281852,
135.933819589987));
#227774=CARTESIAN_POINT('Ctrl Pts',(-194.561871763472,2.83918818442447,
135.874935432001));
#227775=CARTESIAN_POINT('Ctrl Pts',(-194.840319387286,5.80066876223446,
131.156440730899));
#227776=CARTESIAN_POINT('Ctrl Pts',(-195.118767011098,3.43161812597426,
126.114401605713));
#227777=CARTESIAN_POINT('Ctrl Pts',(-195.397214634911,-2.09092192419104,
125.382205695184));
#227778=CARTESIAN_POINT('Ctrl Pts',(-195.675662258724,-5.69200687323938,
129.63270527133));
#227779=CARTESIAN_POINT('Ctrl Pts',(-195.954109882537,-4.06241557577554,
134.95989887212));
#227780=CARTESIAN_POINT('Ctrl Pts',(-196.23255750635,1.30033717579212,136.468355826305));
#227781=CARTESIAN_POINT('Ctrl Pts',(-196.511005130163,5.46814358780935,
132.771877885207));
#227782=CARTESIAN_POINT('Ctrl Pts',(-196.789452753976,4.61099317629508,
127.267347693709));
#227783=CARTESIAN_POINT('Ctrl Pts',(-197.067900377789,-0.483434704694746,
125.013159586548));
#227784=CARTESIAN_POINT('Ctrl Pts',(-197.346348001602,-5.13360970916836,
128.080802310993));
#227785=CARTESIAN_POINT('Ctrl Pts',(-197.624795625414,-5.06624818169292,
133.651262065958));
#227786=CARTESIAN_POINT('Ctrl Pts',(-197.903243249227,-0.343252075224855,
136.605558468718));
#227787=CARTESIAN_POINT('Ctrl Pts',(-198.18169087304,4.69517591957924,134.228837450539));
#227788=CARTESIAN_POINT('Ctrl Pts',(-198.460138496853,5.41896661638458,
128.705189517851));
#227789=CARTESIAN_POINT('Ctrl Pts',(-198.738586120666,1.1629917239694,125.110577275591));
#227790=CARTESIAN_POINT('Ctrl Pts',(-199.017033744479,-4.16171574746965,
126.748273767825));
#227791=CARTESIAN_POINT('Ctrl Pts',(-199.295481368292,-5.6620097581009,
132.113315924113));
#227792=CARTESIAN_POINT('Ctrl Pts',(-199.573928992105,-1.95919340559182,
136.275492099704));
#227793=CARTESIAN_POINT('Ctrl Pts',(-199.852376615917,3.54402597473752,
135.409965722843));
#227794=CARTESIAN_POINT('Ctrl Pts',(-200.13082423973,5.79045861957696,130.312113250549));
#227795=CARTESIAN_POINT('Ctrl Pts',(-200.409271863544,2.71574267265526,
125.666612060922));
#227796=CARTESIAN_POINT('Ctrl Pts',(-200.687719487356,-2.85460811903155,
125.742450801881));
#227797=CARTESIAN_POINT('Ctrl Pts',(-200.966167111169,-5.80171350468764,
130.469937375411));
#227798=CARTESIAN_POINT('Ctrl Pts',(-201.244614734982,-3.41732760899753,
135.504742570997));
#227799=CARTESIAN_POINT('Ctrl Pts',(-201.523062358795,2.10741541362659,
136.220126377805));
#227800=CARTESIAN_POINT('Ctrl Pts',(-201.801509982608,5.69554662409457,
131.958686025817));
#227801=CARTESIAN_POINT('Ctrl Pts',(-202.079957606421,4.04974872994014,
126.636477015578));
#227802=CARTESIAN_POINT('Ctrl Pts',(-202.358405230234,-1.31757040580477,
125.144349423131));
#227803=CARTESIAN_POINT('Ctrl Pts',(-202.636852854047,-5.47410670550813,
128.853495611451));
#227804=CARTESIAN_POINT('Ctrl Pts',(-202.915300477859,-4.6002063678289,
134.355391435336));
#227805=CARTESIAN_POINT('Ctrl Pts',(-203.193748101672,0.501058889310003,
136.594063415189));
#227806=CARTESIAN_POINT('Ctrl Pts',(-203.472195725485,5.14187550526088,
133.512281366733));
#227807=CARTESIAN_POINT('Ctrl Pts',(-203.750643349298,5.05755972645996,
127.942052439074));
#227808=CARTESIAN_POINT('Ctrl Pts',(-204.029090973111,0.325593634571106,
125.002144895921));
#227809=CARTESIAN_POINT('Ctrl Pts',(-204.307538596924,-4.70557710135553,
127.394190146963));
#227810=CARTESIAN_POINT('Ctrl Pts',(-204.585986220737,-5.41255236135747,
132.920015464399));
#227811=CARTESIAN_POINT('Ctrl Pts',(-204.864433844549,-1.14565641915494,
136.50165733308));
#227812=CARTESIAN_POINT('Ctrl Pts',(-205.142881468362,4.17404180382362,
134.847761848621));
#227813=CARTESIAN_POINT('Ctrl Pts',(-205.421329092175,5.6579995223666,129.478178163952));
#227814=CARTESIAN_POINT('Ctrl Pts',(-205.699776715988,1.94253208849746,
125.327291366541));
#227815=CARTESIAN_POINT('Ctrl Pts',(-205.978224339801,-3.55802743673226,
126.209563641112));
#227816=CARTESIAN_POINT('Ctrl Pts',(-206.256671963614,-5.78893356690891,
131.314229868733));
#227817=CARTESIAN_POINT('Ctrl Pts',(-206.535119587427,-2.70009255422283,
135.950351163029));
#227818=CARTESIAN_POINT('Ctrl Pts',(-206.81356721124,2.87000160893922,135.857558541658));
#227819=CARTESIAN_POINT('Ctrl Pts',(-207.092014835053,5.80270450085972,
131.121123890489));
#227820=CARTESIAN_POINT('Ctrl Pts',(-207.370462458865,3.40300543436423,
126.09359926625));
#227821=CARTESIAN_POINT('Ctrl Pts',(-207.648910082679,-2.12388938025395,
125.395034190384));
#227822=CARTESIAN_POINT('Ctrl Pts',(-207.927357706491,-5.69903361218359,
129.667375840811));
#227823=CARTESIAN_POINT('Ctrl Pts',(-208.205805330304,-4.03704436778601,
134.984550956282));
#227824=CARTESIAN_POINT('Ctrl Pts',(-208.484252954117,1.33479143002538,
136.460335364123));
#227825=CARTESIAN_POINT('Ctrl Pts',(-208.76270057793,5.48001911182977,132.738555289606));
#227826=CARTESIAN_POINT('Ctrl Pts',(-209.041148201743,4.58937694367963,
127.239344802146));
#227827=CARTESIAN_POINT('Ctrl Pts',(-209.319595825556,-0.518678432184342,
125.016209688352));
#227828=CARTESIAN_POINT('Ctrl Pts',(-209.598043449369,-5.15009366772074,
128.112102511612));
#227829=CARTESIAN_POINT('Ctrl Pts',(-209.876491073182,-5.04882441868487,
133.682049010123));
#227830=CARTESIAN_POINT('Ctrl Pts',(-210.154938696994,-0.307932177662294,
136.607540458767));
#227831=CARTESIAN_POINT('Ctrl Pts',(-210.433386320807,4.71593469130848,
134.200193134443));
#227832=CARTESIAN_POINT('Ctrl Pts',(-210.71183394462,5.40608796518471,128.672241622749));
#227833=CARTESIAN_POINT('Ctrl Pts',(-210.990281568433,1.12831050113542,
125.103603307488));
#227834=CARTESIAN_POINT('Ctrl Pts',(-211.268729192246,-4.18632919242468,
126.773682462711));
#227835=CARTESIAN_POINT('Ctrl Pts',(-211.547176816059,-5.65393687169752,
132.14775793267));
#227836=CARTESIAN_POINT('Ctrl Pts',(-211.825624439872,-1.92585277605142,
136.287316898656));
#227837=CARTESIAN_POINT('Ctrl Pts',(-212.104072063685,3.57199593764717,
135.388306899624));
#227838=CARTESIAN_POINT('Ctrl Pts',(-212.382519687498,5.78735488635066,
130.276874205606));
#227839=CARTESIAN_POINT('Ctrl Pts',(-212.660967311311,2.68441742250212,
125.650175755035));
#227840=CARTESIAN_POINT('Ctrl Pts',(-212.939414935123,-2.88536851154432,
125.759921397201));
#227841=CARTESIAN_POINT('Ctrl Pts',(-213.217862558936,-5.80364174156953,
130.505260248325));
#227842=CARTESIAN_POINT('Ctrl Pts',(-213.496310182749,-3.38865173475374,
135.525457726916));
#227843=CARTESIAN_POINT('Ctrl Pts',(-213.774757806562,2.14034367146046,
136.20719760043));
#227844=CARTESIAN_POINT('Ctrl Pts',(-214.053205430375,5.7024678052036,131.923994229952));
#227845=CARTESIAN_POINT('Ctrl Pts',(-214.331653054188,4.02430260700449,
126.611902266833));
#227846=CARTESIAN_POINT('Ctrl Pts',(-214.610100678001,-1.35200008892003,
125.152474715061));
#227847=CARTESIAN_POINT('Ctrl Pts',(-214.888548301814,-5.48588075200302,
128.886854197714));
#227848=CARTESIAN_POINT('Ctrl Pts',(-215.166995925626,-4.5785050041694,
134.383328404815));
#227849=CARTESIAN_POINT('Ctrl Pts',(-215.445443549439,0.536293170092427,
136.59090605773));
#227850=CARTESIAN_POINT('Ctrl Pts',(-215.723891173253,5.15826412041666,
133.480931139593));
#227851=CARTESIAN_POINT('Ctrl Pts',(-216.002338797065,5.04004233928969,
127.911318669453));
#227852=CARTESIAN_POINT('Ctrl Pts',(-216.280786420879,0.290267868112,125.000270416672));
#227853=CARTESIAN_POINT('Ctrl Pts',(-216.559234044691,-4.72624859348692,
127.422897512942));
#227854=CARTESIAN_POINT('Ctrl Pts',(-216.837681668504,-5.39957348775117,
132.952924008705));
#227855=CARTESIAN_POINT('Ctrl Pts',(-217.116129292317,-1.11095413060172,
136.508525711168));
#227856=CARTESIAN_POINT('Ctrl Pts',(-217.39457691613,4.19857779944424,134.822278356567));
#227857=CARTESIAN_POINT('Ctrl Pts',(-217.673024539943,5.64982184372931,
129.443760886018));
#227858=CARTESIAN_POINT('Ctrl Pts',(-217.951472163756,1.90915562276867,
125.315568099769));
#227859=CARTESIAN_POINT('Ctrl Pts',(-218.229919787568,-3.58593134807924,
126.231307494954));
#227860=CARTESIAN_POINT('Ctrl Pts',(-218.508367411381,-5.78572259252759,
131.349459303753));
#227861=CARTESIAN_POINT('Ctrl Pts',(-218.786815035194,-2.66871742270537,
135.966692049498));
#227862=CARTESIAN_POINT('Ctrl Pts',(-219.065262659007,2.90070868448967,
135.839994403207));
#227863=CARTESIAN_POINT('Ctrl Pts',(-219.34371028282,5.80452521813531,131.085795312298));
#227864=CARTESIAN_POINT('Ctrl Pts',(-219.622157906633,3.37426664313623,
126.07297148578));
#227865=CARTESIAN_POINT('Ctrl Pts',(-219.900605530446,-2.15677813481551,
125.408063130162));
#227866=CARTESIAN_POINT('Ctrl Pts',(-220.179053154259,-5.70584917134113,
129.702088541682));
#227867=CARTESIAN_POINT('Ctrl Pts',(-220.457500778071,-4.01152356563293,
135.009048141953));
#227868=CARTESIAN_POINT('Ctrl Pts',(-220.735948401884,1.36919622307095,
136.452105317718));
#227869=CARTESIAN_POINT('Ctrl Pts',(-221.014396025697,5.49169157172664,
132.705161021709));
#227870=CARTESIAN_POINT('Ctrl Pts',(-221.29284364951,4.56759065001379,127.211474013555));
#227871=CARTESIAN_POINT('Ctrl Pts',(-221.571291273323,-0.553902939853376,
125.019474272218));
#227872=CARTESIAN_POINT('Ctrl Pts',(-221.849738897136,-5.16638678765824,
128.143502474846));
#227873=CARTESIAN_POINT('Ctrl Pts',(-222.128186520948,-5.03121356963114,
133.712729320486));
#227874=CARTESIAN_POINT('Ctrl Pts',(-222.406634144762,-0.272600869560251,
136.609307409853));
#227875=CARTESIAN_POINT('Ctrl Pts',(-222.685081768574,4.73651871234416,
134.171422984523));
#227876=CARTESIAN_POINT('Ctrl Pts',(-222.963529392388,5.39300898940659,
128.639372734101));
#227877=CARTESIAN_POINT('Ctrl Pts',(-223.2419770162,1.09358746834067,125.096840583045));
#227878=CARTESIAN_POINT('Ctrl Pts',(-223.520424640014,-4.21078751141269,
126.799240515859));
#227879=CARTESIAN_POINT('Ctrl Pts',(-223.798872263826,-5.64565447658353,
132.182150161146));
#227880=CARTESIAN_POINT('Ctrl Pts',(-224.077319887639,-1.89244078332859,
136.298938524645));
#227881=CARTESIAN_POINT('Ctrl Pts',(-224.355767511452,3.59983353893359,
135.366478216591));
#227882=CARTESIAN_POINT('Ctrl Pts',(-224.634215135265,5.78403670056078,
130.241654706868));
#227883=CARTESIAN_POINT('Ctrl Pts',(-224.912662759078,2.65299270027449,
125.633930439363));
#227884=CARTESIAN_POINT('Ctrl Pts',(-225.191110382891,-2.91602198566553,
125.77757891607));
#227885=CARTESIAN_POINT('Ctrl Pts',(-225.469558006704,-5.8053549223724,
130.540594204513));
#227886=CARTESIAN_POINT('Ctrl Pts',(-225.748005630516,-3.35985029277391,
135.545997940844));
#227887=CARTESIAN_POINT('Ctrl Pts',(-226.026453254329,2.17319261807209,
136.194068618944));
#227888=CARTESIAN_POINT('Ctrl Pts',(-226.304900878142,5.7091776792716,131.88926094565));
#227889=CARTESIAN_POINT('Ctrl Pts',(-226.583348501955,3.99870736205508,
126.587482871174));
#227890=CARTESIAN_POINT('Ctrl Pts',(-226.861796125768,-1.38637967317499,
125.160809439701));
#227891=CARTESIAN_POINT('Ctrl Pts',(-227.140243749581,-5.49745151716988,
128.920283837883));
#227892=CARTESIAN_POINT('Ctrl Pts',(-227.418691373394,-4.55663398232247,
134.411132754326));
#227893=CARTESIAN_POINT('Ctrl Pts',(-227.697138997207,0.571507578333558,
136.5875342777));
#227894=CARTESIAN_POINT('Ctrl Pts',(-227.97558662102,5.17446159419872,133.44948173115));
#227895=CARTESIAN_POINT('Ctrl Pts',(-228.254034244832,5.02233819149715,
127.880692102567));
#227896=CARTESIAN_POINT('Ctrl Pts',(-228.532481868645,0.254931345670833,
124.998611010119));
#227897=CARTESIAN_POINT('Ctrl Pts',(-228.810929492458,-4.74674495273865,
127.451730180279));
#227898=CARTESIAN_POINT('Ctrl Pts',(-229.089377116271,-5.38639453096373,
132.985752937203));
#227899=CARTESIAN_POINT('Ctrl Pts',(-229.367824740084,-1.07621067523457,
136.515182719319));
#227900=CARTESIAN_POINT('Ctrl Pts',(-229.646272363897,4.22295821522052,
134.796645979094));
#227901=CARTESIAN_POINT('Ctrl Pts',(-229.92471998771,5.64143480886619,129.409394025606));
#227902=CARTESIAN_POINT('Ctrl Pts',(-230.203167611523,1.87570841257552,
125.304048222223));
#227903=CARTESIAN_POINT('Ctrl Pts',(-230.481615235336,-3.61370238142155,
126.25322080496));
#227904=CARTESIAN_POINT('Ctrl Pts',(-230.760062859148,-5.78229722606833,
131.384668539942));
#227905=CARTESIAN_POINT('Ctrl Pts',(-231.038510482961,-2.63724340088164,
135.982841643878));
#227906=CARTESIAN_POINT('Ctrl Pts',(-231.316958106774,2.93130827321233,
135.822243667495));
#227907=CARTESIAN_POINT('Ctrl Pts',(-231.595405730587,5.80613084659478,
131.050456305442));
#227908=CARTESIAN_POINT('Ctrl Pts',(-231.8738533544,3.34540281721704,126.052519028673));
#227909=CARTESIAN_POINT('Ctrl Pts',(-232.152300978213,-2.18958696916944,
125.42129203173));
#227910=CARTESIAN_POINT('Ctrl Pts',(-232.430748602025,-5.71245329815966,
129.736842087648));
#227911=CARTESIAN_POINT('Ctrl Pts',(-232.709196225839,-3.98585411499877,
135.033389521383));
#227912=CARTESIAN_POINT('Ctrl Pts',(-232.987643849651,1.40355028004735,
136.443665992055));
#227913=CARTESIAN_POINT('Ctrl Pts',(-233.266091473464,5.50316053497282,
132.671696318956));
#227914=CARTESIAN_POINT('Ctrl Pts',(-233.544539097277,4.5456351025967,127.183736360699));
#227915=CARTESIAN_POINT('Ctrl Pts',(-233.82298672109,-0.589106922445798,
125.022953217175));
#227916=CARTESIAN_POINT('Ctrl Pts',(-234.101434344904,-5.18248846523346,
128.175001037157));
#227917=CARTESIAN_POINT('Ctrl Pts',(-234.379881968716,-5.01341628710851,
133.743301860178));
#227918=CARTESIAN_POINT('Ctrl Pts',(-234.658329592529,-0.237259460132118,
136.610859256499));
#227919=CARTESIAN_POINT('Ctrl Pts',(-234.936777216342,4.75692721993639,
134.14252806687));
#227920=CARTESIAN_POINT('Ctrl Pts',(-235.215224840155,5.37973017369771,
128.606584069875));
#227921=CARTESIAN_POINT('Ctrl Pts',(-235.493672463967,1.05882391226032,
125.090289352854));
#227922=CARTESIAN_POINT('Ctrl Pts',(-235.772120087781,-4.23508979812022,
126.824946980203));
#227923=CARTESIAN_POINT('Ctrl Pts',(-236.050567711593,-5.63716287966734,
132.216491335124));
#227924=CARTESIAN_POINT('Ctrl Pts',(-236.329015335406,-1.85895866551617,
136.310356547029));
#227925=CARTESIAN_POINT('Ctrl Pts',(-236.607462959219,3.62753774706455,
135.344480482612));
#227926=CARTESIAN_POINT('Ctrl Pts',(-236.885910583032,5.78050418516386,
130.206456059403));
#227927=CARTESIAN_POINT('Ctrl Pts',(-237.164358206845,2.62146967042642,
125.617876715884));
#227928=CARTESIAN_POINT('Ctrl Pts',(-237.442805830658,-2.94656740551997,
125.795422704185));
#227929=CARTESIAN_POINT('Ctrl Pts',(-237.72125345447,-5.80685298361372,
130.575937934662));
#227930=CARTESIAN_POINT('Ctrl Pts',(-237.999701078284,-3.33092435030571,
135.566362451659));
#227931=CARTESIAN_POINT('Ctrl Pts',(-238.278148702096,2.20596103623244,
136.180739919846));
#227932=CARTESIAN_POINT('Ctrl Pts',(-238.55659632591,5.7156759976606,131.854487459968));
#227933=CARTESIAN_POINT('Ctrl Pts',(-238.835043949722,3.97296394353457,
126.56321973347));
#227934=CARTESIAN_POINT('Ctrl Pts',(-239.113491573535,-1.42070788462113,
125.169353288205));
#227935=CARTESIAN_POINT('Ctrl Pts',(-239.391939197348,-5.50881857224844,
128.95378329321));
#227936=CARTESIAN_POINT('Ctrl Pts',(-239.670386821161,-4.53459411272838,
134.438803453569));
#227937=CARTESIAN_POINT('Ctrl Pts',(-239.948834444974,0.606700809151854,
136.583948200045));
#227938=CARTESIAN_POINT('Ctrl Pts',(-240.227282068787,5.1904673264033,133.417934306771));
#227939=CARTESIAN_POINT('Ctrl Pts',(-240.5057296926,5.00444793911587,127.850173873291));
#227940=CARTESIAN_POINT('Ctrl Pts',(-240.784177316413,0.21958537665436,
124.997166737753));
#227941=CARTESIAN_POINT('Ctrl Pts',(-241.062624940225,-4.76706541961049,
127.48068708057));
#227942=CARTESIAN_POINT('Ctrl Pts',(-241.341072564039,-5.37301597934592,
133.018501033406));
#227943=CARTESIAN_POINT('Ctrl Pts',(-241.619520187851,-1.04142734048567,
136.521628110858));
#227944=CARTESIAN_POINT('Ctrl Pts',(-241.897967811664,4.24718214772698,
134.770865666018));
#227945=CARTESIAN_POINT('Ctrl Pts',(-242.176415435477,5.63283872856131,
129.375078856195));
#227946=CARTESIAN_POINT('Ctrl Pts',(-242.45486305929,1.84219169731802,125.292732160775));
#227947=CARTESIAN_POINT('Ctrl Pts',(-242.733310683103,-3.64133950769301,
126.275302759127));
#227948=CARTESIAN_POINT('Ctrl Pts',(-243.011758306915,-5.77865759445851,
131.419856272607));
#227949=CARTESIAN_POINT('Ctrl Pts',(-243.290205930729,-2.60567165503458,
135.998799347738));
#227950=CARTESIAN_POINT('Ctrl Pts',(-243.568653554541,2.96179924122969,
135.80430699228));
#227951=CARTESIAN_POINT('Ctrl Pts',(-243.847101178355,5.80752132674009,
131.015108179419));
#227952=CARTESIAN_POINT('Ctrl Pts',(-244.125548802166,3.31641502616601,
126.032242652805));
#227953=CARTESIAN_POINT('Ctrl Pts',(-244.403996425981,-2.22231466757369,
125.434720404883));
#227954=CARTESIAN_POINT('Ctrl Pts',(-244.682444049792,-5.71884574792013,
129.771635190908));
#227955=CARTESIAN_POINT('Ctrl Pts',(-244.960891673606,-3.96003696707471,
135.05757419259));
#227956=CARTESIAN_POINT('Ctrl Pts',(-245.239339297418,1.43785232795156,
136.435017699859));
#227957=CARTESIAN_POINT('Ctrl Pts',(-245.517786921232,5.51442557658153,
132.638162421391));
#227958=CARTESIAN_POINT('Ctrl Pts',(-245.796234545044,4.52351111499922,
127.156132871406));
#227959=CARTESIAN_POINT('Ctrl Pts',(-246.074682168857,-0.624289075464052,
125.026646394309));
#227960=CARTESIAN_POINT('Ctrl Pts',(-246.353129792671,-5.19839810379266,
128.206597031353));
#227961=CARTESIAN_POINT('Ctrl Pts',(-246.631577416483,-4.99543323060155,
133.773765496319));
#227962=CARTESIAN_POINT('Ctrl Pts',(-246.910025040296,-0.201909258968066,
136.612195941205));
#227963=CARTESIAN_POINT('Ctrl Pts',(-247.188472664109,4.77715945784187,
134.113509452194));
#227964=CARTESIAN_POINT('Ctrl Pts',(-247.466920287922,5.36625201010822,
128.573876845067));
#227965=CARTESIAN_POINT('Ctrl Pts',(-247.745367911734,1.02402112107033,
125.083949859676));
#227966=CARTESIAN_POINT('Ctrl Pts',(-248.023815535548,-4.25923515201858,
126.850800903184));
#227967=CARTESIAN_POINT('Ctrl Pts',(-248.30226315936,-5.62846239560694,
132.250780182078));
#227968=CARTESIAN_POINT('Ctrl Pts',(-248.580710783174,-1.82540766330725,
136.32157054271));
#227969=CARTESIAN_POINT('Ctrl Pts',(-248.859158406986,3.65510753545023,
135.322314512822));
#227970=CARTESIAN_POINT('Ctrl Pts',(-249.137606030799,5.7767574710584,130.171279567513));
#227971=CARTESIAN_POINT('Ctrl Pts',(-249.416053654612,2.58984950105633,
125.602015179472));
#227972=CARTESIAN_POINT('Ctrl Pts',(-249.694501278425,-2.97700363923603,
125.813452100338));
#227973=CARTESIAN_POINT('Ctrl Pts',(-249.972948902238,-5.80813586978118,
130.611290129096));
#227974=CARTESIAN_POINT('Ctrl Pts',(-250.251396526051,-3.30187497921299,
135.586550504748));
#227975=CARTESIAN_POINT('Ctrl Pts',(-250.529844149864,2.23864771169993,
136.167211997028));
#227976=CARTESIAN_POINT('Ctrl Pts',(-250.808291773676,5.72196251956533,
131.819675061465));
#227977=CARTESIAN_POINT('Ctrl Pts',(-251.08673939749,3.94707330538994,126.539113752772));
#227978=CARTESIAN_POINT('Ctrl Pts',(-251.365187021302,-1.45498345124562,
125.178105944033));
#227979=CARTESIAN_POINT('Ctrl Pts',(-251.643634645115,-5.5199814959705,
128.987351322257));
#227980=CARTESIAN_POINT('Ctrl Pts',(-251.922082268928,-4.51238621219265,
134.466339477392));
#227981=CARTESIAN_POINT('Ctrl Pts',(-252.200529892741,0.641871558658502,
136.580147957277));
#227982=CARTESIAN_POINT('Ctrl Pts',(-252.478977516554,5.20628072353487,
133.386290036154));
#227983=CARTESIAN_POINT('Ctrl Pts',(-252.757425140367,4.98637224582674,
127.819765111179));
#227984=CARTESIAN_POINT('Ctrl Pts',(-253.035872764179,0.184231269403876,
124.995937655572));
#227985=CARTESIAN_POINT('Ctrl Pts',(-253.314320387993,-4.78720923844335,
127.509767136124));
#227986=CARTESIAN_POINT('Ctrl Pts',(-253.592768011806,-5.35943833369967,
133.051167092665));
#227987=CARTESIAN_POINT('Ctrl Pts',(-253.871215635618,-1.00660540571931,
136.527861630253));
#227988=CARTESIAN_POINT('Ctrl Pts',(-254.149663259431,4.27124868131666,
134.744938404161));
#227989=CARTESIAN_POINT('Ctrl Pts',(-254.428110883244,5.62403395537261,
129.340816589823));
#227990=CARTESIAN_POINT('Ctrl Pts',(-254.706558507057,1.80860665472018,
125.281620447135));
#227991=CARTESIAN_POINT('Ctrl Pts',(-254.98500613087,-3.66884158147516,
126.297552326988));
#227992=CARTESIAN_POINT('Ctrl Pts',(-255.263453754682,-5.77480406163408,
131.45502159855));
#227993=CARTESIAN_POINT('Ctrl Pts',(-255.541901378496,-2.57400292253984,
136.014563813166));
#227994=CARTESIAN_POINT('Ctrl Pts',(-255.820349002309,2.99217964199006,
135.78618647082));
#227995=CARTESIAN_POINT('Ctrl Pts',(-256.098796626121,5.80869814913581,
130.979749546569));
#227996=CARTESIAN_POINT('Ctrl Pts',(-256.377244249934,3.28730143236016,
126.01214820295));
#227997=CARTESIAN_POINT('Ctrl Pts',(-256.655691873747,-2.25495451926359,
125.448338134603));
#227998=CARTESIAN_POINT('Ctrl Pts',(-256.93413949756,-5.72503666514098,
129.806484721847));
#227999=CARTESIAN_POINT('Ctrl Pts',(-257.212587121373,-3.93405347634203,
135.081566970265));
#228000=CARTESIAN_POINT('Ctrl Pts',(-257.491034745186,1.47206408278265,
136.426225506557));
#228001=CARTESIAN_POINT('Ctrl Pts',(-257.769482368999,5.52555616721843,
132.604438319186));
#228002=CARTESIAN_POINT('Ctrl Pts',(-258.047929992812,4.50108754276566,
127.128895412351));
#228003=CARTESIAN_POINT('Ctrl Pts',(-258.326377616624,-0.659198908970111,
125.030117734768));
#228004=CARTESIAN_POINT('Ctrl Pts',(-258.604825240438,-5.21458571703409,
128.239112839452));
#228005=CARTESIAN_POINT('Ctrl Pts',(-258.883272864251,-4.97637574492231,
133.802560593787));
#228006=CARTESIAN_POINT('Ctrl Pts',(-259.161720488063,-0.168236736403017,
136.616288572087));
#228007=CARTESIAN_POINT('Ctrl Pts',(-259.440168111876,4.80044487344316,
134.078525892203));
#228008=CARTESIAN_POINT('Ctrl Pts',(-259.672207798387,5.25516631655033,
129.4749169549));
#228009=CARTESIAN_POINT('Ctrl Pts',(-259.857849473896,3.17366342871357,
126.795179433485));
#228010=CARTESIAN_POINT('Ctrl Pts',(-259.9506752748,1.64266665146648,126.102093112095));
#228011=CARTESIAN_POINT('Ctrl Pts',(-259.997093138402,0.835778587061721,
125.962806053044));
#228012=CARTESIAN_POINT('Ctrl Pts',(210.385579563201,-2.29217962691353,
126.082387726892));
#228013=CARTESIAN_POINT('Ctrl Pts',(210.339169886847,-3.0789974560272,126.464330840008));
#228014=CARTESIAN_POINT('Ctrl Pts',(210.246352273192,-4.44507089109247,
127.629120819077));
#228015=CARTESIAN_POINT('Ctrl Pts',(210.060718784933,-5.78798125627161,
130.996088365878));
#228016=CARTESIAN_POINT('Ctrl Pts',(209.828679098422,-3.95783017776954,
135.586872998689));
#228017=CARTESIAN_POINT('Ctrl Pts',(209.550231474609,1.89393692750204,136.720289837399));
#228018=CARTESIAN_POINT('Ctrl Pts',(209.271783850796,5.99602695027556,132.40812259401));
#228019=CARTESIAN_POINT('Ctrl Pts',(208.993336226983,4.59288360023261,126.626877830413));
#228020=CARTESIAN_POINT('Ctrl Pts',(208.71488860317,-1.03344059257722,124.682062423228));
#228021=CARTESIAN_POINT('Ctrl Pts',(208.436440979357,-5.70873650289865,
128.364647771496));
#228022=CARTESIAN_POINT('Ctrl Pts',(208.157993355544,-5.13869562717284,
134.288517668348));
#228023=CARTESIAN_POINT('Ctrl Pts',(207.879545731732,0.153933173725622,
137.010984097728));
#228024=CARTESIAN_POINT('Ctrl Pts',(207.601098107919,5.30490488755997,134.029672582798));
#228025=CARTESIAN_POINT('Ctrl Pts',(207.322650484106,5.58103410012833,128.084559773234));
#228026=CARTESIAN_POINT('Ctrl Pts',(207.044202860293,0.728409521696789,
124.638756607567));
#228027=CARTESIAN_POINT('Ctrl Pts',(206.76575523648,-4.79355811073501,126.858871164077));
#228028=CARTESIAN_POINT('Ctrl Pts',(206.487307612667,-5.91049575314416,
132.704682504842));
#228029=CARTESIAN_POINT('Ctrl Pts',(206.208859988854,-1.59596820864792,
136.804198957117));
#228030=CARTESIAN_POINT('Ctrl Pts',(205.930412365042,4.1851717387407,135.390152799229));
#228031=CARTESIAN_POINT('Ctrl Pts',(205.651964741228,6.12034565262566,129.76198992389));
#228032=CARTESIAN_POINT('Ctrl Pts',(205.373517117416,2.43121966936229,125.091713591677));
#228033=CARTESIAN_POINT('Ctrl Pts',(205.095069493603,-3.49207776276838,
125.671081434371));
#228034=CARTESIAN_POINT('Ctrl Pts',(204.81662186979,-6.20632667560231,130.96768173473));
#228035=CARTESIAN_POINT('Ctrl Pts',(204.538174245977,-3.21726438559061,
136.114198085604));
#228036=CARTESIAN_POINT('Ctrl Pts',(204.259726622164,2.72830660529182,136.381233108793));
#228037=CARTESIAN_POINT('Ctrl Pts',(203.981278998351,6.16669716267351,131.523394807979));
#228038=CARTESIAN_POINT('Ctrl Pts',(203.702831374538,3.9381942601484,126.004799186432));
#228039=CARTESIAN_POINT('Ctrl Pts',(203.424383750725,-1.909316761502,124.896766062528));
#228040=CARTESIAN_POINT('Ctrl Pts',(203.145936126912,-6.00225896230248,
129.217523725228));
#228041=CARTESIAN_POINT('Ctrl Pts',(202.867488503099,-4.57941839934143,
134.996506974633));
#228042=CARTESIAN_POINT('Ctrl Pts',(202.589040879287,1.05168395343957,136.923112517541));
#228043=CARTESIAN_POINT('Ctrl Pts',(202.310593255474,5.71634013176502,133.226883983125));
#228044=CARTESIAN_POINT('Ctrl Pts',(202.032145631661,5.12795898713612,127.30447482202));
#228045=CARTESIAN_POINT('Ctrl Pts',(201.753698007848,-0.172765951628197,
124.598289728405));
#228046=CARTESIAN_POINT('Ctrl Pts',(201.475250384035,-5.31472742110118,
127.595180598346));
#228047=CARTESIAN_POINT('Ctrl Pts',(201.196802760222,-5.57271402936141,
133.541151128878));
#228048=CARTESIAN_POINT('Ctrl Pts',(200.918355136409,-0.709648686901125,
136.972144879116));
#228049=CARTESIAN_POINT('Ctrl Pts',(200.639907512596,4.80554913058071,134.735246206027));
#228050=CARTESIAN_POINT('Ctrl Pts',(200.361459888783,5.90468206117194,128.886055711564));
#228051=CARTESIAN_POINT('Ctrl Pts',(200.083012264971,1.57770063730838,124.799693711321));
#228052=CARTESIAN_POINT('Ctrl Pts',(199.804564641158,-4.19911059728431,
126.231327253625));
#228053=CARTESIAN_POINT('Ctrl Pts',(199.526117017345,-6.11714433092778,
131.865355052293));
#228054=CARTESIAN_POINT('Ctrl Pts',(199.247669393532,-2.4138212635637,136.524380797905));
#228055=CARTESIAN_POINT('Ctrl Pts',(198.969221769719,3.50768562329156,135.926987436306));
#228056=CARTESIAN_POINT('Ctrl Pts',(198.690774145906,6.20580078231077,130.622150282517));
#228057=CARTESIAN_POINT('Ctrl Pts',(198.412326522093,3.20108819260905,125.484755525167));
#228058=CARTESIAN_POINT('Ctrl Pts',(198.13387889828,-2.74526806424844,125.235817970576));
#228059=CARTESIAN_POINT('Ctrl Pts',(197.855431274468,-6.16885708386238,
130.104099070135));
#228060=CARTESIAN_POINT('Ctrl Pts',(197.576983650655,-3.92356780882929,
135.615886322105));
#228061=CARTESIAN_POINT('Ctrl Pts',(197.298536026841,1.92728860557448,136.706116507701));
#228062=CARTESIAN_POINT('Ctrl Pts',(197.020088403029,6.00706094473797,132.372921347066));
#228063=CARTESIAN_POINT('Ctrl Pts',(196.741640779216,4.56663773692898,126.598295504472));
#228064=CARTESIAN_POINT('Ctrl Pts',(196.463193155403,-1.07030245846182,
124.688838023107));
#228065=CARTESIAN_POINT('Ctrl Pts',(196.184745531591,-5.72368698170812,
128.399247046161));
#228066=CARTESIAN_POINT('Ctrl Pts',(195.906297907777,-5.11728278641862,
134.319837945007));
#228067=CARTESIAN_POINT('Ctrl Pts',(195.627850283965,0.191654296427489,
137.009876920548));
#228068=CARTESIAN_POINT('Ctrl Pts',(195.349402660151,5.32447044368961,133.997349569974));
#228069=CARTESIAN_POINT('Ctrl Pts',(195.070955036339,5.56435836804288,128.050621358318));
#228070=CARTESIAN_POINT('Ctrl Pts',(194.792507412526,0.690872786183208,
124.634444998269));
#228071=CARTESIAN_POINT('Ctrl Pts',(194.514059788713,-4.81749113516689,
126.888119675218));
#228072=CARTESIAN_POINT('Ctrl Pts',(194.2356121649,-5.89881605082435,132.740628459178));
#228073=CARTESIAN_POINT('Ctrl Pts',(193.957164541087,-1.55941718895885,
136.81380168864));
#228074=CARTESIAN_POINT('Ctrl Pts',(193.678716917274,4.21300988779493,135.364592151301));
#228075=CARTESIAN_POINT('Ctrl Pts',(193.400269293461,6.11388669464029,129.724752614155));
#228076=CARTESIAN_POINT('Ctrl Pts',(193.121821669648,2.39640030908087,125.077020090361));
#228077=CARTESIAN_POINT('Ctrl Pts',(192.843374045836,-3.52326088986039,
125.692433714928));
#228078=CARTESIAN_POINT('Ctrl Pts',(192.564926422022,-6.20521745188322,
131.005458431507));
#228079=CARTESIAN_POINT('Ctrl Pts',(192.28647879821,-3.1848823173506,136.133684081248));
#228080=CARTESIAN_POINT('Ctrl Pts',(192.008031174397,2.76220407667619,136.36452181979));
#228081=CARTESIAN_POINT('Ctrl Pts',(191.729583550584,6.17095986540858,131.485843042463));
#228082=CARTESIAN_POINT('Ctrl Pts',(191.451135926771,3.90890500597959,125.980915208923));
#228083=CARTESIAN_POINT('Ctrl Pts',(191.172688302958,-1.94524259331895,
124.908498067517));
#228084=CARTESIAN_POINT('Ctrl Pts',(190.894240679145,-6.01180727974115,
129.254090580708));
#228085=CARTESIAN_POINT('Ctrl Pts',(190.615793055332,-4.5538147691942,135.024305522869));
#228086=CARTESIAN_POINT('Ctrl Pts',(190.337345431519,1.08891104802307,136.916597252826));
#228087=CARTESIAN_POINT('Ctrl Pts',(190.058897807707,5.73098080836918,133.192042114338));
#228088=CARTESIAN_POINT('Ctrl Pts',(189.780450183893,5.10655917980125,127.273324325042));
#228089=CARTESIAN_POINT('Ctrl Pts',(189.502002560081,-0.210540865719208,
124.599456387862));
#228090=CARTESIAN_POINT('Ctrl Pts',(189.223554936268,-5.33416414113684,
127.627592311355));
#228091=CARTESIAN_POINT('Ctrl Pts',(188.945107312455,-5.55595115925501,
133.575023114497));
#228092=CARTESIAN_POINT('Ctrl Pts',(188.666659688642,-0.672090485321342,
136.976350437346));
#228093=CARTESIAN_POINT('Ctrl Pts',(188.388212064829,4.82938851117716,134.705920634282));
#228094=CARTESIAN_POINT('Ctrl Pts',(188.109764441016,5.89289539464864,128.850147777659));
#228095=CARTESIAN_POINT('Ctrl Pts',(187.831316817203,1.54111929438253,124.790201052305));
#228096=CARTESIAN_POINT('Ctrl Pts',(187.552869193391,-4.22687014955807,
126.256973159398));
#228097=CARTESIAN_POINT('Ctrl Pts',(187.274421569578,-6.11057242014135,
131.902572188318));
#228098=CARTESIAN_POINT('Ctrl Pts',(186.995973945765,-2.37895715467313,
136.538968434335));
#228099=CARTESIAN_POINT('Ctrl Pts',(186.717526321952,3.53880351742172,135.905540247907));
#228100=CARTESIAN_POINT('Ctrl Pts',(186.439078698139,6.20457663716883,130.584377187674));
#228101=CARTESIAN_POINT('Ctrl Pts',(186.160631074326,3.16864693777749,125.465368152723));
#228102=CARTESIAN_POINT('Ctrl Pts',(185.882183450513,-2.77911450042273,
125.25263236868));
#228103=CARTESIAN_POINT('Ctrl Pts',(185.6037358267,-6.17300548002561,130.14166362836));
#228104=CARTESIAN_POINT('Ctrl Pts',(185.325288202887,-3.89420599156785,
135.639681046572));
#228105=CARTESIAN_POINT('Ctrl Pts',(185.046840579075,1.96317856060187,136.694275209062));
#228106=CARTESIAN_POINT('Ctrl Pts',(184.768392955261,6.0164979221829,132.336325600291));
#228107=CARTESIAN_POINT('Ctrl Pts',(184.489945331449,4.54094961554151,126.570575013045));
#228108=CARTESIAN_POINT('Ctrl Pts',(184.211497707636,-1.10750955006109,
124.695466564429));
#228109=CARTESIAN_POINT('Ctrl Pts',(183.933050083823,-5.73822154400692,
128.434133314579));
#228110=CARTESIAN_POINT('Ctrl Pts',(183.65460246001,-5.09578826671723,134.350923164133));
#228111=CARTESIAN_POINT('Ctrl Pts',(183.376154836197,0.229425484589131,
137.008595292604));
#228112=CARTESIAN_POINT('Ctrl Pts',(183.097707212384,5.34380842361613,133.964878848429));
#228113=CARTESIAN_POINT('Ctrl Pts',(182.819259588571,5.54749248089459,128.016800549989));
#228114=CARTESIAN_POINT('Ctrl Pts',(182.540811964758,0.653301958305029,
124.630353773773));
#228115=CARTESIAN_POINT('Ctrl Pts',(182.262364340946,-4.84124114839195,
126.917517669999));
#228116=CARTESIAN_POINT('Ctrl Pts',(181.983916717133,-5.88692014749505,
132.776500352206));
#228117=CARTESIAN_POINT('Ctrl Pts',(181.70546909332,-1.52280712308763,136.82318296266));
#228118=CARTESIAN_POINT('Ctrl Pts',(181.427021469507,4.24069125417353,135.33886187379));
#228119=CARTESIAN_POINT('Ctrl Pts',(181.148573845694,6.10720153813428,129.687555653153));
#228120=CARTESIAN_POINT('Ctrl Pts',(180.870126221881,2.36149196193127,125.062538635854));
#228121=CARTESIAN_POINT('Ctrl Pts',(180.591678598068,-3.55431336199069,
125.713975516152));
#228122=CARTESIAN_POINT('Ctrl Pts',(180.313230974255,-6.20387834410407,
131.04322762551));
#228123=CARTESIAN_POINT('Ctrl Pts',(180.034783350442,-3.15238220429199,
136.15297262387));
#228124=CARTESIAN_POINT('Ctrl Pts',(179.75633572663,2.79599917883219,136.347604482659));
#228125=CARTESIAN_POINT('Ctrl Pts',(179.477888102817,6.17499390876314,131.448266031944));
#228126=CARTESIAN_POINT('Ctrl Pts',(179.199440479004,3.8794709017638,125.957209961944));
#228127=CARTESIAN_POINT('Ctrl Pts',(178.920992855191,-1.98109634126673,
124.920448547985));
#228128=CARTESIAN_POINT('Ctrl Pts',(178.642545231378,-6.02113282860982,
129.290714880887));
#228129=CARTESIAN_POINT('Ctrl Pts',(178.364097607565,-4.52804239515191,
135.051947700091));
#228130=CARTESIAN_POINT('Ctrl Pts',(178.085649983752,1.12609779228193,136.909855496619));
#228131=CARTESIAN_POINT('Ctrl Pts',(177.807202359939,5.74540912154417,133.157111769304));
#228132=CARTESIAN_POINT('Ctrl Pts',(177.528754736127,5.08497014694685,127.242304671825));
#228133=CARTESIAN_POINT('Ctrl Pts',(177.250307112313,-0.248307978092709,
124.600852972375));
#228134=CARTESIAN_POINT('Ctrl Pts',(176.971859488501,-5.35340320178418,
127.660121740658));
#228135=CARTESIAN_POINT('Ctrl Pts',(176.693411864688,-5.53898241132168,
133.608792432211));
#228136=CARTESIAN_POINT('Ctrl Pts',(176.414964240875,-0.634507379188621,
136.980327290216));
#228137=CARTESIAN_POINT('Ctrl Pts',(176.136516617062,4.85304893701009,134.676450488799));
#228138=CARTESIAN_POINT('Ctrl Pts',(175.858068993249,5.88089036471739,128.814312257825));
#228139=CARTESIAN_POINT('Ctrl Pts',(175.579621369436,1.50448084471559,124.780931250186));
#228140=CARTESIAN_POINT('Ctrl Pts',(175.301173745623,-4.25447307360455,
126.282787570284));
#228141=CARTESIAN_POINT('Ctrl Pts',(175.02272612181,-6.10377407984646,131.939748629711));
#228142=CARTESIAN_POINT('Ctrl Pts',(174.744278497998,-2.34400489265046,
136.553343572764));
#228143=CARTESIAN_POINT('Ctrl Pts',(174.465830874185,3.56979027988629,135.883904033421));
#228144=CARTESIAN_POINT('Ctrl Pts',(174.187383250372,6.20312257915782,130.546612244398));
#228145=CARTESIAN_POINT('Ctrl Pts',(173.908935626559,3.13608826756835,125.446178618609));
#228146=CARTESIAN_POINT('Ctrl Pts',(173.630488002746,-2.81285795548731,
125.269652488117));
#228147=CARTESIAN_POINT('Ctrl Pts',(173.352040378933,-6.17692513320066,
130.179252743065));
#228148=CARTESIAN_POINT('Ctrl Pts',(173.07359275512,-3.86469987307124,135.663296596462));
#228149=CARTESIAN_POINT('Ctrl Pts',(172.795145131307,1.99899576932572,136.682215657471));
#228150=CARTESIAN_POINT('Ctrl Pts',(172.516697507494,6.02571195608475,132.29967308599));
#228151=CARTESIAN_POINT('Ctrl Pts',(172.238249883681,4.51509322759614,126.543011406101));
#228152=CARTESIAN_POINT('Ctrl Pts',(171.959802259869,-1.14467560248665,
124.702321473066));
#228153=CARTESIAN_POINT('Ctrl Pts',(171.681354636056,-5.75254347439624,
128.469107412642));
#228154=CARTESIAN_POINT('Ctrl Pts',(171.402907012243,-5.07410492070761,
134.38187696408));
#228155=CARTESIAN_POINT('Ctrl Pts',(171.12445938843,0.267188171305193,137.007083764462));
#228156=CARTESIAN_POINT('Ctrl Pts',(170.846011764617,5.36294838675633,133.932291012718));
#228157=CARTESIAN_POINT('Ctrl Pts',(170.567564140804,5.53042102937231,127.983083035723));
#228158=CARTESIAN_POINT('Ctrl Pts',(170.289116516991,0.615706922082464,
124.62649132937));
#228159=CARTESIAN_POINT('Ctrl Pts',(170.010668893178,-4.86481176764585,
126.947059693175));
#228160=CARTESIAN_POINT('Ctrl Pts',(169.732221269365,-5.87480610217478,
132.812299166869));
#228161=CARTESIAN_POINT('Ctrl Pts',(169.453773645553,-1.48614062903852,
136.832341207004));
#228162=CARTESIAN_POINT('Ctrl Pts',(169.17532602174,4.26821548017818,135.312963568669));
#228163=CARTESIAN_POINT('Ctrl Pts',(168.896878397927,6.10029007702938,129.650400075769));
#228164=CARTESIAN_POINT('Ctrl Pts',(168.618430774114,2.32649610882855,125.048269946673));
#228165=CARTESIAN_POINT('Ctrl Pts',(168.339983150301,-3.58523412773234,
125.735705943466));
#228166=CARTESIAN_POINT('Ctrl Pts',(168.061535526488,-6.2023093493314,131.08098796821));
#228167=CARTESIAN_POINT('Ctrl Pts',(167.783087902675,-3.11976527855146,
136.172062971709));
#228168=CARTESIAN_POINT('Ctrl Pts',(167.504640278862,2.82969067421049,136.330481738588));
#228169=CARTESIAN_POINT('Ctrl Pts',(167.22619265505,6.17879913544756,131.410665161273));
#228170=CARTESIAN_POINT('Ctrl Pts',(166.947745031236,3.84989304232704,125.933684327914));
#228171=CARTESIAN_POINT('Ctrl Pts',(166.669297407424,-2.01687667896098,
124.93261705898));
#228172=CARTESIAN_POINT('Ctrl Pts',(166.39084978361,-6.03023526218728,129.327395269766));
#228173=CARTESIAN_POINT('Ctrl Pts',(166.112402159798,-4.50210223283349,
135.079432481411));
#228174=CARTESIAN_POINT('Ctrl Pts',(165.833954535985,1.16324280857304,136.902887499053));
#228175=CARTESIAN_POINT('Ctrl Pts',(165.555506912173,5.75962453647134,133.122094242209));
#228176=CARTESIAN_POINT('Ctrl Pts',(165.277059288359,5.06319268865361,127.2114170119));
#228177=CARTESIAN_POINT('Ctrl Pts',(164.998611664547,-0.286065889322858,
124.602479430144));
#228178=CARTESIAN_POINT('Ctrl Pts',(164.720164040733,-5.37244389010723,
127.692767680889));
#228179=CARTESIAN_POINT('Ctrl Pts',(164.441716416921,-5.52180841435808,
133.642457830674));
#228180=CARTESIAN_POINT('Ctrl Pts',(164.163268793108,-0.596900761151562,
136.984075290369));
#228181=CARTESIAN_POINT('Ctrl Pts',(163.884821169295,4.87652953132996,134.646836861603));
#228182=CARTESIAN_POINT('Ctrl Pts',(163.606373545482,5.86866741623098,128.778550479967));
#228183=CARTESIAN_POINT('Ctrl Pts',(163.327925921669,1.46778664595768,124.771884648456));
#228184=CARTESIAN_POINT('Ctrl Pts',(163.049478297856,-4.28191834658676,
126.308769529723));
#228185=CARTESIAN_POINT('Ctrl Pts',(162.771030674043,-6.09674956195837,
131.976882998882));
#228186=CARTESIAN_POINT('Ctrl Pts',(162.49258305023,-2.30896577266445,136.567505680515));
#228187=CARTESIAN_POINT('Ctrl Pts',(162.214135426418,3.60064476245918,135.862079594585));
#228188=CARTESIAN_POINT('Ctrl Pts',(161.935687802605,6.20143866215845,130.508856852083));
#228189=CARTESIAN_POINT('Ctrl Pts',(161.657240178792,3.10341338845521,125.427187633898));
#228190=CARTESIAN_POINT('Ctrl Pts',(161.378792554979,-2.84649717906582,
125.2868776982));
#228191=CARTESIAN_POINT('Ctrl Pts',(161.100344931166,-6.18061589814333,
130.216865021372));
#228192=CARTESIAN_POINT('Ctrl Pts',(160.821897307353,-3.83505054669964,
135.686732096692));
#228193=CARTESIAN_POINT('Ctrl Pts',(160.54344968354,2.0347389045262,136.6699382998));
#228194=CARTESIAN_POINT('Ctrl Pts',(160.265002059727,6.03470270501411,132.262965162335));
#228195=CARTESIAN_POINT('Ctrl Pts',(159.986554435914,4.48906953121078,126.51560570502));
#228196=CARTESIAN_POINT('Ctrl Pts',(159.708106812101,-1.18179923853688,
124.709402495009));
#228197=CARTESIAN_POINT('Ctrl Pts',(159.429659188289,-5.76665224217155,
128.50416804437));
#228198=CARTESIAN_POINT('Ctrl Pts',(159.151211564475,-5.05223355187421,
134.412698197843));
#228199=CARTESIAN_POINT('Ctrl Pts',(158.872763940663,0.304940957265202,
137.005342392132));
#228200=CARTESIAN_POINT('Ctrl Pts',(158.59431631685,5.38188962387183,133.899587270395));
#228201=CARTESIAN_POINT('Ctrl Pts',(158.315868693037,5.51314464606502,127.949470064936));
#228202=CARTESIAN_POINT('Ctrl Pts',(158.037421069224,0.57808907061355,124.622857808186));
#228203=CARTESIAN_POINT('Ctrl Pts',(157.758973445411,-4.88820211951067,
126.976744650055));
#228204=CARTESIAN_POINT('Ctrl Pts',(157.480525821598,-5.86247436375394,
132.848023576631));
#228205=CARTESIAN_POINT('Ctrl Pts',(157.202078197785,-1.44941906550188,
136.841276082311));
#228206=CARTESIAN_POINT('Ctrl Pts',(156.923630573973,4.29558154588865,135.286898195607));
#228207=CARTESIAN_POINT('Ctrl Pts',(156.645182950159,6.09315256743229,129.613287258817));
#228208=CARTESIAN_POINT('Ctrl Pts',(156.366735326347,2.29141404655692,125.034214551549));
#228209=CARTESIAN_POINT('Ctrl Pts',(156.088287702534,-3.61602204130483,
125.757624191644));
#228210=CARTESIAN_POINT('Ctrl Pts',(155.809840078721,-6.2005105257049,131.11873806038));
#228211=CARTESIAN_POINT('Ctrl Pts',(155.531392454908,-3.08703274876129,
136.190954417361));
#228212=CARTESIAN_POINT('Ctrl Pts',(155.252944831095,2.86327731436015,136.313154222067));
#228213=CARTESIAN_POINT('Ctrl Pts',(154.974497207282,6.18237540445775,131.373041823765));
#228214=CARTESIAN_POINT('Ctrl Pts',(154.696049583469,3.82017252368788,125.910339178587));
#228215=CARTESIAN_POINT('Ctrl Pts',(154.417601959656,-2.05258228054818,
124.945003149591));
#228216=CARTESIAN_POINT('Ctrl Pts',(154.139154335844,-6.03911424317947,
129.364130388138));
#228217=CARTESIAN_POINT('Ctrl Pts',(153.860706712031,-4.47599524346119,
135.106758848372));
#228218=CARTESIAN_POINT('Ctrl Pts',(153.582259088218,1.20034472047403,136.895693518332));
#228219=CARTESIAN_POINT('Ctrl Pts',(153.303811464405,5.77362652639317,133.086990830643));
#228220=CARTESIAN_POINT('Ctrl Pts',(153.025363840592,5.04122761189337,127.180662489822));
#228221=CARTESIAN_POINT('Ctrl Pts',(152.746916216779,-0.323813200276178,
124.604335700902));
#228222=CARTESIAN_POINT('Ctrl Pts',(152.468468592966,-5.39128550054617,
127.725528922339));
#228223=CARTESIAN_POINT('Ctrl Pts',(152.190020969154,-5.5044298047531,133.6760180624));
#228224=CARTESIAN_POINT('Ctrl Pts',(151.91157334534,-0.55927202473736,136.987594298923));
#228225=CARTESIAN_POINT('Ctrl Pts',(151.633125721528,4.89982942405471,134.617080850036));
#228226=CARTESIAN_POINT('Ctrl Pts',(151.354678097715,5.85622700211526,128.742863769248));
#228227=CARTESIAN_POINT('Ctrl Pts',(151.076230473902,1.43103805782584,124.763061582343));
#228228=CARTESIAN_POINT('Ctrl Pts',(150.797782850089,-4.3092049515099,126.334918074943));
#228229=CARTESIAN_POINT('Ctrl Pts',(150.519335226276,-6.0894991267732,132.013973919806));
#228230=CARTESIAN_POINT('Ctrl Pts',(150.240887602463,-2.27384109310269,
136.581454232806));
#228231=CARTESIAN_POINT('Ctrl Pts',(149.96243997865,3.63136582181627,135.840067740113));
#228232=CARTESIAN_POINT('Ctrl Pts',(149.683992354837,6.19952494856889,130.471112409769));
#228233=CARTESIAN_POINT('Ctrl Pts',(149.405544731024,3.0706235112177,125.40839590231));
#228234=CARTESIAN_POINT('Ctrl Pts',(149.127097107212,-2.88003092464457,
125.30430736064));
#228235=CARTESIAN_POINT('Ctrl Pts',(148.848649483398,-6.18407763809098,
130.254499069545));
#228236=CARTESIAN_POINT('Ctrl Pts',(148.570201859586,-3.80525911111971,
135.709986678852));
#228237=CARTESIAN_POINT('Ctrl Pts',(148.291754235773,2.07040664172831,136.657443590992));
#228238=CARTESIAN_POINT('Ctrl Pts',(148.01330661196,6.04346983581547,132.226203189553));
#228239=CARTESIAN_POINT('Ctrl Pts',(147.734858988147,4.46287949070312,126.488358925329));
#228240=CARTESIAN_POINT('Ctrl Pts',(147.456411364334,-1.21887908258166,
124.716709367866));
#228241=CARTESIAN_POINT('Ctrl Pts',(147.177963740522,-5.78054732452736,
128.53931391058));
#228242=CARTESIAN_POINT('Ctrl Pts',(146.899516116708,-5.03017497066859,
134.44338572333));
#228243=CARTESIAN_POINT('Ctrl Pts',(146.621068492896,0.342682443525903,
137.003371240143));
#228244=CARTESIAN_POINT('Ctrl Pts',(146.342620869082,5.40063143308812,133.866768833311));
#228245=CARTESIAN_POINT('Ctrl Pts',(146.06417324527,5.49566397115542,127.915962883168));
#228246=CARTESIAN_POINT('Ctrl Pts',(145.785725621457,0.540449797841529,
124.619453344862));
#228247=CARTESIAN_POINT('Ctrl Pts',(145.507277997644,-4.91141133724831,
127.006571440652));
#228248=CARTESIAN_POINT('Ctrl Pts',(145.228830373831,-5.84992538918966,
132.883672257711));
#228249=CARTESIAN_POINT('Ctrl Pts',(144.950382750018,-1.41264379320865,
136.849987257496));
#228250=CARTESIAN_POINT('Ctrl Pts',(144.671935126205,4.32278843724517,135.260666720466));
#228251=CARTESIAN_POINT('Ctrl Pts',(144.393487502392,6.08578927382608,129.576218577526));
#228252=CARTESIAN_POINT('Ctrl Pts',(144.11503987858,2.25624707509518,125.020372971309));
#228253=CARTESIAN_POINT('Ctrl Pts',(143.836592254767,-3.64667596185081,
125.779729448496));
#228254=CARTESIAN_POINT('Ctrl Pts',(143.558144630954,-6.19848193988065,
131.156476503179));
#228255=CARTESIAN_POINT('Ctrl Pts',(143.279697007141,-3.05418582783736,
136.209646260801));
#228256=CARTESIAN_POINT('Ctrl Pts',(143.001249383328,2.89675785471595,136.295622575173));
#228257=CARTESIAN_POINT('Ctrl Pts',(142.722801759515,6.18572258327378,131.335397413564));
#228258=CARTESIAN_POINT('Ctrl Pts',(142.444354135702,3.79031044715096,125.887175379022));
#228259=CARTESIAN_POINT('Ctrl Pts',(142.165906511889,-2.0882118229442,124.957606360848));
#228260=CARTESIAN_POINT('Ctrl Pts',(141.887458888076,-6.04776944257254,
129.400918874772));
#228261=CARTESIAN_POINT('Ctrl Pts',(141.609011264264,-4.44972239443904,
135.133925788383));
#228262=CARTESIAN_POINT('Ctrl Pts',(141.33056364045,1.2374021531599,136.888273821029));
#228263=CARTESIAN_POINT('Ctrl Pts',(141.052116016638,5.78741457246075,133.051802835376));
#228264=CARTESIAN_POINT('Ctrl Pts',(140.773668392825,5.01907573059014,127.15004224521));
#228265=CARTESIAN_POINT('Ctrl Pts',(140.495220769012,-0.361548512212229,
124.606421715863));
#228266=CARTESIAN_POINT('Ctrl Pts',(140.216773145199,-5.4099273349182,127.758404251031));
#228267=CARTESIAN_POINT('Ctrl Pts',(139.938325521386,-5.48684722647749,
133.709471883804));
#228268=CARTESIAN_POINT('Ctrl Pts',(139.659877897573,-0.521622564292735,
136.990884185479));
#228269=CARTESIAN_POINT('Ctrl Pts',(139.38143027376,4.92294775179823,134.58718355672));
#228270=CARTESIAN_POINT('Ctrl Pts',(139.102982649947,5.84356958335437,128.707253448052));
#228271=CARTESIAN_POINT('Ctrl Pts',(138.824535026135,1.39423644205237,124.754462378786));
#228272=CARTESIAN_POINT('Ctrl Pts',(138.546087402322,-4.33633187725888,
126.361232236999));
#228273=CARTESIAN_POINT('Ctrl Pts',(138.267639778509,-6.08202304295846,
132.051020018064));
#228274=CARTESIAN_POINT('Ctrl Pts',(137.989192154696,-2.23863215552307,
136.595188712768));
#228275=CARTESIAN_POINT('Ctrl Pts',(137.710744530883,3.66195231957746,135.817869285661));
#228276=CARTESIAN_POINT('Ctrl Pts',(137.43229690707,6.19738150930245,130.433380316089));
#228277=CARTESIAN_POINT('Ctrl Pts',(137.153849283257,3.03771985089675,125.389804120178));
#228278=CARTESIAN_POINT('Ctrl Pts',(136.875401659444,-2.91345794961824,
125.321940829576));
#228279=CARTESIAN_POINT('Ctrl Pts',(136.596954035631,-6.1873102247676,130.29215349304));
#228280=CARTESIAN_POINT('Ctrl Pts',(136.318506411819,-3.77532667026395,
135.733059481234));
#228281=CARTESIAN_POINT('Ctrl Pts',(136.040058788006,2.10599765925102,136.644731994041));
#228282=CARTESIAN_POINT('Ctrl Pts',(135.761611164193,6.05201302361958,132.189388529871));
#228283=CARTESIAN_POINT('Ctrl Pts',(135.48316354038,4.4365240765547,126.461272076668));
#228284=CARTESIAN_POINT('Ctrl Pts',(135.204715916567,-1.25591376061384,
124.724241820878));
#228285=CARTESIAN_POINT('Ctrl Pts',(134.926268292754,-5.79422820657625,
128.574543708929));
#228286=CARTESIAN_POINT('Ctrl Pts',(134.647820668941,-5.00792999447956,
134.473938403405));
#228287=CARTESIAN_POINT('Ctrl Pts',(134.369373045128,0.380411231562576,
137.001170381535));
#228288=CARTESIAN_POINT('Ctrl Pts',(134.090925421316,5.41917311992063,133.833836917565));
#228289=CARTESIAN_POINT('Ctrl Pts',(133.812477797503,5.4779796523963,127.88256273204));
#228290=CARTESIAN_POINT('Ctrl Pts',(133.53403017369,0.502790498503515,124.616278065551));
#228291=CARTESIAN_POINT('Ctrl Pts',(133.255582549877,-4.93443856083268,
127.036538959725));
#228292=CARTESIAN_POINT('Ctrl Pts',(132.977134926064,-5.83715964348875,
132.919243889133));
#228293=CARTESIAN_POINT('Ctrl Pts',(132.698687302251,-1.37581617488021,
136.858474409763));
#228294=CARTESIAN_POINT('Ctrl Pts',(132.420239678438,4.34983514608645,135.234270115264));
#228295=CARTESIAN_POINT('Ctrl Pts',(132.141792054625,6.07820046906025,129.539195405491));
#228296=CARTESIAN_POINT('Ctrl Pts',(131.863344430812,2.22099649756843,125.006745718858));
#228297=CARTESIAN_POINT('Ctrl Pts',(131.584896806999,-3.67719475347803,
125.802020894903));
#228298=CARTESIAN_POINT('Ctrl Pts',(131.306449183186,-6.1962236670286,131.194201898194));
#228299=CARTESIAN_POINT('Ctrl Pts',(131.028001559374,-3.02122573293442,
136.228137809392));
#228300=CARTESIAN_POINT('Ctrl Pts',(130.749553935561,2.93013105464412,136.277887447547));
#228301=CARTESIAN_POINT('Ctrl Pts',(130.471106311748,6.18884054786473,131.2977333256));
#228302=CARTESIAN_POINT('Ctrl Pts',(130.192658687935,3.76030791926647,125.864193787566));
#228303=CARTESIAN_POINT('Ctrl Pts',(129.914211064122,-2.12376398588317,
124.970426225734));
#228304=CARTESIAN_POINT('Ctrl Pts',(129.635763440309,-6.05620053964477,
129.437759366456));
#228305=CARTESIAN_POINT('Ctrl Pts',(129.357315816496,-4.42328465931731,
135.160932294765));
#228306=CARTESIAN_POINT('Ctrl Pts',(129.078868192683,1.27441373345414,136.880628682086));
#228307=CARTESIAN_POINT('Ctrl Pts',(128.800420568871,5.80098816375315,133.01653156031));
#228308=CARTESIAN_POINT('Ctrl Pts',(128.521972945058,4.99673786558976,127.11955741271));
#228309=CARTESIAN_POINT('Ctrl Pts',(128.243525321245,-0.399270426835251,
124.608737397728));
#228310=CARTESIAN_POINT('Ctrl Pts',(127.965077697432,-5.42836870244348,
127.791392448756));
#228311=CARTESIAN_POINT('Ctrl Pts',(127.686630073619,-5.46906133106002,
133.742818055242));
#228312=CARTESIAN_POINT('Ctrl Pts',(127.408182449806,-0.483953774931917,
136.993944828129));
#228313=CARTESIAN_POINT('Ctrl Pts',(127.129734825993,4.9458836579024,134.557146089508));
#228314=CARTESIAN_POINT('Ctrl Pts',(126.85128720218,5.8306956289736,128.671720835934));
#228315=CARTESIAN_POINT('Ctrl Pts',(126.572839578367,1.35738316233494,124.746087356435));
#228316=CARTESIAN_POINT('Ctrl Pts',(126.294391954555,-4.36329811863544,
126.387711040812));
#228317=CARTESIAN_POINT('Ctrl Pts',(126.015944330741,-6.07432158754323,
132.088019920899));
#228318=CARTESIAN_POINT('Ctrl Pts',(125.737496706929,-2.20334026460562,
136.608708611466));
#228319=CARTESIAN_POINT('Ctrl Pts',(125.459049083116,3.69240312234872,135.795485053802));
#228320=CARTESIAN_POINT('Ctrl Pts',(125.180601459303,6.19500842378515,130.39566196922));
#228321=CARTESIAN_POINT('Ctrl Pts',(124.90215383549,3.00470362674961,125.371412976429));
#228322=CARTESIAN_POINT('Ctrl Pts',(124.623706211677,-2.9467770153362,125.339777451594));
#228323=CARTESIAN_POINT('Ctrl Pts',(124.345258587864,-6.19031353838844,
130.329826896558));
#228324=CARTESIAN_POINT('Ctrl Pts',(124.066810964051,-3.74525433329013,
135.755949648866));
#228325=CARTESIAN_POINT('Ctrl Pts',(123.788363340238,2.14151063825588,136.631803979981));
#228326=CARTESIAN_POINT('Ctrl Pts',(123.509915716426,6.0603319518555,132.152522547471));
#228327=CARTESIAN_POINT('Ctrl Pts',(123.231468092613,4.4100042653751,126.43434616275));
#228328=CARTESIAN_POINT('Ctrl Pts',(122.9530204688,-1.29290190029971,124.731999574929));
#228329=CARTESIAN_POINT('Ctrl Pts',(122.674572844987,-5.80769438136815,
128.609856133963));
#228330=CARTESIAN_POINT('Ctrl Pts',(122.396125221174,-4.98549944760296,
134.504355105923));
#228331=CARTESIAN_POINT('Ctrl Pts',(122.117677597361,0.418125923321227,
136.998739897863));
#228332=CARTESIAN_POINT('Ctrl Pts',(121.839229973548,5.43751399730024,133.80079274346));
#228333=CARTESIAN_POINT('Ctrl Pts',(121.560782349735,5.46009234508668,127.849270849208));
#228334=CARTESIAN_POINT('Ctrl Pts',(121.282334725922,0.465112568078527,
124.613332087916));
#228335=CARTESIAN_POINT('Ctrl Pts',(121.00388710211,-4.95728293698158,127.066646096814));
#228336=CARTESIAN_POINT('Ctrl Pts',(120.725439478297,-5.82417759969065,
132.954737152777));
#228337=CARTESIAN_POINT('Ctrl Pts',(120.446991854484,-1.33893757517749,
136.866737224615));
#228338=CARTESIAN_POINT('Ctrl Pts',(120.168544230671,4.37672067018674,135.207709358136));
#228339=CARTESIAN_POINT('Ctrl Pts',(119.890096606858,6.07038643434081,129.502219114618));
#228340=CARTESIAN_POINT('Ctrl Pts',(119.611648983045,2.18566362019961,124.993333299159));
#228341=CARTESIAN_POINT('Ctrl Pts',(119.333201359232,-3.7075772853013,125.82449770485));
#228342=CARTESIAN_POINT('Ctrl Pts',(119.054753735419,-6.19373579082994,
131.231912847497));
#228343=CARTESIAN_POINT('Ctrl Pts',(118.776306111606,-2.98815368540088,
136.246428377926));
#228344=CARTESIAN_POINT('Ctrl Pts',(118.497858487794,2.96339567748857,136.259949496373));
#228345=CARTESIAN_POINT('Ctrl Pts',(118.219410863981,6.1917291826932,131.26005095553));
#228346=CARTESIAN_POINT('Ctrl Pts',(117.940963240168,3.73016605178927,125.841395255808));
#228347=CARTESIAN_POINT('Ctrl Pts',(117.662515616355,-2.15923745196658,
124.983462269205));
#228348=CARTESIAN_POINT('Ctrl Pts',(117.384067992542,-6.06440722197891,
129.474650498052));
#228349=CARTESIAN_POINT('Ctrl Pts',(117.105620368729,-4.39668301775581,
135.187777366781));
#228350=CARTESIAN_POINT('Ctrl Pts',(116.827172744916,1.31137808987868,136.872758384795));
#228351=CARTESIAN_POINT('Ctrl Pts',(116.548725121103,5.81434679729579,132.981178312436));
#228352=CARTESIAN_POINT('Ctrl Pts',(116.27027749729,4.97421484463032,127.089209121948));
#228353=CARTESIAN_POINT('Ctrl Pts',(115.991829873478,-0.436977546345769,
124.611282660692));
#228354=CARTESIAN_POINT('Ctrl Pts',(115.713382249665,-5.44660891977013,
127.824492293124));
#228355=CARTESIAN_POINT('Ctrl Pts',(115.434934625852,-5.45107277756375,
133.776055341058));
#228356=CARTESIAN_POINT('Ctrl Pts',(115.156487002039,-0.446267052485976,
136.99677611346));
#228357=CARTESIAN_POINT('Ctrl Pts',(114.878039378226,4.9686362924688,134.526969561451));
#228358=CARTESIAN_POINT('Ctrl Pts',(114.599591754413,5.81760561602206,128.636267249567));
#228359=CARTESIAN_POINT('Ctrl Pts',(114.3211441306,1.32047958428524,124.737936825626));
#228360=CARTESIAN_POINT('Ctrl Pts',(114.042696506787,-4.39010267639563,
126.414353505198));
#228361=CARTESIAN_POINT('Ctrl Pts',(113.764248882975,-6.06639504590774,
132.124972257267));
#228362=CARTESIAN_POINT('Ctrl Pts',(113.485801259161,-2.16796672810439,
136.622013427915));
#228363=CARTESIAN_POINT('Ctrl Pts',(113.207353635349,3.72271710176439,135.772915873991));
#228364=CARTESIAN_POINT('Ctrl Pts',(112.928906011536,6.19240577995249,130.357958766832));
#228365=CARTESIAN_POINT('Ctrl Pts',(112.650458387723,2.97157606220462,125.353223152553));
#228366=CARTESIAN_POINT('Ctrl Pts',(112.37201076391,-2.9799868871482,125.357816565752));
#228367=CARTESIAN_POINT('Ctrl Pts',(112.093563140097,-6.19308746766462,
130.367517884098));
#228368=CARTESIAN_POINT('Ctrl Pts',(111.815115516284,-3.71504321453968,
135.778656333547));
#228369=CARTESIAN_POINT('Ctrl Pts',(111.536667892471,2.1769442627965,136.618660027865));
#228370=CARTESIAN_POINT('Ctrl Pts',(111.258220268658,6.06842631226225,132.115606608435));
#228371=CARTESIAN_POINT('Ctrl Pts',(110.979772644846,4.38332103986566,126.407582181323));
#228372=CARTESIAN_POINT('Ctrl Pts',(110.701325021032,-1.32984213103019,
124.739982342551));
#228373=CARTESIAN_POINT('Ctrl Pts',(110.42287739722,-5.82094534990898,128.645249877167));
#228374=CARTESIAN_POINT('Ctrl Pts',(110.144429773407,-4.96288416121089,
134.534634703787));
#228375=CARTESIAN_POINT('Ctrl Pts',(109.865982149594,0.455825121270016,
136.996079879188));
#228376=CARTESIAN_POINT('Ctrl Pts',(109.587534525781,5.45565338559904,133.767637535461));
#228377=CARTESIAN_POINT('Ctrl Pts',(109.309086901968,5.44200271204727,127.816088468313));
#228378=CARTESIAN_POINT('Ctrl Pts',(109.030639278155,0.427417402736423,
124.610615521118));
#228379=CARTESIAN_POINT('Ctrl Pts',(108.752191654342,-4.97994361918818,
127.096891736289));
#228380=CARTESIAN_POINT('Ctrl Pts',(108.473744030529,-5.81097973884976,
132.990150733429));
#228381=CARTESIAN_POINT('Ctrl Pts',(108.195296406717,-1.30200936065053,
136.874775395874));
#228382=CARTESIAN_POINT('Ctrl Pts',(107.916848782904,4.40344401329306,135.180985433302));
#228383=CARTESIAN_POINT('Ctrl Pts',(107.638401159091,6.06234745921968,129.465291075077));
#228384=CARTESIAN_POINT('Ctrl Pts',(107.359953535278,2.15024975226158,124.980136209215));
#228385=CARTESIAN_POINT('Ctrl Pts',(107.081505911465,-3.73782243148481,
125.847159045447));
#228386=CARTESIAN_POINT('Ctrl Pts',(106.803058287652,-6.19101840347381,
131.269607953695));
#228387=CARTESIAN_POINT('Ctrl Pts',(106.524610663839,-2.95497091073364,
136.264517288637));
#228388=CARTESIAN_POINT('Ctrl Pts',(106.246163040026,2.99655049061638,136.241809386346));
#228389=CARTESIAN_POINT('Ctrl Pts',(105.967715416213,6.1943883807198,131.222351699685));
#228390=CARTESIAN_POINT('Ctrl Pts',(105.689267792401,3.69988596163724,125.818780628557));
#228391=CARTESIAN_POINT('Ctrl Pts',(105.410820168588,-2.19463090671215,
124.996714008204));
#228392=CARTESIAN_POINT('Ctrl Pts',(105.132372544775,-6.07238918547325,
129.511590902545));
#228393=CARTESIAN_POINT('Ctrl Pts',(104.853924920962,-4.36991845548819,
135.214460009678));
#228394=CARTESIAN_POINT('Ctrl Pts',(104.575477297149,1.34829385270585,136.864663220793));
#228395=CARTESIAN_POINT('Ctrl Pts',(104.297029673336,5.82748997807964,132.945744401783));
#228396=CARTESIAN_POINT('Ctrl Pts',(104.018582049523,4.95150750231056,127.058998497491));
#228397=CARTESIAN_POINT('Ctrl Pts',(103.74013442571,-0.474668473492613,
124.614057410436));
#228398=CARTESIAN_POINT('Ctrl Pts',(103.461686801897,-5.46464731100027,
127.857702557609));
#228399=CARTESIAN_POINT('Ctrl Pts',(103.183239178085,-5.43288223256107,
133.809182509633));
#228400=CARTESIAN_POINT('Ctrl Pts',(102.904791554272,-0.408563793450433,
136.999377936557));
#228401=CARTESIAN_POINT('Ctrl Pts',(102.626343930459,4.99120481239017,134.496655090749));
#228402=CARTESIAN_POINT('Ctrl Pts',(102.347896306646,5.80430002955499,128.600894002697));
#228403=CARTESIAN_POINT('Ctrl Pts',(102.069448682833,1.28352707537895,124.730011088381));
#228404=CARTESIAN_POINT('Ctrl Pts',(101.79100105902,-4.41674455728669,126.441158642913));
#228405=CARTESIAN_POINT('Ctrl Pts',(101.512553435207,-6.05824371177293,
132.161875657885));
#228406=CARTESIAN_POINT('Ctrl Pts',(101.234105811394,-2.13251285679878,
136.635102669099));
#228407=CARTESIAN_POINT('Ctrl Pts',(100.955658187581,3.75289313452884,135.750162582539));
#228408=CARTESIAN_POINT('Ctrl Pts',(100.677210563769,6.18957367424645,130.320272106026));
#228409=CARTESIAN_POINT('Ctrl Pts',(100.398762939956,2.93833838481571,125.33523532258));
#228410=CARTESIAN_POINT('Ctrl Pts',(100.120315316143,-3.01308633445025,
125.376057503601));
#228411=CARTESIAN_POINT('Ctrl Pts',(99.8418676923298,-6.19563190980719,
130.405225059005));
#228412=CARTESIAN_POINT('Ctrl Pts',(99.5634200685172,-3.68469443349671,
135.801178693871));
#228413=CARTESIAN_POINT('Ctrl Pts',(99.2849724447041,2.2122972198669,136.605300624745));
#228414=CARTESIAN_POINT('Ctrl Pts',(99.0065248208913,6.07629580490035,132.078642080696));
#228415=CARTESIAN_POINT('Ctrl Pts',(98.7280771970783,4.35647538878314,126.380981124141));
#228416=CARTESIAN_POINT('Ctrl Pts',(98.4496295732656,-1.36673308397146,
124.748189827941));
#228417=CARTESIAN_POINT('Ctrl Pts',(98.1711819494526,-5.8339806211792,128.680723627015));
#228418=CARTESIAN_POINT('Ctrl Pts',(97.8927343256397,-4.94008497332115,
134.564776074971));
#228419=CARTESIAN_POINT('Ctrl Pts',(97.6142867018267,0.493507428451318,
136.993190424079));
#228420=CARTESIAN_POINT('Ctrl Pts',(97.3358390780141,5.47359061265531,133.734372522146));
#228421=CARTESIAN_POINT('Ctrl Pts',(97.0573914542009,5.42371142359607,127.783016818942));
#228422=CARTESIAN_POINT('Ctrl Pts',(96.7789438303882,0.389706399285272,
124.608128465823));
#228423=CARTESIAN_POINT('Ctrl Pts',(96.5004962065753,-5.0024197677526,127.127274757387));
#228424=CARTESIAN_POINT('Ctrl Pts',(96.2220485827623,-5.79756655001767,
133.025483318824));
#228425=CARTESIAN_POINT('Ctrl Pts',(95.9436009589496,-1.26503289968789,
136.882588625681));
#228426=CARTESIAN_POINT('Ctrl Pts',(95.6651533351365,4.4300041851621,135.154099331026));
#228427=CARTESIAN_POINT('Ctrl Pts',(95.3867057113237,6.05408384158403,129.428412655251));
#228428=CARTESIAN_POINT('Ctrl Pts',(95.1082580875108,2.11475620602821,124.967154938047));
#228429=CARTESIAN_POINT('Ctrl Pts',(94.8298104636979,-3.76792907128354,
125.870004076972));
#228430=CARTESIAN_POINT('Ctrl Pts',(94.5513628398851,-6.18807160565406,
131.307285819983));
#228431=CARTESIAN_POINT('Ctrl Pts',(94.2729152160721,-2.92167863853249,
136.282403871234));
#228432=CARTESIAN_POINT('Ctrl Pts',(93.9944675922592,3.02959426546386,136.223467789656));
#228433=CARTESIAN_POINT('Ctrl Pts',(93.7160199684464,6.19681804340696,131.184636955029));
#228434=CARTESIAN_POINT('Ctrl Pts',(93.4375723446334,3.66946877085029,125.796350743805));
#228435=CARTESIAN_POINT('Ctrl Pts',(93.1591247208205,-2.22994303860241,
125.010180951684));
#228436=CARTESIAN_POINT('Ctrl Pts',(92.8806770970077,-6.08014613435319,
129.548579211095));
#228437=CARTESIAN_POINT('Ctrl Pts',(92.6022294731947,-4.3429919642852,135.24097923472));
#228438=CARTESIAN_POINT('Ctrl Pts',(92.323781849382,1.38515965400848,136.856343490049));
#228439=CARTESIAN_POINT('Ctrl Pts',(92.045334225569,5.84041721907928,132.910231141365));
#228440=CARTESIAN_POINT('Ctrl Pts',(91.7668866017561,4.9286166800594,127.028926658805));
#228441=CARTESIAN_POINT('Ctrl Pts',(91.4884389779432,-0.512341811624615,
124.617061544141));
#228442=CARTESIAN_POINT('Ctrl Pts',(91.2099913541303,-5.48248320771468,
127.891022011592));
#228443=CARTESIAN_POINT('Ctrl Pts',(90.9315437303175,-5.41449037010934,
133.842198333429));
#228444=CARTESIAN_POINT('Ctrl Pts',(90.6530961065044,-0.370845394933272,
137.00175020101));
#228445=CARTESIAN_POINT('Ctrl Pts',(90.3746484826917,5.01358838138169,134.466203800718));
#228446=CARTESIAN_POINT('Ctrl Pts',(90.0962008588786,5.79077936261581,128.565602406094));
#228447=CARTESIAN_POINT('Ctrl Pts',(89.817753235066,1.24652700490487,124.722310438393));
#228448=CARTESIAN_POINT('Ctrl Pts',(89.5393056112528,-4.44322277408392,
126.468125460682));
#228449=CARTESIAN_POINT('Ctrl Pts',(89.2608579874402,-6.04986788718945,
132.198728755283));
#228450=CARTESIAN_POINT('Ctrl Pts',(88.9824103636271,-2.09697996444503,
136.647975849991));
#228451=CARTESIAN_POINT('Ctrl Pts',(88.7039627398144,3.78293010245805,135.727226022576));
#228452=CARTESIAN_POINT('Ctrl Pts',(88.4255151160013,6.18651221161165,130.282603383299));
#228453=CARTESIAN_POINT('Ctrl Pts',(88.1470674921886,2.9049918262175,125.317450153056));
#228454=CARTESIAN_POINT('Ctrl Pts',(87.8686198683756,-3.04607413073006,
125.394499589218));
#228455=CARTESIAN_POINT('Ctrl Pts',(87.5901722445627,-6.19794677053091,
130.442947024027));
#228456=CARTESIAN_POINT('Ctrl Pts',(87.3117246207499,-3.65420911474647,
135.823515895262));
#228457=CARTESIAN_POINT('Ctrl Pts',(87.033276996937,2.24756819945024,136.59172626566));
#228458=CARTESIAN_POINT('Ctrl Pts',(86.754829373124,6.08394013816284,132.041630333989));
#228459=CARTESIAN_POINT('Ctrl Pts',(86.4763817493112,4.32946830690299,126.35454397691));
#228460=CARTESIAN_POINT('Ctrl Pts',(86.1979341254982,-1.40357339211569,
124.756621726966));
#228461=CARTESIAN_POINT('Ctrl Pts',(85.9194865016854,-5.84679971215209,
128.716276069012));
#228462=CARTESIAN_POINT('Ctrl Pts',(85.6410388778725,-4.91710272876601,
134.594778102578));
#228463=CARTESIAN_POINT('Ctrl Pts',(85.3625912540596,0.531171448533366,
136.990071639606));
#228464=CARTESIAN_POINT('Ctrl Pts',(85.0841436302467,5.49132501379855,133.700998936161));
#228465=CARTESIAN_POINT('Ctrl Pts',(84.8056960064338,5.4052191575235,127.750057126576));
#228466=CARTESIAN_POINT('Ctrl Pts',(84.527248382621,0.351980955120191,124.60587101419));
#228467=CARTESIAN_POINT('Ctrl Pts',(84.2488007588079,-5.02471054981291,
127.157794034254));
#228468=CARTESIAN_POINT('Ctrl Pts',(83.9703531349953,-5.78393853022499,
133.0607335997));
#228469=CARTESIAN_POINT('Ctrl Pts',(83.6919055111822,-1.22800956246596,
136.890176624513));
#228470=CARTESIAN_POINT('Ctrl Pts',(83.4134578873695,4.45640020159694,135.127052047582));
#228471=CARTESIAN_POINT('Ctrl Pts',(83.1350102635564,6.04559588764522,129.391585221682));
#228472=CARTESIAN_POINT('Ctrl Pts',(82.8565626397436,2.07918429672594,124.954389966684));
#228473=CARTESIAN_POINT('Ctrl Pts',(82.5781150159307,-3.79789608908488,
125.893031952893));
#228474=CARTESIAN_POINT('Ctrl Pts',(82.2996673921181,-6.18489550656524,
131.344945050191));
#228475=CARTESIAN_POINT('Ctrl Pts',(82.0212197683047,-2.88827810245507,
136.300087462925));
#228476=CARTESIAN_POINT('Ctrl Pts',(81.7427721444922,3.06252577758164,136.204925385956));
#228477=CARTESIAN_POINT('Ctrl Pts',(81.464324520679,6.19901808072266,131.146908119091));
#228478=CARTESIAN_POINT('Ctrl Pts',(81.1858768968663,3.6389156065486,125.774106432701));
#228479=CARTESIAN_POINT('Ctrl Pts',(80.9074292730533,-2.26517253913331,
125.023862600622));
#228480=CARTESIAN_POINT('Ctrl Pts',(80.6289816492404,-6.08767778118217,
129.585614053086));
#228481=CARTESIAN_POINT('Ctrl Pts',(80.3505340254275,-4.31590454191782,
135.267334059228));
#228482=CARTESIAN_POINT('Ctrl Pts',(80.0720864016147,1.42197412771073,136.847799500855));
#228483=CARTESIAN_POINT('Ctrl Pts',(79.7936387778018,5.85312804127117,132.874639847142));
#228484=CARTESIAN_POINT('Ctrl Pts',(79.5151911539889,4.90554322610457,126.998994720211));
#228485=CARTESIAN_POINT('Ctrl Pts',(79.236743530176,-0.54999616474248,124.62029495049));
#228486=CARTESIAN_POINT('Ctrl Pts',(78.9582959063631,-5.50011594899764,
127.924449420408));
#228487=CARTESIAN_POINT('Ctrl Pts',(78.6798482825503,-5.39589787172579,
133.87510158903));
#228488=CARTESIAN_POINT('Ctrl Pts',(78.4014006587372,-0.333113254603616,
137.003892818912));
#228489=CARTESIAN_POINT('Ctrl Pts',(78.1229530349246,5.035786170012,134.435616819741));
#228490=CARTESIAN_POINT('Ctrl Pts',(77.8445054111114,5.77704411621779,128.530393767498));
#228491=CARTESIAN_POINT('Ctrl Pts',(77.5660577872988,1.20948074391421,124.71483516101));
#228492=CARTESIAN_POINT('Ctrl Pts',(77.2876101634857,-4.46953634562727,
126.49525295924));
#228493=CARTESIAN_POINT('Ctrl Pts',(77.009162539673,-6.04126788252658,132.235530183857));
#228494=CARTESIAN_POINT('Ctrl Pts',(76.73071491586,-2.06136936772754,136.660632493573));
#228495=CARTESIAN_POINT('Ctrl Pts',(76.4522672920471,3.81282689252116,135.704107044024));
#228496=CARTESIAN_POINT('Ctrl Pts',(76.1738196682342,6.18322150549176,130.244953994479));
#228497=CARTESIAN_POINT('Ctrl Pts',(75.8953720444213,2.87153762207887,125.299868303017));
#228498=CARTESIAN_POINT('Ctrl Pts',(75.6169244206085,-3.07894905361277,
125.413142139227));
#228499=CARTESIAN_POINT('Ctrl Pts',(75.3384767967955,-6.20003196405775,
130.480682381363));
#228500=CARTESIAN_POINT('Ctrl Pts',(75.0600291729826,-3.62358838793365,
135.84566711001));
#228501=CARTESIAN_POINT('Ctrl Pts',(74.7815815491698,2.28275589456742,136.577937453613));
#228502=CARTESIAN_POINT('Ctrl Pts',(74.5031339253568,6.09135902878616,132.004572739798));
#228503=CARTESIAN_POINT('Ctrl Pts',(74.224686301544,4.30230079498258,126.328271719272));
#228504=CARTESIAN_POINT('Ctrl Pts',(73.946238677731,-1.44036169033171,124.76527772718));
#228505=CARTESIAN_POINT('Ctrl Pts',(73.6677910539182,-5.85940214781156,
128.75190588575));
#228506=CARTESIAN_POINT('Ctrl Pts',(73.3893434301052,-4.89393827916089,
134.624639674871));
#228507=CARTESIAN_POINT('Ctrl Pts',(73.1108958062924,0.56881578586215,136.986723641335));
#228508=CARTESIAN_POINT('Ctrl Pts',(72.8324481824796,5.50885593187395,133.66751801418));
#228509=CARTESIAN_POINT('Ctrl Pts',(72.5540005586665,5.38652659906729,127.717210612549));
#228510=CARTESIAN_POINT('Ctrl Pts',(72.2755529348538,0.314242468171368,
124.603843249867));
#228511=CARTESIAN_POINT('Ctrl Pts',(71.9971053110409,-5.04681513937595,
127.188448435987));
#228512=CARTESIAN_POINT('Ctrl Pts',(71.7186576872279,-5.77009618446306,
133.095900269846));
#228513=CARTESIAN_POINT('Ctrl Pts',(71.4402100634152,-1.19094072089807,
136.897539111196));
#228514=CARTESIAN_POINT('Ctrl Pts',(71.1617624396021,4.48263108448347,135.099844585217));
#228515=CARTESIAN_POINT('Ctrl Pts',(70.8833148157894,6.03688391192757,129.354810139024));
#228516=CARTESIAN_POINT('Ctrl Pts',(70.6048671919763,2.04353534248492,124.941841768133));
#228517=CARTESIAN_POINT('Ctrl Pts',(70.3264195681636,-3.82772237444985,
125.916241819903));
#228518=CARTESIAN_POINT('Ctrl Pts',(70.0479719443506,-6.18149022389895,
131.382584248845));
#228519=CARTESIAN_POINT('Ctrl Pts',(69.7695243205378,-2.85477054017052,
136.317567408437));
#228520=CARTESIAN_POINT('Ctrl Pts',(69.4910766967249,3.09534380668036,136.186182862342));
#228521=CARTESIAN_POINT('Ctrl Pts',(69.2126290729119,6.20098841114368,131.109166589932));
#228522=CARTESIAN_POINT('Ctrl Pts',(68.934181449099,3.60822760089105,125.752048519516));
#228523=CARTESIAN_POINT('Ctrl Pts',(68.6557338252862,-2.30031810286251,
125.037758448041));
#228524=CARTESIAN_POINT('Ctrl Pts',(68.3772862014732,-6.09498384687224,
129.622694056181));
#228525=CARTESIAN_POINT('Ctrl Pts',(68.0988385776604,-4.28865719212064,
135.293523506613));
#228526=CARTESIAN_POINT('Ctrl Pts',(67.8203909538475,1.45873590963839,136.83903156981));
#228527=CARTESIAN_POINT('Ctrl Pts',(67.5419433300346,5.86562197365073,132.83897183796));
#228528=CARTESIAN_POINT('Ctrl Pts',(67.2634957062218,4.88228799544191,126.969203790852));
#228529=CARTESIAN_POINT('Ctrl Pts',(66.9850480824087,-0.587630137549865,
124.623757509667));
#228530=CARTESIAN_POINT('Ctrl Pts',(66.706600458596,-5.51754488146136,127.957983545393));
#228531=CARTESIAN_POINT('Ctrl Pts',(66.428152834783,-5.37710542636232,133.907891057196));
#228532=CARTESIAN_POINT('Ctrl Pts',(66.1497052109702,-0.295368770640213,
137.00580571087));
#228533=CARTESIAN_POINT('Ctrl Pts',(65.8712575871573,5.05779735573374,134.404895281231));
#228534=CARTESIAN_POINT('Ctrl Pts',(65.5928099633443,5.76309479932555,128.495269391582));
#228535=CARTESIAN_POINT('Ctrl Pts',(65.3143623395316,1.17238966517029,124.707585533234));
#228536=CARTESIAN_POINT('Ctrl Pts',(65.0359147157185,-4.49568429685739,
126.522540133366));
#228537=CARTESIAN_POINT('Ctrl Pts',(64.7574670919057,-6.03244401646077,
132.272278579917));
#228538=CARTESIAN_POINT('Ctrl Pts',(64.4790194680927,-2.02568238621027,
136.673072130848));
#228539=CARTESIAN_POINT('Ctrl Pts',(64.20057184428,3.84258239688126,135.680806503568));
#228540=CARTESIAN_POINT('Ctrl Pts',(63.922124220467,6.17970167782515,130.207325334677));
#228541=CARTESIAN_POINT('Ctrl Pts',(63.6436765966542,2.8379770120581,125.282490423967));
#228542=CARTESIAN_POINT('Ctrl Pts',(63.3652289728412,-3.11170988490585,
125.431984462817));
#228543=CARTESIAN_POINT('Ctrl Pts',(63.0867813490283,-6.20188741312008,
130.518429732716));
#228544=CARTESIAN_POINT('Ctrl Pts',(62.8083337252156,-3.59283338772076,
135.86763151729));
#228545=CARTESIAN_POINT('Ctrl Pts',(62.5298861014024,2.31785900132509,136.563934699553));
#228546=CARTESIAN_POINT('Ctrl Pts',(62.2514384775899,6.09855220186056,131.967470671305));
#228547=CARTESIAN_POINT('Ctrl Pts',(61.9729908537767,4.27497385972414,126.302165324755));
#228548=CARTESIAN_POINT('Ctrl Pts',(61.6945432299639,-1.47709661541541,
124.774157507831));
#228549=CARTESIAN_POINT('Ctrl Pts',(61.416095606151,-5.87178746116934,128.787611756953));
#228550=CARTESIAN_POINT('Ctrl Pts',(61.1376479823382,-4.8705924828735,134.65435968532));
#228551=CARTESIAN_POINT('Ctrl Pts',(60.8592003585251,0.606439045512412,
136.983146553331));
#228552=CARTESIAN_POINT('Ctrl Pts',(60.5807527347125,5.52618271726667,133.633930996847));
#228553=CARTESIAN_POINT('Ctrl Pts',(60.3023051108993,5.36763444088732,127.684478494003));
#228554=CARTESIAN_POINT('Ctrl Pts',(60.0238574870866,0.276492336852797,
124.602045247997));
#228555=CARTESIAN_POINT('Ctrl Pts',(59.7454098632736,-5.06873271734795,
127.219236826675));
#228556=CARTESIAN_POINT('Ctrl Pts',(59.4669622394608,-5.75604002566515,
133.130982026147));
#228557=CARTESIAN_POINT('Ctrl Pts',(59.1885146156479,-1.15382774858414,
136.904675812908));
#228558=CARTESIAN_POINT('Ctrl Pts',(58.9100669918351,4.50869586182645,135.072477952114));
#228559=CARTESIAN_POINT('Ctrl Pts',(58.6316193680221,6.02794823725661,129.318088769994));
#228560=CARTESIAN_POINT('Ctrl Pts',(58.3531717442092,2.00781066429043,124.929510807376));
#228561=CARTESIAN_POINT('Ctrl Pts',(58.0747241203963,-3.85740682215468,
125.939632817953));
#228562=CARTESIAN_POINT('Ctrl Pts',(57.7962764965834,-6.17785588383907,
131.42020202121));
#228563=CARTESIAN_POINT('Ctrl Pts',(57.5178288727705,-2.82115719331391,
136.334843060042));
#228564=CARTESIAN_POINT('Ctrl Pts',(57.2393812489577,3.12804713667602,136.167240913326));
#228565=CARTESIAN_POINT('Ctrl Pts',(56.9609336251447,6.20272896165862,131.071413766074));
#228566=CARTESIAN_POINT('Ctrl Pts',(56.6824860013319,3.57740589103289,125.730177821614));
#228567=CARTESIAN_POINT('Ctrl Pts',(56.404038377519,-2.33537842745856,125.051867979023));
#228568=CARTESIAN_POINT('Ctrl Pts',(56.125590753706,-6.10206406069443,129.659817846364));
#228569=CARTESIAN_POINT('Ctrl Pts',(55.8471431298932,-4.26125092455389,
135.319546606417));
#228570=CARTESIAN_POINT('Ctrl Pts',(55.5686955060803,1.49544363757083,136.830040021814));
#228571=CARTESIAN_POINT('Ctrl Pts',(55.2902478822675,5.87789855325116,132.80322843551));
#228572=CARTESIAN_POINT('Ctrl Pts',(55.0118002584545,4.85885184980179,126.939554974638));
#228573=CARTESIAN_POINT('Ctrl Pts',(54.7333526346416,-0.625242335506623,
124.627449093364));
#228574=CARTESIAN_POINT('Ctrl Pts',(54.4549050108287,-5.53476935927053,
127.991623143927));
#228575=CARTESIAN_POINT('Ctrl Pts',(54.1764573870159,-5.35811373037978,
133.9405655229));
#228576=CARTESIAN_POINT('Ctrl Pts',(53.8980097632029,-0.257613341678002,
137.007488805997));
#228577=CARTESIAN_POINT('Ctrl Pts',(53.61956213939,5.07962112291461,134.374040323585));
#228578=CARTESIAN_POINT('Ctrl Pts',(53.3411145155772,5.74893192883615,128.460230579889));
#228579=CARTESIAN_POINT('Ctrl Pts',(53.0626668917642,1.13525514309568,124.7005618237));
#228580=CARTESIAN_POINT('Ctrl Pts',(52.7842192679514,-4.52166565885288,
126.549985971924));
#228581=CARTESIAN_POINT('Ctrl Pts',(52.5057716441385,-6.0233966159634,132.308972581737));
#228582=CARTESIAN_POINT('Ctrl Pts',(52.2273240203255,-1.98992034228702,
136.685294300858));
#228583=CARTESIAN_POINT('Ctrl Pts',(51.9488763965128,3.87219551293788,135.657325264614));
#228584=CARTESIAN_POINT('Ctrl Pts',(51.6704287726998,6.17595285904027,130.169718798237));
#228585=CARTESIAN_POINT('Ctrl Pts',(51.391981148887,2.80431123975502,125.265317159845));
#228586=CARTESIAN_POINT('Ctrl Pts',(51.113533525074,-3.14435541064497,125.451025861782));
#228587=CARTESIAN_POINT('Ctrl Pts',(50.8350859012611,-6.20351304896362,
130.556187679343));
#228588=CARTESIAN_POINT('Ctrl Pts',(50.5566382774483,-3.5619452537452,135.889408303207));
#228589=CARTESIAN_POINT('Ctrl Pts',(50.2781906536353,2.35287621896542,136.549718522358));
#228590=CARTESIAN_POINT('Ctrl Pts',(49.9997430298226,6.10551939084041,131.930325503341));
#228591=CARTESIAN_POINT('Ctrl Pts',(49.7212954060095,4.2474885137371,126.27622576074));
#228592=CARTESIAN_POINT('Ctrl Pts',(49.4428477821967,-1.51377680614101,
124.783260739875));
#228593=CARTESIAN_POINT('Ctrl Pts',(49.1644001583838,-5.88395519328364,
128.823392359526));
#228594=CARTESIAN_POINT('Ctrl Pts',(48.8859525345709,-4.84706620499019,
134.683937032636));
#228595=CARTESIAN_POINT('Ctrl Pts',(48.607504910758,0.644039833341117,136.97934050814));
#228596=CARTESIAN_POINT('Ctrl Pts',(48.3290572869451,5.54330472792681,133.600239128744));
#228597=CARTESIAN_POINT('Ctrl Pts',(48.0506096631323,5.34854338303893,127.651861983834));
#228598=CARTESIAN_POINT('Ctrl Pts',(47.7721620393193,0.23873196000854,124.600477075203));
#228599=CARTESIAN_POINT('Ctrl Pts',(47.4937144155065,-5.09046247156518,
127.250158065443));
#228600=CARTESIAN_POINT('Ctrl Pts',(47.2152667916935,-5.74177057468722,
133.165977568637));
#228601=CARTESIAN_POINT('Ctrl Pts',(46.9368191678807,-1.11667202075834,
136.911586465198));
#228602=CARTESIAN_POINT('Ctrl Pts',(46.6583715440677,4.53459356778643,135.044953162355));
#228603=CARTESIAN_POINT('Ctrl Pts',(46.379923920255,6.01878919474683,129.281422475313));
#228604=CARTESIAN_POINT('Ctrl Pts',(46.101476296442,1.97201158593325,124.917397541337));
#228605=CARTESIAN_POINT('Ctrl Pts',(45.8230286726291,-3.88694833223118,
125.963204080281));
#228606=CARTESIAN_POINT('Ctrl Pts',(45.5445810488162,-6.17399262105761,
131.457796973343));
#228607=CARTESIAN_POINT('Ctrl Pts',(45.2661334250033,-2.78743930743976,
136.351913777587));
#228608=CARTESIAN_POINT('Ctrl Pts',(44.9876858011905,3.16063455573481,136.148100240809));
#228609=CARTESIAN_POINT('Ctrl Pts',(44.7092381773775,6.20423966777097,131.033651046464));
#228610=CARTESIAN_POINT('Ctrl Pts',(44.4307905535647,3.54645161908363,125.708495149421));
#228611=CARTESIAN_POINT('Ctrl Pts',(44.1523429297517,-2.37035221374829,
125.066190670735));
#228612=CARTESIAN_POINT('Ctrl Pts',(43.8738953059389,-6.10891816028884,
129.696984048001));
#228613=CARTESIAN_POINT('Ctrl Pts',(43.5954476821259,-4.23368675476706,
135.345402394343));
#228614=CARTESIAN_POINT('Ctrl Pts',(43.3170000583131,1.53209595128933,136.820825190051));
#228615=CARTESIAN_POINT('Ctrl Pts',(43.0385524345002,5.88995732515911,132.767410964279));
#228616=CARTESIAN_POINT('Ctrl Pts',(42.7601048106873,4.83523565761953,126.910049370218));
#228617=CARTESIAN_POINT('Ctrl Pts',(42.4816571868744,-0.662831364878718,
124.631369564788));
#228618=CARTESIAN_POINT('Ctrl Pts',(42.2032095630615,-5.55178874416567,
128.025366969483));
#228619=CARTESIAN_POINT('Ctrl Pts',(41.9247619392486,-5.33892348752252,
133.973123775378));
#228620=CARTESIAN_POINT('Ctrl Pts',(41.6463143154357,-0.219848366758665,
137.008942041929));
#228621=CARTESIAN_POINT('Ctrl Pts',(41.3678666916229,5.10125666286673,134.343053090145));
#228622=CARTESIAN_POINT('Ctrl Pts',(41.0894190678099,5.73455602955998,128.425278630796));
#228623=CARTESIAN_POINT('Ctrl Pts',(40.8109714439971,1.09807855372398,124.693764292674));
#228624=CARTESIAN_POINT('Ctrl Pts',(40.5325238201841,-4.5474794688646,126.5775894579));
#228625=CARTESIAN_POINT('Ctrl Pts',(40.2540761963713,-6.01412601628932,
132.345610829607));
#228626=CARTESIAN_POINT('Ctrl Pts',(39.9756285725584,-1.95408456113369,
136.697298550707));
#228627=CARTESIAN_POINT('Ctrl Pts',(39.6971809487455,3.90166514336576,135.633664197272));
#228628=CARTESIAN_POINT('Ctrl Pts',(39.4187333249326,6.171975188051,130.132135778682));
#228629=CARTESIAN_POINT('Ctrl Pts',(39.1402857011198,2.77054155266769,125.248349147017));
#228630=CARTESIAN_POINT('Ctrl Pts',(38.8618380773068,-3.17688442113803,
125.470265630536));
#228631=CARTESIAN_POINT('Ctrl Pts',(38.583390453494,-6.20490881134979,130.593954822108));
#228632=CARTESIAN_POINT('Ctrl Pts',(38.304942829681,-3.53092513057837,135.910996660811));
#228633=CARTESIAN_POINT('Ctrl Pts',(38.0264952058682,2.38780624991219,136.535289448812));
#228634=CARTESIAN_POINT('Ctrl Pts',(37.7480475820552,6.11226033755391,131.893138612335));
#228635=CARTESIAN_POINT('Ctrl Pts',(37.4695999582424,4.21984577550119,126.250453988427));
#228636=CARTESIAN_POINT('Ctrl Pts',(37.1911523344295,-1.55040090331038,
124.792587085991));
#228637=CARTESIAN_POINT('Ctrl Pts',(36.9127047106166,-5.89590489327443,
128.859246367608));
#228638=CARTESIAN_POINT('Ctrl Pts',(36.6342570868037,-4.82336031728617,
134.713370620821));
#228639=CARTESIAN_POINT('Ctrl Pts',(36.3558094629908,0.681616756036961,
136.975305646799));
#228640=CARTESIAN_POINT('Ctrl Pts',(36.0773618391779,5.56022132939171,133.566443658335));
#228641=CARTESIAN_POINT('Ctrl Pts',(35.798914215365,5.32925413294858,127.619362290662));
#228642=CARTESIAN_POINT('Ctrl Pts',(35.5204665915522,0.200962736863706,
124.599138789596));
#228643=CARTESIAN_POINT('Ctrl Pts',(35.2420189677392,-5.11200359682353,
127.281211006494));
#228644=CARTESIAN_POINT('Ctrl Pts',(34.9635713439263,-5.72728836028912,
133.200885600541));
#228645=CARTESIAN_POINT('Ctrl Pts',(34.6851237201134,-1.07947491424015,
136.918270811987));
#228646=CARTESIAN_POINT('Ctrl Pts',(34.4066760963006,4.56032324271418,135.017271235878));
#228647=CARTESIAN_POINT('Ctrl Pts',(34.1282284724876,6.00940712379002,129.244812613665));
#228648=CARTESIAN_POINT('Ctrl Pts',(33.8497808486748,1.93613943396156,124.905502418881));
#228649=CARTESIAN_POINT('Ctrl Pts',(33.5713332248619,-3.91634581000783,
125.986954733445));
#228650=CARTESIAN_POINT('Ctrl Pts',(33.292885601049,-6.16990057870911,131.495367712155));
#228651=CARTESIAN_POINT('Ctrl Pts',(33.0144379772361,-2.753618131977,136.368778928511));
#228652=CARTESIAN_POINT('Ctrl Pts',(32.7359903534233,3.19310485631782,136.128761554055));
#228653=CARTESIAN_POINT('Ctrl Pts',(32.4575427296103,6.20552047350092,130.995879830412));
#228654=CARTESIAN_POINT('Ctrl Pts',(32.1790951057975,3.51536593206519,125.687001306397));
#228655=CARTESIAN_POINT('Ctrl Pts',(31.9006474819845,-2.40523816576522,
125.080725992446));
#228656=CARTESIAN_POINT('Ctrl Pts',(31.6221998581717,-6.11554589167424,
129.734191283883));
#228657=CARTESIAN_POINT('Ctrl Pts',(31.3437522343588,-4.20596570416061,
135.371089912296));
#228658=CARTESIAN_POINT('Ctrl Pts',(31.0653046105458,1.56869149262894,136.811387415981));
#228659=CARTESIAN_POINT('Ctrl Pts',(30.786856986733,5.90179784253235,132.731520751495));
#228660=CARTESIAN_POINT('Ctrl Pts',(30.5084093629201,4.81144029400183,126.880688070935));
#228661=CARTESIAN_POINT('Ctrl Pts',(30.2299617391072,-0.700395832790832,
124.635518778667));
#228662=CARTESIAN_POINT('Ctrl Pts',(29.9515141152943,-5.56860240548724,
128.05921377167));
#228663=CARTESIAN_POINT('Ctrl Pts',(29.6730664914815,-5.31953540889204,
134.005564608172));
#228664=CARTESIAN_POINT('Ctrl Pts',(29.3946188676685,-0.182075245277261,
137.010165364815));
#228665=CARTESIAN_POINT('Ctrl Pts',(29.1161712438556,5.12270317387725,134.311934729152));
#228666=CARTESIAN_POINT('Ctrl Pts',(28.8377236200427,5.71996763420123,128.390414839463));
#228667=CARTESIAN_POINT('Ctrl Pts',(28.5592759962298,1.06086127464794,124.687193192043));
#228668=CARTESIAN_POINT('Ctrl Pts',(28.280828372417,-4.57312477035222,126.605349568435));
#228669=CARTESIAN_POINT('Ctrl Pts',(28.0023807486041,-6.00463256096402,
132.382191965885));
#228670=CARTESIAN_POINT('Ctrl Pts',(27.7239331247912,-1.91817637065835,
136.709084435575));
#228671=CARTESIAN_POINT('Ctrl Pts',(27.4454855009783,3.93099019615694,135.60982417831));
#228672=CARTESIAN_POINT('Ctrl Pts',(27.1670378771654,6.16776881225138,130.094577668667));
#228673=CARTESIAN_POINT('Ctrl Pts',(26.8885902533525,2.73666920214424,125.231587014236));
#228674=CARTESIAN_POINT('Ctrl Pts',(26.6101426295396,-3.20929571101057,
125.48970305614));
#228675=CARTESIAN_POINT('Ctrl Pts',(26.3316950057267,-6.2060746485581,130.631729761538));
#228676=CARTESIAN_POINT('Ctrl Pts',(26.0532473819138,-3.49977416768234,
135.932395790139));
#228677=CARTESIAN_POINT('Ctrl Pts',(25.774799758101,2.42264779982026,136.52064801359));
#228678=CARTESIAN_POINT('Ctrl Pts',(25.4963521342881,6.11877479221284,131.85591137626));
#228679=CARTESIAN_POINT('Ctrl Pts',(25.2179045104751,4.19204666932822,126.224850962798));
#228680=CARTESIAN_POINT('Ctrl Pts',(24.9394568866623,-1.58696754980412,
124.802136200585));
#228681=CARTESIAN_POINT('Ctrl Pts',(24.6610092628494,-5.90763611834117,
128.895172452612));
#228682=CARTESIAN_POINT('Ctrl Pts',(24.3825616390365,-4.79947569819179,
134.742659359205));
#228683=CARTESIAN_POINT('Ctrl Pts',(24.1041140152236,0.719168421173241,
136.97104211882));
#228684=CARTESIAN_POINT('Ctrl Pts',(23.8256663914108,5.57693189481048,133.532545837923));
#228685=CARTESIAN_POINT('Ctrl Pts',(23.5472187675978,5.3097674053865,127.586980618775));
#228686=CARTESIAN_POINT('Ctrl Pts',(23.2687711437849,0.163186066970757,
124.598030440764));
#228687=CARTESIAN_POINT('Ctrl Pts',(22.990323519972,-5.13335529490864,127.312394499151));
#228688=CARTESIAN_POINT('Ctrl Pts',(22.7118758961592,-5.71259391911463,
133.235704828331));
#228689=CARTESIAN_POINT('Ctrl Pts',(22.4334282723462,-1.04223780738205,
136.924728605587));
#228690=CARTESIAN_POINT('Ctrl Pts',(22.1549806485334,4.58588393318709,134.98943319845));
#228691=CARTESIAN_POINT('Ctrl Pts',(21.8765330247205,5.9998023720423,129.208260541641));
#228692=CARTESIAN_POINT('Ctrl Pts',(21.5980854009075,1.90019553763114,124.893825880784));
#228693=CARTESIAN_POINT('Ctrl Pts',(21.3196377770947,-3.94559816615024,
126.010883897355));
#228694=CARTESIAN_POINT('Ctrl Pts',(21.0411901532818,-6.16557990842568,
131.532912845442));
#228695=CARTESIAN_POINT('Ctrl Pts',(20.7627425294689,-2.71969492018171,
136.385437887866));
#228696=CARTESIAN_POINT('Ctrl Pts',(20.484294905656,3.22545683522612,136.109225569666));
#228697=CARTESIAN_POINT('Ctrl Pts',(20.2058472818431,6.20657133138755,130.958101517545));
#228698=CARTESIAN_POINT('Ctrl Pts',(19.9273996580302,3.48414998186958,125.665697089004));
#228699=CARTESIAN_POINT('Ctrl Pts',(19.6489520342174,-2.44003499079723,
125.095473405541));
#228700=CARTESIAN_POINT('Ctrl Pts',(19.3705044104044,-6.12194700925765,
129.771438175283));
#228701=CARTESIAN_POINT('Ctrl Pts',(19.0920567865916,-4.17808879994825,
135.396608208416));
#228702=CARTESIAN_POINT('Ctrl Pts',(18.8136091627787,1.60522890552839,136.801727049323));
#228703=CARTESIAN_POINT('Ctrl Pts',(18.5351615389658,5.91341966661616,132.695559127084));
#228704=CARTESIAN_POINT('Ctrl Pts',(18.2567139151529,4.78746664069464,126.85147216478));
#228705=CARTESIAN_POINT('Ctrl Pts',(17.97826629134,-0.737934347277788,124.63989658125));
#228706=CARTESIAN_POINT('Ctrl Pts',(17.6998186675271,-5.58520972019883,
128.093162296283));
#228707=CARTESIAN_POINT('Ctrl Pts',(17.4213710437142,-5.29995021292075,
134.037886819174));
#228708=CARTESIAN_POINT('Ctrl Pts',(17.1429234199013,-0.144295376930669,
137.011158729324));
#228709=CARTESIAN_POINT('Ctrl Pts',(16.8644757960885,5.14395986123776,134.280686393713));
#228710=CARTESIAN_POINT('Ctrl Pts',(16.5860281722755,5.70516728333829,128.355640497777));
#228711=CARTESIAN_POINT('Ctrl Pts',(16.3075805484627,1.02360468496723,124.6808487653));
#228712=CARTESIAN_POINT('Ctrl Pts',(16.0291329246498,-4.5986006130197,126.633265274869));
#228713=CARTESIAN_POINT('Ctrl Pts',(15.7506853008369,-5.99491660177097,
132.418714635041));
#228714=CARTESIAN_POINT('Ctrl Pts',(15.472237677024,-1.88219710145218,136.720651518731));
#228715=CARTESIAN_POINT('Ctrl Pts',(15.1937900532111,3.96016958466077,135.585806091128));
#228716=CARTESIAN_POINT('Ctrl Pts',(14.9153424293982,6.16333388751023,130.057045859918));
#228717=CARTESIAN_POINT('Ctrl Pts',(14.6368948055853,2.70269544333712,125.215031382631));
#228718=CARTESIAN_POINT('Ctrl Pts',(14.3584471817724,-3.24158807925031,
125.509337418335));
#228719=CARTESIAN_POINT('Ctrl Pts',(14.0799995579596,-6.20701051738803,
130.669511097867));
#228720=CARTESIAN_POINT('Ctrl Pts',(13.8015519341466,-3.46849351936748,
135.953604898237));
#228721=CARTESIAN_POINT('Ctrl Pts',(13.5231043103337,2.45739957762318,136.505794759238));
#228722=CARTESIAN_POINT('Ctrl Pts',(13.2446566865208,6.12506251342167,131.818645174584));
#228723=CARTESIAN_POINT('Ctrl Pts',(12.966209062708,4.16409222532429,126.199417632585));
#228724=CARTESIAN_POINT('Ctrl Pts',(12.687761438895,-1.62347539063169,124.811907729812));
#228725=CARTESIAN_POINT('Ctrl Pts',(12.4093138150822,-5.91914843377905,
128.931169283287));
#228726=CARTESIAN_POINT('Ctrl Pts',(12.1308661912693,-4.77541323276041,
134.771802162479));
#228727=CARTESIAN_POINT('Ctrl Pts',(11.8524185674564,0.756693437259193,
136.96655008219));
#228728=CARTESIAN_POINT('Ctrl Pts',(11.5739709436435,5.59343580496719,133.498546923603));
#228729=CARTESIAN_POINT('Ctrl Pts',(11.2955233198306,5.2900839224404,127.554718168085));
#228730=CARTESIAN_POINT('Ctrl Pts',(11.0170756960177,0.125403350157864,
124.597152069781));
#228731=CARTESIAN_POINT('Ctrl Pts',(10.7386280722048,-5.15451677462551,
127.343707387895));
#228732=CARTESIAN_POINT('Ctrl Pts',(10.460180448392,-5.69768779567166,133.270433961767));
#228733=CARTESIAN_POINT('Ctrl Pts',(10.1817328245791,-1.0049620800187,136.930959606699));
#228734=CARTESIAN_POINT('Ctrl Pts',(9.90328520076621,4.61127469204443,134.961440081617));
#228735=CARTESIAN_POINT('Ctrl Pts',(9.62483757695328,5.98997529541125,129.171767613693));
#228736=CARTESIAN_POINT('Ctrl Pts',(9.34638995314043,1.86418122885626,124.882368359726));
#228737=CARTESIAN_POINT('Ctrl Pts',(9.0679423293275,-3.97470431670162,126.034990685308));
#228738=CARTESIAN_POINT('Ctrl Pts',(8.78949470551463,-6.16103077031137,
131.57043098196));
#228739=CARTESIAN_POINT('Ctrl Pts',(8.5110470817017,-2.68567092909101,136.401890038352));
#228740=CARTESIAN_POINT('Ctrl Pts',(8.2325994578889,3.25768929364524,136.089493011555));
#228741=CARTESIAN_POINT('Ctrl Pts',(7.95415183407592,6.20739220249103,130.920317507753));
#228742=CARTESIAN_POINT('Ctrl Pts',(7.67570421026306,3.45280492521512,125.644583286679));
#228743=CARTESIAN_POINT('Ctrl Pts',(7.39725658645018,-2.47474139943534,
125.110432363552));
#228744=CARTESIAN_POINT('Ctrl Pts',(7.11880896263729,-6.1281212758433,129.808723342005));
#228745=CARTESIAN_POINT('Ctrl Pts',(6.84036133882437,-4.15005707511893,
135.421956337113));
#228746=CARTESIAN_POINT('Ctrl Pts',(6.56191371501151,1.64170683608044,136.791844448048));
#228747=CARTESIAN_POINT('Ctrl Pts',(6.28346609119863,5.92482236675955,132.659527423617));
#228748=CARTESIAN_POINT('Ctrl Pts',(6.00501846738572,4.76331558605049,126.822402734361));
#228749=CARTESIAN_POINT('Ctrl Pts',(5.72657084357281,-0.775445517336138,
124.644502810313));
#228750=CARTESIAN_POINT('Ctrl Pts',(5.44812321975995,-5.60161007291028,
128.127211285347));
#228751=CARTESIAN_POINT('Ctrl Pts',(5.16967559594705,-5.28016862534525,
134.070089210674));
#228752=CARTESIAN_POINT('Ctrl Pts',(4.89122797213414,-0.106510161665837,
137.011922098645));
#228753=CARTESIAN_POINT('Ctrl Pts',(4.6127803483213,5.16502593727395,134.249309241742));
#228754=CARTESIAN_POINT('Ctrl Pts',(4.33433272450837,5.69015552540359,128.320956894316));
#228755=CARTESIAN_POINT('Ctrl Pts',(4.05588510069549,0.986310165238503,
124.674731247541));
#228756=CARTESIAN_POINT('Ctrl Pts',(3.77743747688256,-4.62390605285035,
126.661335542776));
#228757=CARTESIAN_POINT('Ctrl Pts',(3.49898985306972,-5.98497849873861,
132.455177483715));
#228758=CARTESIAN_POINT('Ctrl Pts',(3.22054222925682,-1.84614808674025,
136.731999371551));
#228759=CARTESIAN_POINT('Ctrl Pts',(2.94209460544391,3.9892022276243,135.561610825727));
#228760=CARTESIAN_POINT('Ctrl Pts',(2.66364698163102,6.15867057816533,130.019541743194));
#228761=CARTESIAN_POINT('Ctrl Pts',(2.38519935781816,2.66862153515642,125.198682865676));
#228762=CARTESIAN_POINT('Ctrl Pts',(2.10675173400524,-3.27376032925169,
125.529167989562));
#228763=CARTESIAN_POINT('Ctrl Pts',(1.82830411019233,-6.20771638316062,
130.707297431096));
#228764=CARTESIAN_POINT('Ctrl Pts',(1.54985648637947,-3.43708434474973,
135.974623199195));
#228765=CARTESIAN_POINT('Ctrl Pts',(1.27140886256659,2.49206029558105,136.490730236146));
#228766=CARTESIAN_POINT('Ctrl Pts',(0.992961238753657,6.13112326818657,
131.78134138822));
#228767=CARTESIAN_POINT('Ctrl Pts',(0.714513614940807,4.13598347935162,
126.174154940227));
#228768=CARTESIAN_POINT('Ctrl Pts',(0.436065991127901,-1.65992307298164,
124.821901311585));
#228769=CARTESIAN_POINT('Ctrl Pts',(0.157618367314999,-5.93044141299494,
128.967235525755));
#228770=CARTESIAN_POINT('Ctrl Pts',(-0.120829256497892,-4.75117381263555,
134.800797950748));
#228771=CARTESIAN_POINT('Ctrl Pts',(-0.399276880310752,0.794190413791566,
136.961829703365));
#228772=CARTESIAN_POINT('Ctrl Pts',(-0.67772450412367,5.60973244830296,
133.464448175219));
#228773=CARTESIAN_POINT('Ctrl Pts',(-0.956172127936585,5.27020441348929,
127.522576134092));
#228774=CARTESIAN_POINT('Ctrl Pts',(-1.23461975174943,0.0876159864779326,
124.596503709192));
#228775=CARTESIAN_POINT('Ctrl Pts',(-1.51306737556233,-5.17548725182775,
127.375148512417));
#228776=CARTESIAN_POINT('Ctrl Pts',(-1.79151499937523,-5.6825705423121,
133.305071713949));
#228777=CARTESIAN_POINT('Ctrl Pts',(-2.06996262318813,-0.967649113415911,
136.936963584433));
#228778=CARTESIAN_POINT('Ctrl Pts',(-2.34841024700098,4.63649457842225,
134.933292922676));
#228779=CARTESIAN_POINT('Ctrl Pts',(-2.62685787081389,5.97992625804282,
129.13533518208));
#228780=CARTESIAN_POINT('Ctrl Pts',(-2.90530549462681,1.82809784216042,
124.871130280269));
#228781=CARTESIAN_POINT('Ctrl Pts',(-3.18375311843967,-4.00366318312286,
126.059274204017));
#228782=CARTESIAN_POINT('Ctrl Pts',(-3.46220074225256,-6.15625333293613,
131.607920731459));
#228783=CARTESIAN_POINT('Ctrl Pts',(-3.74064836606547,-2.65154741947636,
136.418134770325));
#228784=CARTESIAN_POINT('Ctrl Pts',(-4.01909598987837,3.28980103718956,
136.06956461092));
#228785=CARTESIAN_POINT('Ctrl Pts',(-4.29754361369122,6.20798305639367,
130.882529201136));
#228786=CARTESIAN_POINT('Ctrl Pts',(-4.57599123750414,3.42133192360438,
125.623660681799));
#228787=CARTESIAN_POINT('Ctrl Pts',(-4.85443886131705,-2.5093561056208,
125.125602312169));
#228788=CARTESIAN_POINT('Ctrl Pts',(-5.13288648512991,-6.13406846264146,
129.846045402432));
#228789=CARTESIAN_POINT('Ctrl Pts',(-5.41133410894279,-4.12187156839848,
135.447133359102));
#228790=CARTESIAN_POINT('Ctrl Pts',(-5.68978173275571,1.67812393258193,
136.781739978358));
#228791=CARTESIAN_POINT('Ctrl Pts',(-5.9682293565686,5.93600552043131,132.623426976261));
#228792=CARTESIAN_POINT('Ctrl Pts',(-6.24667698038146,4.73898802499559,
126.793480856855));
#228793=CARTESIAN_POINT('Ctrl Pts',(-6.52512460419438,-0.812927952975666,
124.649337295173));
#228794=CARTESIAN_POINT('Ctrl Pts',(-6.80357222800728,-5.61780285590049,
128.161359477164));
#228795=CARTESIAN_POINT('Ctrl Pts',(-7.08201985182013,-5.26019137917956,
134.1021705894));
#228796=CARTESIAN_POINT('Ctrl Pts',(-7.36046747563304,-0.0687209996277829,
137.012455444495));
#228797=CARTESIAN_POINT('Ctrl Pts',(-7.63891509944595,5.18590062137458,
134.217804435933));
#228798=CARTESIAN_POINT('Ctrl Pts',(-7.91736272325884,5.67493291666336,
128.286365314294));
#228799=CARTESIAN_POINT('Ctrl Pts',(-8.1958103470717,0.948979097423875,
124.668840865451));
#228800=CARTESIAN_POINT('Ctrl Pts',(-8.47425797088461,-4.64904015214177,
126.689559331999));
#228801=CARTESIAN_POINT('Ctrl Pts',(-8.75270559469752,-5.97481862012702,
132.491579160764));
#228802=CARTESIAN_POINT('Ctrl Pts',(-9.03115321851038,-1.81003066233205,
136.743127573537));
#228803=CARTESIAN_POINT('Ctrl Pts',(-9.30960084232328,4.0180870492325,135.537239278668));
#228804=CARTESIAN_POINT('Ctrl Pts',(-9.58804846613619,6.15377905701727,
129.982066708221));
#228805=CARTESIAN_POINT('Ctrl Pts',(-9.86649608994908,2.63444874022312,
125.182542069172));
#228806=CARTESIAN_POINT('Ctrl Pts',(-10.144943713762,-3.30581126886015,
125.549194034992));
#228807=CARTESIAN_POINT('Ctrl Pts',(-10.4233913375749,-6.20819221971975,
130.745087361036));
#228808=CARTESIAN_POINT('Ctrl Pts',(-10.7018389613878,-3.40554780770759,
135.995449914173));
#228809=CARTESIAN_POINT('Ctrl Pts',(-10.9802865852006,2.52662866932821,
136.475455002538));
#228810=CARTESIAN_POINT('Ctrl Pts',(-11.2587342090136,6.13695683192405,
131.744001399476));
#228811=CARTESIAN_POINT('Ctrl Pts',(-11.5371818328265,4.10772147299012,
126.149063821843));
#228812=CARTESIAN_POINT('Ctrl Pts',(-11.8156294566394,-1.69630924627168,
124.832116575588));
#228813=CARTESIAN_POINT('Ctrl Pts',(-12.0940770804522,-5.94151463752335,
129.003369843568));
#228814=CARTESIAN_POINT('Ctrl Pts',(-12.3725247042651,-4.72675833601782,
134.829645649562));
#228815=CARTESIAN_POINT('Ctrl Pts',(-12.6509723280781,0.83165796130609,
136.956881157257));
#228816=CARTESIAN_POINT('Ctrl Pts',(-12.9294199518909,5.62582122093989,
133.430250856313));
#228817=CARTESIAN_POINT('Ctrl Pts',(-13.2078675757038,5.25012961517551,
127.490555707831));
#228818=CARTESIAN_POINT('Ctrl Pts',(-13.4863151995167,0.0498253761554086,
124.596085383024));
#228819=CARTESIAN_POINT('Ctrl Pts',(-13.7647628233296,-5.19626594944658,
127.406716707655));
#228820=CARTESIAN_POINT('Ctrl Pts',(-14.0432104471424,-5.66724271921134,
133.339616801361));
#228821=CARTESIAN_POINT('Ctrl Pts',(-14.3216580709554,-0.930300290219375,
136.942740316309));
#228822=CARTESIAN_POINT('Ctrl Pts',(-14.6001056947683,4.6615426577884,134.904992764631));
#228823=CARTESIAN_POINT('Ctrl Pts',(-14.8785533185811,5.96965563230779,
129.098964596818));
#228824=CARTESIAN_POINT('Ctrl Pts',(-15.157000942394,1.79194671462675,124.860112058844));
#228825=CARTESIAN_POINT('Ctrl Pts',(-15.4354485662069,-4.03247369233249,
126.08373355365));
#228826=CARTESIAN_POINT('Ctrl Pts',(-15.7138961900198,-6.15124777332969,
131.645380704742));
#228827=CARTESIAN_POINT('Ctrl Pts',(-15.9923438138327,-2.61732565579698,
136.434171481834));
#228828=CARTESIAN_POINT('Ctrl Pts',(-16.2707914376456,3.32179087594663,
136.049441106215));
#228829=CARTESIAN_POINT('Ctrl Pts',(-16.5492390614585,6.2083438712012,130.844737997954));
#228830=CARTESIAN_POINT('Ctrl Pts',(-16.8276866852714,3.38973214328102,
125.602930049661));
#228831=CARTESIAN_POINT('Ctrl Pts',(-17.1061343090842,-2.54387782669295,
125.140982689263));
#228832=CARTESIAN_POINT('Ctrl Pts',(-17.3845819328972,-6.13978834927694,
129.883402973582));
#228833=CARTESIAN_POINT('Ctrl Pts',(-17.66302955671,-4.09353332421128,135.47213834144));
#228834=CARTESIAN_POINT('Ctrl Pts',(-17.9414771805229,1.71447884558397,
136.771414014676));
#228835=CARTESIAN_POINT('Ctrl Pts',(-18.2199248043358,5.94696871323555,
132.587259122732));
#228836=CARTESIAN_POINT('Ctrl Pts',(-18.4983724281487,4.71448485899666,
126.764707603974));
#228837=CARTESIAN_POINT('Ctrl Pts',(-18.7768200519616,-0.850380265270943,
124.654399856686));
#228838=CARTESIAN_POINT('Ctrl Pts',(-19.0552676757745,-5.63378746913994,
128.19560560636));
#228839=CARTESIAN_POINT('Ctrl Pts',(-19.3337152995874,-5.24001921468789,
134.134129766565));
#228840=CARTESIAN_POINT('Ctrl Pts',(-19.6121629234003,-0.0309292911078312,
137.012758747106));
#228841=CARTESIAN_POINT('Ctrl Pts',(-19.8906105472132,5.2065831400206,134.18617314371));
#228842=CARTESIAN_POINT('Ctrl Pts',(-20.1690581710261,5.65950002119693,
128.251867039513));
#228843=CARTESIAN_POINT('Ctrl Pts',(-20.447505794839,0.911612864839816,
124.663177837304));
#228844=CARTESIAN_POINT('Ctrl Pts',(-20.7259534186518,-4.67400197954067,
126.717935596697));
#228845=CARTESIAN_POINT('Ctrl Pts',(-21.0044010424647,-5.96443734241423,
132.527918317308));
#228846=CARTESIAN_POINT('Ctrl Pts',(-21.2828486662776,-1.77384616657202,
136.754035712331));
#228847=CARTESIAN_POINT('Ctrl Pts',(-21.5612962900905,4.0468229791472,135.512692353051));
#228848=CARTESIAN_POINT('Ctrl Pts',(-21.8397439139034,6.14865950532324,
129.944622143653));
#228849=CARTESIAN_POINT('Ctrl Pts',(-22.1181915377163,2.60017832482316,
125.166609591221));
#228850=CARTESIAN_POINT('Ctrl Pts',(-22.3966391615293,-3.33773971041633,
125.569414812551));
#228851=CARTESIAN_POINT('Ctrl Pts',(-22.6750867853421,-6.20843800943312,
130.782879487369));
#228852=CARTESIAN_POINT('Ctrl Pts',(-22.953534409155,-3.37388507683905,
136.016084271426));
#228853=CARTESIAN_POINT('Ctrl Pts',(-23.2319820329679,2.56110341792085,
136.45996962444));
#228854=CARTESIAN_POINT('Ctrl Pts',(-23.5104296567807,6.14256298846929,
131.706626591997));
#228855=CARTESIAN_POINT('Ctrl Pts',(-23.7888772805937,4.07930725349882,
126.124145207193));
#228856=CARTESIAN_POINT('Ctrl Pts',(-24.0673249044065,-1.73263256219878,
124.842553143289));
#228857=CARTESIAN_POINT('Ctrl Pts',(-24.3457725282195,-5.95236769704188,
129.039570897758));
#228858=CARTESIAN_POINT('Ctrl Pts',(-24.6242201520323,-4.70216770763169,
134.858344189959));
#228859=CARTESIAN_POINT('Ctrl Pts',(-24.9026677758452,0.86909469142902,
136.951704627238));
#228860=CARTESIAN_POINT('Ctrl Pts',(-25.1811153996581,5.64170152670257,
133.395956234079));
#228861=CARTESIAN_POINT('Ctrl Pts',(-25.459563023471,5.22986027137813,127.458658075828));
#228862=CARTESIAN_POINT('Ctrl Pts',(-25.7380106472839,0.0120329195352371,
124.595897106778));
#228863=CARTESIAN_POINT('Ctrl Pts',(-26.0164582710968,-5.21685209751974,
127.438410803838));
#228864=CARTESIAN_POINT('Ctrl Pts',(-26.2949058949097,-5.6517048943475,
133.374067943923));
#228865=CARTESIAN_POINT('Ctrl Pts',(-26.5733535187226,-0.892916994403456,
136.948289588268));
#228866=CARTESIAN_POINT('Ctrl Pts',(-26.8518011425354,4.68641800197708,
134.876540656153));
#228867=CARTESIAN_POINT('Ctrl Pts',(-27.1302487663484,5.95916379878798,
129.062657205632));
#228868=CARTESIAN_POINT('Ctrl Pts',(-27.4086963901612,1.75572918584856,
124.849314103734));
#228869=CARTESIAN_POINT('Ctrl Pts',(-27.6871440139742,-4.06113477674652,
126.108367827853));
#228870=CARTESIAN_POINT('Ctrl Pts',(-27.965591637787,-6.1460142769749,131.682809513716));
#228871=CARTESIAN_POINT('Ctrl Pts',(-28.2440392616,-2.5830069061529,136.449999578631));
#228872=CARTESIAN_POINT('Ctrl Pts',(-28.5224868854127,3.3536576245212,136.029123243122));
#228873=CARTESIAN_POINT('Ctrl Pts',(-28.8009345092257,6.20847463354345,
130.806945298572));
#228874=CARTESIAN_POINT('Ctrl Pts',(-29.0793821330386,3.35800675518651,
125.582392158445));
#228875=CARTESIAN_POINT('Ctrl Pts',(-29.3578297568515,-2.57830528343674,
125.156572924908));
#228876=CARTESIAN_POINT('Ctrl Pts',(-29.6362773806644,-6.14528072379723,
129.920794671155));
#228877=CARTESIAN_POINT('Ctrl Pts',(-29.9147250044772,-4.06504339264135,
135.496970357558));
#228878=CARTESIAN_POINT('Ctrl Pts',(-30.1931726282902,1.75077022794215,
136.760866939637));
#228879=CARTESIAN_POINT('Ctrl Pts',(-30.471620252103,5.95771153892721,132.551025203244));
#228880=CARTESIAN_POINT('Ctrl Pts',(-30.750067875916,4.68980699602731,126.736084041921));
#228881=CARTESIAN_POINT('Ctrl Pts',(-31.0285154997288,-0.887801066412759,
124.659690307256));
#228882=CARTESIAN_POINT('Ctrl Pts',(-31.3069631235417,-5.6495633203129,
128.229948403933));
#228883=CARTESIAN_POINT('Ctrl Pts',(-31.5854107473546,-5.21965287935721,
134.16596555791));
#228884=CARTESIAN_POINT('Ctrl Pts',(-31.8638583711675,0.00686356350839004,
137.012831995241));
#228885=CARTESIAN_POINT('Ctrl Pts',(-32.1423059949804,5.22707272681363,
134.154416537178));
#228886=CARTESIAN_POINT('Ctrl Pts',(-32.4207536187933,5.64385741087595,
128.217463348321));
#228887=CARTESIAN_POINT('Ctrl Pts',(-32.6992012426062,0.874212852105795,
124.657742372942));
#228888=CARTESIAN_POINT('Ctrl Pts',(-32.9776488664191,-4.69879061007736,
126.746463285377));
#228889=CARTESIAN_POINT('Ctrl Pts',(-33.2560964902319,-5.9538350502823,
132.564193606789));
#228890=CARTESIAN_POINT('Ctrl Pts',(-33.5345441140448,-1.73759594028995,
136.764723383724));
#228891=CARTESIAN_POINT('Ctrl Pts',(-33.8129917378578,4.07540895254819,
135.487970958469));
#228892=CARTESIAN_POINT('Ctrl Pts',(-34.0914393616706,6.14331211279008,
129.907209437008));
#228893=CARTESIAN_POINT('Ctrl Pts',(-34.3698869854835,2.56581155885918,
125.150886022208));
#228894=CARTESIAN_POINT('Ctrl Pts',(-34.6483346092964,-3.3695444708001,
125.589829572953));
#228895=CARTESIAN_POINT('Ctrl Pts',(-34.9267822331094,-6.2084537431929,
130.820672409693));
#228896=CARTESIAN_POINT('Ctrl Pts',(-35.2052298569221,-3.34209732541825,
136.036525506343));
#228897=CARTESIAN_POINT('Ctrl Pts',(-35.4836774807351,2.59548326388451,
136.444274675672));
#228898=CARTESIAN_POINT('Ctrl Pts',(-35.7621251045479,6.14794153008404,
131.66921835072));
#228899=CARTESIAN_POINT('Ctrl Pts',(-36.0405727283609,4.05074187377708,
126.099400019648));
#228900=CARTESIAN_POINT('Ctrl Pts',(-36.3190203521737,-1.76889167478912,
124.85321062796));
#228901=CARTESIAN_POINT('Ctrl Pts',(-36.5974679759867,-5.96300018938643,
129.075837346879));
#228902=CARTESIAN_POINT('Ctrl Pts',(-36.8759155997995,-4.67740283869194,
134.886892508504));
#228903=CARTESIAN_POINT('Ctrl Pts',(-37.1543632236125,0.906499216928551,
136.946300305126));
#228904=CARTESIAN_POINT('Ctrl Pts',(-37.4328108474252,5.65737277714046,
133.361565579315));
#228905=CARTESIAN_POINT('Ctrl Pts',(-37.7112584712383,5.2093971331851,127.426884420063));
#228906=CARTESIAN_POINT('Ctrl Pts',(-37.9897060950511,-0.0257599829691867,
124.595938887431));
#228907=CARTESIAN_POINT('Ctrl Pts',(-38.268153718864,-5.23724493321992,
127.470229626529));
#228908=CARTESIAN_POINT('Ctrl Pts',(-38.5466013426768,-5.63595764348039,
133.408423865036));
#228909=CARTESIAN_POINT('Ctrl Pts',(-38.8250489664898,-0.855500611219946,
136.953611194679));
#228910=CARTESIAN_POINT('Ctrl Pts',(-39.1034965903026,4.71111968922328,
134.847937651547));
#228911=CARTESIAN_POINT('Ctrl Pts',(-39.3819442141156,5.94845114626212,
129.026414353905));
#228912=CARTESIAN_POINT('Ctrl Pts',(-39.6603918379284,1.71944659787975,
124.838736815064));
#228913=CARTESIAN_POINT('Ctrl Pts',(-39.9388394617414,-4.08964537431793,
126.133176113797));
#228914=CARTESIAN_POINT('Ctrl Pts',(-40.2172870855541,-6.14055303780089,
131.720205771443));
#228915=CARTESIAN_POINT('Ctrl Pts',(-40.495734709367,-2.54859244223803,
136.465618474199));
#228916=CARTESIAN_POINT('Ctrl Pts',(-40.7741823331801,3.3854001020792,136.008611774531));
#228917=CARTESIAN_POINT('Ctrl Pts',(-41.0526299569928,6.20837533857501,
130.769152503414));
#228918=CARTESIAN_POINT('Ctrl Pts',(-41.3310775808058,3.3261569349168,125.562047769191));
#228919=CARTESIAN_POINT('Ctrl Pts',(-41.6095252046187,-2.61263720013008,
125.172372441404));
#228920=CARTESIAN_POINT('Ctrl Pts',(-41.8879728284316,-6.15054538268038,
129.958219109591));
#228921=CARTESIAN_POINT('Ctrl Pts',(-42.1664204522444,-4.03640282939359,
135.521628487296));
#228922=CARTESIAN_POINT('Ctrl Pts',(-42.4448680760573,1.78699673486542,
136.750099144066));
#228923=CARTESIAN_POINT('Ctrl Pts',(-42.7233156998703,5.96823359942677,
132.514726560457));
#228924=CARTESIAN_POINT('Ctrl Pts',(-43.0017633236831,4.66495535053527,
126.707611231352));
#228925=CARTESIAN_POINT('Ctrl Pts',(-43.2802109474961,-0.925188969759574,
124.665208450844));
#228926=CARTESIAN_POINT('Ctrl Pts',(-43.5586585713089,-5.6651298248394,
128.264386597296));
#228927=CARTESIAN_POINT('Ctrl Pts',(-43.8371061951219,-5.19909312786956,
134.197676783747));
#228928=CARTESIAN_POINT('Ctrl Pts',(-44.1155538189346,0.0446561637927345,
137.012675186187));
#228929=CARTESIAN_POINT('Ctrl Pts',(-44.3940014427476,5.24736862250453,
134.122535793092));
#228930=CARTESIAN_POINT('Ctrl Pts',(-44.6724490665605,5.62800566534308,
128.183155515557));
#228931=CARTESIAN_POINT('Ctrl Pts',(-44.9508966903734,0.836780445093053,
124.65253467378));
#228932=CARTESIAN_POINT('Ctrl Pts',(-45.2293443141862,-4.72340512520001,
126.775141340936));
#228933=CARTESIAN_POINT('Ctrl Pts',(-45.5077919379991,-5.94301213660306,
132.600403685011));
#228934=CARTESIAN_POINT('Ctrl Pts',(-45.7862395618121,-1.7012813267513,
136.775190191685));
#228935=CARTESIAN_POINT('Ctrl Pts',(-46.0646871856249,4.10384391017172,
135.463076010984));
#228936=CARTESIAN_POINT('Ctrl Pts',(-46.3431348094379,6.13773707756737,
129.869829974632));
#228937=CARTESIAN_POINT('Ctrl Pts',(-46.6215824332507,2.5313497158043,125.135371944775));
#228938=CARTESIAN_POINT('Ctrl Pts',(-46.9000300570636,-3.40122437147435,
125.610437559721));
#228939=CARTESIAN_POINT('Ctrl Pts',(-47.1784776808764,-6.20823942041608,
130.858464727578));
#228940=CARTESIAN_POINT('Ctrl Pts',(-47.4569253046894,-3.31018573135201,
136.056772861467));
#228941=CARTESIAN_POINT('Ctrl Pts',(-47.7353729285023,2.62976693326135,
136.428370737814));
#228942=CARTESIAN_POINT('Ctrl Pts',(-48.0138205523151,6.15309225746451,
131.631778061822));
#228943=CARTESIAN_POINT('Ctrl Pts',(-48.2922681761281,4.02202639232555,
126.074829176147));
#228944=CARTESIAN_POINT('Ctrl Pts',(-48.570715799941,-1.80508524044794,
124.864088634681));
#228945=CARTESIAN_POINT('Ctrl Pts',(-48.8491634237538,-5.97341172056607,
129.112167847066));
#228946=CARTESIAN_POINT('Ctrl Pts',(-49.1276110475668,-4.65246464686987,
134.915289547327));
#228947=CARTESIAN_POINT('Ctrl Pts',(-49.4060586713796,0.943870151766231,
136.940668391181));
#228948=CARTESIAN_POINT('Ctrl Pts',(-49.6845062951925,5.6728343915496,133.327080166382));
#228949=CARTESIAN_POINT('Ctrl Pts',(-49.9629539190054,5.18874095886556,
127.395235917922));
#228950=CARTESIAN_POINT('Ctrl Pts',(-50.2414015428183,-0.0635519309279763,
124.596210723434));
#228951=CARTESIAN_POINT('Ctrl Pts',(-50.5198491666312,-5.25744370088312,
127.50217199667));
#228952=CARTESIAN_POINT('Ctrl Pts',(-50.798296790444,-5.6200015501302,133.442683291627));
#228953=CARTESIAN_POINT('Ctrl Pts',(-51.076744414257,-0.818052527146474,
136.958704938348));
#228954=CARTESIAN_POINT('Ctrl Pts',(-51.3551920380699,4.73564680419706,
134.819184810706));
#228955=CARTESIAN_POINT('Ctrl Pts',(-51.6336396618827,5.93751807169133,
128.990237384633));
#228956=CARTESIAN_POINT('Ctrl Pts',(-51.9120872856956,1.68310029518491,
124.828380584778));
#228957=CARTESIAN_POINT('Ctrl Pts',(-52.1905349095086,-4.11800442857602,
126.1581574922));
#228958=CARTESIAN_POINT('Ctrl Pts',(-52.4689825333214,-6.13486425817587,
131.757568092191));
#228959=CARTESIAN_POINT('Ctrl Pts',(-52.7474301571343,-2.51408353929296,
136.481027589776));
#228960=CARTESIAN_POINT('Ctrl Pts',(-53.0258777809472,3.41701713239144,
135.987907460498));
#228961=CARTESIAN_POINT('Ctrl Pts',(-53.3043254047601,6.20804598997526,
130.731361012906));
#228962=CARTESIAN_POINT('Ctrl Pts',(-53.5827730285729,3.29418386267868,
125.541897635768));
#228963=CARTESIAN_POINT('Ctrl Pts',(-53.8612206523859,-2.64687230459117,
125.188380653292));
#228964=CARTESIAN_POINT('Ctrl Pts',(-54.1396682761987,-6.15558213084251,
129.995674902111));
#228965=CARTESIAN_POINT('Ctrl Pts',(-54.4181159000117,-4.0076126957546,
135.546111816938));
#228966=CARTESIAN_POINT('Ctrl Pts',(-54.6965635238244,1.82315702396754,
136.739111026966));
#228967=CARTESIAN_POINT('Ctrl Pts',(-54.9750111476374,5.97853450483549,
132.478364539431));
#228968=CARTESIAN_POINT('Ctrl Pts',(-55.2534587714502,4.63993084340721,
126.679290227339));
#228969=CARTESIAN_POINT('Ctrl Pts',(-55.5319063952633,-0.962542589888887,
124.670954082973));
#228970=CARTESIAN_POINT('Ctrl Pts',(-55.810354019076,-5.68048640589689,
128.298918910331));
#228971=CARTESIAN_POINT('Ctrl Pts',(-56.088801642889,-5.1783407220741,134.229262269005));
#228972=CARTESIAN_POINT('Ctrl Pts',(-56.3672492667019,0.0824471093265141,
137.012288325754));
#228973=CARTESIAN_POINT('Ctrl Pts',(-56.6456968905149,5.26747007502141,
134.090532092806));
#228974=CARTESIAN_POINT('Ctrl Pts',(-56.9241445143275,5.6119453719906,128.148944812513));
#228975=CARTESIAN_POINT('Ctrl Pts',(-57.2025921381407,0.799317030873196,
124.64755493279));
#228976=CARTESIAN_POINT('Ctrl Pts',(-57.4810397619534,-4.74784461280872,
126.803968700697));
#228977=CARTESIAN_POINT('Ctrl Pts',(-57.7594873857663,-5.93196900242356,
132.636547210196));
#228978=CARTESIAN_POINT('Ctrl Pts',(-58.0379350095792,-1.66490367160747,
136.785435748359));
#228979=CARTESIAN_POINT('Ctrl Pts',(-58.3163826333922,4.13212679834998,
135.438008433087));
#228980=CARTESIAN_POINT('Ctrl Pts',(-58.5948302572049,6.13193460624012,
129.832485141631));
#228981=CARTESIAN_POINT('Ctrl Pts',(-58.873277881018,2.49679407265481,125.120067933803));
#228982=CARTESIAN_POINT('Ctrl Pts',(-59.1517255048308,-3.43277823852872,
125.631238009216));
#228983=CARTESIAN_POINT('Ctrl Pts',(-59.4301731286437,-6.20779504904446,
130.896255040614));
#228984=CARTESIAN_POINT('Ctrl Pts',(-59.7086207524566,-3.27815147713605,
136.076825586523));
#228985=CARTESIAN_POINT('Ctrl Pts',(-59.9870683762695,2.66395315565763,
136.412258400192));
#228986=CARTESIAN_POINT('Ctrl Pts',(-60.2655160000824,6.15801497974849,
131.594307112665));
#228987=CARTESIAN_POINT('Ctrl Pts',(-60.5439636238952,3.99316187320697,
126.050433587173));
#228988=CARTESIAN_POINT('Ctrl Pts',(-60.8224112477081,-1.84121191800936,
124.875186760365));
#228989=CARTESIAN_POINT('Ctrl Pts',(-61.1008588715211,-5.98360190477769,
129.148561052078));
#228990=CARTESIAN_POINT('Ctrl Pts',(-61.3793064953339,-4.62735405625939,
134.943534254169));
#228991=CARTESIAN_POINT('Ctrl Pts',(-61.6577541191468,0.981206111148332,
136.934809094094));
#228992=CARTESIAN_POINT('Ctrl Pts',(-61.9362017429597,5.68808579699418,
133.292501273148));
#228993=CARTESIAN_POINT('Ctrl Pts',(-62.2146493667725,5.16789251384163,
127.36371374215));
#228994=CARTESIAN_POINT('Ctrl Pts',(-62.4930969905855,-0.10134152394658,
124.596712604715));
#228995=CARTESIAN_POINT('Ctrl Pts',(-62.7715446143984,-5.27744765203657,
127.534236730624));
#228996=CARTESIAN_POINT('Ctrl Pts',(-63.0499922382113,-5.60383720555579,
133.476844954201));
#228997=CARTESIAN_POINT('Ctrl Pts',(-63.3284398620242,-0.780574129835986,
136.963570630527));
#228998=CARTESIAN_POINT('Ctrl Pts',(-63.606887485837,4.75999843803683,134.790283199078));
#228999=CARTESIAN_POINT('Ctrl Pts',(-63.88533510965,5.92636498020503,128.954127638363));
#229000=CARTESIAN_POINT('Ctrl Pts',(-64.1637827334628,1.64669162458969,
124.818245796629));
#229001=CARTESIAN_POINT('Ctrl Pts',(-64.4422303572757,-4.14621088866563,
126.183311037368));
#229002=CARTESIAN_POINT('Ctrl Pts',(-64.7206779810887,-6.12894814889968,
131.794895091487));
#229003=CARTESIAN_POINT('Ctrl Pts',(-64.9991256049015,-2.47948147605779,
136.49622635437));
#229004=CARTESIAN_POINT('Ctrl Pts',(-65.2775732287142,3.44850754387722,
135.967011068231));
#229005=CARTESIAN_POINT('Ctrl Pts',(-65.5560208525274,6.20748659994837,
130.693572227424));
#229006=CARTESIAN_POINT('Ctrl Pts',(-65.83446847634,3.26208872324607,125.521942504845));
#229007=CARTESIAN_POINT('Ctrl Pts',(-66.1129161001531,-2.68100932822562,
125.204596967384));
#229008=CARTESIAN_POINT('Ctrl Pts',(-66.3913637239659,-6.1603907816451,
130.033160660777));
#229009=CARTESIAN_POINT('Ctrl Pts',(-66.6698113477789,-3.97867405855336,
135.570419439246));
#229010=CARTESIAN_POINT('Ctrl Pts',(-66.9482589715917,1.85924975531565,
136.727902995508));
#229011=CARTESIAN_POINT('Ctrl Pts',(-67.2267065954047,5.98861387344954,
132.441940487574));
#229012=CARTESIAN_POINT('Ctrl Pts',(-67.5051542192175,4.61473440193538,
126.651122079325));
#229013=CARTESIAN_POINT('Ctrl Pts',(-67.7836018430304,-0.999860542648545,
124.676926990737));
#229014=CARTESIAN_POINT('Ctrl Pts',(-68.0620494668433,-5.69563249444164,
128.33354406343));
#229015=CARTESIAN_POINT('Ctrl Pts',(-68.3404970906562,-5.15739643095884,
134.260720843274));
#229016=CARTESIAN_POINT('Ctrl Pts',(-68.618944714469,0.120234999752325,
137.011671428276));
#229017=CARTESIAN_POINT('Ctrl Pts',(-68.8973923382821,5.28737633949755,
134.058406622227));
#229018=CARTESIAN_POINT('Ctrl Pts',(-69.1758399620947,5.59567712593856,
128.114832506878));
#229019=CARTESIAN_POINT('Ctrl Pts',(-69.4542875859078,0.761823997666808,
124.642803334499));
#229020=CARTESIAN_POINT('Ctrl Pts',(-69.7327352097205,-4.77210816728929,
126.832944296451));
#229021=CARTESIAN_POINT('Ctrl Pts',(-70.0111828335336,-5.92070605695121,
132.672622843033));
#229022=CARTESIAN_POINT('Ctrl Pts',(-70.2896304573463,-1.62846432284579,
136.795459674095));
#229023=CARTESIAN_POINT('Ctrl Pts',(-70.5680780811594,4.16025656905012,
135.412769153666));
#229024=CARTESIAN_POINT('Ctrl Pts',(-70.8465257049722,6.12590491382102,
129.795176321834));
#229025=CARTESIAN_POINT('Ctrl Pts',(-71.1249733287852,2.46214590988275,
125.104974556385));
#229026=CARTESIAN_POINT('Ctrl Pts',(-71.4034209525978,-3.46420490272305,
125.652230150673));
#229027=CARTESIAN_POINT('Ctrl Pts',(-71.681868576411,-6.20712064554441,
130.93404194847));
#229028=CARTESIAN_POINT('Ctrl Pts',(-71.9603162002238,-3.24599574981168,
136.09668293845));
#229029=CARTESIAN_POINT('Ctrl Pts',(-72.2387638240367,2.69804066428979,
136.395938259856));
#229030=CARTESIAN_POINT('Ctrl Pts',(-72.5172114478495,6.16270951452303,
131.556806891751));
#229031=CARTESIAN_POINT('Ctrl Pts',(-72.7956590716624,3.96414938600637,
126.026214156713));
#229032=CARTESIAN_POINT('Ctrl Pts',(-73.0741066954753,-1.87727036878649,
124.886504593767));
#229033=CARTESIAN_POINT('Ctrl Pts',(-73.3525543192881,-5.99357036442037,
129.185015613353));
#229034=CARTESIAN_POINT('Ctrl Pts',(-73.6310019431012,-4.60207199734241,
134.971625582408));
#229035=CARTESIAN_POINT('Ctrl Pts',(-73.909449566914,1.01850571157763,136.928722630985));
#229036=CARTESIAN_POINT('Ctrl Pts',(-74.187897190727,5.70312642832773,133.257830180947));
#229037=CARTESIAN_POINT('Ctrl Pts',(-74.4663448145398,5.14685257066011,
127.332319060812));
#229038=CARTESIAN_POINT('Ctrl Pts',(-74.7447924383527,-0.139127361718492,
124.597444512675));
#229039=CARTESIAN_POINT('Ctrl Pts',(-75.0232400621657,-5.29725604542678,
127.566422640223));
#229040=CARTESIAN_POINT('Ctrl Pts',(-75.3016876859784,-5.58746520873256,
133.510907586884));
#229041=CARTESIAN_POINT('Ctrl Pts',(-75.5801353097915,-0.743066808063574,
136.968208090913));
#229042=CARTESIAN_POINT('Ctrl Pts',(-75.8585829336042,4.7841736883842,134.761233887624));
#229043=CARTESIAN_POINT('Ctrl Pts',(-76.1370305574171,5.91499228508486,
128.918086453158));
#229044=CARTESIAN_POINT('Ctrl Pts',(-76.41547818123,1.61022193523031,124.808332826166));
#229045=CARTESIAN_POINT('Ctrl Pts',(-76.693925805043,-4.17426370938676,
126.208635817229));
#229046=CARTESIAN_POINT('Ctrl Pts',(-76.9723734288558,-6.12280492919574,
131.832185386163));
#229047=CARTESIAN_POINT('Ctrl Pts',(-77.2508210526686,-2.44478753472383,
136.511214204787));
#229048=CARTESIAN_POINT('Ctrl Pts',(-77.5292686764817,3.47987016964863,
135.945923372052));
#229049=CARTESIAN_POINT('Ctrl Pts',(-77.8077163002943,6.20669718922256,
130.655787547247));
#229050=CARTESIAN_POINT('Ctrl Pts',(-78.0861639241075,3.22987270591563,
125.502183115868));
#229051=CARTESIAN_POINT('Ctrl Pts',(-78.3646115479203,-2.71504700607423,
125.221020782777));
#229052=CARTESIAN_POINT('Ctrl Pts',(-78.6430591717333,-6.16497115690175,
130.070674996542));
#229053=CARTESIAN_POINT('Ctrl Pts',(-78.921506795546,-3.94958799012119,
135.594550453492));
#229054=CARTESIAN_POINT('Ctrl Pts',(-79.199954419359,1.89527359148086,136.71647546501));
#229055=CARTESIAN_POINT('Ctrl Pts',(-79.4784020431719,5.9984713317742,132.405455754592));
#229056=CARTESIAN_POINT('Ctrl Pts',(-79.7568496669848,4.58936695978296,
126.623107831093));
#229057=CARTESIAN_POINT('Ctrl Pts',(-80.0352972907976,-1.0371414452086,
124.683126952807));
#229058=CARTESIAN_POINT('Ctrl Pts',(-80.3137449146107,-5.71056752923021,
128.368260773546));
#229059=CARTESIAN_POINT('Ctrl Pts',(-80.5921925384234,-5.13626103062165,
134.292051340844));
#229060=CARTESIAN_POINT('Ctrl Pts',(-80.8706401622364,0.158018434826916,
137.010824516613));
#229061=CARTESIAN_POINT('Ctrl Pts',(-81.1490877860493,5.30708667829958,
134.026160571776));
#229062=CARTESIAN_POINT('Ctrl Pts',(-81.4275354098621,5.57920153001237,
128.080819862696));
#229063=CARTESIAN_POINT('Ctrl Pts',(-81.705983033675,0.724302734791404,
124.63828005498));
#229064=CARTESIAN_POINT('Ctrl Pts',(-81.984430657488,-4.79619488954742,
126.862067054498));
#229065=CARTESIAN_POINT('Ctrl Pts',(-82.2628782813007,-5.90922371753823,
132.708629246728));
#229066=CARTESIAN_POINT('Ctrl Pts',(-82.5413259051138,-1.59196463073914,
136.805261597452));
#229067=CARTESIAN_POINT('Ctrl Pts',(-82.8197735289264,4.18823217991362,
135.387359107972));
#229068=CARTESIAN_POINT('Ctrl Pts',(-83.0982211527395,6.11964822374235,
129.757904897731));
#229069=CARTESIAN_POINT('Ctrl Pts',(-83.3766687765523,2.42740651138818,
125.090092371815));
#229070=CARTESIAN_POINT('Ctrl Pts',(-83.6551164003652,-3.49550319953123,
125.67341320622));
#229071=CARTESIAN_POINT('Ctrl Pts',(-83.9335640241781,-6.20621623490623,
130.971824050937));
#229072=CARTESIAN_POINT('Ctrl Pts',(-84.2120116479911,-3.21371974092037,
136.116344181428));
#229073=CARTESIAN_POINT('Ctrl Pts',(-84.4904592718038,2.73202819603347,
136.379410921554));
#229074=CARTESIAN_POINT('Ctrl Pts',(-84.7689068956169,6.16717568783019,
131.519278788663));
#229075=CARTESIAN_POINT('Ctrl Pts',(-85.0473545194296,3.9349900057924,126.002171782228));
#229076=CARTESIAN_POINT('Ctrl Pts',(-85.3258021432425,-1.91325925661942,
124.898041715501));
#229077=CARTESIAN_POINT('Ctrl Pts',(-85.6042497670555,-6.00331673010926,
129.221530180052));
#229078=CARTESIAN_POINT('Ctrl Pts',(-85.8826973908683,-4.57661940695503,
134.999562491112));
#229079=CARTESIAN_POINT('Ctrl Pts',(-86.1611450146813,1.05576757090286,
136.922409227389));
#229080=CARTESIAN_POINT('Ctrl Pts',(-86.4395926384942,5.71795572821454,
133.223068174528));
#229081=CARTESIAN_POINT('Ctrl Pts',(-86.718040262307,5.12562190896342,127.301053037252));
#229082=CARTESIAN_POINT('Ctrl Pts',(-86.9964878861199,-0.176908044074368,
124.598406420195));
#229083=CARTESIAN_POINT('Ctrl Pts',(-87.2749355099329,-5.31686814704595,
127.598728532803));
#229084=CARTESIAN_POINT('Ctrl Pts',(-87.5533831337457,-5.57088616633168,
133.544869927476));
#229085=CARTESIAN_POINT('Ctrl Pts',(-87.8318307575586,-0.70553195167748,
136.972617147663));
#229086=CARTESIAN_POINT('Ctrl Pts',(-88.1102783813713,4.80817165941601,
134.732037952774));
#229087=CARTESIAN_POINT('Ctrl Pts',(-88.3887260051845,5.90340040775061,
128.882115164534));
#229088=CARTESIAN_POINT('Ctrl Pts',(-88.6671736289971,1.57369257850503,
124.798642040718));
#229089=CARTESIAN_POINT('Ctrl Pts',(-88.9456212528103,-4.20216185122988,
126.234130893362));
#229090=CARTESIAN_POINT('Ctrl Pts',(-89.2240688766231,-6.11643482670397,
131.869437594414));
#229091=CARTESIAN_POINT('Ctrl Pts',(-89.5025165004358,-2.41000300088966,
136.525990585645));
#229092=CARTESIAN_POINT('Ctrl Pts',(-89.7809641242489,3.51110384754994,
135.924645153375));
#229093=CARTESIAN_POINT('Ctrl Pts',(-90.0594117480617,6.20567778705031,
130.618008372501));
#229094=CARTESIAN_POINT('Ctrl Pts',(-90.3378593718745,3.19753700446471,
125.482620201028));
#229095=CARTESIAN_POINT('Ctrl Pts',(-90.6163069956876,-2.74898407685696,
125.237651490881));
#229096=CARTESIAN_POINT('Ctrl Pts',(-90.8947546195002,-6.16932308688508,
130.108216519297));
#229097=CARTESIAN_POINT('Ctrl Pts',(-91.1732022433134,-3.92035556825405,
135.618503965492));
#229098=CARTESIAN_POINT('Ctrl Pts',(-91.4516498671261,1.93122719758584,
136.70482885892));
#229099=CARTESIAN_POINT('Ctrl Pts',(-91.7300974909391,6.00810651453776,
132.368911692441));
#229100=CARTESIAN_POINT('Ctrl Pts',(-92.0085451147519,4.56382945695037,
126.595248520721));
#229101=CARTESIAN_POINT('Ctrl Pts',(-92.2869927385648,-1.07438391611076,
124.689553739443));
#229102=CARTESIAN_POINT('Ctrl Pts',(-92.5654403623776,-5.72529095683809,
128.403067754236));
#229103=CARTESIAN_POINT('Ctrl Pts',(-92.8438879861907,-5.11493530424405,
134.323252600751));
#229104=CARTESIAN_POINT('Ctrl Pts',(-93.1223356100035,0.195796014469281,
137.009747622148));
#229105=CARTESIAN_POINT('Ctrl Pts',(-93.4007832338166,5.32660036105212,
133.993795136343));
#229106=CARTESIAN_POINT('Ctrl Pts',(-93.6792308576291,5.56251919472255,
128.046908140318));
#229107=CARTESIAN_POINT('Ctrl Pts',(-93.9576784814422,0.686754632612129,
124.633985261843));
#229108=CARTESIAN_POINT('Ctrl Pts',(-94.2361261052551,-4.82010388703947,
126.891335895681));
#229109=CARTESIAN_POINT('Ctrl Pts',(-94.5145737290679,-5.8975224096676,
132.744565087048));
#229110=CARTESIAN_POINT('Ctrl Pts',(-94.7930213528811,-1.55540594779807,
136.814841155217));
#229111=CARTESIAN_POINT('Ctrl Pts',(-95.0714689766937,4.21605259429308,
135.361779237583));
#229112=CARTESIAN_POINT('Ctrl Pts',(-95.3499166005066,6.11316476784841,
129.720672250431));
#229113=CARTESIAN_POINT('Ctrl Pts',(-95.6283642243196,2.39257716445285,
125.075421931555));
#229114=CARTESIAN_POINT('Ctrl Pts',(-95.9068118481323,-3.52667196918255,
125.694786390909));
#229115=CARTESIAN_POINT('Ctrl Pts',(-96.1852594719453,-6.20508185064282,
131.009599947983));
#229116=CARTESIAN_POINT('Ctrl Pts',(-96.4637070957582,-3.18132464646333,
136.135808586901));
#229117=CARTESIAN_POINT('Ctrl Pts',(-96.742154719571,2.76591449146702,136.362676997713));
#229118=CARTESIAN_POINT('Ctrl Pts',(-97.020602343384,6.17141333417382,131.481724194021));
#229119=CARTESIAN_POINT('Ctrl Pts',(-97.299049967197,3.90568481307747,125.978307354616));
#229120=CARTESIAN_POINT('Ctrl Pts',(-97.5774975910097,-1.94917724792726,
124.909797698053));
#229121=CARTESIAN_POINT('Ctrl Pts',(-97.8559452148228,-6.01284064068852,
129.258103399115));
#229122=CARTESIAN_POINT('Ctrl Pts',(-98.1343928386354,-4.55099722825276,
135.027343945068));
#229123=CARTESIAN_POINT('Ctrl Pts',(-98.4128404624484,1.09299030837272,
136.915869117251));
#229124=CARTESIAN_POINT('Ctrl Pts',(-98.6912880862614,5.73257314714861,
133.188216542011));
#229125=CARTESIAN_POINT('Ctrl Pts',(-98.9697357100741,5.10420131546234,
127.269916830042));
#229126=CARTESIAN_POINT('Ctrl Pts',(-99.2481833338871,-0.214682171037078,
124.599598291628));
#229127=CARTESIAN_POINT('Ctrl Pts',(-99.5266309576999,-5.33628323016052,
127.631153211259));
#229128=CARTESIAN_POINT('Ctrl Pts',(-99.8050785815131,-5.55410069269506,
133.578730717485));
#229129=CARTESIAN_POINT('Ctrl Pts',(-100.083526205326,-0.667970951546107,
136.976797637399));
#229130=CARTESIAN_POINT('Ctrl Pts',(-100.361973829139,4.83199146187865,
134.702696476397));
#229131=CARTESIAN_POINT('Ctrl Pts',(-100.640421452952,5.89158977774298,
128.846215105423));
#229132=CARTESIAN_POINT('Ctrl Pts',(-100.918869076765,1.53710490802326,
124.789173799381));
#229133=CARTESIAN_POINT('Ctrl Pts',(-101.197316700577,-4.22990428042106,
126.259795321038));
#229134=CARTESIAN_POINT('Ctrl Pts',(-101.47576432439,-6.10983807746976,
131.906650335846));
#229135=CARTESIAN_POINT('Ctrl Pts',(-101.754211948203,-2.37512916350784,
136.540554949401));
#229136=CARTESIAN_POINT('Ctrl Pts',(-102.032659572016,3.54220742020778,
135.903177200671));
#229137=CARTESIAN_POINT('Ctrl Pts',(-102.311107195829,6.20442843120499,
130.580236103105));
#229138=CARTESIAN_POINT('Ctrl Pts',(-102.589554819642,3.16508281710451,
125.463254485237));
#229139=CARTESIAN_POINT('Ctrl Pts',(-102.868002443455,-2.78281928302352,
125.254488475437));
#229140=CARTESIAN_POINT('Ctrl Pts',(-103.146450067268,-6.1734464103326,
130.145783837928));
#229141=CARTESIAN_POINT('Ctrl Pts',(-103.424897691081,-3.8909778761698,
135.642279087639));
#229142=CARTESIAN_POINT('Ctrl Pts',(-103.703345314893,1.96710924135641,
136.69296360881));
#229143=CARTESIAN_POINT('Ctrl Pts',(-103.981792938706,6.01751906470488,
132.332309655276));
#229144=CARTESIAN_POINT('Ctrl Pts',(-104.260240562519,4.53812283973896,
126.567545180546));
#229145=CARTESIAN_POINT('Ctrl Pts',(-104.538688186332,-1.11158657532129,
124.696207112496));
#229146=CARTESIAN_POINT('Ctrl Pts',(-104.817135810145,-5.73980223168479,
128.437963715717));
#229147=CARTESIAN_POINT('Ctrl Pts',(-105.095583433958,-5.093420042057,134.354323466822));
#229148=CARTESIAN_POINT('Ctrl Pts',(-105.374031057771,0.233566338818549,
137.008440784786));
#229149=CARTESIAN_POINT('Ctrl Pts',(-105.652478681584,5.34591666467016,
133.961311515241));
#229150=CARTESIAN_POINT('Ctrl Pts',(-105.930926305397,5.54563073823764,
128.013098596357));
#229151=CARTESIAN_POINT('Ctrl Pts',(-106.20937392921,0.649181082487974,
124.629919114234));
#229152=CARTESIAN_POINT('Ctrl Pts',(-106.487821553022,-4.84383427380942,
126.920749735436));
#229153=CARTESIAN_POINT('Ctrl Pts',(-106.766269176835,-5.88560256693534,
132.780429032376));
#229154=CARTESIAN_POINT('Ctrl Pts',(-107.044716800648,-1.51878962871805,
136.824197992414));
#229155=CARTESIAN_POINT('Ctrl Pts',(-107.323164424461,4.2437167812931,135.336030490371));
#229156=CARTESIAN_POINT('Ctrl Pts',(-107.601612048274,6.10645478638612,
129.683479759601));
#229157=CARTESIAN_POINT('Ctrl Pts',(-107.880059672087,2.35765915969063,
125.060963779225));
#229158=CARTESIAN_POINT('Ctrl Pts',(-108.1585072959,-3.55771005670707,125.716348912751));
#229159=CARTESIAN_POINT('Ctrl Pts',(-108.436954919713,-6.20371753478999,
131.04736823981));
#229160=CARTESIAN_POINT('Ctrl Pts',(-108.715402543526,-3.14881166685081,
136.155075433609));
#229161=CARTESIAN_POINT('Ctrl Pts',(-108.993850167338,2.79969829492213,
136.345737108415));
#229162=CARTESIAN_POINT('Ctrl Pts',(-109.272297791151,6.17542229652738,
131.444144499421));
#229163=CARTESIAN_POINT('Ctrl Pts',(-109.550745414964,3.87623489377466,
125.954621758183));
#229164=CARTESIAN_POINT('Ctrl Pts',(-109.829193038777,-1.98502301175461,
124.921772105802));
#229165=CARTESIAN_POINT('Ctrl Pts',(-110.10764066259,-6.02214174324697,
129.294733915307));
#229166=CARTESIAN_POINT('Ctrl Pts',(-110.386088286403,-4.52520641067474,
135.054968914823));
#229167=CARTESIAN_POINT('Ctrl Pts',(-110.664535910216,1.13017254468408,
136.909102542919));
#229168=CARTESIAN_POINT('Ctrl Pts',(-110.942983534029,5.74697814347679,
133.153276574838));
#229169=CARTESIAN_POINT('Ctrl Pts',(-111.221431157841,5.08259158390449,
127.238911592946));
#229170=CARTESIAN_POINT('Ctrl Pts',(-111.499878781655,-0.252448342873548,
124.601020082813));
#229171=CARTESIAN_POINT('Ctrl Pts',(-111.778326405467,-5.3555005753377,
127.663695474083));
#229172=CARTESIAN_POINT('Ctrl Pts',(-112.05677402928,-5.53710940981492,
133.612488702192));
#229173=CARTESIAN_POINT('Ctrl Pts',(-112.335221653093,-0.630385199504834,
136.980749405212));
#229174=CARTESIAN_POINT('Ctrl Pts',(-112.613669276906,4.85563221312083,
134.673210545752));
#229175=CARTESIAN_POINT('Ctrl Pts',(-112.892116900719,5.8795608327098,128.810387606114));
#229176=CARTESIAN_POINT('Ctrl Pts',(-113.170564524532,1.50046027955312,
124.779928453004));
#229177=CARTESIAN_POINT('Ctrl Pts',(-113.449012148345,-4.25748996895278,
126.285628149252));
#229178=CARTESIAN_POINT('Ctrl Pts',(-113.727459772158,-6.10301492593933,
131.943822231527));
#229179=CARTESIAN_POINT('Ctrl Pts',(-114.00590739597,-2.3401673148416,136.554906756366));
#229180=CARTESIAN_POINT('Ctrl Pts',(-114.284355019783,3.57317973506622,
135.881520309444));
#229181=CARTESIAN_POINT('Ctrl Pts',(-114.562802643596,6.202949167983,130.542472138726));
#229182=CARTESIAN_POINT('Ctrl Pts',(-114.841250267409,3.13251134643626,
125.444086686097));
#229183=CARTESIAN_POINT('Ctrl Pts',(-115.119697891222,-2.81655137079845,
125.271531112549));
#229184=CARTESIAN_POINT('Ctrl Pts',(-115.398145515035,-6.17734097445314,
130.183375560363));
#229185=CARTESIAN_POINT('Ctrl Pts',(-115.676593138848,-3.86145600246928,
135.665874938939));
#229186=CARTESIAN_POINT('Ctrl Pts',(-115.955040762661,2.00291839317105,
136.680880154352));
#229187=CARTESIAN_POINT('Ctrl Pts',(-116.233488386474,6.02670863349017,
132.295650999397));
#229188=CARTESIAN_POINT('Ctrl Pts',(-116.511936010287,4.51224806071678,
126.539998837124));
#229189=CARTESIAN_POINT('Ctrl Pts',(-116.790383634099,-1.14874804428301,
124.703086825424));
#229190=CARTESIAN_POINT('Ctrl Pts',(-117.068831257912,-5.75410081604829,
128.472947364906));
#229191=CARTESIAN_POINT('Ctrl Pts',(-117.347278881725,-5.07171604131793,
134.385262787713));
#229192=CARTESIAN_POINT('Ctrl Pts',(-117.625726505538,0.271328008281021,
137.006904052952));
#229193=CARTESIAN_POINT('Ctrl Pts',(-117.904174129351,5.3650348733795,133.928710912162));
#229194=CARTESIAN_POINT('Ctrl Pts',(-118.182621753164,5.52853678636705,
127.979392483636));
#229195=CARTESIAN_POINT('Ctrl Pts',(-118.461069376977,0.611583476719488,
124.626081762825));
#229196=CARTESIAN_POINT('Ctrl Pts',(-118.73951700079,-4.86738517051901,
126.95030748382));
#229197=CARTESIAN_POINT('Ctrl Pts',(-119.017964624603,-5.87346463103546,
132.816219753764));
#229198=CARTESIAN_POINT('Ctrl Pts',(-119.296412248415,-1.48211703032935,
136.833331762325));
#229199=CARTESIAN_POINT('Ctrl Pts',(-119.574859872228,4.27122371580729,
135.310113820466));
#229200=CARTESIAN_POINT('Ctrl Pts',(-119.853307496041,6.09951852799569,
129.646328803424));
#229201=CARTESIAN_POINT('Ctrl Pts',(-120.131755119854,2.32265379100196,
125.046718450578));
#229202=CARTESIAN_POINT('Ctrl Pts',(-120.410202743667,-3.58861631197691,
125.738099972737));
#229203=CARTESIAN_POINT('Ctrl Pts',(-120.68865036748,-6.20212333790203,
131.085127526901));
#229204=CARTESIAN_POINT('Ctrl Pts',(-120.967097991293,-3.11618200686478,
136.174144007612));
#229205=CARTESIAN_POINT('Ctrl Pts',(-121.245545615105,2.83337835452712,
136.328591881372));
#229206=CARTESIAN_POINT('Ctrl Pts',(-121.523993238919,6.17920242633619,
131.406541097396));
#229207=CARTESIAN_POINT('Ctrl Pts',(-121.802440862731,3.84664133916317,
125.931115870606));
#229208=CARTESIAN_POINT('Ctrl Pts',(-122.080888486544,-2.02079521982502,
124.933964495032));
#229209=CARTESIAN_POINT('Ctrl Pts',(-122.359336110357,-6.03121969312815,
129.331420371272));
#229210=CARTESIAN_POINT('Ctrl Pts',(-122.63778373417,-4.49924790990888,
135.082436376724));
#229211=CARTESIAN_POINT('Ctrl Pts',(-122.916231357983,1.16731290203685,
136.90210975513));
#229212=CARTESIAN_POINT('Ctrl Pts',(-123.194678981796,5.76117018341619,
133.118249567719));
#229213=CARTESIAN_POINT('Ctrl Pts',(-123.473126605609,5.06079351504635,
127.208038474877));
#229214=CARTESIAN_POINT('Ctrl Pts',(-123.751574229422,-0.290205160143283,
124.602671741062));
#229215=CARTESIAN_POINT('Ctrl Pts',(-124.030021853235,-5.37451947047147,
127.696354115408));
#229216=CARTESIAN_POINT('Ctrl Pts',(-124.308469477047,-5.51991294730918,
133.646142630679));
#229217=CARTESIAN_POINT('Ctrl Pts',(-124.58691710086,-0.592776088308802,
136.984472304668));
#229218=CARTESIAN_POINT('Ctrl Pts',(-124.865364724673,4.87909303712557,
134.64358125345));
#229219=CARTESIAN_POINT('Ctrl Pts',(-125.143812348486,5.86731401838748,
128.774633994209));
#229220=CARTESIAN_POINT('Ctrl Pts',(-125.422259972299,1.46376005097626,
124.770906344175));
#229221=CARTESIAN_POINT('Ctrl Pts',(-125.700707596112,-4.28491789462882,
126.311628420759));
#229222=CARTESIAN_POINT('Ctrl Pts',(-125.979155219925,-6.09596562494584,
131.980951904039));
#229223=CARTESIAN_POINT('Ctrl Pts',(-126.257602843738,-2.30511875041471,
136.569045474729));
#229224=CARTESIAN_POINT('Ctrl Pts',(-126.536050467551,3.60401964443632,
135.859675282198));
#229225=CARTESIAN_POINT('Ctrl Pts',(-126.814498091363,6.20124005219796,
130.50471787872));
#229226=CARTESIAN_POINT('Ctrl Pts',(-127.092945715177,3.09982379940838,
125.42511751388));
#229227=CARTESIAN_POINT('Ctrl Pts',(-127.371393338989,-2.85017909022625,
125.288778770691));
#229228=CARTESIAN_POINT('Ctrl Pts',(-127.649840962802,-6.18100663493216,
130.220990293627));
#229229=CARTESIAN_POINT('Ctrl Pts',(-127.928288586615,-3.83179104109667,
135.689290645038));
#229230=CARTESIAN_POINT('Ctrl Pts',(-128.206736210428,2.03865332610762,
136.6685789433));
#229231=CARTESIAN_POINT('Ctrl Pts',(-128.485183834241,6.03567488037103,
132.258937083203));
#229232=CARTESIAN_POINT('Ctrl Pts',(-128.763631458054,4.48620607868298,
126.512610511197));
#229233=CARTESIAN_POINT('Ctrl Pts',(-129.042079081867,-1.18586694596332,
124.710192623294));
#229234=CARTESIAN_POINT('Ctrl Pts',(-129.32052670568,-5.76818618009069,
128.508017405469));
#229235=CARTESIAN_POINT('Ctrl Pts',(-129.598974329492,-5.04982410627509,
134.416069416958));
#229236=CARTESIAN_POINT('Ctrl Pts',(-129.877421953305,0.30907962358457,
137.005137483589));
#229237=CARTESIAN_POINT('Ctrl Pts',(-130.155869577118,5.38395427874936,
133.895994535135));
#229238=CARTESIAN_POINT('Ctrl Pts',(-130.434317200931,5.51123797253198,
127.945791051148));
#229239=CARTESIAN_POINT('Ctrl Pts',(-130.712764824744,0.573963208500954,
124.622473349811));
#229240=CARTESIAN_POINT('Ctrl Pts',(-130.991212448557,-4.89075570448117,
126.980008045559));
#229241=CARTESIAN_POINT('Ctrl Pts',(-131.26966007237,-5.8611090517438,132.851935924971));
#229242=CARTESIAN_POINT('Ctrl Pts',(-131.548107696183,-1.44538951154951,
136.842242126491));
#229243=CARTESIAN_POINT('Ctrl Pts',(-131.826555319995,4.29857237855583,
135.28403018822));
#229244=CARTESIAN_POINT('Ctrl Pts',(-132.105002943808,6.09235624970348,
129.609220758541));
#229245=CARTESIAN_POINT('Ctrl Pts',(-132.383450567622,2.28756235552218,
125.032686473479));
#229246=CARTESIAN_POINT('Ctrl Pts',(-132.661898191434,-3.6193895897498,
125.760038764874));
#229247=CARTESIAN_POINT('Ctrl Pts',(-132.940345815247,-6.20029931905343,
131.122876410071));
#229248=CARTESIAN_POINT('Ctrl Pts',(-133.21879343906,-3.08343687560774,
136.193013602317));
#229249=CARTESIAN_POINT('Ctrl Pts',(-133.497241062873,2.86695342225543,
136.311241951909));
#229250=CARTESIAN_POINT('Ctrl Pts',(-133.775688686686,6.18275358352724,
131.368915381349));
#229251=CARTESIAN_POINT('Ctrl Pts',(-134.054136310499,3.81690524584148,
125.907790562906));
#229252=CARTESIAN_POINT('Ctrl Pts',(-134.332583934311,-2.05649254658467,
124.946374413949));
#229253=CARTESIAN_POINT('Ctrl Pts',(-134.611031558124,-6.04007415394596,
129.36816140758));
#229254=CARTESIAN_POINT('Ctrl Pts',(-134.889479181937,-4.47312268785726,
135.109745312956));
#229255=CARTESIAN_POINT('Ctrl Pts',(-135.16792680575,1.20441000418008,136.894891013003));
#229256=CARTESIAN_POINT('Ctrl Pts',(-135.446374429563,5.775148741076,133.083136818595));
#229257=CARTESIAN_POINT('Ctrl Pts',(-135.724822053376,5.03880791662344,
127.177298619846));
#229258=CARTESIAN_POINT('Ctrl Pts',(-136.003269677189,-0.327951223754644,
124.604553205172));
#229259=CARTESIAN_POINT('Ctrl Pts',(-136.281717301002,-5.39333921080989,
127.729127925058));
#229260=CARTESIAN_POINT('Ctrl Pts',(-136.560164924815,-5.50251194239939,
133.679691255889));
#229261=CARTESIAN_POINT('Ctrl Pts',(-136.838612548628,-0.555145011576188,
136.987966197812));
#229262=CARTESIAN_POINT('Ctrl Pts',(-137.117060172441,4.90237306454367,
134.613809697415));
#229263=CARTESIAN_POINT('Ctrl Pts',(-137.395507796253,5.8548497885868,128.73895559457));
#229264=CARTESIAN_POINT('Ctrl Pts',(-137.673955420066,1.42700558223168,
124.762107807213));
#229265=CARTESIAN_POINT('Ctrl Pts',(-137.952403043879,-4.3121870410957,
126.33779517211));
#229266=CARTESIAN_POINT('Ctrl Pts',(-138.230850667692,-6.08869043570493,
132.018037977528));
#229267=CARTESIAN_POINT('Ctrl Pts',(-138.509298291505,-2.26998476896503,
136.582970580575));
#229268=CARTESIAN_POINT('Ctrl Pts',(-138.787745915318,3.63472600553235,
135.837642928407));
#229269=CARTESIAN_POINT('Ctrl Pts',(-139.066193539131,6.1993011471828,130.466974722087));
#229270=CARTESIAN_POINT('Ctrl Pts',(-139.344641162943,3.06702138726935,
125.406347671494));
#229271=CARTESIAN_POINT('Ctrl Pts',(-139.623088786757,-2.88370119522,125.306230810748));
#229272=CARTESIAN_POINT('Ctrl Pts',(-139.901536410569,-6.18444325593727,
130.258626643894));
#229273=CARTESIAN_POINT('Ctrl Pts',(-140.179984034382,-3.80198409129777,
135.712525338258));
#229274=CARTESIAN_POINT('Ctrl Pts',(-140.458431658195,2.07431271599591,
136.656060431482));
#229275=CARTESIAN_POINT('Ctrl Pts',(-140.736879282008,6.04441747309895,
132.222169267145));
#229276=CARTESIAN_POINT('Ctrl Pts',(-141.015326905821,4.45999785863389,
126.485381217648));
#229277=CARTESIAN_POINT('Ctrl Pts',(-141.293774529634,-1.22294190490765,
124.717524242802));
#229278=CARTESIAN_POINT('Ctrl Pts',(-141.572222153447,-5.78205780187226,
128.543172537875));
#229279=CARTESIAN_POINT('Ctrl Pts',(-141.85066977726,-5.02774504814366,
134.446742213005));
#229280=CARTESIAN_POINT('Ctrl Pts',(-142.129117401072,0.346819785828787,
137.003141142159));
#229281=CARTESIAN_POINT('Ctrl Pts',(-142.407565024885,5.40267417971275,
133.863163596476));
#229282=CARTESIAN_POINT('Ctrl Pts',(-142.686012648698,5.49373493774783,
127.912295544006));
#229283=CARTESIAN_POINT('Ctrl Pts',(-142.964460272511,0.536321671864061,
124.619094008905));
#229284=CARTESIAN_POINT('Ctrl Pts',(-143.242907896324,-4.91394500969209,
127.00985032009));
#229285=CARTESIAN_POINT('Ctrl Pts',(-143.521355520137,-5.84853628690073,
132.887576222521));
#229286=CARTESIAN_POINT('Ctrl Pts',(-143.79980314395,-1.40860843332932,
136.850928754739));
#229287=CARTESIAN_POINT('Ctrl Pts',(-144.078250767763,4.32576175612421,
135.257780560169));
#229288=CARTESIAN_POINT('Ctrl Pts',(-144.356698391576,6.08496821690962,
129.572157000006));
#229289=CARTESIAN_POINT('Ctrl Pts',(-144.635146015388,2.2523861535788,125.018868367886));
#229290=CARTESIAN_POINT('Ctrl Pts',(-144.913593639201,-3.65002874971022,
125.782164476213));
#229291=CARTESIAN_POINT('Ctrl Pts',(-145.192041263014,-6.19824554583293,
131.160613490521));
#229292=CARTESIAN_POINT('Ctrl Pts',(-145.470488886827,-3.05057748646412,
136.211683518503));
#229293=CARTESIAN_POINT('Ctrl Pts',(-145.74893651064,2.90042225397064,136.293687962933));
#229294=CARTESIAN_POINT('Ctrl Pts',(-146.027384134453,6.18607563651005,
131.33126874552));
#229295=CARTESIAN_POINT('Ctrl Pts',(-146.305831758266,3.78702771569254,
125.884646699409));
#229296=CARTESIAN_POINT('Ctrl Pts',(-146.584279382079,-2.09211366925746,
124.959001402698));
#229297=CARTESIAN_POINT('Ctrl Pts',(-146.862727005891,-6.04870479759444,
129.404955662777));
#229298=CARTESIAN_POINT('Ctrl Pts',(-147.141174629705,-4.4468317125993,
135.136894711575));
#229299=CARTESIAN_POINT('Ctrl Pts',(-147.419622253517,1.24146247646836,
136.887446584034));
#229300=CARTESIAN_POINT('Ctrl Pts',(-147.69806987733,5.78891329847519,133.04793962858));
#229301=CARTESIAN_POINT('Ctrl Pts',(-147.976517501143,5.01663560332014,
127.146693166932));
#229302=CARTESIAN_POINT('Ctrl Pts',(-148.254965124956,-0.365685135012239,
124.606664405427));
#229303=CARTESIAN_POINT('Ctrl Pts',(-148.533412748769,-5.41195909898036,
127.762015688586));
#229304=CARTESIAN_POINT('Ctrl Pts',(-148.811860372582,-5.48490703988586,
133.713133334664));
#229305=CARTESIAN_POINT('Ctrl Pts',(-149.090307996395,-0.517493363741682,
136.991230955176));
#229306=CARTESIAN_POINT('Ctrl Pts',(-149.368755620208,4.92547143272535,
134.583896980843));
#229307=CARTESIAN_POINT('Ctrl Pts',(-149.647203244021,5.84216860517359,
128.703353729273));
#229308=CARTESIAN_POINT('Ctrl Pts',(-149.925650867833,1.39019823527075,
124.753533168151));
#229309=CARTESIAN_POINT('Ctrl Pts',(-150.204098491647,-4.33929639788676,
126.364127433687));
#229310=CARTESIAN_POINT('Ctrl Pts',(-150.482546115459,-6.08118962780021,
132.055079077756));
#229311=CARTESIAN_POINT('Ctrl Pts',(-150.760993739272,-2.23476667239474,
136.596681557904));
#229312=CARTESIAN_POINT('Ctrl Pts',(-151.039441363085,3.66529768052036,
135.81542406449));
#229313=CARTESIAN_POINT('Ctrl Pts',(-151.317888986898,6.19713252478332,
130.429244067412));
#229314=CARTESIAN_POINT('Ctrl Pts',(-151.596336610711,3.03410532552526,
125.387777854462));
#229315=CARTESIAN_POINT('Ctrl Pts',(-151.874784234524,-2.91711644360522,
125.323886586026));
#229316=CARTESIAN_POINT('Ctrl Pts',(-152.153231858337,-6.18765071012318,
130.296283216534));
#229317=CARTESIAN_POINT('Ctrl Pts',(-152.431679482149,-3.77203625758034,
135.735578157629));
#229318=CARTESIAN_POINT('Ctrl Pts',(-152.710127105962,2.10989524146327,
136.643325082775));
#229319=CARTESIAN_POINT('Ctrl Pts',(-152.988574729775,6.0529360877152,132.185348913665));
#229320=CARTESIAN_POINT('Ctrl Pts',(-153.267022353588,4.43362437172323,
126.458311965469));
#229321=CARTESIAN_POINT('Ctrl Pts',(-153.545469977401,-1.25997154729018,
124.725081412269));
#229322=CARTESIAN_POINT('Ctrl Pts',(-153.823917601214,-5.79571516737629,
128.578411459437));
#229323=CARTESIAN_POINT('Ctrl Pts',(-154.102365225027,-5.00547968506979,
134.477280039263));
#229324=CARTESIAN_POINT('Ctrl Pts',(-154.38081284884,0.38454709653853,137.000915102638));
#229325=CARTESIAN_POINT('Ctrl Pts',(-154.659260472653,5.4211938825983,133.830219312748));
#229326=CARTESIAN_POINT('Ctrl Pts',(-154.937708096465,5.47602833059452,
127.8789072034));
#229327=CARTESIAN_POINT('Ctrl Pts',(-155.216155720278,0.498660261630971,
124.615943865326));
#229328=CARTESIAN_POINT('Ctrl Pts',(-155.494603344091,-4.93695222686361,
127.039833201595));
#229329=CARTESIAN_POINT('Ctrl Pts',(-155.773050967904,-5.83574680239484,
132.923139325752));
#229330=CARTESIAN_POINT('Ctrl Pts',(-156.051498591717,-1.37177515860606,
136.85939132518));
#229331=CARTESIAN_POINT('Ctrl Pts',(-156.32994621553,4.3527908409998,135.231365909006));
#229332=CARTESIAN_POINT('Ctrl Pts',(-156.608393839343,6.0773547033811,129.535138901228));
#229333=CARTESIAN_POINT('Ctrl Pts',(-156.886841463156,2.21712648863745,
125.005264645838));
#229334=CARTESIAN_POINT('Ctrl Pts',(-157.165289086968,-3.68053265651321,
125.804476286877));
#229335=CARTESIAN_POINT('Ctrl Pts',(-157.443736710782,-6.19596209434481,
131.19833736989));
#229336=CARTESIAN_POINT('Ctrl Pts',(-157.722184334594,-3.0176050570491,
136.230153064351));
#229337=CARTESIAN_POINT('Ctrl Pts',(-158.000631958407,2.93378360947182,
136.275930564914));
#229338=CARTESIAN_POINT('Ctrl Pts',(-158.27907958222,6.18916846218569,131.293602584915));
#229339=CARTESIAN_POINT('Ctrl Pts',(-158.557527206033,3.7570098558391,125.861685137721));
#229340=CARTESIAN_POINT('Ctrl Pts',(-158.835974829846,-2.12765726788813,
124.971844993383));
#229341=CARTESIAN_POINT('Ctrl Pts',(-159.114422453659,-6.05711130426257,
129.44180177344));
#229342=CARTESIAN_POINT('Ctrl Pts',(-159.392870077472,-4.42037595835707,
135.163883566548));
#229343=CARTESIAN_POINT('Ctrl Pts',(-159.671317701285,1.27846894590735,
136.879776744077));
#229344=CARTESIAN_POINT('Ctrl Pts',(-159.949765325097,5.80246334556346,
133.01265930192));
#229345=CARTESIAN_POINT('Ctrl Pts',(-160.22821294891,4.9942773967397,127.116223250229));
#229346=CARTESIAN_POINT('Ctrl Pts',(-160.506660572723,-0.403405495673234,
124.609005263594));
#229347=CARTESIAN_POINT('Ctrl Pts',(-160.785108196536,-5.43037844501628,
127.795016187323));
#229348=CARTESIAN_POINT('Ctrl Pts',(-161.063555820349,-5.46709889212507,
133.746467627798));
#229349=CARTESIAN_POINT('Ctrl Pts',(-161.342003444162,-0.479822539999598,
136.994266455786));
#229350=CARTESIAN_POINT('Ctrl Pts',(-161.620451067975,4.94838728575097,
134.553844212161));
#229351=CARTESIAN_POINT('Ctrl Pts',(-161.898898691787,5.82927093805496,
128.66782971756));
#229352=CARTESIAN_POINT('Ctrl Pts',(-162.177346315601,1.35333937400316,
124.745182744726));
#229353=CARTESIAN_POINT('Ctrl Pts',(-162.455793939413,-4.36624496045326,
126.390624229737));
#229354=CARTESIAN_POINT('Ctrl Pts',(-162.734241563226,-6.07346347917808,
132.092073832152));
#229355=CARTESIAN_POINT('Ctrl Pts',(-163.012689187039,-2.19946576572379,
136.61017789865));
#229356=CARTESIAN_POINT('Ctrl Pts',(-163.291136810852,3.69573353655413,
135.793019513774));
#229357=CARTESIAN_POINT('Ctrl Pts',(-163.569584434665,6.19473426535967,
130.391527312818));
#229358=CARTESIAN_POINT('Ctrl Pts',(-163.848032058478,3.0010768338922,125.369408750896));
#229359=CARTESIAN_POINT('Ctrl Pts',(-164.126479682291,-2.95042359716811,
125.341745442286));
#229360=CARTESIAN_POINT('Ctrl Pts',(-164.404927306104,-6.19062887863655,
130.333958616169));
#229361=CARTESIAN_POINT('Ctrl Pts',(-164.683374929917,-3.74194864967208,
135.758448248921));
#229362=CARTESIAN_POINT('Ctrl Pts',(-164.961822553729,2.14539958398697,
136.630373369092));
#229363=CARTESIAN_POINT('Ctrl Pts',(-165.240270177542,6.06123040855813,
132.148477387157));
#229364=CARTESIAN_POINT('Ctrl Pts',(-165.518717801355,4.40708659523179,
126.431403757722));
#229365=CARTESIAN_POINT('Ctrl Pts',(-165.797165425168,-1.29695450096345,
124.732863851664));
#229366=CARTESIAN_POINT('Ctrl Pts',(-166.075613048981,-5.80915777052276,
128.613732864363));
#229367=CARTESIAN_POINT('Ctrl Pts',(-166.354060672794,-4.98302884210618,
134.50768176414));
#229368=CARTESIAN_POINT('Ctrl Pts',(-166.632508296607,0.422260157714416,
136.998459447511));
#229369=CARTESIAN_POINT('Ctrl Pts',(-166.91095592042,5.43951270115045,133.797162904712));
#229370=CARTESIAN_POINT('Ctrl Pts',(-167.189403544233,5.45811880719792,
127.845627266545));
#229371=CARTESIAN_POINT('Ctrl Pts',(-167.467851168046,0.460980373357943,
124.613023035806));
#229372=CARTESIAN_POINT('Ctrl Pts',(-167.746298791858,-4.95977650345479,
127.069955579048));
#229373=CARTESIAN_POINT('Ctrl Pts',(-168.024746415672,-5.822741072145,132.958623916859));
#229374=CARTESIAN_POINT('Ctrl Pts',(-168.303194039484,-1.33489105224939,
136.867629524233));
#229375=CARTESIAN_POINT('Ctrl Pts',(-168.581641663297,4.37965863161014,
135.204787213532));
#229376=CARTESIAN_POINT('Ctrl Pts',(-168.86008928711,6.06951599123876,129.498167833929));
#229377=CARTESIAN_POINT('Ctrl Pts',(-169.138536910923,2.18178466725943,
124.991875811423));
#229378=CARTESIAN_POINT('Ctrl Pts',(-169.416984534736,-3.71090017982492,
125.826973370093));
#229379=CARTESIAN_POINT('Ctrl Pts',(-169.695432158549,-6.19344904920226,
131.236046650305));
#229380=CARTESIAN_POINT('Ctrl Pts',(-169.973879782361,-2.98452080916978,
136.248421555465));
#229381=CARTESIAN_POINT('Ctrl Pts',(-170.252327406175,2.96703625254325,
136.257970415857));
#229382=CARTESIAN_POINT('Ctrl Pts',(-170.530775029987,6.19203194594742,
131.25591829527));
#229383=CARTESIAN_POINT('Ctrl Pts',(-170.8092226538,3.72685277860365,125.838906728691));
#229384=CARTESIAN_POINT('Ctrl Pts',(-171.087670277614,-2.16312202539704,
124.984904710079));
#229385=CARTESIAN_POINT('Ctrl Pts',(-171.366117901426,-6.06529336244348,
129.478698374222));
#229386=CARTESIAN_POINT('Ctrl Pts',(-171.644565525239,-4.39375640545797,
135.190710877796));
#229387=CARTESIAN_POINT('Ctrl Pts',(-171.923013149052,1.31542804121008,
136.871881777341));
#229388=CARTESIAN_POINT('Ctrl Pts',(-172.201460772865,5.81579838023838,
132.977297145939));
#229389=CARTESIAN_POINT('Ctrl Pts',(-172.479908396678,4.97173412537368,
127.085889998814));
#229390=CARTESIAN_POINT('Ctrl Pts',(-172.75835602049,-0.441110907994683,
124.611575692932));
#229391=CARTESIAN_POINT('Ctrl Pts',(-173.036803644304,-5.4485965663818,
127.828128198426));
#229392=CARTESIAN_POINT('Ctrl Pts',(-173.315251268116,-5.44908815900415,
133.779692900072));
#229393=CARTESIAN_POINT('Ctrl Pts',(-173.593698891929,-0.442133936257506,
136.997072587158));
#229394=CARTESIAN_POINT('Ctrl Pts',(-173.872146515742,4.97111977446672,
134.523652504987));
#229395=CARTESIAN_POINT('Ctrl Pts',(-174.150594139555,5.81615726515733,
128.632384875785));
#229396=CARTESIAN_POINT('Ctrl Pts',(-174.429041763368,1.31643036424716,
124.737056846366));
#229397=CARTESIAN_POINT('Ctrl Pts',(-174.707489387181,-4.39303173020782,
126.417284578411));
#229398=CARTESIAN_POINT('Ctrl Pts',(-174.985937010994,-6.06551227613263,
132.129020869861));
#229399=CARTESIAN_POINT('Ctrl Pts',(-175.264384634806,-2.16408335703982,
136.623459102702));
#229400=CARTESIAN_POINT('Ctrl Pts',(-175.542832258619,3.72603244582337,
135.770430106468));
#229401=CARTESIAN_POINT('Ctrl Pts',(-175.821279882432,6.19210645777918,
130.353825855915));
#229402=CARTESIAN_POINT('Ctrl Pts',(-176.099727506245,2.96793713625374,
125.351241041473));
#229403=CARTESIAN_POINT('Ctrl Pts',(-176.378175130058,-2.98362142169932,
125.359806717758));
#229404=CARTESIAN_POINT('Ctrl Pts',(-176.656622753871,-6.19337765112022,
130.371651446723));
#229405=CARTESIAN_POINT('Ctrl Pts',(-176.935070377684,-3.71172238248064,
135.781134764673));
#229406=CARTESIAN_POINT('Ctrl Pts',(-177.213518001496,2.18082442793968,
136.617205770365));
#229407=CARTESIAN_POINT('Ctrl Pts',(-177.49196562531,6.06930012827989,132.111556053907));
#229408=CARTESIAN_POINT('Ctrl Pts',(-177.770413249122,4.38038551252508,
126.404657591498));
#229409=CARTESIAN_POINT('Ctrl Pts',(-178.048860872936,-1.33388939551094,
124.740871272604));
#229410=CARTESIAN_POINT('Ctrl Pts',(-178.327308496748,-5.82238511319243,
128.649135443807));
#229411=CARTESIAN_POINT('Ctrl Pts',(-178.605756120561,-4.96039335117553,
134.537946261091));
#229412=CARTESIAN_POINT('Ctrl Pts',(-178.884203744374,0.459957571884186,
136.995774267775));
#229413=CARTESIAN_POINT('Ctrl Pts',(-179.162651368187,5.45762995655925,
133.763995597288));
#229414=CARTESIAN_POINT('Ctrl Pts',(-179.441098991999,5.44000703120181,
127.812456966643));
#229415=CARTESIAN_POINT('Ctrl Pts',(-179.719546615813,0.423283403288203,
124.610331628578));
#229416=CARTESIAN_POINT('Ctrl Pts',(-179.997994239625,-4.98241699370369,
127.100216336253));
#229417=CARTESIAN_POINT('Ctrl Pts',(-180.276441863438,-5.80951957808352,
132.994028680947));
#229418=CARTESIAN_POINT('Ctrl Pts',(-180.554889487251,-1.29795748101432,
136.875643046625));
#229419=CARTESIAN_POINT('Ctrl Pts',(-180.833337111064,4.40636413235919,
135.178045458633));
#229420=CARTESIAN_POINT('Ctrl Pts',(-181.111784734877,6.06145237094964,
129.461245168083));
#229421=CARTESIAN_POINT('Ctrl Pts',(-181.39023235869,2.14636199904753,124.97870236077));
#229422=CARTESIAN_POINT('Ctrl Pts',(-181.668679982503,-3.74113019436597,
125.849654892224));
#229423=CARTESIAN_POINT('Ctrl Pts',(-181.947127606316,-6.19070650352801,
131.273739934436));
#229424=CARTESIAN_POINT('Ctrl Pts',(-182.225575230128,-2.95132596877351,
136.266488314898));
#229425=CARTESIAN_POINT('Ctrl Pts',(-182.504022853942,3.00017895099442,
136.239808181284));
#229426=CARTESIAN_POINT('Ctrl Pts',(-182.782470477755,6.19466598168877,
131.218217272988));
#229427=CARTESIAN_POINT('Ctrl Pts',(-183.060918101567,3.6965576014681,125.81631231638));
#229428=CARTESIAN_POINT('Ctrl Pts',(-183.33936572538,-2.19850662762309,
124.998180068855));
#229429=CARTESIAN_POINT('Ctrl Pts',(-183.617813349193,-6.07325066894868,
129.515644097905));
#229430=CARTESIAN_POINT('Ctrl Pts',(-183.896260973006,-4.36697404029963,
135.217375651221));
#229431=CARTESIAN_POINT('Ctrl Pts',(-184.174708596819,1.35233839284232,
136.863761976378));
#229432=CARTESIAN_POINT('Ctrl Pts',(-184.453156220632,5.8289179083658,132.941854470998));
#229433=CARTESIAN_POINT('Ctrl Pts',(-184.731603844444,4.94900662457131,
127.055694536694));
#229434=CARTESIAN_POINT('Ctrl Pts',(-185.010051468258,-0.478799974789776,
124.614375598192));
#229435=CARTESIAN_POINT('Ctrl Pts',(-185.28849909207,-5.46661278799793,
127.861350494915));
#229436=CARTESIAN_POINT('Ctrl Pts',(-185.566946715884,-5.43087550791776,
133.812807920317));
#229437=CARTESIAN_POINT('Ctrl Pts',(-185.845394339696,-0.404428949079144,
136.999649245311));
#229438=CARTESIAN_POINT('Ctrl Pts',(-186.123841963509,4.99366805651034,
134.493322978084));
#229439=CARTESIAN_POINT('Ctrl Pts',(-186.402289587322,5.80282807241402,
128.59702051737));
#229440=CARTESIAN_POINT('Ctrl Pts',(-186.680737211135,1.27947257368013,
124.729155774178));
#229441=CARTESIAN_POINT('Ctrl Pts',(-186.959184834948,-4.41965571455532,
126.444107491802));
#229442=CARTESIAN_POINT('Ctrl Pts',(-187.237632458761,-6.0573363132998,
132.165918821797));
#229443=CARTESIAN_POINT('Ctrl Pts',(-187.516080082574,-2.12862075745111,
136.636524677919));
#229444=CARTESIAN_POINT('Ctrl Pts',(-187.794527706387,3.75619328558978,
135.74765667963));
#229445=CARTESIAN_POINT('Ctrl Pts',(-188.072975330199,6.18924919941703,
130.316141093742));
#229446=CARTESIAN_POINT('Ctrl Pts',(-188.351422954013,2.93468746061294,
125.333275399398));
#229447=CARTESIAN_POINT('Ctrl Pts',(-188.629870577825,-3.01670868704181,
125.378069743179));
#229448=CARTESIAN_POINT('Ctrl Pts',(-188.908318201638,-6.19589692571743,
130.409360311474));
#229449=CARTESIAN_POINT('Ctrl Pts',(-189.186765825451,-3.68135857605119,
135.80363686423));
#229450=CARTESIAN_POINT('Ctrl Pts',(-189.465213449264,2.21616846064164,
136.603822774524));
#229451=CARTESIAN_POINT('Ctrl Pts',(-189.743661073077,6.07714494785282,
132.07458628205));
#229452=CARTESIAN_POINT('Ctrl Pts',(-190.02210869689,4.35352211302309,126.378074457888));
#229453=CARTESIAN_POINT('Ctrl Pts',(-190.300556320702,-1.37077486229612,
124.749103378371));
#229454=CARTESIAN_POINT('Ctrl Pts',(-190.579003944516,-5.83539670523986,
128.684617885911));
#229455=CARTESIAN_POINT('Ctrl Pts',(-190.857451568328,-4.93757405104588,
134.568072408653));
#229456=CARTESIAN_POINT('Ctrl Pts',(-191.135899192141,0.497637942157669,
136.992859662928));
#229457=CARTESIAN_POINT('Ctrl Pts',(-191.414346815954,5.47554497748281,
133.730718619501));
#229458=CARTESIAN_POINT('Ctrl Pts',(-191.692794439767,5.42169367374449,
127.779397532831));
#229459=CARTESIAN_POINT('Ctrl Pts',(-191.97124206358,0.385570748295746,
124.60786974337));
#229460=CARTESIAN_POINT('Ctrl Pts',(-192.249689687393,-5.00487285865859,
127.130614351886));
#229461=CARTESIAN_POINT('Ctrl Pts',(-192.528137311206,-5.79608281013753,
133.029352306079));
#229462=CARTESIAN_POINT('Ctrl Pts',(-192.806584935019,-1.26097581348702,
136.883431595415));
#229463=CARTESIAN_POINT('Ctrl Pts',(-193.085032558831,4.43290635366497,
135.151141635234));
#229464=CARTESIAN_POINT('Ctrl Pts',(-193.363480182644,6.05316414131348,
129.424372271875));
#229465=CARTESIAN_POINT('Ctrl Pts',(-193.641927806457,2.11085979660312,
124.965744782026));
#229466=CARTESIAN_POINT('Ctrl Pts',(-193.92037543027,-3.77122157995168,
125.872520012798));
#229467=CARTESIAN_POINT('Ctrl Pts',(-194.198823054083,-6.1877345589472,
131.311415825543));
#229468=CARTESIAN_POINT('Ctrl Pts',(-194.477270677896,-2.91802176590892,
136.284352673182));
#229469=CARTESIAN_POINT('Ctrl Pts',(-194.755718301709,3.03321047671203,
136.221444534203));
#229470=CARTESIAN_POINT('Ctrl Pts',(-195.034165925522,6.19707047180361,
131.180500915096));
#229471=CARTESIAN_POINT('Ctrl Pts',(-195.312613549334,3.66612544703105,
125.793902738034));
#229472=CARTESIAN_POINT('Ctrl Pts',(-195.591061173148,-2.23380976337827,
125.011670577786));
#229473=CARTESIAN_POINT('Ctrl Pts',(-195.86950879696,-6.08098292891658,
129.552637575454));
#229474=CARTESIAN_POINT('Ctrl Pts',(-196.147956420774,-4.3400298553121,
135.243876898752));
#229475=CARTESIAN_POINT('Ctrl Pts',(-196.426404044586,1.38919863307876,
136.855417642068));
#229476=CARTESIAN_POINT('Ctrl Pts',(-196.704851668399,5.84182144379631,
132.906332590435));
#229477=CARTESIAN_POINT('Ctrl Pts',(-196.983299292212,4.92609573650846,
127.025637982775));
#229478=CARTESIAN_POINT('Ctrl Pts',(-197.261746916025,-0.516471299475173,
124.617404875624));
#229479=CARTESIAN_POINT('Ctrl Pts',(-197.540194539838,-5.48442644226676,
127.894681845726));
#229480=CARTESIAN_POINT('Ctrl Pts',(-197.81864216365,-5.41246161374207,
133.845811461438));
#229481=CARTESIAN_POINT('Ctrl Pts',(-198.097089787464,-0.36670897563802,
137.001996334766));
#229482=CARTESIAN_POINT('Ctrl Pts',(-198.375537411276,5.01603129634849,
134.462856755322));
#229483=CARTESIAN_POINT('Ctrl Pts',(-198.65398503509,5.78928385374183,128.561737952753));
#229484=CARTESIAN_POINT('Ctrl Pts',(-198.932432658902,1.24246737178614,
124.721479820939));
#229485=CARTESIAN_POINT('Ctrl Pts',(-199.210880282716,-4.44611592693577,
126.471091975977));
#229486=CARTESIAN_POINT('Ctrl Pts',(-199.489327906528,-6.04893589364168,
132.202766320694));
#229487=CARTESIAN_POINT('Ctrl Pts',(-199.767775530341,-2.09307928103787,
136.649374140152));
#229488=CARTESIAN_POINT('Ctrl Pts',(-200.046223154153,3.7862149382325,135.724700077139));
#229489=CARTESIAN_POINT('Ctrl Pts',(-200.324670777967,6.18616259614969,
130.278474422724));
#229490=CARTESIAN_POINT('Ctrl Pts',(-200.603118401779,2.90132903904936,
125.315512490399));
#229491=CARTESIAN_POINT('Ctrl Pts',(-200.881566025592,-3.04968416713424,
125.396533841802));
#229492=CARTESIAN_POINT('Ctrl Pts',(-201.160013649405,-6.1981866090755,
130.447083813107));
#229493=CARTESIAN_POINT('Ctrl Pts',(-201.438461273218,-3.65085835552605,
135.825953713766));
#229494=CARTESIAN_POINT('Ctrl Pts',(-201.716908897031,2.2514303724059,136.590224877478));
#229495=CARTESIAN_POINT('Ctrl Pts',(-201.995356520844,6.08476457658541,
132.037569441512));
#229496=CARTESIAN_POINT('Ctrl Pts',(-202.273804144657,4.32649739215744,
126.35165534194));
#229497=CARTESIAN_POINT('Ctrl Pts',(-202.55225176847,-1.40760953451491,
124.757559863922));
#229498=CARTESIAN_POINT('Ctrl Pts',(-202.830699392283,-5.84819206451709,
128.720178875862));
#229499=CARTESIAN_POINT('Ctrl Pts',(-203.109147016096,-4.91457178729319,
134.59805909049));
#229500=CARTESIAN_POINT('Ctrl Pts',(-203.387594639908,0.535299872273523,
136.989715740974));
#229501=CARTESIAN_POINT('Ctrl Pts',(-203.666042263721,5.49325710007376,
133.697333204442));
#229502=CARTESIAN_POINT('Ctrl Pts',(-203.944489887534,5.40317941343439,
127.746450190138));
#229503=CARTESIAN_POINT('Ctrl Pts',(-204.222937511347,0.347843805837959,
124.605637471411));
#229504=CARTESIAN_POINT('Ctrl Pts',(-204.50138513516,-5.0271432662092,127.161148499539));
#229505=CARTESIAN_POINT('Ctrl Pts',(-204.779832758973,-5.78243126621161,
133.064593483327));
#229506=CARTESIAN_POINT('Ctrl Pts',(-205.058280382786,-1.22394742003769,
136.890994881994));
#229507=CARTESIAN_POINT('Ctrl Pts',(-205.336728006599,4.45928431199552,
135.124076740266));
#229508=CARTESIAN_POINT('Ctrl Pts',(-205.615175630412,6.04465160945437,
129.387550511641));
#229509=CARTESIAN_POINT('Ctrl Pts',(-205.893623254225,2.07527937547198,
124.953003555339));
#229510=CARTESIAN_POINT('Ctrl Pts',(-206.172070878037,-3.80117322153507,
125.89556788454));
#229511=CARTESIAN_POINT('Ctrl Pts',(-206.45051850185,-6.18453332558722,
131.349072927534));
#229512=CARTESIAN_POINT('Ctrl Pts',(-206.728966125663,-2.8846094346739,
136.302013968343));
#229513=CARTESIAN_POINT('Ctrl Pts',(-207.007413749476,3.06612960569919,
136.202880155086));
#229514=CARTESIAN_POINT('Ctrl Pts',(-207.285861373289,6.19924532719362,
131.142770619188));
#229515=CARTESIAN_POINT('Ctrl Pts',(-207.564308997102,3.63555744296752,
125.771678824048));
#229516=CARTESIAN_POINT('Ctrl Pts',(-207.842756620915,-2.26903012449045,
125.025375736976));
#229517=CARTESIAN_POINT('Ctrl Pts',(-208.121204244728,-6.08848985582611,
129.58967743606));
#229518=CARTESIAN_POINT('Ctrl Pts',(-208.399651868541,-4.31292484892225,
135.270213638376));
#229519=CARTESIAN_POINT('Ctrl Pts',(-208.678099492353,1.42600739604885,
136.846849083615));
#229520=CARTESIAN_POINT('Ctrl Pts',(-208.956547116166,5.85450850838505,
132.870732820528));
#229521=CARTESIAN_POINT('Ctrl Pts',(-209.234994739979,4.90300231015654,
126.995721450812));
#229522=CARTESIAN_POINT('Ctrl Pts',(-209.513442363792,-0.554123486127181,
124.620663412976));
#229523=CARTESIAN_POINT('Ctrl Pts',(-209.791889987605,-5.50203686909699,
127.928121015754));
#229524=CARTESIAN_POINT('Ctrl Pts',(-210.070337611418,-5.393847158811,133.878702300482));
#229525=CARTESIAN_POINT('Ctrl Pts',(-210.348785235231,-0.328975413660277,
137.004113768549));
#229526=CARTESIAN_POINT('Ctrl Pts',(-210.627232859043,5.03820866530154,
134.432254965643));
#229527=CARTESIAN_POINT('Ctrl Pts',(-210.905680482857,5.77552511102812,
128.526538489345));
#229528=CARTESIAN_POINT('Ctrl Pts',(-211.184128106669,1.20541612980698,
124.714029271085));
#229529=CARTESIAN_POINT('Ctrl Pts',(-211.462575730482,-4.47241138685473,
126.498237031013));
#229530=CARTESIAN_POINT('Ctrl Pts',(-211.741023354295,-6.04031132844015,
132.239562001151));
#229531=CARTESIAN_POINT('Ctrl Pts',(-212.019470978108,-2.05746024480169,
136.66200701326));
#229532=CARTESIAN_POINT('Ctrl Pts',(-212.297918601921,3.81609629128846,
135.701561149659));
#229533=CARTESIAN_POINT('Ctrl Pts',(-212.576366225734,6.1828467623524,130.240827238612));
#229534=CARTESIAN_POINT('Ctrl Pts',(-212.854813849547,2.86786310767097,
125.297952972686));
#229535=CARTESIAN_POINT('Ctrl Pts',(-213.133261473359,-3.0825466400586,
125.415198329437));
#229536=CARTESIAN_POINT('Ctrl Pts',(-213.411709097173,-6.20024661634941,
130.484820553763));
#229537=CARTESIAN_POINT('Ctrl Pts',(-213.690156720985,-3.62022285110177,
135.848084486325));
#229538=CARTESIAN_POINT('Ctrl Pts',(-213.968604344798,2.28660885659016,
136.576412583105));
#229539=CARTESIAN_POINT('Ctrl Pts',(-214.247051968611,6.09215873212836,
132.00050690397));
#229540=CARTESIAN_POINT('Ctrl Pts',(-214.525499592424,4.29931235134063,
126.325401222624));
#229541=CARTESIAN_POINT('Ctrl Pts',(-214.803947216237,-1.44439204724454,
124.766240415898));
#229542=CARTESIAN_POINT('Ctrl Pts',(-215.08239484005,-5.86077071688603,
128.755817095934));
#229543=CARTESIAN_POINT('Ctrl Pts',(-215.360842463863,-4.89138741227638,
134.627905195436));
#229544=CARTESIAN_POINT('Ctrl Pts',(-215.639290087675,0.572941966656434,
136.986342618411));
#229545=CARTESIAN_POINT('Ctrl Pts',(-215.917737711489,5.51076566800256,
133.66384058922));
#229546=CARTESIAN_POINT('Ctrl Pts',(-216.196185335301,5.38446493632399,
127.713616159441));
#229547=CARTESIAN_POINT('Ctrl Pts',(-216.474632959115,0.310103973899474,
124.603634895418));
#229548=CARTESIAN_POINT('Ctrl Pts',(-216.753080582927,-5.04922739111732,
127.191817647757));
#229549=CARTESIAN_POINT('Ctrl Pts',(-217.031528206741,-5.76856545216855,
133.099750906814));
#229550=CARTESIAN_POINT('Ctrl Pts',(-217.309975830553,-1.18687367276612,
136.898332626102));
#229551=CARTESIAN_POINT('Ctrl Pts',(-217.588423454366,4.48549702990607,
135.096851776628));
#229552=CARTESIAN_POINT('Ctrl Pts',(-217.866871078179,6.03591509080661,
129.350781251827));
#229553=CARTESIAN_POINT('Ctrl Pts',(-218.145318701992,2.03962205410111,
124.94047915284));
#229554=CARTESIAN_POINT('Ctrl Pts',(-218.423766325804,-3.83098400924668,
125.9187976534));
#229555=CARTESIAN_POINT('Ctrl Pts',(-218.702213949618,-6.18110292207006,
131.386709845009));
#229556=CARTESIAN_POINT('Ctrl Pts',(-218.98066157343,-2.85109021317626,
136.319471545938));
#229557=CARTESIAN_POINT('Ctrl Pts',(-219.259109197243,3.09893511812703,
136.18411573184));
#229558=CARTESIAN_POINT('Ctrl Pts',(-219.537556821056,6.20119046726778,
131.105027783371));
#229559=CARTESIAN_POINT('Ctrl Pts',(-219.816004444869,3.6048547219858,125.749641397935));
#229560=CARTESIAN_POINT('Ctrl Pts',(-220.094452068682,-2.30416640585769,
125.039295038577));
#229561=CARTESIAN_POINT('Ctrl Pts',(-220.372899692494,-6.09577117150464,
129.626762307198));
#229562=CARTESIAN_POINT('Ctrl Pts',(-220.651347316308,-4.28566002551621,
135.296384894171));
#229563=CARTESIAN_POINT('Ctrl Pts',(-220.929794940121,1.46276331779004,
136.83805661853));
#229564=CARTESIAN_POINT('Ctrl Pts',(-221.208242563933,5.86697863200795,
132.835056480438));
#229565=CARTESIAN_POINT('Ctrl Pts',(-221.486690187747,4.87972720125093,
126.965946049375));
#229566=CARTESIAN_POINT('Ctrl Pts',(-221.765137811559,-0.591755139529082,
124.624151089502));
#229567=CARTESIAN_POINT('Ctrl Pts',(-222.043585435373,-5.51944341592756,
127.961666765899));
#229568=CARTESIAN_POINT('Ctrl Pts',(-222.322033059185,-5.37503283288975,
133.911479218663));
#229569=CARTESIAN_POINT('Ctrl Pts',(-222.600480682998,-0.29122966137826,
137.006001468201));
#229570=CARTESIAN_POINT('Ctrl Pts',(-222.878928306811,5.06019934158045,
134.401518743003));
#229571=CARTESIAN_POINT('Ctrl Pts',(-223.157375930624,5.7615523541068,128.491423431472));
#229572=CARTESIAN_POINT('Ctrl Pts',(-223.435823554437,1.16832022068962,
124.706804400699));
#229573=CARTESIAN_POINT('Ctrl Pts',(-223.71427117825,-4.49854111992577,
126.525541651043));
#229574=CARTESIAN_POINT('Ctrl Pts',(-223.992718802062,-6.03146293728042,
132.276304499695));
#229575=CARTESIAN_POINT('Ctrl Pts',(-224.271166425875,-2.02176496861996,
136.674422829126));
#229576=CARTESIAN_POINT('Ctrl Pts',(-224.549614049688,3.84583623749284,
135.678240754614));
#229577=CARTESIAN_POINT('Ctrl Pts',(-224.828061673501,6.1793018208946,130.203200936436));
#229578=CARTESIAN_POINT('Ctrl Pts',(-225.106509297314,2.83429090657077,
125.280597496933));
#229579=CARTESIAN_POINT('Ctrl Pts',(-225.384956921127,-3.11529488808334,
125.434062514461));
#229580=CARTESIAN_POINT('Ctrl Pts',(-225.66340454494,-6.20207687120481,
130.522569135094));
#229581=CARTESIAN_POINT('Ctrl Pts',(-225.941852168753,-3.5894531979886,
135.87002836184));
#229582=CARTESIAN_POINT('Ctrl Pts',(-226.220299792565,2.32170260964191,
136.562386403224));
#229583=CARTESIAN_POINT('Ctrl Pts',(-226.498747416378,6.09932714048972,
131.963400042786));
#229584=CARTESIAN_POINT('Ctrl Pts',(-226.777195040191,4.27196799792278,
126.299313072794));
#229585=CARTESIAN_POINT('Ctrl Pts',(-227.055642664004,-1.48112103749588,
124.775144712639));
#229586=CARTESIAN_POINT('Ctrl Pts',(-227.334090287817,-5.87313219624144,
128.79153122554));
#229587=CARTESIAN_POINT('Ctrl Pts',(-227.61253791163,-4.8680217850994,134.65760961753));
#229588=CARTESIAN_POINT('Ctrl Pts',(-227.890985535443,0.610562830463375,
136.982740420231));
#229589=CARTESIAN_POINT('Ctrl Pts',(-228.169433159256,5.52807003248314,
133.630242014917));
#229590=CARTESIAN_POINT('Ctrl Pts',(-228.447880783069,5.36555093588535,
127.680896657417));
#229591=CARTESIAN_POINT('Ctrl Pts',(-228.726328406882,0.272352650944771,
124.601862089598));
#229592=CARTESIAN_POINT('Ctrl Pts',(-229.004776030695,-5.07112441504767,
127.222620660081));
#229593=CARTESIAN_POINT('Ctrl Pts',(-229.283223654507,-5.75448588181141,
133.134823273769));
#229594=CARTESIAN_POINT('Ctrl Pts',(-229.561671278321,-1.14975594545406,
136.905444555836));
#229595=CARTESIAN_POINT('Ctrl Pts',(-229.840118902133,4.51154353607471,
135.069467753152));
#229596=CARTESIAN_POINT('Ctrl Pts',(-230.118566525947,6.0269549091058,129.314065854931));
#229597=CARTESIAN_POINT('Ctrl Pts',(-230.397014149759,2.00388915378425,
124.928172038625));
#229598=CARTESIAN_POINT('Ctrl Pts',(-230.675461773572,-3.86065283843716,
125.942208458593));
#229599=CARTESIAN_POINT('Ctrl Pts',(-230.953909397385,-6.17744347551146,
131.424325183319));
#229600=CARTESIAN_POINT('Ctrl Pts',(-231.232357021197,-2.81746534348149,
136.33672475907));
#229601=CARTESIAN_POINT('Ctrl Pts',(-231.510804645011,3.13162579837364,
136.165151959792));
#229602=CARTESIAN_POINT('Ctrl Pts',(-231.789252268823,6.20290581994918,
131.067273806224));
#229603=CARTESIAN_POINT('Ctrl Pts',(-232.067699892636,3.57401842178686,
125.727791276302));
#229604=CARTESIAN_POINT('Ctrl Pts',(-232.346147516449,-2.33921730549066,
125.053427966802));
#229605=CARTESIAN_POINT('Ctrl Pts',(-232.624595140262,-6.10282660614105,
129.663890814674));
#229606=CARTESIAN_POINT('Ctrl Pts',(-232.903042764075,-4.25823639540172,
135.322389696357));
#229607=CARTESIAN_POINT('Ctrl Pts',(-233.181490387888,1.499465036299,136.829040572621));
#229608=CARTESIAN_POINT('Ctrl Pts',(-233.459938011701,5.87923135258013,
132.799304892167));
#229609=CARTESIAN_POINT('Ctrl Pts',(-233.738385635514,4.85627127225937,
126.9363128818));
#229610=CARTESIAN_POINT('Ctrl Pts',(-234.016833259326,-0.629364865227224,
124.627867775965));
#229611=CARTESIAN_POINT('Ctrl Pts',(-234.29528088314,-5.53664543775268,
127.99531785311));
#229612=CARTESIAN_POINT('Ctrl Pts',(-234.573728506952,-5.35601933315035,
133.944141001422));
#229613=CARTESIAN_POINT('Ctrl Pts',(-234.852176130765,-0.253473117473377,
137.007659363768));
#229614=CARTESIAN_POINT('Ctrl Pts',(-235.130623754578,5.08200251031112,
134.370649226346));
#229615=CARTESIAN_POINT('Ctrl Pts',(-235.409071378391,5.74736610074488,
128.456394080338));
#229616=CARTESIAN_POINT('Ctrl Pts',(-235.687519002204,1.13118101903705,
124.699805477501));
#229617=CARTESIAN_POINT('Ctrl Pts',(-235.965966626017,-4.52450415790052,
126.553004824284));
#229618=CARTESIAN_POINT('Ctrl Pts',(-236.24441424983,-6.0223910480441,132.312992454817));
#229619=CARTESIAN_POINT('Ctrl Pts',(-236.522861873642,-1.98599477519336,
136.686621127679));
#229620=CARTESIAN_POINT('Ctrl Pts',(-236.801309497456,3.87543367482126,
135.654739756147));
#229621=CARTESIAN_POINT('Ctrl Pts',(-237.079757121268,6.1755279031354,130.165596910454));
#229622=CARTESIAN_POINT('Ctrl Pts',(-237.358204745081,2.80061367977841,
125.263446706254));
#229623=CARTESIAN_POINT('Ctrl Pts',(-237.636652368894,-3.14792769771062,
125.453125697856));
#229624=CARTESIAN_POINT('Ctrl Pts',(-237.915099992707,-6.20367730582095,
130.560328158313));
#229625=CARTESIAN_POINT('Ctrl Pts',(-238.19354761652,-3.55855053636696,
135.891784527174));
#229626=CARTESIAN_POINT('Ctrl Pts',(-238.471995240333,2.35671033115007,
136.54814685758));
#229627=CARTESIAN_POINT('Ctrl Pts',(-238.750442864146,6.10626953604027,
131.92625023297));
#229628=CARTESIAN_POINT('Ctrl Pts',(-239.028890487959,4.24446534516054,
126.273391859158));
#229629=CARTESIAN_POINT('Ctrl Pts',(-239.307338111771,-1.51779514426229,
124.784272424193));
#229630=CARTESIAN_POINT('Ctrl Pts',(-239.585785735585,-5.88527604452282,
128.827319941278));
#229631=CARTESIAN_POINT('Ctrl Pts',(-239.864233359397,-4.84447577158576,
134.687171256065));
#229632=CARTESIAN_POINT('Ctrl Pts',(-240.14268098321,0.648161069640796,
136.978909279916));
#229633=CARTESIAN_POINT('Ctrl Pts',(-240.421128607023,5.54516955229552,
133.596538726537));
#229634=CARTESIAN_POINT('Ctrl Pts',(-240.699576230836,5.34643811298351,
127.648292896498));
#229635=CARTESIAN_POINT('Ctrl Pts',(-240.978023854649,0.234591235861842,
124.600319119639));
#229636=CARTESIAN_POINT('Ctrl Pts',(-241.256471478461,-5.09283352659785,
127.253556395099));
#229637=CARTESIAN_POINT('Ctrl Pts',(-241.534919102275,-5.74019307686353,
133.169809284574));
#229638=CARTESIAN_POINT('Ctrl Pts',(-241.813366726087,-1.11259561351327,
136.912330407661));
#229639=CARTESIAN_POINT('Ctrl Pts',(-242.0918143499,4.53742286533832,135.041925684563));
#229640=CARTESIAN_POINT('Ctrl Pts',(-242.370261973713,6.01777139637409,
129.277405681456));
#229641=CARTESIAN_POINT('Ctrl Pts',(-242.648709597526,1.96808199861856,
124.916082668738));
#229642=CARTESIAN_POINT('Ctrl Pts',(-242.927157221339,-3.89017860971679,
125.965799432623));
#229643=CARTESIAN_POINT('Ctrl Pts',(-243.205604845152,-6.1735551215127,
131.461917548614));
#229644=CARTESIAN_POINT('Ctrl Pts',(-243.484052468965,-2.78373607157309,
136.353772968415));
#229645=CARTESIAN_POINT('Ctrl Pts',(-243.762500092778,3.16420043507544,
136.145989541648));
#229646=CARTESIAN_POINT('Ctrl Pts',(-244.040947716591,6.20439132167383,
131.029510086731));
#229647=CARTESIAN_POINT('Ctrl Pts',(-244.319395340403,3.54304968502077,
125.706129268813));
#229648=CARTESIAN_POINT('Ctrl Pts',(-244.597842964216,-2.37418152456686,
125.067773997952));
#229649=CARTESIAN_POINT('Ctrl Pts',(-244.876290588029,-6.10965589829292,
129.701061582678));
#229650=CARTESIAN_POINT('Ctrl Pts',(-245.154738211842,-4.23065497477177,
135.348227081313));
#229651=CARTESIAN_POINT('Ctrl Pts',(-245.433185835655,1.53611119157916,
136.819801279981));
#229652=CARTESIAN_POINT('Ctrl Pts',(-245.711633459468,5.89126621607239,
132.763479380503));
#229653=CARTESIAN_POINT('Ctrl Pts',(-245.990081083281,4.83263539234992,
126.906823046158));
#229654=CARTESIAN_POINT('Ctrl Pts',(-246.268528707094,-0.666951269578287,
124.631813334641));
#229655=CARTESIAN_POINT('Ctrl Pts',(-246.546976330906,-5.55364229714491,
128.029073030433));
#229656=CARTESIAN_POINT('Ctrl Pts',(-246.825423954719,-5.33680736414475,
133.976686438464));
#229657=CARTESIAN_POINT('Ctrl Pts',(-247.103871578532,-0.215707181029578,
137.009087393821));
#229658=CARTESIAN_POINT('Ctrl Pts',(-247.382319202345,5.10361736357064,
134.339647559554));
#229659=CARTESIAN_POINT('Ctrl Pts',(-247.660766826158,5.73296687661779,
128.421451733968));
#229660=CARTESIAN_POINT('Ctrl Pts',(-247.939214449971,1.09399990105564,
124.693032760838));
#229661=CARTESIAN_POINT('Ctrl Pts',(-248.217662073784,-4.55029953871062,
126.580625533077));
#229662=CARTESIAN_POINT('Ctrl Pts',(-248.496109697597,-6.01309599689209,
132.349624507031));
#229663=CARTESIAN_POINT('Ctrl Pts',(-248.77455732141,-1.95015099000055,
136.698601456905));
#229664=CARTESIAN_POINT('Ctrl Pts',(-249.053004945222,3.90488750652966,
135.631059025098));
#229665=CARTESIAN_POINT('Ctrl Pts',(-249.331452569036,6.17152514891849,
130.128016554096));
#229666=CARTESIAN_POINT('Ctrl Pts',(-249.609900192848,2.76683267521693,
125.246501236177));
#229667=CARTESIAN_POINT('Ctrl Pts',(-249.888347816661,-3.18044385971988,
125.472387173231));
#229668=CARTESIAN_POINT('Ctrl Pts',(-250.166795440474,-6.20504786089197,
130.598096224241));
#229669=CARTESIAN_POINT('Ctrl Pts',(-250.445243064287,-3.5275160113489,
135.913352176149));
#229670=CARTESIAN_POINT('Ctrl Pts',(-250.7236906881,2.39163072389511,136.533694473816));
#229671=CARTESIAN_POINT('Ctrl Pts',(-251.002138311913,6.11298566151878,
131.889058851139));
#229672=CARTESIAN_POINT('Ctrl Pts',(-251.280585935725,4.21680541219097,
126.247638542206));
#229673=CARTESIAN_POINT('Ctrl Pts',(-251.559033559539,-1.5544130086051,
124.793623212388));
#229674=CARTESIAN_POINT('Ctrl Pts',(-251.837481183351,-5.89720181167361,
128.863181916876));
#229675=CARTESIAN_POINT('Ctrl Pts',(-252.115928807165,-4.82075024435922,
134.716589015834));
#229676=CARTESIAN_POINT('Ctrl Pts',(-252.394376430977,0.685735291195708,
136.974849339035));
#229677=CARTESIAN_POINT('Ctrl Pts',(-252.67282405479,5.56206359338632,133.562731973716));
#229678=CARTESIAN_POINT('Ctrl Pts',(-252.951271678603,5.32712717665345,
127.615806083426));
#229679=CARTESIAN_POINT('Ctrl Pts',(-253.229719302416,0.196821126400439,
124.599006045371));
#229680=CARTESIAN_POINT('Ctrl Pts',(-253.508166926229,-5.11435391846912,
127.284623701469));
#229681=CARTESIAN_POINT('Ctrl Pts',(-253.786614550041,-5.72568757235024,
133.204707652256));
#229682=CARTESIAN_POINT('Ctrl Pts',(-254.065062173855,-1.07539404373626,
136.918989908584));
#229683=CARTESIAN_POINT('Ctrl Pts',(-254.343509797667,4.56313403947717,
135.014226625117));
#229684=CARTESIAN_POINT('Ctrl Pts',(-254.621957421481,6.00836492926231,
129.240802026269));
#229685=CARTESIAN_POINT('Ctrl Pts',(-254.900405045293,1.9322018468105,124.904211611225));
#229686=CARTESIAN_POINT('Ctrl Pts',(-255.178852669106,-3.91956009939235,
125.989569474605));
#229687=CARTESIAN_POINT('Ctrl Pts',(-255.457300292919,-6.16943824888009,
131.499485975975));
#229688=CARTESIAN_POINT('Ctrl Pts',(-255.735747916732,-2.74990318521692,
136.370614733943));
#229689=CARTESIAN_POINT('Ctrl Pts',(-256.014195540545,3.19665694865877,
136.126630713714));
#229690=CARTESIAN_POINT('Ctrl Pts',(-256.292643164358,6.20564856486739,
130.991735142402));
#229691=CARTESIAN_POINT('Ctrl Pts',(-256.571090788171,3.51194654848645,
125.68466161966));
#229692=CARTESIAN_POINT('Ctrl Pts',(-256.849538411983,-2.40905189372645,
125.082322325773));
#229693=CARTESIAN_POINT('Ctrl Pts',(-257.127986035797,-6.11626988572704,
129.738292634474));
#229694=CARTESIAN_POINT('Ctrl Pts',(-257.406433659609,-4.20289584392431,
135.373859459261));
#229695=CARTESIAN_POINT('Ctrl Pts',(-257.684881283423,1.57266088340656,
136.810408252432));
#229696=CARTESIAN_POINT('Ctrl Pts',(-257.963328907235,5.90315744058412,
132.727450666138));
#229697=CARTESIAN_POINT('Ctrl Pts',(-258.241776531048,4.80867945501638,
126.87772425425));
#229698=CARTESIAN_POINT('Ctrl Pts',(-258.520224154861,-0.704246744852541,
124.635521896935));
#229699=CARTESIAN_POINT('Ctrl Pts',(-258.798671778674,-5.5709361272427,
128.063810879205));
#229700=CARTESIAN_POINT('Ctrl Pts',(-259.077119402487,-5.31644754243966,
134.007449313497));
#229701=CARTESIAN_POINT('Ctrl Pts',(-259.355567026299,-0.179733571114533,
137.013459703814));
#229702=CARTESIAN_POINT('Ctrl Pts',(-259.634014650113,5.12849404027147,
134.30227331953));
#229703=CARTESIAN_POINT('Ctrl Pts',(-259.866054336623,5.61428989304695,
129.384066440553));
#229704=CARTESIAN_POINT('Ctrl Pts',(-260.051696012132,3.39054283699284,
126.521203045511));
#229705=CARTESIAN_POINT('Ctrl Pts',(-260.144521813036,1.754921961264,125.780753115897));
#229706=CARTESIAN_POINT('Ctrl Pts',(-260.190939676638,0.892893391295023,
125.631947563271));
#229707=CARTESIAN_POINT('Ctrl Pts',(210.191733024964,-2.43880115184907,
125.780342085335));
#229708=CARTESIAN_POINT('Ctrl Pts',(210.145323348611,-3.27594855749458,
126.186716565447));
#229709=CARTESIAN_POINT('Ctrl Pts',(210.052505734956,-4.72940422381435,
127.426013481475));
#229710=CARTESIAN_POINT('Ctrl Pts',(209.866872246696,-6.15821517169733,
131.008352419918));
#229711=CARTESIAN_POINT('Ctrl Pts',(209.634832560185,-4.21099667891447,
135.892791108304));
#229712=CARTESIAN_POINT('Ctrl Pts',(209.356384936373,2.01508446636645,137.098708070195));
#229713=CARTESIAN_POINT('Ctrl Pts',(209.07793731256,6.37956871319657,132.510708806665));
#229714=CARTESIAN_POINT('Ctrl Pts',(208.799489688747,4.8866719183268,126.359661034021));
#229715=CARTESIAN_POINT('Ctrl Pts',(208.521042064934,-1.09954563679898,
124.290443595948));
#229716=CARTESIAN_POINT('Ctrl Pts',(208.242594441121,-6.07390144970816,
128.208589139036));
#229717=CARTESIAN_POINT('Ctrl Pts',(207.964146817309,-5.46739734855352,
134.511385201899));
#229718=CARTESIAN_POINT('Ctrl Pts',(207.685699193495,0.163779660617915,
137.407996874876));
#229719=CARTESIAN_POINT('Ctrl Pts',(207.407251569682,5.6442383477931,134.235982835808));
#229720=CARTESIAN_POINT('Ctrl Pts',(207.128803945869,5.93803043711477,127.910585036422));
#229721=CARTESIAN_POINT('Ctrl Pts',(206.850356322057,0.775002953389061,
124.244367681185));
#229722=CARTESIAN_POINT('Ctrl Pts',(206.571908698243,-5.10018277131114,
126.606494049502));
#229723=CARTESIAN_POINT('Ctrl Pts',(206.293461074431,-6.28856642889766,
132.82623846394));
#229724=CARTESIAN_POINT('Ctrl Pts',(206.015013450618,-1.69805588527783,
137.187984519302));
#229725=CARTESIAN_POINT('Ctrl Pts',(205.736565826805,4.45288036648484,135.683487507757));
#229726=CARTESIAN_POINT('Ctrl Pts',(205.458118202992,6.51183958365415,129.695313656966));
#229727=CARTESIAN_POINT('Ctrl Pts',(205.179670579179,2.58673502741873,124.726298504418));
#229728=CARTESIAN_POINT('Ctrl Pts',(204.901222955366,-3.71545195245463,
125.342726181157));
#229729=CARTESIAN_POINT('Ctrl Pts',(204.622775331554,-6.60332046735468,
130.978128730661));
#229730=CARTESIAN_POINT('Ctrl Pts',(204.344327707741,-3.42305986725146,
136.4538470632));
#229731=CARTESIAN_POINT('Ctrl Pts',(204.065880083927,2.90282542147133,136.737963244372));
#229732=CARTESIAN_POINT('Ctrl Pts',(203.787432460115,6.56115601364161,131.569388537382));
#229733=CARTESIAN_POINT('Ctrl Pts',(203.508984836302,4.1901047305044,125.69779051756));
#229734=CARTESIAN_POINT('Ctrl Pts',(203.230537212489,-2.03144808657932,
124.518880964767));
#229735=CARTESIAN_POINT('Ctrl Pts',(202.952089588676,-6.38619936200403,
129.116020142231));
#229736=CARTESIAN_POINT('Ctrl Pts',(202.673641964863,-4.87234540261322,
135.2646617407));
#229737=CARTESIAN_POINT('Ctrl Pts',(202.39519434105,1.1189559521872,137.314504502614));
#229738=CARTESIAN_POINT('Ctrl Pts',(202.116746717238,6.08199145217563,133.381843073553));
#229739=CARTESIAN_POINT('Ctrl Pts',(201.838299093424,5.45597392877388,127.080601183836));
#229740=CARTESIAN_POINT('Ctrl Pts',(201.559851469612,-0.183817095687214,
124.201312298284));
#229741=CARTESIAN_POINT('Ctrl Pts',(201.281403845799,-5.65468918935595,
127.389902241135));
#229742=CARTESIAN_POINT('Ctrl Pts',(201.002956221986,-5.92917816483575,
133.716212626452));
#229743=CARTESIAN_POINT('Ctrl Pts',(200.724508598173,-0.755042063338292,
137.366673267433));
#229744=CARTESIAN_POINT('Ctrl Pts',(200.44606097436,5.11294080853837,134.986689170007));
#229745=CARTESIAN_POINT('Ctrl Pts',(200.167613350547,6.2823808583988,128.763349450982));
#229746=CARTESIAN_POINT('Ctrl Pts',(199.889165726734,1.67861981076543,124.415599285115));
#229747=CARTESIAN_POINT('Ctrl Pts',(199.610718102921,-4.46771083782862,
125.938808675424));
#229748=CARTESIAN_POINT('Ctrl Pts',(199.332270479108,-6.50843348626435,
131.933222605136));
#229749=CARTESIAN_POINT('Ctrl Pts',(199.053822855296,-2.56822371547623,
136.890267516244));
#229750=CARTESIAN_POINT('Ctrl Pts',(198.775375231483,3.73205818513161,136.254661300547));
#229751=CARTESIAN_POINT('Ctrl Pts',(198.49692760767,6.60276093478139,130.610495019181));
#229752=CARTESIAN_POINT('Ctrl Pts',(198.218479983857,3.4058489481713,125.14448175187));
#229753=CARTESIAN_POINT('Ctrl Pts',(197.940032360044,-2.92087183683725,
124.879620661678));
#229754=CARTESIAN_POINT('Ctrl Pts',(197.661584736231,-6.56345409631434,
130.05930615131));
#229755=CARTESIAN_POINT('Ctrl Pts',(197.383137112418,-4.1745426838368,135.923660297497));
#229756=CARTESIAN_POINT('Ctrl Pts',(197.104689488605,2.05056951733907,137.083628129519));
#229757=CARTESIAN_POINT('Ctrl Pts',(196.826241864792,6.39130850797037,132.473255877329));
#229758=CARTESIAN_POINT('Ctrl Pts',(196.54779424098,4.85874721255563,126.329250411482));
#229759=CARTESIAN_POINT('Ctrl Pts',(196.269346617166,-1.13876540820057,
124.297652603739));
#229760=CARTESIAN_POINT('Ctrl Pts',(195.990898993354,-6.0898082506034,128.245401590344));
#229761=CARTESIAN_POINT('Ctrl Pts',(195.712451369541,-5.44461481437399,
134.544708910868));
#229762=CARTESIAN_POINT('Ctrl Pts',(195.434003745728,0.203913652044436,
137.406818876019));
#229763=CARTESIAN_POINT('Ctrl Pts',(195.155556121915,5.66505543396973,134.201592249669));
#229764=CARTESIAN_POINT('Ctrl Pts',(194.877108498102,5.92028802542049,127.874475717408));
#229765=CARTESIAN_POINT('Ctrl Pts',(194.59866087429,0.735065143658737,124.239780275557));
#229766=CARTESIAN_POINT('Ctrl Pts',(194.320213250476,-5.1256466951968,126.637613470433));
#229767=CARTESIAN_POINT('Ctrl Pts',(194.041765626664,-6.2761396229282,132.86448373661));
#229768=CARTESIAN_POINT('Ctrl Pts',(193.763318002851,-1.6591668436545,137.198201498994));
#229769=CARTESIAN_POINT('Ctrl Pts',(193.484870379038,4.48249921013125,135.656291847837));
#229770=CARTESIAN_POINT('Ctrl Pts',(193.206422755225,6.50496747206681,129.655694426079));
#229771=CARTESIAN_POINT('Ctrl Pts',(192.927975131412,2.54968841250072,124.710665118833));
#229772=CARTESIAN_POINT('Ctrl Pts',(192.649527507599,-3.74862973894988,
125.365444281348));
#229773=CARTESIAN_POINT('Ctrl Pts',(192.371079883787,-6.60214029104917,
131.018321851013));
#229774=CARTESIAN_POINT('Ctrl Pts',(192.092632259973,-3.38860644815819,
136.474579499726));
#229775=CARTESIAN_POINT('Ctrl Pts',(191.814184636161,2.93889117796205,136.720183001327));
#229776=CARTESIAN_POINT('Ctrl Pts',(191.535737012347,6.56569138435095,131.529434736241));
#229777=CARTESIAN_POINT('Ctrl Pts',(191.257289388535,4.15894196037717,125.672378777932));
#229778=CARTESIAN_POINT('Ctrl Pts',(190.978841764722,-2.06967194957323,
124.531363418996));
#229779=CARTESIAN_POINT('Ctrl Pts',(190.700394140909,-6.3963584469616,129.154926032595));
#229780=CARTESIAN_POINT('Ctrl Pts',(190.421946517096,-4.84510401107414,
135.294238450423));
#229781=CARTESIAN_POINT('Ctrl Pts',(190.143498893283,1.15856431450073,137.307572482581));
#229782=CARTESIAN_POINT('Ctrl Pts',(189.86505126947,6.09756863406271,133.344772510351));
#229783=CARTESIAN_POINT('Ctrl Pts',(189.586603645657,5.4332052617092,127.047458114672));
#229784=CARTESIAN_POINT('Ctrl Pts',(189.308156021844,-0.224008319322015,
124.202553584261));
#229785=CARTESIAN_POINT('Ctrl Pts',(189.029708398032,-5.67536919831109,
127.424387201254));
#229786=CARTESIAN_POINT('Ctrl Pts',(188.751260774218,-5.91134304125131,
133.752251266956));
#229787=CARTESIAN_POINT('Ctrl Pts',(188.472813150406,-0.71508141444371,
137.371147838333));
#229788=CARTESIAN_POINT('Ctrl Pts',(188.194365526593,5.13830509856852,134.955487759214));
#229789=CARTESIAN_POINT('Ctrl Pts',(187.91591790278,6.26984024615536,128.725144630756));
#229790=CARTESIAN_POINT('Ctrl Pts',(187.637470278967,1.63969850624965,124.405499418827));
#229791=CARTESIAN_POINT('Ctrl Pts',(187.359022655154,-4.49724605717418,
125.966095046791));
#229792=CARTESIAN_POINT('Ctrl Pts',(187.080575031341,-6.5014411967389,131.972820371883));
#229793=CARTESIAN_POINT('Ctrl Pts',(186.802127407528,-2.53112948956026,
136.905788265189));
#229794=CARTESIAN_POINT('Ctrl Pts',(186.523679783716,3.76516656597443,136.231842221641));
#229795=CARTESIAN_POINT('Ctrl Pts',(186.245232159903,6.60145848599114,130.570305731164));
#229796=CARTESIAN_POINT('Ctrl Pts',(185.96678453609,3.3713325565579,125.123854247073));
#229797=CARTESIAN_POINT('Ctrl Pts',(185.688336912277,-2.95688329360047,
124.897510609301));
#229798=CARTESIAN_POINT('Ctrl Pts',(185.409889288464,-6.5678678487195,130.099273563458));
#229799=CARTESIAN_POINT('Ctrl Pts',(185.131441664651,-4.14330270904733,
135.948977074923));
#229800=CARTESIAN_POINT('Ctrl Pts',(184.852994040838,2.08875520864929,137.071029390563));
#229801=CARTESIAN_POINT('Ctrl Pts',(184.574546417025,6.40134913096194,132.434319247607));
#229802=CARTESIAN_POINT('Ctrl Pts',(184.296098793212,4.831415925211,126.299756751549));
#229803=CARTESIAN_POINT('Ctrl Pts',(184.017651169399,-1.17835248801931,
124.304705146227));
#229804=CARTESIAN_POINT('Ctrl Pts',(183.739203545587,-6.10527253047917,
128.282519393244));
#229805=CARTESIAN_POINT('Ctrl Pts',(183.460755921774,-5.42174537657308,
134.577782526619));
#229806=CARTESIAN_POINT('Ctrl Pts',(183.182308297961,0.244100911417136,
137.405455267482));
#229807=CARTESIAN_POINT('Ctrl Pts',(182.903860674148,5.68563038680749,134.167044506474));
#229808=CARTESIAN_POINT('Ctrl Pts',(182.625413050335,5.90234329520773,127.838491527799));
#229809=CARTESIAN_POINT('Ctrl Pts',(182.346965426522,0.695091060812155,
124.23542735186));
#229810=CARTESIAN_POINT('Ctrl Pts',(182.068517802709,-5.15091590138369,
126.668891936874));
#229811=CARTESIAN_POINT('Ctrl Pts',(181.790070178896,-6.263482786439,132.902650210566));
#229812=CARTESIAN_POINT('Ctrl Pts',(181.511622555083,-1.62021497890189,
137.208182855437));
#229813=CARTESIAN_POINT('Ctrl Pts',(181.233174931271,4.51195124234396,135.628915707812));
#229814=CARTESIAN_POINT('Ctrl Pts',(180.954727307458,6.49785469294791,129.61611812487));
#229815=CARTESIAN_POINT('Ctrl Pts',(180.676279683645,2.51254711858197,124.695257343842));
#229816=CARTESIAN_POINT('Ctrl Pts',(180.397832059832,-3.78166851301026,
125.388364025079));
#229817=CARTESIAN_POINT('Ctrl Pts',(180.119384436019,-6.60071552592353,
131.058506988669));
#229818=CARTESIAN_POINT('Ctrl Pts',(179.840936812206,-3.35402743339335,
136.495101852955));
#229819=CARTESIAN_POINT('Ctrl Pts',(179.562489188393,2.97484801707599,136.702183530083));
#229820=CARTESIAN_POINT('Ctrl Pts',(179.28404156458,6.56998346925752,131.489454075275));
#229821=CARTESIAN_POINT('Ctrl Pts',(179.005593940767,4.12762507472721,125.647157201507));
#229822=CARTESIAN_POINT('Ctrl Pts',(178.727146316955,-2.10781911778238,
124.544078323705));
#229823=CARTESIAN_POINT('Ctrl Pts',(178.448698693142,-6.40628051373842,
129.193893042167));
#229824=CARTESIAN_POINT('Ctrl Pts',(178.170251069329,-4.81768308177075,
135.323648786705));
#229825=CARTESIAN_POINT('Ctrl Pts',(177.891803445516,1.19812974544141,137.300399483306));
#229826=CARTESIAN_POINT('Ctrl Pts',(177.613355821703,6.11291986848493,133.307607811431));
#229827=CARTESIAN_POINT('Ctrl Pts',(177.33490819789,5.41023526512845,127.014454258818));
#229828=CARTESIAN_POINT('Ctrl Pts',(177.056460574078,-0.264191242194762,
124.204039502676));
#229829=CARTESIAN_POINT('Ctrl Pts',(176.778012950264,-5.69583890440069,
127.458997407505));
#229830=CARTESIAN_POINT('Ctrl Pts',(176.499565326452,-5.89328887066216,
133.788180672302));
#229831=CARTESIAN_POINT('Ctrl Pts',(176.221117702638,-0.675094267951971,
137.375379074508));
#229832=CARTESIAN_POINT('Ctrl Pts',(175.942670078826,5.16347898681764,134.924132526884));
#229833=CARTESIAN_POINT('Ctrl Pts',(175.664222455013,6.25706730267374,128.687016856641));
#229834=CARTESIAN_POINT('Ctrl Pts',(175.3857748312,1.60071644210391,124.395636664696));
#229835=CARTESIAN_POINT('Ctrl Pts',(175.107327207387,-4.5266146294138,125.993560701866));
#229836=CARTESIAN_POINT('Ctrl Pts',(174.828879583574,-6.49420799391872,
132.012374840923));
#229837=CARTESIAN_POINT('Ctrl Pts',(174.550431959762,-2.49394147171037,
136.92108292349));
#229838=CARTESIAN_POINT('Ctrl Pts',(174.271984335948,3.79813542718566,136.208822025409));
#229839=CARTESIAN_POINT('Ctrl Pts',(173.993536712136,6.59991141772898,130.530125116137));
#229840=CARTESIAN_POINT('Ctrl Pts',(173.715089088322,3.33669123897678,125.103437235529));
#229841=CARTESIAN_POINT('Ctrl Pts',(173.43664146451,-2.99278518196597,124.915619437422));
#229842=CARTESIAN_POINT('Ctrl Pts',(173.158193840697,-6.5720382263662,130.139267102866));
#229843=CARTESIAN_POINT('Ctrl Pts',(172.879746216884,-4.11190920265221,
135.974103216695));
#229844=CARTESIAN_POINT('Ctrl Pts',(172.601298593071,2.12686350036709,137.058198437889));
#229845=CARTESIAN_POINT('Ctrl Pts',(172.322850969258,6.41115254960738,132.395322219168));
#229846=CARTESIAN_POINT('Ctrl Pts',(172.044403345445,4.80390560797255,126.270430011369));
#229847=CARTESIAN_POINT('Ctrl Pts',(171.765955721632,-1.21789590355323,
124.31199853584));
#229848=CARTESIAN_POINT('Ctrl Pts',(171.487508097819,-6.12051057723618,
128.319730643897));
#229849=CARTESIAN_POINT('Ctrl Pts',(171.209060474007,-5.39867503400336,
134.610716316833));
#229850=CARTESIAN_POINT('Ctrl Pts',(170.930612850193,0.284279125540913,
137.403847052956));
#229851=CARTESIAN_POINT('Ctrl Pts',(170.652165226381,5.70599465652041,134.13237215779));
#229852=CARTESIAN_POINT('Ctrl Pts',(170.373717602568,5.88417985149351,127.802617239562));
#229853=CARTESIAN_POINT('Ctrl Pts',(170.095269978755,0.655091221110643,
124.231317842401));
#229854=CARTESIAN_POINT('Ctrl Pts',(169.816822354942,-5.17599423848763,
126.700323644626));
#229855=CARTESIAN_POINT('Ctrl Pts',(169.538374731129,-6.25059385429175,
132.940738931629));
#229856=CARTESIAN_POINT('Ctrl Pts',(169.259927107316,-1.58120307648749,
137.217926915891));
#229857=CARTESIAN_POINT('Ctrl Pts',(168.981479483503,4.54123608254409,135.601360792124));
#229858=CARTESIAN_POINT('Ctrl Pts',(168.703031859691,6.49050113343381,129.576585854424));
#229859=CARTESIAN_POINT('Ctrl Pts',(168.424584235878,2.47531272130571,124.680075943919));
#229860=CARTESIAN_POINT('Ctrl Pts',(168.146136612065,-3.81456715595326,
125.411484460556));
#229861=CARTESIAN_POINT('Ctrl Pts',(167.867688988252,-6.59904616885666,
131.098682708838));
#229862=CARTESIAN_POINT('Ctrl Pts',(167.589241364439,-3.31932413390846,
136.515413333674));
#229863=CARTESIAN_POINT('Ctrl Pts',(167.310793740626,3.01069462210276,136.683965512842));
#229864=CARTESIAN_POINT('Ctrl Pts',(167.032346116813,6.57403210101054,131.449448027918));
#229865=CARTESIAN_POINT('Ctrl Pts',(166.753898493,4.09615523841214,125.622126727152));
#229866=CARTESIAN_POINT('Ctrl Pts',(166.475450869187,-2.14588817997888,
124.557025205477));
#229867=CARTESIAN_POINT('Ctrl Pts',(166.197003245374,-6.41596519343492,
129.232919728208));
#229868=CARTESIAN_POINT('Ctrl Pts',(165.918555621562,-4.79008363144905,
135.352891659104));
#229869=CARTESIAN_POINT('Ctrl Pts',(165.640107997748,1.23765077924384,137.292985770921));
#229870=CARTESIAN_POINT('Ctrl Pts',(165.361660373936,6.12804458641347,133.270350353765));
#229871=CARTESIAN_POINT('Ctrl Pts',(165.083212750123,5.38706479029029,126.981590839339));
#229872=CARTESIAN_POINT('Ctrl Pts',(164.80476512631,-0.304364375363971,
124.205769998417));
#229873=CARTESIAN_POINT('Ctrl Pts',(164.526317502497,-5.71609754908509,
127.493731577419));
#229874=CARTESIAN_POINT('Ctrl Pts',(164.247869878684,-5.8750163220866,133.823999511097));
#229875=CARTESIAN_POINT('Ctrl Pts',(163.969422254871,-0.635082105593798,
137.37936681918));
#229876=CARTESIAN_POINT('Ctrl Pts',(163.690974631059,5.18846154045405,134.892624634889));
#229877=CARTESIAN_POINT('Ctrl Pts',(163.412527007245,6.24406250126218,128.648967541478));
#229878=CARTESIAN_POINT('Ctrl Pts',(163.134079383433,1.56167506282176,124.386011388187));
#229879=CARTESIAN_POINT('Ctrl Pts',(162.85563175962,-4.55581546628373,126.021204622902));
#229880=CARTESIAN_POINT('Ctrl Pts',(162.577184135807,-6.48673414583306,
132.051884546553));
#229881=CARTESIAN_POINT('Ctrl Pts',(162.298736511994,-2.45666103994207,
136.936150924396));
#229882=CARTESIAN_POINT('Ctrl Pts',(162.020288888181,3.83096354709181,136.185601564872));
#229883=CARTESIAN_POINT('Ctrl Pts',(161.741841264368,6.59811978732212,130.489954663008));
#229884=CARTESIAN_POINT('Ctrl Pts',(161.463393640556,3.30192627907479,125.083231473798));
#229885=CARTESIAN_POINT('Ctrl Pts',(161.184946016742,-3.02857617157586,
124.933946475014));
#229886=CARTESIAN_POINT('Ctrl Pts',(160.90649839293,-6.57596507471956,130.179285287561));
#229887=CARTESIAN_POINT('Ctrl Pts',(160.628050769116,-4.08036332794952,
135.999037791754));
#229888=CARTESIAN_POINT('Ctrl Pts',(160.349603145304,2.16489298037573,137.045135746957));
#229889=CARTESIAN_POINT('Ctrl Pts',(160.07115552149,6.42071840063739,132.356266237063));
#229890=CARTESIAN_POINT('Ctrl Pts',(159.792707897678,4.77621728024515,126.241271277656));
#229891=CARTESIAN_POINT('Ctrl Pts',(159.514260273865,-1.25739418950663,
124.319532502318));
#229892=CARTESIAN_POINT('Ctrl Pts',(159.235812650052,-6.13552182622286,
128.357033963427));
#229893=CARTESIAN_POINT('Ctrl Pts',(158.957365026239,-5.37540464154493,
134.643509061136));
#229894=CARTESIAN_POINT('Ctrl Pts',(158.678917402427,0.324446805597038,
137.401994292032));
#229895=CARTESIAN_POINT('Ctrl Pts',(158.400469778613,5.72614748850293,134.097576488416));
#229896=CARTESIAN_POINT('Ctrl Pts',(158.122022154801,5.86579836733105,127.766854182028));
#229897=CARTESIAN_POINT('Ctrl Pts',(157.843574530988,0.615067106763091,
124.22745189946));
#229898=CARTESIAN_POINT('Ctrl Pts',(157.565126907175,-5.20088077722156,
126.731907428977));
#229899=CARTESIAN_POINT('Ctrl Pts',(157.286679283362,-6.23747330409059,
132.978748488409));
#229900=CARTESIAN_POINT('Ctrl Pts',(157.008231659549,-1.54213258201158,
137.227433319288));
#229901=CARTESIAN_POINT('Ctrl Pts',(156.729784035736,4.5703526455712,135.57362812183));
#229902=CARTESIAN_POINT('Ctrl Pts',(156.451336411923,6.48290706601333,129.537099079623));
#229903=CARTESIAN_POINT('Ctrl Pts',(156.172888788111,2.43798660040623,124.665121481617));
#229904=CARTESIAN_POINT('Ctrl Pts',(155.894441164297,-3.84732444870741,
125.434804731043));
#229905=CARTESIAN_POINT('Ctrl Pts',(155.615993540485,-6.59713228170722,
131.138847522794));
#229906=CARTESIAN_POINT('Ctrl Pts',(155.337545916672,-3.28449783564716,
136.535513189234));
#229907=CARTESIAN_POINT('Ctrl Pts',(155.059098292859,3.04642966473303,136.665529624679));
#229908=CARTESIAN_POINT('Ctrl Pts',(154.780650669046,6.57783712958646,131.409418076611));
#229909=CARTESIAN_POINT('Ctrl Pts',(154.502203045233,4.06453361755842,125.597288282381));
#229910=CARTESIAN_POINT('Ctrl Pts',(154.22375542142,-2.18387772549973,124.57020358456));
#229911=CARTESIAN_POINT('Ctrl Pts',(153.945307797607,-6.42541212718171,
129.272004644569));
#229912=CARTESIAN_POINT('Ctrl Pts',(153.666860173794,-4.76230668281685,
135.381965984011));
#229913=CARTESIAN_POINT('Ctrl Pts',(153.388412549982,1.27712595144142,137.285331620145));
#229914=CARTESIAN_POINT('Ctrl Pts',(153.109964926169,6.14294222739622,133.233001517943));
#229915=CARTESIAN_POINT('Ctrl Pts',(152.831517302356,5.36369469578529,126.948869073999));
#229916=CARTESIAN_POINT('Ctrl Pts',(152.553069678543,-0.344526230199219,
124.207745007359));
#229917=CARTESIAN_POINT('Ctrl Pts',(152.27462205473,-5.73614438167267,127.528588423912));
#229918=CARTESIAN_POINT('Ctrl Pts',(151.996174430917,-5.85652607262075,
133.859706456064));
#229919=CARTESIAN_POINT('Ctrl Pts',(151.717726807104,-0.595046410034728,
137.383110924578));
#229920=CARTESIAN_POINT('Ctrl Pts',(151.439279183291,5.21325183374003,134.860965250768));
#229921=CARTESIAN_POINT('Ctrl Pts',(151.160831559478,6.23082632381839,128.610998095198));
#229922=CARTESIAN_POINT('Ctrl Pts',(150.882383935665,1.52257581509584,124.376623945969));
#229923=CARTESIAN_POINT('Ctrl Pts',(150.603936311853,-4.58484748573611,
126.049025785542));
#229924=CARTESIAN_POINT('Ctrl Pts',(150.32548868804,-6.47901992942814,132.091348024725));
#229925=CARTESIAN_POINT('Ctrl Pts',(150.047041064227,-2.41928957569559,
136.950991709558));
#229926=CARTESIAN_POINT('Ctrl Pts',(149.768593440414,3.8636497092349,136.162181700472));
#229927=CARTESIAN_POINT('Ctrl Pts',(149.490145816601,6.59608366116008,130.449795860306));
#229928=CARTESIAN_POINT('Ctrl Pts',(149.211698192788,3.26703896508027,125.06323771061));
#229929=CARTESIAN_POINT('Ctrl Pts',(148.933250568975,-3.06425493618196,
124.95249104296));
#229930=CARTESIAN_POINT('Ctrl Pts',(148.654802945162,-6.57964824826877,
130.219326634649));
#229931=CARTESIAN_POINT('Ctrl Pts',(148.376355321349,-4.04866625388314,
136.02377987614));
#229932=CARTESIAN_POINT('Ctrl Pts',(148.097907697537,2.20284223947883,137.031841801807));
#229933=CARTESIAN_POINT('Ctrl Pts',(147.819460073724,6.43004632958585,132.317152748525));
#229934=CARTESIAN_POINT('Ctrl Pts',(147.541012449911,4.74835196802999,126.212281630895));
#229935=CARTESIAN_POINT('Ctrl Pts',(147.262564826098,-1.29684588225586,
124.327306766486));
#229936=CARTESIAN_POINT('Ctrl Pts',(146.984117202285,-6.15030572119196,
128.394427969547));
#229937=CARTESIAN_POINT('Ctrl Pts',(146.705669578472,-5.35193506149072,
134.676159544383));
#229938=CARTESIAN_POINT('Ctrl Pts',(146.427221954659,0.364602463157475,
137.399897053366));
#229939=CARTESIAN_POINT('Ctrl Pts',(146.148774330846,5.74608813598446,134.062658787717));
#229940=CARTESIAN_POINT('Ctrl Pts',(145.870326707034,5.84719952385297,127.731203680413));
#229941=CARTESIAN_POINT('Ctrl Pts',(145.59187908322,0.575020200877703,124.22382966629));
#229942=CARTESIAN_POINT('Ctrl Pts',(145.313431459408,-5.22557459540567,
126.76364211958));
#229943=CARTESIAN_POINT('Ctrl Pts',(145.034983835595,-6.22412162202233,
133.016677472446));
#229944=CARTESIAN_POINT('Ctrl Pts',(144.756536211782,-1.50300494324566,
137.236701713364));
#229945=CARTESIAN_POINT('Ctrl Pts',(144.478088587969,4.59929985250025,135.545718724575));
#229946=CARTESIAN_POINT('Ctrl Pts',(144.199640964156,6.47507277208744,129.497659263665));
#229947=CARTESIAN_POINT('Ctrl Pts',(143.921193340343,2.40057013901678,124.65039451108));
#229948=CARTESIAN_POINT('Ctrl Pts',(143.64274571653,-3.87993917743928,125.458323972397));
#229949=CARTESIAN_POINT('Ctrl Pts',(143.364298092718,-6.594973935395,131.178999942215));
#229950=CARTESIAN_POINT('Ctrl Pts',(143.085850468904,-3.2495498291107,136.555400674828));
#229951=CARTESIAN_POINT('Ctrl Pts',(142.807402845092,3.08205182079176,136.646876548744));
#229952=CARTESIAN_POINT('Ctrl Pts',(142.528955221279,6.58139841398854,131.369365704677));
#229953=CARTESIAN_POINT('Ctrl Pts',(142.250507597466,4.03276138391676,125.572642787588));
#229954=CARTESIAN_POINT('Ctrl Pts',(141.972059973653,-2.2217863466284,124.583612972623));
#229955=CARTESIAN_POINT('Ctrl Pts',(141.69361234984,-6.43462096491922,129.311146342943));
#229956=CARTESIAN_POINT('Ctrl Pts',(141.415164726027,-4.7343532651591,135.410870684068));
#229957=CARTESIAN_POINT('Ctrl Pts',(141.136717102214,1.31655379926713,137.277437314604));
#229958=CARTESIAN_POINT('Ctrl Pts',(140.858269478402,6.15761223939561,133.195562687939));
#229959=CARTESIAN_POINT('Ctrl Pts',(140.579821854588,5.34012584760095,126.916290175316));
#229960=CARTESIAN_POINT('Ctrl Pts',(140.301374230776,-0.384675318488256,
124.20996445632));
#229961=CARTESIAN_POINT('Ctrl Pts',(140.022926606963,-5.75597865932068,
127.563566655346));
#229962=CARTESIAN_POINT('Ctrl Pts',(139.74447898315,-5.83781880742758,133.895300184066));
#229963=CARTESIAN_POINT('Ctrl Pts',(139.466031359337,-0.554988664812238,
137.386611251964));
#229964=CARTESIAN_POINT('Ctrl Pts',(139.187583735524,5.23784894806212,134.829155547671));
#229965=CARTESIAN_POINT('Ctrl Pts',(138.909136111711,6.21735926081381,128.573109924773));
#229966=CARTESIAN_POINT('Ctrl Pts',(138.630688487898,1.48342014776303,124.367474685896));
#229967=CARTESIAN_POINT('Ctrl Pts',(138.352240864086,-4.61370961197883,
126.077023158863));
#229968=CARTESIAN_POINT('Ctrl Pts',(138.073793240272,-6.47106563055709,
132.130763813104));
#229969=CARTESIAN_POINT('Ctrl Pts',(137.79534561646,-2.38182846378423,136.965604729043));
#229970=CARTESIAN_POINT('Ctrl Pts',(137.516897992647,3.89619270241722,136.138563300043));
#229971=CARTESIAN_POINT('Ctrl Pts',(137.238450368834,6.59380311469226,130.409650196134));
#229972=CARTESIAN_POINT('Ctrl Pts',(136.960002745021,3.23203058975544,125.043456686844));
#229973=CARTESIAN_POINT('Ctrl Pts',(136.681555121208,-3.09982015369448,
124.971252454085));
#229974=CARTESIAN_POINT('Ctrl Pts',(136.403107497395,-6.58308761053252,
130.259389660389));
#229975=CARTESIAN_POINT('Ctrl Pts',(136.124659873582,-4.01681915499975,
136.048328553027));
#229976=CARTESIAN_POINT('Ctrl Pts',(135.846212249769,2.24070987145278,137.018317095051));
#229977=CARTESIAN_POINT('Ctrl Pts',(135.567764625956,6.43913599080291,132.277983202917));
#229978=CARTESIAN_POINT('Ctrl Pts',(135.289317002144,4.72031070388647,126.183462145311));
#229979=CARTESIAN_POINT('Ctrl Pts',(135.010869378331,-1.33624951990408,
124.335321040266));
#229980=CARTESIAN_POINT('Ctrl Pts',(134.732421754518,-6.16486171432077,
128.431911276607));
#229981=CARTESIAN_POINT('Ctrl Pts',(134.453974130705,-5.32826716351462,
134.708666556695));
#229982=CARTESIAN_POINT('Ctrl Pts',(134.175526506892,0.404744610239488,
137.397555414672));
#229983=CARTESIAN_POINT('Ctrl Pts',(133.897078883079,5.76581586005707,134.027620349581));
#229984=CARTESIAN_POINT('Ctrl Pts',(133.618631259266,5.82838401024617,127.695667055759));
#229985=CARTESIAN_POINT('Ctrl Pts',(133.340183635453,0.534951987407334,
124.220451277114));
#229986=CARTESIAN_POINT('Ctrl Pts',(133.06173601164,-5.25007477800144,126.795526540492));
#229987=CARTESIAN_POINT('Ctrl Pts',(132.783288387828,-6.21053930283845,
133.054524478268));
#229988=CARTESIAN_POINT('Ctrl Pts',(132.504840764015,-1.46382161007886,
137.245731754674));
#229989=CARTESIAN_POINT('Ctrl Pts',(132.226393140202,4.62807663068185,135.517633634551));
#229990=CARTESIAN_POINT('Ctrl Pts',(131.947945516389,6.46699854195874,129.458267868007));
#229991=CARTESIAN_POINT('Ctrl Pts',(131.669497892576,2.3630647236181,124.635895578019));
#229992=CARTESIAN_POINT('Ctrl Pts',(131.391050268763,-3.91241013359816,
125.482041313105));
#229993=CARTESIAN_POINT('Ctrl Pts',(131.11260264495,-6.59257120989826,131.219138479237));
#229994=CARTESIAN_POINT('Ctrl Pts',(130.834155021138,-3.2144814093103,136.575075053519));
#229995=CARTESIAN_POINT('Ctrl Pts',(130.555707397324,3.1175597702868,136.628006976231));
#229996=CARTESIAN_POINT('Ctrl Pts',(130.277259773512,6.58471582225214,131.329292396271));
#229997=CARTESIAN_POINT('Ctrl Pts',(129.998812149698,4.0008397148189,125.548191156024));
#229998=CARTESIAN_POINT('Ctrl Pts',(129.720364525886,-2.25961263864694,
124.59725287278));
#229999=CARTESIAN_POINT('Ctrl Pts',(129.441916902073,-6.44359136541048,
129.350343372922));
#230000=CARTESIAN_POINT('Ctrl Pts',(129.16346927826,-4.70622441430021,135.439604688201));
#230001=CARTESIAN_POINT('Ctrl Pts',(128.885021654447,1.35593286170785,137.269303146827));
#230002=CARTESIAN_POINT('Ctrl Pts',(128.606574030634,6.17205407880915,133.158035251063));
#230003=CARTESIAN_POINT('Ctrl Pts',(128.328126406821,5.31635911908928,126.883855350513));
#230004=CARTESIAN_POINT('Ctrl Pts',(128.049678783009,-0.424810152491945,
124.212428263054));
#230005=CARTESIAN_POINT('Ctrl Pts',(127.771231159195,-5.77559964706288,
127.598664975593));
#230006=CARTESIAN_POINT('Ctrl Pts',(127.492783535383,-5.81889521971155,
133.930779376167));
#230007=CARTESIAN_POINT('Ctrl Pts',(127.21433591157,-0.514910354280421,
137.389867671632));
#230008=CARTESIAN_POINT('Ctrl Pts',(126.935888287757,5.26225197196523,134.797196704317));
#230009=CARTESIAN_POINT('Ctrl Pts',(126.657440663944,6.20366181127538,128.535304434163));
#230010=CARTESIAN_POINT('Ctrl Pts',(126.378993040131,1.44420951175126,124.358563947));
#230011=CARTESIAN_POINT('Ctrl Pts',(126.100545416318,-4.64240077551519,
126.105195705413));
#230012=CARTESIAN_POINT('Ctrl Pts',(125.822097792505,-6.46287154396936,
132.170130451126));
#230013=CARTESIAN_POINT('Ctrl Pts',(125.543650168692,-2.34427909234318,
136.979989441362));
#230014=CARTESIAN_POINT('Ctrl Pts',(125.26520254488,3.92859132074607,136.114747238771));
#230015=CARTESIAN_POINT('Ctrl Pts',(124.986754921067,6.59127823242518,130.369519158099));
#230016=CARTESIAN_POINT('Ctrl Pts',(124.708307297254,3.19690245034852,125.023889135492));
#230017=CARTESIAN_POINT('Ctrl Pts',(124.429859673441,-3.13527050623128,
124.990230013179));
#230018=CARTESIAN_POINT('Ctrl Pts',(124.151412049628,-6.58628303406391,
130.299472880227));
#230019=CARTESIAN_POINT('Ctrl Pts',(123.872964425815,-3.98482321140548,
136.072682912751));
#230020=CARTESIAN_POINT('Ctrl Pts',(123.594516802002,2.2784944730983,137.004562127853));
#230021=CARTESIAN_POINT('Ctrl Pts',(123.316069178189,6.44798704746787,132.238759051683));
#230022=CARTESIAN_POINT('Ctrl Pts',(123.037621554376,4.6920945268939,126.154813888819));
#230023=CARTESIAN_POINT('Ctrl Pts',(122.759173930564,-1.37560364233486,
124.343575026687));
#230024=CARTESIAN_POINT('Ctrl Pts',(122.480726306751,-6.17918926623166,
128.46948249565));
#230025=CARTESIAN_POINT('Ctrl Pts',(122.202278682938,-5.30440182463932,
134.741028893516));
#230026=CARTESIAN_POINT('Ctrl Pts',(121.923831059125,0.444871759361186,
137.394969462721));
#230027=CARTESIAN_POINT('Ctrl Pts',(121.645383435312,5.78532992970255,133.992462472369));
#230028=CARTESIAN_POINT('Ctrl Pts',(121.366935811499,5.80935252372653,127.660245624887));
#230029=CARTESIAN_POINT('Ctrl Pts',(121.088488187686,0.494863951094175,
124.21731685712));
#230030=CARTESIAN_POINT('Ctrl Pts',(120.810040563873,-5.27438041714564,
126.827559510225));
#230031=CARTESIAN_POINT('Ctrl Pts',(120.53159294006,-6.19672684983677,133.092288103441));
#230032=CARTESIAN_POINT('Ctrl Pts',(120.253145316248,-1.42458403446405,
137.254523108609));
#230033=CARTESIAN_POINT('Ctrl Pts',(119.974697692435,4.65668191378195,135.489373892464));
#230034=CARTESIAN_POINT('Ctrl Pts',(119.696250068622,6.45868467482089,129.418926352309));
#230035=CARTESIAN_POINT('Ctrl Pts',(119.417802444809,2.32547174398699,124.621625219699));
#230036=CARTESIAN_POINT('Ctrl Pts',(119.139354820996,-3.94473611396066,
125.505955874312));
#230037=CARTESIAN_POINT('Ctrl Pts',(118.860907197183,-6.58992419425096,
131.259261646514));
#230038=CARTESIAN_POINT('Ctrl Pts',(118.58245957337,-3.17929387571916,136.594535596262));
#230039=CARTESIAN_POINT('Ctrl Pts',(118.304011949557,3.15295219745811,136.608921606362));
#230040=CARTESIAN_POINT('Ctrl Pts',(118.025564325744,6.58778923144938,131.289199636326));
#230041=CARTESIAN_POINT('Ctrl Pts',(117.747116701932,3.96876979313418,125.523934293753));
#230042=CARTESIAN_POINT('Ctrl Pts',(117.468669078118,-2.29735519988813,
124.611122779595));
#230043=CARTESIAN_POINT('Ctrl Pts',(117.190221454306,-6.45232299625411,
129.389594282045));
#230044=CARTESIAN_POINT('Ctrl Pts',(116.911773830493,-4.67792117256487,
135.468166931659));
#230045=CARTESIAN_POINT('Ctrl Pts',(116.63332620668,1.39526167955762,137.260929418227));
#230046=CARTESIAN_POINT('Ctrl Pts',(116.354878582867,6.18626721048894,133.120420597908));
#230047=CARTESIAN_POINT('Ctrl Pts',(116.076430959054,5.29239539093549,126.851565801475));
#230048=CARTESIAN_POINT('Ctrl Pts',(115.797983335241,-0.464929244999223,
124.215136336267));
#230049=CARTESIAN_POINT('Ctrl Pts',(115.519535711428,-5.79500661783607,
127.633882084071));
#230050=CARTESIAN_POINT('Ctrl Pts',(115.241088087616,-5.79975601069334,
133.96614271767));
#230051=CARTESIAN_POINT('Ctrl Pts',(114.962640463802,-0.474812963556037,
137.392880062915));
#230052=CARTESIAN_POINT('Ctrl Pts',(114.68419283999,5.28646000118636,134.765089904953));
#230053=CARTESIAN_POINT('Ctrl Pts',(114.405745216177,6.18973448276714,128.497583024264));
#230054=CARTESIAN_POINT('Ctrl Pts',(114.127297592364,1.40494536002493,124.349892059469));
#230055=CARTESIAN_POINT('Ctrl Pts',(113.848849968551,-4.67091991318358,
126.133542381245));
#230056=CARTESIAN_POINT('Ctrl Pts',(113.570402344738,-6.45443797329988,
132.209446480045));
#230057=CARTESIAN_POINT('Ctrl Pts',(113.291954720925,-2.30664285277824,
136.994145313484));
#230058=CARTESIAN_POINT('Ctrl Pts',(113.013507097112,3.96084436367879,136.09073439917));
#230059=CARTESIAN_POINT('Ctrl Pts',(112.735059473299,6.58850910791926,130.329404233275));
#230060=CARTESIAN_POINT('Ctrl Pts',(112.456611849487,3.16165584854565,125.004535781636));
#230061=CARTESIAN_POINT('Ctrl Pts',(112.178164225674,-3.1706046801665,125.00942301702));
#230062=CARTESIAN_POINT('Ctrl Pts',(111.899716601861,-6.58923440045535,
130.339574808866));
#230063=CARTESIAN_POINT('Ctrl Pts',(111.621268978048,-3.9526796087217,136.096842052857));
#230064=CARTESIAN_POINT('Ctrl Pts',(111.342821354235,2.31619464429322,136.990577409908));
#230065=CARTESIAN_POINT('Ctrl Pts',(111.064373730422,6.45659917160154,132.199481748287));
#230066=CARTESIAN_POINT('Ctrl Pts',(110.785926106609,4.66370448261314,126.12633792299));
#230067=CARTESIAN_POINT('Ctrl Pts',(110.507478482796,-1.41490679126679,
124.352068419894));
#230068=CARTESIAN_POINT('Ctrl Pts',(110.229030858983,-6.19328784601188,
128.50714023446));
#230069=CARTESIAN_POINT('Ctrl Pts',(109.950583235171,-5.28033992920373,
134.773245355646));
#230070=CARTESIAN_POINT('Ctrl Pts',(109.672135611358,0.484982423596243,
137.392139293334));
#230071=CARTESIAN_POINT('Ctrl Pts',(109.393687987545,5.80462962181993,133.957186458871));
#230072=CARTESIAN_POINT('Ctrl Pts',(109.115240363732,5.79010576951274,127.624940700352));
#230073=CARTESIAN_POINT('Ctrl Pts',(108.836792739919,0.454757577415474,
124.214426522456));
#230074=CARTESIAN_POINT('Ctrl Pts',(108.558345116106,-5.29849061218381,
126.859739841786));
#230075=CARTESIAN_POINT('Ctrl Pts',(108.279897492293,-6.18268477484283,
133.12996694862));
#230076=CARTESIAN_POINT('Ctrl Pts',(108.00144986848,-1.38529367036394,137.2630754494));
#230077=CARTESIAN_POINT('Ctrl Pts',(107.723002244667,4.68511464182123,135.460940545486));
#230078=CARTESIAN_POINT('Ctrl Pts',(107.444554620855,6.45013147874722,129.379636174388));
#230079=CARTESIAN_POINT('Ctrl Pts',(107.166106997042,2.28779259314522,124.607583964913));
#230080=CARTESIAN_POINT('Ctrl Pts',(106.887659373229,-3.97691592067581,
125.530066769856));
#230081=CARTESIAN_POINT('Ctrl Pts',(106.609211749416,-6.58703298653922,
131.299367957265));
#230082=CARTESIAN_POINT('Ctrl Pts',(106.330764125603,-3.14398853222427,
136.613781581943));
#230083=CARTESIAN_POINT('Ctrl Pts',(106.05231650179,3.18822779082625,136.589621146351));
#230084=CARTESIAN_POINT('Ctrl Pts',(105.773868877977,6.59061852769399,131.249088910493));
#230085=CARTESIAN_POINT('Ctrl Pts',(105.495421254164,3.93655280722527,125.49987309962));
#230086=CARTESIAN_POINT('Ctrl Pts',(105.216973630351,-2.33501263178752,
124.625222179118));
#230087=CARTESIAN_POINT('Ctrl Pts',(104.938526006539,-6.46081553389627,
129.428897615854));
#230088=CARTESIAN_POINT('Ctrl Pts',(104.660078382726,-4.64944458874018,
135.49655635606));
#230089=CARTESIAN_POINT('Ctrl Pts',(104.381630758913,1.43453879547275,137.252316439095));
#230090=CARTESIAN_POINT('Ctrl Pts',(104.1031831351,6.20025110776228,133.082720122298));
#230091=CARTESIAN_POINT('Ctrl Pts',(103.824735511287,5.26823555112421,126.819422724701));
#230092=CARTESIAN_POINT('Ctrl Pts',(103.546287887474,-0.505031109382345,
124.218088575609));
#230093=CARTESIAN_POINT('Ctrl Pts',(103.267840263661,-5.81419885250792,
127.669216675797));
#230094=CARTESIAN_POINT('Ctrl Pts',(102.989392639848,-5.78040188958328,
134.001388898174));
#230095=CARTESIAN_POINT('Ctrl Pts',(102.710945016035,-0.434697978462825,
137.395648314187));
#230096=CARTESIAN_POINT('Ctrl Pts',(102.432497392222,5.31047213868803,134.732836339309));
#230097=CARTESIAN_POINT('Ctrl Pts',(102.15404976841,6.17557779137139,128.459947092858));
#230098=CARTESIAN_POINT('Ctrl Pts',(101.875602144597,1.3656291475316,124.341459344644));
#230099=CARTESIAN_POINT('Ctrl Pts',(101.597154520784,-4.69926596819684,
126.162062135967));
#230100=CARTESIAN_POINT('Ctrl Pts',(101.318706896971,-6.44576523105769,
132.248710442988));
#230101=CARTESIAN_POINT('Ctrl Pts',(101.040259273158,-2.26892113971413,
137.008071820859));
#230102=CARTESIAN_POINT('Ctrl Pts',(100.761811649345,3.99295063606701,136.066525671043));
#230103=CARTESIAN_POINT('Ctrl Pts',(100.483364025532,6.58549584378548,130.289306908136));
#230104=CARTESIAN_POINT('Ctrl Pts',(100.204916401719,3.12629209042249,124.985397342422));
#230105=CARTESIAN_POINT('Ctrl Pts',(99.9264687779064,-3.20582136617937,
125.028830754405));
#230106=CARTESIAN_POINT('Ctrl Pts',(99.6480211540935,-6.5919416003429,130.379693960313));
#230107=CARTESIAN_POINT('Ctrl Pts',(99.3695735302808,-3.92038953804142,
136.120805078117));
#230108=CARTESIAN_POINT('Ctrl Pts',(99.0911259064677,2.35380898804382,136.976363459425));
#230109=CARTESIAN_POINT('Ctrl Pts',(98.812678282655,6.46497204407849,132.160152748165));
#230110=CARTESIAN_POINT('Ctrl Pts',(98.5342306588419,4.63514162304771,126.098035303012));
#230111=CARTESIAN_POINT('Ctrl Pts',(98.2557830350292,-1.45415751030726,
124.36080090516));
#230112=CARTESIAN_POINT('Ctrl Pts',(97.9773354112161,-6.20715693123341,
128.544883097616));
#230113=CARTESIAN_POINT('Ctrl Pts',(97.6988877874034,-5.25608236883021,
134.805314749293));
#230114=CARTESIAN_POINT('Ctrl Pts',(97.4204401635904,0.525075116629235,
137.389065011387));
#230115=CARTESIAN_POINT('Ctrl Pts',(97.1419925397775,5.82371422125203,133.921793616252));
#230116=CARTESIAN_POINT('Ctrl Pts',(96.8635449159648,5.77064446080036,127.589753590393));
#230117=CARTESIAN_POINT('Ctrl Pts',(96.5850972921516,0.414634352527504,
124.211780380221));
#230118=CARTESIAN_POINT('Ctrl Pts',(96.306649668339,-5.32240446970382,126.89206634272));
#230119=CARTESIAN_POINT('Ctrl Pts',(96.0282020445258,-6.16841359819089,
133.1675596176));
#230120=CARTESIAN_POINT('Ctrl Pts',(95.7497544207132,-1.34595197369742,
137.271388460138));
#230121=CARTESIAN_POINT('Ctrl Pts',(95.4713067969001,4.7133737612145,135.432334647225));
#230122=CARTESIAN_POINT('Ctrl Pts',(95.1928591730874,6.44133927067958,129.340398790155));
#230123=CARTESIAN_POINT('Ctrl Pts',(94.9144115492744,2.25002866730758,124.593772333964));
#230124=CARTESIAN_POINT('Ctrl Pts',(94.6359639254615,-4.008948361309,125.554373106298));
#230125=CARTESIAN_POINT('Ctrl Pts',(94.3575163016487,-6.58389769389783,
131.339455925338));
#230126=CARTESIAN_POINT('Ctrl Pts',(94.0790686778357,-3.10856668707799,
136.632812297395));
#230127=CARTESIAN_POINT('Ctrl Pts',(93.8006210540229,3.22338524324122,136.570106311383));
#230128=CARTESIAN_POINT('Ctrl Pts',(93.52217343021,6.59320360614536,131.208961705089));
#230129=CARTESIAN_POINT('Ctrl Pts',(93.2437258063971,3.90418995090443,125.476008465224));
#230130=CARTESIAN_POINT('Ctrl Pts',(92.9652781825842,-2.37258353893516,
124.639550548886));
#230131=CARTESIAN_POINT('Ctrl Pts',(92.6868305587713,-6.46906866364288,
129.468251917951));
#230132=CARTESIAN_POINT('Ctrl Pts',(92.4083829349583,-4.62079571803641,
135.524771909422));
#230133=CARTESIAN_POINT('Ctrl Pts',(92.1299353111456,1.47376275402524,137.24346452859));
#230134=CARTESIAN_POINT('Ctrl Pts',(91.8514876873325,6.21400525245068,133.04493522124));
#230135=CARTESIAN_POINT('Ctrl Pts',(91.5730400635199,5.24388049490719,126.787427311268));
#230136=CARTESIAN_POINT('Ctrl Pts',(91.2945924397067,-0.545114259651984,
124.221284871682));
#230137=CARTESIAN_POINT('Ctrl Pts',(91.016144815894,-5.83317563990314,127.704667441434));
#230138=CARTESIAN_POINT('Ctrl Pts',(90.7376971920811,-5.76083357355547,
134.036516611621));
#230139=CARTESIAN_POINT('Ctrl Pts',(90.4592495682681,-0.394566885476172,
137.398172322869));
#230140=CARTESIAN_POINT('Ctrl Pts',(90.1808019444553,5.33428749469169,134.700437202553));
#230141=CARTESIAN_POINT('Ctrl Pts',(89.9023543206424,6.16119226166949,128.422398034556));
#230142=CARTESIAN_POINT('Ctrl Pts',(89.6239066968295,1.32626233114802,124.333266115003));
#230143=CARTESIAN_POINT('Ctrl Pts',(89.3454590730166,-4.72743789018152,
126.190753912764));
#230144=CARTESIAN_POINT('Ctrl Pts',(89.0670114492037,-6.43685363861442,
132.28792088502));
#230145=CARTESIAN_POINT('Ctrl Pts',(88.7885638253908,-2.23111535094281,
137.021768447433));
#230146=CARTESIAN_POINT('Ctrl Pts',(88.5101162015778,4.02490894820102,136.042121951457));
#230147=CARTESIAN_POINT('Ctrl Pts',(88.2316685777651,6.58223855168135,130.2492286685));
#230148=CARTESIAN_POINT('Ctrl Pts',(87.9532209539521,3.09081248639635,124.966474527032));
#230149=CARTESIAN_POINT('Ctrl Pts',(87.6747733301392,-3.2409192593025,125.048452506173));
#230150=CARTESIAN_POINT('Ctrl Pts',(87.3963257063264,-6.59440453341028,
130.41982884794));
#230151=CARTESIAN_POINT('Ctrl Pts',(87.1178780825135,-3.88795419588509,
136.144571100572));
#230152=CARTESIAN_POINT('Ctrl Pts',(86.8394304587006,2.39133611053674,136.961920803106));
#230153=CARTESIAN_POINT('Ctrl Pts',(86.5609828348878,6.47310535463887,132.120773508667));
#230154=CARTESIAN_POINT('Ctrl Pts',(86.2825352110747,4.60640700660486,126.06990707765));
#230155=CARTESIAN_POINT('Ctrl Pts',(86.004087587262,-1.49335434500641,124.369772158902));
#230156=CARTESIAN_POINT('Ctrl Pts',(85.725639963449,-6.22079600797217,128.582709686544));
#230157=CARTESIAN_POINT('Ctrl Pts',(85.4471923396362,-5.23163004239161,
134.837235886113));
#230158=CARTESIAN_POINT('Ctrl Pts',(85.1687447158232,0.565148352810691,
137.385746730796));
#230159=CARTESIAN_POINT('Ctrl Pts',(84.8902970920103,5.842583020812,133.886285256006));
#230160=CARTESIAN_POINT('Ctrl Pts',(84.6118494681974,5.75096931873532,127.554685598878));
#230161=CARTESIAN_POINT('Ctrl Pts',(84.3334018443846,0.374495763211118,
124.209378528473));
#230162=CARTESIAN_POINT('Ctrl Pts',(84.0549542205716,-5.34612110356891,
126.924537815158));
#230163=CARTESIAN_POINT('Ctrl Pts',(83.7765065967588,-6.15391384870464,
133.205064717373));
#230164=CARTESIAN_POINT('Ctrl Pts',(83.498058972946,-1.30656040228555,137.279461832782));
#230165=CARTESIAN_POINT('Ctrl Pts',(83.2196113491328,4.74145822480973,135.403557257686));
#230166=CARTESIAN_POINT('Ctrl Pts',(82.9411637253203,6.43230837641647,129.301215653567));
#230167=CARTESIAN_POINT('Ctrl Pts',(82.6627161015071,2.21218136583022,124.580190838648));
#230168=CARTESIAN_POINT('Ctrl Pts',(82.3842684776944,-4.04083224888638,
125.578873982957));
#230169=CARTESIAN_POINT('Ctrl Pts',(82.1058208538814,-6.58051843250612,
131.379524065257));
#230170=CARTESIAN_POINT('Ctrl Pts',(81.8273732300686,-3.07302965285007,
136.651627037425));
#230171=CARTESIAN_POINT('Ctrl Pts',(81.5489256062556,3.25842325193051,136.550377824588));
#230172=CARTESIAN_POINT('Ctrl Pts',(81.270477982443,6.59554437101248,131.168819507043));
#230173=CARTESIAN_POINT('Ctrl Pts',(80.9920303586297,3.87168242338918,125.452341274876));
#230174=CARTESIAN_POINT('Ctrl Pts',(80.713582734817,-2.41006652912724,124.654107357959));
#230175=CARTESIAN_POINT('Ctrl Pts',(80.435135111004,-6.47708207967116,129.507655730047));
#230176=CARTESIAN_POINT('Ctrl Pts',(80.1566874871913,-4.59197562204804,
135.552812546207));
#230177=CARTESIAN_POINT('Ctrl Pts',(79.8782398633782,1.51293210175691,137.234374014721));
#230178=CARTESIAN_POINT('Ctrl Pts',(79.5997922395654,6.22752913488936,133.007067294864));
#230179=CARTESIAN_POINT('Ctrl Pts',(79.3213446157525,5.2193311247699,126.755580746775));
#230180=CARTESIAN_POINT('Ctrl Pts',(79.0428969919396,-0.585177210512381,
124.224725106049));
#230181=CARTESIAN_POINT('Ctrl Pts',(78.7644493681267,-5.85193627682986,
127.740233067343));
#230182=CARTESIAN_POINT('Ctrl Pts',(78.4860017443139,-5.74105178772106,
134.071524556339));
#230183=CARTESIAN_POINT('Ctrl Pts',(78.2075541205009,-0.354421171668466,
137.400451995434));
#230184=CARTESIAN_POINT('Ctrl Pts',(77.9291064966881,5.35790518671055,134.667893695246));
#230185=CARTESIAN_POINT('Ctrl Pts',(77.6506588728751,6.14657842672258,128.384937240753));
#230186=CARTESIAN_POINT('Ctrl Pts',(77.3722112490624,1.28684636962602,124.325312674148));
#230187=CARTESIAN_POINT('Ctrl Pts',(77.0937636252493,-4.75543463521666,
126.219616648455));
#230188=CARTESIAN_POINT('Ctrl Pts',(76.8153160014366,-6.42770352619243,
132.327076353179));
#230189=CARTESIAN_POINT('Ctrl Pts',(76.5368683776235,-2.19322688737167,
137.035234685673));
#230190=CARTESIAN_POINT('Ctrl Pts',(76.2584207538107,4.05671811585379,136.017524144697));
#230191=CARTESIAN_POINT('Ctrl Pts',(75.9799731299978,6.57873735230709,130.209170999483));
#230192=CARTESIAN_POINT('Ctrl Pts',(75.7015255061849,3.05521835117689,124.947768036657));
#230193=CARTESIAN_POINT('Ctrl Pts',(75.423077882372,-3.27589705897064,125.068287545233));
#230194=CARTESIAN_POINT('Ctrl Pts',(75.1446302585591,-6.5966231083926,130.459977984534));
#230195=CARTESIAN_POINT('Ctrl Pts',(74.8661826347462,-3.85537478415624,
136.168139239563));
#230196=CARTESIAN_POINT('Ctrl Pts',(74.5877350109334,2.42877462119068,136.94724997613));
#230197=CARTESIAN_POINT('Ctrl Pts',(74.3092873871204,6.48099880189986,132.081345489005));
#230198=CARTESIAN_POINT('Ctrl Pts',(74.0308397633076,4.57750169805637,126.041954289206));
#230199=CARTESIAN_POINT('Ctrl Pts',(73.7523921394947,-1.53249584291112,
124.378981848686));
#230200=CARTESIAN_POINT('Ctrl Pts',(73.4739445156818,-6.23420457082727,
128.620618599563));
#230201=CARTESIAN_POINT('Ctrl Pts',(73.1954968918689,-5.20698385597775,
134.869007583256));
#230202=CARTESIAN_POINT('Ctrl Pts',(72.917049268056,0.605200647212208,137.382184574524));
#230203=CARTESIAN_POINT('Ctrl Pts',(72.6386016442432,5.86123532130951,133.850662693911));
#230204=CARTESIAN_POINT('Ctrl Pts',(72.3601540204302,5.73108107238729,127.519738025268));
#230205=CARTESIAN_POINT('Ctrl Pts',(72.0817063966174,0.334343296816498,
124.207221056211));
#230206=CARTESIAN_POINT('Ctrl Pts',(71.8032587728044,-5.36963963495047,
126.957153055855));
#230207=CARTESIAN_POINT('Ctrl Pts',(71.5248111489915,-6.13918606367764,
133.242480858172));
#230208=CARTESIAN_POINT('Ctrl Pts',(71.2463635251787,-1.26712041579749,
137.287295268168));
#230209=CARTESIAN_POINT('Ctrl Pts',(70.9679159013657,4.76936699192676,135.374609443224));
#230210=CARTESIAN_POINT('Ctrl Pts',(70.689468277553,6.423039130601,129.262088216567));
#230211=CARTESIAN_POINT('Ctrl Pts',(70.4110206537399,2.17425209115883,124.566839982233));
#230212=CARTESIAN_POINT('Ctrl Pts',(70.1325730299272,-4.07256640193864,
125.603568491945));
#230213=CARTESIAN_POINT('Ctrl Pts',(69.8541254061142,-6.57689532758393,
131.419570892283));
#230214=CARTESIAN_POINT('Ctrl Pts',(69.5756777823013,-3.03737874637841,
136.670225104848));
#230215=CARTESIAN_POINT('Ctrl Pts',(69.2972301584884,3.2933405185478,136.530436417012));
#230216=CARTESIAN_POINT('Ctrl Pts',(69.0187825346755,6.5976407355574,131.128663803839));
#230217=CARTESIAN_POINT('Ctrl Pts',(68.7403349108627,3.83903142925813,125.428872405572));
#230218=CARTESIAN_POINT('Ctrl Pts',(68.4618872870498,-2.44746021341752,
124.668892066929));
#230219=CARTESIAN_POINT('Ctrl Pts',(68.1834396632368,-6.48485548504104,
129.547107592018));
#230220=CARTESIAN_POINT('Ctrl Pts',(67.904992039424,-4.56298536871445,135.580677227361));
#230221=CARTESIAN_POINT('Ctrl Pts',(67.6265444156111,1.55204538723279,137.225045234339));
#230222=CARTESIAN_POINT('Ctrl Pts',(67.3480967917982,6.2408222539455,132.969117746385));
#230223=CARTESIAN_POINT('Ctrl Pts',(67.0696491679854,5.19458835039884,126.723884211309));
#230224=CARTESIAN_POINT('Ctrl Pts',(66.7912015441724,-0.625218477415679,
124.228409151229));
#230225=CARTESIAN_POINT('Ctrl Pts',(66.5127539203596,-5.87048006810572,
127.775912235624));
#230226=CARTESIAN_POINT('Ctrl Pts',(66.2343062965465,-5.72105726510147,
134.106411435094));
#230227=CARTESIAN_POINT('Ctrl Pts',(65.9558586727338,-0.314262324654327,
137.402487247406));
#230228=CARTESIAN_POINT('Ctrl Pts',(65.6774110489208,5.3813243395822,134.6352070233));
#230229=CARTESIAN_POINT('Ctrl Pts',(65.398963425108,6.13173682805169,128.347566099575));
#230230=CARTESIAN_POINT('Ctrl Pts',(65.120515801295,1.24738272353907,124.317599316798));
#230231=CARTESIAN_POINT('Ctrl Pts',(64.8420681774823,-4.78325516587229,
126.248649273519));
#230232=CARTESIAN_POINT('Ctrl Pts',(64.5636205536692,-6.41831523285262,
132.366175396547));
#230233=CARTESIAN_POINT('Ctrl Pts',(64.2851729298565,-2.15525715297185,
137.048470036584));
#230234=CARTESIAN_POINT('Ctrl Pts',(64.0067253060435,4.08837696032456,135.992733162246));
#230235=CARTESIAN_POINT('Ctrl Pts',(63.7282776822307,6.57499237540094,130.169135385437));
#230236=CARTESIAN_POINT('Ctrl Pts',(63.4498300584178,3.01951100371835,124.929278564476));
#230237=CARTESIAN_POINT('Ctrl Pts',(63.1713824346048,-3.31075346906837,
125.088335136589));
#230238=CARTESIAN_POINT('Ctrl Pts',(62.892934810792,-6.59859724307971,130.500139882352));
#230239=CARTESIAN_POINT('Ctrl Pts',(62.614487186979,-3.82265251009718,136.191508621766));
#230240=CARTESIAN_POINT('Ctrl Pts',(62.3360395631662,2.46612313270748,136.932351522132));
#230241=CARTESIAN_POINT('Ctrl Pts',(62.0575919393533,6.48865209336687,132.041870150199));
#230242=CARTESIAN_POINT('Ctrl Pts',(61.7791443155403,4.5484267684992,126.014177973478));
#230243=CARTESIAN_POINT('Ctrl Pts',(61.5006966917276,-1.57158055361859,
124.388429633243));
#230244=CARTESIAN_POINT('Ctrl Pts',(61.2222490679146,-6.24738212293903,
128.658608431946));
#230245=CARTESIAN_POINT('Ctrl Pts',(60.9438014441017,-5.18214472286266,
134.900628663412));
#230246=CARTESIAN_POINT('Ctrl Pts',(60.6653538202889,0.645230515680748,
137.378378674564));
#230247=CARTESIAN_POINT('Ctrl Pts',(60.3869061964759,5.87967043157647,133.814927249971));
#230248=CARTESIAN_POINT('Ctrl Pts',(60.108458572663,5.71098045872276,127.484912164554));
#230249=CARTESIAN_POINT('Ctrl Pts',(59.8300109488502,0.294178441208572,
124.205308043382));
#230250=CARTESIAN_POINT('Ctrl Pts',(59.5515633250373,-5.39295919236059,
126.989910856244));
#230251=CARTESIAN_POINT('Ctrl Pts',(59.2731157012244,-6.12423078885343,
133.27980665353));
#230252=CARTESIAN_POINT('Ctrl Pts',(58.9946680774115,-1.2276334756968,137.294888476026));
#230253=CARTESIAN_POINT('Ctrl Pts',(58.7162204535986,4.79709902839574,135.345492276511));
#230254=CARTESIAN_POINT('Ctrl Pts',(58.4377728297857,6.41353187670863,129.223017929039));
#230255=CARTESIAN_POINT('Ctrl Pts',(58.1593252059728,2.13624224877676,124.553720259438));
#230256=CARTESIAN_POINT('Ctrl Pts',(57.8808775821599,-4.10414964454526,
125.628455718198));
#230257=CARTESIAN_POINT('Ctrl Pts',(57.602429958347,-6.57302851338661,131.459594922466));
#230258=CARTESIAN_POINT('Ctrl Pts',(57.3239823345341,-3.00161528872044,
136.688605810505));
#230259=CARTESIAN_POINT('Ctrl Pts',(57.0455347107212,3.32813574922106,136.510282827592));
#230260=CARTESIAN_POINT('Ctrl Pts',(56.7670870869083,6.59949262209846,131.088496083461));
#230261=CARTESIAN_POINT('Ctrl Pts',(56.4886394630955,3.80623817840574,125.405602726962));
#230262=CARTESIAN_POINT('Ctrl Pts',(56.2101918392826,-2.48476320616966,
124.683904127941));
#230263=CARTESIAN_POINT('Ctrl Pts',(55.9317442154696,-6.49238859170611,
129.586606041964));
#230264=CARTESIAN_POINT('Ctrl Pts',(55.6532965916568,-4.53382603227983,
135.608364920346));
#230265=CARTESIAN_POINT('Ctrl Pts',(55.3748489678439,1.59110116109648,137.215478533129));
#230266=CARTESIAN_POINT('Ctrl Pts',(55.096401344031,6.25388411703813,132.931087982032));
#230267=CARTESIAN_POINT('Ctrl Pts',(54.8179537202181,5.1696530886458,126.692338879397));
#230268=CARTESIAN_POINT('Ctrl Pts',(54.5395060964052,-0.665236576618623,
124.23233687071));
#230269=CARTESIAN_POINT('Ctrl Pts',(54.2610584725923,-5.88880632658389,
127.811703624173));
#230270=CARTESIAN_POINT('Ctrl Pts',(53.9826108487795,-5.70085074660091,
134.141175955143));
#230271=CARTESIAN_POINT('Ctrl Pts',(53.7041632249665,-0.274091832533765,
137.40427800337));
#230272=CARTESIAN_POINT('Ctrl Pts',(53.4257156011537,5.40454408550164,134.602378397932));
#230273=CARTESIAN_POINT('Ctrl Pts',(53.1472679773408,6.11666801561766,128.310285995821));
#230274=CARTESIAN_POINT('Ctrl Pts',(52.8688203535278,1.20787285522606,124.310126328773));
#230275=CARTESIAN_POINT('Ctrl Pts',(52.590372729715,-4.81089845124901,126.277850712144));
#230276=CARTESIAN_POINT('Ctrl Pts',(52.3119251059021,-6.40868910648141,
132.405216566294));
#230277=CARTESIAN_POINT('Ctrl Pts',(52.0334774820892,-2.11720755472543,
137.061474009724));
#230278=CARTESIAN_POINT('Ctrl Pts',(51.7550298582764,4.11988430848393,135.967749922743));
#230279=CARTESIAN_POINT('Ctrl Pts',(51.4765822344634,6.57100375973434,130.129123309894));
#230280=CARTESIAN_POINT('Ctrl Pts',(51.1981346106506,2.98369176716867,124.91100679562));
#230281=CARTESIAN_POINT('Ctrl Pts',(50.9196869868376,-3.34548719797895,
125.108594537373));
#230282=CARTESIAN_POINT('Ctrl Pts',(50.6412393630248,-6.60032686431936,
130.540313053181));
#230283=CARTESIAN_POINT('Ctrl Pts',(50.3627917392119,-3.78978858624336,
136.214678381218));
#230284=CARTESIAN_POINT('Ctrl Pts',(50.0843441153989,2.50338026112505,136.917225993175));
#230285=CARTESIAN_POINT('Ctrl Pts',(49.8058964915862,6.49606494544435,132.002348955022));
#230286=CARTESIAN_POINT('Ctrl Pts',(49.5274488677731,4.51918329531533,125.986579159731));
#230287=CARTESIAN_POINT('Ctrl Pts',(49.2490012439603,-1.6106070288309,124.39811516248));
#230288=CARTESIAN_POINT('Ctrl Pts',(48.9705536201474,-6.26032817600901,
128.696677775965));
#230289=CARTESIAN_POINT('Ctrl Pts',(48.6921059963345,-5.15711356346882,
134.932097954848));
#230290=CARTESIAN_POINT('Ctrl Pts',(48.4136583725217,0.685236474895564,
137.374329171949));
#230291=CARTESIAN_POINT('Ctrl Pts',(48.1352107487087,5.89788766849362,133.779080248378));
#230292=CARTESIAN_POINT('Ctrl Pts',(47.8567631248959,5.69066822257687,127.450209307224));
#230293=CARTESIAN_POINT('Ctrl Pts',(47.578315501083,0.254002684709825,124.203639560873));
#230294=CARTESIAN_POINT('Ctrl Pts',(47.29986787727,-5.41607891168467,127.022810002472));
#230295=CARTESIAN_POINT('Ctrl Pts',(47.0214202534572,-6.10904857840509,
133.317040720324));
#230296=CARTESIAN_POINT('Ctrl Pts',(46.7429726296443,-1.18810104518584,
137.302241174989));
#230297=CARTESIAN_POINT('Ctrl Pts',(46.4645250058313,4.82465330659632,135.316206836494));
#230298=CARTESIAN_POINT('Ctrl Pts',(46.1860773820186,6.40378696703385,129.184006238746));
#230299=CARTESIAN_POINT('Ctrl Pts',(45.9076297582056,2.09815324715241,124.54083215642));
#230300=CARTESIAN_POINT('Ctrl Pts',(45.6291821343927,-4.13558080637756,
125.653534739511));
#230301=CARTESIAN_POINT('Ctrl Pts',(45.3507345105798,-6.56891813320061,
131.499594672701));
#230302=CARTESIAN_POINT('Ctrl Pts',(45.072286886767,-2.96574060510383,136.706768473292));
#230303=CARTESIAN_POINT('Ctrl Pts',(44.793839262954,3.36280765460034,136.489917803126));
#230304=CARTESIAN_POINT('Ctrl Pts',(44.5153916391412,6.60109996201359,131.048317834339));
#230305=CARTESIAN_POINT('Ctrl Pts',(44.2369440153282,3.77330388599763,125.38253310131));
#230306=CARTESIAN_POINT('Ctrl Pts',(43.9584963915154,-2.52197412510756,
124.699142984721));
#230307=CARTESIAN_POINT('Ctrl Pts',(43.6800487677024,-6.49968112052436,
129.626149616253));
#230308=CARTESIAN_POINT('Ctrl Pts',(43.4016011438896,-4.50449869325427,
135.635874599185));
#230309=CARTESIAN_POINT('Ctrl Pts',(43.1231535200766,1.6300979761215,137.205674265588));
#230310=CARTESIAN_POINT('Ctrl Pts',(42.8447058962639,6.26671424015497,132.892979411015));
#230311=CARTESIAN_POINT('Ctrl Pts',(42.5662582724509,5.14452626349642,126.660945919963));
#230312=CARTESIAN_POINT('Ctrl Pts',(42.287810648638,-0.705230025235587,
124.236508118946));
#230313=CARTESIAN_POINT('Ctrl Pts',(42.0093630248251,-5.90691437317801,
127.847605906729));
#230314=CARTESIAN_POINT('Ctrl Pts',(41.7309154010123,-5.68043298097947,
134.175816828272));
#230315=CARTESIAN_POINT('Ctrl Pts',(41.4524677771993,-0.233911183839542,
137.405824196969));
#230316=CARTESIAN_POINT('Ctrl Pts',(41.1740201533865,5.42756356405245,134.569409035618));
#230317=CARTESIAN_POINT('Ctrl Pts',(40.8955725295735,6.10137254780096,128.273098310918));
#230318=CARTESIAN_POINT('Ctrl Pts',(40.6171249057607,1.1683182287399,124.302893986988));
#230319=CARTESIAN_POINT('Ctrl Pts',(40.3386772819477,-4.83836346701448,
126.307219882257));
#230320=CARTESIAN_POINT('Ctrl Pts',(40.060229658135,-6.39882550377857,132.444198415735));
#230321=CARTESIAN_POINT('Ctrl Pts',(39.781782034322,-2.07907950257448,137.074246123225));
#230322=CARTESIAN_POINT('Ctrl Pts',(39.5033344105091,4.15123899281517,135.94257535195));
#230323=CARTESIAN_POINT('Ctrl Pts',(39.2248867866962,6.56677165310695,130.089136255519));
#230324=CARTESIAN_POINT('Ctrl Pts',(38.9464391628834,2.94776196882331,124.892953407157));
#230325=CARTESIAN_POINT('Ctrl Pts',(38.6679915390704,-3.38009695863112,
125.129064996863));
#230326=CARTESIAN_POINT('Ctrl Pts',(38.3895439152575,-6.6018119080198,130.58049600839));
#230327=CARTESIAN_POINT('Ctrl Pts',(38.1110962914447,-3.75678423037978,
136.237647659355));
#230328=CARTESIAN_POINT('Ctrl Pts',(37.8326486676317,2.54054462586645,136.901873949744));
#230329=CARTESIAN_POINT('Ctrl Pts',(37.5542010438189,6.50323708344635,131.962783367948));
#230330=CARTESIAN_POINT('Ctrl Pts',(37.275753420006,4.48977236213255,125.959158870647));
#230331=CARTESIAN_POINT('Ctrl Pts',(36.9973057961931,-1.64957382240749,
124.4080380775));
#230332=CARTESIAN_POINT('Ctrl Pts',(36.7188581723802,-6.27304225031618,
128.734825220947));
#230333=CARTESIAN_POINT('Ctrl Pts',(36.4404105485673,-5.13189130533538,
134.96341429146));
#230334=CARTESIAN_POINT('Ctrl Pts',(36.1619629247544,0.725217042420823,
137.370036216732));
#230335=CARTESIAN_POINT('Ctrl Pts',(35.8835153009416,5.91588635701427,133.743123017455));
#230336=CARTESIAN_POINT('Ctrl Pts',(35.6050676771286,5.67014511662727,127.415630739204));
#230337=CARTESIAN_POINT('Ctrl Pts',(35.3266200533158,0.213817516048174,
124.202215670509));
#230338=CARTESIAN_POINT('Ctrl Pts',(35.0481724295028,-5.43899793621292,
127.055849275448));
#230339=CARTESIAN_POINT('Ctrl Pts',(34.76972480569,-6.09363999491508,133.354181678833));
#230340=CARTESIAN_POINT('Ctrl Pts',(34.4912771818771,-1.14852458915375,
137.309353092597));
#230341=CARTESIAN_POINT('Ctrl Pts',(34.2128295580642,4.85202880549439,135.286754208357));
#230342=CARTESIAN_POINT('Ctrl Pts',(33.9343819342512,6.393804762678,129.145054591279));
#230343=CARTESIAN_POINT('Ctrl Pts',(33.6559343104384,2.05998649768791,124.528176150753));
#230344=CARTESIAN_POINT('Ctrl Pts',(33.3774866866255,-4.16685872274224,
125.678804626571));
#230345=CARTESIAN_POINT('Ctrl Pts',(33.0990390628127,-6.56456433933747,
131.539568660782));
#230346=CARTESIAN_POINT('Ctrl Pts',(32.8205914389997,-2.92975602487846,
136.724712420187));
#230347=CARTESIAN_POINT('Ctrl Pts',(32.5421438151868,3.39735494990529,136.469342098247));
#230348=CARTESIAN_POINT('Ctrl Pts',(32.263696191374,6.60246269574222,131.008130545292));
#230349=CARTESIAN_POINT('Ctrl Pts',(31.985248567561,3.74022977242616,125.359664383471));
#230350=CARTESIAN_POINT('Ctrl Pts',(31.7068009437482,-2.55909159136699,
124.714608072585));
#230351=CARTESIAN_POINT('Ctrl Pts',(31.4283533199352,-6.50673280126843,
129.665736849585));
#230352=CARTESIAN_POINT('Ctrl Pts',(31.1499056961224,-4.47500443837311,
135.663205244496));
#230353=CARTESIAN_POINT('Ctrl Pts',(30.8714580723094,1.66903438726656,137.195632795014));
#230354=CARTESIAN_POINT('Ctrl Pts',(30.5930104484966,6.27931214787105,132.854793445461));
#230355=CARTESIAN_POINT('Ctrl Pts',(30.3145628246837,5.11920880603445,126.629706496284));
#230356=CARTESIAN_POINT('Ctrl Pts',(30.0361152008708,-0.745197341294603,
124.240922741373));
#230357=CARTESIAN_POINT('Ctrl Pts',(29.7576675770579,-5.9248035368878,127.883617752917));
#230358=CARTESIAN_POINT('Ctrl Pts',(29.4792199532451,-5.65980472482494,
134.210332770852));
#230359=CARTESIAN_POINT('Ctrl Pts',(29.2007723294321,-0.193721867480399,
137.407125770907));
#230360=CARTESIAN_POINT('Ctrl Pts',(28.9223247056193,5.45038192223944,134.536300158051));
#230361=CARTESIAN_POINT('Ctrl Pts',(28.6438770818064,6.08585099138068,128.236004422871));
#230362=CARTESIAN_POINT('Ctrl Pts',(28.3654294579935,1.12872030979243,124.29590255944));
#230363=CARTESIAN_POINT('Ctrl Pts',(28.0869818341806,-4.86564919544231,
126.336755695574));
#230364=CARTESIAN_POINT('Ctrl Pts',(27.8085342103677,-6.38872479024353,
132.483119500384));
#230365=CARTESIAN_POINT('Ctrl Pts',(27.5300865865548,-2.04087440936798,
137.086785903815));
#230366=CARTESIAN_POINT('Ctrl Pts',(27.2516389627419,4.18243985145892,135.91721038272));
#230367=CARTESIAN_POINT('Ctrl Pts',(26.973191338929,6.56229621234102,130.049175704046));
#230368=CARTESIAN_POINT('Ctrl Pts',(26.6947437151162,2.91172294007416,124.875119068062));
#230369=CARTESIAN_POINT('Ctrl Pts',(26.4162960913032,-3.41458146854746,
125.149745756519));
#230370=CARTESIAN_POINT('Ctrl Pts',(26.1378484674903,-6.60305231915217,
130.620687258984));
#230371=CARTESIAN_POINT('Ctrl Pts',(25.8594008436774,-3.72364066549499,
136.260415605043));
#230372=CARTESIAN_POINT('Ctrl Pts',(25.5809532198646,2.57761484979243,136.886295960714));
#230373=CARTESIAN_POINT('Ctrl Pts',(25.3025055960517,6.51016824160669,131.92317485509));
#230374=CARTESIAN_POINT('Ctrl Pts',(25.0240579722387,4.46019505878377,125.931918122295));
#230375=CARTESIAN_POINT('Ctrl Pts',(24.7456103484259,-1.68847949041943,
124.418198010604));
#230376=CARTESIAN_POINT('Ctrl Pts',(24.467162724613,-6.28552387473587,128.773049353324));
#230377=CARTESIAN_POINT('Ctrl Pts',(24.1887151008001,-5.10647888308236,
134.994576512808));
#230378=CARTESIAN_POINT('Ctrl Pts',(23.9102674769872,0.765170736761864,
137.365499967992));
#230379=CARTESIAN_POINT('Ctrl Pts',(23.6318198531744,5.93366583019039,133.707056889611));
#230380=CARTESIAN_POINT('Ctrl Pts',(23.3533722293614,5.64941190136517,127.381177741815));
#230381=CARTESIAN_POINT('Ctrl Pts',(23.0749246055485,0.173624424299845,
124.201036425055));
#230382=CARTESIAN_POINT('Ctrl Pts',(22.7964769817356,-5.46171541667246,
127.08902745089));
#230383=CARTESIAN_POINT('Ctrl Pts',(22.5180293579228,-6.07800560935413,
133.391228152785));
#230384=CARTESIAN_POINT('Ctrl Pts',(22.2395817341099,-1.10890557412062,
137.316223965318));
#230385=CARTESIAN_POINT('Ctrl Pts',(21.9611341102969,4.87922451068073,135.257135483476));
#230386=CARTESIAN_POINT('Ctrl Pts',(21.6826864864842,6.38358563353538,129.106164430008));
#230387=CARTESIAN_POINT('Ctrl Pts',(21.4042388626712,2.02174341466617,124.515752711409));
#230388=CARTESIAN_POINT('Ctrl Pts',(21.1257912388583,-4.19798223462457,
125.704264442993));
#230389=CARTESIAN_POINT('Ctrl Pts',(20.8473436150454,-6.55996729312864,
131.579515405459));
#230390=CARTESIAN_POINT('Ctrl Pts',(20.5688959912325,-2.89366288146616,
136.742436986267));
#230391=CARTESIAN_POINT('Ctrl Pts',(20.2904483674196,3.43177635497322,136.448556475397));
#230392=CARTESIAN_POINT('Ctrl Pts',(20.0120007436067,6.60358077278748,130.967935705476));
#230393=CARTESIAN_POINT('Ctrl Pts',(19.7335531197938,3.70701706326526,125.336997420853));
#230394=CARTESIAN_POINT('Ctrl Pts',(19.455105495981,-2.59611422954622,124.730298818468));
#230395=CARTESIAN_POINT('Ctrl Pts',(19.176657872168,-6.51354337263571,129.705366275038));
#230396=CARTESIAN_POINT('Ctrl Pts',(18.8982102483552,-4.4453443605568,135.690355843533));
#230397=CARTESIAN_POINT('Ctrl Pts',(18.6197626245423,1.70790895172861,137.1853544935));
#230398=CARTESIAN_POINT('Ctrl Pts',(18.3413150007294,6.29167737336628,132.816531500364));
#230399=CARTESIAN_POINT('Ctrl Pts',(18.0628673769165,5.09370165440758,126.598621765949));
#230400=CARTESIAN_POINT('Ctrl Pts',(17.7844197531036,-0.785137043792105,
124.245580574404));
#230401=CARTESIAN_POINT('Ctrl Pts',(17.5059721292907,-5.94247315482366,
127.919737828307));
#230402=CARTESIAN_POINT('Ctrl Pts',(17.2275245054778,-5.63896674252494,
134.244722503881));
#230403=CARTESIAN_POINT('Ctrl Pts',(16.949076881665,-0.15352537268619,137.408182676953));
#230404=CARTESIAN_POINT('Ctrl Pts',(16.6706292578521,5.47299831451989,134.503052992091));
#230405=CARTESIAN_POINT('Ctrl Pts',(16.3921816340391,6.07010392151387,128.199005706208));
#230406=CARTESIAN_POINT('Ctrl Pts',(16.1137340102263,1.08908056569879,124.289152305198));
#230407=CARTESIAN_POINT('Ctrl Pts',(15.8352863864134,-4.89275462544986,
126.366457057635));
#230408=CARTESIAN_POINT('Ctrl Pts',(15.5568387626005,-6.37838734016194,
132.521978378005));
#230409=CARTESIAN_POINT('Ctrl Pts',(15.2783911387876,-2.00259369080969,
137.099092886824));
#230410=CARTESIAN_POINT('Ctrl Pts',(14.9999435149747,4.21348572825588,135.891655954962));
#230411=CARTESIAN_POINT('Ctrl Pts',(14.7214958911618,6.55757760327567,130.009243136227));
#230412=CARTESIAN_POINT('Ctrl Pts',(14.4430482673489,2.87557601636067,124.857504439193));
#230413=CARTESIAN_POINT('Ctrl Pts',(14.164600643536,-3.44893944989177,125.170636050008));
#230414=CARTESIAN_POINT('Ctrl Pts',(13.8861530197231,-6.60404805175259,
130.660885315664));
#230415=CARTESIAN_POINT('Ctrl Pts',(13.6077053959103,-3.69035911973598,
136.282981374608));
#230416=CARTESIAN_POINT('Ctrl Pts',(13.3292577720973,2.61458955925225,136.870492603333));
#230417=CARTESIAN_POINT('Ctrl Pts',(13.0508101482845,6.5168581630887,131.883524884162));
#230418=CARTESIAN_POINT('Ctrl Pts',(12.7723625244716,4.43045248126686,125.904857924092));
#230419=CARTESIAN_POINT('Ctrl Pts',(12.4939149006587,-1.72732259120293,
124.428594585312));
#230420=CARTESIAN_POINT('Ctrl Pts',(12.2154672768458,-6.29777258675688,
128.811348756686));
#230421=CARTESIAN_POINT('Ctrl Pts',(11.9370196530329,-5.08087723837641,
135.025583464166));
#230422=CARTESIAN_POINT('Ctrl Pts',(11.65857202922,0.805096077419857,137.36072059382));
#230423=CARTESIAN_POINT('Ctrl Pts',(11.3801244054071,5.95122542919731,133.670883201288));
#230424=CARTESIAN_POINT('Ctrl Pts',(11.1016767815943,5.62846934506734,127.346851591727));
#230425=CARTESIAN_POINT('Ctrl Pts',(10.8232291577813,0.13342489883439,124.200101868207));
#230426=CARTESIAN_POINT('Ctrl Pts',(10.5447815339684,-5.4842305112587,127.12234329937));
#230427=CARTESIAN_POINT('Ctrl Pts',(10.2663339101556,-6.06214600106014,
133.428178769409));
#230428=CARTESIAN_POINT('Ctrl Pts',(9.98788628634267,-1.06924546818365,
137.322853538546));
#230429=CARTESIAN_POINT('Ctrl Pts',(9.70943866252976,4.90623941440849,135.227351759386));
#230430=CARTESIAN_POINT('Ctrl Pts',(9.43099103871685,6.37312995827954,129.067337196021));
#230431=CARTESIAN_POINT('Ctrl Pts',(9.15254341490403,1.98342541519871,124.503562298745));
#230432=CARTESIAN_POINT('Ctrl Pts',(8.87409579109107,-4.22895018873139,
125.729913245354));
#230433=CARTESIAN_POINT('Ctrl Pts',(8.59564816727821,-6.55512716491932,
131.61943342649));
#230434=CARTESIAN_POINT('Ctrl Pts',(8.31720054346528,-2.85746251231165,
136.759941514744));
#230435=CARTESIAN_POINT('Ctrl Pts',(8.03875291965246,3.46607059430627,136.427561704794));
#230436=CARTESIAN_POINT('Ctrl Pts',(7.76030529583951,6.60445415171875,130.927734804324));
#230437=CARTESIAN_POINT('Ctrl Pts',(7.48185767202662,3.67366698922382,125.314533053388));
#230438=CARTESIAN_POINT('Ctrl Pts',(7.20341004821377,-2.63304066775796,
124.746214640945));
#230439=CARTESIAN_POINT('Ctrl Pts',(6.92496242440086,-6.52011258225796,
129.745036424131));
#230440=CARTESIAN_POINT('Ctrl Pts',(6.64651480058794,-4.41551955887045,
135.71732539022));
#230441=CARTESIAN_POINT('Ctrl Pts',(6.36806717677509,1.74672022899638,137.174839741911));
#230442=CARTESIAN_POINT('Ctrl Pts',(6.08961955296221,6.30380945844269,132.778194993536));
#230443=CARTESIAN_POINT('Ctrl Pts',(5.81117192914928,5.06800575379271,126.567692880813));
#230444=CARTESIAN_POINT('Ctrl Pts',(5.53272430533639,-0.825047652747706,
124.250481445441));
#230445=CARTESIAN_POINT('Ctrl Pts',(5.25427668152353,-5.95992257223146,
127.955964794454));
#230446=CARTESIAN_POINT('Ctrl Pts',(4.97582905771062,-5.61791980623858,
134.278984753035));
#230447=CARTESIAN_POINT('Ctrl Pts',(4.69738143389771,-0.113323188952861,
137.408994875945));
#230448=CARTESIAN_POINT('Ctrl Pts',(4.41893381008486,5.49541190283514,134.469668769726));
#230449=CARTESIAN_POINT('Ctrl Pts',(4.14048618627195,6.05413192171396,128.162103531929));
#230450=CARTESIAN_POINT('Ctrl Pts',(3.86203856245905,1.0494004653243,124.282643474398));
#230451=CARTESIAN_POINT('Ctrl Pts',(3.58359093864613,-4.91967875263547,
126.396322867843));
#230452=CARTESIAN_POINT('Ctrl Pts',(3.30514331483329,-6.36781353659179,
132.560773608667));
#230453=CARTESIAN_POINT('Ctrl Pts',(3.02669569102039,-1.96423876540577,
137.111166616214));
#230454=CARTESIAN_POINT('Ctrl Pts',(2.74824806720748,4.24437547278969,135.865913015604));
#230455=CARTESIAN_POINT('Ctrl Pts',(2.46980044339459,6.55261600076067,129.969340031779));
#230456=CARTESIAN_POINT('Ctrl Pts',(2.19135281958173,2.83932253712042,124.840110173268));
#230457=CARTESIAN_POINT('Ctrl Pts',(1.91290519576881,-3.48316962951642,
125.191735103234));
#230458=CARTESIAN_POINT('Ctrl Pts',(1.6344575719559,-6.60479906892382,130.701088688872));
#230459=CARTESIAN_POINT('Ctrl Pts',(1.35600994814304,-3.65694082636265,
136.305344131865));
#230460=CARTESIAN_POINT('Ctrl Pts',(1.07756232433016,2.65146738413444,136.854464463202));
#230461=CARTESIAN_POINT('Ctrl Pts',(0.799114700517227,6.52330659999492,
131.843834924404));
#230462=CARTESIAN_POINT('Ctrl Pts',(0.520667076704378,4.40054573170394,
125.877979278764));
#230463=CARTESIAN_POINT('Ctrl Pts',(0.242219452891471,-1.76610168541259,
124.439227416375));
#230464=CARTESIAN_POINT('Ctrl Pts',(-0.03622817092143,-6.30978793249869,
128.849722011837));
#230465=CARTESIAN_POINT('Ctrl Pts',(-0.314675794734322,-5.05508731989592,
135.056433996558));
#230466=CARTESIAN_POINT('Ctrl Pts',(-0.593123418547181,0.844991584946641,
137.355698271319));
#230467=CARTESIAN_POINT('Ctrl Pts',(-0.871571042360099,5.96856450335716,
133.634603292916));
#230468=CARTESIAN_POINT('Ctrl Pts',(-1.15001866617301,5.60731822376822,
127.312653560908));
#230469=CARTESIAN_POINT('Ctrl Pts',(-1.42846628998586,0.0932204292604712,
124.199412034595));
#230470=CARTESIAN_POINT('Ctrl Pts',(-1.70691391379876,-5.50654238566651,
127.155795586355));
#230471=CARTESIAN_POINT('Ctrl Pts',(-1.98536153761166,-6.04606175771675,
133.465032159487));
#230472=CARTESIAN_POINT('Ctrl Pts',(-2.26380916142456,-1.02954574096264,
137.329241566624));
#230473=CARTESIAN_POINT('Ctrl Pts',(-2.5422567852374,4.9330725156305,135.197404139731));
#230474=CARTESIAN_POINT('Ctrl Pts',(-2.82070440905033,6.36243812434939,
129.028574328076));
#230475=CARTESIAN_POINT('Ctrl Pts',(-3.09915203286324,1.94503391917308,
124.491605364478));
#230476=CARTESIAN_POINT('Ctrl Pts',(-3.3775996566761,-4.25976143753379,
125.755750083229));
#230477=CARTESIAN_POINT('Ctrl Pts',(-3.65604728048899,-6.55004413406227,
131.659321244699));
#230478=CARTESIAN_POINT('Ctrl Pts',(-3.9344949043019,-2.82115625883292,
136.777225356981));
#230479=CARTESIAN_POINT('Ctrl Pts',(-4.2129425281148,3.50023639711881,136.406358564405));
#230480=CARTESIAN_POINT('Ctrl Pts',(-4.49139015192765,6.60508280017262,
130.887529331496));
#230481=CARTESIAN_POINT('Ctrl Pts',(-4.76983777574057,3.64018078610111,
125.292272113504));
#230482=CARTESIAN_POINT('Ctrl Pts',(-5.04828539955349,-2.66986953767946,
124.762354950249));
#230483=CARTESIAN_POINT('Ctrl Pts',(-5.32673302336633,-6.52644018671072,
129.784745826872));
#230484=CARTESIAN_POINT('Ctrl Pts',(-5.60518064717923,-4.38553113848304,
135.74411288519));
#230485=CARTESIAN_POINT('Ctrl Pts',(-5.88362827099213,1.7854667809037,137.164088929876));
#230486=CARTESIAN_POINT('Ctrl Pts',(-6.16207589480503,6.31570795354138,
132.739785345549));
#230487=CARTESIAN_POINT('Ctrl Pts',(-6.44052351861788,5.04212205636089,
126.536920986959));
#230488=CARTESIAN_POINT('Ctrl Pts',(-6.71897114243081,-0.864927689259141,
124.255625172881));
#230489=CARTESIAN_POINT('Ctrl Pts',(-6.99741876624371,-5.97715114251656,
127.992297308957));
#230490=CARTESIAN_POINT('Ctrl Pts',(-7.27586639005655,-5.59666469586782,
134.313118248714));
#230491=CARTESIAN_POINT('Ctrl Pts',(-7.55431401386947,-0.0731168059870705,
137.409562337785));
#230492=CARTESIAN_POINT('Ctrl Pts',(-7.83276163768236,5.51762185664139,
134.436148728019));
#230493=CARTESIAN_POINT('Ctrl Pts',(-8.11120926149529,6.03793558382929,
128.125299267457));
#230494=CARTESIAN_POINT('Ctrl Pts',(-8.38965688530811,1.00968147902963,
124.276376308223));
#230495=CARTESIAN_POINT('Ctrl Pts',(-8.66810450912106,-4.94642057931569,
126.426352019512));
#230496=CARTESIAN_POINT('Ctrl Pts',(-8.94655213293394,-6.3570037713493,
132.599503754801));
#230497=CARTESIAN_POINT('Ctrl Pts',(-9.22499975674682,-1.92581105441205,
137.123006644589));
#230498=CARTESIAN_POINT('Ctrl Pts',(-9.50344738055969,4.27510794042973,
135.839982518561));
#230499=CARTESIAN_POINT('Ctrl Pts',(-9.78189500437264,6.54741158865002,
129.929467869325));
#230500=CARTESIAN_POINT('Ctrl Pts',(-10.0603426281855,2.80296384573913,
124.822936914835));
#230501=CARTESIAN_POINT('Ctrl Pts',(-10.3387902519984,-3.51727073900952,
125.213042134361));
#230502=CARTESIAN_POINT('Ctrl Pts',(-10.6172378758113,-6.60530534283666,
130.74129588886));
#230503=CARTESIAN_POINT('Ctrl Pts',(-10.8956854996242,-3.62338702370218,
136.327503048155));
#230504=CARTESIAN_POINT('Ctrl Pts',(-11.174133123437,2.68824695791763,136.838212134247));
#230505=CARTESIAN_POINT('Ctrl Pts',(-11.4525807472499,6.52951331337615,
131.804106446543));
#230506=CARTESIAN_POINT('Ctrl Pts',(-11.7310283710628,4.37047591830066,
125.851283182307));
#230507=CARTESIAN_POINT('Ctrl Pts',(-12.0094759948757,-1.80481533607482,
124.450096109789));
#230508=CARTESIAN_POINT('Ctrl Pts',(-12.2879236186886,-6.32156946672825,
128.88816769684));
#230509=CARTESIAN_POINT('Ctrl Pts',(-12.5663712425015,-5.02911008329581,
135.087126966809));
#230510=CARTESIAN_POINT('Ctrl Pts',(-12.8448188663144,0.884855780999501,
137.350433186591));
#230511=CARTESIAN_POINT('Ctrl Pts',(-13.1232664901273,5.98568241016441,
133.598218508862));
#230512=CARTESIAN_POINT('Ctrl Pts',(-13.4017141139402,5.58595932123025,
127.278584916578));
#230513=CARTESIAN_POINT('Ctrl Pts',(-13.6801617377531,0.0530125053692662,
124.198966949783));
#230514=CARTESIAN_POINT('Ctrl Pts',(-13.958609361566,-5.5286502131212,127.189383072259));
#230515=CARTESIAN_POINT('Ctrl Pts',(-14.2370569853788,-6.02975347533148,
133.501786957402));
#230516=CARTESIAN_POINT('Ctrl Pts',(-14.5155046091917,-0.989807863545592,
137.335387812837));
#230517=CARTESIAN_POINT('Ctrl Pts',(-14.7939522330047,4.95972282003631,
135.167293734234));
#230518=CARTESIAN_POINT('Ctrl Pts',(-15.0723998568175,6.35151052793477,
128.989877262545));
#230519=CARTESIAN_POINT('Ctrl Pts',(-15.3508474806304,1.9065703492003,124.479882351679));
#230520=CARTESIAN_POINT('Ctrl Pts',(-15.6292951044433,-4.29041483930959,
125.781773999224));
#230521=CARTESIAN_POINT('Ctrl Pts',(-15.9077427282562,-6.54471838891106,
131.699177382027));
#230522=CARTESIAN_POINT('Ctrl Pts',(-16.186190352069,-2.78474546637155,
136.794287872519));
#230523=CARTESIAN_POINT('Ctrl Pts',(-16.464637975882,3.53427249738445,136.384947839923));
#230524=CARTESIAN_POINT('Ctrl Pts',(-16.7430855996949,6.60546669485434,
130.847320776822));
#230525=CARTESIAN_POINT('Ctrl Pts',(-17.0215332235078,3.6065596947407,125.270215426085));
#230526=CARTESIAN_POINT('Ctrl Pts',(-17.2999808473206,-2.7065994746034,
124.778719148295));
#230527=CARTESIAN_POINT('Ctrl Pts',(-17.5784284711336,-6.53252595152224,
129.824493011814));
#230528=CARTESIAN_POINT('Ctrl Pts',(-17.8568760949464,-4.35538021062653,
135.770717335825));
#230529=CARTESIAN_POINT('Ctrl Pts',(-18.1353237187593,1.82414717168286,
137.153102455769));
#230530=CARTESIAN_POINT('Ctrl Pts',(-18.4137713425722,6.32737241775927,
132.701303979686));
#230531=CARTESIAN_POINT('Ctrl Pts',(-18.6922189663851,5.01605152124203,
126.506307224649));
#230532=CARTESIAN_POINT('Ctrl Pts',(-18.9706665901979,-0.904775675556959,
124.261011566121));
#230533=CARTESIAN_POINT('Ctrl Pts',(-19.2491142140109,-5.99415822726801,
128.028734025499));
#230534=CARTESIAN_POINT('Ctrl Pts',(-19.5275618378238,-5.57520219902858,
134.347121726088));
#230535=CARTESIAN_POINT('Ctrl Pts',(-19.8060094616367,-0.0329077136511566,
137.409885041447));
#230536=CARTESIAN_POINT('Ctrl Pts',(-20.0844570854496,5.53962735294063,
134.402494109067));
#230537=CARTESIAN_POINT('Ctrl Pts',(-20.3629047092624,6.02151550802112,
128.08859427659));
#230538=CARTESIAN_POINT('Ctrl Pts',(-20.6413523330754,0.969925078616457,
124.270351038909));
#230539=CARTESIAN_POINT('Ctrl Pts',(-20.9197999568882,-4.9729791145623,
126.456543399899));
#230540=CARTESIAN_POINT('Ctrl Pts',(-21.1982475807011,-6.34595844499429,
132.638167381246));
#230541=CARTESIAN_POINT('Ctrl Pts',(-21.476695204514,-1.88731198178147,
137.134612533211));
#230542=CARTESIAN_POINT('Ctrl Pts',(-21.7551428283269,4.30568199237261,
135.813865424697));
#230543=CARTESIAN_POINT('Ctrl Pts',(-22.0335904521398,6.54196455979519,
129.889628126344));
#230544=CARTESIAN_POINT('Ctrl Pts',(-22.3120380759527,2.766501289502,124.805985300257));
#230545=CARTESIAN_POINT('Ctrl Pts',(-22.5904856997656,-3.5512415147419,
125.234556353852));
#230546=CARTESIAN_POINT('Ctrl Pts',(-22.8689333235784,-6.60556685473091,
130.781505425734));
#230547=CARTESIAN_POINT('Ctrl Pts',(-23.1473809473914,-3.58969895510304,
136.349457302372));
#230548=CARTESIAN_POINT('Ctrl Pts',(-23.4258285712042,2.7249269177212,136.821736218705));
#230549=CARTESIAN_POINT('Ctrl Pts',(-23.7042761950172,6.53547807324032,
131.764340922733));
#230550=CARTESIAN_POINT('Ctrl Pts',(-23.98272381883,4.34024415530499,125.824770623956));
#230551=CARTESIAN_POINT('Ctrl Pts',(-24.2611714426429,-1.84346210864104,
124.461200262812));
#230552=CARTESIAN_POINT('Ctrl Pts',(-24.5396190664558,-6.33311675287646,
128.926684387076));
#230553=CARTESIAN_POINT('Ctrl Pts',(-24.8180666902687,-5.00294649117208,
135.117661237576));
#230554=CARTESIAN_POINT('Ctrl Pts',(-25.0965143140816,0.924687188395989,
137.344925534737));
#230555=CARTESIAN_POINT('Ctrl Pts',(-25.3749619378945,6.00257851530871,
133.561730197376));
#230556=CARTESIAN_POINT('Ctrl Pts',(-25.6534095617074,5.56439342891538,
127.244646921163));
#230557=CARTESIAN_POINT('Ctrl Pts',(-25.9318571855203,0.0128026170801758,
124.198766630261));
#230558=CARTESIAN_POINT('Ctrl Pts',(-26.2103048093331,-5.5505531744091,
127.223104512485));
#230559=CARTESIAN_POINT('Ctrl Pts',(-26.4887524331461,-6.01322175821376,
133.538441801192));
#230560=CARTESIAN_POINT('Ctrl Pts',(-26.7672000569589,-0.950033308434149,
137.341292049436));
#230561=CARTESIAN_POINT('Ctrl Pts',(-27.0456476807718,4.98618934008908,
135.137021658645));
#230562=CARTESIAN_POINT('Ctrl Pts',(-27.3240953045847,6.34034757396176,
128.951247433362));
#230563=CARTESIAN_POINT('Ctrl Pts',(-27.6025429283976,1.86803613056208,
124.468393694749));
#230564=CARTESIAN_POINT('Ctrl Pts',(-27.8809905522105,-4.32090925818572,
125.807984029013));
#230565=CARTESIAN_POINT('Ctrl Pts',(-28.1594381760234,-6.53915012681315,
131.739000361591));
#230566=CARTESIAN_POINT('Ctrl Pts',(-28.4378857998363,-2.74823148414282,
136.811128429099));
#230567=CARTESIAN_POINT('Ctrl Pts',(-28.7163334236492,3.56817763388296,
136.36333032473));
#230568=CARTESIAN_POINT('Ctrl Pts',(-28.994781047462,6.60560582153853,130.807110630244));
#230569=CARTESIAN_POINT('Ctrl Pts',(-29.273228671275,3.5728049609845,125.248363808452));
#230570=CARTESIAN_POINT('Ctrl Pts',(-29.5516762950878,-2.74322911748845,
124.795306628702));
#230571=CARTESIAN_POINT('Ctrl Pts',(-29.8301239189007,-6.53836965118233,
129.86427650611));
#230572=CARTESIAN_POINT('Ctrl Pts',(-30.1085715427137,-4.32506789255462,
135.797137756284));
#230573=CARTESIAN_POINT('Ctrl Pts',(-30.3870191665265,1.862759968018,137.141880726698));
#230574=CARTESIAN_POINT('Ctrl Pts',(-30.6654667903394,6.33880241886542,
132.662752321889));
#230575=CARTESIAN_POINT('Ctrl Pts',(-30.9439144141524,4.98979511448915,
126.475852728289));
#230576=CARTESIAN_POINT('Ctrl Pts',(-31.2223620379652,-0.944590135059391,
124.266640425567));
#230577=CARTESIAN_POINT('Ctrl Pts',(-31.5008096617781,-6.01094319628198,
128.065273593905));
#230578=CARTESIAN_POINT('Ctrl Pts',(-31.7792572855909,-5.55353311102158,
134.380993925146));
#230579=CARTESIAN_POINT('Ctrl Pts',(-32.0577049094039,0.00730259809219468,
137.409962974972));
#230580=CARTESIAN_POINT('Ctrl Pts',(-32.3361525332168,5.56142757631112,
134.368706159956));
#230581=CARTESIAN_POINT('Ctrl Pts',(-32.6146001570296,6.0048723027414,128.051989919443));
#230582=CARTESIAN_POINT('Ctrl Pts',(-32.8930477808425,0.930132737272799,
124.264567889721));
#230583=CARTESIAN_POINT('Ctrl Pts',(-33.1714954046555,-4.99935337423901,
126.486895890252));
#230584=CARTESIAN_POINT('Ctrl Pts',(-33.4499430284683,-6.33467796681538,
132.676763055306));
#230585=CARTESIAN_POINT('Ctrl Pts',(-33.7283906522812,-1.84874297411136,
137.145983852021));
#230586=CARTESIAN_POINT('Ctrl Pts',(-34.0068382760941,4.33609649568588,
135.787562701789));
#230587=CARTESIAN_POINT('Ctrl Pts',(-34.285285899907,6.53627511603778,129.849822279112));
#230588=CARTESIAN_POINT('Ctrl Pts',(-34.5637335237199,2.72993621954223,
124.789255957683));
#230589=CARTESIAN_POINT('Ctrl Pts',(-34.8421811475328,-3.58508069791401,
125.256276964487));
#230590=CARTESIAN_POINT('Ctrl Pts',(-35.1206287713457,-6.60558359491616,
130.821715809516));
#230591=CARTESIAN_POINT('Ctrl Pts',(-35.3990763951586,-3.55587786888901,
136.37120608099));
#230592=CARTESIAN_POINT('Ctrl Pts',(-35.6775240189714,2.76150590435573,
136.805037327097));
#230593=CARTESIAN_POINT('Ctrl Pts',(-35.9559716427844,6.54120065856107,
131.724539826499));
#230594=CARTESIAN_POINT('Ctrl Pts',(-36.2344192665972,4.30985156296601,
125.798442586144));
#230595=CARTESIAN_POINT('Ctrl Pts',(-36.5128668904101,-1.8820405710409,
124.472539463974));
#230596=CARTESIAN_POINT('Ctrl Pts',(-36.791314514223,-6.3444293630544,128.965270655295));
#230597=CARTESIAN_POINT('Ctrl Pts',(-37.0697621380359,-4.9765975130263,
135.148035677403));
#230598=CARTESIAN_POINT('Ctrl Pts',(-37.3482097618488,0.964484331168655,
137.339175519844));
#230599=CARTESIAN_POINT('Ctrl Pts',(-37.6266573856617,6.0192521926987,133.525139710547));
#230600=CARTESIAN_POINT('Ctrl Pts',(-37.9051050094746,5.54262134595571,
127.210840832248));
#230601=CARTESIAN_POINT('Ctrl Pts',(-38.1835526332875,-0.0274077456145885,
124.198811083455));
#230602=CARTESIAN_POINT('Ctrl Pts',(-38.4620002571004,-5.5722504579079,
127.256958657474));
#230603=CARTESIAN_POINT('Ctrl Pts',(-38.7404478809132,-5.99646721895241,
133.574995332598));
#230604=CARTESIAN_POINT('Ctrl Pts',(-39.0188955047262,-0.910223549489097,
137.346954057637));
#230605=CARTESIAN_POINT('Ctrl Pts',(-39.297343128539,5.0124710950622,135.106589034709));
#230606=CARTESIAN_POINT('Ctrl Pts',(-39.5757907523519,6.32894967607775,
128.912686271968));
#230607=CARTESIAN_POINT('Ctrl Pts',(-39.8542383761648,1.82943269115809,
124.457139819403));
#230608=CARTESIAN_POINT('Ctrl Pts',(-40.1326859999777,-4.35124356418029,
125.834379201373));
#230609=CARTESIAN_POINT('Ctrl Pts',(-40.4111336237906,-6.53333955410249,
131.778788707735));
#230610=CARTESIAN_POINT('Ctrl Pts',(-40.6895812476035,-2.7116156651858,
136.827746402689));
#230611=CARTESIAN_POINT('Ctrl Pts',(-40.9680288714165,3.60195055024708,
136.34150681987));
#230612=CARTESIAN_POINT('Ctrl Pts',(-41.2464764952292,6.60550017506977,
130.766900381762));
#230613=CARTESIAN_POINT('Ctrl Pts',(-41.5249241190422,3.53891783562657,
125.226718070324));
#230614=CARTESIAN_POINT('Ctrl Pts',(-41.803371742855,-2.77975710900975,
124.812116776814));
#230615=CARTESIAN_POINT('Ctrl Pts',(-42.081819366668,-6.5439710691505,129.904094835568));
#230616=CARTESIAN_POINT('Ctrl Pts',(-42.3602669904808,-4.2945953075014,
135.82337316755));
#230617=CARTESIAN_POINT('Ctrl Pts',(-42.6387146142937,1.90130373909722,
137.130424158489));
#230618=CARTESIAN_POINT('Ctrl Pts',(-42.9171622381066,6.34999753331677,
132.624131800705));
#230619=CARTESIAN_POINT('Ctrl Pts',(-43.1956098619195,4.96335380904355,
126.44555862638));
#230620=CARTESIAN_POINT('Ctrl Pts',(-43.4740574857324,-0.984369592426984,
124.272511542639));
#230621=CARTESIAN_POINT('Ctrl Pts',(-43.7525051095453,-6.02750542758532,
128.101914660188));
#230622=CARTESIAN_POINT('Ctrl Pts',(-44.0309527333582,-5.53165823480283,
134.414733590743));
#230623=CARTESIAN_POINT('Ctrl Pts',(-44.3094003571711,0.0475126392350714,
137.409796135472));
#230624=CARTESIAN_POINT('Ctrl Pts',(-44.5878479809839,5.58302171893757,
134.334786132711));
#230625=CARTESIAN_POINT('Ctrl Pts',(-44.8662956047969,5.98800658471021,
128.015487552405));
#230626=CARTESIAN_POINT('Ctrl Pts',(-45.1447432286098,0.890305929518511,
124.259027074959));
#230627=CARTESIAN_POINT('Ctrl Pts',(-45.4231908524226,-5.02554238103793,
126.517408365848));
#230628=CARTESIAN_POINT('Ctrl Pts',(-45.7016384762356,-6.32316275481482,
132.715289346806));
#230629=CARTESIAN_POINT('Ctrl Pts',(-45.9800861000484,-1.81010546059046,
137.15712017965));
#230630=CARTESIAN_POINT('Ctrl Pts',(-46.2585337238614,4.36635032334889,
135.761075324496));
#230631=CARTESIAN_POINT('Ctrl Pts',(-46.5369813476741,6.53034346820225,
129.810051802649));
#230632=CARTESIAN_POINT('Ctrl Pts',(-46.8154289714873,2.6932699907919,124.772749507024));
#230633=CARTESIAN_POINT('Ctrl Pts',(-47.0938765952999,-3.61878703460243,
125.278203161403));
#230634=CARTESIAN_POINT('Ctrl Pts',(-47.3723242191129,-6.60535556277213,
130.861925550195));
#230635=CARTESIAN_POINT('Ctrl Pts',(-47.6507718429257,-3.52192501831287,
136.392748578105));
#230636=CARTESIAN_POINT('Ctrl Pts',(-47.9292194667387,2.79798256237344,
136.788116078208));
#230637=CARTESIAN_POINT('Ctrl Pts',(-48.2076670905515,6.54668085728591,
131.684704632686));
#230638=CARTESIAN_POINT('Ctrl Pts',(-48.4861147143645,4.27929926749242,
125.772300044465));
#230639=CARTESIAN_POINT('Ctrl Pts',(-48.7645623381774,-1.92054929373528,
124.484113293097));
#230640=CARTESIAN_POINT('Ctrl Pts',(-49.0430099619902,-6.35550687806913,
129.003925071669));
#230641=CARTESIAN_POINT('Ctrl Pts',(-49.3214575858032,-4.95006412522954,
135.178249160753));
#230642=CARTESIAN_POINT('Ctrl Pts',(-49.5999052096159,1.00424573461974,
137.333183354982));
#230643=CARTESIAN_POINT('Ctrl Pts',(-49.878352833429,6.03570282448511,133.488448404247));
#230644=CARTESIAN_POINT('Ctrl Pts',(-50.1568004572417,5.52064387912377,
127.17716790253));
#230645=CARTESIAN_POINT('Ctrl Pts',(-50.4352480810547,-0.0676170927052693,
124.199100307716));
#230646=CARTESIAN_POINT('Ctrl Pts',(-50.7136957048675,-5.5937412596168,
127.290944252747));
#230647=CARTESIAN_POINT('Ctrl Pts',(-50.9921433286805,-5.97949047839309,
133.611446197116));
#230648=CARTESIAN_POINT('Ctrl Pts',(-51.2705909524933,-0.870380061875472,
137.352373627632));
#230649=CARTESIAN_POINT('Ctrl Pts',(-51.5490385763063,5.03856711107574,
135.075996990117));
#230650=CARTESIAN_POINT('Ctrl Pts',(-51.8274862001192,6.31731725663583,
128.874195207264));
#230651=CARTESIAN_POINT('Ctrl Pts',(-52.105933823932,1.79076146145295,124.446121142656));
#230652=CARTESIAN_POINT('Ctrl Pts',(-52.3843814477449,-4.38141663324442,
125.860958538224));
#230653=CARTESIAN_POINT('Ctrl Pts',(-52.6628290715579,-6.52728688609205,
131.818540946088));
#230654=CARTESIAN_POINT('Ctrl Pts',(-52.9412766953706,-2.67489936631311,
136.844141177504));
#230655=CARTESIAN_POINT('Ctrl Pts',(-53.2197243191836,3.63558999500893,
136.319478134021));
#230656=CARTESIAN_POINT('Ctrl Pts',(-53.4981719429964,6.60514975936288,
130.726691521383));
#230657=CARTESIAN_POINT('Ctrl Pts',(-53.7766195668094,3.50489957436681,
125.205279013792));
#230658=CARTESIAN_POINT('Ctrl Pts',(-54.0550671906223,-2.8161820956091,
124.829148969725));
#230659=CARTESIAN_POINT('Ctrl Pts',(-54.3335148144351,-6.54932999786417,
129.943946524707));
#230660=CARTESIAN_POINT('Ctrl Pts',(-54.6119624382481,-4.26396358463975,
135.849422597461));
#230661=CARTESIAN_POINT('Ctrl Pts',(-54.890410062061,1.93977705666721,137.11873317567));
#230662=CARTESIAN_POINT('Ctrl Pts',(-55.1688576858738,6.3609573462743,132.58544384723));
#230663=CARTESIAN_POINT('Ctrl Pts',(-55.4473053096868,4.93672858469731,
126.415426041482));
#230664=CARTESIAN_POINT('Ctrl Pts',(-55.7257529334997,-1.02411257361735,
124.278624699781));
#230665=CARTESIAN_POINT('Ctrl Pts',(-56.0042005573125,-6.0438443074584,
128.138655866601));
#230666=CARTESIAN_POINT('Ctrl Pts',(-56.2826481811254,-5.50957838095395,
134.448339472641));
#230667=CARTESIAN_POINT('Ctrl Pts',(-56.5610958049383,0.0877209197796484,
137.40938452913));
#230668=CARTESIAN_POINT('Ctrl Pts',(-56.8395434287512,5.60440898064107,
134.300735284249));
#230669=CARTESIAN_POINT('Ctrl Pts',(-57.117991052564,5.97091897889293,127.979088528083));
#230670=CARTESIAN_POINT('Ctrl Pts',(-57.396438676377,0.850446131150592,
124.253728799937));
#230671=CARTESIAN_POINT('Ctrl Pts',(-57.6748863001899,-5.05154516451579,
126.548079696037));
#230672=CARTESIAN_POINT('Ctrl Pts',(-57.9533339240027,-6.31141323569307,
132.753744828139));
#230673=CARTESIAN_POINT('Ctrl Pts',(-58.2317815478157,-1.77140087294607,
137.168021103437));
#230674=CARTESIAN_POINT('Ctrl Pts',(-58.5102291716285,4.39644235429495,
135.734404274317));
#230675=CARTESIAN_POINT('Ctrl Pts',(-58.7886767954414,6.52416983608798,
129.770318170665));
#230676=CARTESIAN_POINT('Ctrl Pts',(-59.0671244192543,2.65650396193163,
124.756466559932));
#230677=CARTESIAN_POINT('Ctrl Pts',(-59.3455720430672,-3.6523592758065,
125.300334132115));
#230678=CARTESIAN_POINT('Ctrl Pts',(-59.62401966688,-6.60488276674858,130.902133157784));
#230679=CARTESIAN_POINT('Ctrl Pts',(-59.902467290693,-3.48784166150989,
136.414083995446));
#230680=CARTESIAN_POINT('Ctrl Pts',(-60.1809149145059,2.83435554011865,
136.770973099059));
#230681=CARTESIAN_POINT('Ctrl Pts',(-60.4593625383188,6.55191846634393,
131.644836817403));
#230682=CARTESIAN_POINT('Ctrl Pts',(-60.7378101621316,4.24858840101079,
125.746343967642));
#230683=CARTESIAN_POINT('Ctrl Pts',(-61.0162577859445,-1.95898684976931,
124.49592132131));
#230684=CARTESIAN_POINT('Ctrl Pts',(-61.2947054097575,-6.36634888743926,
129.042646203845));
#230685=CARTESIAN_POINT('Ctrl Pts',(-61.5731530335703,-4.92334731098624,
135.208300568055));
#230686=CARTESIAN_POINT('Ctrl Pts',(-61.8516006573832,1.04396992537583,
137.326949262193));
#230687=CARTESIAN_POINT('Ctrl Pts',(-62.1300482811962,6.05192980108374,
133.451657638088));
#230688=CARTESIAN_POINT('Ctrl Pts',(-62.408495905009,5.49846184280268,127.143629379772));
#230689=CARTESIAN_POINT('Ctrl Pts',(-62.6869435288219,-0.107823934219708,
124.199634292325));
#230690=CARTESIAN_POINT('Ctrl Pts',(-62.9653911526347,-5.61502478318622,
127.325060038955));
#230691=CARTESIAN_POINT('Ctrl Pts',(-63.2438387764477,-5.96229216561512,
133.647793044045));
#230692=CARTESIAN_POINT('Ctrl Pts',(-63.5222864002605,-0.830504322008783,
137.357550558596));
#230693=CARTESIAN_POINT('Ctrl Pts',(-63.8007340240734,5.06447642113188,
135.045246658467));
#230694=CARTESIAN_POINT('Ctrl Pts',(-64.0791816478864,6.30545074667997,
128.835775665549));
#230695=CARTESIAN_POINT('Ctrl Pts',(-64.3576292716992,1.75202387442331,
124.435338072814));
#230696=CARTESIAN_POINT('Ctrl Pts',(-64.6360768955121,-4.41142734730395,
125.887721054655));
#230697=CARTESIAN_POINT('Ctrl Pts',(-64.914524519325,-6.52099234706562,
131.858255603616));
#230698=CARTESIAN_POINT('Ctrl Pts',(-65.1929721431379,-2.63808394806071,
136.860312146029));
#230699=CARTESIAN_POINT('Ctrl Pts',(-65.4714197669508,3.66909472164654,
136.297245083462));
#230700=CARTESIAN_POINT('Ctrl Pts',(-65.7498673907637,6.60455458740261,
130.686485539062));
#230701=CARTESIAN_POINT('Ctrl Pts',(-66.0283150145766,3.4707514377644,125.184047433287));
#230702=CARTESIAN_POINT('Ctrl Pts',(-66.3067626383895,-2.85250272754526,
124.846402576302));
#230703=CARTESIAN_POINT('Ctrl Pts',(-66.5852102622024,-6.55444623874626,
129.983830096806));
#230704=CARTESIAN_POINT('Ctrl Pts',(-66.8636578860152,-4.23317385903938,
135.875285080744));
#230705=CARTESIAN_POINT('Ctrl Pts',(-67.1421055098281,1.978178495085,137.106808211453));
#230706=CARTESIAN_POINT('Ctrl Pts',(-67.4205531336411,6.37168145161813,
132.546689895061));
#230707=CARTESIAN_POINT('Ctrl Pts',(-67.6990007574539,4.90992042805787,
126.385456090168));
#230708=CARTESIAN_POINT('Ctrl Pts',(-67.9774483812669,-1.06381760593968,
124.284979670466));
#230709=CARTESIAN_POINT('Ctrl Pts',(-68.2558960050797,-6.05995923045808,
128.175495851683));
#230710=CARTESIAN_POINT('Ctrl Pts',(-68.5343436288926,-5.48729436765201,
134.481810325563));
#230711=CARTESIAN_POINT('Ctrl Pts',(-68.8127912527054,0.12792594979327,
137.408728171199));
#230712=CARTESIAN_POINT('Ctrl Pts',(-69.0912388765185,5.62558856890878,
134.266554876337));
#230713=CARTESIAN_POINT('Ctrl Pts',(-69.3696865003312,5.9536101184771,127.942794195258));
#230714=CARTESIAN_POINT('Ctrl Pts',(-69.6481341241442,0.810554819188534,
124.248673260987));
#230715=CARTESIAN_POINT('Ctrl Pts',(-69.9265817479571,-5.07736076112986,
126.578908744281));
#230716=CARTESIAN_POINT('Ctrl Pts',(-70.2050293717699,-6.29942984483285,
132.792128074323));
#230717=CARTESIAN_POINT('Ctrl Pts',(-70.4834769955829,-1.73263064539088,
137.178686219444));
#230718=CARTESIAN_POINT('Ctrl Pts',(-70.7619246193956,4.42637147345276,
135.707550539556));
#230719=CARTESIAN_POINT('Ctrl Pts',(-71.0403722432087,6.51775444846118,
129.730622855503));
#230720=CARTESIAN_POINT('Ctrl Pts',(-71.3188198670216,2.6196394953401,124.740407719779));
#230721=CARTESIAN_POINT('Ctrl Pts',(-71.5972674908343,-3.68579617749442,
125.322669056552));
#230722=CARTESIAN_POINT('Ctrl Pts',(-71.8757151146474,-6.6041652243652,
130.942337142376));
#230723=CARTESIAN_POINT('Ctrl Pts',(-72.1541627384602,-3.45362906145158,
136.435211542427));
#230724=CARTESIAN_POINT('Ctrl Pts',(-72.4326103622731,2.87062348977667,
136.753609024891));
#230725=CARTESIAN_POINT('Ctrl Pts',(-72.711057986086,6.55691329165398,131.604937857965));
#230726=CARTESIAN_POINT('Ctrl Pts',(-72.9895056098989,4.21772010152317,
125.720575317484));
#230727=CARTESIAN_POINT('Ctrl Pts',(-73.2679532337117,-1.99735181482566,
124.50796311106));
#230728=CARTESIAN_POINT('Ctrl Pts',(-73.5464008575247,-6.37695498941029,
129.081432616995));
#230729=CARTESIAN_POINT('Ctrl Pts',(-73.8248484813376,-4.89644806029751,
135.238188785743));
#230730=CARTESIAN_POINT('Ctrl Pts',(-74.1032961051504,1.08365543144292,
137.320473472483));
#230731=CARTESIAN_POINT('Ctrl Pts',(-74.3817437289633,6.06793252119795,
133.414768775364));
#230732=CARTESIAN_POINT('Ctrl Pts',(-74.6601913527762,5.47607605895596,
127.110226506756));
#230733=CARTESIAN_POINT('Ctrl Pts',(-74.9386389765891,-0.148026780279403,
124.200413017498));
#230734=CARTESIAN_POINT('Ctrl Pts',(-75.217086600402,-5.63610023994771,
127.359304751927));
#230735=CARTESIAN_POINT('Ctrl Pts',(-75.4955342242149,-5.94487291790794,
133.684034526541));
#230736=CARTESIAN_POINT('Ctrl Pts',(-75.7739818480278,-0.790597807498519,
137.362484658699));
#230737=CARTESIAN_POINT('Ctrl Pts',(-76.0524294718406,5.09019806515201,
135.014339179226));
#230738=CARTESIAN_POINT('Ctrl Pts',(-76.3308770956536,6.29335058592772,
128.797429070474));
#230739=CARTESIAN_POINT('Ctrl Pts',(-76.6093247194664,1.71322136550425,
124.424791009442));
#230740=CARTESIAN_POINT('Ctrl Pts',(-76.8877723432794,-4.44127459430165,
125.914665758975));
#230741=CARTESIAN_POINT('Ctrl Pts',(-77.1662199670922,-6.51445617026952,
131.89793120868));
#230742=CARTESIAN_POINT('Ctrl Pts',(-77.4446675909052,-2.60117077463652,
136.876258709042));
#230743=CARTESIAN_POINT('Ctrl Pts',(-77.7231152147181,3.7024634886308,136.274808492052));
#230744=CARTESIAN_POINT('Ctrl Pts',(-78.0015628385308,6.60371468124315,
130.646283924643));
#230745=CARTESIAN_POINT('Ctrl Pts',(-78.2800104623438,3.43647469119047,
125.163024115555));
#230746=CARTESIAN_POINT('Ctrl Pts',(-78.5584580861567,-2.88871765894464,
124.863876957204));
#230747=CARTESIAN_POINT('Ctrl Pts',(-78.8369057099696,-6.55931960221255,
130.023744073965));
#230748=CARTESIAN_POINT('Ctrl Pts',(-79.1153533337825,-4.20222727162433,
135.900959659057));
#230749=CARTESIAN_POINT('Ctrl Pts',(-79.3938009575953,2.01650663137172,
137.094649707722));
#230750=CARTESIAN_POINT('Ctrl Pts',(-79.6722485814083,6.38216945196263,
132.507871380239));
#230751=CARTESIAN_POINT('Ctrl Pts',(-79.9506962052212,4.88293033251105,
126.355649882987));
#230752=CARTESIAN_POINT('Ctrl Pts',(-80.229143829034,-1.10348321810992,
124.29157621921));
#230753=CARTESIAN_POINT('Ctrl Pts',(-80.507591452847,-6.07584959944043,
128.212433250316));
#230754=CARTESIAN_POINT('Ctrl Pts',(-80.7860390766598,-5.46480702063872,
134.515144909234));
#230755=CARTESIAN_POINT('Ctrl Pts',(-81.0644867004727,0.168126239464741,
137.407827085998));
#230756=CARTESIAN_POINT('Ctrl Pts',(-81.3429343242857,5.64655969892388,
134.232246175545));
#230757=CARTESIAN_POINT('Ctrl Pts',(-81.6213819480984,5.93608064484842,
127.906605898828));
#230758=CARTESIAN_POINT('Ctrl Pts',(-81.8998295719115,0.770633471818905,
124.243860645443));
#230759=CARTESIAN_POINT('Ctrl Pts',(-82.1782771957242,-5.10298821427442,
126.609894368197));
#230760=CARTESIAN_POINT('Ctrl Pts',(-82.4567248195372,-6.28721302628274,
132.830437663053));
#230761=CARTESIAN_POINT('Ctrl Pts',(-82.7351724433501,-1.69379621456928,
137.189115132473));
#230762=CARTESIAN_POINT('Ctrl Pts',(-83.0136200671628,4.45613657178832,
135.680515115291));
#230763=CARTESIAN_POINT('Ctrl Pts',(-83.2920676909759,6.51109754304618,
129.690967328089));
#230764=CARTESIAN_POINT('Ctrl Pts',(-83.5705153147887,2.58267795704331,
124.724573581631));
#230765=CARTESIAN_POINT('Ctrl Pts',(-83.8489629386017,-3.71909650065006,
125.345207107088));
#230766=CARTESIAN_POINT('Ctrl Pts',(-84.1274105624144,-6.60320296221082,
130.982536014198));
#230767=CARTESIAN_POINT('Ctrl Pts',(-84.4058581862275,-3.41928848589759,
136.456130436155));
#230768=CARTESIAN_POINT('Ctrl Pts',(-84.6843058100402,2.90678506742617,
136.736024499134));
#230769=CARTESIAN_POINT('Ctrl Pts',(-84.9627534338533,6.56166514813073,
131.565009232842));
#230770=CARTESIAN_POINT('Ctrl Pts',(-85.241201057666,4.1866955128661,125.694995048862));
#230771=CARTESIAN_POINT('Ctrl Pts',(-85.519648681479,-2.03564276727566,
124.520238216135));
#230772=CARTESIAN_POINT('Ctrl Pts',(-85.7980963052919,-6.38732479096924,
129.120282873878));
#230773=CARTESIAN_POINT('Ctrl Pts',(-86.0765439291047,-4.8693673699251,
135.267912706297));
#230774=CARTESIAN_POINT('Ctrl Pts',(-86.3549915529177,1.12330078225909,
137.313756225814));
#230775=CARTESIAN_POINT('Ctrl Pts',(-86.6334391767305,6.08371039184151,
133.377783183006));
#230776=CARTESIAN_POINT('Ctrl Pts',(-86.9118868005434,5.45348735709659,
127.076960521238));
#230777=CARTESIAN_POINT('Ctrl Pts',(-87.1903344243564,-0.188224141151809,
124.201436454379));
#230778=CARTESIAN_POINT('Ctrl Pts',(-87.4687820481692,-5.65696684894189,
127.39367712271));
#230779=CARTESIAN_POINT('Ctrl Pts',(-87.7472296719821,-5.92723338074904,
133.720169301662));
#230780=CARTESIAN_POINT('Ctrl Pts',(-88.0256772957949,-0.750661997095914,
137.367175745102));
#230781=CARTESIAN_POINT('Ctrl Pts',(-88.3041249196079,5.11573109001074,
134.983275697681));
#230782=CARTESIAN_POINT('Ctrl Pts',(-88.5825725434208,6.28101722275544,
128.759156842984));
#230783=CARTESIAN_POINT('Ctrl Pts',(-88.8610201672337,1.67435537253749,
124.414480343369));
#230784=CARTESIAN_POINT('Ctrl Pts',(-89.1394677910466,-4.47095726823472,
125.941791652735));
#230785=CARTESIAN_POINT('Ctrl Pts',(-89.4179154148595,-6.50767859790483,
131.93756629108));
#230786=CARTESIAN_POINT('Ctrl Pts',(-89.6963630386723,-2.56416121387375,
136.891980275641));
#230787=CARTESIAN_POINT('Ctrl Pts',(-89.9748106624853,3.73569505946763,
136.252169191183));
#230788=CARTESIAN_POINT('Ctrl Pts',(-90.253258286298,6.60263007200808,130.606088167816));
#230789=CARTESIAN_POINT('Ctrl Pts',(-90.5317059101111,3.40207060478355,
125.142209839621));
#230790=CARTESIAN_POINT('Ctrl Pts',(-90.8101535339238,-2.9248255478482,
124.881571464914));
#230791=CARTESIAN_POINT('Ctrl Pts',(-91.0886011577368,-6.56394990767886,
130.063686977158));
#230792=CARTESIAN_POINT('Ctrl Pts',(-91.3670487815497,-4.17112496913288,
135.926445381018));
#230793=CARTESIAN_POINT('Ctrl Pts',(-91.6454964053626,2.05476004526333,
137.082258115016));
#230794=CARTESIAN_POINT('Ctrl Pts',(-91.9239440291755,6.39242095867105,
132.468989741201));
#230795=CARTESIAN_POINT('Ctrl Pts',(-92.2023916529884,4.85575929818535,
126.326008524418));
#230796=CARTESIAN_POINT('Ctrl Pts',(-92.4808392768012,-1.14310794030347,
124.298414101576));
#230797=CARTESIAN_POINT('Ctrl Pts',(-92.7592869006141,-6.09151482558059,
128.249466693771));
#230798=CARTESIAN_POINT('Ctrl Pts',(-93.0377345244271,-5.44211717319261,
134.548341988427));
#230799=CARTESIAN_POINT('Ctrl Pts',(-93.3161821482399,0.208320299155509,
137.406681306919));
#230800=CARTESIAN_POINT('Ctrl Pts',(-93.5946297720528,5.6673215935918,134.197810453193));
#230801=CARTESIAN_POINT('Ctrl Pts',(-93.8730773958657,5.91833120756931,
127.870524979765));
#230802=CARTESIAN_POINT('Ctrl Pts',(-94.1515250196785,0.730683568342929,
124.239291131637));
#230803=CARTESIAN_POINT('Ctrl Pts',(-94.4299726434915,-5.12842657431339,
126.641035419604));
#230804=CARTESIAN_POINT('Ctrl Pts',(-94.7084202673044,-6.27476323274215,
132.868672174754));
#230805=CARTESIAN_POINT('Ctrl Pts',(-94.9868678911172,-1.6548990195065,
137.199307456074));
#230806=CARTESIAN_POINT('Ctrl Pts',(-95.2653155149302,4.48573654634406,
135.653299003326));
#230807=CARTESIAN_POINT('Ctrl Pts',(-95.543763138743,6.50419936651746,129.651353057874));
#230808=CARTESIAN_POINT('Ctrl Pts',(-95.822210762556,2.54562071666526,124.708964732227));
#230809=CARTESIAN_POINT('Ctrl Pts',(-96.1006583863688,-3.75225901131679,
125.367947448562));
#230810=CARTESIAN_POINT('Ctrl Pts',(-96.3791060101818,-6.60199601594203,
131.022728283664));
#230811=CARTESIAN_POINT('Ctrl Pts',(-96.6575536339946,-3.38482120735248,
136.476839901474));
#230812=CARTESIAN_POINT('Ctrl Pts',(-96.9360012578075,2.94283893308538,
136.718220173391));
#230813=CARTESIAN_POINT('Ctrl Pts',(-97.2144488816204,6.5661738596919,131.525052421605));
#230814=CARTESIAN_POINT('Ctrl Pts',(-97.4928965054334,4.15551578466796,
125.669604109659));
#230815=CARTESIAN_POINT('Ctrl Pts',(-97.771344129246,-2.07385828823457,
124.532746181678));
#230816=CARTESIAN_POINT('Ctrl Pts',(-98.0497917530593,-6.39745790785863,
129.15919553488));
#230817=CARTESIAN_POINT('Ctrl Pts',(-98.3282393768718,-4.84210624335443,
135.297471228287));
#230818=CARTESIAN_POINT('Ctrl Pts',(-98.606687000685,1.16290450875192,137.306797771098));
#230819=CARTESIAN_POINT('Ctrl Pts',(-98.8851346244975,6.09926282835875,
133.340702231527));
#230820=CARTESIAN_POINT('Ctrl Pts',(-99.1635822483109,5.43069657425812,
127.043832655902));
#230821=CARTESIAN_POINT('Ctrl Pts',(-99.4420298721233,-0.228414527308866,
124.202704565042));
#230822=CARTESIAN_POINT('Ctrl Pts',(-99.7204774959365,-5.67762383694899,
127.428175877623));
#230823=CARTESIAN_POINT('Ctrl Pts',(-99.9989251197493,-5.90937420777732,
133.756196030418));
#230824=CARTESIAN_POINT('Ctrl Pts',(-100.277372743562,-0.710698370637635,
137.371623643978));
#230825=CARTESIAN_POINT('Ctrl Pts',(-100.555820367375,5.14107454957247,
134.9520573649));
#230826=CARTESIAN_POINT('Ctrl Pts',(-100.834267991188,6.26845111417983,
128.720960401273));
#230827=CARTESIAN_POINT('Ctrl Pts',(-101.112715615001,1.63542733571746,
124.404406456659));
#230828=CARTESIAN_POINT('Ctrl Pts',(-101.391163238814,-4.50047426920288,
125.969097730777));
#230829=CARTESIAN_POINT('Ctrl Pts',(-101.669610862627,-6.50065988111587,
131.977159382129));
#230830=CARTESIAN_POINT('Ctrl Pts',(-101.94805848644,-2.52705663717401,
136.907476263252));
#230831=CARTESIAN_POINT('Ctrl Pts',(-102.226506110253,3.76878820275105,
136.229328019765));
#230832=CARTESIAN_POINT('Ctrl Pts',(-102.504953734065,6.60130079988703,
130.565899758046));
#230833=CARTESIAN_POINT('Ctrl Pts',(-102.783401357878,3.36754045339959,
125.121605376767));
#230834=CARTESIAN_POINT('Ctrl Pts',(-103.061848981691,-2.96082505626518,
124.899485443752));
#230835=CARTESIAN_POINT('Ctrl Pts',(-103.340296605504,-6.56833698356739,
130.103657326284));
#230836=CARTESIAN_POINT('Ctrl Pts',(-103.618744229317,-4.13986810407194,
135.951741302244));
#230837=CARTESIAN_POINT('Ctrl Pts',(-103.89719185313,2.0929373192654,137.06963389251));
#230838=CARTESIAN_POINT('Ctrl Pts',(-104.175639476943,6.40243559186997,
132.430046418718));
#230839=CARTESIAN_POINT('Ctrl Pts',(-104.454087100755,4.82840833191319,
126.296533112833));
#230840=CARTESIAN_POINT('Ctrl Pts',(-104.732534724569,-1.18269030421136,
124.305493064181));
#230841=CARTESIAN_POINT('Ctrl Pts',(-105.010982348381,-6.10695432839948,
128.286594809759));
#230842=CARTESIAN_POINT('Ctrl Pts',(-105.289429972194,-5.41922566609253,
134.581400333014));
#230843=CARTESIAN_POINT('Ctrl Pts',(-105.567877596007,0.248506639461218,
137.40529087642));
#230844=CARTESIAN_POINT('Ctrl Pts',(-105.84632521982,5.68787348357469,134.163248985309));
#230845=CARTESIAN_POINT('Ctrl Pts',(-106.124772843633,5.90036246435008,
127.834552775061));
#230846=CARTESIAN_POINT('Ctrl Pts',(-106.403220467446,0.690706589119241,
124.234964888896));
#230847=CARTESIAN_POINT('Ctrl Pts',(-106.681668091259,-5.1536748986197,
126.672330744555));
#230848=CARTESIAN_POINT('Ctrl Pts',(-106.960115715072,-6.26208092554253,
132.906830192629));
#230849=CARTESIAN_POINT('Ctrl Pts',(-107.238563338885,-1.61594050155245,
137.209262812568));
#230850=CARTESIAN_POINT('Ctrl Pts',(-107.517010962697,4.51517030028232,
135.625903212168));
#230851=CARTESIAN_POINT('Ctrl Pts',(-107.79545858651,6.49706017448951,129.611781512777));
#230852=CARTESIAN_POINT('Ctrl Pts',(-108.073906210323,2.50846914737518,
124.69358174996));
#230853=CARTESIAN_POINT('Ctrl Pts',(-108.352353834136,-3.78528248064593,
125.390889238328));
#230854=CARTESIAN_POINT('Ctrl Pts',(-108.630801457949,-6.60054443028347,
131.062912461436));
#230855=CARTESIAN_POINT('Ctrl Pts',(-108.909249081762,-3.35022850301195,
136.497339170987));
#230856=CARTESIAN_POINT('Ctrl Pts',(-109.187696705575,2.97878375076591,
136.700196707408));
#230857=CARTESIAN_POINT('Ctrl Pts',(-109.466144329388,6.57043925926657,
131.485068904869));
#230858=CARTESIAN_POINT('Ctrl Pts',(-109.7445919532,4.12418207230337,125.644403440746));
#230859=CARTESIAN_POINT('Ctrl Pts',(-110.023039577014,-2.11199696161116,
124.5454865442));
#230860=CARTESIAN_POINT('Ctrl Pts',(-110.301487200826,-6.40735396459295,
129.198169158078));
#230861=CARTESIAN_POINT('Ctrl Pts',(-110.579934824639,-4.81466569075636,
135.326863256411));
#230862=CARTESIAN_POINT('Ctrl Pts',(-110.858382448452,1.20246514338981,
137.299598366182));
#230863=CARTESIAN_POINT('Ctrl Pts',(-111.136830072265,6.11458925444912,
133.303527294979));
#230864=CARTESIAN_POINT('Ctrl Pts',(-111.415277696078,5.407704554961,127.010844138312));
#230865=CARTESIAN_POINT('Ctrl Pts',(-111.693725319891,-0.268596449482207,
124.204217302498));
#230866=CARTESIAN_POINT('Ctrl Pts',(-111.972172943703,-5.69807043851701,
127.462799738304));
#230867=CARTESIAN_POINT('Ctrl Pts',(-112.250620567517,-5.89129606077132,
133.792113377828));
#230868=CARTESIAN_POINT('Ctrl Pts',(-112.529068191329,-0.670708408989202,
137.375828190507));
#230869=CARTESIAN_POINT('Ctrl Pts',(-112.807515815142,5.16622750472631,
134.920685337692));
#230870=CARTESIAN_POINT('Ctrl Pts',(-113.085963438955,6.25565272584325,
128.682841160722));
#230871=CARTESIAN_POINT('Ctrl Pts',(-113.364411062768,1.5964386975353,124.394569722605));
#230872=CARTESIAN_POINT('Ctrl Pts',(-113.642858686581,-4.52982450344111,
125.996582981263));
#230873=CARTESIAN_POINT('Ctrl Pts',(-113.921306310394,-6.49340027998504,
132.016709014688));
#230874=CARTESIAN_POINT('Ctrl Pts',(-114.199753934207,-2.48985841946147,
136.922746097669));
#230875=CARTESIAN_POINT('Ctrl Pts',(-114.47820155802,3.80174169220082,136.206285824184));
#230876=CARTESIAN_POINT('Ctrl Pts',(-114.756649181833,6.59972691413776,
130.525720184532));
#230877=CARTESIAN_POINT('Ctrl Pts',(-115.035096805645,3.3328855165654,125.101211490497));
#230878=CARTESIAN_POINT('Ctrl Pts',(-115.313544429458,-2.99671485022117,
124.917618229914));
#230879=CARTESIAN_POINT('Ctrl Pts',(-115.591992053271,-6.57248066731354,
130.143653640229));
#230880=CARTESIAN_POINT('Ctrl Pts',(-115.870439677084,-4.10845783467579,
135.976846485386));
#230881=CARTESIAN_POINT('Ctrl Pts',(-116.148887300897,2.13103703870585,
137.056777507999));
#230882=CARTESIAN_POINT('Ctrl Pts',(-116.42733492471,6.41221298046361,132.391042855849));
#230883=CARTESIAN_POINT('Ctrl Pts',(-116.705782548523,4.8008784471946,126.267224740454));
#230884=CARTESIAN_POINT('Ctrl Pts',(-116.984230172336,-1.22222884309565,
124.312812844714));
#230885=CARTESIAN_POINT('Ctrl Pts',(-117.262677796149,-6.12216753577917,
128.323816222486));
#230886=CARTESIAN_POINT('Ctrl Pts',(-117.541125419961,-5.39613334759327,
134.614318718005));
#230887=CARTESIAN_POINT('Ctrl Pts',(-117.819573043774,0.288683771261777,
137.403655846021));
#230888=CARTESIAN_POINT('Ctrl Pts',(-118.098020667587,5.70821460731317,
134.128563052582));
#230889=CARTESIAN_POINT('Ctrl Pts',(-118.3764682914,5.88217508103065,127.79869061768));
#230890=CARTESIAN_POINT('Ctrl Pts',(-118.654915915213,0.650704015508265,
124.230882077529));
#230891=CARTESIAN_POINT('Ctrl Pts',(-118.933363539026,-5.17873225160735,
126.703779183394));
#230892=CARTESIAN_POINT('Ctrl Pts',(-119.211811162839,-6.24916657463125,
132.944910302722));
#230893=CARTESIAN_POINT('Ctrl Pts',(-119.490258786652,-1.57692210432836,
137.218980833058));
#230894=CARTESIAN_POINT('Ctrl Pts',(-119.768706410464,4.54443674292479,
135.598328756974));
#230895=CARTESIAN_POINT('Ctrl Pts',(-120.047154034278,6.48968023150711,
129.572254159139));
#230896=CARTESIAN_POINT('Ctrl Pts',(-120.32560165809,2.47122462583917,124.67842520485));
#230897=CARTESIAN_POINT('Ctrl Pts',(-120.604049281903,-3.81816568494053,
125.414031626265));
#230898=CARTESIAN_POINT('Ctrl Pts',(-120.882496905716,-6.59884825902321,
131.103087058474));
#230899=CARTESIAN_POINT('Ctrl Pts',(-121.160944529529,-3.31551165472302,
136.517627485086));
#230900=CARTESIAN_POINT('Ctrl Pts',(-121.439392153342,3.0146181885189,136.68195476905));
#230901=CARTESIAN_POINT('Ctrl Pts',(-121.717839777155,6.57446118879764,
131.445060164237));
#230902=CARTESIAN_POINT('Ctrl Pts',(-121.996287400968,4.0926955368563,125.619393975946));
#230903=CARTESIAN_POINT('Ctrl Pts',(-122.274735024781,-2.15005737416446,
124.5584588316));
#230904=CARTESIAN_POINT('Ctrl Pts',(-122.553182648593,-6.41701259446945,
129.237202299292));
#230905=CARTESIAN_POINT('Ctrl Pts',(-122.831630272406,-4.7870467289504,
135.356087701536));
#230906=CARTESIAN_POINT('Ctrl Pts',(-123.110077896219,1.24198122024032,
137.292158277842));
#230907=CARTESIAN_POINT('Ctrl Pts',(-123.388525520032,6.1296891021858,133.266259750888));
#230908=CARTESIAN_POINT('Ctrl Pts',(-123.666973143845,5.38451215118288,
126.97799619087));
#230909=CARTESIAN_POINT('Ctrl Pts',(-123.945420767658,-0.30876841871475,
124.20597461069));
#230910=CARTESIAN_POINT('Ctrl Pts',(-124.223868391471,-5.71830589598935,
127.497547421752));
#230911=CARTESIAN_POINT('Ctrl Pts',(-124.502316015284,-5.87299960962311,
133.827920012961));
#230912=CARTESIAN_POINT('Ctrl Pts',(-124.780763639097,-0.630693593994696,
137.379789228888));
#230913=CARTESIAN_POINT('Ctrl Pts',(-125.059211262909,5.19118902341993,
134.889160778557));
#230914=CARTESIAN_POINT('Ctrl Pts',(-125.337658886723,6.24262253199412,
128.644800533857));
#230915=CARTESIAN_POINT('Ctrl Pts',(-125.616106510535,1.55739090273089,
124.384970505708));
#230916=CARTESIAN_POINT('Ctrl Pts',(-125.894554134348,-4.55900688336737,
126.024246385717));
#230917=CARTESIAN_POINT('Ctrl Pts',(-126.173001758161,-6.48590006351826,
132.056213723232));
#230918=CARTESIAN_POINT('Ctrl Pts',(-126.451449381974,-2.45256793912933,
136.937789213063));
#230919=CARTESIAN_POINT('Ctrl Pts',(-126.729897005787,3.83455430671493,
136.183043458277));
#230920=CARTESIAN_POINT('Ctrl Pts',(-127.0083446296,6.5979084730801,130.485550936142));
#230921=CARTESIAN_POINT('Ctrl Pts',(-127.286792253413,3.29810707843306,
125.081028936517));
#230922=CARTESIAN_POINT('Ctrl Pts',(-127.565239877225,-3.03249359980603,
124.935969151478));
#230923=CARTESIAN_POINT('Ctrl Pts',(-127.843687501038,-6.57638080537151,
130.183674436914));
#230924=CARTESIAN_POINT('Ctrl Pts',(-128.122135124851,-4.07689532486387,
136.001760000162));
#230925=CARTESIAN_POINT('Ctrl Pts',(-128.400582748664,2.1690577917847,137.043689437881));
#230926=CARTESIAN_POINT('Ctrl Pts',(-128.679030372477,6.42175276214748,
132.351980497887));
#230927=CARTESIAN_POINT('Ctrl Pts',(-128.95747799629,4.77317066415926,126.238084493312));
#230928=CARTESIAN_POINT('Ctrl Pts',(-129.235925620103,-1.26172209184052,
124.320373171937));
#230929=CARTESIAN_POINT('Ctrl Pts',(-129.514373243916,-6.13715388399014,
128.361129552696));
#230930=CARTESIAN_POINT('Ctrl Pts',(-129.792820867728,-5.37284107338758,
134.647095923599));
#230931=CARTESIAN_POINT('Ctrl Pts',(-130.071268491542,0.328850205779251,
137.401776276312));
#230932=CARTESIAN_POINT('Ctrl Pts',(-130.349716115354,5.72834421106097,
134.093753940311));
#230933=CARTESIAN_POINT('Ctrl Pts',(-130.628163739167,5.86376973154965,
127.762939836503));
#230934=CARTESIAN_POINT('Ctrl Pts',(-130.90661136298,0.610677329821333,
124.227042848828));
#230935=CARTESIAN_POINT('Ctrl Pts',(-131.185058986793,-5.20359770476699,
126.735379570785));
#230936=CARTESIAN_POINT('Ctrl Pts',(-131.463506610606,-6.23602065855449,
132.982911093959));
#230937=CARTESIAN_POINT('Ctrl Pts',(-131.741954234419,-1.53784527367628,
137.228461157434));
#230938=CARTESIAN_POINT('Ctrl Pts',(-132.020401858232,4.57353478979242,
135.57057665953));
#230939=CARTESIAN_POINT('Ctrl Pts',(-132.298849482045,6.48205981103755,
129.532772461657));
#230940=CARTESIAN_POINT('Ctrl Pts',(-132.577297105858,2.43388853216508,
124.66349565853));
#230941=CARTESIAN_POINT('Ctrl Pts',(-132.85574472967,-3.85090740570176,
125.437373754826));
#230942=CARTESIAN_POINT('Ctrl Pts',(-133.134192353483,-6.59690756501448,
131.143250586095));
#230943=CARTESIAN_POINT('Ctrl Pts',(-133.412639977296,-3.28067194892964,
136.53770409198));
#230944=CARTESIAN_POINT('Ctrl Pts',(-133.691087601109,3.0503409184865,136.663495034279));
#230945=CARTESIAN_POINT('Ctrl Pts',(-133.969535224922,6.5782394992522,131.405027682246));
#230946=CARTESIAN_POINT('Ctrl Pts',(-134.247982848735,4.06105734507014,
125.59457664199));
#230947=CARTESIAN_POINT('Ctrl Pts',(-134.526430472548,-2.18803811555026,
124.57166256319));
#230948=CARTESIAN_POINT('Ctrl Pts',(-134.804878096361,-6.42643343958478,
129.276293512134));
#230949=CARTESIAN_POINT('Ctrl Pts',(-135.083325720174,-4.75925038136761,
135.385143480741));
#230950=CARTESIAN_POINT('Ctrl Pts',(-135.361773343986,1.28145127501926,
137.284477781773));
#230951=CARTESIAN_POINT('Ctrl Pts',(-135.640220967799,6.14456181203885,
133.228900980221));
#230952=CARTESIAN_POINT('Ctrl Pts',(-135.918668591612,5.36112022232688,
126.945290030769));
#230953=CARTESIAN_POINT('Ctrl Pts',(-136.197116215425,-0.348928946420584,
124.207976424505));
#230954=CARTESIAN_POINT('Ctrl Pts',(-136.475563839238,-5.73832945953392,
127.53241764038));
#230955=CARTESIAN_POINT('Ctrl Pts',(-136.754011463051,-5.85448553231475,
133.863614608987));
#230956=CARTESIAN_POINT('Ctrl Pts',(-137.032459086864,-0.590655408416443,
137.383506612345));
#230957=CARTESIAN_POINT('Ctrl Pts',(-137.310906710677,5.21595818069537,
134.857484855651));
#230958=CARTESIAN_POINT('Ctrl Pts',(-137.58935433449,6.22936101547165,128.606839930282));
#230959=CARTESIAN_POINT('Ctrl Pts',(-137.867801958302,1.51828539823306,
124.375609161675));
#230960=CARTESIAN_POINT('Ctrl Pts',(-138.146249582115,-4.58802032761614,
126.052086919061));
#230961=CARTESIAN_POINT('Ctrl Pts',(-138.424697205928,-6.47815950964009,
132.095672043897));
#230962=CARTESIAN_POINT('Ctrl Pts',(-138.703144829741,-2.41518657799051,
136.952605052004));
#230963=CARTESIAN_POINT('Ctrl Pts',(-138.981592453554,3.86722483040823,
136.159601783301));
#230964=CARTESIAN_POINT('Ctrl Pts',(-139.260040077367,6.59584554409815,
130.445393501362));
#230965=CARTESIAN_POINT('Ctrl Pts',(-139.53848770118,3.26320642772972,125.061058462695));
#230966=CARTESIAN_POINT('Ctrl Pts',(-139.816935324993,-3.06815997922566,
124.954537528447));
#230967=CARTESIAN_POINT('Ctrl Pts',(-140.095382948806,-6.58003725322031,
130.223718233352));
#230968=CARTESIAN_POINT('Ctrl Pts',(-140.373830572619,-4.04518174419624,
136.026480923393));
#230969=CARTESIAN_POINT('Ctrl Pts',(-140.652278196431,2.20699816962987,
137.030370167137));
#230970=CARTESIAN_POINT('Ctrl Pts',(-140.930725820244,6.43105458342049,
132.312860792301));
#230971=CARTESIAN_POINT('Ctrl Pts',(-141.209173444057,4.74528600953044,
126.209113451214));
#230972=CARTESIAN_POINT('Ctrl Pts',(-141.48762106787,-1.30116858700904,
124.328173765698));
#230973=CARTESIAN_POINT('Ctrl Pts',(-141.766068691683,-6.15191281770628,
128.398533417733));
#230974=CARTESIAN_POINT('Ctrl Pts',(-142.044516315496,-5.34934970658085,
134.679730735221));
#230975=CARTESIAN_POINT('Ctrl Pts',(-142.322963939309,0.369004454631186,
137.399652236939));
#230976=CARTESIAN_POINT('Ctrl Pts',(-142.601411563122,5.74826154890666,
134.058822938361));
#230977=CARTESIAN_POINT('Ctrl Pts',(-142.879859186934,5.84514709792562,
127.727301756295));
#230978=CARTESIAN_POINT('Ctrl Pts',(-143.158306810748,0.570628015260733,
124.223447345055));
#230979=CARTESIAN_POINT('Ctrl Pts',(-143.43675443456,-5.22827033670001,
126.767130735766));
#230980=CARTESIAN_POINT('Ctrl Pts',(-143.715202058373,-6.22264366443886,
133.020831158207));
#230981=CARTESIAN_POINT('Ctrl Pts',(-143.993649682186,-1.49871145760156,
137.237703434405));
#230982=CARTESIAN_POINT('Ctrl Pts',(-144.272097305999,4.60246336264661,
135.542647948195));
#230983=CARTESIAN_POINT('Ctrl Pts',(-144.550544929812,6.47419919545755,
129.493337883343));
#230984=CARTESIAN_POINT('Ctrl Pts',(-144.828992553625,2.39646224985712,
124.648793664219));
#230985=CARTESIAN_POINT('Ctrl Pts',(-145.107440177438,-3.8835064296727,
125.460914759058));
#230986=CARTESIAN_POINT('Ctrl Pts',(-145.38588780125,-6.59472242016944,
131.183401556022));
#230987=CARTESIAN_POINT('Ctrl Pts',(-145.664335425064,-3.24571067663155,
136.557568247724));
#230988=CARTESIAN_POINT('Ctrl Pts',(-145.942783048876,3.08595061694992,
136.644818187128));
#230989=CARTESIAN_POINT('Ctrl Pts',(-146.221230672689,6.58177405062243,
131.364972942318));
#230990=CARTESIAN_POINT('Ctrl Pts',(-146.499678296502,4.02926866931097,
125.569952358496));
#230991=CARTESIAN_POINT('Ctrl Pts',(-146.778125920315,-2.22593777837984,
124.585097249699));
#230992=CARTESIAN_POINT('Ctrl Pts',(-147.056573544128,-6.43561615084533,
129.315441348065));
#230993=CARTESIAN_POINT('Ctrl Pts',(-147.335021167941,-4.73127767801157,
135.414029517352));
#230994=CARTESIAN_POINT('Ctrl Pts',(-147.613468791753,1.32087384515067,
137.276557162581));
#230995=CARTESIAN_POINT('Ctrl Pts',(-147.891916415567,6.15920683289404,
133.191452367319));
#230996=CARTESIAN_POINT('Ctrl Pts',(-148.170364039379,5.33752963518947,
126.91272686995));
#230997=CARTESIAN_POINT('Ctrl Pts',(-148.448811663193,-0.389076544435395,
124.210222669761));
#230998=CARTESIAN_POINT('Ctrl Pts',(-148.727259287005,-5.75814038716998,
127.567409102056));
#230999=CARTESIAN_POINT('Ctrl Pts',(-149.005706910818,-5.83575451489182,
133.899195843233));
#231000=CARTESIAN_POINT('Ctrl Pts',(-149.284154534631,-0.550595335885521,
137.386980203127));
#231001=CARTESIAN_POINT('Ctrl Pts',(-149.562602158444,5.24053405872261,
134.825658742734));
#231002=CARTESIAN_POINT('Ctrl Pts',(-149.841049782257,6.21586866768539,
128.568960756646));
#231003=CARTESIAN_POINT('Ctrl Pts',(-150.119497406069,1.47912363311174,
124.366486037389));
#231004=CARTESIAN_POINT('Ctrl Pts',(-150.397945029883,-4.61686376108527,
126.080103549656));
#231005=CARTESIAN_POINT('Ctrl Pts',(-150.676392653695,-6.4701789051783,
132.135082514543));
#231006=CARTESIAN_POINT('Ctrl Pts',(-150.954840277509,-2.37771572122463,
136.967193065487));
#231007=CARTESIAN_POINT('Ctrl Pts',(-151.233287901321,3.89975205266408,
136.135961667893));
#231008=CARTESIAN_POINT('Ctrl Pts',(-151.511735525134,6.59353820363339,
130.405249368239));
#231009=CARTESIAN_POINT('Ctrl Pts',(-151.790183148947,3.22818485771248,
125.041300809049));
#231010=CARTESIAN_POINT('Ctrl Pts',(-152.06863077276,-3.10371266684865,
124.97332267276));
#231011=CARTESIAN_POINT('Ctrl Pts',(-152.347078396573,-6.58344987536885,
130.263783545709));
#231012=CARTESIAN_POINT('Ctrl Pts',(-152.625526020386,-4.01331826783166,
136.051008339035));
#231013=CARTESIAN_POINT('Ctrl Pts',(-152.903973644199,2.24485676634579,
137.016820189321));
#231014=CARTESIAN_POINT('Ctrl Pts',(-153.182421268012,6.44011809960154,
132.273685188686));
#231015=CARTESIAN_POINT('Ctrl Pts',(-153.460868891824,4.71722551658265,
126.180312687687));
#231016=CARTESIAN_POINT('Ctrl Pts',(-153.739316515637,-1.34056686689732,
124.336214336947));
#231017=CARTESIAN_POINT('Ctrl Pts',(-154.01776413945,-6.16644379003131,
128.436026431582));
#231018=CARTESIAN_POINT('Ctrl Pts',(-154.296211763263,-5.32566011765276,
134.712221943579));
#231019=CARTESIAN_POINT('Ctrl Pts',(-154.574659387076,0.409145029887599,
137.397283806609));
#231020=CARTESIAN_POINT('Ctrl Pts',(-154.853107010889,5.7679658828075,134.023771341112));
#231021=CARTESIAN_POINT('Ctrl Pts',(-155.131554634702,5.82630787022557,
127.691777697632));
#231022=CARTESIAN_POINT('Ctrl Pts',(-155.410002258515,0.530557555869813,
124.220095699443));
#231023=CARTESIAN_POINT('Ctrl Pts',(-155.688449882327,-5.25274923315307,
126.799031501784));
#231024=CARTESIAN_POINT('Ctrl Pts',(-155.96689750614,-6.20903608797397,
133.058669090323));
#231025=CARTESIAN_POINT('Ctrl Pts',(-156.245345129953,-1.4595221062231,
137.246707321489));
#231026=CARTESIAN_POINT('Ctrl Pts',(-156.523792753766,4.63122138952822,
135.514543657883));
#231027=CARTESIAN_POINT('Ctrl Pts',(-156.802240377579,6.46609867604585,
129.453951885458));
#231028=CARTESIAN_POINT('Ctrl Pts',(-157.080688001392,2.35894716575843,
124.634319766706));
#231029=CARTESIAN_POINT('Ctrl Pts',(-157.359135625205,-3.9159615488849,
125.484653766641));
#231030=CARTESIAN_POINT('Ctrl Pts',(-157.637583249018,-6.59229290546042,
131.223538480449));
#231031=CARTESIAN_POINT('Ctrl Pts',(-157.916030872831,-3.21062913332988,
136.577219216243));
#231032=CARTESIAN_POINT('Ctrl Pts',(-158.194478496644,3.12144596437753,
136.625924919674));
#231033=CARTESIAN_POINT('Ctrl Pts',(-158.472926120456,6.58506471193526,
131.324897428694));
#231034=CARTESIAN_POINT('Ctrl Pts',(-158.751373744269,3.99733068751967,
125.545522037924));
#231035=CARTESIAN_POINT('Ctrl Pts',(-159.029821368082,-2.26375495826568,
124.598762393297));
#231036=CARTESIAN_POINT('Ctrl Pts',(-159.308268991895,-6.44456038798308,
129.354644356446));
#231037=CARTESIAN_POINT('Ctrl Pts',(-159.586716615708,-4.7031296554214,
135.442744740987));
#231038=CARTESIAN_POINT('Ctrl Pts',(-159.865164239521,1.36024746981527,
137.268396713766));
#231039=CARTESIAN_POINT('Ctrl Pts',(-160.143611863334,6.17362362207528,
133.153915299856));
#231040=CARTESIAN_POINT('Ctrl Pts',(-160.422059487147,5.31374126392856,
126.880307915048));
#231041=CARTESIAN_POINT('Ctrl Pts',(-160.70050711096,-0.429209725076344,
124.212713263223));
#231042=CARTESIAN_POINT('Ctrl Pts',(-160.978954734773,-5.77773794479658,
127.602520510164));
#231043=CARTESIAN_POINT('Ctrl Pts',(-161.257402358585,-5.81680725143943,
133.934662397221));
#231044=CARTESIAN_POINT('Ctrl Pts',(-161.535849982398,-0.51051486084124,
137.390209872519));
#231045=CARTESIAN_POINT('Ctrl Pts',(-161.814297606211,5.26491574683228,
134.793683619137));
#231046=CARTESIAN_POINT('Ctrl Pts',(-162.092745230024,6.20214598860049,
128.531164416574));
#231047=CARTESIAN_POINT('Ctrl Pts',(-162.371192853837,1.43990705852047,
124.357601470914));
#231048=CARTESIAN_POINT('Ctrl Pts',(-162.64964047765,-4.64553611496906,
126.108295239334));
#231049=CARTESIAN_POINT('Ctrl Pts',(-162.928088101462,-6.46195854585841,
132.1744436748));
#231050=CARTESIAN_POINT('Ctrl Pts',(-163.206535725276,-2.34015675732853,
136.981552712947));
#231051=CARTESIAN_POINT('Ctrl Pts',(-163.484983349088,3.93213476817268,
136.112123988049));
#231052=CARTESIAN_POINT('Ctrl Pts',(-163.763430972902,6.5909865371863,130.365120024332));
#231053=CARTESIAN_POINT('Ctrl Pts',(-164.041878596714,3.19304366611785,
125.021756707701));
#231054=CARTESIAN_POINT('Ctrl Pts',(-164.320326220527,-3.13915034525769,
124.99232388833));
#231055=CARTESIAN_POINT('Ctrl Pts',(-164.59877384434,-6.58661854536123,
130.303868889347));
#231056=CARTESIAN_POINT('Ctrl Pts',(-164.877221468153,-3.98130607648258,
136.075341338217));
#231057=CARTESIAN_POINT('Ctrl Pts',(-165.155669091966,2.28263217906914,
137.003040006531));
#231058=CARTESIAN_POINT('Ctrl Pts',(-165.434116715779,6.44894297483741,
132.23445513871));
#231059=CARTESIAN_POINT('Ctrl Pts',(-165.712564339591,4.6889902251094,126.151683269957));
#231060=CARTESIAN_POINT('Ctrl Pts',(-165.991011963405,-1.37991547158711,
124.344494587733));
#231061=CARTESIAN_POINT('Ctrl Pts',(-166.269459587217,-6.18074626251326,
128.473607204924));
#231062=CARTESIAN_POINT('Ctrl Pts',(-166.54790721103,-5.3017731844313,134.744568344699));
#231063=CARTESIAN_POINT('Ctrl Pts',(-166.826354834843,0.449270444124704,
137.394671073086));
#231064=CARTESIAN_POINT('Ctrl Pts',(-167.104802458656,5.78745648261092,
133.988600447415));
#231065=CARTESIAN_POINT('Ctrl Pts',(-167.383250082469,5.8072527465451,127.656368976875));
#231066=CARTESIAN_POINT('Ctrl Pts',(-167.661697706282,0.490467436472931,
124.216988036188));
#231067=CARTESIAN_POINT('Ctrl Pts',(-167.940145330095,-5.27703348705155,
126.831080686747));
#231068=CARTESIAN_POINT('Ctrl Pts',(-168.218592953908,-6.19519843339338,
133.096423488211));
#231069=CARTESIAN_POINT('Ctrl Pts',(-168.49704057772,-1.42027867171577,
137.255472485049));
#231070=CARTESIAN_POINT('Ctrl Pts',(-168.775488201534,4.65980780479824,
135.486264830004));
#231071=CARTESIAN_POINT('Ctrl Pts',(-169.053935825346,6.45775855296945,
129.414615927465));
#231072=CARTESIAN_POINT('Ctrl Pts',(-169.332383449159,2.32134467000579,
124.620074502325));
#231073=CARTESIAN_POINT('Ctrl Pts',(-169.610831072972,-3.94827156070164,
125.508589897919));
#231074=CARTESIAN_POINT('Ctrl Pts',(-169.889278696785,-6.58961911091297,
131.263659872085));
#231075=CARTESIAN_POINT('Ctrl Pts',(-170.167726320598,-3.17542861898582,
136.596656269364));
#231076=CARTESIAN_POINT('Ctrl Pts',(-170.446173944411,3.15682564547787,
136.606815932013));
#231077=CARTESIAN_POINT('Ctrl Pts',(-170.724621568223,6.58811136125304,
131.284802626386));
#231078=CARTESIAN_POINT('Ctrl Pts',(-171.003069192037,3.96524458316956,
125.521286585549));
#231079=CARTESIAN_POINT('Ctrl Pts',(-171.28151681585,-2.30148825387982,
124.612657487621));
#231080=CARTESIAN_POINT('Ctrl Pts',(-171.559964439662,-6.45326581956532,
129.393901084596));
#231081=CARTESIAN_POINT('Ctrl Pts',(-171.838412063475,-4.67480735663214,
135.471288087592));
#231082=CARTESIAN_POINT('Ctrl Pts',(-172.116859687288,1.39957069001038,
137.259996737715));
#231083=CARTESIAN_POINT('Ctrl Pts',(-172.395307311101,6.18781164536257,
133.116291168777));
#231084=CARTESIAN_POINT('Ctrl Pts',(-172.673754934914,5.289755990031,126.848034367363));
#231085=CARTESIAN_POINT('Ctrl Pts',(-172.952202558727,-0.469327001192524,
124.215448112602));
#231086=CARTESIAN_POINT('Ctrl Pts',(-173.23065018254,-5.79712140621875,
127.637750563632));
#231087=CARTESIAN_POINT('Ctrl Pts',(-173.509097806352,-5.79764444405506,
133.970012956726));
#231088=CARTESIAN_POINT('Ctrl Pts',(-173.787545430165,-0.470415468481743,
137.393195500846));
#231089=CARTESIAN_POINT('Ctrl Pts',(-174.065993053978,5.28910234155359,
134.76156066971));
#231090=CARTESIAN_POINT('Ctrl Pts',(-174.344440677791,6.18819348671444,
128.493452310623));
#231091=CARTESIAN_POINT('Ctrl Pts',(-174.622888301604,1.40063712764339,
124.34895579147));
#231092=CARTESIAN_POINT('Ctrl Pts',(-174.901335925417,-4.67403632680454,
126.13666094344));
#231093=CARTESIAN_POINT('Ctrl Pts',(-175.17978354923,-6.45349873628761,
132.213754066126));
#231094=CARTESIAN_POINT('Ctrl Pts',(-175.458231173043,-2.30251107806296,
136.995683462282));
#231095=CARTESIAN_POINT('Ctrl Pts',(-175.736678796856,3.96437177698222,
136.088089627079));
#231096=CARTESIAN_POINT('Ctrl Pts',(-176.015126420669,6.58819063930867,
130.325006956645));
#231097=CARTESIAN_POINT('Ctrl Pts',(-176.293574044481,3.15778415511627,
125.002426882869));
#231098=CARTESIAN_POINT('Ctrl Pts',(-176.572021668294,-3.17447170129595,
125.011540471058));
#231099=CARTESIAN_POINT('Ctrl Pts',(-176.850469292107,-6.58954314578118,
130.343972778891));
#231100=CARTESIAN_POINT('Ctrl Pts',(-177.12891691592,-3.94914635637289,
136.099479019269));
#231101=CARTESIAN_POINT('Ctrl Pts',(-177.407364539733,2.32032300801719,
136.989030129397));
#231102=CARTESIAN_POINT('Ctrl Pts',(-177.685812163546,6.45752888212044,
132.195172096054));
#231103=CARTESIAN_POINT('Ctrl Pts',(-177.964259787359,4.66058118137817,
126.123226258898));
#231104=CARTESIAN_POINT('Ctrl Pts',(-178.242707411172,-1.41921294300185,
124.353014211231));
#231105=CARTESIAN_POINT('Ctrl Pts',(-178.521155034985,-6.19481970517025,
128.511274345191));
#231106=CARTESIAN_POINT('Ctrl Pts',(-178.799602658797,-5.27768979205393,
134.776768739972));
#231107=CARTESIAN_POINT('Ctrl Pts',(-179.078050282611,0.489379210479558,
137.391814133187));
#231108=CARTESIAN_POINT('Ctrl Pts',(-179.356497906423,5.80673262608622,
133.95331156054));
#231109=CARTESIAN_POINT('Ctrl Pts',(-179.634945530236,5.7879824329786,127.621076906106));
#231110=CARTESIAN_POINT('Ctrl Pts',(-179.913393154049,0.450359142625426,
124.214124470449));
#231111=CARTESIAN_POINT('Ctrl Pts',(-180.191840777862,-5.30112219853358,
126.863277103057));
#231112=CARTESIAN_POINT('Ctrl Pts',(-180.470288401675,-6.18113121345664,
133.134092952866));
#231113=CARTESIAN_POINT('Ctrl Pts',(-180.748736025488,-1.38098260826046,
137.263998600285));
#231114=CARTESIAN_POINT('Ctrl Pts',(-181.0271836493,4.68822154917632,135.457812512445));
#231115=CARTESIAN_POINT('Ctrl Pts',(-181.305631273113,6.44917913527537,
129.375331466973));
#231116=CARTESIAN_POINT('Ctrl Pts',(-181.584078896926,2.28365615597197,
124.606058398942));
#231117=CARTESIAN_POINT('Ctrl Pts',(-181.862526520739,-3.98043526786393,
125.532722265928));
#231118=CARTESIAN_POINT('Ctrl Pts',(-182.140974144552,-6.58670113560653,
131.303764244219));
#231119=CARTESIAN_POINT('Ctrl Pts',(-182.419421768365,-3.14011043796568,
136.615878686839));
#231120=CARTESIAN_POINT('Ctrl Pts',(-182.697869392178,3.19208834924215,
136.587491932238));
#231121=CARTESIAN_POINT('Ctrl Pts',(-182.976317015991,6.59091388568205,
131.244690021124));
#231122=CARTESIAN_POINT('Ctrl Pts',(-183.254764639804,3.93301154522339,
125.497246899427));
#231123=CARTESIAN_POINT('Ctrl Pts',(-183.533212263617,-2.33913626699958,
124.626782017781));
#231124=CARTESIAN_POINT('Ctrl Pts',(-183.811659887429,-6.46173212300977,
129.433210077844));
#231125=CARTESIAN_POINT('Ctrl Pts',(-184.090107511242,-4.64631183113728,
135.499658499484));
#231126=CARTESIAN_POINT('Ctrl Pts',(-184.368555135055,1.43884204859816,
137.251357545694));
#231127=CARTESIAN_POINT('Ctrl Pts',(-184.647002758868,6.20177037701405,
133.078581368264));
#231128=CARTESIAN_POINT('Ctrl Pts',(-184.925450382681,5.26557470227994,
126.815907422802));
#231129=CARTESIAN_POINT('Ctrl Pts',(-185.203898006494,-0.50942688622466,
124.218427116558));
#231130=CARTESIAN_POINT('Ctrl Pts',(-185.482345630307,-5.81629005317544,
127.673097957001));
#231131=CARTESIAN_POINT('Ctrl Pts',(-185.76079325412,-5.77826680282389,
134.005246211819));
#231132=CARTESIAN_POINT('Ctrl Pts',(-186.039240877932,-0.430298644703365,
137.395936977472));
#231133=CARTESIAN_POINT('Ctrl Pts',(-186.317688501746,5.31309294664177,
134.729291084778));
#231134=CARTESIAN_POINT('Ctrl Pts',(-186.596136125558,6.17401167904375,
128.455825836229));
#231135=CARTESIAN_POINT('Ctrl Pts',(-186.874583749371,1.36131529564269,
124.340549319425));
#231136=CARTESIAN_POINT('Ctrl Pts',(-187.153031373184,-4.70236334050424,
126.165199610876));
#231137=CARTESIAN_POINT('Ctrl Pts',(-187.431478996997,-6.44479978994851,
132.253012231859));
#231138=CARTESIAN_POINT('Ctrl Pts',(-187.70992662081,-2.26478007840253,
137.009584789872));
#231139=CARTESIAN_POINT('Ctrl Pts',(-187.988374244623,3.99646188453734,
136.063859475589));
#231140=CARTESIAN_POINT('Ctrl Pts',(-188.266821868436,6.58515061360439,
130.284911651585));
#231141=CARTESIAN_POINT('Ctrl Pts',(-188.545269492249,3.12240763126122,
124.983312050825));
#231142=CARTESIAN_POINT('Ctrl Pts',(-188.823717116061,-3.20967542611822,
125.030971708867));
#231143=CARTESIAN_POINT('Ctrl Pts',(-189.102164739874,-6.59222356825658,
130.384093728275));
#231144=CARTESIAN_POINT('Ctrl Pts',(-189.380612363687,-3.91684029919248,
136.123420487763));
#231145=CARTESIAN_POINT('Ctrl Pts',(-189.6590599875,2.35792785654334,136.974791077059));
#231146=CARTESIAN_POINT('Ctrl Pts',(-189.937507611313,6.46587550329532,
132.155837516369));
#231147=CARTESIAN_POINT('Ctrl Pts',(-190.215955235126,4.63199943809816,
126.094942708994));
#231148=CARTESIAN_POINT('Ctrl Pts',(-190.494402858939,-1.45845782495887,
124.361772891742));
#231149=CARTESIAN_POINT('Ctrl Pts',(-190.772850482752,-6.2086635965042,
128.549026456613));
#231150=CARTESIAN_POINT('Ctrl Pts',(-191.051298106565,-5.25341083294129,
134.808821936201));
#231151=CARTESIAN_POINT('Ctrl Pts',(-191.329745730377,0.529469842708527,
137.388713092773));
#231152=CARTESIAN_POINT('Ctrl Pts',(-191.60819335419,5.82579359894846,133.91790598813));
#231153=CARTESIAN_POINT('Ctrl Pts',(-191.886640978003,5.76849764359442,
127.585902793086));
#231154=CARTESIAN_POINT('Ctrl Pts',(-192.165088601816,0.410234160553658,
124.211505108333));
#231155=CARTESIAN_POINT('Ctrl Pts',(-192.443536225629,-5.32501447498302,
126.895619557667));
#231156=CARTESIAN_POINT('Ctrl Pts',(-192.721983849442,-6.16683494942961,
133.171676088433));
#231157=CARTESIAN_POINT('Ctrl Pts',(-193.000431473255,-1.34163537198624,
137.272285351261));
#231158=CARTESIAN_POINT('Ctrl Pts',(-193.278879097068,4.71646156978089,
135.429187759513));
#231159=CARTESIAN_POINT('Ctrl Pts',(-193.557326720881,6.44036074087642,
129.336099959682));
#231160=CARTESIAN_POINT('Ctrl Pts',(-193.835774344694,2.24588302022023,
124.592271975924));
#231161=CARTESIAN_POINT('Ctrl Pts',(-194.114221968506,-4.01245147853337,
125.557049976435));
#231162=CARTESIAN_POINT('Ctrl Pts',(-194.392669592319,-6.58353908766677,
131.343850110767));
#231163=CARTESIAN_POINT('Ctrl Pts',(-194.671117216133,-3.10467589899933,
136.634885756375));
#231164=CARTESIAN_POINT('Ctrl Pts',(-194.949564839945,3.22723276899961,
136.567953636405));
#231165=CARTESIAN_POINT('Ctrl Pts',(-195.228012463758,6.59347218137276,
131.204561099293));
#231166=CARTESIAN_POINT('Ctrl Pts',(-195.506460087571,3.90063276808784,
125.473403870355));
#231167=CARTESIAN_POINT('Ctrl Pts',(-195.784907711384,-2.3766976025655,
124.641135460387));
#231168=CARTESIAN_POINT('Ctrl Pts',(-196.063355335197,-6.46995898459376,
129.472569879579));
#231169=CARTESIAN_POINT('Ctrl Pts',(-196.34180295901,-4.61764413484867,
135.527854925386));
#231170=CARTESIAN_POINT('Ctrl Pts',(-196.620250582823,1.47806009036541,
137.242479457832));
#231171=CARTESIAN_POINT('Ctrl Pts',(-196.898698206635,6.21549929978325,
133.040787295662));
#231172=CARTESIAN_POINT('Ctrl Pts',(-197.177145830448,5.24119829672186,
126.783928271841));
#231173=CARTESIAN_POINT('Ctrl Pts',(-197.455593454261,-0.5495078942556,
124.2216501647));
#231174=CARTESIAN_POINT('Ctrl Pts',(-197.734041078074,-5.83524317536515,
127.708561380459));
#231175=CARTESIAN_POINT('Ctrl Pts',(-198.012488701887,-5.75867504579123,
134.040360856918));
#231176=CARTESIAN_POINT('Ctrl Pts',(-198.2909363257,-0.390165876051177,
137.398434200813));
#231177=CARTESIAN_POINT('Ctrl Pts',(-198.569383949513,5.33688667311775,
134.696876060105));
#231178=CARTESIAN_POINT('Ctrl Pts',(-198.847831573325,6.15960109109908,
128.418286387655));
#231179=CARTESIAN_POINT('Ctrl Pts',(-199.126279197139,1.32194301960288,
124.332382366286));
#231180=CARTESIAN_POINT('Ctrl Pts',(-199.404726820951,-4.73051610640191,
126.193910184127));
#231181=CARTESIAN_POINT('Ctrl Pts',(-199.683174444764,-6.43586202918244,
132.292216717274));
#231182=CARTESIAN_POINT('Ctrl Pts',(-199.961622068577,-2.22696515648391,
137.023256180599));
#231183=CARTESIAN_POINT('Ctrl Pts',(-200.24006969239,4.02840390172748,136.039434431435));
#231184=CARTESIAN_POINT('Ctrl Pts',(-200.518517316203,6.58186657272242,
130.244835594899));
#231185=CARTESIAN_POINT('Ctrl Pts',(-200.796964940016,3.08691540544346,
124.964412919876));
#231186=CARTESIAN_POINT('Ctrl Pts',(-201.075412563829,-3.24476021523692,
125.050616881724));
#231187=CARTESIAN_POINT('Ctrl Pts',(-201.353860187642,-6.59465971346335,
130.424230250803));
#231188=CARTESIAN_POINT('Ctrl Pts',(-201.632307811455,-3.88438910205457,
136.147164856536));
#231189=CARTESIAN_POINT('Ctrl Pts',(-201.910755435267,2.39544533118521,
136.960323377152));
#231190=CARTESIAN_POINT('Ctrl Pts',(-202.18920305908,6.47398252907625,132.116452857208));
#231191=CARTESIAN_POINT('Ctrl Pts',(-202.467650682893,4.60324605437475,
126.066833668302));
#231192=CARTESIAN_POINT('Ctrl Pts',(-202.746098306706,-1.49764866322506,
124.370770304711));
#231193=CARTESIAN_POINT('Ctrl Pts',(-203.024545930519,-6.22227742352606,
128.586862140274));
#231194=CARTESIAN_POINT('Ctrl Pts',(-203.302993554332,-5.22893720675747,
134.840726745644));
#231195=CARTESIAN_POINT('Ctrl Pts',(-203.581441178145,0.569540855237039,
137.385368066758));
#231196=CARTESIAN_POINT('Ctrl Pts',(-203.859888801958,5.84463869488665,
133.882385042152));
#231197=CARTESIAN_POINT('Ctrl Pts',(-204.138336425771,5.7487991004088,127.550847941203));
#231198=CARTESIAN_POINT('Ctrl Pts',(-204.416784049583,0.370093977104817,
124.209130046901));
#231199=CARTESIAN_POINT('Ctrl Pts',(-204.695231673396,-5.34870943106288,
126.928106852114));
#231200=CARTESIAN_POINT('Ctrl Pts',(-204.973679297209,-6.15231017106575,
133.209171502253));
#231201=CARTESIAN_POINT('Ctrl Pts',(-205.252126921022,-1.30223842092043,
137.280332430907));
#231202=CARTESIAN_POINT('Ctrl Pts',(-205.530574544835,4.74452682016742,
135.400391631911));
#231203=CARTESIAN_POINT('Ctrl Pts',(-205.809022168648,6.43130369654214,
129.296922859329));
#231204=CARTESIAN_POINT('Ctrl Pts',(-206.087469792461,2.20802666244648,
124.578715744137));
#231205=CARTESIAN_POINT('Ctrl Pts',(-206.365917416273,-4.04431900633787,
125.581572127967));
#231206=CARTESIAN_POINT('Ctrl Pts',(-206.644365040087,-6.58013308426553,
131.383915986335));
#231207=CARTESIAN_POINT('Ctrl Pts',(-206.922812663899,-3.06912631512495,
136.653676773657));
#231208=CARTESIAN_POINT('Ctrl Pts',(-207.201260287713,3.26225760245914,
136.548201768512));
#231209=CARTESIAN_POINT('Ctrl Pts',(-207.479707911525,6.59578615352751,
131.164417347887));
#231210=CARTESIAN_POINT('Ctrl Pts',(-207.758155535338,3.86810945157081,
125.449758381845));
#231211=CARTESIAN_POINT('Ctrl Pts',(-208.036603159151,-2.41417086872696,
124.655717283569));
#231212=CARTESIAN_POINT('Ctrl Pts',(-208.315050782964,-6.47794609946865,
129.511979031309));
#231213=CARTESIAN_POINT('Ctrl Pts',(-208.593498406777,-4.58880533005852,
135.555876320469));
#231214=CARTESIAN_POINT('Ctrl Pts',(-208.87194603059,1.51722336207232,137.233362803106));
#231215=CARTESIAN_POINT('Ctrl Pts',(-209.150393654402,6.22899790494034,
133.00291035145));
#231216=CARTESIAN_POINT('Ctrl Pts',(-209.428841278216,5.21662767663345,
126.752098099478));
#231217=CARTESIAN_POINT('Ctrl Pts',(-209.707288902028,-0.589568540070009,
124.225117137599));
#231218=CARTESIAN_POINT('Ctrl Pts',(-209.985736525842,-5.85398007047323,
127.744139519898));
#231219=CARTESIAN_POINT('Ctrl Pts',(-210.264184149654,-5.73886989893714,
134.07535559084));
#231220=CARTESIAN_POINT('Ctrl Pts',(-210.542631773467,-0.350018649658268,
137.400687078332));
#231221=CARTESIAN_POINT('Ctrl Pts',(-210.82107939728,5.36048263929459,134.664316796842));
#231222=CARTESIAN_POINT('Ctrl Pts',(-211.099527021093,6.14496225687153,
128.38083535594));
#231223=CARTESIAN_POINT('Ctrl Pts',(-211.377974644906,1.28252175847855,
124.324455234681));
#231224=CARTESIAN_POINT('Ctrl Pts',(-211.656422268719,-4.75849358128477,
126.222791599316));
#231225=CARTESIAN_POINT('Ctrl Pts',(-211.934869892531,-6.4266857851828,
132.331366069634));
#231226=CARTESIAN_POINT('Ctrl Pts',(-212.213317516344,-2.18906771355195,
137.036697127864));
#231227=CARTESIAN_POINT('Ctrl Pts',(-212.491765140157,4.06019664492976,
136.014815399695));
#231228=CARTESIAN_POINT('Ctrl Pts',(-212.770212763971,6.57833863835413,
130.204780271616));
#231229=CARTESIAN_POINT('Ctrl Pts',(-213.048660387783,3.05130879283982,
124.945730190337));
#231230=CARTESIAN_POINT('Ctrl Pts',(-213.327108011596,-3.27972476857289,
125.070475261673));
#231231=CARTESIAN_POINT('Ctrl Pts',(-213.605555635409,-6.59685149112928,
130.464380859201));
#231232=CARTESIAN_POINT('Ctrl Pts',(-213.884003259222,-3.85179396744981,
136.170711245733));
#231233=CARTESIAN_POINT('Ctrl Pts',(-214.162450883035,2.43287404171984,
136.94562756578));
#231234=CARTESIAN_POINT('Ctrl Pts',(-214.440898506847,6.48184965905313,
132.077019577989));
#231235=CARTESIAN_POINT('Ctrl Pts',(-214.71934613066,4.57432209567675,126.038900178414));
#231236=CARTESIAN_POINT('Ctrl Pts',(-214.997793754473,-1.53678400556905,
124.380006116735));
#231237=CARTESIAN_POINT('Ctrl Pts',(-215.276241378286,-6.23566068176903,
128.624779994154));
#231238=CARTESIAN_POINT('Ctrl Pts',(-215.554689002099,-5.20426982038336,
134.872481986055));
#231239=CARTESIAN_POINT('Ctrl Pts',(-215.833136625912,0.609590763220439,
137.381779179092));
#231240=CARTESIAN_POINT('Ctrl Pts',(-216.111584249725,5.86326721558844,
133.846750038845));
#231241=CARTESIAN_POINT('Ctrl Pts',(-216.390031873537,5.72888753335829,
127.51591364943));
#231242=CARTESIAN_POINT('Ctrl Pts',(-216.668479497351,0.329940079686948,
124.206999374164));
#231243=CARTESIAN_POINT('Ctrl Pts',(-216.946927121163,-5.37220618874772,
126.960737782571));
#231244=CARTESIAN_POINT('Ctrl Pts',(-217.225374744977,-6.13755741658593,
133.246577804923));
#231245=CARTESIAN_POINT('Ctrl Pts',(-217.503822368789,-1.26279321493052,
137.288139541036));
#231246=CARTESIAN_POINT('Ctrl Pts',(-217.782269992602,4.77241626036792,
135.37142519669));
#231247=CARTESIAN_POINT('Ctrl Pts',(-218.060717616415,6.4220083378839,129.257801617636));
#231248=CARTESIAN_POINT('Ctrl Pts',(-218.339165240228,2.17008848543354,
124.565390205911));
#231249=CARTESIAN_POINT('Ctrl Pts',(-218.617612864041,-4.07603667041411,
125.606287811847));
#231250=CARTESIAN_POINT('Ctrl Pts',(-218.896060487854,-6.57648325161253,
131.423960386264));
#231251=CARTESIAN_POINT('Ctrl Pts',(-219.174508111666,-3.03346300364714,
136.672251042379));
#231252=CARTESIAN_POINT('Ctrl Pts',(-219.45295573548,3.29716155176439,136.528237060474));
#231253=CARTESIAN_POINT('Ctrl Pts',(-219.731403359293,6.59785571640026,
131.124260254445));
#231254=CARTESIAN_POINT('Ctrl Pts',(-220.009850983105,3.83544280083539,
125.426311310091));
#231255=CARTESIAN_POINT('Ctrl Pts',(-220.288298606918,-2.45155467689987,
124.67052694699));
#231256=CARTESIAN_POINT('Ctrl Pts',(-220.566746230731,-6.48569317166813,
129.551436072715));
#231257=CARTESIAN_POINT('Ctrl Pts',(-220.845193854544,-4.55979648539947,
135.58372164639));
#231258=CARTESIAN_POINT('Ctrl Pts',(-221.123641478357,1.55633041250914,
137.224007919343));
#231259=CARTESIAN_POINT('Ctrl Pts',(-221.40208910217,6.24226569228925,132.964951939167));
#231260=CARTESIAN_POINT('Ctrl Pts',(-221.680536725983,5.19186375248807,
126.720418085194));
#231261=CARTESIAN_POINT('Ctrl Pts',(-221.958984349796,-0.629607339204784,
124.228827906785));
#231262=CARTESIAN_POINT('Ctrl Pts',(-222.237431973609,-5.87250004419688,
127.779831056953));
#231263=CARTESIAN_POINT('Ctrl Pts',(-222.515879597421,-5.71885209614835,
134.110229116839));
#231264=CARTESIAN_POINT('Ctrl Pts',(-222.794327221234,-0.309858453196267,
137.402695526548));
#231265=CARTESIAN_POINT('Ctrl Pts',(-223.072774845047,5.38387997081673,
134.631614501482));
#231266=CARTESIAN_POINT('Ctrl Pts',(-223.35122246886,6.13009571880702,128.343474128844));
#231267=CARTESIAN_POINT('Ctrl Pts',(-223.629670092673,1.24305297303857,
124.316768218352));
#231268=CARTESIAN_POINT('Ctrl Pts',(-223.908117716486,-4.78629472843886,
126.25184278623));
#231269=CARTESIAN_POINT('Ctrl Pts',(-224.186565340298,-6.41727139797729,
132.370458838244));
#231270=CARTESIAN_POINT('Ctrl Pts',(-224.465012964112,-2.15108915391133,
137.049907133607));
#231271=CARTESIAN_POINT('Ctrl Pts',(-224.743460587925,4.09183893605206,
135.990003292637));
#231272=CARTESIAN_POINT('Ctrl Pts',(-225.021908211737,6.57456694122844,
130.164747166004));
#231273=CARTESIAN_POINT('Ctrl Pts',(-225.300355835551,3.01558911286705,
124.927264554503));
#231274=CARTESIAN_POINT('Ctrl Pts',(-225.578803459363,-3.31456779050113,
125.090546112851));
#231275=CARTESIAN_POINT('Ctrl Pts',(-225.857251083176,-6.5987988200372,
130.504544065675));
#231276=CARTESIAN_POINT('Ctrl Pts',(-226.135698706989,-3.8190561032033,
136.194058782834));
#231277=CARTESIAN_POINT('Ctrl Pts',(-226.414146330802,2.47021260121173,
136.930704187504));
#231278=CARTESIAN_POINT('Ctrl Pts',(-226.692593954615,6.48947660170784,
132.037539139922));
#231279=CARTESIAN_POINT('Ctrl Pts',(-226.971041578427,4.54522863379049,
126.011143274415));
#231280=CARTESIAN_POINT('Ctrl Pts',(-227.24948920224,-1.57586240181677,
124.389479985577));
#231281=CARTESIAN_POINT('Ctrl Pts',(-227.527936826054,-6.24881287531301,
128.662778613197));
#231282=CARTESIAN_POINT('Ctrl Pts',(-227.806384449866,-5.17940958787633,
134.904086480733));
#231283=CARTESIAN_POINT('Ctrl Pts',(-228.084832073679,0.649618082593193,
137.377946562762));
#231284=CARTESIAN_POINT('Ctrl Pts',(-228.363279697492,5.88167847076755,
133.811002298682));
#231285=CARTESIAN_POINT('Ctrl Pts',(-228.641727321305,5.70876368027354,
127.481101212267));
#231286=CARTESIAN_POINT('Ctrl Pts',(-228.920174945118,0.289773956218704,
124.205113169075));
#231287=CARTESIAN_POINT('Ctrl Pts',(-229.198622568931,-5.39550387735667,
126.993511139885));
#231288=CARTESIAN_POINT('Ctrl Pts',(-229.477070192744,-6.12257723265909,
133.283893610337));
#231289=CARTESIAN_POINT('Ctrl Pts',(-229.755517816557,-1.22330121567356,
137.295706392352));
#231290=CARTESIAN_POINT('Ctrl Pts',(-230.033965440369,4.80012885692891,
135.34228952721));
#231291=CARTESIAN_POINT('Ctrl Pts',(-230.312413064183,6.41247500934538,
129.218737684256));
#231292=CARTESIAN_POINT('Ctrl Pts',(-230.590860687995,2.13206989499296,
124.552295855027));
#231293=CARTESIAN_POINT('Ctrl Pts',(-230.869308311808,-4.10760329545278,
125.631196112227));
#231294=CARTESIAN_POINT('Ctrl Pts',(-231.147755935621,-6.5725897249546,
131.463981826697));
#231295=CARTESIAN_POINT('Ctrl Pts',(-231.426203559434,-2.99768728608136,
136.690607874263));
#231296=CARTESIAN_POINT('Ctrl Pts',(-231.704651183247,3.33194332353496,
136.508060252089));
#231297=CARTESIAN_POINT('Ctrl Pts',(-231.98309880706,6.59968079330357,131.084091307006));
#231298=CARTESIAN_POINT('Ctrl Pts',(-232.261546430872,3.80263402635669,
125.403063523931));
#231299=CARTESIAN_POINT('Ctrl Pts',(-232.539994054686,-2.48884764181187,
124.685563901874));
#231300=CARTESIAN_POINT('Ctrl Pts',(-232.818441678498,-6.49319991412244,
129.5909395417));
#231301=CARTESIAN_POINT('Ctrl Pts',(-233.096889302311,-4.53061867580467,
135.611389871331));
#231302=CARTESIAN_POINT('Ctrl Pts',(-233.375336926124,1.59537979255065,
137.214415153187));
#231303=CARTESIAN_POINT('Ctrl Pts',(-233.653784549937,6.25530217018742,
132.926913465378));
#231304=CARTESIAN_POINT('Ctrl Pts',(-233.93223217375,5.16690744192206,126.688889402902));
#231305=CARTESIAN_POINT('Ctrl Pts',(-234.210679797563,-0.669622808008655,
124.232782334755));
#231306=CARTESIAN_POINT('Ctrl Pts',(-234.489127421376,-5.89080241027189,
127.815634669064));
#231307=CARTESIAN_POINT('Ctrl Pts',(-234.767575045188,-5.69862237919218,
134.144980142666));
#231308=CARTESIAN_POINT('Ctrl Pts',(-235.046022669002,-0.269686774814632,
137.404459471037));
#231309=CARTESIAN_POINT('Ctrl Pts',(-235.324470292814,5.40707780068583,
134.598770385822));
#231310=CARTESIAN_POINT('Ctrl Pts',(-235.602917916627,6.11500202779203,
128.306204090801));
#231311=CARTESIAN_POINT('Ctrl Pts',(-235.88136554044,1.20353812581378,124.309321602146));
#231312=CARTESIAN_POINT('Ctrl Pts',(-236.159813164253,-4.81391851768082,
126.281062668365));
#231313=CARTESIAN_POINT('Ctrl Pts',(-236.438260788066,-6.40761921642086,
132.40949357451));
#231314=CARTESIAN_POINT('Ctrl Pts',(-236.716708411879,-2.11303088487057,
137.062885708328));
#231315=CARTESIAN_POINT('Ctrl Pts',(-236.995156035692,4.12332960257798,
135.964999029683));
#231316=CARTESIAN_POINT('Ctrl Pts',(-237.273603659505,6.57055162110693,
130.124737761504));
#231317=CARTESIAN_POINT('Ctrl Pts',(-237.552051283318,2.97975768913041,
124.909016696624));
#231318=CARTESIAN_POINT('Ctrl Pts',(-237.83049890713,-3.34928798990126,
125.110828691528));
#231319=CARTESIAN_POINT('Ctrl Pts',(-238.108946530943,-6.60050162802816,
130.544718381962));
#231320=CARTESIAN_POINT('Ctrl Pts',(-238.387394154756,-3.7861767224282,
136.217206602688));
#231321=CARTESIAN_POINT('Ctrl Pts',(-238.665841778569,2.5074596260677,136.915553795314));
#231322=CARTESIAN_POINT('Ctrl Pts',(-238.944289402382,6.49686307441993,
131.998013005973));
#231323=CARTESIAN_POINT('Ctrl Pts',(-239.222737026195,4.51596674678651,
125.983563984846));
#231324=CARTESIAN_POINT('Ctrl Pts',(-239.501184650008,-1.61488240390346,
124.399191560181));
#231325=CARTESIAN_POINT('Ctrl Pts',(-239.77963227382,-6.26173351679718,
128.700856589348));
#231326=CARTESIAN_POINT('Ctrl Pts',(-240.058079897633,-5.15435743044315,
134.935539058562));
#231327=CARTESIAN_POINT('Ctrl Pts',(-240.336527521446,0.689621330129741,
137.373870359787));
#231328=CARTESIAN_POINT('Ctrl Pts',(-240.614975145259,5.89987177818775,
133.775143146303));
#231329=CARTESIAN_POINT('Ctrl Pts',(-240.893422769072,5.68842828685113,
127.446411919705));
#231330=CARTESIAN_POINT('Ctrl Pts',(-241.171870392886,0.249597095069331,
124.203471501526));
#231331=CARTESIAN_POINT('Ctrl Pts',(-241.450318016698,-5.41860163358522,
127.026425709627));
#231332=CARTESIAN_POINT('Ctrl Pts',(-241.728765640511,-6.10737017438111,
133.321117535742));
#231333=CARTESIAN_POINT('Ctrl Pts',(-242.007213264324,-1.18376388654087,
137.303032704464));
#231334=CARTESIAN_POINT('Ctrl Pts',(-242.285660888137,4.82766358294966,
135.312985703106));
#231335=CARTESIAN_POINT('Ctrl Pts',(-242.56410851195,6.40270406418687,129.179732506718));
#231336=CARTESIAN_POINT('Ctrl Pts',(-242.842556135762,2.09397229991911,
124.539433176702));
#231337=CARTESIAN_POINT('Ctrl Pts',(-243.121003759575,-4.13901771174057,
125.65629610612));
#231338=CARTESIAN_POINT('Ctrl Pts',(-243.399451383388,-6.56845264856689,
131.503978824623));
#231339=CARTESIAN_POINT('Ctrl Pts',(-243.677899007202,-2.9618004881116,
136.70874658909));
#231340=CARTESIAN_POINT('Ctrl Pts',(-243.956346631013,3.36660162892119,
136.487672091016));
#231341=CARTESIAN_POINT('Ctrl Pts',(-244.234794254827,6.60126131660758,
131.043911994042));
#231342=CARTESIAN_POINT('Ctrl Pts',(-244.513241878639,3.76968434387551,
125.380015884821));
#231343=CARTESIAN_POINT('Ctrl Pts',(-244.791689502453,-2.52604838156001,
124.70082759102));
#231344=CARTESIAN_POINT('Ctrl Pts',(-245.070137126265,-6.50046604866569,
129.630487974449));
#231345=CARTESIAN_POINT('Ctrl Pts',(-245.348584750079,-4.50127298246883,
135.638879970036));
#231346=CARTESIAN_POINT('Ctrl Pts',(-245.627032373891,1.63437005520677,
137.204584860103));
#231347=CARTESIAN_POINT('Ctrl Pts',(-245.905479997704,6.26810685556324,
132.888796339615));
#231348=CARTESIAN_POINT('Ctrl Pts',(-246.183927621517,5.14175966970064,
126.65751322091));
#231349=CARTESIAN_POINT('Ctrl Pts',(-246.46237524533,-0.709613463692526,
124.236980274974));
#231350=CARTESIAN_POINT('Ctrl Pts',(-246.740822869143,-5.90888649049716,
127.851549029514));
#231351=CARTESIAN_POINT('Ctrl Pts',(-247.019270492956,-5.67818149768794,
134.179607380607));
#231352=CARTESIAN_POINT('Ctrl Pts',(-247.297718116769,-0.229505103091092,
137.405978846438));
#231353=CARTESIAN_POINT('Ctrl Pts',(-247.576165740581,5.43007526929941,
134.565785666913));
#231354=CARTESIAN_POINT('Ctrl Pts',(-247.854613364394,6.09968174312738,
128.269026622868));
#231355=CARTESIAN_POINT('Ctrl Pts',(-248.133060988207,1.16397868104094,
124.302115661998));
#231356=CARTESIAN_POINT('Ctrl Pts',(-248.41150861202,-4.84136392540264,
126.31045016297));
#231357=CARTESIAN_POINT('Ctrl Pts',(-248.689956235833,-6.39772959817725,
132.448468831983));
#231358=CARTESIAN_POINT('Ctrl Pts',(-248.968403859646,-2.07489431669385,
137.075632371099));
#231359=CARTESIAN_POINT('Ctrl Pts',(-249.246851483459,4.15466747760909,
135.939803537374));
#231360=CARTESIAN_POINT('Ctrl Pts',(-249.525299107272,6.56629282677857,
130.08475354068));
#231361=CARTESIAN_POINT('Ctrl Pts',(-249.803746731085,2.94381584937754,
124.890987292882));
#231362=CARTESIAN_POINT('Ctrl Pts',(-250.082194354898,-3.38388408020374,
125.131322246124));
#231363=CARTESIAN_POINT('Ctrl Pts',(-250.36064197871,-6.60195985200274,
130.584902319384));
#231364=CARTESIAN_POINT('Ctrl Pts',(-250.639089602524,-3.75315704348482,
136.240153847548));
#231365=CARTESIAN_POINT('Ctrl Pts',(-250.917537226336,2.54461373609029,
136.900176950603));
#231366=CARTESIAN_POINT('Ctrl Pts',(-251.19598485015,6.50400880347224,131.958442640812));
#231367=CARTESIAN_POINT('Ctrl Pts',(-251.474432473962,4.48653751899202,
125.956163331638));
#231368=CARTESIAN_POINT('Ctrl Pts',(-251.752880097775,-1.65384256596459,
124.409140480742));
#231369=CARTESIAN_POINT('Ctrl Pts',(-252.031327721588,-6.27442212737671,
128.739012511497));
#231370=CARTESIAN_POINT('Ctrl Pts',(-252.309775345401,-5.12911427652582,
134.966838554275));
#231371=CARTESIAN_POINT('Ctrl Pts',(-252.588222969213,0.729599023732927,
137.369550720794));
#231372=CARTESIAN_POINT('Ctrl Pts',(-252.866670593027,5.91784646323776,
133.739173911277));
#231373=CARTESIAN_POINT('Ctrl Pts',(-253.145118216839,5.66788210748017,
127.411847055674));
#231374=CARTESIAN_POINT('Ctrl Pts',(-253.423565840652,0.209410983396998,
124.20207443517));
#231375=CARTESIAN_POINT('Ctrl Pts',(-253.702013464465,-5.44149859849489,
127.059480266814));
#231376=CARTESIAN_POINT('Ctrl Pts',(-253.980461088278,-6.0919368110008,
133.358248211846));
#231377=CARTESIAN_POINT('Ctrl Pts',(-254.258908712091,-1.1441826817532,
137.310118186916));
#231378=CARTESIAN_POINT('Ctrl Pts',(-254.537356335904,4.85501939763767,
135.283514846073));
#231379=CARTESIAN_POINT('Ctrl Pts',(-254.815803959717,6.39269590315201,
129.140787462715));
#231380=CARTESIAN_POINT('Ctrl Pts',(-255.09425158353,2.05579703890082,124.526802775315));
#231381=CARTESIAN_POINT('Ctrl Pts',(-255.372699207342,-4.17027861730954,
125.681586622223));
#231382=CARTESIAN_POINT('Ctrl Pts',(-255.651146831155,-6.5640724361261,
131.5439503534));
#231383=CARTESIAN_POINT('Ctrl Pts',(-255.929594454968,-2.925803447894,136.726665654721));
#231384=CARTESIAN_POINT('Ctrl Pts',(-256.208042078781,3.40113425532747,
136.467074956607));
#231385=CARTESIAN_POINT('Ctrl Pts',(-256.486489702594,6.60259898059897,
131.003720738236));
#231386=CARTESIAN_POINT('Ctrl Pts',(-256.764937326407,3.73659166461274,
125.357175036369));
#231387=CARTESIAN_POINT('Ctrl Pts',(-257.04338495022,-2.56314926818932,
124.716306516944));
#231388=CARTESIAN_POINT('Ctrl Pts',(-257.321832574033,-6.5075031063131,
129.670100547101));
#231389=CARTESIAN_POINT('Ctrl Pts',(-257.600280197845,-4.47173821150659,
135.666151948257));
#231390=CARTESIAN_POINT('Ctrl Pts',(-257.878727821659,1.67325768403046,
137.194590998305));
#231391=CARTESIAN_POINT('Ctrl Pts',(-258.157175445471,6.28075871394982,
132.850463013089));
#231392=CARTESIAN_POINT('Ctrl Pts',(-258.435623069284,5.1162713672671,126.626553096149));
#231393=CARTESIAN_POINT('Ctrl Pts',(-258.714070693097,-0.749294580734974,
124.240926059104));
#231394=CARTESIAN_POINT('Ctrl Pts',(-258.99251831691,-5.92728653745133,
127.888508918958));
#231395=CARTESIAN_POINT('Ctrl Pts',(-259.270965940723,-5.656519339957,134.212338033208));
#231396=CARTESIAN_POINT('Ctrl Pts',(-259.549413564536,-0.191230405826049,
137.41063083554));
#231397=CARTESIAN_POINT('Ctrl Pts',(-259.827861188349,5.45654320709978,
134.526020746857));
#231398=CARTESIAN_POINT('Ctrl Pts',(-260.059900874859,5.97341346954355,
129.293215926205));
#231399=CARTESIAN_POINT('Ctrl Pts',(-260.245542550368,3.60742224527213,
126.247226657536));
#231400=CARTESIAN_POINT('Ctrl Pts',(-260.338368351272,1.86717727106152,
125.459413119698));
#231401=CARTESIAN_POINT('Ctrl Pts',(-260.384786214875,0.950008195528324,
125.301089073499));
#231402=CARTESIAN_POINT('Ctrl Pts',(209.997886486728,-2.58542267678463,
125.478296443779));
#231403=CARTESIAN_POINT('Ctrl Pts',(209.951476810375,-3.47289965896197,
125.909102290886));
#231404=CARTESIAN_POINT('Ctrl Pts',(209.85865919672,-5.01373755653622,127.222906143875));
#231405=CARTESIAN_POINT('Ctrl Pts',(209.67302570846,-6.52844908712303,131.020616473957));
#231406=CARTESIAN_POINT('Ctrl Pts',(209.440986021949,-4.4641631800594,136.198709217918));
#231407=CARTESIAN_POINT('Ctrl Pts',(209.162538398136,2.13623200523086,137.47712630299));
#231408=CARTESIAN_POINT('Ctrl Pts',(208.884090774324,6.76311047611758,132.61329501932));
#231409=CARTESIAN_POINT('Ctrl Pts',(208.60564315051,5.180460236421,126.09244423763));
#231410=CARTESIAN_POINT('Ctrl Pts',(208.327195526698,-1.16565068102074,
123.898824768668));
#231411=CARTESIAN_POINT('Ctrl Pts',(208.048747902884,-6.43906639651766,
128.052530506575));
#231412=CARTESIAN_POINT('Ctrl Pts',(207.770300279072,-5.79609906993421,
134.734252735451));
#231413=CARTESIAN_POINT('Ctrl Pts',(207.491852655259,0.173626147510206,
137.805009652024));
#231414=CARTESIAN_POINT('Ctrl Pts',(207.213405031446,5.98357180802623,134.442293088818));
#231415=CARTESIAN_POINT('Ctrl Pts',(206.934957407633,6.29502677410122,127.736610299611));
#231416=CARTESIAN_POINT('Ctrl Pts',(206.65650978382,0.821596385081328,123.849978754804));
#231417=CARTESIAN_POINT('Ctrl Pts',(206.378062160007,-5.40680743188727,
126.354116934927));
#231418=CARTESIAN_POINT('Ctrl Pts',(206.099614536195,-6.66663710465116,
132.947794423038));
#231419=CARTESIAN_POINT('Ctrl Pts',(205.821166912381,-1.80014356190772,
137.571770081489));
#231420=CARTESIAN_POINT('Ctrl Pts',(205.542719288569,4.72058899422897,135.976822216287));
#231421=CARTESIAN_POINT('Ctrl Pts',(205.264271664756,6.90333351468265,129.628637390042));
#231422=CARTESIAN_POINT('Ctrl Pts',(204.985824040943,2.74225038547515,124.360883417158));
#231423=CARTESIAN_POINT('Ctrl Pts',(204.70737641713,-3.93882614214087,125.014370927945));
#231424=CARTESIAN_POINT('Ctrl Pts',(204.428928793317,-7.00031425910704,
130.988575726592));
#231425=CARTESIAN_POINT('Ctrl Pts',(204.150481169504,-3.62885534891233,
136.793496040797));
#231426=CARTESIAN_POINT('Ctrl Pts',(203.872033545692,3.07734423765085,137.09469337995));
#231427=CARTESIAN_POINT('Ctrl Pts',(203.593585921878,6.95561486460971,131.615382266785));
#231428=CARTESIAN_POINT('Ctrl Pts',(203.315138298066,4.44201520086038,125.390781848689));
#231429=CARTESIAN_POINT('Ctrl Pts',(203.036690674253,-2.15357941165663,
124.140995867004));
#231430=CARTESIAN_POINT('Ctrl Pts',(202.75824305044,-6.77013976170558,129.014516559232));
#231431=CARTESIAN_POINT('Ctrl Pts',(202.479795426627,-5.16527240588502,
135.532816506767));
#231432=CARTESIAN_POINT('Ctrl Pts',(202.201347802814,1.18622795093483,137.705896487686));
#231433=CARTESIAN_POINT('Ctrl Pts',(201.922900179001,6.44764277258624,133.536802163981));
#231434=CARTESIAN_POINT('Ctrl Pts',(201.644452555188,5.78398887041165,126.856727545651));
#231435=CARTESIAN_POINT('Ctrl Pts',(201.366004931376,-0.194868239746226,
123.804334868162));
#231436=CARTESIAN_POINT('Ctrl Pts',(201.087557307562,-5.99465095761073,
127.184623883922));
#231437=CARTESIAN_POINT('Ctrl Pts',(200.80910968375,-6.2856423003101,133.891274124028));
#231438=CARTESIAN_POINT('Ctrl Pts',(200.530662059936,-0.80043543977546,
137.76120165575));
#231439=CARTESIAN_POINT('Ctrl Pts',(200.252214436124,5.42033248649604,135.238132133988));
#231440=CARTESIAN_POINT('Ctrl Pts',(199.973766812311,6.66007965562565,128.640643190398));
#231441=CARTESIAN_POINT('Ctrl Pts',(199.695319188498,1.77953898422249,124.031504858911));
#231442=CARTESIAN_POINT('Ctrl Pts',(199.416871564685,-4.73631107837294,
125.646290097223));
#231443=CARTESIAN_POINT('Ctrl Pts',(199.138423940872,-6.89972264160091,
132.00109015798));
#231444=CARTESIAN_POINT('Ctrl Pts',(198.859976317059,-2.72262616738874,
137.256154234582));
#231445=CARTESIAN_POINT('Ctrl Pts',(198.581528693247,3.95643074697165,136.582335164788));
#231446=CARTESIAN_POINT('Ctrl Pts',(198.303081069434,6.999721087252,130.598839755845));
#231447=CARTESIAN_POINT('Ctrl Pts',(198.024633445621,3.61060970373355,124.804207978572));
#231448=CARTESIAN_POINT('Ctrl Pts',(197.746185821808,-3.09647560942607,
124.523423352781));
#231449=CARTESIAN_POINT('Ctrl Pts',(197.467738197995,-6.9580511087663,130.014513232485));
#231450=CARTESIAN_POINT('Ctrl Pts',(197.189290574182,-4.4255175588443,136.231434272887));
#231451=CARTESIAN_POINT('Ctrl Pts',(196.910842950369,2.17385042910367,137.461139751337));
#231452=CARTESIAN_POINT('Ctrl Pts',(196.632395326556,6.77555607120273,132.573590407591));
#231453=CARTESIAN_POINT('Ctrl Pts',(196.353947702743,5.15085668818228,126.060205318492));
#231454=CARTESIAN_POINT('Ctrl Pts',(196.07550007893,-1.20722835793932,123.90646718437));
#231455=CARTESIAN_POINT('Ctrl Pts',(195.797052455118,-6.45592951949867,
128.091556134528));
#231456=CARTESIAN_POINT('Ctrl Pts',(195.518604831305,-5.77194684232935,
134.769579876729));
#231457=CARTESIAN_POINT('Ctrl Pts',(195.240157207492,0.216173007661386,
137.80376083149));
#231458=CARTESIAN_POINT('Ctrl Pts',(194.961709583679,6.00564042424985,134.405834929363));
#231459=CARTESIAN_POINT('Ctrl Pts',(194.683261959866,6.2762176827981,127.698330076496));
#231460=CARTESIAN_POINT('Ctrl Pts',(194.404814336053,0.779257501134259,
123.845115552844));
#231461=CARTESIAN_POINT('Ctrl Pts',(194.12636671224,-5.43380225522669,126.387107265649));
#231462=CARTESIAN_POINT('Ctrl Pts',(193.847919088427,-6.65346319503207,
132.988339014042));
#231463=CARTESIAN_POINT('Ctrl Pts',(193.569471464615,-1.75891649835014,
137.58260130935));
#231464=CARTESIAN_POINT('Ctrl Pts',(193.291023840801,4.75198853246758,135.947991544374));
#231465=CARTESIAN_POINT('Ctrl Pts',(193.012576216989,6.89604824949333,129.586636238002));
#231466=CARTESIAN_POINT('Ctrl Pts',(192.734128593176,2.70297651592057,124.344310147306));
#231467=CARTESIAN_POINT('Ctrl Pts',(192.455680969363,-3.97399858803937,
125.038454847768));
#231468=CARTESIAN_POINT('Ctrl Pts',(192.17723334555,-6.99906313021511,131.031185270517));
#231469=CARTESIAN_POINT('Ctrl Pts',(191.898785721737,-3.59233057896577,
136.815474918205));
#231470=CARTESIAN_POINT('Ctrl Pts',(191.620338097924,3.11557827924791,137.075844182864));
#231471=CARTESIAN_POINT('Ctrl Pts',(191.341890474111,6.96042290329331,131.573026430018));
#231472=CARTESIAN_POINT('Ctrl Pts',(191.063442850298,4.40897891477476,125.363842346942));
#231473=CARTESIAN_POINT('Ctrl Pts',(190.784995226486,-2.19410130582752,
124.154228770475));
#231474=CARTESIAN_POINT('Ctrl Pts',(190.506547602672,-6.78090961418206,
129.055761484483));
#231475=CARTESIAN_POINT('Ctrl Pts',(190.22809997886,-5.13639325295408,135.564171377977));
#231476=CARTESIAN_POINT('Ctrl Pts',(189.949652355047,1.22821758097839,137.698547712335));
#231477=CARTESIAN_POINT('Ctrl Pts',(189.671204731234,6.46415645975623,133.497502906364));
#231478=CARTESIAN_POINT('Ctrl Pts',(189.392757107421,5.75985134361714,126.821591904301));
#231479=CARTESIAN_POINT('Ctrl Pts',(189.114309483608,-0.237475772924818,
123.80565078066));
#231480=CARTESIAN_POINT('Ctrl Pts',(188.835861859795,-6.01657425548534,
127.221182091151));
#231481=CARTESIAN_POINT('Ctrl Pts',(188.557414235982,-6.2667349232476,133.929479419415));
#231482=CARTESIAN_POINT('Ctrl Pts',(188.278966612169,-0.758072343566082,
137.76594523932));
#231483=CARTESIAN_POINT('Ctrl Pts',(188.000518988357,5.44722168595988,135.205054884148));
#231484=CARTESIAN_POINT('Ctrl Pts',(187.722071364544,6.64678509766207,128.600141483854));
#231485=CARTESIAN_POINT('Ctrl Pts',(187.443623740731,1.73827771811677,124.02079778535));
#231486=CARTESIAN_POINT('Ctrl Pts',(187.165176116918,-4.76762196479028,
125.675216934184));
#231487=CARTESIAN_POINT('Ctrl Pts',(186.886728493105,-6.89230997333645,
132.043068555446));
#231488=CARTESIAN_POINT('Ctrl Pts',(186.608280869292,-2.68330182444739,
137.272608096043));
#231489=CARTESIAN_POINT('Ctrl Pts',(186.329833245479,3.99152961452714,136.558144195375));
#231490=CARTESIAN_POINT('Ctrl Pts',(186.051385621667,6.99834033481346,130.556234274655));
#231491=CARTESIAN_POINT('Ctrl Pts',(185.772937997853,3.5740181753383,124.782340341422));
#231492=CARTESIAN_POINT('Ctrl Pts',(185.494490374041,-3.13465208677821,
124.542388849921));
#231493=CARTESIAN_POINT('Ctrl Pts',(185.216042750227,-6.96273021741339,
130.056883498557));
#231494=CARTESIAN_POINT('Ctrl Pts',(184.937595126415,-4.39239942652681,
136.258273103275));
#231495=CARTESIAN_POINT('Ctrl Pts',(184.659147502602,2.21433185669671,137.447783572063));
#231496=CARTESIAN_POINT('Ctrl Pts',(184.380699878789,6.78620033974098,132.532312894923));
#231497=CARTESIAN_POINT('Ctrl Pts',(184.102252254976,5.12188223488049,126.028938490053));
#231498=CARTESIAN_POINT('Ctrl Pts',(183.823804631163,-1.24919542597752,
123.913943728027));
#231499=CARTESIAN_POINT('Ctrl Pts',(183.54535700735,-6.47232351695142,128.130905471908));
#231500=CARTESIAN_POINT('Ctrl Pts',(183.266909383538,-5.74770248642891,
134.804641889104));
#231501=CARTESIAN_POINT('Ctrl Pts',(182.988461759724,0.258776338245136,
137.80231524236));
#231502=CARTESIAN_POINT('Ctrl Pts',(182.710014135912,6.02745234999885,134.369210164519));
#231503=CARTESIAN_POINT('Ctrl Pts',(182.431566512099,6.25719410952084,127.66018250561));
#231504=CARTESIAN_POINT('Ctrl Pts',(182.153118888286,0.73688016331929,123.840500929948));
#231505=CARTESIAN_POINT('Ctrl Pts',(181.874671264473,-5.46059065437546,
126.420266203747));
#231506=CARTESIAN_POINT('Ctrl Pts',(181.59622364066,-6.64004542538295,133.028800068927));
#231507=CARTESIAN_POINT('Ctrl Pts',(181.317776016847,-1.71762283471616,
137.593182748215));
#231508=CARTESIAN_POINT('Ctrl Pts',(181.039328393035,4.78321123051439,135.918969541833));
#231509=CARTESIAN_POINT('Ctrl Pts',(180.760880769221,6.88850784776155,129.544680596588));
#231510=CARTESIAN_POINT('Ctrl Pts',(180.482433145409,2.66360227523266,124.32797605183));
#231511=CARTESIAN_POINT('Ctrl Pts',(180.203985521595,-4.00902366402984,
125.062752534008));
#231512=CARTESIAN_POINT('Ctrl Pts',(179.925537897783,-6.99755270774298,
131.073786351827));
#231513=CARTESIAN_POINT('Ctrl Pts',(179.64709027397,-3.5556726624947,136.837231082039));
#231514=CARTESIAN_POINT('Ctrl Pts',(179.368642650157,3.15369685531979,137.056762577506));
#231515=CARTESIAN_POINT('Ctrl Pts',(179.090195026344,6.96497302975191,131.530642118605));
#231516=CARTESIAN_POINT('Ctrl Pts',(178.811747402531,4.37577924769062,125.337104441072));
#231517=CARTESIAN_POINT('Ctrl Pts',(178.533299778718,-2.23454189429802,
124.167708099424));
#231518=CARTESIAN_POINT('Ctrl Pts',(178.254852154906,-6.79142819886702,
129.097071203448));
#231519=CARTESIAN_POINT('Ctrl Pts',(177.976404531092,-5.10732376838957,
135.595349873321));
#231520=CARTESIAN_POINT('Ctrl Pts',(177.69795690728,1.27016169860089,137.690943469992));
#231521=CARTESIAN_POINT('Ctrl Pts',(177.419509283467,6.48043061542571,133.458103853558));
#231522=CARTESIAN_POINT('Ctrl Pts',(177.141061659654,5.73550038331004,126.786603845811));
#231523=CARTESIAN_POINT('Ctrl Pts',(176.862614035841,-0.280074506296806,
123.807226032976));
#231524=CARTESIAN_POINT('Ctrl Pts',(176.584166412028,-6.0382746070172,127.257873074351));
#231525=CARTESIAN_POINT('Ctrl Pts',(176.305718788215,-6.24759533000263,
133.967568912391));
#231526=CARTESIAN_POINT('Ctrl Pts',(176.027271164402,-0.71568115671533,
137.770430858802));
#231527=CARTESIAN_POINT('Ctrl Pts',(175.748823540589,5.4739090366252,135.171814564968));
#231528=CARTESIAN_POINT('Ctrl Pts',(175.470375916777,6.63324424063007,128.559721455457));
#231529=CARTESIAN_POINT('Ctrl Pts',(175.191928292964,1.69695203949225,124.010342079205));
#231530=CARTESIAN_POINT('Ctrl Pts',(174.913480669151,-4.79875618522306,
125.704333833448));
#231531=CARTESIAN_POINT('Ctrl Pts',(174.635033045338,-6.88464190799096,
132.085001052137));
#231532=CARTESIAN_POINT('Ctrl Pts',(174.356585421525,-2.64387805077028,
137.288822274217));
#231533=CARTESIAN_POINT('Ctrl Pts',(174.078137797712,4.02648057448505,136.533740017397));
#231534=CARTESIAN_POINT('Ctrl Pts',(173.799690173899,6.99670025630013,130.513637987877));
#231535=CARTESIAN_POINT('Ctrl Pts',(173.521242550086,3.53729421038521,124.76069585245));
#231536=CARTESIAN_POINT('Ctrl Pts',(173.242794926273,-3.17271240844464,
124.561586386726));
#231537=CARTESIAN_POINT('Ctrl Pts',(172.96434730246,-6.96715131953175,130.099281462668));
#231538=CARTESIAN_POINT('Ctrl Pts',(172.685899678648,-4.35911853223319,
136.284909836929));
#231539=CARTESIAN_POINT('Ctrl Pts',(172.407452054835,2.25473123140845,137.434181218309));
#231540=CARTESIAN_POINT('Ctrl Pts',(172.129004431022,6.79659314313001,132.490971352347));
#231541=CARTESIAN_POINT('Ctrl Pts',(171.850556807209,5.09271798834896,125.997848616637));
#231542=CARTESIAN_POINT('Ctrl Pts',(171.572109183396,-1.29111620461978,
123.921675598615));
#231543=CARTESIAN_POINT('Ctrl Pts',(171.293661559583,-6.48847768007612,
128.170353875152));
#231544=CARTESIAN_POINT('Ctrl Pts',(171.01521393577,-5.72324514729908,134.839555669585));
#231545=CARTESIAN_POINT('Ctrl Pts',(170.736766311957,0.301370079776633,
137.800610341449));
#231546=CARTESIAN_POINT('Ctrl Pts',(170.458318688145,6.04904092628448,134.332453302864));
#231547=CARTESIAN_POINT('Ctrl Pts',(170.179871064331,6.23793867361471,127.6221514434));
#231548=CARTESIAN_POINT('Ctrl Pts',(169.901423440519,0.694475520138818,
123.836144355433));
#231549=CARTESIAN_POINT('Ctrl Pts',(169.622975816706,-5.4871767093294,126.453587596077));
#231550=CARTESIAN_POINT('Ctrl Pts',(169.344528192893,-6.62638160640872,
133.06917869639));
#231551=CARTESIAN_POINT('Ctrl Pts',(169.06608056908,-1.67626552393645,137.603512624779));
#231552=CARTESIAN_POINT('Ctrl Pts',(168.787632945267,4.81425668490999,135.88975801558));
#231553=CARTESIAN_POINT('Ctrl Pts',(168.509185321454,6.88071218983824,129.50277163308));
#231554=CARTESIAN_POINT('Ctrl Pts',(168.230737697641,2.62412933378287,124.311881941165));
#231555=CARTESIAN_POINT('Ctrl Pts',(167.952290073828,-4.0439001841742,125.087262977647));
#231556=CARTESIAN_POINT('Ctrl Pts',(167.673842450016,-6.99578298838191,
131.116377449467));
#231557=CARTESIAN_POINT('Ctrl Pts',(167.395394826203,-3.51888298926545,
136.858763695638));
#231558=CARTESIAN_POINT('Ctrl Pts',(167.11694720239,3.19169856999505,137.037449287095));
#231559=CARTESIAN_POINT('Ctrl Pts',(166.838499578577,6.96926506657354,131.488230894564));
#231560=CARTESIAN_POINT('Ctrl Pts',(166.560051954764,4.34241743449723,125.310569126392));
#231561=CARTESIAN_POINT('Ctrl Pts',(166.281604330951,-2.27489968099678,
124.181433351974));
#231562=CARTESIAN_POINT('Ctrl Pts',(166.003156707138,-6.80169512468258,
129.13844418665));
#231563=CARTESIAN_POINT('Ctrl Pts',(165.724709083325,-5.0780650300646,135.626350836796));
#231564=CARTESIAN_POINT('Ctrl Pts',(165.446261459512,1.31205874991464,137.683084042787));
#231565=CARTESIAN_POINT('Ctrl Pts',(165.1678138357,6.49646463635559,133.418606465321));
#231566=CARTESIAN_POINT('Ctrl Pts',(164.889366211887,5.71093689192698,126.751764666776));
#231567=CARTESIAN_POINT('Ctrl Pts',(164.610918588074,-0.322662861405092,
123.809060566689));
#231568=CARTESIAN_POINT('Ctrl Pts',(164.332470964261,-6.05975120806294,
127.29469547395));
#231569=CARTESIAN_POINT('Ctrl Pts',(164.054023340448,-6.22822422981513,
134.00554119152));
#231570=CARTESIAN_POINT('Ctrl Pts',(163.775575716635,-0.673263450036036,
137.774658347991));
#231571=CARTESIAN_POINT('Ctrl Pts',(163.497128092822,5.50039354957815,135.138412408175));
#231572=CARTESIAN_POINT('Ctrl Pts',(163.218680469009,6.61945758629338,128.51938460299));
#231573=CARTESIAN_POINT('Ctrl Pts',(162.940232845196,1.65556347968583,124.000138127916));
#231574=CARTESIAN_POINT('Ctrl Pts',(162.661785221384,-4.82971258598073,
125.733639716082));
#231575=CARTESIAN_POINT('Ctrl Pts',(162.383337597571,-6.87671872970774,
132.126886094224));
#231576=CARTESIAN_POINT('Ctrl Pts',(162.104889973758,-2.60435630721971,
137.304796168278));
#231577=CARTESIAN_POINT('Ctrl Pts',(161.826442349945,4.06128233172446,136.509123535159));
#231578=CARTESIAN_POINT('Ctrl Pts',(161.547994726132,6.99480091248578,130.471052473933));
#231579=CARTESIAN_POINT('Ctrl Pts',(161.269547102319,3.50043916969439,124.739275313697));
#231580=CARTESIAN_POINT('Ctrl Pts',(160.991099478506,-3.21065516408591,
124.581015251828));
#231581=CARTESIAN_POINT('Ctrl Pts',(160.712651854693,-6.97131425129578,
130.141705553748));
#231582=CARTESIAN_POINT('Ctrl Pts',(160.434204230881,-4.32567610919938,
136.311343486817));
#231583=CARTESIAN_POINT('Ctrl Pts',(160.155756607067,2.29504705622523,137.420333194114));
#231584=CARTESIAN_POINT('Ctrl Pts',(159.877308983254,6.80673409626067,132.449567311792));
#231585=CARTESIAN_POINT('Ctrl Pts',(159.598861359442,5.06336502927952,125.966936850291));
#231586=CARTESIAN_POINT('Ctrl Pts',(159.320413735629,-1.33298914047637,
123.929662509627));
#231587=CARTESIAN_POINT('Ctrl Pts',(159.041966111816,-6.50439141027418,
128.209899882485));
#231588=CARTESIAN_POINT('Ctrl Pts',(158.763518488003,-5.69857573121565,
134.874319924428));
#231589=CARTESIAN_POINT('Ctrl Pts',(158.48507086419,0.343952653928878,137.798646191931));
#231590=CARTESIAN_POINT('Ctrl Pts',(158.206623240377,6.07040535313402,134.295565706438));
#231591=CARTESIAN_POINT('Ctrl Pts',(157.928175616564,6.2184520885971,127.584238299121));
#231592=CARTESIAN_POINT('Ctrl Pts',(157.649727992752,0.652045142912632,
123.832045990734));
#231593=CARTESIAN_POINT('Ctrl Pts',(157.371280368939,-5.51355943493244,
126.487070207899));
#231594=CARTESIAN_POINT('Ctrl Pts',(157.092832745126,-6.61247224442723,
133.109473400187));
#231595=CARTESIAN_POINT('Ctrl Pts',(156.814385121313,-1.63484609852131,
137.613590556265));
#231596=CARTESIAN_POINT('Ctrl Pts',(156.5359374975,4.84512374525377,135.860358048054));
#231597=CARTESIAN_POINT('Ctrl Pts',(156.257489873687,6.87266156459436,129.46091090043));
#231598=CARTESIAN_POINT('Ctrl Pts',(155.979042249874,2.58455915425555,124.296028411687));
#231599=CARTESIAN_POINT('Ctrl Pts',(155.700594626061,-4.07862685611001,
125.111985270442));
#231600=CARTESIAN_POINT('Ctrl Pts',(155.422147002248,-6.99375403770952,
131.158956985208));
#231601=CARTESIAN_POINT('Ctrl Pts',(155.143699378435,-3.48196292253304,
136.880071961106));
#231602=CARTESIAN_POINT('Ctrl Pts',(154.865251754623,3.22958201510593,137.017905027291));
#231603=CARTESIAN_POINT('Ctrl Pts',(154.58680413081,6.97329885471516,131.445794329457));
#231604=CARTESIAN_POINT('Ctrl Pts',(154.308356506997,4.30889471142897,125.284237386175));
#231605=CARTESIAN_POINT('Ctrl Pts',(154.029908883184,-2.31517317045128,
124.195404019528));
#231606=CARTESIAN_POINT('Ctrl Pts',(153.751461259371,-6.81171001118396,
129.179878900999));
#231607=CARTESIAN_POINT('Ctrl Pts',(153.473013635558,-5.04861812217248,
135.65717311965));
#231608=CARTESIAN_POINT('Ctrl Pts',(153.194566011745,1.3539071824088,137.674969721956));
#231609=CARTESIAN_POINT('Ctrl Pts',(152.916118387933,6.51225792839928,133.379012205241));
#231610=CARTESIAN_POINT('Ctrl Pts',(152.637670764119,5.68616177967723,126.717075658174));
#231611=CARTESIAN_POINT('Ctrl Pts',(152.359223140307,-0.365239260122265,
123.811154313817));
#231612=CARTESIAN_POINT('Ctrl Pts',(152.080775516494,-6.08100326279917,
127.331647925483));
#231613=CARTESIAN_POINT('Ctrl Pts',(151.802327892681,-6.20862234048841,
134.043394849727));
#231614=CARTESIAN_POINT('Ctrl Pts',(151.523880268868,-0.630820795332096,
137.778627550233));
#231615=CARTESIAN_POINT('Ctrl Pts',(151.245432645055,5.52667424342534,135.104849651499));
#231616=CARTESIAN_POINT('Ctrl Pts',(150.966985021242,6.60542564552152,128.479132421149));
#231617=CARTESIAN_POINT('Ctrl Pts',(150.688537397429,1.61411357236584,123.990186309594));
#231618=CARTESIAN_POINT('Ctrl Pts',(150.410089773616,-4.86049001996232,
125.763133496143));
#231619=CARTESIAN_POINT('Ctrl Pts',(150.131642149803,-6.8685407320831,132.168722129643));
#231620=CARTESIAN_POINT('Ctrl Pts',(149.853194525991,-2.56473805828847,
137.32052918631));
#231621=CARTESIAN_POINT('Ctrl Pts',(149.574746902178,4.09593359665354,136.484295660832));
#231622=CARTESIAN_POINT('Ctrl Pts',(149.296299278365,6.99264237375128,130.428479310845));
#231623=CARTESIAN_POINT('Ctrl Pts',(149.017851654552,3.46345441894284,124.718079518912));
#231624=CARTESIAN_POINT('Ctrl Pts',(148.739404030739,-3.24847894771935,
124.600674725279));
#231625=CARTESIAN_POINT('Ctrl Pts',(148.460956406926,-6.97521885844655,
130.184154199754));
#231626=CARTESIAN_POINT('Ctrl Pts',(148.182508783113,-4.29207339664657,
136.337573073429));
#231627=CARTESIAN_POINT('Ctrl Pts',(147.9040611593,2.33527783722936,137.406240012622));
#231628=CARTESIAN_POINT('Ctrl Pts',(147.625613535487,6.81662282335624,132.408102307496));
#231629=CARTESIAN_POINT('Ctrl Pts',(147.347165911675,5.03382444535687,125.936204336462));
#231630=CARTESIAN_POINT('Ctrl Pts',(147.068718287862,-1.37481268193005,
123.937904165105));
#231631=CARTESIAN_POINT('Ctrl Pts',(146.790270664049,-6.52006411785656,
128.249542028514));
#231632=CARTESIAN_POINT('Ctrl Pts',(146.511823040236,-5.67369515231286,
134.908933365434));
#231633=CARTESIAN_POINT('Ctrl Pts',(146.233375416423,0.386522482789046,
137.796422866589));
#231634=CARTESIAN_POINT('Ctrl Pts',(145.95492779261,6.09154483888081,134.258548742122));
#231635=CARTESIAN_POINT('Ctrl Pts',(145.676480168797,6.19873507655051,127.546444477659));
#231636=CARTESIAN_POINT('Ctrl Pts',(145.398032544984,0.609590603913882,
123.828205987717));
#231637=CARTESIAN_POINT('Ctrl Pts',(145.119584921171,-5.53973785356302,
126.520712798507));
#231638=CARTESIAN_POINT('Ctrl Pts',(144.841137297358,-6.59831785485502,
133.149682687181));
#231639=CARTESIAN_POINT('Ctrl Pts',(144.562689673546,-1.59336609328267,
137.623416169231));
#231640=CARTESIAN_POINT('Ctrl Pts',(144.284242049733,4.87581126775532,135.830770728684));
#231641=CARTESIAN_POINT('Ctrl Pts',(144.00579442592,6.86435627034879,129.419099949804));
#231642=CARTESIAN_POINT('Ctrl Pts',(143.727346802107,2.54489320293839,124.280416050852));
#231643=CARTESIAN_POINT('Ctrl Pts',(143.448899178294,-4.11320239302776,
125.136918496298));
#231644=CARTESIAN_POINT('Ctrl Pts',(143.170451554481,-6.99146593090932,
131.201523381251));
#231645=CARTESIAN_POINT('Ctrl Pts',(142.892003930668,-3.44491383038404,
136.901155088855));
#231646=CARTESIAN_POINT('Ctrl Pts',(142.613556306855,3.26734578686757,136.998130522314));
#231647=CARTESIAN_POINT('Ctrl Pts',(142.335108683042,6.97707424470332,131.403333995789));
#231648=CARTESIAN_POINT('Ctrl Pts',(142.05666105923,4.27521232068256,125.258110196154));
#231649=CARTESIAN_POINT('Ctrl Pts',(141.778213435417,-2.35536087031262,
124.209619584399));
#231650=CARTESIAN_POINT('Ctrl Pts',(141.499765811604,-6.8214724872659,129.221373811115));
#231651=CARTESIAN_POINT('Ctrl Pts',(141.221318187791,-5.01898413587917,
135.687815579753));
#231652=CARTESIAN_POINT('Ctrl Pts',(140.942870563978,1.39570544537436,137.666600808179));
#231653=CARTESIAN_POINT('Ctrl Pts',(140.664422940165,6.52780990633047,133.339322540502));
#231654=CARTESIAN_POINT('Ctrl Pts',(140.385975316352,5.66117596461176,126.68253810542));
#231655=CARTESIAN_POINT('Ctrl Pts',(140.10752769254,-0.407802124764288,
123.813507196776));
#231656=CARTESIAN_POINT('Ctrl Pts',(139.829080068726,-6.10202998372316,
127.368729059661));
#231657=CARTESIAN_POINT('Ctrl Pts',(139.550632444914,-6.18879038837768,
134.081128484328));
#231658=CARTESIAN_POINT('Ctrl Pts',(139.272184821101,-0.588354765331746,
137.78233831845));
#231659=CARTESIAN_POINT('Ctrl Pts',(138.993737197288,5.55275014432601,135.071127538621));
#231660=CARTESIAN_POINT('Ctrl Pts',(138.715289573475,6.59114893827324,128.438966401494));
#231661=CARTESIAN_POINT('Ctrl Pts',(138.436841949662,1.57260385347371,123.980486993006));
#231662=CARTESIAN_POINT('Ctrl Pts',(138.158394325849,-4.8910873466988,125.792814080728));
#231663=CARTESIAN_POINT('Ctrl Pts',(137.879946702036,-6.86010821815569,
132.210507608145));
#231664=CARTESIAN_POINT('Ctrl Pts',(137.601499078223,-2.52502477204539,
137.336020745319));
#231665=CARTESIAN_POINT('Ctrl Pts',(137.32305145441,4.13043308525698,136.459257314423));
#231666=CARTESIAN_POINT('Ctrl Pts',(137.044603830598,6.99022472008204,130.385920076178));
#231667=CARTESIAN_POINT('Ctrl Pts',(136.766156206785,3.42634132861412,124.69710925351));
#231668=CARTESIAN_POINT('Ctrl Pts',(136.487708582972,-3.28618235777073,
124.620564078594));
#231669=CARTESIAN_POINT('Ctrl Pts',(136.209260959159,-6.97886499629743,
130.226625827737));
#231670=CARTESIAN_POINT('Ctrl Pts',(135.930813335346,-4.25831163973555,
136.363597624819));
#231671=CARTESIAN_POINT('Ctrl Pts',(135.652365711533,2.37542208365453,137.391902196061));
#231672=CARTESIAN_POINT('Ctrl Pts',(135.37391808772,6.82625895798624,132.366577875963));
#231673=CARTESIAN_POINT('Ctrl Pts',(135.095470463907,5.00409733121823,125.905652213954));
#231674=CARTESIAN_POINT('Ctrl Pts',(134.817022840094,-1.4165852791943,123.946400259653));
#231675=CARTESIAN_POINT('Ctrl Pts',(134.538575216282,-6.53549522206528,
128.289278844285));
#231676=CARTESIAN_POINT('Ctrl Pts',(134.260127592469,-5.64860433254967,
134.943394709987));
#231677=CARTESIAN_POINT('Ctrl Pts',(133.981679968656,0.429077988916399,
137.793940447809));
#231678=CARTESIAN_POINT('Ctrl Pts',(133.703232344843,6.1124586001935,134.221403781595));
#231679=CARTESIAN_POINT('Ctrl Pts',(133.42478472103,6.17878836809604,127.508771379477));
#231680=CARTESIAN_POINT('Ctrl Pts',(133.146337097217,0.567113476311158,
123.824624488677));
#231681=CARTESIAN_POINT('Ctrl Pts',(132.867889473404,-5.5657109951702,126.554514121259));
#231682=CARTESIAN_POINT('Ctrl Pts',(132.589441849591,-6.58391896218814,
133.189805067404));
#231683=CARTESIAN_POINT('Ctrl Pts',(132.310994225778,-1.55182704527753,
137.632989099587));
#231684=CARTESIAN_POINT('Ctrl Pts',(132.032546601965,4.90631811527725,135.800997153839));
#231685=CARTESIAN_POINT('Ctrl Pts',(131.754098978153,6.85579661485726,129.377340330521));
#231686=CARTESIAN_POINT('Ctrl Pts',(131.47565135434,2.50513294966777,124.265045437181));
#231687=CARTESIAN_POINT('Ctrl Pts',(131.197203730527,-4.14762551371829,
125.162061731307));
#231688=CARTESIAN_POINT('Ctrl Pts',(130.918756106714,-6.98891875276791,
131.244075060281));
#231689=CARTESIAN_POINT('Ctrl Pts',(130.640308482901,-3.4077370856862,136.922012297644));
#231690=CARTESIAN_POINT('Ctrl Pts',(130.361860859088,3.30498848592948,136.978126504915));
#231691=CARTESIAN_POINT('Ctrl Pts',(130.083413235275,6.98059109663955,131.360851466943));
#231692=CARTESIAN_POINT('Ctrl Pts',(129.804965611462,4.24137151037132,125.232188524482));
#231693=CARTESIAN_POINT('Ctrl Pts',(129.526517987649,-2.39546129141071,
124.224079519825));
#231694=CARTESIAN_POINT('Ctrl Pts',(129.248070363836,-6.83098219117618,
129.262927379388));
#231695=CARTESIAN_POINT('Ctrl Pts',(128.969622740024,-4.98916416928312,
135.718277081636));
#231696=CARTESIAN_POINT('Ctrl Pts',(128.691175116211,1.43745198996158,137.657977611568));
#231697=CARTESIAN_POINT('Ctrl Pts',(128.412727492398,6.54311999386511,133.299538941816));
#231698=CARTESIAN_POINT('Ctrl Pts',(128.134279868585,5.63598037258881,126.648153288314));
#231699=CARTESIAN_POINT('Ctrl Pts',(127.855832244772,-0.450349878148651,
123.81611912838));
#231700=CARTESIAN_POINT('Ctrl Pts',(127.577384620959,-6.12283059168226,
127.40593750243));
#231701=CARTESIAN_POINT('Ctrl Pts',(127.298936997146,-6.16872910836309,
134.118740697091));
#231702=CARTESIAN_POINT('Ctrl Pts',(127.020489373333,-0.545866933628919,
137.785790515136));
#231703=CARTESIAN_POINT('Ctrl Pts',(126.742041749521,5.57862028602806,135.037247319125));
#231704=CARTESIAN_POINT('Ctrl Pts',(126.463594125708,6.57662799357718,128.398888032392));
#231705=CARTESIAN_POINT('Ctrl Pts',(126.185146501895,1.53103586116759,123.971040537565));
#231706=CARTESIAN_POINT('Ctrl Pts',(125.906698878082,-4.92150343239493,
125.822680370014));
#231707=CARTESIAN_POINT('Ctrl Pts',(125.628251254269,-6.85142150039552,
132.252240981353));
#231708=CARTESIAN_POINT('Ctrl Pts',(125.349803630456,-2.48521792008072,
137.351270271259));
#231709=CARTESIAN_POINT('Ctrl Pts',(125.071356006643,4.16477951914341,136.434009423738));
#231710=CARTESIAN_POINT('Ctrl Pts',(124.79290838283,6.98754804106521,130.343376346978));
#231711=CARTESIAN_POINT('Ctrl Pts',(124.514460759018,3.38910127394743,124.676365294554));
#231712=CARTESIAN_POINT('Ctrl Pts',(124.236013135205,-3.32376399712637,
124.640682574762));
#231713=CARTESIAN_POINT('Ctrl Pts',(123.957565511392,-6.98225252973936,
130.269118863895));
#231714=CARTESIAN_POINT('Ctrl Pts',(123.679117887579,-4.22439208952083,
136.389416176637));
#231715=CARTESIAN_POINT('Ctrl Pts',(123.400670263766,2.41547830794073,137.377320275725));
#231716=CARTESIAN_POINT('Ctrl Pts',(123.122222639953,6.83564214308024,132.324995555895));
#231717=CARTESIAN_POINT('Ctrl Pts',(122.84377501614,4.97418478841272,125.875281614887));
#231718=CARTESIAN_POINT('Ctrl Pts',(122.565327392328,-1.45830538437,123.955150478444));
#231719=CARTESIAN_POINT('Ctrl Pts',(122.286879768514,-6.55068415109515,
128.329108857337));
#231720=CARTESIAN_POINT('Ctrl Pts',(122.008432144702,-5.62330420167569,
134.977702681109));
#231721=CARTESIAN_POINT('Ctrl Pts',(121.729984520888,0.471617595401148,
137.791199027578));
#231722=CARTESIAN_POINT('Ctrl Pts',(121.451536897076,6.13314586210485,134.184132201278));
#231723=CARTESIAN_POINT('Ctrl Pts',(121.173089273263,6.15861270236637,127.471220400567));
#231724=CARTESIAN_POINT('Ctrl Pts',(120.89464164945,0.52461533410983,123.821301626325));
#231725=CARTESIAN_POINT('Ctrl Pts',(120.616194025637,-5.5914778973097,126.588472923636));
#231726=CARTESIAN_POINT('Ctrl Pts',(120.337746401824,-6.56927609998288,
133.229839054105));
#231727=CARTESIAN_POINT('Ctrl Pts',(120.059298778011,-1.51023049375061,
137.642308992603));
#231728=CARTESIAN_POINT('Ctrl Pts',(119.780851154198,4.93664315737715,135.77103842679));
#231729=CARTESIAN_POINT('Ctrl Pts',(119.502403530385,6.84698291530094,129.33563359));
#231730=CARTESIAN_POINT('Ctrl Pts',(119.223955906573,2.46527986777437,124.249917140239));
#231731=CARTESIAN_POINT('Ctrl Pts',(118.94550828276,-4.18189494262004,125.187414043775));
#231732=CARTESIAN_POINT('Ctrl Pts',(118.667060658947,-6.98611259767199,
131.28661044553));
#231733=CARTESIAN_POINT('Ctrl Pts',(118.388613035134,-3.37043406603744,
136.942642814599));
#231734=CARTESIAN_POINT('Ctrl Pts',(118.110165411321,3.34250871742766,136.95789371635));
#231735=CARTESIAN_POINT('Ctrl Pts',(117.831717787508,6.98384928020556,131.318348317123));
#231736=CARTESIAN_POINT('Ctrl Pts',(117.553270163695,4.20737353447909,125.206473331696));
#231737=CARTESIAN_POINT('Ctrl Pts',(117.274822539882,-2.43547294780967,
124.238783289987));
#231738=CARTESIAN_POINT('Ctrl Pts',(116.99637491607,-6.84023877052931,129.304538066038));
#231739=CARTESIAN_POINT('Ctrl Pts',(116.717927292256,-4.95915932737393,
135.748556496538));
#231740=CARTESIAN_POINT('Ctrl Pts',(116.439479668444,1.47914526923655,137.649100451659));
#231741=CARTESIAN_POINT('Ctrl Pts',(116.161032044631,6.55818762368211,133.259662883379));
#231742=CARTESIAN_POINT('Ctrl Pts',(115.882584420818,5.61057593724064,126.613922481));
#231743=CARTESIAN_POINT('Ctrl Pts',(115.604136797005,-0.49288094365267,
123.818990011842));
#231744=CARTESIAN_POINT('Ctrl Pts',(115.325689173192,-6.14340431590201,
127.443271875017));
#231745=CARTESIAN_POINT('Ctrl Pts',(115.047241549379,-6.14843924382291,
134.156230094282));
#231746=CARTESIAN_POINT('Ctrl Pts',(114.768793925566,-0.5033588746261,137.78898401237));
#231747=CARTESIAN_POINT('Ctrl Pts',(114.490346301753,5.60428370990391,135.003210248456));
#231748=CARTESIAN_POINT('Ctrl Pts',(114.211898677941,6.56186334951224,128.358898798961));
#231749=CARTESIAN_POINT('Ctrl Pts',(113.933451054127,1.48941113576461,123.961847293312));
#231750=CARTESIAN_POINT('Ctrl Pts',(113.655003430315,-4.95173714997151,
125.852731257293));
#231751=CARTESIAN_POINT('Ctrl Pts',(113.376555806502,-6.84248090069202,
132.293920702821));
#231752=CARTESIAN_POINT('Ctrl Pts',(113.098108182689,-2.4453189774521,137.366277199056));
#231753=CARTESIAN_POINT('Ctrl Pts',(112.819660558876,4.19897162559319,136.408552924347));
#231754=CARTESIAN_POINT('Ctrl Pts',(112.541212935063,6.98461243588604,130.300849699721));
#231755=CARTESIAN_POINT('Ctrl Pts',(112.26276531125,3.35173563488669,124.655848410718));
#231756=CARTESIAN_POINT('Ctrl Pts',(111.984317687437,-3.3612224731848,124.661029468288));
#231757=CARTESIAN_POINT('Ctrl Pts',(111.705870063624,-6.98538133324609,
130.311631733633));
#231758=CARTESIAN_POINT('Ctrl Pts',(111.427422439812,-4.1903160029037,136.415027772168));
#231759=CARTESIAN_POINT('Ctrl Pts',(111.148974815999,2.45544502578993,137.362494791951));
#231760=CARTESIAN_POINT('Ctrl Pts',(110.870527192186,6.84477203094083,132.28335688814));
#231761=CARTESIAN_POINT('Ctrl Pts',(110.592079568373,4.94408792536061,125.845093664656));
#231762=CARTESIAN_POINT('Ctrl Pts',(110.31363194456,-1.49997145150339,123.964154497236));
#231763=CARTESIAN_POINT('Ctrl Pts',(110.035184320747,-6.56563034211481,
128.369030591753));
#231764=CARTESIAN_POINT('Ctrl Pts',(109.756736696934,-5.59779569719655,
135.011856007506));
#231765=CARTESIAN_POINT('Ctrl Pts',(109.478289073121,0.514139725922464,
137.788198707481));
#231766=CARTESIAN_POINT('Ctrl Pts',(109.199841449309,6.15360585804082,134.146735382281));
#231767=CARTESIAN_POINT('Ctrl Pts',(108.921393825496,6.13820882697821,127.433792932393));
#231768=CARTESIAN_POINT('Ctrl Pts',(108.642946201683,0.482097752094529,
123.818237523792));
#231769=CARTESIAN_POINT('Ctrl Pts',(108.36449857787,-5.61703760517944,126.622587947283));
#231770=CARTESIAN_POINT('Ctrl Pts',(108.086050954057,-6.5543898108359,133.26978316381));
#231771=CARTESIAN_POINT('Ctrl Pts',(107.807603330244,-1.46857798007734,
137.651375502926));
#231772=CARTESIAN_POINT('Ctrl Pts',(107.529155706431,4.96678527034939,135.740895657668));
#231773=CARTESIAN_POINT('Ctrl Pts',(107.250708082618,6.83791549827476,129.2939812737));
#231774=CARTESIAN_POINT('Ctrl Pts',(106.972260458805,2.42533543402888,124.23503172061));
#231775=CARTESIAN_POINT('Ctrl Pts',(106.693812834992,-4.21600940986681,
125.212974494265));
#231776=CARTESIAN_POINT('Ctrl Pts',(106.415365211179,-6.98304756960462,
131.329127960835));
#231777=CARTESIAN_POINT('Ctrl Pts',(106.136917587367,-3.33300615371489,
136.96304587525));
#231778=CARTESIAN_POINT('Ctrl Pts',(105.858469963554,3.37990509103613,136.937432906355));
#231779=CARTESIAN_POINT('Ctrl Pts',(105.580022339741,6.98684867466819,131.275826121299));
#231780=CARTESIAN_POINT('Ctrl Pts',(105.301574715928,4.1732196528133,125.180965570684));
#231781=CARTESIAN_POINT('Ctrl Pts',(105.023127092115,-2.4753943568629,124.253730350031));
#231782=CARTESIAN_POINT('Ctrl Pts',(104.744679468302,-6.84924188231931,
129.346204329164));
#231783=CARTESIAN_POINT('Ctrl Pts',(104.466231844489,-4.92897072199215,
135.778652702442));
#231784=CARTESIAN_POINT('Ctrl Pts',(104.187784220676,1.52078373823962,137.639969657397));
#231785=CARTESIAN_POINT('Ctrl Pts',(103.909336596864,6.57301223744494,133.219695842813));
#231786=CARTESIAN_POINT('Ctrl Pts',(103.63088897305,5.58496359993783,126.579846951912));
#231787=CARTESIAN_POINT('Ctrl Pts',(103.352441349238,-0.535393745272065,
123.82211974078));
#231788=CARTESIAN_POINT('Ctrl Pts',(103.073993725425,-6.1637503940156,127.480730793984));
#231789=CARTESIAN_POINT('Ctrl Pts',(102.795546101612,-6.12792154660547,
134.193595286717));
#231790=CARTESIAN_POINT('Ctrl Pts',(102.517098477799,-0.460832163475232,
137.791918691816));
#231791=CARTESIAN_POINT('Ctrl Pts',(102.238650853986,5.6297394649859,134.96901758787));
#231792=CARTESIAN_POINT('Ctrl Pts',(101.960203230173,6.54685555318778,128.319000183017));
#231793=CARTESIAN_POINT('Ctrl Pts',(101.68175560636,1.44773121968427,123.952907600908));
#231794=CARTESIAN_POINT('Ctrl Pts',(101.403307982548,-4.981787379107,125.882965629019));
#231795=CARTESIAN_POINT('Ctrl Pts',(101.124860358735,-6.83328675034245,
132.335545228093));
#231796=CARTESIAN_POINT('Ctrl Pts',(100.846412734922,-2.4053294226295,137.38104097262));
#231797=CARTESIAN_POINT('Ctrl Pts',(100.567965111109,4.23300813760519,136.382888759548));
#231798=CARTESIAN_POINT('Ctrl Pts',(100.289517487296,6.98141801332452,130.258341710245));
#231799=CARTESIAN_POINT('Ctrl Pts',(100.011069863483,3.31424579602927,124.635559362262));
#231800=CARTESIAN_POINT('Ctrl Pts',(99.7326222396699,-3.39855639790849,
124.681604005209));
#231801=CARTESIAN_POINT('Ctrl Pts',(99.4541746158571,-6.98825129087862,
130.354162861621));
#231802=CARTESIAN_POINT('Ctrl Pts',(99.1757269920442,-4.15608464258612,
136.440431462363));
#231803=CARTESIAN_POINT('Ctrl Pts',(98.8972793682313,2.49532075622072,137.347426294104));
#231804=CARTESIAN_POINT('Ctrl Pts',(98.6188317444184,6.85364828325664,132.241663415635));
#231805=CARTESIAN_POINT('Ctrl Pts',(98.3403841206056,4.91380785731226,125.815089481885));
#231806=CARTESIAN_POINT('Ctrl Pts',(98.0619364967926,-1.54158193664305,
123.97341198238));
#231807=CARTESIAN_POINT('Ctrl Pts',(97.7834888729798,-6.58033324128762,
128.409042568218));
#231808=CARTESIAN_POINT('Ctrl Pts',(97.5050412491668,-5.57207976433927,
135.045853423614));
#231809=CARTESIAN_POINT('Ctrl Pts',(97.226593625354,0.55664280480716,137.784939598694));
#231810=CARTESIAN_POINT('Ctrl Pts',(96.948146001541,6.17383782984873,134.109214710358));
#231811=CARTESIAN_POINT('Ctrl Pts',(96.6696983777281,6.11757749800464,127.396490361844));
#231812=CARTESIAN_POINT('Ctrl Pts',(96.3912507539153,0.43956230576973,123.815432294619));
#231813=CARTESIAN_POINT('Ctrl Pts',(96.1128031301024,-5.64238917165504,
126.656857928054));
#231814=CARTESIAN_POINT('Ctrl Pts',(95.8343555062895,-6.53926064636413,
133.309635916377));
#231815=CARTESIAN_POINT('Ctrl Pts',(95.5559078824767,-1.42687104770695,
137.660188294596));
#231816=CARTESIAN_POINT('Ctrl Pts',(95.2774602586637,4.99674333726689,135.710569963425));
#231817=CARTESIAN_POINT('Ctrl Pts',(94.9990126348508,6.82859469977515,129.252384925061));
#231818=CARTESIAN_POINT('Ctrl Pts',(94.720565011038,2.38530112858694,124.22038972988));
#231819=CARTESIAN_POINT('Ctrl Pts',(94.442117387225,-4.24996765133445,125.238742135624));
#231820=CARTESIAN_POINT('Ctrl Pts',(94.1636697634123,-6.97972378214161,
131.371626030693));
#231821=CARTESIAN_POINT('Ctrl Pts',(93.885222139599,-3.29545473562348,136.983220723554));
#231822=CARTESIAN_POINT('Ctrl Pts',(93.6067745157866,3.41717622101856,136.91674483311));
#231823=CARTESIAN_POINT('Ctrl Pts',(93.3283268919733,6.98958916888377,131.233286455149));
#231824=CARTESIAN_POINT('Ctrl Pts',(93.0498792681607,4.13891113095855,125.155666186642));
#231825=CARTESIAN_POINT('Ctrl Pts',(92.7714316443476,-2.51522403926791,
124.268920146089));
#231826=CARTESIAN_POINT('Ctrl Pts',(92.4929840205349,-6.85799119293255,
129.387924624807));
#231827=CARTESIAN_POINT('Ctrl Pts',(92.2145363967218,-4.89859947178764,
135.808564584124));
#231828=CARTESIAN_POINT('Ctrl Pts',(91.9360887729091,1.562365854042,137.63058556713));
#231829=CARTESIAN_POINT('Ctrl Pts',(91.6576411490961,6.58759328582208,133.179639301113));
#231830=CARTESIAN_POINT('Ctrl Pts',(91.3791935252832,5.55914430975498,126.545927963732));
#231831=CARTESIAN_POINT('Ctrl Pts',(91.1007459014705,-0.57788670767935,
123.825508199223));
#231832=CARTESIAN_POINT('Ctrl Pts',(90.8222982776573,-6.18386807209161,
127.518312871276));
#231833=CARTESIAN_POINT('Ctrl Pts',(90.5438506538447,-6.10717677700159,
134.230834889814));
#231834=CARTESIAN_POINT('Ctrl Pts',(90.2654030300316,-0.41828837601907,
137.794594444728));
#231835=CARTESIAN_POINT('Ctrl Pts',(89.9869554062187,5.65498660800168,134.934670604388));
#231836=CARTESIAN_POINT('Ctrl Pts',(89.708507782406,6.53160516072318,128.279193663018));
#231837=CARTESIAN_POINT('Ctrl Pts',(89.430060158593,1.40599765739116,123.944221791613));
#231838=CARTESIAN_POINT('Ctrl Pts',(89.1516125347801,-5.01165300627911,
125.913382364846));
#231839=CARTESIAN_POINT('Ctrl Pts',(88.8731649109673,-6.82383939003939,
132.377113014756));
#231840=CARTESIAN_POINT('Ctrl Pts',(88.5947172871542,-2.36525073744058,
137.395561044874));
#231841=CARTESIAN_POINT('Ctrl Pts',(88.3162696633415,4.26688779394398,136.357017880338));
#231842=CARTESIAN_POINT('Ctrl Pts',(88.0378220395285,6.97796489175107,130.2158539537));
#231843=CARTESIAN_POINT('Ctrl Pts',(87.7593744157156,3.2766331465752,124.615498901007));
#231844=CARTESIAN_POINT('Ctrl Pts',(87.4809267919028,-3.43576438787495,
124.702405423128));
#231845=CARTESIAN_POINT('Ctrl Pts',(87.2024791680898,-6.99086229628967,
130.396710671853));
#231846=CARTESIAN_POINT('Ctrl Pts',(86.924031544277,-4.1216992770237,136.465626305881));
#231847=CARTESIAN_POINT('Ctrl Pts',(86.6455839204641,2.53510402162323,137.332115340552));
#231848=CARTESIAN_POINT('Ctrl Pts',(86.3671362966513,6.8622705711149,132.199916683345));
#231849=CARTESIAN_POINT('Ctrl Pts',(86.0886886728382,4.88334570630671,125.785270178391));
#231850=CARTESIAN_POINT('Ctrl Pts',(85.8102410490255,-1.58313529789712,
123.982922590838));
#231851=CARTESIAN_POINT('Ctrl Pts',(85.5317934252125,-6.59479230379227,
128.449143304076));
#231852=CARTESIAN_POINT('Ctrl Pts',(85.2533458013996,-5.5461573560172,135.079693669646));
#231853=CARTESIAN_POINT('Ctrl Pts',(84.9748981775869,0.599125257088023,
137.781421821987));
#231854=CARTESIAN_POINT('Ctrl Pts',(84.6964505537737,6.19384102782544,134.071571575853));
#231855=CARTESIAN_POINT('Ctrl Pts',(84.418002929961,6.09671947994716,127.359314071181));
#231856=CARTESIAN_POINT('Ctrl Pts',(84.1395553061481,0.397010571302045,
123.812886042756));
#231857=CARTESIAN_POINT('Ctrl Pts',(83.8611076823352,-5.66753165732491,
126.691281596061));
#231858=CARTESIAN_POINT('Ctrl Pts',(83.5826600585222,-6.52388916718428,
133.349395835046));
#231859=CARTESIAN_POINT('Ctrl Pts',(83.3042124347095,-1.38511124210516,
137.66874704105));
#231860=CARTESIAN_POINT('Ctrl Pts',(83.0257648108964,5.02651624802251,135.68006246779));
#231861=CARTESIAN_POINT('Ctrl Pts',(82.7473171870836,6.81902086518772,129.210846085452));
#231862=CARTESIAN_POINT('Ctrl Pts',(82.4688695632707,2.34517843493451,124.205991710613));
#231863=CARTESIAN_POINT('Ctrl Pts',(82.1904219394578,-4.28376840868787,
125.264716013022));
#231864=CARTESIAN_POINT('Ctrl Pts',(81.9119743156449,-6.97614135844701,
131.414103080323));
#231865=CARTESIAN_POINT('Ctrl Pts',(81.6335266918322,-3.25778120324508,
137.003166611925));
#231866=CARTESIAN_POINT('Ctrl Pts',(81.355079068019,3.45432072627939,136.895830263219));
#231867=CARTESIAN_POINT('Ctrl Pts',(81.0766314442065,6.99207066130227,131.190730894994));
#231868=CARTESIAN_POINT('Ctrl Pts',(80.7981838203932,4.10444924022979,125.130576117049));
#231869=CARTESIAN_POINT('Ctrl Pts',(80.5197361965806,-2.55496051912119,
124.284352115297));
#231870=CARTESIAN_POINT('Ctrl Pts',(80.2412885727675,-6.86648637816013,
129.429697407007));
#231871=CARTESIAN_POINT('Ctrl Pts',(79.9628409489547,-4.86804670217826,
135.838291033188));
#231872=CARTESIAN_POINT('Ctrl Pts',(79.6843933251418,1.6038900758031,137.620948528586));
#231873=CARTESIAN_POINT('Ctrl Pts',(79.405945701329,6.60193022850756,133.139494742587));
#231874=CARTESIAN_POINT('Ctrl Pts',(79.1274980775159,5.53311902343524,126.512166773338));
#231875=CARTESIAN_POINT('Ctrl Pts',(78.8490504537032,-0.620358256282274,
123.829155261608));
#231876=CARTESIAN_POINT('Ctrl Pts',(78.5706028298902,-6.2037566046621,127.556016714277));
#231877=CARTESIAN_POINT('Ctrl Pts',(78.2921552060774,-6.08620570371632,
134.267947523646));
#231878=CARTESIAN_POINT('Ctrl Pts',(78.0137075822645,-0.375729088733312,
137.797011171955));
#231879=CARTESIAN_POINT('Ctrl Pts',(77.7352599584516,5.68002420340909,134.90017057075));
#231880=CARTESIAN_POINT('Ctrl Pts',(77.4568123346387,6.51611273722737,128.23948071401));
#231881=CARTESIAN_POINT('Ctrl Pts',(77.1783647108257,1.36421199533782,123.935790187287));
#231882=CARTESIAN_POINT('Ctrl Pts',(76.8999170870129,-5.04133292480603,
125.94398033767));
#231883=CARTESIAN_POINT('Ctrl Pts',(76.6214694632,-6.81413916985829,132.418622522501));
#231884=CARTESIAN_POINT('Ctrl Pts',(76.3430218393871,-2.32508440701577,
137.409836877774));
#231885=CARTESIAN_POINT('Ctrl Pts',(76.0645742155741,4.30060933918641,136.33094124537));
#231886=CARTESIAN_POINT('Ctrl Pts',(75.7861265917614,6.97425319912241,130.173388004487));
#231887=CARTESIAN_POINT('Ctrl Pts',(75.5076789679483,3.23889908027492,124.595667770297));
#231888=CARTESIAN_POINT('Ctrl Pts',(75.2292313441357,-3.47284506432852,
124.72343295124));
#231889=CARTESIAN_POINT('Ctrl Pts',(74.9507837203226,-6.99321425272744,
130.439273587703));
#231890=CARTESIAN_POINT('Ctrl Pts',(74.6723360965098,-4.08716118037883,
136.490611369118));
#231891=CARTESIAN_POINT('Ctrl Pts',(74.3938884726969,2.57479334781394,137.316562498648));
#231892=CARTESIAN_POINT('Ctrl Pts',(74.1154408488841,6.87063857501356,132.158118238212));
#231893=CARTESIAN_POINT('Ctrl Pts',(73.836993225071,4.85270260113016,125.755636859138));
#231894=CARTESIAN_POINT('Ctrl Pts',(73.5585456012583,-1.62462999549052,
123.992685970191));
#231895=CARTESIAN_POINT('Ctrl Pts',(73.2800979774453,-6.60900699384299,
128.489331313375));
#231896=CARTESIAN_POINT('Ctrl Pts',(73.0016503536324,-5.52002943279461,
135.113375491641));
#231897=CARTESIAN_POINT('Ctrl Pts',(72.7232027298196,0.641585508562261,
137.777645507711));
#231898=CARTESIAN_POINT('Ctrl Pts',(72.4447551060067,6.21361471074508,134.033807373642));
#231899=CARTESIAN_POINT('Ctrl Pts',(72.1663074821937,6.07563554570727,127.322265437984));
#231900=CARTESIAN_POINT('Ctrl Pts',(71.8878598583809,0.354444125461637,
123.810598862555));
#231901=CARTESIAN_POINT('Ctrl Pts',(71.609412234568,-5.69246413052499,126.725857675724));
#231902=CARTESIAN_POINT('Ctrl Pts',(71.330964610755,-6.5082759428922,133.3890614465));
#231903=CARTESIAN_POINT('Ctrl Pts',(71.0525169869423,-1.34330011069692,
137.677051425141));
#231904=CARTESIAN_POINT('Ctrl Pts',(70.7740693631292,5.05610289937005,135.649374301231));
#231905=CARTESIAN_POINT('Ctrl Pts',(70.4956217393166,6.80919434927445,129.16936629411));
#231906=CARTESIAN_POINT('Ctrl Pts',(70.2171741155033,2.30496883983272,124.191838196331));
#231907=CARTESIAN_POINT('Ctrl Pts',(69.9387264916908,-4.31741042942741,
125.290895163988));
#231908=CARTESIAN_POINT('Ctrl Pts',(69.6602788678776,-6.97230043126892,
131.456557535721));
#231909=CARTESIAN_POINT('Ctrl Pts',(69.3818312440649,-3.21998695258627,
137.02288280126));
#231910=CARTESIAN_POINT('Ctrl Pts',(69.1033836202519,3.49133723041524,136.874689971681));
#231911=CARTESIAN_POINT('Ctrl Pts',(68.8249359964391,6.9942930599711,131.148161017746));
#231912=CARTESIAN_POINT('Ctrl Pts',(68.5464883726262,4.0698352576252,125.105696291628));
#231913=CARTESIAN_POINT('Ctrl Pts',(68.2680407488133,-2.59460232397255,
124.300025685817));
#231914=CARTESIAN_POINT('Ctrl Pts',(67.9895931250004,-6.87472712320984,
129.471521127857));
#231915=CARTESIAN_POINT('Ctrl Pts',(67.7111455011875,-4.83731354530826,
135.867830948109));
#231916=CARTESIAN_POINT('Ctrl Pts',(67.4326978773747,1.64535486482719,137.61105889887));
#231917=CARTESIAN_POINT('Ctrl Pts',(67.1542502535617,6.61602253424027,133.099263654809));
#231918=CARTESIAN_POINT('Ctrl Pts',(66.8758026297489,5.50688870535577,126.478564631767));
#231919=CARTESIAN_POINT('Ctrl Pts',(66.5973550059358,-0.662806817281494,
123.833060792792));
#231920=CARTESIAN_POINT('Ctrl Pts',(66.3189073821232,-6.22341525475008,
127.593840925854));
#231921=CARTESIAN_POINT('Ctrl Pts',(66.0404597583101,-6.0650091038406,134.304931812993));
#231922=CARTESIAN_POINT('Ctrl Pts',(65.7620121344974,-0.333155878668442,
137.799168783944));
#231923=CARTESIAN_POINT('Ctrl Pts',(65.4835645106842,5.70485132343066,134.865518765369));
#231924=CARTESIAN_POINT('Ctrl Pts',(65.2051168868716,6.50037885677781,128.199862807569));
#231925=CARTESIAN_POINT('Ctrl Pts',(64.9266692630585,1.32237578190785,123.927613100363));
#231926=CARTESIAN_POINT('Ctrl Pts',(64.6482216392459,-5.07082603488719,
125.974758413674));
#231927=CARTESIAN_POINT('Ctrl Pts',(64.3697740154327,-6.80418644924447,
132.460072213177));
#231928=CARTESIAN_POINT('Ctrl Pts',(64.09132639162,-2.28483191973344,137.423867942321));
#231929=CARTESIAN_POINT('Ctrl Pts',(63.812878767807,4.33417152376786,136.304659820925));
#231930=CARTESIAN_POINT('Ctrl Pts',(63.5344311439942,6.97028307297671,130.130945436197));
#231931=CARTESIAN_POINT('Ctrl Pts',(63.2559835201813,3.20104499537862,124.576066704985));
#231932=CARTESIAN_POINT('Ctrl Pts',(62.9775358963684,-3.5097970532309,124.744685810362));
#231933=CARTESIAN_POINT('Ctrl Pts',(62.6990882725555,-6.9953070730393,130.481850031987));
#231934=CARTESIAN_POINT('Ctrl Pts',(62.4206406487427,-4.05247163247362,
136.51538572624));
#231935=CARTESIAN_POINT('Ctrl Pts',(62.1421930249296,2.61438726408988,137.300768344709));
#231936=CARTESIAN_POINT('Ctrl Pts',(61.8637454011169,6.87875198487314,132.116269629093));
#231937=CARTESIAN_POINT('Ctrl Pts',(61.5852977773038,4.82187967727427,125.726190622201));
#231938=CARTESIAN_POINT('Ctrl Pts',(61.3068501534911,-1.66606449182178,
124.002701758653));
#231939=CARTESIAN_POINT('Ctrl Pts',(61.0284025296781,-6.62297678470872,
128.529605106938));
#231940=CARTESIAN_POINT('Ctrl Pts',(60.7499549058653,-5.49369696285183,
135.146897641504));
#231941=CARTESIAN_POINT('Ctrl Pts',(60.4715072820523,0.684021985849089,
137.773610795799));
#231942=CARTESIAN_POINT('Ctrl Pts',(60.1930596582395,6.23315814588628,133.995923503096));
#231943=CARTESIAN_POINT('Ctrl Pts',(59.9146120344266,6.05432647655821,127.285345835106));
#231944=CARTESIAN_POINT('Ctrl Pts',(59.6361644106137,0.311864545564345,
123.808570838767));
#231945=CARTESIAN_POINT('Ctrl Pts',(59.3577167868007,-5.71718566737322,
126.760584885814));
#231946=CARTESIAN_POINT('Ctrl Pts',(59.0792691629879,-6.49242155204172,
133.428631280914));
#231947=CARTESIAN_POINT('Ctrl Pts',(58.800821539175,-1.30143920280946,137.685101139145));
#231948=CARTESIAN_POINT('Ctrl Pts',(58.5223739153621,5.08550219496502,135.618506600908));
#231949=CARTESIAN_POINT('Ctrl Pts',(58.2439262915492,6.79911551616065,129.127947088084));
#231950=CARTESIAN_POINT('Ctrl Pts',(57.9654786677363,2.26467383326308,124.1779297115));
#231951=CARTESIAN_POINT('Ctrl Pts',(57.6870310439234,-4.35089246693584,
125.317278618444));
#231952=CARTESIAN_POINT('Ctrl Pts',(57.4085834201106,-6.96820114293417,
131.498987823723));
#231953=CARTESIAN_POINT('Ctrl Pts',(57.1301357962976,-3.18207338412696,
137.042368560968));
#231954=CARTESIAN_POINT('Ctrl Pts',(56.8516881724848,3.52822436176609,136.853324741857));
#231955=CARTESIAN_POINT('Ctrl Pts',(56.5732405486719,6.9962562825383,131.105578400848));
#231956=CARTESIAN_POINT('Ctrl Pts',(56.294792924859,4.03507046577855,125.081027632309));
#231957=CARTESIAN_POINT('Ctrl Pts',(56.0163453010462,-2.63414798488075,
124.315940276861));
#231958=CARTESIAN_POINT('Ctrl Pts',(55.7378976772331,-6.8827131227178,129.513394237565));
#231959=CARTESIAN_POINT('Ctrl Pts',(55.4594500534204,-4.80640114000575,
135.897183234276));
#231960=CARTESIAN_POINT('Ctrl Pts',(55.1810024296073,1.68675868462211,137.600917044446));
#231961=CARTESIAN_POINT('Ctrl Pts',(54.9025548057946,6.62986968082513,133.058947528554));
#231962=CARTESIAN_POINT('Ctrl Pts',(54.6241071819816,5.4804543274898,126.445122784157));
#231963=CARTESIAN_POINT('Ctrl Pts',(54.3456595581689,-0.705230817730614,
123.837224648055));
#231964=CARTESIAN_POINT('Ctrl Pts',(54.0672119343557,-6.24284329389726,
127.63178410442));
#231965=CARTESIAN_POINT('Ctrl Pts',(53.7887643105431,-6.04358776282204,
134.341786387386));
#231966=CARTESIAN_POINT('Ctrl Pts',(53.51031668673,-0.290570323389535,137.801067200743));
#231967=CARTESIAN_POINT('Ctrl Pts',(53.2318690629172,5.72946704808866,134.830716472279));
#231968=CARTESIAN_POINT('Ctrl Pts',(52.9534214391043,6.48440410239917,128.160341411752));
#231969=CARTESIAN_POINT('Ctrl Pts',(52.6749738152913,1.28049056735643,123.919690833848));
#231970=CARTESIAN_POINT('Ctrl Pts',(52.3965261914786,-5.10013124364513,
126.005715452363));
#231971=CARTESIAN_POINT('Ctrl Pts',(52.1180785676656,-6.79398159699943,
132.501460550851));
#231972=CARTESIAN_POINT('Ctrl Pts',(51.8396309438527,-2.24449476716385,
137.43765371859));
#231973=CARTESIAN_POINT('Ctrl Pts',(51.5611833200399,4.36757310402998,136.278174580871));
#231974=CARTESIAN_POINT('Ctrl Pts',(51.2827356962269,6.96605466042841,130.088527821552));
#231975=CARTESIAN_POINT('Ctrl Pts',(51.0042880724141,3.16307229458231,124.556696431394));
#231976=CARTESIAN_POINT('Ctrl Pts',(50.7258404486012,-3.54661898531293,
124.766163212963));
#231977=CARTESIAN_POINT('Ctrl Pts',(50.4473928247883,-6.99714067967511,
130.52443842702));
#231978=CARTESIAN_POINT('Ctrl Pts',(50.1689452009753,-4.0176319187415,136.539948459229));
#231979=CARTESIAN_POINT('Ctrl Pts',(49.8904975771625,2.65388430328469,137.284733463992));
#231980=CARTESIAN_POINT('Ctrl Pts',(49.6120499533496,6.88661050004828,132.074372406703));
#231981=CARTESIAN_POINT('Ctrl Pts',(49.3336023295367,4.79087807689359,125.696932558722));
#231982=CARTESIAN_POINT('Ctrl Pts',(49.0551547057238,-1.7074372515208,124.012969585086));
#231983=CARTESIAN_POINT('Ctrl Pts',(48.776707081911,-6.63670115873435,128.569963192402));
#231984=CARTESIAN_POINT('Ctrl Pts',(48.498259458098,-5.46716092194746,135.180258877061));
#231985=CARTESIAN_POINT('Ctrl Pts',(48.2198118342852,0.72643311645002,137.769317835757));
#231986=CARTESIAN_POINT('Ctrl Pts',(47.9413642104722,6.25247060906043,133.957921368012));
#231987=CARTESIAN_POINT('Ctrl Pts',(47.6629165866595,6.03279306211481,127.248556630613));
#231988=CARTESIAN_POINT('Ctrl Pts',(47.3844689628464,0.269273409411107,
123.806802046542));
#231989=CARTESIAN_POINT('Ctrl Pts',(47.1060213390337,-5.74169535180415,
126.7954619395));
#231990=CARTESIAN_POINT('Ctrl Pts',(46.8275737152206,-6.47632658212296,
133.468103872012));
#231991=CARTESIAN_POINT('Ctrl Pts',(46.5491260914079,-1.25953006961336,
137.69289588478));
#231992=CARTESIAN_POINT('Ctrl Pts',(46.2706784675948,5.11471304540623,135.587460510634));
#231993=CARTESIAN_POINT('Ctrl Pts',(45.9922308437821,6.78878473932087,129.086590002178));
#231994=CARTESIAN_POINT('Ctrl Pts',(45.7137832199691,2.22429490837156,124.164266771503));
#231995=CARTESIAN_POINT('Ctrl Pts',(45.4353355961562,-4.38421328052394,
125.343865398741));
#231996=CARTESIAN_POINT('Ctrl Pts',(45.1568879723434,-6.96384364534361,
131.541392372057));
#231997=CARTESIAN_POINT('Ctrl Pts',(44.8784403485304,-3.1440419027679,137.061623168999));
#231998=CARTESIAN_POINT('Ctrl Pts',(44.5999927247176,3.56498075346585,136.831735365442));
#231999=CARTESIAN_POINT('Ctrl Pts',(44.3215451009046,6.99796025625624,131.062984622213));
#232000=CARTESIAN_POINT('Ctrl Pts',(44.0430974770918,4.00015615291162,125.056571053198));
#232001=CARTESIAN_POINT('Ctrl Pts',(43.7646498532789,-2.67359603646683,
124.332095298706));
#232002=CARTESIAN_POINT('Ctrl Pts',(43.486202229466,-6.8904440807599,129.555315184507));
#232003=CARTESIAN_POINT('Ctrl Pts',(43.2077546056531,-4.77531063174146,
135.926346804027));
#232004=CARTESIAN_POINT('Ctrl Pts',(42.9293069818402,1.72810000095366,137.590523341125));
#232005=CARTESIAN_POINT('Ctrl Pts',(42.6508593580274,6.64347115515083,133.018547857752));
#232006=CARTESIAN_POINT('Ctrl Pts',(42.3724117342144,5.4538168693733,126.411842469708));
#232007=CARTESIAN_POINT('Ctrl Pts',(42.0939641104015,-0.74762868559244,
123.841646673103));
#232008=CARTESIAN_POINT('Ctrl Pts',(41.8155164865887,-6.26204000219037,
127.669844843974));
#232009=CARTESIAN_POINT('Ctrl Pts',(41.5370688627757,-6.02194247443641,
134.378509881167));
#232010=CARTESIAN_POINT('Ctrl Pts',(41.2586212389629,-0.247974000920424,
137.802706352008));
#232011=CARTESIAN_POINT('Ctrl Pts',(40.9801736151499,5.75387046523817,134.795764981093));
#232012=CARTESIAN_POINT('Ctrl Pts',(40.7017259913371,6.46818906604193,128.120917991039));
#232013=CARTESIAN_POINT('Ctrl Pts',(40.4232783675241,1.23855790375582,123.912023681303));
#232014=CARTESIAN_POINT('Ctrl Pts',(40.1448307437113,-5.12924746516435,
126.036850306614));
#232015=CARTESIAN_POINT('Ctrl Pts',(39.8663831198984,-6.78352499126783,
132.542786001862));
#232016=CARTESIAN_POINT('Ctrl Pts',(39.5879354960856,-2.20407444401526,
137.451193695743));
#232017=CARTESIAN_POINT('Ctrl Pts',(39.3094878722726,4.40081284226458,136.251486506627));
#232018=CARTESIAN_POINT('Ctrl Pts',(39.0310402484598,6.96156811816289,130.046136732356));
#232019=CARTESIAN_POINT('Ctrl Pts',(38.7525926246468,3.12498238497894,124.537557667297));
#232020=CARTESIAN_POINT('Ctrl Pts',(38.474145000834,-3.58330949612422,124.78786436319));
#232021=CARTESIAN_POINT('Ctrl Pts',(38.195697377021,-6.9987150046898,130.567037194673));
#232022=CARTESIAN_POINT('Ctrl Pts',(37.9172497532082,-3.98264333018119,
136.564298657899));
#232023=CARTESIAN_POINT('Ctrl Pts',(37.6388021293952,2.69328300182069,137.268458450676));
#232024=CARTESIAN_POINT('Ctrl Pts',(37.3603545055824,6.89421382933879,132.032428123559));
#232025=CARTESIAN_POINT('Ctrl Pts',(37.0819068817695,4.7596989487639,125.667863752866));
#232026=CARTESIAN_POINT('Ctrl Pts',(36.8034592579566,-1.74874674150458,
124.02348906901));
#232027=CARTESIAN_POINT('Ctrl Pts',(36.5250116341437,-6.65017960735793,
128.610404074285));
#232028=CARTESIAN_POINT('Ctrl Pts',(36.2465640103308,-5.44042229338459,
135.213457962098));
#232029=CARTESIAN_POINT('Ctrl Pts',(35.968116386518,0.768817328804687,137.764766786667));
#232030=CARTESIAN_POINT('Ctrl Pts',(35.689668762705,6.27155138463682,133.919802376575));
#232031=CARTESIAN_POINT('Ctrl Pts',(35.4112211388921,6.01103610030595,127.211899187745));
#232032=CARTESIAN_POINT('Ctrl Pts',(35.1327735150793,0.226672295232647,
123.805292551423));
#232033=CARTESIAN_POINT('Ctrl Pts',(34.8543258912663,-5.76599227560232,
126.830487544402));
#232034=CARTESIAN_POINT('Ctrl Pts',(34.5758782674535,-6.45999162954105,
133.507477757125));
#232035=CARTESIAN_POINT('Ctrl Pts',(34.2974306436406,-1.21757426406734,
137.700435373207));
#232036=CARTESIAN_POINT('Ctrl Pts',(34.0189830198277,5.1437343682746,135.556237180835));
#232037=CARTESIAN_POINT('Ctrl Pts',(33.7405353960148,6.778202401566,129.045296568894));
#232038=CARTESIAN_POINT('Ctrl Pts',(33.4620877722019,2.18383356141425,124.150849882625));
#232039=CARTESIAN_POINT('Ctrl Pts',(33.1836401483891,-4.41737163547663,
125.370654519698));
#232040=CARTESIAN_POINT('Ctrl Pts',(32.9051925245761,-6.95922809996586,
131.58376960941));
#232041=CARTESIAN_POINT('Ctrl Pts',(32.6267449007632,-3.10589391777991,
137.080645911863));
#232042=CARTESIAN_POINT('Ctrl Pts',(32.3482972769504,3.60160504349277,136.80992264244));
#232043=CARTESIAN_POINT('Ctrl Pts',(32.0698496531375,6.99940491798352,131.020381260171));
#232044=CARTESIAN_POINT('Ctrl Pts',(31.7914020293246,3.96509361278713,125.032327460544));
#232045=CARTESIAN_POINT('Ctrl Pts',(31.5129544055117,-2.71294501696876,
124.348490152723));
#232046=CARTESIAN_POINT('Ctrl Pts',(31.2345067816988,-6.89791971086261,
129.597282415287));
#232047=CARTESIAN_POINT('Ctrl Pts',(30.9560591578859,-4.74404317258561,
135.955320576696));
#232048=CARTESIAN_POINT('Ctrl Pts',(30.677611534073,1.76937728190418,137.579878174048));
#232049=CARTESIAN_POINT('Ctrl Pts',(30.3991639102601,6.65682645320975,132.978066139427));
#232050=CARTESIAN_POINT('Ctrl Pts',(30.1207162864473,5.42697731806706,126.378724921634));
#232051=CARTESIAN_POINT('Ctrl Pts',(29.8422686626343,-0.789998849798377,
123.846326704078));
#232052=CARTESIAN_POINT('Ctrl Pts',(29.5638210388214,-6.28100466828836,
127.708021734164));
#232053=CARTESIAN_POINT('Ctrl Pts',(29.2853734150086,-6.00007404075783,
134.415100933532));
#232054=CARTESIAN_POINT('Ctrl Pts',(29.0069257911957,-0.205368489683527,
137.804086176998));
#232055=CARTESIAN_POINT('Ctrl Pts',(28.7284781673828,5.77806067060162,134.760665586949));
#232056=CARTESIAN_POINT('Ctrl Pts',(28.4500305435699,6.45173434856014,128.08159400628));
#232057=CARTESIAN_POINT('Ctrl Pts',(28.171582919757,1.19657934493693,123.904611926838));
#232058=CARTESIAN_POINT('Ctrl Pts',(27.8931352959441,-5.15817362053239,
126.068161822712));
#232059=CARTESIAN_POINT('Ctrl Pts',(27.6146876721312,-6.77281701952304,
132.584047034882));
#232060=CARTESIAN_POINT('Ctrl Pts',(27.3362400483183,-2.16357244807759,
137.464487372053));
#232061=CARTESIAN_POINT('Ctrl Pts',(27.0577924245054,4.4338895067609,136.22459658713));
#232062=CARTESIAN_POINT('Ctrl Pts',(26.7793448006925,6.95682361243065,130.003773739425));
#232063=CARTESIAN_POINT('Ctrl Pts',(26.5008971768797,3.08677667800406,124.518651121888));
#232064=CARTESIAN_POINT('Ctrl Pts',(26.2224495530668,-3.61986722608435,
124.809788456898));
#232065=CARTESIAN_POINT('Ctrl Pts',(25.9440019292538,-7.00002998974624,
130.609644756432));
#232066=CARTESIAN_POINT('Ctrl Pts',(25.665554305441,-3.94750716330764,136.588435419948));
#232067=CARTESIAN_POINT('Ctrl Pts',(25.3871066816281,2.7325818997646,137.251943907838));
#232068=CARTESIAN_POINT('Ctrl Pts',(25.1086590578152,6.90156169100052,131.990438333922));
#232069=CARTESIAN_POINT('Ctrl Pts',(24.8302114340022,4.72834344823931,125.638985281792));
#232070=CARTESIAN_POINT('Ctrl Pts',(24.5517638101894,-1.78999143103474,
124.034259820624));
#232071=CARTESIAN_POINT('Ctrl Pts',(24.2733161863765,-6.66341163113055,
128.650926254035));
#232072=CARTESIAN_POINT('Ctrl Pts',(23.9948685625636,-5.41348206797292,
135.246493666413));
#232073=CARTESIAN_POINT('Ctrl Pts',(23.7164209387507,0.811173052350488,
137.759957817164));
#232074=CARTESIAN_POINT('Ctrl Pts',(23.4379733149379,6.29039976557031,133.881567941299));
#232075=CARTESIAN_POINT('Ctrl Pts',(23.159525691125,5.98905639734383,127.175374864857));
#232076=CARTESIAN_POINT('Ctrl Pts',(22.8810780673121,0.184062781628937,
123.804042409345));
#232077=CARTESIAN_POINT('Ctrl Pts',(22.6026304434992,-5.79007553843628,
126.865660402631));
#232078=CARTESIAN_POINT('Ctrl Pts',(22.3241828196863,-6.44341729959363,
133.546751477239));
#232079=CARTESIAN_POINT('Ctrl Pts',(22.0457351958734,-1.17557334085921,
137.707719325048));
#232080=CARTESIAN_POINT('Ctrl Pts',(21.7672875720605,5.17256508817436,135.524837768503));
#232081=CARTESIAN_POINT('Ctrl Pts',(21.4888399482477,6.76736889502847,129.004068318375));
#232082=CARTESIAN_POINT('Ctrl Pts',(21.2103923244347,2.14329129170119,124.137679542035));
#232083=CARTESIAN_POINT('Ctrl Pts',(20.9319447006219,-4.45036630309889,
125.397644988631));
#232084=CARTESIAN_POINT('Ctrl Pts',(20.6534970768089,-6.95435467783159,
131.626117965476));
#232085=CARTESIAN_POINT('Ctrl Pts',(20.3750494529961,-3.06763084275059,
137.099436084669));
#232086=CARTESIAN_POINT('Ctrl Pts',(20.0966018291831,3.6380958747203,136.787887381128));
#232087=CARTESIAN_POINT('Ctrl Pts',(19.8181542053702,7.00059021418742,130.977769893405));
#232088=CARTESIAN_POINT('Ctrl Pts',(19.5397065815574,3.92988414466092,125.0082977527));
#232089=CARTESIAN_POINT('Ctrl Pts',(19.2612589577445,-2.75219346829522,
124.365124231394));
#232090=CARTESIAN_POINT('Ctrl Pts',(18.9828113339316,-6.90513973601376,
129.639294374793));
#232091=CARTESIAN_POINT('Ctrl Pts',(18.7043637101187,-4.71259992116536,
135.98410347865));
#232092=CARTESIAN_POINT('Ctrl Pts',(18.4259160863058,1.81058899792882,137.568981937677));
#232093=CARTESIAN_POINT('Ctrl Pts',(18.1474684624929,6.6699350801164,132.937503873645));
#232094=CARTESIAN_POINT('Ctrl Pts',(17.86902083868,5.39993666812053,126.345771367118));
#232095=CARTESIAN_POINT('Ctrl Pts',(17.5905732148672,-0.832339740306418,
123.851264567558));
#232096=CARTESIAN_POINT('Ctrl Pts',(17.3121255910542,-6.29973658944851,
127.746313360329));
#232097=CARTESIAN_POINT('Ctrl Pts',(17.0336779672413,-5.97798327212915,
134.451558188587));
#232098=CARTESIAN_POINT('Ctrl Pts',(16.7552303434285,-0.162755368441711,
137.805206624583));
#232099=CARTESIAN_POINT('Ctrl Pts',(16.4767827196156,5.80203676780203,134.72541959047));
#232100=CARTESIAN_POINT('Ctrl Pts',(16.1983350958026,6.43504055968944,128.042370914639));
#232101=CARTESIAN_POINT('Ctrl Pts',(15.9198874719898,1.15455644643036,123.897455845098));
#232102=CARTESIAN_POINT('Ctrl Pts',(15.6414398481769,-5.18690863788001,
126.0996488404));
#232103=CARTESIAN_POINT('Ctrl Pts',(15.362992224364,-6.7618580785529,132.625242120967));
#232104=CARTESIAN_POINT('Ctrl Pts',(15.0845446005511,-2.12299028016722,
137.477534254917));
#232105=CARTESIAN_POINT('Ctrl Pts',(14.8060969767383,4.466801871851,136.197505818795));
#232106=CARTESIAN_POINT('Ctrl Pts',(14.5276493529253,6.95182131904109,129.961440412534));
#232107=CARTESIAN_POINT('Ctrl Pts',(14.2492017291125,3.04845658938423,124.499977495755));
#232108=CARTESIAN_POINT('Ctrl Pts',(13.9707541052995,-3.65629082053323,
124.831934681683));
#232109=CARTESIAN_POINT('Ctrl Pts',(13.6923064814867,-7.00108558611715,
130.652259533458));
#232110=CARTESIAN_POINT('Ctrl Pts',(13.4138588576738,-3.91222472010448,
136.612357850978));
#232111=CARTESIAN_POINT('Ctrl Pts',(13.1354112338608,2.77177954088132,137.23519044743));
#232112=CARTESIAN_POINT('Ctrl Pts',(12.856963610048,6.90865381275575,131.94840459374));
#232113=CARTESIAN_POINT('Ctrl Pts',(12.5785159862351,4.6968127372094,125.6102982156));
#232114=CARTESIAN_POINT('Ctrl Pts',(12.3000683624222,-1.83116979177416,
124.045281440813));
#232115=CARTESIAN_POINT('Ctrl Pts',(12.0216207386093,-6.67639673973472,
128.691528230086));
#232116=CARTESIAN_POINT('Ctrl Pts',(11.7431731147965,-5.38634124399241,
135.279364765853));
#232117=CARTESIAN_POINT('Ctrl Pts',(11.4647254909835,0.853498717580522,
137.75489110545));
#232118=CARTESIAN_POINT('Ctrl Pts',(11.1862778671706,6.30901505342741,133.843219478972));
#232119=CARTESIAN_POINT('Ctrl Pts',(10.9078302433578,5.96685476769427,127.13898501537));
#232120=CARTESIAN_POINT('Ctrl Pts',(10.6293826195448,0.141446447510913,
123.803051666633));
#232121=CARTESIAN_POINT('Ctrl Pts',(10.350934995732,-5.81394424789186,126.900979210845));
#232122=CARTESIAN_POINT('Ctrl Pts',(10.0724873719191,-6.42660420644864,
133.585923577051));
#232123=CARTESIAN_POINT('Ctrl Pts',(9.79403974810624,-1.1335288563486,137.714747470394));
#232124=CARTESIAN_POINT('Ctrl Pts',(9.51559212429333,5.20120413677258,135.493263437154));
#232125=CARTESIAN_POINT('Ctrl Pts',(9.23714450048043,6.75628462114785,128.962906778349));
#232126=CARTESIAN_POINT('Ctrl Pts',(8.95869687666756,2.10266960154115,124.124756237763));
#232127=CARTESIAN_POINT('Ctrl Pts',(8.68024925285465,-4.48319606076117,
125.4248358054));
#232128=CARTESIAN_POINT('Ctrl Pts',(8.40180162904178,-6.94922355952728,
131.66843587102));
#232129=CARTESIAN_POINT('Ctrl Pts',(8.12335400522884,-3.0292540955323,137.117992991138));
#232130=CARTESIAN_POINT('Ctrl Pts',(7.84490638141603,3.67445189496732,136.765630398031));
#232131=CARTESIAN_POINT('Ctrl Pts',(7.56645875760307,7.00151610094645,130.935152100895));
#232132=CARTESIAN_POINT('Ctrl Pts',(7.2880111337902,3.89452905323253,124.984482820099));
#232133=CARTESIAN_POINT('Ctrl Pts',(7.00956350997733,-2.79133993608059,
124.381996918337));
#232134=CARTESIAN_POINT('Ctrl Pts',(6.73111588616443,-6.91210388867261,
129.681349506257));
#232135=CARTESIAN_POINT('Ctrl Pts',(6.45266826235151,-4.68098204262199,
136.012694443327));
#232136=CARTESIAN_POINT('Ctrl Pts',(6.17422063853866,1.85173362191231,137.557835035774));
#232137=CARTESIAN_POINT('Ctrl Pts',(5.89577301472578,6.68279655012581,132.896862563455));
#232138=CARTESIAN_POINT('Ctrl Pts',(5.61732539091285,5.37269592153495,126.312983027266));
#232139=CARTESIAN_POINT('Ctrl Pts',(5.33887776709996,-0.874649788159289,
123.856460080569));
#232140=CARTESIAN_POINT('Ctrl Pts',(5.06043014328709,-6.31823507155263,
127.784718303561));
#232141=CARTESIAN_POINT('Ctrl Pts',(4.7819825194742,-5.95567098713191,134.487880295395));
#232142=CARTESIAN_POINT('Ctrl Pts',(4.50353489566127,-0.120136216239877,
137.806067653244));
#232143=CARTESIAN_POINT('Ctrl Pts',(4.22508727184843,5.82579786839633,134.690028297709));
#232144=CARTESIAN_POINT('Ctrl Pts',(3.94663964803551,6.41810831802433,128.003250169541));
#232145=CARTESIAN_POINT('Ctrl Pts',(3.66819202422262,1.11249076541009,123.890555701254));
#232146=CARTESIAN_POINT('Ctrl Pts',(3.3897444004097,-5.21545145242058,126.131310192911));
#232147=CARTESIAN_POINT('Ctrl Pts',(3.11129677659686,-6.75064857444498,
132.666369733619));
#232148=CARTESIAN_POINT('Ctrl Pts',(2.83284915278395,-2.08232944407128,
137.490333860877));
#232149=CARTESIAN_POINT('Ctrl Pts',(2.55440152897106,4.49954871795507,136.170215205482));
#232150=CARTESIAN_POINT('Ctrl Pts',(2.27595390515816,6.94656142335602,129.919138320362));
#232151=CARTESIAN_POINT('Ctrl Pts',(1.9975062813453,3.01002353908442,124.481537480858));
#232152=CARTESIAN_POINT('Ctrl Pts',(1.71905865753238,-3.69257892978116,
124.854302216906));
#232153=CARTESIAN_POINT('Ctrl Pts',(1.44061103371947,-7.00188175468703,
130.694879946647));
#232154=CARTESIAN_POINT('Ctrl Pts',(1.16216340990662,-3.87679730797559,
136.636065064534));
#232155=CARTESIAN_POINT('Ctrl Pts',(0.883715786093727,2.81087447268782,
137.218198690258));
#232156=CARTESIAN_POINT('Ctrl Pts',(0.605268162280799,6.91548993180329,
131.906328460586));
#232157=CARTESIAN_POINT('Ctrl Pts',(0.326820538467947,4.66510798405627,
125.5818036173));
#232158=CARTESIAN_POINT('Ctrl Pts',(0.0483729146550416,-1.87228029784353,
124.056553521165));
#232159=CARTESIAN_POINT('Ctrl Pts',(-0.23007470915786,-6.68913445200245,
128.732208497919));
#232160=CARTESIAN_POINT('Ctrl Pts',(-0.508522332970751,-5.35900082715629,
135.312070042369));
#232161=CARTESIAN_POINT('Ctrl Pts',(-0.786969956783612,0.895792756101716,
137.749566839272));
#232162=CARTESIAN_POINT('Ctrl Pts',(-1.06541758059653,6.32739655841135,
133.804758410613));
#232163=CARTESIAN_POINT('Ctrl Pts',(-1.34386520440944,5.94443203404716,
127.102730987725));
#232164=CARTESIAN_POINT('Ctrl Pts',(-1.62231282822229,0.0988248720430084,
123.802320359999));
#232165=CARTESIAN_POINT('Ctrl Pts',(-1.90076045203519,-5.83759751950527,
126.936442660293));
#232166=CARTESIAN_POINT('Ctrl Pts',(-2.17920807584809,-6.40955297312139,
133.624992605024));
#232167=CARTESIAN_POINT('Ctrl Pts',(-2.45765569966099,-1.09144236850938,
137.721519548813));
#232168=CARTESIAN_POINT('Ctrl Pts',(-2.73610332347384,5.22965045283876,
135.461515356786));
#232169=CARTESIAN_POINT('Ctrl Pts',(-3.01455094728676,6.74494999065597,
128.921813474073));
#232170=CARTESIAN_POINT('Ctrl Pts',(-3.29299857109967,2.06196999618574,
124.112080448687));
#232171=CARTESIAN_POINT('Ctrl Pts',(-3.57144619491253,-4.51585969194472,
125.452225962441));
#232172=CARTESIAN_POINT('Ctrl Pts',(-3.84989381872542,-6.94383493518842,
131.710721757939));
#232173=CARTESIAN_POINT('Ctrl Pts',(-4.12834144253832,-2.99076509818949,
137.136315943637));
#232174=CARTESIAN_POINT('Ctrl Pts',(-4.40678906635123,3.71067175704807,
136.743152517891));
#232175=CARTESIAN_POINT('Ctrl Pts',(-4.68523669016409,7.00218254395157,
130.892529461858));
#232176=CARTESIAN_POINT('Ctrl Pts',(-4.963684313977,3.85902964859785,124.960883545208));
#232177=CARTESIAN_POINT('Ctrl Pts',(-5.24213193778992,-2.83038296973812,
124.399107588329));
#232178=CARTESIAN_POINT('Ctrl Pts',(-5.52057956160276,-6.91881191077996,
129.723446251312));
#232179=CARTESIAN_POINT('Ctrl Pts',(-5.79902718541567,-4.6491907085676,
136.041092411279));
#232180=CARTESIAN_POINT('Ctrl Pts',(-6.07747480922856,1.89280962922548,
137.546437881394));
#232181=CARTESIAN_POINT('Ctrl Pts',(-6.35592243304147,6.69541038665145,
132.856143714835));
#232182=CARTESIAN_POINT('Ctrl Pts',(-6.63437005685431,5.34525608772619,
126.280361117063));
#232183=CARTESIAN_POINT('Ctrl Pts',(-6.91281768066725,-0.916927425542613,
123.86191305059));
#232184=CARTESIAN_POINT('Ctrl Pts',(-7.19126530448013,-6.33649942913263,
127.823235140749));
#232185=CARTESIAN_POINT('Ctrl Pts',(-7.469712928293,-5.93313801255607,134.524065908027));
#232186=CARTESIAN_POINT('Ctrl Pts',(-7.74816055210589,-0.0775126123463511,
137.806669231077));
#232187=CARTESIAN_POINT('Ctrl Pts',(-8.02660817591882,5.84934309190818,
134.654493020103));
#232188=CARTESIAN_POINT('Ctrl Pts',(-8.3050557997317,6.40093825099524,127.964233220621));
#232189=CARTESIAN_POINT('Ctrl Pts',(-8.58350342354456,1.07038386063539,
123.883911750995));
#232190=CARTESIAN_POINT('Ctrl Pts',(-8.86195104735747,-5.2438010064896,
126.163144707024));
#232191=CARTESIAN_POINT('Ctrl Pts',(-9.14039867117038,-6.73918892257159,
132.707428348838));
#232192=CARTESIAN_POINT('Ctrl Pts',(-9.41884629498326,-2.04159144649203,
137.50288571564));
#232193=CARTESIAN_POINT('Ctrl Pts',(-9.69729391879612,4.53212883162697,
136.142725758454));
#232194=CARTESIAN_POINT('Ctrl Pts',(-9.97574154260907,6.94104412028278,
129.876869030427));
#232195=CARTESIAN_POINT('Ctrl Pts',(-10.254189166422,2.97147895125515,124.463331760497));
#232196=CARTESIAN_POINT('Ctrl Pts',(-10.5326367902348,-3.72873020915888,
124.876890233732));
#232197=CARTESIAN_POINT('Ctrl Pts',(-10.8110844140478,-7.00241846595355,
130.737504416682));
#232198=CARTESIAN_POINT('Ctrl Pts',(-11.0895320378606,-3.84122623969676,
136.659556182137));
#232199=CARTESIAN_POINT('Ctrl Pts',(-11.3679796616735,2.84986524650705,
137.200969265957));
#232200=CARTESIAN_POINT('Ctrl Pts',(-11.6464272854864,6.92206979482823,
131.864211493609));
#232201=CARTESIAN_POINT('Ctrl Pts',(-11.9248749092993,4.6332303636112,125.553502542771));
#232202=CARTESIAN_POINT('Ctrl Pts',(-12.2033225331122,-1.91332142587795,
124.068075643991));
#232203=CARTESIAN_POINT('Ctrl Pts',(-12.4817701569251,-6.70162429593314,
128.77296555011));
#232204=CARTESIAN_POINT('Ctrl Pts',(-12.760217780738,-5.33146183057377,
135.344608284054));
#232205=CARTESIAN_POINT('Ctrl Pts',(-13.0386654045509,0.938053600692905,
137.743985215925));
#232206=CARTESIAN_POINT('Ctrl Pts',(-13.3171130283637,6.34554359938892,
133.766186161411));
#232207=CARTESIAN_POINT('Ctrl Pts',(-13.5955606521767,5.92178902728497,
127.066614125326));
#232208=CARTESIAN_POINT('Ctrl Pts',(-13.8740082759896,0.0561996345831295,
123.801848516541));
#232209=CARTESIAN_POINT('Ctrl Pts',(-14.1524558998025,-5.86103447679583,
126.972049436864));
#232210=CARTESIAN_POINT('Ctrl Pts',(-14.4309035236153,-6.39226423145161,
133.663957113442));
#232211=CARTESIAN_POINT('Ctrl Pts',(-14.7093511474282,-1.04931543687181,
137.728035309365));
#232212=CARTESIAN_POINT('Ctrl Pts',(-14.9877987712411,5.25790298228423,
135.429594703837));
#232213=CARTESIAN_POINT('Ctrl Pts',(-15.266246395054,6.73336542356173,128.880789928272));
#232214=CARTESIAN_POINT('Ctrl Pts',(-15.5446940188669,2.02119398377386,
124.099652644515));
#232215=CARTESIAN_POINT('Ctrl Pts',(-15.8231416426798,-4.54835598628669,
125.479814444798));
#232216=CARTESIAN_POINT('Ctrl Pts',(-16.1015892664927,-6.93818900449243,
131.752974059312));
#232217=CARTESIAN_POINT('Ctrl Pts',(-16.3800368903055,-2.95216527694612,
137.154404263204));
#232218=CARTESIAN_POINT('Ctrl Pts',(-16.6584845141185,3.74675411882228,
136.720454573632));
#232219=CARTESIAN_POINT('Ctrl Pts',(-16.9369321379314,7.00258951850748,
130.849903555692));
#232220=CARTESIAN_POINT('Ctrl Pts',(-17.2153797617442,3.82338724620039,
124.93750080251));
#232221=CARTESIAN_POINT('Ctrl Pts',(-17.4938273855571,-2.86932112251383,
124.416455607327));
#232222=CARTESIAN_POINT('Ctrl Pts',(-17.77227500937,-6.92526355376757,129.765583050046));
#232223=CARTESIAN_POINT('Ctrl Pts',(-18.0507226331829,-4.61722709704176,
136.069296330209));
#232224=CARTESIAN_POINT('Ctrl Pts',(-18.3291702569958,1.93381549778173,
137.534790896862));
#232225=CARTESIAN_POINT('Ctrl Pts',(-18.6076178808087,6.70777612228299,
132.81534883664));
#232226=CARTESIAN_POINT('Ctrl Pts',(-18.8860655046216,5.31761818348739,
126.247906845325));
#232227=CARTESIAN_POINT('Ctrl Pts',(-19.1645131284344,-0.959171085842972,
123.867623275557));
#232228=CARTESIAN_POINT('Ctrl Pts',(-19.4429607522474,-6.35452898539608,
127.861862444637));
#232229=CARTESIAN_POINT('Ctrl Pts',(-19.7214083760603,-5.91038518336925,
134.560113685611));
#232230=CARTESIAN_POINT('Ctrl Pts',(-19.9998559998732,-0.0348861361944895,
137.807011335788));
#232231=CARTESIAN_POINT('Ctrl Pts',(-20.278303623686,5.87267156586067,134.618815074426));
#232232=CARTESIAN_POINT('Ctrl Pts',(-20.5567512474989,6.38353099484532,
127.925321513668));
#232233=CARTESIAN_POINT('Ctrl Pts',(-20.8351988713118,1.02823729239309,
123.877524240513));
#232234=CARTESIAN_POINT('Ctrl Pts',(-21.1136464951247,-5.27195624958391,
126.1951512031));
#232235=CARTESIAN_POINT('Ctrl Pts',(-21.3920941189376,-6.72747954757436,
132.748416445183));
#232236=CARTESIAN_POINT('Ctrl Pts',(-21.6705417427505,-2.00077779699093,
137.515189354092));
#232237=CARTESIAN_POINT('Ctrl Pts',(-21.9489893665634,4.56454100559805,
136.115038496344));
#232238=CARTESIAN_POINT('Ctrl Pts',(-22.2274369903762,6.93526961426714,
129.834634109035));
#232239=CARTESIAN_POINT('Ctrl Pts',(-22.5058846141892,2.93282425418085,
124.445361009293));
#232240=CARTESIAN_POINT('Ctrl Pts',(-22.784332238002,-3.76474331906749,
124.899697895151));
#232241=CARTESIAN_POINT('Ctrl Pts',(-23.062779861815,-7.0026957000287,130.780131364099));
#232242=CARTESIAN_POINT('Ctrl Pts',(-23.3412274856278,-3.80551283336702,
136.682830333316));
#232243=CARTESIAN_POINT('Ctrl Pts',(-23.6196751094408,2.88875041752152,
137.183502812971));
#232244=CARTESIAN_POINT('Ctrl Pts',(-23.8981227332536,6.92839315801137,
131.822055253468));
#232245=CARTESIAN_POINT('Ctrl Pts',(-24.1765703570665,4.60118105711114,
125.525396040718));
#232246=CARTESIAN_POINT('Ctrl Pts',(-24.4550179808794,-1.95429165508329,
124.079847382335));
#232247=CARTESIAN_POINT('Ctrl Pts',(-24.7334656046923,-6.71386580871103,
128.813797876394));
#232248=CARTESIAN_POINT('Ctrl Pts',(-25.0119132285052,-5.30372527471246,
135.376978285193));
#232249=CARTESIAN_POINT('Ctrl Pts',(-25.290360852318,0.980279685362951,
137.738146442235));
#232250=CARTESIAN_POINT('Ctrl Pts',(-25.568808476131,6.36345550391485,133.727504160674));
#232251=CARTESIAN_POINT('Ctrl Pts',(-25.8472560999438,5.89892658645264,
127.030635766497));
#232252=CARTESIAN_POINT('Ctrl Pts',(-26.1257037237567,0.0135723146251221,
123.801636153745));
#232253=CARTESIAN_POINT('Ctrl Pts',(-26.4041513475696,-5.88425425129846,
127.007798221134));
#232254=CARTESIAN_POINT('Ctrl Pts',(-26.6825989713826,-6.37473862207999,
133.70281565846));
#232255=CARTESIAN_POINT('Ctrl Pts',(-26.9610465951954,-1.00714962246484,
137.734294510605));
#232256=CARTESIAN_POINT('Ctrl Pts',(-27.2394942190083,5.28596067820108,
135.397502661138));
#232257=CARTESIAN_POINT('Ctrl Pts',(-27.5179418428212,6.72153134913555,
128.839837661092));
#232258=CARTESIAN_POINT('Ctrl Pts',(-27.7963894666341,1.98034307527561,
124.087473285763));
#232259=CARTESIAN_POINT('Ctrl Pts',(-28.0748370904469,-4.58068373962494,
125.507600230172));
#232260=CARTESIAN_POINT('Ctrl Pts',(-28.3532847142599,-6.93228597665136,
131.795191209466));
#232261=CARTESIAN_POINT('Ctrl Pts',(-28.6317323380727,-2.91345606213275,
137.172257279568));
#232262=CARTESIAN_POINT('Ctrl Pts',(-28.9101799618857,3.78269764324474,
136.697537406337));
#232263=CARTESIAN_POINT('Ctrl Pts',(-29.1886275856985,7.00273700953358,
130.807275961916));
#232264=CARTESIAN_POINT('Ctrl Pts',(-29.4670752095115,3.78760316678249,
124.914335458459));
#232265=CARTESIAN_POINT('Ctrl Pts',(-29.7455228333243,-2.90815295154017,
124.434040332496));
#232266=CARTESIAN_POINT('Ctrl Pts',(-30.0239704571372,-6.93145857856742,
129.807758341064));
#232267=CARTESIAN_POINT('Ctrl Pts',(-30.3024180809501,-4.5850923924679,
136.097305155009));
#232268=CARTESIAN_POINT('Ctrl Pts',(-30.580865704763,1.97474970809384,137.52289451376));
#232269=CARTESIAN_POINT('Ctrl Pts',(-30.8593133285759,6.71989329880362,
132.774479440534));
#232270=CARTESIAN_POINT('Ctrl Pts',(-31.1377609523888,5.28978323295099,
126.215621414657));
#232271=CARTESIAN_POINT('Ctrl Pts',(-31.4162085762017,-1.00137920370602,
123.873590543879));
#232272=CARTESIAN_POINT('Ctrl Pts',(-31.6946562000146,-6.37232307225107,
127.900598783877));
#232273=CARTESIAN_POINT('Ctrl Pts',(-31.9731038238274,-5.88741334268594,
134.596022292384));
#232274=CARTESIAN_POINT('Ctrl Pts',(-32.2515514476404,0.00774163267598956,
137.807093954702));
#232275=CARTESIAN_POINT('Ctrl Pts',(-32.5299990714533,5.89578242580862,
134.582995782735));
#232276=CARTESIAN_POINT('Ctrl Pts',(-32.8084466952661,6.36588719460685,
127.886516490566));
#232277=CARTESIAN_POINT('Ctrl Pts',(-33.086894319079,0.9860526224398,123.8713934065));
#232278=CARTESIAN_POINT('Ctrl Pts',(-33.365341942892,-5.29991613840065,
126.227328495126));
#232279=CARTESIAN_POINT('Ctrl Pts',(-33.6437895667048,-6.71552088334846,
132.789332503824));
#232280=CARTESIAN_POINT('Ctrl Pts',(-33.9222371905177,-1.95989000793276,
137.527244320318));
#232281=CARTESIAN_POINT('Ctrl Pts',(-34.2006848143306,4.59678403882356,
136.08715444511));
#232282=CARTESIAN_POINT('Ctrl Pts',(-34.4791324381435,6.9292381192855,129.792435121214));
#232283=CARTESIAN_POINT('Ctrl Pts',(-34.7575800619564,2.89406088022529,
124.427625893158));
#232284=CARTESIAN_POINT('Ctrl Pts',(-35.0360276857693,-3.80061692502793,
124.922724356021));
#232285=CARTESIAN_POINT('Ctrl Pts',(-35.3144753095821,-7.00271344663942,
130.822759209339));
#232286=CARTESIAN_POINT('Ctrl Pts',(-35.592922933395,-3.76965841235978,
136.705886655638));
#232287=CARTESIAN_POINT('Ctrl Pts',(-35.8713705572079,2.92752854482695,
137.165799978524));
#232288=CARTESIAN_POINT('Ctrl Pts',(-36.1498181810209,6.9344597870381,131.779861302279));
#232289=CARTESIAN_POINT('Ctrl Pts',(-36.4282658048337,4.56896125215494,
125.49748515264));
#232290=CARTESIAN_POINT('Ctrl Pts',(-36.7067134286466,-1.99518946729269,
124.091868299989));
#232291=CARTESIAN_POINT('Ctrl Pts',(-36.9851610524595,-6.72585853672236,
128.854703963711));
#232292=CARTESIAN_POINT('Ctrl Pts',(-37.2636086762724,-5.27579218736066,
135.409178846303));
#232293=CARTESIAN_POINT('Ctrl Pts',(-37.5420563000852,1.02246944540875,
137.732050734562));
#232294=CARTESIAN_POINT('Ctrl Pts',(-37.8205039238982,6.38113160825695,
133.688713841779));
#232295=CARTESIAN_POINT('Ctrl Pts',(-38.0989515477111,5.87584555872632,
126.994797244432));
#232296=CARTESIAN_POINT('Ctrl Pts',(-38.377399171524,-0.0290555082599903,
123.801683279478));
#232297=CARTESIAN_POINT('Ctrl Pts',(-38.6558467953367,-5.90725598259587,
127.04368768842));
#232298=CARTESIAN_POINT('Ctrl Pts',(-38.9342944191497,-6.35697679442443,
133.741566800161));
#232299=CARTESIAN_POINT('Ctrl Pts',(-39.2127420429625,-0.964946487758246,
137.740296920595));
#232300=CARTESIAN_POINT('Ctrl Pts',(-39.4911896667755,5.31382250090111,
135.365240417872));
#232301=CARTESIAN_POINT('Ctrl Pts',(-39.7696372905882,6.70944820589337,
128.798958190032));
#232302=CARTESIAN_POINT('Ctrl Pts',(-40.0480849144012,1.93941878443644,
124.07554282374));
#232303=CARTESIAN_POINT('Ctrl Pts',(-40.3265325382142,-4.61284175404266,
125.535582288951));
#232304=CARTESIAN_POINT('Ctrl Pts',(-40.604980162027,-6.9261260704041,131.837371644027));
#232305=CARTESIAN_POINT('Ctrl Pts',(-40.8834277858398,-2.87463888813357,
137.18987433118));
#232306=CARTESIAN_POINT('Ctrl Pts',(-41.1618754096529,3.81850099841496,
136.674401865208));
#232307=CARTESIAN_POINT('Ctrl Pts',(-41.4403230334656,7.00262501156454,
130.76464826011));
#232308=CARTESIAN_POINT('Ctrl Pts',(-41.7187706572786,3.75167873633635,
124.891388371457));
#232309=CARTESIAN_POINT('Ctrl Pts',(-41.9972182810916,-2.94687701788942,
124.451861112224));
#232310=CARTESIAN_POINT('Ctrl Pts',(-42.2756659049044,-6.93739675562063,
129.849970561546));
#232311=CARTESIAN_POINT('Ctrl Pts',(-42.5541135287174,-4.55278778560923,
136.125117847804));
#232312=CARTESIAN_POINT('Ctrl Pts',(-42.8325611525302,2.01561074332903,
137.510749172913));
#232313=CARTESIAN_POINT('Ctrl Pts',(-43.1110087763431,6.73176146720674,
132.733537040953));
#232314=CARTESIAN_POINT('Ctrl Pts',(-43.389456400156,5.26175226755184,126.183506021407));
#232315=CARTESIAN_POINT('Ctrl Pts',(-43.6679040239687,-1.0435502150944,
123.879814634434));
#232316=CARTESIAN_POINT('Ctrl Pts',(-43.9463516477818,-6.38988103033122,
127.93944272308));
#232317=CARTESIAN_POINT('Ctrl Pts',(-44.2247992715946,-5.86422334173611,
134.631790397739));
#232318=CARTESIAN_POINT('Ctrl Pts',(-44.5032468954075,0.050369114677416,
137.806917084757));
#232319=CARTESIAN_POINT('Ctrl Pts',(-44.7816945192204,5.91867481537061,
134.547036472328));
#232320=CARTESIAN_POINT('Ctrl Pts',(-45.0601421430334,6.34800750407734,
127.847819589252));
#232321=CARTESIAN_POINT('Ctrl Pts',(-45.3385897668461,0.943831413943965,
123.865519476137));
#232322=CARTESIAN_POINT('Ctrl Pts',(-45.6170373906592,-5.32767963687585,
126.25967539076));
#232323=CARTESIAN_POINT('Ctrl Pts',(-45.895485014472,-6.7033133730266,132.830175008601));
#232324=CARTESIAN_POINT('Ctrl Pts',(-46.1739326382849,-1.91892959442962,
137.539050167615));
#232325=CARTESIAN_POINT('Ctrl Pts',(-46.4523802620978,4.62885673652604,
136.059074638009));
#232326=CARTESIAN_POINT('Ctrl Pts',(-46.7308278859106,6.92294985883713,
129.750273630666));
#232327=CARTESIAN_POINT('Ctrl Pts',(-47.0092755097235,2.8551902657795,124.410127069272));
#232328=CARTESIAN_POINT('Ctrl Pts',(-47.2877231335364,-3.83634969773052,
124.945968763085));
#232329=CARTESIAN_POINT('Ctrl Pts',(-47.5661707573492,-7.00247170512816,
130.865386372813));
#232330=CARTESIAN_POINT('Ctrl Pts',(-47.8446183811622,-3.73366430527375,
136.728724294741));
#232331=CARTESIAN_POINT('Ctrl Pts',(-48.123066004975,2.96619819148554,137.147861418602));
#232332=CARTESIAN_POINT('Ctrl Pts',(-48.4015136287881,6.9402694571073,131.737631203552));
#232333=CARTESIAN_POINT('Ctrl Pts',(-48.6799612526008,4.53657214265928,
125.469770912784));
#232334=CARTESIAN_POINT('Ctrl Pts',(-48.9584088764139,-2.03601334702262,
124.104137951514));
#232335=CARTESIAN_POINT('Ctrl Pts',(-49.2368565002267,-6.7376020355722,
128.895682296272));
#232336=CARTESIAN_POINT('Ctrl Pts',(-49.5153041240395,-5.24766360358919,
135.441208774179));
#232337=CARTESIAN_POINT('Ctrl Pts',(-49.7937517478526,1.06462131747325,
137.725698318783));
#232338=CARTESIAN_POINT('Ctrl Pts',(-50.0721993716652,6.39857125742062,
133.649816642113));
#232339=CARTESIAN_POINT('Ctrl Pts',(-50.3506469954783,5.85254679938199,
126.959099887138));
#232340=CARTESIAN_POINT('Ctrl Pts',(-50.6290946192911,-0.0716822544825644,
123.801989891996));
#232341=CARTESIAN_POINT('Ctrl Pts',(-50.907542243104,-5.93003881835047,
127.079716508824));
#232342=CARTESIAN_POINT('Ctrl Pts',(-51.1859898669169,-6.33897940665598,
133.780209102606));
#232343=CARTESIAN_POINT('Ctrl Pts',(-51.4644374907297,-0.922707596604453,
137.746042316915));
#232344=CARTESIAN_POINT('Ctrl Pts',(-51.7428851145428,5.34148741795441,
135.332809169526));
#232345=CARTESIAN_POINT('Ctrl Pts',(-52.0213327383556,6.69711644158035,
128.758153029896));
#232346=CARTESIAN_POINT('Ctrl Pts',(-52.2997803621686,1.89842262772099,
124.063861700536));
#232347=CARTESIAN_POINT('Ctrl Pts',(-52.5782279859813,-4.64482883791282,
125.563759584248));
#232348=CARTESIAN_POINT('Ctrl Pts',(-52.8566756097944,-6.91970951400822,
131.879513799985));
#232349=CARTESIAN_POINT('Ctrl Pts',(-53.135123233607,-2.83571519333325,
137.207254765232));
#232350=CARTESIAN_POINT('Ctrl Pts',(-53.4135708574202,3.85416285762642,
136.651048807542));
#232351=CARTESIAN_POINT('Ctrl Pts',(-53.6920184812329,7.0022535287505,130.72202202986));
#232352=CARTESIAN_POINT('Ctrl Pts',(-53.9704661050458,3.71561528605495,
124.868660391816));
#232353=CARTESIAN_POINT('Ctrl Pts',(-54.2489137288587,-2.98549188662705,
124.469917286158));
#232354=CARTESIAN_POINT('Ctrl Pts',(-54.5273613526715,-6.94307786488582,
129.892218147303));
#232355=CARTESIAN_POINT('Ctrl Pts',(-54.8058089764845,-4.5203144735249,
136.152733377983));
#232356=CARTESIAN_POINT('Ctrl Pts',(-55.0842566002972,2.05639708936689,
137.498355324372));
#232357=CARTESIAN_POINT('Ctrl Pts',(-55.3627042241104,6.74338018771311,
132.69252315503));
#232358=CARTESIAN_POINT('Ctrl Pts',(-55.6411518479232,5.23352632598741,
126.151561855625));
#232359=CARTESIAN_POINT('Ctrl Pts',(-55.919599471736,-1.08568255734582,
123.886295316588));
#232360=CARTESIAN_POINT('Ctrl Pts',(-56.1980470955489,-6.40720220901991,
127.978392822871));
#232361=CARTESIAN_POINT('Ctrl Pts',(-56.4764947193619,-5.8408160398338,
134.667416676276));
#232362=CARTESIAN_POINT('Ctrl Pts',(-56.7549423431748,0.0929947302327828,
137.806480732508));
#232363=CARTESIAN_POINT('Ctrl Pts',(-57.0333899669875,5.94134788626073,
134.510938475691));
#232364=CARTESIAN_POINT('Ctrl Pts',(-57.3118375908005,6.32989258579528,
127.809232243652));
#232365=CARTESIAN_POINT('Ctrl Pts',(-57.5902852146133,0.901575231427987,
123.859902667085));
#232366=CARTESIAN_POINT('Ctrl Pts',(-57.8687328384263,-5.35524571622284,
126.292190691378));
#232367=CARTESIAN_POINT('Ctrl Pts',(-58.1471804622391,-6.69085746896258,
132.870942446081));
#232368=CARTESIAN_POINT('Ctrl Pts',(-58.4256280860521,-1.87789807428466,
137.550606458515));
#232369=CARTESIAN_POINT('Ctrl Pts',(-58.7040757098649,4.6607579102399,136.030800115547));
#232370=CARTESIAN_POINT('Ctrl Pts',(-58.9825233336777,6.91640506593584,
129.708151199698));
#232371=CARTESIAN_POINT('Ctrl Pts',(-59.2609709574908,2.81621385120844,
124.392865186062));
#232372=CARTESIAN_POINT('Ctrl Pts',(-59.5394185813036,-3.87194031308425,
124.969430255013));
#232373=CARTESIAN_POINT('Ctrl Pts',(-59.8178662051166,-7.00197048445272,
130.908011274954));
#232374=CARTESIAN_POINT('Ctrl Pts',(-60.0963138289294,-3.69753184588372,
136.751342404371));
#232375=CARTESIAN_POINT('Ctrl Pts',(-60.3747614527424,3.00475792457964,
137.129687797925));
#232376=CARTESIAN_POINT('Ctrl Pts',(-60.6532090765552,6.94582195293937,
131.695366522141));
#232377=CARTESIAN_POINT('Ctrl Pts',(-60.9316567003681,4.50401492881459,
125.442254348109));
#232378=CARTESIAN_POINT('Ctrl Pts',(-61.210104324181,-2.07676178152925,
124.116655882255));
#232379=CARTESIAN_POINT('Ctrl Pts',(-61.4885519479939,-6.74909587010084,
128.93673135561));
#232380=CARTESIAN_POINT('Ctrl Pts',(-61.7669995718066,-5.21934056571308,
135.473066881942));
#232381=CARTESIAN_POINT('Ctrl Pts',(-62.0454471956197,1.10673373960332,
137.719089430292));
#232382=CARTESIAN_POINT('Ctrl Pts',(-62.3238948194324,6.41577380517329,
133.610814003028));
#232383=CARTESIAN_POINT('Ctrl Pts',(-62.6023424432454,5.82903117176375,
126.923545017394));
#232384=CARTESIAN_POINT('Ctrl Pts',(-62.8807900670583,-0.114306344492842,
123.802555979936));
#232385=CARTESIAN_POINT('Ctrl Pts',(-63.1592376908712,-5.95260191433588,
127.115883347286));
#232386=CARTESIAN_POINT('Ctrl Pts',(-63.4376853146842,-6.32074712567447,
133.818741133891));
#232387=CARTESIAN_POINT('Ctrl Pts',(-63.716132938497,-0.880434514181572,
137.751530486667));
#232388=CARTESIAN_POINT('Ctrl Pts',(-63.99458056231,5.36895440422691,135.300210117855));
#232389=CARTESIAN_POINT('Ctrl Pts',(-64.2730281861228,6.6845365131549,128.717423692735));
#232390=CARTESIAN_POINT('Ctrl Pts',(-64.5514758099358,1.85735612425694,
124.052430348997));
#232391=CARTESIAN_POINT('Ctrl Pts',(-64.8299234337484,-4.67664380594228,
125.592131071942));
#232392=CARTESIAN_POINT('Ctrl Pts',(-65.1083710575615,-6.91303654523158,
131.921616115747));
#232393=CARTESIAN_POINT('Ctrl Pts',(-65.3868186813742,-2.79668642006362,
137.224397937687));
#232394=CARTESIAN_POINT('Ctrl Pts',(-65.6652663051872,3.88968189941585,
136.627479098696));
#232395=CARTESIAN_POINT('Ctrl Pts',(-65.9437139290001,7.00162257485687,
130.679398850698));
#232396=CARTESIAN_POINT('Ctrl Pts',(-66.2221615528129,3.67941415228271,
124.846152361731));
#232397=CARTESIAN_POINT('Ctrl Pts',(-66.500609176626,-3.02399612686491,
124.48820818522));
#232398=CARTESIAN_POINT('Ctrl Pts',(-66.7790568004388,-6.94850169584742,
129.934499532835));
#232399=CARTESIAN_POINT('Ctrl Pts',(-67.0575044242516,-4.48767365952541,
136.180150722241));
#232400=CARTESIAN_POINT('Ctrl Pts',(-67.3359520480646,2.09710723485436,
137.485713427398));
#232401=CARTESIAN_POINT('Ctrl Pts',(-67.6143996718775,6.75474902978674,
132.651439302549));
#232402=CARTESIAN_POINT('Ctrl Pts',(-67.8928472956903,5.20510645418034,
126.119790101011));
#232403=CARTESIAN_POINT('Ctrl Pts',(-68.1712949195033,-1.12777466923081,
123.893032350195));
#232404=CARTESIAN_POINT('Ctrl Pts',(-68.449742543316,-6.42428596647451,
128.017447639935));
#232405=CARTESIAN_POINT('Ctrl Pts',(-68.728190167129,-5.81719230434518,
134.702899807851));
#232406=CARTESIAN_POINT('Ctrl Pts',(-69.0066377909419,0.135616899834216,
137.805784914121));
#232407=CARTESIAN_POINT('Ctrl Pts',(-69.2850854147548,5.96380079832,134.474703130449));
#232408=CARTESIAN_POINT('Ctrl Pts',(-69.5635330385676,6.31154311101565,
127.770755883637));
#232409=CARTESIAN_POINT('Ctrl Pts',(-69.8419806623805,0.859285640710264,
123.854543187474));
#232410=CARTESIAN_POINT('Ctrl Pts',(-70.1204282861936,-5.38261335497044,
126.324873192109));
#232411=CARTESIAN_POINT('Ctrl Pts',(-70.3988759100064,-6.67815363271447,
132.911633305611));
#232412=CARTESIAN_POINT('Ctrl Pts',(-70.6773235338194,-1.83679696793597,
137.561912764793));
#232413=CARTESIAN_POINT('Ctrl Pts',(-70.9557711576322,4.69248637785542,
136.002331925448));
#232414=CARTESIAN_POINT('Ctrl Pts',(-71.2342187814451,6.90960398310133,
129.666069389173));
#232415=CARTESIAN_POINT('Ctrl Pts',(-71.5126664052579,2.77713308079745,
124.375840883174));
#232416=CARTESIAN_POINT('Ctrl Pts',(-71.7911140290708,-3.90738745226578,
124.993107962432));
#232417=CARTESIAN_POINT('Ctrl Pts',(-72.0695616528837,-7.00120980318599,
130.950632336283));
#232418=CARTESIAN_POINT('Ctrl Pts',(-72.3480092766965,-3.66126237309149,
136.773740146404));
#232419=CARTESIAN_POINT('Ctrl Pts',(-72.6264569005095,3.04320631526353,
137.111279789924));
#232420=CARTESIAN_POINT('Ctrl Pts',(-72.9049045243223,6.95111706878496,
131.653068824177));
#232421=CARTESIAN_POINT('Ctrl Pts',(-73.1833521481353,4.47129081703998,
125.414936478256));
#232422=CARTESIAN_POINT('Ctrl Pts',(-73.4617997719481,-2.11743326086482,
124.129421628353));
#232423=CARTESIAN_POINT('Ctrl Pts',(-73.7402473957612,-6.76033961440018,
128.977849620639));
#232424=CARTESIAN_POINT('Ctrl Pts',(-74.018695019574,-5.19082412325261,
135.504751989078));
#232425=CARTESIAN_POINT('Ctrl Pts',(-74.2971426433868,1.14880515130821,
137.712224313981));
#232426=CARTESIAN_POINT('Ctrl Pts',(-74.5755902671998,6.43273861406817,
133.571707369781));
#232427=CARTESIAN_POINT('Ctrl Pts',(-74.8540378910127,5.80529954725181,
126.8881339527));
#232428=CARTESIAN_POINT('Ctrl Pts',(-75.1324855148255,-0.156926198840311,
123.803381522322));
#232429=CARTESIAN_POINT('Ctrl Pts',(-75.4109331386384,-5.97494443446864,
127.15218686363));
#232430=CARTESIAN_POINT('Ctrl Pts',(-75.6893807624512,-6.30228062708332,
133.857161466198));
#232431=CARTESIAN_POINT('Ctrl Pts',(-75.9678283862644,-0.838128806933456,
137.756761226486));
#232432=CARTESIAN_POINT('Ctrl Pts',(-76.2462760100769,5.3962224419198,135.267444470826));
#232433=CARTESIAN_POINT('Ctrl Pts',(-76.52472363389,6.67170888677059,128.676771687789));
#232434=CARTESIAN_POINT('Ctrl Pts',(-76.8031712577027,1.81622079577817,
124.041249192718));
#232435=CARTESIAN_POINT('Ctrl Pts',(-77.0816188815158,-4.70828547921653,
125.620695700721));
#232436=CARTESIAN_POINT('Ctrl Pts',(-77.3600665053286,-6.90610741134329,
131.963677031195));
#232437=CARTESIAN_POINT('Ctrl Pts',(-77.6385141291417,-2.75755401454922,
137.241303213299));
#232438=CARTESIAN_POINT('Ctrl Pts',(-77.9169617529544,3.92505680761298,
136.603693612052));
#232439=CARTESIAN_POINT('Ctrl Pts',(-78.1954093767674,7.00073217326374,
130.636780302039));
#232440=CARTESIAN_POINT('Ctrl Pts',(-78.4738570005803,3.6430766764653,124.823865115242));
#232441=CARTESIAN_POINT('Ctrl Pts',(-78.7523046243931,-3.06238831181505,
124.506733131632));
#232442=CARTESIAN_POINT('Ctrl Pts',(-79.0307522482061,-6.95366804752337,
129.976813151389));
#232443=CARTESIAN_POINT('Ctrl Pts',(-79.3091998720188,-4.45486655312747,
136.207368864621));
#232444=CARTESIAN_POINT('Ctrl Pts',(-79.5876474958318,2.13773967126259,
137.472823950436));
#232445=CARTESIAN_POINT('Ctrl Pts',(-79.8660951196445,6.76586757215105,
132.610287005887));
#232446=CARTESIAN_POINT('Ctrl Pts',(-80.1445427434577,5.17649370523912,
126.08819193488));
#232447=CARTESIAN_POINT('Ctrl Pts',(-80.4229903672703,-1.16982499101125,
123.900025485612));
#232448=CARTESIAN_POINT('Ctrl Pts',(-80.7014379910835,-6.44113166965063,
128.056605727087));
#232449=CARTESIAN_POINT('Ctrl Pts',(-80.9798856148961,-5.7933530106558,
134.738238477622));
#232450=CARTESIAN_POINT('Ctrl Pts',(-81.2583332387092,0.17823404410257,
137.804829655383));
#232451=CARTESIAN_POINT('Ctrl Pts',(-81.5367808625219,5.98603271954817,
134.438331779315));
#232452=CARTESIAN_POINT('Ctrl Pts',(-81.815228486335,6.29295975968447,127.732391934959));
#232453=CARTESIAN_POINT('Ctrl Pts',(-82.0936761101477,0.816964208846405,
123.849441235906));
#232454=CARTESIAN_POINT('Ctrl Pts',(-82.3721237339607,-5.40978153900143,
126.357721681897));
#232455=CARTESIAN_POINT('Ctrl Pts',(-82.6505713577735,-6.66520233502723,
132.952246079378));
#232456=CARTESIAN_POINT('Ctrl Pts',(-82.9290189815866,-1.79562779839943,
137.572968667493));
#232457=CARTESIAN_POINT('Ctrl Pts',(-83.2074666053992,4.72404096366304,
135.97367112261));
#232458=CARTESIAN_POINT('Ctrl Pts',(-83.4859142292123,6.90254686235,129.624029758449));
#232459=CARTESIAN_POINT('Ctrl Pts',(-83.7643618530252,2.73794940269844,
124.359054791448));
#232460=CARTESIAN_POINT('Ctrl Pts',(-84.0428094768383,-3.94268980176888,
125.017001007954));
#232461=CARTESIAN_POINT('Ctrl Pts',(-84.3212571006508,-7.00018968951541,
130.99324797746));
#232462=CARTESIAN_POINT('Ctrl Pts',(-84.5997047244641,-3.62485723087481,
136.795916690882));
#232463=CARTESIAN_POINT('Ctrl Pts',(-84.8781523482765,3.08154193881888,
137.092638076712));
#232464=CARTESIAN_POINT('Ctrl Pts',(-85.1565999720898,6.95615460843127,
131.61073967702));
#232465=CARTESIAN_POINT('Ctrl Pts',(-85.4350475959023,4.4384010199398,125.387818315495));
#232466=CARTESIAN_POINT('Ctrl Pts',(-85.7134952197154,-2.1580262779319,
124.142434716771));
#232467=CARTESIAN_POINT('Ctrl Pts',(-85.9919428435283,-6.7713328518292,
129.019035567703));
#232468=CARTESIAN_POINT('Ctrl Pts',(-86.2703904673411,-5.16211533289519,
135.536262921482));
#232469=CARTESIAN_POINT('Ctrl Pts',(-86.5488380911541,1.19083399361533,
137.70510322424));
#232470=CARTESIAN_POINT('Ctrl Pts',(-86.827285714967,6.4494650554685,133.532498191482));
#232471=CARTESIAN_POINT('Ctrl Pts',(-87.1057333387799,5.78135280522977,
126.852868005224));
#232472=CARTESIAN_POINT('Ctrl Pts',(-87.3841809625928,-0.199540238229241,
123.804466488563));
#232473=CARTESIAN_POINT('Ctrl Pts',(-87.6626285864056,-5.99706555083783,
127.188625712615));
#232474=CARTESIAN_POINT('Ctrl Pts',(-87.9410762102187,-6.28358059516641,
133.895468675847));
#232475=CARTESIAN_POINT('Ctrl Pts',(-88.2195238340314,-0.795792042514341,
137.761734342542));
#232476=CARTESIAN_POINT('Ctrl Pts',(-88.4979714578443,5.42329052060546,
135.234513442586));
#232477=CARTESIAN_POINT('Ctrl Pts',(-88.7764190816572,6.65863403776028,
128.636198521433));
#232478=CARTESIAN_POINT('Ctrl Pts',(-89.0548667054699,1.77501816656995,
124.03031864602));
#232479=CARTESIAN_POINT('Ctrl Pts',(-89.3333143292831,-4.73975268523957,
125.649452412109));
#232480=CARTESIAN_POINT('Ctrl Pts',(-89.6117619530957,-6.8989223691057,
132.005694987746));
#232481=CARTESIAN_POINT('Ctrl Pts',(-89.8902095769088,-2.71831942685781,
137.257969965635));
#232482=CARTESIAN_POINT('Ctrl Pts',(-90.1686572007216,3.9602862713853,136.579693228991));
#232483=CARTESIAN_POINT('Ctrl Pts',(-90.4471048245344,6.99958235696585,
130.59416796313));
#232484=CARTESIAN_POINT('Ctrl Pts',(-90.7255524483476,3.60660420510239,
124.801799478213));
#232485=CARTESIAN_POINT('Ctrl Pts',(-91.0040000721602,-3.10066701883943,
124.525491438947));
#232486=CARTESIAN_POINT('Ctrl Pts',(-91.2824476959735,-6.95857672847263,
130.019157435019));
#232487=CARTESIAN_POINT('Ctrl Pts',(-91.560895319786,-4.4218943700117,136.234386796543));
#232488=CARTESIAN_POINT('Ctrl Pts',(-91.8393429435991,2.17829289294083,
137.459687371113));
#232489=CARTESIAN_POINT('Ctrl Pts',(-92.1177905674117,6.77673540280433,
132.56906778996));
#232490=CARTESIAN_POINT('Ctrl Pts',(-92.3962381912249,5.14768913942031,
126.056768528114));
#232491=CARTESIAN_POINT('Ctrl Pts',(-92.6746858150375,-1.21183196449619,
123.907274463707));
#232492=CARTESIAN_POINT('Ctrl Pts',(-92.9531334388505,-6.45773869432309,
128.095865633305));
#232493=CARTESIAN_POINT('Ctrl Pts',(-93.2315810626634,-5.76929904214118,
134.773431376103));
#232494=CARTESIAN_POINT('Ctrl Pts',(-93.5100286864763,0.220844583841736,
137.803614991691));
#232495=CARTESIAN_POINT('Ctrl Pts',(-93.7884763102892,6.00804282613147,
134.401825770043));
#232496=CARTESIAN_POINT('Ctrl Pts',(-94.0669239341021,6.27414322041607,
127.694141819211));
#232497=CARTESIAN_POINT('Ctrl Pts',(-94.3453715579151,0.774612504073732,
123.844597001431));
#232498=CARTESIAN_POINT('Ctrl Pts',(-94.6238191817278,-5.43674926158731,
126.390734943524));
#232499=CARTESIAN_POINT('Ctrl Pts',(-94.9022668055408,-6.65200405581671,
132.99277926246));
#232500=CARTESIAN_POINT('Ctrl Pts',(-95.1807144293538,-1.75439209121494,
137.583773756932));
#232501=CARTESIAN_POINT('Ctrl Pts',(-95.4591620531666,4.75542049839504,
135.94481876907));
#232502=CARTESIAN_POINT('Ctrl Pts',(-95.7376096769794,6.89523396518648,
129.582033865318));
#232503=CARTESIAN_POINT('Ctrl Pts',(-96.0160573007924,2.69866426887766,
124.342507532899));
#232504=CARTESIAN_POINT('Ctrl Pts',(-96.2945049246052,-3.97784605345104,
125.041108506217));
#232505=CARTESIAN_POINT('Ctrl Pts',(-96.5729525484182,-6.99891018124123,
131.035856619345));
#232506=CARTESIAN_POINT('Ctrl Pts',(-96.8514001722308,-3.58831776824163,
136.817871216047));
#232507=CARTESIAN_POINT('Ctrl Pts',(-97.129847796044,3.11976337470375,137.073763349068));
#232508=CARTESIAN_POINT('Ctrl Pts',(-97.4082954198568,6.96093438520996,
131.56838064919));
#232509=CARTESIAN_POINT('Ctrl Pts',(-97.6867430436697,4.40534675625846,
125.360900864701));
#232510=CARTESIAN_POINT('Ctrl Pts',(-97.9651906674826,-2.1985393285419,
124.155694665303));
#232511=CARTESIAN_POINT('Ctrl Pts',(-98.2436382912955,-6.78207517502872,
129.060287670645));
#232512=CARTESIAN_POINT('Ctrl Pts',(-98.5220859151084,-5.13321525845608,
135.567598511506));
#232513=CARTESIAN_POINT('Ctrl Pts',(-98.8005335389213,1.23281870913114,
137.697726424945));
#232514=CARTESIAN_POINT('Ctrl Pts',(-99.0789811627341,6.4659525095689,133.493187921042));
#232515=CARTESIAN_POINT('Ctrl Pts',(-99.3574287865471,5.7571918330539,126.817748481762));
#232516=CARTESIAN_POINT('Ctrl Pts',(-99.6358764103599,-0.242146883580649,
123.805810838454));
#232517=CARTESIAN_POINT('Ctrl Pts',(-99.9143240341728,-6.01896444373747,
127.225198543987));
#232518=CARTESIAN_POINT('Ctrl Pts',(-100.192771657986,-6.26464772285957,
133.93366134335));
#232519=CARTESIAN_POINT('Ctrl Pts',(-100.471219281798,-0.753425789729175,
137.766449650557));
#232520=CARTESIAN_POINT('Ctrl Pts',(-100.749666905611,5.45015763726631,
135.201418253402));
#232521=CARTESIAN_POINT('Ctrl Pts',(-101.028114529424,6.64531245061667,
128.595705697122));
#232522=CARTESIAN_POINT('Ctrl Pts',(-101.306562153237,1.73374976341167,
124.019639113937));
#232523=CARTESIAN_POINT('Ctrl Pts',(-101.58500977705,-4.77104425798471,
125.678400140516));
#232524=CARTESIAN_POINT('Ctrl Pts',(-101.863457400863,-6.89148168476197,
132.047668428412));
#232525=CARTESIAN_POINT('Ctrl Pts',(-102.141905024676,-2.67898411084018,
137.274397577103));
#232526=CARTESIAN_POINT('Ctrl Pts',(-102.420352648489,3.99536898529432,
136.555478838857));
#232527=CARTESIAN_POINT('Ctrl Pts',(-102.698800272302,6.99817316856906,
130.551563412989));
#232528=CARTESIAN_POINT('Ctrl Pts',(-102.977247896115,3.56999808969468,
124.779956268296));
#232529=CARTESIAN_POINT('Ctrl Pts',(-103.255695519928,-3.13883082950684,
124.544482412068));
#232530=CARTESIAN_POINT('Ctrl Pts',(-103.53414314374,-6.96322755680218,
130.061530814641));
#232531=CARTESIAN_POINT('Ctrl Pts',(-103.812590767553,-4.38875833197407,
136.261203516848));
#232532=CARTESIAN_POINT('Ctrl Pts',(-104.091038391366,2.21876539717438,
137.44630417621));
#232533=CARTESIAN_POINT('Ctrl Pts',(-104.369486015179,6.78735211903507,
132.52778318216));
#232534=CARTESIAN_POINT('Ctrl Pts',(-104.647933638992,5.11869382408742,
126.02552104512));
#232535=CARTESIAN_POINT('Ctrl Pts',(-104.926381262805,-1.25379403310144,
123.914779015865));
#232536=CARTESIAN_POINT('Ctrl Pts',(-105.204828886617,-6.47410642511416,
128.135225903801));
#232537=CARTESIAN_POINT('Ctrl Pts',(-105.483276510431,-5.74503129012806,
134.808477199207));
#232538=CARTESIAN_POINT('Ctrl Pts',(-105.761724134243,0.263446940103889,
137.802140968053));
#232539=CARTESIAN_POINT('Ctrl Pts',(-106.040171758056,6.02983030247923,
134.365186455377));
#232540=CARTESIAN_POINT('Ctrl Pts',(-106.318619381869,6.25509419046252,
127.656006953765));
#232541=CARTESIAN_POINT('Ctrl Pts',(-106.597067005682,0.732232095750508,
123.840010663559));
#232542=CARTESIAN_POINT('Ctrl Pts',(-106.875514629495,-5.46351552342998,
126.423911753675));
#232543=CARTESIAN_POINT('Ctrl Pts',(-107.153962253308,-6.63855928414971,
133.033231352883));
#232544=CARTESIAN_POINT('Ctrl Pts',(-107.432409877121,-1.71309137438684,
137.594327632723));
#232545=CARTESIAN_POINT('Ctrl Pts',(-107.710857500934,4.78662381927155,
135.915775933963));
#232546=CARTESIAN_POINT('Ctrl Pts',(-107.989305124746,6.8876655625929,129.540083265954));
#232547=CARTESIAN_POINT('Ctrl Pts',(-108.26775274856,2.65927913505975,124.326199720693));
#232548=CARTESIAN_POINT('Ctrl Pts',(-108.546200372372,-4.0128549045848,
125.065429563905));
#232549=CARTESIAN_POINT('Ctrl Pts',(-108.824647996185,-6.99737132577695,
131.078456683062));
#232550=CARTESIAN_POINT('Ctrl Pts',(-109.103095619998,-3.5516453391731,
136.839602908365));
#232551=CARTESIAN_POINT('Ctrl Pts',(-109.381543243811,3.1578692066097,137.054656306401));
#232552=CARTESIAN_POINT('Ctrl Pts',(-109.659990867624,6.96545622200577,
131.525993310316));
#232553=CARTESIAN_POINT('Ctrl Pts',(-109.938438491437,4.37212925083209,
125.334185123311));
#232554=CARTESIAN_POINT('Ctrl Pts',(-110.21688611525,-2.23897091146772,
124.169200982596));
#232555=CARTESIAN_POINT('Ctrl Pts',(-110.495333739063,-6.79256618593892,
129.10160440085));
#232556=CARTESIAN_POINT('Ctrl Pts',(-110.773781362875,-5.10412497083799,
135.598757597999));
#232557=CARTESIAN_POINT('Ctrl Pts',(-111.052228986688,1.27475774209554,
137.690094189444));
#232558=CARTESIAN_POINT('Ctrl Pts',(-111.330676610501,6.48220036542147,
133.453778015119));
#232559=CARTESIAN_POINT('Ctrl Pts',(-111.609124234314,5.73281752601749,
126.782776683677));
#232560=CARTESIAN_POINT('Ctrl Pts',(-111.887571858127,-0.284744556090853,
123.807414522182));
#232561=CARTESIAN_POINT('Ctrl Pts',(-112.16601948194,-6.04064030169634,
127.261904002525));
#232562=CARTESIAN_POINT('Ctrl Pts',(-112.444467105753,-6.24548271172772,
133.971738053464));
#232563=CARTESIAN_POINT('Ctrl Pts',(-112.722914729566,-0.71103161847358,
137.770906975801));
#232564=CARTESIAN_POINT('Ctrl Pts',(-113.001362353379,5.47682279633179,
135.16816012963));
#232565=CARTESIAN_POINT('Ctrl Pts',(-113.279809977192,6.63174461897671,
128.55529471533));
#232566=CARTESIAN_POINT('Ctrl Pts',(-113.558257601004,1.69241711551747,
124.009210992206));
#232567=CARTESIAN_POINT('Ctrl Pts',(-113.836705224817,-4.80215903792943,
125.707537813274));
#232568=CARTESIAN_POINT('Ctrl Pts',(-114.11515284863,-6.88378563403075,
132.089595797848));
#232569=CARTESIAN_POINT('Ctrl Pts',(-114.393600472443,-2.63954952408134,
137.290585438973));
#232570=CARTESIAN_POINT('Ctrl Pts',(-114.672048096256,4.03030364933543,
136.531051338922));
#232571=CARTESIAN_POINT('Ctrl Pts',(-114.950495720069,6.99650466029252,
130.508968230339));
#232572=CARTESIAN_POINT('Ctrl Pts',(-115.228943343882,3.53325968669456,
124.758336294896));
#232573=CARTESIAN_POINT('Ctrl Pts',(-115.507390967695,-3.17687832964389,
124.563705347279));
#232574=CARTESIAN_POINT('Ctrl Pts',(-115.785838591507,-6.96762036017394,
130.103931720095));
#232575=CARTESIAN_POINT('Ctrl Pts',(-116.06428621532,-4.35545966688232,
136.287818031834));
#232576=CARTESIAN_POINT('Ctrl Pts',(-116.342733839133,2.25915568424066,
137.432674861647));
#232577=CARTESIAN_POINT('Ctrl Pts',(-116.621181462946,6.79771732743703,
132.486434712303));
#232578=CARTESIAN_POINT('Ctrl Pts',(-116.899629086759,5.08950883367243,
125.994450643782));
#232579=CARTESIAN_POINT('Ctrl Pts',(-117.178076710572,-1.2957096419083,
123.922538864004));
#232580=CARTESIAN_POINT('Ctrl Pts',(-117.456524334385,-6.49023425551004,
128.174685080065));
#232581=CARTESIAN_POINT('Ctrl Pts',(-117.734971958198,-5.7205506538686,
134.843374648297));
#232582=CARTESIAN_POINT('Ctrl Pts',(-118.013419582011,0.306039534242538,
137.800407639092));
#232583=CARTESIAN_POINT('Ctrl Pts',(-118.291867205823,6.05139434124684,
134.328415193001));
#232584=CARTESIAN_POINT('Ctrl Pts',(-118.570314829636,6.23581337569426,
127.617988751722));
#232585=CARTESIAN_POINT('Ctrl Pts',(-118.848762453449,0.689824554297045,
123.835682392233));
#232586=CARTESIAN_POINT('Ctrl Pts',(-119.127210077262,-5.49007933269568,
126.457250882969));
#232587=CARTESIAN_POINT('Ctrl Pts',(-119.405657701075,-6.62486851822702,
133.073600851681));
#232588=CARTESIAN_POINT('Ctrl Pts',(-119.684105324888,-1.67172717832737,
137.60462990379));
#232589=CARTESIAN_POINT('Ctrl Pts',(-119.962552948701,4.81764977004229,
135.886543693482));
#232590=CARTESIAN_POINT('Ctrl Pts',(-120.241000572514,6.87984193501854,
129.498179514853));
#232591=CARTESIAN_POINT('Ctrl Pts',(-120.519448196327,2.61979546067638,
124.310131959122));
#232592=CARTESIAN_POINT('Ctrl Pts',(-120.79789582014,-4.04771505790416,
125.089963279793));
#232593=CARTESIAN_POINT('Ctrl Pts',(-121.076343443952,-6.9955731801444,
131.121046590047));
#232594=CARTESIAN_POINT('Ctrl Pts',(-121.354791067765,-3.51484130258126,
136.86111096256));
#232595=CARTESIAN_POINT('Ctrl Pts',(-121.633238691578,3.19585802251066,
137.035317656727));
#232596=CARTESIAN_POINT('Ctrl Pts',(-121.911686315391,6.96971995125911,
131.483579231079));
#232597=CARTESIAN_POINT('Ctrl Pts',(-122.190133939204,4.3387497345494,125.307672081285));
#232598=CARTESIAN_POINT('Ctrl Pts',(-122.468581563017,-2.2793195285039,
124.182953168171));
#232599=CARTESIAN_POINT('Ctrl Pts',(-122.74702918683,-6.80280549581075,
129.142984227312));
#232600=CARTESIAN_POINT('Ctrl Pts',(-123.025476810643,-5.07484554799192,
135.629739026348));
#232601=CARTESIAN_POINT('Ctrl Pts',(-123.303924434456,1.31664953844379,
137.682206800553));
#232602=CARTESIAN_POINT('Ctrl Pts',(-123.582372058268,6.49820802095541,
133.414269934058));
#232603=CARTESIAN_POINT('Ctrl Pts',(-123.860819682081,5.7082307873194,126.747953906865));
#232604=CARTESIAN_POINT('Ctrl Pts',(-124.139267305894,-0.327331677286216,
123.809277480321));
#232605=CARTESIAN_POINT('Ctrl Pts',(-124.417714929707,-6.06209232150722,
127.298740728095));
#232606=CARTESIAN_POINT('Ctrl Pts',(-124.69616255352,-6.22608627193705,
134.009697395242));
#232607=CARTESIAN_POINT('Ctrl Pts',(-124.974610177333,-0.668611099680587,
137.77510615311));
#232608=CARTESIAN_POINT('Ctrl Pts',(-125.253057801146,5.50328500971429,
135.134740303665));
#232609=CARTESIAN_POINT('Ctrl Pts',(-125.531505424959,6.61793104560076,
128.514967073503));
#232610=CARTESIAN_POINT('Ctrl Pts',(-125.809953048772,1.6510217544855,123.999034667242));
#232611=CARTESIAN_POINT('Ctrl Pts',(-126.088400672584,-4.8330958721059,
125.736864350674));
#232612=CARTESIAN_POINT('Ctrl Pts',(-126.366848296398,-6.87583450209069,
132.131475542423));
#232613=CARTESIAN_POINT('Ctrl Pts',(-126.64529592021,-2.60001712784396,
137.306532951397));
#232614=CARTESIAN_POINT('Ctrl Pts',(-126.923743544023,4.06508896899354,
136.506411634357));
#232615=CARTESIAN_POINT('Ctrl Pts',(-127.202191167836,6.99457689396224,
130.466383993564));
#232616=CARTESIAN_POINT('Ctrl Pts',(-127.480638791649,3.49639035745773,
124.736940359153));
#232617=CARTESIAN_POINT('Ctrl Pts',(-127.759086415462,-3.21480810938582,
124.583159532264));
#232618=CARTESIAN_POINT('Ctrl Pts',(-128.037534039275,-6.97175497581086,
130.146358580199));
#232619=CARTESIAN_POINT('Ctrl Pts',(-128.315981663087,-4.32199960863106,
136.314229355287));
#232620=CARTESIAN_POINT('Ctrl Pts',(-128.594429286901,2.29946225746178,
137.418799932461));
#232621=CARTESIAN_POINT('Ctrl Pts',(-128.872876910713,6.80783064392392,
132.44502391257));
#232622=CARTESIAN_POINT('Ctrl Pts',(-129.151324534526,5.06013524963555,
125.963558475429));
#232623=CARTESIAN_POINT('Ctrl Pts',(-129.429772158339,-1.33757723771771,
123.930553720578));
#232624=CARTESIAN_POINT('Ctrl Pts',(-129.708219782152,-6.50612158788957,
128.214241699924));
#232625=CARTESIAN_POINT('Ctrl Pts',(-129.986667405965,-5.69585804050008,
134.878122430239));
#232626=CARTESIAN_POINT('Ctrl Pts',(-130.265115029778,0.348620787973942,
137.798415069035));
#232627=CARTESIAN_POINT('Ctrl Pts',(-130.543562653591,6.07273414337257,
134.291513345486));
#232628=CARTESIAN_POINT('Ctrl Pts',(-130.822010277403,6.21630149056731,
127.58008862186));
#232629=CARTESIAN_POINT('Ctrl Pts',(-131.100457901217,0.647391451141708,
123.831612347843));
#232630=CARTESIAN_POINT('Ctrl Pts',(-131.378905525029,-5.5164397050528,
126.490751096011));
#232631=CARTESIAN_POINT('Ctrl Pts',(-131.657353148842,-6.61093226536518,
133.113886262947));
#232632=CARTESIAN_POINT('Ctrl Pts',(-131.935800772655,-1.63030103580305,
137.614680188378));
#232633=CARTESIAN_POINT('Ctrl Pts',(-132.214248396468,4.848497201029,135.857123130838));
#232634=CARTESIAN_POINT('Ctrl Pts',(-132.492696020281,6.87176337237162,
129.456324164773));
#232635=CARTESIAN_POINT('Ctrl Pts',(-132.771143644094,2.58021470880796,
124.294304843582));
#232636=CARTESIAN_POINT('Ctrl Pts',(-133.049591267907,-4.08242522165371,
125.114708744776));
#232637=CARTESIAN_POINT('Ctrl Pts',(-133.32803889172,-6.99351581097555,
131.163624762118));
#232638=CARTESIAN_POINT('Ctrl Pts',(-133.606486515532,-3.47790702225152,
136.882394581644));
#232639=CARTESIAN_POINT('Ctrl Pts',(-133.884934139345,3.23372841471757,
137.015748116649));
#232640=CARTESIAN_POINT('Ctrl Pts',(-134.163381763158,6.97372541497715,
131.441139983145));
#232641=CARTESIAN_POINT('Ctrl Pts',(-134.441829386971,4.30520944429882,
125.281362721075));
#232642=CARTESIAN_POINT('Ctrl Pts',(-134.720277010784,-2.31958368451587,
124.196950712432));
#232643=CARTESIAN_POINT('Ctrl Pts',(-134.998724634597,-6.81279272522359,
129.184425616688));
#232644=CARTESIAN_POINT('Ctrl Pts',(-135.27717225841,-5.04537807487797,
135.660541648527));
#232645=CARTESIAN_POINT('Ctrl Pts',(-135.555619882223,1.35849254585843,
137.674064550544));
#232646=CARTESIAN_POINT('Ctrl Pts',(-135.834067506036,6.51397488300169,
133.374665141848));
#232647=CARTESIAN_POINT('Ctrl Pts',(-136.112515129848,5.68343252803032,
126.713281441693));
#232648=CARTESIAN_POINT('Ctrl Pts',(-136.390962753662,-0.369906669086523,
123.811399643837));
#232649=CARTESIAN_POINT('Ctrl Pts',(-136.669410377474,-6.08331970825794,
127.335707355701));
#232650=CARTESIAN_POINT('Ctrl Pts',(-136.947858001288,-6.20645912223011,
134.047537962086));
#232651=CARTESIAN_POINT('Ctrl Pts',(-137.2263056251,-0.626165805256695,
137.779047026878));
#232652=CARTESIAN_POINT('Ctrl Pts',(-137.504753248913,5.52954329684707,
135.101160013885));
#232653=CARTESIAN_POINT('Ctrl Pts',(-137.783200872726,6.60387224235649,
128.474724265995));
#232654=CARTESIAN_POINT('Ctrl Pts',(-138.061648496539,1.60956521423443,
123.989110516135));
#232655=CARTESIAN_POINT('Ctrl Pts',(-138.340096120352,-4.86385361413656,
125.766378666012));
#232656=CARTESIAN_POINT('Ctrl Pts',(-138.618543744165,-6.86762858357524,
132.173306110266));
#232657=CARTESIAN_POINT('Ctrl Pts',(-138.896991367977,-2.56038838701599,
137.322239523433));
#232658=CARTESIAN_POINT('Ctrl Pts',(-139.17543899179,4.09972365528409,136.481560638194));
#232659=CARTESIAN_POINT('Ctrl Pts',(-139.453886615603,6.99238994101352,
130.423812280637));
#232660=CARTESIAN_POINT('Ctrl Pts',(-139.732334239416,3.45939146819007,
124.715769253897));
#232661=CARTESIAN_POINT('Ctrl Pts',(-140.010781863229,-3.25261876323132,
124.602844246145));
#232662=CARTESIAN_POINT('Ctrl Pts',(-140.289229487042,-6.97563125050334,
130.188809822811));
#232663=CARTESIAN_POINT('Ctrl Pts',(-140.567677110855,-4.28837939709471,
136.340436508528));
#232664=CARTESIAN_POINT('Ctrl Pts',(-140.846124734668,2.33968362326381,
137.404679902793));
#232665=CARTESIAN_POINT('Ctrl Pts',(-141.124572358481,6.81769169374202,
132.403552317457));
#232666=CARTESIAN_POINT('Ctrl Pts',(-141.403019982293,5.03057416042698,
125.932845684778));
#232667=CARTESIAN_POINT('Ctrl Pts',(-141.681467606106,-1.37939526911043,
123.938823288595));
#232668=CARTESIAN_POINT('Ctrl Pts',(-141.959915229919,-6.52176783354029,
128.253894297592));
#232669=CARTESIAN_POINT('Ctrl Pts',(-142.238362853732,-5.67095436501806,
134.912719257437));
#232670=CARTESIAN_POINT('Ctrl Pts',(-142.516810477545,0.39118912343359,
137.796163331718));
#232671=CARTESIAN_POINT('Ctrl Pts',(-142.795258101358,6.09384891810056,
134.254482280245));
#232672=CARTESIAN_POINT('Ctrl Pts',(-143.073705725171,6.19655925810344,
127.542307968582));
#232673=CARTESIAN_POINT('Ctrl Pts',(-143.352153348984,0.604934358657401,
123.827800681205));
#232674=CARTESIAN_POINT('Ctrl Pts',(-143.630600972796,-5.54259566370794,
126.524411151443));
#232675=CARTESIAN_POINT('Ctrl Pts',(-143.90904859661,-6.59675104197701,
133.154086093891));
#232676=CARTESIAN_POINT('Ctrl Pts',(-144.187496220422,-1.58881448187379,
137.624478114069));
#232677=CARTESIAN_POINT('Ctrl Pts',(-144.465943844235,4.87916496916901,
135.827515336221));
#232678=CARTESIAN_POINT('Ctrl Pts',(-144.744391468048,6.86343017400547,
129.41451876668));
#232679=CARTESIAN_POINT('Ctrl Pts',(-145.022839091861,2.54053834613545,
124.278718960552));
#232680=CARTESIAN_POINT('Ctrl Pts',(-145.301286715674,-4.11698410963516,
125.139665041902));
#232681=CARTESIAN_POINT('Ctrl Pts',(-145.579734339487,-6.99119929450595,
131.206189621523));
#232682=CARTESIAN_POINT('Ctrl Pts',(-145.8581819633,-3.44084386679896,136.903452976945));
#232683=CARTESIAN_POINT('Ctrl Pts',(-146.136629587113,3.27147897992919,
136.995948411323));
#232684=CARTESIAN_POINT('Ctrl Pts',(-146.415077210925,6.97747246473481,
131.398677139117));
#232685=CARTESIAN_POINT('Ctrl Pts',(-146.693524834738,4.27150962292939,
125.255258017582));
#232686=CARTESIAN_POINT('Ctrl Pts',(-146.971972458551,-2.35976188750221,
124.211193096699));
#232687=CARTESIAN_POINT('Ctrl Pts',(-147.250420082364,-6.82252750409623,
129.225927033352));
#232688=CARTESIAN_POINT('Ctrl Pts',(-147.528867706177,-5.01572364342383,
135.69116432313));
#232689=CARTESIAN_POINT('Ctrl Pts',(-147.80731532999,1.40028521383297,137.665667741127));
#232690=CARTESIAN_POINT('Ctrl Pts',(-148.085762953803,6.52950036731291,
133.334965106058));
#232691=CARTESIAN_POINT('Ctrl Pts',(-148.364210577616,5.65842366705879,
126.678760572968));
#232692=CARTESIAN_POINT('Ctrl Pts',(-148.642658201429,-0.412467953858535,
123.813780934094));
#232693=CARTESIAN_POINT('Ctrl Pts',(-148.921105825242,-6.10432167535963,
127.372802515528));
#232694=CARTESIAN_POINT('Ctrl Pts',(-149.199553449054,-6.18660198989778,
134.085258351801));
#232695=CARTESIAN_POINT('Ctrl Pts',(-149.478001072867,-0.583697308029368,
137.782729451077));
#232696=CARTESIAN_POINT('Ctrl Pts',(-149.75644869668,5.55559668471987,135.067420504625));
#232697=CARTESIAN_POINT('Ctrl Pts',(-150.034896320493,6.58956873019717,
128.434567784019));
#232698=CARTESIAN_POINT('Ctrl Pts',(-150.313343944306,1.56804903095274,
123.979438906626));
#232699=CARTESIAN_POINT('Ctrl Pts',(-150.591791568119,-4.89443112428377,
125.796079665625));
#232700=CARTESIAN_POINT('Ctrl Pts',(-150.870239191931,-6.85916818255639,
132.21508595133));
#232701=CARTESIAN_POINT('Ctrl Pts',(-151.148686815745,-2.52066477005453,
137.33770457307));
#232702=CARTESIAN_POINT('Ctrl Pts',(-151.427134439557,4.13420642480782,
136.456499271296));
#232703=CARTESIAN_POINT('Ctrl Pts',(-151.705582063371,6.98994388248347,
130.381254669068));
#232704=CARTESIAN_POINT('Ctrl Pts',(-151.984029687183,3.42226438989971,
124.694823763634));
#232705=CARTESIAN_POINT('Ctrl Pts',(-152.262477310996,-3.29030889009209,
124.622758759495));
#232706=CARTESIAN_POINT('Ctrl Pts',(-152.540924934809,-6.97924904061452,
130.231283874884));
#232707=CARTESIAN_POINT('Ctrl Pts',(-152.819372558622,-4.25460027808296,
136.366438520441));
#232708=CARTESIAN_POINT('Ctrl Pts',(-153.097820182435,2.37981829122829,
137.390315295868));
#232709=CARTESIAN_POINT('Ctrl Pts',(-153.376267806248,6.82730011148789,
132.362021463707));
#232710=CARTESIAN_POINT('Ctrl Pts',(-153.654715430061,5.00082666144207,
125.902313409905));
#232711=CARTESIAN_POINT('Ctrl Pts',(-153.933163053873,-1.42116218650446,
123.947347261623));
#232712=CARTESIAN_POINT('Ctrl Pts',(-154.211610677687,-6.53717241268631,
128.293641403726));
#232713=CARTESIAN_POINT('Ctrl Pts',(-154.490058301499,-5.64584055023574,
134.947163847896));
#232714=CARTESIAN_POINT('Ctrl Pts',(-154.768505925312,0.433742963236675,
137.79365251058));
#232715=CARTESIAN_POINT('Ctrl Pts',(-155.046953549125,6.11473788301669,
134.217323369476));
#232716=CARTESIAN_POINT('Ctrl Pts',(-155.325401172938,6.17658740985663,
127.504648191865));
#232717=CARTESIAN_POINT('Ctrl Pts',(-155.603848796751,0.562454850108638,
123.824247533559));
#232718=CARTESIAN_POINT('Ctrl Pts',(-155.882296420564,-5.5685462394425,
126.558229801974));
#232719=CARTESIAN_POINT('Ctrl Pts',(-156.160744044376,-6.5823253735531,
133.194198854895));
#232720=CARTESIAN_POINT('Ctrl Pts',(-156.43919166819,-1.54726905384013,
137.634023317798));
#232721=CARTESIAN_POINT('Ctrl Pts',(-156.717639292002,4.90965193805665,
135.79772140676));
#232722=CARTESIAN_POINT('Ctrl Pts',(-156.996086915816,6.8548426487106,129.372764869687));
#232723=CARTESIAN_POINT('Ctrl Pts',(-157.274534539628,2.50076784287941,
124.263374887574));
#232724=CARTESIAN_POINT('Ctrl Pts',(-157.552982163441,-4.15139044125659,
125.164831246407));
#232725=CARTESIAN_POINT('Ctrl Pts',(-157.831429787254,-6.98862371657603,
131.248739591007));
#232726=CARTESIAN_POINT('Ctrl Pts',(-158.109877411067,-3.40365320961064,
136.924285368134));
#232727=CARTESIAN_POINT('Ctrl Pts',(-158.38832503488,3.30910831928323,136.975919274434));
#232728=CARTESIAN_POINT('Ctrl Pts',(-158.666772658693,6.98096096168483,
131.356192272474));
#232729=CARTESIAN_POINT('Ctrl Pts',(-158.945220282506,4.23765151920024,
125.229358938127));
#232730=CARTESIAN_POINT('Ctrl Pts',(-159.223667906319,-2.39985264864321,
124.225679793212));
#232731=CARTESIAN_POINT('Ctrl Pts',(-159.502115530131,-6.8320094717036,
129.267486939452));
#232732=CARTESIAN_POINT('Ctrl Pts',(-159.780563153944,-4.98588335248574,
135.721605915426));
#232733=CARTESIAN_POINT('Ctrl Pts',(-160.059010777757,1.44202599372318,
137.657016683454));
#232734=CARTESIAN_POINT('Ctrl Pts',(-160.33745840157,6.54478389858708,133.295171297791));
#232735=CARTESIAN_POINT('Ctrl Pts',(-160.615906025383,5.63320513111742,
126.644392579866));
#232736=CARTESIAN_POINT('Ctrl Pts',(-160.894353649196,-0.455013954479453,
123.816421262852));
#232737=CARTESIAN_POINT('Ctrl Pts',(-161.172801273009,-6.12509744457689,
127.410024833003));
#232738=CARTESIAN_POINT('Ctrl Pts',(-161.451248896821,-6.16651561075379,
134.122857166646));
#232739=CARTESIAN_POINT('Ctrl Pts',(-161.729696520635,-0.541207181682879,
137.786153289251));
#232740=CARTESIAN_POINT('Ctrl Pts',(-162.008144144447,5.58144420791359,
135.033523026113));
#232741=CARTESIAN_POINT('Ctrl Pts',(-162.286591768261,6.57502103914602,
128.394499115588));
#232742=CARTESIAN_POINT('Ctrl Pts',(-162.565039392073,1.52647474303778,
123.970020197102));
#232743=CARTESIAN_POINT('Ctrl Pts',(-162.843487015886,-4.92482726948487,
125.825966248931));
#232744=CARTESIAN_POINT('Ctrl Pts',(-163.121934639699,-6.85045361253876,
132.256813517449));
#232745=CARTESIAN_POINT('Ctrl Pts',(-163.400382263512,-2.48084774893327,
137.352927527244));
#232746=CARTESIAN_POINT('Ctrl Pts',(-163.678829887325,4.16853599979124,
136.431228462323));
#232747=CARTESIAN_POINT('Ctrl Pts',(-163.957277511138,6.98723880901292,
130.338712735846));
#232748=CARTESIAN_POINT('Ctrl Pts',(-164.23572513495,3.3850104983435,124.674104664506));
#232749=CARTESIAN_POINT('Ctrl Pts',(-164.514172758764,-3.32787709334726,
124.642902334375));
#232750=CARTESIAN_POINT('Ctrl Pts',(-164.792620382576,-6.98260821208591,
130.273779162525));
#232751=CARTESIAN_POINT('Ctrl Pts',(-165.07106800639,-4.22066350329308,
136.392234427513));
#232752=CARTESIAN_POINT('Ctrl Pts',(-165.349515630202,2.4198647741513,137.37570664397));
#232753=CARTESIAN_POINT('Ctrl Pts',(-165.627963254015,6.83665554111671,
132.320432890263));
#232754=CARTESIAN_POINT('Ctrl Pts',(-165.906410877828,4.97089385498702,
125.871962782194));
#232755=CARTESIAN_POINT('Ctrl Pts',(-166.184858501641,-1.46287644221077,
123.956125323802));
#232756=CARTESIAN_POINT('Ctrl Pts',(-166.463306125454,-6.55233475450377,
128.333481545486));
#232757=CARTESIAN_POINT('Ctrl Pts',(-166.741753749267,-5.62051752675643,
134.981454925258));
#232758=CARTESIAN_POINT('Ctrl Pts',(-167.020201373079,0.476280730534997,
137.790882698662));
#232759=CARTESIAN_POINT('Ctrl Pts',(-167.298648996893,6.13540026407138,
134.180037990117));
#232760=CARTESIAN_POINT('Ctrl Pts',(-167.577096620705,6.15638668589229,
127.467110687205));
#232761=CARTESIAN_POINT('Ctrl Pts',(-167.855544244518,0.519954499587912,
123.820953036571));
#232762=CARTESIAN_POINT('Ctrl Pts',(-168.133991868331,-5.5942904706483,
126.592205794446));
#232763=CARTESIAN_POINT('Ctrl Pts',(-168.412439492144,-6.56765579464175,
133.234223059563));
#232764=CARTESIAN_POINT('Ctrl Pts',(-168.690887115956,-1.50566629118217,
137.643315445865));
#232765=CARTESIAN_POINT('Ctrl Pts',(-168.96933473977,4.93995697798634,135.767742446477));
#232766=CARTESIAN_POINT('Ctrl Pts',(-169.247782363582,6.84600111470013,
129.331064021001));
#232767=CARTESIAN_POINT('Ctrl Pts',(-169.526229987396,2.46090467275213,
124.248273193229));
#232768=CARTESIAN_POINT('Ctrl Pts',(-169.804677611208,-4.18564294157836,
125.190206425745));
#232769=CARTESIAN_POINT('Ctrl Pts',(-170.083125235021,-6.98578917262369,
131.291273093865));
#232770=CARTESIAN_POINT('Ctrl Pts',(-170.361572858834,-3.36633642880185,
136.944890983262));
#232771=CARTESIAN_POINT('Ctrl Pts',(-170.640020482647,3.34661503841248,
136.955661448171));
#232772=CARTESIAN_POINT('Ctrl Pts',(-170.91846810646,6.98419077655865,131.313686957504));
#232773=CARTESIAN_POINT('Ctrl Pts',(-171.196915730273,4.20363638773547,
125.203666442409));
#232774=CARTESIAN_POINT('Ctrl Pts',(-171.475363354086,-2.43985448236259,
124.240410265162));
#232775=CARTESIAN_POINT('Ctrl Pts',(-171.753810977898,-6.84123827668714,
129.309103794972));
#232776=CARTESIAN_POINT('Ctrl Pts',(-172.032258601712,-4.9558583078063,
135.751865297389));
#232777=CARTESIAN_POINT('Ctrl Pts',(-172.310706225524,1.48371333881067,
137.648111698089));
#232778=CARTESIAN_POINT('Ctrl Pts',(-172.589153849337,6.55982491048677,
133.255285191615));
#232779=CARTESIAN_POINT('Ctrl Pts',(-172.86760147315,5.60777785468832,126.610178735912));
#232780=CARTESIAN_POINT('Ctrl Pts',(-173.146049096963,-0.497543094390354,
123.819320532272));
#232781=CARTESIAN_POINT('Ctrl Pts',(-173.424496720776,-6.14564624605571,
127.447372928838));
#232782=CARTESIAN_POINT('Ctrl Pts',(-173.702944344589,-6.14620072910595,
134.160333013378));
#232783=CARTESIAN_POINT('Ctrl Pts',(-173.981391968402,-0.498697000705985,
137.789318414533));
#232784=CARTESIAN_POINT('Ctrl Pts',(-174.259839592215,5.60708490864046,
134.999468834432));
#232785=CARTESIAN_POINT('Ctrl Pts',(-174.538287216028,6.56022970827155,
128.354519745462));
#232786=CARTESIAN_POINT('Ctrl Pts',(-174.81673483984,1.48484389103961,123.960854736574));
#232787=CARTESIAN_POINT('Ctrl Pts',(-175.095182463654,-4.95504092340126,
125.85603730847));
#232788=CARTESIAN_POINT('Ctrl Pts',(-175.373630087466,-6.8414851964426,
132.298487262391));
#232789=CARTESIAN_POINT('Ctrl Pts',(-175.652077711279,-2.44093879908611,
137.367907821863));
#232790=CARTESIAN_POINT('Ctrl Pts',(-175.930525335092,4.20271110814107,
136.405749147692));
#232791=CARTESIAN_POINT('Ctrl Pts',(-176.208972958905,6.98427482083815,
130.296188057377));
#232792=CARTESIAN_POINT('Ctrl Pts',(-176.487420582718,3.3476311739788,124.653612724266));
#232793=CARTESIAN_POINT('Ctrl Pts',(-176.765868206531,-3.36532198089259,
124.663274224357));
#232794=CARTESIAN_POINT('Ctrl Pts',(-177.044315830343,-6.98570864044213,
130.316294111058));
#232795=CARTESIAN_POINT('Ctrl Pts',(-177.322763454156,-4.18657033026512,
136.417823273865));
#232796=CARTESIAN_POINT('Ctrl Pts',(-177.601211077969,2.4598215880947,137.360854488428));
#232797=CARTESIAN_POINT('Ctrl Pts',(-177.879658701782,6.84575763596098,
132.278788138201));
#232798=CARTESIAN_POINT('Ctrl Pts',(-178.158106325595,4.94077685023126,
125.841794926299));
#232799=CARTESIAN_POINT('Ctrl Pts',(-178.436553949408,-1.50453649049278,
123.965157149858));
#232800=CARTESIAN_POINT('Ctrl Pts',(-178.715001573221,-6.56725429714808,
128.373413246577));
#232801=CARTESIAN_POINT('Ctrl Pts',(-178.993449197033,-5.59498623293233,
135.015591218853));
#232802=CARTESIAN_POINT('Ctrl Pts',(-179.271896820847,0.518800849074927,
137.787853998597));
#232803=CARTESIAN_POINT('Ctrl Pts',(-179.550344444659,6.15583529561319,
134.142627523792));
#232804=CARTESIAN_POINT('Ctrl Pts',(-179.828792068472,6.13595783475539,
127.429696845569));
#232805=CARTESIAN_POINT('Ctrl Pts',(-180.107239692285,0.477434881962636,
123.81791731232));
#232806=CARTESIAN_POINT('Ctrl Pts',(-180.385687316098,-5.61982740336347,
126.626337869861));
#232807=CARTESIAN_POINT('Ctrl Pts',(-180.664134939911,-6.55274284882976,
133.274157224785));
#232808=CARTESIAN_POINT('Ctrl Pts',(-180.942582563724,-1.4640077355066,
137.652354153945));
#232809=CARTESIAN_POINT('Ctrl Pts',(-181.221030187537,4.97007896599344,
135.737579566256));
#232810=CARTESIAN_POINT('Ctrl Pts',(-181.499477811349,6.83690589960112,
129.289417765863));
#232811=CARTESIAN_POINT('Ctrl Pts',(-181.777925435163,2.42095031289641,
124.233414437113));
#232812=CARTESIAN_POINT('Ctrl Pts',(-182.056373058975,-4.21974034136189,
125.215789639631));
#232813=CARTESIAN_POINT('Ctrl Pts',(-182.334820682789,-6.98269576768506,
131.333788554001));
#232814=CARTESIAN_POINT('Ctrl Pts',(-182.613268306601,-3.32889490715784,
136.965269058779));
#232815=CARTESIAN_POINT('Ctrl Pts',(-182.891715930414,3.38399774748988,
136.935175683191));
#232816=CARTESIAN_POINT('Ctrl Pts',(-183.170163554227,6.98716178967534,
131.27116276926));
#232817=CARTESIAN_POINT('Ctrl Pts',(-183.44861117804,4.16946548897866,125.178181482475));
#232818=CARTESIAN_POINT('Ctrl Pts',(-183.727058801853,-2.47976590637605,
124.255383966707));
#232819=CARTESIAN_POINT('Ctrl Pts',(-184.005506425666,-6.85021357707087,
129.350776057783));
#232820=CARTESIAN_POINT('Ctrl Pts',(-184.283954049479,-4.92564962197493,
135.781941347746));
#232821=CARTESIAN_POINT('Ctrl Pts',(-184.562401673291,1.52534570435398,
137.63895311501));
#232822=CARTESIAN_POINT('Ctrl Pts',(-184.840849297105,6.5746228456623,133.215308265529));
#232823=CARTESIAN_POINT('Ctrl Pts',(-185.119296920917,5.58214277998856,
126.576120308909));
#232824=CARTESIAN_POINT('Ctrl Pts',(-185.39774454473,-0.540053797659538,
123.822478634922));
#232825=CARTESIAN_POINT('Ctrl Pts',(-185.676192168543,-6.16596731835295,
127.484845419088));
#232826=CARTESIAN_POINT('Ctrl Pts',(-185.954639792356,-6.12565809773001,
134.197684503321));
#232827=CARTESIAN_POINT('Ctrl Pts',(-186.233087416169,-0.456168340327589,
137.792224709632));
#232828=CARTESIAN_POINT('Ctrl Pts',(-186.511535039982,5.63251783677319,
134.965259191474));
#232829=CARTESIAN_POINT('Ctrl Pts',(-186.789982663795,6.54519528567348,
128.314631155089));
#232830=CARTESIAN_POINT('Ctrl Pts',(-187.068430287608,1.44315801760525,
123.951942864674));
#232831=CARTESIAN_POINT('Ctrl Pts',(-187.346877911421,-4.98507096645316,
125.886291729948));
#232832=CARTESIAN_POINT('Ctrl Pts',(-187.625325535233,-6.83226326659722,
132.340105641921));
#232833=CARTESIAN_POINT('Ctrl Pts',(-187.903773159046,-2.40093939935397,
137.382644901827));
#232834=CARTESIAN_POINT('Ctrl Pts',(-188.182220782859,4.23673048348491,
136.380062271549));
#232835=CARTESIAN_POINT('Ctrl Pts',(-188.460668406672,6.98105202779173,
130.25368220943));
#232836=CARTESIAN_POINT('Ctrl Pts',(-188.739116030485,3.31012780190951,
124.633348702251));
#232837=CARTESIAN_POINT('Ctrl Pts',(-189.017563654298,-3.40264216519462,
124.683873674555));
#232838=CARTESIAN_POINT('Ctrl Pts',(-189.296011278111,-6.98855021079573,
130.358827145076));
#232839=CARTESIAN_POINT('Ctrl Pts',(-189.574458901924,-4.15232202233378,
136.443204111294));
#232840=CARTESIAN_POINT('Ctrl Pts',(-189.852906525736,2.49968725244504,
137.345759379595));
#232841=CARTESIAN_POINT('Ctrl Pts',(-190.13135414955,6.85460605873784,132.237088750687));
#232842=CARTESIAN_POINT('Ctrl Pts',(-190.409801773362,4.91047676317321,
125.8118109601));
#232843=CARTESIAN_POINT('Ctrl Pts',(-190.688249397175,-1.5461407876216,
123.974442405114));
#232844=CARTESIAN_POINT('Ctrl Pts',(-190.966697020988,-6.58193048776853,
128.413435027317));
#232845=CARTESIAN_POINT('Ctrl Pts',(-191.245144644801,-5.56924761483672,
135.049571463749));
#232846=CARTESIAN_POINT('Ctrl Pts',(-191.523592268614,0.561301743259386,
137.784566522618));
#232847=CARTESIAN_POINT('Ctrl Pts',(-191.802039892427,6.17604222041412,
134.105093356759));
#232848=CARTESIAN_POINT('Ctrl Pts',(-192.08048751624,6.11530161344434,127.39240805334));
#232849=CARTESIAN_POINT('Ctrl Pts',(-192.358935140053,0.43489757281158,
123.815140473294));
#232850=CARTESIAN_POINT('Ctrl Pts',(-192.637382763865,-5.64515609130746,
126.660624763449));
#232851=CARTESIAN_POINT('Ctrl Pts',(-192.915830387678,-6.53758708872167,
133.313999870785));
#232852=CARTESIAN_POINT('Ctrl Pts',(-193.194278011491,-1.42229493048546,
137.661139107108));
#232853=CARTESIAN_POINT('Ctrl Pts',(-193.472725635304,5.00001678589681,
135.707233883791));
#232854=CARTESIAN_POINT('Ctrl Pts',(-193.751173259117,6.82755734043935,
129.247827647489));
#232855=CARTESIAN_POINT('Ctrl Pts',(-194.02962088293,2.38090624383734,124.218799169824));
#232856=CARTESIAN_POINT('Ctrl Pts',(-194.308068506743,-4.25368137711504,
125.241579940071));
#232857=CARTESIAN_POINT('Ctrl Pts',(-194.586516130556,-6.97934361638637,
131.376284395991));
#232858=CARTESIAN_POINT('Ctrl Pts',(-194.864963754369,-3.29133003208973,
136.985418839569));
#232859=CARTESIAN_POINT('Ctrl Pts',(-195.143411378181,3.42125506128717,
136.914462738605));
#232860=CARTESIAN_POINT('Ctrl Pts',(-195.421859001994,6.98987389094189,
131.22862128349));
#232861=CARTESIAN_POINT('Ctrl Pts',(-195.700306625807,4.13514008914463,
125.152905002676));
#232862=CARTESIAN_POINT('Ctrl Pts',(-195.97875424962,-2.51958544175274,
124.270600342989));
#232863=CARTESIAN_POINT('Ctrl Pts',(-196.257201873433,-6.85893504027095,
129.392502183704));
#232864=CARTESIAN_POINT('Ctrl Pts',(-196.535649497246,-4.89525841438522,
135.811832952018));
#232865=CARTESIAN_POINT('Ctrl Pts',(-196.814097121059,1.56692154765205,
137.629541273595));
#232866=CARTESIAN_POINT('Ctrl Pts',(-197.092544744872,6.58917715577019,
133.175242000891));
#232867=CARTESIAN_POINT('Ctrl Pts',(-197.370992368684,5.55630085693524,
126.542218560906));
#232868=CARTESIAN_POINT('Ctrl Pts',(-197.649439992498,-0.582544489036021,
123.825895453776));
#232869=CARTESIAN_POINT('Ctrl Pts',(-197.92788761631,-6.18605990846357,
127.522440915193));
#232870=CARTESIAN_POINT('Ctrl Pts',(-198.206335240123,-6.10488847784037,
134.234910252398));
#232871=CARTESIAN_POINT('Ctrl Pts',(-198.484782863936,-0.413622776464342,
137.79487206686));
#232872=CARTESIAN_POINT('Ctrl Pts',(-198.763230487749,5.657742049887,134.930895364888));
#232873=CARTESIAN_POINT('Ctrl Pts',(-199.041678111562,6.52991832845634,
128.274834822558));
#232874=CARTESIAN_POINT('Ctrl Pts',(-199.320125735375,1.40141866741961,
123.943284911633));
#232875=CARTESIAN_POINT('Ctrl Pts',(-199.598573359188,-5.01491628586802,
125.916728392279));
#232876=CARTESIAN_POINT('Ctrl Pts',(-199.877020983,-6.82278816472322,132.381667113854));
#232877=CARTESIAN_POINT('Ctrl Pts',(-200.155468606814,-2.36085103192995,
137.397138221046));
#232878=CARTESIAN_POINT('Ctrl Pts',(-200.433916230626,4.27059286522247,
136.354168785731));
#232879=CARTESIAN_POINT('Ctrl Pts',(-200.712363854439,6.97757054929515,
130.211196767073));
#232880=CARTESIAN_POINT('Ctrl Pts',(-200.990811478252,3.27250177183757,
124.613313349352));
#232881=CARTESIAN_POINT('Ctrl Pts',(-201.269259102065,-3.43983626333961,
124.704699921646));
#232882=CARTESIAN_POINT('Ctrl Pts',(-201.547706725878,-6.9911328178512,
130.401376688499));
#232883=CARTESIAN_POINT('Ctrl Pts',(-201.826154349691,-4.1179198485831,
136.468375999304));
#232884=CARTESIAN_POINT('Ctrl Pts',(-202.104601973504,2.53946028996452,
137.330421876826));
#232885=CARTESIAN_POINT('Ctrl Pts',(-202.383049597317,6.86320048156709,
132.195336272904));
#232886=CARTESIAN_POINT('Ctrl Pts',(-202.66149722113,4.87999471659204,125.782011994664));
#232887=CARTESIAN_POINT('Ctrl Pts',(-202.939944844942,-1.5876877919352,
123.983980745501));
#232888=CARTESIAN_POINT('Ctrl Pts',(-203.218392468755,-6.59636278253501,
128.453545404684));
#232889=CARTESIAN_POINT('Ctrl Pts',(-203.496840092568,-5.54330262622176,
135.083394400798));
#232890=CARTESIAN_POINT('Ctrl Pts',(-203.775287716381,0.603781838200554,
137.781020392543));
#232891=CARTESIAN_POINT('Ctrl Pts',(-204.053735340194,6.19602028969954,
134.067436879861));
#232892=CARTESIAN_POINT('Ctrl Pts',(-204.332182964007,6.09441878738321,
127.355245692268));
#232893=CARTESIAN_POINT('Ctrl Pts',(-204.61063058782,0.392344148371673,
123.812622622391));
#232894=CARTESIAN_POINT('Ctrl Pts',(-204.889078211633,-5.67027559591653,
126.69506520469));
#232895=CARTESIAN_POINT('Ctrl Pts',(-205.167525835445,-6.5221890759199,
133.353749521179));
#232896=CARTESIAN_POINT('Ctrl Pts',(-205.445973459259,-1.38052942180316,
137.66966997982));
#232897=CARTESIAN_POINT('Ctrl Pts',(-205.724421083071,5.02976932833932,
135.676706523556));
#232898=CARTESIAN_POINT('Ctrl Pts',(-206.002868706884,6.8179557836299,129.206295207017));
#232899=CARTESIAN_POINT('Ctrl Pts',(-206.281316330697,2.340773949421,124.204427932937));
#232900=CARTESIAN_POINT('Ctrl Pts',(-206.55976395451,-4.28746479114066,
125.267576371395));
#232901=CARTESIAN_POINT('Ctrl Pts',(-206.838211578323,-6.97573284294384,
131.418759045136));
#232902=CARTESIAN_POINT('Ctrl Pts',(-207.116659202136,-3.253643195576,137.005339578972));
#232903=CARTESIAN_POINT('Ctrl Pts',(-207.395106825949,3.4583855992191,136.893523381939));
#232904=CARTESIAN_POINT('Ctrl Pts',(-207.673554449762,6.99232697986142,
131.186064076586));
#232905=CARTESIAN_POINT('Ctrl Pts',(-207.952002073574,4.10066146017411,
125.127837939644));
#232906=CARTESIAN_POINT('Ctrl Pts',(-208.230449697387,-2.55931161296347,
124.286058830161));
#232907=CARTESIAN_POINT('Ctrl Pts',(-208.5088973212,-6.86740234311116,129.434280626559));
#232908=CARTESIAN_POINT('Ctrl Pts',(-208.787344945013,-4.86468581119477,
135.841539002563));
#232909=CARTESIAN_POINT('Ctrl Pts',(-209.065792568826,1.60843932809579,
137.619876522599));
#232910=CARTESIAN_POINT('Ctrl Pts',(-209.344240192639,6.60348730149562,
133.135087882371));
#232911=CARTESIAN_POINT('Ctrl Pts',(-209.622687816452,5.53025304311036,
126.508474748144));
#232912=CARTESIAN_POINT('Ctrl Pts',(-209.901135440264,-0.625013594012848,
123.829570862223));
#232913=CARTESIAN_POINT('Ctrl Pts',(-210.179583064078,-6.20592327184948,
127.56015802404));
#232914=CARTESIAN_POINT('Ctrl Pts',(-210.45803068789,-6.08389263906328,
134.272008881199));
#232915=CARTESIAN_POINT('Ctrl Pts',(-210.736478311703,-0.371061885656257,
137.797260388114));
#232916=CARTESIAN_POINT('Ctrl Pts',(-211.014925935516,5.68275661328764,
134.896378628042));
#232917=CARTESIAN_POINT('Ctrl Pts',(-211.293373559329,6.51439940271492,
128.235132222534));
#232918=CARTESIAN_POINT('Ctrl Pts',(-211.571821183142,1.35962738715011,
123.934881198276));
#232919=CARTESIAN_POINT('Ctrl Pts',(-211.850268806955,-5.04457577571481,
125.947346167619));
#232920=CARTESIAN_POINT('Ctrl Pts',(-212.128716430768,-6.81306024192543,
132.423170138115));
#232921=CARTESIAN_POINT('Ctrl Pts',(-212.40716405458,-2.32067518230222,
137.411387242468));
#232922=CARTESIAN_POINT('Ctrl Pts',(-212.685611678394,4.30429699857105,
136.32806964973));
#232923=CARTESIAN_POINT('Ctrl Pts',(-212.964059302206,6.97383051435588,
130.168733304621));
#232924=CARTESIAN_POINT('Ctrl Pts',(-213.24250692602,3.23475447800865,124.593507407987));
#232925=CARTESIAN_POINT('Ctrl Pts',(-213.520954549832,-3.47690289708716,
124.725752193909));
#232926=CARTESIAN_POINT('Ctrl Pts',(-213.799402173646,-6.99345636590915,
130.443941164641));
#232927=CARTESIAN_POINT('Ctrl Pts',(-214.077849797458,-4.08336508379785,
136.49333800514));
#232928=CARTESIAN_POINT('Ctrl Pts',(-214.356297421271,2.57913922684953,
137.314842548456));
#232929=CARTESIAN_POINT('Ctrl Pts',(-214.634745045084,6.87154058597789,
132.153532252007));
#232930=CARTESIAN_POINT('Ctrl Pts',(-214.913192668897,4.84933184001288,
125.752399134204));
#232931=CARTESIAN_POINT('Ctrl Pts',(-215.19164029271,-1.62917596389355,
123.993771817573));
#232932=CARTESIAN_POINT('Ctrl Pts',(-215.470087916522,-6.61055064665203,
128.493742892374));
#232933=CARTESIAN_POINT('Ctrl Pts',(-215.748535540335,-5.51715222849034,
135.117058776675));
#232934=CARTESIAN_POINT('Ctrl Pts',(-216.026983164148,0.646239559784443,
137.777215739773));
#232935=CARTESIAN_POINT('Ctrl Pts',(-216.305430787961,6.21576876317433,
134.029659488472));
#232936=CARTESIAN_POINT('Ctrl Pts',(-216.583878411774,6.0733101303926,127.318211139417));
#232937=CARTESIAN_POINT('Ctrl Pts',(-216.862326035587,0.349776185474419,
123.810363852911));
#232938=CARTESIAN_POINT('Ctrl Pts',(-217.1407736594,-5.69518498637811,126.729657917385));
#232939=CARTESIAN_POINT('Ctrl Pts',(-217.419221283213,-6.50654938100331,
133.393404703032));
#232940=CARTESIAN_POINT('Ctrl Pts',(-217.697668907026,-1.33871275709491,
137.67794645597));
#232941=CARTESIAN_POINT('Ctrl Pts',(-217.976116530838,5.05933549082977,
135.64599861675));
#232942=CARTESIAN_POINT('Ctrl Pts',(-218.254564154652,6.80810158496121,
129.164821983446));
#232943=CARTESIAN_POINT('Ctrl Pts',(-218.533011778464,2.30055491676597,
124.190301258982));
#232944=CARTESIAN_POINT('Ctrl Pts',(-218.811459402277,-4.32108933158155,
125.293777970294));
#232945=CARTESIAN_POINT('Ctrl Pts',(-219.08990702609,-6.97186358115499,
131.461210927519));
#232946=CARTESIAN_POINT('Ctrl Pts',(-219.368354649903,-3.21583579411804,
137.02503053882));
#232947=CARTESIAN_POINT('Ctrl Pts',(-219.646802273716,3.49538798540175,
136.872358389107));
#232948=CARTESIAN_POINT('Ctrl Pts',(-219.925249897529,6.99452096553273,
131.143492725519));
#232949=CARTESIAN_POINT('Ctrl Pts',(-220.203697521342,4.06603087968498,
125.102981222246));
#232950=CARTESIAN_POINT('Ctrl Pts',(-220.482145145155,-2.59894294794204,
124.301758855404));
#232951=CARTESIAN_POINT('Ctrl Pts',(-220.760592768967,-6.87561517183164,
129.476109838232));
#232952=CARTESIAN_POINT('Ctrl Pts',(-221.03904039278,-4.83393294528274,
135.87105839861));
#232953=CARTESIAN_POINT('Ctrl Pts',(-221.317488016593,1.64989750722823,
137.609959220154));
#232954=CARTESIAN_POINT('Ctrl Pts',(-221.595935640406,6.61755275257056,
133.094847397895));
#232955=CARTESIAN_POINT('Ctrl Pts',(-221.874383264219,5.5040003037252,126.474890121013));
#232956=CARTESIAN_POINT('Ctrl Pts',(-222.152830888031,-0.667459538880483,
123.83350472407));
#232957=CARTESIAN_POINT('Ctrl Pts',(-222.431278511845,-6.22555667246622,
127.597995348007));
#232958=CARTESIAN_POINT('Ctrl Pts',(-222.709726135657,-6.06267135940695,
134.308979015016));
#232959=CARTESIAN_POINT('Ctrl Pts',(-222.988173759471,-0.328487245014279,
137.799389584896));
#232960=CARTESIAN_POINT('Ctrl Pts',(-223.266621383283,5.70756060005303,
134.861710259961));
#232961=CARTESIAN_POINT('Ctrl Pts',(-223.545069007096,6.49863908350723,
128.195524826214));
#232962=CARTESIAN_POINT('Ctrl Pts',(-223.823516630909,1.31778572538753,
123.926732036005));
#232963=CARTESIAN_POINT('Ctrl Pts',(-224.101964254722,-5.07404833695195,
125.978143921416));
#232964=CARTESIAN_POINT('Ctrl Pts',(-224.380411878535,-6.80307985867417,
132.464613176793));
#232965=CARTESIAN_POINT('Ctrl Pts',(-224.658859502348,-2.28041333920269,
137.425391438088));
#232966=CARTESIAN_POINT('Ctrl Pts',(-224.937307126161,4.33784163461131,
136.30176583066));
#232967=CARTESIAN_POINT('Ctrl Pts',(-225.215754749974,6.96983206156226,
130.126293395573));
#232968=CARTESIAN_POINT('Ctrl Pts',(-225.494202373786,3.19688731916334,
124.573931612073));
#232969=CARTESIAN_POINT('Ctrl Pts',(-225.7726499976,-3.51384069291894,124.747029711241));
#232970=CARTESIAN_POINT('Ctrl Pts',(-226.051097621412,-6.9955207688696,
130.486518996257));
#232971=CARTESIAN_POINT('Ctrl Pts',(-226.329545245225,-4.04865900841799,
136.518089203828));
#232972=CARTESIAN_POINT('Ctrl Pts',(-226.607992869038,2.61872259278156,
137.299021971784));
#232973=CARTESIAN_POINT('Ctrl Pts',(-226.886440492851,6.87962606292594,
132.111678237058));
#232974=CARTESIAN_POINT('Ctrl Pts',(-227.164888116664,4.81848926965818,
125.722973476035));
#232975=CARTESIAN_POINT('Ctrl Pts',(-227.443335740477,-1.67060376613766,
124.003815258517));
#232976=CARTESIAN_POINT('Ctrl Pts',(-227.72178336429,-6.62449355438458,
128.534026000853));
#232977=CARTESIAN_POINT('Ctrl Pts',(-228.000230988102,-5.49079739065326,
135.150563343936));
#232978=CARTESIAN_POINT('Ctrl Pts',(-228.278678611916,0.688673334723007,
137.773152705292));
#232979=CARTESIAN_POINT('Ctrl Pts',(-228.557126235728,6.23528690905198,
133.991762582447));
#232980=CARTESIAN_POINT('Ctrl Pts',(-228.835573859542,6.05197642466173,
127.281305767118));
#232981=CARTESIAN_POINT('Ctrl Pts',(-229.114021483354,0.307195261492642,
123.808364248553));
#232982=CARTESIAN_POINT('Ctrl Pts',(-229.392469107167,-5.7198833396657,
126.764401619687));
#232983=CARTESIAN_POINT('Ctrl Pts',(-229.670916730979,-6.49066858350677,
133.432963946903));
#232984=CARTESIAN_POINT('Ctrl Pts',(-229.949364354793,-1.29684648589306,
137.685968228869));
#232985=CARTESIAN_POINT('Ctrl Pts',(-230.227811978605,5.0887141777831,135.615111301269));
#232986=CARTESIAN_POINT('Ctrl Pts',(-230.506259602419,6.79799510958498,
129.123409513582));
#232987=CARTESIAN_POINT('Ctrl Pts',(-230.784707226231,2.26025063620168,
124.176419671429));
#232988=CARTESIAN_POINT('Ctrl Pts',(-231.063154850045,-4.35455375246839,
125.32018376586));
#232989=CARTESIAN_POINT('Ctrl Pts',(-231.341602473857,-6.96773597439774,
131.503638470075));
#232990=CARTESIAN_POINT('Ctrl Pts',(-231.62005009767,-3.17790922868121,
137.044490989456));
#232991=CARTESIAN_POINT('Ctrl Pts',(-231.898497721483,3.53226084869627,
136.850968544386));
#232992=CARTESIAN_POINT('Ctrl Pts',(-232.176945345296,6.99645576665798,
131.100908807788));
#232993=CARTESIAN_POINT('Ctrl Pts',(-232.455392969109,4.03124963092651,
125.078335771559));
#232994=CARTESIAN_POINT('Ctrl Pts',(-232.733840592922,-2.63847797813309,
124.317699836946));
#232995=CARTESIAN_POINT('Ctrl Pts',(-233.012288216734,-6.88357322210384,
129.517988268725));
#232996=CARTESIAN_POINT('Ctrl Pts',(-233.290735840548,-4.80300095620762,
135.900390046307));
#232997=CARTESIAN_POINT('Ctrl Pts',(-233.56918346436,1.6912945488023,137.599789733751));
#232998=CARTESIAN_POINT('Ctrl Pts',(-233.847631088173,6.63137298779474,
133.05452203859));
#232999=CARTESIAN_POINT('Ctrl Pts',(-234.126078711986,5.47754361158473,
126.441465924004));
#233000=CARTESIAN_POINT('Ctrl Pts',(-234.404526335799,-0.709880750790079,
123.837696893545));
#233001=CARTESIAN_POINT('Ctrl Pts',(-234.682973959612,-6.24495938279112,
127.635951485018));
#233002=CARTESIAN_POINT('Ctrl Pts',(-234.961421583425,-6.04122542523402,
134.345819283911));
#233003=CARTESIAN_POINT('Ctrl Pts',(-235.239869207238,-0.285900432155891,
137.801259578306));
#233004=CARTESIAN_POINT('Ctrl Pts',(-235.518316831051,5.73215309106056,
134.826891545298));
#233005=CARTESIAN_POINT('Ctrl Pts',(-235.796764454864,6.48263795483918,
128.156014101264));
#233006=CARTESIAN_POINT('Ctrl Pts',(-236.075212078676,1.27589523259052,
123.918837726791));
#233007=CARTESIAN_POINT('Ctrl Pts',(-236.353659702489,-5.10333287746112,
126.009120512446));
#233008=CARTESIAN_POINT('Ctrl Pts',(-236.632107326302,-6.79284738479763,
132.505994694203));
#233009=CARTESIAN_POINT('Ctrl Pts',(-236.910554950115,-2.24006699454776,
137.439150288976));
#233010=CARTESIAN_POINT('Ctrl Pts',(-237.189002573928,4.3712255303347,136.275258303218));
#233011=CARTESIAN_POINT('Ctrl Pts',(-237.467450197741,6.96557533907847,
130.083878612554));
#233012=CARTESIAN_POINT('Ctrl Pts',(-237.745897821554,3.15890169848239,
124.554586686994));
#233013=CARTESIAN_POINT('Ctrl Pts',(-238.024345445366,-3.55064828209192,
124.768531685198));
#233014=CARTESIAN_POINT('Ctrl Pts',(-238.30279306918,-6.99732595023538,
130.529108605612));
#233015=CARTESIAN_POINT('Ctrl Pts',(-238.581240692992,-4.01380290848946,
136.542628678202));
#233016=CARTESIAN_POINT('Ctrl Pts',(-238.859688316805,2.65820892098533,
137.282960733047));
#233017=CARTESIAN_POINT('Ctrl Pts',(-239.138135940618,6.88745661279959,
132.069775778975));
#233018=CARTESIAN_POINT('Ctrl Pts',(-239.416583564431,4.78746814841248,
125.693736110535));
#233019=CARTESIAN_POINT('Ctrl Pts',(-239.695031188244,-1.71196966354462,
124.014110696169));
#233020=CARTESIAN_POINT('Ctrl Pts',(-239.973478812057,-6.63819098907155,
128.574393237416));
#233021=CARTESIAN_POINT('Ctrl Pts',(-240.25192643587,-5.46423908930053,
135.183906861057));
#233022=CARTESIAN_POINT('Ctrl Pts',(-240.530374059683,0.731081590618679,
137.768831439659));
#233023=CARTESIAN_POINT('Ctrl Pts',(-240.808821683496,6.25457400407998,
133.95374756607));
#233024=CARTESIAN_POINT('Ctrl Pts',(-241.087269307308,6.03041846071876,
127.244530942912));
#233025=CARTESIAN_POINT('Ctrl Pts',(-241.365716931122,0.264602954276818,
123.806623883412));
#233026=CARTESIAN_POINT('Ctrl Pts',(-241.644164554934,-5.74436974057257,
126.799295024156));
#233027=CARTESIAN_POINT('Ctrl Pts',(-241.922612178747,-6.47454727189872,
133.472425786911));
#233028=CARTESIAN_POINT('Ctrl Pts',(-242.20105980256,-1.25493215956847,
137.693735001267));
#233029=CARTESIAN_POINT('Ctrl Pts',(-242.479507426373,5.11790430056101,
135.584045721651));
#233030=CARTESIAN_POINT('Ctrl Pts',(-242.757955050186,6.78763673199965,
129.082059331979));
#233031=CARTESIAN_POINT('Ctrl Pts',(-243.036402673998,2.21986260121965,
124.162783684665));
#233032=CARTESIAN_POINT('Ctrl Pts',(-243.314850297812,-4.38785681376436,
125.346792779616));
#233033=CARTESIAN_POINT('Ctrl Pts',(-243.593297921624,-6.96335017562108,
131.54604010063));
#233034=CARTESIAN_POINT('Ctrl Pts',(-243.871745545438,-3.13986490465013,
137.063720209766));
#233035=CARTESIAN_POINT('Ctrl Pts',(-244.15019316925,3.56900282276695,136.829354640385));
#233036=CARTESIAN_POINT('Ctrl Pts',(-244.428640793064,6.99813131154132,
131.058313901354));
#233037=CARTESIAN_POINT('Ctrl Pts',(-244.707088416876,3.99631900273028,
125.053902500829));
#233038=CARTESIAN_POINT('Ctrl Pts',(-244.985536040689,-2.67791523855318,
124.333881184089));
#233039=CARTESIAN_POINT('Ctrl Pts',(-245.263983664501,-6.89127619903846,
129.559914366219));
#233040=CARTESIAN_POINT('Ctrl Pts',(-245.542431288315,-4.7718909901659,
135.929532858758));
#233041=CARTESIAN_POINT('Ctrl Pts',(-245.820878912128,1.73262891883438,
137.589368440225));
#233042=CARTESIAN_POINT('Ctrl Pts',(-246.09932653594,6.6449474950541,133.014113298726));
#233043=CARTESIAN_POINT('Ctrl Pts',(-246.377774159753,5.45088394705135,
126.408203395661));
#233044=CARTESIAN_POINT('Ctrl Pts',(-246.656221783566,-0.752275657806765,
123.842147215306));
#233045=CARTESIAN_POINT('Ctrl Pts',(-246.934669407379,-6.26413068384941,
127.674025028594));
#233046=CARTESIAN_POINT('Ctrl Pts',(-247.213117031192,-6.01955563123113,
134.382528322752));
#233047=CARTESIAN_POINT('Ctrl Pts',(-247.491564655005,-0.243303025152602,
137.802870299053));
#233048=CARTESIAN_POINT('Ctrl Pts',(-247.770012278818,5.75653317502817,
134.791923774272));
#233049=CARTESIAN_POINT('Ctrl Pts',(-248.048459902631,6.46639660963695,
128.116601511768));
#233050=CARTESIAN_POINT('Ctrl Pts',(-248.326907526444,1.23395746102625,
123.91119856316));
#233051=CARTESIAN_POINT('Ctrl Pts',(-248.605355150257,-5.13242831209467,
126.040274792862));
#233052=CARTESIAN_POINT('Ctrl Pts',(-248.883802774069,-6.78236319946242,
132.547313156937));
#233053=CARTESIAN_POINT('Ctrl Pts',(-249.162250397883,-2.19963764338714,
137.452663285294));
#233054=CARTESIAN_POINT('Ctrl Pts',(-249.440698021695,4.40444744868852,
136.24854804965));
#233055=CARTESIAN_POINT('Ctrl Pts',(-249.719145645508,6.96106050463867,
130.041490527264));
#233056=CARTESIAN_POINT('Ctrl Pts',(-249.997593269321,3.12079902353814,
124.535473349588));
#233057=CARTESIAN_POINT('Ctrl Pts',(-250.276040893134,-3.58732430068758,
124.790257319018));
#233058=CARTESIAN_POINT('Ctrl Pts',(-250.554488516946,-6.99887184311352,
130.571708414529));
#233059=CARTESIAN_POINT('Ctrl Pts',(-250.83293614076,-3.97879807562073,
136.566955518948));
#233060=CARTESIAN_POINT('Ctrl Pts',(-251.111383764572,2.69759674828547,
137.26665942739));
#233061=CARTESIAN_POINT('Ctrl Pts',(-251.389831388386,6.89503194542569,
132.027826430486));
#233062=CARTESIAN_POINT('Ctrl Pts',(-251.668279012198,4.75626962579305,
125.66468812107));
#233063=CARTESIAN_POINT('Ctrl Pts',(-251.946726636011,-1.75327212332407,
124.024657749096));
#233064=CARTESIAN_POINT('Ctrl Pts',(-252.225174259824,-6.65164244307981,
128.614843106116));
#233065=CARTESIAN_POINT('Ctrl Pts',(-252.503621883637,-5.43747830869239,
135.217088092717));
#233066=CARTESIAN_POINT('Ctrl Pts',(-252.78206950745,0.773462756270139,
137.764252102553));
#233067=CARTESIAN_POINT('Ctrl Pts',(-253.060517131263,6.2736293330892,133.91561584884));
#233068=CARTESIAN_POINT('Ctrl Pts',(-253.338964755075,6.00863703830687,
127.207888027921));
#233069=CARTESIAN_POINT('Ctrl Pts',(-253.617412378889,0.222000840393564,
123.805142824969));
#233070=CARTESIAN_POINT('Ctrl Pts',(-253.895860002702,-5.76864327852066,
126.83433683216));
#233071=CARTESIAN_POINT('Ctrl Pts',(-254.174307626514,-6.45818604965135,
133.511788771436));
#233072=CARTESIAN_POINT('Ctrl Pts',(-254.452755250327,-1.21297131977014,
137.701246465247));
#233073=CARTESIAN_POINT('Ctrl Pts',(-254.73120287414,5.14690475579816,135.55280306703));
#233074=CARTESIAN_POINT('Ctrl Pts',(-255.009650497953,6.7770268770417,129.040772899161));
#233075=CARTESIAN_POINT('Ctrl Pts',(-255.288098121766,2.17939223099114,
124.149393939406));
#233076=CARTESIAN_POINT('Ctrl Pts',(-255.566545745579,-4.42099713522674,
125.37360376984));
#233077=CARTESIAN_POINT('Ctrl Pts',(-255.844993369392,-6.95870662337211,
131.588414730824));
#233078=CARTESIAN_POINT('Ctrl Pts',(-256.123440993205,-3.10170371057109,
137.082716575498));
#233079=CARTESIAN_POINT('Ctrl Pts',(-256.401888617018,3.60561156199617,
136.807519199501));
#233080=CARTESIAN_POINT('Ctrl Pts',(-256.68033624083,6.99954939633056,131.01570633407));
#233081=CARTESIAN_POINT('Ctrl Pts',(-256.958783864643,3.96123678073902,
125.029688453078));
#233082=CARTESIAN_POINT('Ctrl Pts',(-257.237231488456,-2.71724664265218,
124.350290708114));
#233083=CARTESIAN_POINT('Ctrl Pts',(-257.515679112269,-6.89873632689917,
129.601908459729));
#233084=CARTESIAN_POINT('Ctrl Pts',(-257.794126736082,-4.74058057908887,
135.958444437253));
#233085=CARTESIAN_POINT('Ctrl Pts',(-258.072574359895,1.77385448465437,
137.578773744179));
#233086=CARTESIAN_POINT('Ctrl Pts',(-258.351021983707,6.6583599873155,132.973475360041));
#233087=CARTESIAN_POINT('Ctrl Pts',(-258.629469607521,5.42386327951784,
126.375381938049));
#233088=CARTESIAN_POINT('Ctrl Pts',(-258.907917231333,-0.794342416617398,
123.846330221273));
#233089=CARTESIAN_POINT('Ctrl Pts',(-259.186364855146,-6.28363694765996,
127.713206958712));
#233090=CARTESIAN_POINT('Ctrl Pts',(-259.464812478959,-5.99659113747434,
134.41722675292));
#233091=CARTESIAN_POINT('Ctrl Pts',(-259.743260102772,-0.202727240537578,
137.807801967267));
#233092=CARTESIAN_POINT('Ctrl Pts',(-260.021707726585,5.7845923739281,134.749768174183));
#233093=CARTESIAN_POINT('Ctrl Pts',(-260.253747413096,6.33253704604016,
129.202365411857));
#233094=CARTESIAN_POINT('Ctrl Pts',(-260.439389088604,3.82430165355141,
125.973250269562));
#233095=CARTESIAN_POINT('Ctrl Pts',(-260.532214889509,1.97943258085903,
125.138073123498));
#233096=CARTESIAN_POINT('Ctrl Pts',(-260.578632753112,1.00712299976162,
124.970230583726));
#233097=CARTESIAN_POINT('Ctrl Pts',(207.955458783725,-5.89986192518215,
130.414453211936));
#233098=CARTESIAN_POINT('Ctrl Pts',(207.964054739687,-5.87737129978886,
130.750371489811));
#233099=CARTESIAN_POINT('Ctrl Pts',(207.961523532031,-5.84640950003041,
131.085475744573));
#233100=CARTESIAN_POINT('Ctrl Pts',(207.946544851276,-5.80258759547012,
131.456229395558));
#233101=CARTESIAN_POINT('Ctrl Pts',(207.944935584475,-5.7981622731838,131.492794197297));
#233102=CARTESIAN_POINT('Ctrl Pts',(207.943168852932,-5.79356696020855,
131.52989605424));
#233103=CARTESIAN_POINT('Ctrl Pts',(207.943142385322,-5.79349817258261,
131.53045124226));
#233104=CARTESIAN_POINT('Ctrl Pts',(207.94310533414,-5.79340195614918,131.531227539937));
#233105=CARTESIAN_POINT('Ctrl Pts',(207.94309477597,-5.79337454689547,131.531448653929));
#233106=CARTESIAN_POINT('Ctrl Pts',(207.943077748303,-5.79333035677605,
131.531805092076));
#233107=CARTESIAN_POINT('Ctrl Pts',(207.943071281854,-5.7933135783506,131.531940415657));
#233108=CARTESIAN_POINT('Ctrl Pts',(207.943059016683,-5.79328176025719,
131.532197017465));
#233109=CARTESIAN_POINT('Ctrl Pts',(207.943053218331,-5.79326672089837,
131.53231829545));
#233110=CARTESIAN_POINT('Ctrl Pts',(207.943040063266,-5.79323260617857,
131.53259337706));
#233111=CARTESIAN_POINT('Ctrl Pts',(207.943032705692,-5.7932135301817,131.532747180222));
#233112=CARTESIAN_POINT('Ctrl Pts',(207.943010733002,-5.7931565741522,131.533206352869));
#233113=CARTESIAN_POINT('Ctrl Pts',(207.942996111113,-5.79311868898518,
131.533511720278));
#233114=CARTESIAN_POINT('Ctrl Pts',(207.942874410758,-5.79280350296,131.536051743128));
#233115=CARTESIAN_POINT('Ctrl Pts',(207.942766851691,-5.79252583105091,
131.538286329208));
#233116=CARTESIAN_POINT('Ctrl Pts',(207.941632120879,-5.78960574275957,
131.561753268497));
#233117=CARTESIAN_POINT('Ctrl Pts',(207.940561232304,-5.786929583699,131.582979183399));
#233118=CARTESIAN_POINT('Ctrl Pts',(207.935616314913,-5.77491032228197,
131.677081722506));
#233119=CARTESIAN_POINT('Ctrl Pts',(207.93126593134,-5.76519996462025,131.749881133765));
#233120=CARTESIAN_POINT('Ctrl Pts',(207.908432950335,-5.71778482372917,
132.090906340396));
#233121=CARTESIAN_POINT('Ctrl Pts',(207.883444286136,-5.67508447486567,
132.357688125701));
#233122=CARTESIAN_POINT('Ctrl Pts',(207.851560096185,-5.62714347058168,
132.623000814592));
#233123=CARTESIAN_POINT('Origin',(213.235140564004,0.,130.804360617566));
#233124=CARTESIAN_POINT('',(207.935358922621,4.83993619626808,129.931218342011));
#233125=CARTESIAN_POINT('',(207.344471284167,2.40266844899661,126.515070645963));
#233126=CARTESIAN_POINT('Ctrl Pts',(207.932945971377,4.83234977408945,129.889167346526));
#233127=CARTESIAN_POINT('Ctrl Pts',(207.913056351572,4.7697277774651,129.558514356806));
#233128=CARTESIAN_POINT('Ctrl Pts',(207.882216843952,4.67183438727748,129.22996814172));
#233129=CARTESIAN_POINT('Ctrl Pts',(207.767461666534,4.28964812743425,128.310813320659));
#233130=CARTESIAN_POINT('Ctrl Pts',(207.660120443156,3.9118143497335,127.760719114158));
#233131=CARTESIAN_POINT('Ctrl Pts',(207.486761489502,3.17206573993542,127.02097050436));
#233132=CARTESIAN_POINT('Ctrl Pts',(207.410948455005,2.80990088697428,126.741872036394));
#233133=CARTESIAN_POINT('Ctrl Pts',(207.345096392365,2.41028028844146,126.517201652278));
#233134=CARTESIAN_POINT('',(207.776993964391,4.32587057920753,133.142886646627));
#233135=CARTESIAN_POINT('Ctrl Pts',(207.778436608163,4.32133082450553,133.15282457677));
#233136=CARTESIAN_POINT('Ctrl Pts',(207.80166991443,4.4022999262327,133.003836011816));
#233137=CARTESIAN_POINT('Ctrl Pts',(207.823382325825,4.47588902830909,132.850000075013));
#233138=CARTESIAN_POINT('Ctrl Pts',(207.918593342393,4.79298445822067,132.087388166203));
#233139=CARTESIAN_POINT('Ctrl Pts',(207.96044672069,4.91825,131.426623044073));
#233140=CARTESIAN_POINT('Ctrl Pts',(207.96044672069,4.91825,130.532140837719));
#233141=CARTESIAN_POINT('Ctrl Pts',(207.953011753591,4.89537008512156,130.252332639368));
#233142=CARTESIAN_POINT('Ctrl Pts',(207.93776844465,4.84751183684522,129.97320957585));
#233143=CARTESIAN_POINT('Ctrl Pts',(207.777553167153,4.32872518108459,133.139167112577));
#233144=CARTESIAN_POINT('Ctrl Pts',(207.769784873384,4.39355921696334,133.018964978353));
#233145=CARTESIAN_POINT('Ctrl Pts',(207.762016579614,4.45347444860551,132.895890200518));
#233146=CARTESIAN_POINT('Ctrl Pts',(207.754248285845,4.50820764817201,132.770383726144));
#233147=CARTESIAN_POINT('Ctrl Pts',(207.746488411523,4.5628815266944,132.645013278445));
#233148=CARTESIAN_POINT('Ctrl Pts',(207.7387285372,4.61238439418871,132.517216734316));
#233149=CARTESIAN_POINT('Ctrl Pts',(207.730968662878,4.6564985492191,132.387460211281));
#233150=CARTESIAN_POINT('Ctrl Pts',(207.723215343369,4.70057544075838,132.257813294358));
#233151=CARTESIAN_POINT('Ctrl Pts',(207.715462023859,4.73927255412797,132.126210061989));
#233152=CARTESIAN_POINT('Ctrl Pts',(207.707708704349,4.77242014607768,131.993136884074));
#233153=CARTESIAN_POINT('Ctrl Pts',(207.699619190911,4.80700506034141,131.854293481633));
#233154=CARTESIAN_POINT('Ctrl Pts',(207.691529677474,4.83554820242537,131.71385019373));
#233155=CARTESIAN_POINT('Ctrl Pts',(207.683440164036,4.85791441337539,131.572377944727));
#233156=CARTESIAN_POINT('Ctrl Pts',(207.675693401989,4.87933297154286,131.436899852299));
#233157=CARTESIAN_POINT('Ctrl Pts',(207.667946639943,4.89508723941358,131.30047862999));
#233158=CARTESIAN_POINT('Ctrl Pts',(207.660199877896,4.9051107445793,131.163626043001));
#233159=CARTESIAN_POINT('Ctrl Pts',(207.652453621073,4.91513359603885,131.02678238117));
#233160=CARTESIAN_POINT('Ctrl Pts',(207.644707364249,4.91942639951774,130.889507800467));
#233161=CARTESIAN_POINT('Ctrl Pts',(207.636961107426,4.91797464963016,130.752318249297));
#233162=CARTESIAN_POINT('Ctrl Pts',(207.629213678398,4.91652268005615,130.615107937881));
#233163=CARTESIAN_POINT('Ctrl Pts',(207.62146624937,4.90932443143035,130.47798307252));
#233164=CARTESIAN_POINT('Ctrl Pts',(207.613718820343,4.89641751401577,130.341458261837));
#233165=CARTESIAN_POINT('Ctrl Pts',(207.605968541273,4.88350584854127,130.204883227854));
#233166=CARTESIAN_POINT('Ctrl Pts',(207.598218262203,4.8648813720697,130.068909076728));
#233167=CARTESIAN_POINT('Ctrl Pts',(207.590467983133,4.84063335749527,129.934043571425));
#233168=CARTESIAN_POINT('Ctrl Pts',(207.582708968004,4.81635801073261,129.79902604669));
#233169=CARTESIAN_POINT('Ctrl Pts',(207.574949952875,4.78644654020057,129.665120047497));
#233170=CARTESIAN_POINT('Ctrl Pts',(207.567190937746,4.751039073567,129.532821871031));
#233171=CARTESIAN_POINT('Ctrl Pts',(207.559426780275,4.71560814038174,129.400436013003));
#233172=CARTESIAN_POINT('Ctrl Pts',(207.551662622803,4.67467407196882,129.269660472309));
#233173=CARTESIAN_POINT('Ctrl Pts',(207.543898465331,4.62842600073996,129.140973765936));
#233174=CARTESIAN_POINT('Ctrl Pts',(207.536123292545,4.58211231555991,129.01210448669));
#233175=CARTESIAN_POINT('Ctrl Pts',(207.528348119759,4.53046972426244,128.885330318326));
#233176=CARTESIAN_POINT('Ctrl Pts',(207.520572946973,4.47373451129918,128.761107675586));
#233177=CARTESIAN_POINT('Ctrl Pts',(207.518235425263,4.45667768238356,128.723761479917));
#233178=CARTESIAN_POINT('Ctrl Pts',(207.515897903554,4.43916086859752,128.686645716714));
#233179=CARTESIAN_POINT('Ctrl Pts',(207.513560381844,4.42119126588729,128.649772291936));
#233180=CARTESIAN_POINT('Ctrl Pts',(207.505787242456,4.36143557419401,128.527154277599));
#233181=CARTESIAN_POINT('Ctrl Pts',(207.498014103069,4.29648027204063,128.406829765919));
#233182=CARTESIAN_POINT('Ctrl Pts',(207.490240963681,4.2265243627226,128.289271181023));
#233183=CARTESIAN_POINT('Ctrl Pts',(207.48247687602,4.15664991620944,128.171849491667));
#233184=CARTESIAN_POINT('Ctrl Pts',(207.474712788358,4.08178664354628,128.057187654845));
#233185=CARTESIAN_POINT('Ctrl Pts',(207.466948700697,4.00218085216552,127.94573656235));
#233186=CARTESIAN_POINT('Ctrl Pts',(207.459191971722,3.92265050996814,127.834391101541));
#233187=CARTESIAN_POINT('Ctrl Pts',(207.451435242747,3.83838681773448,127.726250646596));
#233188=CARTESIAN_POINT('Ctrl Pts',(207.443678513772,3.74968088678163,127.621739636393));
#233189=CARTESIAN_POINT('Ctrl Pts',(207.435927455956,3.66103981118161,127.517305037071));
#233190=CARTESIAN_POINT('Ctrl Pts',(207.42817639814,3.56796321247351,127.416494898379));
#233191=CARTESIAN_POINT('Ctrl Pts',(207.420425340323,3.47078398382534,127.319702585546));
#233192=CARTESIAN_POINT('Ctrl Pts',(207.412678122975,3.37365290521867,127.222958231046));
#233193=CARTESIAN_POINT('Ctrl Pts',(207.404930905627,3.27242351943269,127.130228014992));
#233194=CARTESIAN_POINT('Ctrl Pts',(207.39718368828,3.16746701561529,127.041869984024));
#233195=CARTESIAN_POINT('Ctrl Pts',(207.389438629274,3.06253975223555,126.95353656923));
#233196=CARTESIAN_POINT('Ctrl Pts',(207.381693570268,2.95388773802827,126.869573164603));
#233197=CARTESIAN_POINT('Ctrl Pts',(207.373948511262,2.84191651249237,126.790298635169));
#233198=CARTESIAN_POINT('Ctrl Pts',(207.366203026905,2.72993913761875,126.711019752064));
#233199=CARTESIAN_POINT('Ctrl Pts',(207.358457542549,2.61464250564787,126.636430485188));
#233200=CARTESIAN_POINT('Ctrl Pts',(207.350712058193,2.49646231867335,126.566807201508));
#233201=CARTESIAN_POINT('Ctrl Pts',(207.348840169584,2.46790114216212,126.549981006311));
#233202=CARTESIAN_POINT('Ctrl Pts',(207.346968280974,2.43917167189546,126.533444654371));
#233203=CARTESIAN_POINT('Ctrl Pts',(207.345096392365,2.41028028844147,126.517201652278));
#233204=CARTESIAN_POINT('Origin',(210.,0.,130.804360617566));
#233205=CARTESIAN_POINT('',(177.987468637443,-4.44881802408841,134.718337674492));
#233206=CARTESIAN_POINT('Ctrl Pts',(177.987171124066,-4.4381842494261,134.71721777451));
#233207=CARTESIAN_POINT('Ctrl Pts',(177.917908154705,-4.66808213043419,
134.456454574234));
#233208=CARTESIAN_POINT('Ctrl Pts',(177.848867591835,-4.8807856187837,134.168285242348));
#233209=CARTESIAN_POINT('Ctrl Pts',(177.78566632542,-5.06704185329145,133.859359376894));
#233210=CARTESIAN_POINT('',(178.188375192211,-5.91592736650928,130.798890494443));
#233211=CARTESIAN_POINT('Ctrl Pts',(178.188375192211,-5.91592736650928,
130.798890494443));
#233212=CARTESIAN_POINT('Ctrl Pts',(178.121415174441,-5.90292116165263,
132.221415516948));
#233213=CARTESIAN_POINT('Ctrl Pts',(178.054455156671,-5.38193783986145,
133.652419557679));
#233214=CARTESIAN_POINT('Ctrl Pts',(177.987495138901,-4.44976524376727,
134.718437431289));
#233215=CARTESIAN_POINT('',(178.530363299101,-1.97902084214117,125.22872231614));
#233216=CARTESIAN_POINT('Ctrl Pts',(178.531594387824,-1.96435919885661,
125.223211676679));
#233217=CARTESIAN_POINT('Ctrl Pts',(178.524172743157,-2.11222423528786,
125.275254732254));
#233218=CARTESIAN_POINT('Ctrl Pts',(178.516751098491,-2.25823691125162,
125.333254551213));
#233219=CARTESIAN_POINT('Ctrl Pts',(178.509329453824,-2.40188156402355,
125.397060411835));
#233220=CARTESIAN_POINT('Ctrl Pts',(178.501916303098,-2.54536181804821,
125.460793247784));
#233221=CARTESIAN_POINT('Ctrl Pts',(178.494503152372,-2.6864791055858,125.530318748188));
#233222=CARTESIAN_POINT('Ctrl Pts',(178.487090001645,-2.82473377071421,
125.605436720538));
#233223=CARTESIAN_POINT('Ctrl Pts',(178.479683718601,-2.96286035412852,
125.68048510219));
#233224=CARTESIAN_POINT('Ctrl Pts',(178.472277435556,-3.09812926890283,
125.761115464114));
#233225=CARTESIAN_POINT('Ctrl Pts',(178.464871152512,-3.23006177761989,
125.847079964299));
#233226=CARTESIAN_POINT('Ctrl Pts',(178.457470116298,-3.36190082143372,
125.932983564681));
#233227=CARTESIAN_POINT('Ctrl Pts',(178.450069080084,-3.4904078540771,126.024213575878));
#233228=CARTESIAN_POINT('Ctrl Pts',(178.44266804387,-3.61512975619378,126.120476822212));
#233229=CARTESIAN_POINT('Ctrl Pts',(178.434930662265,-3.74551973448816,
126.221114820727));
#233230=CARTESIAN_POINT('Ctrl Pts',(178.427193280659,-3.87177211423748,
126.327254051388));
#233231=CARTESIAN_POINT('Ctrl Pts',(178.419455899053,-3.99340362608919,
126.438509263977));
#233232=CARTESIAN_POINT('Ctrl Pts',(178.412059409808,-4.10967631562484,
126.544862811636));
#233233=CARTESIAN_POINT('Ctrl Pts',(178.404662920563,-4.22172630043844,
126.65589090558));
#233234=CARTESIAN_POINT('Ctrl Pts',(178.397266431318,-4.32916618737662,
126.77121659775));
#233235=CARTESIAN_POINT('Ctrl Pts',(178.389869952312,-4.43660592557766,
126.886542130267));
#233236=CARTESIAN_POINT('Ctrl Pts',(178.382473473307,-4.53943532371603,
127.006164976397));
#233237=CARTESIAN_POINT('Ctrl Pts',(178.375076994301,-4.63730509265252,
127.129672598134));
#233238=CARTESIAN_POINT('Ctrl Pts',(178.367679065145,-4.73519404990068,
127.253204434731));
#233239=CARTESIAN_POINT('Ctrl Pts',(178.360281135988,-4.8281212100497,127.380622270841));
#233240=CARTESIAN_POINT('Ctrl Pts',(178.352883206831,-4.915778785888,127.511482015079));
#233241=CARTESIAN_POINT('Ctrl Pts',(178.345482366543,-5.00347085553144,
127.642393253447));
#233242=CARTESIAN_POINT('Ctrl Pts',(178.338081526255,-5.08588900471472,
127.776748786709));
#233243=CARTESIAN_POINT('Ctrl Pts',(178.330680685967,-5.16276990799104,
127.914077337394));
#233244=CARTESIAN_POINT('Ctrl Pts',(178.323271586729,-5.23973660633535,
128.05155913956));
#233245=CARTESIAN_POINT('Ctrl Pts',(178.31586248749,-5.3111535380145,128.192020258013));
#233246=CARTESIAN_POINT('Ctrl Pts',(178.308453388251,-5.37680400071853,
128.334966096564));
#233247=CARTESIAN_POINT('Ctrl Pts',(178.301039443423,-5.44249739916783,
128.478005422438));
#233248=CARTESIAN_POINT('Ctrl Pts',(178.293625498594,-5.5024166726957,128.623532362135));
#233249=CARTESIAN_POINT('Ctrl Pts',(178.286211553766,-5.55639422987409,
128.771034838277));
#233250=CARTESIAN_POINT('Ctrl Pts',(178.278787443269,-5.6104457986575,128.918739563197));
#233251=CARTESIAN_POINT('Ctrl Pts',(178.271363332772,-5.65853927118603,
129.068424878913));
#233252=CARTESIAN_POINT('Ctrl Pts',(178.263939222275,-5.70055742603375,
129.219565490431));
#233253=CARTESIAN_POINT('Ctrl Pts',(178.261616443294,-5.71370363216299,
129.266852803277));
#233254=CARTESIAN_POINT('Ctrl Pts',(178.259293664312,-5.72625552043617,
129.314282511711));
#233255=CARTESIAN_POINT('Ctrl Pts',(178.256970885331,-5.73821053949377,
129.361838393494));
#233256=CARTESIAN_POINT('Ctrl Pts',(178.247172129819,-5.78864336578615,
129.562455181601));
#233257=CARTESIAN_POINT('Ctrl Pts',(178.237373374307,-5.82857446158499,
129.765810079934));
#233258=CARTESIAN_POINT('Ctrl Pts',(178.227574618795,-5.85776135301491,
129.970956457734));
#233259=CARTESIAN_POINT('Ctrl Pts',(178.217994260587,-5.88629771913931,
130.171530477754));
#233260=CARTESIAN_POINT('Ctrl Pts',(178.20841390238,-5.90456354448122,130.373817290498));
#233261=CARTESIAN_POINT('Ctrl Pts',(178.198833544173,-5.9123765717479,130.576909883677));
#233262=CARTESIAN_POINT('Ctrl Pts',(178.195347434846,-5.91521958310856,
130.650811398412));
#233263=CARTESIAN_POINT('Ctrl Pts',(178.19186132552,-5.91667897563865,130.724819368433));
#233264=CARTESIAN_POINT('Ctrl Pts',(178.188375216193,-5.91674747022219,
130.798889226584));
#233265=CARTESIAN_POINT('Ctrl Pts',(178.183768748222,-3.73415024100118,
126.214801538512));
#233266=CARTESIAN_POINT('Ctrl Pts',(178.294473067275,-3.30324972789069,
125.864212903054));
#233267=CARTESIAN_POINT('Ctrl Pts',(178.40360148388,-2.80660255836622,125.563909715843));
#233268=CARTESIAN_POINT('Ctrl Pts',(178.502989322817,-2.18499290349215,
125.304971384407));
#233269=CARTESIAN_POINT('Ctrl Pts',(178.516732714955,-2.09380460320336,
125.26960931481));
#233270=CARTESIAN_POINT('Ctrl Pts',(178.52971317936,-2.00179946419882,125.236530746994));
#233271=CARTESIAN_POINT('Origin',(213.235140564004,0.,130.804360617566));
#233272=CARTESIAN_POINT('',(206.764859435946,-4.91824826123457,130.808496238813));
#233273=CARTESIAN_POINT('Ctrl Pts',(206.834782106149,-4.76405452823405,
129.582490119308));
#233274=CARTESIAN_POINT('Ctrl Pts',(206.827070043619,-4.79800979989384,
129.714881208167));
#233275=CARTESIAN_POINT('Ctrl Pts',(206.819357981088,-4.82644926951694,
129.84871625431));
#233276=CARTESIAN_POINT('Ctrl Pts',(206.811645918557,-4.84926402357277,
129.983494311653));
#233277=CARTESIAN_POINT('Ctrl Pts',(206.803848171462,-4.8723322600444,130.119769815232));
#233278=CARTESIAN_POINT('Ctrl Pts',(206.796050424368,-4.8896499380063,130.257009012014));
#233279=CARTESIAN_POINT('Ctrl Pts',(206.788252677274,-4.90115795633873,
130.394685441948));
#233280=CARTESIAN_POINT('Ctrl Pts',(206.78045493018,-4.91266597467115,130.532361871882));
#233281=CARTESIAN_POINT('Ctrl Pts',(206.772657183085,-4.9183643194193,130.67047511888));
#233282=CARTESIAN_POINT('Ctrl Pts',(206.764859435991,-4.91824826123525,
130.80849623801));
#233283=CARTESIAN_POINT('Ctrl Pts',(206.764859435946,-4.91824826123457,
130.808496238813));
#233284=CARTESIAN_POINT('Ctrl Pts',(206.755633759936,-4.91811095036783,
130.971791882044));
#233285=CARTESIAN_POINT('Ctrl Pts',(206.746408083927,-4.9098372427412,131.134736331661));
#233286=CARTESIAN_POINT('Ctrl Pts',(206.737182407917,-4.89355472835045,
131.296605661359));
#233287=CARTESIAN_POINT('Ctrl Pts',(206.727886086852,-4.87714753159103,
131.459714495655));
#233288=CARTESIAN_POINT('Ctrl Pts',(206.718589765787,-4.85260850573713,
131.621731650502));
#233289=CARTESIAN_POINT('Ctrl Pts',(206.709293444722,-4.82011683649341,
131.781937594102));
#233290=CARTESIAN_POINT('Ctrl Pts',(206.699922676766,-4.7873649671415,131.94342650053));
#233291=CARTESIAN_POINT('Ctrl Pts',(206.69055190881,-4.74653262850223,132.103075044456));
#233292=CARTESIAN_POINT('Ctrl Pts',(206.681181140855,-4.69785138332069,
132.260168105777));
#233293=CARTESIAN_POINT('Ctrl Pts',(206.680193264038,-4.69271935212153,
132.27672903163));
#233294=CARTESIAN_POINT('Ctrl Pts',(206.679205387222,-4.68750013448521,
132.293261576894));
#233295=CARTESIAN_POINT('Ctrl Pts',(206.678217510405,-4.68219403218519,
132.309764917902));
#233296=CARTESIAN_POINT('Ctrl Pts',(206.670443203729,-4.64043653180415,
132.439641469363));
#233297=CARTESIAN_POINT('Ctrl Pts',(206.662668897052,-4.59320493957362,
132.567985005214));
#233298=CARTESIAN_POINT('Ctrl Pts',(206.654894590376,-4.54062928664211,
132.694299437684));
#233299=CARTESIAN_POINT('Ctrl Pts',(206.647129865258,-4.48811843135327,
132.820458192059));
#233300=CARTESIAN_POINT('Ctrl Pts',(206.639365140141,-4.43027676906317,
132.944592461411));
#233301=CARTESIAN_POINT('Ctrl Pts',(206.631600415024,-4.36728419816986,
133.066220868536));
#233302=CARTESIAN_POINT('Ctrl Pts',(206.623843402325,-4.30435419549641,
133.187728466606));
#233303=CARTESIAN_POINT('Ctrl Pts',(206.616086389625,-4.23628364434482,
133.306734810711));
#233304=CARTESIAN_POINT('Ctrl Pts',(206.608329376926,-4.16330052534937,
133.422778421914));
#233305=CARTESIAN_POINT('Ctrl Pts',(206.600578214196,-4.09037244674563,
133.538734518553));
#233306=CARTESIAN_POINT('Ctrl Pts',(206.592827051467,-4.01253938183014,
133.651732000017));
#233307=CARTESIAN_POINT('Ctrl Pts',(206.585075888737,-3.93007506123518,
133.761334252139));
#233308=CARTESIAN_POINT('Ctrl Pts',(206.577328020864,-3.84764579449751,
133.870889914636));
#233309=CARTESIAN_POINT('Ctrl Pts',(206.569580152991,-3.76058942214285,
133.977052906525));
#233310=CARTESIAN_POINT('Ctrl Pts',(206.561832285118,-3.66922266005811,
134.079416057313));
#233311=CARTESIAN_POINT('Ctrl Pts',(206.554086038175,-3.577875012784,134.181757792739));
#233312=CARTESIAN_POINT('Ctrl Pts',(206.546339791231,-3.48221902964024,
134.280300976796));
#233313=CARTESIAN_POINT('Ctrl Pts',(206.538593544287,-3.38261107228556,
134.374672284095));
#233314=CARTESIAN_POINT('Ctrl Pts',(206.530847240371,-3.28300238233128,
134.469044285479));
#233315=CARTESIAN_POINT('Ctrl Pts',(206.523100936455,-3.17944194398242,
134.559244079983));
#233316=CARTESIAN_POINT('Ctrl Pts',(206.515354632539,-3.07232196606475,
134.644936199342));
#233317=CARTESIAN_POINT('Ctrl Pts',(206.507606594067,-2.96517800179731,
134.730647506916));
#233318=CARTESIAN_POINT('Ctrl Pts',(206.499858555595,-2.85447321715903,
134.811848886652));
#233319=CARTESIAN_POINT('Ctrl Pts',(206.492110517123,-2.74063145552457,
134.888246302485));
#233320=CARTESIAN_POINT('Ctrl Pts',(206.484354244035,-2.62666870285167,
134.964724913502));
#233321=CARTESIAN_POINT('Ctrl Pts',(206.476597970948,-2.50956263835897,
135.036389143314));
#233322=CARTESIAN_POINT('Ctrl Pts',(206.46884169786,-2.38976501336611,135.102989031769));
#233323=CARTESIAN_POINT('Ctrl Pts',(206.461081285113,-2.26990345028647,
135.169624465748));
#233324=CARTESIAN_POINT('Ctrl Pts',(206.453320872367,-2.14734781348686,
135.231189997141));
#233325=CARTESIAN_POINT('Ctrl Pts',(206.44556045962,-2.02257190409865,135.28748296201));
#233326=CARTESIAN_POINT('Ctrl Pts',(206.437787589017,-1.8975956908752,135.343866294457));
#233327=CARTESIAN_POINT('Ctrl Pts',(206.430014718413,-1.77039244561536,
135.394960000609));
#233328=CARTESIAN_POINT('Ctrl Pts',(206.422241847809,-1.64145412060007,
135.440610333928));
#233329=CARTESIAN_POINT('Ctrl Pts',(206.41475119407,-1.5171972796397,135.484603198007));
#233330=CARTESIAN_POINT('Ctrl Pts',(206.407260540331,-1.39132946298595,
135.523541019782));
#233331=CARTESIAN_POINT('Ctrl Pts',(206.399769886592,-1.26429990602564,
135.557331142419));
#233332=CARTESIAN_POINT('Ctrl Pts',(206.391995539368,-1.13245935939483,
135.592400998174));
#233333=CARTESIAN_POINT('Ctrl Pts',(206.384221192143,-0.998949706372701,
135.622036643276));
#233334=CARTESIAN_POINT('Ctrl Pts',(206.376446844919,-0.864258611065781,
135.646079332619));
#233335=CARTESIAN_POINT('Ctrl Pts',(206.368682078737,-0.72973350798047,
135.670092391946));
#233336=CARTESIAN_POINT('Ctrl Pts',(206.360917312556,-0.594030240801939,
135.688526141918));
#233337=CARTESIAN_POINT('Ctrl Pts',(206.353152546374,-0.457651051086741,
135.70127174377));
#233338=CARTESIAN_POINT('Ctrl Pts',(206.345395492141,-0.321407312868765,
135.71400468672));
#233339=CARTESIAN_POINT('Ctrl Pts',(206.337638437907,-0.184489374829276,
135.721060688077));
#233340=CARTESIAN_POINT('Ctrl Pts',(206.329881383673,-0.0474087266159011,
135.722382117635));
#233341=CARTESIAN_POINT('Ctrl Pts',(206.322130178985,0.0895685499512351,
135.723702550711));
#233342=CARTESIAN_POINT('Ctrl Pts',(206.314378974297,0.226707903104169,
135.719297015699));
#233343=CARTESIAN_POINT('Ctrl Pts',(206.306627769608,0.363494034138324,
135.709159813216));
#233344=CARTESIAN_POINT('Ctrl Pts',(206.298879859279,0.500222029349606,
135.699026919171));
#233345=CARTESIAN_POINT('Ctrl Pts',(206.29113194895,0.636596711948773,135.68316723157));
#233346=CARTESIAN_POINT('Ctrl Pts',(206.283384038621,0.772104320862591,
135.661627130761));
#233347=CARTESIAN_POINT('Ctrl Pts',(206.275637748924,0.907583585626675,
135.640091535498));
#233348=CARTESIAN_POINT('Ctrl Pts',(206.267891459227,1.04219575158091,135.612877951706));
#233349=CARTESIAN_POINT('Ctrl Pts',(206.26014516953,1.17543410337159,135.580084408902));
#233350=CARTESIAN_POINT('Ctrl Pts',(206.252398822603,1.30867343952879,135.547290623819));
#233351=CARTESIAN_POINT('Ctrl Pts',(206.244652475676,1.44053856163545,135.508916890901));
#233352=CARTESIAN_POINT('Ctrl Pts',(206.236906128749,1.57053522864704,135.465111861526));
#233353=CARTESIAN_POINT('Ctrl Pts',(206.229158047049,1.70056100805719,135.421297022135));
#233354=CARTESIAN_POINT('Ctrl Pts',(206.221409965348,1.8287171293106,135.372048590765));
#233355=CARTESIAN_POINT('Ctrl Pts',(206.213661883648,1.95452711044093,135.317564228866));
#233356=CARTESIAN_POINT('Ctrl Pts',(206.20590556723,2.08047080333817,135.263021960589));
#233357=CARTESIAN_POINT('Ctrl Pts',(206.198149250812,2.2040630157501,135.203232801142));
#233358=CARTESIAN_POINT('Ctrl Pts',(206.190392934394,2.32484926327892,135.138441715738));
#233359=CARTESIAN_POINT('Ctrl Pts',(206.182632478194,2.44569997811104,135.073616049356));
#233360=CARTESIAN_POINT('Ctrl Pts',(206.174872021993,2.5637414075819,135.003783336419));
#233361=CARTESIAN_POINT('Ctrl Pts',(206.167111565792,2.67854694058481,134.929232657955));
#233362=CARTESIAN_POINT('Ctrl Pts',(206.159338651962,2.79353676750179,134.8545623055));
#233363=CARTESIAN_POINT('Ctrl Pts',(206.151565738131,2.90527999882711,134.775159079624));
#233364=CARTESIAN_POINT('Ctrl Pts',(206.143792824301,3.01338136800174,134.691353773397));
#233365=CARTESIAN_POINT('Ctrl Pts',(206.136302637127,3.1175507318328,134.61059674412));
#233366=CARTESIAN_POINT('Ctrl Pts',(206.128812449953,3.21833832869957,134.525752506211));
#233367=CARTESIAN_POINT('Ctrl Pts',(206.12132226278,3.31542344251232,134.43714886619));
#233368=CARTESIAN_POINT('Ctrl Pts',(206.113547928467,3.41619156940981,134.345183965593));
#233369=CARTESIAN_POINT('Ctrl Pts',(206.105773594154,3.51328995165438,134.248877485937));
#233370=CARTESIAN_POINT('Ctrl Pts',(206.097999259841,3.60632143845033,134.148553905203));
#233371=CARTESIAN_POINT('Ctrl Pts',(206.090234506665,3.69923827267255,134.048353963863));
#233372=CARTESIAN_POINT('Ctrl Pts',(206.082469753489,3.78809792067824,133.944147055788));
#233373=CARTESIAN_POINT('Ctrl Pts',(206.074705000313,3.87253733969881,133.836296899076));
#233374=CARTESIAN_POINT('Ctrl Pts',(206.066947959165,3.95689289267469,133.72855386018));
#233375=CARTESIAN_POINT('Ctrl Pts',(206.059190918017,4.03683671393217,133.617175079492));
#233376=CARTESIAN_POINT('Ctrl Pts',(206.051433876869,4.11204384499684,133.502559735371));
#233377=CARTESIAN_POINT('Ctrl Pts',(206.043682685331,4.18719426211104,133.388030823066));
#233378=CARTESIAN_POINT('Ctrl Pts',(206.035931493794,4.2576148851709,133.270270530956));
#233379=CARTESIAN_POINT('Ctrl Pts',(206.028180302257,4.32302238761605,133.14970931204));
#233380=CARTESIAN_POINT('Ctrl Pts',(206.020432405131,4.38840209056044,133.029199334061));
#233381=CARTESIAN_POINT('Ctrl Pts',(206.012684508006,4.44877272459587,132.90589113992));
#233382=CARTESIAN_POINT('Ctrl Pts',(206.00493661088,4.50389561038913,132.780242039417));
#233383=CARTESIAN_POINT('Ctrl Pts',(205.997190334417,4.55900696588485,132.654619221492));
#233384=CARTESIAN_POINT('Ctrl Pts',(205.989444057953,4.60887259954457,132.52665682896));
#233385=CARTESIAN_POINT('Ctrl Pts',(205.98169778149,4.65330109429353,132.396834161568));
#233386=CARTESIAN_POINT('Ctrl Pts',(205.973951447814,4.69772991718062,132.267010535338));
#233387=CARTESIAN_POINT('Ctrl Pts',(205.966205114138,4.73672139443581,132.135326976735));
#233388=CARTESIAN_POINT('Ctrl Pts',(205.958458780463,4.77013344123859,132.002279652926));
#233389=CARTESIAN_POINT('Ctrl Pts',(205.950710712019,4.80355297056946,131.869202533566));
#233390=CARTESIAN_POINT('Ctrl Pts',(205.942962643575,4.83139048788632,131.734761420386));
#233391=CARTESIAN_POINT('Ctrl Pts',(205.935214575131,4.85355474113685,131.599464030518));
#233392=CARTESIAN_POINT('Ctrl Pts',(205.927458271901,4.87574255095105,131.464022844171));
#233393=CARTESIAN_POINT('Ctrl Pts',(205.919701968672,4.89224498852538,131.327723949617));
#233394=CARTESIAN_POINT('Ctrl Pts',(205.911945665443,4.90302249002199,131.191082125681));
#233395=CARTESIAN_POINT('Ctrl Pts',(205.904185222415,4.91380574383149,131.054367371435));
#233396=CARTESIAN_POINT('Ctrl Pts',(205.896424779388,4.91885795864703,130.917309713606));
#233397=CARTESIAN_POINT('Ctrl Pts',(205.88866433636,4.91819175271269,130.780424326105));
#233398=CARTESIAN_POINT('Ctrl Pts',(205.880891435541,4.91752447732209,130.643319197341));
#233399=CARTESIAN_POINT('Ctrl Pts',(205.873118534722,4.91112045540052,130.506387282292));
#233400=CARTESIAN_POINT('Ctrl Pts',(205.865345633904,4.89904434121163,130.370139930193));
#233401=CARTESIAN_POINT('Ctrl Pts',(205.857855302258,4.8874072314151,130.238845594031));
#233402=CARTESIAN_POINT('Ctrl Pts',(205.850364970613,4.87050330540731,130.108187218426));
#233403=CARTESIAN_POINT('Ctrl Pts',(205.842874638967,4.84843500802732,129.978611844975));
#233404=CARTESIAN_POINT('Ctrl Pts',(205.835100308635,4.82552998301369,129.844123573455));
#233405=CARTESIAN_POINT('Ctrl Pts',(205.827325978302,4.79698868437903,129.710376028441));
#233406=CARTESIAN_POINT('Ctrl Pts',(205.81955164797,4.76286943415894,129.577878731987));
#233407=CARTESIAN_POINT('Ctrl Pts',(205.811786898866,4.72879223313221,129.445544727644));
#233408=CARTESIAN_POINT('Ctrl Pts',(205.804022149762,4.68915085502848,129.31445828105));
#233409=CARTESIAN_POINT('Ctrl Pts',(205.796257400658,4.64405507193892,129.185121428534));
#233410=CARTESIAN_POINT('Ctrl Pts',(205.788500363668,4.59900407893947,129.055913036128));
#233411=CARTESIAN_POINT('Ctrl Pts',(205.780743326677,4.54850958977095,128.928451146412));
#233412=CARTESIAN_POINT('Ctrl Pts',(205.772986289687,4.49273179575291,128.803224921535));
#233413=CARTESIAN_POINT('Ctrl Pts',(205.765235102389,4.43699606456529,128.67809313154));
#233414=CARTESIAN_POINT('Ctrl Pts',(205.757483915091,4.37598511729972,128.555194006304));
#233415=CARTESIAN_POINT('Ctrl Pts',(205.749732727793,4.30990796060895,128.434998586643));
#233416=CARTESIAN_POINT('Ctrl Pts',(205.741984835016,4.24385888898434,128.314854254173));
#233417=CARTESIAN_POINT('Ctrl Pts',(205.73423694224,4.17274807866374,128.197411683559));
#233418=CARTESIAN_POINT('Ctrl Pts',(205.726489049463,4.09683126462683,128.083118869452));
#233419=CARTESIAN_POINT('Ctrl Pts',(205.718742777414,4.0209303311019,127.968849963467));
#233420=CARTESIAN_POINT('Ctrl Pts',(205.710996505366,3.94022560970842,127.85772982891));
#233421=CARTESIAN_POINT('Ctrl Pts',(205.703250233317,3.85501688262898,127.750178583511));
#233422=CARTESIAN_POINT('Ctrl Pts',(205.695503904118,3.76980752690164,127.642626544626));
#233423=CARTESIAN_POINT('Ctrl Pts',(205.68775757492,3.68009434196701,127.538643753886));
#233424=CARTESIAN_POINT('Ctrl Pts',(205.680011245721,3.58621796636794,127.438617941692));
#233425=CARTESIAN_POINT('Ctrl Pts',(205.672263181812,3.49232056812825,127.338569729755));
#233426=CARTESIAN_POINT('Ctrl Pts',(205.664515117904,3.39425839154965,127.242480544672));
#233427=CARTESIAN_POINT('Ctrl Pts',(205.656767053995,3.29240926887433,127.150701592872));
#233428=CARTESIAN_POINT('Ctrl Pts',(205.649010755368,3.19045189995416,127.058825097503));
#233429=CARTESIAN_POINT('Ctrl Pts',(205.641254456741,3.0846998358618,126.971268248513));
#233430=CARTESIAN_POINT('Ctrl Pts',(205.633498158114,2.97556478881364,126.888342582614));
#233431=CARTESIAN_POINT('Ctrl Pts',(205.625737719733,2.86637149332416,126.805372656956));
#233432=CARTESIAN_POINT('Ctrl Pts',(205.617977281351,2.75379193784736,126.727039062836));
#233433=CARTESIAN_POINT('Ctrl Pts',(205.61021684297,2.63826637271815,126.653609648273));
#233434=CARTESIAN_POINT('Ctrl Pts',(205.602443946826,2.52255535542982,126.580062358127));
#233435=CARTESIAN_POINT('Ctrl Pts',(205.594671050682,2.40388921667307,126.511435175415));
#233436=CARTESIAN_POINT('Ctrl Pts',(205.586898154538,2.2827331157452,126.447950101467));
#233437=CARTESIAN_POINT('Ctrl Pts',(205.579407774743,2.16598059601619,126.386772477791));
#233438=CARTESIAN_POINT('Ctrl Pts',(205.571917394949,2.04691625263489,126.330369789491));
#233439=CARTESIAN_POINT('Ctrl Pts',(205.564427015154,1.92597157701165,126.278897486897));
#233440=CARTESIAN_POINT('Ctrl Pts',(205.556652678921,1.80044195106122,126.225473895836));
#233441=CARTESIAN_POINT('Ctrl Pts',(205.548878342688,1.67248897498338,126.177192652376));
#233442=CARTESIAN_POINT('Ctrl Pts',(205.541104006456,1.54257284960153,126.134280097257));
#233443=CARTESIAN_POINT('Ctrl Pts',(205.533339251373,1.412816833816,126.091420427889));
#233444=CARTESIAN_POINT('Ctrl Pts',(205.525574496289,1.28110285028441,126.053916403621));
#233445=CARTESIAN_POINT('Ctrl Pts',(205.517809741206,1.14791261180821,126.021947032549));
#233446=CARTESIAN_POINT('Ctrl Pts',(205.510052698165,1.01485465937561,125.990009413817));
#233447=CARTESIAN_POINT('Ctrl Pts',(205.502295655124,0.88032374757524,125.963595599504));
#233448=CARTESIAN_POINT('Ctrl Pts',(205.494538612083,0.744818010538801,
125.942835219743));
#233449=CARTESIAN_POINT('Ctrl Pts',(205.48678741867,0.609414459097139,125.922090495495));
#233450=CARTESIAN_POINT('Ctrl Pts',(205.479036225256,0.473037930525041,
125.906990778956));
#233451=CARTESIAN_POINT('Ctrl Pts',(205.471285031842,0.33619769877146,125.897614835498));
#233452=CARTESIAN_POINT('Ctrl Pts',(205.463537132872,0.199415627413407,
125.888242877042));
#233453=CARTESIAN_POINT('Ctrl Pts',(205.455789233902,0.0621706340948198,
125.884589879799));
#233454=CARTESIAN_POINT('Ctrl Pts',(205.448041334933,-0.0750221388880692,
125.88668283825));
#233455=CARTESIAN_POINT('Ctrl Pts',(205.440295056645,-0.212186214308715,
125.888775358903));
#233456=CARTESIAN_POINT('Ctrl Pts',(205.432548778357,-0.349297700448874,
125.896611438603));
#233457=CARTESIAN_POINT('Ctrl Pts',(205.424802500068,-0.485841100123671,
125.910165945515));
#233458=CARTESIAN_POINT('Ctrl Pts',(205.41705616459,-0.622385507893228,
125.9237205525));
#233459=CARTESIAN_POINT('Ctrl Pts',(205.409309829111,-0.758361431775545,
125.942993632321));
#233460=CARTESIAN_POINT('Ctrl Pts',(205.401563493633,-0.89325853914859,
125.967908173394));
#233461=CARTESIAN_POINT('Ctrl Pts',(205.393815423409,-1.02818585590989,
125.992828293927));
#233462=CARTESIAN_POINT('Ctrl Pts',(205.386067353186,-1.16203349102794,
126.02339231868));
#233463=CARTESIAN_POINT('Ctrl Pts',(205.378319282963,-1.29430173647038,
126.059472201863));
#233464=CARTESIAN_POINT('Ctrl Pts',(205.370562978002,-1.42671055811762,
126.095590431159));
#233465=CARTESIAN_POINT('Ctrl Pts',(205.36280667304,-1.55753625913267,126.137236126444));
#233466=CARTESIAN_POINT('Ctrl Pts',(205.355050368079,-1.68629419381508,
126.184231295306));
#233467=CARTESIAN_POINT('Ctrl Pts',(205.347289923343,-1.81512085051228,
126.231251546915));
#233468=CARTESIAN_POINT('Ctrl Pts',(205.339529478607,-1.94187718064387,
126.283626812052));
#233469=CARTESIAN_POINT('Ctrl Pts',(205.331769033871,-2.06609986951013,
126.341131473582));
#233470=CARTESIAN_POINT('Ctrl Pts',(205.323996131401,-2.19052197132574,
126.398728446543));
#233471=CARTESIAN_POINT('Ctrl Pts',(205.316223228931,-2.31240195646745,
126.461471091301));
#233472=CARTESIAN_POINT('Ctrl Pts',(205.308450326461,-2.43130161847012,
126.52908805286));
#233473=CARTESIAN_POINT('Ctrl Pts',(205.300960014754,-2.54587857780558,
126.594246739811));
#233474=CARTESIAN_POINT('Ctrl Pts',(205.293469703048,-2.65768789450607,
126.663931314284));
#233475=CARTESIAN_POINT('Ctrl Pts',(205.285979391341,-2.7663655623862,126.737862783097));
#233476=CARTESIAN_POINT('Ctrl Pts',(205.278237672039,-2.87869092774278,
126.814275715097));
#233477=CARTESIAN_POINT('Ctrl Pts',(205.270495952738,-2.98803353029666,
126.895472526408));
#233478=CARTESIAN_POINT('Ctrl Pts',(205.262754233436,-3.09395614481765,
126.981191979323));
#233479=CARTESIAN_POINT('Ctrl Pts',(205.255024754641,-3.19971128407027,
127.066775900384));
#233480=CARTESIAN_POINT('Ctrl Pts',(205.247295275847,-3.30205689954337,
127.156867976875));
#233481=CARTESIAN_POINT('Ctrl Pts',(205.239565797052,-3.40058421415425,
127.251163456565));
#233482=CARTESIAN_POINT('Ctrl Pts',(205.231843383955,-3.4990214626426,127.345372738552));
#233483=CARTESIAN_POINT('Ctrl Pts',(205.224120970858,-3.59364706915702,
127.443777510556));
#233484=CARTESIAN_POINT('Ctrl Pts',(205.216398557761,-3.68408468413249,
127.546032349475));
#233485=CARTESIAN_POINT('Ctrl Pts',(205.208681492833,-3.77445966639361,
127.648216371643));
#233486=CARTESIAN_POINT('Ctrl Pts',(205.200964427906,-3.86065216668493,
127.75424486186));
#233487=CARTESIAN_POINT('Ctrl Pts',(205.193247362978,-3.94232245691661,
127.863735393538));
#233488=CARTESIAN_POINT('Ctrl Pts',(205.185533932859,-4.02395427969229,
127.97317435417));
#233489=CARTESIAN_POINT('Ctrl Pts',(205.177820502739,-4.1010678957911,128.086071795385));
#233490=CARTESIAN_POINT('Ctrl Pts',(205.17010707262,-4.17336396541682,128.202012394391));
#233491=CARTESIAN_POINT('Ctrl Pts',(205.162394028974,-4.24565641272213,
128.317947184313));
#233492=CARTESIAN_POINT('Ctrl Pts',(205.154680985329,-4.31313157631286,
128.436924499339));
#233493=CARTESIAN_POINT('Ctrl Pts',(205.146967941683,-4.37553364940197,
128.558500349105));
#233494=CARTESIAN_POINT('Ctrl Pts',(205.139255293534,-4.43793252273594,
128.680069964896));
#233495=CARTESIAN_POINT('Ctrl Pts',(205.131542645386,-4.49525864776658,
128.804237496571));
#233496=CARTESIAN_POINT('Ctrl Pts',(205.123829997237,-4.54730272990832,
128.930535400245));
#233497=CARTESIAN_POINT('Ctrl Pts',(205.116113219495,-4.59937467808288,
129.056900927775));
#233498=CARTESIAN_POINT('Ctrl Pts',(205.108396441753,-4.64615878721881,
129.185398739042));
#233499=CARTESIAN_POINT('Ctrl Pts',(205.100679664011,-4.68749433319855,
129.315542314773));
#233500=CARTESIAN_POINT('Ctrl Pts',(205.0954453069,-4.71553259168844,129.403819828246));
#233501=CARTESIAN_POINT('Ctrl Pts',(205.090210949789,-4.74106497151865,
129.49285418659));
#233502=CARTESIAN_POINT('Ctrl Pts',(205.084976592678,-4.76405452823405,
129.582490119308));
#233503=CARTESIAN_POINT('Ctrl Pts',(210.579426101437,-2.14555810197798,
126.384433368448));
#233504=CARTESIAN_POINT('Ctrl Pts',(210.533016425084,-2.88204635455982,
126.741945114569));
#233505=CARTESIAN_POINT('Ctrl Pts',(210.440198811428,-4.16073755837059,
127.832228156677));
#233506=CARTESIAN_POINT('Ctrl Pts',(210.254565323169,-5.41774734084591,
130.983824311839));
#233507=CARTESIAN_POINT('Ctrl Pts',(210.022525636658,-3.70466367662459,
135.280954889074));
#233508=CARTESIAN_POINT('Ctrl Pts',(209.744078012845,1.77278938863763,136.341871604603));
#233509=CARTESIAN_POINT('Ctrl Pts',(209.465630389032,5.61248518735455,132.305536381355));
#233510=CARTESIAN_POINT('Ctrl Pts',(209.187182765219,4.2990952821384,126.894094626803));
#233511=CARTESIAN_POINT('Ctrl Pts',(208.908735141406,-0.967335548355457,
125.073681250508));
#233512=CARTESIAN_POINT('Ctrl Pts',(208.630287517594,-5.34357155608916,
128.520706403956));
#233513=CARTESIAN_POINT('Ctrl Pts',(208.351839893781,-4.80999390579215,
134.065650134797));
#233514=CARTESIAN_POINT('Ctrl Pts',(208.073392269968,0.144086686833323,
136.613971320579));
#233515=CARTESIAN_POINT('Ctrl Pts',(207.794944646155,4.96557142732685,133.823362329787));
#233516=CARTESIAN_POINT('Ctrl Pts',(207.516497022342,5.22403776314189,128.258534510045));
#233517=CARTESIAN_POINT('Ctrl Pts',(207.238049398529,0.681816090004523,
125.033145533949));
#233518=CARTESIAN_POINT('Ctrl Pts',(206.959601774716,-4.48693345015888,
127.111248278652));
#233519=CARTESIAN_POINT('Ctrl Pts',(206.681154150904,-5.53242507739068,
132.583126545744));
#233520=CARTESIAN_POINT('Ctrl Pts',(206.40270652709,-1.49388053201802,136.420413394932));
#233521=CARTESIAN_POINT('Ctrl Pts',(206.124258903278,3.91746311099657,135.0968180907));
#233522=CARTESIAN_POINT('Ctrl Pts',(205.845811279465,5.72885172159717,129.828666190814));
#233523=CARTESIAN_POINT('Ctrl Pts',(205.567363655652,2.27570431130586,125.457128678938));
#233524=CARTESIAN_POINT('Ctrl Pts',(205.288916031839,-3.26870357308214,
125.999436687584));
#233525=CARTESIAN_POINT('Ctrl Pts',(205.010468408026,-5.80933288384994,
130.9572347388));
#233526=CARTESIAN_POINT('Ctrl Pts',(204.732020784213,-3.01146890392974,
135.774549108008));
#233527=CARTESIAN_POINT('Ctrl Pts',(204.4535731604,2.5537877891123,136.024502973214));
#233528=CARTESIAN_POINT('Ctrl Pts',(204.175125536587,5.77223831170541,131.477401078575));
#233529=CARTESIAN_POINT('Ctrl Pts',(203.896677912775,3.6862837897924,126.311807855303));
#233530=CARTESIAN_POINT('Ctrl Pts',(203.618230288961,-1.78718543642468,
125.274651160291));
#233531=CARTESIAN_POINT('Ctrl Pts',(203.339782665149,-5.61831856260093,
129.319027308227));
#233532=CARTESIAN_POINT('Ctrl Pts',(203.061335041336,-4.28649139606962,
134.728352208566));
#233533=CARTESIAN_POINT('Ctrl Pts',(202.782887417523,0.984411954691954,
136.531720532469));
#233534=CARTESIAN_POINT('Ctrl Pts',(202.50443979371,5.3506888113544,133.071924892697));
#233535=CARTESIAN_POINT('Ctrl Pts',(202.225992169897,4.79994404549834,127.528348460205));
#233536=CARTESIAN_POINT('Ctrl Pts',(201.947544546084,-0.161714807569177,
124.995267158526));
#233537=CARTESIAN_POINT('Ctrl Pts',(201.669096922271,-4.97476565284641,
127.800458955558));
#233538=CARTESIAN_POINT('Ctrl Pts',(201.390649298458,-5.21624989388704,
133.366089631302));
#233539=CARTESIAN_POINT('Ctrl Pts',(201.112201674645,-0.664255310463968,
136.577616490799));
#233540=CARTESIAN_POINT('Ctrl Pts',(200.833754050833,4.49815745262305,134.483803242045));
#233541=CARTESIAN_POINT('Ctrl Pts',(200.55530642702,5.52698326394509,129.008761972148));
#233542=CARTESIAN_POINT('Ctrl Pts',(200.276858803207,1.47678146385132,125.183788137525));
#233543=CARTESIAN_POINT('Ctrl Pts',(199.998411179394,-3.93051035674001,
126.523845831826));
#233544=CARTESIAN_POINT('Ctrl Pts',(199.719963555581,-5.7258551755912,131.79748749945));
#233545=CARTESIAN_POINT('Ctrl Pts',(199.441515931768,-2.25941881165118,
136.158494079568));
#233546=CARTESIAN_POINT('Ctrl Pts',(199.163068307955,3.28331306145151,135.599313572066));
#233547=CARTESIAN_POINT('Ctrl Pts',(198.884620684142,5.80884062984016,130.633805545853));
#233548=CARTESIAN_POINT('Ctrl Pts',(198.606173060329,2.99632743704681,125.825029298466));
#233549=CARTESIAN_POINT('Ctrl Pts',(198.327725436517,-2.56966429165962,
125.592015279473));
#233550=CARTESIAN_POINT('Ctrl Pts',(198.049277812704,-5.77426007141042,
130.148891988961));
#233551=CARTESIAN_POINT('Ctrl Pts',(197.770830188891,-3.6725929338218,135.308112346714));
#233552=CARTESIAN_POINT('Ctrl Pts',(197.492382565078,1.80400769380988,136.328604885883));
#233553=CARTESIAN_POINT('Ctrl Pts',(197.213934941265,5.62281338150559,132.272586816804));
#233554=CARTESIAN_POINT('Ctrl Pts',(196.935487317452,4.27452826130232,126.867340597462));
#233555=CARTESIAN_POINT('Ctrl Pts',(196.657039693639,-1.00183950872307,
125.080023442474));
#233556=CARTESIAN_POINT('Ctrl Pts',(196.378592069827,-5.35756571281285,
128.553092501978));
#233557=CARTESIAN_POINT('Ctrl Pts',(196.100144446013,-4.78995075846325,
134.094966979145));
#233558=CARTESIAN_POINT('Ctrl Pts',(195.821696822201,0.179394940810534,
136.612934965078));
#233559=CARTESIAN_POINT('Ctrl Pts',(195.543249198387,4.98388545340951,133.79310689028));
#233560=CARTESIAN_POINT('Ctrl Pts',(195.264801574575,5.20842871066526,128.22676699923));
#233561=CARTESIAN_POINT('Ctrl Pts',(194.986353950762,0.64668042870769,125.029109720981));
#233562=CARTESIAN_POINT('Ctrl Pts',(194.70790632695,-4.50933557513701,127.138625880003));
#233563=CARTESIAN_POINT('Ctrl Pts',(194.429458703136,-5.52149247872048,
132.616773181746));
#233564=CARTESIAN_POINT('Ctrl Pts',(194.151011079324,-1.4596675342632,136.429401878284));
#233565=CARTESIAN_POINT('Ctrl Pts',(193.87256345551,3.9435205654586,135.072892454764));
#233566=CARTESIAN_POINT('Ctrl Pts',(193.594115831698,5.72280591721378,129.793810802232));
#233567=CARTESIAN_POINT('Ctrl Pts',(193.315668207884,2.24311220566103,125.443375061888));
#233568=CARTESIAN_POINT('Ctrl Pts',(193.037220584072,-3.29789204077089,
126.019423148508));
#233569=CARTESIAN_POINT('Ctrl Pts',(192.758772960259,-5.80829461271728,
130.992595012001));
#233570=CARTESIAN_POINT('Ctrl Pts',(192.480325336446,-2.98115818654302,
135.792788662769));
#233571=CARTESIAN_POINT('Ctrl Pts',(192.201877712633,2.58551697539033,136.008860638253));
#233572=CARTESIAN_POINT('Ctrl Pts',(191.92343008882,5.77622834646622,131.442251348686));
#233573=CARTESIAN_POINT('Ctrl Pts',(191.644982465007,3.658868051582,126.289451639914));
#233574=CARTESIAN_POINT('Ctrl Pts',(191.366534841194,-1.82081323706467,
125.285632716038));
#233575=CARTESIAN_POINT('Ctrl Pts',(191.088087217381,-5.6272561125207,129.35325512882));
#233576=CARTESIAN_POINT('Ctrl Pts',(190.809639593569,-4.26252552731426,
134.754372595315));
#233577=CARTESIAN_POINT('Ctrl Pts',(190.531191969755,1.01925778154541,136.525622023071));
#233578=CARTESIAN_POINT('Ctrl Pts',(190.252744345943,5.36439298267566,133.039311718326));
#233579=CARTESIAN_POINT('Ctrl Pts',(189.974296722129,4.77991309789331,127.499190535413));
#233580=CARTESIAN_POINT('Ctrl Pts',(189.695849098317,-0.197073412116412,
124.996359191464));
#233581=CARTESIAN_POINT('Ctrl Pts',(189.417401474504,-4.99295908396257,
127.830797421458));
#233582=CARTESIAN_POINT('Ctrl Pts',(189.138953850692,-5.20055927725872,
133.397794962038));
#233583=CARTESIAN_POINT('Ctrl Pts',(188.860506226878,-0.629099556198964,
136.581553036358));
#233584=CARTESIAN_POINT('Ctrl Pts',(188.582058603065,4.52047192378579,134.456353509349));
#233585=CARTESIAN_POINT('Ctrl Pts',(188.303610979253,5.51595054314194,128.975150924561));
#233586=CARTESIAN_POINT('Ctrl Pts',(188.02516335544,1.44254008251539,125.174902685784));
#233587=CARTESIAN_POINT('Ctrl Pts',(187.746715731627,-3.95649424194195,
126.547851272005));
#233588=CARTESIAN_POINT('Ctrl Pts',(187.468268107814,-5.71970364354381,
131.832324004755));
#233589=CARTESIAN_POINT('Ctrl Pts',(187.189820484001,-2.22678481978599,
136.172148603481));
#233590=CARTESIAN_POINT('Ctrl Pts',(186.911372860188,3.312440468869,135.579238274173));
#233591=CARTESIAN_POINT('Ctrl Pts',(186.632925236375,5.80769478834652,130.598448644184));
#233592=CARTESIAN_POINT('Ctrl Pts',(186.354477612562,2.96596131899707,125.806882058373));
#233593=CARTESIAN_POINT('Ctrl Pts',(186.076029988749,-2.60134570724499,
125.607754128061));
#233594=CARTESIAN_POINT('Ctrl Pts',(185.797582364937,-5.7781431113317,130.184053693262));
#233595=CARTESIAN_POINT('Ctrl Pts',(185.519134741124,-3.64510927408837,
135.33038501822));
#233596=CARTESIAN_POINT('Ctrl Pts',(185.240687117311,1.83760191255446,136.317521027561));
#233597=CARTESIAN_POINT('Ctrl Pts',(184.962239493498,5.63164671340385,132.238331952975));
#233598=CARTESIAN_POINT('Ctrl Pts',(184.683791869685,4.25048330587202,126.841393274542));
#233599=CARTESIAN_POINT('Ctrl Pts',(184.405344245872,-1.03666661210287,
125.086227982629));
#233600=CARTESIAN_POINT('Ctrl Pts',(184.126896622059,-5.37117055753467,
128.585747235914));
#233601=CARTESIAN_POINT('Ctrl Pts',(183.848448998247,-4.7698311568614,134.124063801647));
#233602=CARTESIAN_POINT('Ctrl Pts',(183.570001374433,0.214750057761129,
136.611735317726));
#233603=CARTESIAN_POINT('Ctrl Pts',(183.291553750621,5.00198646042476,133.762713190383));
#233604=CARTESIAN_POINT('Ctrl Pts',(183.013106126807,5.19264166658148,128.195109572179));
#233605=CARTESIAN_POINT('Ctrl Pts',(182.734658502995,0.611512855797894,
125.025280195685));
#233606=CARTESIAN_POINT('Ctrl Pts',(182.456210879182,-4.53156639540017,
127.166143403126));
#233607=CARTESIAN_POINT('Ctrl Pts',(182.177763255369,-5.5103575085511,132.650350493844));
#233608=CARTESIAN_POINT('Ctrl Pts',(181.899315631556,-1.42539926727337,
136.438183069882));
#233609=CARTESIAN_POINT('Ctrl Pts',(181.620868007743,3.96943126600311,135.048808039769));
#233610=CARTESIAN_POINT('Ctrl Pts',(181.34242038393,5.71654838332065,129.758993181434));
#233611=CARTESIAN_POINT('Ctrl Pts',(181.063972760118,2.21043680528058,125.429819927867));
#233612=CARTESIAN_POINT('Ctrl Pts',(180.785525136304,-3.32695821097111,
126.039587007222));
#233613=CARTESIAN_POINT('Ctrl Pts',(180.507077512492,-5.80704116228462,
131.027948262352));
#233614=CARTESIAN_POINT('Ctrl Pts',(180.228629888679,-2.95073697519064,
135.810843394787));
#233615=CARTESIAN_POINT('Ctrl Pts',(179.950182264866,2.61715034058839,135.993025435236));
#233616=CARTESIAN_POINT('Ctrl Pts',(179.671734641053,5.78000434826875,131.407077988614));
#233617=CARTESIAN_POINT('Ctrl Pts',(179.39328701724,3.63131672880039,126.26726272238));
#233618=CARTESIAN_POINT('Ctrl Pts',(179.114839393428,-1.8543735647511,125.296818772266));
#233619=CARTESIAN_POINT('Ctrl Pts',(178.836391769614,-5.63598514348121,
129.387536719606));
#233620=CARTESIAN_POINT('Ctrl Pts',(178.557944145802,-4.23840170853308,
134.780246613475));
#233621=CARTESIAN_POINT('Ctrl Pts',(178.279496521988,1.05406583912245,136.519311509933));
#233622=CARTESIAN_POINT('Ctrl Pts',(178.001048898175,5.3778983746034,133.006615727177));
#233623=CARTESIAN_POINT('Ctrl Pts',(177.722601274363,4.75970502876524,127.470155084831));
#233624=CARTESIAN_POINT('Ctrl Pts',(177.44415365055,-0.232424713990654,
124.997666442073));
#233625=CARTESIAN_POINT('Ctrl Pts',(177.165706026737,-5.01096749916768,
127.861246073811));
#233626=CARTESIAN_POINT('Ctrl Pts',(176.887258402924,-5.18467595198119,
133.429404192122));
#233627=CARTESIAN_POINT('Ctrl Pts',(176.608810779111,-0.593920490425269,
136.585275505922));
#233628=CARTESIAN_POINT('Ctrl Pts',(176.330363155298,4.54261888720253,134.428768450716));
#233629=CARTESIAN_POINT('Ctrl Pts',(176.051915531486,5.50471342676105,128.941607659011));
#233630=CARTESIAN_POINT('Ctrl Pts',(175.773467907672,1.40824524732727,125.166225835676));
#233631=CARTESIAN_POINT('Ctrl Pts',(175.49502028386,-3.98233151779528,126.572014438702));
#233632=CARTESIAN_POINT('Ctrl Pts',(175.216572660047,-5.7133401657742,131.867122418498));
#233633=CARTESIAN_POINT('Ctrl Pts',(174.938125036234,-2.19406831359054,
136.185604222037));
#233634=CARTESIAN_POINT('Ctrl Pts',(174.659677412421,3.34144513258691,135.558986041432));
#233635=CARTESIAN_POINT('Ctrl Pts',(174.381229788608,5.80633374058666,130.563099372659));
#233636=CARTESIAN_POINT('Ctrl Pts',(174.102782164795,2.93548529615992,125.788920001687));
#233637=CARTESIAN_POINT('Ctrl Pts',(173.824334540982,-2.63293072900865,
125.623685538813));
#233638=CARTESIAN_POINT('Ctrl Pts',(173.54588691717,-5.7818120400351,130.219238383264));
#233639=CARTESIAN_POINT('Ctrl Pts',(173.267439293356,-3.61749054349026,
135.352489976228));
#233640=CARTESIAN_POINT('Ctrl Pts',(172.988991669544,1.87112803828436,136.306232877052));
#233641=CARTESIAN_POINT('Ctrl Pts',(172.71054404573,5.64027136256211,132.204023952811));
#233642=CARTESIAN_POINT('Ctrl Pts',(172.432096421918,4.22628084721974,126.815592800833));
#233643=CARTESIAN_POINT('Ctrl Pts',(172.153648798105,-1.07145530142008,
125.092644410292));
#233644=CARTESIAN_POINT('Ctrl Pts',(171.875201174292,-5.38457637155629,
128.618484181386));
#233645=CARTESIAN_POINT('Ctrl Pts',(171.596753550479,-4.74953480741189,
134.153037611328));
#233646=CARTESIAN_POINT('Ctrl Pts',(171.318305926666,0.25009721706947,136.610320475968));
#233647=CARTESIAN_POINT('Ctrl Pts',(171.039858302853,5.01990211699227,133.732209867644));
#233648=CARTESIAN_POINT('Ctrl Pts',(170.76141067904,5.1766622072511,128.163548831885));
#233649=CARTESIAN_POINT('Ctrl Pts',(170.482963055228,0.576322623054293,
125.021664816339));
#233650=CARTESIAN_POINT('Ctrl Pts',(170.204515431414,-4.55362929680409,
127.193795741725));
#233651=CARTESIAN_POINT('Ctrl Pts',(169.926067807602,-5.4990183500578,132.683859402108));
#233652=CARTESIAN_POINT('Ctrl Pts',(169.647620183788,-1.39107818158956,
136.446755498118));
#233653=CARTESIAN_POINT('Ctrl Pts',(169.369172559976,3.99519487781229,135.024566345214));
#233654=CARTESIAN_POINT('Ctrl Pts',(169.090724936163,5.71007902062496,129.724214297113));
#233655=CARTESIAN_POINT('Ctrl Pts',(168.81227731235,2.17767949635139,125.416463949427));
#233656=CARTESIAN_POINT('Ctrl Pts',(168.533829688537,-3.35590109951139,
126.059927426375));
#233657=CARTESIAN_POINT('Ctrl Pts',(168.255382064725,-5.80557252980615,
131.063293227581));
#233658=CARTESIAN_POINT('Ctrl Pts',(167.976934440911,-2.92020642319446,
135.828712609743));
#233659=CARTESIAN_POINT('Ctrl Pts',(167.698486817099,2.64868672631821,135.976997964335));
#233660=CARTESIAN_POINT('Ctrl Pts',(167.420039193286,5.78356616988455,131.371882294628));
#233661=CARTESIAN_POINT('Ctrl Pts',(167.141591569473,3.60363084624196,126.245241928676));
#233662=CARTESIAN_POINT('Ctrl Pts',(166.86314394566,-1.88786517794308,125.308208912483));
#233663=CARTESIAN_POINT('Ctrl Pts',(166.584696321847,-5.64450533093961,
129.421870811324));
#233664=CARTESIAN_POINT('Ctrl Pts',(166.306248698034,-4.21412083421794,
134.805973303719));
#233665=CARTESIAN_POINT('Ctrl Pts',(166.027801074221,1.08883483790225,136.512789227187));
#233666=CARTESIAN_POINT('Ctrl Pts',(165.749353450409,5.3912044865292,132.973838130654));
#233667=CARTESIAN_POINT('Ctrl Pts',(165.470905826595,4.73932058701693,127.441243184462));
#233668=CARTESIAN_POINT('Ctrl Pts',(165.192458202783,-0.267767403281747,
124.999188861871));
#233669=CARTESIAN_POINT('Ctrl Pts',(164.914010578969,-5.02879023112935,
127.891803784357));
#233670=CARTESIAN_POINT('Ctrl Pts',(164.635562955157,-5.16860050662956,
133.46091615025));
#233671=CARTESIAN_POINT('Ctrl Pts',(164.357115331344,-0.55871941670932,
136.588783761558));
#233672=CARTESIAN_POINT('Ctrl Pts',(164.078667707531,4.56459752220588,134.401049088318));
#233673=CARTESIAN_POINT('Ctrl Pts',(163.800220083718,5.49327233119978,128.908133418456));
#233674=CARTESIAN_POINT('Ctrl Pts',(163.521772459905,1.37389822909362,125.157757908727));
#233675=CARTESIAN_POINT('Ctrl Pts',(163.243324836092,-4.00802122688977,
126.596334436543));
#233676=CARTESIAN_POINT('Ctrl Pts',(162.964877212279,-5.70676497808368,
131.901881451211));
#233677=CARTESIAN_POINT('Ctrl Pts',(162.686429588467,-2.16127050538683,
136.198860436632));
#233678=CARTESIAN_POINT('Ctrl Pts',(162.407981964654,3.37032597782655,135.538557624299));
#233679=CARTESIAN_POINT('Ctrl Pts',(162.129534340841,5.80475753699479,130.527759041158));
#233680=CARTESIAN_POINT('Ctrl Pts',(161.851086717028,2.90490049783562,125.771143793998));
#233681=CARTESIAN_POINT('Ctrl Pts',(161.572639093215,-2.66441818655578,
125.639808921385));
#233682=CARTESIAN_POINT('Ctrl Pts',(161.294191469402,-5.7852667215671,130.254444755185));
#233683=CARTESIAN_POINT('Ctrl Pts',(161.015743845589,-3.58973776544978,
135.37442640163));
#233684=CARTESIAN_POINT('Ctrl Pts',(160.737296221776,1.90458482867669,136.294740852644));
#233685=CARTESIAN_POINT('Ctrl Pts',(160.458848597964,5.64868700939082,132.169664087608));
#233686=CARTESIAN_POINT('Ctrl Pts',(160.18040097415,4.20192178217643,126.789940132385));
#233687=CARTESIAN_POINT('Ctrl Pts',(159.901953350338,-1.10620428756715,
125.099272487699));
#233688=CARTESIAN_POINT('Ctrl Pts',(159.623505726525,-5.39778265812024,
128.651302125312));
#233689=CARTESIAN_POINT('Ctrl Pts',(159.345058102712,-4.72906246220349,
134.18188733455));
#233690=CARTESIAN_POINT('Ctrl Pts',(159.066610478899,0.285435108933367,
136.608690492233));
#233691=CARTESIAN_POINT('Ctrl Pts',(158.788162855086,5.03763175924073,133.701598052375));
#233692=CARTESIAN_POINT('Ctrl Pts',(158.509715231273,5.16049092479898,128.132085947844));
#233693=CARTESIAN_POINT('Ctrl Pts',(158.23126760746,0.541111034464008,125.018263716911));
#233694=CARTESIAN_POINT('Ctrl Pts',(157.952819983648,-4.57552346179978,
127.221581871133));
#233695=CARTESIAN_POINT('Ctrl Pts',(157.674372359834,-5.48747542341729,
132.717298664853));
#233696=CARTESIAN_POINT('Ctrl Pts',(157.395924736022,-1.35670554899215,
136.455118845335));
#233697=CARTESIAN_POINT('Ctrl Pts',(157.117477112209,4.02081044620608,135.000168269382));
#233698=CARTESIAN_POINT('Ctrl Pts',(156.839029488396,5.70339806885126,129.68947543801));
#233699=CARTESIAN_POINT('Ctrl Pts',(156.560581864583,2.1448414927076,125.403307621479));
#233700=CARTESIAN_POINT('Ctrl Pts',(156.28213424077,-3.38471963390224,126.080443652244));
#233701=CARTESIAN_POINT('Ctrl Pts',(156.003686616957,-5.8038887697026,131.098628597966));
#233702=CARTESIAN_POINT('Ctrl Pts',(155.725238993144,-2.88956766187541,
135.846395645489));
#233703=CARTESIAN_POINT('Ctrl Pts',(155.446791369331,2.68012496398725,135.960778819456));
#233704=CARTESIAN_POINT('Ctrl Pts',(155.168343745519,5.78691367932904,131.336665570917));
#233705=CARTESIAN_POINT('Ctrl Pts',(154.889896121706,3.57581142981733,126.223390074792));
#233706=CARTESIAN_POINT('Ctrl Pts',(154.611448497893,-1.92128683559663,
125.319802714623));
#233707=CARTESIAN_POINT('Ctrl Pts',(154.33300087408,-5.65281635917722,129.456256131708));
#233708=CARTESIAN_POINT('Ctrl Pts',(154.054553250267,-4.18968380410554,
134.831551712731));
#233709=CARTESIAN_POINT('Ctrl Pts',(153.776105626454,1.12356348950664,136.50605541652));
#233710=CARTESIAN_POINT('Ctrl Pts',(153.497658002641,5.40431082539012,132.940980143345));
#233711=CARTESIAN_POINT('Ctrl Pts',(153.219210378828,4.71876052800142,127.412455905645));
#233712=CARTESIAN_POINT('Ctrl Pts',(152.940762755016,-0.303100170353132,
125.000926394444));
#233713=CARTESIAN_POINT('Ctrl Pts',(152.662315131202,-5.04642661941966,
127.922469420767));
#233714=CARTESIAN_POINT('Ctrl Pts',(152.38386750739,-5.15233353688545,133.492329668737));
#233715=CARTESIAN_POINT('Ctrl Pts',(152.105419883576,-0.523497639439988,
136.592077673268));
#233716=CARTESIAN_POINT('Ctrl Pts',(151.826972259764,4.58640701436939,134.373196449306));
#233717=CARTESIAN_POINT('Ctrl Pts',(151.548524635951,5.48162768041213,128.874729443297));
#233718=CARTESIAN_POINT('Ctrl Pts',(151.270077012138,1.33950030055583,125.149499218718));
#233719=CARTESIAN_POINT('Ctrl Pts',(150.991629388325,-4.03356241728369,
126.620810364342));
#233720=CARTESIAN_POINT('Ctrl Pts',(150.713181764512,-5.69997832411825,
131.936599814887));
#233721=CARTESIAN_POINT('Ctrl Pts',(150.434734140699,-2.1283926105098,136.211916756054));
#233722=CARTESIAN_POINT('Ctrl Pts',(150.156286516886,3.39908193439765,135.517953779753));
#233723=CARTESIAN_POINT('Ctrl Pts',(149.877838893074,5.8029662359777,130.49242895923));
#233724=CARTESIAN_POINT('Ctrl Pts',(149.599391269261,2.87420805735513,125.753554094008));
#233725=CARTESIAN_POINT('Ctrl Pts',(149.320943645448,-2.69580691310719,
125.65612367832));
#233726=CARTESIAN_POINT('Ctrl Pts',(149.042496021635,-5.7885070279132,130.289671504441));
#233727=CARTESIAN_POINT('Ctrl Pts',(148.764048397822,-3.56185196835627,
135.396193481562));
#233728=CARTESIAN_POINT('Ctrl Pts',(148.485600774009,1.93797104397778,136.283045380177));
#233729=CARTESIAN_POINT('Ctrl Pts',(148.207153150196,5.6568933420451,132.135253630582));
#233730=CARTESIAN_POINT('Ctrl Pts',(147.928705526383,4.17740701337624,126.764436219762));
#233731=CARTESIAN_POINT('Ctrl Pts',(147.65025790257,-1.14091228290746,125.106111969245));
#233732=CARTESIAN_POINT('Ctrl Pts',(147.371810278758,-5.41078892786276,
128.684199851613));
#233733=CARTESIAN_POINT('Ctrl Pts',(147.093362654945,-4.70841487984645,
134.210611902278));
#233734=CARTESIAN_POINT('Ctrl Pts',(146.814915031132,0.320762423894332,
136.60684542692));
#233735=CARTESIAN_POINT('Ctrl Pts',(146.536467407319,5.05517473019176,133.670878878906));
#233736=CARTESIAN_POINT('Ctrl Pts',(146.258019783506,5.14412841845787,128.100722085923));
#233737=CARTESIAN_POINT('Ctrl Pts',(145.979572159693,0.505879394805349,
125.015077023433));
#233738=CARTESIAN_POINT('Ctrl Pts',(145.70112453588,-4.59724807909095,127.249500761725));
#233739=CARTESIAN_POINT('Ctrl Pts',(145.422676912067,-5.47572915635697,
132.750667042976));
#233740=CARTESIAN_POINT('Ctrl Pts',(145.144229288255,-1.32228264317164,
136.463272801628));
#233741=CARTESIAN_POINT('Ctrl Pts',(144.865781664442,4.0462770219901,134.975614716357));
#233742=CARTESIAN_POINT('Ctrl Pts',(144.587334040629,5.69650577556471,129.654777891387));
#233743=CARTESIAN_POINT('Ctrl Pts',(144.308886416816,2.11192401117359,125.390351431538));
#233744=CARTESIAN_POINT('Ctrl Pts',(144.030438793003,-3.41341274626234,
126.101134924595));
#233745=CARTESIAN_POINT('Ctrl Pts',(143.75199116919,-5.80198994436631,131.133953064144));
#233746=CARTESIAN_POINT('Ctrl Pts',(143.473543545377,-2.85882182656403,
135.863891846773));
#233747=CARTESIAN_POINT('Ctrl Pts',(143.195095921564,2.71146388864014,135.944368601604));
#233748=CARTESIAN_POINT('Ctrl Pts',(142.916648297751,5.790046752559,131.301429122451));
#233749=CARTESIAN_POINT('Ctrl Pts',(142.638200673938,3.54785951038517,126.201707970457));
#233750=CARTESIAN_POINT('Ctrl Pts',(142.359753050125,-1.95463729925998,
125.331599749072));
#233751=CARTESIAN_POINT('Ctrl Pts',(142.081305426313,-5.66091792022584,
129.490691406602));
#233752=CARTESIAN_POINT('Ctrl Pts',(141.8028578025,-4.16509152371897,134.856980892698));
#233753=CARTESIAN_POINT('Ctrl Pts',(141.524410178687,1.15825050705268,136.499110327454));
#233754=CARTESIAN_POINT('Ctrl Pts',(141.245962554874,5.41721690552589,132.908042982814));
#233755=CARTESIAN_POINT('Ctrl Pts',(140.967514931061,4.69802561357932,127.383794315106));
#233756=CARTESIAN_POINT('Ctrl Pts',(140.689067307248,-0.338421705936203,
125.002878975406));
#233757=CARTESIAN_POINT('Ctrl Pts',(140.410619683435,-5.06387601051571,
127.953241846716));
#233758=CARTESIAN_POINT('Ctrl Pts',(140.132172059623,-5.13587564552739,
133.523643583541));
#233759=CARTESIAN_POINT('Ctrl Pts',(139.85372443581,-0.48825646377323,136.595157118993));
#233760=CARTESIAN_POINT('Ctrl Pts',(139.575276811997,4.60804655553434,134.34521156577));
#233761=CARTESIAN_POINT('Ctrl Pts',(139.296829188184,5.46977990589493,128.841396971331));
#233762=CARTESIAN_POINT('Ctrl Pts',(139.018381564371,1.30505273634171,125.141450071677));
#233763=CARTESIAN_POINT('Ctrl Pts',(138.739933940558,-4.05895414253892,
126.645441315135));
#233764=CARTESIAN_POINT('Ctrl Pts',(138.461486316745,-5.69298045535984,
131.971276223022));
#233765=CARTESIAN_POINT('Ctrl Pts',(138.183038692932,-2.09543584726193,
136.224772696493));
#233766=CARTESIAN_POINT('Ctrl Pts',(137.904591069119,3.42771193673771,135.49717527128));
#233767=CARTESIAN_POINT('Ctrl Pts',(137.626143445306,5.80095990391266,130.457110436044));
#233768=CARTESIAN_POINT('Ctrl Pts',(137.347695821494,2.84340911203807,125.736151553513));
#233769=CARTESIAN_POINT('Ctrl Pts',(137.069248197681,-2.727095745542,125.672629205068));
#233770=CARTESIAN_POINT('Ctrl Pts',(136.790800573868,-5.7915328390027,130.324917325691));
#233771=CARTESIAN_POINT('Ctrl Pts',(136.512352950055,-3.53383418552815,
135.417790409441));
#233772=CARTESIAN_POINT('Ctrl Pts',(136.233905326242,1.97128544704926,136.271146893031));
#233773=CARTESIAN_POINT('Ctrl Pts',(135.955457702429,5.66489005643625,132.100793856825));
#233774=CARTESIAN_POINT('Ctrl Pts',(135.677010078616,4.15273744922295,126.739082008025));
#233775=CARTESIAN_POINT('Ctrl Pts',(135.398562454803,-1.17557800132362,
125.113162601491));
#233776=CARTESIAN_POINT('Ctrl Pts',(135.12011483099,-5.42359469883174,128.717176141249));
#233777=CARTESIAN_POINT('Ctrl Pts',(134.841667207177,-4.68759282544451,
134.239210250113));
#233778=CARTESIAN_POINT('Ctrl Pts',(134.563219583365,0.356077852885664,
136.604785348398));
#233779=CARTESIAN_POINT('Ctrl Pts',(134.284771959552,5.0725303797842,133.640053485549));
#233780=CARTESIAN_POINT('Ctrl Pts',(134.006324335739,5.12757529454644,128.069458408322));
#233781=CARTESIAN_POINT('Ctrl Pts',(133.727876711926,0.470629009599695,
125.012104853988));
#233782=CARTESIAN_POINT('Ctrl Pts',(133.449429088113,-4.61880234366392,
127.277551378957));
#233783=CARTESIAN_POINT('Ctrl Pts',(133.1709814643,-5.46377998413907,132.783963299997));
#233784=CARTESIAN_POINT('Ctrl Pts',(132.892533840487,-1.28781073968153,
136.47121706485));
#233785=CARTESIAN_POINT('Ctrl Pts',(132.614086216674,4.07159366149105,134.950906595976));
#233786=CARTESIAN_POINT('Ctrl Pts',(132.335638592862,5.68940239616175,129.620122942976));
#233787=CARTESIAN_POINT('Ctrl Pts',(132.057190969048,2.07892827151876,125.377595859696));
#233788=CARTESIAN_POINT('Ctrl Pts',(131.778743345236,-3.44197937335791,
126.122000476702));
#233789=CARTESIAN_POINT('Ctrl Pts',(131.500295721423,-5.79987612415893,
131.169265317152));
#233790=CARTESIAN_POINT('Ctrl Pts',(131.22184809761,-2.82797005655853,135.881200565267));
#233791=CARTESIAN_POINT('Ctrl Pts',(130.943400473797,2.74270233900145,135.927767918864));
#233792=CARTESIAN_POINT('Ctrl Pts',(130.664952849984,5.79296527347731,131.26617425493));
#233793=CARTESIAN_POINT('Ctrl Pts',(130.386505226171,3.51977612371406,126.180196419108));
#233794=CARTESIAN_POINT('Ctrl Pts',(130.108057602358,-1.98791533311939,
125.343599578688));
#233795=CARTESIAN_POINT('Ctrl Pts',(129.829609978546,-5.66880971387908,
129.52517535999));
#233796=CARTESIAN_POINT('Ctrl Pts',(129.551162354732,-4.14034490433441,
134.882259901329));
#233797=CARTESIAN_POINT('Ctrl Pts',(129.27271473092,1.19289460520041,136.491954217345));
#233798=CARTESIAN_POINT('Ctrl Pts',(128.994267107107,5.42992224869717,132.875027869557));
#233799=CARTESIAN_POINT('Ctrl Pts',(128.715819483294,4.67711661209022,127.355259474909));
#233800=CARTESIAN_POINT('Ctrl Pts',(128.437371859481,-0.373730701178542,
125.005046532403));
#233801=CARTESIAN_POINT('Ctrl Pts',(128.158924235668,-5.0811377578241,127.984119921918));
#233802=CARTESIAN_POINT('Ctrl Pts',(127.880476611855,-5.11922744240848,
133.554856734316));
#233803=CARTESIAN_POINT('Ctrl Pts',(127.602028988042,-0.452997195583419,
136.598021984625));
#233804=CARTESIAN_POINT('Ctrl Pts',(127.323581364229,4.62951534383955,134.3170954747));
#233805=CARTESIAN_POINT('Ctrl Pts',(127.045133740417,5.45772944667181,128.808137237705));
#233806=CARTESIAN_POINT('Ctrl Pts',(126.766686116604,1.2705568129186,125.133610765869));
#233807=CARTESIAN_POINT('Ctrl Pts',(126.488238492791,-4.08419546175569,
126.67022637621));
#233808=CARTESIAN_POINT('Ctrl Pts',(126.209790868978,-5.68577163111709,
132.005909390672));
#233809=CARTESIAN_POINT('Ctrl Pts',(125.931343245165,-2.06240143686808,
136.237427781569));
#233810=CARTESIAN_POINT('Ctrl Pts',(125.652895621352,3.45621492395137,135.476222868834));
#233811=CARTESIAN_POINT('Ctrl Pts',(125.374447997539,5.79873861514512,130.421804780342));
#233812=CARTESIAN_POINT('Ctrl Pts',(125.096000373726,2.8125048031507,125.718936817367));
#233813=CARTESIAN_POINT('Ctrl Pts',(124.817552749914,-2.75828352444112,
125.68932489001));
#233814=CARTESIAN_POINT('Ctrl Pts',(124.5391051261,-5.79434404271298,130.36018091289));
#233815=CARTESIAN_POINT('Ctrl Pts',(124.260657502288,-3.50568545517477,
135.439216384981));
#233816=CARTESIAN_POINT('Ctrl Pts',(123.982209878475,2.00452680341345,136.25904583211));
#233817=CARTESIAN_POINT('Ctrl Pts',(123.703762254662,5.67267685624313,132.066286043259));
#233818=CARTESIAN_POINT('Ctrl Pts',(123.425314630849,4.12791400385628,126.71387843668));
#233819=CARTESIAN_POINT('Ctrl Pts',(123.146867007036,-1.21020015826455,
125.120424123171));
#233820=CARTESIAN_POINT('Ctrl Pts',(122.868419383223,-5.43619949650465,
128.750229772276));
#233821=CARTESIAN_POINT('Ctrl Pts',(122.58997175941,-4.66659707056658,134.267681318331));
#233822=CARTESIAN_POINT('Ctrl Pts',(122.311524135597,0.391380087281262,
136.602510333005));
#233823=CARTESIAN_POINT('Ctrl Pts',(122.033076511785,5.08969806489794,133.609123014551));
#233824=CARTESIAN_POINT('Ctrl Pts',(121.754628887972,5.11083216644683,128.038296073528));
#233825=CARTESIAN_POINT('Ctrl Pts',(121.476181264159,0.435361185062875,
125.00934731871));
#233826=CARTESIAN_POINT('Ctrl Pts',(121.197733640346,-4.64018545681751,
127.305732683402));
#233827=CARTESIAN_POINT('Ctrl Pts',(120.919286016533,-5.45162834954452,
132.817186202114));
#233828=CARTESIAN_POINT('Ctrl Pts',(120.64083839272,-1.25329111589093,136.478951340622));
#233829=CARTESIAN_POINT('Ctrl Pts',(120.362390768907,4.09675942659154,134.92604482381));
#233830=CARTESIAN_POINT('Ctrl Pts',(120.083943145094,5.68208819386074,129.585511876926));
#233831=CARTESIAN_POINT('Ctrl Pts',(119.805495521281,2.04585549641223,125.36504137862));
#233832=CARTESIAN_POINT('Ctrl Pts',(119.527047897469,-3.47041845664194,
126.143039535386));
#233833=CARTESIAN_POINT('Ctrl Pts',(119.248600273655,-5.79754738740892,
131.204564048482));
#233834=CARTESIAN_POINT('Ctrl Pts',(118.970152649843,-2.7970134950826,135.898321159589));
#233835=CARTESIAN_POINT('Ctrl Pts',(118.69170502603,2.77383915751901,135.910977386384));
#233836=CARTESIAN_POINT('Ctrl Pts',(118.413257402217,5.795669133937,131.230902274733));
#233837=CARTESIAN_POINT('Ctrl Pts',(118.134809778404,3.49156231044436,126.158856217863));
#233838=CARTESIAN_POINT('Ctrl Pts',(117.856362154591,-2.02111970404504,
125.355801758813));
#233839=CARTESIAN_POINT('Ctrl Pts',(117.577914530778,-5.67649144770371,
129.559706714059));
#233840=CARTESIAN_POINT('Ctrl Pts',(117.299466906965,-4.11544486294674,
134.907387801903));
#233841=CARTESIAN_POINT('Ctrl Pts',(117.021019283153,1.22749450019975,136.484587351363));
#233842=CARTESIAN_POINT('Ctrl Pts',(116.74257165934,5.44242638410263,132.841936026965));
#233843=CARTESIAN_POINT('Ctrl Pts',(116.464124035527,4.65603429832517,127.326852442422));
#233844=CARTESIAN_POINT('Ctrl Pts',(116.185676411714,-0.409025847692317,
125.007428985116));
#233845=CARTESIAN_POINT('Ctrl Pts',(115.907228787901,-5.09821122170419,
128.015102502178));
#233846=CARTESIAN_POINT('Ctrl Pts',(115.628781164088,-5.10238954443416,
133.585967964446));
#233847=CARTESIAN_POINT('Ctrl Pts',(115.350333540275,-0.417721141415912,
136.600672164005));
#233848=CARTESIAN_POINT('Ctrl Pts',(115.071885916462,4.65081258375125,134.288849217947));
#233849=CARTESIAN_POINT('Ctrl Pts',(114.793438292649,5.44547674927697,128.77495147487));
#233850=CARTESIAN_POINT('Ctrl Pts',(114.514990668836,1.23601380854556,125.125981591782));
#233851=CARTESIAN_POINT('Ctrl Pts',(114.236543045024,-4.10928543960769,
126.695164629152));
#233852=CARTESIAN_POINT('Ctrl Pts',(113.958095421211,-5.67835211851559,
132.040498034489));
#233853=CARTESIAN_POINT('Ctrl Pts',(113.679647797398,-2.02929060343055,
136.249881542344));
#233854=CARTESIAN_POINT('Ctrl Pts',(113.401200173585,3.48458983985001,135.455097348814));
#233855=CARTESIAN_POINT('Ctrl Pts',(113.122752549772,5.79630245198571,130.386513300387));
#233856=CARTESIAN_POINT('Ctrl Pts',(112.844304925959,2.78149627586357,125.701910523471));
#233857=CARTESIAN_POINT('Ctrl Pts',(112.565857302146,-2.78936909412988,
125.706210114483));
#233858=CARTESIAN_POINT('Ctrl Pts',(112.287409678333,-5.7969405348739,130.395460959329));
#233859=CARTESIAN_POINT('Ctrl Pts',(112.008962054521,-3.47740682035766,
135.460470614237));
#233860=CARTESIAN_POINT('Ctrl Pts',(111.730514430707,2.03769388129978,136.246742645822));
#233861=CARTESIAN_POINT('Ctrl Pts',(111.452066806895,5.68025345292297,132.031731468582));
#233862=CARTESIAN_POINT('Ctrl Pts',(111.173619183082,4.10293759711819,126.688826439658));
#233863=CARTESIAN_POINT('Ctrl Pts',(110.895171559269,-1.24477747079359,
125.127896265209));
#233864=CARTESIAN_POINT('Ctrl Pts',(110.616723935456,-5.44860285380605,
128.783359519875));
#233865=CARTESIAN_POINT('Ctrl Pts',(110.338276311643,-4.64542839321807,
134.296024051927));
#233866=CARTESIAN_POINT('Ctrl Pts',(110.05982868783,0.426667818943798,136.600020465042));
#233867=CARTESIAN_POINT('Ctrl Pts',(109.781381064017,5.10667714937814,133.57808861205));
#233868=CARTESIAN_POINT('Ctrl Pts',(109.502933440204,5.0938996545818,128.007236236273));
#233869=CARTESIAN_POINT('Ctrl Pts',(109.224485816392,0.400077228057368,
125.006804519781));
#233870=CARTESIAN_POINT('Ctrl Pts',(108.946038192578,-4.66139662619255,
127.334043630792));
#233871=CARTESIAN_POINT('Ctrl Pts',(108.667590568766,-5.43927470285667,
132.850334518237));
#233872=CARTESIAN_POINT('Ctrl Pts',(108.389142944953,-1.21872505093712,
136.486475342347));
#233873=CARTESIAN_POINT('Ctrl Pts',(108.11069532114,4.1217733847649,134.901030321119));
#233874=CARTESIAN_POINT('Ctrl Pts',(107.832247697327,5.67456343969215,129.550945975765));
#233875=CARTESIAN_POINT('Ctrl Pts',(107.553800073514,2.01270691137792,125.352688453517));
#233876=CARTESIAN_POINT('Ctrl Pts',(107.275352449701,-3.49872894229381,
126.164251321038));
#233877=CARTESIAN_POINT('Ctrl Pts',(106.996904825888,-5.7950038204084,131.239847950126));
#233878=CARTESIAN_POINT('Ctrl Pts',(106.718457202076,-2.76595328924301,
135.91525299533));
#233879=CARTESIAN_POINT('Ctrl Pts',(106.440009578262,2.80487319040651,135.893997626342));
#233880=CARTESIAN_POINT('Ctrl Pts',(106.16156195445,5.7981582337456,131.195614488879));
#233881=CARTESIAN_POINT('Ctrl Pts',(105.883114330637,3.46321911604922,126.137688157493));
#233882=CARTESIAN_POINT('Ctrl Pts',(105.604666706824,-2.05424918163679,
125.36820583729));
#233883=CARTESIAN_POINT('Ctrl Pts',(105.326219083011,-5.68396283705021,
129.594284189235));
#233884=CARTESIAN_POINT('Ctrl Pts',(105.047771459198,-4.09039232223623,
134.932363663296));
#233885=CARTESIAN_POINT('Ctrl Pts',(104.769323835385,1.26204890993897,136.47701000249));
#233886=CARTESIAN_POINT('Ctrl Pts',(104.490876211572,5.45472884839698,132.808768681268));
#233887=CARTESIAN_POINT('Ctrl Pts',(104.21242858776,4.63477945349693,127.29857427028));
#233888=CARTESIAN_POINT('Ctrl Pts',(103.933980963947,-0.444305837602887,
125.010026245263));
#233889=CARTESIAN_POINT('Ctrl Pts',(103.655533340134,-5.1150957694926,128.046188439421));
#233890=CARTESIAN_POINT('Ctrl Pts',(103.377085716321,-5.08536257553889,
133.616976121092));
#233891=CARTESIAN_POINT('Ctrl Pts',(103.098638092508,-0.38242960843803,
136.603107558928));
#233892=CARTESIAN_POINT('Ctrl Pts',(102.820190468695,4.6719374860923,134.260473842188));
#233893=CARTESIAN_POINT('Ctrl Pts',(102.541742844882,5.4330222677386,128.741840912539));
#233894=CARTESIAN_POINT('Ctrl Pts',(102.263295221069,1.2014250032263,125.118562832119));
#233895=CARTESIAN_POINT('Ctrl Pts',(101.984847597256,-4.13422314637653,
126.720255149861));
#233896=CARTESIAN_POINT('Ctrl Pts',(101.706399973443,-5.67072219248816,
132.07504087278));
#233897=CARTESIAN_POINT('Ctrl Pts',(101.427952349631,-1.99610457388343,
136.262133517338));
#233898=CARTESIAN_POINT('Ctrl Pts',(101.149504725818,3.51283563299066,135.433799494034));
#233899=CARTESIAN_POINT('Ctrl Pts',(100.871057102005,5.7936515047074,130.351237303918));
#233900=CARTESIAN_POINT('Ctrl Pts',(100.592609478192,2.75038467920892,125.685073302739));
#233901=CARTESIAN_POINT('Ctrl Pts',(100.314161854379,-2.82035130272114,
125.723284252797));
#233902=CARTESIAN_POINT('Ctrl Pts',(100.035714230566,-5.79932221927147,
130.430756157697));
#233903=CARTESIAN_POINT('Ctrl Pts',(99.7572666067534,-3.44899932895201,
135.481552309624));
#233904=CARTESIAN_POINT('Ctrl Pts',(99.4788189829407,2.07078545168999,136.234237790066));
#233905=CARTESIAN_POINT('Ctrl Pts',(99.2003713591278,5.6876195657222,131.997131413226));
#233906=CARTESIAN_POINT('Ctrl Pts',(98.9219237353147,4.07780915451857,126.663926945268));
#233907=CARTESIAN_POINT('Ctrl Pts',(98.6434761115021,-1.27930865763567,
125.13557875072));
#233908=CARTESIAN_POINT('Ctrl Pts',(98.3650284876889,-5.460804311125,128.816564156414));
#233909=CARTESIAN_POINT('Ctrl Pts',(98.0865808638763,-4.62408757781209,
134.324237400649));
#233910=CARTESIAN_POINT('Ctrl Pts',(97.8081332400632,0.461939740273397,
136.597315836771));
#233911=CARTESIAN_POINT('Ctrl Pts',(97.5296856162504,5.12346700405862,133.546951428038));
#233912=CARTESIAN_POINT('Ctrl Pts',(97.2512379924375,5.07677838639178,127.97628004749));
#233913=CARTESIAN_POINT('Ctrl Pts',(96.9727903686245,0.364778446043045,
125.004476551425));
#233914=CARTESIAN_POINT('Ctrl Pts',(96.6943427448119,-4.68243506580139,
127.362483172053));
#233915=CARTESIAN_POINT('Ctrl Pts',(96.4158951209985,-5.42671950184442,
132.883407020047));
#233916=CARTESIAN_POINT('Ctrl Pts',(96.1374474971861,-1.18411382567837,
136.493788791223));
#233917=CARTESIAN_POINT('Ctrl Pts',(95.8589998733729,4.14663460910971,134.875864014826));
#233918=CARTESIAN_POINT('Ctrl Pts',(95.5805522495601,5.66682841248846,129.516426520346));
#233919=CARTESIAN_POINT('Ctrl Pts',(95.3021046257473,1.97948374474885,125.340537542131));
#233920=CARTESIAN_POINT('Ctrl Pts',(95.0236570019342,-3.52690978125809,
126.185635047646));
#233921=CARTESIAN_POINT('Ctrl Pts',(94.7452093781216,-5.79224551741027,
131.275115714627));
#233922=CARTESIAN_POINT('Ctrl Pts',(94.4667617543085,-2.73479058998699,
135.931995445075));
#233923=CARTESIAN_POINT('Ctrl Pts',(94.1883141304955,2.8358032876865,135.876829267928));
#233924=CARTESIAN_POINT('Ctrl Pts',(93.909866506683,5.80043248066857,131.160312204968));
#233925=CARTESIAN_POINT('Ctrl Pts',(93.6314188828698,3.43474759079615,126.116693022386));
#233926=CARTESIAN_POINT('Ctrl Pts',(93.352971259057,-2.08730253826965,125.380811354481));
#233927=CARTESIAN_POINT('Ctrl Pts',(93.0745236352441,-5.69122360506351,
129.628906504239));
#233928=CARTESIAN_POINT('Ctrl Pts',(92.7960760114314,-4.06518821053398,
134.957186560018));
#233929=CARTESIAN_POINT('Ctrl Pts',(92.5176283876181,1.29655655399172,136.469222451509));
#233930=CARTESIAN_POINT('Ctrl Pts',(92.2391807638055,5.46682918570788,132.775527061492));
#233931=CARTESIAN_POINT('Ctrl Pts',(91.9607331399925,4.61335286521161,127.270426006341));
#233932=CARTESIAN_POINT('Ctrl Pts',(91.6822855161797,-0.479569363597252,
125.012838216602));
#233933=CARTESIAN_POINT('Ctrl Pts',(91.4038378923669,-5.13179077552621,
128.077376581749));
#233934=CARTESIAN_POINT('Ctrl Pts',(91.1253902685539,-5.06814716666323,
133.647880055237));
#233935=CARTESIAN_POINT('Ctrl Pts',(90.846942644741,-0.347123904390365,
136.605328079151));
#233936=CARTESIAN_POINT('Ctrl Pts',(90.5684950209282,4.69288926807169,134.231970398883));
#233937=CARTESIAN_POINT('Ctrl Pts',(90.2900473971151,5.42036646356212,128.708806777632));
#233938=CARTESIAN_POINT('Ctrl Pts',(90.0115997733025,1.16679167866171,125.111354761782));
#233939=CARTESIAN_POINT('Ctrl Pts',(89.7331521494893,-4.15900765798632,
126.7454970086));
#233940=CARTESIAN_POINT('Ctrl Pts',(89.4547045256766,-5.66288213576447,
132.109536625546));
#233941=CARTESIAN_POINT('Ctrl Pts',(89.1762569018636,-1.96284457794726,
136.274183252551));
#233942=CARTESIAN_POINT('Ctrl Pts',(88.8978092780507,3.5409512567151,135.412330093694));
#233943=CARTESIAN_POINT('Ctrl Pts',(88.619361654238,5.79078587154194,130.3159780981));
#233944=CARTESIAN_POINT('Ctrl Pts',(88.3409140304249,2.71917116603865,125.668425779081));
#233945=CARTESIAN_POINT('Ctrl Pts',(88.0624664066122,-2.85122900215762,
125.740546672265));
#233946=CARTESIAN_POINT('Ctrl Pts',(87.7840187827991,-5.80148900765152,
130.466065200115));
#233947=CARTESIAN_POINT('Ctrl Pts',(87.5055711589863,-3.42046403360785,
135.502460689953));
#233948=CARTESIAN_POINT('Ctrl Pts',(87.2271235351733,2.10380028836375,136.221531728214));
#233949=CARTESIAN_POINT('Ctrl Pts',(86.9486759113605,5.69477492168681,131.962487159311));
#233950=CARTESIAN_POINT('Ctrl Pts',(86.6702282875477,4.05252960720113,126.63918087617));
#233951=CARTESIAN_POINT('Ctrl Pts',(86.3917806637346,-1.31379243922498,
125.14347129503));
#233952=CARTESIAN_POINT('Ctrl Pts',(86.113333039922,-5.47280341633199,128.849842451481));
#233953=CARTESIAN_POINT('Ctrl Pts',(85.8348854161089,-4.6025754151404,134.352320319043));
#233954=CARTESIAN_POINT('Ctrl Pts',(85.5564377922961,0.497194544256039,
136.594396548415));
#233955=CARTESIAN_POINT('Ctrl Pts',(85.2779901684829,5.1400670067851,133.515712616316));
#233956=CARTESIAN_POINT('Ctrl Pts',(84.9995425446705,5.05946899631168,127.945428654274));
#233957=CARTESIAN_POINT('Ctrl Pts',(84.7210949208572,0.329466147029263,
125.002363499906));
#233958=CARTESIAN_POINT('Ctrl Pts',(84.4426472970446,-4.70329999605691,
127.391050253351));
#233959=CARTESIAN_POINT('Ctrl Pts',(84.1641996732315,-5.41396321174535,
132.916402482027));
#233960=CARTESIAN_POINT('Ctrl Pts',(83.8857520494189,-1.14945872264635,
136.500891416245));
#233961=CARTESIAN_POINT('Ctrl Pts',(83.6073044256056,4.17134217838416,134.850546837477));
#233962=CARTESIAN_POINT('Ctrl Pts',(83.328856801793,5.65888339887398,129.481954789796));
#233963=CARTESIAN_POINT('Ctrl Pts',(83.05040917798,1.94618722762166,125.328589094719));
#233964=CARTESIAN_POINT('Ctrl Pts',(82.7719615541671,-3.5549599292834,126.207189922827));
#233965=CARTESIAN_POINT('Ctrl Pts',(82.4935139303543,-5.78927258062435,
131.310366035126));
#233966=CARTESIAN_POINT('Ctrl Pts',(82.2150663065413,-2.70352655206008,
135.948547888425));
#233967=CARTESIAN_POINT('Ctrl Pts',(81.9366186827285,2.86662830323276,135.859472947324));
#233968=CARTESIAN_POINT('Ctrl Pts',(81.6581710589156,5.80249179043285,131.124996731141));
#233969=CARTESIAN_POINT('Ctrl Pts',(81.3797234351026,3.40614878970799,126.095871590527));
#233970=CARTESIAN_POINT('Ctrl Pts',(81.1012758112897,-2.12027854913937,
125.393617843285));
#233971=CARTESIAN_POINT('Ctrl Pts',(80.822828187477,-5.6982734826932,129.663572376127));
#233972=CARTESIAN_POINT('Ctrl Pts',(80.5443805636639,-4.03983346178761,
134.981855572247));
#233973=CARTESIAN_POINT('Ctrl Pts',(80.2659329398512,1.33101615366455,136.461224986989));
#233974=CARTESIAN_POINT('Ctrl Pts',(79.9874853160382,5.47872694765296,132.742212399419));
#233975=CARTESIAN_POINT('Ctrl Pts',(79.7090376922254,4.59175532743923,127.242408693648));
#233976=CARTESIAN_POINT('Ctrl Pts',(79.4305900684125,-0.514815118972584,
125.015864794932));
#233977=CARTESIAN_POINT('Ctrl Pts',(79.1521424445996,-5.1482956211654,128.108665773475));
#233978=CARTESIAN_POINT('Ctrl Pts',(78.8736948207867,-5.05074395573051,
133.678678621723));
#233979=CARTESIAN_POINT('Ctrl Pts',(78.5952471969738,-0.31180533753877,
136.607333642391));
#233980=CARTESIAN_POINT('Ctrl Pts',(78.3167995731609,4.71366715331346,134.203339944237));
#233981=CARTESIAN_POINT('Ctrl Pts',(78.0383519493481,5.407509805713,128.675850294243));
#233982=CARTESIAN_POINT('Ctrl Pts',(77.7599043255351,1.1321151182024,125.104357647873));
#233983=CARTESIAN_POINT('Ctrl Pts',(77.4814567017223,-4.18363805603787,
126.770889270024));
#233984=CARTESIAN_POINT('Ctrl Pts',(77.2030090779094,-5.65483223886072,
132.143984014535));
#233985=CARTESIAN_POINT('Ctrl Pts',(76.9245614540965,-1.92951184808342,
136.286030301474));
#233986=CARTESIAN_POINT('Ctrl Pts',(76.6461138302835,3.56893566918854,135.390689943351));
#233987=CARTESIAN_POINT('Ctrl Pts',(76.3676662064707,5.78770565867644,130.280736989476));
#233988=CARTESIAN_POINT('Ctrl Pts',(76.0892185826578,2.68785689298084,125.651968569378));
#233989=CARTESIAN_POINT('Ctrl Pts',(75.8107709588449,-2.8820010482549,125.75799673322));
#233990=CARTESIAN_POINT('Ctrl Pts',(75.532323335032,-5.8034408197229,130.501386778194));
#233991=CARTESIAN_POINT('Ctrl Pts',(75.2538757112192,-3.39180199171105,
135.523194980456));
#233992=CARTESIAN_POINT('Ctrl Pts',(74.9754280874062,2.13673716794415,136.208624931095));
#233993=CARTESIAN_POINT('Ctrl Pts',(74.6969804635933,5.70171925567246,131.92779999059));
#233994=CARTESIAN_POINT('Ctrl Pts',(74.4185328397805,4.02709989190878,126.61458914934));
#233995=CARTESIAN_POINT('Ctrl Pts',(74.1400852159675,-1.34822753775231,
125.151573605674));
#233996=CARTESIAN_POINT('Ctrl Pts',(73.8616375921548,-5.48459972479585,
128.883193171938));
#233997=CARTESIAN_POINT('Ctrl Pts',(73.5831899683417,-4.58089270234404,
134.380271766487));
#233998=CARTESIAN_POINT('Ctrl Pts',(73.3047423445289,0.532430924512096,
136.591262708148));
#233999=CARTESIAN_POINT('Ctrl Pts',(73.026294720716,5.15647654243839,133.484373334449));
#234000=CARTESIAN_POINT('Ctrl Pts',(72.7478470969032,5.04197212574731,127.914683199832));
#234001=CARTESIAN_POINT('Ctrl Pts',(72.46939947309,0.294141639526237,125.000465443524));
#234002=CARTESIAN_POINT('Ctrl Pts',(72.1909518492774,-4.72399064380143,
127.419743816117));
#234003=CARTESIAN_POINT('Ctrl Pts',(71.9125042254643,-5.40100630524849,
132.949319681519));
#234004=CARTESIAN_POINT('Ctrl Pts',(71.6340566016516,-1.11476102599866,
136.507782954223));
#234005=CARTESIAN_POINT('Ctrl Pts',(71.3556089778387,4.19589517704018,134.82507972721));
#234006=CARTESIAN_POINT('Ctrl Pts',(71.0771613540258,5.65072869325411,129.447532061481));
#234007=CARTESIAN_POINT('Ctrl Pts',(70.7987137302128,1.91281859381102,125.316843554035));
#234008=CARTESIAN_POINT('Ctrl Pts',(70.5202661064001,-3.58287834696108,
126.22891514786));
#234009=CARTESIAN_POINT('Ctrl Pts',(70.241818482587,-5.78608512021397,131.345597605407));
#234010=CARTESIAN_POINT('Ctrl Pts',(69.9633708587742,-2.67216233396265,
135.964909712024));
#234011=CARTESIAN_POINT('Ctrl Pts',(69.6849232349613,2.89734709481291,135.841929307673));
#234012=CARTESIAN_POINT('Ctrl Pts',(69.4064756111484,5.80433608672999,131.089669376025));
#234013=CARTESIAN_POINT('Ctrl Pts',(69.1280279873355,3.37742377252397,126.07522463346));
#234014=CARTESIAN_POINT('Ctrl Pts',(68.8495803635227,-2.15317599230747,
125.406624829152));
#234015=CARTESIAN_POINT('Ctrl Pts',(68.5711327397097,-5.70511220870344,
129.698280520343));
#234016=CARTESIAN_POINT('Ctrl Pts',(68.2926851158969,-4.01432901552682,
135.006369785865));
#234017=CARTESIAN_POINT('Ctrl Pts',(68.014237492084,1.36542643204398,136.45301790528));
#234018=CARTESIAN_POINT('Ctrl Pts',(67.735789868271,5.49042169335597,132.708825929535));
#234019=CARTESIAN_POINT('Ctrl Pts',(67.4573422444582,4.56998764048497,127.214523370394));
#234020=CARTESIAN_POINT('Ctrl Pts',(67.1788946206453,-0.550041797684044,
125.019105868103));
#234021=CARTESIAN_POINT('Ctrl Pts',(66.9004469968323,-5.164609694817,128.140054855163));
#234022=CARTESIAN_POINT('Ctrl Pts',(66.6219993730196,-5.03315358762317,
133.709370679297));
#234023=CARTESIAN_POINT('Ctrl Pts',(66.3435517492066,-0.2764752166261,136.609124174332));
#234024=CARTESIAN_POINT('Ctrl Pts',(66.0651041253938,4.73427037188528,134.174583539162));
#234025=CARTESIAN_POINT('Ctrl Pts',(65.7866565015808,5.39445277059944,128.642972683589));
#234026=CARTESIAN_POINT('Ctrl Pts',(65.508208877768,1.0973966068015,125.097571749668));
#234027=CARTESIAN_POINT('Ctrl Pts',(65.2297612539551,-4.20811342784249,
126.796430993211));
#234028=CARTESIAN_POINT('Ctrl Pts',(64.9513136301422,-5.64657280006891,
132.178381763287));
#234029=CARTESIAN_POINT('Ctrl Pts',(64.6728660063292,-1.89610761944867,
136.297674225111));
#234030=CARTESIAN_POINT('Ctrl Pts',(64.3944183825164,3.59678783343796,135.368879844889));
#234031=CARTESIAN_POINT('Ctrl Pts',(64.1159707587035,5.78441098024938,130.245515283918));
#234032=CARTESIAN_POINT('Ctrl Pts',(63.8375231348906,2.65644302039782,125.635702283457));
#234033=CARTESIAN_POINT('Ctrl Pts',(63.5590755110777,-2.91266630074331,
125.775633789045));
#234034=CARTESIAN_POINT('Ctrl Pts',(63.2806278872649,-5.80517758316048,
130.53671958308));
#234035=CARTESIAN_POINT('Ctrl Pts',(63.0021802634519,-3.36301426534433,
135.543754412816));
#234036=CARTESIAN_POINT('Ctrl Pts',(62.723732639639,2.16959486994269,136.195517876976));
#234037=CARTESIAN_POINT('Ctrl Pts',(62.4452850158262,5.70845231035428,131.893071192411));
#234038=CARTESIAN_POINT('Ctrl Pts',(62.1668373920132,4.00152095094907,126.590152676031));
#234039=CARTESIAN_POINT('Ctrl Pts',(61.8883897682004,-1.38261267721222,
125.159885382419));
#234040=CARTESIAN_POINT('Ctrl Pts',(61.6099421443874,-5.49619279939966,
128.916615081961));
#234041=CARTESIAN_POINT('Ctrl Pts',(61.3314945205747,-4.55904024288434,
134.408090707227));
#234042=CARTESIAN_POINT('Ctrl Pts',(61.0530468967616,0.567647575344072,
136.587914432096));
#234043=CARTESIAN_POINT('Ctrl Pts',(60.7745992729488,5.17269500295686,133.452934743723));
#234044=CARTESIAN_POINT('Ctrl Pts',(60.496151649136,5.02428842305186,127.884044823451));
#234045=CARTESIAN_POINT('Ctrl Pts',(60.2177040253229,0.258806232497024,
124.998782452612));
#234046=CARTESIAN_POINT('Ctrl Pts',(59.9392564015102,-4.74450624233532,
127.448562797104));
#234047=CARTESIAN_POINT('Ctrl Pts',(59.6608087776971,-5.38784926247686,
132.982157398764));
#234048=CARTESIAN_POINT('Ctrl Pts',(59.3823611538844,-1.08002202147149,
136.514463149789));
#234049=CARTESIAN_POINT('Ctrl Pts',(59.1039135300714,4.22029269525717,134.799463627718));
#234050=CARTESIAN_POINT('Ctrl Pts',(58.8254659062585,5.64236459780459,129.413159610949));
#234051=CARTESIAN_POINT('Ctrl Pts',(58.5470182824457,1.8793790798041,125.305301355313));
#234052=CARTESIAN_POINT('Ctrl Pts',(58.2685706586328,-3.61066399976409,
126.250809917708));
#234053=CARTESIAN_POINT('Ctrl Pts',(57.9901230348199,-5.78268325429153,
131.380809119953));
#234054=CARTESIAN_POINT('Ctrl Pts',(57.711675411007,-2.64069909790739,135.981080309579));
#234055=CARTESIAN_POINT('Ctrl Pts',(57.4332277871941,2.92795852413098,135.824198999061));
#234056=CARTESIAN_POINT('Ctrl Pts',(57.1547801633813,5.80596530121877,131.054331448687));
#234057=CARTESIAN_POINT('Ctrl Pts',(56.8763325395683,3.34857360366007,126.054752916266));
#234058=CARTESIAN_POINT('Ctrl Pts',(56.5978849157555,-2.18599364874745,
125.419831830104));
#234059=CARTESIAN_POINT('Ctrl Pts',(56.3194372919424,-5.71173952968275,
129.733029650764));
#234060=CARTESIAN_POINT('Ctrl Pts',(56.0409896681298,-3.98867581682796,
135.030728292487));
#234061=CARTESIAN_POINT('Ctrl Pts',(55.7625420443167,1.39978611404518,136.444601510497));
#234062=CARTESIAN_POINT('Ctrl Pts',(55.4840944205039,5.50191298946419,132.675368888989));
#234063=CARTESIAN_POINT('Ctrl Pts',(55.2056467966909,4.54805061095778,127.186771069878));
#234064=CARTESIAN_POINT('Ctrl Pts',(54.9271991728781,-0.585248094394635,
125.022561316018));
#234065=CARTESIAN_POINT('Ctrl Pts',(54.6487515490652,-5.18073239195715,
128.171542663682));
#234066=CARTESIAN_POINT('Ctrl Pts',(54.3703039252523,-5.01537671415865,
133.739955090657));
#234067=CARTESIAN_POINT('Ctrl Pts',(54.0918563014394,-0.241134850822232,
136.610699608625));
#234068=CARTESIAN_POINT('Ctrl Pts',(53.8134086776265,4.75469816032759,134.145702249237));
#234069=CARTESIAN_POINT('Ctrl Pts',(53.5349610538137,5.38119584205463,128.610175163959));
#234070=CARTESIAN_POINT('Ctrl Pts',(53.2565134300007,1.06263743096531,125.090997318624));
#234071=CARTESIAN_POINT('Ctrl Pts',(52.9780658061879,-4.23243286645675,
126.822121231705));
#234072=CARTESIAN_POINT('Ctrl Pts',(52.6996181823749,-5.63810412544538,
132.21272859718));
#234073=CARTESIAN_POINT('Ctrl Pts',(52.4211705585621,-1.86263312984859,
136.309114591992));
#234074=CARTESIAN_POINT('Ctrl Pts',(52.1427229347491,3.62450671739182,135.346900606486));
#234075=CARTESIAN_POINT('Ctrl Pts',(51.8642753109363,5.7809019583462,130.210314286579));
#234076=CARTESIAN_POINT('Ctrl Pts',(51.5858276871234,2.62493071234137,125.619627524071));
#234077=CARTESIAN_POINT('Ctrl Pts',(51.3073800633105,-2.94322362331098,
125.793457186192));
#234078=CARTESIAN_POINT('Ctrl Pts',(51.0289324394976,-5.80669923360788,
130.572062305503));
#234079=CARTESIAN_POINT('Ctrl Pts',(50.7504848156848,-3.33410192124705,
135.564138225197));
#234080=CARTESIAN_POINT('Ctrl Pts',(50.4720371918718,2.20237217680579,136.182211051539));
#234081=CARTESIAN_POINT('Ctrl Pts',(50.193589568059,5.71497383623647,131.858302051661));
#234082=CARTESIAN_POINT('Ctrl Pts',(49.915141944246,3.97579373215887,126.565872361749));
#234083=CARTESIAN_POINT('Ctrl Pts',(49.6366943204332,-1.41694658345112,
125.168406317271));
#234084=CARTESIAN_POINT('Ctrl Pts',(49.3582466966203,-5.50758221055828,
128.950106943089));
#234085=CARTESIAN_POINT('Ctrl Pts',(49.0797990728074,-4.53701884651156,
134.435776110423));
#234086=CARTESIAN_POINT('Ctrl Pts',(48.8013514489945,0.602843191786665,
136.584351844331));
#234087=CARTESIAN_POINT('Ctrl Pts',(48.5229038251815,5.18872178735999,133.421398009111));
#234088=CARTESIAN_POINT('Ctrl Pts',(48.2444562013688,5.006418543501,127.853514660444));
#234089=CARTESIAN_POINT('Ctrl Pts',(47.9660085775558,0.223461235307256,
124.997314589534));
#234090=CARTESIAN_POINT('Ctrl Pts',(47.6875609537429,-4.7648460314457,127.477506128414));
#234091=CARTESIAN_POINT('Ctrl Pts',(47.40911332993,-5.37449257096935,133.014914416948));
#234092=CARTESIAN_POINT('Ctrl Pts',(47.1306657061172,-1.04524299633083,
136.520931755405));
#234093=CARTESIAN_POINT('Ctrl Pts',(46.8522180823042,4.24453382897653,134.773699488214));
#234094=CARTESIAN_POINT('Ctrl Pts',(46.5737704584914,5.6337914224598,129.378838711881));
#234095=CARTESIAN_POINT('Ctrl Pts',(46.2953228346785,1.84586992471411,125.293962926255));
#234096=CARTESIAN_POINT('Ctrl Pts',(46.0168752108656,-3.63831585808481,
126.272873421051));
#234097=CARTESIAN_POINT('Ctrl Pts',(45.7384275870526,-5.77906710891461,
131.415999273987));
#234098=CARTESIAN_POINT('Ctrl Pts',(45.4599799632399,-2.60913800977569,
135.997059081882));
#234099=CARTESIAN_POINT('Ctrl Pts',(45.1815323394269,2.95846145686929,135.806282678493));
#234100=CARTESIAN_POINT('Ctrl Pts',(44.903084715614,5.80737937352832,131.018984258588));
#234101=CARTESIAN_POINT('Ctrl Pts',(44.6246370918012,3.31959935216964,126.034457197533));
#234102=CARTESIAN_POINT('Ctrl Pts',(44.3461894679882,-2.21873030238901,
125.43323835675));
#234103=CARTESIAN_POINT('Ctrl Pts',(44.0677418441753,-5.7181552000533,129.767818479747));
#234104=CARTESIAN_POINT('Ctrl Pts',(43.7892942203624,-3.96287481627985,
135.054930189501));
#234105=CARTESIAN_POINT('Ctrl Pts',(43.5108465965496,1.43409392645716,136.435976114513));
#234106=CARTESIAN_POINT('Ctrl Pts',(43.2323989727367,5.51320041016325,132.641842517543));
#234107=CARTESIAN_POINT('Ctrl Pts',(42.9539513489238,4.52594505174265,127.159152820475));
#234108=CARTESIAN_POINT('Ctrl Pts',(42.6755037251109,-0.620432704521861,
125.026231010632));
#234109=CARTESIAN_POINT('Ctrl Pts',(42.397056101298,-5.19666311515333,128.203128032237));
#234110=CARTESIAN_POINT('Ctrl Pts',(42.1186084774851,-4.99741399406557,
133.770430722483));
#234111=CARTESIAN_POINT('Ctrl Pts',(41.8401608536722,-0.205785549677785,
136.612059886891));
#234112=CARTESIAN_POINT('Ctrl Pts',(41.5617132298594,4.77494976168102,134.11669714467));
#234113=CARTESIAN_POINT('Ctrl Pts',(41.2832656060464,5.36773951131901,128.577458950676));
#234114=CARTESIAN_POINT('Ctrl Pts',(41.0048179822336,1.02783887870806,125.084634598359));
#234115=CARTESIAN_POINT('Ctrl Pts',(40.7263703584206,-4.25659547071474,
126.847959033542));
#234116=CARTESIAN_POINT('Ctrl Pts',(40.4479227346078,-5.62942652880005,
132.24702324348));
#234117=CARTESIAN_POINT('Ctrl Pts',(40.1694751107948,-1.82908961969292,
136.320350978189));
#234118=CARTESIAN_POINT('Ctrl Pts',(39.891027486982,3.65209129391637,135.324753042595));
#234119=CARTESIAN_POINT('Ctrl Pts',(39.6125798631691,5.77717872299504,130.175135301845));
#234120=CARTESIAN_POINT('Ctrl Pts',(39.3341322393562,2.59332113651206,125.603744886877));
#234121=CARTESIAN_POINT('Ctrl Pts',(39.0556846155433,-2.97367188364494,
125.811466264208));
#234122=CARTESIAN_POINT('Ctrl Pts',(38.7772369917304,-5.80800571467979,
130.607413635826));
#234123=CARTESIAN_POINT('Ctrl Pts',(38.4987893679175,-3.30506603077697,
135.584345662267));
#234124=CARTESIAN_POINT('Ctrl Pts',(38.2203417441046,2.23506787395795,136.16870494788));
#234125=CARTESIAN_POINT('Ctrl Pts',(37.9418941202917,5.72128359166147,131.823493856722));
#234126=CARTESIAN_POINT('Ctrl Pts',(37.6634464964789,3.94991918886983,126.541749106207));
#234127=CARTESIAN_POINT('Ctrl Pts',(37.3849988726659,-1.45122798421329,
125.177136094481));
#234128=CARTESIAN_POINT('Ctrl Pts',(37.1065512488531,-5.51876753623267,
128.983667514269));
#234129=CARTESIAN_POINT('Ctrl Pts',(36.8281036250402,-4.51482932923697,
134.463326950183));
#234130=CARTESIAN_POINT('Ctrl Pts',(36.5496560012273,0.6380164696531,136.580575076865));
#234131=CARTESIAN_POINT('Ctrl Pts',(36.2712083774144,5.20455630176915,133.389764299214));
#234132=CARTESIAN_POINT('Ctrl Pts',(35.9927607536015,4.9883631492699,127.82309384212));
#234133=CARTESIAN_POINT('Ctrl Pts',(35.7143131297886,0.188107957679239,
124.996061908681));
#234134=CARTESIAN_POINT('Ctrl Pts',(35.4358655059757,-4.78500925743413,
127.50657273754));
#234135=CARTESIAN_POINT('Ctrl Pts',(35.1574178821628,-5.36093672566315,
133.047589522248));
#234136=CARTESIAN_POINT('Ctrl Pts',(34.87897025835,-1.01042523932657,136.527188531377));
#234137=CARTESIAN_POINT('Ctrl Pts',(34.6005226345371,4.26861767993396,134.747788263399));
#234138=CARTESIAN_POINT('Ctrl Pts',(34.3220750107242,5.62500948490202,129.34457063605));
#234139=CARTESIAN_POINT('Ctrl Pts',(34.0436273869112,1.81229237023524,125.282828687009));
#234140=CARTESIAN_POINT('Ctrl Pts',(33.7651797630984,-3.66583289727342,
126.295104840318));
#234141=CARTESIAN_POINT('Ctrl Pts',(33.4867321392855,-5.77523681808073,
131.451166763527));
#234142=CARTESIAN_POINT('Ctrl Pts',(33.2082845154725,-2.57748023907555,
136.012845436834));
#234143=CARTESIAN_POINT('Ctrl Pts',(32.9298368916598,2.98885476273036,135.788181009863));
#234144=CARTESIAN_POINT('Ctrl Pts',(32.6513892678468,5.80857825125962,130.983629115531));
#234145=CARTESIAN_POINT('Ctrl Pts',(32.3729416440339,3.29050209170421,126.014338229324));
#234146=CARTESIAN_POINT('Ctrl Pts',(32.094494020221,-2.25138474016344,125.446843912307));
#234147=CARTESIAN_POINT('Ctrl Pts',(31.8160463964081,-5.72435898208005,
129.802645718181));
#234148=CARTESIAN_POINT('Ctrl Pts',(31.5375987725953,-3.93692696994811,
135.078974580096));
#234149=CARTESIAN_POINT('Ctrl Pts',(31.2591511487823,1.46834859799131,136.427142036947));
#234150=CARTESIAN_POINT('Ctrl Pts',(30.9807035249695,5.52428353719365,132.608248057529));
#234151=CARTESIAN_POINT('Ctrl Pts',(30.7022559011566,4.50367178196922,127.131669645585));
#234152=CARTESIAN_POINT('Ctrl Pts',(30.4238082773436,-0.655594324287056,
125.030114815962));
#234153=CARTESIAN_POINT('Ctrl Pts',(30.1453606535308,-5.21240127408669,
128.234809790423));
#234154=CARTESIAN_POINT('Ctrl Pts',(29.8669130297179,-4.97926609295916,
133.80079644549));
#234155=CARTESIAN_POINT('Ctrl Pts',(29.588465405905,-0.170428623074124,
136.613204958723));
#234156=CARTESIAN_POINT('Ctrl Pts',(29.3100177820921,4.79502442551506,134.087569300254));
#234157=CARTESIAN_POINT('Ctrl Pts',(29.0315701582792,5.35408427702179,128.544825256054));
#234158=CARTESIAN_POINT('Ctrl Pts',(28.7531225344664,0.99300223950345,125.078483824645));
#234159=CARTESIAN_POINT('Ctrl Pts',(28.4746749106534,-4.28060034526213,
126.873943441297));
#234160=CARTESIAN_POINT('Ctrl Pts',(28.1962272868406,-5.6205403316845,132.281264431386));
#234161=CARTESIAN_POINT('Ctrl Pts',(27.9177796630277,-1.79547833194873,
136.331382967337));
#234162=CARTESIAN_POINT('Ctrl Pts',(27.6393320392148,3.67954054085496,135.3024379739));
#234163=CARTESIAN_POINT('Ctrl Pts',(27.3608844154018,5.77324141216173,130.139979633288));
#234164=CARTESIAN_POINT('Ctrl Pts',(27.082436791589,2.56161546421434,125.58805496041));
#234165=CARTESIAN_POINT('Ctrl Pts',(26.8039891677761,-3.00400995347367,
125.82966035576));
#234166=CARTESIAN_POINT('Ctrl Pts',(26.5255415439632,-5.80909697796402,
130.642772264091));
#234167=CARTESIAN_POINT('Ctrl Pts',(26.2470939201503,-3.27590766986969,
135.604375975235));
#234168=CARTESIAN_POINT('Ctrl Pts',(25.9686462963375,2.2676807498481,136.155000066467));
#234169=CARTESIAN_POINT('Ctrl Pts',(25.6901986725246,5.727381342819,131.788647897428));
#234170=CARTESIAN_POINT('Ctrl Pts',(25.4117510487116,3.92389827987267,126.517783803302));
#234171=CARTESIAN_POINT('Ctrl Pts',(25.1333034248988,-1.48545560918882,
125.186074390566));
#234172=CARTESIAN_POINT('Ctrl Pts',(24.8548558010858,-5.5297483619465,129.017295551901));
#234173=CARTESIAN_POINT('Ctrl Pts',(24.576408177273,-4.49247251330123,134.490742205601));
#234174=CARTESIAN_POINT('Ctrl Pts',(24.2979605534601,0.673166105584617,
136.576584269648));
#234175=CARTESIAN_POINT('Ctrl Pts',(24.0195129296472,5.22019795943058,133.358034786234));
#234176=CARTESIAN_POINT('Ctrl Pts',(23.7410653058343,4.97012290940784,127.792783495733));
#234177=CARTESIAN_POINT('Ctrl Pts',(23.4626176820214,0.152747709641667,
124.995024456474));
#234178=CARTESIAN_POINT('Ctrl Pts',(23.1841700582085,-4.80499517314482,
127.53576154741));
#234179=CARTESIAN_POINT('Ctrl Pts',(22.9057224343956,-5.34718222887511,
133.080181503877));
#234180=CARTESIAN_POINT('Ctrl Pts',(22.6272748105827,-0.975570040643468,
136.533233245855));
#234181=CARTESIAN_POINT('Ctrl Pts',(22.3488271867698,4.29254335569345,134.721730913422));
#234182=CARTESIAN_POINT('Ctrl Pts',(22.070379562957,5.61601911054919,129.310356653276));
#234183=CARTESIAN_POINT('Ctrl Pts',(21.791931939144,1.77864766059611,125.27189905016));
#234184=CARTESIAN_POINT('Ctrl Pts',(21.5134843153312,-3.69321409767591,
126.317503351717));
#234185=CARTESIAN_POINT('Ctrl Pts',(21.2350366915183,-5.77119252372273,
131.486310285425));
#234186=CARTESIAN_POINT('Ctrl Pts',(20.9565890677054,-2.54572695889727,
136.028438789465));
#234187=CARTESIAN_POINT('Ctrl Pts',(20.6781414438925,3.01913731547902,135.769894663934));
#234188=CARTESIAN_POINT('Ctrl Pts',(20.3996938200796,5.80956188998761,130.948267329615));
#234189=CARTESIAN_POINT('Ctrl Pts',(20.1212461962667,3.26128290047392,125.994396757156));
#234190=CARTESIAN_POINT('Ctrl Pts',(19.8427985724538,-2.28395575204823,
125.460647992615));
#234191=CARTESIAN_POINT('Ctrl Pts',(19.5643509486409,-5.7303506458796,129.837510075529));
#234192=CARTESIAN_POINT('Ctrl Pts',(19.285903324828,-3.91083323933969,135.102860573299));
#234193=CARTESIAN_POINT('Ctrl Pts',(19.0074557010152,1.50254885932817,136.418099605148));
#234194=CARTESIAN_POINT('Ctrl Pts',(18.7290080772022,5.53516195986603,132.574586753804));
#234195=CARTESIAN_POINT('Ctrl Pts',(18.4505604533894,4.48123162698169,127.104322563612));
#234196=CARTESIAN_POINT('Ctrl Pts',(18.1721128295765,-0.690731650763477,
125.034212588094));
#234197=CARTESIAN_POINT('Ctrl Pts',(17.8936652057636,-5.22794628557398,
128.26658676426));
#234198=CARTESIAN_POINT('Ctrl Pts',(17.6152175819507,-4.96093368331654,
133.831051134467));
#234199=CARTESIAN_POINT('Ctrl Pts',(17.3367699581378,-0.135065381175154,
136.614134781694));
#234200=CARTESIAN_POINT('Ctrl Pts',(17.0583223343249,4.81492140795562,134.058319795333));
#234201=CARTESIAN_POINT('Ctrl Pts',(16.779874710512,5.34023064516271,128.512275289347));
#234202=CARTESIAN_POINT('Ctrl Pts',(16.5014270866992,0.958128804235671,
125.0725452254));
#234203=CARTESIAN_POINT('Ctrl Pts',(16.2229794628862,-4.30444660058956,
126.900073492105));
#234204=CARTESIAN_POINT('Ctrl Pts',(15.9445318390734,-5.61144586338,132.315450892077));
#234205=CARTESIAN_POINT('Ctrl Pts',(15.6660842152604,-1.76180051209467,
136.342210150638));
#234206=CARTESIAN_POINT('Ctrl Pts',(15.3876365914476,3.70685344106567,135.279956227294));
#234207=CARTESIAN_POINT('Ctrl Pts',(15.1091889676347,5.76909017174479,130.104848583611));
#234208=CARTESIAN_POINT('Ctrl Pts',(14.8307413438218,2.52981487031356,125.572558326068));
#234209=CARTESIAN_POINT('Ctrl Pts',(14.5522937200089,-3.03423670860886,
125.848038786661));
#234210=CARTESIAN_POINT('Ctrl Pts',(14.273846096196,-5.80997298302346,130.678136880072));
#234211=CARTESIAN_POINT('Ctrl Pts',(13.9953984723831,-3.24662791899898,
135.624228421867));
#234212=CARTESIAN_POINT('Ctrl Pts',(13.7169508485702,2.30020959599411,136.141096915141));
#234213=CARTESIAN_POINT('Ctrl Pts',(13.4385032247574,5.73326686375462,131.753765465006));
#234214=CARTESIAN_POINT('Ctrl Pts',(13.1600556009444,3.89773196938174,126.493977341077));
#234215=CARTESIAN_POINT('Ctrl Pts',(12.8816079771316,-1.51962819006047,
125.195220874312));
#234216=CARTESIAN_POINT('Ctrl Pts',(12.6031603533186,-5.54052428080121,
129.050989809886));
#234217=CARTESIAN_POINT('Ctrl Pts',(12.3247127295058,-4.46994922714442,
134.518020860792));
#234218=CARTESIAN_POINT('Ctrl Pts',(12.0462651056929,0.708290797098533,
136.572379570561));
#234219=CARTESIAN_POINT('Ctrl Pts',(11.76781748188,5.23564618073708,133.326210645918));
#234220=CARTESIAN_POINT('Ctrl Pts',(11.4893698580671,4.95169849981347,127.762584744442));
#234221=CARTESIAN_POINT('Ctrl Pts',(11.2109222342542,0.117381801481337,
124.994202271355));
#234222=CARTESIAN_POINT('Ctrl Pts',(10.9324746104413,-4.82480303799234,
127.565071476419));
#234223=CARTESIAN_POINT('Ctrl Pts',(10.6540269866284,-5.33322959028317,
133.112689154126));
#234224=CARTESIAN_POINT('Ctrl Pts',(10.3755793628155,-0.940678691853753,
136.539065674851));
#234225=CARTESIAN_POINT('Ctrl Pts',(10.0971317390026,4.31630996968034,134.695528403849));
#234226=CARTESIAN_POINT('Ctrl Pts',(9.81868411518972,5.60682063254294,129.276198031366));
#234227=CARTESIAN_POINT('Ctrl Pts',(9.54023649137686,1.74493704251384,125.261174420708));
#234228=CARTESIAN_POINT('Ctrl Pts',(9.26178886756394,-3.72045844467185,
126.340068125262));
#234229=CARTESIAN_POINT('Ctrl Pts',(8.98334124375105,-5.76693437570339,
131.52142853743));
#234230=CARTESIAN_POINT('Ctrl Pts',(8.70489361993813,-2.51387934587036,
136.043838561958));
#234231=CARTESIAN_POINT('Ctrl Pts',(8.42644599612531,3.0493079929842,135.751424318317));
#234232=CARTESIAN_POINT('Ctrl Pts',(8.14799837231237,5.81033025326331,130.912900211183));
#234233=CARTESIAN_POINT('Ctrl Pts',(7.86955074849947,3.23194286120641,125.974633519968));
#234234=CARTESIAN_POINT('Ctrl Pts',(7.59110312468663,-2.3164421311127,125.47465008616));
#234235=CARTESIAN_POINT('Ctrl Pts',(7.31265550087371,-5.73612996942864,
129.872410259879));
#234236=CARTESIAN_POINT('Ctrl Pts',(7.0342078770608,-3.88459459136738,135.126587284006));
#234237=CARTESIAN_POINT('Ctrl Pts',(6.75576025324794,1.53669344316449,136.408849154185));
#234238=CARTESIAN_POINT('Ctrl Pts',(6.47731262943506,5.54583527507644,132.540859853697));
#234239=CARTESIAN_POINT('Ctrl Pts',(6.19886500562214,4.45862541830825,127.077112587908));
#234240=CARTESIAN_POINT('Ctrl Pts',(5.92041738180924,-0.725843381924555,
125.038524175185));
#234241=CARTESIAN_POINT('Ctrl Pts',(5.64196975799638,-5.24329757358911,
128.29845777624));
#234242=CARTESIAN_POINT('Ctrl Pts',(5.36352213418349,-4.94241744445191,
133.861193668313));
#234243=CARTESIAN_POINT('Ctrl Pts',(5.08507451037056,-0.0996971343788212,
136.614849321347));
#234244=CARTESIAN_POINT('Ctrl Pts',(4.80662688655771,4.83463997171276,134.028949713759));
#234245=CARTESIAN_POINT('Ctrl Pts',(4.5281792627448,5.32617912909322,128.479810256704));
#234246=CARTESIAN_POINT('Ctrl Pts',(4.24973163893191,0.923219865152705,
125.066819020683));
#234247=CARTESIAN_POINT('Ctrl Pts',(3.97128401511898,-4.32813335306523,
126.926348217707));
#234248=CARTESIAN_POINT('Ctrl Pts',(3.69283639130614,-5.60214346088543,
132.349581358763));
#234249=CARTESIAN_POINT('Ctrl Pts',(3.41438876749324,-1.72805740807474,
136.352832126888));
#234250=CARTESIAN_POINT('Ctrl Pts',(3.13594114368033,3.73402898245891,135.257308635848));
#234251=CARTESIAN_POINT('Ctrl Pts',(2.85749351986744,5.76472515556999,130.06974345461));
#234252=CARTESIAN_POINT('Ctrl Pts',(2.5790458960546,2.49792053319242,125.557255558086));
#234253=CARTESIAN_POINT('Ctrl Pts',(2.30059827224166,-3.06435102898697,
125.866600875889));
#234254=CARTESIAN_POINT('Ctrl Pts',(2.02215064842876,-5.81063369739741,
130.713506173321));
#234255=CARTESIAN_POINT('Ctrl Pts',(1.74370302461591,-3.21722786313679,
135.643902266527));
#234256=CARTESIAN_POINT('Ctrl Pts',(1.46525540080302,2.33265320702766,136.12699600909));
#234257=CARTESIAN_POINT('Ctrl Pts',(1.18680777699008,5.73893993637821,131.718847852038));
#234258=CARTESIAN_POINT('Ctrl Pts',(0.908360153177235,3.87142122699929,
126.47033060169));
#234259=CARTESIAN_POINT('Ctrl Pts',(0.629912529364331,-1.55374446055069,
125.204575206795));
#234260=CARTESIAN_POINT('Ctrl Pts',(0.351464905551429,-5.55109489349118,
129.084749039672));
#234261=CARTESIAN_POINT('Ctrl Pts',(0.0730172817385382,-4.44726030537518,
134.545161904937));
#234262=CARTESIAN_POINT('Ctrl Pts',(-0.205430342074321,0.743389242636492,
136.56796113541));
#234263=CARTESIAN_POINT('Ctrl Pts',(-0.48387796588724,5.25090039324876,
133.294293057522));
#234264=CARTESIAN_POINT('Ctrl Pts',(-0.762325589700153,4.93309060321035,
127.732498707276));
#234265=CARTESIAN_POINT('Ctrl Pts',(-1.040773213513,0.0820115436953976,
124.993595383789));
#234266=CARTESIAN_POINT('Ctrl Pts',(-1.3192208373259,-4.84443211798899,
127.594501438479));
#234267=CARTESIAN_POINT('Ctrl Pts',(-1.5976684611388,-5.31907932690746,
133.145111268411));
#234268=CARTESIAN_POINT('Ctrl Pts',(-1.8761160849517,-0.905752485869179,
136.544685602242));
#234269=CARTESIAN_POINT('Ctrl Pts',(-2.15456370876455,4.33991664121397,
134.669181705622));
#234270=CARTESIAN_POINT('Ctrl Pts',(-2.43301133257747,5.59741439173625,
129.242096036083));
#234271=CARTESIAN_POINT('Ctrl Pts',(-2.71145895639038,1.71116176514775,
125.250655196059));
#234272=CARTESIAN_POINT('Ctrl Pts',(-2.98990658020324,-3.74756492871192,
126.362798324807));
#234273=CARTESIAN_POINT('Ctrl Pts',(-3.26835420401613,-5.76246253181,131.556520218218));
#234274=CARTESIAN_POINT('Ctrl Pts',(-3.54680182782904,-2.48193858011979,
136.059044183669));
#234275=CARTESIAN_POINT('Ctrl Pts',(-3.82524945164193,3.0793656772603,135.732770657435));
#234276=CARTESIAN_POINT('Ctrl Pts',(-4.1036970754548,5.81088331261472,130.877529070775));
#234277=CARTESIAN_POINT('Ctrl Pts',(-4.38214469926771,3.20248306110764,
125.955049250094));
#234278=CARTESIAN_POINT('Ctrl Pts',(-4.66059232308062,-2.34884267356213,
125.488849674089));
#234279=CARTESIAN_POINT('Ctrl Pts',(-4.93903994689347,-5.7416967385722,
129.907344977992));
#234280=CARTESIAN_POINT('Ctrl Pts',(-5.21748757070636,-3.85821199831392,
135.150153833014));
#234281=CARTESIAN_POINT('Ctrl Pts',(-5.49593519451928,1.57078108426016,
136.399391026839));
#234282=CARTESIAN_POINT('Ctrl Pts',(-5.77438281833216,5.55630308732125,
132.507068606974));
#234283=CARTESIAN_POINT('Ctrl Pts',(-6.05283044214503,4.43585399363028,
127.050040726751));
#234284=CARTESIAN_POINT('Ctrl Pts',(-6.33127806595794,-0.76092821669219,
125.043049417465));
#234285=CARTESIAN_POINT('Ctrl Pts',(-6.60972568977086,-5.25845456928442,
128.330421645371));
#234286=CARTESIAN_POINT('Ctrl Pts',(-6.88817331358369,-4.92371806249131,
133.891222930087));
#234287=CARTESIAN_POINT('Ctrl Pts',(-7.16662093739661,-0.0643251932685087,
136.615348551203));
#234288=CARTESIAN_POINT('Ctrl Pts',(-7.44506856120951,4.8541793861078,133.999460143849));
#234289=CARTESIAN_POINT('Ctrl Pts',(-7.72351618502242,5.3119302494974,128.44743136113));
#234290=CARTESIAN_POINT('Ctrl Pts',(-8.00196380883526,0.888276715818123,
125.06130542268));
#234291=CARTESIAN_POINT('Ctrl Pts',(-8.28041143264819,-4.35165972496785,
126.952766644486));
#234292=CARTESIAN_POINT('Ctrl Pts',(-8.55885905646108,-5.59263346890473,
132.383654566726));
#234293=CARTESIAN_POINT('Ctrl Pts',(-8.83730668027396,-1.69425027025207,
136.363248502487));
#234294=CARTESIAN_POINT('Ctrl Pts',(-9.11575430408684,3.76106615803527,
135.234496038775));
#234295=CARTESIAN_POINT('Ctrl Pts',(-9.39420192789976,5.7601465253845,130.034665547118));
#234296=CARTESIAN_POINT('Ctrl Pts',(-9.67264955171265,2.4659336347071,125.542147223509));
#234297=CARTESIAN_POINT('Ctrl Pts',(-9.95109717552551,-3.09435179871079,
125.885345935621));
#234298=CARTESIAN_POINT('Ctrl Pts',(-10.2295447993384,-5.81107909660284,
130.748878833214));
#234299=CARTESIAN_POINT('Ctrl Pts',(-10.5079924231513,-3.18770859171301,
135.663396780189));
#234300=CARTESIAN_POINT('Ctrl Pts',(-10.7864400469642,2.36501038073878,
136.112697870828));
#234301=CARTESIAN_POINT('Ctrl Pts',(-11.0648876707771,5.74440035047196,
131.683896352409));
#234302=CARTESIAN_POINT('Ctrl Pts',(-11.34333529459,3.84496702767957,126.446844461378));
#234303=CARTESIAN_POINT('Ctrl Pts',(-11.6217829184029,-1.58780315646856,
125.214137041385));
#234304=CARTESIAN_POINT('Ctrl Pts',(-11.9002305422157,-5.56145980831845,
129.118571990297));
#234305=CARTESIAN_POINT('Ctrl Pts',(-12.1786781660286,-4.42440658873985,
134.572164332316));
#234306=CARTESIAN_POINT('Ctrl Pts',(-12.4571257898416,0.778460141612691,
136.563329127923));
#234307=CARTESIAN_POINT('Ctrl Pts',(-12.7355734136544,5.26596003171537,
133.262283203764));
#234308=CARTESIAN_POINT('Ctrl Pts',(-13.0140210374673,4.91429990912079,
127.702526499083));
#234309=CARTESIAN_POINT('Ctrl Pts',(-13.2924686612802,0.0466382469415425,
124.993203816266));
#234310=CARTESIAN_POINT('Ctrl Pts',(-13.5709162850931,-4.86388168577195,
127.624050343051));
#234311=CARTESIAN_POINT('Ctrl Pts',(-13.849363908906,-5.30473196309121,
133.177446645321));
#234312=CARTESIAN_POINT('Ctrl Pts',(-14.1278115327188,-0.87079271689315,
136.550092819781));
#234313=CARTESIAN_POINT('Ctrl Pts',(-14.4062591565318,4.36336249554048,
134.642691795028));
#234314=CARTESIAN_POINT('Ctrl Pts',(-14.6847067803446,5.58780073668082,
129.20805193109));
#234315=CARTESIAN_POINT('Ctrl Pts',(-14.9631544041576,1.67732308005318,
125.240341766008));
#234316=CARTESIAN_POINT('Ctrl Pts',(-15.2416020279704,-3.77453254535539,
126.385693108075));
#234317=CARTESIAN_POINT('Ctrl Pts',(-15.5200496517834,-5.75777715774833,
131.591584027456));
#234318=CARTESIAN_POINT('Ctrl Pts',(-15.7984972755962,-2.44990584522241,
136.074055091149));
#234319=CARTESIAN_POINT('Ctrl Pts',(-16.0769448994091,3.1093092545088,135.713934372506));
#234320=CARTESIAN_POINT('Ctrl Pts',(-16.355392523222,5.81122104754806,130.842155219084));
#234321=CARTESIAN_POINT('Ctrl Pts',(-16.6338401470349,3.17290459182133,
125.935644673236));
#234322=CARTESIAN_POINT('Ctrl Pts',(-16.9122877708478,-2.38115617878252,
125.50324623023));
#234323=CARTESIAN_POINT('Ctrl Pts',(-17.1907353946607,-5.74705074703162,
129.94231293535));
#234324=CARTESIAN_POINT('Ctrl Pts',(-17.4691830184736,-3.83168643779603,
135.173559347056));
#234325=CARTESIAN_POINT('Ctrl Pts',(-17.7476306422864,1.6048105194851,136.389725573584));
#234326=CARTESIAN_POINT('Ctrl Pts',(-18.0260782660994,5.56656500871184,
132.473214265779));
#234327=CARTESIAN_POINT('Ctrl Pts',(-18.3045258899123,4.4129181967513,127.023107983299));
#234328=CARTESIAN_POINT('Ctrl Pts',(-18.5829735137251,-0.795984854984928,
125.047788147249));
#234329=CARTESIAN_POINT('Ctrl Pts',(-18.861421137538,-5.27341671101187,
128.362477187221));
#234330=CARTESIAN_POINT('Ctrl Pts',(-19.1398687613509,-4.90483623034722,
133.921137807042));
#234331=CARTESIAN_POINT('Ctrl Pts',(-19.4183163851638,-0.0289508685644962,
136.615632452765));
#234332=CARTESIAN_POINT('Ctrl Pts',(-19.6967640089767,4.87353892710056,
133.969852178351));
#234333=CARTESIAN_POINT('Ctrl Pts',(-19.9752116327896,5.29748453437273,
128.415139802436));
#234334=CARTESIAN_POINT('Ctrl Pts',(-20.2536592566025,0.853300651063172,
125.056004635698));
#234335=CARTESIAN_POINT('Ctrl Pts',(-20.5321068804154,-4.37502484451904,
126.979327793496));
#234336=CARTESIAN_POINT('Ctrl Pts',(-20.8105545042282,-5.58291623983416,
132.417669253371));
#234337=CARTESIAN_POINT('Ctrl Pts',(-21.0890021280412,-1.66038035136256,
136.37345889145));
#234338=CARTESIAN_POINT('Ctrl Pts',(-21.367449751854,3.78796396592178,135.211519281404));
#234339=CARTESIAN_POINT('Ctrl Pts',(-21.6458973756669,5.75535445085128,
129.999616160961));
#234340=CARTESIAN_POINT('Ctrl Pts',(-21.9243449994798,2.43385536014432,
125.527233882186));
#234341=CARTESIAN_POINT('Ctrl Pts',(-22.2027926232928,-3.12423790609075,
125.904273271251));
#234342=CARTESIAN_POINT('Ctrl Pts',(-22.4812402471056,-5.81130916413533,
130.784253549004));
#234343=CARTESIAN_POINT('Ctrl Pts',(-22.7596878709185,-3.15807119857507,
135.682711240481));
#234344=CARTESIAN_POINT('Ctrl Pts',(-23.0381354947314,2.39727991812053,
136.098203030175));
#234345=CARTESIAN_POINT('Ctrl Pts',(-23.3165831185443,5.74964790369824,
131.648912261261));
#234346=CARTESIAN_POINT('Ctrl Pts',(-23.5950307423572,3.81837035169266,
126.423519790431));
#234347=CARTESIAN_POINT('Ctrl Pts',(-23.8734783661701,-1.62180301575654,
125.223906023766));
#234348=CARTESIAN_POINT('Ctrl Pts',(-24.151925989983,-5.57161864120731,
129.15245740844));
#234349=CARTESIAN_POINT('Ctrl Pts',(-24.4303736137958,-4.4013889240913,
134.599027142342));
#234350=CARTESIAN_POINT('Ctrl Pts',(-24.7088212376087,0.813502194462058,
136.558483719739));
#234351=CARTESIAN_POINT('Ctrl Pts',(-24.9872688614217,5.28082453809644,
133.230182270781));
#234352=CARTESIAN_POINT('Ctrl Pts',(-25.2657164852345,4.89532711384086,
127.672669230493));
#234353=CARTESIAN_POINT('Ctrl Pts',(-25.5441641090475,0.0112632219902977,
124.993027583295));
#234354=CARTESIAN_POINT('Ctrl Pts',(-25.8226117328602,-4.88315102063038,
127.65371709519));
#234355=CARTESIAN_POINT('Ctrl Pts',(-26.1010593566733,-5.29018803048126,
133.209694086655));
#234356=CARTESIAN_POINT('Ctrl Pts',(-26.3795069804861,-0.835800680372761,
136.555287127099));
#234357=CARTESIAN_POINT('Ctrl Pts',(-26.6579546042989,4.38664666386508,
134.616059653661));
#234358=CARTESIAN_POINT('Ctrl Pts',(-26.9364022281119,5.57798002361419,
129.174066977901));
#234359=CARTESIAN_POINT('Ctrl Pts',(-27.2148498519247,1.64342224113504,
125.23023451272));
#234360=CARTESIAN_POINT('Ctrl Pts',(-27.4932974757377,-3.80136029530733,
126.408751626694));
#234361=CARTESIAN_POINT('Ctrl Pts',(-27.7717450995505,-5.75287842713667,
131.626618665841));
#234362=CARTESIAN_POINT('Ctrl Pts',(-28.0501927233634,-2.41778232816299,
136.088870728161));
#234363=CARTESIAN_POINT('Ctrl Pts',(-28.3286403471763,3.13913761515943,
135.694916161515));
#234364=CARTESIAN_POINT('Ctrl Pts',(-28.6070879709892,5.8113434455484,130.8067799669));
#234365=CARTESIAN_POINT('Ctrl Pts',(-28.8855355948021,3.14320854938853,
125.916420508438));
#234366=CARTESIAN_POINT('Ctrl Pts',(-29.163983218615,-2.41338144938502,
125.517839221114));
#234367=CARTESIAN_POINT('Ctrl Pts',(-29.4424308424279,-5.75219179641212,
129.977312836202));
#234368=CARTESIAN_POINT('Ctrl Pts',(-29.7208784662408,-3.80501889272807,
135.196802958832));
#234369=CARTESIAN_POINT('Ctrl Pts',(-29.9993260900537,1.6387804878663,136.379853152576));
#234370=CARTESIAN_POINT('Ctrl Pts',(-30.2777737138665,5.576620658989,132.439298084597));
#234371=CARTESIAN_POINT('Ctrl Pts',(-30.5562213376795,4.38981887756547,
126.996315355552));
#234372=CARTESIAN_POINT('Ctrl Pts',(-30.8346689614924,-0.831011997766135,
125.052740188944));
#234373=CARTESIAN_POINT('Ctrl Pts',(-31.1131165853052,-5.2881834443438,
128.394623213959));
#234374=CARTESIAN_POINT('Ctrl Pts',(-31.3915642091181,-4.88577264769286,
133.950937190672));
#234375=CARTESIAN_POINT('Ctrl Pts',(-31.670011832931,0.00642452892459172,
136.615701015511));
#234376=CARTESIAN_POINT('Ctrl Pts',(-31.9484594567439,4.89271787731614,
133.940126914399));
#234377=CARTESIAN_POINT('Ctrl Pts',(-32.2269070805568,5.28284251901049,
128.382936777197));
#234378=CARTESIAN_POINT('Ctrl Pts',(-32.5053547043697,0.818292966938792,
125.050916856162));
#234379=CARTESIAN_POINT('Ctrl Pts',(-32.7838023281826,-4.3982278459157,
127.006030680504));
#234380=CARTESIAN_POINT('Ctrl Pts',(-33.0622499519955,-5.57299213374921,
132.451624158271));
#234381=CARTESIAN_POINT('Ctrl Pts',(-33.3406975758084,-1.62644890646854,
136.383462915428));
#234382=CARTESIAN_POINT('Ctrl Pts',(-33.6191451996212,3.81472140941051,
135.188379215148));
#234383=CARTESIAN_POINT('Ctrl Pts',(-33.8975928234342,5.75034910954236,
129.964596594906));
#234384=CARTESIAN_POINT('Ctrl Pts',(-34.176040447247,2.40168689817613,125.512516086734));
#234385=CARTESIAN_POINT('Ctrl Pts',(-34.4544880710599,-3.15400824368619,
125.923382181419));
#234386=CARTESIAN_POINT('Ctrl Pts',(-34.7329356948729,-5.81132389146964,
130.81962900987));
#234387=CARTESIAN_POINT('Ctrl Pts',(-35.0113833186857,-3.1283167819475,
135.701844931696));
#234388=CARTESIAN_POINT('Ctrl Pts',(-35.2898309424986,2.42946062341331,
136.083512024245));
#234389=CARTESIAN_POINT('Ctrl Pts',(-35.5682785663115,5.75468240160701,
131.613896874941));
#234390=CARTESIAN_POINT('Ctrl Pts',(-35.8467261901244,3.79163218458816,
126.400357453152));
#234391=CARTESIAN_POINT('Ctrl Pts',(-36.1251738139373,-1.65574277853735,
125.233881791944));
#234392=CARTESIAN_POINT('Ctrl Pts',(-36.4036214377501,-5.58157101571846,
129.186404038463));
#234393=CARTESIAN_POINT('Ctrl Pts',(-36.6820690615631,-4.37820816435757,
134.625749339604));
#234394=CARTESIAN_POINT('Ctrl Pts',(-36.960516685376,0.848514102688449,
136.553425090409));
#234395=CARTESIAN_POINT('Ctrl Pts',(-37.2389643091888,5.29549336158222,
133.197991448084));
#234396=CARTESIAN_POINT('Ctrl Pts',(-37.5174119330018,4.87617292041449,
127.64292800788));
#234397=CARTESIAN_POINT('Ctrl Pts',(-37.7958595568146,-0.0241122203237842,
124.993066691407));
#234398=CARTESIAN_POINT('Ctrl Pts',(-38.0743071806275,-4.90223940853195,
127.683500595584));
#234399=CARTESIAN_POINT('Ctrl Pts',(-38.3527548044404,-5.27544806800837,
133.241852397473));
#234400=CARTESIAN_POINT('Ctrl Pts',(-38.6312024282533,-0.800777672950798,
136.560268331721));
#234401=CARTESIAN_POINT('Ctrl Pts',(-38.9096500520661,4.40976828338437,
134.589286268384));
#234402=CARTESIAN_POINT('Ctrl Pts',(-39.1880976758791,5.56795261644649,
129.140142435842));
#234403=CARTESIAN_POINT('Ctrl Pts',(-39.4665452996919,1.6094605046014,125.220333810727));
#234404=CARTESIAN_POINT('Ctrl Pts',(-39.7449929235049,-3.82804718445556,
126.43197302622));
#234405=CARTESIAN_POINT('Ctrl Pts',(-40.0234405473177,-5.74776652149929,
131.661622835152));
#234406=CARTESIAN_POINT('Ctrl Pts',(-40.3018881711306,-2.38556921929025,
136.103490545709));
#234407=CARTESIAN_POINT('Ctrl Pts',(-40.5803357949436,3.16884965391132,
135.675716729192));
#234408=CARTESIAN_POINT('Ctrl Pts',(-40.8587834187564,5.81125050208024,
130.771404625066));
#234409=CARTESIAN_POINT('Ctrl Pts',(-41.1372310425694,3.11339603420704,
125.897377468058));
#234410=CARTESIAN_POINT('Ctrl Pts',(-41.4156786663821,-2.4455172912504,
125.532628105994));
#234411=CARTESIAN_POINT('Ctrl Pts',(-41.6941262901951,-5.75711969621025,
130.012343383614));
#234412=CARTESIAN_POINT('Ctrl Pts',(-41.9725739140079,-3.77821035128576,
135.219883807042));
#234413=CARTESIAN_POINT('Ctrl Pts',(-42.2510215378209,1.67268973063362,
136.369774129642));
#234414=CARTESIAN_POINT('Ctrl Pts',(-42.5294691616338,5.58646966553678,
132.405321320208));
#234415=CARTESIAN_POINT('Ctrl Pts',(-42.8079167854466,4.366556892027,126.969663836325));
#234416=CARTESIAN_POINT('Ctrl Pts',(-43.0863644092596,-0.866008347092154,
125.057905359049));
#234417=CARTESIAN_POINT('Ctrl Pts',(-43.3648120330724,-5.3027542220935,
128.426858534403));
#234418=CARTESIAN_POINT('Ctrl Pts',(-43.6432596568854,-4.86652802093628,
133.98061997675));
#234419=CARTESIAN_POINT('Ctrl Pts',(-43.9217072806982,0.0417996883503892,
136.615554236903));
#234420=CARTESIAN_POINT('Ctrl Pts',(-44.2001549045111,4.9117155260715,133.910285453475));
#234421=CARTESIAN_POINT('Ctrl Pts',(-44.478602528324,5.26800474597596,128.350823478709));
#234422=CARTESIAN_POINT('Ctrl Pts',(-44.7570501521369,0.783254960667603,
125.046042272601));
#234423=CARTESIAN_POINT('Ctrl Pts',(-45.0354977759497,-4.42126786936209,
127.032874316024));
#234424=CARTESIAN_POINT('Ctrl Pts',(-45.3139453997627,-5.56286151839129,
132.485518023215));
#234425=CARTESIAN_POINT('Ctrl Pts',(-45.5923930235756,-1.59245719291215,
136.393260203719));
#234426=CARTESIAN_POINT('Ctrl Pts',(-45.8708406473885,3.84133749699455,
135.165076697471));
#234427=CARTESIAN_POINT('Ctrl Pts',(-46.1492882712014,5.74513068693249,
129.929608146614));
#234428=CARTESIAN_POINT('Ctrl Pts',(-46.4277358950142,2.3694294408167,125.497994382526));
#234429=CARTESIAN_POINT('Ctrl Pts',(-46.7061835188271,-3.18366170834627,
125.942671958037));
#234430=CARTESIAN_POINT('Ctrl Pts',(-46.98463114264,-5.81112327806003,130.85500390496));
#234431=CARTESIAN_POINT('Ctrl Pts',(-47.263078766453,-3.09844644439114,
135.720797144829));
#234432=CARTESIAN_POINT('Ctrl Pts',(-47.5415263902657,2.46155130414924,
136.068625397419));
#234433=CARTESIAN_POINT('Ctrl Pts',(-47.8199740140787,5.75950365764311,
131.578851490957));
#234434=CARTESIAN_POINT('Ctrl Pts',(-48.0984216378915,3.76475351715869,
126.377358307829));
#234435=CARTESIAN_POINT('Ctrl Pts',(-48.3768692617045,-1.6896211871606,
125.244063976264));
#234436=CARTESIAN_POINT('Ctrl Pts',(-48.6553168855173,-5.59131656306301,
129.220410622463));
#234437=CARTESIAN_POINT('Ctrl Pts',(-48.9337645093303,-4.35486516851022,
134.652329933902));
#234438=CARTESIAN_POINT('Ctrl Pts',(-49.2122121331431,0.883494568912716,
136.548153427379));
#234439=CARTESIAN_POINT('Ctrl Pts',(-49.4906597569561,5.3099659586141,133.165711928516));
#234440=CARTESIAN_POINT('Ctrl Pts',(-49.7691073807689,4.85683803860733,
127.613303933314));
#234441=CARTESIAN_POINT('Ctrl Pts',(-50.0475550045819,-0.0594867691506708,
124.993321139153));
#234442=CARTESIAN_POINT('Ctrl Pts',(-50.3260026283946,-4.92114614214944,
127.713399740592));
#234443=CARTESIAN_POINT('Ctrl Pts',(-50.6044502522077,-5.26051262186729,
133.273920386136));
#234444=CARTESIAN_POINT('Ctrl Pts',(-50.8828978760204,-0.765724992417492,
136.565036249065));
#234445=CARTESIAN_POINT('Ctrl Pts',(-51.1613454998334,4.4327264973184,134.562372631296));
#234446=CARTESIAN_POINT('Ctrl Pts',(-51.4397931236463,5.55771888674681,
129.106279562002));
#234447=CARTESIAN_POINT('Ctrl Pts',(-51.7182407474591,1.57543912891688,
125.210640026899));
#234448=CARTESIAN_POINT('Ctrl Pts',(-51.9966883712721,-3.85459222390762,
126.455356446176));
#234449=CARTESIAN_POINT('Ctrl Pts',(-52.2751359950849,-5.7424416302597,
131.696595238295));
#234450=CARTESIAN_POINT('Ctrl Pts',(-52.5535836188979,-2.35326771227282,
136.117914002047));
#234451=CARTESIAN_POINT('Ctrl Pts',(-52.8320312427106,3.19844426977395,
135.656336786975));
#234452=CARTESIAN_POINT('Ctrl Pts',(-53.1104788665238,5.81094222058764,
130.736030504428));
#234453=CARTESIAN_POINT('Ctrl Pts',(-53.3889264903363,3.08346815099054,
125.878516257743));
#234454=CARTESIAN_POINT('Ctrl Pts',(-53.6673741141495,-2.47756251357323,
125.547612336859));
#234455=CARTESIAN_POINT('Ctrl Pts',(-53.9458217379622,-5.76183426382087,
130.047403279515));
#234456=CARTESIAN_POINT('Ctrl Pts',(-54.2242693617753,-3.75126180686946,
135.242801036416));
#234457=CARTESIAN_POINT('Ctrl Pts',(-54.502716985588,1.70653699126786,136.359488878264));
#234458=CARTESIAN_POINT('Ctrl Pts',(-54.7811646094011,5.59611166339667,
132.371285231631));
#234459=CARTESIAN_POINT('Ctrl Pts',(-55.0596122332138,4.3431331021171,126.943154413196));
#234460=CARTESIAN_POINT('Ctrl Pts',(-55.3380598570268,-0.900972606160421,
125.063283466166));
#234461=CARTESIAN_POINT('Ctrl Pts',(-55.6165074808396,-5.31712850433539,
128.459181954061));
#234462=CARTESIAN_POINT('Ctrl Pts',(-55.8949551046525,-4.84710306319425,
134.01018506537));
#234463=CARTESIAN_POINT('Ctrl Pts',(-56.1734027284654,0.0771732988733811,
136.615192122377));
#234464=CARTESIAN_POINT('Ctrl Pts',(-56.4518503522783,4.93053116940174,
133.880328901363));
#234465=CARTESIAN_POINT('Ctrl Pts',(-56.7302979760911,5.25297176508825,
128.318801096944));
#234466=CARTESIAN_POINT('Ctrl Pts',(-57.0087455999042,0.748187930595796,
125.041381065643));
#234467=CARTESIAN_POINT('Ctrl Pts',(-57.2871932237169,-4.44414406110167,
127.059857705357));
#234468=CARTESIAN_POINT('Ctrl Pts',(-57.5656408475299,-5.55252476915405,
132.519349592253));
#234469=CARTESIAN_POINT('Ctrl Pts',(-57.8440884713427,-1.55840647026886,
136.402850393281));
#234470=CARTESIAN_POINT('Ctrl Pts',(-58.1225360951557,3.867811242405,135.141612591857));
#234471=CARTESIAN_POINT('Ctrl Pts',(-58.4009837189685,5.73969937639226,
129.894652112598));
#234472=CARTESIAN_POINT('Ctrl Pts',(-58.6794313427815,2.33708418337799,
125.483669307672));
#234473=CARTESIAN_POINT('Ctrl Pts',(-58.9578789665944,-3.21319720125095,
125.962141886319));
#234474=CARTESIAN_POINT('Ctrl Pts',(-59.2363265904072,-5.81070733134035,
130.890376923444));
#234475=CARTESIAN_POINT('Ctrl Pts',(-59.5147742142201,-3.06846129276222,
135.739567177598));
#234476=CARTESIAN_POINT('Ctrl Pts',(-59.793221838033,2.49355077119662,136.053543701326));
#234477=CARTESIAN_POINT('Ctrl Pts',(-60.071669461846,5.76411149315304,131.543777407928));
#234478=CARTESIAN_POINT('Ctrl Pts',(-60.3501170856587,3.73773534540316,
126.354523206705));
#234479=CARTESIAN_POINT('Ctrl Pts',(-60.6285647094717,-1.72343698624942,
125.254452199421));
#234480=CARTESIAN_POINT('Ctrl Pts',(-60.9070123332846,-5.6008549221161,
129.254475900312));
#234481=CARTESIAN_POINT('Ctrl Pts',(-61.1854599570975,-4.33136080153256,
134.678767940282));
#234482=CARTESIAN_POINT('Ctrl Pts',(-61.4639075809103,0.918442296920838,
136.542668925995));
#234483=CARTESIAN_POINT('Ctrl Pts',(-61.7423552047232,5.32424179290464,
133.133344908207));
#234484=CARTESIAN_POINT('Ctrl Pts',(-62.0208028285362,4.83732318488056,
127.583798104527));
#234485=CARTESIAN_POINT('Ctrl Pts',(-62.299250452349,-0.0948591136734494,
124.993790917104));
#234486=CARTESIAN_POINT('Ctrl Pts',(-62.5776980761619,-4.93987052088691,
127.743413422294));
#234487=CARTESIAN_POINT('Ctrl Pts',(-62.8561456999749,-5.24538224549645,
133.305896864355));
#234488=CARTESIAN_POINT('Ctrl Pts',(-63.1345933237877,-0.730643937663188,
136.569590702456));
#234489=CARTESIAN_POINT('Ctrl Pts',(-63.4130409476006,4.45552045494177,
134.53531973969));
#234490=CARTESIAN_POINT('Ctrl Pts',(-63.6914885714135,5.5472792137301,129.072479611178));
#234491=CARTESIAN_POINT('Ctrl Pts',(-63.9699361952264,1.54135937475606,
125.201153520444));
#234492=CARTESIAN_POINT('Ctrl Pts',(-64.2483838190392,-3.88099443002729,
126.478901020081));
#234493=CARTESIAN_POINT('Ctrl Pts',(-64.5268314428522,-5.73690395073373,
131.731534579357));
#234494=CARTESIAN_POINT('Ctrl Pts',(-64.805279066665,-2.32087900405488,
136.132140562712));
#234495=CARTESIAN_POINT('Ctrl Pts',(-65.083726690478,3.22792036610792,135.636777052998));
#234496=CARTESIAN_POINT('Ctrl Pts',(-65.3621743142908,5.81041861249411,
130.700658915789));
#234497=CARTESIAN_POINT('Ctrl Pts',(-65.6406219381037,3.05342600872776,
125.859837576403));
#234498=CARTESIAN_POINT('Ctrl Pts',(-65.9190695619166,-2.50951592890599,
125.562791358466));
#234499=CARTESIAN_POINT('Ctrl Pts',(-66.1975171857295,-5.76633532454392,
130.082491224748));
#234500=CARTESIAN_POINT('Ctrl Pts',(-66.4759648095424,-3.72417425806736,
135.26555379775));
#234501=CARTESIAN_POINT('Ctrl Pts',(-66.7544124333553,1.74032101554631,
136.348997779564));
#234502=CARTESIAN_POINT('Ctrl Pts',(-67.0328600571681,5.60554629528092,
132.337191080086));
#234503=CARTESIAN_POINT('Ctrl Pts',(-67.3113076809811,4.31954837581292,
126.916788068483));
#234504=CARTESIAN_POINT('Ctrl Pts',(-67.5897553047939,-0.935903479357421,
125.068874311009));
#234505=CARTESIAN_POINT('Ctrl Pts',(-67.8682029286069,-5.33130575842519,
128.491592275178));
#234506=CARTESIAN_POINT('Ctrl Pts',(-68.1466505524197,-4.82749849426569,
134.039631360986));
#234507=CARTESIAN_POINT('Ctrl Pts',(-68.4250981762326,0.112544049711387,
136.614614685353));
#234508=CARTESIAN_POINT('Ctrl Pts',(-68.7035458000455,4.94916411008632,
133.850258368115));
#234509=CARTESIAN_POINT('Ctrl Pts',(-68.9819934238584,5.23774413340002,
128.286870818499));
#234510=CARTESIAN_POINT('Ctrl Pts',(-69.2604410476712,0.713093176145084,
125.036933408012));
#234511=CARTESIAN_POINT('Ctrl Pts',(-69.5388886714842,-4.46685557344872,
127.086979848621));
#234512=CARTESIAN_POINT('Ctrl Pts',(-69.8173362952971,-5.54198226906957,
132.553117611744));
#234513=CARTESIAN_POINT('Ctrl Pts',(-70.09578391911,-1.52429800030071,136.412233128746));
#234514=CARTESIAN_POINT('Ctrl Pts',(-70.3742315429229,3.89414166464747,
135.117987767775));
#234515=CARTESIAN_POINT('Ctrl Pts',(-70.6526791667357,5.73405537918087,
129.859729788164));
#234516=CARTESIAN_POINT('Ctrl Pts',(-70.9311267905487,2.3046523244254,125.469541392991));
#234517=CARTESIAN_POINT('Ctrl Pts',(-71.2095744143614,-3.24261362795168,
125.981791244794));
#234518=CARTESIAN_POINT('Ctrl Pts',(-71.4880220381746,-5.81007606672361,
130.925746754563));
#234519=CARTESIAN_POINT('Ctrl Pts',(-71.7664696619872,-3.03836243817177,
135.758154334473));
#234520=CARTESIAN_POINT('Ctrl Pts',(-72.0449172858002,2.52545783880292,
136.038267494822));
#234521=CARTESIAN_POINT('Ctrl Pts',(-72.3233649096131,5.76850573739207,
131.508675925537));
#234522=CARTESIAN_POINT('Ctrl Pts',(-72.601812533426,3.71057867048956,126.331852995942));
#234523=CARTESIAN_POINT('Ctrl Pts',(-72.8802601572389,-1.75718892274731,
125.265046076474));
#234524=CARTESIAN_POINT('Ctrl Pts',(-73.1587077810518,-5.61018573943046,
129.28859860971));
#234525=CARTESIAN_POINT('Ctrl Pts',(-73.4371554048648,-4.30769593438731,
134.705062379074));
#234526=CARTESIAN_POINT('Ctrl Pts',(-73.7156030286775,0.953355991712339,
136.536971789486));
#234527=CARTESIAN_POINT('Ctrl Pts',(-73.9940506524905,5.33832033545752,
133.100891586529));
#234528=CARTESIAN_POINT('Ctrl Pts',(-74.2724982763033,4.81762908236426,
127.554411614868));
#234529=CARTESIAN_POINT('Ctrl Pts',(-74.5509459001162,-0.130227943157576,
124.994476007852));
#234530=CARTESIAN_POINT('Ctrl Pts',(-74.8293935239292,-4.95841185090586,
127.77354052852));
#234531=CARTESIAN_POINT('Ctrl Pts',(-75.107841147742,-5.23005749955717,
133.337780647228));
#234532=CARTESIAN_POINT('Ctrl Pts',(-75.3862887715549,-0.695535808628632,
136.573931523126));
#234533=CARTESIAN_POINT('Ctrl Pts',(-75.6647363953679,4.4781493116164,134.508128596022));
#234534=CARTESIAN_POINT('Ctrl Pts',(-75.9431840191806,5.53663398424198,
129.038743835842));
#234535=CARTESIAN_POINT('Ctrl Pts',(-76.2216316429937,1.50722250495638,
125.191874642891));
#234536=CARTESIAN_POINT('Ctrl Pts',(-76.5000792668064,-3.90725282447187,
126.502605875483));
#234537=CARTESIAN_POINT('Ctrl Pts',(-76.7785268906195,-5.73115368812196,
131.766439563647));
#234538=CARTESIAN_POINT('Ctrl Pts',(-77.0569745144322,-2.28840429481114,
136.146169700531));
#234539=CARTESIAN_POINT('Ctrl Pts',(-77.3354221382452,3.25727685066645,
135.617038252052));
#234540=CARTESIAN_POINT('Ctrl Pts',(-77.613869762058,5.80967969720196,130.665291169852));
#234541=CARTESIAN_POINT('Ctrl Pts',(-77.8923173858709,3.0232707206408,125.841342116181));
#234542=CARTESIAN_POINT('Ctrl Pts',(-78.1707650096839,-2.54137635320382,
125.57816460835));
#234543=CARTESIAN_POINT('Ctrl Pts',(-78.4492126334967,-5.77062271159095,
130.117605919119));
#234544=CARTESIAN_POINT('Ctrl Pts',(-78.7276602573096,-3.69694870861804,
135.288141247929));
#234545=CARTESIAN_POINT('Ctrl Pts',(-79.0061078811224,1.77404055158998,
136.338301222296));
#234546=CARTESIAN_POINT('Ctrl Pts',(-79.2845555049354,5.61477321158579,
132.303040128944));
#234547=CARTESIAN_POINT('Ctrl Pts',(-79.5630031287483,4.29580358705489,
126.8905657792));
#234548=CARTESIAN_POINT('Ctrl Pts',(-79.8414507525611,-0.970799672307275,
125.074677686406));
#234549=CARTESIAN_POINT('Ctrl Pts',(-80.1198983763742,-5.34528545901998,
128.524088296775));
#234550=CARTESIAN_POINT('Ctrl Pts',(-80.3983460001869,-4.80771504060458,
134.068957772455));
#234551=CARTESIAN_POINT('Ctrl Pts',(-80.6767936239998,0.147910630189091,
136.613821947228));
#234552=CARTESIAN_POINT('Ctrl Pts',(-80.9552412478128,4.96761365767528,
133.820074968005));
#234553=CARTESIAN_POINT('Ctrl Pts',(-81.2336888716256,5.22232241517632,
128.255033826564));
#234554=CARTESIAN_POINT('Ctrl Pts',(-81.5121364954386,0.6779719977639,125.032699464516));
#234555=CARTESIAN_POINT('Ctrl Pts',(-81.7905841192513,-4.48940156482041,
127.114239740797));
#234556=CARTESIAN_POINT('Ctrl Pts',(-82.0690317430644,-5.53123440879372,
132.586820830401));
#234557=CARTESIAN_POINT('Ctrl Pts',(-82.3474793668772,-1.490133046909,136.421408062431));
#234558=CARTESIAN_POINT('Ctrl Pts',(-82.62592699069,3.92032778803891,135.094203100652));
#234559=CARTESIAN_POINT('Ctrl Pts',(-82.9043746145031,5.72819890443852,
129.824842467372));
#234560=CARTESIAN_POINT('Ctrl Pts',(-83.1828222383158,2.27213506573304,
125.455611161998));
#234561=CARTESIAN_POINT('Ctrl Pts',(-83.4612698621288,-3.27190989841242,
126.001619305352));
#234562=CARTESIAN_POINT('Ctrl Pts',(-83.7397174859417,-5.80922950760163,
130.961112087674));
#234563=CARTESIAN_POINT('Ctrl Pts',(-84.0181651097544,-3.00815099594316,
135.776557926701));
#234564=CARTESIAN_POINT('Ctrl Pts',(-84.2966127335676,2.55727132464077,
136.022797343974));
#234565=CARTESIAN_POINT('Ctrl Pts',(-84.5750603573801,5.77268622752965,
131.473548344486));
#234566=CARTESIAN_POINT('Ctrl Pts',(-84.8535079811934,3.68328449871872,
126.309348515594));
#234567=CARTESIAN_POINT('Ctrl Pts',(-85.131955605006,-1.79087574596318,
125.275845214866));
#234568=CARTESIAN_POINT('Ctrl Pts',(-85.4104032288191,-5.61930866924928,
129.322777486226));
#234569=CARTESIAN_POINT('Ctrl Pts',(-85.6888508526319,-4.28387144398495,
134.731212275928));
#234570=CARTESIAN_POINT('Ctrl Pts',(-85.9672984764448,0.98823435954663,
136.531062228962));
#234571=CARTESIAN_POINT('Ctrl Pts',(-86.2457461002577,5.35220106458756,
133.068353166051));
#234572=CARTESIAN_POINT('Ctrl Pts',(-86.5241937240705,4.79775646083024,
127.525145553266));
#234573=CARTESIAN_POINT('Ctrl Pts',(-86.8026413478836,-0.165591946996939,
124.995376386011));
#234574=CARTESIAN_POINT('Ctrl Pts',(-87.0810889716963,-4.97676944515001,
127.803779942897));
#234575=CARTESIAN_POINT('Ctrl Pts',(-87.3595365955093,-5.21453895191432,
133.36957055329));
#234576=CARTESIAN_POINT('Ctrl Pts',(-87.6379842193221,-0.660401906259044,
136.578058550223));
#234577=CARTESIAN_POINT('Ctrl Pts',(-87.916431843135,4.50061222882128,134.480800207869));
#234578=CARTESIAN_POINT('Ctrl Pts',(-88.1948794669479,5.52578359274576,
129.005073486085));
#234579=CARTESIAN_POINT('Ctrl Pts',(-88.4733270907608,1.47302978447255,
125.182803738068));
#234580=CARTESIAN_POINT('Ctrl Pts',(-88.7517747145737,-3.93336643422502,
126.526470133988));
#234581=CARTESIAN_POINT('Ctrl Pts',(-89.0302223383866,-5.7251910555031,
131.801308897747));
#234582=CARTESIAN_POINT('Ctrl Pts',(-89.3086699621995,-2.25584478790559,
136.16000089565));
#234583=CARTESIAN_POINT('Ctrl Pts',(-89.5871175860123,3.28651263563227,
135.597121115567));
#234584=CARTESIAN_POINT('Ctrl Pts',(-89.8655652098253,5.80872550209253,
130.629928577187));
#234585=CARTESIAN_POINT('Ctrl Pts',(-90.1440128336381,2.99300340414587,
125.823030562435));
#234586=CARTESIAN_POINT('Ctrl Pts',(-90.4224604574511,-2.57314260586573,
125.593731516848));
#234587=CARTESIAN_POINT('Ctrl Pts',(-90.7009080812639,-5.77469626609129,
130.152746061436));
#234588=CARTESIAN_POINT('Ctrl Pts',(-90.9793557050769,-3.66958616737523,
135.310562549967));
#234589=CARTESIAN_POINT('Ctrl Pts',(-91.2578033288896,1.80769434990835,
136.327399602824));
#234590=CARTESIAN_POINT('Ctrl Pts',(-91.5362509527026,5.62379207040447,
132.268833643682));
#234591=CARTESIAN_POINT('Ctrl Pts',(-91.8146985765155,4.27189961571542,
126.864488517025));
#234592=CARTESIAN_POINT('Ctrl Pts',(-92.0931462003284,-1.00565989191805,
125.080693377311));
#234593=CARTESIAN_POINT('Ctrl Pts',(-92.3715938241412,-5.3590670880956,
128.556668814702));
#234594=CARTESIAN_POINT('Ctrl Pts',(-92.6500414479542,-4.78775343529548,
134.098163213075));
#234595=CARTESIAN_POINT('Ctrl Pts',(-92.928489071767,0.183271729783054,
136.612813937377));
#234596=CARTESIAN_POINT('Ctrl Pts',(-93.2069366955801,4.98587912851244,
133.789779819492));
#234597=CARTESIAN_POINT('Ctrl Pts',(-93.4853843193926,5.2067071818758,128.223291300872));
#234598=CARTESIAN_POINT('Ctrl Pts',(-93.7638319432059,0.642825696881324,
125.028679392048));
#234599=CARTESIAN_POINT('Ctrl Pts',(-94.0422795670186,-4.51178119976554,
127.14163637176));
#234600=CARTESIAN_POINT('Ctrl Pts',(-94.3207271908314,-5.52028158659305,
132.62045799934));
#234601=CARTESIAN_POINT('Ctrl Pts',(-94.5991748146444,-1.45591287608963,
136.430374854359));
#234602=CARTESIAN_POINT('Ctrl Pts',(-94.8776224384574,3.94636864224209,
135.07025947184));
#234603=CARTESIAN_POINT('Ctrl Pts',(-95.1560700622702,5.7221301691794,129.789991442987));
#234604=CARTESIAN_POINT('Ctrl Pts',(-95.4345176860831,2.23953361224044,
125.441879130882));
#234605=CARTESIAN_POINT('Ctrl Pts',(-95.7129653098959,-3.30108492704829,
126.021625333256));
#234606=CARTESIAN_POINT('Ctrl Pts',(-95.9914129337089,-5.80816768534362,
130.996471612301));
#234607=CARTESIAN_POINT('Ctrl Pts',(-96.2698605575217,-2.97782808557417,
135.794777272329));
#234608=CARTESIAN_POINT('Ctrl Pts',(-96.5483081813347,2.58899004984866,
136.007133822036));
#234609=CARTESIAN_POINT('Ctrl Pts',(-96.8267558051475,5.77665280865574,
131.438395966436));
#234610=CARTESIAN_POINT('Ctrl Pts',(-97.1052034289604,3.65585384148698,
126.287010599573));
#234611=CARTESIAN_POINT('Ctrl Pts',(-97.3836510527732,-1.82449620761995,
125.286849214428));
#234612=CARTESIAN_POINT('Ctrl Pts',(-97.6620986765863,-5.62822337351841,
129.35701126335));
#234613=CARTESIAN_POINT('Ctrl Pts',(-97.9405463003989,-4.25988821315111,
134.757216661848));
#234614=CARTESIAN_POINT('Ctrl Pts',(-98.2189939242121,1.02307610799351,
136.524940463405));
#234615=CARTESIAN_POINT('Ctrl Pts',(-98.4974415480248,5.36588346593846,
133.035730852497));
#234616=CARTESIAN_POINT('Ctrl Pts',(-98.7758891718378,4.77770605666655,
127.496001004183));
#234617=CARTESIAN_POINT('Ctrl Pts',(-99.0543367956506,-0.200949814765295,
124.996492018215));
#234618=CARTESIAN_POINT('Ctrl Pts',(-99.3327844194636,-4.99494262337204,
127.834130544897));
#234619=CARTESIAN_POINT('Ctrl Pts',(-99.6112320432764,-5.19882717761281,
133.401265404553));
#234620=CARTESIAN_POINT('Ctrl Pts',(-99.8896796670892,-0.625243532454567,
136.581971630822));
#234621=CARTESIAN_POINT('Ctrl Pts',(-100.168127290903,4.5229083741848,134.453335587896));
#234622=CARTESIAN_POINT('Ctrl Pts',(-100.446574914715,5.51472844130613,
128.971469809575));
#234623=CARTESIAN_POINT('Ctrl Pts',(-100.725022538528,1.43878248032906,
125.173941142103));
#234624=CARTESIAN_POINT('Ctrl Pts',(-101.003470162341,-3.95933429163924,
126.550492911299));
#234625=CARTESIAN_POINT('Ctrl Pts',(-101.281917786154,-5.71901627382367,
131.836141289563));
#234626=CARTESIAN_POINT('Ctrl Pts',(-101.560365409967,-2.22320168984167,
136.17363363555));
#234627=CARTESIAN_POINT('Ctrl Pts',(-101.83881303378,3.31562663766449,135.577026381578));
#234628=CARTESIAN_POINT('Ctrl Pts',(-102.117260657593,5.80755606252295,
130.594572448163));
#234629=CARTESIAN_POINT('Ctrl Pts',(-102.395708281405,2.96262518080941,
125.804903593708));
#234630=CARTESIAN_POINT('Ctrl Pts',(-102.674155905219,-2.60481350978186,
125.609491507123));
#234631=CARTESIAN_POINT('Ctrl Pts',(-102.952603529031,-5.77855583709781,
130.187910349571));
#234632=CARTESIAN_POINT('Ctrl Pts',(-103.231051152844,-3.64208764826766,
135.332816873036));
#234633=CARTESIAN_POINT('Ctrl Pts',(-103.509498776657,1.84128116344741,
136.316293325111));
#234634=CARTESIAN_POINT('Ctrl Pts',(-103.78794640047,5.63260253753978,132.234572891835));
#234635=CARTESIAN_POINT('Ctrl Pts',(-104.066394024283,4.24783734756473,
126.838557248259));
#234636=CARTESIAN_POINT('Ctrl Pts',(-104.344841648096,-1.04048284643121,
125.086921160811));
#234637=CARTESIAN_POINT('Ctrl Pts',(-104.623289271909,-5.3726501349701,
128.589332621676));
#234638=CARTESIAN_POINT('Ctrl Pts',(-104.901736895722,-4.76761441802147,
134.12724660063));
#234639=CARTESIAN_POINT('Ctrl Pts',(-105.180184519534,0.218626038175886,
136.611590693152));
#234640=CARTESIAN_POINT('Ctrl Pts',(-105.458632143348,5.00395984576562,
133.759374045173));
#234641=CARTESIAN_POINT('Ctrl Pts',(-105.73707976716,5.1908990121252,128.191644417652));
#234642=CARTESIAN_POINT('Ctrl Pts',(-106.015527390973,0.607655575856702,
125.024873339572));
#234643=CARTESIAN_POINT('Ctrl Pts',(-106.293975014786,-4.53399364899913,
127.169168726316));
#234644=CARTESIAN_POINT('Ctrl Pts',(-106.572422638599,-5.50912420832816,
132.654027872123));
#234645=CARTESIAN_POINT('Ctrl Pts',(-106.850870262412,-1.42163875588365,
136.43913317226));
#234646=CARTESIAN_POINT('Ctrl Pts',(-107.129317886225,3.97226326230387,
135.046157768576));
#234647=CARTESIAN_POINT('Ctrl Pts',(-107.407765510038,5.71584939828273,
129.755178006424));
#234648=CARTESIAN_POINT('Ctrl Pts',(-107.686213133851,2.20684917200607,
125.428345808491));
#234649=CARTESIAN_POINT('Ctrl Pts',(-107.964660757664,-3.3301376327682,
126.041808587174));
#234650=CARTESIAN_POINT('Ctrl Pts',(-108.243108381476,-5.80689063929651,
131.031824018185));
#234651=CARTESIAN_POINT('Ctrl Pts',(-108.521556005289,-2.94739483068967,
135.812811696231));
#234652=CARTESIAN_POINT('Ctrl Pts',(-108.800003629102,2.62061283907833,
135.991277509423));
#234653=CARTESIAN_POINT('Ctrl Pts',(-109.078451252915,5.7804053337882,131.403220093974));
#234654=CARTESIAN_POINT('Ctrl Pts',(-109.356898876728,3.62828771524594,
126.264840075618));
#234655=CARTESIAN_POINT('Ctrl Pts',(-109.635346500541,-1.85804906189805,
125.298057667405));
#234656=CARTESIAN_POINT('Ctrl Pts',(-109.913794124354,-5.636929521901,129.391298672536));
#234657=CARTESIAN_POINT('Ctrl Pts',(-110.192241748167,-4.2357471305931,
134.783074573235));
#234658=CARTESIAN_POINT('Ctrl Pts',(-110.470689371979,1.05787994597834,
136.518606719657));
#234659=CARTESIAN_POINT('Ctrl Pts',(-110.749136995792,5.37936703250445,
133.003025854698));
#234660=CARTESIAN_POINT('Ctrl Pts',(-111.027584619605,4.75747861284798,
127.466979047582));
#234661=CARTESIAN_POINT('Ctrl Pts',(-111.306032243418,-0.23630023626489,
124.997822863128));
#234662=CARTESIAN_POINT('Ctrl Pts',(-111.584479867231,-5.01293071215839,
127.864591209862));
#234663=CARTESIAN_POINT('Ctrl Pts',(-111.862927491044,-5.18292275885852,
133.432864026556));
#234664=CARTESIAN_POINT('Ctrl Pts',(-112.141375114857,-0.590061990020461,
136.585670619917));
#234665=CARTESIAN_POINT('Ctrl Pts',(-112.41982273867,4.54503692151536,134.425735753813));
#234666=CARTESIAN_POINT('Ctrl Pts',(-112.698270362483,5.50346893957634,
128.937934051507));
#234667=CARTESIAN_POINT('Ctrl Pts',(-112.976717986295,1.40448186157095,
125.165287183403));
#234668=CARTESIAN_POINT('Ctrl Pts',(-113.255165610108,-3.98515543446448,
126.574673317241));
#234669=CARTESIAN_POINT('Ctrl Pts',(-113.533613233921,-5.71262957189362,
131.870935448366));
#234670=CARTESIAN_POINT('Ctrl Pts',(-113.812060857734,-2.19047621022174,
136.187067415062));
#234671=CARTESIAN_POINT('Ctrl Pts',(-114.090508481547,3.34461777793161,
135.556754794705));
#234672=CARTESIAN_POINT('Ctrl Pts',(-114.36895610536,5.80617142182825,130.559224092919));
#234673=CARTESIAN_POINT('Ctrl Pts',(-114.647403729173,2.9321371763071,125.786961881698));
#234674=CARTESIAN_POINT('Ctrl Pts',(-114.925851352986,-2.63638789137572,
125.625443995184));
#234675=CARTESIAN_POINT('Ctrl Pts',(-115.204298976799,-5.78220128159277,
130.223097480497));
#234676=CARTESIAN_POINT('Ctrl Pts',(-115.482746600612,-3.61445417026275,
135.354903392492));
#234677=CARTESIAN_POINT('Ctrl Pts',(-115.761194224424,1.87479974763623,
136.304982800703));
#234678=CARTESIAN_POINT('Ctrl Pts',(-116.039641848237,5.64120428651674,
132.200259142944));
#234679=CARTESIAN_POINT('Ctrl Pts',(-116.31808947205,4.22361767423897,126.812772933795));
#234680=CARTESIAN_POINT('Ctrl Pts',(-116.596537095863,-1.07526724547036,
125.093360806132));
#234681=CARTESIAN_POINT('Ctrl Pts',(-116.874984719676,-5.38603409631742,
128.622078507325));
#234682=CARTESIAN_POINT('Ctrl Pts',(-117.153432343489,-4.7472987350426,
134.156206857421));
#234683=CARTESIAN_POINT('Ctrl Pts',(-117.431879967302,0.253972245300257,
136.610152259881));
#234684=CARTESIAN_POINT('Ctrl Pts',(-117.710327591115,5.02185513944583,
133.728858771743));
#234685=CARTESIAN_POINT('Ctrl Pts',(-117.988775214928,5.17489849170343,
128.160094349593));
#234686=CARTESIAN_POINT('Ctrl Pts',(-118.26722283874,0.572462937930709,
125.021281448121));
#234687=CARTESIAN_POINT('Ctrl Pts',(-118.545670462553,-4.55603808943068,
127.196835784245));
#234688=CARTESIAN_POINT('Ctrl Pts',(-118.824118086366,-5.49776268743969,
132.687529204804));
#234689=CARTESIAN_POINT('Ctrl Pts',(-119.102565710179,-1.38731195633035,
136.447682691592));
#234690=CARTESIAN_POINT('Ctrl Pts',(-119.381013333992,3.99801068868978,
135.021898883958));
#234691=CARTESIAN_POINT('Ctrl Pts',(-119.659460957805,5.70935682448427,
129.720403447709));
#234692=CARTESIAN_POINT('Ctrl Pts',(-119.937908581618,2.17408295616475,
125.415011696306));
#234693=CARTESIAN_POINT('Ctrl Pts',(-120.216356205431,-3.3590669390133,
126.062168319208));
#234694=CARTESIAN_POINT('Ctrl Pts',(-120.494803829244,-5.80539841678086,
131.067167995328));
#234695=CARTESIAN_POINT('Ctrl Pts',(-120.773251453056,-2.91685235900652,
135.830660530138));
#234696=CARTESIAN_POINT('Ctrl Pts',(-121.051699076869,2.65213852053535,
135.975228993696));
#234697=CARTESIAN_POINT('Ctrl Pts',(-121.330146700682,5.78394366387473,
131.368022030553));
#234698=CARTESIAN_POINT('Ctrl Pts',(-121.608594324495,3.60058714147007,
126.242837765265));
#234699=CARTESIAN_POINT('Ctrl Pts',(-121.887041948308,-1.89153306548558,
125.309470158462));
#234700=CARTESIAN_POINT('Ctrl Pts',(-122.165489572121,-5.64542679178685,
129.425638443252));
#234701=CARTESIAN_POINT('Ctrl Pts',(-122.443937195934,-4.21144909086733,
134.808785051914));
#234702=CARTESIAN_POINT('Ctrl Pts',(-122.722384819747,1.09264458383337,
136.512061232418));
#234703=CARTESIAN_POINT('Ctrl Pts',(-123.00083244356,5.39265126464657,132.97023938455));
#234704=CARTESIAN_POINT('Ctrl Pts',(-123.279280067372,4.73707487890982,
127.438080758883));
#234705=CARTESIAN_POINT('Ctrl Pts',(-123.557727691185,-0.27164190157181,
124.999368871432));
#234706=CARTESIAN_POINT('Ctrl Pts',(-123.836175314998,-5.03073304495359,
127.895160809065));
#234707=CARTESIAN_POINT('Ctrl Pts',(-124.114622938811,-5.16682628499523,
133.464365248398));
#234708=CARTESIAN_POINT('Ctrl Pts',(-124.393070562624,-0.554858582622917,
136.589155380447));
#234709=CARTESIAN_POINT('Ctrl Pts',(-124.671518186437,4.56699705083122,
134.398001728342));
#234710=CARTESIAN_POINT('Ctrl Pts',(-124.94996581025,5.49200550478084,128.904467454562));
#234711=CARTESIAN_POINT('Ctrl Pts',(-125.228413434063,1.37012919922165,
125.156842182641));
#234712=CARTESIAN_POINT('Ctrl Pts',(-125.506861057876,-4.0108289058903,
126.599010455801));
#234713=CARTESIAN_POINT('Ctrl Pts',(-125.785308681688,-5.70603118637341,
131.905690084846));
#234714=CARTESIAN_POINT('Ctrl Pts',(-126.063756305501,-2.1576695617001,
136.200301736396));
#234715=CARTESIAN_POINT('Ctrl Pts',(-126.342203929314,3.37348498215772,
135.536307106118));
#234716=CARTESIAN_POINT('Ctrl Pts',(-126.620651553127,5.8045716313158,130.523884821299));
#234717=CARTESIAN_POINT('Ctrl Pts',(-126.89909917694,2.90154052038371,125.769206091244));
#234718=CARTESIAN_POINT('Ctrl Pts',(-127.177546800753,-2.66786458064647,
125.641588389905));
#234719=CARTESIAN_POINT('Ctrl Pts',(-127.455994424566,-5.7856324644928,
130.258306150342));
#234720=CARTESIAN_POINT('Ctrl Pts',(-127.734442048379,-3.5866867573295,
135.376821289913));
#234721=CARTESIAN_POINT('Ctrl Pts',(-128.012889672192,1.90824886043053,
136.293468448719));
#234722=CARTESIAN_POINT('Ctrl Pts',(-128.291337296005,5.64959699859458,
132.16589366852));
#234723=CARTESIAN_POINT('Ctrl Pts',(-128.569784919818,4.19924149320669,
126.787136529081));
#234724=CARTESIAN_POINT('Ctrl Pts',(-128.84823254363,-1.11001180008614,
125.100012074652));
#234725=CARTESIAN_POINT('Ctrl Pts',(-129.126680167443,-5.39921847619124,
128.654905258242));
#234726=CARTESIAN_POINT('Ctrl Pts',(-129.405127791256,-4.72680713916258,
134.185042910317));
#234727=CARTESIAN_POINT('Ctrl Pts',(-129.683575415069,0.289309041389885,
136.608498690867));
#234728=CARTESIAN_POINT('Ctrl Pts',(-129.962023038882,5.03956434643776,
133.69823512996));
#234729=CARTESIAN_POINT('Ctrl Pts',(-130.240470662695,5.15870621351431,
128.128642265792));
#234730=CARTESIAN_POINT('Ctrl Pts',(-130.518918286508,0.537249087180579,
125.017903850796));
#234731=CARTESIAN_POINT('Ctrl Pts',(-130.79736591032,-4.57791370419536,
127.224636520332));
#234732=CARTESIAN_POINT('Ctrl Pts',(-131.075813534134,-5.4861974449331,
132.720960755981));
#234733=CARTESIAN_POINT('Ctrl Pts',(-131.354261157946,-1.35293374942274,
136.456023095549));
#234734=CARTESIAN_POINT('Ctrl Pts',(-131.632708781759,4.02360996731925,
134.99748371691));
#234735=CARTESIAN_POINT('Ctrl Pts',(-131.911156405572,5.7026526883694,129.685669055425));
#234736=CARTESIAN_POINT('Ctrl Pts',(-132.189604029385,2.1412361788793,125.401877288427));
#234737=CARTESIAN_POINT('Ctrl Pts',(-132.468051653198,-3.38787177379785,
126.082703774923));
#234738=CARTESIAN_POINT('Ctrl Pts',(-132.746499277011,-5.80369107309236,
131.102502234048));
#234739=CARTESIAN_POINT('Ctrl Pts',(-133.024946900823,-2.88620180228584,
135.848323112653));
#234740=CARTESIAN_POINT('Ctrl Pts',(-133.303394524637,2.68356592602436,
135.95898886954));
#234741=CARTESIAN_POINT('Ctrl Pts',(-133.581842148449,5.78726766780228,
131.332803080451));
#234742=CARTESIAN_POINT('Ctrl Pts',(-133.860289772262,3.57275314661281,
126.221004483821));
#234743=CARTESIAN_POINT('Ctrl Pts',(-134.138737396075,-1.92494697761906,
125.321086264707));
#234744=CARTESIAN_POINT('Ctrl Pts',(-134.417185019888,-5.65371486830715,
129.460029303025));
#234745=CARTESIAN_POINT('Ctrl Pts',(-134.695632643701,-4.1869949943469,
134.834347145171));
#234746=CARTESIAN_POINT('Ctrl Pts',(-134.974080267514,1.1273687333409,136.505304244234));
#234747=CARTESIAN_POINT('Ctrl Pts',(-135.252527891327,5.40573567011315,
132.937372656969));
#234748=CARTESIAN_POINT('Ctrl Pts',(-135.53097551514,4.71649561092,127.409307208922));
#234749=CARTESIAN_POINT('Ctrl Pts',(-135.809423138953,-0.306973501088704,
125.001129985841));
#234750=CARTESIAN_POINT('Ctrl Pts',(-136.087870762765,-5.04834896208586,
127.925838209736));
#234751=CARTESIAN_POINT('Ctrl Pts',(-136.366318386578,-5.15053835248403,
133.49576790279));
#234752=CARTESIAN_POINT('Ctrl Pts',(-136.644766010391,-0.519634614735935,
136.592425783278));
#234753=CARTESIAN_POINT('Ctrl Pts',(-136.923213634204,4.58878794839197,
134.37013453918));
#234754=CARTESIAN_POINT('Ctrl Pts',(-137.201661258017,5.48033856170195,
128.871071258858));
#234755=CARTESIAN_POINT('Ctrl Pts',(-137.48010888183,1.33572576623031,125.148606452753));
#234756=CARTESIAN_POINT('Ctrl Pts',(-137.758556505643,-4.03635375457527,
126.623503425159));
#234757=CARTESIAN_POINT('Ctrl Pts',(-138.037004129456,-5.69922136176977,
131.940403911158));
#234758=CARTESIAN_POINT('Ctrl Pts',(-138.315451753269,-2.12478295993955,
136.213336109146));
#234759=CARTESIAN_POINT('Ctrl Pts',(-138.593899377082,3.40222718065648,
135.515684073514));
#234760=CARTESIAN_POINT('Ctrl Pts',(-138.872347000894,5.80275675026745,
130.488555942812));
#234761=CARTESIAN_POINT('Ctrl Pts',(-139.150794624707,2.870836346809,125.751636880291));
#234762=CARTESIAN_POINT('Ctrl Pts',(-139.42924224852,-2.69924241121433,
125.65792409305));
#234763=CARTESIAN_POINT('Ctrl Pts',(-139.707689872333,-5.78884925865424,
130.293535054436));
#234764=CARTESIAN_POINT('Ctrl Pts',(-139.986137496146,-3.55878643839929,
135.398569753122));
#234765=CARTESIAN_POINT('Ctrl Pts',(-140.264585119959,1.94162726236197,
136.281750695826));
#234766=CARTESIAN_POINT('Ctrl Pts',(-140.543032743772,5.65778036277742,
132.131477741989));
#234767=CARTESIAN_POINT('Ctrl Pts',(-140.821480367585,4.17470970773734,
126.761648984083));
#234768=CARTESIAN_POINT('Ctrl Pts',(-141.099927991397,-1.14471522280625,
125.106874719905));
#234769=CARTESIAN_POINT('Ctrl Pts',(-141.37837561521,-5.41220278603824,
128.687811658017));
#234770=CARTESIAN_POINT('Ctrl Pts',(-141.656823239023,-4.70614038970644,
134.213753690789));
#234771=CARTESIAN_POINT('Ctrl Pts',(-141.935270862836,0.324635117026387,
136.60663004738));
#234772=CARTESIAN_POINT('Ctrl Pts',(-142.213718486649,5.05708681051884,
133.667504254592));
#234773=CARTESIAN_POINT('Ctrl Pts',(-142.492166110462,5.14232277757003,
128.097289331719));
#234774=CARTESIAN_POINT('Ctrl Pts',(-142.770613734275,0.502015328467386,
125.014740672754));
#234775=CARTESIAN_POINT('Ctrl Pts',(-143.049061358088,-4.59961968268416,
127.252569904414));
#234776=CARTESIAN_POINT('Ctrl Pts',(-143.327508981901,-5.4744289093626,
132.754321286837));
#234777=CARTESIAN_POINT('Ctrl Pts',(-143.605956605714,-1.31850540905707,
136.464154075075));
#234778=CARTESIAN_POINT('Ctrl Pts',(-143.884404229526,4.04906014960179,
134.972913172143));
#234779=CARTESIAN_POINT('Ctrl Pts',(-144.162851853339,5.69573723836169,
129.650976116669));
#234780=CARTESIAN_POINT('Ctrl Pts',(-144.441299477152,2.10831005730047,
125.388943071553));
#234781=CARTESIAN_POINT('Ctrl Pts',(-144.719747100965,-3.41655106974776,
126.103414193369));
#234782=CARTESIAN_POINT('Ctrl Pts',(-144.998194724778,-5.80176867149642,
131.13782542502));
#234783=CARTESIAN_POINT('Ctrl Pts',(-145.276642348591,-2.85544429629671,
135.865798789283));
#234784=CARTESIAN_POINT('Ctrl Pts',(-145.555089972404,2.71489389099137,
135.942557738738));
#234785=CARTESIAN_POINT('Ctrl Pts',(-145.833537596217,5.79037722239768,
131.29756454872));
#234786=CARTESIAN_POINT('Ctrl Pts',(-146.111985220029,3.54478676207412,
126.199341040322));
#234787=CARTESIAN_POINT('Ctrl Pts',(-146.390432843843,-1.95828956013508,
125.332905555698));
#234788=CARTESIAN_POINT('Ctrl Pts',(-146.668880467655,-5.66179344434354,
129.49446997749));
#234789=CARTESIAN_POINT('Ctrl Pts',(-146.947328091469,-4.16238574718705,
134.859759905796));
#234790=CARTESIAN_POINT('Ctrl Pts',(-147.225775715281,1.16205110778606,
136.498336005488));
#234791=CARTESIAN_POINT('Ctrl Pts',(-147.504223339094,5.41861976405632,
132.904426889841));
#234792=CARTESIAN_POINT('Ctrl Pts',(-147.782670962907,4.6957415714508,127.380659463914));
#234793=CARTESIAN_POINT('Ctrl Pts',(-148.06111858672,-0.342293725589094,
125.003106141093));
#234794=CARTESIAN_POINT('Ctrl Pts',(-148.339566210533,-5.06577781079073,
127.956622275114));
#234795=CARTESIAN_POINT('Ctrl Pts',(-148.618013834346,-5.1340595648799,
133.527070826096));
#234796=CARTESIAN_POINT('Ctrl Pts',(-148.896461458158,-0.48439139159784,
136.595481707227));
#234797=CARTESIAN_POINT('Ctrl Pts',(-149.174909081971,4.61040880672808,
134.342135218952));
#234798=CARTESIAN_POINT('Ctrl Pts',(-149.453356705784,5.4684685426618,128.837746701901));
#234799=CARTESIAN_POINT('Ctrl Pts',(-149.731804329597,1.30127283742975,
125.140580298914));
#234800=CARTESIAN_POINT('Ctrl Pts',(-150.01025195341,-4.06172903468827,
126.648151317718));
#234801=CARTESIAN_POINT('Ctrl Pts',(-150.288699577223,-5.69220035042211,
131.975075640969));
#234802=CARTESIAN_POINT('Ctrl Pts',(-150.567147201036,-2.09181762356486,
136.226170050321));
#234803=CARTESIAN_POINT('Ctrl Pts',(-150.845594824849,3.43084330837664,
135.494886461086));
#234804=CARTESIAN_POINT('Ctrl Pts',(-151.124042448661,5.80072684593324,
130.453238766583));
#234805=CARTESIAN_POINT('Ctrl Pts',(-151.402490072475,2.84002579333802,
125.734254899877));
#234806=CARTESIAN_POINT('Ctrl Pts',(-151.680937696287,-2.73052022036177,
125.674450499292));
#234807=CARTESIAN_POINT('Ctrl Pts',(-151.9593853201,-5.79185154487752,130.32878288736));
#234808=CARTESIAN_POINT('Ctrl Pts',(-152.237832943913,-3.53075424732904,
135.420147976222));
#234809=CARTESIAN_POINT('Ctrl Pts',(-152.516280567726,1.97493371658077,
136.269829976228));
#234810=CARTESIAN_POINT('Ctrl Pts',(-152.794728191539,5.66575407582884,
132.097012638644));
#234811=CARTESIAN_POINT('Ctrl Pts',(-153.073175815352,4.15002322686382,
126.736311243251));
#234812=CARTESIAN_POINT('Ctrl Pts',(-153.351623439165,-1.17937622768304,
125.113948487592));
#234813=CARTESIAN_POINT('Ctrl Pts',(-153.630071062978,-5.42498654472129,
128.720796487292));
#234814=CARTESIAN_POINT('Ctrl Pts',(-153.90851868679,-4.6852992524868,134.242338134946));
#234815=CARTESIAN_POINT('Ctrl Pts',(-154.186966310604,0.359949163189457,
136.604546398667));
#234816=CARTESIAN_POINT('Ctrl Pts',(-154.465413934416,5.0744218823891,133.636667284384));
#234817=CARTESIAN_POINT('Ctrl Pts',(-154.743861558229,5.12574879096345,
128.066036709167));
#234818=CARTESIAN_POINT('Ctrl Pts',(-155.022309182042,0.466762967392146,
125.011792031209));
#234819=CARTESIAN_POINT('Ctrl Pts',(-155.300756805855,-4.62115522057418,
127.280634901405));
#234820=CARTESIAN_POINT('Ctrl Pts',(-155.579204429668,-5.46245751681569,
132.787609561181));
#234821=CARTESIAN_POINT('Ctrl Pts',(-155.857652053481,-1.28402821098903,
136.472075328871));
#234822=CARTESIAN_POINT('Ctrl Pts',(-156.136099677293,4.07436029247137,
134.948188160129));
#234823=CARTESIAN_POINT('Ctrl Pts',(-156.414547301107,5.68861073071636,
129.616325916999));
#234824=CARTESIAN_POINT('Ctrl Pts',(-156.692994924919,2.07530581151645,
125.376209524969));
#234825=CARTESIAN_POINT('Ctrl Pts',(-156.971442548732,-3.44510376414151,
126.124298807112));
#234826=CARTESIAN_POINT('Ctrl Pts',(-157.249890172545,-5.79963128322921,
131.173136259331));
#234827=CARTESIAN_POINT('Ctrl Pts',(-157.528337796358,-2.82458098076833,
135.883086912459));
#234828=CARTESIAN_POINT('Ctrl Pts',(-157.806785420171,2.74612125456611,
135.925936210153));
#234829=CARTESIAN_POINT('Ctrl Pts',(-158.085233043984,5.79327221243612,
131.262307741136));
#234830=CARTESIAN_POINT('Ctrl Pts',(-158.363680667797,3.51668902415852,
126.177848237519));
#234831=CARTESIAN_POINT('Ctrl Pts',(-158.64212829161,-1.9915595775106,125.344927593469));
#234832=CARTESIAN_POINT('Ctrl Pts',(-158.920575915422,-5.66966222054205,
129.528959190434));
#234833=CARTESIAN_POINT('Ctrl Pts',(-159.199023539236,-4.13762226129274,
134.885022392109));
#234834=CARTESIAN_POINT('Ctrl Pts',(-159.477471163048,1.19669042199943,
136.491156774389));
#234835=CARTESIAN_POINT('Ctrl Pts',(-159.755918786861,5.43130306905165,
132.871403303985));
#234836=CARTESIAN_POINT('Ctrl Pts',(-160.034366410674,4.67481352955083,
127.352138585409));
#234837=CARTESIAN_POINT('Ctrl Pts',(-160.312814034487,-0.377601266270116,
125.005297263965));
#234838=CARTESIAN_POINT('Ctrl Pts',(-160.5912616583,-5.08301894523598,127.987511864483));
#234839=CARTESIAN_POINT('Ctrl Pts',(-160.869709282113,-5.1173905328107,
133.558272858373));
#234840=CARTESIAN_POINT('Ctrl Pts',(-161.148156905926,-0.449130219157962,
136.598323039052));
#234841=CARTESIAN_POINT('Ctrl Pts',(-161.426604529739,4.63185882466967,
134.314004805186));
#234842=CARTESIAN_POINT('Ctrl Pts',(-161.705052153551,5.45639588750942,
128.804495018547));
#234843=CARTESIAN_POINT('Ctrl Pts',(-161.983499777364,1.26677168948586,
125.13276401854));
#234844=CARTESIAN_POINT('Ctrl Pts',(-162.261947401177,-4.08695380593746,
126.67295322014));
#234845=CARTESIAN_POINT('Ctrl Pts',(-162.54039502499,-5.68496841249774,
132.009703989503));
#234846=CARTESIAN_POINT('Ctrl Pts',(-162.818842648803,-2.05877477411906,
136.238803084352));
#234847=CARTESIAN_POINT('Ctrl Pts',(-163.097290272616,3.45933230493559,
135.473915039499));
#234848=CARTESIAN_POINT('Ctrl Pts',(-163.375737896429,5.79848199353304,
130.417934601304));
#234849=CARTESIAN_POINT('Ctrl Pts',(-163.654185520242,2.80911000166655,
125.717060794092));
#234850=CARTESIAN_POINT('Ctrl Pts',(-163.932633144055,-2.76169684907854,
125.691166996241));
#234851=CARTESIAN_POINT('Ctrl Pts',(-164.211080767867,-5.79463921191188,
130.36404834299));
#234852=CARTESIAN_POINT('Ctrl Pts',(-164.489528391681,-3.50259122286156,
135.441555159625));
#234853=CARTESIAN_POINT('Ctrl Pts',(-164.767976015493,2.00816698890481,
136.257706731653));
#234854=CARTESIAN_POINT('Ctrl Pts',(-165.046423639306,5.67351784227885,
132.062499635604));
#234855=CARTESIAN_POINT('Ctrl Pts',(-165.324871263119,4.12518296535417,
126.711124245485));
#234856=CARTESIAN_POINT('Ctrl Pts',(-165.603318886932,-1.21399353033979,
125.121233115594));
#234857=CARTESIAN_POINT('Ctrl Pts',(-165.881766510745,-5.43756927853226,
128.753858523801));
#234858=CARTESIAN_POINT('Ctrl Pts',(-166.160214134558,-4.66428449978105,
134.270795183582));
#234859=CARTESIAN_POINT('Ctrl Pts',(-166.438661758371,0.395249871304121,
136.602247821935));
#234860=CARTESIAN_POINT('Ctrl Pts',(-166.717109382183,5.09156891968999,
133.60572536201));
#234861=CARTESIAN_POINT('Ctrl Pts',(-166.995557005996,5.10898486785074,
128.034885556215));
#234862=CARTESIAN_POINT('Ctrl Pts',(-167.274004629809,0.431493310242956,
125.009058035423));
#234863=CARTESIAN_POINT('Ctrl Pts',(-167.552452253622,-4.64251951985801,
127.30883047135));
#234864=CARTESIAN_POINT('Ctrl Pts',(-167.830899877435,-5.45028371089662,
132.820824345507));
#234865=CARTESIAN_POINT('Ctrl Pts',(-168.109347501248,-1.24950343278299,
136.479786563416));
#234866=CARTESIAN_POINT('Ctrl Pts',(-168.387795125061,4.09950945842204,
134.923309597059));
#234867=CARTESIAN_POINT('Ctrl Pts',(-168.666242748874,5.68127342950807,
129.581719740392));
#234868=CARTESIAN_POINT('Ctrl Pts',(-168.944690372687,2.04222466451309,
125.36367712052));
#234869=CARTESIAN_POINT('Ctrl Pts',(-169.223137996499,-3.47352879894819,
126.145356842267));
#234870=CARTESIAN_POINT('Ctrl Pts',(-169.501585620313,-5.79727898749155,
131.208433428525));
#234871=CARTESIAN_POINT('Ctrl Pts',(-169.780033244125,-2.79361299935373,
135.900186841566));
#234872=CARTESIAN_POINT('Ctrl Pts',(-170.058480867939,2.77724685960862,
135.909124899701));
#234873=CARTESIAN_POINT('Ctrl Pts',(-170.336928491751,5.79595253064181,
131.227033964152));
#234874=CARTESIAN_POINT('Ctrl Pts',(-170.615376115564,3.48846097403773,
126.156526871832));
#234875=CARTESIAN_POINT('Ctrl Pts',(-170.893823739377,-2.02475579691427,
125.357151932539));
#234876=CARTESIAN_POINT('Ctrl Pts',(-171.17227136319,-5.67732090532164,
129.563495663847));
#234877=CARTESIAN_POINT('Ctrl Pts',(-171.450718987003,-4.11270545428381,
134.910133667999));
#234878=CARTESIAN_POINT('Ctrl Pts',(-171.729166610815,1.23128539240979,
136.483766816968));
#234879=CARTESIAN_POINT('Ctrl Pts',(-172.007614234629,5.44378511511418,
132.838303123102));
#234880=CARTESIAN_POINT('Ctrl Pts',(-172.286061858441,4.65371226071637,
127.323745630264));
#234881=CARTESIAN_POINT('Ctrl Pts',(-172.564509482254,-0.412894814796852,
125.00770327326));
#234882=CARTESIAN_POINT('Ctrl Pts',(-172.842957106067,-5.10007172654484,
128.018505833219));
#234883=CARTESIAN_POINT('Ctrl Pts',(-173.12140472988,-5.10053187395325,
133.589372843419));
#234884=CARTESIAN_POINT('Ctrl Pts',(-173.399852353693,-0.413852404033268,
136.600949673471));
#234885=CARTESIAN_POINT('Ctrl Pts',(-173.678299977506,4.65313720737985,
134.285744340263));
#234886=CARTESIAN_POINT('Ctrl Pts',(-173.956747601319,5.44412104360021,
128.771317440947));
#234887=CARTESIAN_POINT('Ctrl Pts',(-174.235195225131,1.23222360085094,
125.125157901261));
#234888=CARTESIAN_POINT('Ctrl Pts',(-174.513642848945,-4.11202713361109,
126.697908213384));
#234889=CARTESIAN_POINT('Ctrl Pts',(-174.792090472757,-5.67752581597763,
132.044287673595));
#234890=CARTESIAN_POINT('Ctrl Pts',(-175.070538096571,-2.02565563601667,
136.251234743121));
#234891=CARTESIAN_POINT('Ctrl Pts',(-175.348985720383,3.48769311466452,
135.452770585855));
#234892=CARTESIAN_POINT('Ctrl Pts',(-175.627433344196,5.79602227624969,
130.382644755183));
#234893=CARTESIAN_POINT('Ctrl Pts',(-175.905880968009,2.77809011739122,
125.700055200075));
#234894=CARTESIAN_POINT('Ctrl Pts',(-176.184328591822,-2.79277114210269,
125.708072964459));
#234895=CARTESIAN_POINT('Ctrl Pts',(-176.462776215635,-5.79721215645926,
130.399330114555));
#234896=CARTESIAN_POINT('Ctrl Pts',(-176.741223839448,-3.47429840858841,
135.462790510077));
#234897=CARTESIAN_POINT('Ctrl Pts',(-177.019671463261,2.04132584786218,
136.245381411334));
#234898=CARTESIAN_POINT('Ctrl Pts',(-177.298119087073,5.68107137443935,
132.02794001176));
#234899=CARTESIAN_POINT('Ctrl Pts',(-177.576566710886,4.10018984367198,
126.686088924097));
#234900=CARTESIAN_POINT('Ctrl Pts',(-177.855014334699,-1.24856584802001,
125.128728333976));
#234901=CARTESIAN_POINT('Ctrl Pts',(-178.133461958512,-5.4499505212146,
128.786996542421));
#234902=CARTESIAN_POINT('Ctrl Pts',(-178.411909582325,-4.64309691029714,
134.29912378221));
#234903=CARTESIAN_POINT('Ctrl Pts',(-178.690357206138,0.430535933288815,
136.599734402363));
#234904=CARTESIAN_POINT('Ctrl Pts',(-178.968804829951,5.10852728703229,
133.574679634036));
#234905=CARTESIAN_POINT('Ctrl Pts',(-179.247252453763,5.09203162942501,
128.00383702718));
#234906=CARTESIAN_POINT('Ctrl Pts',(-179.525700077576,0.396207663951002,
125.006538786706));
#234907=CARTESIAN_POINT('Ctrl Pts',(-179.80414770139,-4.66371178887382,
127.337155569449));
#234908=CARTESIAN_POINT('Ctrl Pts',(-180.082595325202,-5.43790794271038,
132.853964409027));
#234909=CARTESIAN_POINT('Ctrl Pts',(-180.361042949015,-1.2149323537682,
136.487287492965));
#234910=CARTESIAN_POINT('Ctrl Pts',(-180.639490572828,4.12450671554208,
134.898278404822));
#234911=CARTESIAN_POINT('Ctrl Pts',(-180.917938196641,5.67372560662389,
129.547158869193));
#234912=CARTESIAN_POINT('Ctrl Pts',(-181.196385820454,2.00906784212309,
125.351346322599));
#234913=CARTESIAN_POINT('Ctrl Pts',(-181.474833444267,-3.50182512086801,
126.166587518521));
#234914=CARTESIAN_POINT('Ctrl Pts',(-181.75328106808,-5.79471187144949,
131.243715624654));
#234915=CARTESIAN_POINT('Ctrl Pts',(-182.031728691892,-2.76254149958135,
135.917097942958));
#234916=CARTESIAN_POINT('Ctrl Pts',(-182.310176315705,2.80826955274668,
135.892124430331));
#234917=CARTESIAN_POINT('Ctrl Pts',(-182.588623939518,5.79841807769547,
131.191744524852));
#234918=CARTESIAN_POINT('Ctrl Pts',(-182.867071563331,3.46010365771282,
126.135377733334));
#234919=CARTESIAN_POINT('Ctrl Pts',(-183.145519187144,-2.05787698824661,
125.369578119929));
#234920=CARTESIAN_POINT('Ctrl Pts',(-183.423966810957,-5.68476921488759,
129.598078117967));
#234921=CARTESIAN_POINT('Ctrl Pts',(-183.70241443477,-4.08763624946197,
134.93509280296));
#234922=CARTESIAN_POINT('Ctrl Pts',(-183.980862058583,1.26583473708647,
136.476166407061));
#234923=CARTESIAN_POINT('Ctrl Pts',(-184.259309682396,5.45606543971754,
132.805127573733));
#234924=CARTESIAN_POINT('Ctrl Pts',(-184.537757306209,4.63243854686269,
127.295481650585));
#234925=CARTESIAN_POINT('Ctrl Pts',(-184.816204930021,-0.448173063354899,
125.010324079826));
#234926=CARTESIAN_POINT('Ctrl Pts',(-185.094652553834,-5.11693552282041,
128.049603032828));
#234927=CARTESIAN_POINT('Ctrl Pts',(-185.373100177647,-5.08348421301165,
133.620369628814));
#234928=CARTESIAN_POINT('Ctrl Pts',(-185.65154780146,-0.378559253454916,
136.60336151315));
#234929=CARTESIAN_POINT('Ctrl Pts',(-185.929995425273,4.67424316637891,
134.257354871388));
#234930=CARTESIAN_POINT('Ctrl Pts',(-186.208443049086,5.4316444657843,128.73821519851));
#234931=CARTESIAN_POINT('Ctrl Pts',(-186.486890672899,1.19762985171755,
125.117762228929));
#234932=CARTESIAN_POINT('Ctrl Pts',(-186.765338296712,-4.13694808860639,
126.72301537273));
#234933=CARTESIAN_POINT('Ctrl Pts',(-187.043785920525,-5.66987283665109,
132.078825411735));
#234934=CARTESIAN_POINT('Ctrl Pts',(-187.322233544337,-1.99246143649967,
136.263464565965));
#234935=CARTESIAN_POINT('Ctrl Pts',(-187.600681168151,3.51592468664221,
135.43145388367));
#234936=CARTESIAN_POINT('Ctrl Pts',(-187.879128791963,5.79334778522967,
130.347370535898));
#234937=CARTESIAN_POINT('Ctrl Pts',(-188.157576415776,2.74696728996466,
125.683238747971));
#234938=CARTESIAN_POINT('Ctrl Pts',(-188.436024039589,-2.82374194796541,
125.72516777749));
#234939=CARTESIAN_POINT('Ctrl Pts',(-188.714471663402,-5.79957028317828,
130.434626894674));
#234940=CARTESIAN_POINT('Ctrl Pts',(-188.992919287215,-3.44587685290989,
135.483853240698));
#234941=CARTESIAN_POINT('Ctrl Pts',(-189.271366911028,2.07440906473995,
136.232854471987));
#234942=CARTESIAN_POINT('Ctrl Pts',(-189.54981453484,5.68841439241029,131.993335047731));
#234943=CARTESIAN_POINT('Ctrl Pts',(-189.828262158654,4.07504478794802,
126.661206206783));
#234944=CARTESIAN_POINT('Ctrl Pts',(-190.106709782466,-1.28309189963338,
125.136433864998));
#234945=CARTESIAN_POINT('Ctrl Pts',(-190.385157406279,-5.46212981397553,
128.820209315208));
#234946=CARTESIAN_POINT('Ctrl Pts',(-190.663605030092,-4.62173726915045,
134.327322881104));
#234947=CARTESIAN_POINT('Ctrl Pts',(-190.942052653905,0.465806041606811,
136.597006233083));
#234948=CARTESIAN_POINT('Ctrl Pts',(-191.220500277718,5.12529635601715,
133.543531250871));
#234949=CARTESIAN_POINT('Ctrl Pts',(-191.49894790153,5.07488970389458,127.972892272577));
#234950=CARTESIAN_POINT('Ctrl Pts',(-191.777395525344,0.360907336037817,
125.004234378408));
#234951=CARTESIAN_POINT('Ctrl Pts',(-192.055843149156,-4.68473124233415,
127.365609146106));
#234952=CARTESIAN_POINT('Ctrl Pts',(-192.33429077297,-5.42533067084548,
132.887028523726));
#234953=CARTESIAN_POINT('Ctrl Pts',(-192.612738396782,-1.1803162549878,
136.494577839569));
#234954=CARTESIAN_POINT('Ctrl Pts',(-192.891186020595,4.14935113754904,
134.873095510955));
#234955=CARTESIAN_POINT('Ctrl Pts',(-193.169633644408,5.66596754175055,
129.512644584067));
#234956=CARTESIAN_POINT('Ctrl Pts',(-193.448081268221,1.97583657298603,
125.339217588127));
#234957=CARTESIAN_POINT('Ctrl Pts',(-193.726528892034,-3.52999168137001,
126.187990049162));
#234958=CARTESIAN_POINT('Ctrl Pts',(-194.004976515847,-5.79193003022761,
131.27898154032));
#234959=CARTESIAN_POINT('Ctrl Pts',(-194.28342413966,-2.73136763281852,
135.933819589987));
#234960=CARTESIAN_POINT('Ctrl Pts',(-194.561871763472,2.83918818442447,
135.874935432001));
#234961=CARTESIAN_POINT('Ctrl Pts',(-194.840319387286,5.80066876223446,
131.156440730899));
#234962=CARTESIAN_POINT('Ctrl Pts',(-195.118767011098,3.43161812597426,
126.114401605713));
#234963=CARTESIAN_POINT('Ctrl Pts',(-195.397214634911,-2.09092192419104,
125.382205695184));
#234964=CARTESIAN_POINT('Ctrl Pts',(-195.675662258724,-5.69200687323938,
129.63270527133));
#234965=CARTESIAN_POINT('Ctrl Pts',(-195.954109882537,-4.06241557577554,
134.95989887212));
#234966=CARTESIAN_POINT('Ctrl Pts',(-196.23255750635,1.30033717579212,136.468355826305));
#234967=CARTESIAN_POINT('Ctrl Pts',(-196.511005130163,5.46814358780935,
132.771877885207));
#234968=CARTESIAN_POINT('Ctrl Pts',(-196.789452753976,4.61099317629508,
127.267347693709));
#234969=CARTESIAN_POINT('Ctrl Pts',(-197.067900377789,-0.483434704694746,
125.013159586548));
#234970=CARTESIAN_POINT('Ctrl Pts',(-197.346348001602,-5.13360970916836,
128.080802310993));
#234971=CARTESIAN_POINT('Ctrl Pts',(-197.624795625414,-5.06624818169292,
133.651262065958));
#234972=CARTESIAN_POINT('Ctrl Pts',(-197.903243249227,-0.343252075224855,
136.605558468718));
#234973=CARTESIAN_POINT('Ctrl Pts',(-198.18169087304,4.69517591957924,134.228837450539));
#234974=CARTESIAN_POINT('Ctrl Pts',(-198.460138496853,5.41896661638458,
128.705189517851));
#234975=CARTESIAN_POINT('Ctrl Pts',(-198.738586120666,1.1629917239694,125.110577275591));
#234976=CARTESIAN_POINT('Ctrl Pts',(-199.017033744479,-4.16171574746965,
126.748273767825));
#234977=CARTESIAN_POINT('Ctrl Pts',(-199.295481368292,-5.6620097581009,
132.113315924113));
#234978=CARTESIAN_POINT('Ctrl Pts',(-199.573928992105,-1.95919340559182,
136.275492099704));
#234979=CARTESIAN_POINT('Ctrl Pts',(-199.852376615917,3.54402597473752,
135.409965722843));
#234980=CARTESIAN_POINT('Ctrl Pts',(-200.13082423973,5.79045861957696,130.312113250549));
#234981=CARTESIAN_POINT('Ctrl Pts',(-200.409271863544,2.71574267265526,
125.666612060922));
#234982=CARTESIAN_POINT('Ctrl Pts',(-200.687719487356,-2.85460811903155,
125.742450801881));
#234983=CARTESIAN_POINT('Ctrl Pts',(-200.966167111169,-5.80171350468764,
130.469937375411));
#234984=CARTESIAN_POINT('Ctrl Pts',(-201.244614734982,-3.41732760899753,
135.504742570997));
#234985=CARTESIAN_POINT('Ctrl Pts',(-201.523062358795,2.10741541362659,
136.220126377805));
#234986=CARTESIAN_POINT('Ctrl Pts',(-201.801509982608,5.69554662409457,
131.958686025817));
#234987=CARTESIAN_POINT('Ctrl Pts',(-202.079957606421,4.04974872994014,
126.636477015578));
#234988=CARTESIAN_POINT('Ctrl Pts',(-202.358405230234,-1.31757040580477,
125.144349423131));
#234989=CARTESIAN_POINT('Ctrl Pts',(-202.636852854047,-5.47410670550813,
128.853495611451));
#234990=CARTESIAN_POINT('Ctrl Pts',(-202.915300477859,-4.6002063678289,
134.355391435336));
#234991=CARTESIAN_POINT('Ctrl Pts',(-203.193748101672,0.501058889310003,
136.594063415189));
#234992=CARTESIAN_POINT('Ctrl Pts',(-203.472195725485,5.14187550526088,
133.512281366733));
#234993=CARTESIAN_POINT('Ctrl Pts',(-203.750643349298,5.05755972645996,
127.942052439074));
#234994=CARTESIAN_POINT('Ctrl Pts',(-204.029090973111,0.325593634571106,
125.002144895921));
#234995=CARTESIAN_POINT('Ctrl Pts',(-204.307538596924,-4.70557710135553,
127.394190146963));
#234996=CARTESIAN_POINT('Ctrl Pts',(-204.585986220737,-5.41255236135747,
132.920015464399));
#234997=CARTESIAN_POINT('Ctrl Pts',(-204.864433844549,-1.14565641915494,
136.50165733308));
#234998=CARTESIAN_POINT('Ctrl Pts',(-205.142881468362,4.17404180382362,
134.847761848621));
#234999=CARTESIAN_POINT('Ctrl Pts',(-205.421329092175,5.6579995223666,129.478178163952));
#235000=CARTESIAN_POINT('Ctrl Pts',(-205.699776715988,1.94253208849746,
125.327291366541));
#235001=CARTESIAN_POINT('Ctrl Pts',(-205.978224339801,-3.55802743673226,
126.209563641112));
#235002=CARTESIAN_POINT('Ctrl Pts',(-206.256671963614,-5.78893356690891,
131.314229868733));
#235003=CARTESIAN_POINT('Ctrl Pts',(-206.535119587427,-2.70009255422283,
135.950351163029));
#235004=CARTESIAN_POINT('Ctrl Pts',(-206.81356721124,2.87000160893922,135.857558541658));
#235005=CARTESIAN_POINT('Ctrl Pts',(-207.092014835053,5.80270450085972,
131.121123890489));
#235006=CARTESIAN_POINT('Ctrl Pts',(-207.370462458865,3.40300543436423,
126.09359926625));
#235007=CARTESIAN_POINT('Ctrl Pts',(-207.648910082679,-2.12388938025395,
125.395034190384));
#235008=CARTESIAN_POINT('Ctrl Pts',(-207.927357706491,-5.69903361218359,
129.667375840811));
#235009=CARTESIAN_POINT('Ctrl Pts',(-208.205805330304,-4.03704436778601,
134.984550956282));
#235010=CARTESIAN_POINT('Ctrl Pts',(-208.484252954117,1.33479143002538,
136.460335364123));
#235011=CARTESIAN_POINT('Ctrl Pts',(-208.76270057793,5.48001911182977,132.738555289606));
#235012=CARTESIAN_POINT('Ctrl Pts',(-209.041148201743,4.58937694367963,
127.239344802146));
#235013=CARTESIAN_POINT('Ctrl Pts',(-209.319595825556,-0.518678432184342,
125.016209688352));
#235014=CARTESIAN_POINT('Ctrl Pts',(-209.598043449369,-5.15009366772074,
128.112102511612));
#235015=CARTESIAN_POINT('Ctrl Pts',(-209.876491073182,-5.04882441868487,
133.682049010123));
#235016=CARTESIAN_POINT('Ctrl Pts',(-210.154938696994,-0.307932177662294,
136.607540458767));
#235017=CARTESIAN_POINT('Ctrl Pts',(-210.433386320807,4.71593469130848,
134.200193134443));
#235018=CARTESIAN_POINT('Ctrl Pts',(-210.71183394462,5.40608796518471,128.672241622749));
#235019=CARTESIAN_POINT('Ctrl Pts',(-210.990281568433,1.12831050113542,
125.103603307488));
#235020=CARTESIAN_POINT('Ctrl Pts',(-211.268729192246,-4.18632919242468,
126.773682462711));
#235021=CARTESIAN_POINT('Ctrl Pts',(-211.547176816059,-5.65393687169752,
132.14775793267));
#235022=CARTESIAN_POINT('Ctrl Pts',(-211.825624439872,-1.92585277605142,
136.287316898656));
#235023=CARTESIAN_POINT('Ctrl Pts',(-212.104072063685,3.57199593764717,
135.388306899624));
#235024=CARTESIAN_POINT('Ctrl Pts',(-212.382519687498,5.78735488635066,
130.276874205606));
#235025=CARTESIAN_POINT('Ctrl Pts',(-212.660967311311,2.68441742250212,
125.650175755035));
#235026=CARTESIAN_POINT('Ctrl Pts',(-212.939414935123,-2.88536851154432,
125.759921397201));
#235027=CARTESIAN_POINT('Ctrl Pts',(-213.217862558936,-5.80364174156953,
130.505260248325));
#235028=CARTESIAN_POINT('Ctrl Pts',(-213.496310182749,-3.38865173475374,
135.525457726916));
#235029=CARTESIAN_POINT('Ctrl Pts',(-213.774757806562,2.14034367146046,
136.20719760043));
#235030=CARTESIAN_POINT('Ctrl Pts',(-214.053205430375,5.7024678052036,131.923994229952));
#235031=CARTESIAN_POINT('Ctrl Pts',(-214.331653054188,4.02430260700449,
126.611902266833));
#235032=CARTESIAN_POINT('Ctrl Pts',(-214.610100678001,-1.35200008892003,
125.152474715061));
#235033=CARTESIAN_POINT('Ctrl Pts',(-214.888548301814,-5.48588075200302,
128.886854197714));
#235034=CARTESIAN_POINT('Ctrl Pts',(-215.166995925626,-4.5785050041694,
134.383328404815));
#235035=CARTESIAN_POINT('Ctrl Pts',(-215.445443549439,0.536293170092427,
136.59090605773));
#235036=CARTESIAN_POINT('Ctrl Pts',(-215.723891173253,5.15826412041666,
133.480931139593));
#235037=CARTESIAN_POINT('Ctrl Pts',(-216.002338797065,5.04004233928969,
127.911318669453));
#235038=CARTESIAN_POINT('Ctrl Pts',(-216.280786420879,0.290267868112,125.000270416672));
#235039=CARTESIAN_POINT('Ctrl Pts',(-216.559234044691,-4.72624859348692,
127.422897512942));
#235040=CARTESIAN_POINT('Ctrl Pts',(-216.837681668504,-5.39957348775117,
132.952924008705));
#235041=CARTESIAN_POINT('Ctrl Pts',(-217.116129292317,-1.11095413060172,
136.508525711168));
#235042=CARTESIAN_POINT('Ctrl Pts',(-217.39457691613,4.19857779944424,134.822278356567));
#235043=CARTESIAN_POINT('Ctrl Pts',(-217.673024539943,5.64982184372931,
129.443760886018));
#235044=CARTESIAN_POINT('Ctrl Pts',(-217.951472163756,1.90915562276867,
125.315568099769));
#235045=CARTESIAN_POINT('Ctrl Pts',(-218.229919787568,-3.58593134807924,
126.231307494954));
#235046=CARTESIAN_POINT('Ctrl Pts',(-218.508367411381,-5.78572259252759,
131.349459303753));
#235047=CARTESIAN_POINT('Ctrl Pts',(-218.786815035194,-2.66871742270537,
135.966692049498));
#235048=CARTESIAN_POINT('Ctrl Pts',(-219.065262659007,2.90070868448967,
135.839994403207));
#235049=CARTESIAN_POINT('Ctrl Pts',(-219.34371028282,5.80452521813531,131.085795312298));
#235050=CARTESIAN_POINT('Ctrl Pts',(-219.622157906633,3.37426664313623,
126.07297148578));
#235051=CARTESIAN_POINT('Ctrl Pts',(-219.900605530446,-2.15677813481551,
125.408063130162));
#235052=CARTESIAN_POINT('Ctrl Pts',(-220.179053154259,-5.70584917134113,
129.702088541682));
#235053=CARTESIAN_POINT('Ctrl Pts',(-220.457500778071,-4.01152356563293,
135.009048141953));
#235054=CARTESIAN_POINT('Ctrl Pts',(-220.735948401884,1.36919622307095,
136.452105317718));
#235055=CARTESIAN_POINT('Ctrl Pts',(-221.014396025697,5.49169157172664,
132.705161021709));
#235056=CARTESIAN_POINT('Ctrl Pts',(-221.29284364951,4.56759065001379,127.211474013555));
#235057=CARTESIAN_POINT('Ctrl Pts',(-221.571291273323,-0.553902939853376,
125.019474272218));
#235058=CARTESIAN_POINT('Ctrl Pts',(-221.849738897136,-5.16638678765824,
128.143502474846));
#235059=CARTESIAN_POINT('Ctrl Pts',(-222.128186520948,-5.03121356963114,
133.712729320486));
#235060=CARTESIAN_POINT('Ctrl Pts',(-222.406634144762,-0.272600869560251,
136.609307409853));
#235061=CARTESIAN_POINT('Ctrl Pts',(-222.685081768574,4.73651871234416,
134.171422984523));
#235062=CARTESIAN_POINT('Ctrl Pts',(-222.963529392388,5.39300898940659,
128.639372734101));
#235063=CARTESIAN_POINT('Ctrl Pts',(-223.2419770162,1.09358746834067,125.096840583045));
#235064=CARTESIAN_POINT('Ctrl Pts',(-223.520424640014,-4.21078751141269,
126.799240515859));
#235065=CARTESIAN_POINT('Ctrl Pts',(-223.798872263826,-5.64565447658353,
132.182150161146));
#235066=CARTESIAN_POINT('Ctrl Pts',(-224.077319887639,-1.89244078332859,
136.298938524645));
#235067=CARTESIAN_POINT('Ctrl Pts',(-224.355767511452,3.59983353893359,
135.366478216591));
#235068=CARTESIAN_POINT('Ctrl Pts',(-224.634215135265,5.78403670056078,
130.241654706868));
#235069=CARTESIAN_POINT('Ctrl Pts',(-224.912662759078,2.65299270027449,
125.633930439363));
#235070=CARTESIAN_POINT('Ctrl Pts',(-225.191110382891,-2.91602198566553,
125.77757891607));
#235071=CARTESIAN_POINT('Ctrl Pts',(-225.469558006704,-5.8053549223724,
130.540594204513));
#235072=CARTESIAN_POINT('Ctrl Pts',(-225.748005630516,-3.35985029277391,
135.545997940844));
#235073=CARTESIAN_POINT('Ctrl Pts',(-226.026453254329,2.17319261807209,
136.194068618944));
#235074=CARTESIAN_POINT('Ctrl Pts',(-226.304900878142,5.7091776792716,131.88926094565));
#235075=CARTESIAN_POINT('Ctrl Pts',(-226.583348501955,3.99870736205508,
126.587482871174));
#235076=CARTESIAN_POINT('Ctrl Pts',(-226.861796125768,-1.38637967317499,
125.160809439701));
#235077=CARTESIAN_POINT('Ctrl Pts',(-227.140243749581,-5.49745151716988,
128.920283837883));
#235078=CARTESIAN_POINT('Ctrl Pts',(-227.418691373394,-4.55663398232247,
134.411132754326));
#235079=CARTESIAN_POINT('Ctrl Pts',(-227.697138997207,0.571507578333558,
136.5875342777));
#235080=CARTESIAN_POINT('Ctrl Pts',(-227.97558662102,5.17446159419872,133.44948173115));
#235081=CARTESIAN_POINT('Ctrl Pts',(-228.254034244832,5.02233819149715,
127.880692102567));
#235082=CARTESIAN_POINT('Ctrl Pts',(-228.532481868645,0.254931345670833,
124.998611010119));
#235083=CARTESIAN_POINT('Ctrl Pts',(-228.810929492458,-4.74674495273865,
127.451730180279));
#235084=CARTESIAN_POINT('Ctrl Pts',(-229.089377116271,-5.38639453096373,
132.985752937203));
#235085=CARTESIAN_POINT('Ctrl Pts',(-229.367824740084,-1.07621067523457,
136.515182719319));
#235086=CARTESIAN_POINT('Ctrl Pts',(-229.646272363897,4.22295821522052,
134.796645979094));
#235087=CARTESIAN_POINT('Ctrl Pts',(-229.92471998771,5.64143480886619,129.409394025606));
#235088=CARTESIAN_POINT('Ctrl Pts',(-230.203167611523,1.87570841257552,
125.304048222223));
#235089=CARTESIAN_POINT('Ctrl Pts',(-230.481615235336,-3.61370238142155,
126.25322080496));
#235090=CARTESIAN_POINT('Ctrl Pts',(-230.760062859148,-5.78229722606833,
131.384668539942));
#235091=CARTESIAN_POINT('Ctrl Pts',(-231.038510482961,-2.63724340088164,
135.982841643878));
#235092=CARTESIAN_POINT('Ctrl Pts',(-231.316958106774,2.93130827321233,
135.822243667495));
#235093=CARTESIAN_POINT('Ctrl Pts',(-231.595405730587,5.80613084659478,
131.050456305442));
#235094=CARTESIAN_POINT('Ctrl Pts',(-231.8738533544,3.34540281721704,126.052519028673));
#235095=CARTESIAN_POINT('Ctrl Pts',(-232.152300978213,-2.18958696916944,
125.42129203173));
#235096=CARTESIAN_POINT('Ctrl Pts',(-232.430748602025,-5.71245329815966,
129.736842087648));
#235097=CARTESIAN_POINT('Ctrl Pts',(-232.709196225839,-3.98585411499877,
135.033389521383));
#235098=CARTESIAN_POINT('Ctrl Pts',(-232.987643849651,1.40355028004735,
136.443665992055));
#235099=CARTESIAN_POINT('Ctrl Pts',(-233.266091473464,5.50316053497282,
132.671696318956));
#235100=CARTESIAN_POINT('Ctrl Pts',(-233.544539097277,4.5456351025967,127.183736360699));
#235101=CARTESIAN_POINT('Ctrl Pts',(-233.82298672109,-0.589106922445798,
125.022953217175));
#235102=CARTESIAN_POINT('Ctrl Pts',(-234.101434344904,-5.18248846523346,
128.175001037157));
#235103=CARTESIAN_POINT('Ctrl Pts',(-234.379881968716,-5.01341628710851,
133.743301860178));
#235104=CARTESIAN_POINT('Ctrl Pts',(-234.658329592529,-0.237259460132118,
136.610859256499));
#235105=CARTESIAN_POINT('Ctrl Pts',(-234.936777216342,4.75692721993639,
134.14252806687));
#235106=CARTESIAN_POINT('Ctrl Pts',(-235.215224840155,5.37973017369771,
128.606584069875));
#235107=CARTESIAN_POINT('Ctrl Pts',(-235.493672463967,1.05882391226032,
125.090289352854));
#235108=CARTESIAN_POINT('Ctrl Pts',(-235.772120087781,-4.23508979812022,
126.824946980203));
#235109=CARTESIAN_POINT('Ctrl Pts',(-236.050567711593,-5.63716287966734,
132.216491335124));
#235110=CARTESIAN_POINT('Ctrl Pts',(-236.329015335406,-1.85895866551617,
136.310356547029));
#235111=CARTESIAN_POINT('Ctrl Pts',(-236.607462959219,3.62753774706455,
135.344480482612));
#235112=CARTESIAN_POINT('Ctrl Pts',(-236.885910583032,5.78050418516386,
130.206456059403));
#235113=CARTESIAN_POINT('Ctrl Pts',(-237.164358206845,2.62146967042642,
125.617876715884));
#235114=CARTESIAN_POINT('Ctrl Pts',(-237.442805830658,-2.94656740551997,
125.795422704185));
#235115=CARTESIAN_POINT('Ctrl Pts',(-237.72125345447,-5.80685298361372,
130.575937934662));
#235116=CARTESIAN_POINT('Ctrl Pts',(-237.999701078284,-3.33092435030571,
135.566362451659));
#235117=CARTESIAN_POINT('Ctrl Pts',(-238.278148702096,2.20596103623244,
136.180739919846));
#235118=CARTESIAN_POINT('Ctrl Pts',(-238.55659632591,5.7156759976606,131.854487459968));
#235119=CARTESIAN_POINT('Ctrl Pts',(-238.835043949722,3.97296394353457,
126.56321973347));
#235120=CARTESIAN_POINT('Ctrl Pts',(-239.113491573535,-1.42070788462113,
125.169353288205));
#235121=CARTESIAN_POINT('Ctrl Pts',(-239.391939197348,-5.50881857224844,
128.95378329321));
#235122=CARTESIAN_POINT('Ctrl Pts',(-239.670386821161,-4.53459411272838,
134.438803453569));
#235123=CARTESIAN_POINT('Ctrl Pts',(-239.948834444974,0.606700809151854,
136.583948200045));
#235124=CARTESIAN_POINT('Ctrl Pts',(-240.227282068787,5.1904673264033,133.417934306771));
#235125=CARTESIAN_POINT('Ctrl Pts',(-240.5057296926,5.00444793911587,127.850173873291));
#235126=CARTESIAN_POINT('Ctrl Pts',(-240.784177316413,0.21958537665436,
124.997166737753));
#235127=CARTESIAN_POINT('Ctrl Pts',(-241.062624940225,-4.76706541961049,
127.48068708057));
#235128=CARTESIAN_POINT('Ctrl Pts',(-241.341072564039,-5.37301597934592,
133.018501033406));
#235129=CARTESIAN_POINT('Ctrl Pts',(-241.619520187851,-1.04142734048567,
136.521628110858));
#235130=CARTESIAN_POINT('Ctrl Pts',(-241.897967811664,4.24718214772698,
134.770865666018));
#235131=CARTESIAN_POINT('Ctrl Pts',(-242.176415435477,5.63283872856131,
129.375078856195));
#235132=CARTESIAN_POINT('Ctrl Pts',(-242.45486305929,1.84219169731802,125.292732160775));
#235133=CARTESIAN_POINT('Ctrl Pts',(-242.733310683103,-3.64133950769301,
126.275302759127));
#235134=CARTESIAN_POINT('Ctrl Pts',(-243.011758306915,-5.77865759445851,
131.419856272607));
#235135=CARTESIAN_POINT('Ctrl Pts',(-243.290205930729,-2.60567165503458,
135.998799347738));
#235136=CARTESIAN_POINT('Ctrl Pts',(-243.568653554541,2.96179924122969,
135.80430699228));
#235137=CARTESIAN_POINT('Ctrl Pts',(-243.847101178355,5.80752132674009,
131.015108179419));
#235138=CARTESIAN_POINT('Ctrl Pts',(-244.125548802166,3.31641502616601,
126.032242652805));
#235139=CARTESIAN_POINT('Ctrl Pts',(-244.403996425981,-2.22231466757369,
125.434720404883));
#235140=CARTESIAN_POINT('Ctrl Pts',(-244.682444049792,-5.71884574792013,
129.771635190908));
#235141=CARTESIAN_POINT('Ctrl Pts',(-244.960891673606,-3.96003696707471,
135.05757419259));
#235142=CARTESIAN_POINT('Ctrl Pts',(-245.239339297418,1.43785232795156,
136.435017699859));
#235143=CARTESIAN_POINT('Ctrl Pts',(-245.517786921232,5.51442557658153,
132.638162421391));
#235144=CARTESIAN_POINT('Ctrl Pts',(-245.796234545044,4.52351111499922,
127.156132871406));
#235145=CARTESIAN_POINT('Ctrl Pts',(-246.074682168857,-0.624289075464052,
125.026646394309));
#235146=CARTESIAN_POINT('Ctrl Pts',(-246.353129792671,-5.19839810379266,
128.206597031353));
#235147=CARTESIAN_POINT('Ctrl Pts',(-246.631577416483,-4.99543323060155,
133.773765496319));
#235148=CARTESIAN_POINT('Ctrl Pts',(-246.910025040296,-0.201909258968066,
136.612195941205));
#235149=CARTESIAN_POINT('Ctrl Pts',(-247.188472664109,4.77715945784187,
134.113509452194));
#235150=CARTESIAN_POINT('Ctrl Pts',(-247.466920287922,5.36625201010822,
128.573876845067));
#235151=CARTESIAN_POINT('Ctrl Pts',(-247.745367911734,1.02402112107033,
125.083949859676));
#235152=CARTESIAN_POINT('Ctrl Pts',(-248.023815535548,-4.25923515201858,
126.850800903184));
#235153=CARTESIAN_POINT('Ctrl Pts',(-248.30226315936,-5.62846239560694,
132.250780182078));
#235154=CARTESIAN_POINT('Ctrl Pts',(-248.580710783174,-1.82540766330725,
136.32157054271));
#235155=CARTESIAN_POINT('Ctrl Pts',(-248.859158406986,3.65510753545023,
135.322314512822));
#235156=CARTESIAN_POINT('Ctrl Pts',(-249.137606030799,5.7767574710584,130.171279567513));
#235157=CARTESIAN_POINT('Ctrl Pts',(-249.416053654612,2.58984950105633,
125.602015179472));
#235158=CARTESIAN_POINT('Ctrl Pts',(-249.694501278425,-2.97700363923603,
125.813452100338));
#235159=CARTESIAN_POINT('Ctrl Pts',(-249.972948902238,-5.80813586978118,
130.611290129096));
#235160=CARTESIAN_POINT('Ctrl Pts',(-250.251396526051,-3.30187497921299,
135.586550504748));
#235161=CARTESIAN_POINT('Ctrl Pts',(-250.529844149864,2.23864771169993,
136.167211997028));
#235162=CARTESIAN_POINT('Ctrl Pts',(-250.808291773676,5.72196251956533,
131.819675061465));
#235163=CARTESIAN_POINT('Ctrl Pts',(-251.08673939749,3.94707330538994,126.539113752772));
#235164=CARTESIAN_POINT('Ctrl Pts',(-251.365187021302,-1.45498345124562,
125.178105944033));
#235165=CARTESIAN_POINT('Ctrl Pts',(-251.643634645115,-5.5199814959705,
128.987351322257));
#235166=CARTESIAN_POINT('Ctrl Pts',(-251.922082268928,-4.51238621219265,
134.466339477392));
#235167=CARTESIAN_POINT('Ctrl Pts',(-252.200529892741,0.641871558658502,
136.580147957277));
#235168=CARTESIAN_POINT('Ctrl Pts',(-252.478977516554,5.20628072353487,
133.386290036154));
#235169=CARTESIAN_POINT('Ctrl Pts',(-252.757425140367,4.98637224582674,
127.819765111179));
#235170=CARTESIAN_POINT('Ctrl Pts',(-253.035872764179,0.184231269403876,
124.995937655572));
#235171=CARTESIAN_POINT('Ctrl Pts',(-253.314320387993,-4.78720923844335,
127.509767136124));
#235172=CARTESIAN_POINT('Ctrl Pts',(-253.592768011806,-5.35943833369967,
133.051167092665));
#235173=CARTESIAN_POINT('Ctrl Pts',(-253.871215635618,-1.00660540571931,
136.527861630253));
#235174=CARTESIAN_POINT('Ctrl Pts',(-254.149663259431,4.27124868131666,
134.744938404161));
#235175=CARTESIAN_POINT('Ctrl Pts',(-254.428110883244,5.62403395537261,
129.340816589823));
#235176=CARTESIAN_POINT('Ctrl Pts',(-254.706558507057,1.80860665472018,
125.281620447135));
#235177=CARTESIAN_POINT('Ctrl Pts',(-254.98500613087,-3.66884158147516,
126.297552326988));
#235178=CARTESIAN_POINT('Ctrl Pts',(-255.263453754682,-5.77480406163408,
131.45502159855));
#235179=CARTESIAN_POINT('Ctrl Pts',(-255.541901378496,-2.57400292253984,
136.014563813166));
#235180=CARTESIAN_POINT('Ctrl Pts',(-255.820349002309,2.99217964199006,
135.78618647082));
#235181=CARTESIAN_POINT('Ctrl Pts',(-256.098796626121,5.80869814913581,
130.979749546569));
#235182=CARTESIAN_POINT('Ctrl Pts',(-256.377244249934,3.28730143236016,
126.01214820295));
#235183=CARTESIAN_POINT('Ctrl Pts',(-256.655691873747,-2.25495451926359,
125.448338134603));
#235184=CARTESIAN_POINT('Ctrl Pts',(-256.93413949756,-5.72503666514098,
129.806484721847));
#235185=CARTESIAN_POINT('Ctrl Pts',(-257.212587121373,-3.93405347634203,
135.081566970265));
#235186=CARTESIAN_POINT('Ctrl Pts',(-257.491034745186,1.47206408278265,
136.426225506557));
#235187=CARTESIAN_POINT('Ctrl Pts',(-257.769482368999,5.52555616721843,
132.604438319186));
#235188=CARTESIAN_POINT('Ctrl Pts',(-258.047929992812,4.50108754276566,
127.128895412351));
#235189=CARTESIAN_POINT('Ctrl Pts',(-258.326377616624,-0.659198908970111,
125.030117734768));
#235190=CARTESIAN_POINT('Ctrl Pts',(-258.604825240438,-5.21458571703409,
128.239112839452));
#235191=CARTESIAN_POINT('Ctrl Pts',(-258.883272864251,-4.97637574492231,
133.802560593787));
#235192=CARTESIAN_POINT('Ctrl Pts',(-259.161720488063,-0.168236736403017,
136.616288572087));
#235193=CARTESIAN_POINT('Ctrl Pts',(-259.440168111876,4.80044487344316,
134.078525892203));
#235194=CARTESIAN_POINT('Ctrl Pts',(-259.672207798387,5.25516631655033,
129.4749169549));
#235195=CARTESIAN_POINT('Ctrl Pts',(-259.857849473896,3.17366342871357,
126.795179433485));
#235196=CARTESIAN_POINT('Ctrl Pts',(-259.9506752748,1.64266665146648,126.102093112095));
#235197=CARTESIAN_POINT('Ctrl Pts',(-259.997093138402,0.835778587061721,
125.962806053044));
#235198=CARTESIAN_POINT('Ctrl Pts',(210.385579563201,-2.29217962691353,
126.082387726892));
#235199=CARTESIAN_POINT('Ctrl Pts',(210.339169886847,-3.0789974560272,126.464330840008));
#235200=CARTESIAN_POINT('Ctrl Pts',(210.246352273192,-4.44507089109247,
127.629120819077));
#235201=CARTESIAN_POINT('Ctrl Pts',(210.060718784933,-5.78798125627161,
130.996088365878));
#235202=CARTESIAN_POINT('Ctrl Pts',(209.828679098422,-3.95783017776954,
135.586872998689));
#235203=CARTESIAN_POINT('Ctrl Pts',(209.550231474609,1.89393692750204,136.720289837399));
#235204=CARTESIAN_POINT('Ctrl Pts',(209.271783850796,5.99602695027556,132.40812259401));
#235205=CARTESIAN_POINT('Ctrl Pts',(208.993336226983,4.59288360023261,126.626877830413));
#235206=CARTESIAN_POINT('Ctrl Pts',(208.71488860317,-1.03344059257722,124.682062423228));
#235207=CARTESIAN_POINT('Ctrl Pts',(208.436440979357,-5.70873650289865,
128.364647771496));
#235208=CARTESIAN_POINT('Ctrl Pts',(208.157993355544,-5.13869562717284,
134.288517668348));
#235209=CARTESIAN_POINT('Ctrl Pts',(207.879545731732,0.153933173725622,
137.010984097728));
#235210=CARTESIAN_POINT('Ctrl Pts',(207.601098107919,5.30490488755997,134.029672582798));
#235211=CARTESIAN_POINT('Ctrl Pts',(207.322650484106,5.58103410012833,128.084559773234));
#235212=CARTESIAN_POINT('Ctrl Pts',(207.044202860293,0.728409521696789,
124.638756607567));
#235213=CARTESIAN_POINT('Ctrl Pts',(206.76575523648,-4.79355811073501,126.858871164077));
#235214=CARTESIAN_POINT('Ctrl Pts',(206.487307612667,-5.91049575314416,
132.704682504842));
#235215=CARTESIAN_POINT('Ctrl Pts',(206.208859988854,-1.59596820864792,
136.804198957117));
#235216=CARTESIAN_POINT('Ctrl Pts',(205.930412365042,4.1851717387407,135.390152799229));
#235217=CARTESIAN_POINT('Ctrl Pts',(205.651964741228,6.12034565262566,129.76198992389));
#235218=CARTESIAN_POINT('Ctrl Pts',(205.373517117416,2.43121966936229,125.091713591677));
#235219=CARTESIAN_POINT('Ctrl Pts',(205.095069493603,-3.49207776276838,
125.671081434371));
#235220=CARTESIAN_POINT('Ctrl Pts',(204.81662186979,-6.20632667560231,130.96768173473));
#235221=CARTESIAN_POINT('Ctrl Pts',(204.538174245977,-3.21726438559061,
136.114198085604));
#235222=CARTESIAN_POINT('Ctrl Pts',(204.259726622164,2.72830660529182,136.381233108793));
#235223=CARTESIAN_POINT('Ctrl Pts',(203.981278998351,6.16669716267351,131.523394807979));
#235224=CARTESIAN_POINT('Ctrl Pts',(203.702831374538,3.9381942601484,126.004799186432));
#235225=CARTESIAN_POINT('Ctrl Pts',(203.424383750725,-1.909316761502,124.896766062528));
#235226=CARTESIAN_POINT('Ctrl Pts',(203.145936126912,-6.00225896230248,
129.217523725228));
#235227=CARTESIAN_POINT('Ctrl Pts',(202.867488503099,-4.57941839934143,
134.996506974633));
#235228=CARTESIAN_POINT('Ctrl Pts',(202.589040879287,1.05168395343957,136.923112517541));
#235229=CARTESIAN_POINT('Ctrl Pts',(202.310593255474,5.71634013176502,133.226883983125));
#235230=CARTESIAN_POINT('Ctrl Pts',(202.032145631661,5.12795898713612,127.30447482202));
#235231=CARTESIAN_POINT('Ctrl Pts',(201.753698007848,-0.172765951628197,
124.598289728405));
#235232=CARTESIAN_POINT('Ctrl Pts',(201.475250384035,-5.31472742110118,
127.595180598346));
#235233=CARTESIAN_POINT('Ctrl Pts',(201.196802760222,-5.57271402936141,
133.541151128878));
#235234=CARTESIAN_POINT('Ctrl Pts',(200.918355136409,-0.709648686901125,
136.972144879116));
#235235=CARTESIAN_POINT('Ctrl Pts',(200.639907512596,4.80554913058071,134.735246206027));
#235236=CARTESIAN_POINT('Ctrl Pts',(200.361459888783,5.90468206117194,128.886055711564));
#235237=CARTESIAN_POINT('Ctrl Pts',(200.083012264971,1.57770063730838,124.799693711321));
#235238=CARTESIAN_POINT('Ctrl Pts',(199.804564641158,-4.19911059728431,
126.231327253625));
#235239=CARTESIAN_POINT('Ctrl Pts',(199.526117017345,-6.11714433092778,
131.865355052293));
#235240=CARTESIAN_POINT('Ctrl Pts',(199.247669393532,-2.4138212635637,136.524380797905));
#235241=CARTESIAN_POINT('Ctrl Pts',(198.969221769719,3.50768562329156,135.926987436306));
#235242=CARTESIAN_POINT('Ctrl Pts',(198.690774145906,6.20580078231077,130.622150282517));
#235243=CARTESIAN_POINT('Ctrl Pts',(198.412326522093,3.20108819260905,125.484755525167));
#235244=CARTESIAN_POINT('Ctrl Pts',(198.13387889828,-2.74526806424844,125.235817970576));
#235245=CARTESIAN_POINT('Ctrl Pts',(197.855431274468,-6.16885708386238,
130.104099070135));
#235246=CARTESIAN_POINT('Ctrl Pts',(197.576983650655,-3.92356780882929,
135.615886322105));
#235247=CARTESIAN_POINT('Ctrl Pts',(197.298536026841,1.92728860557448,136.706116507701));
#235248=CARTESIAN_POINT('Ctrl Pts',(197.020088403029,6.00706094473797,132.372921347066));
#235249=CARTESIAN_POINT('Ctrl Pts',(196.741640779216,4.56663773692898,126.598295504472));
#235250=CARTESIAN_POINT('Ctrl Pts',(196.463193155403,-1.07030245846182,
124.688838023107));
#235251=CARTESIAN_POINT('Ctrl Pts',(196.184745531591,-5.72368698170812,
128.399247046161));
#235252=CARTESIAN_POINT('Ctrl Pts',(195.906297907777,-5.11728278641862,
134.319837945007));
#235253=CARTESIAN_POINT('Ctrl Pts',(195.627850283965,0.191654296427489,
137.009876920548));
#235254=CARTESIAN_POINT('Ctrl Pts',(195.349402660151,5.32447044368961,133.997349569974));
#235255=CARTESIAN_POINT('Ctrl Pts',(195.070955036339,5.56435836804288,128.050621358318));
#235256=CARTESIAN_POINT('Ctrl Pts',(194.792507412526,0.690872786183208,
124.634444998269));
#235257=CARTESIAN_POINT('Ctrl Pts',(194.514059788713,-4.81749113516689,
126.888119675218));
#235258=CARTESIAN_POINT('Ctrl Pts',(194.2356121649,-5.89881605082435,132.740628459178));
#235259=CARTESIAN_POINT('Ctrl Pts',(193.957164541087,-1.55941718895885,
136.81380168864));
#235260=CARTESIAN_POINT('Ctrl Pts',(193.678716917274,4.21300988779493,135.364592151301));
#235261=CARTESIAN_POINT('Ctrl Pts',(193.400269293461,6.11388669464029,129.724752614155));
#235262=CARTESIAN_POINT('Ctrl Pts',(193.121821669648,2.39640030908087,125.077020090361));
#235263=CARTESIAN_POINT('Ctrl Pts',(192.843374045836,-3.52326088986039,
125.692433714928));
#235264=CARTESIAN_POINT('Ctrl Pts',(192.564926422022,-6.20521745188322,
131.005458431507));
#235265=CARTESIAN_POINT('Ctrl Pts',(192.28647879821,-3.1848823173506,136.133684081248));
#235266=CARTESIAN_POINT('Ctrl Pts',(192.008031174397,2.76220407667619,136.36452181979));
#235267=CARTESIAN_POINT('Ctrl Pts',(191.729583550584,6.17095986540858,131.485843042463));
#235268=CARTESIAN_POINT('Ctrl Pts',(191.451135926771,3.90890500597959,125.980915208923));
#235269=CARTESIAN_POINT('Ctrl Pts',(191.172688302958,-1.94524259331895,
124.908498067517));
#235270=CARTESIAN_POINT('Ctrl Pts',(190.894240679145,-6.01180727974115,
129.254090580708));
#235271=CARTESIAN_POINT('Ctrl Pts',(190.615793055332,-4.5538147691942,135.024305522869));
#235272=CARTESIAN_POINT('Ctrl Pts',(190.337345431519,1.08891104802307,136.916597252826));
#235273=CARTESIAN_POINT('Ctrl Pts',(190.058897807707,5.73098080836918,133.192042114338));
#235274=CARTESIAN_POINT('Ctrl Pts',(189.780450183893,5.10655917980125,127.273324325042));
#235275=CARTESIAN_POINT('Ctrl Pts',(189.502002560081,-0.210540865719208,
124.599456387862));
#235276=CARTESIAN_POINT('Ctrl Pts',(189.223554936268,-5.33416414113684,
127.627592311355));
#235277=CARTESIAN_POINT('Ctrl Pts',(188.945107312455,-5.55595115925501,
133.575023114497));
#235278=CARTESIAN_POINT('Ctrl Pts',(188.666659688642,-0.672090485321342,
136.976350437346));
#235279=CARTESIAN_POINT('Ctrl Pts',(188.388212064829,4.82938851117716,134.705920634282));
#235280=CARTESIAN_POINT('Ctrl Pts',(188.109764441016,5.89289539464864,128.850147777659));
#235281=CARTESIAN_POINT('Ctrl Pts',(187.831316817203,1.54111929438253,124.790201052305));
#235282=CARTESIAN_POINT('Ctrl Pts',(187.552869193391,-4.22687014955807,
126.256973159398));
#235283=CARTESIAN_POINT('Ctrl Pts',(187.274421569578,-6.11057242014135,
131.902572188318));
#235284=CARTESIAN_POINT('Ctrl Pts',(186.995973945765,-2.37895715467313,
136.538968434335));
#235285=CARTESIAN_POINT('Ctrl Pts',(186.717526321952,3.53880351742172,135.905540247907));
#235286=CARTESIAN_POINT('Ctrl Pts',(186.439078698139,6.20457663716883,130.584377187674));
#235287=CARTESIAN_POINT('Ctrl Pts',(186.160631074326,3.16864693777749,125.465368152723));
#235288=CARTESIAN_POINT('Ctrl Pts',(185.882183450513,-2.77911450042273,
125.25263236868));
#235289=CARTESIAN_POINT('Ctrl Pts',(185.6037358267,-6.17300548002561,130.14166362836));
#235290=CARTESIAN_POINT('Ctrl Pts',(185.325288202887,-3.89420599156785,
135.639681046572));
#235291=CARTESIAN_POINT('Ctrl Pts',(185.046840579075,1.96317856060187,136.694275209062));
#235292=CARTESIAN_POINT('Ctrl Pts',(184.768392955261,6.0164979221829,132.336325600291));
#235293=CARTESIAN_POINT('Ctrl Pts',(184.489945331449,4.54094961554151,126.570575013045));
#235294=CARTESIAN_POINT('Ctrl Pts',(184.211497707636,-1.10750955006109,
124.695466564429));
#235295=CARTESIAN_POINT('Ctrl Pts',(183.933050083823,-5.73822154400692,
128.434133314579));
#235296=CARTESIAN_POINT('Ctrl Pts',(183.65460246001,-5.09578826671723,134.350923164133));
#235297=CARTESIAN_POINT('Ctrl Pts',(183.376154836197,0.229425484589131,
137.008595292604));
#235298=CARTESIAN_POINT('Ctrl Pts',(183.097707212384,5.34380842361613,133.964878848429));
#235299=CARTESIAN_POINT('Ctrl Pts',(182.819259588571,5.54749248089459,128.016800549989));
#235300=CARTESIAN_POINT('Ctrl Pts',(182.540811964758,0.653301958305029,
124.630353773773));
#235301=CARTESIAN_POINT('Ctrl Pts',(182.262364340946,-4.84124114839195,
126.917517669999));
#235302=CARTESIAN_POINT('Ctrl Pts',(181.983916717133,-5.88692014749505,
132.776500352206));
#235303=CARTESIAN_POINT('Ctrl Pts',(181.70546909332,-1.52280712308763,136.82318296266));
#235304=CARTESIAN_POINT('Ctrl Pts',(181.427021469507,4.24069125417353,135.33886187379));
#235305=CARTESIAN_POINT('Ctrl Pts',(181.148573845694,6.10720153813428,129.687555653153));
#235306=CARTESIAN_POINT('Ctrl Pts',(180.870126221881,2.36149196193127,125.062538635854));
#235307=CARTESIAN_POINT('Ctrl Pts',(180.591678598068,-3.55431336199069,
125.713975516152));
#235308=CARTESIAN_POINT('Ctrl Pts',(180.313230974255,-6.20387834410407,
131.04322762551));
#235309=CARTESIAN_POINT('Ctrl Pts',(180.034783350442,-3.15238220429199,
136.15297262387));
#235310=CARTESIAN_POINT('Ctrl Pts',(179.75633572663,2.79599917883219,136.347604482659));
#235311=CARTESIAN_POINT('Ctrl Pts',(179.477888102817,6.17499390876314,131.448266031944));
#235312=CARTESIAN_POINT('Ctrl Pts',(179.199440479004,3.8794709017638,125.957209961944));
#235313=CARTESIAN_POINT('Ctrl Pts',(178.920992855191,-1.98109634126673,
124.920448547985));
#235314=CARTESIAN_POINT('Ctrl Pts',(178.642545231378,-6.02113282860982,
129.290714880887));
#235315=CARTESIAN_POINT('Ctrl Pts',(178.364097607565,-4.52804239515191,
135.051947700091));
#235316=CARTESIAN_POINT('Ctrl Pts',(178.085649983752,1.12609779228193,136.909855496619));
#235317=CARTESIAN_POINT('Ctrl Pts',(177.807202359939,5.74540912154417,133.157111769304));
#235318=CARTESIAN_POINT('Ctrl Pts',(177.528754736127,5.08497014694685,127.242304671825));
#235319=CARTESIAN_POINT('Ctrl Pts',(177.250307112313,-0.248307978092709,
124.600852972375));
#235320=CARTESIAN_POINT('Ctrl Pts',(176.971859488501,-5.35340320178418,
127.660121740658));
#235321=CARTESIAN_POINT('Ctrl Pts',(176.693411864688,-5.53898241132168,
133.608792432211));
#235322=CARTESIAN_POINT('Ctrl Pts',(176.414964240875,-0.634507379188621,
136.980327290216));
#235323=CARTESIAN_POINT('Ctrl Pts',(176.136516617062,4.85304893701009,134.676450488799));
#235324=CARTESIAN_POINT('Ctrl Pts',(175.858068993249,5.88089036471739,128.814312257825));
#235325=CARTESIAN_POINT('Ctrl Pts',(175.579621369436,1.50448084471559,124.780931250186));
#235326=CARTESIAN_POINT('Ctrl Pts',(175.301173745623,-4.25447307360455,
126.282787570284));
#235327=CARTESIAN_POINT('Ctrl Pts',(175.02272612181,-6.10377407984646,131.939748629711));
#235328=CARTESIAN_POINT('Ctrl Pts',(174.744278497998,-2.34400489265046,
136.553343572764));
#235329=CARTESIAN_POINT('Ctrl Pts',(174.465830874185,3.56979027988629,135.883904033421));
#235330=CARTESIAN_POINT('Ctrl Pts',(174.187383250372,6.20312257915782,130.546612244398));
#235331=CARTESIAN_POINT('Ctrl Pts',(173.908935626559,3.13608826756835,125.446178618609));
#235332=CARTESIAN_POINT('Ctrl Pts',(173.630488002746,-2.81285795548731,
125.269652488117));
#235333=CARTESIAN_POINT('Ctrl Pts',(173.352040378933,-6.17692513320066,
130.179252743065));
#235334=CARTESIAN_POINT('Ctrl Pts',(173.07359275512,-3.86469987307124,135.663296596462));
#235335=CARTESIAN_POINT('Ctrl Pts',(172.795145131307,1.99899576932572,136.682215657471));
#235336=CARTESIAN_POINT('Ctrl Pts',(172.516697507494,6.02571195608475,132.29967308599));
#235337=CARTESIAN_POINT('Ctrl Pts',(172.238249883681,4.51509322759614,126.543011406101));
#235338=CARTESIAN_POINT('Ctrl Pts',(171.959802259869,-1.14467560248665,
124.702321473066));
#235339=CARTESIAN_POINT('Ctrl Pts',(171.681354636056,-5.75254347439624,
128.469107412642));
#235340=CARTESIAN_POINT('Ctrl Pts',(171.402907012243,-5.07410492070761,
134.38187696408));
#235341=CARTESIAN_POINT('Ctrl Pts',(171.12445938843,0.267188171305193,137.007083764462));
#235342=CARTESIAN_POINT('Ctrl Pts',(170.846011764617,5.36294838675633,133.932291012718));
#235343=CARTESIAN_POINT('Ctrl Pts',(170.567564140804,5.53042102937231,127.983083035723));
#235344=CARTESIAN_POINT('Ctrl Pts',(170.289116516991,0.615706922082464,
124.62649132937));
#235345=CARTESIAN_POINT('Ctrl Pts',(170.010668893178,-4.86481176764585,
126.947059693175));
#235346=CARTESIAN_POINT('Ctrl Pts',(169.732221269365,-5.87480610217478,
132.812299166869));
#235347=CARTESIAN_POINT('Ctrl Pts',(169.453773645553,-1.48614062903852,
136.832341207004));
#235348=CARTESIAN_POINT('Ctrl Pts',(169.17532602174,4.26821548017818,135.312963568669));
#235349=CARTESIAN_POINT('Ctrl Pts',(168.896878397927,6.10029007702938,129.650400075769));
#235350=CARTESIAN_POINT('Ctrl Pts',(168.618430774114,2.32649610882855,125.048269946673));
#235351=CARTESIAN_POINT('Ctrl Pts',(168.339983150301,-3.58523412773234,
125.735705943466));
#235352=CARTESIAN_POINT('Ctrl Pts',(168.061535526488,-6.2023093493314,131.08098796821));
#235353=CARTESIAN_POINT('Ctrl Pts',(167.783087902675,-3.11976527855146,
136.172062971709));
#235354=CARTESIAN_POINT('Ctrl Pts',(167.504640278862,2.82969067421049,136.330481738588));
#235355=CARTESIAN_POINT('Ctrl Pts',(167.22619265505,6.17879913544756,131.410665161273));
#235356=CARTESIAN_POINT('Ctrl Pts',(166.947745031236,3.84989304232704,125.933684327914));
#235357=CARTESIAN_POINT('Ctrl Pts',(166.669297407424,-2.01687667896098,
124.93261705898));
#235358=CARTESIAN_POINT('Ctrl Pts',(166.39084978361,-6.03023526218728,129.327395269766));
#235359=CARTESIAN_POINT('Ctrl Pts',(166.112402159798,-4.50210223283349,
135.079432481411));
#235360=CARTESIAN_POINT('Ctrl Pts',(165.833954535985,1.16324280857304,136.902887499053));
#235361=CARTESIAN_POINT('Ctrl Pts',(165.555506912173,5.75962453647134,133.122094242209));
#235362=CARTESIAN_POINT('Ctrl Pts',(165.277059288359,5.06319268865361,127.2114170119));
#235363=CARTESIAN_POINT('Ctrl Pts',(164.998611664547,-0.286065889322858,
124.602479430144));
#235364=CARTESIAN_POINT('Ctrl Pts',(164.720164040733,-5.37244389010723,
127.692767680889));
#235365=CARTESIAN_POINT('Ctrl Pts',(164.441716416921,-5.52180841435808,
133.642457830674));
#235366=CARTESIAN_POINT('Ctrl Pts',(164.163268793108,-0.596900761151562,
136.984075290369));
#235367=CARTESIAN_POINT('Ctrl Pts',(163.884821169295,4.87652953132996,134.646836861603));
#235368=CARTESIAN_POINT('Ctrl Pts',(163.606373545482,5.86866741623098,128.778550479967));
#235369=CARTESIAN_POINT('Ctrl Pts',(163.327925921669,1.46778664595768,124.771884648456));
#235370=CARTESIAN_POINT('Ctrl Pts',(163.049478297856,-4.28191834658676,
126.308769529723));
#235371=CARTESIAN_POINT('Ctrl Pts',(162.771030674043,-6.09674956195837,
131.976882998882));
#235372=CARTESIAN_POINT('Ctrl Pts',(162.49258305023,-2.30896577266445,136.567505680515));
#235373=CARTESIAN_POINT('Ctrl Pts',(162.214135426418,3.60064476245918,135.862079594585));
#235374=CARTESIAN_POINT('Ctrl Pts',(161.935687802605,6.20143866215845,130.508856852083));
#235375=CARTESIAN_POINT('Ctrl Pts',(161.657240178792,3.10341338845521,125.427187633898));
#235376=CARTESIAN_POINT('Ctrl Pts',(161.378792554979,-2.84649717906582,
125.2868776982));
#235377=CARTESIAN_POINT('Ctrl Pts',(161.100344931166,-6.18061589814333,
130.216865021372));
#235378=CARTESIAN_POINT('Ctrl Pts',(160.821897307353,-3.83505054669964,
135.686732096692));
#235379=CARTESIAN_POINT('Ctrl Pts',(160.54344968354,2.0347389045262,136.6699382998));
#235380=CARTESIAN_POINT('Ctrl Pts',(160.265002059727,6.03470270501411,132.262965162335));
#235381=CARTESIAN_POINT('Ctrl Pts',(159.986554435914,4.48906953121078,126.51560570502));
#235382=CARTESIAN_POINT('Ctrl Pts',(159.708106812101,-1.18179923853688,
124.709402495009));
#235383=CARTESIAN_POINT('Ctrl Pts',(159.429659188289,-5.76665224217155,
128.50416804437));
#235384=CARTESIAN_POINT('Ctrl Pts',(159.151211564475,-5.05223355187421,
134.412698197843));
#235385=CARTESIAN_POINT('Ctrl Pts',(158.872763940663,0.304940957265202,
137.005342392132));
#235386=CARTESIAN_POINT('Ctrl Pts',(158.59431631685,5.38188962387183,133.899587270395));
#235387=CARTESIAN_POINT('Ctrl Pts',(158.315868693037,5.51314464606502,127.949470064936));
#235388=CARTESIAN_POINT('Ctrl Pts',(158.037421069224,0.57808907061355,124.622857808186));
#235389=CARTESIAN_POINT('Ctrl Pts',(157.758973445411,-4.88820211951067,
126.976744650055));
#235390=CARTESIAN_POINT('Ctrl Pts',(157.480525821598,-5.86247436375394,
132.848023576631));
#235391=CARTESIAN_POINT('Ctrl Pts',(157.202078197785,-1.44941906550188,
136.841276082311));
#235392=CARTESIAN_POINT('Ctrl Pts',(156.923630573973,4.29558154588865,135.286898195607));
#235393=CARTESIAN_POINT('Ctrl Pts',(156.645182950159,6.09315256743229,129.613287258817));
#235394=CARTESIAN_POINT('Ctrl Pts',(156.366735326347,2.29141404655692,125.034214551549));
#235395=CARTESIAN_POINT('Ctrl Pts',(156.088287702534,-3.61602204130483,
125.757624191644));
#235396=CARTESIAN_POINT('Ctrl Pts',(155.809840078721,-6.2005105257049,131.11873806038));
#235397=CARTESIAN_POINT('Ctrl Pts',(155.531392454908,-3.08703274876129,
136.190954417361));
#235398=CARTESIAN_POINT('Ctrl Pts',(155.252944831095,2.86327731436015,136.313154222067));
#235399=CARTESIAN_POINT('Ctrl Pts',(154.974497207282,6.18237540445775,131.373041823765));
#235400=CARTESIAN_POINT('Ctrl Pts',(154.696049583469,3.82017252368788,125.910339178587));
#235401=CARTESIAN_POINT('Ctrl Pts',(154.417601959656,-2.05258228054818,
124.945003149591));
#235402=CARTESIAN_POINT('Ctrl Pts',(154.139154335844,-6.03911424317947,
129.364130388138));
#235403=CARTESIAN_POINT('Ctrl Pts',(153.860706712031,-4.47599524346119,
135.106758848372));
#235404=CARTESIAN_POINT('Ctrl Pts',(153.582259088218,1.20034472047403,136.895693518332));
#235405=CARTESIAN_POINT('Ctrl Pts',(153.303811464405,5.77362652639317,133.086990830643));
#235406=CARTESIAN_POINT('Ctrl Pts',(153.025363840592,5.04122761189337,127.180662489822));
#235407=CARTESIAN_POINT('Ctrl Pts',(152.746916216779,-0.323813200276178,
124.604335700902));
#235408=CARTESIAN_POINT('Ctrl Pts',(152.468468592966,-5.39128550054617,
127.725528922339));
#235409=CARTESIAN_POINT('Ctrl Pts',(152.190020969154,-5.5044298047531,133.6760180624));
#235410=CARTESIAN_POINT('Ctrl Pts',(151.91157334534,-0.55927202473736,136.987594298923));
#235411=CARTESIAN_POINT('Ctrl Pts',(151.633125721528,4.89982942405471,134.617080850036));
#235412=CARTESIAN_POINT('Ctrl Pts',(151.354678097715,5.85622700211526,128.742863769248));
#235413=CARTESIAN_POINT('Ctrl Pts',(151.076230473902,1.43103805782584,124.763061582343));
#235414=CARTESIAN_POINT('Ctrl Pts',(150.797782850089,-4.3092049515099,126.334918074943));
#235415=CARTESIAN_POINT('Ctrl Pts',(150.519335226276,-6.0894991267732,132.013973919806));
#235416=CARTESIAN_POINT('Ctrl Pts',(150.240887602463,-2.27384109310269,
136.581454232806));
#235417=CARTESIAN_POINT('Ctrl Pts',(149.96243997865,3.63136582181627,135.840067740113));
#235418=CARTESIAN_POINT('Ctrl Pts',(149.683992354837,6.19952494856889,130.471112409769));
#235419=CARTESIAN_POINT('Ctrl Pts',(149.405544731024,3.0706235112177,125.40839590231));
#235420=CARTESIAN_POINT('Ctrl Pts',(149.127097107212,-2.88003092464457,
125.30430736064));
#235421=CARTESIAN_POINT('Ctrl Pts',(148.848649483398,-6.18407763809098,
130.254499069545));
#235422=CARTESIAN_POINT('Ctrl Pts',(148.570201859586,-3.80525911111971,
135.709986678852));
#235423=CARTESIAN_POINT('Ctrl Pts',(148.291754235773,2.07040664172831,136.657443590992));
#235424=CARTESIAN_POINT('Ctrl Pts',(148.01330661196,6.04346983581547,132.226203189553));
#235425=CARTESIAN_POINT('Ctrl Pts',(147.734858988147,4.46287949070312,126.488358925329));
#235426=CARTESIAN_POINT('Ctrl Pts',(147.456411364334,-1.21887908258166,
124.716709367866));
#235427=CARTESIAN_POINT('Ctrl Pts',(147.177963740522,-5.78054732452736,
128.53931391058));
#235428=CARTESIAN_POINT('Ctrl Pts',(146.899516116708,-5.03017497066859,
134.44338572333));
#235429=CARTESIAN_POINT('Ctrl Pts',(146.621068492896,0.342682443525903,
137.003371240143));
#235430=CARTESIAN_POINT('Ctrl Pts',(146.342620869082,5.40063143308812,133.866768833311));
#235431=CARTESIAN_POINT('Ctrl Pts',(146.06417324527,5.49566397115542,127.915962883168));
#235432=CARTESIAN_POINT('Ctrl Pts',(145.785725621457,0.540449797841529,
124.619453344862));
#235433=CARTESIAN_POINT('Ctrl Pts',(145.507277997644,-4.91141133724831,
127.006571440652));
#235434=CARTESIAN_POINT('Ctrl Pts',(145.228830373831,-5.84992538918966,
132.883672257711));
#235435=CARTESIAN_POINT('Ctrl Pts',(144.950382750018,-1.41264379320865,
136.849987257496));
#235436=CARTESIAN_POINT('Ctrl Pts',(144.671935126205,4.32278843724517,135.260666720466));
#235437=CARTESIAN_POINT('Ctrl Pts',(144.393487502392,6.08578927382608,129.576218577526));
#235438=CARTESIAN_POINT('Ctrl Pts',(144.11503987858,2.25624707509518,125.020372971309));
#235439=CARTESIAN_POINT('Ctrl Pts',(143.836592254767,-3.64667596185081,
125.779729448496));
#235440=CARTESIAN_POINT('Ctrl Pts',(143.558144630954,-6.19848193988065,
131.156476503179));
#235441=CARTESIAN_POINT('Ctrl Pts',(143.279697007141,-3.05418582783736,
136.209646260801));
#235442=CARTESIAN_POINT('Ctrl Pts',(143.001249383328,2.89675785471595,136.295622575173));
#235443=CARTESIAN_POINT('Ctrl Pts',(142.722801759515,6.18572258327378,131.335397413564));
#235444=CARTESIAN_POINT('Ctrl Pts',(142.444354135702,3.79031044715096,125.887175379022));
#235445=CARTESIAN_POINT('Ctrl Pts',(142.165906511889,-2.0882118229442,124.957606360848));
#235446=CARTESIAN_POINT('Ctrl Pts',(141.887458888076,-6.04776944257254,
129.400918874772));
#235447=CARTESIAN_POINT('Ctrl Pts',(141.609011264264,-4.44972239443904,
135.133925788383));
#235448=CARTESIAN_POINT('Ctrl Pts',(141.33056364045,1.2374021531599,136.888273821029));
#235449=CARTESIAN_POINT('Ctrl Pts',(141.052116016638,5.78741457246075,133.051802835376));
#235450=CARTESIAN_POINT('Ctrl Pts',(140.773668392825,5.01907573059014,127.15004224521));
#235451=CARTESIAN_POINT('Ctrl Pts',(140.495220769012,-0.361548512212229,
124.606421715863));
#235452=CARTESIAN_POINT('Ctrl Pts',(140.216773145199,-5.4099273349182,127.758404251031));
#235453=CARTESIAN_POINT('Ctrl Pts',(139.938325521386,-5.48684722647749,
133.709471883804));
#235454=CARTESIAN_POINT('Ctrl Pts',(139.659877897573,-0.521622564292735,
136.990884185479));
#235455=CARTESIAN_POINT('Ctrl Pts',(139.38143027376,4.92294775179823,134.58718355672));
#235456=CARTESIAN_POINT('Ctrl Pts',(139.102982649947,5.84356958335437,128.707253448052));
#235457=CARTESIAN_POINT('Ctrl Pts',(138.824535026135,1.39423644205237,124.754462378786));
#235458=CARTESIAN_POINT('Ctrl Pts',(138.546087402322,-4.33633187725888,
126.361232236999));
#235459=CARTESIAN_POINT('Ctrl Pts',(138.267639778509,-6.08202304295846,
132.051020018064));
#235460=CARTESIAN_POINT('Ctrl Pts',(137.989192154696,-2.23863215552307,
136.595188712768));
#235461=CARTESIAN_POINT('Ctrl Pts',(137.710744530883,3.66195231957746,135.817869285661));
#235462=CARTESIAN_POINT('Ctrl Pts',(137.43229690707,6.19738150930245,130.433380316089));
#235463=CARTESIAN_POINT('Ctrl Pts',(137.153849283257,3.03771985089675,125.389804120178));
#235464=CARTESIAN_POINT('Ctrl Pts',(136.875401659444,-2.91345794961824,
125.321940829576));
#235465=CARTESIAN_POINT('Ctrl Pts',(136.596954035631,-6.1873102247676,130.29215349304));
#235466=CARTESIAN_POINT('Ctrl Pts',(136.318506411819,-3.77532667026395,
135.733059481234));
#235467=CARTESIAN_POINT('Ctrl Pts',(136.040058788006,2.10599765925102,136.644731994041));
#235468=CARTESIAN_POINT('Ctrl Pts',(135.761611164193,6.05201302361958,132.189388529871));
#235469=CARTESIAN_POINT('Ctrl Pts',(135.48316354038,4.4365240765547,126.461272076668));
#235470=CARTESIAN_POINT('Ctrl Pts',(135.204715916567,-1.25591376061384,
124.724241820878));
#235471=CARTESIAN_POINT('Ctrl Pts',(134.926268292754,-5.79422820657625,
128.574543708929));
#235472=CARTESIAN_POINT('Ctrl Pts',(134.647820668941,-5.00792999447956,
134.473938403405));
#235473=CARTESIAN_POINT('Ctrl Pts',(134.369373045128,0.380411231562576,
137.001170381535));
#235474=CARTESIAN_POINT('Ctrl Pts',(134.090925421316,5.41917311992063,133.833836917565));
#235475=CARTESIAN_POINT('Ctrl Pts',(133.812477797503,5.4779796523963,127.88256273204));
#235476=CARTESIAN_POINT('Ctrl Pts',(133.53403017369,0.502790498503515,124.616278065551));
#235477=CARTESIAN_POINT('Ctrl Pts',(133.255582549877,-4.93443856083268,
127.036538959725));
#235478=CARTESIAN_POINT('Ctrl Pts',(132.977134926064,-5.83715964348875,
132.919243889133));
#235479=CARTESIAN_POINT('Ctrl Pts',(132.698687302251,-1.37581617488021,
136.858474409763));
#235480=CARTESIAN_POINT('Ctrl Pts',(132.420239678438,4.34983514608645,135.234270115264));
#235481=CARTESIAN_POINT('Ctrl Pts',(132.141792054625,6.07820046906025,129.539195405491));
#235482=CARTESIAN_POINT('Ctrl Pts',(131.863344430812,2.22099649756843,125.006745718858));
#235483=CARTESIAN_POINT('Ctrl Pts',(131.584896806999,-3.67719475347803,
125.802020894903));
#235484=CARTESIAN_POINT('Ctrl Pts',(131.306449183186,-6.1962236670286,131.194201898194));
#235485=CARTESIAN_POINT('Ctrl Pts',(131.028001559374,-3.02122573293442,
136.228137809392));
#235486=CARTESIAN_POINT('Ctrl Pts',(130.749553935561,2.93013105464412,136.277887447547));
#235487=CARTESIAN_POINT('Ctrl Pts',(130.471106311748,6.18884054786473,131.2977333256));
#235488=CARTESIAN_POINT('Ctrl Pts',(130.192658687935,3.76030791926647,125.864193787566));
#235489=CARTESIAN_POINT('Ctrl Pts',(129.914211064122,-2.12376398588317,
124.970426225734));
#235490=CARTESIAN_POINT('Ctrl Pts',(129.635763440309,-6.05620053964477,
129.437759366456));
#235491=CARTESIAN_POINT('Ctrl Pts',(129.357315816496,-4.42328465931731,
135.160932294765));
#235492=CARTESIAN_POINT('Ctrl Pts',(129.078868192683,1.27441373345414,136.880628682086));
#235493=CARTESIAN_POINT('Ctrl Pts',(128.800420568871,5.80098816375315,133.01653156031));
#235494=CARTESIAN_POINT('Ctrl Pts',(128.521972945058,4.99673786558976,127.11955741271));
#235495=CARTESIAN_POINT('Ctrl Pts',(128.243525321245,-0.399270426835251,
124.608737397728));
#235496=CARTESIAN_POINT('Ctrl Pts',(127.965077697432,-5.42836870244348,
127.791392448756));
#235497=CARTESIAN_POINT('Ctrl Pts',(127.686630073619,-5.46906133106002,
133.742818055242));
#235498=CARTESIAN_POINT('Ctrl Pts',(127.408182449806,-0.483953774931917,
136.993944828129));
#235499=CARTESIAN_POINT('Ctrl Pts',(127.129734825993,4.9458836579024,134.557146089508));
#235500=CARTESIAN_POINT('Ctrl Pts',(126.85128720218,5.8306956289736,128.671720835934));
#235501=CARTESIAN_POINT('Ctrl Pts',(126.572839578367,1.35738316233494,124.746087356435));
#235502=CARTESIAN_POINT('Ctrl Pts',(126.294391954555,-4.36329811863544,
126.387711040812));
#235503=CARTESIAN_POINT('Ctrl Pts',(126.015944330741,-6.07432158754323,
132.088019920899));
#235504=CARTESIAN_POINT('Ctrl Pts',(125.737496706929,-2.20334026460562,
136.608708611466));
#235505=CARTESIAN_POINT('Ctrl Pts',(125.459049083116,3.69240312234872,135.795485053802));
#235506=CARTESIAN_POINT('Ctrl Pts',(125.180601459303,6.19500842378515,130.39566196922));
#235507=CARTESIAN_POINT('Ctrl Pts',(124.90215383549,3.00470362674961,125.371412976429));
#235508=CARTESIAN_POINT('Ctrl Pts',(124.623706211677,-2.9467770153362,125.339777451594));
#235509=CARTESIAN_POINT('Ctrl Pts',(124.345258587864,-6.19031353838844,
130.329826896558));
#235510=CARTESIAN_POINT('Ctrl Pts',(124.066810964051,-3.74525433329013,
135.755949648866));
#235511=CARTESIAN_POINT('Ctrl Pts',(123.788363340238,2.14151063825588,136.631803979981));
#235512=CARTESIAN_POINT('Ctrl Pts',(123.509915716426,6.0603319518555,132.152522547471));
#235513=CARTESIAN_POINT('Ctrl Pts',(123.231468092613,4.4100042653751,126.43434616275));
#235514=CARTESIAN_POINT('Ctrl Pts',(122.9530204688,-1.29290190029971,124.731999574929));
#235515=CARTESIAN_POINT('Ctrl Pts',(122.674572844987,-5.80769438136815,
128.609856133963));
#235516=CARTESIAN_POINT('Ctrl Pts',(122.396125221174,-4.98549944760296,
134.504355105923));
#235517=CARTESIAN_POINT('Ctrl Pts',(122.117677597361,0.418125923321227,
136.998739897863));
#235518=CARTESIAN_POINT('Ctrl Pts',(121.839229973548,5.43751399730024,133.80079274346));
#235519=CARTESIAN_POINT('Ctrl Pts',(121.560782349735,5.46009234508668,127.849270849208));
#235520=CARTESIAN_POINT('Ctrl Pts',(121.282334725922,0.465112568078527,
124.613332087916));
#235521=CARTESIAN_POINT('Ctrl Pts',(121.00388710211,-4.95728293698158,127.066646096814));
#235522=CARTESIAN_POINT('Ctrl Pts',(120.725439478297,-5.82417759969065,
132.954737152777));
#235523=CARTESIAN_POINT('Ctrl Pts',(120.446991854484,-1.33893757517749,
136.866737224615));
#235524=CARTESIAN_POINT('Ctrl Pts',(120.168544230671,4.37672067018674,135.207709358136));
#235525=CARTESIAN_POINT('Ctrl Pts',(119.890096606858,6.07038643434081,129.502219114618));
#235526=CARTESIAN_POINT('Ctrl Pts',(119.611648983045,2.18566362019961,124.993333299159));
#235527=CARTESIAN_POINT('Ctrl Pts',(119.333201359232,-3.7075772853013,125.82449770485));
#235528=CARTESIAN_POINT('Ctrl Pts',(119.054753735419,-6.19373579082994,
131.231912847497));
#235529=CARTESIAN_POINT('Ctrl Pts',(118.776306111606,-2.98815368540088,
136.246428377926));
#235530=CARTESIAN_POINT('Ctrl Pts',(118.497858487794,2.96339567748857,136.259949496373));
#235531=CARTESIAN_POINT('Ctrl Pts',(118.219410863981,6.1917291826932,131.26005095553));
#235532=CARTESIAN_POINT('Ctrl Pts',(117.940963240168,3.73016605178927,125.841395255808));
#235533=CARTESIAN_POINT('Ctrl Pts',(117.662515616355,-2.15923745196658,
124.983462269205));
#235534=CARTESIAN_POINT('Ctrl Pts',(117.384067992542,-6.06440722197891,
129.474650498052));
#235535=CARTESIAN_POINT('Ctrl Pts',(117.105620368729,-4.39668301775581,
135.187777366781));
#235536=CARTESIAN_POINT('Ctrl Pts',(116.827172744916,1.31137808987868,136.872758384795));
#235537=CARTESIAN_POINT('Ctrl Pts',(116.548725121103,5.81434679729579,132.981178312436));
#235538=CARTESIAN_POINT('Ctrl Pts',(116.27027749729,4.97421484463032,127.089209121948));
#235539=CARTESIAN_POINT('Ctrl Pts',(115.991829873478,-0.436977546345769,
124.611282660692));
#235540=CARTESIAN_POINT('Ctrl Pts',(115.713382249665,-5.44660891977013,
127.824492293124));
#235541=CARTESIAN_POINT('Ctrl Pts',(115.434934625852,-5.45107277756375,
133.776055341058));
#235542=CARTESIAN_POINT('Ctrl Pts',(115.156487002039,-0.446267052485976,
136.99677611346));
#235543=CARTESIAN_POINT('Ctrl Pts',(114.878039378226,4.9686362924688,134.526969561451));
#235544=CARTESIAN_POINT('Ctrl Pts',(114.599591754413,5.81760561602206,128.636267249567));
#235545=CARTESIAN_POINT('Ctrl Pts',(114.3211441306,1.32047958428524,124.737936825626));
#235546=CARTESIAN_POINT('Ctrl Pts',(114.042696506787,-4.39010267639563,
126.414353505198));
#235547=CARTESIAN_POINT('Ctrl Pts',(113.764248882975,-6.06639504590774,
132.124972257267));
#235548=CARTESIAN_POINT('Ctrl Pts',(113.485801259161,-2.16796672810439,
136.622013427915));
#235549=CARTESIAN_POINT('Ctrl Pts',(113.207353635349,3.72271710176439,135.772915873991));
#235550=CARTESIAN_POINT('Ctrl Pts',(112.928906011536,6.19240577995249,130.357958766832));
#235551=CARTESIAN_POINT('Ctrl Pts',(112.650458387723,2.97157606220462,125.353223152553));
#235552=CARTESIAN_POINT('Ctrl Pts',(112.37201076391,-2.9799868871482,125.357816565752));
#235553=CARTESIAN_POINT('Ctrl Pts',(112.093563140097,-6.19308746766462,
130.367517884098));
#235554=CARTESIAN_POINT('Ctrl Pts',(111.815115516284,-3.71504321453968,
135.778656333547));
#235555=CARTESIAN_POINT('Ctrl Pts',(111.536667892471,2.1769442627965,136.618660027865));
#235556=CARTESIAN_POINT('Ctrl Pts',(111.258220268658,6.06842631226225,132.115606608435));
#235557=CARTESIAN_POINT('Ctrl Pts',(110.979772644846,4.38332103986566,126.407582181323));
#235558=CARTESIAN_POINT('Ctrl Pts',(110.701325021032,-1.32984213103019,
124.739982342551));
#235559=CARTESIAN_POINT('Ctrl Pts',(110.42287739722,-5.82094534990898,128.645249877167));
#235560=CARTESIAN_POINT('Ctrl Pts',(110.144429773407,-4.96288416121089,
134.534634703787));
#235561=CARTESIAN_POINT('Ctrl Pts',(109.865982149594,0.455825121270016,
136.996079879188));
#235562=CARTESIAN_POINT('Ctrl Pts',(109.587534525781,5.45565338559904,133.767637535461));
#235563=CARTESIAN_POINT('Ctrl Pts',(109.309086901968,5.44200271204727,127.816088468313));
#235564=CARTESIAN_POINT('Ctrl Pts',(109.030639278155,0.427417402736423,
124.610615521118));
#235565=CARTESIAN_POINT('Ctrl Pts',(108.752191654342,-4.97994361918818,
127.096891736289));
#235566=CARTESIAN_POINT('Ctrl Pts',(108.473744030529,-5.81097973884976,
132.990150733429));
#235567=CARTESIAN_POINT('Ctrl Pts',(108.195296406717,-1.30200936065053,
136.874775395874));
#235568=CARTESIAN_POINT('Ctrl Pts',(107.916848782904,4.40344401329306,135.180985433302));
#235569=CARTESIAN_POINT('Ctrl Pts',(107.638401159091,6.06234745921968,129.465291075077));
#235570=CARTESIAN_POINT('Ctrl Pts',(107.359953535278,2.15024975226158,124.980136209215));
#235571=CARTESIAN_POINT('Ctrl Pts',(107.081505911465,-3.73782243148481,
125.847159045447));
#235572=CARTESIAN_POINT('Ctrl Pts',(106.803058287652,-6.19101840347381,
131.269607953695));
#235573=CARTESIAN_POINT('Ctrl Pts',(106.524610663839,-2.95497091073364,
136.264517288637));
#235574=CARTESIAN_POINT('Ctrl Pts',(106.246163040026,2.99655049061638,136.241809386346));
#235575=CARTESIAN_POINT('Ctrl Pts',(105.967715416213,6.1943883807198,131.222351699685));
#235576=CARTESIAN_POINT('Ctrl Pts',(105.689267792401,3.69988596163724,125.818780628557));
#235577=CARTESIAN_POINT('Ctrl Pts',(105.410820168588,-2.19463090671215,
124.996714008204));
#235578=CARTESIAN_POINT('Ctrl Pts',(105.132372544775,-6.07238918547325,
129.511590902545));
#235579=CARTESIAN_POINT('Ctrl Pts',(104.853924920962,-4.36991845548819,
135.214460009678));
#235580=CARTESIAN_POINT('Ctrl Pts',(104.575477297149,1.34829385270585,136.864663220793));
#235581=CARTESIAN_POINT('Ctrl Pts',(104.297029673336,5.82748997807964,132.945744401783));
#235582=CARTESIAN_POINT('Ctrl Pts',(104.018582049523,4.95150750231056,127.058998497491));
#235583=CARTESIAN_POINT('Ctrl Pts',(103.74013442571,-0.474668473492613,
124.614057410436));
#235584=CARTESIAN_POINT('Ctrl Pts',(103.461686801897,-5.46464731100027,
127.857702557609));
#235585=CARTESIAN_POINT('Ctrl Pts',(103.183239178085,-5.43288223256107,
133.809182509633));
#235586=CARTESIAN_POINT('Ctrl Pts',(102.904791554272,-0.408563793450433,
136.999377936557));
#235587=CARTESIAN_POINT('Ctrl Pts',(102.626343930459,4.99120481239017,134.496655090749));
#235588=CARTESIAN_POINT('Ctrl Pts',(102.347896306646,5.80430002955499,128.600894002697));
#235589=CARTESIAN_POINT('Ctrl Pts',(102.069448682833,1.28352707537895,124.730011088381));
#235590=CARTESIAN_POINT('Ctrl Pts',(101.79100105902,-4.41674455728669,126.441158642913));
#235591=CARTESIAN_POINT('Ctrl Pts',(101.512553435207,-6.05824371177293,
132.161875657885));
#235592=CARTESIAN_POINT('Ctrl Pts',(101.234105811394,-2.13251285679878,
136.635102669099));
#235593=CARTESIAN_POINT('Ctrl Pts',(100.955658187581,3.75289313452884,135.750162582539));
#235594=CARTESIAN_POINT('Ctrl Pts',(100.677210563769,6.18957367424645,130.320272106026));
#235595=CARTESIAN_POINT('Ctrl Pts',(100.398762939956,2.93833838481571,125.33523532258));
#235596=CARTESIAN_POINT('Ctrl Pts',(100.120315316143,-3.01308633445025,
125.376057503601));
#235597=CARTESIAN_POINT('Ctrl Pts',(99.8418676923298,-6.19563190980719,
130.405225059005));
#235598=CARTESIAN_POINT('Ctrl Pts',(99.5634200685172,-3.68469443349671,
135.801178693871));
#235599=CARTESIAN_POINT('Ctrl Pts',(99.2849724447041,2.2122972198669,136.605300624745));
#235600=CARTESIAN_POINT('Ctrl Pts',(99.0065248208913,6.07629580490035,132.078642080696));
#235601=CARTESIAN_POINT('Ctrl Pts',(98.7280771970783,4.35647538878314,126.380981124141));
#235602=CARTESIAN_POINT('Ctrl Pts',(98.4496295732656,-1.36673308397146,
124.748189827941));
#235603=CARTESIAN_POINT('Ctrl Pts',(98.1711819494526,-5.8339806211792,128.680723627015));
#235604=CARTESIAN_POINT('Ctrl Pts',(97.8927343256397,-4.94008497332115,
134.564776074971));
#235605=CARTESIAN_POINT('Ctrl Pts',(97.6142867018267,0.493507428451318,
136.993190424079));
#235606=CARTESIAN_POINT('Ctrl Pts',(97.3358390780141,5.47359061265531,133.734372522146));
#235607=CARTESIAN_POINT('Ctrl Pts',(97.0573914542009,5.42371142359607,127.783016818942));
#235608=CARTESIAN_POINT('Ctrl Pts',(96.7789438303882,0.389706399285272,
124.608128465823));
#235609=CARTESIAN_POINT('Ctrl Pts',(96.5004962065753,-5.0024197677526,127.127274757387));
#235610=CARTESIAN_POINT('Ctrl Pts',(96.2220485827623,-5.79756655001767,
133.025483318824));
#235611=CARTESIAN_POINT('Ctrl Pts',(95.9436009589496,-1.26503289968789,
136.882588625681));
#235612=CARTESIAN_POINT('Ctrl Pts',(95.6651533351365,4.4300041851621,135.154099331026));
#235613=CARTESIAN_POINT('Ctrl Pts',(95.3867057113237,6.05408384158403,129.428412655251));
#235614=CARTESIAN_POINT('Ctrl Pts',(95.1082580875108,2.11475620602821,124.967154938047));
#235615=CARTESIAN_POINT('Ctrl Pts',(94.8298104636979,-3.76792907128354,
125.870004076972));
#235616=CARTESIAN_POINT('Ctrl Pts',(94.5513628398851,-6.18807160565406,
131.307285819983));
#235617=CARTESIAN_POINT('Ctrl Pts',(94.2729152160721,-2.92167863853249,
136.282403871234));
#235618=CARTESIAN_POINT('Ctrl Pts',(93.9944675922592,3.02959426546386,136.223467789656));
#235619=CARTESIAN_POINT('Ctrl Pts',(93.7160199684464,6.19681804340696,131.184636955029));
#235620=CARTESIAN_POINT('Ctrl Pts',(93.4375723446334,3.66946877085029,125.796350743805));
#235621=CARTESIAN_POINT('Ctrl Pts',(93.1591247208205,-2.22994303860241,
125.010180951684));
#235622=CARTESIAN_POINT('Ctrl Pts',(92.8806770970077,-6.08014613435319,
129.548579211095));
#235623=CARTESIAN_POINT('Ctrl Pts',(92.6022294731947,-4.3429919642852,135.24097923472));
#235624=CARTESIAN_POINT('Ctrl Pts',(92.323781849382,1.38515965400848,136.856343490049));
#235625=CARTESIAN_POINT('Ctrl Pts',(92.045334225569,5.84041721907928,132.910231141365));
#235626=CARTESIAN_POINT('Ctrl Pts',(91.7668866017561,4.9286166800594,127.028926658805));
#235627=CARTESIAN_POINT('Ctrl Pts',(91.4884389779432,-0.512341811624615,
124.617061544141));
#235628=CARTESIAN_POINT('Ctrl Pts',(91.2099913541303,-5.48248320771468,
127.891022011592));
#235629=CARTESIAN_POINT('Ctrl Pts',(90.9315437303175,-5.41449037010934,
133.842198333429));
#235630=CARTESIAN_POINT('Ctrl Pts',(90.6530961065044,-0.370845394933272,
137.00175020101));
#235631=CARTESIAN_POINT('Ctrl Pts',(90.3746484826917,5.01358838138169,134.466203800718));
#235632=CARTESIAN_POINT('Ctrl Pts',(90.0962008588786,5.79077936261581,128.565602406094));
#235633=CARTESIAN_POINT('Ctrl Pts',(89.817753235066,1.24652700490487,124.722310438393));
#235634=CARTESIAN_POINT('Ctrl Pts',(89.5393056112528,-4.44322277408392,
126.468125460682));
#235635=CARTESIAN_POINT('Ctrl Pts',(89.2608579874402,-6.04986788718945,
132.198728755283));
#235636=CARTESIAN_POINT('Ctrl Pts',(88.9824103636271,-2.09697996444503,
136.647975849991));
#235637=CARTESIAN_POINT('Ctrl Pts',(88.7039627398144,3.78293010245805,135.727226022576));
#235638=CARTESIAN_POINT('Ctrl Pts',(88.4255151160013,6.18651221161165,130.282603383299));
#235639=CARTESIAN_POINT('Ctrl Pts',(88.1470674921886,2.9049918262175,125.317450153056));
#235640=CARTESIAN_POINT('Ctrl Pts',(87.8686198683756,-3.04607413073006,
125.394499589218));
#235641=CARTESIAN_POINT('Ctrl Pts',(87.5901722445627,-6.19794677053091,
130.442947024027));
#235642=CARTESIAN_POINT('Ctrl Pts',(87.3117246207499,-3.65420911474647,
135.823515895262));
#235643=CARTESIAN_POINT('Ctrl Pts',(87.033276996937,2.24756819945024,136.59172626566));
#235644=CARTESIAN_POINT('Ctrl Pts',(86.754829373124,6.08394013816284,132.041630333989));
#235645=CARTESIAN_POINT('Ctrl Pts',(86.4763817493112,4.32946830690299,126.35454397691));
#235646=CARTESIAN_POINT('Ctrl Pts',(86.1979341254982,-1.40357339211569,
124.756621726966));
#235647=CARTESIAN_POINT('Ctrl Pts',(85.9194865016854,-5.84679971215209,
128.716276069012));
#235648=CARTESIAN_POINT('Ctrl Pts',(85.6410388778725,-4.91710272876601,
134.594778102578));
#235649=CARTESIAN_POINT('Ctrl Pts',(85.3625912540596,0.531171448533366,
136.990071639606));
#235650=CARTESIAN_POINT('Ctrl Pts',(85.0841436302467,5.49132501379855,133.700998936161));
#235651=CARTESIAN_POINT('Ctrl Pts',(84.8056960064338,5.4052191575235,127.750057126576));
#235652=CARTESIAN_POINT('Ctrl Pts',(84.527248382621,0.351980955120191,124.60587101419));
#235653=CARTESIAN_POINT('Ctrl Pts',(84.2488007588079,-5.02471054981291,
127.157794034254));
#235654=CARTESIAN_POINT('Ctrl Pts',(83.9703531349953,-5.78393853022499,
133.0607335997));
#235655=CARTESIAN_POINT('Ctrl Pts',(83.6919055111822,-1.22800956246596,
136.890176624513));
#235656=CARTESIAN_POINT('Ctrl Pts',(83.4134578873695,4.45640020159694,135.127052047582));
#235657=CARTESIAN_POINT('Ctrl Pts',(83.1350102635564,6.04559588764522,129.391585221682));
#235658=CARTESIAN_POINT('Ctrl Pts',(82.8565626397436,2.07918429672594,124.954389966684));
#235659=CARTESIAN_POINT('Ctrl Pts',(82.5781150159307,-3.79789608908488,
125.893031952893));
#235660=CARTESIAN_POINT('Ctrl Pts',(82.2996673921181,-6.18489550656524,
131.344945050191));
#235661=CARTESIAN_POINT('Ctrl Pts',(82.0212197683047,-2.88827810245507,
136.300087462925));
#235662=CARTESIAN_POINT('Ctrl Pts',(81.7427721444922,3.06252577758164,136.204925385956));
#235663=CARTESIAN_POINT('Ctrl Pts',(81.464324520679,6.19901808072266,131.146908119091));
#235664=CARTESIAN_POINT('Ctrl Pts',(81.1858768968663,3.6389156065486,125.774106432701));
#235665=CARTESIAN_POINT('Ctrl Pts',(80.9074292730533,-2.26517253913331,
125.023862600622));
#235666=CARTESIAN_POINT('Ctrl Pts',(80.6289816492404,-6.08767778118217,
129.585614053086));
#235667=CARTESIAN_POINT('Ctrl Pts',(80.3505340254275,-4.31590454191782,
135.267334059228));
#235668=CARTESIAN_POINT('Ctrl Pts',(80.0720864016147,1.42197412771073,136.847799500855));
#235669=CARTESIAN_POINT('Ctrl Pts',(79.7936387778018,5.85312804127117,132.874639847142));
#235670=CARTESIAN_POINT('Ctrl Pts',(79.5151911539889,4.90554322610457,126.998994720211));
#235671=CARTESIAN_POINT('Ctrl Pts',(79.236743530176,-0.54999616474248,124.62029495049));
#235672=CARTESIAN_POINT('Ctrl Pts',(78.9582959063631,-5.50011594899764,
127.924449420408));
#235673=CARTESIAN_POINT('Ctrl Pts',(78.6798482825503,-5.39589787172579,
133.87510158903));
#235674=CARTESIAN_POINT('Ctrl Pts',(78.4014006587372,-0.333113254603616,
137.003892818912));
#235675=CARTESIAN_POINT('Ctrl Pts',(78.1229530349246,5.035786170012,134.435616819741));
#235676=CARTESIAN_POINT('Ctrl Pts',(77.8445054111114,5.77704411621779,128.530393767498));
#235677=CARTESIAN_POINT('Ctrl Pts',(77.5660577872988,1.20948074391421,124.71483516101));
#235678=CARTESIAN_POINT('Ctrl Pts',(77.2876101634857,-4.46953634562727,
126.49525295924));
#235679=CARTESIAN_POINT('Ctrl Pts',(77.009162539673,-6.04126788252658,132.235530183857));
#235680=CARTESIAN_POINT('Ctrl Pts',(76.73071491586,-2.06136936772754,136.660632493573));
#235681=CARTESIAN_POINT('Ctrl Pts',(76.4522672920471,3.81282689252116,135.704107044024));
#235682=CARTESIAN_POINT('Ctrl Pts',(76.1738196682342,6.18322150549176,130.244953994479));
#235683=CARTESIAN_POINT('Ctrl Pts',(75.8953720444213,2.87153762207887,125.299868303017));
#235684=CARTESIAN_POINT('Ctrl Pts',(75.6169244206085,-3.07894905361277,
125.413142139227));
#235685=CARTESIAN_POINT('Ctrl Pts',(75.3384767967955,-6.20003196405775,
130.480682381363));
#235686=CARTESIAN_POINT('Ctrl Pts',(75.0600291729826,-3.62358838793365,
135.84566711001));
#235687=CARTESIAN_POINT('Ctrl Pts',(74.7815815491698,2.28275589456742,136.577937453613));
#235688=CARTESIAN_POINT('Ctrl Pts',(74.5031339253568,6.09135902878616,132.004572739798));
#235689=CARTESIAN_POINT('Ctrl Pts',(74.224686301544,4.30230079498258,126.328271719272));
#235690=CARTESIAN_POINT('Ctrl Pts',(73.946238677731,-1.44036169033171,124.76527772718));
#235691=CARTESIAN_POINT('Ctrl Pts',(73.6677910539182,-5.85940214781156,
128.75190588575));
#235692=CARTESIAN_POINT('Ctrl Pts',(73.3893434301052,-4.89393827916089,
134.624639674871));
#235693=CARTESIAN_POINT('Ctrl Pts',(73.1108958062924,0.56881578586215,136.986723641335));
#235694=CARTESIAN_POINT('Ctrl Pts',(72.8324481824796,5.50885593187395,133.66751801418));
#235695=CARTESIAN_POINT('Ctrl Pts',(72.5540005586665,5.38652659906729,127.717210612549));
#235696=CARTESIAN_POINT('Ctrl Pts',(72.2755529348538,0.314242468171368,
124.603843249867));
#235697=CARTESIAN_POINT('Ctrl Pts',(71.9971053110409,-5.04681513937595,
127.188448435987));
#235698=CARTESIAN_POINT('Ctrl Pts',(71.7186576872279,-5.77009618446306,
133.095900269846));
#235699=CARTESIAN_POINT('Ctrl Pts',(71.4402100634152,-1.19094072089807,
136.897539111196));
#235700=CARTESIAN_POINT('Ctrl Pts',(71.1617624396021,4.48263108448347,135.099844585217));
#235701=CARTESIAN_POINT('Ctrl Pts',(70.8833148157894,6.03688391192757,129.354810139024));
#235702=CARTESIAN_POINT('Ctrl Pts',(70.6048671919763,2.04353534248492,124.941841768133));
#235703=CARTESIAN_POINT('Ctrl Pts',(70.3264195681636,-3.82772237444985,
125.916241819903));
#235704=CARTESIAN_POINT('Ctrl Pts',(70.0479719443506,-6.18149022389895,
131.382584248845));
#235705=CARTESIAN_POINT('Ctrl Pts',(69.7695243205378,-2.85477054017052,
136.317567408437));
#235706=CARTESIAN_POINT('Ctrl Pts',(69.4910766967249,3.09534380668036,136.186182862342));
#235707=CARTESIAN_POINT('Ctrl Pts',(69.2126290729119,6.20098841114368,131.109166589932));
#235708=CARTESIAN_POINT('Ctrl Pts',(68.934181449099,3.60822760089105,125.752048519516));
#235709=CARTESIAN_POINT('Ctrl Pts',(68.6557338252862,-2.30031810286251,
125.037758448041));
#235710=CARTESIAN_POINT('Ctrl Pts',(68.3772862014732,-6.09498384687224,
129.622694056181));
#235711=CARTESIAN_POINT('Ctrl Pts',(68.0988385776604,-4.28865719212064,
135.293523506613));
#235712=CARTESIAN_POINT('Ctrl Pts',(67.8203909538475,1.45873590963839,136.83903156981));
#235713=CARTESIAN_POINT('Ctrl Pts',(67.5419433300346,5.86562197365073,132.83897183796));
#235714=CARTESIAN_POINT('Ctrl Pts',(67.2634957062218,4.88228799544191,126.969203790852));
#235715=CARTESIAN_POINT('Ctrl Pts',(66.9850480824087,-0.587630137549865,
124.623757509667));
#235716=CARTESIAN_POINT('Ctrl Pts',(66.706600458596,-5.51754488146136,127.957983545393));
#235717=CARTESIAN_POINT('Ctrl Pts',(66.428152834783,-5.37710542636232,133.907891057196));
#235718=CARTESIAN_POINT('Ctrl Pts',(66.1497052109702,-0.295368770640213,
137.00580571087));
#235719=CARTESIAN_POINT('Ctrl Pts',(65.8712575871573,5.05779735573374,134.404895281231));
#235720=CARTESIAN_POINT('Ctrl Pts',(65.5928099633443,5.76309479932555,128.495269391582));
#235721=CARTESIAN_POINT('Ctrl Pts',(65.3143623395316,1.17238966517029,124.707585533234));
#235722=CARTESIAN_POINT('Ctrl Pts',(65.0359147157185,-4.49568429685739,
126.522540133366));
#235723=CARTESIAN_POINT('Ctrl Pts',(64.7574670919057,-6.03244401646077,
132.272278579917));
#235724=CARTESIAN_POINT('Ctrl Pts',(64.4790194680927,-2.02568238621027,
136.673072130848));
#235725=CARTESIAN_POINT('Ctrl Pts',(64.20057184428,3.84258239688126,135.680806503568));
#235726=CARTESIAN_POINT('Ctrl Pts',(63.922124220467,6.17970167782515,130.207325334677));
#235727=CARTESIAN_POINT('Ctrl Pts',(63.6436765966542,2.8379770120581,125.282490423967));
#235728=CARTESIAN_POINT('Ctrl Pts',(63.3652289728412,-3.11170988490585,
125.431984462817));
#235729=CARTESIAN_POINT('Ctrl Pts',(63.0867813490283,-6.20188741312008,
130.518429732716));
#235730=CARTESIAN_POINT('Ctrl Pts',(62.8083337252156,-3.59283338772076,
135.86763151729));
#235731=CARTESIAN_POINT('Ctrl Pts',(62.5298861014024,2.31785900132509,136.563934699553));
#235732=CARTESIAN_POINT('Ctrl Pts',(62.2514384775899,6.09855220186056,131.967470671305));
#235733=CARTESIAN_POINT('Ctrl Pts',(61.9729908537767,4.27497385972414,126.302165324755));
#235734=CARTESIAN_POINT('Ctrl Pts',(61.6945432299639,-1.47709661541541,
124.774157507831));
#235735=CARTESIAN_POINT('Ctrl Pts',(61.416095606151,-5.87178746116934,128.787611756953));
#235736=CARTESIAN_POINT('Ctrl Pts',(61.1376479823382,-4.8705924828735,134.65435968532));
#235737=CARTESIAN_POINT('Ctrl Pts',(60.8592003585251,0.606439045512412,
136.983146553331));
#235738=CARTESIAN_POINT('Ctrl Pts',(60.5807527347125,5.52618271726667,133.633930996847));
#235739=CARTESIAN_POINT('Ctrl Pts',(60.3023051108993,5.36763444088732,127.684478494003));
#235740=CARTESIAN_POINT('Ctrl Pts',(60.0238574870866,0.276492336852797,
124.602045247997));
#235741=CARTESIAN_POINT('Ctrl Pts',(59.7454098632736,-5.06873271734795,
127.219236826675));
#235742=CARTESIAN_POINT('Ctrl Pts',(59.4669622394608,-5.75604002566515,
133.130982026147));
#235743=CARTESIAN_POINT('Ctrl Pts',(59.1885146156479,-1.15382774858414,
136.904675812908));
#235744=CARTESIAN_POINT('Ctrl Pts',(58.9100669918351,4.50869586182645,135.072477952114));
#235745=CARTESIAN_POINT('Ctrl Pts',(58.6316193680221,6.02794823725661,129.318088769994));
#235746=CARTESIAN_POINT('Ctrl Pts',(58.3531717442092,2.00781066429043,124.929510807376));
#235747=CARTESIAN_POINT('Ctrl Pts',(58.0747241203963,-3.85740682215468,
125.939632817953));
#235748=CARTESIAN_POINT('Ctrl Pts',(57.7962764965834,-6.17785588383907,
131.42020202121));
#235749=CARTESIAN_POINT('Ctrl Pts',(57.5178288727705,-2.82115719331391,
136.334843060042));
#235750=CARTESIAN_POINT('Ctrl Pts',(57.2393812489577,3.12804713667602,136.167240913326));
#235751=CARTESIAN_POINT('Ctrl Pts',(56.9609336251447,6.20272896165862,131.071413766074));
#235752=CARTESIAN_POINT('Ctrl Pts',(56.6824860013319,3.57740589103289,125.730177821614));
#235753=CARTESIAN_POINT('Ctrl Pts',(56.404038377519,-2.33537842745856,125.051867979023));
#235754=CARTESIAN_POINT('Ctrl Pts',(56.125590753706,-6.10206406069443,129.659817846364));
#235755=CARTESIAN_POINT('Ctrl Pts',(55.8471431298932,-4.26125092455389,
135.319546606417));
#235756=CARTESIAN_POINT('Ctrl Pts',(55.5686955060803,1.49544363757083,136.830040021814));
#235757=CARTESIAN_POINT('Ctrl Pts',(55.2902478822675,5.87789855325116,132.80322843551));
#235758=CARTESIAN_POINT('Ctrl Pts',(55.0118002584545,4.85885184980179,126.939554974638));
#235759=CARTESIAN_POINT('Ctrl Pts',(54.7333526346416,-0.625242335506623,
124.627449093364));
#235760=CARTESIAN_POINT('Ctrl Pts',(54.4549050108287,-5.53476935927053,
127.991623143927));
#235761=CARTESIAN_POINT('Ctrl Pts',(54.1764573870159,-5.35811373037978,
133.9405655229));
#235762=CARTESIAN_POINT('Ctrl Pts',(53.8980097632029,-0.257613341678002,
137.007488805997));
#235763=CARTESIAN_POINT('Ctrl Pts',(53.61956213939,5.07962112291461,134.374040323585));
#235764=CARTESIAN_POINT('Ctrl Pts',(53.3411145155772,5.74893192883615,128.460230579889));
#235765=CARTESIAN_POINT('Ctrl Pts',(53.0626668917642,1.13525514309568,124.7005618237));
#235766=CARTESIAN_POINT('Ctrl Pts',(52.7842192679514,-4.52166565885288,
126.549985971924));
#235767=CARTESIAN_POINT('Ctrl Pts',(52.5057716441385,-6.0233966159634,132.308972581737));
#235768=CARTESIAN_POINT('Ctrl Pts',(52.2273240203255,-1.98992034228702,
136.685294300858));
#235769=CARTESIAN_POINT('Ctrl Pts',(51.9488763965128,3.87219551293788,135.657325264614));
#235770=CARTESIAN_POINT('Ctrl Pts',(51.6704287726998,6.17595285904027,130.169718798237));
#235771=CARTESIAN_POINT('Ctrl Pts',(51.391981148887,2.80431123975502,125.265317159845));
#235772=CARTESIAN_POINT('Ctrl Pts',(51.113533525074,-3.14435541064497,125.451025861782));
#235773=CARTESIAN_POINT('Ctrl Pts',(50.8350859012611,-6.20351304896362,
130.556187679343));
#235774=CARTESIAN_POINT('Ctrl Pts',(50.5566382774483,-3.5619452537452,135.889408303207));
#235775=CARTESIAN_POINT('Ctrl Pts',(50.2781906536353,2.35287621896542,136.549718522358));
#235776=CARTESIAN_POINT('Ctrl Pts',(49.9997430298226,6.10551939084041,131.930325503341));
#235777=CARTESIAN_POINT('Ctrl Pts',(49.7212954060095,4.2474885137371,126.27622576074));
#235778=CARTESIAN_POINT('Ctrl Pts',(49.4428477821967,-1.51377680614101,
124.783260739875));
#235779=CARTESIAN_POINT('Ctrl Pts',(49.1644001583838,-5.88395519328364,
128.823392359526));
#235780=CARTESIAN_POINT('Ctrl Pts',(48.8859525345709,-4.84706620499019,
134.683937032636));
#235781=CARTESIAN_POINT('Ctrl Pts',(48.607504910758,0.644039833341117,136.97934050814));
#235782=CARTESIAN_POINT('Ctrl Pts',(48.3290572869451,5.54330472792681,133.600239128744));
#235783=CARTESIAN_POINT('Ctrl Pts',(48.0506096631323,5.34854338303893,127.651861983834));
#235784=CARTESIAN_POINT('Ctrl Pts',(47.7721620393193,0.23873196000854,124.600477075203));
#235785=CARTESIAN_POINT('Ctrl Pts',(47.4937144155065,-5.09046247156518,
127.250158065443));
#235786=CARTESIAN_POINT('Ctrl Pts',(47.2152667916935,-5.74177057468722,
133.165977568637));
#235787=CARTESIAN_POINT('Ctrl Pts',(46.9368191678807,-1.11667202075834,
136.911586465198));
#235788=CARTESIAN_POINT('Ctrl Pts',(46.6583715440677,4.53459356778643,135.044953162355));
#235789=CARTESIAN_POINT('Ctrl Pts',(46.379923920255,6.01878919474683,129.281422475313));
#235790=CARTESIAN_POINT('Ctrl Pts',(46.101476296442,1.97201158593325,124.917397541337));
#235791=CARTESIAN_POINT('Ctrl Pts',(45.8230286726291,-3.88694833223118,
125.963204080281));
#235792=CARTESIAN_POINT('Ctrl Pts',(45.5445810488162,-6.17399262105761,
131.457796973343));
#235793=CARTESIAN_POINT('Ctrl Pts',(45.2661334250033,-2.78743930743976,
136.351913777587));
#235794=CARTESIAN_POINT('Ctrl Pts',(44.9876858011905,3.16063455573481,136.148100240809));
#235795=CARTESIAN_POINT('Ctrl Pts',(44.7092381773775,6.20423966777097,131.033651046464));
#235796=CARTESIAN_POINT('Ctrl Pts',(44.4307905535647,3.54645161908363,125.708495149421));
#235797=CARTESIAN_POINT('Ctrl Pts',(44.1523429297517,-2.37035221374829,
125.066190670735));
#235798=CARTESIAN_POINT('Ctrl Pts',(43.8738953059389,-6.10891816028884,
129.696984048001));
#235799=CARTESIAN_POINT('Ctrl Pts',(43.5954476821259,-4.23368675476706,
135.345402394343));
#235800=CARTESIAN_POINT('Ctrl Pts',(43.3170000583131,1.53209595128933,136.820825190051));
#235801=CARTESIAN_POINT('Ctrl Pts',(43.0385524345002,5.88995732515911,132.767410964279));
#235802=CARTESIAN_POINT('Ctrl Pts',(42.7601048106873,4.83523565761953,126.910049370218));
#235803=CARTESIAN_POINT('Ctrl Pts',(42.4816571868744,-0.662831364878718,
124.631369564788));
#235804=CARTESIAN_POINT('Ctrl Pts',(42.2032095630615,-5.55178874416567,
128.025366969483));
#235805=CARTESIAN_POINT('Ctrl Pts',(41.9247619392486,-5.33892348752252,
133.973123775378));
#235806=CARTESIAN_POINT('Ctrl Pts',(41.6463143154357,-0.219848366758665,
137.008942041929));
#235807=CARTESIAN_POINT('Ctrl Pts',(41.3678666916229,5.10125666286673,134.343053090145));
#235808=CARTESIAN_POINT('Ctrl Pts',(41.0894190678099,5.73455602955998,128.425278630796));
#235809=CARTESIAN_POINT('Ctrl Pts',(40.8109714439971,1.09807855372398,124.693764292674));
#235810=CARTESIAN_POINT('Ctrl Pts',(40.5325238201841,-4.5474794688646,126.5775894579));
#235811=CARTESIAN_POINT('Ctrl Pts',(40.2540761963713,-6.01412601628932,
132.345610829607));
#235812=CARTESIAN_POINT('Ctrl Pts',(39.9756285725584,-1.95408456113369,
136.697298550707));
#235813=CARTESIAN_POINT('Ctrl Pts',(39.6971809487455,3.90166514336576,135.633664197272));
#235814=CARTESIAN_POINT('Ctrl Pts',(39.4187333249326,6.171975188051,130.132135778682));
#235815=CARTESIAN_POINT('Ctrl Pts',(39.1402857011198,2.77054155266769,125.248349147017));
#235816=CARTESIAN_POINT('Ctrl Pts',(38.8618380773068,-3.17688442113803,
125.470265630536));
#235817=CARTESIAN_POINT('Ctrl Pts',(38.583390453494,-6.20490881134979,130.593954822108));
#235818=CARTESIAN_POINT('Ctrl Pts',(38.304942829681,-3.53092513057837,135.910996660811));
#235819=CARTESIAN_POINT('Ctrl Pts',(38.0264952058682,2.38780624991219,136.535289448812));
#235820=CARTESIAN_POINT('Ctrl Pts',(37.7480475820552,6.11226033755391,131.893138612335));
#235821=CARTESIAN_POINT('Ctrl Pts',(37.4695999582424,4.21984577550119,126.250453988427));
#235822=CARTESIAN_POINT('Ctrl Pts',(37.1911523344295,-1.55040090331038,
124.792587085991));
#235823=CARTESIAN_POINT('Ctrl Pts',(36.9127047106166,-5.89590489327443,
128.859246367608));
#235824=CARTESIAN_POINT('Ctrl Pts',(36.6342570868037,-4.82336031728617,
134.713370620821));
#235825=CARTESIAN_POINT('Ctrl Pts',(36.3558094629908,0.681616756036961,
136.975305646799));
#235826=CARTESIAN_POINT('Ctrl Pts',(36.0773618391779,5.56022132939171,133.566443658335));
#235827=CARTESIAN_POINT('Ctrl Pts',(35.798914215365,5.32925413294858,127.619362290662));
#235828=CARTESIAN_POINT('Ctrl Pts',(35.5204665915522,0.200962736863706,
124.599138789596));
#235829=CARTESIAN_POINT('Ctrl Pts',(35.2420189677392,-5.11200359682353,
127.281211006494));
#235830=CARTESIAN_POINT('Ctrl Pts',(34.9635713439263,-5.72728836028912,
133.200885600541));
#235831=CARTESIAN_POINT('Ctrl Pts',(34.6851237201134,-1.07947491424015,
136.918270811987));
#235832=CARTESIAN_POINT('Ctrl Pts',(34.4066760963006,4.56032324271418,135.017271235878));
#235833=CARTESIAN_POINT('Ctrl Pts',(34.1282284724876,6.00940712379002,129.244812613665));
#235834=CARTESIAN_POINT('Ctrl Pts',(33.8497808486748,1.93613943396156,124.905502418881));
#235835=CARTESIAN_POINT('Ctrl Pts',(33.5713332248619,-3.91634581000783,
125.986954733445));
#235836=CARTESIAN_POINT('Ctrl Pts',(33.292885601049,-6.16990057870911,131.495367712155));
#235837=CARTESIAN_POINT('Ctrl Pts',(33.0144379772361,-2.753618131977,136.368778928511));
#235838=CARTESIAN_POINT('Ctrl Pts',(32.7359903534233,3.19310485631782,136.128761554055));
#235839=CARTESIAN_POINT('Ctrl Pts',(32.4575427296103,6.20552047350092,130.995879830412));
#235840=CARTESIAN_POINT('Ctrl Pts',(32.1790951057975,3.51536593206519,125.687001306397));
#235841=CARTESIAN_POINT('Ctrl Pts',(31.9006474819845,-2.40523816576522,
125.080725992446));
#235842=CARTESIAN_POINT('Ctrl Pts',(31.6221998581717,-6.11554589167424,
129.734191283883));
#235843=CARTESIAN_POINT('Ctrl Pts',(31.3437522343588,-4.20596570416061,
135.371089912296));
#235844=CARTESIAN_POINT('Ctrl Pts',(31.0653046105458,1.56869149262894,136.811387415981));
#235845=CARTESIAN_POINT('Ctrl Pts',(30.786856986733,5.90179784253235,132.731520751495));
#235846=CARTESIAN_POINT('Ctrl Pts',(30.5084093629201,4.81144029400183,126.880688070935));
#235847=CARTESIAN_POINT('Ctrl Pts',(30.2299617391072,-0.700395832790832,
124.635518778667));
#235848=CARTESIAN_POINT('Ctrl Pts',(29.9515141152943,-5.56860240548724,
128.05921377167));
#235849=CARTESIAN_POINT('Ctrl Pts',(29.6730664914815,-5.31953540889204,
134.005564608172));
#235850=CARTESIAN_POINT('Ctrl Pts',(29.3946188676685,-0.182075245277261,
137.010165364815));
#235851=CARTESIAN_POINT('Ctrl Pts',(29.1161712438556,5.12270317387725,134.311934729152));
#235852=CARTESIAN_POINT('Ctrl Pts',(28.8377236200427,5.71996763420123,128.390414839463));
#235853=CARTESIAN_POINT('Ctrl Pts',(28.5592759962298,1.06086127464794,124.687193192043));
#235854=CARTESIAN_POINT('Ctrl Pts',(28.280828372417,-4.57312477035222,126.605349568435));
#235855=CARTESIAN_POINT('Ctrl Pts',(28.0023807486041,-6.00463256096402,
132.382191965885));
#235856=CARTESIAN_POINT('Ctrl Pts',(27.7239331247912,-1.91817637065835,
136.709084435575));
#235857=CARTESIAN_POINT('Ctrl Pts',(27.4454855009783,3.93099019615694,135.60982417831));
#235858=CARTESIAN_POINT('Ctrl Pts',(27.1670378771654,6.16776881225138,130.094577668667));
#235859=CARTESIAN_POINT('Ctrl Pts',(26.8885902533525,2.73666920214424,125.231587014236));
#235860=CARTESIAN_POINT('Ctrl Pts',(26.6101426295396,-3.20929571101057,
125.48970305614));
#235861=CARTESIAN_POINT('Ctrl Pts',(26.3316950057267,-6.2060746485581,130.631729761538));
#235862=CARTESIAN_POINT('Ctrl Pts',(26.0532473819138,-3.49977416768234,
135.932395790139));
#235863=CARTESIAN_POINT('Ctrl Pts',(25.774799758101,2.42264779982026,136.52064801359));
#235864=CARTESIAN_POINT('Ctrl Pts',(25.4963521342881,6.11877479221284,131.85591137626));
#235865=CARTESIAN_POINT('Ctrl Pts',(25.2179045104751,4.19204666932822,126.224850962798));
#235866=CARTESIAN_POINT('Ctrl Pts',(24.9394568866623,-1.58696754980412,
124.802136200585));
#235867=CARTESIAN_POINT('Ctrl Pts',(24.6610092628494,-5.90763611834117,
128.895172452612));
#235868=CARTESIAN_POINT('Ctrl Pts',(24.3825616390365,-4.79947569819179,
134.742659359205));
#235869=CARTESIAN_POINT('Ctrl Pts',(24.1041140152236,0.719168421173241,
136.97104211882));
#235870=CARTESIAN_POINT('Ctrl Pts',(23.8256663914108,5.57693189481048,133.532545837923));
#235871=CARTESIAN_POINT('Ctrl Pts',(23.5472187675978,5.3097674053865,127.586980618775));
#235872=CARTESIAN_POINT('Ctrl Pts',(23.2687711437849,0.163186066970757,
124.598030440764));
#235873=CARTESIAN_POINT('Ctrl Pts',(22.990323519972,-5.13335529490864,127.312394499151));
#235874=CARTESIAN_POINT('Ctrl Pts',(22.7118758961592,-5.71259391911463,
133.235704828331));
#235875=CARTESIAN_POINT('Ctrl Pts',(22.4334282723462,-1.04223780738205,
136.924728605587));
#235876=CARTESIAN_POINT('Ctrl Pts',(22.1549806485334,4.58588393318709,134.98943319845));
#235877=CARTESIAN_POINT('Ctrl Pts',(21.8765330247205,5.9998023720423,129.208260541641));
#235878=CARTESIAN_POINT('Ctrl Pts',(21.5980854009075,1.90019553763114,124.893825880784));
#235879=CARTESIAN_POINT('Ctrl Pts',(21.3196377770947,-3.94559816615024,
126.010883897355));
#235880=CARTESIAN_POINT('Ctrl Pts',(21.0411901532818,-6.16557990842568,
131.532912845442));
#235881=CARTESIAN_POINT('Ctrl Pts',(20.7627425294689,-2.71969492018171,
136.385437887866));
#235882=CARTESIAN_POINT('Ctrl Pts',(20.484294905656,3.22545683522612,136.109225569666));
#235883=CARTESIAN_POINT('Ctrl Pts',(20.2058472818431,6.20657133138755,130.958101517545));
#235884=CARTESIAN_POINT('Ctrl Pts',(19.9273996580302,3.48414998186958,125.665697089004));
#235885=CARTESIAN_POINT('Ctrl Pts',(19.6489520342174,-2.44003499079723,
125.095473405541));
#235886=CARTESIAN_POINT('Ctrl Pts',(19.3705044104044,-6.12194700925765,
129.771438175283));
#235887=CARTESIAN_POINT('Ctrl Pts',(19.0920567865916,-4.17808879994825,
135.396608208416));
#235888=CARTESIAN_POINT('Ctrl Pts',(18.8136091627787,1.60522890552839,136.801727049323));
#235889=CARTESIAN_POINT('Ctrl Pts',(18.5351615389658,5.91341966661616,132.695559127084));
#235890=CARTESIAN_POINT('Ctrl Pts',(18.2567139151529,4.78746664069464,126.85147216478));
#235891=CARTESIAN_POINT('Ctrl Pts',(17.97826629134,-0.737934347277788,124.63989658125));
#235892=CARTESIAN_POINT('Ctrl Pts',(17.6998186675271,-5.58520972019883,
128.093162296283));
#235893=CARTESIAN_POINT('Ctrl Pts',(17.4213710437142,-5.29995021292075,
134.037886819174));
#235894=CARTESIAN_POINT('Ctrl Pts',(17.1429234199013,-0.144295376930669,
137.011158729324));
#235895=CARTESIAN_POINT('Ctrl Pts',(16.8644757960885,5.14395986123776,134.280686393713));
#235896=CARTESIAN_POINT('Ctrl Pts',(16.5860281722755,5.70516728333829,128.355640497777));
#235897=CARTESIAN_POINT('Ctrl Pts',(16.3075805484627,1.02360468496723,124.6808487653));
#235898=CARTESIAN_POINT('Ctrl Pts',(16.0291329246498,-4.5986006130197,126.633265274869));
#235899=CARTESIAN_POINT('Ctrl Pts',(15.7506853008369,-5.99491660177097,
132.418714635041));
#235900=CARTESIAN_POINT('Ctrl Pts',(15.472237677024,-1.88219710145218,136.720651518731));
#235901=CARTESIAN_POINT('Ctrl Pts',(15.1937900532111,3.96016958466077,135.585806091128));
#235902=CARTESIAN_POINT('Ctrl Pts',(14.9153424293982,6.16333388751023,130.057045859918));
#235903=CARTESIAN_POINT('Ctrl Pts',(14.6368948055853,2.70269544333712,125.215031382631));
#235904=CARTESIAN_POINT('Ctrl Pts',(14.3584471817724,-3.24158807925031,
125.509337418335));
#235905=CARTESIAN_POINT('Ctrl Pts',(14.0799995579596,-6.20701051738803,
130.669511097867));
#235906=CARTESIAN_POINT('Ctrl Pts',(13.8015519341466,-3.46849351936748,
135.953604898237));
#235907=CARTESIAN_POINT('Ctrl Pts',(13.5231043103337,2.45739957762318,136.505794759238));
#235908=CARTESIAN_POINT('Ctrl Pts',(13.2446566865208,6.12506251342167,131.818645174584));
#235909=CARTESIAN_POINT('Ctrl Pts',(12.966209062708,4.16409222532429,126.199417632585));
#235910=CARTESIAN_POINT('Ctrl Pts',(12.687761438895,-1.62347539063169,124.811907729812));
#235911=CARTESIAN_POINT('Ctrl Pts',(12.4093138150822,-5.91914843377905,
128.931169283287));
#235912=CARTESIAN_POINT('Ctrl Pts',(12.1308661912693,-4.77541323276041,
134.771802162479));
#235913=CARTESIAN_POINT('Ctrl Pts',(11.8524185674564,0.756693437259193,
136.96655008219));
#235914=CARTESIAN_POINT('Ctrl Pts',(11.5739709436435,5.59343580496719,133.498546923603));
#235915=CARTESIAN_POINT('Ctrl Pts',(11.2955233198306,5.2900839224404,127.554718168085));
#235916=CARTESIAN_POINT('Ctrl Pts',(11.0170756960177,0.125403350157864,
124.597152069781));
#235917=CARTESIAN_POINT('Ctrl Pts',(10.7386280722048,-5.15451677462551,
127.343707387895));
#235918=CARTESIAN_POINT('Ctrl Pts',(10.460180448392,-5.69768779567166,133.270433961767));
#235919=CARTESIAN_POINT('Ctrl Pts',(10.1817328245791,-1.0049620800187,136.930959606699));
#235920=CARTESIAN_POINT('Ctrl Pts',(9.90328520076621,4.61127469204443,134.961440081617));
#235921=CARTESIAN_POINT('Ctrl Pts',(9.62483757695328,5.98997529541125,129.171767613693));
#235922=CARTESIAN_POINT('Ctrl Pts',(9.34638995314043,1.86418122885626,124.882368359726));
#235923=CARTESIAN_POINT('Ctrl Pts',(9.0679423293275,-3.97470431670162,126.034990685308));
#235924=CARTESIAN_POINT('Ctrl Pts',(8.78949470551463,-6.16103077031137,
131.57043098196));
#235925=CARTESIAN_POINT('Ctrl Pts',(8.5110470817017,-2.68567092909101,136.401890038352));
#235926=CARTESIAN_POINT('Ctrl Pts',(8.2325994578889,3.25768929364524,136.089493011555));
#235927=CARTESIAN_POINT('Ctrl Pts',(7.95415183407592,6.20739220249103,130.920317507753));
#235928=CARTESIAN_POINT('Ctrl Pts',(7.67570421026306,3.45280492521512,125.644583286679));
#235929=CARTESIAN_POINT('Ctrl Pts',(7.39725658645018,-2.47474139943534,
125.110432363552));
#235930=CARTESIAN_POINT('Ctrl Pts',(7.11880896263729,-6.1281212758433,129.808723342005));
#235931=CARTESIAN_POINT('Ctrl Pts',(6.84036133882437,-4.15005707511893,
135.421956337113));
#235932=CARTESIAN_POINT('Ctrl Pts',(6.56191371501151,1.64170683608044,136.791844448048));
#235933=CARTESIAN_POINT('Ctrl Pts',(6.28346609119863,5.92482236675955,132.659527423617));
#235934=CARTESIAN_POINT('Ctrl Pts',(6.00501846738572,4.76331558605049,126.822402734361));
#235935=CARTESIAN_POINT('Ctrl Pts',(5.72657084357281,-0.775445517336138,
124.644502810313));
#235936=CARTESIAN_POINT('Ctrl Pts',(5.44812321975995,-5.60161007291028,
128.127211285347));
#235937=CARTESIAN_POINT('Ctrl Pts',(5.16967559594705,-5.28016862534525,
134.070089210674));
#235938=CARTESIAN_POINT('Ctrl Pts',(4.89122797213414,-0.106510161665837,
137.011922098645));
#235939=CARTESIAN_POINT('Ctrl Pts',(4.6127803483213,5.16502593727395,134.249309241742));
#235940=CARTESIAN_POINT('Ctrl Pts',(4.33433272450837,5.69015552540359,128.320956894316));
#235941=CARTESIAN_POINT('Ctrl Pts',(4.05588510069549,0.986310165238503,
124.674731247541));
#235942=CARTESIAN_POINT('Ctrl Pts',(3.77743747688256,-4.62390605285035,
126.661335542776));
#235943=CARTESIAN_POINT('Ctrl Pts',(3.49898985306972,-5.98497849873861,
132.455177483715));
#235944=CARTESIAN_POINT('Ctrl Pts',(3.22054222925682,-1.84614808674025,
136.731999371551));
#235945=CARTESIAN_POINT('Ctrl Pts',(2.94209460544391,3.9892022276243,135.561610825727));
#235946=CARTESIAN_POINT('Ctrl Pts',(2.66364698163102,6.15867057816533,130.019541743194));
#235947=CARTESIAN_POINT('Ctrl Pts',(2.38519935781816,2.66862153515642,125.198682865676));
#235948=CARTESIAN_POINT('Ctrl Pts',(2.10675173400524,-3.27376032925169,
125.529167989562));
#235949=CARTESIAN_POINT('Ctrl Pts',(1.82830411019233,-6.20771638316062,
130.707297431096));
#235950=CARTESIAN_POINT('Ctrl Pts',(1.54985648637947,-3.43708434474973,
135.974623199195));
#235951=CARTESIAN_POINT('Ctrl Pts',(1.27140886256659,2.49206029558105,136.490730236146));
#235952=CARTESIAN_POINT('Ctrl Pts',(0.992961238753657,6.13112326818657,
131.78134138822));
#235953=CARTESIAN_POINT('Ctrl Pts',(0.714513614940807,4.13598347935162,
126.174154940227));
#235954=CARTESIAN_POINT('Ctrl Pts',(0.436065991127901,-1.65992307298164,
124.821901311585));
#235955=CARTESIAN_POINT('Ctrl Pts',(0.157618367314999,-5.93044141299494,
128.967235525755));
#235956=CARTESIAN_POINT('Ctrl Pts',(-0.120829256497892,-4.75117381263555,
134.800797950748));
#235957=CARTESIAN_POINT('Ctrl Pts',(-0.399276880310752,0.794190413791566,
136.961829703365));
#235958=CARTESIAN_POINT('Ctrl Pts',(-0.67772450412367,5.60973244830296,
133.464448175219));
#235959=CARTESIAN_POINT('Ctrl Pts',(-0.956172127936585,5.27020441348929,
127.522576134092));
#235960=CARTESIAN_POINT('Ctrl Pts',(-1.23461975174943,0.0876159864779326,
124.596503709192));
#235961=CARTESIAN_POINT('Ctrl Pts',(-1.51306737556233,-5.17548725182775,
127.375148512417));
#235962=CARTESIAN_POINT('Ctrl Pts',(-1.79151499937523,-5.6825705423121,
133.305071713949));
#235963=CARTESIAN_POINT('Ctrl Pts',(-2.06996262318813,-0.967649113415911,
136.936963584433));
#235964=CARTESIAN_POINT('Ctrl Pts',(-2.34841024700098,4.63649457842225,
134.933292922676));
#235965=CARTESIAN_POINT('Ctrl Pts',(-2.62685787081389,5.97992625804282,
129.13533518208));
#235966=CARTESIAN_POINT('Ctrl Pts',(-2.90530549462681,1.82809784216042,
124.871130280269));
#235967=CARTESIAN_POINT('Ctrl Pts',(-3.18375311843967,-4.00366318312286,
126.059274204017));
#235968=CARTESIAN_POINT('Ctrl Pts',(-3.46220074225256,-6.15625333293613,
131.607920731459));
#235969=CARTESIAN_POINT('Ctrl Pts',(-3.74064836606547,-2.65154741947636,
136.418134770325));
#235970=CARTESIAN_POINT('Ctrl Pts',(-4.01909598987837,3.28980103718956,
136.06956461092));
#235971=CARTESIAN_POINT('Ctrl Pts',(-4.29754361369122,6.20798305639367,
130.882529201136));
#235972=CARTESIAN_POINT('Ctrl Pts',(-4.57599123750414,3.42133192360438,
125.623660681799));
#235973=CARTESIAN_POINT('Ctrl Pts',(-4.85443886131705,-2.5093561056208,
125.125602312169));
#235974=CARTESIAN_POINT('Ctrl Pts',(-5.13288648512991,-6.13406846264146,
129.846045402432));
#235975=CARTESIAN_POINT('Ctrl Pts',(-5.41133410894279,-4.12187156839848,
135.447133359102));
#235976=CARTESIAN_POINT('Ctrl Pts',(-5.68978173275571,1.67812393258193,
136.781739978358));
#235977=CARTESIAN_POINT('Ctrl Pts',(-5.9682293565686,5.93600552043131,132.623426976261));
#235978=CARTESIAN_POINT('Ctrl Pts',(-6.24667698038146,4.73898802499559,
126.793480856855));
#235979=CARTESIAN_POINT('Ctrl Pts',(-6.52512460419438,-0.812927952975666,
124.649337295173));
#235980=CARTESIAN_POINT('Ctrl Pts',(-6.80357222800728,-5.61780285590049,
128.161359477164));
#235981=CARTESIAN_POINT('Ctrl Pts',(-7.08201985182013,-5.26019137917956,
134.1021705894));
#235982=CARTESIAN_POINT('Ctrl Pts',(-7.36046747563304,-0.0687209996277829,
137.012455444495));
#235983=CARTESIAN_POINT('Ctrl Pts',(-7.63891509944595,5.18590062137458,
134.217804435933));
#235984=CARTESIAN_POINT('Ctrl Pts',(-7.91736272325884,5.67493291666336,
128.286365314294));
#235985=CARTESIAN_POINT('Ctrl Pts',(-8.1958103470717,0.948979097423875,
124.668840865451));
#235986=CARTESIAN_POINT('Ctrl Pts',(-8.47425797088461,-4.64904015214177,
126.689559331999));
#235987=CARTESIAN_POINT('Ctrl Pts',(-8.75270559469752,-5.97481862012702,
132.491579160764));
#235988=CARTESIAN_POINT('Ctrl Pts',(-9.03115321851038,-1.81003066233205,
136.743127573537));
#235989=CARTESIAN_POINT('Ctrl Pts',(-9.30960084232328,4.0180870492325,135.537239278668));
#235990=CARTESIAN_POINT('Ctrl Pts',(-9.58804846613619,6.15377905701727,
129.982066708221));
#235991=CARTESIAN_POINT('Ctrl Pts',(-9.86649608994908,2.63444874022312,
125.182542069172));
#235992=CARTESIAN_POINT('Ctrl Pts',(-10.144943713762,-3.30581126886015,
125.549194034992));
#235993=CARTESIAN_POINT('Ctrl Pts',(-10.4233913375749,-6.20819221971975,
130.745087361036));
#235994=CARTESIAN_POINT('Ctrl Pts',(-10.7018389613878,-3.40554780770759,
135.995449914173));
#235995=CARTESIAN_POINT('Ctrl Pts',(-10.9802865852006,2.52662866932821,
136.475455002538));
#235996=CARTESIAN_POINT('Ctrl Pts',(-11.2587342090136,6.13695683192405,
131.744001399476));
#235997=CARTESIAN_POINT('Ctrl Pts',(-11.5371818328265,4.10772147299012,
126.149063821843));
#235998=CARTESIAN_POINT('Ctrl Pts',(-11.8156294566394,-1.69630924627168,
124.832116575588));
#235999=CARTESIAN_POINT('Ctrl Pts',(-12.0940770804522,-5.94151463752335,
129.003369843568));
#236000=CARTESIAN_POINT('Ctrl Pts',(-12.3725247042651,-4.72675833601782,
134.829645649562));
#236001=CARTESIAN_POINT('Ctrl Pts',(-12.6509723280781,0.83165796130609,
136.956881157257));
#236002=CARTESIAN_POINT('Ctrl Pts',(-12.9294199518909,5.62582122093989,
133.430250856313));
#236003=CARTESIAN_POINT('Ctrl Pts',(-13.2078675757038,5.25012961517551,
127.490555707831));
#236004=CARTESIAN_POINT('Ctrl Pts',(-13.4863151995167,0.0498253761554086,
124.596085383024));
#236005=CARTESIAN_POINT('Ctrl Pts',(-13.7647628233296,-5.19626594944658,
127.406716707655));
#236006=CARTESIAN_POINT('Ctrl Pts',(-14.0432104471424,-5.66724271921134,
133.339616801361));
#236007=CARTESIAN_POINT('Ctrl Pts',(-14.3216580709554,-0.930300290219375,
136.942740316309));
#236008=CARTESIAN_POINT('Ctrl Pts',(-14.6001056947683,4.6615426577884,134.904992764631));
#236009=CARTESIAN_POINT('Ctrl Pts',(-14.8785533185811,5.96965563230779,
129.098964596818));
#236010=CARTESIAN_POINT('Ctrl Pts',(-15.157000942394,1.79194671462675,124.860112058844));
#236011=CARTESIAN_POINT('Ctrl Pts',(-15.4354485662069,-4.03247369233249,
126.08373355365));
#236012=CARTESIAN_POINT('Ctrl Pts',(-15.7138961900198,-6.15124777332969,
131.645380704742));
#236013=CARTESIAN_POINT('Ctrl Pts',(-15.9923438138327,-2.61732565579698,
136.434171481834));
#236014=CARTESIAN_POINT('Ctrl Pts',(-16.2707914376456,3.32179087594663,
136.049441106215));
#236015=CARTESIAN_POINT('Ctrl Pts',(-16.5492390614585,6.2083438712012,130.844737997954));
#236016=CARTESIAN_POINT('Ctrl Pts',(-16.8276866852714,3.38973214328102,
125.602930049661));
#236017=CARTESIAN_POINT('Ctrl Pts',(-17.1061343090842,-2.54387782669295,
125.140982689263));
#236018=CARTESIAN_POINT('Ctrl Pts',(-17.3845819328972,-6.13978834927694,
129.883402973582));
#236019=CARTESIAN_POINT('Ctrl Pts',(-17.66302955671,-4.09353332421128,135.47213834144));
#236020=CARTESIAN_POINT('Ctrl Pts',(-17.9414771805229,1.71447884558397,
136.771414014676));
#236021=CARTESIAN_POINT('Ctrl Pts',(-18.2199248043358,5.94696871323555,
132.587259122732));
#236022=CARTESIAN_POINT('Ctrl Pts',(-18.4983724281487,4.71448485899666,
126.764707603974));
#236023=CARTESIAN_POINT('Ctrl Pts',(-18.7768200519616,-0.850380265270943,
124.654399856686));
#236024=CARTESIAN_POINT('Ctrl Pts',(-19.0552676757745,-5.63378746913994,
128.19560560636));
#236025=CARTESIAN_POINT('Ctrl Pts',(-19.3337152995874,-5.24001921468789,
134.134129766565));
#236026=CARTESIAN_POINT('Ctrl Pts',(-19.6121629234003,-0.0309292911078312,
137.012758747106));
#236027=CARTESIAN_POINT('Ctrl Pts',(-19.8906105472132,5.2065831400206,134.18617314371));
#236028=CARTESIAN_POINT('Ctrl Pts',(-20.1690581710261,5.65950002119693,
128.251867039513));
#236029=CARTESIAN_POINT('Ctrl Pts',(-20.447505794839,0.911612864839816,
124.663177837304));
#236030=CARTESIAN_POINT('Ctrl Pts',(-20.7259534186518,-4.67400197954067,
126.717935596697));
#236031=CARTESIAN_POINT('Ctrl Pts',(-21.0044010424647,-5.96443734241423,
132.527918317308));
#236032=CARTESIAN_POINT('Ctrl Pts',(-21.2828486662776,-1.77384616657202,
136.754035712331));
#236033=CARTESIAN_POINT('Ctrl Pts',(-21.5612962900905,4.0468229791472,135.512692353051));
#236034=CARTESIAN_POINT('Ctrl Pts',(-21.8397439139034,6.14865950532324,
129.944622143653));
#236035=CARTESIAN_POINT('Ctrl Pts',(-22.1181915377163,2.60017832482316,
125.166609591221));
#236036=CARTESIAN_POINT('Ctrl Pts',(-22.3966391615293,-3.33773971041633,
125.569414812551));
#236037=CARTESIAN_POINT('Ctrl Pts',(-22.6750867853421,-6.20843800943312,
130.782879487369));
#236038=CARTESIAN_POINT('Ctrl Pts',(-22.953534409155,-3.37388507683905,
136.016084271426));
#236039=CARTESIAN_POINT('Ctrl Pts',(-23.2319820329679,2.56110341792085,
136.45996962444));
#236040=CARTESIAN_POINT('Ctrl Pts',(-23.5104296567807,6.14256298846929,
131.706626591997));
#236041=CARTESIAN_POINT('Ctrl Pts',(-23.7888772805937,4.07930725349882,
126.124145207193));
#236042=CARTESIAN_POINT('Ctrl Pts',(-24.0673249044065,-1.73263256219878,
124.842553143289));
#236043=CARTESIAN_POINT('Ctrl Pts',(-24.3457725282195,-5.95236769704188,
129.039570897758));
#236044=CARTESIAN_POINT('Ctrl Pts',(-24.6242201520323,-4.70216770763169,
134.858344189959));
#236045=CARTESIAN_POINT('Ctrl Pts',(-24.9026677758452,0.86909469142902,
136.951704627238));
#236046=CARTESIAN_POINT('Ctrl Pts',(-25.1811153996581,5.64170152670257,
133.395956234079));
#236047=CARTESIAN_POINT('Ctrl Pts',(-25.459563023471,5.22986027137813,127.458658075828));
#236048=CARTESIAN_POINT('Ctrl Pts',(-25.7380106472839,0.0120329195352371,
124.595897106778));
#236049=CARTESIAN_POINT('Ctrl Pts',(-26.0164582710968,-5.21685209751974,
127.438410803838));
#236050=CARTESIAN_POINT('Ctrl Pts',(-26.2949058949097,-5.6517048943475,
133.374067943923));
#236051=CARTESIAN_POINT('Ctrl Pts',(-26.5733535187226,-0.892916994403456,
136.948289588268));
#236052=CARTESIAN_POINT('Ctrl Pts',(-26.8518011425354,4.68641800197708,
134.876540656153));
#236053=CARTESIAN_POINT('Ctrl Pts',(-27.1302487663484,5.95916379878798,
129.062657205632));
#236054=CARTESIAN_POINT('Ctrl Pts',(-27.4086963901612,1.75572918584856,
124.849314103734));
#236055=CARTESIAN_POINT('Ctrl Pts',(-27.6871440139742,-4.06113477674652,
126.108367827853));
#236056=CARTESIAN_POINT('Ctrl Pts',(-27.965591637787,-6.1460142769749,131.682809513716));
#236057=CARTESIAN_POINT('Ctrl Pts',(-28.2440392616,-2.5830069061529,136.449999578631));
#236058=CARTESIAN_POINT('Ctrl Pts',(-28.5224868854127,3.3536576245212,136.029123243122));
#236059=CARTESIAN_POINT('Ctrl Pts',(-28.8009345092257,6.20847463354345,
130.806945298572));
#236060=CARTESIAN_POINT('Ctrl Pts',(-29.0793821330386,3.35800675518651,
125.582392158445));
#236061=CARTESIAN_POINT('Ctrl Pts',(-29.3578297568515,-2.57830528343674,
125.156572924908));
#236062=CARTESIAN_POINT('Ctrl Pts',(-29.6362773806644,-6.14528072379723,
129.920794671155));
#236063=CARTESIAN_POINT('Ctrl Pts',(-29.9147250044772,-4.06504339264135,
135.496970357558));
#236064=CARTESIAN_POINT('Ctrl Pts',(-30.1931726282902,1.75077022794215,
136.760866939637));
#236065=CARTESIAN_POINT('Ctrl Pts',(-30.471620252103,5.95771153892721,132.551025203244));
#236066=CARTESIAN_POINT('Ctrl Pts',(-30.750067875916,4.68980699602731,126.736084041921));
#236067=CARTESIAN_POINT('Ctrl Pts',(-31.0285154997288,-0.887801066412759,
124.659690307256));
#236068=CARTESIAN_POINT('Ctrl Pts',(-31.3069631235417,-5.6495633203129,
128.229948403933));
#236069=CARTESIAN_POINT('Ctrl Pts',(-31.5854107473546,-5.21965287935721,
134.16596555791));
#236070=CARTESIAN_POINT('Ctrl Pts',(-31.8638583711675,0.00686356350839004,
137.012831995241));
#236071=CARTESIAN_POINT('Ctrl Pts',(-32.1423059949804,5.22707272681363,
134.154416537178));
#236072=CARTESIAN_POINT('Ctrl Pts',(-32.4207536187933,5.64385741087595,
128.217463348321));
#236073=CARTESIAN_POINT('Ctrl Pts',(-32.6992012426062,0.874212852105795,
124.657742372942));
#236074=CARTESIAN_POINT('Ctrl Pts',(-32.9776488664191,-4.69879061007736,
126.746463285377));
#236075=CARTESIAN_POINT('Ctrl Pts',(-33.2560964902319,-5.9538350502823,
132.564193606789));
#236076=CARTESIAN_POINT('Ctrl Pts',(-33.5345441140448,-1.73759594028995,
136.764723383724));
#236077=CARTESIAN_POINT('Ctrl Pts',(-33.8129917378578,4.07540895254819,
135.487970958469));
#236078=CARTESIAN_POINT('Ctrl Pts',(-34.0914393616706,6.14331211279008,
129.907209437008));
#236079=CARTESIAN_POINT('Ctrl Pts',(-34.3698869854835,2.56581155885918,
125.150886022208));
#236080=CARTESIAN_POINT('Ctrl Pts',(-34.6483346092964,-3.3695444708001,
125.589829572953));
#236081=CARTESIAN_POINT('Ctrl Pts',(-34.9267822331094,-6.2084537431929,
130.820672409693));
#236082=CARTESIAN_POINT('Ctrl Pts',(-35.2052298569221,-3.34209732541825,
136.036525506343));
#236083=CARTESIAN_POINT('Ctrl Pts',(-35.4836774807351,2.59548326388451,
136.444274675672));
#236084=CARTESIAN_POINT('Ctrl Pts',(-35.7621251045479,6.14794153008404,
131.66921835072));
#236085=CARTESIAN_POINT('Ctrl Pts',(-36.0405727283609,4.05074187377708,
126.099400019648));
#236086=CARTESIAN_POINT('Ctrl Pts',(-36.3190203521737,-1.76889167478912,
124.85321062796));
#236087=CARTESIAN_POINT('Ctrl Pts',(-36.5974679759867,-5.96300018938643,
129.075837346879));
#236088=CARTESIAN_POINT('Ctrl Pts',(-36.8759155997995,-4.67740283869194,
134.886892508504));
#236089=CARTESIAN_POINT('Ctrl Pts',(-37.1543632236125,0.906499216928551,
136.946300305126));
#236090=CARTESIAN_POINT('Ctrl Pts',(-37.4328108474252,5.65737277714046,
133.361565579315));
#236091=CARTESIAN_POINT('Ctrl Pts',(-37.7112584712383,5.2093971331851,127.426884420063));
#236092=CARTESIAN_POINT('Ctrl Pts',(-37.9897060950511,-0.0257599829691867,
124.595938887431));
#236093=CARTESIAN_POINT('Ctrl Pts',(-38.268153718864,-5.23724493321992,
127.470229626529));
#236094=CARTESIAN_POINT('Ctrl Pts',(-38.5466013426768,-5.63595764348039,
133.408423865036));
#236095=CARTESIAN_POINT('Ctrl Pts',(-38.8250489664898,-0.855500611219946,
136.953611194679));
#236096=CARTESIAN_POINT('Ctrl Pts',(-39.1034965903026,4.71111968922328,
134.847937651547));
#236097=CARTESIAN_POINT('Ctrl Pts',(-39.3819442141156,5.94845114626212,
129.026414353905));
#236098=CARTESIAN_POINT('Ctrl Pts',(-39.6603918379284,1.71944659787975,
124.838736815064));
#236099=CARTESIAN_POINT('Ctrl Pts',(-39.9388394617414,-4.08964537431793,
126.133176113797));
#236100=CARTESIAN_POINT('Ctrl Pts',(-40.2172870855541,-6.14055303780089,
131.720205771443));
#236101=CARTESIAN_POINT('Ctrl Pts',(-40.495734709367,-2.54859244223803,
136.465618474199));
#236102=CARTESIAN_POINT('Ctrl Pts',(-40.7741823331801,3.3854001020792,136.008611774531));
#236103=CARTESIAN_POINT('Ctrl Pts',(-41.0526299569928,6.20837533857501,
130.769152503414));
#236104=CARTESIAN_POINT('Ctrl Pts',(-41.3310775808058,3.3261569349168,125.562047769191));
#236105=CARTESIAN_POINT('Ctrl Pts',(-41.6095252046187,-2.61263720013008,
125.172372441404));
#236106=CARTESIAN_POINT('Ctrl Pts',(-41.8879728284316,-6.15054538268038,
129.958219109591));
#236107=CARTESIAN_POINT('Ctrl Pts',(-42.1664204522444,-4.03640282939359,
135.521628487296));
#236108=CARTESIAN_POINT('Ctrl Pts',(-42.4448680760573,1.78699673486542,
136.750099144066));
#236109=CARTESIAN_POINT('Ctrl Pts',(-42.7233156998703,5.96823359942677,
132.514726560457));
#236110=CARTESIAN_POINT('Ctrl Pts',(-43.0017633236831,4.66495535053527,
126.707611231352));
#236111=CARTESIAN_POINT('Ctrl Pts',(-43.2802109474961,-0.925188969759574,
124.665208450844));
#236112=CARTESIAN_POINT('Ctrl Pts',(-43.5586585713089,-5.6651298248394,
128.264386597296));
#236113=CARTESIAN_POINT('Ctrl Pts',(-43.8371061951219,-5.19909312786956,
134.197676783747));
#236114=CARTESIAN_POINT('Ctrl Pts',(-44.1155538189346,0.0446561637927345,
137.012675186187));
#236115=CARTESIAN_POINT('Ctrl Pts',(-44.3940014427476,5.24736862250453,
134.122535793092));
#236116=CARTESIAN_POINT('Ctrl Pts',(-44.6724490665605,5.62800566534308,
128.183155515557));
#236117=CARTESIAN_POINT('Ctrl Pts',(-44.9508966903734,0.836780445093053,
124.65253467378));
#236118=CARTESIAN_POINT('Ctrl Pts',(-45.2293443141862,-4.72340512520001,
126.775141340936));
#236119=CARTESIAN_POINT('Ctrl Pts',(-45.5077919379991,-5.94301213660306,
132.600403685011));
#236120=CARTESIAN_POINT('Ctrl Pts',(-45.7862395618121,-1.7012813267513,
136.775190191685));
#236121=CARTESIAN_POINT('Ctrl Pts',(-46.0646871856249,4.10384391017172,
135.463076010984));
#236122=CARTESIAN_POINT('Ctrl Pts',(-46.3431348094379,6.13773707756737,
129.869829974632));
#236123=CARTESIAN_POINT('Ctrl Pts',(-46.6215824332507,2.5313497158043,125.135371944775));
#236124=CARTESIAN_POINT('Ctrl Pts',(-46.9000300570636,-3.40122437147435,
125.610437559721));
#236125=CARTESIAN_POINT('Ctrl Pts',(-47.1784776808764,-6.20823942041608,
130.858464727578));
#236126=CARTESIAN_POINT('Ctrl Pts',(-47.4569253046894,-3.31018573135201,
136.056772861467));
#236127=CARTESIAN_POINT('Ctrl Pts',(-47.7353729285023,2.62976693326135,
136.428370737814));
#236128=CARTESIAN_POINT('Ctrl Pts',(-48.0138205523151,6.15309225746451,
131.631778061822));
#236129=CARTESIAN_POINT('Ctrl Pts',(-48.2922681761281,4.02202639232555,
126.074829176147));
#236130=CARTESIAN_POINT('Ctrl Pts',(-48.570715799941,-1.80508524044794,
124.864088634681));
#236131=CARTESIAN_POINT('Ctrl Pts',(-48.8491634237538,-5.97341172056607,
129.112167847066));
#236132=CARTESIAN_POINT('Ctrl Pts',(-49.1276110475668,-4.65246464686987,
134.915289547327));
#236133=CARTESIAN_POINT('Ctrl Pts',(-49.4060586713796,0.943870151766231,
136.940668391181));
#236134=CARTESIAN_POINT('Ctrl Pts',(-49.6845062951925,5.6728343915496,133.327080166382));
#236135=CARTESIAN_POINT('Ctrl Pts',(-49.9629539190054,5.18874095886556,
127.395235917922));
#236136=CARTESIAN_POINT('Ctrl Pts',(-50.2414015428183,-0.0635519309279763,
124.596210723434));
#236137=CARTESIAN_POINT('Ctrl Pts',(-50.5198491666312,-5.25744370088312,
127.50217199667));
#236138=CARTESIAN_POINT('Ctrl Pts',(-50.798296790444,-5.6200015501302,133.442683291627));
#236139=CARTESIAN_POINT('Ctrl Pts',(-51.076744414257,-0.818052527146474,
136.958704938348));
#236140=CARTESIAN_POINT('Ctrl Pts',(-51.3551920380699,4.73564680419706,
134.819184810706));
#236141=CARTESIAN_POINT('Ctrl Pts',(-51.6336396618827,5.93751807169133,
128.990237384633));
#236142=CARTESIAN_POINT('Ctrl Pts',(-51.9120872856956,1.68310029518491,
124.828380584778));
#236143=CARTESIAN_POINT('Ctrl Pts',(-52.1905349095086,-4.11800442857602,
126.1581574922));
#236144=CARTESIAN_POINT('Ctrl Pts',(-52.4689825333214,-6.13486425817587,
131.757568092191));
#236145=CARTESIAN_POINT('Ctrl Pts',(-52.7474301571343,-2.51408353929296,
136.481027589776));
#236146=CARTESIAN_POINT('Ctrl Pts',(-53.0258777809472,3.41701713239144,
135.987907460498));
#236147=CARTESIAN_POINT('Ctrl Pts',(-53.3043254047601,6.20804598997526,
130.731361012906));
#236148=CARTESIAN_POINT('Ctrl Pts',(-53.5827730285729,3.29418386267868,
125.541897635768));
#236149=CARTESIAN_POINT('Ctrl Pts',(-53.8612206523859,-2.64687230459117,
125.188380653292));
#236150=CARTESIAN_POINT('Ctrl Pts',(-54.1396682761987,-6.15558213084251,
129.995674902111));
#236151=CARTESIAN_POINT('Ctrl Pts',(-54.4181159000117,-4.0076126957546,
135.546111816938));
#236152=CARTESIAN_POINT('Ctrl Pts',(-54.6965635238244,1.82315702396754,
136.739111026966));
#236153=CARTESIAN_POINT('Ctrl Pts',(-54.9750111476374,5.97853450483549,
132.478364539431));
#236154=CARTESIAN_POINT('Ctrl Pts',(-55.2534587714502,4.63993084340721,
126.679290227339));
#236155=CARTESIAN_POINT('Ctrl Pts',(-55.5319063952633,-0.962542589888887,
124.670954082973));
#236156=CARTESIAN_POINT('Ctrl Pts',(-55.810354019076,-5.68048640589689,
128.298918910331));
#236157=CARTESIAN_POINT('Ctrl Pts',(-56.088801642889,-5.1783407220741,134.229262269005));
#236158=CARTESIAN_POINT('Ctrl Pts',(-56.3672492667019,0.0824471093265141,
137.012288325754));
#236159=CARTESIAN_POINT('Ctrl Pts',(-56.6456968905149,5.26747007502141,
134.090532092806));
#236160=CARTESIAN_POINT('Ctrl Pts',(-56.9241445143275,5.6119453719906,128.148944812513));
#236161=CARTESIAN_POINT('Ctrl Pts',(-57.2025921381407,0.799317030873196,
124.64755493279));
#236162=CARTESIAN_POINT('Ctrl Pts',(-57.4810397619534,-4.74784461280872,
126.803968700697));
#236163=CARTESIAN_POINT('Ctrl Pts',(-57.7594873857663,-5.93196900242356,
132.636547210196));
#236164=CARTESIAN_POINT('Ctrl Pts',(-58.0379350095792,-1.66490367160747,
136.785435748359));
#236165=CARTESIAN_POINT('Ctrl Pts',(-58.3163826333922,4.13212679834998,
135.438008433087));
#236166=CARTESIAN_POINT('Ctrl Pts',(-58.5948302572049,6.13193460624012,
129.832485141631));
#236167=CARTESIAN_POINT('Ctrl Pts',(-58.873277881018,2.49679407265481,125.120067933803));
#236168=CARTESIAN_POINT('Ctrl Pts',(-59.1517255048308,-3.43277823852872,
125.631238009216));
#236169=CARTESIAN_POINT('Ctrl Pts',(-59.4301731286437,-6.20779504904446,
130.896255040614));
#236170=CARTESIAN_POINT('Ctrl Pts',(-59.7086207524566,-3.27815147713605,
136.076825586523));
#236171=CARTESIAN_POINT('Ctrl Pts',(-59.9870683762695,2.66395315565763,
136.412258400192));
#236172=CARTESIAN_POINT('Ctrl Pts',(-60.2655160000824,6.15801497974849,
131.594307112665));
#236173=CARTESIAN_POINT('Ctrl Pts',(-60.5439636238952,3.99316187320697,
126.050433587173));
#236174=CARTESIAN_POINT('Ctrl Pts',(-60.8224112477081,-1.84121191800936,
124.875186760365));
#236175=CARTESIAN_POINT('Ctrl Pts',(-61.1008588715211,-5.98360190477769,
129.148561052078));
#236176=CARTESIAN_POINT('Ctrl Pts',(-61.3793064953339,-4.62735405625939,
134.943534254169));
#236177=CARTESIAN_POINT('Ctrl Pts',(-61.6577541191468,0.981206111148332,
136.934809094094));
#236178=CARTESIAN_POINT('Ctrl Pts',(-61.9362017429597,5.68808579699418,
133.292501273148));
#236179=CARTESIAN_POINT('Ctrl Pts',(-62.2146493667725,5.16789251384163,
127.36371374215));
#236180=CARTESIAN_POINT('Ctrl Pts',(-62.4930969905855,-0.10134152394658,
124.596712604715));
#236181=CARTESIAN_POINT('Ctrl Pts',(-62.7715446143984,-5.27744765203657,
127.534236730624));
#236182=CARTESIAN_POINT('Ctrl Pts',(-63.0499922382113,-5.60383720555579,
133.476844954201));
#236183=CARTESIAN_POINT('Ctrl Pts',(-63.3284398620242,-0.780574129835986,
136.963570630527));
#236184=CARTESIAN_POINT('Ctrl Pts',(-63.606887485837,4.75999843803683,134.790283199078));
#236185=CARTESIAN_POINT('Ctrl Pts',(-63.88533510965,5.92636498020503,128.954127638363));
#236186=CARTESIAN_POINT('Ctrl Pts',(-64.1637827334628,1.64669162458969,
124.818245796629));
#236187=CARTESIAN_POINT('Ctrl Pts',(-64.4422303572757,-4.14621088866563,
126.183311037368));
#236188=CARTESIAN_POINT('Ctrl Pts',(-64.7206779810887,-6.12894814889968,
131.794895091487));
#236189=CARTESIAN_POINT('Ctrl Pts',(-64.9991256049015,-2.47948147605779,
136.49622635437));
#236190=CARTESIAN_POINT('Ctrl Pts',(-65.2775732287142,3.44850754387722,
135.967011068231));
#236191=CARTESIAN_POINT('Ctrl Pts',(-65.5560208525274,6.20748659994837,
130.693572227424));
#236192=CARTESIAN_POINT('Ctrl Pts',(-65.83446847634,3.26208872324607,125.521942504845));
#236193=CARTESIAN_POINT('Ctrl Pts',(-66.1129161001531,-2.68100932822562,
125.204596967384));
#236194=CARTESIAN_POINT('Ctrl Pts',(-66.3913637239659,-6.1603907816451,
130.033160660777));
#236195=CARTESIAN_POINT('Ctrl Pts',(-66.6698113477789,-3.97867405855336,
135.570419439246));
#236196=CARTESIAN_POINT('Ctrl Pts',(-66.9482589715917,1.85924975531565,
136.727902995508));
#236197=CARTESIAN_POINT('Ctrl Pts',(-67.2267065954047,5.98861387344954,
132.441940487574));
#236198=CARTESIAN_POINT('Ctrl Pts',(-67.5051542192175,4.61473440193538,
126.651122079325));
#236199=CARTESIAN_POINT('Ctrl Pts',(-67.7836018430304,-0.999860542648545,
124.676926990737));
#236200=CARTESIAN_POINT('Ctrl Pts',(-68.0620494668433,-5.69563249444164,
128.33354406343));
#236201=CARTESIAN_POINT('Ctrl Pts',(-68.3404970906562,-5.15739643095884,
134.260720843274));
#236202=CARTESIAN_POINT('Ctrl Pts',(-68.618944714469,0.120234999752325,
137.011671428276));
#236203=CARTESIAN_POINT('Ctrl Pts',(-68.8973923382821,5.28737633949755,
134.058406622227));
#236204=CARTESIAN_POINT('Ctrl Pts',(-69.1758399620947,5.59567712593856,
128.114832506878));
#236205=CARTESIAN_POINT('Ctrl Pts',(-69.4542875859078,0.761823997666808,
124.642803334499));
#236206=CARTESIAN_POINT('Ctrl Pts',(-69.7327352097205,-4.77210816728929,
126.832944296451));
#236207=CARTESIAN_POINT('Ctrl Pts',(-70.0111828335336,-5.92070605695121,
132.672622843033));
#236208=CARTESIAN_POINT('Ctrl Pts',(-70.2896304573463,-1.62846432284579,
136.795459674095));
#236209=CARTESIAN_POINT('Ctrl Pts',(-70.5680780811594,4.16025656905012,
135.412769153666));
#236210=CARTESIAN_POINT('Ctrl Pts',(-70.8465257049722,6.12590491382102,
129.795176321834));
#236211=CARTESIAN_POINT('Ctrl Pts',(-71.1249733287852,2.46214590988275,
125.104974556385));
#236212=CARTESIAN_POINT('Ctrl Pts',(-71.4034209525978,-3.46420490272305,
125.652230150673));
#236213=CARTESIAN_POINT('Ctrl Pts',(-71.681868576411,-6.20712064554441,
130.93404194847));
#236214=CARTESIAN_POINT('Ctrl Pts',(-71.9603162002238,-3.24599574981168,
136.09668293845));
#236215=CARTESIAN_POINT('Ctrl Pts',(-72.2387638240367,2.69804066428979,
136.395938259856));
#236216=CARTESIAN_POINT('Ctrl Pts',(-72.5172114478495,6.16270951452303,
131.556806891751));
#236217=CARTESIAN_POINT('Ctrl Pts',(-72.7956590716624,3.96414938600637,
126.026214156713));
#236218=CARTESIAN_POINT('Ctrl Pts',(-73.0741066954753,-1.87727036878649,
124.886504593767));
#236219=CARTESIAN_POINT('Ctrl Pts',(-73.3525543192881,-5.99357036442037,
129.185015613353));
#236220=CARTESIAN_POINT('Ctrl Pts',(-73.6310019431012,-4.60207199734241,
134.971625582408));
#236221=CARTESIAN_POINT('Ctrl Pts',(-73.909449566914,1.01850571157763,136.928722630985));
#236222=CARTESIAN_POINT('Ctrl Pts',(-74.187897190727,5.70312642832773,133.257830180947));
#236223=CARTESIAN_POINT('Ctrl Pts',(-74.4663448145398,5.14685257066011,
127.332319060812));
#236224=CARTESIAN_POINT('Ctrl Pts',(-74.7447924383527,-0.139127361718492,
124.597444512675));
#236225=CARTESIAN_POINT('Ctrl Pts',(-75.0232400621657,-5.29725604542678,
127.566422640223));
#236226=CARTESIAN_POINT('Ctrl Pts',(-75.3016876859784,-5.58746520873256,
133.510907586884));
#236227=CARTESIAN_POINT('Ctrl Pts',(-75.5801353097915,-0.743066808063574,
136.968208090913));
#236228=CARTESIAN_POINT('Ctrl Pts',(-75.8585829336042,4.7841736883842,134.761233887624));
#236229=CARTESIAN_POINT('Ctrl Pts',(-76.1370305574171,5.91499228508486,
128.918086453158));
#236230=CARTESIAN_POINT('Ctrl Pts',(-76.41547818123,1.61022193523031,124.808332826166));
#236231=CARTESIAN_POINT('Ctrl Pts',(-76.693925805043,-4.17426370938676,
126.208635817229));
#236232=CARTESIAN_POINT('Ctrl Pts',(-76.9723734288558,-6.12280492919574,
131.832185386163));
#236233=CARTESIAN_POINT('Ctrl Pts',(-77.2508210526686,-2.44478753472383,
136.511214204787));
#236234=CARTESIAN_POINT('Ctrl Pts',(-77.5292686764817,3.47987016964863,
135.945923372052));
#236235=CARTESIAN_POINT('Ctrl Pts',(-77.8077163002943,6.20669718922256,
130.655787547247));
#236236=CARTESIAN_POINT('Ctrl Pts',(-78.0861639241075,3.22987270591563,
125.502183115868));
#236237=CARTESIAN_POINT('Ctrl Pts',(-78.3646115479203,-2.71504700607423,
125.221020782777));
#236238=CARTESIAN_POINT('Ctrl Pts',(-78.6430591717333,-6.16497115690175,
130.070674996542));
#236239=CARTESIAN_POINT('Ctrl Pts',(-78.921506795546,-3.94958799012119,
135.594550453492));
#236240=CARTESIAN_POINT('Ctrl Pts',(-79.199954419359,1.89527359148086,136.71647546501));
#236241=CARTESIAN_POINT('Ctrl Pts',(-79.4784020431719,5.9984713317742,132.405455754592));
#236242=CARTESIAN_POINT('Ctrl Pts',(-79.7568496669848,4.58936695978296,
126.623107831093));
#236243=CARTESIAN_POINT('Ctrl Pts',(-80.0352972907976,-1.0371414452086,
124.683126952807));
#236244=CARTESIAN_POINT('Ctrl Pts',(-80.3137449146107,-5.71056752923021,
128.368260773546));
#236245=CARTESIAN_POINT('Ctrl Pts',(-80.5921925384234,-5.13626103062165,
134.292051340844));
#236246=CARTESIAN_POINT('Ctrl Pts',(-80.8706401622364,0.158018434826916,
137.010824516613));
#236247=CARTESIAN_POINT('Ctrl Pts',(-81.1490877860493,5.30708667829958,
134.026160571776));
#236248=CARTESIAN_POINT('Ctrl Pts',(-81.4275354098621,5.57920153001237,
128.080819862696));
#236249=CARTESIAN_POINT('Ctrl Pts',(-81.705983033675,0.724302734791404,
124.63828005498));
#236250=CARTESIAN_POINT('Ctrl Pts',(-81.984430657488,-4.79619488954742,
126.862067054498));
#236251=CARTESIAN_POINT('Ctrl Pts',(-82.2628782813007,-5.90922371753823,
132.708629246728));
#236252=CARTESIAN_POINT('Ctrl Pts',(-82.5413259051138,-1.59196463073914,
136.805261597452));
#236253=CARTESIAN_POINT('Ctrl Pts',(-82.8197735289264,4.18823217991362,
135.387359107972));
#236254=CARTESIAN_POINT('Ctrl Pts',(-83.0982211527395,6.11964822374235,
129.757904897731));
#236255=CARTESIAN_POINT('Ctrl Pts',(-83.3766687765523,2.42740651138818,
125.090092371815));
#236256=CARTESIAN_POINT('Ctrl Pts',(-83.6551164003652,-3.49550319953123,
125.67341320622));
#236257=CARTESIAN_POINT('Ctrl Pts',(-83.9335640241781,-6.20621623490623,
130.971824050937));
#236258=CARTESIAN_POINT('Ctrl Pts',(-84.2120116479911,-3.21371974092037,
136.116344181428));
#236259=CARTESIAN_POINT('Ctrl Pts',(-84.4904592718038,2.73202819603347,
136.379410921554));
#236260=CARTESIAN_POINT('Ctrl Pts',(-84.7689068956169,6.16717568783019,
131.519278788663));
#236261=CARTESIAN_POINT('Ctrl Pts',(-85.0473545194296,3.9349900057924,126.002171782228));
#236262=CARTESIAN_POINT('Ctrl Pts',(-85.3258021432425,-1.91325925661942,
124.898041715501));
#236263=CARTESIAN_POINT('Ctrl Pts',(-85.6042497670555,-6.00331673010926,
129.221530180052));
#236264=CARTESIAN_POINT('Ctrl Pts',(-85.8826973908683,-4.57661940695503,
134.999562491112));
#236265=CARTESIAN_POINT('Ctrl Pts',(-86.1611450146813,1.05576757090286,
136.922409227389));
#236266=CARTESIAN_POINT('Ctrl Pts',(-86.4395926384942,5.71795572821454,
133.223068174528));
#236267=CARTESIAN_POINT('Ctrl Pts',(-86.718040262307,5.12562190896342,127.301053037252));
#236268=CARTESIAN_POINT('Ctrl Pts',(-86.9964878861199,-0.176908044074368,
124.598406420195));
#236269=CARTESIAN_POINT('Ctrl Pts',(-87.2749355099329,-5.31686814704595,
127.598728532803));
#236270=CARTESIAN_POINT('Ctrl Pts',(-87.5533831337457,-5.57088616633168,
133.544869927476));
#236271=CARTESIAN_POINT('Ctrl Pts',(-87.8318307575586,-0.70553195167748,
136.972617147663));
#236272=CARTESIAN_POINT('Ctrl Pts',(-88.1102783813713,4.80817165941601,
134.732037952774));
#236273=CARTESIAN_POINT('Ctrl Pts',(-88.3887260051845,5.90340040775061,
128.882115164534));
#236274=CARTESIAN_POINT('Ctrl Pts',(-88.6671736289971,1.57369257850503,
124.798642040718));
#236275=CARTESIAN_POINT('Ctrl Pts',(-88.9456212528103,-4.20216185122988,
126.234130893362));
#236276=CARTESIAN_POINT('Ctrl Pts',(-89.2240688766231,-6.11643482670397,
131.869437594414));
#236277=CARTESIAN_POINT('Ctrl Pts',(-89.5025165004358,-2.41000300088966,
136.525990585645));
#236278=CARTESIAN_POINT('Ctrl Pts',(-89.7809641242489,3.51110384754994,
135.924645153375));
#236279=CARTESIAN_POINT('Ctrl Pts',(-90.0594117480617,6.20567778705031,
130.618008372501));
#236280=CARTESIAN_POINT('Ctrl Pts',(-90.3378593718745,3.19753700446471,
125.482620201028));
#236281=CARTESIAN_POINT('Ctrl Pts',(-90.6163069956876,-2.74898407685696,
125.237651490881));
#236282=CARTESIAN_POINT('Ctrl Pts',(-90.8947546195002,-6.16932308688508,
130.108216519297));
#236283=CARTESIAN_POINT('Ctrl Pts',(-91.1732022433134,-3.92035556825405,
135.618503965492));
#236284=CARTESIAN_POINT('Ctrl Pts',(-91.4516498671261,1.93122719758584,
136.70482885892));
#236285=CARTESIAN_POINT('Ctrl Pts',(-91.7300974909391,6.00810651453776,
132.368911692441));
#236286=CARTESIAN_POINT('Ctrl Pts',(-92.0085451147519,4.56382945695037,
126.595248520721));
#236287=CARTESIAN_POINT('Ctrl Pts',(-92.2869927385648,-1.07438391611076,
124.689553739443));
#236288=CARTESIAN_POINT('Ctrl Pts',(-92.5654403623776,-5.72529095683809,
128.403067754236));
#236289=CARTESIAN_POINT('Ctrl Pts',(-92.8438879861907,-5.11493530424405,
134.323252600751));
#236290=CARTESIAN_POINT('Ctrl Pts',(-93.1223356100035,0.195796014469281,
137.009747622148));
#236291=CARTESIAN_POINT('Ctrl Pts',(-93.4007832338166,5.32660036105212,
133.993795136343));
#236292=CARTESIAN_POINT('Ctrl Pts',(-93.6792308576291,5.56251919472255,
128.046908140318));
#236293=CARTESIAN_POINT('Ctrl Pts',(-93.9576784814422,0.686754632612129,
124.633985261843));
#236294=CARTESIAN_POINT('Ctrl Pts',(-94.2361261052551,-4.82010388703947,
126.891335895681));
#236295=CARTESIAN_POINT('Ctrl Pts',(-94.5145737290679,-5.8975224096676,
132.744565087048));
#236296=CARTESIAN_POINT('Ctrl Pts',(-94.7930213528811,-1.55540594779807,
136.814841155217));
#236297=CARTESIAN_POINT('Ctrl Pts',(-95.0714689766937,4.21605259429308,
135.361779237583));
#236298=CARTESIAN_POINT('Ctrl Pts',(-95.3499166005066,6.11316476784841,
129.720672250431));
#236299=CARTESIAN_POINT('Ctrl Pts',(-95.6283642243196,2.39257716445285,
125.075421931555));
#236300=CARTESIAN_POINT('Ctrl Pts',(-95.9068118481323,-3.52667196918255,
125.694786390909));
#236301=CARTESIAN_POINT('Ctrl Pts',(-96.1852594719453,-6.20508185064282,
131.009599947983));
#236302=CARTESIAN_POINT('Ctrl Pts',(-96.4637070957582,-3.18132464646333,
136.135808586901));
#236303=CARTESIAN_POINT('Ctrl Pts',(-96.742154719571,2.76591449146702,136.362676997713));
#236304=CARTESIAN_POINT('Ctrl Pts',(-97.020602343384,6.17141333417382,131.481724194021));
#236305=CARTESIAN_POINT('Ctrl Pts',(-97.299049967197,3.90568481307747,125.978307354616));
#236306=CARTESIAN_POINT('Ctrl Pts',(-97.5774975910097,-1.94917724792726,
124.909797698053));
#236307=CARTESIAN_POINT('Ctrl Pts',(-97.8559452148228,-6.01284064068852,
129.258103399115));
#236308=CARTESIAN_POINT('Ctrl Pts',(-98.1343928386354,-4.55099722825276,
135.027343945068));
#236309=CARTESIAN_POINT('Ctrl Pts',(-98.4128404624484,1.09299030837272,
136.915869117251));
#236310=CARTESIAN_POINT('Ctrl Pts',(-98.6912880862614,5.73257314714861,
133.188216542011));
#236311=CARTESIAN_POINT('Ctrl Pts',(-98.9697357100741,5.10420131546234,
127.269916830042));
#236312=CARTESIAN_POINT('Ctrl Pts',(-99.2481833338871,-0.214682171037078,
124.599598291628));
#236313=CARTESIAN_POINT('Ctrl Pts',(-99.5266309576999,-5.33628323016052,
127.631153211259));
#236314=CARTESIAN_POINT('Ctrl Pts',(-99.8050785815131,-5.55410069269506,
133.578730717485));
#236315=CARTESIAN_POINT('Ctrl Pts',(-100.083526205326,-0.667970951546107,
136.976797637399));
#236316=CARTESIAN_POINT('Ctrl Pts',(-100.361973829139,4.83199146187865,
134.702696476397));
#236317=CARTESIAN_POINT('Ctrl Pts',(-100.640421452952,5.89158977774298,
128.846215105423));
#236318=CARTESIAN_POINT('Ctrl Pts',(-100.918869076765,1.53710490802326,
124.789173799381));
#236319=CARTESIAN_POINT('Ctrl Pts',(-101.197316700577,-4.22990428042106,
126.259795321038));
#236320=CARTESIAN_POINT('Ctrl Pts',(-101.47576432439,-6.10983807746976,
131.906650335846));
#236321=CARTESIAN_POINT('Ctrl Pts',(-101.754211948203,-2.37512916350784,
136.540554949401));
#236322=CARTESIAN_POINT('Ctrl Pts',(-102.032659572016,3.54220742020778,
135.903177200671));
#236323=CARTESIAN_POINT('Ctrl Pts',(-102.311107195829,6.20442843120499,
130.580236103105));
#236324=CARTESIAN_POINT('Ctrl Pts',(-102.589554819642,3.16508281710451,
125.463254485237));
#236325=CARTESIAN_POINT('Ctrl Pts',(-102.868002443455,-2.78281928302352,
125.254488475437));
#236326=CARTESIAN_POINT('Ctrl Pts',(-103.146450067268,-6.1734464103326,
130.145783837928));
#236327=CARTESIAN_POINT('Ctrl Pts',(-103.424897691081,-3.8909778761698,
135.642279087639));
#236328=CARTESIAN_POINT('Ctrl Pts',(-103.703345314893,1.96710924135641,
136.69296360881));
#236329=CARTESIAN_POINT('Ctrl Pts',(-103.981792938706,6.01751906470488,
132.332309655276));
#236330=CARTESIAN_POINT('Ctrl Pts',(-104.260240562519,4.53812283973896,
126.567545180546));
#236331=CARTESIAN_POINT('Ctrl Pts',(-104.538688186332,-1.11158657532129,
124.696207112496));
#236332=CARTESIAN_POINT('Ctrl Pts',(-104.817135810145,-5.73980223168479,
128.437963715717));
#236333=CARTESIAN_POINT('Ctrl Pts',(-105.095583433958,-5.093420042057,134.354323466822));
#236334=CARTESIAN_POINT('Ctrl Pts',(-105.374031057771,0.233566338818549,
137.008440784786));
#236335=CARTESIAN_POINT('Ctrl Pts',(-105.652478681584,5.34591666467016,
133.961311515241));
#236336=CARTESIAN_POINT('Ctrl Pts',(-105.930926305397,5.54563073823764,
128.013098596357));
#236337=CARTESIAN_POINT('Ctrl Pts',(-106.20937392921,0.649181082487974,
124.629919114234));
#236338=CARTESIAN_POINT('Ctrl Pts',(-106.487821553022,-4.84383427380942,
126.920749735436));
#236339=CARTESIAN_POINT('Ctrl Pts',(-106.766269176835,-5.88560256693534,
132.780429032376));
#236340=CARTESIAN_POINT('Ctrl Pts',(-107.044716800648,-1.51878962871805,
136.824197992414));
#236341=CARTESIAN_POINT('Ctrl Pts',(-107.323164424461,4.2437167812931,135.336030490371));
#236342=CARTESIAN_POINT('Ctrl Pts',(-107.601612048274,6.10645478638612,
129.683479759601));
#236343=CARTESIAN_POINT('Ctrl Pts',(-107.880059672087,2.35765915969063,
125.060963779225));
#236344=CARTESIAN_POINT('Ctrl Pts',(-108.1585072959,-3.55771005670707,125.716348912751));
#236345=CARTESIAN_POINT('Ctrl Pts',(-108.436954919713,-6.20371753478999,
131.04736823981));
#236346=CARTESIAN_POINT('Ctrl Pts',(-108.715402543526,-3.14881166685081,
136.155075433609));
#236347=CARTESIAN_POINT('Ctrl Pts',(-108.993850167338,2.79969829492213,
136.345737108415));
#236348=CARTESIAN_POINT('Ctrl Pts',(-109.272297791151,6.17542229652738,
131.444144499421));
#236349=CARTESIAN_POINT('Ctrl Pts',(-109.550745414964,3.87623489377466,
125.954621758183));
#236350=CARTESIAN_POINT('Ctrl Pts',(-109.829193038777,-1.98502301175461,
124.921772105802));
#236351=CARTESIAN_POINT('Ctrl Pts',(-110.10764066259,-6.02214174324697,
129.294733915307));
#236352=CARTESIAN_POINT('Ctrl Pts',(-110.386088286403,-4.52520641067474,
135.054968914823));
#236353=CARTESIAN_POINT('Ctrl Pts',(-110.664535910216,1.13017254468408,
136.909102542919));
#236354=CARTESIAN_POINT('Ctrl Pts',(-110.942983534029,5.74697814347679,
133.153276574838));
#236355=CARTESIAN_POINT('Ctrl Pts',(-111.221431157841,5.08259158390449,
127.238911592946));
#236356=CARTESIAN_POINT('Ctrl Pts',(-111.499878781655,-0.252448342873548,
124.601020082813));
#236357=CARTESIAN_POINT('Ctrl Pts',(-111.778326405467,-5.3555005753377,
127.663695474083));
#236358=CARTESIAN_POINT('Ctrl Pts',(-112.05677402928,-5.53710940981492,
133.612488702192));
#236359=CARTESIAN_POINT('Ctrl Pts',(-112.335221653093,-0.630385199504834,
136.980749405212));
#236360=CARTESIAN_POINT('Ctrl Pts',(-112.613669276906,4.85563221312083,
134.673210545752));
#236361=CARTESIAN_POINT('Ctrl Pts',(-112.892116900719,5.8795608327098,128.810387606114));
#236362=CARTESIAN_POINT('Ctrl Pts',(-113.170564524532,1.50046027955312,
124.779928453004));
#236363=CARTESIAN_POINT('Ctrl Pts',(-113.449012148345,-4.25748996895278,
126.285628149252));
#236364=CARTESIAN_POINT('Ctrl Pts',(-113.727459772158,-6.10301492593933,
131.943822231527));
#236365=CARTESIAN_POINT('Ctrl Pts',(-114.00590739597,-2.3401673148416,136.554906756366));
#236366=CARTESIAN_POINT('Ctrl Pts',(-114.284355019783,3.57317973506622,
135.881520309444));
#236367=CARTESIAN_POINT('Ctrl Pts',(-114.562802643596,6.202949167983,130.542472138726));
#236368=CARTESIAN_POINT('Ctrl Pts',(-114.841250267409,3.13251134643626,
125.444086686097));
#236369=CARTESIAN_POINT('Ctrl Pts',(-115.119697891222,-2.81655137079845,
125.271531112549));
#236370=CARTESIAN_POINT('Ctrl Pts',(-115.398145515035,-6.17734097445314,
130.183375560363));
#236371=CARTESIAN_POINT('Ctrl Pts',(-115.676593138848,-3.86145600246928,
135.665874938939));
#236372=CARTESIAN_POINT('Ctrl Pts',(-115.955040762661,2.00291839317105,
136.680880154352));
#236373=CARTESIAN_POINT('Ctrl Pts',(-116.233488386474,6.02670863349017,
132.295650999397));
#236374=CARTESIAN_POINT('Ctrl Pts',(-116.511936010287,4.51224806071678,
126.539998837124));
#236375=CARTESIAN_POINT('Ctrl Pts',(-116.790383634099,-1.14874804428301,
124.703086825424));
#236376=CARTESIAN_POINT('Ctrl Pts',(-117.068831257912,-5.75410081604829,
128.472947364906));
#236377=CARTESIAN_POINT('Ctrl Pts',(-117.347278881725,-5.07171604131793,
134.385262787713));
#236378=CARTESIAN_POINT('Ctrl Pts',(-117.625726505538,0.271328008281021,
137.006904052952));
#236379=CARTESIAN_POINT('Ctrl Pts',(-117.904174129351,5.3650348733795,133.928710912162));
#236380=CARTESIAN_POINT('Ctrl Pts',(-118.182621753164,5.52853678636705,
127.979392483636));
#236381=CARTESIAN_POINT('Ctrl Pts',(-118.461069376977,0.611583476719488,
124.626081762825));
#236382=CARTESIAN_POINT('Ctrl Pts',(-118.73951700079,-4.86738517051901,
126.95030748382));
#236383=CARTESIAN_POINT('Ctrl Pts',(-119.017964624603,-5.87346463103546,
132.816219753764));
#236384=CARTESIAN_POINT('Ctrl Pts',(-119.296412248415,-1.48211703032935,
136.833331762325));
#236385=CARTESIAN_POINT('Ctrl Pts',(-119.574859872228,4.27122371580729,
135.310113820466));
#236386=CARTESIAN_POINT('Ctrl Pts',(-119.853307496041,6.09951852799569,
129.646328803424));
#236387=CARTESIAN_POINT('Ctrl Pts',(-120.131755119854,2.32265379100196,
125.046718450578));
#236388=CARTESIAN_POINT('Ctrl Pts',(-120.410202743667,-3.58861631197691,
125.738099972737));
#236389=CARTESIAN_POINT('Ctrl Pts',(-120.68865036748,-6.20212333790203,
131.085127526901));
#236390=CARTESIAN_POINT('Ctrl Pts',(-120.967097991293,-3.11618200686478,
136.174144007612));
#236391=CARTESIAN_POINT('Ctrl Pts',(-121.245545615105,2.83337835452712,
136.328591881372));
#236392=CARTESIAN_POINT('Ctrl Pts',(-121.523993238919,6.17920242633619,
131.406541097396));
#236393=CARTESIAN_POINT('Ctrl Pts',(-121.802440862731,3.84664133916317,
125.931115870606));
#236394=CARTESIAN_POINT('Ctrl Pts',(-122.080888486544,-2.02079521982502,
124.933964495032));
#236395=CARTESIAN_POINT('Ctrl Pts',(-122.359336110357,-6.03121969312815,
129.331420371272));
#236396=CARTESIAN_POINT('Ctrl Pts',(-122.63778373417,-4.49924790990888,
135.082436376724));
#236397=CARTESIAN_POINT('Ctrl Pts',(-122.916231357983,1.16731290203685,
136.90210975513));
#236398=CARTESIAN_POINT('Ctrl Pts',(-123.194678981796,5.76117018341619,
133.118249567719));
#236399=CARTESIAN_POINT('Ctrl Pts',(-123.473126605609,5.06079351504635,
127.208038474877));
#236400=CARTESIAN_POINT('Ctrl Pts',(-123.751574229422,-0.290205160143283,
124.602671741062));
#236401=CARTESIAN_POINT('Ctrl Pts',(-124.030021853235,-5.37451947047147,
127.696354115408));
#236402=CARTESIAN_POINT('Ctrl Pts',(-124.308469477047,-5.51991294730918,
133.646142630679));
#236403=CARTESIAN_POINT('Ctrl Pts',(-124.58691710086,-0.592776088308802,
136.984472304668));
#236404=CARTESIAN_POINT('Ctrl Pts',(-124.865364724673,4.87909303712557,
134.64358125345));
#236405=CARTESIAN_POINT('Ctrl Pts',(-125.143812348486,5.86731401838748,
128.774633994209));
#236406=CARTESIAN_POINT('Ctrl Pts',(-125.422259972299,1.46376005097626,
124.770906344175));
#236407=CARTESIAN_POINT('Ctrl Pts',(-125.700707596112,-4.28491789462882,
126.311628420759));
#236408=CARTESIAN_POINT('Ctrl Pts',(-125.979155219925,-6.09596562494584,
131.980951904039));
#236409=CARTESIAN_POINT('Ctrl Pts',(-126.257602843738,-2.30511875041471,
136.569045474729));
#236410=CARTESIAN_POINT('Ctrl Pts',(-126.536050467551,3.60401964443632,
135.859675282198));
#236411=CARTESIAN_POINT('Ctrl Pts',(-126.814498091363,6.20124005219796,
130.50471787872));
#236412=CARTESIAN_POINT('Ctrl Pts',(-127.092945715177,3.09982379940838,
125.42511751388));
#236413=CARTESIAN_POINT('Ctrl Pts',(-127.371393338989,-2.85017909022625,
125.288778770691));
#236414=CARTESIAN_POINT('Ctrl Pts',(-127.649840962802,-6.18100663493216,
130.220990293627));
#236415=CARTESIAN_POINT('Ctrl Pts',(-127.928288586615,-3.83179104109667,
135.689290645038));
#236416=CARTESIAN_POINT('Ctrl Pts',(-128.206736210428,2.03865332610762,
136.6685789433));
#236417=CARTESIAN_POINT('Ctrl Pts',(-128.485183834241,6.03567488037103,
132.258937083203));
#236418=CARTESIAN_POINT('Ctrl Pts',(-128.763631458054,4.48620607868298,
126.512610511197));
#236419=CARTESIAN_POINT('Ctrl Pts',(-129.042079081867,-1.18586694596332,
124.710192623294));
#236420=CARTESIAN_POINT('Ctrl Pts',(-129.32052670568,-5.76818618009069,
128.508017405469));
#236421=CARTESIAN_POINT('Ctrl Pts',(-129.598974329492,-5.04982410627509,
134.416069416958));
#236422=CARTESIAN_POINT('Ctrl Pts',(-129.877421953305,0.30907962358457,
137.005137483589));
#236423=CARTESIAN_POINT('Ctrl Pts',(-130.155869577118,5.38395427874936,
133.895994535135));
#236424=CARTESIAN_POINT('Ctrl Pts',(-130.434317200931,5.51123797253198,
127.945791051148));
#236425=CARTESIAN_POINT('Ctrl Pts',(-130.712764824744,0.573963208500954,
124.622473349811));
#236426=CARTESIAN_POINT('Ctrl Pts',(-130.991212448557,-4.89075570448117,
126.980008045559));
#236427=CARTESIAN_POINT('Ctrl Pts',(-131.26966007237,-5.8611090517438,132.851935924971));
#236428=CARTESIAN_POINT('Ctrl Pts',(-131.548107696183,-1.44538951154951,
136.842242126491));
#236429=CARTESIAN_POINT('Ctrl Pts',(-131.826555319995,4.29857237855583,
135.28403018822));
#236430=CARTESIAN_POINT('Ctrl Pts',(-132.105002943808,6.09235624970348,
129.609220758541));
#236431=CARTESIAN_POINT('Ctrl Pts',(-132.383450567622,2.28756235552218,
125.032686473479));
#236432=CARTESIAN_POINT('Ctrl Pts',(-132.661898191434,-3.6193895897498,
125.760038764874));
#236433=CARTESIAN_POINT('Ctrl Pts',(-132.940345815247,-6.20029931905343,
131.122876410071));
#236434=CARTESIAN_POINT('Ctrl Pts',(-133.21879343906,-3.08343687560774,
136.193013602317));
#236435=CARTESIAN_POINT('Ctrl Pts',(-133.497241062873,2.86695342225543,
136.311241951909));
#236436=CARTESIAN_POINT('Ctrl Pts',(-133.775688686686,6.18275358352724,
131.368915381349));
#236437=CARTESIAN_POINT('Ctrl Pts',(-134.054136310499,3.81690524584148,
125.907790562906));
#236438=CARTESIAN_POINT('Ctrl Pts',(-134.332583934311,-2.05649254658467,
124.946374413949));
#236439=CARTESIAN_POINT('Ctrl Pts',(-134.611031558124,-6.04007415394596,
129.36816140758));
#236440=CARTESIAN_POINT('Ctrl Pts',(-134.889479181937,-4.47312268785726,
135.109745312956));
#236441=CARTESIAN_POINT('Ctrl Pts',(-135.16792680575,1.20441000418008,136.894891013003));
#236442=CARTESIAN_POINT('Ctrl Pts',(-135.446374429563,5.775148741076,133.083136818595));
#236443=CARTESIAN_POINT('Ctrl Pts',(-135.724822053376,5.03880791662344,
127.177298619846));
#236444=CARTESIAN_POINT('Ctrl Pts',(-136.003269677189,-0.327951223754644,
124.604553205172));
#236445=CARTESIAN_POINT('Ctrl Pts',(-136.281717301002,-5.39333921080989,
127.729127925058));
#236446=CARTESIAN_POINT('Ctrl Pts',(-136.560164924815,-5.50251194239939,
133.679691255889));
#236447=CARTESIAN_POINT('Ctrl Pts',(-136.838612548628,-0.555145011576188,
136.987966197812));
#236448=CARTESIAN_POINT('Ctrl Pts',(-137.117060172441,4.90237306454367,
134.613809697415));
#236449=CARTESIAN_POINT('Ctrl Pts',(-137.395507796253,5.8548497885868,128.73895559457));
#236450=CARTESIAN_POINT('Ctrl Pts',(-137.673955420066,1.42700558223168,
124.762107807213));
#236451=CARTESIAN_POINT('Ctrl Pts',(-137.952403043879,-4.3121870410957,
126.33779517211));
#236452=CARTESIAN_POINT('Ctrl Pts',(-138.230850667692,-6.08869043570493,
132.018037977528));
#236453=CARTESIAN_POINT('Ctrl Pts',(-138.509298291505,-2.26998476896503,
136.582970580575));
#236454=CARTESIAN_POINT('Ctrl Pts',(-138.787745915318,3.63472600553235,
135.837642928407));
#236455=CARTESIAN_POINT('Ctrl Pts',(-139.066193539131,6.1993011471828,130.466974722087));
#236456=CARTESIAN_POINT('Ctrl Pts',(-139.344641162943,3.06702138726935,
125.406347671494));
#236457=CARTESIAN_POINT('Ctrl Pts',(-139.623088786757,-2.88370119522,125.306230810748));
#236458=CARTESIAN_POINT('Ctrl Pts',(-139.901536410569,-6.18444325593727,
130.258626643894));
#236459=CARTESIAN_POINT('Ctrl Pts',(-140.179984034382,-3.80198409129777,
135.712525338258));
#236460=CARTESIAN_POINT('Ctrl Pts',(-140.458431658195,2.07431271599591,
136.656060431482));
#236461=CARTESIAN_POINT('Ctrl Pts',(-140.736879282008,6.04441747309895,
132.222169267145));
#236462=CARTESIAN_POINT('Ctrl Pts',(-141.015326905821,4.45999785863389,
126.485381217648));
#236463=CARTESIAN_POINT('Ctrl Pts',(-141.293774529634,-1.22294190490765,
124.717524242802));
#236464=CARTESIAN_POINT('Ctrl Pts',(-141.572222153447,-5.78205780187226,
128.543172537875));
#236465=CARTESIAN_POINT('Ctrl Pts',(-141.85066977726,-5.02774504814366,
134.446742213005));
#236466=CARTESIAN_POINT('Ctrl Pts',(-142.129117401072,0.346819785828787,
137.003141142159));
#236467=CARTESIAN_POINT('Ctrl Pts',(-142.407565024885,5.40267417971275,
133.863163596476));
#236468=CARTESIAN_POINT('Ctrl Pts',(-142.686012648698,5.49373493774783,
127.912295544006));
#236469=CARTESIAN_POINT('Ctrl Pts',(-142.964460272511,0.536321671864061,
124.619094008905));
#236470=CARTESIAN_POINT('Ctrl Pts',(-143.242907896324,-4.91394500969209,
127.00985032009));
#236471=CARTESIAN_POINT('Ctrl Pts',(-143.521355520137,-5.84853628690073,
132.887576222521));
#236472=CARTESIAN_POINT('Ctrl Pts',(-143.79980314395,-1.40860843332932,
136.850928754739));
#236473=CARTESIAN_POINT('Ctrl Pts',(-144.078250767763,4.32576175612421,
135.257780560169));
#236474=CARTESIAN_POINT('Ctrl Pts',(-144.356698391576,6.08496821690962,
129.572157000006));
#236475=CARTESIAN_POINT('Ctrl Pts',(-144.635146015388,2.2523861535788,125.018868367886));
#236476=CARTESIAN_POINT('Ctrl Pts',(-144.913593639201,-3.65002874971022,
125.782164476213));
#236477=CARTESIAN_POINT('Ctrl Pts',(-145.192041263014,-6.19824554583293,
131.160613490521));
#236478=CARTESIAN_POINT('Ctrl Pts',(-145.470488886827,-3.05057748646412,
136.211683518503));
#236479=CARTESIAN_POINT('Ctrl Pts',(-145.74893651064,2.90042225397064,136.293687962933));
#236480=CARTESIAN_POINT('Ctrl Pts',(-146.027384134453,6.18607563651005,
131.33126874552));
#236481=CARTESIAN_POINT('Ctrl Pts',(-146.305831758266,3.78702771569254,
125.884646699409));
#236482=CARTESIAN_POINT('Ctrl Pts',(-146.584279382079,-2.09211366925746,
124.959001402698));
#236483=CARTESIAN_POINT('Ctrl Pts',(-146.862727005891,-6.04870479759444,
129.404955662777));
#236484=CARTESIAN_POINT('Ctrl Pts',(-147.141174629705,-4.4468317125993,
135.136894711575));
#236485=CARTESIAN_POINT('Ctrl Pts',(-147.419622253517,1.24146247646836,
136.887446584034));
#236486=CARTESIAN_POINT('Ctrl Pts',(-147.69806987733,5.78891329847519,133.04793962858));
#236487=CARTESIAN_POINT('Ctrl Pts',(-147.976517501143,5.01663560332014,
127.146693166932));
#236488=CARTESIAN_POINT('Ctrl Pts',(-148.254965124956,-0.365685135012239,
124.606664405427));
#236489=CARTESIAN_POINT('Ctrl Pts',(-148.533412748769,-5.41195909898036,
127.762015688586));
#236490=CARTESIAN_POINT('Ctrl Pts',(-148.811860372582,-5.48490703988586,
133.713133334664));
#236491=CARTESIAN_POINT('Ctrl Pts',(-149.090307996395,-0.517493363741682,
136.991230955176));
#236492=CARTESIAN_POINT('Ctrl Pts',(-149.368755620208,4.92547143272535,
134.583896980843));
#236493=CARTESIAN_POINT('Ctrl Pts',(-149.647203244021,5.84216860517359,
128.703353729273));
#236494=CARTESIAN_POINT('Ctrl Pts',(-149.925650867833,1.39019823527075,
124.753533168151));
#236495=CARTESIAN_POINT('Ctrl Pts',(-150.204098491647,-4.33929639788676,
126.364127433687));
#236496=CARTESIAN_POINT('Ctrl Pts',(-150.482546115459,-6.08118962780021,
132.055079077756));
#236497=CARTESIAN_POINT('Ctrl Pts',(-150.760993739272,-2.23476667239474,
136.596681557904));
#236498=CARTESIAN_POINT('Ctrl Pts',(-151.039441363085,3.66529768052036,
135.81542406449));
#236499=CARTESIAN_POINT('Ctrl Pts',(-151.317888986898,6.19713252478332,
130.429244067412));
#236500=CARTESIAN_POINT('Ctrl Pts',(-151.596336610711,3.03410532552526,
125.387777854462));
#236501=CARTESIAN_POINT('Ctrl Pts',(-151.874784234524,-2.91711644360522,
125.323886586026));
#236502=CARTESIAN_POINT('Ctrl Pts',(-152.153231858337,-6.18765071012318,
130.296283216534));
#236503=CARTESIAN_POINT('Ctrl Pts',(-152.431679482149,-3.77203625758034,
135.735578157629));
#236504=CARTESIAN_POINT('Ctrl Pts',(-152.710127105962,2.10989524146327,
136.643325082775));
#236505=CARTESIAN_POINT('Ctrl Pts',(-152.988574729775,6.0529360877152,132.185348913665));
#236506=CARTESIAN_POINT('Ctrl Pts',(-153.267022353588,4.43362437172323,
126.458311965469));
#236507=CARTESIAN_POINT('Ctrl Pts',(-153.545469977401,-1.25997154729018,
124.725081412269));
#236508=CARTESIAN_POINT('Ctrl Pts',(-153.823917601214,-5.79571516737629,
128.578411459437));
#236509=CARTESIAN_POINT('Ctrl Pts',(-154.102365225027,-5.00547968506979,
134.477280039263));
#236510=CARTESIAN_POINT('Ctrl Pts',(-154.38081284884,0.38454709653853,137.000915102638));
#236511=CARTESIAN_POINT('Ctrl Pts',(-154.659260472653,5.4211938825983,133.830219312748));
#236512=CARTESIAN_POINT('Ctrl Pts',(-154.937708096465,5.47602833059452,
127.8789072034));
#236513=CARTESIAN_POINT('Ctrl Pts',(-155.216155720278,0.498660261630971,
124.615943865326));
#236514=CARTESIAN_POINT('Ctrl Pts',(-155.494603344091,-4.93695222686361,
127.039833201595));
#236515=CARTESIAN_POINT('Ctrl Pts',(-155.773050967904,-5.83574680239484,
132.923139325752));
#236516=CARTESIAN_POINT('Ctrl Pts',(-156.051498591717,-1.37177515860606,
136.85939132518));
#236517=CARTESIAN_POINT('Ctrl Pts',(-156.32994621553,4.3527908409998,135.231365909006));
#236518=CARTESIAN_POINT('Ctrl Pts',(-156.608393839343,6.0773547033811,129.535138901228));
#236519=CARTESIAN_POINT('Ctrl Pts',(-156.886841463156,2.21712648863745,
125.005264645838));
#236520=CARTESIAN_POINT('Ctrl Pts',(-157.165289086968,-3.68053265651321,
125.804476286877));
#236521=CARTESIAN_POINT('Ctrl Pts',(-157.443736710782,-6.19596209434481,
131.19833736989));
#236522=CARTESIAN_POINT('Ctrl Pts',(-157.722184334594,-3.0176050570491,
136.230153064351));
#236523=CARTESIAN_POINT('Ctrl Pts',(-158.000631958407,2.93378360947182,
136.275930564914));
#236524=CARTESIAN_POINT('Ctrl Pts',(-158.27907958222,6.18916846218569,131.293602584915));
#236525=CARTESIAN_POINT('Ctrl Pts',(-158.557527206033,3.7570098558391,125.861685137721));
#236526=CARTESIAN_POINT('Ctrl Pts',(-158.835974829846,-2.12765726788813,
124.971844993383));
#236527=CARTESIAN_POINT('Ctrl Pts',(-159.114422453659,-6.05711130426257,
129.44180177344));
#236528=CARTESIAN_POINT('Ctrl Pts',(-159.392870077472,-4.42037595835707,
135.163883566548));
#236529=CARTESIAN_POINT('Ctrl Pts',(-159.671317701285,1.27846894590735,
136.879776744077));
#236530=CARTESIAN_POINT('Ctrl Pts',(-159.949765325097,5.80246334556346,
133.01265930192));
#236531=CARTESIAN_POINT('Ctrl Pts',(-160.22821294891,4.9942773967397,127.116223250229));
#236532=CARTESIAN_POINT('Ctrl Pts',(-160.506660572723,-0.403405495673234,
124.609005263594));
#236533=CARTESIAN_POINT('Ctrl Pts',(-160.785108196536,-5.43037844501628,
127.795016187323));
#236534=CARTESIAN_POINT('Ctrl Pts',(-161.063555820349,-5.46709889212507,
133.746467627798));
#236535=CARTESIAN_POINT('Ctrl Pts',(-161.342003444162,-0.479822539999598,
136.994266455786));
#236536=CARTESIAN_POINT('Ctrl Pts',(-161.620451067975,4.94838728575097,
134.553844212161));
#236537=CARTESIAN_POINT('Ctrl Pts',(-161.898898691787,5.82927093805496,
128.66782971756));
#236538=CARTESIAN_POINT('Ctrl Pts',(-162.177346315601,1.35333937400316,
124.745182744726));
#236539=CARTESIAN_POINT('Ctrl Pts',(-162.455793939413,-4.36624496045326,
126.390624229737));
#236540=CARTESIAN_POINT('Ctrl Pts',(-162.734241563226,-6.07346347917808,
132.092073832152));
#236541=CARTESIAN_POINT('Ctrl Pts',(-163.012689187039,-2.19946576572379,
136.61017789865));
#236542=CARTESIAN_POINT('Ctrl Pts',(-163.291136810852,3.69573353655413,
135.793019513774));
#236543=CARTESIAN_POINT('Ctrl Pts',(-163.569584434665,6.19473426535967,
130.391527312818));
#236544=CARTESIAN_POINT('Ctrl Pts',(-163.848032058478,3.0010768338922,125.369408750896));
#236545=CARTESIAN_POINT('Ctrl Pts',(-164.126479682291,-2.95042359716811,
125.341745442286));
#236546=CARTESIAN_POINT('Ctrl Pts',(-164.404927306104,-6.19062887863655,
130.333958616169));
#236547=CARTESIAN_POINT('Ctrl Pts',(-164.683374929917,-3.74194864967208,
135.758448248921));
#236548=CARTESIAN_POINT('Ctrl Pts',(-164.961822553729,2.14539958398697,
136.630373369092));
#236549=CARTESIAN_POINT('Ctrl Pts',(-165.240270177542,6.06123040855813,
132.148477387157));
#236550=CARTESIAN_POINT('Ctrl Pts',(-165.518717801355,4.40708659523179,
126.431403757722));
#236551=CARTESIAN_POINT('Ctrl Pts',(-165.797165425168,-1.29695450096345,
124.732863851664));
#236552=CARTESIAN_POINT('Ctrl Pts',(-166.075613048981,-5.80915777052276,
128.613732864363));
#236553=CARTESIAN_POINT('Ctrl Pts',(-166.354060672794,-4.98302884210618,
134.50768176414));
#236554=CARTESIAN_POINT('Ctrl Pts',(-166.632508296607,0.422260157714416,
136.998459447511));
#236555=CARTESIAN_POINT('Ctrl Pts',(-166.91095592042,5.43951270115045,133.797162904712));
#236556=CARTESIAN_POINT('Ctrl Pts',(-167.189403544233,5.45811880719792,
127.845627266545));
#236557=CARTESIAN_POINT('Ctrl Pts',(-167.467851168046,0.460980373357943,
124.613023035806));
#236558=CARTESIAN_POINT('Ctrl Pts',(-167.746298791858,-4.95977650345479,
127.069955579048));
#236559=CARTESIAN_POINT('Ctrl Pts',(-168.024746415672,-5.822741072145,132.958623916859));
#236560=CARTESIAN_POINT('Ctrl Pts',(-168.303194039484,-1.33489105224939,
136.867629524233));
#236561=CARTESIAN_POINT('Ctrl Pts',(-168.581641663297,4.37965863161014,
135.204787213532));
#236562=CARTESIAN_POINT('Ctrl Pts',(-168.86008928711,6.06951599123876,129.498167833929));
#236563=CARTESIAN_POINT('Ctrl Pts',(-169.138536910923,2.18178466725943,
124.991875811423));
#236564=CARTESIAN_POINT('Ctrl Pts',(-169.416984534736,-3.71090017982492,
125.826973370093));
#236565=CARTESIAN_POINT('Ctrl Pts',(-169.695432158549,-6.19344904920226,
131.236046650305));
#236566=CARTESIAN_POINT('Ctrl Pts',(-169.973879782361,-2.98452080916978,
136.248421555465));
#236567=CARTESIAN_POINT('Ctrl Pts',(-170.252327406175,2.96703625254325,
136.257970415857));
#236568=CARTESIAN_POINT('Ctrl Pts',(-170.530775029987,6.19203194594742,
131.25591829527));
#236569=CARTESIAN_POINT('Ctrl Pts',(-170.8092226538,3.72685277860365,125.838906728691));
#236570=CARTESIAN_POINT('Ctrl Pts',(-171.087670277614,-2.16312202539704,
124.984904710079));
#236571=CARTESIAN_POINT('Ctrl Pts',(-171.366117901426,-6.06529336244348,
129.478698374222));
#236572=CARTESIAN_POINT('Ctrl Pts',(-171.644565525239,-4.39375640545797,
135.190710877796));
#236573=CARTESIAN_POINT('Ctrl Pts',(-171.923013149052,1.31542804121008,
136.871881777341));
#236574=CARTESIAN_POINT('Ctrl Pts',(-172.201460772865,5.81579838023838,
132.977297145939));
#236575=CARTESIAN_POINT('Ctrl Pts',(-172.479908396678,4.97173412537368,
127.085889998814));
#236576=CARTESIAN_POINT('Ctrl Pts',(-172.75835602049,-0.441110907994683,
124.611575692932));
#236577=CARTESIAN_POINT('Ctrl Pts',(-173.036803644304,-5.4485965663818,
127.828128198426));
#236578=CARTESIAN_POINT('Ctrl Pts',(-173.315251268116,-5.44908815900415,
133.779692900072));
#236579=CARTESIAN_POINT('Ctrl Pts',(-173.593698891929,-0.442133936257506,
136.997072587158));
#236580=CARTESIAN_POINT('Ctrl Pts',(-173.872146515742,4.97111977446672,
134.523652504987));
#236581=CARTESIAN_POINT('Ctrl Pts',(-174.150594139555,5.81615726515733,
128.632384875785));
#236582=CARTESIAN_POINT('Ctrl Pts',(-174.429041763368,1.31643036424716,
124.737056846366));
#236583=CARTESIAN_POINT('Ctrl Pts',(-174.707489387181,-4.39303173020782,
126.417284578411));
#236584=CARTESIAN_POINT('Ctrl Pts',(-174.985937010994,-6.06551227613263,
132.129020869861));
#236585=CARTESIAN_POINT('Ctrl Pts',(-175.264384634806,-2.16408335703982,
136.623459102702));
#236586=CARTESIAN_POINT('Ctrl Pts',(-175.542832258619,3.72603244582337,
135.770430106468));
#236587=CARTESIAN_POINT('Ctrl Pts',(-175.821279882432,6.19210645777918,
130.353825855915));
#236588=CARTESIAN_POINT('Ctrl Pts',(-176.099727506245,2.96793713625374,
125.351241041473));
#236589=CARTESIAN_POINT('Ctrl Pts',(-176.378175130058,-2.98362142169932,
125.359806717758));
#236590=CARTESIAN_POINT('Ctrl Pts',(-176.656622753871,-6.19337765112022,
130.371651446723));
#236591=CARTESIAN_POINT('Ctrl Pts',(-176.935070377684,-3.71172238248064,
135.781134764673));
#236592=CARTESIAN_POINT('Ctrl Pts',(-177.213518001496,2.18082442793968,
136.617205770365));
#236593=CARTESIAN_POINT('Ctrl Pts',(-177.49196562531,6.06930012827989,132.111556053907));
#236594=CARTESIAN_POINT('Ctrl Pts',(-177.770413249122,4.38038551252508,
126.404657591498));
#236595=CARTESIAN_POINT('Ctrl Pts',(-178.048860872936,-1.33388939551094,
124.740871272604));
#236596=CARTESIAN_POINT('Ctrl Pts',(-178.327308496748,-5.82238511319243,
128.649135443807));
#236597=CARTESIAN_POINT('Ctrl Pts',(-178.605756120561,-4.96039335117553,
134.537946261091));
#236598=CARTESIAN_POINT('Ctrl Pts',(-178.884203744374,0.459957571884186,
136.995774267775));
#236599=CARTESIAN_POINT('Ctrl Pts',(-179.162651368187,5.45762995655925,
133.763995597288));
#236600=CARTESIAN_POINT('Ctrl Pts',(-179.441098991999,5.44000703120181,
127.812456966643));
#236601=CARTESIAN_POINT('Ctrl Pts',(-179.719546615813,0.423283403288203,
124.610331628578));
#236602=CARTESIAN_POINT('Ctrl Pts',(-179.997994239625,-4.98241699370369,
127.100216336253));
#236603=CARTESIAN_POINT('Ctrl Pts',(-180.276441863438,-5.80951957808352,
132.994028680947));
#236604=CARTESIAN_POINT('Ctrl Pts',(-180.554889487251,-1.29795748101432,
136.875643046625));
#236605=CARTESIAN_POINT('Ctrl Pts',(-180.833337111064,4.40636413235919,
135.178045458633));
#236606=CARTESIAN_POINT('Ctrl Pts',(-181.111784734877,6.06145237094964,
129.461245168083));
#236607=CARTESIAN_POINT('Ctrl Pts',(-181.39023235869,2.14636199904753,124.97870236077));
#236608=CARTESIAN_POINT('Ctrl Pts',(-181.668679982503,-3.74113019436597,
125.849654892224));
#236609=CARTESIAN_POINT('Ctrl Pts',(-181.947127606316,-6.19070650352801,
131.273739934436));
#236610=CARTESIAN_POINT('Ctrl Pts',(-182.225575230128,-2.95132596877351,
136.266488314898));
#236611=CARTESIAN_POINT('Ctrl Pts',(-182.504022853942,3.00017895099442,
136.239808181284));
#236612=CARTESIAN_POINT('Ctrl Pts',(-182.782470477755,6.19466598168877,
131.218217272988));
#236613=CARTESIAN_POINT('Ctrl Pts',(-183.060918101567,3.6965576014681,125.81631231638));
#236614=CARTESIAN_POINT('Ctrl Pts',(-183.33936572538,-2.19850662762309,
124.998180068855));
#236615=CARTESIAN_POINT('Ctrl Pts',(-183.617813349193,-6.07325066894868,
129.515644097905));
#236616=CARTESIAN_POINT('Ctrl Pts',(-183.896260973006,-4.36697404029963,
135.217375651221));
#236617=CARTESIAN_POINT('Ctrl Pts',(-184.174708596819,1.35233839284232,
136.863761976378));
#236618=CARTESIAN_POINT('Ctrl Pts',(-184.453156220632,5.8289179083658,132.941854470998));
#236619=CARTESIAN_POINT('Ctrl Pts',(-184.731603844444,4.94900662457131,
127.055694536694));
#236620=CARTESIAN_POINT('Ctrl Pts',(-185.010051468258,-0.478799974789776,
124.614375598192));
#236621=CARTESIAN_POINT('Ctrl Pts',(-185.28849909207,-5.46661278799793,
127.861350494915));
#236622=CARTESIAN_POINT('Ctrl Pts',(-185.566946715884,-5.43087550791776,
133.812807920317));
#236623=CARTESIAN_POINT('Ctrl Pts',(-185.845394339696,-0.404428949079144,
136.999649245311));
#236624=CARTESIAN_POINT('Ctrl Pts',(-186.123841963509,4.99366805651034,
134.493322978084));
#236625=CARTESIAN_POINT('Ctrl Pts',(-186.402289587322,5.80282807241402,
128.59702051737));
#236626=CARTESIAN_POINT('Ctrl Pts',(-186.680737211135,1.27947257368013,
124.729155774178));
#236627=CARTESIAN_POINT('Ctrl Pts',(-186.959184834948,-4.41965571455532,
126.444107491802));
#236628=CARTESIAN_POINT('Ctrl Pts',(-187.237632458761,-6.0573363132998,
132.165918821797));
#236629=CARTESIAN_POINT('Ctrl Pts',(-187.516080082574,-2.12862075745111,
136.636524677919));
#236630=CARTESIAN_POINT('Ctrl Pts',(-187.794527706387,3.75619328558978,
135.74765667963));
#236631=CARTESIAN_POINT('Ctrl Pts',(-188.072975330199,6.18924919941703,
130.316141093742));
#236632=CARTESIAN_POINT('Ctrl Pts',(-188.351422954013,2.93468746061294,
125.333275399398));
#236633=CARTESIAN_POINT('Ctrl Pts',(-188.629870577825,-3.01670868704181,
125.378069743179));
#236634=CARTESIAN_POINT('Ctrl Pts',(-188.908318201638,-6.19589692571743,
130.409360311474));
#236635=CARTESIAN_POINT('Ctrl Pts',(-189.186765825451,-3.68135857605119,
135.80363686423));
#236636=CARTESIAN_POINT('Ctrl Pts',(-189.465213449264,2.21616846064164,
136.603822774524));
#236637=CARTESIAN_POINT('Ctrl Pts',(-189.743661073077,6.07714494785282,
132.07458628205));
#236638=CARTESIAN_POINT('Ctrl Pts',(-190.02210869689,4.35352211302309,126.378074457888));
#236639=CARTESIAN_POINT('Ctrl Pts',(-190.300556320702,-1.37077486229612,
124.749103378371));
#236640=CARTESIAN_POINT('Ctrl Pts',(-190.579003944516,-5.83539670523986,
128.684617885911));
#236641=CARTESIAN_POINT('Ctrl Pts',(-190.857451568328,-4.93757405104588,
134.568072408653));
#236642=CARTESIAN_POINT('Ctrl Pts',(-191.135899192141,0.497637942157669,
136.992859662928));
#236643=CARTESIAN_POINT('Ctrl Pts',(-191.414346815954,5.47554497748281,
133.730718619501));
#236644=CARTESIAN_POINT('Ctrl Pts',(-191.692794439767,5.42169367374449,
127.779397532831));
#236645=CARTESIAN_POINT('Ctrl Pts',(-191.97124206358,0.385570748295746,
124.60786974337));
#236646=CARTESIAN_POINT('Ctrl Pts',(-192.249689687393,-5.00487285865859,
127.130614351886));
#236647=CARTESIAN_POINT('Ctrl Pts',(-192.528137311206,-5.79608281013753,
133.029352306079));
#236648=CARTESIAN_POINT('Ctrl Pts',(-192.806584935019,-1.26097581348702,
136.883431595415));
#236649=CARTESIAN_POINT('Ctrl Pts',(-193.085032558831,4.43290635366497,
135.151141635234));
#236650=CARTESIAN_POINT('Ctrl Pts',(-193.363480182644,6.05316414131348,
129.424372271875));
#236651=CARTESIAN_POINT('Ctrl Pts',(-193.641927806457,2.11085979660312,
124.965744782026));
#236652=CARTESIAN_POINT('Ctrl Pts',(-193.92037543027,-3.77122157995168,
125.872520012798));
#236653=CARTESIAN_POINT('Ctrl Pts',(-194.198823054083,-6.1877345589472,
131.311415825543));
#236654=CARTESIAN_POINT('Ctrl Pts',(-194.477270677896,-2.91802176590892,
136.284352673182));
#236655=CARTESIAN_POINT('Ctrl Pts',(-194.755718301709,3.03321047671203,
136.221444534203));
#236656=CARTESIAN_POINT('Ctrl Pts',(-195.034165925522,6.19707047180361,
131.180500915096));
#236657=CARTESIAN_POINT('Ctrl Pts',(-195.312613549334,3.66612544703105,
125.793902738034));
#236658=CARTESIAN_POINT('Ctrl Pts',(-195.591061173148,-2.23380976337827,
125.011670577786));
#236659=CARTESIAN_POINT('Ctrl Pts',(-195.86950879696,-6.08098292891658,
129.552637575454));
#236660=CARTESIAN_POINT('Ctrl Pts',(-196.147956420774,-4.3400298553121,
135.243876898752));
#236661=CARTESIAN_POINT('Ctrl Pts',(-196.426404044586,1.38919863307876,
136.855417642068));
#236662=CARTESIAN_POINT('Ctrl Pts',(-196.704851668399,5.84182144379631,
132.906332590435));
#236663=CARTESIAN_POINT('Ctrl Pts',(-196.983299292212,4.92609573650846,
127.025637982775));
#236664=CARTESIAN_POINT('Ctrl Pts',(-197.261746916025,-0.516471299475173,
124.617404875624));
#236665=CARTESIAN_POINT('Ctrl Pts',(-197.540194539838,-5.48442644226676,
127.894681845726));
#236666=CARTESIAN_POINT('Ctrl Pts',(-197.81864216365,-5.41246161374207,
133.845811461438));
#236667=CARTESIAN_POINT('Ctrl Pts',(-198.097089787464,-0.36670897563802,
137.001996334766));
#236668=CARTESIAN_POINT('Ctrl Pts',(-198.375537411276,5.01603129634849,
134.462856755322));
#236669=CARTESIAN_POINT('Ctrl Pts',(-198.65398503509,5.78928385374183,128.561737952753));
#236670=CARTESIAN_POINT('Ctrl Pts',(-198.932432658902,1.24246737178614,
124.721479820939));
#236671=CARTESIAN_POINT('Ctrl Pts',(-199.210880282716,-4.44611592693577,
126.471091975977));
#236672=CARTESIAN_POINT('Ctrl Pts',(-199.489327906528,-6.04893589364168,
132.202766320694));
#236673=CARTESIAN_POINT('Ctrl Pts',(-199.767775530341,-2.09307928103787,
136.649374140152));
#236674=CARTESIAN_POINT('Ctrl Pts',(-200.046223154153,3.7862149382325,135.724700077139));
#236675=CARTESIAN_POINT('Ctrl Pts',(-200.324670777967,6.18616259614969,
130.278474422724));
#236676=CARTESIAN_POINT('Ctrl Pts',(-200.603118401779,2.90132903904936,
125.315512490399));
#236677=CARTESIAN_POINT('Ctrl Pts',(-200.881566025592,-3.04968416713424,
125.396533841802));
#236678=CARTESIAN_POINT('Ctrl Pts',(-201.160013649405,-6.1981866090755,
130.447083813107));
#236679=CARTESIAN_POINT('Ctrl Pts',(-201.438461273218,-3.65085835552605,
135.825953713766));
#236680=CARTESIAN_POINT('Ctrl Pts',(-201.716908897031,2.2514303724059,136.590224877478));
#236681=CARTESIAN_POINT('Ctrl Pts',(-201.995356520844,6.08476457658541,
132.037569441512));
#236682=CARTESIAN_POINT('Ctrl Pts',(-202.273804144657,4.32649739215744,
126.35165534194));
#236683=CARTESIAN_POINT('Ctrl Pts',(-202.55225176847,-1.40760953451491,
124.757559863922));
#236684=CARTESIAN_POINT('Ctrl Pts',(-202.830699392283,-5.84819206451709,
128.720178875862));
#236685=CARTESIAN_POINT('Ctrl Pts',(-203.109147016096,-4.91457178729319,
134.59805909049));
#236686=CARTESIAN_POINT('Ctrl Pts',(-203.387594639908,0.535299872273523,
136.989715740974));
#236687=CARTESIAN_POINT('Ctrl Pts',(-203.666042263721,5.49325710007376,
133.697333204442));
#236688=CARTESIAN_POINT('Ctrl Pts',(-203.944489887534,5.40317941343439,
127.746450190138));
#236689=CARTESIAN_POINT('Ctrl Pts',(-204.222937511347,0.347843805837959,
124.605637471411));
#236690=CARTESIAN_POINT('Ctrl Pts',(-204.50138513516,-5.0271432662092,127.161148499539));
#236691=CARTESIAN_POINT('Ctrl Pts',(-204.779832758973,-5.78243126621161,
133.064593483327));
#236692=CARTESIAN_POINT('Ctrl Pts',(-205.058280382786,-1.22394742003769,
136.890994881994));
#236693=CARTESIAN_POINT('Ctrl Pts',(-205.336728006599,4.45928431199552,
135.124076740266));
#236694=CARTESIAN_POINT('Ctrl Pts',(-205.615175630412,6.04465160945437,
129.387550511641));
#236695=CARTESIAN_POINT('Ctrl Pts',(-205.893623254225,2.07527937547198,
124.953003555339));
#236696=CARTESIAN_POINT('Ctrl Pts',(-206.172070878037,-3.80117322153507,
125.89556788454));
#236697=CARTESIAN_POINT('Ctrl Pts',(-206.45051850185,-6.18453332558722,
131.349072927534));
#236698=CARTESIAN_POINT('Ctrl Pts',(-206.728966125663,-2.8846094346739,
136.302013968343));
#236699=CARTESIAN_POINT('Ctrl Pts',(-207.007413749476,3.06612960569919,
136.202880155086));
#236700=CARTESIAN_POINT('Ctrl Pts',(-207.285861373289,6.19924532719362,
131.142770619188));
#236701=CARTESIAN_POINT('Ctrl Pts',(-207.564308997102,3.63555744296752,
125.771678824048));
#236702=CARTESIAN_POINT('Ctrl Pts',(-207.842756620915,-2.26903012449045,
125.025375736976));
#236703=CARTESIAN_POINT('Ctrl Pts',(-208.121204244728,-6.08848985582611,
129.58967743606));
#236704=CARTESIAN_POINT('Ctrl Pts',(-208.399651868541,-4.31292484892225,
135.270213638376));
#236705=CARTESIAN_POINT('Ctrl Pts',(-208.678099492353,1.42600739604885,
136.846849083615));
#236706=CARTESIAN_POINT('Ctrl Pts',(-208.956547116166,5.85450850838505,
132.870732820528));
#236707=CARTESIAN_POINT('Ctrl Pts',(-209.234994739979,4.90300231015654,
126.995721450812));
#236708=CARTESIAN_POINT('Ctrl Pts',(-209.513442363792,-0.554123486127181,
124.620663412976));
#236709=CARTESIAN_POINT('Ctrl Pts',(-209.791889987605,-5.50203686909699,
127.928121015754));
#236710=CARTESIAN_POINT('Ctrl Pts',(-210.070337611418,-5.393847158811,133.878702300482));
#236711=CARTESIAN_POINT('Ctrl Pts',(-210.348785235231,-0.328975413660277,
137.004113768549));
#236712=CARTESIAN_POINT('Ctrl Pts',(-210.627232859043,5.03820866530154,
134.432254965643));
#236713=CARTESIAN_POINT('Ctrl Pts',(-210.905680482857,5.77552511102812,
128.526538489345));
#236714=CARTESIAN_POINT('Ctrl Pts',(-211.184128106669,1.20541612980698,
124.714029271085));
#236715=CARTESIAN_POINT('Ctrl Pts',(-211.462575730482,-4.47241138685473,
126.498237031013));
#236716=CARTESIAN_POINT('Ctrl Pts',(-211.741023354295,-6.04031132844015,
132.239562001151));
#236717=CARTESIAN_POINT('Ctrl Pts',(-212.019470978108,-2.05746024480169,
136.66200701326));
#236718=CARTESIAN_POINT('Ctrl Pts',(-212.297918601921,3.81609629128846,
135.701561149659));
#236719=CARTESIAN_POINT('Ctrl Pts',(-212.576366225734,6.1828467623524,130.240827238612));
#236720=CARTESIAN_POINT('Ctrl Pts',(-212.854813849547,2.86786310767097,
125.297952972686));
#236721=CARTESIAN_POINT('Ctrl Pts',(-213.133261473359,-3.0825466400586,
125.415198329437));
#236722=CARTESIAN_POINT('Ctrl Pts',(-213.411709097173,-6.20024661634941,
130.484820553763));
#236723=CARTESIAN_POINT('Ctrl Pts',(-213.690156720985,-3.62022285110177,
135.848084486325));
#236724=CARTESIAN_POINT('Ctrl Pts',(-213.968604344798,2.28660885659016,
136.576412583105));
#236725=CARTESIAN_POINT('Ctrl Pts',(-214.247051968611,6.09215873212836,
132.00050690397));
#236726=CARTESIAN_POINT('Ctrl Pts',(-214.525499592424,4.29931235134063,
126.325401222624));
#236727=CARTESIAN_POINT('Ctrl Pts',(-214.803947216237,-1.44439204724454,
124.766240415898));
#236728=CARTESIAN_POINT('Ctrl Pts',(-215.08239484005,-5.86077071688603,
128.755817095934));
#236729=CARTESIAN_POINT('Ctrl Pts',(-215.360842463863,-4.89138741227638,
134.627905195436));
#236730=CARTESIAN_POINT('Ctrl Pts',(-215.639290087675,0.572941966656434,
136.986342618411));
#236731=CARTESIAN_POINT('Ctrl Pts',(-215.917737711489,5.51076566800256,
133.66384058922));
#236732=CARTESIAN_POINT('Ctrl Pts',(-216.196185335301,5.38446493632399,
127.713616159441));
#236733=CARTESIAN_POINT('Ctrl Pts',(-216.474632959115,0.310103973899474,
124.603634895418));
#236734=CARTESIAN_POINT('Ctrl Pts',(-216.753080582927,-5.04922739111732,
127.191817647757));
#236735=CARTESIAN_POINT('Ctrl Pts',(-217.031528206741,-5.76856545216855,
133.099750906814));
#236736=CARTESIAN_POINT('Ctrl Pts',(-217.309975830553,-1.18687367276612,
136.898332626102));
#236737=CARTESIAN_POINT('Ctrl Pts',(-217.588423454366,4.48549702990607,
135.096851776628));
#236738=CARTESIAN_POINT('Ctrl Pts',(-217.866871078179,6.03591509080661,
129.350781251827));
#236739=CARTESIAN_POINT('Ctrl Pts',(-218.145318701992,2.03962205410111,
124.94047915284));
#236740=CARTESIAN_POINT('Ctrl Pts',(-218.423766325804,-3.83098400924668,
125.9187976534));
#236741=CARTESIAN_POINT('Ctrl Pts',(-218.702213949618,-6.18110292207006,
131.386709845009));
#236742=CARTESIAN_POINT('Ctrl Pts',(-218.98066157343,-2.85109021317626,
136.319471545938));
#236743=CARTESIAN_POINT('Ctrl Pts',(-219.259109197243,3.09893511812703,
136.18411573184));
#236744=CARTESIAN_POINT('Ctrl Pts',(-219.537556821056,6.20119046726778,
131.105027783371));
#236745=CARTESIAN_POINT('Ctrl Pts',(-219.816004444869,3.6048547219858,125.749641397935));
#236746=CARTESIAN_POINT('Ctrl Pts',(-220.094452068682,-2.30416640585769,
125.039295038577));
#236747=CARTESIAN_POINT('Ctrl Pts',(-220.372899692494,-6.09577117150464,
129.626762307198));
#236748=CARTESIAN_POINT('Ctrl Pts',(-220.651347316308,-4.28566002551621,
135.296384894171));
#236749=CARTESIAN_POINT('Ctrl Pts',(-220.929794940121,1.46276331779004,
136.83805661853));
#236750=CARTESIAN_POINT('Ctrl Pts',(-221.208242563933,5.86697863200795,
132.835056480438));
#236751=CARTESIAN_POINT('Ctrl Pts',(-221.486690187747,4.87972720125093,
126.965946049375));
#236752=CARTESIAN_POINT('Ctrl Pts',(-221.765137811559,-0.591755139529082,
124.624151089502));
#236753=CARTESIAN_POINT('Ctrl Pts',(-222.043585435373,-5.51944341592756,
127.961666765899));
#236754=CARTESIAN_POINT('Ctrl Pts',(-222.322033059185,-5.37503283288975,
133.911479218663));
#236755=CARTESIAN_POINT('Ctrl Pts',(-222.600480682998,-0.29122966137826,
137.006001468201));
#236756=CARTESIAN_POINT('Ctrl Pts',(-222.878928306811,5.06019934158045,
134.401518743003));
#236757=CARTESIAN_POINT('Ctrl Pts',(-223.157375930624,5.7615523541068,128.491423431472));
#236758=CARTESIAN_POINT('Ctrl Pts',(-223.435823554437,1.16832022068962,
124.706804400699));
#236759=CARTESIAN_POINT('Ctrl Pts',(-223.71427117825,-4.49854111992577,
126.525541651043));
#236760=CARTESIAN_POINT('Ctrl Pts',(-223.992718802062,-6.03146293728042,
132.276304499695));
#236761=CARTESIAN_POINT('Ctrl Pts',(-224.271166425875,-2.02176496861996,
136.674422829126));
#236762=CARTESIAN_POINT('Ctrl Pts',(-224.549614049688,3.84583623749284,
135.678240754614));
#236763=CARTESIAN_POINT('Ctrl Pts',(-224.828061673501,6.1793018208946,130.203200936436));
#236764=CARTESIAN_POINT('Ctrl Pts',(-225.106509297314,2.83429090657077,
125.280597496933));
#236765=CARTESIAN_POINT('Ctrl Pts',(-225.384956921127,-3.11529488808334,
125.434062514461));
#236766=CARTESIAN_POINT('Ctrl Pts',(-225.66340454494,-6.20207687120481,
130.522569135094));
#236767=CARTESIAN_POINT('Ctrl Pts',(-225.941852168753,-3.5894531979886,
135.87002836184));
#236768=CARTESIAN_POINT('Ctrl Pts',(-226.220299792565,2.32170260964191,
136.562386403224));
#236769=CARTESIAN_POINT('Ctrl Pts',(-226.498747416378,6.09932714048972,
131.963400042786));
#236770=CARTESIAN_POINT('Ctrl Pts',(-226.777195040191,4.27196799792278,
126.299313072794));
#236771=CARTESIAN_POINT('Ctrl Pts',(-227.055642664004,-1.48112103749588,
124.775144712639));
#236772=CARTESIAN_POINT('Ctrl Pts',(-227.334090287817,-5.87313219624144,
128.79153122554));
#236773=CARTESIAN_POINT('Ctrl Pts',(-227.61253791163,-4.8680217850994,134.65760961753));
#236774=CARTESIAN_POINT('Ctrl Pts',(-227.890985535443,0.610562830463375,
136.982740420231));
#236775=CARTESIAN_POINT('Ctrl Pts',(-228.169433159256,5.52807003248314,
133.630242014917));
#236776=CARTESIAN_POINT('Ctrl Pts',(-228.447880783069,5.36555093588535,
127.680896657417));
#236777=CARTESIAN_POINT('Ctrl Pts',(-228.726328406882,0.272352650944771,
124.601862089598));
#236778=CARTESIAN_POINT('Ctrl Pts',(-229.004776030695,-5.07112441504767,
127.222620660081));
#236779=CARTESIAN_POINT('Ctrl Pts',(-229.283223654507,-5.75448588181141,
133.134823273769));
#236780=CARTESIAN_POINT('Ctrl Pts',(-229.561671278321,-1.14975594545406,
136.905444555836));
#236781=CARTESIAN_POINT('Ctrl Pts',(-229.840118902133,4.51154353607471,
135.069467753152));
#236782=CARTESIAN_POINT('Ctrl Pts',(-230.118566525947,6.0269549091058,129.314065854931));
#236783=CARTESIAN_POINT('Ctrl Pts',(-230.397014149759,2.00388915378425,
124.928172038625));
#236784=CARTESIAN_POINT('Ctrl Pts',(-230.675461773572,-3.86065283843716,
125.942208458593));
#236785=CARTESIAN_POINT('Ctrl Pts',(-230.953909397385,-6.17744347551146,
131.424325183319));
#236786=CARTESIAN_POINT('Ctrl Pts',(-231.232357021197,-2.81746534348149,
136.33672475907));
#236787=CARTESIAN_POINT('Ctrl Pts',(-231.510804645011,3.13162579837364,
136.165151959792));
#236788=CARTESIAN_POINT('Ctrl Pts',(-231.789252268823,6.20290581994918,
131.067273806224));
#236789=CARTESIAN_POINT('Ctrl Pts',(-232.067699892636,3.57401842178686,
125.727791276302));
#236790=CARTESIAN_POINT('Ctrl Pts',(-232.346147516449,-2.33921730549066,
125.053427966802));
#236791=CARTESIAN_POINT('Ctrl Pts',(-232.624595140262,-6.10282660614105,
129.663890814674));
#236792=CARTESIAN_POINT('Ctrl Pts',(-232.903042764075,-4.25823639540172,
135.322389696357));
#236793=CARTESIAN_POINT('Ctrl Pts',(-233.181490387888,1.499465036299,136.829040572621));
#236794=CARTESIAN_POINT('Ctrl Pts',(-233.459938011701,5.87923135258013,
132.799304892167));
#236795=CARTESIAN_POINT('Ctrl Pts',(-233.738385635514,4.85627127225937,
126.9363128818));
#236796=CARTESIAN_POINT('Ctrl Pts',(-234.016833259326,-0.629364865227224,
124.627867775965));
#236797=CARTESIAN_POINT('Ctrl Pts',(-234.29528088314,-5.53664543775268,
127.99531785311));
#236798=CARTESIAN_POINT('Ctrl Pts',(-234.573728506952,-5.35601933315035,
133.944141001422));
#236799=CARTESIAN_POINT('Ctrl Pts',(-234.852176130765,-0.253473117473377,
137.007659363768));
#236800=CARTESIAN_POINT('Ctrl Pts',(-235.130623754578,5.08200251031112,
134.370649226346));
#236801=CARTESIAN_POINT('Ctrl Pts',(-235.409071378391,5.74736610074488,
128.456394080338));
#236802=CARTESIAN_POINT('Ctrl Pts',(-235.687519002204,1.13118101903705,
124.699805477501));
#236803=CARTESIAN_POINT('Ctrl Pts',(-235.965966626017,-4.52450415790052,
126.553004824284));
#236804=CARTESIAN_POINT('Ctrl Pts',(-236.24441424983,-6.0223910480441,132.312992454817));
#236805=CARTESIAN_POINT('Ctrl Pts',(-236.522861873642,-1.98599477519336,
136.686621127679));
#236806=CARTESIAN_POINT('Ctrl Pts',(-236.801309497456,3.87543367482126,
135.654739756147));
#236807=CARTESIAN_POINT('Ctrl Pts',(-237.079757121268,6.1755279031354,130.165596910454));
#236808=CARTESIAN_POINT('Ctrl Pts',(-237.358204745081,2.80061367977841,
125.263446706254));
#236809=CARTESIAN_POINT('Ctrl Pts',(-237.636652368894,-3.14792769771062,
125.453125697856));
#236810=CARTESIAN_POINT('Ctrl Pts',(-237.915099992707,-6.20367730582095,
130.560328158313));
#236811=CARTESIAN_POINT('Ctrl Pts',(-238.19354761652,-3.55855053636696,
135.891784527174));
#236812=CARTESIAN_POINT('Ctrl Pts',(-238.471995240333,2.35671033115007,
136.54814685758));
#236813=CARTESIAN_POINT('Ctrl Pts',(-238.750442864146,6.10626953604027,
131.92625023297));
#236814=CARTESIAN_POINT('Ctrl Pts',(-239.028890487959,4.24446534516054,
126.273391859158));
#236815=CARTESIAN_POINT('Ctrl Pts',(-239.307338111771,-1.51779514426229,
124.784272424193));
#236816=CARTESIAN_POINT('Ctrl Pts',(-239.585785735585,-5.88527604452282,
128.827319941278));
#236817=CARTESIAN_POINT('Ctrl Pts',(-239.864233359397,-4.84447577158576,
134.687171256065));
#236818=CARTESIAN_POINT('Ctrl Pts',(-240.14268098321,0.648161069640796,
136.978909279916));
#236819=CARTESIAN_POINT('Ctrl Pts',(-240.421128607023,5.54516955229552,
133.596538726537));
#236820=CARTESIAN_POINT('Ctrl Pts',(-240.699576230836,5.34643811298351,
127.648292896498));
#236821=CARTESIAN_POINT('Ctrl Pts',(-240.978023854649,0.234591235861842,
124.600319119639));
#236822=CARTESIAN_POINT('Ctrl Pts',(-241.256471478461,-5.09283352659785,
127.253556395099));
#236823=CARTESIAN_POINT('Ctrl Pts',(-241.534919102275,-5.74019307686353,
133.169809284574));
#236824=CARTESIAN_POINT('Ctrl Pts',(-241.813366726087,-1.11259561351327,
136.912330407661));
#236825=CARTESIAN_POINT('Ctrl Pts',(-242.0918143499,4.53742286533832,135.041925684563));
#236826=CARTESIAN_POINT('Ctrl Pts',(-242.370261973713,6.01777139637409,
129.277405681456));
#236827=CARTESIAN_POINT('Ctrl Pts',(-242.648709597526,1.96808199861856,
124.916082668738));
#236828=CARTESIAN_POINT('Ctrl Pts',(-242.927157221339,-3.89017860971679,
125.965799432623));
#236829=CARTESIAN_POINT('Ctrl Pts',(-243.205604845152,-6.1735551215127,
131.461917548614));
#236830=CARTESIAN_POINT('Ctrl Pts',(-243.484052468965,-2.78373607157309,
136.353772968415));
#236831=CARTESIAN_POINT('Ctrl Pts',(-243.762500092778,3.16420043507544,
136.145989541648));
#236832=CARTESIAN_POINT('Ctrl Pts',(-244.040947716591,6.20439132167383,
131.029510086731));
#236833=CARTESIAN_POINT('Ctrl Pts',(-244.319395340403,3.54304968502077,
125.706129268813));
#236834=CARTESIAN_POINT('Ctrl Pts',(-244.597842964216,-2.37418152456686,
125.067773997952));
#236835=CARTESIAN_POINT('Ctrl Pts',(-244.876290588029,-6.10965589829292,
129.701061582678));
#236836=CARTESIAN_POINT('Ctrl Pts',(-245.154738211842,-4.23065497477177,
135.348227081313));
#236837=CARTESIAN_POINT('Ctrl Pts',(-245.433185835655,1.53611119157916,
136.819801279981));
#236838=CARTESIAN_POINT('Ctrl Pts',(-245.711633459468,5.89126621607239,
132.763479380503));
#236839=CARTESIAN_POINT('Ctrl Pts',(-245.990081083281,4.83263539234992,
126.906823046158));
#236840=CARTESIAN_POINT('Ctrl Pts',(-246.268528707094,-0.666951269578287,
124.631813334641));
#236841=CARTESIAN_POINT('Ctrl Pts',(-246.546976330906,-5.55364229714491,
128.029073030433));
#236842=CARTESIAN_POINT('Ctrl Pts',(-246.825423954719,-5.33680736414475,
133.976686438464));
#236843=CARTESIAN_POINT('Ctrl Pts',(-247.103871578532,-0.215707181029578,
137.009087393821));
#236844=CARTESIAN_POINT('Ctrl Pts',(-247.382319202345,5.10361736357064,
134.339647559554));
#236845=CARTESIAN_POINT('Ctrl Pts',(-247.660766826158,5.73296687661779,
128.421451733968));
#236846=CARTESIAN_POINT('Ctrl Pts',(-247.939214449971,1.09399990105564,
124.693032760838));
#236847=CARTESIAN_POINT('Ctrl Pts',(-248.217662073784,-4.55029953871062,
126.580625533077));
#236848=CARTESIAN_POINT('Ctrl Pts',(-248.496109697597,-6.01309599689209,
132.349624507031));
#236849=CARTESIAN_POINT('Ctrl Pts',(-248.77455732141,-1.95015099000055,
136.698601456905));
#236850=CARTESIAN_POINT('Ctrl Pts',(-249.053004945222,3.90488750652966,
135.631059025098));
#236851=CARTESIAN_POINT('Ctrl Pts',(-249.331452569036,6.17152514891849,
130.128016554096));
#236852=CARTESIAN_POINT('Ctrl Pts',(-249.609900192848,2.76683267521693,
125.246501236177));
#236853=CARTESIAN_POINT('Ctrl Pts',(-249.888347816661,-3.18044385971988,
125.472387173231));
#236854=CARTESIAN_POINT('Ctrl Pts',(-250.166795440474,-6.20504786089197,
130.598096224241));
#236855=CARTESIAN_POINT('Ctrl Pts',(-250.445243064287,-3.5275160113489,
135.913352176149));
#236856=CARTESIAN_POINT('Ctrl Pts',(-250.7236906881,2.39163072389511,136.533694473816));
#236857=CARTESIAN_POINT('Ctrl Pts',(-251.002138311913,6.11298566151878,
131.889058851139));
#236858=CARTESIAN_POINT('Ctrl Pts',(-251.280585935725,4.21680541219097,
126.247638542206));
#236859=CARTESIAN_POINT('Ctrl Pts',(-251.559033559539,-1.5544130086051,
124.793623212388));
#236860=CARTESIAN_POINT('Ctrl Pts',(-251.837481183351,-5.89720181167361,
128.863181916876));
#236861=CARTESIAN_POINT('Ctrl Pts',(-252.115928807165,-4.82075024435922,
134.716589015834));
#236862=CARTESIAN_POINT('Ctrl Pts',(-252.394376430977,0.685735291195708,
136.974849339035));
#236863=CARTESIAN_POINT('Ctrl Pts',(-252.67282405479,5.56206359338632,133.562731973716));
#236864=CARTESIAN_POINT('Ctrl Pts',(-252.951271678603,5.32712717665345,
127.615806083426));
#236865=CARTESIAN_POINT('Ctrl Pts',(-253.229719302416,0.196821126400439,
124.599006045371));
#236866=CARTESIAN_POINT('Ctrl Pts',(-253.508166926229,-5.11435391846912,
127.284623701469));
#236867=CARTESIAN_POINT('Ctrl Pts',(-253.786614550041,-5.72568757235024,
133.204707652256));
#236868=CARTESIAN_POINT('Ctrl Pts',(-254.065062173855,-1.07539404373626,
136.918989908584));
#236869=CARTESIAN_POINT('Ctrl Pts',(-254.343509797667,4.56313403947717,
135.014226625117));
#236870=CARTESIAN_POINT('Ctrl Pts',(-254.621957421481,6.00836492926231,
129.240802026269));
#236871=CARTESIAN_POINT('Ctrl Pts',(-254.900405045293,1.9322018468105,124.904211611225));
#236872=CARTESIAN_POINT('Ctrl Pts',(-255.178852669106,-3.91956009939235,
125.989569474605));
#236873=CARTESIAN_POINT('Ctrl Pts',(-255.457300292919,-6.16943824888009,
131.499485975975));
#236874=CARTESIAN_POINT('Ctrl Pts',(-255.735747916732,-2.74990318521692,
136.370614733943));
#236875=CARTESIAN_POINT('Ctrl Pts',(-256.014195540545,3.19665694865877,
136.126630713714));
#236876=CARTESIAN_POINT('Ctrl Pts',(-256.292643164358,6.20564856486739,
130.991735142402));
#236877=CARTESIAN_POINT('Ctrl Pts',(-256.571090788171,3.51194654848645,
125.68466161966));
#236878=CARTESIAN_POINT('Ctrl Pts',(-256.849538411983,-2.40905189372645,
125.082322325773));
#236879=CARTESIAN_POINT('Ctrl Pts',(-257.127986035797,-6.11626988572704,
129.738292634474));
#236880=CARTESIAN_POINT('Ctrl Pts',(-257.406433659609,-4.20289584392431,
135.373859459261));
#236881=CARTESIAN_POINT('Ctrl Pts',(-257.684881283423,1.57266088340656,
136.810408252432));
#236882=CARTESIAN_POINT('Ctrl Pts',(-257.963328907235,5.90315744058412,
132.727450666138));
#236883=CARTESIAN_POINT('Ctrl Pts',(-258.241776531048,4.80867945501638,
126.87772425425));
#236884=CARTESIAN_POINT('Ctrl Pts',(-258.520224154861,-0.704246744852541,
124.635521896935));
#236885=CARTESIAN_POINT('Ctrl Pts',(-258.798671778674,-5.5709361272427,
128.063810879205));
#236886=CARTESIAN_POINT('Ctrl Pts',(-259.077119402487,-5.31644754243966,
134.007449313497));
#236887=CARTESIAN_POINT('Ctrl Pts',(-259.355567026299,-0.179733571114533,
137.013459703814));
#236888=CARTESIAN_POINT('Ctrl Pts',(-259.634014650113,5.12849404027147,
134.30227331953));
#236889=CARTESIAN_POINT('Ctrl Pts',(-259.866054336623,5.61428989304695,
129.384066440553));
#236890=CARTESIAN_POINT('Ctrl Pts',(-260.051696012132,3.39054283699284,
126.521203045511));
#236891=CARTESIAN_POINT('Ctrl Pts',(-260.144521813036,1.754921961264,125.780753115897));
#236892=CARTESIAN_POINT('Ctrl Pts',(-260.190939676638,0.892893391295023,
125.631947563271));
#236893=CARTESIAN_POINT('Ctrl Pts',(210.191733024964,-2.43880115184907,
125.780342085335));
#236894=CARTESIAN_POINT('Ctrl Pts',(210.145323348611,-3.27594855749458,
126.186716565447));
#236895=CARTESIAN_POINT('Ctrl Pts',(210.052505734956,-4.72940422381435,
127.426013481475));
#236896=CARTESIAN_POINT('Ctrl Pts',(209.866872246696,-6.15821517169733,
131.008352419918));
#236897=CARTESIAN_POINT('Ctrl Pts',(209.634832560185,-4.21099667891447,
135.892791108304));
#236898=CARTESIAN_POINT('Ctrl Pts',(209.356384936373,2.01508446636645,137.098708070195));
#236899=CARTESIAN_POINT('Ctrl Pts',(209.07793731256,6.37956871319657,132.510708806665));
#236900=CARTESIAN_POINT('Ctrl Pts',(208.799489688747,4.8866719183268,126.359661034021));
#236901=CARTESIAN_POINT('Ctrl Pts',(208.521042064934,-1.09954563679898,
124.290443595948));
#236902=CARTESIAN_POINT('Ctrl Pts',(208.242594441121,-6.07390144970816,
128.208589139036));
#236903=CARTESIAN_POINT('Ctrl Pts',(207.964146817309,-5.46739734855352,
134.511385201899));
#236904=CARTESIAN_POINT('Ctrl Pts',(207.685699193495,0.163779660617915,
137.407996874876));
#236905=CARTESIAN_POINT('Ctrl Pts',(207.407251569682,5.6442383477931,134.235982835808));
#236906=CARTESIAN_POINT('Ctrl Pts',(207.128803945869,5.93803043711477,127.910585036422));
#236907=CARTESIAN_POINT('Ctrl Pts',(206.850356322057,0.775002953389061,
124.244367681185));
#236908=CARTESIAN_POINT('Ctrl Pts',(206.571908698243,-5.10018277131114,
126.606494049502));
#236909=CARTESIAN_POINT('Ctrl Pts',(206.293461074431,-6.28856642889766,
132.82623846394));
#236910=CARTESIAN_POINT('Ctrl Pts',(206.015013450618,-1.69805588527783,
137.187984519302));
#236911=CARTESIAN_POINT('Ctrl Pts',(205.736565826805,4.45288036648484,135.683487507757));
#236912=CARTESIAN_POINT('Ctrl Pts',(205.458118202992,6.51183958365415,129.695313656966));
#236913=CARTESIAN_POINT('Ctrl Pts',(205.179670579179,2.58673502741873,124.726298504418));
#236914=CARTESIAN_POINT('Ctrl Pts',(204.901222955366,-3.71545195245463,
125.342726181157));
#236915=CARTESIAN_POINT('Ctrl Pts',(204.622775331554,-6.60332046735468,
130.978128730661));
#236916=CARTESIAN_POINT('Ctrl Pts',(204.344327707741,-3.42305986725146,
136.4538470632));
#236917=CARTESIAN_POINT('Ctrl Pts',(204.065880083927,2.90282542147133,136.737963244372));
#236918=CARTESIAN_POINT('Ctrl Pts',(203.787432460115,6.56115601364161,131.569388537382));
#236919=CARTESIAN_POINT('Ctrl Pts',(203.508984836302,4.1901047305044,125.69779051756));
#236920=CARTESIAN_POINT('Ctrl Pts',(203.230537212489,-2.03144808657932,
124.518880964767));
#236921=CARTESIAN_POINT('Ctrl Pts',(202.952089588676,-6.38619936200403,
129.116020142231));
#236922=CARTESIAN_POINT('Ctrl Pts',(202.673641964863,-4.87234540261322,
135.2646617407));
#236923=CARTESIAN_POINT('Ctrl Pts',(202.39519434105,1.1189559521872,137.314504502614));
#236924=CARTESIAN_POINT('Ctrl Pts',(202.116746717238,6.08199145217563,133.381843073553));
#236925=CARTESIAN_POINT('Ctrl Pts',(201.838299093424,5.45597392877388,127.080601183836));
#236926=CARTESIAN_POINT('Ctrl Pts',(201.559851469612,-0.183817095687214,
124.201312298284));
#236927=CARTESIAN_POINT('Ctrl Pts',(201.281403845799,-5.65468918935595,
127.389902241135));
#236928=CARTESIAN_POINT('Ctrl Pts',(201.002956221986,-5.92917816483575,
133.716212626452));
#236929=CARTESIAN_POINT('Ctrl Pts',(200.724508598173,-0.755042063338292,
137.366673267433));
#236930=CARTESIAN_POINT('Ctrl Pts',(200.44606097436,5.11294080853837,134.986689170007));
#236931=CARTESIAN_POINT('Ctrl Pts',(200.167613350547,6.2823808583988,128.763349450982));
#236932=CARTESIAN_POINT('Ctrl Pts',(199.889165726734,1.67861981076543,124.415599285115));
#236933=CARTESIAN_POINT('Ctrl Pts',(199.610718102921,-4.46771083782862,
125.938808675424));
#236934=CARTESIAN_POINT('Ctrl Pts',(199.332270479108,-6.50843348626435,
131.933222605136));
#236935=CARTESIAN_POINT('Ctrl Pts',(199.053822855296,-2.56822371547623,
136.890267516244));
#236936=CARTESIAN_POINT('Ctrl Pts',(198.775375231483,3.73205818513161,136.254661300547));
#236937=CARTESIAN_POINT('Ctrl Pts',(198.49692760767,6.60276093478139,130.610495019181));
#236938=CARTESIAN_POINT('Ctrl Pts',(198.218479983857,3.4058489481713,125.14448175187));
#236939=CARTESIAN_POINT('Ctrl Pts',(197.940032360044,-2.92087183683725,
124.879620661678));
#236940=CARTESIAN_POINT('Ctrl Pts',(197.661584736231,-6.56345409631434,
130.05930615131));
#236941=CARTESIAN_POINT('Ctrl Pts',(197.383137112418,-4.1745426838368,135.923660297497));
#236942=CARTESIAN_POINT('Ctrl Pts',(197.104689488605,2.05056951733907,137.083628129519));
#236943=CARTESIAN_POINT('Ctrl Pts',(196.826241864792,6.39130850797037,132.473255877329));
#236944=CARTESIAN_POINT('Ctrl Pts',(196.54779424098,4.85874721255563,126.329250411482));
#236945=CARTESIAN_POINT('Ctrl Pts',(196.269346617166,-1.13876540820057,
124.297652603739));
#236946=CARTESIAN_POINT('Ctrl Pts',(195.990898993354,-6.0898082506034,128.245401590344));
#236947=CARTESIAN_POINT('Ctrl Pts',(195.712451369541,-5.44461481437399,
134.544708910868));
#236948=CARTESIAN_POINT('Ctrl Pts',(195.434003745728,0.203913652044436,
137.406818876019));
#236949=CARTESIAN_POINT('Ctrl Pts',(195.155556121915,5.66505543396973,134.201592249669));
#236950=CARTESIAN_POINT('Ctrl Pts',(194.877108498102,5.92028802542049,127.874475717408));
#236951=CARTESIAN_POINT('Ctrl Pts',(194.59866087429,0.735065143658737,124.239780275557));
#236952=CARTESIAN_POINT('Ctrl Pts',(194.320213250476,-5.1256466951968,126.637613470433));
#236953=CARTESIAN_POINT('Ctrl Pts',(194.041765626664,-6.2761396229282,132.86448373661));
#236954=CARTESIAN_POINT('Ctrl Pts',(193.763318002851,-1.6591668436545,137.198201498994));
#236955=CARTESIAN_POINT('Ctrl Pts',(193.484870379038,4.48249921013125,135.656291847837));
#236956=CARTESIAN_POINT('Ctrl Pts',(193.206422755225,6.50496747206681,129.655694426079));
#236957=CARTESIAN_POINT('Ctrl Pts',(192.927975131412,2.54968841250072,124.710665118833));
#236958=CARTESIAN_POINT('Ctrl Pts',(192.649527507599,-3.74862973894988,
125.365444281348));
#236959=CARTESIAN_POINT('Ctrl Pts',(192.371079883787,-6.60214029104917,
131.018321851013));
#236960=CARTESIAN_POINT('Ctrl Pts',(192.092632259973,-3.38860644815819,
136.474579499726));
#236961=CARTESIAN_POINT('Ctrl Pts',(191.814184636161,2.93889117796205,136.720183001327));
#236962=CARTESIAN_POINT('Ctrl Pts',(191.535737012347,6.56569138435095,131.529434736241));
#236963=CARTESIAN_POINT('Ctrl Pts',(191.257289388535,4.15894196037717,125.672378777932));
#236964=CARTESIAN_POINT('Ctrl Pts',(190.978841764722,-2.06967194957323,
124.531363418996));
#236965=CARTESIAN_POINT('Ctrl Pts',(190.700394140909,-6.3963584469616,129.154926032595));
#236966=CARTESIAN_POINT('Ctrl Pts',(190.421946517096,-4.84510401107414,
135.294238450423));
#236967=CARTESIAN_POINT('Ctrl Pts',(190.143498893283,1.15856431450073,137.307572482581));
#236968=CARTESIAN_POINT('Ctrl Pts',(189.86505126947,6.09756863406271,133.344772510351));
#236969=CARTESIAN_POINT('Ctrl Pts',(189.586603645657,5.4332052617092,127.047458114672));
#236970=CARTESIAN_POINT('Ctrl Pts',(189.308156021844,-0.224008319322015,
124.202553584261));
#236971=CARTESIAN_POINT('Ctrl Pts',(189.029708398032,-5.67536919831109,
127.424387201254));
#236972=CARTESIAN_POINT('Ctrl Pts',(188.751260774218,-5.91134304125131,
133.752251266956));
#236973=CARTESIAN_POINT('Ctrl Pts',(188.472813150406,-0.71508141444371,
137.371147838333));
#236974=CARTESIAN_POINT('Ctrl Pts',(188.194365526593,5.13830509856852,134.955487759214));
#236975=CARTESIAN_POINT('Ctrl Pts',(187.91591790278,6.26984024615536,128.725144630756));
#236976=CARTESIAN_POINT('Ctrl Pts',(187.637470278967,1.63969850624965,124.405499418827));
#236977=CARTESIAN_POINT('Ctrl Pts',(187.359022655154,-4.49724605717418,
125.966095046791));
#236978=CARTESIAN_POINT('Ctrl Pts',(187.080575031341,-6.5014411967389,131.972820371883));
#236979=CARTESIAN_POINT('Ctrl Pts',(186.802127407528,-2.53112948956026,
136.905788265189));
#236980=CARTESIAN_POINT('Ctrl Pts',(186.523679783716,3.76516656597443,136.231842221641));
#236981=CARTESIAN_POINT('Ctrl Pts',(186.245232159903,6.60145848599114,130.570305731164));
#236982=CARTESIAN_POINT('Ctrl Pts',(185.96678453609,3.3713325565579,125.123854247073));
#236983=CARTESIAN_POINT('Ctrl Pts',(185.688336912277,-2.95688329360047,
124.897510609301));
#236984=CARTESIAN_POINT('Ctrl Pts',(185.409889288464,-6.5678678487195,130.099273563458));
#236985=CARTESIAN_POINT('Ctrl Pts',(185.131441664651,-4.14330270904733,
135.948977074923));
#236986=CARTESIAN_POINT('Ctrl Pts',(184.852994040838,2.08875520864929,137.071029390563));
#236987=CARTESIAN_POINT('Ctrl Pts',(184.574546417025,6.40134913096194,132.434319247607));
#236988=CARTESIAN_POINT('Ctrl Pts',(184.296098793212,4.831415925211,126.299756751549));
#236989=CARTESIAN_POINT('Ctrl Pts',(184.017651169399,-1.17835248801931,
124.304705146227));
#236990=CARTESIAN_POINT('Ctrl Pts',(183.739203545587,-6.10527253047917,
128.282519393244));
#236991=CARTESIAN_POINT('Ctrl Pts',(183.460755921774,-5.42174537657308,
134.577782526619));
#236992=CARTESIAN_POINT('Ctrl Pts',(183.182308297961,0.244100911417136,
137.405455267482));
#236993=CARTESIAN_POINT('Ctrl Pts',(182.903860674148,5.68563038680749,134.167044506474));
#236994=CARTESIAN_POINT('Ctrl Pts',(182.625413050335,5.90234329520773,127.838491527799));
#236995=CARTESIAN_POINT('Ctrl Pts',(182.346965426522,0.695091060812155,
124.23542735186));
#236996=CARTESIAN_POINT('Ctrl Pts',(182.068517802709,-5.15091590138369,
126.668891936874));
#236997=CARTESIAN_POINT('Ctrl Pts',(181.790070178896,-6.263482786439,132.902650210566));
#236998=CARTESIAN_POINT('Ctrl Pts',(181.511622555083,-1.62021497890189,
137.208182855437));
#236999=CARTESIAN_POINT('Ctrl Pts',(181.233174931271,4.51195124234396,135.628915707812));
#237000=CARTESIAN_POINT('Ctrl Pts',(180.954727307458,6.49785469294791,129.61611812487));
#237001=CARTESIAN_POINT('Ctrl Pts',(180.676279683645,2.51254711858197,124.695257343842));
#237002=CARTESIAN_POINT('Ctrl Pts',(180.397832059832,-3.78166851301026,
125.388364025079));
#237003=CARTESIAN_POINT('Ctrl Pts',(180.119384436019,-6.60071552592353,
131.058506988669));
#237004=CARTESIAN_POINT('Ctrl Pts',(179.840936812206,-3.35402743339335,
136.495101852955));
#237005=CARTESIAN_POINT('Ctrl Pts',(179.562489188393,2.97484801707599,136.702183530083));
#237006=CARTESIAN_POINT('Ctrl Pts',(179.28404156458,6.56998346925752,131.489454075275));
#237007=CARTESIAN_POINT('Ctrl Pts',(179.005593940767,4.12762507472721,125.647157201507));
#237008=CARTESIAN_POINT('Ctrl Pts',(178.727146316955,-2.10781911778238,
124.544078323705));
#237009=CARTESIAN_POINT('Ctrl Pts',(178.448698693142,-6.40628051373842,
129.193893042167));
#237010=CARTESIAN_POINT('Ctrl Pts',(178.170251069329,-4.81768308177075,
135.323648786705));
#237011=CARTESIAN_POINT('Ctrl Pts',(177.891803445516,1.19812974544141,137.300399483306));
#237012=CARTESIAN_POINT('Ctrl Pts',(177.613355821703,6.11291986848493,133.307607811431));
#237013=CARTESIAN_POINT('Ctrl Pts',(177.33490819789,5.41023526512845,127.014454258818));
#237014=CARTESIAN_POINT('Ctrl Pts',(177.056460574078,-0.264191242194762,
124.204039502676));
#237015=CARTESIAN_POINT('Ctrl Pts',(176.778012950264,-5.69583890440069,
127.458997407505));
#237016=CARTESIAN_POINT('Ctrl Pts',(176.499565326452,-5.89328887066216,
133.788180672302));
#237017=CARTESIAN_POINT('Ctrl Pts',(176.221117702638,-0.675094267951971,
137.375379074508));
#237018=CARTESIAN_POINT('Ctrl Pts',(175.942670078826,5.16347898681764,134.924132526884));
#237019=CARTESIAN_POINT('Ctrl Pts',(175.664222455013,6.25706730267374,128.687016856641));
#237020=CARTESIAN_POINT('Ctrl Pts',(175.3857748312,1.60071644210391,124.395636664696));
#237021=CARTESIAN_POINT('Ctrl Pts',(175.107327207387,-4.5266146294138,125.993560701866));
#237022=CARTESIAN_POINT('Ctrl Pts',(174.828879583574,-6.49420799391872,
132.012374840923));
#237023=CARTESIAN_POINT('Ctrl Pts',(174.550431959762,-2.49394147171037,
136.92108292349));
#237024=CARTESIAN_POINT('Ctrl Pts',(174.271984335948,3.79813542718566,136.208822025409));
#237025=CARTESIAN_POINT('Ctrl Pts',(173.993536712136,6.59991141772898,130.530125116137));
#237026=CARTESIAN_POINT('Ctrl Pts',(173.715089088322,3.33669123897678,125.103437235529));
#237027=CARTESIAN_POINT('Ctrl Pts',(173.43664146451,-2.99278518196597,124.915619437422));
#237028=CARTESIAN_POINT('Ctrl Pts',(173.158193840697,-6.5720382263662,130.139267102866));
#237029=CARTESIAN_POINT('Ctrl Pts',(172.879746216884,-4.11190920265221,
135.974103216695));
#237030=CARTESIAN_POINT('Ctrl Pts',(172.601298593071,2.12686350036709,137.058198437889));
#237031=CARTESIAN_POINT('Ctrl Pts',(172.322850969258,6.41115254960738,132.395322219168));
#237032=CARTESIAN_POINT('Ctrl Pts',(172.044403345445,4.80390560797255,126.270430011369));
#237033=CARTESIAN_POINT('Ctrl Pts',(171.765955721632,-1.21789590355323,
124.31199853584));
#237034=CARTESIAN_POINT('Ctrl Pts',(171.487508097819,-6.12051057723618,
128.319730643897));
#237035=CARTESIAN_POINT('Ctrl Pts',(171.209060474007,-5.39867503400336,
134.610716316833));
#237036=CARTESIAN_POINT('Ctrl Pts',(170.930612850193,0.284279125540913,
137.403847052956));
#237037=CARTESIAN_POINT('Ctrl Pts',(170.652165226381,5.70599465652041,134.13237215779));
#237038=CARTESIAN_POINT('Ctrl Pts',(170.373717602568,5.88417985149351,127.802617239562));
#237039=CARTESIAN_POINT('Ctrl Pts',(170.095269978755,0.655091221110643,
124.231317842401));
#237040=CARTESIAN_POINT('Ctrl Pts',(169.816822354942,-5.17599423848763,
126.700323644626));
#237041=CARTESIAN_POINT('Ctrl Pts',(169.538374731129,-6.25059385429175,
132.940738931629));
#237042=CARTESIAN_POINT('Ctrl Pts',(169.259927107316,-1.58120307648749,
137.217926915891));
#237043=CARTESIAN_POINT('Ctrl Pts',(168.981479483503,4.54123608254409,135.601360792124));
#237044=CARTESIAN_POINT('Ctrl Pts',(168.703031859691,6.49050113343381,129.576585854424));
#237045=CARTESIAN_POINT('Ctrl Pts',(168.424584235878,2.47531272130571,124.680075943919));
#237046=CARTESIAN_POINT('Ctrl Pts',(168.146136612065,-3.81456715595326,
125.411484460556));
#237047=CARTESIAN_POINT('Ctrl Pts',(167.867688988252,-6.59904616885666,
131.098682708838));
#237048=CARTESIAN_POINT('Ctrl Pts',(167.589241364439,-3.31932413390846,
136.515413333674));
#237049=CARTESIAN_POINT('Ctrl Pts',(167.310793740626,3.01069462210276,136.683965512842));
#237050=CARTESIAN_POINT('Ctrl Pts',(167.032346116813,6.57403210101054,131.449448027918));
#237051=CARTESIAN_POINT('Ctrl Pts',(166.753898493,4.09615523841214,125.622126727152));
#237052=CARTESIAN_POINT('Ctrl Pts',(166.475450869187,-2.14588817997888,
124.557025205477));
#237053=CARTESIAN_POINT('Ctrl Pts',(166.197003245374,-6.41596519343492,
129.232919728208));
#237054=CARTESIAN_POINT('Ctrl Pts',(165.918555621562,-4.79008363144905,
135.352891659104));
#237055=CARTESIAN_POINT('Ctrl Pts',(165.640107997748,1.23765077924384,137.292985770921));
#237056=CARTESIAN_POINT('Ctrl Pts',(165.361660373936,6.12804458641347,133.270350353765));
#237057=CARTESIAN_POINT('Ctrl Pts',(165.083212750123,5.38706479029029,126.981590839339));
#237058=CARTESIAN_POINT('Ctrl Pts',(164.80476512631,-0.304364375363971,
124.205769998417));
#237059=CARTESIAN_POINT('Ctrl Pts',(164.526317502497,-5.71609754908509,
127.493731577419));
#237060=CARTESIAN_POINT('Ctrl Pts',(164.247869878684,-5.8750163220866,133.823999511097));
#237061=CARTESIAN_POINT('Ctrl Pts',(163.969422254871,-0.635082105593798,
137.37936681918));
#237062=CARTESIAN_POINT('Ctrl Pts',(163.690974631059,5.18846154045405,134.892624634889));
#237063=CARTESIAN_POINT('Ctrl Pts',(163.412527007245,6.24406250126218,128.648967541478));
#237064=CARTESIAN_POINT('Ctrl Pts',(163.134079383433,1.56167506282176,124.386011388187));
#237065=CARTESIAN_POINT('Ctrl Pts',(162.85563175962,-4.55581546628373,126.021204622902));
#237066=CARTESIAN_POINT('Ctrl Pts',(162.577184135807,-6.48673414583306,
132.051884546553));
#237067=CARTESIAN_POINT('Ctrl Pts',(162.298736511994,-2.45666103994207,
136.936150924396));
#237068=CARTESIAN_POINT('Ctrl Pts',(162.020288888181,3.83096354709181,136.185601564872));
#237069=CARTESIAN_POINT('Ctrl Pts',(161.741841264368,6.59811978732212,130.489954663008));
#237070=CARTESIAN_POINT('Ctrl Pts',(161.463393640556,3.30192627907479,125.083231473798));
#237071=CARTESIAN_POINT('Ctrl Pts',(161.184946016742,-3.02857617157586,
124.933946475014));
#237072=CARTESIAN_POINT('Ctrl Pts',(160.90649839293,-6.57596507471956,130.179285287561));
#237073=CARTESIAN_POINT('Ctrl Pts',(160.628050769116,-4.08036332794952,
135.999037791754));
#237074=CARTESIAN_POINT('Ctrl Pts',(160.349603145304,2.16489298037573,137.045135746957));
#237075=CARTESIAN_POINT('Ctrl Pts',(160.07115552149,6.42071840063739,132.356266237063));
#237076=CARTESIAN_POINT('Ctrl Pts',(159.792707897678,4.77621728024515,126.241271277656));
#237077=CARTESIAN_POINT('Ctrl Pts',(159.514260273865,-1.25739418950663,
124.319532502318));
#237078=CARTESIAN_POINT('Ctrl Pts',(159.235812650052,-6.13552182622286,
128.357033963427));
#237079=CARTESIAN_POINT('Ctrl Pts',(158.957365026239,-5.37540464154493,
134.643509061136));
#237080=CARTESIAN_POINT('Ctrl Pts',(158.678917402427,0.324446805597038,
137.401994292032));
#237081=CARTESIAN_POINT('Ctrl Pts',(158.400469778613,5.72614748850293,134.097576488416));
#237082=CARTESIAN_POINT('Ctrl Pts',(158.122022154801,5.86579836733105,127.766854182028));
#237083=CARTESIAN_POINT('Ctrl Pts',(157.843574530988,0.615067106763091,
124.22745189946));
#237084=CARTESIAN_POINT('Ctrl Pts',(157.565126907175,-5.20088077722156,
126.731907428977));
#237085=CARTESIAN_POINT('Ctrl Pts',(157.286679283362,-6.23747330409059,
132.978748488409));
#237086=CARTESIAN_POINT('Ctrl Pts',(157.008231659549,-1.54213258201158,
137.227433319288));
#237087=CARTESIAN_POINT('Ctrl Pts',(156.729784035736,4.5703526455712,135.57362812183));
#237088=CARTESIAN_POINT('Ctrl Pts',(156.451336411923,6.48290706601333,129.537099079623));
#237089=CARTESIAN_POINT('Ctrl Pts',(156.172888788111,2.43798660040623,124.665121481617));
#237090=CARTESIAN_POINT('Ctrl Pts',(155.894441164297,-3.84732444870741,
125.434804731043));
#237091=CARTESIAN_POINT('Ctrl Pts',(155.615993540485,-6.59713228170722,
131.138847522794));
#237092=CARTESIAN_POINT('Ctrl Pts',(155.337545916672,-3.28449783564716,
136.535513189234));
#237093=CARTESIAN_POINT('Ctrl Pts',(155.059098292859,3.04642966473303,136.665529624679));
#237094=CARTESIAN_POINT('Ctrl Pts',(154.780650669046,6.57783712958646,131.409418076611));
#237095=CARTESIAN_POINT('Ctrl Pts',(154.502203045233,4.06453361755842,125.597288282381));
#237096=CARTESIAN_POINT('Ctrl Pts',(154.22375542142,-2.18387772549973,124.57020358456));
#237097=CARTESIAN_POINT('Ctrl Pts',(153.945307797607,-6.42541212718171,
129.272004644569));
#237098=CARTESIAN_POINT('Ctrl Pts',(153.666860173794,-4.76230668281685,
135.381965984011));
#237099=CARTESIAN_POINT('Ctrl Pts',(153.388412549982,1.27712595144142,137.285331620145));
#237100=CARTESIAN_POINT('Ctrl Pts',(153.109964926169,6.14294222739622,133.233001517943));
#237101=CARTESIAN_POINT('Ctrl Pts',(152.831517302356,5.36369469578529,126.948869073999));
#237102=CARTESIAN_POINT('Ctrl Pts',(152.553069678543,-0.344526230199219,
124.207745007359));
#237103=CARTESIAN_POINT('Ctrl Pts',(152.27462205473,-5.73614438167267,127.528588423912));
#237104=CARTESIAN_POINT('Ctrl Pts',(151.996174430917,-5.85652607262075,
133.859706456064));
#237105=CARTESIAN_POINT('Ctrl Pts',(151.717726807104,-0.595046410034728,
137.383110924578));
#237106=CARTESIAN_POINT('Ctrl Pts',(151.439279183291,5.21325183374003,134.860965250768));
#237107=CARTESIAN_POINT('Ctrl Pts',(151.160831559478,6.23082632381839,128.610998095198));
#237108=CARTESIAN_POINT('Ctrl Pts',(150.882383935665,1.52257581509584,124.376623945969));
#237109=CARTESIAN_POINT('Ctrl Pts',(150.603936311853,-4.58484748573611,
126.049025785542));
#237110=CARTESIAN_POINT('Ctrl Pts',(150.32548868804,-6.47901992942814,132.091348024725));
#237111=CARTESIAN_POINT('Ctrl Pts',(150.047041064227,-2.41928957569559,
136.950991709558));
#237112=CARTESIAN_POINT('Ctrl Pts',(149.768593440414,3.8636497092349,136.162181700472));
#237113=CARTESIAN_POINT('Ctrl Pts',(149.490145816601,6.59608366116008,130.449795860306));
#237114=CARTESIAN_POINT('Ctrl Pts',(149.211698192788,3.26703896508027,125.06323771061));
#237115=CARTESIAN_POINT('Ctrl Pts',(148.933250568975,-3.06425493618196,
124.95249104296));
#237116=CARTESIAN_POINT('Ctrl Pts',(148.654802945162,-6.57964824826877,
130.219326634649));
#237117=CARTESIAN_POINT('Ctrl Pts',(148.376355321349,-4.04866625388314,
136.02377987614));
#237118=CARTESIAN_POINT('Ctrl Pts',(148.097907697537,2.20284223947883,137.031841801807));
#237119=CARTESIAN_POINT('Ctrl Pts',(147.819460073724,6.43004632958585,132.317152748525));
#237120=CARTESIAN_POINT('Ctrl Pts',(147.541012449911,4.74835196802999,126.212281630895));
#237121=CARTESIAN_POINT('Ctrl Pts',(147.262564826098,-1.29684588225586,
124.327306766486));
#237122=CARTESIAN_POINT('Ctrl Pts',(146.984117202285,-6.15030572119196,
128.394427969547));
#237123=CARTESIAN_POINT('Ctrl Pts',(146.705669578472,-5.35193506149072,
134.676159544383));
#237124=CARTESIAN_POINT('Ctrl Pts',(146.427221954659,0.364602463157475,
137.399897053366));
#237125=CARTESIAN_POINT('Ctrl Pts',(146.148774330846,5.74608813598446,134.062658787717));
#237126=CARTESIAN_POINT('Ctrl Pts',(145.870326707034,5.84719952385297,127.731203680413));
#237127=CARTESIAN_POINT('Ctrl Pts',(145.59187908322,0.575020200877703,124.22382966629));
#237128=CARTESIAN_POINT('Ctrl Pts',(145.313431459408,-5.22557459540567,
126.76364211958));
#237129=CARTESIAN_POINT('Ctrl Pts',(145.034983835595,-6.22412162202233,
133.016677472446));
#237130=CARTESIAN_POINT('Ctrl Pts',(144.756536211782,-1.50300494324566,
137.236701713364));
#237131=CARTESIAN_POINT('Ctrl Pts',(144.478088587969,4.59929985250025,135.545718724575));
#237132=CARTESIAN_POINT('Ctrl Pts',(144.199640964156,6.47507277208744,129.497659263665));
#237133=CARTESIAN_POINT('Ctrl Pts',(143.921193340343,2.40057013901678,124.65039451108));
#237134=CARTESIAN_POINT('Ctrl Pts',(143.64274571653,-3.87993917743928,125.458323972397));
#237135=CARTESIAN_POINT('Ctrl Pts',(143.364298092718,-6.594973935395,131.178999942215));
#237136=CARTESIAN_POINT('Ctrl Pts',(143.085850468904,-3.2495498291107,136.555400674828));
#237137=CARTESIAN_POINT('Ctrl Pts',(142.807402845092,3.08205182079176,136.646876548744));
#237138=CARTESIAN_POINT('Ctrl Pts',(142.528955221279,6.58139841398854,131.369365704677));
#237139=CARTESIAN_POINT('Ctrl Pts',(142.250507597466,4.03276138391676,125.572642787588));
#237140=CARTESIAN_POINT('Ctrl Pts',(141.972059973653,-2.2217863466284,124.583612972623));
#237141=CARTESIAN_POINT('Ctrl Pts',(141.69361234984,-6.43462096491922,129.311146342943));
#237142=CARTESIAN_POINT('Ctrl Pts',(141.415164726027,-4.7343532651591,135.410870684068));
#237143=CARTESIAN_POINT('Ctrl Pts',(141.136717102214,1.31655379926713,137.277437314604));
#237144=CARTESIAN_POINT('Ctrl Pts',(140.858269478402,6.15761223939561,133.195562687939));
#237145=CARTESIAN_POINT('Ctrl Pts',(140.579821854588,5.34012584760095,126.916290175316));
#237146=CARTESIAN_POINT('Ctrl Pts',(140.301374230776,-0.384675318488256,
124.20996445632));
#237147=CARTESIAN_POINT('Ctrl Pts',(140.022926606963,-5.75597865932068,
127.563566655346));
#237148=CARTESIAN_POINT('Ctrl Pts',(139.74447898315,-5.83781880742758,133.895300184066));
#237149=CARTESIAN_POINT('Ctrl Pts',(139.466031359337,-0.554988664812238,
137.386611251964));
#237150=CARTESIAN_POINT('Ctrl Pts',(139.187583735524,5.23784894806212,134.829155547671));
#237151=CARTESIAN_POINT('Ctrl Pts',(138.909136111711,6.21735926081381,128.573109924773));
#237152=CARTESIAN_POINT('Ctrl Pts',(138.630688487898,1.48342014776303,124.367474685896));
#237153=CARTESIAN_POINT('Ctrl Pts',(138.352240864086,-4.61370961197883,
126.077023158863));
#237154=CARTESIAN_POINT('Ctrl Pts',(138.073793240272,-6.47106563055709,
132.130763813104));
#237155=CARTESIAN_POINT('Ctrl Pts',(137.79534561646,-2.38182846378423,136.965604729043));
#237156=CARTESIAN_POINT('Ctrl Pts',(137.516897992647,3.89619270241722,136.138563300043));
#237157=CARTESIAN_POINT('Ctrl Pts',(137.238450368834,6.59380311469226,130.409650196134));
#237158=CARTESIAN_POINT('Ctrl Pts',(136.960002745021,3.23203058975544,125.043456686844));
#237159=CARTESIAN_POINT('Ctrl Pts',(136.681555121208,-3.09982015369448,
124.971252454085));
#237160=CARTESIAN_POINT('Ctrl Pts',(136.403107497395,-6.58308761053252,
130.259389660389));
#237161=CARTESIAN_POINT('Ctrl Pts',(136.124659873582,-4.01681915499975,
136.048328553027));
#237162=CARTESIAN_POINT('Ctrl Pts',(135.846212249769,2.24070987145278,137.018317095051));
#237163=CARTESIAN_POINT('Ctrl Pts',(135.567764625956,6.43913599080291,132.277983202917));
#237164=CARTESIAN_POINT('Ctrl Pts',(135.289317002144,4.72031070388647,126.183462145311));
#237165=CARTESIAN_POINT('Ctrl Pts',(135.010869378331,-1.33624951990408,
124.335321040266));
#237166=CARTESIAN_POINT('Ctrl Pts',(134.732421754518,-6.16486171432077,
128.431911276607));
#237167=CARTESIAN_POINT('Ctrl Pts',(134.453974130705,-5.32826716351462,
134.708666556695));
#237168=CARTESIAN_POINT('Ctrl Pts',(134.175526506892,0.404744610239488,
137.397555414672));
#237169=CARTESIAN_POINT('Ctrl Pts',(133.897078883079,5.76581586005707,134.027620349581));
#237170=CARTESIAN_POINT('Ctrl Pts',(133.618631259266,5.82838401024617,127.695667055759));
#237171=CARTESIAN_POINT('Ctrl Pts',(133.340183635453,0.534951987407334,
124.220451277114));
#237172=CARTESIAN_POINT('Ctrl Pts',(133.06173601164,-5.25007477800144,126.795526540492));
#237173=CARTESIAN_POINT('Ctrl Pts',(132.783288387828,-6.21053930283845,
133.054524478268));
#237174=CARTESIAN_POINT('Ctrl Pts',(132.504840764015,-1.46382161007886,
137.245731754674));
#237175=CARTESIAN_POINT('Ctrl Pts',(132.226393140202,4.62807663068185,135.517633634551));
#237176=CARTESIAN_POINT('Ctrl Pts',(131.947945516389,6.46699854195874,129.458267868007));
#237177=CARTESIAN_POINT('Ctrl Pts',(131.669497892576,2.3630647236181,124.635895578019));
#237178=CARTESIAN_POINT('Ctrl Pts',(131.391050268763,-3.91241013359816,
125.482041313105));
#237179=CARTESIAN_POINT('Ctrl Pts',(131.11260264495,-6.59257120989826,131.219138479237));
#237180=CARTESIAN_POINT('Ctrl Pts',(130.834155021138,-3.2144814093103,136.575075053519));
#237181=CARTESIAN_POINT('Ctrl Pts',(130.555707397324,3.1175597702868,136.628006976231));
#237182=CARTESIAN_POINT('Ctrl Pts',(130.277259773512,6.58471582225214,131.329292396271));
#237183=CARTESIAN_POINT('Ctrl Pts',(129.998812149698,4.0008397148189,125.548191156024));
#237184=CARTESIAN_POINT('Ctrl Pts',(129.720364525886,-2.25961263864694,
124.59725287278));
#237185=CARTESIAN_POINT('Ctrl Pts',(129.441916902073,-6.44359136541048,
129.350343372922));
#237186=CARTESIAN_POINT('Ctrl Pts',(129.16346927826,-4.70622441430021,135.439604688201));
#237187=CARTESIAN_POINT('Ctrl Pts',(128.885021654447,1.35593286170785,137.269303146827));
#237188=CARTESIAN_POINT('Ctrl Pts',(128.606574030634,6.17205407880915,133.158035251063));
#237189=CARTESIAN_POINT('Ctrl Pts',(128.328126406821,5.31635911908928,126.883855350513));
#237190=CARTESIAN_POINT('Ctrl Pts',(128.049678783009,-0.424810152491945,
124.212428263054));
#237191=CARTESIAN_POINT('Ctrl Pts',(127.771231159195,-5.77559964706288,
127.598664975593));
#237192=CARTESIAN_POINT('Ctrl Pts',(127.492783535383,-5.81889521971155,
133.930779376167));
#237193=CARTESIAN_POINT('Ctrl Pts',(127.21433591157,-0.514910354280421,
137.389867671632));
#237194=CARTESIAN_POINT('Ctrl Pts',(126.935888287757,5.26225197196523,134.797196704317));
#237195=CARTESIAN_POINT('Ctrl Pts',(126.657440663944,6.20366181127538,128.535304434163));
#237196=CARTESIAN_POINT('Ctrl Pts',(126.378993040131,1.44420951175126,124.358563947));
#237197=CARTESIAN_POINT('Ctrl Pts',(126.100545416318,-4.64240077551519,
126.105195705413));
#237198=CARTESIAN_POINT('Ctrl Pts',(125.822097792505,-6.46287154396936,
132.170130451126));
#237199=CARTESIAN_POINT('Ctrl Pts',(125.543650168692,-2.34427909234318,
136.979989441362));
#237200=CARTESIAN_POINT('Ctrl Pts',(125.26520254488,3.92859132074607,136.114747238771));
#237201=CARTESIAN_POINT('Ctrl Pts',(124.986754921067,6.59127823242518,130.369519158099));
#237202=CARTESIAN_POINT('Ctrl Pts',(124.708307297254,3.19690245034852,125.023889135492));
#237203=CARTESIAN_POINT('Ctrl Pts',(124.429859673441,-3.13527050623128,
124.990230013179));
#237204=CARTESIAN_POINT('Ctrl Pts',(124.151412049628,-6.58628303406391,
130.299472880227));
#237205=CARTESIAN_POINT('Ctrl Pts',(123.872964425815,-3.98482321140548,
136.072682912751));
#237206=CARTESIAN_POINT('Ctrl Pts',(123.594516802002,2.2784944730983,137.004562127853));
#237207=CARTESIAN_POINT('Ctrl Pts',(123.316069178189,6.44798704746787,132.238759051683));
#237208=CARTESIAN_POINT('Ctrl Pts',(123.037621554376,4.6920945268939,126.154813888819));
#237209=CARTESIAN_POINT('Ctrl Pts',(122.759173930564,-1.37560364233486,
124.343575026687));
#237210=CARTESIAN_POINT('Ctrl Pts',(122.480726306751,-6.17918926623166,
128.46948249565));
#237211=CARTESIAN_POINT('Ctrl Pts',(122.202278682938,-5.30440182463932,
134.741028893516));
#237212=CARTESIAN_POINT('Ctrl Pts',(121.923831059125,0.444871759361186,
137.394969462721));
#237213=CARTESIAN_POINT('Ctrl Pts',(121.645383435312,5.78532992970255,133.992462472369));
#237214=CARTESIAN_POINT('Ctrl Pts',(121.366935811499,5.80935252372653,127.660245624887));
#237215=CARTESIAN_POINT('Ctrl Pts',(121.088488187686,0.494863951094175,
124.21731685712));
#237216=CARTESIAN_POINT('Ctrl Pts',(120.810040563873,-5.27438041714564,
126.827559510225));
#237217=CARTESIAN_POINT('Ctrl Pts',(120.53159294006,-6.19672684983677,133.092288103441));
#237218=CARTESIAN_POINT('Ctrl Pts',(120.253145316248,-1.42458403446405,
137.254523108609));
#237219=CARTESIAN_POINT('Ctrl Pts',(119.974697692435,4.65668191378195,135.489373892464));
#237220=CARTESIAN_POINT('Ctrl Pts',(119.696250068622,6.45868467482089,129.418926352309));
#237221=CARTESIAN_POINT('Ctrl Pts',(119.417802444809,2.32547174398699,124.621625219699));
#237222=CARTESIAN_POINT('Ctrl Pts',(119.139354820996,-3.94473611396066,
125.505955874312));
#237223=CARTESIAN_POINT('Ctrl Pts',(118.860907197183,-6.58992419425096,
131.259261646514));
#237224=CARTESIAN_POINT('Ctrl Pts',(118.58245957337,-3.17929387571916,136.594535596262));
#237225=CARTESIAN_POINT('Ctrl Pts',(118.304011949557,3.15295219745811,136.608921606362));
#237226=CARTESIAN_POINT('Ctrl Pts',(118.025564325744,6.58778923144938,131.289199636326));
#237227=CARTESIAN_POINT('Ctrl Pts',(117.747116701932,3.96876979313418,125.523934293753));
#237228=CARTESIAN_POINT('Ctrl Pts',(117.468669078118,-2.29735519988813,
124.611122779595));
#237229=CARTESIAN_POINT('Ctrl Pts',(117.190221454306,-6.45232299625411,
129.389594282045));
#237230=CARTESIAN_POINT('Ctrl Pts',(116.911773830493,-4.67792117256487,
135.468166931659));
#237231=CARTESIAN_POINT('Ctrl Pts',(116.63332620668,1.39526167955762,137.260929418227));
#237232=CARTESIAN_POINT('Ctrl Pts',(116.354878582867,6.18626721048894,133.120420597908));
#237233=CARTESIAN_POINT('Ctrl Pts',(116.076430959054,5.29239539093549,126.851565801475));
#237234=CARTESIAN_POINT('Ctrl Pts',(115.797983335241,-0.464929244999223,
124.215136336267));
#237235=CARTESIAN_POINT('Ctrl Pts',(115.519535711428,-5.79500661783607,
127.633882084071));
#237236=CARTESIAN_POINT('Ctrl Pts',(115.241088087616,-5.79975601069334,
133.96614271767));
#237237=CARTESIAN_POINT('Ctrl Pts',(114.962640463802,-0.474812963556037,
137.392880062915));
#237238=CARTESIAN_POINT('Ctrl Pts',(114.68419283999,5.28646000118636,134.765089904953));
#237239=CARTESIAN_POINT('Ctrl Pts',(114.405745216177,6.18973448276714,128.497583024264));
#237240=CARTESIAN_POINT('Ctrl Pts',(114.127297592364,1.40494536002493,124.349892059469));
#237241=CARTESIAN_POINT('Ctrl Pts',(113.848849968551,-4.67091991318358,
126.133542381245));
#237242=CARTESIAN_POINT('Ctrl Pts',(113.570402344738,-6.45443797329988,
132.209446480045));
#237243=CARTESIAN_POINT('Ctrl Pts',(113.291954720925,-2.30664285277824,
136.994145313484));
#237244=CARTESIAN_POINT('Ctrl Pts',(113.013507097112,3.96084436367879,136.09073439917));
#237245=CARTESIAN_POINT('Ctrl Pts',(112.735059473299,6.58850910791926,130.329404233275));
#237246=CARTESIAN_POINT('Ctrl Pts',(112.456611849487,3.16165584854565,125.004535781636));
#237247=CARTESIAN_POINT('Ctrl Pts',(112.178164225674,-3.1706046801665,125.00942301702));
#237248=CARTESIAN_POINT('Ctrl Pts',(111.899716601861,-6.58923440045535,
130.339574808866));
#237249=CARTESIAN_POINT('Ctrl Pts',(111.621268978048,-3.9526796087217,136.096842052857));
#237250=CARTESIAN_POINT('Ctrl Pts',(111.342821354235,2.31619464429322,136.990577409908));
#237251=CARTESIAN_POINT('Ctrl Pts',(111.064373730422,6.45659917160154,132.199481748287));
#237252=CARTESIAN_POINT('Ctrl Pts',(110.785926106609,4.66370448261314,126.12633792299));
#237253=CARTESIAN_POINT('Ctrl Pts',(110.507478482796,-1.41490679126679,
124.352068419894));
#237254=CARTESIAN_POINT('Ctrl Pts',(110.229030858983,-6.19328784601188,
128.50714023446));
#237255=CARTESIAN_POINT('Ctrl Pts',(109.950583235171,-5.28033992920373,
134.773245355646));
#237256=CARTESIAN_POINT('Ctrl Pts',(109.672135611358,0.484982423596243,
137.392139293334));
#237257=CARTESIAN_POINT('Ctrl Pts',(109.393687987545,5.80462962181993,133.957186458871));
#237258=CARTESIAN_POINT('Ctrl Pts',(109.115240363732,5.79010576951274,127.624940700352));
#237259=CARTESIAN_POINT('Ctrl Pts',(108.836792739919,0.454757577415474,
124.214426522456));
#237260=CARTESIAN_POINT('Ctrl Pts',(108.558345116106,-5.29849061218381,
126.859739841786));
#237261=CARTESIAN_POINT('Ctrl Pts',(108.279897492293,-6.18268477484283,
133.12996694862));
#237262=CARTESIAN_POINT('Ctrl Pts',(108.00144986848,-1.38529367036394,137.2630754494));
#237263=CARTESIAN_POINT('Ctrl Pts',(107.723002244667,4.68511464182123,135.460940545486));
#237264=CARTESIAN_POINT('Ctrl Pts',(107.444554620855,6.45013147874722,129.379636174388));
#237265=CARTESIAN_POINT('Ctrl Pts',(107.166106997042,2.28779259314522,124.607583964913));
#237266=CARTESIAN_POINT('Ctrl Pts',(106.887659373229,-3.97691592067581,
125.530066769856));
#237267=CARTESIAN_POINT('Ctrl Pts',(106.609211749416,-6.58703298653922,
131.299367957265));
#237268=CARTESIAN_POINT('Ctrl Pts',(106.330764125603,-3.14398853222427,
136.613781581943));
#237269=CARTESIAN_POINT('Ctrl Pts',(106.05231650179,3.18822779082625,136.589621146351));
#237270=CARTESIAN_POINT('Ctrl Pts',(105.773868877977,6.59061852769399,131.249088910493));
#237271=CARTESIAN_POINT('Ctrl Pts',(105.495421254164,3.93655280722527,125.49987309962));
#237272=CARTESIAN_POINT('Ctrl Pts',(105.216973630351,-2.33501263178752,
124.625222179118));
#237273=CARTESIAN_POINT('Ctrl Pts',(104.938526006539,-6.46081553389627,
129.428897615854));
#237274=CARTESIAN_POINT('Ctrl Pts',(104.660078382726,-4.64944458874018,
135.49655635606));
#237275=CARTESIAN_POINT('Ctrl Pts',(104.381630758913,1.43453879547275,137.252316439095));
#237276=CARTESIAN_POINT('Ctrl Pts',(104.1031831351,6.20025110776228,133.082720122298));
#237277=CARTESIAN_POINT('Ctrl Pts',(103.824735511287,5.26823555112421,126.819422724701));
#237278=CARTESIAN_POINT('Ctrl Pts',(103.546287887474,-0.505031109382345,
124.218088575609));
#237279=CARTESIAN_POINT('Ctrl Pts',(103.267840263661,-5.81419885250792,
127.669216675797));
#237280=CARTESIAN_POINT('Ctrl Pts',(102.989392639848,-5.78040188958328,
134.001388898174));
#237281=CARTESIAN_POINT('Ctrl Pts',(102.710945016035,-0.434697978462825,
137.395648314187));
#237282=CARTESIAN_POINT('Ctrl Pts',(102.432497392222,5.31047213868803,134.732836339309));
#237283=CARTESIAN_POINT('Ctrl Pts',(102.15404976841,6.17557779137139,128.459947092858));
#237284=CARTESIAN_POINT('Ctrl Pts',(101.875602144597,1.3656291475316,124.341459344644));
#237285=CARTESIAN_POINT('Ctrl Pts',(101.597154520784,-4.69926596819684,
126.162062135967));
#237286=CARTESIAN_POINT('Ctrl Pts',(101.318706896971,-6.44576523105769,
132.248710442988));
#237287=CARTESIAN_POINT('Ctrl Pts',(101.040259273158,-2.26892113971413,
137.008071820859));
#237288=CARTESIAN_POINT('Ctrl Pts',(100.761811649345,3.99295063606701,136.066525671043));
#237289=CARTESIAN_POINT('Ctrl Pts',(100.483364025532,6.58549584378548,130.289306908136));
#237290=CARTESIAN_POINT('Ctrl Pts',(100.204916401719,3.12629209042249,124.985397342422));
#237291=CARTESIAN_POINT('Ctrl Pts',(99.9264687779064,-3.20582136617937,
125.028830754405));
#237292=CARTESIAN_POINT('Ctrl Pts',(99.6480211540935,-6.5919416003429,130.379693960313));
#237293=CARTESIAN_POINT('Ctrl Pts',(99.3695735302808,-3.92038953804142,
136.120805078117));
#237294=CARTESIAN_POINT('Ctrl Pts',(99.0911259064677,2.35380898804382,136.976363459425));
#237295=CARTESIAN_POINT('Ctrl Pts',(98.812678282655,6.46497204407849,132.160152748165));
#237296=CARTESIAN_POINT('Ctrl Pts',(98.5342306588419,4.63514162304771,126.098035303012));
#237297=CARTESIAN_POINT('Ctrl Pts',(98.2557830350292,-1.45415751030726,
124.36080090516));
#237298=CARTESIAN_POINT('Ctrl Pts',(97.9773354112161,-6.20715693123341,
128.544883097616));
#237299=CARTESIAN_POINT('Ctrl Pts',(97.6988877874034,-5.25608236883021,
134.805314749293));
#237300=CARTESIAN_POINT('Ctrl Pts',(97.4204401635904,0.525075116629235,
137.389065011387));
#237301=CARTESIAN_POINT('Ctrl Pts',(97.1419925397775,5.82371422125203,133.921793616252));
#237302=CARTESIAN_POINT('Ctrl Pts',(96.8635449159648,5.77064446080036,127.589753590393));
#237303=CARTESIAN_POINT('Ctrl Pts',(96.5850972921516,0.414634352527504,
124.211780380221));
#237304=CARTESIAN_POINT('Ctrl Pts',(96.306649668339,-5.32240446970382,126.89206634272));
#237305=CARTESIAN_POINT('Ctrl Pts',(96.0282020445258,-6.16841359819089,
133.1675596176));
#237306=CARTESIAN_POINT('Ctrl Pts',(95.7497544207132,-1.34595197369742,
137.271388460138));
#237307=CARTESIAN_POINT('Ctrl Pts',(95.4713067969001,4.7133737612145,135.432334647225));
#237308=CARTESIAN_POINT('Ctrl Pts',(95.1928591730874,6.44133927067958,129.340398790155));
#237309=CARTESIAN_POINT('Ctrl Pts',(94.9144115492744,2.25002866730758,124.593772333964));
#237310=CARTESIAN_POINT('Ctrl Pts',(94.6359639254615,-4.008948361309,125.554373106298));
#237311=CARTESIAN_POINT('Ctrl Pts',(94.3575163016487,-6.58389769389783,
131.339455925338));
#237312=CARTESIAN_POINT('Ctrl Pts',(94.0790686778357,-3.10856668707799,
136.632812297395));
#237313=CARTESIAN_POINT('Ctrl Pts',(93.8006210540229,3.22338524324122,136.570106311383));
#237314=CARTESIAN_POINT('Ctrl Pts',(93.52217343021,6.59320360614536,131.208961705089));
#237315=CARTESIAN_POINT('Ctrl Pts',(93.2437258063971,3.90418995090443,125.476008465224));
#237316=CARTESIAN_POINT('Ctrl Pts',(92.9652781825842,-2.37258353893516,
124.639550548886));
#237317=CARTESIAN_POINT('Ctrl Pts',(92.6868305587713,-6.46906866364288,
129.468251917951));
#237318=CARTESIAN_POINT('Ctrl Pts',(92.4083829349583,-4.62079571803641,
135.524771909422));
#237319=CARTESIAN_POINT('Ctrl Pts',(92.1299353111456,1.47376275402524,137.24346452859));
#237320=CARTESIAN_POINT('Ctrl Pts',(91.8514876873325,6.21400525245068,133.04493522124));
#237321=CARTESIAN_POINT('Ctrl Pts',(91.5730400635199,5.24388049490719,126.787427311268));
#237322=CARTESIAN_POINT('Ctrl Pts',(91.2945924397067,-0.545114259651984,
124.221284871682));
#237323=CARTESIAN_POINT('Ctrl Pts',(91.016144815894,-5.83317563990314,127.704667441434));
#237324=CARTESIAN_POINT('Ctrl Pts',(90.7376971920811,-5.76083357355547,
134.036516611621));
#237325=CARTESIAN_POINT('Ctrl Pts',(90.4592495682681,-0.394566885476172,
137.398172322869));
#237326=CARTESIAN_POINT('Ctrl Pts',(90.1808019444553,5.33428749469169,134.700437202553));
#237327=CARTESIAN_POINT('Ctrl Pts',(89.9023543206424,6.16119226166949,128.422398034556));
#237328=CARTESIAN_POINT('Ctrl Pts',(89.6239066968295,1.32626233114802,124.333266115003));
#237329=CARTESIAN_POINT('Ctrl Pts',(89.3454590730166,-4.72743789018152,
126.190753912764));
#237330=CARTESIAN_POINT('Ctrl Pts',(89.0670114492037,-6.43685363861442,
132.28792088502));
#237331=CARTESIAN_POINT('Ctrl Pts',(88.7885638253908,-2.23111535094281,
137.021768447433));
#237332=CARTESIAN_POINT('Ctrl Pts',(88.5101162015778,4.02490894820102,136.042121951457));
#237333=CARTESIAN_POINT('Ctrl Pts',(88.2316685777651,6.58223855168135,130.2492286685));
#237334=CARTESIAN_POINT('Ctrl Pts',(87.9532209539521,3.09081248639635,124.966474527032));
#237335=CARTESIAN_POINT('Ctrl Pts',(87.6747733301392,-3.2409192593025,125.048452506173));
#237336=CARTESIAN_POINT('Ctrl Pts',(87.3963257063264,-6.59440453341028,
130.41982884794));
#237337=CARTESIAN_POINT('Ctrl Pts',(87.1178780825135,-3.88795419588509,
136.144571100572));
#237338=CARTESIAN_POINT('Ctrl Pts',(86.8394304587006,2.39133611053674,136.961920803106));
#237339=CARTESIAN_POINT('Ctrl Pts',(86.5609828348878,6.47310535463887,132.120773508667));
#237340=CARTESIAN_POINT('Ctrl Pts',(86.2825352110747,4.60640700660486,126.06990707765));
#237341=CARTESIAN_POINT('Ctrl Pts',(86.004087587262,-1.49335434500641,124.369772158902));
#237342=CARTESIAN_POINT('Ctrl Pts',(85.725639963449,-6.22079600797217,128.582709686544));
#237343=CARTESIAN_POINT('Ctrl Pts',(85.4471923396362,-5.23163004239161,
134.837235886113));
#237344=CARTESIAN_POINT('Ctrl Pts',(85.1687447158232,0.565148352810691,
137.385746730796));
#237345=CARTESIAN_POINT('Ctrl Pts',(84.8902970920103,5.842583020812,133.886285256006));
#237346=CARTESIAN_POINT('Ctrl Pts',(84.6118494681974,5.75096931873532,127.554685598878));
#237347=CARTESIAN_POINT('Ctrl Pts',(84.3334018443846,0.374495763211118,
124.209378528473));
#237348=CARTESIAN_POINT('Ctrl Pts',(84.0549542205716,-5.34612110356891,
126.924537815158));
#237349=CARTESIAN_POINT('Ctrl Pts',(83.7765065967588,-6.15391384870464,
133.205064717373));
#237350=CARTESIAN_POINT('Ctrl Pts',(83.498058972946,-1.30656040228555,137.279461832782));
#237351=CARTESIAN_POINT('Ctrl Pts',(83.2196113491328,4.74145822480973,135.403557257686));
#237352=CARTESIAN_POINT('Ctrl Pts',(82.9411637253203,6.43230837641647,129.301215653567));
#237353=CARTESIAN_POINT('Ctrl Pts',(82.6627161015071,2.21218136583022,124.580190838648));
#237354=CARTESIAN_POINT('Ctrl Pts',(82.3842684776944,-4.04083224888638,
125.578873982957));
#237355=CARTESIAN_POINT('Ctrl Pts',(82.1058208538814,-6.58051843250612,
131.379524065257));
#237356=CARTESIAN_POINT('Ctrl Pts',(81.8273732300686,-3.07302965285007,
136.651627037425));
#237357=CARTESIAN_POINT('Ctrl Pts',(81.5489256062556,3.25842325193051,136.550377824588));
#237358=CARTESIAN_POINT('Ctrl Pts',(81.270477982443,6.59554437101248,131.168819507043));
#237359=CARTESIAN_POINT('Ctrl Pts',(80.9920303586297,3.87168242338918,125.452341274876));
#237360=CARTESIAN_POINT('Ctrl Pts',(80.713582734817,-2.41006652912724,124.654107357959));
#237361=CARTESIAN_POINT('Ctrl Pts',(80.435135111004,-6.47708207967116,129.507655730047));
#237362=CARTESIAN_POINT('Ctrl Pts',(80.1566874871913,-4.59197562204804,
135.552812546207));
#237363=CARTESIAN_POINT('Ctrl Pts',(79.8782398633782,1.51293210175691,137.234374014721));
#237364=CARTESIAN_POINT('Ctrl Pts',(79.5997922395654,6.22752913488936,133.007067294864));
#237365=CARTESIAN_POINT('Ctrl Pts',(79.3213446157525,5.2193311247699,126.755580746775));
#237366=CARTESIAN_POINT('Ctrl Pts',(79.0428969919396,-0.585177210512381,
124.224725106049));
#237367=CARTESIAN_POINT('Ctrl Pts',(78.7644493681267,-5.85193627682986,
127.740233067343));
#237368=CARTESIAN_POINT('Ctrl Pts',(78.4860017443139,-5.74105178772106,
134.071524556339));
#237369=CARTESIAN_POINT('Ctrl Pts',(78.2075541205009,-0.354421171668466,
137.400451995434));
#237370=CARTESIAN_POINT('Ctrl Pts',(77.9291064966881,5.35790518671055,134.667893695246));
#237371=CARTESIAN_POINT('Ctrl Pts',(77.6506588728751,6.14657842672258,128.384937240753));
#237372=CARTESIAN_POINT('Ctrl Pts',(77.3722112490624,1.28684636962602,124.325312674148));
#237373=CARTESIAN_POINT('Ctrl Pts',(77.0937636252493,-4.75543463521666,
126.219616648455));
#237374=CARTESIAN_POINT('Ctrl Pts',(76.8153160014366,-6.42770352619243,
132.327076353179));
#237375=CARTESIAN_POINT('Ctrl Pts',(76.5368683776235,-2.19322688737167,
137.035234685673));
#237376=CARTESIAN_POINT('Ctrl Pts',(76.2584207538107,4.05671811585379,136.017524144697));
#237377=CARTESIAN_POINT('Ctrl Pts',(75.9799731299978,6.57873735230709,130.209170999483));
#237378=CARTESIAN_POINT('Ctrl Pts',(75.7015255061849,3.05521835117689,124.947768036657));
#237379=CARTESIAN_POINT('Ctrl Pts',(75.423077882372,-3.27589705897064,125.068287545233));
#237380=CARTESIAN_POINT('Ctrl Pts',(75.1446302585591,-6.5966231083926,130.459977984534));
#237381=CARTESIAN_POINT('Ctrl Pts',(74.8661826347462,-3.85537478415624,
136.168139239563));
#237382=CARTESIAN_POINT('Ctrl Pts',(74.5877350109334,2.42877462119068,136.94724997613));
#237383=CARTESIAN_POINT('Ctrl Pts',(74.3092873871204,6.48099880189986,132.081345489005));
#237384=CARTESIAN_POINT('Ctrl Pts',(74.0308397633076,4.57750169805637,126.041954289206));
#237385=CARTESIAN_POINT('Ctrl Pts',(73.7523921394947,-1.53249584291112,
124.378981848686));
#237386=CARTESIAN_POINT('Ctrl Pts',(73.4739445156818,-6.23420457082727,
128.620618599563));
#237387=CARTESIAN_POINT('Ctrl Pts',(73.1954968918689,-5.20698385597775,
134.869007583256));
#237388=CARTESIAN_POINT('Ctrl Pts',(72.917049268056,0.605200647212208,137.382184574524));
#237389=CARTESIAN_POINT('Ctrl Pts',(72.6386016442432,5.86123532130951,133.850662693911));
#237390=CARTESIAN_POINT('Ctrl Pts',(72.3601540204302,5.73108107238729,127.519738025268));
#237391=CARTESIAN_POINT('Ctrl Pts',(72.0817063966174,0.334343296816498,
124.207221056211));
#237392=CARTESIAN_POINT('Ctrl Pts',(71.8032587728044,-5.36963963495047,
126.957153055855));
#237393=CARTESIAN_POINT('Ctrl Pts',(71.5248111489915,-6.13918606367764,
133.242480858172));
#237394=CARTESIAN_POINT('Ctrl Pts',(71.2463635251787,-1.26712041579749,
137.287295268168));
#237395=CARTESIAN_POINT('Ctrl Pts',(70.9679159013657,4.76936699192676,135.374609443224));
#237396=CARTESIAN_POINT('Ctrl Pts',(70.689468277553,6.423039130601,129.262088216567));
#237397=CARTESIAN_POINT('Ctrl Pts',(70.4110206537399,2.17425209115883,124.566839982233));
#237398=CARTESIAN_POINT('Ctrl Pts',(70.1325730299272,-4.07256640193864,
125.603568491945));
#237399=CARTESIAN_POINT('Ctrl Pts',(69.8541254061142,-6.57689532758393,
131.419570892283));
#237400=CARTESIAN_POINT('Ctrl Pts',(69.5756777823013,-3.03737874637841,
136.670225104848));
#237401=CARTESIAN_POINT('Ctrl Pts',(69.2972301584884,3.2933405185478,136.530436417012));
#237402=CARTESIAN_POINT('Ctrl Pts',(69.0187825346755,6.5976407355574,131.128663803839));
#237403=CARTESIAN_POINT('Ctrl Pts',(68.7403349108627,3.83903142925813,125.428872405572));
#237404=CARTESIAN_POINT('Ctrl Pts',(68.4618872870498,-2.44746021341752,
124.668892066929));
#237405=CARTESIAN_POINT('Ctrl Pts',(68.1834396632368,-6.48485548504104,
129.547107592018));
#237406=CARTESIAN_POINT('Ctrl Pts',(67.904992039424,-4.56298536871445,135.580677227361));
#237407=CARTESIAN_POINT('Ctrl Pts',(67.6265444156111,1.55204538723279,137.225045234339));
#237408=CARTESIAN_POINT('Ctrl Pts',(67.3480967917982,6.2408222539455,132.969117746385));
#237409=CARTESIAN_POINT('Ctrl Pts',(67.0696491679854,5.19458835039884,126.723884211309));
#237410=CARTESIAN_POINT('Ctrl Pts',(66.7912015441724,-0.625218477415679,
124.228409151229));
#237411=CARTESIAN_POINT('Ctrl Pts',(66.5127539203596,-5.87048006810572,
127.775912235624));
#237412=CARTESIAN_POINT('Ctrl Pts',(66.2343062965465,-5.72105726510147,
134.106411435094));
#237413=CARTESIAN_POINT('Ctrl Pts',(65.9558586727338,-0.314262324654327,
137.402487247406));
#237414=CARTESIAN_POINT('Ctrl Pts',(65.6774110489208,5.3813243395822,134.6352070233));
#237415=CARTESIAN_POINT('Ctrl Pts',(65.398963425108,6.13173682805169,128.347566099575));
#237416=CARTESIAN_POINT('Ctrl Pts',(65.120515801295,1.24738272353907,124.317599316798));
#237417=CARTESIAN_POINT('Ctrl Pts',(64.8420681774823,-4.78325516587229,
126.248649273519));
#237418=CARTESIAN_POINT('Ctrl Pts',(64.5636205536692,-6.41831523285262,
132.366175396547));
#237419=CARTESIAN_POINT('Ctrl Pts',(64.2851729298565,-2.15525715297185,
137.048470036584));
#237420=CARTESIAN_POINT('Ctrl Pts',(64.0067253060435,4.08837696032456,135.992733162246));
#237421=CARTESIAN_POINT('Ctrl Pts',(63.7282776822307,6.57499237540094,130.169135385437));
#237422=CARTESIAN_POINT('Ctrl Pts',(63.4498300584178,3.01951100371835,124.929278564476));
#237423=CARTESIAN_POINT('Ctrl Pts',(63.1713824346048,-3.31075346906837,
125.088335136589));
#237424=CARTESIAN_POINT('Ctrl Pts',(62.892934810792,-6.59859724307971,130.500139882352));
#237425=CARTESIAN_POINT('Ctrl Pts',(62.614487186979,-3.82265251009718,136.191508621766));
#237426=CARTESIAN_POINT('Ctrl Pts',(62.3360395631662,2.46612313270748,136.932351522132));
#237427=CARTESIAN_POINT('Ctrl Pts',(62.0575919393533,6.48865209336687,132.041870150199));
#237428=CARTESIAN_POINT('Ctrl Pts',(61.7791443155403,4.5484267684992,126.014177973478));
#237429=CARTESIAN_POINT('Ctrl Pts',(61.5006966917276,-1.57158055361859,
124.388429633243));
#237430=CARTESIAN_POINT('Ctrl Pts',(61.2222490679146,-6.24738212293903,
128.658608431946));
#237431=CARTESIAN_POINT('Ctrl Pts',(60.9438014441017,-5.18214472286266,
134.900628663412));
#237432=CARTESIAN_POINT('Ctrl Pts',(60.6653538202889,0.645230515680748,
137.378378674564));
#237433=CARTESIAN_POINT('Ctrl Pts',(60.3869061964759,5.87967043157647,133.814927249971));
#237434=CARTESIAN_POINT('Ctrl Pts',(60.108458572663,5.71098045872276,127.484912164554));
#237435=CARTESIAN_POINT('Ctrl Pts',(59.8300109488502,0.294178441208572,
124.205308043382));
#237436=CARTESIAN_POINT('Ctrl Pts',(59.5515633250373,-5.39295919236059,
126.989910856244));
#237437=CARTESIAN_POINT('Ctrl Pts',(59.2731157012244,-6.12423078885343,
133.27980665353));
#237438=CARTESIAN_POINT('Ctrl Pts',(58.9946680774115,-1.2276334756968,137.294888476026));
#237439=CARTESIAN_POINT('Ctrl Pts',(58.7162204535986,4.79709902839574,135.345492276511));
#237440=CARTESIAN_POINT('Ctrl Pts',(58.4377728297857,6.41353187670863,129.223017929039));
#237441=CARTESIAN_POINT('Ctrl Pts',(58.1593252059728,2.13624224877676,124.553720259438));
#237442=CARTESIAN_POINT('Ctrl Pts',(57.8808775821599,-4.10414964454526,
125.628455718198));
#237443=CARTESIAN_POINT('Ctrl Pts',(57.602429958347,-6.57302851338661,131.459594922466));
#237444=CARTESIAN_POINT('Ctrl Pts',(57.3239823345341,-3.00161528872044,
136.688605810505));
#237445=CARTESIAN_POINT('Ctrl Pts',(57.0455347107212,3.32813574922106,136.510282827592));
#237446=CARTESIAN_POINT('Ctrl Pts',(56.7670870869083,6.59949262209846,131.088496083461));
#237447=CARTESIAN_POINT('Ctrl Pts',(56.4886394630955,3.80623817840574,125.405602726962));
#237448=CARTESIAN_POINT('Ctrl Pts',(56.2101918392826,-2.48476320616966,
124.683904127941));
#237449=CARTESIAN_POINT('Ctrl Pts',(55.9317442154696,-6.49238859170611,
129.586606041964));
#237450=CARTESIAN_POINT('Ctrl Pts',(55.6532965916568,-4.53382603227983,
135.608364920346));
#237451=CARTESIAN_POINT('Ctrl Pts',(55.3748489678439,1.59110116109648,137.215478533129));
#237452=CARTESIAN_POINT('Ctrl Pts',(55.096401344031,6.25388411703813,132.931087982032));
#237453=CARTESIAN_POINT('Ctrl Pts',(54.8179537202181,5.1696530886458,126.692338879397));
#237454=CARTESIAN_POINT('Ctrl Pts',(54.5395060964052,-0.665236576618623,
124.23233687071));
#237455=CARTESIAN_POINT('Ctrl Pts',(54.2610584725923,-5.88880632658389,
127.811703624173));
#237456=CARTESIAN_POINT('Ctrl Pts',(53.9826108487795,-5.70085074660091,
134.141175955143));
#237457=CARTESIAN_POINT('Ctrl Pts',(53.7041632249665,-0.274091832533765,
137.40427800337));
#237458=CARTESIAN_POINT('Ctrl Pts',(53.4257156011537,5.40454408550164,134.602378397932));
#237459=CARTESIAN_POINT('Ctrl Pts',(53.1472679773408,6.11666801561766,128.310285995821));
#237460=CARTESIAN_POINT('Ctrl Pts',(52.8688203535278,1.20787285522606,124.310126328773));
#237461=CARTESIAN_POINT('Ctrl Pts',(52.590372729715,-4.81089845124901,126.277850712144));
#237462=CARTESIAN_POINT('Ctrl Pts',(52.3119251059021,-6.40868910648141,
132.405216566294));
#237463=CARTESIAN_POINT('Ctrl Pts',(52.0334774820892,-2.11720755472543,
137.061474009724));
#237464=CARTESIAN_POINT('Ctrl Pts',(51.7550298582764,4.11988430848393,135.967749922743));
#237465=CARTESIAN_POINT('Ctrl Pts',(51.4765822344634,6.57100375973434,130.129123309894));
#237466=CARTESIAN_POINT('Ctrl Pts',(51.1981346106506,2.98369176716867,124.91100679562));
#237467=CARTESIAN_POINT('Ctrl Pts',(50.9196869868376,-3.34548719797895,
125.108594537373));
#237468=CARTESIAN_POINT('Ctrl Pts',(50.6412393630248,-6.60032686431936,
130.540313053181));
#237469=CARTESIAN_POINT('Ctrl Pts',(50.3627917392119,-3.78978858624336,
136.214678381218));
#237470=CARTESIAN_POINT('Ctrl Pts',(50.0843441153989,2.50338026112505,136.917225993175));
#237471=CARTESIAN_POINT('Ctrl Pts',(49.8058964915862,6.49606494544435,132.002348955022));
#237472=CARTESIAN_POINT('Ctrl Pts',(49.5274488677731,4.51918329531533,125.986579159731));
#237473=CARTESIAN_POINT('Ctrl Pts',(49.2490012439603,-1.6106070288309,124.39811516248));
#237474=CARTESIAN_POINT('Ctrl Pts',(48.9705536201474,-6.26032817600901,
128.696677775965));
#237475=CARTESIAN_POINT('Ctrl Pts',(48.6921059963345,-5.15711356346882,
134.932097954848));
#237476=CARTESIAN_POINT('Ctrl Pts',(48.4136583725217,0.685236474895564,
137.374329171949));
#237477=CARTESIAN_POINT('Ctrl Pts',(48.1352107487087,5.89788766849362,133.779080248378));
#237478=CARTESIAN_POINT('Ctrl Pts',(47.8567631248959,5.69066822257687,127.450209307224));
#237479=CARTESIAN_POINT('Ctrl Pts',(47.578315501083,0.254002684709825,124.203639560873));
#237480=CARTESIAN_POINT('Ctrl Pts',(47.29986787727,-5.41607891168467,127.022810002472));
#237481=CARTESIAN_POINT('Ctrl Pts',(47.0214202534572,-6.10904857840509,
133.317040720324));
#237482=CARTESIAN_POINT('Ctrl Pts',(46.7429726296443,-1.18810104518584,
137.302241174989));
#237483=CARTESIAN_POINT('Ctrl Pts',(46.4645250058313,4.82465330659632,135.316206836494));
#237484=CARTESIAN_POINT('Ctrl Pts',(46.1860773820186,6.40378696703385,129.184006238746));
#237485=CARTESIAN_POINT('Ctrl Pts',(45.9076297582056,2.09815324715241,124.54083215642));
#237486=CARTESIAN_POINT('Ctrl Pts',(45.6291821343927,-4.13558080637756,
125.653534739511));
#237487=CARTESIAN_POINT('Ctrl Pts',(45.3507345105798,-6.56891813320061,
131.499594672701));
#237488=CARTESIAN_POINT('Ctrl Pts',(45.072286886767,-2.96574060510383,136.706768473292));
#237489=CARTESIAN_POINT('Ctrl Pts',(44.793839262954,3.36280765460034,136.489917803126));
#237490=CARTESIAN_POINT('Ctrl Pts',(44.5153916391412,6.60109996201359,131.048317834339));
#237491=CARTESIAN_POINT('Ctrl Pts',(44.2369440153282,3.77330388599763,125.38253310131));
#237492=CARTESIAN_POINT('Ctrl Pts',(43.9584963915154,-2.52197412510756,
124.699142984721));
#237493=CARTESIAN_POINT('Ctrl Pts',(43.6800487677024,-6.49968112052436,
129.626149616253));
#237494=CARTESIAN_POINT('Ctrl Pts',(43.4016011438896,-4.50449869325427,
135.635874599185));
#237495=CARTESIAN_POINT('Ctrl Pts',(43.1231535200766,1.6300979761215,137.205674265588));
#237496=CARTESIAN_POINT('Ctrl Pts',(42.8447058962639,6.26671424015497,132.892979411015));
#237497=CARTESIAN_POINT('Ctrl Pts',(42.5662582724509,5.14452626349642,126.660945919963));
#237498=CARTESIAN_POINT('Ctrl Pts',(42.287810648638,-0.705230025235587,
124.236508118946));
#237499=CARTESIAN_POINT('Ctrl Pts',(42.0093630248251,-5.90691437317801,
127.847605906729));
#237500=CARTESIAN_POINT('Ctrl Pts',(41.7309154010123,-5.68043298097947,
134.175816828272));
#237501=CARTESIAN_POINT('Ctrl Pts',(41.4524677771993,-0.233911183839542,
137.405824196969));
#237502=CARTESIAN_POINT('Ctrl Pts',(41.1740201533865,5.42756356405245,134.569409035618));
#237503=CARTESIAN_POINT('Ctrl Pts',(40.8955725295735,6.10137254780096,128.273098310918));
#237504=CARTESIAN_POINT('Ctrl Pts',(40.6171249057607,1.1683182287399,124.302893986988));
#237505=CARTESIAN_POINT('Ctrl Pts',(40.3386772819477,-4.83836346701448,
126.307219882257));
#237506=CARTESIAN_POINT('Ctrl Pts',(40.060229658135,-6.39882550377857,132.444198415735));
#237507=CARTESIAN_POINT('Ctrl Pts',(39.781782034322,-2.07907950257448,137.074246123225));
#237508=CARTESIAN_POINT('Ctrl Pts',(39.5033344105091,4.15123899281517,135.94257535195));
#237509=CARTESIAN_POINT('Ctrl Pts',(39.2248867866962,6.56677165310695,130.089136255519));
#237510=CARTESIAN_POINT('Ctrl Pts',(38.9464391628834,2.94776196882331,124.892953407157));
#237511=CARTESIAN_POINT('Ctrl Pts',(38.6679915390704,-3.38009695863112,
125.129064996863));
#237512=CARTESIAN_POINT('Ctrl Pts',(38.3895439152575,-6.6018119080198,130.58049600839));
#237513=CARTESIAN_POINT('Ctrl Pts',(38.1110962914447,-3.75678423037978,
136.237647659355));
#237514=CARTESIAN_POINT('Ctrl Pts',(37.8326486676317,2.54054462586645,136.901873949744));
#237515=CARTESIAN_POINT('Ctrl Pts',(37.5542010438189,6.50323708344635,131.962783367948));
#237516=CARTESIAN_POINT('Ctrl Pts',(37.275753420006,4.48977236213255,125.959158870647));
#237517=CARTESIAN_POINT('Ctrl Pts',(36.9973057961931,-1.64957382240749,
124.4080380775));
#237518=CARTESIAN_POINT('Ctrl Pts',(36.7188581723802,-6.27304225031618,
128.734825220947));
#237519=CARTESIAN_POINT('Ctrl Pts',(36.4404105485673,-5.13189130533538,
134.96341429146));
#237520=CARTESIAN_POINT('Ctrl Pts',(36.1619629247544,0.725217042420823,
137.370036216732));
#237521=CARTESIAN_POINT('Ctrl Pts',(35.8835153009416,5.91588635701427,133.743123017455));
#237522=CARTESIAN_POINT('Ctrl Pts',(35.6050676771286,5.67014511662727,127.415630739204));
#237523=CARTESIAN_POINT('Ctrl Pts',(35.3266200533158,0.213817516048174,
124.202215670509));
#237524=CARTESIAN_POINT('Ctrl Pts',(35.0481724295028,-5.43899793621292,
127.055849275448));
#237525=CARTESIAN_POINT('Ctrl Pts',(34.76972480569,-6.09363999491508,133.354181678833));
#237526=CARTESIAN_POINT('Ctrl Pts',(34.4912771818771,-1.14852458915375,
137.309353092597));
#237527=CARTESIAN_POINT('Ctrl Pts',(34.2128295580642,4.85202880549439,135.286754208357));
#237528=CARTESIAN_POINT('Ctrl Pts',(33.9343819342512,6.393804762678,129.145054591279));
#237529=CARTESIAN_POINT('Ctrl Pts',(33.6559343104384,2.05998649768791,124.528176150753));
#237530=CARTESIAN_POINT('Ctrl Pts',(33.3774866866255,-4.16685872274224,
125.678804626571));
#237531=CARTESIAN_POINT('Ctrl Pts',(33.0990390628127,-6.56456433933747,
131.539568660782));
#237532=CARTESIAN_POINT('Ctrl Pts',(32.8205914389997,-2.92975602487846,
136.724712420187));
#237533=CARTESIAN_POINT('Ctrl Pts',(32.5421438151868,3.39735494990529,136.469342098247));
#237534=CARTESIAN_POINT('Ctrl Pts',(32.263696191374,6.60246269574222,131.008130545292));
#237535=CARTESIAN_POINT('Ctrl Pts',(31.985248567561,3.74022977242616,125.359664383471));
#237536=CARTESIAN_POINT('Ctrl Pts',(31.7068009437482,-2.55909159136699,
124.714608072585));
#237537=CARTESIAN_POINT('Ctrl Pts',(31.4283533199352,-6.50673280126843,
129.665736849585));
#237538=CARTESIAN_POINT('Ctrl Pts',(31.1499056961224,-4.47500443837311,
135.663205244496));
#237539=CARTESIAN_POINT('Ctrl Pts',(30.8714580723094,1.66903438726656,137.195632795014));
#237540=CARTESIAN_POINT('Ctrl Pts',(30.5930104484966,6.27931214787105,132.854793445461));
#237541=CARTESIAN_POINT('Ctrl Pts',(30.3145628246837,5.11920880603445,126.629706496284));
#237542=CARTESIAN_POINT('Ctrl Pts',(30.0361152008708,-0.745197341294603,
124.240922741373));
#237543=CARTESIAN_POINT('Ctrl Pts',(29.7576675770579,-5.9248035368878,127.883617752917));
#237544=CARTESIAN_POINT('Ctrl Pts',(29.4792199532451,-5.65980472482494,
134.210332770852));
#237545=CARTESIAN_POINT('Ctrl Pts',(29.2007723294321,-0.193721867480399,
137.407125770907));
#237546=CARTESIAN_POINT('Ctrl Pts',(28.9223247056193,5.45038192223944,134.536300158051));
#237547=CARTESIAN_POINT('Ctrl Pts',(28.6438770818064,6.08585099138068,128.236004422871));
#237548=CARTESIAN_POINT('Ctrl Pts',(28.3654294579935,1.12872030979243,124.29590255944));
#237549=CARTESIAN_POINT('Ctrl Pts',(28.0869818341806,-4.86564919544231,
126.336755695574));
#237550=CARTESIAN_POINT('Ctrl Pts',(27.8085342103677,-6.38872479024353,
132.483119500384));
#237551=CARTESIAN_POINT('Ctrl Pts',(27.5300865865548,-2.04087440936798,
137.086785903815));
#237552=CARTESIAN_POINT('Ctrl Pts',(27.2516389627419,4.18243985145892,135.91721038272));
#237553=CARTESIAN_POINT('Ctrl Pts',(26.973191338929,6.56229621234102,130.049175704046));
#237554=CARTESIAN_POINT('Ctrl Pts',(26.6947437151162,2.91172294007416,124.875119068062));
#237555=CARTESIAN_POINT('Ctrl Pts',(26.4162960913032,-3.41458146854746,
125.149745756519));
#237556=CARTESIAN_POINT('Ctrl Pts',(26.1378484674903,-6.60305231915217,
130.620687258984));
#237557=CARTESIAN_POINT('Ctrl Pts',(25.8594008436774,-3.72364066549499,
136.260415605043));
#237558=CARTESIAN_POINT('Ctrl Pts',(25.5809532198646,2.57761484979243,136.886295960714));
#237559=CARTESIAN_POINT('Ctrl Pts',(25.3025055960517,6.51016824160669,131.92317485509));
#237560=CARTESIAN_POINT('Ctrl Pts',(25.0240579722387,4.46019505878377,125.931918122295));
#237561=CARTESIAN_POINT('Ctrl Pts',(24.7456103484259,-1.68847949041943,
124.418198010604));
#237562=CARTESIAN_POINT('Ctrl Pts',(24.467162724613,-6.28552387473587,128.773049353324));
#237563=CARTESIAN_POINT('Ctrl Pts',(24.1887151008001,-5.10647888308236,
134.994576512808));
#237564=CARTESIAN_POINT('Ctrl Pts',(23.9102674769872,0.765170736761864,
137.365499967992));
#237565=CARTESIAN_POINT('Ctrl Pts',(23.6318198531744,5.93366583019039,133.707056889611));
#237566=CARTESIAN_POINT('Ctrl Pts',(23.3533722293614,5.64941190136517,127.381177741815));
#237567=CARTESIAN_POINT('Ctrl Pts',(23.0749246055485,0.173624424299845,
124.201036425055));
#237568=CARTESIAN_POINT('Ctrl Pts',(22.7964769817356,-5.46171541667246,
127.08902745089));
#237569=CARTESIAN_POINT('Ctrl Pts',(22.5180293579228,-6.07800560935413,
133.391228152785));
#237570=CARTESIAN_POINT('Ctrl Pts',(22.2395817341099,-1.10890557412062,
137.316223965318));
#237571=CARTESIAN_POINT('Ctrl Pts',(21.9611341102969,4.87922451068073,135.257135483476));
#237572=CARTESIAN_POINT('Ctrl Pts',(21.6826864864842,6.38358563353538,129.106164430008));
#237573=CARTESIAN_POINT('Ctrl Pts',(21.4042388626712,2.02174341466617,124.515752711409));
#237574=CARTESIAN_POINT('Ctrl Pts',(21.1257912388583,-4.19798223462457,
125.704264442993));
#237575=CARTESIAN_POINT('Ctrl Pts',(20.8473436150454,-6.55996729312864,
131.579515405459));
#237576=CARTESIAN_POINT('Ctrl Pts',(20.5688959912325,-2.89366288146616,
136.742436986267));
#237577=CARTESIAN_POINT('Ctrl Pts',(20.2904483674196,3.43177635497322,136.448556475397));
#237578=CARTESIAN_POINT('Ctrl Pts',(20.0120007436067,6.60358077278748,130.967935705476));
#237579=CARTESIAN_POINT('Ctrl Pts',(19.7335531197938,3.70701706326526,125.336997420853));
#237580=CARTESIAN_POINT('Ctrl Pts',(19.455105495981,-2.59611422954622,124.730298818468));
#237581=CARTESIAN_POINT('Ctrl Pts',(19.176657872168,-6.51354337263571,129.705366275038));
#237582=CARTESIAN_POINT('Ctrl Pts',(18.8982102483552,-4.4453443605568,135.690355843533));
#237583=CARTESIAN_POINT('Ctrl Pts',(18.6197626245423,1.70790895172861,137.1853544935));
#237584=CARTESIAN_POINT('Ctrl Pts',(18.3413150007294,6.29167737336628,132.816531500364));
#237585=CARTESIAN_POINT('Ctrl Pts',(18.0628673769165,5.09370165440758,126.598621765949));
#237586=CARTESIAN_POINT('Ctrl Pts',(17.7844197531036,-0.785137043792105,
124.245580574404));
#237587=CARTESIAN_POINT('Ctrl Pts',(17.5059721292907,-5.94247315482366,
127.919737828307));
#237588=CARTESIAN_POINT('Ctrl Pts',(17.2275245054778,-5.63896674252494,
134.244722503881));
#237589=CARTESIAN_POINT('Ctrl Pts',(16.949076881665,-0.15352537268619,137.408182676953));
#237590=CARTESIAN_POINT('Ctrl Pts',(16.6706292578521,5.47299831451989,134.503052992091));
#237591=CARTESIAN_POINT('Ctrl Pts',(16.3921816340391,6.07010392151387,128.199005706208));
#237592=CARTESIAN_POINT('Ctrl Pts',(16.1137340102263,1.08908056569879,124.289152305198));
#237593=CARTESIAN_POINT('Ctrl Pts',(15.8352863864134,-4.89275462544986,
126.366457057635));
#237594=CARTESIAN_POINT('Ctrl Pts',(15.5568387626005,-6.37838734016194,
132.521978378005));
#237595=CARTESIAN_POINT('Ctrl Pts',(15.2783911387876,-2.00259369080969,
137.099092886824));
#237596=CARTESIAN_POINT('Ctrl Pts',(14.9999435149747,4.21348572825588,135.891655954962));
#237597=CARTESIAN_POINT('Ctrl Pts',(14.7214958911618,6.55757760327567,130.009243136227));
#237598=CARTESIAN_POINT('Ctrl Pts',(14.4430482673489,2.87557601636067,124.857504439193));
#237599=CARTESIAN_POINT('Ctrl Pts',(14.164600643536,-3.44893944989177,125.170636050008));
#237600=CARTESIAN_POINT('Ctrl Pts',(13.8861530197231,-6.60404805175259,
130.660885315664));
#237601=CARTESIAN_POINT('Ctrl Pts',(13.6077053959103,-3.69035911973598,
136.282981374608));
#237602=CARTESIAN_POINT('Ctrl Pts',(13.3292577720973,2.61458955925225,136.870492603333));
#237603=CARTESIAN_POINT('Ctrl Pts',(13.0508101482845,6.5168581630887,131.883524884162));
#237604=CARTESIAN_POINT('Ctrl Pts',(12.7723625244716,4.43045248126686,125.904857924092));
#237605=CARTESIAN_POINT('Ctrl Pts',(12.4939149006587,-1.72732259120293,
124.428594585312));
#237606=CARTESIAN_POINT('Ctrl Pts',(12.2154672768458,-6.29777258675688,
128.811348756686));
#237607=CARTESIAN_POINT('Ctrl Pts',(11.9370196530329,-5.08087723837641,
135.025583464166));
#237608=CARTESIAN_POINT('Ctrl Pts',(11.65857202922,0.805096077419857,137.36072059382));
#237609=CARTESIAN_POINT('Ctrl Pts',(11.3801244054071,5.95122542919731,133.670883201288));
#237610=CARTESIAN_POINT('Ctrl Pts',(11.1016767815943,5.62846934506734,127.346851591727));
#237611=CARTESIAN_POINT('Ctrl Pts',(10.8232291577813,0.13342489883439,124.200101868207));
#237612=CARTESIAN_POINT('Ctrl Pts',(10.5447815339684,-5.4842305112587,127.12234329937));
#237613=CARTESIAN_POINT('Ctrl Pts',(10.2663339101556,-6.06214600106014,
133.428178769409));
#237614=CARTESIAN_POINT('Ctrl Pts',(9.98788628634267,-1.06924546818365,
137.322853538546));
#237615=CARTESIAN_POINT('Ctrl Pts',(9.70943866252976,4.90623941440849,135.227351759386));
#237616=CARTESIAN_POINT('Ctrl Pts',(9.43099103871685,6.37312995827954,129.067337196021));
#237617=CARTESIAN_POINT('Ctrl Pts',(9.15254341490403,1.98342541519871,124.503562298745));
#237618=CARTESIAN_POINT('Ctrl Pts',(8.87409579109107,-4.22895018873139,
125.729913245354));
#237619=CARTESIAN_POINT('Ctrl Pts',(8.59564816727821,-6.55512716491932,
131.61943342649));
#237620=CARTESIAN_POINT('Ctrl Pts',(8.31720054346528,-2.85746251231165,
136.759941514744));
#237621=CARTESIAN_POINT('Ctrl Pts',(8.03875291965246,3.46607059430627,136.427561704794));
#237622=CARTESIAN_POINT('Ctrl Pts',(7.76030529583951,6.60445415171875,130.927734804324));
#237623=CARTESIAN_POINT('Ctrl Pts',(7.48185767202662,3.67366698922382,125.314533053388));
#237624=CARTESIAN_POINT('Ctrl Pts',(7.20341004821377,-2.63304066775796,
124.746214640945));
#237625=CARTESIAN_POINT('Ctrl Pts',(6.92496242440086,-6.52011258225796,
129.745036424131));
#237626=CARTESIAN_POINT('Ctrl Pts',(6.64651480058794,-4.41551955887045,
135.71732539022));
#237627=CARTESIAN_POINT('Ctrl Pts',(6.36806717677509,1.74672022899638,137.174839741911));
#237628=CARTESIAN_POINT('Ctrl Pts',(6.08961955296221,6.30380945844269,132.778194993536));
#237629=CARTESIAN_POINT('Ctrl Pts',(5.81117192914928,5.06800575379271,126.567692880813));
#237630=CARTESIAN_POINT('Ctrl Pts',(5.53272430533639,-0.825047652747706,
124.250481445441));
#237631=CARTESIAN_POINT('Ctrl Pts',(5.25427668152353,-5.95992257223146,
127.955964794454));
#237632=CARTESIAN_POINT('Ctrl Pts',(4.97582905771062,-5.61791980623858,
134.278984753035));
#237633=CARTESIAN_POINT('Ctrl Pts',(4.69738143389771,-0.113323188952861,
137.408994875945));
#237634=CARTESIAN_POINT('Ctrl Pts',(4.41893381008486,5.49541190283514,134.469668769726));
#237635=CARTESIAN_POINT('Ctrl Pts',(4.14048618627195,6.05413192171396,128.162103531929));
#237636=CARTESIAN_POINT('Ctrl Pts',(3.86203856245905,1.0494004653243,124.282643474398));
#237637=CARTESIAN_POINT('Ctrl Pts',(3.58359093864613,-4.91967875263547,
126.396322867843));
#237638=CARTESIAN_POINT('Ctrl Pts',(3.30514331483329,-6.36781353659179,
132.560773608667));
#237639=CARTESIAN_POINT('Ctrl Pts',(3.02669569102039,-1.96423876540577,
137.111166616214));
#237640=CARTESIAN_POINT('Ctrl Pts',(2.74824806720748,4.24437547278969,135.865913015604));
#237641=CARTESIAN_POINT('Ctrl Pts',(2.46980044339459,6.55261600076067,129.969340031779));
#237642=CARTESIAN_POINT('Ctrl Pts',(2.19135281958173,2.83932253712042,124.840110173268));
#237643=CARTESIAN_POINT('Ctrl Pts',(1.91290519576881,-3.48316962951642,
125.191735103234));
#237644=CARTESIAN_POINT('Ctrl Pts',(1.6344575719559,-6.60479906892382,130.701088688872));
#237645=CARTESIAN_POINT('Ctrl Pts',(1.35600994814304,-3.65694082636265,
136.305344131865));
#237646=CARTESIAN_POINT('Ctrl Pts',(1.07756232433016,2.65146738413444,136.854464463202));
#237647=CARTESIAN_POINT('Ctrl Pts',(0.799114700517227,6.52330659999492,
131.843834924404));
#237648=CARTESIAN_POINT('Ctrl Pts',(0.520667076704378,4.40054573170394,
125.877979278764));
#237649=CARTESIAN_POINT('Ctrl Pts',(0.242219452891471,-1.76610168541259,
124.439227416375));
#237650=CARTESIAN_POINT('Ctrl Pts',(-0.03622817092143,-6.30978793249869,
128.849722011837));
#237651=CARTESIAN_POINT('Ctrl Pts',(-0.314675794734322,-5.05508731989592,
135.056433996558));
#237652=CARTESIAN_POINT('Ctrl Pts',(-0.593123418547181,0.844991584946641,
137.355698271319));
#237653=CARTESIAN_POINT('Ctrl Pts',(-0.871571042360099,5.96856450335716,
133.634603292916));
#237654=CARTESIAN_POINT('Ctrl Pts',(-1.15001866617301,5.60731822376822,
127.312653560908));
#237655=CARTESIAN_POINT('Ctrl Pts',(-1.42846628998586,0.0932204292604712,
124.199412034595));
#237656=CARTESIAN_POINT('Ctrl Pts',(-1.70691391379876,-5.50654238566651,
127.155795586355));
#237657=CARTESIAN_POINT('Ctrl Pts',(-1.98536153761166,-6.04606175771675,
133.465032159487));
#237658=CARTESIAN_POINT('Ctrl Pts',(-2.26380916142456,-1.02954574096264,
137.329241566624));
#237659=CARTESIAN_POINT('Ctrl Pts',(-2.5422567852374,4.9330725156305,135.197404139731));
#237660=CARTESIAN_POINT('Ctrl Pts',(-2.82070440905033,6.36243812434939,
129.028574328076));
#237661=CARTESIAN_POINT('Ctrl Pts',(-3.09915203286324,1.94503391917308,
124.491605364478));
#237662=CARTESIAN_POINT('Ctrl Pts',(-3.3775996566761,-4.25976143753379,
125.755750083229));
#237663=CARTESIAN_POINT('Ctrl Pts',(-3.65604728048899,-6.55004413406227,
131.659321244699));
#237664=CARTESIAN_POINT('Ctrl Pts',(-3.9344949043019,-2.82115625883292,
136.777225356981));
#237665=CARTESIAN_POINT('Ctrl Pts',(-4.2129425281148,3.50023639711881,136.406358564405));
#237666=CARTESIAN_POINT('Ctrl Pts',(-4.49139015192765,6.60508280017262,
130.887529331496));
#237667=CARTESIAN_POINT('Ctrl Pts',(-4.76983777574057,3.64018078610111,
125.292272113504));
#237668=CARTESIAN_POINT('Ctrl Pts',(-5.04828539955349,-2.66986953767946,
124.762354950249));
#237669=CARTESIAN_POINT('Ctrl Pts',(-5.32673302336633,-6.52644018671072,
129.784745826872));
#237670=CARTESIAN_POINT('Ctrl Pts',(-5.60518064717923,-4.38553113848304,
135.74411288519));
#237671=CARTESIAN_POINT('Ctrl Pts',(-5.88362827099213,1.7854667809037,137.164088929876));
#237672=CARTESIAN_POINT('Ctrl Pts',(-6.16207589480503,6.31570795354138,
132.739785345549));
#237673=CARTESIAN_POINT('Ctrl Pts',(-6.44052351861788,5.04212205636089,
126.536920986959));
#237674=CARTESIAN_POINT('Ctrl Pts',(-6.71897114243081,-0.864927689259141,
124.255625172881));
#237675=CARTESIAN_POINT('Ctrl Pts',(-6.99741876624371,-5.97715114251656,
127.992297308957));
#237676=CARTESIAN_POINT('Ctrl Pts',(-7.27586639005655,-5.59666469586782,
134.313118248714));
#237677=CARTESIAN_POINT('Ctrl Pts',(-7.55431401386947,-0.0731168059870705,
137.409562337785));
#237678=CARTESIAN_POINT('Ctrl Pts',(-7.83276163768236,5.51762185664139,
134.436148728019));
#237679=CARTESIAN_POINT('Ctrl Pts',(-8.11120926149529,6.03793558382929,
128.125299267457));
#237680=CARTESIAN_POINT('Ctrl Pts',(-8.38965688530811,1.00968147902963,
124.276376308223));
#237681=CARTESIAN_POINT('Ctrl Pts',(-8.66810450912106,-4.94642057931569,
126.426352019512));
#237682=CARTESIAN_POINT('Ctrl Pts',(-8.94655213293394,-6.3570037713493,
132.599503754801));
#237683=CARTESIAN_POINT('Ctrl Pts',(-9.22499975674682,-1.92581105441205,
137.123006644589));
#237684=CARTESIAN_POINT('Ctrl Pts',(-9.50344738055969,4.27510794042973,
135.839982518561));
#237685=CARTESIAN_POINT('Ctrl Pts',(-9.78189500437264,6.54741158865002,
129.929467869325));
#237686=CARTESIAN_POINT('Ctrl Pts',(-10.0603426281855,2.80296384573913,
124.822936914835));
#237687=CARTESIAN_POINT('Ctrl Pts',(-10.3387902519984,-3.51727073900952,
125.213042134361));
#237688=CARTESIAN_POINT('Ctrl Pts',(-10.6172378758113,-6.60530534283666,
130.74129588886));
#237689=CARTESIAN_POINT('Ctrl Pts',(-10.8956854996242,-3.62338702370218,
136.327503048155));
#237690=CARTESIAN_POINT('Ctrl Pts',(-11.174133123437,2.68824695791763,136.838212134247));
#237691=CARTESIAN_POINT('Ctrl Pts',(-11.4525807472499,6.52951331337615,
131.804106446543));
#237692=CARTESIAN_POINT('Ctrl Pts',(-11.7310283710628,4.37047591830066,
125.851283182307));
#237693=CARTESIAN_POINT('Ctrl Pts',(-12.0094759948757,-1.80481533607482,
124.450096109789));
#237694=CARTESIAN_POINT('Ctrl Pts',(-12.2879236186886,-6.32156946672825,
128.88816769684));
#237695=CARTESIAN_POINT('Ctrl Pts',(-12.5663712425015,-5.02911008329581,
135.087126966809));
#237696=CARTESIAN_POINT('Ctrl Pts',(-12.8448188663144,0.884855780999501,
137.350433186591));
#237697=CARTESIAN_POINT('Ctrl Pts',(-13.1232664901273,5.98568241016441,
133.598218508862));
#237698=CARTESIAN_POINT('Ctrl Pts',(-13.4017141139402,5.58595932123025,
127.278584916578));
#237699=CARTESIAN_POINT('Ctrl Pts',(-13.6801617377531,0.0530125053692662,
124.198966949783));
#237700=CARTESIAN_POINT('Ctrl Pts',(-13.958609361566,-5.5286502131212,127.189383072259));
#237701=CARTESIAN_POINT('Ctrl Pts',(-14.2370569853788,-6.02975347533148,
133.501786957402));
#237702=CARTESIAN_POINT('Ctrl Pts',(-14.5155046091917,-0.989807863545592,
137.335387812837));
#237703=CARTESIAN_POINT('Ctrl Pts',(-14.7939522330047,4.95972282003631,
135.167293734234));
#237704=CARTESIAN_POINT('Ctrl Pts',(-15.0723998568175,6.35151052793477,
128.989877262545));
#237705=CARTESIAN_POINT('Ctrl Pts',(-15.3508474806304,1.9065703492003,124.479882351679));
#237706=CARTESIAN_POINT('Ctrl Pts',(-15.6292951044433,-4.29041483930959,
125.781773999224));
#237707=CARTESIAN_POINT('Ctrl Pts',(-15.9077427282562,-6.54471838891106,
131.699177382027));
#237708=CARTESIAN_POINT('Ctrl Pts',(-16.186190352069,-2.78474546637155,
136.794287872519));
#237709=CARTESIAN_POINT('Ctrl Pts',(-16.464637975882,3.53427249738445,136.384947839923));
#237710=CARTESIAN_POINT('Ctrl Pts',(-16.7430855996949,6.60546669485434,
130.847320776822));
#237711=CARTESIAN_POINT('Ctrl Pts',(-17.0215332235078,3.6065596947407,125.270215426085));
#237712=CARTESIAN_POINT('Ctrl Pts',(-17.2999808473206,-2.7065994746034,
124.778719148295));
#237713=CARTESIAN_POINT('Ctrl Pts',(-17.5784284711336,-6.53252595152224,
129.824493011814));
#237714=CARTESIAN_POINT('Ctrl Pts',(-17.8568760949464,-4.35538021062653,
135.770717335825));
#237715=CARTESIAN_POINT('Ctrl Pts',(-18.1353237187593,1.82414717168286,
137.153102455769));
#237716=CARTESIAN_POINT('Ctrl Pts',(-18.4137713425722,6.32737241775927,
132.701303979686));
#237717=CARTESIAN_POINT('Ctrl Pts',(-18.6922189663851,5.01605152124203,
126.506307224649));
#237718=CARTESIAN_POINT('Ctrl Pts',(-18.9706665901979,-0.904775675556959,
124.261011566121));
#237719=CARTESIAN_POINT('Ctrl Pts',(-19.2491142140109,-5.99415822726801,
128.028734025499));
#237720=CARTESIAN_POINT('Ctrl Pts',(-19.5275618378238,-5.57520219902858,
134.347121726088));
#237721=CARTESIAN_POINT('Ctrl Pts',(-19.8060094616367,-0.0329077136511566,
137.409885041447));
#237722=CARTESIAN_POINT('Ctrl Pts',(-20.0844570854496,5.53962735294063,
134.402494109067));
#237723=CARTESIAN_POINT('Ctrl Pts',(-20.3629047092624,6.02151550802112,
128.08859427659));
#237724=CARTESIAN_POINT('Ctrl Pts',(-20.6413523330754,0.969925078616457,
124.270351038909));
#237725=CARTESIAN_POINT('Ctrl Pts',(-20.9197999568882,-4.9729791145623,
126.456543399899));
#237726=CARTESIAN_POINT('Ctrl Pts',(-21.1982475807011,-6.34595844499429,
132.638167381246));
#237727=CARTESIAN_POINT('Ctrl Pts',(-21.476695204514,-1.88731198178147,
137.134612533211));
#237728=CARTESIAN_POINT('Ctrl Pts',(-21.7551428283269,4.30568199237261,
135.813865424697));
#237729=CARTESIAN_POINT('Ctrl Pts',(-22.0335904521398,6.54196455979519,
129.889628126344));
#237730=CARTESIAN_POINT('Ctrl Pts',(-22.3120380759527,2.766501289502,124.805985300257));
#237731=CARTESIAN_POINT('Ctrl Pts',(-22.5904856997656,-3.5512415147419,
125.234556353852));
#237732=CARTESIAN_POINT('Ctrl Pts',(-22.8689333235784,-6.60556685473091,
130.781505425734));
#237733=CARTESIAN_POINT('Ctrl Pts',(-23.1473809473914,-3.58969895510304,
136.349457302372));
#237734=CARTESIAN_POINT('Ctrl Pts',(-23.4258285712042,2.7249269177212,136.821736218705));
#237735=CARTESIAN_POINT('Ctrl Pts',(-23.7042761950172,6.53547807324032,
131.764340922733));
#237736=CARTESIAN_POINT('Ctrl Pts',(-23.98272381883,4.34024415530499,125.824770623956));
#237737=CARTESIAN_POINT('Ctrl Pts',(-24.2611714426429,-1.84346210864104,
124.461200262812));
#237738=CARTESIAN_POINT('Ctrl Pts',(-24.5396190664558,-6.33311675287646,
128.926684387076));
#237739=CARTESIAN_POINT('Ctrl Pts',(-24.8180666902687,-5.00294649117208,
135.117661237576));
#237740=CARTESIAN_POINT('Ctrl Pts',(-25.0965143140816,0.924687188395989,
137.344925534737));
#237741=CARTESIAN_POINT('Ctrl Pts',(-25.3749619378945,6.00257851530871,
133.561730197376));
#237742=CARTESIAN_POINT('Ctrl Pts',(-25.6534095617074,5.56439342891538,
127.244646921163));
#237743=CARTESIAN_POINT('Ctrl Pts',(-25.9318571855203,0.0128026170801758,
124.198766630261));
#237744=CARTESIAN_POINT('Ctrl Pts',(-26.2103048093331,-5.5505531744091,
127.223104512485));
#237745=CARTESIAN_POINT('Ctrl Pts',(-26.4887524331461,-6.01322175821376,
133.538441801192));
#237746=CARTESIAN_POINT('Ctrl Pts',(-26.7672000569589,-0.950033308434149,
137.341292049436));
#237747=CARTESIAN_POINT('Ctrl Pts',(-27.0456476807718,4.98618934008908,
135.137021658645));
#237748=CARTESIAN_POINT('Ctrl Pts',(-27.3240953045847,6.34034757396176,
128.951247433362));
#237749=CARTESIAN_POINT('Ctrl Pts',(-27.6025429283976,1.86803613056208,
124.468393694749));
#237750=CARTESIAN_POINT('Ctrl Pts',(-27.8809905522105,-4.32090925818572,
125.807984029013));
#237751=CARTESIAN_POINT('Ctrl Pts',(-28.1594381760234,-6.53915012681315,
131.739000361591));
#237752=CARTESIAN_POINT('Ctrl Pts',(-28.4378857998363,-2.74823148414282,
136.811128429099));
#237753=CARTESIAN_POINT('Ctrl Pts',(-28.7163334236492,3.56817763388296,
136.36333032473));
#237754=CARTESIAN_POINT('Ctrl Pts',(-28.994781047462,6.60560582153853,130.807110630244));
#237755=CARTESIAN_POINT('Ctrl Pts',(-29.273228671275,3.5728049609845,125.248363808452));
#237756=CARTESIAN_POINT('Ctrl Pts',(-29.5516762950878,-2.74322911748845,
124.795306628702));
#237757=CARTESIAN_POINT('Ctrl Pts',(-29.8301239189007,-6.53836965118233,
129.86427650611));
#237758=CARTESIAN_POINT('Ctrl Pts',(-30.1085715427137,-4.32506789255462,
135.797137756284));
#237759=CARTESIAN_POINT('Ctrl Pts',(-30.3870191665265,1.862759968018,137.141880726698));
#237760=CARTESIAN_POINT('Ctrl Pts',(-30.6654667903394,6.33880241886542,
132.662752321889));
#237761=CARTESIAN_POINT('Ctrl Pts',(-30.9439144141524,4.98979511448915,
126.475852728289));
#237762=CARTESIAN_POINT('Ctrl Pts',(-31.2223620379652,-0.944590135059391,
124.266640425567));
#237763=CARTESIAN_POINT('Ctrl Pts',(-31.5008096617781,-6.01094319628198,
128.065273593905));
#237764=CARTESIAN_POINT('Ctrl Pts',(-31.7792572855909,-5.55353311102158,
134.380993925146));
#237765=CARTESIAN_POINT('Ctrl Pts',(-32.0577049094039,0.00730259809219468,
137.409962974972));
#237766=CARTESIAN_POINT('Ctrl Pts',(-32.3361525332168,5.56142757631112,
134.368706159956));
#237767=CARTESIAN_POINT('Ctrl Pts',(-32.6146001570296,6.0048723027414,128.051989919443));
#237768=CARTESIAN_POINT('Ctrl Pts',(-32.8930477808425,0.930132737272799,
124.264567889721));
#237769=CARTESIAN_POINT('Ctrl Pts',(-33.1714954046555,-4.99935337423901,
126.486895890252));
#237770=CARTESIAN_POINT('Ctrl Pts',(-33.4499430284683,-6.33467796681538,
132.676763055306));
#237771=CARTESIAN_POINT('Ctrl Pts',(-33.7283906522812,-1.84874297411136,
137.145983852021));
#237772=CARTESIAN_POINT('Ctrl Pts',(-34.0068382760941,4.33609649568588,
135.787562701789));
#237773=CARTESIAN_POINT('Ctrl Pts',(-34.285285899907,6.53627511603778,129.849822279112));
#237774=CARTESIAN_POINT('Ctrl Pts',(-34.5637335237199,2.72993621954223,
124.789255957683));
#237775=CARTESIAN_POINT('Ctrl Pts',(-34.8421811475328,-3.58508069791401,
125.256276964487));
#237776=CARTESIAN_POINT('Ctrl Pts',(-35.1206287713457,-6.60558359491616,
130.821715809516));
#237777=CARTESIAN_POINT('Ctrl Pts',(-35.3990763951586,-3.55587786888901,
136.37120608099));
#237778=CARTESIAN_POINT('Ctrl Pts',(-35.6775240189714,2.76150590435573,
136.805037327097));
#237779=CARTESIAN_POINT('Ctrl Pts',(-35.9559716427844,6.54120065856107,
131.724539826499));
#237780=CARTESIAN_POINT('Ctrl Pts',(-36.2344192665972,4.30985156296601,
125.798442586144));
#237781=CARTESIAN_POINT('Ctrl Pts',(-36.5128668904101,-1.8820405710409,
124.472539463974));
#237782=CARTESIAN_POINT('Ctrl Pts',(-36.791314514223,-6.3444293630544,128.965270655295));
#237783=CARTESIAN_POINT('Ctrl Pts',(-37.0697621380359,-4.9765975130263,
135.148035677403));
#237784=CARTESIAN_POINT('Ctrl Pts',(-37.3482097618488,0.964484331168655,
137.339175519844));
#237785=CARTESIAN_POINT('Ctrl Pts',(-37.6266573856617,6.0192521926987,133.525139710547));
#237786=CARTESIAN_POINT('Ctrl Pts',(-37.9051050094746,5.54262134595571,
127.210840832248));
#237787=CARTESIAN_POINT('Ctrl Pts',(-38.1835526332875,-0.0274077456145885,
124.198811083455));
#237788=CARTESIAN_POINT('Ctrl Pts',(-38.4620002571004,-5.5722504579079,
127.256958657474));
#237789=CARTESIAN_POINT('Ctrl Pts',(-38.7404478809132,-5.99646721895241,
133.574995332598));
#237790=CARTESIAN_POINT('Ctrl Pts',(-39.0188955047262,-0.910223549489097,
137.346954057637));
#237791=CARTESIAN_POINT('Ctrl Pts',(-39.297343128539,5.0124710950622,135.106589034709));
#237792=CARTESIAN_POINT('Ctrl Pts',(-39.5757907523519,6.32894967607775,
128.912686271968));
#237793=CARTESIAN_POINT('Ctrl Pts',(-39.8542383761648,1.82943269115809,
124.457139819403));
#237794=CARTESIAN_POINT('Ctrl Pts',(-40.1326859999777,-4.35124356418029,
125.834379201373));
#237795=CARTESIAN_POINT('Ctrl Pts',(-40.4111336237906,-6.53333955410249,
131.778788707735));
#237796=CARTESIAN_POINT('Ctrl Pts',(-40.6895812476035,-2.7116156651858,
136.827746402689));
#237797=CARTESIAN_POINT('Ctrl Pts',(-40.9680288714165,3.60195055024708,
136.34150681987));
#237798=CARTESIAN_POINT('Ctrl Pts',(-41.2464764952292,6.60550017506977,
130.766900381762));
#237799=CARTESIAN_POINT('Ctrl Pts',(-41.5249241190422,3.53891783562657,
125.226718070324));
#237800=CARTESIAN_POINT('Ctrl Pts',(-41.803371742855,-2.77975710900975,
124.812116776814));
#237801=CARTESIAN_POINT('Ctrl Pts',(-42.081819366668,-6.5439710691505,129.904094835568));
#237802=CARTESIAN_POINT('Ctrl Pts',(-42.3602669904808,-4.2945953075014,
135.82337316755));
#237803=CARTESIAN_POINT('Ctrl Pts',(-42.6387146142937,1.90130373909722,
137.130424158489));
#237804=CARTESIAN_POINT('Ctrl Pts',(-42.9171622381066,6.34999753331677,
132.624131800705));
#237805=CARTESIAN_POINT('Ctrl Pts',(-43.1956098619195,4.96335380904355,
126.44555862638));
#237806=CARTESIAN_POINT('Ctrl Pts',(-43.4740574857324,-0.984369592426984,
124.272511542639));
#237807=CARTESIAN_POINT('Ctrl Pts',(-43.7525051095453,-6.02750542758532,
128.101914660188));
#237808=CARTESIAN_POINT('Ctrl Pts',(-44.0309527333582,-5.53165823480283,
134.414733590743));
#237809=CARTESIAN_POINT('Ctrl Pts',(-44.3094003571711,0.0475126392350714,
137.409796135472));
#237810=CARTESIAN_POINT('Ctrl Pts',(-44.5878479809839,5.58302171893757,
134.334786132711));
#237811=CARTESIAN_POINT('Ctrl Pts',(-44.8662956047969,5.98800658471021,
128.015487552405));
#237812=CARTESIAN_POINT('Ctrl Pts',(-45.1447432286098,0.890305929518511,
124.259027074959));
#237813=CARTESIAN_POINT('Ctrl Pts',(-45.4231908524226,-5.02554238103793,
126.517408365848));
#237814=CARTESIAN_POINT('Ctrl Pts',(-45.7016384762356,-6.32316275481482,
132.715289346806));
#237815=CARTESIAN_POINT('Ctrl Pts',(-45.9800861000484,-1.81010546059046,
137.15712017965));
#237816=CARTESIAN_POINT('Ctrl Pts',(-46.2585337238614,4.36635032334889,
135.761075324496));
#237817=CARTESIAN_POINT('Ctrl Pts',(-46.5369813476741,6.53034346820225,
129.810051802649));
#237818=CARTESIAN_POINT('Ctrl Pts',(-46.8154289714873,2.6932699907919,124.772749507024));
#237819=CARTESIAN_POINT('Ctrl Pts',(-47.0938765952999,-3.61878703460243,
125.278203161403));
#237820=CARTESIAN_POINT('Ctrl Pts',(-47.3723242191129,-6.60535556277213,
130.861925550195));
#237821=CARTESIAN_POINT('Ctrl Pts',(-47.6507718429257,-3.52192501831287,
136.392748578105));
#237822=CARTESIAN_POINT('Ctrl Pts',(-47.9292194667387,2.79798256237344,
136.788116078208));
#237823=CARTESIAN_POINT('Ctrl Pts',(-48.2076670905515,6.54668085728591,
131.684704632686));
#237824=CARTESIAN_POINT('Ctrl Pts',(-48.4861147143645,4.27929926749242,
125.772300044465));
#237825=CARTESIAN_POINT('Ctrl Pts',(-48.7645623381774,-1.92054929373528,
124.484113293097));
#237826=CARTESIAN_POINT('Ctrl Pts',(-49.0430099619902,-6.35550687806913,
129.003925071669));
#237827=CARTESIAN_POINT('Ctrl Pts',(-49.3214575858032,-4.95006412522954,
135.178249160753));
#237828=CARTESIAN_POINT('Ctrl Pts',(-49.5999052096159,1.00424573461974,
137.333183354982));
#237829=CARTESIAN_POINT('Ctrl Pts',(-49.878352833429,6.03570282448511,133.488448404247));
#237830=CARTESIAN_POINT('Ctrl Pts',(-50.1568004572417,5.52064387912377,
127.17716790253));
#237831=CARTESIAN_POINT('Ctrl Pts',(-50.4352480810547,-0.0676170927052693,
124.199100307716));
#237832=CARTESIAN_POINT('Ctrl Pts',(-50.7136957048675,-5.5937412596168,
127.290944252747));
#237833=CARTESIAN_POINT('Ctrl Pts',(-50.9921433286805,-5.97949047839309,
133.611446197116));
#237834=CARTESIAN_POINT('Ctrl Pts',(-51.2705909524933,-0.870380061875472,
137.352373627632));
#237835=CARTESIAN_POINT('Ctrl Pts',(-51.5490385763063,5.03856711107574,
135.075996990117));
#237836=CARTESIAN_POINT('Ctrl Pts',(-51.8274862001192,6.31731725663583,
128.874195207264));
#237837=CARTESIAN_POINT('Ctrl Pts',(-52.105933823932,1.79076146145295,124.446121142656));
#237838=CARTESIAN_POINT('Ctrl Pts',(-52.3843814477449,-4.38141663324442,
125.860958538224));
#237839=CARTESIAN_POINT('Ctrl Pts',(-52.6628290715579,-6.52728688609205,
131.818540946088));
#237840=CARTESIAN_POINT('Ctrl Pts',(-52.9412766953706,-2.67489936631311,
136.844141177504));
#237841=CARTESIAN_POINT('Ctrl Pts',(-53.2197243191836,3.63558999500893,
136.319478134021));
#237842=CARTESIAN_POINT('Ctrl Pts',(-53.4981719429964,6.60514975936288,
130.726691521383));
#237843=CARTESIAN_POINT('Ctrl Pts',(-53.7766195668094,3.50489957436681,
125.205279013792));
#237844=CARTESIAN_POINT('Ctrl Pts',(-54.0550671906223,-2.8161820956091,
124.829148969725));
#237845=CARTESIAN_POINT('Ctrl Pts',(-54.3335148144351,-6.54932999786417,
129.943946524707));
#237846=CARTESIAN_POINT('Ctrl Pts',(-54.6119624382481,-4.26396358463975,
135.849422597461));
#237847=CARTESIAN_POINT('Ctrl Pts',(-54.890410062061,1.93977705666721,137.11873317567));
#237848=CARTESIAN_POINT('Ctrl Pts',(-55.1688576858738,6.3609573462743,132.58544384723));
#237849=CARTESIAN_POINT('Ctrl Pts',(-55.4473053096868,4.93672858469731,
126.415426041482));
#237850=CARTESIAN_POINT('Ctrl Pts',(-55.7257529334997,-1.02411257361735,
124.278624699781));
#237851=CARTESIAN_POINT('Ctrl Pts',(-56.0042005573125,-6.0438443074584,
128.138655866601));
#237852=CARTESIAN_POINT('Ctrl Pts',(-56.2826481811254,-5.50957838095395,
134.448339472641));
#237853=CARTESIAN_POINT('Ctrl Pts',(-56.5610958049383,0.0877209197796484,
137.40938452913));
#237854=CARTESIAN_POINT('Ctrl Pts',(-56.8395434287512,5.60440898064107,
134.300735284249));
#237855=CARTESIAN_POINT('Ctrl Pts',(-57.117991052564,5.97091897889293,127.979088528083));
#237856=CARTESIAN_POINT('Ctrl Pts',(-57.396438676377,0.850446131150592,
124.253728799937));
#237857=CARTESIAN_POINT('Ctrl Pts',(-57.6748863001899,-5.05154516451579,
126.548079696037));
#237858=CARTESIAN_POINT('Ctrl Pts',(-57.9533339240027,-6.31141323569307,
132.753744828139));
#237859=CARTESIAN_POINT('Ctrl Pts',(-58.2317815478157,-1.77140087294607,
137.168021103437));
#237860=CARTESIAN_POINT('Ctrl Pts',(-58.5102291716285,4.39644235429495,
135.734404274317));
#237861=CARTESIAN_POINT('Ctrl Pts',(-58.7886767954414,6.52416983608798,
129.770318170665));
#237862=CARTESIAN_POINT('Ctrl Pts',(-59.0671244192543,2.65650396193163,
124.756466559932));
#237863=CARTESIAN_POINT('Ctrl Pts',(-59.3455720430672,-3.6523592758065,
125.300334132115));
#237864=CARTESIAN_POINT('Ctrl Pts',(-59.62401966688,-6.60488276674858,130.902133157784));
#237865=CARTESIAN_POINT('Ctrl Pts',(-59.902467290693,-3.48784166150989,
136.414083995446));
#237866=CARTESIAN_POINT('Ctrl Pts',(-60.1809149145059,2.83435554011865,
136.770973099059));
#237867=CARTESIAN_POINT('Ctrl Pts',(-60.4593625383188,6.55191846634393,
131.644836817403));
#237868=CARTESIAN_POINT('Ctrl Pts',(-60.7378101621316,4.24858840101079,
125.746343967642));
#237869=CARTESIAN_POINT('Ctrl Pts',(-61.0162577859445,-1.95898684976931,
124.49592132131));
#237870=CARTESIAN_POINT('Ctrl Pts',(-61.2947054097575,-6.36634888743926,
129.042646203845));
#237871=CARTESIAN_POINT('Ctrl Pts',(-61.5731530335703,-4.92334731098624,
135.208300568055));
#237872=CARTESIAN_POINT('Ctrl Pts',(-61.8516006573832,1.04396992537583,
137.326949262193));
#237873=CARTESIAN_POINT('Ctrl Pts',(-62.1300482811962,6.05192980108374,
133.451657638088));
#237874=CARTESIAN_POINT('Ctrl Pts',(-62.408495905009,5.49846184280268,127.143629379772));
#237875=CARTESIAN_POINT('Ctrl Pts',(-62.6869435288219,-0.107823934219708,
124.199634292325));
#237876=CARTESIAN_POINT('Ctrl Pts',(-62.9653911526347,-5.61502478318622,
127.325060038955));
#237877=CARTESIAN_POINT('Ctrl Pts',(-63.2438387764477,-5.96229216561512,
133.647793044045));
#237878=CARTESIAN_POINT('Ctrl Pts',(-63.5222864002605,-0.830504322008783,
137.357550558596));
#237879=CARTESIAN_POINT('Ctrl Pts',(-63.8007340240734,5.06447642113188,
135.045246658467));
#237880=CARTESIAN_POINT('Ctrl Pts',(-64.0791816478864,6.30545074667997,
128.835775665549));
#237881=CARTESIAN_POINT('Ctrl Pts',(-64.3576292716992,1.75202387442331,
124.435338072814));
#237882=CARTESIAN_POINT('Ctrl Pts',(-64.6360768955121,-4.41142734730395,
125.887721054655));
#237883=CARTESIAN_POINT('Ctrl Pts',(-64.914524519325,-6.52099234706562,
131.858255603616));
#237884=CARTESIAN_POINT('Ctrl Pts',(-65.1929721431379,-2.63808394806071,
136.860312146029));
#237885=CARTESIAN_POINT('Ctrl Pts',(-65.4714197669508,3.66909472164654,
136.297245083462));
#237886=CARTESIAN_POINT('Ctrl Pts',(-65.7498673907637,6.60455458740261,
130.686485539062));
#237887=CARTESIAN_POINT('Ctrl Pts',(-66.0283150145766,3.4707514377644,125.184047433287));
#237888=CARTESIAN_POINT('Ctrl Pts',(-66.3067626383895,-2.85250272754526,
124.846402576302));
#237889=CARTESIAN_POINT('Ctrl Pts',(-66.5852102622024,-6.55444623874626,
129.983830096806));
#237890=CARTESIAN_POINT('Ctrl Pts',(-66.8636578860152,-4.23317385903938,
135.875285080744));
#237891=CARTESIAN_POINT('Ctrl Pts',(-67.1421055098281,1.978178495085,137.106808211453));
#237892=CARTESIAN_POINT('Ctrl Pts',(-67.4205531336411,6.37168145161813,
132.546689895061));
#237893=CARTESIAN_POINT('Ctrl Pts',(-67.6990007574539,4.90992042805787,
126.385456090168));
#237894=CARTESIAN_POINT('Ctrl Pts',(-67.9774483812669,-1.06381760593968,
124.284979670466));
#237895=CARTESIAN_POINT('Ctrl Pts',(-68.2558960050797,-6.05995923045808,
128.175495851683));
#237896=CARTESIAN_POINT('Ctrl Pts',(-68.5343436288926,-5.48729436765201,
134.481810325563));
#237897=CARTESIAN_POINT('Ctrl Pts',(-68.8127912527054,0.12792594979327,
137.408728171199));
#237898=CARTESIAN_POINT('Ctrl Pts',(-69.0912388765185,5.62558856890878,
134.266554876337));
#237899=CARTESIAN_POINT('Ctrl Pts',(-69.3696865003312,5.9536101184771,127.942794195258));
#237900=CARTESIAN_POINT('Ctrl Pts',(-69.6481341241442,0.810554819188534,
124.248673260987));
#237901=CARTESIAN_POINT('Ctrl Pts',(-69.9265817479571,-5.07736076112986,
126.578908744281));
#237902=CARTESIAN_POINT('Ctrl Pts',(-70.2050293717699,-6.29942984483285,
132.792128074323));
#237903=CARTESIAN_POINT('Ctrl Pts',(-70.4834769955829,-1.73263064539088,
137.178686219444));
#237904=CARTESIAN_POINT('Ctrl Pts',(-70.7619246193956,4.42637147345276,
135.707550539556));
#237905=CARTESIAN_POINT('Ctrl Pts',(-71.0403722432087,6.51775444846118,
129.730622855503));
#237906=CARTESIAN_POINT('Ctrl Pts',(-71.3188198670216,2.6196394953401,124.740407719779));
#237907=CARTESIAN_POINT('Ctrl Pts',(-71.5972674908343,-3.68579617749442,
125.322669056552));
#237908=CARTESIAN_POINT('Ctrl Pts',(-71.8757151146474,-6.6041652243652,
130.942337142376));
#237909=CARTESIAN_POINT('Ctrl Pts',(-72.1541627384602,-3.45362906145158,
136.435211542427));
#237910=CARTESIAN_POINT('Ctrl Pts',(-72.4326103622731,2.87062348977667,
136.753609024891));
#237911=CARTESIAN_POINT('Ctrl Pts',(-72.711057986086,6.55691329165398,131.604937857965));
#237912=CARTESIAN_POINT('Ctrl Pts',(-72.9895056098989,4.21772010152317,
125.720575317484));
#237913=CARTESIAN_POINT('Ctrl Pts',(-73.2679532337117,-1.99735181482566,
124.50796311106));
#237914=CARTESIAN_POINT('Ctrl Pts',(-73.5464008575247,-6.37695498941029,
129.081432616995));
#237915=CARTESIAN_POINT('Ctrl Pts',(-73.8248484813376,-4.89644806029751,
135.238188785743));
#237916=CARTESIAN_POINT('Ctrl Pts',(-74.1032961051504,1.08365543144292,
137.320473472483));
#237917=CARTESIAN_POINT('Ctrl Pts',(-74.3817437289633,6.06793252119795,
133.414768775364));
#237918=CARTESIAN_POINT('Ctrl Pts',(-74.6601913527762,5.47607605895596,
127.110226506756));
#237919=CARTESIAN_POINT('Ctrl Pts',(-74.9386389765891,-0.148026780279403,
124.200413017498));
#237920=CARTESIAN_POINT('Ctrl Pts',(-75.217086600402,-5.63610023994771,
127.359304751927));
#237921=CARTESIAN_POINT('Ctrl Pts',(-75.4955342242149,-5.94487291790794,
133.684034526541));
#237922=CARTESIAN_POINT('Ctrl Pts',(-75.7739818480278,-0.790597807498519,
137.362484658699));
#237923=CARTESIAN_POINT('Ctrl Pts',(-76.0524294718406,5.09019806515201,
135.014339179226));
#237924=CARTESIAN_POINT('Ctrl Pts',(-76.3308770956536,6.29335058592772,
128.797429070474));
#237925=CARTESIAN_POINT('Ctrl Pts',(-76.6093247194664,1.71322136550425,
124.424791009442));
#237926=CARTESIAN_POINT('Ctrl Pts',(-76.8877723432794,-4.44127459430165,
125.914665758975));
#237927=CARTESIAN_POINT('Ctrl Pts',(-77.1662199670922,-6.51445617026952,
131.89793120868));
#237928=CARTESIAN_POINT('Ctrl Pts',(-77.4446675909052,-2.60117077463652,
136.876258709042));
#237929=CARTESIAN_POINT('Ctrl Pts',(-77.7231152147181,3.7024634886308,136.274808492052));
#237930=CARTESIAN_POINT('Ctrl Pts',(-78.0015628385308,6.60371468124315,
130.646283924643));
#237931=CARTESIAN_POINT('Ctrl Pts',(-78.2800104623438,3.43647469119047,
125.163024115555));
#237932=CARTESIAN_POINT('Ctrl Pts',(-78.5584580861567,-2.88871765894464,
124.863876957204));
#237933=CARTESIAN_POINT('Ctrl Pts',(-78.8369057099696,-6.55931960221255,
130.023744073965));
#237934=CARTESIAN_POINT('Ctrl Pts',(-79.1153533337825,-4.20222727162433,
135.900959659057));
#237935=CARTESIAN_POINT('Ctrl Pts',(-79.3938009575953,2.01650663137172,
137.094649707722));
#237936=CARTESIAN_POINT('Ctrl Pts',(-79.6722485814083,6.38216945196263,
132.507871380239));
#237937=CARTESIAN_POINT('Ctrl Pts',(-79.9506962052212,4.88293033251105,
126.355649882987));
#237938=CARTESIAN_POINT('Ctrl Pts',(-80.229143829034,-1.10348321810992,
124.29157621921));
#237939=CARTESIAN_POINT('Ctrl Pts',(-80.507591452847,-6.07584959944043,
128.212433250316));
#237940=CARTESIAN_POINT('Ctrl Pts',(-80.7860390766598,-5.46480702063872,
134.515144909234));
#237941=CARTESIAN_POINT('Ctrl Pts',(-81.0644867004727,0.168126239464741,
137.407827085998));
#237942=CARTESIAN_POINT('Ctrl Pts',(-81.3429343242857,5.64655969892388,
134.232246175545));
#237943=CARTESIAN_POINT('Ctrl Pts',(-81.6213819480984,5.93608064484842,
127.906605898828));
#237944=CARTESIAN_POINT('Ctrl Pts',(-81.8998295719115,0.770633471818905,
124.243860645443));
#237945=CARTESIAN_POINT('Ctrl Pts',(-82.1782771957242,-5.10298821427442,
126.609894368197));
#237946=CARTESIAN_POINT('Ctrl Pts',(-82.4567248195372,-6.28721302628274,
132.830437663053));
#237947=CARTESIAN_POINT('Ctrl Pts',(-82.7351724433501,-1.69379621456928,
137.189115132473));
#237948=CARTESIAN_POINT('Ctrl Pts',(-83.0136200671628,4.45613657178832,
135.680515115291));
#237949=CARTESIAN_POINT('Ctrl Pts',(-83.2920676909759,6.51109754304618,
129.690967328089));
#237950=CARTESIAN_POINT('Ctrl Pts',(-83.5705153147887,2.58267795704331,
124.724573581631));
#237951=CARTESIAN_POINT('Ctrl Pts',(-83.8489629386017,-3.71909650065006,
125.345207107088));
#237952=CARTESIAN_POINT('Ctrl Pts',(-84.1274105624144,-6.60320296221082,
130.982536014198));
#237953=CARTESIAN_POINT('Ctrl Pts',(-84.4058581862275,-3.41928848589759,
136.456130436155));
#237954=CARTESIAN_POINT('Ctrl Pts',(-84.6843058100402,2.90678506742617,
136.736024499134));
#237955=CARTESIAN_POINT('Ctrl Pts',(-84.9627534338533,6.56166514813073,
131.565009232842));
#237956=CARTESIAN_POINT('Ctrl Pts',(-85.241201057666,4.1866955128661,125.694995048862));
#237957=CARTESIAN_POINT('Ctrl Pts',(-85.519648681479,-2.03564276727566,
124.520238216135));
#237958=CARTESIAN_POINT('Ctrl Pts',(-85.7980963052919,-6.38732479096924,
129.120282873878));
#237959=CARTESIAN_POINT('Ctrl Pts',(-86.0765439291047,-4.8693673699251,
135.267912706297));
#237960=CARTESIAN_POINT('Ctrl Pts',(-86.3549915529177,1.12330078225909,
137.313756225814));
#237961=CARTESIAN_POINT('Ctrl Pts',(-86.6334391767305,6.08371039184151,
133.377783183006));
#237962=CARTESIAN_POINT('Ctrl Pts',(-86.9118868005434,5.45348735709659,
127.076960521238));
#237963=CARTESIAN_POINT('Ctrl Pts',(-87.1903344243564,-0.188224141151809,
124.201436454379));
#237964=CARTESIAN_POINT('Ctrl Pts',(-87.4687820481692,-5.65696684894189,
127.39367712271));
#237965=CARTESIAN_POINT('Ctrl Pts',(-87.7472296719821,-5.92723338074904,
133.720169301662));
#237966=CARTESIAN_POINT('Ctrl Pts',(-88.0256772957949,-0.750661997095914,
137.367175745102));
#237967=CARTESIAN_POINT('Ctrl Pts',(-88.3041249196079,5.11573109001074,
134.983275697681));
#237968=CARTESIAN_POINT('Ctrl Pts',(-88.5825725434208,6.28101722275544,
128.759156842984));
#237969=CARTESIAN_POINT('Ctrl Pts',(-88.8610201672337,1.67435537253749,
124.414480343369));
#237970=CARTESIAN_POINT('Ctrl Pts',(-89.1394677910466,-4.47095726823472,
125.941791652735));
#237971=CARTESIAN_POINT('Ctrl Pts',(-89.4179154148595,-6.50767859790483,
131.93756629108));
#237972=CARTESIAN_POINT('Ctrl Pts',(-89.6963630386723,-2.56416121387375,
136.891980275641));
#237973=CARTESIAN_POINT('Ctrl Pts',(-89.9748106624853,3.73569505946763,
136.252169191183));
#237974=CARTESIAN_POINT('Ctrl Pts',(-90.253258286298,6.60263007200808,130.606088167816));
#237975=CARTESIAN_POINT('Ctrl Pts',(-90.5317059101111,3.40207060478355,
125.142209839621));
#237976=CARTESIAN_POINT('Ctrl Pts',(-90.8101535339238,-2.9248255478482,
124.881571464914));
#237977=CARTESIAN_POINT('Ctrl Pts',(-91.0886011577368,-6.56394990767886,
130.063686977158));
#237978=CARTESIAN_POINT('Ctrl Pts',(-91.3670487815497,-4.17112496913288,
135.926445381018));
#237979=CARTESIAN_POINT('Ctrl Pts',(-91.6454964053626,2.05476004526333,
137.082258115016));
#237980=CARTESIAN_POINT('Ctrl Pts',(-91.9239440291755,6.39242095867105,
132.468989741201));
#237981=CARTESIAN_POINT('Ctrl Pts',(-92.2023916529884,4.85575929818535,
126.326008524418));
#237982=CARTESIAN_POINT('Ctrl Pts',(-92.4808392768012,-1.14310794030347,
124.298414101576));
#237983=CARTESIAN_POINT('Ctrl Pts',(-92.7592869006141,-6.09151482558059,
128.249466693771));
#237984=CARTESIAN_POINT('Ctrl Pts',(-93.0377345244271,-5.44211717319261,
134.548341988427));
#237985=CARTESIAN_POINT('Ctrl Pts',(-93.3161821482399,0.208320299155509,
137.406681306919));
#237986=CARTESIAN_POINT('Ctrl Pts',(-93.5946297720528,5.6673215935918,134.197810453193));
#237987=CARTESIAN_POINT('Ctrl Pts',(-93.8730773958657,5.91833120756931,
127.870524979765));
#237988=CARTESIAN_POINT('Ctrl Pts',(-94.1515250196785,0.730683568342929,
124.239291131637));
#237989=CARTESIAN_POINT('Ctrl Pts',(-94.4299726434915,-5.12842657431339,
126.641035419604));
#237990=CARTESIAN_POINT('Ctrl Pts',(-94.7084202673044,-6.27476323274215,
132.868672174754));
#237991=CARTESIAN_POINT('Ctrl Pts',(-94.9868678911172,-1.6548990195065,
137.199307456074));
#237992=CARTESIAN_POINT('Ctrl Pts',(-95.2653155149302,4.48573654634406,
135.653299003326));
#237993=CARTESIAN_POINT('Ctrl Pts',(-95.543763138743,6.50419936651746,129.651353057874));
#237994=CARTESIAN_POINT('Ctrl Pts',(-95.822210762556,2.54562071666526,124.708964732227));
#237995=CARTESIAN_POINT('Ctrl Pts',(-96.1006583863688,-3.75225901131679,
125.367947448562));
#237996=CARTESIAN_POINT('Ctrl Pts',(-96.3791060101818,-6.60199601594203,
131.022728283664));
#237997=CARTESIAN_POINT('Ctrl Pts',(-96.6575536339946,-3.38482120735248,
136.476839901474));
#237998=CARTESIAN_POINT('Ctrl Pts',(-96.9360012578075,2.94283893308538,
136.718220173391));
#237999=CARTESIAN_POINT('Ctrl Pts',(-97.2144488816204,6.5661738596919,131.525052421605));
#238000=CARTESIAN_POINT('Ctrl Pts',(-97.4928965054334,4.15551578466796,
125.669604109659));
#238001=CARTESIAN_POINT('Ctrl Pts',(-97.771344129246,-2.07385828823457,
124.532746181678));
#238002=CARTESIAN_POINT('Ctrl Pts',(-98.0497917530593,-6.39745790785863,
129.15919553488));
#238003=CARTESIAN_POINT('Ctrl Pts',(-98.3282393768718,-4.84210624335443,
135.297471228287));
#238004=CARTESIAN_POINT('Ctrl Pts',(-98.606687000685,1.16290450875192,137.306797771098));
#238005=CARTESIAN_POINT('Ctrl Pts',(-98.8851346244975,6.09926282835875,
133.340702231527));
#238006=CARTESIAN_POINT('Ctrl Pts',(-99.1635822483109,5.43069657425812,
127.043832655902));
#238007=CARTESIAN_POINT('Ctrl Pts',(-99.4420298721233,-0.228414527308866,
124.202704565042));
#238008=CARTESIAN_POINT('Ctrl Pts',(-99.7204774959365,-5.67762383694899,
127.428175877623));
#238009=CARTESIAN_POINT('Ctrl Pts',(-99.9989251197493,-5.90937420777732,
133.756196030418));
#238010=CARTESIAN_POINT('Ctrl Pts',(-100.277372743562,-0.710698370637635,
137.371623643978));
#238011=CARTESIAN_POINT('Ctrl Pts',(-100.555820367375,5.14107454957247,
134.9520573649));
#238012=CARTESIAN_POINT('Ctrl Pts',(-100.834267991188,6.26845111417983,
128.720960401273));
#238013=CARTESIAN_POINT('Ctrl Pts',(-101.112715615001,1.63542733571746,
124.404406456659));
#238014=CARTESIAN_POINT('Ctrl Pts',(-101.391163238814,-4.50047426920288,
125.969097730777));
#238015=CARTESIAN_POINT('Ctrl Pts',(-101.669610862627,-6.50065988111587,
131.977159382129));
#238016=CARTESIAN_POINT('Ctrl Pts',(-101.94805848644,-2.52705663717401,
136.907476263252));
#238017=CARTESIAN_POINT('Ctrl Pts',(-102.226506110253,3.76878820275105,
136.229328019765));
#238018=CARTESIAN_POINT('Ctrl Pts',(-102.504953734065,6.60130079988703,
130.565899758046));
#238019=CARTESIAN_POINT('Ctrl Pts',(-102.783401357878,3.36754045339959,
125.121605376767));
#238020=CARTESIAN_POINT('Ctrl Pts',(-103.061848981691,-2.96082505626518,
124.899485443752));
#238021=CARTESIAN_POINT('Ctrl Pts',(-103.340296605504,-6.56833698356739,
130.103657326284));
#238022=CARTESIAN_POINT('Ctrl Pts',(-103.618744229317,-4.13986810407194,
135.951741302244));
#238023=CARTESIAN_POINT('Ctrl Pts',(-103.89719185313,2.0929373192654,137.06963389251));
#238024=CARTESIAN_POINT('Ctrl Pts',(-104.175639476943,6.40243559186997,
132.430046418718));
#238025=CARTESIAN_POINT('Ctrl Pts',(-104.454087100755,4.82840833191319,
126.296533112833));
#238026=CARTESIAN_POINT('Ctrl Pts',(-104.732534724569,-1.18269030421136,
124.305493064181));
#238027=CARTESIAN_POINT('Ctrl Pts',(-105.010982348381,-6.10695432839948,
128.286594809759));
#238028=CARTESIAN_POINT('Ctrl Pts',(-105.289429972194,-5.41922566609253,
134.581400333014));
#238029=CARTESIAN_POINT('Ctrl Pts',(-105.567877596007,0.248506639461218,
137.40529087642));
#238030=CARTESIAN_POINT('Ctrl Pts',(-105.84632521982,5.68787348357469,134.163248985309));
#238031=CARTESIAN_POINT('Ctrl Pts',(-106.124772843633,5.90036246435008,
127.834552775061));
#238032=CARTESIAN_POINT('Ctrl Pts',(-106.403220467446,0.690706589119241,
124.234964888896));
#238033=CARTESIAN_POINT('Ctrl Pts',(-106.681668091259,-5.1536748986197,
126.672330744555));
#238034=CARTESIAN_POINT('Ctrl Pts',(-106.960115715072,-6.26208092554253,
132.906830192629));
#238035=CARTESIAN_POINT('Ctrl Pts',(-107.238563338885,-1.61594050155245,
137.209262812568));
#238036=CARTESIAN_POINT('Ctrl Pts',(-107.517010962697,4.51517030028232,
135.625903212168));
#238037=CARTESIAN_POINT('Ctrl Pts',(-107.79545858651,6.49706017448951,129.611781512777));
#238038=CARTESIAN_POINT('Ctrl Pts',(-108.073906210323,2.50846914737518,
124.69358174996));
#238039=CARTESIAN_POINT('Ctrl Pts',(-108.352353834136,-3.78528248064593,
125.390889238328));
#238040=CARTESIAN_POINT('Ctrl Pts',(-108.630801457949,-6.60054443028347,
131.062912461436));
#238041=CARTESIAN_POINT('Ctrl Pts',(-108.909249081762,-3.35022850301195,
136.497339170987));
#238042=CARTESIAN_POINT('Ctrl Pts',(-109.187696705575,2.97878375076591,
136.700196707408));
#238043=CARTESIAN_POINT('Ctrl Pts',(-109.466144329388,6.57043925926657,
131.485068904869));
#238044=CARTESIAN_POINT('Ctrl Pts',(-109.7445919532,4.12418207230337,125.644403440746));
#238045=CARTESIAN_POINT('Ctrl Pts',(-110.023039577014,-2.11199696161116,
124.5454865442));
#238046=CARTESIAN_POINT('Ctrl Pts',(-110.301487200826,-6.40735396459295,
129.198169158078));
#238047=CARTESIAN_POINT('Ctrl Pts',(-110.579934824639,-4.81466569075636,
135.326863256411));
#238048=CARTESIAN_POINT('Ctrl Pts',(-110.858382448452,1.20246514338981,
137.299598366182));
#238049=CARTESIAN_POINT('Ctrl Pts',(-111.136830072265,6.11458925444912,
133.303527294979));
#238050=CARTESIAN_POINT('Ctrl Pts',(-111.415277696078,5.407704554961,127.010844138312));
#238051=CARTESIAN_POINT('Ctrl Pts',(-111.693725319891,-0.268596449482207,
124.204217302498));
#238052=CARTESIAN_POINT('Ctrl Pts',(-111.972172943703,-5.69807043851701,
127.462799738304));
#238053=CARTESIAN_POINT('Ctrl Pts',(-112.250620567517,-5.89129606077132,
133.792113377828));
#238054=CARTESIAN_POINT('Ctrl Pts',(-112.529068191329,-0.670708408989202,
137.375828190507));
#238055=CARTESIAN_POINT('Ctrl Pts',(-112.807515815142,5.16622750472631,
134.920685337692));
#238056=CARTESIAN_POINT('Ctrl Pts',(-113.085963438955,6.25565272584325,
128.682841160722));
#238057=CARTESIAN_POINT('Ctrl Pts',(-113.364411062768,1.5964386975353,124.394569722605));
#238058=CARTESIAN_POINT('Ctrl Pts',(-113.642858686581,-4.52982450344111,
125.996582981263));
#238059=CARTESIAN_POINT('Ctrl Pts',(-113.921306310394,-6.49340027998504,
132.016709014688));
#238060=CARTESIAN_POINT('Ctrl Pts',(-114.199753934207,-2.48985841946147,
136.922746097669));
#238061=CARTESIAN_POINT('Ctrl Pts',(-114.47820155802,3.80174169220082,136.206285824184));
#238062=CARTESIAN_POINT('Ctrl Pts',(-114.756649181833,6.59972691413776,
130.525720184532));
#238063=CARTESIAN_POINT('Ctrl Pts',(-115.035096805645,3.3328855165654,125.101211490497));
#238064=CARTESIAN_POINT('Ctrl Pts',(-115.313544429458,-2.99671485022117,
124.917618229914));
#238065=CARTESIAN_POINT('Ctrl Pts',(-115.591992053271,-6.57248066731354,
130.143653640229));
#238066=CARTESIAN_POINT('Ctrl Pts',(-115.870439677084,-4.10845783467579,
135.976846485386));
#238067=CARTESIAN_POINT('Ctrl Pts',(-116.148887300897,2.13103703870585,
137.056777507999));
#238068=CARTESIAN_POINT('Ctrl Pts',(-116.42733492471,6.41221298046361,132.391042855849));
#238069=CARTESIAN_POINT('Ctrl Pts',(-116.705782548523,4.8008784471946,126.267224740454));
#238070=CARTESIAN_POINT('Ctrl Pts',(-116.984230172336,-1.22222884309565,
124.312812844714));
#238071=CARTESIAN_POINT('Ctrl Pts',(-117.262677796149,-6.12216753577917,
128.323816222486));
#238072=CARTESIAN_POINT('Ctrl Pts',(-117.541125419961,-5.39613334759327,
134.614318718005));
#238073=CARTESIAN_POINT('Ctrl Pts',(-117.819573043774,0.288683771261777,
137.403655846021));
#238074=CARTESIAN_POINT('Ctrl Pts',(-118.098020667587,5.70821460731317,
134.128563052582));
#238075=CARTESIAN_POINT('Ctrl Pts',(-118.3764682914,5.88217508103065,127.79869061768));
#238076=CARTESIAN_POINT('Ctrl Pts',(-118.654915915213,0.650704015508265,
124.230882077529));
#238077=CARTESIAN_POINT('Ctrl Pts',(-118.933363539026,-5.17873225160735,
126.703779183394));
#238078=CARTESIAN_POINT('Ctrl Pts',(-119.211811162839,-6.24916657463125,
132.944910302722));
#238079=CARTESIAN_POINT('Ctrl Pts',(-119.490258786652,-1.57692210432836,
137.218980833058));
#238080=CARTESIAN_POINT('Ctrl Pts',(-119.768706410464,4.54443674292479,
135.598328756974));
#238081=CARTESIAN_POINT('Ctrl Pts',(-120.047154034278,6.48968023150711,
129.572254159139));
#238082=CARTESIAN_POINT('Ctrl Pts',(-120.32560165809,2.47122462583917,124.67842520485));
#238083=CARTESIAN_POINT('Ctrl Pts',(-120.604049281903,-3.81816568494053,
125.414031626265));
#238084=CARTESIAN_POINT('Ctrl Pts',(-120.882496905716,-6.59884825902321,
131.103087058474));
#238085=CARTESIAN_POINT('Ctrl Pts',(-121.160944529529,-3.31551165472302,
136.517627485086));
#238086=CARTESIAN_POINT('Ctrl Pts',(-121.439392153342,3.0146181885189,136.68195476905));
#238087=CARTESIAN_POINT('Ctrl Pts',(-121.717839777155,6.57446118879764,
131.445060164237));
#238088=CARTESIAN_POINT('Ctrl Pts',(-121.996287400968,4.0926955368563,125.619393975946));
#238089=CARTESIAN_POINT('Ctrl Pts',(-122.274735024781,-2.15005737416446,
124.5584588316));
#238090=CARTESIAN_POINT('Ctrl Pts',(-122.553182648593,-6.41701259446945,
129.237202299292));
#238091=CARTESIAN_POINT('Ctrl Pts',(-122.831630272406,-4.7870467289504,
135.356087701536));
#238092=CARTESIAN_POINT('Ctrl Pts',(-123.110077896219,1.24198122024032,
137.292158277842));
#238093=CARTESIAN_POINT('Ctrl Pts',(-123.388525520032,6.1296891021858,133.266259750888));
#238094=CARTESIAN_POINT('Ctrl Pts',(-123.666973143845,5.38451215118288,
126.97799619087));
#238095=CARTESIAN_POINT('Ctrl Pts',(-123.945420767658,-0.30876841871475,
124.20597461069));
#238096=CARTESIAN_POINT('Ctrl Pts',(-124.223868391471,-5.71830589598935,
127.497547421752));
#238097=CARTESIAN_POINT('Ctrl Pts',(-124.502316015284,-5.87299960962311,
133.827920012961));
#238098=CARTESIAN_POINT('Ctrl Pts',(-124.780763639097,-0.630693593994696,
137.379789228888));
#238099=CARTESIAN_POINT('Ctrl Pts',(-125.059211262909,5.19118902341993,
134.889160778557));
#238100=CARTESIAN_POINT('Ctrl Pts',(-125.337658886723,6.24262253199412,
128.644800533857));
#238101=CARTESIAN_POINT('Ctrl Pts',(-125.616106510535,1.55739090273089,
124.384970505708));
#238102=CARTESIAN_POINT('Ctrl Pts',(-125.894554134348,-4.55900688336737,
126.024246385717));
#238103=CARTESIAN_POINT('Ctrl Pts',(-126.173001758161,-6.48590006351826,
132.056213723232));
#238104=CARTESIAN_POINT('Ctrl Pts',(-126.451449381974,-2.45256793912933,
136.937789213063));
#238105=CARTESIAN_POINT('Ctrl Pts',(-126.729897005787,3.83455430671493,
136.183043458277));
#238106=CARTESIAN_POINT('Ctrl Pts',(-127.0083446296,6.5979084730801,130.485550936142));
#238107=CARTESIAN_POINT('Ctrl Pts',(-127.286792253413,3.29810707843306,
125.081028936517));
#238108=CARTESIAN_POINT('Ctrl Pts',(-127.565239877225,-3.03249359980603,
124.935969151478));
#238109=CARTESIAN_POINT('Ctrl Pts',(-127.843687501038,-6.57638080537151,
130.183674436914));
#238110=CARTESIAN_POINT('Ctrl Pts',(-128.122135124851,-4.07689532486387,
136.001760000162));
#238111=CARTESIAN_POINT('Ctrl Pts',(-128.400582748664,2.1690577917847,137.043689437881));
#238112=CARTESIAN_POINT('Ctrl Pts',(-128.679030372477,6.42175276214748,
132.351980497887));
#238113=CARTESIAN_POINT('Ctrl Pts',(-128.95747799629,4.77317066415926,126.238084493312));
#238114=CARTESIAN_POINT('Ctrl Pts',(-129.235925620103,-1.26172209184052,
124.320373171937));
#238115=CARTESIAN_POINT('Ctrl Pts',(-129.514373243916,-6.13715388399014,
128.361129552696));
#238116=CARTESIAN_POINT('Ctrl Pts',(-129.792820867728,-5.37284107338758,
134.647095923599));
#238117=CARTESIAN_POINT('Ctrl Pts',(-130.071268491542,0.328850205779251,
137.401776276312));
#238118=CARTESIAN_POINT('Ctrl Pts',(-130.349716115354,5.72834421106097,
134.093753940311));
#238119=CARTESIAN_POINT('Ctrl Pts',(-130.628163739167,5.86376973154965,
127.762939836503));
#238120=CARTESIAN_POINT('Ctrl Pts',(-130.90661136298,0.610677329821333,
124.227042848828));
#238121=CARTESIAN_POINT('Ctrl Pts',(-131.185058986793,-5.20359770476699,
126.735379570785));
#238122=CARTESIAN_POINT('Ctrl Pts',(-131.463506610606,-6.23602065855449,
132.982911093959));
#238123=CARTESIAN_POINT('Ctrl Pts',(-131.741954234419,-1.53784527367628,
137.228461157434));
#238124=CARTESIAN_POINT('Ctrl Pts',(-132.020401858232,4.57353478979242,
135.57057665953));
#238125=CARTESIAN_POINT('Ctrl Pts',(-132.298849482045,6.48205981103755,
129.532772461657));
#238126=CARTESIAN_POINT('Ctrl Pts',(-132.577297105858,2.43388853216508,
124.66349565853));
#238127=CARTESIAN_POINT('Ctrl Pts',(-132.85574472967,-3.85090740570176,
125.437373754826));
#238128=CARTESIAN_POINT('Ctrl Pts',(-133.134192353483,-6.59690756501448,
131.143250586095));
#238129=CARTESIAN_POINT('Ctrl Pts',(-133.412639977296,-3.28067194892964,
136.53770409198));
#238130=CARTESIAN_POINT('Ctrl Pts',(-133.691087601109,3.0503409184865,136.663495034279));
#238131=CARTESIAN_POINT('Ctrl Pts',(-133.969535224922,6.5782394992522,131.405027682246));
#238132=CARTESIAN_POINT('Ctrl Pts',(-134.247982848735,4.06105734507014,
125.59457664199));
#238133=CARTESIAN_POINT('Ctrl Pts',(-134.526430472548,-2.18803811555026,
124.57166256319));
#238134=CARTESIAN_POINT('Ctrl Pts',(-134.804878096361,-6.42643343958478,
129.276293512134));
#238135=CARTESIAN_POINT('Ctrl Pts',(-135.083325720174,-4.75925038136761,
135.385143480741));
#238136=CARTESIAN_POINT('Ctrl Pts',(-135.361773343986,1.28145127501926,
137.284477781773));
#238137=CARTESIAN_POINT('Ctrl Pts',(-135.640220967799,6.14456181203885,
133.228900980221));
#238138=CARTESIAN_POINT('Ctrl Pts',(-135.918668591612,5.36112022232688,
126.945290030769));
#238139=CARTESIAN_POINT('Ctrl Pts',(-136.197116215425,-0.348928946420584,
124.207976424505));
#238140=CARTESIAN_POINT('Ctrl Pts',(-136.475563839238,-5.73832945953392,
127.53241764038));
#238141=CARTESIAN_POINT('Ctrl Pts',(-136.754011463051,-5.85448553231475,
133.863614608987));
#238142=CARTESIAN_POINT('Ctrl Pts',(-137.032459086864,-0.590655408416443,
137.383506612345));
#238143=CARTESIAN_POINT('Ctrl Pts',(-137.310906710677,5.21595818069537,
134.857484855651));
#238144=CARTESIAN_POINT('Ctrl Pts',(-137.58935433449,6.22936101547165,128.606839930282));
#238145=CARTESIAN_POINT('Ctrl Pts',(-137.867801958302,1.51828539823306,
124.375609161675));
#238146=CARTESIAN_POINT('Ctrl Pts',(-138.146249582115,-4.58802032761614,
126.052086919061));
#238147=CARTESIAN_POINT('Ctrl Pts',(-138.424697205928,-6.47815950964009,
132.095672043897));
#238148=CARTESIAN_POINT('Ctrl Pts',(-138.703144829741,-2.41518657799051,
136.952605052004));
#238149=CARTESIAN_POINT('Ctrl Pts',(-138.981592453554,3.86722483040823,
136.159601783301));
#238150=CARTESIAN_POINT('Ctrl Pts',(-139.260040077367,6.59584554409815,
130.445393501362));
#238151=CARTESIAN_POINT('Ctrl Pts',(-139.53848770118,3.26320642772972,125.061058462695));
#238152=CARTESIAN_POINT('Ctrl Pts',(-139.816935324993,-3.06815997922566,
124.954537528447));
#238153=CARTESIAN_POINT('Ctrl Pts',(-140.095382948806,-6.58003725322031,
130.223718233352));
#238154=CARTESIAN_POINT('Ctrl Pts',(-140.373830572619,-4.04518174419624,
136.026480923393));
#238155=CARTESIAN_POINT('Ctrl Pts',(-140.652278196431,2.20699816962987,
137.030370167137));
#238156=CARTESIAN_POINT('Ctrl Pts',(-140.930725820244,6.43105458342049,
132.312860792301));
#238157=CARTESIAN_POINT('Ctrl Pts',(-141.209173444057,4.74528600953044,
126.209113451214));
#238158=CARTESIAN_POINT('Ctrl Pts',(-141.48762106787,-1.30116858700904,
124.328173765698));
#238159=CARTESIAN_POINT('Ctrl Pts',(-141.766068691683,-6.15191281770628,
128.398533417733));
#238160=CARTESIAN_POINT('Ctrl Pts',(-142.044516315496,-5.34934970658085,
134.679730735221));
#238161=CARTESIAN_POINT('Ctrl Pts',(-142.322963939309,0.369004454631186,
137.399652236939));
#238162=CARTESIAN_POINT('Ctrl Pts',(-142.601411563122,5.74826154890666,
134.058822938361));
#238163=CARTESIAN_POINT('Ctrl Pts',(-142.879859186934,5.84514709792562,
127.727301756295));
#238164=CARTESIAN_POINT('Ctrl Pts',(-143.158306810748,0.570628015260733,
124.223447345055));
#238165=CARTESIAN_POINT('Ctrl Pts',(-143.43675443456,-5.22827033670001,
126.767130735766));
#238166=CARTESIAN_POINT('Ctrl Pts',(-143.715202058373,-6.22264366443886,
133.020831158207));
#238167=CARTESIAN_POINT('Ctrl Pts',(-143.993649682186,-1.49871145760156,
137.237703434405));
#238168=CARTESIAN_POINT('Ctrl Pts',(-144.272097305999,4.60246336264661,
135.542647948195));
#238169=CARTESIAN_POINT('Ctrl Pts',(-144.550544929812,6.47419919545755,
129.493337883343));
#238170=CARTESIAN_POINT('Ctrl Pts',(-144.828992553625,2.39646224985712,
124.648793664219));
#238171=CARTESIAN_POINT('Ctrl Pts',(-145.107440177438,-3.8835064296727,
125.460914759058));
#238172=CARTESIAN_POINT('Ctrl Pts',(-145.38588780125,-6.59472242016944,
131.183401556022));
#238173=CARTESIAN_POINT('Ctrl Pts',(-145.664335425064,-3.24571067663155,
136.557568247724));
#238174=CARTESIAN_POINT('Ctrl Pts',(-145.942783048876,3.08595061694992,
136.644818187128));
#238175=CARTESIAN_POINT('Ctrl Pts',(-146.221230672689,6.58177405062243,
131.364972942318));
#238176=CARTESIAN_POINT('Ctrl Pts',(-146.499678296502,4.02926866931097,
125.569952358496));
#238177=CARTESIAN_POINT('Ctrl Pts',(-146.778125920315,-2.22593777837984,
124.585097249699));
#238178=CARTESIAN_POINT('Ctrl Pts',(-147.056573544128,-6.43561615084533,
129.315441348065));
#238179=CARTESIAN_POINT('Ctrl Pts',(-147.335021167941,-4.73127767801157,
135.414029517352));
#238180=CARTESIAN_POINT('Ctrl Pts',(-147.613468791753,1.32087384515067,
137.276557162581));
#238181=CARTESIAN_POINT('Ctrl Pts',(-147.891916415567,6.15920683289404,
133.191452367319));
#238182=CARTESIAN_POINT('Ctrl Pts',(-148.170364039379,5.33752963518947,
126.91272686995));
#238183=CARTESIAN_POINT('Ctrl Pts',(-148.448811663193,-0.389076544435395,
124.210222669761));
#238184=CARTESIAN_POINT('Ctrl Pts',(-148.727259287005,-5.75814038716998,
127.567409102056));
#238185=CARTESIAN_POINT('Ctrl Pts',(-149.005706910818,-5.83575451489182,
133.899195843233));
#238186=CARTESIAN_POINT('Ctrl Pts',(-149.284154534631,-0.550595335885521,
137.386980203127));
#238187=CARTESIAN_POINT('Ctrl Pts',(-149.562602158444,5.24053405872261,
134.825658742734));
#238188=CARTESIAN_POINT('Ctrl Pts',(-149.841049782257,6.21586866768539,
128.568960756646));
#238189=CARTESIAN_POINT('Ctrl Pts',(-150.119497406069,1.47912363311174,
124.366486037389));
#238190=CARTESIAN_POINT('Ctrl Pts',(-150.397945029883,-4.61686376108527,
126.080103549656));
#238191=CARTESIAN_POINT('Ctrl Pts',(-150.676392653695,-6.4701789051783,
132.135082514543));
#238192=CARTESIAN_POINT('Ctrl Pts',(-150.954840277509,-2.37771572122463,
136.967193065487));
#238193=CARTESIAN_POINT('Ctrl Pts',(-151.233287901321,3.89975205266408,
136.135961667893));
#238194=CARTESIAN_POINT('Ctrl Pts',(-151.511735525134,6.59353820363339,
130.405249368239));
#238195=CARTESIAN_POINT('Ctrl Pts',(-151.790183148947,3.22818485771248,
125.041300809049));
#238196=CARTESIAN_POINT('Ctrl Pts',(-152.06863077276,-3.10371266684865,
124.97332267276));
#238197=CARTESIAN_POINT('Ctrl Pts',(-152.347078396573,-6.58344987536885,
130.263783545709));
#238198=CARTESIAN_POINT('Ctrl Pts',(-152.625526020386,-4.01331826783166,
136.051008339035));
#238199=CARTESIAN_POINT('Ctrl Pts',(-152.903973644199,2.24485676634579,
137.016820189321));
#238200=CARTESIAN_POINT('Ctrl Pts',(-153.182421268012,6.44011809960154,
132.273685188686));
#238201=CARTESIAN_POINT('Ctrl Pts',(-153.460868891824,4.71722551658265,
126.180312687687));
#238202=CARTESIAN_POINT('Ctrl Pts',(-153.739316515637,-1.34056686689732,
124.336214336947));
#238203=CARTESIAN_POINT('Ctrl Pts',(-154.01776413945,-6.16644379003131,
128.436026431582));
#238204=CARTESIAN_POINT('Ctrl Pts',(-154.296211763263,-5.32566011765276,
134.712221943579));
#238205=CARTESIAN_POINT('Ctrl Pts',(-154.574659387076,0.409145029887599,
137.397283806609));
#238206=CARTESIAN_POINT('Ctrl Pts',(-154.853107010889,5.7679658828075,134.023771341112));
#238207=CARTESIAN_POINT('Ctrl Pts',(-155.131554634702,5.82630787022557,
127.691777697632));
#238208=CARTESIAN_POINT('Ctrl Pts',(-155.410002258515,0.530557555869813,
124.220095699443));
#238209=CARTESIAN_POINT('Ctrl Pts',(-155.688449882327,-5.25274923315307,
126.799031501784));
#238210=CARTESIAN_POINT('Ctrl Pts',(-155.96689750614,-6.20903608797397,
133.058669090323));
#238211=CARTESIAN_POINT('Ctrl Pts',(-156.245345129953,-1.4595221062231,
137.246707321489));
#238212=CARTESIAN_POINT('Ctrl Pts',(-156.523792753766,4.63122138952822,
135.514543657883));
#238213=CARTESIAN_POINT('Ctrl Pts',(-156.802240377579,6.46609867604585,
129.453951885458));
#238214=CARTESIAN_POINT('Ctrl Pts',(-157.080688001392,2.35894716575843,
124.634319766706));
#238215=CARTESIAN_POINT('Ctrl Pts',(-157.359135625205,-3.9159615488849,
125.484653766641));
#238216=CARTESIAN_POINT('Ctrl Pts',(-157.637583249018,-6.59229290546042,
131.223538480449));
#238217=CARTESIAN_POINT('Ctrl Pts',(-157.916030872831,-3.21062913332988,
136.577219216243));
#238218=CARTESIAN_POINT('Ctrl Pts',(-158.194478496644,3.12144596437753,
136.625924919674));
#238219=CARTESIAN_POINT('Ctrl Pts',(-158.472926120456,6.58506471193526,
131.324897428694));
#238220=CARTESIAN_POINT('Ctrl Pts',(-158.751373744269,3.99733068751967,
125.545522037924));
#238221=CARTESIAN_POINT('Ctrl Pts',(-159.029821368082,-2.26375495826568,
124.598762393297));
#238222=CARTESIAN_POINT('Ctrl Pts',(-159.308268991895,-6.44456038798308,
129.354644356446));
#238223=CARTESIAN_POINT('Ctrl Pts',(-159.586716615708,-4.7031296554214,
135.442744740987));
#238224=CARTESIAN_POINT('Ctrl Pts',(-159.865164239521,1.36024746981527,
137.268396713766));
#238225=CARTESIAN_POINT('Ctrl Pts',(-160.143611863334,6.17362362207528,
133.153915299856));
#238226=CARTESIAN_POINT('Ctrl Pts',(-160.422059487147,5.31374126392856,
126.880307915048));
#238227=CARTESIAN_POINT('Ctrl Pts',(-160.70050711096,-0.429209725076344,
124.212713263223));
#238228=CARTESIAN_POINT('Ctrl Pts',(-160.978954734773,-5.77773794479658,
127.602520510164));
#238229=CARTESIAN_POINT('Ctrl Pts',(-161.257402358585,-5.81680725143943,
133.934662397221));
#238230=CARTESIAN_POINT('Ctrl Pts',(-161.535849982398,-0.51051486084124,
137.390209872519));
#238231=CARTESIAN_POINT('Ctrl Pts',(-161.814297606211,5.26491574683228,
134.793683619137));
#238232=CARTESIAN_POINT('Ctrl Pts',(-162.092745230024,6.20214598860049,
128.531164416574));
#238233=CARTESIAN_POINT('Ctrl Pts',(-162.371192853837,1.43990705852047,
124.357601470914));
#238234=CARTESIAN_POINT('Ctrl Pts',(-162.64964047765,-4.64553611496906,
126.108295239334));
#238235=CARTESIAN_POINT('Ctrl Pts',(-162.928088101462,-6.46195854585841,
132.1744436748));
#238236=CARTESIAN_POINT('Ctrl Pts',(-163.206535725276,-2.34015675732853,
136.981552712947));
#238237=CARTESIAN_POINT('Ctrl Pts',(-163.484983349088,3.93213476817268,
136.112123988049));
#238238=CARTESIAN_POINT('Ctrl Pts',(-163.763430972902,6.5909865371863,130.365120024332));
#238239=CARTESIAN_POINT('Ctrl Pts',(-164.041878596714,3.19304366611785,
125.021756707701));
#238240=CARTESIAN_POINT('Ctrl Pts',(-164.320326220527,-3.13915034525769,
124.99232388833));
#238241=CARTESIAN_POINT('Ctrl Pts',(-164.59877384434,-6.58661854536123,
130.303868889347));
#238242=CARTESIAN_POINT('Ctrl Pts',(-164.877221468153,-3.98130607648258,
136.075341338217));
#238243=CARTESIAN_POINT('Ctrl Pts',(-165.155669091966,2.28263217906914,
137.003040006531));
#238244=CARTESIAN_POINT('Ctrl Pts',(-165.434116715779,6.44894297483741,
132.23445513871));
#238245=CARTESIAN_POINT('Ctrl Pts',(-165.712564339591,4.6889902251094,126.151683269957));
#238246=CARTESIAN_POINT('Ctrl Pts',(-165.991011963405,-1.37991547158711,
124.344494587733));
#238247=CARTESIAN_POINT('Ctrl Pts',(-166.269459587217,-6.18074626251326,
128.473607204924));
#238248=CARTESIAN_POINT('Ctrl Pts',(-166.54790721103,-5.3017731844313,134.744568344699));
#238249=CARTESIAN_POINT('Ctrl Pts',(-166.826354834843,0.449270444124704,
137.394671073086));
#238250=CARTESIAN_POINT('Ctrl Pts',(-167.104802458656,5.78745648261092,
133.988600447415));
#238251=CARTESIAN_POINT('Ctrl Pts',(-167.383250082469,5.8072527465451,127.656368976875));
#238252=CARTESIAN_POINT('Ctrl Pts',(-167.661697706282,0.490467436472931,
124.216988036188));
#238253=CARTESIAN_POINT('Ctrl Pts',(-167.940145330095,-5.27703348705155,
126.831080686747));
#238254=CARTESIAN_POINT('Ctrl Pts',(-168.218592953908,-6.19519843339338,
133.096423488211));
#238255=CARTESIAN_POINT('Ctrl Pts',(-168.49704057772,-1.42027867171577,
137.255472485049));
#238256=CARTESIAN_POINT('Ctrl Pts',(-168.775488201534,4.65980780479824,
135.486264830004));
#238257=CARTESIAN_POINT('Ctrl Pts',(-169.053935825346,6.45775855296945,
129.414615927465));
#238258=CARTESIAN_POINT('Ctrl Pts',(-169.332383449159,2.32134467000579,
124.620074502325));
#238259=CARTESIAN_POINT('Ctrl Pts',(-169.610831072972,-3.94827156070164,
125.508589897919));
#238260=CARTESIAN_POINT('Ctrl Pts',(-169.889278696785,-6.58961911091297,
131.263659872085));
#238261=CARTESIAN_POINT('Ctrl Pts',(-170.167726320598,-3.17542861898582,
136.596656269364));
#238262=CARTESIAN_POINT('Ctrl Pts',(-170.446173944411,3.15682564547787,
136.606815932013));
#238263=CARTESIAN_POINT('Ctrl Pts',(-170.724621568223,6.58811136125304,
131.284802626386));
#238264=CARTESIAN_POINT('Ctrl Pts',(-171.003069192037,3.96524458316956,
125.521286585549));
#238265=CARTESIAN_POINT('Ctrl Pts',(-171.28151681585,-2.30148825387982,
124.612657487621));
#238266=CARTESIAN_POINT('Ctrl Pts',(-171.559964439662,-6.45326581956532,
129.393901084596));
#238267=CARTESIAN_POINT('Ctrl Pts',(-171.838412063475,-4.67480735663214,
135.471288087592));
#238268=CARTESIAN_POINT('Ctrl Pts',(-172.116859687288,1.39957069001038,
137.259996737715));
#238269=CARTESIAN_POINT('Ctrl Pts',(-172.395307311101,6.18781164536257,
133.116291168777));
#238270=CARTESIAN_POINT('Ctrl Pts',(-172.673754934914,5.289755990031,126.848034367363));
#238271=CARTESIAN_POINT('Ctrl Pts',(-172.952202558727,-0.469327001192524,
124.215448112602));
#238272=CARTESIAN_POINT('Ctrl Pts',(-173.23065018254,-5.79712140621875,
127.637750563632));
#238273=CARTESIAN_POINT('Ctrl Pts',(-173.509097806352,-5.79764444405506,
133.970012956726));
#238274=CARTESIAN_POINT('Ctrl Pts',(-173.787545430165,-0.470415468481743,
137.393195500846));
#238275=CARTESIAN_POINT('Ctrl Pts',(-174.065993053978,5.28910234155359,
134.76156066971));
#238276=CARTESIAN_POINT('Ctrl Pts',(-174.344440677791,6.18819348671444,
128.493452310623));
#238277=CARTESIAN_POINT('Ctrl Pts',(-174.622888301604,1.40063712764339,
124.34895579147));
#238278=CARTESIAN_POINT('Ctrl Pts',(-174.901335925417,-4.67403632680454,
126.13666094344));
#238279=CARTESIAN_POINT('Ctrl Pts',(-175.17978354923,-6.45349873628761,
132.213754066126));
#238280=CARTESIAN_POINT('Ctrl Pts',(-175.458231173043,-2.30251107806296,
136.995683462282));
#238281=CARTESIAN_POINT('Ctrl Pts',(-175.736678796856,3.96437177698222,
136.088089627079));
#238282=CARTESIAN_POINT('Ctrl Pts',(-176.015126420669,6.58819063930867,
130.325006956645));
#238283=CARTESIAN_POINT('Ctrl Pts',(-176.293574044481,3.15778415511627,
125.002426882869));
#238284=CARTESIAN_POINT('Ctrl Pts',(-176.572021668294,-3.17447170129595,
125.011540471058));
#238285=CARTESIAN_POINT('Ctrl Pts',(-176.850469292107,-6.58954314578118,
130.343972778891));
#238286=CARTESIAN_POINT('Ctrl Pts',(-177.12891691592,-3.94914635637289,
136.099479019269));
#238287=CARTESIAN_POINT('Ctrl Pts',(-177.407364539733,2.32032300801719,
136.989030129397));
#238288=CARTESIAN_POINT('Ctrl Pts',(-177.685812163546,6.45752888212044,
132.195172096054));
#238289=CARTESIAN_POINT('Ctrl Pts',(-177.964259787359,4.66058118137817,
126.123226258898));
#238290=CARTESIAN_POINT('Ctrl Pts',(-178.242707411172,-1.41921294300185,
124.353014211231));
#238291=CARTESIAN_POINT('Ctrl Pts',(-178.521155034985,-6.19481970517025,
128.511274345191));
#238292=CARTESIAN_POINT('Ctrl Pts',(-178.799602658797,-5.27768979205393,
134.776768739972));
#238293=CARTESIAN_POINT('Ctrl Pts',(-179.078050282611,0.489379210479558,
137.391814133187));
#238294=CARTESIAN_POINT('Ctrl Pts',(-179.356497906423,5.80673262608622,
133.95331156054));
#238295=CARTESIAN_POINT('Ctrl Pts',(-179.634945530236,5.7879824329786,127.621076906106));
#238296=CARTESIAN_POINT('Ctrl Pts',(-179.913393154049,0.450359142625426,
124.214124470449));
#238297=CARTESIAN_POINT('Ctrl Pts',(-180.191840777862,-5.30112219853358,
126.863277103057));
#238298=CARTESIAN_POINT('Ctrl Pts',(-180.470288401675,-6.18113121345664,
133.134092952866));
#238299=CARTESIAN_POINT('Ctrl Pts',(-180.748736025488,-1.38098260826046,
137.263998600285));
#238300=CARTESIAN_POINT('Ctrl Pts',(-181.0271836493,4.68822154917632,135.457812512445));
#238301=CARTESIAN_POINT('Ctrl Pts',(-181.305631273113,6.44917913527537,
129.375331466973));
#238302=CARTESIAN_POINT('Ctrl Pts',(-181.584078896926,2.28365615597197,
124.606058398942));
#238303=CARTESIAN_POINT('Ctrl Pts',(-181.862526520739,-3.98043526786393,
125.532722265928));
#238304=CARTESIAN_POINT('Ctrl Pts',(-182.140974144552,-6.58670113560653,
131.303764244219));
#238305=CARTESIAN_POINT('Ctrl Pts',(-182.419421768365,-3.14011043796568,
136.615878686839));
#238306=CARTESIAN_POINT('Ctrl Pts',(-182.697869392178,3.19208834924215,
136.587491932238));
#238307=CARTESIAN_POINT('Ctrl Pts',(-182.976317015991,6.59091388568205,
131.244690021124));
#238308=CARTESIAN_POINT('Ctrl Pts',(-183.254764639804,3.93301154522339,
125.497246899427));
#238309=CARTESIAN_POINT('Ctrl Pts',(-183.533212263617,-2.33913626699958,
124.626782017781));
#238310=CARTESIAN_POINT('Ctrl Pts',(-183.811659887429,-6.46173212300977,
129.433210077844));
#238311=CARTESIAN_POINT('Ctrl Pts',(-184.090107511242,-4.64631183113728,
135.499658499484));
#238312=CARTESIAN_POINT('Ctrl Pts',(-184.368555135055,1.43884204859816,
137.251357545694));
#238313=CARTESIAN_POINT('Ctrl Pts',(-184.647002758868,6.20177037701405,
133.078581368264));
#238314=CARTESIAN_POINT('Ctrl Pts',(-184.925450382681,5.26557470227994,
126.815907422802));
#238315=CARTESIAN_POINT('Ctrl Pts',(-185.203898006494,-0.50942688622466,
124.218427116558));
#238316=CARTESIAN_POINT('Ctrl Pts',(-185.482345630307,-5.81629005317544,
127.673097957001));
#238317=CARTESIAN_POINT('Ctrl Pts',(-185.76079325412,-5.77826680282389,
134.005246211819));
#238318=CARTESIAN_POINT('Ctrl Pts',(-186.039240877932,-0.430298644703365,
137.395936977472));
#238319=CARTESIAN_POINT('Ctrl Pts',(-186.317688501746,5.31309294664177,
134.729291084778));
#238320=CARTESIAN_POINT('Ctrl Pts',(-186.596136125558,6.17401167904375,
128.455825836229));
#238321=CARTESIAN_POINT('Ctrl Pts',(-186.874583749371,1.36131529564269,
124.340549319425));
#238322=CARTESIAN_POINT('Ctrl Pts',(-187.153031373184,-4.70236334050424,
126.165199610876));
#238323=CARTESIAN_POINT('Ctrl Pts',(-187.431478996997,-6.44479978994851,
132.253012231859));
#238324=CARTESIAN_POINT('Ctrl Pts',(-187.70992662081,-2.26478007840253,
137.009584789872));
#238325=CARTESIAN_POINT('Ctrl Pts',(-187.988374244623,3.99646188453734,
136.063859475589));
#238326=CARTESIAN_POINT('Ctrl Pts',(-188.266821868436,6.58515061360439,
130.284911651585));
#238327=CARTESIAN_POINT('Ctrl Pts',(-188.545269492249,3.12240763126122,
124.983312050825));
#238328=CARTESIAN_POINT('Ctrl Pts',(-188.823717116061,-3.20967542611822,
125.030971708867));
#238329=CARTESIAN_POINT('Ctrl Pts',(-189.102164739874,-6.59222356825658,
130.384093728275));
#238330=CARTESIAN_POINT('Ctrl Pts',(-189.380612363687,-3.91684029919248,
136.123420487763));
#238331=CARTESIAN_POINT('Ctrl Pts',(-189.6590599875,2.35792785654334,136.974791077059));
#238332=CARTESIAN_POINT('Ctrl Pts',(-189.937507611313,6.46587550329532,
132.155837516369));
#238333=CARTESIAN_POINT('Ctrl Pts',(-190.215955235126,4.63199943809816,
126.094942708994));
#238334=CARTESIAN_POINT('Ctrl Pts',(-190.494402858939,-1.45845782495887,
124.361772891742));
#238335=CARTESIAN_POINT('Ctrl Pts',(-190.772850482752,-6.2086635965042,
128.549026456613));
#238336=CARTESIAN_POINT('Ctrl Pts',(-191.051298106565,-5.25341083294129,
134.808821936201));
#238337=CARTESIAN_POINT('Ctrl Pts',(-191.329745730377,0.529469842708527,
137.388713092773));
#238338=CARTESIAN_POINT('Ctrl Pts',(-191.60819335419,5.82579359894846,133.91790598813));
#238339=CARTESIAN_POINT('Ctrl Pts',(-191.886640978003,5.76849764359442,
127.585902793086));
#238340=CARTESIAN_POINT('Ctrl Pts',(-192.165088601816,0.410234160553658,
124.211505108333));
#238341=CARTESIAN_POINT('Ctrl Pts',(-192.443536225629,-5.32501447498302,
126.895619557667));
#238342=CARTESIAN_POINT('Ctrl Pts',(-192.721983849442,-6.16683494942961,
133.171676088433));
#238343=CARTESIAN_POINT('Ctrl Pts',(-193.000431473255,-1.34163537198624,
137.272285351261));
#238344=CARTESIAN_POINT('Ctrl Pts',(-193.278879097068,4.71646156978089,
135.429187759513));
#238345=CARTESIAN_POINT('Ctrl Pts',(-193.557326720881,6.44036074087642,
129.336099959682));
#238346=CARTESIAN_POINT('Ctrl Pts',(-193.835774344694,2.24588302022023,
124.592271975924));
#238347=CARTESIAN_POINT('Ctrl Pts',(-194.114221968506,-4.01245147853337,
125.557049976435));
#238348=CARTESIAN_POINT('Ctrl Pts',(-194.392669592319,-6.58353908766677,
131.343850110767));
#238349=CARTESIAN_POINT('Ctrl Pts',(-194.671117216133,-3.10467589899933,
136.634885756375));
#238350=CARTESIAN_POINT('Ctrl Pts',(-194.949564839945,3.22723276899961,
136.567953636405));
#238351=CARTESIAN_POINT('Ctrl Pts',(-195.228012463758,6.59347218137276,
131.204561099293));
#238352=CARTESIAN_POINT('Ctrl Pts',(-195.506460087571,3.90063276808784,
125.473403870355));
#238353=CARTESIAN_POINT('Ctrl Pts',(-195.784907711384,-2.3766976025655,
124.641135460387));
#238354=CARTESIAN_POINT('Ctrl Pts',(-196.063355335197,-6.46995898459376,
129.472569879579));
#238355=CARTESIAN_POINT('Ctrl Pts',(-196.34180295901,-4.61764413484867,
135.527854925386));
#238356=CARTESIAN_POINT('Ctrl Pts',(-196.620250582823,1.47806009036541,
137.242479457832));
#238357=CARTESIAN_POINT('Ctrl Pts',(-196.898698206635,6.21549929978325,
133.040787295662));
#238358=CARTESIAN_POINT('Ctrl Pts',(-197.177145830448,5.24119829672186,
126.783928271841));
#238359=CARTESIAN_POINT('Ctrl Pts',(-197.455593454261,-0.5495078942556,
124.2216501647));
#238360=CARTESIAN_POINT('Ctrl Pts',(-197.734041078074,-5.83524317536515,
127.708561380459));
#238361=CARTESIAN_POINT('Ctrl Pts',(-198.012488701887,-5.75867504579123,
134.040360856918));
#238362=CARTESIAN_POINT('Ctrl Pts',(-198.2909363257,-0.390165876051177,
137.398434200813));
#238363=CARTESIAN_POINT('Ctrl Pts',(-198.569383949513,5.33688667311775,
134.696876060105));
#238364=CARTESIAN_POINT('Ctrl Pts',(-198.847831573325,6.15960109109908,
128.418286387655));
#238365=CARTESIAN_POINT('Ctrl Pts',(-199.126279197139,1.32194301960288,
124.332382366286));
#238366=CARTESIAN_POINT('Ctrl Pts',(-199.404726820951,-4.73051610640191,
126.193910184127));
#238367=CARTESIAN_POINT('Ctrl Pts',(-199.683174444764,-6.43586202918244,
132.292216717274));
#238368=CARTESIAN_POINT('Ctrl Pts',(-199.961622068577,-2.22696515648391,
137.023256180599));
#238369=CARTESIAN_POINT('Ctrl Pts',(-200.24006969239,4.02840390172748,136.039434431435));
#238370=CARTESIAN_POINT('Ctrl Pts',(-200.518517316203,6.58186657272242,
130.244835594899));
#238371=CARTESIAN_POINT('Ctrl Pts',(-200.796964940016,3.08691540544346,
124.964412919876));
#238372=CARTESIAN_POINT('Ctrl Pts',(-201.075412563829,-3.24476021523692,
125.050616881724));
#238373=CARTESIAN_POINT('Ctrl Pts',(-201.353860187642,-6.59465971346335,
130.424230250803));
#238374=CARTESIAN_POINT('Ctrl Pts',(-201.632307811455,-3.88438910205457,
136.147164856536));
#238375=CARTESIAN_POINT('Ctrl Pts',(-201.910755435267,2.39544533118521,
136.960323377152));
#238376=CARTESIAN_POINT('Ctrl Pts',(-202.18920305908,6.47398252907625,132.116452857208));
#238377=CARTESIAN_POINT('Ctrl Pts',(-202.467650682893,4.60324605437475,
126.066833668302));
#238378=CARTESIAN_POINT('Ctrl Pts',(-202.746098306706,-1.49764866322506,
124.370770304711));
#238379=CARTESIAN_POINT('Ctrl Pts',(-203.024545930519,-6.22227742352606,
128.586862140274));
#238380=CARTESIAN_POINT('Ctrl Pts',(-203.302993554332,-5.22893720675747,
134.840726745644));
#238381=CARTESIAN_POINT('Ctrl Pts',(-203.581441178145,0.569540855237039,
137.385368066758));
#238382=CARTESIAN_POINT('Ctrl Pts',(-203.859888801958,5.84463869488665,
133.882385042152));
#238383=CARTESIAN_POINT('Ctrl Pts',(-204.138336425771,5.7487991004088,127.550847941203));
#238384=CARTESIAN_POINT('Ctrl Pts',(-204.416784049583,0.370093977104817,
124.209130046901));
#238385=CARTESIAN_POINT('Ctrl Pts',(-204.695231673396,-5.34870943106288,
126.928106852114));
#238386=CARTESIAN_POINT('Ctrl Pts',(-204.973679297209,-6.15231017106575,
133.209171502253));
#238387=CARTESIAN_POINT('Ctrl Pts',(-205.252126921022,-1.30223842092043,
137.280332430907));
#238388=CARTESIAN_POINT('Ctrl Pts',(-205.530574544835,4.74452682016742,
135.400391631911));
#238389=CARTESIAN_POINT('Ctrl Pts',(-205.809022168648,6.43130369654214,
129.296922859329));
#238390=CARTESIAN_POINT('Ctrl Pts',(-206.087469792461,2.20802666244648,
124.578715744137));
#238391=CARTESIAN_POINT('Ctrl Pts',(-206.365917416273,-4.04431900633787,
125.581572127967));
#238392=CARTESIAN_POINT('Ctrl Pts',(-206.644365040087,-6.58013308426553,
131.383915986335));
#238393=CARTESIAN_POINT('Ctrl Pts',(-206.922812663899,-3.06912631512495,
136.653676773657));
#238394=CARTESIAN_POINT('Ctrl Pts',(-207.201260287713,3.26225760245914,
136.548201768512));
#238395=CARTESIAN_POINT('Ctrl Pts',(-207.479707911525,6.59578615352751,
131.164417347887));
#238396=CARTESIAN_POINT('Ctrl Pts',(-207.758155535338,3.86810945157081,
125.449758381845));
#238397=CARTESIAN_POINT('Ctrl Pts',(-208.036603159151,-2.41417086872696,
124.655717283569));
#238398=CARTESIAN_POINT('Ctrl Pts',(-208.315050782964,-6.47794609946865,
129.511979031309));
#238399=CARTESIAN_POINT('Ctrl Pts',(-208.593498406777,-4.58880533005852,
135.555876320469));
#238400=CARTESIAN_POINT('Ctrl Pts',(-208.87194603059,1.51722336207232,137.233362803106));
#238401=CARTESIAN_POINT('Ctrl Pts',(-209.150393654402,6.22899790494034,
133.00291035145));
#238402=CARTESIAN_POINT('Ctrl Pts',(-209.428841278216,5.21662767663345,
126.752098099478));
#238403=CARTESIAN_POINT('Ctrl Pts',(-209.707288902028,-0.589568540070009,
124.225117137599));
#238404=CARTESIAN_POINT('Ctrl Pts',(-209.985736525842,-5.85398007047323,
127.744139519898));
#238405=CARTESIAN_POINT('Ctrl Pts',(-210.264184149654,-5.73886989893714,
134.07535559084));
#238406=CARTESIAN_POINT('Ctrl Pts',(-210.542631773467,-0.350018649658268,
137.400687078332));
#238407=CARTESIAN_POINT('Ctrl Pts',(-210.82107939728,5.36048263929459,134.664316796842));
#238408=CARTESIAN_POINT('Ctrl Pts',(-211.099527021093,6.14496225687153,
128.38083535594));
#238409=CARTESIAN_POINT('Ctrl Pts',(-211.377974644906,1.28252175847855,
124.324455234681));
#238410=CARTESIAN_POINT('Ctrl Pts',(-211.656422268719,-4.75849358128477,
126.222791599316));
#238411=CARTESIAN_POINT('Ctrl Pts',(-211.934869892531,-6.4266857851828,
132.331366069634));
#238412=CARTESIAN_POINT('Ctrl Pts',(-212.213317516344,-2.18906771355195,
137.036697127864));
#238413=CARTESIAN_POINT('Ctrl Pts',(-212.491765140157,4.06019664492976,
136.014815399695));
#238414=CARTESIAN_POINT('Ctrl Pts',(-212.770212763971,6.57833863835413,
130.204780271616));
#238415=CARTESIAN_POINT('Ctrl Pts',(-213.048660387783,3.05130879283982,
124.945730190337));
#238416=CARTESIAN_POINT('Ctrl Pts',(-213.327108011596,-3.27972476857289,
125.070475261673));
#238417=CARTESIAN_POINT('Ctrl Pts',(-213.605555635409,-6.59685149112928,
130.464380859201));
#238418=CARTESIAN_POINT('Ctrl Pts',(-213.884003259222,-3.85179396744981,
136.170711245733));
#238419=CARTESIAN_POINT('Ctrl Pts',(-214.162450883035,2.43287404171984,
136.94562756578));
#238420=CARTESIAN_POINT('Ctrl Pts',(-214.440898506847,6.48184965905313,
132.077019577989));
#238421=CARTESIAN_POINT('Ctrl Pts',(-214.71934613066,4.57432209567675,126.038900178414));
#238422=CARTESIAN_POINT('Ctrl Pts',(-214.997793754473,-1.53678400556905,
124.380006116735));
#238423=CARTESIAN_POINT('Ctrl Pts',(-215.276241378286,-6.23566068176903,
128.624779994154));
#238424=CARTESIAN_POINT('Ctrl Pts',(-215.554689002099,-5.20426982038336,
134.872481986055));
#238425=CARTESIAN_POINT('Ctrl Pts',(-215.833136625912,0.609590763220439,
137.381779179092));
#238426=CARTESIAN_POINT('Ctrl Pts',(-216.111584249725,5.86326721558844,
133.846750038845));
#238427=CARTESIAN_POINT('Ctrl Pts',(-216.390031873537,5.72888753335829,
127.51591364943));
#238428=CARTESIAN_POINT('Ctrl Pts',(-216.668479497351,0.329940079686948,
124.206999374164));
#238429=CARTESIAN_POINT('Ctrl Pts',(-216.946927121163,-5.37220618874772,
126.960737782571));
#238430=CARTESIAN_POINT('Ctrl Pts',(-217.225374744977,-6.13755741658593,
133.246577804923));
#238431=CARTESIAN_POINT('Ctrl Pts',(-217.503822368789,-1.26279321493052,
137.288139541036));
#238432=CARTESIAN_POINT('Ctrl Pts',(-217.782269992602,4.77241626036792,
135.37142519669));
#238433=CARTESIAN_POINT('Ctrl Pts',(-218.060717616415,6.4220083378839,129.257801617636));
#238434=CARTESIAN_POINT('Ctrl Pts',(-218.339165240228,2.17008848543354,
124.565390205911));
#238435=CARTESIAN_POINT('Ctrl Pts',(-218.617612864041,-4.07603667041411,
125.606287811847));
#238436=CARTESIAN_POINT('Ctrl Pts',(-218.896060487854,-6.57648325161253,
131.423960386264));
#238437=CARTESIAN_POINT('Ctrl Pts',(-219.174508111666,-3.03346300364714,
136.672251042379));
#238438=CARTESIAN_POINT('Ctrl Pts',(-219.45295573548,3.29716155176439,136.528237060474));
#238439=CARTESIAN_POINT('Ctrl Pts',(-219.731403359293,6.59785571640026,
131.124260254445));
#238440=CARTESIAN_POINT('Ctrl Pts',(-220.009850983105,3.83544280083539,
125.426311310091));
#238441=CARTESIAN_POINT('Ctrl Pts',(-220.288298606918,-2.45155467689987,
124.67052694699));
#238442=CARTESIAN_POINT('Ctrl Pts',(-220.566746230731,-6.48569317166813,
129.551436072715));
#238443=CARTESIAN_POINT('Ctrl Pts',(-220.845193854544,-4.55979648539947,
135.58372164639));
#238444=CARTESIAN_POINT('Ctrl Pts',(-221.123641478357,1.55633041250914,
137.224007919343));
#238445=CARTESIAN_POINT('Ctrl Pts',(-221.40208910217,6.24226569228925,132.964951939167));
#238446=CARTESIAN_POINT('Ctrl Pts',(-221.680536725983,5.19186375248807,
126.720418085194));
#238447=CARTESIAN_POINT('Ctrl Pts',(-221.958984349796,-0.629607339204784,
124.228827906785));
#238448=CARTESIAN_POINT('Ctrl Pts',(-222.237431973609,-5.87250004419688,
127.779831056953));
#238449=CARTESIAN_POINT('Ctrl Pts',(-222.515879597421,-5.71885209614835,
134.110229116839));
#238450=CARTESIAN_POINT('Ctrl Pts',(-222.794327221234,-0.309858453196267,
137.402695526548));
#238451=CARTESIAN_POINT('Ctrl Pts',(-223.072774845047,5.38387997081673,
134.631614501482));
#238452=CARTESIAN_POINT('Ctrl Pts',(-223.35122246886,6.13009571880702,128.343474128844));
#238453=CARTESIAN_POINT('Ctrl Pts',(-223.629670092673,1.24305297303857,
124.316768218352));
#238454=CARTESIAN_POINT('Ctrl Pts',(-223.908117716486,-4.78629472843886,
126.25184278623));
#238455=CARTESIAN_POINT('Ctrl Pts',(-224.186565340298,-6.41727139797729,
132.370458838244));
#238456=CARTESIAN_POINT('Ctrl Pts',(-224.465012964112,-2.15108915391133,
137.049907133607));
#238457=CARTESIAN_POINT('Ctrl Pts',(-224.743460587925,4.09183893605206,
135.990003292637));
#238458=CARTESIAN_POINT('Ctrl Pts',(-225.021908211737,6.57456694122844,
130.164747166004));
#238459=CARTESIAN_POINT('Ctrl Pts',(-225.300355835551,3.01558911286705,
124.927264554503));
#238460=CARTESIAN_POINT('Ctrl Pts',(-225.578803459363,-3.31456779050113,
125.090546112851));
#238461=CARTESIAN_POINT('Ctrl Pts',(-225.857251083176,-6.5987988200372,
130.504544065675));
#238462=CARTESIAN_POINT('Ctrl Pts',(-226.135698706989,-3.8190561032033,
136.194058782834));
#238463=CARTESIAN_POINT('Ctrl Pts',(-226.414146330802,2.47021260121173,
136.930704187504));
#238464=CARTESIAN_POINT('Ctrl Pts',(-226.692593954615,6.48947660170784,
132.037539139922));
#238465=CARTESIAN_POINT('Ctrl Pts',(-226.971041578427,4.54522863379049,
126.011143274415));
#238466=CARTESIAN_POINT('Ctrl Pts',(-227.24948920224,-1.57586240181677,
124.389479985577));
#238467=CARTESIAN_POINT('Ctrl Pts',(-227.527936826054,-6.24881287531301,
128.662778613197));
#238468=CARTESIAN_POINT('Ctrl Pts',(-227.806384449866,-5.17940958787633,
134.904086480733));
#238469=CARTESIAN_POINT('Ctrl Pts',(-228.084832073679,0.649618082593193,
137.377946562762));
#238470=CARTESIAN_POINT('Ctrl Pts',(-228.363279697492,5.88167847076755,
133.811002298682));
#238471=CARTESIAN_POINT('Ctrl Pts',(-228.641727321305,5.70876368027354,
127.481101212267));
#238472=CARTESIAN_POINT('Ctrl Pts',(-228.920174945118,0.289773956218704,
124.205113169075));
#238473=CARTESIAN_POINT('Ctrl Pts',(-229.198622568931,-5.39550387735667,
126.993511139885));
#238474=CARTESIAN_POINT('Ctrl Pts',(-229.477070192744,-6.12257723265909,
133.283893610337));
#238475=CARTESIAN_POINT('Ctrl Pts',(-229.755517816557,-1.22330121567356,
137.295706392352));
#238476=CARTESIAN_POINT('Ctrl Pts',(-230.033965440369,4.80012885692891,
135.34228952721));
#238477=CARTESIAN_POINT('Ctrl Pts',(-230.312413064183,6.41247500934538,
129.218737684256));
#238478=CARTESIAN_POINT('Ctrl Pts',(-230.590860687995,2.13206989499296,
124.552295855027));
#238479=CARTESIAN_POINT('Ctrl Pts',(-230.869308311808,-4.10760329545278,
125.631196112227));
#238480=CARTESIAN_POINT('Ctrl Pts',(-231.147755935621,-6.5725897249546,
131.463981826697));
#238481=CARTESIAN_POINT('Ctrl Pts',(-231.426203559434,-2.99768728608136,
136.690607874263));
#238482=CARTESIAN_POINT('Ctrl Pts',(-231.704651183247,3.33194332353496,
136.508060252089));
#238483=CARTESIAN_POINT('Ctrl Pts',(-231.98309880706,6.59968079330357,131.084091307006));
#238484=CARTESIAN_POINT('Ctrl Pts',(-232.261546430872,3.80263402635669,
125.403063523931));
#238485=CARTESIAN_POINT('Ctrl Pts',(-232.539994054686,-2.48884764181187,
124.685563901874));
#238486=CARTESIAN_POINT('Ctrl Pts',(-232.818441678498,-6.49319991412244,
129.5909395417));
#238487=CARTESIAN_POINT('Ctrl Pts',(-233.096889302311,-4.53061867580467,
135.611389871331));
#238488=CARTESIAN_POINT('Ctrl Pts',(-233.375336926124,1.59537979255065,
137.214415153187));
#238489=CARTESIAN_POINT('Ctrl Pts',(-233.653784549937,6.25530217018742,
132.926913465378));
#238490=CARTESIAN_POINT('Ctrl Pts',(-233.93223217375,5.16690744192206,126.688889402902));
#238491=CARTESIAN_POINT('Ctrl Pts',(-234.210679797563,-0.669622808008655,
124.232782334755));
#238492=CARTESIAN_POINT('Ctrl Pts',(-234.489127421376,-5.89080241027189,
127.815634669064));
#238493=CARTESIAN_POINT('Ctrl Pts',(-234.767575045188,-5.69862237919218,
134.144980142666));
#238494=CARTESIAN_POINT('Ctrl Pts',(-235.046022669002,-0.269686774814632,
137.404459471037));
#238495=CARTESIAN_POINT('Ctrl Pts',(-235.324470292814,5.40707780068583,
134.598770385822));
#238496=CARTESIAN_POINT('Ctrl Pts',(-235.602917916627,6.11500202779203,
128.306204090801));
#238497=CARTESIAN_POINT('Ctrl Pts',(-235.88136554044,1.20353812581378,124.309321602146));
#238498=CARTESIAN_POINT('Ctrl Pts',(-236.159813164253,-4.81391851768082,
126.281062668365));
#238499=CARTESIAN_POINT('Ctrl Pts',(-236.438260788066,-6.40761921642086,
132.40949357451));
#238500=CARTESIAN_POINT('Ctrl Pts',(-236.716708411879,-2.11303088487057,
137.062885708328));
#238501=CARTESIAN_POINT('Ctrl Pts',(-236.995156035692,4.12332960257798,
135.964999029683));
#238502=CARTESIAN_POINT('Ctrl Pts',(-237.273603659505,6.57055162110693,
130.124737761504));
#238503=CARTESIAN_POINT('Ctrl Pts',(-237.552051283318,2.97975768913041,
124.909016696624));
#238504=CARTESIAN_POINT('Ctrl Pts',(-237.83049890713,-3.34928798990126,
125.110828691528));
#238505=CARTESIAN_POINT('Ctrl Pts',(-238.108946530943,-6.60050162802816,
130.544718381962));
#238506=CARTESIAN_POINT('Ctrl Pts',(-238.387394154756,-3.7861767224282,
136.217206602688));
#238507=CARTESIAN_POINT('Ctrl Pts',(-238.665841778569,2.5074596260677,136.915553795314));
#238508=CARTESIAN_POINT('Ctrl Pts',(-238.944289402382,6.49686307441993,
131.998013005973));
#238509=CARTESIAN_POINT('Ctrl Pts',(-239.222737026195,4.51596674678651,
125.983563984846));
#238510=CARTESIAN_POINT('Ctrl Pts',(-239.501184650008,-1.61488240390346,
124.399191560181));
#238511=CARTESIAN_POINT('Ctrl Pts',(-239.77963227382,-6.26173351679718,
128.700856589348));
#238512=CARTESIAN_POINT('Ctrl Pts',(-240.058079897633,-5.15435743044315,
134.935539058562));
#238513=CARTESIAN_POINT('Ctrl Pts',(-240.336527521446,0.689621330129741,
137.373870359787));
#238514=CARTESIAN_POINT('Ctrl Pts',(-240.614975145259,5.89987177818775,
133.775143146303));
#238515=CARTESIAN_POINT('Ctrl Pts',(-240.893422769072,5.68842828685113,
127.446411919705));
#238516=CARTESIAN_POINT('Ctrl Pts',(-241.171870392886,0.249597095069331,
124.203471501526));
#238517=CARTESIAN_POINT('Ctrl Pts',(-241.450318016698,-5.41860163358522,
127.026425709627));
#238518=CARTESIAN_POINT('Ctrl Pts',(-241.728765640511,-6.10737017438111,
133.321117535742));
#238519=CARTESIAN_POINT('Ctrl Pts',(-242.007213264324,-1.18376388654087,
137.303032704464));
#238520=CARTESIAN_POINT('Ctrl Pts',(-242.285660888137,4.82766358294966,
135.312985703106));
#238521=CARTESIAN_POINT('Ctrl Pts',(-242.56410851195,6.40270406418687,129.179732506718));
#238522=CARTESIAN_POINT('Ctrl Pts',(-242.842556135762,2.09397229991911,
124.539433176702));
#238523=CARTESIAN_POINT('Ctrl Pts',(-243.121003759575,-4.13901771174057,
125.65629610612));
#238524=CARTESIAN_POINT('Ctrl Pts',(-243.399451383388,-6.56845264856689,
131.503978824623));
#238525=CARTESIAN_POINT('Ctrl Pts',(-243.677899007202,-2.9618004881116,
136.70874658909));
#238526=CARTESIAN_POINT('Ctrl Pts',(-243.956346631013,3.36660162892119,
136.487672091016));
#238527=CARTESIAN_POINT('Ctrl Pts',(-244.234794254827,6.60126131660758,
131.043911994042));
#238528=CARTESIAN_POINT('Ctrl Pts',(-244.513241878639,3.76968434387551,
125.380015884821));
#238529=CARTESIAN_POINT('Ctrl Pts',(-244.791689502453,-2.52604838156001,
124.70082759102));
#238530=CARTESIAN_POINT('Ctrl Pts',(-245.070137126265,-6.50046604866569,
129.630487974449));
#238531=CARTESIAN_POINT('Ctrl Pts',(-245.348584750079,-4.50127298246883,
135.638879970036));
#238532=CARTESIAN_POINT('Ctrl Pts',(-245.627032373891,1.63437005520677,
137.204584860103));
#238533=CARTESIAN_POINT('Ctrl Pts',(-245.905479997704,6.26810685556324,
132.888796339615));
#238534=CARTESIAN_POINT('Ctrl Pts',(-246.183927621517,5.14175966970064,
126.65751322091));
#238535=CARTESIAN_POINT('Ctrl Pts',(-246.46237524533,-0.709613463692526,
124.236980274974));
#238536=CARTESIAN_POINT('Ctrl Pts',(-246.740822869143,-5.90888649049716,
127.851549029514));
#238537=CARTESIAN_POINT('Ctrl Pts',(-247.019270492956,-5.67818149768794,
134.179607380607));
#238538=CARTESIAN_POINT('Ctrl Pts',(-247.297718116769,-0.229505103091092,
137.405978846438));
#238539=CARTESIAN_POINT('Ctrl Pts',(-247.576165740581,5.43007526929941,
134.565785666913));
#238540=CARTESIAN_POINT('Ctrl Pts',(-247.854613364394,6.09968174312738,
128.269026622868));
#238541=CARTESIAN_POINT('Ctrl Pts',(-248.133060988207,1.16397868104094,
124.302115661998));
#238542=CARTESIAN_POINT('Ctrl Pts',(-248.41150861202,-4.84136392540264,
126.31045016297));
#238543=CARTESIAN_POINT('Ctrl Pts',(-248.689956235833,-6.39772959817725,
132.448468831983));
#238544=CARTESIAN_POINT('Ctrl Pts',(-248.968403859646,-2.07489431669385,
137.075632371099));
#238545=CARTESIAN_POINT('Ctrl Pts',(-249.246851483459,4.15466747760909,
135.939803537374));
#238546=CARTESIAN_POINT('Ctrl Pts',(-249.525299107272,6.56629282677857,
130.08475354068));
#238547=CARTESIAN_POINT('Ctrl Pts',(-249.803746731085,2.94381584937754,
124.890987292882));
#238548=CARTESIAN_POINT('Ctrl Pts',(-250.082194354898,-3.38388408020374,
125.131322246124));
#238549=CARTESIAN_POINT('Ctrl Pts',(-250.36064197871,-6.60195985200274,
130.584902319384));
#238550=CARTESIAN_POINT('Ctrl Pts',(-250.639089602524,-3.75315704348482,
136.240153847548));
#238551=CARTESIAN_POINT('Ctrl Pts',(-250.917537226336,2.54461373609029,
136.900176950603));
#238552=CARTESIAN_POINT('Ctrl Pts',(-251.19598485015,6.50400880347224,131.958442640812));
#238553=CARTESIAN_POINT('Ctrl Pts',(-251.474432473962,4.48653751899202,
125.956163331638));
#238554=CARTESIAN_POINT('Ctrl Pts',(-251.752880097775,-1.65384256596459,
124.409140480742));
#238555=CARTESIAN_POINT('Ctrl Pts',(-252.031327721588,-6.27442212737671,
128.739012511497));
#238556=CARTESIAN_POINT('Ctrl Pts',(-252.309775345401,-5.12911427652582,
134.966838554275));
#238557=CARTESIAN_POINT('Ctrl Pts',(-252.588222969213,0.729599023732927,
137.369550720794));
#238558=CARTESIAN_POINT('Ctrl Pts',(-252.866670593027,5.91784646323776,
133.739173911277));
#238559=CARTESIAN_POINT('Ctrl Pts',(-253.145118216839,5.66788210748017,
127.411847055674));
#238560=CARTESIAN_POINT('Ctrl Pts',(-253.423565840652,0.209410983396998,
124.20207443517));
#238561=CARTESIAN_POINT('Ctrl Pts',(-253.702013464465,-5.44149859849489,
127.059480266814));
#238562=CARTESIAN_POINT('Ctrl Pts',(-253.980461088278,-6.0919368110008,
133.358248211846));
#238563=CARTESIAN_POINT('Ctrl Pts',(-254.258908712091,-1.1441826817532,
137.310118186916));
#238564=CARTESIAN_POINT('Ctrl Pts',(-254.537356335904,4.85501939763767,
135.283514846073));
#238565=CARTESIAN_POINT('Ctrl Pts',(-254.815803959717,6.39269590315201,
129.140787462715));
#238566=CARTESIAN_POINT('Ctrl Pts',(-255.09425158353,2.05579703890082,124.526802775315));
#238567=CARTESIAN_POINT('Ctrl Pts',(-255.372699207342,-4.17027861730954,
125.681586622223));
#238568=CARTESIAN_POINT('Ctrl Pts',(-255.651146831155,-6.5640724361261,
131.5439503534));
#238569=CARTESIAN_POINT('Ctrl Pts',(-255.929594454968,-2.925803447894,136.726665654721));
#238570=CARTESIAN_POINT('Ctrl Pts',(-256.208042078781,3.40113425532747,
136.467074956607));
#238571=CARTESIAN_POINT('Ctrl Pts',(-256.486489702594,6.60259898059897,
131.003720738236));
#238572=CARTESIAN_POINT('Ctrl Pts',(-256.764937326407,3.73659166461274,
125.357175036369));
#238573=CARTESIAN_POINT('Ctrl Pts',(-257.04338495022,-2.56314926818932,
124.716306516944));
#238574=CARTESIAN_POINT('Ctrl Pts',(-257.321832574033,-6.5075031063131,
129.670100547101));
#238575=CARTESIAN_POINT('Ctrl Pts',(-257.600280197845,-4.47173821150659,
135.666151948257));
#238576=CARTESIAN_POINT('Ctrl Pts',(-257.878727821659,1.67325768403046,
137.194590998305));
#238577=CARTESIAN_POINT('Ctrl Pts',(-258.157175445471,6.28075871394982,
132.850463013089));
#238578=CARTESIAN_POINT('Ctrl Pts',(-258.435623069284,5.1162713672671,126.626553096149));
#238579=CARTESIAN_POINT('Ctrl Pts',(-258.714070693097,-0.749294580734974,
124.240926059104));
#238580=CARTESIAN_POINT('Ctrl Pts',(-258.99251831691,-5.92728653745133,
127.888508918958));
#238581=CARTESIAN_POINT('Ctrl Pts',(-259.270965940723,-5.656519339957,134.212338033208));
#238582=CARTESIAN_POINT('Ctrl Pts',(-259.549413564536,-0.191230405826049,
137.41063083554));
#238583=CARTESIAN_POINT('Ctrl Pts',(-259.827861188349,5.45654320709978,
134.526020746857));
#238584=CARTESIAN_POINT('Ctrl Pts',(-260.059900874859,5.97341346954355,
129.293215926205));
#238585=CARTESIAN_POINT('Ctrl Pts',(-260.245542550368,3.60742224527213,
126.247226657536));
#238586=CARTESIAN_POINT('Ctrl Pts',(-260.338368351272,1.86717727106152,
125.459413119698));
#238587=CARTESIAN_POINT('Ctrl Pts',(-260.384786214875,0.950008195528324,
125.301089073499));
#238588=CARTESIAN_POINT('Ctrl Pts',(209.997886486728,-2.58542267678463,
125.478296443779));
#238589=CARTESIAN_POINT('Ctrl Pts',(209.951476810375,-3.47289965896197,
125.909102290886));
#238590=CARTESIAN_POINT('Ctrl Pts',(209.85865919672,-5.01373755653622,127.222906143875));
#238591=CARTESIAN_POINT('Ctrl Pts',(209.67302570846,-6.52844908712303,131.020616473957));
#238592=CARTESIAN_POINT('Ctrl Pts',(209.440986021949,-4.4641631800594,136.198709217918));
#238593=CARTESIAN_POINT('Ctrl Pts',(209.162538398136,2.13623200523086,137.47712630299));
#238594=CARTESIAN_POINT('Ctrl Pts',(208.884090774324,6.76311047611758,132.61329501932));
#238595=CARTESIAN_POINT('Ctrl Pts',(208.60564315051,5.180460236421,126.09244423763));
#238596=CARTESIAN_POINT('Ctrl Pts',(208.327195526698,-1.16565068102074,
123.898824768668));
#238597=CARTESIAN_POINT('Ctrl Pts',(208.048747902884,-6.43906639651766,
128.052530506575));
#238598=CARTESIAN_POINT('Ctrl Pts',(207.770300279072,-5.79609906993421,
134.734252735451));
#238599=CARTESIAN_POINT('Ctrl Pts',(207.491852655259,0.173626147510206,
137.805009652024));
#238600=CARTESIAN_POINT('Ctrl Pts',(207.213405031446,5.98357180802623,134.442293088818));
#238601=CARTESIAN_POINT('Ctrl Pts',(206.934957407633,6.29502677410122,127.736610299611));
#238602=CARTESIAN_POINT('Ctrl Pts',(206.65650978382,0.821596385081328,123.849978754804));
#238603=CARTESIAN_POINT('Ctrl Pts',(206.378062160007,-5.40680743188727,
126.354116934927));
#238604=CARTESIAN_POINT('Ctrl Pts',(206.099614536195,-6.66663710465116,
132.947794423038));
#238605=CARTESIAN_POINT('Ctrl Pts',(205.821166912381,-1.80014356190772,
137.571770081489));
#238606=CARTESIAN_POINT('Ctrl Pts',(205.542719288569,4.72058899422897,135.976822216287));
#238607=CARTESIAN_POINT('Ctrl Pts',(205.264271664756,6.90333351468265,129.628637390042));
#238608=CARTESIAN_POINT('Ctrl Pts',(204.985824040943,2.74225038547515,124.360883417158));
#238609=CARTESIAN_POINT('Ctrl Pts',(204.70737641713,-3.93882614214087,125.014370927945));
#238610=CARTESIAN_POINT('Ctrl Pts',(204.428928793317,-7.00031425910704,
130.988575726592));
#238611=CARTESIAN_POINT('Ctrl Pts',(204.150481169504,-3.62885534891233,
136.793496040797));
#238612=CARTESIAN_POINT('Ctrl Pts',(203.872033545692,3.07734423765085,137.09469337995));
#238613=CARTESIAN_POINT('Ctrl Pts',(203.593585921878,6.95561486460971,131.615382266785));
#238614=CARTESIAN_POINT('Ctrl Pts',(203.315138298066,4.44201520086038,125.390781848689));
#238615=CARTESIAN_POINT('Ctrl Pts',(203.036690674253,-2.15357941165663,
124.140995867004));
#238616=CARTESIAN_POINT('Ctrl Pts',(202.75824305044,-6.77013976170558,129.014516559232));
#238617=CARTESIAN_POINT('Ctrl Pts',(202.479795426627,-5.16527240588502,
135.532816506767));
#238618=CARTESIAN_POINT('Ctrl Pts',(202.201347802814,1.18622795093483,137.705896487686));
#238619=CARTESIAN_POINT('Ctrl Pts',(201.922900179001,6.44764277258624,133.536802163981));
#238620=CARTESIAN_POINT('Ctrl Pts',(201.644452555188,5.78398887041165,126.856727545651));
#238621=CARTESIAN_POINT('Ctrl Pts',(201.366004931376,-0.194868239746226,
123.804334868162));
#238622=CARTESIAN_POINT('Ctrl Pts',(201.087557307562,-5.99465095761073,
127.184623883922));
#238623=CARTESIAN_POINT('Ctrl Pts',(200.80910968375,-6.2856423003101,133.891274124028));
#238624=CARTESIAN_POINT('Ctrl Pts',(200.530662059936,-0.80043543977546,
137.76120165575));
#238625=CARTESIAN_POINT('Ctrl Pts',(200.252214436124,5.42033248649604,135.238132133988));
#238626=CARTESIAN_POINT('Ctrl Pts',(199.973766812311,6.66007965562565,128.640643190398));
#238627=CARTESIAN_POINT('Ctrl Pts',(199.695319188498,1.77953898422249,124.031504858911));
#238628=CARTESIAN_POINT('Ctrl Pts',(199.416871564685,-4.73631107837294,
125.646290097223));
#238629=CARTESIAN_POINT('Ctrl Pts',(199.138423940872,-6.89972264160091,
132.00109015798));
#238630=CARTESIAN_POINT('Ctrl Pts',(198.859976317059,-2.72262616738874,
137.256154234582));
#238631=CARTESIAN_POINT('Ctrl Pts',(198.581528693247,3.95643074697165,136.582335164788));
#238632=CARTESIAN_POINT('Ctrl Pts',(198.303081069434,6.999721087252,130.598839755845));
#238633=CARTESIAN_POINT('Ctrl Pts',(198.024633445621,3.61060970373355,124.804207978572));
#238634=CARTESIAN_POINT('Ctrl Pts',(197.746185821808,-3.09647560942607,
124.523423352781));
#238635=CARTESIAN_POINT('Ctrl Pts',(197.467738197995,-6.9580511087663,130.014513232485));
#238636=CARTESIAN_POINT('Ctrl Pts',(197.189290574182,-4.4255175588443,136.231434272887));
#238637=CARTESIAN_POINT('Ctrl Pts',(196.910842950369,2.17385042910367,137.461139751337));
#238638=CARTESIAN_POINT('Ctrl Pts',(196.632395326556,6.77555607120273,132.573590407591));
#238639=CARTESIAN_POINT('Ctrl Pts',(196.353947702743,5.15085668818228,126.060205318492));
#238640=CARTESIAN_POINT('Ctrl Pts',(196.07550007893,-1.20722835793932,123.90646718437));
#238641=CARTESIAN_POINT('Ctrl Pts',(195.797052455118,-6.45592951949867,
128.091556134528));
#238642=CARTESIAN_POINT('Ctrl Pts',(195.518604831305,-5.77194684232935,
134.769579876729));
#238643=CARTESIAN_POINT('Ctrl Pts',(195.240157207492,0.216173007661386,
137.80376083149));
#238644=CARTESIAN_POINT('Ctrl Pts',(194.961709583679,6.00564042424985,134.405834929363));
#238645=CARTESIAN_POINT('Ctrl Pts',(194.683261959866,6.2762176827981,127.698330076496));
#238646=CARTESIAN_POINT('Ctrl Pts',(194.404814336053,0.779257501134259,
123.845115552844));
#238647=CARTESIAN_POINT('Ctrl Pts',(194.12636671224,-5.43380225522669,126.387107265649));
#238648=CARTESIAN_POINT('Ctrl Pts',(193.847919088427,-6.65346319503207,
132.988339014042));
#238649=CARTESIAN_POINT('Ctrl Pts',(193.569471464615,-1.75891649835014,
137.58260130935));
#238650=CARTESIAN_POINT('Ctrl Pts',(193.291023840801,4.75198853246758,135.947991544374));
#238651=CARTESIAN_POINT('Ctrl Pts',(193.012576216989,6.89604824949333,129.586636238002));
#238652=CARTESIAN_POINT('Ctrl Pts',(192.734128593176,2.70297651592057,124.344310147306));
#238653=CARTESIAN_POINT('Ctrl Pts',(192.455680969363,-3.97399858803937,
125.038454847768));
#238654=CARTESIAN_POINT('Ctrl Pts',(192.17723334555,-6.99906313021511,131.031185270517));
#238655=CARTESIAN_POINT('Ctrl Pts',(191.898785721737,-3.59233057896577,
136.815474918205));
#238656=CARTESIAN_POINT('Ctrl Pts',(191.620338097924,3.11557827924791,137.075844182864));
#238657=CARTESIAN_POINT('Ctrl Pts',(191.341890474111,6.96042290329331,131.573026430018));
#238658=CARTESIAN_POINT('Ctrl Pts',(191.063442850298,4.40897891477476,125.363842346942));
#238659=CARTESIAN_POINT('Ctrl Pts',(190.784995226486,-2.19410130582752,
124.154228770475));
#238660=CARTESIAN_POINT('Ctrl Pts',(190.506547602672,-6.78090961418206,
129.055761484483));
#238661=CARTESIAN_POINT('Ctrl Pts',(190.22809997886,-5.13639325295408,135.564171377977));
#238662=CARTESIAN_POINT('Ctrl Pts',(189.949652355047,1.22821758097839,137.698547712335));
#238663=CARTESIAN_POINT('Ctrl Pts',(189.671204731234,6.46415645975623,133.497502906364));
#238664=CARTESIAN_POINT('Ctrl Pts',(189.392757107421,5.75985134361714,126.821591904301));
#238665=CARTESIAN_POINT('Ctrl Pts',(189.114309483608,-0.237475772924818,
123.80565078066));
#238666=CARTESIAN_POINT('Ctrl Pts',(188.835861859795,-6.01657425548534,
127.221182091151));
#238667=CARTESIAN_POINT('Ctrl Pts',(188.557414235982,-6.2667349232476,133.929479419415));
#238668=CARTESIAN_POINT('Ctrl Pts',(188.278966612169,-0.758072343566082,
137.76594523932));
#238669=CARTESIAN_POINT('Ctrl Pts',(188.000518988357,5.44722168595988,135.205054884148));
#238670=CARTESIAN_POINT('Ctrl Pts',(187.722071364544,6.64678509766207,128.600141483854));
#238671=CARTESIAN_POINT('Ctrl Pts',(187.443623740731,1.73827771811677,124.02079778535));
#238672=CARTESIAN_POINT('Ctrl Pts',(187.165176116918,-4.76762196479028,
125.675216934184));
#238673=CARTESIAN_POINT('Ctrl Pts',(186.886728493105,-6.89230997333645,
132.043068555446));
#238674=CARTESIAN_POINT('Ctrl Pts',(186.608280869292,-2.68330182444739,
137.272608096043));
#238675=CARTESIAN_POINT('Ctrl Pts',(186.329833245479,3.99152961452714,136.558144195375));
#238676=CARTESIAN_POINT('Ctrl Pts',(186.051385621667,6.99834033481346,130.556234274655));
#238677=CARTESIAN_POINT('Ctrl Pts',(185.772937997853,3.5740181753383,124.782340341422));
#238678=CARTESIAN_POINT('Ctrl Pts',(185.494490374041,-3.13465208677821,
124.542388849921));
#238679=CARTESIAN_POINT('Ctrl Pts',(185.216042750227,-6.96273021741339,
130.056883498557));
#238680=CARTESIAN_POINT('Ctrl Pts',(184.937595126415,-4.39239942652681,
136.258273103275));
#238681=CARTESIAN_POINT('Ctrl Pts',(184.659147502602,2.21433185669671,137.447783572063));
#238682=CARTESIAN_POINT('Ctrl Pts',(184.380699878789,6.78620033974098,132.532312894923));
#238683=CARTESIAN_POINT('Ctrl Pts',(184.102252254976,5.12188223488049,126.028938490053));
#238684=CARTESIAN_POINT('Ctrl Pts',(183.823804631163,-1.24919542597752,
123.913943728027));
#238685=CARTESIAN_POINT('Ctrl Pts',(183.54535700735,-6.47232351695142,128.130905471908));
#238686=CARTESIAN_POINT('Ctrl Pts',(183.266909383538,-5.74770248642891,
134.804641889104));
#238687=CARTESIAN_POINT('Ctrl Pts',(182.988461759724,0.258776338245136,
137.80231524236));
#238688=CARTESIAN_POINT('Ctrl Pts',(182.710014135912,6.02745234999885,134.369210164519));
#238689=CARTESIAN_POINT('Ctrl Pts',(182.431566512099,6.25719410952084,127.66018250561));
#238690=CARTESIAN_POINT('Ctrl Pts',(182.153118888286,0.73688016331929,123.840500929948));
#238691=CARTESIAN_POINT('Ctrl Pts',(181.874671264473,-5.46059065437546,
126.420266203747));
#238692=CARTESIAN_POINT('Ctrl Pts',(181.59622364066,-6.64004542538295,133.028800068927));
#238693=CARTESIAN_POINT('Ctrl Pts',(181.317776016847,-1.71762283471616,
137.593182748215));
#238694=CARTESIAN_POINT('Ctrl Pts',(181.039328393035,4.78321123051439,135.918969541833));
#238695=CARTESIAN_POINT('Ctrl Pts',(180.760880769221,6.88850784776155,129.544680596588));
#238696=CARTESIAN_POINT('Ctrl Pts',(180.482433145409,2.66360227523266,124.32797605183));
#238697=CARTESIAN_POINT('Ctrl Pts',(180.203985521595,-4.00902366402984,
125.062752534008));
#238698=CARTESIAN_POINT('Ctrl Pts',(179.925537897783,-6.99755270774298,
131.073786351827));
#238699=CARTESIAN_POINT('Ctrl Pts',(179.64709027397,-3.5556726624947,136.837231082039));
#238700=CARTESIAN_POINT('Ctrl Pts',(179.368642650157,3.15369685531979,137.056762577506));
#238701=CARTESIAN_POINT('Ctrl Pts',(179.090195026344,6.96497302975191,131.530642118605));
#238702=CARTESIAN_POINT('Ctrl Pts',(178.811747402531,4.37577924769062,125.337104441072));
#238703=CARTESIAN_POINT('Ctrl Pts',(178.533299778718,-2.23454189429802,
124.167708099424));
#238704=CARTESIAN_POINT('Ctrl Pts',(178.254852154906,-6.79142819886702,
129.097071203448));
#238705=CARTESIAN_POINT('Ctrl Pts',(177.976404531092,-5.10732376838957,
135.595349873321));
#238706=CARTESIAN_POINT('Ctrl Pts',(177.69795690728,1.27016169860089,137.690943469992));
#238707=CARTESIAN_POINT('Ctrl Pts',(177.419509283467,6.48043061542571,133.458103853558));
#238708=CARTESIAN_POINT('Ctrl Pts',(177.141061659654,5.73550038331004,126.786603845811));
#238709=CARTESIAN_POINT('Ctrl Pts',(176.862614035841,-0.280074506296806,
123.807226032976));
#238710=CARTESIAN_POINT('Ctrl Pts',(176.584166412028,-6.0382746070172,127.257873074351));
#238711=CARTESIAN_POINT('Ctrl Pts',(176.305718788215,-6.24759533000263,
133.967568912391));
#238712=CARTESIAN_POINT('Ctrl Pts',(176.027271164402,-0.71568115671533,
137.770430858802));
#238713=CARTESIAN_POINT('Ctrl Pts',(175.748823540589,5.4739090366252,135.171814564968));
#238714=CARTESIAN_POINT('Ctrl Pts',(175.470375916777,6.63324424063007,128.559721455457));
#238715=CARTESIAN_POINT('Ctrl Pts',(175.191928292964,1.69695203949225,124.010342079205));
#238716=CARTESIAN_POINT('Ctrl Pts',(174.913480669151,-4.79875618522306,
125.704333833448));
#238717=CARTESIAN_POINT('Ctrl Pts',(174.635033045338,-6.88464190799096,
132.085001052137));
#238718=CARTESIAN_POINT('Ctrl Pts',(174.356585421525,-2.64387805077028,
137.288822274217));
#238719=CARTESIAN_POINT('Ctrl Pts',(174.078137797712,4.02648057448505,136.533740017397));
#238720=CARTESIAN_POINT('Ctrl Pts',(173.799690173899,6.99670025630013,130.513637987877));
#238721=CARTESIAN_POINT('Ctrl Pts',(173.521242550086,3.53729421038521,124.76069585245));
#238722=CARTESIAN_POINT('Ctrl Pts',(173.242794926273,-3.17271240844464,
124.561586386726));
#238723=CARTESIAN_POINT('Ctrl Pts',(172.96434730246,-6.96715131953175,130.099281462668));
#238724=CARTESIAN_POINT('Ctrl Pts',(172.685899678648,-4.35911853223319,
136.284909836929));
#238725=CARTESIAN_POINT('Ctrl Pts',(172.407452054835,2.25473123140845,137.434181218309));
#238726=CARTESIAN_POINT('Ctrl Pts',(172.129004431022,6.79659314313001,132.490971352347));
#238727=CARTESIAN_POINT('Ctrl Pts',(171.850556807209,5.09271798834896,125.997848616637));
#238728=CARTESIAN_POINT('Ctrl Pts',(171.572109183396,-1.29111620461978,
123.921675598615));
#238729=CARTESIAN_POINT('Ctrl Pts',(171.293661559583,-6.48847768007612,
128.170353875152));
#238730=CARTESIAN_POINT('Ctrl Pts',(171.01521393577,-5.72324514729908,134.839555669585));
#238731=CARTESIAN_POINT('Ctrl Pts',(170.736766311957,0.301370079776633,
137.800610341449));
#238732=CARTESIAN_POINT('Ctrl Pts',(170.458318688145,6.04904092628448,134.332453302864));
#238733=CARTESIAN_POINT('Ctrl Pts',(170.179871064331,6.23793867361471,127.6221514434));
#238734=CARTESIAN_POINT('Ctrl Pts',(169.901423440519,0.694475520138818,
123.836144355433));
#238735=CARTESIAN_POINT('Ctrl Pts',(169.622975816706,-5.4871767093294,126.453587596077));
#238736=CARTESIAN_POINT('Ctrl Pts',(169.344528192893,-6.62638160640872,
133.06917869639));
#238737=CARTESIAN_POINT('Ctrl Pts',(169.06608056908,-1.67626552393645,137.603512624779));
#238738=CARTESIAN_POINT('Ctrl Pts',(168.787632945267,4.81425668490999,135.88975801558));
#238739=CARTESIAN_POINT('Ctrl Pts',(168.509185321454,6.88071218983824,129.50277163308));
#238740=CARTESIAN_POINT('Ctrl Pts',(168.230737697641,2.62412933378287,124.311881941165));
#238741=CARTESIAN_POINT('Ctrl Pts',(167.952290073828,-4.0439001841742,125.087262977647));
#238742=CARTESIAN_POINT('Ctrl Pts',(167.673842450016,-6.99578298838191,
131.116377449467));
#238743=CARTESIAN_POINT('Ctrl Pts',(167.395394826203,-3.51888298926545,
136.858763695638));
#238744=CARTESIAN_POINT('Ctrl Pts',(167.11694720239,3.19169856999505,137.037449287095));
#238745=CARTESIAN_POINT('Ctrl Pts',(166.838499578577,6.96926506657354,131.488230894564));
#238746=CARTESIAN_POINT('Ctrl Pts',(166.560051954764,4.34241743449723,125.310569126392));
#238747=CARTESIAN_POINT('Ctrl Pts',(166.281604330951,-2.27489968099678,
124.181433351974));
#238748=CARTESIAN_POINT('Ctrl Pts',(166.003156707138,-6.80169512468258,
129.13844418665));
#238749=CARTESIAN_POINT('Ctrl Pts',(165.724709083325,-5.0780650300646,135.626350836796));
#238750=CARTESIAN_POINT('Ctrl Pts',(165.446261459512,1.31205874991464,137.683084042787));
#238751=CARTESIAN_POINT('Ctrl Pts',(165.1678138357,6.49646463635559,133.418606465321));
#238752=CARTESIAN_POINT('Ctrl Pts',(164.889366211887,5.71093689192698,126.751764666776));
#238753=CARTESIAN_POINT('Ctrl Pts',(164.610918588074,-0.322662861405092,
123.809060566689));
#238754=CARTESIAN_POINT('Ctrl Pts',(164.332470964261,-6.05975120806294,
127.29469547395));
#238755=CARTESIAN_POINT('Ctrl Pts',(164.054023340448,-6.22822422981513,
134.00554119152));
#238756=CARTESIAN_POINT('Ctrl Pts',(163.775575716635,-0.673263450036036,
137.774658347991));
#238757=CARTESIAN_POINT('Ctrl Pts',(163.497128092822,5.50039354957815,135.138412408175));
#238758=CARTESIAN_POINT('Ctrl Pts',(163.218680469009,6.61945758629338,128.51938460299));
#238759=CARTESIAN_POINT('Ctrl Pts',(162.940232845196,1.65556347968583,124.000138127916));
#238760=CARTESIAN_POINT('Ctrl Pts',(162.661785221384,-4.82971258598073,
125.733639716082));
#238761=CARTESIAN_POINT('Ctrl Pts',(162.383337597571,-6.87671872970774,
132.126886094224));
#238762=CARTESIAN_POINT('Ctrl Pts',(162.104889973758,-2.60435630721971,
137.304796168278));
#238763=CARTESIAN_POINT('Ctrl Pts',(161.826442349945,4.06128233172446,136.509123535159));
#238764=CARTESIAN_POINT('Ctrl Pts',(161.547994726132,6.99480091248578,130.471052473933));
#238765=CARTESIAN_POINT('Ctrl Pts',(161.269547102319,3.50043916969439,124.739275313697));
#238766=CARTESIAN_POINT('Ctrl Pts',(160.991099478506,-3.21065516408591,
124.581015251828));
#238767=CARTESIAN_POINT('Ctrl Pts',(160.712651854693,-6.97131425129578,
130.141705553748));
#238768=CARTESIAN_POINT('Ctrl Pts',(160.434204230881,-4.32567610919938,
136.311343486817));
#238769=CARTESIAN_POINT('Ctrl Pts',(160.155756607067,2.29504705622523,137.420333194114));
#238770=CARTESIAN_POINT('Ctrl Pts',(159.877308983254,6.80673409626067,132.449567311792));
#238771=CARTESIAN_POINT('Ctrl Pts',(159.598861359442,5.06336502927952,125.966936850291));
#238772=CARTESIAN_POINT('Ctrl Pts',(159.320413735629,-1.33298914047637,
123.929662509627));
#238773=CARTESIAN_POINT('Ctrl Pts',(159.041966111816,-6.50439141027418,
128.209899882485));
#238774=CARTESIAN_POINT('Ctrl Pts',(158.763518488003,-5.69857573121565,
134.874319924428));
#238775=CARTESIAN_POINT('Ctrl Pts',(158.48507086419,0.343952653928878,137.798646191931));
#238776=CARTESIAN_POINT('Ctrl Pts',(158.206623240377,6.07040535313402,134.295565706438));
#238777=CARTESIAN_POINT('Ctrl Pts',(157.928175616564,6.2184520885971,127.584238299121));
#238778=CARTESIAN_POINT('Ctrl Pts',(157.649727992752,0.652045142912632,
123.832045990734));
#238779=CARTESIAN_POINT('Ctrl Pts',(157.371280368939,-5.51355943493244,
126.487070207899));
#238780=CARTESIAN_POINT('Ctrl Pts',(157.092832745126,-6.61247224442723,
133.109473400187));
#238781=CARTESIAN_POINT('Ctrl Pts',(156.814385121313,-1.63484609852131,
137.613590556265));
#238782=CARTESIAN_POINT('Ctrl Pts',(156.5359374975,4.84512374525377,135.860358048054));
#238783=CARTESIAN_POINT('Ctrl Pts',(156.257489873687,6.87266156459436,129.46091090043));
#238784=CARTESIAN_POINT('Ctrl Pts',(155.979042249874,2.58455915425555,124.296028411687));
#238785=CARTESIAN_POINT('Ctrl Pts',(155.700594626061,-4.07862685611001,
125.111985270442));
#238786=CARTESIAN_POINT('Ctrl Pts',(155.422147002248,-6.99375403770952,
131.158956985208));
#238787=CARTESIAN_POINT('Ctrl Pts',(155.143699378435,-3.48196292253304,
136.880071961106));
#238788=CARTESIAN_POINT('Ctrl Pts',(154.865251754623,3.22958201510593,137.017905027291));
#238789=CARTESIAN_POINT('Ctrl Pts',(154.58680413081,6.97329885471516,131.445794329457));
#238790=CARTESIAN_POINT('Ctrl Pts',(154.308356506997,4.30889471142897,125.284237386175));
#238791=CARTESIAN_POINT('Ctrl Pts',(154.029908883184,-2.31517317045128,
124.195404019528));
#238792=CARTESIAN_POINT('Ctrl Pts',(153.751461259371,-6.81171001118396,
129.179878900999));
#238793=CARTESIAN_POINT('Ctrl Pts',(153.473013635558,-5.04861812217248,
135.65717311965));
#238794=CARTESIAN_POINT('Ctrl Pts',(153.194566011745,1.3539071824088,137.674969721956));
#238795=CARTESIAN_POINT('Ctrl Pts',(152.916118387933,6.51225792839928,133.379012205241));
#238796=CARTESIAN_POINT('Ctrl Pts',(152.637670764119,5.68616177967723,126.717075658174));
#238797=CARTESIAN_POINT('Ctrl Pts',(152.359223140307,-0.365239260122265,
123.811154313817));
#238798=CARTESIAN_POINT('Ctrl Pts',(152.080775516494,-6.08100326279917,
127.331647925483));
#238799=CARTESIAN_POINT('Ctrl Pts',(151.802327892681,-6.20862234048841,
134.043394849727));
#238800=CARTESIAN_POINT('Ctrl Pts',(151.523880268868,-0.630820795332096,
137.778627550233));
#238801=CARTESIAN_POINT('Ctrl Pts',(151.245432645055,5.52667424342534,135.104849651499));
#238802=CARTESIAN_POINT('Ctrl Pts',(150.966985021242,6.60542564552152,128.479132421149));
#238803=CARTESIAN_POINT('Ctrl Pts',(150.688537397429,1.61411357236584,123.990186309594));
#238804=CARTESIAN_POINT('Ctrl Pts',(150.410089773616,-4.86049001996232,
125.763133496143));
#238805=CARTESIAN_POINT('Ctrl Pts',(150.131642149803,-6.8685407320831,132.168722129643));
#238806=CARTESIAN_POINT('Ctrl Pts',(149.853194525991,-2.56473805828847,
137.32052918631));
#238807=CARTESIAN_POINT('Ctrl Pts',(149.574746902178,4.09593359665354,136.484295660832));
#238808=CARTESIAN_POINT('Ctrl Pts',(149.296299278365,6.99264237375128,130.428479310845));
#238809=CARTESIAN_POINT('Ctrl Pts',(149.017851654552,3.46345441894284,124.718079518912));
#238810=CARTESIAN_POINT('Ctrl Pts',(148.739404030739,-3.24847894771935,
124.600674725279));
#238811=CARTESIAN_POINT('Ctrl Pts',(148.460956406926,-6.97521885844655,
130.184154199754));
#238812=CARTESIAN_POINT('Ctrl Pts',(148.182508783113,-4.29207339664657,
136.337573073429));
#238813=CARTESIAN_POINT('Ctrl Pts',(147.9040611593,2.33527783722936,137.406240012622));
#238814=CARTESIAN_POINT('Ctrl Pts',(147.625613535487,6.81662282335624,132.408102307496));
#238815=CARTESIAN_POINT('Ctrl Pts',(147.347165911675,5.03382444535687,125.936204336462));
#238816=CARTESIAN_POINT('Ctrl Pts',(147.068718287862,-1.37481268193005,
123.937904165105));
#238817=CARTESIAN_POINT('Ctrl Pts',(146.790270664049,-6.52006411785656,
128.249542028514));
#238818=CARTESIAN_POINT('Ctrl Pts',(146.511823040236,-5.67369515231286,
134.908933365434));
#238819=CARTESIAN_POINT('Ctrl Pts',(146.233375416423,0.386522482789046,
137.796422866589));
#238820=CARTESIAN_POINT('Ctrl Pts',(145.95492779261,6.09154483888081,134.258548742122));
#238821=CARTESIAN_POINT('Ctrl Pts',(145.676480168797,6.19873507655051,127.546444477659));
#238822=CARTESIAN_POINT('Ctrl Pts',(145.398032544984,0.609590603913882,
123.828205987717));
#238823=CARTESIAN_POINT('Ctrl Pts',(145.119584921171,-5.53973785356302,
126.520712798507));
#238824=CARTESIAN_POINT('Ctrl Pts',(144.841137297358,-6.59831785485502,
133.149682687181));
#238825=CARTESIAN_POINT('Ctrl Pts',(144.562689673546,-1.59336609328267,
137.623416169231));
#238826=CARTESIAN_POINT('Ctrl Pts',(144.284242049733,4.87581126775532,135.830770728684));
#238827=CARTESIAN_POINT('Ctrl Pts',(144.00579442592,6.86435627034879,129.419099949804));
#238828=CARTESIAN_POINT('Ctrl Pts',(143.727346802107,2.54489320293839,124.280416050852));
#238829=CARTESIAN_POINT('Ctrl Pts',(143.448899178294,-4.11320239302776,
125.136918496298));
#238830=CARTESIAN_POINT('Ctrl Pts',(143.170451554481,-6.99146593090932,
131.201523381251));
#238831=CARTESIAN_POINT('Ctrl Pts',(142.892003930668,-3.44491383038404,
136.901155088855));
#238832=CARTESIAN_POINT('Ctrl Pts',(142.613556306855,3.26734578686757,136.998130522314));
#238833=CARTESIAN_POINT('Ctrl Pts',(142.335108683042,6.97707424470332,131.403333995789));
#238834=CARTESIAN_POINT('Ctrl Pts',(142.05666105923,4.27521232068256,125.258110196154));
#238835=CARTESIAN_POINT('Ctrl Pts',(141.778213435417,-2.35536087031262,
124.209619584399));
#238836=CARTESIAN_POINT('Ctrl Pts',(141.499765811604,-6.8214724872659,129.221373811115));
#238837=CARTESIAN_POINT('Ctrl Pts',(141.221318187791,-5.01898413587917,
135.687815579753));
#238838=CARTESIAN_POINT('Ctrl Pts',(140.942870563978,1.39570544537436,137.666600808179));
#238839=CARTESIAN_POINT('Ctrl Pts',(140.664422940165,6.52780990633047,133.339322540502));
#238840=CARTESIAN_POINT('Ctrl Pts',(140.385975316352,5.66117596461176,126.68253810542));
#238841=CARTESIAN_POINT('Ctrl Pts',(140.10752769254,-0.407802124764288,
123.813507196776));
#238842=CARTESIAN_POINT('Ctrl Pts',(139.829080068726,-6.10202998372316,
127.368729059661));
#238843=CARTESIAN_POINT('Ctrl Pts',(139.550632444914,-6.18879038837768,
134.081128484328));
#238844=CARTESIAN_POINT('Ctrl Pts',(139.272184821101,-0.588354765331746,
137.78233831845));
#238845=CARTESIAN_POINT('Ctrl Pts',(138.993737197288,5.55275014432601,135.071127538621));
#238846=CARTESIAN_POINT('Ctrl Pts',(138.715289573475,6.59114893827324,128.438966401494));
#238847=CARTESIAN_POINT('Ctrl Pts',(138.436841949662,1.57260385347371,123.980486993006));
#238848=CARTESIAN_POINT('Ctrl Pts',(138.158394325849,-4.8910873466988,125.792814080728));
#238849=CARTESIAN_POINT('Ctrl Pts',(137.879946702036,-6.86010821815569,
132.210507608145));
#238850=CARTESIAN_POINT('Ctrl Pts',(137.601499078223,-2.52502477204539,
137.336020745319));
#238851=CARTESIAN_POINT('Ctrl Pts',(137.32305145441,4.13043308525698,136.459257314423));
#238852=CARTESIAN_POINT('Ctrl Pts',(137.044603830598,6.99022472008204,130.385920076178));
#238853=CARTESIAN_POINT('Ctrl Pts',(136.766156206785,3.42634132861412,124.69710925351));
#238854=CARTESIAN_POINT('Ctrl Pts',(136.487708582972,-3.28618235777073,
124.620564078594));
#238855=CARTESIAN_POINT('Ctrl Pts',(136.209260959159,-6.97886499629743,
130.226625827737));
#238856=CARTESIAN_POINT('Ctrl Pts',(135.930813335346,-4.25831163973555,
136.363597624819));
#238857=CARTESIAN_POINT('Ctrl Pts',(135.652365711533,2.37542208365453,137.391902196061));
#238858=CARTESIAN_POINT('Ctrl Pts',(135.37391808772,6.82625895798624,132.366577875963));
#238859=CARTESIAN_POINT('Ctrl Pts',(135.095470463907,5.00409733121823,125.905652213954));
#238860=CARTESIAN_POINT('Ctrl Pts',(134.817022840094,-1.4165852791943,123.946400259653));
#238861=CARTESIAN_POINT('Ctrl Pts',(134.538575216282,-6.53549522206528,
128.289278844285));
#238862=CARTESIAN_POINT('Ctrl Pts',(134.260127592469,-5.64860433254967,
134.943394709987));
#238863=CARTESIAN_POINT('Ctrl Pts',(133.981679968656,0.429077988916399,
137.793940447809));
#238864=CARTESIAN_POINT('Ctrl Pts',(133.703232344843,6.1124586001935,134.221403781595));
#238865=CARTESIAN_POINT('Ctrl Pts',(133.42478472103,6.17878836809604,127.508771379477));
#238866=CARTESIAN_POINT('Ctrl Pts',(133.146337097217,0.567113476311158,
123.824624488677));
#238867=CARTESIAN_POINT('Ctrl Pts',(132.867889473404,-5.5657109951702,126.554514121259));
#238868=CARTESIAN_POINT('Ctrl Pts',(132.589441849591,-6.58391896218814,
133.189805067404));
#238869=CARTESIAN_POINT('Ctrl Pts',(132.310994225778,-1.55182704527753,
137.632989099587));
#238870=CARTESIAN_POINT('Ctrl Pts',(132.032546601965,4.90631811527725,135.800997153839));
#238871=CARTESIAN_POINT('Ctrl Pts',(131.754098978153,6.85579661485726,129.377340330521));
#238872=CARTESIAN_POINT('Ctrl Pts',(131.47565135434,2.50513294966777,124.265045437181));
#238873=CARTESIAN_POINT('Ctrl Pts',(131.197203730527,-4.14762551371829,
125.162061731307));
#238874=CARTESIAN_POINT('Ctrl Pts',(130.918756106714,-6.98891875276791,
131.244075060281));
#238875=CARTESIAN_POINT('Ctrl Pts',(130.640308482901,-3.4077370856862,136.922012297644));
#238876=CARTESIAN_POINT('Ctrl Pts',(130.361860859088,3.30498848592948,136.978126504915));
#238877=CARTESIAN_POINT('Ctrl Pts',(130.083413235275,6.98059109663955,131.360851466943));
#238878=CARTESIAN_POINT('Ctrl Pts',(129.804965611462,4.24137151037132,125.232188524482));
#238879=CARTESIAN_POINT('Ctrl Pts',(129.526517987649,-2.39546129141071,
124.224079519825));
#238880=CARTESIAN_POINT('Ctrl Pts',(129.248070363836,-6.83098219117618,
129.262927379388));
#238881=CARTESIAN_POINT('Ctrl Pts',(128.969622740024,-4.98916416928312,
135.718277081636));
#238882=CARTESIAN_POINT('Ctrl Pts',(128.691175116211,1.43745198996158,137.657977611568));
#238883=CARTESIAN_POINT('Ctrl Pts',(128.412727492398,6.54311999386511,133.299538941816));
#238884=CARTESIAN_POINT('Ctrl Pts',(128.134279868585,5.63598037258881,126.648153288314));
#238885=CARTESIAN_POINT('Ctrl Pts',(127.855832244772,-0.450349878148651,
123.81611912838));
#238886=CARTESIAN_POINT('Ctrl Pts',(127.577384620959,-6.12283059168226,
127.40593750243));
#238887=CARTESIAN_POINT('Ctrl Pts',(127.298936997146,-6.16872910836309,
134.118740697091));
#238888=CARTESIAN_POINT('Ctrl Pts',(127.020489373333,-0.545866933628919,
137.785790515136));
#238889=CARTESIAN_POINT('Ctrl Pts',(126.742041749521,5.57862028602806,135.037247319125));
#238890=CARTESIAN_POINT('Ctrl Pts',(126.463594125708,6.57662799357718,128.398888032392));
#238891=CARTESIAN_POINT('Ctrl Pts',(126.185146501895,1.53103586116759,123.971040537565));
#238892=CARTESIAN_POINT('Ctrl Pts',(125.906698878082,-4.92150343239493,
125.822680370014));
#238893=CARTESIAN_POINT('Ctrl Pts',(125.628251254269,-6.85142150039552,
132.252240981353));
#238894=CARTESIAN_POINT('Ctrl Pts',(125.349803630456,-2.48521792008072,
137.351270271259));
#238895=CARTESIAN_POINT('Ctrl Pts',(125.071356006643,4.16477951914341,136.434009423738));
#238896=CARTESIAN_POINT('Ctrl Pts',(124.79290838283,6.98754804106521,130.343376346978));
#238897=CARTESIAN_POINT('Ctrl Pts',(124.514460759018,3.38910127394743,124.676365294554));
#238898=CARTESIAN_POINT('Ctrl Pts',(124.236013135205,-3.32376399712637,
124.640682574762));
#238899=CARTESIAN_POINT('Ctrl Pts',(123.957565511392,-6.98225252973936,
130.269118863895));
#238900=CARTESIAN_POINT('Ctrl Pts',(123.679117887579,-4.22439208952083,
136.389416176637));
#238901=CARTESIAN_POINT('Ctrl Pts',(123.400670263766,2.41547830794073,137.377320275725));
#238902=CARTESIAN_POINT('Ctrl Pts',(123.122222639953,6.83564214308024,132.324995555895));
#238903=CARTESIAN_POINT('Ctrl Pts',(122.84377501614,4.97418478841272,125.875281614887));
#238904=CARTESIAN_POINT('Ctrl Pts',(122.565327392328,-1.45830538437,123.955150478444));
#238905=CARTESIAN_POINT('Ctrl Pts',(122.286879768514,-6.55068415109515,
128.329108857337));
#238906=CARTESIAN_POINT('Ctrl Pts',(122.008432144702,-5.62330420167569,
134.977702681109));
#238907=CARTESIAN_POINT('Ctrl Pts',(121.729984520888,0.471617595401148,
137.791199027578));
#238908=CARTESIAN_POINT('Ctrl Pts',(121.451536897076,6.13314586210485,134.184132201278));
#238909=CARTESIAN_POINT('Ctrl Pts',(121.173089273263,6.15861270236637,127.471220400567));
#238910=CARTESIAN_POINT('Ctrl Pts',(120.89464164945,0.52461533410983,123.821301626325));
#238911=CARTESIAN_POINT('Ctrl Pts',(120.616194025637,-5.5914778973097,126.588472923636));
#238912=CARTESIAN_POINT('Ctrl Pts',(120.337746401824,-6.56927609998288,
133.229839054105));
#238913=CARTESIAN_POINT('Ctrl Pts',(120.059298778011,-1.51023049375061,
137.642308992603));
#238914=CARTESIAN_POINT('Ctrl Pts',(119.780851154198,4.93664315737715,135.77103842679));
#238915=CARTESIAN_POINT('Ctrl Pts',(119.502403530385,6.84698291530094,129.33563359));
#238916=CARTESIAN_POINT('Ctrl Pts',(119.223955906573,2.46527986777437,124.249917140239));
#238917=CARTESIAN_POINT('Ctrl Pts',(118.94550828276,-4.18189494262004,125.187414043775));
#238918=CARTESIAN_POINT('Ctrl Pts',(118.667060658947,-6.98611259767199,
131.28661044553));
#238919=CARTESIAN_POINT('Ctrl Pts',(118.388613035134,-3.37043406603744,
136.942642814599));
#238920=CARTESIAN_POINT('Ctrl Pts',(118.110165411321,3.34250871742766,136.95789371635));
#238921=CARTESIAN_POINT('Ctrl Pts',(117.831717787508,6.98384928020556,131.318348317123));
#238922=CARTESIAN_POINT('Ctrl Pts',(117.553270163695,4.20737353447909,125.206473331696));
#238923=CARTESIAN_POINT('Ctrl Pts',(117.274822539882,-2.43547294780967,
124.238783289987));
#238924=CARTESIAN_POINT('Ctrl Pts',(116.99637491607,-6.84023877052931,129.304538066038));
#238925=CARTESIAN_POINT('Ctrl Pts',(116.717927292256,-4.95915932737393,
135.748556496538));
#238926=CARTESIAN_POINT('Ctrl Pts',(116.439479668444,1.47914526923655,137.649100451659));
#238927=CARTESIAN_POINT('Ctrl Pts',(116.161032044631,6.55818762368211,133.259662883379));
#238928=CARTESIAN_POINT('Ctrl Pts',(115.882584420818,5.61057593724064,126.613922481));
#238929=CARTESIAN_POINT('Ctrl Pts',(115.604136797005,-0.49288094365267,
123.818990011842));
#238930=CARTESIAN_POINT('Ctrl Pts',(115.325689173192,-6.14340431590201,
127.443271875017));
#238931=CARTESIAN_POINT('Ctrl Pts',(115.047241549379,-6.14843924382291,
134.156230094282));
#238932=CARTESIAN_POINT('Ctrl Pts',(114.768793925566,-0.5033588746261,137.78898401237));
#238933=CARTESIAN_POINT('Ctrl Pts',(114.490346301753,5.60428370990391,135.003210248456));
#238934=CARTESIAN_POINT('Ctrl Pts',(114.211898677941,6.56186334951224,128.358898798961));
#238935=CARTESIAN_POINT('Ctrl Pts',(113.933451054127,1.48941113576461,123.961847293312));
#238936=CARTESIAN_POINT('Ctrl Pts',(113.655003430315,-4.95173714997151,
125.852731257293));
#238937=CARTESIAN_POINT('Ctrl Pts',(113.376555806502,-6.84248090069202,
132.293920702821));
#238938=CARTESIAN_POINT('Ctrl Pts',(113.098108182689,-2.4453189774521,137.366277199056));
#238939=CARTESIAN_POINT('Ctrl Pts',(112.819660558876,4.19897162559319,136.408552924347));
#238940=CARTESIAN_POINT('Ctrl Pts',(112.541212935063,6.98461243588604,130.300849699721));
#238941=CARTESIAN_POINT('Ctrl Pts',(112.26276531125,3.35173563488669,124.655848410718));
#238942=CARTESIAN_POINT('Ctrl Pts',(111.984317687437,-3.3612224731848,124.661029468288));
#238943=CARTESIAN_POINT('Ctrl Pts',(111.705870063624,-6.98538133324609,
130.311631733633));
#238944=CARTESIAN_POINT('Ctrl Pts',(111.427422439812,-4.1903160029037,136.415027772168));
#238945=CARTESIAN_POINT('Ctrl Pts',(111.148974815999,2.45544502578993,137.362494791951));
#238946=CARTESIAN_POINT('Ctrl Pts',(110.870527192186,6.84477203094083,132.28335688814));
#238947=CARTESIAN_POINT('Ctrl Pts',(110.592079568373,4.94408792536061,125.845093664656));
#238948=CARTESIAN_POINT('Ctrl Pts',(110.31363194456,-1.49997145150339,123.964154497236));
#238949=CARTESIAN_POINT('Ctrl Pts',(110.035184320747,-6.56563034211481,
128.369030591753));
#238950=CARTESIAN_POINT('Ctrl Pts',(109.756736696934,-5.59779569719655,
135.011856007506));
#238951=CARTESIAN_POINT('Ctrl Pts',(109.478289073121,0.514139725922464,
137.788198707481));
#238952=CARTESIAN_POINT('Ctrl Pts',(109.199841449309,6.15360585804082,134.146735382281));
#238953=CARTESIAN_POINT('Ctrl Pts',(108.921393825496,6.13820882697821,127.433792932393));
#238954=CARTESIAN_POINT('Ctrl Pts',(108.642946201683,0.482097752094529,
123.818237523792));
#238955=CARTESIAN_POINT('Ctrl Pts',(108.36449857787,-5.61703760517944,126.622587947283));
#238956=CARTESIAN_POINT('Ctrl Pts',(108.086050954057,-6.5543898108359,133.26978316381));
#238957=CARTESIAN_POINT('Ctrl Pts',(107.807603330244,-1.46857798007734,
137.651375502926));
#238958=CARTESIAN_POINT('Ctrl Pts',(107.529155706431,4.96678527034939,135.740895657668));
#238959=CARTESIAN_POINT('Ctrl Pts',(107.250708082618,6.83791549827476,129.2939812737));
#238960=CARTESIAN_POINT('Ctrl Pts',(106.972260458805,2.42533543402888,124.23503172061));
#238961=CARTESIAN_POINT('Ctrl Pts',(106.693812834992,-4.21600940986681,
125.212974494265));
#238962=CARTESIAN_POINT('Ctrl Pts',(106.415365211179,-6.98304756960462,
131.329127960835));
#238963=CARTESIAN_POINT('Ctrl Pts',(106.136917587367,-3.33300615371489,
136.96304587525));
#238964=CARTESIAN_POINT('Ctrl Pts',(105.858469963554,3.37990509103613,136.937432906355));
#238965=CARTESIAN_POINT('Ctrl Pts',(105.580022339741,6.98684867466819,131.275826121299));
#238966=CARTESIAN_POINT('Ctrl Pts',(105.301574715928,4.1732196528133,125.180965570684));
#238967=CARTESIAN_POINT('Ctrl Pts',(105.023127092115,-2.4753943568629,124.253730350031));
#238968=CARTESIAN_POINT('Ctrl Pts',(104.744679468302,-6.84924188231931,
129.346204329164));
#238969=CARTESIAN_POINT('Ctrl Pts',(104.466231844489,-4.92897072199215,
135.778652702442));
#238970=CARTESIAN_POINT('Ctrl Pts',(104.187784220676,1.52078373823962,137.639969657397));
#238971=CARTESIAN_POINT('Ctrl Pts',(103.909336596864,6.57301223744494,133.219695842813));
#238972=CARTESIAN_POINT('Ctrl Pts',(103.63088897305,5.58496359993783,126.579846951912));
#238973=CARTESIAN_POINT('Ctrl Pts',(103.352441349238,-0.535393745272065,
123.82211974078));
#238974=CARTESIAN_POINT('Ctrl Pts',(103.073993725425,-6.1637503940156,127.480730793984));
#238975=CARTESIAN_POINT('Ctrl Pts',(102.795546101612,-6.12792154660547,
134.193595286717));
#238976=CARTESIAN_POINT('Ctrl Pts',(102.517098477799,-0.460832163475232,
137.791918691816));
#238977=CARTESIAN_POINT('Ctrl Pts',(102.238650853986,5.6297394649859,134.96901758787));
#238978=CARTESIAN_POINT('Ctrl Pts',(101.960203230173,6.54685555318778,128.319000183017));
#238979=CARTESIAN_POINT('Ctrl Pts',(101.68175560636,1.44773121968427,123.952907600908));
#238980=CARTESIAN_POINT('Ctrl Pts',(101.403307982548,-4.981787379107,125.882965629019));
#238981=CARTESIAN_POINT('Ctrl Pts',(101.124860358735,-6.83328675034245,
132.335545228093));
#238982=CARTESIAN_POINT('Ctrl Pts',(100.846412734922,-2.4053294226295,137.38104097262));
#238983=CARTESIAN_POINT('Ctrl Pts',(100.567965111109,4.23300813760519,136.382888759548));
#238984=CARTESIAN_POINT('Ctrl Pts',(100.289517487296,6.98141801332452,130.258341710245));
#238985=CARTESIAN_POINT('Ctrl Pts',(100.011069863483,3.31424579602927,124.635559362262));
#238986=CARTESIAN_POINT('Ctrl Pts',(99.7326222396699,-3.39855639790849,
124.681604005209));
#238987=CARTESIAN_POINT('Ctrl Pts',(99.4541746158571,-6.98825129087862,
130.354162861621));
#238988=CARTESIAN_POINT('Ctrl Pts',(99.1757269920442,-4.15608464258612,
136.440431462363));
#238989=CARTESIAN_POINT('Ctrl Pts',(98.8972793682313,2.49532075622072,137.347426294104));
#238990=CARTESIAN_POINT('Ctrl Pts',(98.6188317444184,6.85364828325664,132.241663415635));
#238991=CARTESIAN_POINT('Ctrl Pts',(98.3403841206056,4.91380785731226,125.815089481885));
#238992=CARTESIAN_POINT('Ctrl Pts',(98.0619364967926,-1.54158193664305,
123.97341198238));
#238993=CARTESIAN_POINT('Ctrl Pts',(97.7834888729798,-6.58033324128762,
128.409042568218));
#238994=CARTESIAN_POINT('Ctrl Pts',(97.5050412491668,-5.57207976433927,
135.045853423614));
#238995=CARTESIAN_POINT('Ctrl Pts',(97.226593625354,0.55664280480716,137.784939598694));
#238996=CARTESIAN_POINT('Ctrl Pts',(96.948146001541,6.17383782984873,134.109214710358));
#238997=CARTESIAN_POINT('Ctrl Pts',(96.6696983777281,6.11757749800464,127.396490361844));
#238998=CARTESIAN_POINT('Ctrl Pts',(96.3912507539153,0.43956230576973,123.815432294619));
#238999=CARTESIAN_POINT('Ctrl Pts',(96.1128031301024,-5.64238917165504,
126.656857928054));
#239000=CARTESIAN_POINT('Ctrl Pts',(95.8343555062895,-6.53926064636413,
133.309635916377));
#239001=CARTESIAN_POINT('Ctrl Pts',(95.5559078824767,-1.42687104770695,
137.660188294596));
#239002=CARTESIAN_POINT('Ctrl Pts',(95.2774602586637,4.99674333726689,135.710569963425));
#239003=CARTESIAN_POINT('Ctrl Pts',(94.9990126348508,6.82859469977515,129.252384925061));
#239004=CARTESIAN_POINT('Ctrl Pts',(94.720565011038,2.38530112858694,124.22038972988));
#239005=CARTESIAN_POINT('Ctrl Pts',(94.442117387225,-4.24996765133445,125.238742135624));
#239006=CARTESIAN_POINT('Ctrl Pts',(94.1636697634123,-6.97972378214161,
131.371626030693));
#239007=CARTESIAN_POINT('Ctrl Pts',(93.885222139599,-3.29545473562348,136.983220723554));
#239008=CARTESIAN_POINT('Ctrl Pts',(93.6067745157866,3.41717622101856,136.91674483311));
#239009=CARTESIAN_POINT('Ctrl Pts',(93.3283268919733,6.98958916888377,131.233286455149));
#239010=CARTESIAN_POINT('Ctrl Pts',(93.0498792681607,4.13891113095855,125.155666186642));
#239011=CARTESIAN_POINT('Ctrl Pts',(92.7714316443476,-2.51522403926791,
124.268920146089));
#239012=CARTESIAN_POINT('Ctrl Pts',(92.4929840205349,-6.85799119293255,
129.387924624807));
#239013=CARTESIAN_POINT('Ctrl Pts',(92.2145363967218,-4.89859947178764,
135.808564584124));
#239014=CARTESIAN_POINT('Ctrl Pts',(91.9360887729091,1.562365854042,137.63058556713));
#239015=CARTESIAN_POINT('Ctrl Pts',(91.6576411490961,6.58759328582208,133.179639301113));
#239016=CARTESIAN_POINT('Ctrl Pts',(91.3791935252832,5.55914430975498,126.545927963732));
#239017=CARTESIAN_POINT('Ctrl Pts',(91.1007459014705,-0.57788670767935,
123.825508199223));
#239018=CARTESIAN_POINT('Ctrl Pts',(90.8222982776573,-6.18386807209161,
127.518312871276));
#239019=CARTESIAN_POINT('Ctrl Pts',(90.5438506538447,-6.10717677700159,
134.230834889814));
#239020=CARTESIAN_POINT('Ctrl Pts',(90.2654030300316,-0.41828837601907,
137.794594444728));
#239021=CARTESIAN_POINT('Ctrl Pts',(89.9869554062187,5.65498660800168,134.934670604388));
#239022=CARTESIAN_POINT('Ctrl Pts',(89.708507782406,6.53160516072318,128.279193663018));
#239023=CARTESIAN_POINT('Ctrl Pts',(89.430060158593,1.40599765739116,123.944221791613));
#239024=CARTESIAN_POINT('Ctrl Pts',(89.1516125347801,-5.01165300627911,
125.913382364846));
#239025=CARTESIAN_POINT('Ctrl Pts',(88.8731649109673,-6.82383939003939,
132.377113014756));
#239026=CARTESIAN_POINT('Ctrl Pts',(88.5947172871542,-2.36525073744058,
137.395561044874));
#239027=CARTESIAN_POINT('Ctrl Pts',(88.3162696633415,4.26688779394398,136.357017880338));
#239028=CARTESIAN_POINT('Ctrl Pts',(88.0378220395285,6.97796489175107,130.2158539537));
#239029=CARTESIAN_POINT('Ctrl Pts',(87.7593744157156,3.2766331465752,124.615498901007));
#239030=CARTESIAN_POINT('Ctrl Pts',(87.4809267919028,-3.43576438787495,
124.702405423128));
#239031=CARTESIAN_POINT('Ctrl Pts',(87.2024791680898,-6.99086229628967,
130.396710671853));
#239032=CARTESIAN_POINT('Ctrl Pts',(86.924031544277,-4.1216992770237,136.465626305881));
#239033=CARTESIAN_POINT('Ctrl Pts',(86.6455839204641,2.53510402162323,137.332115340552));
#239034=CARTESIAN_POINT('Ctrl Pts',(86.3671362966513,6.8622705711149,132.199916683345));
#239035=CARTESIAN_POINT('Ctrl Pts',(86.0886886728382,4.88334570630671,125.785270178391));
#239036=CARTESIAN_POINT('Ctrl Pts',(85.8102410490255,-1.58313529789712,
123.982922590838));
#239037=CARTESIAN_POINT('Ctrl Pts',(85.5317934252125,-6.59479230379227,
128.449143304076));
#239038=CARTESIAN_POINT('Ctrl Pts',(85.2533458013996,-5.5461573560172,135.079693669646));
#239039=CARTESIAN_POINT('Ctrl Pts',(84.9748981775869,0.599125257088023,
137.781421821987));
#239040=CARTESIAN_POINT('Ctrl Pts',(84.6964505537737,6.19384102782544,134.071571575853));
#239041=CARTESIAN_POINT('Ctrl Pts',(84.418002929961,6.09671947994716,127.359314071181));
#239042=CARTESIAN_POINT('Ctrl Pts',(84.1395553061481,0.397010571302045,
123.812886042756));
#239043=CARTESIAN_POINT('Ctrl Pts',(83.8611076823352,-5.66753165732491,
126.691281596061));
#239044=CARTESIAN_POINT('Ctrl Pts',(83.5826600585222,-6.52388916718428,
133.349395835046));
#239045=CARTESIAN_POINT('Ctrl Pts',(83.3042124347095,-1.38511124210516,
137.66874704105));
#239046=CARTESIAN_POINT('Ctrl Pts',(83.0257648108964,5.02651624802251,135.68006246779));
#239047=CARTESIAN_POINT('Ctrl Pts',(82.7473171870836,6.81902086518772,129.210846085452));
#239048=CARTESIAN_POINT('Ctrl Pts',(82.4688695632707,2.34517843493451,124.205991710613));
#239049=CARTESIAN_POINT('Ctrl Pts',(82.1904219394578,-4.28376840868787,
125.264716013022));
#239050=CARTESIAN_POINT('Ctrl Pts',(81.9119743156449,-6.97614135844701,
131.414103080323));
#239051=CARTESIAN_POINT('Ctrl Pts',(81.6335266918322,-3.25778120324508,
137.003166611925));
#239052=CARTESIAN_POINT('Ctrl Pts',(81.355079068019,3.45432072627939,136.895830263219));
#239053=CARTESIAN_POINT('Ctrl Pts',(81.0766314442065,6.99207066130227,131.190730894994));
#239054=CARTESIAN_POINT('Ctrl Pts',(80.7981838203932,4.10444924022979,125.130576117049));
#239055=CARTESIAN_POINT('Ctrl Pts',(80.5197361965806,-2.55496051912119,
124.284352115297));
#239056=CARTESIAN_POINT('Ctrl Pts',(80.2412885727675,-6.86648637816013,
129.429697407007));
#239057=CARTESIAN_POINT('Ctrl Pts',(79.9628409489547,-4.86804670217826,
135.838291033188));
#239058=CARTESIAN_POINT('Ctrl Pts',(79.6843933251418,1.6038900758031,137.620948528586));
#239059=CARTESIAN_POINT('Ctrl Pts',(79.405945701329,6.60193022850756,133.139494742587));
#239060=CARTESIAN_POINT('Ctrl Pts',(79.1274980775159,5.53311902343524,126.512166773338));
#239061=CARTESIAN_POINT('Ctrl Pts',(78.8490504537032,-0.620358256282274,
123.829155261608));
#239062=CARTESIAN_POINT('Ctrl Pts',(78.5706028298902,-6.2037566046621,127.556016714277));
#239063=CARTESIAN_POINT('Ctrl Pts',(78.2921552060774,-6.08620570371632,
134.267947523646));
#239064=CARTESIAN_POINT('Ctrl Pts',(78.0137075822645,-0.375729088733312,
137.797011171955));
#239065=CARTESIAN_POINT('Ctrl Pts',(77.7352599584516,5.68002420340909,134.90017057075));
#239066=CARTESIAN_POINT('Ctrl Pts',(77.4568123346387,6.51611273722737,128.23948071401));
#239067=CARTESIAN_POINT('Ctrl Pts',(77.1783647108257,1.36421199533782,123.935790187287));
#239068=CARTESIAN_POINT('Ctrl Pts',(76.8999170870129,-5.04133292480603,
125.94398033767));
#239069=CARTESIAN_POINT('Ctrl Pts',(76.6214694632,-6.81413916985829,132.418622522501));
#239070=CARTESIAN_POINT('Ctrl Pts',(76.3430218393871,-2.32508440701577,
137.409836877774));
#239071=CARTESIAN_POINT('Ctrl Pts',(76.0645742155741,4.30060933918641,136.33094124537));
#239072=CARTESIAN_POINT('Ctrl Pts',(75.7861265917614,6.97425319912241,130.173388004487));
#239073=CARTESIAN_POINT('Ctrl Pts',(75.5076789679483,3.23889908027492,124.595667770297));
#239074=CARTESIAN_POINT('Ctrl Pts',(75.2292313441357,-3.47284506432852,
124.72343295124));
#239075=CARTESIAN_POINT('Ctrl Pts',(74.9507837203226,-6.99321425272744,
130.439273587703));
#239076=CARTESIAN_POINT('Ctrl Pts',(74.6723360965098,-4.08716118037883,
136.490611369118));
#239077=CARTESIAN_POINT('Ctrl Pts',(74.3938884726969,2.57479334781394,137.316562498648));
#239078=CARTESIAN_POINT('Ctrl Pts',(74.1154408488841,6.87063857501356,132.158118238212));
#239079=CARTESIAN_POINT('Ctrl Pts',(73.836993225071,4.85270260113016,125.755636859138));
#239080=CARTESIAN_POINT('Ctrl Pts',(73.5585456012583,-1.62462999549052,
123.992685970191));
#239081=CARTESIAN_POINT('Ctrl Pts',(73.2800979774453,-6.60900699384299,
128.489331313375));
#239082=CARTESIAN_POINT('Ctrl Pts',(73.0016503536324,-5.52002943279461,
135.113375491641));
#239083=CARTESIAN_POINT('Ctrl Pts',(72.7232027298196,0.641585508562261,
137.777645507711));
#239084=CARTESIAN_POINT('Ctrl Pts',(72.4447551060067,6.21361471074508,134.033807373642));
#239085=CARTESIAN_POINT('Ctrl Pts',(72.1663074821937,6.07563554570727,127.322265437984));
#239086=CARTESIAN_POINT('Ctrl Pts',(71.8878598583809,0.354444125461637,
123.810598862555));
#239087=CARTESIAN_POINT('Ctrl Pts',(71.609412234568,-5.69246413052499,126.725857675724));
#239088=CARTESIAN_POINT('Ctrl Pts',(71.330964610755,-6.5082759428922,133.3890614465));
#239089=CARTESIAN_POINT('Ctrl Pts',(71.0525169869423,-1.34330011069692,
137.677051425141));
#239090=CARTESIAN_POINT('Ctrl Pts',(70.7740693631292,5.05610289937005,135.649374301231));
#239091=CARTESIAN_POINT('Ctrl Pts',(70.4956217393166,6.80919434927445,129.16936629411));
#239092=CARTESIAN_POINT('Ctrl Pts',(70.2171741155033,2.30496883983272,124.191838196331));
#239093=CARTESIAN_POINT('Ctrl Pts',(69.9387264916908,-4.31741042942741,
125.290895163988));
#239094=CARTESIAN_POINT('Ctrl Pts',(69.6602788678776,-6.97230043126892,
131.456557535721));
#239095=CARTESIAN_POINT('Ctrl Pts',(69.3818312440649,-3.21998695258627,
137.02288280126));
#239096=CARTESIAN_POINT('Ctrl Pts',(69.1033836202519,3.49133723041524,136.874689971681));
#239097=CARTESIAN_POINT('Ctrl Pts',(68.8249359964391,6.9942930599711,131.148161017746));
#239098=CARTESIAN_POINT('Ctrl Pts',(68.5464883726262,4.0698352576252,125.105696291628));
#239099=CARTESIAN_POINT('Ctrl Pts',(68.2680407488133,-2.59460232397255,
124.300025685817));
#239100=CARTESIAN_POINT('Ctrl Pts',(67.9895931250004,-6.87472712320984,
129.471521127857));
#239101=CARTESIAN_POINT('Ctrl Pts',(67.7111455011875,-4.83731354530826,
135.867830948109));
#239102=CARTESIAN_POINT('Ctrl Pts',(67.4326978773747,1.64535486482719,137.61105889887));
#239103=CARTESIAN_POINT('Ctrl Pts',(67.1542502535617,6.61602253424027,133.099263654809));
#239104=CARTESIAN_POINT('Ctrl Pts',(66.8758026297489,5.50688870535577,126.478564631767));
#239105=CARTESIAN_POINT('Ctrl Pts',(66.5973550059358,-0.662806817281494,
123.833060792792));
#239106=CARTESIAN_POINT('Ctrl Pts',(66.3189073821232,-6.22341525475008,
127.593840925854));
#239107=CARTESIAN_POINT('Ctrl Pts',(66.0404597583101,-6.0650091038406,134.304931812993));
#239108=CARTESIAN_POINT('Ctrl Pts',(65.7620121344974,-0.333155878668442,
137.799168783944));
#239109=CARTESIAN_POINT('Ctrl Pts',(65.4835645106842,5.70485132343066,134.865518765369));
#239110=CARTESIAN_POINT('Ctrl Pts',(65.2051168868716,6.50037885677781,128.199862807569));
#239111=CARTESIAN_POINT('Ctrl Pts',(64.9266692630585,1.32237578190785,123.927613100363));
#239112=CARTESIAN_POINT('Ctrl Pts',(64.6482216392459,-5.07082603488719,
125.974758413674));
#239113=CARTESIAN_POINT('Ctrl Pts',(64.3697740154327,-6.80418644924447,
132.460072213177));
#239114=CARTESIAN_POINT('Ctrl Pts',(64.09132639162,-2.28483191973344,137.423867942321));
#239115=CARTESIAN_POINT('Ctrl Pts',(63.812878767807,4.33417152376786,136.304659820925));
#239116=CARTESIAN_POINT('Ctrl Pts',(63.5344311439942,6.97028307297671,130.130945436197));
#239117=CARTESIAN_POINT('Ctrl Pts',(63.2559835201813,3.20104499537862,124.576066704985));
#239118=CARTESIAN_POINT('Ctrl Pts',(62.9775358963684,-3.5097970532309,124.744685810362));
#239119=CARTESIAN_POINT('Ctrl Pts',(62.6990882725555,-6.9953070730393,130.481850031987));
#239120=CARTESIAN_POINT('Ctrl Pts',(62.4206406487427,-4.05247163247362,
136.51538572624));
#239121=CARTESIAN_POINT('Ctrl Pts',(62.1421930249296,2.61438726408988,137.300768344709));
#239122=CARTESIAN_POINT('Ctrl Pts',(61.8637454011169,6.87875198487314,132.116269629093));
#239123=CARTESIAN_POINT('Ctrl Pts',(61.5852977773038,4.82187967727427,125.726190622201));
#239124=CARTESIAN_POINT('Ctrl Pts',(61.3068501534911,-1.66606449182178,
124.002701758653));
#239125=CARTESIAN_POINT('Ctrl Pts',(61.0284025296781,-6.62297678470872,
128.529605106938));
#239126=CARTESIAN_POINT('Ctrl Pts',(60.7499549058653,-5.49369696285183,
135.146897641504));
#239127=CARTESIAN_POINT('Ctrl Pts',(60.4715072820523,0.684021985849089,
137.773610795799));
#239128=CARTESIAN_POINT('Ctrl Pts',(60.1930596582395,6.23315814588628,133.995923503096));
#239129=CARTESIAN_POINT('Ctrl Pts',(59.9146120344266,6.05432647655821,127.285345835106));
#239130=CARTESIAN_POINT('Ctrl Pts',(59.6361644106137,0.311864545564345,
123.808570838767));
#239131=CARTESIAN_POINT('Ctrl Pts',(59.3577167868007,-5.71718566737322,
126.760584885814));
#239132=CARTESIAN_POINT('Ctrl Pts',(59.0792691629879,-6.49242155204172,
133.428631280914));
#239133=CARTESIAN_POINT('Ctrl Pts',(58.800821539175,-1.30143920280946,137.685101139145));
#239134=CARTESIAN_POINT('Ctrl Pts',(58.5223739153621,5.08550219496502,135.618506600908));
#239135=CARTESIAN_POINT('Ctrl Pts',(58.2439262915492,6.79911551616065,129.127947088084));
#239136=CARTESIAN_POINT('Ctrl Pts',(57.9654786677363,2.26467383326308,124.1779297115));
#239137=CARTESIAN_POINT('Ctrl Pts',(57.6870310439234,-4.35089246693584,
125.317278618444));
#239138=CARTESIAN_POINT('Ctrl Pts',(57.4085834201106,-6.96820114293417,
131.498987823723));
#239139=CARTESIAN_POINT('Ctrl Pts',(57.1301357962976,-3.18207338412696,
137.042368560968));
#239140=CARTESIAN_POINT('Ctrl Pts',(56.8516881724848,3.52822436176609,136.853324741857));
#239141=CARTESIAN_POINT('Ctrl Pts',(56.5732405486719,6.9962562825383,131.105578400848));
#239142=CARTESIAN_POINT('Ctrl Pts',(56.294792924859,4.03507046577855,125.081027632309));
#239143=CARTESIAN_POINT('Ctrl Pts',(56.0163453010462,-2.63414798488075,
124.315940276861));
#239144=CARTESIAN_POINT('Ctrl Pts',(55.7378976772331,-6.8827131227178,129.513394237565));
#239145=CARTESIAN_POINT('Ctrl Pts',(55.4594500534204,-4.80640114000575,
135.897183234276));
#239146=CARTESIAN_POINT('Ctrl Pts',(55.1810024296073,1.68675868462211,137.600917044446));
#239147=CARTESIAN_POINT('Ctrl Pts',(54.9025548057946,6.62986968082513,133.058947528554));
#239148=CARTESIAN_POINT('Ctrl Pts',(54.6241071819816,5.4804543274898,126.445122784157));
#239149=CARTESIAN_POINT('Ctrl Pts',(54.3456595581689,-0.705230817730614,
123.837224648055));
#239150=CARTESIAN_POINT('Ctrl Pts',(54.0672119343557,-6.24284329389726,
127.63178410442));
#239151=CARTESIAN_POINT('Ctrl Pts',(53.7887643105431,-6.04358776282204,
134.341786387386));
#239152=CARTESIAN_POINT('Ctrl Pts',(53.51031668673,-0.290570323389535,137.801067200743));
#239153=CARTESIAN_POINT('Ctrl Pts',(53.2318690629172,5.72946704808866,134.830716472279));
#239154=CARTESIAN_POINT('Ctrl Pts',(52.9534214391043,6.48440410239917,128.160341411752));
#239155=CARTESIAN_POINT('Ctrl Pts',(52.6749738152913,1.28049056735643,123.919690833848));
#239156=CARTESIAN_POINT('Ctrl Pts',(52.3965261914786,-5.10013124364513,
126.005715452363));
#239157=CARTESIAN_POINT('Ctrl Pts',(52.1180785676656,-6.79398159699943,
132.501460550851));
#239158=CARTESIAN_POINT('Ctrl Pts',(51.8396309438527,-2.24449476716385,
137.43765371859));
#239159=CARTESIAN_POINT('Ctrl Pts',(51.5611833200399,4.36757310402998,136.278174580871));
#239160=CARTESIAN_POINT('Ctrl Pts',(51.2827356962269,6.96605466042841,130.088527821552));
#239161=CARTESIAN_POINT('Ctrl Pts',(51.0042880724141,3.16307229458231,124.556696431394));
#239162=CARTESIAN_POINT('Ctrl Pts',(50.7258404486012,-3.54661898531293,
124.766163212963));
#239163=CARTESIAN_POINT('Ctrl Pts',(50.4473928247883,-6.99714067967511,
130.52443842702));
#239164=CARTESIAN_POINT('Ctrl Pts',(50.1689452009753,-4.0176319187415,136.539948459229));
#239165=CARTESIAN_POINT('Ctrl Pts',(49.8904975771625,2.65388430328469,137.284733463992));
#239166=CARTESIAN_POINT('Ctrl Pts',(49.6120499533496,6.88661050004828,132.074372406703));
#239167=CARTESIAN_POINT('Ctrl Pts',(49.3336023295367,4.79087807689359,125.696932558722));
#239168=CARTESIAN_POINT('Ctrl Pts',(49.0551547057238,-1.7074372515208,124.012969585086));
#239169=CARTESIAN_POINT('Ctrl Pts',(48.776707081911,-6.63670115873435,128.569963192402));
#239170=CARTESIAN_POINT('Ctrl Pts',(48.498259458098,-5.46716092194746,135.180258877061));
#239171=CARTESIAN_POINT('Ctrl Pts',(48.2198118342852,0.72643311645002,137.769317835757));
#239172=CARTESIAN_POINT('Ctrl Pts',(47.9413642104722,6.25247060906043,133.957921368012));
#239173=CARTESIAN_POINT('Ctrl Pts',(47.6629165866595,6.03279306211481,127.248556630613));
#239174=CARTESIAN_POINT('Ctrl Pts',(47.3844689628464,0.269273409411107,
123.806802046542));
#239175=CARTESIAN_POINT('Ctrl Pts',(47.1060213390337,-5.74169535180415,
126.7954619395));
#239176=CARTESIAN_POINT('Ctrl Pts',(46.8275737152206,-6.47632658212296,
133.468103872012));
#239177=CARTESIAN_POINT('Ctrl Pts',(46.5491260914079,-1.25953006961336,
137.69289588478));
#239178=CARTESIAN_POINT('Ctrl Pts',(46.2706784675948,5.11471304540623,135.587460510634));
#239179=CARTESIAN_POINT('Ctrl Pts',(45.9922308437821,6.78878473932087,129.086590002178));
#239180=CARTESIAN_POINT('Ctrl Pts',(45.7137832199691,2.22429490837156,124.164266771503));
#239181=CARTESIAN_POINT('Ctrl Pts',(45.4353355961562,-4.38421328052394,
125.343865398741));
#239182=CARTESIAN_POINT('Ctrl Pts',(45.1568879723434,-6.96384364534361,
131.541392372057));
#239183=CARTESIAN_POINT('Ctrl Pts',(44.8784403485304,-3.1440419027679,137.061623168999));
#239184=CARTESIAN_POINT('Ctrl Pts',(44.5999927247176,3.56498075346585,136.831735365442));
#239185=CARTESIAN_POINT('Ctrl Pts',(44.3215451009046,6.99796025625624,131.062984622213));
#239186=CARTESIAN_POINT('Ctrl Pts',(44.0430974770918,4.00015615291162,125.056571053198));
#239187=CARTESIAN_POINT('Ctrl Pts',(43.7646498532789,-2.67359603646683,
124.332095298706));
#239188=CARTESIAN_POINT('Ctrl Pts',(43.486202229466,-6.8904440807599,129.555315184507));
#239189=CARTESIAN_POINT('Ctrl Pts',(43.2077546056531,-4.77531063174146,
135.926346804027));
#239190=CARTESIAN_POINT('Ctrl Pts',(42.9293069818402,1.72810000095366,137.590523341125));
#239191=CARTESIAN_POINT('Ctrl Pts',(42.6508593580274,6.64347115515083,133.018547857752));
#239192=CARTESIAN_POINT('Ctrl Pts',(42.3724117342144,5.4538168693733,126.411842469708));
#239193=CARTESIAN_POINT('Ctrl Pts',(42.0939641104015,-0.74762868559244,
123.841646673103));
#239194=CARTESIAN_POINT('Ctrl Pts',(41.8155164865887,-6.26204000219037,
127.669844843974));
#239195=CARTESIAN_POINT('Ctrl Pts',(41.5370688627757,-6.02194247443641,
134.378509881167));
#239196=CARTESIAN_POINT('Ctrl Pts',(41.2586212389629,-0.247974000920424,
137.802706352008));
#239197=CARTESIAN_POINT('Ctrl Pts',(40.9801736151499,5.75387046523817,134.795764981093));
#239198=CARTESIAN_POINT('Ctrl Pts',(40.7017259913371,6.46818906604193,128.120917991039));
#239199=CARTESIAN_POINT('Ctrl Pts',(40.4232783675241,1.23855790375582,123.912023681303));
#239200=CARTESIAN_POINT('Ctrl Pts',(40.1448307437113,-5.12924746516435,
126.036850306614));
#239201=CARTESIAN_POINT('Ctrl Pts',(39.8663831198984,-6.78352499126783,
132.542786001862));
#239202=CARTESIAN_POINT('Ctrl Pts',(39.5879354960856,-2.20407444401526,
137.451193695743));
#239203=CARTESIAN_POINT('Ctrl Pts',(39.3094878722726,4.40081284226458,136.251486506627));
#239204=CARTESIAN_POINT('Ctrl Pts',(39.0310402484598,6.96156811816289,130.046136732356));
#239205=CARTESIAN_POINT('Ctrl Pts',(38.7525926246468,3.12498238497894,124.537557667297));
#239206=CARTESIAN_POINT('Ctrl Pts',(38.474145000834,-3.58330949612422,124.78786436319));
#239207=CARTESIAN_POINT('Ctrl Pts',(38.195697377021,-6.9987150046898,130.567037194673));
#239208=CARTESIAN_POINT('Ctrl Pts',(37.9172497532082,-3.98264333018119,
136.564298657899));
#239209=CARTESIAN_POINT('Ctrl Pts',(37.6388021293952,2.69328300182069,137.268458450676));
#239210=CARTESIAN_POINT('Ctrl Pts',(37.3603545055824,6.89421382933879,132.032428123559));
#239211=CARTESIAN_POINT('Ctrl Pts',(37.0819068817695,4.7596989487639,125.667863752866));
#239212=CARTESIAN_POINT('Ctrl Pts',(36.8034592579566,-1.74874674150458,
124.02348906901));
#239213=CARTESIAN_POINT('Ctrl Pts',(36.5250116341437,-6.65017960735793,
128.610404074285));
#239214=CARTESIAN_POINT('Ctrl Pts',(36.2465640103308,-5.44042229338459,
135.213457962098));
#239215=CARTESIAN_POINT('Ctrl Pts',(35.968116386518,0.768817328804687,137.764766786667));
#239216=CARTESIAN_POINT('Ctrl Pts',(35.689668762705,6.27155138463682,133.919802376575));
#239217=CARTESIAN_POINT('Ctrl Pts',(35.4112211388921,6.01103610030595,127.211899187745));
#239218=CARTESIAN_POINT('Ctrl Pts',(35.1327735150793,0.226672295232647,
123.805292551423));
#239219=CARTESIAN_POINT('Ctrl Pts',(34.8543258912663,-5.76599227560232,
126.830487544402));
#239220=CARTESIAN_POINT('Ctrl Pts',(34.5758782674535,-6.45999162954105,
133.507477757125));
#239221=CARTESIAN_POINT('Ctrl Pts',(34.2974306436406,-1.21757426406734,
137.700435373207));
#239222=CARTESIAN_POINT('Ctrl Pts',(34.0189830198277,5.1437343682746,135.556237180835));
#239223=CARTESIAN_POINT('Ctrl Pts',(33.7405353960148,6.778202401566,129.045296568894));
#239224=CARTESIAN_POINT('Ctrl Pts',(33.4620877722019,2.18383356141425,124.150849882625));
#239225=CARTESIAN_POINT('Ctrl Pts',(33.1836401483891,-4.41737163547663,
125.370654519698));
#239226=CARTESIAN_POINT('Ctrl Pts',(32.9051925245761,-6.95922809996586,
131.58376960941));
#239227=CARTESIAN_POINT('Ctrl Pts',(32.6267449007632,-3.10589391777991,
137.080645911863));
#239228=CARTESIAN_POINT('Ctrl Pts',(32.3482972769504,3.60160504349277,136.80992264244));
#239229=CARTESIAN_POINT('Ctrl Pts',(32.0698496531375,6.99940491798352,131.020381260171));
#239230=CARTESIAN_POINT('Ctrl Pts',(31.7914020293246,3.96509361278713,125.032327460544));
#239231=CARTESIAN_POINT('Ctrl Pts',(31.5129544055117,-2.71294501696876,
124.348490152723));
#239232=CARTESIAN_POINT('Ctrl Pts',(31.2345067816988,-6.89791971086261,
129.597282415287));
#239233=CARTESIAN_POINT('Ctrl Pts',(30.9560591578859,-4.74404317258561,
135.955320576696));
#239234=CARTESIAN_POINT('Ctrl Pts',(30.677611534073,1.76937728190418,137.579878174048));
#239235=CARTESIAN_POINT('Ctrl Pts',(30.3991639102601,6.65682645320975,132.978066139427));
#239236=CARTESIAN_POINT('Ctrl Pts',(30.1207162864473,5.42697731806706,126.378724921634));
#239237=CARTESIAN_POINT('Ctrl Pts',(29.8422686626343,-0.789998849798377,
123.846326704078));
#239238=CARTESIAN_POINT('Ctrl Pts',(29.5638210388214,-6.28100466828836,
127.708021734164));
#239239=CARTESIAN_POINT('Ctrl Pts',(29.2853734150086,-6.00007404075783,
134.415100933532));
#239240=CARTESIAN_POINT('Ctrl Pts',(29.0069257911957,-0.205368489683527,
137.804086176998));
#239241=CARTESIAN_POINT('Ctrl Pts',(28.7284781673828,5.77806067060162,134.760665586949));
#239242=CARTESIAN_POINT('Ctrl Pts',(28.4500305435699,6.45173434856014,128.08159400628));
#239243=CARTESIAN_POINT('Ctrl Pts',(28.171582919757,1.19657934493693,123.904611926838));
#239244=CARTESIAN_POINT('Ctrl Pts',(27.8931352959441,-5.15817362053239,
126.068161822712));
#239245=CARTESIAN_POINT('Ctrl Pts',(27.6146876721312,-6.77281701952304,
132.584047034882));
#239246=CARTESIAN_POINT('Ctrl Pts',(27.3362400483183,-2.16357244807759,
137.464487372053));
#239247=CARTESIAN_POINT('Ctrl Pts',(27.0577924245054,4.4338895067609,136.22459658713));
#239248=CARTESIAN_POINT('Ctrl Pts',(26.7793448006925,6.95682361243065,130.003773739425));
#239249=CARTESIAN_POINT('Ctrl Pts',(26.5008971768797,3.08677667800406,124.518651121888));
#239250=CARTESIAN_POINT('Ctrl Pts',(26.2224495530668,-3.61986722608435,
124.809788456898));
#239251=CARTESIAN_POINT('Ctrl Pts',(25.9440019292538,-7.00002998974624,
130.609644756432));
#239252=CARTESIAN_POINT('Ctrl Pts',(25.665554305441,-3.94750716330764,136.588435419948));
#239253=CARTESIAN_POINT('Ctrl Pts',(25.3871066816281,2.7325818997646,137.251943907838));
#239254=CARTESIAN_POINT('Ctrl Pts',(25.1086590578152,6.90156169100052,131.990438333922));
#239255=CARTESIAN_POINT('Ctrl Pts',(24.8302114340022,4.72834344823931,125.638985281792));
#239256=CARTESIAN_POINT('Ctrl Pts',(24.5517638101894,-1.78999143103474,
124.034259820624));
#239257=CARTESIAN_POINT('Ctrl Pts',(24.2733161863765,-6.66341163113055,
128.650926254035));
#239258=CARTESIAN_POINT('Ctrl Pts',(23.9948685625636,-5.41348206797292,
135.246493666413));
#239259=CARTESIAN_POINT('Ctrl Pts',(23.7164209387507,0.811173052350488,
137.759957817164));
#239260=CARTESIAN_POINT('Ctrl Pts',(23.4379733149379,6.29039976557031,133.881567941299));
#239261=CARTESIAN_POINT('Ctrl Pts',(23.159525691125,5.98905639734383,127.175374864857));
#239262=CARTESIAN_POINT('Ctrl Pts',(22.8810780673121,0.184062781628937,
123.804042409345));
#239263=CARTESIAN_POINT('Ctrl Pts',(22.6026304434992,-5.79007553843628,
126.865660402631));
#239264=CARTESIAN_POINT('Ctrl Pts',(22.3241828196863,-6.44341729959363,
133.546751477239));
#239265=CARTESIAN_POINT('Ctrl Pts',(22.0457351958734,-1.17557334085921,
137.707719325048));
#239266=CARTESIAN_POINT('Ctrl Pts',(21.7672875720605,5.17256508817436,135.524837768503));
#239267=CARTESIAN_POINT('Ctrl Pts',(21.4888399482477,6.76736889502847,129.004068318375));
#239268=CARTESIAN_POINT('Ctrl Pts',(21.2103923244347,2.14329129170119,124.137679542035));
#239269=CARTESIAN_POINT('Ctrl Pts',(20.9319447006219,-4.45036630309889,
125.397644988631));
#239270=CARTESIAN_POINT('Ctrl Pts',(20.6534970768089,-6.95435467783159,
131.626117965476));
#239271=CARTESIAN_POINT('Ctrl Pts',(20.3750494529961,-3.06763084275059,
137.099436084669));
#239272=CARTESIAN_POINT('Ctrl Pts',(20.0966018291831,3.6380958747203,136.787887381128));
#239273=CARTESIAN_POINT('Ctrl Pts',(19.8181542053702,7.00059021418742,130.977769893405));
#239274=CARTESIAN_POINT('Ctrl Pts',(19.5397065815574,3.92988414466092,125.0082977527));
#239275=CARTESIAN_POINT('Ctrl Pts',(19.2612589577445,-2.75219346829522,
124.365124231394));
#239276=CARTESIAN_POINT('Ctrl Pts',(18.9828113339316,-6.90513973601376,
129.639294374793));
#239277=CARTESIAN_POINT('Ctrl Pts',(18.7043637101187,-4.71259992116536,
135.98410347865));
#239278=CARTESIAN_POINT('Ctrl Pts',(18.4259160863058,1.81058899792882,137.568981937677));
#239279=CARTESIAN_POINT('Ctrl Pts',(18.1474684624929,6.6699350801164,132.937503873645));
#239280=CARTESIAN_POINT('Ctrl Pts',(17.86902083868,5.39993666812053,126.345771367118));
#239281=CARTESIAN_POINT('Ctrl Pts',(17.5905732148672,-0.832339740306418,
123.851264567558));
#239282=CARTESIAN_POINT('Ctrl Pts',(17.3121255910542,-6.29973658944851,
127.746313360329));
#239283=CARTESIAN_POINT('Ctrl Pts',(17.0336779672413,-5.97798327212915,
134.451558188587));
#239284=CARTESIAN_POINT('Ctrl Pts',(16.7552303434285,-0.162755368441711,
137.805206624583));
#239285=CARTESIAN_POINT('Ctrl Pts',(16.4767827196156,5.80203676780203,134.72541959047));
#239286=CARTESIAN_POINT('Ctrl Pts',(16.1983350958026,6.43504055968944,128.042370914639));
#239287=CARTESIAN_POINT('Ctrl Pts',(15.9198874719898,1.15455644643036,123.897455845098));
#239288=CARTESIAN_POINT('Ctrl Pts',(15.6414398481769,-5.18690863788001,
126.0996488404));
#239289=CARTESIAN_POINT('Ctrl Pts',(15.362992224364,-6.7618580785529,132.625242120967));
#239290=CARTESIAN_POINT('Ctrl Pts',(15.0845446005511,-2.12299028016722,
137.477534254917));
#239291=CARTESIAN_POINT('Ctrl Pts',(14.8060969767383,4.466801871851,136.197505818795));
#239292=CARTESIAN_POINT('Ctrl Pts',(14.5276493529253,6.95182131904109,129.961440412534));
#239293=CARTESIAN_POINT('Ctrl Pts',(14.2492017291125,3.04845658938423,124.499977495755));
#239294=CARTESIAN_POINT('Ctrl Pts',(13.9707541052995,-3.65629082053323,
124.831934681683));
#239295=CARTESIAN_POINT('Ctrl Pts',(13.6923064814867,-7.00108558611715,
130.652259533458));
#239296=CARTESIAN_POINT('Ctrl Pts',(13.4138588576738,-3.91222472010448,
136.612357850978));
#239297=CARTESIAN_POINT('Ctrl Pts',(13.1354112338608,2.77177954088132,137.23519044743));
#239298=CARTESIAN_POINT('Ctrl Pts',(12.856963610048,6.90865381275575,131.94840459374));
#239299=CARTESIAN_POINT('Ctrl Pts',(12.5785159862351,4.6968127372094,125.6102982156));
#239300=CARTESIAN_POINT('Ctrl Pts',(12.3000683624222,-1.83116979177416,
124.045281440813));
#239301=CARTESIAN_POINT('Ctrl Pts',(12.0216207386093,-6.67639673973472,
128.691528230086));
#239302=CARTESIAN_POINT('Ctrl Pts',(11.7431731147965,-5.38634124399241,
135.279364765853));
#239303=CARTESIAN_POINT('Ctrl Pts',(11.4647254909835,0.853498717580522,
137.75489110545));
#239304=CARTESIAN_POINT('Ctrl Pts',(11.1862778671706,6.30901505342741,133.843219478972));
#239305=CARTESIAN_POINT('Ctrl Pts',(10.9078302433578,5.96685476769427,127.13898501537));
#239306=CARTESIAN_POINT('Ctrl Pts',(10.6293826195448,0.141446447510913,
123.803051666633));
#239307=CARTESIAN_POINT('Ctrl Pts',(10.350934995732,-5.81394424789186,126.900979210845));
#239308=CARTESIAN_POINT('Ctrl Pts',(10.0724873719191,-6.42660420644864,
133.585923577051));
#239309=CARTESIAN_POINT('Ctrl Pts',(9.79403974810624,-1.1335288563486,137.714747470394));
#239310=CARTESIAN_POINT('Ctrl Pts',(9.51559212429333,5.20120413677258,135.493263437154));
#239311=CARTESIAN_POINT('Ctrl Pts',(9.23714450048043,6.75628462114785,128.962906778349));
#239312=CARTESIAN_POINT('Ctrl Pts',(8.95869687666756,2.10266960154115,124.124756237763));
#239313=CARTESIAN_POINT('Ctrl Pts',(8.68024925285465,-4.48319606076117,
125.4248358054));
#239314=CARTESIAN_POINT('Ctrl Pts',(8.40180162904178,-6.94922355952728,
131.66843587102));
#239315=CARTESIAN_POINT('Ctrl Pts',(8.12335400522884,-3.0292540955323,137.117992991138));
#239316=CARTESIAN_POINT('Ctrl Pts',(7.84490638141603,3.67445189496732,136.765630398031));
#239317=CARTESIAN_POINT('Ctrl Pts',(7.56645875760307,7.00151610094645,130.935152100895));
#239318=CARTESIAN_POINT('Ctrl Pts',(7.2880111337902,3.89452905323253,124.984482820099));
#239319=CARTESIAN_POINT('Ctrl Pts',(7.00956350997733,-2.79133993608059,
124.381996918337));
#239320=CARTESIAN_POINT('Ctrl Pts',(6.73111588616443,-6.91210388867261,
129.681349506257));
#239321=CARTESIAN_POINT('Ctrl Pts',(6.45266826235151,-4.68098204262199,
136.012694443327));
#239322=CARTESIAN_POINT('Ctrl Pts',(6.17422063853866,1.85173362191231,137.557835035774));
#239323=CARTESIAN_POINT('Ctrl Pts',(5.89577301472578,6.68279655012581,132.896862563455));
#239324=CARTESIAN_POINT('Ctrl Pts',(5.61732539091285,5.37269592153495,126.312983027266));
#239325=CARTESIAN_POINT('Ctrl Pts',(5.33887776709996,-0.874649788159289,
123.856460080569));
#239326=CARTESIAN_POINT('Ctrl Pts',(5.06043014328709,-6.31823507155263,
127.784718303561));
#239327=CARTESIAN_POINT('Ctrl Pts',(4.7819825194742,-5.95567098713191,134.487880295395));
#239328=CARTESIAN_POINT('Ctrl Pts',(4.50353489566127,-0.120136216239877,
137.806067653244));
#239329=CARTESIAN_POINT('Ctrl Pts',(4.22508727184843,5.82579786839633,134.690028297709));
#239330=CARTESIAN_POINT('Ctrl Pts',(3.94663964803551,6.41810831802433,128.003250169541));
#239331=CARTESIAN_POINT('Ctrl Pts',(3.66819202422262,1.11249076541009,123.890555701254));
#239332=CARTESIAN_POINT('Ctrl Pts',(3.3897444004097,-5.21545145242058,126.131310192911));
#239333=CARTESIAN_POINT('Ctrl Pts',(3.11129677659686,-6.75064857444498,
132.666369733619));
#239334=CARTESIAN_POINT('Ctrl Pts',(2.83284915278395,-2.08232944407128,
137.490333860877));
#239335=CARTESIAN_POINT('Ctrl Pts',(2.55440152897106,4.49954871795507,136.170215205482));
#239336=CARTESIAN_POINT('Ctrl Pts',(2.27595390515816,6.94656142335602,129.919138320362));
#239337=CARTESIAN_POINT('Ctrl Pts',(1.9975062813453,3.01002353908442,124.481537480858));
#239338=CARTESIAN_POINT('Ctrl Pts',(1.71905865753238,-3.69257892978116,
124.854302216906));
#239339=CARTESIAN_POINT('Ctrl Pts',(1.44061103371947,-7.00188175468703,
130.694879946647));
#239340=CARTESIAN_POINT('Ctrl Pts',(1.16216340990662,-3.87679730797559,
136.636065064534));
#239341=CARTESIAN_POINT('Ctrl Pts',(0.883715786093727,2.81087447268782,
137.218198690258));
#239342=CARTESIAN_POINT('Ctrl Pts',(0.605268162280799,6.91548993180329,
131.906328460586));
#239343=CARTESIAN_POINT('Ctrl Pts',(0.326820538467947,4.66510798405627,
125.5818036173));
#239344=CARTESIAN_POINT('Ctrl Pts',(0.0483729146550416,-1.87228029784353,
124.056553521165));
#239345=CARTESIAN_POINT('Ctrl Pts',(-0.23007470915786,-6.68913445200245,
128.732208497919));
#239346=CARTESIAN_POINT('Ctrl Pts',(-0.508522332970751,-5.35900082715629,
135.312070042369));
#239347=CARTESIAN_POINT('Ctrl Pts',(-0.786969956783612,0.895792756101716,
137.749566839272));
#239348=CARTESIAN_POINT('Ctrl Pts',(-1.06541758059653,6.32739655841135,
133.804758410613));
#239349=CARTESIAN_POINT('Ctrl Pts',(-1.34386520440944,5.94443203404716,
127.102730987725));
#239350=CARTESIAN_POINT('Ctrl Pts',(-1.62231282822229,0.0988248720430084,
123.802320359999));
#239351=CARTESIAN_POINT('Ctrl Pts',(-1.90076045203519,-5.83759751950527,
126.936442660293));
#239352=CARTESIAN_POINT('Ctrl Pts',(-2.17920807584809,-6.40955297312139,
133.624992605024));
#239353=CARTESIAN_POINT('Ctrl Pts',(-2.45765569966099,-1.09144236850938,
137.721519548813));
#239354=CARTESIAN_POINT('Ctrl Pts',(-2.73610332347384,5.22965045283876,
135.461515356786));
#239355=CARTESIAN_POINT('Ctrl Pts',(-3.01455094728676,6.74494999065597,
128.921813474073));
#239356=CARTESIAN_POINT('Ctrl Pts',(-3.29299857109967,2.06196999618574,
124.112080448687));
#239357=CARTESIAN_POINT('Ctrl Pts',(-3.57144619491253,-4.51585969194472,
125.452225962441));
#239358=CARTESIAN_POINT('Ctrl Pts',(-3.84989381872542,-6.94383493518842,
131.710721757939));
#239359=CARTESIAN_POINT('Ctrl Pts',(-4.12834144253832,-2.99076509818949,
137.136315943637));
#239360=CARTESIAN_POINT('Ctrl Pts',(-4.40678906635123,3.71067175704807,
136.743152517891));
#239361=CARTESIAN_POINT('Ctrl Pts',(-4.68523669016409,7.00218254395157,
130.892529461858));
#239362=CARTESIAN_POINT('Ctrl Pts',(-4.963684313977,3.85902964859785,124.960883545208));
#239363=CARTESIAN_POINT('Ctrl Pts',(-5.24213193778992,-2.83038296973812,
124.399107588329));
#239364=CARTESIAN_POINT('Ctrl Pts',(-5.52057956160276,-6.91881191077996,
129.723446251312));
#239365=CARTESIAN_POINT('Ctrl Pts',(-5.79902718541567,-4.6491907085676,
136.041092411279));
#239366=CARTESIAN_POINT('Ctrl Pts',(-6.07747480922856,1.89280962922548,
137.546437881394));
#239367=CARTESIAN_POINT('Ctrl Pts',(-6.35592243304147,6.69541038665145,
132.856143714835));
#239368=CARTESIAN_POINT('Ctrl Pts',(-6.63437005685431,5.34525608772619,
126.280361117063));
#239369=CARTESIAN_POINT('Ctrl Pts',(-6.91281768066725,-0.916927425542613,
123.86191305059));
#239370=CARTESIAN_POINT('Ctrl Pts',(-7.19126530448013,-6.33649942913263,
127.823235140749));
#239371=CARTESIAN_POINT('Ctrl Pts',(-7.469712928293,-5.93313801255607,134.524065908027));
#239372=CARTESIAN_POINT('Ctrl Pts',(-7.74816055210589,-0.0775126123463511,
137.806669231077));
#239373=CARTESIAN_POINT('Ctrl Pts',(-8.02660817591882,5.84934309190818,
134.654493020103));
#239374=CARTESIAN_POINT('Ctrl Pts',(-8.3050557997317,6.40093825099524,127.964233220621));
#239375=CARTESIAN_POINT('Ctrl Pts',(-8.58350342354456,1.07038386063539,
123.883911750995));
#239376=CARTESIAN_POINT('Ctrl Pts',(-8.86195104735747,-5.2438010064896,
126.163144707024));
#239377=CARTESIAN_POINT('Ctrl Pts',(-9.14039867117038,-6.73918892257159,
132.707428348838));
#239378=CARTESIAN_POINT('Ctrl Pts',(-9.41884629498326,-2.04159144649203,
137.50288571564));
#239379=CARTESIAN_POINT('Ctrl Pts',(-9.69729391879612,4.53212883162697,
136.142725758454));
#239380=CARTESIAN_POINT('Ctrl Pts',(-9.97574154260907,6.94104412028278,
129.876869030427));
#239381=CARTESIAN_POINT('Ctrl Pts',(-10.254189166422,2.97147895125515,124.463331760497));
#239382=CARTESIAN_POINT('Ctrl Pts',(-10.5326367902348,-3.72873020915888,
124.876890233732));
#239383=CARTESIAN_POINT('Ctrl Pts',(-10.8110844140478,-7.00241846595355,
130.737504416682));
#239384=CARTESIAN_POINT('Ctrl Pts',(-11.0895320378606,-3.84122623969676,
136.659556182137));
#239385=CARTESIAN_POINT('Ctrl Pts',(-11.3679796616735,2.84986524650705,
137.200969265957));
#239386=CARTESIAN_POINT('Ctrl Pts',(-11.6464272854864,6.92206979482823,
131.864211493609));
#239387=CARTESIAN_POINT('Ctrl Pts',(-11.9248749092993,4.6332303636112,125.553502542771));
#239388=CARTESIAN_POINT('Ctrl Pts',(-12.2033225331122,-1.91332142587795,
124.068075643991));
#239389=CARTESIAN_POINT('Ctrl Pts',(-12.4817701569251,-6.70162429593314,
128.77296555011));
#239390=CARTESIAN_POINT('Ctrl Pts',(-12.760217780738,-5.33146183057377,
135.344608284054));
#239391=CARTESIAN_POINT('Ctrl Pts',(-13.0386654045509,0.938053600692905,
137.743985215925));
#239392=CARTESIAN_POINT('Ctrl Pts',(-13.3171130283637,6.34554359938892,
133.766186161411));
#239393=CARTESIAN_POINT('Ctrl Pts',(-13.5955606521767,5.92178902728497,
127.066614125326));
#239394=CARTESIAN_POINT('Ctrl Pts',(-13.8740082759896,0.0561996345831295,
123.801848516541));
#239395=CARTESIAN_POINT('Ctrl Pts',(-14.1524558998025,-5.86103447679583,
126.972049436864));
#239396=CARTESIAN_POINT('Ctrl Pts',(-14.4309035236153,-6.39226423145161,
133.663957113442));
#239397=CARTESIAN_POINT('Ctrl Pts',(-14.7093511474282,-1.04931543687181,
137.728035309365));
#239398=CARTESIAN_POINT('Ctrl Pts',(-14.9877987712411,5.25790298228423,
135.429594703837));
#239399=CARTESIAN_POINT('Ctrl Pts',(-15.266246395054,6.73336542356173,128.880789928272));
#239400=CARTESIAN_POINT('Ctrl Pts',(-15.5446940188669,2.02119398377386,
124.099652644515));
#239401=CARTESIAN_POINT('Ctrl Pts',(-15.8231416426798,-4.54835598628669,
125.479814444798));
#239402=CARTESIAN_POINT('Ctrl Pts',(-16.1015892664927,-6.93818900449243,
131.752974059312));
#239403=CARTESIAN_POINT('Ctrl Pts',(-16.3800368903055,-2.95216527694612,
137.154404263204));
#239404=CARTESIAN_POINT('Ctrl Pts',(-16.6584845141185,3.74675411882228,
136.720454573632));
#239405=CARTESIAN_POINT('Ctrl Pts',(-16.9369321379314,7.00258951850748,
130.849903555692));
#239406=CARTESIAN_POINT('Ctrl Pts',(-17.2153797617442,3.82338724620039,
124.93750080251));
#239407=CARTESIAN_POINT('Ctrl Pts',(-17.4938273855571,-2.86932112251383,
124.416455607327));
#239408=CARTESIAN_POINT('Ctrl Pts',(-17.77227500937,-6.92526355376757,129.765583050046));
#239409=CARTESIAN_POINT('Ctrl Pts',(-18.0507226331829,-4.61722709704176,
136.069296330209));
#239410=CARTESIAN_POINT('Ctrl Pts',(-18.3291702569958,1.93381549778173,
137.534790896862));
#239411=CARTESIAN_POINT('Ctrl Pts',(-18.6076178808087,6.70777612228299,
132.81534883664));
#239412=CARTESIAN_POINT('Ctrl Pts',(-18.8860655046216,5.31761818348739,
126.247906845325));
#239413=CARTESIAN_POINT('Ctrl Pts',(-19.1645131284344,-0.959171085842972,
123.867623275557));
#239414=CARTESIAN_POINT('Ctrl Pts',(-19.4429607522474,-6.35452898539608,
127.861862444637));
#239415=CARTESIAN_POINT('Ctrl Pts',(-19.7214083760603,-5.91038518336925,
134.560113685611));
#239416=CARTESIAN_POINT('Ctrl Pts',(-19.9998559998732,-0.0348861361944895,
137.807011335788));
#239417=CARTESIAN_POINT('Ctrl Pts',(-20.278303623686,5.87267156586067,134.618815074426));
#239418=CARTESIAN_POINT('Ctrl Pts',(-20.5567512474989,6.38353099484532,
127.925321513668));
#239419=CARTESIAN_POINT('Ctrl Pts',(-20.8351988713118,1.02823729239309,
123.877524240513));
#239420=CARTESIAN_POINT('Ctrl Pts',(-21.1136464951247,-5.27195624958391,
126.1951512031));
#239421=CARTESIAN_POINT('Ctrl Pts',(-21.3920941189376,-6.72747954757436,
132.748416445183));
#239422=CARTESIAN_POINT('Ctrl Pts',(-21.6705417427505,-2.00077779699093,
137.515189354092));
#239423=CARTESIAN_POINT('Ctrl Pts',(-21.9489893665634,4.56454100559805,
136.115038496344));
#239424=CARTESIAN_POINT('Ctrl Pts',(-22.2274369903762,6.93526961426714,
129.834634109035));
#239425=CARTESIAN_POINT('Ctrl Pts',(-22.5058846141892,2.93282425418085,
124.445361009293));
#239426=CARTESIAN_POINT('Ctrl Pts',(-22.784332238002,-3.76474331906749,
124.899697895151));
#239427=CARTESIAN_POINT('Ctrl Pts',(-23.062779861815,-7.0026957000287,130.780131364099));
#239428=CARTESIAN_POINT('Ctrl Pts',(-23.3412274856278,-3.80551283336702,
136.682830333316));
#239429=CARTESIAN_POINT('Ctrl Pts',(-23.6196751094408,2.88875041752152,
137.183502812971));
#239430=CARTESIAN_POINT('Ctrl Pts',(-23.8981227332536,6.92839315801137,
131.822055253468));
#239431=CARTESIAN_POINT('Ctrl Pts',(-24.1765703570665,4.60118105711114,
125.525396040718));
#239432=CARTESIAN_POINT('Ctrl Pts',(-24.4550179808794,-1.95429165508329,
124.079847382335));
#239433=CARTESIAN_POINT('Ctrl Pts',(-24.7334656046923,-6.71386580871103,
128.813797876394));
#239434=CARTESIAN_POINT('Ctrl Pts',(-25.0119132285052,-5.30372527471246,
135.376978285193));
#239435=CARTESIAN_POINT('Ctrl Pts',(-25.290360852318,0.980279685362951,
137.738146442235));
#239436=CARTESIAN_POINT('Ctrl Pts',(-25.568808476131,6.36345550391485,133.727504160674));
#239437=CARTESIAN_POINT('Ctrl Pts',(-25.8472560999438,5.89892658645264,
127.030635766497));
#239438=CARTESIAN_POINT('Ctrl Pts',(-26.1257037237567,0.0135723146251221,
123.801636153745));
#239439=CARTESIAN_POINT('Ctrl Pts',(-26.4041513475696,-5.88425425129846,
127.007798221134));
#239440=CARTESIAN_POINT('Ctrl Pts',(-26.6825989713826,-6.37473862207999,
133.70281565846));
#239441=CARTESIAN_POINT('Ctrl Pts',(-26.9610465951954,-1.00714962246484,
137.734294510605));
#239442=CARTESIAN_POINT('Ctrl Pts',(-27.2394942190083,5.28596067820108,
135.397502661138));
#239443=CARTESIAN_POINT('Ctrl Pts',(-27.5179418428212,6.72153134913555,
128.839837661092));
#239444=CARTESIAN_POINT('Ctrl Pts',(-27.7963894666341,1.98034307527561,
124.087473285763));
#239445=CARTESIAN_POINT('Ctrl Pts',(-28.0748370904469,-4.58068373962494,
125.507600230172));
#239446=CARTESIAN_POINT('Ctrl Pts',(-28.3532847142599,-6.93228597665136,
131.795191209466));
#239447=CARTESIAN_POINT('Ctrl Pts',(-28.6317323380727,-2.91345606213275,
137.172257279568));
#239448=CARTESIAN_POINT('Ctrl Pts',(-28.9101799618857,3.78269764324474,
136.697537406337));
#239449=CARTESIAN_POINT('Ctrl Pts',(-29.1886275856985,7.00273700953358,
130.807275961916));
#239450=CARTESIAN_POINT('Ctrl Pts',(-29.4670752095115,3.78760316678249,
124.914335458459));
#239451=CARTESIAN_POINT('Ctrl Pts',(-29.7455228333243,-2.90815295154017,
124.434040332496));
#239452=CARTESIAN_POINT('Ctrl Pts',(-30.0239704571372,-6.93145857856742,
129.807758341064));
#239453=CARTESIAN_POINT('Ctrl Pts',(-30.3024180809501,-4.5850923924679,
136.097305155009));
#239454=CARTESIAN_POINT('Ctrl Pts',(-30.580865704763,1.97474970809384,137.52289451376));
#239455=CARTESIAN_POINT('Ctrl Pts',(-30.8593133285759,6.71989329880362,
132.774479440534));
#239456=CARTESIAN_POINT('Ctrl Pts',(-31.1377609523888,5.28978323295099,
126.215621414657));
#239457=CARTESIAN_POINT('Ctrl Pts',(-31.4162085762017,-1.00137920370602,
123.873590543879));
#239458=CARTESIAN_POINT('Ctrl Pts',(-31.6946562000146,-6.37232307225107,
127.900598783877));
#239459=CARTESIAN_POINT('Ctrl Pts',(-31.9731038238274,-5.88741334268594,
134.596022292384));
#239460=CARTESIAN_POINT('Ctrl Pts',(-32.2515514476404,0.00774163267598956,
137.807093954702));
#239461=CARTESIAN_POINT('Ctrl Pts',(-32.5299990714533,5.89578242580862,
134.582995782735));
#239462=CARTESIAN_POINT('Ctrl Pts',(-32.8084466952661,6.36588719460685,
127.886516490566));
#239463=CARTESIAN_POINT('Ctrl Pts',(-33.086894319079,0.9860526224398,123.8713934065));
#239464=CARTESIAN_POINT('Ctrl Pts',(-33.365341942892,-5.29991613840065,
126.227328495126));
#239465=CARTESIAN_POINT('Ctrl Pts',(-33.6437895667048,-6.71552088334846,
132.789332503824));
#239466=CARTESIAN_POINT('Ctrl Pts',(-33.9222371905177,-1.95989000793276,
137.527244320318));
#239467=CARTESIAN_POINT('Ctrl Pts',(-34.2006848143306,4.59678403882356,
136.08715444511));
#239468=CARTESIAN_POINT('Ctrl Pts',(-34.4791324381435,6.9292381192855,129.792435121214));
#239469=CARTESIAN_POINT('Ctrl Pts',(-34.7575800619564,2.89406088022529,
124.427625893158));
#239470=CARTESIAN_POINT('Ctrl Pts',(-35.0360276857693,-3.80061692502793,
124.922724356021));
#239471=CARTESIAN_POINT('Ctrl Pts',(-35.3144753095821,-7.00271344663942,
130.822759209339));
#239472=CARTESIAN_POINT('Ctrl Pts',(-35.592922933395,-3.76965841235978,
136.705886655638));
#239473=CARTESIAN_POINT('Ctrl Pts',(-35.8713705572079,2.92752854482695,
137.165799978524));
#239474=CARTESIAN_POINT('Ctrl Pts',(-36.1498181810209,6.9344597870381,131.779861302279));
#239475=CARTESIAN_POINT('Ctrl Pts',(-36.4282658048337,4.56896125215494,
125.49748515264));
#239476=CARTESIAN_POINT('Ctrl Pts',(-36.7067134286466,-1.99518946729269,
124.091868299989));
#239477=CARTESIAN_POINT('Ctrl Pts',(-36.9851610524595,-6.72585853672236,
128.854703963711));
#239478=CARTESIAN_POINT('Ctrl Pts',(-37.2636086762724,-5.27579218736066,
135.409178846303));
#239479=CARTESIAN_POINT('Ctrl Pts',(-37.5420563000852,1.02246944540875,
137.732050734562));
#239480=CARTESIAN_POINT('Ctrl Pts',(-37.8205039238982,6.38113160825695,
133.688713841779));
#239481=CARTESIAN_POINT('Ctrl Pts',(-38.0989515477111,5.87584555872632,
126.994797244432));
#239482=CARTESIAN_POINT('Ctrl Pts',(-38.377399171524,-0.0290555082599903,
123.801683279478));
#239483=CARTESIAN_POINT('Ctrl Pts',(-38.6558467953367,-5.90725598259587,
127.04368768842));
#239484=CARTESIAN_POINT('Ctrl Pts',(-38.9342944191497,-6.35697679442443,
133.741566800161));
#239485=CARTESIAN_POINT('Ctrl Pts',(-39.2127420429625,-0.964946487758246,
137.740296920595));
#239486=CARTESIAN_POINT('Ctrl Pts',(-39.4911896667755,5.31382250090111,
135.365240417872));
#239487=CARTESIAN_POINT('Ctrl Pts',(-39.7696372905882,6.70944820589337,
128.798958190032));
#239488=CARTESIAN_POINT('Ctrl Pts',(-40.0480849144012,1.93941878443644,
124.07554282374));
#239489=CARTESIAN_POINT('Ctrl Pts',(-40.3265325382142,-4.61284175404266,
125.535582288951));
#239490=CARTESIAN_POINT('Ctrl Pts',(-40.604980162027,-6.9261260704041,131.837371644027));
#239491=CARTESIAN_POINT('Ctrl Pts',(-40.8834277858398,-2.87463888813357,
137.18987433118));
#239492=CARTESIAN_POINT('Ctrl Pts',(-41.1618754096529,3.81850099841496,
136.674401865208));
#239493=CARTESIAN_POINT('Ctrl Pts',(-41.4403230334656,7.00262501156454,
130.76464826011));
#239494=CARTESIAN_POINT('Ctrl Pts',(-41.7187706572786,3.75167873633635,
124.891388371457));
#239495=CARTESIAN_POINT('Ctrl Pts',(-41.9972182810916,-2.94687701788942,
124.451861112224));
#239496=CARTESIAN_POINT('Ctrl Pts',(-42.2756659049044,-6.93739675562063,
129.849970561546));
#239497=CARTESIAN_POINT('Ctrl Pts',(-42.5541135287174,-4.55278778560923,
136.125117847804));
#239498=CARTESIAN_POINT('Ctrl Pts',(-42.8325611525302,2.01561074332903,
137.510749172913));
#239499=CARTESIAN_POINT('Ctrl Pts',(-43.1110087763431,6.73176146720674,
132.733537040953));
#239500=CARTESIAN_POINT('Ctrl Pts',(-43.389456400156,5.26175226755184,126.183506021407));
#239501=CARTESIAN_POINT('Ctrl Pts',(-43.6679040239687,-1.0435502150944,
123.879814634434));
#239502=CARTESIAN_POINT('Ctrl Pts',(-43.9463516477818,-6.38988103033122,
127.93944272308));
#239503=CARTESIAN_POINT('Ctrl Pts',(-44.2247992715946,-5.86422334173611,
134.631790397739));
#239504=CARTESIAN_POINT('Ctrl Pts',(-44.5032468954075,0.050369114677416,
137.806917084757));
#239505=CARTESIAN_POINT('Ctrl Pts',(-44.7816945192204,5.91867481537061,
134.547036472328));
#239506=CARTESIAN_POINT('Ctrl Pts',(-45.0601421430334,6.34800750407734,
127.847819589252));
#239507=CARTESIAN_POINT('Ctrl Pts',(-45.3385897668461,0.943831413943965,
123.865519476137));
#239508=CARTESIAN_POINT('Ctrl Pts',(-45.6170373906592,-5.32767963687585,
126.25967539076));
#239509=CARTESIAN_POINT('Ctrl Pts',(-45.895485014472,-6.7033133730266,132.830175008601));
#239510=CARTESIAN_POINT('Ctrl Pts',(-46.1739326382849,-1.91892959442962,
137.539050167615));
#239511=CARTESIAN_POINT('Ctrl Pts',(-46.4523802620978,4.62885673652604,
136.059074638009));
#239512=CARTESIAN_POINT('Ctrl Pts',(-46.7308278859106,6.92294985883713,
129.750273630666));
#239513=CARTESIAN_POINT('Ctrl Pts',(-47.0092755097235,2.8551902657795,124.410127069272));
#239514=CARTESIAN_POINT('Ctrl Pts',(-47.2877231335364,-3.83634969773052,
124.945968763085));
#239515=CARTESIAN_POINT('Ctrl Pts',(-47.5661707573492,-7.00247170512816,
130.865386372813));
#239516=CARTESIAN_POINT('Ctrl Pts',(-47.8446183811622,-3.73366430527375,
136.728724294741));
#239517=CARTESIAN_POINT('Ctrl Pts',(-48.123066004975,2.96619819148554,137.147861418602));
#239518=CARTESIAN_POINT('Ctrl Pts',(-48.4015136287881,6.9402694571073,131.737631203552));
#239519=CARTESIAN_POINT('Ctrl Pts',(-48.6799612526008,4.53657214265928,
125.469770912784));
#239520=CARTESIAN_POINT('Ctrl Pts',(-48.9584088764139,-2.03601334702262,
124.104137951514));
#239521=CARTESIAN_POINT('Ctrl Pts',(-49.2368565002267,-6.7376020355722,
128.895682296272));
#239522=CARTESIAN_POINT('Ctrl Pts',(-49.5153041240395,-5.24766360358919,
135.441208774179));
#239523=CARTESIAN_POINT('Ctrl Pts',(-49.7937517478526,1.06462131747325,
137.725698318783));
#239524=CARTESIAN_POINT('Ctrl Pts',(-50.0721993716652,6.39857125742062,
133.649816642113));
#239525=CARTESIAN_POINT('Ctrl Pts',(-50.3506469954783,5.85254679938199,
126.959099887138));
#239526=CARTESIAN_POINT('Ctrl Pts',(-50.6290946192911,-0.0716822544825644,
123.801989891996));
#239527=CARTESIAN_POINT('Ctrl Pts',(-50.907542243104,-5.93003881835047,
127.079716508824));
#239528=CARTESIAN_POINT('Ctrl Pts',(-51.1859898669169,-6.33897940665598,
133.780209102606));
#239529=CARTESIAN_POINT('Ctrl Pts',(-51.4644374907297,-0.922707596604453,
137.746042316915));
#239530=CARTESIAN_POINT('Ctrl Pts',(-51.7428851145428,5.34148741795441,
135.332809169526));
#239531=CARTESIAN_POINT('Ctrl Pts',(-52.0213327383556,6.69711644158035,
128.758153029896));
#239532=CARTESIAN_POINT('Ctrl Pts',(-52.2997803621686,1.89842262772099,
124.063861700536));
#239533=CARTESIAN_POINT('Ctrl Pts',(-52.5782279859813,-4.64482883791282,
125.563759584248));
#239534=CARTESIAN_POINT('Ctrl Pts',(-52.8566756097944,-6.91970951400822,
131.879513799985));
#239535=CARTESIAN_POINT('Ctrl Pts',(-53.135123233607,-2.83571519333325,
137.207254765232));
#239536=CARTESIAN_POINT('Ctrl Pts',(-53.4135708574202,3.85416285762642,
136.651048807542));
#239537=CARTESIAN_POINT('Ctrl Pts',(-53.6920184812329,7.0022535287505,130.72202202986));
#239538=CARTESIAN_POINT('Ctrl Pts',(-53.9704661050458,3.71561528605495,
124.868660391816));
#239539=CARTESIAN_POINT('Ctrl Pts',(-54.2489137288587,-2.98549188662705,
124.469917286158));
#239540=CARTESIAN_POINT('Ctrl Pts',(-54.5273613526715,-6.94307786488582,
129.892218147303));
#239541=CARTESIAN_POINT('Ctrl Pts',(-54.8058089764845,-4.5203144735249,
136.152733377983));
#239542=CARTESIAN_POINT('Ctrl Pts',(-55.0842566002972,2.05639708936689,
137.498355324372));
#239543=CARTESIAN_POINT('Ctrl Pts',(-55.3627042241104,6.74338018771311,
132.69252315503));
#239544=CARTESIAN_POINT('Ctrl Pts',(-55.6411518479232,5.23352632598741,
126.151561855625));
#239545=CARTESIAN_POINT('Ctrl Pts',(-55.919599471736,-1.08568255734582,
123.886295316588));
#239546=CARTESIAN_POINT('Ctrl Pts',(-56.1980470955489,-6.40720220901991,
127.978392822871));
#239547=CARTESIAN_POINT('Ctrl Pts',(-56.4764947193619,-5.8408160398338,
134.667416676276));
#239548=CARTESIAN_POINT('Ctrl Pts',(-56.7549423431748,0.0929947302327828,
137.806480732508));
#239549=CARTESIAN_POINT('Ctrl Pts',(-57.0333899669875,5.94134788626073,
134.510938475691));
#239550=CARTESIAN_POINT('Ctrl Pts',(-57.3118375908005,6.32989258579528,
127.809232243652));
#239551=CARTESIAN_POINT('Ctrl Pts',(-57.5902852146133,0.901575231427987,
123.859902667085));
#239552=CARTESIAN_POINT('Ctrl Pts',(-57.8687328384263,-5.35524571622284,
126.292190691378));
#239553=CARTESIAN_POINT('Ctrl Pts',(-58.1471804622391,-6.69085746896258,
132.870942446081));
#239554=CARTESIAN_POINT('Ctrl Pts',(-58.4256280860521,-1.87789807428466,
137.550606458515));
#239555=CARTESIAN_POINT('Ctrl Pts',(-58.7040757098649,4.6607579102399,136.030800115547));
#239556=CARTESIAN_POINT('Ctrl Pts',(-58.9825233336777,6.91640506593584,
129.708151199698));
#239557=CARTESIAN_POINT('Ctrl Pts',(-59.2609709574908,2.81621385120844,
124.392865186062));
#239558=CARTESIAN_POINT('Ctrl Pts',(-59.5394185813036,-3.87194031308425,
124.969430255013));
#239559=CARTESIAN_POINT('Ctrl Pts',(-59.8178662051166,-7.00197048445272,
130.908011274954));
#239560=CARTESIAN_POINT('Ctrl Pts',(-60.0963138289294,-3.69753184588372,
136.751342404371));
#239561=CARTESIAN_POINT('Ctrl Pts',(-60.3747614527424,3.00475792457964,
137.129687797925));
#239562=CARTESIAN_POINT('Ctrl Pts',(-60.6532090765552,6.94582195293937,
131.695366522141));
#239563=CARTESIAN_POINT('Ctrl Pts',(-60.9316567003681,4.50401492881459,
125.442254348109));
#239564=CARTESIAN_POINT('Ctrl Pts',(-61.210104324181,-2.07676178152925,
124.116655882255));
#239565=CARTESIAN_POINT('Ctrl Pts',(-61.4885519479939,-6.74909587010084,
128.93673135561));
#239566=CARTESIAN_POINT('Ctrl Pts',(-61.7669995718066,-5.21934056571308,
135.473066881942));
#239567=CARTESIAN_POINT('Ctrl Pts',(-62.0454471956197,1.10673373960332,
137.719089430292));
#239568=CARTESIAN_POINT('Ctrl Pts',(-62.3238948194324,6.41577380517329,
133.610814003028));
#239569=CARTESIAN_POINT('Ctrl Pts',(-62.6023424432454,5.82903117176375,
126.923545017394));
#239570=CARTESIAN_POINT('Ctrl Pts',(-62.8807900670583,-0.114306344492842,
123.802555979936));
#239571=CARTESIAN_POINT('Ctrl Pts',(-63.1592376908712,-5.95260191433588,
127.115883347286));
#239572=CARTESIAN_POINT('Ctrl Pts',(-63.4376853146842,-6.32074712567447,
133.818741133891));
#239573=CARTESIAN_POINT('Ctrl Pts',(-63.716132938497,-0.880434514181572,
137.751530486667));
#239574=CARTESIAN_POINT('Ctrl Pts',(-63.99458056231,5.36895440422691,135.300210117855));
#239575=CARTESIAN_POINT('Ctrl Pts',(-64.2730281861228,6.6845365131549,128.717423692735));
#239576=CARTESIAN_POINT('Ctrl Pts',(-64.5514758099358,1.85735612425694,
124.052430348997));
#239577=CARTESIAN_POINT('Ctrl Pts',(-64.8299234337484,-4.67664380594228,
125.592131071942));
#239578=CARTESIAN_POINT('Ctrl Pts',(-65.1083710575615,-6.91303654523158,
131.921616115747));
#239579=CARTESIAN_POINT('Ctrl Pts',(-65.3868186813742,-2.79668642006362,
137.224397937687));
#239580=CARTESIAN_POINT('Ctrl Pts',(-65.6652663051872,3.88968189941585,
136.627479098696));
#239581=CARTESIAN_POINT('Ctrl Pts',(-65.9437139290001,7.00162257485687,
130.679398850698));
#239582=CARTESIAN_POINT('Ctrl Pts',(-66.2221615528129,3.67941415228271,
124.846152361731));
#239583=CARTESIAN_POINT('Ctrl Pts',(-66.500609176626,-3.02399612686491,
124.48820818522));
#239584=CARTESIAN_POINT('Ctrl Pts',(-66.7790568004388,-6.94850169584742,
129.934499532835));
#239585=CARTESIAN_POINT('Ctrl Pts',(-67.0575044242516,-4.48767365952541,
136.180150722241));
#239586=CARTESIAN_POINT('Ctrl Pts',(-67.3359520480646,2.09710723485436,
137.485713427398));
#239587=CARTESIAN_POINT('Ctrl Pts',(-67.6143996718775,6.75474902978674,
132.651439302549));
#239588=CARTESIAN_POINT('Ctrl Pts',(-67.8928472956903,5.20510645418034,
126.119790101011));
#239589=CARTESIAN_POINT('Ctrl Pts',(-68.1712949195033,-1.12777466923081,
123.893032350195));
#239590=CARTESIAN_POINT('Ctrl Pts',(-68.449742543316,-6.42428596647451,
128.017447639935));
#239591=CARTESIAN_POINT('Ctrl Pts',(-68.728190167129,-5.81719230434518,
134.702899807851));
#239592=CARTESIAN_POINT('Ctrl Pts',(-69.0066377909419,0.135616899834216,
137.805784914121));
#239593=CARTESIAN_POINT('Ctrl Pts',(-69.2850854147548,5.96380079832,134.474703130449));
#239594=CARTESIAN_POINT('Ctrl Pts',(-69.5635330385676,6.31154311101565,
127.770755883637));
#239595=CARTESIAN_POINT('Ctrl Pts',(-69.8419806623805,0.859285640710264,
123.854543187474));
#239596=CARTESIAN_POINT('Ctrl Pts',(-70.1204282861936,-5.38261335497044,
126.324873192109));
#239597=CARTESIAN_POINT('Ctrl Pts',(-70.3988759100064,-6.67815363271447,
132.911633305611));
#239598=CARTESIAN_POINT('Ctrl Pts',(-70.6773235338194,-1.83679696793597,
137.561912764793));
#239599=CARTESIAN_POINT('Ctrl Pts',(-70.9557711576322,4.69248637785542,
136.002331925448));
#239600=CARTESIAN_POINT('Ctrl Pts',(-71.2342187814451,6.90960398310133,
129.666069389173));
#239601=CARTESIAN_POINT('Ctrl Pts',(-71.5126664052579,2.77713308079745,
124.375840883174));
#239602=CARTESIAN_POINT('Ctrl Pts',(-71.7911140290708,-3.90738745226578,
124.993107962432));
#239603=CARTESIAN_POINT('Ctrl Pts',(-72.0695616528837,-7.00120980318599,
130.950632336283));
#239604=CARTESIAN_POINT('Ctrl Pts',(-72.3480092766965,-3.66126237309149,
136.773740146404));
#239605=CARTESIAN_POINT('Ctrl Pts',(-72.6264569005095,3.04320631526353,
137.111279789924));
#239606=CARTESIAN_POINT('Ctrl Pts',(-72.9049045243223,6.95111706878496,
131.653068824177));
#239607=CARTESIAN_POINT('Ctrl Pts',(-73.1833521481353,4.47129081703998,
125.414936478256));
#239608=CARTESIAN_POINT('Ctrl Pts',(-73.4617997719481,-2.11743326086482,
124.129421628353));
#239609=CARTESIAN_POINT('Ctrl Pts',(-73.7402473957612,-6.76033961440018,
128.977849620639));
#239610=CARTESIAN_POINT('Ctrl Pts',(-74.018695019574,-5.19082412325261,
135.504751989078));
#239611=CARTESIAN_POINT('Ctrl Pts',(-74.2971426433868,1.14880515130821,
137.712224313981));
#239612=CARTESIAN_POINT('Ctrl Pts',(-74.5755902671998,6.43273861406817,
133.571707369781));
#239613=CARTESIAN_POINT('Ctrl Pts',(-74.8540378910127,5.80529954725181,
126.8881339527));
#239614=CARTESIAN_POINT('Ctrl Pts',(-75.1324855148255,-0.156926198840311,
123.803381522322));
#239615=CARTESIAN_POINT('Ctrl Pts',(-75.4109331386384,-5.97494443446864,
127.15218686363));
#239616=CARTESIAN_POINT('Ctrl Pts',(-75.6893807624512,-6.30228062708332,
133.857161466198));
#239617=CARTESIAN_POINT('Ctrl Pts',(-75.9678283862644,-0.838128806933456,
137.756761226486));
#239618=CARTESIAN_POINT('Ctrl Pts',(-76.2462760100769,5.3962224419198,135.267444470826));
#239619=CARTESIAN_POINT('Ctrl Pts',(-76.52472363389,6.67170888677059,128.676771687789));
#239620=CARTESIAN_POINT('Ctrl Pts',(-76.8031712577027,1.81622079577817,
124.041249192718));
#239621=CARTESIAN_POINT('Ctrl Pts',(-77.0816188815158,-4.70828547921653,
125.620695700721));
#239622=CARTESIAN_POINT('Ctrl Pts',(-77.3600665053286,-6.90610741134329,
131.963677031195));
#239623=CARTESIAN_POINT('Ctrl Pts',(-77.6385141291417,-2.75755401454922,
137.241303213299));
#239624=CARTESIAN_POINT('Ctrl Pts',(-77.9169617529544,3.92505680761298,
136.603693612052));
#239625=CARTESIAN_POINT('Ctrl Pts',(-78.1954093767674,7.00073217326374,
130.636780302039));
#239626=CARTESIAN_POINT('Ctrl Pts',(-78.4738570005803,3.6430766764653,124.823865115242));
#239627=CARTESIAN_POINT('Ctrl Pts',(-78.7523046243931,-3.06238831181505,
124.506733131632));
#239628=CARTESIAN_POINT('Ctrl Pts',(-79.0307522482061,-6.95366804752337,
129.976813151389));
#239629=CARTESIAN_POINT('Ctrl Pts',(-79.3091998720188,-4.45486655312747,
136.207368864621));
#239630=CARTESIAN_POINT('Ctrl Pts',(-79.5876474958318,2.13773967126259,
137.472823950436));
#239631=CARTESIAN_POINT('Ctrl Pts',(-79.8660951196445,6.76586757215105,
132.610287005887));
#239632=CARTESIAN_POINT('Ctrl Pts',(-80.1445427434577,5.17649370523912,
126.08819193488));
#239633=CARTESIAN_POINT('Ctrl Pts',(-80.4229903672703,-1.16982499101125,
123.900025485612));
#239634=CARTESIAN_POINT('Ctrl Pts',(-80.7014379910835,-6.44113166965063,
128.056605727087));
#239635=CARTESIAN_POINT('Ctrl Pts',(-80.9798856148961,-5.7933530106558,
134.738238477622));
#239636=CARTESIAN_POINT('Ctrl Pts',(-81.2583332387092,0.17823404410257,
137.804829655383));
#239637=CARTESIAN_POINT('Ctrl Pts',(-81.5367808625219,5.98603271954817,
134.438331779315));
#239638=CARTESIAN_POINT('Ctrl Pts',(-81.815228486335,6.29295975968447,127.732391934959));
#239639=CARTESIAN_POINT('Ctrl Pts',(-82.0936761101477,0.816964208846405,
123.849441235906));
#239640=CARTESIAN_POINT('Ctrl Pts',(-82.3721237339607,-5.40978153900143,
126.357721681897));
#239641=CARTESIAN_POINT('Ctrl Pts',(-82.6505713577735,-6.66520233502723,
132.952246079378));
#239642=CARTESIAN_POINT('Ctrl Pts',(-82.9290189815866,-1.79562779839943,
137.572968667493));
#239643=CARTESIAN_POINT('Ctrl Pts',(-83.2074666053992,4.72404096366304,
135.97367112261));
#239644=CARTESIAN_POINT('Ctrl Pts',(-83.4859142292123,6.90254686235,129.624029758449));
#239645=CARTESIAN_POINT('Ctrl Pts',(-83.7643618530252,2.73794940269844,
124.359054791448));
#239646=CARTESIAN_POINT('Ctrl Pts',(-84.0428094768383,-3.94268980176888,
125.017001007954));
#239647=CARTESIAN_POINT('Ctrl Pts',(-84.3212571006508,-7.00018968951541,
130.99324797746));
#239648=CARTESIAN_POINT('Ctrl Pts',(-84.5997047244641,-3.62485723087481,
136.795916690882));
#239649=CARTESIAN_POINT('Ctrl Pts',(-84.8781523482765,3.08154193881888,
137.092638076712));
#239650=CARTESIAN_POINT('Ctrl Pts',(-85.1565999720898,6.95615460843127,
131.61073967702));
#239651=CARTESIAN_POINT('Ctrl Pts',(-85.4350475959023,4.4384010199398,125.387818315495));
#239652=CARTESIAN_POINT('Ctrl Pts',(-85.7134952197154,-2.1580262779319,
124.142434716771));
#239653=CARTESIAN_POINT('Ctrl Pts',(-85.9919428435283,-6.7713328518292,
129.019035567703));
#239654=CARTESIAN_POINT('Ctrl Pts',(-86.2703904673411,-5.16211533289519,
135.536262921482));
#239655=CARTESIAN_POINT('Ctrl Pts',(-86.5488380911541,1.19083399361533,
137.70510322424));
#239656=CARTESIAN_POINT('Ctrl Pts',(-86.827285714967,6.4494650554685,133.532498191482));
#239657=CARTESIAN_POINT('Ctrl Pts',(-87.1057333387799,5.78135280522977,
126.852868005224));
#239658=CARTESIAN_POINT('Ctrl Pts',(-87.3841809625928,-0.199540238229241,
123.804466488563));
#239659=CARTESIAN_POINT('Ctrl Pts',(-87.6626285864056,-5.99706555083783,
127.188625712615));
#239660=CARTESIAN_POINT('Ctrl Pts',(-87.9410762102187,-6.28358059516641,
133.895468675847));
#239661=CARTESIAN_POINT('Ctrl Pts',(-88.2195238340314,-0.795792042514341,
137.761734342542));
#239662=CARTESIAN_POINT('Ctrl Pts',(-88.4979714578443,5.42329052060546,
135.234513442586));
#239663=CARTESIAN_POINT('Ctrl Pts',(-88.7764190816572,6.65863403776028,
128.636198521433));
#239664=CARTESIAN_POINT('Ctrl Pts',(-89.0548667054699,1.77501816656995,
124.03031864602));
#239665=CARTESIAN_POINT('Ctrl Pts',(-89.3333143292831,-4.73975268523957,
125.649452412109));
#239666=CARTESIAN_POINT('Ctrl Pts',(-89.6117619530957,-6.8989223691057,
132.005694987746));
#239667=CARTESIAN_POINT('Ctrl Pts',(-89.8902095769088,-2.71831942685781,
137.257969965635));
#239668=CARTESIAN_POINT('Ctrl Pts',(-90.1686572007216,3.9602862713853,136.579693228991));
#239669=CARTESIAN_POINT('Ctrl Pts',(-90.4471048245344,6.99958235696585,
130.59416796313));
#239670=CARTESIAN_POINT('Ctrl Pts',(-90.7255524483476,3.60660420510239,
124.801799478213));
#239671=CARTESIAN_POINT('Ctrl Pts',(-91.0040000721602,-3.10066701883943,
124.525491438947));
#239672=CARTESIAN_POINT('Ctrl Pts',(-91.2824476959735,-6.95857672847263,
130.019157435019));
#239673=CARTESIAN_POINT('Ctrl Pts',(-91.560895319786,-4.4218943700117,136.234386796543));
#239674=CARTESIAN_POINT('Ctrl Pts',(-91.8393429435991,2.17829289294083,
137.459687371113));
#239675=CARTESIAN_POINT('Ctrl Pts',(-92.1177905674117,6.77673540280433,
132.56906778996));
#239676=CARTESIAN_POINT('Ctrl Pts',(-92.3962381912249,5.14768913942031,
126.056768528114));
#239677=CARTESIAN_POINT('Ctrl Pts',(-92.6746858150375,-1.21183196449619,
123.907274463707));
#239678=CARTESIAN_POINT('Ctrl Pts',(-92.9531334388505,-6.45773869432309,
128.095865633305));
#239679=CARTESIAN_POINT('Ctrl Pts',(-93.2315810626634,-5.76929904214118,
134.773431376103));
#239680=CARTESIAN_POINT('Ctrl Pts',(-93.5100286864763,0.220844583841736,
137.803614991691));
#239681=CARTESIAN_POINT('Ctrl Pts',(-93.7884763102892,6.00804282613147,
134.401825770043));
#239682=CARTESIAN_POINT('Ctrl Pts',(-94.0669239341021,6.27414322041607,
127.694141819211));
#239683=CARTESIAN_POINT('Ctrl Pts',(-94.3453715579151,0.774612504073732,
123.844597001431));
#239684=CARTESIAN_POINT('Ctrl Pts',(-94.6238191817278,-5.43674926158731,
126.390734943524));
#239685=CARTESIAN_POINT('Ctrl Pts',(-94.9022668055408,-6.65200405581671,
132.99277926246));
#239686=CARTESIAN_POINT('Ctrl Pts',(-95.1807144293538,-1.75439209121494,
137.583773756932));
#239687=CARTESIAN_POINT('Ctrl Pts',(-95.4591620531666,4.75542049839504,
135.94481876907));
#239688=CARTESIAN_POINT('Ctrl Pts',(-95.7376096769794,6.89523396518648,
129.582033865318));
#239689=CARTESIAN_POINT('Ctrl Pts',(-96.0160573007924,2.69866426887766,
124.342507532899));
#239690=CARTESIAN_POINT('Ctrl Pts',(-96.2945049246052,-3.97784605345104,
125.041108506217));
#239691=CARTESIAN_POINT('Ctrl Pts',(-96.5729525484182,-6.99891018124123,
131.035856619345));
#239692=CARTESIAN_POINT('Ctrl Pts',(-96.8514001722308,-3.58831776824163,
136.817871216047));
#239693=CARTESIAN_POINT('Ctrl Pts',(-97.129847796044,3.11976337470375,137.073763349068));
#239694=CARTESIAN_POINT('Ctrl Pts',(-97.4082954198568,6.96093438520996,
131.56838064919));
#239695=CARTESIAN_POINT('Ctrl Pts',(-97.6867430436697,4.40534675625846,
125.360900864701));
#239696=CARTESIAN_POINT('Ctrl Pts',(-97.9651906674826,-2.1985393285419,
124.155694665303));
#239697=CARTESIAN_POINT('Ctrl Pts',(-98.2436382912955,-6.78207517502872,
129.060287670645));
#239698=CARTESIAN_POINT('Ctrl Pts',(-98.5220859151084,-5.13321525845608,
135.567598511506));
#239699=CARTESIAN_POINT('Ctrl Pts',(-98.8005335389213,1.23281870913114,
137.697726424945));
#239700=CARTESIAN_POINT('Ctrl Pts',(-99.0789811627341,6.4659525095689,133.493187921042));
#239701=CARTESIAN_POINT('Ctrl Pts',(-99.3574287865471,5.7571918330539,126.817748481762));
#239702=CARTESIAN_POINT('Ctrl Pts',(-99.6358764103599,-0.242146883580649,
123.805810838454));
#239703=CARTESIAN_POINT('Ctrl Pts',(-99.9143240341728,-6.01896444373747,
127.225198543987));
#239704=CARTESIAN_POINT('Ctrl Pts',(-100.192771657986,-6.26464772285957,
133.93366134335));
#239705=CARTESIAN_POINT('Ctrl Pts',(-100.471219281798,-0.753425789729175,
137.766449650557));
#239706=CARTESIAN_POINT('Ctrl Pts',(-100.749666905611,5.45015763726631,
135.201418253402));
#239707=CARTESIAN_POINT('Ctrl Pts',(-101.028114529424,6.64531245061667,
128.595705697122));
#239708=CARTESIAN_POINT('Ctrl Pts',(-101.306562153237,1.73374976341167,
124.019639113937));
#239709=CARTESIAN_POINT('Ctrl Pts',(-101.58500977705,-4.77104425798471,
125.678400140516));
#239710=CARTESIAN_POINT('Ctrl Pts',(-101.863457400863,-6.89148168476197,
132.047668428412));
#239711=CARTESIAN_POINT('Ctrl Pts',(-102.141905024676,-2.67898411084018,
137.274397577103));
#239712=CARTESIAN_POINT('Ctrl Pts',(-102.420352648489,3.99536898529432,
136.555478838857));
#239713=CARTESIAN_POINT('Ctrl Pts',(-102.698800272302,6.99817316856906,
130.551563412989));
#239714=CARTESIAN_POINT('Ctrl Pts',(-102.977247896115,3.56999808969468,
124.779956268296));
#239715=CARTESIAN_POINT('Ctrl Pts',(-103.255695519928,-3.13883082950684,
124.544482412068));
#239716=CARTESIAN_POINT('Ctrl Pts',(-103.53414314374,-6.96322755680218,
130.061530814641));
#239717=CARTESIAN_POINT('Ctrl Pts',(-103.812590767553,-4.38875833197407,
136.261203516848));
#239718=CARTESIAN_POINT('Ctrl Pts',(-104.091038391366,2.21876539717438,
137.44630417621));
#239719=CARTESIAN_POINT('Ctrl Pts',(-104.369486015179,6.78735211903507,
132.52778318216));
#239720=CARTESIAN_POINT('Ctrl Pts',(-104.647933638992,5.11869382408742,
126.02552104512));
#239721=CARTESIAN_POINT('Ctrl Pts',(-104.926381262805,-1.25379403310144,
123.914779015865));
#239722=CARTESIAN_POINT('Ctrl Pts',(-105.204828886617,-6.47410642511416,
128.135225903801));
#239723=CARTESIAN_POINT('Ctrl Pts',(-105.483276510431,-5.74503129012806,
134.808477199207));
#239724=CARTESIAN_POINT('Ctrl Pts',(-105.761724134243,0.263446940103889,
137.802140968053));
#239725=CARTESIAN_POINT('Ctrl Pts',(-106.040171758056,6.02983030247923,
134.365186455377));
#239726=CARTESIAN_POINT('Ctrl Pts',(-106.318619381869,6.25509419046252,
127.656006953765));
#239727=CARTESIAN_POINT('Ctrl Pts',(-106.597067005682,0.732232095750508,
123.840010663559));
#239728=CARTESIAN_POINT('Ctrl Pts',(-106.875514629495,-5.46351552342998,
126.423911753675));
#239729=CARTESIAN_POINT('Ctrl Pts',(-107.153962253308,-6.63855928414971,
133.033231352883));
#239730=CARTESIAN_POINT('Ctrl Pts',(-107.432409877121,-1.71309137438684,
137.594327632723));
#239731=CARTESIAN_POINT('Ctrl Pts',(-107.710857500934,4.78662381927155,
135.915775933963));
#239732=CARTESIAN_POINT('Ctrl Pts',(-107.989305124746,6.8876655625929,129.540083265954));
#239733=CARTESIAN_POINT('Ctrl Pts',(-108.26775274856,2.65927913505975,124.326199720693));
#239734=CARTESIAN_POINT('Ctrl Pts',(-108.546200372372,-4.0128549045848,
125.065429563905));
#239735=CARTESIAN_POINT('Ctrl Pts',(-108.824647996185,-6.99737132577695,
131.078456683062));
#239736=CARTESIAN_POINT('Ctrl Pts',(-109.103095619998,-3.5516453391731,
136.839602908365));
#239737=CARTESIAN_POINT('Ctrl Pts',(-109.381543243811,3.1578692066097,137.054656306401));
#239738=CARTESIAN_POINT('Ctrl Pts',(-109.659990867624,6.96545622200577,
131.525993310316));
#239739=CARTESIAN_POINT('Ctrl Pts',(-109.938438491437,4.37212925083209,
125.334185123311));
#239740=CARTESIAN_POINT('Ctrl Pts',(-110.21688611525,-2.23897091146772,
124.169200982596));
#239741=CARTESIAN_POINT('Ctrl Pts',(-110.495333739063,-6.79256618593892,
129.10160440085));
#239742=CARTESIAN_POINT('Ctrl Pts',(-110.773781362875,-5.10412497083799,
135.598757597999));
#239743=CARTESIAN_POINT('Ctrl Pts',(-111.052228986688,1.27475774209554,
137.690094189444));
#239744=CARTESIAN_POINT('Ctrl Pts',(-111.330676610501,6.48220036542147,
133.453778015119));
#239745=CARTESIAN_POINT('Ctrl Pts',(-111.609124234314,5.73281752601749,
126.782776683677));
#239746=CARTESIAN_POINT('Ctrl Pts',(-111.887571858127,-0.284744556090853,
123.807414522182));
#239747=CARTESIAN_POINT('Ctrl Pts',(-112.16601948194,-6.04064030169634,
127.261904002525));
#239748=CARTESIAN_POINT('Ctrl Pts',(-112.444467105753,-6.24548271172772,
133.971738053464));
#239749=CARTESIAN_POINT('Ctrl Pts',(-112.722914729566,-0.71103161847358,
137.770906975801));
#239750=CARTESIAN_POINT('Ctrl Pts',(-113.001362353379,5.47682279633179,
135.16816012963));
#239751=CARTESIAN_POINT('Ctrl Pts',(-113.279809977192,6.63174461897671,
128.55529471533));
#239752=CARTESIAN_POINT('Ctrl Pts',(-113.558257601004,1.69241711551747,
124.009210992206));
#239753=CARTESIAN_POINT('Ctrl Pts',(-113.836705224817,-4.80215903792943,
125.707537813274));
#239754=CARTESIAN_POINT('Ctrl Pts',(-114.11515284863,-6.88378563403075,
132.089595797848));
#239755=CARTESIAN_POINT('Ctrl Pts',(-114.393600472443,-2.63954952408134,
137.290585438973));
#239756=CARTESIAN_POINT('Ctrl Pts',(-114.672048096256,4.03030364933543,
136.531051338922));
#239757=CARTESIAN_POINT('Ctrl Pts',(-114.950495720069,6.99650466029252,
130.508968230339));
#239758=CARTESIAN_POINT('Ctrl Pts',(-115.228943343882,3.53325968669456,
124.758336294896));
#239759=CARTESIAN_POINT('Ctrl Pts',(-115.507390967695,-3.17687832964389,
124.563705347279));
#239760=CARTESIAN_POINT('Ctrl Pts',(-115.785838591507,-6.96762036017394,
130.103931720095));
#239761=CARTESIAN_POINT('Ctrl Pts',(-116.06428621532,-4.35545966688232,
136.287818031834));
#239762=CARTESIAN_POINT('Ctrl Pts',(-116.342733839133,2.25915568424066,
137.432674861647));
#239763=CARTESIAN_POINT('Ctrl Pts',(-116.621181462946,6.79771732743703,
132.486434712303));
#239764=CARTESIAN_POINT('Ctrl Pts',(-116.899629086759,5.08950883367243,
125.994450643782));
#239765=CARTESIAN_POINT('Ctrl Pts',(-117.178076710572,-1.2957096419083,
123.922538864004));
#239766=CARTESIAN_POINT('Ctrl Pts',(-117.456524334385,-6.49023425551004,
128.174685080065));
#239767=CARTESIAN_POINT('Ctrl Pts',(-117.734971958198,-5.7205506538686,
134.843374648297));
#239768=CARTESIAN_POINT('Ctrl Pts',(-118.013419582011,0.306039534242538,
137.800407639092));
#239769=CARTESIAN_POINT('Ctrl Pts',(-118.291867205823,6.05139434124684,
134.328415193001));
#239770=CARTESIAN_POINT('Ctrl Pts',(-118.570314829636,6.23581337569426,
127.617988751722));
#239771=CARTESIAN_POINT('Ctrl Pts',(-118.848762453449,0.689824554297045,
123.835682392233));
#239772=CARTESIAN_POINT('Ctrl Pts',(-119.127210077262,-5.49007933269568,
126.457250882969));
#239773=CARTESIAN_POINT('Ctrl Pts',(-119.405657701075,-6.62486851822702,
133.073600851681));
#239774=CARTESIAN_POINT('Ctrl Pts',(-119.684105324888,-1.67172717832737,
137.60462990379));
#239775=CARTESIAN_POINT('Ctrl Pts',(-119.962552948701,4.81764977004229,
135.886543693482));
#239776=CARTESIAN_POINT('Ctrl Pts',(-120.241000572514,6.87984193501854,
129.498179514853));
#239777=CARTESIAN_POINT('Ctrl Pts',(-120.519448196327,2.61979546067638,
124.310131959122));
#239778=CARTESIAN_POINT('Ctrl Pts',(-120.79789582014,-4.04771505790416,
125.089963279793));
#239779=CARTESIAN_POINT('Ctrl Pts',(-121.076343443952,-6.9955731801444,
131.121046590047));
#239780=CARTESIAN_POINT('Ctrl Pts',(-121.354791067765,-3.51484130258126,
136.86111096256));
#239781=CARTESIAN_POINT('Ctrl Pts',(-121.633238691578,3.19585802251066,
137.035317656727));
#239782=CARTESIAN_POINT('Ctrl Pts',(-121.911686315391,6.96971995125911,
131.483579231079));
#239783=CARTESIAN_POINT('Ctrl Pts',(-122.190133939204,4.3387497345494,125.307672081285));
#239784=CARTESIAN_POINT('Ctrl Pts',(-122.468581563017,-2.2793195285039,
124.182953168171));
#239785=CARTESIAN_POINT('Ctrl Pts',(-122.74702918683,-6.80280549581075,
129.142984227312));
#239786=CARTESIAN_POINT('Ctrl Pts',(-123.025476810643,-5.07484554799192,
135.629739026348));
#239787=CARTESIAN_POINT('Ctrl Pts',(-123.303924434456,1.31664953844379,
137.682206800553));
#239788=CARTESIAN_POINT('Ctrl Pts',(-123.582372058268,6.49820802095541,
133.414269934058));
#239789=CARTESIAN_POINT('Ctrl Pts',(-123.860819682081,5.7082307873194,126.747953906865));
#239790=CARTESIAN_POINT('Ctrl Pts',(-124.139267305894,-0.327331677286216,
123.809277480321));
#239791=CARTESIAN_POINT('Ctrl Pts',(-124.417714929707,-6.06209232150722,
127.298740728095));
#239792=CARTESIAN_POINT('Ctrl Pts',(-124.69616255352,-6.22608627193705,
134.009697395242));
#239793=CARTESIAN_POINT('Ctrl Pts',(-124.974610177333,-0.668611099680587,
137.77510615311));
#239794=CARTESIAN_POINT('Ctrl Pts',(-125.253057801146,5.50328500971429,
135.134740303665));
#239795=CARTESIAN_POINT('Ctrl Pts',(-125.531505424959,6.61793104560076,
128.514967073503));
#239796=CARTESIAN_POINT('Ctrl Pts',(-125.809953048772,1.6510217544855,123.999034667242));
#239797=CARTESIAN_POINT('Ctrl Pts',(-126.088400672584,-4.8330958721059,
125.736864350674));
#239798=CARTESIAN_POINT('Ctrl Pts',(-126.366848296398,-6.87583450209069,
132.131475542423));
#239799=CARTESIAN_POINT('Ctrl Pts',(-126.64529592021,-2.60001712784396,
137.306532951397));
#239800=CARTESIAN_POINT('Ctrl Pts',(-126.923743544023,4.06508896899354,
136.506411634357));
#239801=CARTESIAN_POINT('Ctrl Pts',(-127.202191167836,6.99457689396224,
130.466383993564));
#239802=CARTESIAN_POINT('Ctrl Pts',(-127.480638791649,3.49639035745773,
124.736940359153));
#239803=CARTESIAN_POINT('Ctrl Pts',(-127.759086415462,-3.21480810938582,
124.583159532264));
#239804=CARTESIAN_POINT('Ctrl Pts',(-128.037534039275,-6.97175497581086,
130.146358580199));
#239805=CARTESIAN_POINT('Ctrl Pts',(-128.315981663087,-4.32199960863106,
136.314229355287));
#239806=CARTESIAN_POINT('Ctrl Pts',(-128.594429286901,2.29946225746178,
137.418799932461));
#239807=CARTESIAN_POINT('Ctrl Pts',(-128.872876910713,6.80783064392392,
132.44502391257));
#239808=CARTESIAN_POINT('Ctrl Pts',(-129.151324534526,5.06013524963555,
125.963558475429));
#239809=CARTESIAN_POINT('Ctrl Pts',(-129.429772158339,-1.33757723771771,
123.930553720578));
#239810=CARTESIAN_POINT('Ctrl Pts',(-129.708219782152,-6.50612158788957,
128.214241699924));
#239811=CARTESIAN_POINT('Ctrl Pts',(-129.986667405965,-5.69585804050008,
134.878122430239));
#239812=CARTESIAN_POINT('Ctrl Pts',(-130.265115029778,0.348620787973942,
137.798415069035));
#239813=CARTESIAN_POINT('Ctrl Pts',(-130.543562653591,6.07273414337257,
134.291513345486));
#239814=CARTESIAN_POINT('Ctrl Pts',(-130.822010277403,6.21630149056731,
127.58008862186));
#239815=CARTESIAN_POINT('Ctrl Pts',(-131.100457901217,0.647391451141708,
123.831612347843));
#239816=CARTESIAN_POINT('Ctrl Pts',(-131.378905525029,-5.5164397050528,
126.490751096011));
#239817=CARTESIAN_POINT('Ctrl Pts',(-131.657353148842,-6.61093226536518,
133.113886262947));
#239818=CARTESIAN_POINT('Ctrl Pts',(-131.935800772655,-1.63030103580305,
137.614680188378));
#239819=CARTESIAN_POINT('Ctrl Pts',(-132.214248396468,4.848497201029,135.857123130838));
#239820=CARTESIAN_POINT('Ctrl Pts',(-132.492696020281,6.87176337237162,
129.456324164773));
#239821=CARTESIAN_POINT('Ctrl Pts',(-132.771143644094,2.58021470880796,
124.294304843582));
#239822=CARTESIAN_POINT('Ctrl Pts',(-133.049591267907,-4.08242522165371,
125.114708744776));
#239823=CARTESIAN_POINT('Ctrl Pts',(-133.32803889172,-6.99351581097555,
131.163624762118));
#239824=CARTESIAN_POINT('Ctrl Pts',(-133.606486515532,-3.47790702225152,
136.882394581644));
#239825=CARTESIAN_POINT('Ctrl Pts',(-133.884934139345,3.23372841471757,
137.015748116649));
#239826=CARTESIAN_POINT('Ctrl Pts',(-134.163381763158,6.97372541497715,
131.441139983145));
#239827=CARTESIAN_POINT('Ctrl Pts',(-134.441829386971,4.30520944429882,
125.281362721075));
#239828=CARTESIAN_POINT('Ctrl Pts',(-134.720277010784,-2.31958368451587,
124.196950712432));
#239829=CARTESIAN_POINT('Ctrl Pts',(-134.998724634597,-6.81279272522359,
129.184425616688));
#239830=CARTESIAN_POINT('Ctrl Pts',(-135.27717225841,-5.04537807487797,
135.660541648527));
#239831=CARTESIAN_POINT('Ctrl Pts',(-135.555619882223,1.35849254585843,
137.674064550544));
#239832=CARTESIAN_POINT('Ctrl Pts',(-135.834067506036,6.51397488300169,
133.374665141848));
#239833=CARTESIAN_POINT('Ctrl Pts',(-136.112515129848,5.68343252803032,
126.713281441693));
#239834=CARTESIAN_POINT('Ctrl Pts',(-136.390962753662,-0.369906669086523,
123.811399643837));
#239835=CARTESIAN_POINT('Ctrl Pts',(-136.669410377474,-6.08331970825794,
127.335707355701));
#239836=CARTESIAN_POINT('Ctrl Pts',(-136.947858001288,-6.20645912223011,
134.047537962086));
#239837=CARTESIAN_POINT('Ctrl Pts',(-137.2263056251,-0.626165805256695,
137.779047026878));
#239838=CARTESIAN_POINT('Ctrl Pts',(-137.504753248913,5.52954329684707,
135.101160013885));
#239839=CARTESIAN_POINT('Ctrl Pts',(-137.783200872726,6.60387224235649,
128.474724265995));
#239840=CARTESIAN_POINT('Ctrl Pts',(-138.061648496539,1.60956521423443,
123.989110516135));
#239841=CARTESIAN_POINT('Ctrl Pts',(-138.340096120352,-4.86385361413656,
125.766378666012));
#239842=CARTESIAN_POINT('Ctrl Pts',(-138.618543744165,-6.86762858357524,
132.173306110266));
#239843=CARTESIAN_POINT('Ctrl Pts',(-138.896991367977,-2.56038838701599,
137.322239523433));
#239844=CARTESIAN_POINT('Ctrl Pts',(-139.17543899179,4.09972365528409,136.481560638194));
#239845=CARTESIAN_POINT('Ctrl Pts',(-139.453886615603,6.99238994101352,
130.423812280637));
#239846=CARTESIAN_POINT('Ctrl Pts',(-139.732334239416,3.45939146819007,
124.715769253897));
#239847=CARTESIAN_POINT('Ctrl Pts',(-140.010781863229,-3.25261876323132,
124.602844246145));
#239848=CARTESIAN_POINT('Ctrl Pts',(-140.289229487042,-6.97563125050334,
130.188809822811));
#239849=CARTESIAN_POINT('Ctrl Pts',(-140.567677110855,-4.28837939709471,
136.340436508528));
#239850=CARTESIAN_POINT('Ctrl Pts',(-140.846124734668,2.33968362326381,
137.404679902793));
#239851=CARTESIAN_POINT('Ctrl Pts',(-141.124572358481,6.81769169374202,
132.403552317457));
#239852=CARTESIAN_POINT('Ctrl Pts',(-141.403019982293,5.03057416042698,
125.932845684778));
#239853=CARTESIAN_POINT('Ctrl Pts',(-141.681467606106,-1.37939526911043,
123.938823288595));
#239854=CARTESIAN_POINT('Ctrl Pts',(-141.959915229919,-6.52176783354029,
128.253894297592));
#239855=CARTESIAN_POINT('Ctrl Pts',(-142.238362853732,-5.67095436501806,
134.912719257437));
#239856=CARTESIAN_POINT('Ctrl Pts',(-142.516810477545,0.39118912343359,
137.796163331718));
#239857=CARTESIAN_POINT('Ctrl Pts',(-142.795258101358,6.09384891810056,
134.254482280245));
#239858=CARTESIAN_POINT('Ctrl Pts',(-143.073705725171,6.19655925810344,
127.542307968582));
#239859=CARTESIAN_POINT('Ctrl Pts',(-143.352153348984,0.604934358657401,
123.827800681205));
#239860=CARTESIAN_POINT('Ctrl Pts',(-143.630600972796,-5.54259566370794,
126.524411151443));
#239861=CARTESIAN_POINT('Ctrl Pts',(-143.90904859661,-6.59675104197701,
133.154086093891));
#239862=CARTESIAN_POINT('Ctrl Pts',(-144.187496220422,-1.58881448187379,
137.624478114069));
#239863=CARTESIAN_POINT('Ctrl Pts',(-144.465943844235,4.87916496916901,
135.827515336221));
#239864=CARTESIAN_POINT('Ctrl Pts',(-144.744391468048,6.86343017400547,
129.41451876668));
#239865=CARTESIAN_POINT('Ctrl Pts',(-145.022839091861,2.54053834613545,
124.278718960552));
#239866=CARTESIAN_POINT('Ctrl Pts',(-145.301286715674,-4.11698410963516,
125.139665041902));
#239867=CARTESIAN_POINT('Ctrl Pts',(-145.579734339487,-6.99119929450595,
131.206189621523));
#239868=CARTESIAN_POINT('Ctrl Pts',(-145.8581819633,-3.44084386679896,136.903452976945));
#239869=CARTESIAN_POINT('Ctrl Pts',(-146.136629587113,3.27147897992919,
136.995948411323));
#239870=CARTESIAN_POINT('Ctrl Pts',(-146.415077210925,6.97747246473481,
131.398677139117));
#239871=CARTESIAN_POINT('Ctrl Pts',(-146.693524834738,4.27150962292939,
125.255258017582));
#239872=CARTESIAN_POINT('Ctrl Pts',(-146.971972458551,-2.35976188750221,
124.211193096699));
#239873=CARTESIAN_POINT('Ctrl Pts',(-147.250420082364,-6.82252750409623,
129.225927033352));
#239874=CARTESIAN_POINT('Ctrl Pts',(-147.528867706177,-5.01572364342383,
135.69116432313));
#239875=CARTESIAN_POINT('Ctrl Pts',(-147.80731532999,1.40028521383297,137.665667741127));
#239876=CARTESIAN_POINT('Ctrl Pts',(-148.085762953803,6.52950036731291,
133.334965106058));
#239877=CARTESIAN_POINT('Ctrl Pts',(-148.364210577616,5.65842366705879,
126.678760572968));
#239878=CARTESIAN_POINT('Ctrl Pts',(-148.642658201429,-0.412467953858535,
123.813780934094));
#239879=CARTESIAN_POINT('Ctrl Pts',(-148.921105825242,-6.10432167535963,
127.372802515528));
#239880=CARTESIAN_POINT('Ctrl Pts',(-149.199553449054,-6.18660198989778,
134.085258351801));
#239881=CARTESIAN_POINT('Ctrl Pts',(-149.478001072867,-0.583697308029368,
137.782729451077));
#239882=CARTESIAN_POINT('Ctrl Pts',(-149.75644869668,5.55559668471987,135.067420504625));
#239883=CARTESIAN_POINT('Ctrl Pts',(-150.034896320493,6.58956873019717,
128.434567784019));
#239884=CARTESIAN_POINT('Ctrl Pts',(-150.313343944306,1.56804903095274,
123.979438906626));
#239885=CARTESIAN_POINT('Ctrl Pts',(-150.591791568119,-4.89443112428377,
125.796079665625));
#239886=CARTESIAN_POINT('Ctrl Pts',(-150.870239191931,-6.85916818255639,
132.21508595133));
#239887=CARTESIAN_POINT('Ctrl Pts',(-151.148686815745,-2.52066477005453,
137.33770457307));
#239888=CARTESIAN_POINT('Ctrl Pts',(-151.427134439557,4.13420642480782,
136.456499271296));
#239889=CARTESIAN_POINT('Ctrl Pts',(-151.705582063371,6.98994388248347,
130.381254669068));
#239890=CARTESIAN_POINT('Ctrl Pts',(-151.984029687183,3.42226438989971,
124.694823763634));
#239891=CARTESIAN_POINT('Ctrl Pts',(-152.262477310996,-3.29030889009209,
124.622758759495));
#239892=CARTESIAN_POINT('Ctrl Pts',(-152.540924934809,-6.97924904061452,
130.231283874884));
#239893=CARTESIAN_POINT('Ctrl Pts',(-152.819372558622,-4.25460027808296,
136.366438520441));
#239894=CARTESIAN_POINT('Ctrl Pts',(-153.097820182435,2.37981829122829,
137.390315295868));
#239895=CARTESIAN_POINT('Ctrl Pts',(-153.376267806248,6.82730011148789,
132.362021463707));
#239896=CARTESIAN_POINT('Ctrl Pts',(-153.654715430061,5.00082666144207,
125.902313409905));
#239897=CARTESIAN_POINT('Ctrl Pts',(-153.933163053873,-1.42116218650446,
123.947347261623));
#239898=CARTESIAN_POINT('Ctrl Pts',(-154.211610677687,-6.53717241268631,
128.293641403726));
#239899=CARTESIAN_POINT('Ctrl Pts',(-154.490058301499,-5.64584055023574,
134.947163847896));
#239900=CARTESIAN_POINT('Ctrl Pts',(-154.768505925312,0.433742963236675,
137.79365251058));
#239901=CARTESIAN_POINT('Ctrl Pts',(-155.046953549125,6.11473788301669,
134.217323369476));
#239902=CARTESIAN_POINT('Ctrl Pts',(-155.325401172938,6.17658740985663,
127.504648191865));
#239903=CARTESIAN_POINT('Ctrl Pts',(-155.603848796751,0.562454850108638,
123.824247533559));
#239904=CARTESIAN_POINT('Ctrl Pts',(-155.882296420564,-5.5685462394425,
126.558229801974));
#239905=CARTESIAN_POINT('Ctrl Pts',(-156.160744044376,-6.5823253735531,
133.194198854895));
#239906=CARTESIAN_POINT('Ctrl Pts',(-156.43919166819,-1.54726905384013,
137.634023317798));
#239907=CARTESIAN_POINT('Ctrl Pts',(-156.717639292002,4.90965193805665,
135.79772140676));
#239908=CARTESIAN_POINT('Ctrl Pts',(-156.996086915816,6.8548426487106,129.372764869687));
#239909=CARTESIAN_POINT('Ctrl Pts',(-157.274534539628,2.50076784287941,
124.263374887574));
#239910=CARTESIAN_POINT('Ctrl Pts',(-157.552982163441,-4.15139044125659,
125.164831246407));
#239911=CARTESIAN_POINT('Ctrl Pts',(-157.831429787254,-6.98862371657603,
131.248739591007));
#239912=CARTESIAN_POINT('Ctrl Pts',(-158.109877411067,-3.40365320961064,
136.924285368134));
#239913=CARTESIAN_POINT('Ctrl Pts',(-158.38832503488,3.30910831928323,136.975919274434));
#239914=CARTESIAN_POINT('Ctrl Pts',(-158.666772658693,6.98096096168483,
131.356192272474));
#239915=CARTESIAN_POINT('Ctrl Pts',(-158.945220282506,4.23765151920024,
125.229358938127));
#239916=CARTESIAN_POINT('Ctrl Pts',(-159.223667906319,-2.39985264864321,
124.225679793212));
#239917=CARTESIAN_POINT('Ctrl Pts',(-159.502115530131,-6.8320094717036,
129.267486939452));
#239918=CARTESIAN_POINT('Ctrl Pts',(-159.780563153944,-4.98588335248574,
135.721605915426));
#239919=CARTESIAN_POINT('Ctrl Pts',(-160.059010777757,1.44202599372318,
137.657016683454));
#239920=CARTESIAN_POINT('Ctrl Pts',(-160.33745840157,6.54478389858708,133.295171297791));
#239921=CARTESIAN_POINT('Ctrl Pts',(-160.615906025383,5.63320513111742,
126.644392579866));
#239922=CARTESIAN_POINT('Ctrl Pts',(-160.894353649196,-0.455013954479453,
123.816421262852));
#239923=CARTESIAN_POINT('Ctrl Pts',(-161.172801273009,-6.12509744457689,
127.410024833003));
#239924=CARTESIAN_POINT('Ctrl Pts',(-161.451248896821,-6.16651561075379,
134.122857166646));
#239925=CARTESIAN_POINT('Ctrl Pts',(-161.729696520635,-0.541207181682879,
137.786153289251));
#239926=CARTESIAN_POINT('Ctrl Pts',(-162.008144144447,5.58144420791359,
135.033523026113));
#239927=CARTESIAN_POINT('Ctrl Pts',(-162.286591768261,6.57502103914602,
128.394499115588));
#239928=CARTESIAN_POINT('Ctrl Pts',(-162.565039392073,1.52647474303778,
123.970020197102));
#239929=CARTESIAN_POINT('Ctrl Pts',(-162.843487015886,-4.92482726948487,
125.825966248931));
#239930=CARTESIAN_POINT('Ctrl Pts',(-163.121934639699,-6.85045361253876,
132.256813517449));
#239931=CARTESIAN_POINT('Ctrl Pts',(-163.400382263512,-2.48084774893327,
137.352927527244));
#239932=CARTESIAN_POINT('Ctrl Pts',(-163.678829887325,4.16853599979124,
136.431228462323));
#239933=CARTESIAN_POINT('Ctrl Pts',(-163.957277511138,6.98723880901292,
130.338712735846));
#239934=CARTESIAN_POINT('Ctrl Pts',(-164.23572513495,3.3850104983435,124.674104664506));
#239935=CARTESIAN_POINT('Ctrl Pts',(-164.514172758764,-3.32787709334726,
124.642902334375));
#239936=CARTESIAN_POINT('Ctrl Pts',(-164.792620382576,-6.98260821208591,
130.273779162525));
#239937=CARTESIAN_POINT('Ctrl Pts',(-165.07106800639,-4.22066350329308,
136.392234427513));
#239938=CARTESIAN_POINT('Ctrl Pts',(-165.349515630202,2.4198647741513,137.37570664397));
#239939=CARTESIAN_POINT('Ctrl Pts',(-165.627963254015,6.83665554111671,
132.320432890263));
#239940=CARTESIAN_POINT('Ctrl Pts',(-165.906410877828,4.97089385498702,
125.871962782194));
#239941=CARTESIAN_POINT('Ctrl Pts',(-166.184858501641,-1.46287644221077,
123.956125323802));
#239942=CARTESIAN_POINT('Ctrl Pts',(-166.463306125454,-6.55233475450377,
128.333481545486));
#239943=CARTESIAN_POINT('Ctrl Pts',(-166.741753749267,-5.62051752675643,
134.981454925258));
#239944=CARTESIAN_POINT('Ctrl Pts',(-167.020201373079,0.476280730534997,
137.790882698662));
#239945=CARTESIAN_POINT('Ctrl Pts',(-167.298648996893,6.13540026407138,
134.180037990117));
#239946=CARTESIAN_POINT('Ctrl Pts',(-167.577096620705,6.15638668589229,
127.467110687205));
#239947=CARTESIAN_POINT('Ctrl Pts',(-167.855544244518,0.519954499587912,
123.820953036571));
#239948=CARTESIAN_POINT('Ctrl Pts',(-168.133991868331,-5.5942904706483,
126.592205794446));
#239949=CARTESIAN_POINT('Ctrl Pts',(-168.412439492144,-6.56765579464175,
133.234223059563));
#239950=CARTESIAN_POINT('Ctrl Pts',(-168.690887115956,-1.50566629118217,
137.643315445865));
#239951=CARTESIAN_POINT('Ctrl Pts',(-168.96933473977,4.93995697798634,135.767742446477));
#239952=CARTESIAN_POINT('Ctrl Pts',(-169.247782363582,6.84600111470013,
129.331064021001));
#239953=CARTESIAN_POINT('Ctrl Pts',(-169.526229987396,2.46090467275213,
124.248273193229));
#239954=CARTESIAN_POINT('Ctrl Pts',(-169.804677611208,-4.18564294157836,
125.190206425745));
#239955=CARTESIAN_POINT('Ctrl Pts',(-170.083125235021,-6.98578917262369,
131.291273093865));
#239956=CARTESIAN_POINT('Ctrl Pts',(-170.361572858834,-3.36633642880185,
136.944890983262));
#239957=CARTESIAN_POINT('Ctrl Pts',(-170.640020482647,3.34661503841248,
136.955661448171));
#239958=CARTESIAN_POINT('Ctrl Pts',(-170.91846810646,6.98419077655865,131.313686957504));
#239959=CARTESIAN_POINT('Ctrl Pts',(-171.196915730273,4.20363638773547,
125.203666442409));
#239960=CARTESIAN_POINT('Ctrl Pts',(-171.475363354086,-2.43985448236259,
124.240410265162));
#239961=CARTESIAN_POINT('Ctrl Pts',(-171.753810977898,-6.84123827668714,
129.309103794972));
#239962=CARTESIAN_POINT('Ctrl Pts',(-172.032258601712,-4.9558583078063,
135.751865297389));
#239963=CARTESIAN_POINT('Ctrl Pts',(-172.310706225524,1.48371333881067,
137.648111698089));
#239964=CARTESIAN_POINT('Ctrl Pts',(-172.589153849337,6.55982491048677,
133.255285191615));
#239965=CARTESIAN_POINT('Ctrl Pts',(-172.86760147315,5.60777785468832,126.610178735912));
#239966=CARTESIAN_POINT('Ctrl Pts',(-173.146049096963,-0.497543094390354,
123.819320532272));
#239967=CARTESIAN_POINT('Ctrl Pts',(-173.424496720776,-6.14564624605571,
127.447372928838));
#239968=CARTESIAN_POINT('Ctrl Pts',(-173.702944344589,-6.14620072910595,
134.160333013378));
#239969=CARTESIAN_POINT('Ctrl Pts',(-173.981391968402,-0.498697000705985,
137.789318414533));
#239970=CARTESIAN_POINT('Ctrl Pts',(-174.259839592215,5.60708490864046,
134.999468834432));
#239971=CARTESIAN_POINT('Ctrl Pts',(-174.538287216028,6.56022970827155,
128.354519745462));
#239972=CARTESIAN_POINT('Ctrl Pts',(-174.81673483984,1.48484389103961,123.960854736574));
#239973=CARTESIAN_POINT('Ctrl Pts',(-175.095182463654,-4.95504092340126,
125.85603730847));
#239974=CARTESIAN_POINT('Ctrl Pts',(-175.373630087466,-6.8414851964426,
132.298487262391));
#239975=CARTESIAN_POINT('Ctrl Pts',(-175.652077711279,-2.44093879908611,
137.367907821863));
#239976=CARTESIAN_POINT('Ctrl Pts',(-175.930525335092,4.20271110814107,
136.405749147692));
#239977=CARTESIAN_POINT('Ctrl Pts',(-176.208972958905,6.98427482083815,
130.296188057377));
#239978=CARTESIAN_POINT('Ctrl Pts',(-176.487420582718,3.3476311739788,124.653612724266));
#239979=CARTESIAN_POINT('Ctrl Pts',(-176.765868206531,-3.36532198089259,
124.663274224357));
#239980=CARTESIAN_POINT('Ctrl Pts',(-177.044315830343,-6.98570864044213,
130.316294111058));
#239981=CARTESIAN_POINT('Ctrl Pts',(-177.322763454156,-4.18657033026512,
136.417823273865));
#239982=CARTESIAN_POINT('Ctrl Pts',(-177.601211077969,2.4598215880947,137.360854488428));
#239983=CARTESIAN_POINT('Ctrl Pts',(-177.879658701782,6.84575763596098,
132.278788138201));
#239984=CARTESIAN_POINT('Ctrl Pts',(-178.158106325595,4.94077685023126,
125.841794926299));
#239985=CARTESIAN_POINT('Ctrl Pts',(-178.436553949408,-1.50453649049278,
123.965157149858));
#239986=CARTESIAN_POINT('Ctrl Pts',(-178.715001573221,-6.56725429714808,
128.373413246577));
#239987=CARTESIAN_POINT('Ctrl Pts',(-178.993449197033,-5.59498623293233,
135.015591218853));
#239988=CARTESIAN_POINT('Ctrl Pts',(-179.271896820847,0.518800849074927,
137.787853998597));
#239989=CARTESIAN_POINT('Ctrl Pts',(-179.550344444659,6.15583529561319,
134.142627523792));
#239990=CARTESIAN_POINT('Ctrl Pts',(-179.828792068472,6.13595783475539,
127.429696845569));
#239991=CARTESIAN_POINT('Ctrl Pts',(-180.107239692285,0.477434881962636,
123.81791731232));
#239992=CARTESIAN_POINT('Ctrl Pts',(-180.385687316098,-5.61982740336347,
126.626337869861));
#239993=CARTESIAN_POINT('Ctrl Pts',(-180.664134939911,-6.55274284882976,
133.274157224785));
#239994=CARTESIAN_POINT('Ctrl Pts',(-180.942582563724,-1.4640077355066,
137.652354153945));
#239995=CARTESIAN_POINT('Ctrl Pts',(-181.221030187537,4.97007896599344,
135.737579566256));
#239996=CARTESIAN_POINT('Ctrl Pts',(-181.499477811349,6.83690589960112,
129.289417765863));
#239997=CARTESIAN_POINT('Ctrl Pts',(-181.777925435163,2.42095031289641,
124.233414437113));
#239998=CARTESIAN_POINT('Ctrl Pts',(-182.056373058975,-4.21974034136189,
125.215789639631));
#239999=CARTESIAN_POINT('Ctrl Pts',(-182.334820682789,-6.98269576768506,
131.333788554001));
#240000=CARTESIAN_POINT('Ctrl Pts',(-182.613268306601,-3.32889490715784,
136.965269058779));
#240001=CARTESIAN_POINT('Ctrl Pts',(-182.891715930414,3.38399774748988,
136.935175683191));
#240002=CARTESIAN_POINT('Ctrl Pts',(-183.170163554227,6.98716178967534,
131.27116276926));
#240003=CARTESIAN_POINT('Ctrl Pts',(-183.44861117804,4.16946548897866,125.178181482475));
#240004=CARTESIAN_POINT('Ctrl Pts',(-183.727058801853,-2.47976590637605,
124.255383966707));
#240005=CARTESIAN_POINT('Ctrl Pts',(-184.005506425666,-6.85021357707087,
129.350776057783));
#240006=CARTESIAN_POINT('Ctrl Pts',(-184.283954049479,-4.92564962197493,
135.781941347746));
#240007=CARTESIAN_POINT('Ctrl Pts',(-184.562401673291,1.52534570435398,
137.63895311501));
#240008=CARTESIAN_POINT('Ctrl Pts',(-184.840849297105,6.5746228456623,133.215308265529));
#240009=CARTESIAN_POINT('Ctrl Pts',(-185.119296920917,5.58214277998856,
126.576120308909));
#240010=CARTESIAN_POINT('Ctrl Pts',(-185.39774454473,-0.540053797659538,
123.822478634922));
#240011=CARTESIAN_POINT('Ctrl Pts',(-185.676192168543,-6.16596731835295,
127.484845419088));
#240012=CARTESIAN_POINT('Ctrl Pts',(-185.954639792356,-6.12565809773001,
134.197684503321));
#240013=CARTESIAN_POINT('Ctrl Pts',(-186.233087416169,-0.456168340327589,
137.792224709632));
#240014=CARTESIAN_POINT('Ctrl Pts',(-186.511535039982,5.63251783677319,
134.965259191474));
#240015=CARTESIAN_POINT('Ctrl Pts',(-186.789982663795,6.54519528567348,
128.314631155089));
#240016=CARTESIAN_POINT('Ctrl Pts',(-187.068430287608,1.44315801760525,
123.951942864674));
#240017=CARTESIAN_POINT('Ctrl Pts',(-187.346877911421,-4.98507096645316,
125.886291729948));
#240018=CARTESIAN_POINT('Ctrl Pts',(-187.625325535233,-6.83226326659722,
132.340105641921));
#240019=CARTESIAN_POINT('Ctrl Pts',(-187.903773159046,-2.40093939935397,
137.382644901827));
#240020=CARTESIAN_POINT('Ctrl Pts',(-188.182220782859,4.23673048348491,
136.380062271549));
#240021=CARTESIAN_POINT('Ctrl Pts',(-188.460668406672,6.98105202779173,
130.25368220943));
#240022=CARTESIAN_POINT('Ctrl Pts',(-188.739116030485,3.31012780190951,
124.633348702251));
#240023=CARTESIAN_POINT('Ctrl Pts',(-189.017563654298,-3.40264216519462,
124.683873674555));
#240024=CARTESIAN_POINT('Ctrl Pts',(-189.296011278111,-6.98855021079573,
130.358827145076));
#240025=CARTESIAN_POINT('Ctrl Pts',(-189.574458901924,-4.15232202233378,
136.443204111294));
#240026=CARTESIAN_POINT('Ctrl Pts',(-189.852906525736,2.49968725244504,
137.345759379595));
#240027=CARTESIAN_POINT('Ctrl Pts',(-190.13135414955,6.85460605873784,132.237088750687));
#240028=CARTESIAN_POINT('Ctrl Pts',(-190.409801773362,4.91047676317321,
125.8118109601));
#240029=CARTESIAN_POINT('Ctrl Pts',(-190.688249397175,-1.5461407876216,
123.974442405114));
#240030=CARTESIAN_POINT('Ctrl Pts',(-190.966697020988,-6.58193048776853,
128.413435027317));
#240031=CARTESIAN_POINT('Ctrl Pts',(-191.245144644801,-5.56924761483672,
135.049571463749));
#240032=CARTESIAN_POINT('Ctrl Pts',(-191.523592268614,0.561301743259386,
137.784566522618));
#240033=CARTESIAN_POINT('Ctrl Pts',(-191.802039892427,6.17604222041412,
134.105093356759));
#240034=CARTESIAN_POINT('Ctrl Pts',(-192.08048751624,6.11530161344434,127.39240805334));
#240035=CARTESIAN_POINT('Ctrl Pts',(-192.358935140053,0.43489757281158,
123.815140473294));
#240036=CARTESIAN_POINT('Ctrl Pts',(-192.637382763865,-5.64515609130746,
126.660624763449));
#240037=CARTESIAN_POINT('Ctrl Pts',(-192.915830387678,-6.53758708872167,
133.313999870785));
#240038=CARTESIAN_POINT('Ctrl Pts',(-193.194278011491,-1.42229493048546,
137.661139107108));
#240039=CARTESIAN_POINT('Ctrl Pts',(-193.472725635304,5.00001678589681,
135.707233883791));
#240040=CARTESIAN_POINT('Ctrl Pts',(-193.751173259117,6.82755734043935,
129.247827647489));
#240041=CARTESIAN_POINT('Ctrl Pts',(-194.02962088293,2.38090624383734,124.218799169824));
#240042=CARTESIAN_POINT('Ctrl Pts',(-194.308068506743,-4.25368137711504,
125.241579940071));
#240043=CARTESIAN_POINT('Ctrl Pts',(-194.586516130556,-6.97934361638637,
131.376284395991));
#240044=CARTESIAN_POINT('Ctrl Pts',(-194.864963754369,-3.29133003208973,
136.985418839569));
#240045=CARTESIAN_POINT('Ctrl Pts',(-195.143411378181,3.42125506128717,
136.914462738605));
#240046=CARTESIAN_POINT('Ctrl Pts',(-195.421859001994,6.98987389094189,
131.22862128349));
#240047=CARTESIAN_POINT('Ctrl Pts',(-195.700306625807,4.13514008914463,
125.152905002676));
#240048=CARTESIAN_POINT('Ctrl Pts',(-195.97875424962,-2.51958544175274,
124.270600342989));
#240049=CARTESIAN_POINT('Ctrl Pts',(-196.257201873433,-6.85893504027095,
129.392502183704));
#240050=CARTESIAN_POINT('Ctrl Pts',(-196.535649497246,-4.89525841438522,
135.811832952018));
#240051=CARTESIAN_POINT('Ctrl Pts',(-196.814097121059,1.56692154765205,
137.629541273595));
#240052=CARTESIAN_POINT('Ctrl Pts',(-197.092544744872,6.58917715577019,
133.175242000891));
#240053=CARTESIAN_POINT('Ctrl Pts',(-197.370992368684,5.55630085693524,
126.542218560906));
#240054=CARTESIAN_POINT('Ctrl Pts',(-197.649439992498,-0.582544489036021,
123.825895453776));
#240055=CARTESIAN_POINT('Ctrl Pts',(-197.92788761631,-6.18605990846357,
127.522440915193));
#240056=CARTESIAN_POINT('Ctrl Pts',(-198.206335240123,-6.10488847784037,
134.234910252398));
#240057=CARTESIAN_POINT('Ctrl Pts',(-198.484782863936,-0.413622776464342,
137.79487206686));
#240058=CARTESIAN_POINT('Ctrl Pts',(-198.763230487749,5.657742049887,134.930895364888));
#240059=CARTESIAN_POINT('Ctrl Pts',(-199.041678111562,6.52991832845634,
128.274834822558));
#240060=CARTESIAN_POINT('Ctrl Pts',(-199.320125735375,1.40141866741961,
123.943284911633));
#240061=CARTESIAN_POINT('Ctrl Pts',(-199.598573359188,-5.01491628586802,
125.916728392279));
#240062=CARTESIAN_POINT('Ctrl Pts',(-199.877020983,-6.82278816472322,132.381667113854));
#240063=CARTESIAN_POINT('Ctrl Pts',(-200.155468606814,-2.36085103192995,
137.397138221046));
#240064=CARTESIAN_POINT('Ctrl Pts',(-200.433916230626,4.27059286522247,
136.354168785731));
#240065=CARTESIAN_POINT('Ctrl Pts',(-200.712363854439,6.97757054929515,
130.211196767073));
#240066=CARTESIAN_POINT('Ctrl Pts',(-200.990811478252,3.27250177183757,
124.613313349352));
#240067=CARTESIAN_POINT('Ctrl Pts',(-201.269259102065,-3.43983626333961,
124.704699921646));
#240068=CARTESIAN_POINT('Ctrl Pts',(-201.547706725878,-6.9911328178512,
130.401376688499));
#240069=CARTESIAN_POINT('Ctrl Pts',(-201.826154349691,-4.1179198485831,
136.468375999304));
#240070=CARTESIAN_POINT('Ctrl Pts',(-202.104601973504,2.53946028996452,
137.330421876826));
#240071=CARTESIAN_POINT('Ctrl Pts',(-202.383049597317,6.86320048156709,
132.195336272904));
#240072=CARTESIAN_POINT('Ctrl Pts',(-202.66149722113,4.87999471659204,125.782011994664));
#240073=CARTESIAN_POINT('Ctrl Pts',(-202.939944844942,-1.5876877919352,
123.983980745501));
#240074=CARTESIAN_POINT('Ctrl Pts',(-203.218392468755,-6.59636278253501,
128.453545404684));
#240075=CARTESIAN_POINT('Ctrl Pts',(-203.496840092568,-5.54330262622176,
135.083394400798));
#240076=CARTESIAN_POINT('Ctrl Pts',(-203.775287716381,0.603781838200554,
137.781020392543));
#240077=CARTESIAN_POINT('Ctrl Pts',(-204.053735340194,6.19602028969954,
134.067436879861));
#240078=CARTESIAN_POINT('Ctrl Pts',(-204.332182964007,6.09441878738321,
127.355245692268));
#240079=CARTESIAN_POINT('Ctrl Pts',(-204.61063058782,0.392344148371673,
123.812622622391));
#240080=CARTESIAN_POINT('Ctrl Pts',(-204.889078211633,-5.67027559591653,
126.69506520469));
#240081=CARTESIAN_POINT('Ctrl Pts',(-205.167525835445,-6.5221890759199,
133.353749521179));
#240082=CARTESIAN_POINT('Ctrl Pts',(-205.445973459259,-1.38052942180316,
137.66966997982));
#240083=CARTESIAN_POINT('Ctrl Pts',(-205.724421083071,5.02976932833932,
135.676706523556));
#240084=CARTESIAN_POINT('Ctrl Pts',(-206.002868706884,6.8179557836299,129.206295207017));
#240085=CARTESIAN_POINT('Ctrl Pts',(-206.281316330697,2.340773949421,124.204427932937));
#240086=CARTESIAN_POINT('Ctrl Pts',(-206.55976395451,-4.28746479114066,
125.267576371395));
#240087=CARTESIAN_POINT('Ctrl Pts',(-206.838211578323,-6.97573284294384,
131.418759045136));
#240088=CARTESIAN_POINT('Ctrl Pts',(-207.116659202136,-3.253643195576,137.005339578972));
#240089=CARTESIAN_POINT('Ctrl Pts',(-207.395106825949,3.4583855992191,136.893523381939));
#240090=CARTESIAN_POINT('Ctrl Pts',(-207.673554449762,6.99232697986142,
131.186064076586));
#240091=CARTESIAN_POINT('Ctrl Pts',(-207.952002073574,4.10066146017411,
125.127837939644));
#240092=CARTESIAN_POINT('Ctrl Pts',(-208.230449697387,-2.55931161296347,
124.286058830161));
#240093=CARTESIAN_POINT('Ctrl Pts',(-208.5088973212,-6.86740234311116,129.434280626559));
#240094=CARTESIAN_POINT('Ctrl Pts',(-208.787344945013,-4.86468581119477,
135.841539002563));
#240095=CARTESIAN_POINT('Ctrl Pts',(-209.065792568826,1.60843932809579,
137.619876522599));
#240096=CARTESIAN_POINT('Ctrl Pts',(-209.344240192639,6.60348730149562,
133.135087882371));
#240097=CARTESIAN_POINT('Ctrl Pts',(-209.622687816452,5.53025304311036,
126.508474748144));
#240098=CARTESIAN_POINT('Ctrl Pts',(-209.901135440264,-0.625013594012848,
123.829570862223));
#240099=CARTESIAN_POINT('Ctrl Pts',(-210.179583064078,-6.20592327184948,
127.56015802404));
#240100=CARTESIAN_POINT('Ctrl Pts',(-210.45803068789,-6.08389263906328,
134.272008881199));
#240101=CARTESIAN_POINT('Ctrl Pts',(-210.736478311703,-0.371061885656257,
137.797260388114));
#240102=CARTESIAN_POINT('Ctrl Pts',(-211.014925935516,5.68275661328764,
134.896378628042));
#240103=CARTESIAN_POINT('Ctrl Pts',(-211.293373559329,6.51439940271492,
128.235132222534));
#240104=CARTESIAN_POINT('Ctrl Pts',(-211.571821183142,1.35962738715011,
123.934881198276));
#240105=CARTESIAN_POINT('Ctrl Pts',(-211.850268806955,-5.04457577571481,
125.947346167619));
#240106=CARTESIAN_POINT('Ctrl Pts',(-212.128716430768,-6.81306024192543,
132.423170138115));
#240107=CARTESIAN_POINT('Ctrl Pts',(-212.40716405458,-2.32067518230222,
137.411387242468));
#240108=CARTESIAN_POINT('Ctrl Pts',(-212.685611678394,4.30429699857105,
136.32806964973));
#240109=CARTESIAN_POINT('Ctrl Pts',(-212.964059302206,6.97383051435588,
130.168733304621));
#240110=CARTESIAN_POINT('Ctrl Pts',(-213.24250692602,3.23475447800865,124.593507407987));
#240111=CARTESIAN_POINT('Ctrl Pts',(-213.520954549832,-3.47690289708716,
124.725752193909));
#240112=CARTESIAN_POINT('Ctrl Pts',(-213.799402173646,-6.99345636590915,
130.443941164641));
#240113=CARTESIAN_POINT('Ctrl Pts',(-214.077849797458,-4.08336508379785,
136.49333800514));
#240114=CARTESIAN_POINT('Ctrl Pts',(-214.356297421271,2.57913922684953,
137.314842548456));
#240115=CARTESIAN_POINT('Ctrl Pts',(-214.634745045084,6.87154058597789,
132.153532252007));
#240116=CARTESIAN_POINT('Ctrl Pts',(-214.913192668897,4.84933184001288,
125.752399134204));
#240117=CARTESIAN_POINT('Ctrl Pts',(-215.19164029271,-1.62917596389355,
123.993771817573));
#240118=CARTESIAN_POINT('Ctrl Pts',(-215.470087916522,-6.61055064665203,
128.493742892374));
#240119=CARTESIAN_POINT('Ctrl Pts',(-215.748535540335,-5.51715222849034,
135.117058776675));
#240120=CARTESIAN_POINT('Ctrl Pts',(-216.026983164148,0.646239559784443,
137.777215739773));
#240121=CARTESIAN_POINT('Ctrl Pts',(-216.305430787961,6.21576876317433,
134.029659488472));
#240122=CARTESIAN_POINT('Ctrl Pts',(-216.583878411774,6.0733101303926,127.318211139417));
#240123=CARTESIAN_POINT('Ctrl Pts',(-216.862326035587,0.349776185474419,
123.810363852911));
#240124=CARTESIAN_POINT('Ctrl Pts',(-217.1407736594,-5.69518498637811,126.729657917385));
#240125=CARTESIAN_POINT('Ctrl Pts',(-217.419221283213,-6.50654938100331,
133.393404703032));
#240126=CARTESIAN_POINT('Ctrl Pts',(-217.697668907026,-1.33871275709491,
137.67794645597));
#240127=CARTESIAN_POINT('Ctrl Pts',(-217.976116530838,5.05933549082977,
135.64599861675));
#240128=CARTESIAN_POINT('Ctrl Pts',(-218.254564154652,6.80810158496121,
129.164821983446));
#240129=CARTESIAN_POINT('Ctrl Pts',(-218.533011778464,2.30055491676597,
124.190301258982));
#240130=CARTESIAN_POINT('Ctrl Pts',(-218.811459402277,-4.32108933158155,
125.293777970294));
#240131=CARTESIAN_POINT('Ctrl Pts',(-219.08990702609,-6.97186358115499,
131.461210927519));
#240132=CARTESIAN_POINT('Ctrl Pts',(-219.368354649903,-3.21583579411804,
137.02503053882));
#240133=CARTESIAN_POINT('Ctrl Pts',(-219.646802273716,3.49538798540175,
136.872358389107));
#240134=CARTESIAN_POINT('Ctrl Pts',(-219.925249897529,6.99452096553273,
131.143492725519));
#240135=CARTESIAN_POINT('Ctrl Pts',(-220.203697521342,4.06603087968498,
125.102981222246));
#240136=CARTESIAN_POINT('Ctrl Pts',(-220.482145145155,-2.59894294794204,
124.301758855404));
#240137=CARTESIAN_POINT('Ctrl Pts',(-220.760592768967,-6.87561517183164,
129.476109838232));
#240138=CARTESIAN_POINT('Ctrl Pts',(-221.03904039278,-4.83393294528274,
135.87105839861));
#240139=CARTESIAN_POINT('Ctrl Pts',(-221.317488016593,1.64989750722823,
137.609959220154));
#240140=CARTESIAN_POINT('Ctrl Pts',(-221.595935640406,6.61755275257056,
133.094847397895));
#240141=CARTESIAN_POINT('Ctrl Pts',(-221.874383264219,5.5040003037252,126.474890121013));
#240142=CARTESIAN_POINT('Ctrl Pts',(-222.152830888031,-0.667459538880483,
123.83350472407));
#240143=CARTESIAN_POINT('Ctrl Pts',(-222.431278511845,-6.22555667246622,
127.597995348007));
#240144=CARTESIAN_POINT('Ctrl Pts',(-222.709726135657,-6.06267135940695,
134.308979015016));
#240145=CARTESIAN_POINT('Ctrl Pts',(-222.988173759471,-0.328487245014279,
137.799389584896));
#240146=CARTESIAN_POINT('Ctrl Pts',(-223.266621383283,5.70756060005303,
134.861710259961));
#240147=CARTESIAN_POINT('Ctrl Pts',(-223.545069007096,6.49863908350723,
128.195524826214));
#240148=CARTESIAN_POINT('Ctrl Pts',(-223.823516630909,1.31778572538753,
123.926732036005));
#240149=CARTESIAN_POINT('Ctrl Pts',(-224.101964254722,-5.07404833695195,
125.978143921416));
#240150=CARTESIAN_POINT('Ctrl Pts',(-224.380411878535,-6.80307985867417,
132.464613176793));
#240151=CARTESIAN_POINT('Ctrl Pts',(-224.658859502348,-2.28041333920269,
137.425391438088));
#240152=CARTESIAN_POINT('Ctrl Pts',(-224.937307126161,4.33784163461131,
136.30176583066));
#240153=CARTESIAN_POINT('Ctrl Pts',(-225.215754749974,6.96983206156226,
130.126293395573));
#240154=CARTESIAN_POINT('Ctrl Pts',(-225.494202373786,3.19688731916334,
124.573931612073));
#240155=CARTESIAN_POINT('Ctrl Pts',(-225.7726499976,-3.51384069291894,124.747029711241));
#240156=CARTESIAN_POINT('Ctrl Pts',(-226.051097621412,-6.9955207688696,
130.486518996257));
#240157=CARTESIAN_POINT('Ctrl Pts',(-226.329545245225,-4.04865900841799,
136.518089203828));
#240158=CARTESIAN_POINT('Ctrl Pts',(-226.607992869038,2.61872259278156,
137.299021971784));
#240159=CARTESIAN_POINT('Ctrl Pts',(-226.886440492851,6.87962606292594,
132.111678237058));
#240160=CARTESIAN_POINT('Ctrl Pts',(-227.164888116664,4.81848926965818,
125.722973476035));
#240161=CARTESIAN_POINT('Ctrl Pts',(-227.443335740477,-1.67060376613766,
124.003815258517));
#240162=CARTESIAN_POINT('Ctrl Pts',(-227.72178336429,-6.62449355438458,
128.534026000853));
#240163=CARTESIAN_POINT('Ctrl Pts',(-228.000230988102,-5.49079739065326,
135.150563343936));
#240164=CARTESIAN_POINT('Ctrl Pts',(-228.278678611916,0.688673334723007,
137.773152705292));
#240165=CARTESIAN_POINT('Ctrl Pts',(-228.557126235728,6.23528690905198,
133.991762582447));
#240166=CARTESIAN_POINT('Ctrl Pts',(-228.835573859542,6.05197642466173,
127.281305767118));
#240167=CARTESIAN_POINT('Ctrl Pts',(-229.114021483354,0.307195261492642,
123.808364248553));
#240168=CARTESIAN_POINT('Ctrl Pts',(-229.392469107167,-5.7198833396657,
126.764401619687));
#240169=CARTESIAN_POINT('Ctrl Pts',(-229.670916730979,-6.49066858350677,
133.432963946903));
#240170=CARTESIAN_POINT('Ctrl Pts',(-229.949364354793,-1.29684648589306,
137.685968228869));
#240171=CARTESIAN_POINT('Ctrl Pts',(-230.227811978605,5.0887141777831,135.615111301269));
#240172=CARTESIAN_POINT('Ctrl Pts',(-230.506259602419,6.79799510958498,
129.123409513582));
#240173=CARTESIAN_POINT('Ctrl Pts',(-230.784707226231,2.26025063620168,
124.176419671429));
#240174=CARTESIAN_POINT('Ctrl Pts',(-231.063154850045,-4.35455375246839,
125.32018376586));
#240175=CARTESIAN_POINT('Ctrl Pts',(-231.341602473857,-6.96773597439774,
131.503638470075));
#240176=CARTESIAN_POINT('Ctrl Pts',(-231.62005009767,-3.17790922868121,
137.044490989456));
#240177=CARTESIAN_POINT('Ctrl Pts',(-231.898497721483,3.53226084869627,
136.850968544386));
#240178=CARTESIAN_POINT('Ctrl Pts',(-232.176945345296,6.99645576665798,
131.100908807788));
#240179=CARTESIAN_POINT('Ctrl Pts',(-232.455392969109,4.03124963092651,
125.078335771559));
#240180=CARTESIAN_POINT('Ctrl Pts',(-232.733840592922,-2.63847797813309,
124.317699836946));
#240181=CARTESIAN_POINT('Ctrl Pts',(-233.012288216734,-6.88357322210384,
129.517988268725));
#240182=CARTESIAN_POINT('Ctrl Pts',(-233.290735840548,-4.80300095620762,
135.900390046307));
#240183=CARTESIAN_POINT('Ctrl Pts',(-233.56918346436,1.6912945488023,137.599789733751));
#240184=CARTESIAN_POINT('Ctrl Pts',(-233.847631088173,6.63137298779474,
133.05452203859));
#240185=CARTESIAN_POINT('Ctrl Pts',(-234.126078711986,5.47754361158473,
126.441465924004));
#240186=CARTESIAN_POINT('Ctrl Pts',(-234.404526335799,-0.709880750790079,
123.837696893545));
#240187=CARTESIAN_POINT('Ctrl Pts',(-234.682973959612,-6.24495938279112,
127.635951485018));
#240188=CARTESIAN_POINT('Ctrl Pts',(-234.961421583425,-6.04122542523402,
134.345819283911));
#240189=CARTESIAN_POINT('Ctrl Pts',(-235.239869207238,-0.285900432155891,
137.801259578306));
#240190=CARTESIAN_POINT('Ctrl Pts',(-235.518316831051,5.73215309106056,
134.826891545298));
#240191=CARTESIAN_POINT('Ctrl Pts',(-235.796764454864,6.48263795483918,
128.156014101264));
#240192=CARTESIAN_POINT('Ctrl Pts',(-236.075212078676,1.27589523259052,
123.918837726791));
#240193=CARTESIAN_POINT('Ctrl Pts',(-236.353659702489,-5.10333287746112,
126.009120512446));
#240194=CARTESIAN_POINT('Ctrl Pts',(-236.632107326302,-6.79284738479763,
132.505994694203));
#240195=CARTESIAN_POINT('Ctrl Pts',(-236.910554950115,-2.24006699454776,
137.439150288976));
#240196=CARTESIAN_POINT('Ctrl Pts',(-237.189002573928,4.3712255303347,136.275258303218));
#240197=CARTESIAN_POINT('Ctrl Pts',(-237.467450197741,6.96557533907847,
130.083878612554));
#240198=CARTESIAN_POINT('Ctrl Pts',(-237.745897821554,3.15890169848239,
124.554586686994));
#240199=CARTESIAN_POINT('Ctrl Pts',(-238.024345445366,-3.55064828209192,
124.768531685198));
#240200=CARTESIAN_POINT('Ctrl Pts',(-238.30279306918,-6.99732595023538,
130.529108605612));
#240201=CARTESIAN_POINT('Ctrl Pts',(-238.581240692992,-4.01380290848946,
136.542628678202));
#240202=CARTESIAN_POINT('Ctrl Pts',(-238.859688316805,2.65820892098533,
137.282960733047));
#240203=CARTESIAN_POINT('Ctrl Pts',(-239.138135940618,6.88745661279959,
132.069775778975));
#240204=CARTESIAN_POINT('Ctrl Pts',(-239.416583564431,4.78746814841248,
125.693736110535));
#240205=CARTESIAN_POINT('Ctrl Pts',(-239.695031188244,-1.71196966354462,
124.014110696169));
#240206=CARTESIAN_POINT('Ctrl Pts',(-239.973478812057,-6.63819098907155,
128.574393237416));
#240207=CARTESIAN_POINT('Ctrl Pts',(-240.25192643587,-5.46423908930053,
135.183906861057));
#240208=CARTESIAN_POINT('Ctrl Pts',(-240.530374059683,0.731081590618679,
137.768831439659));
#240209=CARTESIAN_POINT('Ctrl Pts',(-240.808821683496,6.25457400407998,
133.95374756607));
#240210=CARTESIAN_POINT('Ctrl Pts',(-241.087269307308,6.03041846071876,
127.244530942912));
#240211=CARTESIAN_POINT('Ctrl Pts',(-241.365716931122,0.264602954276818,
123.806623883412));
#240212=CARTESIAN_POINT('Ctrl Pts',(-241.644164554934,-5.74436974057257,
126.799295024156));
#240213=CARTESIAN_POINT('Ctrl Pts',(-241.922612178747,-6.47454727189872,
133.472425786911));
#240214=CARTESIAN_POINT('Ctrl Pts',(-242.20105980256,-1.25493215956847,
137.693735001267));
#240215=CARTESIAN_POINT('Ctrl Pts',(-242.479507426373,5.11790430056101,
135.584045721651));
#240216=CARTESIAN_POINT('Ctrl Pts',(-242.757955050186,6.78763673199965,
129.082059331979));
#240217=CARTESIAN_POINT('Ctrl Pts',(-243.036402673998,2.21986260121965,
124.162783684665));
#240218=CARTESIAN_POINT('Ctrl Pts',(-243.314850297812,-4.38785681376436,
125.346792779616));
#240219=CARTESIAN_POINT('Ctrl Pts',(-243.593297921624,-6.96335017562108,
131.54604010063));
#240220=CARTESIAN_POINT('Ctrl Pts',(-243.871745545438,-3.13986490465013,
137.063720209766));
#240221=CARTESIAN_POINT('Ctrl Pts',(-244.15019316925,3.56900282276695,136.829354640385));
#240222=CARTESIAN_POINT('Ctrl Pts',(-244.428640793064,6.99813131154132,
131.058313901354));
#240223=CARTESIAN_POINT('Ctrl Pts',(-244.707088416876,3.99631900273028,
125.053902500829));
#240224=CARTESIAN_POINT('Ctrl Pts',(-244.985536040689,-2.67791523855318,
124.333881184089));
#240225=CARTESIAN_POINT('Ctrl Pts',(-245.263983664501,-6.89127619903846,
129.559914366219));
#240226=CARTESIAN_POINT('Ctrl Pts',(-245.542431288315,-4.7718909901659,
135.929532858758));
#240227=CARTESIAN_POINT('Ctrl Pts',(-245.820878912128,1.73262891883438,
137.589368440225));
#240228=CARTESIAN_POINT('Ctrl Pts',(-246.09932653594,6.6449474950541,133.014113298726));
#240229=CARTESIAN_POINT('Ctrl Pts',(-246.377774159753,5.45088394705135,
126.408203395661));
#240230=CARTESIAN_POINT('Ctrl Pts',(-246.656221783566,-0.752275657806765,
123.842147215306));
#240231=CARTESIAN_POINT('Ctrl Pts',(-246.934669407379,-6.26413068384941,
127.674025028594));
#240232=CARTESIAN_POINT('Ctrl Pts',(-247.213117031192,-6.01955563123113,
134.382528322752));
#240233=CARTESIAN_POINT('Ctrl Pts',(-247.491564655005,-0.243303025152602,
137.802870299053));
#240234=CARTESIAN_POINT('Ctrl Pts',(-247.770012278818,5.75653317502817,
134.791923774272));
#240235=CARTESIAN_POINT('Ctrl Pts',(-248.048459902631,6.46639660963695,
128.116601511768));
#240236=CARTESIAN_POINT('Ctrl Pts',(-248.326907526444,1.23395746102625,
123.91119856316));
#240237=CARTESIAN_POINT('Ctrl Pts',(-248.605355150257,-5.13242831209467,
126.040274792862));
#240238=CARTESIAN_POINT('Ctrl Pts',(-248.883802774069,-6.78236319946242,
132.547313156937));
#240239=CARTESIAN_POINT('Ctrl Pts',(-249.162250397883,-2.19963764338714,
137.452663285294));
#240240=CARTESIAN_POINT('Ctrl Pts',(-249.440698021695,4.40444744868852,
136.24854804965));
#240241=CARTESIAN_POINT('Ctrl Pts',(-249.719145645508,6.96106050463867,
130.041490527264));
#240242=CARTESIAN_POINT('Ctrl Pts',(-249.997593269321,3.12079902353814,
124.535473349588));
#240243=CARTESIAN_POINT('Ctrl Pts',(-250.276040893134,-3.58732430068758,
124.790257319018));
#240244=CARTESIAN_POINT('Ctrl Pts',(-250.554488516946,-6.99887184311352,
130.571708414529));
#240245=CARTESIAN_POINT('Ctrl Pts',(-250.83293614076,-3.97879807562073,
136.566955518948));
#240246=CARTESIAN_POINT('Ctrl Pts',(-251.111383764572,2.69759674828547,
137.26665942739));
#240247=CARTESIAN_POINT('Ctrl Pts',(-251.389831388386,6.89503194542569,
132.027826430486));
#240248=CARTESIAN_POINT('Ctrl Pts',(-251.668279012198,4.75626962579305,
125.66468812107));
#240249=CARTESIAN_POINT('Ctrl Pts',(-251.946726636011,-1.75327212332407,
124.024657749096));
#240250=CARTESIAN_POINT('Ctrl Pts',(-252.225174259824,-6.65164244307981,
128.614843106116));
#240251=CARTESIAN_POINT('Ctrl Pts',(-252.503621883637,-5.43747830869239,
135.217088092717));
#240252=CARTESIAN_POINT('Ctrl Pts',(-252.78206950745,0.773462756270139,
137.764252102553));
#240253=CARTESIAN_POINT('Ctrl Pts',(-253.060517131263,6.2736293330892,133.91561584884));
#240254=CARTESIAN_POINT('Ctrl Pts',(-253.338964755075,6.00863703830687,
127.207888027921));
#240255=CARTESIAN_POINT('Ctrl Pts',(-253.617412378889,0.222000840393564,
123.805142824969));
#240256=CARTESIAN_POINT('Ctrl Pts',(-253.895860002702,-5.76864327852066,
126.83433683216));
#240257=CARTESIAN_POINT('Ctrl Pts',(-254.174307626514,-6.45818604965135,
133.511788771436));
#240258=CARTESIAN_POINT('Ctrl Pts',(-254.452755250327,-1.21297131977014,
137.701246465247));
#240259=CARTESIAN_POINT('Ctrl Pts',(-254.73120287414,5.14690475579816,135.55280306703));
#240260=CARTESIAN_POINT('Ctrl Pts',(-255.009650497953,6.7770268770417,129.040772899161));
#240261=CARTESIAN_POINT('Ctrl Pts',(-255.288098121766,2.17939223099114,
124.149393939406));
#240262=CARTESIAN_POINT('Ctrl Pts',(-255.566545745579,-4.42099713522674,
125.37360376984));
#240263=CARTESIAN_POINT('Ctrl Pts',(-255.844993369392,-6.95870662337211,
131.588414730824));
#240264=CARTESIAN_POINT('Ctrl Pts',(-256.123440993205,-3.10170371057109,
137.082716575498));
#240265=CARTESIAN_POINT('Ctrl Pts',(-256.401888617018,3.60561156199617,
136.807519199501));
#240266=CARTESIAN_POINT('Ctrl Pts',(-256.68033624083,6.99954939633056,131.01570633407));
#240267=CARTESIAN_POINT('Ctrl Pts',(-256.958783864643,3.96123678073902,
125.029688453078));
#240268=CARTESIAN_POINT('Ctrl Pts',(-257.237231488456,-2.71724664265218,
124.350290708114));
#240269=CARTESIAN_POINT('Ctrl Pts',(-257.515679112269,-6.89873632689917,
129.601908459729));
#240270=CARTESIAN_POINT('Ctrl Pts',(-257.794126736082,-4.74058057908887,
135.958444437253));
#240271=CARTESIAN_POINT('Ctrl Pts',(-258.072574359895,1.77385448465437,
137.578773744179));
#240272=CARTESIAN_POINT('Ctrl Pts',(-258.351021983707,6.6583599873155,132.973475360041));
#240273=CARTESIAN_POINT('Ctrl Pts',(-258.629469607521,5.42386327951784,
126.375381938049));
#240274=CARTESIAN_POINT('Ctrl Pts',(-258.907917231333,-0.794342416617398,
123.846330221273));
#240275=CARTESIAN_POINT('Ctrl Pts',(-259.186364855146,-6.28363694765996,
127.713206958712));
#240276=CARTESIAN_POINT('Ctrl Pts',(-259.464812478959,-5.99659113747434,
134.41722675292));
#240277=CARTESIAN_POINT('Ctrl Pts',(-259.743260102772,-0.202727240537578,
137.807801967267));
#240278=CARTESIAN_POINT('Ctrl Pts',(-260.021707726585,5.7845923739281,134.749768174183));
#240279=CARTESIAN_POINT('Ctrl Pts',(-260.253747413096,6.33253704604016,
129.202365411857));
#240280=CARTESIAN_POINT('Ctrl Pts',(-260.439389088604,3.82430165355141,
125.973250269562));
#240281=CARTESIAN_POINT('Ctrl Pts',(-260.532214889509,1.97943258085903,
125.138073123498));
#240282=CARTESIAN_POINT('Ctrl Pts',(-260.578632753112,1.00712299976162,
124.970230583726));
#240283=CARTESIAN_POINT('',(177.476367722506,5.62666147572432,130.804360632945));
#240284=CARTESIAN_POINT('Ctrl Pts',(177.727351910922,4.07805626267757,128.049722934653));
#240285=CARTESIAN_POINT('Ctrl Pts',(177.71910609987,4.13364155314972,128.094597587437));
#240286=CARTESIAN_POINT('Ctrl Pts',(177.710836728767,4.1882073110253,128.140733789961));
#240287=CARTESIAN_POINT('Ctrl Pts',(177.668436485582,4.46292964568284,128.384086882844));
#240288=CARTESIAN_POINT('Ctrl Pts',(177.634553719226,4.66558123475735,128.601241704498));
#240289=CARTESIAN_POINT('Ctrl Pts',(177.567013746104,5.05830116010295,129.120170708466));
#240290=CARTESIAN_POINT('Ctrl Pts',(177.534914197562,5.23713864285283,129.429348263662));
#240291=CARTESIAN_POINT('Ctrl Pts',(177.491184739739,5.49518559902329,130.065605691881));
#240292=CARTESIAN_POINT('Ctrl Pts',(177.478557559001,5.57905246121522,130.386047316322));
#240293=CARTESIAN_POINT('Ctrl Pts',(177.476455077554,5.62086138792093,130.74479140865));
#240294=CARTESIAN_POINT('Ctrl Pts',(177.476367722476,5.62395081735113,130.774568592934));
#240295=CARTESIAN_POINT('Ctrl Pts',(177.476367722506,5.62666147433654,130.804360633071));
#240296=CARTESIAN_POINT('Ctrl Pts',(207.343245771341,2.3877455813801,126.510892848288));
#240297=CARTESIAN_POINT('Ctrl Pts',(207.275858229453,2.15528266814333,126.281350675543));
#240298=CARTESIAN_POINT('Ctrl Pts',(207.205844547368,1.89354568495696,126.064552767189));
#240299=CARTESIAN_POINT('Ctrl Pts',(207.10286979807,1.39124105048774,125.761845041447));
#240300=CARTESIAN_POINT('Ctrl Pts',(207.06364877788,1.14897513173755,125.652900568378));
#240301=CARTESIAN_POINT('Ctrl Pts',(207.039544129699,0.852522970188626,
125.586612482375));
#240302=CARTESIAN_POINT('Ctrl Pts',(207.036751493533,0.812407362098567,
125.578958169151));
#240303=CARTESIAN_POINT('Ctrl Pts',(207.034346644558,0.770380885625219,
125.572377570558));
#240304=CARTESIAN_POINT('Ctrl Pts',(207.034253959284,0.76874693830571,125.572123968997));
#240305=CARTESIAN_POINT('Ctrl Pts',(207.034033708417,0.76482971591445,125.571521376621));
#240306=CARTESIAN_POINT('Ctrl Pts',(207.03390689775,0.762546089248627,125.571174470768));
#240307=CARTESIAN_POINT('Ctrl Pts',(207.033710514163,0.758964574572171,
125.570637298871));
#240308=CARTESIAN_POINT('Ctrl Pts',(207.033639889101,0.757667190070412,
125.570444129042));
#240309=CARTESIAN_POINT('Ctrl Pts',(207.033544370583,0.755899632091822,
125.570182888153));
#240310=CARTESIAN_POINT('Ctrl Pts',(207.033519040958,0.755429661562308,
125.570113613793));
#240311=CARTESIAN_POINT('Ctrl Pts',(207.033487449577,0.75484194224604,125.570027216002));
#240312=CARTESIAN_POINT('Ctrl Pts',(207.033481126023,0.754724221366939,
125.570009922105));
#240313=CARTESIAN_POINT('Ctrl Pts',(207.033468679808,0.75449236414991,125.569975883918));
#240314=CARTESIAN_POINT('Ctrl Pts',(207.033462556857,0.754378227124989,
125.569959138824));
#240315=CARTESIAN_POINT('Ctrl Pts',(207.033453376976,0.7542069949192,125.569934033751));
#240316=CARTESIAN_POINT('Ctrl Pts',(207.033450317046,0.754149899488901,
125.569925665499));
#240317=CARTESIAN_POINT('Ctrl Pts',(207.033444862271,0.754048085319076,
125.5699107479));
#240318=CARTESIAN_POINT('Ctrl Pts',(207.033442467482,0.754003374824332,
125.569904198698));
#240319=CARTESIAN_POINT('Ctrl Pts',(207.033437443175,0.75390954752979,125.569890458394));
#240320=CARTESIAN_POINT('Ctrl Pts',(207.033434813833,0.753860431646158,
125.569883267775));
#240321=CARTESIAN_POINT('Ctrl Pts',(207.033427919641,0.753731612570639,
125.569864413858));
#240322=CARTESIAN_POINT('Ctrl Pts',(207.033423655866,0.753651906963209,
125.569852753528));
#240323=CARTESIAN_POINT('Ctrl Pts',(207.03340516309,0.753306051493517,125.569802180728));
#240324=CARTESIAN_POINT('Ctrl Pts',(207.033390953313,0.753039892352538,
125.569763321276));
#240325=CARTESIAN_POINT('Ctrl Pts',(207.032637262426,0.738901169539525,
125.567702230136));
#240326=CARTESIAN_POINT('Ctrl Pts',(207.031955337296,0.72500443032654,125.565838715569));
#240327=CARTESIAN_POINT('Ctrl Pts',(207.02839943031,0.645577309011463,125.556126262888));
#240328=CARTESIAN_POINT('Ctrl Pts',(207.026791222654,0.58006201298121,125.55175022771));
#240329=CARTESIAN_POINT('Ctrl Pts',(207.026066210465,0.390615670661435,
125.549775550373));
#240330=CARTESIAN_POINT('Ctrl Pts',(207.030357517256,0.268505495823795,
125.561416336111));
#240331=CARTESIAN_POINT('Ctrl Pts',(207.051180759308,-0.0272120970339418,
125.618546972655));
#240332=CARTESIAN_POINT('Ctrl Pts',(207.072035822298,-0.195505216489052,
125.676082796202));
#240333=CARTESIAN_POINT('Ctrl Pts',(207.11742615221,-0.475952586113691,
125.805214506685));
#240334=CARTESIAN_POINT('Ctrl Pts',(207.139776849114,-0.591942288014956,
125.869844509151));
#240335=CARTESIAN_POINT('Ctrl Pts',(207.16361981536,-0.702841334627603,
125.940658199356));
#240336=CARTESIAN_POINT('Ctrl Pts',(207.300060471638,3.90699806772733,135.242283170685));
#240337=CARTESIAN_POINT('Ctrl Pts',(207.34413274425,3.94262575384843,135.097475191392));
#240338=CARTESIAN_POINT('Ctrl Pts',(207.386092965017,3.97836208698807,134.951861709998));
#240339=CARTESIAN_POINT('Ctrl Pts',(207.469685208882,4.05173223617054,134.644592220037));
#240340=CARTESIAN_POINT('Ctrl Pts',(207.510886564299,4.08921616848532,134.482726191452));
#240341=CARTESIAN_POINT('Ctrl Pts',(207.592391673631,4.16413723955857,134.138864482574));
#240342=CARTESIAN_POINT('Ctrl Pts',(207.632065558946,4.20108743265175,133.956753701393));
#240343=CARTESIAN_POINT('Ctrl Pts',(207.710182522622,4.27216743944126,133.563382656296));
#240344=CARTESIAN_POINT('Ctrl Pts',(207.747210242616,4.30461553044184,133.35420995967));
#240345=CARTESIAN_POINT('Ctrl Pts',(207.780393500533,4.3310565938262,133.140241056514));
#240346=CARTESIAN_POINT('Ctrl Pts',(178.535810555027,-1.96534307107584,
125.221017543274));
#240347=CARTESIAN_POINT('Ctrl Pts',(178.572363368561,-1.60399563351745,
125.128167470391));
#240348=CARTESIAN_POINT('Ctrl Pts',(178.600500782542,-1.23860474272998,
125.059173954896));
#240349=CARTESIAN_POINT('Ctrl Pts',(178.621003548882,-0.856428478077489,
125.009278016813));
#240350=CARTESIAN_POINT('Ctrl Pts',(178.621801810245,-0.841279080621699,
125.007336534832));
#240351=CARTESIAN_POINT('Ctrl Pts',(178.623990647172,-0.798973658475563,
125.002015992207));
#240352=CARTESIAN_POINT('Ctrl Pts',(178.625349900214,-0.771805929769255,
124.998715493147));
#240353=CARTESIAN_POINT('Ctrl Pts',(178.62668571351,-0.744165676501276,
124.995474921175));
#240354=CARTESIAN_POINT('Ctrl Pts',(178.626707795983,-0.743708481662123,
124.995421351801));
#240355=CARTESIAN_POINT('Ctrl Pts',(178.626816871274,-0.741448850750257,
124.995156752781));
#240356=CARTESIAN_POINT('Ctrl Pts',(178.626903676827,-0.739646350809624,
124.994946190002));
#240357=CARTESIAN_POINT('Ctrl Pts',(178.627010610293,-0.737420683462579,
124.9946868197));
#240358=CARTESIAN_POINT('Ctrl Pts',(178.627030927358,-0.736997579512831,
124.994637540787));
#240359=CARTESIAN_POINT('Ctrl Pts',(178.62706240287,-0.736341738602775,
124.99456119827));
#240360=CARTESIAN_POINT('Ctrl Pts',(178.627073568876,-0.736109006983649,
124.99453411582));
#240361=CARTESIAN_POINT('Ctrl Pts',(178.627094018329,-0.735682652195354,
124.994484517351));
#240362=CARTESIAN_POINT('Ctrl Pts',(178.627103302812,-0.735489029217585,
124.994461998755));
#240363=CARTESIAN_POINT('Ctrl Pts',(178.627123488216,-0.735067966852662,
124.994413041381));
#240364=CARTESIAN_POINT('Ctrl Pts',(178.627134388279,-0.734840526798812,
124.994386604746));
#240365=CARTESIAN_POINT('Ctrl Pts',(178.627164443798,-0.734213203786545,
124.994313709709));
#240366=CARTESIAN_POINT('Ctrl Pts',(178.627183592622,-0.733813317949453,
124.994267267836));
#240367=CARTESIAN_POINT('Ctrl Pts',(178.62728583349,-0.73167710034013,124.994019305302));
#240368=CARTESIAN_POINT('Ctrl Pts',(178.627368749657,-0.729940710022163,
124.993818222811));
#240369=CARTESIAN_POINT('Ctrl Pts',(178.629059143694,-0.69446056615761,
124.989719045218));
#240370=CARTESIAN_POINT('Ctrl Pts',(178.630596698252,-0.660693007946553,
124.985995081663));
#240371=CARTESIAN_POINT('Ctrl Pts',(178.634998934465,-0.559328070586893,
124.975343706825));
#240372=CARTESIAN_POINT('Ctrl Pts',(178.637653366489,-0.491663502550943,
124.968936267428));
#240373=CARTESIAN_POINT('Ctrl Pts',(178.652290692225,-0.0741053585462007,
124.933657265026));
#240374=CARTESIAN_POINT('Ctrl Pts',(178.65706528323,0.278036573125624,124.922313922981));
#240375=CARTESIAN_POINT('Ctrl Pts',(178.654556968681,0.629286258110217,
124.928317377817));
#240376=CARTESIAN_POINT('Ctrl Pts',(177.476367722506,5.62666147433657,130.804360633071));
#240377=CARTESIAN_POINT('Ctrl Pts',(177.476367722745,5.64800886896215,131.038983619647));
#240378=CARTESIAN_POINT('Ctrl Pts',(177.481815845156,5.64587111696085,131.2745273672));
#240379=CARTESIAN_POINT('Ctrl Pts',(177.493340279704,5.61850113655357,131.523613241248));
#240380=CARTESIAN_POINT('Ctrl Pts',(177.494046319909,5.61678087678775,131.538405721014));
#240381=CARTESIAN_POINT('Ctrl Pts',(177.494830441239,5.6148248201693,131.554346920936));
#240382=CARTESIAN_POINT('Ctrl Pts',(177.494887671502,5.61468180143515,131.555507707183));
#240383=CARTESIAN_POINT('Ctrl Pts',(177.494958749217,5.61450386495011,131.556946013306));
#240384=CARTESIAN_POINT('Ctrl Pts',(177.494972474835,5.61446948972427,131.557223606544));
#240385=CARTESIAN_POINT('Ctrl Pts',(177.494993809106,5.61441603657773,131.557654841551));
#240386=CARTESIAN_POINT('Ctrl Pts',(177.495001412615,5.61439698152929,131.557808486065));
#240387=CARTESIAN_POINT('Ctrl Pts',(177.495015372434,5.61436198892514,131.558090486421));
#240388=CARTESIAN_POINT('Ctrl Pts',(177.495021728047,5.6143460544523,131.558218842378));
#240389=CARTESIAN_POINT('Ctrl Pts',(177.49503551666,5.61431147766019,131.558497241617));
#240390=CARTESIAN_POINT('Ctrl Pts',(177.495042950192,5.61429283288377,131.558647283569));
#240391=CARTESIAN_POINT('Ctrl Pts',(177.495063575169,5.6142410896851,131.559063463467));
#240392=CARTESIAN_POINT('Ctrl Pts',(177.49507677126,5.61420797059531,131.559329598846));
#240393=CARTESIAN_POINT('Ctrl Pts',(177.495147761058,5.614029731868,131.560760544247));
#240394=CARTESIAN_POINT('Ctrl Pts',(177.495205678106,5.61388406288704,131.561925280089));
#240395=CARTESIAN_POINT('Ctrl Pts',(177.498353203655,5.60595394007177,131.625077226177));
#240396=CARTESIAN_POINT('Ctrl Pts',(177.501809975298,5.59653185305586,131.686815725141));
#240397=CARTESIAN_POINT('Ctrl Pts',(177.517258408342,5.55180098308332,131.935795836193));
#240398=CARTESIAN_POINT('Ctrl Pts',(177.53216773447,5.50319392797717,132.119815974191));
#240399=CARTESIAN_POINT('Ctrl Pts',(177.579958465937,5.33412594249757,132.604732031663));
#240400=CARTESIAN_POINT('Ctrl Pts',(177.61742104521,5.18961629328228,132.891229558403));
#240401=CARTESIAN_POINT('Ctrl Pts',(177.722598493876,4.74529882642138,133.563053730255));
#240402=CARTESIAN_POINT('Ctrl Pts',(177.794691730185,4.41119386074116,133.919144338343));
#240403=CARTESIAN_POINT('Ctrl Pts',(177.927395241577,3.71809800550664,134.49513348593));
#240404=CARTESIAN_POINT('Ctrl Pts',(177.989174049252,3.36304316837917,134.730227794869));
#240405=CARTESIAN_POINT('Ctrl Pts',(178.082682503228,2.74398222802927,135.062813747627));
#240406=CARTESIAN_POINT('Ctrl Pts',(178.117862998488,2.48723912541729,135.181048337578));
#240407=CARTESIAN_POINT('Ctrl Pts',(178.197858320915,1.82144645103899,135.441236023159));
#240408=CARTESIAN_POINT('Ctrl Pts',(178.238066467768,1.40117430183672,135.563242037453));
#240409=CARTESIAN_POINT('Ctrl Pts',(178.266323014416,0.960634556419806,
135.647607167646));
#240410=CARTESIAN_POINT('Ctrl Pts',(178.267150551097,0.947540843553741,
135.650075767119));
#240411=CARTESIAN_POINT('Ctrl Pts',(178.268982584149,0.918113096294057,
135.655536346135));
#240412=CARTESIAN_POINT('Ctrl Pts',(178.26998060066,0.901773160982638,135.658507888363));
#240413=CARTESIAN_POINT('Ctrl Pts',(178.271818928666,0.871078974814065,
135.663976038944));
#240414=CARTESIAN_POINT('Ctrl Pts',(178.27266304642,0.856736664322277,135.666484646891));
#240415=CARTESIAN_POINT('Ctrl Pts',(178.273548891525,0.841415948934087,
135.669115076619));
#240416=CARTESIAN_POINT('Ctrl Pts',(178.273604905292,0.840446016661627,
135.669281394459));
#240417=CARTESIAN_POINT('Ctrl Pts',(178.273680705371,0.83913187483764,135.66950644962));
#240418=CARTESIAN_POINT('Ctrl Pts',(178.27370054899,0.838787699115299,135.669565365371));
#240419=CARTESIAN_POINT('Ctrl Pts',(178.273733193885,0.838221249282319,
135.669662286179));
#240420=CARTESIAN_POINT('Ctrl Pts',(178.273745999974,0.837998977982071,
135.66970030622));
#240421=CARTESIAN_POINT('Ctrl Pts',(178.273770748392,0.837569307966119,
135.669773780926));
#240422=CARTESIAN_POINT('Ctrl Pts',(178.273782691233,0.837361908358778,
135.669809237174));
#240423=CARTESIAN_POINT('Ctrl Pts',(178.273810458122,0.8368795828714,135.669891671306));
#240424=CARTESIAN_POINT('Ctrl Pts',(178.273826279791,0.836604657560614,
135.669938641801));
#240425=CARTESIAN_POINT('Ctrl Pts',(178.273876010189,0.835740219580388,
135.670086276272));
#240426=CARTESIAN_POINT('Ctrl Pts',(178.273909899986,0.835150695482057,
135.670186881322));
#240427=CARTESIAN_POINT('Ctrl Pts',(178.274371088221,0.827122245215414,
135.671555914787));
#240428=CARTESIAN_POINT('Ctrl Pts',(178.274794555457,0.819681066691097,
135.672812421509));
#240429=CARTESIAN_POINT('Ctrl Pts',(178.28084223278,0.712402304277549,135.69074942723));
#240430=CARTESIAN_POINT('Ctrl Pts',(178.285775955922,0.612166885418918,
135.705288668747));
#240431=CARTESIAN_POINT('Ctrl Pts',(178.299419217276,0.288637961509831,
135.745352837328));
#240432=CARTESIAN_POINT('Ctrl Pts',(178.305399847096,0.0641175829676573,
135.762692232661));
#240433=CARTESIAN_POINT('Ctrl Pts',(178.311924012651,-0.490333735750563,
135.781624064638));
#240434=CARTESIAN_POINT('Ctrl Pts',(178.308617172973,-0.821441843563681,
135.772121437776));
#240435=CARTESIAN_POINT('Ctrl Pts',(178.285319321399,-1.5965832586439,135.704101279333));
#240436=CARTESIAN_POINT('Ctrl Pts',(178.259606239746,-2.04175646283672,
135.628895105993));
#240437=CARTESIAN_POINT('Ctrl Pts',(178.197253864959,-2.79960490124737,
135.437212662791));
#240438=CARTESIAN_POINT('Ctrl Pts',(178.164853130157,-3.11943053718718,
135.335366999488));
#240439=CARTESIAN_POINT('Ctrl Pts',(178.08645413946,-3.78099261367155,135.075940074041));
#240440=CARTESIAN_POINT('Ctrl Pts',(178.038838181365,-4.12315427920155,
134.911670696906));
#240441=CARTESIAN_POINT('Ctrl Pts',(177.9874951389,-4.44976524376849,134.718437431287));
#240442=CARTESIAN_POINT('Origin',(192.718407221598,12.,130.804360617566));
#240443=CARTESIAN_POINT('',(177.476367722507,-12.,130.804360617566));
#240444=CARTESIAN_POINT('Origin',(192.718407221598,-12.,130.804360617566));
#240445=CARTESIAN_POINT('',(177.476367722506,12.,130.804360617566));
#240446=CARTESIAN_POINT('',(177.476367722507,12.,130.804360617566));
#240447=CARTESIAN_POINT('',(177.476367722506,12.,130.804360617566));
#240448=CARTESIAN_POINT('Origin',(192.718407221598,12.,130.804360617566));
#240449=CARTESIAN_POINT('Origin',(192.718407221598,-12.,130.804360617566));
#240450=CARTESIAN_POINT('Origin',(192.718407221598,12.,130.804360617566));
#240451=CARTESIAN_POINT('',(0.,0.,0.));
#240452=CARTESIAN_POINT('Origin',(192.718407221598,22.,130.804360617566));
#240453=CARTESIAN_POINT('',(186.217299572429,17.,130.804360617566));
#240454=CARTESIAN_POINT('Origin',(192.718407221598,17.,130.804360617566));
#240455=CARTESIAN_POINT('',(186.217299572429,22.,130.804360617566));
#240456=CARTESIAN_POINT('',(186.217299572428,22.,130.804360617566));
#240457=CARTESIAN_POINT('Origin',(192.718407221598,22.,130.804360617566));
#240458=CARTESIAN_POINT('Origin',(200.401984582636,22.,117.640683052811));
#240459=CARTESIAN_POINT('',(200.401984582636,22.,117.640683052811));
#240460=CARTESIAN_POINT('',(27.6628184943316,22.,16.8136353382454));
#240461=CARTESIAN_POINT('',(200.401984582636,22.,117.640683052811));
#240462=CARTESIAN_POINT('',(200.401984582636,17.,117.640683052811));
#240463=CARTESIAN_POINT('',(200.401984582636,22.,117.640683052811));
#240464=CARTESIAN_POINT('',(27.6628184943316,17.,16.8136353382454));
#240465=CARTESIAN_POINT('',(200.401984582636,17.,117.640683052811));
#240466=CARTESIAN_POINT('',(27.6628184943316,22.,16.8136353382454));
#240467=CARTESIAN_POINT('Origin',(192.718407221598,22.,130.804360617566));
#240468=CARTESIAN_POINT('',(185.034829860561,22.,143.96803818232));
#240469=CARTESIAN_POINT('Origin',(192.718407221598,22.,130.804360617566));
#240470=CARTESIAN_POINT('',(185.034829860561,17.,143.96803818232));
#240471=CARTESIAN_POINT('',(185.034829860561,22.,143.96803818232));
#240472=CARTESIAN_POINT('Origin',(192.718407221598,17.,130.804360617566));
#240473=CARTESIAN_POINT('Origin',(12.2956637722558,22.,43.1409904677544));
#240474=CARTESIAN_POINT('',(12.2956637722558,22.,43.1409904677544));
#240475=CARTESIAN_POINT('',(12.2956637722558,22.,43.1409904677544));
#240476=CARTESIAN_POINT('',(12.2956637722558,17.,43.1409904677544));
#240477=CARTESIAN_POINT('',(12.2956637722558,22.,43.1409904677544));
#240478=CARTESIAN_POINT('',(12.2956637722558,17.,43.1409904677544));
#240479=CARTESIAN_POINT('Origin',(106.348824177446,17.,80.3908367602827));
#240480=CARTESIAN_POINT('Origin',(19.9792411332937,17.,29.9773129029999));
#240481=CARTESIAN_POINT('Origin',(106.348824177446,22.,80.3908367602827));
#240482=CARTESIAN_POINT('Origin',(19.9792411332937,22.,29.9773129029999));
#240483=CARTESIAN_POINT('',(12.4213924902778,22.,29.9773129029999));
#240484=CARTESIAN_POINT('Origin',(19.9792411332937,22.,29.9773129029999));
#240485=CARTESIAN_POINT('Origin',(19.9792411332937,-22.,29.9773129029999));
#240486=CARTESIAN_POINT('',(12.4213924902778,-22.,29.9773129029999));
#240487=CARTESIAN_POINT('Origin',(19.9792411332937,-22.,29.9773129029999));
#240488=CARTESIAN_POINT('',(12.4213924902778,-22.,29.9773129029999));
#240489=CARTESIAN_POINT('Origin',(192.718407221598,-22.,130.804360617566));
#240490=CARTESIAN_POINT('',(186.217299572429,-22.,130.804360617566));
#240491=CARTESIAN_POINT('Origin',(192.718407221598,-22.,130.804360617566));
#240492=CARTESIAN_POINT('',(186.217299572429,-17.,130.804360617566));
#240493=CARTESIAN_POINT('',(186.217299572428,-22.,130.804360617566));
#240494=CARTESIAN_POINT('Origin',(192.718407221598,-17.,130.804360617566));
#240495=CARTESIAN_POINT('Origin',(200.401984582636,-22.,117.640683052811));
#240496=CARTESIAN_POINT('',(200.401984582636,-22.,117.640683052811));
#240497=CARTESIAN_POINT('',(27.6628184943316,-22.,16.8136353382454));
#240498=CARTESIAN_POINT('',(200.401984582636,-22.,117.640683052811));
#240499=CARTESIAN_POINT('',(27.6628184943316,-17.,16.8136353382454));
#240500=CARTESIAN_POINT('',(27.6628184943316,-22.,16.8136353382454));
#240501=CARTESIAN_POINT('',(200.401984582636,-17.,117.640683052811));
#240502=CARTESIAN_POINT('',(200.401984582636,-17.,117.640683052811));
#240503=CARTESIAN_POINT('',(200.401984582636,-22.,117.640683052811));
#240504=CARTESIAN_POINT('Origin',(192.718407221598,-22.,130.804360617566));
#240505=CARTESIAN_POINT('',(185.034829860561,-22.,143.96803818232));
#240506=CARTESIAN_POINT('Origin',(192.718407221598,-22.,130.804360617566));
#240507=CARTESIAN_POINT('',(185.034829860561,-17.,143.96803818232));
#240508=CARTESIAN_POINT('Origin',(192.718407221598,-17.,130.804360617566));
#240509=CARTESIAN_POINT('',(185.034829860561,-22.,143.96803818232));
#240510=CARTESIAN_POINT('Origin',(12.2956637722558,-22.,43.1409904677544));
#240511=CARTESIAN_POINT('',(12.2956637722558,-22.,43.1409904677544));
#240512=CARTESIAN_POINT('',(12.2956637722558,-22.,43.1409904677544));
#240513=CARTESIAN_POINT('',(12.2956637722558,-17.,43.1409904677544));
#240514=CARTESIAN_POINT('',(12.2956637722558,-17.,43.1409904677544));
#240515=CARTESIAN_POINT('',(12.2956637722558,-22.,43.1409904677544));
#240516=CARTESIAN_POINT('Origin',(19.9792411332937,-22.,29.9773129029999));
#240517=CARTESIAN_POINT('',(12.2956637722558,-22.,43.1409904677544));
#240518=CARTESIAN_POINT('Origin',(19.9792411332937,-17.,29.9773129029999));
#240519=CARTESIAN_POINT('Origin',(19.9792411332937,-22.,29.9773129029999));
#240520=CARTESIAN_POINT('Origin',(106.348824177446,-17.,80.3908367602827));
#240521=CARTESIAN_POINT('Origin',(106.348824177446,-22.,80.3908367602827));
#240522=CARTESIAN_POINT('',(0.,0.,0.));
#240523=CARTESIAN_POINT('Origin',(19.9792411332937,17.,231.631408332131));
#240524=CARTESIAN_POINT('',(13.4123053085775,-17.,235.37258862514));
#240525=CARTESIAN_POINT('',(12.4213924902778,-17.,231.631408332131));
#240526=CARTESIAN_POINT('Origin',(19.9792411332937,-17.,231.631408332131));
#240527=CARTESIAN_POINT('',(12.4213924902778,17.,231.631408332131));
#240528=CARTESIAN_POINT('',(12.4213924902778,17.,231.631408332131));
#240529=CARTESIAN_POINT('',(13.4123053085775,17.,235.37258862514));
#240530=CARTESIAN_POINT('Origin',(19.9792411332937,17.,231.631408332131));
#240531=CARTESIAN_POINT('',(13.4123053085775,12.,235.37258862514));
#240532=CARTESIAN_POINT('',(13.4123053085775,17.,235.37258862514));
#240533=CARTESIAN_POINT('',(26.4691126286313,12.,227.758083651093));
#240534=CARTESIAN_POINT('Origin',(19.9792411332937,12.,231.631408332131));
#240535=CARTESIAN_POINT('',(26.4691126286313,17.,227.758083651093));
#240536=CARTESIAN_POINT('',(26.4691126286313,17.,227.758083651093));
#240537=CARTESIAN_POINT('Origin',(19.9792411332937,17.,231.631408332131));
#240538=CARTESIAN_POINT('',(26.4691126286313,-17.,227.758083651093));
#240539=CARTESIAN_POINT('Origin',(19.9792411332937,-17.,231.631408332131));
#240540=CARTESIAN_POINT('',(26.4691126286313,-12.,227.758083651093));
#240541=CARTESIAN_POINT('',(26.4691126286313,17.,227.758083651093));
#240542=CARTESIAN_POINT('',(13.4123053085775,-12.,235.37258862514));
#240543=CARTESIAN_POINT('Origin',(19.9792411332937,-12.,231.631408332131));
#240544=CARTESIAN_POINT('',(13.4123053085775,17.,235.37258862514));
#240545=CARTESIAN_POINT('Origin',(19.9792411332937,17.,231.631408332131));
#240546=CARTESIAN_POINT('',(29.4368821049519,12.,243.584349198005));
#240547=CARTESIAN_POINT('',(4.7372016342019,12.,231.631408332131));
#240548=CARTESIAN_POINT('Origin',(19.9792411332937,12.,231.631408332131));
#240549=CARTESIAN_POINT('',(29.4368821049519,17.,243.584349198005));
#240550=CARTESIAN_POINT('',(29.4368821049519,17.,243.584349198005));
#240551=CARTESIAN_POINT('',(6.77425985905829,17.,239.243782313943));
#240552=CARTESIAN_POINT('Origin',(19.9792411332937,17.,231.631408332131));
#240553=CARTESIAN_POINT('',(6.77425985905829,12.,239.243782313943));
#240554=CARTESIAN_POINT('',(6.77425985905829,17.,239.243782313943));
#240555=CARTESIAN_POINT('Origin',(19.9792411332937,12.,231.631408332131));
#240556=CARTESIAN_POINT('',(4.7372016342019,-12.,231.631408332131));
#240557=CARTESIAN_POINT('',(4.7372016342019,17.,231.631408332131));
#240558=CARTESIAN_POINT('',(6.77425985905829,-12.,239.243782313943));
#240559=CARTESIAN_POINT('Origin',(19.9792411332937,-12.,231.631408332131));
#240560=CARTESIAN_POINT('',(6.77425985905829,-17.,239.243782313943));
#240561=CARTESIAN_POINT('',(6.77425985905829,17.,239.243782313943));
#240562=CARTESIAN_POINT('',(29.4368821049519,-17.,243.584349198005));
#240563=CARTESIAN_POINT('Origin',(19.9792411332937,-17.,231.631408332131));
#240564=CARTESIAN_POINT('',(29.4368821049519,-12.,243.584349198005));
#240565=CARTESIAN_POINT('',(29.4368821049519,17.,243.584349198005));
#240566=CARTESIAN_POINT('Origin',(19.9792411332937,-12.,231.631408332131));
#240567=CARTESIAN_POINT('Origin',(19.9021768039151,17.,231.499263944101));
#240568=CARTESIAN_POINT('Origin',(19.9021768039151,12.,231.499263944101));
#240569=CARTESIAN_POINT('Origin',(19.9021768039151,17.,231.499263944101));
#240570=CARTESIAN_POINT('Origin',(27.5756840334628,17.,244.668814235966));
#240571=CARTESIAN_POINT('',(200.391914451146,12.,143.97391090943));
#240572=CARTESIAN_POINT('',(27.5756840334628,12.,244.668814235966));
#240573=CARTESIAN_POINT('',(200.391914451146,17.,143.97391090943));
#240574=CARTESIAN_POINT('',(200.391914451146,17.,143.97391090943));
#240575=CARTESIAN_POINT('',(27.5756840334628,17.,244.668814235966));
#240576=CARTESIAN_POINT('Origin',(106.310292012757,12.,181.151812280833));
#240577=CARTESIAN_POINT('',(12.2286695743674,12.,218.329713652237));
#240578=CARTESIAN_POINT('Origin',(19.9021768039151,12.,231.499263944101));
#240579=CARTESIAN_POINT('',(185.044899992051,12.,117.634810325701));
#240580=CARTESIAN_POINT('',(185.044899992051,12.,117.634810325701));
#240581=CARTESIAN_POINT('Origin',(192.718407221598,12.,130.804360617566));
#240582=CARTESIAN_POINT('',(189.517108648379,12.,136.462636689939));
#240583=CARTESIAN_POINT('Origin',(192.718407221598,12.,130.804360617566));
#240584=CARTESIAN_POINT('Origin',(106.310292012757,12.,181.151812280833));
#240585=CARTESIAN_POINT('Origin',(192.718407221598,17.,130.804360617566));
#240586=CARTESIAN_POINT('',(189.517108648379,17.,136.462636689939));
#240587=CARTESIAN_POINT('',(189.517108648378,17.,136.462636689939));
#240588=CARTESIAN_POINT('Origin',(192.718407221598,17.,130.804360617566));
#240589=CARTESIAN_POINT('Origin',(185.044899992051,17.,117.634810325701));
#240590=CARTESIAN_POINT('',(185.044899992051,17.,117.634810325701));
#240591=CARTESIAN_POINT('',(12.2286695743674,17.,218.329713652237));
#240592=CARTESIAN_POINT('',(185.044899992051,17.,117.634810325701));
#240593=CARTESIAN_POINT('',(185.044899992051,17.,117.634810325701));
#240594=CARTESIAN_POINT('',(12.2286695743674,17.,218.329713652237));
#240595=CARTESIAN_POINT('Origin',(192.718407221598,17.,130.804360617566));
#240596=CARTESIAN_POINT('Origin',(192.718407221598,17.,130.804360617566));
#240597=CARTESIAN_POINT('Origin',(19.9021768039151,17.,231.499263944101));
#240598=CARTESIAN_POINT('Origin',(19.9021768039151,17.,231.499263944101));
#240599=CARTESIAN_POINT('Origin',(106.310292012757,17.,181.151812280833));
#240600=CARTESIAN_POINT('Origin',(19.9021768039151,-17.,231.499263944101));
#240601=CARTESIAN_POINT('Origin',(19.9021768039151,-17.,231.499263944101));
#240602=CARTESIAN_POINT('Origin',(19.9021768039151,-12.,231.499263944101));
#240603=CARTESIAN_POINT('Origin',(106.310292012757,-17.,181.151812280833));
#240604=CARTESIAN_POINT('',(12.2286695743674,-17.,218.329713652237));
#240605=CARTESIAN_POINT('Origin',(19.9021768039151,-17.,231.499263944101));
#240606=CARTESIAN_POINT('',(185.044899992051,-17.,117.634810325701));
#240607=CARTESIAN_POINT('',(185.044899992051,-17.,117.634810325701));
#240608=CARTESIAN_POINT('',(200.391914451146,-17.,143.97391090943));
#240609=CARTESIAN_POINT('Origin',(192.718407221598,-17.,130.804360617566));
#240610=CARTESIAN_POINT('',(27.5756840334628,-17.,244.668814235966));
#240611=CARTESIAN_POINT('',(189.517108648379,-17.,136.462636689939));
#240612=CARTESIAN_POINT('Origin',(192.718407221598,-17.,130.804360617566));
#240613=CARTESIAN_POINT('Origin',(106.310292012757,-12.,181.151812280833));
#240614=CARTESIAN_POINT('',(200.391914451146,-12.,143.97391090943));
#240615=CARTESIAN_POINT('',(27.5756840334628,-12.,244.668814235966));
#240616=CARTESIAN_POINT('',(185.044899992051,-12.,117.634810325701));
#240617=CARTESIAN_POINT('Origin',(192.718407221598,-12.,130.804360617566));
#240618=CARTESIAN_POINT('',(12.2286695743674,-12.,218.329713652237));
#240619=CARTESIAN_POINT('',(185.044899992051,-12.,117.634810325701));
#240620=CARTESIAN_POINT('Origin',(19.9021768039151,-12.,231.499263944101));
#240621=CARTESIAN_POINT('',(189.517108648379,-12.,136.462636689939));
#240622=CARTESIAN_POINT('Origin',(192.718407221598,-12.,130.804360617566));
#240623=CARTESIAN_POINT('Origin',(192.718407221598,-17.,130.804360617566));
#240624=CARTESIAN_POINT('',(189.517108648378,-17.,136.462636689939));
#240625=CARTESIAN_POINT('Origin',(185.044899992051,-17.,117.634810325701));
#240626=CARTESIAN_POINT('',(12.2286695743674,-17.,218.329713652237));
#240627=CARTESIAN_POINT('',(185.044899992051,-17.,117.634810325701));
#240628=CARTESIAN_POINT('Origin',(192.718407221598,-17.,130.804360617566));
#240629=CARTESIAN_POINT('',(200.391914451146,-17.,143.97391090943));
#240630=CARTESIAN_POINT('Origin',(27.5756840334628,-17.,244.668814235966));
#240631=CARTESIAN_POINT('Origin',(19.9021768039151,-17.,231.499263944101));
#240632=CARTESIAN_POINT('Origin',(106.310292012757,-12.,181.151812280833));
#240633=CARTESIAN_POINT('',(0.,0.,0.));
#240634=CARTESIAN_POINT('Origin',(-39.9751670169646,25.,260.358721235131));
#240635=CARTESIAN_POINT('',(-49.9751670169646,25.,256.608721235131));
#240636=CARTESIAN_POINT('',(-39.9751670169646,35.,256.608721235131));
#240637=CARTESIAN_POINT('Origin',(-39.9751670169646,25.,256.608721235131));
#240638=CARTESIAN_POINT('',(-49.9751670169646,25.,261.608721235131));
#240639=CARTESIAN_POINT('',(-49.9751670169646,25.,260.358721235131));
#240640=CARTESIAN_POINT('',(-39.9751670169646,35.,261.608721235131));
#240641=CARTESIAN_POINT('Origin',(-39.9751670169646,25.,261.608721235131));
#240642=CARTESIAN_POINT('',(-39.9751670169646,35.,260.358721235131));
#240643=CARTESIAN_POINT('Origin',(-19.9792411332937,0.,231.631408332131));
#240644=CARTESIAN_POINT('',(-12.4213924902778,25.,231.631408332131));
#240645=CARTESIAN_POINT('Origin',(-19.9792411332937,25.,231.631408332131));
#240646=CARTESIAN_POINT('',(-12.4213924902778,22.,231.631408332131));
#240647=CARTESIAN_POINT('',(-12.4213924902778,0.,231.631408332131));
#240648=CARTESIAN_POINT('Origin',(-19.9792411332937,22.,231.631408332131));
#240649=CARTESIAN_POINT('Origin',(-35.0075079285187,0.,224.577877459809));
#240650=CARTESIAN_POINT('',(-35.0075079285187,22.,224.577877459809));
#240651=CARTESIAN_POINT('',(-27.0075079285187,22.,216.577877459809));
#240652=CARTESIAN_POINT('',(-33.010424909369,22.,222.58079444066));
#240653=CARTESIAN_POINT('',(-35.0075079285187,25.,224.577877459809));
#240654=CARTESIAN_POINT('',(-35.0075079285187,0.,224.577877459809));
#240655=CARTESIAN_POINT('',(-27.0075079285187,25.,216.577877459809));
#240656=CARTESIAN_POINT('',(-35.0075079285187,25.,224.577877459809));
#240657=CARTESIAN_POINT('',(-27.0075079285187,0.,216.577877459809));
#240658=CARTESIAN_POINT('Origin',(39.9751670169646,25.,260.358721235131));
#240659=CARTESIAN_POINT('',(49.9751670169646,25.,256.608721235131));
#240660=CARTESIAN_POINT('',(39.9751670169646,35.,256.608721235131));
#240661=CARTESIAN_POINT('Origin',(39.9751670169646,25.,256.608721235131));
#240662=CARTESIAN_POINT('',(39.9751670169646,35.,261.608721235131));
#240663=CARTESIAN_POINT('',(39.9751670169646,35.,260.358721235131));
#240664=CARTESIAN_POINT('',(49.9751670169646,25.,261.608721235131));
#240665=CARTESIAN_POINT('Origin',(39.9751670169646,25.,261.608721235131));
#240666=CARTESIAN_POINT('',(49.9751670169646,25.,260.358721235131));
#240667=CARTESIAN_POINT('Origin',(24.9875835084823,35.,259.108721235131));
#240668=CARTESIAN_POINT('',(0.,35.,256.608721235131));
#240669=CARTESIAN_POINT('',(0.,35.,261.608721235131));
#240670=CARTESIAN_POINT('Origin',(26.255630946389,19.,248.608721235131));
#240671=CARTESIAN_POINT('',(-35.0075079285187,22.,248.608721235131));
#240672=CARTESIAN_POINT('',(35.0075079285187,22.,248.608721235131));
#240673=CARTESIAN_POINT('',(26.255630946389,22.,248.608721235131));
#240674=CARTESIAN_POINT('',(35.0075079285187,19.,251.608721235131));
#240675=CARTESIAN_POINT('Origin',(35.0075079285187,19.,248.608721235131));
#240676=CARTESIAN_POINT('',(-35.0075079285187,19.,251.608721235131));
#240677=CARTESIAN_POINT('',(26.255630946389,19.,251.608721235131));
#240678=CARTESIAN_POINT('Origin',(-35.0075079285187,19.,248.608721235131));
#240679=CARTESIAN_POINT('Origin',(17.5037539642593,22.,234.09329934747));
#240680=CARTESIAN_POINT('',(-35.0075079285187,22.,242.851010291301));
#240681=CARTESIAN_POINT('',(27.0075079285187,22.,216.577877459809));
#240682=CARTESIAN_POINT('',(-22.255630946389,22.,216.577877459809));
#240683=CARTESIAN_POINT('',(35.0075079285187,22.,224.577877459809));
#240684=CARTESIAN_POINT('',(33.010424909369,22.,222.58079444066));
#240685=CARTESIAN_POINT('',(35.0075079285187,22.,242.851010291301));
#240686=CARTESIAN_POINT('',(12.4213924902778,22.,231.631408332131));
#240687=CARTESIAN_POINT('Origin',(19.9792411332937,22.,231.631408332131));
#240688=CARTESIAN_POINT('Origin',(8.75187698212967,19.5,251.108721235131));
#240689=CARTESIAN_POINT('',(35.0075079285187,19.5,256.608721235131));
#240690=CARTESIAN_POINT('',(35.0075079285187,25.,251.108721235131));
#240691=CARTESIAN_POINT('Origin',(35.0075079285187,19.5,251.108721235131));
#240692=CARTESIAN_POINT('',(-35.0075079285187,25.,251.108721235131));
#240693=CARTESIAN_POINT('',(8.75187698212967,25.,251.108721235131));
#240694=CARTESIAN_POINT('',(-35.0075079285187,19.5,256.608721235131));
#240695=CARTESIAN_POINT('Origin',(-35.0075079285187,19.5,251.108721235131));
#240696=CARTESIAN_POINT('',(8.75187698212967,19.5,256.608721235131));
#240697=CARTESIAN_POINT('Origin',(17.5037539642593,25.,254.108721235131));
#240698=CARTESIAN_POINT('',(35.0075079285187,25.,224.577877459809));
#240699=CARTESIAN_POINT('',(35.0075079285187,25.,256.608721235131));
#240700=CARTESIAN_POINT('',(27.0075079285187,25.,216.577877459809));
#240701=CARTESIAN_POINT('',(35.0075079285187,25.,224.577877459809));
#240702=CARTESIAN_POINT('',(27.0075079285187,25.,216.577877459809));
#240703=CARTESIAN_POINT('',(-35.0075079285187,25.,256.608721235131));
#240704=CARTESIAN_POINT('',(12.4213924902778,25.,231.631408332131));
#240705=CARTESIAN_POINT('Origin',(19.9792411332937,25.,231.631408332131));
#240706=CARTESIAN_POINT('Origin',(19.9792411332937,0.,231.631408332131));
#240707=CARTESIAN_POINT('',(12.4213924902778,0.,231.631408332131));
#240708=CARTESIAN_POINT('Origin',(27.0075079285187,0.,216.577877459809));
#240709=CARTESIAN_POINT('',(27.0075079285187,0.,216.577877459809));
#240710=CARTESIAN_POINT('Origin',(35.0075079285187,0.,224.577877459809));
#240711=CARTESIAN_POINT('',(35.0075079285187,0.,224.577877459809));
#240712=CARTESIAN_POINT('Origin',(-39.9751670169646,-25.,260.358721235131));
#240713=CARTESIAN_POINT('',(-49.9751670169646,-25.,256.608721235131));
#240714=CARTESIAN_POINT('',(-39.9751670169646,-35.,256.608721235131));
#240715=CARTESIAN_POINT('Origin',(-39.9751670169646,-25.,256.608721235131));
#240716=CARTESIAN_POINT('',(-39.9751670169646,-35.,261.608721235131));
#240717=CARTESIAN_POINT('',(-39.9751670169646,-35.,260.358721235131));
#240718=CARTESIAN_POINT('',(-49.9751670169646,-25.,261.608721235131));
#240719=CARTESIAN_POINT('Origin',(-39.9751670169646,-25.,261.608721235131));
#240720=CARTESIAN_POINT('',(-49.9751670169646,-25.,260.358721235131));
#240721=CARTESIAN_POINT('Origin',(-49.9751670169646,0.,261.608721235131));
#240722=CARTESIAN_POINT('',(-49.9751670169646,0.,261.608721235131));
#240723=CARTESIAN_POINT('',(-49.9751670169646,0.,256.608721235131));
#240724=CARTESIAN_POINT('Origin',(-35.0075079285187,0.,256.608721235131));
#240725=CARTESIAN_POINT('',(-35.0075079285187,-19.5,256.608721235131));
#240726=CARTESIAN_POINT('',(-35.0075079285187,-25.,251.108721235131));
#240727=CARTESIAN_POINT('Origin',(-35.0075079285187,-19.5,251.108721235131));
#240728=CARTESIAN_POINT('',(-35.0075079285187,0.,256.608721235131));
#240729=CARTESIAN_POINT('',(-35.0075079285187,-19.,251.608721235131));
#240730=CARTESIAN_POINT('',(-35.0075079285187,0.,251.608721235131));
#240731=CARTESIAN_POINT('',(-35.0075079285187,-22.,248.608721235131));
#240732=CARTESIAN_POINT('Origin',(-35.0075079285187,-19.,248.608721235131));
#240733=CARTESIAN_POINT('',(-35.0075079285187,-22.,224.577877459809));
#240734=CARTESIAN_POINT('',(-35.0075079285187,-22.,242.851010291301));
#240735=CARTESIAN_POINT('',(-35.0075079285187,-25.,224.577877459809));
#240736=CARTESIAN_POINT('',(-35.0075079285187,0.,224.577877459809));
#240737=CARTESIAN_POINT('',(-35.0075079285187,-25.,256.608721235131));
#240738=CARTESIAN_POINT('Origin',(-19.9792411332937,0.,231.631408332131));
#240739=CARTESIAN_POINT('',(-12.4213924902778,-22.,231.631408332131));
#240740=CARTESIAN_POINT('Origin',(-19.9792411332937,-22.,231.631408332131));
#240741=CARTESIAN_POINT('',(-12.4213924902778,-25.,231.631408332131));
#240742=CARTESIAN_POINT('',(-12.4213924902778,0.,231.631408332131));
#240743=CARTESIAN_POINT('Origin',(-19.9792411332937,-25.,231.631408332131));
#240744=CARTESIAN_POINT('Origin',(-35.0075079285187,0.,224.577877459809));
#240745=CARTESIAN_POINT('',(-27.0075079285187,-22.,216.577877459809));
#240746=CARTESIAN_POINT('',(-33.010424909369,-22.,222.58079444066));
#240747=CARTESIAN_POINT('',(-27.0075079285187,-25.,216.577877459809));
#240748=CARTESIAN_POINT('',(-27.0075079285187,0.,216.577877459809));
#240749=CARTESIAN_POINT('',(-35.0075079285187,-25.,224.577877459809));
#240750=CARTESIAN_POINT('Origin',(39.9751670169646,-25.,260.358721235131));
#240751=CARTESIAN_POINT('',(49.9751670169646,-25.,256.608721235131));
#240752=CARTESIAN_POINT('',(39.9751670169646,-35.,256.608721235131));
#240753=CARTESIAN_POINT('Origin',(39.9751670169646,-25.,256.608721235131));
#240754=CARTESIAN_POINT('',(49.9751670169646,-25.,261.608721235131));
#240755=CARTESIAN_POINT('',(49.9751670169646,-25.,260.358721235131));
#240756=CARTESIAN_POINT('',(39.9751670169646,-35.,261.608721235131));
#240757=CARTESIAN_POINT('Origin',(39.9751670169646,-25.,261.608721235131));
#240758=CARTESIAN_POINT('',(39.9751670169646,-35.,260.358721235131));
#240759=CARTESIAN_POINT('Origin',(24.9875835084823,-35.,259.108721235131));
#240760=CARTESIAN_POINT('',(0.,-35.,261.608721235131));
#240761=CARTESIAN_POINT('',(0.,-35.,256.608721235131));
#240762=CARTESIAN_POINT('Origin',(49.9751670169646,0.,256.608721235131));
#240763=CARTESIAN_POINT('',(49.9751670169646,0.,256.608721235131));
#240764=CARTESIAN_POINT('',(35.0075079285187,-19.5,256.608721235131));
#240765=CARTESIAN_POINT('',(8.75187698212967,-19.5,256.608721235131));
#240766=CARTESIAN_POINT('',(35.0075079285187,0.,256.608721235131));
#240767=CARTESIAN_POINT('Origin',(49.9751670169646,0.,261.608721235131));
#240768=CARTESIAN_POINT('',(49.9751670169646,0.,261.608721235131));
#240769=CARTESIAN_POINT('Origin',(0.,0.,261.608721235131));
#240770=CARTESIAN_POINT('Origin',(26.255630946389,-19.,248.608721235131));
#240771=CARTESIAN_POINT('',(35.0075079285187,-22.,248.608721235131));
#240772=CARTESIAN_POINT('',(26.255630946389,-22.,248.608721235131));
#240773=CARTESIAN_POINT('',(35.0075079285187,-19.,251.608721235131));
#240774=CARTESIAN_POINT('',(26.255630946389,-19.,251.608721235131));
#240775=CARTESIAN_POINT('Origin',(35.0075079285187,-19.,248.608721235131));
#240776=CARTESIAN_POINT('Origin',(17.5037539642593,-22.,234.09329934747));
#240777=CARTESIAN_POINT('',(35.0075079285187,-22.,224.577877459809));
#240778=CARTESIAN_POINT('',(35.0075079285187,-22.,242.851010291301));
#240779=CARTESIAN_POINT('',(27.0075079285187,-22.,216.577877459809));
#240780=CARTESIAN_POINT('',(33.010424909369,-22.,222.58079444066));
#240781=CARTESIAN_POINT('',(-22.255630946389,-22.,216.577877459809));
#240782=CARTESIAN_POINT('',(12.4213924902778,-22.,231.631408332131));
#240783=CARTESIAN_POINT('Origin',(19.9792411332937,-22.,231.631408332131));
#240784=CARTESIAN_POINT('Origin',(8.75187698212967,-19.5,251.108721235131));
#240785=CARTESIAN_POINT('',(35.0075079285187,-25.,251.108721235131));
#240786=CARTESIAN_POINT('Origin',(35.0075079285187,-19.5,251.108721235131));
#240787=CARTESIAN_POINT('',(8.75187698212967,-25.,251.108721235131));
#240788=CARTESIAN_POINT('Origin',(17.5037539642593,-25.,254.108721235131));
#240789=CARTESIAN_POINT('',(27.0075079285187,-25.,216.577877459809));
#240790=CARTESIAN_POINT('',(27.0075079285187,-25.,216.577877459809));
#240791=CARTESIAN_POINT('',(35.0075079285187,-25.,224.577877459809));
#240792=CARTESIAN_POINT('',(35.0075079285187,-25.,224.577877459809));
#240793=CARTESIAN_POINT('',(35.0075079285187,-25.,256.608721235131));
#240794=CARTESIAN_POINT('',(12.4213924902778,-25.,231.631408332131));
#240795=CARTESIAN_POINT('Origin',(19.9792411332937,-25.,231.631408332131));
#240796=CARTESIAN_POINT('Origin',(35.0075079285187,0.,256.608721235131));
#240797=CARTESIAN_POINT('',(35.0075079285187,0.,224.577877459809));
#240798=CARTESIAN_POINT('',(35.0075079285187,0.,251.608721235131));
#240799=CARTESIAN_POINT('Origin',(19.9792411332937,0.,231.631408332131));
#240800=CARTESIAN_POINT('',(12.4213924902778,0.,231.631408332131));
#240801=CARTESIAN_POINT('Origin',(27.0075079285187,0.,216.577877459809));
#240802=CARTESIAN_POINT('',(27.0075079285187,0.,216.577877459809));
#240803=CARTESIAN_POINT('Origin',(35.0075079285187,0.,224.577877459809));
#240804=CARTESIAN_POINT('Origin',(35.0075079285187,0.,251.608721235131));
#240805=CARTESIAN_POINT('',(0.,0.,0.));
#240806=CARTESIAN_POINT('Origin',(213.235140564004,0.,130.804360617566));
#240807=CARTESIAN_POINT('',(-205.820054717884,-4.76405452823395,129.582490119308));
#240808=CARTESIAN_POINT('',(-206.164998470905,-4.76405452823394,129.582490119308));
#240809=CARTESIAN_POINT('',(213.235140564004,-4.76405452823405,129.582490119308));
#240810=CARTESIAN_POINT('',(-206.235140563976,-4.91824935292959,130.806883494435));
#240811=CARTESIAN_POINT('Ctrl Pts',(-206.164998470905,-4.76405452823394,
129.582490119308));
#240812=CARTESIAN_POINT('Ctrl Pts',(-206.172665944474,-4.79776118631657,
129.713911867602));
#240813=CARTESIAN_POINT('Ctrl Pts',(-206.180333418043,-4.82600172992664,
129.846636618208));
#240814=CARTESIAN_POINT('Ctrl Pts',(-206.188000891612,-4.84869920343357,
129.980164586805));
#240815=CARTESIAN_POINT('Ctrl Pts',(-206.195857503673,-4.87195657008729,
130.116986375504));
#240816=CARTESIAN_POINT('Ctrl Pts',(-206.203714115733,-4.88939378574457,
130.254651075192));
#240817=CARTESIAN_POINT('Ctrl Pts',(-206.211570727794,-4.90098467145666,
130.392617599839));
#240818=CARTESIAN_POINT('Ctrl Pts',(-206.219427339854,-4.91257555716875,
130.530584124486));
#240819=CARTESIAN_POINT('Ctrl Pts',(-206.227283951915,-4.91832015787954,
130.668852025862));
#240820=CARTESIAN_POINT('Ctrl Pts',(-206.235140563975,-4.91824935292959,
130.806883494435));
#240821=CARTESIAN_POINT('',(-207.389991015301,2.65316544558642,126.664162929598));
#240822=CARTESIAN_POINT('Ctrl Pts',(-206.235140564013,-4.91824935292925,
130.806883495092));
#240823=CARTESIAN_POINT('Ctrl Pts',(-206.243296577379,-4.91817584971133,
130.950175093808));
#240824=CARTESIAN_POINT('Ctrl Pts',(-206.251452590746,-4.9118408081057,
131.09330184757));
#240825=CARTESIAN_POINT('Ctrl Pts',(-206.259608604113,-4.89928367079141,
131.235872582194));
#240826=CARTESIAN_POINT('Ctrl Pts',(-206.267382938232,-4.88731417335877,
131.371771394107));
#240827=CARTESIAN_POINT('Ctrl Pts',(-206.275157272351,-4.86966698677397,
131.507387058606));
#240828=CARTESIAN_POINT('Ctrl Pts',(-206.28293160647,-4.846359096209,131.64220700748));
#240829=CARTESIAN_POINT('Ctrl Pts',(-206.290696359417,-4.82307993053606,
131.776860802817));
#240830=CARTESIAN_POINT('Ctrl Pts',(-206.298461112364,-4.79415400762733,
131.910720452176));
#240831=CARTESIAN_POINT('Ctrl Pts',(-206.306225865311,-4.75965019918353,
132.043276693784));
#240832=CARTESIAN_POINT('Ctrl Pts',(-206.313982906196,-4.72518066040869,
132.175701278665));
#240833=CARTESIAN_POINT('Ctrl Pts',(-206.321739947081,-4.68514435886508,
132.306824656126));
#240834=CARTESIAN_POINT('Ctrl Pts',(-206.329496987965,-4.63966146046592,
132.436146324933));
#240835=CARTESIAN_POINT('Ctrl Pts',(-206.337248179205,-4.59421286107431,
132.565370471264));
#240836=CARTESIAN_POINT('Ctrl Pts',(-206.344999370445,-4.5433259693909,
132.69279524599));
#240837=CARTESIAN_POINT('Ctrl Pts',(-206.352750561685,-4.48717107061851,
132.817934267946));
#240838=CARTESIAN_POINT('Ctrl Pts',(-206.360498458462,-4.43104003917615,
132.943020102479));
#240839=CARTESIAN_POINT('Ctrl Pts',(-206.368246355239,-4.36964561366111,
133.065821760543));
#240840=CARTESIAN_POINT('Ctrl Pts',(-206.375994252016,-4.30320651608381,
133.185872058318));
#240841=CARTESIAN_POINT('Ctrl Pts',(-206.3837405281,-4.23678131613346,133.305897244159));
#240842=CARTESIAN_POINT('Ctrl Pts',(-206.391486804184,-4.16531373223735,
133.423171872606));
#240843=CARTESIAN_POINT('Ctrl Pts',(-206.399233080268,-4.08906864095504,
133.537252988674));
#240844=CARTESIAN_POINT('Ctrl Pts',(-206.406979413534,-4.01282298684869,
133.651334946862));
#240845=CARTESIAN_POINT('Ctrl Pts',(-206.414725746799,-3.93179997222957,
133.762223020581));
#240846=CARTESIAN_POINT('Ctrl Pts',(-206.422472080064,-3.84630781202687,
133.869503237028));
#240847=CARTESIAN_POINT('Ctrl Pts',(-206.430220148067,-3.76079650644777,
133.976807478135));
#240848=CARTESIAN_POINT('Ctrl Pts',(-206.43796821607,-3.67081430735097,
134.080501948538));
#240849=CARTESIAN_POINT('Ctrl Pts',(-206.445716284073,-3.5767094513966,
134.180206076527));
#240850=CARTESIAN_POINT('Ctrl Pts',(-206.453472586815,-3.48250457968159,
134.280016171251));
#240851=CARTESIAN_POINT('Ctrl Pts',(-206.461228889557,-3.38416856715666,
134.375827166964));
#240852=CARTESIAN_POINT('Ctrl Pts',(-206.468985192298,-3.28208662334993,
134.467295296116));
#240853=CARTESIAN_POINT('Ctrl Pts',(-206.476745634812,-3.17995019533615,
134.558812244563));
#240854=CARTESIAN_POINT('Ctrl Pts',(-206.484506077326,-3.07406415392714,
134.645981459434));
#240855=CARTESIAN_POINT('Ctrl Pts',(-206.49226651984,-2.96484568166884,
134.728500414565));
#240856=CARTESIAN_POINT('Ctrl Pts',(-206.500039420106,-2.8554518822229,
134.811151836448));
#240857=CARTESIAN_POINT('Ctrl Pts',(-206.507812320371,-2.74271528361125,
134.889137858572));
#240858=CARTESIAN_POINT('Ctrl Pts',(-206.515585220636,-2.62708159836639,
134.962199640186));
#240859=CARTESIAN_POINT('Ctrl Pts',(-206.523075556399,-2.51565148882853,
135.032605442017));
#240860=CARTESIAN_POINT('Ctrl Pts',(-206.530565892162,-2.40153153536177,
135.098438650812));
#240861=CARTESIAN_POINT('Ctrl Pts',(-206.538056227925,-2.2851392588354,
135.159509481868));
#240862=CARTESIAN_POINT('Ctrl Pts',(-206.545830562044,-2.16433393378268,
135.222895832038));
#240863=CARTESIAN_POINT('Ctrl Pts',(-206.553604896163,-2.04069789899693,
135.281352333429));
#240864=CARTESIAN_POINT('Ctrl Pts',(-206.561379230282,-1.91467157352999,
135.334616220511));
#240865=CARTESIAN_POINT('Ctrl Pts',(-206.56914398323,-1.78880056424624,
135.387814464613));
#240866=CARTESIAN_POINT('Ctrl Pts',(-206.576908736177,-1.66054548224971,
135.435832676627));
#240867=CARTESIAN_POINT('Ctrl Pts',(-206.584673489124,-1.53037201072842,
135.478453531841));
#240868=CARTESIAN_POINT('Ctrl Pts',(-206.592430530009,-1.40032782933418,
135.521032055421));
#240869=CARTESIAN_POINT('Ctrl Pts',(-206.600187570894,-1.26836941934266,
135.55822376943));
#240870=CARTESIAN_POINT('Ctrl Pts',(-206.607944611779,-1.13498281922694,
135.589859239712));
#240871=CARTESIAN_POINT('Ctrl Pts',(-206.615695803019,-1.00169680698415,
135.62147085344));
#240872=CARTESIAN_POINT('Ctrl Pts',(-206.623446994259,-0.866985127212026,
135.647534473537));
#240873=CARTESIAN_POINT('Ctrl Pts',(-206.631198185499,-0.731349029471388,
135.667930464869));
#240874=CARTESIAN_POINT('Ctrl Pts',(-206.638946082276,-0.595770580690315,
135.688317787359));
#240875=CARTESIAN_POINT('Ctrl Pts',(-206.646693979053,-0.459268881202547,
135.703042214174));
#240876=CARTESIAN_POINT('Ctrl Pts',(-206.65444187583,-0.322355210575576,
135.712035238068));
#240877=CARTESIAN_POINT('Ctrl Pts',(-206.662188151914,-0.185470179336983,
135.721026380815));
#240878=CARTESIAN_POINT('Ctrl Pts',(-206.669934427998,-0.0481737382443191,
135.724288479683));
#240879=CARTESIAN_POINT('Ctrl Pts',(-206.677680704082,0.0890182698783709,
135.721804954834));
#240880=CARTESIAN_POINT('Ctrl Pts',(-206.685427037348,0.226211290721486,
135.719321411652));
#240881=CARTESIAN_POINT('Ctrl Pts',(-206.693173370613,0.36329948615519,
135.711092167198));
#240882=CARTESIAN_POINT('Ctrl Pts',(-206.700919703878,0.499767971438338,
135.697152769009));
#240883=CARTESIAN_POINT('Ctrl Pts',(-206.708667771881,0.636267017892372,
135.683210249189));
#240884=CARTESIAN_POINT('Ctrl Pts',(-206.716415839884,0.772145689173082,
135.66355507079));
#240885=CARTESIAN_POINT('Ctrl Pts',(-206.724163907887,0.906895569102237,
135.638274506874));
#240886=CARTESIAN_POINT('Ctrl Pts',(-206.731920210629,1.04178866280751,
135.612967074473));
#240887=CARTESIAN_POINT('Ctrl Pts',(-206.739676513371,1.17555018377165,
135.582022385611));
#240888=CARTESIAN_POINT('Ctrl Pts',(-206.747432816113,1.30768269545861,
135.545578713214));
#240889=CARTESIAN_POINT('Ctrl Pts',(-206.755193258627,1.4398857302455,135.509115589732));
#240890=CARTESIAN_POINT('Ctrl Pts',(-206.762953701141,1.57045765127054,
135.467147754108));
#240891=CARTESIAN_POINT('Ctrl Pts',(-206.770714143655,1.69891843734635,
135.419862671053));
#240892=CARTESIAN_POINT('Ctrl Pts',(-206.77848704392,1.82758544008018,135.372501681785));
#240893=CARTESIAN_POINT('Ctrl Pts',(-206.786259944186,1.9541341744678,135.319806538378));
#240894=CARTESIAN_POINT('Ctrl Pts',(-206.794032844451,2.07810595194281,
135.262012321659));
#240895=CARTESIAN_POINT('Ctrl Pts',(-206.801523180213,2.19757104304053,
135.206319070292));
#240896=CARTESIAN_POINT('Ctrl Pts',(-206.809013515975,2.31464300846158,
135.145891178822));
#240897=CARTESIAN_POINT('Ctrl Pts',(-206.816503851737,2.42893649673259,
135.080977336111));
#240898=CARTESIAN_POINT('Ctrl Pts',(-206.824278185856,2.5475634573503,135.013602265324));
#240899=CARTESIAN_POINT('Ctrl Pts',(-206.832052519975,2.66357286432491,
134.941180934586));
#240900=CARTESIAN_POINT('Ctrl Pts',(-206.839826854094,2.77650558831772,
134.86394184973));
#240901=CARTESIAN_POINT('Ctrl Pts',(-206.847591607042,2.88929913282099,
134.786797955144));
#240902=CARTESIAN_POINT('Ctrl Pts',(-206.855356359989,2.99902321915925,
134.704848338791));
#240903=CARTESIAN_POINT('Ctrl Pts',(-206.863121112936,3.1052432927571,134.618367323812));
#240904=CARTESIAN_POINT('Ctrl Pts',(-206.870878153821,3.21135786708041,
134.531972202995));
#240905=CARTESIAN_POINT('Ctrl Pts',(-206.878635194706,3.31397505326374,
134.441054885293));
#240906=CARTESIAN_POINT('Ctrl Pts',(-206.886392235591,3.41268958588663,
134.345932705337));
#240907=CARTESIAN_POINT('Ctrl Pts',(-206.894143426831,3.51132967711271,
134.250882257758));
#240908=CARTESIAN_POINT('Ctrl Pts',(-206.901894618071,3.6060726922938,134.151633529634));
#240909=CARTESIAN_POINT('Ctrl Pts',(-206.909645809311,3.69654704137007,
134.048543570705));
#240910=CARTESIAN_POINT('Ctrl Pts',(-206.917393706088,3.78698293643439,
133.945497427759));
#240911=CARTESIAN_POINT('Ctrl Pts',(-206.925141602865,3.87315351654314,
133.838613594408));
#240912=CARTESIAN_POINT('Ctrl Pts',(-206.932889499642,3.95472478551692,
133.728285194794));
#240913=CARTESIAN_POINT('Ctrl Pts',(-206.940635775726,4.0362789915397,133.617979873503));
#240914=CARTESIAN_POINT('Ctrl Pts',(-206.948382051811,4.11323556776735,
133.504231733294));
#240915=CARTESIAN_POINT('Ctrl Pts',(-206.956128327895,4.18530173946635,
133.387465805536));
#240916=CARTESIAN_POINT('Ctrl Pts',(-206.96387466116,4.25736844314155,133.270699015839));
#240917=CARTESIAN_POINT('Ctrl Pts',(-206.971620994426,4.32454446491532,
133.150914726844));
#240918=CARTESIAN_POINT('Ctrl Pts',(-206.979367327691,4.38658140415818,
133.028565339977));
#240919=CARTESIAN_POINT('Ctrl Pts',(-206.987115395694,4.44863223614336,
132.906188553813));
#240920=CARTESIAN_POINT('Ctrl Pts',(-206.994863463697,4.50554151874139,
132.781245875352));
#240921=CARTESIAN_POINT('Ctrl Pts',(-207.0026115317,4.55710786588625,132.654212222743));
#240922=CARTESIAN_POINT('Ctrl Pts',(-207.010367834442,4.60872901835857,
132.527043557257));
#240923=CARTESIAN_POINT('Ctrl Pts',(-207.018124137184,4.65499574460735,
132.397779841151));
#240924=CARTESIAN_POINT('Ctrl Pts',(-207.025880439925,4.69575550096411,
132.266914321765));
#240925=CARTESIAN_POINT('Ctrl Pts',(-207.03364088244,4.73653701203008,132.13597895551));
#240926=CARTESIAN_POINT('Ctrl Pts',(-207.041401324954,4.77180559603988,
132.003440460087));
#240927=CARTESIAN_POINT('Ctrl Pts',(-207.049161767468,4.80145950918554,
131.86980402017));
#240928=CARTESIAN_POINT('Ctrl Pts',(-207.056934667734,4.83116102542514,
131.735953055175));
#240929=CARTESIAN_POINT('Ctrl Pts',(-207.064707567999,4.85522979093357,
131.601001008726));
#240930=CARTESIAN_POINT('Ctrl Pts',(-207.072480468265,4.87361565349489,
131.465460855434));
#240931=CARTESIAN_POINT('Ctrl Pts',(-207.079970804027,4.89133314364086,
131.33484792812));
#240932=CARTESIAN_POINT('Ctrl Pts',(-207.087461139788,4.90377370409151,
131.203689216588));
#240933=CARTESIAN_POINT('Ctrl Pts',(-207.09495147555,4.91093827194779,131.072443350353));
#240934=CARTESIAN_POINT('Ctrl Pts',(-207.102725809669,4.91837448657198,
130.936221257207));
#240935=CARTESIAN_POINT('Ctrl Pts',(-207.110500143789,4.92015028810036,
130.79947375931));
#240936=CARTESIAN_POINT('Ctrl Pts',(-207.118274477908,4.91620975433994,
130.66271064816));
#240937=CARTESIAN_POINT('Ctrl Pts',(-207.126039230855,4.91227407693521,
130.526116085322));
#240938=CARTESIAN_POINT('Ctrl Pts',(-207.133803983802,4.90263609258996,
130.389506334569));
#240939=CARTESIAN_POINT('Ctrl Pts',(-207.141568736749,4.88729170976703,
130.253395277329));
#240940=CARTESIAN_POINT('Ctrl Pts',(-207.149325777634,4.87196256720145,
130.11741940751));
#240941=CARTESIAN_POINT('Ctrl Pts',(-207.157082818519,4.85093834860235,
129.981941631508));
#240942=CARTESIAN_POINT('Ctrl Pts',(-207.164839859404,4.824266980725,129.847474437717));
#240943=CARTESIAN_POINT('Ctrl Pts',(-207.172591050644,4.79761572593367,
129.713108646683));
#240944=CARTESIAN_POINT('Ctrl Pts',(-207.180342241884,4.76532587402565,
129.579752302914));
#240945=CARTESIAN_POINT('Ctrl Pts',(-207.188093433124,4.72749696755391,
129.447911029756));
#240946=CARTESIAN_POINT('Ctrl Pts',(-207.195841329901,4.68968413937648,
129.316125792657));
#240947=CARTESIAN_POINT('Ctrl Pts',(-207.203589226679,4.64633704665318,
129.185854720425));
#240948=CARTESIAN_POINT('Ctrl Pts',(-207.211337123456,4.59760590276493,
129.057591306706));
#240949=CARTESIAN_POINT('Ctrl Pts',(-207.21908339954,4.54888495238146,128.929354722929));
#240950=CARTESIAN_POINT('Ctrl Pts',(-207.226829675624,4.49478232972868,
128.80312532759));
#240951=CARTESIAN_POINT('Ctrl Pts',(-207.234575951708,4.43549737384086,
128.6793791802));
#240952=CARTESIAN_POINT('Ctrl Pts',(-207.242322284973,4.37621198032504,
128.555632119344));
#240953=CARTESIAN_POINT('Ctrl Pts',(-207.250068618239,4.31174434616012,
128.434368695606));
#240954=CARTESIAN_POINT('Ctrl Pts',(-207.257814951504,4.24234082287173,
128.316042429493));
#240955=CARTESIAN_POINT('Ctrl Pts',(-207.265563019507,4.17292175714561,
128.197689665032));
#240956=CARTESIAN_POINT('Ctrl Pts',(-207.27331108751,4.09856480052667,128.082275704225));
#240957=CARTESIAN_POINT('Ctrl Pts',(-207.281059155513,4.01956066101754,
127.970226683734));
#240958=CARTESIAN_POINT('Ctrl Pts',(-207.288815458255,3.94047255496867,
127.858058576209));
#240959=CARTESIAN_POINT('Ctrl Pts',(-207.296571760996,3.85672762533503,
127.749262873077));
#240960=CARTESIAN_POINT('Ctrl Pts',(-207.304328063738,3.76865840149488,
127.644234525882));
#240961=CARTESIAN_POINT('Ctrl Pts',(-207.312088506252,3.68054217245802,
127.539150121895));
#240962=CARTESIAN_POINT('Ctrl Pts',(-207.319848948767,3.58809731371382,
127.437837369101));
#240963=CARTESIAN_POINT('Ctrl Pts',(-207.327609391281,3.4916938564228,127.340654932101));
#240964=CARTESIAN_POINT('Ctrl Pts',(-207.335382291546,3.3951356437441,127.243316489227));
#240965=CARTESIAN_POINT('Ctrl Pts',(-207.343155191812,3.29460642069608,
127.15012187765));
#240966=CARTESIAN_POINT('Ctrl Pts',(-207.350928092077,3.19051065884962,
127.061390567156));
#240967=CARTESIAN_POINT('Ctrl Pts',(-207.358418427839,3.09019904014599,
126.975884863298));
#240968=CARTESIAN_POINT('Ctrl Pts',(-207.365908763601,2.98657592832593,
126.894523780142));
#240969=CARTESIAN_POINT('Ctrl Pts',(-207.373399099363,2.88002768791472,
126.817554429733));
#240970=CARTESIAN_POINT('Ctrl Pts',(-207.378631136696,2.80560320424821,
126.763790950015));
#240971=CARTESIAN_POINT('Ctrl Pts',(-207.383863174029,2.72959351183089,
126.712054947007));
#240972=CARTESIAN_POINT('Ctrl Pts',(-207.389095211362,2.65211837414998,
126.662446664815));
#240973=CARTESIAN_POINT('',(-207.161386959855,0.717556610101921,125.938940090646));
#240974=CARTESIAN_POINT('Ctrl Pts',(-207.16240288731,0.705992749060373,
125.937045412982));
#240975=CARTESIAN_POINT('Ctrl Pts',(-207.181988187458,1.10669090187245,
125.995165748024));
#240976=CARTESIAN_POINT('Ctrl Pts',(-207.218876175974,1.50830544278856,
126.105044865929));
#240977=CARTESIAN_POINT('Ctrl Pts',(-207.303250137215,2.1584231714227,126.375368867204));
#240978=CARTESIAN_POINT('Ctrl Pts',(-207.34444557399,2.41814945805675,126.511911515592));
#240979=CARTESIAN_POINT('Ctrl Pts',(-207.388495272009,2.66099574923083,
126.668144389529));
#240980=CARTESIAN_POINT('',(-205.889859436046,-4.91824930584068,130.806973680448));
#240981=CARTESIAN_POINT('Ctrl Pts',(-205.889859436046,-4.91824930584068,
130.806973680447));
#240982=CARTESIAN_POINT('Ctrl Pts',(-205.898419073697,-4.91816863288146,
130.958814544507));
#240983=CARTESIAN_POINT('Ctrl Pts',(-205.906978711349,-4.91105222461682,
131.11040905316));
#240984=CARTESIAN_POINT('Ctrl Pts',(-205.915538349,-4.89699280558849,131.261136847809));
#240985=CARTESIAN_POINT('Ctrl Pts',(-205.924144711242,-4.88285664025042,
131.412687421976));
#240986=CARTESIAN_POINT('Ctrl Pts',(-205.932751073485,-4.86170154469193,
131.563361562213));
#240987=CARTESIAN_POINT('Ctrl Pts',(-205.941357435727,-4.8336719627189,
131.712544750507));
#240988=CARTESIAN_POINT('Ctrl Pts',(-205.949987994199,-4.80556357739427,
131.862147357658));
#240989=CARTESIAN_POINT('Ctrl Pts',(-205.95861855267,-4.77054211518795,
132.010250401408));
#240990=CARTESIAN_POINT('Ctrl Pts',(-205.967249111142,-4.72880199806623,
132.15625363315));
#240991=CARTESIAN_POINT('Ctrl Pts',(-205.975911032462,-4.68691020026427,
132.302787430473));
#240992=CARTESIAN_POINT('Ctrl Pts',(-205.984572953782,-4.63825094856085,
132.447205915682));
#240993=CARTESIAN_POINT('Ctrl Pts',(-205.993234875102,-4.58306805029199,
132.588925076725));
#240994=CARTESIAN_POINT('Ctrl Pts',(-205.995739908888,-4.5671091169981,
132.629910358551));
#240995=CARTESIAN_POINT('Ctrl Pts',(-205.998244942673,-4.55060485959071,
132.67067003316));
#240996=CARTESIAN_POINT('Ctrl Pts',(-206.000749976459,-4.53356188569129,
132.711190366418));
#240997=CARTESIAN_POINT('Ctrl Pts',(-206.008524310578,-4.48066927631869,
132.836944602228));
#240998=CARTESIAN_POINT('Ctrl Pts',(-206.016298644698,-4.42245657148283,
132.960695612929));
#240999=CARTESIAN_POINT('Ctrl Pts',(-206.024072978817,-4.35909645044119,
133.081960494246));
#241000=CARTESIAN_POINT('Ctrl Pts',(-206.031837731764,-4.29581441508608,
133.203075927434));
#241001=CARTESIAN_POINT('Ctrl Pts',(-206.039602484712,-4.22739776497256,
133.321710984359));
#241002=CARTESIAN_POINT('Ctrl Pts',(-206.047367237659,-4.15406757846652,
133.437401752078));
#241003=CARTESIAN_POINT('Ctrl Pts',(-206.055124278544,-4.0808102245355,
133.552977614096));
#241004=CARTESIAN_POINT('Ctrl Pts',(-206.06288131943,-4.00264925397073,
133.665614678334));
#241005=CARTESIAN_POINT('Ctrl Pts',(-206.070638360315,-3.91985191488636,
133.774873035965));
#241006=CARTESIAN_POINT('Ctrl Pts',(-206.078389551555,-3.83711701391935,
133.884049001019));
#241007=CARTESIAN_POINT('Ctrl Pts',(-206.086140742796,-3.7497529388275,
133.989851020585));
#241008=CARTESIAN_POINT('Ctrl Pts',(-206.093891934036,-3.65807035220528,
134.091867934792));
#241009=CARTESIAN_POINT('Ctrl Pts',(-206.101639830814,-3.5664267331282,
134.193841489089));
#241010=CARTESIAN_POINT('Ctrl Pts',(-206.109387727591,-3.47046851394157,
134.292032847568));
#241011=CARTESIAN_POINT('Ctrl Pts',(-206.117135624368,-3.37054661931243,
134.386063920401));
#241012=CARTESIAN_POINT('Ctrl Pts',(-206.124881900453,-3.2706456261893,
134.480075323962));
#241013=CARTESIAN_POINT('Ctrl Pts',(-206.132628176537,-3.16678289131879,
134.569927905073));
#241014=CARTESIAN_POINT('Ctrl Pts',(-206.140374452621,-3.0593458918801,
134.655280738308));
#241015=CARTESIAN_POINT('Ctrl Pts',(-206.148120785887,-2.95190809936603,
134.740634201599));
#241016=CARTESIAN_POINT('Ctrl Pts',(-206.155867119153,-2.84089629575584,
134.821487607538));
#241017=CARTESIAN_POINT('Ctrl Pts',(-206.163613452418,-2.72673037768329,
134.897540861572));
#241018=CARTESIAN_POINT('Ctrl Pts',(-206.171361520422,-2.61253889294479,
134.973611147205));
#241019=CARTESIAN_POINT('Ctrl Pts',(-206.179109588425,-2.49519221352086,
135.044878925172));
#241020=CARTESIAN_POINT('Ctrl Pts',(-206.186857656428,-2.37513814799737,
135.11108812699));
#241021=CARTESIAN_POINT('Ctrl Pts',(-206.19461395917,-2.25495648758455,
135.177367696735));
#241022=CARTESIAN_POINT('Ctrl Pts',(-206.202370261912,-2.13206203597101,
135.238577761457));
#241023=CARTESIAN_POINT('Ctrl Pts',(-206.210126564654,-2.00692657135467,
135.294508588367));
#241024=CARTESIAN_POINT('Ctrl Pts',(-206.217887007169,-1.88172431817278,
135.350469267244));
#241025=CARTESIAN_POINT('Ctrl Pts',(-206.225647449683,-1.75427903178613,
135.401144949441));
#241026=CARTESIAN_POINT('Ctrl Pts',(-206.233407892198,-1.6250803440804,
135.446374936564));
#241027=CARTESIAN_POINT('Ctrl Pts',(-206.241180792463,-1.49567425517145,
135.491677530877));
#241028=CARTESIAN_POINT('Ctrl Pts',(-206.248953692729,-1.36450951455032,
135.531516847299));
#241029=CARTESIAN_POINT('Ctrl Pts',(-206.256726592995,-1.23208958293334,
135.565782497858));
#241030=CARTESIAN_POINT('Ctrl Pts',(-206.264216928754,-1.10448344942972,
135.598802505697));
#241031=CARTESIAN_POINT('Ctrl Pts',(-206.271707264513,-0.975712100315515,
135.626646980716));
#241032=CARTESIAN_POINT('Ctrl Pts',(-206.279197600272,-0.846231065683617,
135.649262685304));
#241033=CARTESIAN_POINT('Ctrl Pts',(-206.286971934391,-0.711840718217051,
135.672735871215));
#241034=CARTESIAN_POINT('Ctrl Pts',(-206.29474626851,-0.576260099220195,
135.690650318037));
#241035=CARTESIAN_POINT('Ctrl Pts',(-206.302520602629,-0.439988827093508,
135.702890284163));
#241036=CARTESIAN_POINT('Ctrl Pts',(-206.310285355577,-0.303885497130804,
135.715115165626));
#241037=CARTESIAN_POINT('Ctrl Pts',(-206.318050108524,-0.16709359326881,
135.721679446316));
#241038=CARTESIAN_POINT('Ctrl Pts',(-206.325814861471,-0.030122916862644,
135.722518369446));
#241039=CARTESIAN_POINT('Ctrl Pts',(-206.333571902356,0.106711718336767,
135.723356459347));
#241040=CARTESIAN_POINT('Ctrl Pts',(-206.341328943241,0.243724384301109,
135.718480505712));
#241041=CARTESIAN_POINT('Ctrl Pts',(-206.349085984126,0.380400519141976,
135.707877570482));
#241042=CARTESIAN_POINT('Ctrl Pts',(-206.356837175366,0.516973585446189,
135.697282631009));
#241043=CARTESIAN_POINT('Ctrl Pts',(-206.364588366606,0.653210237545264,
135.68096933629));
#241044=CARTESIAN_POINT('Ctrl Pts',(-206.372339557846,0.78859663427342,
135.658976813612));
#241045=CARTESIAN_POINT('Ctrl Pts',(-206.380087454624,0.9239254881716,135.636993638342));
#241046=CARTESIAN_POINT('Ctrl Pts',(-206.387835351401,1.0584044203597,135.60933609858));
#241047=CARTESIAN_POINT('Ctrl Pts',(-206.395583248178,1.19152564980452,
135.576095070399));
#241048=CARTESIAN_POINT('Ctrl Pts',(-206.403329524262,1.3246190331579,135.542860995525));
#241049=CARTESIAN_POINT('Ctrl Pts',(-206.411075800346,1.45635489958587,
135.504045849998));
#241050=CARTESIAN_POINT('Ctrl Pts',(-206.41882207643,1.58623697799247,135.459791350823));
#241051=CARTESIAN_POINT('Ctrl Pts',(-206.426568409696,1.71612001515889,
135.41553652497));
#241052=CARTESIAN_POINT('Ctrl Pts',(-206.434314742961,1.84414886692504,
135.365842391443));
#241053=CARTESIAN_POINT('Ctrl Pts',(-206.442061076226,1.96984409085683,
135.310900012736));
#241054=CARTESIAN_POINT('Ctrl Pts',(-206.449809144229,2.09556746336268,
135.255945330063));
#241055=CARTESIAN_POINT('Ctrl Pts',(-206.457557212232,2.21895580995249,
135.195740220041));
#241056=CARTESIAN_POINT('Ctrl Pts',(-206.465305280235,2.33955164148073,
135.130523025445));
#241057=CARTESIAN_POINT('Ctrl Pts',(-206.473061582977,2.46027564369365,
135.065236517239));
#241058=CARTESIAN_POINT('Ctrl Pts',(-206.480817885719,2.57820085766173,
134.99492746967));
#241059=CARTESIAN_POINT('Ctrl Pts',(-206.488574188461,2.69289582161183,
134.919879437405));
#241060=CARTESIAN_POINT('Ctrl Pts',(-206.496334630975,2.80765200171758,
134.844791349744));
#241061=CARTESIAN_POINT('Ctrl Pts',(-206.504095073489,2.91917417867433,
134.764959464925));
#241062=CARTESIAN_POINT('Ctrl Pts',(-206.511855516003,3.02706249437732,
134.68070886271));
#241063=CARTESIAN_POINT('Ctrl Pts',(-206.519628416269,3.13512400198284,
134.59632301395));
#241064=CARTESIAN_POINT('Ctrl Pts',(-206.527401316534,3.23953969337777,
134.507504526547));
#241065=CARTESIAN_POINT('Ctrl Pts',(-206.5351742168,3.33994456322253,134.414617308869));
#241066=CARTESIAN_POINT('Ctrl Pts',(-206.542664552561,3.43669946314165,
134.325106775525));
#241067=CARTESIAN_POINT('Ctrl Pts',(-206.550154888323,3.52972986821838,
134.231818411375));
#241068=CARTESIAN_POINT('Ctrl Pts',(-206.557645224085,3.61874476299928,
134.13510669056));
#241069=CARTESIAN_POINT('Ctrl Pts',(-206.565419558204,3.71113468457249,
134.034728115454));
#241070=CARTESIAN_POINT('Ctrl Pts',(-206.573193892323,3.79949125235512,
133.930343496942));
#241071=CARTESIAN_POINT('Ctrl Pts',(-206.580968226442,3.88344703370601,
133.82231061697));
#241072=CARTESIAN_POINT('Ctrl Pts',(-206.588732979389,3.9672993470595,133.714410877866));
#241073=CARTESIAN_POINT('Ctrl Pts',(-206.596497732336,4.04676142767885,
133.602872129055));
#241074=CARTESIAN_POINT('Ctrl Pts',(-206.604262485283,4.12150323375985,
133.488088278229));
#241075=CARTESIAN_POINT('Ctrl Pts',(-206.612019526168,4.19617080522537,
133.373418432341));
#241076=CARTESIAN_POINT('Ctrl Pts',(-206.619776567053,4.2661272200117,133.255510224025));
#241077=CARTESIAN_POINT('Ctrl Pts',(-206.627533607938,4.33108345969385,
133.134789575433));
#241078=CARTESIAN_POINT('Ctrl Pts',(-206.635284799178,4.39599071537045,
133.014159963221));
#241079=CARTESIAN_POINT('Ctrl Pts',(-206.643035990418,4.45590511673205,
132.890722475119));
#241080=CARTESIAN_POINT('Ctrl Pts',(-206.650787181658,4.51058183897033,
132.764930569506));
#241081=CARTESIAN_POINT('Ctrl Pts',(-206.658535078435,4.56523532214318,
132.639192128808));
#241082=CARTESIAN_POINT('Ctrl Pts',(-206.666282975212,4.61465539831717,
132.511101618704));
#241083=CARTESIAN_POINT('Ctrl Pts',(-206.674030871989,4.65864405605593,
132.381135370495));
#241084=CARTESIAN_POINT('Ctrl Pts',(-206.681777148073,4.70262351231578,
132.251196308424));
#241085=CARTESIAN_POINT('Ctrl Pts',(-206.689523424157,4.74117368471374,
132.119382658775));
#241086=CARTESIAN_POINT('Ctrl Pts',(-206.697269700241,4.77414555713005,
131.986188549981));
#241087=CARTESIAN_POINT('Ctrl Pts',(-206.705016033506,4.80711767293719,
131.852993457978));
#241088=CARTESIAN_POINT('Ctrl Pts',(-206.712762366772,4.83451131264874,
131.718418266004));
#241089=CARTESIAN_POINT('Ctrl Pts',(-206.720508700037,4.8562280722051,131.582969616504));
#241090=CARTESIAN_POINT('Ctrl Pts',(-206.72825676804,4.87794969507915,131.447490634218));
#241091=CARTESIAN_POINT('Ctrl Pts',(-206.736004836043,4.89399184618037,
131.311138191135));
#241092=CARTESIAN_POINT('Ctrl Pts',(-206.743752904046,4.90430776597871,
131.174426015923));
#241093=CARTESIAN_POINT('Ctrl Pts',(-206.751509206787,4.91463464965938,
131.037568541384));
#241094=CARTESIAN_POINT('Ctrl Pts',(-206.759265509529,4.91922311531838,
130.900350961453));
#241095=CARTESIAN_POINT('Ctrl Pts',(-206.767021812271,4.91807850989876,
130.763289545363));
#241096=CARTESIAN_POINT('Ctrl Pts',(-206.774782254785,4.91693329356877,
130.626154975468));
#241097=CARTESIAN_POINT('Ctrl Pts',(-206.782542697299,4.91004892864024,
130.489177125775));
#241098=CARTESIAN_POINT('Ctrl Pts',(-206.790303139813,4.89748278085339,
130.352868121787));
#241099=CARTESIAN_POINT('Ctrl Pts',(-206.798076040079,4.88489646077053,
130.216340302485));
#241100=CARTESIAN_POINT('Ctrl Pts',(-206.805848940344,4.86661018354394,
130.080483862156));
#241101=CARTESIAN_POINT('Ctrl Pts',(-206.813621840609,4.84273282128629,
129.945802591492));
#241102=CARTESIAN_POINT('Ctrl Pts',(-206.821112176372,4.81972346128801,
129.816017324245));
#241103=CARTESIAN_POINT('Ctrl Pts',(-206.828602512135,4.79152252480077,
129.687323570165));
#241104=CARTESIAN_POINT('Ctrl Pts',(-206.836092847897,4.75827093999596,
129.560157770724));
#241105=CARTESIAN_POINT('Ctrl Pts',(-206.843867182016,4.72375861124946,
129.428170441356));
#241106=CARTESIAN_POINT('Ctrl Pts',(-206.851641516135,4.68369575848463,
129.29741112245));
#241107=CARTESIAN_POINT('Ctrl Pts',(-206.859415850255,4.63818478746673,
129.168382335371));
#241108=CARTESIAN_POINT('Ctrl Pts',(-206.867180603202,4.59272990465331,
129.039512564742));
#241109=CARTESIAN_POINT('Ctrl Pts',(-206.874945356149,4.54184039188006,
128.912369447615));
#241110=CARTESIAN_POINT('Ctrl Pts',(-206.882710109096,4.4856692591883,128.787443574236));
#241111=CARTESIAN_POINT('Ctrl Pts',(-206.890467149981,4.42955391645741,
128.662641778997));
#241112=CARTESIAN_POINT('Ctrl Pts',(-206.898224190866,4.36816755243845,
128.540053199304));
#241113=CARTESIAN_POINT('Ctrl Pts',(-206.905981231751,4.30171228598306,
128.420151215873));
#241114=CARTESIAN_POINT('Ctrl Pts',(-206.913732422991,4.23530713396096,
128.300339651459));
#241115=CARTESIAN_POINT('Ctrl Pts',(-206.921483614231,4.16384087671486,
128.183210991282));
#241116=CARTESIAN_POINT('Ctrl Pts',(-206.929234805471,4.08756268783238,
128.069216318714));
#241117=CARTESIAN_POINT('Ctrl Pts',(-206.936982702249,4.01131691921485,
127.955270096924));
#241118=CARTESIAN_POINT('Ctrl Pts',(-206.944730599026,3.93026350367536,
127.844455537692));
#241119=CARTESIAN_POINT('Ctrl Pts',(-206.952478495803,3.844696162211,127.737196702354));
#241120=CARTESIAN_POINT('Ctrl Pts',(-206.960224771887,3.75914671958986,
127.629960303251));
#241121=CARTESIAN_POINT('Ctrl Pts',(-206.967971047971,3.66908547280403,
127.526278454052));
#241122=CARTESIAN_POINT('Ctrl Pts',(-206.975717324055,3.5748475992442,127.426543614726));
#241123=CARTESIAN_POINT('Ctrl Pts',(-206.983463657321,3.48060903004192,
127.326808039179));
#241124=CARTESIAN_POINT('Ctrl Pts',(-206.991209990586,3.38219404105675,
127.231019815818));
#241125=CARTESIAN_POINT('Ctrl Pts',(-206.998956323851,3.27997569512705,
127.13953558738));
#241126=CARTESIAN_POINT('Ctrl Pts',(-207.006704391854,3.17773445810738,
127.048030871684));
#241127=CARTESIAN_POINT('Ctrl Pts',(-207.014452459857,3.07168846055954,
126.960832329545));
#241128=CARTESIAN_POINT('Ctrl Pts',(-207.022200527861,2.96224464229277,
126.878256983974));
#241129=CARTESIAN_POINT('Ctrl Pts',(-207.029956830602,2.85268450583369,
126.795593876342));
#241130=CARTESIAN_POINT('Ctrl Pts',(-207.037713133344,2.73971964740063,
126.717564016553));
#241131=CARTESIAN_POINT('Ctrl Pts',(-207.045469436086,2.62378730907338,
126.644441962202));
#241132=CARTESIAN_POINT('Ctrl Pts',(-207.0532298786,2.50779309416619,126.571280880408));
#241133=CARTESIAN_POINT('Ctrl Pts',(-207.060990321115,2.38882858239987,
126.50303301797));
#241134=CARTESIAN_POINT('Ctrl Pts',(-207.068750763629,2.26735564704684,
126.439926927807));
#241135=CARTESIAN_POINT('Ctrl Pts',(-207.076523663894,2.14568771255446,
126.376719534146));
#241136=CARTESIAN_POINT('Ctrl Pts',(-207.08429656416,2.02150366214178,126.318670572596));
#241137=CARTESIAN_POINT('Ctrl Pts',(-207.092069464425,1.89528619722091,
126.265960757139));
#241138=CARTESIAN_POINT('Ctrl Pts',(-207.099559800187,1.77365705507833,
126.215167076244));
#241139=CARTESIAN_POINT('Ctrl Pts',(-207.107050135949,1.65014005997225,
126.16933120521));
#241140=CARTESIAN_POINT('Ctrl Pts',(-207.114540471711,1.52517857759403,
126.12857048445));
#241141=CARTESIAN_POINT('Ctrl Pts',(-207.122366202396,1.39462169226328,
126.08598462003));
#241142=CARTESIAN_POINT('Ctrl Pts',(-207.130191933081,1.26207165493998,
126.048803145944));
#241143=CARTESIAN_POINT('Ctrl Pts',(-207.138017663766,1.12801622149789,
126.017215072825));
#241144=CARTESIAN_POINT('Ctrl Pts',(-207.145843394452,0.993960788056163,
125.985626999705));
#241145=CARTESIAN_POINT('Ctrl Pts',(-207.153669125137,0.858400328457906,
125.959632493955));
#241146=CARTESIAN_POINT('Ctrl Pts',(-207.161494855822,0.721842234581774,
125.939370704845));
#241147=CARTESIAN_POINT('Ctrl Pts',(-205.820054717884,-4.76405452823395,
129.582490119308));
#241148=CARTESIAN_POINT('Ctrl Pts',(-205.827905852165,-4.79858606955834,
129.717128074842));
#241149=CARTESIAN_POINT('Ctrl Pts',(-205.835756986446,-4.82742791349959,
129.853316954026));
#241150=CARTESIAN_POINT('Ctrl Pts',(-205.843608120727,-4.85045202410955,
129.99054354702));
#241151=CARTESIAN_POINT('Ctrl Pts',(-205.851456131429,-4.87346697456125,
130.12771554432));
#241152=CARTESIAN_POINT('Ctrl Pts',(-205.859304142131,-4.8906687356244,
130.265924063211));
#241153=CARTESIAN_POINT('Ctrl Pts',(-205.867152152832,-4.9019802890764,
130.404645333887));
#241154=CARTESIAN_POINT('Ctrl Pts',(-205.87472124722,-4.91288983278145,
130.538436485711));
#241155=CARTESIAN_POINT('Ctrl Pts',(-205.882290341607,-4.91832064309359,
130.672704230441));
#241156=CARTESIAN_POINT('Ctrl Pts',(-205.889859435995,-4.91824930584116,
130.806973679544));
#241157=CARTESIAN_POINT('Origin',(213.235140564004,0.,130.804360617566));
#241158=CARTESIAN_POINT('',(-204.070038127516,-4.76405452823409,129.582490119308));
#241159=CARTESIAN_POINT('',(-204.415385129731,-4.7580624943176,129.583982083009));
#241160=CARTESIAN_POINT('',(213.235140564004,-4.76405452823405,129.582490119308));
#241161=CARTESIAN_POINT('',(-204.485140564013,-4.91500524972814,130.807513005812));
#241162=CARTESIAN_POINT('Ctrl Pts',(-204.415385129731,-4.7580624943176,
129.583982083009));
#241163=CARTESIAN_POINT('Ctrl Pts',(-204.438636941158,-4.85784969763347,
129.983485013898));
#241164=CARTESIAN_POINT('Ctrl Pts',(-204.461888752586,-4.90979750657223,
130.395767923279));
#241165=CARTESIAN_POINT('Ctrl Pts',(-204.485140564013,-4.91220180825584,
130.807511207739));
#241166=CARTESIAN_POINT('Ctrl Pts',(-204.485140564013,-4.91824898839283,
130.807515086282));
#241167=CARTESIAN_POINT('Ctrl Pts',(-204.49387773296,-4.91814963363141,
130.962422774028));
#241168=CARTESIAN_POINT('Ctrl Pts',(-204.502614901907,-4.91072767197462,
131.117052050995));
#241169=CARTESIAN_POINT('Ctrl Pts',(-204.511352070854,-4.8960860736549,
131.27075553806));
#241170=CARTESIAN_POINT('Ctrl Pts',(-204.520123591854,-4.88138690875277,
131.425063343332));
#241171=CARTESIAN_POINT('Ctrl Pts',(-204.528895112854,-4.85941133515114,
131.578437879815));
#241172=CARTESIAN_POINT('Ctrl Pts',(-204.537666633853,-4.83031338638245,
131.73024163143));
#241173=CARTESIAN_POINT('Ctrl Pts',(-204.546486847053,-4.8010539099665,
131.882888071409));
#241174=CARTESIAN_POINT('Ctrl Pts',(-204.555307060253,-4.76459286084652,
132.033946055602));
#241175=CARTESIAN_POINT('Ctrl Pts',(-204.564127273453,-4.72113560423765,
132.182787862255));
#241176=CARTESIAN_POINT('Ctrl Pts',(-204.572392469381,-4.68041292189577,
132.322263707821));
#241177=CARTESIAN_POINT('Ctrl Pts',(-204.580657665308,-4.63354733828304,
132.459793589481));
#241178=CARTESIAN_POINT('Ctrl Pts',(-204.588922861235,-4.58074515708572,
132.594879220747));
#241179=CARTESIAN_POINT('Ctrl Pts',(-204.596697195354,-4.53107884518496,
132.721942250031));
#241180=CARTESIAN_POINT('Ctrl Pts',(-204.604471529473,-4.47604305081149,
132.847138467984));
#241181=CARTESIAN_POINT('Ctrl Pts',(-204.612245863592,-4.41579807394511,
132.969980721057));
#241182=CARTESIAN_POINT('Ctrl Pts',(-204.620010616539,-4.35562734362847,
133.092671582031));
#241183=CARTESIAN_POINT('Ctrl Pts',(-204.627775369486,-4.29026037490912,
133.213013902697));
#241184=CARTESIAN_POINT('Ctrl Pts',(-204.635540122433,-4.21990633574634,
133.330538279574));
#241185=CARTESIAN_POINT('Ctrl Pts',(-204.643297163318,-4.14962217320707,
133.447945929583));
#241186=CARTESIAN_POINT('Ctrl Pts',(-204.651054204203,-4.07436099688629,
133.562540872303));
#241187=CARTESIAN_POINT('Ctrl Pts',(-204.658811245088,-3.99437874200781,
133.673876522365));
#241188=CARTESIAN_POINT('Ctrl Pts',(-204.666562436328,-3.91445680236981,
133.785128213348));
#241189=CARTESIAN_POINT('Ctrl Pts',(-204.674313627568,-3.82982109772313,
133.89312518765));
#241190=CARTESIAN_POINT('Ctrl Pts',(-204.682064818808,-3.74077169726714,
133.997448491619));
#241191=CARTESIAN_POINT('Ctrl Pts',(-204.689812715585,-3.65176014518169,
134.101727455401));
#241192=CARTESIAN_POINT('Ctrl Pts',(-204.697560612362,-3.55833888168141,
134.202335557629));
#241193=CARTESIAN_POINT('Ctrl Pts',(-204.705308509139,-3.46084906882826,
134.298885876495));
#241194=CARTESIAN_POINT('Ctrl Pts',(-204.713054785223,-3.36337964874233,
134.395415999115));
#241195=CARTESIAN_POINT('Ctrl Pts',(-204.720801061307,-3.26184364970766,
134.487889751746));
#241196=CARTESIAN_POINT('Ctrl Pts',(-204.728547337392,-3.15661972277871,
134.575956432107));
#241197=CARTESIAN_POINT('Ctrl Pts',(-204.736293670657,-3.05139501911078,
134.664023762557));
#241198=CARTESIAN_POINT('Ctrl Pts',(-204.744040003922,-2.94248263304068,
134.747683704894));
#241199=CARTESIAN_POINT('Ctrl Pts',(-204.751786337187,-2.83029466646686,
134.826625547114));
#241200=CARTESIAN_POINT('Ctrl Pts',(-204.75953440519,-2.71808157617563,
134.905585067812));
#241201=CARTESIAN_POINT('Ctrl Pts',(-204.767282473193,-2.60259176539364,
134.979824160965));
#241202=CARTESIAN_POINT('Ctrl Pts',(-204.775030541196,-2.48426636236587,
135.04907541403));
#241203=CARTESIAN_POINT('Ctrl Pts',(-204.782786843938,-2.36581520169152,
135.11840026815));
#241204=CARTESIAN_POINT('Ctrl Pts',(-204.79054314668,-2.24452276654071,
135.182726494795));
#241205=CARTESIAN_POINT('Ctrl Pts',(-204.798299449421,-2.12085532938707,
135.241832390356));
#241206=CARTESIAN_POINT('Ctrl Pts',(-204.806059891935,-1.99712188719867,
135.300969832514));
#241207=CARTESIAN_POINT('Ctrl Pts',(-204.81382033445,-1.87101127650509,
135.354881238147));
#241208=CARTESIAN_POINT('Ctrl Pts',(-204.821580776964,-1.74300886894293,
135.403393466469));
#241209=CARTESIAN_POINT('Ctrl Pts',(-204.829353677229,-1.61480098055263,
135.451983570926));
#241210=CARTESIAN_POINT('Ctrl Pts',(-204.837126577494,-1.48469559792147,
135.495157054964));
#241211=CARTESIAN_POINT('Ctrl Pts',(-204.84489947776,-1.35319320086527,
135.532790718946));
#241212=CARTESIAN_POINT('Ctrl Pts',(-204.852389813522,-1.22647124717054,
135.569056304449));
#241213=CARTESIAN_POINT('Ctrl Pts',(-204.859880149284,-1.09845238493452,
135.600177777234));
#241214=CARTESIAN_POINT('Ctrl Pts',(-204.867370485047,-0.969590637356454,
135.626090292532));
#241215=CARTESIAN_POINT('Ctrl Pts',(-204.875144819166,-0.835843057454864,
135.652985288723));
#241216=CARTESIAN_POINT('Ctrl Pts',(-204.882919153285,-0.700763742363002,
135.674353730114));
#241217=CARTESIAN_POINT('Ctrl Pts',(-204.890693487405,-0.564849194214768,
135.690067163225));
#241218=CARTESIAN_POINT('Ctrl Pts',(-204.898458240352,-0.42910214860009,
135.705761230934));
#241219=CARTESIAN_POINT('Ctrl Pts',(-204.906222993299,-0.292522302678767,
135.715814112706));
#241220=CARTESIAN_POINT('Ctrl Pts',(-204.913987746246,-0.155617639284803,
135.720148063423));
#241221=CARTESIAN_POINT('Ctrl Pts',(-204.921744787131,-0.0188489515325352,
135.724477709599));
#241222=CARTESIAN_POINT('Ctrl Pts',(-204.929501828017,0.118243523436565,
135.723099716129));
#241223=CARTESIAN_POINT('Ctrl Pts',(-204.937258868902,0.255145721463766,
135.715988018267));
#241224=CARTESIAN_POINT('Ctrl Pts',(-204.945010060142,0.391944680478308,
135.708881683392));
#241225=CARTESIAN_POINT('Ctrl Pts',(-204.952761251382,0.528553259298798,
135.696050270647));
#241226=CARTESIAN_POINT('Ctrl Pts',(-204.960512442623,0.664456785619391,
135.677519782065));
#241227=CARTESIAN_POINT('Ctrl Pts',(-204.9682603394,0.80030254931577,135.658997169436));
#241228=CARTESIAN_POINT('Ctrl Pts',(-204.976008236177,0.935443469955528,
135.634780351368));
#241229=CARTESIAN_POINT('Ctrl Pts',(-204.983756132954,1.06936961283493,
135.604947216477));
#241230=CARTESIAN_POINT('Ctrl Pts',(-204.991502409038,1.20326774125236,
135.575120322035));
#241231=CARTESIAN_POINT('Ctrl Pts',(-204.999248685123,1.33595121596879,
135.53967953249));
#241232=CARTESIAN_POINT('Ctrl Pts',(-205.006994961207,1.46692031107978,
135.49875385455));
#241233=CARTESIAN_POINT('Ctrl Pts',(-205.014741294472,1.59789037297505,
135.457827874506));
#241234=CARTESIAN_POINT('Ctrl Pts',(-205.022487627738,1.72714565684219,
135.411417041884));
#241235=CARTESIAN_POINT('Ctrl Pts',(-205.030233961003,1.85420200073023,
135.359700122256));
#241236=CARTESIAN_POINT('Ctrl Pts',(-205.037982029006,1.98128679800571,
135.307971620982));
#241237=CARTESIAN_POINT('Ctrl Pts',(-205.04573009701,2.10617131336159,135.250934815567));
#241238=CARTESIAN_POINT('Ctrl Pts',(-205.053478165013,2.22839212445938,
135.188816296684));
#241239=CARTESIAN_POINT('Ctrl Pts',(-205.061234467755,2.35074283328949,
135.1266317575));
#241240=CARTESIAN_POINT('Ctrl Pts',(-205.068990770497,2.47042383351275,
135.059354893381));
#241241=CARTESIAN_POINT('Ctrl Pts',(-205.076747073239,2.58699656794278,
134.987258156348));
#241242=CARTESIAN_POINT('Ctrl Pts',(-205.084507515753,2.70363152075111,
134.915122939117));
#241243=CARTESIAN_POINT('Ctrl Pts',(-205.092267958267,2.81715457866475,
134.838162942302));
#241244=CARTESIAN_POINT('Ctrl Pts',(-205.100028400782,2.9271577182112,134.756692935985));
#241245=CARTESIAN_POINT('Ctrl Pts',(-205.107801301047,3.03733744456286,
134.67509214678));
#241246=CARTESIAN_POINT('Ctrl Pts',(-205.115574201313,3.1439856567345,134.588967126286));
#241247=CARTESIAN_POINT('Ctrl Pts',(-205.123347101578,3.24672818181712,
134.498672349932));
#241248=CARTESIAN_POINT('Ctrl Pts',(-205.130837437339,3.3457357573013,134.411660016153));
#241249=CARTESIAN_POINT('Ctrl Pts',(-205.1383277731,3.4411164558133,134.320776037914));
#241250=CARTESIAN_POINT('Ctrl Pts',(-205.145818108861,3.53257031098373,
134.226367347609));
#241251=CARTESIAN_POINT('Ctrl Pts',(-205.15359244298,3.62749166688566,134.128379123099));
#241252=CARTESIAN_POINT('Ctrl Pts',(-205.161366777099,3.71848321111434,
134.026283234194));
#241253=CARTESIAN_POINT('Ctrl Pts',(-205.169141111218,3.80516850058741,
133.920427969957));
#241254=CARTESIAN_POINT('Ctrl Pts',(-205.176905864165,3.89174695818848,
133.814703162873));
#241255=CARTESIAN_POINT('Ctrl Pts',(-205.184670617112,3.97402947520282,
133.705228498512));
#241256=CARTESIAN_POINT('Ctrl Pts',(-205.192435370059,4.05167606532983,
133.592389334085));
#241257=CARTESIAN_POINT('Ctrl Pts',(-205.200192410944,4.1292455357689,133.479662243106));
#241258=CARTESIAN_POINT('Ctrl Pts',(-205.207949451829,4.2021880222257,133.363577622127));
#241259=CARTESIAN_POINT('Ctrl Pts',(-205.215706492714,4.27020373145505,
133.24455387925));
#241260=CARTESIAN_POINT('Ctrl Pts',(-205.223457683954,4.33816814950907,
133.125619893103));
#241261=CARTESIAN_POINT('Ctrl Pts',(-205.231208875195,4.40121299226405,
133.003751534774));
#241262=CARTESIAN_POINT('Ctrl Pts',(-205.238960066435,4.45908194301358,
132.879395867385));
#241263=CARTESIAN_POINT('Ctrl Pts',(-205.246707963212,4.51692629791526,
132.755093054471));
#241264=CARTESIAN_POINT('Ctrl Pts',(-205.254455859989,4.56959897162442,
132.628305388855));
#241265=CARTESIAN_POINT('Ctrl Pts',(-205.262203756766,4.61688986187661,
132.499503993744));
#241266=CARTESIAN_POINT('Ctrl Pts',(-205.26995003285,4.66417085989403,132.370729541109));
#241267=CARTESIAN_POINT('Ctrl Pts',(-205.277696308934,4.70607217897284,
132.239942563603));
#241268=CARTESIAN_POINT('Ctrl Pts',(-205.285442585018,4.74243224205182,
132.107633226059));
#241269=CARTESIAN_POINT('Ctrl Pts',(-205.293188918284,4.77879257353258,
131.975322911837));
#241270=CARTESIAN_POINT('Ctrl Pts',(-205.300935251549,4.80961146379121,
131.841490592143));
#241271=CARTESIAN_POINT('Ctrl Pts',(-205.308681584814,4.83477761200457,
131.706640233295));
#241272=CARTESIAN_POINT('Ctrl Pts',(-205.316429652817,4.8599493960023,131.571759675644));
#241273=CARTESIAN_POINT('Ctrl Pts',(-205.32417772082,4.8794658472645,131.435861009436));
#241274=CARTESIAN_POINT('Ctrl Pts',(-205.331925788823,4.89326711184883,
131.299456602804));
#241275=CARTESIAN_POINT('Ctrl Pts',(-205.339682091565,4.90708304458142,
131.162907223945));
#241276=CARTESIAN_POINT('Ctrl Pts',(-205.347438394307,4.91517161741112,
131.025851420532));
#241277=CARTESIAN_POINT('Ctrl Pts',(-205.355194697049,4.91752500106838,
130.888805430121));
#241278=CARTESIAN_POINT('Ctrl Pts',(-205.362955139563,4.91987964079736,
130.751686294138));
#241279=CARTESIAN_POINT('Ctrl Pts',(-205.370715582077,4.91649300161557,
130.614577372247));
#241280=CARTESIAN_POINT('Ctrl Pts',(-205.378476024592,4.9074093618528,130.477992087068));
#241281=CARTESIAN_POINT('Ctrl Pts',(-205.386248924857,4.89831114022507,
130.341187543064));
#241282=CARTESIAN_POINT('Ctrl Pts',(-205.394021825122,4.88349768500393,
130.204908704434));
#241283=CARTESIAN_POINT('Ctrl Pts',(-205.401794725388,4.86306497681123,
130.069661976073));
#241284=CARTESIAN_POINT('Ctrl Pts',(-205.40928506115,4.84337504902889,129.939331806958));
#241285=CARTESIAN_POINT('Ctrl Pts',(-205.416775396912,4.81846738151463,
129.809960313757));
#241286=CARTESIAN_POINT('Ctrl Pts',(-205.424265732673,4.78847171916799,
129.681987392107));
#241287=CARTESIAN_POINT('Ctrl Pts',(-205.432040066792,4.75733876216599,
129.549162338233));
#241288=CARTESIAN_POINT('Ctrl Pts',(-205.439814400911,4.72062575157316,
129.417423253277));
#241289=CARTESIAN_POINT('Ctrl Pts',(-205.44758873503,4.67842223616104,129.287275108211));
#241290=CARTESIAN_POINT('Ctrl Pts',(-205.455353487977,4.63627073280972,
129.157287359103));
#241291=CARTESIAN_POINT('Ctrl Pts',(-205.463118240924,4.58864230750925,
129.028887017024));
#241292=CARTESIAN_POINT('Ctrl Pts',(-205.470882993871,4.53567740129338,
128.902568417062));
#241293=CARTESIAN_POINT('Ctrl Pts',(-205.478640034756,4.48276510056905,
128.776375278515));
#241294=CARTESIAN_POINT('Ctrl Pts',(-205.486397075641,4.4245270169024,128.652260125658));
#241295=CARTESIAN_POINT('Ctrl Pts',(-205.494154116526,4.36115312330836,
128.530701342838));
#241296=CARTESIAN_POINT('Ctrl Pts',(-205.501905307766,4.29782702046055,
128.409234228441));
#241297=CARTESIAN_POINT('Ctrl Pts',(-205.509656499006,4.22937299657398,
128.290319992233));
#241298=CARTESIAN_POINT('Ctrl Pts',(-205.517407690246,4.15602863307309,
128.174415929255));
#241299=CARTESIAN_POINT('Ctrl Pts',(-205.525155587023,4.08271544288332,
128.058561128595));
#241300=CARTESIAN_POINT('Ctrl Pts',(-205.5329034838,4.00451625573041,127.94571428621));
#241301=CARTESIAN_POINT('Ctrl Pts',(-205.540651380577,3.92171387550616,
127.836306820688));
#241302=CARTESIAN_POINT('Ctrl Pts',(-205.548397656661,3.83892881575483,
127.726922240849));
#241303=CARTESIAN_POINT('Ctrl Pts',(-205.556143932745,3.75154271395995,
127.62097591841));
#241304=CARTESIAN_POINT('Ctrl Pts',(-205.563890208829,3.65988062332928,
127.518868738794));
#241305=CARTESIAN_POINT('Ctrl Pts',(-205.571636542094,3.56821785606976,
127.416760805445));
#241306=CARTESIAN_POINT('Ctrl Pts',(-205.579382875359,3.47227929816279,
127.318492362404));
#241307=CARTESIAN_POINT('Ctrl Pts',(-205.587129208625,3.37242878993213,
127.224429456309));
#241308=CARTESIAN_POINT('Ctrl Pts',(-205.594877276628,3.27255592087287,
127.130345485479));
#241309=CARTESIAN_POINT('Ctrl Pts',(-205.60262534463,3.16876964276772,127.040469193703));
#241310=CARTESIAN_POINT('Ctrl Pts',(-205.610373412633,3.06146867291942,
126.955127885289));
#241311=CARTESIAN_POINT('Ctrl Pts',(-205.618129715375,2.95405366232302,
126.869695875116));
#241312=CARTESIAN_POINT('Ctrl Pts',(-205.625886018117,2.84311680448129,
126.788808720195));
#241313=CARTESIAN_POINT('Ctrl Pts',(-205.633642320859,2.72908819275771,
126.712752046521));
#241314=CARTESIAN_POINT('Ctrl Pts',(-205.641402763373,2.61499872053071,
126.63665477911));
#241315=CARTESIAN_POINT('Ctrl Pts',(-205.649163205887,2.4978145402187,126.565393333214));
#241316=CARTESIAN_POINT('Ctrl Pts',(-205.656923648401,2.37799154233177,
126.499207973687));
#241317=CARTESIAN_POINT('Ctrl Pts',(-205.664696548666,2.25797619393123,
126.432916367546));
#241318=CARTESIAN_POINT('Ctrl Pts',(-205.672469448932,2.13531391299143,
126.371717305886));
#241319=CARTESIAN_POINT('Ctrl Pts',(-205.680242349197,2.01048263216247,
126.315803761708));
#241320=CARTESIAN_POINT('Ctrl Pts',(-205.68773268496,1.89018928280237,126.261922815689));
#241321=CARTESIAN_POINT('Ctrl Pts',(-205.695223020723,1.76788217886368,
126.212949889631));
#241322=CARTESIAN_POINT('Ctrl Pts',(-205.702713356486,1.64400154729095,
126.169013599812));
#241323=CARTESIAN_POINT('Ctrl Pts',(-205.710487690606,1.5154239439371,126.123411452216));
#241324=CARTESIAN_POINT('Ctrl Pts',(-205.718262024725,1.38474384172379,
126.083090954468));
#241325=CARTESIAN_POINT('Ctrl Pts',(-205.726036358844,1.25243449033019,
126.048249715796));
#241326=CARTESIAN_POINT('Ctrl Pts',(-205.733801111791,1.12028819838735,
126.013451415837));
#241327=CARTESIAN_POINT('Ctrl Pts',(-205.741565864738,0.986517026841535,
125.984119037703));
#241328=CARTESIAN_POINT('Ctrl Pts',(-205.749330617686,0.85161278561181,
125.960401624564));
#241329=CARTESIAN_POINT('Ctrl Pts',(-205.757087658571,0.716842533176288,
125.936707767895));
#241330=CARTESIAN_POINT('Ctrl Pts',(-205.764844699456,0.5809418331833,125.918617845271));
#241331=CARTESIAN_POINT('Ctrl Pts',(-205.772601740341,0.444415848987914,
125.906230605442));
#241332=CARTESIAN_POINT('Ctrl Pts',(-205.780352931581,0.307992820099411,
125.893852706927));
#241333=CARTESIAN_POINT('Ctrl Pts',(-205.788104122822,0.170945833354071,
125.88716896663));
#241334=CARTESIAN_POINT('Ctrl Pts',(-205.795855314062,0.0337880425846281,
125.886226679711));
#241335=CARTESIAN_POINT('Ctrl Pts',(-205.803603210839,-0.103311452464748,
125.885284793289));
#241336=CARTESIAN_POINT('Ctrl Pts',(-205.811351107616,-0.240521267733049,
125.890079509413));
#241337=CARTESIAN_POINT('Ctrl Pts',(-205.819099004394,-0.377325576133052,
125.900606089442));
#241338=CARTESIAN_POINT('Ctrl Pts',(-205.826845280478,-0.514101268020897,
125.911130467538));
#241339=CARTESIAN_POINT('Ctrl Pts',(-205.834591556562,-0.650471232192675,
125.927384294722));
#241340=CARTESIAN_POINT('Ctrl Pts',(-205.842337832646,-0.785922493189801,
125.949310782889));
#241341=CARTESIAN_POINT('Ctrl Pts',(-205.850084165912,-0.921374754057551,
125.971237432912));
#241342=CARTESIAN_POINT('Ctrl Pts',(-205.857830499177,-1.05590791227709,
125.998836764999));
#241343=CARTESIAN_POINT('Ctrl Pts',(-205.865576832443,-1.18901733786065,
126.032000527132));
#241344=CARTESIAN_POINT('Ctrl Pts',(-205.873324900446,-1.32215657237697,
126.065171716059));
#241345=CARTESIAN_POINT('Ctrl Pts',(-205.881072968449,-1.45387106051707,
126.103909720158));
#241346=CARTESIAN_POINT('Ctrl Pts',(-205.888821036452,-1.58366991545586,
126.148056003241));
#241347=CARTESIAN_POINT('Ctrl Pts',(-205.896577339194,-1.71360672216248,
126.19224920552));
#241348=CARTESIAN_POINT('Ctrl Pts',(-205.904333641936,-1.8416234578902,
126.241862042909));
#241349=CARTESIAN_POINT('Ctrl Pts',(-205.912089944678,-1.96724734143226,
126.296687053506));
#241350=CARTESIAN_POINT('Ctrl Pts',(-205.919850387192,-2.09293827422343,
126.351541325862));
#241351=CARTESIAN_POINT('Ctrl Pts',(-205.927610829707,-2.21623345872856,
126.411613143427));
#241352=CARTESIAN_POINT('Ctrl Pts',(-205.935371272221,-2.33668433336452,
126.476648821627));
#241353=CARTESIAN_POINT('Ctrl Pts',(-205.943144172487,-2.45732856643756,
126.541788900871));
#241354=CARTESIAN_POINT('Ctrl Pts',(-205.950917072752,-2.57511902930189,
126.61190856411));
#241355=CARTESIAN_POINT('Ctrl Pts',(-205.958689973018,-2.68963503403625,
126.68671001969));
#241356=CARTESIAN_POINT('Ctrl Pts',(-205.966180308779,-2.79998809352685,
126.758792253932));
#241357=CARTESIAN_POINT('Ctrl Pts',(-205.973670644539,-2.90730038036246,
126.835221621603));
#241358=CARTESIAN_POINT('Ctrl Pts',(-205.9811609803,-3.0112257326097,126.915697267549));
#241359=CARTESIAN_POINT('Ctrl Pts',(-205.988843416406,-3.11781639876974,
126.998236826237));
#241360=CARTESIAN_POINT('Ctrl Pts',(-205.996525852513,-3.22119867281582,
127.085307874707));
#241361=CARTESIAN_POINT('Ctrl Pts',(-206.004208288619,-3.32095599792357,
127.1766293262));
#241362=CARTESIAN_POINT('Ctrl Pts',(-206.01188194727,-3.42059934675241,
127.267846439699));
#241363=CARTESIAN_POINT('Ctrl Pts',(-206.019555605921,-3.5166256876976,
127.363304034671));
#241364=CARTESIAN_POINT('Ctrl Pts',(-206.027229264572,-3.60864870074115,
127.462678762999));
#241365=CARTESIAN_POINT('Ctrl Pts',(-206.034895912193,-3.70058763704767,
127.561962697703));
#241366=CARTESIAN_POINT('Ctrl Pts',(-206.042562559813,-3.78853024788272,
127.665156357538));
#241367=CARTESIAN_POINT('Ctrl Pts',(-206.050229207433,-3.87212489877666,
127.771897620137));
#241368=CARTESIAN_POINT('Ctrl Pts',(-206.057890604246,-3.95566229656263,
127.878565776755));
#241369=CARTESIAN_POINT('Ctrl Pts',(-206.065552001059,-4.03485741114901,
127.988776389217));
#241370=CARTESIAN_POINT('Ctrl Pts',(-206.073213397872,-4.10939732791692,
128.102132525082));
#241371=CARTESIAN_POINT('Ctrl Pts',(-206.080872341447,-4.18391337642932,
128.215452363439));
#241372=CARTESIAN_POINT('Ctrl Pts',(-206.088531285021,-4.25377696648902,
128.331915391257));
#241373=CARTESIAN_POINT('Ctrl Pts',(-206.096190228596,-4.31871736387104,
128.451094080707));
#241374=CARTESIAN_POINT('Ctrl Pts',(-206.103847441602,-4.38364308771443,
128.570245841263));
#241375=CARTESIAN_POINT('Ctrl Pts',(-206.111504654608,-4.44364764309317,
128.692111689209));
#241376=CARTESIAN_POINT('Ctrl Pts',(-206.119161867614,-4.49850566380742,
128.816238424341));
#241377=CARTESIAN_POINT('Ctrl Pts',(-206.1268221242,-4.55338548942266,128.940414497221));
#241378=CARTESIAN_POINT('Ctrl Pts',(-206.134482380787,-4.60311452764392,
129.066852887145));
#241379=CARTESIAN_POINT('Ctrl Pts',(-206.142142637373,-4.64751508729958,
129.195079232654));
#241380=CARTESIAN_POINT('Ctrl Pts',(-206.14976124855,-4.69167426085744,
129.322608468546));
#241381=CARTESIAN_POINT('Ctrl Pts',(-206.157379859728,-4.73056267205465,
129.451905880375));
#241382=CARTESIAN_POINT('Ctrl Pts',(-206.164998470905,-4.76405452823394,
129.582490119308));
#241383=CARTESIAN_POINT('',(-204.139859435948,-4.91824831916273,130.80029447038));
#241384=CARTESIAN_POINT('Ctrl Pts',(-204.139859435995,-4.91824831916343,
130.800294471219));
#241385=CARTESIAN_POINT('Ctrl Pts',(-204.147784635894,-4.91836431326766,
130.94059630973));
#241386=CARTESIAN_POINT('Ctrl Pts',(-204.155709835794,-4.91247201397862,
131.080987232013));
#241387=CARTESIAN_POINT('Ctrl Pts',(-204.163635035693,-4.900578301156,131.220912387145));
#241388=CARTESIAN_POINT('Ctrl Pts',(-204.171354581511,-4.88899322289429,
131.357206570228));
#241389=CARTESIAN_POINT('Ctrl Pts',(-204.179074127329,-4.87171440627009,
131.493058448163));
#241390=CARTESIAN_POINT('Ctrl Pts',(-204.186793673146,-4.84880093828704,
131.627957924122));
#241391=CARTESIAN_POINT('Ctrl Pts',(-204.194513059106,-4.8258879448005,
131.762854606557));
#241392=CARTESIAN_POINT('Ctrl Pts',(-204.202232445066,-4.79734059760185,
131.896798538118));
#241393=CARTESIAN_POINT('Ctrl Pts',(-204.209951831025,-4.76326941003805,
132.029288203138));
#241394=CARTESIAN_POINT('Ctrl Pts',(-204.217672755543,-4.72919143171145,
132.161804274807));
#241395=CARTESIAN_POINT('Ctrl Pts',(-204.225393680062,-4.68958752045796,
132.29286512203));
#241396=CARTESIAN_POINT('Ctrl Pts',(-204.23311460458,-4.6446184041067,132.421983238183));
#241397=CARTESIAN_POINT('Ctrl Pts',(-204.24119374033,-4.59756295178294,
132.55709177159));
#241398=CARTESIAN_POINT('Ctrl Pts',(-204.24927287608,-4.54463267751754,
132.69007253139));
#241399=CARTESIAN_POINT('Ctrl Pts',(-204.25735201183,-4.48606813212016,
132.820390323814));
#241400=CARTESIAN_POINT('Ctrl Pts',(-204.265085528802,-4.43000892977471,
132.945133228333));
#241401=CARTESIAN_POINT('Ctrl Pts',(-204.272819045774,-4.36878776769414,
133.067435961724));
#241402=CARTESIAN_POINT('Ctrl Pts',(-204.280552562746,-4.30266231755848,
133.186855117783));
#241403=CARTESIAN_POINT('Ctrl Pts',(-204.288291669847,-4.23648906901836,
133.306360595297));
#241404=CARTESIAN_POINT('Ctrl Pts',(-204.296030776948,-4.16540467691822,
133.422978009958));
#241405=CARTESIAN_POINT('Ctrl Pts',(-204.303769884048,-4.08970977527734,
133.53629345285));
#241406=CARTESIAN_POINT('Ctrl Pts',(-204.311519964139,-4.01390754867324,
133.649769561459));
#241407=CARTESIAN_POINT('Ctrl Pts',(-204.319270044229,-3.93348199885383,
133.759934040129));
#241408=CARTESIAN_POINT('Ctrl Pts',(-204.32702012432,-3.84877374515481,
133.866406293435));
#241409=CARTESIAN_POINT('Ctrl Pts',(-204.328034827407,-3.83768305634567,
133.880346500872));
#241410=CARTESIAN_POINT('Ctrl Pts',(-204.329049530494,-3.82651900354742,
133.894223468265));
#241411=CARTESIAN_POINT('Ctrl Pts',(-204.330064233581,-3.81528239632779,
133.908036389739));
#241412=CARTESIAN_POINT('Ctrl Pts',(-204.3378385677,-3.72919106576708,134.013866625264));
#241413=CARTESIAN_POINT('Ctrl Pts',(-204.345612901819,-3.63855667661419,
134.116279706243));
#241414=CARTESIAN_POINT('Ctrl Pts',(-204.353387235938,-3.54368061892281,
134.21486068846));
#241415=CARTESIAN_POINT('Ctrl Pts',(-204.361151988886,-3.44892148749296,
134.313320178428));
#241416=CARTESIAN_POINT('Ctrl Pts',(-204.368916741833,-3.3499313571539,
134.407956687445));
#241417=CARTESIAN_POINT('Ctrl Pts',(-204.37668149478,-3.24705273251776,
134.498387094833));
#241418=CARTESIAN_POINT('Ctrl Pts',(-204.384438535665,-3.14427628838194,
134.588727685466));
#241419=CARTESIAN_POINT('Ctrl Pts',(-204.39219557655,-3.03761932746507,
134.674870231555));
#241420=CARTESIAN_POINT('Ctrl Pts',(-204.399952617435,-2.92746192108998,
134.756467620554));
#241421=CARTESIAN_POINT('Ctrl Pts',(-204.407703808675,-2.81738758527178,
134.838003476328));
#241422=CARTESIAN_POINT('Ctrl Pts',(-204.415454999916,-2.70381837107695,
134.915000765548));
#241423=CARTESIAN_POINT('Ctrl Pts',(-204.423206191156,-2.58716793923965,
134.987152163492));
#241424=CARTESIAN_POINT('Ctrl Pts',(-204.430954087933,-2.47056708694779,
135.059272895167));
#241425=CARTESIAN_POINT('Ctrl Pts',(-204.43870198471,-2.35088795351289,
135.126551626789));
#241426=CARTESIAN_POINT('Ctrl Pts',(-204.446449881487,-2.22857354968108,
135.188724082901));
#241427=CARTESIAN_POINT('Ctrl Pts',(-204.454196157571,-2.1062847313861,
135.250883533874));
#241428=CARTESIAN_POINT('Ctrl Pts',(-204.461942433656,-1.98136208744859,
135.307938656849));
#241429=CARTESIAN_POINT('Ctrl Pts',(-204.46968870974,-1.85427326821161,
135.359671112943));
#241430=CARTESIAN_POINT('Ctrl Pts',(-204.477435043005,-1.72718351083332,
135.411403950916));
#241431=CARTESIAN_POINT('Ctrl Pts',(-204.485181376271,-1.59792790836239,
135.457813896205));
#241432=CARTESIAN_POINT('Ctrl Pts',(-204.492927709536,-1.46699375409005,
135.498730904192));
#241433=CARTESIAN_POINT('Ctrl Pts',(-204.500675777539,-1.33603027802187,
135.53965707526));
#241434=CARTESIAN_POINT('Ctrl Pts',(-204.508423845542,-1.20338787525171,
135.575087744666));
#241435=CARTESIAN_POINT('Ctrl Pts',(-204.516171913545,-1.06956825840305,
135.604902962251));
#241436=CARTESIAN_POINT('Ctrl Pts',(-204.523928216287,-0.935606416472946,
135.634749867804));
#241437=CARTESIAN_POINT('Ctrl Pts',(-204.531684519029,-0.800465243359993,
135.658969314318));
#241438=CARTESIAN_POINT('Ctrl Pts',(-204.539440821771,-0.664656438594865,
135.677492555153));
#241439=CARTESIAN_POINT('Ctrl Pts',(-204.547201264285,-0.528775148581879,
135.696025682401));
#241440=CARTESIAN_POINT('Ctrl Pts',(-204.5549617068,-0.392225905948943,
135.708856509484));
#241441=CARTESIAN_POINT('Ctrl Pts',(-204.562722149314,-0.255523769358385,
135.715968365116));
#241442=CARTESIAN_POINT('Ctrl Pts',(-204.570495049579,-0.118602186361955,
135.72309163733));
#241443=CARTESIAN_POINT('Ctrl Pts',(-204.578267949845,0.0184723898871198,
135.724477588372));
#241444=CARTESIAN_POINT('Ctrl Pts',(-204.58604085011,0.155185762840657,
135.720161716218));
#241445=CARTESIAN_POINT('Ctrl Pts',(-204.593531185872,0.286929260314916,
135.716002736889));
#241446=CARTESIAN_POINT('Ctrl Pts',(-204.601021521633,0.418337052633677,
135.70654931052));
#241447=CARTESIAN_POINT('Ctrl Pts',(-204.608511857394,0.548956999130425,
135.691878318363));
#241448=CARTESIAN_POINT('Ctrl Pts',(-204.616286191514,0.684529440611316,
135.676651071078));
#241449=CARTESIAN_POINT('Ctrl Pts',(-204.624060525633,0.819682567332442,
135.655754564432));
#241450=CARTESIAN_POINT('Ctrl Pts',(-204.631834859752,0.953904366288411,
135.62921807893));
#241451=CARTESIAN_POINT('Ctrl Pts',(-204.639599612699,1.08796074887291,
135.602714297274));
#241452=CARTESIAN_POINT('Ctrl Pts',(-204.647364365646,1.22108770756962,
135.570584441822));
#241453=CARTESIAN_POINT('Ctrl Pts',(-204.655129118593,1.35277777999265,
135.532909585321));
#241454=CARTESIAN_POINT('Ctrl Pts',(-204.662886159478,1.48433705597924,
135.495272148018));
#241455=CARTESIAN_POINT('Ctrl Pts',(-204.670643200363,1.6144619123036,135.452100776427));
#241456=CARTESIAN_POINT('Ctrl Pts',(-204.678400241248,1.74265487551586,
135.403527612506));
#241457=CARTESIAN_POINT('Ctrl Pts',(-204.686151432488,1.8707511674172,135.354991077985));
#241458=CARTESIAN_POINT('Ctrl Pts',(-204.693902623728,1.99691810186812,
135.301060997223));
#241459=CARTESIAN_POINT('Ctrl Pts',(-204.701653814969,2.12067352414457,
135.241919278191));
#241460=CARTESIAN_POINT('Ctrl Pts',(-204.709401711746,2.24437634706579,
135.182802695968));
#241461=CARTESIAN_POINT('Ctrl Pts',(-204.717149608523,2.36566934435866,
135.118479049337));
#241462=CARTESIAN_POINT('Ctrl Pts',(-204.7248975053,2.48409071546674,135.049178208445));
#241463=CARTESIAN_POINT('Ctrl Pts',(-204.732643781384,2.60248731537686,
134.979891863794));
#241464=CARTESIAN_POINT('Ctrl Pts',(-204.740390057468,2.71801314667377,
134.905630593073));
#241465=CARTESIAN_POINT('Ctrl Pts',(-204.748136333552,2.83023173824012,
134.826669826262));
#241466=CARTESIAN_POINT('Ctrl Pts',(-204.755882666818,2.94245115817848,
134.74770847658));
#241467=CARTESIAN_POINT('Ctrl Pts',(-204.763629000083,3.05136296992693,
134.664047786568));
#241468=CARTESIAN_POINT('Ctrl Pts',(-204.771375333349,3.15656071620505,
134.576005816602));
#241469=CARTESIAN_POINT('Ctrl Pts',(-204.779123401352,3.26178202078891,
134.487944130248));
#241470=CARTESIAN_POINT('Ctrl Pts',(-204.786871469354,3.36328730507665,
134.395499462426));
#241471=CARTESIAN_POINT('Ctrl Pts',(-204.794619537357,3.46070446367402,
134.299029082186));
#241472=CARTESIAN_POINT('Ctrl Pts',(-204.802375840099,3.55822515838696,
134.202456172077));
#241473=CARTESIAN_POINT('Ctrl Pts',(-204.810132142841,3.65164876974275,
134.101849278174));
#241474=CARTESIAN_POINT('Ctrl Pts',(-204.817888445583,3.74064087315327,
133.997601748548));
#241475=CARTESIAN_POINT('Ctrl Pts',(-204.825648888097,3.82968047432912,
133.893298578876));
#241476=CARTESIAN_POINT('Ctrl Pts',(-204.833409330612,3.91428361358645,
133.785351209223));
#241477=CARTESIAN_POINT('Ctrl Pts',(-204.841169773126,3.99415786311061,
133.67418396179));
#241478=CARTESIAN_POINT('Ctrl Pts',(-204.848942673391,4.07416033387079,
133.562838258822));
#241479=CARTESIAN_POINT('Ctrl Pts',(-204.856715573657,4.14941853042956,
133.448262676063));
#241480=CARTESIAN_POINT('Ctrl Pts',(-204.864488473922,4.21968438244643,
133.330909009154));
#241481=CARTESIAN_POINT('Ctrl Pts',(-204.871978809684,4.28739589375082,
133.217821443638));
#241482=CARTESIAN_POINT('Ctrl Pts',(-204.879469145446,4.35047157997676,
133.102154538428));
#241483=CARTESIAN_POINT('Ctrl Pts',(-204.886959481207,4.40873173042483,
132.984330248466));
#241484=CARTESIAN_POINT('Ctrl Pts',(-204.894733815326,4.4692008321869,132.862038614734));
#241485=CARTESIAN_POINT('Ctrl Pts',(-204.902508149446,4.52467357561692,
132.737035389221));
#241486=CARTESIAN_POINT('Ctrl Pts',(-204.910282483565,4.57489783969652,
132.609767169797));
#241487=CARTESIAN_POINT('Ctrl Pts',(-204.918047236512,4.62506020685945,
132.48265579708));
#241488=CARTESIAN_POINT('Ctrl Pts',(-204.925811989459,4.66998682248568,
132.35328534469));
#241489=CARTESIAN_POINT('Ctrl Pts',(-204.933576742406,4.70947159955726,
132.222126576906));
#241490=CARTESIAN_POINT('Ctrl Pts',(-204.941333783291,4.74891715979151,
132.091098077859));
#241491=CARTESIAN_POINT('Ctrl Pts',(-204.949090824176,4.78293152551465,
131.958285170043));
#241492=CARTESIAN_POINT('Ctrl Pts',(-204.956847865061,4.81135697494726,
131.824177817914));
#241493=CARTESIAN_POINT('Ctrl Pts',(-204.964599056301,4.8397609885273,131.690171597184));
#241494=CARTESIAN_POINT('Ctrl Pts',(-204.972350247541,4.86258439407255,
131.55487325603));
#241495=CARTESIAN_POINT('Ctrl Pts',(-204.980101438781,4.87971961950594,
131.418786770581));
#241496=CARTESIAN_POINT('Ctrl Pts',(-204.987849335558,4.89684756201144,
131.282758125518));
#241497=CARTESIAN_POINT('Ctrl Pts',(-204.995597232335,4.90829208414323,
131.145942389504));
#241498=CARTESIAN_POINT('Ctrl Pts',(-205.003345129112,4.91399696768572,
131.008852338855));
#241499=CARTESIAN_POINT('Ctrl Pts',(-205.011091405196,4.91970065788955,
130.871790964489));
#241500=CARTESIAN_POINT('Ctrl Pts',(-205.01883768128,4.91966708133521,130.734455780001));
#241501=CARTESIAN_POINT('Ctrl Pts',(-205.026583957365,4.91389204176511,
130.597362877536));
#241502=CARTESIAN_POINT('Ctrl Pts',(-205.03433029063,4.90811695956499,130.460268963083));
#241503=CARTESIAN_POINT('Ctrl Pts',(-205.042076623895,4.89660034623337,
130.323417724839));
#241504=CARTESIAN_POINT('Ctrl Pts',(-205.04982295716,4.87939009488483,130.18732304623));
#241505=CARTESIAN_POINT('Ctrl Pts',(-205.057571025163,4.86217598941975,
130.051197890161));
#241506=CARTESIAN_POINT('Ctrl Pts',(-205.065319093166,4.83926575777492,
129.915830018667));
#241507=CARTESIAN_POINT('Ctrl Pts',(-205.073067161169,4.81075884846427,
129.781725607202));
#241508=CARTESIAN_POINT('Ctrl Pts',(-205.080823463911,4.78222164167122,
129.647478667972));
#241509=CARTESIAN_POINT('Ctrl Pts',(-205.088579766653,4.74807595643261,
129.514498254231));
#241510=CARTESIAN_POINT('Ctrl Pts',(-205.096336069395,4.70847196296183,
129.383278341094));
#241511=CARTESIAN_POINT('Ctrl Pts',(-205.104096511909,4.66884683164728,
129.251988391939));
#241512=CARTESIAN_POINT('Ctrl Pts',(-205.111856954423,4.62375771564571,
129.122461184739));
#241513=CARTESIAN_POINT('Ctrl Pts',(-205.119617396937,4.5734035448659,128.99517210381));
#241514=CARTESIAN_POINT('Ctrl Pts',(-205.127390297203,4.52296854110091,
128.867678687148));
#241515=CARTESIAN_POINT('Ctrl Pts',(-205.135163197468,4.46725175190091,
128.742430933815));
#241516=CARTESIAN_POINT('Ctrl Pts',(-205.142936097734,4.40649919765708,
128.619881758994));
#241517=CARTESIAN_POINT('Ctrl Pts',(-205.150426433496,4.34795515178448,
128.501787555357));
#241518=CARTESIAN_POINT('Ctrl Pts',(-205.157916769258,4.28473525768429,
128.386199406543));
#241519=CARTESIAN_POINT('Ctrl Pts',(-205.16540710502,4.21709737997774,128.273496585208));
#241520=CARTESIAN_POINT('Ctrl Pts',(-205.17318143914,4.14689499158213,128.15652060215));
#241521=CARTESIAN_POINT('Ctrl Pts',(-205.180955773259,4.0717106105036,128.042282515269));
#241522=CARTESIAN_POINT('Ctrl Pts',(-205.188730107378,3.9917836946099,127.931235838176));
#241523=CARTESIAN_POINT('Ctrl Pts',(-205.196494860325,3.91195528149677,
127.820326016188));
#241524=CARTESIAN_POINT('Ctrl Pts',(-205.204259613272,3.82739618907955,
127.712600092508));
#241525=CARTESIAN_POINT('Ctrl Pts',(-205.212024366219,3.73839108960982,
127.608485913572));
#241526=CARTESIAN_POINT('Ctrl Pts',(-205.219781407104,3.64947439125963,
127.504475142307));
#241527=CARTESIAN_POINT('Ctrl Pts',(-205.227538447989,3.55612072597651,
127.404069272277));
#241528=CARTESIAN_POINT('Ctrl Pts',(-205.235295488874,3.45865706226162,
127.307665837039));
#241529=CARTESIAN_POINT('Ctrl Pts',(-205.243046680114,3.36126689665303,
127.21133510038));
#241530=CARTESIAN_POINT('Ctrl Pts',(-205.250797871354,3.2597731785813,127.119001064663));
#241531=CARTESIAN_POINT('Ctrl Pts',(-205.258549062594,3.15454177209991,
127.031026644728));
#241532=CARTESIAN_POINT('Ctrl Pts',(-205.266296959371,3.04935509177414,
126.943089616268));
#241533=CARTESIAN_POINT('Ctrl Pts',(-205.274044856149,2.94043418200212,
126.859508768447));
#241534=CARTESIAN_POINT('Ctrl Pts',(-205.281792752926,2.82818006870287,
126.780608567366));
#241535=CARTESIAN_POINT('Ctrl Pts',(-205.28953902901,2.71594943654389,126.701724870505));
#241536=CARTESIAN_POINT('Ctrl Pts',(-205.297285305094,2.60038730735141,
126.627520097597));
#241537=CARTESIAN_POINT('Ctrl Pts',(-205.305031581178,2.48192561588327,
126.558276739482));
#241538=CARTESIAN_POINT('Ctrl Pts',(-205.312777914443,2.36346304995832,
126.489032870229));
#241539=CARTESIAN_POINT('Ctrl Pts',(-205.320524247709,2.24210121658067,
126.424750686145));
#241540=CARTESIAN_POINT('Ctrl Pts',(-205.328270580974,2.11829834782731,
126.365667659938));
#241541=CARTESIAN_POINT('Ctrl Pts',(-205.336018648977,1.99446775428004,
126.306571402498));
#241542=CARTESIAN_POINT('Ctrl Pts',(-205.34376671698,1.86819539035735,126.252676788146));
#241543=CARTESIAN_POINT('Ctrl Pts',(-205.351514784983,1.73996087015536,
126.204173748228));
#241544=CARTESIAN_POINT('Ctrl Pts',(-205.359271087725,1.61159006077877,
126.155619158702));
#241545=CARTESIAN_POINT('Ctrl Pts',(-205.367027390467,1.48125329557024,
126.112467728895));
#241546=CARTESIAN_POINT('Ctrl Pts',(-205.374783693208,1.34944734045477,
126.07486012197));
#241547=CARTESIAN_POINT('Ctrl Pts',(-205.382544135723,1.21757103653245,
126.037232442734));
#241548=CARTESIAN_POINT('Ctrl Pts',(-205.390304578237,1.0842243601514,126.005154573647));
#241549=CARTESIAN_POINT('Ctrl Pts',(-205.398065020751,0.94991479207595,
125.978716106177));
#241550=CARTESIAN_POINT('Ctrl Pts',(-205.405837921016,0.815389618358384,
125.952235197333));
#241551=CARTESIAN_POINT('Ctrl Pts',(-205.413610821282,0.679898850757354,
125.931411840046));
#241552=CARTESIAN_POINT('Ctrl Pts',(-205.421383721547,0.543956519674996,
125.916283862113));
#241553=CARTESIAN_POINT('Ctrl Pts',(-205.428874057309,0.412956034745918,
125.901705824283));
#241554=CARTESIAN_POINT('Ctrl Pts',(-205.436364393071,0.281536554534047,
125.892416293839));
#241555=CARTESIAN_POINT('Ctrl Pts',(-205.443854728833,0.150156553991709,
125.888403328106));
#241556=CARTESIAN_POINT('Ctrl Pts',(-205.451629062952,0.0137952407976317,
125.884238209558));
#241557=CARTESIAN_POINT('Ctrl Pts',(-205.459403397071,-0.122955491538462,
125.885744482312));
#241558=CARTESIAN_POINT('Ctrl Pts',(-205.46717773119,-0.259584656345014,
125.892965818867));
#241559=CARTESIAN_POINT('Ctrl Pts',(-205.474942484137,-0.396045437916839,
125.900178255769));
#241560=CARTESIAN_POINT('Ctrl Pts',(-205.482707237084,-0.532384563386209,
125.913091721957));
#241561=CARTESIAN_POINT('Ctrl Pts',(-205.490471990031,-0.668088201124236,
125.931697976051));
#241562=CARTESIAN_POINT('Ctrl Pts',(-205.498229030916,-0.803657056095805,
125.950285750151));
#241563=CARTESIAN_POINT('Ctrl Pts',(-205.505986071801,-0.938591294568638,
125.974555007365));
#241564=CARTESIAN_POINT('Ctrl Pts',(-205.513743112686,-1.07237972584027,
126.004445536431));
#241565=CARTESIAN_POINT('Ctrl Pts',(-205.521494303926,-1.20606726621606,
126.034313524817));
#241566=CARTESIAN_POINT('Ctrl Pts',(-205.529245495166,-1.33861033923932,
126.069794262592));
#241567=CARTESIAN_POINT('Ctrl Pts',(-205.536996686406,-1.4695058559177,
126.110776102302));
#241568=CARTESIAN_POINT('Ctrl Pts',(-205.544744583183,-1.60034573850956,
126.151740523638));
#241569=CARTESIAN_POINT('Ctrl Pts',(-205.55249247996,-1.72953908518632,
126.198201280005));
#241570=CARTESIAN_POINT('Ctrl Pts',(-205.560240376737,-1.85659614912279,
126.249996358796));
#241571=CARTESIAN_POINT('Ctrl Pts',(-205.567986652821,-1.98362663546017,
126.301780603172));
#241572=CARTESIAN_POINT('Ctrl Pts',(-205.575732928906,-2.10852136608529,
126.358896803041));
#241573=CARTESIAN_POINT('Ctrl Pts',(-205.58347920499,-2.23080920216611,
126.421134252657));
#241574=CARTESIAN_POINT('Ctrl Pts',(-205.591225538255,-2.35309794094813,
126.483372161696));
#241575=CARTESIAN_POINT('Ctrl Pts',(-205.59897187152,-2.47277939835213,
126.550731218584));
#241576=CARTESIAN_POINT('Ctrl Pts',(-205.606718204785,-2.58940609623158,
126.622954259497));
#241577=CARTESIAN_POINT('Ctrl Pts',(-205.614466272788,-2.70605891185186,
126.69519347426));
#241578=CARTESIAN_POINT('Ctrl Pts',(-205.622214340791,-2.81965527435539,
126.77229863474));
#241579=CARTESIAN_POINT('Ctrl Pts',(-205.629962408794,-2.92977614598774,
126.853968890547));
#241580=CARTESIAN_POINT('Ctrl Pts',(-205.637718711536,-3.04001405539247,
126.935725946473));
#241581=CARTESIAN_POINT('Ctrl Pts',(-205.645475014278,-3.14676878064829,
127.022057556528));
#241582=CARTESIAN_POINT('Ctrl Pts',(-205.65323131702,-3.24965346373534,
127.112621809344));
#241583=CARTESIAN_POINT('Ctrl Pts',(-205.660991759534,-3.35259305947554,
127.203234399029));
#241584=CARTESIAN_POINT('Ctrl Pts',(-205.668752202048,-3.45165821498836,
127.298083862653));
#241585=CARTESIAN_POINT('Ctrl Pts',(-205.676512644562,-3.54649924868453,
127.396791668655));
#241586=CARTESIAN_POINT('Ctrl Pts',(-205.684285544827,-3.64149252962784,
127.495657929191));
#241587=CARTESIAN_POINT('Ctrl Pts',(-205.692058445093,-3.73224787929608,
127.598394616017));
#241588=CARTESIAN_POINT('Ctrl Pts',(-205.699831345358,-3.81845562610398,
127.704589707648));
#241589=CARTESIAN_POINT('Ctrl Pts',(-205.707321681121,-3.90152950417868,
127.806924340218));
#241590=CARTESIAN_POINT('Ctrl Pts',(-205.714812016883,-3.98038048839516,
127.912470052807));
#241591=CARTESIAN_POINT('Ctrl Pts',(-205.722302352646,-4.05477080955335,
128.020834662146));
#241592=CARTESIAN_POINT('Ctrl Pts',(-205.730448383082,-4.13567316687673,
128.138685374571));
#241593=CARTESIAN_POINT('Ctrl Pts',(-205.738594413519,-4.21155944536966,
128.260249366182));
#241594=CARTESIAN_POINT('Ctrl Pts',(-205.746740443956,-4.28207823747369,
128.385065465946));
#241595=CARTESIAN_POINT('Ctrl Pts',(-205.754614573043,-4.35024322610434,
128.505715405734));
#241596=CARTESIAN_POINT('Ctrl Pts',(-205.76248870213,-4.41339304358188,
128.629403491818));
#241597=CARTESIAN_POINT('Ctrl Pts',(-205.770362831217,-4.47125192901984,
128.755680737805));
#241598=CARTESIAN_POINT('Ctrl Pts',(-205.778228904709,-4.52905162216871,
128.881828796388));
#241599=CARTESIAN_POINT('Ctrl Pts',(-205.786094978202,-4.58157099847426,
129.010560404246));
#241600=CARTESIAN_POINT('Ctrl Pts',(-205.793961051694,-4.62857939142672,
129.141400642173));
#241601=CARTESIAN_POINT('Ctrl Pts',(-205.801819026306,-4.67553938470417,
129.272106167454));
#241602=CARTESIAN_POINT('Ctrl Pts',(-205.809677000917,-4.7169995704176,
129.404915645517));
#241603=CARTESIAN_POINT('Ctrl Pts',(-205.817534975528,-4.75277695961418,
129.539333252383));
#241604=CARTESIAN_POINT('Ctrl Pts',(-205.818374889647,-4.75660109188932,
129.553700726375));
#241605=CARTESIAN_POINT('Ctrl Pts',(-205.819214803765,-4.76036034493871,
129.568086554707));
#241606=CARTESIAN_POINT('Ctrl Pts',(-205.820054717884,-4.76405452823395,
129.582490119308));
#241607=CARTESIAN_POINT('Ctrl Pts',(-204.070038127516,-4.76405452823409,
129.582490119308));
#241608=CARTESIAN_POINT('Ctrl Pts',(-204.079301788646,-4.80448438634937,
129.740125522491));
#241609=CARTESIAN_POINT('Ctrl Pts',(-204.088565449776,-4.837125792116,129.899922785572));
#241610=CARTESIAN_POINT('Ctrl Pts',(-204.097829110906,-4.86177557562907,
130.061177386649));
#241611=CARTESIAN_POINT('Ctrl Pts',(-204.106997320508,-4.88617137106238,
130.220770441836));
#241612=CARTESIAN_POINT('Ctrl Pts',(-204.11616553011,-4.9027393278596,130.381790901728));
#241613=CARTESIAN_POINT('Ctrl Pts',(-204.125333739712,-4.91132906577983,
130.543535254293));
#241614=CARTESIAN_POINT('Ctrl Pts',(-204.130175638457,-4.91586546307692,
130.628955397563));
#241615=CARTESIAN_POINT('Ctrl Pts',(-204.135017537202,-4.91817745258136,
130.71457709991));
#241616=CARTESIAN_POINT('Ctrl Pts',(-204.139859435948,-4.91824831916273,
130.80029447038));
#241617=CARTESIAN_POINT('Origin',(213.235140564004,0.,130.804360617566));
#241618=CARTESIAN_POINT('',(-202.319765235154,-4.76405452823411,129.582490119309));
#241619=CARTESIAN_POINT('',(-202.665364488388,-4.77027151308326,129.580941132323));
#241620=CARTESIAN_POINT('',(213.235140564004,-4.76405452823405,129.582490119308));
#241621=CARTESIAN_POINT('',(-202.735140564013,-4.91326211273809,130.800663901985));
#241622=CARTESIAN_POINT('Ctrl Pts',(-202.665364488388,-4.77027151308407,
129.580941132326));
#241623=CARTESIAN_POINT('Ctrl Pts',(-202.688623180263,-4.86916182929373,
129.978023072962));
#241624=CARTESIAN_POINT('Ctrl Pts',(-202.711881872138,-4.91612258108715,
130.389021896046));
#241625=CARTESIAN_POINT('Ctrl Pts',(-202.735140564013,-4.91326211273809,
130.800663901985));
#241626=CARTESIAN_POINT('Ctrl Pts',(-202.735140564013,-4.91326211273809,
130.800663901985));
#241627=CARTESIAN_POINT('Ctrl Pts',(-202.796172748794,-4.90575607440281,
131.880836901629));
#241628=CARTESIAN_POINT('Ctrl Pts',(-202.950020808181,-4.02207680521533,
134.614867738963));
#241629=CARTESIAN_POINT('Ctrl Pts',(-203.19668474217,0.501577616433585,
136.600057273287));
#241630=CARTESIAN_POINT('Ctrl Pts',(-203.475132365984,5.14719869251641,
133.515084773622));
#241631=CARTESIAN_POINT('Ctrl Pts',(-203.753579989796,5.06279562480976,
127.939089200777));
#241632=CARTESIAN_POINT('Ctrl Pts',(-204.032027613609,0.325930709221482,
124.996138083671));
#241633=CARTESIAN_POINT('Ctrl Pts',(-204.25262932692,-3.66416944143293,
126.893211472255));
#241634=CARTESIAN_POINT('Ctrl Pts',(-204.380415165628,-4.60798580335201,
128.983142737816));
#241635=CARTESIAN_POINT('Ctrl Pts',(-204.415385129731,-4.7580624943176,
129.583982083009));
#241636=CARTESIAN_POINT('',(-202.389859436034,-4.91824990320504,130.803384849354));
#241637=CARTESIAN_POINT('Ctrl Pts',(-202.389859436034,-4.91824990320504,
130.803384849353));
#241638=CARTESIAN_POINT('Ctrl Pts',(-202.397592511015,-4.91827683063906,
130.939109551199));
#241639=CARTESIAN_POINT('Ctrl Pts',(-202.405325585996,-4.91268128621269,
131.075059385912));
#241640=CARTESIAN_POINT('Ctrl Pts',(-202.413058660977,-4.90143341606133,
131.210726869139));
#241641=CARTESIAN_POINT('Ctrl Pts',(-202.42078228894,-4.89019928673439,
131.346228615827));
#241642=CARTESIAN_POINT('Ctrl Pts',(-202.428505916903,-4.87332660037077,
131.481448306892));
#241643=CARTESIAN_POINT('Ctrl Pts',(-202.436229544867,-4.8508374788153,
131.615876986237));
#241644=CARTESIAN_POINT('Ctrl Pts',(-202.443945635588,-4.82837030367676,
131.750174480918));
#241645=CARTESIAN_POINT('Ctrl Pts',(-202.451661726309,-4.80029766335863,
131.883682112162));
#241646=CARTESIAN_POINT('Ctrl Pts',(-202.45937781703,-4.76669356115084,
132.015894998664));
#241647=CARTESIAN_POINT('Ctrl Pts',(-202.467088273264,-4.73311399751808,
132.148011339935));
#241648=CARTESIAN_POINT('Ctrl Pts',(-202.474798729498,-4.69401110747945,
132.278834436168));
#241649=CARTESIAN_POINT('Ctrl Pts',(-202.482509185732,-4.64951007925511,
132.407868985304));
#241650=CARTESIAN_POINT('Ctrl Pts',(-202.490216665053,-4.6050262323335,
132.536853715778));
#241651=CARTESIAN_POINT('Ctrl Pts',(-202.497924144375,-4.55514851955673,
132.664050898828));
#241652=CARTESIAN_POINT('Ctrl Pts',(-202.505631623696,-4.50005207787166,
132.788980066968));
#241653=CARTESIAN_POINT('Ctrl Pts',(-202.513337751278,-4.44496529901407,
132.913887324999));
#241654=CARTESIAN_POINT('Ctrl Pts',(-202.521043878859,-4.38466177095691,
133.036526997411));
#241655=CARTESIAN_POINT('Ctrl Pts',(-202.528750006441,-4.31936471923195,
133.156438738028));
#241656=CARTESIAN_POINT('Ctrl Pts',(-202.536456496514,-4.25406459597308,
133.27635611922));
#241657=CARTESIAN_POINT('Ctrl Pts',(-202.544162986588,-4.18377067092648,
133.39354496595));
#241658=CARTESIAN_POINT('Ctrl Pts',(-202.551869476661,-4.10875183304938,
133.507570087236));
#241659=CARTESIAN_POINT('Ctrl Pts',(-202.559578043381,-4.03371278004685,
133.621625934566));
#241660=CARTESIAN_POINT('Ctrl Pts',(-202.567286610102,-3.95394649875435,
133.732516030231));
#241661=CARTESIAN_POINT('Ctrl Pts',(-202.574995176822,-3.86976457714697,
133.839835074708));
#241662=CARTESIAN_POINT('Ctrl Pts',(-202.582712029366,-3.78549216965473,
133.947269474815));
#241663=CARTESIAN_POINT('Ctrl Pts',(-202.590428881909,-3.69679488857133,
134.051124847371));
#241664=CARTESIAN_POINT('Ctrl Pts',(-202.598145734452,-3.60402417816858,
134.151029526448));
#241665=CARTESIAN_POINT('Ctrl Pts',(-202.605867103336,-3.51119917307237,
134.250992675422));
#241666=CARTESIAN_POINT('Ctrl Pts',(-202.61358847222,-3.41429627095629,
134.347000247896));
#241667=CARTESIAN_POINT('Ctrl Pts',(-202.621309841104,-3.31370214936235,
134.438719037949));
#241668=CARTESIAN_POINT('Ctrl Pts',(-202.629042866836,-3.21295616217193,
134.530576294631));
#241669=CARTESIAN_POINT('Ctrl Pts',(-202.636775892567,-3.10850812896895,
134.618131584567));
#241670=CARTESIAN_POINT('Ctrl Pts',(-202.644508918298,-3.00077647222385,
134.701093046954));
#241671=CARTESIAN_POINT('Ctrl Pts',(-202.649465442433,-2.93172529156538,
134.754267639271));
#241672=CARTESIAN_POINT('Ctrl Pts',(-202.654421966569,-2.86132571321719,
134.80555585624));
#241673=CARTESIAN_POINT('Ctrl Pts',(-202.659378490704,-2.7896934030652,
134.8548906791));
#241674=CARTESIAN_POINT('Ctrl Pts',(-202.667152824823,-2.67733774865093,
134.932272607676));
#241675=CARTESIAN_POINT('Ctrl Pts',(-202.674927158942,-2.56158200219939,
135.005098693772));
#241676=CARTESIAN_POINT('Ctrl Pts',(-202.682701493061,-2.4428319884996,
135.07305537574));
#241677=CARTESIAN_POINT('Ctrl Pts',(-202.690466246008,-2.32422832357901,
135.140928307171));
#241678=CARTESIAN_POINT('Ctrl Pts',(-202.698230998955,-2.20263806981494,
135.203943582563));
#241679=CARTESIAN_POINT('Ctrl Pts',(-202.705995751903,-2.078497570351,135.261829732719));
#241680=CARTESIAN_POINT('Ctrl Pts',(-202.713752792788,-1.95448036898086,
135.319658389536));
#241681=CARTESIAN_POINT('Ctrl Pts',(-202.721509833673,-1.82791831461926,
135.372367894886));
#241682=CARTESIAN_POINT('Ctrl Pts',(-202.729266874558,-1.69927368819759,
135.419731891375));
#241683=CARTESIAN_POINT('Ctrl Pts',(-202.737018065798,-1.57072607368995,
135.467060170305));
#241684=CARTESIAN_POINT('Ctrl Pts',(-202.744769257038,-1.44009937847901,
135.50905082948));
#241685=CARTESIAN_POINT('Ctrl Pts',(-202.752520448278,-1.30787694231266,
135.545525133407));
#241686=CARTESIAN_POINT('Ctrl Pts',(-202.760268345055,-1.17571070420829,
135.581983934782));
#241687=CARTESIAN_POINT('Ctrl Pts',(-202.768016241832,-1.04195045020032,
135.612930940387));
#241688=CARTESIAN_POINT('Ctrl Pts',(-202.77576413861,-0.907095593932953,
135.638236975725));
#241689=CARTESIAN_POINT('Ctrl Pts',(-202.783510414694,-0.772268946394382,
135.663537717586));
#241690=CARTESIAN_POINT('Ctrl Pts',(-202.791256690778,-0.636348536039387,
135.683199764143));
#241691=CARTESIAN_POINT('Ctrl Pts',(-202.799002966862,-0.49984451854849,
135.697144949598));
#241692=CARTESIAN_POINT('Ctrl Pts',(-202.806749300127,-0.363339493416131,
135.711090237993));
#241693=CARTESIAN_POINT('Ctrl Pts',(-202.814495633393,-0.226251241492333,
135.719318541345));
#241694=CARTESIAN_POINT('Ctrl Pts',(-202.822241966658,-0.0890952027191759,
135.721803561551));
#241695=CARTESIAN_POINT('Ctrl Pts',(-202.829990034661,0.0480915511977042,
135.724289138261));
#241696=CARTESIAN_POINT('Ctrl Pts',(-202.837738102664,0.18534573134494,
135.721028865417));
#241697=CARTESIAN_POINT('Ctrl Pts',(-202.845486170667,0.322152132501905,
135.712048572808));
#241698=CARTESIAN_POINT('Ctrl Pts',(-202.853242473409,0.459103933130223,
135.703058735837));
#241699=CARTESIAN_POINT('Ctrl Pts',(-202.860998776151,0.595606613349426,
135.688336760683));
#241700=CARTESIAN_POINT('Ctrl Pts',(-202.868755078893,0.731149768151804,
135.667960424194));
#241701=CARTESIAN_POINT('Ctrl Pts',(-202.876515521407,0.866765266417027,
135.647573212241));
#241702=CARTESIAN_POINT('Ctrl Pts',(-202.884275963921,1.00141983514607,
135.62152569974));
#241703=CARTESIAN_POINT('Ctrl Pts',(-202.892036406435,1.1346144753236,135.589946585333));
#241704=CARTESIAN_POINT('Ctrl Pts',(-202.899809306701,1.268022931362,135.558316777328));
#241705=CARTESIAN_POINT('Ctrl Pts',(-202.907582206966,1.39996639904794,
135.521137728808));
#241706=CARTESIAN_POINT('Ctrl Pts',(-202.915355107232,1.52996136298433,
135.478587964441));
#241707=CARTESIAN_POINT('Ctrl Pts',(-202.922845442994,1.65523068254303,
135.437584991186));
#241708=CARTESIAN_POINT('Ctrl Pts',(-202.930335778755,1.77869041621811,
135.391595108432));
#241709=CARTESIAN_POINT('Ctrl Pts',(-202.937826114517,1.89992823133841,
135.340819123743));
#241710=CARTESIAN_POINT('Ctrl Pts',(-202.945600448637,2.02576281507001,
135.28811795216));
#241711=CARTESIAN_POINT('Ctrl Pts',(-202.953374782756,2.14960227229255,
135.230093642708));
#241712=CARTESIAN_POINT('Ctrl Pts',(-202.961149116875,2.27096343650089,
135.166918139545));
#241713=CARTESIAN_POINT('Ctrl Pts',(-202.968913869822,2.39217503392037,
135.103820494544));
#241714=CARTESIAN_POINT('Ctrl Pts',(-202.976678622769,2.51091407195934,
135.03558446602));
#241715=CARTESIAN_POINT('Ctrl Pts',(-202.984443375716,2.62671630176767,
134.962430426086));
#241716=CARTESIAN_POINT('Ctrl Pts',(-202.992200416601,2.74240351516851,
134.889349043777));
#241717=CARTESIAN_POINT('Ctrl Pts',(-202.999957457486,2.85515939666273,
134.811359578162));
#241718=CARTESIAN_POINT('Ctrl Pts',(-203.007714498371,2.96454363122682,
134.728728607581));
#241719=CARTESIAN_POINT('Ctrl Pts',(-203.015465689611,3.07384537828889,
134.646159949657));
#241720=CARTESIAN_POINT('Ctrl Pts',(-203.023216880851,3.1797802285859,134.558956988398));
#241721=CARTESIAN_POINT('Ctrl Pts',(-203.030968072092,3.28193654994615,
134.467429760324));
#241722=CARTESIAN_POINT('Ctrl Pts',(-203.038715968869,3.38404945214513,
134.375941433763));
#241723=CARTESIAN_POINT('Ctrl Pts',(-203.046463865646,3.48238672899254,
134.280132756231));
#241724=CARTESIAN_POINT('Ctrl Pts',(-203.054211762423,3.57656975705238,
134.1803540766));
#241725=CARTESIAN_POINT('Ctrl Pts',(-203.061958038507,3.67073308405285,
134.080596268517));
#241726=CARTESIAN_POINT('Ctrl Pts',(-203.069704314591,3.76074362251624,
133.976870394256));
#241727=CARTESIAN_POINT('Ctrl Pts',(-203.077450590675,3.84625985773754,
133.869563411715));
#241728=CARTESIAN_POINT('Ctrl Pts',(-203.085196923941,3.93177672422038,
133.762255637058));
#241729=CARTESIAN_POINT('Ctrl Pts',(-203.092943257206,4.01279897759957,
133.651367007122));
#241730=CARTESIAN_POINT('Ctrl Pts',(-203.100689590471,4.08902588465788,
133.537316961363));
#241731=CARTESIAN_POINT('Ctrl Pts',(-203.108437658474,4.1652698622036,133.423241374886));
#241732=CARTESIAN_POINT('Ctrl Pts',(-203.116185726477,4.23671613931385,
133.306003288778));
#241733=CARTESIAN_POINT('Ctrl Pts',(-203.12393379448,4.30310796631424,133.186050121415));
#241734=CARTESIAN_POINT('Ctrl Pts',(-203.131690097222,4.36957035533834,
133.065969466397));
#241735=CARTESIAN_POINT('Ctrl Pts',(-203.139446399964,4.43096737361537,
132.943168308397));
#241736=CARTESIAN_POINT('Ctrl Pts',(-203.147202702706,4.48708857063544,
132.818118105888));
#241737=CARTESIAN_POINT('Ctrl Pts',(-203.15496314522,4.54323972122798,132.693001160321));
#241738=CARTESIAN_POINT('Ctrl Pts',(-203.162723587734,4.59410929477576,
132.565633141281));
#241739=CARTESIAN_POINT('Ctrl Pts',(-203.170484030249,4.63953584793378,
132.436503435532));
#241740=CARTESIAN_POINT('Ctrl Pts',(-203.178256930514,4.68503532382784,
132.307166439315));
#241741=CARTESIAN_POINT('Ctrl Pts',(-203.18602983078,4.72507420452498,132.176062479243));
#241742=CARTESIAN_POINT('Ctrl Pts',(-203.193802731045,4.75954133600245,
132.043694847459));
#241743=CARTESIAN_POINT('Ctrl Pts',(-203.201293066807,4.79275550043213,
131.916139112508));
#241744=CARTESIAN_POINT('Ctrl Pts',(-203.208783402569,4.82079591129226,
131.787410287015));
#241745=CARTESIAN_POINT('Ctrl Pts',(-203.21627373833,4.84360863779292,131.657963819527));
#241746=CARTESIAN_POINT('Ctrl Pts',(-203.224048072449,4.86728631575333,
131.523609349876));
#241747=CARTESIAN_POINT('Ctrl Pts',(-203.231822406569,4.8854070724529,131.388056150618));
#241748=CARTESIAN_POINT('Ctrl Pts',(-203.239596740688,4.89785440608457,
131.251803663437));
#241749=CARTESIAN_POINT('Ctrl Pts',(-203.247361493635,4.91028639949003,
131.115719095268));
#241750=CARTESIAN_POINT('Ctrl Pts',(-203.255126246582,4.91705884657044,
130.978937339527));
#241751=CARTESIAN_POINT('Ctrl Pts',(-203.262890999529,4.91810621478259,
130.841968098429));
#241752=CARTESIAN_POINT('Ctrl Pts',(-203.270648040414,4.91915254273387,
130.705134897112));
#241753=CARTESIAN_POINT('Ctrl Pts',(-203.278405081299,4.91448510469911,
130.568114969434));
#241754=CARTESIAN_POINT('Ctrl Pts',(-203.286162122184,4.90409017955869,
130.431422857));
#241755=CARTESIAN_POINT('Ctrl Pts',(-203.293913313424,4.89370309331222,
130.294833825151));
#241756=CARTESIAN_POINT('Ctrl Pts',(-203.301664504664,4.8775971464774,130.158572504755));
#241757=CARTESIAN_POINT('Ctrl Pts',(-203.309415695904,4.85581068431517,
130.023152795927));
#241758=CARTESIAN_POINT('Ctrl Pts',(-203.317163592681,4.8340334819805,129.887790644087));
#241759=CARTESIAN_POINT('Ctrl Pts',(-203.324911489458,4.8065806282877,129.753269777556));
#241760=CARTESIAN_POINT('Ctrl Pts',(-203.332659386236,4.77354222644985,
129.620098115078));
#241761=CARTESIAN_POINT('Ctrl Pts',(-203.34040566232,4.74051073553344,129.48695430924));
#241762=CARTESIAN_POINT('Ctrl Pts',(-203.348151938404,4.70189611451706,
129.355159525316));
#241763=CARTESIAN_POINT('Ctrl Pts',(-203.355898214488,4.65783932500118,
129.225210249497));
#241764=CARTESIAN_POINT('Ctrl Pts',(-203.363644547753,4.61378221026816,
129.095260014422));
#241765=CARTESIAN_POINT('Ctrl Pts',(-203.371390881019,4.56428297240465,
128.967155684899));
#241766=CARTESIAN_POINT('Ctrl Pts',(-203.379137214284,4.50953194405326,
128.841376993573));
#241767=CARTESIAN_POINT('Ctrl Pts',(-203.386885282287,4.45476865458861,
128.715570134981));
#241768=CARTESIAN_POINT('Ctrl Pts',(-203.39463335029,4.39475139034221,128.592090309345));
#241769=CARTESIAN_POINT('Ctrl Pts',(-203.402381418293,4.32971779759376,
128.471395367996));
#241770=CARTESIAN_POINT('Ctrl Pts',(-203.410137721035,4.26461508636893,
128.350572150628));
#241771=CARTESIAN_POINT('Ctrl Pts',(-203.417894023777,4.19448558231854,
128.232540074813));
#241772=CARTESIAN_POINT('Ctrl Pts',(-203.425650326518,4.11961218316801,
128.117731033348));
#241773=CARTESIAN_POINT('Ctrl Pts',(-203.433410769033,4.04469882182997,
128.002860714841));
#241774=CARTESIAN_POINT('Ctrl Pts',(-203.441171211547,3.96503674722332,
127.891217176486));
#241775=CARTESIAN_POINT('Ctrl Pts',(-203.448931654061,3.88095043022052,
127.783200770641));
#241776=CARTESIAN_POINT('Ctrl Pts',(-203.456704554326,3.79672913039707,
127.675010967273));
#241777=CARTESIAN_POINT('Ctrl Pts',(-203.464477454592,3.70806964875335,
127.570460230171));
#241778=CARTESIAN_POINT('Ctrl Pts',(-203.472250354857,3.61533533775766,
127.469914118061));
#241779=CARTESIAN_POINT('Ctrl Pts',(-203.479740690619,3.52597215254956,
127.373023110385));
#241780=CARTESIAN_POINT('Ctrl Pts',(-203.487231026381,3.4328254728641,127.279850844024));
#241781=CARTESIAN_POINT('Ctrl Pts',(-203.494721362143,3.3362493295539,127.190688873543));
#241782=CARTESIAN_POINT('Ctrl Pts',(-203.502495696262,3.23601147241738,
127.098146299852));
#241783=CARTESIAN_POINT('Ctrl Pts',(-203.510270030382,3.13176143843621,
127.009630978764));
#241784=CARTESIAN_POINT('Ctrl Pts',(-203.518044364501,3.0238564499707,126.92551088698));
#241785=CARTESIAN_POINT('Ctrl Pts',(-203.525809117448,2.91608444475944,
126.84149446569));
#241786=CARTESIAN_POINT('Ctrl Pts',(-203.533573870395,2.80466675286709,
126.761862734097));
#241787=CARTESIAN_POINT('Ctrl Pts',(-203.541338623342,2.68999677926315,
126.686946333084));
#241788=CARTESIAN_POINT('Ctrl Pts',(-203.549095664227,2.57544069749386,
126.612104340097));
#241789=CARTESIAN_POINT('Ctrl Pts',(-203.556852705112,2.45763908746732,
126.541968570097));
#241790=CARTESIAN_POINT('Ctrl Pts',(-203.564609745997,2.33701743100642,
126.476828689357));
#241791=CARTESIAN_POINT('Ctrl Pts',(-203.572360937237,2.2164867362748,126.411737931106));
#241792=CARTESIAN_POINT('Ctrl Pts',(-203.580112128477,2.09314057063032,
126.35163574828));
#241793=CARTESIAN_POINT('Ctrl Pts',(-203.587863319717,1.96743201934503,
126.29676765549));
#241794=CARTESIAN_POINT('Ctrl Pts',(-203.595611216494,1.84177689754726,
126.241922883103));
#241795=CARTESIAN_POINT('Ctrl Pts',(-203.603359113271,1.71376174471187,
126.192307932205));
#241796=CARTESIAN_POINT('Ctrl Pts',(-203.611107010048,1.58386259025,126.148121538899));
#241797=CARTESIAN_POINT('Ctrl Pts',(-203.618853286132,1.45399060789093,
126.103944388434));
#241798=CARTESIAN_POINT('Ctrl Pts',(-203.626599562217,1.32223577767975,
126.06519366274));
#241799=CARTESIAN_POINT('Ctrl Pts',(-203.634345838301,1.18909200069798,
126.032019129745));
#241800=CARTESIAN_POINT('Ctrl Pts',(-203.642092171566,1.05594724087891,
125.998844351863));
#241801=CARTESIAN_POINT('Ctrl Pts',(-203.649838504831,0.921413893196879,
125.97124594334));
#241802=CARTESIAN_POINT('Ctrl Pts',(-203.657584838097,0.785998449754042,
125.949323079144));
#241803=CARTESIAN_POINT('Ctrl Pts',(-203.6653329061,0.650552680961736,125.927395305475));
#241804=CARTESIAN_POINT('Ctrl Pts',(-203.673080974103,0.514224809194846,
125.911145667744));
#241805=CARTESIAN_POINT('Ctrl Pts',(-203.680829042106,0.377528491365758,
125.900621707234));
#241806=CARTESIAN_POINT('Ctrl Pts',(-203.688585344847,0.240686891063561,
125.890086561733));
#241807=CARTESIAN_POINT('Ctrl Pts',(-203.696341647589,0.103476452891485,
125.88528927959));
#241808=CARTESIAN_POINT('Ctrl Pts',(-203.704097950331,-0.0335865463790532,
125.886225299541));
#241809=CARTESIAN_POINT('Ctrl Pts',(-203.711858392845,-0.17072270029919,
125.887161819075));
#241810=CARTESIAN_POINT('Ctrl Pts',(-203.719618835359,-0.307710868205461,
125.893837719063));
#241811=CARTESIAN_POINT('Ctrl Pts',(-203.727379277873,-0.44403883788848,
125.906196413199));
#241812=CARTESIAN_POINT('Ctrl Pts',(-203.735152178139,-0.580585653331063,
125.918574946608));
#241813=CARTESIAN_POINT('Ctrl Pts',(-203.742925078404,-0.716469764941721,
125.936654452284));
#241814=CARTESIAN_POINT('Ctrl Pts',(-203.75069797867,-0.851187216928724,
125.960326824926));
#241815=CARTESIAN_POINT('Ctrl Pts',(-203.758188314432,-0.981007350205763,
125.983138647196));
#241816=CARTESIAN_POINT('Ctrl Pts',(-203.765678650194,-1.10974387227684,
126.011143701039));
#241817=CARTESIAN_POINT('Ctrl Pts',(-203.773168985956,-1.23696012770498,
126.044201722637));
#241818=CARTESIAN_POINT('Ctrl Pts',(-203.780943320075,-1.36899982612075,
126.078513149172));
#241819=CARTESIAN_POINT('Ctrl Pts',(-203.788717654194,-1.4998199624505,
126.118376962119));
#241820=CARTESIAN_POINT('Ctrl Pts',(-203.796491988313,-1.62891786006441,
126.163691520586));
#241821=CARTESIAN_POINT('Ctrl Pts',(-203.80425674126,-1.75785665605768,
126.20895023291));
#241822=CARTESIAN_POINT('Ctrl Pts',(-203.812021494207,-1.88507707112989,
126.259646196572));
#241823=CARTESIAN_POINT('Ctrl Pts',(-203.819786247154,-2.01008828274693,
126.315627148305));
#241824=CARTESIAN_POINT('Ctrl Pts',(-203.827543288039,-2.13497533146623,
126.371552498967));
#241825=CARTESIAN_POINT('Ctrl Pts',(-203.835300328924,-2.25765718879851,
126.432752232951));
#241826=CARTESIAN_POINT('Ctrl Pts',(-203.843057369809,-2.37766016698767,
126.499024952043));
#241827=CARTESIAN_POINT('Ctrl Pts',(-203.850808561049,-2.49757264999765,
126.565247694363));
#241828=CARTESIAN_POINT('Ctrl Pts',(-203.858559752289,-2.61480993401946,
126.63653561897));
#241829=CARTESIAN_POINT('Ctrl Pts',(-203.866310943529,-2.72892055700057,
126.712640239036));
#241830=CARTESIAN_POINT('Ctrl Pts',(-203.874058840306,-2.84298267992244,
126.788712512608));
#241831=CARTESIAN_POINT('Ctrl Pts',(-203.881806737083,-2.95392046033182,
126.869597193392));
#241832=CARTESIAN_POINT('Ctrl Pts',(-203.88955463386,-3.06130939039301,
126.955001206081));
#241833=CARTESIAN_POINT('Ctrl Pts',(-203.897300909944,-3.16867585700537,
127.040387354091));
#241834=CARTESIAN_POINT('Ctrl Pts',(-203.905047186028,-3.27249464402813,
127.130290710461));
#241835=CARTESIAN_POINT('Ctrl Pts',(-203.912793462112,-3.3723727818643,
127.224376695446));
#241836=CARTESIAN_POINT('Ctrl Pts',(-203.920539795377,-3.47225165697833,
127.318463374952));
#241837=CARTESIAN_POINT('Ctrl Pts',(-203.928286128643,-3.56818954027803,
127.416732476603));
#241838=CARTESIAN_POINT('Ctrl Pts',(-203.936032461908,-3.65982922170008,
127.518811480741));
#241839=CARTESIAN_POINT('Ctrl Pts',(-203.943780529911,-3.75148942519278,
127.620913344764));
#241840=CARTESIAN_POINT('Ctrl Pts',(-203.951528597914,-3.83884925031249,
127.726826518173));
#241841=CARTESIAN_POINT('Ctrl Pts',(-203.959276665916,-3.92159105512307,
127.836144544084));
#241842=CARTESIAN_POINT('Ctrl Pts',(-203.967032968658,-4.00442079890878,
127.945578754494));
#241843=CARTESIAN_POINT('Ctrl Pts',(-203.9747892714,-4.08262248162509,128.05842473395));
#241844=CARTESIAN_POINT('Ctrl Pts',(-203.982545574142,-4.15592088058601,
128.174245658708));
#241845=CARTESIAN_POINT('Ctrl Pts',(-203.990306016656,-4.22925840110944,
128.290128400581));
#241846=CARTESIAN_POINT('Ctrl Pts',(-203.99806645917,-4.29768722825386,
128.408988912957));
#241847=CARTESIAN_POINT('Ctrl Pts',(-204.005826901684,-4.36097810647042,
128.530365670917));
#241848=CARTESIAN_POINT('Ctrl Pts',(-204.013599801949,-4.42437058482357,
128.651937273624));
#241849=CARTESIAN_POINT('Ctrl Pts',(-204.021372702215,-4.48260846613932,
128.776032839594));
#241850=CARTESIAN_POINT('Ctrl Pts',(-204.02914560248,-4.53551030205551,
128.902169942989));
#241851=CARTESIAN_POINT('Ctrl Pts',(-204.036635938243,-4.58648902298876,
129.023721644965));
#241852=CARTESIAN_POINT('Ctrl Pts',(-204.044126274005,-4.63251281279301,
129.147168742662));
#241853=CARTESIAN_POINT('Ctrl Pts',(-204.051616609768,-4.67346365646167,
129.272068049473));
#241854=CARTESIAN_POINT('Ctrl Pts',(-204.057757115684,-4.70703476806217,
129.374459311585));
#241855=CARTESIAN_POINT('Ctrl Pts',(-204.0638976216,-4.73725521212647,129.477999992541));
#241856=CARTESIAN_POINT('Ctrl Pts',(-204.070038127516,-4.76405452823409,
129.582490119308));
#241857=CARTESIAN_POINT('Ctrl Pts',(-202.319765235154,-4.76405452823412,
129.582490119309));
#241858=CARTESIAN_POINT('Ctrl Pts',(-202.327527427096,-4.79811327357253,
129.715284650469));
#241859=CARTESIAN_POINT('Ctrl Pts',(-202.335289619037,-4.82658544150759,
129.849387011775));
#241860=CARTESIAN_POINT('Ctrl Pts',(-202.343051810979,-4.84939821559733,
129.984287444574));
#241861=CARTESIAN_POINT('Ctrl Pts',(-202.350825702342,-4.87224537382299,
130.11939120358));
#241862=CARTESIAN_POINT('Ctrl Pts',(-202.358599593705,-4.88941605217232,
130.255295049384));
#241863=CARTESIAN_POINT('Ctrl Pts',(-202.366373485068,-4.90088936486764,
130.391484733277));
#241864=CARTESIAN_POINT('Ctrl Pts',(-202.371225945676,-4.90805100313769,
130.476494292247));
#241865=CARTESIAN_POINT('Ctrl Pts',(-202.376078406283,-4.91299384376543,
130.561615199731));
#241866=CARTESIAN_POINT('Ctrl Pts',(-202.380930866891,-4.91572308414765,
130.646722987294));
#241867=CARTESIAN_POINT('Ctrl Pts',(-202.383907056592,-4.91739702604547,
130.698922673462));
#241868=CARTESIAN_POINT('Ctrl Pts',(-202.386883246294,-4.9182395397714,
130.751149164821));
#241869=CARTESIAN_POINT('Ctrl Pts',(-202.389859435995,-4.9182499032049,
130.803384848665));
#241870=CARTESIAN_POINT('Origin',(213.235140564004,0.,130.804360617566));
#241871=CARTESIAN_POINT('',(-200.569853205643,-4.76405452823395,129.582490119308));
#241872=CARTESIAN_POINT('',(-200.91504706349,-4.76405452823395,129.582490119308));
#241873=CARTESIAN_POINT('',(213.235140564004,-4.76405452823405,129.582490119308));
#241874=CARTESIAN_POINT('',(-200.985142080239,-4.92392244591489,130.802667972596));
#241875=CARTESIAN_POINT('Ctrl Pts',(-200.91504706349,-4.76405452823395,
129.582490119308));
#241876=CARTESIAN_POINT('Ctrl Pts',(-200.922810977094,-4.79810171876979,
129.715239598469));
#241877=CARTESIAN_POINT('Ctrl Pts',(-200.930574890699,-4.82656335624725,
129.849285219688));
#241878=CARTESIAN_POINT('Ctrl Pts',(-200.938338804304,-4.84936942606639,
129.984117219523));
#241879=CARTESIAN_POINT('Ctrl Pts',(-200.946113769782,-4.87220796015882,
130.119141151722));
#241880=CARTESIAN_POINT('Ctrl Pts',(-200.953888735261,-4.88937480602331,
130.254953310856));
#241881=CARTESIAN_POINT('Ctrl Pts',(-200.96166370074,-4.90085188096385,
130.39104003575));
#241882=CARTESIAN_POINT('Ctrl Pts',(-200.964143717715,-4.90451277704879,
130.434448252648));
#241883=CARTESIAN_POINT('Ctrl Pts',(-200.966623734691,-4.90759516567256,
130.477884416332));
#241884=CARTESIAN_POINT('Ctrl Pts',(-200.969103751666,-4.91009957319356,
130.521331919685));
#241885=CARTESIAN_POINT('Ctrl Pts',(-200.974449355782,-4.91549775041753,
130.614981743472));
#241886=CARTESIAN_POINT('Ctrl Pts',(-200.979794959898,-4.91821692815383,
130.708787473997));
#241887=CARTESIAN_POINT('Ctrl Pts',(-200.985140564013,-4.91824970017718,
130.802643292019));
#241888=CARTESIAN_POINT('Ctrl Pts',(-200.985142543985,-4.92565748492521,
130.802675521279));
#241889=CARTESIAN_POINT('Ctrl Pts',(-201.072612154484,-4.9187069394712,
132.340745200837));
#241890=CARTESIAN_POINT('Ctrl Pts',(-201.252897639586,-3.31467917127183,
135.523358464972));
#241891=CARTESIAN_POINT('Ctrl Pts',(-201.525998999293,2.10959714028603,
136.225733113176));
#241892=CARTESIAN_POINT('Ctrl Pts',(-201.804446623106,5.70144300590434,
131.959881054809));
#241893=CARTESIAN_POINT('Ctrl Pts',(-202.082894246919,4.05394128007133,
126.632162164928));
#241894=CARTESIAN_POINT('Ctrl Pts',(-202.361341870732,-1.31893443610527,
125.138489829794));
#241895=CARTESIAN_POINT('Ctrl Pts',(-202.555498617888,-4.22021631041374,
127.727491303473));
#241896=CARTESIAN_POINT('Ctrl Pts',(-202.65683949044,-4.73402528963851,
129.435398865923));
#241897=CARTESIAN_POINT('Ctrl Pts',(-202.665364488388,-4.77027151308407,
129.580941132326));
#241898=CARTESIAN_POINT('',(-200.639859436051,-4.91824790596759,130.808899113513));
#241899=CARTESIAN_POINT('Ctrl Pts',(-200.639859436051,-4.91824790596758,
130.808899113514));
#241900=CARTESIAN_POINT('Ctrl Pts',(-200.649775499558,-4.91808625878195,
130.984071889128));
#241901=CARTESIAN_POINT('Ctrl Pts',(-200.659691563065,-4.9085624689396,
131.15882584626));
#241902=CARTESIAN_POINT('Ctrl Pts',(-200.669607626572,-4.8898314044626,
131.332311276654));
#241903=CARTESIAN_POINT('Ctrl Pts',(-200.679740109887,-4.87069153125199,
131.50958305668));
#241904=CARTESIAN_POINT('Ctrl Pts',(-200.689872593201,-4.84193809215862,
131.685530583323));
#241905=CARTESIAN_POINT('Ctrl Pts',(-200.700005076516,-4.80378435667934,
131.859272422895));
#241906=CARTESIAN_POINT('Ctrl Pts',(-200.703418425682,-4.7909314343376,
131.917801170958));
#241907=CARTESIAN_POINT('Ctrl Pts',(-200.706831774848,-4.77701213815199,
131.976079801564));
#241908=CARTESIAN_POINT('Ctrl Pts',(-200.710245124013,-4.76203582549044,
132.034075161371));
#241909=CARTESIAN_POINT('Ctrl Pts',(-200.718019458133,-4.72792538063196,
132.166166923039));
#241910=CARTESIAN_POINT('Ctrl Pts',(-200.725793792252,-4.68826069982342,
132.297047573819));
#241911=CARTESIAN_POINT('Ctrl Pts',(-200.733568126371,-4.64314265885356,
132.426214282985));
#241912=CARTESIAN_POINT('Ctrl Pts',(-200.741332879318,-4.59808022183689,
132.555221805726));
#241913=CARTESIAN_POINT('Ctrl Pts',(-200.749097632265,-4.5475779246939,
132.682519224107));
#241914=CARTESIAN_POINT('Ctrl Pts',(-200.756862385212,-4.49178728356926,
132.807615484443));
#241915=CARTESIAN_POINT('Ctrl Pts',(-200.764619426097,-4.43605205449589,
132.932587497409));
#241916=CARTESIAN_POINT('Ctrl Pts',(-200.772376466982,-4.37503909228266,
133.055362348256));
#241917=CARTESIAN_POINT('Ctrl Pts',(-200.780133507867,-4.30894907403695,
133.175466043281));
#241918=CARTESIAN_POINT('Ctrl Pts',(-200.787884699107,-4.2429088947882,
133.295479167176));
#241919=CARTESIAN_POINT('Ctrl Pts',(-200.795635890348,-4.17179946792055,
133.412824803525));
#241920=CARTESIAN_POINT('Ctrl Pts',(-200.803387081588,-4.09586859292485,
133.527051112645));
#241921=CARTESIAN_POINT('Ctrl Pts',(-200.811134978365,-4.01996999057645,
133.641228872536));
#241922=CARTESIAN_POINT('Ctrl Pts',(-200.818882875142,-3.93925423187122,
133.752289617197));
#241923=CARTESIAN_POINT('Ctrl Pts',(-200.826630771919,-3.85401374574893,
133.859808393274));
#241924=CARTESIAN_POINT('Ctrl Pts',(-200.834377048003,-3.76879109009876,
133.96730467874));
#241925=CARTESIAN_POINT('Ctrl Pts',(-200.842123324087,-3.67904583235511,
134.071260163147));
#241926=CARTESIAN_POINT('Ctrl Pts',(-200.849869600171,-3.58511195384299,
134.17128136818));
#241927=CARTESIAN_POINT('Ctrl Pts',(-200.857615933436,-3.49117738193219,
134.271303311546));
#241928=CARTESIAN_POINT('Ctrl Pts',(-200.865362266702,-3.39305439520117,
134.367390632596));
#241929=CARTESIAN_POINT('Ctrl Pts',(-200.873108599967,-3.29111496926247,
134.459185554768));
#241930=CARTESIAN_POINT('Ctrl Pts',(-200.88085666797,-3.18915271469628,
134.551001033777));
#241931=CARTESIAN_POINT('Ctrl Pts',(-200.888604735973,-3.08337261071428,
134.638521939557));
#241932=CARTESIAN_POINT('Ctrl Pts',(-200.896352803976,-2.9741806303318,
134.721430011981));
#241933=CARTESIAN_POINT('Ctrl Pts',(-200.904109106718,-2.86487259941302,
134.80442620009));
#241934=CARTESIAN_POINT('Ctrl Pts',(-200.91186540946,-2.75214576027803,
134.882799524622));
#241935=CARTESIAN_POINT('Ctrl Pts',(-200.919621712202,-2.63643651732246,
134.956274098436));
#241936=CARTESIAN_POINT('Ctrl Pts',(-200.927382154716,-2.52066551685999,
135.029787887842));
#241937=CARTESIAN_POINT('Ctrl Pts',(-200.93514259723,-2.40190927914698,
135.098397521213));
#241938=CARTESIAN_POINT('Ctrl Pts',(-200.942903039744,-2.28062897968,135.161873040904));
#241939=CARTESIAN_POINT('Ctrl Pts',(-200.95067594001,-2.15915399030956,
135.225450457134));
#241940=CARTESIAN_POINT('Ctrl Pts',(-200.958448840275,-2.03514719618037,
135.283877123337));
#241941=CARTESIAN_POINT('Ctrl Pts',(-200.966221740541,-1.90909074643751,
135.336970857192));
#241942=CARTESIAN_POINT('Ctrl Pts',(-200.973712076303,-1.78761676615949,
135.388134500087));
#241943=CARTESIAN_POINT('Ctrl Pts',(-200.981202412065,-1.66423985179437,
135.434346102061));
#241944=CARTESIAN_POINT('Ctrl Pts',(-200.988692747827,-1.5394030098361,
135.47548697379));
#241945=CARTESIAN_POINT('Ctrl Pts',(-200.996467081946,-1.40983294107218,
135.518187714174));
#241946=CARTESIAN_POINT('Ctrl Pts',(-201.004241416065,-1.27827961399708,
135.555560883532));
#241947=CARTESIAN_POINT('Ctrl Pts',(-201.012015750184,-1.14522060017088,
135.587419559231));
#241948=CARTESIAN_POINT('Ctrl Pts',(-201.019780503131,-1.01232556968741,
135.61923897196));
#241949=CARTESIAN_POINT('Ctrl Pts',(-201.027545256078,-0.877928921160667,
135.645557323121));
#241950=CARTESIAN_POINT('Ctrl Pts',(-201.035310009025,-0.742525690139992,
135.666236661027));
#241951=CARTESIAN_POINT('Ctrl Pts',(-201.04306704991,-0.607256943517217,
135.686895459924));
#241952=CARTESIAN_POINT('Ctrl Pts',(-201.050824090795,-0.470983987934914,
135.701926332662));
#241953=CARTESIAN_POINT('Ctrl Pts',(-201.05858113168,-0.33421407859659,
135.711241909402));
#241954=CARTESIAN_POINT('Ctrl Pts',(-201.066332322921,-0.197547308510626,
135.720550461193));
#241955=CARTESIAN_POINT('Ctrl Pts',(-201.074083514161,-0.0603847190823009,
135.724152269219));
#241956=CARTESIAN_POINT('Ctrl Pts',(-201.081834705401,0.076759602487468,
135.722011583823));
#241957=CARTESIAN_POINT('Ctrl Pts',(-201.089582602178,0.213845634062312,
135.719871808275));
#241958=CARTESIAN_POINT('Ctrl Pts',(-201.097330498955,0.350913023122092,
135.711994399786));
#241959=CARTESIAN_POINT('Ctrl Pts',(-201.105078395732,0.487446179389158,
135.698395689437));
#241960=CARTESIAN_POINT('Ctrl Pts',(-201.112824671816,0.623950775863247,
135.684799823644));
#241961=CARTESIAN_POINT('Ctrl Pts',(-201.1205709479,0.759920973027649,135.665485075162));
#241962=CARTESIAN_POINT('Ctrl Pts',(-201.128317223985,0.894845201367628,
135.640519747298));
#241963=CARTESIAN_POINT('Ctrl Pts',(-201.13606355725,1.02977042568743,135.615554235145));
#241964=CARTESIAN_POINT('Ctrl Pts',(-201.143809890515,1.16364928133632,
135.584938131512));
#241965=CARTESIAN_POINT('Ctrl Pts',(-201.151556223781,1.29597969885603,
135.548791003045));
#241966=CARTESIAN_POINT('Ctrl Pts',(-201.159304291784,1.42833975085505,
135.512635779679));
#241967=CARTESIAN_POINT('Ctrl Pts',(-201.167052359787,1.55915029763305,
135.470947169741));
#241968=CARTESIAN_POINT('Ctrl Pts',(-201.17480042779,1.68792413960081,135.423894702455));
#241969=CARTESIAN_POINT('Ctrl Pts',(-201.182556730532,1.81683484394041,
135.376792227247));
#241970=CARTESIAN_POINT('Ctrl Pts',(-201.190313033273,1.94370415157494,
135.324314641176));
#241971=CARTESIAN_POINT('Ctrl Pts',(-201.198069336015,2.06806406360551,
135.266679979885));
#241972=CARTESIAN_POINT('Ctrl Pts',(-201.205829778529,2.19249035026554,
135.209014557239));
#241973=CARTESIAN_POINT('Ctrl Pts',(-201.213590221043,2.31440422521268,
135.14618675382));
#241974=CARTESIAN_POINT('Ctrl Pts',(-201.221350663558,2.4333629419461,135.07846027191));
#241975=CARTESIAN_POINT('Ctrl Pts',(-201.229123563823,2.55251262177229,
135.010625069439));
#241976=CARTESIAN_POINT('Ctrl Pts',(-201.236896464089,2.66869733203954,
134.937875681717));
#241977=CARTESIAN_POINT('Ctrl Pts',(-201.244669364354,2.7815031842106,134.860519280479));
#241978=CARTESIAN_POINT('Ctrl Pts',(-201.252159700116,2.89020825951414,
134.785974979276));
#241979=CARTESIAN_POINT('Ctrl Pts',(-201.259650035878,2.99577562489767,
134.707152986653));
#241980=CARTESIAN_POINT('Ctrl Pts',(-201.26714037164,3.09786596784007,134.624361862042));
#241981=CARTESIAN_POINT('Ctrl Pts',(-201.274914705759,3.20382709716525,
134.538431686777));
#241982=CARTESIAN_POINT('Ctrl Pts',(-201.282689039878,3.30637798966232,
134.447953257853));
#241983=CARTESIAN_POINT('Ctrl Pts',(-201.290463373997,3.40510324293289,
134.353227333501));
#241984=CARTESIAN_POINT('Ctrl Pts',(-201.298228126944,3.50370682615185,
134.258618150384));
#241985=CARTESIAN_POINT('Ctrl Pts',(-201.305992879892,3.59849387170741,
134.159772155332));
#241986=CARTESIAN_POINT('Ctrl Pts',(-201.313757632839,3.68908073813156,
134.057031269514));
#241987=CARTESIAN_POINT('Ctrl Pts',(-201.321514673724,3.77957763240292,
133.954392427393));
#241988=CARTESIAN_POINT('Ctrl Pts',(-201.329271714609,3.86588239247803,
133.847866684276));
#241989=CARTESIAN_POINT('Ctrl Pts',(-201.337028755494,3.94764732780846,
133.737833582798));
#241990=CARTESIAN_POINT('Ctrl Pts',(-201.344779946734,4.02935060356523,
133.627883458138));
#241991=CARTESIAN_POINT('Ctrl Pts',(-201.352531137974,4.10652063663432,
133.514431552222));
#241992=CARTESIAN_POINT('Ctrl Pts',(-201.360282329214,4.1788494731278,133.397891057611));
#241993=CARTESIAN_POINT('Ctrl Pts',(-201.368030225991,4.25114756793644,
133.281400095818));
#241994=CARTESIAN_POINT('Ctrl Pts',(-201.375778122768,4.31860835291871,
133.161823487747));
#241995=CARTESIAN_POINT('Ctrl Pts',(-201.383526019545,4.38096687873627,
133.039603841449));
#241996=CARTESIAN_POINT('Ctrl Pts',(-201.39127229563,4.44331236049435,132.917409760867));
#241997=CARTESIAN_POINT('Ctrl Pts',(-201.399018571714,4.50055752839833,
132.792574089773));
#241998=CARTESIAN_POINT('Ctrl Pts',(-201.406764847798,4.55248333213625,
132.665564145695));
#241999=CARTESIAN_POINT('Ctrl Pts',(-201.414511181063,4.60440951917872,
132.538553264059));
#242000=CARTESIAN_POINT('Ctrl Pts',(-201.422257514328,4.65101611574979,
132.409368439302));
#242001=CARTESIAN_POINT('Ctrl Pts',(-201.430003847594,4.69213233585013,
132.278496705371));
#242002=CARTESIAN_POINT('Ctrl Pts',(-201.437751915597,4.73325776364294,
132.147595663623));
#242003=CARTESIAN_POINT('Ctrl Pts',(-201.4454999836,4.76889025117849,132.015007333899));
#242004=CARTESIAN_POINT('Ctrl Pts',(-201.453248051603,4.79890908491508,
131.881233245698));
#242005=CARTESIAN_POINT('Ctrl Pts',(-201.461004354345,4.82895982302535,
131.747316980804));
#242006=CARTESIAN_POINT('Ctrl Pts',(-201.468760657086,4.85338490335348,
131.612212822058));
#242007=CARTESIAN_POINT('Ctrl Pts',(-201.476516959828,4.87211480062235,
131.476432363778));
#242008=CARTESIAN_POINT('Ctrl Pts',(-201.484277402342,4.89085469460135,
131.340579435379));
#242009=CARTESIAN_POINT('Ctrl Pts',(-201.492037844857,4.90389331153006,
131.204049877203));
#242010=CARTESIAN_POINT('Ctrl Pts',(-201.499798287371,4.91121319630827,
131.067358721946));
#242011=CARTESIAN_POINT('Ctrl Pts',(-201.507571187636,4.91854483161535,
130.930448137912));
#242012=CARTESIAN_POINT('Ctrl Pts',(-201.515344087902,4.92013938522368,
130.793375829575));
#242013=CARTESIAN_POINT('Ctrl Pts',(-201.523116988167,4.91603157254995,
130.656656046912));
#242014=CARTESIAN_POINT('Ctrl Pts',(-201.530607323929,4.9120730892139,130.524906372726));
#242015=CARTESIAN_POINT('Ctrl Pts',(-201.538097659691,4.90281965408166,
130.39348434606));
#242016=CARTESIAN_POINT('Ctrl Pts',(-201.545587995453,4.88834746023548,
130.262842224056));
#242017=CARTESIAN_POINT('Ctrl Pts',(-201.553362329572,4.87332654876078,
130.127246766288));
#242018=CARTESIAN_POINT('Ctrl Pts',(-201.561136663691,4.8526357463644,129.992061995147));
#242019=CARTESIAN_POINT('Ctrl Pts',(-201.56891099781,4.82630355432022,129.857799967604));
#242020=CARTESIAN_POINT('Ctrl Pts',(-201.576675750757,4.80000381434937,
129.723703406011));
#242021=CARTESIAN_POINT('Ctrl Pts',(-201.584440503704,4.76807659267288,
129.590527705303));
#242022=CARTESIAN_POINT('Ctrl Pts',(-201.592205256651,4.73060218967124,
129.458780450657));
#242023=CARTESIAN_POINT('Ctrl Pts',(-201.599962297536,4.69316500677496,
129.327164049242));
#242024=CARTESIAN_POINT('Ctrl Pts',(-201.607719338421,4.65019171305585,
129.196973644122));
#242025=CARTESIAN_POINT('Ctrl Pts',(-201.615476379306,4.60181369324896,
129.068706909269));
#242026=CARTESIAN_POINT('Ctrl Pts',(-201.623227570546,4.5534721556832,128.940536901358));
#242027=CARTESIAN_POINT('Ctrl Pts',(-201.630978761786,4.49973414196849,
128.814288040604));
#242028=CARTESIAN_POINT('Ctrl Pts',(-201.638729953027,4.44078082610854,
128.690442758006));
#242029=CARTESIAN_POINT('Ctrl Pts',(-201.646477849804,4.38185256698038,
128.566650112956));
#242030=CARTESIAN_POINT('Ctrl Pts',(-201.654225746581,4.31771358212929,
128.445259366479));
#242031=CARTESIAN_POINT('Ctrl Pts',(-201.661973643358,4.24859303865466,
128.326732668419));
#242032=CARTESIAN_POINT('Ctrl Pts',(-201.669719919442,4.17948695370766,
128.208230763589));
#242033=CARTESIAN_POINT('Ctrl Pts',(-201.677466195526,4.10540157962988,
128.092592053057));
#242034=CARTESIAN_POINT('Ctrl Pts',(-201.68521247161,4.0266116818476,127.980253426592));
#242035=CARTESIAN_POINT('Ctrl Pts',(-201.692958804875,3.9478212024563,127.86791397087));
#242036=CARTESIAN_POINT('Ctrl Pts',(-201.700705138141,3.86432635455989,
127.758874967912));
#242037=CARTESIAN_POINT('Ctrl Pts',(-201.708451471406,3.77644457960803,
127.65354335856));
#242038=CARTESIAN_POINT('Ctrl Pts',(-201.716199539409,3.68854312414213,
127.548188160925));
#242039=CARTESIAN_POINT('Ctrl Pts',(-201.723947607412,3.59625303713412,
127.446542309132));
#242040=CARTESIAN_POINT('Ctrl Pts',(-201.731695675415,3.49993102093752,
127.348978451846));
#242041=CARTESIAN_POINT('Ctrl Pts',(-201.739451978156,3.40350663255572,
127.251310902531));
#242042=CARTESIAN_POINT('Ctrl Pts',(-201.747208280898,3.30304202998784,
127.157734292792));
#242043=CARTESIAN_POINT('Ctrl Pts',(-201.75496458364,3.19893005191173,127.068583645439));
#242044=CARTESIAN_POINT('Ctrl Pts',(-201.762725026154,3.09476250613789,
126.979385415701));
#242045=CARTESIAN_POINT('Ctrl Pts',(-201.770485468669,2.98694401306269,
126.894618096892));
#242046=CARTESIAN_POINT('Ctrl Pts',(-201.778245911183,2.87589844937092,
126.814574762234));
#242047=CARTESIAN_POINT('Ctrl Pts',(-201.786018811448,2.76467462548215,
126.73440293491));
#242048=CARTESIAN_POINT('Ctrl Pts',(-201.793791711714,2.65021370556392,
126.658970460966));
#242049=CARTESIAN_POINT('Ctrl Pts',(-201.801564611979,2.5329671072149,126.588526098011));
#242050=CARTESIAN_POINT('Ctrl Pts',(-201.809054947741,2.41998271804094,
126.520642565088));
#242051=CARTESIAN_POINT('Ctrl Pts',(-201.816545283503,2.3044119372224,126.45739092656));
#242052=CARTESIAN_POINT('Ctrl Pts',(-201.824035619265,2.18667644572457,
126.398951535061));
#242053=CARTESIAN_POINT('Ctrl Pts',(-201.831809953384,2.06447697728321,
126.338296396273));
#242054=CARTESIAN_POINT('Ctrl Pts',(-201.839584287503,1.93955831659402,
126.282633483449));
#242055=CARTESIAN_POINT('Ctrl Pts',(-201.847358621622,1.81236667732486,
126.232215596963));
#242056=CARTESIAN_POINT('Ctrl Pts',(-201.85512337457,1.68533179038399,126.181859846017));
#242057=CARTESIAN_POINT('Ctrl Pts',(-201.862888127517,1.55602985846499,
126.136736402609));
#242058=CARTESIAN_POINT('Ctrl Pts',(-201.870652880464,1.42493133167005,
126.097052069943));
#242059=CARTESIAN_POINT('Ctrl Pts',(-201.878409921349,1.29396301378008,
126.057407152316));
#242060=CARTESIAN_POINT('Ctrl Pts',(-201.886166962234,1.16120202383286,
126.023190707344));
#242061=CARTESIAN_POINT('Ctrl Pts',(-201.893924003119,1.02713808569387,
125.994561202266));
#242062=CARTESIAN_POINT('Ctrl Pts',(-201.901675194359,0.893175246212959,
125.965953286921));
#242063=CARTESIAN_POINT('Ctrl Pts',(-201.909426385599,0.757911795070179,
125.942924006762));
#242064=CARTESIAN_POINT('Ctrl Pts',(-201.917177576839,0.621851544102284,
125.925581700706));
#242065=CARTESIAN_POINT('Ctrl Pts',(-201.924925473616,0.485849122370762,
125.908246765593));
#242066=CARTESIAN_POINT('Ctrl Pts',(-201.932673370393,0.349050961400987,
125.896594046454));
#242067=CARTESIAN_POINT('Ctrl Pts',(-201.940421267171,0.211969751361186,
125.890680541797));
#242068=CARTESIAN_POINT('Ctrl Pts',(-201.948167543255,0.0749172157553973,
125.884768274118));
#242069=CARTESIAN_POINT('Ctrl Pts',(-201.955913819339,-0.0624178607984672,
125.884592849862));
#242070=CARTESIAN_POINT('Ctrl Pts',(-201.963660095423,-0.199519393139578,
125.890159250684));
#242071=CARTESIAN_POINT('Ctrl Pts',(-201.971406428688,-0.336621937532869,
125.895725692597));
#242072=CARTESIAN_POINT('Ctrl Pts',(-201.979152761954,-0.473490543629981,
125.907034028304));
#242073=CARTESIAN_POINT('Ctrl Pts',(-201.986899095219,-0.609611255716637,
125.92403714679));
#242074=CARTESIAN_POINT('Ctrl Pts',(-201.994647163222,-0.745762451093156,
125.941044073007));
#242075=CARTESIAN_POINT('Ctrl Pts',(-202.002395231225,-0.881165031306035,
125.963748271266));
#242076=CARTESIAN_POINT('Ctrl Pts',(-202.010143299228,-1.01531267014358,
125.99205106348));
#242077=CARTESIAN_POINT('Ctrl Pts',(-202.01789960197,-1.14960288268788,
126.020383936239));
#242078=CARTESIAN_POINT('Ctrl Pts',(-202.025655904712,-1.28263510636064,
126.054327208385));
#242079=CARTESIAN_POINT('Ctrl Pts',(-202.033412207453,-1.41391513808278,
126.093731461625));
#242080=CARTESIAN_POINT('Ctrl Pts',(-202.041172649968,-1.54526523791097,
126.133156746102));
#242081=CARTESIAN_POINT('Ctrl Pts',(-202.048933092482,-1.67486091308033,
126.178048691531));
#242082=CARTESIAN_POINT('Ctrl Pts',(-202.056693534996,-1.80222647708686,
126.228209091689));
#242083=CARTESIAN_POINT('Ctrl Pts',(-202.064466435261,-1.92979649960372,
126.278450013774));
#242084=CARTESIAN_POINT('Ctrl Pts',(-202.072239335527,-2.0551288993706,
126.333976132696));
#242085=CARTESIAN_POINT('Ctrl Pts',(-202.080012235792,-2.17777038732706,
126.394542117607));
#242086=CARTESIAN_POINT('Ctrl Pts',(-202.087502571554,-2.29595354828237,
126.452906376411));
#242087=CARTESIAN_POINT('Ctrl Pts',(-202.094992907316,-2.41163777316133,
126.515950291816));
#242088=CARTESIAN_POINT('Ctrl Pts',(-202.102483243079,-2.52444339732246,
126.583416576689));
#242089=CARTESIAN_POINT('Ctrl Pts',(-202.110258818857,-2.64154478059957,
126.653452050026));
#242090=CARTESIAN_POINT('Ctrl Pts',(-202.118034394636,-2.7559149798318,
126.728475270979));
#242091=CARTESIAN_POINT('Ctrl Pts',(-202.125809970415,-2.86709990176267,
126.808247353929));
#242092=CARTESIAN_POINT('Ctrl Pts',(-202.133891439779,-2.98265887332797,
126.891157695595));
#242093=CARTESIAN_POINT('Ctrl Pts',(-202.141972909144,-3.09477643568045,
126.979198038385));
#242094=CARTESIAN_POINT('Ctrl Pts',(-202.150054378508,-3.20297036422735,
127.072047138183));
#242095=CARTESIAN_POINT('Ctrl Pts',(-202.157810400925,-3.30680724058814,
127.161157133776));
#242096=CARTESIAN_POINT('Ctrl Pts',(-202.165566423341,-3.40702999075184,
127.254695853762));
#242097=CARTESIAN_POINT('Ctrl Pts',(-202.173322445758,-3.50324203012239,
127.352335365503));
#242098=CARTESIAN_POINT('Ctrl Pts',(-202.181073173471,-3.59938838965428,
127.44990822293));
#242099=CARTESIAN_POINT('Ctrl Pts',(-202.188823901183,-3.69152921254174,
127.551576025106));
#242100=CARTESIAN_POINT('Ctrl Pts',(-202.196574628896,-3.77930256283194,
127.65697198553));
#242101=CARTESIAN_POINT('Ctrl Pts',(-202.20432174412,-3.86703500338546,
127.762318822604));
#242102=CARTESIAN_POINT('Ctrl Pts',(-202.212068859344,-3.95040377296826,
127.871390059986));
#242103=CARTESIAN_POINT('Ctrl Pts',(-202.219815974568,-4.02908552554411,
127.983783922925));
#242104=CARTESIAN_POINT('Ctrl Pts',(-202.227561156713,-4.10774764526049,
128.096149741079));
#242105=CARTESIAN_POINT('Ctrl Pts',(-202.235306338858,-4.18172485302055,
128.211836213856));
#242106=CARTESIAN_POINT('Ctrl Pts',(-202.243051521003,-4.25073589056795,
128.330410850263));
#242107=CARTESIAN_POINT('Ctrl Pts',(-202.250798386813,-4.31976192988371,
128.449011262681));
#242108=CARTESIAN_POINT('Ctrl Pts',(-202.258545252622,-4.38381944209067,
128.570500757135));
#242109=CARTESIAN_POINT('Ctrl Pts',(-202.266292118432,-4.44267209747922,
128.694420405906));
#242110=CARTESIAN_POINT('Ctrl Pts',(-202.274040018994,-4.50153261384766,
128.818356606689));
#242111=CARTESIAN_POINT('Ctrl Pts',(-202.281787919557,-4.55518672851136,
128.944723251757));
#242112=CARTESIAN_POINT('Ctrl Pts',(-202.289535820119,-4.60344577788972,
129.07304030274));
#242113=CARTESIAN_POINT('Ctrl Pts',(-202.297288826251,-4.6517366281298,
129.201441909736));
#242114=CARTESIAN_POINT('Ctrl Pts',(-202.305041832382,-4.6946251865411,
129.331796119675));
#242115=CARTESIAN_POINT('Ctrl Pts',(-202.312794838514,-4.73197225875476,
129.463606499588));
#242116=CARTESIAN_POINT('Ctrl Pts',(-202.315118304061,-4.74316464453239,
129.503108193671));
#242117=CARTESIAN_POINT('Ctrl Pts',(-202.317441769608,-4.75385968611253,
129.542740584605));
#242118=CARTESIAN_POINT('Ctrl Pts',(-202.319765235154,-4.76405452823412,
129.582490119309));
#242119=CARTESIAN_POINT('Ctrl Pts',(-200.569853205643,-4.76405452823395,
129.582490119308));
#242120=CARTESIAN_POINT('Ctrl Pts',(-200.577513488277,-4.79778564433713,
129.714007229053));
#242121=CARTESIAN_POINT('Ctrl Pts',(-200.58517377091,-4.82606367990543,
129.846911054034));
#242122=CARTESIAN_POINT('Ctrl Pts',(-200.592834053543,-4.84879096813837,
129.980704615463));
#242123=CARTESIAN_POINT('Ctrl Pts',(-200.600671617285,-4.87204423159276,
130.117594547097));
#242124=CARTESIAN_POINT('Ctrl Pts',(-200.608509181027,-4.88948659380923,
130.255415469519));
#242125=CARTESIAN_POINT('Ctrl Pts',(-200.616346744769,-4.90106945198536,
130.393627992473));
#242126=CARTESIAN_POINT('Ctrl Pts',(-200.624184308511,-4.9126523101615,
130.531840515427));
#242127=CARTESIAN_POINT('Ctrl Pts',(-200.632021872253,-4.91837567036258,
130.670444191001));
#242128=CARTESIAN_POINT('Ctrl Pts',(-200.639859435995,-4.91824790596849,
130.808899112527));
#242129=CARTESIAN_POINT('Origin',(213.235140564004,0.,130.804360617566));
#242130=CARTESIAN_POINT('',(-198.820145221536,-4.76405452823399,129.582490119308));
#242131=CARTESIAN_POINT('',(-199.165100499421,-4.76405452823391,129.582490119308));
#242132=CARTESIAN_POINT('',(213.235140564004,-4.76405452823405,129.582490119308));
#242133=CARTESIAN_POINT('',(-199.235140563976,-4.91824791219353,130.808892361601));
#242134=CARTESIAN_POINT('Ctrl Pts',(-199.165100499421,-4.76405452823391,
129.582490119308));
#242135=CARTESIAN_POINT('Ctrl Pts',(-199.172747479307,-4.79772404353953,
129.713767048478));
#242136=CARTESIAN_POINT('Ctrl Pts',(-199.180394459193,-4.8259562660387,
129.846409655637));
#242137=CARTESIAN_POINT('Ctrl Pts',(-199.188041439078,-4.84865793162383,
129.979921823839));
#242138=CARTESIAN_POINT('Ctrl Pts',(-199.195891293228,-4.87196187206307,
130.116976067901));
#242139=CARTESIAN_POINT('Ctrl Pts',(-199.203741147378,-4.8894376250516,
130.254946212889));
#242140=CARTESIAN_POINT('Ctrl Pts',(-199.211591001527,-4.90104104578751,
130.393289176079));
#242141=CARTESIAN_POINT('Ctrl Pts',(-199.219440855677,-4.91264446652345,
130.53163213927));
#242142=CARTESIAN_POINT('Ctrl Pts',(-199.227290709826,-4.91837556944563,
130.67034746391));
#242143=CARTESIAN_POINT('Ctrl Pts',(-199.235140563976,-4.91824791219353,
130.808892361601));
#242144=CARTESIAN_POINT('Ctrl Pts',(-199.235140564013,-4.91824791219293,
130.80889236225));
#242145=CARTESIAN_POINT('Ctrl Pts',(-199.245686804809,-4.91807640527225,
130.995026757141));
#242146=CARTESIAN_POINT('Ctrl Pts',(-199.256233045605,-4.90733475277425,
131.180693350563));
#242147=CARTESIAN_POINT('Ctrl Pts',(-199.266779286401,-4.88620319730163,
131.364897304304));
#242148=CARTESIAN_POINT('Ctrl Pts',(-199.277325527197,-4.86507164182904,
131.549101258045));
#242149=CARTESIAN_POINT('Ctrl Pts',(-199.287871767993,-4.83355032983892,
131.731843197017));
#242150=CARTESIAN_POINT('Ctrl Pts',(-199.298418008789,-4.79186565731639,
131.912154183503));
#242151=CARTESIAN_POINT('Ctrl Pts',(-199.306192342908,-4.76113711829408,
132.045073380155));
#242152=CARTESIAN_POINT('Ctrl Pts',(-199.313966677027,-4.72482524621133,
132.176923596683));
#242153=CARTESIAN_POINT('Ctrl Pts',(-199.321741011146,-4.68301805246697,
132.307199591897));
#242154=CARTESIAN_POINT('Ctrl Pts',(-199.329505764093,-4.64126238235248,
132.43731503359));
#242155=CARTESIAN_POINT('Ctrl Pts',(-199.337270517041,-4.59402498413645,
132.565859745473));
#242156=CARTESIAN_POINT('Ctrl Pts',(-199.345035269988,-4.54144479361619,
132.692338967293));
#242157=CARTESIAN_POINT('Ctrl Pts',(-199.352792310873,-4.48891682648241,
132.818692568166));
#242158=CARTESIAN_POINT('Ctrl Pts',(-199.360549351758,-4.43105677640118,
132.942984402826));
#242159=CARTESIAN_POINT('Ctrl Pts',(-199.368306392643,-4.36805315947013,
133.064735510928));
#242160=CARTESIAN_POINT('Ctrl Pts',(-199.376057583883,-4.3050970540568,
133.186394805573));
#242161=CARTESIAN_POINT('Ctrl Pts',(-199.383808775123,-4.2370052812737,
133.305516841482));
#242162=CARTESIAN_POINT('Ctrl Pts',(-199.391559966363,-4.16401402959605,
133.421643602615));
#242163=CARTESIAN_POINT('Ctrl Pts',(-199.39930786314,-4.09105380114736,
133.537721006777));
#242164=CARTESIAN_POINT('Ctrl Pts',(-199.407055759917,-4.01319844317672,
133.650805337891));
#242165=CARTESIAN_POINT('Ctrl Pts',(-199.414803656695,-3.93072944517622,
133.76046431861));
#242166=CARTESIAN_POINT('Ctrl Pts',(-199.422549932779,-3.84827769791228,
133.870100361034));
#242167=CARTESIAN_POINT('Ctrl Pts',(-199.430296208863,-3.76121446504357,
133.976312165972));
#242168=CARTESIAN_POINT('Ctrl Pts',(-199.438042484947,-3.66986357811492,
134.078697860509));
#242169=CARTESIAN_POINT('Ctrl Pts',(-199.445788818212,-3.57851201685465,
134.181084310835));
#242170=CARTESIAN_POINT('Ctrl Pts',(-199.453535151478,-3.48287299866424,
134.279644302673));
#242171=CARTESIAN_POINT('Ctrl Pts',(-199.461281484743,-3.38330924806213,
134.374010683676));
#242172=CARTESIAN_POINT('Ctrl Pts',(-199.469029552746,-3.28372320084826,
134.468398197375));
#242173=CARTESIAN_POINT('Ctrl Pts',(-199.476777620749,-3.18021095598737,
134.558589962581));
#242174=CARTESIAN_POINT('Ctrl Pts',(-199.484525688752,-3.07317023273365,
134.644257462943));
#242175=CARTESIAN_POINT('Ctrl Pts',(-199.492281991494,-2.9660157453259,
134.730016011745));
#242176=CARTESIAN_POINT('Ctrl Pts',(-199.500038294236,-2.85532559400969,
134.811240445636));
#242177=CARTESIAN_POINT('Ctrl Pts',(-199.507794596978,-2.74152900080911,
134.887643830891));
#242178=CARTESIAN_POINT('Ctrl Pts',(-199.515555039492,-2.62767167094008,
134.964087994933));
#242179=CARTESIAN_POINT('Ctrl Pts',(-199.523315482006,-2.51070492874323,
135.035705779087));
#242180=CARTESIAN_POINT('Ctrl Pts',(-199.53107592452,-2.39108393133343,
135.102255532035));
#242181=CARTESIAN_POINT('Ctrl Pts',(-199.538848824786,-2.27127090767914,
135.168912116555));
#242182=CARTESIAN_POINT('Ctrl Pts',(-199.546621725051,-2.14879546379233,
135.230484236534));
#242183=CARTESIAN_POINT('Ctrl Pts',(-199.554394625317,-2.02413494276591,
135.286777465202));
#242184=CARTESIAN_POINT('Ctrl Pts',(-199.561884961079,-1.90400614567938,
135.341024293215));
#242185=CARTESIAN_POINT('Ctrl Pts',(-199.569375296841,-1.781848665018,135.390369253178));
#242186=CARTESIAN_POINT('Ctrl Pts',(-199.576865632603,-1.65810233422333,
135.43468238951));
#242187=CARTESIAN_POINT('Ctrl Pts',(-199.584639966722,-1.52966412368488,
135.480675671875));
#242188=CARTESIAN_POINT('Ctrl Pts',(-199.592414300841,-1.39910734850033,
135.52139372814));
#242189=CARTESIAN_POINT('Ctrl Pts',(-199.60018863496,-1.26690465470224,
135.556637509582));
#242190=CARTESIAN_POINT('Ctrl Pts',(-199.607953387907,-1.13486488890897,
135.591837856214));
#242191=CARTESIAN_POINT('Ctrl Pts',(-199.615718140854,-1.00118361465327,
135.621577251914));
#242192=CARTESIAN_POINT('Ctrl Pts',(-199.623482893801,-0.866352185939986,
135.645705157301));
#242193=CARTESIAN_POINT('Ctrl Pts',(-199.631239934686,-0.731654673702493,
135.669809098511));
#242194=CARTESIAN_POINT('Ctrl Pts',(-199.638996975571,-0.595809662696144,
135.688312572326));
#242195=CARTESIAN_POINT('Ctrl Pts',(-199.646754016456,-0.459322013378897,
135.701115292912));
#242196=CARTESIAN_POINT('Ctrl Pts',(-199.654505207696,-0.322937290459533,
135.713908358867));
#242197=CARTESIAN_POINT('Ctrl Pts',(-199.662256398937,-0.185911281514558,
135.721009192091));
#242198=CARTESIAN_POINT('Ctrl Pts',(-199.670007590177,-0.0487569940496048,
135.722368935781));
#242199=CARTESIAN_POINT('Ctrl Pts',(-199.677755486954,0.0883389991842788,
135.723728101544));
#242200=CARTESIAN_POINT('Ctrl Pts',(-199.685503383731,0.225562772370937,
135.719351027109));
#242201=CARTESIAN_POINT('Ctrl Pts',(-199.693251280508,0.362398486389647,
135.709240881096));
#242202=CARTESIAN_POINT('Ctrl Pts',(-199.700997556592,0.499205577326821,
135.699132849906));
#242203=CARTESIAN_POINT('Ctrl Pts',(-199.708743832676,0.635624380899426,
135.683294161272));
#242204=CARTESIAN_POINT('Ctrl Pts',(-199.71649010876,0.771141751181498,
135.661780041713));
#242205=CARTESIAN_POINT('Ctrl Pts',(-199.724236442026,0.906660121822196,
135.640265763343));
#242206=CARTESIAN_POINT('Ctrl Pts',(-199.731982775291,1.04127665976482,
135.613076031752));
#242207=CARTESIAN_POINT('Ctrl Pts',(-199.739729108556,1.17448640787711,
135.580317562536));
#242208=CARTESIAN_POINT('Ctrl Pts',(-199.747477176559,1.3077259873887,135.547551757289));
#242209=CARTESIAN_POINT('Ctrl Pts',(-199.755225244562,1.43955777059391,
135.509214826219));
#242210=CARTESIAN_POINT('Ctrl Pts',(-199.762973312565,1.56949039041183,
135.465463810685));
#242211=CARTESIAN_POINT('Ctrl Pts',(-199.770729615307,1.69956110416447,
135.421666296052));
#242212=CARTESIAN_POINT('Ctrl Pts',(-199.778485918049,1.82772825133692,
135.372443327376));
#242213=CARTESIAN_POINT('Ctrl Pts',(-199.786242220791,1.95351842146964,
135.318000926616));
#242214=CARTESIAN_POINT('Ctrl Pts',(-199.794002663305,2.07937572960363,
135.263529468307));
#242215=CARTESIAN_POINT('Ctrl Pts',(-199.801763105819,2.20285318096146,
135.203833197122));
#242216=CARTESIAN_POINT('Ctrl Pts',(-199.809523548333,2.32350144390913,
135.139164431195));
#242217=CARTESIAN_POINT('Ctrl Pts',(-199.817296448599,2.44434338215913,
135.074391853224));
#242218=CARTESIAN_POINT('Ctrl Pts',(-199.825069348864,2.56234671955976,
135.004631028427));
#242219=CARTESIAN_POINT('Ctrl Pts',(-199.83284224913,2.67708986376302,134.930178466652));
#242220=CARTESIAN_POINT('Ctrl Pts',(-199.840332584892,2.78766180565022,
134.858432443034));
#242221=CARTESIAN_POINT('Ctrl Pts',(-199.847822920653,2.89520622014493,
134.782330051055));
#242222=CARTESIAN_POINT('Ctrl Pts',(-199.855313256415,2.99937603121739,
134.702171090878));
#242223=CARTESIAN_POINT('Ctrl Pts',(-199.863087590534,3.1074954723416,134.618972879359));
#242224=CARTESIAN_POINT('Ctrl Pts',(-199.870861924653,3.21232185228549,
134.531140870842));
#242225=CARTESIAN_POINT('Ctrl Pts',(-199.878636258772,3.31343222899665,
134.438965125122));
#242226=CARTESIAN_POINT('Ctrl Pts',(-199.886401011719,3.414417996205,134.346902977771));
#242227=CARTESIAN_POINT('Ctrl Pts',(-199.894165764666,3.51169658615192,
134.25050800549));
#242228=CARTESIAN_POINT('Ctrl Pts',(-199.901930517614,3.60487575695146,
134.150112228108));
#242229=CARTESIAN_POINT('Ctrl Pts',(-199.909687558499,3.69796238088497,
134.049816165227));
#242230=CARTESIAN_POINT('Ctrl Pts',(-199.917444599384,3.78695742409865,
133.945527489707));
#242231=CARTESIAN_POINT('Ctrl Pts',(-199.925201640269,3.87150362387128,
133.837616748006));
#242232=CARTESIAN_POINT('Ctrl Pts',(-199.932952831509,3.95598606669709,
133.729787382635));
#242233=CARTESIAN_POINT('Ctrl Pts',(-199.940704022749,4.03602610367543,
133.618341694337));
#242234=CARTESIAN_POINT('Ctrl Pts',(-199.948455213989,4.11130533710608,
133.50368488256));
#242235=CARTESIAN_POINT('Ctrl Pts',(-199.956203110766,4.18655257485428,
133.389076802986));
#242236=CARTESIAN_POINT('Ctrl Pts',(-199.963951007543,4.25704281945193,
133.271260640578));
#242237=CARTESIAN_POINT('Ctrl Pts',(-199.97169890432,4.32249991310147,133.150672098111));
#242238=CARTESIAN_POINT('Ctrl Pts',(-199.979445180404,4.38794331453812,
133.030108780168));
#242239=CARTESIAN_POINT('Ctrl Pts',(-199.987191456488,4.44835547276005,
132.906774579053));
#242240=CARTESIAN_POINT('Ctrl Pts',(-199.994937732572,4.50350548349756,
132.781131070251));
#242241=CARTESIAN_POINT('Ctrl Pts',(-200.002684065838,4.55865590134,132.655486633977));
#242242=CARTESIAN_POINT('Ctrl Pts',(-200.010430399103,4.60854393704874,
132.527533213996));
#242243=CARTESIAN_POINT('Ctrl Pts',(-200.018176732369,4.65298643181374,
132.397753327433));
#242244=CARTESIAN_POINT('Ctrl Pts',(-200.025924800372,4.69743887916725,
132.267944377564));
#242245=CARTESIAN_POINT('Ctrl Pts',(-200.033672868375,4.73644323229192,
132.136308517008));
#242246=CARTESIAN_POINT('Ctrl Pts',(-200.041420936378,4.76986601862287,
132.003344031499));
#242247=CARTESIAN_POINT('Ctrl Pts',(-200.04917723912,4.80332432708882,131.870238229753));
#242248=CARTESIAN_POINT('Ctrl Pts',(-200.056933541861,4.83118912317878,
131.735801362048));
#242249=CARTESIAN_POINT('Ctrl Pts',(-200.064689844603,4.85337784908269,
131.600543081913));
#242250=CARTESIAN_POINT('Ctrl Pts',(-200.072450287117,4.87557841777776,
131.465212610361));
#242251=CARTESIAN_POINT('Ctrl Pts',(-200.080210729631,4.89209683270756,
131.329060240733));
#242252=CARTESIAN_POINT('Ctrl Pts',(-200.087971172146,4.90290250153954,
131.192600392573));
#242253=CARTESIAN_POINT('Ctrl Pts',(-200.095744072411,4.9137255165904,131.05592148695));
#242254=CARTESIAN_POINT('Ctrl Pts',(-200.103516972676,4.91881744521724,
130.918934507362));
#242255=CARTESIAN_POINT('Ctrl Pts',(-200.111289872942,4.91819986858887,
130.782154422205));
#242256=CARTESIAN_POINT('Ctrl Pts',(-200.118780208704,4.91760474242652,
130.650346637671));
#242257=CARTESIAN_POINT('Ctrl Pts',(-200.126270544466,4.91170802767491,
130.518731274167));
#242258=CARTESIAN_POINT('Ctrl Pts',(-200.133760880228,4.90057435163176,
130.387762385898));
#242259=CARTESIAN_POINT('Ctrl Pts',(-200.141535214347,4.88901853887747,
130.251827772423));
#242260=CARTESIAN_POINT('Ctrl Pts',(-200.149309548466,4.87178420146617,
130.116159024119));
#242261=CARTESIAN_POINT('Ctrl Pts',(-200.157083882586,4.8488867644099,129.981268758518));
#242262=CARTESIAN_POINT('Ctrl Pts',(-200.164848635533,4.8260175463984,129.846544733114));
#242263=CARTESIAN_POINT('Ctrl Pts',(-200.17261338848,4.79749918019917,129.712597663223));
#242264=CARTESIAN_POINT('Ctrl Pts',(-200.180378141427,4.76339898717628,
129.57993701788));
#242265=CARTESIAN_POINT('Ctrl Pts',(-200.188135182312,4.72933266294583,
129.44740813296));
#242266=CARTESIAN_POINT('Ctrl Pts',(-200.195892223197,4.68969564130355,
129.316163506122));
#242267=CARTESIAN_POINT('Ctrl Pts',(-200.203649264082,4.64460656425249,
129.186704002025));
#242268=CARTESIAN_POINT('Ctrl Pts',(-200.211400455322,4.59955148922512,
129.057342124347));
#242269=CARTESIAN_POINT('Ctrl Pts',(-200.219151646562,4.5490526704274,128.929763057648));
#242270=CARTESIAN_POINT('Ctrl Pts',(-200.226902837802,4.49327891189645,
128.80445369913));
#242271=CARTESIAN_POINT('Ctrl Pts',(-200.23465073458,4.43752885870062,128.679197600433));
#242272=CARTESIAN_POINT('Ctrl Pts',(-200.242398631357,4.37650848356419,
128.556209647663));
#242273=CARTESIAN_POINT('Ctrl Pts',(-200.250146528134,4.31043508553766,
128.435957688192));
#242274=CARTESIAN_POINT('Ctrl Pts',(-200.257892804218,4.2443755086418,128.315730882839));
#242275=CARTESIAN_POINT('Ctrl Pts',(-200.265639080302,4.17326519940549,
128.198239274858));
#242276=CARTESIAN_POINT('Ctrl Pts',(-200.273385356386,4.09736768495884,
128.083926623374));
#242277=CARTESIAN_POINT('Ctrl Pts',(-200.281131689651,4.02146961025387,
127.96961312806));
#242278=CARTESIAN_POINT('Ctrl Pts',(-200.288878022917,3.94078447607879,
127.85847896178));
#242279=CARTESIAN_POINT('Ctrl Pts',(-200.296624356182,3.85561923594436,
127.75093903352));
#242280=CARTESIAN_POINT('Ctrl Pts',(-200.304372424185,3.770434923645,127.643375022439));
#242281=CARTESIAN_POINT('Ctrl Pts',(-200.312120492188,3.68076875163644,
127.53940715748));
#242282=CARTESIAN_POINT('Ctrl Pts',(-200.319868560191,3.58696779663645,
127.439417068501));
#242283=CARTESIAN_POINT('Ctrl Pts',(-200.327624862933,3.49306714886511,
127.339320708866));
#242284=CARTESIAN_POINT('Ctrl Pts',(-200.335381165675,3.39502320753719,
127.243210855946));
#242285=CARTESIAN_POINT('Ctrl Pts',(-200.343137468417,3.29322013408638,
127.151432448145));
#242286=CARTESIAN_POINT('Ctrl Pts',(-200.350897910931,3.19136272527004,
127.059605055445));
#242287=CARTESIAN_POINT('Ctrl Pts',(-200.358658353445,3.08574248742091,
126.972113963648));
#242288=CARTESIAN_POINT('Ctrl Pts',(-200.366418795959,2.97677568036702,
126.88926296728));
#242289=CARTESIAN_POINT('Ctrl Pts',(-200.374191696225,2.86763395012082,
126.806278971137));
#242290=CARTESIAN_POINT('Ctrl Pts',(-200.38196459649,2.75513523632046,126.727950178812));
#242291=CARTESIAN_POINT('Ctrl Pts',(-200.389737496756,2.63972446161173,
126.654536786454));
#242292=CARTESIAN_POINT('Ctrl Pts',(-200.397227832518,2.52850915926618,
126.583792155825));
#242293=CARTESIAN_POINT('Ctrl Pts',(-200.40471816828,2.41459010805134,126.517611910091));
#242294=CARTESIAN_POINT('Ctrl Pts',(-200.412208504042,2.29838424926308,
126.456187103866));
#242295=CARTESIAN_POINT('Ctrl Pts',(-200.419982838161,2.17777241001932,
126.392433357444));
#242296=CARTESIAN_POINT('Ctrl Pts',(-200.42775717228,2.05431486939034,126.333600821259));
#242297=CARTESIAN_POINT('Ctrl Pts',(-200.435531506399,1.92845124462011,
126.279953600108));
#242298=CARTESIAN_POINT('Ctrl Pts',(-200.443296259346,1.8027427355183,126.226372494363));
#242299=CARTESIAN_POINT('Ctrl Pts',(-200.451061012293,1.67463439851077,
126.177964140413));
#242300=CARTESIAN_POINT('Ctrl Pts',(-200.45882576524,1.54459125316685,126.134947279347));
#242301=CARTESIAN_POINT('Ctrl Pts',(-200.466582806125,1.41467726850817,
126.091973143233));
#242302=CARTESIAN_POINT('Ctrl Pts',(-200.47433984701,1.28283266852345,126.054379965485));
#242303=CARTESIAN_POINT('Ctrl Pts',(-200.482096887895,1.14954297373518,
126.022338658809));
#242304=CARTESIAN_POINT('Ctrl Pts',(-200.489848079135,1.01635379374277,
125.990321514731));
#242305=CARTESIAN_POINT('Ctrl Pts',(-200.497599270375,0.881722066640452,
125.963847999343));
#242306=CARTESIAN_POINT('Ctrl Pts',(-200.505350461615,0.746148675539075,
125.94303927286));
#242307=CARTESIAN_POINT('Ctrl Pts',(-200.513098358392,0.61063290674527,
125.922239390641));
#242308=CARTESIAN_POINT('Ctrl Pts',(-200.520846255169,0.474176655614721,
125.90709956781));
#242309=CARTESIAN_POINT('Ctrl Pts',(-200.528594151946,0.337290990834222,
125.897689867454));
#242310=CARTESIAN_POINT('Ctrl Pts',(-200.53634042803,0.200433959583882,
125.888282135405));
#242311=CARTESIAN_POINT('Ctrl Pts',(-200.544086704114,0.0631480831462334,
125.884602168507));
#242312=CARTESIAN_POINT('Ctrl Pts',(-200.551832980198,-0.0740508485073515,
125.886668116572));
#242313=CARTESIAN_POINT('Ctrl Pts',(-200.559579313464,-0.211250792932096,
125.888734079886));
#242314=CARTESIAN_POINT('Ctrl Pts',(-200.567325646729,-0.348363400371211,
125.896546036912));
#242315=CARTESIAN_POINT('Ctrl Pts',(-200.575071979994,-0.484873680273991,
125.910070007408));
#242316=CARTESIAN_POINT('Ctrl Pts',(-200.582820047997,-0.621414530707646,
125.923597006504));
#242317=CARTESIAN_POINT('Ctrl Pts',(-200.590568116,-0.757352396209157,125.942838525925));
#242318=CARTESIAN_POINT('Ctrl Pts',(-200.598316184003,-0.892178597326069,
125.967708840461));
#242319=CARTESIAN_POINT('Ctrl Pts',(-200.606072486745,-1.0271480933338,
125.992605587463));
#242320=CARTESIAN_POINT('Ctrl Pts',(-200.613828789487,-1.16100317971131,
126.023143008933));
#242321=CARTESIAN_POINT('Ctrl Pts',(-200.621585092229,-1.29324600137144,
126.059184346611));
#242322=CARTESIAN_POINT('Ctrl Pts',(-200.629345534743,-1.42555940500761,
126.095244920636));
#242323=CARTESIAN_POINT('Ctrl Pts',(-200.637105977257,-1.55625845688736,
126.136815145853));
#242324=CARTESIAN_POINT('Ctrl Pts',(-200.644866419771,-1.68486256746866,
126.183709019442));
#242325=CARTESIAN_POINT('Ctrl Pts',(-200.652639320036,-1.8136731247852,
126.23067817124));
#242326=CARTESIAN_POINT('Ctrl Pts',(-200.660412220302,-1.94038165889755,
126.28298789975));
#242327=CARTESIAN_POINT('Ctrl Pts',(-200.668185120567,-2.06452876785875,
126.340404521323));
#242328=CARTESIAN_POINT('Ctrl Pts',(-200.675675456329,-2.18416281670689,
126.395733904081));
#242329=CARTESIAN_POINT('Ctrl Pts',(-200.683165792092,-2.30141816157879,
126.455805188864));
#242330=CARTESIAN_POINT('Ctrl Pts',(-200.690656127854,-2.41590869586259,
126.520370860837));
#242331=CARTESIAN_POINT('Ctrl Pts',(-200.698431549059,-2.53475678976688,
126.587393930419));
#242332=CARTESIAN_POINT('Ctrl Pts',(-200.706206970264,-2.65100197297227,
126.659472618184));
#242333=CARTESIAN_POINT('Ctrl Pts',(-200.713982391469,-2.7641842313008,
126.736379718161));
#242334=CARTESIAN_POINT('Ctrl Pts',(-200.721747993784,-2.87722356178429,
126.813189698976));
#242335=CARTESIAN_POINT('Ctrl Pts',(-200.729513596099,-2.98720734372281,
126.894815740927));
#242336=CARTESIAN_POINT('Ctrl Pts',(-200.737279198413,-3.09370005168907,
126.980984746339));
#242337=CARTESIAN_POINT('Ctrl Pts',(-200.745035419852,-3.20006411607945,
127.067049659281));
#242338=CARTESIAN_POINT('Ctrl Pts',(-200.752791641291,-3.30294520389971,
127.15764636104));
#242339=CARTESIAN_POINT('Ctrl Pts',(-200.76054786273,-3.40193722042223,
127.252458843754));
#242340=CARTESIAN_POINT('Ctrl Pts',(-200.768298765275,-3.50086135232833,
127.347206308003));
#242341=CARTESIAN_POINT('Ctrl Pts',(-200.776049667819,-3.5959014377128,
127.446163532372));
#242342=CARTESIAN_POINT('Ctrl Pts',(-200.783800570363,-3.68668484751337,
127.548974634673));
#242343=CARTESIAN_POINT('Ctrl Pts',(-200.791547836284,-3.77742566291104,
127.651737499334));
#242344=CARTESIAN_POINT('Ctrl Pts',(-200.799295102205,-3.86391351900049,
127.758350351215));
#242345=CARTESIAN_POINT('Ctrl Pts',(-200.807042368126,-3.94581330905367,
127.868421178035));
#242346=CARTESIAN_POINT('Ctrl Pts',(-200.814787676884,-4.0276924090674,
127.97846419807));
#242347=CARTESIAN_POINT('Ctrl Pts',(-200.822532985642,-4.10498551777313,
128.091963140353));
#242348=CARTESIAN_POINT('Ctrl Pts',(-200.8302782944,-4.17739867669816,128.208494026537));
#242349=CARTESIAN_POINT('Ctrl Pts',(-200.838025646966,-4.24983094378865,
128.325055662539));
#242350=CARTESIAN_POINT('Ctrl Pts',(-200.845772999533,-4.31738047721026,
128.444650511683));
#242351=CARTESIAN_POINT('Ctrl Pts',(-200.8535203521,-4.37979740039574,128.566826753244));
#242352=CARTESIAN_POINT('Ctrl Pts',(-200.861268696023,-4.4422223104952,
128.689018628564));
#242353=CARTESIAN_POINT('Ctrl Pts',(-200.869017039946,-4.49951313147677,
128.813792202435));
#242354=CARTESIAN_POINT('Ctrl Pts',(-200.87676538387,-4.55146701346846,
128.940673120208));
#242355=CARTESIAN_POINT('Ctrl Pts',(-200.884519834436,-4.60346184147747,
129.067654035672));
#242356=CARTESIAN_POINT('Ctrl Pts',(-200.892274285003,-4.65011118842505,
129.19674524743));
#242357=CARTESIAN_POINT('Ctrl Pts',(-200.90002873557,-4.69126111778874,
129.327454328317));
#242358=CARTESIAN_POINT('Ctrl Pts',(-200.905034844876,-4.71782664201108,
129.411837346905));
#242359=CARTESIAN_POINT('Ctrl Pts',(-200.910040954183,-4.74210117247926,
129.496894318409));
#242360=CARTESIAN_POINT('Ctrl Pts',(-200.91504706349,-4.76405452823395,
129.582490119308));
#242361=CARTESIAN_POINT('',(-198.889859435951,-4.91824989448309,130.8033418354));
#242362=CARTESIAN_POINT('Ctrl Pts',(-198.889859435995,-4.91824989448325,
130.803341836187));
#242363=CARTESIAN_POINT('Ctrl Pts',(-198.897858632837,-4.91827931260921,
130.945360229872));
#242364=CARTESIAN_POINT('Ctrl Pts',(-198.905857829679,-4.91215304597155,
131.087301810736));
#242365=CARTESIAN_POINT('Ctrl Pts',(-198.913857026521,-4.89991714960293,
131.228618781338));
#242366=CARTESIAN_POINT('Ctrl Pts',(-198.921862893465,-4.88767105037535,
131.370053588597));
#242367=CARTESIAN_POINT('Ctrl Pts',(-198.929868760409,-4.86930519372858,
131.510862395327));
#242368=CARTESIAN_POINT('Ctrl Pts',(-198.937874627353,-4.84491724488214,
131.650504785391));
#242369=CARTESIAN_POINT('Ctrl Pts',(-198.945888336214,-4.82050540752001,
131.790283958152));
#242370=CARTESIAN_POINT('Ctrl Pts',(-198.953902045075,-4.79005977639878,
131.928894088689));
#242371=CARTESIAN_POINT('Ctrl Pts',(-198.961915753937,-4.75372862315488,
132.065807104698));
#242372=CARTESIAN_POINT('Ctrl Pts',(-198.969944216913,-4.71733058028216,
132.202972192552));
#242373=CARTESIAN_POINT('Ctrl Pts',(-198.977972679889,-4.67502545496002,
132.338433581101));
#242374=CARTESIAN_POINT('Ctrl Pts',(-198.986001142865,-4.62701107698537,
132.471679290152));
#242375=CARTESIAN_POINT('Ctrl Pts',(-198.994038134277,-4.57894569453759,
132.605066542788));
#242376=CARTESIAN_POINT('Ctrl Pts',(-199.002075125689,-4.52515909597119,
132.736233095487));
#242377=CARTESIAN_POINT('Ctrl Pts',(-199.0101121171,-4.46589624387441,132.864689183948));
#242378=CARTESIAN_POINT('Ctrl Pts',(-199.018163714144,-4.40652569334159,
132.993378715777));
#242379=CARTESIAN_POINT('Ctrl Pts',(-199.026215311188,-4.34165916726409,
133.119347629071));
#242380=CARTESIAN_POINT('Ctrl Pts',(-199.034266908231,-4.27158681882194,
133.242131958723));
#242381=CARTESIAN_POINT('Ctrl Pts',(-199.036031065866,-4.25623350843576,
133.269034809357));
#242382=CARTESIAN_POINT('Ctrl Pts',(-199.037795223501,-4.2406304385508,
133.295784893293));
#242383=CARTESIAN_POINT('Ctrl Pts',(-199.039559381137,-4.2247809262074,
133.322377533326));
#242384=CARTESIAN_POINT('Ctrl Pts',(-199.047333715256,-4.15493489763892,
133.439566646481));
#242385=CARTESIAN_POINT('Ctrl Pts',(-199.055108049375,-4.08009856624961,
133.554033039613));
#242386=CARTESIAN_POINT('Ctrl Pts',(-199.062882383494,-4.00051000845862,
133.665322472384));
#242387=CARTESIAN_POINT('Ctrl Pts',(-199.070647136441,-3.92101953645207,
133.776474750875));
#242388=CARTESIAN_POINT('Ctrl Pts',(-199.078411889388,-3.83678871636238,
133.884457544366));
#242389=CARTESIAN_POINT('Ctrl Pts',(-199.086176642335,-3.74810091690515,
133.988842141958));
#242390=CARTESIAN_POINT('Ctrl Pts',(-199.09393368322,-3.65950120342062,
134.093123063297));
#242391=CARTESIAN_POINT('Ctrl Pts',(-199.101690724105,-3.56645357147556,
134.193812604699));
#242392=CARTESIAN_POINT('Ctrl Pts',(-199.10944776499,-3.46928377810122,
134.290512239269));
#242393=CARTESIAN_POINT('Ctrl Pts',(-199.11719895623,-3.37218726122407,
134.387138951893));
#242394=CARTESIAN_POINT('Ctrl Pts',(-199.12495014747,-3.27097504630834,
134.47978147189));
#242395=CARTESIAN_POINT('Ctrl Pts',(-199.132701338711,-3.16601189112494,
134.568075772537));
#242396=CARTESIAN_POINT('Ctrl Pts',(-199.140449235488,-3.06109334808233,
134.65633254575));
#242397=CARTESIAN_POINT('Ctrl Pts',(-199.148197132265,-2.95242733417478,
134.740244524213));
#242398=CARTESIAN_POINT('Ctrl Pts',(-199.155945029042,-2.84041388590054,
134.819486022741));
#242399=CARTESIAN_POINT('Ctrl Pts',(-199.163691305126,-2.72842386842495,
134.898710945656));
#242400=CARTESIAN_POINT('Ctrl Pts',(-199.17143758121,-2.61308812831208,
134.973267106223));
#242401=CARTESIAN_POINT('Ctrl Pts',(-199.179183857294,-2.49483773851418,
135.042870700247));
#242402=CARTESIAN_POINT('Ctrl Pts',(-199.186930190559,-2.3765864758186,
135.112474808069));
#242403=CARTESIAN_POINT('Ctrl Pts',(-199.194676523825,-2.25542085743659,
135.177126078077));
#242404=CARTESIAN_POINT('Ctrl Pts',(-199.20242285709,-2.13179839053741,
135.236585643961));
#242405=CARTESIAN_POINT('Ctrl Pts',(-199.210170925093,-2.0081482392444,
135.296058525402));
#242406=CARTESIAN_POINT('Ctrl Pts',(-199.217918993096,-1.88204049687381,
135.350337219758));
#242407=CARTESIAN_POINT('Ctrl Pts',(-199.225667061099,-1.75395419721453,
135.399230336783));
#242408=CARTESIAN_POINT('Ctrl Pts',(-199.233423363841,-1.6257317659112,
135.448175417994));
#242409=CARTESIAN_POINT('Ctrl Pts',(-199.241179666583,-1.49552694252251,
135.491723348206));
#242410=CARTESIAN_POINT('Ctrl Pts',(-199.248935969325,-1.3638360625422,
135.529731952923));
#242411=CARTESIAN_POINT('Ctrl Pts',(-199.256696411839,-1.23207489517375,
135.567760843976));
#242412=CARTESIAN_POINT('Ctrl Pts',(-199.264456854353,-1.0988264704442,
135.600244425895));
#242413=CARTESIAN_POINT('Ctrl Pts',(-199.272217296867,-0.96459799408161,
135.627091563028));
#242414=CARTESIAN_POINT('Ctrl Pts',(-199.279990197133,-0.830154042252889,
135.653981797568));
#242415=CARTESIAN_POINT('Ctrl Pts',(-199.287763097398,-0.694727281372439,
135.675217445693));
#242416=CARTESIAN_POINT('Ctrl Pts',(-199.295535997664,-0.558831624326638,
135.690759115248));
#242417=CARTESIAN_POINT('Ctrl Pts',(-199.303026333426,-0.427876116714585,
135.705735805968));
#242418=CARTESIAN_POINT('Ctrl Pts',(-199.310516669188,-0.296485519363162,
135.715425289075));
#242419=CARTESIAN_POINT('Ctrl Pts',(-199.31800700495,-0.16511834145049,
135.719838111749));
#242420=CARTESIAN_POINT('Ctrl Pts',(-199.325781339069,-0.0287703370596385,
135.724418247935));
#242421=CARTESIAN_POINT('Ctrl Pts',(-199.333555673188,0.10798434643372,
135.723328204347));
#242422=CARTESIAN_POINT('Ctrl Pts',(-199.341330007307,0.244634857648935,
135.716522753421));
#242423=CARTESIAN_POINT('Ctrl Pts',(-199.349094760254,0.381116959321885,
135.709725689604));
#242424=CARTESIAN_POINT('Ctrl Pts',(-199.356859513201,0.517494757427955,
135.69722725263));
#242425=CARTESIAN_POINT('Ctrl Pts',(-199.364624266149,0.653254397634356,
135.679034119912));
#242426=CARTESIAN_POINT('Ctrl Pts',(-199.372381307034,0.788879199452228,
135.660859056869));
#242427=CARTESIAN_POINT('Ctrl Pts',(-199.380138347918,0.923886680191096,
135.637000605475));
#242428=CARTESIAN_POINT('Ctrl Pts',(-199.387895388803,1.05776546825392,
135.607517420823));
#242429=CARTESIAN_POINT('Ctrl Pts',(-199.395646580044,1.19154329728142,
135.578056469669));
#242430=CARTESIAN_POINT('Ctrl Pts',(-199.403397771284,1.32419374753591,
135.542979311759));
#242431=CARTESIAN_POINT('Ctrl Pts',(-199.411148962524,1.45521339253885,
135.5023960628));
#242432=CARTESIAN_POINT('Ctrl Pts',(-199.418896859301,1.58617735069778,
135.461830062804));
#242433=CARTESIAN_POINT('Ctrl Pts',(-199.426644756078,1.71551150952141,
135.415762741745));
#242434=CARTESIAN_POINT('Ctrl Pts',(-199.434392652855,1.84272563134234,
135.364354620862));
#242435=CARTESIAN_POINT('Ctrl Pts',(-199.442138928939,1.96991314271106,
135.312957253449));
#242436=CARTESIAN_POINT('Ctrl Pts',(-199.449885205023,2.09498113689857,
135.256221454736));
#242437=CARTESIAN_POINT('Ctrl Pts',(-199.457631481108,2.21745783593928,
135.194356495506));
#242438=CARTESIAN_POINT('Ctrl Pts',(-199.465377814373,2.33993543907532,
135.132491079603));
#242439=CARTESIAN_POINT('Ctrl Pts',(-199.473124147638,2.45982135992249,
135.065496603904));
#242440=CARTESIAN_POINT('Ctrl Pts',(-199.480870480904,2.57666733968873,
134.993628869073));
#242441=CARTESIAN_POINT('Ctrl Pts',(-199.488618548907,2.69353948630213,
134.92174503996));
#242442=CARTESIAN_POINT('Ctrl Pts',(-199.49636661691,2.80737000422098,134.844985984877));
#242443=CARTESIAN_POINT('Ctrl Pts',(-199.504114684913,2.91773894194668,
134.763651277413));
#242444=CARTESIAN_POINT('Ctrl Pts',(-199.511870987655,3.02822518109265,
134.682230126454));
#242445=CARTESIAN_POINT('Ctrl Pts',(-199.519627290396,3.13524217559271,
134.596223840941));
#242446=CARTESIAN_POINT('Ctrl Pts',(-199.527383593138,3.23840202855827,
134.505973153196));
#242447=CARTESIAN_POINT('Ctrl Pts',(-199.535144035652,3.34161694104344,
134.41567429594));
#242448=CARTESIAN_POINT('Ctrl Pts',(-199.542904478166,3.44097032683412,
134.321126791907));
#242449=CARTESIAN_POINT('Ctrl Pts',(-199.550664920681,3.5361113538409,134.222708106593));
#242450=CARTESIAN_POINT('Ctrl Pts',(-199.558437820946,3.63140510967045,
134.124131430869));
#242451=CARTESIAN_POINT('Ctrl Pts',(-199.566210721212,3.72247273410093,
134.021671447976));
#242452=CARTESIAN_POINT('Ctrl Pts',(-199.573983621477,3.80900330292975,
133.915739234959));
#242453=CARTESIAN_POINT('Ctrl Pts',(-199.581473957239,3.89238826762382,
133.813657924713));
#242454=CARTESIAN_POINT('Ctrl Pts',(-199.588964293001,3.97156013144357,
133.708352696285));
#242455=CARTESIAN_POINT('Ctrl Pts',(-199.596454628763,4.04627993261936,
133.600215007441));
#242456=CARTESIAN_POINT('Ctrl Pts',(-199.604228962882,4.12383275776765,
133.487977245255));
#242457=CARTESIAN_POINT('Ctrl Pts',(-199.612003297001,4.1968349200723,133.372332461753));
#242458=CARTESIAN_POINT('Ctrl Pts',(-199.61977763112,4.26497224065351,133.253686004066));
#242459=CARTESIAN_POINT('Ctrl Pts',(-199.627542384067,4.33302558807671,
133.135185767535));
#242460=CARTESIAN_POINT('Ctrl Pts',(-199.635307137014,4.39622583016546,
133.013691553092));
#242461=CARTESIAN_POINT('Ctrl Pts',(-199.643071889961,4.45430083399845,
132.889639290248));
#242462=CARTESIAN_POINT('Ctrl Pts',(-199.650828930846,4.51231815691907,
132.765710237859));
#242463=CARTESIAN_POINT('Ctrl Pts',(-199.658585971731,4.56522020713492,
132.639228544949));
#242464=CARTESIAN_POINT('Ctrl Pts',(-199.666343012616,4.61277992399897,
132.510656147435));
#242465=CARTESIAN_POINT('Ctrl Pts',(-199.674094203857,4.66030377571063,
132.382180707367));
#242466=CARTESIAN_POINT('Ctrl Pts',(-199.681845395097,4.70249317785453,
132.251618066054));
#242467=CARTESIAN_POINT('Ctrl Pts',(-199.689596586337,4.73916865958453,
132.11945129068));
#242468=CARTESIAN_POINT('Ctrl Pts',(-199.697344483114,4.77582855325628,
131.987340689712));
#242469=CARTESIAN_POINT('Ctrl Pts',(-199.705092379891,4.80697908336153,
131.853627686671));
#242470=CARTESIAN_POINT('Ctrl Pts',(-199.712840276668,4.83249031553063,
131.718811498042));
#242471=CARTESIAN_POINT('Ctrl Pts',(-199.720586552752,4.85799621129998,
131.584023510052));
#242472=CARTESIAN_POINT('Ctrl Pts',(-199.728332828836,4.87786508281496,
131.448133179379));
#242473=CARTESIAN_POINT('Ctrl Pts',(-199.73607910492,4.89201798799939,131.311650542156));
#242474=CARTESIAN_POINT('Ctrl Pts',(-199.743825438185,4.9061709976573,131.17516689745));
#242475=CARTESIAN_POINT('Ctrl Pts',(-199.751571771451,4.91460791646383,
131.038091326349));
#242476=CARTESIAN_POINT('Ctrl Pts',(-199.759318104716,4.91730166193535,
130.900939228179));
#242477=CARTESIAN_POINT('Ctrl Pts',(-199.767066172719,4.91999601065249,
130.763756415746));
#242478=CARTESIAN_POINT('Ctrl Pts',(-199.774814240722,4.91694461908141,
130.626497432957));
#242479=CARTESIAN_POINT('Ctrl Pts',(-199.782562308725,4.90817253292527,
130.489677523743));
#242480=CARTESIAN_POINT('Ctrl Pts',(-199.790318611467,4.89939112369156,
130.352712200701));
#242481=CARTESIAN_POINT('Ctrl Pts',(-199.798074914209,4.88487689942825,
130.21618727421));
#242482=CARTESIAN_POINT('Ctrl Pts',(-199.805831216951,4.8647068601427,130.080613267049));
#242483=CARTESIAN_POINT('Ctrl Pts',(-199.813591659465,4.84452605549987,
129.944966899958));
#242484=CARTESIAN_POINT('Ctrl Pts',(-199.821352101979,4.81868349449313,
129.810272847277));
#242485=CARTESIAN_POINT('Ctrl Pts',(-199.829112544493,4.78730711622281,
129.6770303033));
#242486=CARTESIAN_POINT('Ctrl Pts',(-199.836885444758,4.75588036980463,
129.543573866563));
#242487=CARTESIAN_POINT('Ctrl Pts',(-199.844658345024,4.71890215983434,
129.411573971483));
#242488=CARTESIAN_POINT('Ctrl Pts',(-199.852431245289,4.67655027494581,
129.281514404581));
#242489=CARTESIAN_POINT('Ctrl Pts',(-199.859921581051,4.63573798775117,
129.156182830536));
#242490=CARTESIAN_POINT('Ctrl Pts',(-199.867411916813,4.58993604295062,
129.032653251052));
#242491=CARTESIAN_POINT('Ctrl Pts',(-199.874902252575,4.53934462037534,
128.911338303918));
#242492=CARTESIAN_POINT('Ctrl Pts',(-199.882676586694,4.48683500863597,
128.78542366369));
#242493=CARTESIAN_POINT('Ctrl Pts',(-199.890450920813,4.42899922894786,
128.66149604675));
#242494=CARTESIAN_POINT('Ctrl Pts',(-199.898225254932,4.36600848997413,
128.540038880715));
#242495=CARTESIAN_POINT('Ctrl Pts',(-199.905990007879,4.30309538145654,
128.418731399783));
#242496=CARTESIAN_POINT('Ctrl Pts',(-199.913754760827,4.23504013255191,
128.299888655622));
#242497=CARTESIAN_POINT('Ctrl Pts',(-199.921519513774,4.16206240861067,
128.183975231916));
#242498=CARTESIAN_POINT('Ctrl Pts',(-199.929276554659,4.08915716717364,
128.068176935055));
#242499=CARTESIAN_POINT('Ctrl Pts',(-199.937033595544,4.01133938712683,
127.95530249744));
#242500=CARTESIAN_POINT('Ctrl Pts',(-199.944790636429,3.9288749764153,127.84579263927));
#242501=CARTESIAN_POINT('Ctrl Pts',(-199.952541827669,3.84647275275725,
127.736365363336));
#242502=CARTESIAN_POINT('Ctrl Pts',(-199.960293018909,3.75943110728714,
127.630297927647));
#242503=CARTESIAN_POINT('Ctrl Pts',(-199.968044210149,3.6680594497312,127.528002435722));
#242504=CARTESIAN_POINT('Ctrl Pts',(-199.975792106926,3.57672662756702,
127.425750422109));
#242505=CARTESIAN_POINT('Ctrl Pts',(-199.983540003703,3.48106771357534,
127.327267454637));
#242506=CARTESIAN_POINT('Ctrl Pts',(-199.99128790048,3.38143248002231,127.232932689475));
#242507=CARTESIAN_POINT('Ctrl Pts',(-199.999034176564,3.2818180880128,127.138617657112));
#242508=CARTESIAN_POINT('Ctrl Pts',(-200.006780452648,3.17822931458165,
127.048449369756));
#242509=CARTESIAN_POINT('Ctrl Pts',(-200.014526728732,3.07105259745354,
126.962769930601));
#242510=CARTESIAN_POINT('Ctrl Pts',(-200.022273061998,2.9638750891711,126.87708985898));
#242511=CARTESIAN_POINT('Ctrl Pts',(-200.030019395263,2.85310988972064,
126.795898945805));
#242512=CARTESIAN_POINT('Ctrl Pts',(-200.037765728529,2.73917598040633,
126.719498562262));
#242513=CARTESIAN_POINT('Ctrl Pts',(-200.045513796531,2.62521655638345,
126.643081069382));
#242514=CARTESIAN_POINT('Ctrl Pts',(-200.053261864534,2.50808733510855,
126.571456458597));
#242515=CARTESIAN_POINT('Ctrl Pts',(-200.061009932537,2.38823534370891,
126.504882160176));
#242516=CARTESIAN_POINT('Ctrl Pts',(-200.068766235279,2.26825597218606,
126.438237105799));
#242517=CARTESIAN_POINT('Ctrl Pts',(-200.076522538021,2.14554839219856,
126.37665327616));
#242518=CARTESIAN_POINT('Ctrl Pts',(-200.084278840763,2.02058374140458,
126.320341839007));
#242519=CARTESIAN_POINT('Ctrl Pts',(-200.092039283277,1.89555239321386,
126.264000346744));
#242520=CARTESIAN_POINT('Ctrl Pts',(-200.099799725791,1.76826193649607,
126.212936999659));
#242521=CARTESIAN_POINT('Ctrl Pts',(-200.107560168305,1.63920151175827,
126.167313985673));
#242522=CARTESIAN_POINT('Ctrl Pts',(-200.115333068571,1.50993390776888,
126.121617733575));
#242523=CARTESIAN_POINT('Ctrl Pts',(-200.123105968836,1.37889103187466,
126.081379381333));
#242524=CARTESIAN_POINT('Ctrl Pts',(-200.130878869102,1.24657600647687,
126.046710848765));
#242525=CARTESIAN_POINT('Ctrl Pts',(-200.138369204864,1.11907096553192,
126.01330260468));
#242526=CARTESIAN_POINT('Ctrl Pts',(-200.145859540626,0.99038496183093,
125.985066322929));
#242527=CARTESIAN_POINT('Ctrl Pts',(-200.153349876388,0.860973361320397,
125.962056627357));
#242528=CARTESIAN_POINT('Ctrl Pts',(-200.161124210507,0.726655080644413,
125.938174512183));
#242529=CARTESIAN_POINT('Ctrl Pts',(-200.168898544626,0.591129615061729,
125.919847487573));
#242530=CARTESIAN_POINT('Ctrl Pts',(-200.176672878745,0.454896228380958,
125.907192815264));
#242531=CARTESIAN_POINT('Ctrl Pts',(-200.184437631692,0.318830737174114,
125.894553738707));
#242532=CARTESIAN_POINT('Ctrl Pts',(-200.19220238464,0.182059446335804,
125.887573140922));
#242533=CARTESIAN_POINT('Ctrl Pts',(-200.199967137587,0.0450919577624086,
125.886317330054));
#242534=CARTESIAN_POINT('Ctrl Pts',(-200.207724178472,-0.0917394927708051,
125.885062766475));
#242535=CARTESIAN_POINT('Ctrl Pts',(-200.215481219357,-0.228766364827308,
125.8895216781));
#242536=CARTESIAN_POINT('Ctrl Pts',(-200.223238260242,-0.365474138281122,
125.899708569077));
#242537=CARTESIAN_POINT('Ctrl Pts',(-200.230989451482,-0.502078819338985,
125.90988777804));
#242538=CARTESIAN_POINT('Ctrl Pts',(-200.238740642722,-0.638364492456307,
125.925786339691));
#242539=CARTESIAN_POINT('Ctrl Pts',(-200.246491833962,-0.773817199757398,
125.947366690881));
#242540=CARTESIAN_POINT('Ctrl Pts',(-200.254239730739,-0.909212336044752,
125.968937869845));
#242541=CARTESIAN_POINT('Ctrl Pts',(-200.261987627516,-1.04377482537243,
125.996185973889));
#242542=CARTESIAN_POINT('Ctrl Pts',(-200.269735524293,-1.17699661246376,
126.029021672868));
#242543=CARTESIAN_POINT('Ctrl Pts',(-200.277481800377,-1.31019053242917,
126.061850503327));
#242544=CARTESIAN_POINT('Ctrl Pts',(-200.285228076462,-1.44204392861639,
126.100264510403));
#242545=CARTESIAN_POINT('Ctrl Pts',(-200.292974352546,-1.57206010089031,
126.144123488225));
#242546=CARTESIAN_POINT('Ctrl Pts',(-200.300720685811,-1.70207723291426,
126.187982789804));
#242547=CARTESIAN_POINT('Ctrl Pts',(-200.308467019076,-1.83025674350794,
126.237287017366));
#242548=CARTESIAN_POINT('Ctrl Pts',(-200.316213352342,-1.9561186109295,
126.29184656856));
#242549=CARTESIAN_POINT('Ctrl Pts',(-200.323961420345,-2.08200866424412,
126.346418337987));
#242550=CARTESIAN_POINT('Ctrl Pts',(-200.331709488348,-2.20557968295316,
126.40624761746));
#242551=CARTESIAN_POINT('Ctrl Pts',(-200.339457556351,-2.32637345459673,
126.471097457747));
#242552=CARTESIAN_POINT('Ctrl Pts',(-200.347213859093,-2.44729560729777,
126.536016221215));
#242553=CARTESIAN_POINT('Ctrl Pts',(-200.354970161835,-2.56543427159992,
126.605966019329));
#242554=CARTESIAN_POINT('Ctrl Pts',(-200.362726464576,-2.68035712468567,
126.68066461196));
#242555=CARTESIAN_POINT('Ctrl Pts',(-200.370486907091,-2.79534131555868,
126.75540307348));
#242556=CARTESIAN_POINT('Ctrl Pts',(-200.378247349605,-2.90710595674912,
126.834895153379));
#242557=CARTESIAN_POINT('Ctrl Pts',(-200.386007792119,-3.01525020257337,
126.918816990429));
#242558=CARTESIAN_POINT('Ctrl Pts',(-200.393780692384,-3.12356805114131,
127.002873546263));
#242559=CARTESIAN_POINT('Ctrl Pts',(-200.40155359265,-3.22825359181314,
127.091373816816));
#242560=CARTESIAN_POINT('Ctrl Pts',(-200.409326492915,-3.32894071332805,
127.183955006361));
#242561=CARTESIAN_POINT('Ctrl Pts',(-200.416816828677,-3.42596760435925,
127.273170636466));
#242562=CARTESIAN_POINT('Ctrl Pts',(-200.424307164439,-3.51928151621706,
127.366175415959));
#242563=CARTESIAN_POINT('Ctrl Pts',(-200.431797500201,-3.60859035589865,
127.462615758093));
#242564=CARTESIAN_POINT('Ctrl Pts',(-200.439483530572,-3.70023250333136,
127.561575727608));
#242565=CARTESIAN_POINT('Ctrl Pts',(-200.447169560944,-3.78796263802236,
127.664483128439));
#242566=CARTESIAN_POINT('Ctrl Pts',(-200.454855591315,-3.87141551944836,
127.770992038202));
#242567=CARTESIAN_POINT('Ctrl Pts',(-200.462532485089,-3.95476919812291,
127.877374337873));
#242568=CARTESIAN_POINT('Ctrl Pts',(-200.470209378863,-4.03385548881044,
127.987349321958));
#242569=CARTESIAN_POINT('Ctrl Pts',(-200.477886272637,-4.10834596593192,
128.100534349717));
#242570=CARTESIAN_POINT('Ctrl Pts',(-200.48555463187,-4.18275363065011,
128.213593547645));
#242571=CARTESIAN_POINT('Ctrl Pts',(-200.493222991104,-4.25257543216279,
128.329855354119));
#242572=CARTESIAN_POINT('Ctrl Pts',(-200.500891350337,-4.3175236951057,
128.44890477958));
#242573=CARTESIAN_POINT('Ctrl Pts',(-200.508554665913,-4.38242924007743,
128.567875903488));
#242574=CARTESIAN_POINT('Ctrl Pts',(-200.516217981489,-4.44246742915597,
128.689630650553));
#242575=CARTESIAN_POINT('Ctrl Pts',(-200.523881297066,-4.49739444895502,
128.813725986849));
#242576=CARTESIAN_POINT('Ctrl Pts',(-200.531543281829,-4.55231193011296,
128.937799772716));
#242577=CARTESIAN_POINT('Ctrl Pts',(-200.539205266592,-4.60211982992361,
129.064212980692));
#242578=CARTESIAN_POINT('Ctrl Pts',(-200.546867251355,-4.64662086241272,
129.192499077765));
#242579=CARTESIAN_POINT('Ctrl Pts',(-200.554529236118,-4.69112189490171,
129.320785174837));
#242580=CARTESIAN_POINT('Ctrl Pts',(-200.56219122088,-4.73031591701161,
129.450943786207));
#242581=CARTESIAN_POINT('Ctrl Pts',(-200.569853205643,-4.76405452823395,
129.582490119308));
#242582=CARTESIAN_POINT('Ctrl Pts',(-198.820145221536,-4.76405452823399,
129.582490119308));
#242583=CARTESIAN_POINT('Ctrl Pts',(-198.828426476198,-4.80034991023985,
129.72400526289));
#242584=CARTESIAN_POINT('Ctrl Pts',(-198.836707730859,-4.83037656394087,
129.867298369273));
#242585=CARTESIAN_POINT('Ctrl Pts',(-198.844988985521,-4.85397223469977,
130.011809920598));
#242586=CARTESIAN_POINT('Ctrl Pts',(-198.853248087719,-4.87750478673457,
130.155934901657));
#242587=CARTESIAN_POINT('Ctrl Pts',(-198.861507189918,-4.89464061291577,
130.301271527841));
#242588=CARTESIAN_POINT('Ctrl Pts',(-198.869766292116,-4.90526800462946,
130.44724877898));
#242589=CARTESIAN_POINT('Ctrl Pts',(-198.876464006728,-4.91388628238558,
130.5656289545));
#242590=CARTESIAN_POINT('Ctrl Pts',(-198.883161721339,-4.91822526271462,
130.684430063471));
#242591=CARTESIAN_POINT('Ctrl Pts',(-198.889859435951,-4.91824989448309,
130.803341835399));
#242592=CARTESIAN_POINT('Origin',(213.235140564004,0.,130.804360617566));
#242593=CARTESIAN_POINT('',(-197.069830899744,-4.76405452823391,129.582490119308));
#242594=CARTESIAN_POINT('',(-197.415422870675,-4.76405452823413,129.582490119309));
#242595=CARTESIAN_POINT('',(213.235140564004,-4.76405452823405,129.582490119308));
#242596=CARTESIAN_POINT('',(-197.485140563979,-4.91824998893204,130.804030662974));
#242597=CARTESIAN_POINT('Ctrl Pts',(-197.415422870675,-4.76405452823413,
129.582490119309));
#242598=CARTESIAN_POINT('Ctrl Pts',(-197.423600431488,-4.79992281658223,
129.722340031201));
#242599=CARTESIAN_POINT('Ctrl Pts',(-197.431777992302,-4.82966733555782,
129.863920110019));
#242600=CARTESIAN_POINT('Ctrl Pts',(-197.439955553115,-4.85313234200592,
130.006683030144));
#242601=CARTESIAN_POINT('Ctrl Pts',(-197.448116021641,-4.87654830318953,
130.149147555073));
#242602=CARTESIAN_POINT('Ctrl Pts',(-197.456276490167,-4.89371087298272,
130.292789672346));
#242603=CARTESIAN_POINT('Ctrl Pts',(-197.464436958693,-4.90451488430555,
130.437050377952));
#242604=CARTESIAN_POINT('Ctrl Pts',(-197.471338160455,-4.91365169572061,
130.559049774504));
#242605=CARTESIAN_POINT('Ctrl Pts',(-197.478239362217,-4.91824176802981,
130.681491218841));
#242606=CARTESIAN_POINT('Ctrl Pts',(-197.485140563979,-4.91824998893204,
130.804030662974));
#242607=CARTESIAN_POINT('Ctrl Pts',(-197.485140564012,-4.91824998893207,
130.804030663556));
#242608=CARTESIAN_POINT('Ctrl Pts',(-197.493215691151,-4.91825960822969,
130.947414616808));
#242609=CARTESIAN_POINT('Ctrl Pts',(-197.501290818289,-4.91199470079414,
131.0906909398));
#242610=CARTESIAN_POINT('Ctrl Pts',(-197.509365945428,-4.8995093582954,
131.233302467326));
#242611=CARTESIAN_POINT('Ctrl Pts',(-197.517450328902,-4.88700970413012,
131.37607746723));
#242612=CARTESIAN_POINT('Ctrl Pts',(-197.525534712377,-4.86827541990526,
131.518185812766));
#242613=CARTESIAN_POINT('Ctrl Pts',(-197.533619095851,-4.84341207736157,
131.659078413899));
#242614=CARTESIAN_POINT('Ctrl Pts',(-197.541721259799,-4.81849405136742,
131.800280888636));
#242615=CARTESIAN_POINT('Ctrl Pts',(-197.549823423746,-4.78742007700962,
131.940261937201));
#242616=CARTESIAN_POINT('Ctrl Pts',(-197.557925587693,-4.75034662328381,
132.078483853818));
#242617=CARTESIAN_POINT('Ctrl Pts',(-197.566036944332,-4.71323110612685,
132.216862596612));
#242618=CARTESIAN_POINT('Ctrl Pts',(-197.57414830097,-4.67010262962301,
132.353477900727));
#242619=CARTESIAN_POINT('Ctrl Pts',(-197.582259657609,-4.62116662589813,
132.487810075728));
#242620=CARTESIAN_POINT('Ctrl Pts',(-197.590389437885,-4.57211947193716,
132.622447364588));
#242621=CARTESIAN_POINT('Ctrl Pts',(-197.598519218162,-4.51723854412096,
132.754790839472));
#242622=CARTESIAN_POINT('Ctrl Pts',(-197.606648998438,-4.45677700646237,
132.884341813916));
#242623=CARTESIAN_POINT('Ctrl Pts',(-197.613676754263,-4.40451127368774,
132.996331632124));
#242624=CARTESIAN_POINT('Ctrl Pts',(-197.620704510087,-4.34807614872925,
133.106234993745));
#242625=CARTESIAN_POINT('Ctrl Pts',(-197.627732265912,-4.28766139771813,
133.213747012692));
#242626=CARTESIAN_POINT('Ctrl Pts',(-197.635506600031,-4.22082861755148,
133.332680336215));
#242627=CARTESIAN_POINT('Ctrl Pts',(-197.64328093415,-4.14893767964865,
133.449019171949));
#242628=CARTESIAN_POINT('Ctrl Pts',(-197.651055268269,-4.0722149913182,
133.562303352103));
#242629=CARTESIAN_POINT('Ctrl Pts',(-197.658820021216,-3.99558685684443,
133.675447919629));
#242630=CARTESIAN_POINT('Ctrl Pts',(-197.666584774163,-3.91413903715416,
133.785545001383));
#242631=CARTESIAN_POINT('Ctrl Pts',(-197.67434952711,-3.82814386857856,
133.892158794903));
#242632=CARTESIAN_POINT('Ctrl Pts',(-197.682106567995,-3.74223411161671,
133.9986666981));
#242633=CARTESIAN_POINT('Ctrl Pts',(-197.68986360888,-3.65178623765968,
134.101697895584));
#242634=CARTESIAN_POINT('Ctrl Pts',(-197.697620649765,-3.55711572780408,
134.200845677375));
#242635=CARTESIAN_POINT('Ctrl Pts',(-197.705371841005,-3.46251660971625,
134.299918691053));
#242636=CARTESIAN_POINT('Ctrl Pts',(-197.713123032246,-3.36370146283428,
134.395113836446));
#242637=CARTESIAN_POINT('Ctrl Pts',(-197.720874223486,-3.26102563669002,
134.486057897266));
#242638=CARTESIAN_POINT('Ctrl Pts',(-197.728622120263,-3.15839345051069,
134.576963304434));
#242639=CARTESIAN_POINT('Ctrl Pts',(-197.73637001704,-3.05190414073299,
134.663620961979));
#242640=CARTESIAN_POINT('Ctrl Pts',(-197.744117913817,-2.94194930255022,
134.745695082405));
#242641=CARTESIAN_POINT('Ctrl Pts',(-197.751864189901,-2.83201746454923,
134.827752034693));
#242642=CARTESIAN_POINT('Ctrl Pts',(-197.759610465985,-2.71862185314553,
134.905227123207));
#242643=CARTESIAN_POINT('Ctrl Pts',(-197.767356742069,-2.6021861586238,
134.977825635793));
#242644=CARTESIAN_POINT('Ctrl Pts',(-197.775103075335,-2.48574960460007,
135.050424684285));
#242645=CARTESIAN_POINT('Ctrl Pts',(-197.7828494086,-2.3662732544387,135.118146878164));
#242646=CARTESIAN_POINT('Ctrl Pts',(-197.790595741865,-2.24420837078515,
135.180741753961));
#242647=CARTESIAN_POINT('Ctrl Pts',(-197.798343809868,-2.12211615154708,
135.243350647447));
#242648=CARTESIAN_POINT('Ctrl Pts',(-197.806091877871,-1.9974345931365,
135.300829759648));
#242649=CARTESIAN_POINT('Ctrl Pts',(-197.813839945874,-1.87063768933132,
135.352975538369));
#242650=CARTESIAN_POINT('Ctrl Pts',(-197.821596248616,-1.74370602426839,
135.405176738244));
#242651=CARTESIAN_POINT('Ctrl Pts',(-197.829352551358,-1.61465488491918,
135.452033132601));
#242652=CARTESIAN_POINT('Ctrl Pts',(-197.8371088541,-1.48397681704943,135.493389927451));
#242653=CARTESIAN_POINT('Ctrl Pts',(-197.844869296614,-1.35322900236022,
135.534768795668));
#242654=CARTESIAN_POINT('Ctrl Pts',(-197.852629739128,-1.22085290607787,
135.57064211333));
#242655=CARTESIAN_POINT('Ctrl Pts',(-197.860390181642,-1.08735324310278,
135.600905831281));
#242656=CARTESIAN_POINT('Ctrl Pts',(-197.868163081908,-0.953639274617129,
135.631218131239));
#242657=CARTESIAN_POINT('Ctrl Pts',(-197.875935982173,-0.818798519968866,
135.65590276613));
#242658=CARTESIAN_POINT('Ctrl Pts',(-197.883708882439,-0.683343719454388,
135.674907242287));
#242659=CARTESIAN_POINT('Ctrl Pts',(-197.891199218201,-0.55281304212647,
135.693220857867));
#242660=CARTESIAN_POINT('Ctrl Pts',(-197.898689553963,-0.421712494577103,
135.706260090511));
#242661=CARTESIAN_POINT('Ctrl Pts',(-197.906179889725,-0.290500705819022,
135.714023783448));
#242662=CARTESIAN_POINT('Ctrl Pts',(-197.913954223844,-0.154313982210954,
135.722081839163));
#242663=CARTESIAN_POINT('Ctrl Pts',(-197.921728557963,-0.0175760168504587,
135.724481939496));
#242664=CARTESIAN_POINT('Ctrl Pts',(-197.929502892082,0.119203659386324,
135.721165835397));
#242665=CARTESIAN_POINT('Ctrl Pts',(-197.937267645029,0.255814766896124,
135.7178538181));
#242666=CARTESIAN_POINT('Ctrl Pts',(-197.945032397976,0.392467095903496,
135.708839622631));
#242667=CARTESIAN_POINT('Ctrl Pts',(-197.952797150924,0.528646789015383,
135.694116811382));
#242668=CARTESIAN_POINT('Ctrl Pts',(-197.960554191809,0.664691226536644,
135.679408623037));
#242669=CARTESIAN_POINT('Ctrl Pts',(-197.968311232694,0.800263576161697,
135.659003143977));
#242670=CARTESIAN_POINT('Ctrl Pts',(-197.976068273579,0.93485113602674,
135.632945960704));
#242671=CARTESIAN_POINT('Ctrl Pts',(-197.983819464819,1.0693372023654,135.606908427356));
#242672=CARTESIAN_POINT('Ctrl Pts',(-197.991570656059,1.20283957483479,
135.575227747049));
#242673=CARTESIAN_POINT('Ctrl Pts',(-197.999321847299,1.33485218089917,
135.538001152889));
#242674=CARTESIAN_POINT('Ctrl Pts',(-198.007069744076,1.46680867808496,
135.500790381023));
#242675=CARTESIAN_POINT('Ctrl Pts',(-198.014817640853,1.59727629273097,
135.458038489407));
#242676=CARTESIAN_POINT('Ctrl Pts',(-198.02256553763,1.72576085053872,135.409893436822));
#242677=CARTESIAN_POINT('Ctrl Pts',(-198.030311813714,1.85421853214679,
135.361758455145));
#242678=CARTESIAN_POINT('Ctrl Pts',(-198.038058089798,1.98069361612735,
135.308232693516));
#242679=CARTESIAN_POINT('Ctrl Pts',(-198.045804365883,2.1047091378518,135.249513315454));
#242680=CARTESIAN_POINT('Ctrl Pts',(-198.053550699148,2.22872557503048,
135.19079350394));
#242681=CARTESIAN_POINT('Ctrl Pts',(-198.061297032413,2.35028206036682,
135.126880166801));
#242682=CARTESIAN_POINT('Ctrl Pts',(-198.069043365679,2.46892395336895,
135.058017582459));
#242683=CARTESIAN_POINT('Ctrl Pts',(-198.076791433682,2.58759241540058,
134.989139576819));
#242684=CARTESIAN_POINT('Ctrl Pts',(-198.084539501685,2.70334464822494,
134.915310314712));
#242685=CARTESIAN_POINT('Ctrl Pts',(-198.092287569688,2.8157531924012,134.836818555596));
#242686=CARTESIAN_POINT('Ctrl Pts',(-198.10004387243,2.92828120571605,134.758243374504));
#242687=CARTESIAN_POINT('Ctrl Pts',(-198.107800175171,3.03745811039781,
134.674996021732));
#242688=CARTESIAN_POINT('Ctrl Pts',(-198.115556477913,3.14288744086359,
134.587407220049));
#242689=CARTESIAN_POINT('Ctrl Pts',(-198.123316920427,3.24837304213745,
134.499771669587));
#242690=CARTESIAN_POINT('Ctrl Pts',(-198.131077362942,3.35010679377825,
134.407790315149));
#242691=CARTESIAN_POINT('Ctrl Pts',(-198.138837805456,3.44772834555247,
134.311831546565));
#242692=CARTESIAN_POINT('Ctrl Pts',(-198.146610705722,3.54550660810803,
134.215718736448));
#242693=CARTESIAN_POINT('Ctrl Pts',(-198.154383605987,3.6391592121027,134.115616038787));
#242694=CARTESIAN_POINT('Ctrl Pts',(-198.162156506252,3.7283648444739,134.011926462407));
#242695=CARTESIAN_POINT('Ctrl Pts',(-198.169646842014,3.81432762741104,
133.912006263309));
#242696=CARTESIAN_POINT('Ctrl Pts',(-198.177137177776,3.89616095138074,
133.808755683444));
#242697=CARTESIAN_POINT('Ctrl Pts',(-198.184627513538,3.97361594297526,
133.702559955126));
#242698=CARTESIAN_POINT('Ctrl Pts',(-198.192401847657,4.05400766411971,
133.592337783489));
#242699=CARTESIAN_POINT('Ctrl Pts',(-198.200176181776,4.12993714679204,
133.478593573467));
#242700=CARTESIAN_POINT('Ctrl Pts',(-198.207950515895,4.20107997053173,
133.361724522781));
#242701=CARTESIAN_POINT('Ctrl Pts',(-198.215715268842,4.27213511709918,
133.244999502756));
#242702=CARTESIAN_POINT('Ctrl Pts',(-198.22348002179,4.33841514090281,133.125157635332));
#242703=CARTESIAN_POINT('Ctrl Pts',(-198.231244774737,4.39963687332856,
133.002627763603));
#242704=CARTESIAN_POINT('Ctrl Pts',(-198.239001815622,4.46079779946676,
132.88021959027));
#242705=CARTESIAN_POINT('Ctrl Pts',(-198.246758856507,4.5169102585312,132.755129073059));
#242706=CARTESIAN_POINT('Ctrl Pts',(-198.254515897392,4.56773547585683,
132.627812203186));
#242707=CARTESIAN_POINT('Ctrl Pts',(-198.262267088632,4.61852236549037,
132.500591343955));
#242708=CARTESIAN_POINT('Ctrl Pts',(-198.270018279872,4.66402980520103,
132.371147835464));
#242709=CARTESIAN_POINT('Ctrl Pts',(-198.277769471112,4.70406605538651,
132.239960007737));
#242710=CARTESIAN_POINT('Ctrl Pts',(-198.285517367889,4.74408528909782,
132.108827938336));
#242711=CARTESIAN_POINT('Ctrl Pts',(-198.293265264666,4.77863784444936,
131.975953397409));
#242712=CARTESIAN_POINT('Ctrl Pts',(-198.301013161443,4.80758109007599,
131.841832123124));
#242713=CARTESIAN_POINT('Ctrl Pts',(-198.308759437527,4.83651828139958,
131.707738904118));
#242714=CARTESIAN_POINT('Ctrl Pts',(-198.316505713611,4.8598484144299,131.572399852405));
#242715=CARTESIAN_POINT('Ctrl Pts',(-198.324251989695,4.87747955738707,
131.436322823533));
#242716=CARTESIAN_POINT('Ctrl Pts',(-198.331998322961,4.89511083049331,
131.300244790173));
#242717=CARTESIAN_POINT('Ctrl Pts',(-198.339744656226,4.90704297934507,
131.163429156507));
#242718=CARTESIAN_POINT('Ctrl Pts',(-198.347490989491,4.91323577800568,
131.026390462913));
#242719=CARTESIAN_POINT('Ctrl Pts',(-198.355239057494,4.91942996350062,
130.889321080454));
#242720=CARTESIAN_POINT('Ctrl Pts',(-198.362987125497,4.91988222358433,
130.752028929157));
#242721=CARTESIAN_POINT('Ctrl Pts',(-198.3707351935,4.91460444749664,130.615029724296));
#242722=CARTESIAN_POINT('Ctrl Pts',(-198.378491496242,4.9093210621257,130.47788491505));
#242723=CARTESIAN_POINT('Ctrl Pts',(-198.386247798984,4.8982954903254,130.341034065488));
#242724=CARTESIAN_POINT('Ctrl Pts',(-198.394004101726,4.88159167919793,
130.204989497069));
#242725=CARTESIAN_POINT('Ctrl Pts',(-198.40176454424,4.86487895274352,130.068872317568));
#242726=CARTESIAN_POINT('Ctrl Pts',(-198.409524986754,4.84248201195462,
129.93356266222));
#242727=CARTESIAN_POINT('Ctrl Pts',(-198.417285429268,4.8145160155251,129.799562827584));
#242728=CARTESIAN_POINT('Ctrl Pts',(-198.425058329534,4.78650512559541,
129.665347884518));
#242729=CARTESIAN_POINT('Ctrl Pts',(-198.432831229799,4.7529074110492,129.532447343168));
#242730=CARTESIAN_POINT('Ctrl Pts',(-198.440604130065,4.71388825706518,
129.401349369428));
#242731=CARTESIAN_POINT('Ctrl Pts',(-198.448094465827,4.67628754761169,
129.275017137248));
#242732=CARTESIAN_POINT('Ctrl Pts',(-198.455584801589,4.6336528210575,129.150358983697));
#242733=CARTESIAN_POINT('Ctrl Pts',(-198.463075137351,4.58617366210336,
129.027792520495));
#242734=CARTESIAN_POINT('Ctrl Pts',(-198.47084947147,4.53689431640671,128.900578912589));
#242735=CARTESIAN_POINT('Ctrl Pts',(-198.478623805589,4.48223983117683,
128.775215764509));
#242736=CARTESIAN_POINT('Ctrl Pts',(-198.486398139708,4.42236902292319,
128.652190715446));
#242737=CARTESIAN_POINT('Ctrl Pts',(-198.494162892655,4.36257200009024,
128.529317283763));
#242738=CARTESIAN_POINT('Ctrl Pts',(-198.501927645602,4.29757161477436,
128.408776565947));
#242739=CARTESIAN_POINT('Ctrl Pts',(-198.509692398549,4.22757560526325,
128.29103859994));
#242740=CARTESIAN_POINT('Ctrl Pts',(-198.517449439434,4.15764911677518,
128.173417572941));
#242741=CARTESIAN_POINT('Ctrl Pts',(-198.525206480319,4.08273707664526,
128.058594091884));
#242742=CARTESIAN_POINT('Ctrl Pts',(-198.532963521204,4.0030940596596,127.947015519049));
#242743=CARTESIAN_POINT('Ctrl Pts',(-198.540714712445,3.92351110209268,
127.835521088484));
#242744=CARTESIAN_POINT('Ctrl Pts',(-198.548465903685,3.8392044951129,127.727267012445));
#242745=CARTESIAN_POINT('Ctrl Pts',(-198.556217094925,3.7504730313789,127.622673155951));
#242746=CARTESIAN_POINT('Ctrl Pts',(-198.563964991702,3.66177928088409,
127.518123754636));
#242747=CARTESIAN_POINT('Ctrl Pts',(-198.571712888479,3.56866466656006,
127.417231776227));
#242748=CARTESIAN_POINT('Ctrl Pts',(-198.579460785256,3.47146917123165,
127.320385179121));
#242749=CARTESIAN_POINT('Ctrl Pts',(-198.58720706134,3.37429400710557,127.223558840235));
#242750=CARTESIAN_POINT('Ctrl Pts',(-198.594953337424,3.27303993667195,
127.130776475282));
#242751=CARTESIAN_POINT('Ctrl Pts',(-198.602699613508,3.16808454181421,
127.042389937401));
#242752=CARTESIAN_POINT('Ctrl Pts',(-198.610445946774,3.06312837219946,
126.954002747071));
#242753=CARTESIAN_POINT('Ctrl Pts',(-198.618192280039,2.95447112269024,
126.870011700402));
#242754=CARTESIAN_POINT('Ctrl Pts',(-198.625938613304,2.84252394757572,
126.790728762256));
#242755=CARTESIAN_POINT('Ctrl Pts',(-198.633686681307,2.73055170266768,
126.711428069246));
#242756=CARTESIAN_POINT('Ctrl Pts',(-198.64143474931,2.61528838508869,126.636837808705));
#242757=CARTESIAN_POINT('Ctrl Pts',(-198.649182817313,2.49717430712868,
126.567226734584));
#242758=CARTESIAN_POINT('Ctrl Pts',(-198.656939120055,2.37893469612088,
126.497541676984));
#242759=CARTESIAN_POINT('Ctrl Pts',(-198.664695422797,2.2578386096946,126.432846575844));
#242760=CARTESIAN_POINT('Ctrl Pts',(-198.672451725539,2.13435164337421,
126.373364552918));
#242761=CARTESIAN_POINT('Ctrl Pts',(-198.680212168053,2.01079876834144,
126.313850782646));
#242762=CARTESIAN_POINT('Ctrl Pts',(-198.687972610567,1.88485282955681,
126.259555789408));
#242763=CARTESIAN_POINT('Ctrl Pts',(-198.695733053081,1.75699866942774,
126.210654190493));
#242764=CARTESIAN_POINT('Ctrl Pts',(-198.703505953346,1.62893926645082,
126.161674090391));
#242765=CARTESIAN_POINT('Ctrl Pts',(-198.711278853612,1.49896589169275,
126.1181048103));
#242766=CARTESIAN_POINT('Ctrl Pts',(-198.719051753877,1.36757864767384,
126.080071072573));
#242767=CARTESIAN_POINT('Ctrl Pts',(-198.726542089639,1.24096766091596,
126.043419957014));
#242768=CARTESIAN_POINT('Ctrl Pts',(-198.734032425402,1.11304411471436,
126.011908983002));
#242769=CARTESIAN_POINT('Ctrl Pts',(-198.741522761164,0.984261832800122,
125.985604376896));
#242770=CARTESIAN_POINT('Ctrl Pts',(-198.749297095283,0.850596731528147,
125.958302423656));
#242771=CARTESIAN_POINT('Ctrl Pts',(-198.757071429402,0.715583080302673,
125.936522946273));
#242772=CARTESIAN_POINT('Ctrl Pts',(-198.764845763521,0.579716987989611,
125.920395908814));
#242773=CARTESIAN_POINT('Ctrl Pts',(-198.772610516468,0.444018338491886,
125.904288746487));
#242774=CARTESIAN_POINT('Ctrl Pts',(-198.780375269415,0.307469722715481,
125.89382020921));
#242775=CARTESIAN_POINT('Ctrl Pts',(-198.788140022362,0.170578884512039,
125.889069587865));
#242776=CARTESIAN_POINT('Ctrl Pts',(-198.795897063247,0.0338240082189226,
125.884323684905));
#242777=CARTESIAN_POINT('Ctrl Pts',(-198.803654104132,-0.103272025883022,
125.885284409655));
#242778=CARTESIAN_POINT('Ctrl Pts',(-198.811411145017,-0.240195235348314,
125.891979391377));
#242779=CARTESIAN_POINT('Ctrl Pts',(-198.819162336258,-0.377015189955682,
125.898669324361));
#242780=CARTESIAN_POINT('Ctrl Pts',(-198.826913527498,-0.513662190418549,
125.911084888148));
#242781=CARTESIAN_POINT('Ctrl Pts',(-198.834664718738,-0.649621487673782,
125.929201647312));
#242782=CARTESIAN_POINT('Ctrl Pts',(-198.842412615515,-0.785522998601034,
125.947310706369));
#242783=CARTESIAN_POINT('Ctrl Pts',(-198.850160512292,-0.920737000939123,
125.971116089789));
#242784=CARTESIAN_POINT('Ctrl Pts',(-198.857908409069,-1.05475332528018,
126.000541461383));
#242785=CARTESIAN_POINT('Ctrl Pts',(-198.865654685153,-1.18874161629487,
126.029960677823));
#242786=CARTESIAN_POINT('Ctrl Pts',(-198.873400961237,-1.32153234600044,
126.064997460351));
#242787=CARTESIAN_POINT('Ctrl Pts',(-198.881147237321,-1.45262539815508,
126.105524323851));
#242788=CARTESIAN_POINT('Ctrl Pts',(-198.888893570586,-1.58371941800903,
126.14605148651));
#242789=CARTESIAN_POINT('Ctrl Pts',(-198.896639903852,-1.71311536178222,
126.192068695536));
#242790=CARTESIAN_POINT('Ctrl Pts',(-198.904386237117,-1.84032852566538,
126.243398659807));
#242791=CARTESIAN_POINT('Ctrl Pts',(-198.91213430512,-1.96757017805508,
126.294740119068));
#242792=CARTESIAN_POINT('Ctrl Pts',(-198.919882373123,-2.09262771536865,
126.351396554784));
#242793=CARTESIAN_POINT('Ctrl Pts',(-198.927630441126,-2.2150370277501,
126.413142787829));
#242794=CARTESIAN_POINT('Ctrl Pts',(-198.935386743868,-2.33757643820495,
126.474954645506));
#242795=CARTESIAN_POINT('Ctrl Pts',(-198.94314304661,-2.4574616517044,126.541866930204));
#242796=CARTESIAN_POINT('Ctrl Pts',(-198.950899349351,-2.57425328384323,
126.613608525981));
#242797=CARTESIAN_POINT('Ctrl Pts',(-198.958659791866,-2.69110725119298,
126.685388412409));
#242798=CARTESIAN_POINT('Ctrl Pts',(-198.96642023438,-2.80486402303167,
126.762002527609));
#242799=CARTESIAN_POINT('Ctrl Pts',(-198.974180676894,-2.91511461972486,
126.843137344842));
#242800=CARTESIAN_POINT('Ctrl Pts',(-198.981953577159,-3.02554220046346,
126.924402406887));
#242801=CARTESIAN_POINT('Ctrl Pts',(-198.989726477425,-3.13245205358369,
127.010202427981));
#242802=CARTESIAN_POINT('Ctrl Pts',(-198.99749937769,-3.23546892900845,
127.100184073188));
#242803=CARTESIAN_POINT('Ctrl Pts',(-199.004989713452,-3.33474088152516,
127.186894658939));
#242804=CARTESIAN_POINT('Ctrl Pts',(-199.012480049214,-3.43039775782205,
127.277487910186));
#242805=CARTESIAN_POINT('Ctrl Pts',(-199.019970384976,-3.52213853697615,
127.371617809133));
#242806=CARTESIAN_POINT('Ctrl Pts',(-199.027641276347,-3.6160907406696,
127.468016722693));
#242807=CARTESIAN_POINT('Ctrl Pts',(-199.035312167719,-3.70625045185473,
127.568448295507));
#242808=CARTESIAN_POINT('Ctrl Pts',(-199.04298305909,-3.79224452810265,
127.672577658679));
#242809=CARTESIAN_POINT('Ctrl Pts',(-199.0506449325,-3.87813750901698,127.776584606526));
#242810=CARTESIAN_POINT('Ctrl Pts',(-199.058306805909,-3.9598743377894,
127.884280395336));
#242811=CARTESIAN_POINT('Ctrl Pts',(-199.065968679319,-4.03711767976908,
127.995292462075));
#242812=CARTESIAN_POINT('Ctrl Pts',(-199.073623311162,-4.11428801574521,
128.106199606536));
#242813=CARTESIAN_POINT('Ctrl Pts',(-199.081277943005,-4.1869730825278,
128.220416467907));
#242814=CARTESIAN_POINT('Ctrl Pts',(-199.088932574849,-4.25487528640376,
128.337536878494));
#242815=CARTESIAN_POINT('Ctrl Pts',(-199.096581319393,-4.32272526561704,
128.454567209913));
#242816=CARTESIAN_POINT('Ctrl Pts',(-199.104230063938,-4.38579950174855,
128.574496299718));
#242817=CARTESIAN_POINT('Ctrl Pts',(-199.111878808483,-4.44384363448245,
128.696888953517));
#242818=CARTESIAN_POINT('Ctrl Pts',(-199.119524183703,-4.50186219837772,
128.819227692512));
#242819=CARTESIAN_POINT('Ctrl Pts',(-199.127169558923,-4.55485489515574,
128.944027473816));
#242820=CARTESIAN_POINT('Ctrl Pts',(-199.134814934143,-4.60261344758878,
129.070828813827));
#242821=CARTESIAN_POINT('Ctrl Pts',(-199.142459303634,-4.65036571750983,
129.197613473455));
#242822=CARTESIAN_POINT('Ctrl Pts',(-199.150103673125,-4.69288506876711,
129.32639879276));
#242823=CARTESIAN_POINT('Ctrl Pts',(-199.157748042617,-4.73001164933185,
129.456706040278));
#242824=CARTESIAN_POINT('Ctrl Pts',(-199.160198861551,-4.74191459655825,
129.498483124697));
#242825=CARTESIAN_POINT('Ctrl Pts',(-199.162649680486,-4.75326361641396,
129.540416517897));
#242826=CARTESIAN_POINT('Ctrl Pts',(-199.165100499421,-4.76405452823391,
129.582490119308));
#242827=CARTESIAN_POINT('',(-197.13985943604,-4.91824821858491,130.800174582878));
#242828=CARTESIAN_POINT('Ctrl Pts',(-197.13985943604,-4.91824821858491,
130.800174582878));
#242829=CARTESIAN_POINT('Ctrl Pts',(-197.147506112978,-4.91836287925791,
130.93489149106));
#242830=CARTESIAN_POINT('Ctrl Pts',(-197.155152789915,-4.91293828803124,
131.069802457209));
#242831=CARTESIAN_POINT('Ctrl Pts',(-197.162799466852,-4.9019533167259,
131.204406543854));
#242832=CARTESIAN_POINT('Ctrl Pts',(-197.170439161222,-4.89097837635308,
131.338887716705));
#242833=CARTESIAN_POINT('Ctrl Pts',(-197.178078855592,-4.87445318757935,
131.473062167562));
#242834=CARTESIAN_POINT('Ctrl Pts',(-197.185718549962,-4.85240867394315,
131.606428646814));
#242835=CARTESIAN_POINT('Ctrl Pts',(-197.193353528545,-4.83037776781788,
131.73971280237));
#242836=CARTESIAN_POINT('Ctrl Pts',(-197.200988507129,-4.80283437820965,
131.872189581299));
#242837=CARTESIAN_POINT('Ctrl Pts',(-197.208623485712,-4.76986124614636,
132.003363017485));
#242838=CARTESIAN_POINT('Ctrl Pts',(-197.216256000669,-4.73689875372977,
132.134494127118));
#242839=CARTESIAN_POINT('Ctrl Pts',(-197.223888515626,-4.69851009985092,
132.264322339006));
#242840=CARTESIAN_POINT('Ctrl Pts',(-197.231521030583,-4.6548290030468,
132.392362511423));
#242841=CARTESIAN_POINT('Ctrl Pts',(-197.239152849597,-4.61115188914653,
132.520391008958));
#242842=CARTESIAN_POINT('Ctrl Pts',(-197.24678466861,-4.56218342217936,
132.646631409198));
#242843=CARTESIAN_POINT('Ctrl Pts',(-197.254416487624,-4.50810682560393,
132.770614902099));
#242844=CARTESIAN_POINT('Ctrl Pts',(-197.262049377602,-4.45402264051946,
132.894615793466));
#242845=CARTESIAN_POINT('Ctrl Pts',(-197.26968226758,-4.39482906232151,
133.016358777953));
#242846=CARTESIAN_POINT('Ctrl Pts',(-197.277315157558,-4.33075673716147,
133.135396684647));
#242847=CARTESIAN_POINT('Ctrl Pts',(-197.284955576458,-4.26662121241328,
133.254552007817));
#242848=CARTESIAN_POINT('Ctrl Pts',(-197.292595995358,-4.19759752046628,
133.37099656774));
#242849=CARTESIAN_POINT('Ctrl Pts',(-197.300236414258,-4.1239615861599,
133.484309105574));
#242850=CARTESIAN_POINT('Ctrl Pts',(-197.307880546064,-4.05028986803414,
133.597676708309));
#242851=CARTESIAN_POINT('Ctrl Pts',(-197.315524677871,-3.97200167824627,
133.707908929455));
#242852=CARTESIAN_POINT('Ctrl Pts',(-197.323168809677,-3.88941447193958,
133.814616109707));
#242853=CARTESIAN_POINT('Ctrl Pts',(-197.330825110679,-3.8066957896451,
133.921493164115));
#242854=CARTESIAN_POINT('Ctrl Pts',(-197.33848141168,-3.71966467800465,
134.024833657621));
#242855=CARTESIAN_POINT('Ctrl Pts',(-197.346137712681,-3.62867730838004,
134.124282913968));
#242856=CARTESIAN_POINT('Ctrl Pts',(-197.35371635454,-3.53861283886426,
134.222723439874));
#242857=CARTESIAN_POINT('Ctrl Pts',(-197.3612949964,-3.44467233174058,134.317351104802));
#242858=CARTESIAN_POINT('Ctrl Pts',(-197.368873638259,-3.34723265001436,
134.407861227969));
#242859=CARTESIAN_POINT('Ctrl Pts',(-197.376647972378,-3.24727692493325,
134.500708462567));
#242860=CARTESIAN_POINT('Ctrl Pts',(-197.384422306497,-3.14329678401998,
134.589540674901));
#242861=CARTESIAN_POINT('Ctrl Pts',(-197.392196640617,-3.03564832798573,
134.673988802715));
#242862=CARTESIAN_POINT('Ctrl Pts',(-197.399961393564,-2.92813253905301,
134.758332855758));
#242863=CARTESIAN_POINT('Ctrl Pts',(-197.407726146511,-2.81695773483861,
134.83830333563));
#242864=CARTESIAN_POINT('Ctrl Pts',(-197.415490899458,-2.70251631213269,
134.91356840559));
#242865=CARTESIAN_POINT('Ctrl Pts',(-197.423247940343,-2.58818855426113,
134.988758721222));
#242866=CARTESIAN_POINT('Ctrl Pts',(-197.431004981228,-2.47060095904148,
135.059252713936));
#242867=CARTESIAN_POINT('Ctrl Pts',(-197.438762022113,-2.35017812468133,
135.124759423784));
#242868=CARTESIAN_POINT('Ctrl Pts',(-197.446513213353,-2.22984610211716,
135.190216734512));
#242869=CARTESIAN_POINT('Ctrl Pts',(-197.454264404593,-2.1066834381736,
135.250694062248));
#242870=CARTESIAN_POINT('Ctrl Pts',(-197.462015595833,-1.98114246876202,
135.305944514481));
#242871=CARTESIAN_POINT('Ctrl Pts',(-197.46976349261,-1.85565485761151,
135.361171483799));
#242872=CARTESIAN_POINT('Ctrl Pts',(-197.477511389387,-1.72779130857727,
135.411175838973));
#242873=CARTESIAN_POINT('Ctrl Pts',(-197.485259286164,-1.59802724398115,
135.455757395954));
#242874=CARTESIAN_POINT('Ctrl Pts',(-197.493005562248,-1.46829032322996,
135.500329627433));
#242875=CARTESIAN_POINT('Ctrl Pts',(-197.500751838333,-1.33665404717749,
135.539481190017));
#242876=CARTESIAN_POINT('Ctrl Pts',(-197.508498114417,-1.20361185877549,
135.573060813208));
#242877=CARTESIAN_POINT('Ctrl Pts',(-197.516244447682,-1.0705686882861,
135.606640684276));
#242878=CARTESIAN_POINT('Ctrl Pts',(-197.523990780947,-0.936119963815441,
135.634648438198));
#242879=CARTESIAN_POINT('Ctrl Pts',(-197.531737114213,-0.800771873265166,
135.656983358877));
#242880=CARTESIAN_POINT('Ctrl Pts',(-197.539485182216,-0.665393472448266,
135.679323281307));
#242881=CARTESIAN_POINT('Ctrl Pts',(-197.547233250219,-0.52911569045003,
135.695987778918));
#242882=CARTESIAN_POINT('Ctrl Pts',(-197.554981318222,-0.392452037104296,
135.706927747252));
#242883=CARTESIAN_POINT('Ctrl Pts',(-197.562737620963,-0.255643136002026,
135.717879342714));
#242884=CARTESIAN_POINT('Ctrl Pts',(-197.570493923705,-0.118447934655994,
135.723094224012));
#242885=CARTESIAN_POINT('Ctrl Pts',(-197.578250226447,0.0186172786708312,
135.722575381018));
#242886=CARTESIAN_POINT('Ctrl Pts',(-197.586010668961,0.155755647829336,
135.722056261102));
#242887=CARTESIAN_POINT('Ctrl Pts',(-197.593771111476,0.292763500359275,
135.715797336897));
#242888=CARTESIAN_POINT('Ctrl Pts',(-197.60153155399,0.429128454194537,
135.703853635451));
#242889=CARTESIAN_POINT('Ctrl Pts',(-197.609304454255,0.565712313159607,
135.691890760914));
#242890=CARTESIAN_POINT('Ctrl Pts',(-197.617077354521,0.701650823160877,
135.674224923474));
#242891=CARTESIAN_POINT('Ctrl Pts',(-197.624850254786,0.836439701705548,
135.650962694064));
#242892=CARTESIAN_POINT('Ctrl Pts',(-197.632340590548,0.966328665002057,
135.628546105287));
#242893=CARTESIAN_POINT('Ctrl Pts',(-197.63983092631,1.09514982852237,135.600933010851));
#242894=CARTESIAN_POINT('Ctrl Pts',(-197.647321262072,1.2224661119373,135.568262344897));
#242895=CARTESIAN_POINT('Ctrl Pts',(-197.655095596191,1.35460963093539,
135.534352960713));
#242896=CARTESIAN_POINT('Ctrl Pts',(-197.66286993031,1.48555049305068,135.494887503906));
#242897=CARTESIAN_POINT('Ctrl Pts',(-197.670644264429,1.61478571462178,
135.449966084925));
#242898=CARTESIAN_POINT('Ctrl Pts',(-197.678409017376,1.74386166533168,
135.405100027578));
#242899=CARTESIAN_POINT('Ctrl Pts',(-197.686173770323,1.87123579220267,
135.354791513917));
#242900=CARTESIAN_POINT('Ctrl Pts',(-197.693938523271,1.99641681153709,
135.29919131261));
#242901=CARTESIAN_POINT('Ctrl Pts',(-197.701695564156,2.1214734993187,135.243646334207));
#242902=CARTESIAN_POINT('Ctrl Pts',(-197.70945260504,2.24434105933608,135.182820285069));
#242903=CARTESIAN_POINT('Ctrl Pts',(-197.717209645925,2.36454519304033,
135.116913120733));
#242904=CARTESIAN_POINT('Ctrl Pts',(-197.724960837166,2.4846586798728,135.051055657502));
#242905=CARTESIAN_POINT('Ctrl Pts',(-197.732712028406,2.60211239678094,
134.98012489306));
#242906=CARTESIAN_POINT('Ctrl Pts',(-197.740463219646,2.7164541274949,134.904367938988));
#242907=CARTESIAN_POINT('Ctrl Pts',(-197.748211116423,2.83074725992267,
134.828643183643));
#242908=CARTESIAN_POINT('Ctrl Pts',(-197.7559590132,2.94193071162179,134.748096533953));
#242909=CARTESIAN_POINT('Ctrl Pts',(-197.763706909977,3.04957908470244,
134.663019771812));
#242910=CARTESIAN_POINT('Ctrl Pts',(-197.771453186061,3.15720494006407,
134.577960805895));
#242911=CARTESIAN_POINT('Ctrl Pts',(-197.779199462145,3.26129688109708,
134.488373854626));
#242912=CARTESIAN_POINT('Ctrl Pts',(-197.786945738229,3.361460921679,134.394592300135));
#242913=CARTESIAN_POINT('Ctrl Pts',(-197.794692071495,3.46162570164924,
134.30081005337));
#242914=CARTESIAN_POINT('Ctrl Pts',(-197.80243840476,3.55786223791384,134.20283340881));
#242915=CARTESIAN_POINT('Ctrl Pts',(-197.810184738026,3.64981218824234,
134.101033797161));
#242916=CARTESIAN_POINT('Ctrl Pts',(-197.817932806029,3.74178273012479,
133.999211388194));
#242917=CARTESIAN_POINT('Ctrl Pts',(-197.825680874032,3.82946451386792,
133.893564598623));
#242918=CARTESIAN_POINT('Ctrl Pts',(-197.833428942035,3.91253866189194,
133.784498916656));
#242919=CARTESIAN_POINT('Ctrl Pts',(-197.841185244776,3.99570110210896,
133.675317318384));
#242920=CARTESIAN_POINT('Ctrl Pts',(-197.848941547518,4.07424588694472,
133.562709880643));
#242921=CARTESIAN_POINT('Ctrl Pts',(-197.85669785026,4.14789646544683,133.44711258747));
#242922=CARTESIAN_POINT('Ctrl Pts',(-197.864458292774,4.22158635348026,
133.331453596542));
#242923=CARTESIAN_POINT('Ctrl Pts',(-197.872218735289,4.29037663418042,
133.212801908529));
#242924=CARTESIAN_POINT('Ctrl Pts',(-197.879979177803,4.35403664833725,
133.091618348439));
#242925=CARTESIAN_POINT('Ctrl Pts',(-197.887752078068,4.41779885520026,
132.970240253739));
#242926=CARTESIAN_POINT('Ctrl Pts',(-197.895524978334,4.4764141709775,132.846322518647));
#242927=CARTESIAN_POINT('Ctrl Pts',(-197.903297878599,4.52969967980894,
132.720347014501));
#242928=CARTESIAN_POINT('Ctrl Pts',(-197.910788214361,4.58104812617597,
132.598951037243));
#242929=CARTESIAN_POINT('Ctrl Pts',(-197.918278550123,4.62744743329827,
132.475644591939));
#242930=CARTESIAN_POINT('Ctrl Pts',(-197.925768885885,4.66877823780837,
132.350870503945));
#242931=CARTESIAN_POINT('Ctrl Pts',(-197.933543220004,4.71167611233399,
132.221365568478));
#242932=CARTESIAN_POINT('Ctrl Pts',(-197.941317554123,4.74924944018407,
132.089869269341));
#242933=CARTESIAN_POINT('Ctrl Pts',(-197.949091888242,4.78131057215974,
131.956858893076));
#242934=CARTESIAN_POINT('Ctrl Pts',(-197.956856641189,4.81333219165545,
131.824012440213));
#242935=CARTESIAN_POINT('Ctrl Pts',(-197.964621394136,4.83985504116094,
131.689655999366));
#242936=CARTESIAN_POINT('Ctrl Pts',(-197.972386147084,4.86074041578861,
131.554284395572));
#242937=CARTESIAN_POINT('Ctrl Pts',(-197.980143187969,4.88160504676788,
131.419047244763));
#242938=CARTESIAN_POINT('Ctrl Pts',(-197.987900228854,4.89684328634105,
131.282797321412));
#242939=CARTESIAN_POINT('Ctrl Pts',(-197.995657269739,4.90636699281359,
131.146041747173));
#242940=CARTESIAN_POINT('Ctrl Pts',(-198.003408460979,4.91588351738501,
131.009389301376));
#242941=CARTESIAN_POINT('Ctrl Pts',(-198.011159652219,4.91969405935185,
130.872232352118));
#242942=CARTESIAN_POINT('Ctrl Pts',(-198.018910843459,4.91776208674575,
130.7350849316));
#242943=CARTESIAN_POINT('Ctrl Pts',(-198.026658740236,4.91583093527955,
130.597995802394));
#242944=CARTESIAN_POINT('Ctrl Pts',(-198.034406637013,4.90816212914558,
130.460916583982));
#242945=CARTESIAN_POINT('Ctrl Pts',(-198.04215453379,4.89477121476498,130.324362890896));
#242946=CARTESIAN_POINT('Ctrl Pts',(-198.049900809875,4.881383101475,130.187837761899));
#242947=CARTESIAN_POINT('Ctrl Pts',(-198.057647085959,4.86227529885319,
130.051838328427));
#242948=CARTESIAN_POINT('Ctrl Pts',(-198.065393362043,4.83751533160561,
129.916876263349));
#242949=CARTESIAN_POINT('Ctrl Pts',(-198.073139695308,4.81275518158554,
129.78191320201));
#242950=CARTESIAN_POINT('Ctrl Pts',(-198.080886028573,4.78234285423304,
129.647987908893));
#242951=CARTESIAN_POINT('Ctrl Pts',(-198.088632361839,4.74639715199262,
129.515602634834));
#242952=CARTESIAN_POINT('Ctrl Pts',(-198.096380429842,4.71044339996136,
129.38318771401));
#242953=CARTESIAN_POINT('Ctrl Pts',(-198.104128497845,4.66895390968266,
129.25231387574));
#242954=CARTESIAN_POINT('Ctrl Pts',(-198.111876565848,4.62209746874859,
129.123468577045));
#242955=CARTESIAN_POINT('Ctrl Pts',(-198.11963286859,4.57519122823157,128.994486340033));
#242956=CARTESIAN_POINT('Ctrl Pts',(-198.127389171331,4.52290677641864,
128.867537317358));
#242957=CARTESIAN_POINT('Ctrl Pts',(-198.135145474073,4.46546143648297,
128.743089839191));
#242958=CARTESIAN_POINT('Ctrl Pts',(-198.142905916588,4.40798543623973,
128.618575939658));
#242959=CARTESIAN_POINT('Ctrl Pts',(-198.150666359102,4.34534323773866,
128.496566592663));
#242960=CARTESIAN_POINT('Ctrl Pts',(-198.158426801616,4.27779786917148,
128.377504945506));
#242961=CARTESIAN_POINT('Ctrl Pts',(-198.166199701881,4.21014407078227,
128.258252170022));
#242962=CARTESIAN_POINT('Ctrl Pts',(-198.173972602147,4.13757158065354,
128.141956882111));
#242963=CARTESIAN_POINT('Ctrl Pts',(-198.181745502412,4.06038694029745,
128.029033437293));
#242964=CARTESIAN_POINT('Ctrl Pts',(-198.189235838174,3.98600815603532,
127.920215044132));
#242965=CARTESIAN_POINT('Ctrl Pts',(-198.196726173936,3.90734691024696,
127.81452784734));
#242966=CARTESIAN_POINT('Ctrl Pts',(-198.204216509698,3.8247112456301,127.712311628619));
#242967=CARTESIAN_POINT('Ctrl Pts',(-198.211990843817,3.73894242467187,
127.606219850896));
#242968=CARTESIAN_POINT('Ctrl Pts',(-198.219765177936,3.64862016552164,
127.503531384384));
#242969=CARTESIAN_POINT('Ctrl Pts',(-198.227539512055,3.55404459388961,
127.404662088704));
#242970=CARTESIAN_POINT('Ctrl Pts',(-198.235304265002,3.45958557819766,
127.305914640596));
#242971=CARTESIAN_POINT('Ctrl Pts',(-198.24306901795,3.36088394735533,127.210977278024));
#242972=CARTESIAN_POINT('Ctrl Pts',(-198.250833770897,3.25828103830071,
127.12023416236));
#242973=CARTESIAN_POINT('Ctrl Pts',(-198.258590811782,3.15578003590126,
127.029581174037));
#242974=CARTESIAN_POINT('Ctrl Pts',(-198.266347852667,3.04938575729155,
126.943114399854));
#242975=CARTESIAN_POINT('Ctrl Pts',(-198.274104893552,2.93947721554274,
126.861182107556));
#242976=CARTESIAN_POINT('Ctrl Pts',(-198.281856084792,2.82965155668068,
126.779311601038));
#242977=CARTESIAN_POINT('Ctrl Pts',(-198.289607276032,2.71631722179468,
126.701969002842));
#242978=CARTESIAN_POINT('Ctrl Pts',(-198.297358467272,2.59988693431213,
126.629462895311));
#242979=CARTESIAN_POINT('Ctrl Pts',(-198.305106364049,2.48350613280748,
126.556987604809));
#242980=CARTESIAN_POINT('Ctrl Pts',(-198.312854260826,2.36403232703562,
126.489344922703));
#242981=CARTESIAN_POINT('Ctrl Pts',(-198.320602157603,2.24190772132709,
126.4268004716));
#242982=CARTESIAN_POINT('Ctrl Pts',(-198.328348433687,2.11980866145337,
126.364269103447));
#242983=CARTESIAN_POINT('Ctrl Pts',(-198.336094709771,1.99506025231821,
126.306834023191));
#242984=CARTESIAN_POINT('Ctrl Pts',(-198.343840985855,1.8681294775501,126.254714992069));
#242985=CARTESIAN_POINT('Ctrl Pts',(-198.351587319121,1.74119776580766,
126.202595576215));
#242986=CARTESIAN_POINT('Ctrl Pts',(-198.359333652386,1.61208401795031,
126.155792436301));
#242987=CARTESIAN_POINT('Ctrl Pts',(-198.367079985652,1.48127500745482,
126.114477099312));
#242988=CARTESIAN_POINT('Ctrl Pts',(-198.374828053655,1.35043670318858,
126.07315251004));
#242989=CARTESIAN_POINT('Ctrl Pts',(-198.382576121657,1.21790275358034,
126.037318286899));
#242990=CARTESIAN_POINT('Ctrl Pts',(-198.39032418966,1.08417450384265,126.007095906534));
#242991=CARTESIAN_POINT('Ctrl Pts',(-198.398080492402,0.950304126129575,
125.976841405463));
#242992=CARTESIAN_POINT('Ctrl Pts',(-198.405836795144,0.81523729464666,
125.952210747888));
#242993=CARTESIAN_POINT('Ctrl Pts',(-198.413593097886,0.679485497313303,
125.933274237564));
#242994=CARTESIAN_POINT('Ctrl Pts',(-198.4213535404,0.543661245157932,125.914327620255));
#242995=CARTESIAN_POINT('Ctrl Pts',(-198.429113982914,0.407151687636302,
125.901081243678));
#242996=CARTESIAN_POINT('Ctrl Pts',(-198.436874425429,0.270471830283358,
125.893553346707));
#242997=CARTESIAN_POINT('Ctrl Pts',(-198.444647325694,0.133572562289896,
125.886013365287));
#242998=CARTESIAN_POINT('Ctrl Pts',(-198.45242022596,-0.00349716067967948,
125.884210212806));
#242999=CARTESIAN_POINT('Ctrl Pts',(-198.460193126225,-0.140223036415281,
125.888109956487));
#243000=CARTESIAN_POINT('Ctrl Pts',(-198.467683461987,-0.271978582175825,
125.891867934663));
#243001=CARTESIAN_POINT('Ctrl Pts',(-198.475173797749,-0.403414538811383,
125.900921357127));
#243002=CARTESIAN_POINT('Ctrl Pts',(-198.482664133511,-0.534078533749533,
125.915194719144));
#243003=CARTESIAN_POINT('Ctrl Pts',(-198.49043846763,-0.669696693770792,
125.930009260021));
#243004=CARTESIAN_POINT('Ctrl Pts',(-198.498212801749,-0.804912796249909,
125.950494310249));
#243005=CARTESIAN_POINT('Ctrl Pts',(-198.505987135868,-0.939214741433294,
125.97662214785));
#243006=CARTESIAN_POINT('Ctrl Pts',(-198.513751888815,-1.07335117147142,
126.002717785227));
#243007=CARTESIAN_POINT('Ctrl Pts',(-198.521516641762,-1.20657530576016,
126.034442299186));
#243008=CARTESIAN_POINT('Ctrl Pts',(-198.529281394709,-1.33837943750662,
126.071716161899));
#243009=CARTESIAN_POINT('Ctrl Pts',(-198.537038435594,-1.47005265953166,
126.108953003685));
#243010=CARTESIAN_POINT('Ctrl Pts',(-198.544795476479,-1.60030831193102,
126.151728120008));
#243011=CARTESIAN_POINT('Ctrl Pts',(-198.552552517364,-1.72864852136443,
126.199910883658));
#243012=CARTESIAN_POINT('Ctrl Pts',(-198.560303708605,-1.85689194844843,
126.248057312312));
#243013=CARTESIAN_POINT('Ctrl Pts',(-198.568054899845,-1.9832224431181,
126.301603134525));
#243014=CARTESIAN_POINT('Ctrl Pts',(-198.575806091085,-2.10715729921745,
126.36036791068));
#243015=CARTESIAN_POINT('Ctrl Pts',(-198.583553987862,-2.23103947969604,
126.419107710238));
#243016=CARTESIAN_POINT('Ctrl Pts',(-198.591301884639,-2.3525276942214,
126.483061884765));
#243017=CARTESIAN_POINT('Ctrl Pts',(-198.599049781416,-2.47115944473042,
126.552001970742));
#243018=CARTESIAN_POINT('Ctrl Pts',(-198.6067960575,-2.58976638003497,126.620927635939));
#243019=CARTESIAN_POINT('Ctrl Pts',(-198.614542333584,-2.70551770198718,
126.694836941795));
#243020=CARTESIAN_POINT('Ctrl Pts',(-198.622288609669,-2.81797610317734,
126.773455788074));
#243021=CARTESIAN_POINT('Ctrl Pts',(-198.630034942934,-2.93043533450971,
126.852075214699));
#243022=CARTESIAN_POINT('Ctrl Pts',(-198.637781276199,-3.03960127614829,
126.93540402711));
#243023=CARTESIAN_POINT('Ctrl Pts',(-198.645527609465,-3.14506650462893,
127.023125403517));
#243024=CARTESIAN_POINT('Ctrl Pts',(-198.653275677468,-3.25055535131611,
127.110866424519));
#243025=CARTESIAN_POINT('Ctrl Pts',(-198.661023745471,-3.35234153520745,
127.203001716974));
#243026=CARTESIAN_POINT('Ctrl Pts',(-198.668771813474,-3.4500518652282,
127.299175146049));
#243027=CARTESIAN_POINT('Ctrl Pts',(-198.676528116215,-3.54786604295059,
127.395450789389));
#243028=CARTESIAN_POINT('Ctrl Pts',(-198.684284418957,-3.64159543435231,
127.49577286795));
#243029=CARTESIAN_POINT('Ctrl Pts',(-198.692040721699,-3.73090441917804,
127.599749053358));
#243030=CARTESIAN_POINT('Ctrl Pts',(-198.699801164213,-3.82026107089802,
127.703780733986));
#243031=CARTESIAN_POINT('Ctrl Pts',(-198.707561606727,-3.90519237294011,
127.81147010078));
#243032=CARTESIAN_POINT('Ctrl Pts',(-198.715322049242,-3.98540460735336,
127.922393723553));
#243033=CARTESIAN_POINT('Ctrl Pts',(-198.723094949507,-4.06574560556619,
128.033495410773));
#243034=CARTESIAN_POINT('Ctrl Pts',(-198.730867849773,-4.14135218219585,
128.147841402763));
#243035=CARTESIAN_POINT('Ctrl Pts',(-198.738640750038,-4.21197489294038,
128.264980661014));
#243036=CARTESIAN_POINT('Ctrl Pts',(-198.7461310858,-4.28003029026089,128.37786161217));
#243037=CARTESIAN_POINT('Ctrl Pts',(-198.753621421562,-4.34345773459829,
128.493336000931));
#243038=CARTESIAN_POINT('Ctrl Pts',(-198.761111757324,-4.40207623179987,
128.610982421285));
#243039=CARTESIAN_POINT('Ctrl Pts',(-198.769439516326,-4.46724830596083,
128.741781769581));
#243040=CARTESIAN_POINT('Ctrl Pts',(-198.777767275329,-4.52666005472299,
128.87563467257));
#243041=CARTESIAN_POINT('Ctrl Pts',(-198.786095034331,-4.58003551060785,
129.012027561443));
#243042=CARTESIAN_POINT('Ctrl Pts',(-198.794402369264,-4.63328006164643,
129.148085942819));
#243043=CARTESIAN_POINT('Ctrl Pts',(-198.802709704197,-4.6805177289175,
129.2866716051));
#243044=CARTESIAN_POINT('Ctrl Pts',(-198.811017039129,-4.72151946632294,
129.427248787817));
#243045=CARTESIAN_POINT('Ctrl Pts',(-198.814059766598,-4.73653717220337,
129.478737990889));
#243046=CARTESIAN_POINT('Ctrl Pts',(-198.817102494067,-4.75071875239664,
129.530494131717));
#243047=CARTESIAN_POINT('Ctrl Pts',(-198.820145221536,-4.76405452823399,
129.582490119308));
#243048=CARTESIAN_POINT('Ctrl Pts',(-197.069830899744,-4.76405452823391,
129.582490119308));
#243049=CARTESIAN_POINT('Ctrl Pts',(-197.076695937978,-4.79406056862158,
129.699483215374));
#243050=CARTESIAN_POINT('Ctrl Pts',(-197.083560976212,-4.81971881788819,
129.817443076));
#243051=CARTESIAN_POINT('Ctrl Pts',(-197.090426014446,-4.84098812800867,
129.936019090873));
#243052=CARTESIAN_POINT('Ctrl Pts',(-197.102330337474,-4.87787018599897,
130.14163588954));
#243053=CARTESIAN_POINT('Ctrl Pts',(-197.114234660503,-4.90165998726396,
130.349666738386));
#243054=CARTESIAN_POINT('Ctrl Pts',(-197.126138983531,-4.91211451822462,
130.558771484364));
#243055=CARTESIAN_POINT('Ctrl Pts',(-197.130712467685,-4.91613101135752,
130.639106774339));
#243056=CARTESIAN_POINT('Ctrl Pts',(-197.13528595184,-4.91817963992249,
130.719600281634));
#243057=CARTESIAN_POINT('Ctrl Pts',(-197.139859435995,-4.91824821858423,
130.80017458208));
#243058=CARTESIAN_POINT('Origin',(213.235140564004,0.,130.804360617566));
#243059=CARTESIAN_POINT('',(-195.319719904489,-4.76405452823413,129.582490119309));
#243060=CARTESIAN_POINT('',(-195.665141276266,-4.76405452823396,129.582490119308));
#243061=CARTESIAN_POINT('',(213.235140564004,-4.76405452823405,129.582490119308));
#243062=CARTESIAN_POINT('',(-195.735140564062,-4.91824801533315,130.799942227414));
#243063=CARTESIAN_POINT('Ctrl Pts',(-195.665141276266,-4.76405452823396,
129.582490119308));
#243064=CARTESIAN_POINT('Ctrl Pts',(-195.669627150585,-4.78364500634694,
129.658873096143));
#243065=CARTESIAN_POINT('Ctrl Pts',(-195.674113024903,-4.80138190659694,
129.735664461695));
#243066=CARTESIAN_POINT('Ctrl Pts',(-195.678598899222,-4.81725278166829,
129.812766597813));
#243067=CARTESIAN_POINT('Ctrl Pts',(-195.689674595893,-4.85643823041579,
130.00313302623));
#243068=CARTESIAN_POINT('Ctrl Pts',(-195.700750292564,-4.88435001913631,
130.195892860283));
#243069=CARTESIAN_POINT('Ctrl Pts',(-195.711825989234,-4.90075931060626,
130.38994386838));
#243070=CARTESIAN_POINT('Ctrl Pts',(-195.71959751416,-4.91227327866349,
130.526104354821));
#243071=CARTESIAN_POINT('Ctrl Pts',(-195.727369039086,-4.91812490136763,
130.662900256424));
#243072=CARTESIAN_POINT('Ctrl Pts',(-195.735140564012,-4.91824801533235,
130.799942226527));
#243073=CARTESIAN_POINT('Ctrl Pts',(-195.735140564062,-4.91824801533315,
130.799942227414));
#243074=CARTESIAN_POINT('Ctrl Pts',(-195.742788954033,-4.91836917860973,
130.934812853151));
#243075=CARTESIAN_POINT('Ctrl Pts',(-195.750437344004,-4.91293844047973,
131.069862221547));
#243076=CARTESIAN_POINT('Ctrl Pts',(-195.758085733975,-4.90193846711678,
131.204588461551));
#243077=CARTESIAN_POINT('Ctrl Pts',(-195.765727802631,-4.89094758511626,
131.339203351733));
#243078=CARTESIAN_POINT('Ctrl Pts',(-195.773369871288,-4.87439665663672,
131.473495244947));
#243079=CARTESIAN_POINT('Ctrl Pts',(-195.781011939945,-4.85232041130353,
131.606962441977));
#243080=CARTESIAN_POINT('Ctrl Pts',(-195.788650174382,-4.83025524218319,
131.740362675125));
#243081=CARTESIAN_POINT('Ctrl Pts',(-195.796288408819,-4.80267033378295,
131.872938638019));
#243082=CARTESIAN_POINT('Ctrl Pts',(-195.803926643255,-4.7696521975637,
132.00419434637));
#243083=CARTESIAN_POINT('Ctrl Pts',(-195.811563004816,-4.73664215730885,
132.13541787115));
#243084=CARTESIAN_POINT('Ctrl Pts',(-195.819199366377,-4.69820163590381,
132.265321394214));
#243085=CARTESIAN_POINT('Ctrl Pts',(-195.826835727938,-4.65446802695667,
132.393420228952));
#243086=CARTESIAN_POINT('Ctrl Pts',(-195.834471981253,-4.6107350379391,
132.521517247872));
#243087=CARTESIAN_POINT('Ctrl Pts',(-195.842108234567,-4.56170924103285,
132.647809247807));
#243088=CARTESIAN_POINT('Ctrl Pts',(-195.849744487881,-4.50757738476626,
132.771828325775));
#243089=CARTESIAN_POINT('Ctrl Pts',(-195.857382397285,-4.4534337888199,
132.895874299998));
#243090=CARTESIAN_POINT('Ctrl Pts',(-195.865020306688,-4.39418209327545,
133.01764600283));
#243091=CARTESIAN_POINT('Ctrl Pts',(-195.872658216092,-4.33005626833118,
133.136697594846));
#243092=CARTESIAN_POINT('Ctrl Pts',(-195.880303983217,-4.26586447207508,
133.255871664657));
#243093=CARTESIAN_POINT('Ctrl Pts',(-195.887949750342,-4.19678872589688,
133.37231968092));
#243094=CARTESIAN_POINT('Ctrl Pts',(-195.895595517468,-4.12310800759558,
133.485622152777));
#243095=CARTESIAN_POINT('Ctrl Pts',(-195.903245518399,-4.04938648895914,
133.59898736532));
#243096=CARTESIAN_POINT('Ctrl Pts',(-195.91089551933,-3.9710551549251,133.709203237835));
#243097=CARTESIAN_POINT('Ctrl Pts',(-195.918545520261,-3.88843420921999,
133.815882236792));
#243098=CARTESIAN_POINT('Ctrl Pts',(-195.926207035089,-3.8056889120232,
133.922721796641));
#243099=CARTESIAN_POINT('Ctrl Pts',(-195.933868549917,-3.71864137075232,
134.026013545911));
#243100=CARTESIAN_POINT('Ctrl Pts',(-195.941530064745,-3.62765000128713,
134.125405412606));
#243101=CARTESIAN_POINT('Ctrl Pts',(-195.946702217508,-3.56622334173219,
134.192503098836));
#243102=CARTESIAN_POINT('Ctrl Pts',(-195.951874370271,-3.50300009789946,
134.257824245905));
#243103=CARTESIAN_POINT('Ctrl Pts',(-195.957046523035,-3.43809892864949,
134.321271025768));
#243104=CARTESIAN_POINT('Ctrl Pts',(-195.964820857154,-3.34054508645473,
134.416638755225));
#243105=CARTESIAN_POINT('Ctrl Pts',(-195.972595191273,-3.23886568121659,
134.508095467405));
#243106=CARTESIAN_POINT('Ctrl Pts',(-195.980369525392,-3.13340727972664,
134.595263133044));
#243107=CARTESIAN_POINT('Ctrl Pts',(-195.988134278339,-3.02807884629143,
134.682323372325));
#243108=CARTESIAN_POINT('Ctrl Pts',(-195.995899031286,-2.91898098165016,
134.765104835671));
#243109=CARTESIAN_POINT('Ctrl Pts',(-196.003663784233,-2.80649748679672,
134.843265780986));
#243110=CARTESIAN_POINT('Ctrl Pts',(-196.011420825118,-2.69412571213581,
134.921349095749));
#243111=CARTESIAN_POINT('Ctrl Pts',(-196.019177866003,-2.5783753180853,
134.994820803471));
#243112=CARTESIAN_POINT('Ctrl Pts',(-196.026934906888,-2.45966333968881,
135.063379203801));
#243113=CARTESIAN_POINT('Ctrl Pts',(-196.034686098128,-2.34104088291883,
135.131885903706));
#243114=CARTESIAN_POINT('Ctrl Pts',(-196.042437289368,-2.21946162434935,
135.195486476388));
#243115=CARTESIAN_POINT('Ctrl Pts',(-196.050188480608,-2.09537145223453,
135.253922566754));
#243116=CARTESIAN_POINT('Ctrl Pts',(-196.057936377386,-1.9713340217529,
135.312333820223));
#243117=CARTESIAN_POINT('Ctrl Pts',(-196.065684274163,-1.84478815328316,
135.365584790931));
#243118=CARTESIAN_POINT('Ctrl Pts',(-196.07343217094,-1.71620400590661,
135.413463227902));
#243119=CARTESIAN_POINT('Ctrl Pts',(-196.081178447024,-1.58764675556175,
135.461331649737));
#243120=CARTESIAN_POINT('Ctrl Pts',(-196.088924723108,-1.45705244052956,
135.503829636831));
#243121=CARTESIAN_POINT('Ctrl Pts',(-196.096670999192,-1.32491048285849,
135.540793375973));
#243122=CARTESIAN_POINT('Ctrl Pts',(-196.104417332458,-1.19276754974533,
135.577757387973));
#243123=CARTESIAN_POINT('Ctrl Pts',(-196.112163665723,-1.05907732770887,
135.60918696518));
#243124=CARTESIAN_POINT('Ctrl Pts',(-196.119909998988,-0.92434326967486,
135.634968507087));
#243125=CARTESIAN_POINT('Ctrl Pts',(-196.127658066991,-0.789579038882551,
135.660755822592));
#243126=CARTESIAN_POINT('Ctrl Pts',(-196.135406134994,-0.653770890862492,
135.680892512449));
#243127=CARTESIAN_POINT('Ctrl Pts',(-196.143154202997,-0.517430915145343,
135.695316384137));
#243128=CARTESIAN_POINT('Ctrl Pts',(-196.150910505739,-0.380946035680092,
135.709755585687));
#243129=CARTESIAN_POINT('Ctrl Pts',(-196.158666808481,-0.243928588819814,
135.718469799092));
#243130=CARTESIAN_POINT('Ctrl Pts',(-196.166423111223,-0.106894770994205,
135.721448838295));
#243131=CARTESIAN_POINT('Ctrl Pts',(-196.174183553737,0.0302121859059867,
135.724429467501));
#243132=CARTESIAN_POINT('Ctrl Pts',(-196.181943996251,0.167335140487332,
135.721668830999));
#243133=CARTESIAN_POINT('Ctrl Pts',(-196.189704438765,0.303960473328762,
135.713208862639));
#243134=CARTESIAN_POINT('Ctrl Pts',(-196.197477339031,0.440805129283496,
135.704735313586));
#243135=CARTESIAN_POINT('Ctrl Pts',(-196.205250239296,0.577150178099871,
135.690544190408));
#243136=CARTESIAN_POINT('Ctrl Pts',(-196.213023139562,0.712488781964307,
135.670729160748));
#243137=CARTESIAN_POINT('Ctrl Pts',(-196.220513475324,0.842907486683093,
135.651634457327));
#243138=CARTESIAN_POINT('Ctrl Pts',(-196.228003811086,0.972391346940213,
135.627317691741));
#243139=CARTESIAN_POINT('Ctrl Pts',(-196.235494146848,1.10049987933717,
135.597906599204));
#243140=CARTESIAN_POINT('Ctrl Pts',(-196.243268480967,1.23346568567565,
135.567380376155));
#243141=CARTESIAN_POINT('Ctrl Pts',(-196.251042815086,1.3653710100103,135.531269199705));
#243142=CARTESIAN_POINT('Ctrl Pts',(-196.258817149205,1.49571047779856,
135.48966031226));
#243143=CARTESIAN_POINT('Ctrl Pts',(-196.266581902152,1.62588931384153,
135.448102704051));
#243144=CARTESIAN_POINT('Ctrl Pts',(-196.274346655099,1.75450576414976,
135.401060983704));
#243145=CARTESIAN_POINT('Ctrl Pts',(-196.282111408047,1.88106485760708,
135.348673333915));
#243146=CARTESIAN_POINT('Ctrl Pts',(-196.289868448932,2.00749825078861,
135.296337716279));
#243147=CARTESIAN_POINT('Ctrl Pts',(-196.297625489817,2.1318779946668,135.238666884213));
#243148=CARTESIAN_POINT('Ctrl Pts',(-196.305382530702,2.25372484256268,
135.1758486247));
#243149=CARTESIAN_POINT('Ctrl Pts',(-196.313133721942,2.37547980480323,
135.113077736925));
#243150=CARTESIAN_POINT('Ctrl Pts',(-196.320884913182,2.49470532685751,
135.045167326451));
#243151=CARTESIAN_POINT('Ctrl Pts',(-196.328636104422,2.61094303377791,
134.972352884457));
#243152=CARTESIAN_POINT('Ctrl Pts',(-196.336384001199,2.72713133657197,
134.899569390544));
#243153=CARTESIAN_POINT('Ctrl Pts',(-196.344131897976,2.8403340193372,134.82188621783));
#243154=CARTESIAN_POINT('Ctrl Pts',(-196.351879794753,2.95011837684841,
134.739584197629));
#243155=CARTESIAN_POINT('Ctrl Pts',(-196.359626070838,3.05987976983901,
134.657299393235));
#243156=CARTESIAN_POINT('Ctrl Pts',(-196.367372346922,3.16622394720568,
134.57039789747));
#243157=CARTESIAN_POINT('Ctrl Pts',(-196.375118623006,3.26874854368119,
134.479202929922));
#243158=CARTESIAN_POINT('Ctrl Pts',(-196.382864956271,3.37127389696957,
134.388007289193));
#243159=CARTESIAN_POINT('Ctrl Pts',(-196.390611289537,3.46997932098188,
134.292518373281));
#243160=CARTESIAN_POINT('Ctrl Pts',(-196.398357622802,3.56449711178872,
134.19309834754));
#243161=CARTESIAN_POINT('Ctrl Pts',(-196.406105690805,3.6590360691996,134.093656057373));
#243162=CARTESIAN_POINT('Ctrl Pts',(-196.413853758808,3.74938525798013,
133.990281188891));
#243163=CARTESIAN_POINT('Ctrl Pts',(-196.421601826811,3.83521555689988,
133.883370960941));
#243164=CARTESIAN_POINT('Ctrl Pts',(-196.429358129553,3.92113707728282,
133.776347107529));
#243165=CARTESIAN_POINT('Ctrl Pts',(-196.437114432295,4.00252986868535,
133.665780694151));
#243166=CARTESIAN_POINT('Ctrl Pts',(-196.444870735037,4.07910634450957,
133.552100505671));
#243167=CARTESIAN_POINT('Ctrl Pts',(-196.452631177551,4.1557236915046,133.438359642651));
#243168=CARTESIAN_POINT('Ctrl Pts',(-196.460391620065,4.22751939619557,
133.321502025975));
#243169=CARTESIAN_POINT('Ctrl Pts',(-196.468152062579,4.29425111487522,
133.20198244448));
#243170=CARTESIAN_POINT('Ctrl Pts',(-196.475924962845,4.36108995723385,
133.082270999541));
#243171=CARTESIAN_POINT('Ctrl Pts',(-196.48369786311,4.42284839268908,132.959889399764));
#243172=CARTESIAN_POINT('Ctrl Pts',(-196.491470763375,4.47933126826296,
132.835314691803));
#243173=CARTESIAN_POINT('Ctrl Pts',(-196.498961099137,4.53376084903658,
132.715268588265));
#243174=CARTESIAN_POINT('Ctrl Pts',(-196.506451434899,4.58329165474819,
132.593186343692));
#243175=CARTESIAN_POINT('Ctrl Pts',(-196.513941770661,4.62779306061534,
132.469507593247));
#243176=CARTESIAN_POINT('Ctrl Pts',(-196.52171610478,4.67398175081282,132.341139525385));
#243177=CARTESIAN_POINT('Ctrl Pts',(-196.529490438899,4.71489844511337,
132.210644867334));
#243178=CARTESIAN_POINT('Ctrl Pts',(-196.537264773018,4.75034337573913,
132.078495961661));
#243179=CARTESIAN_POINT('Ctrl Pts',(-196.545029525966,4.7857446236558,131.946509917703));
#243180=CARTESIAN_POINT('Ctrl Pts',(-196.552794278913,4.81568742506033,
131.812874056546));
#243181=CARTESIAN_POINT('Ctrl Pts',(-196.56055903186,4.84002049298939,131.67807950253));
#243182=CARTESIAN_POINT('Ctrl Pts',(-196.568316072745,4.86432939297227,
131.543418828366));
#243183=CARTESIAN_POINT('Ctrl Pts',(-196.57607311363,4.88303957834233,131.407602133804));
#243184=CARTESIAN_POINT('Ctrl Pts',(-196.583830154515,4.89604999507073,
131.271134126099));
#243185=CARTESIAN_POINT('Ctrl Pts',(-196.591581345755,4.90905060054271,
131.134769029979));
#243186=CARTESIAN_POINT('Ctrl Pts',(-196.599332536995,4.91635995580379,
130.997753985968));
#243187=CARTESIAN_POINT('Ctrl Pts',(-196.607083728235,4.91792842339693,
130.860601926624));
#243188=CARTESIAN_POINT('Ctrl Pts',(-196.614831625012,4.91949622434951,
130.723508160564));
#243189=CARTESIAN_POINT('Ctrl Pts',(-196.622579521789,4.91532798620717,
130.586277885118));
#243190=CARTESIAN_POINT('Ctrl Pts',(-196.630327418567,4.90542609256398,
130.449426943632));
#243191=CARTESIAN_POINT('Ctrl Pts',(-196.638073694651,4.89552627018349,
130.312604628412));
#243192=CARTESIAN_POINT('Ctrl Pts',(-196.645819970735,4.87989520608599,
130.176161879023));
#243193=CARTESIAN_POINT('Ctrl Pts',(-196.653566246819,4.85858734580939,
130.04061192484));
#243194=CARTESIAN_POINT('Ctrl Pts',(-196.661312580084,4.83727932824304,
129.905060970058));
#243195=CARTESIAN_POINT('Ctrl Pts',(-196.669058913349,4.81029449159206,
129.770403209857));
#243196=CARTESIAN_POINT('Ctrl Pts',(-196.676805246615,4.77773878287119,
129.637143763186));
#243197=CARTESIAN_POINT('Ctrl Pts',(-196.684553314618,4.74517578352494,
129.503854473986));
#243198=CARTESIAN_POINT('Ctrl Pts',(-196.692301382621,4.70703952237994,
129.371964501156));
#243199=CARTESIAN_POINT('Ctrl Pts',(-196.700049450624,4.6634862928383,129.2419654502));
#243200=CARTESIAN_POINT('Ctrl Pts',(-196.707805753366,4.61988677440618,
129.111828234706));
#243201=CARTESIAN_POINT('Ctrl Pts',(-196.715562056108,4.57085891131053,
128.98358632697));
#243202=CARTESIAN_POINT('Ctrl Pts',(-196.723318358849,4.51660800481933,
128.857713450434));
#243203=CARTESIAN_POINT('Ctrl Pts',(-196.731078801364,4.46232814298588,
128.731773391754));
#243204=CARTESIAN_POINT('Ctrl Pts',(-196.738839243878,4.40281985259029,
128.608205235819));
#243205=CARTESIAN_POINT('Ctrl Pts',(-196.746599686392,4.33833476766696,
128.487458697727));
#243206=CARTESIAN_POINT('Ctrl Pts',(-196.754372586657,4.27374616556059,
128.366518326573));
#243207=CARTESIAN_POINT('Ctrl Pts',(-196.762145486923,4.20416500253837,
128.248408961719));
#243208=CARTESIAN_POINT('Ctrl Pts',(-196.769918387188,4.12988714651096,
128.133552646262));
#243209=CARTESIAN_POINT('Ctrl Pts',(-196.77740872295,4.05830947764578,128.022871647178));
#243210=CARTESIAN_POINT('Ctrl Pts',(-196.784899058712,3.98237083808165,
127.915211542331));
#243211=CARTESIAN_POINT('Ctrl Pts',(-196.792389394474,3.90237049944579,
127.810919863592));
#243212=CARTESIAN_POINT('Ctrl Pts',(-196.800163728593,3.81933692365392,
127.702673934153));
#243213=CARTESIAN_POINT('Ctrl Pts',(-196.807938062712,3.73166454474996,
127.597714010231));
#243214=CARTESIAN_POINT('Ctrl Pts',(-196.815712396831,3.63964277854941,
127.49646347481));
#243215=CARTESIAN_POINT('Ctrl Pts',(-196.823477149778,3.54773442095174,
127.395337721625));
#243216=CARTESIAN_POINT('Ctrl Pts',(-196.831241902725,3.4514876017493,127.297912547587));
#243217=CARTESIAN_POINT('Ctrl Pts',(-196.839006655673,3.35123374346011,
127.204580699405));
#243218=CARTESIAN_POINT('Ctrl Pts',(-196.846763696558,3.25107945871658,
127.111341549731));
#243219=CARTESIAN_POINT('Ctrl Pts',(-196.854520737442,3.14692633926754,
127.022187899961));
#243220=CARTESIAN_POINT('Ctrl Pts',(-196.862277778327,3.03914438745001,
126.937477576313));
#243221=CARTESIAN_POINT('Ctrl Pts',(-196.870028969567,2.93144371484062,
126.852831133378));
#243222=CARTESIAN_POINT('Ctrl Pts',(-196.877780160808,2.82011996290654,
126.772621587719));
#243223=CARTESIAN_POINT('Ctrl Pts',(-196.885531352048,2.70557784607938,
126.697167953312));
#243224=CARTESIAN_POINT('Ctrl Pts',(-196.893279248825,2.59108441270722,
126.621746388711));
#243225=CARTESIAN_POINT('Ctrl Pts',(-196.901027145602,2.47337566088124,
126.551076929597));
#243226=CARTESIAN_POINT('Ctrl Pts',(-196.908775042379,2.35288687260822,
126.485436396512));
#243227=CARTESIAN_POINT('Ctrl Pts',(-196.916521318463,2.23242328799227,
126.419809594011));
#243228=CARTESIAN_POINT('Ctrl Pts',(-196.924267594547,2.10918116671744,
126.359209812087));
#243229=CARTESIAN_POINT('Ctrl Pts',(-196.932013870631,1.98362173233724,
126.30386865718));
#243230=CARTESIAN_POINT('Ctrl Pts',(-196.939760203896,1.85806137110565,
126.248527093757));
#243231=CARTESIAN_POINT('Ctrl Pts',(-196.947506537162,1.73018402039162,
126.198444392494));
#243232=CARTESIAN_POINT('Ctrl Pts',(-196.955252870427,1.60047191802326,
126.153804446298));
#243233=CARTESIAN_POINT('Ctrl Pts',(-196.96300093843,1.47073076752877,126.109154503295));
#243234=CARTESIAN_POINT('Ctrl Pts',(-196.970749006433,1.33915441739122,
126.069949867965));
#243235=CARTESIAN_POINT('Ctrl Pts',(-196.978497074436,1.2062409496441,126.036324771025));
#243236=CARTESIAN_POINT('Ctrl Pts',(-196.986253377178,1.07318621988194,
126.002663936931));
#243237=CARTESIAN_POINT('Ctrl Pts',(-196.99400967992,0.938791913329507,
125.974594583081));
#243238=CARTESIAN_POINT('Ctrl Pts',(-197.001765982662,0.803567557284923,
125.952200042793));
#243239=CARTESIAN_POINT('Ctrl Pts',(-197.009526425176,0.668271027929991,
125.929793549866));
#243240=CARTESIAN_POINT('Ctrl Pts',(-197.01728686769,0.532143954180493,
125.913067953334));
#243241=CARTESIAN_POINT('Ctrl Pts',(-197.025047310204,0.395700708427855,
125.902054628355));
#243242=CARTESIAN_POINT('Ctrl Pts',(-197.032820210469,0.259038431864272,
125.89102362381));
#243243=CARTESIAN_POINT('Ctrl Pts',(-197.040593110735,0.122059359953858,
125.885723230215));
#243244=CARTESIAN_POINT('Ctrl Pts',(-197.048366011,-0.0147215066600589,
125.886132650123));
#243245=CARTESIAN_POINT('Ctrl Pts',(-197.055856346762,-0.146530044246793,
125.886527186585));
#243246=CARTESIAN_POINT('Ctrl Pts',(-197.063346682525,-0.27815422914227,
125.89222359833));
#243247=CARTESIAN_POINT('Ctrl Pts',(-197.070837018287,-0.409139909314695,
125.903157949128));
#243248=CARTESIAN_POINT('Ctrl Pts',(-197.078611352406,-0.545091951359064,
125.914506879159));
#243249=CARTESIAN_POINT('Ctrl Pts',(-197.086385686525,-0.680786770288788,
125.931534731873));
#243250=CARTESIAN_POINT('Ctrl Pts',(-197.094160020644,-0.815711725690703,
125.954226862393));
#243251=CARTESIAN_POINT('Ctrl Pts',(-197.101924773591,-0.950470398142942,
125.976891026889));
#243252=CARTESIAN_POINT('Ctrl Pts',(-197.109689526538,-1.08446071302349,
126.005205515426));
#243253=CARTESIAN_POINT('Ctrl Pts',(-197.117454279485,-1.21717309943613,
126.039103782042));
#243254=CARTESIAN_POINT('Ctrl Pts',(-197.12521132037,-1.3497536740364,126.072968380422));
#243255=CARTESIAN_POINT('Ctrl Pts',(-197.132968361255,-1.48105846969448,
126.112405624185));
#243256=CARTESIAN_POINT('Ctrl Pts',(-197.14072540214,-1.61058644177957,
126.157297633696));
#243257=CARTESIAN_POINT('Ctrl Pts',(-197.148476593381,-1.74001673581351,
126.202155789794));
#243258=CARTESIAN_POINT('Ctrl Pts',(-197.156227784621,-1.86767250538385,
126.252460396493));
#243259=CARTESIAN_POINT('Ctrl Pts',(-197.163978975861,-1.99306659696161,
126.308043390926));
#243260=CARTESIAN_POINT('Ctrl Pts',(-197.171726872638,-2.11840739270528,
126.363602761105));
#243261=CARTESIAN_POINT('Ctrl Pts',(-197.179474769415,-2.24148806567971,
126.424435898852));
#243262=CARTESIAN_POINT('Ctrl Pts',(-197.187222666192,-2.3618404383649,
126.490326217355));
#243263=CARTESIAN_POINT('Ctrl Pts',(-197.194968942276,-2.48216763592822,
126.556202753023));
#243264=CARTESIAN_POINT('Ctrl Pts',(-197.20271521836,-2.59976732564188,
126.627134177688));
#243265=CARTESIAN_POINT('Ctrl Pts',(-197.210461494444,-2.71419534785042,
126.702857639851));
#243266=CARTESIAN_POINT('Ctrl Pts',(-197.21820782771,-2.82862421474047,
126.778581660986));
#243267=CARTESIAN_POINT('Ctrl Pts',(-197.225954160975,-2.93988104136766,
126.859097574447));
#243268=CARTESIAN_POINT('Ctrl Pts',(-197.23370049424,-3.0475504520959,126.944099058496));
#243269=CARTESIAN_POINT('Ctrl Pts',(-197.241448562243,-3.15524397464228,
127.029119578039));
#243270=CARTESIAN_POINT('Ctrl Pts',(-197.249196630246,-3.25934817585858,
127.118627424824));
#243271=CARTESIAN_POINT('Ctrl Pts',(-197.256944698249,-3.35948089813607,
127.21227610331));
#243272=CARTESIAN_POINT('Ctrl Pts',(-197.264701000991,-3.45972004266226,
127.306024312726));
#243273=CARTESIAN_POINT('Ctrl Pts',(-197.272457303733,-3.55597899047717,
127.403921877684));
#243274=CARTESIAN_POINT('Ctrl Pts',(-197.280213606475,-3.64791221894775,
127.505585162135));
#243275=CARTESIAN_POINT('Ctrl Pts',(-197.287974048989,-3.73989451495042,
127.607302707342));
#243276=CARTESIAN_POINT('Ctrl Pts',(-197.295734491503,-3.82754624145586,
127.712789676336));
#243277=CARTESIAN_POINT('Ctrl Pts',(-197.303494934017,-3.91056297081482,
127.821630272095));
#243278=CARTESIAN_POINT('Ctrl Pts',(-197.311267834283,-3.99371296599786,
127.930645588441));
#243279=CARTESIAN_POINT('Ctrl Pts',(-197.319040734548,-4.07221287151127,
128.043024968882));
#243280=CARTESIAN_POINT('Ctrl Pts',(-197.326813634813,-4.14580181441111,
128.158323887261));
#243281=CARTESIAN_POINT('Ctrl Pts',(-197.334303970575,-4.21671561387579,
128.269431399534));
#243282=CARTESIAN_POINT('Ctrl Pts',(-197.341794306337,-4.2830691483762,
128.383249603762));
#243283=CARTESIAN_POINT('Ctrl Pts',(-197.349284642099,-4.3446707290067,
128.499361849885));
#243284=CARTESIAN_POINT('Ctrl Pts',(-197.357505688457,-4.41228177691909,
128.626801284969));
#243285=CARTESIAN_POINT('Ctrl Pts',(-197.365726734815,-4.47436294437082,
128.757370335874));
#243286=CARTESIAN_POINT('Ctrl Pts',(-197.373947781172,-4.5306305492326,
128.890576437242));
#243287=CARTESIAN_POINT('Ctrl Pts',(-197.382149938232,-4.58676886939006,
129.023476474196));
#243288=CARTESIAN_POINT('Ctrl Pts',(-197.390352095292,-4.63712013449305,
129.159001183372));
#243289=CARTESIAN_POINT('Ctrl Pts',(-197.398554252352,-4.68144684635498,
129.296634353534));
#243290=CARTESIAN_POINT('Ctrl Pts',(-197.404177125126,-4.71183439678685,
129.390986826878));
#243291=CARTESIAN_POINT('Ctrl Pts',(-197.409799997901,-4.73939157229638,
129.48632962842));
#243292=CARTESIAN_POINT('Ctrl Pts',(-197.415422870675,-4.76405452823413,
129.582490119309));
#243293=CARTESIAN_POINT('',(-195.389859435957,-4.9182490946383,130.807344841003));
#243294=CARTESIAN_POINT('Ctrl Pts',(-195.389859435995,-4.9182490946379,
130.807344841668));
#243295=CARTESIAN_POINT('Ctrl Pts',(-195.39981971452,-4.91814286233046,
130.982424504574));
#243296=CARTESIAN_POINT('Ctrl Pts',(-195.409779993045,-4.90868858456078,
131.157218844946));
#243297=CARTESIAN_POINT('Ctrl Pts',(-195.41974027157,-4.88997301345931,
131.330998054651));
#243298=CARTESIAN_POINT('Ctrl Pts',(-195.427514605689,-4.87536487749105,
131.466638602838));
#243299=CARTESIAN_POINT('Ctrl Pts',(-195.435288939808,-4.85508562687483,
131.601885723498));
#243300=CARTESIAN_POINT('Ctrl Pts',(-195.443063273927,-4.82916220422726,
131.736227275282));
#243301=CARTESIAN_POINT('Ctrl Pts',(-195.450828026874,-4.80327072988126,
131.87040326311));
#243302=CARTESIAN_POINT('Ctrl Pts',(-195.458592779821,-4.77174899711198,
132.003675522438));
#243303=CARTESIAN_POINT('Ctrl Pts',(-195.466357532768,-4.73467576101327,
132.135536226031));
#243304=CARTESIAN_POINT('Ctrl Pts',(-195.474114573653,-4.69763934657529,
132.267265963715));
#243305=CARTESIAN_POINT('Ctrl Pts',(-195.481871614538,-4.65506250671518,
132.397586561726));
#243306=CARTESIAN_POINT('Ctrl Pts',(-195.489628655423,-4.60707511081103,
132.525999948508));
#243307=CARTESIAN_POINT('Ctrl Pts',(-195.497379846663,-4.55912390257549,
132.654316497755));
#243308=CARTESIAN_POINT('Ctrl Pts',(-195.505131037903,-4.50577039587603,
132.780728333762));
#243309=CARTESIAN_POINT('Ctrl Pts',(-195.512882229143,-4.44719429552313,
132.904752476331));
#243310=CARTESIAN_POINT('Ctrl Pts',(-195.52063012592,-4.38864309157538,
133.028723905332));
#243311=CARTESIAN_POINT('Ctrl Pts',(-195.528378022698,-4.32487387548738,
133.150309306542));
#243312=CARTESIAN_POINT('Ctrl Pts',(-195.536125919475,-4.2561144066719,
133.269045834753));
#243313=CARTESIAN_POINT('Ctrl Pts',(-195.543872195559,-4.18736932085501,
133.387757525841));
#243314=CARTESIAN_POINT('Ctrl Pts',(-195.551618471643,-4.11363625439252,
133.503621191137));
#243315=CARTESIAN_POINT('Ctrl Pts',(-195.559364747727,-4.03518864169585,
133.616199106603));
#243316=CARTESIAN_POINT('Ctrl Pts',(-195.567111080992,-3.95674044991661,
133.728777853093));
#243317=CARTESIAN_POINT('Ctrl Pts',(-195.574857414257,-3.87357786597965,
133.838070480587));
#243318=CARTESIAN_POINT('Ctrl Pts',(-195.582603747523,-3.78601709127631,
133.943669083943));
#243319=CARTESIAN_POINT('Ctrl Pts',(-195.590351815526,-3.69843670794469,
134.049291335373));
#243320=CARTESIAN_POINT('Ctrl Pts',(-195.598099883529,-3.60645642342602,
134.151217615629));
#243321=CARTESIAN_POINT('Ctrl Pts',(-195.605847951532,-3.51043180420721,
134.24907419209));
#243322=CARTESIAN_POINT('Ctrl Pts',(-195.613604254274,-3.41430512888052,
134.347034771685));
#243323=CARTESIAN_POINT('Ctrl Pts',(-195.621360557015,-3.3141258066689,
134.440916727675));
#243324=CARTESIAN_POINT('Ctrl Pts',(-195.629116859757,-3.21028565473641,
134.530383843137));
#243325=CARTESIAN_POINT('Ctrl Pts',(-195.636877302271,-3.10639008018798,
134.619898709892));
#243326=CARTESIAN_POINT('Ctrl Pts',(-195.644637744786,-2.99883008908042,
134.704993798469));
#243327=CARTESIAN_POINT('Ctrl Pts',(-195.6523981873,-2.88802866412109,134.78537474687));
#243328=CARTESIAN_POINT('Ctrl Pts',(-195.660171087565,-2.77704937087823,
134.865884729904));
#243329=CARTESIAN_POINT('Ctrl Pts',(-195.667943987831,-2.66281857163852,
134.941665234117));
#243330=CARTESIAN_POINT('Ctrl Pts',(-195.675716888096,-2.54578692477708,
135.012466129092));
#243331=CARTESIAN_POINT('Ctrl Pts',(-195.683207223858,-2.43300967306273,
135.080693233198));
#243332=CARTESIAN_POINT('Ctrl Pts',(-195.69069755962,-2.31763194379055,
135.144296336452));
#243333=CARTESIAN_POINT('Ctrl Pts',(-195.698187895382,-2.20007486704126,
135.2030938036));
#243334=CARTESIAN_POINT('Ctrl Pts',(-195.705962229501,-2.07806057799752,
135.264120594585));
#243335=CARTESIAN_POINT('Ctrl Pts',(-195.71373656362,-1.95331191468248,
135.320163459015));
#243336=CARTESIAN_POINT('Ctrl Pts',(-195.721510897739,-1.82627431925977,
135.370968239566));
#243337=CARTESIAN_POINT('Ctrl Pts',(-195.729275650686,-1.69939328631975,
135.421710407767));
#243338=CARTESIAN_POINT('Ctrl Pts',(-195.737040403634,-1.57022929355805,
135.467227192768));
#243339=CARTESIAN_POINT('Ctrl Pts',(-195.744805156581,-1.43925215945998,
135.507310360439));
#243340=CARTESIAN_POINT('Ctrl Pts',(-195.752562197466,-1.30840511369795,
135.547353716943));
#243341=CARTESIAN_POINT('Ctrl Pts',(-195.760319238351,-1.17574888177873,
135.581974082212));
#243342=CARTESIAN_POINT('Ctrl Pts',(-195.768076279236,-1.04177270297969,
135.611011499191));
#243343=CARTESIAN_POINT('Ctrl Pts',(-195.775827470476,-0.907897556659447,
135.640027018828));
#243344=CARTESIAN_POINT('Ctrl Pts',(-195.783578661716,-0.772704825255148,
135.663467887734));
#243345=CARTESIAN_POINT('Ctrl Pts',(-195.791329852956,-0.63669798852352,
135.681224234063));
#243346=CARTESIAN_POINT('Ctrl Pts',(-195.799077749733,-0.500748958325419,
135.698973033471));
#243347=CARTESIAN_POINT('Ctrl Pts',(-195.80682564651,-0.363986897864043,
135.711042065181));
#243348=CARTESIAN_POINT('Ctrl Pts',(-195.814573543287,-0.226924321449017,
135.717372770496));
#243349=CARTESIAN_POINT('Ctrl Pts',(-195.822319819371,-0.0898904155702491,
135.723702151564));
#243350=CARTESIAN_POINT('Ctrl Pts',(-195.830066095455,0.0474434909258787,
135.724295575739));
#243351=CARTESIAN_POINT('Ctrl Pts',(-195.837812371539,0.184561330431458,
135.719146490604));
#243352=CARTESIAN_POINT('Ctrl Pts',(-195.845558704805,0.321680182109967,
135.713997367458));
#243353=CARTESIAN_POINT('Ctrl Pts',(-195.85330503807,0.458582572925475,
135.703105665086));
#243354=CARTESIAN_POINT('Ctrl Pts',(-195.861051371335,0.594754406154578,
135.686516929982));
#243355=CARTESIAN_POINT('Ctrl Pts',(-195.868799439338,0.730956734121398,
135.669924479945));
#243356=CARTESIAN_POINT('Ctrl Pts',(-195.876547507341,0.866427790928436,
135.647632505728));
#243357=CARTESIAN_POINT('Ctrl Pts',(-195.884295575344,1.00066095236712,
135.619738143878));
#243358=CARTESIAN_POINT('Ctrl Pts',(-195.892051878086,1.13503677840698,
135.591814135568));
#243359=CARTESIAN_POINT('Ctrl Pts',(-195.899808180828,1.26817169752809,
135.558275924972));
#243360=CARTESIAN_POINT('Ctrl Pts',(-195.90756448357,1.39957105416255,135.519271425508));
#243361=CARTESIAN_POINT('Ctrl Pts',(-195.915324926084,1.53104054259037,
135.480246108168));
#243362=CARTESIAN_POINT('Ctrl Pts',(-195.923085368598,1.66077225312122,
135.435748815331));
#243363=CARTESIAN_POINT('Ctrl Pts',(-195.930845811113,1.78828989818289,
135.385976304478));
#243364=CARTESIAN_POINT('Ctrl Pts',(-195.938618711378,1.91601224588891,
135.336123894371));
#243365=CARTESIAN_POINT('Ctrl Pts',(-195.946391611643,2.04151306753059,
135.280979501355));
#243366=CARTESIAN_POINT('Ctrl Pts',(-195.954164511909,2.16433832944441,
135.220787075484));
#243367=CARTESIAN_POINT('Ctrl Pts',(-195.961654847671,2.28269858371017,
135.162782795908));
#243368=CARTESIAN_POINT('Ctrl Pts',(-195.969145183433,2.39857415673948,
135.100091275505));
#243369=CARTESIAN_POINT('Ctrl Pts',(-195.976635519195,2.5115846025559,135.032968644648));
#243370=CARTESIAN_POINT('Ctrl Pts',(-195.984409853314,2.6288798737734,134.963301038841));
#243371=CARTESIAN_POINT('Ctrl Pts',(-195.992184187433,2.74346002251183,
134.888638992476));
#243372=CARTESIAN_POINT('Ctrl Pts',(-195.999958521552,2.85487044664782,
134.809219890419));
#243373=CARTESIAN_POINT('Ctrl Pts',(-196.007723274499,2.9661435673931,134.729898665308));
#243374=CARTESIAN_POINT('Ctrl Pts',(-196.015488027446,3.07425442081109,
134.645832274185));
#243375=CARTESIAN_POINT('Ctrl Pts',(-196.023252780394,3.17877386526114,
134.557303433015));
#243376=CARTESIAN_POINT('Ctrl Pts',(-196.031009821279,3.2831894995255,134.468862519938));
#243377=CARTESIAN_POINT('Ctrl Pts',(-196.038766862164,3.38402052698728,
134.375968228082));
#243378=CARTESIAN_POINT('Ctrl Pts',(-196.046523903049,3.48086792546511,
134.278945707612));
#243379=CARTESIAN_POINT('Ctrl Pts',(-196.054275094289,3.57764229056651,
134.181996352578));
#243380=CARTESIAN_POINT('Ctrl Pts',(-196.062026285529,3.67043873104742,
134.080925241009));
#243381=CARTESIAN_POINT('Ctrl Pts',(-196.069777476769,3.75889266550496,
133.976096576266));
#243382=CARTESIAN_POINT('Ctrl Pts',(-196.077525373546,3.84730900468066,
133.871312466503));
#243383=CARTESIAN_POINT('Ctrl Pts',(-196.085273270323,3.93138625714945,
133.762774278175));
#243384=CARTESIAN_POINT('Ctrl Pts',(-196.0930211671,4.01079812931765,133.650881551682));
#243385=CARTESIAN_POINT('Ctrl Pts',(-196.100767443184,4.09019339023412,
133.539012230735));
#243386=CARTESIAN_POINT('Ctrl Pts',(-196.108513719268,4.16492498582819,
133.423790085964));
#243387=CARTESIAN_POINT('Ctrl Pts',(-196.116259995352,4.23470845621583,
133.30564575792));
#243388=CARTESIAN_POINT('Ctrl Pts',(-196.124006328618,4.30449244172929,
133.187500557761));
#243389=CARTESIAN_POINT('Ctrl Pts',(-196.131752661883,4.36932803031741,
133.066433467914));
#243390=CARTESIAN_POINT('Ctrl Pts',(-196.139498995149,4.42897565969853,
132.942901631505));
#243391=CARTESIAN_POINT('Ctrl Pts',(-196.147247063151,4.48863664675259,
132.819342130998));
#243392=CARTESIAN_POINT('Ctrl Pts',(-196.154995131154,4.54310719277129,
132.69331713759));
#243393=CARTESIAN_POINT('Ctrl Pts',(-196.162743199157,4.59219517872211,
132.565305393254));
#243394=CARTESIAN_POINT('Ctrl Pts',(-196.170499501899,4.64133533596847,
132.437157596512));
#243395=CARTESIAN_POINT('Ctrl Pts',(-196.178255804641,4.68508136532905,
132.307019196435));
#243396=CARTESIAN_POINT('Ctrl Pts',(-196.186012107383,4.72329033713375,
132.175386311577));
#243397=CARTESIAN_POINT('Ctrl Pts',(-196.193772549897,4.76151970221726,
132.043683170285));
#243398=CARTESIAN_POINT('Ctrl Pts',(-196.201532992411,4.79420602793986,
131.910484334337));
#243399=CARTESIAN_POINT('Ctrl Pts',(-196.209293434926,4.8212574068754,131.776296870182));
#243400=CARTESIAN_POINT('Ctrl Pts',(-196.217066335191,4.84835221108591,
131.641893996397));
#243401=CARTESIAN_POINT('Ctrl Pts',(-196.224839235456,4.86979393109643,
131.50649970938));
#243402=CARTESIAN_POINT('Ctrl Pts',(-196.232612135722,4.88554239271103,
131.370627861474));
#243403=CARTESIAN_POINT('Ctrl Pts',(-196.240102471484,4.900718358078,131.23969529748));
#243404=CARTESIAN_POINT('Ctrl Pts',(-196.247592807246,4.91060778408717,
131.108319598021));
#243405=CARTESIAN_POINT('Ctrl Pts',(-196.255083143008,4.91522052013289,
130.976959287794));
#243406=CARTESIAN_POINT('Ctrl Pts',(-196.262857477127,4.92000814946778,
130.84061841148));
#243407=CARTESIAN_POINT('Ctrl Pts',(-196.270631811246,4.91912622449037,
130.703862227485));
#243408=CARTESIAN_POINT('Ctrl Pts',(-196.278406145365,4.91252874026042,
130.567201517771));
#243409=CARTESIAN_POINT('Ctrl Pts',(-196.286170898312,4.90593938684015,
130.430709230169));
#243410=CARTESIAN_POINT('Ctrl Pts',(-196.293935651259,4.89364850813207,
130.294312569492));
#243411=CARTESIAN_POINT('Ctrl Pts',(-196.301700404207,4.87566199954319,
130.158525399642));
#243412=CARTESIAN_POINT('Ctrl Pts',(-196.309457445092,4.85769335540821,
130.022873095524));
#243413=CARTESIAN_POINT('Ctrl Pts',(-196.317214485976,4.8340403900447,129.88782946262));
#243414=CARTESIAN_POINT('Ctrl Pts',(-196.324971526861,4.8047609802586,129.753905961198));
#243415=CARTESIAN_POINT('Ctrl Pts',(-196.332722718102,4.77550365030315,
129.620083452531));
#243416=CARTESIAN_POINT('Ctrl Pts',(-196.340473909342,4.74062840441648,
129.48737977442));
#243417=CARTESIAN_POINT('Ctrl Pts',(-196.348225100582,4.70024459204801,
129.35629852034));
#243418=CARTESIAN_POINT('Ctrl Pts',(-196.355972997359,4.65987794387701,
129.225272979288));
#243419=CARTESIAN_POINT('Ctrl Pts',(-196.363720894136,4.61400750073638,
129.095868863611));
#243420=CARTESIAN_POINT('Ctrl Pts',(-196.371468790913,4.56279303762065,
128.968576654693));
#243421=CARTESIAN_POINT('Ctrl Pts',(-196.379215066997,4.51158928746668,
128.841311072562));
#243422=CARTESIAN_POINT('Ctrl Pts',(-196.386961343081,4.45504388664914,
128.716156880974));
#243423=CARTESIAN_POINT('Ctrl Pts',(-196.394707619166,4.39336538774464,
128.593586175822));
#243424=CARTESIAN_POINT('Ctrl Pts',(-196.402453952431,4.33168643354339,
128.471014565882));
#243425=CARTESIAN_POINT('Ctrl Pts',(-196.410200285696,4.26487448138624,
128.351026829673));
#243426=CARTESIAN_POINT('Ctrl Pts',(-196.417946618962,4.19318464946682,
128.234071614754));
#243427=CARTESIAN_POINT('Ctrl Pts',(-196.425694686965,4.1214787631067,128.117090208526));
#243428=CARTESIAN_POINT('Ctrl Pts',(-196.433442754968,4.04489302757999,
128.003143008206));
#243429=CARTESIAN_POINT('Ctrl Pts',(-196.441190822971,3.96372637703559,
127.892650420707));
#243430=CARTESIAN_POINT('Ctrl Pts',(-196.448947125713,3.88247346160899,
127.782040400371));
#243431=CARTESIAN_POINT('Ctrl Pts',(-196.456703428454,3.79663013733879,
127.674892642869));
#243432=CARTESIAN_POINT('Ctrl Pts',(-196.464459731196,3.70653654583702,
127.571595563178));
#243433=CARTESIAN_POINT('Ctrl Pts',(-196.47222017371,3.6163948686728,127.468243350725));
#243434=CARTESIAN_POINT('Ctrl Pts',(-196.479980616225,3.52199867306387,
127.368746194777));
#243435=CARTESIAN_POINT('Ctrl Pts',(-196.487741058739,3.42372489016486,
127.273455501457));
#243436=CARTESIAN_POINT('Ctrl Pts',(-196.495513959004,3.32529334946519,
127.178011839056));
#243437=CARTESIAN_POINT('Ctrl Pts',(-196.50328685927,3.22297207464116,127.086788393428));
#243438=CARTESIAN_POINT('Ctrl Pts',(-196.511059759535,3.11717166908787,
127.000096714005));
#243439=CARTESIAN_POINT('Ctrl Pts',(-196.518550095297,3.01521737477187,
126.916556495492));
#243440=CARTESIAN_POINT('Ctrl Pts',(-196.526040431059,2.91003275438475,
126.837224466721));
#243441=CARTESIAN_POINT('Ctrl Pts',(-196.533530766821,2.80200890157942,
126.762340184915));
#243442=CARTESIAN_POINT('Ctrl Pts',(-196.54130510094,2.68988929156167,126.684616642804));
#243443=CARTESIAN_POINT('Ctrl Pts',(-196.549079435059,2.57435573883828,
126.61143857336));
#243444=CARTESIAN_POINT('Ctrl Pts',(-196.556853769178,2.45581311194474,
126.543120771969));
#243445=CARTESIAN_POINT('Ctrl Pts',(-196.564618522125,2.33741657824439,
126.474887166163));
#243446=CARTESIAN_POINT('Ctrl Pts',(-196.572383275073,2.2160186845002,126.411502103747));
#243447=CARTESIAN_POINT('Ctrl Pts',(-196.58014802802,2.09205494557583,126.353238380737));
#243448=CARTESIAN_POINT('Ctrl Pts',(-196.587905068905,1.96821432918454,
126.295032526079));
#243449=CARTESIAN_POINT('Ctrl Pts',(-196.59566210979,1.84181329065324,126.241938053517));
#243450=CARTESIAN_POINT('Ctrl Pts',(-196.603419150675,1.71331341981801,
126.194182726424));
#243451=CARTESIAN_POINT('Ctrl Pts',(-196.611170341915,1.58491045173478,
126.146463411995));
#243452=CARTESIAN_POINT('Ctrl Pts',(-196.618921533155,1.45441216669993,
126.104075364592));
#243453=CARTESIAN_POINT('Ctrl Pts',(-196.626672724395,1.32230135821319,
126.067198789998));
#243454=CARTESIAN_POINT('Ctrl Pts',(-196.634420621172,1.19024670034405,
126.030337888932));
#243455=CARTESIAN_POINT('Ctrl Pts',(-196.642168517949,1.05658125794433,
125.99898390647));
#243456=CARTESIAN_POINT('Ctrl Pts',(-196.649916414726,0.921804049182246,
125.973267536553));
#243457=CARTESIAN_POINT('Ctrl Pts',(-196.65766269081,0.78705503290714,125.947556545946));
#243458=CARTESIAN_POINT('Ctrl Pts',(-196.665408966895,0.651195096632955,
125.927480895489));
#243459=CARTESIAN_POINT('Ctrl Pts',(-196.673155242979,0.514734155767422,
125.913120303353));
#243460=CARTESIAN_POINT('Ctrl Pts',(-196.680901576244,0.378272207578036,
125.89875960521));
#243461=CARTESIAN_POINT('Ctrl Pts',(-196.688647909509,0.241209634762758,
125.890114090488));
#243462=CARTESIAN_POINT('Ctrl Pts',(-196.696394242775,0.104061794833803,
125.88721162599));
#243463=CARTESIAN_POINT('Ctrl Pts',(-196.704142310778,-0.0331167584028003,
125.884308511505));
#243464=CARTESIAN_POINT('Ctrl Pts',(-196.711890378781,-0.170380225947006,
125.887151014736));
#243465=CARTESIAN_POINT('Ctrl Pts',(-196.719638446784,-0.307213326347598,
125.895714874124));
#243466=CARTESIAN_POINT('Ctrl Pts',(-196.727394749525,-0.444191854595816,
125.904287835283));
#243467=CARTESIAN_POINT('Ctrl Pts',(-196.735151052267,-0.580738711172077,
125.918594275041));
#243468=CARTESIAN_POINT('Ctrl Pts',(-196.742907355009,-0.716343256706872,
125.93855797041));
#243469=CARTESIAN_POINT('Ctrl Pts',(-196.750667797523,-0.852020178470593,
125.958532321004));
#243470=CARTESIAN_POINT('Ctrl Pts',(-196.758428240037,-0.986753403156911,
125.984169870666));
#243471=CARTESIAN_POINT('Ctrl Pts',(-196.766188682552,-1.12004354234743,
126.015343440133));
#243472=CARTESIAN_POINT('Ctrl Pts',(-196.773961582817,-1.25354765070231,
126.046567052181));
#243473=CARTESIAN_POINT('Ctrl Pts',(-196.781734483082,-1.38560366746973,
126.083344337961));
#243474=CARTESIAN_POINT('Ctrl Pts',(-196.789507383348,-1.51572753612455,
126.125498245286));
#243475=CARTESIAN_POINT('Ctrl Pts',(-196.79699771911,-1.64112107439117,
126.166119751901));
#243476=CARTESIAN_POINT('Ctrl Pts',(-196.804488054872,-1.76472021359313,
126.211733652672));
#243477=CARTESIAN_POINT('Ctrl Pts',(-196.811978390634,-1.88611201178001,
126.262140395965));
#243478=CARTESIAN_POINT('Ctrl Pts',(-196.819753120516,-2.01211283081602,
126.31446098957));
#243479=CARTESIAN_POINT('Ctrl Pts',(-196.827527850399,-2.13613453277524,
126.372111311885));
#243480=CARTESIAN_POINT('Ctrl Pts',(-196.835302580282,-2.25769335655606,
126.434920862831));
#243481=CARTESIAN_POINT('Ctrl Pts',(-196.84306763844,-2.37910096178886,
126.49765227902));
#243482=CARTESIAN_POINT('Ctrl Pts',(-196.850832696599,-2.49805144108238,
126.565529975486));
#243483=CARTESIAN_POINT('Ctrl Pts',(-196.858597754758,-2.61407982358089,
126.638334964927));
#243484=CARTESIAN_POINT('Ctrl Pts',(-196.866355010688,-2.72999162227744,
126.711066800866));
#243485=CARTESIAN_POINT('Ctrl Pts',(-196.874112266618,-2.84298683835341,
126.788715870278));
#243486=CARTESIAN_POINT('Ctrl Pts',(-196.881869522548,-2.95262431338359,
126.871016909407));
#243487=CARTESIAN_POINT('Ctrl Pts',(-196.889701246598,-3.06331428645066,
126.954108022204));
#243488=CARTESIAN_POINT('Ctrl Pts',(-196.897532970648,-3.17058134690447,
127.041940717171));
#243489=CARTESIAN_POINT('Ctrl Pts',(-196.905364694697,-3.27400009449339,
127.134196255612));
#243490=CARTESIAN_POINT('Ctrl Pts',(-196.913112250324,-3.37630738911646,
127.225460313357));
#243491=CARTESIAN_POINT('Ctrl Pts',(-196.92085980595,-3.47484838652523,
127.321052344723));
#243492=CARTESIAN_POINT('Ctrl Pts',(-196.928607361577,-3.56924381249012,
127.420622792394));
#243493=CARTESIAN_POINT('Ctrl Pts',(-196.936353185915,-3.66361814461469,
127.520170989801));
#243494=CARTESIAN_POINT('Ctrl Pts',(-196.944099010253,-3.75384847999537,
127.623695550915));
#243495=CARTESIAN_POINT('Ctrl Pts',(-196.951844834592,-3.83959259305698,
127.730810263034));
#243496=CARTESIAN_POINT('Ctrl Pts',(-196.959590605432,-3.92533611390858,
127.837924235343));
#243497=CARTESIAN_POINT('Ctrl Pts',(-196.967336376272,-4.00659323053975,
127.948628003653));
#243498=CARTESIAN_POINT('Ctrl Pts',(-196.975082147112,-4.08306244107213,
128.062502823149));
#243499=CARTESIAN_POINT('Ctrl Pts',(-196.982977876498,-4.16101209969199,
128.178582265363));
#243500=CARTESIAN_POINT('Ctrl Pts',(-196.990873605884,-4.23398630132602,
128.297956468713));
#243501=CARTESIAN_POINT('Ctrl Pts',(-196.99876933527,-4.30171285759348,
128.420152247202));
#243502=CARTESIAN_POINT('Ctrl Pts',(-197.006523360613,-4.36822393061056,
128.540154987535));
#243503=CARTESIAN_POINT('Ctrl Pts',(-197.014277385956,-4.42967400356862,
128.662878498698));
#243504=CARTESIAN_POINT('Ctrl Pts',(-197.0220314113,-4.48585278789196,128.787851795899));
#243505=CARTESIAN_POINT('Ctrl Pts',(-197.029997992707,-4.54357156476701,
128.916250904981));
#243506=CARTESIAN_POINT('Ctrl Pts',(-197.037964574115,-4.59572572575124,
129.047024507953));
#243507=CARTESIAN_POINT('Ctrl Pts',(-197.045931155522,-4.64214130697621,
129.179643057938));
#243508=CARTESIAN_POINT('Ctrl Pts',(-197.053897736929,-4.68855688820118,
129.312261607922));
#243509=CARTESIAN_POINT('Ctrl Pts',(-197.061864318336,-4.72923380978975,
129.446724666572));
#243510=CARTESIAN_POINT('Ctrl Pts',(-197.069830899744,-4.76405452823391,
129.582490119308));
#243511=CARTESIAN_POINT('Ctrl Pts',(-195.319719904489,-4.76405452823413,
129.582490119309));
#243512=CARTESIAN_POINT('Ctrl Pts',(-195.327375268945,-4.79771771013328,
129.713742354623));
#243513=CARTESIAN_POINT('Ctrl Pts',(-195.335030633401,-4.82593039702568,
129.846300244023));
#243514=CARTESIAN_POINT('Ctrl Pts',(-195.342685997857,-4.84861431659377,
129.979665357836));
#243515=CARTESIAN_POINT('Ctrl Pts',(-195.35054823754,-4.87191123650242,
130.116634472268));
#243516=CARTESIAN_POINT('Ctrl Pts',(-195.358410477224,-4.88937627244404,
130.25445460389));
#243517=CARTESIAN_POINT('Ctrl Pts',(-195.366272716907,-4.90098169012487,
130.392582114532));
#243518=CARTESIAN_POINT('Ctrl Pts',(-195.37413495659,-4.91258710780571,
130.530709625174));
#243519=CARTESIAN_POINT('Ctrl Pts',(-195.381997196274,-4.91833295009223,
130.669144059767));
#243520=CARTESIAN_POINT('Ctrl Pts',(-195.389859435957,-4.9182490946383,
130.807344841003));
#243521=CARTESIAN_POINT('Origin',(213.235140564004,0.,130.804360617566));
#243522=CARTESIAN_POINT('',(-193.570047426085,-4.7640545282341,129.582490119308));
#243523=CARTESIAN_POINT('',(-193.914998640423,-4.76405452823412,129.582490119309));
#243524=CARTESIAN_POINT('',(213.235140564004,-4.76405452823405,129.582490119308));
#243525=CARTESIAN_POINT('',(-193.985140563976,-4.91824942956879,130.80672938227));
#243526=CARTESIAN_POINT('Ctrl Pts',(-193.914998640423,-4.76405452823412,
129.582490119309));
#243527=CARTESIAN_POINT('Ctrl Pts',(-193.92267052425,-4.79777746561117,
129.713975340325));
#243528=CARTESIAN_POINT('Ctrl Pts',(-193.930342408077,-4.82602859703584,
129.84676320345));
#243529=CARTESIAN_POINT('Ctrl Pts',(-193.938014291904,-4.84873130167584,
129.980353441233));
#243530=CARTESIAN_POINT('Ctrl Pts',(-193.945868670583,-4.87197404665051,
130.117121455314));
#243531=CARTESIAN_POINT('Ctrl Pts',(-193.953723049261,-4.88940102937192,
130.254730049252));
#243532=CARTESIAN_POINT('Ctrl Pts',(-193.96157742794,-4.90098647655538,
130.392639086527));
#243533=CARTESIAN_POINT('Ctrl Pts',(-193.969431806619,-4.91257192373883,
130.530548123802));
#243534=CARTESIAN_POINT('Ctrl Pts',(-193.977286185297,-4.91831588080072,
130.668757158678));
#243535=CARTESIAN_POINT('Ctrl Pts',(-193.985140563975,-4.91824942956879,
130.806729382271));
#243536=CARTESIAN_POINT('Ctrl Pts',(-193.985140564012,-4.91824942956849,
130.806729382913));
#243537=CARTESIAN_POINT('Ctrl Pts',(-193.992731428123,-4.91818520775937,
130.940072635538));
#243538=CARTESIAN_POINT('Ctrl Pts',(-194.000322292233,-4.91269870967798,
131.073280898492));
#243539=CARTESIAN_POINT('Ctrl Pts',(-194.007913156344,-4.90181963422078,
131.206041256965));
#243540=CARTESIAN_POINT('Ctrl Pts',(-194.015687490463,-4.89067761319646,
131.342010412719));
#243541=CARTESIAN_POINT('Ctrl Pts',(-194.023461824582,-4.87385628461547,
131.47773098801));
#243542=CARTESIAN_POINT('Ctrl Pts',(-194.031236158701,-4.85136951318697,
131.612690320732));
#243543=CARTESIAN_POINT('Ctrl Pts',(-194.039000911648,-4.82891045469462,
131.747483328137));
#243544=CARTESIAN_POINT('Ctrl Pts',(-194.046765664595,-4.80079990939565,
131.881516577692));
#243545=CARTESIAN_POINT('Ctrl Pts',(-194.054530417543,-4.76710364769382,
132.014280397818));
#243546=CARTESIAN_POINT('Ctrl Pts',(-194.062287458428,-4.73344085359424,
132.146912355046));
#243547=CARTESIAN_POINT('Ctrl Pts',(-194.070044499313,-4.69420347904607,
132.278277015427));
#243548=CARTESIAN_POINT('Ctrl Pts',(-194.077801540198,-4.64950864104312,
132.407873155517));
#243549=CARTESIAN_POINT('Ctrl Pts',(-194.085552731438,-4.604847507765,132.53737156615));
#243550=CARTESIAN_POINT('Ctrl Pts',(-194.093303922678,-4.55473722966819,
132.665103742946));
#243551=CARTESIAN_POINT('Ctrl Pts',(-194.101055113918,-4.49934512806033,
132.790582277175));
#243552=CARTESIAN_POINT('Ctrl Pts',(-194.108803010695,-4.44397656957337,
132.91600747968));
#243553=CARTESIAN_POINT('Ctrl Pts',(-194.116550907472,-4.38333081010158,
133.039180587809));
#243554=CARTESIAN_POINT('Ctrl Pts',(-194.124298804249,-4.3176237237225,
133.159633094977));
#243555=CARTESIAN_POINT('Ctrl Pts',(-194.132045080334,-4.25193038184923,
133.280060406077));
#243556=CARTESIAN_POINT('Ctrl Pts',(-194.139791356418,-4.18117800603018,
133.397767905166));
#243557=CARTESIAN_POINT('Ctrl Pts',(-194.147537632502,-4.10562877152469,
133.512311033089));
#243558=CARTESIAN_POINT('Ctrl Pts',(-194.155283965767,-4.03007897933201,
133.626855006542));
#243559=CARTESIAN_POINT('Ctrl Pts',(-194.163030299033,-3.94973247305859,
133.73823423585));
#243560=CARTESIAN_POINT('Ctrl Pts',(-194.170776632298,-3.86489494195318,
133.846032879688));
#243561=CARTESIAN_POINT('Ctrl Pts',(-194.178524700301,-3.78003841207102,
133.953855664285));
#243562=CARTESIAN_POINT('Ctrl Pts',(-194.186272768304,-3.69068909780753,
134.058095960657));
#243563=CARTESIAN_POINT('Ctrl Pts',(-194.194020836307,-3.59719291272284,
134.158371084329));
#243564=CARTESIAN_POINT('Ctrl Pts',(-194.201777139049,-3.50359735877989,
134.258752781596));
#243565=CARTESIAN_POINT('Ctrl Pts',(-194.209533441791,-3.40584639691667,
134.355160601374));
#243566=CARTESIAN_POINT('Ctrl Pts',(-194.217289744533,-3.30432313691359,
134.447248437601));
#243567=CARTESIAN_POINT('Ctrl Pts',(-194.225050187047,-3.20274569088985,
134.539385423878));
#243568=CARTESIAN_POINT('Ctrl Pts',(-194.232810629561,-3.09739223505416,
134.627197582094));
#243569=CARTESIAN_POINT('Ctrl Pts',(-194.240571072075,-2.9886781026604,
134.71037985218));
#243570=CARTESIAN_POINT('Ctrl Pts',(-194.248343972341,-2.87978945269014,
134.793695653831));
#243571=CARTESIAN_POINT('Ctrl Pts',(-194.256116872606,-2.76752966587593,
134.87236649073));
#243572=CARTESIAN_POINT('Ctrl Pts',(-194.263889772872,-2.65234287085514,
134.946130813741));
#243573=CARTESIAN_POINT('Ctrl Pts',(-194.271380108634,-2.54134340597169,
135.01721361781));
#243574=CARTESIAN_POINT('Ctrl Pts',(-194.278870444396,-2.427626312325,135.083740287406));
#243575=CARTESIAN_POINT('Ctrl Pts',(-194.286360780158,-2.31160794777514,
135.145518499777));
#243576=CARTESIAN_POINT('Ctrl Pts',(-194.294135114277,-2.19119071166986,
135.209639051847));
#243577=CARTESIAN_POINT('Ctrl Pts',(-194.301909448396,-2.06791280888925,
135.268847077811));
#243578=CARTESIAN_POINT('Ctrl Pts',(-194.309683782515,-1.94221305079689,
135.32287713605));
#243579=CARTESIAN_POINT('Ctrl Pts',(-194.317448535462,-1.81666820642226,
135.376840607072));
#243580=CARTESIAN_POINT('Ctrl Pts',(-194.325213288409,-1.68870780118061,
135.425638654508));
#243581=CARTESIAN_POINT('Ctrl Pts',(-194.332978041356,-1.55879618671472,
135.469051122925));
#243582=CARTESIAN_POINT('Ctrl Pts',(-194.340735082241,-1.42901360229611,
135.512420473466));
#243583=CARTESIAN_POINT('Ctrl Pts',(-194.348492123126,-1.29728403370762,
135.550414766694));
#243584=CARTESIAN_POINT('Ctrl Pts',(-194.356249164011,-1.1640924790234,
135.582861612939));
#243585=CARTESIAN_POINT('Ctrl Pts',(-194.364000355251,-1.03100136512646,
135.615283990765));
#243586=CARTESIAN_POINT('Ctrl Pts',(-194.371751546491,-0.896450837902563,
135.642167156194));
#243587=CARTESIAN_POINT('Ctrl Pts',(-194.379502737732,-0.760941409372517,
135.66338842506));
#243588=CARTESIAN_POINT('Ctrl Pts',(-194.387250634509,-0.625489575964244,
135.684600674321));
#243589=CARTESIAN_POINT('Ctrl Pts',(-194.394998531286,-0.489080037301672,
135.700155752914));
#243590=CARTESIAN_POINT('Ctrl Pts',(-194.402746428063,-0.352223646456436,
135.709982042562));
#243591=CARTESIAN_POINT('Ctrl Pts',(-194.410492704147,-0.215395883017882,
135.719806276762));
#243592=CARTESIAN_POINT('Ctrl Pts',(-194.418238980231,-0.0781218430315514,
135.723904077597));
#243593=CARTESIAN_POINT('Ctrl Pts',(-194.425985256315,0.0590827411620631,
135.722255725455));
#243594=CARTESIAN_POINT('Ctrl Pts',(-194.433731589581,0.196288338168563,
135.720607361145));
#243595=CARTESIAN_POINT('Ctrl Pts',(-194.441477922846,0.333424087422282,
135.713212763916));
#243596=CARTESIAN_POINT('Ctrl Pts',(-194.449224256111,0.469974897333745,
135.700104346396));
#243597=CARTESIAN_POINT('Ctrl Pts',(-194.456972324114,0.606556286852497,
135.686992993336));
#243598=CARTESIAN_POINT('Ctrl Pts',(-194.464720392117,0.742552087266234,
135.668165311142));
#243599=CARTESIAN_POINT('Ctrl Pts',(-194.47246846012,0.877453360560609,
135.643705476381));
#243600=CARTESIAN_POINT('Ctrl Pts',(-194.480224762862,1.0124980085334,135.619219645417));
#243601=CARTESIAN_POINT('Ctrl Pts',(-194.487981065604,1.1464454203106,135.589089774232));
#243602=CARTESIAN_POINT('Ctrl Pts',(-194.495737368346,1.27879732686596,
135.553451105154));
#243603=CARTESIAN_POINT('Ctrl Pts',(-194.50349781086,1.41121987361924,135.517793414645));
#243604=CARTESIAN_POINT('Ctrl Pts',(-194.511258253374,1.54204484557664,
135.476621184933));
#243605=CARTESIAN_POINT('Ctrl Pts',(-194.519018695888,1.67079108929357,
135.430118955227));
#243606=CARTESIAN_POINT('Ctrl Pts',(-194.526791596154,1.79974400791011,
135.383542076013));
#243607=CARTESIAN_POINT('Ctrl Pts',(-194.534564496419,1.92661116793729,
135.33161824699));
#243608=CARTESIAN_POINT('Ctrl Pts',(-194.542337396684,2.05093245830343,
135.274579752461));
#243609=CARTESIAN_POINT('Ctrl Pts',(-194.549827732446,2.17073435661631,
135.21961475088));
#243610=CARTESIAN_POINT('Ctrl Pts',(-194.557318068208,2.28817199468981,
135.159900629281));
#243611=CARTESIAN_POINT('Ctrl Pts',(-194.56480840397,2.40285851435058,135.095683726179));
#243612=CARTESIAN_POINT('Ctrl Pts',(-194.572582738089,2.52189340826435,
135.029032019675));
#243613=CARTESIAN_POINT('Ctrl Pts',(-194.580357072209,2.63834151504885,
134.957318212925));
#243614=CARTESIAN_POINT('Ctrl Pts',(-194.588131406328,2.75174232289214,
134.880768012676));
#243615=CARTESIAN_POINT('Ctrl Pts',(-194.595896159275,2.86500337437468,
134.804312153707));
#243616=CARTESIAN_POINT('Ctrl Pts',(-194.603660912222,2.97522427835457,
134.723031977348));
#243617=CARTESIAN_POINT('Ctrl Pts',(-194.611425665169,3.08196881842492,
134.637199156398));
#243618=CARTESIAN_POINT('Ctrl Pts',(-194.619182706054,3.18860733831322,
134.551451585816));
#243619=CARTESIAN_POINT('Ctrl Pts',(-194.626939746939,3.29177606275606,
134.461160612539));
#243620=CARTESIAN_POINT('Ctrl Pts',(-194.634696787824,3.39106780213559,
134.366641098356));
#243621=CARTESIAN_POINT('Ctrl Pts',(-194.642447979064,3.49028466484221,
134.272192862074));
#243622=CARTESIAN_POINT('Ctrl Pts',(-194.650199170304,3.58563007983292,
134.173522700424));
#243623=CARTESIAN_POINT('Ctrl Pts',(-194.657950361544,3.6767302904695,134.070985394556));
#243624=CARTESIAN_POINT('Ctrl Pts',(-194.665698258321,3.76779178108626,
133.968491669778));
#243625=CARTESIAN_POINT('Ctrl Pts',(-194.673446155098,3.85461139688462,
133.862134361516));
#243626=CARTESIAN_POINT('Ctrl Pts',(-194.681194051876,3.93685275481512,
133.752304553499));
#243627=CARTESIAN_POINT('Ctrl Pts',(-194.68894032796,4.01907690962669,133.64249771951));
#243628=CARTESIAN_POINT('Ctrl Pts',(-194.696686604044,4.09672447724247,
133.529220143312));
#243629=CARTESIAN_POINT('Ctrl Pts',(-194.704432880128,4.1695001010668,133.412895066199));
#243630=CARTESIAN_POINT('Ctrl Pts',(-194.712179213393,4.24227626210415,
133.2965691304));
#243631=CARTESIAN_POINT('Ctrl Pts',(-194.719925546659,4.31018020022778,
133.177195980241));
#243632=CARTESIAN_POINT('Ctrl Pts',(-194.727671879924,4.3729607655146,133.055226496682));
#243633=CARTESIAN_POINT('Ctrl Pts',(-194.735419947927,4.43575539007363,
132.933229698903));
#243634=CARTESIAN_POINT('Ctrl Pts',(-194.74316801593,4.49342417982122,132.808635758297));
#243635=CARTESIAN_POINT('Ctrl Pts',(-194.750916083933,4.54576286146099,
132.681918358319));
#243636=CARTESIAN_POINT('Ctrl Pts',(-194.758672386675,4.59815716927451,
132.555066281581));
#243637=CARTESIAN_POINT('Ctrl Pts',(-194.766428689417,4.64520990323737,
132.426086599126));
#243638=CARTESIAN_POINT('Ctrl Pts',(-194.774184992159,4.68676551997081,
132.295471620581));
#243639=CARTESIAN_POINT('Ctrl Pts',(-194.781945434673,4.72834331618813,
132.164786928889));
#243640=CARTESIAN_POINT('Ctrl Pts',(-194.789705877187,4.76441804619331,
132.032465578979));
#243641=CARTESIAN_POINT('Ctrl Pts',(-194.797466319701,4.79488489286097,
131.899012126821));
#243642=CARTESIAN_POINT('Ctrl Pts',(-194.805239219967,4.82540064761563,
131.765344443334));
#243643=CARTESIAN_POINT('Ctrl Pts',(-194.813012120232,4.85029045859629,
131.630541410641));
#243644=CARTESIAN_POINT('Ctrl Pts',(-194.820785020498,4.86950105189414,
131.495115688559));
#243645=CARTESIAN_POINT('Ctrl Pts',(-194.82827535626,4.88801329173705,131.36461303259));
#243646=CARTESIAN_POINT('Ctrl Pts',(-194.835765692022,4.90125202199734,
131.233532480348));
#243647=CARTESIAN_POINT('Ctrl Pts',(-194.843256027784,4.90921538795057,
131.102332658552));
#243648=CARTESIAN_POINT('Ctrl Pts',(-194.851030361903,4.91748068734433,
130.966158355635));
#243649=CARTESIAN_POINT('Ctrl Pts',(-194.858804696022,4.92008887680447,
130.82942420116));
#243650=CARTESIAN_POINT('Ctrl Pts',(-194.866579030141,4.91698093192857,
130.692639636767));
#243651=CARTESIAN_POINT('Ctrl Pts',(-194.874343783088,4.91387681731697,
130.556023647124));
#243652=CARTESIAN_POINT('Ctrl Pts',(-194.882108536035,4.90507059386854,
130.419357758287));
#243653=CARTESIAN_POINT('Ctrl Pts',(-194.889873288982,4.89055504197982,
130.283155817256));
#243654=CARTESIAN_POINT('Ctrl Pts',(-194.897630329867,4.87605390714187,
130.147089153914));
#243655=CARTESIAN_POINT('Ctrl Pts',(-194.905387370752,4.85585476974856,
130.011485907615));
#243656=CARTESIAN_POINT('Ctrl Pts',(-194.913144411637,4.83000243600482,
129.876858849003));
#243657=CARTESIAN_POINT('Ctrl Pts',(-194.920895602877,4.80416959770702,
129.742333313703));
#243658=CARTESIAN_POINT('Ctrl Pts',(-194.928646794117,4.77269212197063,
129.608782883225));
#243659=CARTESIAN_POINT('Ctrl Pts',(-194.936397985358,4.73566647163151,
129.476713777489));
#243660=CARTESIAN_POINT('Ctrl Pts',(-194.944145882135,4.69865655818142,
129.344700804647));
#243661=CARTESIAN_POINT('Ctrl Pts',(-194.951893778912,4.6561032655712,129.214168279979));
#243662=CARTESIAN_POINT('Ctrl Pts',(-194.959641675689,4.6081538003628,129.08561060238));
#243663=CARTESIAN_POINT('Ctrl Pts',(-194.967387951773,4.56021436514899,
128.957079816276));
#243664=CARTESIAN_POINT('Ctrl Pts',(-194.975134227857,4.50688113905005,
128.830523421655));
#243665=CARTESIAN_POINT('Ctrl Pts',(-194.982880503941,4.44835055949762,
128.706418682641));
#243666=CARTESIAN_POINT('Ctrl Pts',(-194.990626837206,4.38981954788566,
128.582313027514));
#243667=CARTESIAN_POINT('Ctrl Pts',(-194.998373170472,4.32609127303541,
128.460659417719));
#243668=CARTESIAN_POINT('Ctrl Pts',(-195.006119503737,4.25740932120014,
128.341912864971));
#243669=CARTESIAN_POINT('Ctrl Pts',(-195.01386757174,4.18871198851806,128.223139719757));
#243670=CARTESIAN_POINT('Ctrl Pts',(-195.021615639743,4.11505896709885,
128.107275265403));
#243671=CARTESIAN_POINT('Ctrl Pts',(-195.029363707746,4.03673836554418,
127.994747400299));
#243672=CARTESIAN_POINT('Ctrl Pts',(-195.037120010488,3.95833452392204,
127.88209993924));
#243673=CARTESIAN_POINT('Ctrl Pts',(-195.04487631323,3.87525341621253,127.772796472684));
#243674=CARTESIAN_POINT('Ctrl Pts',(-195.052632615971,3.78782516145076,
127.667233969058));
#243675=CARTESIAN_POINT('Ctrl Pts',(-195.060393058486,3.70035024359701,
127.561615123545));
#243676=CARTESIAN_POINT('Ctrl Pts',(-195.068153501,3.60852381712407,127.459741509747));
#243677=CARTESIAN_POINT('Ctrl Pts',(-195.075913943514,3.51271372304341,
127.361974038107));
#243678=CARTESIAN_POINT('Ctrl Pts',(-195.083686843779,3.41674982609412,
127.264049621441));
#243679=CARTESIAN_POINT('Ctrl Pts',(-195.091459744045,3.31678976767184,
127.170244786629));
#243680=CARTESIAN_POINT('Ctrl Pts',(-195.09923264431,3.21323606715028,127.080881459673));
#243681=CARTESIAN_POINT('Ctrl Pts',(-195.106722980072,3.11344680447899,
126.994766714744));
#243682=CARTESIAN_POINT('Ctrl Pts',(-195.114213315834,3.01032088056308,
126.912776355728));
#243683=CARTESIAN_POINT('Ctrl Pts',(-195.121703651596,2.90424314852822,
126.835159842003));
#243684=CARTESIAN_POINT('Ctrl Pts',(-195.129477985715,2.79414344704178,
126.75460047457));
#243685=CARTESIAN_POINT('Ctrl Pts',(-195.137252319834,2.68051492048119,
126.678497980498));
#243686=CARTESIAN_POINT('Ctrl Pts',(-195.145026653953,2.56375427239589,
126.60717738434));
#243687=CARTESIAN_POINT('Ctrl Pts',(-195.1527914069,2.44713752137415,126.535944684443));
#243688=CARTESIAN_POINT('Ctrl Pts',(-195.160556159847,2.32739665963895,
126.469482358469));
#243689=CARTESIAN_POINT('Ctrl Pts',(-195.168320912794,2.20496009885318,
126.408074227331));
#243690=CARTESIAN_POINT('Ctrl Pts',(-195.176077953679,2.0826451437853,126.346727087614));
#243691=CARTESIAN_POINT('Ctrl Pts',(-195.183834994564,1.95764016503764,
126.290424327054));
#243692=CARTESIAN_POINT('Ctrl Pts',(-195.191592035449,1.83040078992447,
126.23940541398));
#243693=CARTESIAN_POINT('Ctrl Pts',(-195.19934322669,1.70325736701403,126.188424974666));
#243694=CARTESIAN_POINT('Ctrl Pts',(-195.20709441793,1.57388326299252,126.142720596667));
#243695=CARTESIAN_POINT('Ctrl Pts',(-195.21484560917,1.44275651553619,126.102484747301));
#243696=CARTESIAN_POINT('Ctrl Pts',(-195.222593505947,1.31168550044528,
126.062265999245));
#243697=CARTESIAN_POINT('Ctrl Pts',(-195.230341402724,1.17886369649157,
126.027511271472));
#243698=CARTESIAN_POINT('Ctrl Pts',(-195.238089299501,1.04478662420943,
125.998363949613));
#243699=CARTESIAN_POINT('Ctrl Pts',(-195.245835575585,0.910737597960802,
125.969222724746));
#243700=CARTESIAN_POINT('Ctrl Pts',(-195.253581851669,0.775434207459803,
125.945686655733));
#243701=CARTESIAN_POINT('Ctrl Pts',(-195.261328127753,0.63938416776216,
125.927848447119));
#243702=CARTESIAN_POINT('Ctrl Pts',(-195.269074461019,0.503333123773844,
125.910010106827));
#243703=CARTESIAN_POINT('Ctrl Pts',(-195.276820794284,0.366535807238244,
125.897869761689));
#243704=CARTESIAN_POINT('Ctrl Pts',(-195.284567127549,0.229506696718071,
125.891468420635));
#243705=CARTESIAN_POINT('Ctrl Pts',(-195.292315195552,0.0924468994788774,
125.885065646046));
#243706=CARTESIAN_POINT('Ctrl Pts',(-195.300063263555,-0.0448444045725537,
125.884404451203));
#243707=CARTESIAN_POINT('Ctrl Pts',(-195.307811331558,-0.181851482666569,
125.889473731711));
#243708=CARTESIAN_POINT('Ctrl Pts',(-195.3155676343,-0.319004173513774,
125.89454839991));
#243709=CARTESIAN_POINT('Ctrl Pts',(-195.323323937042,-0.455871643647917,
125.905365695246));
#243710=CARTESIAN_POINT('Ctrl Pts',(-195.331080239784,-0.591941474886092,
125.921862450356));
#243711=CARTESIAN_POINT('Ctrl Pts',(-195.338840682298,-0.728083930690183,
125.938368010281));
#243712=CARTESIAN_POINT('Ctrl Pts',(-195.346601124812,-0.863427513682498,
125.960559006873));
#243713=CARTESIAN_POINT('Ctrl Pts',(-195.354361567326,-0.997469752634241,
125.98832104598));
#243714=CARTESIAN_POINT('Ctrl Pts',(-195.362134467592,-1.13172716808766,
126.016127651178));
#243715=CARTESIAN_POINT('Ctrl Pts',(-195.369907367857,-1.26467868554271,
126.049523074818));
#243716=CARTESIAN_POINT('Ctrl Pts',(-195.377680268122,-1.39583588798348,
126.088342674818));
#243717=CARTESIAN_POINT('Ctrl Pts',(-195.385170603885,-1.52222519575403,
126.12575108458));
#243718=CARTESIAN_POINT('Ctrl Pts',(-195.392660939647,-1.64694808775228,
126.168196053275));
#243719=CARTESIAN_POINT('Ctrl Pts',(-195.400151275409,-1.76958666422382,
126.215488631958));
#243720=CARTESIAN_POINT('Ctrl Pts',(-195.407925865569,-1.89687931172836,
126.264575939728));
#243721=CARTESIAN_POINT('Ctrl Pts',(-195.415700455729,-2.02232956017334,
126.319041551411));
#243722=CARTESIAN_POINT('Ctrl Pts',(-195.423475045889,-2.1454494812566,
126.378727376336));
#243723=CARTESIAN_POINT('Ctrl Pts',(-195.431239995709,-2.26841673604816,
126.438339192008));
#243724=CARTESIAN_POINT('Ctrl Pts',(-195.43900494553,-2.38905906452119,
126.503158172355));
#243725=CARTESIAN_POINT('Ctrl Pts',(-195.44676989535,-2.50690607821073,
126.57297727668));
#243726=CARTESIAN_POINT('Ctrl Pts',(-195.454527074191,-2.62463515337862,
126.642726507686));
#243727=CARTESIAN_POINT('Ctrl Pts',(-195.462284253032,-2.73957414685786,
126.717465706102));
#243728=CARTESIAN_POINT('Ctrl Pts',(-195.470041431874,-2.85127528719056,
126.796940961583));
#243729=CARTESIAN_POINT('Ctrl Pts',(-195.478170592057,-2.96833285167254,
126.880227307771));
#243730=CARTESIAN_POINT('Ctrl Pts',(-195.48629975224,-3.08183394409786,
126.968714999343));
#243731=CARTESIAN_POINT('Ctrl Pts',(-195.494428912423,-3.19129454302132,
127.0620588924));
#243732=CARTESIAN_POINT('Ctrl Pts',(-195.50217647144,-3.29561681384803,
127.151021011987));
#243733=CARTESIAN_POINT('Ctrl Pts',(-195.509924030457,-3.39626895266872,
127.244393515566));
#243734=CARTESIAN_POINT('Ctrl Pts',(-195.517671589474,-3.49286418306127,
127.341835114239));
#243735=CARTESIAN_POINT('Ctrl Pts',(-195.525417525999,-3.58943918449754,
127.43925630671));
#243736=CARTESIAN_POINT('Ctrl Pts',(-195.533163462523,-3.68195869289281,
127.540744621327));
#243737=CARTESIAN_POINT('Ctrl Pts',(-195.540909399048,-3.77007218189079,
127.645921318508));
#243738=CARTESIAN_POINT('Ctrl Pts',(-195.548655390858,-3.85818629978034,
127.751098766365));
#243739=CARTESIAN_POINT('Ctrl Pts',(-195.556401382667,-3.94189408507239,
127.859964349216));
#243740=CARTESIAN_POINT('Ctrl Pts',(-195.564147374477,-4.02088502556128,
127.972105919677));
#243741=CARTESIAN_POINT('Ctrl Pts',(-195.571895099012,-4.09989363577994,
128.084272575435));
#243742=CARTESIAN_POINT('Ctrl Pts',(-195.579642823547,-4.17418307720177,
128.199716357132));
#243743=CARTESIAN_POINT('Ctrl Pts',(-195.587390548081,-4.24348615363837,
128.317996137772));
#243744=CARTESIAN_POINT('Ctrl Pts',(-195.595145422041,-4.31285318138828,
128.436385064323));
#243745=CARTESIAN_POINT('Ctrl Pts',(-195.602900296001,-4.37722445952681,
128.557614877344));
#243746=CARTESIAN_POINT('Ctrl Pts',(-195.610655169961,-4.43637859937377,
128.681219551711));
#243747=CARTESIAN_POINT('Ctrl Pts',(-195.61841422265,-4.49556461454609,
128.804890830702));
#243748=CARTESIAN_POINT('Ctrl Pts',(-195.626173275339,-4.54952773652002,
128.930939161969));
#243749=CARTESIAN_POINT('Ctrl Pts',(-195.633932328028,-4.59809510986851,
129.05887947384));
#243750=CARTESIAN_POINT('Ctrl Pts',(-195.64170116025,-4.64672369767602,
129.186981042053));
#243751=CARTESIAN_POINT('Ctrl Pts',(-195.649469992472,-4.68994283555458,
129.316978981968));
#243752=CARTESIAN_POINT('Ctrl Pts',(-195.657238824693,-4.72762969271982,
129.448373688789));
#243753=CARTESIAN_POINT('Ctrl Pts',(-195.659872975218,-4.74040804237829,
129.492925228326));
#243754=CARTESIAN_POINT('Ctrl Pts',(-195.662507125742,-4.7525508024199,
129.537637266952));
#243755=CARTESIAN_POINT('Ctrl Pts',(-195.665141276266,-4.76405452823396,
129.582490119308));
#243756=CARTESIAN_POINT('',(-193.639859436047,-4.91824923219391,130.807108803159));
#243757=CARTESIAN_POINT('Ctrl Pts',(-193.639859436047,-4.91824923219391,
130.80710880316));
#243758=CARTESIAN_POINT('Ctrl Pts',(-193.648453682647,-4.91816405453979,
130.959545717499));
#243759=CARTESIAN_POINT('Ctrl Pts',(-193.657047929247,-4.91098784782448,
131.11172896582));
#243760=CARTESIAN_POINT('Ctrl Pts',(-193.665642175847,-4.89681553245056,
131.263033380711));
#243761=CARTESIAN_POINT('Ctrl Pts',(-193.674285738832,-4.88256189204551,
131.415206026086));
#243762=CARTESIAN_POINT('Ctrl Pts',(-193.682929301818,-4.86123170846623,
131.566489499949));
#243763=CARTESIAN_POINT('Ctrl Pts',(-193.691572864804,-4.83297164334981,
131.716264207359));
#243764=CARTESIAN_POINT('Ctrl Pts',(-193.700242045639,-4.8046278208643,
131.866482818043));
#243765=CARTESIAN_POINT('Ctrl Pts',(-193.708911226474,-4.76931309557723,
132.015183498403));
#243766=CARTESIAN_POINT('Ctrl Pts',(-193.717580407309,-4.7272241103825,
132.161760806426));
#243767=CARTESIAN_POINT('Ctrl Pts',(-193.726281692355,-4.6849792588291,
132.308880927995));
#243768=CARTESIAN_POINT('Ctrl Pts',(-193.734982977401,-4.63590999828547,
132.453861718932));
#243769=CARTESIAN_POINT('Ctrl Pts',(-193.743684262447,-4.5802623667498,
132.596113869059));
#243770=CARTESIAN_POINT('Ctrl Pts',(-193.745474351195,-4.56881414978355,
132.625378968644));
#243771=CARTESIAN_POINT('Ctrl Pts',(-193.747264439944,-4.55708766805062,
132.654528665305));
#243772=CARTESIAN_POINT('Ctrl Pts',(-193.749054528692,-4.5450853031912,
132.683557959309));
#243773=CARTESIAN_POINT('Ctrl Pts',(-193.756828862811,-4.49295917552469,
132.809631837505));
#243774=CARTESIAN_POINT('Ctrl Pts',(-193.76460319693,-4.4355008567645,132.933734912639));
#243775=CARTESIAN_POINT('Ctrl Pts',(-193.772377531049,-4.37288008339332,
133.055383238235));
#243776=CARTESIAN_POINT('Ctrl Pts',(-193.780142283997,-4.31033648452892,
133.17688164314));
#243777=CARTESIAN_POINT('Ctrl Pts',(-193.787907036944,-4.24264326728463,
133.295930973597));
#243778=CARTESIAN_POINT('Ctrl Pts',(-193.795671789891,-4.17001868196047,
133.412065979489));
#243779=CARTESIAN_POINT('Ctrl Pts',(-193.803428830776,-4.09746622839829,
133.528085638456));
#243780=CARTESIAN_POINT('Ctrl Pts',(-193.811185871661,-4.01999235975909,
133.641196403798));
#243781=CARTESIAN_POINT('Ctrl Pts',(-193.818942912546,-3.93786164135559,
133.750956748026));
#243782=CARTESIAN_POINT('Ctrl Pts',(-193.826694103786,-3.8557928583656,
133.860634321124));
#243783=CARTESIAN_POINT('Ctrl Pts',(-193.834445295026,-3.76907444885508,
133.966966190343));
#243784=CARTESIAN_POINT('Ctrl Pts',(-193.842196486266,-3.67801456681571,
134.069539312338));
#243785=CARTESIAN_POINT('Ctrl Pts',(-193.849944383043,-3.58699338765545,
134.172068838019));
#243786=CARTESIAN_POINT('Ctrl Pts',(-193.85769227982,-3.4916346650259,134.270842502153));
#243787=CARTESIAN_POINT('Ctrl Pts',(-193.865440176597,-3.39228701555218,
134.365480085741));
#243788=CARTESIAN_POINT('Ctrl Pts',(-193.873186452681,-3.29296014746504,
134.460097873187));
#243789=CARTESIAN_POINT('Ctrl Pts',(-193.880932728766,-3.18964629509992,
134.550581031482));
#243790=CARTESIAN_POINT('Ctrl Pts',(-193.88867900485,-3.0827308531471,134.636586282836));
#243791=CARTESIAN_POINT('Ctrl Pts',(-193.896425338115,-2.97581462196864,
134.722592169061));
#243792=CARTESIAN_POINT('Ctrl Pts',(-193.90417167138,-2.86529705278595,
134.804119837331));
#243793=CARTESIAN_POINT('Ctrl Pts',(-193.911918004646,-2.75159620769232,
134.880866642621));
#243794=CARTESIAN_POINT('Ctrl Pts',(-193.919666072649,-2.63786990008324,
134.957630634827));
#243795=CARTESIAN_POINT('Ctrl Pts',(-193.927414140652,-2.52095922202,135.029611414911));
#243796=CARTESIAN_POINT('Ctrl Pts',(-193.935162208655,-2.40131041503007,
135.096550193198));
#243797=CARTESIAN_POINT('Ctrl Pts',(-193.942918511396,-2.28153444386374,
135.163560114816));
#243798=CARTESIAN_POINT('Ctrl Pts',(-193.950674814138,-2.15901487224249,
135.225517138867));
#243799=CARTESIAN_POINT('Ctrl Pts',(-193.95843111688,-2.03422219292027,
135.2822086646));
#243800=CARTESIAN_POINT('Ctrl Pts',(-193.966191559394,-1.90936290798765,
135.338930448309));
#243801=CARTESIAN_POINT('Ctrl Pts',(-193.973952001908,-1.78222846013368,
135.390380987236));
#243802=CARTESIAN_POINT('Ctrl Pts',(-193.981712444423,-1.65330749395548,
135.436396605437));
#243803=CARTESIAN_POINT('Ctrl Pts',(-193.989485344688,-1.52417957239731,
135.482486091993));
#243804=CARTESIAN_POINT('Ctrl Pts',(-193.997258244953,-1.39325977518751,
135.523123107292));
#243805=CARTESIAN_POINT('Ctrl Pts',(-194.005031145219,-1.26105088175151,
135.5581942007));
#243806=CARTESIAN_POINT('Ctrl Pts',(-194.012521480981,-1.133648114606,135.591990371525));
#243807=CARTESIAN_POINT('Ctrl Pts',(-194.020011816743,-1.00504864850035,
135.620618198415));
#243808=CARTESIAN_POINT('Ctrl Pts',(-194.027502152505,-0.875707681015639,
135.644021671804));
#243809=CARTESIAN_POINT('Ctrl Pts',(-194.035276486624,-0.741462711436587,
135.668312495));
#243810=CARTESIAN_POINT('Ctrl Pts',(-194.043050820743,-0.605993654757619,
135.687051927619));
#243811=CARTESIAN_POINT('Ctrl Pts',(-194.050825154862,-0.469799415570403,
135.70012118888));
#243812=CARTESIAN_POINT('Ctrl Pts',(-194.058589907809,-0.333773023610957,
135.713174343443));
#243813=CARTESIAN_POINT('Ctrl Pts',(-194.066354660756,-0.197023612826312,
135.720571193658));
#243814=CARTESIAN_POINT('Ctrl Pts',(-194.074119413703,-0.0600605809332014,
135.722243880629));
#243815=CARTESIAN_POINT('Ctrl Pts',(-194.081876454588,0.0767664173457922,
135.723914906265));
#243816=CARTESIAN_POINT('Ctrl Pts',(-194.089633495473,0.213806226096077,
135.719873077956));
#243817=CARTESIAN_POINT('Ctrl Pts',(-194.097390536358,0.35054437172053,
135.710102325601));
#243818=CARTESIAN_POINT('Ctrl Pts',(-194.105141727599,0.487179402045514,
135.700338941446));
#243819=CARTESIAN_POINT('Ctrl Pts',(-194.112892918839,0.6235128336498,135.684855260145));
#243820=CARTESIAN_POINT('Ctrl Pts',(-194.120644110079,0.759030596709005,
135.663687280362));
#243821=CARTESIAN_POINT('Ctrl Pts',(-194.128392006856,0.894490761104039,
135.642528297535));
#243822=CARTESIAN_POINT('Ctrl Pts',(-194.136139903633,1.02913556100334,
135.615689881632));
#243823=CARTESIAN_POINT('Ctrl Pts',(-194.14388780041,1.16245667159326,135.583259816039));
#243824=CARTESIAN_POINT('Ctrl Pts',(-194.151634076494,1.29574989428092,
135.550836534117));
#243825=CARTESIAN_POINT('Ctrl Pts',(-194.159380352578,1.42771959875601,
135.512824021355));
#243826=CARTESIAN_POINT('Ctrl Pts',(-194.167126628662,1.55786866044568,
135.469360971189));
#243827=CARTESIAN_POINT('Ctrl Pts',(-194.174872961928,1.68801868286598,
135.425897600189));
#243828=CARTESIAN_POINT('Ctrl Pts',(-194.182619295193,1.81634766484947,
135.376983735339));
#243829=CARTESIAN_POINT('Ctrl Pts',(-194.190365628458,1.9423750097934,135.322807517091));
#243830=CARTESIAN_POINT('Ctrl Pts',(-194.198113696461,2.06843057768725,
135.268619166455));
#243831=CARTESIAN_POINT('Ctrl Pts',(-194.205861764464,2.19218312376924,
135.209166271782));
#243832=CARTESIAN_POINT('Ctrl Pts',(-194.213609832467,2.31317371650994,
135.144684386566));
#243833=CARTESIAN_POINT('Ctrl Pts',(-194.221366135209,2.43429289949258,
135.080133969235));
#243834=CARTESIAN_POINT('Ctrl Pts',(-194.229122437951,2.55264391970813,
135.010544068579));
#243835=CARTESIAN_POINT('Ctrl Pts',(-194.236878740693,2.66779359729971,
134.93619560758));
#243836=CARTESIAN_POINT('Ctrl Pts',(-194.244639183207,2.78300473374162,
134.861807464569));
#243837=CARTESIAN_POINT('Ctrl Pts',(-194.252399625721,2.8950108037929,134.782655925994));
#243838=CARTESIAN_POINT('Ctrl Pts',(-194.260160068235,3.00340997790441,
134.699063631548));
#243839=CARTESIAN_POINT('Ctrl Pts',(-194.2679329685,3.11198316399314,134.615337147331));
#243840=CARTESIAN_POINT('Ctrl Pts',(-194.275705868766,3.2169375841494,134.527155913481));
#243841=CARTESIAN_POINT('Ctrl Pts',(-194.283478769031,3.3179060245828,134.434881609729));
#243842=CARTESIAN_POINT('Ctrl Pts',(-194.290969104794,3.41520400788394,
134.345961709343));
#243843=CARTESIAN_POINT('Ctrl Pts',(-194.298459440556,3.50880056207708,
134.253241376088));
#243844=CARTESIAN_POINT('Ctrl Pts',(-194.305949776318,3.59840251931591,
134.157073306044));
#243845=CARTESIAN_POINT('Ctrl Pts',(-194.313724110437,3.69140176199619,
134.057258994396));
#243846=CARTESIAN_POINT('Ctrl Pts',(-194.321498444556,3.78039211153777,
133.953414161395));
#243847=CARTESIAN_POINT('Ctrl Pts',(-194.329272778675,3.8650039641869,133.845894345691));
#243848=CARTESIAN_POINT('Ctrl Pts',(-194.337037531622,3.94951154028939,
133.73850703855));
#243849=CARTESIAN_POINT('Ctrl Pts',(-194.344802284569,4.02965111668345,
133.627454064531));
#243850=CARTESIAN_POINT('Ctrl Pts',(-194.352567037516,4.10509025985185,
133.513127314971));
#243851=CARTESIAN_POINT('Ctrl Pts',(-194.360324078401,4.18045447579975,
133.39891411635));
#243852=CARTESIAN_POINT('Ctrl Pts',(-194.368081119286,4.25112733518645,
133.281433937151));
#243853=CARTESIAN_POINT('Ctrl Pts',(-194.375838160171,4.31681723223276,
133.1611109323));
#243854=CARTESIAN_POINT('Ctrl Pts',(-194.383589351411,4.38245759201679,
133.040878663962));
#243855=CARTESIAN_POINT('Ctrl Pts',(-194.391340542651,4.44312228232928,
132.917808178837));
#243856=CARTESIAN_POINT('Ctrl Pts',(-194.399091733892,4.49856372256806,
132.792351436583));
#243857=CARTESIAN_POINT('Ctrl Pts',(-194.406839630669,4.55398159871571,
132.666948016791));
#243858=CARTESIAN_POINT('Ctrl Pts',(-194.414587527446,4.60418048254142,
132.539160713937));
#243859=CARTESIAN_POINT('Ctrl Pts',(-194.422335424223,4.64895946671369,
132.409464645146));
#243860=CARTESIAN_POINT('Ctrl Pts',(-194.430081700307,4.69372908408779,
132.279795705977));
#243861=CARTESIAN_POINT('Ctrl Pts',(-194.437827976391,4.73308092933866,
132.14821916437));
#243862=CARTESIAN_POINT('Ctrl Pts',(-194.445574252475,4.76686298120744,
132.015228232499));
#243863=CARTESIAN_POINT('Ctrl Pts',(-194.45332058574,4.80064528244769,131.882236318919));
#243864=CARTESIAN_POINT('Ctrl Pts',(-194.461066919006,4.82885761200875,
131.747830373172));
#243865=CARTESIAN_POINT('Ctrl Pts',(-194.468813252271,4.85139848357786,
131.612516429299));
#243866=CARTESIAN_POINT('Ctrl Pts',(-194.476561320274,4.87394440301884,
131.477172182808));
#243867=CARTESIAN_POINT('Ctrl Pts',(-194.484309388277,4.89081627291814,
131.340919919146));
#243868=CARTESIAN_POINT('Ctrl Pts',(-194.49205745628,4.90196420739985,131.204273072824));
#243869=CARTESIAN_POINT('Ctrl Pts',(-194.499813759022,4.913123990039,131.067480996608));
#243870=CARTESIAN_POINT('Ctrl Pts',(-194.507570061764,4.91854765303973,
130.930293890293));
#243871=CARTESIAN_POINT('Ctrl Pts',(-194.515326364506,4.91823740056867,
130.793228046095));
#243872=CARTESIAN_POINT('Ctrl Pts',(-194.52308680702,4.91792698250651,130.656089045728));
#243873=CARTESIAN_POINT('Ctrl Pts',(-194.530847249534,4.91187656817852,
130.519071826834));
#243874=CARTESIAN_POINT('Ctrl Pts',(-194.538607692048,4.90014040480876,
130.382688854626));
#243875=CARTESIAN_POINT('Ctrl Pts',(-194.546380592313,4.88838540150768,
130.246086948365));
#243876=CARTESIAN_POINT('Ctrl Pts',(-194.554153492579,4.8709264597954,130.110121711381));
#243877=CARTESIAN_POINT('Ctrl Pts',(-194.561926392844,4.84786938305054,
129.975297587766));
#243878=CARTESIAN_POINT('Ctrl Pts',(-194.569416728606,4.8256504891227,129.845374660647));
#243879=CARTESIAN_POINT('Ctrl Pts',(-194.576907064368,4.79823347054425,
129.71651162387));
#243880=CARTESIAN_POINT('Ctrl Pts',(-194.58439740013,4.76575659613236,129.589145768693));
#243881=CARTESIAN_POINT('Ctrl Pts',(-194.592171734249,4.73204835115597,
129.456950798405));
#243882=CARTESIAN_POINT('Ctrl Pts',(-194.599946068368,4.69278220975143,
129.325950028211));
#243883=CARTESIAN_POINT('Ctrl Pts',(-194.607720402487,4.64805751679649,
129.196646593539));
#243884=CARTESIAN_POINT('Ctrl Pts',(-194.615485155434,4.60338794302845,
129.067502513795));
#243885=CARTESIAN_POINT('Ctrl Pts',(-194.623249908382,4.55327332936175,
128.940051973427));
#243886=CARTESIAN_POINT('Ctrl Pts',(-194.631014661329,4.49786369664073,
128.814786485009));
#243887=CARTESIAN_POINT('Ctrl Pts',(-194.638771702214,4.44250909754792,
128.689645412039));
#243888=CARTESIAN_POINT('Ctrl Pts',(-194.646528743099,4.38187010235564,
128.566685427407));
#243889=CARTESIAN_POINT('Ctrl Pts',(-194.654285783984,4.31614594456795,
128.446381133412));
#243890=CARTESIAN_POINT('Ctrl Pts',(-194.662036975224,4.250471349879,128.326167561822));
#243891=CARTESIAN_POINT('Ctrl Pts',(-194.669788166464,4.17971941213704,
128.208606036374));
#243892=CARTESIAN_POINT('Ctrl Pts',(-194.677539357704,4.10413655444054,
128.094149148879));
#243893=CARTESIAN_POINT('Ctrl Pts',(-194.685287254481,4.0285858214747,127.979740908613));
#243894=CARTESIAN_POINT('Ctrl Pts',(-194.693035151258,3.94820846734261,
127.868435007373));
#243895=CARTESIAN_POINT('Ctrl Pts',(-194.700783048035,3.86329562621768,
127.760657286598));
#243896=CARTESIAN_POINT('Ctrl Pts',(-194.708529324119,3.77840054702884,
127.652902110599));
#243897=CARTESIAN_POINT('Ctrl Pts',(-194.716275600204,3.68897210971447,
127.548673954013));
#243898=CARTESIAN_POINT('Ctrl Pts',(-194.724021876288,3.59534309643996,
127.448367309858));
#243899=CARTESIAN_POINT('Ctrl Pts',(-194.731768209553,3.50171339201721,
127.348059925262));
#243900=CARTESIAN_POINT('Ctrl Pts',(-194.739514542818,3.40388331653783,
127.251674396663));
#243901=CARTESIAN_POINT('Ctrl Pts',(-194.747260876084,3.3022237549426,127.159569631132));
#243902=CARTESIAN_POINT('Ctrl Pts',(-194.755008944087,3.20054142739355,
127.067444239377));
#243903=CARTESIAN_POINT('Ctrl Pts',(-194.76275701209,3.09502819690908,126.979601780738));
#243904=CARTESIAN_POINT('Ctrl Pts',(-194.770505080093,2.98608906594972,
126.896361749511));
#243905=CARTESIAN_POINT('Ctrl Pts',(-194.778261382835,2.87703415318544,
126.813033249789));
#243906=CARTESIAN_POINT('Ctrl Pts',(-194.786017685576,2.76454637763411,
126.734317186555));
#243907=CARTESIAN_POINT('Ctrl Pts',(-194.793773988318,2.6490613019644,126.660490773937));
#243908=CARTESIAN_POINT('Ctrl Pts',(-194.801534430832,2.53351458843263,
126.58662495794));
#243909=CARTESIAN_POINT('Ctrl Pts',(-194.809294873347,2.41496772491371,
126.517654189227));
#243910=CARTESIAN_POINT('Ctrl Pts',(-194.817055315861,2.29388118485612,
126.453809828038));
#243911=CARTESIAN_POINT('Ctrl Pts',(-194.824828216126,2.17260026593488,
126.389862978213));
#243912=CARTESIAN_POINT('Ctrl Pts',(-194.832601116392,2.04877187687075,
126.331059148613));
#243913=CARTESIAN_POINT('Ctrl Pts',(-194.840374016657,1.92287761007517,
126.277581988213));
#243914=CARTESIAN_POINT('Ctrl Pts',(-194.847864352419,1.80155991698648,
126.226048857294));
#243915=CARTESIAN_POINT('Ctrl Pts',(-194.855354688181,1.67832422631585,
126.179461952482));
#243916=CARTESIAN_POINT('Ctrl Pts',(-194.862845023943,1.55361318125574,
126.13794131091));
#243917=CARTESIAN_POINT('Ctrl Pts',(-194.870619358062,1.42417367901689,
126.094846401594));
#243918=CARTESIAN_POINT('Ctrl Pts',(-194.878393692181,1.29273471235955,
126.05707300227));
#243919=CARTESIAN_POINT('Ctrl Pts',(-194.886168026301,1.15977328170358,
126.024809488271));
#243920=CARTESIAN_POINT('Ctrl Pts',(-194.893932779248,1.02697571412778,
125.992585736169));
#243921=CARTESIAN_POINT('Ctrl Pts',(-194.901697532195,0.892659792124973,
125.965858449745));
#243922=CARTESIAN_POINT('Ctrl Pts',(-194.909462285142,0.757320129074038,
125.944767086765));
#243923=CARTESIAN_POINT('Ctrl Pts',(-194.917219326027,0.6221148872844,125.923696672025));
#243924=CARTESIAN_POINT('Ctrl Pts',(-194.924976366912,0.485888311715355,
125.908251100908));
#243925=CARTESIAN_POINT('Ctrl Pts',(-194.932733407797,0.349147389297095,
125.89851928676));
#243926=CARTESIAN_POINT('Ctrl Pts',(-194.940484599037,0.212509584271935,
125.888794811448));
#243927=CARTESIAN_POINT('Ctrl Pts',(-194.948235790277,0.0753585928360218,
125.884775544365));
#243928=CARTESIAN_POINT('Ctrl Pts',(-194.955986981517,-0.0617916090006001,
125.886498799707));
#243929=CARTESIAN_POINT('Ctrl Pts',(-194.963734878294,-0.198883518342653,
125.888221322619));
#243930=CARTESIAN_POINT('Ctrl Pts',(-194.971482775071,-0.335974248637008,
125.895681508637));
#243931=CARTESIAN_POINT('Ctrl Pts',(-194.979230671849,-0.472548162288011,
125.908864596036));
#243932=CARTESIAN_POINT('Ctrl Pts',(-194.986976947933,-0.60909350762047,
125.922044925817));
#243933=CARTESIAN_POINT('Ctrl Pts',(-194.994723224017,-0.745121862430249,
125.940945738326));
#243934=CARTESIAN_POINT('Ctrl Pts',(-195.002469500101,-0.880121451680396,
125.965500287613));
#243935=CARTESIAN_POINT('Ctrl Pts',(-195.010215833366,-1.01512203746703,
125.990055018157));
#243936=CARTESIAN_POINT('Ctrl Pts',(-195.017962166632,-1.14909345788622,
126.020263498794));
#243937=CARTESIAN_POINT('Ctrl Pts',(-195.025708499897,-1.28153328188549,
126.056007691559));
#243938=CARTESIAN_POINT('Ctrl Pts',(-195.0334565679,-1.41400276486489,126.091759888988));
#243939=CARTESIAN_POINT('Ctrl Pts',(-195.041204635903,-1.54493959152582,
126.133050163519));
#243940=CARTESIAN_POINT('Ctrl Pts',(-195.048952703906,-1.67385604854705,
126.179710469583));
#243941=CARTESIAN_POINT('Ctrl Pts',(-195.056709006648,-1.80290951951275,
126.226420366775));
#243942=CARTESIAN_POINT('Ctrl Pts',(-195.06446530939,-1.92993796321751,
126.278511563241));
#243943=CARTESIAN_POINT('Ctrl Pts',(-195.072221612131,-2.0544727193047,
126.335767448779));
#243944=CARTESIAN_POINT('Ctrl Pts',(-195.079982054646,-2.17907394334121,
126.393053893507));
#243945=CARTESIAN_POINT('Ctrl Pts',(-195.08774249716,-2.30117847981346,
126.455510342012));
#243946=CARTESIAN_POINT('Ctrl Pts',(-195.095502939674,-2.42034278165234,
126.522874440804));
#243947=CARTESIAN_POINT('Ctrl Pts',(-195.10327583994,-2.53969837660744,
126.590346678427));
#243948=CARTESIAN_POINT('Ctrl Pts',(-195.111048740205,-2.65610397282664,
126.662742102887));
#243949=CARTESIAN_POINT('Ctrl Pts',(-195.11882164047,-2.76914474876468,
126.739754803605));
#243950=CARTESIAN_POINT('Ctrl Pts',(-195.126311976232,-2.87807620776515,
126.813967898668));
#243951=CARTESIAN_POINT('Ctrl Pts',(-195.133802311994,-2.98388299120046,
126.892468215446));
#243952=CARTESIAN_POINT('Ctrl Pts',(-195.141292647756,-3.08622484897237,
126.974948228689));
#243953=CARTESIAN_POINT('Ctrl Pts',(-195.148964038384,-3.19104049321887,
127.059421931958));
#243954=CARTESIAN_POINT('Ctrl Pts',(-195.156635429012,-3.29257225117811,
127.148353103153));
#243955=CARTESIAN_POINT('Ctrl Pts',(-195.164306819639,-3.39040972582631,
127.241453805211));
#243956=CARTESIAN_POINT('Ctrl Pts',(-195.171969427545,-3.48813518957756,
127.334447919347));
#243957=CARTESIAN_POINT('Ctrl Pts',(-195.17963203545,-3.58217448966821,
127.431601801204));
#243958=CARTESIAN_POINT('Ctrl Pts',(-195.187294643356,-3.67214823682183,
127.532585810324));
#243959=CARTESIAN_POINT('Ctrl Pts',(-195.194950242633,-3.76203968920446,
127.633477454101));
#243960=CARTESIAN_POINT('Ctrl Pts',(-195.20260584191,-3.84787271682651,
127.738191961579));
#243961=CARTESIAN_POINT('Ctrl Pts',(-195.210261441187,-3.92930333398827,
127.846361568883));
#243962=CARTESIAN_POINT('Ctrl Pts',(-195.217911799506,-4.01067820443681,
127.954457124187));
#243963=CARTESIAN_POINT('Ctrl Pts',(-195.225562157824,-4.0876564179061,
128.066002754977));
#243964=CARTESIAN_POINT('Ctrl Pts',(-195.233212516142,-4.15993336229173,
128.180596625933));
#243965=CARTESIAN_POINT('Ctrl Pts',(-195.24086026656,-4.23218566846759,
128.295151433424));
#243966=CARTESIAN_POINT('Ctrl Pts',(-195.248508016977,-4.29973967457936,
128.412752077692));
#243967=CARTESIAN_POINT('Ctrl Pts',(-195.256155767394,-4.36233354812221,
128.532966975454));
#243968=CARTESIAN_POINT('Ctrl Pts',(-195.263801822143,-4.42491354327928,
128.65315521903));
#243969=CARTESIAN_POINT('Ctrl Pts',(-195.271447876892,-4.48253541118757,
128.775956204889));
#243970=CARTESIAN_POINT('Ctrl Pts',(-195.279093931642,-4.53498317575593,
128.900913571255));
#243971=CARTESIAN_POINT('Ctrl Pts',(-195.286742468474,-4.58744796606283,
129.025911501627));
#243972=CARTESIAN_POINT('Ctrl Pts',(-195.294391005307,-4.63473514030973,
129.153066840563));
#243973=CARTESIAN_POINT('Ctrl Pts',(-195.30203954214,-4.67667684027603,
129.281903132404));
#243974=CARTESIAN_POINT('Ctrl Pts',(-195.307932996256,-4.70899432657831,
129.38117581568));
#243975=CARTESIAN_POINT('Ctrl Pts',(-195.313826450373,-4.73813905169708,
129.481446069613));
#243976=CARTESIAN_POINT('Ctrl Pts',(-195.319719904489,-4.76405452823413,
129.582490119309));
#243977=CARTESIAN_POINT('Ctrl Pts',(-193.570047426085,-4.76405452823409,
129.582490119308));
#243978=CARTESIAN_POINT('Ctrl Pts',(-193.577886143416,-4.79853512568151,
129.71692944544));
#243979=CARTESIAN_POINT('Ctrl Pts',(-193.585724860747,-4.82734183515294,
129.852911410386));
#243980=CARTESIAN_POINT('Ctrl Pts',(-193.593563578078,-4.85034802871446,
129.989923963893));
#243981=CARTESIAN_POINT('Ctrl Pts',(-193.601399678027,-4.87334654040656,
130.126890768305));
#243982=CARTESIAN_POINT('Ctrl Pts',(-193.609235777976,-4.8905483261116,
130.264887104432));
#243983=CARTESIAN_POINT('Ctrl Pts',(-193.617071877925,-4.90187780366035,
130.40339046845));
#243984=CARTESIAN_POINT('Ctrl Pts',(-193.624667730615,-4.91285993036604,
130.537647453052));
#243985=CARTESIAN_POINT('Ctrl Pts',(-193.632263583305,-4.91832451473222,
130.672380489236));
#243986=CARTESIAN_POINT('Ctrl Pts',(-193.639859435995,-4.91824923219442,
130.807108802231));
#243987=CARTESIAN_POINT('Origin',(213.235140564004,0.,130.804360617566));
#243988=CARTESIAN_POINT('',(-191.820046567589,-4.76405452823394,129.582490119308));
#243989=CARTESIAN_POINT('',(-192.165295998532,-4.76405452823416,129.582490119309));
#243990=CARTESIAN_POINT('',(213.235140564004,-4.76405452823405,129.582490119308));
#243991=CARTESIAN_POINT('',(-192.235140564068,-4.9182489107902,130.807633843951));
#243992=CARTESIAN_POINT('Ctrl Pts',(-192.165295998532,-4.76405452823416,
129.582490119309));
#243993=CARTESIAN_POINT('Ctrl Pts',(-192.173087299489,-4.79834001608084,
129.716168716068));
#243994=CARTESIAN_POINT('Ctrl Pts',(-192.180878600447,-4.82701148740486,
129.851356535398));
#243995=CARTESIAN_POINT('Ctrl Pts',(-192.188669901404,-4.84994811259561,
129.987545848092));
#243996=CARTESIAN_POINT('Ctrl Pts',(-192.196460544,-4.87288279965338,130.12372365286));
#243997=CARTESIAN_POINT('Ctrl Pts',(-192.204251186596,-4.89008353206788,
130.260902405253));
#243998=CARTESIAN_POINT('Ctrl Pts',(-192.212041829192,-4.90148064217082,
130.398564391703));
#243999=CARTESIAN_POINT('Ctrl Pts',(-192.219741407466,-4.9127445321833,
130.534617256005));
#244000=CARTESIAN_POINT('Ctrl Pts',(-192.227440985739,-4.91833974990952,
130.671141747254));
#244001=CARTESIAN_POINT('Ctrl Pts',(-192.235140564013,-4.91824891079085,
130.807633842979));
#244002=CARTESIAN_POINT('Ctrl Pts',(-192.235140564068,-4.9182489107902,
130.80763384395));
#244003=CARTESIAN_POINT('Ctrl Pts',(-192.243918515748,-4.9181453490622,
130.963242499187));
#244004=CARTESIAN_POINT('Ctrl Pts',(-192.252696467428,-4.91065281771742,
131.118565439462));
#244005=CARTESIAN_POINT('Ctrl Pts',(-192.261474419109,-4.89587660554873,
131.272949270588));
#244006=CARTESIAN_POINT('Ctrl Pts',(-192.270289110367,-4.88103854845119,
131.42797926576));
#244007=CARTESIAN_POINT('Ctrl Pts',(-192.279103801625,-4.85885582307568,
131.582062100835));
#244008=CARTESIAN_POINT('Ctrl Pts',(-192.287918492883,-4.8294847853578,
131.734554022454));
#244009=CARTESIAN_POINT('Ctrl Pts',(-192.296783739358,-4.79994529486645,
131.887920536499));
#244010=CARTESIAN_POINT('Ctrl Pts',(-192.305648985834,-4.76313489578936,
132.039677664175));
#244011=CARTESIAN_POINT('Ctrl Pts',(-192.314514232309,-4.71926132012198,
132.189191168536));
#244012=CARTESIAN_POINT('Ctrl Pts',(-192.322085292695,-4.68179259416399,
132.316878060629));
#244013=CARTESIAN_POINT('Ctrl Pts',(-192.329656353081,-4.63917323850466,
132.442928873986));
#244014=CARTESIAN_POINT('Ctrl Pts',(-192.337227413468,-4.59155968143751,
132.566961750635));
#244015=CARTESIAN_POINT('Ctrl Pts',(-192.345001747587,-4.54266775846242,
132.694324758674));
#244016=CARTESIAN_POINT('Ctrl Pts',(-192.352776081706,-4.48839508868817,
132.819853675534));
#244017=CARTESIAN_POINT('Ctrl Pts',(-192.360550415825,-4.42889900368266,
132.943060380899));
#244018=CARTESIAN_POINT('Ctrl Pts',(-192.368315168772,-4.3694762422846,
133.06611524501));
#244019=CARTESIAN_POINT('Ctrl Pts',(-192.376079921719,-4.30484304252658,
133.186853243304));
#244020=CARTESIAN_POINT('Ctrl Pts',(-192.383844674666,-4.23520571110023,
133.304803707733));
#244021=CARTESIAN_POINT('Ctrl Pts',(-192.391601715551,-4.16563754445317,
133.422637022098));
#244022=CARTESIAN_POINT('Ctrl Pts',(-192.399358756436,-4.09107533448945,
133.537687977781));
#244023=CARTESIAN_POINT('Ctrl Pts',(-192.407115797321,-4.01177229319911,
133.64950843974));
#244024=CARTESIAN_POINT('Ctrl Pts',(-192.414866988561,-3.9325290549492,
133.761244577018));
#244025=CARTESIAN_POINT('Ctrl Pts',(-192.422618179801,-3.84855232664149,
133.869754751943));
#244026=CARTESIAN_POINT('Ctrl Pts',(-192.430369371041,-3.76013962162594,
133.974618192019));
#244027=CARTESIAN_POINT('Ctrl Pts',(-192.438117267819,-3.67176449436839,
134.079437062336));
#244028=CARTESIAN_POINT('Ctrl Pts',(-192.445865164596,-3.57895739182149,
134.180611982277));
#244029=CARTESIAN_POINT('Ctrl Pts',(-192.453613061373,-3.4820571144234,
134.27775396045));
#244030=CARTESIAN_POINT('Ctrl Pts',(-192.461359337457,-3.38517710647442,
134.374875618616));
#244031=CARTESIAN_POINT('Ctrl Pts',(-192.469105613541,-3.28420590264548,
134.467965736369));
#244032=CARTESIAN_POINT('Ctrl Pts',(-192.476851889625,-3.17952001215119,
134.556671312968));
#244033=CARTESIAN_POINT('Ctrl Pts',(-192.48459822289,-3.07483334888957,
134.645377544372));
#244034=CARTESIAN_POINT('Ctrl Pts',(-192.492344556156,-2.96643224252753,
134.729698917291));
#244035=CARTESIAN_POINT('Ctrl Pts',(-192.500090889421,-2.85472689593607,
134.809322216897));
#244036=CARTESIAN_POINT('Ctrl Pts',(-192.507838957424,-2.7429965337069,
134.888963347589));
#244037=CARTESIAN_POINT('Ctrl Pts',(-192.515587025427,-2.62796077711468,
134.963904084522));
#244038=CARTESIAN_POINT('Ctrl Pts',(-192.52333509343,-2.51005911841526,
135.033874334834));
#244039=CARTESIAN_POINT('Ctrl Pts',(-192.531091396171,-2.39203215242945,
135.103918950361));
#244040=CARTESIAN_POINT('Ctrl Pts',(-192.538847698913,-2.27113353654513,
135.16898232667));
#244041=CARTESIAN_POINT('Ctrl Pts',(-192.546604001655,-2.14782818502421,
135.228839925927));
#244042=CARTESIAN_POINT('Ctrl Pts',(-192.554364444169,-2.02445702172452,
135.288729472987));
#244043=CARTESIAN_POINT('Ctrl Pts',(-192.562124886684,-1.89867692159537,
135.343407550848));
#244044=CARTESIAN_POINT('Ctrl Pts',(-192.569885329198,-1.77097219332344,
135.392698067337));
#244045=CARTESIAN_POINT('Ctrl Pts',(-192.577658229463,-1.64306246208459,
135.442067709339));
#244046=CARTESIAN_POINT('Ctrl Pts',(-192.585431129729,-1.51322229925508,
135.486032381865));
#244047=CARTESIAN_POINT('Ctrl Pts',(-192.593204029994,-1.38195142542684,
135.524465840997));
#244048=CARTESIAN_POINT('Ctrl Pts',(-192.600694365756,-1.25545257851221,
135.561502147082));
#244049=CARTESIAN_POINT('Ctrl Pts',(-192.608184701518,-1.12762553341084,
135.593402330408));
#244050=CARTESIAN_POINT('Ctrl Pts',(-192.61567503728,-0.998923910181445,
135.620098783639));
#244051=CARTESIAN_POINT('Ctrl Pts',(-192.623449371399,-0.865342525790616,
135.647807441008));
#244052=CARTESIAN_POINT('Ctrl Pts',(-192.631223705518,-0.730395789175812,
135.669997752622));
#244053=CARTESIAN_POINT('Ctrl Pts',(-192.638998039637,-0.594579411339083,
135.68653824503));
#244054=CARTESIAN_POINT('Ctrl Pts',(-192.646762792585,-0.45893041504978,
135.70305835276));
#244055=CARTESIAN_POINT('Ctrl Pts',(-192.654527545532,-0.32241429438374,
135.713942448564));
#244056=CARTESIAN_POINT('Ctrl Pts',(-192.662292298479,-0.185538549506594,
135.719109696527));
#244057=CARTESIAN_POINT('Ctrl Pts',(-192.670049339364,-0.0487987515492415,
135.724271812306));
#244058=CARTESIAN_POINT('Ctrl Pts',(-192.677806380249,0.0882995716484737,
135.723728365175));
#244059=CARTESIAN_POINT('Ctrl Pts',(-192.685563421134,0.225242524115774,
135.717450161614));
#244060=CARTESIAN_POINT('Ctrl Pts',(-192.693314612374,0.362082206837544,
135.711176692494));
#244061=CARTESIAN_POINT('Ctrl Pts',(-192.701065803614,0.498766363066561,
135.69917709268));
#244062=CARTESIAN_POINT('Ctrl Pts',(-192.708816994854,0.63478017175093,
135.681474230765));
#244063=CARTESIAN_POINT('Ctrl Pts',(-192.716564891631,0.770736170938507,
135.663778893039));
#244064=CARTESIAN_POINT('Ctrl Pts',(-192.724312788408,0.906022002373333,
135.640385164795));
#244065=CARTESIAN_POINT('Ctrl Pts',(-192.732060685185,1.04012726666948,
135.611367829089));
#244066=CARTESIAN_POINT('Ctrl Pts',(-192.73980696127,1.17420447903531,135.582356563184));
#244067=CARTESIAN_POINT('Ctrl Pts',(-192.747553237354,1.30710123357782,
135.547724112247));
#244068=CARTESIAN_POINT('Ctrl Pts',(-192.755299513438,1.4383170283509,135.507596438621));
#244069=CARTESIAN_POINT('Ctrl Pts',(-192.763045846703,1.56953379172899,
135.467468468782));
#244070=CARTESIAN_POINT('Ctrl Pts',(-192.770792179969,1.69906919670432,
135.421845309648));
#244071=CARTESIAN_POINT('Ctrl Pts',(-192.778538513234,1.82643800209956,
135.370902776244));
#244072=CARTESIAN_POINT('Ctrl Pts',(-192.786286581237,1.95383533085548,
135.319948834614));
#244073=CARTESIAN_POINT('Ctrl Pts',(-192.79403464924,2.07906473161203,135.263673293452));
#244074=CARTESIAN_POINT('Ctrl Pts',(-192.801782717243,2.20166141129512,
135.202299918251));
#244075=CARTESIAN_POINT('Ctrl Pts',(-192.809539019985,2.32438838818846,
135.140861314697));
#244076=CARTESIAN_POINT('Ctrl Pts',(-192.817295322727,2.44447670436585,
135.074314229283));
#244077=CARTESIAN_POINT('Ctrl Pts',(-192.825051625468,2.56148615227356,
135.002928439361));
#244078=CARTESIAN_POINT('Ctrl Pts',(-192.832812067983,2.67855805164703,
134.931504548693));
#244079=CARTESIAN_POINT('Ctrl Pts',(-192.840572510497,2.79254748358488,
134.855237024847));
#244080=CARTESIAN_POINT('Ctrl Pts',(-192.848332953011,2.90304451607954,
134.774438148315));
#244081=CARTESIAN_POINT('Ctrl Pts',(-192.856105853276,3.01371892821992,
134.693509566255));
#244082=CARTESIAN_POINT('Ctrl Pts',(-192.863878753542,3.12088943189119,
134.608035339398));
#244083=CARTESIAN_POINT('Ctrl Pts',(-192.871651653807,3.22417970332439,
134.518367658912));
#244084=CARTESIAN_POINT('Ctrl Pts',(-192.879141989569,3.32371511321709,
134.431959624473));
#244085=CARTESIAN_POINT('Ctrl Pts',(-192.886632325331,3.41964728113286,
134.341657939474));
#244086=CARTESIAN_POINT('Ctrl Pts',(-192.894122661093,3.51167413438388,
134.247807703902));
#244087=CARTESIAN_POINT('Ctrl Pts',(-192.901896995212,3.60719021374836,
134.150399108123));
#244088=CARTESIAN_POINT('Ctrl Pts',(-192.909671329331,3.69880155876895,
134.048859002174));
#244089=CARTESIAN_POINT('Ctrl Pts',(-192.91744566345,3.78612961320351,133.943533377151));
#244090=CARTESIAN_POINT('Ctrl Pts',(-192.925210416397,3.87335004361548,
133.838337556548));
#244091=CARTESIAN_POINT('Ctrl Pts',(-192.932975169344,3.95629743948013,
133.729365797536));
#244092=CARTESIAN_POINT('Ctrl Pts',(-192.940739922292,4.0346294750173,133.61700138059));
#244093=CARTESIAN_POINT('Ctrl Pts',(-192.948496963177,4.11288371007249,
133.504748565566));
#244094=CARTESIAN_POINT('Ctrl Pts',(-192.956254004062,4.18653148511081,
133.389110116985));
#244095=CARTESIAN_POINT('Ctrl Pts',(-192.964011044947,4.25527046547266,
133.27050261027));
#244096=CARTESIAN_POINT('Ctrl Pts',(-192.971762236187,4.32395760923461,
133.151984546398));
#244097=CARTESIAN_POINT('Ctrl Pts',(-192.979513427427,4.38774313120223,
133.03050221786));
#244098=CARTESIAN_POINT('Ctrl Pts',(-192.987264618667,4.44636799801797,
132.906501119222));
#244099=CARTESIAN_POINT('Ctrl Pts',(-192.995012515444,4.50496794770152,
132.782552724358));
#244100=CARTESIAN_POINT('Ctrl Pts',(-193.002760412221,4.55841143801551,
132.656088041339));
#244101=CARTESIAN_POINT('Ctrl Pts',(-193.010508308998,4.60648550272751,
132.527576905692));
#244102=CARTESIAN_POINT('Ctrl Pts',(-193.018254585082,4.65454951138154,
132.399092651803));
#244103=CARTESIAN_POINT('Ctrl Pts',(-193.026000861166,4.69724619158006,
132.268563162699));
#244104=CARTESIAN_POINT('Ctrl Pts',(-193.03374713725,4.73441098548304,132.136477610565));
#244105=CARTESIAN_POINT('Ctrl Pts',(-193.041493470516,4.77157605372813,
132.004391083406));
#244106=CARTESIAN_POINT('Ctrl Pts',(-193.049239803781,4.80320904830049,
131.870748846647));
#244107=CARTESIAN_POINT('Ctrl Pts',(-193.056986137046,4.82919560265308,
131.736054179751));
#244108=CARTESIAN_POINT('Ctrl Pts',(-193.064734205049,4.8551879765143,131.601329348918));
#244109=CARTESIAN_POINT('Ctrl Pts',(-193.072482273053,4.87553131993598,
131.465552002776));
#244110=CARTESIAN_POINT('Ctrl Pts',(-193.080230341056,4.89016266115448,
131.329234135616));
#244111=CARTESIAN_POINT('Ctrl Pts',(-193.087986643797,4.90480955273655,
131.192771388205));
#244112=CARTESIAN_POINT('Ctrl Pts',(-193.095742946539,4.91373227328045,
131.055767361558));
#244113=CARTESIAN_POINT('Ctrl Pts',(-193.103499249281,4.91691985117717,
130.918738236006));
#244114=CARTESIAN_POINT('Ctrl Pts',(-193.111259691795,4.92010913038018,
130.781635973883));
#244115=CARTESIAN_POINT('Ctrl Pts',(-193.119020134309,4.91755717486896,
130.644508976869));
#244116=CARTESIAN_POINT('Ctrl Pts',(-193.126780576824,4.90930513680369,
130.507870927605));
#244117=CARTESIAN_POINT('Ctrl Pts',(-193.134553477089,4.90103985183434,
130.371013534815));
#244118=CARTESIAN_POINT('Ctrl Pts',(-193.142326377354,4.88705623904379,
130.23464704741));
#244119=CARTESIAN_POINT('Ctrl Pts',(-193.15009927762,4.86744719464528,130.099278445164));
#244120=CARTESIAN_POINT('Ctrl Pts',(-193.157589613382,4.84855098840286,
129.968830832581));
#244121=CARTESIAN_POINT('Ctrl Pts',(-193.165079949144,4.82443130336841,
129.839310116289));
#244122=CARTESIAN_POINT('Ctrl Pts',(-193.172570284906,4.79521520426802,
129.711156973565));
#244123=CARTESIAN_POINT('Ctrl Pts',(-193.180344619025,4.76489136789024,
129.578144865484));
#244124=CARTESIAN_POINT('Ctrl Pts',(-193.188118953144,4.7289809707059,129.44618473883));
#244125=CARTESIAN_POINT('Ctrl Pts',(-193.195893287263,4.68757048592578,
129.31578210033));
#244126=CARTESIAN_POINT('Ctrl Pts',(-193.20365804021,4.64621103586719,129.185540171426));
#244127=CARTESIAN_POINT('Ctrl Pts',(-193.211422793157,4.59936510233688,
129.056852280564));
#244128=CARTESIAN_POINT('Ctrl Pts',(-193.219187546105,4.54717011460856,
128.930213608575));
#244129=CARTESIAN_POINT('Ctrl Pts',(-193.22694458699,4.49502696767788,128.8037007159));
#244130=CARTESIAN_POINT('Ctrl Pts',(-193.234701627874,4.43754548719051,
128.679233350863));
#244131=CARTESIAN_POINT('Ctrl Pts',(-193.242458668759,4.37491273058033,
128.557291045366));
#244132=CARTESIAN_POINT('Ctrl Pts',(-193.25020986,4.31232720581922,128.435440697511));
#244133=CARTESIAN_POINT('Ctrl Pts',(-193.25796105124,4.24459831493363,128.316111965434));
#244134=CARTESIAN_POINT('Ctrl Pts',(-193.26571224248,4.17196085126148,128.19976358193));
#244135=CARTESIAN_POINT('Ctrl Pts',(-193.273460139257,4.09935426044897,
128.083464649593));
#244136=CARTESIAN_POINT('Ctrl Pts',(-193.281208036034,4.02184345290365,
127.97014387735));
#244137=CARTESIAN_POINT('Ctrl Pts',(-193.288955932811,3.93970860111024,
127.860234397303));
#244138=CARTESIAN_POINT('Ctrl Pts',(-193.296702208895,3.8575909301572,127.75034790795));
#244139=CARTESIAN_POINT('Ctrl Pts',(-193.304448484979,3.77085137275848,
127.643871604446));
#244140=CARTESIAN_POINT('Ctrl Pts',(-193.312194761063,3.67981253579604,
127.541208343476));
#244141=CARTESIAN_POINT('Ctrl Pts',(-193.319941094329,3.58877302680572,
127.43854432467));
#244142=CARTESIAN_POINT('Ctrl Pts',(-193.327687427594,3.49343443432112,
127.339693697082));
#244143=CARTESIAN_POINT('Ctrl Pts',(-193.335433760859,3.39415836369511,
127.24502471537));
#244144=CARTESIAN_POINT('Ctrl Pts',(-193.343181828862,3.29486006088155,
127.150334533197));
#244145=CARTESIAN_POINT('Ctrl Pts',(-193.350929896865,3.19162280819176,
127.059828130087));
#244146=CARTESIAN_POINT('Ctrl Pts',(-193.358677964868,3.08484332314698,
126.97383523139));
#244147=CARTESIAN_POINT('Ctrl Pts',(-193.36643426761,2.97795035159466,126.887750938417));
#244148=CARTESIAN_POINT('Ctrl Pts',(-193.374190570352,2.86750793222474,
126.806189978007));
#244149=CARTESIAN_POINT('Ctrl Pts',(-193.381946873094,2.7539444117456,126.729440588962));
#244150=CARTESIAN_POINT('Ctrl Pts',(-193.389707315608,2.64032027899594,
126.652650236458));
#244151=CARTESIAN_POINT('Ctrl Pts',(-193.397467758122,2.52357205848088,
126.580676777505));
#244152=CARTESIAN_POINT('Ctrl Pts',(-193.405228200636,2.40415416970356,
126.513763247642));
#244153=CARTESIAN_POINT('Ctrl Pts',(-193.413001100902,2.28454458072975,
126.446742302241));
#244154=CARTESIAN_POINT('Ctrl Pts',(-193.420774001167,2.16225710849449,
126.384797694339));
#244155=CARTESIAN_POINT('Ctrl Pts',(-193.428546901433,2.03776850211148,
126.328125302672));
#244156=CARTESIAN_POINT('Ctrl Pts',(-193.436037237195,1.91780537013702,
126.273513095191));
#244157=CARTESIAN_POINT('Ctrl Pts',(-193.443527572957,1.79579864438425,
126.223796558439));
#244158=CARTESIAN_POINT('Ctrl Pts',(-193.451017908719,1.67218776071735,
126.179106986098));
#244159=CARTESIAN_POINT('Ctrl Pts',(-193.458792242838,1.54389013282677,
126.132722995039));
#244160=CARTESIAN_POINT('Ctrl Pts',(-193.466566576957,1.41345789412949,
126.091607757464));
#244161=CARTESIAN_POINT('Ctrl Pts',(-193.474340911076,1.28136308263296,
126.055961759744));
#244162=CARTESIAN_POINT('Ctrl Pts',(-193.482105664023,1.1494310661863,126.020359692531));
#244163=CARTESIAN_POINT('Ctrl Pts',(-193.48987041697,1.01584092762441,125.990213554768));
#244164=CARTESIAN_POINT('Ctrl Pts',(-193.497635169917,0.88108356048614,
125.965675380651));
#244165=CARTESIAN_POINT('Ctrl Pts',(-193.505392210802,0.746460036264656,
125.941161578194));
#244166=CARTESIAN_POINT('Ctrl Pts',(-193.513149251688,0.610671972693172,
125.922244724601));
#244167=CARTESIAN_POINT('Ctrl Pts',(-193.520906292573,0.47422392265558,
125.909026641862));
#244168=CARTESIAN_POINT('Ctrl Pts',(-193.528657483813,0.337878769153747,
125.895818526982));
#244169=CARTESIAN_POINT('Ctrl Pts',(-193.536408675053,0.200875007398296,
125.888300666612));
#244170=CARTESIAN_POINT('Ctrl Pts',(-193.544159866293,0.0637254938153366,
125.886523478748));
#244171=CARTESIAN_POINT('Ctrl Pts',(-193.55190776307,-0.0733657275659535,
125.884747046236));
#244172=CARTESIAN_POINT('Ctrl Pts',(-193.559655659847,-0.210602187450144,
125.888706438433));
#244173=CARTESIAN_POINT('Ctrl Pts',(-193.567403556624,-0.347468039461664,
125.898400056773));
#244174=CARTESIAN_POINT('Ctrl Pts',(-193.575149832708,-0.48430526208743,
125.908091647417));
#244175=CARTESIAN_POINT('Ctrl Pts',(-193.582896108792,-0.620771641297166,
125.923515050776));
#244176=CARTESIAN_POINT('Ctrl Pts',(-193.590642384876,-0.756353865451232,
125.944616602423));
#244177=CARTESIAN_POINT('Ctrl Pts',(-193.598388718142,-0.891937090442292,
125.965718309837));
#244178=CARTESIAN_POINT('Ctrl Pts',(-193.606135051407,-1.02663576103986,
125.992498189051));
#244179=CARTESIAN_POINT('Ctrl Pts',(-193.613881384672,-1.15994459764504,
126.02485106188));
#244180=CARTESIAN_POINT('Ctrl Pts',(-193.621629452675,-1.29328328784007,
126.05721117991));
#244181=CARTESIAN_POINT('Ctrl Pts',(-193.629377520678,-1.42523114484017,
126.095146682807));
#244182=CARTESIAN_POINT('Ctrl Pts',(-193.637125588681,-1.55529632586053,
126.138502025488));
#244183=CARTESIAN_POINT('Ctrl Pts',(-193.644881891423,-1.68549974170325,
126.181903446744));
#244184=CARTESIAN_POINT('Ctrl Pts',(-193.652638194165,-1.81381611299879,
126.230736090713));
#244185=CARTESIAN_POINT('Ctrl Pts',(-193.660394496907,-1.93977140442049,
126.284795377292));
#244186=CARTESIAN_POINT('Ctrl Pts',(-193.668154939421,-2.06579392197332,
126.33888351694));
#244187=CARTESIAN_POINT('Ctrl Pts',(-193.675915381935,-2.1894524963065,
126.398203688727));
#244188=CARTESIAN_POINT('Ctrl Pts',(-193.683675824449,-2.31029702989768,
126.462504943301));
#244189=CARTESIAN_POINT('Ctrl Pts',(-193.691448724715,-2.43133555386226,
126.526909419958));
#244190=CARTESIAN_POINT('Ctrl Pts',(-193.69922162498,-2.54955067263316,
126.596310760058));
#244191=CARTESIAN_POINT('Ctrl Pts',(-193.706994525246,-2.6645198933412,
126.670413738313));
#244192=CARTESIAN_POINT('Ctrl Pts',(-193.714484861008,-2.77530969328494,
126.741822886652));
#244193=CARTESIAN_POINT('Ctrl Pts',(-193.72197519677,-2.88308523914618,
126.817597597928));
#244194=CARTESIAN_POINT('Ctrl Pts',(-193.729465532532,-2.98749854401419,
126.897439129743));
#244195=CARTESIAN_POINT('Ctrl Pts',(-193.737196078694,-3.0952603185036,
126.97984112973));
#244196=CARTESIAN_POINT('Ctrl Pts',(-193.744926624856,-3.19980039402153,
127.066850545295));
#244197=CARTESIAN_POINT('Ctrl Pts',(-193.752657171018,-3.30069311752396,
127.158183440517));
#244198=CARTESIAN_POINT('Ctrl Pts',(-193.760334883215,-3.40089629561768,
127.248892126417));
#244199=CARTESIAN_POINT('Ctrl Pts',(-193.768012595413,-3.49750149279864,
127.343865140785));
#244200=CARTESIAN_POINT('Ctrl Pts',(-193.77569030761,-3.5901203904032,127.44278083346));
#244201=CARTESIAN_POINT('Ctrl Pts',(-193.783361016429,-3.68265480383977,
127.54160629822));
#244202=CARTESIAN_POINT('Ctrl Pts',(-193.791031725249,-3.77120987628044,
127.644366999939));
#244203=CARTESIAN_POINT('Ctrl Pts',(-193.798702434068,-3.855431774176,127.750702336557));
#244204=CARTESIAN_POINT('Ctrl Pts',(-193.80636789687,-3.93959607249805,
127.856964950164));
#244205=CARTESIAN_POINT('Ctrl Pts',(-193.814033359672,-4.01943284300044,
127.966797023577));
#244206=CARTESIAN_POINT('Ctrl Pts',(-193.821698822474,-4.09462678788818,
128.079802941464));
#244207=CARTESIAN_POINT('Ctrl Pts',(-193.829473807303,-4.17089508320833,
128.194423456868));
#244208=CARTESIAN_POINT('Ctrl Pts',(-193.837248792132,-4.24238657353508,
128.312308902551));
#244209=CARTESIAN_POINT('Ctrl Pts',(-193.845023776961,-4.30881615492087,
128.433013657378));
#244210=CARTESIAN_POINT('Ctrl Pts',(-193.852685093457,-4.37427455244702,
128.551953738889));
#244211=CARTESIAN_POINT('Ctrl Pts',(-193.860346409954,-4.43481787122632,
128.673630879259));
#244212=CARTESIAN_POINT('Ctrl Pts',(-193.86800772645,-4.49021873156322,
128.79759236856));
#244213=CARTESIAN_POINT('Ctrl Pts',(-193.875839545445,-4.54685253732966,
128.924312619201));
#244214=CARTESIAN_POINT('Ctrl Pts',(-193.883671364441,-4.5981120887347,
129.053419710477));
#244215=CARTESIAN_POINT('Ctrl Pts',(-193.891503183436,-4.64380612801652,
129.184407621984));
#244216=CARTESIAN_POINT('Ctrl Pts',(-193.899335002432,-4.68950016729845,
129.315395533491));
#244217=CARTESIAN_POINT('Ctrl Pts',(-193.907166821427,-4.72962857139135,
129.448263836065));
#244218=CARTESIAN_POINT('Ctrl Pts',(-193.914998640423,-4.76405452823412,
129.582490119309));
#244219=CARTESIAN_POINT('',(-191.889859435946,-4.91824838362704,130.800373206121));
#244220=CARTESIAN_POINT('Ctrl Pts',(-191.889859435995,-4.91824838362774,
130.800373206994));
#244221=CARTESIAN_POINT('Ctrl Pts',(-191.897713992238,-4.91836113829842,
130.939449799867));
#244222=CARTESIAN_POINT('Ctrl Pts',(-191.90556854848,-4.91257017733928,
131.078607516704));
#244223=CARTESIAN_POINT('Ctrl Pts',(-191.913423104722,-4.90088344947465,
131.217306712311));
#244224=CARTESIAN_POINT('Ctrl Pts',(-191.921150059273,-4.88938657908931,
131.353752661333));
#244225=CARTESIAN_POINT('Ctrl Pts',(-191.928877013823,-4.87218410818176,
131.489754471933));
#244226=CARTESIAN_POINT('Ctrl Pts',(-191.936603968374,-4.84933606598093,
131.624801219728));
#244227=CARTESIAN_POINT('Ctrl Pts',(-191.944330975815,-4.82648786738739,
131.759848891906));
#244228=CARTESIAN_POINT('Ctrl Pts',(-191.952057983256,-4.7979940857108,
131.893941100987));
#244229=CARTESIAN_POINT('Ctrl Pts',(-191.959784990697,-4.76396615906066,
132.02657561413));
#244230=CARTESIAN_POINT('Ctrl Pts',(-191.967513741978,-4.72993055294498,
132.159240060396));
#244231=CARTESIAN_POINT('Ctrl Pts',(-191.97524249326,-4.69035841421798,
132.290445775788));
#244232=CARTESIAN_POINT('Ctrl Pts',(-191.982971244541,-4.64541136803275,
132.419704631778));
#244233=CARTESIAN_POINT('Ctrl Pts',(-191.990921039647,-4.59917882738299,
132.552660316771));
#244234=CARTESIAN_POINT('Ctrl Pts',(-191.998870834754,-4.54725946423311,
132.6835556899));
#244235=CARTESIAN_POINT('Ctrl Pts',(-192.00682062986,-4.48988223286208,
132.811881625558));
#244236=CARTESIAN_POINT('Ctrl Pts',(-192.01456223062,-4.43400763331795,
132.936846879103));
#244237=CARTESIAN_POINT('Ctrl Pts',(-192.022303831381,-4.37295770825076,
133.059375276236));
#244238=CARTESIAN_POINT('Ctrl Pts',(-192.030045432141,-4.30699015546567,
133.179022459434));
#244239=CARTESIAN_POINT('Ctrl Pts',(-192.03809932442,-4.23836151127706,
133.30349613804));
#244240=CARTESIAN_POINT('Ctrl Pts',(-192.046153216699,-4.16441045295695,
133.424850879837));
#244241=CARTESIAN_POINT('Ctrl Pts',(-192.054207108978,-4.08547567197879,
133.542621305698));
#244242=CARTESIAN_POINT('Ctrl Pts',(-192.062261001257,-4.00654089100041,
133.660391731559));
#244243=CARTESIAN_POINT('Ctrl Pts',(-192.070314893536,-3.9226227251379,
133.77457750615));
#244244=CARTESIAN_POINT('Ctrl Pts',(-192.078368785815,-3.83410466332919,
133.88475417897));
#244245=CARTESIAN_POINT('Ctrl Pts',(-192.086143119934,-3.74865914652369,
133.99110651607));
#244246=CARTESIAN_POINT('Ctrl Pts',(-192.093917454053,-3.65864985410877,
134.094069416823));
#244247=CARTESIAN_POINT('Ctrl Pts',(-192.101691788172,-3.56437564467085,
134.193226110054));
#244248=CARTESIAN_POINT('Ctrl Pts',(-192.109456541119,-3.47021761977078,
134.292260601523));
#244249=CARTESIAN_POINT('Ctrl Pts',(-192.117221294066,-3.37180540278206,
134.387497938163));
#244250=CARTESIAN_POINT('Ctrl Pts',(-192.124986047013,-3.26947915980666,
134.478552921473));
#244251=CARTESIAN_POINT('Ctrl Pts',(-192.132743087898,-3.16725454869806,
134.56951746769));
#244252=CARTESIAN_POINT('Ctrl Pts',(-192.140500128783,-3.06112393801676,
134.656307668951));
#244253=CARTESIAN_POINT('Ctrl Pts',(-192.148257169668,-2.95146527907113,
134.738574105538));
#244254=CARTESIAN_POINT('Ctrl Pts',(-192.156008360908,-2.84188931457368,
134.820778504364));
#244255=CARTESIAN_POINT('Ctrl Pts',(-192.163759552148,-2.72879090890884,
134.898465695044));
#244256=CARTESIAN_POINT('Ctrl Pts',(-192.171510743389,-2.6125818443738,
134.971325840477));
#244257=CARTESIAN_POINT('Ctrl Pts',(-192.179258640166,-2.49642217179069,
135.044155018405));
#244258=CARTESIAN_POINT('Ctrl Pts',(-192.187006536943,-2.37715480046932,
135.112161024362));
#244259=CARTESIAN_POINT('Ctrl Pts',(-192.19475443372,-2.25522112422815,
135.175076891054));
#244260=CARTESIAN_POINT('Ctrl Pts',(-192.202500709804,-2.13331295388346,
135.237979597104));
#244261=CARTESIAN_POINT('Ctrl Pts',(-192.210246985888,-2.00873993520163,
135.29579410257));
#244262=CARTESIAN_POINT('Ctrl Pts',(-192.217993261972,-1.88196838077047,
135.348299225897));
#244263=CARTESIAN_POINT('Ctrl Pts',(-192.225739595237,-1.75519589054102,
135.400804736805));
#244264=CARTESIAN_POINT('Ctrl Pts',(-192.233485928503,-1.62622519338845,
135.448000637764));
#244265=CARTESIAN_POINT('Ctrl Pts',(-192.241232261768,-1.49554253846573,
135.489713921015));
#244266=CARTESIAN_POINT('Ctrl Pts',(-192.248980329771,-1.36483061806836,
135.531436545666));
#244267=CARTESIAN_POINT('Ctrl Pts',(-192.256728397774,-1.2324063493972,
135.567673990578));
#244268=CARTESIAN_POINT('Ctrl Pts',(-192.264476465777,-1.09877070560949,
135.598303253747));
#244269=CARTESIAN_POINT('Ctrl Pts',(-192.272232768519,-0.964993032269096,
135.628965070061));
#244270=CARTESIAN_POINT('Ctrl Pts',(-192.279989071261,-0.830001793655666,
135.654006710523));
#244271=CARTESIAN_POINT('Ctrl Pts',(-192.287745374002,-0.694308261338982,
135.673356314908));
#244272=CARTESIAN_POINT('Ctrl Pts',(-192.295505816517,-0.558542305298078,
135.69271624676));
#244273=CARTESIAN_POINT('Ctrl Pts',(-192.303266259031,-0.422073697493207,
135.706378050116));
#244274=CARTESIAN_POINT('Ctrl Pts',(-192.311026701545,-0.28541738556099,
135.714321918688));
#244275=CARTESIAN_POINT('Ctrl Pts',(-192.31879960181,-0.148541700785455,
135.722278539464));
#244276=CARTESIAN_POINT('Ctrl Pts',(-192.326572502076,-0.0114781008894383,
135.72449887668));
#244277=CARTESIAN_POINT('Ctrl Pts',(-192.334345402341,0.125259011019499,
135.721015297596));
#244278=CARTESIAN_POINT('Ctrl Pts',(-192.341835738103,0.257025384489433,
135.717658355386));
#244279=CARTESIAN_POINT('Ctrl Pts',(-192.349326073865,0.388488287825575,
135.709005020696));
#244280=CARTESIAN_POINT('Ctrl Pts',(-192.356816409627,0.519195120740406,
135.695129421047));
#244281=CARTESIAN_POINT('Ctrl Pts',(-192.364590743746,0.654857742953279,
135.680727723819));
#244282=CARTESIAN_POINT('Ctrl Pts',(-192.372365077865,0.790135568566218,
135.66065431978));
#244283=CARTESIAN_POINT('Ctrl Pts',(-192.380139411984,0.924516415821493,
135.634935372124));
#244284=CARTESIAN_POINT('Ctrl Pts',(-192.387904164931,1.05873165069249,
135.609248120773));
#244285=CARTESIAN_POINT('Ctrl Pts',(-192.395668917878,1.19205172640386,
135.577929242197));
#244286=CARTESIAN_POINT('Ctrl Pts',(-192.403433670826,1.32396869645902,
135.541056718573));
#244287=CARTESIAN_POINT('Ctrl Pts',(-192.411190711711,1.45575464472018,
135.504220817259));
#244288=CARTESIAN_POINT('Ctrl Pts',(-192.418947752595,1.58613988652435,
135.461842352468));
#244289=CARTESIAN_POINT('Ctrl Pts',(-192.42670479348,1.71462615325309,135.414050435448));
#244290=CARTESIAN_POINT('Ctrl Pts',(-192.43445598472,1.84301552748845,135.366294558683));
#244291=CARTESIAN_POINT('Ctrl Pts',(-192.442207175961,1.96950841206677,
135.313133491062));
#244292=CARTESIAN_POINT('Ctrl Pts',(-192.449958367201,2.0936215538718,135.254746202171));
#244293=CARTESIAN_POINT('Ctrl Pts',(-192.457706263978,2.21768194428091,
135.196383729436));
#244294=CARTESIAN_POINT('Ctrl Pts',(-192.465454160755,2.33936425058921,
135.132799619475));
#244295=CARTESIAN_POINT('Ctrl Pts',(-192.473202057532,2.45820528151151,
135.064220927065));
#244296=CARTESIAN_POINT('Ctrl Pts',(-192.480948333616,2.57702145345207,
134.99565657984));
#244297=CARTESIAN_POINT('Ctrl Pts',(-192.4886946097,2.6929971937552,134.922099923534));
#244298=CARTESIAN_POINT('Ctrl Pts',(-192.496440885784,2.80569436276991,
134.843823726102));
#244299=CARTESIAN_POINT('Ctrl Pts',(-192.50418721905,2.91839236368936,134.765546950852));
#244300=CARTESIAN_POINT('Ctrl Pts',(-192.511933552315,3.0278114239197,134.682550787991));
#244301=CARTESIAN_POINT('Ctrl Pts',(-192.51967988558,3.13354315758743,134.59515081778));
#244302=CARTESIAN_POINT('Ctrl Pts',(-192.527427953583,3.23929856914339,
134.507731274952));
#244303=CARTESIAN_POINT('Ctrl Pts',(-192.535176021586,3.34136470970479,
134.415906211393));
#244304=CARTESIAN_POINT('Ctrl Pts',(-192.542924089589,3.43936730597353,
134.320030624421));
#244305=CARTESIAN_POINT('Ctrl Pts',(-192.550680392331,3.53747406056822,
134.224053139734));
#244306=CARTESIAN_POINT('Ctrl Pts',(-192.558436695073,3.63150836371962,
134.124016805884));
#244307=CARTESIAN_POINT('Ctrl Pts',(-192.566192997815,3.72113340261438,
134.020312927916));
#244308=CARTESIAN_POINT('Ctrl Pts',(-192.573953440329,3.81080627709143,
133.916553700066));
#244309=CARTESIAN_POINT('Ctrl Pts',(-192.581713882843,3.896064955127,133.80912333375));
#244310=CARTESIAN_POINT('Ctrl Pts',(-192.589474325357,3.97661443135476,
133.698444363217));
#244311=CARTESIAN_POINT('Ctrl Pts',(-192.597247225623,4.05729321275217,
133.587587720975));
#244312=CARTESIAN_POINT('Ctrl Pts',(-192.605020125888,4.13324746904369,
133.47347237904));
#244313=CARTESIAN_POINT('Ctrl Pts',(-192.612793026153,4.20422638427667,
133.356548614609));
#244314=CARTESIAN_POINT('Ctrl Pts',(-192.620283361916,4.27262503715757,
133.243875323526));
#244315=CARTESIAN_POINT('Ctrl Pts',(-192.627773697678,4.3364036520234,133.128594520953));
#244316=CARTESIAN_POINT('Ctrl Pts',(-192.63526403344,4.39537995294483,133.011127060068));
#244317=CARTESIAN_POINT('Ctrl Pts',(-192.643038367559,4.45659235823986,
132.889205784701));
#244318=CARTESIAN_POINT('Ctrl Pts',(-192.650812701678,4.51282500400254,
132.764542553542));
#244319=CARTESIAN_POINT('Ctrl Pts',(-192.658587035797,4.56382305531772,
132.637582421454));
#244320=CARTESIAN_POINT('Ctrl Pts',(-192.666351788744,4.6147582560922,132.510778756383));
#244321=CARTESIAN_POINT('Ctrl Pts',(-192.674116541692,4.66047155399552,
132.381684181989));
#244322=CARTESIAN_POINT('Ctrl Pts',(-192.681881294639,4.70075400015228,
132.250768199319));
#244323=CARTESIAN_POINT('Ctrl Pts',(-192.689638335524,4.74099643721574,
132.119982244248));
#244324=CARTESIAN_POINT('Ctrl Pts',(-192.697395376409,4.77581864259817,
131.987378852245));
#244325=CARTESIAN_POINT('Ctrl Pts',(-192.705152417294,4.80505991488965,
131.853447018593));
#244326=CARTESIAN_POINT('Ctrl Pts',(-192.712903608534,4.83427913611028,
131.71961618398));
#244327=CARTESIAN_POINT('Ctrl Pts',(-192.720654799774,4.85792571819555,
131.584459282138));
#244328=CARTESIAN_POINT('Ctrl Pts',(-192.728405991014,4.87588902321573,
131.448479625036));
#244329=CARTESIAN_POINT('Ctrl Pts',(-192.736153887791,4.89384469335207,
131.312557762916));
#244330=CARTESIAN_POINT('Ctrl Pts',(-192.743901784568,4.90612183966131,
131.175814227835));
#244331=CARTESIAN_POINT('Ctrl Pts',(-192.751649681345,4.91266112355447,
131.038761444392));
#244332=CARTESIAN_POINT('Ctrl Pts',(-192.759395957429,4.9191990395704,130.901737329437));
#244333=CARTESIAN_POINT('Ctrl Pts',(-192.767142233513,4.92000146188634,
130.764404485061));
#244334=CARTESIAN_POINT('Ctrl Pts',(-192.774888509598,4.91506105272305,
130.627278968305));
#244335=CARTESIAN_POINT('Ctrl Pts',(-192.782634842863,4.91012060709078,
130.490152439319));
#244336=CARTESIAN_POINT('Ctrl Pts',(-192.790381176128,4.89943725946526,
130.353233631717));
#244337=CARTESIAN_POINT('Ctrl Pts',(-192.798127509394,4.88305577391945,
130.217036710942));
#244338=CARTESIAN_POINT('Ctrl Pts',(-192.805875577397,4.86667061985355,
130.080809289811));
#244339=CARTESIAN_POINT('Ctrl Pts',(-192.8136236454,4.84458483533778,129.945304465287));
#244340=CARTESIAN_POINT('Ctrl Pts',(-192.821371713403,4.81689478580987,
129.811029008818));
#244341=CARTESIAN_POINT('Ctrl Pts',(-192.829128016144,4.78917530696777,
129.676610842796));
#244342=CARTESIAN_POINT('Ctrl Pts',(-192.836884318886,4.75583974389208,
129.543425038395));
#244343=CARTESIAN_POINT('Ctrl Pts',(-192.844640621628,4.71703525704713,
129.41196647571));
#244344=CARTESIAN_POINT('Ctrl Pts',(-192.852401064142,4.67821005907918,
129.280437749632));
#244345=CARTESIAN_POINT('Ctrl Pts',(-192.860161506656,4.63391024734856,
129.150638472024));
#244346=CARTESIAN_POINT('Ctrl Pts',(-192.867921949171,4.58433185427907,
129.023045229337));
#244347=CARTESIAN_POINT('Ctrl Pts',(-192.875694849436,4.53467387357166,
128.895247162649));
#244348=CARTESIAN_POINT('Ctrl Pts',(-192.883467749701,4.47972053529839,
128.769662565957));
#244349=CARTESIAN_POINT('Ctrl Pts',(-192.891240649967,4.41971509826897,
128.646745843647));
#244350=CARTESIAN_POINT('Ctrl Pts',(-192.898730985729,4.36189101002015,
128.528297453802));
#244351=CARTESIAN_POINT('Ctrl Pts',(-192.906221321491,4.29937590510965,
128.412326609133));
#244352=CARTESIAN_POINT('Ctrl Pts',(-192.913711657253,4.23242533464076,
128.299214144964));
#244353=CARTESIAN_POINT('Ctrl Pts',(-192.921485991372,4.16293631294325,
128.181812987336));
#244354=CARTESIAN_POINT('Ctrl Pts',(-192.929260325491,4.08844872451645,
128.067119348354));
#244355=CARTESIAN_POINT('Ctrl Pts',(-192.93703465961,4.00919926212544,127.955588190875));
#244356=CARTESIAN_POINT('Ctrl Pts',(-192.944799412557,3.93004746761452,
127.844194485581));
#244357=CARTESIAN_POINT('Ctrl Pts',(-192.952564165504,3.84614570015536,
127.735955822617));
#244358=CARTESIAN_POINT('Ctrl Pts',(-192.960328918452,3.75777602230254,
127.631301773374));
#244359=CARTESIAN_POINT('Ctrl Pts',(-192.968085959337,3.66949411445908,
127.526751668006));
#244360=CARTESIAN_POINT('Ctrl Pts',(-192.975843000222,3.57675337783237,
127.425779388006));
#244361=CARTESIAN_POINT('Ctrl Pts',(-192.983600041107,3.47987835496601,
127.328784449916));
#244362=CARTESIAN_POINT('Ctrl Pts',(-192.991351232347,3.38307638630784,
127.231862656463));
#244363=CARTESIAN_POINT('Ctrl Pts',(-192.999102423587,3.28214661216284,
127.138912510412));
#244364=CARTESIAN_POINT('Ctrl Pts',(-193.006853614827,3.17745268064025,
127.050299146999));
#244365=CARTESIAN_POINT('Ctrl Pts',(-193.014601511604,3.07280324683178,
126.961723446631));
#244366=CARTESIAN_POINT('Ctrl Pts',(-193.022349408381,2.96439313545571,
126.877481114876));
#244367=CARTESIAN_POINT('Ctrl Pts',(-193.030097305158,2.85262138988372,
126.797899052983));
#244368=CARTESIAN_POINT('Ctrl Pts',(-193.037843581242,2.74087302455107,
126.718333637942));
#244369=CARTESIAN_POINT('Ctrl Pts',(-193.045589857326,2.62576474197169,
126.643426780396));
#244370=CARTESIAN_POINT('Ctrl Pts',(-193.053336133411,2.50772674929877,
126.573463595261));
#244371=CARTESIAN_POINT('Ctrl Pts',(-193.061082466676,2.38968788529636,
126.503499893673));
#244372=CARTESIAN_POINT('Ctrl Pts',(-193.068828799941,2.26871960437203,
126.438480136662));
#244373=CARTESIAN_POINT('Ctrl Pts',(-193.076575133207,2.145278684549,126.378644581926));
#244374=CARTESIAN_POINT('Ctrl Pts',(-193.08432320121,2.02181012098801,126.318795627432));
#244375=CARTESIAN_POINT('Ctrl Pts',(-193.092071269213,1.89586816841405,
126.264133355903));
#244376=CARTESIAN_POINT('Ctrl Pts',(-193.099819337216,1.7679312758711,126.214850614712));
#244377=CARTESIAN_POINT('Ctrl Pts',(-193.107575639958,1.63985841047612,
126.165515495237));
#244378=CARTESIAN_POINT('Ctrl Pts',(-193.115331942699,1.50978673510698,
126.121571468042));
#244379=CARTESIAN_POINT('Ctrl Pts',(-193.123088245441,1.37821215022817,
126.08316221764));
#244380=CARTESIAN_POINT('Ctrl Pts',(-193.130848687956,1.24656734003178,
126.044732467064));
#244381=CARTESIAN_POINT('Ctrl Pts',(-193.13860913047,1.11341840134966,126.011843473238));
#244382=CARTESIAN_POINT('Ctrl Pts',(-193.146369572984,0.979272260174981,
125.98458791515));
#244383=CARTESIAN_POINT('Ctrl Pts',(-193.154142473249,0.844910775705553,
125.957288604021));
#244384=CARTESIAN_POINT('Ctrl Pts',(-193.161915373515,0.70954927612074,
125.935640861783));
#244385=CARTESIAN_POINT('Ctrl Pts',(-193.16968827378,0.573701552030352,
125.919685644582));
#244386=CARTESIAN_POINT('Ctrl Pts',(-193.177178609542,0.442792234891523,
125.904310439715));
#244387=CARTESIAN_POINT('Ctrl Pts',(-193.184668945304,0.311431737587399,
125.894221093707));
#244388=CARTESIAN_POINT('Ctrl Pts',(-193.192159281066,0.180078599274265,
125.889408454972));
#244389=CARTESIAN_POINT('Ctrl Pts',(-193.199933615185,0.0437451667967284,
125.884413343577));
#244390=CARTESIAN_POINT('Ctrl Pts',(-193.207707949304,-0.0930122009763956,
125.885087147901));
#244391=CARTESIAN_POINT('Ctrl Pts',(-193.215482283423,-0.229682792687816,
125.891476650155));
#244392=CARTESIAN_POINT('Ctrl Pts',(-193.22324703637,-0.366184950108441,
125.897858277918));
#244393=CARTESIAN_POINT('Ctrl Pts',(-193.231011789318,-0.502600157464022,
125.909941569895));
#244394=CARTESIAN_POINT('Ctrl Pts',(-193.238776542265,-0.638414542478167,
125.927721412698));
#244395=CARTESIAN_POINT('Ctrl Pts',(-193.24653358315,-0.774094034730837,
125.945483596311));
#244396=CARTESIAN_POINT('Ctrl Pts',(-193.254290624035,-0.909173507043042,
125.968931020864));
#244397=CARTESIAN_POINT('Ctrl Pts',(-193.26204766492,-1.04314141166046,
125.998006587974));
#244398=CARTESIAN_POINT('Ctrl Pts',(-193.26979885616,-1.17700829003943,
126.027060228972));
#244399=CARTESIAN_POINT('Ctrl Pts',(-193.2775500474,-1.30976488866881,126.061733482066));
#244400=CARTESIAN_POINT('Ctrl Pts',(-193.28530123864,-1.44090744824757,
126.101917764316));
#244401=CARTESIAN_POINT('Ctrl Pts',(-193.293049135417,-1.57199426873999,
126.142084967174));
#244402=CARTESIAN_POINT('Ctrl Pts',(-193.300797032194,-1.70146804157518,
126.187758426161));
#244403=CARTESIAN_POINT('Ctrl Pts',(-193.308544928971,-1.82883804278507,
126.238779112898));
#244404=CARTESIAN_POINT('Ctrl Pts',(-193.316291205055,-1.95618140093683,
126.289789127208));
#244405=CARTESIAN_POINT('Ctrl Pts',(-193.324037481139,-2.08142150007336,
126.346143999172));
#244406=CARTESIAN_POINT('Ctrl Pts',(-193.331783757224,-2.20408592746605,
126.407635894906));
#244407=CARTESIAN_POINT('Ctrl Pts',(-193.339530090489,-2.32675126033885,
126.469128244559));
#244408=CARTESIAN_POINT('Ctrl Pts',(-193.347276423754,-2.44684053402099,
126.53575751844));
#244409=CARTESIAN_POINT('Ctrl Pts',(-193.35502275702,-2.5639047132275,126.607269281415));
#244410=CARTESIAN_POINT('Ctrl Pts',(-193.362770825023,-2.68099510814607,
126.678797058955));
#244411=CARTESIAN_POINT('Ctrl Pts',(-193.370518893026,-2.79505872696956,
126.755209297555));
#244412=CARTESIAN_POINT('Ctrl Pts',(-193.378266961029,-2.90567470834559,
126.836207703201));
#244413=CARTESIAN_POINT('Ctrl Pts',(-193.38602326377,-3.01640825370252,
126.917292194916));
#244414=CARTESIAN_POINT('Ctrl Pts',(-193.393779566512,-3.12368652605522,
127.002972359134));
#244415=CARTESIAN_POINT('Ctrl Pts',(-193.401535869254,-3.22712059323985,
127.092908645738));
#244416=CARTESIAN_POINT('Ctrl Pts',(-193.409296311768,-3.33060986630048,
127.182892934046));
#244417=CARTESIAN_POINT('Ctrl Pts',(-193.417056754283,-3.4302505619723,
127.277137602611));
#244418=CARTESIAN_POINT('Ctrl Pts',(-193.424817196797,-3.52569070091577,
127.375266255497));
#244419=CARTESIAN_POINT('Ctrl Pts',(-193.432590097062,-3.62128404884331,
127.473552433207));
#244420=CARTESIAN_POINT('Ctrl Pts',(-193.440362997328,-3.71266310439815,
127.57573476299));
#244421=CARTESIAN_POINT('Ctrl Pts',(-193.448135897593,-3.79951569364077,
127.68140311605));
#244422=CARTESIAN_POINT('Ctrl Pts',(-193.455626233355,-3.88321097249688,
127.783230158314));
#244423=CARTESIAN_POINT('Ctrl Pts',(-193.463116569117,-3.9627029824913,
127.888293927058));
#244424=CARTESIAN_POINT('Ctrl Pts',(-193.470606904879,-4.03775157149843,
127.996203693646));
#244425=CARTESIAN_POINT('Ctrl Pts',(-193.47889361498,-4.12077934492612,
128.115586453127));
#244426=CARTESIAN_POINT('Ctrl Pts',(-193.48718032508,-4.19864109136327,
128.238845638589));
#244427=CARTESIAN_POINT('Ctrl Pts',(-193.495467035181,-4.27096326554449,
128.365496979133));
#244428=CARTESIAN_POINT('Ctrl Pts',(-193.503328207986,-4.33957156751243,
128.485644548189));
#244429=CARTESIAN_POINT('Ctrl Pts',(-193.511189380792,-4.40319473039249,
128.608844226595));
#244430=CARTESIAN_POINT('Ctrl Pts',(-193.519050553597,-4.46155570869261,
128.734649594082));
#244431=CARTESIAN_POINT('Ctrl Pts',(-193.526903815789,-4.51985795897289,
128.86032836499));
#244432=CARTESIAN_POINT('Ctrl Pts',(-193.534757077982,-4.57290840298805,
128.988607267093));
#244433=CARTESIAN_POINT('Ctrl Pts',(-193.542610340174,-4.62047497514472,
129.119013749244));
#244434=CARTESIAN_POINT('Ctrl Pts',(-193.550455704939,-4.66799371322391,
129.249289091533));
#244435=CARTESIAN_POINT('Ctrl Pts',(-193.558301069704,-4.71003943508657,
129.381687398499));
#244436=CARTESIAN_POINT('Ctrl Pts',(-193.566146434469,-4.74642766497959,
129.515715017094));
#244437=CARTESIAN_POINT('Ctrl Pts',(-193.567446765008,-4.75245883472166,
129.537929434235));
#244438=CARTESIAN_POINT('Ctrl Pts',(-193.568747095547,-4.75833469270917,
129.560188567407));
#244439=CARTESIAN_POINT('Ctrl Pts',(-193.570047426085,-4.76405452823409,
129.582490119308));
#244440=CARTESIAN_POINT('Ctrl Pts',(-191.820046567589,-4.76405452823394,
129.582490119308));
#244441=CARTESIAN_POINT('Ctrl Pts',(-191.82924828616,-4.80421977364591,
129.739093801576));
#244442=CARTESIAN_POINT('Ctrl Pts',(-191.83845000473,-4.83669951198726,
129.897836547039));
#244443=CARTESIAN_POINT('Ctrl Pts',(-191.847651723301,-4.86129257036642,
130.058024495031));
#244444=CARTESIAN_POINT('Ctrl Pts',(-191.856764218548,-4.88564716520422,
130.216659200447));
#244445=CARTESIAN_POINT('Ctrl Pts',(-191.865876713795,-4.90226722063982,
130.376711144536));
#244446=CARTESIAN_POINT('Ctrl Pts',(-191.874989209043,-4.91100407682167,
130.537486077864));
#244447=CARTESIAN_POINT('Ctrl Pts',(-191.879945951344,-4.91575649023196,
130.624939611869));
#244448=CARTESIAN_POINT('Ctrl Pts',(-191.884902693645,-4.9181772279881,
130.712606716241));
#244449=CARTESIAN_POINT('Ctrl Pts',(-191.889859435946,-4.91824838362704,
130.800373206121));
#244450=CARTESIAN_POINT('Origin',(213.235140564004,0.,130.804360617566));
#244451=CARTESIAN_POINT('',(-190.06976504276,-4.76405452823418,129.582490119309));
#244452=CARTESIAN_POINT('',(-190.415359814329,-4.76405452823405,129.582490119308));
#244453=CARTESIAN_POINT('',(213.235140564004,-4.76405452823405,129.582490119308));
#244454=CARTESIAN_POINT('',(-190.485140563957,-4.91824868249715,130.800760671037));
#244455=CARTESIAN_POINT('Ctrl Pts',(-190.415359814329,-4.76405452823405,
129.582490119308));
#244456=CARTESIAN_POINT('Ctrl Pts',(-190.424329050674,-4.80323055054687,
129.735236835727));
#244457=CARTESIAN_POINT('Ctrl Pts',(-190.433298287018,-4.83509936457335,
129.890036533855));
#244458=CARTESIAN_POINT('Ctrl Pts',(-190.442267523362,-4.85946771299443,
130.04623357751));
#244459=CARTESIAN_POINT('Ctrl Pts',(-190.451168803988,-4.88365143381179,
130.201247189058));
#244460=CARTESIAN_POINT('Ctrl Pts',(-190.460070084614,-4.9004478339706,
130.357636916376));
#244461=CARTESIAN_POINT('Ctrl Pts',(-190.46897136524,-4.90971529438901,
130.51474226431));
#244462=CARTESIAN_POINT('Ctrl Pts',(-190.474361098146,-4.9153267494672,
130.609869684625));
#244463=CARTESIAN_POINT('Ctrl Pts',(-190.479750831051,-4.9181787794553,
130.705259101589));
#244464=CARTESIAN_POINT('Ctrl Pts',(-190.485140563957,-4.91824868249715,
130.800760671037));
#244465=CARTESIAN_POINT('Ctrl Pts',(-190.485140564012,-4.91824868249786,
130.800760672006));
#244466=CARTESIAN_POINT('Ctrl Pts',(-190.492903044254,-4.9183493592558,
130.938305344235));
#244467=CARTESIAN_POINT('Ctrl Pts',(-190.500665524497,-4.91267582439302,
131.075902460375));
#244468=CARTESIAN_POINT('Ctrl Pts',(-190.508428004739,-4.90124163143306,
131.213033509752));
#244469=CARTESIAN_POINT('Ctrl Pts',(-190.516189892968,-4.88980831051287,
131.350154100696));
#244470=CARTESIAN_POINT('Ctrl Pts',(-190.523951781197,-4.87261523719499,
131.486808308646));
#244471=CARTESIAN_POINT('Ctrl Pts',(-190.531713669427,-4.8497279622425,
131.622481485619));
#244472=CARTESIAN_POINT('Ctrl Pts',(-190.539476617656,-4.8268375616964,
131.758173190757));
#244473=CARTESIAN_POINT('Ctrl Pts',(-190.547239565885,-4.7982514760145,
131.892883215297));
#244474=CARTESIAN_POINT('Ctrl Pts',(-190.555002514114,-4.76408655954542,
132.026106219424));
#244475=CARTESIAN_POINT('Ctrl Pts',(-190.562768174686,-4.72990970599202,
132.159375771132));
#244476=CARTESIAN_POINT('Ctrl Pts',(-190.570533835258,-4.69015023823709,
132.291156892345));
#244477=CARTESIAN_POINT('Ctrl Pts',(-190.57829949583,-4.64497503635937,
132.420958889895));
#244478=CARTESIAN_POINT('Ctrl Pts',(-190.586074494797,-4.59974551020291,
132.550916977504));
#244479=CARTESIAN_POINT('Ctrl Pts',(-190.593849493765,-4.54908737022984,
132.678890820855));
#244480=CARTESIAN_POINT('Ctrl Pts',(-190.601624492733,-4.49321610342936,
132.804408644585));
#244481=CARTESIAN_POINT('Ctrl Pts',(-190.609404441072,-4.4373092703673,
132.930006369846));
#244482=CARTESIAN_POINT('Ctrl Pts',(-190.617184389411,-4.37618287100597,
133.053144613246));
#244483=CARTESIAN_POINT('Ctrl Pts',(-190.62496433775,-4.31009818111834,
133.173376601391));
#244484=CARTESIAN_POINT('Ctrl Pts',(-190.632757105409,-4.24390460094357,
133.293806700412));
#244485=CARTESIAN_POINT('Ctrl Pts',(-190.640549873068,-4.17273660894555,
133.411320645231));
#244486=CARTESIAN_POINT('Ctrl Pts',(-190.648342640727,-4.09689905135302,
133.52550030996));
#244487=CARTESIAN_POINT('Ctrl Pts',(-190.654408984015,-4.0378626885938,
133.614384397484));
#244488=CARTESIAN_POINT('Ctrl Pts',(-190.660475327302,-3.97599746982579,
133.701248499452));
#244489=CARTESIAN_POINT('Ctrl Pts',(-190.66654167059,-3.91146342789147,
133.78591003268));
#244490=CARTESIAN_POINT('Ctrl Pts',(-190.674316004709,-3.82875970007991,
133.894408186373));
#244491=CARTESIAN_POINT('Ctrl Pts',(-190.682090338828,-3.74140718917245,
133.999634468692));
#244492=CARTESIAN_POINT('Ctrl Pts',(-190.689864672947,-3.64969402101185,
134.101164617729));
#244493=CARTESIAN_POINT('Ctrl Pts',(-190.697629425894,-3.55809388113412,
134.202569639932));
#244494=CARTESIAN_POINT('Ctrl Pts',(-190.705394178841,-3.46214403645708,
134.300287304914));
#244495=CARTESIAN_POINT('Ctrl Pts',(-190.713158931788,-3.36217471257771,
134.393923859049));
#244496=CARTESIAN_POINT('Ctrl Pts',(-190.720915972673,-3.26230467964042,
134.487467412037));
#244497=CARTESIAN_POINT('Ctrl Pts',(-190.728673013558,-3.15842339566355,
134.576937655122));
#244498=CARTESIAN_POINT('Ctrl Pts',(-190.736430054443,-3.05089977217039,
134.661975637584));
#244499=CARTESIAN_POINT('Ctrl Pts',(-190.744181245683,-2.94345723307797,
134.746949492243));
#244500=CARTESIAN_POINT('Ctrl Pts',(-190.751932436923,-2.83237812705361,
134.827497497584));
#244501=CARTESIAN_POINT('Ctrl Pts',(-190.759683628163,-2.7180661956855,
134.903299409299));
#244502=CARTESIAN_POINT('Ctrl Pts',(-190.76743152494,-2.60380284993743,
134.979069103179));
#244503=CARTESIAN_POINT('Ctrl Pts',(-190.775179421717,-2.48630973685419,
135.050096499908));
#244504=CARTESIAN_POINT('Ctrl Pts',(-190.782927318495,-2.36602129387989,
135.116103455376));
#244505=CARTESIAN_POINT('Ctrl Pts',(-190.790673594579,-2.24575801265473,
135.182096603612));
#244506=CARTESIAN_POINT('Ctrl Pts',(-190.798419870663,-2.12270090711924,
135.243071211466));
#244507=CARTESIAN_POINT('Ctrl Pts',(-190.806166146747,-1.99731049376025,
135.298794269765));
#244508=CARTESIAN_POINT('Ctrl Pts',(-190.813912480012,-1.87191915479789,
135.354517739398));
#244509=CARTESIAN_POINT('Ctrl Pts',(-190.821658813278,-1.74419483091776,
135.404989423349));
#244510=CARTESIAN_POINT('Ctrl Pts',(-190.829405146543,-1.61461919800756,
135.450023961796));
#244511=CARTESIAN_POINT('Ctrl Pts',(-190.837153214546,-1.4850145475326,
135.495068585417));
#244512=CARTESIAN_POINT('Ctrl Pts',(-190.844901282549,-1.35355813227166,
135.534673512303));
#244513=CARTESIAN_POINT('Ctrl Pts',(-190.852649350552,-1.22074762339899,
135.56870299637));
#244514=CARTESIAN_POINT('Ctrl Pts',(-190.860405653294,-1.0877959619372,
135.602768647377));
#244515=CARTESIAN_POINT('Ctrl Pts',(-190.868161956036,-0.953487711347482,
135.631246921252));
#244516=CARTESIAN_POINT('Ctrl Pts',(-190.875918258778,-0.818332142929902,
135.654052934234));
#244517=CARTESIAN_POINT('Ctrl Pts',(-190.883678701292,-0.683104437916002,
135.676871119472));
#244518=CARTESIAN_POINT('Ctrl Pts',(-190.891439143806,-0.54702890166007,
135.694010962518));
#244519=CARTESIAN_POINT('Ctrl Pts',(-190.89919958632,-0.410619808675805,
135.705439522789));
#244520=CARTESIAN_POINT('Ctrl Pts',(-190.906972486586,-0.273991739705651,
135.7168864292));
#244521=CARTESIAN_POINT('Ctrl Pts',(-190.914745386851,-0.137029434847546,
135.722603715419));
#244522=CARTESIAN_POINT('Ctrl Pts',(-190.922518287116,-0.00024795565964834,
135.722610611316));
#244523=CARTESIAN_POINT('Ctrl Pts',(-190.930008622879,0.131561172230973,
135.722617256529));
#244524=CARTESIAN_POINT('Ctrl Pts',(-190.937498958641,0.263202085368852,
135.717321489911));
#244525=CARTESIAN_POINT('Ctrl Pts',(-190.944989294403,0.394220439225914,
135.706785865114));
#244526=CARTESIAN_POINT('Ctrl Pts',(-190.952763628522,0.530206393788766,
135.695850778901));
#244527=CARTESIAN_POINT('Ctrl Pts',(-190.960537962641,0.665952411115588,
135.67923601341));
#244528=CARTESIAN_POINT('Ctrl Pts',(-190.96831229676,0.800945808593782,
135.656954653151));
#244529=CARTESIAN_POINT('Ctrl Pts',(-190.976077049707,0.935772838774291,
135.634700752677));
#244530=CARTESIAN_POINT('Ctrl Pts',(-190.983841802654,1.06984871258484,
135.606794215719));
#244531=CARTESIAN_POINT('Ctrl Pts',(-190.991606555601,1.20266365894648,
135.57330003697));
#244532=CARTESIAN_POINT('Ctrl Pts',(-190.999363596486,1.33534669163104,
135.539839125113));
#244533=CARTESIAN_POINT('Ctrl Pts',(-191.007120637371,1.46677091249836,
135.500801710651));
#244534=CARTESIAN_POINT('Ctrl Pts',(-191.014877678256,1.59643492045341,
135.456304147668));
#244535=CARTESIAN_POINT('Ctrl Pts',(-191.022628869497,1.7260011477716,135.411840140643));
#244536=CARTESIAN_POINT('Ctrl Pts',(-191.030380060737,1.85380943596783,
135.361924307202));
#244537=CARTESIAN_POINT('Ctrl Pts',(-191.038131251977,1.97937212224398,
135.306723226706));
#244538=CARTESIAN_POINT('Ctrl Pts',(-191.045879148754,2.10488144102913,
135.251545608142));
#244539=CARTESIAN_POINT('Ctrl Pts',(-191.053627045531,2.22814669904816,
135.191087367399));
#244540=CARTESIAN_POINT('Ctrl Pts',(-191.061374942308,2.34869906173386,
135.125563665319));
#244541=CARTESIAN_POINT('Ctrl Pts',(-191.069121218392,2.46922620746376,
135.060053669385));
#244542=CARTESIAN_POINT('Ctrl Pts',(-191.076867494477,2.58704124332095,
134.989480506272));
#244543=CARTESIAN_POINT('Ctrl Pts',(-191.084613770561,2.70169921167772,
134.914105674394));
#244544=CARTESIAN_POINT('Ctrl Pts',(-191.092360103826,2.81635802641402,
134.838730286115));
#244545=CARTESIAN_POINT('Ctrl Pts',(-191.100106437091,2.927859400452,134.758553373108));
#244546=CARTESIAN_POINT('Ctrl Pts',(-191.107852770357,3.03578702774157,
134.673879991428));
#244547=CARTESIAN_POINT('Ctrl Pts',(-191.11560083836,3.14373882467452,134.589187647732));
#244548=CARTESIAN_POINT('Ctrl Pts',(-191.123348906363,3.24811497478342,
134.49999707292));
#244549=CARTESIAN_POINT('Ctrl Pts',(-191.131096974365,3.34853226761644,
134.406653597771));
#244550=CARTESIAN_POINT('Ctrl Pts',(-191.138853277107,3.44905628514341,
134.313210916065));
#244551=CARTESIAN_POINT('Ctrl Pts',(-191.146609579849,3.54561275360605,
134.215606783686));
#244552=CARTESIAN_POINT('Ctrl Pts',(-191.154365882591,3.63785498431555,
134.114223783256));
#244553=CARTESIAN_POINT('Ctrl Pts',(-191.162126325105,3.73014644748118,
134.012786671666));
#244554=CARTESIAN_POINT('Ctrl Pts',(-191.16988676762,3.81811883403782,133.907566972984));
#244555=CARTESIAN_POINT('Ctrl Pts',(-191.177647210134,3.9014664522032,133.798979555734));
#244556=CARTESIAN_POINT('Ctrl Pts',(-191.185420110399,3.98494786736428,
133.690217824322));
#244557=CARTESIAN_POINT('Ctrl Pts',(-191.193193010664,4.06378945344856,
133.578077891125));
#244558=CARTESIAN_POINT('Ctrl Pts',(-191.20096591093,4.1377289857357,133.463003486231));
#244559=CARTESIAN_POINT('Ctrl Pts',(-191.208456246692,4.20898062978117,
133.352112325811));
#244560=CARTESIAN_POINT('Ctrl Pts',(-191.215946582454,4.27568028039896,
133.238496606114));
#244561=CARTESIAN_POINT('Ctrl Pts',(-191.223436918216,4.33763498143187,
133.122572391835));
#244562=CARTESIAN_POINT('Ctrl Pts',(-191.231211252335,4.40193871378563,
133.002252875736));
#244563=CARTESIAN_POINT('Ctrl Pts',(-191.238985586454,4.46133427916974,
132.879065220246));
#244564=CARTESIAN_POINT('Ctrl Pts',(-191.246759920573,4.51555556847681,
132.753447832264));
#244565=CARTESIAN_POINT('Ctrl Pts',(-191.25452467352,4.56971003489071,132.627985256485));
#244566=CARTESIAN_POINT('Ctrl Pts',(-191.262289426467,4.61870275977333,
132.500099261741));
#244567=CARTESIAN_POINT('Ctrl Pts',(-191.270054179414,4.66231288128167,
132.370253864098));
#244568=CARTESIAN_POINT('Ctrl Pts',(-191.277811220299,4.70587968860265,
132.240537430734));
#244569=CARTESIAN_POINT('Ctrl Pts',(-191.285568261184,4.74407440781323,
132.108865835533));
#244570=CARTESIAN_POINT('Ctrl Pts',(-191.293325302069,4.77672391135812,
131.975723813658));
#244571=CARTESIAN_POINT('Ctrl Pts',(-191.301076493309,4.80934879365846,
131.842682195218));
#244572=CARTESIAN_POINT('Ctrl Pts',(-191.30882768455,4.83643669095588,131.708172735403));
#244573=CARTESIAN_POINT('Ctrl Pts',(-191.31657887579,4.85786415753015,131.572695758949));
#244574=CARTESIAN_POINT('Ctrl Pts',(-191.324326772567,4.87928251685945,
131.437276363824));
#244575=CARTESIAN_POINT('Ctrl Pts',(-191.332074669344,4.89504516953697,
131.300890655304));
#244576=CARTESIAN_POINT('Ctrl Pts',(-191.339822566121,4.9050797199358,131.164049376877));
#244577=CARTESIAN_POINT('Ctrl Pts',(-191.347568842205,4.91511217132304,
131.027236722695));
#244578=CARTESIAN_POINT('Ctrl Pts',(-191.355315118289,4.91941887513359,
130.889969077825));
#244579=CARTESIAN_POINT('Ctrl Pts',(-191.363061394373,4.91797932692134,
130.752762144001));
#244580=CARTESIAN_POINT('Ctrl Pts',(-191.370807727638,4.91653976808269,
130.615554197346));
#244581=CARTESIAN_POINT('Ctrl Pts',(-191.378554060904,4.90935387668189,
130.478407353576));
#244582=CARTESIAN_POINT('Ctrl Pts',(-191.386300394169,4.89645328142879,
130.341836753008));
#244583=CARTESIAN_POINT('Ctrl Pts',(-191.394048462172,4.88354979717682,
130.205235568402));
#244584=CARTESIAN_POINT('Ctrl Pts',(-191.401796530175,4.86492909924203,
130.069211272942));
#244585=CARTESIAN_POINT('Ctrl Pts',(-191.409544598178,4.84067458957936,
129.934272932157));
#244586=CARTESIAN_POINT('Ctrl Pts',(-191.41730090092,4.81639430193517,129.799191177297));
#244587=CARTESIAN_POINT('Ctrl Pts',(-191.425057203662,4.78646831079896,
129.665198068094));
#244588=CARTESIAN_POINT('Ctrl Pts',(-191.432813506404,4.75103110006152,
129.532792078812));
#244589=CARTESIAN_POINT('Ctrl Pts',(-191.440573948918,4.71557497541762,
129.400315420467));
#244590=CARTESIAN_POINT('Ctrl Pts',(-191.448334391432,4.67460188671874,
129.269427942878));
#244591=CARTESIAN_POINT('Ctrl Pts',(-191.456094833946,4.6282956407281,129.14061107977));
#244592=CARTESIAN_POINT('Ctrl Pts',(-191.463867734212,4.58191505984064,
129.011587428397));
#244593=CARTESIAN_POINT('Ctrl Pts',(-191.471640634477,4.53018436116495,
128.884641396051));
#244594=CARTESIAN_POINT('Ctrl Pts',(-191.479413534742,4.47333512852615,
128.760233446768));
#244595=CARTESIAN_POINT('Ctrl Pts',(-191.486903870504,4.41855250868881,
128.640348039807));
#244596=CARTESIAN_POINT('Ctrl Pts',(-191.494394206266,4.35901717633166,
128.522819662996));
#244597=CARTESIAN_POINT('Ctrl Pts',(-191.501884542028,4.29497488095036,
128.408035548944));
#244598=CARTESIAN_POINT('Ctrl Pts',(-191.509658876147,4.22850440247415,
128.28889936032));
#244599=CARTESIAN_POINT('Ctrl Pts',(-191.517433210267,4.15696789296251,
128.172342252175));
#244600=CARTESIAN_POINT('Ctrl Pts',(-191.525207544386,4.08059035808282,
128.058825079275));
#244601=CARTESIAN_POINT('Ctrl Pts',(-191.532972297333,4.0043069516886,127.945447806144));
#244602=CARTESIAN_POINT('Ctrl Pts',(-191.54073705028,3.92319460690395,127.835103335206));
#244603=CARTESIAN_POINT('Ctrl Pts',(-191.548501803227,3.83752433236579,
127.728228295802));
#244604=CARTESIAN_POINT('Ctrl Pts',(-191.556258844112,3.75193914675227,
127.621459406194));
#244605=CARTESIAN_POINT('Ctrl Pts',(-191.564015884997,3.6618052832676,127.518153393728));
#244606=CARTESIAN_POINT('Ctrl Pts',(-191.571772925882,3.5674369836618,127.418717926717));
#244607=CARTESIAN_POINT('Ctrl Pts',(-191.579524117122,3.47313984792494,
127.319357444764));
#244608=CARTESIAN_POINT('Ctrl Pts',(-191.587275308362,3.37461490002521,
127.223861980993));
#244609=CARTESIAN_POINT('Ctrl Pts',(-191.595026499602,3.27221635190649,
127.132605831525));
#244610=CARTESIAN_POINT('Ctrl Pts',(-191.602774396379,3.16986132590188,
127.041388468354));
#244611=CARTESIAN_POINT('Ctrl Pts',(-191.610522293156,3.06363626547616,
126.954407095373));
#244612=CARTESIAN_POINT('Ctrl Pts',(-191.618270189933,2.95393174198714,
126.871998690406));
#244613=CARTESIAN_POINT('Ctrl Pts',(-191.626016466018,2.84425016631949,
126.789607523499));
#244614=CARTESIAN_POINT('Ctrl Pts',(-191.633762742102,2.73109088767587,
126.711787656611));
#244615=CARTESIAN_POINT('Ctrl Pts',(-191.641509018186,2.61487669737603,
126.638835090094));
#244616=CARTESIAN_POINT('Ctrl Pts',(-191.649255351451,2.49866164920991,
126.565881985059));
#244617=CARTESIAN_POINT('Ctrl Pts',(-191.657001684716,2.37939197551846,
126.497796459953));
#244618=CARTESIAN_POINT('Ctrl Pts',(-191.664748017982,2.25751817453226,
126.434830350574));
#244619=CARTESIAN_POINT('Ctrl Pts',(-191.672496085985,2.1356170807535,126.371850140372));
#244620=CARTESIAN_POINT('Ctrl Pts',(-191.680244153988,2.01111104650626,
126.313991806636));
#244621=CARTESIAN_POINT('Ctrl Pts',(-191.687992221991,1.88447344383008,
126.261460343292));
#244622=CARTESIAN_POINT('Ctrl Pts',(-191.695748524732,1.75770124920225,
126.208873048883));
#244623=CARTESIAN_POINT('Ctrl Pts',(-191.703504827474,1.62879332235594,
126.161624084286));
#244624=CARTESIAN_POINT('Ctrl Pts',(-191.711261130216,1.49824173563579,
126.119869741911));
#244625=CARTESIAN_POINT('Ctrl Pts',(-191.71902157273,1.36762046960263,126.078093113985));
#244626=CARTESIAN_POINT('Ctrl Pts',(-191.726782015244,1.23535417251634,
126.041817055184));
#244627=CARTESIAN_POINT('Ctrl Pts',(-191.734542457759,1.10194724024969,
126.01114715036));
#244628=CARTESIAN_POINT('Ctrl Pts',(-191.742315358024,0.968326151332061,
125.980428011482));
#244629=CARTESIAN_POINT('Ctrl Pts',(-191.750088258289,0.833561152794384,
125.955333082055));
#244630=CARTESIAN_POINT('Ctrl Pts',(-191.757861158555,0.698164822785404,
125.935916416106));
#244631=CARTESIAN_POINT('Ctrl Pts',(-191.765351494317,0.567690490411714,
125.917205594873));
#244632=CARTESIAN_POINT('Ctrl Pts',(-191.772841830079,0.436630237048816,
125.903767397656));
#244633=CARTESIAN_POINT('Ctrl Pts',(-191.780332165842,0.305442686064309,
125.895604377129));
#244634=CARTESIAN_POINT('Ctrl Pts',(-191.788106499961,0.169281119213901,
125.887131853198));
#244635=CARTESIAN_POINT('Ctrl Pts',(-191.79588083408,0.0325510922944527,
125.884315580651));
#244636=CARTESIAN_POINT('Ctrl Pts',(-191.803655168199,-0.104238043468105,
125.887215359106));
#244637=CARTESIAN_POINT('Ctrl Pts',(-191.811419921146,-0.240858598845289,
125.890111563843));
#244638=CARTESIAN_POINT('Ctrl Pts',(-191.819184674093,-0.377537730998018,
125.898709794876));
#244639=CARTESIAN_POINT('Ctrl Pts',(-191.82694942704,-0.513761604507242,
125.913018053787));
#244640=CARTESIAN_POINT('Ctrl Pts',(-191.834706467925,-0.649850178545986,
125.927312101534));
#244641=CARTESIAN_POINT('Ctrl Pts',(-191.84246350881,-0.785484007468369,
125.94730485048));
#244642=CARTESIAN_POINT('Ctrl Pts',(-191.850220549695,-0.920150253035749,
125.972952274822));
#244643=CARTESIAN_POINT('Ctrl Pts',(-191.857971740935,-1.05471494573815,
125.998580358241));
#244644=CARTESIAN_POINT('Ctrl Pts',(-191.865722932175,-1.18831312492588,
126.029854556506));
#244645=CARTESIAN_POINT('Ctrl Pts',(-191.873474123415,-1.32043842446319,
126.066679177273));
#244646=CARTESIAN_POINT('Ctrl Pts',(-191.881222020193,-1.4525075672249,
126.103488146594));
#244647=CARTESIAN_POINT('Ctrl Pts',(-191.88896991697,-1.58310469960573,
126.145842741646));
#244648=CARTESIAN_POINT('Ctrl Pts',(-191.896717813747,-1.71173519926051,
126.193596508428));
#244649=CARTESIAN_POINT('Ctrl Pts',(-191.904464089831,-1.84033879218771,
126.241340286152));
#244650=CARTESIAN_POINT('Ctrl Pts',(-191.912210365915,-1.96697620435051,
126.294480853203));
#244651=CARTESIAN_POINT('Ctrl Pts',(-191.919956641999,-2.09116987323163,
126.352822498692));
#244652=CARTESIAN_POINT('Ctrl Pts',(-191.927702975264,-2.21536445888204,
126.411164574845));
#244653=CARTESIAN_POINT('Ctrl Pts',(-191.93544930853,-2.33711491138994,
126.474707639814));
#244654=CARTESIAN_POINT('Ctrl Pts',(-191.943195641795,-2.45596584886988,
126.543208800078));
#244655=CARTESIAN_POINT('Ctrl Pts',(-191.950943709798,-2.57484340219369,
126.611725300701));
#244656=CARTESIAN_POINT('Ctrl Pts',(-191.958691777801,-2.69081980973953,
126.685201910856));
#244657=CARTESIAN_POINT('Ctrl Pts',(-191.966439845804,-2.80346673516209,
126.763351173462));
#244658=CARTESIAN_POINT('Ctrl Pts',(-191.974196148546,-2.91623338307735,
126.841583494034));
#244659=CARTESIAN_POINT('Ctrl Pts',(-191.981952451288,-3.02566315836508,
126.924498164268));
#244660=CARTESIAN_POINT('Ctrl Pts',(-191.98970875403,-3.13135859067244,
127.011765669628));
#244661=CARTESIAN_POINT('Ctrl Pts',(-191.997469196544,-3.23711043581445,
127.099079752284));
#244662=CARTESIAN_POINT('Ctrl Pts',(-192.005229639058,-3.33912367583414,
127.190751038126));
#244663=CARTESIAN_POINT('Ctrl Pts',(-192.012990081572,-3.43703684091518,
127.286412235811));
#244664=CARTESIAN_POINT('Ctrl Pts',(-192.020762981838,-3.53510718490086,
127.382226997343));
#244665=CARTESIAN_POINT('Ctrl Pts',(-192.028535882103,-3.62906403328069,
127.482044185023));
#244666=CARTESIAN_POINT('Ctrl Pts',(-192.036308782368,-3.71858484786014,
127.58546176986));
#244667=CARTESIAN_POINT('Ctrl Pts',(-192.04379911813,-3.80485135533908,
127.685119864993));
#244668=CARTESIAN_POINT('Ctrl Pts',(-192.051289453892,-3.88699855951138,
127.78812089412));
#244669=CARTESIAN_POINT('Ctrl Pts',(-192.058779789654,-3.9647764156074,
127.894080384196));
#244670=CARTESIAN_POINT('Ctrl Pts',(-192.066605571333,-4.04603746191827,
128.004785145967));
#244671=CARTESIAN_POINT('Ctrl Pts',(-192.074431353011,-4.12278666815336,
128.119070688909));
#244672=CARTESIAN_POINT('Ctrl Pts',(-192.08225713469,-4.19469433982913,
128.236536157463));
#244673=CARTESIAN_POINT('Ctrl Pts',(-192.090069792819,-4.26648142497111,
128.353804640724));
#244674=CARTESIAN_POINT('Ctrl Pts',(-192.097882450948,-4.33344294894402,
128.474242102797));
#244675=CARTESIAN_POINT('Ctrl Pts',(-192.105695109077,-4.3952906467389,
128.597416306264));
#244676=CARTESIAN_POINT('Ctrl Pts',(-192.113500201717,-4.4570784535094,
128.720471232385));
#244677=CARTESIAN_POINT('Ctrl Pts',(-192.121305294356,-4.51376211373051,
128.846257287088));
#244678=CARTESIAN_POINT('Ctrl Pts',(-192.129110386996,-4.5650974649776,
128.974314662472));
#244679=CARTESIAN_POINT('Ctrl Pts',(-192.136908171869,-4.61638475186583,
129.102252140057));
#244680=CARTESIAN_POINT('Ctrl Pts',(-192.144705956742,-4.66233355954381,
129.232456348203));
#244681=CARTESIAN_POINT('Ctrl Pts',(-192.152503741615,-4.70274661817135,
129.364444888164));
#244682=CARTESIAN_POINT('Ctrl Pts',(-192.156767827254,-4.72484580989491,
129.436620569713));
#244683=CARTESIAN_POINT('Ctrl Pts',(-192.161031912893,-4.7452904916293,
129.50932942537));
#244684=CARTESIAN_POINT('Ctrl Pts',(-192.165295998532,-4.76405452823416,
129.582490119309));
#244685=CARTESIAN_POINT('',(-190.13985943604,-4.91824986400714,130.803204030469));
#244686=CARTESIAN_POINT('Ctrl Pts',(-190.13985943604,-4.91824986400714,
130.803204030469));
#244687=CARTESIAN_POINT('Ctrl Pts',(-190.147585601233,-4.91828175505972,
130.938816960416));
#244688=CARTESIAN_POINT('Ctrl Pts',(-190.155311766426,-4.91270043226599,
131.074655996844));
#244689=CARTESIAN_POINT('Ctrl Pts',(-190.163037931618,-4.90147587807679,
131.210214383264));
#244690=CARTESIAN_POINT('Ctrl Pts',(-190.170754697744,-4.89026497882958,
131.345607859624));
#244691=CARTESIAN_POINT('Ctrl Pts',(-190.178471463869,-4.87342453696202,
131.48072097409));
#244692=CARTESIAN_POINT('Ctrl Pts',(-190.186188229995,-4.85097651155595,
131.615045480403));
#244693=CARTESIAN_POINT('Ctrl Pts',(-190.193897512807,-4.82855025506256,
131.749239725884));
#244694=CARTESIAN_POINT('Ctrl Pts',(-190.201606795619,-4.80052729930736,
131.882646496431));
#244695=CARTESIAN_POINT('Ctrl Pts',(-190.209316078432,-4.76698148662643,
132.014761612551));
#244696=CARTESIAN_POINT('Ctrl Pts',(-190.217019786611,-4.73345993114099,
132.14678119537));
#244697=CARTESIAN_POINT('Ctrl Pts',(-190.224723494791,-4.69442356335619,
132.277510599873));
#244698=CARTESIAN_POINT('Ctrl Pts',(-190.232427202971,-4.6499974110266,
132.406455227739));
#244699=CARTESIAN_POINT('Ctrl Pts',(-190.240128016859,-4.60558794964859,
132.535351410974));
#244700=CARTESIAN_POINT('Ctrl Pts',(-190.247828830748,-4.55579285811654,
132.662463776619));
#244701=CARTESIAN_POINT('Ctrl Pts',(-190.255529644636,-4.50078711110052,
132.787312569342));
#244702=CARTESIAN_POINT('Ctrl Pts',(-190.263229171694,-4.44579055572119,
132.912140499431));
#244703=CARTESIAN_POINT('Ctrl Pts',(-190.270928698752,-4.38558523610426,
133.034705246309));
#244704=CARTESIAN_POINT('Ctrl Pts',(-190.27862822581,-4.32039420672799,
133.1545471976));
#244705=CARTESIAN_POINT('Ctrl Pts',(-190.286328185659,-4.25519951295482,
133.274395885223));
#244706=CARTESIAN_POINT('Ctrl Pts',(-190.294028145508,-4.18501874133744,
133.391521124698));
#244707=CARTESIAN_POINT('Ctrl Pts',(-190.301728105358,-4.1101205931154,
133.505488488021));
#244708=CARTESIAN_POINT('Ctrl Pts',(-190.309430217604,-4.03520150834462,
133.619487709051));
#244709=CARTESIAN_POINT('Ctrl Pts',(-190.317132329851,-3.95556264143853,
133.73032696698));
#244710=CARTESIAN_POINT('Ctrl Pts',(-190.324834442098,-3.87151536636673,
133.837601760384));
#244711=CARTESIAN_POINT('Ctrl Pts',(-190.332544856977,-3.78737749100206,
133.944992192609));
#244712=CARTESIAN_POINT('Ctrl Pts',(-190.340255271856,-3.69882196354237,
134.048810176041));
#244713=CARTESIAN_POINT('Ctrl Pts',(-190.347965686736,-3.60619996799212,
134.148684892117));
#244714=CARTESIAN_POINT('Ctrl Pts',(-190.3556806963,-3.51352277841163,134.248619124166));
#244715=CARTESIAN_POINT('Ctrl Pts',(-190.363395705863,-3.41677457553636,
134.344605130585));
#244716=CARTESIAN_POINT('Ctrl Pts',(-190.371110715427,-3.31634172458628,
134.43631059358));
#244717=CARTESIAN_POINT('Ctrl Pts',(-190.378837231148,-3.21575908819369,
134.528152826001));
#244718=CARTESIAN_POINT('Ctrl Pts',(-190.386563746869,-3.11148113317161,
134.615701512883));
#244719=CARTESIAN_POINT('Ctrl Pts',(-190.394290262589,-3.00392586603647,
134.698665748633));
#244720=CARTESIAN_POINT('Ctrl Pts',(-190.398754522705,-2.94178211240861,
134.746601188372));
#244721=CARTESIAN_POINT('Ctrl Pts',(-190.403218782821,-2.87854480706385,
134.793006993218));
#244722=CARTESIAN_POINT('Ctrl Pts',(-190.407683042937,-2.81429844266184,
134.837833976612));
#244723=CARTESIAN_POINT('Ctrl Pts',(-190.415457377056,-2.70241591570069,
134.915898412238));
#244724=CARTESIAN_POINT('Ctrl Pts',(-190.423231711176,-2.58710562699183,
134.989427787118));
#244725=CARTESIAN_POINT('Ctrl Pts',(-190.431006045295,-2.46877148506654,
135.058106075045));
#244726=CARTESIAN_POINT('Ctrl Pts',(-190.438770798242,-2.35058317939566,
135.126699723119));
#244727=CARTESIAN_POINT('Ctrl Pts',(-190.446535551189,-2.2293787702848,
135.19045398537));
#244728=CARTESIAN_POINT('Ctrl Pts',(-190.454300304136,-2.1055929402831,
135.249094741485));
#244729=CARTESIAN_POINT('Ctrl Pts',(-190.462057345021,-1.98193005611249,
135.307677254775));
#244730=CARTESIAN_POINT('Ctrl Pts',(-190.469814385906,-1.85569120437271,
135.361156202688));
#244731=CARTESIAN_POINT('Ctrl Pts',(-190.477571426791,-1.72733727952841,
135.409302417986));
#244732=CARTESIAN_POINT('Ctrl Pts',(-190.485322618031,-1.59908014737782,
135.457412325848));
#244733=CARTESIAN_POINT('Ctrl Pts',(-190.493073809271,-1.46871148143803,
135.500197368803));
#244734=CARTESIAN_POINT('Ctrl Pts',(-190.500825000511,-1.3367135244881,
135.537475872443));
#244735=CARTESIAN_POINT('Ctrl Pts',(-190.508572897288,-1.2047716701905,
135.574738531725));
#244736=CARTESIAN_POINT('Ctrl Pts',(-190.516320794066,-1.07120227765744,
135.606499200586));
#244737=CARTESIAN_POINT('Ctrl Pts',(-190.524068690843,-0.9365039649583,
135.632625666848));
#244738=CARTESIAN_POINT('Ctrl Pts',(-190.531814966927,-0.80183382824242,
135.658746668017));
#244739=CARTESIAN_POINT('Ctrl Pts',(-190.539561243011,-0.666035624636225,
135.679235736398));
#244740=CARTESIAN_POINT('Ctrl Pts',(-190.547307519095,-0.529619024550856,
135.69401160218));
#244741=CARTESIAN_POINT('Ctrl Pts',(-190.55505385236,-0.39320141746932,
135.708787577034));
#244742=CARTESIAN_POINT('Ctrl Pts',(-190.562800185626,-0.25616579349155,
135.717850223034));
#244743=CARTESIAN_POINT('Ctrl Pts',(-190.570546518891,-0.119027422925699,
135.721170104936));
#244744=CARTESIAN_POINT('Ctrl Pts',(-190.578294586894,0.0181416588272017,
135.724490730303));
#244745=CARTESIAN_POINT('Ctrl Pts',(-190.586042654897,0.155413142178313,
135.722066023016));
#244746=CARTESIAN_POINT('Ctrl Pts',(-190.5937907229,0.292271674219316,135.713918676185));
#244747=CARTESIAN_POINT('Ctrl Pts',(-190.601547025642,0.429275661136996,
135.705762670257));
#244748=CARTESIAN_POINT('Ctrl Pts',(-190.609303328384,0.565865429118824,
135.691871898426));
#244749=CARTESIAN_POINT('Ctrl Pts',(-190.617059631125,0.70153010916397,
135.672321029118));
#244750=CARTESIAN_POINT('Ctrl Pts',(-190.62482007364,0.837267197534009,
135.652759724922));
#244751=CARTESIAN_POINT('Ctrl Pts',(-190.632580516154,0.972077830027677,
135.627532375601));
#244752=CARTESIAN_POINT('Ctrl Pts',(-190.640340958668,1.1054622334498,135.596764639862));
#244753=CARTESIAN_POINT('Ctrl Pts',(-190.648113858933,1.23906075735725,
135.565947513022));
#244754=CARTESIAN_POINT('Ctrl Pts',(-190.655886759199,1.37122809985715,
135.529572330681));
#244755=CARTESIAN_POINT('Ctrl Pts',(-190.663659659464,1.50147966778053,
135.487814670905));
#244756=CARTESIAN_POINT('Ctrl Pts',(-190.671149995226,1.62699626312459,
135.447575007244));
#244757=CARTESIAN_POINT('Ctrl Pts',(-190.678640330988,1.75073366284605,
135.402337511017));
#244758=CARTESIAN_POINT('Ctrl Pts',(-190.68613066675,1.8722783195407,135.352300476082));
#244759=CARTESIAN_POINT('Ctrl Pts',(-190.693905000869,1.99843137883754,
135.300366271758));
#244760=CARTESIAN_POINT('Ctrl Pts',(-190.701679334988,2.12262175204157,
135.243096883288));
#244761=CARTESIAN_POINT('Ctrl Pts',(-190.709453669107,2.24436523492668,
135.180661310475));
#244762=CARTESIAN_POINT('Ctrl Pts',(-190.717218422054,2.36595867984999,
135.118302683924));
#244763=CARTESIAN_POINT('Ctrl Pts',(-190.724983175001,2.48511089000259,
135.050790717883));
#244764=CARTESIAN_POINT('Ctrl Pts',(-190.732747927949,2.6013562836682,134.978342954366));
#244765=CARTESIAN_POINT('Ctrl Pts',(-190.740504968834,2.71748622077004,
134.90596714699));
#244766=CARTESIAN_POINT('Ctrl Pts',(-190.748262009719,2.83071475717223,
134.828665503394));
#244767=CARTESIAN_POINT('Ctrl Pts',(-190.756019050603,2.94059996327127,
134.746701916656));
#244768=CARTESIAN_POINT('Ctrl Pts',(-190.763770241844,3.05040230408146,
134.664800139296));
#244769=CARTESIAN_POINT('Ctrl Pts',(-190.771521433084,3.15686602082719,
134.578243649209));
#244770=CARTESIAN_POINT('Ctrl Pts',(-190.779272624324,3.25957760168308,
134.487339971446));
#244771=CARTESIAN_POINT('Ctrl Pts',(-190.787020521101,3.36224552737705,
134.396474930171));
#244772=CARTESIAN_POINT('Ctrl Pts',(-190.794768417878,3.46116419687574,
134.301266634669));
#244773=CARTESIAN_POINT('Ctrl Pts',(-190.802516314655,3.55595286108516,
134.20206312253));
#244774=CARTESIAN_POINT('Ctrl Pts',(-190.810262590739,3.65072169754968,
134.102880361628));
#244775=CARTESIAN_POINT('Ctrl Pts',(-190.818008866823,3.74136197716383,
133.999704328862));
#244776=CARTESIAN_POINT('Ctrl Pts',(-190.825755142907,3.82752983602749,
133.892919896068));
#244777=CARTESIAN_POINT('Ctrl Pts',(-190.833501476173,3.91369833096282,
133.786134675015));
#244778=CARTESIAN_POINT('Ctrl Pts',(-190.841247809438,3.99539409375177,
133.675741305042));
#244779=CARTESIAN_POINT('Ctrl Pts',(-190.848994142703,4.07231384350195,
133.562157387185));
#244780=CARTESIAN_POINT('Ctrl Pts',(-190.856742210706,4.14925081889687,
133.448548032997));
#244781=CARTESIAN_POINT('Ctrl Pts',(-190.864490278709,4.2214094337795,133.331747032808));
#244782=CARTESIAN_POINT('Ctrl Pts',(-190.872238346712,4.28853021966979,
133.212200233794));
#244783=CARTESIAN_POINT('Ctrl Pts',(-190.879994649454,4.3557223423298,133.092526379021));
#244784=CARTESIAN_POINT('Ctrl Pts',(-190.887750952196,4.41786574856622,
132.970101237319));
#244785=CARTESIAN_POINT('Ctrl Pts',(-190.895507254938,4.47474712186675,
132.845394977356));
#244786=CARTESIAN_POINT('Ctrl Pts',(-190.903267697452,4.53165885446903,
132.720622157908));
#244787=CARTESIAN_POINT('Ctrl Pts',(-190.911028139966,4.5833028108051,132.593566156235));
#244788=CARTESIAN_POINT('Ctrl Pts',(-190.91878858248,4.62951457148501,132.464715367283));
#244789=CARTESIAN_POINT('Ctrl Pts',(-190.926561482746,4.67580051538552,
132.335657735606));
#244790=CARTESIAN_POINT('Ctrl Pts',(-190.934334383011,4.71663672127184,
132.204799932619));
#244791=CARTESIAN_POINT('Ctrl Pts',(-190.942107283277,4.75190897349856,
132.072644564513));
#244792=CARTESIAN_POINT('Ctrl Pts',(-190.949597619039,4.78589899051188,
131.945293376915));
#244793=CARTESIAN_POINT('Ctrl Pts',(-190.957087954801,4.81472249074796,
131.816737626403));
#244794=CARTESIAN_POINT('Ctrl Pts',(-190.964578290563,4.83832277197152,
131.687432424795));
#244795=CARTESIAN_POINT('Ctrl Pts',(-190.972352624682,4.86281786503052,
131.553224577167));
#244796=CARTESIAN_POINT('Ctrl Pts',(-190.980126958801,4.88176343679289,
131.417784195585));
#244797=CARTESIAN_POINT('Ctrl Pts',(-190.98790129292,4.89503994736683,131.281610003299));
#244798=CARTESIAN_POINT('Ctrl Pts',(-190.995666045867,4.90830009582805,
131.145603633535));
#244799=CARTESIAN_POINT('Ctrl Pts',(-191.003430798814,4.91590504680117,
131.008865637851));
#244800=CARTESIAN_POINT('Ctrl Pts',(-191.011195551762,4.91778616625509,
130.871905310104));
#244801=CARTESIAN_POINT('Ctrl Pts',(-191.018952592647,4.91966541735466,
130.735081013285));
#244802=CARTESIAN_POINT('Ctrl Pts',(-191.026709633532,4.9158321449874,130.59803521225));
#244803=CARTESIAN_POINT('Ctrl Pts',(-191.034466674417,4.90626949612716,
130.461282355544));
#244804=CARTESIAN_POINT('Ctrl Pts',(-191.042217865657,4.89671405853478,
130.324632625231));
#244805=CARTESIAN_POINT('Ctrl Pts',(-191.049969056897,4.88143787143859,
130.18827578797));
#244806=CARTESIAN_POINT('Ctrl Pts',(-191.057720248137,4.86047615113323,
130.052725967776));
#244807=CARTESIAN_POINT('Ctrl Pts',(-191.065468144914,4.83952334011826,
129.917233759872));
#244808=CARTESIAN_POINT('Ctrl Pts',(-191.073216041691,4.81288986175936,
129.782548272388));
#244809=CARTESIAN_POINT('Ctrl Pts',(-191.080963938468,4.78066272575466,
129.649177963143));
#244810=CARTESIAN_POINT('Ctrl Pts',(-191.088710214552,4.74844233097209,
129.515835552091));
#244811=CARTESIAN_POINT('Ctrl Pts',(-191.096456490636,4.71063069765271,
129.383808151861));
#244812=CARTESIAN_POINT('Ctrl Pts',(-191.104202766721,4.66736576253298,
129.253593097518));
#244813=CARTESIAN_POINT('Ctrl Pts',(-191.111949099986,4.62410050804126,
129.123377081957));
#244814=CARTESIAN_POINT('Ctrl Pts',(-191.119695433251,4.57538199469793,
128.994973810001));
#244815=CARTESIAN_POINT('Ctrl Pts',(-191.127441766517,4.52139763135042,
128.868864164012));
#244816=CARTESIAN_POINT('Ctrl Pts',(-191.13518983452,4.46740117857896,128.742726276643));
#244817=CARTESIAN_POINT('Ctrl Pts',(-191.142937902523,4.40813668305963,
128.618883396679));
#244818=CARTESIAN_POINT('Ctrl Pts',(-191.150685970526,4.34383899959804,
128.49779481359));
#244819=CARTESIAN_POINT('Ctrl Pts',(-191.158442273267,4.2794729797934,128.376577536114));
#244820=CARTESIAN_POINT('Ctrl Pts',(-191.166198576009,4.21006326982718,
128.258120748965));
#244821=CARTESIAN_POINT('Ctrl Pts',(-191.173954878751,4.13589013312932,
128.142858059013));
#244822=CARTESIAN_POINT('Ctrl Pts',(-191.181715321265,4.0616774079951,128.027533849893));
#244823=CARTESIAN_POINT('Ctrl Pts',(-191.18947576378,3.98269641524828,127.915407454376));
#244824=CARTESIAN_POINT('Ctrl Pts',(-191.197236206294,3.89926918269119,
127.806881192547));
#244825=CARTESIAN_POINT('Ctrl Pts',(-191.205009106559,3.81570802533407,
127.698180714727));
#244826=CARTESIAN_POINT('Ctrl Pts',(-191.212782006825,3.72768661635664,
127.59309221928));
#244827=CARTESIAN_POINT('Ctrl Pts',(-191.22055490709,3.63556607623541,127.491983469984));
#244828=CARTESIAN_POINT('Ctrl Pts',(-191.228045242852,3.54679434978573,
127.394550278402));
#244829=CARTESIAN_POINT('Ctrl Pts',(-191.235535578614,3.4542165619243,127.300812728031));
#244830=CARTESIAN_POINT('Ctrl Pts',(-191.243025914376,3.35818496216893,
127.21106452312));
#244831=CARTESIAN_POINT('Ctrl Pts',(-191.250800248495,3.25851229511997,
127.11791348774));
#244832=CARTESIAN_POINT('Ctrl Pts',(-191.258574582614,3.15480301053301,
127.02876520709));
#244833=CARTESIAN_POINT('Ctrl Pts',(-191.266348916733,3.04741208417123,
126.943989825563));
#244834=CARTESIAN_POINT('Ctrl Pts',(-191.27411366968,2.94015350752896,126.859318922119));
#244835=CARTESIAN_POINT('Ctrl Pts',(-191.281878422628,2.82922262090105,
126.779010434803));
#244836=CARTESIAN_POINT('Ctrl Pts',(-191.289643175575,2.71501080926322,
126.703397393141));
#244837=CARTESIAN_POINT('Ctrl Pts',(-191.29740021646,2.60091243440618,126.627859451418));
#244838=CARTESIAN_POINT('Ctrl Pts',(-191.305157257345,2.48353994330888,
126.557007889035));
#244839=CARTESIAN_POINT('Ctrl Pts',(-191.31291429823,2.3633170466302,126.491134956926));
#244840=CARTESIAN_POINT('Ctrl Pts',(-191.32066548947,2.24318481097262,126.425311700106));
#244841=CARTESIAN_POINT('Ctrl Pts',(-191.32841668071,2.12020678969177,126.364459787714));
#244842=CARTESIAN_POINT('Ctrl Pts',(-191.33616787195,1.99483456514794,126.30882748787));
#244843=CARTESIAN_POINT('Ctrl Pts',(-191.343915768727,1.86951562714447,
126.253218833238));
#244844=CARTESIAN_POINT('Ctrl Pts',(-191.351663665504,1.74180486642149,
126.20282553702));
#244845=CARTESIAN_POINT('Ctrl Pts',(-191.359411562281,1.61217709380733,
126.157849229363));
#244846=CARTESIAN_POINT('Ctrl Pts',(-191.367157838366,1.48257643652876,
126.112882329779));
#244847=CARTESIAN_POINT('Ctrl Pts',(-191.37490411445,1.35105993409509,126.073330292999));
#244848=CARTESIAN_POINT('Ctrl Pts',(-191.382650390534,1.21812056675712,
126.03934589069));
#244849=CARTESIAN_POINT('Ctrl Pts',(-191.390396723799,1.08518021809113,
126.005361237516));
#244850=CARTESIAN_POINT('Ctrl Pts',(-191.398143057064,0.950817362346455,
125.976944397655));
#244851=CARTESIAN_POINT('Ctrl Pts',(-191.40588939033,0.815537878534929,
125.9541976274));
#244852=CARTESIAN_POINT('Ctrl Pts',(-191.413637458333,0.68022809982115,
125.931445763164));
#244853=CARTESIAN_POINT('Ctrl Pts',(-191.421385526336,0.544001670051006,
125.914366560051));
#244854=CARTESIAN_POINT('Ctrl Pts',(-191.429133594339,0.407371947222745,
125.90301068524));
#244855=CARTESIAN_POINT('Ctrl Pts',(-191.436889897081,0.270597012698589,
125.89164274127));
#244856=CARTESIAN_POINT('Ctrl Pts',(-191.444646199823,0.133418319135421,
125.886010309127));
#244857=CARTESIAN_POINT('Ctrl Pts',(-191.452402502564,-0.00364783849507481,
125.886111970357));
#244858=CARTESIAN_POINT('Ctrl Pts',(-191.460162945079,-0.14078715246088,
125.886213685846));
#244859=CARTESIAN_POINT('Ctrl Pts',(-191.467923387593,-0.277813420392517,
125.892055576286));
#244860=CARTESIAN_POINT('Ctrl Pts',(-191.475683830107,-0.414214095113777,
125.903584174398));
#244861=CARTESIAN_POINT('Ctrl Pts',(-191.483456730372,-0.550833732307181,
125.91513127924));
#244862=CARTESIAN_POINT('Ctrl Pts',(-191.491229630638,-0.686825381383332,
125.93238328479));
#244863=CARTESIAN_POINT('Ctrl Pts',(-191.499002530903,-0.821684437819978,
125.95523515547));
#244864=CARTESIAN_POINT('Ctrl Pts',(-191.506492866665,-0.951641027862406,
125.977256303091));
#244865=CARTESIAN_POINT('Ctrl Pts',(-191.513983202427,-1.08054563945036,
126.004477182315));
#244866=CARTESIAN_POINT('Ctrl Pts',(-191.521473538189,-1.20796077141146,
126.036760189968));
#244867=CARTESIAN_POINT('Ctrl Pts',(-191.529247872308,-1.3402068868303,
126.07026721767));
#244868=CARTESIAN_POINT('Ctrl Pts',(-191.537022206427,-1.47126726171084,
126.109333952733));
#244869=CARTESIAN_POINT('Ctrl Pts',(-191.544796540546,-1.6006386100197,
126.153861816081));
#244870=CARTESIAN_POINT('Ctrl Pts',(-191.552561293493,-1.72985051970473,
126.198334802817));
#244871=CARTESIAN_POINT('Ctrl Pts',(-191.560326046441,-1.85737717839847,
126.248255400426));
#244872=CARTESIAN_POINT('Ctrl Pts',(-191.568090799388,-1.98272684579087,
126.303474336234));
#244873=CARTESIAN_POINT('Ctrl Pts',(-191.575847840273,-2.10795201412615,
126.358638427817));
#244874=CARTESIAN_POINT('Ctrl Pts',(-191.583604881158,-2.2310041385998,
126.419090228625));
#244875=CARTESIAN_POINT('Ctrl Pts',(-191.591361922043,-2.35140831426397,
126.484631227649));
#244876=CARTESIAN_POINT('Ctrl Pts',(-191.599113113283,-2.47172169220282,
126.550122801696));
#244877=CARTESIAN_POINT('Ctrl Pts',(-191.606864304523,-2.58939075392098,
126.62069574888));
#244878=CARTESIAN_POINT('Ctrl Pts',(-191.614615495763,-2.70396253312058,
126.696104335154));
#244879=CARTESIAN_POINT('Ctrl Pts',(-191.62236339254,-2.81848561625756,
126.771480870767));
#244880=CARTESIAN_POINT('Ctrl Pts',(-191.630111289317,-2.92991370925743,
126.851688743189));
#244881=CARTESIAN_POINT('Ctrl Pts',(-191.637859186094,-3.03782052811709,
126.936437466642));
#244882=CARTESIAN_POINT('Ctrl Pts',(-191.645605462178,-3.14570477519644,
127.02116846249));
#244883=CARTESIAN_POINT('Ctrl Pts',(-191.653351738262,-3.25006890594588,
127.110438178736));
#244884=CARTESIAN_POINT('Ctrl Pts',(-191.661098014347,-3.35051792136731,
127.203914433953));
#244885=CARTESIAN_POINT('Ctrl Pts',(-191.668844347612,-3.45096767828041,
127.29739137919));
#244886=CARTESIAN_POINT('Ctrl Pts',(-191.676590680877,-3.54750197598732,
127.395074659016));
#244887=CARTESIAN_POINT('Ctrl Pts',(-191.684337014142,-3.63976134341008,
127.496593935117));
#244888=CARTESIAN_POINT('Ctrl Pts',(-191.692085082145,-3.73204137167862,
127.598135945756));
#244889=CARTESIAN_POINT('Ctrl Pts',(-191.699833150149,-3.82004430177213,
127.70351537279));
#244890=CARTESIAN_POINT('Ctrl Pts',(-191.707581218151,-3.90345002342118,
127.812327700442));
#244891=CARTESIAN_POINT('Ctrl Pts',(-191.715337520893,-3.98694438966386,
127.921255675131));
#244892=CARTESIAN_POINT('Ctrl Pts',(-191.723093823635,-4.06583154899084,
128.033623527975));
#244893=CARTESIAN_POINT('Ctrl Pts',(-191.730850126377,-4.13983362474526,
128.148996118683));
#244894=CARTESIAN_POINT('Ctrl Pts',(-191.738610568891,-4.21387519763547,
128.264430287216));
#244895=CARTESIAN_POINT('Ctrl Pts',(-191.746371011405,-4.28302629462755,
128.38287205169));
#244896=CARTESIAN_POINT('Ctrl Pts',(-191.754131453919,-4.34705485498703,
128.503861291282));
#244897=CARTESIAN_POINT('Ctrl Pts',(-191.761904354185,-4.41118619967579,
128.625044753542));
#244898=CARTESIAN_POINT('Ctrl Pts',(-191.76967725445,-4.47017840691058,
128.748783509796));
#244899=CARTESIAN_POINT('Ctrl Pts',(-191.777450154716,-4.52384709502806,
128.874596247674));
#244900=CARTESIAN_POINT('Ctrl Pts',(-191.784940490478,-4.57556479114977,
128.995835375627));
#244901=CARTESIAN_POINT('Ctrl Pts',(-191.79243082624,-4.62233918575824,
129.119000026256));
#244902=CARTESIAN_POINT('Ctrl Pts',(-191.799921162002,-4.6640495682308,
129.243647739556));
#244903=CARTESIAN_POINT('Ctrl Pts',(-191.806629630531,-4.70140607627558,
129.355284292103));
#244904=CARTESIAN_POINT('Ctrl Pts',(-191.81333809906,-4.73477224984779,
129.468318960301));
#244905=CARTESIAN_POINT('Ctrl Pts',(-191.820046567589,-4.76405452823394,
129.582490119308));
#244906=CARTESIAN_POINT('Ctrl Pts',(-190.06976504276,-4.76405452823418,
129.582490119309));
#244907=CARTESIAN_POINT('Ctrl Pts',(-190.077527632497,-4.79811061399697,
129.715274280825));
#244908=CARTESIAN_POINT('Ctrl Pts',(-190.085290222234,-4.82658033576797,
129.849363494492));
#244909=CARTESIAN_POINT('Ctrl Pts',(-190.093052811971,-4.84939154448578,
129.984247996782));
#244910=CARTESIAN_POINT('Ctrl Pts',(-190.100826943755,-4.87223667075837,
130.119333056286));
#244911=CARTESIAN_POINT('Ctrl Pts',(-190.10860107554,-4.88940643253583,
130.255215378942));
#244912=CARTESIAN_POINT('Ctrl Pts',(-190.116375207325,-4.90088061235472,
130.391380852994));
#244913=CARTESIAN_POINT('Ctrl Pts',(-190.120661944591,-4.90720759465933,
130.466463914131));
#244914=CARTESIAN_POINT('Ctrl Pts',(-190.124948681858,-4.91180373898945,
130.541633066273));
#244915=CARTESIAN_POINT('Ctrl Pts',(-190.129235419125,-4.91467242218679,
130.616802506313));
#244916=CARTESIAN_POINT('Ctrl Pts',(-190.132776758081,-4.91704228507516,
130.678901125798));
#244917=CARTESIAN_POINT('Ctrl Pts',(-190.136318097038,-4.91823524652186,
130.741044945587));
#244918=CARTESIAN_POINT('Ctrl Pts',(-190.139859435995,-4.91824986400696,
130.803204029673));
#244919=CARTESIAN_POINT('Origin',(213.235140564004,0.,130.804360617566));
#244920=CARTESIAN_POINT('',(-188.319844903182,-4.76405452823404,129.582490119308));
#244921=CARTESIAN_POINT('',(-188.665047832579,-4.76405452823406,129.582490119308));
#244922=CARTESIAN_POINT('',(213.235140564004,-4.76405452823405,129.582490119308));
#244923=CARTESIAN_POINT('',(-188.735140564044,-4.9182496381179,130.802473913264));
#244924=CARTESIAN_POINT('Ctrl Pts',(-188.665047832579,-4.76405452823406,
129.582490119308));
#244925=CARTESIAN_POINT('Ctrl Pts',(-188.672812177752,-4.7980988056188,
129.715228240137));
#244926=CARTESIAN_POINT('Ctrl Pts',(-188.680576522925,-4.82655782458609,
129.849259699109));
#244927=CARTESIAN_POINT('Ctrl Pts',(-188.688340868098,-4.84936224031761,
129.984074737716));
#244928=CARTESIAN_POINT('Ctrl Pts',(-188.696116115444,-4.87219867648161,
130.119079074566));
#244929=CARTESIAN_POINT('Ctrl Pts',(-188.703891362791,-4.88936461210996,
130.254868801069));
#244930=CARTESIAN_POINT('Ctrl Pts',(-188.711666610137,-4.90084263355078,
130.390930401361));
#244931=CARTESIAN_POINT('Ctrl Pts',(-188.713580508058,-4.90366797921412,
130.424422328024));
#244932=CARTESIAN_POINT('Ctrl Pts',(-188.715494405978,-4.90614893497245,
130.457930736052));
#244933=CARTESIAN_POINT('Ctrl Pts',(-188.717408303899,-4.90828572440508,
130.491447993817));
#244934=CARTESIAN_POINT('Ctrl Pts',(-188.72331905727,-4.91488484090139,
130.594960434142));
#244935=CARTESIAN_POINT('Ctrl Pts',(-188.729229810641,-4.9182098228819,
130.6986838224));
#244936=CARTESIAN_POINT('Ctrl Pts',(-188.735140564012,-4.91824963811768,
130.802473912695));
#244937=CARTESIAN_POINT('Ctrl Pts',(-188.735140564045,-4.9182496381179,
130.802473913264));
#244938=CARTESIAN_POINT('Ctrl Pts',(-188.742840932869,-4.91830150830916,
130.937688821655));
#244939=CARTESIAN_POINT('Ctrl Pts',(-188.750541301692,-4.91277307334292,
131.073131498441));
#244940=CARTESIAN_POINT('Ctrl Pts',(-188.758241670516,-4.90163420131192,
131.208297764941));
#244941=CARTESIAN_POINT('Ctrl Pts',(-188.76593290635,-4.89050854049381,
131.343303718052));
#244942=CARTESIAN_POINT('Ctrl Pts',(-188.773624142184,-4.87378571052704,
131.478033519156));
#244943=CARTESIAN_POINT('Ctrl Pts',(-188.781315378017,-4.85148756347388,
131.611981496418));
#244944=CARTESIAN_POINT('Ctrl Pts',(-188.788999416841,-4.82921028172503,
131.745804132983));
#244945=CARTESIAN_POINT('Ctrl Pts',(-188.796683455665,-4.80136812688925,
131.87884601002));
#244946=CARTESIAN_POINT('Ctrl Pts',(-188.804367494489,-4.76803483755962,
132.010605555511));
#244947=CARTESIAN_POINT('Ctrl Pts',(-188.812346179207,-4.73342337706943,
132.147417445207));
#244948=CARTESIAN_POINT('Ctrl Pts',(-188.820324863925,-4.69289129475855,
132.282846262811));
#244949=CARTESIAN_POINT('Ctrl Pts',(-188.828303548642,-4.64657983212241,
132.416340433263));
#244950=CARTESIAN_POINT('Ctrl Pts',(-188.835979763627,-4.6020240242359,
132.544773876606));
#244951=CARTESIAN_POINT('Ctrl Pts',(-188.843655978612,-4.55211916674477,
132.671416266738));
#244952=CARTESIAN_POINT('Ctrl Pts',(-188.851332193597,-4.49704201443896,
132.795791305004));
#244953=CARTESIAN_POINT('Ctrl Pts',(-188.859007503027,-4.44197135952829,
132.920151670875));
#244954=CARTESIAN_POINT('Ctrl Pts',(-188.866682812457,-4.3817297846288,
133.042244852048));
#244955=CARTESIAN_POINT('Ctrl Pts',(-188.874358121887,-4.31654198168248,
133.161615033804));
#244956=CARTESIAN_POINT('Ctrl Pts',(-188.882034263867,-4.25134710773214,
133.280998163795));
#244957=CARTESIAN_POINT('Ctrl Pts',(-188.889710405848,-4.18120513001891,
133.397657356846));
#244958=CARTESIAN_POINT('Ctrl Pts',(-188.897386547828,-4.10638618677583,
133.511162336857));
#244959=CARTESIAN_POINT('Ctrl Pts',(-188.905065260793,-4.03154218428859,
133.624705333297));
#244960=CARTESIAN_POINT('Ctrl Pts',(-188.912743973757,-3.95201832019808,
133.735091682711));
#244961=CARTESIAN_POINT('Ctrl Pts',(-188.920422686722,-3.86812714267184,
133.841921394016));
#244962=CARTESIAN_POINT('Ctrl Pts',(-188.928109823954,-3.78414392866631,
133.94886830752));
#244963=CARTESIAN_POINT('Ctrl Pts',(-188.935796961185,-3.69578408429893,
134.052250480927));
#244964=CARTESIAN_POINT('Ctrl Pts',(-188.943484098417,-3.60339959857195,
134.151702009703));
#244965=CARTESIAN_POINT('Ctrl Pts',(-188.951176241949,-3.5109549468263,
134.251218306957));
#244966=CARTESIAN_POINT('Ctrl Pts',(-188.958868385481,-3.41448071785227,
134.346798583313));
#244967=CARTESIAN_POINT('Ctrl Pts',(-188.966560529013,-3.31436367286446,
134.438115769815));
#244968=CARTESIAN_POINT('Ctrl Pts',(-188.974263479165,-3.21410597437231,
134.529561246983));
#244969=CARTESIAN_POINT('Ctrl Pts',(-188.981966429318,-3.11019555105514,
134.616731427316));
#244970=CARTESIAN_POINT('Ctrl Pts',(-188.98966937947,-3.00305014572403,
134.699341090529));
#244971=CARTESIAN_POINT('Ctrl Pts',(-188.991731562218,-2.97436588814104,
134.721456801895));
#244972=CARTESIAN_POINT('Ctrl Pts',(-188.993793744965,-2.94544992466852,
134.743245908247));
#244973=CARTESIAN_POINT('Ctrl Pts',(-188.995855927712,-2.91631057808861,
134.764703490933));
#244974=CARTESIAN_POINT('Ctrl Pts',(-189.003630261831,-2.80645658157905,
134.84559759084));
#244975=CARTESIAN_POINT('Ctrl Pts',(-189.01140459595,-2.69306021115118,
134.92204557856));
#244976=CARTESIAN_POINT('Ctrl Pts',(-189.01917893007,-2.57651717925398,
134.993721223614));
#244977=CARTESIAN_POINT('Ctrl Pts',(-189.026943683017,-2.46011777622816,
135.065308534842));
#244978=CARTESIAN_POINT('Ctrl Pts',(-189.034708435964,-2.34057975758224,
135.132135002961));
#244979=CARTESIAN_POINT('Ctrl Pts',(-189.042473188911,-2.21833066914151,
135.193915504436));
#244980=CARTESIAN_POINT('Ctrl Pts',(-189.050230229796,-2.09620300021883,
135.255634644646));
#244981=CARTESIAN_POINT('Ctrl Pts',(-189.057987270681,-1.97136996672141,
135.312317616571));
#244982=CARTESIAN_POINT('Ctrl Pts',(-189.065744311566,-1.84428646499388,
135.363723566218));
#244983=CARTESIAN_POINT('Ctrl Pts',(-189.073495502806,-1.71729879792339,
135.415090750238));
#244984=CARTESIAN_POINT('Ctrl Pts',(-189.081246694046,-1.58806440155843,
135.461188686808));
#244985=CARTESIAN_POINT('Ctrl Pts',(-189.088997885286,-1.4570607255567,
135.501823454517));
#244986=CARTESIAN_POINT('Ctrl Pts',(-189.096745782063,-1.32611272961209,
135.542440951367));
#244987=CARTESIAN_POINT('Ctrl Pts',(-189.10449367884,-1.19339732231602,
135.57759978204));
#244988=CARTESIAN_POINT('Ctrl Pts',(-189.112241575618,-1.05940958549109,
135.607155053378));
#244989=CARTESIAN_POINT('Ctrl Pts',(-189.119987851702,-0.925449876012263,
135.636704142391));
#244990=CARTESIAN_POINT('Ctrl Pts',(-189.127734127786,-0.790218747924846,
135.660651919364));
#244991=CARTESIAN_POINT('Ctrl Pts',(-189.13548040387,-0.65422363177214,
135.678904134874));
#244992=CARTESIAN_POINT('Ctrl Pts',(-189.143226737135,-0.518227511734195,
135.697156485118));
#244993=CARTESIAN_POINT('Ctrl Pts',(-189.150973070401,-0.381467779868424,
135.709713137999));
#244994=CARTESIAN_POINT('Ctrl Pts',(-189.158719403666,-0.244458787537432,
135.716531518878));
#244995=CARTESIAN_POINT('Ctrl Pts',(-189.166467471669,-0.107419112992374,
135.723351426686));
#244996=CARTESIAN_POINT('Ctrl Pts',(-189.174215539672,0.0298695426863131,
135.72443048597));
#244997=CARTESIAN_POINT('Ctrl Pts',(-189.181963607675,0.166891415319874,
135.71977823136));
#244998=CARTESIAN_POINT('Ctrl Pts',(-189.189719910417,0.304058916429691,
135.715121032278));
#244999=CARTESIAN_POINT('Ctrl Pts',(-189.197476213158,0.440958676729197,
135.704720364546));
#245000=CARTESIAN_POINT('Ctrl Pts',(-189.2052325159,0.577078088149238,135.688637835607));
#245001=CARTESIAN_POINT('Ctrl Pts',(-189.212992958415,0.713270150598,135.672546722939));
#245002=CARTESIAN_POINT('Ctrl Pts',(-189.220753400929,0.848680648448811,
135.650767768445));
#245003=CARTESIAN_POINT('Ctrl Pts',(-189.228513843443,0.982806764623835,
135.623413836395));
#245004=CARTESIAN_POINT('Ctrl Pts',(-189.236286743708,1.1171481919477,135.596015993386));
#245005=CARTESIAN_POINT('Ctrl Pts',(-189.244059643974,1.25020073776289,
135.563025383117));
#245006=CARTESIAN_POINT('Ctrl Pts',(-189.251832544239,1.38147548620193,
135.524605160333));
#245007=CARTESIAN_POINT('Ctrl Pts',(-189.259322880001,1.50797806687371,
135.487581609423));
#245008=CARTESIAN_POINT('Ctrl Pts',(-189.266813215763,1.63282956904491,
135.445516450911));
#245009=CARTESIAN_POINT('Ctrl Pts',(-189.274303551525,1.75561151980122,
135.398597360926));
#245010=CARTESIAN_POINT('Ctrl Pts',(-189.282077885644,1.88304878554009,
135.349899319384));
#245011=CARTESIAN_POINT('Ctrl Pts',(-189.289852219764,2.0086601508045,135.295817746099));
#245012=CARTESIAN_POINT('Ctrl Pts',(-189.297626553883,2.1319572564113,135.23650922962));
#245013=CARTESIAN_POINT('Ctrl Pts',(-189.30539130683,2.25510240935448,135.177273805588));
#245014=CARTESIAN_POINT('Ctrl Pts',(-189.313156059777,2.37593862856379,
135.112824423354));
#245015=CARTESIAN_POINT('Ctrl Pts',(-189.320920812724,2.49399493257179,
135.043366673094));
#245016=CARTESIAN_POINT('Ctrl Pts',(-189.328677853609,2.61193398139434,
134.973977909251));
#245017=CARTESIAN_POINT('Ctrl Pts',(-189.336434894494,2.72709827484188,
134.899590873599));
#245018=CARTESIAN_POINT('Ctrl Pts',(-189.344191935379,2.8390392930429,134.820458095847));
#245019=CARTESIAN_POINT('Ctrl Pts',(-189.351943126619,2.95089589565147,
134.741384992739));
#245020=CARTESIAN_POINT('Ctrl Pts',(-189.359694317859,3.0595337432095,134.657573495689));
#245021=CARTESIAN_POINT('Ctrl Pts',(-189.3674455091,3.16453161094203,134.569320477358));
#245022=CARTESIAN_POINT('Ctrl Pts',(-189.375193405877,3.26948485177972,
134.481104968915));
#245023=CARTESIAN_POINT('Ctrl Pts',(-189.382941302654,3.37080089117263,
134.388451944842));
#245024=CARTESIAN_POINT('Ctrl Pts',(-189.390689199431,3.46809022258434,
134.291699613207));
#245025=CARTESIAN_POINT('Ctrl Pts',(-189.398435475515,3.5653592031655,134.194967520073));
#245026=CARTESIAN_POINT('Ctrl Pts',(-189.406181751599,3.65860287410479,
134.094138100479));
#245027=CARTESIAN_POINT('Ctrl Pts',(-189.413928027683,3.74746766208944,
133.989587325996));
#245028=CARTESIAN_POINT('Ctrl Pts',(-189.421674360949,3.83633310605366,
133.885035779743));
#245029=CARTESIAN_POINT('Ctrl Pts',(-189.429420694214,3.92081934936079,
133.776763121682));
#245030=CARTESIAN_POINT('Ctrl Pts',(-189.437167027479,4.00061255328625,
133.665179077551));
#245031=CARTESIAN_POINT('Ctrl Pts',(-189.444915095482,4.08042362634638,
133.553570044946));
#245032=CARTESIAN_POINT('Ctrl Pts',(-189.452663163485,4.15553934133821,
133.438648468607));
#245033=CARTESIAN_POINT('Ctrl Pts',(-189.460411231488,4.22568893687965,
133.320853429245));
#245034=CARTESIAN_POINT('Ctrl Pts',(-189.46816753423,4.29591308824612,133.202933195913));
#245035=CARTESIAN_POINT('Ctrl Pts',(-189.475923836972,4.36116037632517,
133.08213373541));
#245036=CARTESIAN_POINT('Ctrl Pts',(-189.483680139714,4.42120555602244,
132.958919619751));
#245037=CARTESIAN_POINT('Ctrl Pts',(-189.491440582228,4.4812827836402,132.835639741008));
#245038=CARTESIAN_POINT('Ctrl Pts',(-189.499201024743,4.53615221408563,
132.709942997256));
#245039=CARTESIAN_POINT('Ctrl Pts',(-189.506961467257,4.58563701835403,
132.582313428639));
#245040=CARTESIAN_POINT('Ctrl Pts',(-189.514734367522,4.63520126002316,
132.454478977708));
#245041=CARTESIAN_POINT('Ctrl Pts',(-189.522507267788,4.67936347626291,
132.324705871978));
#245042=CARTESIAN_POINT('Ctrl Pts',(-189.530280168053,4.7179966628129,132.193493639341));
#245043=CARTESIAN_POINT('Ctrl Pts',(-189.537770503815,4.7552254357191,132.06705130187));
#245044=CARTESIAN_POINT('Ctrl Pts',(-189.545260839577,4.78732011310547,
131.939272951445));
#245045=CARTESIAN_POINT('Ctrl Pts',(-189.552751175338,4.81421239738261,
131.810612104714));
#245046=CARTESIAN_POINT('Ctrl Pts',(-189.560525509457,4.84212431079291,
131.677073042868));
#245047=CARTESIAN_POINT('Ctrl Pts',(-189.568299843577,4.86451996267185,
131.542160232397));
#245048=CARTESIAN_POINT('Ctrl Pts',(-189.576074177696,4.88126712533379,
131.406369183648));
#245049=CARTESIAN_POINT('Ctrl Pts',(-189.583838930643,4.89799364861444,
131.27074548523));
#245050=CARTESIAN_POINT('Ctrl Pts',(-189.59160368359,4.90908548611105,131.134246086389));
#245051=CARTESIAN_POINT('Ctrl Pts',(-189.599368436537,4.91446102967388,
130.997378363685));
#245052=CARTESIAN_POINT('Ctrl Pts',(-189.607125477422,4.91983123417105,
130.860646579932));
#245053=CARTESIAN_POINT('Ctrl Pts',(-189.614882518307,4.91949642797885,
130.723547588459));
#245054=CARTESIAN_POINT('Ctrl Pts',(-189.622639559192,4.91342663554939,
130.586595240213));
#245055=CARTESIAN_POINT('Ctrl Pts',(-189.630390750432,4.90736142039758,
130.449746168797));
#245056=CARTESIAN_POINT('Ctrl Pts',(-189.638141941672,4.8955698444968,130.313043909499));
#245057=CARTESIAN_POINT('Ctrl Pts',(-189.645893132912,4.87807399294504,
130.177003317574));
#245058=CARTESIAN_POINT('Ctrl Pts',(-189.653641029689,4.86058557759692,
130.04102054653));
#245059=CARTESIAN_POINT('Ctrl Pts',(-189.661388926466,4.83739775844842,
129.905699270483));
#245060=CARTESIAN_POINT('Ctrl Pts',(-189.669136823243,4.80858454172782,
129.771550002034));
#245061=CARTESIAN_POINT('Ctrl Pts',(-189.676883099327,4.77977735211094,
129.637428794719));
#245062=CARTESIAN_POINT('Ctrl Pts',(-189.684629375411,4.74534718751536,
129.504479489374));
#245063=CARTESIAN_POINT('Ctrl Pts',(-189.692375651495,4.70541924846024,
129.373202779059));
#245064=CARTESIAN_POINT('Ctrl Pts',(-189.700121984761,4.66549101466631,
129.241925099689));
#245065=CARTESIAN_POINT('Ctrl Pts',(-189.707868318026,4.62006503919849,
129.112320414033));
#245066=CARTESIAN_POINT('Ctrl Pts',(-189.715614651291,4.56931639842622,
128.984874230265));
#245067=CARTESIAN_POINT('Ctrl Pts',(-189.723362719294,4.51855639284751,
128.857399505808));
#245068=CARTESIAN_POINT('Ctrl Pts',(-189.731110787297,4.46247149468235,
128.732084608271));
#245069=CARTESIAN_POINT('Ctrl Pts',(-189.7388588553,4.40128476182806,128.609394670723));
#245070=CARTESIAN_POINT('Ctrl Pts',(-189.746615158042,4.34003299898604,
128.48657433685));
#245071=CARTESIAN_POINT('Ctrl Pts',(-189.754371460784,4.2736687446074,128.366384886397));
#245072=CARTESIAN_POINT('Ctrl Pts',(-189.762127763526,4.20246110581043,
128.249266936964));
#245073=CARTESIAN_POINT('Ctrl Pts',(-189.76988820604,4.13121546135242,128.132086478155));
#245074=CARTESIAN_POINT('Ctrl Pts',(-189.777648648554,4.0551214983341,128.017981112027));
#245075=CARTESIAN_POINT('Ctrl Pts',(-189.785409091068,3.97449087304063,
127.907361245351));
#245076=CARTESIAN_POINT('Ctrl Pts',(-189.793181991334,3.89373081230961,
127.796563801844));
#245077=CARTESIAN_POINT('Ctrl Pts',(-189.800954891599,3.80841977969454,
127.689263345051));
#245078=CARTESIAN_POINT('Ctrl Pts',(-189.808727791865,3.71890939325291,
127.585836734281));
#245079=CARTESIAN_POINT('Ctrl Pts',(-189.816218127627,3.63265293481907,
127.486169941325));
#245080=CARTESIAN_POINT('Ctrl Pts',(-189.823708463389,3.54249734681371,
127.390100460701));
#245081=CARTESIAN_POINT('Ctrl Pts',(-189.831198799151,3.44878726912054,
127.29793088993));
#245082=CARTESIAN_POINT('Ctrl Pts',(-189.83897313327,3.3515241453514,127.20226668187));
#245083=CARTESIAN_POINT('Ctrl Pts',(-189.846747467389,3.25012357385693,
127.110500916178));
#245084=CARTESIAN_POINT('Ctrl Pts',(-189.854521801508,3.14493096923238,
127.023012675196));
#245085=CARTESIAN_POINT('Ctrl Pts',(-189.862286554456,3.03986800509226,
126.935632255653));
#245086=CARTESIAN_POINT('Ctrl Pts',(-189.870051307403,2.93102260408373,
126.852519119373));
#245087=CARTESIAN_POINT('Ctrl Pts',(-189.87781606035,2.81877752527758,126.774016175029));
#245088=CARTESIAN_POINT('Ctrl Pts',(-189.885573101235,2.70664392986547,
126.695591200915));
#245089=CARTESIAN_POINT('Ctrl Pts',(-189.89333014212,2.59111769456779,126.621767529126));
#245090=CARTESIAN_POINT('Ctrl Pts',(-189.901087183005,2.47261493422438,
126.552848127928));
#245091=CARTESIAN_POINT('Ctrl Pts',(-189.908838374245,2.35420153773453,
126.483980699386));
#245092=CARTESIAN_POINT('Ctrl Pts',(-189.916589565485,2.23281642057723,
126.420010375857));
#245093=CARTESIAN_POINT('Ctrl Pts',(-189.924340756725,2.10890468259733,
126.361196868364));
#245094=CARTESIAN_POINT('Ctrl Pts',(-189.932088653502,1.98504561041135,
126.302408358181));
#245095=CARTESIAN_POINT('Ctrl Pts',(-189.93983655028,1.8586624057305,126.248772472034));
#245096=CARTESIAN_POINT('Ctrl Pts',(-189.947584447057,1.73022457943941,
126.200502890919));
#245097=CARTESIAN_POINT('Ctrl Pts',(-189.955330723141,1.60181361957279,
126.15224340676));
#245098=CARTESIAN_POINT('Ctrl Pts',(-189.963076999225,1.47134925869841,
126.109348132341));
#245099=CARTESIAN_POINT('Ctrl Pts',(-189.970823275309,1.33932041800663,
126.071982369749));
#245100=CARTESIAN_POINT('Ctrl Pts',(-189.978569608574,1.20729060270813,
126.034616331331));
#245101=CARTESIAN_POINT('Ctrl Pts',(-189.98631594184,1.07369666073754,126.002779992655));
#245102=CARTESIAN_POINT('Ctrl Pts',(-189.994062275105,0.939041696927769,
125.976588486041));
#245103=CARTESIAN_POINT('Ctrl Pts',(-190.001810343108,0.804356578073038,
125.95039111402));
#245104=CARTESIAN_POINT('Ctrl Pts',(-190.009558411111,0.668610348265179,
125.929841164149));
#245105=CARTESIAN_POINT('Ctrl Pts',(-190.017306479114,0.532314905370259,
125.915002387285));
#245106=CARTESIAN_POINT('Ctrl Pts',(-190.025062781856,0.395874606056136,
125.900147839592));
#245107=CARTESIAN_POINT('Ctrl Pts',(-190.032819084598,0.258884316919199,
125.891016632574));
#245108=CARTESIAN_POINT('Ctrl Pts',(-190.040575387339,0.12186020099531,
125.887620523366));
#245109=CARTESIAN_POINT('Ctrl Pts',(-190.048335829854,-0.0152370488249634,
125.884222601552));
#245110=CARTESIAN_POINT('Ctrl Pts',(-190.056096272368,-0.152367770690179,
125.886565870162));
#245111=CARTESIAN_POINT('Ctrl Pts',(-190.063856714882,-0.28901821992613,
125.894609958821));
#245112=CARTESIAN_POINT('Ctrl Pts',(-190.071629615147,-0.42588803259445,
125.902666960564));
#245113=CARTESIAN_POINT('Ctrl Pts',(-190.079402515413,-0.562275642767436,
125.916443030582));
#245114=CARTESIAN_POINT('Ctrl Pts',(-190.087175415678,-0.697673929887046,
125.935846044305));
#245115=CARTESIAN_POINT('Ctrl Pts',(-190.09466575144,-0.82815014822142,
125.954543709606));
#245116=CARTESIAN_POINT('Ctrl Pts',(-190.102156087202,-0.957707420585213,
125.978466258228));
#245117=CARTESIAN_POINT('Ctrl Pts',(-190.109646422964,-1.0859048768382,
126.007487296229));
#245118=CARTESIAN_POINT('Ctrl Pts',(-190.117420757083,-1.21896297860964,
126.037608675706));
#245119=CARTESIAN_POINT('Ctrl Pts',(-190.125195091202,-1.35097760196638,
126.073318210457));
#245120=CARTESIAN_POINT('Ctrl Pts',(-190.132969425321,-1.48144310917082,
126.114530196667));
#245121=CARTESIAN_POINT('Ctrl Pts',(-190.140734178268,-1.61174782929803,
126.155691392787));
#245122=CARTESIAN_POINT('Ctrl Pts',(-190.148498931215,-1.74050686267825,
126.202341431007));
#245123=CARTESIAN_POINT('Ctrl Pts',(-190.156263684163,-1.86722481990743,
126.254343635793));
#245124=CARTESIAN_POINT('Ctrl Pts',(-190.164020725047,-1.9938169190744,
126.306294191256));
#245125=CARTESIAN_POINT('Ctrl Pts',(-190.171777765932,-2.11837161700793,
126.363586187039));
#245126=CARTESIAN_POINT('Ctrl Pts',(-190.179534806817,-2.24040909768993,
126.42603329569));
#245127=CARTESIAN_POINT('Ctrl Pts',(-190.187285998058,-2.36235454895925,
126.488433312491));
#245128=CARTESIAN_POINT('Ctrl Pts',(-190.195037189298,-2.48178621469771,
126.55598052693));
#245129=CARTESIAN_POINT('Ctrl Pts',(-190.202788380538,-2.59824500532673,
126.628440844056));
#245130=CARTESIAN_POINT('Ctrl Pts',(-190.210536277315,-2.71465429786326,
126.700870363613));
#245131=CARTESIAN_POINT('Ctrl Pts',(-190.218284174092,-2.82809289713704,
126.778208626477));
#245132=CARTESIAN_POINT('Ctrl Pts',(-190.226032070869,-2.93812724517321,
126.860176119641));
#245133=CARTESIAN_POINT('Ctrl Pts',(-190.233778346953,-3.04813857639583,
126.942126466972));
#245134=CARTESIAN_POINT('Ctrl Pts',(-190.241524623037,-3.15474675944337,
127.028703885119));
#245135=CARTESIAN_POINT('Ctrl Pts',(-190.249270899121,-3.25754844714305,
127.119586380653));
#245136=CARTESIAN_POINT('Ctrl Pts',(-190.257017232387,-3.36035089370159,
127.210469547061));
#245137=CARTESIAN_POINT('Ctrl Pts',(-190.264763565652,-3.45934649593055,
127.305657595318));
#245138=CARTESIAN_POINT('Ctrl Pts',(-190.272509898917,-3.55416644929697,
127.404789480909));
#245139=CARTESIAN_POINT('Ctrl Pts',(-190.28025796692,-3.64900763693438,
127.503943566399));
#245140=CARTESIAN_POINT('Ctrl Pts',(-190.288006034923,-3.73967104476384,
127.607042964203));
#245141=CARTESIAN_POINT('Ctrl Pts',(-190.295754102926,-3.82582634408186,
127.713691459046));
#245142=CARTESIAN_POINT('Ctrl Pts',(-190.303510405668,-3.91207321027691,
127.820453301177));
#245143=CARTESIAN_POINT('Ctrl Pts',(-190.31126670841,-3.99380215080234,
127.930771470759));
#245144=CARTESIAN_POINT('Ctrl Pts',(-190.319023011152,-4.07072427531871,
128.044218060228));
#245145=CARTESIAN_POINT('Ctrl Pts',(-190.326783453666,-4.14768745548943,
128.157725199558));
#245146=CARTESIAN_POINT('Ctrl Pts',(-190.33454389618,-4.21983850201565,
128.274363753527));
#245147=CARTESIAN_POINT('Ctrl Pts',(-190.342304338694,-4.28693368809188,
128.393679673019));
#245148=CARTESIAN_POINT('Ctrl Pts',(-190.35007723896,-4.35413658131705,
128.513187129016));
#245149=CARTESIAN_POINT('Ctrl Pts',(-190.357850139225,-4.41626721820383,
128.635380190496));
#245150=CARTESIAN_POINT('Ctrl Pts',(-190.36562303949,-4.47312899471228,
128.759782406989));
#245151=CARTESIAN_POINT('Ctrl Pts',(-190.373113375253,-4.52792370242032,
128.879662289568));
#245152=CARTESIAN_POINT('Ctrl Pts',(-190.380603711015,-4.57782585506955,
129.001593213935));
#245153=CARTESIAN_POINT('Ctrl Pts',(-190.388094046777,-4.62270349038433,
129.125135944543));
#245154=CARTESIAN_POINT('Ctrl Pts',(-190.397182635961,-4.67715690927988,
129.275039655247));
#245155=CARTESIAN_POINT('Ctrl Pts',(-190.406271225145,-4.72435719403422,
129.427710815754));
#245156=CARTESIAN_POINT('Ctrl Pts',(-190.415359814329,-4.76405452823405,
129.582490119308));
#245157=CARTESIAN_POINT('',(-188.389859436034,-4.91824789781227,130.808907942626));
#245158=CARTESIAN_POINT('Ctrl Pts',(-188.389859436034,-4.91824789781227,
130.808907942627));
#245159=CARTESIAN_POINT('Ctrl Pts',(-188.399867117337,-4.9180844751749,
130.985660875825));
#245160=CARTESIAN_POINT('Ctrl Pts',(-188.409874798639,-4.90838934841572,
131.161987856138));
#245161=CARTESIAN_POINT('Ctrl Pts',(-188.419882479942,-4.88932061848566,
131.33702087716));
#245162=CARTESIAN_POINT('Ctrl Pts',(-188.430125673914,-4.86980314050388,
131.516172983589));
#245163=CARTESIAN_POINT('Ctrl Pts',(-188.440368867886,-4.84046566695456,
131.693969810191));
#245164=CARTESIAN_POINT('Ctrl Pts',(-188.450612061858,-4.80152560262522,
131.86950612398));
#245165=CARTESIAN_POINT('Ctrl Pts',(-188.453257933321,-4.79146717697613,
131.914848087107));
#245166=CARTESIAN_POINT('Ctrl Pts',(-188.455903804784,-4.78076829602226,
131.960039341272));
#245167=CARTESIAN_POINT('Ctrl Pts',(-188.458549676247,-4.76943321745608,
132.005064513923));
#245168=CARTESIAN_POINT('Ctrl Pts',(-188.466324010366,-4.73612748463049,
132.137361468194));
#245169=CARTESIAN_POINT('Ctrl Pts',(-188.474098344485,-4.69726024638632,
132.268481144229));
#245170=CARTESIAN_POINT('Ctrl Pts',(-188.481872678604,-4.65292931576995,
132.397920106556));
#245171=CARTESIAN_POINT('Ctrl Pts',(-188.489637431551,-4.60865301906372,
132.527199546929));
#245172=CARTESIAN_POINT('Ctrl Pts',(-188.497402184498,-4.55892655312866,
132.654802028599));
#245173=CARTESIAN_POINT('Ctrl Pts',(-188.505166937445,-4.503898442119,132.780235584657));
#245174=CARTESIAN_POINT('Ctrl Pts',(-188.51292397833,-4.44892498580481,
132.90554455834));
#245175=CARTESIAN_POINT('Ctrl Pts',(-188.520681019215,-4.38866051938554,
133.028688537671));
#245176=CARTESIAN_POINT('Ctrl Pts',(-188.5284380601,-4.32330283091627,133.149192316152));
#245177=CARTESIAN_POINT('Ctrl Pts',(-188.53618925134,-4.25799442918837,
133.269605221796));
#245178=CARTESIAN_POINT('Ctrl Pts',(-188.54394044258,-4.18760063600923,
133.387381547266));
#245179=CARTESIAN_POINT('Ctrl Pts',(-188.551691633821,-4.11236649580212,
133.502067952824));
#245180=CARTESIAN_POINT('Ctrl Pts',(-188.559439530598,-4.03716433211143,
133.6167056136));
#245181=CARTESIAN_POINT('Ctrl Pts',(-188.567187427375,-3.95712612715828,
133.728255640296));
#245182=CARTESIAN_POINT('Ctrl Pts',(-188.574935324152,-3.87254171765271,
133.836291307331));
#245183=CARTESIAN_POINT('Ctrl Pts',(-188.582681600236,-3.78797500138217,
133.944304375634));
#245184=CARTESIAN_POINT('Ctrl Pts',(-188.59042787632,-3.69886421295048,
134.048804238843));
#245185=CARTESIAN_POINT('Ctrl Pts',(-188.598174152404,-3.60554093228053,
134.149395392893));
#245186=CARTESIAN_POINT('Ctrl Pts',(-188.605920485669,-3.51221696271946,
134.249987289485));
#245187=CARTESIAN_POINT('Ctrl Pts',(-188.613666818935,-3.41468070477701,
134.34667013273));
#245188=CARTESIAN_POINT('Ctrl Pts',(-188.6214131522,-3.31330194928639,134.439083888374));
#245189=CARTESIAN_POINT('Ctrl Pts',(-188.629161220203,-3.21190049072653,
134.531518339438));
#245190=CARTESIAN_POINT('Ctrl Pts',(-188.636909288206,-3.10665511120062,
134.619681537175));
#245191=CARTESIAN_POINT('Ctrl Pts',(-188.644657356209,-2.99796983886249,
134.703252756081));
#245192=CARTESIAN_POINT('Ctrl Pts',(-188.652413658951,-2.88916905452341,
134.786912795473));
#245193=CARTESIAN_POINT('Ctrl Pts',(-188.660169961693,-2.77692138462799,
134.865970868193));
#245194=CARTESIAN_POINT('Ctrl Pts',(-188.667926264434,-2.661661546083,134.940148435697));
#245195=CARTESIAN_POINT('Ctrl Pts',(-188.675686706949,-2.54634018989178,
135.014365594003));
#245196=CARTESIAN_POINT('Ctrl Pts',(-188.683447149463,-2.4280037987698,
135.083696859122));
#245197=CARTESIAN_POINT('Ctrl Pts',(-188.691207591977,-2.30711213985166,
135.147909470365));
#245198=CARTESIAN_POINT('Ctrl Pts',(-188.698980492242,-2.18602641491037,
135.212225161391));
#245199=CARTESIAN_POINT('Ctrl Pts',(-188.706753392507,-2.06237757804144,
135.271405609637));
#245200=CARTESIAN_POINT('Ctrl Pts',(-188.714526292773,-1.93664666046133,
135.325265701177));
#245201=CARTESIAN_POINT('Ctrl Pts',(-188.722016628535,-1.81548637842552,
135.377167842728));
#245202=CARTESIAN_POINT('Ctrl Pts',(-188.729506964298,-1.69239305308073,
135.424129618806));
#245203=CARTESIAN_POINT('Ctrl Pts',(-188.73699730006,-1.56780896021745,
135.466029645582));
#245204=CARTESIAN_POINT('Ctrl Pts',(-188.744771634179,-1.43850122361313,
135.509518324605));
#245205=CARTESIAN_POINT('Ctrl Pts',(-188.752545968298,-1.30717783500581,
135.547691603967));
#245206=CARTESIAN_POINT('Ctrl Pts',(-188.760320302418,-1.17431521925618,
135.580359657382));
#245207=CARTESIAN_POINT('Ctrl Pts',(-188.768085055365,-1.04161634480655,
135.612987450341));
#245208=CARTESIAN_POINT('Ctrl Pts',(-188.775849808312,-0.907382393612003,
135.64012342443));
#245209=CARTESIAN_POINT('Ctrl Pts',(-188.783614561259,-0.772107552298939,
135.661626617095));
#245210=CARTESIAN_POINT('Ctrl Pts',(-188.791371602144,-0.636967067865308,
135.683108452486));
#245211=CARTESIAN_POINT('Ctrl Pts',(-188.799128643029,-0.500788134293892,
135.698968578897));
#245212=CARTESIAN_POINT('Ctrl Pts',(-188.806885683914,-0.36407746554492,
135.709116540299));
#245213=CARTESIAN_POINT('Ctrl Pts',(-188.814636875154,-0.227469891374892,
135.719256849044));
#245214=CARTESIAN_POINT('Ctrl Pts',(-188.822388066394,-0.0903317684798211,
135.72369353795));
#245215=CARTESIAN_POINT('Ctrl Pts',(-188.830139257634,0.0468230430825336,
135.722387728628));
#245216=CARTESIAN_POINT('Ctrl Pts',(-188.837887154411,0.183919560191437,
135.721082474309));
#245217=CARTESIAN_POINT('Ctrl Pts',(-188.845635051188,0.321032361730929,
135.714039579871));
#245218=CARTESIAN_POINT('Ctrl Pts',(-188.853382947965,0.457645767564134,
135.70127223755));
#245219=CARTESIAN_POINT('Ctrl Pts',(-188.861129224049,0.594230596817883,
135.688507565881));
#245220=CARTESIAN_POINT('Ctrl Pts',(-188.868875500133,0.730315849125278,
135.670020864439));
#245221=CARTESIAN_POINT('Ctrl Pts',(-188.876621776217,0.865389548668166,
135.645877321199));
#245222=CARTESIAN_POINT('Ctrl Pts',(-188.884368109483,1.0004642452946,135.621733599736));
#245223=CARTESIAN_POINT('Ctrl Pts',(-188.892114442748,1.1345269893911,135.591933021942));
#245224=CARTESIAN_POINT('Ctrl Pts',(-188.899860776013,1.26707499296545,
135.556592096009));
#245225=CARTESIAN_POINT('Ctrl Pts',(-188.907608844016,1.39965267974599,
135.52124325572));
#245226=CARTESIAN_POINT('Ctrl Pts',(-188.915356912019,1.53071457330889,
135.480351699103));
#245227=CARTESIAN_POINT('Ctrl Pts',(-188.923104980022,1.65977245111908,
135.434083986516));
#245228=CARTESIAN_POINT('Ctrl Pts',(-188.930861282764,1.7889674931778,135.387767100054));
#245229=CARTESIAN_POINT('Ctrl Pts',(-188.938617585506,1.91615389617927,
135.336062775758));
#245230=CARTESIAN_POINT('Ctrl Pts',(-188.946373888248,2.04086234265069,
135.279186196385));
#245231=CARTESIAN_POINT('Ctrl Pts',(-188.954134330762,2.16563734977488,
135.222279260269));
#245232=CARTESIAN_POINT('Ctrl Pts',(-188.961894773276,2.2879314166124,135.160194745264));
#245233=CARTESIAN_POINT('Ctrl Pts',(-188.96965521579,2.40730019963481,135.093193653642));
#245234=CARTESIAN_POINT('Ctrl Pts',(-188.977428116055,2.5268606040248,135.02608500592));
#245235=CARTESIAN_POINT('Ctrl Pts',(-188.985201016321,2.64348600783031,
134.954044215384));
#245236=CARTESIAN_POINT('Ctrl Pts',(-188.992973916586,2.75676066034094,
134.877375928622));
#245237=CARTESIAN_POINT('Ctrl Pts',(-189.000464252348,2.86591749391118,
134.803494727199));
#245238=CARTESIAN_POINT('Ctrl Pts',(-189.00795458811,2.97196271521771,134.725316813482));
#245239=CARTESIAN_POINT('Ctrl Pts',(-189.015444923872,3.07455513973725,
134.643148675693));
#245240=CARTESIAN_POINT('Ctrl Pts',(-189.023219257991,3.18103738721459,
134.557865107985));
#245241=CARTESIAN_POINT('Ctrl Pts',(-189.03099359211,3.2841371475586,134.468012611807));
#245242=CARTESIAN_POINT('Ctrl Pts',(-189.038767926229,3.38343719526661,
134.373889411145));
#245243=CARTESIAN_POINT('Ctrl Pts',(-189.046532679176,3.48261486454052,
134.279882208915));
#245244=CARTESIAN_POINT('Ctrl Pts',(-189.054297432124,3.57800185753944,
134.1816150409));
#245245=CARTESIAN_POINT('Ctrl Pts',(-189.062062185071,3.66921245853213,
134.079427486601));
#245246=CARTESIAN_POINT('Ctrl Pts',(-189.069819225956,3.76033246787007,
133.977341426422));
#245247=CARTESIAN_POINT('Ctrl Pts',(-189.077576266841,3.84728408135189,
133.87134301855));
#245248=CARTESIAN_POINT('Ctrl Pts',(-189.085333307726,3.92971730448732,
133.7618096821));
#245249=CARTESIAN_POINT('Ctrl Pts',(-189.093084498966,4.01208836408783,
133.652358945591));
#245250=CARTESIAN_POINT('Ctrl Pts',(-189.100835690206,4.0899475813276,133.539378897572));
#245251=CARTESIAN_POINT('Ctrl Pts',(-189.108586881446,4.16298449280398,
133.423280848343));
#245252=CARTESIAN_POINT('Ctrl Pts',(-189.116334778223,4.23599036164477,
133.307232143882));
#245253=CARTESIAN_POINT('Ctrl Pts',(-189.124082675,4.30417779348807,133.188068404235));
#245254=CARTESIAN_POINT('Ctrl Pts',(-189.131830571777,4.36727914962361,
133.06623061643));
#245255=CARTESIAN_POINT('Ctrl Pts',(-189.139576847861,4.43036730631575,
132.944418314464));
#245256=CARTESIAN_POINT('Ctrl Pts',(-189.147323123945,4.48837132376201,
132.819933423872));
#245257=CARTESIAN_POINT('Ctrl Pts',(-189.15506940003,4.54106931101448,132.6932419201));
#245258=CARTESIAN_POINT('Ctrl Pts',(-189.162815733295,4.59376768727144,
132.56654948112));
#245259=CARTESIAN_POINT('Ctrl Pts',(-189.17056206656,4.64115980502555,132.437650757441));
#245260=CARTESIAN_POINT('Ctrl Pts',(-189.178308399826,4.68307191672785,
132.307031734363));
#245261=CARTESIAN_POINT('Ctrl Pts',(-189.186056467829,4.72499341435691,
132.17638346006));
#245262=CARTESIAN_POINT('Ctrl Pts',(-189.193804535832,4.76143234450105,
132.044014491957));
#245263=CARTESIAN_POINT('Ctrl Pts',(-189.201552603835,4.7922649429027,131.910425615442));
#245264=CARTESIAN_POINT('Ctrl Pts',(-189.209308906576,4.82313031055689,
131.776694759079));
#245265=CARTESIAN_POINT('Ctrl Pts',(-189.217065209318,4.84837735570641,
131.641741785897));
#245266=CARTESIAN_POINT('Ctrl Pts',(-189.22482151206,4.86793344014249,131.506077857516));
#245267=CARTESIAN_POINT('Ctrl Pts',(-189.232581954574,4.8874999622497,131.37034152121));
#245268=CARTESIAN_POINT('Ctrl Pts',(-189.240342397089,4.90136943177558,
131.233893862373));
#245269=CARTESIAN_POINT('Ctrl Pts',(-189.248102839603,4.90952125879313,
131.097249797903));
#245270=CARTESIAN_POINT('Ctrl Pts',(-189.255875739868,4.91768617184709,
130.960386380249));
#245271=CARTESIAN_POINT('Ctrl Pts',(-189.263648640134,4.92011509395886,
130.823326318046));
#245272=CARTESIAN_POINT('Ctrl Pts',(-189.271421540399,4.91683960951637,
130.686584063062));
#245273=CARTESIAN_POINT('Ctrl Pts',(-189.278911876161,4.91368319718378,
130.554812733478));
#245274=CARTESIAN_POINT('Ctrl Pts',(-189.286402211923,4.90522993667453,
130.423336813468));
#245275=CARTESIAN_POINT('Ctrl Pts',(-189.293892547685,4.8915532666416,130.292609015607));
#245276=CARTESIAN_POINT('Ctrl Pts',(-189.301666881805,4.87735804150758,
130.156924633557));
#245277=CARTESIAN_POINT('Ctrl Pts',(-189.309441215924,4.85749053053571,
130.021616416288));
#245278=CARTESIAN_POINT('Ctrl Pts',(-189.317215550043,4.83197611743572,
129.887196584783));
#245279=CARTESIAN_POINT('Ctrl Pts',(-189.32498030299,4.80649314856966,129.752942413707));
#245280=CARTESIAN_POINT('Ctrl Pts',(-189.332745055937,4.77537719672058,
129.619574830376));
#245281=CARTESIAN_POINT('Ctrl Pts',(-189.340509808884,4.73870547096616,
129.487601899374));
#245282=CARTESIAN_POINT('Ctrl Pts',(-189.348266849769,4.70207016808673,
129.355760045747));
#245283=CARTESIAN_POINT('Ctrl Pts',(-189.356023890654,4.6598901765116,129.225310462118));
#245284=CARTESIAN_POINT('Ctrl Pts',(-189.363780931539,4.61229384905882,
129.096751613012));
#245285=CARTESIAN_POINT('Ctrl Pts',(-189.371532122779,4.56473341436676,
128.968289711134));
#245286=CARTESIAN_POINT('Ctrl Pts',(-189.379283314019,4.5117649089419,128.841716070937));
#245287=CARTESIAN_POINT('Ctrl Pts',(-189.387034505259,4.45356656673678,
128.717514217338));
#245288=CARTESIAN_POINT('Ctrl Pts',(-189.394782402037,4.39539296037968,
128.59336515284));
#245289=CARTESIAN_POINT('Ctrl Pts',(-189.402530298814,4.33199410380397,
128.471586223247));
#245290=CARTESIAN_POINT('Ctrl Pts',(-189.410278195591,4.26359634662585,
128.352640964845));
#245291=CARTESIAN_POINT('Ctrl Pts',(-189.418024471675,4.19521289678404,
128.233720587227));
#245292=CARTESIAN_POINT('Ctrl Pts',(-189.425770747759,4.12183282098978,
128.117633040512));
#245293=CARTESIAN_POINT('Ctrl Pts',(-189.433517023843,4.04372822010655,
128.004816878952));
#245294=CARTESIAN_POINT('Ctrl Pts',(-189.441263357108,3.9656230426728,127.891999884608));
#245295=CARTESIAN_POINT('Ctrl Pts',(-189.449009690374,3.88279349310222,
127.782454645051));
#245296=CARTESIAN_POINT('Ctrl Pts',(-189.456756023639,3.7955545297986,127.676590025942));
#245297=CARTESIAN_POINT('Ctrl Pts',(-189.464504091642,3.70829602993413,
127.570701699186));
#245298=CARTESIAN_POINT('Ctrl Pts',(-189.472252159645,3.61662639999776,
127.4684959347));
#245299=CARTESIAN_POINT('Ctrl Pts',(-189.480000227648,3.5209000673159,127.370347545594));
#245300=CARTESIAN_POINT('Ctrl Pts',(-189.48775653039,3.42507199554838,127.272094843212));
#245301=CARTESIAN_POINT('Ctrl Pts',(-189.495512833132,3.32517888174022,
127.17790841068));
#245302=CARTESIAN_POINT('Ctrl Pts',(-189.503269135873,3.22161151791196,
127.08812565592));
#245303=CARTESIAN_POINT('Ctrl Pts',(-189.511029578388,3.11798887706327,
126.998294981402));
#245304=CARTESIAN_POINT('Ctrl Pts',(-189.518790020902,3.01068838434436,
126.912872911365));
#245305=CARTESIAN_POINT('Ctrl Pts',(-189.526550463416,2.90013212456667,
126.832155093861));
#245306=CARTESIAN_POINT('Ctrl Pts',(-189.534323363681,2.78939839006606,
126.751307700949));
#245307=CARTESIAN_POINT('Ctrl Pts',(-189.542096263947,2.67539876972268,
126.675179868487));
#245308=CARTESIAN_POINT('Ctrl Pts',(-189.549869164212,2.55858315851329,
126.604023097381));
#245309=CARTESIAN_POINT('Ctrl Pts',(-189.557359499974,2.44601408901245,
126.535453054138));
#245310=CARTESIAN_POINT('Ctrl Pts',(-189.564849835736,2.33083048013107,
126.471499075371));
#245311=CARTESIAN_POINT('Ctrl Pts',(-189.572340171498,2.21345290716398,
126.412344077266));
#245312=CARTESIAN_POINT('Ctrl Pts',(-189.580114505617,2.0916249278412,126.350946199428));
#245313=CARTESIAN_POINT('Ctrl Pts',(-189.587888839736,1.96704741755451,
126.294523902565));
#245314=CARTESIAN_POINT('Ctrl Pts',(-189.595663173855,1.84016504283681,
126.243332698596));
#245315=CARTESIAN_POINT('Ctrl Pts',(-189.603427926802,1.7134390393065,126.192204583211));
#245316=CARTESIAN_POINT('Ctrl Pts',(-189.61119267975,1.58441418226004,126.146294878277));
#245317=CARTESIAN_POINT('Ctrl Pts',(-189.618957432697,1.45355965421348,
126.105813246927));
#245318=CARTESIAN_POINT('Ctrl Pts',(-189.626714473582,1.3228350927289,126.065371822503));
#245319=CARTESIAN_POINT('Ctrl Pts',(-189.634471514467,1.19028484774728,
126.030347857655));
#245320=CARTESIAN_POINT('Ctrl Pts',(-189.642228555352,1.0563976694256,126.000902797773));
#245321=CARTESIAN_POINT('Ctrl Pts',(-189.649979746592,0.922611456466401,
125.971479942639));
#245322=CARTESIAN_POINT('Ctrl Pts',(-189.657730937832,0.787490697206884,
125.94762770214));
#245323=CARTESIAN_POINT('Ctrl Pts',(-189.665482129072,0.651538534659585,
125.92945748003));
#245324=CARTESIAN_POINT('Ctrl Pts',(-189.673230025849,0.515644155408197,
125.91129498075));
#245325=CARTESIAN_POINT('Ctrl Pts',(-189.680977922626,0.378919462400322,
125.898809748275));
#245326=CARTESIAN_POINT('Ctrl Pts',(-189.688725819403,0.241876789339127,
125.892061900949));
#245327=CARTESIAN_POINT('Ctrl Pts',(-189.696472095488,0.104862782650838,
125.885315465126));
#245328=CARTESIAN_POINT('Ctrl Pts',(-189.704218371572,-0.0324686815449168,
125.884304046529));
#245329=CARTESIAN_POINT('Ctrl Pts',(-189.711964647656,-0.169601557973934,
125.889035768278));
#245330=CARTESIAN_POINT('Ctrl Pts',(-189.719710980921,-0.30673544668688,
125.893767524955));
#245331=CARTESIAN_POINT('Ctrl Pts',(-189.727457314187,-0.443670353975256,
125.904242493092));
#245332=CARTESIAN_POINT('Ctrl Pts',(-189.735203647452,-0.57989204686906,
125.92041669114));
#245333=CARTESIAN_POINT('Ctrl Pts',(-189.742951715455,-0.716144245666308,
125.936594511287));
#245334=CARTESIAN_POINT('Ctrl Pts',(-189.750699783458,-0.851682524082018,
125.958474054952));
#245335=CARTESIAN_POINT('Ctrl Pts',(-189.758447851461,-0.985999964604032,
125.985959728028));
#245336=CARTESIAN_POINT('Ctrl Pts',(-189.766204154203,-1.12046015930041,
126.013474613205));
#245337=CARTESIAN_POINT('Ctrl Pts',(-189.773960456944,-1.25369654052637,
126.046607451556));
#245338=CARTESIAN_POINT('Ctrl Pts',(-189.781716759686,-1.38521400480768,
126.085211835912));
#245339=CARTESIAN_POINT('Ctrl Pts',(-189.7894772022,-1.51680166391959,126.12383682459));
#245340=CARTESIAN_POINT('Ctrl Pts',(-189.797237644715,-1.64666820799493,
126.167939052618));
#245341=CARTESIAN_POINT('Ctrl Pts',(-189.804998087229,-1.77433675280554,
126.217323213081));
#245342=CARTESIAN_POINT('Ctrl Pts',(-189.812770987494,-1.90221024249816,
126.266786649383));
#245343=CARTESIAN_POINT('Ctrl Pts',(-189.82054388776,-2.02787832339203,
126.321548805643));
#245344=CARTESIAN_POINT('Ctrl Pts',(-189.828316788025,-2.1508862214266,
126.38136711486));
#245345=CARTESIAN_POINT('Ctrl Pts',(-189.835807123787,-2.26942247252908,
126.439010877864));
#245346=CARTESIAN_POINT('Ctrl Pts',(-189.843297459549,-2.38548832025277,
126.501349422499));
#245347=CARTESIAN_POINT('Ctrl Pts',(-189.850787795311,-2.49870254081068,
126.568127777524));
#245348=CARTESIAN_POINT('Ctrl Pts',(-189.858563333984,-2.61622751943143,
126.637448793101));
#245349=CARTESIAN_POINT('Ctrl Pts',(-189.866338872658,-2.73105175223908,
126.711774041575));
#245350=CARTESIAN_POINT('Ctrl Pts',(-189.874114411331,-2.84271970669593,
126.790867409441));
#245351=CARTESIAN_POINT('Ctrl Pts',(-189.882266520974,-2.95979576362285,
126.873791285713));
#245352=CARTESIAN_POINT('Ctrl Pts',(-189.890418630616,-3.07340178179484,
126.961956537243));
#245353=CARTESIAN_POINT('Ctrl Pts',(-189.898570740259,-3.18304092391845,
127.055036206534));
#245354=CARTESIAN_POINT('Ctrl Pts',(-189.906326693971,-3.28735209593799,
127.14359262176));
#245355=CARTESIAN_POINT('Ctrl Pts',(-189.914082647682,-3.38807246231964,
127.236596825632));
#245356=CARTESIAN_POINT('Ctrl Pts',(-189.921838601394,-3.48480374559348,
127.333722935929));
#245357=CARTESIAN_POINT('Ctrl Pts',(-189.929589286311,-3.58146931712576,
127.43078306627));
#245358=CARTESIAN_POINT('Ctrl Pts',(-189.937339971229,-3.67415092233515,
127.531959256202));
#245359=CARTESIAN_POINT('Ctrl Pts',(-189.945090656146,-3.7624847314623,
127.636886591151));
#245360=CARTESIAN_POINT('Ctrl Pts',(-189.952837754435,-3.8507776641283,
127.741765370987));
#245361=CARTESIAN_POINT('Ctrl Pts',(-189.960584852723,-3.93472655359425,
127.850391542837));
#245362=CARTESIAN_POINT('Ctrl Pts',(-189.968331951012,-4.01400597908118,
127.962365004902));
#245363=CARTESIAN_POINT('Ctrl Pts',(-189.976077142051,-4.09326588685833,
128.07431090035));
#245364=CARTESIAN_POINT('Ctrl Pts',(-189.983822333091,-4.1678583942436,
128.189602126264));
#245365=CARTESIAN_POINT('Ctrl Pts',(-189.99156752413,-4.23750000942929,
128.307807647452));
#245366=CARTESIAN_POINT('Ctrl Pts',(-189.999314507378,-4.30715773942337,
128.426040520954));
#245367=CARTESIAN_POINT('Ctrl Pts',(-190.007061490626,-4.37186208637682,
128.54718870223));
#245368=CARTESIAN_POINT('Ctrl Pts',(-190.014808473873,-4.43137434301563,
128.67079447269));
#245369=CARTESIAN_POINT('Ctrl Pts',(-190.022556509817,-4.49089468645619,
128.794417039275));
#245370=CARTESIAN_POINT('Ctrl Pts',(-190.030304545761,-4.54522137225773,
128.920497504471));
#245371=CARTESIAN_POINT('Ctrl Pts',(-190.038052581704,-4.59416325289056,
129.04855679359));
#245372=CARTESIAN_POINT('Ctrl Pts',(-190.045805933935,-4.64313871481742,
129.176703950126));
#245373=CARTESIAN_POINT('Ctrl Pts',(-190.053559286166,-4.68672186348919,
129.30683227332));
#245374=CARTESIAN_POINT('Ctrl Pts',(-190.061312638396,-4.72477092847605,
129.438446002399));
#245375=CARTESIAN_POINT('Ctrl Pts',(-190.064130106518,-4.73859746756062,
129.486272732696));
#245376=CARTESIAN_POINT('Ctrl Pts',(-190.066947574639,-4.75169371319282,
129.534295489064));
#245377=CARTESIAN_POINT('Ctrl Pts',(-190.06976504276,-4.76405452823418,
129.582490119309));
#245378=CARTESIAN_POINT('Ctrl Pts',(-188.319844903182,-4.76405452823404,
129.582490119308));
#245379=CARTESIAN_POINT('Ctrl Pts',(-188.327501512409,-4.79776899317125,
129.71394230641));
#245380=CARTESIAN_POINT('Ctrl Pts',(-188.335158121637,-4.82603476089132,
129.846775959306));
#245381=CARTESIAN_POINT('Ctrl Pts',(-188.342814730864,-4.84875524607537,
129.980494350411));
#245382=CARTESIAN_POINT('Ctrl Pts',(-188.350655515053,-4.87202225836387,
130.117429254037));
#245383=CARTESIAN_POINT('Ctrl Pts',(-188.358496299241,-4.88947373540814,
130.255291565461));
#245384=CARTESIAN_POINT('Ctrl Pts',(-188.36633708343,-4.90106215269356,
130.393540902929));
#245385=CARTESIAN_POINT('Ctrl Pts',(-188.374177867618,-4.91265056997894,
130.531790240396));
#245386=CARTESIAN_POINT('Ctrl Pts',(-188.382018651807,-4.91837593560674,
130.670426153596));
#245387=CARTESIAN_POINT('Ctrl Pts',(-188.389859435995,-4.91824789781291,
130.808907941932));
#245388=CARTESIAN_POINT('Origin',(213.235140564004,0.,130.804360617566));
#245389=CARTESIAN_POINT('',(-186.570144995258,-4.76405452823391,129.582490119308));
#245390=CARTESIAN_POINT('',(-186.915092859931,-4.76405452823404,129.582490119308));
#245391=CARTESIAN_POINT('',(213.235140564004,-4.76405452823405,129.582490119308));
#245392=CARTESIAN_POINT('',(-186.985140563973,-4.91824792938353,130.808873666935));
#245393=CARTESIAN_POINT('Ctrl Pts',(-186.915092859931,-4.76405452823404,
129.582490119308));
#245394=CARTESIAN_POINT('Ctrl Pts',(-186.922737472684,-4.79771251131355,
129.713722084504));
#245395=CARTESIAN_POINT('Ctrl Pts',(-186.930382085436,-4.82593597496495,
129.846315094707));
#245396=CARTESIAN_POINT('Ctrl Pts',(-186.938026698189,-4.84863265225042,
129.979773165545));
#245397=CARTESIAN_POINT('Ctrl Pts',(-186.945879009153,-4.87194598068921,
130.116857188863));
#245398=CARTESIAN_POINT('Ctrl Pts',(-186.953731320117,-4.88942783458341,
130.2548535049));
#245399=CARTESIAN_POINT('Ctrl Pts',(-186.961583631081,-4.90103510324496,
130.393218331659));
#245400=CARTESIAN_POINT('Ctrl Pts',(-186.969435942045,-4.91264237190651,
130.531583158419));
#245401=CARTESIAN_POINT('Ctrl Pts',(-186.977288253009,-4.91837507169744,
130.670316037513));
#245402=CARTESIAN_POINT('Ctrl Pts',(-186.985140563973,-4.91824792938353,
130.808873666936));
#245403=CARTESIAN_POINT('Ctrl Pts',(-186.985140564012,-4.9182479293829,
130.808873667626));
#245404=CARTESIAN_POINT('Ctrl Pts',(-186.995772027482,-4.91807578782115,
130.996470718023));
#245405=CARTESIAN_POINT('Ctrl Pts',(-187.006403490951,-4.90716688700063,
131.183595083917));
#245406=CARTESIAN_POINT('Ctrl Pts',(-187.017034954421,-4.88570371797789,
131.369234269489));
#245407=CARTESIAN_POINT('Ctrl Pts',(-187.026930823288,-4.86572559297847,
131.542029016165));
#245408=CARTESIAN_POINT('Ctrl Pts',(-187.036826692156,-4.83660372490796,
131.71353778882));
#245409=CARTESIAN_POINT('Ctrl Pts',(-187.046722561023,-4.79852032900577,
131.882964212321));
#245410=CARTESIAN_POINT('Ctrl Pts',(-187.054496895142,-4.76860147618899,
132.016067999625));
#245411=CARTESIAN_POINT('Ctrl Pts',(-187.062271229261,-4.73309288657269,
132.148136813944));
#245412=CARTESIAN_POINT('Ctrl Pts',(-187.07004556338,-4.69207949437852,
132.278664887699));
#245413=CARTESIAN_POINT('Ctrl Pts',(-187.077810316327,-4.65111664752476,
132.409032097269));
#245414=CARTESIAN_POINT('Ctrl Pts',(-187.085575069274,-4.60466261265512,
132.537861974965));
#245415=CARTESIAN_POINT('Ctrl Pts',(-187.093339822221,-4.55285331124662,
132.66465892396));
#245416=CARTESIAN_POINT('Ctrl Pts',(-187.101096863106,-4.50109546756681,
132.791329936437));
#245417=CARTESIAN_POINT('Ctrl Pts',(-187.108853903991,-4.44399308917469,
132.915971678803));
#245418=CARTESIAN_POINT('Ctrl Pts',(-187.116610944876,-4.38173177310754,
133.038104052036));
#245419=CARTESIAN_POINT('Ctrl Pts',(-187.124362136116,-4.31951740878307,
133.160144324298));
#245420=CARTESIAN_POINT('Ctrl Pts',(-187.132113327356,-4.25215202722686,
133.279678647097));
#245421=CARTESIAN_POINT('Ctrl Pts',(-187.139864518596,-4.17986902446443,
133.396247575136));
#245422=CARTESIAN_POINT('Ctrl Pts',(-187.147612415373,-4.1076167439063,
133.512766958271));
#245423=CARTESIAN_POINT('Ctrl Pts',(-187.15536031215,-4.03045120483651,
133.626323121855));
#245424=CARTESIAN_POINT('Ctrl Pts',(-187.163108208927,-3.9486512601369,
133.736482083044));
#245425=CARTESIAN_POINT('Ctrl Pts',(-187.170854485011,-3.86686842622231,
133.846618001354));
#245426=CARTESIAN_POINT('Ctrl Pts',(-187.178600761095,-3.78045334783767,
133.953357817043));
#245427=CARTESIAN_POINT('Ctrl Pts',(-187.186347037179,-3.68972740421345,
134.056297693387));
#245428=CARTESIAN_POINT('Ctrl Pts',(-187.194093370445,-3.59900079087104,
134.159238329609));
#245429=CARTESIAN_POINT('Ctrl Pts',(-187.20183970371,-3.50396350729632,
134.258378677208));
#245430=CARTESIAN_POINT('Ctrl Pts',(-187.209586036975,-3.40497603632671,
134.353349382629));
#245431=CARTESIAN_POINT('Ctrl Pts',(-187.217334104978,-3.30596639779917,
134.44834135608));
#245432=CARTESIAN_POINT('Ctrl Pts',(-187.225082172981,-3.20300509365603,
134.539161558656));
#245433=CARTESIAN_POINT('Ctrl Pts',(-187.232830240984,-3.09648783601041,
134.625479059062));
#245434=CARTESIAN_POINT('Ctrl Pts',(-187.240586543725,-2.98985737055593,
134.711888298734));
#245435=CARTESIAN_POINT('Ctrl Pts',(-187.248342846467,-2.8796637062563,
134.793785030094));
#245436=CARTESIAN_POINT('Ctrl Pts',(-187.256099149209,-2.76633431053606,
134.870879711933));
#245437=CARTESIAN_POINT('Ctrl Pts',(-187.263859591723,-2.65294442750473,
134.948015541525));
#245438=CARTESIAN_POINT('Ctrl Pts',(-187.271620034237,-2.53641581021152,
135.020344008526));
#245439=CARTESIAN_POINT('Ctrl Pts',(-187.279380476751,-2.41720213633815,
135.087620695425));
#245440=CARTESIAN_POINT('Ctrl Pts',(-187.287153377017,-2.2977970900922,
135.155005380835));
#245441=CARTESIAN_POINT('Ctrl Pts',(-187.294926277282,-2.1756987223634,
135.217321902815));
#245442=CARTESIAN_POINT('Ctrl Pts',(-187.302699177547,-2.05138318386969,
135.274372932475));
#245443=CARTESIAN_POINT('Ctrl Pts',(-187.31018951331,-1.93158682832274,
135.329350013508));
#245444=CARTESIAN_POINT('Ctrl Pts',(-187.317679849073,-1.80973198772532,
135.379437666485));
#245445=CARTESIAN_POINT('Ctrl Pts',(-187.325170184835,-1.68625769629345,
135.424503260839));
#245446=CARTESIAN_POINT('Ctrl Pts',(-187.332944518954,-1.5581018395823,
135.471277530897));
#245447=CARTESIAN_POINT('Ctrl Pts',(-187.340718853073,-1.42779534567859,
135.512789568897));
#245448=CARTESIAN_POINT('Ctrl Pts',(-187.348493187192,-1.29580964019177,
135.548837452675));
#245449=CARTESIAN_POINT('Ctrl Pts',(-187.356257940139,-1.16398659529106,
135.584840910658));
#245450=CARTESIAN_POINT('Ctrl Pts',(-187.364022693087,-1.03048882998293,
135.615393511214));
#245451=CARTESIAN_POINT('Ctrl Pts',(-187.371787446034,-0.895806772792648,
135.640341726743));
#245452=CARTESIAN_POINT('Ctrl Pts',(-187.379544486919,-0.761258483720252,
135.665265163353));
#245453=CARTESIAN_POINT('Ctrl Pts',(-187.387301527804,-0.625528625504841,
135.68459522148));
#245454=CARTESIAN_POINT('Ctrl Pts',(-187.395058568689,-0.48912143878214,
135.698228543923));
#245455=CARTESIAN_POINT('Ctrl Pts',(-187.402809759929,-0.352817117779854,
135.711851585371));
#245456=CARTESIAN_POINT('Ctrl Pts',(-187.410560951169,-0.215836872397206,
135.719786403242));
#245457=CARTESIAN_POINT('Ctrl Pts',(-187.418312142409,-0.0786934032297544,
135.721981018816));
#245458=CARTESIAN_POINT('Ctrl Pts',(-187.426060039186,0.0583917763046921,
135.72417470162));
#245459=CARTESIAN_POINT('Ctrl Pts',(-187.433807935963,0.195639651546684,
135.720633028339));
#245460=CARTESIAN_POINT('Ctrl Pts',(-187.44155583274,0.33253437364453,135.711356027473));
#245461=CARTESIAN_POINT('Ctrl Pts',(-187.449302108824,0.469400460317623,
135.702080967155));
#245462=CARTESIAN_POINT('Ctrl Pts',(-187.457048384909,0.605913150958659,
135.687072991952));
#245463=CARTESIAN_POINT('Ctrl Pts',(-187.464794660993,0.741558972969566,
135.666384203698));
#245464=CARTESIAN_POINT('Ctrl Pts',(-187.472540994258,0.877205796287302,
135.645695262725));
#245465=CARTESIAN_POINT('Ctrl Pts',(-187.480287327523,1.01198535171049,
135.619325483972));
#245466=CARTESIAN_POINT('Ctrl Pts',(-187.488033660789,1.14539204185446,
135.587378507242));
#245467=CARTESIAN_POINT('Ctrl Pts',(-187.495781728792,1.27882860750151,
135.555424376208));
#245468=CARTESIAN_POINT('Ctrl Pts',(-187.503529796795,1.41089131594959,
135.517890652914));
#245469=CARTESIAN_POINT('Ctrl Pts',(-187.511277864798,1.54108785326631,
135.474931384722));
#245470=CARTESIAN_POINT('Ctrl Pts',(-187.51903416754,1.67142276501208,135.431926458909));
#245471=CARTESIAN_POINT('Ctrl Pts',(-187.526790470281,1.79988717172503,
135.383484592025));
#245472=CARTESIAN_POINT('Ctrl Pts',(-187.534546773023,1.92600641760273,
135.329808920425));
#245473=CARTESIAN_POINT('Ctrl Pts',(-187.542307215538,2.05219297711968,
135.276104600504));
#245474=CARTESIAN_POINT('Ctrl Pts',(-187.550067658052,2.17603152887269,
135.217161077647));
#245475=CARTESIAN_POINT('Ctrl Pts',(-187.557828100566,2.29707121362073,
135.153227930103));
#245476=CARTESIAN_POINT('Ctrl Pts',(-187.565601000831,2.41830520201613,
135.089192151395));
#245477=CARTESIAN_POINT('Ctrl Pts',(-187.573373901097,2.53673100702913,
135.020150938914));
#245478=CARTESIAN_POINT('Ctrl Pts',(-187.581146801362,2.65192523918329,
134.94639823066));
#245479=CARTESIAN_POINT('Ctrl Pts',(-187.588637137124,2.7629318708422,134.875326619122));
#245480=CARTESIAN_POINT('Ctrl Pts',(-187.596127472886,2.87093754965219,
134.799880290516));
#245481=CARTESIAN_POINT('Ctrl Pts',(-187.603617808648,2.9755933810453,134.720356926704));
#245482=CARTESIAN_POINT('Ctrl Pts',(-187.611392142768,3.08421727009468,
134.637818410382));
#245483=CARTESIAN_POINT('Ctrl Pts',(-187.619166476887,3.18957636621408,
134.550626137116));
#245484=CARTESIAN_POINT('Ctrl Pts',(-187.626940811006,3.29124596951094,
134.45906758676));
#245485=CARTESIAN_POINT('Ctrl Pts',(-187.634705563953,3.3927902741082,134.367621874136));
#245486=CARTESIAN_POINT('Ctrl Pts',(-187.6424703169,3.49065384526458,134.271820850219));
#245487=CARTESIAN_POINT('Ctrl Pts',(-187.650235069847,3.58444242726253,
134.171994140998));
#245488=CARTESIAN_POINT('Ctrl Pts',(-187.657992110732,3.67813785711891,
134.072266581071));
#245489=CARTESIAN_POINT('Ctrl Pts',(-187.665749151617,3.76776608622933,
133.968521575866));
#245490=CARTESIAN_POINT('Ctrl Pts',(-187.673506192502,3.85296760287033,
133.861127490216));
#245491=CARTESIAN_POINT('Ctrl Pts',(-187.681257383742,3.93810486838475,
133.753814391282));
#245492=CARTESIAN_POINT('Ctrl Pts',(-187.689008574982,4.01882182394327,
133.642857994237));
#245493=CARTESIAN_POINT('Ctrl Pts',(-187.696759766223,4.0947976111808,133.528661552846));
#245494=CARTESIAN_POINT('Ctrl Pts',(-187.704507663,4.17074110668214,133.414513647989));
#245495=CARTESIAN_POINT('Ctrl Pts',(-187.712255559777,4.24194722567974,
133.297128762567));
#245496=CARTESIAN_POINT('Ctrl Pts',(-187.720003456554,4.30813716324615,
133.176940910234));
#245497=CARTESIAN_POINT('Ctrl Pts',(-187.727749732638,4.37431325530452,
133.056778198609));
#245498=CARTESIAN_POINT('Ctrl Pts',(-187.735496008722,4.43547506451776,
132.933814028545));
#245499=CARTESIAN_POINT('Ctrl Pts',(-187.743242284806,4.4913888811533,132.808508561395));
#245500=CARTESIAN_POINT('Ctrl Pts',(-187.750988618071,4.54730311053187,
132.683202169268));
#245501=CARTESIAN_POINT('Ctrl Pts',(-187.758734951337,4.59796911071568,
132.555554802601));
#245502=CARTESIAN_POINT('Ctrl Pts',(-187.766481284602,4.64320078906951,
132.426047854639));
#245503=CARTESIAN_POINT('Ctrl Pts',(-187.774229352605,4.68844259674417,
132.296511904493));
#245504=CARTESIAN_POINT('Ctrl Pts',(-187.781977420608,4.72824753205442,
132.165115913412));
#245505=CARTESIAN_POINT('Ctrl Pts',(-187.789725488611,4.76247909170162,
132.032357345414));
#245506=CARTESIAN_POINT('Ctrl Pts',(-187.797481791353,4.79674703305773,
131.899457680029));
#245507=CARTESIAN_POINT('Ctrl Pts',(-187.805238094095,4.82542966824893,
131.765192924051));
#245508=CARTESIAN_POINT('Ctrl Pts',(-187.812994396837,4.8484413385891,131.630072219011));
#245509=CARTESIAN_POINT('Ctrl Pts',(-187.820754839351,4.87146529095061,
131.494879395982));
#245510=CARTESIAN_POINT('Ctrl Pts',(-187.828515281865,4.88881219795085,
131.358830101222));
#245511=CARTESIAN_POINT('Ctrl Pts',(-187.836275724379,4.90044833640633,
131.22243855852));
#245512=CARTESIAN_POINT('Ctrl Pts',(-187.844048624645,4.91210315422426,
131.085828068006));
#245513=CARTESIAN_POINT('Ctrl Pts',(-187.85182152491,4.9180288671356,130.948874622484));
#245514=CARTESIAN_POINT('Ctrl Pts',(-187.859594425176,4.91824392115051,
130.812093312181));
#245515=CARTESIAN_POINT('Ctrl Pts',(-187.867084760937,4.9184511574103,130.68028434704));
#245516=CARTESIAN_POINT('Ctrl Pts',(-187.874575096699,4.91335573198571,
130.548635527089));
#245517=CARTESIAN_POINT('Ctrl Pts',(-187.882065432461,4.90301950702024,
130.417601291526));
#245518=CARTESIAN_POINT('Ctrl Pts',(-187.88983976658,4.89229138094348,130.281598853093));
#245519=CARTESIAN_POINT('Ctrl Pts',(-187.897614100699,4.87588321702286,
130.145827708113));
#245520=CARTESIAN_POINT('Ctrl Pts',(-187.905388434818,4.85380731953623,
130.010800558518));
#245521=CARTESIAN_POINT('Ctrl Pts',(-187.913153187766,4.83175862862026,
129.875939817817));
#245522=CARTESIAN_POINT('Ctrl Pts',(-187.920917940713,4.80405616463346,
129.741821630265));
#245523=CARTESIAN_POINT('Ctrl Pts',(-187.92868269366,4.77076414640998,129.608955865263));
#245524=CARTESIAN_POINT('Ctrl Pts',(-187.936439734545,4.73750519428833,
129.476222064411));
#245525=CARTESIAN_POINT('Ctrl Pts',(-187.94419677543,4.69866783032351,129.344738587432));
#245526=CARTESIAN_POINT('Ctrl Pts',(-187.951953816315,4.65436764541508,
129.21500701191));
#245527=CARTESIAN_POINT('Ctrl Pts',(-187.959705007555,4.61010086762063,
129.085373267977));
#245528=CARTESIAN_POINT('Ctrl Pts',(-187.967456198795,4.56037959443934,
128.95748916438));
#245529=CARTESIAN_POINT('Ctrl Pts',(-187.975207390035,4.50536966289933,
128.831842616856));
#245530=CARTESIAN_POINT('Ctrl Pts',(-187.982955286812,4.45038311204773,
128.706249472466));
#245531=CARTESIAN_POINT('Ctrl Pts',(-187.990703183589,4.39011253005438,
128.582892350036));
#245532=CARTESIAN_POINT('Ctrl Pts',(-187.998451080366,4.32477236402399,
128.462240411028));
#245533=CARTESIAN_POINT('Ctrl Pts',(-188.006197356451,4.25944586574759,
128.341613709804));
#245534=CARTESIAN_POINT('Ctrl Pts',(-188.013943632535,4.18905207878634,
128.223691410034));
#245535=CARTESIAN_POINT('Ctrl Pts',(-188.021689908619,4.11385182410005,
128.108918866786));
#245536=CARTESIAN_POINT('Ctrl Pts',(-188.029436241884,4.03865101430267,
127.994145476313));
#245537=CARTESIAN_POINT('Ctrl Pts',(-188.03718257515,3.95864388025005,127.882522215779));
#245538=CARTESIAN_POINT('Ctrl Pts',(-188.044928908415,3.87413484409709,
127.774465854995));
#245539=CARTESIAN_POINT('Ctrl Pts',(-188.052676976418,3.78960688273153,
127.666385295739));
#245540=CARTESIAN_POINT('Ctrl Pts',(-188.060425044421,3.70057525393309,
127.561873533624));
#245541=CARTESIAN_POINT('Ctrl Pts',(-188.068173112424,3.60738470489975,
127.461314304193));
#245542=CARTESIAN_POINT('Ctrl Pts',(-188.075929415166,3.51409511184179,
127.360648199217));
#245543=CARTESIAN_POINT('Ctrl Pts',(-188.083685717908,3.416638034995,127.26394330569));
#245544=CARTESIAN_POINT('Ctrl Pts',(-188.091442020649,3.31539552893747,
127.171546894128));
#245545=CARTESIAN_POINT('Ctrl Pts',(-188.099202463164,3.21409898670611,
127.079101167818));
#245546=CARTESIAN_POINT('Ctrl Pts',(-188.106962905678,3.10901328886408,
126.990968756662));
#245547=CARTESIAN_POINT('Ctrl Pts',(-188.114723348192,3.00055283824357,
126.907455983448));
#245548=CARTESIAN_POINT('Ctrl Pts',(-188.122496248457,2.89191827727905,
126.823809148117));
#245549=CARTESIAN_POINT('Ctrl Pts',(-188.130269148723,2.77989845741056,
126.744796995441));
#245550=CARTESIAN_POINT('Ctrl Pts',(-188.138042048988,2.66493670915268,
126.670682425119));
#245551=CARTESIAN_POINT('Ctrl Pts',(-188.14553238475,2.55415411001514,126.599262106112));
#245552=CARTESIAN_POINT('Ctrl Pts',(-188.153022720512,2.44064002739613,
126.532389628946));
#245553=CARTESIAN_POINT('Ctrl Pts',(-188.160513056274,2.32481023186287,
126.470258582735));
#245554=CARTESIAN_POINT('Ctrl Pts',(-188.168287390393,2.2045887144261,126.405771819022));
#245555=CARTESIAN_POINT('Ctrl Pts',(-188.176061724512,2.0814915915248,126.346188851776));
#245556=CARTESIAN_POINT('Ctrl Pts',(-188.183836058631,1.95595686457699,
126.291776456975));
#245557=CARTESIAN_POINT('Ctrl Pts',(-188.191600811579,1.83057684796112,
126.237431120589));
#245558=CARTESIAN_POINT('Ctrl Pts',(-188.199365564526,1.70276555989438,
126.188243831725));
#245559=CARTESIAN_POINT('Ctrl Pts',(-188.207130317473,1.5729866797913,126.144436158125));
#245560=CARTESIAN_POINT('Ctrl Pts',(-188.214887358358,1.4433366979015,126.100671994924));
#245561=CARTESIAN_POINT('Ctrl Pts',(-188.222644399243,1.3117233810346,126.062276938189));
#245562=CARTESIAN_POINT('Ctrl Pts',(-188.230401440128,1.17863120032339,
126.029424852959));
#245563=CARTESIAN_POINT('Ctrl Pts',(-188.238152631368,1.04563938546079,
125.996597541742));
#245564=CARTESIAN_POINT('Ctrl Pts',(-188.245903822608,0.911171304574001,
125.969304975312));
#245565=CARTESIAN_POINT('Ctrl Pts',(-188.253655013848,0.775727093957084,
125.947671360654));
#245566=CARTESIAN_POINT('Ctrl Pts',(-188.261402910625,0.640340450742956,
125.92604694086));
#245567=CARTESIAN_POINT('Ctrl Pts',(-188.269150807402,0.503978888229026,
125.910076750604));
#245568=CARTESIAN_POINT('Ctrl Pts',(-188.276898704179,0.36715303913928,
125.899833962694));
#245569=CARTESIAN_POINT('Ctrl Pts',(-188.284644980264,0.230355811067541,
125.889593317354));
#245570=CARTESIAN_POINT('Ctrl Pts',(-188.292391256348,0.0930948792217825,
125.885077720542));
#245571=CARTESIAN_POINT('Ctrl Pts',(-188.300137532432,-0.0441140864660505,
125.886308461491));
#245572=CARTESIAN_POINT('Ctrl Pts',(-188.307883865697,-0.181324064999486,
125.887539211525));
#245573=CARTESIAN_POINT('Ctrl Pts',(-188.315630198963,-0.318481685660068,
125.894516380455));
#245574=CARTESIAN_POINT('Ctrl Pts',(-188.323376532228,-0.455071760591299,
125.907209123563));
#245575=CARTESIAN_POINT('Ctrl Pts',(-188.331124600231,-0.591692423922576,
125.919904709124));
#245576=CARTESIAN_POINT('Ctrl Pts',(-188.338872668234,-0.727744899400813,
125.938318379674));
#245577=CARTESIAN_POINT('Ctrl Pts',(-188.346620736237,-0.862719995164512,
125.962367508066));
#245578=CARTESIAN_POINT('Ctrl Pts',(-188.354377038979,-0.997838544066398,
125.986442196158));
#245579=CARTESIAN_POINT('Ctrl Pts',(-188.362133341721,-1.13187704037199,
126.016164237938));
#245580=CARTESIAN_POINT('Ctrl Pts',(-188.369889644462,-1.26433680573185,
126.051399908264));
#245581=CARTESIAN_POINT('Ctrl Pts',(-188.377650086977,-1.39686726885678,
126.086654384927));
#245582=CARTESIAN_POINT('Ctrl Pts',(-188.385410529491,-1.52781694894612,
126.12742823772));
#245583=CARTESIAN_POINT('Ctrl Pts',(-188.393170972005,-1.65670413311006,
126.173538392751));
#245584=CARTESIAN_POINT('Ctrl Pts',(-188.40094387227,-1.78579821842409,
126.219722567897));
#245585=CARTESIAN_POINT('Ctrl Pts',(-188.408716772536,-1.91282282908581,
126.271260016418));
#245586=CARTESIAN_POINT('Ctrl Pts',(-188.416489672801,-2.03731714916122,
126.327919855506));
#245587=CARTESIAN_POINT('Ctrl Pts',(-188.423980008563,-2.15728578711929,
126.382519966725));
#245588=CARTESIAN_POINT('Ctrl Pts',(-188.431470344325,-2.27490463047672,
126.441876371959));
#245589=CARTESIAN_POINT('Ctrl Pts',(-188.438960680087,-2.38978607308234,
126.505743911299));
#245590=CARTESIAN_POINT('Ctrl Pts',(-188.446736064809,-2.50903939390405,
126.572041965939));
#245591=CARTESIAN_POINT('Ctrl Pts',(-188.454511449531,-2.62572065138844,
126.643411342122));
#245592=CARTESIAN_POINT('Ctrl Pts',(-188.462286834253,-2.73936846326012,
126.719627641594));
#245593=CARTESIAN_POINT('Ctrl Pts',(-188.470052407546,-2.85287286776605,
126.795747766942));
#245594=CARTESIAN_POINT('Ctrl Pts',(-188.477817980839,-2.96335112181759,
126.876702429187));
#245595=CARTESIAN_POINT('Ctrl Pts',(-188.485583554132,-3.07036605036914,
126.96222119021));
#245596=CARTESIAN_POINT('Ctrl Pts',(-188.493339764738,-3.177251954663,127.047636844174));
#245597=CARTESIAN_POINT('Ctrl Pts',(-188.501095975344,-3.28068254643464,
127.137605394597));
#245598=CARTESIAN_POINT('Ctrl Pts',(-188.508852185949,-3.38024981628517,
127.23181331319));
#245599=CARTESIAN_POINT('Ctrl Pts',(-188.516603088238,-3.47974894273336,
127.325956756297));
#245600=CARTESIAN_POINT('Ctrl Pts',(-188.524353990527,-3.57538972474253,
127.424333527832));
#245601=CARTESIAN_POINT('Ctrl Pts',(-188.532104892816,-3.66679737349336,
127.526590020919));
#245602=CARTESIAN_POINT('Ctrl Pts',(-188.539852169042,-3.75816225948245,
127.628798675886));
#245603=CARTESIAN_POINT('Ctrl Pts',(-188.547599445267,-3.84529769319432,
127.734883149714));
#245604=CARTESIAN_POINT('Ctrl Pts',(-188.555346721492,-3.92786618611514,
127.844453476037));
#245605=CARTESIAN_POINT('Ctrl Pts',(-188.563092051104,-4.01041393253067,
127.953996271261));
#245606=CARTESIAN_POINT('Ctrl Pts',(-188.570837380716,-4.08839678790403,
128.067022863189));
#245607=CARTESIAN_POINT('Ctrl Pts',(-188.578582710328,-4.1615182156311,
128.183111067548));
#245608=CARTESIAN_POINT('Ctrl Pts',(-188.586330187877,-4.23465992141677,
128.299231465526));
#245609=CARTESIAN_POINT('Ctrl Pts',(-188.594077665427,-4.302937292578,128.41841484449));
#245610=CARTESIAN_POINT('Ctrl Pts',(-188.601825142976,-4.36609769469263,
128.540210891311));
#245611=CARTESIAN_POINT('Ctrl Pts',(-188.609573616128,-4.42926621333887,
128.662022589734));
#245612=CARTESIAN_POINT('Ctrl Pts',(-188.617322089279,-4.48731628029937,
128.78644727399));
#245613=CARTESIAN_POINT('Ctrl Pts',(-188.625070562431,-4.54004215253343,
128.913011808985));
#245614=CARTESIAN_POINT('Ctrl Pts',(-188.632825393423,-4.59281128782829,
129.03968019374));
#245615=CARTESIAN_POINT('Ctrl Pts',(-188.640580224415,-4.64024735853174,
129.168491572479));
#245616=CARTESIAN_POINT('Ctrl Pts',(-188.648335055407,-4.68219341291706,
129.298954391149));
#245617=CARTESIAN_POINT('Ctrl Pts',(-188.653905981131,-4.7123266748338,
129.392676443031));
#245618=CARTESIAN_POINT('Ctrl Pts',(-188.659476906855,-4.73962772385923,
129.487250379779));
#245619=CARTESIAN_POINT('Ctrl Pts',(-188.665047832579,-4.76405452823406,
129.582490119308));
#245620=CARTESIAN_POINT('',(-186.639859435958,-4.91824992550734,130.803504611091));
#245621=CARTESIAN_POINT('Ctrl Pts',(-186.639859435995,-4.91824992550745,
130.803504611754));
#245622=CARTESIAN_POINT('Ctrl Pts',(-186.647875869329,-4.91827469762084,
130.945834772432));
#245623=CARTESIAN_POINT('Ctrl Pts',(-186.655892302664,-4.91211675181942,
131.08808080582));
#245624=CARTESIAN_POINT('Ctrl Pts',(-186.663908735998,-4.89982403781472,
131.229692794756));
#245625=CARTESIAN_POINT('Ctrl Pts',(-186.671932409808,-4.88752022097909,
131.371432688235));
#245626=CARTESIAN_POINT('Ctrl Pts',(-186.679956083619,-4.86907061660121,
131.512537046391));
#245627=CARTESIAN_POINT('Ctrl Pts',(-186.68797975743,-4.84457475465937,
131.652463505792));
#245628=CARTESIAN_POINT('Ctrl Pts',(-186.696303438758,-4.81916298525302,
131.797621856561));
#245629=CARTESIAN_POINT('Ctrl Pts',(-186.704627120086,-4.78724414801483,
131.941512102986));
#245630=CARTESIAN_POINT('Ctrl Pts',(-186.712950801415,-4.74898628261018,
132.083544869377));
#245631=CARTESIAN_POINT('Ctrl Pts',(-186.720998349268,-4.71199760050266,
132.220865778145));
#245632=CARTESIAN_POINT('Ctrl Pts',(-186.729045897121,-4.6690839408078,
132.356450179057));
#245633=CARTESIAN_POINT('Ctrl Pts',(-186.737093444975,-4.62044665828881,
132.489785116144));
#245634=CARTESIAN_POINT('Ctrl Pts',(-186.745555193041,-4.56930605760306,
132.629982685208));
#245635=CARTESIAN_POINT('Ctrl Pts',(-186.754016941106,-4.51183726098221,
132.767692681952));
#245636=CARTESIAN_POINT('Ctrl Pts',(-186.762478689172,-4.44832931978521,
132.902347587316));
#245637=CARTESIAN_POINT('Ctrl Pts',(-186.770940437238,-4.38482137858837,
133.037002492679));
#245638=CARTESIAN_POINT('Ctrl Pts',(-186.779402185303,-4.31527456651344,
133.168601951196));
#245639=CARTESIAN_POINT('Ctrl Pts',(-186.787863933369,-4.2400305344674,
133.29661343967));
#245640=CARTESIAN_POINT('Ctrl Pts',(-186.795638267488,-4.17089916337693,
133.414225554185));
#245641=CARTESIAN_POINT('Ctrl Pts',(-186.803412601607,-4.09676100795466,
133.529145376511));
#245642=CARTESIAN_POINT('Ctrl Pts',(-186.811186935727,-4.0178513751189,
133.64091722549));
#245643=CARTESIAN_POINT('Ctrl Pts',(-186.818951688674,-3.93903899135325,
133.752551325653));
#245644=CARTESIAN_POINT('Ctrl Pts',(-186.826716441621,-3.85546705377721,
133.861044855384));
#245645=CARTESIAN_POINT('Ctrl Pts',(-186.834481194568,-3.76741631617132,
133.965967386781));
#245646=CARTESIAN_POINT('Ctrl Pts',(-186.842238235453,-3.67945303179932,
134.070785707641));
#245647=CARTESIAN_POINT('Ctrl Pts',(-186.849995276338,-3.5870200496273,
134.172039790846));
#245648=CARTESIAN_POINT('Ctrl Pts',(-186.857752317224,-3.49044069470467,
134.269329133909));
#245649=CARTESIAN_POINT('Ctrl Pts',(-186.865503508464,-3.39393417102474,
134.366545110322));
#245650=CARTESIAN_POINT('Ctrl Pts',(-186.873254699704,-3.29328777264913,
134.459802021349));
#245651=CARTESIAN_POINT('Ctrl Pts',(-186.881005890944,-3.18886403465664,
134.548733626626));
#245652=CARTESIAN_POINT('Ctrl Pts',(-186.888753787722,-3.08448467953826,
134.637627433597));
#245653=CARTESIAN_POINT('Ctrl Pts',(-186.896501684499,-2.97633147498796,
134.722199338236));
#245654=CARTESIAN_POINT('Ctrl Pts',(-186.904249581276,-2.86480246755412,
134.802121226256));
#245655=CARTESIAN_POINT('Ctrl Pts',(-186.91199585736,-2.75329678958435,
134.882026396341));
#245656=CARTESIAN_POINT('Ctrl Pts',(-186.919742133444,-2.63841703088417,
134.957283256941));
#245657=CARTESIAN_POINT('Ctrl Pts',(-186.927488409529,-2.52059252882238,
135.027605385058));
#245658=CARTESIAN_POINT('Ctrl Pts',(-186.935234742794,-2.40276715700672,
135.097928032277));
#245659=CARTESIAN_POINT('Ctrl Pts',(-186.94298107606,-2.2819973341713,135.163315673957));
#245660=CARTESIAN_POINT('Ctrl Pts',(-186.950727409325,-2.15873910496181,
135.223526663237));
#245661=CARTESIAN_POINT('Ctrl Pts',(-186.958475477328,-2.03545327292633,
135.28375113635));
#245662=CARTESIAN_POINT('Ctrl Pts',(-186.966223545331,-1.90967827685561,
135.338796478669));
#245663=CARTESIAN_POINT('Ctrl Pts',(-186.973971613335,-1.78189197661644,
135.388468387478));
#245664=CARTESIAN_POINT('Ctrl Pts',(-186.981727916077,-1.65396986357687,
135.438193088183));
#245665=CARTESIAN_POINT('Ctrl Pts',(-186.989484218819,-1.52403254119107,
135.482532805269));
#245666=CARTESIAN_POINT('Ctrl Pts',(-186.997240521561,-1.3925754703003,
135.521342345538));
#245667=CARTESIAN_POINT('Ctrl Pts',(-187.005000964075,-1.2610482368127,
135.560172599627));
#245668=CARTESIAN_POINT('Ctrl Pts',(-187.012761406589,-1.12800001764879,
135.59346670068));
#245669=CARTESIAN_POINT('Ctrl Pts',(-187.020521849103,-0.993937454370752,
135.621130427231));
#245670=CARTESIAN_POINT('Ctrl Pts',(-187.028294749369,-0.85965968196463,
135.648838562051));
#245671=CARTESIAN_POINT('Ctrl Pts',(-187.036067649635,-0.724364697643503,
135.670898197859));
#245672=CARTESIAN_POINT('Ctrl Pts',(-187.0438405499,-0.588566164980932,
135.687266814898));
#245673=CARTESIAN_POINT('Ctrl Pts',(-187.051330885661,-0.457704251061874,
135.703040391474));
#245674=CARTESIAN_POINT('Ctrl Pts',(-187.058821221422,-0.326375070731452,
135.713529506913));
#245675=CARTESIAN_POINT('Ctrl Pts',(-187.066311557182,-0.19503718887608,
135.718741917125));
#245676=CARTESIAN_POINT('Ctrl Pts',(-187.074085891301,-0.0587195912883398,
135.724151957455));
#245677=CARTESIAN_POINT('Ctrl Pts',(-187.08186022542,0.0780391938607504,
135.723894398637));
#245678=CARTESIAN_POINT('Ctrl Pts',(-187.089634559539,0.214728599968461,
135.717920904248));
#245679=CARTESIAN_POINT('Ctrl Pts',(-187.097399312486,0.351249548599797,
135.711954771656));
#245680=CARTESIAN_POINT('Ctrl Pts',(-187.105164065433,0.48770090147341,
135.700286736615));
#245681=CARTESIAN_POINT('Ctrl Pts',(-187.11292881838,0.62356877312973,135.682920348437));
#245682=CARTESIAN_POINT('Ctrl Pts',(-187.120685859265,0.759301698900149,
135.665571208801));
#245683=CARTESIAN_POINT('Ctrl Pts',(-187.12844290015,0.894451911427142,
135.642535028303));
#245684=CARTESIAN_POINT('Ctrl Pts',(-187.136199941035,1.028507691538,135.613867348089));
#245685=CARTESIAN_POINT('Ctrl Pts',(-187.143951132275,1.16246237914208,
135.585221286396));
#245686=CARTESIAN_POINT('Ctrl Pts',(-187.151702323515,1.2953238963055,135.550952259327));
#245687=CARTESIAN_POINT('Ctrl Pts',(-187.159453514755,1.42658815557148,
135.511167316049));
#245688=CARTESIAN_POINT('Ctrl Pts',(-187.167201411532,1.55779662402658,
135.471399282433));
#245689=CARTESIAN_POINT('Ctrl Pts',(-187.174949308309,1.68740881144558,
135.42612010863));
#245690=CARTESIAN_POINT('Ctrl Pts',(-187.182697205086,1.81493351210572,
135.375487328688));
#245691=CARTESIAN_POINT('Ctrl Pts',(-187.19044348117,1.94243153734725,135.324865140033));
#245692=CARTESIAN_POINT('Ctrl Pts',(-187.198189757255,2.0678425812239,135.268891716883));
#245693=CARTESIAN_POINT('Ctrl Pts',(-187.205936033339,2.19069360062039,
135.207773454299));
#245694=CARTESIAN_POINT('Ctrl Pts',(-187.213682366604,2.31354552687536,
135.146654740553));
#245695=CARTESIAN_POINT('Ctrl Pts',(-187.221428699869,2.43383704090215,
135.080391285736));
#245696=CARTESIAN_POINT('Ctrl Pts',(-187.229175033134,2.55111833508265,
135.009236157092));
#245697=CARTESIAN_POINT('Ctrl Pts',(-187.236923101137,2.66842589359566,
134.938065093751));
#245698=CARTESIAN_POINT('Ctrl Pts',(-187.24467116914,2.78272155665276,134.862000379508));
#245699=CARTESIAN_POINT('Ctrl Pts',(-187.252419237143,2.89358355694662,
134.78133902604));
#245700=CARTESIAN_POINT('Ctrl Pts',(-187.260175539885,3.00456338269382,
134.700591944726));
#245701=CARTESIAN_POINT('Ctrl Pts',(-187.267931842627,3.11210193908768,
134.615238695533));
#245702=CARTESIAN_POINT('Ctrl Pts',(-187.275688145368,3.21580926229213,
134.52561764323));
#245703=CARTESIAN_POINT('Ctrl Pts',(-187.283448587883,3.31957193721782,
134.435948757473));
#245704=CARTESIAN_POINT('Ctrl Pts',(-187.291209030397,3.41949901971309,
134.342007797447));
#245705=CARTESIAN_POINT('Ctrl Pts',(-187.298969472911,3.51523738644899,
134.244170086041));
#245706=CARTESIAN_POINT('Ctrl Pts',(-187.306742373176,3.61112944091017,
134.146175316856));
#245707=CARTESIAN_POINT('Ctrl Pts',(-187.314515273441,3.70281908106574,
134.044271586789));
#245708=CARTESIAN_POINT('Ctrl Pts',(-187.322288173707,3.7899928861312,133.938868072586));
#245709=CARTESIAN_POINT('Ctrl Pts',(-187.329778509469,3.87399770381394,
133.837296241609));
#245710=CARTESIAN_POINT('Ctrl Pts',(-187.337268845232,3.95380912358556,
133.732474905839));
#245711=CARTESIAN_POINT('Ctrl Pts',(-187.344759180995,4.02918580518921,
133.624794061163));
#245712=CARTESIAN_POINT('Ctrl Pts',(-187.352533515114,4.10742041657999,
133.513030464541));
#245713=CARTESIAN_POINT('Ctrl Pts',(-187.360307849233,4.181125188946,133.39783220855));
#245714=CARTESIAN_POINT('Ctrl Pts',(-187.368082183353,4.24998348176541,
133.279602720315));
#245715=CARTESIAN_POINT('Ctrl Pts',(-187.3758469363,4.31875691289296,133.161518939358));
#245716=CARTESIAN_POINT('Ctrl Pts',(-187.383611689247,4.38269555379604,
133.040411693732));
#245717=CARTESIAN_POINT('Ctrl Pts',(-187.391376442194,4.44152462296868,
132.916715248319));
#245718=CARTESIAN_POINT('Ctrl Pts',(-187.399133483079,4.50029526228031,
132.793141659959));
#245719=CARTESIAN_POINT('Ctrl Pts',(-187.406890523964,4.55396626230861,
132.666984340256));
#245720=CARTESIAN_POINT('Ctrl Pts',(-187.414647564849,4.60230775467839,
132.538703834385));
#245721=CARTESIAN_POINT('Ctrl Pts',(-187.42239875609,4.6506127923528,132.410520065842));
#245722=CARTESIAN_POINT('Ctrl Pts',(-187.43014994733,4.69359618468073,132.280216662417));
#245723=CARTESIAN_POINT('Ctrl Pts',(-187.43790113857,4.73107552357416,132.148275589853));
#245724=CARTESIAN_POINT('Ctrl Pts',(-187.445649035347,4.76853893274882,
132.016390595764));
#245725=CARTESIAN_POINT('Ctrl Pts',(-187.453396932125,4.80050283470879,
131.882869692232));
#245726=CARTESIAN_POINT('Ctrl Pts',(-187.461144828902,4.82683425861936,
131.748211295543));
#245727=CARTESIAN_POINT('Ctrl Pts',(-187.468891104986,4.85316017456368,
131.613581066489));
#245728=CARTESIAN_POINT('Ctrl Pts',(-187.47663738107,4.87385588096731,131.477814201007));
#245729=CARTESIAN_POINT('Ctrl Pts',(-187.484383657154,4.88883933248194,
131.34142024524));
#245730=CARTESIAN_POINT('Ctrl Pts',(-187.49212999042,4.90382289460099,131.205025282644));
#245731=CARTESIAN_POINT('Ctrl Pts',(-187.499876323685,4.91309407499838,
131.068003609154));
#245732=CARTESIAN_POINT('Ctrl Pts',(-187.507622656951,4.91662265431028,
130.930870449686));
#245733=CARTESIAN_POINT('Ctrl Pts',(-187.515370724954,4.92015202382305,
130.793706580197));
#245734=CARTESIAN_POINT('Ctrl Pts',(-187.523118792957,4.91793622317329,
130.65643156581));
#245735=CARTESIAN_POINT('Ctrl Pts',(-187.53086686096,4.90999716116407,130.519560793372));
#245736=CARTESIAN_POINT('Ctrl Pts',(-187.538623163702,4.90204966142525,
130.382544553048));
#245737=CARTESIAN_POINT('Ctrl Pts',(-187.546379466444,4.88836677205368,
130.245933803843));
#245738=CARTESIAN_POINT('Ctrl Pts',(-187.554135769186,4.86902238393298,
130.110239527799));
#245739=CARTESIAN_POINT('Ctrl Pts',(-187.5618962117,4.8496676711299,129.974472827634));
#245740=CARTESIAN_POINT('Ctrl Pts',(-187.569656654214,4.82464550985388,
129.839623959516));
#245741=CARTESIAN_POINT('Ctrl Pts',(-187.577417096728,4.79408079809747,
129.706192887293));
#245742=CARTESIAN_POINT('Ctrl Pts',(-187.585189996994,4.76346702115233,
129.572547619668));
#245743=CARTESIAN_POINT('Ctrl Pts',(-187.59296289726,4.72729301712821,129.440325073378));
#245744=CARTESIAN_POINT('Ctrl Pts',(-187.600735797525,4.6857336264191,129.310010108232));
#245745=CARTESIAN_POINT('Ctrl Pts',(-187.608226133286,4.64568502424898,
129.184432420329));
#245746=CARTESIAN_POINT('Ctrl Pts',(-187.615716469048,4.60063588766843,
129.060626320137));
#245747=CARTESIAN_POINT('Ctrl Pts',(-187.623206804809,4.55078388095632,
128.939005656351));
#245748=CARTESIAN_POINT('Ctrl Pts',(-187.630981138928,4.49904172025193,
128.812773708119));
#245749=CARTESIAN_POINT('Ctrl Pts',(-187.638755473047,4.4419613947056,128.688496324464));
#245750=CARTESIAN_POINT('Ctrl Pts',(-187.646529807166,4.37971116704724,
128.566657966242));
#245751=CARTESIAN_POINT('Ctrl Pts',(-187.654294560113,4.31753765723083,
128.444969762907));
#245752=CARTESIAN_POINT('Ctrl Pts',(-187.66205931306,4.25020709874698,128.325714949011));
#245753=CARTESIAN_POINT('Ctrl Pts',(-187.669824066007,4.17793632482349,
128.209359436792));
#245754=CARTESIAN_POINT('Ctrl Pts',(-187.677581106892,4.1057373312515,128.093119490508));
#245755=CARTESIAN_POINT('Ctrl Pts',(-187.685338147778,4.02860809172652,
127.979773445279));
#245756=CARTESIAN_POINT('Ctrl Pts',(-187.693095188663,3.94681182647804,
127.869763631799));
#245757=CARTESIAN_POINT('Ctrl Pts',(-187.700846379903,3.86507724442891,
127.759836777574));
#245758=CARTESIAN_POINT('Ctrl Pts',(-187.708597571143,3.77868287422416,
127.653241459867));
#245759=CARTESIAN_POINT('Ctrl Pts',(-187.716348762383,3.68793561126631,
127.550391658025));
#245760=CARTESIAN_POINT('Ctrl Pts',(-187.72409665916,3.59722691831658,127.447585570094));
#245761=CARTESIAN_POINT('Ctrl Pts',(-187.731844555937,3.50216927043818,
127.348522124323));
#245762=CARTESIAN_POINT('Ctrl Pts',(-187.739592452715,3.40311012538557,
127.253582599019));
#245763=CARTESIAN_POINT('Ctrl Pts',(-187.747338728799,3.30407170137063,
127.158662933017));
#245764=CARTESIAN_POINT('Ctrl Pts',(-187.755085004883,3.20103372715624,
127.067865742005));
#245765=CARTESIAN_POINT('Ctrl Pts',(-187.762831280967,3.09438055082806,
126.981535475193));
#245766=CARTESIAN_POINT('Ctrl Pts',(-187.770577614232,2.9877265872108,126.895204571112));
#245767=CARTESIAN_POINT('Ctrl Pts',(-187.778323947498,2.87745767211547,
126.813340903009));
#245768=CARTESIAN_POINT('Ctrl Pts',(-187.786070280763,2.76399094455158,
126.736248386944));
#245769=CARTESIAN_POINT('Ctrl Pts',(-187.793818348766,2.6504988069003,126.659138606544));
#245770=CARTESIAN_POINT('Ctrl Pts',(-187.801566416769,2.53380775509228,
126.586802323981));
#245771=CARTESIAN_POINT('Ctrl Pts',(-187.809314484772,2.41436324092127,
126.519499685938));
#245772=CARTESIAN_POINT('Ctrl Pts',(-187.817070787514,2.29479177969936,
126.452125517851));
#245773=CARTESIAN_POINT('Ctrl Pts',(-187.824827090256,2.17246135144864,
126.389795873351));
#245774=CARTESIAN_POINT('Ctrl Pts',(-187.832583392998,2.0478417996602,126.33272478422));
#245775=CARTESIAN_POINT('Ctrl Pts',(-187.840343835512,1.92315573466474,
126.27562323453));
#245776=CARTESIAN_POINT('Ctrl Pts',(-187.848104278026,1.79617847343045,
126.223785980392));
#245777=CARTESIAN_POINT('Ctrl Pts',(-187.855864720541,1.66739816011783,
126.177378184259));
#245778=CARTESIAN_POINT('Ctrl Pts',(-187.863637620806,1.53841111721335,
126.130895890211));
#245779=CARTESIAN_POINT('Ctrl Pts',(-187.871410521072,1.40761561151015,
126.089860588313));
#245780=CARTESIAN_POINT('Ctrl Pts',(-187.879183421337,1.27551407480012,
126.054387258958));
#245781=CARTESIAN_POINT('Ctrl Pts',(-187.886673757098,1.14821476170498,
126.02020347448));
#245782=CARTESIAN_POINT('Ctrl Pts',(-187.89416409286,1.01970302453186,125.991184367656));
#245783=CARTESIAN_POINT('Ctrl Pts',(-187.901654428621,0.890433888279403,
125.967387333259));
#245784=CARTESIAN_POINT('Ctrl Pts',(-187.90942876274,0.756263473425365,
125.942688027067));
#245785=CARTESIAN_POINT('Ctrl Pts',(-187.917203096859,0.620852080617946,
125.923536360038));
#245786=CARTESIAN_POINT('Ctrl Pts',(-187.924977430978,0.484698250610068,
125.910052630899));
#245787=CARTESIAN_POINT('Ctrl Pts',(-187.932742183925,0.34871221802889,
125.89658551925));
#245788=CARTESIAN_POINT('Ctrl Pts',(-187.940506936872,0.211985954126687,
125.888772485131));
#245789=CARTESIAN_POINT('Ctrl Pts',(-187.948271689819,0.0750286477215531,
125.886682937551));
#245790=CARTESIAN_POINT('Ctrl Pts',(-187.956028730704,-0.0617926307557264,
125.884595465339));
#245791=CARTESIAN_POINT('Ctrl Pts',(-187.963785771589,-0.198844106680892,
125.888220172887));
#245792=CARTESIAN_POINT('Ctrl Pts',(-187.971542812474,-0.33561135775171,
125.897574696105));
#245793=CARTESIAN_POINT('Ctrl Pts',(-187.979294003714,-0.472275471574414,
125.906922165004));
#245794=CARTESIAN_POINT('Ctrl Pts',(-187.987045194954,-0.608655398690284,
125.921990822516));
#245795=CARTESIAN_POINT('Ctrl Pts',(-187.994796386194,-0.744236962088531,
125.942746234795));
#245796=CARTESIAN_POINT('Ctrl Pts',(-188.002544282971,-0.879760899705762,
125.963492825471));
#245797=CARTESIAN_POINT('Ctrl Pts',(-188.010292179749,-1.01448676284468,
125.989921304604));
#245798=CARTESIAN_POINT('Ctrl Pts',(-188.018040076526,-1.14790596186375,
126.021945436382));
#245799=CARTESIAN_POINT('Ctrl Pts',(-188.02578635261,-1.28129725246294,
126.053962869403));
#245800=CARTESIAN_POINT('Ctrl Pts',(-188.033532628694,-1.41338204267613,
126.091573535708));
#245801=CARTESIAN_POINT('Ctrl Pts',(-188.041278904778,-1.54366278809802,
126.134640255581));
#245802=CARTESIAN_POINT('Ctrl Pts',(-188.049025238043,-1.67394449522224,
126.177707293362));
#245803=CARTESIAN_POINT('Ctrl Pts',(-188.056771571308,-1.80242175977307,
126.226230342367));
#245804=CARTESIAN_POINT('Ctrl Pts',(-188.064517904574,-1.928613414739,126.280022725787));
#245805=CARTESIAN_POINT('Ctrl Pts',(-188.072265972577,-2.05483332945198,
126.333827155638));
#245806=CARTESIAN_POINT('Ctrl Pts',(-188.080014040579,-2.17876625648171,
126.392903114748));
#245807=CARTESIAN_POINT('Ctrl Pts',(-188.087762108582,-2.29995254948067,
126.457016447543));
#245808=CARTESIAN_POINT('Ctrl Pts',(-188.095518411324,-2.42126764071347,
126.52119792075));
#245809=CARTESIAN_POINT('Ctrl Pts',(-188.103274714066,-2.53982992045492,
126.590427279275));
#245810=CARTESIAN_POINT('Ctrl Pts',(-188.111031016808,-2.65520535582168,
126.664424919887));
#245811=CARTESIAN_POINT('Ctrl Pts',(-188.118791459322,-2.77064237053186,
126.738462055268));
#245812=CARTESIAN_POINT('Ctrl Pts',(-188.126551901836,-2.88288883183471,
126.817272319268));
#245813=CARTESIAN_POINT('Ctrl Pts',(-188.13431234435,-2.99154193003811,
126.900534296721));
#245814=CARTESIAN_POINT('Ctrl Pts',(-188.142085244616,-3.1003694478408,
126.983929933691));
#245815=CARTESIAN_POINT('Ctrl Pts',(-188.149858144881,-3.20559177519847,
127.071791313939));
#245816=CARTESIAN_POINT('Ctrl Pts',(-188.157631045146,-3.30684059919295,
127.163757877081));
#245817=CARTESIAN_POINT('Ctrl Pts',(-188.165121380909,-3.4044087734147,
127.252381224011));
#245818=CARTESIAN_POINT('Ctrl Pts',(-188.172611716672,-3.49828710288302,
127.344816252083));
#245819=CARTESIAN_POINT('Ctrl Pts',(-188.180102052434,-3.58818134762388,
127.440711159156));
#245820=CARTESIAN_POINT('Ctrl Pts',(-188.187783968033,-3.6803748116775,
127.539058764095));
#245821=CARTESIAN_POINT('Ctrl Pts',(-188.195465883631,-3.76868519027518,
127.641374004402));
#245822=CARTESIAN_POINT('Ctrl Pts',(-188.20314779923,-3.85274535651832,
127.747313630631));
#245823=CARTESIAN_POINT('Ctrl Pts',(-188.210820609535,-3.93670588713396,
127.85312768774));
#245824=CARTESIAN_POINT('Ctrl Pts',(-188.21849341984,-4.01642597523958,
127.962557278402));
#245825=CARTESIAN_POINT('Ctrl Pts',(-188.226166230145,-4.09157506968238,
128.075222198274));
#245826=CARTESIAN_POINT('Ctrl Pts',(-188.233972786232,-4.16803409802803,
128.189850995414));
#245827=CARTESIAN_POINT('Ctrl Pts',(-188.241779342318,-4.23976097868823,
128.307828684763));
#245828=CARTESIAN_POINT('Ctrl Pts',(-188.249585898404,-4.3064496647105,
128.428718736344));
#245829=CARTESIAN_POINT('Ctrl Pts',(-188.257245164482,-4.37188010355881,
128.547327897795));
#245830=CARTESIAN_POINT('Ctrl Pts',(-188.26490443056,-4.43246057085316,
128.668740130964));
#245831=CARTESIAN_POINT('Ctrl Pts',(-188.272563696638,-4.4879455798733,
128.792513820567));
#245832=CARTESIAN_POINT('Ctrl Pts',(-188.280443897728,-4.54503107920871,
128.919857818529));
#245833=CARTESIAN_POINT('Ctrl Pts',(-188.288324098819,-4.59672247009533,
129.049701204745));
#245834=CARTESIAN_POINT('Ctrl Pts',(-188.29620429991,-4.64280362102202,
129.181536659422));
#245835=CARTESIAN_POINT('Ctrl Pts',(-188.304084501,-4.68888477194858,129.3133721141));
#245836=CARTESIAN_POINT('Ctrl Pts',(-188.311964702091,-4.72935551781386,
129.447199204311));
#245837=CARTESIAN_POINT('Ctrl Pts',(-188.319844903182,-4.76405452823404,
129.582490119308));
#245838=CARTESIAN_POINT('Ctrl Pts',(-186.570144995258,-4.76405452823391,
129.582490119308));
#245839=CARTESIAN_POINT('Ctrl Pts',(-186.57840025716,-4.80024267923322,
129.723587170822));
#245840=CARTESIAN_POINT('Ctrl Pts',(-186.586655519063,-4.83019874442568,
129.866450467451));
#245841=CARTESIAN_POINT('Ctrl Pts',(-186.594910780965,-4.8537620318651,
130.010523606257));
#245842=CARTESIAN_POINT('Ctrl Pts',(-186.603145195941,-4.87726581518243,
130.154232918679));
#245843=CARTESIAN_POINT('Ctrl Pts',(-186.611379610917,-4.89440896454415,
130.299145675755));
#245844=CARTESIAN_POINT('Ctrl Pts',(-186.619614025893,-4.90508133671532,
130.444693906975));
#245845=CARTESIAN_POINT('Ctrl Pts',(-186.626362495915,-4.9138278213004,
130.563977168498));
#245846=CARTESIAN_POINT('Ctrl Pts',(-186.633110965936,-4.91822907159551,
130.683686883876));
#245847=CARTESIAN_POINT('Ctrl Pts',(-186.639859435957,-4.91824992550734,
130.803504611091));
#245848=CARTESIAN_POINT('Origin',(213.235140564004,0.,130.804360617566));
#245849=CARTESIAN_POINT('',(-184.819837330039,-4.76405452823405,129.582490119308));
#245850=CARTESIAN_POINT('',(-185.165421073984,-4.76405452823401,129.582490119308));
#245851=CARTESIAN_POINT('',(213.235140564004,-4.76405452823405,129.582490119308));
#245852=CARTESIAN_POINT('',(-185.235140563977,-4.91824999726717,130.804196661748));
#245853=CARTESIAN_POINT('Ctrl Pts',(-185.165421073984,-4.76405452823401,
129.582490119308));
#245854=CARTESIAN_POINT('Ctrl Pts',(-185.17357585509,-4.79982922771808,
129.72197512964));
#245855=CARTESIAN_POINT('Ctrl Pts',(-185.181730636195,-4.82951156155369,
129.863179394967));
#245856=CARTESIAN_POINT('Ctrl Pts',(-185.189885417301,-4.85294732447109,
130.005558183663));
#245857=CARTESIAN_POINT('Ctrl Pts',(-185.198024167137,-4.87633701563996,
130.147657073652));
#245858=CARTESIAN_POINT('Ctrl Pts',(-185.206162916974,-4.89350457056318,
130.29092555989));
#245859=CARTESIAN_POINT('Ctrl Pts',(-185.21430166681,-4.90434637358492,
130.434807224395));
#245860=CARTESIAN_POINT('Ctrl Pts',(-185.221247965866,-4.9135996873744,
130.557608034144));
#245861=CARTESIAN_POINT('Ctrl Pts',(-185.228194264921,-4.91824588552851,
130.680855148721));
#245862=CARTESIAN_POINT('Ctrl Pts',(-185.235140563977,-4.91824999726717,
130.804196661748));
#245863=CARTESIAN_POINT('Ctrl Pts',(-185.235140564012,-4.91824999726719,
130.804196662373));
#245864=CARTESIAN_POINT('Ctrl Pts',(-185.243235275636,-4.91825478877005,
130.947929889419));
#245865=CARTESIAN_POINT('Ctrl Pts',(-185.251329987261,-4.91195447570265,
131.09154808551));
#245866=CARTESIAN_POINT('Ctrl Pts',(-185.259424698885,-4.89940510202952,
131.234491654236));
#245867=CARTESIAN_POINT('Ctrl Pts',(-185.267529366981,-4.88684029266407,
131.377611043127));
#245868=CARTESIAN_POINT('Ctrl Pts',(-185.275634035077,-4.86801111637512,
131.520053813894));
#245869=CARTESIAN_POINT('Ctrl Pts',(-185.283738703172,-4.84302506459005,
131.661268597604));
#245870=CARTESIAN_POINT('Ctrl Pts',(-185.291861849205,-4.8179820467862,
131.802805338704));
#245871=CARTESIAN_POINT('Ctrl Pts',(-185.299984995237,-4.78675414792536,
131.9431081626));
#245872=CARTESIAN_POINT('Ctrl Pts',(-185.308108141269,-4.74949972502816,
132.081637182942));
#245873=CARTESIAN_POINT('Ctrl Pts',(-185.316240943695,-4.71220101591753,
132.220330879723));
#245874=CARTESIAN_POINT('Ctrl Pts',(-185.324373746121,-4.66886158835768,
132.357246244439));
#245875=CARTESIAN_POINT('Ctrl Pts',(-185.332506548547,-4.61968871556572,
132.491861501647));
#245876=CARTESIAN_POINT('Ctrl Pts',(-185.340657905423,-4.57040365811858,
132.626783874656));
#245877=CARTESIAN_POINT('Ctrl Pts',(-185.3488092623,-4.51525867281962,132.759395335421));
#245878=CARTESIAN_POINT('Ctrl Pts',(-185.356960619176,-4.45450870042069,
132.889195215412));
#245879=CARTESIAN_POINT('Ctrl Pts',(-185.363319352166,-4.40711869413288,
132.990449864361));
#245880=CARTESIAN_POINT('Ctrl Pts',(-185.369678085156,-4.35631884409728,
133.08999403756));
#245881=CARTESIAN_POINT('Ctrl Pts',(-185.376036818146,-4.3022485761293,
133.187602160443));
#245882=CARTESIAN_POINT('Ctrl Pts',(-185.383811152265,-4.23614101511718,
133.306940110507));
#245883=CARTESIAN_POINT('Ctrl Pts',(-185.391585486384,-4.16495959670137,
133.423714411295));
#245884=CARTESIAN_POINT('Ctrl Pts',(-185.399359820503,-4.08892792282361,
133.537463525335));
#245885=CARTESIAN_POINT('Ctrl Pts',(-185.40712457345,-4.01298995118897,
133.651072453757));
#245886=CARTESIAN_POINT('Ctrl Pts',(-185.414889326397,-3.93221383272465,
133.761663291662));
#245887=CARTESIAN_POINT('Ctrl Pts',(-185.422654079344,-3.84686924586274,
133.868798586874));
#245888=CARTESIAN_POINT('Ctrl Pts',(-185.430411120229,-3.76160942444742,
133.9758274738));
#245889=CARTESIAN_POINT('Ctrl Pts',(-185.438168161114,-3.67179040642328,
134.079407344235));
#245890=CARTESIAN_POINT('Ctrl Pts',(-185.445925201999,-3.57772519128268,
134.179129575311));
#245891=CARTESIAN_POINT('Ctrl Pts',(-185.453676393239,-3.48373091145266,
134.278776605077));
#245892=CARTESIAN_POINT('Ctrl Pts',(-185.461427584479,-3.38549707525688,
134.37457150257));
#245893=CARTESIAN_POINT('Ctrl Pts',(-185.469178775719,-3.28337675376989,
134.466138895303));
#245894=CARTESIAN_POINT('Ctrl Pts',(-185.476926672496,-3.18129983614355,
134.557667369451));
#245895=CARTESIAN_POINT('Ctrl Pts',(-185.484674569273,-3.07534000912483,
134.644971652084));
#245896=CARTESIAN_POINT('Ctrl Pts',(-185.49242246605,-2.96588681661787,
134.727713578174));
#245897=CARTESIAN_POINT('Ctrl Pts',(-185.500168742134,-2.85645651935925,
134.810438196437));
#245898=CARTESIAN_POINT('Ctrl Pts',(-185.507915018218,-2.74353462176835,
134.888602120789));
#245899=CARTESIAN_POINT('Ctrl Pts',(-185.515661294302,-2.62754301228335,
134.961908065413));
#245900=CARTESIAN_POINT('Ctrl Pts',(-185.523407627568,-2.51155054657478,
135.035214551166));
#245901=CARTESIAN_POINT('Ctrl Pts',(-185.531153960833,-2.39248865425077,
135.103662776763));
#245902=CARTESIAN_POINT('Ctrl Pts',(-185.538900294098,-2.27080706495366,
135.166999536415));
#245903=CARTESIAN_POINT('Ctrl Pts',(-185.546648362101,-2.14909822590848,
135.230350479895));
#245904=CARTESIAN_POINT('Ctrl Pts',(-185.554396430104,-2.02476886923059,
135.288587499175));
#245905=CARTESIAN_POINT('Ctrl Pts',(-185.562144498107,-1.89829174083592,
135.341504160499));
#245906=CARTESIAN_POINT('Ctrl Pts',(-185.569900800848,-1.77168019104392,
135.394477062279));
#245907=CARTESIAN_POINT('Ctrl Pts',(-185.57765710359,-1.64291667088637,
135.442118159409));
#245908=CARTESIAN_POINT('Ctrl Pts',(-185.585413406332,-1.51249277472832,
135.484269662504));
#245909=CARTESIAN_POINT('Ctrl Pts',(-185.593173848846,-1.38199926740991,
135.526443663125));
#245910=CARTESIAN_POINT('Ctrl Pts',(-185.60093429136,-1.24984399481776,
135.563122127009));
#245911=CARTESIAN_POINT('Ctrl Pts',(-185.608694733874,-1.11653102912432,
135.594197934584));
#245912=CARTESIAN_POINT('Ctrl Pts',(-185.61646763414,-0.983004057623368,
135.625323627805));
#245913=CARTESIAN_POINT('Ctrl Pts',(-185.624240534405,-0.848316063641948,
135.650828619293));
#245914=CARTESIAN_POINT('Ctrl Pts',(-185.63201343467,-0.712979458432716,
135.670657295159));
#245915=CARTESIAN_POINT('Ctrl Pts',(-185.639503770433,-0.582562679703454,
135.689765148714));
#245916=CARTESIAN_POINT('Ctrl Pts',(-185.646994106196,-0.451543934645043,
135.703602186016));
#245917=CARTESIAN_POINT('Ctrl Pts',(-185.654484441958,-0.320381836731385,
135.712164458511));
#245918=CARTESIAN_POINT('Ctrl Pts',(-185.662258776077,-0.184246688020785,
135.721051372169));
#245919=CARTESIAN_POINT('Ctrl Pts',(-185.670033110196,-0.047525866190644,
135.72428379084));
#245920=CARTESIAN_POINT('Ctrl Pts',(-185.677807444315,0.0892714619018228,
135.721800364893));
#245921=CARTESIAN_POINT('Ctrl Pts',(-185.685572197262,0.225900199513344,
135.719319999546));
#245922=CARTESIAN_POINT('Ctrl Pts',(-185.69333695021,0.362604868635719,
135.711137812602));
#245923=CARTESIAN_POINT('Ctrl Pts',(-185.701101703157,0.498871660584027,
135.697244238578));
#245924=CARTESIAN_POINT('Ctrl Pts',(-185.708858744042,0.635003110433547,
135.683364463847));
#245925=CARTESIAN_POINT('Ctrl Pts',(-185.716615784927,0.770697162159242,
135.663784630225));
#245926=CARTESIAN_POINT('Ctrl Pts',(-185.724372825812,0.905440845898517,
135.638547202409));
#245927=CARTESIAN_POINT('Ctrl Pts',(-185.732124017052,1.04008291837792,
135.613328806334));
#245928=CARTESIAN_POINT('Ctrl Pts',(-185.739875208292,1.17377566665088,
135.58246137983));
#245929=CARTESIAN_POINT('Ctrl Pts',(-185.747626399532,1.3060124356725,135.546039073595));
#245930=CARTESIAN_POINT('Ctrl Pts',(-185.755374296309,1.43819300053959,
135.509632247811));
#245931=CARTESIAN_POINT('Ctrl Pts',(-185.763122193086,1.56891844082116,
135.46767534169));
#245932=CARTESIAN_POINT('Ctrl Pts',(-185.770870089863,1.69769369070752,
135.420313303094));
#245933=CARTESIAN_POINT('Ctrl Pts',(-185.778616365947,1.82644200358802,
135.372961171615));
#245934=CARTESIAN_POINT('Ctrl Pts',(-185.786362642032,1.95324057078163,
135.320206291428));
#245935=CARTESIAN_POINT('Ctrl Pts',(-185.794108918116,2.07761123630648,
135.262242918981));
#245936=CARTESIAN_POINT('Ctrl Pts',(-185.801855251381,2.20198281990683,
135.204279118662));
#245937=CARTESIAN_POINT('Ctrl Pts',(-185.809601584646,2.32392611170664,
135.141106914518));
#245938=CARTESIAN_POINT('Ctrl Pts',(-185.817347917912,2.44298499264541,
135.072967812918));
#245939=CARTESIAN_POINT('Ctrl Pts',(-185.825095985915,2.56207053599523,
135.004813452038));
#245940=CARTESIAN_POINT('Ctrl Pts',(-185.832844053918,2.67827004387223,
134.931690174513));
#245941=CARTESIAN_POINT('Ctrl Pts',(-185.840592121921,2.79115430699464,
134.853884132382));
#245942=CARTESIAN_POINT('Ctrl Pts',(-185.848348424663,2.9041585448554,134.775995397063));
#245943=CARTESIAN_POINT('Ctrl Pts',(-185.856104727404,3.01384017700653,
134.693414177478));
#245944=CARTESIAN_POINT('Ctrl Pts',(-185.863861030146,3.11980073200734,
134.606468776873));
#245945=CARTESIAN_POINT('Ctrl Pts',(-185.871621472661,3.22581784134676,
134.519476970889));
#245946=CARTESIAN_POINT('Ctrl Pts',(-185.879381915175,3.32810962470852,
134.428116602875));
#245947=CARTESIAN_POINT('Ctrl Pts',(-185.887142357689,3.42631349604209,
134.33275386228));
#245948=CARTESIAN_POINT('Ctrl Pts',(-185.894915257954,3.52467501294806,
134.237238036947));
#245949=CARTESIAN_POINT('Ctrl Pts',(-185.90268815822,3.61893523531003,134.13770728394));
#245950=CARTESIAN_POINT('Ctrl Pts',(-185.910461058485,3.70877040278946,
134.034562648692));
#245951=CARTESIAN_POINT('Ctrl Pts',(-185.917951394247,3.79533983565013,
133.935167580741));
#245952=CARTESIAN_POINT('Ctrl Pts',(-185.925441730009,3.8778001590255,133.832417056538));
#245953=CARTESIAN_POINT('Ctrl Pts',(-185.932932065771,3.9559001591004,133.726694786296));
#245954=CARTESIAN_POINT('Ctrl Pts',(-185.94070639989,4.03696134441601,133.616964024045));
#245955=CARTESIAN_POINT('Ctrl Pts',(-185.948480734009,4.11358181358176,
133.503684125752));
#245956=CARTESIAN_POINT('Ctrl Pts',(-185.956255068128,4.18543473429262,
133.38725030694));
#245957=CARTESIAN_POINT('Ctrl Pts',(-185.964019821076,4.25719910270018,
133.270959982405));
#245958=CARTESIAN_POINT('Ctrl Pts',(-185.971784574023,4.32420740995068,
133.15152380069));
#245959=CARTESIAN_POINT('Ctrl Pts',(-185.97954932697,4.38617388218686,133.029368873219));
#245960=CARTESIAN_POINT('Ctrl Pts',(-185.987306367855,4.44807880844942,
132.907335271742));
#245961=CARTESIAN_POINT('Ctrl Pts',(-185.99506340874,4.50495168936313,132.782588644633));
#245962=CARTESIAN_POINT('Ctrl Pts',(-186.002820449625,4.55655097893896,
132.655583521171));
#245963=CARTESIAN_POINT('Ctrl Pts',(-186.010571640865,4.60811135708892,
132.52867417326));
#245964=CARTESIAN_POINT('Ctrl Pts',(-186.018322832105,4.65440591302887,
132.399510079759));
#245965=CARTESIAN_POINT('Ctrl Pts',(-186.026074023345,4.69523999897835,
132.268568394657));
#245966=CARTESIAN_POINT('Ctrl Pts',(-186.033821920122,4.73605672935219,
132.137682363264));
#245967=CARTESIAN_POINT('Ctrl Pts',(-186.041569816899,4.77141748956988,
132.005020615405));
#245968=CARTESIAN_POINT('Ctrl Pts',(-186.049317713676,4.80117663320995,
131.871078011827));
#245969=CARTESIAN_POINT('Ctrl Pts',(-186.05706398976,4.83092955187871,131.737163426154));
#245970=CARTESIAN_POINT('Ctrl Pts',(-186.064810265844,4.85508309987727,
131.601968899102));
#245971=CARTESIAN_POINT('Ctrl Pts',(-186.072556541928,4.87354225566816,
131.466001717194));
#245972=CARTESIAN_POINT('Ctrl Pts',(-186.080302875194,4.89200154772027,
131.330033531608));
#245973=CARTESIAN_POINT('Ctrl Pts',(-186.088049208459,4.90476631109189,
131.193293067196));
#245974=CARTESIAN_POINT('Ctrl Pts',(-186.095795541724,4.91179318843833,
131.056294609935));
#245975=CARTESIAN_POINT('Ctrl Pts',(-186.103543609727,4.91882163940525,
130.919265472818));
#245976=CARTESIAN_POINT('Ctrl Pts',(-186.11129167773,4.92010962740263,130.781978618262));
#245977=CARTESIAN_POINT('Ctrl Pts',(-186.119039745733,4.91566590214478,
130.644949824358));
#245978=CARTESIAN_POINT('Ctrl Pts',(-186.126796048475,4.91121745404283,
130.507775394621));
#245979=CARTESIAN_POINT('Ctrl Pts',(-186.134552351217,4.90102513648487,
130.370859964803));
#245980=CARTESIAN_POINT('Ctrl Pts',(-186.142308653959,4.88514977674217,
130.234716236135));
#245981=CARTESIAN_POINT('Ctrl Pts',(-186.150069096473,4.86926594384197,
130.09849984346));
#245982=CARTESIAN_POINT('Ctrl Pts',(-186.157829538987,4.84769308629387,
129.963056358551));
#245983=CARTESIAN_POINT('Ctrl Pts',(-186.165589981501,4.82054330303636,
129.828888769663));
#245984=CARTESIAN_POINT('Ctrl Pts',(-186.173362881767,4.79334993653653,
129.694505803051));
#245985=CARTESIAN_POINT('Ctrl Pts',(-186.181135782032,4.76056184779475,
129.561403205215));
#245986=CARTESIAN_POINT('Ctrl Pts',(-186.188908682298,4.72234144732119,
129.430070139751));
#245987=CARTESIAN_POINT('Ctrl Pts',(-186.19639901806,4.68551045467694,129.303511362027));
#245988=CARTESIAN_POINT('Ctrl Pts',(-186.203889353822,4.6436353476091,129.178595988423));
#245989=CARTESIAN_POINT('Ctrl Pts',(-186.211379689583,4.59690316518476,
129.05574277698));
#245990=CARTESIAN_POINT('Ctrl Pts',(-186.219154023703,4.54839911785924,
128.928231548683));
#245991=CARTESIAN_POINT('Ctrl Pts',(-186.226928357822,4.49450876631522,
128.802538025928));
#245992=CARTESIAN_POINT('Ctrl Pts',(-186.234702691941,4.43538795572149,
128.679150805632));
#245993=CARTESIAN_POINT('Ctrl Pts',(-186.242467444888,4.37634000624273,
128.555915649057));
#245994=CARTESIAN_POINT('Ctrl Pts',(-186.250232197835,4.31207459079579,
128.434981488786));
#245995=CARTESIAN_POINT('Ctrl Pts',(-186.257996950782,4.2427965825651,128.316819618613));
#245996=CARTESIAN_POINT('Ctrl Pts',(-186.265753991667,4.17358738222901,
128.198775108475));
#245997=CARTESIAN_POINT('Ctrl Pts',(-186.273511032552,4.09937569316561,
128.083497743981));
#245998=CARTESIAN_POINT('Ctrl Pts',(-186.281268073437,4.02041336222315,
127.971436428789));
#245999=CARTESIAN_POINT('Ctrl Pts',(-186.289019264677,3.94151057738879,
127.859459619907));
#246000=CARTESIAN_POINT('Ctrl Pts',(-186.296770455917,3.85786450570213,
127.750694351319));
#246001=CARTESIAN_POINT('Ctrl Pts',(-186.304521647158,3.76977137844832,
127.645562299102));
#246002=CARTESIAN_POINT('Ctrl Pts',(-186.312269543935,3.68171569312366,
127.540474930812));
#246003=CARTESIAN_POINT('Ctrl Pts',(-186.320017440712,3.58921696210682,
127.439018006611));
#246004=CARTESIAN_POINT('Ctrl Pts',(-186.327765337489,3.49261280031067,
127.341581547281));
#246005=CARTESIAN_POINT('Ctrl Pts',(-186.335511613573,3.39602884602262,
127.244165469557));
#246006=CARTESIAN_POINT('Ctrl Pts',(-186.343257889657,3.29534144418254,
127.15076846138));
#246007=CARTESIAN_POINT('Ctrl Pts',(-186.351004165741,3.19092602784825,
127.061744667819));
#246008=CARTESIAN_POINT('Ctrl Pts',(-186.358750499007,3.08650984074266,
126.972720217104));
#246009=CARTESIAN_POINT('Ctrl Pts',(-186.366496832272,2.97836588174077,
126.888069299076));
#246010=CARTESIAN_POINT('Ctrl Pts',(-186.374243165537,2.86690339849536,
126.808106375629));
#246011=CARTESIAN_POINT('Ctrl Pts',(-186.38199123354,2.75541595399981,126.728125545041));
#246012=CARTESIAN_POINT('Ctrl Pts',(-186.389739301543,2.64060882406983,
126.652835025955));
#246013=CARTESIAN_POINT('Ctrl Pts',(-186.397487369546,2.52292067685579,
126.582506247648));
#246014=CARTESIAN_POINT('Ctrl Pts',(-186.405243672288,2.40510744927854,
126.512102723079));
#246015=CARTESIAN_POINT('Ctrl Pts',(-186.41299997503,2.2844074239254,126.44667167434));
#246016=CARTESIAN_POINT('Ctrl Pts',(-186.420756277772,2.16128482948886,
126.386439053264));
#246017=CARTESIAN_POINT('Ctrl Pts',(-186.428516720286,2.03809652081653,
126.326174284226));
#246018=CARTESIAN_POINT('Ctrl Pts',(-186.4362771628,1.9124834245532,126.271113628271));
#246019=CARTESIAN_POINT('Ctrl Pts',(-186.444037605315,1.78492931117828,
126.221434650829));
#246020=CARTESIAN_POINT('Ctrl Pts',(-186.45181050558,1.65717043661684,126.171675924281));
#246021=CARTESIAN_POINT('Ctrl Pts',(-186.459583405845,1.52746468853852,
126.127316266604));
#246022=CARTESIAN_POINT('Ctrl Pts',(-186.467356306111,1.39631140097754,
126.088483442109));
#246023=CARTESIAN_POINT('Ctrl Pts',(-186.474846641873,1.26992586577211,
126.051062288597));
#246024=CARTESIAN_POINT('Ctrl Pts',(-186.482336977635,1.14219650594113,
126.018773191476));
#246025=CARTESIAN_POINT('Ctrl Pts',(-186.489827313397,1.0135767336687,125.991685138431));
#246026=CARTESIAN_POINT('Ctrl Pts',(-186.497601647516,0.880080303639861,
125.963570033623));
#246027=CARTESIAN_POINT('Ctrl Pts',(-186.505375981635,0.745201731765015,
125.940969093346));
#246028=CARTESIAN_POINT('Ctrl Pts',(-186.513150315754,0.609436326590159,
125.924015299217));
#246029=CARTESIAN_POINT('Ctrl Pts',(-186.520915068702,0.47383824014311,
125.907082399123));
#246030=CARTESIAN_POINT('Ctrl Pts',(-186.528679821649,0.337355879254183,
125.895782845622));
#246031=CARTESIAN_POINT('Ctrl Pts',(-186.536444574596,0.200496495701578,
125.890199018909));
#246032=CARTESIAN_POINT('Ctrl Pts',(-186.544201615481,0.0637730428177244,
125.884620738132));
#246033=CARTESIAN_POINT('Ctrl Pts',(-186.551958656366,-0.0733262994167068,
125.88474690261));
#246034=CARTESIAN_POINT('Ctrl Pts',(-186.559715697251,-0.2102877262663,
125.89060826985));
#246035=CARTESIAN_POINT('Ctrl Pts',(-186.567466888491,-0.34714586943757,
125.896465216988));
#246036=CARTESIAN_POINT('Ctrl Pts',(-186.575218079731,-0.483865915208605,
125.908048741667));
#246037=CARTESIAN_POINT('Ctrl Pts',(-186.582969270971,-0.619932975308011,
125.925337542336));
#246038=CARTESIAN_POINT('Ctrl Pts',(-186.590717167748,-0.755942203277722,
125.942618994804));
#246039=CARTESIAN_POINT('Ctrl Pts',(-186.598465064525,-0.891298610539438,
125.965600851155));
#246040=CARTESIAN_POINT('Ctrl Pts',(-186.606212961302,-1.02549157245746,
125.994209882161));
#246041=CARTESIAN_POINT('Ctrl Pts',(-186.613959237386,-1.15965646410071,
126.022812928774));
#246042=CARTESIAN_POINT('Ctrl Pts',(-186.62170551347,-1.29265801234209,
126.057040727289));
#246043=CARTESIAN_POINT('Ctrl Pts',(-186.629451789554,-1.42399533416772,
126.096768839303));
#246044=CARTESIAN_POINT('Ctrl Pts',(-186.63719812282,-1.55533362549545,
126.136497244581));
#246045=CARTESIAN_POINT('Ctrl Pts',(-186.644944456085,-1.68500729167432,
126.181725931178));
#246046=CARTESIAN_POINT('Ctrl Pts',(-186.65269078935,-1.81253055865413,
126.232280561788));
#246047=CARTESIAN_POINT('Ctrl Pts',(-186.660438857353,-1.94008238358522,
126.282846513757));
#246048=CARTESIAN_POINT('Ctrl Pts',(-186.668186925356,-2.06548248767706,
126.338740639035));
#246049=CARTESIAN_POINT('Ctrl Pts',(-186.675934993359,-2.18826539894326,
126.399740587837));
#246050=CARTESIAN_POINT('Ctrl Pts',(-186.683691296101,-2.31117880534887,
126.460805368111));
#246051=CARTESIAN_POINT('Ctrl Pts',(-186.691447598843,-2.43146911172216,
126.526986637757));
#246052=CARTESIAN_POINT('Ctrl Pts',(-186.699203901585,-2.54869529143897,
126.598015960516));
#246053=CARTESIAN_POINT('Ctrl Pts',(-186.706964344099,-2.66598403829782,
126.669083193762));
#246054=CARTESIAN_POINT('Ctrl Pts',(-186.714724786613,-2.7802050743521,
126.745003419722));
#246055=CARTESIAN_POINT('Ctrl Pts',(-186.722485229127,-2.89094751901861,
126.825465607041));
#246056=CARTESIAN_POINT('Ctrl Pts',(-186.730258129393,-3.00186773728824,
126.906056959406));
#246057=CARTESIAN_POINT('Ctrl Pts',(-186.738031029658,-3.10929789869776,
126.991204600203));
#246058=CARTESIAN_POINT('Ctrl Pts',(-186.745803929924,-3.21286060927254,
127.080557485299));
#246059=CARTESIAN_POINT('Ctrl Pts',(-186.753294265686,-3.31265855445779,
127.166662167953));
#246060=CARTESIAN_POINT('Ctrl Pts',(-186.760784601447,-3.40886512528903,
127.256671450161));
#246061=CARTESIAN_POINT('Ctrl Pts',(-186.768274937209,-3.50117720011197,
127.350241152939));
#246062=CARTESIAN_POINT('Ctrl Pts',(-186.775943029108,-3.5956799694917,
127.446031395543));
#246063=CARTESIAN_POINT('Ctrl Pts',(-186.783611121006,-3.68641809312052,
127.545874838496));
#246064=CARTESIAN_POINT('Ctrl Pts',(-186.791279212905,-3.77301654595831,
127.649439191219));
#246065=CARTESIAN_POINT('Ctrl Pts',(-186.798938310547,-3.85951342349731,
127.75288206856));
#246066=CARTESIAN_POINT('Ctrl Pts',(-186.806597408188,-3.94188002817934,
127.860036873487));
#246067=CARTESIAN_POINT('Ctrl Pts',(-186.81425650583,-4.0197769009932,127.970533394756));
#246068=CARTESIAN_POINT('Ctrl Pts',(-186.821908387342,-4.09760038214203,
128.080925810129));
#246069=CARTESIAN_POINT('Ctrl Pts',(-186.829560268854,-4.17096227552672,
128.194653354138));
#246070=CARTESIAN_POINT('Ctrl Pts',(-186.837212150366,-4.23956264999936,
128.311311961958));
#246071=CARTESIAN_POINT('Ctrl Pts',(-186.844858218946,-4.30811091057845,
128.427881947313));
#246072=CARTESIAN_POINT('Ctrl Pts',(-186.852504287526,-4.37190464719919,
128.547378219883));
#246073=CARTESIAN_POINT('Ctrl Pts',(-186.860150356106,-4.43068697554932,
128.669367412144));
#246074=CARTESIAN_POINT('Ctrl Pts',(-186.867793074609,-4.48944354879428,
128.791303155613));
#246075=CARTESIAN_POINT('Ctrl Pts',(-186.875435793112,-4.54319290765865,
128.915729283918));
#246076=CARTESIAN_POINT('Ctrl Pts',(-186.883078511615,-4.59172410237677,
129.04218785925));
#246077=CARTESIAN_POINT('Ctrl Pts',(-186.890720376631,-4.64024987745937,
129.168632312543));
#246078=CARTESIAN_POINT('Ctrl Pts',(-186.898362241647,-4.68355850002953,
129.297108387139));
#246079=CARTESIAN_POINT('Ctrl Pts',(-186.906004106664,-4.72148732126051,
129.427138581119));
#246080=CARTESIAN_POINT('Ctrl Pts',(-186.909033691086,-4.73652403883128,
129.478688490636));
#246081=CARTESIAN_POINT('Ctrl Pts',(-186.912063275508,-4.75071576216139,
129.530482472835));
#246082=CARTESIAN_POINT('Ctrl Pts',(-186.915092859931,-4.76405452823404,
129.582490119308));
#246083=CARTESIAN_POINT('',(-184.889859436036,-4.91824816211532,130.800108753356));
#246084=CARTESIAN_POINT('Ctrl Pts',(-184.889859436036,-4.91824816211532,
130.800108753357));
#246085=CARTESIAN_POINT('Ctrl Pts',(-184.897506058226,-4.91836465031066,
130.934853849735));
#246086=CARTESIAN_POINT('Ctrl Pts',(-184.905152680416,-4.91293956817794,
131.069789576618));
#246087=CARTESIAN_POINT('Ctrl Pts',(-184.912799302606,-4.90195264080868,
131.204414826104));
#246088=CARTESIAN_POINT('Ctrl Pts',(-184.920439094191,-4.89097552788502,
131.338919817018));
#246089=CARTESIAN_POINT('Ctrl Pts',(-184.928078885776,-4.87444648449873,
131.473114482282));
#246090=CARTESIAN_POINT('Ctrl Pts',(-184.935718677362,-4.85239729067965,
131.60649751106));
#246091=CARTESIAN_POINT('Ctrl Pts',(-184.943353957593,-4.83036111707372,
131.739801776167));
#246092=CARTESIAN_POINT('Ctrl Pts',(-184.950989237825,-4.80281134123516,
131.872294960994));
#246093=CARTESIAN_POINT('Ctrl Pts',(-184.958624518056,-4.76983155314398,
132.003481135751));
#246094=CARTESIAN_POINT('Ctrl Pts',(-184.96625747086,-4.73686181813173,
132.134627321622));
#246095=CARTESIAN_POINT('Ctrl Pts',(-184.973890423664,-4.69846545941638,
132.264466898419));
#246096=CARTESIAN_POINT('Ctrl Pts',(-184.981523376467,-4.65477702326063,
132.392514868961));
#246097=CARTESIAN_POINT('Ctrl Pts',(-184.989155769078,-4.61109179346305,
132.520553441876));
#246098=CARTESIAN_POINT('Ctrl Pts',(-184.996788161688,-4.56211538887205,
132.646800288048));
#246099=CARTESIAN_POINT('Ctrl Pts',(-185.004420554298,-4.50803182670943,
132.770786846));
#246100=CARTESIAN_POINT('Ctrl Pts',(-185.012054153287,-4.45393971608056,
132.89479300131));
#246101=CARTESIAN_POINT('Ctrl Pts',(-185.019687752276,-4.39473900456917,
133.016537788303));
#246102=CARTESIAN_POINT('Ctrl Pts',(-185.027321351264,-4.33066108607502,
133.13557438298));
#246103=CARTESIAN_POINT('Ctrl Pts',(-185.034962554895,-4.26651933273594,
133.254729562698));
#246104=CARTESIAN_POINT('Ctrl Pts',(-185.042603758525,-4.19749086029851,
133.371170805936));
#246105=CARTESIAN_POINT('Ctrl Pts',(-185.050244962156,-4.12385227870567,
133.484477302696));
#246106=CARTESIAN_POINT('Ctrl Pts',(-185.057889999776,-4.05017674879779,
133.597840651233));
#246107=CARTESIAN_POINT('Ctrl Pts',(-185.065535037397,-3.9718867376698,
133.708065792888));
#246108=CARTESIAN_POINT('Ctrl Pts',(-185.073180075017,-3.88930031472982,
133.814763601278));
#246109=CARTESIAN_POINT('Ctrl Pts',(-185.080837121003,-3.80658417000405,
133.921629004168));
#246110=CARTESIAN_POINT('Ctrl Pts',(-185.088494166989,-3.7195583925844,
134.024955697636));
#246111=CARTESIAN_POINT('Ctrl Pts',(-185.096151212975,-3.62857964916102,
134.124389652408));
#246112=CARTESIAN_POINT('Ctrl Pts',(-185.103160205481,-3.54530088447839,
134.215408022297));
#246113=CARTESIAN_POINT('Ctrl Pts',(-185.110169197986,-3.45871056569238,
134.303164978857));
#246114=CARTESIAN_POINT('Ctrl Pts',(-185.117178190492,-3.36910616455944,
134.387418908248));
#246115=CARTESIAN_POINT('Ctrl Pts',(-185.124952524611,-3.26971747889623,
134.480872881472));
#246116=CARTESIAN_POINT('Ctrl Pts',(-185.13272685873,-3.1662800113838,134.570336404582));
#246117=CARTESIAN_POINT('Ctrl Pts',(-185.140501192849,-3.05914760954894,
134.655438254474));
#246118=CARTESIAN_POINT('Ctrl Pts',(-185.148265945796,-2.95214723882493,
134.740435223941));
#246119=CARTESIAN_POINT('Ctrl Pts',(-185.156030698744,-2.84146129743104,
134.821080974734));
#246120=CARTESIAN_POINT('Ctrl Pts',(-185.163795451691,-2.7274801549028,
134.897041287629));
#246121=CARTESIAN_POINT('Ctrl Pts',(-185.171552492576,-2.61361222005217,
134.972926155671));
#246122=CARTESIAN_POINT('Ctrl Pts',(-185.179309533461,-2.4964559204001,
135.044134631363));
#246123=CARTESIAN_POINT('Ctrl Pts',(-185.187066574346,-2.37643407513157,
135.110373175496));
#246124=CARTESIAN_POINT('Ctrl Pts',(-185.194817765586,-2.25650273927002,
135.176561768628));
#246125=CARTESIAN_POINT('Ctrl Pts',(-185.202568956826,-2.13371049990436,
135.237787701952));
#246126=CARTESIAN_POINT('Ctrl Pts',(-185.210320148066,-2.00850818166039,
135.293801334037));
#246127=CARTESIAN_POINT('Ctrl Pts',(-185.218068044844,-1.88335907774139,
135.349791158833));
#246128=CARTESIAN_POINT('Ctrl Pts',(-185.225815941621,-1.75580228842462,
135.400572929258));
#246129=CARTESIAN_POINT('Ctrl Pts',(-185.233563838398,-1.62631200864633,
135.445943570938));
#246130=CARTESIAN_POINT('Ctrl Pts',(-185.241310114482,-1.49684881544309,
135.491304722058));
#246131=CARTESIAN_POINT('Ctrl Pts',(-185.249056390566,-1.36545330497909,
135.531256866629));
#246132=CARTESIAN_POINT('Ctrl Pts',(-185.25680266665,-1.23261799023726,
135.56564573323));
#246133=CARTESIAN_POINT('Ctrl Pts',(-185.264548999916,-1.09978169493548,
135.600034853681));
#246134=CARTESIAN_POINT('Ctrl Pts',(-185.272295333181,-0.965505952635501,
135.628860516231));
#246135=CARTESIAN_POINT('Ctrl Pts',(-185.280041666446,-0.830296328772982,
135.65201892534));
#246136=CARTESIAN_POINT('Ctrl Pts',(-185.287789734449,-0.695056425652861,
135.675182520613));
#246137=CARTESIAN_POINT('Ctrl Pts',(-185.295537802453,-0.558882610093101,
135.692676271008));
#246138=CARTESIAN_POINT('Ctrl Pts',(-185.303285870456,-0.42228808350065,
135.704447947097));
#246139=CARTESIAN_POINT('Ctrl Pts',(-185.311042173197,-0.285548382619655,
135.716232134264));
#246140=CARTESIAN_POINT('Ctrl Pts',(-185.318798475939,-0.148387467644769,
135.722282065073));
#246141=CARTESIAN_POINT('Ctrl Pts',(-185.326554778681,-0.0113216354735307,
135.722597586549));
#246142=CARTESIAN_POINT('Ctrl Pts',(-185.334315221195,0.125817352859683,
135.722913276428));
#246143=CARTESIAN_POINT('Ctrl Pts',(-185.34207566371,0.262860766800342,
135.717488473873));
#246144=CARTESIAN_POINT('Ctrl Pts',(-185.349836106224,0.399295898810333,
135.706375085894));
#246145=CARTESIAN_POINT('Ctrl Pts',(-185.357609006489,0.535950048605996,
135.695243857718));
#246146=CARTESIAN_POINT('Ctrl Pts',(-185.365381906755,0.671993576948554,
135.678405843878));
#246147=CARTESIAN_POINT('Ctrl Pts',(-185.37315480702,0.806921561960867,
135.655964543624));
#246148=CARTESIAN_POINT('Ctrl Pts',(-185.380645142782,0.936944574849048,
135.634339041161));
#246149=CARTESIAN_POINT('Ctrl Pts',(-185.388135478544,1.06593144034985,
135.60751062932));
#246150=CARTESIAN_POINT('Ctrl Pts',(-185.395625814305,1.19344424050067,
135.575615579032));
#246151=CARTESIAN_POINT('Ctrl Pts',(-185.403400148425,1.32579172723165,
135.542511218217));
#246152=CARTESIAN_POINT('Ctrl Pts',(-185.411174482543,1.45697040075332,
135.503843566807));
#246153=CARTESIAN_POINT('Ctrl Pts',(-185.418948816663,1.5864766773227,135.459709671591));
#246154=CARTESIAN_POINT('Ctrl Pts',(-185.42671356961,1.71582334898017,135.415630167457));
#246155=CARTESIAN_POINT('Ctrl Pts',(-185.434478322557,1.84350135810591,
135.366097948359));
#246156=CARTESIAN_POINT('Ctrl Pts',(-185.442243075504,1.9690185123329,135.31126078959));
#246157=CARTESIAN_POINT('Ctrl Pts',(-185.450000116389,2.09441100115318,
135.25647809586));
#246158=CARTESIAN_POINT('Ctrl Pts',(-185.457757157274,2.21764655014518,
135.196401103399));
#246159=CARTESIAN_POINT('Ctrl Pts',(-185.465514198159,2.33824965236156,
135.13122687685));
#246160=CARTESIAN_POINT('Ctrl Pts',(-185.473265389399,2.45876180684023,
135.066101798692));
#246161=CARTESIAN_POINT('Ctrl Pts',(-185.481016580639,2.5766451232984,134.995887322545));
#246162=CARTESIAN_POINT('Ctrl Pts',(-185.488767771879,2.69144588960641,
134.920827802644));
#246163=CARTESIAN_POINT('Ctrl Pts',(-185.496515668657,2.80619786252648,
134.84580018504));
#246164=CARTESIAN_POINT('Ctrl Pts',(-185.504263565434,2.91786956457255,
134.76593183292));
#246165=CARTESIAN_POINT('Ctrl Pts',(-185.512011462211,3.02603382957723,
134.681511933256));
#246166=CARTESIAN_POINT('Ctrl Pts',(-185.519757738295,3.13417546894943,
134.597109692414));
#246167=CARTESIAN_POINT('Ctrl Pts',(-185.527504014379,3.23881082260025,
134.508158038173));
#246168=CARTESIAN_POINT('Ctrl Pts',(-185.535250290463,3.33954388231524,
134.414987948182));
#246169=CARTESIAN_POINT('Ctrl Pts',(-185.542996623729,3.44027768561866,
134.32181717043));
#246170=CARTESIAN_POINT('Ctrl Pts',(-185.550742956994,3.53710885048758,
134.224428160262));
#246171=CARTESIAN_POINT('Ctrl Pts',(-185.558489290259,3.62967678032664,
134.123190160169));
#246172=CARTESIAN_POINT('Ctrl Pts',(-185.566237358262,3.72226544011165,
134.021929488529));
#246173=CARTESIAN_POINT('Ctrl Pts',(-185.573985426265,3.81058870130834,
133.916818400254));
#246174=CARTESIAN_POINT('Ctrl Pts',(-185.581733494268,3.89432522392317,
133.808260434939));
#246175=CARTESIAN_POINT('Ctrl Pts',(-185.58948979701,3.97815074271105,133.699587092927));
#246176=CARTESIAN_POINT('Ctrl Pts',(-185.597246099752,4.05737954572931,
133.58745986594));
#246177=CARTESIAN_POINT('Ctrl Pts',(-185.605002402494,4.13173243319085,
133.472313046493));
#246178=CARTESIAN_POINT('Ctrl Pts',(-185.612762845008,4.20612500502695,
133.357104769722));
#246179=CARTESIAN_POINT('Ctrl Pts',(-185.620523287522,4.27563627770473,
133.238874026014));
#246180=CARTESIAN_POINT('Ctrl Pts',(-185.628283730036,4.3400327911151,133.118080227749));
#246181=CARTESIAN_POINT('Ctrl Pts',(-185.636056630302,4.40453267952583,
132.997092520555));
#246182=CARTESIAN_POINT('Ctrl Pts',(-185.643829530567,4.46390123172262,
132.873533889436));
#246183=CARTESIAN_POINT('Ctrl Pts',(-185.651602430833,4.51795260194687,
132.74788508334));
#246184=CARTESIAN_POINT('Ctrl Pts',(-185.659092766595,4.57003906871526,
132.626803927838));
#246185=CARTESIAN_POINT('Ctrl Pts',(-185.666583102356,4.61718811749639,
132.50378221287));
#246186=CARTESIAN_POINT('Ctrl Pts',(-185.674073438118,4.65927769153067,
132.37926202899));
#246187=CARTESIAN_POINT('Ctrl Pts',(-185.681847772237,4.70296310455798,
132.250020624489));
#246188=CARTESIAN_POINT('Ctrl Pts',(-185.689622106357,4.74133619155718,
132.118755481185));
#246189=CARTESIAN_POINT('Ctrl Pts',(-185.697396440476,4.77420640142745,
131.985942734505));
#246190=CARTESIAN_POINT('Ctrl Pts',(-185.705161193423,4.80703610170175,
131.853293667665));
#246191=CARTESIAN_POINT('Ctrl Pts',(-185.71292594637,4.83437632559071,131.719101168244));
#246192=CARTESIAN_POINT('Ctrl Pts',(-185.720690699317,4.85608535863617,
131.583859207776));
#246193=CARTESIAN_POINT('Ctrl Pts',(-185.728447740202,4.87777282996403,
131.448751571529));
#246194=CARTESIAN_POINT('Ctrl Pts',(-185.736204781087,4.89384017916371,
131.312596932063));
#246195=CARTESIAN_POINT('Ctrl Pts',(-185.743961821972,4.90419617918031,
131.175901865092));
#246196=CARTESIAN_POINT('Ctrl Pts',(-185.751713013212,4.9145443696567,131.039309880935));
#246197=CARTESIAN_POINT('Ctrl Pts',(-185.759464204452,4.91918975430297,
130.902178668729));
#246198=CARTESIAN_POINT('Ctrl Pts',(-185.767215395692,4.91809267276772,
130.76502202877));
#246199=CARTESIAN_POINT('Ctrl Pts',(-185.774963292469,4.91699605752139,
130.627923684042));
#246200=CARTESIAN_POINT('Ctrl Pts',(-185.782711189246,4.91016183358293,
130.490800323191));
#246201=CARTESIAN_POINT('Ctrl Pts',(-185.790459086024,4.89760240839343,
130.354167645832));
#246202=CARTESIAN_POINT('Ctrl Pts',(-185.798205362108,4.88504561036494,
130.217563549084));
#246203=CARTESIAN_POINT('Ctrl Pts',(-185.805951638192,4.86676602891934,
130.081450320748));
#246204=CARTESIAN_POINT('Ctrl Pts',(-185.813697914276,4.84282807281364,
129.946340035256));
#246205=CARTESIAN_POINT('Ctrl Pts',(-185.821444247541,4.81888994000336,
129.81122875241));
#246206=CARTESIAN_POINT('Ctrl Pts',(-185.829190580807,4.78929341739268,
129.677120812149));
#246207=CARTESIAN_POINT('Ctrl Pts',(-185.836936914072,4.75415424788159,
129.54451917919));
#246208=CARTESIAN_POINT('Ctrl Pts',(-185.844684982075,4.71900720919718,
129.411887851015));
#246209=CARTESIAN_POINT('Ctrl Pts',(-185.852433050078,4.67831515382283,
129.280763879231));
#246210=CARTESIAN_POINT('Ctrl Pts',(-185.860181118081,4.63224389893416,
129.151635739286));
#246211=CARTESIAN_POINT('Ctrl Pts',(-185.867937420823,4.5861236789676,129.022370360416));
#246212=CARTESIAN_POINT('Ctrl Pts',(-185.875693723564,4.5346129705982,128.895105419515));
#246213=CARTESIAN_POINT('Ctrl Pts',(-185.883450026306,4.47792624211395,
128.770310560983));
#246214=CARTESIAN_POINT('Ctrl Pts',(-185.89121046882,4.42120925821574,128.645449095676));
#246215=CARTESIAN_POINT('Ctrl Pts',(-185.898970911335,4.35931092585522,
128.52306068839));
#246216=CARTESIAN_POINT('Ctrl Pts',(-185.906731353849,4.29249157078739,
128.403590079339));
#246217=CARTESIAN_POINT('Ctrl Pts',(-185.914504254114,4.22556495135886,
128.28392768546));
#246218=CARTESIAN_POINT('Ctrl Pts',(-185.922277154379,4.15370172825647,
128.167192782885));
#246219=CARTESIAN_POINT('Ctrl Pts',(-185.930050054645,4.07720591501325,
128.053801585463));
#246220=CARTESIAN_POINT('Ctrl Pts',(-185.937540390407,4.00349091726232,
127.944532443683));
#246221=CARTESIAN_POINT('Ctrl Pts',(-185.945030726169,3.92547447684811,
127.838368371698));
#246222=CARTESIAN_POINT('Ctrl Pts',(-185.952521061931,3.84346256241335,
127.73565102006));
#246223=CARTESIAN_POINT('Ctrl Pts',(-185.96029539605,3.75834114131641,127.629039108815));
#246224=CARTESIAN_POINT('Ctrl Pts',(-185.968069730169,3.66864564947082,
127.525802727655));
#246225=CARTESIAN_POINT('Ctrl Pts',(-185.975844064288,3.57467367557063,
127.426359555446));
#246226=CARTESIAN_POINT('Ctrl Pts',(-185.983608817235,3.48081751372976,
127.32703893806));
#246227=CARTESIAN_POINT('Ctrl Pts',(-185.991373570182,3.38269562227221,
127.231502509616));
#246228=CARTESIAN_POINT('Ctrl Pts',(-185.99913832313,3.28064699331261,127.140136502181));
#246229=CARTESIAN_POINT('Ctrl Pts',(-186.006895364015,3.17869972048965,
127.048861240753));
#246230=CARTESIAN_POINT('Ctrl Pts',(-186.0146524049,3.07283376091616,126.961748416427));
#246231=CARTESIAN_POINT('Ctrl Pts',(-186.022409445785,2.96342600063647,
126.879148597655));
#246232=CARTESIAN_POINT('Ctrl Pts',(-186.030160637025,2.85410074559971,
126.79661106805));
#246233=CARTESIAN_POINT('Ctrl Pts',(-186.037911828265,2.74123931688351,
126.718580004569));
#246234=CARTESIAN_POINT('Ctrl Pts',(-186.045663019505,2.6252525518401,126.6453664962));
#246235=CARTESIAN_POINT('Ctrl Pts',(-186.053410916282,2.50931508426635,
126.572184105526));
#246236=CARTESIAN_POINT('Ctrl Pts',(-186.061158813059,2.39025525227261,
126.503815405716));
#246237=CARTESIAN_POINT('Ctrl Pts',(-186.068906709836,2.26851363507625,
126.440528706278));
#246238=CARTESIAN_POINT('Ctrl Pts',(-186.07665298592,2.14679748360143,126.377255245054));
#246239=CARTESIAN_POINT('Ctrl Pts',(-186.084399262004,2.02240100940056,
126.319061849963));
#246240=CARTESIAN_POINT('Ctrl Pts',(-186.092145538088,1.89578984970093,
126.266171120832));
#246241=CARTESIAN_POINT('Ctrl Pts',(-186.099891871354,1.769177755387,126.213280001273));
#246242=CARTESIAN_POINT('Ctrl Pts',(-186.107638204619,1.64035130370563,
126.165691776484));
#246243=CARTESIAN_POINT('Ctrl Pts',(-186.115384537884,1.50979621498143,
126.123580933397));
#246244=CARTESIAN_POINT('Ctrl Pts',(-186.123132605887,1.37921188934978,
126.081460659879));
#246245=CARTESIAN_POINT('Ctrl Pts',(-186.13088067389,1.24689852837551,126.044820328894));
#246246=CARTESIAN_POINT('Ctrl Pts',(-186.138628741893,1.11335672851959,
126.013784466667));
#246247=CARTESIAN_POINT('Ctrl Pts',(-186.146385044635,0.979672998849801,
125.982715619156));
#246248=CARTESIAN_POINT('Ctrl Pts',(-186.154141347377,0.844758603646081,
125.957263227791));
#246249=CARTESIAN_POINT('Ctrl Pts',(-186.161897650119,0.709124593392249,
125.937500708595));
#246250=CARTESIAN_POINT('Ctrl Pts',(-186.169658092633,0.573418191182914,
125.917727641549));
#246251=CARTESIAN_POINT('Ctrl Pts',(-186.177418535147,0.436991797321192,
125.903650537974));
#246252=CARTESIAN_POINT('Ctrl Pts',(-186.185178977661,0.300360296774949,
125.895290771391));
#246253=CARTESIAN_POINT('Ctrl Pts',(-186.192951877927,0.163509463214826,
125.886917584969));
#246254=CARTESIAN_POINT('Ctrl Pts',(-186.200724778192,0.0264532561306669,
125.884280083587));
#246255=CARTESIAN_POINT('Ctrl Pts',(-186.208497678457,-0.110293825237829,
125.887347465803));
#246256=CARTESIAN_POINT('Ctrl Pts',(-186.215988014219,-0.242069805751984,
125.890303340948));
#246257=CARTESIAN_POINT('Ctrl Pts',(-186.223478349981,-0.37355843793483,
125.898556507699));
#246258=CARTESIAN_POINT('Ctrl Pts',(-186.230968685743,-0.504306897976589,
125.91203421644));
#246259=CARTESIAN_POINT('Ctrl Pts',(-186.238743019862,-0.640012725620837,
125.926022936604));
#246260=CARTESIAN_POINT('Ctrl Pts',(-186.246517353981,-0.775351021172049,
125.945684508496));
#246261=CARTESIAN_POINT('Ctrl Pts',(-186.2542916881,-0.909809525613153,
125.970994327949));
#246262=CARTESIAN_POINT('Ctrl Pts',(-186.262056441047,-1.0441023219648,
125.996272955312));
#246263=CARTESIAN_POINT('Ctrl Pts',(-186.269821193994,-1.17751710403923,
126.02718590837));
#246264=CARTESIAN_POINT('Ctrl Pts',(-186.277585946941,-1.3095456903417,
126.063656751323));
#246265=CARTESIAN_POINT('Ctrl Pts',(-186.285342987826,-1.44144314399063,
126.100091370921));
#246266=CARTESIAN_POINT('Ctrl Pts',(-186.293100028711,-1.57195676732722,
126.142072791592));
#246267=CARTESIAN_POINT('Ctrl Pts',(-186.300857069596,-1.7005879010708,
126.189473419245));
#246268=CARTESIAN_POINT('Ctrl Pts',(-186.308608260836,-1.8291220330753,
126.236838301715));
#246269=CARTESIAN_POINT('Ctrl Pts',(-186.316359452076,-1.95577613574888,
126.289614122268));
#246270=CARTESIAN_POINT('Ctrl Pts',(-186.324110643316,-2.08006641349185,
126.347623383));
#246271=CARTESIAN_POINT('Ctrl Pts',(-186.331858540093,-2.20430386455207,
126.40560798825));
#246272=CARTESIAN_POINT('Ctrl Pts',(-186.33960643687,-2.32617913539421,
126.46882144461));
#246273=CARTESIAN_POINT('Ctrl Pts',(-186.347354333647,-2.4452283458019,
126.537038108148));
#246274=CARTESIAN_POINT('Ctrl Pts',(-186.355100609731,-2.56425265368117,
126.605240502231));
#246275=CARTESIAN_POINT('Ctrl Pts',(-186.362846885815,-2.68045173795131,
126.678443827566));
#246276=CARTESIAN_POINT('Ctrl Pts',(-186.370593161899,-2.79338663077894,
126.756376651011));
#246277=CARTESIAN_POINT('Ctrl Pts',(-186.378339495165,-2.90632235726645,
126.834310049738));
#246278=CARTESIAN_POINT('Ctrl Pts',(-186.38608582843,-3.01599352244523,
126.916972794186));
#246279=CARTESIAN_POINT('Ctrl Pts',(-186.393832161695,-3.12199078181559,
127.004050548538));
#246280=CARTESIAN_POINT('Ctrl Pts',(-186.401580229698,-3.2280117785374,
127.091147803349));
#246281=CARTESIAN_POINT('Ctrl Pts',(-186.409328297701,-3.33035693024278,
127.182661787357));
#246282=CARTESIAN_POINT('Ctrl Pts',(-186.417076365704,-3.42865088487751,
127.278238644048));
#246283=CARTESIAN_POINT('Ctrl Pts',(-186.424832668446,-3.52704930749682,
127.373917080959));
#246284=CARTESIAN_POINT('Ctrl Pts',(-186.432588971188,-3.62138765127686,
127.473666743374));
#246285=CARTESIAN_POINT('Ctrl Pts',(-186.440345273929,-3.71132791396644,
127.577097353202));
#246286=CARTESIAN_POINT('Ctrl Pts',(-186.448105716444,-3.8013161804825,
127.680583167061));
#246287=CARTESIAN_POINT('Ctrl Pts',(-186.455866158958,-3.8869014446861,
127.787753537677));
#246288=CARTESIAN_POINT('Ctrl Pts',(-186.463626601472,-3.96778741652845,
127.898186830653));
#246289=CARTESIAN_POINT('Ctrl Pts',(-186.471399501737,-4.04880323371331,
128.008797400955));
#246290=CARTESIAN_POINT('Ctrl Pts',(-186.479172402003,-4.12510446603694,
128.122681035685));
#246291=CARTESIAN_POINT('Ctrl Pts',(-186.486945302268,-4.19643892821958,
128.239388223129));
#246292=CARTESIAN_POINT('Ctrl Pts',(-186.494435638031,-4.26518020302876,
128.351852810354));
#246293=CARTESIAN_POINT('Ctrl Pts',(-186.501925973793,-4.32930939758988,
128.466938958798));
#246294=CARTESIAN_POINT('Ctrl Pts',(-186.509416309556,-4.38864295588559,
128.584226372018));
#246295=CARTESIAN_POINT('Ctrl Pts',(-186.517717331537,-4.45439824205773,
128.714207914373));
#246296=CARTESIAN_POINT('Ctrl Pts',(-186.526018353518,-4.51445011624346,
128.847261066043));
#246297=CARTESIAN_POINT('Ctrl Pts',(-186.534319375498,-4.56852078633726,
128.982877461645));
#246298=CARTESIAN_POINT('Ctrl Pts',(-186.542600349557,-4.62246086954897,
129.118166328066));
#246299=CARTESIAN_POINT('Ctrl Pts',(-186.550881323616,-4.670448438029,129.256005807444));
#246300=CARTESIAN_POINT('Ctrl Pts',(-186.559162297674,-4.71225244919594,
129.39586499544));
#246301=CARTESIAN_POINT('Ctrl Pts',(-186.562823196869,-4.73073339959214,
129.45769472526));
#246302=CARTESIAN_POINT('Ctrl Pts',(-186.566484096064,-4.74800643982495,
129.519918866165));
#246303=CARTESIAN_POINT('Ctrl Pts',(-186.570144995258,-4.76405452823391,
129.582490119308));
#246304=CARTESIAN_POINT('Ctrl Pts',(-184.819837330039,-4.76405452823405,
129.582490119308));
#246305=CARTESIAN_POINT('Ctrl Pts',(-184.826135075586,-4.79157558581711,
129.689794305134));
#246306=CARTESIAN_POINT('Ctrl Pts',(-184.832432821132,-4.8154390765796,
129.797910017712));
#246307=CARTESIAN_POINT('Ctrl Pts',(-184.838730566679,-4.83561259437176,
129.906566710451));
#246308=CARTESIAN_POINT('Ctrl Pts',(-184.850410110173,-4.87302558235891,
130.108077006377));
#246309=CARTESIAN_POINT('Ctrl Pts',(-184.862089653666,-4.89785094753426,
130.311991589822));
#246310=CARTESIAN_POINT('Ctrl Pts',(-184.87376919716,-4.90985019127264,
130.517038217186));
#246311=CARTESIAN_POINT('Ctrl Pts',(-184.879132610105,-4.91536041512924,
130.611198552825));
#246312=CARTESIAN_POINT('Ctrl Pts',(-184.88449602305,-4.9181664561817,130.705597270812));
#246313=CARTESIAN_POINT('Ctrl Pts',(-184.889859435995,-4.9182481621147,
130.800108752638));
#246314=CARTESIAN_POINT('Origin',(213.235140564004,0.,130.804360617566));
#246315=CARTESIAN_POINT('',(-183.069718605797,-4.76405452823406,129.582490119308));
#246316=CARTESIAN_POINT('',(-183.415149158805,-4.76405452823414,129.582490119309));
#246317=CARTESIAN_POINT('',(213.235140564004,-4.76405452823405,129.582490119308));
#246318=CARTESIAN_POINT('',(-183.485140564052,-4.91824798071509,130.799903859564));
#246319=CARTESIAN_POINT('Ctrl Pts',(-183.415149158805,-4.76405452823414,
129.582490119309));
#246320=CARTESIAN_POINT('Ctrl Pts',(-183.419067256354,-4.78116185622988,
129.649191331524));
#246321=CARTESIAN_POINT('Ctrl Pts',(-183.422985353904,-4.79685563415493,
129.716203290357));
#246322=CARTESIAN_POINT('Ctrl Pts',(-183.426903451454,-4.81112741488386,
129.783460984765));
#246323=CARTESIAN_POINT('Ctrl Pts',(-183.437819003722,-4.85088762159933,
129.970836329416));
#246324=CARTESIAN_POINT('Ctrl Pts',(-183.448734555991,-4.87971282541858,
130.160606736013));
#246325=CARTESIAN_POINT('Ctrl Pts',(-183.459650108259,-4.89737607248764,
130.351712114724));
#246326=CARTESIAN_POINT('Ctrl Pts',(-183.468146926843,-4.91112539109944,
130.500471214907));
#246327=CARTESIAN_POINT('Ctrl Pts',(-183.476643745428,-4.91811217802289,
130.650039045172));
#246328=CARTESIAN_POINT('Ctrl Pts',(-183.485140564012,-4.91824798071445,
130.799903858857));
#246329=CARTESIAN_POINT('Ctrl Pts',(-183.485140564052,-4.91824798071509,
130.799903859564));
#246330=CARTESIAN_POINT('Ctrl Pts',(-183.492790120517,-4.91837024179223,
130.934824870645));
#246331=CARTESIAN_POINT('Ctrl Pts',(-183.500439676982,-4.91293645195532,
131.069920615074));
#246332=CARTESIAN_POINT('Ctrl Pts',(-183.508089233447,-4.90193026440357,
131.204688914623));
#246333=CARTESIAN_POINT('Ctrl Pts',(-183.515732635828,-4.89093293135145,
131.339348792808));
#246334=CARTESIAN_POINT('Ctrl Pts',(-183.52337603821,-4.8743721510898,131.473681350422));
#246335=CARTESIAN_POINT('Ctrl Pts',(-183.531019440591,-4.85228364227142,
131.607184706296));
#246336=CARTESIAN_POINT('Ctrl Pts',(-183.538659228572,-4.83020557863537,
131.740624931294));
#246337=CARTESIAN_POINT('Ctrl Pts',(-183.546299016552,-4.80260504893871,
131.873236337474));
#246338=CARTESIAN_POINT('Ctrl Pts',(-183.553938804532,-4.76956954354201,
132.004522869854));
#246339=CARTESIAN_POINT('Ctrl Pts',(-183.561576868312,-4.73654149382951,
132.135779772569));
#246340=CARTESIAN_POINT('Ctrl Pts',(-183.569214932091,-4.69808100518792,
132.265712005344));
#246341=CARTESIAN_POINT('Ctrl Pts',(-183.576852995871,-4.65432642489983,
132.393834930973));
#246342=CARTESIAN_POINT('Ctrl Pts',(-183.584491098882,-4.6105716198721,
132.521958514688));
#246343=CARTESIAN_POINT('Ctrl Pts',(-183.592129201894,-4.56152279959267,
132.648272391449));
#246344=CARTESIAN_POINT('Ctrl Pts',(-183.599767304905,-4.50736762758277,
132.772308821234));
#246345=CARTESIAN_POINT('Ctrl Pts',(-183.607407210404,-4.45319967569707,
132.89637452191));
#246346=CARTESIAN_POINT('Ctrl Pts',(-183.615047115903,-4.39392313754426,
133.018161337874));
#246347=CARTESIAN_POINT('Ctrl Pts',(-183.622687021401,-4.32977284733201,
133.137223698205));
#246348=CARTESIAN_POINT('Ctrl Pts',(-183.63033486744,-4.26555588247997,
133.256409806066));
#246349=CARTESIAN_POINT('Ctrl Pts',(-183.637982713479,-4.19645524369809,
133.372865449847));
#246350=CARTESIAN_POINT('Ctrl Pts',(-183.645630559517,-4.12275070500498,
133.486171514494));
#246351=CARTESIAN_POINT('Ctrl Pts',(-183.653282768779,-4.04900411665295,
133.599542222126));
#246352=CARTESIAN_POINT('Ctrl Pts',(-183.66093497804,-3.97064863261913,
133.709759445809));
#246353=CARTESIAN_POINT('Ctrl Pts',(-183.668587187302,-3.8880051776028,
133.816436114866));
#246354=CARTESIAN_POINT('Ctrl Pts',(-183.676250761655,-3.80523898019318,
133.923271220542));
#246355=CARTESIAN_POINT('Ctrl Pts',(-183.683914336009,-3.71817235596996,
134.026554965782));
#246356=CARTESIAN_POINT('Ctrl Pts',(-183.691577910362,-3.62716431972376,
134.125935855344));
#246357=CARTESIAN_POINT('Ctrl Pts',(-183.696168965331,-3.5726436903536,
134.1854724509));
#246358=CARTESIAN_POINT('Ctrl Pts',(-183.700760020299,-3.51670920889025,
134.243609084722));
#246359=CARTESIAN_POINT('Ctrl Pts',(-183.705351075268,-3.45944366050394,
134.300277181544));
#246360=CARTESIAN_POINT('Ctrl Pts',(-183.713125409387,-3.36247215619332,
134.396236981985));
#246361=CARTESIAN_POINT('Ctrl Pts',(-183.720899743506,-3.26135135780418,
134.488310951084));
#246362=CARTESIAN_POINT('Ctrl Pts',(-183.728674077625,-3.15642552453558,
134.57611895693));
#246363=CARTESIAN_POINT('Ctrl Pts',(-183.736438830572,-3.05162900297956,
134.663818747256));
#246364=CARTESIAN_POINT('Ctrl Pts',(-183.744203583519,-2.94303707393275,
134.74726278652));
#246365=CARTESIAN_POINT('Ctrl Pts',(-183.751968336466,-2.83103145099696,
134.826107002654));
#246366=CARTESIAN_POINT('Ctrl Pts',(-183.759725377351,-2.71913707362488,
134.9048729096));
#246367=CARTESIAN_POINT('Ctrl Pts',(-183.767482418236,-2.60383606730024,
134.979047861564));
#246368=CARTESIAN_POINT('Ctrl Pts',(-183.775239459121,-2.48554362280428,
135.048327625171));
#246369=CARTESIAN_POINT('Ctrl Pts',(-183.782990650361,-2.36734038356073,
135.117555144369));
#246370=CARTESIAN_POINT('Ctrl Pts',(-183.790741841601,-2.24615053231144,
135.181894626134));
#246371=CARTESIAN_POINT('Ctrl Pts',(-183.798493032841,-2.12241837636851,
135.241085005913));
#246372=CARTESIAN_POINT('Ctrl Pts',(-183.806240929618,-1.99873880989235,
135.300250228202));
#246373=CARTESIAN_POINT('Ctrl Pts',(-183.813988826396,-1.87251943979781,
135.354270532912));
#246374=CARTESIAN_POINT('Ctrl Pts',(-183.821736723173,-1.7442291244233,
135.402930811008));
#246375=CARTESIAN_POINT('Ctrl Pts',(-183.829482999257,-1.61596564461714,
135.451580910423));
#246376=CARTESIAN_POINT('Ctrl Pts',(-183.837229275341,-1.48563244650519,
135.494873074791));
#246377=CARTESIAN_POINT('Ctrl Pts',(-183.844975551425,-1.35371794589048,
135.532640514682));
#246378=CARTESIAN_POINT('Ctrl Pts',(-183.85272188469,-1.22180247151308,
135.570408233365));
#246379=CARTESIAN_POINT('Ctrl Pts',(-183.860468217956,-1.08830604720463,
135.602651038582));
#246380=CARTESIAN_POINT('Ctrl Pts',(-183.868214551221,-0.953731425044513,
135.62925226727));
#246381=CARTESIAN_POINT('Ctrl Pts',(-183.875962619224,-0.81912666583066,
135.655859453118));
#246382=CARTESIAN_POINT('Ctrl Pts',(-183.883710687227,-0.683443611768262,
135.676822472633));
#246383=CARTESIAN_POINT('Ctrl Pts',(-183.89145875523,-0.547193964316623,
135.69207601721));
#246384=CARTESIAN_POINT('Ctrl Pts',(-183.899215057972,-0.410799509118467,
135.707345773435));
#246385=CARTESIAN_POINT('Ctrl Pts',(-183.906971360713,-0.273837646764738,
135.716893889475));
#246386=CARTESIAN_POINT('Ctrl Pts',(-183.914727663455,-0.136824502115776,
135.720707037228));
#246387=CARTESIAN_POINT('Ctrl Pts',(-183.922488105969,0.000261770573871722,
135.724522220172));
#246388=CARTESIAN_POINT('Ctrl Pts',(-183.930248548483,0.137398989362215,
135.722596341163));
#246389=CARTESIAN_POINT('Ctrl Pts',(-183.938008990998,0.274073289081115,
135.714968206726));
#246390=CARTESIAN_POINT('Ctrl Pts',(-183.945781891263,0.410966990519299,
135.70732782693));
#246391=CARTESIAN_POINT('Ctrl Pts',(-183.953554791528,0.547395898572235,
135.693966937693));
#246392=CARTESIAN_POINT('Ctrl Pts',(-183.961327691794,0.682852614635353,
135.674976119655));
#246393=CARTESIAN_POINT('Ctrl Pts',(-183.968818027556,0.813385137877262,
135.656675665687));
#246394=CARTESIAN_POINT('Ctrl Pts',(-183.976308363318,0.943014622152609,
135.633147555643));
#246395=CARTESIAN_POINT('Ctrl Pts',(-183.98379869908,1.07129981466353,135.604516841024));
#246396=CARTESIAN_POINT('Ctrl Pts',(-183.991573033199,1.20444897923751,
135.574800584158));
#246397=CARTESIAN_POINT('Ctrl Pts',(-183.999347367318,1.3365716786525,135.539493021914));
#246398=CARTESIAN_POINT('Ctrl Pts',(-184.007121701437,1.46716201666007,
135.49867831872));
#246399=CARTESIAN_POINT('Ctrl Pts',(-184.014886454385,1.5975914137469,135.457913916001));
#246400=CARTESIAN_POINT('Ctrl Pts',(-184.022651207332,1.72649183739355,
135.411655992067));
#246401=CARTESIAN_POINT('Ctrl Pts',(-184.030415960279,1.85336748449725,
135.360039714024));
#246402=CARTESIAN_POINT('Ctrl Pts',(-184.038173001164,1.98011711691926,
135.308474701997));
#246403=CARTESIAN_POINT('Ctrl Pts',(-184.045930042049,2.10484561505189,
135.251562073242));
#246404=CARTESIAN_POINT('Ctrl Pts',(-184.053687082934,2.22707259798284,
135.189486693954));
#246405=CARTESIAN_POINT('Ctrl Pts',(-184.061438274174,2.34920740859568,
135.127458126191));
#246406=CARTESIAN_POINT('Ctrl Pts',(-184.069189465414,2.46884411162038,
135.060274733533));
#246407=CARTESIAN_POINT('Ctrl Pts',(-184.076940656654,2.58552290710035,
134.988169212538));
#246408=CARTESIAN_POINT('Ctrl Pts',(-184.084688553431,2.70215211097956,
134.916094338312));
#246409=CARTESIAN_POINT('Ctrl Pts',(-184.092436450208,2.81582557588218,
134.839101701749));
#246410=CARTESIAN_POINT('Ctrl Pts',(-184.100184346985,2.92610889510012,
134.757469494958));
#246411=CARTESIAN_POINT('Ctrl Pts',(-184.107930623069,3.03636914542542,
134.675854363865));
#246412=CARTESIAN_POINT('Ctrl Pts',(-184.115676899153,3.14324034655068,
134.589601825376));
#246413=CARTESIAN_POINT('Ctrl Pts',(-184.123423175237,3.24631817313421,
134.499032643779));
#246414=CARTESIAN_POINT('Ctrl Pts',(-184.131169508503,3.34939676061442,
134.40846279362));
#246415=CARTESIAN_POINT('Ctrl Pts',(-184.138915841768,3.44868162397767,
134.313576494829));
#246416=CARTESIAN_POINT('Ctrl Pts',(-184.146662175034,3.54380286150397,
134.214733667732));
#246417=CARTESIAN_POINT('Ctrl Pts',(-184.154410243036,3.63894540077176,
134.115868705469));
#246418=CARTESIAN_POINT('Ctrl Pts',(-184.162158311039,3.72992218775639,
134.013045733441));
#246419=CARTESIAN_POINT('Ctrl Pts',(-184.169906379042,3.81640168934142,
133.906659959682));
#246420=CARTESIAN_POINT('Ctrl Pts',(-184.177662681784,3.90297310236997,
133.800161117856));
#246421=CARTESIAN_POINT('Ctrl Pts',(-184.185418984526,3.98503743489305,
133.690092214043));
#246422=CARTESIAN_POINT('Ctrl Pts',(-184.193175287268,4.06230449550591,
133.576880274537));
#246423=CARTESIAN_POINT('Ctrl Pts',(-184.200935729782,4.13961279587571,
133.463607910411));
#246424=CARTESIAN_POINT('Ctrl Pts',(-184.208696172296,4.21211851583949,
133.34718949967));
#246425=CARTESIAN_POINT('Ctrl Pts',(-184.21645661481,4.27957654775137,133.228078347508));
#246426=CARTESIAN_POINT('Ctrl Pts',(-184.224229515076,4.34714286928472,
133.108775987551));
#246427=CARTESIAN_POINT('Ctrl Pts',(-184.232002415341,4.40964513203329,
132.986772596348));
#246428=CARTESIAN_POINT('Ctrl Pts',(-184.239775315607,4.46688528271646,
132.862544023765));
#246429=CARTESIAN_POINT('Ctrl Pts',(-184.247265651369,4.52204460974522,
132.742831472703));
#246430=CARTESIAN_POINT('Ctrl Pts',(-184.254755987131,4.57231764704277,
132.621052998097));
#246431=CARTESIAN_POINT('Ctrl Pts',(-184.262246322894,4.61757109606277,
132.497647431814));
#246432=CARTESIAN_POINT('Ctrl Pts',(-184.270020657013,4.66454034335519,
132.369562905981));
#246433=CARTESIAN_POINT('Ctrl Pts',(-184.277794991132,4.70625063758659,
132.239319737225));
#246434=CARTESIAN_POINT('Ctrl Pts',(-184.285569325251,4.74249933939709,
132.107389043318));
#246435=CARTESIAN_POINT('Ctrl Pts',(-184.293334078198,4.77870336792206,
131.975620942201));
#246436=CARTESIAN_POINT('Ctrl Pts',(-184.301098831145,4.80945909397288,
131.842169827338));
#246437=CARTESIAN_POINT('Ctrl Pts',(-184.308863584092,4.83461224377596,
131.707525893045));
#246438=CARTESIAN_POINT('Ctrl Pts',(-184.316620624977,4.85974041111613,
131.573015689005));
#246439=CARTESIAN_POINT('Ctrl Pts',(-184.324377665862,4.87927700459897,
131.437315405021));
#246440=CARTESIAN_POINT('Ctrl Pts',(-184.332134706747,4.89311789977162,
131.300929123851));
#246441=CARTESIAN_POINT('Ctrl Pts',(-184.339885897987,4.9069483574176,131.164645692637));
#246442=CARTESIAN_POINT('Ctrl Pts',(-184.347637089227,4.91509162671567,
131.027677681317));
#246443=CARTESIAN_POINT('Ctrl Pts',(-184.355388280468,4.91749494876237,
130.89053771079));
#246444=CARTESIAN_POINT('Ctrl Pts',(-184.363136177245,4.91989724933307,
130.75345602841));
#246445=CARTESIAN_POINT('Ctrl Pts',(-184.370884074022,4.9165644480558,130.616202922275));
#246446=CARTESIAN_POINT('Ctrl Pts',(-184.378631970799,4.90749578839558,
130.479294240683));
#246447=CARTESIAN_POINT('Ctrl Pts',(-184.386378246883,4.89842902570346,
130.342414197436));
#246448=CARTESIAN_POINT('Ctrl Pts',(-184.394124522967,4.88362881695607,
130.205878825291));
#246449=CARTESIAN_POINT('Ctrl Pts',(-184.401870799051,4.86314648250967,
130.070201675542));
#246450=CARTESIAN_POINT('Ctrl Pts',(-184.409617132316,4.84266399686724,
129.934523524254));
#246451=CARTESIAN_POINT('Ctrl Pts',(-184.417363465582,4.81649936018953,
129.799703994589));
#246452=CARTESIAN_POINT('Ctrl Pts',(-184.425109798847,4.78475544272591,
129.666248841067));
#246453=CARTESIAN_POINT('Ctrl Pts',(-184.43285786685,4.75300441643203,129.532763801189));
#246454=CARTESIAN_POINT('Ctrl Pts',(-184.440605934853,4.7156717135631,129.400644125729));
#246455=CARTESIAN_POINT('Ctrl Pts',(-184.448354002856,4.67291063208325,
129.270382362484));
#246456=CARTESIAN_POINT('Ctrl Pts',(-184.456110305598,4.6301041036172,129.139982155487));
#246457=CARTESIAN_POINT('Ctrl Pts',(-184.46386660834,4.58185779378596,129.011444177258));
#246458=CARTESIAN_POINT('Ctrl Pts',(-184.471622911082,4.52837411636472,
128.885243392189));
#246459=CARTESIAN_POINT('Ctrl Pts',(-184.479383353596,4.47486189309462,
128.758975249962));
#246460=CARTESIAN_POINT('Ctrl Pts',(-184.48714379611,4.41610689968782,128.635047139604));
#246461=CARTESIAN_POINT('Ctrl Pts',(-184.494904238624,4.35235802797307,
128.513910299651));
#246462=CARTESIAN_POINT('Ctrl Pts',(-184.50267713889,4.28850682091009,128.392579000088));
#246463=CARTESIAN_POINT('Ctrl Pts',(-184.510450039155,4.21964591229296,
128.274048263238));
#246464=CARTESIAN_POINT('Ctrl Pts',(-184.518222939421,4.14606859545448,
128.15874192541));
#246465=CARTESIAN_POINT('Ctrl Pts',(-184.525713275183,4.07516599941415,
128.047627263403));
#246466=CARTESIAN_POINT('Ctrl Pts',(-184.533203610945,3.99988412443292,
127.939506893194));
#246467=CARTESIAN_POINT('Ctrl Pts',(-184.540693946706,3.92052012106803,
127.83473016197));
#246468=CARTESIAN_POINT('Ctrl Pts',(-184.548468280826,3.83814700739212,
127.725980789134));
#246469=CARTESIAN_POINT('Ctrl Pts',(-184.556242614945,3.75111517370212,
127.620489123221));
#246470=CARTESIAN_POINT('Ctrl Pts',(-184.564016949064,3.65971145319893,
127.518680301129));
#246471=CARTESIAN_POINT('Ctrl Pts',(-184.571781702011,3.56842037961253,
127.41699694931));
#246472=CARTESIAN_POINT('Ctrl Pts',(-184.579546454958,3.47276839832737,
127.318987698628));
#246473=CARTESIAN_POINT('Ctrl Pts',(-184.587311207905,3.37308453496028,
127.225047305978));
#246474=CARTESIAN_POINT('Ctrl Pts',(-184.59506824879,3.27349967901132,127.13120021625));
#246475=CARTESIAN_POINT('Ctrl Pts',(-184.602825289675,3.16989119284842,
127.04141420869));
#246476=CARTESIAN_POINT('Ctrl Pts',(-184.61058233056,3.06262689376355,126.956049355194));
#246477=CARTESIAN_POINT('Ctrl Pts',(-184.6183335218,2.95544348352117,126.870748875999));
#246478=CARTESIAN_POINT('Ctrl Pts',(-184.62608471304,2.84461005242828,126.789863157161));
#246479=CARTESIAN_POINT('Ctrl Pts',(-184.63383590428,2.73052936548945,126.713713670358));
#246480=CARTESIAN_POINT('Ctrl Pts',(-184.641583801057,2.61649716588561,
126.637596549119));
#246481=CARTESIAN_POINT('Ctrl Pts',(-184.649331697835,2.49922077998541,
126.566211872763));
#246482=CARTESIAN_POINT('Ctrl Pts',(-184.657079594612,2.37913379664567,
126.499839106392));
#246483=CARTESIAN_POINT('Ctrl Pts',(-184.664825870696,2.25907193291407,
126.433480223773));
#246484=CARTESIAN_POINT('Ctrl Pts',(-184.67257214678,2.13620098310233,126.372131354849));
#246485=CARTESIAN_POINT('Ctrl Pts',(-184.680318422864,2.01098075236442,
126.316026909371));
#246486=CARTESIAN_POINT('Ctrl Pts',(-184.688064756129,1.88575959727938,
126.259922049742));
#246487=CARTESIAN_POINT('Ctrl Pts',(-184.695811089395,1.75818948345372,
126.209061850666));
#246488=CARTESIAN_POINT('Ctrl Pts',(-184.70355742266,1.62875152037251,126.163633137161));
#246489=CARTESIAN_POINT('Ctrl Pts',(-184.711305490663,1.49928457055711,
126.118194250211));
#246490=CARTESIAN_POINT('Ctrl Pts',(-184.719053558666,1.36794930796729,
126.078189398663));
#246491=CARTESIAN_POINT('Ctrl Pts',(-184.726801626669,1.23524298830775,
126.043755842715));
#246492=CARTESIAN_POINT('Ctrl Pts',(-184.734557929411,1.10239562679191,
126.009285690373));
#246493=CARTESIAN_POINT('Ctrl Pts',(-184.742314232153,0.968174676377767,
125.980398760293));
#246494=CARTESIAN_POINT('Ctrl Pts',(-184.750070534895,0.833089147649478,
125.957181485889));
#246495=CARTESIAN_POINT('Ctrl Pts',(-184.757830977409,0.697931519707528,
125.933951819726));
#246496=CARTESIAN_POINT('Ctrl Pts',(-184.765591419923,0.561908781530276,
125.916397888946));
#246497=CARTESIAN_POINT('Ctrl Pts',(-184.773351862437,0.425535104989546,
125.904554199255));
#246498=CARTESIAN_POINT('Ctrl Pts',(-184.781124762703,0.288942509316547,
125.892691497022));
#246499=CARTESIAN_POINT('Ctrl Pts',(-184.788897662968,0.1519982403108,125.886557371142));
#246500=CARTESIAN_POINT('Ctrl Pts',(-184.796670563234,0.0152174156738462,
125.886134159506));
#246501=CARTESIAN_POINT('Ctrl Pts',(-184.804160898996,-0.116591081455591,
125.885726332679));
#246502=CARTESIAN_POINT('Ctrl Pts',(-184.811651234757,-0.248247503329108,
125.89062140511));
#246503=CARTESIAN_POINT('Ctrl Pts',(-184.819141570519,-0.379297317131378,
125.900758206306));
#246504=CARTESIAN_POINT('Ctrl Pts',(-184.826915904638,-0.515315924457791,
125.9112793474));
#246505=CARTESIAN_POINT('Ctrl Pts',(-184.834690238758,-0.651111882649554,
125.92748087175));
#246506=CARTESIAN_POINT('Ctrl Pts',(-184.842464572877,-0.786172471644022,
125.949351255337));
#246507=CARTESIAN_POINT('Ctrl Pts',(-184.850229325824,-0.921066610532533,
125.971194685631));
#246508=CARTESIAN_POINT('Ctrl Pts',(-184.857994078771,-1.05522680121144,
125.998693012488));
#246509=CARTESIAN_POINT('Ctrl Pts',(-184.865758831718,-1.18814307714153,
126.031782793084));
#246510=CARTESIAN_POINT('Ctrl Pts',(-184.873515872603,-1.3209273387533,
126.064839708443));
#246511=CARTESIAN_POINT('Ctrl Pts',(-184.881272913488,-1.45246976733426,
126.103476931965));
#246512=CARTESIAN_POINT('Ctrl Pts',(-184.889029954373,-1.58226860997003,
126.147579636201));
#246513=CARTESIAN_POINT('Ctrl Pts',(-184.896781145613,-1.71196957028905,
126.191649082245));
#246514=CARTESIAN_POINT('Ctrl Pts',(-184.904532336853,-1.83992919311302,
126.241175680014));
#246515=CARTESIAN_POINT('Ctrl Pts',(-184.912283528093,-1.96565931089237,
126.295994335197));
#246516=CARTESIAN_POINT('Ctrl Pts',(-184.92003142487,-2.09133599001719,
126.350789690989));
#246517=CARTESIAN_POINT('Ctrl Pts',(-184.927779321648,-2.21478469116771,
126.410872474649));
#246518=CARTESIAN_POINT('Ctrl Pts',(-184.935527218425,-2.33553592707272,
126.476028953304));
#246519=CARTESIAN_POINT('Ctrl Pts',(-184.943273494509,-2.45626190442228,
126.541171802628));
#246520=CARTESIAN_POINT('Ctrl Pts',(-184.951019770593,-2.57429119500066,
126.611386050408));
#246521=CARTESIAN_POINT('Ctrl Pts',(-184.958766046677,-2.68917804732998,
126.686411553741));
#246522=CARTESIAN_POINT('Ctrl Pts',(-184.966512379942,-2.8040657477281,
126.761437610895));
#246523=CARTESIAN_POINT('Ctrl Pts',(-184.974258713208,-2.9158106362426,
126.8412747807));
#246524=CARTESIAN_POINT('Ctrl Pts',(-184.982005046473,-3.02399548026597,
126.925619275606));
#246525=CARTESIAN_POINT('Ctrl Pts',(-184.989753114476,-3.1322045515355,
127.009982658877));
#246526=CARTESIAN_POINT('Ctrl Pts',(-184.997501182479,-3.2368516836113,
127.098855135468));
#246527=CARTESIAN_POINT('Ctrl Pts',(-185.005249250482,-3.33755261674843,
127.19189254256));
#246528=CARTESIAN_POINT('Ctrl Pts',(-185.013005553224,-3.43836057603525,
127.285028830915));
#246529=CARTESIAN_POINT('Ctrl Pts',(-185.020761855966,-3.53521367065951,
127.382338626523));
#246530=CARTESIAN_POINT('Ctrl Pts',(-185.028518158708,-3.62776404908838,
127.483440403733));
#246531=CARTESIAN_POINT('Ctrl Pts',(-185.036278601222,-3.72036382444085,
127.584596142007));
#246532=CARTESIAN_POINT('Ctrl Pts',(-185.044039043736,-3.80865605608395,
127.689547595635));
#246533=CARTESIAN_POINT('Ctrl Pts',(-185.05179948625,-3.89233379093432,
127.797880828435));
#246534=CARTESIAN_POINT('Ctrl Pts',(-185.059572386516,-3.976145852713,127.906387967359));
#246535=CARTESIAN_POINT('Ctrl Pts',(-185.067345286781,-4.05532838899046,
128.018287414464));
#246536=CARTESIAN_POINT('Ctrl Pts',(-185.075118187046,-4.12961782569921,
128.133136239838));
#246537=CARTESIAN_POINT('Ctrl Pts',(-185.082608522808,-4.20120665425939,
128.243810021123));
#246538=CARTESIAN_POINT('Ctrl Pts',(-185.09009885857,-4.26825180309765,
128.357222203767));
#246539=CARTESIAN_POINT('Ctrl Pts',(-185.097589194332,-4.33055905059273,
128.472957312295));
#246540=CARTESIAN_POINT('Ctrl Pts',(-185.10578677954,-4.39874944774409,
128.599620314307));
#246541=CARTESIAN_POINT('Ctrl Pts',(-185.113984364748,-4.46146195184884,
128.729431206875));
#246542=CARTESIAN_POINT('Ctrl Pts',(-185.122181949956,-4.51841101832934,
128.86190214132));
#246543=CARTESIAN_POINT('Ctrl Pts',(-185.130360998453,-4.57523130928227,
128.994073527142));
#246544=CARTESIAN_POINT('Ctrl Pts',(-185.13854004695,-4.62631401768098,
129.128892662092));
#246545=CARTESIAN_POINT('Ctrl Pts',(-185.146719095448,-4.6714196002999,
129.265847705552));
#246546=CARTESIAN_POINT('Ctrl Pts',(-185.152953088293,-4.70579864566502,
129.370233534949));
#246547=CARTESIAN_POINT('Ctrl Pts',(-185.159187081138,-4.73670625024354,
129.475859598491));
#246548=CARTESIAN_POINT('Ctrl Pts',(-185.165421073984,-4.76405452823401,
129.582490119308));
#246549=CARTESIAN_POINT('',(-183.139859435957,-4.91824917715616,130.807205596086));
#246550=CARTESIAN_POINT('Ctrl Pts',(-183.139859435995,-4.91824917715577,
130.807205596751));
#246551=CARTESIAN_POINT('Ctrl Pts',(-183.149254565264,-4.91815366403183,
130.972323621388));
#246552=CARTESIAN_POINT('Ctrl Pts',(-183.158649694533,-4.90974370090652,
131.137198293807));
#246553=CARTESIAN_POINT('Ctrl Pts',(-183.168044823802,-4.89308820514277,
131.301221643601));
#246554=CARTESIAN_POINT('Ctrl Pts',(-183.175819157921,-4.87930602234573,
131.436948602553));
#246555=CARTESIAN_POINT('Ctrl Pts',(-183.18359349204,-4.85985043506831,
131.572316662951));
#246556=CARTESIAN_POINT('Ctrl Pts',(-183.191367826159,-4.83474526787819,
131.70681352893));
#246557=CARTESIAN_POINT('Ctrl Pts',(-183.199132579106,-4.80967104056291,
131.841144639542));
#246558=CARTESIAN_POINT('Ctrl Pts',(-183.206897332053,-4.77896115788808,
131.974606311377));
#246559=CARTESIAN_POINT('Ctrl Pts',(-183.214662085,-4.74269128219991,132.106690247209));
#246560=CARTESIAN_POINT('Ctrl Pts',(-183.222419125885,-4.70645743026349,
132.238642995413));
#246561=CARTESIAN_POINT('Ctrl Pts',(-183.23017616677,-4.664674677723,132.369220356194));
#246562=CARTESIAN_POINT('Ctrl Pts',(-183.237933207655,-4.61746985964742,
132.497923476673));
#246563=CARTESIAN_POINT('Ctrl Pts',(-183.245684398895,-4.57030063909242,
132.626529541128));
#246564=CARTESIAN_POINT('Ctrl Pts',(-183.253435590136,-4.5177176256354,
132.753263812955));
#246565=CARTESIAN_POINT('Ctrl Pts',(-183.261186781376,-4.45989758071983,
132.877642226993));
#246566=CARTESIAN_POINT('Ctrl Pts',(-183.268934678153,-4.40210211086567,
133.001967776888));
#246567=CARTESIAN_POINT('Ctrl Pts',(-183.27668257493,-4.33907420112053,
133.123939106722));
#246568=CARTESIAN_POINT('Ctrl Pts',(-183.284430471707,-4.27103878920714,
133.243091993423));
#246569=CARTESIAN_POINT('Ctrl Pts',(-183.292176747791,-4.20301760883524,
133.362219955909));
#246570=CARTESIAN_POINT('Ctrl Pts',(-183.299923023875,-4.12999120349208,
133.478530308623));
#246571=CARTESIAN_POINT('Ctrl Pts',(-183.307669299959,-4.05223033797251,
133.591583671165));
#246572=CARTESIAN_POINT('Ctrl Pts',(-183.315415633224,-3.97446889844,133.704637868242));
#246573=CARTESIAN_POINT('Ctrl Pts',(-183.32316196649,-3.89197315055749,
133.814434705049));
#246574=CARTESIAN_POINT('Ctrl Pts',(-183.330908299755,-3.80505680682347,
133.920564359196));
#246575=CARTESIAN_POINT('Ctrl Pts',(-183.338656367758,-3.7181209987768,
134.026717780342));
#246576=CARTESIAN_POINT('Ctrl Pts',(-183.346404435761,-3.62676287263744,
134.129202082239));
#246577=CARTESIAN_POINT('Ctrl Pts',(-183.354152503764,-3.53133571328797,
134.227641374757));
#246578=CARTESIAN_POINT('Ctrl Pts',(-183.361908806506,-3.43580713281808,
134.326185289727));
#246579=CARTESIAN_POINT('Ctrl Pts',(-183.369665109248,-3.33620115280986,
134.420675326271));
#246580=CARTESIAN_POINT('Ctrl Pts',(-183.37742141199,-3.23290753652007,
134.510772888592));
#246581=CARTESIAN_POINT('Ctrl Pts',(-183.385181854504,-3.12955878931717,
134.600918538695));
#246582=CARTESIAN_POINT('Ctrl Pts',(-183.392942297018,-3.02251878900405,
134.686666798853));
#246583=CARTESIAN_POINT('Ctrl Pts',(-183.400702739532,-2.91220871858613,
134.767720737703));
#246584=CARTESIAN_POINT('Ctrl Pts',(-183.408475639798,-2.80172156865031,
134.848904791531));
#246585=CARTESIAN_POINT('Ctrl Pts',(-183.416248540063,-2.68795418328053,
134.925379247005));
#246586=CARTESIAN_POINT('Ctrl Pts',(-183.424021440328,-2.57135568988743,
134.996891235055));
#246587=CARTESIAN_POINT('Ctrl Pts',(-183.43151177609,-2.45899584542431,
135.065803582211));
#246588=CARTESIAN_POINT('Ctrl Pts',(-183.439002111852,-2.34400742397867,
135.130107844031));
#246589=CARTESIAN_POINT('Ctrl Pts',(-183.446492447614,-2.22681044216329,
135.18961982509));
#246590=CARTESIAN_POINT('Ctrl Pts',(-183.454266781733,-2.1051699011596,
135.251388221));
#246591=CARTESIAN_POINT('Ctrl Pts',(-183.462041115852,-1.98076469797066,
135.308189427607));
#246592=CARTESIAN_POINT('Ctrl Pts',(-183.469815449971,-1.85403871937935,
135.359766580764));
#246593=CARTESIAN_POINT('Ctrl Pts',(-183.477580202919,-1.72746891923083,
135.41128016969));
#246594=CARTESIAN_POINT('Ctrl Pts',(-183.485344955866,-1.59858439316792,
135.457582369257));
#246595=CARTESIAN_POINT('Ctrl Pts',(-183.493109708813,-1.467853683391,135.49846208927));
#246596=CARTESIAN_POINT('Ctrl Pts',(-183.500866749698,-1.33725281719802,
135.539301206969));
#246597=CARTESIAN_POINT('Ctrl Pts',(-183.508623790583,-1.204809787081,135.57472844694));
#246598=CARTESIAN_POINT('Ctrl Pts',(-183.516380831468,-1.07101284954884,
135.60458087695));
#246599=CARTESIAN_POINT('Ctrl Pts',(-183.524132022708,-0.937316809328249,
135.634410795011));
#246600=CARTESIAN_POINT('Ctrl Pts',(-183.531883213948,-0.802269273954129,
135.65867418614));
#246601=CARTESIAN_POINT('Ctrl Pts',(-183.539634405188,-0.66637304503378,
135.677258115703));
#246602=CARTESIAN_POINT('Ctrl Pts',(-183.547382301965,-0.530534575635689,
135.695834146601));
#246603=CARTESIAN_POINT('Ctrl Pts',(-183.555130198743,-0.393848516679804,
135.708735464179));
#246604=CARTESIAN_POINT('Ctrl Pts',(-183.56287809552,-0.256827016516643,
135.715900391006));
#246605=CARTESIAN_POINT('Ctrl Pts',(-183.570624371604,-0.119834178297475,
135.723063819085));
#246606=CARTESIAN_POINT('Ctrl Pts',(-183.578370647688,0.01749357137839,
135.724493222735));
#246607=CARTESIAN_POINT('Ctrl Pts',(-183.586116923772,0.15464021435102,
135.720178908207));
#246608=CARTESIAN_POINT('Ctrl Pts',(-183.593863257037,0.291787869708826,
135.715864561833));
#246609=CARTESIAN_POINT('Ctrl Pts',(-183.601609590303,0.42875402492383,
135.705806424969));
#246610=CARTESIAN_POINT('Ctrl Pts',(-183.609355923568,0.565024315543222,
135.690046913814));
#246611=CARTESIAN_POINT('Ctrl Pts',(-183.617103991571,0.701325122949181,
135.674283873426));
#246612=CARTESIAN_POINT('Ctrl Pts',(-183.624852059574,0.836929367365514,
135.652816963002));
#246613=CARTESIAN_POINT('Ctrl Pts',(-183.632600127577,0.971329842672489,
135.625740233323));
#246614=CARTESIAN_POINT('Ctrl Pts',(-183.640356430319,1.10587316040419,
135.598634726173));
#246615=CARTESIAN_POINT('Ctrl Pts',(-183.648112733061,1.23920976945106,
135.565907567004));
#246616=CARTESIAN_POINT('Ctrl Pts',(-183.655869035803,1.37084412301909,
135.527703655382));
#246617=CARTESIAN_POINT('Ctrl Pts',(-183.663629478317,1.50254873380541,
135.489479353182));
#246618=CARTESIAN_POINT('Ctrl Pts',(-183.671389920831,1.63254890835973,
135.445772598521));
#246619=CARTESIAN_POINT('Ctrl Pts',(-183.679150363345,1.76036717021572,
135.396777245936));
#246620=CARTESIAN_POINT('Ctrl Pts',(-183.686923263611,1.88839061729247,
135.347703241661));
#246621=CARTESIAN_POINT('Ctrl Pts',(-183.694696163876,2.01422479326663,
135.293323829465));
#246622=CARTESIAN_POINT('Ctrl Pts',(-183.702469064142,2.13741418789364,
135.233880191051));
#246623=CARTESIAN_POINT('Ctrl Pts',(-183.709959399904,2.25612533772893,
135.176597478624));
#246624=CARTESIAN_POINT('Ctrl Pts',(-183.717449735665,2.37238038492857,
135.114612487253));
#246625=CARTESIAN_POINT('Ctrl Pts',(-183.724940071427,2.48579733142663,
135.048179026684));
#246626=CARTESIAN_POINT('Ctrl Pts',(-183.732714405547,2.60351451592501,
134.979226721265));
#246627=CARTESIAN_POINT('Ctrl Pts',(-183.740488739666,2.71854703082651,
134.905263540102));
#246628=CARTESIAN_POINT('Ctrl Pts',(-183.748263073785,2.83043883740145,
134.826524096371));
#246629=CARTESIAN_POINT('Ctrl Pts',(-183.756027826732,2.94219274732453,
134.747881691967));
#246630=CARTESIAN_POINT('Ctrl Pts',(-183.763792579679,3.05081333368219,
134.664474959851));
#246631=CARTESIAN_POINT('Ctrl Pts',(-183.771557332626,3.15586974181246,
134.57658399844));
#246632=CARTESIAN_POINT('Ctrl Pts',(-183.779314373511,3.26082180643742,
134.488780331571));
#246633=CARTESIAN_POINT('Ctrl Pts',(-183.787071414396,3.36221643965492,
134.396501547914));
#246634=CARTESIAN_POINT('Ctrl Pts',(-183.794828455281,3.45965264739519,
134.300070362649));
#246635=CARTESIAN_POINT('Ctrl Pts',(-183.802579646521,3.55701537773313,
134.203711896892));
#246636=CARTESIAN_POINT('Ctrl Pts',(-183.810330837761,3.65042534745426,
134.103207536208));
#246637=CARTESIAN_POINT('Ctrl Pts',(-183.818082029001,3.73951576490132,
133.998919257903));
#246638=CARTESIAN_POINT('Ctrl Pts',(-183.825829925778,3.82856831654428,
133.894675304899));
#246639=CARTESIAN_POINT('Ctrl Pts',(-183.833577822555,3.91330471401534,
133.786650929633));
#246640=CARTESIAN_POINT('Ctrl Pts',(-183.841325719332,3.99339623765048,
133.675243678859));
#246641=CARTESIAN_POINT('Ctrl Pts',(-183.849071995416,4.07347100786544,
133.56385973208));
#246642=CARTESIAN_POINT('Ctrl Pts',(-183.8568182715,4.14890260875522,133.449094634542));
#246643=CARTESIAN_POINT('Ctrl Pts',(-183.864564547585,4.21940396427489,
133.33137728723));
#246644=CARTESIAN_POINT('Ctrl Pts',(-183.87231088085,4.28990584021965,133.213659070955));
#246645=CARTESIAN_POINT('Ctrl Pts',(-183.880057214115,4.35547719729329,
133.092988896832));
#246646=CARTESIAN_POINT('Ctrl Pts',(-183.887803547381,4.41587569489273,
132.969822441232));
#246647=CARTESIAN_POINT('Ctrl Pts',(-183.895551615384,4.47628771831701,
132.846628403359));
#246648=CARTESIAN_POINT('Ctrl Pts',(-183.903299683387,4.53152440502785,
132.720937322577));
#246649=CARTESIAN_POINT('Ctrl Pts',(-183.911047751389,4.58139072531399,
132.593226762504));
#246650=CARTESIAN_POINT('Ctrl Pts',(-183.918804054131,4.63131004411868,
132.465380470129));
#246651=CARTESIAN_POINT('Ctrl Pts',(-183.926560356873,4.67584745234577,
132.335510775713));
#246652=CARTESIAN_POINT('Ctrl Pts',(-183.934316659615,4.71485700295889,
132.204112918564));
#246653=CARTESIAN_POINT('Ctrl Pts',(-183.942077102129,4.75388737414372,
132.072644930422));
#246654=CARTESIAN_POINT('Ctrl Pts',(-183.949837544643,4.78738391338526,
131.939647533283));
#246655=CARTESIAN_POINT('Ctrl Pts',(-183.957597987157,4.81525162830277,
131.805627224733));
#246656=CARTESIAN_POINT('Ctrl Pts',(-183.965370887423,4.84316407895025,
131.671391774886));
#246657=CARTESIAN_POINT('Ctrl Pts',(-183.973143787688,4.86542958515006,
131.536130518247));
#246658=CARTESIAN_POINT('Ctrl Pts',(-183.980916687954,4.88200484548556,
131.400357053089));
#246659=CARTESIAN_POINT('Ctrl Pts',(-183.988407023716,4.8979775533577,131.269519295378));
#246660=CARTESIAN_POINT('Ctrl Pts',(-183.995897359478,4.90866651731051,
131.138206229746));
#246661=CARTESIAN_POINT('Ctrl Pts',(-184.00338769524,4.91407879538588,131.006876432353));
#246662=CARTESIAN_POINT('Ctrl Pts',(-184.011162029359,4.91969628162939,
130.870567225777));
#246663=CARTESIAN_POINT('Ctrl Pts',(-184.018936363479,4.91964684670001,
130.73380820703));
#246664=CARTESIAN_POINT('Ctrl Pts',(-184.026710697598,4.91388137723509,
130.597109868563));
#246665=CARTESIAN_POINT('Ctrl Pts',(-184.034475450545,4.90812301319603,
130.460579998582));
#246666=CARTESIAN_POINT('Ctrl Pts',(-184.042240203492,4.89666264739697,
130.324111046953));
#246667=CARTESIAN_POINT('Ctrl Pts',(-184.050004956439,4.87950304710029,
130.188216903941));
#246668=CARTESIAN_POINT('Ctrl Pts',(-184.057761997324,4.86236048996048,
130.052457732909));
#246669=CARTESIAN_POINT('Ctrl Pts',(-184.065519038209,4.83953001175498,
129.917272619736));
#246670=CARTESIAN_POINT('Ctrl Pts',(-184.073276079094,4.81106637481358,
129.783173367529));
#246671=CARTESIAN_POINT('Ctrl Pts',(-184.081027270334,4.78262420252226,
129.649175240611));
#246672=CARTESIAN_POINT('Ctrl Pts',(-184.088778461574,4.74855740774753,
129.516261725672));
#246673=CARTESIAN_POINT('Ctrl Pts',(-184.096529652814,4.70897227239641,
129.384937072495));
#246674=CARTESIAN_POINT('Ctrl Pts',(-184.104277549591,4.66940396178373,
129.253668235799));
#246675=CARTESIAN_POINT('Ctrl Pts',(-184.112025446369,4.62432208809752,
129.123987291273));
#246676=CARTESIAN_POINT('Ctrl Pts',(-184.119773343146,4.57388343767266,
128.996385683812));
#246677=CARTESIAN_POINT('Ctrl Pts',(-184.12751961923,4.52345533792613,128.868810767856));
#246678=CARTESIAN_POINT('Ctrl Pts',(-184.135265895314,4.46767283385089,
128.74331468718));
#246679=CARTESIAN_POINT('Ctrl Pts',(-184.143012171398,4.40674160037786,
128.620370798451));
#246680=CARTESIAN_POINT('Ctrl Pts',(-184.150758504663,4.3458099171244,128.497426002177));
#246681=CARTESIAN_POINT('Ctrl Pts',(-184.158504837929,4.2797296022448,128.377033785747));
#246682=CARTESIAN_POINT('Ctrl Pts',(-184.166251171194,4.20875303816093,
128.259644341383));
#246683=CARTESIAN_POINT('Ctrl Pts',(-184.173999239197,4.13776057936755,
128.142228608466));
#246684=CARTESIAN_POINT('Ctrl Pts',(-184.1817473072,4.06186989174729,128.027817320214));
#246685=CARTESIAN_POINT('Ctrl Pts',(-184.189495375203,3.98137734477428,
127.916832695447));
#246686=CARTESIAN_POINT('Ctrl Pts',(-184.197251677945,3.90079924936458,
127.8057301149));
#246687=CARTESIAN_POINT('Ctrl Pts',(-184.205007980687,3.81560975438436,
127.698061789918));
#246688=CARTESIAN_POINT('Ctrl Pts',(-184.212764283429,3.72614663075139,
127.594218198819));
#246689=CARTESIAN_POINT('Ctrl Pts',(-184.220524725943,3.63663575795566,
127.490319183269));
#246690=CARTESIAN_POINT('Ctrl Pts',(-184.228285168457,3.54284697871845,
127.390249254338));
#246691=CARTESIAN_POINT('Ctrl Pts',(-184.236045610971,3.44515507810191,
127.294362106124));
#246692=CARTESIAN_POINT('Ctrl Pts',(-184.243818511237,3.34730635377383,
127.198321031346));
#246693=CARTESIAN_POINT('Ctrl Pts',(-184.251591411502,3.2455422777318,127.106476417236));
#246694=CARTESIAN_POINT('Ctrl Pts',(-184.259364311768,3.14027154927359,
127.01914230691));
#246695=CARTESIAN_POINT('Ctrl Pts',(-184.26685464753,3.03882767695724,126.934983011478));
#246696=CARTESIAN_POINT('Ctrl Pts',(-184.274344983291,2.93412792197492,
126.855012163906));
#246697=CARTESIAN_POINT('Ctrl Pts',(-184.281835319053,2.82656191248064,
126.779471697681));
#246698=CARTESIAN_POINT('Ctrl Pts',(-184.289609653172,2.71491750504099,
126.701067091717));
#246699=CARTESIAN_POINT('Ctrl Pts',(-184.297383987292,2.59983154856586,
126.627187092566));
#246700=CARTESIAN_POINT('Ctrl Pts',(-184.305158321411,2.4817069878406,126.55814895433));
#246701=CARTESIAN_POINT('Ctrl Pts',(-184.312923074358,2.36372800507934,
126.489195899429));
#246702=CARTESIAN_POINT('Ctrl Pts',(-184.320687827305,2.2427182034227,126.425073027955));
#246703=CARTESIAN_POINT('Ctrl Pts',(-184.328452580252,2.11911142907846,
126.366055781973));
#246704=CARTESIAN_POINT('Ctrl Pts',(-184.336209621137,1.99562742272505,
126.307097152752));
#246705=CARTESIAN_POINT('Ctrl Pts',(-184.343966662022,1.8695519272367,126.253234224909));
#246706=CARTESIAN_POINT('Ctrl Pts',(-184.351723702907,1.74134513743703,
126.204697567426));
#246707=CARTESIAN_POINT('Ctrl Pts',(-184.359474894147,1.61323502937467,
126.156197511813));
#246708=CARTESIAN_POINT('Ctrl Pts',(-184.367226085387,1.48299719024648,
126.113015869661));
#246709=CARTESIAN_POINT('Ctrl Pts',(-184.374977276627,1.35111330764339,
126.075335782316));
#246710=CARTESIAN_POINT('Ctrl Pts',(-184.382725173404,1.2192854792087,126.037671710014));
#246711=CARTESIAN_POINT('Ctrl Pts',(-184.390473070181,1.08581337391095,
126.005504648981));
#246712=CARTESIAN_POINT('Ctrl Pts',(-184.398220966959,0.951195205101593,
125.978968328405));
#246713=CARTESIAN_POINT('Ctrl Pts',(-184.405967243043,0.816605195511116,
125.952437558655));
#246714=CARTESIAN_POINT('Ctrl Pts',(-184.413713519127,0.680869982589351,
125.931535262159));
#246715=CARTESIAN_POINT('Ctrl Pts',(-184.421459795211,0.544498987029324,
125.916344259612));
#246716=CARTESIAN_POINT('Ctrl Pts',(-184.429206128476,0.408126984809772,
125.901153144929));
#246717=CARTESIAN_POINT('Ctrl Pts',(-184.436952461741,0.271119579148865,
125.891673451605));
#246718=CARTESIAN_POINT('Ctrl Pts',(-184.444698795007,0.133991948377302,
125.887936183054));
#246719=CARTESIAN_POINT('Ctrl Pts',(-184.45244686301,-0.00316639117658285,
125.884198077567));
#246720=CARTESIAN_POINT('Ctrl Pts',(-184.460194931013,-0.140444618670646,
125.886204966446));
#246721=CARTESIAN_POINT('Ctrl Pts',(-184.467942999016,-0.277327314513638,
125.893935725245));
#246722=CARTESIAN_POINT('Ctrl Pts',(-184.475699301758,-0.41435549091451,
125.901674700386));
#246723=CARTESIAN_POINT('Ctrl Pts',(-184.4834556045,-0.550986904952897,
125.915149675607));
#246724=CARTESIAN_POINT('Ctrl Pts',(-184.491211907241,-0.686710462729283,
125.934287537737));
#246725=CARTESIAN_POINT('Ctrl Pts',(-184.498972349756,-0.822506460255012,
125.95343561432));
#246726=CARTESIAN_POINT('Ctrl Pts',(-184.50673279227,-0.957393251687999,
125.978252529597));
#246727=CARTESIAN_POINT('Ctrl Pts',(-184.514493234784,-1.09087068368609,
126.00861414658));
#246728=CARTESIAN_POINT('Ctrl Pts',(-184.522266135049,-1.22456238550795,
126.039024502726));
#246729=CARTESIAN_POINT('Ctrl Pts',(-184.530039035315,-1.35683982936047,
126.074997244652));
#246730=CARTESIAN_POINT('Ctrl Pts',(-184.53781193558,-1.48721788992002,
126.116358270041));
#246731=CARTESIAN_POINT('Ctrl Pts',(-184.545302271342,-1.61285637957678,
126.156215717975));
#246732=CARTESIAN_POINT('Ctrl Pts',(-184.552792607104,-1.73673089353513,
126.201076390584));
#246733=CARTESIAN_POINT('Ctrl Pts',(-184.560282942866,-1.85842728276808,
126.250743253627));
#246734=CARTESIAN_POINT('Ctrl Pts',(-184.568057639186,-1.98474371230457,
126.302295652556));
#246735=CARTESIAN_POINT('Ctrl Pts',(-184.575832335506,-2.10911352182145,
126.359189682738));
#246736=CARTESIAN_POINT('Ctrl Pts',(-184.583607031826,-2.23105192754482,
126.421257794326));
#246737=CARTESIAN_POINT('Ctrl Pts',(-184.591372063905,-2.35283875923919,
126.483248752913));
#246738=CARTESIAN_POINT('Ctrl Pts',(-184.599137095985,-2.4721998557502,
126.550400819786));
#246739=CARTESIAN_POINT('Ctrl Pts',(-184.606902128064,-2.5886689263795,
126.622497844579));
#246740=CARTESIAN_POINT('Ctrl Pts',(-184.614659365366,-2.70502108178013,
126.694522496164));
#246741=CARTESIAN_POINT('Ctrl Pts',(-184.622416602668,-2.81848665856598,
126.771482022306));
#246742=CARTESIAN_POINT('Ctrl Pts',(-184.63017383997,-2.92862289471845,
126.85311385192));
#246743=CARTESIAN_POINT('Ctrl Pts',(-184.63807648539,-3.0408236162226,126.936275856545));
#246744=CARTESIAN_POINT('Ctrl Pts',(-184.645979130809,-3.1495685597896,
127.02428690553));
#246745=CARTESIAN_POINT('Ctrl Pts',(-184.653881776229,-3.25441882467343,
127.116821983719));
#246746=CARTESIAN_POINT('Ctrl Pts',(-184.66162933114,-3.35721138861581,
127.207541048209));
#246747=CARTESIAN_POINT('Ctrl Pts',(-184.669376886051,-3.45626042849622,
127.30260793449));
#246748=CARTESIAN_POINT('Ctrl Pts',(-184.677124440961,-3.55118486455092,
127.401675042864));
#246749=CARTESIAN_POINT('Ctrl Pts',(-184.684870290526,-3.64608840639422,
127.500720345166));
#246750=CARTESIAN_POINT('Ctrl Pts',(-184.69261614009,-3.73686888073763,
127.603763835403));
#246751=CARTESIAN_POINT('Ctrl Pts',(-184.700361989654,-3.82318206752826,
127.710421067247));
#246752=CARTESIAN_POINT('Ctrl Pts',(-184.708107811659,-3.90949494721215,
127.817077919599));
#246753=CARTESIAN_POINT('Ctrl Pts',(-184.715853633663,-3.99134032571703,
127.927348183657));
#246754=CARTESIAN_POINT('Ctrl Pts',(-184.723599455667,-4.06841453913728,
128.040814670737));
#246755=CARTESIAN_POINT('Ctrl Pts',(-184.731619278531,-4.1482151773007,
128.158294923565));
#246756=CARTESIAN_POINT('Ctrl Pts',(-184.739639101396,-4.22290061394825,
128.279201330047));
#246757=CARTESIAN_POINT('Ctrl Pts',(-184.74765892426,-4.29218348010272,
128.403039307197));
#246758=CARTESIAN_POINT('Ctrl Pts',(-184.755413217867,-4.35917245170187,
128.522777118212));
#246759=CARTESIAN_POINT('Ctrl Pts',(-184.763167511474,-4.42111077918117,
128.645255083161));
#246760=CARTESIAN_POINT('Ctrl Pts',(-184.770921805081,-4.4777865008787,
128.770002951115));
#246761=CARTESIAN_POINT('Ctrl Pts',(-184.779074392574,-4.53737333151672,
128.901158406353));
#246762=CARTESIAN_POINT('Ctrl Pts',(-184.787226980067,-4.59114243408741,
129.034822659559));
#246763=CARTESIAN_POINT('Ctrl Pts',(-184.79537956756,-4.63890608312226,
129.170428729612));
#246764=CARTESIAN_POINT('Ctrl Pts',(-184.803532155053,-4.68666973215712,
129.306034799666));
#246765=CARTESIAN_POINT('Ctrl Pts',(-184.811684742546,-4.72842783798587,
129.443582194741));
#246766=CARTESIAN_POINT('Ctrl Pts',(-184.819837330039,-4.76405452823405,
129.582490119308));
#246767=CARTESIAN_POINT('Ctrl Pts',(-183.069718605797,-4.76405452823406,
129.582490119308));
#246768=CARTESIAN_POINT('Ctrl Pts',(-183.077377441043,-4.79772994797449,
129.71379006978));
#246769=CARTESIAN_POINT('Ctrl Pts',(-183.085036276289,-4.825950394775,129.846394602858));
#246770=CARTESIAN_POINT('Ctrl Pts',(-183.092695111536,-4.84863804824104,
129.97980489498));
#246771=CARTESIAN_POINT('Ctrl Pts',(-183.100555832273,-4.87192374408618,
130.116731857903));
#246772=CARTESIAN_POINT('Ctrl Pts',(-183.10841655301,-4.88938085774212,
130.254507194701));
#246773=CARTESIAN_POINT('Ctrl Pts',(-183.116277273746,-4.90098218359303,
130.392587987825));
#246774=CARTESIAN_POINT('Ctrl Pts',(-183.124137994483,-4.91258350944392,
130.530668780949));
#246775=CARTESIAN_POINT('Ctrl Pts',(-183.13199871522,-4.91832909109846,
130.669054577283));
#246776=CARTESIAN_POINT('Ctrl Pts',(-183.139859435957,-4.91824917715616,
130.807205596086));
#246777=CARTESIAN_POINT('Origin',(213.235140564004,0.,130.804360617566));
#246778=CARTESIAN_POINT('',(-181.320039938991,-4.76405452823418,129.582490119309));
#246779=CARTESIAN_POINT('',(-181.664999290689,-4.76405452823418,129.582490119309));
#246780=CARTESIAN_POINT('',(213.235140564004,-4.76405452823405,129.582490119308));
#246781=CARTESIAN_POINT('',(-181.735140563977,-4.91824950327072,130.806571064885));
#246782=CARTESIAN_POINT('Ctrl Pts',(-181.664999290689,-4.76405452823418,
129.582490119309));
#246783=CARTESIAN_POINT('Ctrl Pts',(-181.672675880478,-4.79779503273996,
129.714043834293));
#246784=CARTESIAN_POINT('Ctrl Pts',(-181.680352470268,-4.82605765331497,
129.846900063432));
#246785=CARTESIAN_POINT('Ctrl Pts',(-181.688029060058,-4.84876606521478,
129.980558027547));
#246786=CARTESIAN_POINT('Ctrl Pts',(-181.695880977377,-4.87199312014276,
130.117268638917));
#246787=CARTESIAN_POINT('Ctrl Pts',(-181.703732894697,-4.88940914158996,
130.254817604855));
#246788=CARTESIAN_POINT('Ctrl Pts',(-181.711584812017,-4.90098872141958,
130.392665809464));
#246789=CARTESIAN_POINT('Ctrl Pts',(-181.719436729337,-4.9125683012492,
130.530514014073));
#246790=CARTESIAN_POINT('Ctrl Pts',(-181.727288646657,-4.91831148526274,
130.668661014282));
#246791=CARTESIAN_POINT('Ctrl Pts',(-181.735140563977,-4.91824950327072,
130.806571064884));
#246792=CARTESIAN_POINT('Ctrl Pts',(-181.735140564012,-4.91824950327044,
130.806571065507));
#246793=CARTESIAN_POINT('Ctrl Pts',(-181.742166278867,-4.91819404319526,
130.929969803894));
#246794=CARTESIAN_POINT('Ctrl Pts',(-181.749191993722,-4.91349490493225,
131.053259845395));
#246795=CARTESIAN_POINT('Ctrl Pts',(-181.756217708576,-4.90417395891944,
131.176195047328));
#246796=CARTESIAN_POINT('Ctrl Pts',(-181.763992042696,-4.89385982717492,
131.312229508533));
#246797=CARTESIAN_POINT('Ctrl Pts',(-181.771766376815,-4.87786497991832,
131.448049965438));
#246798=CARTESIAN_POINT('Ctrl Pts',(-181.779540710934,-4.85620016088216,
131.583143681036));
#246799=CARTESIAN_POINT('Ctrl Pts',(-181.787305463881,-4.83456204179922,
131.718070905703));
#246800=CARTESIAN_POINT('Ctrl Pts',(-181.795070216828,-4.80726791575691,
131.852272788801));
#246801=CARTESIAN_POINT('Ctrl Pts',(-181.802834969775,-4.77438044942487,
131.98523926783));
#246802=CARTESIAN_POINT('Ctrl Pts',(-181.81059201066,-4.74152564738802,
132.118073682678));
#246803=CARTESIAN_POINT('Ctrl Pts',(-181.818349051545,-4.70308865379099,
132.249674758213));
#246804=CARTESIAN_POINT('Ctrl Pts',(-181.82610609243,-4.6591835323683,132.379540567352));
#246805=CARTESIAN_POINT('Ctrl Pts',(-181.833857283671,-4.61531152013915,
132.509308443675));
#246806=CARTESIAN_POINT('Ctrl Pts',(-181.841608474911,-4.56597971248463,
132.637343289375));
#246807=CARTESIAN_POINT('Ctrl Pts',(-181.849359666151,-4.51135246061705,
132.763156686223));
#246808=CARTESIAN_POINT('Ctrl Pts',(-181.857107562928,-4.45674842678867,
132.888916609021));
#246809=CARTESIAN_POINT('Ctrl Pts',(-181.864855459705,-4.39685358061205,
133.012456602989));
#246810=CARTESIAN_POINT('Ctrl Pts',(-181.872603356482,-4.33188094023251,
133.133306856136));
#246811=CARTESIAN_POINT('Ctrl Pts',(-181.880349632566,-4.26692189072869,
133.254131830015));
#246812=CARTESIAN_POINT('Ctrl Pts',(-181.888095908651,-4.19688734474357,
133.372267838051));
#246813=CARTESIAN_POINT('Ctrl Pts',(-181.895842184735,-4.12203676652123,
133.487268733389));
#246814=CARTESIAN_POINT('Ctrl Pts',(-181.903588518,-4.04718563576903,133.602270477636));
#246815=CARTESIAN_POINT('Ctrl Pts',(-181.911334851265,-3.9675186151122,
133.714136735334));
#246816=CARTESIAN_POINT('Ctrl Pts',(-181.919081184531,-3.88333885679162,
133.822449812045));
#246817=CARTESIAN_POINT('Ctrl Pts',(-181.926829252534,-3.79914024699795,
133.930787144718));
#246818=CARTESIAN_POINT('Ctrl Pts',(-181.934577320537,-3.71042712844116,
134.035569404395));
#246819=CARTESIAN_POINT('Ctrl Pts',(-181.94232538854,-3.61754307876341,
134.136411808018));
#246820=CARTESIAN_POINT('Ctrl Pts',(-181.950081691281,-3.52456031081195,
134.237361388148));
#246821=CARTESIAN_POINT('Ctrl Pts',(-181.957837994024,-3.42739802181008,
134.334362459562));
#246822=CARTESIAN_POINT('Ctrl Pts',(-181.965594296765,-3.32643720759424,
134.427066590514));
#246823=CARTESIAN_POINT('Ctrl Pts',(-181.97335473928,-3.22542250755198,
134.519820200452));
#246824=CARTESIAN_POINT('Ctrl Pts',(-181.981115181794,-3.12060554120253,
134.608272048101));
#246825=CARTESIAN_POINT('Ctrl Pts',(-181.988875624308,-3.01239977711739,
134.692114550793));
#246826=CARTESIAN_POINT('Ctrl Pts',(-181.996648524573,-2.90402031153368,
134.776091644914));
#246827=CARTESIAN_POINT('Ctrl Pts',(-182.004421424839,-2.79224149634652,
134.85544438141));
#246828=CARTESIAN_POINT('Ctrl Pts',(-182.012194325104,-2.67750585984077,
134.929908512454));
#246829=CARTESIAN_POINT('Ctrl Pts',(-182.019684660866,-2.5669411527255,
135.001665684771));
#246830=CARTESIAN_POINT('Ctrl Pts',(-182.027174996628,-2.4536311327147,
135.068883350007));
#246831=CARTESIAN_POINT('Ctrl Pts',(-182.03466533239,-2.33799097923109,
135.131366654485));
#246832=CARTESIAN_POINT('Ctrl Pts',(-182.042439666509,-2.21796629417824,
135.196219032444));
#246833=CARTESIAN_POINT('Ctrl Pts',(-182.050214000628,-2.09505109151086,
135.256176389005));
#246834=CARTESIAN_POINT('Ctrl Pts',(-182.057988334747,-1.96968255864387,
135.310970616298));
#246835=CARTESIAN_POINT('Ctrl Pts',(-182.065753087694,-1.84446853128913,
135.365697314603));
#246836=CARTESIAN_POINT('Ctrl Pts',(-182.073517840642,-1.71680754442264,
135.415273389231));
#246837=CARTESIAN_POINT('Ctrl Pts',(-182.081282593589,-1.5871626009352,
135.459475862186));
#246838=CARTESIAN_POINT('Ctrl Pts',(-182.089039634474,-1.45764642263331,
135.503634432622));
#246839=CARTESIAN_POINT('Ctrl Pts',(-182.096796675359,-1.32615057673516,
135.542429897177));
#246840=CARTESIAN_POINT('Ctrl Pts',(-182.104553716244,-1.19315900294414,
135.575686917055));
#246841=CARTESIAN_POINT('Ctrl Pts',(-182.112304907484,-1.06026771913327,
135.608918857555));
#246842=CARTESIAN_POINT('Ctrl Pts',(-182.120056098724,-0.925883330276927,
135.636620572151));
#246843=CARTESIAN_POINT('Ctrl Pts',(-182.127807289964,-0.790505592309228,
135.65866633219));
#246844=CARTESIAN_POINT('Ctrl Pts',(-182.135555186741,-0.655185393491669,
135.680702722192));
#246845=CARTESIAN_POINT('Ctrl Pts',(-182.143303083518,-0.518873070360332,
135.697087876165));
#246846=CARTESIAN_POINT('Ctrl Pts',(-182.151050980295,-0.382079030561141,
135.70774706745));
#246847=CARTESIAN_POINT('Ctrl Pts',(-182.15879725638,-0.245313605126137,
135.718404029062));
#246848=CARTESIAN_POINT('Ctrl Pts',(-182.166543532464,-0.108067052986587,
135.723337380018));
#246849=CARTESIAN_POINT('Ctrl Pts',(-182.174289808548,0.0291450231112156,
135.722524261664));
#246850=CARTESIAN_POINT('Ctrl Pts',(-182.182036141813,0.16635811207758,
135.721711137307));
#246851=CARTESIAN_POINT('Ctrl Pts',(-182.189782475079,0.303536333536031,
135.715151461312));
#246852=CARTESIAN_POINT('Ctrl Pts',(-182.197528808344,0.440164408135673,
135.702874510198));
#246853=CARTESIAN_POINT('Ctrl Pts',(-182.205276876347,0.576823079645122,
135.690594809746));
#246854=CARTESIAN_POINT('Ctrl Pts',(-182.21302494435,0.712930969817092,
135.672595321422));
#246855=CARTESIAN_POINT('Ctrl Pts',(-182.220773012353,0.847978637660013,
135.648957122186));
#246856=CARTESIAN_POINT('Ctrl Pts',(-182.228529315095,0.983169835771588,
135.62529379999));
#246857=CARTESIAN_POINT('Ctrl Pts',(-182.236285617837,1.1172981748916,135.595979862955));
#246858=CARTESIAN_POINT('Ctrl Pts',(-182.244041920579,1.24986457196712,
135.5611475178));
#246859=CARTESIAN_POINT('Ctrl Pts',(-182.251802363093,1.38250172372027,
135.526296581574));
#246860=CARTESIAN_POINT('Ctrl Pts',(-182.259562805607,1.51357489884223,
135.485921483424));
#246861=CARTESIAN_POINT('Ctrl Pts',(-182.267323248121,1.64260182946052,
135.440203830225));
#246862=CARTESIAN_POINT('Ctrl Pts',(-182.275096148387,1.77183588556232,
135.39441278699));
#246863=CARTESIAN_POINT('Ctrl Pts',(-182.282869048652,1.89901677012015,
135.343262196406));
#246864=CARTESIAN_POINT('Ctrl Pts',(-182.290641948918,2.02368296660664,
135.286981537649));
#246865=CARTESIAN_POINT('Ctrl Pts',(-182.298132284679,2.14381723283161,
135.232746822602));
#246866=CARTESIAN_POINT('Ctrl Pts',(-182.305622620441,2.26161619186303,
135.173748683604));
#246867=CARTESIAN_POINT('Ctrl Pts',(-182.313112956203,2.37669149316271,
135.11023109969));
#246868=CARTESIAN_POINT('Ctrl Pts',(-182.320887290322,2.49612990949109,
135.044305227274));
#246869=CARTESIAN_POINT('Ctrl Pts',(-182.328661624441,2.61301240105838,
134.973301601892));
#246870=CARTESIAN_POINT('Ctrl Pts',(-182.33643595856,2.72687709064381,134.897443122845));
#246871=CARTESIAN_POINT('Ctrl Pts',(-182.344200711507,2.84060145217569,
134.821678132594));
#246872=CARTESIAN_POINT('Ctrl Pts',(-182.351965464454,2.9513150895211,134.741070408096));
#246873=CARTESIAN_POINT('Ctrl Pts',(-182.359730217402,3.05858014060573,
134.655888961742));
#246874=CARTESIAN_POINT('Ctrl Pts',(-182.367487258287,3.16573865452946,
134.570792118802));
#246875=CARTESIAN_POINT('Ctrl Pts',(-182.375244299171,3.26945509427675,
134.481130835716));
#246876=CARTESIAN_POINT('Ctrl Pts',(-182.383001340056,3.369320361121,134.387217489761));
#246877=CARTESIAN_POINT('Ctrl Pts',(-182.390752531297,3.46911031879082,
134.29337496459));
#246878=CARTESIAN_POINT('Ctrl Pts',(-182.398503722537,3.56505460053173,
134.195287025673));
#246879=CARTESIAN_POINT('Ctrl Pts',(-182.406254913777,3.6567772969768,134.093306172423));
#246880=CARTESIAN_POINT('Ctrl Pts',(-182.414002810554,3.74846100882897,
133.991368663756));
#246881=CARTESIAN_POINT('Ctrl Pts',(-182.421750707331,3.83592644318413,
133.885541821693));
#246882=CARTESIAN_POINT('Ctrl Pts',(-182.429498604108,3.91883484258758,
133.776214675056));
#246883=CARTESIAN_POINT('Ctrl Pts',(-182.437244880192,4.00172589934117,
133.666910397302));
#246884=CARTESIAN_POINT('Ctrl Pts',(-182.444991156276,4.08006158108549,
133.554107582659));
#246885=CARTESIAN_POINT('Ctrl Pts',(-182.45273743236,4.15354396030729,133.438227666658));
#246886=CARTESIAN_POINT('Ctrl Pts',(-182.460483765626,4.22702688195942,
133.322346895258));
#246887=CARTESIAN_POINT('Ctrl Pts',(-182.468230098891,4.29565622022754,
133.203389307352));
#246888=CARTESIAN_POINT('Ctrl Pts',(-182.475976432157,4.35917808520141,
133.081804246726));
#246889=CARTESIAN_POINT('Ctrl Pts',(-182.48372450016,4.42271417545642,132.960191957968));
#246890=CARTESIAN_POINT('Ctrl Pts',(-182.491472568163,4.48114033541539,
132.83595137209));
#246891=CARTESIAN_POINT('Ctrl Pts',(-182.499220636166,4.53424941212098,
132.709554920303));
#246892=CARTESIAN_POINT('Ctrl Pts',(-182.506976938907,4.58741493378524,
132.583024132863));
#246893=CARTESIAN_POINT('Ctrl Pts',(-182.514733241649,4.63525193190573,
132.45433326345));
#246894=CARTESIAN_POINT('Ctrl Pts',(-182.522489544391,4.67760186915715,
132.323973665732));
#246895=CARTESIAN_POINT('Ctrl Pts',(-182.530249986905,4.71997440984532,
132.193544491172));
#246896=CARTESIAN_POINT('Ctrl Pts',(-182.53801042942,4.75685394908354,132.06144518999));
#246897=CARTESIAN_POINT('Ctrl Pts',(-182.545770871934,4.78813260031306,
131.928179670759));
#246898=CARTESIAN_POINT('Ctrl Pts',(-182.553543772199,4.81946146281031,
131.794700221885));
#246899=CARTESIAN_POINT('Ctrl Pts',(-182.561316672464,4.84517139696213,
131.660051198124));
#246900=CARTESIAN_POINT('Ctrl Pts',(-182.56908957273,4.86520600914096,131.524744925501));
#246901=CARTESIAN_POINT('Ctrl Pts',(-182.576579908492,4.88451231270299,
131.394357376703));
#246902=CARTESIAN_POINT('Ctrl Pts',(-182.584070244254,4.89854872220694,
131.263359840987));
#246903=CARTESIAN_POINT('Ctrl Pts',(-182.591560580016,4.90731059117172,
131.132210925289));
#246904=CARTESIAN_POINT('Ctrl Pts',(-182.599334914135,4.91640466906136,
130.99608945859));
#246905=CARTESIAN_POINT('Ctrl Pts',(-182.607109248254,4.91984514980589,
130.859373714271));
#246906=CARTESIAN_POINT('Ctrl Pts',(-182.614883582373,4.91756990898058,
130.722572765236));
#246907=CARTESIAN_POINT('Ctrl Pts',(-182.62264833532,4.91529747218625,130.585940411145));
#246908=CARTESIAN_POINT('Ctrl Pts',(-182.630413088267,4.90732333595251,
130.449223448429));
#246909=CARTESIAN_POINT('Ctrl Pts',(-182.638177841215,4.89363715287714,
130.31293567062));
#246910=CARTESIAN_POINT('Ctrl Pts',(-182.6459348821,4.87996456311174,130.176783255754));
#246911=CARTESIAN_POINT('Ctrl Pts',(-182.653691922985,4.86059125541069,
130.041059563987));
#246912=CARTESIAN_POINT('Ctrl Pts',(-182.66144896387,4.83555891376832,129.906277629209));
#246913=CARTESIAN_POINT('Ctrl Pts',(-182.66920015511,4.81054544920946,129.771597334537));
#246914=CARTESIAN_POINT('Ctrl Pts',(-182.67695134635,4.77988151605426,129.63785776611));
#246915=CARTESIAN_POINT('Ctrl Pts',(-182.68470253759,4.74366049384699,129.505565721666));
#246916=CARTESIAN_POINT('Ctrl Pts',(-182.692450434367,4.70745486654033,
129.37332990487));
#246917=CARTESIAN_POINT('Ctrl Pts',(-182.700198331144,4.66569695087129,
129.242540764698));
#246918=CARTESIAN_POINT('Ctrl Pts',(-182.707946227921,4.618530941128,129.11369358697));
#246919=CARTESIAN_POINT('Ctrl Pts',(-182.715692504005,4.57137479749729,
128.984873361295));
#246920=CARTESIAN_POINT('Ctrl Pts',(-182.72343878009,4.51881294423457,128.857994656986));
#246921=CARTESIAN_POINT('Ctrl Pts',(-182.731185056174,4.46103890988972,
128.733535925094));
#246922=CARTESIAN_POINT('Ctrl Pts',(-182.738931389439,4.40326444907,128.609076274477));
#246923=CARTESIAN_POINT('Ctrl Pts',(-182.746677722704,4.34027789500933,
128.487036986544));
#246924=CARTESIAN_POINT('Ctrl Pts',(-182.75442405597,4.27232005966242,128.36787454736));
#246925=CARTESIAN_POINT('Ctrl Pts',(-182.762172123973,4.20434700562956,
128.248685422574));
#246926=CARTESIAN_POINT('Ctrl Pts',(-182.769920191976,4.13140064865017,
128.132374768074));
#246927=CARTESIAN_POINT('Ctrl Pts',(-182.777668259979,4.05376648724896,
128.019372228119));
#246928=CARTESIAN_POINT('Ctrl Pts',(-182.78542456272,3.97604981533704,127.906249587719));
#246929=CARTESIAN_POINT('Ctrl Pts',(-182.793180865462,3.89363560815299,
127.796442408019));
#246930=CARTESIAN_POINT('Ctrl Pts',(-182.800937168204,3.80685156215607,
127.69034965962));
#246931=CARTESIAN_POINT('Ctrl Pts',(-182.808697610718,3.72002119690079,
127.584200286326));
#246932=CARTESIAN_POINT('Ctrl Pts',(-182.816458053233,3.62881660536122,
127.481769586489));
#246933=CARTESIAN_POINT('Ctrl Pts',(-182.824218495747,3.5336034247693,127.383420703016));
#246934=CARTESIAN_POINT('Ctrl Pts',(-182.831991396012,3.43823739952725,
127.284913941185));
#246935=CARTESIAN_POINT('Ctrl Pts',(-182.839764296278,3.33885020978783,
127.190502359112));
#246936=CARTESIAN_POINT('Ctrl Pts',(-182.847537196543,3.23584240781202,
127.100510327084));
#246937=CARTESIAN_POINT('Ctrl Pts',(-182.855027532305,3.1365791988993,127.013789732096));
#246938=CARTESIAN_POINT('Ctrl Pts',(-182.862517868067,3.03395428425488,
126.931173135403));
#246939=CARTESIAN_POINT('Ctrl Pts',(-182.870008203829,2.92835099134394,
126.852912334468));
#246940=CARTESIAN_POINT('Ctrl Pts',(-182.877782537948,2.818743717485,126.77168425148));
#246941=CARTESIAN_POINT('Ctrl Pts',(-182.885556872067,2.70558055367971,
126.694891478318));
#246942=CARTESIAN_POINT('Ctrl Pts',(-182.893331206186,2.58925621761079,
126.622861448361));
#246943=CARTESIAN_POINT('Ctrl Pts',(-182.901095959133,2.47307524088987,
126.550920188978));
#246944=CARTESIAN_POINT('Ctrl Pts',(-182.90886071208,2.35374117271796,126.483730197785));
#246945=CARTESIAN_POINT('Ctrl Pts',(-182.916625465027,2.23168068912202,
126.4215778983));
#246946=CARTESIAN_POINT('Ctrl Pts',(-182.924382505912,2.10974143771914,
126.359487329355));
#246947=CARTESIAN_POINT('Ctrl Pts',(-182.932139546797,1.98508150590871,
126.302424671168));
#246948=CARTESIAN_POINT('Ctrl Pts',(-182.939896587682,1.85815505485159,
126.250632161166));
#246949=CARTESIAN_POINT('Ctrl Pts',(-182.947647778922,1.73132432001839,
126.198878708298));
#246950=CARTESIAN_POINT('Ctrl Pts',(-182.955398970163,1.60223082852072,
126.152387640204));
#246951=CARTESIAN_POINT('Ctrl Pts',(-182.963150161403,1.47135143757472,
126.111354330585));
#246952=CARTESIAN_POINT('Ctrl Pts',(-182.97089805818,1.34052767386137,126.070338461217));
#246953=CARTESIAN_POINT('Ctrl Pts',(-182.978645954957,1.20791989268096,
126.034775853349));
#246954=CARTESIAN_POINT('Ctrl Pts',(-182.986393851734,1.07402273255796,
126.004812906328));
#246955=CARTESIAN_POINT('Ctrl Pts',(-182.994140127818,0.940153580834378,
125.97485622691));
#246956=CARTESIAN_POINT('Ctrl Pts',(-183.001886403902,0.804995967924261,
125.950496963824));
#246957=CARTESIAN_POINT('Ctrl Pts',(-183.009632679986,0.669057035157692,
125.931830910504));
#246958=CARTESIAN_POINT('Ctrl Pts',(-183.017379013251,0.533117098920988,
125.913164719394));
#246959=CARTESIAN_POINT('Ctrl Pts',(-183.025125346517,0.39639621864993,
125.900191875094));
#246960=CARTESIAN_POINT('Ctrl Pts',(-183.032871679782,0.259408613742112,
125.892956517554));
#246961=CARTESIAN_POINT('Ctrl Pts',(-183.040619747785,0.122390331409793,
125.885719539705));
#246962=CARTESIAN_POINT('Ctrl Pts',(-183.048367815788,-0.0148944040710403,
125.884222625977));
#246963=CARTESIAN_POINT('Ctrl Pts',(-183.056115883791,-0.151929801890471,
125.888457811591));
#246964=CARTESIAN_POINT('Ctrl Pts',(-183.063872186533,-0.289110842561633,
125.89269749841));
#246965=CARTESIAN_POINT('Ctrl Pts',(-183.071628489275,-0.426041624805545,
125.902681442188));
#246966=CARTESIAN_POINT('Ctrl Pts',(-183.079384792016,-0.562209355415556,
125.918349595967));
#246967=CARTESIAN_POINT('Ctrl Pts',(-183.08714523453,-0.698449762843326,
125.934026112312));
#246968=CARTESIAN_POINT('Ctrl Pts',(-183.094905677045,-0.833925921127289,
125.955392822951));
#246969=CARTESIAN_POINT('Ctrl Pts',(-183.102666119559,-0.968134671998613,
125.982338394538));
#246970=CARTESIAN_POINT('Ctrl Pts',(-183.110439019824,-1.10255886667133,
126.009327221549));
#246971=CARTESIAN_POINT('Ctrl Pts',(-183.11821192009,-1.2357112082651,126.041912712826));
#246972=CARTESIAN_POINT('Ctrl Pts',(-183.125984820355,-1.36710228659016,
126.079933202471));
#246973=CARTESIAN_POINT('Ctrl Pts',(-183.133475156117,-1.49371696826858,
126.116571551551));
#246974=CARTESIAN_POINT('Ctrl Pts',(-183.14096549188,-1.61869592401328,
126.158256510196));
#246975=CARTESIAN_POINT('Ctrl Pts',(-183.148455827642,-1.74162011162668,
126.204801676833));
#246976=CARTESIAN_POINT('Ctrl Pts',(-183.15623038486,-1.86920866845707,
126.253113003952));
#246977=CARTESIAN_POINT('Ctrl Pts',(-183.164004942078,-1.99498761497027,
126.306813704835));
#246978=CARTESIAN_POINT('Ctrl Pts',(-183.171779499296,-2.11846807574788,
126.365748663978));
#246979=CARTESIAN_POINT('Ctrl Pts',(-183.179544423664,-2.24179554147299,
126.424610601388));
#246980=CARTESIAN_POINT('Ctrl Pts',(-183.187309348032,-2.36282983852742,
126.488693725991));
#246981=CARTESIAN_POINT('Ctrl Pts',(-183.195074272399,-2.48109933137568,
126.557793866607));
#246982=CARTESIAN_POINT('Ctrl Pts',(-183.202831433245,-2.59925057609296,
126.626824919564));
#246983=CARTESIAN_POINT('Ctrl Pts',(-183.210588594091,-2.71464218244685,
126.700862809964));
#246984=CARTESIAN_POINT('Ctrl Pts',(-183.218345754937,-2.82682484457249,
126.779656360033));
#246985=CARTESIAN_POINT('Ctrl Pts',(-183.226097014844,-2.93892216838622,
126.858389971173));
#246986=CARTESIAN_POINT('Ctrl Pts',(-183.233848274751,-3.04781508831774,
126.941871817109));
#246987=CARTESIAN_POINT('Ctrl Pts',(-183.241599534659,-3.15308146877894,
127.029806297684));
#246988=CARTESIAN_POINT('Ctrl Pts',(-183.249347240883,-3.25829958826959,
127.11770046336));
#246989=CARTESIAN_POINT('Ctrl Pts',(-183.257094947108,-3.35989417716957,
127.210042951671));
#246990=CARTESIAN_POINT('Ctrl Pts',(-183.264842653332,-3.45747473226868,
127.30649676398));
#246991=CARTESIAN_POINT('Ctrl Pts',(-183.272588665805,-3.55503395496101,
127.402929490203));
#246992=CARTESIAN_POINT('Ctrl Pts',(-183.280334678278,-3.6485806119105,
127.503471477585));
#246993=CARTESIAN_POINT('Ctrl Pts',(-183.28808069075,-3.73776002458828,
127.607747869501));
#246994=CARTESIAN_POINT('Ctrl Pts',(-183.295826687299,-3.82693925393412,
127.71202404705));
#246995=CARTESIAN_POINT('Ctrl Pts',(-183.303572683848,-3.91175100311841,
127.820034316536));
#246996=CARTESIAN_POINT('Ctrl Pts',(-183.311318680397,-3.9918802286738,
127.931369962791));
#246997=CARTESIAN_POINT('Ctrl Pts',(-183.319066338468,-4.07202664200908,
128.042729490627));
#246998=CARTESIAN_POINT('Ctrl Pts',(-183.326813996539,-4.14748830531724,
128.157415497046));
#246999=CARTESIAN_POINT('Ctrl Pts',(-183.33456165461,-4.21799316285316,
128.274989798444));
#247000=CARTESIAN_POINT('Ctrl Pts',(-183.342316556619,-4.28856394132185,
128.392674029965));
#247001=CARTESIAN_POINT('Ctrl Pts',(-183.350071458629,-4.35416845854172,
128.5132516133));
#247002=CARTESIAN_POINT('Ctrl Pts',(-183.357826360638,-4.4145801711371,
128.636258919051));
#247003=CARTESIAN_POINT('Ctrl Pts',(-183.365585372232,-4.47502389793923,
128.759331410527));
#247004=CARTESIAN_POINT('Ctrl Pts',(-183.373344383826,-4.53026917973013,
128.884835832641));
#247005=CARTESIAN_POINT('Ctrl Pts',(-183.38110339542,-4.58013779618434,
129.012288958713));
#247006=CARTESIAN_POINT('Ctrl Pts',(-183.388872575828,-4.63007176950502,
129.139909122444));
#247007=CARTESIAN_POINT('Ctrl Pts',(-183.396641756236,-4.67461487900791,
129.269482721212));
#247008=CARTESIAN_POINT('Ctrl Pts',(-183.404410936644,-4.71363875007996,
129.400511339244));
#247009=CARTESIAN_POINT('Ctrl Pts',(-183.407990344031,-4.73161778069228,
129.460878685434));
#247010=CARTESIAN_POINT('Ctrl Pts',(-183.411569751418,-4.74842600050534,
129.52155472689));
#247011=CARTESIAN_POINT('Ctrl Pts',(-183.415149158805,-4.76405452823414,
129.582490119309));
#247012=CARTESIAN_POINT('',(-181.389859436049,-4.91824915695527,130.807240306567));
#247013=CARTESIAN_POINT('Ctrl Pts',(-181.389859436049,-4.91824915695527,
130.807240306567));
#247014=CARTESIAN_POINT('Ctrl Pts',(-181.398817739788,-4.91815613411647,
130.966114927541));
#247015=CARTESIAN_POINT('Ctrl Pts',(-181.407776043528,-4.91036021059812,
131.124708256897));
#247016=CARTESIAN_POINT('Ctrl Pts',(-181.416734347267,-4.89497108865333,
131.282315744903));
#247017=CARTESIAN_POINT('Ctrl Pts',(-181.425417497863,-4.88005464160356,
131.43508233925));
#247018=CARTESIAN_POINT('Ctrl Pts',(-181.434100648459,-4.8580046953391,
131.58692260436));
#247019=CARTESIAN_POINT('Ctrl Pts',(-181.442783799056,-4.82897206538774,
131.737212081736));
#247020=CARTESIAN_POINT('Ctrl Pts',(-181.451879679367,-4.79855944910979,
131.89464515665));
#247021=CARTESIAN_POINT('Ctrl Pts',(-181.460975559678,-4.76048430540328,
132.050376121223));
#247022=CARTESIAN_POINT('Ctrl Pts',(-181.47007143999,-4.71497645596076,
132.203710495987));
#247023=CARTESIAN_POINT('Ctrl Pts',(-181.479167320301,-4.66946860651813,
132.35704487075));
#247024=CARTESIAN_POINT('Ctrl Pts',(-181.488263200613,-4.61652822818693,
132.507982437687));
#247025=CARTESIAN_POINT('Ctrl Pts',(-181.497359080924,-4.5564403008889,
132.65585591784));
#247026=CARTESIAN_POINT('Ctrl Pts',(-181.505133415044,-4.50508258647963,
132.782244766713));
#247027=CARTESIAN_POINT('Ctrl Pts',(-181.512907749162,-4.44838078293223,
132.906695307599));
#247028=CARTESIAN_POINT('Ctrl Pts',(-181.520682083282,-4.386501677665,133.028722569754));
#247029=CARTESIAN_POINT('Ctrl Pts',(-181.528446836229,-4.32469883286472,
133.150599444214));
#247030=CARTESIAN_POINT('Ctrl Pts',(-181.536211589176,-4.25773155688373,
133.27005863679));
#247031=CARTESIAN_POINT('Ctrl Pts',(-181.543976342123,-4.18581526386889,
133.386633577433));
#247032=CARTESIAN_POINT('Ctrl Pts',(-181.551733383008,-4.11397039913011,
133.503092734203));
#247033=CARTESIAN_POINT('Ctrl Pts',(-181.559490423893,-4.0371865032356,
133.616673009293));
#247034=CARTESIAN_POINT('Ctrl Pts',(-181.567247464778,-3.95572544889312,
133.72693127291));
#247035=CARTESIAN_POINT('Ctrl Pts',(-181.574998656018,-3.87432582496551,
133.837106389913));
#247036=CARTESIAN_POINT('Ctrl Pts',(-181.582749847258,-3.78825629441504,
133.943964168621));
#247037=CARTESIAN_POINT('Ctrl Pts',(-181.590501038498,-3.69782249121197,
134.047089697521));
#247038=CARTESIAN_POINT('Ctrl Pts',(-181.598248935275,-3.60742712478753,
134.150171395321));
#247039=CARTESIAN_POINT('Ctrl Pts',(-181.605996832053,-3.51267143226317,
134.249523705019));
#247040=CARTESIAN_POINT('Ctrl Pts',(-181.61374472883,-3.41390170930395,
134.344764292532));
#247041=CARTESIAN_POINT('Ctrl Pts',(-181.621491004914,-3.31515264684154,
134.439984957767));
#247042=CARTESIAN_POINT('Ctrl Pts',(-181.629237280998,-3.21239150530955,
134.531095340363));
#247043=CARTESIAN_POINT('Ctrl Pts',(-181.636983557082,-3.10600158262843,
134.617749822881));
#247044=CARTESIAN_POINT('Ctrl Pts',(-181.644729890347,-2.99961087460092,
134.704404945062));
#247045=CARTESIAN_POINT('Ctrl Pts',(-181.652476223613,-2.88959163510988,
134.786603854625));
#247046=CARTESIAN_POINT('Ctrl Pts',(-181.660222556878,-2.77636007621668,
134.864041367291));
#247047=CARTESIAN_POINT('Ctrl Pts',(-181.667970624881,-2.66310315990082,
134.941496221552));
#247048=CARTESIAN_POINT('Ctrl Pts',(-181.675718692884,-2.54663281535994,
135.01418733648));
#247049=CARTESIAN_POINT('Ctrl Pts',(-181.683466760887,-2.4273937005275,
135.081853210796));
#247050=CARTESIAN_POINT('Ctrl Pts',(-181.691223063629,-2.30802785694534,
135.149591001208));
#247051=CARTESIAN_POINT('Ctrl Pts',(-181.698979366371,-2.18588770531916,
135.212292688746));
#247052=CARTESIAN_POINT('Ctrl Pts',(-181.706735669113,-2.06144243552465,
135.269742812577));
#247053=CARTESIAN_POINT('Ctrl Pts',(-181.714496111627,-1.93693074554234,
135.327223599268));
#247054=CARTESIAN_POINT('Ctrl Pts',(-181.722256554141,-1.81011184722903,
135.379447088406));
#247055=CARTESIAN_POINT('Ctrl Pts',(-181.730016996655,-1.68147337978646,
135.426246632557));
#247056=CARTESIAN_POINT('Ctrl Pts',(-181.737789896921,-1.55262841045597,
135.473121303491));
#247057=CARTESIAN_POINT('Ctrl Pts',(-181.745562797186,-1.42195840793301,
135.514554511845));
#247058=CARTESIAN_POINT('Ctrl Pts',(-181.753335697452,-1.28996545172147,
135.550429748527));
#247059=CARTESIAN_POINT('Ctrl Pts',(-181.760826033214,-1.16277077193805,
135.585000829992));
#247060=CARTESIAN_POINT('Ctrl Pts',(-181.768316368976,-1.03434795419006,
135.614410947926));
#247061=CARTESIAN_POINT('Ctrl Pts',(-181.775806704738,-0.905151846678698,
135.638601322884));
#247062=CARTESIAN_POINT('Ctrl Pts',(-181.783581038857,-0.771057229483291,
135.663708883261));
#247063=CARTESIAN_POINT('Ctrl Pts',(-181.791355372976,-0.635704754977355,
135.68327260728));
#247064=CARTESIAN_POINT('Ctrl Pts',(-181.799129707095,-0.499592595456683,
135.697170679388));
#247065=CARTESIAN_POINT('Ctrl Pts',(-181.806894460042,-0.363648182007928,
135.711051623364));
#247066=CARTESIAN_POINT('Ctrl Pts',(-181.814659212989,-0.226946331599816,
135.719280769009));
#247067=CARTESIAN_POINT('Ctrl Pts',(-181.822423965936,-0.08999601943478,
135.721787157839));
#247068=CARTESIAN_POINT('Ctrl Pts',(-181.830181006821,0.0468182717495528,
135.724291057289));
#247069=CARTESIAN_POINT('Ctrl Pts',(-181.837938047706,0.18388014522574,
135.721083504079));
#247070=CARTESIAN_POINT('Ctrl Pts',(-181.845695088591,0.320675234751949,
135.712145296657));
#247071=CARTESIAN_POINT('Ctrl Pts',(-181.853446279831,0.457367166036849,
135.703213829606));
#247072=CARTESIAN_POINT('Ctrl Pts',(-181.861197471071,0.593792325261312,
135.688560335476));
#247073=CARTESIAN_POINT('Ctrl Pts',(-181.868948662312,0.7294364329914,135.668217682975));
#247074=CARTESIAN_POINT('Ctrl Pts',(-181.876696559089,0.865022888357463,
135.647883676643));
#247075=CARTESIAN_POINT('Ctrl Pts',(-181.884444455866,0.999828566655742,
135.621865379108));
#247076=CARTESIAN_POINT('Ctrl Pts',(-181.892192352643,1.13334461812831,
135.59024747781));
#247077=CARTESIAN_POINT('Ctrl Pts',(-181.899938628727,1.26683274092118,
135.558636190296));
#247078=CARTESIAN_POINT('Ctrl Pts',(-181.907684904811,1.39903139325775,
135.521427718866));
#247079=CARTESIAN_POINT('Ctrl Pts',(-181.915431180895,1.5294426155094,135.478757728249));
#247080=CARTESIAN_POINT('Ctrl Pts',(-181.92317751416,1.65985480042725,135.436087422652));
#247081=CARTESIAN_POINT('Ctrl Pts',(-181.930923847426,1.78847915735103,
135.387955639));
#247082=CARTESIAN_POINT('Ctrl Pts',(-181.938670180691,1.91483395331802,
135.334547588732));
#247083=CARTESIAN_POINT('Ctrl Pts',(-181.946418248694,2.0412170455653,135.281127578101));
#247084=CARTESIAN_POINT('Ctrl Pts',(-181.954166316697,2.16532920544419,
135.222429101825));
#247085=CARTESIAN_POINT('Ctrl Pts',(-181.9619143847,2.2867100760472,135.158684915388));
#247086=CARTESIAN_POINT('Ctrl Pts',(-181.969670687442,2.40821995168409,
135.094872980871));
#247087=CARTESIAN_POINT('Ctrl Pts',(-181.977426990184,2.52699239260691,
135.026004805807));
#247088=CARTESIAN_POINT('Ctrl Pts',(-181.985183292925,2.64259251692664,
134.952358671083));
#247089=CARTESIAN_POINT('Ctrl Pts',(-181.99294373544,2.75825434051338,134.8786732292));
#247090=CARTESIAN_POINT('Ctrl Pts',(-182.000704177954,2.87074015323274,
134.80020496986));
#247091=CARTESIAN_POINT('Ctrl Pts',(-182.008464620468,2.97964616898119,
134.717274080726));
#247092=CARTESIAN_POINT('Ctrl Pts',(-182.016237520733,3.08872701033434,
134.634210063566));
#247093=CARTESIAN_POINT('Ctrl Pts',(-182.024010420999,3.19421627012777,
134.546669350855));
#247094=CARTESIAN_POINT('Ctrl Pts',(-182.031783321264,3.29574453972754,
134.455011380287));
#247095=CARTESIAN_POINT('Ctrl Pts',(-182.039273657026,3.39358200099335,
134.366685407822));
#247096=CARTESIAN_POINT('Ctrl Pts',(-182.046763992788,3.48774123604373,
134.274536541253));
#247097=CARTESIAN_POINT('Ctrl Pts',(-182.05425432855,3.57792693550293,134.178915685527));
#247098=CARTESIAN_POINT('Ctrl Pts',(-182.062028662669,3.67153205316809,
134.079669335994));
#247099=CARTESIAN_POINT('Ctrl Pts',(-182.069802996788,3.76115288689754,
133.976368136514));
#247100=CARTESIAN_POINT('Ctrl Pts',(-182.077577330907,3.84641767552078,
133.869365369266));
#247101=CARTESIAN_POINT('Ctrl Pts',(-182.085342083855,3.93157738291237,
133.762494473365));
#247102=CARTESIAN_POINT('Ctrl Pts',(-182.093106836802,4.01239148547918,
133.651931389249));
#247103=CARTESIAN_POINT('Ctrl Pts',(-182.100871589749,4.0885251703094,133.538065977375));
#247104=CARTESIAN_POINT('Ctrl Pts',(-182.108628630634,4.16458323809056,
133.424313658233));
#247105=CARTESIAN_POINT('Ctrl Pts',(-182.116385671519,4.23596992326855,
133.307265861425));
#247106=CARTESIAN_POINT('Ctrl Pts',(-182.124142712404,4.30239104351552,
133.187344958928));
#247107=CARTESIAN_POINT('Ctrl Pts',(-182.131893903644,4.36876207507913,
133.067514489717));
#247108=CARTESIAN_POINT('Ctrl Pts',(-182.139645094884,4.43017480638999,
132.944815567991));
#247109=CARTESIAN_POINT('Ctrl Pts',(-182.147396286124,4.48637891022631,
132.819698637943));
#247110=CARTESIAN_POINT('Ctrl Pts',(-182.155144182901,4.54255912581914,
132.694634885927));
#247111=CARTESIAN_POINT('Ctrl Pts',(-182.162892079678,4.59353495715868,
132.56715552553));
#247112=CARTESIAN_POINT('Ctrl Pts',(-182.170639976455,4.639102608463,132.437734442094));
#247113=CARTESIAN_POINT('Ctrl Pts',(-182.178386252539,4.68466072799699,
132.308340430758));
#247114=CARTESIAN_POINT('Ctrl Pts',(-182.186132528623,4.724812787904,132.177005872811));
#247115=CARTESIAN_POINT('Ctrl Pts',(-182.193878804708,4.75940376741928,
132.044223045892));
#247116=CARTESIAN_POINT('Ctrl Pts',(-182.201625137973,4.79399500227735,
131.911439238801));
#247117=CARTESIAN_POINT('Ctrl Pts',(-182.209371471238,4.82302497627006,
131.777207519742));
#247118=CARTESIAN_POINT('Ctrl Pts',(-182.217117804504,4.8463891245921,131.642033295606));
#247119=CARTESIAN_POINT('Ctrl Pts',(-182.224865872507,4.86975850515314,
131.506828800141));
#247120=CARTESIAN_POINT('Ctrl Pts',(-182.23261394051,4.88745946865773,131.370681764779));
#247121=CARTESIAN_POINT('Ctrl Pts',(-182.240362008513,4.89943900473265,
131.234105310848));
#247122=CARTESIAN_POINT('Ctrl Pts',(-182.248118311254,4.91143127280104,
131.097383701837));
#247123=CARTESIAN_POINT('Ctrl Pts',(-182.255874613996,4.91768993216839,
130.960232152658));
#247124=CARTESIAN_POINT('Ctrl Pts',(-182.263630916738,4.91821404414322,
130.823166959378));
#247125=CARTESIAN_POINT('Ctrl Pts',(-182.271391359252,4.9187384358524,130.686028610276));
#247126=CARTESIAN_POINT('Ctrl Pts',(-182.279151801766,4.91352219632619,
130.548977099404));
#247127=CARTESIAN_POINT('Ctrl Pts',(-182.28691224428,4.90261645226236,130.4125252127));
#247128=CARTESIAN_POINT('Ctrl Pts',(-182.294685144546,4.89169320132999,
130.275854281314));
#247129=CARTESIAN_POINT('Ctrl Pts',(-182.302458044811,4.8750622420806,130.139785285917));
#247130=CARTESIAN_POINT('Ctrl Pts',(-182.310230945077,4.85282630523814,
130.004823305311));
#247131=CARTESIAN_POINT('Ctrl Pts',(-182.317721280839,4.83139870070879,
129.874767532648));
#247132=CARTESIAN_POINT('Ctrl Pts',(-182.325211616601,4.80476661598463,
129.74573998823));
#247133=CARTESIAN_POINT('Ctrl Pts',(-182.332701952363,4.77306565540504,
129.618178796894));
#247134=CARTESIAN_POINT('Ctrl Pts',(-182.340476286482,4.74016274326992,
129.485781084218));
#247135=CARTESIAN_POINT('Ctrl Pts',(-182.348250620601,4.70169476824667,
129.354543717016));
#247136=CARTESIAN_POINT('Ctrl Pts',(-182.35602495472,4.65775801064424,129.224970426138));
#247137=CARTESIAN_POINT('Ctrl Pts',(-182.363789707667,4.61387540116881,
129.09555682276));
#247138=CARTESIAN_POINT('Ctrl Pts',(-182.371554460614,4.56453754362383,
128.967803581878));
#247139=CARTESIAN_POINT('Ctrl Pts',(-182.379319213561,4.50989146409757,
128.842203120177));
#247140=CARTESIAN_POINT('Ctrl Pts',(-182.387076254446,4.45529965982786,
128.716727406625));
#247141=CARTESIAN_POINT('Ctrl Pts',(-182.394833295331,4.39541028046255,
128.593400573383));
#247142=CARTESIAN_POINT('Ctrl Pts',(-182.402590336216,4.33041966677546,
128.472698426745));
#247143=CARTESIAN_POINT('Ctrl Pts',(-182.410341527457,4.26547806301561,
128.352087302535));
#247144=CARTESIAN_POINT('Ctrl Pts',(-182.418092718697,4.19544306651655,
128.234097268103));
#247145=CARTESIAN_POINT('Ctrl Pts',(-182.425843909937,4.1205583407563,128.119182406921));
#247146=CARTESIAN_POINT('Ctrl Pts',(-182.433591806714,4.04570544300221,
128.00431638762));
#247147=CARTESIAN_POINT('Ctrl Pts',(-182.441339703491,3.96600712868981,
127.892523268852));
#247148=CARTESIAN_POINT('Ctrl Pts',(-182.449087600268,3.88175193438076,
127.784230656384));
#247149=CARTESIAN_POINT('Ctrl Pts',(-182.456833876352,3.79751436444203,
127.675960696395));
#247150=CARTESIAN_POINT('Ctrl Pts',(-182.464580152436,3.70872205040214,
127.571190094635));
#247151=CARTESIAN_POINT('Ctrl Pts',(-182.47232642852,3.61570536686982,127.470315362551));
#247152=CARTESIAN_POINT('Ctrl Pts',(-182.480072761786,3.52268799670936,
127.369439885832));
#247153=CARTESIAN_POINT('Ctrl Pts',(-182.487819095051,3.42544645986479,
127.272460623597));
#247154=CARTESIAN_POINT('Ctrl Pts',(-182.495565428317,3.32434944963606,
127.179738733948));
#247155=CARTESIAN_POINT('Ctrl Pts',(-182.50331349632,3.22322979943299,127.086996079874));
#247156=CARTESIAN_POINT('Ctrl Pts',(-182.511061564323,3.11825324584275,
126.998512959771));
#247157=CARTESIAN_POINT('Ctrl Pts',(-182.518809632326,3.00982283896963,
126.914611327378));
#247158=CARTESIAN_POINT('Ctrl Pts',(-182.526565935067,2.9012771909699,126.830620523332));
#247159=CARTESIAN_POINT('Ctrl Pts',(-182.534322237809,2.78927066657606,
126.751221173508));
#247160=CARTESIAN_POINT('Ctrl Pts',(-182.542078540551,2.67423713290575,
126.676693138288));
#247161=CARTESIAN_POINT('Ctrl Pts',(-182.549838983065,2.55914220237462,
126.602125325212));
#247162=CARTESIAN_POINT('Ctrl Pts',(-182.557599425579,2.44101737989998,
126.532434205961));
#247163=CARTESIAN_POINT('Ctrl Pts',(-182.565359868094,2.32032172204335,
126.467853939523));
#247164=CARTESIAN_POINT('Ctrl Pts',(-182.573132768359,2.19943231280187,
126.403170003107));
#247165=CARTESIAN_POINT('Ctrl Pts',(-182.580905668624,2.07596417359235,
126.343613484455));
#247166=CARTESIAN_POINT('Ctrl Pts',(-182.58867856889,1.95039776998001,126.289370960728));
#247167=CARTESIAN_POINT('Ctrl Pts',(-182.596168904652,1.82939602142133,
126.237100289366));
#247168=CARTESIAN_POINT('Ctrl Pts',(-182.603659240414,1.70644620173451,
126.189764077074));
#247169=CARTESIAN_POINT('Ctrl Pts',(-182.611149576176,1.5819902152108,126.147485053255));
#247170=CARTESIAN_POINT('Ctrl Pts',(-182.618923910295,1.45281544213099,
126.103603007398));
#247171=CARTESIAN_POINT('Ctrl Pts',(-182.626698244414,1.3216088481364,126.065030201631));
#247172=CARTESIAN_POINT('Ctrl Pts',(-182.634472578533,1.18884627811505,
126.031957911432));
#247173=CARTESIAN_POINT('Ctrl Pts',(-182.64223733148,1.05624732609592,125.998926379875));
#247174=CARTESIAN_POINT('Ctrl Pts',(-182.650002084427,0.922096589234707,
125.971381969506));
#247175=CARTESIAN_POINT('Ctrl Pts',(-182.657766837375,0.786887822827249,
125.949467146357));
#247176=CARTESIAN_POINT('Ctrl Pts',(-182.66552387826,0.651813347672695,
125.92757408932));
#247177=CARTESIAN_POINT('Ctrl Pts',(-182.673280919145,0.515683317642029,
125.911299554543));
#247178=CARTESIAN_POINT('Ctrl Pts',(-182.68103796003,0.379004169031384,
125.900735539896));
#247179=CARTESIAN_POINT('Ctrl Pts',(-182.68878915127,0.242428091229729,
125.890179491655));
#247180=CARTESIAN_POINT('Ctrl Pts',(-182.69654034251,0.105304107303662,
125.885325422026));
#247181=CARTESIAN_POINT('Ctrl Pts',(-182.70429153375,-0.0318540434016616,
125.886213773233));
#247182=CARTESIAN_POINT('Ctrl Pts',(-182.712039430527,-0.168953898234309,
125.887101746867));
#247183=CARTESIAN_POINT('Ctrl Pts',(-182.719787327304,-0.306087500824971,
125.893727284479));
#247184=CARTESIAN_POINT('Ctrl Pts',(-182.727535224081,-0.442739133272749,
125.906078763449));
#247185=CARTESIAN_POINT('Ctrl Pts',(-182.735281500165,-0.579362181144514,
125.918427658756));
#247186=CARTESIAN_POINT('Ctrl Pts',(-182.743027776249,-0.715503070274265,
125.936500077871));
#247187=CARTESIAN_POINT('Ctrl Pts',(-182.750774052334,-0.85064962880552,
125.960232391403));
#247188=CARTESIAN_POINT('Ctrl Pts',(-182.758520385599,-0.985797184958153,
125.98396488012));
#247189=CARTESIAN_POINT('Ctrl Pts',(-182.766266718864,-1.11995001079294,
126.013357279003));
#247190=CARTESIAN_POINT('Ctrl Pts',(-182.77401305213,-1.25260496603569,
126.048294610711));
#247191=CARTESIAN_POINT('Ctrl Pts',(-182.781761120133,-1.38528962843572,
126.083239766392));
#247192=CARTESIAN_POINT('Ctrl Pts',(-182.789509188136,-1.51647537476105,
126.123732226282));
#247193=CARTESIAN_POINT('Ctrl Pts',(-182.797257256139,-1.6456734777856,
126.169606916773));
#247194=CARTESIAN_POINT('Ctrl Pts',(-182.80501355888,-1.7750088940917,126.215530363432));
#247195=CARTESIAN_POINT('Ctrl Pts',(-182.812769861622,-1.902352078152,126.266847336577));
#247196=CARTESIAN_POINT('Ctrl Pts',(-182.820526164364,-2.02723305972525,
126.323344082888));
#247197=CARTESIAN_POINT('Ctrl Pts',(-182.828286606878,-2.15218069403846,
126.379870983214));
#247198=CARTESIAN_POINT('Ctrl Pts',(-182.836047049393,-2.27466315832567,
126.441582989575));
#247199=CARTESIAN_POINT('Ctrl Pts',(-182.843807491907,-2.39423531671549,
126.508220453338));
#247200=CARTESIAN_POINT('Ctrl Pts',(-182.851580392172,-2.51399942294907,
126.574964889473));
#247201=CARTESIAN_POINT('Ctrl Pts',(-182.859353292438,-2.63084355393906,
126.646650378709));
#247202=CARTESIAN_POINT('Ctrl Pts',(-182.867126192703,-2.74435103366134,
126.722973541272));
#247203=CARTESIAN_POINT('Ctrl Pts',(-182.874616528465,-2.85373223058731,
126.796522164628));
#247204=CARTESIAN_POINT('Ctrl Pts',(-182.882106864227,-2.9600149073766,
126.874376951055));
#247205=CARTESIAN_POINT('Ctrl Pts',(-182.889597199989,-3.06285694824154,
126.956232452197));
#247206=CARTESIAN_POINT('Ctrl Pts',(-182.897271718051,-3.16822780545898,
127.040100724848));
#247207=CARTESIAN_POINT('Ctrl Pts',(-182.904946236112,-3.27033860869109,
127.128449457481));
#247208=CARTESIAN_POINT('Ctrl Pts',(-182.912620754173,-3.36877703830128,
127.220992881942));
#247209=CARTESIAN_POINT('Ctrl Pts',(-182.920286491824,-3.46710284456976,
127.313430427532));
#247210=CARTESIAN_POINT('Ctrl Pts',(-182.927952229474,-3.56176434009002,
127.410052852803));
#247211=CARTESIAN_POINT('Ctrl Pts',(-182.935617967125,-3.65237997082311,
127.510532508628));
#247212=CARTESIAN_POINT('Ctrl Pts',(-182.943276696308,-3.74291275542632,
127.610920300052));
#247213=CARTESIAN_POINT('Ctrl Pts',(-182.95093542549,-3.82940676294885,
127.715158013987));
#247214=CARTESIAN_POINT('Ctrl Pts',(-182.958594154673,-3.9115156180739,
127.822879671448));
#247215=CARTESIAN_POINT('Ctrl Pts',(-182.966247640976,-3.99356826453599,
127.930527586676));
#247216=CARTESIAN_POINT('Ctrl Pts',(-182.973901127278,-4.07124148666013,
128.041654383705));
#247217=CARTESIAN_POINT('Ctrl Pts',(-182.98155461358,-4.14422807866773,
128.15585977851));
#247218=CARTESIAN_POINT('Ctrl Pts',(-182.989205542012,-4.2171902778377,
128.270027004747));
#247219=CARTESIAN_POINT('Ctrl Pts',(-182.996856470444,-4.28546874152419,
128.387270447522));
#247220=CARTESIAN_POINT('Ctrl Pts',(-183.004507398876,-4.34879885726115,
128.50715980754));
#247221=CARTESIAN_POINT('Ctrl Pts',(-183.012156622058,-4.41211485788887,
128.627022446441));
#247222=CARTESIAN_POINT('Ctrl Pts',(-183.019805845239,-4.47048452011149,
128.749529472692));
#247223=CARTESIAN_POINT('Ctrl Pts',(-183.027455068421,-4.52368893671273,
128.874225527381));
#247224=CARTESIAN_POINT('Ctrl Pts',(-183.035106947243,-4.57691182470863,
128.998964873778));
#247225=CARTESIAN_POINT('Ctrl Pts',(-183.042758826066,-4.62496572459593,
129.125894397969));
#247226=CARTESIAN_POINT('Ctrl Pts',(-183.050410704888,-4.66767971122647,
129.254538312944));
#247227=CARTESIAN_POINT('Ctrl Pts',(-183.056846671858,-4.7036062873606,
129.362740233909));
#247228=CARTESIAN_POINT('Ctrl Pts',(-183.063282638827,-4.73575598385233,
129.472154524254));
#247229=CARTESIAN_POINT('Ctrl Pts',(-183.069718605797,-4.76405452823406,
129.582490119308));
#247230=CARTESIAN_POINT('Ctrl Pts',(-181.320039938991,-4.76405452823418,
129.582490119309));
#247231=CARTESIAN_POINT('Ctrl Pts',(-181.327866674491,-4.79848591795568,
129.716737585264));
#247232=CARTESIAN_POINT('Ctrl Pts',(-181.33569340999,-4.82725862397902,
129.852519526693));
#247233=CARTESIAN_POINT('Ctrl Pts',(-181.34352014549,-4.8502474171004,129.989325001528));
#247234=CARTESIAN_POINT('Ctrl Pts',(-181.351344753954,-4.8732299626622,
130.126093297362));
#247235=CARTESIAN_POINT('Ctrl Pts',(-181.359169362417,-4.89043165683097,
130.263884199659));
#247236=CARTESIAN_POINT('Ctrl Pts',(-181.366993970881,-4.90177834412933,
130.40217642155));
#247237=CARTESIAN_POINT('Ctrl Pts',(-181.374615792586,-4.91283096458077,
130.536884587887));
#247238=CARTESIAN_POINT('Ctrl Pts',(-181.38223761429,-4.91832830176703,
130.672068059881));
#247239=CARTESIAN_POINT('Ctrl Pts',(-181.389859435995,-4.91824915695583,
130.807240305618));
#247240=CARTESIAN_POINT('Origin',(213.235140564004,0.,130.804360617566));
#247241=CARTESIAN_POINT('',(-179.570054719422,-4.76405452823393,129.582490119308));
#247242=CARTESIAN_POINT('',(-179.915287826822,-4.76405452823417,129.582490119309));
#247243=CARTESIAN_POINT('',(213.235140564004,-4.76405452823405,129.582490119308));
#247244=CARTESIAN_POINT('',(-179.985140564067,-4.91824883331974,130.807748249335));
#247245=CARTESIAN_POINT('Ctrl Pts',(-179.915287826822,-4.76405452823417,
129.582490119309));
#247246=CARTESIAN_POINT('Ctrl Pts',(-179.92306888399,-4.79829769999019,
129.716003726273));
#247247=CARTESIAN_POINT('Ctrl Pts',(-179.930849941158,-4.82693968418732,
129.851018898772));
#247248=CARTESIAN_POINT('Ctrl Pts',(-179.938630998326,-4.84986100741504,
129.987028817588));
#247249=CARTESIAN_POINT('Ctrl Pts',(-179.946411829481,-4.87278166485761,
130.123034785786));
#247250=CARTESIAN_POINT('Ctrl Pts',(-179.954192660636,-4.88998191732996,
130.260035064349));
#247251=CARTESIAN_POINT('Ctrl Pts',(-179.961973491791,-4.90139348051783,
130.397512965935));
#247252=CARTESIAN_POINT('Ctrl Pts',(-179.969695849198,-4.91271928463228,
130.533957706923));
#247253=CARTESIAN_POINT('Ctrl Pts',(-179.977418206605,-4.91834311166686,
130.670872539273));
#247254=CARTESIAN_POINT('Ctrl Pts',(-179.985140564012,-4.91824883332041,
130.807748248363));
#247255=CARTESIAN_POINT('Ctrl Pts',(-179.985140564067,-4.91824883331974,
130.807748249336));
#247256=CARTESIAN_POINT('Ctrl Pts',(-179.993960729007,-4.91814115236676,
130.964082159672));
#247257=CARTESIAN_POINT('Ctrl Pts',(-180.002780893947,-4.91057552406498,
131.120123073993));
#247258=CARTESIAN_POINT('Ctrl Pts',(-180.011601058887,-4.89565957716396,
131.27521130199));
#247259=CARTESIAN_POINT('Ctrl Pts',(-180.020460543816,-4.88067713548981,
131.43099090792));
#247260=CARTESIAN_POINT('Ctrl Pts',(-180.029320028745,-4.85827880522494,
131.585809153203));
#247261=CARTESIAN_POINT('Ctrl Pts',(-180.038179513674,-4.82862329315814,
131.739015717199));
#247262=CARTESIAN_POINT('Ctrl Pts',(-180.047091538771,-4.79879191244734,
131.893130855312));
#247263=CARTESIAN_POINT('Ctrl Pts',(-180.056003563869,-4.7616171115927,
132.045614980022));
#247264=CARTESIAN_POINT('Ctrl Pts',(-180.064915588966,-4.71730902760369,
132.195826966634));
#247265=CARTESIAN_POINT('Ctrl Pts',(-180.071787714544,-4.68314275069523,
132.311656491802));
#247266=CARTESIAN_POINT('Ctrl Pts',(-180.078659840122,-4.64473597477464,
132.426135393135));
#247267=CARTESIAN_POINT('Ctrl Pts',(-180.0855319657,-4.60220406385651,132.538978966691));
#247268=CARTESIAN_POINT('Ctrl Pts',(-180.093306299819,-4.55408834151546,
132.666637234001));
#247269=CARTESIAN_POINT('Ctrl Pts',(-180.101080633938,-4.50058080743443,
132.792494198247));
#247270=CARTESIAN_POINT('Ctrl Pts',(-180.108854968057,-4.44183581893942,
132.916060790433));
#247271=CARTESIAN_POINT('Ctrl Pts',(-180.116619721004,-4.3831632283927,
133.039475097838));
#247272=CARTESIAN_POINT('Ctrl Pts',(-180.124384473951,-4.31926619260353,
133.160604299769));
#247273=CARTESIAN_POINT('Ctrl Pts',(-180.132149226898,-4.25034814935119,
133.27897648105));
#247274=CARTESIAN_POINT('Ctrl Pts',(-180.139906267783,-4.1814985564708,
133.397231093413));
#247275=CARTESIAN_POINT('Ctrl Pts',(-180.147663308668,-4.10763807579476,
133.512733798804));
#247276=CARTESIAN_POINT('Ctrl Pts',(-180.155420349553,-4.02901718669648,
133.62503492911));
#247277=CARTESIAN_POINT('Ctrl Pts',(-180.163171540793,-3.95045558622215,
133.73725137226));
#247278=CARTESIAN_POINT('Ctrl Pts',(-180.170922732034,-3.8671409460421,
133.846270726925));
#247279=CARTESIAN_POINT('Ctrl Pts',(-180.178673923274,-3.77936821263246,
133.951670417354));
#247280=CARTESIAN_POINT('Ctrl Pts',(-180.186421820051,-3.69163278497605,
134.057025310104));
#247281=CARTESIAN_POINT('Ctrl Pts',(-180.194169716828,-3.5994432823843,
134.158763298683));
#247282=CARTESIAN_POINT('Ctrl Pts',(-180.201917613605,-3.50313613111719,
134.256493336533));
#247283=CARTESIAN_POINT('Ctrl Pts',(-180.209663889689,-3.40684912522998,
134.354202931366));
#247284=CARTESIAN_POINT('Ctrl Pts',(-180.217410165773,-3.30644645813239,
134.447905964751));
#247285=CARTESIAN_POINT('Ctrl Pts',(-180.225156441857,-3.20230248324751,
134.537247150571));
#247286=CARTESIAN_POINT('Ctrl Pts',(-180.232902775123,-3.0981577395956,
134.626588995887));
#247287=CARTESIAN_POINT('Ctrl Pts',(-180.240649108388,-2.99027192978512,
134.711568674828));
#247288=CARTESIAN_POINT('Ctrl Pts',(-180.248395441653,-2.8790533424594,
134.79187048135));
#247289=CARTESIAN_POINT('Ctrl Pts',(-180.256143509656,-2.76780984850203,
134.872190270904));
#247290=CARTESIAN_POINT('Ctrl Pts',(-180.263891577659,-2.65323240879196,
134.947829874661));
#247291=CARTESIAN_POINT('Ctrl Pts',(-180.271639645662,-2.53575886331033,
135.018516529447));
#247292=CARTESIAN_POINT('Ctrl Pts',(-180.279395948404,-2.41816046554677,
135.089278310851));
#247293=CARTESIAN_POINT('Ctrl Pts',(-180.287152251146,-2.29766014887279,
135.155076425877));
#247294=CARTESIAN_POINT('Ctrl Pts',(-180.294908553888,-2.17472145211095,
135.215683510784));
#247295=CARTESIAN_POINT('Ctrl Pts',(-180.302668996402,-2.05171713926471,
135.276322943517));
#247296=CARTESIAN_POINT('Ctrl Pts',(-180.310429438916,-1.92627221052881,
135.331765667491));
#247297=CARTESIAN_POINT('Ctrl Pts',(-180.31818988143,-1.79886989369378,
135.381832645669));
#247298=CARTESIAN_POINT('Ctrl Pts',(-180.325962781696,-1.67126305934953,
135.431979995805));
#247299=CARTESIAN_POINT('Ctrl Pts',(-180.333735681961,-1.54169292759772,
135.476734227691));
#247300=CARTESIAN_POINT('Ctrl Pts',(-180.341508582227,-1.41065844128908,
135.515966057808));
#247301=CARTESIAN_POINT('Ctrl Pts',(-180.348998917989,-1.28438738861264,
135.553771712082));
#247302=CARTESIAN_POINT('Ctrl Pts',(-180.356489253751,-1.15675689732088,
135.586449423876));
#247303=CARTESIAN_POINT('Ctrl Pts',(-180.363979589513,-1.02822016752291,
135.613928825794));
#247304=CARTESIAN_POINT('Ctrl Pts',(-180.371753923632,-0.894809928547707,
135.642450117588));
#247305=CARTESIAN_POINT('Ctrl Pts',(-180.379528257751,-0.760000770908441,
135.665461477155));
#247306=CARTESIAN_POINT('Ctrl Pts',(-180.38730259187,-0.624287596106585,
135.682828415948));
#247307=CARTESIAN_POINT('Ctrl Pts',(-180.395067344817,-0.488741675663636,
135.700173951541));
#247308=CARTESIAN_POINT('Ctrl Pts',(-180.402832097764,-0.352294338905479,
135.711888858062));
#247309=CARTESIAN_POINT('Ctrl Pts',(-180.410596850712,-0.215452584523784,
135.717889211797));
#247310=CARTESIAN_POINT('Ctrl Pts',(-180.418353891597,-0.0787467433016716,
135.723883605896));
#247311=CARTESIAN_POINT('Ctrl Pts',(-180.426110932482,0.0583523478990269,
135.72417472524));
#247312=CARTESIAN_POINT('Ctrl Pts',(-180.433867973367,0.195330980338071,
135.718730248619));
#247313=CARTESIAN_POINT('Ctrl Pts',(-180.441619164607,0.332206316124668,
135.713289877721));
#247314=CARTESIAN_POINT('Ctrl Pts',(-180.449370355847,0.468960984882857,
135.702122535486));
#247315=CARTESIAN_POINT('Ctrl Pts',(-180.457121547087,0.605080035891566,
135.685247956223));
#247316=CARTESIAN_POINT('Ctrl Pts',(-180.464869443864,0.741141232672686,
135.668380549107));
#247317=CARTESIAN_POINT('Ctrl Pts',(-180.472617340641,0.876566961838184,
135.645810777549));
#247318=CARTESIAN_POINT('Ctrl Pts',(-180.480365237418,1.01084637823296,
135.617610316274));
#247319=CARTESIAN_POINT('Ctrl Pts',(-180.488111513502,1.14509770626855,
135.589415753928));
#247320=CARTESIAN_POINT('Ctrl Pts',(-180.495857789587,1.27820281610075,
135.555592924915));
#247321=CARTESIAN_POINT('Ctrl Pts',(-180.503604065671,1.40966044828803,
135.516264742549));
#247322=CARTESIAN_POINT('Ctrl Pts',(-180.511350398936,1.54111905086551,
135.476936269871));
#247323=CARTESIAN_POINT('Ctrl Pts',(-180.519096732201,1.67092977696887,
135.432102474804));
#247324=CARTESIAN_POINT('Ctrl Pts',(-180.526843065467,1.7986063241752,135.381936215318));
#247325=CARTESIAN_POINT('Ctrl Pts',(-180.53459113347,1.9263114636592,135.331758721446));
#247326=CARTESIAN_POINT('Ctrl Pts',(-180.542339201473,2.05188110939729,
135.276246529846));
#247327=CARTESIAN_POINT('Ctrl Pts',(-180.550087269476,2.17484911480286,
135.215620572538));
#247328=CARTESIAN_POINT('Ctrl Pts',(-180.557843572218,2.29794781206775,
135.154930181241));
#247329=CARTESIAN_POINT('Ctrl Pts',(-180.56559987496,2.41843899428399,135.089115340456));
#247330=CARTESIAN_POINT('Ctrl Pts',(-180.573356177701,2.53588081984257,
135.018443142868));
#247331=CARTESIAN_POINT('Ctrl Pts',(-180.581116620216,2.65338532763989,
134.9477332254));
#247332=CARTESIAN_POINT('Ctrl Pts',(-180.58887706273,2.76783690968252,134.87216100064));
#247333=CARTESIAN_POINT('Ctrl Pts',(-180.596637505244,2.87882374061796,
134.792036247924));
#247334=CARTESIAN_POINT('Ctrl Pts',(-180.604410405509,2.98998873746736,
134.711782871843));
#247335=CARTESIAN_POINT('Ctrl Pts',(-180.612183305775,3.09767756139703,
134.6269626059));
#247336=CARTESIAN_POINT('Ctrl Pts',(-180.61995620604,3.2015117517228,134.537925343948));
#247337=CARTESIAN_POINT('Ctrl Pts',(-180.627446541802,3.30157130768515,
134.452124810741));
#247338=CARTESIAN_POINT('Ctrl Pts',(-180.634936877564,3.39805139018646,
134.362408765159));
#247339=CARTESIAN_POINT('Ctrl Pts',(-180.642427213326,3.49064783141407,
134.269120461992));
#247340=CARTESIAN_POINT('Ctrl Pts',(-180.650201547445,3.58675509485719,
134.172295104453));
#247341=CARTESIAN_POINT('Ctrl Pts',(-180.657975881564,3.67898284597718,
134.071314544067));
#247342=CARTESIAN_POINT('Ctrl Pts',(-180.665750215683,3.76695042939966,
133.966522461138));
#247343=CARTESIAN_POINT('Ctrl Pts',(-180.67351496863,3.85480960063723,133.861859525086));
#247344=CARTESIAN_POINT('Ctrl Pts',(-180.681279721577,3.93841880170574,
133.75339470941));
#247345=CARTESIAN_POINT('Ctrl Pts',(-180.689044474525,4.01743338003051,
133.64150920365));
#247346=CARTESIAN_POINT('Ctrl Pts',(-180.69680151541,4.09636947996217,133.529734824151));
#247347=CARTESIAN_POINT('Ctrl Pts',(-180.704558556295,4.17071981453642,
133.414546832993));
#247348=CARTESIAN_POINT('Ctrl Pts',(-180.71231559718,4.24017951888239,133.296359957484));
#247349=CARTESIAN_POINT('Ctrl Pts',(-180.72006678842,4.30958684312489,133.178262207617));
#247350=CARTESIAN_POINT('Ctrl Pts',(-180.72781797966,4.37411068070913,133.057170410442));
#247351=CARTESIAN_POINT('Ctrl Pts',(-180.7355691709,4.433489291225,132.933528475461));
#247352=CARTESIAN_POINT('Ctrl Pts',(-180.743317067677,4.4928426642475,132.8099390916));
#247353=CARTESIAN_POINT('Ctrl Pts',(-180.751064964454,4.5470549907979,132.683802077373));
#247354=CARTESIAN_POINT('Ctrl Pts',(-180.758812861231,4.59591044856734,
132.555585963217));
#247355=CARTESIAN_POINT('Ctrl Pts',(-180.766559137315,4.64475568682821,
132.427396669107));
#247356=CARTESIAN_POINT('Ctrl Pts',(-180.774305413399,4.68824614600501,
132.297129505223));
#247357=CARTESIAN_POINT('Ctrl Pts',(-180.782051689483,4.72621429357663,
132.165272632978));
#247358=CARTESIAN_POINT('Ctrl Pts',(-180.789798022749,4.76418272142055,
132.033414787394));
#247359=CARTESIAN_POINT('Ctrl Pts',(-180.797544356014,4.79662864813414,
131.899967585733));
#247360=CARTESIAN_POINT('Ctrl Pts',(-180.80529068928,4.82343464568437,131.765433601949));
#247361=CARTESIAN_POINT('Ctrl Pts',(-180.813038757283,4.85024664625185,
131.630869490213));
#247362=CARTESIAN_POINT('Ctrl Pts',(-180.820786825286,4.87141612800267,
131.495218495417));
#247363=CARTESIAN_POINT('Ctrl Pts',(-180.828534893288,4.88687700368533,
131.358992219038));
#247364=CARTESIAN_POINT('Ctrl Pts',(-180.83629119603,4.90235431137068,131.222621159752));
#247365=CARTESIAN_POINT('Ctrl Pts',(-180.844047498772,4.91211084899382,
131.085673986604));
#247366=CARTESIAN_POINT('Ctrl Pts',(-180.851803801514,4.91613250301284,
130.948666803576));
#247367=CARTESIAN_POINT('Ctrl Pts',(-180.859564244028,4.92015630350971,
130.811586495688));
#247368=CARTESIAN_POINT('Ctrl Pts',(-180.867324686542,4.91843912623242,
130.674446504842));
#247369=CARTESIAN_POINT('Ctrl Pts',(-180.875085129057,4.91101899564668,
130.537760754668));
#247370=CARTESIAN_POINT('Ctrl Pts',(-180.882858029322,4.90358695360859,
130.400855584392));
#247371=CARTESIAN_POINT('Ctrl Pts',(-180.890630929587,4.89043370141627,
130.264406501322));
#247372=CARTESIAN_POINT('Ctrl Pts',(-180.898403829853,4.871649047432,130.128921041323));
#247373=CARTESIAN_POINT('Ctrl Pts',(-180.905894165615,4.85354726293575,
129.998360819063));
#247374=CARTESIAN_POINT('Ctrl Pts',(-180.913384501377,4.83021645414565,
129.86869567912));
#247375=CARTESIAN_POINT('Ctrl Pts',(-180.920874837139,4.80178100090587,
129.74036706409));
#247376=CARTESIAN_POINT('Ctrl Pts',(-180.928649171258,4.77226740881377,
129.607172830616));
#247377=CARTESIAN_POINT('Ctrl Pts',(-180.936423505377,4.73716095571161,
129.474996552097));
#247378=CARTESIAN_POINT('Ctrl Pts',(-180.944197839496,4.69654503604511,
129.344344252281));
#247379=CARTESIAN_POINT('Ctrl Pts',(-180.951962592443,4.65597917186976,
129.213852969748));
#247380=CARTESIAN_POINT('Ctrl Pts',(-180.95972734539,4.60991746600389,129.08488229868));
#247381=CARTESIAN_POINT('Ctrl Pts',(-180.967492098337,4.55849433086872,
128.957928247308));
#247382=CARTESIAN_POINT('Ctrl Pts',(-180.975249139222,4.5071222699163,128.831100288489));
#247383=CARTESIAN_POINT('Ctrl Pts',(-180.983006180107,4.45039952260687,
128.706285323457));
#247384=CARTESIAN_POINT('Ctrl Pts',(-180.990763220992,4.38851022386175,
128.583964013902));
#247385=CARTESIAN_POINT('Ctrl Pts',(-180.998514412233,4.32666759631816,
128.461734947799));
#247386=CARTESIAN_POINT('Ctrl Pts',(-181.006265603473,4.2596663481538,128.341996141624));
#247387=CARTESIAN_POINT('Ctrl Pts',(-181.014016794713,4.18773847591968,
128.225207748928));
#247388=CARTESIAN_POINT('Ctrl Pts',(-181.02176469149,4.11584117494989,128.108468994414));
#247389=CARTESIAN_POINT('Ctrl Pts',(-181.029512588267,4.03902161920529,
127.994678491457));
#247390=CARTESIAN_POINT('Ctrl Pts',(-181.037260485044,3.95755733938158,
127.884271069623));
#247391=CARTESIAN_POINT('Ctrl Pts',(-181.045006761128,3.87611010012927,
127.773886742641));
#247392=CARTESIAN_POINT('Ctrl Pts',(-181.052753037212,3.79002030129498,
127.666884403591));
#247393=CARTESIAN_POINT('Ctrl Pts',(-181.060499313296,3.6996080914805,127.563668865493));
#247394=CARTESIAN_POINT('Ctrl Pts',(-181.068245646562,3.6091952142635,127.460452565482));
#247395=CARTESIAN_POINT('Ctrl Pts',(-181.075991979827,3.51446012000957,
127.361023416295));
#247396=CARTESIAN_POINT('Ctrl Pts',(-181.083738313092,3.41576216570124,
127.26575186696));
#247397=CARTESIAN_POINT('Ctrl Pts',(-181.091486381095,3.3170421086705,127.170458982223));
#247398=CARTESIAN_POINT('Ctrl Pts',(-181.099234449098,3.2143577068925,127.079325821528));
#247399=CARTESIAN_POINT('Ctrl Pts',(-181.106982517101,3.10810366340641,
126.992684519047));
#247400=CARTESIAN_POINT('Ctrl Pts',(-181.114738819843,3.00173669185833,
126.905951133159));
#247401=CARTESIAN_POINT('Ctrl Pts',(-181.122495122585,2.89179280344652,
126.82371938953));
#247402=CARTESIAN_POINT('Ctrl Pts',(-181.130251425327,2.77869858235167,
126.746280129092));
#247403=CARTESIAN_POINT('Ctrl Pts',(-181.138011867841,2.66554399946583,
126.668799536988));
#247404=CARTESIAN_POINT('Ctrl Pts',(-181.145772310355,2.54923606489846,
126.596116731981));
#247405=CARTESIAN_POINT('Ctrl Pts',(-181.153532752869,2.43022771030707,
126.528477511288));
#247406=CARTESIAN_POINT('Ctrl Pts',(-181.161305653134,2.31102831293982,
126.460729710112));
#247407=CARTESIAN_POINT('Ctrl Pts',(-181.1690785534,2.18912018081892,126.398041851348));
#247408=CARTESIAN_POINT('Ctrl Pts',(-181.176851453665,2.06497886185556,
126.340612712208));
#247409=CARTESIAN_POINT('Ctrl Pts',(-181.184341789427,1.94535039252626,
126.285271266929));
#247410=CARTESIAN_POINT('Ctrl Pts',(-181.19183212519,1.82364856594436,126.23481296174));
#247411=CARTESIAN_POINT('Ctrl Pts',(-181.199322460952,1.70031201061043,
126.189371762859));
#247412=CARTESIAN_POINT('Ctrl Pts',(-181.207096795071,1.57229911229676,
126.142207647111));
#247413=CARTESIAN_POINT('Ctrl Pts',(-181.21487112919,1.44211957032787,126.100299193248));
#247414=CARTESIAN_POINT('Ctrl Pts',(-181.222645463309,1.31024419354801,
126.063849757355));
#247415=CARTESIAN_POINT('Ctrl Pts',(-181.230410216256,1.17853134138399,
126.027445242135));
#247416=CARTESIAN_POINT('Ctrl Pts',(-181.238174969203,1.04512718603475,
125.996486461819));
#247417=CARTESIAN_POINT('Ctrl Pts',(-181.24593972215,0.910521686468727,
125.971128435995));
#247418=CARTESIAN_POINT('Ctrl Pts',(-181.253696763035,0.776049878982477,
125.94579559612));
#247419=CARTESIAN_POINT('Ctrl Pts',(-181.26145380392,0.640379483506111,
125.926052512528));
#247420=CARTESIAN_POINT('Ctrl Pts',(-181.269210844805,0.504014423755966,
125.91200407668));
#247421=CARTESIAN_POINT('Ctrl Pts',(-181.276962036045,0.36775219795833,
125.897966234867));
#247422=CARTESIAN_POINT('Ctrl Pts',(-181.284713227285,0.230796737915274,
125.889614533002));
#247423=CARTESIAN_POINT('Ctrl Pts',(-181.292464418526,0.0936605836422182,
125.887002510048));
#247424=CARTESIAN_POINT('Ctrl Pts',(-181.300212315303,-0.0434172841072315,
125.884391597274));
#247425=CARTESIAN_POINT('Ctrl Pts',(-181.30796021208,-0.180675303261666,
125.887515518829));
#247426=CARTESIAN_POINT('Ctrl Pts',(-181.315708108857,-0.317597627272033,
125.89637581628));
#247427=CARTESIAN_POINT('Ctrl Pts',(-181.323454384941,-0.454491310083921,
125.905234260348));
#247428=CARTESIAN_POINT('Ctrl Pts',(-181.331200661025,-0.591049047521525,
125.919826668363));
#247429=CARTESIAN_POINT('Ctrl Pts',(-181.338946937109,-0.726757210785079,
125.940102501566));
#247430=CARTESIAN_POINT('Ctrl Pts',(-181.346693270374,-0.862466375815651,
125.96037848444));
#247431=CARTESIAN_POINT('Ctrl Pts',(-181.35443960364,-0.997325567484876,
125.986337918446));
#247432=CARTESIAN_POINT('Ctrl Pts',(-181.362185936905,-1.13082887530605,
126.017878703125));
#247433=CARTESIAN_POINT('Ctrl Pts',(-181.369934004908,-1.26436208026681,
126.049426551144));
#247434=CARTESIAN_POINT('Ctrl Pts',(-181.377682072911,-1.39653841675175,
126.086558147126));
#247435=CARTESIAN_POINT('Ctrl Pts',(-181.385430140914,-1.52686510424168,
126.12912094286));
#247436=CARTESIAN_POINT('Ctrl Pts',(-181.393186443656,-1.65733030448651,
126.171728974839));
#247437=CARTESIAN_POINT('Ctrl Pts',(-181.400942746398,-1.78594155654096,
126.21977961588));
#247438=CARTESIAN_POINT('Ctrl Pts',(-181.408699049139,-1.91222358852397,
126.273071175256));
#247439=CARTESIAN_POINT('Ctrl Pts',(-181.416459491654,-2.03857302102973,
126.326391177942));
#247440=CARTESIAN_POINT('Ctrl Pts',(-181.424219934168,-2.16259040297888,
126.384957505823));
#247441=CARTESIAN_POINT('Ctrl Pts',(-181.431980376682,-2.28382411758841,
126.448521954068));
#247442=CARTESIAN_POINT('Ctrl Pts',(-181.439753276947,-2.40525244731925,
126.512188441609));
#247443=CARTESIAN_POINT('Ctrl Pts',(-181.447526177213,-2.52388784149363,
126.580868886882));
#247444=CARTESIAN_POINT('Ctrl Pts',(-181.455299077478,-2.63930601795003,
126.654270641901));
#247445=CARTESIAN_POINT('Ctrl Pts',(-181.46278941324,-2.75052845296859,
126.725004058236));
#247446=CARTESIAN_POINT('Ctrl Pts',(-181.470279749002,-2.85876326417252,
126.800121305243));
#247447=CARTESIAN_POINT('Ctrl Pts',(-181.477770084764,-2.96366065256876,
126.879325764356));
#247448=CARTESIAN_POINT('Ctrl Pts',(-181.485571301677,-3.07291173377017,
126.961817549197));
#247449=CARTESIAN_POINT('Ctrl Pts',(-181.493372518591,-3.17890946479242,
127.049020518601));
#247450=CARTESIAN_POINT('Ctrl Pts',(-181.501173735504,-3.28121524436916,
127.140645347158));
#247451=CARTESIAN_POINT('Ctrl Pts',(-181.508855785267,-3.38195825643629,
127.230870564611));
#247452=CARTESIAN_POINT('Ctrl Pts',(-181.516537835029,-3.47912097019819,
127.325383261093));
#247453=CARTESIAN_POINT('Ctrl Pts',(-181.524219884791,-3.57231315162841,
127.423863345092));
#247454=CARTESIAN_POINT('Ctrl Pts',(-181.531894943118,-3.66542051884068,
127.522253802353));
#247455=CARTESIAN_POINT('Ctrl Pts',(-181.539570001446,-3.75456426629303,
127.624604178921));
#247456=CARTESIAN_POINT('Ctrl Pts',(-181.547245059773,-3.83938845729224,
127.730555266456));
#247457=CARTESIAN_POINT('Ctrl Pts',(-181.554914880889,-3.92415476700669,
127.836434056396));
#247458=CARTESIAN_POINT('Ctrl Pts',(-181.562584702005,-4.00460713403721,
127.945908359317));
#247459=CARTESIAN_POINT('Ctrl Pts',(-181.570254523121,-4.08042798415152,
128.058583764169));
#247460=CARTESIAN_POINT('Ctrl Pts',(-181.578149920418,-4.15847879212069,
128.174573051728));
#247461=CARTESIAN_POINT('Ctrl Pts',(-181.586045317716,-4.2316211508202,
128.293954320808));
#247462=CARTESIAN_POINT('Ctrl Pts',(-181.593940715013,-4.29955471667743,
128.416262566648));
#247463=CARTESIAN_POINT('Ctrl Pts',(-181.60160643385,-4.36551208345984,
128.535012844653));
#247464=CARTESIAN_POINT('Ctrl Pts',(-181.609272152686,-4.42655931303819,
128.656521791086));
#247465=CARTESIAN_POINT('Ctrl Pts',(-181.616937871523,-4.48246715571917,
128.780337084996));
#247466=CARTESIAN_POINT('Ctrl Pts',(-181.624948108051,-4.54088764480406,
128.909716965876));
#247467=CARTESIAN_POINT('Ctrl Pts',(-181.632958344578,-4.59369582612956,
129.041614905708));
#247468=CARTESIAN_POINT('Ctrl Pts',(-181.640968581106,-4.6406858403334,
129.175490458889));
#247469=CARTESIAN_POINT('Ctrl Pts',(-181.648978817634,-4.68767585453736,
129.30936601207));
#247470=CARTESIAN_POINT('Ctrl Pts',(-181.656989054161,-4.72884756406629,
129.445218700358));
#247471=CARTESIAN_POINT('Ctrl Pts',(-181.664999290689,-4.76405452823418,
129.582490119309));
#247472=CARTESIAN_POINT('',(-179.639859435944,-4.91824845113006,130.800457355239));
#247473=CARTESIAN_POINT('Ctrl Pts',(-179.639859435995,-4.91824845113077,
130.80045735614));
#247474=CARTESIAN_POINT('Ctrl Pts',(-179.647643348581,-4.91835785303648,
130.938307654795));
#247475=CARTESIAN_POINT('Ctrl Pts',(-179.655427261166,-4.91266728495612,
131.076231294055));
#247476=CARTESIAN_POINT('Ctrl Pts',(-179.663211173751,-4.90118571413701,
131.213703576513));
#247477=CARTESIAN_POINT('Ctrl Pts',(-179.670945887216,-4.88977671391655,
131.350306949481));
#247478=CARTESIAN_POINT('Ctrl Pts',(-179.67868060068,-4.87264975986795,
131.486464261715));
#247479=CARTESIAN_POINT('Ctrl Pts',(-179.686415314144,-4.84986584312386,
131.62166372303));
#247480=CARTESIAN_POINT('Ctrl Pts',(-179.694150299485,-4.82708112551935,
131.75686793664));
#247481=CARTESIAN_POINT('Ctrl Pts',(-179.701885284826,-4.79863911424742,
131.891113845955));
#247482=CARTESIAN_POINT('Ctrl Pts',(-179.709620270168,-4.76465219127589,
132.023898463912));
#247483=CARTESIAN_POINT('Ctrl Pts',(-179.717357210254,-4.73065667930619,
132.156716638506));
#247484=CARTESIAN_POINT('Ctrl Pts',(-179.725094150341,-4.69111356423603,
132.288072407442));
#247485=CARTESIAN_POINT('Ctrl Pts',(-179.732831090427,-4.64618538712646,
132.417476983782));
#247486=CARTESIAN_POINT('Ctrl Pts',(-179.740651277729,-4.6007737959558,
132.54827391556));
#247487=CARTESIAN_POINT('Ctrl Pts',(-179.748471465031,-4.54986071193366,
132.677077031875));
#247488=CARTESIAN_POINT('Ctrl Pts',(-179.756291652332,-4.4936638437746,
132.803402468467));
#247489=CARTESIAN_POINT('Ctrl Pts',(-179.764041702127,-4.43797099273028,
132.928594920532));
#247490=CARTESIAN_POINT('Ctrl Pts',(-179.771791751921,-4.37708898469712,
133.051353633612));
#247491=CARTESIAN_POINT('Ctrl Pts',(-179.779541801716,-4.31127556038019,
133.171233259887));
#247492=CARTESIAN_POINT('Ctrl Pts',(-179.787397057771,-4.24456872447766,
133.292740241798));
#247493=CARTESIAN_POINT('Ctrl Pts',(-179.795252313826,-4.17279583022991,
133.41128904481));
#247494=CARTESIAN_POINT('Ctrl Pts',(-179.803107569882,-4.09626958239033,
133.526447789367));
#247495=CARTESIAN_POINT('Ctrl Pts',(-179.810962825937,-4.01974333455076,
133.641606533924));
#247496=CARTESIAN_POINT('Ctrl Pts',(-179.818818081992,-3.93846402808792,
133.753374925537));
#247497=CARTESIAN_POINT('Ctrl Pts',(-179.826673338047,-3.85278485618213,
133.861357823072));
#247498=CARTESIAN_POINT('Ctrl Pts',(-179.834447672166,-3.76798831934649,
133.968228320824));
#247499=CARTESIAN_POINT('Ctrl Pts',(-179.842222006285,-3.67860745899652,
134.071737226023));
#247500=CARTESIAN_POINT('Ctrl Pts',(-179.849996340404,-3.58493859117706,
134.171465955982));
#247501=CARTESIAN_POINT('Ctrl Pts',(-179.857761093352,-3.491385161866,134.271071779194));
#247502=CARTESIAN_POINT('Ctrl Pts',(-179.865525846299,-3.39355450492741,
134.366906414405));
#247503=CARTESIAN_POINT('Ctrl Pts',(-179.873290599246,-3.29178443534814,
134.458582599562));
#247504=CARTESIAN_POINT('Ctrl Pts',(-179.881047640131,-3.19011544523642,
134.550167730639));
#247505=CARTESIAN_POINT('Ctrl Pts',(-179.888804681016,-3.08451511749853,
134.637602371029));
#247506=CARTESIAN_POINT('Ctrl Pts',(-179.896561721901,-2.97535926942331,
134.720534806792));
#247507=CARTESIAN_POINT('Ctrl Pts',(-179.904312913141,-2.86628573662238,
134.803404702559));
#247508=CARTESIAN_POINT('Ctrl Pts',(-179.912064104381,-2.75366233038859,
134.881778915971));
#247509=CARTESIAN_POINT('Ctrl Pts',(-179.919815295621,-2.63789893932337,
134.955345109035));
#247510=CARTESIAN_POINT('Ctrl Pts',(-179.927563192398,-2.52218475078761,
135.028880034504));
#247511=CARTESIAN_POINT('Ctrl Pts',(-179.935311089175,-2.40333356107528,
135.097610794808));
#247512=CARTESIAN_POINT('Ctrl Pts',(-179.943058985952,-2.28178513072117,
135.161267740712));
#247513=CARTESIAN_POINT('Ctrl Pts',(-179.950805262036,-2.16026212567808,
135.224911370955));
#247514=CARTESIAN_POINT('Ctrl Pts',(-179.958551538121,-2.03604334835015,
135.283483116575));
#247515=CARTESIAN_POINT('Ctrl Pts',(-179.966297814205,-1.9095937562906,
135.336758961538));
#247516=CARTESIAN_POINT('Ctrl Pts',(-179.97404414747,-1.78314323080907,
135.39003519977));
#247517=CARTESIAN_POINT('Ctrl Pts',(-179.981790480735,-1.65446221802928,
135.438015307539));
#247518=CARTESIAN_POINT('Ctrl Pts',(-179.989536814001,-1.5240359049478,
135.480523320352));
#247519=CARTESIAN_POINT('Ctrl Pts',(-179.997284882004,-1.393580383798,135.52304085254));
#247520=CARTESIAN_POINT('Ctrl Pts',(-180.005032950007,-1.26137915625431,
135.560083730166));
#247521=CARTESIAN_POINT('Ctrl Pts',(-180.01278101801,-1.12793243744398,
135.59152590394));
#247522=CARTESIAN_POINT('Ctrl Pts',(-180.020537320752,-0.994343889872685,
135.62300149483));
#247523=CARTESIAN_POINT('Ctrl Pts',(-180.028293623494,-0.859507587907298,
135.648864401312));
#247524=CARTESIAN_POINT('Ctrl Pts',(-180.036049926235,-0.723934356211346,
135.66903965224));
#247525=CARTESIAN_POINT('Ctrl Pts',(-180.04381036875,-0.588288764999606,
135.689225671307));
#247526=CARTESIAN_POINT('Ctrl Pts',(-180.051570811264,-0.45190584891694,
135.703717944691));
#247527=CARTESIAN_POINT('Ctrl Pts',(-180.059331253778,-0.315300425492684,
135.71249353184));
#247528=CARTESIAN_POINT('Ctrl Pts',(-180.067104154043,-0.178475710915488,
135.721283206341));
#247529=CARTESIAN_POINT('Ctrl Pts',(-180.074877054309,-0.0414281663132729,
135.724337847456));
#247530=CARTESIAN_POINT('Ctrl Pts',(-180.082649954574,0.0953276177084138,
135.721686690525));
#247531=CARTESIAN_POINT('Ctrl Pts',(-180.090140290336,0.227111984512766,
135.719131909827));
#247532=CARTESIAN_POINT('Ctrl Pts',(-180.097630626098,0.358625127450248,
135.71127898747));
#247533=CARTESIAN_POINT('Ctrl Pts',(-180.10512096186,0.489414003383709,
135.698199294494));
#247534=CARTESIAN_POINT('Ctrl Pts',(-180.112895295979,0.625161779301939,
135.684623680983));
#247535=CARTESIAN_POINT('Ctrl Pts',(-180.120669630098,0.76055929103879,
135.665374123379));
#247536=CARTESIAN_POINT('Ctrl Pts',(-180.128443964217,0.895094207063287,
135.640473666594));
#247537=CARTESIAN_POINT('Ctrl Pts',(-180.136208717164,1.02946332082715,
135.615603897398));
#247538=CARTESIAN_POINT('Ctrl Pts',(-180.143973470111,1.16297157332996,
135.58509715623));
#247539=CARTESIAN_POINT('Ctrl Pts',(-180.151738223059,1.29511055278657,
135.549028331807));
#247540=CARTESIAN_POINT('Ctrl Pts',(-180.159495263944,1.42711828994595,
135.512995331449));
#247541=CARTESIAN_POINT('Ctrl Pts',(-180.167252304829,1.55775908575723,
135.471411343807));
#247542=CARTESIAN_POINT('Ctrl Pts',(-180.175009345714,1.68653389489693,
135.424402444635));
#247543=CARTESIAN_POINT('Ctrl Pts',(-180.182760536954,1.81521159395151,
135.377428995238));
#247544=CARTESIAN_POINT('Ctrl Pts',(-180.190511728194,1.94202574141753,
135.325038910659));
#247545=CARTESIAN_POINT('Ctrl Pts',(-180.198262919434,2.06649200369359,
135.267408215472));
#247546=CARTESIAN_POINT('Ctrl Pts',(-180.206010816211,2.19090536448777,
135.209802014867));
#247547=CARTESIAN_POINT('Ctrl Pts',(-180.213758712988,2.31297247082939,
135.146959797708));
#247548=CARTESIAN_POINT('Ctrl Pts',(-180.221506609765,2.43222875786826,
135.079105794989));
#247549=CARTESIAN_POINT('Ctrl Pts',(-180.229252885849,2.55146009906276,
135.011265985864));
#247550=CARTESIAN_POINT('Ctrl Pts',(-180.236999161933,2.6678814508488,134.938416669642));
#247551=CARTESIAN_POINT('Ctrl Pts',(-180.244745438018,2.78105302127715,
134.860827942141));
#247552=CARTESIAN_POINT('Ctrl Pts',(-180.252491771283,2.89422542711247,
134.783238641898));
#247553=CARTESIAN_POINT('Ctrl Pts',(-180.260238104548,3.00414768126175,
134.700910081639));
#247554=CARTESIAN_POINT('Ctrl Pts',(-180.267984437814,3.11040948439129,
134.61415534982));
#247555=CARTESIAN_POINT('Ctrl Pts',(-180.275732505817,3.21669508411531,
134.52738118988));
#247556=CARTESIAN_POINT('Ctrl Pts',(-180.28348057382,3.31931829885344,134.436179133193));
#247557=CARTESIAN_POINT('Ctrl Pts',(-180.291228641823,3.41790270127258,
134.340901892192));
#247558=CARTESIAN_POINT('Ctrl Pts',(-180.298984944565,3.51659188036738,
134.245523389406));
#247559=CARTESIAN_POINT('Ctrl Pts',(-180.306741247306,3.61123339083883,
134.146061322491));
#247560=CARTESIAN_POINT('Ctrl Pts',(-180.314497550048,3.70148804412907,
134.042904938966));
#247561=CARTESIAN_POINT('Ctrl Pts',(-180.322257992563,3.79179086904529,
133.939693497773));
#247562=CARTESIAN_POINT('Ctrl Pts',(-180.330018435077,3.87770192656671,
133.832784115665));
#247563=CARTESIAN_POINT('Ctrl Pts',(-180.337778877591,3.95892364470687,
133.722597523282));
#247564=CARTESIAN_POINT('Ctrl Pts',(-180.345551777856,4.04027574715952,
133.612234049598));
#247565=CARTESIAN_POINT('Ctrl Pts',(-180.353324678122,4.1169232486707,133.498583177072));
#247566=CARTESIAN_POINT('Ctrl Pts',(-180.361097578387,4.18861259696973,
133.38209364777));
#247567=CARTESIAN_POINT('Ctrl Pts',(-180.368587914149,4.25769585688294,
133.269838806279));
#247568=CARTESIAN_POINT('Ctrl Pts',(-180.376078249911,4.32217503704249,
133.154948378128));
#247569=CARTESIAN_POINT('Ctrl Pts',(-180.383568585673,4.3818653030435,133.037842099129));
#247570=CARTESIAN_POINT('Ctrl Pts',(-180.391342919792,4.44381874362301,
132.916295699966));
#247571=CARTESIAN_POINT('Ctrl Pts',(-180.399117253911,4.50080920799675,
132.791977082604));
#247572=CARTESIAN_POINT('Ctrl Pts',(-180.40689158803,4.5525791567958,132.665329742406));
#247573=CARTESIAN_POINT('Ctrl Pts',(-180.414656340977,4.60428530375948,
132.538838483737));
#247574=CARTESIAN_POINT('Ctrl Pts',(-180.422421093925,4.65078359001705,
132.410024570987));
#247575=CARTESIAN_POINT('Ctrl Pts',(-180.430185846872,4.69186221257831,
132.27935622457));
#247576=CARTESIAN_POINT('Ctrl Pts',(-180.437942887757,4.73290003527265,
132.148817659796));
#247577=CARTESIAN_POINT('Ctrl Pts',(-180.445699928642,4.76852878996476,
132.016428697274));
#247578=CARTESIAN_POINT('Ctrl Pts',(-180.453456969527,4.79858480156904,
131.882677344994));
#247579=CARTESIAN_POINT('Ctrl Pts',(-180.461208160767,4.8286181477013,131.749026855648));
#247580=CARTESIAN_POINT('Ctrl Pts',(-180.468959352007,4.85308703009387,
131.614016401407));
#247581=CARTESIAN_POINT('Ctrl Pts',(-180.476710543247,4.87187774906408,
131.478148611429));
#247582=CARTESIAN_POINT('Ctrl Pts',(-180.484458440024,4.89066048147738,
131.342338568887));
#247583=CARTESIAN_POINT('Ctrl Pts',(-180.492206336801,4.90376979703001,
131.205672301821));
#247584=CARTESIAN_POINT('Ctrl Pts',(-180.499954233578,4.91114323895842,
131.068661864126));
#247585=CARTESIAN_POINT('Ctrl Pts',(-180.507700509662,4.91851513852172,
130.93168008606));
#247586=CARTESIAN_POINT('Ctrl Pts',(-180.515446785746,4.92015352997405,
130.794354670717));
#247587=CARTESIAN_POINT('Ctrl Pts',(-180.523193061831,4.91604793428645,
130.657201620906));
#247588=CARTESIAN_POINT('Ctrl Pts',(-180.530939395096,4.91194230829228,
130.520047558662));
#247589=CARTESIAN_POINT('Ctrl Pts',(-180.538685728361,4.9020926222485,130.38306625528));
#247590=CARTESIAN_POINT('Ctrl Pts',(-180.546432061627,4.88654050952772,
130.246772139166));
#247591=CARTESIAN_POINT('Ctrl Pts',(-180.55418012963,4.8709849140191,130.110447500929));
#247592=CARTESIAN_POINT('Ctrl Pts',(-180.561928197633,4.84972439502942,
129.974810744557));
#247593=CARTESIAN_POINT('Ctrl Pts',(-180.569676265636,4.82285223134933,
129.84036921871));
#247594=CARTESIAN_POINT('Ctrl Pts',(-180.577432568377,4.795951507614,129.70578480681));
#247595=CARTESIAN_POINT('Ctrl Pts',(-180.585188871119,4.76342730196317,
129.572398547));
#247596=CARTESIAN_POINT('Ctrl Pts',(-180.592945173861,4.72542375965904,
129.440706206012));
#247597=CARTESIAN_POINT('Ctrl Pts',(-180.600705616375,4.68739993372011,
129.308943576857));
#247598=CARTESIAN_POINT('Ctrl Pts',(-180.608466058889,4.64389106780674,
129.178877038601));
#247599=CARTESIAN_POINT('Ctrl Pts',(-180.616226501404,4.59509028959371,
129.050984362171));
#247600=CARTESIAN_POINT('Ctrl Pts',(-180.623999401669,4.54621117203903,
128.922886381063));
#247601=CARTESIAN_POINT('Ctrl Pts',(-180.631772301934,4.49202332100907,
128.796969594594));
#247602=CARTESIAN_POINT('Ctrl Pts',(-180.6395452022,4.43276722471806,128.67368987952));
#247603=CARTESIAN_POINT('Ctrl Pts',(-180.647035537962,4.37566523678433,
128.554891692612));
#247604=CARTESIAN_POINT('Ctrl Pts',(-180.654525873724,4.31385723758189,
128.438542449427));
#247605=CARTESIAN_POINT('Ctrl Pts',(-180.662016209486,4.24759645522655,
128.325024533844));
#247606=CARTESIAN_POINT('Ctrl Pts',(-180.669790543605,4.17882337516859,
128.207202551989));
#247607=CARTESIAN_POINT('Ctrl Pts',(-180.677564877724,4.10503533955871,
128.092057610922));
#247608=CARTESIAN_POINT('Ctrl Pts',(-180.685339211843,4.02646626728858,
127.980046105886));
#247609=CARTESIAN_POINT('Ctrl Pts',(-180.69310396479,3.94799402437853,127.86817264502));
#247610=CARTESIAN_POINT('Ctrl Pts',(-180.700868717737,3.86475269088806,
127.759425253595));
#247611=CARTESIAN_POINT('Ctrl Pts',(-180.708633470684,3.77702170922281,
127.654235212037));
#247612=CARTESIAN_POINT('Ctrl Pts',(-180.71639051157,3.68937786320486,127.54914964671));
#247613=CARTESIAN_POINT('Ctrl Pts',(-180.724147552455,3.59725349177691,
127.447614698306));
#247614=CARTESIAN_POINT('Ctrl Pts',(-180.73190459334,3.50097069949896,127.350031851547));
#247615=CARTESIAN_POINT('Ctrl Pts',(-180.73965578458,3.40476051482377,127.252522592771));
#247616=CARTESIAN_POINT('Ctrl Pts',(-180.74740697582,3.30439842459542,127.158959780689));
#247617=CARTESIAN_POINT('Ctrl Pts',(-180.75515816706,3.20024584750376,127.0697107574));
#247618=CARTESIAN_POINT('Ctrl Pts',(-180.762906063837,3.09613753803588,
126.980499667328));
#247619=CARTESIAN_POINT('Ctrl Pts',(-180.770653960614,2.98824224223235,
126.89559897327));
#247620=CARTESIAN_POINT('Ctrl Pts',(-180.778401857391,2.87695700613077,
126.815337999508));
#247621=CARTESIAN_POINT('Ctrl Pts',(-180.786148133475,2.76569504850156,
126.735093814613));
#247622=CARTESIAN_POINT('Ctrl Pts',(-180.793894409559,2.65104487791537,
126.659487648129));
#247623=CARTESIAN_POINT('Ctrl Pts',(-180.801640685643,2.53343495797927,
126.588807228485));
#247624=CARTESIAN_POINT('Ctrl Pts',(-180.809387018909,2.41582416987298,
126.518126287095));
#247625=CARTESIAN_POINT('Ctrl Pts',(-180.817133352174,2.29525392392618,
126.452371366488));
#247626=CARTESIAN_POINT('Ctrl Pts',(-180.82487968544,2.17217952718222,126.39178550045));
#247627=CARTESIAN_POINT('Ctrl Pts',(-180.832627753443,2.04907756878062,
126.331186066628));
#247628=CARTESIAN_POINT('Ctrl Pts',(-180.840375821446,1.92347069438084,
126.275758163452));
#247629=CARTESIAN_POINT('Ctrl Pts',(-180.848123889449,1.79583617024562,
126.225697547178));
#247630=CARTESIAN_POINT('Ctrl Pts',(-180.855880192191,1.66806599461945,
126.175583725885));
#247631=CARTESIAN_POINT('Ctrl Pts',(-180.863636494932,1.53826422894359,
126.130848729665));
#247632=CARTESIAN_POINT('Ctrl Pts',(-180.871392797674,1.40692588984619,
126.091639259053));
#247633=CARTESIAN_POINT('Ctrl Pts',(-180.879153240188,1.2755174515227,126.052408861167));
#247634=CARTESIAN_POINT('Ctrl Pts',(-180.886913682703,1.14257118442251,
126.018709961316));
#247635=CARTESIAN_POINT('Ctrl Pts',(-180.894674125217,1.00859344098332,
125.990638322574));
#247636=CARTESIAN_POINT('Ctrl Pts',(-180.902447025482,0.874400624576381,
125.962521620745));
#247637=CARTESIAN_POINT('Ctrl Pts',(-180.910219925748,0.739173408878079,
125.940050295721));
#247638=CARTESIAN_POINT('Ctrl Pts',(-180.917992826013,0.603425325667191,
125.923268430479));
#247639=CARTESIAN_POINT('Ctrl Pts',(-180.925483161775,0.472612027210911,
125.907096628309));
#247640=CARTESIAN_POINT('Ctrl Pts',(-180.932973497537,0.341315380425482,
125.896207840602));
#247641=CARTESIAN_POINT('Ctrl Pts',(-180.940463833299,0.20999397167983,
125.890595707199));
#247642=CARTESIAN_POINT('Ctrl Pts',(-180.948238167418,0.0736934718059715,
125.884770788052));
#247643=CARTESIAN_POINT('Ctrl Pts',(-180.956012501537,-0.0630654638079416,
125.884612098978));
#247644=CARTESIAN_POINT('Ctrl Pts',(-180.963786835656,-0.199772418043521,
125.890169530165));
#247645=CARTESIAN_POINT('Ctrl Pts',(-180.971551588603,-0.336310893175113,
125.895720112316));
#247646=CARTESIAN_POINT('Ctrl Pts',(-180.97931634155,-0.472797127501037,
125.90697278233));
#247647=CARTESIAN_POINT('Ctrl Pts',(-180.987081094497,-0.608717227139118,
125.923925555004));
#247648=CARTESIAN_POINT('Ctrl Pts',(-180.994838135382,-0.744502329018101,
125.940861489945));
#247649=CARTESIAN_POINT('Ctrl Pts',(-181.002595176267,-0.87972202974887,
125.963486212983));
#247650=CARTESIAN_POINT('Ctrl Pts',(-181.010352217152,-1.01386444348082,
125.99174574073));
#247651=CARTESIAN_POINT('Ctrl Pts',(-181.018103408392,-1.14790569937564,
126.019983957747));
#247652=CARTESIAN_POINT('Ctrl Pts',(-181.025854599632,-1.28087090426565,
126.053848441329));
#247653=CARTESIAN_POINT('Ctrl Pts',(-181.033605790873,-1.41225564720813,
126.093233677074));
#247654=CARTESIAN_POINT('Ctrl Pts',(-181.04135368765,-1.54358454812987,
126.132602173044));
#247655=CARTESIAN_POINT('Ctrl Pts',(-181.049101584427,-1.67333394942435,
126.177486642203));
#247656=CARTESIAN_POINT('Ctrl Pts',(-181.056849481204,-1.80101216816459,
126.227731046296));
#247657=CARTESIAN_POINT('Ctrl Pts',(-181.064595757288,-1.92866367937423,
126.277964940342));
#247658=CARTESIAN_POINT('Ctrl Pts',(-181.072342033372,-2.05424450620277,
126.333556396151));
#247659=CARTESIAN_POINT('Ctrl Pts',(-181.080088309456,-2.17728097953044,
126.394300459396));
#247660=CARTESIAN_POINT('Ctrl Pts',(-181.087834642722,-2.3003183610849,
126.455044971041));
#247661=CARTESIAN_POINT('Ctrl Pts',(-181.095580975987,-2.42081100109293,
126.520941992941));
#247662=CARTESIAN_POINT('Ctrl Pts',(-181.103327309252,-2.53830832377024,
126.591739828084));
#247663=CARTESIAN_POINT('Ctrl Pts',(-181.111075377255,-2.65583195915813,
126.662553517911));
#247664=CARTESIAN_POINT('Ctrl Pts',(-181.118823445258,-2.77035860763099,
126.738270003146));
#247665=CARTESIAN_POINT('Ctrl Pts',(-181.126571513261,-2.88146559983368,
126.818593557203));
#247666=CARTESIAN_POINT('Ctrl Pts',(-181.134327816003,-2.99269067787002,
126.89900248009));
#247667=CARTESIAN_POINT('Ctrl Pts',(-181.142084118745,-3.1004885220833,
126.984028023559));
#247668=CARTESIAN_POINT('Ctrl Pts',(-181.149840421487,-3.20446814057772,
127.073333011326));
#247669=CARTESIAN_POINT('Ctrl Pts',(-181.157600864001,-3.30850325612586,
127.162685663855));
#247670=CARTESIAN_POINT('Ctrl Pts',(-181.165361306515,-3.40871579973424,
127.25632204509));
#247671=CARTESIAN_POINT('Ctrl Pts',(-181.173121749029,-3.5047515073558,
127.353867908664));
#247672=CARTESIAN_POINT('Ctrl Pts',(-181.180894649295,-3.60094138002062,
127.451570361518));
#247673=CARTESIAN_POINT('Ctrl Pts',(-181.18866754956,-3.69294075537735,
127.55319454785));
#247674=CARTESIAN_POINT('Ctrl Pts',(-181.196440449825,-3.78043496869995,
127.658332246758));
#247675=CARTESIAN_POINT('Ctrl Pts',(-181.203930785587,-3.86474854698411,
127.759647925484));
#247676=CARTESIAN_POINT('Ctrl Pts',(-181.21142112135,-3.94487863715625,
127.864225857211));
#247677=CARTESIAN_POINT('Ctrl Pts',(-181.218911457112,-4.02058271306412,
127.971676782418));
#247678=CARTESIAN_POINT('Ctrl Pts',(-181.226774298583,-4.10005166699623,
128.084471404409));
#247679=CARTESIAN_POINT('Ctrl Pts',(-181.234637140055,-4.174892552443,128.200785850527));
#247680=CARTESIAN_POINT('Ctrl Pts',(-181.242499981526,-4.24478179121977,
128.320208728605));
#247681=CARTESIAN_POINT('Ctrl Pts',(-181.250349252588,-4.31455040877096,
128.439425495782));
#247682=CARTESIAN_POINT('Ctrl Pts',(-181.25819852365,-4.37938421453783,
128.56173968249));
#247683=CARTESIAN_POINT('Ctrl Pts',(-181.266047794713,-4.43900175716958,
128.686709451216));
#247684=CARTESIAN_POINT('Ctrl Pts',(-181.273889191536,-4.49855949261664,
128.811553852646));
#247685=CARTESIAN_POINT('Ctrl Pts',(-181.281730588359,-4.55291121398804,
128.939048195462));
#247686=CARTESIAN_POINT('Ctrl Pts',(-181.289571985181,-4.60182013260226,
129.0687239823));
#247687=CARTESIAN_POINT('Ctrl Pts',(-181.297405522347,-4.65068002839995,
129.198269791365));
#247688=CARTESIAN_POINT('Ctrl Pts',(-181.305239059512,-4.69410785428418,
129.329992335658));
#247689=CARTESIAN_POINT('Ctrl Pts',(-181.313072596677,-4.73191416286347,
129.463401476581));
#247690=CARTESIAN_POINT('Ctrl Pts',(-181.315395044115,-4.74312278581986,
129.502953943239));
#247691=CARTESIAN_POINT('Ctrl Pts',(-181.317717491553,-4.75383761304045,
129.542654522032));
#247692=CARTESIAN_POINT('Ctrl Pts',(-181.320039938991,-4.76405452823418,
129.582490119309));
#247693=CARTESIAN_POINT('Ctrl Pts',(-179.570054719422,-4.76405452823393,
129.582490119308));
#247694=CARTESIAN_POINT('Ctrl Pts',(-179.579197174056,-4.80396699441805,
129.738108219203));
#247695=CARTESIAN_POINT('Ctrl Pts',(-179.58833962869,-4.8362916101084,129.895843536568));
#247696=CARTESIAN_POINT('Ctrl Pts',(-179.597482083324,-4.86082915223956,
130.055012223801));
#247697=CARTESIAN_POINT('Ctrl Pts',(-179.606541047858,-4.88514261430456,
130.212727361621));
#247698=CARTESIAN_POINT('Ctrl Pts',(-179.615600012392,-4.90181051144224,
130.371849719594));
#247699=CARTESIAN_POINT('Ctrl Pts',(-179.624658976926,-4.91068588618086,
130.53169380667));
#247700=CARTESIAN_POINT('Ctrl Pts',(-179.629725796599,-4.91565002122716,
130.621097089119));
#247701=CARTESIAN_POINT('Ctrl Pts',(-179.634792616271,-4.91817723760474,
130.710725797053));
#247702=CARTESIAN_POINT('Ctrl Pts',(-179.639859435944,-4.91824845113006,
130.800457355239));
#247703=CARTESIAN_POINT('Origin',(213.235140564004,0.,130.804360617566));
#247704=CARTESIAN_POINT('',(-177.819765072025,-4.76405452823413,129.582490119309));
#247705=CARTESIAN_POINT('',(-178.165366640417,-4.76405452823403,129.582490119308));
#247706=CARTESIAN_POINT('',(213.235140564004,-4.76405452823405,129.582490119308));
#247707=CARTESIAN_POINT('',(-177.725096247279,-4.0820853165969,128.06104828928));
#247708=CARTESIAN_POINT('Ctrl Pts',(-177.725096247279,-4.08208531659689,
128.06104828928));
#247709=CARTESIAN_POINT('Ctrl Pts',(-177.732985316008,-4.16002539388626,
128.177024163335));
#247710=CARTESIAN_POINT('Ctrl Pts',(-177.740874384737,-4.23303079411445,
128.296341548097));
#247711=CARTESIAN_POINT('Ctrl Pts',(-177.748763453466,-4.30081646430476,
128.418535644341));
#247712=CARTESIAN_POINT('Ctrl Pts',(-177.756510780686,-4.36738424129978,
128.538534300783));
#247713=CARTESIAN_POINT('Ctrl Pts',(-177.764258107907,-4.42891811933753,
128.661306795764));
#247714=CARTESIAN_POINT('Ctrl Pts',(-177.772005435128,-4.48519447304636,
128.786387971207));
#247715=CARTESIAN_POINT('Ctrl Pts',(-177.779965374611,-4.54301523588223,
128.91490178747));
#247716=CARTESIAN_POINT('Ctrl Pts',(-177.787925314094,-4.59528555643844,
129.045852432001));
#247717=CARTESIAN_POINT('Ctrl Pts',(-177.795885253576,-4.64181608494743,
129.178714132003));
#247718=CARTESIAN_POINT('Ctrl Pts',(-177.803845193059,-4.68834661345641,
129.311575832005));
#247719=CARTESIAN_POINT('Ctrl Pts',(-177.811805132542,-4.72913724299794,
129.446348154116));
#247720=CARTESIAN_POINT('Ctrl Pts',(-177.819765072025,-4.76405452823413,
129.582490119309));
#247721=CARTESIAN_POINT('',(-177.981041338087,-3.00808041127123,126.914654376525));
#247722=CARTESIAN_POINT('Ctrl Pts',(-177.981095179098,-3.00961479406227,
126.914450354609));
#247723=CARTESIAN_POINT('Ctrl Pts',(-177.946925114628,-3.17693683926483,
127.043907043471));
#247724=CARTESIAN_POINT('Ctrl Pts',(-177.912218584466,-3.33351065782883,
127.182415422253));
#247725=CARTESIAN_POINT('Ctrl Pts',(-177.8272197828,-3.69621327019491,127.545118034619));
#247726=CARTESIAN_POINT('Ctrl Pts',(-177.774444409595,-3.90151116845466,
127.792249968281));
#247727=CARTESIAN_POINT('Ctrl Pts',(-177.725144769241,-4.08256462727749,
128.061761644584));
#247728=CARTESIAN_POINT('Ctrl Pts',(-177.981095179098,-3.00961479406228,
126.914450354609));
#247729=CARTESIAN_POINT('Ctrl Pts',(-177.988841298821,-3.11812387474683,
126.998403585517));
#247730=CARTESIAN_POINT('Ctrl Pts',(-177.996587418545,-3.22313694139555,
127.086915601532));
#247731=CARTESIAN_POINT('Ctrl Pts',(-178.004333538268,-3.32425823831933,
127.17965508091));
#247732=CARTESIAN_POINT('Ctrl Pts',(-178.012080203021,-3.42538665030451,
127.272401085591));
#247733=CARTESIAN_POINT('Ctrl Pts',(-178.019826867774,-3.52262245944916,
127.36937488135));
#247734=CARTESIAN_POINT('Ctrl Pts',(-178.027573532527,-3.61560540807819,
127.470206962502));
#247735=CARTESIAN_POINT('Ctrl Pts',(-178.035322419979,-3.70861503568729,
127.571067974734));
#247736=CARTESIAN_POINT('Ctrl Pts',(-178.043071307431,-3.79736910967914,
127.675789187946));
#247737=CARTESIAN_POINT('Ctrl Pts',(-178.050820194884,-3.88154670282093,
127.783966892185));
#247738=CARTESIAN_POINT('Ctrl Pts',(-178.058577545204,-3.96581622965968,
127.892262741597));
#247739=CARTESIAN_POINT('Ctrl Pts',(-178.066334895524,-4.04549905361132,
128.004022312041));
#247740=CARTESIAN_POINT('Ctrl Pts',(-178.074092245844,-4.12031647581515,
128.118811287983));
#247741=CARTESIAN_POINT('Ctrl Pts',(-178.081854174614,-4.19517805584832,
128.233668013278));
#247742=CARTESIAN_POINT('Ctrl Pts',(-178.089616103383,-4.2651683139012,
128.351557370489));
#247743=CARTESIAN_POINT('Ctrl Pts',(-178.097378032152,-4.33005433352629,
128.472020048264));
#247744=CARTESIAN_POINT('Ctrl Pts',(-178.10515176728,-4.39503904867666,
128.592665956994));
#247745=CARTESIAN_POINT('Ctrl Pts',(-178.112925502409,-4.45490384678247,
128.715892653527));
#247746=CARTESIAN_POINT('Ctrl Pts',(-178.120699237537,-4.50946352571929,
128.841219824676));
#247747=CARTESIAN_POINT('Ctrl Pts',(-178.125932358028,-4.54619199268115,
128.925587529081));
#247748=CARTESIAN_POINT('Ctrl Pts',(-178.131165478519,-4.58051734944699,
129.010906720745));
#247749=CARTESIAN_POINT('Ctrl Pts',(-178.13639859901,-4.61239592518718,
129.097027348454));
#247750=CARTESIAN_POINT('Ctrl Pts',(-178.145370171086,-4.66704800905346,
129.244671076535));
#247751=CARTESIAN_POINT('Ctrl Pts',(-178.154341743163,-4.71465032755617,
129.395057764512));
#247752=CARTESIAN_POINT('Ctrl Pts',(-178.163313315239,-4.75495695955518,
129.547552209225));
#247753=CARTESIAN_POINT('Ctrl Pts',(-178.163997756965,-4.75803195472055,
129.559186018774));
#247754=CARTESIAN_POINT('Ctrl Pts',(-178.164682198691,-4.7610645102698,
129.570832084646));
#247755=CARTESIAN_POINT('Ctrl Pts',(-178.165366640417,-4.76405452823403,
129.582490119308));
#247756=CARTESIAN_POINT('Ctrl Pts',(210.579426101437,-2.14555810197798,
126.384433368448));
#247757=CARTESIAN_POINT('Ctrl Pts',(210.533016425084,-2.88204635455982,
126.741945114569));
#247758=CARTESIAN_POINT('Ctrl Pts',(210.440198811428,-4.16073755837059,
127.832228156677));
#247759=CARTESIAN_POINT('Ctrl Pts',(210.254565323169,-5.41774734084591,
130.983824311839));
#247760=CARTESIAN_POINT('Ctrl Pts',(210.022525636658,-3.70466367662459,
135.280954889074));
#247761=CARTESIAN_POINT('Ctrl Pts',(209.744078012845,1.77278938863763,136.341871604603));
#247762=CARTESIAN_POINT('Ctrl Pts',(209.465630389032,5.61248518735455,132.305536381355));
#247763=CARTESIAN_POINT('Ctrl Pts',(209.187182765219,4.2990952821384,126.894094626803));
#247764=CARTESIAN_POINT('Ctrl Pts',(208.908735141406,-0.967335548355457,
125.073681250508));
#247765=CARTESIAN_POINT('Ctrl Pts',(208.630287517594,-5.34357155608916,
128.520706403956));
#247766=CARTESIAN_POINT('Ctrl Pts',(208.351839893781,-4.80999390579215,
134.065650134797));
#247767=CARTESIAN_POINT('Ctrl Pts',(208.073392269968,0.144086686833323,
136.613971320579));
#247768=CARTESIAN_POINT('Ctrl Pts',(207.794944646155,4.96557142732685,133.823362329787));
#247769=CARTESIAN_POINT('Ctrl Pts',(207.516497022342,5.22403776314189,128.258534510045));
#247770=CARTESIAN_POINT('Ctrl Pts',(207.238049398529,0.681816090004523,
125.033145533949));
#247771=CARTESIAN_POINT('Ctrl Pts',(206.959601774716,-4.48693345015888,
127.111248278652));
#247772=CARTESIAN_POINT('Ctrl Pts',(206.681154150904,-5.53242507739068,
132.583126545744));
#247773=CARTESIAN_POINT('Ctrl Pts',(206.40270652709,-1.49388053201802,136.420413394932));
#247774=CARTESIAN_POINT('Ctrl Pts',(206.124258903278,3.91746311099657,135.0968180907));
#247775=CARTESIAN_POINT('Ctrl Pts',(205.845811279465,5.72885172159717,129.828666190814));
#247776=CARTESIAN_POINT('Ctrl Pts',(205.567363655652,2.27570431130586,125.457128678938));
#247777=CARTESIAN_POINT('Ctrl Pts',(205.288916031839,-3.26870357308214,
125.999436687584));
#247778=CARTESIAN_POINT('Ctrl Pts',(205.010468408026,-5.80933288384994,
130.9572347388));
#247779=CARTESIAN_POINT('Ctrl Pts',(204.732020784213,-3.01146890392974,
135.774549108008));
#247780=CARTESIAN_POINT('Ctrl Pts',(204.4535731604,2.5537877891123,136.024502973214));
#247781=CARTESIAN_POINT('Ctrl Pts',(204.175125536587,5.77223831170541,131.477401078575));
#247782=CARTESIAN_POINT('Ctrl Pts',(203.896677912775,3.6862837897924,126.311807855303));
#247783=CARTESIAN_POINT('Ctrl Pts',(203.618230288961,-1.78718543642468,
125.274651160291));
#247784=CARTESIAN_POINT('Ctrl Pts',(203.339782665149,-5.61831856260093,
129.319027308227));
#247785=CARTESIAN_POINT('Ctrl Pts',(203.061335041336,-4.28649139606962,
134.728352208566));
#247786=CARTESIAN_POINT('Ctrl Pts',(202.782887417523,0.984411954691954,
136.531720532469));
#247787=CARTESIAN_POINT('Ctrl Pts',(202.50443979371,5.3506888113544,133.071924892697));
#247788=CARTESIAN_POINT('Ctrl Pts',(202.225992169897,4.79994404549834,127.528348460205));
#247789=CARTESIAN_POINT('Ctrl Pts',(201.947544546084,-0.161714807569177,
124.995267158526));
#247790=CARTESIAN_POINT('Ctrl Pts',(201.669096922271,-4.97476565284641,
127.800458955558));
#247791=CARTESIAN_POINT('Ctrl Pts',(201.390649298458,-5.21624989388704,
133.366089631302));
#247792=CARTESIAN_POINT('Ctrl Pts',(201.112201674645,-0.664255310463968,
136.577616490799));
#247793=CARTESIAN_POINT('Ctrl Pts',(200.833754050833,4.49815745262305,134.483803242045));
#247794=CARTESIAN_POINT('Ctrl Pts',(200.55530642702,5.52698326394509,129.008761972148));
#247795=CARTESIAN_POINT('Ctrl Pts',(200.276858803207,1.47678146385132,125.183788137525));
#247796=CARTESIAN_POINT('Ctrl Pts',(199.998411179394,-3.93051035674001,
126.523845831826));
#247797=CARTESIAN_POINT('Ctrl Pts',(199.719963555581,-5.7258551755912,131.79748749945));
#247798=CARTESIAN_POINT('Ctrl Pts',(199.441515931768,-2.25941881165118,
136.158494079568));
#247799=CARTESIAN_POINT('Ctrl Pts',(199.163068307955,3.28331306145151,135.599313572066));
#247800=CARTESIAN_POINT('Ctrl Pts',(198.884620684142,5.80884062984016,130.633805545853));
#247801=CARTESIAN_POINT('Ctrl Pts',(198.606173060329,2.99632743704681,125.825029298466));
#247802=CARTESIAN_POINT('Ctrl Pts',(198.327725436517,-2.56966429165962,
125.592015279473));
#247803=CARTESIAN_POINT('Ctrl Pts',(198.049277812704,-5.77426007141042,
130.148891988961));
#247804=CARTESIAN_POINT('Ctrl Pts',(197.770830188891,-3.6725929338218,135.308112346714));
#247805=CARTESIAN_POINT('Ctrl Pts',(197.492382565078,1.80400769380988,136.328604885883));
#247806=CARTESIAN_POINT('Ctrl Pts',(197.213934941265,5.62281338150559,132.272586816804));
#247807=CARTESIAN_POINT('Ctrl Pts',(196.935487317452,4.27452826130232,126.867340597462));
#247808=CARTESIAN_POINT('Ctrl Pts',(196.657039693639,-1.00183950872307,
125.080023442474));
#247809=CARTESIAN_POINT('Ctrl Pts',(196.378592069827,-5.35756571281285,
128.553092501978));
#247810=CARTESIAN_POINT('Ctrl Pts',(196.100144446013,-4.78995075846325,
134.094966979145));
#247811=CARTESIAN_POINT('Ctrl Pts',(195.821696822201,0.179394940810534,
136.612934965078));
#247812=CARTESIAN_POINT('Ctrl Pts',(195.543249198387,4.98388545340951,133.79310689028));
#247813=CARTESIAN_POINT('Ctrl Pts',(195.264801574575,5.20842871066526,128.22676699923));
#247814=CARTESIAN_POINT('Ctrl Pts',(194.986353950762,0.64668042870769,125.029109720981));
#247815=CARTESIAN_POINT('Ctrl Pts',(194.70790632695,-4.50933557513701,127.138625880003));
#247816=CARTESIAN_POINT('Ctrl Pts',(194.429458703136,-5.52149247872048,
132.616773181746));
#247817=CARTESIAN_POINT('Ctrl Pts',(194.151011079324,-1.4596675342632,136.429401878284));
#247818=CARTESIAN_POINT('Ctrl Pts',(193.87256345551,3.9435205654586,135.072892454764));
#247819=CARTESIAN_POINT('Ctrl Pts',(193.594115831698,5.72280591721378,129.793810802232));
#247820=CARTESIAN_POINT('Ctrl Pts',(193.315668207884,2.24311220566103,125.443375061888));
#247821=CARTESIAN_POINT('Ctrl Pts',(193.037220584072,-3.29789204077089,
126.019423148508));
#247822=CARTESIAN_POINT('Ctrl Pts',(192.758772960259,-5.80829461271728,
130.992595012001));
#247823=CARTESIAN_POINT('Ctrl Pts',(192.480325336446,-2.98115818654302,
135.792788662769));
#247824=CARTESIAN_POINT('Ctrl Pts',(192.201877712633,2.58551697539033,136.008860638253));
#247825=CARTESIAN_POINT('Ctrl Pts',(191.92343008882,5.77622834646622,131.442251348686));
#247826=CARTESIAN_POINT('Ctrl Pts',(191.644982465007,3.658868051582,126.289451639914));
#247827=CARTESIAN_POINT('Ctrl Pts',(191.366534841194,-1.82081323706467,
125.285632716038));
#247828=CARTESIAN_POINT('Ctrl Pts',(191.088087217381,-5.6272561125207,129.35325512882));
#247829=CARTESIAN_POINT('Ctrl Pts',(190.809639593569,-4.26252552731426,
134.754372595315));
#247830=CARTESIAN_POINT('Ctrl Pts',(190.531191969755,1.01925778154541,136.525622023071));
#247831=CARTESIAN_POINT('Ctrl Pts',(190.252744345943,5.36439298267566,133.039311718326));
#247832=CARTESIAN_POINT('Ctrl Pts',(189.974296722129,4.77991309789331,127.499190535413));
#247833=CARTESIAN_POINT('Ctrl Pts',(189.695849098317,-0.197073412116412,
124.996359191464));
#247834=CARTESIAN_POINT('Ctrl Pts',(189.417401474504,-4.99295908396257,
127.830797421458));
#247835=CARTESIAN_POINT('Ctrl Pts',(189.138953850692,-5.20055927725872,
133.397794962038));
#247836=CARTESIAN_POINT('Ctrl Pts',(188.860506226878,-0.629099556198964,
136.581553036358));
#247837=CARTESIAN_POINT('Ctrl Pts',(188.582058603065,4.52047192378579,134.456353509349));
#247838=CARTESIAN_POINT('Ctrl Pts',(188.303610979253,5.51595054314194,128.975150924561));
#247839=CARTESIAN_POINT('Ctrl Pts',(188.02516335544,1.44254008251539,125.174902685784));
#247840=CARTESIAN_POINT('Ctrl Pts',(187.746715731627,-3.95649424194195,
126.547851272005));
#247841=CARTESIAN_POINT('Ctrl Pts',(187.468268107814,-5.71970364354381,
131.832324004755));
#247842=CARTESIAN_POINT('Ctrl Pts',(187.189820484001,-2.22678481978599,
136.172148603481));
#247843=CARTESIAN_POINT('Ctrl Pts',(186.911372860188,3.312440468869,135.579238274173));
#247844=CARTESIAN_POINT('Ctrl Pts',(186.632925236375,5.80769478834652,130.598448644184));
#247845=CARTESIAN_POINT('Ctrl Pts',(186.354477612562,2.96596131899707,125.806882058373));
#247846=CARTESIAN_POINT('Ctrl Pts',(186.076029988749,-2.60134570724499,
125.607754128061));
#247847=CARTESIAN_POINT('Ctrl Pts',(185.797582364937,-5.7781431113317,130.184053693262));
#247848=CARTESIAN_POINT('Ctrl Pts',(185.519134741124,-3.64510927408837,
135.33038501822));
#247849=CARTESIAN_POINT('Ctrl Pts',(185.240687117311,1.83760191255446,136.317521027561));
#247850=CARTESIAN_POINT('Ctrl Pts',(184.962239493498,5.63164671340385,132.238331952975));
#247851=CARTESIAN_POINT('Ctrl Pts',(184.683791869685,4.25048330587202,126.841393274542));
#247852=CARTESIAN_POINT('Ctrl Pts',(184.405344245872,-1.03666661210287,
125.086227982629));
#247853=CARTESIAN_POINT('Ctrl Pts',(184.126896622059,-5.37117055753467,
128.585747235914));
#247854=CARTESIAN_POINT('Ctrl Pts',(183.848448998247,-4.7698311568614,134.124063801647));
#247855=CARTESIAN_POINT('Ctrl Pts',(183.570001374433,0.214750057761129,
136.611735317726));
#247856=CARTESIAN_POINT('Ctrl Pts',(183.291553750621,5.00198646042476,133.762713190383));
#247857=CARTESIAN_POINT('Ctrl Pts',(183.013106126807,5.19264166658148,128.195109572179));
#247858=CARTESIAN_POINT('Ctrl Pts',(182.734658502995,0.611512855797894,
125.025280195685));
#247859=CARTESIAN_POINT('Ctrl Pts',(182.456210879182,-4.53156639540017,
127.166143403126));
#247860=CARTESIAN_POINT('Ctrl Pts',(182.177763255369,-5.5103575085511,132.650350493844));
#247861=CARTESIAN_POINT('Ctrl Pts',(181.899315631556,-1.42539926727337,
136.438183069882));
#247862=CARTESIAN_POINT('Ctrl Pts',(181.620868007743,3.96943126600311,135.048808039769));
#247863=CARTESIAN_POINT('Ctrl Pts',(181.34242038393,5.71654838332065,129.758993181434));
#247864=CARTESIAN_POINT('Ctrl Pts',(181.063972760118,2.21043680528058,125.429819927867));
#247865=CARTESIAN_POINT('Ctrl Pts',(180.785525136304,-3.32695821097111,
126.039587007222));
#247866=CARTESIAN_POINT('Ctrl Pts',(180.507077512492,-5.80704116228462,
131.027948262352));
#247867=CARTESIAN_POINT('Ctrl Pts',(180.228629888679,-2.95073697519064,
135.810843394787));
#247868=CARTESIAN_POINT('Ctrl Pts',(179.950182264866,2.61715034058839,135.993025435236));
#247869=CARTESIAN_POINT('Ctrl Pts',(179.671734641053,5.78000434826875,131.407077988614));
#247870=CARTESIAN_POINT('Ctrl Pts',(179.39328701724,3.63131672880039,126.26726272238));
#247871=CARTESIAN_POINT('Ctrl Pts',(179.114839393428,-1.8543735647511,125.296818772266));
#247872=CARTESIAN_POINT('Ctrl Pts',(178.836391769614,-5.63598514348121,
129.387536719606));
#247873=CARTESIAN_POINT('Ctrl Pts',(178.557944145802,-4.23840170853308,
134.780246613475));
#247874=CARTESIAN_POINT('Ctrl Pts',(178.279496521988,1.05406583912245,136.519311509933));
#247875=CARTESIAN_POINT('Ctrl Pts',(178.001048898175,5.3778983746034,133.006615727177));
#247876=CARTESIAN_POINT('Ctrl Pts',(177.722601274363,4.75970502876524,127.470155084831));
#247877=CARTESIAN_POINT('Ctrl Pts',(177.44415365055,-0.232424713990654,
124.997666442073));
#247878=CARTESIAN_POINT('Ctrl Pts',(177.165706026737,-5.01096749916768,
127.861246073811));
#247879=CARTESIAN_POINT('Ctrl Pts',(176.887258402924,-5.18467595198119,
133.429404192122));
#247880=CARTESIAN_POINT('Ctrl Pts',(176.608810779111,-0.593920490425269,
136.585275505922));
#247881=CARTESIAN_POINT('Ctrl Pts',(176.330363155298,4.54261888720253,134.428768450716));
#247882=CARTESIAN_POINT('Ctrl Pts',(176.051915531486,5.50471342676105,128.941607659011));
#247883=CARTESIAN_POINT('Ctrl Pts',(175.773467907672,1.40824524732727,125.166225835676));
#247884=CARTESIAN_POINT('Ctrl Pts',(175.49502028386,-3.98233151779528,126.572014438702));
#247885=CARTESIAN_POINT('Ctrl Pts',(175.216572660047,-5.7133401657742,131.867122418498));
#247886=CARTESIAN_POINT('Ctrl Pts',(174.938125036234,-2.19406831359054,
136.185604222037));
#247887=CARTESIAN_POINT('Ctrl Pts',(174.659677412421,3.34144513258691,135.558986041432));
#247888=CARTESIAN_POINT('Ctrl Pts',(174.381229788608,5.80633374058666,130.563099372659));
#247889=CARTESIAN_POINT('Ctrl Pts',(174.102782164795,2.93548529615992,125.788920001687));
#247890=CARTESIAN_POINT('Ctrl Pts',(173.824334540982,-2.63293072900865,
125.623685538813));
#247891=CARTESIAN_POINT('Ctrl Pts',(173.54588691717,-5.7818120400351,130.219238383264));
#247892=CARTESIAN_POINT('Ctrl Pts',(173.267439293356,-3.61749054349026,
135.352489976228));
#247893=CARTESIAN_POINT('Ctrl Pts',(172.988991669544,1.87112803828436,136.306232877052));
#247894=CARTESIAN_POINT('Ctrl Pts',(172.71054404573,5.64027136256211,132.204023952811));
#247895=CARTESIAN_POINT('Ctrl Pts',(172.432096421918,4.22628084721974,126.815592800833));
#247896=CARTESIAN_POINT('Ctrl Pts',(172.153648798105,-1.07145530142008,
125.092644410292));
#247897=CARTESIAN_POINT('Ctrl Pts',(171.875201174292,-5.38457637155629,
128.618484181386));
#247898=CARTESIAN_POINT('Ctrl Pts',(171.596753550479,-4.74953480741189,
134.153037611328));
#247899=CARTESIAN_POINT('Ctrl Pts',(171.318305926666,0.25009721706947,136.610320475968));
#247900=CARTESIAN_POINT('Ctrl Pts',(171.039858302853,5.01990211699227,133.732209867644));
#247901=CARTESIAN_POINT('Ctrl Pts',(170.76141067904,5.1766622072511,128.163548831885));
#247902=CARTESIAN_POINT('Ctrl Pts',(170.482963055228,0.576322623054293,
125.021664816339));
#247903=CARTESIAN_POINT('Ctrl Pts',(170.204515431414,-4.55362929680409,
127.193795741725));
#247904=CARTESIAN_POINT('Ctrl Pts',(169.926067807602,-5.4990183500578,132.683859402108));
#247905=CARTESIAN_POINT('Ctrl Pts',(169.647620183788,-1.39107818158956,
136.446755498118));
#247906=CARTESIAN_POINT('Ctrl Pts',(169.369172559976,3.99519487781229,135.024566345214));
#247907=CARTESIAN_POINT('Ctrl Pts',(169.090724936163,5.71007902062496,129.724214297113));
#247908=CARTESIAN_POINT('Ctrl Pts',(168.81227731235,2.17767949635139,125.416463949427));
#247909=CARTESIAN_POINT('Ctrl Pts',(168.533829688537,-3.35590109951139,
126.059927426375));
#247910=CARTESIAN_POINT('Ctrl Pts',(168.255382064725,-5.80557252980615,
131.063293227581));
#247911=CARTESIAN_POINT('Ctrl Pts',(167.976934440911,-2.92020642319446,
135.828712609743));
#247912=CARTESIAN_POINT('Ctrl Pts',(167.698486817099,2.64868672631821,135.976997964335));
#247913=CARTESIAN_POINT('Ctrl Pts',(167.420039193286,5.78356616988455,131.371882294628));
#247914=CARTESIAN_POINT('Ctrl Pts',(167.141591569473,3.60363084624196,126.245241928676));
#247915=CARTESIAN_POINT('Ctrl Pts',(166.86314394566,-1.88786517794308,125.308208912483));
#247916=CARTESIAN_POINT('Ctrl Pts',(166.584696321847,-5.64450533093961,
129.421870811324));
#247917=CARTESIAN_POINT('Ctrl Pts',(166.306248698034,-4.21412083421794,
134.805973303719));
#247918=CARTESIAN_POINT('Ctrl Pts',(166.027801074221,1.08883483790225,136.512789227187));
#247919=CARTESIAN_POINT('Ctrl Pts',(165.749353450409,5.3912044865292,132.973838130654));
#247920=CARTESIAN_POINT('Ctrl Pts',(165.470905826595,4.73932058701693,127.441243184462));
#247921=CARTESIAN_POINT('Ctrl Pts',(165.192458202783,-0.267767403281747,
124.999188861871));
#247922=CARTESIAN_POINT('Ctrl Pts',(164.914010578969,-5.02879023112935,
127.891803784357));
#247923=CARTESIAN_POINT('Ctrl Pts',(164.635562955157,-5.16860050662956,
133.46091615025));
#247924=CARTESIAN_POINT('Ctrl Pts',(164.357115331344,-0.55871941670932,
136.588783761558));
#247925=CARTESIAN_POINT('Ctrl Pts',(164.078667707531,4.56459752220588,134.401049088318));
#247926=CARTESIAN_POINT('Ctrl Pts',(163.800220083718,5.49327233119978,128.908133418456));
#247927=CARTESIAN_POINT('Ctrl Pts',(163.521772459905,1.37389822909362,125.157757908727));
#247928=CARTESIAN_POINT('Ctrl Pts',(163.243324836092,-4.00802122688977,
126.596334436543));
#247929=CARTESIAN_POINT('Ctrl Pts',(162.964877212279,-5.70676497808368,
131.901881451211));
#247930=CARTESIAN_POINT('Ctrl Pts',(162.686429588467,-2.16127050538683,
136.198860436632));
#247931=CARTESIAN_POINT('Ctrl Pts',(162.407981964654,3.37032597782655,135.538557624299));
#247932=CARTESIAN_POINT('Ctrl Pts',(162.129534340841,5.80475753699479,130.527759041158));
#247933=CARTESIAN_POINT('Ctrl Pts',(161.851086717028,2.90490049783562,125.771143793998));
#247934=CARTESIAN_POINT('Ctrl Pts',(161.572639093215,-2.66441818655578,
125.639808921385));
#247935=CARTESIAN_POINT('Ctrl Pts',(161.294191469402,-5.7852667215671,130.254444755185));
#247936=CARTESIAN_POINT('Ctrl Pts',(161.015743845589,-3.58973776544978,
135.37442640163));
#247937=CARTESIAN_POINT('Ctrl Pts',(160.737296221776,1.90458482867669,136.294740852644));
#247938=CARTESIAN_POINT('Ctrl Pts',(160.458848597964,5.64868700939082,132.169664087608));
#247939=CARTESIAN_POINT('Ctrl Pts',(160.18040097415,4.20192178217643,126.789940132385));
#247940=CARTESIAN_POINT('Ctrl Pts',(159.901953350338,-1.10620428756715,
125.099272487699));
#247941=CARTESIAN_POINT('Ctrl Pts',(159.623505726525,-5.39778265812024,
128.651302125312));
#247942=CARTESIAN_POINT('Ctrl Pts',(159.345058102712,-4.72906246220349,
134.18188733455));
#247943=CARTESIAN_POINT('Ctrl Pts',(159.066610478899,0.285435108933367,
136.608690492233));
#247944=CARTESIAN_POINT('Ctrl Pts',(158.788162855086,5.03763175924073,133.701598052375));
#247945=CARTESIAN_POINT('Ctrl Pts',(158.509715231273,5.16049092479898,128.132085947844));
#247946=CARTESIAN_POINT('Ctrl Pts',(158.23126760746,0.541111034464008,125.018263716911));
#247947=CARTESIAN_POINT('Ctrl Pts',(157.952819983648,-4.57552346179978,
127.221581871133));
#247948=CARTESIAN_POINT('Ctrl Pts',(157.674372359834,-5.48747542341729,
132.717298664853));
#247949=CARTESIAN_POINT('Ctrl Pts',(157.395924736022,-1.35670554899215,
136.455118845335));
#247950=CARTESIAN_POINT('Ctrl Pts',(157.117477112209,4.02081044620608,135.000168269382));
#247951=CARTESIAN_POINT('Ctrl Pts',(156.839029488396,5.70339806885126,129.68947543801));
#247952=CARTESIAN_POINT('Ctrl Pts',(156.560581864583,2.1448414927076,125.403307621479));
#247953=CARTESIAN_POINT('Ctrl Pts',(156.28213424077,-3.38471963390224,126.080443652244));
#247954=CARTESIAN_POINT('Ctrl Pts',(156.003686616957,-5.8038887697026,131.098628597966));
#247955=CARTESIAN_POINT('Ctrl Pts',(155.725238993144,-2.88956766187541,
135.846395645489));
#247956=CARTESIAN_POINT('Ctrl Pts',(155.446791369331,2.68012496398725,135.960778819456));
#247957=CARTESIAN_POINT('Ctrl Pts',(155.168343745519,5.78691367932904,131.336665570917));
#247958=CARTESIAN_POINT('Ctrl Pts',(154.889896121706,3.57581142981733,126.223390074792));
#247959=CARTESIAN_POINT('Ctrl Pts',(154.611448497893,-1.92128683559663,
125.319802714623));
#247960=CARTESIAN_POINT('Ctrl Pts',(154.33300087408,-5.65281635917722,129.456256131708));
#247961=CARTESIAN_POINT('Ctrl Pts',(154.054553250267,-4.18968380410554,
134.831551712731));
#247962=CARTESIAN_POINT('Ctrl Pts',(153.776105626454,1.12356348950664,136.50605541652));
#247963=CARTESIAN_POINT('Ctrl Pts',(153.497658002641,5.40431082539012,132.940980143345));
#247964=CARTESIAN_POINT('Ctrl Pts',(153.219210378828,4.71876052800142,127.412455905645));
#247965=CARTESIAN_POINT('Ctrl Pts',(152.940762755016,-0.303100170353132,
125.000926394444));
#247966=CARTESIAN_POINT('Ctrl Pts',(152.662315131202,-5.04642661941966,
127.922469420767));
#247967=CARTESIAN_POINT('Ctrl Pts',(152.38386750739,-5.15233353688545,133.492329668737));
#247968=CARTESIAN_POINT('Ctrl Pts',(152.105419883576,-0.523497639439988,
136.592077673268));
#247969=CARTESIAN_POINT('Ctrl Pts',(151.826972259764,4.58640701436939,134.373196449306));
#247970=CARTESIAN_POINT('Ctrl Pts',(151.548524635951,5.48162768041213,128.874729443297));
#247971=CARTESIAN_POINT('Ctrl Pts',(151.270077012138,1.33950030055583,125.149499218718));
#247972=CARTESIAN_POINT('Ctrl Pts',(150.991629388325,-4.03356241728369,
126.620810364342));
#247973=CARTESIAN_POINT('Ctrl Pts',(150.713181764512,-5.69997832411825,
131.936599814887));
#247974=CARTESIAN_POINT('Ctrl Pts',(150.434734140699,-2.1283926105098,136.211916756054));
#247975=CARTESIAN_POINT('Ctrl Pts',(150.156286516886,3.39908193439765,135.517953779753));
#247976=CARTESIAN_POINT('Ctrl Pts',(149.877838893074,5.8029662359777,130.49242895923));
#247977=CARTESIAN_POINT('Ctrl Pts',(149.599391269261,2.87420805735513,125.753554094008));
#247978=CARTESIAN_POINT('Ctrl Pts',(149.320943645448,-2.69580691310719,
125.65612367832));
#247979=CARTESIAN_POINT('Ctrl Pts',(149.042496021635,-5.7885070279132,130.289671504441));
#247980=CARTESIAN_POINT('Ctrl Pts',(148.764048397822,-3.56185196835627,
135.396193481562));
#247981=CARTESIAN_POINT('Ctrl Pts',(148.485600774009,1.93797104397778,136.283045380177));
#247982=CARTESIAN_POINT('Ctrl Pts',(148.207153150196,5.6568933420451,132.135253630582));
#247983=CARTESIAN_POINT('Ctrl Pts',(147.928705526383,4.17740701337624,126.764436219762));
#247984=CARTESIAN_POINT('Ctrl Pts',(147.65025790257,-1.14091228290746,125.106111969245));
#247985=CARTESIAN_POINT('Ctrl Pts',(147.371810278758,-5.41078892786276,
128.684199851613));
#247986=CARTESIAN_POINT('Ctrl Pts',(147.093362654945,-4.70841487984645,
134.210611902278));
#247987=CARTESIAN_POINT('Ctrl Pts',(146.814915031132,0.320762423894332,
136.60684542692));
#247988=CARTESIAN_POINT('Ctrl Pts',(146.536467407319,5.05517473019176,133.670878878906));
#247989=CARTESIAN_POINT('Ctrl Pts',(146.258019783506,5.14412841845787,128.100722085923));
#247990=CARTESIAN_POINT('Ctrl Pts',(145.979572159693,0.505879394805349,
125.015077023433));
#247991=CARTESIAN_POINT('Ctrl Pts',(145.70112453588,-4.59724807909095,127.249500761725));
#247992=CARTESIAN_POINT('Ctrl Pts',(145.422676912067,-5.47572915635697,
132.750667042976));
#247993=CARTESIAN_POINT('Ctrl Pts',(145.144229288255,-1.32228264317164,
136.463272801628));
#247994=CARTESIAN_POINT('Ctrl Pts',(144.865781664442,4.0462770219901,134.975614716357));
#247995=CARTESIAN_POINT('Ctrl Pts',(144.587334040629,5.69650577556471,129.654777891387));
#247996=CARTESIAN_POINT('Ctrl Pts',(144.308886416816,2.11192401117359,125.390351431538));
#247997=CARTESIAN_POINT('Ctrl Pts',(144.030438793003,-3.41341274626234,
126.101134924595));
#247998=CARTESIAN_POINT('Ctrl Pts',(143.75199116919,-5.80198994436631,131.133953064144));
#247999=CARTESIAN_POINT('Ctrl Pts',(143.473543545377,-2.85882182656403,
135.863891846773));
#248000=CARTESIAN_POINT('Ctrl Pts',(143.195095921564,2.71146388864014,135.944368601604));
#248001=CARTESIAN_POINT('Ctrl Pts',(142.916648297751,5.790046752559,131.301429122451));
#248002=CARTESIAN_POINT('Ctrl Pts',(142.638200673938,3.54785951038517,126.201707970457));
#248003=CARTESIAN_POINT('Ctrl Pts',(142.359753050125,-1.95463729925998,
125.331599749072));
#248004=CARTESIAN_POINT('Ctrl Pts',(142.081305426313,-5.66091792022584,
129.490691406602));
#248005=CARTESIAN_POINT('Ctrl Pts',(141.8028578025,-4.16509152371897,134.856980892698));
#248006=CARTESIAN_POINT('Ctrl Pts',(141.524410178687,1.15825050705268,136.499110327454));
#248007=CARTESIAN_POINT('Ctrl Pts',(141.245962554874,5.41721690552589,132.908042982814));
#248008=CARTESIAN_POINT('Ctrl Pts',(140.967514931061,4.69802561357932,127.383794315106));
#248009=CARTESIAN_POINT('Ctrl Pts',(140.689067307248,-0.338421705936203,
125.002878975406));
#248010=CARTESIAN_POINT('Ctrl Pts',(140.410619683435,-5.06387601051571,
127.953241846716));
#248011=CARTESIAN_POINT('Ctrl Pts',(140.132172059623,-5.13587564552739,
133.523643583541));
#248012=CARTESIAN_POINT('Ctrl Pts',(139.85372443581,-0.48825646377323,136.595157118993));
#248013=CARTESIAN_POINT('Ctrl Pts',(139.575276811997,4.60804655553434,134.34521156577));
#248014=CARTESIAN_POINT('Ctrl Pts',(139.296829188184,5.46977990589493,128.841396971331));
#248015=CARTESIAN_POINT('Ctrl Pts',(139.018381564371,1.30505273634171,125.141450071677));
#248016=CARTESIAN_POINT('Ctrl Pts',(138.739933940558,-4.05895414253892,
126.645441315135));
#248017=CARTESIAN_POINT('Ctrl Pts',(138.461486316745,-5.69298045535984,
131.971276223022));
#248018=CARTESIAN_POINT('Ctrl Pts',(138.183038692932,-2.09543584726193,
136.224772696493));
#248019=CARTESIAN_POINT('Ctrl Pts',(137.904591069119,3.42771193673771,135.49717527128));
#248020=CARTESIAN_POINT('Ctrl Pts',(137.626143445306,5.80095990391266,130.457110436044));
#248021=CARTESIAN_POINT('Ctrl Pts',(137.347695821494,2.84340911203807,125.736151553513));
#248022=CARTESIAN_POINT('Ctrl Pts',(137.069248197681,-2.727095745542,125.672629205068));
#248023=CARTESIAN_POINT('Ctrl Pts',(136.790800573868,-5.7915328390027,130.324917325691));
#248024=CARTESIAN_POINT('Ctrl Pts',(136.512352950055,-3.53383418552815,
135.417790409441));
#248025=CARTESIAN_POINT('Ctrl Pts',(136.233905326242,1.97128544704926,136.271146893031));
#248026=CARTESIAN_POINT('Ctrl Pts',(135.955457702429,5.66489005643625,132.100793856825));
#248027=CARTESIAN_POINT('Ctrl Pts',(135.677010078616,4.15273744922295,126.739082008025));
#248028=CARTESIAN_POINT('Ctrl Pts',(135.398562454803,-1.17557800132362,
125.113162601491));
#248029=CARTESIAN_POINT('Ctrl Pts',(135.12011483099,-5.42359469883174,128.717176141249));
#248030=CARTESIAN_POINT('Ctrl Pts',(134.841667207177,-4.68759282544451,
134.239210250113));
#248031=CARTESIAN_POINT('Ctrl Pts',(134.563219583365,0.356077852885664,
136.604785348398));
#248032=CARTESIAN_POINT('Ctrl Pts',(134.284771959552,5.0725303797842,133.640053485549));
#248033=CARTESIAN_POINT('Ctrl Pts',(134.006324335739,5.12757529454644,128.069458408322));
#248034=CARTESIAN_POINT('Ctrl Pts',(133.727876711926,0.470629009599695,
125.012104853988));
#248035=CARTESIAN_POINT('Ctrl Pts',(133.449429088113,-4.61880234366392,
127.277551378957));
#248036=CARTESIAN_POINT('Ctrl Pts',(133.1709814643,-5.46377998413907,132.783963299997));
#248037=CARTESIAN_POINT('Ctrl Pts',(132.892533840487,-1.28781073968153,
136.47121706485));
#248038=CARTESIAN_POINT('Ctrl Pts',(132.614086216674,4.07159366149105,134.950906595976));
#248039=CARTESIAN_POINT('Ctrl Pts',(132.335638592862,5.68940239616175,129.620122942976));
#248040=CARTESIAN_POINT('Ctrl Pts',(132.057190969048,2.07892827151876,125.377595859696));
#248041=CARTESIAN_POINT('Ctrl Pts',(131.778743345236,-3.44197937335791,
126.122000476702));
#248042=CARTESIAN_POINT('Ctrl Pts',(131.500295721423,-5.79987612415893,
131.169265317152));
#248043=CARTESIAN_POINT('Ctrl Pts',(131.22184809761,-2.82797005655853,135.881200565267));
#248044=CARTESIAN_POINT('Ctrl Pts',(130.943400473797,2.74270233900145,135.927767918864));
#248045=CARTESIAN_POINT('Ctrl Pts',(130.664952849984,5.79296527347731,131.26617425493));
#248046=CARTESIAN_POINT('Ctrl Pts',(130.386505226171,3.51977612371406,126.180196419108));
#248047=CARTESIAN_POINT('Ctrl Pts',(130.108057602358,-1.98791533311939,
125.343599578688));
#248048=CARTESIAN_POINT('Ctrl Pts',(129.829609978546,-5.66880971387908,
129.52517535999));
#248049=CARTESIAN_POINT('Ctrl Pts',(129.551162354732,-4.14034490433441,
134.882259901329));
#248050=CARTESIAN_POINT('Ctrl Pts',(129.27271473092,1.19289460520041,136.491954217345));
#248051=CARTESIAN_POINT('Ctrl Pts',(128.994267107107,5.42992224869717,132.875027869557));
#248052=CARTESIAN_POINT('Ctrl Pts',(128.715819483294,4.67711661209022,127.355259474909));
#248053=CARTESIAN_POINT('Ctrl Pts',(128.437371859481,-0.373730701178542,
125.005046532403));
#248054=CARTESIAN_POINT('Ctrl Pts',(128.158924235668,-5.0811377578241,127.984119921918));
#248055=CARTESIAN_POINT('Ctrl Pts',(127.880476611855,-5.11922744240848,
133.554856734316));
#248056=CARTESIAN_POINT('Ctrl Pts',(127.602028988042,-0.452997195583419,
136.598021984625));
#248057=CARTESIAN_POINT('Ctrl Pts',(127.323581364229,4.62951534383955,134.3170954747));
#248058=CARTESIAN_POINT('Ctrl Pts',(127.045133740417,5.45772944667181,128.808137237705));
#248059=CARTESIAN_POINT('Ctrl Pts',(126.766686116604,1.2705568129186,125.133610765869));
#248060=CARTESIAN_POINT('Ctrl Pts',(126.488238492791,-4.08419546175569,
126.67022637621));
#248061=CARTESIAN_POINT('Ctrl Pts',(126.209790868978,-5.68577163111709,
132.005909390672));
#248062=CARTESIAN_POINT('Ctrl Pts',(125.931343245165,-2.06240143686808,
136.237427781569));
#248063=CARTESIAN_POINT('Ctrl Pts',(125.652895621352,3.45621492395137,135.476222868834));
#248064=CARTESIAN_POINT('Ctrl Pts',(125.374447997539,5.79873861514512,130.421804780342));
#248065=CARTESIAN_POINT('Ctrl Pts',(125.096000373726,2.8125048031507,125.718936817367));
#248066=CARTESIAN_POINT('Ctrl Pts',(124.817552749914,-2.75828352444112,
125.68932489001));
#248067=CARTESIAN_POINT('Ctrl Pts',(124.5391051261,-5.79434404271298,130.36018091289));
#248068=CARTESIAN_POINT('Ctrl Pts',(124.260657502288,-3.50568545517477,
135.439216384981));
#248069=CARTESIAN_POINT('Ctrl Pts',(123.982209878475,2.00452680341345,136.25904583211));
#248070=CARTESIAN_POINT('Ctrl Pts',(123.703762254662,5.67267685624313,132.066286043259));
#248071=CARTESIAN_POINT('Ctrl Pts',(123.425314630849,4.12791400385628,126.71387843668));
#248072=CARTESIAN_POINT('Ctrl Pts',(123.146867007036,-1.21020015826455,
125.120424123171));
#248073=CARTESIAN_POINT('Ctrl Pts',(122.868419383223,-5.43619949650465,
128.750229772276));
#248074=CARTESIAN_POINT('Ctrl Pts',(122.58997175941,-4.66659707056658,134.267681318331));
#248075=CARTESIAN_POINT('Ctrl Pts',(122.311524135597,0.391380087281262,
136.602510333005));
#248076=CARTESIAN_POINT('Ctrl Pts',(122.033076511785,5.08969806489794,133.609123014551));
#248077=CARTESIAN_POINT('Ctrl Pts',(121.754628887972,5.11083216644683,128.038296073528));
#248078=CARTESIAN_POINT('Ctrl Pts',(121.476181264159,0.435361185062875,
125.00934731871));
#248079=CARTESIAN_POINT('Ctrl Pts',(121.197733640346,-4.64018545681751,
127.305732683402));
#248080=CARTESIAN_POINT('Ctrl Pts',(120.919286016533,-5.45162834954452,
132.817186202114));
#248081=CARTESIAN_POINT('Ctrl Pts',(120.64083839272,-1.25329111589093,136.478951340622));
#248082=CARTESIAN_POINT('Ctrl Pts',(120.362390768907,4.09675942659154,134.92604482381));
#248083=CARTESIAN_POINT('Ctrl Pts',(120.083943145094,5.68208819386074,129.585511876926));
#248084=CARTESIAN_POINT('Ctrl Pts',(119.805495521281,2.04585549641223,125.36504137862));
#248085=CARTESIAN_POINT('Ctrl Pts',(119.527047897469,-3.47041845664194,
126.143039535386));
#248086=CARTESIAN_POINT('Ctrl Pts',(119.248600273655,-5.79754738740892,
131.204564048482));
#248087=CARTESIAN_POINT('Ctrl Pts',(118.970152649843,-2.7970134950826,135.898321159589));
#248088=CARTESIAN_POINT('Ctrl Pts',(118.69170502603,2.77383915751901,135.910977386384));
#248089=CARTESIAN_POINT('Ctrl Pts',(118.413257402217,5.795669133937,131.230902274733));
#248090=CARTESIAN_POINT('Ctrl Pts',(118.134809778404,3.49156231044436,126.158856217863));
#248091=CARTESIAN_POINT('Ctrl Pts',(117.856362154591,-2.02111970404504,
125.355801758813));
#248092=CARTESIAN_POINT('Ctrl Pts',(117.577914530778,-5.67649144770371,
129.559706714059));
#248093=CARTESIAN_POINT('Ctrl Pts',(117.299466906965,-4.11544486294674,
134.907387801903));
#248094=CARTESIAN_POINT('Ctrl Pts',(117.021019283153,1.22749450019975,136.484587351363));
#248095=CARTESIAN_POINT('Ctrl Pts',(116.74257165934,5.44242638410263,132.841936026965));
#248096=CARTESIAN_POINT('Ctrl Pts',(116.464124035527,4.65603429832517,127.326852442422));
#248097=CARTESIAN_POINT('Ctrl Pts',(116.185676411714,-0.409025847692317,
125.007428985116));
#248098=CARTESIAN_POINT('Ctrl Pts',(115.907228787901,-5.09821122170419,
128.015102502178));
#248099=CARTESIAN_POINT('Ctrl Pts',(115.628781164088,-5.10238954443416,
133.585967964446));
#248100=CARTESIAN_POINT('Ctrl Pts',(115.350333540275,-0.417721141415912,
136.600672164005));
#248101=CARTESIAN_POINT('Ctrl Pts',(115.071885916462,4.65081258375125,134.288849217947));
#248102=CARTESIAN_POINT('Ctrl Pts',(114.793438292649,5.44547674927697,128.77495147487));
#248103=CARTESIAN_POINT('Ctrl Pts',(114.514990668836,1.23601380854556,125.125981591782));
#248104=CARTESIAN_POINT('Ctrl Pts',(114.236543045024,-4.10928543960769,
126.695164629152));
#248105=CARTESIAN_POINT('Ctrl Pts',(113.958095421211,-5.67835211851559,
132.040498034489));
#248106=CARTESIAN_POINT('Ctrl Pts',(113.679647797398,-2.02929060343055,
136.249881542344));
#248107=CARTESIAN_POINT('Ctrl Pts',(113.401200173585,3.48458983985001,135.455097348814));
#248108=CARTESIAN_POINT('Ctrl Pts',(113.122752549772,5.79630245198571,130.386513300387));
#248109=CARTESIAN_POINT('Ctrl Pts',(112.844304925959,2.78149627586357,125.701910523471));
#248110=CARTESIAN_POINT('Ctrl Pts',(112.565857302146,-2.78936909412988,
125.706210114483));
#248111=CARTESIAN_POINT('Ctrl Pts',(112.287409678333,-5.7969405348739,130.395460959329));
#248112=CARTESIAN_POINT('Ctrl Pts',(112.008962054521,-3.47740682035766,
135.460470614237));
#248113=CARTESIAN_POINT('Ctrl Pts',(111.730514430707,2.03769388129978,136.246742645822));
#248114=CARTESIAN_POINT('Ctrl Pts',(111.452066806895,5.68025345292297,132.031731468582));
#248115=CARTESIAN_POINT('Ctrl Pts',(111.173619183082,4.10293759711819,126.688826439658));
#248116=CARTESIAN_POINT('Ctrl Pts',(110.895171559269,-1.24477747079359,
125.127896265209));
#248117=CARTESIAN_POINT('Ctrl Pts',(110.616723935456,-5.44860285380605,
128.783359519875));
#248118=CARTESIAN_POINT('Ctrl Pts',(110.338276311643,-4.64542839321807,
134.296024051927));
#248119=CARTESIAN_POINT('Ctrl Pts',(110.05982868783,0.426667818943798,136.600020465042));
#248120=CARTESIAN_POINT('Ctrl Pts',(109.781381064017,5.10667714937814,133.57808861205));
#248121=CARTESIAN_POINT('Ctrl Pts',(109.502933440204,5.0938996545818,128.007236236273));
#248122=CARTESIAN_POINT('Ctrl Pts',(109.224485816392,0.400077228057368,
125.006804519781));
#248123=CARTESIAN_POINT('Ctrl Pts',(108.946038192578,-4.66139662619255,
127.334043630792));
#248124=CARTESIAN_POINT('Ctrl Pts',(108.667590568766,-5.43927470285667,
132.850334518237));
#248125=CARTESIAN_POINT('Ctrl Pts',(108.389142944953,-1.21872505093712,
136.486475342347));
#248126=CARTESIAN_POINT('Ctrl Pts',(108.11069532114,4.1217733847649,134.901030321119));
#248127=CARTESIAN_POINT('Ctrl Pts',(107.832247697327,5.67456343969215,129.550945975765));
#248128=CARTESIAN_POINT('Ctrl Pts',(107.553800073514,2.01270691137792,125.352688453517));
#248129=CARTESIAN_POINT('Ctrl Pts',(107.275352449701,-3.49872894229381,
126.164251321038));
#248130=CARTESIAN_POINT('Ctrl Pts',(106.996904825888,-5.7950038204084,131.239847950126));
#248131=CARTESIAN_POINT('Ctrl Pts',(106.718457202076,-2.76595328924301,
135.91525299533));
#248132=CARTESIAN_POINT('Ctrl Pts',(106.440009578262,2.80487319040651,135.893997626342));
#248133=CARTESIAN_POINT('Ctrl Pts',(106.16156195445,5.7981582337456,131.195614488879));
#248134=CARTESIAN_POINT('Ctrl Pts',(105.883114330637,3.46321911604922,126.137688157493));
#248135=CARTESIAN_POINT('Ctrl Pts',(105.604666706824,-2.05424918163679,
125.36820583729));
#248136=CARTESIAN_POINT('Ctrl Pts',(105.326219083011,-5.68396283705021,
129.594284189235));
#248137=CARTESIAN_POINT('Ctrl Pts',(105.047771459198,-4.09039232223623,
134.932363663296));
#248138=CARTESIAN_POINT('Ctrl Pts',(104.769323835385,1.26204890993897,136.47701000249));
#248139=CARTESIAN_POINT('Ctrl Pts',(104.490876211572,5.45472884839698,132.808768681268));
#248140=CARTESIAN_POINT('Ctrl Pts',(104.21242858776,4.63477945349693,127.29857427028));
#248141=CARTESIAN_POINT('Ctrl Pts',(103.933980963947,-0.444305837602887,
125.010026245263));
#248142=CARTESIAN_POINT('Ctrl Pts',(103.655533340134,-5.1150957694926,128.046188439421));
#248143=CARTESIAN_POINT('Ctrl Pts',(103.377085716321,-5.08536257553889,
133.616976121092));
#248144=CARTESIAN_POINT('Ctrl Pts',(103.098638092508,-0.38242960843803,
136.603107558928));
#248145=CARTESIAN_POINT('Ctrl Pts',(102.820190468695,4.6719374860923,134.260473842188));
#248146=CARTESIAN_POINT('Ctrl Pts',(102.541742844882,5.4330222677386,128.741840912539));
#248147=CARTESIAN_POINT('Ctrl Pts',(102.263295221069,1.2014250032263,125.118562832119));
#248148=CARTESIAN_POINT('Ctrl Pts',(101.984847597256,-4.13422314637653,
126.720255149861));
#248149=CARTESIAN_POINT('Ctrl Pts',(101.706399973443,-5.67072219248816,
132.07504087278));
#248150=CARTESIAN_POINT('Ctrl Pts',(101.427952349631,-1.99610457388343,
136.262133517338));
#248151=CARTESIAN_POINT('Ctrl Pts',(101.149504725818,3.51283563299066,135.433799494034));
#248152=CARTESIAN_POINT('Ctrl Pts',(100.871057102005,5.7936515047074,130.351237303918));
#248153=CARTESIAN_POINT('Ctrl Pts',(100.592609478192,2.75038467920892,125.685073302739));
#248154=CARTESIAN_POINT('Ctrl Pts',(100.314161854379,-2.82035130272114,
125.723284252797));
#248155=CARTESIAN_POINT('Ctrl Pts',(100.035714230566,-5.79932221927147,
130.430756157697));
#248156=CARTESIAN_POINT('Ctrl Pts',(99.7572666067534,-3.44899932895201,
135.481552309624));
#248157=CARTESIAN_POINT('Ctrl Pts',(99.4788189829407,2.07078545168999,136.234237790066));
#248158=CARTESIAN_POINT('Ctrl Pts',(99.2003713591278,5.6876195657222,131.997131413226));
#248159=CARTESIAN_POINT('Ctrl Pts',(98.9219237353147,4.07780915451857,126.663926945268));
#248160=CARTESIAN_POINT('Ctrl Pts',(98.6434761115021,-1.27930865763567,
125.13557875072));
#248161=CARTESIAN_POINT('Ctrl Pts',(98.3650284876889,-5.460804311125,128.816564156414));
#248162=CARTESIAN_POINT('Ctrl Pts',(98.0865808638763,-4.62408757781209,
134.324237400649));
#248163=CARTESIAN_POINT('Ctrl Pts',(97.8081332400632,0.461939740273397,
136.597315836771));
#248164=CARTESIAN_POINT('Ctrl Pts',(97.5296856162504,5.12346700405862,133.546951428038));
#248165=CARTESIAN_POINT('Ctrl Pts',(97.2512379924375,5.07677838639178,127.97628004749));
#248166=CARTESIAN_POINT('Ctrl Pts',(96.9727903686245,0.364778446043045,
125.004476551425));
#248167=CARTESIAN_POINT('Ctrl Pts',(96.6943427448119,-4.68243506580139,
127.362483172053));
#248168=CARTESIAN_POINT('Ctrl Pts',(96.4158951209985,-5.42671950184442,
132.883407020047));
#248169=CARTESIAN_POINT('Ctrl Pts',(96.1374474971861,-1.18411382567837,
136.493788791223));
#248170=CARTESIAN_POINT('Ctrl Pts',(95.8589998733729,4.14663460910971,134.875864014826));
#248171=CARTESIAN_POINT('Ctrl Pts',(95.5805522495601,5.66682841248846,129.516426520346));
#248172=CARTESIAN_POINT('Ctrl Pts',(95.3021046257473,1.97948374474885,125.340537542131));
#248173=CARTESIAN_POINT('Ctrl Pts',(95.0236570019342,-3.52690978125809,
126.185635047646));
#248174=CARTESIAN_POINT('Ctrl Pts',(94.7452093781216,-5.79224551741027,
131.275115714627));
#248175=CARTESIAN_POINT('Ctrl Pts',(94.4667617543085,-2.73479058998699,
135.931995445075));
#248176=CARTESIAN_POINT('Ctrl Pts',(94.1883141304955,2.8358032876865,135.876829267928));
#248177=CARTESIAN_POINT('Ctrl Pts',(93.909866506683,5.80043248066857,131.160312204968));
#248178=CARTESIAN_POINT('Ctrl Pts',(93.6314188828698,3.43474759079615,126.116693022386));
#248179=CARTESIAN_POINT('Ctrl Pts',(93.352971259057,-2.08730253826965,125.380811354481));
#248180=CARTESIAN_POINT('Ctrl Pts',(93.0745236352441,-5.69122360506351,
129.628906504239));
#248181=CARTESIAN_POINT('Ctrl Pts',(92.7960760114314,-4.06518821053398,
134.957186560018));
#248182=CARTESIAN_POINT('Ctrl Pts',(92.5176283876181,1.29655655399172,136.469222451509));
#248183=CARTESIAN_POINT('Ctrl Pts',(92.2391807638055,5.46682918570788,132.775527061492));
#248184=CARTESIAN_POINT('Ctrl Pts',(91.9607331399925,4.61335286521161,127.270426006341));
#248185=CARTESIAN_POINT('Ctrl Pts',(91.6822855161797,-0.479569363597252,
125.012838216602));
#248186=CARTESIAN_POINT('Ctrl Pts',(91.4038378923669,-5.13179077552621,
128.077376581749));
#248187=CARTESIAN_POINT('Ctrl Pts',(91.1253902685539,-5.06814716666323,
133.647880055237));
#248188=CARTESIAN_POINT('Ctrl Pts',(90.846942644741,-0.347123904390365,
136.605328079151));
#248189=CARTESIAN_POINT('Ctrl Pts',(90.5684950209282,4.69288926807169,134.231970398883));
#248190=CARTESIAN_POINT('Ctrl Pts',(90.2900473971151,5.42036646356212,128.708806777632));
#248191=CARTESIAN_POINT('Ctrl Pts',(90.0115997733025,1.16679167866171,125.111354761782));
#248192=CARTESIAN_POINT('Ctrl Pts',(89.7331521494893,-4.15900765798632,
126.7454970086));
#248193=CARTESIAN_POINT('Ctrl Pts',(89.4547045256766,-5.66288213576447,
132.109536625546));
#248194=CARTESIAN_POINT('Ctrl Pts',(89.1762569018636,-1.96284457794726,
136.274183252551));
#248195=CARTESIAN_POINT('Ctrl Pts',(88.8978092780507,3.5409512567151,135.412330093694));
#248196=CARTESIAN_POINT('Ctrl Pts',(88.619361654238,5.79078587154194,130.3159780981));
#248197=CARTESIAN_POINT('Ctrl Pts',(88.3409140304249,2.71917116603865,125.668425779081));
#248198=CARTESIAN_POINT('Ctrl Pts',(88.0624664066122,-2.85122900215762,
125.740546672265));
#248199=CARTESIAN_POINT('Ctrl Pts',(87.7840187827991,-5.80148900765152,
130.466065200115));
#248200=CARTESIAN_POINT('Ctrl Pts',(87.5055711589863,-3.42046403360785,
135.502460689953));
#248201=CARTESIAN_POINT('Ctrl Pts',(87.2271235351733,2.10380028836375,136.221531728214));
#248202=CARTESIAN_POINT('Ctrl Pts',(86.9486759113605,5.69477492168681,131.962487159311));
#248203=CARTESIAN_POINT('Ctrl Pts',(86.6702282875477,4.05252960720113,126.63918087617));
#248204=CARTESIAN_POINT('Ctrl Pts',(86.3917806637346,-1.31379243922498,
125.14347129503));
#248205=CARTESIAN_POINT('Ctrl Pts',(86.113333039922,-5.47280341633199,128.849842451481));
#248206=CARTESIAN_POINT('Ctrl Pts',(85.8348854161089,-4.6025754151404,134.352320319043));
#248207=CARTESIAN_POINT('Ctrl Pts',(85.5564377922961,0.497194544256039,
136.594396548415));
#248208=CARTESIAN_POINT('Ctrl Pts',(85.2779901684829,5.1400670067851,133.515712616316));
#248209=CARTESIAN_POINT('Ctrl Pts',(84.9995425446705,5.05946899631168,127.945428654274));
#248210=CARTESIAN_POINT('Ctrl Pts',(84.7210949208572,0.329466147029263,
125.002363499906));
#248211=CARTESIAN_POINT('Ctrl Pts',(84.4426472970446,-4.70329999605691,
127.391050253351));
#248212=CARTESIAN_POINT('Ctrl Pts',(84.1641996732315,-5.41396321174535,
132.916402482027));
#248213=CARTESIAN_POINT('Ctrl Pts',(83.8857520494189,-1.14945872264635,
136.500891416245));
#248214=CARTESIAN_POINT('Ctrl Pts',(83.6073044256056,4.17134217838416,134.850546837477));
#248215=CARTESIAN_POINT('Ctrl Pts',(83.328856801793,5.65888339887398,129.481954789796));
#248216=CARTESIAN_POINT('Ctrl Pts',(83.05040917798,1.94618722762166,125.328589094719));
#248217=CARTESIAN_POINT('Ctrl Pts',(82.7719615541671,-3.5549599292834,126.207189922827));
#248218=CARTESIAN_POINT('Ctrl Pts',(82.4935139303543,-5.78927258062435,
131.310366035126));
#248219=CARTESIAN_POINT('Ctrl Pts',(82.2150663065413,-2.70352655206008,
135.948547888425));
#248220=CARTESIAN_POINT('Ctrl Pts',(81.9366186827285,2.86662830323276,135.859472947324));
#248221=CARTESIAN_POINT('Ctrl Pts',(81.6581710589156,5.80249179043285,131.124996731141));
#248222=CARTESIAN_POINT('Ctrl Pts',(81.3797234351026,3.40614878970799,126.095871590527));
#248223=CARTESIAN_POINT('Ctrl Pts',(81.1012758112897,-2.12027854913937,
125.393617843285));
#248224=CARTESIAN_POINT('Ctrl Pts',(80.822828187477,-5.6982734826932,129.663572376127));
#248225=CARTESIAN_POINT('Ctrl Pts',(80.5443805636639,-4.03983346178761,
134.981855572247));
#248226=CARTESIAN_POINT('Ctrl Pts',(80.2659329398512,1.33101615366455,136.461224986989));
#248227=CARTESIAN_POINT('Ctrl Pts',(79.9874853160382,5.47872694765296,132.742212399419));
#248228=CARTESIAN_POINT('Ctrl Pts',(79.7090376922254,4.59175532743923,127.242408693648));
#248229=CARTESIAN_POINT('Ctrl Pts',(79.4305900684125,-0.514815118972584,
125.015864794932));
#248230=CARTESIAN_POINT('Ctrl Pts',(79.1521424445996,-5.1482956211654,128.108665773475));
#248231=CARTESIAN_POINT('Ctrl Pts',(78.8736948207867,-5.05074395573051,
133.678678621723));
#248232=CARTESIAN_POINT('Ctrl Pts',(78.5952471969738,-0.31180533753877,
136.607333642391));
#248233=CARTESIAN_POINT('Ctrl Pts',(78.3167995731609,4.71366715331346,134.203339944237));
#248234=CARTESIAN_POINT('Ctrl Pts',(78.0383519493481,5.407509805713,128.675850294243));
#248235=CARTESIAN_POINT('Ctrl Pts',(77.7599043255351,1.1321151182024,125.104357647873));
#248236=CARTESIAN_POINT('Ctrl Pts',(77.4814567017223,-4.18363805603787,
126.770889270024));
#248237=CARTESIAN_POINT('Ctrl Pts',(77.2030090779094,-5.65483223886072,
132.143984014535));
#248238=CARTESIAN_POINT('Ctrl Pts',(76.9245614540965,-1.92951184808342,
136.286030301474));
#248239=CARTESIAN_POINT('Ctrl Pts',(76.6461138302835,3.56893566918854,135.390689943351));
#248240=CARTESIAN_POINT('Ctrl Pts',(76.3676662064707,5.78770565867644,130.280736989476));
#248241=CARTESIAN_POINT('Ctrl Pts',(76.0892185826578,2.68785689298084,125.651968569378));
#248242=CARTESIAN_POINT('Ctrl Pts',(75.8107709588449,-2.8820010482549,125.75799673322));
#248243=CARTESIAN_POINT('Ctrl Pts',(75.532323335032,-5.8034408197229,130.501386778194));
#248244=CARTESIAN_POINT('Ctrl Pts',(75.2538757112192,-3.39180199171105,
135.523194980456));
#248245=CARTESIAN_POINT('Ctrl Pts',(74.9754280874062,2.13673716794415,136.208624931095));
#248246=CARTESIAN_POINT('Ctrl Pts',(74.6969804635933,5.70171925567246,131.92779999059));
#248247=CARTESIAN_POINT('Ctrl Pts',(74.4185328397805,4.02709989190878,126.61458914934));
#248248=CARTESIAN_POINT('Ctrl Pts',(74.1400852159675,-1.34822753775231,
125.151573605674));
#248249=CARTESIAN_POINT('Ctrl Pts',(73.8616375921548,-5.48459972479585,
128.883193171938));
#248250=CARTESIAN_POINT('Ctrl Pts',(73.5831899683417,-4.58089270234404,
134.380271766487));
#248251=CARTESIAN_POINT('Ctrl Pts',(73.3047423445289,0.532430924512096,
136.591262708148));
#248252=CARTESIAN_POINT('Ctrl Pts',(73.026294720716,5.15647654243839,133.484373334449));
#248253=CARTESIAN_POINT('Ctrl Pts',(72.7478470969032,5.04197212574731,127.914683199832));
#248254=CARTESIAN_POINT('Ctrl Pts',(72.46939947309,0.294141639526237,125.000465443524));
#248255=CARTESIAN_POINT('Ctrl Pts',(72.1909518492774,-4.72399064380143,
127.419743816117));
#248256=CARTESIAN_POINT('Ctrl Pts',(71.9125042254643,-5.40100630524849,
132.949319681519));
#248257=CARTESIAN_POINT('Ctrl Pts',(71.6340566016516,-1.11476102599866,
136.507782954223));
#248258=CARTESIAN_POINT('Ctrl Pts',(71.3556089778387,4.19589517704018,134.82507972721));
#248259=CARTESIAN_POINT('Ctrl Pts',(71.0771613540258,5.65072869325411,129.447532061481));
#248260=CARTESIAN_POINT('Ctrl Pts',(70.7987137302128,1.91281859381102,125.316843554035));
#248261=CARTESIAN_POINT('Ctrl Pts',(70.5202661064001,-3.58287834696108,
126.22891514786));
#248262=CARTESIAN_POINT('Ctrl Pts',(70.241818482587,-5.78608512021397,131.345597605407));
#248263=CARTESIAN_POINT('Ctrl Pts',(69.9633708587742,-2.67216233396265,
135.964909712024));
#248264=CARTESIAN_POINT('Ctrl Pts',(69.6849232349613,2.89734709481291,135.841929307673));
#248265=CARTESIAN_POINT('Ctrl Pts',(69.4064756111484,5.80433608672999,131.089669376025));
#248266=CARTESIAN_POINT('Ctrl Pts',(69.1280279873355,3.37742377252397,126.07522463346));
#248267=CARTESIAN_POINT('Ctrl Pts',(68.8495803635227,-2.15317599230747,
125.406624829152));
#248268=CARTESIAN_POINT('Ctrl Pts',(68.5711327397097,-5.70511220870344,
129.698280520343));
#248269=CARTESIAN_POINT('Ctrl Pts',(68.2926851158969,-4.01432901552682,
135.006369785865));
#248270=CARTESIAN_POINT('Ctrl Pts',(68.014237492084,1.36542643204398,136.45301790528));
#248271=CARTESIAN_POINT('Ctrl Pts',(67.735789868271,5.49042169335597,132.708825929535));
#248272=CARTESIAN_POINT('Ctrl Pts',(67.4573422444582,4.56998764048497,127.214523370394));
#248273=CARTESIAN_POINT('Ctrl Pts',(67.1788946206453,-0.550041797684044,
125.019105868103));
#248274=CARTESIAN_POINT('Ctrl Pts',(66.9004469968323,-5.164609694817,128.140054855163));
#248275=CARTESIAN_POINT('Ctrl Pts',(66.6219993730196,-5.03315358762317,
133.709370679297));
#248276=CARTESIAN_POINT('Ctrl Pts',(66.3435517492066,-0.2764752166261,136.609124174332));
#248277=CARTESIAN_POINT('Ctrl Pts',(66.0651041253938,4.73427037188528,134.174583539162));
#248278=CARTESIAN_POINT('Ctrl Pts',(65.7866565015808,5.39445277059944,128.642972683589));
#248279=CARTESIAN_POINT('Ctrl Pts',(65.508208877768,1.0973966068015,125.097571749668));
#248280=CARTESIAN_POINT('Ctrl Pts',(65.2297612539551,-4.20811342784249,
126.796430993211));
#248281=CARTESIAN_POINT('Ctrl Pts',(64.9513136301422,-5.64657280006891,
132.178381763287));
#248282=CARTESIAN_POINT('Ctrl Pts',(64.6728660063292,-1.89610761944867,
136.297674225111));
#248283=CARTESIAN_POINT('Ctrl Pts',(64.3944183825164,3.59678783343796,135.368879844889));
#248284=CARTESIAN_POINT('Ctrl Pts',(64.1159707587035,5.78441098024938,130.245515283918));
#248285=CARTESIAN_POINT('Ctrl Pts',(63.8375231348906,2.65644302039782,125.635702283457));
#248286=CARTESIAN_POINT('Ctrl Pts',(63.5590755110777,-2.91266630074331,
125.775633789045));
#248287=CARTESIAN_POINT('Ctrl Pts',(63.2806278872649,-5.80517758316048,
130.53671958308));
#248288=CARTESIAN_POINT('Ctrl Pts',(63.0021802634519,-3.36301426534433,
135.543754412816));
#248289=CARTESIAN_POINT('Ctrl Pts',(62.723732639639,2.16959486994269,136.195517876976));
#248290=CARTESIAN_POINT('Ctrl Pts',(62.4452850158262,5.70845231035428,131.893071192411));
#248291=CARTESIAN_POINT('Ctrl Pts',(62.1668373920132,4.00152095094907,126.590152676031));
#248292=CARTESIAN_POINT('Ctrl Pts',(61.8883897682004,-1.38261267721222,
125.159885382419));
#248293=CARTESIAN_POINT('Ctrl Pts',(61.6099421443874,-5.49619279939966,
128.916615081961));
#248294=CARTESIAN_POINT('Ctrl Pts',(61.3314945205747,-4.55904024288434,
134.408090707227));
#248295=CARTESIAN_POINT('Ctrl Pts',(61.0530468967616,0.567647575344072,
136.587914432096));
#248296=CARTESIAN_POINT('Ctrl Pts',(60.7745992729488,5.17269500295686,133.452934743723));
#248297=CARTESIAN_POINT('Ctrl Pts',(60.496151649136,5.02428842305186,127.884044823451));
#248298=CARTESIAN_POINT('Ctrl Pts',(60.2177040253229,0.258806232497024,
124.998782452612));
#248299=CARTESIAN_POINT('Ctrl Pts',(59.9392564015102,-4.74450624233532,
127.448562797104));
#248300=CARTESIAN_POINT('Ctrl Pts',(59.6608087776971,-5.38784926247686,
132.982157398764));
#248301=CARTESIAN_POINT('Ctrl Pts',(59.3823611538844,-1.08002202147149,
136.514463149789));
#248302=CARTESIAN_POINT('Ctrl Pts',(59.1039135300714,4.22029269525717,134.799463627718));
#248303=CARTESIAN_POINT('Ctrl Pts',(58.8254659062585,5.64236459780459,129.413159610949));
#248304=CARTESIAN_POINT('Ctrl Pts',(58.5470182824457,1.8793790798041,125.305301355313));
#248305=CARTESIAN_POINT('Ctrl Pts',(58.2685706586328,-3.61066399976409,
126.250809917708));
#248306=CARTESIAN_POINT('Ctrl Pts',(57.9901230348199,-5.78268325429153,
131.380809119953));
#248307=CARTESIAN_POINT('Ctrl Pts',(57.711675411007,-2.64069909790739,135.981080309579));
#248308=CARTESIAN_POINT('Ctrl Pts',(57.4332277871941,2.92795852413098,135.824198999061));
#248309=CARTESIAN_POINT('Ctrl Pts',(57.1547801633813,5.80596530121877,131.054331448687));
#248310=CARTESIAN_POINT('Ctrl Pts',(56.8763325395683,3.34857360366007,126.054752916266));
#248311=CARTESIAN_POINT('Ctrl Pts',(56.5978849157555,-2.18599364874745,
125.419831830104));
#248312=CARTESIAN_POINT('Ctrl Pts',(56.3194372919424,-5.71173952968275,
129.733029650764));
#248313=CARTESIAN_POINT('Ctrl Pts',(56.0409896681298,-3.98867581682796,
135.030728292487));
#248314=CARTESIAN_POINT('Ctrl Pts',(55.7625420443167,1.39978611404518,136.444601510497));
#248315=CARTESIAN_POINT('Ctrl Pts',(55.4840944205039,5.50191298946419,132.675368888989));
#248316=CARTESIAN_POINT('Ctrl Pts',(55.2056467966909,4.54805061095778,127.186771069878));
#248317=CARTESIAN_POINT('Ctrl Pts',(54.9271991728781,-0.585248094394635,
125.022561316018));
#248318=CARTESIAN_POINT('Ctrl Pts',(54.6487515490652,-5.18073239195715,
128.171542663682));
#248319=CARTESIAN_POINT('Ctrl Pts',(54.3703039252523,-5.01537671415865,
133.739955090657));
#248320=CARTESIAN_POINT('Ctrl Pts',(54.0918563014394,-0.241134850822232,
136.610699608625));
#248321=CARTESIAN_POINT('Ctrl Pts',(53.8134086776265,4.75469816032759,134.145702249237));
#248322=CARTESIAN_POINT('Ctrl Pts',(53.5349610538137,5.38119584205463,128.610175163959));
#248323=CARTESIAN_POINT('Ctrl Pts',(53.2565134300007,1.06263743096531,125.090997318624));
#248324=CARTESIAN_POINT('Ctrl Pts',(52.9780658061879,-4.23243286645675,
126.822121231705));
#248325=CARTESIAN_POINT('Ctrl Pts',(52.6996181823749,-5.63810412544538,
132.21272859718));
#248326=CARTESIAN_POINT('Ctrl Pts',(52.4211705585621,-1.86263312984859,
136.309114591992));
#248327=CARTESIAN_POINT('Ctrl Pts',(52.1427229347491,3.62450671739182,135.346900606486));
#248328=CARTESIAN_POINT('Ctrl Pts',(51.8642753109363,5.7809019583462,130.210314286579));
#248329=CARTESIAN_POINT('Ctrl Pts',(51.5858276871234,2.62493071234137,125.619627524071));
#248330=CARTESIAN_POINT('Ctrl Pts',(51.3073800633105,-2.94322362331098,
125.793457186192));
#248331=CARTESIAN_POINT('Ctrl Pts',(51.0289324394976,-5.80669923360788,
130.572062305503));
#248332=CARTESIAN_POINT('Ctrl Pts',(50.7504848156848,-3.33410192124705,
135.564138225197));
#248333=CARTESIAN_POINT('Ctrl Pts',(50.4720371918718,2.20237217680579,136.182211051539));
#248334=CARTESIAN_POINT('Ctrl Pts',(50.193589568059,5.71497383623647,131.858302051661));
#248335=CARTESIAN_POINT('Ctrl Pts',(49.915141944246,3.97579373215887,126.565872361749));
#248336=CARTESIAN_POINT('Ctrl Pts',(49.6366943204332,-1.41694658345112,
125.168406317271));
#248337=CARTESIAN_POINT('Ctrl Pts',(49.3582466966203,-5.50758221055828,
128.950106943089));
#248338=CARTESIAN_POINT('Ctrl Pts',(49.0797990728074,-4.53701884651156,
134.435776110423));
#248339=CARTESIAN_POINT('Ctrl Pts',(48.8013514489945,0.602843191786665,
136.584351844331));
#248340=CARTESIAN_POINT('Ctrl Pts',(48.5229038251815,5.18872178735999,133.421398009111));
#248341=CARTESIAN_POINT('Ctrl Pts',(48.2444562013688,5.006418543501,127.853514660444));
#248342=CARTESIAN_POINT('Ctrl Pts',(47.9660085775558,0.223461235307256,
124.997314589534));
#248343=CARTESIAN_POINT('Ctrl Pts',(47.6875609537429,-4.7648460314457,127.477506128414));
#248344=CARTESIAN_POINT('Ctrl Pts',(47.40911332993,-5.37449257096935,133.014914416948));
#248345=CARTESIAN_POINT('Ctrl Pts',(47.1306657061172,-1.04524299633083,
136.520931755405));
#248346=CARTESIAN_POINT('Ctrl Pts',(46.8522180823042,4.24453382897653,134.773699488214));
#248347=CARTESIAN_POINT('Ctrl Pts',(46.5737704584914,5.6337914224598,129.378838711881));
#248348=CARTESIAN_POINT('Ctrl Pts',(46.2953228346785,1.84586992471411,125.293962926255));
#248349=CARTESIAN_POINT('Ctrl Pts',(46.0168752108656,-3.63831585808481,
126.272873421051));
#248350=CARTESIAN_POINT('Ctrl Pts',(45.7384275870526,-5.77906710891461,
131.415999273987));
#248351=CARTESIAN_POINT('Ctrl Pts',(45.4599799632399,-2.60913800977569,
135.997059081882));
#248352=CARTESIAN_POINT('Ctrl Pts',(45.1815323394269,2.95846145686929,135.806282678493));
#248353=CARTESIAN_POINT('Ctrl Pts',(44.903084715614,5.80737937352832,131.018984258588));
#248354=CARTESIAN_POINT('Ctrl Pts',(44.6246370918012,3.31959935216964,126.034457197533));
#248355=CARTESIAN_POINT('Ctrl Pts',(44.3461894679882,-2.21873030238901,
125.43323835675));
#248356=CARTESIAN_POINT('Ctrl Pts',(44.0677418441753,-5.7181552000533,129.767818479747));
#248357=CARTESIAN_POINT('Ctrl Pts',(43.7892942203624,-3.96287481627985,
135.054930189501));
#248358=CARTESIAN_POINT('Ctrl Pts',(43.5108465965496,1.43409392645716,136.435976114513));
#248359=CARTESIAN_POINT('Ctrl Pts',(43.2323989727367,5.51320041016325,132.641842517543));
#248360=CARTESIAN_POINT('Ctrl Pts',(42.9539513489238,4.52594505174265,127.159152820475));
#248361=CARTESIAN_POINT('Ctrl Pts',(42.6755037251109,-0.620432704521861,
125.026231010632));
#248362=CARTESIAN_POINT('Ctrl Pts',(42.397056101298,-5.19666311515333,128.203128032237));
#248363=CARTESIAN_POINT('Ctrl Pts',(42.1186084774851,-4.99741399406557,
133.770430722483));
#248364=CARTESIAN_POINT('Ctrl Pts',(41.8401608536722,-0.205785549677785,
136.612059886891));
#248365=CARTESIAN_POINT('Ctrl Pts',(41.5617132298594,4.77494976168102,134.11669714467));
#248366=CARTESIAN_POINT('Ctrl Pts',(41.2832656060464,5.36773951131901,128.577458950676));
#248367=CARTESIAN_POINT('Ctrl Pts',(41.0048179822336,1.02783887870806,125.084634598359));
#248368=CARTESIAN_POINT('Ctrl Pts',(40.7263703584206,-4.25659547071474,
126.847959033542));
#248369=CARTESIAN_POINT('Ctrl Pts',(40.4479227346078,-5.62942652880005,
132.24702324348));
#248370=CARTESIAN_POINT('Ctrl Pts',(40.1694751107948,-1.82908961969292,
136.320350978189));
#248371=CARTESIAN_POINT('Ctrl Pts',(39.891027486982,3.65209129391637,135.324753042595));
#248372=CARTESIAN_POINT('Ctrl Pts',(39.6125798631691,5.77717872299504,130.175135301845));
#248373=CARTESIAN_POINT('Ctrl Pts',(39.3341322393562,2.59332113651206,125.603744886877));
#248374=CARTESIAN_POINT('Ctrl Pts',(39.0556846155433,-2.97367188364494,
125.811466264208));
#248375=CARTESIAN_POINT('Ctrl Pts',(38.7772369917304,-5.80800571467979,
130.607413635826));
#248376=CARTESIAN_POINT('Ctrl Pts',(38.4987893679175,-3.30506603077697,
135.584345662267));
#248377=CARTESIAN_POINT('Ctrl Pts',(38.2203417441046,2.23506787395795,136.16870494788));
#248378=CARTESIAN_POINT('Ctrl Pts',(37.9418941202917,5.72128359166147,131.823493856722));
#248379=CARTESIAN_POINT('Ctrl Pts',(37.6634464964789,3.94991918886983,126.541749106207));
#248380=CARTESIAN_POINT('Ctrl Pts',(37.3849988726659,-1.45122798421329,
125.177136094481));
#248381=CARTESIAN_POINT('Ctrl Pts',(37.1065512488531,-5.51876753623267,
128.983667514269));
#248382=CARTESIAN_POINT('Ctrl Pts',(36.8281036250402,-4.51482932923697,
134.463326950183));
#248383=CARTESIAN_POINT('Ctrl Pts',(36.5496560012273,0.6380164696531,136.580575076865));
#248384=CARTESIAN_POINT('Ctrl Pts',(36.2712083774144,5.20455630176915,133.389764299214));
#248385=CARTESIAN_POINT('Ctrl Pts',(35.9927607536015,4.9883631492699,127.82309384212));
#248386=CARTESIAN_POINT('Ctrl Pts',(35.7143131297886,0.188107957679239,
124.996061908681));
#248387=CARTESIAN_POINT('Ctrl Pts',(35.4358655059757,-4.78500925743413,
127.50657273754));
#248388=CARTESIAN_POINT('Ctrl Pts',(35.1574178821628,-5.36093672566315,
133.047589522248));
#248389=CARTESIAN_POINT('Ctrl Pts',(34.87897025835,-1.01042523932657,136.527188531377));
#248390=CARTESIAN_POINT('Ctrl Pts',(34.6005226345371,4.26861767993396,134.747788263399));
#248391=CARTESIAN_POINT('Ctrl Pts',(34.3220750107242,5.62500948490202,129.34457063605));
#248392=CARTESIAN_POINT('Ctrl Pts',(34.0436273869112,1.81229237023524,125.282828687009));
#248393=CARTESIAN_POINT('Ctrl Pts',(33.7651797630984,-3.66583289727342,
126.295104840318));
#248394=CARTESIAN_POINT('Ctrl Pts',(33.4867321392855,-5.77523681808073,
131.451166763527));
#248395=CARTESIAN_POINT('Ctrl Pts',(33.2082845154725,-2.57748023907555,
136.012845436834));
#248396=CARTESIAN_POINT('Ctrl Pts',(32.9298368916598,2.98885476273036,135.788181009863));
#248397=CARTESIAN_POINT('Ctrl Pts',(32.6513892678468,5.80857825125962,130.983629115531));
#248398=CARTESIAN_POINT('Ctrl Pts',(32.3729416440339,3.29050209170421,126.014338229324));
#248399=CARTESIAN_POINT('Ctrl Pts',(32.094494020221,-2.25138474016344,125.446843912307));
#248400=CARTESIAN_POINT('Ctrl Pts',(31.8160463964081,-5.72435898208005,
129.802645718181));
#248401=CARTESIAN_POINT('Ctrl Pts',(31.5375987725953,-3.93692696994811,
135.078974580096));
#248402=CARTESIAN_POINT('Ctrl Pts',(31.2591511487823,1.46834859799131,136.427142036947));
#248403=CARTESIAN_POINT('Ctrl Pts',(30.9807035249695,5.52428353719365,132.608248057529));
#248404=CARTESIAN_POINT('Ctrl Pts',(30.7022559011566,4.50367178196922,127.131669645585));
#248405=CARTESIAN_POINT('Ctrl Pts',(30.4238082773436,-0.655594324287056,
125.030114815962));
#248406=CARTESIAN_POINT('Ctrl Pts',(30.1453606535308,-5.21240127408669,
128.234809790423));
#248407=CARTESIAN_POINT('Ctrl Pts',(29.8669130297179,-4.97926609295916,
133.80079644549));
#248408=CARTESIAN_POINT('Ctrl Pts',(29.588465405905,-0.170428623074124,
136.613204958723));
#248409=CARTESIAN_POINT('Ctrl Pts',(29.3100177820921,4.79502442551506,134.087569300254));
#248410=CARTESIAN_POINT('Ctrl Pts',(29.0315701582792,5.35408427702179,128.544825256054));
#248411=CARTESIAN_POINT('Ctrl Pts',(28.7531225344664,0.99300223950345,125.078483824645));
#248412=CARTESIAN_POINT('Ctrl Pts',(28.4746749106534,-4.28060034526213,
126.873943441297));
#248413=CARTESIAN_POINT('Ctrl Pts',(28.1962272868406,-5.6205403316845,132.281264431386));
#248414=CARTESIAN_POINT('Ctrl Pts',(27.9177796630277,-1.79547833194873,
136.331382967337));
#248415=CARTESIAN_POINT('Ctrl Pts',(27.6393320392148,3.67954054085496,135.3024379739));
#248416=CARTESIAN_POINT('Ctrl Pts',(27.3608844154018,5.77324141216173,130.139979633288));
#248417=CARTESIAN_POINT('Ctrl Pts',(27.082436791589,2.56161546421434,125.58805496041));
#248418=CARTESIAN_POINT('Ctrl Pts',(26.8039891677761,-3.00400995347367,
125.82966035576));
#248419=CARTESIAN_POINT('Ctrl Pts',(26.5255415439632,-5.80909697796402,
130.642772264091));
#248420=CARTESIAN_POINT('Ctrl Pts',(26.2470939201503,-3.27590766986969,
135.604375975235));
#248421=CARTESIAN_POINT('Ctrl Pts',(25.9686462963375,2.2676807498481,136.155000066467));
#248422=CARTESIAN_POINT('Ctrl Pts',(25.6901986725246,5.727381342819,131.788647897428));
#248423=CARTESIAN_POINT('Ctrl Pts',(25.4117510487116,3.92389827987267,126.517783803302));
#248424=CARTESIAN_POINT('Ctrl Pts',(25.1333034248988,-1.48545560918882,
125.186074390566));
#248425=CARTESIAN_POINT('Ctrl Pts',(24.8548558010858,-5.5297483619465,129.017295551901));
#248426=CARTESIAN_POINT('Ctrl Pts',(24.576408177273,-4.49247251330123,134.490742205601));
#248427=CARTESIAN_POINT('Ctrl Pts',(24.2979605534601,0.673166105584617,
136.576584269648));
#248428=CARTESIAN_POINT('Ctrl Pts',(24.0195129296472,5.22019795943058,133.358034786234));
#248429=CARTESIAN_POINT('Ctrl Pts',(23.7410653058343,4.97012290940784,127.792783495733));
#248430=CARTESIAN_POINT('Ctrl Pts',(23.4626176820214,0.152747709641667,
124.995024456474));
#248431=CARTESIAN_POINT('Ctrl Pts',(23.1841700582085,-4.80499517314482,
127.53576154741));
#248432=CARTESIAN_POINT('Ctrl Pts',(22.9057224343956,-5.34718222887511,
133.080181503877));
#248433=CARTESIAN_POINT('Ctrl Pts',(22.6272748105827,-0.975570040643468,
136.533233245855));
#248434=CARTESIAN_POINT('Ctrl Pts',(22.3488271867698,4.29254335569345,134.721730913422));
#248435=CARTESIAN_POINT('Ctrl Pts',(22.070379562957,5.61601911054919,129.310356653276));
#248436=CARTESIAN_POINT('Ctrl Pts',(21.791931939144,1.77864766059611,125.27189905016));
#248437=CARTESIAN_POINT('Ctrl Pts',(21.5134843153312,-3.69321409767591,
126.317503351717));
#248438=CARTESIAN_POINT('Ctrl Pts',(21.2350366915183,-5.77119252372273,
131.486310285425));
#248439=CARTESIAN_POINT('Ctrl Pts',(20.9565890677054,-2.54572695889727,
136.028438789465));
#248440=CARTESIAN_POINT('Ctrl Pts',(20.6781414438925,3.01913731547902,135.769894663934));
#248441=CARTESIAN_POINT('Ctrl Pts',(20.3996938200796,5.80956188998761,130.948267329615));
#248442=CARTESIAN_POINT('Ctrl Pts',(20.1212461962667,3.26128290047392,125.994396757156));
#248443=CARTESIAN_POINT('Ctrl Pts',(19.8427985724538,-2.28395575204823,
125.460647992615));
#248444=CARTESIAN_POINT('Ctrl Pts',(19.5643509486409,-5.7303506458796,129.837510075529));
#248445=CARTESIAN_POINT('Ctrl Pts',(19.285903324828,-3.91083323933969,135.102860573299));
#248446=CARTESIAN_POINT('Ctrl Pts',(19.0074557010152,1.50254885932817,136.418099605148));
#248447=CARTESIAN_POINT('Ctrl Pts',(18.7290080772022,5.53516195986603,132.574586753804));
#248448=CARTESIAN_POINT('Ctrl Pts',(18.4505604533894,4.48123162698169,127.104322563612));
#248449=CARTESIAN_POINT('Ctrl Pts',(18.1721128295765,-0.690731650763477,
125.034212588094));
#248450=CARTESIAN_POINT('Ctrl Pts',(17.8936652057636,-5.22794628557398,
128.26658676426));
#248451=CARTESIAN_POINT('Ctrl Pts',(17.6152175819507,-4.96093368331654,
133.831051134467));
#248452=CARTESIAN_POINT('Ctrl Pts',(17.3367699581378,-0.135065381175154,
136.614134781694));
#248453=CARTESIAN_POINT('Ctrl Pts',(17.0583223343249,4.81492140795562,134.058319795333));
#248454=CARTESIAN_POINT('Ctrl Pts',(16.779874710512,5.34023064516271,128.512275289347));
#248455=CARTESIAN_POINT('Ctrl Pts',(16.5014270866992,0.958128804235671,
125.0725452254));
#248456=CARTESIAN_POINT('Ctrl Pts',(16.2229794628862,-4.30444660058956,
126.900073492105));
#248457=CARTESIAN_POINT('Ctrl Pts',(15.9445318390734,-5.61144586338,132.315450892077));
#248458=CARTESIAN_POINT('Ctrl Pts',(15.6660842152604,-1.76180051209467,
136.342210150638));
#248459=CARTESIAN_POINT('Ctrl Pts',(15.3876365914476,3.70685344106567,135.279956227294));
#248460=CARTESIAN_POINT('Ctrl Pts',(15.1091889676347,5.76909017174479,130.104848583611));
#248461=CARTESIAN_POINT('Ctrl Pts',(14.8307413438218,2.52981487031356,125.572558326068));
#248462=CARTESIAN_POINT('Ctrl Pts',(14.5522937200089,-3.03423670860886,
125.848038786661));
#248463=CARTESIAN_POINT('Ctrl Pts',(14.273846096196,-5.80997298302346,130.678136880072));
#248464=CARTESIAN_POINT('Ctrl Pts',(13.9953984723831,-3.24662791899898,
135.624228421867));
#248465=CARTESIAN_POINT('Ctrl Pts',(13.7169508485702,2.30020959599411,136.141096915141));
#248466=CARTESIAN_POINT('Ctrl Pts',(13.4385032247574,5.73326686375462,131.753765465006));
#248467=CARTESIAN_POINT('Ctrl Pts',(13.1600556009444,3.89773196938174,126.493977341077));
#248468=CARTESIAN_POINT('Ctrl Pts',(12.8816079771316,-1.51962819006047,
125.195220874312));
#248469=CARTESIAN_POINT('Ctrl Pts',(12.6031603533186,-5.54052428080121,
129.050989809886));
#248470=CARTESIAN_POINT('Ctrl Pts',(12.3247127295058,-4.46994922714442,
134.518020860792));
#248471=CARTESIAN_POINT('Ctrl Pts',(12.0462651056929,0.708290797098533,
136.572379570561));
#248472=CARTESIAN_POINT('Ctrl Pts',(11.76781748188,5.23564618073708,133.326210645918));
#248473=CARTESIAN_POINT('Ctrl Pts',(11.4893698580671,4.95169849981347,127.762584744442));
#248474=CARTESIAN_POINT('Ctrl Pts',(11.2109222342542,0.117381801481337,
124.994202271355));
#248475=CARTESIAN_POINT('Ctrl Pts',(10.9324746104413,-4.82480303799234,
127.565071476419));
#248476=CARTESIAN_POINT('Ctrl Pts',(10.6540269866284,-5.33322959028317,
133.112689154126));
#248477=CARTESIAN_POINT('Ctrl Pts',(10.3755793628155,-0.940678691853753,
136.539065674851));
#248478=CARTESIAN_POINT('Ctrl Pts',(10.0971317390026,4.31630996968034,134.695528403849));
#248479=CARTESIAN_POINT('Ctrl Pts',(9.81868411518972,5.60682063254294,129.276198031366));
#248480=CARTESIAN_POINT('Ctrl Pts',(9.54023649137686,1.74493704251384,125.261174420708));
#248481=CARTESIAN_POINT('Ctrl Pts',(9.26178886756394,-3.72045844467185,
126.340068125262));
#248482=CARTESIAN_POINT('Ctrl Pts',(8.98334124375105,-5.76693437570339,
131.52142853743));
#248483=CARTESIAN_POINT('Ctrl Pts',(8.70489361993813,-2.51387934587036,
136.043838561958));
#248484=CARTESIAN_POINT('Ctrl Pts',(8.42644599612531,3.0493079929842,135.751424318317));
#248485=CARTESIAN_POINT('Ctrl Pts',(8.14799837231237,5.81033025326331,130.912900211183));
#248486=CARTESIAN_POINT('Ctrl Pts',(7.86955074849947,3.23194286120641,125.974633519968));
#248487=CARTESIAN_POINT('Ctrl Pts',(7.59110312468663,-2.3164421311127,125.47465008616));
#248488=CARTESIAN_POINT('Ctrl Pts',(7.31265550087371,-5.73612996942864,
129.872410259879));
#248489=CARTESIAN_POINT('Ctrl Pts',(7.0342078770608,-3.88459459136738,135.126587284006));
#248490=CARTESIAN_POINT('Ctrl Pts',(6.75576025324794,1.53669344316449,136.408849154185));
#248491=CARTESIAN_POINT('Ctrl Pts',(6.47731262943506,5.54583527507644,132.540859853697));
#248492=CARTESIAN_POINT('Ctrl Pts',(6.19886500562214,4.45862541830825,127.077112587908));
#248493=CARTESIAN_POINT('Ctrl Pts',(5.92041738180924,-0.725843381924555,
125.038524175185));
#248494=CARTESIAN_POINT('Ctrl Pts',(5.64196975799638,-5.24329757358911,
128.29845777624));
#248495=CARTESIAN_POINT('Ctrl Pts',(5.36352213418349,-4.94241744445191,
133.861193668313));
#248496=CARTESIAN_POINT('Ctrl Pts',(5.08507451037056,-0.0996971343788212,
136.614849321347));
#248497=CARTESIAN_POINT('Ctrl Pts',(4.80662688655771,4.83463997171276,134.028949713759));
#248498=CARTESIAN_POINT('Ctrl Pts',(4.5281792627448,5.32617912909322,128.479810256704));
#248499=CARTESIAN_POINT('Ctrl Pts',(4.24973163893191,0.923219865152705,
125.066819020683));
#248500=CARTESIAN_POINT('Ctrl Pts',(3.97128401511898,-4.32813335306523,
126.926348217707));
#248501=CARTESIAN_POINT('Ctrl Pts',(3.69283639130614,-5.60214346088543,
132.349581358763));
#248502=CARTESIAN_POINT('Ctrl Pts',(3.41438876749324,-1.72805740807474,
136.352832126888));
#248503=CARTESIAN_POINT('Ctrl Pts',(3.13594114368033,3.73402898245891,135.257308635848));
#248504=CARTESIAN_POINT('Ctrl Pts',(2.85749351986744,5.76472515556999,130.06974345461));
#248505=CARTESIAN_POINT('Ctrl Pts',(2.5790458960546,2.49792053319242,125.557255558086));
#248506=CARTESIAN_POINT('Ctrl Pts',(2.30059827224166,-3.06435102898697,
125.866600875889));
#248507=CARTESIAN_POINT('Ctrl Pts',(2.02215064842876,-5.81063369739741,
130.713506173321));
#248508=CARTESIAN_POINT('Ctrl Pts',(1.74370302461591,-3.21722786313679,
135.643902266527));
#248509=CARTESIAN_POINT('Ctrl Pts',(1.46525540080302,2.33265320702766,136.12699600909));
#248510=CARTESIAN_POINT('Ctrl Pts',(1.18680777699008,5.73893993637821,131.718847852038));
#248511=CARTESIAN_POINT('Ctrl Pts',(0.908360153177235,3.87142122699929,
126.47033060169));
#248512=CARTESIAN_POINT('Ctrl Pts',(0.629912529364331,-1.55374446055069,
125.204575206795));
#248513=CARTESIAN_POINT('Ctrl Pts',(0.351464905551429,-5.55109489349118,
129.084749039672));
#248514=CARTESIAN_POINT('Ctrl Pts',(0.0730172817385382,-4.44726030537518,
134.545161904937));
#248515=CARTESIAN_POINT('Ctrl Pts',(-0.205430342074321,0.743389242636492,
136.56796113541));
#248516=CARTESIAN_POINT('Ctrl Pts',(-0.48387796588724,5.25090039324876,
133.294293057522));
#248517=CARTESIAN_POINT('Ctrl Pts',(-0.762325589700153,4.93309060321035,
127.732498707276));
#248518=CARTESIAN_POINT('Ctrl Pts',(-1.040773213513,0.0820115436953976,
124.993595383789));
#248519=CARTESIAN_POINT('Ctrl Pts',(-1.3192208373259,-4.84443211798899,
127.594501438479));
#248520=CARTESIAN_POINT('Ctrl Pts',(-1.5976684611388,-5.31907932690746,
133.145111268411));
#248521=CARTESIAN_POINT('Ctrl Pts',(-1.8761160849517,-0.905752485869179,
136.544685602242));
#248522=CARTESIAN_POINT('Ctrl Pts',(-2.15456370876455,4.33991664121397,
134.669181705622));
#248523=CARTESIAN_POINT('Ctrl Pts',(-2.43301133257747,5.59741439173625,
129.242096036083));
#248524=CARTESIAN_POINT('Ctrl Pts',(-2.71145895639038,1.71116176514775,
125.250655196059));
#248525=CARTESIAN_POINT('Ctrl Pts',(-2.98990658020324,-3.74756492871192,
126.362798324807));
#248526=CARTESIAN_POINT('Ctrl Pts',(-3.26835420401613,-5.76246253181,131.556520218218));
#248527=CARTESIAN_POINT('Ctrl Pts',(-3.54680182782904,-2.48193858011979,
136.059044183669));
#248528=CARTESIAN_POINT('Ctrl Pts',(-3.82524945164193,3.0793656772603,135.732770657435));
#248529=CARTESIAN_POINT('Ctrl Pts',(-4.1036970754548,5.81088331261472,130.877529070775));
#248530=CARTESIAN_POINT('Ctrl Pts',(-4.38214469926771,3.20248306110764,
125.955049250094));
#248531=CARTESIAN_POINT('Ctrl Pts',(-4.66059232308062,-2.34884267356213,
125.488849674089));
#248532=CARTESIAN_POINT('Ctrl Pts',(-4.93903994689347,-5.7416967385722,
129.907344977992));
#248533=CARTESIAN_POINT('Ctrl Pts',(-5.21748757070636,-3.85821199831392,
135.150153833014));
#248534=CARTESIAN_POINT('Ctrl Pts',(-5.49593519451928,1.57078108426016,
136.399391026839));
#248535=CARTESIAN_POINT('Ctrl Pts',(-5.77438281833216,5.55630308732125,
132.507068606974));
#248536=CARTESIAN_POINT('Ctrl Pts',(-6.05283044214503,4.43585399363028,
127.050040726751));
#248537=CARTESIAN_POINT('Ctrl Pts',(-6.33127806595794,-0.76092821669219,
125.043049417465));
#248538=CARTESIAN_POINT('Ctrl Pts',(-6.60972568977086,-5.25845456928442,
128.330421645371));
#248539=CARTESIAN_POINT('Ctrl Pts',(-6.88817331358369,-4.92371806249131,
133.891222930087));
#248540=CARTESIAN_POINT('Ctrl Pts',(-7.16662093739661,-0.0643251932685087,
136.615348551203));
#248541=CARTESIAN_POINT('Ctrl Pts',(-7.44506856120951,4.8541793861078,133.999460143849));
#248542=CARTESIAN_POINT('Ctrl Pts',(-7.72351618502242,5.3119302494974,128.44743136113));
#248543=CARTESIAN_POINT('Ctrl Pts',(-8.00196380883526,0.888276715818123,
125.06130542268));
#248544=CARTESIAN_POINT('Ctrl Pts',(-8.28041143264819,-4.35165972496785,
126.952766644486));
#248545=CARTESIAN_POINT('Ctrl Pts',(-8.55885905646108,-5.59263346890473,
132.383654566726));
#248546=CARTESIAN_POINT('Ctrl Pts',(-8.83730668027396,-1.69425027025207,
136.363248502487));
#248547=CARTESIAN_POINT('Ctrl Pts',(-9.11575430408684,3.76106615803527,
135.234496038775));
#248548=CARTESIAN_POINT('Ctrl Pts',(-9.39420192789976,5.7601465253845,130.034665547118));
#248549=CARTESIAN_POINT('Ctrl Pts',(-9.67264955171265,2.4659336347071,125.542147223509));
#248550=CARTESIAN_POINT('Ctrl Pts',(-9.95109717552551,-3.09435179871079,
125.885345935621));
#248551=CARTESIAN_POINT('Ctrl Pts',(-10.2295447993384,-5.81107909660284,
130.748878833214));
#248552=CARTESIAN_POINT('Ctrl Pts',(-10.5079924231513,-3.18770859171301,
135.663396780189));
#248553=CARTESIAN_POINT('Ctrl Pts',(-10.7864400469642,2.36501038073878,
136.112697870828));
#248554=CARTESIAN_POINT('Ctrl Pts',(-11.0648876707771,5.74440035047196,
131.683896352409));
#248555=CARTESIAN_POINT('Ctrl Pts',(-11.34333529459,3.84496702767957,126.446844461378));
#248556=CARTESIAN_POINT('Ctrl Pts',(-11.6217829184029,-1.58780315646856,
125.214137041385));
#248557=CARTESIAN_POINT('Ctrl Pts',(-11.9002305422157,-5.56145980831845,
129.118571990297));
#248558=CARTESIAN_POINT('Ctrl Pts',(-12.1786781660286,-4.42440658873985,
134.572164332316));
#248559=CARTESIAN_POINT('Ctrl Pts',(-12.4571257898416,0.778460141612691,
136.563329127923));
#248560=CARTESIAN_POINT('Ctrl Pts',(-12.7355734136544,5.26596003171537,
133.262283203764));
#248561=CARTESIAN_POINT('Ctrl Pts',(-13.0140210374673,4.91429990912079,
127.702526499083));
#248562=CARTESIAN_POINT('Ctrl Pts',(-13.2924686612802,0.0466382469415425,
124.993203816266));
#248563=CARTESIAN_POINT('Ctrl Pts',(-13.5709162850931,-4.86388168577195,
127.624050343051));
#248564=CARTESIAN_POINT('Ctrl Pts',(-13.849363908906,-5.30473196309121,
133.177446645321));
#248565=CARTESIAN_POINT('Ctrl Pts',(-14.1278115327188,-0.87079271689315,
136.550092819781));
#248566=CARTESIAN_POINT('Ctrl Pts',(-14.4062591565318,4.36336249554048,
134.642691795028));
#248567=CARTESIAN_POINT('Ctrl Pts',(-14.6847067803446,5.58780073668082,
129.20805193109));
#248568=CARTESIAN_POINT('Ctrl Pts',(-14.9631544041576,1.67732308005318,
125.240341766008));
#248569=CARTESIAN_POINT('Ctrl Pts',(-15.2416020279704,-3.77453254535539,
126.385693108075));
#248570=CARTESIAN_POINT('Ctrl Pts',(-15.5200496517834,-5.75777715774833,
131.591584027456));
#248571=CARTESIAN_POINT('Ctrl Pts',(-15.7984972755962,-2.44990584522241,
136.074055091149));
#248572=CARTESIAN_POINT('Ctrl Pts',(-16.0769448994091,3.1093092545088,135.713934372506));
#248573=CARTESIAN_POINT('Ctrl Pts',(-16.355392523222,5.81122104754806,130.842155219084));
#248574=CARTESIAN_POINT('Ctrl Pts',(-16.6338401470349,3.17290459182133,
125.935644673236));
#248575=CARTESIAN_POINT('Ctrl Pts',(-16.9122877708478,-2.38115617878252,
125.50324623023));
#248576=CARTESIAN_POINT('Ctrl Pts',(-17.1907353946607,-5.74705074703162,
129.94231293535));
#248577=CARTESIAN_POINT('Ctrl Pts',(-17.4691830184736,-3.83168643779603,
135.173559347056));
#248578=CARTESIAN_POINT('Ctrl Pts',(-17.7476306422864,1.6048105194851,136.389725573584));
#248579=CARTESIAN_POINT('Ctrl Pts',(-18.0260782660994,5.56656500871184,
132.473214265779));
#248580=CARTESIAN_POINT('Ctrl Pts',(-18.3045258899123,4.4129181967513,127.023107983299));
#248581=CARTESIAN_POINT('Ctrl Pts',(-18.5829735137251,-0.795984854984928,
125.047788147249));
#248582=CARTESIAN_POINT('Ctrl Pts',(-18.861421137538,-5.27341671101187,
128.362477187221));
#248583=CARTESIAN_POINT('Ctrl Pts',(-19.1398687613509,-4.90483623034722,
133.921137807042));
#248584=CARTESIAN_POINT('Ctrl Pts',(-19.4183163851638,-0.0289508685644962,
136.615632452765));
#248585=CARTESIAN_POINT('Ctrl Pts',(-19.6967640089767,4.87353892710056,
133.969852178351));
#248586=CARTESIAN_POINT('Ctrl Pts',(-19.9752116327896,5.29748453437273,
128.415139802436));
#248587=CARTESIAN_POINT('Ctrl Pts',(-20.2536592566025,0.853300651063172,
125.056004635698));
#248588=CARTESIAN_POINT('Ctrl Pts',(-20.5321068804154,-4.37502484451904,
126.979327793496));
#248589=CARTESIAN_POINT('Ctrl Pts',(-20.8105545042282,-5.58291623983416,
132.417669253371));
#248590=CARTESIAN_POINT('Ctrl Pts',(-21.0890021280412,-1.66038035136256,
136.37345889145));
#248591=CARTESIAN_POINT('Ctrl Pts',(-21.367449751854,3.78796396592178,135.211519281404));
#248592=CARTESIAN_POINT('Ctrl Pts',(-21.6458973756669,5.75535445085128,
129.999616160961));
#248593=CARTESIAN_POINT('Ctrl Pts',(-21.9243449994798,2.43385536014432,
125.527233882186));
#248594=CARTESIAN_POINT('Ctrl Pts',(-22.2027926232928,-3.12423790609075,
125.904273271251));
#248595=CARTESIAN_POINT('Ctrl Pts',(-22.4812402471056,-5.81130916413533,
130.784253549004));
#248596=CARTESIAN_POINT('Ctrl Pts',(-22.7596878709185,-3.15807119857507,
135.682711240481));
#248597=CARTESIAN_POINT('Ctrl Pts',(-23.0381354947314,2.39727991812053,
136.098203030175));
#248598=CARTESIAN_POINT('Ctrl Pts',(-23.3165831185443,5.74964790369824,
131.648912261261));
#248599=CARTESIAN_POINT('Ctrl Pts',(-23.5950307423572,3.81837035169266,
126.423519790431));
#248600=CARTESIAN_POINT('Ctrl Pts',(-23.8734783661701,-1.62180301575654,
125.223906023766));
#248601=CARTESIAN_POINT('Ctrl Pts',(-24.151925989983,-5.57161864120731,
129.15245740844));
#248602=CARTESIAN_POINT('Ctrl Pts',(-24.4303736137958,-4.4013889240913,
134.599027142342));
#248603=CARTESIAN_POINT('Ctrl Pts',(-24.7088212376087,0.813502194462058,
136.558483719739));
#248604=CARTESIAN_POINT('Ctrl Pts',(-24.9872688614217,5.28082453809644,
133.230182270781));
#248605=CARTESIAN_POINT('Ctrl Pts',(-25.2657164852345,4.89532711384086,
127.672669230493));
#248606=CARTESIAN_POINT('Ctrl Pts',(-25.5441641090475,0.0112632219902977,
124.993027583295));
#248607=CARTESIAN_POINT('Ctrl Pts',(-25.8226117328602,-4.88315102063038,
127.65371709519));
#248608=CARTESIAN_POINT('Ctrl Pts',(-26.1010593566733,-5.29018803048126,
133.209694086655));
#248609=CARTESIAN_POINT('Ctrl Pts',(-26.3795069804861,-0.835800680372761,
136.555287127099));
#248610=CARTESIAN_POINT('Ctrl Pts',(-26.6579546042989,4.38664666386508,
134.616059653661));
#248611=CARTESIAN_POINT('Ctrl Pts',(-26.9364022281119,5.57798002361419,
129.174066977901));
#248612=CARTESIAN_POINT('Ctrl Pts',(-27.2148498519247,1.64342224113504,
125.23023451272));
#248613=CARTESIAN_POINT('Ctrl Pts',(-27.4932974757377,-3.80136029530733,
126.408751626694));
#248614=CARTESIAN_POINT('Ctrl Pts',(-27.7717450995505,-5.75287842713667,
131.626618665841));
#248615=CARTESIAN_POINT('Ctrl Pts',(-28.0501927233634,-2.41778232816299,
136.088870728161));
#248616=CARTESIAN_POINT('Ctrl Pts',(-28.3286403471763,3.13913761515943,
135.694916161515));
#248617=CARTESIAN_POINT('Ctrl Pts',(-28.6070879709892,5.8113434455484,130.8067799669));
#248618=CARTESIAN_POINT('Ctrl Pts',(-28.8855355948021,3.14320854938853,
125.916420508438));
#248619=CARTESIAN_POINT('Ctrl Pts',(-29.163983218615,-2.41338144938502,
125.517839221114));
#248620=CARTESIAN_POINT('Ctrl Pts',(-29.4424308424279,-5.75219179641212,
129.977312836202));
#248621=CARTESIAN_POINT('Ctrl Pts',(-29.7208784662408,-3.80501889272807,
135.196802958832));
#248622=CARTESIAN_POINT('Ctrl Pts',(-29.9993260900537,1.6387804878663,136.379853152576));
#248623=CARTESIAN_POINT('Ctrl Pts',(-30.2777737138665,5.576620658989,132.439298084597));
#248624=CARTESIAN_POINT('Ctrl Pts',(-30.5562213376795,4.38981887756547,
126.996315355552));
#248625=CARTESIAN_POINT('Ctrl Pts',(-30.8346689614924,-0.831011997766135,
125.052740188944));
#248626=CARTESIAN_POINT('Ctrl Pts',(-31.1131165853052,-5.2881834443438,
128.394623213959));
#248627=CARTESIAN_POINT('Ctrl Pts',(-31.3915642091181,-4.88577264769286,
133.950937190672));
#248628=CARTESIAN_POINT('Ctrl Pts',(-31.670011832931,0.00642452892459172,
136.615701015511));
#248629=CARTESIAN_POINT('Ctrl Pts',(-31.9484594567439,4.89271787731614,
133.940126914399));
#248630=CARTESIAN_POINT('Ctrl Pts',(-32.2269070805568,5.28284251901049,
128.382936777197));
#248631=CARTESIAN_POINT('Ctrl Pts',(-32.5053547043697,0.818292966938792,
125.050916856162));
#248632=CARTESIAN_POINT('Ctrl Pts',(-32.7838023281826,-4.3982278459157,
127.006030680504));
#248633=CARTESIAN_POINT('Ctrl Pts',(-33.0622499519955,-5.57299213374921,
132.451624158271));
#248634=CARTESIAN_POINT('Ctrl Pts',(-33.3406975758084,-1.62644890646854,
136.383462915428));
#248635=CARTESIAN_POINT('Ctrl Pts',(-33.6191451996212,3.81472140941051,
135.188379215148));
#248636=CARTESIAN_POINT('Ctrl Pts',(-33.8975928234342,5.75034910954236,
129.964596594906));
#248637=CARTESIAN_POINT('Ctrl Pts',(-34.176040447247,2.40168689817613,125.512516086734));
#248638=CARTESIAN_POINT('Ctrl Pts',(-34.4544880710599,-3.15400824368619,
125.923382181419));
#248639=CARTESIAN_POINT('Ctrl Pts',(-34.7329356948729,-5.81132389146964,
130.81962900987));
#248640=CARTESIAN_POINT('Ctrl Pts',(-35.0113833186857,-3.1283167819475,
135.701844931696));
#248641=CARTESIAN_POINT('Ctrl Pts',(-35.2898309424986,2.42946062341331,
136.083512024245));
#248642=CARTESIAN_POINT('Ctrl Pts',(-35.5682785663115,5.75468240160701,
131.613896874941));
#248643=CARTESIAN_POINT('Ctrl Pts',(-35.8467261901244,3.79163218458816,
126.400357453152));
#248644=CARTESIAN_POINT('Ctrl Pts',(-36.1251738139373,-1.65574277853735,
125.233881791944));
#248645=CARTESIAN_POINT('Ctrl Pts',(-36.4036214377501,-5.58157101571846,
129.186404038463));
#248646=CARTESIAN_POINT('Ctrl Pts',(-36.6820690615631,-4.37820816435757,
134.625749339604));
#248647=CARTESIAN_POINT('Ctrl Pts',(-36.960516685376,0.848514102688449,
136.553425090409));
#248648=CARTESIAN_POINT('Ctrl Pts',(-37.2389643091888,5.29549336158222,
133.197991448084));
#248649=CARTESIAN_POINT('Ctrl Pts',(-37.5174119330018,4.87617292041449,
127.64292800788));
#248650=CARTESIAN_POINT('Ctrl Pts',(-37.7958595568146,-0.0241122203237842,
124.993066691407));
#248651=CARTESIAN_POINT('Ctrl Pts',(-38.0743071806275,-4.90223940853195,
127.683500595584));
#248652=CARTESIAN_POINT('Ctrl Pts',(-38.3527548044404,-5.27544806800837,
133.241852397473));
#248653=CARTESIAN_POINT('Ctrl Pts',(-38.6312024282533,-0.800777672950798,
136.560268331721));
#248654=CARTESIAN_POINT('Ctrl Pts',(-38.9096500520661,4.40976828338437,
134.589286268384));
#248655=CARTESIAN_POINT('Ctrl Pts',(-39.1880976758791,5.56795261644649,
129.140142435842));
#248656=CARTESIAN_POINT('Ctrl Pts',(-39.4665452996919,1.6094605046014,125.220333810727));
#248657=CARTESIAN_POINT('Ctrl Pts',(-39.7449929235049,-3.82804718445556,
126.43197302622));
#248658=CARTESIAN_POINT('Ctrl Pts',(-40.0234405473177,-5.74776652149929,
131.661622835152));
#248659=CARTESIAN_POINT('Ctrl Pts',(-40.3018881711306,-2.38556921929025,
136.103490545709));
#248660=CARTESIAN_POINT('Ctrl Pts',(-40.5803357949436,3.16884965391132,
135.675716729192));
#248661=CARTESIAN_POINT('Ctrl Pts',(-40.8587834187564,5.81125050208024,
130.771404625066));
#248662=CARTESIAN_POINT('Ctrl Pts',(-41.1372310425694,3.11339603420704,
125.897377468058));
#248663=CARTESIAN_POINT('Ctrl Pts',(-41.4156786663821,-2.4455172912504,
125.532628105994));
#248664=CARTESIAN_POINT('Ctrl Pts',(-41.6941262901951,-5.75711969621025,
130.012343383614));
#248665=CARTESIAN_POINT('Ctrl Pts',(-41.9725739140079,-3.77821035128576,
135.219883807042));
#248666=CARTESIAN_POINT('Ctrl Pts',(-42.2510215378209,1.67268973063362,
136.369774129642));
#248667=CARTESIAN_POINT('Ctrl Pts',(-42.5294691616338,5.58646966553678,
132.405321320208));
#248668=CARTESIAN_POINT('Ctrl Pts',(-42.8079167854466,4.366556892027,126.969663836325));
#248669=CARTESIAN_POINT('Ctrl Pts',(-43.0863644092596,-0.866008347092154,
125.057905359049));
#248670=CARTESIAN_POINT('Ctrl Pts',(-43.3648120330724,-5.3027542220935,
128.426858534403));
#248671=CARTESIAN_POINT('Ctrl Pts',(-43.6432596568854,-4.86652802093628,
133.98061997675));
#248672=CARTESIAN_POINT('Ctrl Pts',(-43.9217072806982,0.0417996883503892,
136.615554236903));
#248673=CARTESIAN_POINT('Ctrl Pts',(-44.2001549045111,4.9117155260715,133.910285453475));
#248674=CARTESIAN_POINT('Ctrl Pts',(-44.478602528324,5.26800474597596,128.350823478709));
#248675=CARTESIAN_POINT('Ctrl Pts',(-44.7570501521369,0.783254960667603,
125.046042272601));
#248676=CARTESIAN_POINT('Ctrl Pts',(-45.0354977759497,-4.42126786936209,
127.032874316024));
#248677=CARTESIAN_POINT('Ctrl Pts',(-45.3139453997627,-5.56286151839129,
132.485518023215));
#248678=CARTESIAN_POINT('Ctrl Pts',(-45.5923930235756,-1.59245719291215,
136.393260203719));
#248679=CARTESIAN_POINT('Ctrl Pts',(-45.8708406473885,3.84133749699455,
135.165076697471));
#248680=CARTESIAN_POINT('Ctrl Pts',(-46.1492882712014,5.74513068693249,
129.929608146614));
#248681=CARTESIAN_POINT('Ctrl Pts',(-46.4277358950142,2.3694294408167,125.497994382526));
#248682=CARTESIAN_POINT('Ctrl Pts',(-46.7061835188271,-3.18366170834627,
125.942671958037));
#248683=CARTESIAN_POINT('Ctrl Pts',(-46.98463114264,-5.81112327806003,130.85500390496));
#248684=CARTESIAN_POINT('Ctrl Pts',(-47.263078766453,-3.09844644439114,
135.720797144829));
#248685=CARTESIAN_POINT('Ctrl Pts',(-47.5415263902657,2.46155130414924,
136.068625397419));
#248686=CARTESIAN_POINT('Ctrl Pts',(-47.8199740140787,5.75950365764311,
131.578851490957));
#248687=CARTESIAN_POINT('Ctrl Pts',(-48.0984216378915,3.76475351715869,
126.377358307829));
#248688=CARTESIAN_POINT('Ctrl Pts',(-48.3768692617045,-1.6896211871606,
125.244063976264));
#248689=CARTESIAN_POINT('Ctrl Pts',(-48.6553168855173,-5.59131656306301,
129.220410622463));
#248690=CARTESIAN_POINT('Ctrl Pts',(-48.9337645093303,-4.35486516851022,
134.652329933902));
#248691=CARTESIAN_POINT('Ctrl Pts',(-49.2122121331431,0.883494568912716,
136.548153427379));
#248692=CARTESIAN_POINT('Ctrl Pts',(-49.4906597569561,5.3099659586141,133.165711928516));
#248693=CARTESIAN_POINT('Ctrl Pts',(-49.7691073807689,4.85683803860733,
127.613303933314));
#248694=CARTESIAN_POINT('Ctrl Pts',(-50.0475550045819,-0.0594867691506708,
124.993321139153));
#248695=CARTESIAN_POINT('Ctrl Pts',(-50.3260026283946,-4.92114614214944,
127.713399740592));
#248696=CARTESIAN_POINT('Ctrl Pts',(-50.6044502522077,-5.26051262186729,
133.273920386136));
#248697=CARTESIAN_POINT('Ctrl Pts',(-50.8828978760204,-0.765724992417492,
136.565036249065));
#248698=CARTESIAN_POINT('Ctrl Pts',(-51.1613454998334,4.4327264973184,134.562372631296));
#248699=CARTESIAN_POINT('Ctrl Pts',(-51.4397931236463,5.55771888674681,
129.106279562002));
#248700=CARTESIAN_POINT('Ctrl Pts',(-51.7182407474591,1.57543912891688,
125.210640026899));
#248701=CARTESIAN_POINT('Ctrl Pts',(-51.9966883712721,-3.85459222390762,
126.455356446176));
#248702=CARTESIAN_POINT('Ctrl Pts',(-52.2751359950849,-5.7424416302597,
131.696595238295));
#248703=CARTESIAN_POINT('Ctrl Pts',(-52.5535836188979,-2.35326771227282,
136.117914002047));
#248704=CARTESIAN_POINT('Ctrl Pts',(-52.8320312427106,3.19844426977395,
135.656336786975));
#248705=CARTESIAN_POINT('Ctrl Pts',(-53.1104788665238,5.81094222058764,
130.736030504428));
#248706=CARTESIAN_POINT('Ctrl Pts',(-53.3889264903363,3.08346815099054,
125.878516257743));
#248707=CARTESIAN_POINT('Ctrl Pts',(-53.6673741141495,-2.47756251357323,
125.547612336859));
#248708=CARTESIAN_POINT('Ctrl Pts',(-53.9458217379622,-5.76183426382087,
130.047403279515));
#248709=CARTESIAN_POINT('Ctrl Pts',(-54.2242693617753,-3.75126180686946,
135.242801036416));
#248710=CARTESIAN_POINT('Ctrl Pts',(-54.502716985588,1.70653699126786,136.359488878264));
#248711=CARTESIAN_POINT('Ctrl Pts',(-54.7811646094011,5.59611166339667,
132.371285231631));
#248712=CARTESIAN_POINT('Ctrl Pts',(-55.0596122332138,4.3431331021171,126.943154413196));
#248713=CARTESIAN_POINT('Ctrl Pts',(-55.3380598570268,-0.900972606160421,
125.063283466166));
#248714=CARTESIAN_POINT('Ctrl Pts',(-55.6165074808396,-5.31712850433539,
128.459181954061));
#248715=CARTESIAN_POINT('Ctrl Pts',(-55.8949551046525,-4.84710306319425,
134.01018506537));
#248716=CARTESIAN_POINT('Ctrl Pts',(-56.1734027284654,0.0771732988733811,
136.615192122377));
#248717=CARTESIAN_POINT('Ctrl Pts',(-56.4518503522783,4.93053116940174,
133.880328901363));
#248718=CARTESIAN_POINT('Ctrl Pts',(-56.7302979760911,5.25297176508825,
128.318801096944));
#248719=CARTESIAN_POINT('Ctrl Pts',(-57.0087455999042,0.748187930595796,
125.041381065643));
#248720=CARTESIAN_POINT('Ctrl Pts',(-57.2871932237169,-4.44414406110167,
127.059857705357));
#248721=CARTESIAN_POINT('Ctrl Pts',(-57.5656408475299,-5.55252476915405,
132.519349592253));
#248722=CARTESIAN_POINT('Ctrl Pts',(-57.8440884713427,-1.55840647026886,
136.402850393281));
#248723=CARTESIAN_POINT('Ctrl Pts',(-58.1225360951557,3.867811242405,135.141612591857));
#248724=CARTESIAN_POINT('Ctrl Pts',(-58.4009837189685,5.73969937639226,
129.894652112598));
#248725=CARTESIAN_POINT('Ctrl Pts',(-58.6794313427815,2.33708418337799,
125.483669307672));
#248726=CARTESIAN_POINT('Ctrl Pts',(-58.9578789665944,-3.21319720125095,
125.962141886319));
#248727=CARTESIAN_POINT('Ctrl Pts',(-59.2363265904072,-5.81070733134035,
130.890376923444));
#248728=CARTESIAN_POINT('Ctrl Pts',(-59.5147742142201,-3.06846129276222,
135.739567177598));
#248729=CARTESIAN_POINT('Ctrl Pts',(-59.793221838033,2.49355077119662,136.053543701326));
#248730=CARTESIAN_POINT('Ctrl Pts',(-60.071669461846,5.76411149315304,131.543777407928));
#248731=CARTESIAN_POINT('Ctrl Pts',(-60.3501170856587,3.73773534540316,
126.354523206705));
#248732=CARTESIAN_POINT('Ctrl Pts',(-60.6285647094717,-1.72343698624942,
125.254452199421));
#248733=CARTESIAN_POINT('Ctrl Pts',(-60.9070123332846,-5.6008549221161,
129.254475900312));
#248734=CARTESIAN_POINT('Ctrl Pts',(-61.1854599570975,-4.33136080153256,
134.678767940282));
#248735=CARTESIAN_POINT('Ctrl Pts',(-61.4639075809103,0.918442296920838,
136.542668925995));
#248736=CARTESIAN_POINT('Ctrl Pts',(-61.7423552047232,5.32424179290464,
133.133344908207));
#248737=CARTESIAN_POINT('Ctrl Pts',(-62.0208028285362,4.83732318488056,
127.583798104527));
#248738=CARTESIAN_POINT('Ctrl Pts',(-62.299250452349,-0.0948591136734494,
124.993790917104));
#248739=CARTESIAN_POINT('Ctrl Pts',(-62.5776980761619,-4.93987052088691,
127.743413422294));
#248740=CARTESIAN_POINT('Ctrl Pts',(-62.8561456999749,-5.24538224549645,
133.305896864355));
#248741=CARTESIAN_POINT('Ctrl Pts',(-63.1345933237877,-0.730643937663188,
136.569590702456));
#248742=CARTESIAN_POINT('Ctrl Pts',(-63.4130409476006,4.45552045494177,
134.53531973969));
#248743=CARTESIAN_POINT('Ctrl Pts',(-63.6914885714135,5.5472792137301,129.072479611178));
#248744=CARTESIAN_POINT('Ctrl Pts',(-63.9699361952264,1.54135937475606,
125.201153520444));
#248745=CARTESIAN_POINT('Ctrl Pts',(-64.2483838190392,-3.88099443002729,
126.478901020081));
#248746=CARTESIAN_POINT('Ctrl Pts',(-64.5268314428522,-5.73690395073373,
131.731534579357));
#248747=CARTESIAN_POINT('Ctrl Pts',(-64.805279066665,-2.32087900405488,
136.132140562712));
#248748=CARTESIAN_POINT('Ctrl Pts',(-65.083726690478,3.22792036610792,135.636777052998));
#248749=CARTESIAN_POINT('Ctrl Pts',(-65.3621743142908,5.81041861249411,
130.700658915789));
#248750=CARTESIAN_POINT('Ctrl Pts',(-65.6406219381037,3.05342600872776,
125.859837576403));
#248751=CARTESIAN_POINT('Ctrl Pts',(-65.9190695619166,-2.50951592890599,
125.562791358466));
#248752=CARTESIAN_POINT('Ctrl Pts',(-66.1975171857295,-5.76633532454392,
130.082491224748));
#248753=CARTESIAN_POINT('Ctrl Pts',(-66.4759648095424,-3.72417425806736,
135.26555379775));
#248754=CARTESIAN_POINT('Ctrl Pts',(-66.7544124333553,1.74032101554631,
136.348997779564));
#248755=CARTESIAN_POINT('Ctrl Pts',(-67.0328600571681,5.60554629528092,
132.337191080086));
#248756=CARTESIAN_POINT('Ctrl Pts',(-67.3113076809811,4.31954837581292,
126.916788068483));
#248757=CARTESIAN_POINT('Ctrl Pts',(-67.5897553047939,-0.935903479357421,
125.068874311009));
#248758=CARTESIAN_POINT('Ctrl Pts',(-67.8682029286069,-5.33130575842519,
128.491592275178));
#248759=CARTESIAN_POINT('Ctrl Pts',(-68.1466505524197,-4.82749849426569,
134.039631360986));
#248760=CARTESIAN_POINT('Ctrl Pts',(-68.4250981762326,0.112544049711387,
136.614614685353));
#248761=CARTESIAN_POINT('Ctrl Pts',(-68.7035458000455,4.94916411008632,
133.850258368115));
#248762=CARTESIAN_POINT('Ctrl Pts',(-68.9819934238584,5.23774413340002,
128.286870818499));
#248763=CARTESIAN_POINT('Ctrl Pts',(-69.2604410476712,0.713093176145084,
125.036933408012));
#248764=CARTESIAN_POINT('Ctrl Pts',(-69.5388886714842,-4.46685557344872,
127.086979848621));
#248765=CARTESIAN_POINT('Ctrl Pts',(-69.8173362952971,-5.54198226906957,
132.553117611744));
#248766=CARTESIAN_POINT('Ctrl Pts',(-70.09578391911,-1.52429800030071,136.412233128746));
#248767=CARTESIAN_POINT('Ctrl Pts',(-70.3742315429229,3.89414166464747,
135.117987767775));
#248768=CARTESIAN_POINT('Ctrl Pts',(-70.6526791667357,5.73405537918087,
129.859729788164));
#248769=CARTESIAN_POINT('Ctrl Pts',(-70.9311267905487,2.3046523244254,125.469541392991));
#248770=CARTESIAN_POINT('Ctrl Pts',(-71.2095744143614,-3.24261362795168,
125.981791244794));
#248771=CARTESIAN_POINT('Ctrl Pts',(-71.4880220381746,-5.81007606672361,
130.925746754563));
#248772=CARTESIAN_POINT('Ctrl Pts',(-71.7664696619872,-3.03836243817177,
135.758154334473));
#248773=CARTESIAN_POINT('Ctrl Pts',(-72.0449172858002,2.52545783880292,
136.038267494822));
#248774=CARTESIAN_POINT('Ctrl Pts',(-72.3233649096131,5.76850573739207,
131.508675925537));
#248775=CARTESIAN_POINT('Ctrl Pts',(-72.601812533426,3.71057867048956,126.331852995942));
#248776=CARTESIAN_POINT('Ctrl Pts',(-72.8802601572389,-1.75718892274731,
125.265046076474));
#248777=CARTESIAN_POINT('Ctrl Pts',(-73.1587077810518,-5.61018573943046,
129.28859860971));
#248778=CARTESIAN_POINT('Ctrl Pts',(-73.4371554048648,-4.30769593438731,
134.705062379074));
#248779=CARTESIAN_POINT('Ctrl Pts',(-73.7156030286775,0.953355991712339,
136.536971789486));
#248780=CARTESIAN_POINT('Ctrl Pts',(-73.9940506524905,5.33832033545752,
133.100891586529));
#248781=CARTESIAN_POINT('Ctrl Pts',(-74.2724982763033,4.81762908236426,
127.554411614868));
#248782=CARTESIAN_POINT('Ctrl Pts',(-74.5509459001162,-0.130227943157576,
124.994476007852));
#248783=CARTESIAN_POINT('Ctrl Pts',(-74.8293935239292,-4.95841185090586,
127.77354052852));
#248784=CARTESIAN_POINT('Ctrl Pts',(-75.107841147742,-5.23005749955717,
133.337780647228));
#248785=CARTESIAN_POINT('Ctrl Pts',(-75.3862887715549,-0.695535808628632,
136.573931523126));
#248786=CARTESIAN_POINT('Ctrl Pts',(-75.6647363953679,4.4781493116164,134.508128596022));
#248787=CARTESIAN_POINT('Ctrl Pts',(-75.9431840191806,5.53663398424198,
129.038743835842));
#248788=CARTESIAN_POINT('Ctrl Pts',(-76.2216316429937,1.50722250495638,
125.191874642891));
#248789=CARTESIAN_POINT('Ctrl Pts',(-76.5000792668064,-3.90725282447187,
126.502605875483));
#248790=CARTESIAN_POINT('Ctrl Pts',(-76.7785268906195,-5.73115368812196,
131.766439563647));
#248791=CARTESIAN_POINT('Ctrl Pts',(-77.0569745144322,-2.28840429481114,
136.146169700531));
#248792=CARTESIAN_POINT('Ctrl Pts',(-77.3354221382452,3.25727685066645,
135.617038252052));
#248793=CARTESIAN_POINT('Ctrl Pts',(-77.613869762058,5.80967969720196,130.665291169852));
#248794=CARTESIAN_POINT('Ctrl Pts',(-77.8923173858709,3.0232707206408,125.841342116181));
#248795=CARTESIAN_POINT('Ctrl Pts',(-78.1707650096839,-2.54137635320382,
125.57816460835));
#248796=CARTESIAN_POINT('Ctrl Pts',(-78.4492126334967,-5.77062271159095,
130.117605919119));
#248797=CARTESIAN_POINT('Ctrl Pts',(-78.7276602573096,-3.69694870861804,
135.288141247929));
#248798=CARTESIAN_POINT('Ctrl Pts',(-79.0061078811224,1.77404055158998,
136.338301222296));
#248799=CARTESIAN_POINT('Ctrl Pts',(-79.2845555049354,5.61477321158579,
132.303040128944));
#248800=CARTESIAN_POINT('Ctrl Pts',(-79.5630031287483,4.29580358705489,
126.8905657792));
#248801=CARTESIAN_POINT('Ctrl Pts',(-79.8414507525611,-0.970799672307275,
125.074677686406));
#248802=CARTESIAN_POINT('Ctrl Pts',(-80.1198983763742,-5.34528545901998,
128.524088296775));
#248803=CARTESIAN_POINT('Ctrl Pts',(-80.3983460001869,-4.80771504060458,
134.068957772455));
#248804=CARTESIAN_POINT('Ctrl Pts',(-80.6767936239998,0.147910630189091,
136.613821947228));
#248805=CARTESIAN_POINT('Ctrl Pts',(-80.9552412478128,4.96761365767528,
133.820074968005));
#248806=CARTESIAN_POINT('Ctrl Pts',(-81.2336888716256,5.22232241517632,
128.255033826564));
#248807=CARTESIAN_POINT('Ctrl Pts',(-81.5121364954386,0.6779719977639,125.032699464516));
#248808=CARTESIAN_POINT('Ctrl Pts',(-81.7905841192513,-4.48940156482041,
127.114239740797));
#248809=CARTESIAN_POINT('Ctrl Pts',(-82.0690317430644,-5.53123440879372,
132.586820830401));
#248810=CARTESIAN_POINT('Ctrl Pts',(-82.3474793668772,-1.490133046909,136.421408062431));
#248811=CARTESIAN_POINT('Ctrl Pts',(-82.62592699069,3.92032778803891,135.094203100652));
#248812=CARTESIAN_POINT('Ctrl Pts',(-82.9043746145031,5.72819890443852,
129.824842467372));
#248813=CARTESIAN_POINT('Ctrl Pts',(-83.1828222383158,2.27213506573304,
125.455611161998));
#248814=CARTESIAN_POINT('Ctrl Pts',(-83.4612698621288,-3.27190989841242,
126.001619305352));
#248815=CARTESIAN_POINT('Ctrl Pts',(-83.7397174859417,-5.80922950760163,
130.961112087674));
#248816=CARTESIAN_POINT('Ctrl Pts',(-84.0181651097544,-3.00815099594316,
135.776557926701));
#248817=CARTESIAN_POINT('Ctrl Pts',(-84.2966127335676,2.55727132464077,
136.022797343974));
#248818=CARTESIAN_POINT('Ctrl Pts',(-84.5750603573801,5.77268622752965,
131.473548344486));
#248819=CARTESIAN_POINT('Ctrl Pts',(-84.8535079811934,3.68328449871872,
126.309348515594));
#248820=CARTESIAN_POINT('Ctrl Pts',(-85.131955605006,-1.79087574596318,
125.275845214866));
#248821=CARTESIAN_POINT('Ctrl Pts',(-85.4104032288191,-5.61930866924928,
129.322777486226));
#248822=CARTESIAN_POINT('Ctrl Pts',(-85.6888508526319,-4.28387144398495,
134.731212275928));
#248823=CARTESIAN_POINT('Ctrl Pts',(-85.9672984764448,0.98823435954663,
136.531062228962));
#248824=CARTESIAN_POINT('Ctrl Pts',(-86.2457461002577,5.35220106458756,
133.068353166051));
#248825=CARTESIAN_POINT('Ctrl Pts',(-86.5241937240705,4.79775646083024,
127.525145553266));
#248826=CARTESIAN_POINT('Ctrl Pts',(-86.8026413478836,-0.165591946996939,
124.995376386011));
#248827=CARTESIAN_POINT('Ctrl Pts',(-87.0810889716963,-4.97676944515001,
127.803779942897));
#248828=CARTESIAN_POINT('Ctrl Pts',(-87.3595365955093,-5.21453895191432,
133.36957055329));
#248829=CARTESIAN_POINT('Ctrl Pts',(-87.6379842193221,-0.660401906259044,
136.578058550223));
#248830=CARTESIAN_POINT('Ctrl Pts',(-87.916431843135,4.50061222882128,134.480800207869));
#248831=CARTESIAN_POINT('Ctrl Pts',(-88.1948794669479,5.52578359274576,
129.005073486085));
#248832=CARTESIAN_POINT('Ctrl Pts',(-88.4733270907608,1.47302978447255,
125.182803738068));
#248833=CARTESIAN_POINT('Ctrl Pts',(-88.7517747145737,-3.93336643422502,
126.526470133988));
#248834=CARTESIAN_POINT('Ctrl Pts',(-89.0302223383866,-5.7251910555031,
131.801308897747));
#248835=CARTESIAN_POINT('Ctrl Pts',(-89.3086699621995,-2.25584478790559,
136.16000089565));
#248836=CARTESIAN_POINT('Ctrl Pts',(-89.5871175860123,3.28651263563227,
135.597121115567));
#248837=CARTESIAN_POINT('Ctrl Pts',(-89.8655652098253,5.80872550209253,
130.629928577187));
#248838=CARTESIAN_POINT('Ctrl Pts',(-90.1440128336381,2.99300340414587,
125.823030562435));
#248839=CARTESIAN_POINT('Ctrl Pts',(-90.4224604574511,-2.57314260586573,
125.593731516848));
#248840=CARTESIAN_POINT('Ctrl Pts',(-90.7009080812639,-5.77469626609129,
130.152746061436));
#248841=CARTESIAN_POINT('Ctrl Pts',(-90.9793557050769,-3.66958616737523,
135.310562549967));
#248842=CARTESIAN_POINT('Ctrl Pts',(-91.2578033288896,1.80769434990835,
136.327399602824));
#248843=CARTESIAN_POINT('Ctrl Pts',(-91.5362509527026,5.62379207040447,
132.268833643682));
#248844=CARTESIAN_POINT('Ctrl Pts',(-91.8146985765155,4.27189961571542,
126.864488517025));
#248845=CARTESIAN_POINT('Ctrl Pts',(-92.0931462003284,-1.00565989191805,
125.080693377311));
#248846=CARTESIAN_POINT('Ctrl Pts',(-92.3715938241412,-5.3590670880956,
128.556668814702));
#248847=CARTESIAN_POINT('Ctrl Pts',(-92.6500414479542,-4.78775343529548,
134.098163213075));
#248848=CARTESIAN_POINT('Ctrl Pts',(-92.928489071767,0.183271729783054,
136.612813937377));
#248849=CARTESIAN_POINT('Ctrl Pts',(-93.2069366955801,4.98587912851244,
133.789779819492));
#248850=CARTESIAN_POINT('Ctrl Pts',(-93.4853843193926,5.2067071818758,128.223291300872));
#248851=CARTESIAN_POINT('Ctrl Pts',(-93.7638319432059,0.642825696881324,
125.028679392048));
#248852=CARTESIAN_POINT('Ctrl Pts',(-94.0422795670186,-4.51178119976554,
127.14163637176));
#248853=CARTESIAN_POINT('Ctrl Pts',(-94.3207271908314,-5.52028158659305,
132.62045799934));
#248854=CARTESIAN_POINT('Ctrl Pts',(-94.5991748146444,-1.45591287608963,
136.430374854359));
#248855=CARTESIAN_POINT('Ctrl Pts',(-94.8776224384574,3.94636864224209,
135.07025947184));
#248856=CARTESIAN_POINT('Ctrl Pts',(-95.1560700622702,5.7221301691794,129.789991442987));
#248857=CARTESIAN_POINT('Ctrl Pts',(-95.4345176860831,2.23953361224044,
125.441879130882));
#248858=CARTESIAN_POINT('Ctrl Pts',(-95.7129653098959,-3.30108492704829,
126.021625333256));
#248859=CARTESIAN_POINT('Ctrl Pts',(-95.9914129337089,-5.80816768534362,
130.996471612301));
#248860=CARTESIAN_POINT('Ctrl Pts',(-96.2698605575217,-2.97782808557417,
135.794777272329));
#248861=CARTESIAN_POINT('Ctrl Pts',(-96.5483081813347,2.58899004984866,
136.007133822036));
#248862=CARTESIAN_POINT('Ctrl Pts',(-96.8267558051475,5.77665280865574,
131.438395966436));
#248863=CARTESIAN_POINT('Ctrl Pts',(-97.1052034289604,3.65585384148698,
126.287010599573));
#248864=CARTESIAN_POINT('Ctrl Pts',(-97.3836510527732,-1.82449620761995,
125.286849214428));
#248865=CARTESIAN_POINT('Ctrl Pts',(-97.6620986765863,-5.62822337351841,
129.35701126335));
#248866=CARTESIAN_POINT('Ctrl Pts',(-97.9405463003989,-4.25988821315111,
134.757216661848));
#248867=CARTESIAN_POINT('Ctrl Pts',(-98.2189939242121,1.02307610799351,
136.524940463405));
#248868=CARTESIAN_POINT('Ctrl Pts',(-98.4974415480248,5.36588346593846,
133.035730852497));
#248869=CARTESIAN_POINT('Ctrl Pts',(-98.7758891718378,4.77770605666655,
127.496001004183));
#248870=CARTESIAN_POINT('Ctrl Pts',(-99.0543367956506,-0.200949814765295,
124.996492018215));
#248871=CARTESIAN_POINT('Ctrl Pts',(-99.3327844194636,-4.99494262337204,
127.834130544897));
#248872=CARTESIAN_POINT('Ctrl Pts',(-99.6112320432764,-5.19882717761281,
133.401265404553));
#248873=CARTESIAN_POINT('Ctrl Pts',(-99.8896796670892,-0.625243532454567,
136.581971630822));
#248874=CARTESIAN_POINT('Ctrl Pts',(-100.168127290903,4.5229083741848,134.453335587896));
#248875=CARTESIAN_POINT('Ctrl Pts',(-100.446574914715,5.51472844130613,
128.971469809575));
#248876=CARTESIAN_POINT('Ctrl Pts',(-100.725022538528,1.43878248032906,
125.173941142103));
#248877=CARTESIAN_POINT('Ctrl Pts',(-101.003470162341,-3.95933429163924,
126.550492911299));
#248878=CARTESIAN_POINT('Ctrl Pts',(-101.281917786154,-5.71901627382367,
131.836141289563));
#248879=CARTESIAN_POINT('Ctrl Pts',(-101.560365409967,-2.22320168984167,
136.17363363555));
#248880=CARTESIAN_POINT('Ctrl Pts',(-101.83881303378,3.31562663766449,135.577026381578));
#248881=CARTESIAN_POINT('Ctrl Pts',(-102.117260657593,5.80755606252295,
130.594572448163));
#248882=CARTESIAN_POINT('Ctrl Pts',(-102.395708281405,2.96262518080941,
125.804903593708));
#248883=CARTESIAN_POINT('Ctrl Pts',(-102.674155905219,-2.60481350978186,
125.609491507123));
#248884=CARTESIAN_POINT('Ctrl Pts',(-102.952603529031,-5.77855583709781,
130.187910349571));
#248885=CARTESIAN_POINT('Ctrl Pts',(-103.231051152844,-3.64208764826766,
135.332816873036));
#248886=CARTESIAN_POINT('Ctrl Pts',(-103.509498776657,1.84128116344741,
136.316293325111));
#248887=CARTESIAN_POINT('Ctrl Pts',(-103.78794640047,5.63260253753978,132.234572891835));
#248888=CARTESIAN_POINT('Ctrl Pts',(-104.066394024283,4.24783734756473,
126.838557248259));
#248889=CARTESIAN_POINT('Ctrl Pts',(-104.344841648096,-1.04048284643121,
125.086921160811));
#248890=CARTESIAN_POINT('Ctrl Pts',(-104.623289271909,-5.3726501349701,
128.589332621676));
#248891=CARTESIAN_POINT('Ctrl Pts',(-104.901736895722,-4.76761441802147,
134.12724660063));
#248892=CARTESIAN_POINT('Ctrl Pts',(-105.180184519534,0.218626038175886,
136.611590693152));
#248893=CARTESIAN_POINT('Ctrl Pts',(-105.458632143348,5.00395984576562,
133.759374045173));
#248894=CARTESIAN_POINT('Ctrl Pts',(-105.73707976716,5.1908990121252,128.191644417652));
#248895=CARTESIAN_POINT('Ctrl Pts',(-106.015527390973,0.607655575856702,
125.024873339572));
#248896=CARTESIAN_POINT('Ctrl Pts',(-106.293975014786,-4.53399364899913,
127.169168726316));
#248897=CARTESIAN_POINT('Ctrl Pts',(-106.572422638599,-5.50912420832816,
132.654027872123));
#248898=CARTESIAN_POINT('Ctrl Pts',(-106.850870262412,-1.42163875588365,
136.43913317226));
#248899=CARTESIAN_POINT('Ctrl Pts',(-107.129317886225,3.97226326230387,
135.046157768576));
#248900=CARTESIAN_POINT('Ctrl Pts',(-107.407765510038,5.71584939828273,
129.755178006424));
#248901=CARTESIAN_POINT('Ctrl Pts',(-107.686213133851,2.20684917200607,
125.428345808491));
#248902=CARTESIAN_POINT('Ctrl Pts',(-107.964660757664,-3.3301376327682,
126.041808587174));
#248903=CARTESIAN_POINT('Ctrl Pts',(-108.243108381476,-5.80689063929651,
131.031824018185));
#248904=CARTESIAN_POINT('Ctrl Pts',(-108.521556005289,-2.94739483068967,
135.812811696231));
#248905=CARTESIAN_POINT('Ctrl Pts',(-108.800003629102,2.62061283907833,
135.991277509423));
#248906=CARTESIAN_POINT('Ctrl Pts',(-109.078451252915,5.7804053337882,131.403220093974));
#248907=CARTESIAN_POINT('Ctrl Pts',(-109.356898876728,3.62828771524594,
126.264840075618));
#248908=CARTESIAN_POINT('Ctrl Pts',(-109.635346500541,-1.85804906189805,
125.298057667405));
#248909=CARTESIAN_POINT('Ctrl Pts',(-109.913794124354,-5.636929521901,129.391298672536));
#248910=CARTESIAN_POINT('Ctrl Pts',(-110.192241748167,-4.2357471305931,
134.783074573235));
#248911=CARTESIAN_POINT('Ctrl Pts',(-110.470689371979,1.05787994597834,
136.518606719657));
#248912=CARTESIAN_POINT('Ctrl Pts',(-110.749136995792,5.37936703250445,
133.003025854698));
#248913=CARTESIAN_POINT('Ctrl Pts',(-111.027584619605,4.75747861284798,
127.466979047582));
#248914=CARTESIAN_POINT('Ctrl Pts',(-111.306032243418,-0.23630023626489,
124.997822863128));
#248915=CARTESIAN_POINT('Ctrl Pts',(-111.584479867231,-5.01293071215839,
127.864591209862));
#248916=CARTESIAN_POINT('Ctrl Pts',(-111.862927491044,-5.18292275885852,
133.432864026556));
#248917=CARTESIAN_POINT('Ctrl Pts',(-112.141375114857,-0.590061990020461,
136.585670619917));
#248918=CARTESIAN_POINT('Ctrl Pts',(-112.41982273867,4.54503692151536,134.425735753813));
#248919=CARTESIAN_POINT('Ctrl Pts',(-112.698270362483,5.50346893957634,
128.937934051507));
#248920=CARTESIAN_POINT('Ctrl Pts',(-112.976717986295,1.40448186157095,
125.165287183403));
#248921=CARTESIAN_POINT('Ctrl Pts',(-113.255165610108,-3.98515543446448,
126.574673317241));
#248922=CARTESIAN_POINT('Ctrl Pts',(-113.533613233921,-5.71262957189362,
131.870935448366));
#248923=CARTESIAN_POINT('Ctrl Pts',(-113.812060857734,-2.19047621022174,
136.187067415062));
#248924=CARTESIAN_POINT('Ctrl Pts',(-114.090508481547,3.34461777793161,
135.556754794705));
#248925=CARTESIAN_POINT('Ctrl Pts',(-114.36895610536,5.80617142182825,130.559224092919));
#248926=CARTESIAN_POINT('Ctrl Pts',(-114.647403729173,2.9321371763071,125.786961881698));
#248927=CARTESIAN_POINT('Ctrl Pts',(-114.925851352986,-2.63638789137572,
125.625443995184));
#248928=CARTESIAN_POINT('Ctrl Pts',(-115.204298976799,-5.78220128159277,
130.223097480497));
#248929=CARTESIAN_POINT('Ctrl Pts',(-115.482746600612,-3.61445417026275,
135.354903392492));
#248930=CARTESIAN_POINT('Ctrl Pts',(-115.761194224424,1.87479974763623,
136.304982800703));
#248931=CARTESIAN_POINT('Ctrl Pts',(-116.039641848237,5.64120428651674,
132.200259142944));
#248932=CARTESIAN_POINT('Ctrl Pts',(-116.31808947205,4.22361767423897,126.812772933795));
#248933=CARTESIAN_POINT('Ctrl Pts',(-116.596537095863,-1.07526724547036,
125.093360806132));
#248934=CARTESIAN_POINT('Ctrl Pts',(-116.874984719676,-5.38603409631742,
128.622078507325));
#248935=CARTESIAN_POINT('Ctrl Pts',(-117.153432343489,-4.7472987350426,
134.156206857421));
#248936=CARTESIAN_POINT('Ctrl Pts',(-117.431879967302,0.253972245300257,
136.610152259881));
#248937=CARTESIAN_POINT('Ctrl Pts',(-117.710327591115,5.02185513944583,
133.728858771743));
#248938=CARTESIAN_POINT('Ctrl Pts',(-117.988775214928,5.17489849170343,
128.160094349593));
#248939=CARTESIAN_POINT('Ctrl Pts',(-118.26722283874,0.572462937930709,
125.021281448121));
#248940=CARTESIAN_POINT('Ctrl Pts',(-118.545670462553,-4.55603808943068,
127.196835784245));
#248941=CARTESIAN_POINT('Ctrl Pts',(-118.824118086366,-5.49776268743969,
132.687529204804));
#248942=CARTESIAN_POINT('Ctrl Pts',(-119.102565710179,-1.38731195633035,
136.447682691592));
#248943=CARTESIAN_POINT('Ctrl Pts',(-119.381013333992,3.99801068868978,
135.021898883958));
#248944=CARTESIAN_POINT('Ctrl Pts',(-119.659460957805,5.70935682448427,
129.720403447709));
#248945=CARTESIAN_POINT('Ctrl Pts',(-119.937908581618,2.17408295616475,
125.415011696306));
#248946=CARTESIAN_POINT('Ctrl Pts',(-120.216356205431,-3.3590669390133,
126.062168319208));
#248947=CARTESIAN_POINT('Ctrl Pts',(-120.494803829244,-5.80539841678086,
131.067167995328));
#248948=CARTESIAN_POINT('Ctrl Pts',(-120.773251453056,-2.91685235900652,
135.830660530138));
#248949=CARTESIAN_POINT('Ctrl Pts',(-121.051699076869,2.65213852053535,
135.975228993696));
#248950=CARTESIAN_POINT('Ctrl Pts',(-121.330146700682,5.78394366387473,
131.368022030553));
#248951=CARTESIAN_POINT('Ctrl Pts',(-121.608594324495,3.60058714147007,
126.242837765265));
#248952=CARTESIAN_POINT('Ctrl Pts',(-121.887041948308,-1.89153306548558,
125.309470158462));
#248953=CARTESIAN_POINT('Ctrl Pts',(-122.165489572121,-5.64542679178685,
129.425638443252));
#248954=CARTESIAN_POINT('Ctrl Pts',(-122.443937195934,-4.21144909086733,
134.808785051914));
#248955=CARTESIAN_POINT('Ctrl Pts',(-122.722384819747,1.09264458383337,
136.512061232418));
#248956=CARTESIAN_POINT('Ctrl Pts',(-123.00083244356,5.39265126464657,132.97023938455));
#248957=CARTESIAN_POINT('Ctrl Pts',(-123.279280067372,4.73707487890982,
127.438080758883));
#248958=CARTESIAN_POINT('Ctrl Pts',(-123.557727691185,-0.27164190157181,
124.999368871432));
#248959=CARTESIAN_POINT('Ctrl Pts',(-123.836175314998,-5.03073304495359,
127.895160809065));
#248960=CARTESIAN_POINT('Ctrl Pts',(-124.114622938811,-5.16682628499523,
133.464365248398));
#248961=CARTESIAN_POINT('Ctrl Pts',(-124.393070562624,-0.554858582622917,
136.589155380447));
#248962=CARTESIAN_POINT('Ctrl Pts',(-124.671518186437,4.56699705083122,
134.398001728342));
#248963=CARTESIAN_POINT('Ctrl Pts',(-124.94996581025,5.49200550478084,128.904467454562));
#248964=CARTESIAN_POINT('Ctrl Pts',(-125.228413434063,1.37012919922165,
125.156842182641));
#248965=CARTESIAN_POINT('Ctrl Pts',(-125.506861057876,-4.0108289058903,
126.599010455801));
#248966=CARTESIAN_POINT('Ctrl Pts',(-125.785308681688,-5.70603118637341,
131.905690084846));
#248967=CARTESIAN_POINT('Ctrl Pts',(-126.063756305501,-2.1576695617001,
136.200301736396));
#248968=CARTESIAN_POINT('Ctrl Pts',(-126.342203929314,3.37348498215772,
135.536307106118));
#248969=CARTESIAN_POINT('Ctrl Pts',(-126.620651553127,5.8045716313158,130.523884821299));
#248970=CARTESIAN_POINT('Ctrl Pts',(-126.89909917694,2.90154052038371,125.769206091244));
#248971=CARTESIAN_POINT('Ctrl Pts',(-127.177546800753,-2.66786458064647,
125.641588389905));
#248972=CARTESIAN_POINT('Ctrl Pts',(-127.455994424566,-5.7856324644928,
130.258306150342));
#248973=CARTESIAN_POINT('Ctrl Pts',(-127.734442048379,-3.5866867573295,
135.376821289913));
#248974=CARTESIAN_POINT('Ctrl Pts',(-128.012889672192,1.90824886043053,
136.293468448719));
#248975=CARTESIAN_POINT('Ctrl Pts',(-128.291337296005,5.64959699859458,
132.16589366852));
#248976=CARTESIAN_POINT('Ctrl Pts',(-128.569784919818,4.19924149320669,
126.787136529081));
#248977=CARTESIAN_POINT('Ctrl Pts',(-128.84823254363,-1.11001180008614,
125.100012074652));
#248978=CARTESIAN_POINT('Ctrl Pts',(-129.126680167443,-5.39921847619124,
128.654905258242));
#248979=CARTESIAN_POINT('Ctrl Pts',(-129.405127791256,-4.72680713916258,
134.185042910317));
#248980=CARTESIAN_POINT('Ctrl Pts',(-129.683575415069,0.289309041389885,
136.608498690867));
#248981=CARTESIAN_POINT('Ctrl Pts',(-129.962023038882,5.03956434643776,
133.69823512996));
#248982=CARTESIAN_POINT('Ctrl Pts',(-130.240470662695,5.15870621351431,
128.128642265792));
#248983=CARTESIAN_POINT('Ctrl Pts',(-130.518918286508,0.537249087180579,
125.017903850796));
#248984=CARTESIAN_POINT('Ctrl Pts',(-130.79736591032,-4.57791370419536,
127.224636520332));
#248985=CARTESIAN_POINT('Ctrl Pts',(-131.075813534134,-5.4861974449331,
132.720960755981));
#248986=CARTESIAN_POINT('Ctrl Pts',(-131.354261157946,-1.35293374942274,
136.456023095549));
#248987=CARTESIAN_POINT('Ctrl Pts',(-131.632708781759,4.02360996731925,
134.99748371691));
#248988=CARTESIAN_POINT('Ctrl Pts',(-131.911156405572,5.7026526883694,129.685669055425));
#248989=CARTESIAN_POINT('Ctrl Pts',(-132.189604029385,2.1412361788793,125.401877288427));
#248990=CARTESIAN_POINT('Ctrl Pts',(-132.468051653198,-3.38787177379785,
126.082703774923));
#248991=CARTESIAN_POINT('Ctrl Pts',(-132.746499277011,-5.80369107309236,
131.102502234048));
#248992=CARTESIAN_POINT('Ctrl Pts',(-133.024946900823,-2.88620180228584,
135.848323112653));
#248993=CARTESIAN_POINT('Ctrl Pts',(-133.303394524637,2.68356592602436,
135.95898886954));
#248994=CARTESIAN_POINT('Ctrl Pts',(-133.581842148449,5.78726766780228,
131.332803080451));
#248995=CARTESIAN_POINT('Ctrl Pts',(-133.860289772262,3.57275314661281,
126.221004483821));
#248996=CARTESIAN_POINT('Ctrl Pts',(-134.138737396075,-1.92494697761906,
125.321086264707));
#248997=CARTESIAN_POINT('Ctrl Pts',(-134.417185019888,-5.65371486830715,
129.460029303025));
#248998=CARTESIAN_POINT('Ctrl Pts',(-134.695632643701,-4.1869949943469,
134.834347145171));
#248999=CARTESIAN_POINT('Ctrl Pts',(-134.974080267514,1.1273687333409,136.505304244234));
#249000=CARTESIAN_POINT('Ctrl Pts',(-135.252527891327,5.40573567011315,
132.937372656969));
#249001=CARTESIAN_POINT('Ctrl Pts',(-135.53097551514,4.71649561092,127.409307208922));
#249002=CARTESIAN_POINT('Ctrl Pts',(-135.809423138953,-0.306973501088704,
125.001129985841));
#249003=CARTESIAN_POINT('Ctrl Pts',(-136.087870762765,-5.04834896208586,
127.925838209736));
#249004=CARTESIAN_POINT('Ctrl Pts',(-136.366318386578,-5.15053835248403,
133.49576790279));
#249005=CARTESIAN_POINT('Ctrl Pts',(-136.644766010391,-0.519634614735935,
136.592425783278));
#249006=CARTESIAN_POINT('Ctrl Pts',(-136.923213634204,4.58878794839197,
134.37013453918));
#249007=CARTESIAN_POINT('Ctrl Pts',(-137.201661258017,5.48033856170195,
128.871071258858));
#249008=CARTESIAN_POINT('Ctrl Pts',(-137.48010888183,1.33572576623031,125.148606452753));
#249009=CARTESIAN_POINT('Ctrl Pts',(-137.758556505643,-4.03635375457527,
126.623503425159));
#249010=CARTESIAN_POINT('Ctrl Pts',(-138.037004129456,-5.69922136176977,
131.940403911158));
#249011=CARTESIAN_POINT('Ctrl Pts',(-138.315451753269,-2.12478295993955,
136.213336109146));
#249012=CARTESIAN_POINT('Ctrl Pts',(-138.593899377082,3.40222718065648,
135.515684073514));
#249013=CARTESIAN_POINT('Ctrl Pts',(-138.872347000894,5.80275675026745,
130.488555942812));
#249014=CARTESIAN_POINT('Ctrl Pts',(-139.150794624707,2.870836346809,125.751636880291));
#249015=CARTESIAN_POINT('Ctrl Pts',(-139.42924224852,-2.69924241121433,
125.65792409305));
#249016=CARTESIAN_POINT('Ctrl Pts',(-139.707689872333,-5.78884925865424,
130.293535054436));
#249017=CARTESIAN_POINT('Ctrl Pts',(-139.986137496146,-3.55878643839929,
135.398569753122));
#249018=CARTESIAN_POINT('Ctrl Pts',(-140.264585119959,1.94162726236197,
136.281750695826));
#249019=CARTESIAN_POINT('Ctrl Pts',(-140.543032743772,5.65778036277742,
132.131477741989));
#249020=CARTESIAN_POINT('Ctrl Pts',(-140.821480367585,4.17470970773734,
126.761648984083));
#249021=CARTESIAN_POINT('Ctrl Pts',(-141.099927991397,-1.14471522280625,
125.106874719905));
#249022=CARTESIAN_POINT('Ctrl Pts',(-141.37837561521,-5.41220278603824,
128.687811658017));
#249023=CARTESIAN_POINT('Ctrl Pts',(-141.656823239023,-4.70614038970644,
134.213753690789));
#249024=CARTESIAN_POINT('Ctrl Pts',(-141.935270862836,0.324635117026387,
136.60663004738));
#249025=CARTESIAN_POINT('Ctrl Pts',(-142.213718486649,5.05708681051884,
133.667504254592));
#249026=CARTESIAN_POINT('Ctrl Pts',(-142.492166110462,5.14232277757003,
128.097289331719));
#249027=CARTESIAN_POINT('Ctrl Pts',(-142.770613734275,0.502015328467386,
125.014740672754));
#249028=CARTESIAN_POINT('Ctrl Pts',(-143.049061358088,-4.59961968268416,
127.252569904414));
#249029=CARTESIAN_POINT('Ctrl Pts',(-143.327508981901,-5.4744289093626,
132.754321286837));
#249030=CARTESIAN_POINT('Ctrl Pts',(-143.605956605714,-1.31850540905707,
136.464154075075));
#249031=CARTESIAN_POINT('Ctrl Pts',(-143.884404229526,4.04906014960179,
134.972913172143));
#249032=CARTESIAN_POINT('Ctrl Pts',(-144.162851853339,5.69573723836169,
129.650976116669));
#249033=CARTESIAN_POINT('Ctrl Pts',(-144.441299477152,2.10831005730047,
125.388943071553));
#249034=CARTESIAN_POINT('Ctrl Pts',(-144.719747100965,-3.41655106974776,
126.103414193369));
#249035=CARTESIAN_POINT('Ctrl Pts',(-144.998194724778,-5.80176867149642,
131.13782542502));
#249036=CARTESIAN_POINT('Ctrl Pts',(-145.276642348591,-2.85544429629671,
135.865798789283));
#249037=CARTESIAN_POINT('Ctrl Pts',(-145.555089972404,2.71489389099137,
135.942557738738));
#249038=CARTESIAN_POINT('Ctrl Pts',(-145.833537596217,5.79037722239768,
131.29756454872));
#249039=CARTESIAN_POINT('Ctrl Pts',(-146.111985220029,3.54478676207412,
126.199341040322));
#249040=CARTESIAN_POINT('Ctrl Pts',(-146.390432843843,-1.95828956013508,
125.332905555698));
#249041=CARTESIAN_POINT('Ctrl Pts',(-146.668880467655,-5.66179344434354,
129.49446997749));
#249042=CARTESIAN_POINT('Ctrl Pts',(-146.947328091469,-4.16238574718705,
134.859759905796));
#249043=CARTESIAN_POINT('Ctrl Pts',(-147.225775715281,1.16205110778606,
136.498336005488));
#249044=CARTESIAN_POINT('Ctrl Pts',(-147.504223339094,5.41861976405632,
132.904426889841));
#249045=CARTESIAN_POINT('Ctrl Pts',(-147.782670962907,4.6957415714508,127.380659463914));
#249046=CARTESIAN_POINT('Ctrl Pts',(-148.06111858672,-0.342293725589094,
125.003106141093));
#249047=CARTESIAN_POINT('Ctrl Pts',(-148.339566210533,-5.06577781079073,
127.956622275114));
#249048=CARTESIAN_POINT('Ctrl Pts',(-148.618013834346,-5.1340595648799,
133.527070826096));
#249049=CARTESIAN_POINT('Ctrl Pts',(-148.896461458158,-0.48439139159784,
136.595481707227));
#249050=CARTESIAN_POINT('Ctrl Pts',(-149.174909081971,4.61040880672808,
134.342135218952));
#249051=CARTESIAN_POINT('Ctrl Pts',(-149.453356705784,5.4684685426618,128.837746701901));
#249052=CARTESIAN_POINT('Ctrl Pts',(-149.731804329597,1.30127283742975,
125.140580298914));
#249053=CARTESIAN_POINT('Ctrl Pts',(-150.01025195341,-4.06172903468827,
126.648151317718));
#249054=CARTESIAN_POINT('Ctrl Pts',(-150.288699577223,-5.69220035042211,
131.975075640969));
#249055=CARTESIAN_POINT('Ctrl Pts',(-150.567147201036,-2.09181762356486,
136.226170050321));
#249056=CARTESIAN_POINT('Ctrl Pts',(-150.845594824849,3.43084330837664,
135.494886461086));
#249057=CARTESIAN_POINT('Ctrl Pts',(-151.124042448661,5.80072684593324,
130.453238766583));
#249058=CARTESIAN_POINT('Ctrl Pts',(-151.402490072475,2.84002579333802,
125.734254899877));
#249059=CARTESIAN_POINT('Ctrl Pts',(-151.680937696287,-2.73052022036177,
125.674450499292));
#249060=CARTESIAN_POINT('Ctrl Pts',(-151.9593853201,-5.79185154487752,130.32878288736));
#249061=CARTESIAN_POINT('Ctrl Pts',(-152.237832943913,-3.53075424732904,
135.420147976222));
#249062=CARTESIAN_POINT('Ctrl Pts',(-152.516280567726,1.97493371658077,
136.269829976228));
#249063=CARTESIAN_POINT('Ctrl Pts',(-152.794728191539,5.66575407582884,
132.097012638644));
#249064=CARTESIAN_POINT('Ctrl Pts',(-153.073175815352,4.15002322686382,
126.736311243251));
#249065=CARTESIAN_POINT('Ctrl Pts',(-153.351623439165,-1.17937622768304,
125.113948487592));
#249066=CARTESIAN_POINT('Ctrl Pts',(-153.630071062978,-5.42498654472129,
128.720796487292));
#249067=CARTESIAN_POINT('Ctrl Pts',(-153.90851868679,-4.6852992524868,134.242338134946));
#249068=CARTESIAN_POINT('Ctrl Pts',(-154.186966310604,0.359949163189457,
136.604546398667));
#249069=CARTESIAN_POINT('Ctrl Pts',(-154.465413934416,5.0744218823891,133.636667284384));
#249070=CARTESIAN_POINT('Ctrl Pts',(-154.743861558229,5.12574879096345,
128.066036709167));
#249071=CARTESIAN_POINT('Ctrl Pts',(-155.022309182042,0.466762967392146,
125.011792031209));
#249072=CARTESIAN_POINT('Ctrl Pts',(-155.300756805855,-4.62115522057418,
127.280634901405));
#249073=CARTESIAN_POINT('Ctrl Pts',(-155.579204429668,-5.46245751681569,
132.787609561181));
#249074=CARTESIAN_POINT('Ctrl Pts',(-155.857652053481,-1.28402821098903,
136.472075328871));
#249075=CARTESIAN_POINT('Ctrl Pts',(-156.136099677293,4.07436029247137,
134.948188160129));
#249076=CARTESIAN_POINT('Ctrl Pts',(-156.414547301107,5.68861073071636,
129.616325916999));
#249077=CARTESIAN_POINT('Ctrl Pts',(-156.692994924919,2.07530581151645,
125.376209524969));
#249078=CARTESIAN_POINT('Ctrl Pts',(-156.971442548732,-3.44510376414151,
126.124298807112));
#249079=CARTESIAN_POINT('Ctrl Pts',(-157.249890172545,-5.79963128322921,
131.173136259331));
#249080=CARTESIAN_POINT('Ctrl Pts',(-157.528337796358,-2.82458098076833,
135.883086912459));
#249081=CARTESIAN_POINT('Ctrl Pts',(-157.806785420171,2.74612125456611,
135.925936210153));
#249082=CARTESIAN_POINT('Ctrl Pts',(-158.085233043984,5.79327221243612,
131.262307741136));
#249083=CARTESIAN_POINT('Ctrl Pts',(-158.363680667797,3.51668902415852,
126.177848237519));
#249084=CARTESIAN_POINT('Ctrl Pts',(-158.64212829161,-1.9915595775106,125.344927593469));
#249085=CARTESIAN_POINT('Ctrl Pts',(-158.920575915422,-5.66966222054205,
129.528959190434));
#249086=CARTESIAN_POINT('Ctrl Pts',(-159.199023539236,-4.13762226129274,
134.885022392109));
#249087=CARTESIAN_POINT('Ctrl Pts',(-159.477471163048,1.19669042199943,
136.491156774389));
#249088=CARTESIAN_POINT('Ctrl Pts',(-159.755918786861,5.43130306905165,
132.871403303985));
#249089=CARTESIAN_POINT('Ctrl Pts',(-160.034366410674,4.67481352955083,
127.352138585409));
#249090=CARTESIAN_POINT('Ctrl Pts',(-160.312814034487,-0.377601266270116,
125.005297263965));
#249091=CARTESIAN_POINT('Ctrl Pts',(-160.5912616583,-5.08301894523598,127.987511864483));
#249092=CARTESIAN_POINT('Ctrl Pts',(-160.869709282113,-5.1173905328107,
133.558272858373));
#249093=CARTESIAN_POINT('Ctrl Pts',(-161.148156905926,-0.449130219157962,
136.598323039052));
#249094=CARTESIAN_POINT('Ctrl Pts',(-161.426604529739,4.63185882466967,
134.314004805186));
#249095=CARTESIAN_POINT('Ctrl Pts',(-161.705052153551,5.45639588750942,
128.804495018547));
#249096=CARTESIAN_POINT('Ctrl Pts',(-161.983499777364,1.26677168948586,
125.13276401854));
#249097=CARTESIAN_POINT('Ctrl Pts',(-162.261947401177,-4.08695380593746,
126.67295322014));
#249098=CARTESIAN_POINT('Ctrl Pts',(-162.54039502499,-5.68496841249774,
132.009703989503));
#249099=CARTESIAN_POINT('Ctrl Pts',(-162.818842648803,-2.05877477411906,
136.238803084352));
#249100=CARTESIAN_POINT('Ctrl Pts',(-163.097290272616,3.45933230493559,
135.473915039499));
#249101=CARTESIAN_POINT('Ctrl Pts',(-163.375737896429,5.79848199353304,
130.417934601304));
#249102=CARTESIAN_POINT('Ctrl Pts',(-163.654185520242,2.80911000166655,
125.717060794092));
#249103=CARTESIAN_POINT('Ctrl Pts',(-163.932633144055,-2.76169684907854,
125.691166996241));
#249104=CARTESIAN_POINT('Ctrl Pts',(-164.211080767867,-5.79463921191188,
130.36404834299));
#249105=CARTESIAN_POINT('Ctrl Pts',(-164.489528391681,-3.50259122286156,
135.441555159625));
#249106=CARTESIAN_POINT('Ctrl Pts',(-164.767976015493,2.00816698890481,
136.257706731653));
#249107=CARTESIAN_POINT('Ctrl Pts',(-165.046423639306,5.67351784227885,
132.062499635604));
#249108=CARTESIAN_POINT('Ctrl Pts',(-165.324871263119,4.12518296535417,
126.711124245485));
#249109=CARTESIAN_POINT('Ctrl Pts',(-165.603318886932,-1.21399353033979,
125.121233115594));
#249110=CARTESIAN_POINT('Ctrl Pts',(-165.881766510745,-5.43756927853226,
128.753858523801));
#249111=CARTESIAN_POINT('Ctrl Pts',(-166.160214134558,-4.66428449978105,
134.270795183582));
#249112=CARTESIAN_POINT('Ctrl Pts',(-166.438661758371,0.395249871304121,
136.602247821935));
#249113=CARTESIAN_POINT('Ctrl Pts',(-166.717109382183,5.09156891968999,
133.60572536201));
#249114=CARTESIAN_POINT('Ctrl Pts',(-166.995557005996,5.10898486785074,
128.034885556215));
#249115=CARTESIAN_POINT('Ctrl Pts',(-167.274004629809,0.431493310242956,
125.009058035423));
#249116=CARTESIAN_POINT('Ctrl Pts',(-167.552452253622,-4.64251951985801,
127.30883047135));
#249117=CARTESIAN_POINT('Ctrl Pts',(-167.830899877435,-5.45028371089662,
132.820824345507));
#249118=CARTESIAN_POINT('Ctrl Pts',(-168.109347501248,-1.24950343278299,
136.479786563416));
#249119=CARTESIAN_POINT('Ctrl Pts',(-168.387795125061,4.09950945842204,
134.923309597059));
#249120=CARTESIAN_POINT('Ctrl Pts',(-168.666242748874,5.68127342950807,
129.581719740392));
#249121=CARTESIAN_POINT('Ctrl Pts',(-168.944690372687,2.04222466451309,
125.36367712052));
#249122=CARTESIAN_POINT('Ctrl Pts',(-169.223137996499,-3.47352879894819,
126.145356842267));
#249123=CARTESIAN_POINT('Ctrl Pts',(-169.501585620313,-5.79727898749155,
131.208433428525));
#249124=CARTESIAN_POINT('Ctrl Pts',(-169.780033244125,-2.79361299935373,
135.900186841566));
#249125=CARTESIAN_POINT('Ctrl Pts',(-170.058480867939,2.77724685960862,
135.909124899701));
#249126=CARTESIAN_POINT('Ctrl Pts',(-170.336928491751,5.79595253064181,
131.227033964152));
#249127=CARTESIAN_POINT('Ctrl Pts',(-170.615376115564,3.48846097403773,
126.156526871832));
#249128=CARTESIAN_POINT('Ctrl Pts',(-170.893823739377,-2.02475579691427,
125.357151932539));
#249129=CARTESIAN_POINT('Ctrl Pts',(-171.17227136319,-5.67732090532164,
129.563495663847));
#249130=CARTESIAN_POINT('Ctrl Pts',(-171.450718987003,-4.11270545428381,
134.910133667999));
#249131=CARTESIAN_POINT('Ctrl Pts',(-171.729166610815,1.23128539240979,
136.483766816968));
#249132=CARTESIAN_POINT('Ctrl Pts',(-172.007614234629,5.44378511511418,
132.838303123102));
#249133=CARTESIAN_POINT('Ctrl Pts',(-172.286061858441,4.65371226071637,
127.323745630264));
#249134=CARTESIAN_POINT('Ctrl Pts',(-172.564509482254,-0.412894814796852,
125.00770327326));
#249135=CARTESIAN_POINT('Ctrl Pts',(-172.842957106067,-5.10007172654484,
128.018505833219));
#249136=CARTESIAN_POINT('Ctrl Pts',(-173.12140472988,-5.10053187395325,
133.589372843419));
#249137=CARTESIAN_POINT('Ctrl Pts',(-173.399852353693,-0.413852404033268,
136.600949673471));
#249138=CARTESIAN_POINT('Ctrl Pts',(-173.678299977506,4.65313720737985,
134.285744340263));
#249139=CARTESIAN_POINT('Ctrl Pts',(-173.956747601319,5.44412104360021,
128.771317440947));
#249140=CARTESIAN_POINT('Ctrl Pts',(-174.235195225131,1.23222360085094,
125.125157901261));
#249141=CARTESIAN_POINT('Ctrl Pts',(-174.513642848945,-4.11202713361109,
126.697908213384));
#249142=CARTESIAN_POINT('Ctrl Pts',(-174.792090472757,-5.67752581597763,
132.044287673595));
#249143=CARTESIAN_POINT('Ctrl Pts',(-175.070538096571,-2.02565563601667,
136.251234743121));
#249144=CARTESIAN_POINT('Ctrl Pts',(-175.348985720383,3.48769311466452,
135.452770585855));
#249145=CARTESIAN_POINT('Ctrl Pts',(-175.627433344196,5.79602227624969,
130.382644755183));
#249146=CARTESIAN_POINT('Ctrl Pts',(-175.905880968009,2.77809011739122,
125.700055200075));
#249147=CARTESIAN_POINT('Ctrl Pts',(-176.184328591822,-2.79277114210269,
125.708072964459));
#249148=CARTESIAN_POINT('Ctrl Pts',(-176.462776215635,-5.79721215645926,
130.399330114555));
#249149=CARTESIAN_POINT('Ctrl Pts',(-176.741223839448,-3.47429840858841,
135.462790510077));
#249150=CARTESIAN_POINT('Ctrl Pts',(-177.019671463261,2.04132584786218,
136.245381411334));
#249151=CARTESIAN_POINT('Ctrl Pts',(-177.298119087073,5.68107137443935,
132.02794001176));
#249152=CARTESIAN_POINT('Ctrl Pts',(-177.576566710886,4.10018984367198,
126.686088924097));
#249153=CARTESIAN_POINT('Ctrl Pts',(-177.855014334699,-1.24856584802001,
125.128728333976));
#249154=CARTESIAN_POINT('Ctrl Pts',(-178.133461958512,-5.4499505212146,
128.786996542421));
#249155=CARTESIAN_POINT('Ctrl Pts',(-178.411909582325,-4.64309691029714,
134.29912378221));
#249156=CARTESIAN_POINT('Ctrl Pts',(-178.690357206138,0.430535933288815,
136.599734402363));
#249157=CARTESIAN_POINT('Ctrl Pts',(-178.968804829951,5.10852728703229,
133.574679634036));
#249158=CARTESIAN_POINT('Ctrl Pts',(-179.247252453763,5.09203162942501,
128.00383702718));
#249159=CARTESIAN_POINT('Ctrl Pts',(-179.525700077576,0.396207663951002,
125.006538786706));
#249160=CARTESIAN_POINT('Ctrl Pts',(-179.80414770139,-4.66371178887382,
127.337155569449));
#249161=CARTESIAN_POINT('Ctrl Pts',(-180.082595325202,-5.43790794271038,
132.853964409027));
#249162=CARTESIAN_POINT('Ctrl Pts',(-180.361042949015,-1.2149323537682,
136.487287492965));
#249163=CARTESIAN_POINT('Ctrl Pts',(-180.639490572828,4.12450671554208,
134.898278404822));
#249164=CARTESIAN_POINT('Ctrl Pts',(-180.917938196641,5.67372560662389,
129.547158869193));
#249165=CARTESIAN_POINT('Ctrl Pts',(-181.196385820454,2.00906784212309,
125.351346322599));
#249166=CARTESIAN_POINT('Ctrl Pts',(-181.474833444267,-3.50182512086801,
126.166587518521));
#249167=CARTESIAN_POINT('Ctrl Pts',(-181.75328106808,-5.79471187144949,
131.243715624654));
#249168=CARTESIAN_POINT('Ctrl Pts',(-182.031728691892,-2.76254149958135,
135.917097942958));
#249169=CARTESIAN_POINT('Ctrl Pts',(-182.310176315705,2.80826955274668,
135.892124430331));
#249170=CARTESIAN_POINT('Ctrl Pts',(-182.588623939518,5.79841807769547,
131.191744524852));
#249171=CARTESIAN_POINT('Ctrl Pts',(-182.867071563331,3.46010365771282,
126.135377733334));
#249172=CARTESIAN_POINT('Ctrl Pts',(-183.145519187144,-2.05787698824661,
125.369578119929));
#249173=CARTESIAN_POINT('Ctrl Pts',(-183.423966810957,-5.68476921488759,
129.598078117967));
#249174=CARTESIAN_POINT('Ctrl Pts',(-183.70241443477,-4.08763624946197,
134.93509280296));
#249175=CARTESIAN_POINT('Ctrl Pts',(-183.980862058583,1.26583473708647,
136.476166407061));
#249176=CARTESIAN_POINT('Ctrl Pts',(-184.259309682396,5.45606543971754,
132.805127573733));
#249177=CARTESIAN_POINT('Ctrl Pts',(-184.537757306209,4.63243854686269,
127.295481650585));
#249178=CARTESIAN_POINT('Ctrl Pts',(-184.816204930021,-0.448173063354899,
125.010324079826));
#249179=CARTESIAN_POINT('Ctrl Pts',(-185.094652553834,-5.11693552282041,
128.049603032828));
#249180=CARTESIAN_POINT('Ctrl Pts',(-185.373100177647,-5.08348421301165,
133.620369628814));
#249181=CARTESIAN_POINT('Ctrl Pts',(-185.65154780146,-0.378559253454916,
136.60336151315));
#249182=CARTESIAN_POINT('Ctrl Pts',(-185.929995425273,4.67424316637891,
134.257354871388));
#249183=CARTESIAN_POINT('Ctrl Pts',(-186.208443049086,5.4316444657843,128.73821519851));
#249184=CARTESIAN_POINT('Ctrl Pts',(-186.486890672899,1.19762985171755,
125.117762228929));
#249185=CARTESIAN_POINT('Ctrl Pts',(-186.765338296712,-4.13694808860639,
126.72301537273));
#249186=CARTESIAN_POINT('Ctrl Pts',(-187.043785920525,-5.66987283665109,
132.078825411735));
#249187=CARTESIAN_POINT('Ctrl Pts',(-187.322233544337,-1.99246143649967,
136.263464565965));
#249188=CARTESIAN_POINT('Ctrl Pts',(-187.600681168151,3.51592468664221,
135.43145388367));
#249189=CARTESIAN_POINT('Ctrl Pts',(-187.879128791963,5.79334778522967,
130.347370535898));
#249190=CARTESIAN_POINT('Ctrl Pts',(-188.157576415776,2.74696728996466,
125.683238747971));
#249191=CARTESIAN_POINT('Ctrl Pts',(-188.436024039589,-2.82374194796541,
125.72516777749));
#249192=CARTESIAN_POINT('Ctrl Pts',(-188.714471663402,-5.79957028317828,
130.434626894674));
#249193=CARTESIAN_POINT('Ctrl Pts',(-188.992919287215,-3.44587685290989,
135.483853240698));
#249194=CARTESIAN_POINT('Ctrl Pts',(-189.271366911028,2.07440906473995,
136.232854471987));
#249195=CARTESIAN_POINT('Ctrl Pts',(-189.54981453484,5.68841439241029,131.993335047731));
#249196=CARTESIAN_POINT('Ctrl Pts',(-189.828262158654,4.07504478794802,
126.661206206783));
#249197=CARTESIAN_POINT('Ctrl Pts',(-190.106709782466,-1.28309189963338,
125.136433864998));
#249198=CARTESIAN_POINT('Ctrl Pts',(-190.385157406279,-5.46212981397553,
128.820209315208));
#249199=CARTESIAN_POINT('Ctrl Pts',(-190.663605030092,-4.62173726915045,
134.327322881104));
#249200=CARTESIAN_POINT('Ctrl Pts',(-190.942052653905,0.465806041606811,
136.597006233083));
#249201=CARTESIAN_POINT('Ctrl Pts',(-191.220500277718,5.12529635601715,
133.543531250871));
#249202=CARTESIAN_POINT('Ctrl Pts',(-191.49894790153,5.07488970389458,127.972892272577));
#249203=CARTESIAN_POINT('Ctrl Pts',(-191.777395525344,0.360907336037817,
125.004234378408));
#249204=CARTESIAN_POINT('Ctrl Pts',(-192.055843149156,-4.68473124233415,
127.365609146106));
#249205=CARTESIAN_POINT('Ctrl Pts',(-192.33429077297,-5.42533067084548,
132.887028523726));
#249206=CARTESIAN_POINT('Ctrl Pts',(-192.612738396782,-1.1803162549878,
136.494577839569));
#249207=CARTESIAN_POINT('Ctrl Pts',(-192.891186020595,4.14935113754904,
134.873095510955));
#249208=CARTESIAN_POINT('Ctrl Pts',(-193.169633644408,5.66596754175055,
129.512644584067));
#249209=CARTESIAN_POINT('Ctrl Pts',(-193.448081268221,1.97583657298603,
125.339217588127));
#249210=CARTESIAN_POINT('Ctrl Pts',(-193.726528892034,-3.52999168137001,
126.187990049162));
#249211=CARTESIAN_POINT('Ctrl Pts',(-194.004976515847,-5.79193003022761,
131.27898154032));
#249212=CARTESIAN_POINT('Ctrl Pts',(-194.28342413966,-2.73136763281852,
135.933819589987));
#249213=CARTESIAN_POINT('Ctrl Pts',(-194.561871763472,2.83918818442447,
135.874935432001));
#249214=CARTESIAN_POINT('Ctrl Pts',(-194.840319387286,5.80066876223446,
131.156440730899));
#249215=CARTESIAN_POINT('Ctrl Pts',(-195.118767011098,3.43161812597426,
126.114401605713));
#249216=CARTESIAN_POINT('Ctrl Pts',(-195.397214634911,-2.09092192419104,
125.382205695184));
#249217=CARTESIAN_POINT('Ctrl Pts',(-195.675662258724,-5.69200687323938,
129.63270527133));
#249218=CARTESIAN_POINT('Ctrl Pts',(-195.954109882537,-4.06241557577554,
134.95989887212));
#249219=CARTESIAN_POINT('Ctrl Pts',(-196.23255750635,1.30033717579212,136.468355826305));
#249220=CARTESIAN_POINT('Ctrl Pts',(-196.511005130163,5.46814358780935,
132.771877885207));
#249221=CARTESIAN_POINT('Ctrl Pts',(-196.789452753976,4.61099317629508,
127.267347693709));
#249222=CARTESIAN_POINT('Ctrl Pts',(-197.067900377789,-0.483434704694746,
125.013159586548));
#249223=CARTESIAN_POINT('Ctrl Pts',(-197.346348001602,-5.13360970916836,
128.080802310993));
#249224=CARTESIAN_POINT('Ctrl Pts',(-197.624795625414,-5.06624818169292,
133.651262065958));
#249225=CARTESIAN_POINT('Ctrl Pts',(-197.903243249227,-0.343252075224855,
136.605558468718));
#249226=CARTESIAN_POINT('Ctrl Pts',(-198.18169087304,4.69517591957924,134.228837450539));
#249227=CARTESIAN_POINT('Ctrl Pts',(-198.460138496853,5.41896661638458,
128.705189517851));
#249228=CARTESIAN_POINT('Ctrl Pts',(-198.738586120666,1.1629917239694,125.110577275591));
#249229=CARTESIAN_POINT('Ctrl Pts',(-199.017033744479,-4.16171574746965,
126.748273767825));
#249230=CARTESIAN_POINT('Ctrl Pts',(-199.295481368292,-5.6620097581009,
132.113315924113));
#249231=CARTESIAN_POINT('Ctrl Pts',(-199.573928992105,-1.95919340559182,
136.275492099704));
#249232=CARTESIAN_POINT('Ctrl Pts',(-199.852376615917,3.54402597473752,
135.409965722843));
#249233=CARTESIAN_POINT('Ctrl Pts',(-200.13082423973,5.79045861957696,130.312113250549));
#249234=CARTESIAN_POINT('Ctrl Pts',(-200.409271863544,2.71574267265526,
125.666612060922));
#249235=CARTESIAN_POINT('Ctrl Pts',(-200.687719487356,-2.85460811903155,
125.742450801881));
#249236=CARTESIAN_POINT('Ctrl Pts',(-200.966167111169,-5.80171350468764,
130.469937375411));
#249237=CARTESIAN_POINT('Ctrl Pts',(-201.244614734982,-3.41732760899753,
135.504742570997));
#249238=CARTESIAN_POINT('Ctrl Pts',(-201.523062358795,2.10741541362659,
136.220126377805));
#249239=CARTESIAN_POINT('Ctrl Pts',(-201.801509982608,5.69554662409457,
131.958686025817));
#249240=CARTESIAN_POINT('Ctrl Pts',(-202.079957606421,4.04974872994014,
126.636477015578));
#249241=CARTESIAN_POINT('Ctrl Pts',(-202.358405230234,-1.31757040580477,
125.144349423131));
#249242=CARTESIAN_POINT('Ctrl Pts',(-202.636852854047,-5.47410670550813,
128.853495611451));
#249243=CARTESIAN_POINT('Ctrl Pts',(-202.915300477859,-4.6002063678289,
134.355391435336));
#249244=CARTESIAN_POINT('Ctrl Pts',(-203.193748101672,0.501058889310003,
136.594063415189));
#249245=CARTESIAN_POINT('Ctrl Pts',(-203.472195725485,5.14187550526088,
133.512281366733));
#249246=CARTESIAN_POINT('Ctrl Pts',(-203.750643349298,5.05755972645996,
127.942052439074));
#249247=CARTESIAN_POINT('Ctrl Pts',(-204.029090973111,0.325593634571106,
125.002144895921));
#249248=CARTESIAN_POINT('Ctrl Pts',(-204.307538596924,-4.70557710135553,
127.394190146963));
#249249=CARTESIAN_POINT('Ctrl Pts',(-204.585986220737,-5.41255236135747,
132.920015464399));
#249250=CARTESIAN_POINT('Ctrl Pts',(-204.864433844549,-1.14565641915494,
136.50165733308));
#249251=CARTESIAN_POINT('Ctrl Pts',(-205.142881468362,4.17404180382362,
134.847761848621));
#249252=CARTESIAN_POINT('Ctrl Pts',(-205.421329092175,5.6579995223666,129.478178163952));
#249253=CARTESIAN_POINT('Ctrl Pts',(-205.699776715988,1.94253208849746,
125.327291366541));
#249254=CARTESIAN_POINT('Ctrl Pts',(-205.978224339801,-3.55802743673226,
126.209563641112));
#249255=CARTESIAN_POINT('Ctrl Pts',(-206.256671963614,-5.78893356690891,
131.314229868733));
#249256=CARTESIAN_POINT('Ctrl Pts',(-206.535119587427,-2.70009255422283,
135.950351163029));
#249257=CARTESIAN_POINT('Ctrl Pts',(-206.81356721124,2.87000160893922,135.857558541658));
#249258=CARTESIAN_POINT('Ctrl Pts',(-207.092014835053,5.80270450085972,
131.121123890489));
#249259=CARTESIAN_POINT('Ctrl Pts',(-207.370462458865,3.40300543436423,
126.09359926625));
#249260=CARTESIAN_POINT('Ctrl Pts',(-207.648910082679,-2.12388938025395,
125.395034190384));
#249261=CARTESIAN_POINT('Ctrl Pts',(-207.927357706491,-5.69903361218359,
129.667375840811));
#249262=CARTESIAN_POINT('Ctrl Pts',(-208.205805330304,-4.03704436778601,
134.984550956282));
#249263=CARTESIAN_POINT('Ctrl Pts',(-208.484252954117,1.33479143002538,
136.460335364123));
#249264=CARTESIAN_POINT('Ctrl Pts',(-208.76270057793,5.48001911182977,132.738555289606));
#249265=CARTESIAN_POINT('Ctrl Pts',(-209.041148201743,4.58937694367963,
127.239344802146));
#249266=CARTESIAN_POINT('Ctrl Pts',(-209.319595825556,-0.518678432184342,
125.016209688352));
#249267=CARTESIAN_POINT('Ctrl Pts',(-209.598043449369,-5.15009366772074,
128.112102511612));
#249268=CARTESIAN_POINT('Ctrl Pts',(-209.876491073182,-5.04882441868487,
133.682049010123));
#249269=CARTESIAN_POINT('Ctrl Pts',(-210.154938696994,-0.307932177662294,
136.607540458767));
#249270=CARTESIAN_POINT('Ctrl Pts',(-210.433386320807,4.71593469130848,
134.200193134443));
#249271=CARTESIAN_POINT('Ctrl Pts',(-210.71183394462,5.40608796518471,128.672241622749));
#249272=CARTESIAN_POINT('Ctrl Pts',(-210.990281568433,1.12831050113542,
125.103603307488));
#249273=CARTESIAN_POINT('Ctrl Pts',(-211.268729192246,-4.18632919242468,
126.773682462711));
#249274=CARTESIAN_POINT('Ctrl Pts',(-211.547176816059,-5.65393687169752,
132.14775793267));
#249275=CARTESIAN_POINT('Ctrl Pts',(-211.825624439872,-1.92585277605142,
136.287316898656));
#249276=CARTESIAN_POINT('Ctrl Pts',(-212.104072063685,3.57199593764717,
135.388306899624));
#249277=CARTESIAN_POINT('Ctrl Pts',(-212.382519687498,5.78735488635066,
130.276874205606));
#249278=CARTESIAN_POINT('Ctrl Pts',(-212.660967311311,2.68441742250212,
125.650175755035));
#249279=CARTESIAN_POINT('Ctrl Pts',(-212.939414935123,-2.88536851154432,
125.759921397201));
#249280=CARTESIAN_POINT('Ctrl Pts',(-213.217862558936,-5.80364174156953,
130.505260248325));
#249281=CARTESIAN_POINT('Ctrl Pts',(-213.496310182749,-3.38865173475374,
135.525457726916));
#249282=CARTESIAN_POINT('Ctrl Pts',(-213.774757806562,2.14034367146046,
136.20719760043));
#249283=CARTESIAN_POINT('Ctrl Pts',(-214.053205430375,5.7024678052036,131.923994229952));
#249284=CARTESIAN_POINT('Ctrl Pts',(-214.331653054188,4.02430260700449,
126.611902266833));
#249285=CARTESIAN_POINT('Ctrl Pts',(-214.610100678001,-1.35200008892003,
125.152474715061));
#249286=CARTESIAN_POINT('Ctrl Pts',(-214.888548301814,-5.48588075200302,
128.886854197714));
#249287=CARTESIAN_POINT('Ctrl Pts',(-215.166995925626,-4.5785050041694,
134.383328404815));
#249288=CARTESIAN_POINT('Ctrl Pts',(-215.445443549439,0.536293170092427,
136.59090605773));
#249289=CARTESIAN_POINT('Ctrl Pts',(-215.723891173253,5.15826412041666,
133.480931139593));
#249290=CARTESIAN_POINT('Ctrl Pts',(-216.002338797065,5.04004233928969,
127.911318669453));
#249291=CARTESIAN_POINT('Ctrl Pts',(-216.280786420879,0.290267868112,125.000270416672));
#249292=CARTESIAN_POINT('Ctrl Pts',(-216.559234044691,-4.72624859348692,
127.422897512942));
#249293=CARTESIAN_POINT('Ctrl Pts',(-216.837681668504,-5.39957348775117,
132.952924008705));
#249294=CARTESIAN_POINT('Ctrl Pts',(-217.116129292317,-1.11095413060172,
136.508525711168));
#249295=CARTESIAN_POINT('Ctrl Pts',(-217.39457691613,4.19857779944424,134.822278356567));
#249296=CARTESIAN_POINT('Ctrl Pts',(-217.673024539943,5.64982184372931,
129.443760886018));
#249297=CARTESIAN_POINT('Ctrl Pts',(-217.951472163756,1.90915562276867,
125.315568099769));
#249298=CARTESIAN_POINT('Ctrl Pts',(-218.229919787568,-3.58593134807924,
126.231307494954));
#249299=CARTESIAN_POINT('Ctrl Pts',(-218.508367411381,-5.78572259252759,
131.349459303753));
#249300=CARTESIAN_POINT('Ctrl Pts',(-218.786815035194,-2.66871742270537,
135.966692049498));
#249301=CARTESIAN_POINT('Ctrl Pts',(-219.065262659007,2.90070868448967,
135.839994403207));
#249302=CARTESIAN_POINT('Ctrl Pts',(-219.34371028282,5.80452521813531,131.085795312298));
#249303=CARTESIAN_POINT('Ctrl Pts',(-219.622157906633,3.37426664313623,
126.07297148578));
#249304=CARTESIAN_POINT('Ctrl Pts',(-219.900605530446,-2.15677813481551,
125.408063130162));
#249305=CARTESIAN_POINT('Ctrl Pts',(-220.179053154259,-5.70584917134113,
129.702088541682));
#249306=CARTESIAN_POINT('Ctrl Pts',(-220.457500778071,-4.01152356563293,
135.009048141953));
#249307=CARTESIAN_POINT('Ctrl Pts',(-220.735948401884,1.36919622307095,
136.452105317718));
#249308=CARTESIAN_POINT('Ctrl Pts',(-221.014396025697,5.49169157172664,
132.705161021709));
#249309=CARTESIAN_POINT('Ctrl Pts',(-221.29284364951,4.56759065001379,127.211474013555));
#249310=CARTESIAN_POINT('Ctrl Pts',(-221.571291273323,-0.553902939853376,
125.019474272218));
#249311=CARTESIAN_POINT('Ctrl Pts',(-221.849738897136,-5.16638678765824,
128.143502474846));
#249312=CARTESIAN_POINT('Ctrl Pts',(-222.128186520948,-5.03121356963114,
133.712729320486));
#249313=CARTESIAN_POINT('Ctrl Pts',(-222.406634144762,-0.272600869560251,
136.609307409853));
#249314=CARTESIAN_POINT('Ctrl Pts',(-222.685081768574,4.73651871234416,
134.171422984523));
#249315=CARTESIAN_POINT('Ctrl Pts',(-222.963529392388,5.39300898940659,
128.639372734101));
#249316=CARTESIAN_POINT('Ctrl Pts',(-223.2419770162,1.09358746834067,125.096840583045));
#249317=CARTESIAN_POINT('Ctrl Pts',(-223.520424640014,-4.21078751141269,
126.799240515859));
#249318=CARTESIAN_POINT('Ctrl Pts',(-223.798872263826,-5.64565447658353,
132.182150161146));
#249319=CARTESIAN_POINT('Ctrl Pts',(-224.077319887639,-1.89244078332859,
136.298938524645));
#249320=CARTESIAN_POINT('Ctrl Pts',(-224.355767511452,3.59983353893359,
135.366478216591));
#249321=CARTESIAN_POINT('Ctrl Pts',(-224.634215135265,5.78403670056078,
130.241654706868));
#249322=CARTESIAN_POINT('Ctrl Pts',(-224.912662759078,2.65299270027449,
125.633930439363));
#249323=CARTESIAN_POINT('Ctrl Pts',(-225.191110382891,-2.91602198566553,
125.77757891607));
#249324=CARTESIAN_POINT('Ctrl Pts',(-225.469558006704,-5.8053549223724,
130.540594204513));
#249325=CARTESIAN_POINT('Ctrl Pts',(-225.748005630516,-3.35985029277391,
135.545997940844));
#249326=CARTESIAN_POINT('Ctrl Pts',(-226.026453254329,2.17319261807209,
136.194068618944));
#249327=CARTESIAN_POINT('Ctrl Pts',(-226.304900878142,5.7091776792716,131.88926094565));
#249328=CARTESIAN_POINT('Ctrl Pts',(-226.583348501955,3.99870736205508,
126.587482871174));
#249329=CARTESIAN_POINT('Ctrl Pts',(-226.861796125768,-1.38637967317499,
125.160809439701));
#249330=CARTESIAN_POINT('Ctrl Pts',(-227.140243749581,-5.49745151716988,
128.920283837883));
#249331=CARTESIAN_POINT('Ctrl Pts',(-227.418691373394,-4.55663398232247,
134.411132754326));
#249332=CARTESIAN_POINT('Ctrl Pts',(-227.697138997207,0.571507578333558,
136.5875342777));
#249333=CARTESIAN_POINT('Ctrl Pts',(-227.97558662102,5.17446159419872,133.44948173115));
#249334=CARTESIAN_POINT('Ctrl Pts',(-228.254034244832,5.02233819149715,
127.880692102567));
#249335=CARTESIAN_POINT('Ctrl Pts',(-228.532481868645,0.254931345670833,
124.998611010119));
#249336=CARTESIAN_POINT('Ctrl Pts',(-228.810929492458,-4.74674495273865,
127.451730180279));
#249337=CARTESIAN_POINT('Ctrl Pts',(-229.089377116271,-5.38639453096373,
132.985752937203));
#249338=CARTESIAN_POINT('Ctrl Pts',(-229.367824740084,-1.07621067523457,
136.515182719319));
#249339=CARTESIAN_POINT('Ctrl Pts',(-229.646272363897,4.22295821522052,
134.796645979094));
#249340=CARTESIAN_POINT('Ctrl Pts',(-229.92471998771,5.64143480886619,129.409394025606));
#249341=CARTESIAN_POINT('Ctrl Pts',(-230.203167611523,1.87570841257552,
125.304048222223));
#249342=CARTESIAN_POINT('Ctrl Pts',(-230.481615235336,-3.61370238142155,
126.25322080496));
#249343=CARTESIAN_POINT('Ctrl Pts',(-230.760062859148,-5.78229722606833,
131.384668539942));
#249344=CARTESIAN_POINT('Ctrl Pts',(-231.038510482961,-2.63724340088164,
135.982841643878));
#249345=CARTESIAN_POINT('Ctrl Pts',(-231.316958106774,2.93130827321233,
135.822243667495));
#249346=CARTESIAN_POINT('Ctrl Pts',(-231.595405730587,5.80613084659478,
131.050456305442));
#249347=CARTESIAN_POINT('Ctrl Pts',(-231.8738533544,3.34540281721704,126.052519028673));
#249348=CARTESIAN_POINT('Ctrl Pts',(-232.152300978213,-2.18958696916944,
125.42129203173));
#249349=CARTESIAN_POINT('Ctrl Pts',(-232.430748602025,-5.71245329815966,
129.736842087648));
#249350=CARTESIAN_POINT('Ctrl Pts',(-232.709196225839,-3.98585411499877,
135.033389521383));
#249351=CARTESIAN_POINT('Ctrl Pts',(-232.987643849651,1.40355028004735,
136.443665992055));
#249352=CARTESIAN_POINT('Ctrl Pts',(-233.266091473464,5.50316053497282,
132.671696318956));
#249353=CARTESIAN_POINT('Ctrl Pts',(-233.544539097277,4.5456351025967,127.183736360699));
#249354=CARTESIAN_POINT('Ctrl Pts',(-233.82298672109,-0.589106922445798,
125.022953217175));
#249355=CARTESIAN_POINT('Ctrl Pts',(-234.101434344904,-5.18248846523346,
128.175001037157));
#249356=CARTESIAN_POINT('Ctrl Pts',(-234.379881968716,-5.01341628710851,
133.743301860178));
#249357=CARTESIAN_POINT('Ctrl Pts',(-234.658329592529,-0.237259460132118,
136.610859256499));
#249358=CARTESIAN_POINT('Ctrl Pts',(-234.936777216342,4.75692721993639,
134.14252806687));
#249359=CARTESIAN_POINT('Ctrl Pts',(-235.215224840155,5.37973017369771,
128.606584069875));
#249360=CARTESIAN_POINT('Ctrl Pts',(-235.493672463967,1.05882391226032,
125.090289352854));
#249361=CARTESIAN_POINT('Ctrl Pts',(-235.772120087781,-4.23508979812022,
126.824946980203));
#249362=CARTESIAN_POINT('Ctrl Pts',(-236.050567711593,-5.63716287966734,
132.216491335124));
#249363=CARTESIAN_POINT('Ctrl Pts',(-236.329015335406,-1.85895866551617,
136.310356547029));
#249364=CARTESIAN_POINT('Ctrl Pts',(-236.607462959219,3.62753774706455,
135.344480482612));
#249365=CARTESIAN_POINT('Ctrl Pts',(-236.885910583032,5.78050418516386,
130.206456059403));
#249366=CARTESIAN_POINT('Ctrl Pts',(-237.164358206845,2.62146967042642,
125.617876715884));
#249367=CARTESIAN_POINT('Ctrl Pts',(-237.442805830658,-2.94656740551997,
125.795422704185));
#249368=CARTESIAN_POINT('Ctrl Pts',(-237.72125345447,-5.80685298361372,
130.575937934662));
#249369=CARTESIAN_POINT('Ctrl Pts',(-237.999701078284,-3.33092435030571,
135.566362451659));
#249370=CARTESIAN_POINT('Ctrl Pts',(-238.278148702096,2.20596103623244,
136.180739919846));
#249371=CARTESIAN_POINT('Ctrl Pts',(-238.55659632591,5.7156759976606,131.854487459968));
#249372=CARTESIAN_POINT('Ctrl Pts',(-238.835043949722,3.97296394353457,
126.56321973347));
#249373=CARTESIAN_POINT('Ctrl Pts',(-239.113491573535,-1.42070788462113,
125.169353288205));
#249374=CARTESIAN_POINT('Ctrl Pts',(-239.391939197348,-5.50881857224844,
128.95378329321));
#249375=CARTESIAN_POINT('Ctrl Pts',(-239.670386821161,-4.53459411272838,
134.438803453569));
#249376=CARTESIAN_POINT('Ctrl Pts',(-239.948834444974,0.606700809151854,
136.583948200045));
#249377=CARTESIAN_POINT('Ctrl Pts',(-240.227282068787,5.1904673264033,133.417934306771));
#249378=CARTESIAN_POINT('Ctrl Pts',(-240.5057296926,5.00444793911587,127.850173873291));
#249379=CARTESIAN_POINT('Ctrl Pts',(-240.784177316413,0.21958537665436,
124.997166737753));
#249380=CARTESIAN_POINT('Ctrl Pts',(-241.062624940225,-4.76706541961049,
127.48068708057));
#249381=CARTESIAN_POINT('Ctrl Pts',(-241.341072564039,-5.37301597934592,
133.018501033406));
#249382=CARTESIAN_POINT('Ctrl Pts',(-241.619520187851,-1.04142734048567,
136.521628110858));
#249383=CARTESIAN_POINT('Ctrl Pts',(-241.897967811664,4.24718214772698,
134.770865666018));
#249384=CARTESIAN_POINT('Ctrl Pts',(-242.176415435477,5.63283872856131,
129.375078856195));
#249385=CARTESIAN_POINT('Ctrl Pts',(-242.45486305929,1.84219169731802,125.292732160775));
#249386=CARTESIAN_POINT('Ctrl Pts',(-242.733310683103,-3.64133950769301,
126.275302759127));
#249387=CARTESIAN_POINT('Ctrl Pts',(-243.011758306915,-5.77865759445851,
131.419856272607));
#249388=CARTESIAN_POINT('Ctrl Pts',(-243.290205930729,-2.60567165503458,
135.998799347738));
#249389=CARTESIAN_POINT('Ctrl Pts',(-243.568653554541,2.96179924122969,
135.80430699228));
#249390=CARTESIAN_POINT('Ctrl Pts',(-243.847101178355,5.80752132674009,
131.015108179419));
#249391=CARTESIAN_POINT('Ctrl Pts',(-244.125548802166,3.31641502616601,
126.032242652805));
#249392=CARTESIAN_POINT('Ctrl Pts',(-244.403996425981,-2.22231466757369,
125.434720404883));
#249393=CARTESIAN_POINT('Ctrl Pts',(-244.682444049792,-5.71884574792013,
129.771635190908));
#249394=CARTESIAN_POINT('Ctrl Pts',(-244.960891673606,-3.96003696707471,
135.05757419259));
#249395=CARTESIAN_POINT('Ctrl Pts',(-245.239339297418,1.43785232795156,
136.435017699859));
#249396=CARTESIAN_POINT('Ctrl Pts',(-245.517786921232,5.51442557658153,
132.638162421391));
#249397=CARTESIAN_POINT('Ctrl Pts',(-245.796234545044,4.52351111499922,
127.156132871406));
#249398=CARTESIAN_POINT('Ctrl Pts',(-246.074682168857,-0.624289075464052,
125.026646394309));
#249399=CARTESIAN_POINT('Ctrl Pts',(-246.353129792671,-5.19839810379266,
128.206597031353));
#249400=CARTESIAN_POINT('Ctrl Pts',(-246.631577416483,-4.99543323060155,
133.773765496319));
#249401=CARTESIAN_POINT('Ctrl Pts',(-246.910025040296,-0.201909258968066,
136.612195941205));
#249402=CARTESIAN_POINT('Ctrl Pts',(-247.188472664109,4.77715945784187,
134.113509452194));
#249403=CARTESIAN_POINT('Ctrl Pts',(-247.466920287922,5.36625201010822,
128.573876845067));
#249404=CARTESIAN_POINT('Ctrl Pts',(-247.745367911734,1.02402112107033,
125.083949859676));
#249405=CARTESIAN_POINT('Ctrl Pts',(-248.023815535548,-4.25923515201858,
126.850800903184));
#249406=CARTESIAN_POINT('Ctrl Pts',(-248.30226315936,-5.62846239560694,
132.250780182078));
#249407=CARTESIAN_POINT('Ctrl Pts',(-248.580710783174,-1.82540766330725,
136.32157054271));
#249408=CARTESIAN_POINT('Ctrl Pts',(-248.859158406986,3.65510753545023,
135.322314512822));
#249409=CARTESIAN_POINT('Ctrl Pts',(-249.137606030799,5.7767574710584,130.171279567513));
#249410=CARTESIAN_POINT('Ctrl Pts',(-249.416053654612,2.58984950105633,
125.602015179472));
#249411=CARTESIAN_POINT('Ctrl Pts',(-249.694501278425,-2.97700363923603,
125.813452100338));
#249412=CARTESIAN_POINT('Ctrl Pts',(-249.972948902238,-5.80813586978118,
130.611290129096));
#249413=CARTESIAN_POINT('Ctrl Pts',(-250.251396526051,-3.30187497921299,
135.586550504748));
#249414=CARTESIAN_POINT('Ctrl Pts',(-250.529844149864,2.23864771169993,
136.167211997028));
#249415=CARTESIAN_POINT('Ctrl Pts',(-250.808291773676,5.72196251956533,
131.819675061465));
#249416=CARTESIAN_POINT('Ctrl Pts',(-251.08673939749,3.94707330538994,126.539113752772));
#249417=CARTESIAN_POINT('Ctrl Pts',(-251.365187021302,-1.45498345124562,
125.178105944033));
#249418=CARTESIAN_POINT('Ctrl Pts',(-251.643634645115,-5.5199814959705,
128.987351322257));
#249419=CARTESIAN_POINT('Ctrl Pts',(-251.922082268928,-4.51238621219265,
134.466339477392));
#249420=CARTESIAN_POINT('Ctrl Pts',(-252.200529892741,0.641871558658502,
136.580147957277));
#249421=CARTESIAN_POINT('Ctrl Pts',(-252.478977516554,5.20628072353487,
133.386290036154));
#249422=CARTESIAN_POINT('Ctrl Pts',(-252.757425140367,4.98637224582674,
127.819765111179));
#249423=CARTESIAN_POINT('Ctrl Pts',(-253.035872764179,0.184231269403876,
124.995937655572));
#249424=CARTESIAN_POINT('Ctrl Pts',(-253.314320387993,-4.78720923844335,
127.509767136124));
#249425=CARTESIAN_POINT('Ctrl Pts',(-253.592768011806,-5.35943833369967,
133.051167092665));
#249426=CARTESIAN_POINT('Ctrl Pts',(-253.871215635618,-1.00660540571931,
136.527861630253));
#249427=CARTESIAN_POINT('Ctrl Pts',(-254.149663259431,4.27124868131666,
134.744938404161));
#249428=CARTESIAN_POINT('Ctrl Pts',(-254.428110883244,5.62403395537261,
129.340816589823));
#249429=CARTESIAN_POINT('Ctrl Pts',(-254.706558507057,1.80860665472018,
125.281620447135));
#249430=CARTESIAN_POINT('Ctrl Pts',(-254.98500613087,-3.66884158147516,
126.297552326988));
#249431=CARTESIAN_POINT('Ctrl Pts',(-255.263453754682,-5.77480406163408,
131.45502159855));
#249432=CARTESIAN_POINT('Ctrl Pts',(-255.541901378496,-2.57400292253984,
136.014563813166));
#249433=CARTESIAN_POINT('Ctrl Pts',(-255.820349002309,2.99217964199006,
135.78618647082));
#249434=CARTESIAN_POINT('Ctrl Pts',(-256.098796626121,5.80869814913581,
130.979749546569));
#249435=CARTESIAN_POINT('Ctrl Pts',(-256.377244249934,3.28730143236016,
126.01214820295));
#249436=CARTESIAN_POINT('Ctrl Pts',(-256.655691873747,-2.25495451926359,
125.448338134603));
#249437=CARTESIAN_POINT('Ctrl Pts',(-256.93413949756,-5.72503666514098,
129.806484721847));
#249438=CARTESIAN_POINT('Ctrl Pts',(-257.212587121373,-3.93405347634203,
135.081566970265));
#249439=CARTESIAN_POINT('Ctrl Pts',(-257.491034745186,1.47206408278265,
136.426225506557));
#249440=CARTESIAN_POINT('Ctrl Pts',(-257.769482368999,5.52555616721843,
132.604438319186));
#249441=CARTESIAN_POINT('Ctrl Pts',(-258.047929992812,4.50108754276566,
127.128895412351));
#249442=CARTESIAN_POINT('Ctrl Pts',(-258.326377616624,-0.659198908970111,
125.030117734768));
#249443=CARTESIAN_POINT('Ctrl Pts',(-258.604825240438,-5.21458571703409,
128.239112839452));
#249444=CARTESIAN_POINT('Ctrl Pts',(-258.883272864251,-4.97637574492231,
133.802560593787));
#249445=CARTESIAN_POINT('Ctrl Pts',(-259.161720488063,-0.168236736403017,
136.616288572087));
#249446=CARTESIAN_POINT('Ctrl Pts',(-259.440168111876,4.80044487344316,
134.078525892203));
#249447=CARTESIAN_POINT('Ctrl Pts',(-259.672207798387,5.25516631655033,
129.4749169549));
#249448=CARTESIAN_POINT('Ctrl Pts',(-259.857849473896,3.17366342871357,
126.795179433485));
#249449=CARTESIAN_POINT('Ctrl Pts',(-259.9506752748,1.64266665146648,126.102093112095));
#249450=CARTESIAN_POINT('Ctrl Pts',(-259.997093138402,0.835778587061721,
125.962806053044));
#249451=CARTESIAN_POINT('Ctrl Pts',(210.385579563201,-2.29217962691353,
126.082387726892));
#249452=CARTESIAN_POINT('Ctrl Pts',(210.339169886847,-3.0789974560272,126.464330840008));
#249453=CARTESIAN_POINT('Ctrl Pts',(210.246352273192,-4.44507089109247,
127.629120819077));
#249454=CARTESIAN_POINT('Ctrl Pts',(210.060718784933,-5.78798125627161,
130.996088365878));
#249455=CARTESIAN_POINT('Ctrl Pts',(209.828679098422,-3.95783017776954,
135.586872998689));
#249456=CARTESIAN_POINT('Ctrl Pts',(209.550231474609,1.89393692750204,136.720289837399));
#249457=CARTESIAN_POINT('Ctrl Pts',(209.271783850796,5.99602695027556,132.40812259401));
#249458=CARTESIAN_POINT('Ctrl Pts',(208.993336226983,4.59288360023261,126.626877830413));
#249459=CARTESIAN_POINT('Ctrl Pts',(208.71488860317,-1.03344059257722,124.682062423228));
#249460=CARTESIAN_POINT('Ctrl Pts',(208.436440979357,-5.70873650289865,
128.364647771496));
#249461=CARTESIAN_POINT('Ctrl Pts',(208.157993355544,-5.13869562717284,
134.288517668348));
#249462=CARTESIAN_POINT('Ctrl Pts',(207.879545731732,0.153933173725622,
137.010984097728));
#249463=CARTESIAN_POINT('Ctrl Pts',(207.601098107919,5.30490488755997,134.029672582798));
#249464=CARTESIAN_POINT('Ctrl Pts',(207.322650484106,5.58103410012833,128.084559773234));
#249465=CARTESIAN_POINT('Ctrl Pts',(207.044202860293,0.728409521696789,
124.638756607567));
#249466=CARTESIAN_POINT('Ctrl Pts',(206.76575523648,-4.79355811073501,126.858871164077));
#249467=CARTESIAN_POINT('Ctrl Pts',(206.487307612667,-5.91049575314416,
132.704682504842));
#249468=CARTESIAN_POINT('Ctrl Pts',(206.208859988854,-1.59596820864792,
136.804198957117));
#249469=CARTESIAN_POINT('Ctrl Pts',(205.930412365042,4.1851717387407,135.390152799229));
#249470=CARTESIAN_POINT('Ctrl Pts',(205.651964741228,6.12034565262566,129.76198992389));
#249471=CARTESIAN_POINT('Ctrl Pts',(205.373517117416,2.43121966936229,125.091713591677));
#249472=CARTESIAN_POINT('Ctrl Pts',(205.095069493603,-3.49207776276838,
125.671081434371));
#249473=CARTESIAN_POINT('Ctrl Pts',(204.81662186979,-6.20632667560231,130.96768173473));
#249474=CARTESIAN_POINT('Ctrl Pts',(204.538174245977,-3.21726438559061,
136.114198085604));
#249475=CARTESIAN_POINT('Ctrl Pts',(204.259726622164,2.72830660529182,136.381233108793));
#249476=CARTESIAN_POINT('Ctrl Pts',(203.981278998351,6.16669716267351,131.523394807979));
#249477=CARTESIAN_POINT('Ctrl Pts',(203.702831374538,3.9381942601484,126.004799186432));
#249478=CARTESIAN_POINT('Ctrl Pts',(203.424383750725,-1.909316761502,124.896766062528));
#249479=CARTESIAN_POINT('Ctrl Pts',(203.145936126912,-6.00225896230248,
129.217523725228));
#249480=CARTESIAN_POINT('Ctrl Pts',(202.867488503099,-4.57941839934143,
134.996506974633));
#249481=CARTESIAN_POINT('Ctrl Pts',(202.589040879287,1.05168395343957,136.923112517541));
#249482=CARTESIAN_POINT('Ctrl Pts',(202.310593255474,5.71634013176502,133.226883983125));
#249483=CARTESIAN_POINT('Ctrl Pts',(202.032145631661,5.12795898713612,127.30447482202));
#249484=CARTESIAN_POINT('Ctrl Pts',(201.753698007848,-0.172765951628197,
124.598289728405));
#249485=CARTESIAN_POINT('Ctrl Pts',(201.475250384035,-5.31472742110118,
127.595180598346));
#249486=CARTESIAN_POINT('Ctrl Pts',(201.196802760222,-5.57271402936141,
133.541151128878));
#249487=CARTESIAN_POINT('Ctrl Pts',(200.918355136409,-0.709648686901125,
136.972144879116));
#249488=CARTESIAN_POINT('Ctrl Pts',(200.639907512596,4.80554913058071,134.735246206027));
#249489=CARTESIAN_POINT('Ctrl Pts',(200.361459888783,5.90468206117194,128.886055711564));
#249490=CARTESIAN_POINT('Ctrl Pts',(200.083012264971,1.57770063730838,124.799693711321));
#249491=CARTESIAN_POINT('Ctrl Pts',(199.804564641158,-4.19911059728431,
126.231327253625));
#249492=CARTESIAN_POINT('Ctrl Pts',(199.526117017345,-6.11714433092778,
131.865355052293));
#249493=CARTESIAN_POINT('Ctrl Pts',(199.247669393532,-2.4138212635637,136.524380797905));
#249494=CARTESIAN_POINT('Ctrl Pts',(198.969221769719,3.50768562329156,135.926987436306));
#249495=CARTESIAN_POINT('Ctrl Pts',(198.690774145906,6.20580078231077,130.622150282517));
#249496=CARTESIAN_POINT('Ctrl Pts',(198.412326522093,3.20108819260905,125.484755525167));
#249497=CARTESIAN_POINT('Ctrl Pts',(198.13387889828,-2.74526806424844,125.235817970576));
#249498=CARTESIAN_POINT('Ctrl Pts',(197.855431274468,-6.16885708386238,
130.104099070135));
#249499=CARTESIAN_POINT('Ctrl Pts',(197.576983650655,-3.92356780882929,
135.615886322105));
#249500=CARTESIAN_POINT('Ctrl Pts',(197.298536026841,1.92728860557448,136.706116507701));
#249501=CARTESIAN_POINT('Ctrl Pts',(197.020088403029,6.00706094473797,132.372921347066));
#249502=CARTESIAN_POINT('Ctrl Pts',(196.741640779216,4.56663773692898,126.598295504472));
#249503=CARTESIAN_POINT('Ctrl Pts',(196.463193155403,-1.07030245846182,
124.688838023107));
#249504=CARTESIAN_POINT('Ctrl Pts',(196.184745531591,-5.72368698170812,
128.399247046161));
#249505=CARTESIAN_POINT('Ctrl Pts',(195.906297907777,-5.11728278641862,
134.319837945007));
#249506=CARTESIAN_POINT('Ctrl Pts',(195.627850283965,0.191654296427489,
137.009876920548));
#249507=CARTESIAN_POINT('Ctrl Pts',(195.349402660151,5.32447044368961,133.997349569974));
#249508=CARTESIAN_POINT('Ctrl Pts',(195.070955036339,5.56435836804288,128.050621358318));
#249509=CARTESIAN_POINT('Ctrl Pts',(194.792507412526,0.690872786183208,
124.634444998269));
#249510=CARTESIAN_POINT('Ctrl Pts',(194.514059788713,-4.81749113516689,
126.888119675218));
#249511=CARTESIAN_POINT('Ctrl Pts',(194.2356121649,-5.89881605082435,132.740628459178));
#249512=CARTESIAN_POINT('Ctrl Pts',(193.957164541087,-1.55941718895885,
136.81380168864));
#249513=CARTESIAN_POINT('Ctrl Pts',(193.678716917274,4.21300988779493,135.364592151301));
#249514=CARTESIAN_POINT('Ctrl Pts',(193.400269293461,6.11388669464029,129.724752614155));
#249515=CARTESIAN_POINT('Ctrl Pts',(193.121821669648,2.39640030908087,125.077020090361));
#249516=CARTESIAN_POINT('Ctrl Pts',(192.843374045836,-3.52326088986039,
125.692433714928));
#249517=CARTESIAN_POINT('Ctrl Pts',(192.564926422022,-6.20521745188322,
131.005458431507));
#249518=CARTESIAN_POINT('Ctrl Pts',(192.28647879821,-3.1848823173506,136.133684081248));
#249519=CARTESIAN_POINT('Ctrl Pts',(192.008031174397,2.76220407667619,136.36452181979));
#249520=CARTESIAN_POINT('Ctrl Pts',(191.729583550584,6.17095986540858,131.485843042463));
#249521=CARTESIAN_POINT('Ctrl Pts',(191.451135926771,3.90890500597959,125.980915208923));
#249522=CARTESIAN_POINT('Ctrl Pts',(191.172688302958,-1.94524259331895,
124.908498067517));
#249523=CARTESIAN_POINT('Ctrl Pts',(190.894240679145,-6.01180727974115,
129.254090580708));
#249524=CARTESIAN_POINT('Ctrl Pts',(190.615793055332,-4.5538147691942,135.024305522869));
#249525=CARTESIAN_POINT('Ctrl Pts',(190.337345431519,1.08891104802307,136.916597252826));
#249526=CARTESIAN_POINT('Ctrl Pts',(190.058897807707,5.73098080836918,133.192042114338));
#249527=CARTESIAN_POINT('Ctrl Pts',(189.780450183893,5.10655917980125,127.273324325042));
#249528=CARTESIAN_POINT('Ctrl Pts',(189.502002560081,-0.210540865719208,
124.599456387862));
#249529=CARTESIAN_POINT('Ctrl Pts',(189.223554936268,-5.33416414113684,
127.627592311355));
#249530=CARTESIAN_POINT('Ctrl Pts',(188.945107312455,-5.55595115925501,
133.575023114497));
#249531=CARTESIAN_POINT('Ctrl Pts',(188.666659688642,-0.672090485321342,
136.976350437346));
#249532=CARTESIAN_POINT('Ctrl Pts',(188.388212064829,4.82938851117716,134.705920634282));
#249533=CARTESIAN_POINT('Ctrl Pts',(188.109764441016,5.89289539464864,128.850147777659));
#249534=CARTESIAN_POINT('Ctrl Pts',(187.831316817203,1.54111929438253,124.790201052305));
#249535=CARTESIAN_POINT('Ctrl Pts',(187.552869193391,-4.22687014955807,
126.256973159398));
#249536=CARTESIAN_POINT('Ctrl Pts',(187.274421569578,-6.11057242014135,
131.902572188318));
#249537=CARTESIAN_POINT('Ctrl Pts',(186.995973945765,-2.37895715467313,
136.538968434335));
#249538=CARTESIAN_POINT('Ctrl Pts',(186.717526321952,3.53880351742172,135.905540247907));
#249539=CARTESIAN_POINT('Ctrl Pts',(186.439078698139,6.20457663716883,130.584377187674));
#249540=CARTESIAN_POINT('Ctrl Pts',(186.160631074326,3.16864693777749,125.465368152723));
#249541=CARTESIAN_POINT('Ctrl Pts',(185.882183450513,-2.77911450042273,
125.25263236868));
#249542=CARTESIAN_POINT('Ctrl Pts',(185.6037358267,-6.17300548002561,130.14166362836));
#249543=CARTESIAN_POINT('Ctrl Pts',(185.325288202887,-3.89420599156785,
135.639681046572));
#249544=CARTESIAN_POINT('Ctrl Pts',(185.046840579075,1.96317856060187,136.694275209062));
#249545=CARTESIAN_POINT('Ctrl Pts',(184.768392955261,6.0164979221829,132.336325600291));
#249546=CARTESIAN_POINT('Ctrl Pts',(184.489945331449,4.54094961554151,126.570575013045));
#249547=CARTESIAN_POINT('Ctrl Pts',(184.211497707636,-1.10750955006109,
124.695466564429));
#249548=CARTESIAN_POINT('Ctrl Pts',(183.933050083823,-5.73822154400692,
128.434133314579));
#249549=CARTESIAN_POINT('Ctrl Pts',(183.65460246001,-5.09578826671723,134.350923164133));
#249550=CARTESIAN_POINT('Ctrl Pts',(183.376154836197,0.229425484589131,
137.008595292604));
#249551=CARTESIAN_POINT('Ctrl Pts',(183.097707212384,5.34380842361613,133.964878848429));
#249552=CARTESIAN_POINT('Ctrl Pts',(182.819259588571,5.54749248089459,128.016800549989));
#249553=CARTESIAN_POINT('Ctrl Pts',(182.540811964758,0.653301958305029,
124.630353773773));
#249554=CARTESIAN_POINT('Ctrl Pts',(182.262364340946,-4.84124114839195,
126.917517669999));
#249555=CARTESIAN_POINT('Ctrl Pts',(181.983916717133,-5.88692014749505,
132.776500352206));
#249556=CARTESIAN_POINT('Ctrl Pts',(181.70546909332,-1.52280712308763,136.82318296266));
#249557=CARTESIAN_POINT('Ctrl Pts',(181.427021469507,4.24069125417353,135.33886187379));
#249558=CARTESIAN_POINT('Ctrl Pts',(181.148573845694,6.10720153813428,129.687555653153));
#249559=CARTESIAN_POINT('Ctrl Pts',(180.870126221881,2.36149196193127,125.062538635854));
#249560=CARTESIAN_POINT('Ctrl Pts',(180.591678598068,-3.55431336199069,
125.713975516152));
#249561=CARTESIAN_POINT('Ctrl Pts',(180.313230974255,-6.20387834410407,
131.04322762551));
#249562=CARTESIAN_POINT('Ctrl Pts',(180.034783350442,-3.15238220429199,
136.15297262387));
#249563=CARTESIAN_POINT('Ctrl Pts',(179.75633572663,2.79599917883219,136.347604482659));
#249564=CARTESIAN_POINT('Ctrl Pts',(179.477888102817,6.17499390876314,131.448266031944));
#249565=CARTESIAN_POINT('Ctrl Pts',(179.199440479004,3.8794709017638,125.957209961944));
#249566=CARTESIAN_POINT('Ctrl Pts',(178.920992855191,-1.98109634126673,
124.920448547985));
#249567=CARTESIAN_POINT('Ctrl Pts',(178.642545231378,-6.02113282860982,
129.290714880887));
#249568=CARTESIAN_POINT('Ctrl Pts',(178.364097607565,-4.52804239515191,
135.051947700091));
#249569=CARTESIAN_POINT('Ctrl Pts',(178.085649983752,1.12609779228193,136.909855496619));
#249570=CARTESIAN_POINT('Ctrl Pts',(177.807202359939,5.74540912154417,133.157111769304));
#249571=CARTESIAN_POINT('Ctrl Pts',(177.528754736127,5.08497014694685,127.242304671825));
#249572=CARTESIAN_POINT('Ctrl Pts',(177.250307112313,-0.248307978092709,
124.600852972375));
#249573=CARTESIAN_POINT('Ctrl Pts',(176.971859488501,-5.35340320178418,
127.660121740658));
#249574=CARTESIAN_POINT('Ctrl Pts',(176.693411864688,-5.53898241132168,
133.608792432211));
#249575=CARTESIAN_POINT('Ctrl Pts',(176.414964240875,-0.634507379188621,
136.980327290216));
#249576=CARTESIAN_POINT('Ctrl Pts',(176.136516617062,4.85304893701009,134.676450488799));
#249577=CARTESIAN_POINT('Ctrl Pts',(175.858068993249,5.88089036471739,128.814312257825));
#249578=CARTESIAN_POINT('Ctrl Pts',(175.579621369436,1.50448084471559,124.780931250186));
#249579=CARTESIAN_POINT('Ctrl Pts',(175.301173745623,-4.25447307360455,
126.282787570284));
#249580=CARTESIAN_POINT('Ctrl Pts',(175.02272612181,-6.10377407984646,131.939748629711));
#249581=CARTESIAN_POINT('Ctrl Pts',(174.744278497998,-2.34400489265046,
136.553343572764));
#249582=CARTESIAN_POINT('Ctrl Pts',(174.465830874185,3.56979027988629,135.883904033421));
#249583=CARTESIAN_POINT('Ctrl Pts',(174.187383250372,6.20312257915782,130.546612244398));
#249584=CARTESIAN_POINT('Ctrl Pts',(173.908935626559,3.13608826756835,125.446178618609));
#249585=CARTESIAN_POINT('Ctrl Pts',(173.630488002746,-2.81285795548731,
125.269652488117));
#249586=CARTESIAN_POINT('Ctrl Pts',(173.352040378933,-6.17692513320066,
130.179252743065));
#249587=CARTESIAN_POINT('Ctrl Pts',(173.07359275512,-3.86469987307124,135.663296596462));
#249588=CARTESIAN_POINT('Ctrl Pts',(172.795145131307,1.99899576932572,136.682215657471));
#249589=CARTESIAN_POINT('Ctrl Pts',(172.516697507494,6.02571195608475,132.29967308599));
#249590=CARTESIAN_POINT('Ctrl Pts',(172.238249883681,4.51509322759614,126.543011406101));
#249591=CARTESIAN_POINT('Ctrl Pts',(171.959802259869,-1.14467560248665,
124.702321473066));
#249592=CARTESIAN_POINT('Ctrl Pts',(171.681354636056,-5.75254347439624,
128.469107412642));
#249593=CARTESIAN_POINT('Ctrl Pts',(171.402907012243,-5.07410492070761,
134.38187696408));
#249594=CARTESIAN_POINT('Ctrl Pts',(171.12445938843,0.267188171305193,137.007083764462));
#249595=CARTESIAN_POINT('Ctrl Pts',(170.846011764617,5.36294838675633,133.932291012718));
#249596=CARTESIAN_POINT('Ctrl Pts',(170.567564140804,5.53042102937231,127.983083035723));
#249597=CARTESIAN_POINT('Ctrl Pts',(170.289116516991,0.615706922082464,
124.62649132937));
#249598=CARTESIAN_POINT('Ctrl Pts',(170.010668893178,-4.86481176764585,
126.947059693175));
#249599=CARTESIAN_POINT('Ctrl Pts',(169.732221269365,-5.87480610217478,
132.812299166869));
#249600=CARTESIAN_POINT('Ctrl Pts',(169.453773645553,-1.48614062903852,
136.832341207004));
#249601=CARTESIAN_POINT('Ctrl Pts',(169.17532602174,4.26821548017818,135.312963568669));
#249602=CARTESIAN_POINT('Ctrl Pts',(168.896878397927,6.10029007702938,129.650400075769));
#249603=CARTESIAN_POINT('Ctrl Pts',(168.618430774114,2.32649610882855,125.048269946673));
#249604=CARTESIAN_POINT('Ctrl Pts',(168.339983150301,-3.58523412773234,
125.735705943466));
#249605=CARTESIAN_POINT('Ctrl Pts',(168.061535526488,-6.2023093493314,131.08098796821));
#249606=CARTESIAN_POINT('Ctrl Pts',(167.783087902675,-3.11976527855146,
136.172062971709));
#249607=CARTESIAN_POINT('Ctrl Pts',(167.504640278862,2.82969067421049,136.330481738588));
#249608=CARTESIAN_POINT('Ctrl Pts',(167.22619265505,6.17879913544756,131.410665161273));
#249609=CARTESIAN_POINT('Ctrl Pts',(166.947745031236,3.84989304232704,125.933684327914));
#249610=CARTESIAN_POINT('Ctrl Pts',(166.669297407424,-2.01687667896098,
124.93261705898));
#249611=CARTESIAN_POINT('Ctrl Pts',(166.39084978361,-6.03023526218728,129.327395269766));
#249612=CARTESIAN_POINT('Ctrl Pts',(166.112402159798,-4.50210223283349,
135.079432481411));
#249613=CARTESIAN_POINT('Ctrl Pts',(165.833954535985,1.16324280857304,136.902887499053));
#249614=CARTESIAN_POINT('Ctrl Pts',(165.555506912173,5.75962453647134,133.122094242209));
#249615=CARTESIAN_POINT('Ctrl Pts',(165.277059288359,5.06319268865361,127.2114170119));
#249616=CARTESIAN_POINT('Ctrl Pts',(164.998611664547,-0.286065889322858,
124.602479430144));
#249617=CARTESIAN_POINT('Ctrl Pts',(164.720164040733,-5.37244389010723,
127.692767680889));
#249618=CARTESIAN_POINT('Ctrl Pts',(164.441716416921,-5.52180841435808,
133.642457830674));
#249619=CARTESIAN_POINT('Ctrl Pts',(164.163268793108,-0.596900761151562,
136.984075290369));
#249620=CARTESIAN_POINT('Ctrl Pts',(163.884821169295,4.87652953132996,134.646836861603));
#249621=CARTESIAN_POINT('Ctrl Pts',(163.606373545482,5.86866741623098,128.778550479967));
#249622=CARTESIAN_POINT('Ctrl Pts',(163.327925921669,1.46778664595768,124.771884648456));
#249623=CARTESIAN_POINT('Ctrl Pts',(163.049478297856,-4.28191834658676,
126.308769529723));
#249624=CARTESIAN_POINT('Ctrl Pts',(162.771030674043,-6.09674956195837,
131.976882998882));
#249625=CARTESIAN_POINT('Ctrl Pts',(162.49258305023,-2.30896577266445,136.567505680515));
#249626=CARTESIAN_POINT('Ctrl Pts',(162.214135426418,3.60064476245918,135.862079594585));
#249627=CARTESIAN_POINT('Ctrl Pts',(161.935687802605,6.20143866215845,130.508856852083));
#249628=CARTESIAN_POINT('Ctrl Pts',(161.657240178792,3.10341338845521,125.427187633898));
#249629=CARTESIAN_POINT('Ctrl Pts',(161.378792554979,-2.84649717906582,
125.2868776982));
#249630=CARTESIAN_POINT('Ctrl Pts',(161.100344931166,-6.18061589814333,
130.216865021372));
#249631=CARTESIAN_POINT('Ctrl Pts',(160.821897307353,-3.83505054669964,
135.686732096692));
#249632=CARTESIAN_POINT('Ctrl Pts',(160.54344968354,2.0347389045262,136.6699382998));
#249633=CARTESIAN_POINT('Ctrl Pts',(160.265002059727,6.03470270501411,132.262965162335));
#249634=CARTESIAN_POINT('Ctrl Pts',(159.986554435914,4.48906953121078,126.51560570502));
#249635=CARTESIAN_POINT('Ctrl Pts',(159.708106812101,-1.18179923853688,
124.709402495009));
#249636=CARTESIAN_POINT('Ctrl Pts',(159.429659188289,-5.76665224217155,
128.50416804437));
#249637=CARTESIAN_POINT('Ctrl Pts',(159.151211564475,-5.05223355187421,
134.412698197843));
#249638=CARTESIAN_POINT('Ctrl Pts',(158.872763940663,0.304940957265202,
137.005342392132));
#249639=CARTESIAN_POINT('Ctrl Pts',(158.59431631685,5.38188962387183,133.899587270395));
#249640=CARTESIAN_POINT('Ctrl Pts',(158.315868693037,5.51314464606502,127.949470064936));
#249641=CARTESIAN_POINT('Ctrl Pts',(158.037421069224,0.57808907061355,124.622857808186));
#249642=CARTESIAN_POINT('Ctrl Pts',(157.758973445411,-4.88820211951067,
126.976744650055));
#249643=CARTESIAN_POINT('Ctrl Pts',(157.480525821598,-5.86247436375394,
132.848023576631));
#249644=CARTESIAN_POINT('Ctrl Pts',(157.202078197785,-1.44941906550188,
136.841276082311));
#249645=CARTESIAN_POINT('Ctrl Pts',(156.923630573973,4.29558154588865,135.286898195607));
#249646=CARTESIAN_POINT('Ctrl Pts',(156.645182950159,6.09315256743229,129.613287258817));
#249647=CARTESIAN_POINT('Ctrl Pts',(156.366735326347,2.29141404655692,125.034214551549));
#249648=CARTESIAN_POINT('Ctrl Pts',(156.088287702534,-3.61602204130483,
125.757624191644));
#249649=CARTESIAN_POINT('Ctrl Pts',(155.809840078721,-6.2005105257049,131.11873806038));
#249650=CARTESIAN_POINT('Ctrl Pts',(155.531392454908,-3.08703274876129,
136.190954417361));
#249651=CARTESIAN_POINT('Ctrl Pts',(155.252944831095,2.86327731436015,136.313154222067));
#249652=CARTESIAN_POINT('Ctrl Pts',(154.974497207282,6.18237540445775,131.373041823765));
#249653=CARTESIAN_POINT('Ctrl Pts',(154.696049583469,3.82017252368788,125.910339178587));
#249654=CARTESIAN_POINT('Ctrl Pts',(154.417601959656,-2.05258228054818,
124.945003149591));
#249655=CARTESIAN_POINT('Ctrl Pts',(154.139154335844,-6.03911424317947,
129.364130388138));
#249656=CARTESIAN_POINT('Ctrl Pts',(153.860706712031,-4.47599524346119,
135.106758848372));
#249657=CARTESIAN_POINT('Ctrl Pts',(153.582259088218,1.20034472047403,136.895693518332));
#249658=CARTESIAN_POINT('Ctrl Pts',(153.303811464405,5.77362652639317,133.086990830643));
#249659=CARTESIAN_POINT('Ctrl Pts',(153.025363840592,5.04122761189337,127.180662489822));
#249660=CARTESIAN_POINT('Ctrl Pts',(152.746916216779,-0.323813200276178,
124.604335700902));
#249661=CARTESIAN_POINT('Ctrl Pts',(152.468468592966,-5.39128550054617,
127.725528922339));
#249662=CARTESIAN_POINT('Ctrl Pts',(152.190020969154,-5.5044298047531,133.6760180624));
#249663=CARTESIAN_POINT('Ctrl Pts',(151.91157334534,-0.55927202473736,136.987594298923));
#249664=CARTESIAN_POINT('Ctrl Pts',(151.633125721528,4.89982942405471,134.617080850036));
#249665=CARTESIAN_POINT('Ctrl Pts',(151.354678097715,5.85622700211526,128.742863769248));
#249666=CARTESIAN_POINT('Ctrl Pts',(151.076230473902,1.43103805782584,124.763061582343));
#249667=CARTESIAN_POINT('Ctrl Pts',(150.797782850089,-4.3092049515099,126.334918074943));
#249668=CARTESIAN_POINT('Ctrl Pts',(150.519335226276,-6.0894991267732,132.013973919806));
#249669=CARTESIAN_POINT('Ctrl Pts',(150.240887602463,-2.27384109310269,
136.581454232806));
#249670=CARTESIAN_POINT('Ctrl Pts',(149.96243997865,3.63136582181627,135.840067740113));
#249671=CARTESIAN_POINT('Ctrl Pts',(149.683992354837,6.19952494856889,130.471112409769));
#249672=CARTESIAN_POINT('Ctrl Pts',(149.405544731024,3.0706235112177,125.40839590231));
#249673=CARTESIAN_POINT('Ctrl Pts',(149.127097107212,-2.88003092464457,
125.30430736064));
#249674=CARTESIAN_POINT('Ctrl Pts',(148.848649483398,-6.18407763809098,
130.254499069545));
#249675=CARTESIAN_POINT('Ctrl Pts',(148.570201859586,-3.80525911111971,
135.709986678852));
#249676=CARTESIAN_POINT('Ctrl Pts',(148.291754235773,2.07040664172831,136.657443590992));
#249677=CARTESIAN_POINT('Ctrl Pts',(148.01330661196,6.04346983581547,132.226203189553));
#249678=CARTESIAN_POINT('Ctrl Pts',(147.734858988147,4.46287949070312,126.488358925329));
#249679=CARTESIAN_POINT('Ctrl Pts',(147.456411364334,-1.21887908258166,
124.716709367866));
#249680=CARTESIAN_POINT('Ctrl Pts',(147.177963740522,-5.78054732452736,
128.53931391058));
#249681=CARTESIAN_POINT('Ctrl Pts',(146.899516116708,-5.03017497066859,
134.44338572333));
#249682=CARTESIAN_POINT('Ctrl Pts',(146.621068492896,0.342682443525903,
137.003371240143));
#249683=CARTESIAN_POINT('Ctrl Pts',(146.342620869082,5.40063143308812,133.866768833311));
#249684=CARTESIAN_POINT('Ctrl Pts',(146.06417324527,5.49566397115542,127.915962883168));
#249685=CARTESIAN_POINT('Ctrl Pts',(145.785725621457,0.540449797841529,
124.619453344862));
#249686=CARTESIAN_POINT('Ctrl Pts',(145.507277997644,-4.91141133724831,
127.006571440652));
#249687=CARTESIAN_POINT('Ctrl Pts',(145.228830373831,-5.84992538918966,
132.883672257711));
#249688=CARTESIAN_POINT('Ctrl Pts',(144.950382750018,-1.41264379320865,
136.849987257496));
#249689=CARTESIAN_POINT('Ctrl Pts',(144.671935126205,4.32278843724517,135.260666720466));
#249690=CARTESIAN_POINT('Ctrl Pts',(144.393487502392,6.08578927382608,129.576218577526));
#249691=CARTESIAN_POINT('Ctrl Pts',(144.11503987858,2.25624707509518,125.020372971309));
#249692=CARTESIAN_POINT('Ctrl Pts',(143.836592254767,-3.64667596185081,
125.779729448496));
#249693=CARTESIAN_POINT('Ctrl Pts',(143.558144630954,-6.19848193988065,
131.156476503179));
#249694=CARTESIAN_POINT('Ctrl Pts',(143.279697007141,-3.05418582783736,
136.209646260801));
#249695=CARTESIAN_POINT('Ctrl Pts',(143.001249383328,2.89675785471595,136.295622575173));
#249696=CARTESIAN_POINT('Ctrl Pts',(142.722801759515,6.18572258327378,131.335397413564));
#249697=CARTESIAN_POINT('Ctrl Pts',(142.444354135702,3.79031044715096,125.887175379022));
#249698=CARTESIAN_POINT('Ctrl Pts',(142.165906511889,-2.0882118229442,124.957606360848));
#249699=CARTESIAN_POINT('Ctrl Pts',(141.887458888076,-6.04776944257254,
129.400918874772));
#249700=CARTESIAN_POINT('Ctrl Pts',(141.609011264264,-4.44972239443904,
135.133925788383));
#249701=CARTESIAN_POINT('Ctrl Pts',(141.33056364045,1.2374021531599,136.888273821029));
#249702=CARTESIAN_POINT('Ctrl Pts',(141.052116016638,5.78741457246075,133.051802835376));
#249703=CARTESIAN_POINT('Ctrl Pts',(140.773668392825,5.01907573059014,127.15004224521));
#249704=CARTESIAN_POINT('Ctrl Pts',(140.495220769012,-0.361548512212229,
124.606421715863));
#249705=CARTESIAN_POINT('Ctrl Pts',(140.216773145199,-5.4099273349182,127.758404251031));
#249706=CARTESIAN_POINT('Ctrl Pts',(139.938325521386,-5.48684722647749,
133.709471883804));
#249707=CARTESIAN_POINT('Ctrl Pts',(139.659877897573,-0.521622564292735,
136.990884185479));
#249708=CARTESIAN_POINT('Ctrl Pts',(139.38143027376,4.92294775179823,134.58718355672));
#249709=CARTESIAN_POINT('Ctrl Pts',(139.102982649947,5.84356958335437,128.707253448052));
#249710=CARTESIAN_POINT('Ctrl Pts',(138.824535026135,1.39423644205237,124.754462378786));
#249711=CARTESIAN_POINT('Ctrl Pts',(138.546087402322,-4.33633187725888,
126.361232236999));
#249712=CARTESIAN_POINT('Ctrl Pts',(138.267639778509,-6.08202304295846,
132.051020018064));
#249713=CARTESIAN_POINT('Ctrl Pts',(137.989192154696,-2.23863215552307,
136.595188712768));
#249714=CARTESIAN_POINT('Ctrl Pts',(137.710744530883,3.66195231957746,135.817869285661));
#249715=CARTESIAN_POINT('Ctrl Pts',(137.43229690707,6.19738150930245,130.433380316089));
#249716=CARTESIAN_POINT('Ctrl Pts',(137.153849283257,3.03771985089675,125.389804120178));
#249717=CARTESIAN_POINT('Ctrl Pts',(136.875401659444,-2.91345794961824,
125.321940829576));
#249718=CARTESIAN_POINT('Ctrl Pts',(136.596954035631,-6.1873102247676,130.29215349304));
#249719=CARTESIAN_POINT('Ctrl Pts',(136.318506411819,-3.77532667026395,
135.733059481234));
#249720=CARTESIAN_POINT('Ctrl Pts',(136.040058788006,2.10599765925102,136.644731994041));
#249721=CARTESIAN_POINT('Ctrl Pts',(135.761611164193,6.05201302361958,132.189388529871));
#249722=CARTESIAN_POINT('Ctrl Pts',(135.48316354038,4.4365240765547,126.461272076668));
#249723=CARTESIAN_POINT('Ctrl Pts',(135.204715916567,-1.25591376061384,
124.724241820878));
#249724=CARTESIAN_POINT('Ctrl Pts',(134.926268292754,-5.79422820657625,
128.574543708929));
#249725=CARTESIAN_POINT('Ctrl Pts',(134.647820668941,-5.00792999447956,
134.473938403405));
#249726=CARTESIAN_POINT('Ctrl Pts',(134.369373045128,0.380411231562576,
137.001170381535));
#249727=CARTESIAN_POINT('Ctrl Pts',(134.090925421316,5.41917311992063,133.833836917565));
#249728=CARTESIAN_POINT('Ctrl Pts',(133.812477797503,5.4779796523963,127.88256273204));
#249729=CARTESIAN_POINT('Ctrl Pts',(133.53403017369,0.502790498503515,124.616278065551));
#249730=CARTESIAN_POINT('Ctrl Pts',(133.255582549877,-4.93443856083268,
127.036538959725));
#249731=CARTESIAN_POINT('Ctrl Pts',(132.977134926064,-5.83715964348875,
132.919243889133));
#249732=CARTESIAN_POINT('Ctrl Pts',(132.698687302251,-1.37581617488021,
136.858474409763));
#249733=CARTESIAN_POINT('Ctrl Pts',(132.420239678438,4.34983514608645,135.234270115264));
#249734=CARTESIAN_POINT('Ctrl Pts',(132.141792054625,6.07820046906025,129.539195405491));
#249735=CARTESIAN_POINT('Ctrl Pts',(131.863344430812,2.22099649756843,125.006745718858));
#249736=CARTESIAN_POINT('Ctrl Pts',(131.584896806999,-3.67719475347803,
125.802020894903));
#249737=CARTESIAN_POINT('Ctrl Pts',(131.306449183186,-6.1962236670286,131.194201898194));
#249738=CARTESIAN_POINT('Ctrl Pts',(131.028001559374,-3.02122573293442,
136.228137809392));
#249739=CARTESIAN_POINT('Ctrl Pts',(130.749553935561,2.93013105464412,136.277887447547));
#249740=CARTESIAN_POINT('Ctrl Pts',(130.471106311748,6.18884054786473,131.2977333256));
#249741=CARTESIAN_POINT('Ctrl Pts',(130.192658687935,3.76030791926647,125.864193787566));
#249742=CARTESIAN_POINT('Ctrl Pts',(129.914211064122,-2.12376398588317,
124.970426225734));
#249743=CARTESIAN_POINT('Ctrl Pts',(129.635763440309,-6.05620053964477,
129.437759366456));
#249744=CARTESIAN_POINT('Ctrl Pts',(129.357315816496,-4.42328465931731,
135.160932294765));
#249745=CARTESIAN_POINT('Ctrl Pts',(129.078868192683,1.27441373345414,136.880628682086));
#249746=CARTESIAN_POINT('Ctrl Pts',(128.800420568871,5.80098816375315,133.01653156031));
#249747=CARTESIAN_POINT('Ctrl Pts',(128.521972945058,4.99673786558976,127.11955741271));
#249748=CARTESIAN_POINT('Ctrl Pts',(128.243525321245,-0.399270426835251,
124.608737397728));
#249749=CARTESIAN_POINT('Ctrl Pts',(127.965077697432,-5.42836870244348,
127.791392448756));
#249750=CARTESIAN_POINT('Ctrl Pts',(127.686630073619,-5.46906133106002,
133.742818055242));
#249751=CARTESIAN_POINT('Ctrl Pts',(127.408182449806,-0.483953774931917,
136.993944828129));
#249752=CARTESIAN_POINT('Ctrl Pts',(127.129734825993,4.9458836579024,134.557146089508));
#249753=CARTESIAN_POINT('Ctrl Pts',(126.85128720218,5.8306956289736,128.671720835934));
#249754=CARTESIAN_POINT('Ctrl Pts',(126.572839578367,1.35738316233494,124.746087356435));
#249755=CARTESIAN_POINT('Ctrl Pts',(126.294391954555,-4.36329811863544,
126.387711040812));
#249756=CARTESIAN_POINT('Ctrl Pts',(126.015944330741,-6.07432158754323,
132.088019920899));
#249757=CARTESIAN_POINT('Ctrl Pts',(125.737496706929,-2.20334026460562,
136.608708611466));
#249758=CARTESIAN_POINT('Ctrl Pts',(125.459049083116,3.69240312234872,135.795485053802));
#249759=CARTESIAN_POINT('Ctrl Pts',(125.180601459303,6.19500842378515,130.39566196922));
#249760=CARTESIAN_POINT('Ctrl Pts',(124.90215383549,3.00470362674961,125.371412976429));
#249761=CARTESIAN_POINT('Ctrl Pts',(124.623706211677,-2.9467770153362,125.339777451594));
#249762=CARTESIAN_POINT('Ctrl Pts',(124.345258587864,-6.19031353838844,
130.329826896558));
#249763=CARTESIAN_POINT('Ctrl Pts',(124.066810964051,-3.74525433329013,
135.755949648866));
#249764=CARTESIAN_POINT('Ctrl Pts',(123.788363340238,2.14151063825588,136.631803979981));
#249765=CARTESIAN_POINT('Ctrl Pts',(123.509915716426,6.0603319518555,132.152522547471));
#249766=CARTESIAN_POINT('Ctrl Pts',(123.231468092613,4.4100042653751,126.43434616275));
#249767=CARTESIAN_POINT('Ctrl Pts',(122.9530204688,-1.29290190029971,124.731999574929));
#249768=CARTESIAN_POINT('Ctrl Pts',(122.674572844987,-5.80769438136815,
128.609856133963));
#249769=CARTESIAN_POINT('Ctrl Pts',(122.396125221174,-4.98549944760296,
134.504355105923));
#249770=CARTESIAN_POINT('Ctrl Pts',(122.117677597361,0.418125923321227,
136.998739897863));
#249771=CARTESIAN_POINT('Ctrl Pts',(121.839229973548,5.43751399730024,133.80079274346));
#249772=CARTESIAN_POINT('Ctrl Pts',(121.560782349735,5.46009234508668,127.849270849208));
#249773=CARTESIAN_POINT('Ctrl Pts',(121.282334725922,0.465112568078527,
124.613332087916));
#249774=CARTESIAN_POINT('Ctrl Pts',(121.00388710211,-4.95728293698158,127.066646096814));
#249775=CARTESIAN_POINT('Ctrl Pts',(120.725439478297,-5.82417759969065,
132.954737152777));
#249776=CARTESIAN_POINT('Ctrl Pts',(120.446991854484,-1.33893757517749,
136.866737224615));
#249777=CARTESIAN_POINT('Ctrl Pts',(120.168544230671,4.37672067018674,135.207709358136));
#249778=CARTESIAN_POINT('Ctrl Pts',(119.890096606858,6.07038643434081,129.502219114618));
#249779=CARTESIAN_POINT('Ctrl Pts',(119.611648983045,2.18566362019961,124.993333299159));
#249780=CARTESIAN_POINT('Ctrl Pts',(119.333201359232,-3.7075772853013,125.82449770485));
#249781=CARTESIAN_POINT('Ctrl Pts',(119.054753735419,-6.19373579082994,
131.231912847497));
#249782=CARTESIAN_POINT('Ctrl Pts',(118.776306111606,-2.98815368540088,
136.246428377926));
#249783=CARTESIAN_POINT('Ctrl Pts',(118.497858487794,2.96339567748857,136.259949496373));
#249784=CARTESIAN_POINT('Ctrl Pts',(118.219410863981,6.1917291826932,131.26005095553));
#249785=CARTESIAN_POINT('Ctrl Pts',(117.940963240168,3.73016605178927,125.841395255808));
#249786=CARTESIAN_POINT('Ctrl Pts',(117.662515616355,-2.15923745196658,
124.983462269205));
#249787=CARTESIAN_POINT('Ctrl Pts',(117.384067992542,-6.06440722197891,
129.474650498052));
#249788=CARTESIAN_POINT('Ctrl Pts',(117.105620368729,-4.39668301775581,
135.187777366781));
#249789=CARTESIAN_POINT('Ctrl Pts',(116.827172744916,1.31137808987868,136.872758384795));
#249790=CARTESIAN_POINT('Ctrl Pts',(116.548725121103,5.81434679729579,132.981178312436));
#249791=CARTESIAN_POINT('Ctrl Pts',(116.27027749729,4.97421484463032,127.089209121948));
#249792=CARTESIAN_POINT('Ctrl Pts',(115.991829873478,-0.436977546345769,
124.611282660692));
#249793=CARTESIAN_POINT('Ctrl Pts',(115.713382249665,-5.44660891977013,
127.824492293124));
#249794=CARTESIAN_POINT('Ctrl Pts',(115.434934625852,-5.45107277756375,
133.776055341058));
#249795=CARTESIAN_POINT('Ctrl Pts',(115.156487002039,-0.446267052485976,
136.99677611346));
#249796=CARTESIAN_POINT('Ctrl Pts',(114.878039378226,4.9686362924688,134.526969561451));
#249797=CARTESIAN_POINT('Ctrl Pts',(114.599591754413,5.81760561602206,128.636267249567));
#249798=CARTESIAN_POINT('Ctrl Pts',(114.3211441306,1.32047958428524,124.737936825626));
#249799=CARTESIAN_POINT('Ctrl Pts',(114.042696506787,-4.39010267639563,
126.414353505198));
#249800=CARTESIAN_POINT('Ctrl Pts',(113.764248882975,-6.06639504590774,
132.124972257267));
#249801=CARTESIAN_POINT('Ctrl Pts',(113.485801259161,-2.16796672810439,
136.622013427915));
#249802=CARTESIAN_POINT('Ctrl Pts',(113.207353635349,3.72271710176439,135.772915873991));
#249803=CARTESIAN_POINT('Ctrl Pts',(112.928906011536,6.19240577995249,130.357958766832));
#249804=CARTESIAN_POINT('Ctrl Pts',(112.650458387723,2.97157606220462,125.353223152553));
#249805=CARTESIAN_POINT('Ctrl Pts',(112.37201076391,-2.9799868871482,125.357816565752));
#249806=CARTESIAN_POINT('Ctrl Pts',(112.093563140097,-6.19308746766462,
130.367517884098));
#249807=CARTESIAN_POINT('Ctrl Pts',(111.815115516284,-3.71504321453968,
135.778656333547));
#249808=CARTESIAN_POINT('Ctrl Pts',(111.536667892471,2.1769442627965,136.618660027865));
#249809=CARTESIAN_POINT('Ctrl Pts',(111.258220268658,6.06842631226225,132.115606608435));
#249810=CARTESIAN_POINT('Ctrl Pts',(110.979772644846,4.38332103986566,126.407582181323));
#249811=CARTESIAN_POINT('Ctrl Pts',(110.701325021032,-1.32984213103019,
124.739982342551));
#249812=CARTESIAN_POINT('Ctrl Pts',(110.42287739722,-5.82094534990898,128.645249877167));
#249813=CARTESIAN_POINT('Ctrl Pts',(110.144429773407,-4.96288416121089,
134.534634703787));
#249814=CARTESIAN_POINT('Ctrl Pts',(109.865982149594,0.455825121270016,
136.996079879188));
#249815=CARTESIAN_POINT('Ctrl Pts',(109.587534525781,5.45565338559904,133.767637535461));
#249816=CARTESIAN_POINT('Ctrl Pts',(109.309086901968,5.44200271204727,127.816088468313));
#249817=CARTESIAN_POINT('Ctrl Pts',(109.030639278155,0.427417402736423,
124.610615521118));
#249818=CARTESIAN_POINT('Ctrl Pts',(108.752191654342,-4.97994361918818,
127.096891736289));
#249819=CARTESIAN_POINT('Ctrl Pts',(108.473744030529,-5.81097973884976,
132.990150733429));
#249820=CARTESIAN_POINT('Ctrl Pts',(108.195296406717,-1.30200936065053,
136.874775395874));
#249821=CARTESIAN_POINT('Ctrl Pts',(107.916848782904,4.40344401329306,135.180985433302));
#249822=CARTESIAN_POINT('Ctrl Pts',(107.638401159091,6.06234745921968,129.465291075077));
#249823=CARTESIAN_POINT('Ctrl Pts',(107.359953535278,2.15024975226158,124.980136209215));
#249824=CARTESIAN_POINT('Ctrl Pts',(107.081505911465,-3.73782243148481,
125.847159045447));
#249825=CARTESIAN_POINT('Ctrl Pts',(106.803058287652,-6.19101840347381,
131.269607953695));
#249826=CARTESIAN_POINT('Ctrl Pts',(106.524610663839,-2.95497091073364,
136.264517288637));
#249827=CARTESIAN_POINT('Ctrl Pts',(106.246163040026,2.99655049061638,136.241809386346));
#249828=CARTESIAN_POINT('Ctrl Pts',(105.967715416213,6.1943883807198,131.222351699685));
#249829=CARTESIAN_POINT('Ctrl Pts',(105.689267792401,3.69988596163724,125.818780628557));
#249830=CARTESIAN_POINT('Ctrl Pts',(105.410820168588,-2.19463090671215,
124.996714008204));
#249831=CARTESIAN_POINT('Ctrl Pts',(105.132372544775,-6.07238918547325,
129.511590902545));
#249832=CARTESIAN_POINT('Ctrl Pts',(104.853924920962,-4.36991845548819,
135.214460009678));
#249833=CARTESIAN_POINT('Ctrl Pts',(104.575477297149,1.34829385270585,136.864663220793));
#249834=CARTESIAN_POINT('Ctrl Pts',(104.297029673336,5.82748997807964,132.945744401783));
#249835=CARTESIAN_POINT('Ctrl Pts',(104.018582049523,4.95150750231056,127.058998497491));
#249836=CARTESIAN_POINT('Ctrl Pts',(103.74013442571,-0.474668473492613,
124.614057410436));
#249837=CARTESIAN_POINT('Ctrl Pts',(103.461686801897,-5.46464731100027,
127.857702557609));
#249838=CARTESIAN_POINT('Ctrl Pts',(103.183239178085,-5.43288223256107,
133.809182509633));
#249839=CARTESIAN_POINT('Ctrl Pts',(102.904791554272,-0.408563793450433,
136.999377936557));
#249840=CARTESIAN_POINT('Ctrl Pts',(102.626343930459,4.99120481239017,134.496655090749));
#249841=CARTESIAN_POINT('Ctrl Pts',(102.347896306646,5.80430002955499,128.600894002697));
#249842=CARTESIAN_POINT('Ctrl Pts',(102.069448682833,1.28352707537895,124.730011088381));
#249843=CARTESIAN_POINT('Ctrl Pts',(101.79100105902,-4.41674455728669,126.441158642913));
#249844=CARTESIAN_POINT('Ctrl Pts',(101.512553435207,-6.05824371177293,
132.161875657885));
#249845=CARTESIAN_POINT('Ctrl Pts',(101.234105811394,-2.13251285679878,
136.635102669099));
#249846=CARTESIAN_POINT('Ctrl Pts',(100.955658187581,3.75289313452884,135.750162582539));
#249847=CARTESIAN_POINT('Ctrl Pts',(100.677210563769,6.18957367424645,130.320272106026));
#249848=CARTESIAN_POINT('Ctrl Pts',(100.398762939956,2.93833838481571,125.33523532258));
#249849=CARTESIAN_POINT('Ctrl Pts',(100.120315316143,-3.01308633445025,
125.376057503601));
#249850=CARTESIAN_POINT('Ctrl Pts',(99.8418676923298,-6.19563190980719,
130.405225059005));
#249851=CARTESIAN_POINT('Ctrl Pts',(99.5634200685172,-3.68469443349671,
135.801178693871));
#249852=CARTESIAN_POINT('Ctrl Pts',(99.2849724447041,2.2122972198669,136.605300624745));
#249853=CARTESIAN_POINT('Ctrl Pts',(99.0065248208913,6.07629580490035,132.078642080696));
#249854=CARTESIAN_POINT('Ctrl Pts',(98.7280771970783,4.35647538878314,126.380981124141));
#249855=CARTESIAN_POINT('Ctrl Pts',(98.4496295732656,-1.36673308397146,
124.748189827941));
#249856=CARTESIAN_POINT('Ctrl Pts',(98.1711819494526,-5.8339806211792,128.680723627015));
#249857=CARTESIAN_POINT('Ctrl Pts',(97.8927343256397,-4.94008497332115,
134.564776074971));
#249858=CARTESIAN_POINT('Ctrl Pts',(97.6142867018267,0.493507428451318,
136.993190424079));
#249859=CARTESIAN_POINT('Ctrl Pts',(97.3358390780141,5.47359061265531,133.734372522146));
#249860=CARTESIAN_POINT('Ctrl Pts',(97.0573914542009,5.42371142359607,127.783016818942));
#249861=CARTESIAN_POINT('Ctrl Pts',(96.7789438303882,0.389706399285272,
124.608128465823));
#249862=CARTESIAN_POINT('Ctrl Pts',(96.5004962065753,-5.0024197677526,127.127274757387));
#249863=CARTESIAN_POINT('Ctrl Pts',(96.2220485827623,-5.79756655001767,
133.025483318824));
#249864=CARTESIAN_POINT('Ctrl Pts',(95.9436009589496,-1.26503289968789,
136.882588625681));
#249865=CARTESIAN_POINT('Ctrl Pts',(95.6651533351365,4.4300041851621,135.154099331026));
#249866=CARTESIAN_POINT('Ctrl Pts',(95.3867057113237,6.05408384158403,129.428412655251));
#249867=CARTESIAN_POINT('Ctrl Pts',(95.1082580875108,2.11475620602821,124.967154938047));
#249868=CARTESIAN_POINT('Ctrl Pts',(94.8298104636979,-3.76792907128354,
125.870004076972));
#249869=CARTESIAN_POINT('Ctrl Pts',(94.5513628398851,-6.18807160565406,
131.307285819983));
#249870=CARTESIAN_POINT('Ctrl Pts',(94.2729152160721,-2.92167863853249,
136.282403871234));
#249871=CARTESIAN_POINT('Ctrl Pts',(93.9944675922592,3.02959426546386,136.223467789656));
#249872=CARTESIAN_POINT('Ctrl Pts',(93.7160199684464,6.19681804340696,131.184636955029));
#249873=CARTESIAN_POINT('Ctrl Pts',(93.4375723446334,3.66946877085029,125.796350743805));
#249874=CARTESIAN_POINT('Ctrl Pts',(93.1591247208205,-2.22994303860241,
125.010180951684));
#249875=CARTESIAN_POINT('Ctrl Pts',(92.8806770970077,-6.08014613435319,
129.548579211095));
#249876=CARTESIAN_POINT('Ctrl Pts',(92.6022294731947,-4.3429919642852,135.24097923472));
#249877=CARTESIAN_POINT('Ctrl Pts',(92.323781849382,1.38515965400848,136.856343490049));
#249878=CARTESIAN_POINT('Ctrl Pts',(92.045334225569,5.84041721907928,132.910231141365));
#249879=CARTESIAN_POINT('Ctrl Pts',(91.7668866017561,4.9286166800594,127.028926658805));
#249880=CARTESIAN_POINT('Ctrl Pts',(91.4884389779432,-0.512341811624615,
124.617061544141));
#249881=CARTESIAN_POINT('Ctrl Pts',(91.2099913541303,-5.48248320771468,
127.891022011592));
#249882=CARTESIAN_POINT('Ctrl Pts',(90.9315437303175,-5.41449037010934,
133.842198333429));
#249883=CARTESIAN_POINT('Ctrl Pts',(90.6530961065044,-0.370845394933272,
137.00175020101));
#249884=CARTESIAN_POINT('Ctrl Pts',(90.3746484826917,5.01358838138169,134.466203800718));
#249885=CARTESIAN_POINT('Ctrl Pts',(90.0962008588786,5.79077936261581,128.565602406094));
#249886=CARTESIAN_POINT('Ctrl Pts',(89.817753235066,1.24652700490487,124.722310438393));
#249887=CARTESIAN_POINT('Ctrl Pts',(89.5393056112528,-4.44322277408392,
126.468125460682));
#249888=CARTESIAN_POINT('Ctrl Pts',(89.2608579874402,-6.04986788718945,
132.198728755283));
#249889=CARTESIAN_POINT('Ctrl Pts',(88.9824103636271,-2.09697996444503,
136.647975849991));
#249890=CARTESIAN_POINT('Ctrl Pts',(88.7039627398144,3.78293010245805,135.727226022576));
#249891=CARTESIAN_POINT('Ctrl Pts',(88.4255151160013,6.18651221161165,130.282603383299));
#249892=CARTESIAN_POINT('Ctrl Pts',(88.1470674921886,2.9049918262175,125.317450153056));
#249893=CARTESIAN_POINT('Ctrl Pts',(87.8686198683756,-3.04607413073006,
125.394499589218));
#249894=CARTESIAN_POINT('Ctrl Pts',(87.5901722445627,-6.19794677053091,
130.442947024027));
#249895=CARTESIAN_POINT('Ctrl Pts',(87.3117246207499,-3.65420911474647,
135.823515895262));
#249896=CARTESIAN_POINT('Ctrl Pts',(87.033276996937,2.24756819945024,136.59172626566));
#249897=CARTESIAN_POINT('Ctrl Pts',(86.754829373124,6.08394013816284,132.041630333989));
#249898=CARTESIAN_POINT('Ctrl Pts',(86.4763817493112,4.32946830690299,126.35454397691));
#249899=CARTESIAN_POINT('Ctrl Pts',(86.1979341254982,-1.40357339211569,
124.756621726966));
#249900=CARTESIAN_POINT('Ctrl Pts',(85.9194865016854,-5.84679971215209,
128.716276069012));
#249901=CARTESIAN_POINT('Ctrl Pts',(85.6410388778725,-4.91710272876601,
134.594778102578));
#249902=CARTESIAN_POINT('Ctrl Pts',(85.3625912540596,0.531171448533366,
136.990071639606));
#249903=CARTESIAN_POINT('Ctrl Pts',(85.0841436302467,5.49132501379855,133.700998936161));
#249904=CARTESIAN_POINT('Ctrl Pts',(84.8056960064338,5.4052191575235,127.750057126576));
#249905=CARTESIAN_POINT('Ctrl Pts',(84.527248382621,0.351980955120191,124.60587101419));
#249906=CARTESIAN_POINT('Ctrl Pts',(84.2488007588079,-5.02471054981291,
127.157794034254));
#249907=CARTESIAN_POINT('Ctrl Pts',(83.9703531349953,-5.78393853022499,
133.0607335997));
#249908=CARTESIAN_POINT('Ctrl Pts',(83.6919055111822,-1.22800956246596,
136.890176624513));
#249909=CARTESIAN_POINT('Ctrl Pts',(83.4134578873695,4.45640020159694,135.127052047582));
#249910=CARTESIAN_POINT('Ctrl Pts',(83.1350102635564,6.04559588764522,129.391585221682));
#249911=CARTESIAN_POINT('Ctrl Pts',(82.8565626397436,2.07918429672594,124.954389966684));
#249912=CARTESIAN_POINT('Ctrl Pts',(82.5781150159307,-3.79789608908488,
125.893031952893));
#249913=CARTESIAN_POINT('Ctrl Pts',(82.2996673921181,-6.18489550656524,
131.344945050191));
#249914=CARTESIAN_POINT('Ctrl Pts',(82.0212197683047,-2.88827810245507,
136.300087462925));
#249915=CARTESIAN_POINT('Ctrl Pts',(81.7427721444922,3.06252577758164,136.204925385956));
#249916=CARTESIAN_POINT('Ctrl Pts',(81.464324520679,6.19901808072266,131.146908119091));
#249917=CARTESIAN_POINT('Ctrl Pts',(81.1858768968663,3.6389156065486,125.774106432701));
#249918=CARTESIAN_POINT('Ctrl Pts',(80.9074292730533,-2.26517253913331,
125.023862600622));
#249919=CARTESIAN_POINT('Ctrl Pts',(80.6289816492404,-6.08767778118217,
129.585614053086));
#249920=CARTESIAN_POINT('Ctrl Pts',(80.3505340254275,-4.31590454191782,
135.267334059228));
#249921=CARTESIAN_POINT('Ctrl Pts',(80.0720864016147,1.42197412771073,136.847799500855));
#249922=CARTESIAN_POINT('Ctrl Pts',(79.7936387778018,5.85312804127117,132.874639847142));
#249923=CARTESIAN_POINT('Ctrl Pts',(79.5151911539889,4.90554322610457,126.998994720211));
#249924=CARTESIAN_POINT('Ctrl Pts',(79.236743530176,-0.54999616474248,124.62029495049));
#249925=CARTESIAN_POINT('Ctrl Pts',(78.9582959063631,-5.50011594899764,
127.924449420408));
#249926=CARTESIAN_POINT('Ctrl Pts',(78.6798482825503,-5.39589787172579,
133.87510158903));
#249927=CARTESIAN_POINT('Ctrl Pts',(78.4014006587372,-0.333113254603616,
137.003892818912));
#249928=CARTESIAN_POINT('Ctrl Pts',(78.1229530349246,5.035786170012,134.435616819741));
#249929=CARTESIAN_POINT('Ctrl Pts',(77.8445054111114,5.77704411621779,128.530393767498));
#249930=CARTESIAN_POINT('Ctrl Pts',(77.5660577872988,1.20948074391421,124.71483516101));
#249931=CARTESIAN_POINT('Ctrl Pts',(77.2876101634857,-4.46953634562727,
126.49525295924));
#249932=CARTESIAN_POINT('Ctrl Pts',(77.009162539673,-6.04126788252658,132.235530183857));
#249933=CARTESIAN_POINT('Ctrl Pts',(76.73071491586,-2.06136936772754,136.660632493573));
#249934=CARTESIAN_POINT('Ctrl Pts',(76.4522672920471,3.81282689252116,135.704107044024));
#249935=CARTESIAN_POINT('Ctrl Pts',(76.1738196682342,6.18322150549176,130.244953994479));
#249936=CARTESIAN_POINT('Ctrl Pts',(75.8953720444213,2.87153762207887,125.299868303017));
#249937=CARTESIAN_POINT('Ctrl Pts',(75.6169244206085,-3.07894905361277,
125.413142139227));
#249938=CARTESIAN_POINT('Ctrl Pts',(75.3384767967955,-6.20003196405775,
130.480682381363));
#249939=CARTESIAN_POINT('Ctrl Pts',(75.0600291729826,-3.62358838793365,
135.84566711001));
#249940=CARTESIAN_POINT('Ctrl Pts',(74.7815815491698,2.28275589456742,136.577937453613));
#249941=CARTESIAN_POINT('Ctrl Pts',(74.5031339253568,6.09135902878616,132.004572739798));
#249942=CARTESIAN_POINT('Ctrl Pts',(74.224686301544,4.30230079498258,126.328271719272));
#249943=CARTESIAN_POINT('Ctrl Pts',(73.946238677731,-1.44036169033171,124.76527772718));
#249944=CARTESIAN_POINT('Ctrl Pts',(73.6677910539182,-5.85940214781156,
128.75190588575));
#249945=CARTESIAN_POINT('Ctrl Pts',(73.3893434301052,-4.89393827916089,
134.624639674871));
#249946=CARTESIAN_POINT('Ctrl Pts',(73.1108958062924,0.56881578586215,136.986723641335));
#249947=CARTESIAN_POINT('Ctrl Pts',(72.8324481824796,5.50885593187395,133.66751801418));
#249948=CARTESIAN_POINT('Ctrl Pts',(72.5540005586665,5.38652659906729,127.717210612549));
#249949=CARTESIAN_POINT('Ctrl Pts',(72.2755529348538,0.314242468171368,
124.603843249867));
#249950=CARTESIAN_POINT('Ctrl Pts',(71.9971053110409,-5.04681513937595,
127.188448435987));
#249951=CARTESIAN_POINT('Ctrl Pts',(71.7186576872279,-5.77009618446306,
133.095900269846));
#249952=CARTESIAN_POINT('Ctrl Pts',(71.4402100634152,-1.19094072089807,
136.897539111196));
#249953=CARTESIAN_POINT('Ctrl Pts',(71.1617624396021,4.48263108448347,135.099844585217));
#249954=CARTESIAN_POINT('Ctrl Pts',(70.8833148157894,6.03688391192757,129.354810139024));
#249955=CARTESIAN_POINT('Ctrl Pts',(70.6048671919763,2.04353534248492,124.941841768133));
#249956=CARTESIAN_POINT('Ctrl Pts',(70.3264195681636,-3.82772237444985,
125.916241819903));
#249957=CARTESIAN_POINT('Ctrl Pts',(70.0479719443506,-6.18149022389895,
131.382584248845));
#249958=CARTESIAN_POINT('Ctrl Pts',(69.7695243205378,-2.85477054017052,
136.317567408437));
#249959=CARTESIAN_POINT('Ctrl Pts',(69.4910766967249,3.09534380668036,136.186182862342));
#249960=CARTESIAN_POINT('Ctrl Pts',(69.2126290729119,6.20098841114368,131.109166589932));
#249961=CARTESIAN_POINT('Ctrl Pts',(68.934181449099,3.60822760089105,125.752048519516));
#249962=CARTESIAN_POINT('Ctrl Pts',(68.6557338252862,-2.30031810286251,
125.037758448041));
#249963=CARTESIAN_POINT('Ctrl Pts',(68.3772862014732,-6.09498384687224,
129.622694056181));
#249964=CARTESIAN_POINT('Ctrl Pts',(68.0988385776604,-4.28865719212064,
135.293523506613));
#249965=CARTESIAN_POINT('Ctrl Pts',(67.8203909538475,1.45873590963839,136.83903156981));
#249966=CARTESIAN_POINT('Ctrl Pts',(67.5419433300346,5.86562197365073,132.83897183796));
#249967=CARTESIAN_POINT('Ctrl Pts',(67.2634957062218,4.88228799544191,126.969203790852));
#249968=CARTESIAN_POINT('Ctrl Pts',(66.9850480824087,-0.587630137549865,
124.623757509667));
#249969=CARTESIAN_POINT('Ctrl Pts',(66.706600458596,-5.51754488146136,127.957983545393));
#249970=CARTESIAN_POINT('Ctrl Pts',(66.428152834783,-5.37710542636232,133.907891057196));
#249971=CARTESIAN_POINT('Ctrl Pts',(66.1497052109702,-0.295368770640213,
137.00580571087));
#249972=CARTESIAN_POINT('Ctrl Pts',(65.8712575871573,5.05779735573374,134.404895281231));
#249973=CARTESIAN_POINT('Ctrl Pts',(65.5928099633443,5.76309479932555,128.495269391582));
#249974=CARTESIAN_POINT('Ctrl Pts',(65.3143623395316,1.17238966517029,124.707585533234));
#249975=CARTESIAN_POINT('Ctrl Pts',(65.0359147157185,-4.49568429685739,
126.522540133366));
#249976=CARTESIAN_POINT('Ctrl Pts',(64.7574670919057,-6.03244401646077,
132.272278579917));
#249977=CARTESIAN_POINT('Ctrl Pts',(64.4790194680927,-2.02568238621027,
136.673072130848));
#249978=CARTESIAN_POINT('Ctrl Pts',(64.20057184428,3.84258239688126,135.680806503568));
#249979=CARTESIAN_POINT('Ctrl Pts',(63.922124220467,6.17970167782515,130.207325334677));
#249980=CARTESIAN_POINT('Ctrl Pts',(63.6436765966542,2.8379770120581,125.282490423967));
#249981=CARTESIAN_POINT('Ctrl Pts',(63.3652289728412,-3.11170988490585,
125.431984462817));
#249982=CARTESIAN_POINT('Ctrl Pts',(63.0867813490283,-6.20188741312008,
130.518429732716));
#249983=CARTESIAN_POINT('Ctrl Pts',(62.8083337252156,-3.59283338772076,
135.86763151729));
#249984=CARTESIAN_POINT('Ctrl Pts',(62.5298861014024,2.31785900132509,136.563934699553));
#249985=CARTESIAN_POINT('Ctrl Pts',(62.2514384775899,6.09855220186056,131.967470671305));
#249986=CARTESIAN_POINT('Ctrl Pts',(61.9729908537767,4.27497385972414,126.302165324755));
#249987=CARTESIAN_POINT('Ctrl Pts',(61.6945432299639,-1.47709661541541,
124.774157507831));
#249988=CARTESIAN_POINT('Ctrl Pts',(61.416095606151,-5.87178746116934,128.787611756953));
#249989=CARTESIAN_POINT('Ctrl Pts',(61.1376479823382,-4.8705924828735,134.65435968532));
#249990=CARTESIAN_POINT('Ctrl Pts',(60.8592003585251,0.606439045512412,
136.983146553331));
#249991=CARTESIAN_POINT('Ctrl Pts',(60.5807527347125,5.52618271726667,133.633930996847));
#249992=CARTESIAN_POINT('Ctrl Pts',(60.3023051108993,5.36763444088732,127.684478494003));
#249993=CARTESIAN_POINT('Ctrl Pts',(60.0238574870866,0.276492336852797,
124.602045247997));
#249994=CARTESIAN_POINT('Ctrl Pts',(59.7454098632736,-5.06873271734795,
127.219236826675));
#249995=CARTESIAN_POINT('Ctrl Pts',(59.4669622394608,-5.75604002566515,
133.130982026147));
#249996=CARTESIAN_POINT('Ctrl Pts',(59.1885146156479,-1.15382774858414,
136.904675812908));
#249997=CARTESIAN_POINT('Ctrl Pts',(58.9100669918351,4.50869586182645,135.072477952114));
#249998=CARTESIAN_POINT('Ctrl Pts',(58.6316193680221,6.02794823725661,129.318088769994));
#249999=CARTESIAN_POINT('Ctrl Pts',(58.3531717442092,2.00781066429043,124.929510807376));
#250000=CARTESIAN_POINT('Ctrl Pts',(58.0747241203963,-3.85740682215468,
125.939632817953));
#250001=CARTESIAN_POINT('Ctrl Pts',(57.7962764965834,-6.17785588383907,
131.42020202121));
#250002=CARTESIAN_POINT('Ctrl Pts',(57.5178288727705,-2.82115719331391,
136.334843060042));
#250003=CARTESIAN_POINT('Ctrl Pts',(57.2393812489577,3.12804713667602,136.167240913326));
#250004=CARTESIAN_POINT('Ctrl Pts',(56.9609336251447,6.20272896165862,131.071413766074));
#250005=CARTESIAN_POINT('Ctrl Pts',(56.6824860013319,3.57740589103289,125.730177821614));
#250006=CARTESIAN_POINT('Ctrl Pts',(56.404038377519,-2.33537842745856,125.051867979023));
#250007=CARTESIAN_POINT('Ctrl Pts',(56.125590753706,-6.10206406069443,129.659817846364));
#250008=CARTESIAN_POINT('Ctrl Pts',(55.8471431298932,-4.26125092455389,
135.319546606417));
#250009=CARTESIAN_POINT('Ctrl Pts',(55.5686955060803,1.49544363757083,136.830040021814));
#250010=CARTESIAN_POINT('Ctrl Pts',(55.2902478822675,5.87789855325116,132.80322843551));
#250011=CARTESIAN_POINT('Ctrl Pts',(55.0118002584545,4.85885184980179,126.939554974638));
#250012=CARTESIAN_POINT('Ctrl Pts',(54.7333526346416,-0.625242335506623,
124.627449093364));
#250013=CARTESIAN_POINT('Ctrl Pts',(54.4549050108287,-5.53476935927053,
127.991623143927));
#250014=CARTESIAN_POINT('Ctrl Pts',(54.1764573870159,-5.35811373037978,
133.9405655229));
#250015=CARTESIAN_POINT('Ctrl Pts',(53.8980097632029,-0.257613341678002,
137.007488805997));
#250016=CARTESIAN_POINT('Ctrl Pts',(53.61956213939,5.07962112291461,134.374040323585));
#250017=CARTESIAN_POINT('Ctrl Pts',(53.3411145155772,5.74893192883615,128.460230579889));
#250018=CARTESIAN_POINT('Ctrl Pts',(53.0626668917642,1.13525514309568,124.7005618237));
#250019=CARTESIAN_POINT('Ctrl Pts',(52.7842192679514,-4.52166565885288,
126.549985971924));
#250020=CARTESIAN_POINT('Ctrl Pts',(52.5057716441385,-6.0233966159634,132.308972581737));
#250021=CARTESIAN_POINT('Ctrl Pts',(52.2273240203255,-1.98992034228702,
136.685294300858));
#250022=CARTESIAN_POINT('Ctrl Pts',(51.9488763965128,3.87219551293788,135.657325264614));
#250023=CARTESIAN_POINT('Ctrl Pts',(51.6704287726998,6.17595285904027,130.169718798237));
#250024=CARTESIAN_POINT('Ctrl Pts',(51.391981148887,2.80431123975502,125.265317159845));
#250025=CARTESIAN_POINT('Ctrl Pts',(51.113533525074,-3.14435541064497,125.451025861782));
#250026=CARTESIAN_POINT('Ctrl Pts',(50.8350859012611,-6.20351304896362,
130.556187679343));
#250027=CARTESIAN_POINT('Ctrl Pts',(50.5566382774483,-3.5619452537452,135.889408303207));
#250028=CARTESIAN_POINT('Ctrl Pts',(50.2781906536353,2.35287621896542,136.549718522358));
#250029=CARTESIAN_POINT('Ctrl Pts',(49.9997430298226,6.10551939084041,131.930325503341));
#250030=CARTESIAN_POINT('Ctrl Pts',(49.7212954060095,4.2474885137371,126.27622576074));
#250031=CARTESIAN_POINT('Ctrl Pts',(49.4428477821967,-1.51377680614101,
124.783260739875));
#250032=CARTESIAN_POINT('Ctrl Pts',(49.1644001583838,-5.88395519328364,
128.823392359526));
#250033=CARTESIAN_POINT('Ctrl Pts',(48.8859525345709,-4.84706620499019,
134.683937032636));
#250034=CARTESIAN_POINT('Ctrl Pts',(48.607504910758,0.644039833341117,136.97934050814));
#250035=CARTESIAN_POINT('Ctrl Pts',(48.3290572869451,5.54330472792681,133.600239128744));
#250036=CARTESIAN_POINT('Ctrl Pts',(48.0506096631323,5.34854338303893,127.651861983834));
#250037=CARTESIAN_POINT('Ctrl Pts',(47.7721620393193,0.23873196000854,124.600477075203));
#250038=CARTESIAN_POINT('Ctrl Pts',(47.4937144155065,-5.09046247156518,
127.250158065443));
#250039=CARTESIAN_POINT('Ctrl Pts',(47.2152667916935,-5.74177057468722,
133.165977568637));
#250040=CARTESIAN_POINT('Ctrl Pts',(46.9368191678807,-1.11667202075834,
136.911586465198));
#250041=CARTESIAN_POINT('Ctrl Pts',(46.6583715440677,4.53459356778643,135.044953162355));
#250042=CARTESIAN_POINT('Ctrl Pts',(46.379923920255,6.01878919474683,129.281422475313));
#250043=CARTESIAN_POINT('Ctrl Pts',(46.101476296442,1.97201158593325,124.917397541337));
#250044=CARTESIAN_POINT('Ctrl Pts',(45.8230286726291,-3.88694833223118,
125.963204080281));
#250045=CARTESIAN_POINT('Ctrl Pts',(45.5445810488162,-6.17399262105761,
131.457796973343));
#250046=CARTESIAN_POINT('Ctrl Pts',(45.2661334250033,-2.78743930743976,
136.351913777587));
#250047=CARTESIAN_POINT('Ctrl Pts',(44.9876858011905,3.16063455573481,136.148100240809));
#250048=CARTESIAN_POINT('Ctrl Pts',(44.7092381773775,6.20423966777097,131.033651046464));
#250049=CARTESIAN_POINT('Ctrl Pts',(44.4307905535647,3.54645161908363,125.708495149421));
#250050=CARTESIAN_POINT('Ctrl Pts',(44.1523429297517,-2.37035221374829,
125.066190670735));
#250051=CARTESIAN_POINT('Ctrl Pts',(43.8738953059389,-6.10891816028884,
129.696984048001));
#250052=CARTESIAN_POINT('Ctrl Pts',(43.5954476821259,-4.23368675476706,
135.345402394343));
#250053=CARTESIAN_POINT('Ctrl Pts',(43.3170000583131,1.53209595128933,136.820825190051));
#250054=CARTESIAN_POINT('Ctrl Pts',(43.0385524345002,5.88995732515911,132.767410964279));
#250055=CARTESIAN_POINT('Ctrl Pts',(42.7601048106873,4.83523565761953,126.910049370218));
#250056=CARTESIAN_POINT('Ctrl Pts',(42.4816571868744,-0.662831364878718,
124.631369564788));
#250057=CARTESIAN_POINT('Ctrl Pts',(42.2032095630615,-5.55178874416567,
128.025366969483));
#250058=CARTESIAN_POINT('Ctrl Pts',(41.9247619392486,-5.33892348752252,
133.973123775378));
#250059=CARTESIAN_POINT('Ctrl Pts',(41.6463143154357,-0.219848366758665,
137.008942041929));
#250060=CARTESIAN_POINT('Ctrl Pts',(41.3678666916229,5.10125666286673,134.343053090145));
#250061=CARTESIAN_POINT('Ctrl Pts',(41.0894190678099,5.73455602955998,128.425278630796));
#250062=CARTESIAN_POINT('Ctrl Pts',(40.8109714439971,1.09807855372398,124.693764292674));
#250063=CARTESIAN_POINT('Ctrl Pts',(40.5325238201841,-4.5474794688646,126.5775894579));
#250064=CARTESIAN_POINT('Ctrl Pts',(40.2540761963713,-6.01412601628932,
132.345610829607));
#250065=CARTESIAN_POINT('Ctrl Pts',(39.9756285725584,-1.95408456113369,
136.697298550707));
#250066=CARTESIAN_POINT('Ctrl Pts',(39.6971809487455,3.90166514336576,135.633664197272));
#250067=CARTESIAN_POINT('Ctrl Pts',(39.4187333249326,6.171975188051,130.132135778682));
#250068=CARTESIAN_POINT('Ctrl Pts',(39.1402857011198,2.77054155266769,125.248349147017));
#250069=CARTESIAN_POINT('Ctrl Pts',(38.8618380773068,-3.17688442113803,
125.470265630536));
#250070=CARTESIAN_POINT('Ctrl Pts',(38.583390453494,-6.20490881134979,130.593954822108));
#250071=CARTESIAN_POINT('Ctrl Pts',(38.304942829681,-3.53092513057837,135.910996660811));
#250072=CARTESIAN_POINT('Ctrl Pts',(38.0264952058682,2.38780624991219,136.535289448812));
#250073=CARTESIAN_POINT('Ctrl Pts',(37.7480475820552,6.11226033755391,131.893138612335));
#250074=CARTESIAN_POINT('Ctrl Pts',(37.4695999582424,4.21984577550119,126.250453988427));
#250075=CARTESIAN_POINT('Ctrl Pts',(37.1911523344295,-1.55040090331038,
124.792587085991));
#250076=CARTESIAN_POINT('Ctrl Pts',(36.9127047106166,-5.89590489327443,
128.859246367608));
#250077=CARTESIAN_POINT('Ctrl Pts',(36.6342570868037,-4.82336031728617,
134.713370620821));
#250078=CARTESIAN_POINT('Ctrl Pts',(36.3558094629908,0.681616756036961,
136.975305646799));
#250079=CARTESIAN_POINT('Ctrl Pts',(36.0773618391779,5.56022132939171,133.566443658335));
#250080=CARTESIAN_POINT('Ctrl Pts',(35.798914215365,5.32925413294858,127.619362290662));
#250081=CARTESIAN_POINT('Ctrl Pts',(35.5204665915522,0.200962736863706,
124.599138789596));
#250082=CARTESIAN_POINT('Ctrl Pts',(35.2420189677392,-5.11200359682353,
127.281211006494));
#250083=CARTESIAN_POINT('Ctrl Pts',(34.9635713439263,-5.72728836028912,
133.200885600541));
#250084=CARTESIAN_POINT('Ctrl Pts',(34.6851237201134,-1.07947491424015,
136.918270811987));
#250085=CARTESIAN_POINT('Ctrl Pts',(34.4066760963006,4.56032324271418,135.017271235878));
#250086=CARTESIAN_POINT('Ctrl Pts',(34.1282284724876,6.00940712379002,129.244812613665));
#250087=CARTESIAN_POINT('Ctrl Pts',(33.8497808486748,1.93613943396156,124.905502418881));
#250088=CARTESIAN_POINT('Ctrl Pts',(33.5713332248619,-3.91634581000783,
125.986954733445));
#250089=CARTESIAN_POINT('Ctrl Pts',(33.292885601049,-6.16990057870911,131.495367712155));
#250090=CARTESIAN_POINT('Ctrl Pts',(33.0144379772361,-2.753618131977,136.368778928511));
#250091=CARTESIAN_POINT('Ctrl Pts',(32.7359903534233,3.19310485631782,136.128761554055));
#250092=CARTESIAN_POINT('Ctrl Pts',(32.4575427296103,6.20552047350092,130.995879830412));
#250093=CARTESIAN_POINT('Ctrl Pts',(32.1790951057975,3.51536593206519,125.687001306397));
#250094=CARTESIAN_POINT('Ctrl Pts',(31.9006474819845,-2.40523816576522,
125.080725992446));
#250095=CARTESIAN_POINT('Ctrl Pts',(31.6221998581717,-6.11554589167424,
129.734191283883));
#250096=CARTESIAN_POINT('Ctrl Pts',(31.3437522343588,-4.20596570416061,
135.371089912296));
#250097=CARTESIAN_POINT('Ctrl Pts',(31.0653046105458,1.56869149262894,136.811387415981));
#250098=CARTESIAN_POINT('Ctrl Pts',(30.786856986733,5.90179784253235,132.731520751495));
#250099=CARTESIAN_POINT('Ctrl Pts',(30.5084093629201,4.81144029400183,126.880688070935));
#250100=CARTESIAN_POINT('Ctrl Pts',(30.2299617391072,-0.700395832790832,
124.635518778667));
#250101=CARTESIAN_POINT('Ctrl Pts',(29.9515141152943,-5.56860240548724,
128.05921377167));
#250102=CARTESIAN_POINT('Ctrl Pts',(29.6730664914815,-5.31953540889204,
134.005564608172));
#250103=CARTESIAN_POINT('Ctrl Pts',(29.3946188676685,-0.182075245277261,
137.010165364815));
#250104=CARTESIAN_POINT('Ctrl Pts',(29.1161712438556,5.12270317387725,134.311934729152));
#250105=CARTESIAN_POINT('Ctrl Pts',(28.8377236200427,5.71996763420123,128.390414839463));
#250106=CARTESIAN_POINT('Ctrl Pts',(28.5592759962298,1.06086127464794,124.687193192043));
#250107=CARTESIAN_POINT('Ctrl Pts',(28.280828372417,-4.57312477035222,126.605349568435));
#250108=CARTESIAN_POINT('Ctrl Pts',(28.0023807486041,-6.00463256096402,
132.382191965885));
#250109=CARTESIAN_POINT('Ctrl Pts',(27.7239331247912,-1.91817637065835,
136.709084435575));
#250110=CARTESIAN_POINT('Ctrl Pts',(27.4454855009783,3.93099019615694,135.60982417831));
#250111=CARTESIAN_POINT('Ctrl Pts',(27.1670378771654,6.16776881225138,130.094577668667));
#250112=CARTESIAN_POINT('Ctrl Pts',(26.8885902533525,2.73666920214424,125.231587014236));
#250113=CARTESIAN_POINT('Ctrl Pts',(26.6101426295396,-3.20929571101057,
125.48970305614));
#250114=CARTESIAN_POINT('Ctrl Pts',(26.3316950057267,-6.2060746485581,130.631729761538));
#250115=CARTESIAN_POINT('Ctrl Pts',(26.0532473819138,-3.49977416768234,
135.932395790139));
#250116=CARTESIAN_POINT('Ctrl Pts',(25.774799758101,2.42264779982026,136.52064801359));
#250117=CARTESIAN_POINT('Ctrl Pts',(25.4963521342881,6.11877479221284,131.85591137626));
#250118=CARTESIAN_POINT('Ctrl Pts',(25.2179045104751,4.19204666932822,126.224850962798));
#250119=CARTESIAN_POINT('Ctrl Pts',(24.9394568866623,-1.58696754980412,
124.802136200585));
#250120=CARTESIAN_POINT('Ctrl Pts',(24.6610092628494,-5.90763611834117,
128.895172452612));
#250121=CARTESIAN_POINT('Ctrl Pts',(24.3825616390365,-4.79947569819179,
134.742659359205));
#250122=CARTESIAN_POINT('Ctrl Pts',(24.1041140152236,0.719168421173241,
136.97104211882));
#250123=CARTESIAN_POINT('Ctrl Pts',(23.8256663914108,5.57693189481048,133.532545837923));
#250124=CARTESIAN_POINT('Ctrl Pts',(23.5472187675978,5.3097674053865,127.586980618775));
#250125=CARTESIAN_POINT('Ctrl Pts',(23.2687711437849,0.163186066970757,
124.598030440764));
#250126=CARTESIAN_POINT('Ctrl Pts',(22.990323519972,-5.13335529490864,127.312394499151));
#250127=CARTESIAN_POINT('Ctrl Pts',(22.7118758961592,-5.71259391911463,
133.235704828331));
#250128=CARTESIAN_POINT('Ctrl Pts',(22.4334282723462,-1.04223780738205,
136.924728605587));
#250129=CARTESIAN_POINT('Ctrl Pts',(22.1549806485334,4.58588393318709,134.98943319845));
#250130=CARTESIAN_POINT('Ctrl Pts',(21.8765330247205,5.9998023720423,129.208260541641));
#250131=CARTESIAN_POINT('Ctrl Pts',(21.5980854009075,1.90019553763114,124.893825880784));
#250132=CARTESIAN_POINT('Ctrl Pts',(21.3196377770947,-3.94559816615024,
126.010883897355));
#250133=CARTESIAN_POINT('Ctrl Pts',(21.0411901532818,-6.16557990842568,
131.532912845442));
#250134=CARTESIAN_POINT('Ctrl Pts',(20.7627425294689,-2.71969492018171,
136.385437887866));
#250135=CARTESIAN_POINT('Ctrl Pts',(20.484294905656,3.22545683522612,136.109225569666));
#250136=CARTESIAN_POINT('Ctrl Pts',(20.2058472818431,6.20657133138755,130.958101517545));
#250137=CARTESIAN_POINT('Ctrl Pts',(19.9273996580302,3.48414998186958,125.665697089004));
#250138=CARTESIAN_POINT('Ctrl Pts',(19.6489520342174,-2.44003499079723,
125.095473405541));
#250139=CARTESIAN_POINT('Ctrl Pts',(19.3705044104044,-6.12194700925765,
129.771438175283));
#250140=CARTESIAN_POINT('Ctrl Pts',(19.0920567865916,-4.17808879994825,
135.396608208416));
#250141=CARTESIAN_POINT('Ctrl Pts',(18.8136091627787,1.60522890552839,136.801727049323));
#250142=CARTESIAN_POINT('Ctrl Pts',(18.5351615389658,5.91341966661616,132.695559127084));
#250143=CARTESIAN_POINT('Ctrl Pts',(18.2567139151529,4.78746664069464,126.85147216478));
#250144=CARTESIAN_POINT('Ctrl Pts',(17.97826629134,-0.737934347277788,124.63989658125));
#250145=CARTESIAN_POINT('Ctrl Pts',(17.6998186675271,-5.58520972019883,
128.093162296283));
#250146=CARTESIAN_POINT('Ctrl Pts',(17.4213710437142,-5.29995021292075,
134.037886819174));
#250147=CARTESIAN_POINT('Ctrl Pts',(17.1429234199013,-0.144295376930669,
137.011158729324));
#250148=CARTESIAN_POINT('Ctrl Pts',(16.8644757960885,5.14395986123776,134.280686393713));
#250149=CARTESIAN_POINT('Ctrl Pts',(16.5860281722755,5.70516728333829,128.355640497777));
#250150=CARTESIAN_POINT('Ctrl Pts',(16.3075805484627,1.02360468496723,124.6808487653));
#250151=CARTESIAN_POINT('Ctrl Pts',(16.0291329246498,-4.5986006130197,126.633265274869));
#250152=CARTESIAN_POINT('Ctrl Pts',(15.7506853008369,-5.99491660177097,
132.418714635041));
#250153=CARTESIAN_POINT('Ctrl Pts',(15.472237677024,-1.88219710145218,136.720651518731));
#250154=CARTESIAN_POINT('Ctrl Pts',(15.1937900532111,3.96016958466077,135.585806091128));
#250155=CARTESIAN_POINT('Ctrl Pts',(14.9153424293982,6.16333388751023,130.057045859918));
#250156=CARTESIAN_POINT('Ctrl Pts',(14.6368948055853,2.70269544333712,125.215031382631));
#250157=CARTESIAN_POINT('Ctrl Pts',(14.3584471817724,-3.24158807925031,
125.509337418335));
#250158=CARTESIAN_POINT('Ctrl Pts',(14.0799995579596,-6.20701051738803,
130.669511097867));
#250159=CARTESIAN_POINT('Ctrl Pts',(13.8015519341466,-3.46849351936748,
135.953604898237));
#250160=CARTESIAN_POINT('Ctrl Pts',(13.5231043103337,2.45739957762318,136.505794759238));
#250161=CARTESIAN_POINT('Ctrl Pts',(13.2446566865208,6.12506251342167,131.818645174584));
#250162=CARTESIAN_POINT('Ctrl Pts',(12.966209062708,4.16409222532429,126.199417632585));
#250163=CARTESIAN_POINT('Ctrl Pts',(12.687761438895,-1.62347539063169,124.811907729812));
#250164=CARTESIAN_POINT('Ctrl Pts',(12.4093138150822,-5.91914843377905,
128.931169283287));
#250165=CARTESIAN_POINT('Ctrl Pts',(12.1308661912693,-4.77541323276041,
134.771802162479));
#250166=CARTESIAN_POINT('Ctrl Pts',(11.8524185674564,0.756693437259193,
136.96655008219));
#250167=CARTESIAN_POINT('Ctrl Pts',(11.5739709436435,5.59343580496719,133.498546923603));
#250168=CARTESIAN_POINT('Ctrl Pts',(11.2955233198306,5.2900839224404,127.554718168085));
#250169=CARTESIAN_POINT('Ctrl Pts',(11.0170756960177,0.125403350157864,
124.597152069781));
#250170=CARTESIAN_POINT('Ctrl Pts',(10.7386280722048,-5.15451677462551,
127.343707387895));
#250171=CARTESIAN_POINT('Ctrl Pts',(10.460180448392,-5.69768779567166,133.270433961767));
#250172=CARTESIAN_POINT('Ctrl Pts',(10.1817328245791,-1.0049620800187,136.930959606699));
#250173=CARTESIAN_POINT('Ctrl Pts',(9.90328520076621,4.61127469204443,134.961440081617));
#250174=CARTESIAN_POINT('Ctrl Pts',(9.62483757695328,5.98997529541125,129.171767613693));
#250175=CARTESIAN_POINT('Ctrl Pts',(9.34638995314043,1.86418122885626,124.882368359726));
#250176=CARTESIAN_POINT('Ctrl Pts',(9.0679423293275,-3.97470431670162,126.034990685308));
#250177=CARTESIAN_POINT('Ctrl Pts',(8.78949470551463,-6.16103077031137,
131.57043098196));
#250178=CARTESIAN_POINT('Ctrl Pts',(8.5110470817017,-2.68567092909101,136.401890038352));
#250179=CARTESIAN_POINT('Ctrl Pts',(8.2325994578889,3.25768929364524,136.089493011555));
#250180=CARTESIAN_POINT('Ctrl Pts',(7.95415183407592,6.20739220249103,130.920317507753));
#250181=CARTESIAN_POINT('Ctrl Pts',(7.67570421026306,3.45280492521512,125.644583286679));
#250182=CARTESIAN_POINT('Ctrl Pts',(7.39725658645018,-2.47474139943534,
125.110432363552));
#250183=CARTESIAN_POINT('Ctrl Pts',(7.11880896263729,-6.1281212758433,129.808723342005));
#250184=CARTESIAN_POINT('Ctrl Pts',(6.84036133882437,-4.15005707511893,
135.421956337113));
#250185=CARTESIAN_POINT('Ctrl Pts',(6.56191371501151,1.64170683608044,136.791844448048));
#250186=CARTESIAN_POINT('Ctrl Pts',(6.28346609119863,5.92482236675955,132.659527423617));
#250187=CARTESIAN_POINT('Ctrl Pts',(6.00501846738572,4.76331558605049,126.822402734361));
#250188=CARTESIAN_POINT('Ctrl Pts',(5.72657084357281,-0.775445517336138,
124.644502810313));
#250189=CARTESIAN_POINT('Ctrl Pts',(5.44812321975995,-5.60161007291028,
128.127211285347));
#250190=CARTESIAN_POINT('Ctrl Pts',(5.16967559594705,-5.28016862534525,
134.070089210674));
#250191=CARTESIAN_POINT('Ctrl Pts',(4.89122797213414,-0.106510161665837,
137.011922098645));
#250192=CARTESIAN_POINT('Ctrl Pts',(4.6127803483213,5.16502593727395,134.249309241742));
#250193=CARTESIAN_POINT('Ctrl Pts',(4.33433272450837,5.69015552540359,128.320956894316));
#250194=CARTESIAN_POINT('Ctrl Pts',(4.05588510069549,0.986310165238503,
124.674731247541));
#250195=CARTESIAN_POINT('Ctrl Pts',(3.77743747688256,-4.62390605285035,
126.661335542776));
#250196=CARTESIAN_POINT('Ctrl Pts',(3.49898985306972,-5.98497849873861,
132.455177483715));
#250197=CARTESIAN_POINT('Ctrl Pts',(3.22054222925682,-1.84614808674025,
136.731999371551));
#250198=CARTESIAN_POINT('Ctrl Pts',(2.94209460544391,3.9892022276243,135.561610825727));
#250199=CARTESIAN_POINT('Ctrl Pts',(2.66364698163102,6.15867057816533,130.019541743194));
#250200=CARTESIAN_POINT('Ctrl Pts',(2.38519935781816,2.66862153515642,125.198682865676));
#250201=CARTESIAN_POINT('Ctrl Pts',(2.10675173400524,-3.27376032925169,
125.529167989562));
#250202=CARTESIAN_POINT('Ctrl Pts',(1.82830411019233,-6.20771638316062,
130.707297431096));
#250203=CARTESIAN_POINT('Ctrl Pts',(1.54985648637947,-3.43708434474973,
135.974623199195));
#250204=CARTESIAN_POINT('Ctrl Pts',(1.27140886256659,2.49206029558105,136.490730236146));
#250205=CARTESIAN_POINT('Ctrl Pts',(0.992961238753657,6.13112326818657,
131.78134138822));
#250206=CARTESIAN_POINT('Ctrl Pts',(0.714513614940807,4.13598347935162,
126.174154940227));
#250207=CARTESIAN_POINT('Ctrl Pts',(0.436065991127901,-1.65992307298164,
124.821901311585));
#250208=CARTESIAN_POINT('Ctrl Pts',(0.157618367314999,-5.93044141299494,
128.967235525755));
#250209=CARTESIAN_POINT('Ctrl Pts',(-0.120829256497892,-4.75117381263555,
134.800797950748));
#250210=CARTESIAN_POINT('Ctrl Pts',(-0.399276880310752,0.794190413791566,
136.961829703365));
#250211=CARTESIAN_POINT('Ctrl Pts',(-0.67772450412367,5.60973244830296,
133.464448175219));
#250212=CARTESIAN_POINT('Ctrl Pts',(-0.956172127936585,5.27020441348929,
127.522576134092));
#250213=CARTESIAN_POINT('Ctrl Pts',(-1.23461975174943,0.0876159864779326,
124.596503709192));
#250214=CARTESIAN_POINT('Ctrl Pts',(-1.51306737556233,-5.17548725182775,
127.375148512417));
#250215=CARTESIAN_POINT('Ctrl Pts',(-1.79151499937523,-5.6825705423121,
133.305071713949));
#250216=CARTESIAN_POINT('Ctrl Pts',(-2.06996262318813,-0.967649113415911,
136.936963584433));
#250217=CARTESIAN_POINT('Ctrl Pts',(-2.34841024700098,4.63649457842225,
134.933292922676));
#250218=CARTESIAN_POINT('Ctrl Pts',(-2.62685787081389,5.97992625804282,
129.13533518208));
#250219=CARTESIAN_POINT('Ctrl Pts',(-2.90530549462681,1.82809784216042,
124.871130280269));
#250220=CARTESIAN_POINT('Ctrl Pts',(-3.18375311843967,-4.00366318312286,
126.059274204017));
#250221=CARTESIAN_POINT('Ctrl Pts',(-3.46220074225256,-6.15625333293613,
131.607920731459));
#250222=CARTESIAN_POINT('Ctrl Pts',(-3.74064836606547,-2.65154741947636,
136.418134770325));
#250223=CARTESIAN_POINT('Ctrl Pts',(-4.01909598987837,3.28980103718956,
136.06956461092));
#250224=CARTESIAN_POINT('Ctrl Pts',(-4.29754361369122,6.20798305639367,
130.882529201136));
#250225=CARTESIAN_POINT('Ctrl Pts',(-4.57599123750414,3.42133192360438,
125.623660681799));
#250226=CARTESIAN_POINT('Ctrl Pts',(-4.85443886131705,-2.5093561056208,
125.125602312169));
#250227=CARTESIAN_POINT('Ctrl Pts',(-5.13288648512991,-6.13406846264146,
129.846045402432));
#250228=CARTESIAN_POINT('Ctrl Pts',(-5.41133410894279,-4.12187156839848,
135.447133359102));
#250229=CARTESIAN_POINT('Ctrl Pts',(-5.68978173275571,1.67812393258193,
136.781739978358));
#250230=CARTESIAN_POINT('Ctrl Pts',(-5.9682293565686,5.93600552043131,132.623426976261));
#250231=CARTESIAN_POINT('Ctrl Pts',(-6.24667698038146,4.73898802499559,
126.793480856855));
#250232=CARTESIAN_POINT('Ctrl Pts',(-6.52512460419438,-0.812927952975666,
124.649337295173));
#250233=CARTESIAN_POINT('Ctrl Pts',(-6.80357222800728,-5.61780285590049,
128.161359477164));
#250234=CARTESIAN_POINT('Ctrl Pts',(-7.08201985182013,-5.26019137917956,
134.1021705894));
#250235=CARTESIAN_POINT('Ctrl Pts',(-7.36046747563304,-0.0687209996277829,
137.012455444495));
#250236=CARTESIAN_POINT('Ctrl Pts',(-7.63891509944595,5.18590062137458,
134.217804435933));
#250237=CARTESIAN_POINT('Ctrl Pts',(-7.91736272325884,5.67493291666336,
128.286365314294));
#250238=CARTESIAN_POINT('Ctrl Pts',(-8.1958103470717,0.948979097423875,
124.668840865451));
#250239=CARTESIAN_POINT('Ctrl Pts',(-8.47425797088461,-4.64904015214177,
126.689559331999));
#250240=CARTESIAN_POINT('Ctrl Pts',(-8.75270559469752,-5.97481862012702,
132.491579160764));
#250241=CARTESIAN_POINT('Ctrl Pts',(-9.03115321851038,-1.81003066233205,
136.743127573537));
#250242=CARTESIAN_POINT('Ctrl Pts',(-9.30960084232328,4.0180870492325,135.537239278668));
#250243=CARTESIAN_POINT('Ctrl Pts',(-9.58804846613619,6.15377905701727,
129.982066708221));
#250244=CARTESIAN_POINT('Ctrl Pts',(-9.86649608994908,2.63444874022312,
125.182542069172));
#250245=CARTESIAN_POINT('Ctrl Pts',(-10.144943713762,-3.30581126886015,
125.549194034992));
#250246=CARTESIAN_POINT('Ctrl Pts',(-10.4233913375749,-6.20819221971975,
130.745087361036));
#250247=CARTESIAN_POINT('Ctrl Pts',(-10.7018389613878,-3.40554780770759,
135.995449914173));
#250248=CARTESIAN_POINT('Ctrl Pts',(-10.9802865852006,2.52662866932821,
136.475455002538));
#250249=CARTESIAN_POINT('Ctrl Pts',(-11.2587342090136,6.13695683192405,
131.744001399476));
#250250=CARTESIAN_POINT('Ctrl Pts',(-11.5371818328265,4.10772147299012,
126.149063821843));
#250251=CARTESIAN_POINT('Ctrl Pts',(-11.8156294566394,-1.69630924627168,
124.832116575588));
#250252=CARTESIAN_POINT('Ctrl Pts',(-12.0940770804522,-5.94151463752335,
129.003369843568));
#250253=CARTESIAN_POINT('Ctrl Pts',(-12.3725247042651,-4.72675833601782,
134.829645649562));
#250254=CARTESIAN_POINT('Ctrl Pts',(-12.6509723280781,0.83165796130609,
136.956881157257));
#250255=CARTESIAN_POINT('Ctrl Pts',(-12.9294199518909,5.62582122093989,
133.430250856313));
#250256=CARTESIAN_POINT('Ctrl Pts',(-13.2078675757038,5.25012961517551,
127.490555707831));
#250257=CARTESIAN_POINT('Ctrl Pts',(-13.4863151995167,0.0498253761554086,
124.596085383024));
#250258=CARTESIAN_POINT('Ctrl Pts',(-13.7647628233296,-5.19626594944658,
127.406716707655));
#250259=CARTESIAN_POINT('Ctrl Pts',(-14.0432104471424,-5.66724271921134,
133.339616801361));
#250260=CARTESIAN_POINT('Ctrl Pts',(-14.3216580709554,-0.930300290219375,
136.942740316309));
#250261=CARTESIAN_POINT('Ctrl Pts',(-14.6001056947683,4.6615426577884,134.904992764631));
#250262=CARTESIAN_POINT('Ctrl Pts',(-14.8785533185811,5.96965563230779,
129.098964596818));
#250263=CARTESIAN_POINT('Ctrl Pts',(-15.157000942394,1.79194671462675,124.860112058844));
#250264=CARTESIAN_POINT('Ctrl Pts',(-15.4354485662069,-4.03247369233249,
126.08373355365));
#250265=CARTESIAN_POINT('Ctrl Pts',(-15.7138961900198,-6.15124777332969,
131.645380704742));
#250266=CARTESIAN_POINT('Ctrl Pts',(-15.9923438138327,-2.61732565579698,
136.434171481834));
#250267=CARTESIAN_POINT('Ctrl Pts',(-16.2707914376456,3.32179087594663,
136.049441106215));
#250268=CARTESIAN_POINT('Ctrl Pts',(-16.5492390614585,6.2083438712012,130.844737997954));
#250269=CARTESIAN_POINT('Ctrl Pts',(-16.8276866852714,3.38973214328102,
125.602930049661));
#250270=CARTESIAN_POINT('Ctrl Pts',(-17.1061343090842,-2.54387782669295,
125.140982689263));
#250271=CARTESIAN_POINT('Ctrl Pts',(-17.3845819328972,-6.13978834927694,
129.883402973582));
#250272=CARTESIAN_POINT('Ctrl Pts',(-17.66302955671,-4.09353332421128,135.47213834144));
#250273=CARTESIAN_POINT('Ctrl Pts',(-17.9414771805229,1.71447884558397,
136.771414014676));
#250274=CARTESIAN_POINT('Ctrl Pts',(-18.2199248043358,5.94696871323555,
132.587259122732));
#250275=CARTESIAN_POINT('Ctrl Pts',(-18.4983724281487,4.71448485899666,
126.764707603974));
#250276=CARTESIAN_POINT('Ctrl Pts',(-18.7768200519616,-0.850380265270943,
124.654399856686));
#250277=CARTESIAN_POINT('Ctrl Pts',(-19.0552676757745,-5.63378746913994,
128.19560560636));
#250278=CARTESIAN_POINT('Ctrl Pts',(-19.3337152995874,-5.24001921468789,
134.134129766565));
#250279=CARTESIAN_POINT('Ctrl Pts',(-19.6121629234003,-0.0309292911078312,
137.012758747106));
#250280=CARTESIAN_POINT('Ctrl Pts',(-19.8906105472132,5.2065831400206,134.18617314371));
#250281=CARTESIAN_POINT('Ctrl Pts',(-20.1690581710261,5.65950002119693,
128.251867039513));
#250282=CARTESIAN_POINT('Ctrl Pts',(-20.447505794839,0.911612864839816,
124.663177837304));
#250283=CARTESIAN_POINT('Ctrl Pts',(-20.7259534186518,-4.67400197954067,
126.717935596697));
#250284=CARTESIAN_POINT('Ctrl Pts',(-21.0044010424647,-5.96443734241423,
132.527918317308));
#250285=CARTESIAN_POINT('Ctrl Pts',(-21.2828486662776,-1.77384616657202,
136.754035712331));
#250286=CARTESIAN_POINT('Ctrl Pts',(-21.5612962900905,4.0468229791472,135.512692353051));
#250287=CARTESIAN_POINT('Ctrl Pts',(-21.8397439139034,6.14865950532324,
129.944622143653));
#250288=CARTESIAN_POINT('Ctrl Pts',(-22.1181915377163,2.60017832482316,
125.166609591221));
#250289=CARTESIAN_POINT('Ctrl Pts',(-22.3966391615293,-3.33773971041633,
125.569414812551));
#250290=CARTESIAN_POINT('Ctrl Pts',(-22.6750867853421,-6.20843800943312,
130.782879487369));
#250291=CARTESIAN_POINT('Ctrl Pts',(-22.953534409155,-3.37388507683905,
136.016084271426));
#250292=CARTESIAN_POINT('Ctrl Pts',(-23.2319820329679,2.56110341792085,
136.45996962444));
#250293=CARTESIAN_POINT('Ctrl Pts',(-23.5104296567807,6.14256298846929,
131.706626591997));
#250294=CARTESIAN_POINT('Ctrl Pts',(-23.7888772805937,4.07930725349882,
126.124145207193));
#250295=CARTESIAN_POINT('Ctrl Pts',(-24.0673249044065,-1.73263256219878,
124.842553143289));
#250296=CARTESIAN_POINT('Ctrl Pts',(-24.3457725282195,-5.95236769704188,
129.039570897758));
#250297=CARTESIAN_POINT('Ctrl Pts',(-24.6242201520323,-4.70216770763169,
134.858344189959));
#250298=CARTESIAN_POINT('Ctrl Pts',(-24.9026677758452,0.86909469142902,
136.951704627238));
#250299=CARTESIAN_POINT('Ctrl Pts',(-25.1811153996581,5.64170152670257,
133.395956234079));
#250300=CARTESIAN_POINT('Ctrl Pts',(-25.459563023471,5.22986027137813,127.458658075828));
#250301=CARTESIAN_POINT('Ctrl Pts',(-25.7380106472839,0.0120329195352371,
124.595897106778));
#250302=CARTESIAN_POINT('Ctrl Pts',(-26.0164582710968,-5.21685209751974,
127.438410803838));
#250303=CARTESIAN_POINT('Ctrl Pts',(-26.2949058949097,-5.6517048943475,
133.374067943923));
#250304=CARTESIAN_POINT('Ctrl Pts',(-26.5733535187226,-0.892916994403456,
136.948289588268));
#250305=CARTESIAN_POINT('Ctrl Pts',(-26.8518011425354,4.68641800197708,
134.876540656153));
#250306=CARTESIAN_POINT('Ctrl Pts',(-27.1302487663484,5.95916379878798,
129.062657205632));
#250307=CARTESIAN_POINT('Ctrl Pts',(-27.4086963901612,1.75572918584856,
124.849314103734));
#250308=CARTESIAN_POINT('Ctrl Pts',(-27.6871440139742,-4.06113477674652,
126.108367827853));
#250309=CARTESIAN_POINT('Ctrl Pts',(-27.965591637787,-6.1460142769749,131.682809513716));
#250310=CARTESIAN_POINT('Ctrl Pts',(-28.2440392616,-2.5830069061529,136.449999578631));
#250311=CARTESIAN_POINT('Ctrl Pts',(-28.5224868854127,3.3536576245212,136.029123243122));
#250312=CARTESIAN_POINT('Ctrl Pts',(-28.8009345092257,6.20847463354345,
130.806945298572));
#250313=CARTESIAN_POINT('Ctrl Pts',(-29.0793821330386,3.35800675518651,
125.582392158445));
#250314=CARTESIAN_POINT('Ctrl Pts',(-29.3578297568515,-2.57830528343674,
125.156572924908));
#250315=CARTESIAN_POINT('Ctrl Pts',(-29.6362773806644,-6.14528072379723,
129.920794671155));
#250316=CARTESIAN_POINT('Ctrl Pts',(-29.9147250044772,-4.06504339264135,
135.496970357558));
#250317=CARTESIAN_POINT('Ctrl Pts',(-30.1931726282902,1.75077022794215,
136.760866939637));
#250318=CARTESIAN_POINT('Ctrl Pts',(-30.471620252103,5.95771153892721,132.551025203244));
#250319=CARTESIAN_POINT('Ctrl Pts',(-30.750067875916,4.68980699602731,126.736084041921));
#250320=CARTESIAN_POINT('Ctrl Pts',(-31.0285154997288,-0.887801066412759,
124.659690307256));
#250321=CARTESIAN_POINT('Ctrl Pts',(-31.3069631235417,-5.6495633203129,
128.229948403933));
#250322=CARTESIAN_POINT('Ctrl Pts',(-31.5854107473546,-5.21965287935721,
134.16596555791));
#250323=CARTESIAN_POINT('Ctrl Pts',(-31.8638583711675,0.00686356350839004,
137.012831995241));
#250324=CARTESIAN_POINT('Ctrl Pts',(-32.1423059949804,5.22707272681363,
134.154416537178));
#250325=CARTESIAN_POINT('Ctrl Pts',(-32.4207536187933,5.64385741087595,
128.217463348321));
#250326=CARTESIAN_POINT('Ctrl Pts',(-32.6992012426062,0.874212852105795,
124.657742372942));
#250327=CARTESIAN_POINT('Ctrl Pts',(-32.9776488664191,-4.69879061007736,
126.746463285377));
#250328=CARTESIAN_POINT('Ctrl Pts',(-33.2560964902319,-5.9538350502823,
132.564193606789));
#250329=CARTESIAN_POINT('Ctrl Pts',(-33.5345441140448,-1.73759594028995,
136.764723383724));
#250330=CARTESIAN_POINT('Ctrl Pts',(-33.8129917378578,4.07540895254819,
135.487970958469));
#250331=CARTESIAN_POINT('Ctrl Pts',(-34.0914393616706,6.14331211279008,
129.907209437008));
#250332=CARTESIAN_POINT('Ctrl Pts',(-34.3698869854835,2.56581155885918,
125.150886022208));
#250333=CARTESIAN_POINT('Ctrl Pts',(-34.6483346092964,-3.3695444708001,
125.589829572953));
#250334=CARTESIAN_POINT('Ctrl Pts',(-34.9267822331094,-6.2084537431929,
130.820672409693));
#250335=CARTESIAN_POINT('Ctrl Pts',(-35.2052298569221,-3.34209732541825,
136.036525506343));
#250336=CARTESIAN_POINT('Ctrl Pts',(-35.4836774807351,2.59548326388451,
136.444274675672));
#250337=CARTESIAN_POINT('Ctrl Pts',(-35.7621251045479,6.14794153008404,
131.66921835072));
#250338=CARTESIAN_POINT('Ctrl Pts',(-36.0405727283609,4.05074187377708,
126.099400019648));
#250339=CARTESIAN_POINT('Ctrl Pts',(-36.3190203521737,-1.76889167478912,
124.85321062796));
#250340=CARTESIAN_POINT('Ctrl Pts',(-36.5974679759867,-5.96300018938643,
129.075837346879));
#250341=CARTESIAN_POINT('Ctrl Pts',(-36.8759155997995,-4.67740283869194,
134.886892508504));
#250342=CARTESIAN_POINT('Ctrl Pts',(-37.1543632236125,0.906499216928551,
136.946300305126));
#250343=CARTESIAN_POINT('Ctrl Pts',(-37.4328108474252,5.65737277714046,
133.361565579315));
#250344=CARTESIAN_POINT('Ctrl Pts',(-37.7112584712383,5.2093971331851,127.426884420063));
#250345=CARTESIAN_POINT('Ctrl Pts',(-37.9897060950511,-0.0257599829691867,
124.595938887431));
#250346=CARTESIAN_POINT('Ctrl Pts',(-38.268153718864,-5.23724493321992,
127.470229626529));
#250347=CARTESIAN_POINT('Ctrl Pts',(-38.5466013426768,-5.63595764348039,
133.408423865036));
#250348=CARTESIAN_POINT('Ctrl Pts',(-38.8250489664898,-0.855500611219946,
136.953611194679));
#250349=CARTESIAN_POINT('Ctrl Pts',(-39.1034965903026,4.71111968922328,
134.847937651547));
#250350=CARTESIAN_POINT('Ctrl Pts',(-39.3819442141156,5.94845114626212,
129.026414353905));
#250351=CARTESIAN_POINT('Ctrl Pts',(-39.6603918379284,1.71944659787975,
124.838736815064));
#250352=CARTESIAN_POINT('Ctrl Pts',(-39.9388394617414,-4.08964537431793,
126.133176113797));
#250353=CARTESIAN_POINT('Ctrl Pts',(-40.2172870855541,-6.14055303780089,
131.720205771443));
#250354=CARTESIAN_POINT('Ctrl Pts',(-40.495734709367,-2.54859244223803,
136.465618474199));
#250355=CARTESIAN_POINT('Ctrl Pts',(-40.7741823331801,3.3854001020792,136.008611774531));
#250356=CARTESIAN_POINT('Ctrl Pts',(-41.0526299569928,6.20837533857501,
130.769152503414));
#250357=CARTESIAN_POINT('Ctrl Pts',(-41.3310775808058,3.3261569349168,125.562047769191));
#250358=CARTESIAN_POINT('Ctrl Pts',(-41.6095252046187,-2.61263720013008,
125.172372441404));
#250359=CARTESIAN_POINT('Ctrl Pts',(-41.8879728284316,-6.15054538268038,
129.958219109591));
#250360=CARTESIAN_POINT('Ctrl Pts',(-42.1664204522444,-4.03640282939359,
135.521628487296));
#250361=CARTESIAN_POINT('Ctrl Pts',(-42.4448680760573,1.78699673486542,
136.750099144066));
#250362=CARTESIAN_POINT('Ctrl Pts',(-42.7233156998703,5.96823359942677,
132.514726560457));
#250363=CARTESIAN_POINT('Ctrl Pts',(-43.0017633236831,4.66495535053527,
126.707611231352));
#250364=CARTESIAN_POINT('Ctrl Pts',(-43.2802109474961,-0.925188969759574,
124.665208450844));
#250365=CARTESIAN_POINT('Ctrl Pts',(-43.5586585713089,-5.6651298248394,
128.264386597296));
#250366=CARTESIAN_POINT('Ctrl Pts',(-43.8371061951219,-5.19909312786956,
134.197676783747));
#250367=CARTESIAN_POINT('Ctrl Pts',(-44.1155538189346,0.0446561637927345,
137.012675186187));
#250368=CARTESIAN_POINT('Ctrl Pts',(-44.3940014427476,5.24736862250453,
134.122535793092));
#250369=CARTESIAN_POINT('Ctrl Pts',(-44.6724490665605,5.62800566534308,
128.183155515557));
#250370=CARTESIAN_POINT('Ctrl Pts',(-44.9508966903734,0.836780445093053,
124.65253467378));
#250371=CARTESIAN_POINT('Ctrl Pts',(-45.2293443141862,-4.72340512520001,
126.775141340936));
#250372=CARTESIAN_POINT('Ctrl Pts',(-45.5077919379991,-5.94301213660306,
132.600403685011));
#250373=CARTESIAN_POINT('Ctrl Pts',(-45.7862395618121,-1.7012813267513,
136.775190191685));
#250374=CARTESIAN_POINT('Ctrl Pts',(-46.0646871856249,4.10384391017172,
135.463076010984));
#250375=CARTESIAN_POINT('Ctrl Pts',(-46.3431348094379,6.13773707756737,
129.869829974632));
#250376=CARTESIAN_POINT('Ctrl Pts',(-46.6215824332507,2.5313497158043,125.135371944775));
#250377=CARTESIAN_POINT('Ctrl Pts',(-46.9000300570636,-3.40122437147435,
125.610437559721));
#250378=CARTESIAN_POINT('Ctrl Pts',(-47.1784776808764,-6.20823942041608,
130.858464727578));
#250379=CARTESIAN_POINT('Ctrl Pts',(-47.4569253046894,-3.31018573135201,
136.056772861467));
#250380=CARTESIAN_POINT('Ctrl Pts',(-47.7353729285023,2.62976693326135,
136.428370737814));
#250381=CARTESIAN_POINT('Ctrl Pts',(-48.0138205523151,6.15309225746451,
131.631778061822));
#250382=CARTESIAN_POINT('Ctrl Pts',(-48.2922681761281,4.02202639232555,
126.074829176147));
#250383=CARTESIAN_POINT('Ctrl Pts',(-48.570715799941,-1.80508524044794,
124.864088634681));
#250384=CARTESIAN_POINT('Ctrl Pts',(-48.8491634237538,-5.97341172056607,
129.112167847066));
#250385=CARTESIAN_POINT('Ctrl Pts',(-49.1276110475668,-4.65246464686987,
134.915289547327));
#250386=CARTESIAN_POINT('Ctrl Pts',(-49.4060586713796,0.943870151766231,
136.940668391181));
#250387=CARTESIAN_POINT('Ctrl Pts',(-49.6845062951925,5.6728343915496,133.327080166382));
#250388=CARTESIAN_POINT('Ctrl Pts',(-49.9629539190054,5.18874095886556,
127.395235917922));
#250389=CARTESIAN_POINT('Ctrl Pts',(-50.2414015428183,-0.0635519309279763,
124.596210723434));
#250390=CARTESIAN_POINT('Ctrl Pts',(-50.5198491666312,-5.25744370088312,
127.50217199667));
#250391=CARTESIAN_POINT('Ctrl Pts',(-50.798296790444,-5.6200015501302,133.442683291627));
#250392=CARTESIAN_POINT('Ctrl Pts',(-51.076744414257,-0.818052527146474,
136.958704938348));
#250393=CARTESIAN_POINT('Ctrl Pts',(-51.3551920380699,4.73564680419706,
134.819184810706));
#250394=CARTESIAN_POINT('Ctrl Pts',(-51.6336396618827,5.93751807169133,
128.990237384633));
#250395=CARTESIAN_POINT('Ctrl Pts',(-51.9120872856956,1.68310029518491,
124.828380584778));
#250396=CARTESIAN_POINT('Ctrl Pts',(-52.1905349095086,-4.11800442857602,
126.1581574922));
#250397=CARTESIAN_POINT('Ctrl Pts',(-52.4689825333214,-6.13486425817587,
131.757568092191));
#250398=CARTESIAN_POINT('Ctrl Pts',(-52.7474301571343,-2.51408353929296,
136.481027589776));
#250399=CARTESIAN_POINT('Ctrl Pts',(-53.0258777809472,3.41701713239144,
135.987907460498));
#250400=CARTESIAN_POINT('Ctrl Pts',(-53.3043254047601,6.20804598997526,
130.731361012906));
#250401=CARTESIAN_POINT('Ctrl Pts',(-53.5827730285729,3.29418386267868,
125.541897635768));
#250402=CARTESIAN_POINT('Ctrl Pts',(-53.8612206523859,-2.64687230459117,
125.188380653292));
#250403=CARTESIAN_POINT('Ctrl Pts',(-54.1396682761987,-6.15558213084251,
129.995674902111));
#250404=CARTESIAN_POINT('Ctrl Pts',(-54.4181159000117,-4.0076126957546,
135.546111816938));
#250405=CARTESIAN_POINT('Ctrl Pts',(-54.6965635238244,1.82315702396754,
136.739111026966));
#250406=CARTESIAN_POINT('Ctrl Pts',(-54.9750111476374,5.97853450483549,
132.478364539431));
#250407=CARTESIAN_POINT('Ctrl Pts',(-55.2534587714502,4.63993084340721,
126.679290227339));
#250408=CARTESIAN_POINT('Ctrl Pts',(-55.5319063952633,-0.962542589888887,
124.670954082973));
#250409=CARTESIAN_POINT('Ctrl Pts',(-55.810354019076,-5.68048640589689,
128.298918910331));
#250410=CARTESIAN_POINT('Ctrl Pts',(-56.088801642889,-5.1783407220741,134.229262269005));
#250411=CARTESIAN_POINT('Ctrl Pts',(-56.3672492667019,0.0824471093265141,
137.012288325754));
#250412=CARTESIAN_POINT('Ctrl Pts',(-56.6456968905149,5.26747007502141,
134.090532092806));
#250413=CARTESIAN_POINT('Ctrl Pts',(-56.9241445143275,5.6119453719906,128.148944812513));
#250414=CARTESIAN_POINT('Ctrl Pts',(-57.2025921381407,0.799317030873196,
124.64755493279));
#250415=CARTESIAN_POINT('Ctrl Pts',(-57.4810397619534,-4.74784461280872,
126.803968700697));
#250416=CARTESIAN_POINT('Ctrl Pts',(-57.7594873857663,-5.93196900242356,
132.636547210196));
#250417=CARTESIAN_POINT('Ctrl Pts',(-58.0379350095792,-1.66490367160747,
136.785435748359));
#250418=CARTESIAN_POINT('Ctrl Pts',(-58.3163826333922,4.13212679834998,
135.438008433087));
#250419=CARTESIAN_POINT('Ctrl Pts',(-58.5948302572049,6.13193460624012,
129.832485141631));
#250420=CARTESIAN_POINT('Ctrl Pts',(-58.873277881018,2.49679407265481,125.120067933803));
#250421=CARTESIAN_POINT('Ctrl Pts',(-59.1517255048308,-3.43277823852872,
125.631238009216));
#250422=CARTESIAN_POINT('Ctrl Pts',(-59.4301731286437,-6.20779504904446,
130.896255040614));
#250423=CARTESIAN_POINT('Ctrl Pts',(-59.7086207524566,-3.27815147713605,
136.076825586523));
#250424=CARTESIAN_POINT('Ctrl Pts',(-59.9870683762695,2.66395315565763,
136.412258400192));
#250425=CARTESIAN_POINT('Ctrl Pts',(-60.2655160000824,6.15801497974849,
131.594307112665));
#250426=CARTESIAN_POINT('Ctrl Pts',(-60.5439636238952,3.99316187320697,
126.050433587173));
#250427=CARTESIAN_POINT('Ctrl Pts',(-60.8224112477081,-1.84121191800936,
124.875186760365));
#250428=CARTESIAN_POINT('Ctrl Pts',(-61.1008588715211,-5.98360190477769,
129.148561052078));
#250429=CARTESIAN_POINT('Ctrl Pts',(-61.3793064953339,-4.62735405625939,
134.943534254169));
#250430=CARTESIAN_POINT('Ctrl Pts',(-61.6577541191468,0.981206111148332,
136.934809094094));
#250431=CARTESIAN_POINT('Ctrl Pts',(-61.9362017429597,5.68808579699418,
133.292501273148));
#250432=CARTESIAN_POINT('Ctrl Pts',(-62.2146493667725,5.16789251384163,
127.36371374215));
#250433=CARTESIAN_POINT('Ctrl Pts',(-62.4930969905855,-0.10134152394658,
124.596712604715));
#250434=CARTESIAN_POINT('Ctrl Pts',(-62.7715446143984,-5.27744765203657,
127.534236730624));
#250435=CARTESIAN_POINT('Ctrl Pts',(-63.0499922382113,-5.60383720555579,
133.476844954201));
#250436=CARTESIAN_POINT('Ctrl Pts',(-63.3284398620242,-0.780574129835986,
136.963570630527));
#250437=CARTESIAN_POINT('Ctrl Pts',(-63.606887485837,4.75999843803683,134.790283199078));
#250438=CARTESIAN_POINT('Ctrl Pts',(-63.88533510965,5.92636498020503,128.954127638363));
#250439=CARTESIAN_POINT('Ctrl Pts',(-64.1637827334628,1.64669162458969,
124.818245796629));
#250440=CARTESIAN_POINT('Ctrl Pts',(-64.4422303572757,-4.14621088866563,
126.183311037368));
#250441=CARTESIAN_POINT('Ctrl Pts',(-64.7206779810887,-6.12894814889968,
131.794895091487));
#250442=CARTESIAN_POINT('Ctrl Pts',(-64.9991256049015,-2.47948147605779,
136.49622635437));
#250443=CARTESIAN_POINT('Ctrl Pts',(-65.2775732287142,3.44850754387722,
135.967011068231));
#250444=CARTESIAN_POINT('Ctrl Pts',(-65.5560208525274,6.20748659994837,
130.693572227424));
#250445=CARTESIAN_POINT('Ctrl Pts',(-65.83446847634,3.26208872324607,125.521942504845));
#250446=CARTESIAN_POINT('Ctrl Pts',(-66.1129161001531,-2.68100932822562,
125.204596967384));
#250447=CARTESIAN_POINT('Ctrl Pts',(-66.3913637239659,-6.1603907816451,
130.033160660777));
#250448=CARTESIAN_POINT('Ctrl Pts',(-66.6698113477789,-3.97867405855336,
135.570419439246));
#250449=CARTESIAN_POINT('Ctrl Pts',(-66.9482589715917,1.85924975531565,
136.727902995508));
#250450=CARTESIAN_POINT('Ctrl Pts',(-67.2267065954047,5.98861387344954,
132.441940487574));
#250451=CARTESIAN_POINT('Ctrl Pts',(-67.5051542192175,4.61473440193538,
126.651122079325));
#250452=CARTESIAN_POINT('Ctrl Pts',(-67.7836018430304,-0.999860542648545,
124.676926990737));
#250453=CARTESIAN_POINT('Ctrl Pts',(-68.0620494668433,-5.69563249444164,
128.33354406343));
#250454=CARTESIAN_POINT('Ctrl Pts',(-68.3404970906562,-5.15739643095884,
134.260720843274));
#250455=CARTESIAN_POINT('Ctrl Pts',(-68.618944714469,0.120234999752325,
137.011671428276));
#250456=CARTESIAN_POINT('Ctrl Pts',(-68.8973923382821,5.28737633949755,
134.058406622227));
#250457=CARTESIAN_POINT('Ctrl Pts',(-69.1758399620947,5.59567712593856,
128.114832506878));
#250458=CARTESIAN_POINT('Ctrl Pts',(-69.4542875859078,0.761823997666808,
124.642803334499));
#250459=CARTESIAN_POINT('Ctrl Pts',(-69.7327352097205,-4.77210816728929,
126.832944296451));
#250460=CARTESIAN_POINT('Ctrl Pts',(-70.0111828335336,-5.92070605695121,
132.672622843033));
#250461=CARTESIAN_POINT('Ctrl Pts',(-70.2896304573463,-1.62846432284579,
136.795459674095));
#250462=CARTESIAN_POINT('Ctrl Pts',(-70.5680780811594,4.16025656905012,
135.412769153666));
#250463=CARTESIAN_POINT('Ctrl Pts',(-70.8465257049722,6.12590491382102,
129.795176321834));
#250464=CARTESIAN_POINT('Ctrl Pts',(-71.1249733287852,2.46214590988275,
125.104974556385));
#250465=CARTESIAN_POINT('Ctrl Pts',(-71.4034209525978,-3.46420490272305,
125.652230150673));
#250466=CARTESIAN_POINT('Ctrl Pts',(-71.681868576411,-6.20712064554441,
130.93404194847));
#250467=CARTESIAN_POINT('Ctrl Pts',(-71.9603162002238,-3.24599574981168,
136.09668293845));
#250468=CARTESIAN_POINT('Ctrl Pts',(-72.2387638240367,2.69804066428979,
136.395938259856));
#250469=CARTESIAN_POINT('Ctrl Pts',(-72.5172114478495,6.16270951452303,
131.556806891751));
#250470=CARTESIAN_POINT('Ctrl Pts',(-72.7956590716624,3.96414938600637,
126.026214156713));
#250471=CARTESIAN_POINT('Ctrl Pts',(-73.0741066954753,-1.87727036878649,
124.886504593767));
#250472=CARTESIAN_POINT('Ctrl Pts',(-73.3525543192881,-5.99357036442037,
129.185015613353));
#250473=CARTESIAN_POINT('Ctrl Pts',(-73.6310019431012,-4.60207199734241,
134.971625582408));
#250474=CARTESIAN_POINT('Ctrl Pts',(-73.909449566914,1.01850571157763,136.928722630985));
#250475=CARTESIAN_POINT('Ctrl Pts',(-74.187897190727,5.70312642832773,133.257830180947));
#250476=CARTESIAN_POINT('Ctrl Pts',(-74.4663448145398,5.14685257066011,
127.332319060812));
#250477=CARTESIAN_POINT('Ctrl Pts',(-74.7447924383527,-0.139127361718492,
124.597444512675));
#250478=CARTESIAN_POINT('Ctrl Pts',(-75.0232400621657,-5.29725604542678,
127.566422640223));
#250479=CARTESIAN_POINT('Ctrl Pts',(-75.3016876859784,-5.58746520873256,
133.510907586884));
#250480=CARTESIAN_POINT('Ctrl Pts',(-75.5801353097915,-0.743066808063574,
136.968208090913));
#250481=CARTESIAN_POINT('Ctrl Pts',(-75.8585829336042,4.7841736883842,134.761233887624));
#250482=CARTESIAN_POINT('Ctrl Pts',(-76.1370305574171,5.91499228508486,
128.918086453158));
#250483=CARTESIAN_POINT('Ctrl Pts',(-76.41547818123,1.61022193523031,124.808332826166));
#250484=CARTESIAN_POINT('Ctrl Pts',(-76.693925805043,-4.17426370938676,
126.208635817229));
#250485=CARTESIAN_POINT('Ctrl Pts',(-76.9723734288558,-6.12280492919574,
131.832185386163));
#250486=CARTESIAN_POINT('Ctrl Pts',(-77.2508210526686,-2.44478753472383,
136.511214204787));
#250487=CARTESIAN_POINT('Ctrl Pts',(-77.5292686764817,3.47987016964863,
135.945923372052));
#250488=CARTESIAN_POINT('Ctrl Pts',(-77.8077163002943,6.20669718922256,
130.655787547247));
#250489=CARTESIAN_POINT('Ctrl Pts',(-78.0861639241075,3.22987270591563,
125.502183115868));
#250490=CARTESIAN_POINT('Ctrl Pts',(-78.3646115479203,-2.71504700607423,
125.221020782777));
#250491=CARTESIAN_POINT('Ctrl Pts',(-78.6430591717333,-6.16497115690175,
130.070674996542));
#250492=CARTESIAN_POINT('Ctrl Pts',(-78.921506795546,-3.94958799012119,
135.594550453492));
#250493=CARTESIAN_POINT('Ctrl Pts',(-79.199954419359,1.89527359148086,136.71647546501));
#250494=CARTESIAN_POINT('Ctrl Pts',(-79.4784020431719,5.9984713317742,132.405455754592));
#250495=CARTESIAN_POINT('Ctrl Pts',(-79.7568496669848,4.58936695978296,
126.623107831093));
#250496=CARTESIAN_POINT('Ctrl Pts',(-80.0352972907976,-1.0371414452086,
124.683126952807));
#250497=CARTESIAN_POINT('Ctrl Pts',(-80.3137449146107,-5.71056752923021,
128.368260773546));
#250498=CARTESIAN_POINT('Ctrl Pts',(-80.5921925384234,-5.13626103062165,
134.292051340844));
#250499=CARTESIAN_POINT('Ctrl Pts',(-80.8706401622364,0.158018434826916,
137.010824516613));
#250500=CARTESIAN_POINT('Ctrl Pts',(-81.1490877860493,5.30708667829958,
134.026160571776));
#250501=CARTESIAN_POINT('Ctrl Pts',(-81.4275354098621,5.57920153001237,
128.080819862696));
#250502=CARTESIAN_POINT('Ctrl Pts',(-81.705983033675,0.724302734791404,
124.63828005498));
#250503=CARTESIAN_POINT('Ctrl Pts',(-81.984430657488,-4.79619488954742,
126.862067054498));
#250504=CARTESIAN_POINT('Ctrl Pts',(-82.2628782813007,-5.90922371753823,
132.708629246728));
#250505=CARTESIAN_POINT('Ctrl Pts',(-82.5413259051138,-1.59196463073914,
136.805261597452));
#250506=CARTESIAN_POINT('Ctrl Pts',(-82.8197735289264,4.18823217991362,
135.387359107972));
#250507=CARTESIAN_POINT('Ctrl Pts',(-83.0982211527395,6.11964822374235,
129.757904897731));
#250508=CARTESIAN_POINT('Ctrl Pts',(-83.3766687765523,2.42740651138818,
125.090092371815));
#250509=CARTESIAN_POINT('Ctrl Pts',(-83.6551164003652,-3.49550319953123,
125.67341320622));
#250510=CARTESIAN_POINT('Ctrl Pts',(-83.9335640241781,-6.20621623490623,
130.971824050937));
#250511=CARTESIAN_POINT('Ctrl Pts',(-84.2120116479911,-3.21371974092037,
136.116344181428));
#250512=CARTESIAN_POINT('Ctrl Pts',(-84.4904592718038,2.73202819603347,
136.379410921554));
#250513=CARTESIAN_POINT('Ctrl Pts',(-84.7689068956169,6.16717568783019,
131.519278788663));
#250514=CARTESIAN_POINT('Ctrl Pts',(-85.0473545194296,3.9349900057924,126.002171782228));
#250515=CARTESIAN_POINT('Ctrl Pts',(-85.3258021432425,-1.91325925661942,
124.898041715501));
#250516=CARTESIAN_POINT('Ctrl Pts',(-85.6042497670555,-6.00331673010926,
129.221530180052));
#250517=CARTESIAN_POINT('Ctrl Pts',(-85.8826973908683,-4.57661940695503,
134.999562491112));
#250518=CARTESIAN_POINT('Ctrl Pts',(-86.1611450146813,1.05576757090286,
136.922409227389));
#250519=CARTESIAN_POINT('Ctrl Pts',(-86.4395926384942,5.71795572821454,
133.223068174528));
#250520=CARTESIAN_POINT('Ctrl Pts',(-86.718040262307,5.12562190896342,127.301053037252));
#250521=CARTESIAN_POINT('Ctrl Pts',(-86.9964878861199,-0.176908044074368,
124.598406420195));
#250522=CARTESIAN_POINT('Ctrl Pts',(-87.2749355099329,-5.31686814704595,
127.598728532803));
#250523=CARTESIAN_POINT('Ctrl Pts',(-87.5533831337457,-5.57088616633168,
133.544869927476));
#250524=CARTESIAN_POINT('Ctrl Pts',(-87.8318307575586,-0.70553195167748,
136.972617147663));
#250525=CARTESIAN_POINT('Ctrl Pts',(-88.1102783813713,4.80817165941601,
134.732037952774));
#250526=CARTESIAN_POINT('Ctrl Pts',(-88.3887260051845,5.90340040775061,
128.882115164534));
#250527=CARTESIAN_POINT('Ctrl Pts',(-88.6671736289971,1.57369257850503,
124.798642040718));
#250528=CARTESIAN_POINT('Ctrl Pts',(-88.9456212528103,-4.20216185122988,
126.234130893362));
#250529=CARTESIAN_POINT('Ctrl Pts',(-89.2240688766231,-6.11643482670397,
131.869437594414));
#250530=CARTESIAN_POINT('Ctrl Pts',(-89.5025165004358,-2.41000300088966,
136.525990585645));
#250531=CARTESIAN_POINT('Ctrl Pts',(-89.7809641242489,3.51110384754994,
135.924645153375));
#250532=CARTESIAN_POINT('Ctrl Pts',(-90.0594117480617,6.20567778705031,
130.618008372501));
#250533=CARTESIAN_POINT('Ctrl Pts',(-90.3378593718745,3.19753700446471,
125.482620201028));
#250534=CARTESIAN_POINT('Ctrl Pts',(-90.6163069956876,-2.74898407685696,
125.237651490881));
#250535=CARTESIAN_POINT('Ctrl Pts',(-90.8947546195002,-6.16932308688508,
130.108216519297));
#250536=CARTESIAN_POINT('Ctrl Pts',(-91.1732022433134,-3.92035556825405,
135.618503965492));
#250537=CARTESIAN_POINT('Ctrl Pts',(-91.4516498671261,1.93122719758584,
136.70482885892));
#250538=CARTESIAN_POINT('Ctrl Pts',(-91.7300974909391,6.00810651453776,
132.368911692441));
#250539=CARTESIAN_POINT('Ctrl Pts',(-92.0085451147519,4.56382945695037,
126.595248520721));
#250540=CARTESIAN_POINT('Ctrl Pts',(-92.2869927385648,-1.07438391611076,
124.689553739443));
#250541=CARTESIAN_POINT('Ctrl Pts',(-92.5654403623776,-5.72529095683809,
128.403067754236));
#250542=CARTESIAN_POINT('Ctrl Pts',(-92.8438879861907,-5.11493530424405,
134.323252600751));
#250543=CARTESIAN_POINT('Ctrl Pts',(-93.1223356100035,0.195796014469281,
137.009747622148));
#250544=CARTESIAN_POINT('Ctrl Pts',(-93.4007832338166,5.32660036105212,
133.993795136343));
#250545=CARTESIAN_POINT('Ctrl Pts',(-93.6792308576291,5.56251919472255,
128.046908140318));
#250546=CARTESIAN_POINT('Ctrl Pts',(-93.9576784814422,0.686754632612129,
124.633985261843));
#250547=CARTESIAN_POINT('Ctrl Pts',(-94.2361261052551,-4.82010388703947,
126.891335895681));
#250548=CARTESIAN_POINT('Ctrl Pts',(-94.5145737290679,-5.8975224096676,
132.744565087048));
#250549=CARTESIAN_POINT('Ctrl Pts',(-94.7930213528811,-1.55540594779807,
136.814841155217));
#250550=CARTESIAN_POINT('Ctrl Pts',(-95.0714689766937,4.21605259429308,
135.361779237583));
#250551=CARTESIAN_POINT('Ctrl Pts',(-95.3499166005066,6.11316476784841,
129.720672250431));
#250552=CARTESIAN_POINT('Ctrl Pts',(-95.6283642243196,2.39257716445285,
125.075421931555));
#250553=CARTESIAN_POINT('Ctrl Pts',(-95.9068118481323,-3.52667196918255,
125.694786390909));
#250554=CARTESIAN_POINT('Ctrl Pts',(-96.1852594719453,-6.20508185064282,
131.009599947983));
#250555=CARTESIAN_POINT('Ctrl Pts',(-96.4637070957582,-3.18132464646333,
136.135808586901));
#250556=CARTESIAN_POINT('Ctrl Pts',(-96.742154719571,2.76591449146702,136.362676997713));
#250557=CARTESIAN_POINT('Ctrl Pts',(-97.020602343384,6.17141333417382,131.481724194021));
#250558=CARTESIAN_POINT('Ctrl Pts',(-97.299049967197,3.90568481307747,125.978307354616));
#250559=CARTESIAN_POINT('Ctrl Pts',(-97.5774975910097,-1.94917724792726,
124.909797698053));
#250560=CARTESIAN_POINT('Ctrl Pts',(-97.8559452148228,-6.01284064068852,
129.258103399115));
#250561=CARTESIAN_POINT('Ctrl Pts',(-98.1343928386354,-4.55099722825276,
135.027343945068));
#250562=CARTESIAN_POINT('Ctrl Pts',(-98.4128404624484,1.09299030837272,
136.915869117251));
#250563=CARTESIAN_POINT('Ctrl Pts',(-98.6912880862614,5.73257314714861,
133.188216542011));
#250564=CARTESIAN_POINT('Ctrl Pts',(-98.9697357100741,5.10420131546234,
127.269916830042));
#250565=CARTESIAN_POINT('Ctrl Pts',(-99.2481833338871,-0.214682171037078,
124.599598291628));
#250566=CARTESIAN_POINT('Ctrl Pts',(-99.5266309576999,-5.33628323016052,
127.631153211259));
#250567=CARTESIAN_POINT('Ctrl Pts',(-99.8050785815131,-5.55410069269506,
133.578730717485));
#250568=CARTESIAN_POINT('Ctrl Pts',(-100.083526205326,-0.667970951546107,
136.976797637399));
#250569=CARTESIAN_POINT('Ctrl Pts',(-100.361973829139,4.83199146187865,
134.702696476397));
#250570=CARTESIAN_POINT('Ctrl Pts',(-100.640421452952,5.89158977774298,
128.846215105423));
#250571=CARTESIAN_POINT('Ctrl Pts',(-100.918869076765,1.53710490802326,
124.789173799381));
#250572=CARTESIAN_POINT('Ctrl Pts',(-101.197316700577,-4.22990428042106,
126.259795321038));
#250573=CARTESIAN_POINT('Ctrl Pts',(-101.47576432439,-6.10983807746976,
131.906650335846));
#250574=CARTESIAN_POINT('Ctrl Pts',(-101.754211948203,-2.37512916350784,
136.540554949401));
#250575=CARTESIAN_POINT('Ctrl Pts',(-102.032659572016,3.54220742020778,
135.903177200671));
#250576=CARTESIAN_POINT('Ctrl Pts',(-102.311107195829,6.20442843120499,
130.580236103105));
#250577=CARTESIAN_POINT('Ctrl Pts',(-102.589554819642,3.16508281710451,
125.463254485237));
#250578=CARTESIAN_POINT('Ctrl Pts',(-102.868002443455,-2.78281928302352,
125.254488475437));
#250579=CARTESIAN_POINT('Ctrl Pts',(-103.146450067268,-6.1734464103326,
130.145783837928));
#250580=CARTESIAN_POINT('Ctrl Pts',(-103.424897691081,-3.8909778761698,
135.642279087639));
#250581=CARTESIAN_POINT('Ctrl Pts',(-103.703345314893,1.96710924135641,
136.69296360881));
#250582=CARTESIAN_POINT('Ctrl Pts',(-103.981792938706,6.01751906470488,
132.332309655276));
#250583=CARTESIAN_POINT('Ctrl Pts',(-104.260240562519,4.53812283973896,
126.567545180546));
#250584=CARTESIAN_POINT('Ctrl Pts',(-104.538688186332,-1.11158657532129,
124.696207112496));
#250585=CARTESIAN_POINT('Ctrl Pts',(-104.817135810145,-5.73980223168479,
128.437963715717));
#250586=CARTESIAN_POINT('Ctrl Pts',(-105.095583433958,-5.093420042057,134.354323466822));
#250587=CARTESIAN_POINT('Ctrl Pts',(-105.374031057771,0.233566338818549,
137.008440784786));
#250588=CARTESIAN_POINT('Ctrl Pts',(-105.652478681584,5.34591666467016,
133.961311515241));
#250589=CARTESIAN_POINT('Ctrl Pts',(-105.930926305397,5.54563073823764,
128.013098596357));
#250590=CARTESIAN_POINT('Ctrl Pts',(-106.20937392921,0.649181082487974,
124.629919114234));
#250591=CARTESIAN_POINT('Ctrl Pts',(-106.487821553022,-4.84383427380942,
126.920749735436));
#250592=CARTESIAN_POINT('Ctrl Pts',(-106.766269176835,-5.88560256693534,
132.780429032376));
#250593=CARTESIAN_POINT('Ctrl Pts',(-107.044716800648,-1.51878962871805,
136.824197992414));
#250594=CARTESIAN_POINT('Ctrl Pts',(-107.323164424461,4.2437167812931,135.336030490371));
#250595=CARTESIAN_POINT('Ctrl Pts',(-107.601612048274,6.10645478638612,
129.683479759601));
#250596=CARTESIAN_POINT('Ctrl Pts',(-107.880059672087,2.35765915969063,
125.060963779225));
#250597=CARTESIAN_POINT('Ctrl Pts',(-108.1585072959,-3.55771005670707,125.716348912751));
#250598=CARTESIAN_POINT('Ctrl Pts',(-108.436954919713,-6.20371753478999,
131.04736823981));
#250599=CARTESIAN_POINT('Ctrl Pts',(-108.715402543526,-3.14881166685081,
136.155075433609));
#250600=CARTESIAN_POINT('Ctrl Pts',(-108.993850167338,2.79969829492213,
136.345737108415));
#250601=CARTESIAN_POINT('Ctrl Pts',(-109.272297791151,6.17542229652738,
131.444144499421));
#250602=CARTESIAN_POINT('Ctrl Pts',(-109.550745414964,3.87623489377466,
125.954621758183));
#250603=CARTESIAN_POINT('Ctrl Pts',(-109.829193038777,-1.98502301175461,
124.921772105802));
#250604=CARTESIAN_POINT('Ctrl Pts',(-110.10764066259,-6.02214174324697,
129.294733915307));
#250605=CARTESIAN_POINT('Ctrl Pts',(-110.386088286403,-4.52520641067474,
135.054968914823));
#250606=CARTESIAN_POINT('Ctrl Pts',(-110.664535910216,1.13017254468408,
136.909102542919));
#250607=CARTESIAN_POINT('Ctrl Pts',(-110.942983534029,5.74697814347679,
133.153276574838));
#250608=CARTESIAN_POINT('Ctrl Pts',(-111.221431157841,5.08259158390449,
127.238911592946));
#250609=CARTESIAN_POINT('Ctrl Pts',(-111.499878781655,-0.252448342873548,
124.601020082813));
#250610=CARTESIAN_POINT('Ctrl Pts',(-111.778326405467,-5.3555005753377,
127.663695474083));
#250611=CARTESIAN_POINT('Ctrl Pts',(-112.05677402928,-5.53710940981492,
133.612488702192));
#250612=CARTESIAN_POINT('Ctrl Pts',(-112.335221653093,-0.630385199504834,
136.980749405212));
#250613=CARTESIAN_POINT('Ctrl Pts',(-112.613669276906,4.85563221312083,
134.673210545752));
#250614=CARTESIAN_POINT('Ctrl Pts',(-112.892116900719,5.8795608327098,128.810387606114));
#250615=CARTESIAN_POINT('Ctrl Pts',(-113.170564524532,1.50046027955312,
124.779928453004));
#250616=CARTESIAN_POINT('Ctrl Pts',(-113.449012148345,-4.25748996895278,
126.285628149252));
#250617=CARTESIAN_POINT('Ctrl Pts',(-113.727459772158,-6.10301492593933,
131.943822231527));
#250618=CARTESIAN_POINT('Ctrl Pts',(-114.00590739597,-2.3401673148416,136.554906756366));
#250619=CARTESIAN_POINT('Ctrl Pts',(-114.284355019783,3.57317973506622,
135.881520309444));
#250620=CARTESIAN_POINT('Ctrl Pts',(-114.562802643596,6.202949167983,130.542472138726));
#250621=CARTESIAN_POINT('Ctrl Pts',(-114.841250267409,3.13251134643626,
125.444086686097));
#250622=CARTESIAN_POINT('Ctrl Pts',(-115.119697891222,-2.81655137079845,
125.271531112549));
#250623=CARTESIAN_POINT('Ctrl Pts',(-115.398145515035,-6.17734097445314,
130.183375560363));
#250624=CARTESIAN_POINT('Ctrl Pts',(-115.676593138848,-3.86145600246928,
135.665874938939));
#250625=CARTESIAN_POINT('Ctrl Pts',(-115.955040762661,2.00291839317105,
136.680880154352));
#250626=CARTESIAN_POINT('Ctrl Pts',(-116.233488386474,6.02670863349017,
132.295650999397));
#250627=CARTESIAN_POINT('Ctrl Pts',(-116.511936010287,4.51224806071678,
126.539998837124));
#250628=CARTESIAN_POINT('Ctrl Pts',(-116.790383634099,-1.14874804428301,
124.703086825424));
#250629=CARTESIAN_POINT('Ctrl Pts',(-117.068831257912,-5.75410081604829,
128.472947364906));
#250630=CARTESIAN_POINT('Ctrl Pts',(-117.347278881725,-5.07171604131793,
134.385262787713));
#250631=CARTESIAN_POINT('Ctrl Pts',(-117.625726505538,0.271328008281021,
137.006904052952));
#250632=CARTESIAN_POINT('Ctrl Pts',(-117.904174129351,5.3650348733795,133.928710912162));
#250633=CARTESIAN_POINT('Ctrl Pts',(-118.182621753164,5.52853678636705,
127.979392483636));
#250634=CARTESIAN_POINT('Ctrl Pts',(-118.461069376977,0.611583476719488,
124.626081762825));
#250635=CARTESIAN_POINT('Ctrl Pts',(-118.73951700079,-4.86738517051901,
126.95030748382));
#250636=CARTESIAN_POINT('Ctrl Pts',(-119.017964624603,-5.87346463103546,
132.816219753764));
#250637=CARTESIAN_POINT('Ctrl Pts',(-119.296412248415,-1.48211703032935,
136.833331762325));
#250638=CARTESIAN_POINT('Ctrl Pts',(-119.574859872228,4.27122371580729,
135.310113820466));
#250639=CARTESIAN_POINT('Ctrl Pts',(-119.853307496041,6.09951852799569,
129.646328803424));
#250640=CARTESIAN_POINT('Ctrl Pts',(-120.131755119854,2.32265379100196,
125.046718450578));
#250641=CARTESIAN_POINT('Ctrl Pts',(-120.410202743667,-3.58861631197691,
125.738099972737));
#250642=CARTESIAN_POINT('Ctrl Pts',(-120.68865036748,-6.20212333790203,
131.085127526901));
#250643=CARTESIAN_POINT('Ctrl Pts',(-120.967097991293,-3.11618200686478,
136.174144007612));
#250644=CARTESIAN_POINT('Ctrl Pts',(-121.245545615105,2.83337835452712,
136.328591881372));
#250645=CARTESIAN_POINT('Ctrl Pts',(-121.523993238919,6.17920242633619,
131.406541097396));
#250646=CARTESIAN_POINT('Ctrl Pts',(-121.802440862731,3.84664133916317,
125.931115870606));
#250647=CARTESIAN_POINT('Ctrl Pts',(-122.080888486544,-2.02079521982502,
124.933964495032));
#250648=CARTESIAN_POINT('Ctrl Pts',(-122.359336110357,-6.03121969312815,
129.331420371272));
#250649=CARTESIAN_POINT('Ctrl Pts',(-122.63778373417,-4.49924790990888,
135.082436376724));
#250650=CARTESIAN_POINT('Ctrl Pts',(-122.916231357983,1.16731290203685,
136.90210975513));
#250651=CARTESIAN_POINT('Ctrl Pts',(-123.194678981796,5.76117018341619,
133.118249567719));
#250652=CARTESIAN_POINT('Ctrl Pts',(-123.473126605609,5.06079351504635,
127.208038474877));
#250653=CARTESIAN_POINT('Ctrl Pts',(-123.751574229422,-0.290205160143283,
124.602671741062));
#250654=CARTESIAN_POINT('Ctrl Pts',(-124.030021853235,-5.37451947047147,
127.696354115408));
#250655=CARTESIAN_POINT('Ctrl Pts',(-124.308469477047,-5.51991294730918,
133.646142630679));
#250656=CARTESIAN_POINT('Ctrl Pts',(-124.58691710086,-0.592776088308802,
136.984472304668));
#250657=CARTESIAN_POINT('Ctrl Pts',(-124.865364724673,4.87909303712557,
134.64358125345));
#250658=CARTESIAN_POINT('Ctrl Pts',(-125.143812348486,5.86731401838748,
128.774633994209));
#250659=CARTESIAN_POINT('Ctrl Pts',(-125.422259972299,1.46376005097626,
124.770906344175));
#250660=CARTESIAN_POINT('Ctrl Pts',(-125.700707596112,-4.28491789462882,
126.311628420759));
#250661=CARTESIAN_POINT('Ctrl Pts',(-125.979155219925,-6.09596562494584,
131.980951904039));
#250662=CARTESIAN_POINT('Ctrl Pts',(-126.257602843738,-2.30511875041471,
136.569045474729));
#250663=CARTESIAN_POINT('Ctrl Pts',(-126.536050467551,3.60401964443632,
135.859675282198));
#250664=CARTESIAN_POINT('Ctrl Pts',(-126.814498091363,6.20124005219796,
130.50471787872));
#250665=CARTESIAN_POINT('Ctrl Pts',(-127.092945715177,3.09982379940838,
125.42511751388));
#250666=CARTESIAN_POINT('Ctrl Pts',(-127.371393338989,-2.85017909022625,
125.288778770691));
#250667=CARTESIAN_POINT('Ctrl Pts',(-127.649840962802,-6.18100663493216,
130.220990293627));
#250668=CARTESIAN_POINT('Ctrl Pts',(-127.928288586615,-3.83179104109667,
135.689290645038));
#250669=CARTESIAN_POINT('Ctrl Pts',(-128.206736210428,2.03865332610762,
136.6685789433));
#250670=CARTESIAN_POINT('Ctrl Pts',(-128.485183834241,6.03567488037103,
132.258937083203));
#250671=CARTESIAN_POINT('Ctrl Pts',(-128.763631458054,4.48620607868298,
126.512610511197));
#250672=CARTESIAN_POINT('Ctrl Pts',(-129.042079081867,-1.18586694596332,
124.710192623294));
#250673=CARTESIAN_POINT('Ctrl Pts',(-129.32052670568,-5.76818618009069,
128.508017405469));
#250674=CARTESIAN_POINT('Ctrl Pts',(-129.598974329492,-5.04982410627509,
134.416069416958));
#250675=CARTESIAN_POINT('Ctrl Pts',(-129.877421953305,0.30907962358457,
137.005137483589));
#250676=CARTESIAN_POINT('Ctrl Pts',(-130.155869577118,5.38395427874936,
133.895994535135));
#250677=CARTESIAN_POINT('Ctrl Pts',(-130.434317200931,5.51123797253198,
127.945791051148));
#250678=CARTESIAN_POINT('Ctrl Pts',(-130.712764824744,0.573963208500954,
124.622473349811));
#250679=CARTESIAN_POINT('Ctrl Pts',(-130.991212448557,-4.89075570448117,
126.980008045559));
#250680=CARTESIAN_POINT('Ctrl Pts',(-131.26966007237,-5.8611090517438,132.851935924971));
#250681=CARTESIAN_POINT('Ctrl Pts',(-131.548107696183,-1.44538951154951,
136.842242126491));
#250682=CARTESIAN_POINT('Ctrl Pts',(-131.826555319995,4.29857237855583,
135.28403018822));
#250683=CARTESIAN_POINT('Ctrl Pts',(-132.105002943808,6.09235624970348,
129.609220758541));
#250684=CARTESIAN_POINT('Ctrl Pts',(-132.383450567622,2.28756235552218,
125.032686473479));
#250685=CARTESIAN_POINT('Ctrl Pts',(-132.661898191434,-3.6193895897498,
125.760038764874));
#250686=CARTESIAN_POINT('Ctrl Pts',(-132.940345815247,-6.20029931905343,
131.122876410071));
#250687=CARTESIAN_POINT('Ctrl Pts',(-133.21879343906,-3.08343687560774,
136.193013602317));
#250688=CARTESIAN_POINT('Ctrl Pts',(-133.497241062873,2.86695342225543,
136.311241951909));
#250689=CARTESIAN_POINT('Ctrl Pts',(-133.775688686686,6.18275358352724,
131.368915381349));
#250690=CARTESIAN_POINT('Ctrl Pts',(-134.054136310499,3.81690524584148,
125.907790562906));
#250691=CARTESIAN_POINT('Ctrl Pts',(-134.332583934311,-2.05649254658467,
124.946374413949));
#250692=CARTESIAN_POINT('Ctrl Pts',(-134.611031558124,-6.04007415394596,
129.36816140758));
#250693=CARTESIAN_POINT('Ctrl Pts',(-134.889479181937,-4.47312268785726,
135.109745312956));
#250694=CARTESIAN_POINT('Ctrl Pts',(-135.16792680575,1.20441000418008,136.894891013003));
#250695=CARTESIAN_POINT('Ctrl Pts',(-135.446374429563,5.775148741076,133.083136818595));
#250696=CARTESIAN_POINT('Ctrl Pts',(-135.724822053376,5.03880791662344,
127.177298619846));
#250697=CARTESIAN_POINT('Ctrl Pts',(-136.003269677189,-0.327951223754644,
124.604553205172));
#250698=CARTESIAN_POINT('Ctrl Pts',(-136.281717301002,-5.39333921080989,
127.729127925058));
#250699=CARTESIAN_POINT('Ctrl Pts',(-136.560164924815,-5.50251194239939,
133.679691255889));
#250700=CARTESIAN_POINT('Ctrl Pts',(-136.838612548628,-0.555145011576188,
136.987966197812));
#250701=CARTESIAN_POINT('Ctrl Pts',(-137.117060172441,4.90237306454367,
134.613809697415));
#250702=CARTESIAN_POINT('Ctrl Pts',(-137.395507796253,5.8548497885868,128.73895559457));
#250703=CARTESIAN_POINT('Ctrl Pts',(-137.673955420066,1.42700558223168,
124.762107807213));
#250704=CARTESIAN_POINT('Ctrl Pts',(-137.952403043879,-4.3121870410957,
126.33779517211));
#250705=CARTESIAN_POINT('Ctrl Pts',(-138.230850667692,-6.08869043570493,
132.018037977528));
#250706=CARTESIAN_POINT('Ctrl Pts',(-138.509298291505,-2.26998476896503,
136.582970580575));
#250707=CARTESIAN_POINT('Ctrl Pts',(-138.787745915318,3.63472600553235,
135.837642928407));
#250708=CARTESIAN_POINT('Ctrl Pts',(-139.066193539131,6.1993011471828,130.466974722087));
#250709=CARTESIAN_POINT('Ctrl Pts',(-139.344641162943,3.06702138726935,
125.406347671494));
#250710=CARTESIAN_POINT('Ctrl Pts',(-139.623088786757,-2.88370119522,125.306230810748));
#250711=CARTESIAN_POINT('Ctrl Pts',(-139.901536410569,-6.18444325593727,
130.258626643894));
#250712=CARTESIAN_POINT('Ctrl Pts',(-140.179984034382,-3.80198409129777,
135.712525338258));
#250713=CARTESIAN_POINT('Ctrl Pts',(-140.458431658195,2.07431271599591,
136.656060431482));
#250714=CARTESIAN_POINT('Ctrl Pts',(-140.736879282008,6.04441747309895,
132.222169267145));
#250715=CARTESIAN_POINT('Ctrl Pts',(-141.015326905821,4.45999785863389,
126.485381217648));
#250716=CARTESIAN_POINT('Ctrl Pts',(-141.293774529634,-1.22294190490765,
124.717524242802));
#250717=CARTESIAN_POINT('Ctrl Pts',(-141.572222153447,-5.78205780187226,
128.543172537875));
#250718=CARTESIAN_POINT('Ctrl Pts',(-141.85066977726,-5.02774504814366,
134.446742213005));
#250719=CARTESIAN_POINT('Ctrl Pts',(-142.129117401072,0.346819785828787,
137.003141142159));
#250720=CARTESIAN_POINT('Ctrl Pts',(-142.407565024885,5.40267417971275,
133.863163596476));
#250721=CARTESIAN_POINT('Ctrl Pts',(-142.686012648698,5.49373493774783,
127.912295544006));
#250722=CARTESIAN_POINT('Ctrl Pts',(-142.964460272511,0.536321671864061,
124.619094008905));
#250723=CARTESIAN_POINT('Ctrl Pts',(-143.242907896324,-4.91394500969209,
127.00985032009));
#250724=CARTESIAN_POINT('Ctrl Pts',(-143.521355520137,-5.84853628690073,
132.887576222521));
#250725=CARTESIAN_POINT('Ctrl Pts',(-143.79980314395,-1.40860843332932,
136.850928754739));
#250726=CARTESIAN_POINT('Ctrl Pts',(-144.078250767763,4.32576175612421,
135.257780560169));
#250727=CARTESIAN_POINT('Ctrl Pts',(-144.356698391576,6.08496821690962,
129.572157000006));
#250728=CARTESIAN_POINT('Ctrl Pts',(-144.635146015388,2.2523861535788,125.018868367886));
#250729=CARTESIAN_POINT('Ctrl Pts',(-144.913593639201,-3.65002874971022,
125.782164476213));
#250730=CARTESIAN_POINT('Ctrl Pts',(-145.192041263014,-6.19824554583293,
131.160613490521));
#250731=CARTESIAN_POINT('Ctrl Pts',(-145.470488886827,-3.05057748646412,
136.211683518503));
#250732=CARTESIAN_POINT('Ctrl Pts',(-145.74893651064,2.90042225397064,136.293687962933));
#250733=CARTESIAN_POINT('Ctrl Pts',(-146.027384134453,6.18607563651005,
131.33126874552));
#250734=CARTESIAN_POINT('Ctrl Pts',(-146.305831758266,3.78702771569254,
125.884646699409));
#250735=CARTESIAN_POINT('Ctrl Pts',(-146.584279382079,-2.09211366925746,
124.959001402698));
#250736=CARTESIAN_POINT('Ctrl Pts',(-146.862727005891,-6.04870479759444,
129.404955662777));
#250737=CARTESIAN_POINT('Ctrl Pts',(-147.141174629705,-4.4468317125993,
135.136894711575));
#250738=CARTESIAN_POINT('Ctrl Pts',(-147.419622253517,1.24146247646836,
136.887446584034));
#250739=CARTESIAN_POINT('Ctrl Pts',(-147.69806987733,5.78891329847519,133.04793962858));
#250740=CARTESIAN_POINT('Ctrl Pts',(-147.976517501143,5.01663560332014,
127.146693166932));
#250741=CARTESIAN_POINT('Ctrl Pts',(-148.254965124956,-0.365685135012239,
124.606664405427));
#250742=CARTESIAN_POINT('Ctrl Pts',(-148.533412748769,-5.41195909898036,
127.762015688586));
#250743=CARTESIAN_POINT('Ctrl Pts',(-148.811860372582,-5.48490703988586,
133.713133334664));
#250744=CARTESIAN_POINT('Ctrl Pts',(-149.090307996395,-0.517493363741682,
136.991230955176));
#250745=CARTESIAN_POINT('Ctrl Pts',(-149.368755620208,4.92547143272535,
134.583896980843));
#250746=CARTESIAN_POINT('Ctrl Pts',(-149.647203244021,5.84216860517359,
128.703353729273));
#250747=CARTESIAN_POINT('Ctrl Pts',(-149.925650867833,1.39019823527075,
124.753533168151));
#250748=CARTESIAN_POINT('Ctrl Pts',(-150.204098491647,-4.33929639788676,
126.364127433687));
#250749=CARTESIAN_POINT('Ctrl Pts',(-150.482546115459,-6.08118962780021,
132.055079077756));
#250750=CARTESIAN_POINT('Ctrl Pts',(-150.760993739272,-2.23476667239474,
136.596681557904));
#250751=CARTESIAN_POINT('Ctrl Pts',(-151.039441363085,3.66529768052036,
135.81542406449));
#250752=CARTESIAN_POINT('Ctrl Pts',(-151.317888986898,6.19713252478332,
130.429244067412));
#250753=CARTESIAN_POINT('Ctrl Pts',(-151.596336610711,3.03410532552526,
125.387777854462));
#250754=CARTESIAN_POINT('Ctrl Pts',(-151.874784234524,-2.91711644360522,
125.323886586026));
#250755=CARTESIAN_POINT('Ctrl Pts',(-152.153231858337,-6.18765071012318,
130.296283216534));
#250756=CARTESIAN_POINT('Ctrl Pts',(-152.431679482149,-3.77203625758034,
135.735578157629));
#250757=CARTESIAN_POINT('Ctrl Pts',(-152.710127105962,2.10989524146327,
136.643325082775));
#250758=CARTESIAN_POINT('Ctrl Pts',(-152.988574729775,6.0529360877152,132.185348913665));
#250759=CARTESIAN_POINT('Ctrl Pts',(-153.267022353588,4.43362437172323,
126.458311965469));
#250760=CARTESIAN_POINT('Ctrl Pts',(-153.545469977401,-1.25997154729018,
124.725081412269));
#250761=CARTESIAN_POINT('Ctrl Pts',(-153.823917601214,-5.79571516737629,
128.578411459437));
#250762=CARTESIAN_POINT('Ctrl Pts',(-154.102365225027,-5.00547968506979,
134.477280039263));
#250763=CARTESIAN_POINT('Ctrl Pts',(-154.38081284884,0.38454709653853,137.000915102638));
#250764=CARTESIAN_POINT('Ctrl Pts',(-154.659260472653,5.4211938825983,133.830219312748));
#250765=CARTESIAN_POINT('Ctrl Pts',(-154.937708096465,5.47602833059452,
127.8789072034));
#250766=CARTESIAN_POINT('Ctrl Pts',(-155.216155720278,0.498660261630971,
124.615943865326));
#250767=CARTESIAN_POINT('Ctrl Pts',(-155.494603344091,-4.93695222686361,
127.039833201595));
#250768=CARTESIAN_POINT('Ctrl Pts',(-155.773050967904,-5.83574680239484,
132.923139325752));
#250769=CARTESIAN_POINT('Ctrl Pts',(-156.051498591717,-1.37177515860606,
136.85939132518));
#250770=CARTESIAN_POINT('Ctrl Pts',(-156.32994621553,4.3527908409998,135.231365909006));
#250771=CARTESIAN_POINT('Ctrl Pts',(-156.608393839343,6.0773547033811,129.535138901228));
#250772=CARTESIAN_POINT('Ctrl Pts',(-156.886841463156,2.21712648863745,
125.005264645838));
#250773=CARTESIAN_POINT('Ctrl Pts',(-157.165289086968,-3.68053265651321,
125.804476286877));
#250774=CARTESIAN_POINT('Ctrl Pts',(-157.443736710782,-6.19596209434481,
131.19833736989));
#250775=CARTESIAN_POINT('Ctrl Pts',(-157.722184334594,-3.0176050570491,
136.230153064351));
#250776=CARTESIAN_POINT('Ctrl Pts',(-158.000631958407,2.93378360947182,
136.275930564914));
#250777=CARTESIAN_POINT('Ctrl Pts',(-158.27907958222,6.18916846218569,131.293602584915));
#250778=CARTESIAN_POINT('Ctrl Pts',(-158.557527206033,3.7570098558391,125.861685137721));
#250779=CARTESIAN_POINT('Ctrl Pts',(-158.835974829846,-2.12765726788813,
124.971844993383));
#250780=CARTESIAN_POINT('Ctrl Pts',(-159.114422453659,-6.05711130426257,
129.44180177344));
#250781=CARTESIAN_POINT('Ctrl Pts',(-159.392870077472,-4.42037595835707,
135.163883566548));
#250782=CARTESIAN_POINT('Ctrl Pts',(-159.671317701285,1.27846894590735,
136.879776744077));
#250783=CARTESIAN_POINT('Ctrl Pts',(-159.949765325097,5.80246334556346,
133.01265930192));
#250784=CARTESIAN_POINT('Ctrl Pts',(-160.22821294891,4.9942773967397,127.116223250229));
#250785=CARTESIAN_POINT('Ctrl Pts',(-160.506660572723,-0.403405495673234,
124.609005263594));
#250786=CARTESIAN_POINT('Ctrl Pts',(-160.785108196536,-5.43037844501628,
127.795016187323));
#250787=CARTESIAN_POINT('Ctrl Pts',(-161.063555820349,-5.46709889212507,
133.746467627798));
#250788=CARTESIAN_POINT('Ctrl Pts',(-161.342003444162,-0.479822539999598,
136.994266455786));
#250789=CARTESIAN_POINT('Ctrl Pts',(-161.620451067975,4.94838728575097,
134.553844212161));
#250790=CARTESIAN_POINT('Ctrl Pts',(-161.898898691787,5.82927093805496,
128.66782971756));
#250791=CARTESIAN_POINT('Ctrl Pts',(-162.177346315601,1.35333937400316,
124.745182744726));
#250792=CARTESIAN_POINT('Ctrl Pts',(-162.455793939413,-4.36624496045326,
126.390624229737));
#250793=CARTESIAN_POINT('Ctrl Pts',(-162.734241563226,-6.07346347917808,
132.092073832152));
#250794=CARTESIAN_POINT('Ctrl Pts',(-163.012689187039,-2.19946576572379,
136.61017789865));
#250795=CARTESIAN_POINT('Ctrl Pts',(-163.291136810852,3.69573353655413,
135.793019513774));
#250796=CARTESIAN_POINT('Ctrl Pts',(-163.569584434665,6.19473426535967,
130.391527312818));
#250797=CARTESIAN_POINT('Ctrl Pts',(-163.848032058478,3.0010768338922,125.369408750896));
#250798=CARTESIAN_POINT('Ctrl Pts',(-164.126479682291,-2.95042359716811,
125.341745442286));
#250799=CARTESIAN_POINT('Ctrl Pts',(-164.404927306104,-6.19062887863655,
130.333958616169));
#250800=CARTESIAN_POINT('Ctrl Pts',(-164.683374929917,-3.74194864967208,
135.758448248921));
#250801=CARTESIAN_POINT('Ctrl Pts',(-164.961822553729,2.14539958398697,
136.630373369092));
#250802=CARTESIAN_POINT('Ctrl Pts',(-165.240270177542,6.06123040855813,
132.148477387157));
#250803=CARTESIAN_POINT('Ctrl Pts',(-165.518717801355,4.40708659523179,
126.431403757722));
#250804=CARTESIAN_POINT('Ctrl Pts',(-165.797165425168,-1.29695450096345,
124.732863851664));
#250805=CARTESIAN_POINT('Ctrl Pts',(-166.075613048981,-5.80915777052276,
128.613732864363));
#250806=CARTESIAN_POINT('Ctrl Pts',(-166.354060672794,-4.98302884210618,
134.50768176414));
#250807=CARTESIAN_POINT('Ctrl Pts',(-166.632508296607,0.422260157714416,
136.998459447511));
#250808=CARTESIAN_POINT('Ctrl Pts',(-166.91095592042,5.43951270115045,133.797162904712));
#250809=CARTESIAN_POINT('Ctrl Pts',(-167.189403544233,5.45811880719792,
127.845627266545));
#250810=CARTESIAN_POINT('Ctrl Pts',(-167.467851168046,0.460980373357943,
124.613023035806));
#250811=CARTESIAN_POINT('Ctrl Pts',(-167.746298791858,-4.95977650345479,
127.069955579048));
#250812=CARTESIAN_POINT('Ctrl Pts',(-168.024746415672,-5.822741072145,132.958623916859));
#250813=CARTESIAN_POINT('Ctrl Pts',(-168.303194039484,-1.33489105224939,
136.867629524233));
#250814=CARTESIAN_POINT('Ctrl Pts',(-168.581641663297,4.37965863161014,
135.204787213532));
#250815=CARTESIAN_POINT('Ctrl Pts',(-168.86008928711,6.06951599123876,129.498167833929));
#250816=CARTESIAN_POINT('Ctrl Pts',(-169.138536910923,2.18178466725943,
124.991875811423));
#250817=CARTESIAN_POINT('Ctrl Pts',(-169.416984534736,-3.71090017982492,
125.826973370093));
#250818=CARTESIAN_POINT('Ctrl Pts',(-169.695432158549,-6.19344904920226,
131.236046650305));
#250819=CARTESIAN_POINT('Ctrl Pts',(-169.973879782361,-2.98452080916978,
136.248421555465));
#250820=CARTESIAN_POINT('Ctrl Pts',(-170.252327406175,2.96703625254325,
136.257970415857));
#250821=CARTESIAN_POINT('Ctrl Pts',(-170.530775029987,6.19203194594742,
131.25591829527));
#250822=CARTESIAN_POINT('Ctrl Pts',(-170.8092226538,3.72685277860365,125.838906728691));
#250823=CARTESIAN_POINT('Ctrl Pts',(-171.087670277614,-2.16312202539704,
124.984904710079));
#250824=CARTESIAN_POINT('Ctrl Pts',(-171.366117901426,-6.06529336244348,
129.478698374222));
#250825=CARTESIAN_POINT('Ctrl Pts',(-171.644565525239,-4.39375640545797,
135.190710877796));
#250826=CARTESIAN_POINT('Ctrl Pts',(-171.923013149052,1.31542804121008,
136.871881777341));
#250827=CARTESIAN_POINT('Ctrl Pts',(-172.201460772865,5.81579838023838,
132.977297145939));
#250828=CARTESIAN_POINT('Ctrl Pts',(-172.479908396678,4.97173412537368,
127.085889998814));
#250829=CARTESIAN_POINT('Ctrl Pts',(-172.75835602049,-0.441110907994683,
124.611575692932));
#250830=CARTESIAN_POINT('Ctrl Pts',(-173.036803644304,-5.4485965663818,
127.828128198426));
#250831=CARTESIAN_POINT('Ctrl Pts',(-173.315251268116,-5.44908815900415,
133.779692900072));
#250832=CARTESIAN_POINT('Ctrl Pts',(-173.593698891929,-0.442133936257506,
136.997072587158));
#250833=CARTESIAN_POINT('Ctrl Pts',(-173.872146515742,4.97111977446672,
134.523652504987));
#250834=CARTESIAN_POINT('Ctrl Pts',(-174.150594139555,5.81615726515733,
128.632384875785));
#250835=CARTESIAN_POINT('Ctrl Pts',(-174.429041763368,1.31643036424716,
124.737056846366));
#250836=CARTESIAN_POINT('Ctrl Pts',(-174.707489387181,-4.39303173020782,
126.417284578411));
#250837=CARTESIAN_POINT('Ctrl Pts',(-174.985937010994,-6.06551227613263,
132.129020869861));
#250838=CARTESIAN_POINT('Ctrl Pts',(-175.264384634806,-2.16408335703982,
136.623459102702));
#250839=CARTESIAN_POINT('Ctrl Pts',(-175.542832258619,3.72603244582337,
135.770430106468));
#250840=CARTESIAN_POINT('Ctrl Pts',(-175.821279882432,6.19210645777918,
130.353825855915));
#250841=CARTESIAN_POINT('Ctrl Pts',(-176.099727506245,2.96793713625374,
125.351241041473));
#250842=CARTESIAN_POINT('Ctrl Pts',(-176.378175130058,-2.98362142169932,
125.359806717758));
#250843=CARTESIAN_POINT('Ctrl Pts',(-176.656622753871,-6.19337765112022,
130.371651446723));
#250844=CARTESIAN_POINT('Ctrl Pts',(-176.935070377684,-3.71172238248064,
135.781134764673));
#250845=CARTESIAN_POINT('Ctrl Pts',(-177.213518001496,2.18082442793968,
136.617205770365));
#250846=CARTESIAN_POINT('Ctrl Pts',(-177.49196562531,6.06930012827989,132.111556053907));
#250847=CARTESIAN_POINT('Ctrl Pts',(-177.770413249122,4.38038551252508,
126.404657591498));
#250848=CARTESIAN_POINT('Ctrl Pts',(-178.048860872936,-1.33388939551094,
124.740871272604));
#250849=CARTESIAN_POINT('Ctrl Pts',(-178.327308496748,-5.82238511319243,
128.649135443807));
#250850=CARTESIAN_POINT('Ctrl Pts',(-178.605756120561,-4.96039335117553,
134.537946261091));
#250851=CARTESIAN_POINT('Ctrl Pts',(-178.884203744374,0.459957571884186,
136.995774267775));
#250852=CARTESIAN_POINT('Ctrl Pts',(-179.162651368187,5.45762995655925,
133.763995597288));
#250853=CARTESIAN_POINT('Ctrl Pts',(-179.441098991999,5.44000703120181,
127.812456966643));
#250854=CARTESIAN_POINT('Ctrl Pts',(-179.719546615813,0.423283403288203,
124.610331628578));
#250855=CARTESIAN_POINT('Ctrl Pts',(-179.997994239625,-4.98241699370369,
127.100216336253));
#250856=CARTESIAN_POINT('Ctrl Pts',(-180.276441863438,-5.80951957808352,
132.994028680947));
#250857=CARTESIAN_POINT('Ctrl Pts',(-180.554889487251,-1.29795748101432,
136.875643046625));
#250858=CARTESIAN_POINT('Ctrl Pts',(-180.833337111064,4.40636413235919,
135.178045458633));
#250859=CARTESIAN_POINT('Ctrl Pts',(-181.111784734877,6.06145237094964,
129.461245168083));
#250860=CARTESIAN_POINT('Ctrl Pts',(-181.39023235869,2.14636199904753,124.97870236077));
#250861=CARTESIAN_POINT('Ctrl Pts',(-181.668679982503,-3.74113019436597,
125.849654892224));
#250862=CARTESIAN_POINT('Ctrl Pts',(-181.947127606316,-6.19070650352801,
131.273739934436));
#250863=CARTESIAN_POINT('Ctrl Pts',(-182.225575230128,-2.95132596877351,
136.266488314898));
#250864=CARTESIAN_POINT('Ctrl Pts',(-182.504022853942,3.00017895099442,
136.239808181284));
#250865=CARTESIAN_POINT('Ctrl Pts',(-182.782470477755,6.19466598168877,
131.218217272988));
#250866=CARTESIAN_POINT('Ctrl Pts',(-183.060918101567,3.6965576014681,125.81631231638));
#250867=CARTESIAN_POINT('Ctrl Pts',(-183.33936572538,-2.19850662762309,
124.998180068855));
#250868=CARTESIAN_POINT('Ctrl Pts',(-183.617813349193,-6.07325066894868,
129.515644097905));
#250869=CARTESIAN_POINT('Ctrl Pts',(-183.896260973006,-4.36697404029963,
135.217375651221));
#250870=CARTESIAN_POINT('Ctrl Pts',(-184.174708596819,1.35233839284232,
136.863761976378));
#250871=CARTESIAN_POINT('Ctrl Pts',(-184.453156220632,5.8289179083658,132.941854470998));
#250872=CARTESIAN_POINT('Ctrl Pts',(-184.731603844444,4.94900662457131,
127.055694536694));
#250873=CARTESIAN_POINT('Ctrl Pts',(-185.010051468258,-0.478799974789776,
124.614375598192));
#250874=CARTESIAN_POINT('Ctrl Pts',(-185.28849909207,-5.46661278799793,
127.861350494915));
#250875=CARTESIAN_POINT('Ctrl Pts',(-185.566946715884,-5.43087550791776,
133.812807920317));
#250876=CARTESIAN_POINT('Ctrl Pts',(-185.845394339696,-0.404428949079144,
136.999649245311));
#250877=CARTESIAN_POINT('Ctrl Pts',(-186.123841963509,4.99366805651034,
134.493322978084));
#250878=CARTESIAN_POINT('Ctrl Pts',(-186.402289587322,5.80282807241402,
128.59702051737));
#250879=CARTESIAN_POINT('Ctrl Pts',(-186.680737211135,1.27947257368013,
124.729155774178));
#250880=CARTESIAN_POINT('Ctrl Pts',(-186.959184834948,-4.41965571455532,
126.444107491802));
#250881=CARTESIAN_POINT('Ctrl Pts',(-187.237632458761,-6.0573363132998,
132.165918821797));
#250882=CARTESIAN_POINT('Ctrl Pts',(-187.516080082574,-2.12862075745111,
136.636524677919));
#250883=CARTESIAN_POINT('Ctrl Pts',(-187.794527706387,3.75619328558978,
135.74765667963));
#250884=CARTESIAN_POINT('Ctrl Pts',(-188.072975330199,6.18924919941703,
130.316141093742));
#250885=CARTESIAN_POINT('Ctrl Pts',(-188.351422954013,2.93468746061294,
125.333275399398));
#250886=CARTESIAN_POINT('Ctrl Pts',(-188.629870577825,-3.01670868704181,
125.378069743179));
#250887=CARTESIAN_POINT('Ctrl Pts',(-188.908318201638,-6.19589692571743,
130.409360311474));
#250888=CARTESIAN_POINT('Ctrl Pts',(-189.186765825451,-3.68135857605119,
135.80363686423));
#250889=CARTESIAN_POINT('Ctrl Pts',(-189.465213449264,2.21616846064164,
136.603822774524));
#250890=CARTESIAN_POINT('Ctrl Pts',(-189.743661073077,6.07714494785282,
132.07458628205));
#250891=CARTESIAN_POINT('Ctrl Pts',(-190.02210869689,4.35352211302309,126.378074457888));
#250892=CARTESIAN_POINT('Ctrl Pts',(-190.300556320702,-1.37077486229612,
124.749103378371));
#250893=CARTESIAN_POINT('Ctrl Pts',(-190.579003944516,-5.83539670523986,
128.684617885911));
#250894=CARTESIAN_POINT('Ctrl Pts',(-190.857451568328,-4.93757405104588,
134.568072408653));
#250895=CARTESIAN_POINT('Ctrl Pts',(-191.135899192141,0.497637942157669,
136.992859662928));
#250896=CARTESIAN_POINT('Ctrl Pts',(-191.414346815954,5.47554497748281,
133.730718619501));
#250897=CARTESIAN_POINT('Ctrl Pts',(-191.692794439767,5.42169367374449,
127.779397532831));
#250898=CARTESIAN_POINT('Ctrl Pts',(-191.97124206358,0.385570748295746,
124.60786974337));
#250899=CARTESIAN_POINT('Ctrl Pts',(-192.249689687393,-5.00487285865859,
127.130614351886));
#250900=CARTESIAN_POINT('Ctrl Pts',(-192.528137311206,-5.79608281013753,
133.029352306079));
#250901=CARTESIAN_POINT('Ctrl Pts',(-192.806584935019,-1.26097581348702,
136.883431595415));
#250902=CARTESIAN_POINT('Ctrl Pts',(-193.085032558831,4.43290635366497,
135.151141635234));
#250903=CARTESIAN_POINT('Ctrl Pts',(-193.363480182644,6.05316414131348,
129.424372271875));
#250904=CARTESIAN_POINT('Ctrl Pts',(-193.641927806457,2.11085979660312,
124.965744782026));
#250905=CARTESIAN_POINT('Ctrl Pts',(-193.92037543027,-3.77122157995168,
125.872520012798));
#250906=CARTESIAN_POINT('Ctrl Pts',(-194.198823054083,-6.1877345589472,
131.311415825543));
#250907=CARTESIAN_POINT('Ctrl Pts',(-194.477270677896,-2.91802176590892,
136.284352673182));
#250908=CARTESIAN_POINT('Ctrl Pts',(-194.755718301709,3.03321047671203,
136.221444534203));
#250909=CARTESIAN_POINT('Ctrl Pts',(-195.034165925522,6.19707047180361,
131.180500915096));
#250910=CARTESIAN_POINT('Ctrl Pts',(-195.312613549334,3.66612544703105,
125.793902738034));
#250911=CARTESIAN_POINT('Ctrl Pts',(-195.591061173148,-2.23380976337827,
125.011670577786));
#250912=CARTESIAN_POINT('Ctrl Pts',(-195.86950879696,-6.08098292891658,
129.552637575454));
#250913=CARTESIAN_POINT('Ctrl Pts',(-196.147956420774,-4.3400298553121,
135.243876898752));
#250914=CARTESIAN_POINT('Ctrl Pts',(-196.426404044586,1.38919863307876,
136.855417642068));
#250915=CARTESIAN_POINT('Ctrl Pts',(-196.704851668399,5.84182144379631,
132.906332590435));
#250916=CARTESIAN_POINT('Ctrl Pts',(-196.983299292212,4.92609573650846,
127.025637982775));
#250917=CARTESIAN_POINT('Ctrl Pts',(-197.261746916025,-0.516471299475173,
124.617404875624));
#250918=CARTESIAN_POINT('Ctrl Pts',(-197.540194539838,-5.48442644226676,
127.894681845726));
#250919=CARTESIAN_POINT('Ctrl Pts',(-197.81864216365,-5.41246161374207,
133.845811461438));
#250920=CARTESIAN_POINT('Ctrl Pts',(-198.097089787464,-0.36670897563802,
137.001996334766));
#250921=CARTESIAN_POINT('Ctrl Pts',(-198.375537411276,5.01603129634849,
134.462856755322));
#250922=CARTESIAN_POINT('Ctrl Pts',(-198.65398503509,5.78928385374183,128.561737952753));
#250923=CARTESIAN_POINT('Ctrl Pts',(-198.932432658902,1.24246737178614,
124.721479820939));
#250924=CARTESIAN_POINT('Ctrl Pts',(-199.210880282716,-4.44611592693577,
126.471091975977));
#250925=CARTESIAN_POINT('Ctrl Pts',(-199.489327906528,-6.04893589364168,
132.202766320694));
#250926=CARTESIAN_POINT('Ctrl Pts',(-199.767775530341,-2.09307928103787,
136.649374140152));
#250927=CARTESIAN_POINT('Ctrl Pts',(-200.046223154153,3.7862149382325,135.724700077139));
#250928=CARTESIAN_POINT('Ctrl Pts',(-200.324670777967,6.18616259614969,
130.278474422724));
#250929=CARTESIAN_POINT('Ctrl Pts',(-200.603118401779,2.90132903904936,
125.315512490399));
#250930=CARTESIAN_POINT('Ctrl Pts',(-200.881566025592,-3.04968416713424,
125.396533841802));
#250931=CARTESIAN_POINT('Ctrl Pts',(-201.160013649405,-6.1981866090755,
130.447083813107));
#250932=CARTESIAN_POINT('Ctrl Pts',(-201.438461273218,-3.65085835552605,
135.825953713766));
#250933=CARTESIAN_POINT('Ctrl Pts',(-201.716908897031,2.2514303724059,136.590224877478));
#250934=CARTESIAN_POINT('Ctrl Pts',(-201.995356520844,6.08476457658541,
132.037569441512));
#250935=CARTESIAN_POINT('Ctrl Pts',(-202.273804144657,4.32649739215744,
126.35165534194));
#250936=CARTESIAN_POINT('Ctrl Pts',(-202.55225176847,-1.40760953451491,
124.757559863922));
#250937=CARTESIAN_POINT('Ctrl Pts',(-202.830699392283,-5.84819206451709,
128.720178875862));
#250938=CARTESIAN_POINT('Ctrl Pts',(-203.109147016096,-4.91457178729319,
134.59805909049));
#250939=CARTESIAN_POINT('Ctrl Pts',(-203.387594639908,0.535299872273523,
136.989715740974));
#250940=CARTESIAN_POINT('Ctrl Pts',(-203.666042263721,5.49325710007376,
133.697333204442));
#250941=CARTESIAN_POINT('Ctrl Pts',(-203.944489887534,5.40317941343439,
127.746450190138));
#250942=CARTESIAN_POINT('Ctrl Pts',(-204.222937511347,0.347843805837959,
124.605637471411));
#250943=CARTESIAN_POINT('Ctrl Pts',(-204.50138513516,-5.0271432662092,127.161148499539));
#250944=CARTESIAN_POINT('Ctrl Pts',(-204.779832758973,-5.78243126621161,
133.064593483327));
#250945=CARTESIAN_POINT('Ctrl Pts',(-205.058280382786,-1.22394742003769,
136.890994881994));
#250946=CARTESIAN_POINT('Ctrl Pts',(-205.336728006599,4.45928431199552,
135.124076740266));
#250947=CARTESIAN_POINT('Ctrl Pts',(-205.615175630412,6.04465160945437,
129.387550511641));
#250948=CARTESIAN_POINT('Ctrl Pts',(-205.893623254225,2.07527937547198,
124.953003555339));
#250949=CARTESIAN_POINT('Ctrl Pts',(-206.172070878037,-3.80117322153507,
125.89556788454));
#250950=CARTESIAN_POINT('Ctrl Pts',(-206.45051850185,-6.18453332558722,
131.349072927534));
#250951=CARTESIAN_POINT('Ctrl Pts',(-206.728966125663,-2.8846094346739,
136.302013968343));
#250952=CARTESIAN_POINT('Ctrl Pts',(-207.007413749476,3.06612960569919,
136.202880155086));
#250953=CARTESIAN_POINT('Ctrl Pts',(-207.285861373289,6.19924532719362,
131.142770619188));
#250954=CARTESIAN_POINT('Ctrl Pts',(-207.564308997102,3.63555744296752,
125.771678824048));
#250955=CARTESIAN_POINT('Ctrl Pts',(-207.842756620915,-2.26903012449045,
125.025375736976));
#250956=CARTESIAN_POINT('Ctrl Pts',(-208.121204244728,-6.08848985582611,
129.58967743606));
#250957=CARTESIAN_POINT('Ctrl Pts',(-208.399651868541,-4.31292484892225,
135.270213638376));
#250958=CARTESIAN_POINT('Ctrl Pts',(-208.678099492353,1.42600739604885,
136.846849083615));
#250959=CARTESIAN_POINT('Ctrl Pts',(-208.956547116166,5.85450850838505,
132.870732820528));
#250960=CARTESIAN_POINT('Ctrl Pts',(-209.234994739979,4.90300231015654,
126.995721450812));
#250961=CARTESIAN_POINT('Ctrl Pts',(-209.513442363792,-0.554123486127181,
124.620663412976));
#250962=CARTESIAN_POINT('Ctrl Pts',(-209.791889987605,-5.50203686909699,
127.928121015754));
#250963=CARTESIAN_POINT('Ctrl Pts',(-210.070337611418,-5.393847158811,133.878702300482));
#250964=CARTESIAN_POINT('Ctrl Pts',(-210.348785235231,-0.328975413660277,
137.004113768549));
#250965=CARTESIAN_POINT('Ctrl Pts',(-210.627232859043,5.03820866530154,
134.432254965643));
#250966=CARTESIAN_POINT('Ctrl Pts',(-210.905680482857,5.77552511102812,
128.526538489345));
#250967=CARTESIAN_POINT('Ctrl Pts',(-211.184128106669,1.20541612980698,
124.714029271085));
#250968=CARTESIAN_POINT('Ctrl Pts',(-211.462575730482,-4.47241138685473,
126.498237031013));
#250969=CARTESIAN_POINT('Ctrl Pts',(-211.741023354295,-6.04031132844015,
132.239562001151));
#250970=CARTESIAN_POINT('Ctrl Pts',(-212.019470978108,-2.05746024480169,
136.66200701326));
#250971=CARTESIAN_POINT('Ctrl Pts',(-212.297918601921,3.81609629128846,
135.701561149659));
#250972=CARTESIAN_POINT('Ctrl Pts',(-212.576366225734,6.1828467623524,130.240827238612));
#250973=CARTESIAN_POINT('Ctrl Pts',(-212.854813849547,2.86786310767097,
125.297952972686));
#250974=CARTESIAN_POINT('Ctrl Pts',(-213.133261473359,-3.0825466400586,
125.415198329437));
#250975=CARTESIAN_POINT('Ctrl Pts',(-213.411709097173,-6.20024661634941,
130.484820553763));
#250976=CARTESIAN_POINT('Ctrl Pts',(-213.690156720985,-3.62022285110177,
135.848084486325));
#250977=CARTESIAN_POINT('Ctrl Pts',(-213.968604344798,2.28660885659016,
136.576412583105));
#250978=CARTESIAN_POINT('Ctrl Pts',(-214.247051968611,6.09215873212836,
132.00050690397));
#250979=CARTESIAN_POINT('Ctrl Pts',(-214.525499592424,4.29931235134063,
126.325401222624));
#250980=CARTESIAN_POINT('Ctrl Pts',(-214.803947216237,-1.44439204724454,
124.766240415898));
#250981=CARTESIAN_POINT('Ctrl Pts',(-215.08239484005,-5.86077071688603,
128.755817095934));
#250982=CARTESIAN_POINT('Ctrl Pts',(-215.360842463863,-4.89138741227638,
134.627905195436));
#250983=CARTESIAN_POINT('Ctrl Pts',(-215.639290087675,0.572941966656434,
136.986342618411));
#250984=CARTESIAN_POINT('Ctrl Pts',(-215.917737711489,5.51076566800256,
133.66384058922));
#250985=CARTESIAN_POINT('Ctrl Pts',(-216.196185335301,5.38446493632399,
127.713616159441));
#250986=CARTESIAN_POINT('Ctrl Pts',(-216.474632959115,0.310103973899474,
124.603634895418));
#250987=CARTESIAN_POINT('Ctrl Pts',(-216.753080582927,-5.04922739111732,
127.191817647757));
#250988=CARTESIAN_POINT('Ctrl Pts',(-217.031528206741,-5.76856545216855,
133.099750906814));
#250989=CARTESIAN_POINT('Ctrl Pts',(-217.309975830553,-1.18687367276612,
136.898332626102));
#250990=CARTESIAN_POINT('Ctrl Pts',(-217.588423454366,4.48549702990607,
135.096851776628));
#250991=CARTESIAN_POINT('Ctrl Pts',(-217.866871078179,6.03591509080661,
129.350781251827));
#250992=CARTESIAN_POINT('Ctrl Pts',(-218.145318701992,2.03962205410111,
124.94047915284));
#250993=CARTESIAN_POINT('Ctrl Pts',(-218.423766325804,-3.83098400924668,
125.9187976534));
#250994=CARTESIAN_POINT('Ctrl Pts',(-218.702213949618,-6.18110292207006,
131.386709845009));
#250995=CARTESIAN_POINT('Ctrl Pts',(-218.98066157343,-2.85109021317626,
136.319471545938));
#250996=CARTESIAN_POINT('Ctrl Pts',(-219.259109197243,3.09893511812703,
136.18411573184));
#250997=CARTESIAN_POINT('Ctrl Pts',(-219.537556821056,6.20119046726778,
131.105027783371));
#250998=CARTESIAN_POINT('Ctrl Pts',(-219.816004444869,3.6048547219858,125.749641397935));
#250999=CARTESIAN_POINT('Ctrl Pts',(-220.094452068682,-2.30416640585769,
125.039295038577));
#251000=CARTESIAN_POINT('Ctrl Pts',(-220.372899692494,-6.09577117150464,
129.626762307198));
#251001=CARTESIAN_POINT('Ctrl Pts',(-220.651347316308,-4.28566002551621,
135.296384894171));
#251002=CARTESIAN_POINT('Ctrl Pts',(-220.929794940121,1.46276331779004,
136.83805661853));
#251003=CARTESIAN_POINT('Ctrl Pts',(-221.208242563933,5.86697863200795,
132.835056480438));
#251004=CARTESIAN_POINT('Ctrl Pts',(-221.486690187747,4.87972720125093,
126.965946049375));
#251005=CARTESIAN_POINT('Ctrl Pts',(-221.765137811559,-0.591755139529082,
124.624151089502));
#251006=CARTESIAN_POINT('Ctrl Pts',(-222.043585435373,-5.51944341592756,
127.961666765899));
#251007=CARTESIAN_POINT('Ctrl Pts',(-222.322033059185,-5.37503283288975,
133.911479218663));
#251008=CARTESIAN_POINT('Ctrl Pts',(-222.600480682998,-0.29122966137826,
137.006001468201));
#251009=CARTESIAN_POINT('Ctrl Pts',(-222.878928306811,5.06019934158045,
134.401518743003));
#251010=CARTESIAN_POINT('Ctrl Pts',(-223.157375930624,5.7615523541068,128.491423431472));
#251011=CARTESIAN_POINT('Ctrl Pts',(-223.435823554437,1.16832022068962,
124.706804400699));
#251012=CARTESIAN_POINT('Ctrl Pts',(-223.71427117825,-4.49854111992577,
126.525541651043));
#251013=CARTESIAN_POINT('Ctrl Pts',(-223.992718802062,-6.03146293728042,
132.276304499695));
#251014=CARTESIAN_POINT('Ctrl Pts',(-224.271166425875,-2.02176496861996,
136.674422829126));
#251015=CARTESIAN_POINT('Ctrl Pts',(-224.549614049688,3.84583623749284,
135.678240754614));
#251016=CARTESIAN_POINT('Ctrl Pts',(-224.828061673501,6.1793018208946,130.203200936436));
#251017=CARTESIAN_POINT('Ctrl Pts',(-225.106509297314,2.83429090657077,
125.280597496933));
#251018=CARTESIAN_POINT('Ctrl Pts',(-225.384956921127,-3.11529488808334,
125.434062514461));
#251019=CARTESIAN_POINT('Ctrl Pts',(-225.66340454494,-6.20207687120481,
130.522569135094));
#251020=CARTESIAN_POINT('Ctrl Pts',(-225.941852168753,-3.5894531979886,
135.87002836184));
#251021=CARTESIAN_POINT('Ctrl Pts',(-226.220299792565,2.32170260964191,
136.562386403224));
#251022=CARTESIAN_POINT('Ctrl Pts',(-226.498747416378,6.09932714048972,
131.963400042786));
#251023=CARTESIAN_POINT('Ctrl Pts',(-226.777195040191,4.27196799792278,
126.299313072794));
#251024=CARTESIAN_POINT('Ctrl Pts',(-227.055642664004,-1.48112103749588,
124.775144712639));
#251025=CARTESIAN_POINT('Ctrl Pts',(-227.334090287817,-5.87313219624144,
128.79153122554));
#251026=CARTESIAN_POINT('Ctrl Pts',(-227.61253791163,-4.8680217850994,134.65760961753));
#251027=CARTESIAN_POINT('Ctrl Pts',(-227.890985535443,0.610562830463375,
136.982740420231));
#251028=CARTESIAN_POINT('Ctrl Pts',(-228.169433159256,5.52807003248314,
133.630242014917));
#251029=CARTESIAN_POINT('Ctrl Pts',(-228.447880783069,5.36555093588535,
127.680896657417));
#251030=CARTESIAN_POINT('Ctrl Pts',(-228.726328406882,0.272352650944771,
124.601862089598));
#251031=CARTESIAN_POINT('Ctrl Pts',(-229.004776030695,-5.07112441504767,
127.222620660081));
#251032=CARTESIAN_POINT('Ctrl Pts',(-229.283223654507,-5.75448588181141,
133.134823273769));
#251033=CARTESIAN_POINT('Ctrl Pts',(-229.561671278321,-1.14975594545406,
136.905444555836));
#251034=CARTESIAN_POINT('Ctrl Pts',(-229.840118902133,4.51154353607471,
135.069467753152));
#251035=CARTESIAN_POINT('Ctrl Pts',(-230.118566525947,6.0269549091058,129.314065854931));
#251036=CARTESIAN_POINT('Ctrl Pts',(-230.397014149759,2.00388915378425,
124.928172038625));
#251037=CARTESIAN_POINT('Ctrl Pts',(-230.675461773572,-3.86065283843716,
125.942208458593));
#251038=CARTESIAN_POINT('Ctrl Pts',(-230.953909397385,-6.17744347551146,
131.424325183319));
#251039=CARTESIAN_POINT('Ctrl Pts',(-231.232357021197,-2.81746534348149,
136.33672475907));
#251040=CARTESIAN_POINT('Ctrl Pts',(-231.510804645011,3.13162579837364,
136.165151959792));
#251041=CARTESIAN_POINT('Ctrl Pts',(-231.789252268823,6.20290581994918,
131.067273806224));
#251042=CARTESIAN_POINT('Ctrl Pts',(-232.067699892636,3.57401842178686,
125.727791276302));
#251043=CARTESIAN_POINT('Ctrl Pts',(-232.346147516449,-2.33921730549066,
125.053427966802));
#251044=CARTESIAN_POINT('Ctrl Pts',(-232.624595140262,-6.10282660614105,
129.663890814674));
#251045=CARTESIAN_POINT('Ctrl Pts',(-232.903042764075,-4.25823639540172,
135.322389696357));
#251046=CARTESIAN_POINT('Ctrl Pts',(-233.181490387888,1.499465036299,136.829040572621));
#251047=CARTESIAN_POINT('Ctrl Pts',(-233.459938011701,5.87923135258013,
132.799304892167));
#251048=CARTESIAN_POINT('Ctrl Pts',(-233.738385635514,4.85627127225937,
126.9363128818));
#251049=CARTESIAN_POINT('Ctrl Pts',(-234.016833259326,-0.629364865227224,
124.627867775965));
#251050=CARTESIAN_POINT('Ctrl Pts',(-234.29528088314,-5.53664543775268,
127.99531785311));
#251051=CARTESIAN_POINT('Ctrl Pts',(-234.573728506952,-5.35601933315035,
133.944141001422));
#251052=CARTESIAN_POINT('Ctrl Pts',(-234.852176130765,-0.253473117473377,
137.007659363768));
#251053=CARTESIAN_POINT('Ctrl Pts',(-235.130623754578,5.08200251031112,
134.370649226346));
#251054=CARTESIAN_POINT('Ctrl Pts',(-235.409071378391,5.74736610074488,
128.456394080338));
#251055=CARTESIAN_POINT('Ctrl Pts',(-235.687519002204,1.13118101903705,
124.699805477501));
#251056=CARTESIAN_POINT('Ctrl Pts',(-235.965966626017,-4.52450415790052,
126.553004824284));
#251057=CARTESIAN_POINT('Ctrl Pts',(-236.24441424983,-6.0223910480441,132.312992454817));
#251058=CARTESIAN_POINT('Ctrl Pts',(-236.522861873642,-1.98599477519336,
136.686621127679));
#251059=CARTESIAN_POINT('Ctrl Pts',(-236.801309497456,3.87543367482126,
135.654739756147));
#251060=CARTESIAN_POINT('Ctrl Pts',(-237.079757121268,6.1755279031354,130.165596910454));
#251061=CARTESIAN_POINT('Ctrl Pts',(-237.358204745081,2.80061367977841,
125.263446706254));
#251062=CARTESIAN_POINT('Ctrl Pts',(-237.636652368894,-3.14792769771062,
125.453125697856));
#251063=CARTESIAN_POINT('Ctrl Pts',(-237.915099992707,-6.20367730582095,
130.560328158313));
#251064=CARTESIAN_POINT('Ctrl Pts',(-238.19354761652,-3.55855053636696,
135.891784527174));
#251065=CARTESIAN_POINT('Ctrl Pts',(-238.471995240333,2.35671033115007,
136.54814685758));
#251066=CARTESIAN_POINT('Ctrl Pts',(-238.750442864146,6.10626953604027,
131.92625023297));
#251067=CARTESIAN_POINT('Ctrl Pts',(-239.028890487959,4.24446534516054,
126.273391859158));
#251068=CARTESIAN_POINT('Ctrl Pts',(-239.307338111771,-1.51779514426229,
124.784272424193));
#251069=CARTESIAN_POINT('Ctrl Pts',(-239.585785735585,-5.88527604452282,
128.827319941278));
#251070=CARTESIAN_POINT('Ctrl Pts',(-239.864233359397,-4.84447577158576,
134.687171256065));
#251071=CARTESIAN_POINT('Ctrl Pts',(-240.14268098321,0.648161069640796,
136.978909279916));
#251072=CARTESIAN_POINT('Ctrl Pts',(-240.421128607023,5.54516955229552,
133.596538726537));
#251073=CARTESIAN_POINT('Ctrl Pts',(-240.699576230836,5.34643811298351,
127.648292896498));
#251074=CARTESIAN_POINT('Ctrl Pts',(-240.978023854649,0.234591235861842,
124.600319119639));
#251075=CARTESIAN_POINT('Ctrl Pts',(-241.256471478461,-5.09283352659785,
127.253556395099));
#251076=CARTESIAN_POINT('Ctrl Pts',(-241.534919102275,-5.74019307686353,
133.169809284574));
#251077=CARTESIAN_POINT('Ctrl Pts',(-241.813366726087,-1.11259561351327,
136.912330407661));
#251078=CARTESIAN_POINT('Ctrl Pts',(-242.0918143499,4.53742286533832,135.041925684563));
#251079=CARTESIAN_POINT('Ctrl Pts',(-242.370261973713,6.01777139637409,
129.277405681456));
#251080=CARTESIAN_POINT('Ctrl Pts',(-242.648709597526,1.96808199861856,
124.916082668738));
#251081=CARTESIAN_POINT('Ctrl Pts',(-242.927157221339,-3.89017860971679,
125.965799432623));
#251082=CARTESIAN_POINT('Ctrl Pts',(-243.205604845152,-6.1735551215127,
131.461917548614));
#251083=CARTESIAN_POINT('Ctrl Pts',(-243.484052468965,-2.78373607157309,
136.353772968415));
#251084=CARTESIAN_POINT('Ctrl Pts',(-243.762500092778,3.16420043507544,
136.145989541648));
#251085=CARTESIAN_POINT('Ctrl Pts',(-244.040947716591,6.20439132167383,
131.029510086731));
#251086=CARTESIAN_POINT('Ctrl Pts',(-244.319395340403,3.54304968502077,
125.706129268813));
#251087=CARTESIAN_POINT('Ctrl Pts',(-244.597842964216,-2.37418152456686,
125.067773997952));
#251088=CARTESIAN_POINT('Ctrl Pts',(-244.876290588029,-6.10965589829292,
129.701061582678));
#251089=CARTESIAN_POINT('Ctrl Pts',(-245.154738211842,-4.23065497477177,
135.348227081313));
#251090=CARTESIAN_POINT('Ctrl Pts',(-245.433185835655,1.53611119157916,
136.819801279981));
#251091=CARTESIAN_POINT('Ctrl Pts',(-245.711633459468,5.89126621607239,
132.763479380503));
#251092=CARTESIAN_POINT('Ctrl Pts',(-245.990081083281,4.83263539234992,
126.906823046158));
#251093=CARTESIAN_POINT('Ctrl Pts',(-246.268528707094,-0.666951269578287,
124.631813334641));
#251094=CARTESIAN_POINT('Ctrl Pts',(-246.546976330906,-5.55364229714491,
128.029073030433));
#251095=CARTESIAN_POINT('Ctrl Pts',(-246.825423954719,-5.33680736414475,
133.976686438464));
#251096=CARTESIAN_POINT('Ctrl Pts',(-247.103871578532,-0.215707181029578,
137.009087393821));
#251097=CARTESIAN_POINT('Ctrl Pts',(-247.382319202345,5.10361736357064,
134.339647559554));
#251098=CARTESIAN_POINT('Ctrl Pts',(-247.660766826158,5.73296687661779,
128.421451733968));
#251099=CARTESIAN_POINT('Ctrl Pts',(-247.939214449971,1.09399990105564,
124.693032760838));
#251100=CARTESIAN_POINT('Ctrl Pts',(-248.217662073784,-4.55029953871062,
126.580625533077));
#251101=CARTESIAN_POINT('Ctrl Pts',(-248.496109697597,-6.01309599689209,
132.349624507031));
#251102=CARTESIAN_POINT('Ctrl Pts',(-248.77455732141,-1.95015099000055,
136.698601456905));
#251103=CARTESIAN_POINT('Ctrl Pts',(-249.053004945222,3.90488750652966,
135.631059025098));
#251104=CARTESIAN_POINT('Ctrl Pts',(-249.331452569036,6.17152514891849,
130.128016554096));
#251105=CARTESIAN_POINT('Ctrl Pts',(-249.609900192848,2.76683267521693,
125.246501236177));
#251106=CARTESIAN_POINT('Ctrl Pts',(-249.888347816661,-3.18044385971988,
125.472387173231));
#251107=CARTESIAN_POINT('Ctrl Pts',(-250.166795440474,-6.20504786089197,
130.598096224241));
#251108=CARTESIAN_POINT('Ctrl Pts',(-250.445243064287,-3.5275160113489,
135.913352176149));
#251109=CARTESIAN_POINT('Ctrl Pts',(-250.7236906881,2.39163072389511,136.533694473816));
#251110=CARTESIAN_POINT('Ctrl Pts',(-251.002138311913,6.11298566151878,
131.889058851139));
#251111=CARTESIAN_POINT('Ctrl Pts',(-251.280585935725,4.21680541219097,
126.247638542206));
#251112=CARTESIAN_POINT('Ctrl Pts',(-251.559033559539,-1.5544130086051,
124.793623212388));
#251113=CARTESIAN_POINT('Ctrl Pts',(-251.837481183351,-5.89720181167361,
128.863181916876));
#251114=CARTESIAN_POINT('Ctrl Pts',(-252.115928807165,-4.82075024435922,
134.716589015834));
#251115=CARTESIAN_POINT('Ctrl Pts',(-252.394376430977,0.685735291195708,
136.974849339035));
#251116=CARTESIAN_POINT('Ctrl Pts',(-252.67282405479,5.56206359338632,133.562731973716));
#251117=CARTESIAN_POINT('Ctrl Pts',(-252.951271678603,5.32712717665345,
127.615806083426));
#251118=CARTESIAN_POINT('Ctrl Pts',(-253.229719302416,0.196821126400439,
124.599006045371));
#251119=CARTESIAN_POINT('Ctrl Pts',(-253.508166926229,-5.11435391846912,
127.284623701469));
#251120=CARTESIAN_POINT('Ctrl Pts',(-253.786614550041,-5.72568757235024,
133.204707652256));
#251121=CARTESIAN_POINT('Ctrl Pts',(-254.065062173855,-1.07539404373626,
136.918989908584));
#251122=CARTESIAN_POINT('Ctrl Pts',(-254.343509797667,4.56313403947717,
135.014226625117));
#251123=CARTESIAN_POINT('Ctrl Pts',(-254.621957421481,6.00836492926231,
129.240802026269));
#251124=CARTESIAN_POINT('Ctrl Pts',(-254.900405045293,1.9322018468105,124.904211611225));
#251125=CARTESIAN_POINT('Ctrl Pts',(-255.178852669106,-3.91956009939235,
125.989569474605));
#251126=CARTESIAN_POINT('Ctrl Pts',(-255.457300292919,-6.16943824888009,
131.499485975975));
#251127=CARTESIAN_POINT('Ctrl Pts',(-255.735747916732,-2.74990318521692,
136.370614733943));
#251128=CARTESIAN_POINT('Ctrl Pts',(-256.014195540545,3.19665694865877,
136.126630713714));
#251129=CARTESIAN_POINT('Ctrl Pts',(-256.292643164358,6.20564856486739,
130.991735142402));
#251130=CARTESIAN_POINT('Ctrl Pts',(-256.571090788171,3.51194654848645,
125.68466161966));
#251131=CARTESIAN_POINT('Ctrl Pts',(-256.849538411983,-2.40905189372645,
125.082322325773));
#251132=CARTESIAN_POINT('Ctrl Pts',(-257.127986035797,-6.11626988572704,
129.738292634474));
#251133=CARTESIAN_POINT('Ctrl Pts',(-257.406433659609,-4.20289584392431,
135.373859459261));
#251134=CARTESIAN_POINT('Ctrl Pts',(-257.684881283423,1.57266088340656,
136.810408252432));
#251135=CARTESIAN_POINT('Ctrl Pts',(-257.963328907235,5.90315744058412,
132.727450666138));
#251136=CARTESIAN_POINT('Ctrl Pts',(-258.241776531048,4.80867945501638,
126.87772425425));
#251137=CARTESIAN_POINT('Ctrl Pts',(-258.520224154861,-0.704246744852541,
124.635521896935));
#251138=CARTESIAN_POINT('Ctrl Pts',(-258.798671778674,-5.5709361272427,
128.063810879205));
#251139=CARTESIAN_POINT('Ctrl Pts',(-259.077119402487,-5.31644754243966,
134.007449313497));
#251140=CARTESIAN_POINT('Ctrl Pts',(-259.355567026299,-0.179733571114533,
137.013459703814));
#251141=CARTESIAN_POINT('Ctrl Pts',(-259.634014650113,5.12849404027147,
134.30227331953));
#251142=CARTESIAN_POINT('Ctrl Pts',(-259.866054336623,5.61428989304695,
129.384066440553));
#251143=CARTESIAN_POINT('Ctrl Pts',(-260.051696012132,3.39054283699284,
126.521203045511));
#251144=CARTESIAN_POINT('Ctrl Pts',(-260.144521813036,1.754921961264,125.780753115897));
#251145=CARTESIAN_POINT('Ctrl Pts',(-260.190939676638,0.892893391295023,
125.631947563271));
#251146=CARTESIAN_POINT('Ctrl Pts',(210.191733024964,-2.43880115184907,
125.780342085335));
#251147=CARTESIAN_POINT('Ctrl Pts',(210.145323348611,-3.27594855749458,
126.186716565447));
#251148=CARTESIAN_POINT('Ctrl Pts',(210.052505734956,-4.72940422381435,
127.426013481475));
#251149=CARTESIAN_POINT('Ctrl Pts',(209.866872246696,-6.15821517169733,
131.008352419918));
#251150=CARTESIAN_POINT('Ctrl Pts',(209.634832560185,-4.21099667891447,
135.892791108304));
#251151=CARTESIAN_POINT('Ctrl Pts',(209.356384936373,2.01508446636645,137.098708070195));
#251152=CARTESIAN_POINT('Ctrl Pts',(209.07793731256,6.37956871319657,132.510708806665));
#251153=CARTESIAN_POINT('Ctrl Pts',(208.799489688747,4.8866719183268,126.359661034021));
#251154=CARTESIAN_POINT('Ctrl Pts',(208.521042064934,-1.09954563679898,
124.290443595948));
#251155=CARTESIAN_POINT('Ctrl Pts',(208.242594441121,-6.07390144970816,
128.208589139036));
#251156=CARTESIAN_POINT('Ctrl Pts',(207.964146817309,-5.46739734855352,
134.511385201899));
#251157=CARTESIAN_POINT('Ctrl Pts',(207.685699193495,0.163779660617915,
137.407996874876));
#251158=CARTESIAN_POINT('Ctrl Pts',(207.407251569682,5.6442383477931,134.235982835808));
#251159=CARTESIAN_POINT('Ctrl Pts',(207.128803945869,5.93803043711477,127.910585036422));
#251160=CARTESIAN_POINT('Ctrl Pts',(206.850356322057,0.775002953389061,
124.244367681185));
#251161=CARTESIAN_POINT('Ctrl Pts',(206.571908698243,-5.10018277131114,
126.606494049502));
#251162=CARTESIAN_POINT('Ctrl Pts',(206.293461074431,-6.28856642889766,
132.82623846394));
#251163=CARTESIAN_POINT('Ctrl Pts',(206.015013450618,-1.69805588527783,
137.187984519302));
#251164=CARTESIAN_POINT('Ctrl Pts',(205.736565826805,4.45288036648484,135.683487507757));
#251165=CARTESIAN_POINT('Ctrl Pts',(205.458118202992,6.51183958365415,129.695313656966));
#251166=CARTESIAN_POINT('Ctrl Pts',(205.179670579179,2.58673502741873,124.726298504418));
#251167=CARTESIAN_POINT('Ctrl Pts',(204.901222955366,-3.71545195245463,
125.342726181157));
#251168=CARTESIAN_POINT('Ctrl Pts',(204.622775331554,-6.60332046735468,
130.978128730661));
#251169=CARTESIAN_POINT('Ctrl Pts',(204.344327707741,-3.42305986725146,
136.4538470632));
#251170=CARTESIAN_POINT('Ctrl Pts',(204.065880083927,2.90282542147133,136.737963244372));
#251171=CARTESIAN_POINT('Ctrl Pts',(203.787432460115,6.56115601364161,131.569388537382));
#251172=CARTESIAN_POINT('Ctrl Pts',(203.508984836302,4.1901047305044,125.69779051756));
#251173=CARTESIAN_POINT('Ctrl Pts',(203.230537212489,-2.03144808657932,
124.518880964767));
#251174=CARTESIAN_POINT('Ctrl Pts',(202.952089588676,-6.38619936200403,
129.116020142231));
#251175=CARTESIAN_POINT('Ctrl Pts',(202.673641964863,-4.87234540261322,
135.2646617407));
#251176=CARTESIAN_POINT('Ctrl Pts',(202.39519434105,1.1189559521872,137.314504502614));
#251177=CARTESIAN_POINT('Ctrl Pts',(202.116746717238,6.08199145217563,133.381843073553));
#251178=CARTESIAN_POINT('Ctrl Pts',(201.838299093424,5.45597392877388,127.080601183836));
#251179=CARTESIAN_POINT('Ctrl Pts',(201.559851469612,-0.183817095687214,
124.201312298284));
#251180=CARTESIAN_POINT('Ctrl Pts',(201.281403845799,-5.65468918935595,
127.389902241135));
#251181=CARTESIAN_POINT('Ctrl Pts',(201.002956221986,-5.92917816483575,
133.716212626452));
#251182=CARTESIAN_POINT('Ctrl Pts',(200.724508598173,-0.755042063338292,
137.366673267433));
#251183=CARTESIAN_POINT('Ctrl Pts',(200.44606097436,5.11294080853837,134.986689170007));
#251184=CARTESIAN_POINT('Ctrl Pts',(200.167613350547,6.2823808583988,128.763349450982));
#251185=CARTESIAN_POINT('Ctrl Pts',(199.889165726734,1.67861981076543,124.415599285115));
#251186=CARTESIAN_POINT('Ctrl Pts',(199.610718102921,-4.46771083782862,
125.938808675424));
#251187=CARTESIAN_POINT('Ctrl Pts',(199.332270479108,-6.50843348626435,
131.933222605136));
#251188=CARTESIAN_POINT('Ctrl Pts',(199.053822855296,-2.56822371547623,
136.890267516244));
#251189=CARTESIAN_POINT('Ctrl Pts',(198.775375231483,3.73205818513161,136.254661300547));
#251190=CARTESIAN_POINT('Ctrl Pts',(198.49692760767,6.60276093478139,130.610495019181));
#251191=CARTESIAN_POINT('Ctrl Pts',(198.218479983857,3.4058489481713,125.14448175187));
#251192=CARTESIAN_POINT('Ctrl Pts',(197.940032360044,-2.92087183683725,
124.879620661678));
#251193=CARTESIAN_POINT('Ctrl Pts',(197.661584736231,-6.56345409631434,
130.05930615131));
#251194=CARTESIAN_POINT('Ctrl Pts',(197.383137112418,-4.1745426838368,135.923660297497));
#251195=CARTESIAN_POINT('Ctrl Pts',(197.104689488605,2.05056951733907,137.083628129519));
#251196=CARTESIAN_POINT('Ctrl Pts',(196.826241864792,6.39130850797037,132.473255877329));
#251197=CARTESIAN_POINT('Ctrl Pts',(196.54779424098,4.85874721255563,126.329250411482));
#251198=CARTESIAN_POINT('Ctrl Pts',(196.269346617166,-1.13876540820057,
124.297652603739));
#251199=CARTESIAN_POINT('Ctrl Pts',(195.990898993354,-6.0898082506034,128.245401590344));
#251200=CARTESIAN_POINT('Ctrl Pts',(195.712451369541,-5.44461481437399,
134.544708910868));
#251201=CARTESIAN_POINT('Ctrl Pts',(195.434003745728,0.203913652044436,
137.406818876019));
#251202=CARTESIAN_POINT('Ctrl Pts',(195.155556121915,5.66505543396973,134.201592249669));
#251203=CARTESIAN_POINT('Ctrl Pts',(194.877108498102,5.92028802542049,127.874475717408));
#251204=CARTESIAN_POINT('Ctrl Pts',(194.59866087429,0.735065143658737,124.239780275557));
#251205=CARTESIAN_POINT('Ctrl Pts',(194.320213250476,-5.1256466951968,126.637613470433));
#251206=CARTESIAN_POINT('Ctrl Pts',(194.041765626664,-6.2761396229282,132.86448373661));
#251207=CARTESIAN_POINT('Ctrl Pts',(193.763318002851,-1.6591668436545,137.198201498994));
#251208=CARTESIAN_POINT('Ctrl Pts',(193.484870379038,4.48249921013125,135.656291847837));
#251209=CARTESIAN_POINT('Ctrl Pts',(193.206422755225,6.50496747206681,129.655694426079));
#251210=CARTESIAN_POINT('Ctrl Pts',(192.927975131412,2.54968841250072,124.710665118833));
#251211=CARTESIAN_POINT('Ctrl Pts',(192.649527507599,-3.74862973894988,
125.365444281348));
#251212=CARTESIAN_POINT('Ctrl Pts',(192.371079883787,-6.60214029104917,
131.018321851013));
#251213=CARTESIAN_POINT('Ctrl Pts',(192.092632259973,-3.38860644815819,
136.474579499726));
#251214=CARTESIAN_POINT('Ctrl Pts',(191.814184636161,2.93889117796205,136.720183001327));
#251215=CARTESIAN_POINT('Ctrl Pts',(191.535737012347,6.56569138435095,131.529434736241));
#251216=CARTESIAN_POINT('Ctrl Pts',(191.257289388535,4.15894196037717,125.672378777932));
#251217=CARTESIAN_POINT('Ctrl Pts',(190.978841764722,-2.06967194957323,
124.531363418996));
#251218=CARTESIAN_POINT('Ctrl Pts',(190.700394140909,-6.3963584469616,129.154926032595));
#251219=CARTESIAN_POINT('Ctrl Pts',(190.421946517096,-4.84510401107414,
135.294238450423));
#251220=CARTESIAN_POINT('Ctrl Pts',(190.143498893283,1.15856431450073,137.307572482581));
#251221=CARTESIAN_POINT('Ctrl Pts',(189.86505126947,6.09756863406271,133.344772510351));
#251222=CARTESIAN_POINT('Ctrl Pts',(189.586603645657,5.4332052617092,127.047458114672));
#251223=CARTESIAN_POINT('Ctrl Pts',(189.308156021844,-0.224008319322015,
124.202553584261));
#251224=CARTESIAN_POINT('Ctrl Pts',(189.029708398032,-5.67536919831109,
127.424387201254));
#251225=CARTESIAN_POINT('Ctrl Pts',(188.751260774218,-5.91134304125131,
133.752251266956));
#251226=CARTESIAN_POINT('Ctrl Pts',(188.472813150406,-0.71508141444371,
137.371147838333));
#251227=CARTESIAN_POINT('Ctrl Pts',(188.194365526593,5.13830509856852,134.955487759214));
#251228=CARTESIAN_POINT('Ctrl Pts',(187.91591790278,6.26984024615536,128.725144630756));
#251229=CARTESIAN_POINT('Ctrl Pts',(187.637470278967,1.63969850624965,124.405499418827));
#251230=CARTESIAN_POINT('Ctrl Pts',(187.359022655154,-4.49724605717418,
125.966095046791));
#251231=CARTESIAN_POINT('Ctrl Pts',(187.080575031341,-6.5014411967389,131.972820371883));
#251232=CARTESIAN_POINT('Ctrl Pts',(186.802127407528,-2.53112948956026,
136.905788265189));
#251233=CARTESIAN_POINT('Ctrl Pts',(186.523679783716,3.76516656597443,136.231842221641));
#251234=CARTESIAN_POINT('Ctrl Pts',(186.245232159903,6.60145848599114,130.570305731164));
#251235=CARTESIAN_POINT('Ctrl Pts',(185.96678453609,3.3713325565579,125.123854247073));
#251236=CARTESIAN_POINT('Ctrl Pts',(185.688336912277,-2.95688329360047,
124.897510609301));
#251237=CARTESIAN_POINT('Ctrl Pts',(185.409889288464,-6.5678678487195,130.099273563458));
#251238=CARTESIAN_POINT('Ctrl Pts',(185.131441664651,-4.14330270904733,
135.948977074923));
#251239=CARTESIAN_POINT('Ctrl Pts',(184.852994040838,2.08875520864929,137.071029390563));
#251240=CARTESIAN_POINT('Ctrl Pts',(184.574546417025,6.40134913096194,132.434319247607));
#251241=CARTESIAN_POINT('Ctrl Pts',(184.296098793212,4.831415925211,126.299756751549));
#251242=CARTESIAN_POINT('Ctrl Pts',(184.017651169399,-1.17835248801931,
124.304705146227));
#251243=CARTESIAN_POINT('Ctrl Pts',(183.739203545587,-6.10527253047917,
128.282519393244));
#251244=CARTESIAN_POINT('Ctrl Pts',(183.460755921774,-5.42174537657308,
134.577782526619));
#251245=CARTESIAN_POINT('Ctrl Pts',(183.182308297961,0.244100911417136,
137.405455267482));
#251246=CARTESIAN_POINT('Ctrl Pts',(182.903860674148,5.68563038680749,134.167044506474));
#251247=CARTESIAN_POINT('Ctrl Pts',(182.625413050335,5.90234329520773,127.838491527799));
#251248=CARTESIAN_POINT('Ctrl Pts',(182.346965426522,0.695091060812155,
124.23542735186));
#251249=CARTESIAN_POINT('Ctrl Pts',(182.068517802709,-5.15091590138369,
126.668891936874));
#251250=CARTESIAN_POINT('Ctrl Pts',(181.790070178896,-6.263482786439,132.902650210566));
#251251=CARTESIAN_POINT('Ctrl Pts',(181.511622555083,-1.62021497890189,
137.208182855437));
#251252=CARTESIAN_POINT('Ctrl Pts',(181.233174931271,4.51195124234396,135.628915707812));
#251253=CARTESIAN_POINT('Ctrl Pts',(180.954727307458,6.49785469294791,129.61611812487));
#251254=CARTESIAN_POINT('Ctrl Pts',(180.676279683645,2.51254711858197,124.695257343842));
#251255=CARTESIAN_POINT('Ctrl Pts',(180.397832059832,-3.78166851301026,
125.388364025079));
#251256=CARTESIAN_POINT('Ctrl Pts',(180.119384436019,-6.60071552592353,
131.058506988669));
#251257=CARTESIAN_POINT('Ctrl Pts',(179.840936812206,-3.35402743339335,
136.495101852955));
#251258=CARTESIAN_POINT('Ctrl Pts',(179.562489188393,2.97484801707599,136.702183530083));
#251259=CARTESIAN_POINT('Ctrl Pts',(179.28404156458,6.56998346925752,131.489454075275));
#251260=CARTESIAN_POINT('Ctrl Pts',(179.005593940767,4.12762507472721,125.647157201507));
#251261=CARTESIAN_POINT('Ctrl Pts',(178.727146316955,-2.10781911778238,
124.544078323705));
#251262=CARTESIAN_POINT('Ctrl Pts',(178.448698693142,-6.40628051373842,
129.193893042167));
#251263=CARTESIAN_POINT('Ctrl Pts',(178.170251069329,-4.81768308177075,
135.323648786705));
#251264=CARTESIAN_POINT('Ctrl Pts',(177.891803445516,1.19812974544141,137.300399483306));
#251265=CARTESIAN_POINT('Ctrl Pts',(177.613355821703,6.11291986848493,133.307607811431));
#251266=CARTESIAN_POINT('Ctrl Pts',(177.33490819789,5.41023526512845,127.014454258818));
#251267=CARTESIAN_POINT('Ctrl Pts',(177.056460574078,-0.264191242194762,
124.204039502676));
#251268=CARTESIAN_POINT('Ctrl Pts',(176.778012950264,-5.69583890440069,
127.458997407505));
#251269=CARTESIAN_POINT('Ctrl Pts',(176.499565326452,-5.89328887066216,
133.788180672302));
#251270=CARTESIAN_POINT('Ctrl Pts',(176.221117702638,-0.675094267951971,
137.375379074508));
#251271=CARTESIAN_POINT('Ctrl Pts',(175.942670078826,5.16347898681764,134.924132526884));
#251272=CARTESIAN_POINT('Ctrl Pts',(175.664222455013,6.25706730267374,128.687016856641));
#251273=CARTESIAN_POINT('Ctrl Pts',(175.3857748312,1.60071644210391,124.395636664696));
#251274=CARTESIAN_POINT('Ctrl Pts',(175.107327207387,-4.5266146294138,125.993560701866));
#251275=CARTESIAN_POINT('Ctrl Pts',(174.828879583574,-6.49420799391872,
132.012374840923));
#251276=CARTESIAN_POINT('Ctrl Pts',(174.550431959762,-2.49394147171037,
136.92108292349));
#251277=CARTESIAN_POINT('Ctrl Pts',(174.271984335948,3.79813542718566,136.208822025409));
#251278=CARTESIAN_POINT('Ctrl Pts',(173.993536712136,6.59991141772898,130.530125116137));
#251279=CARTESIAN_POINT('Ctrl Pts',(173.715089088322,3.33669123897678,125.103437235529));
#251280=CARTESIAN_POINT('Ctrl Pts',(173.43664146451,-2.99278518196597,124.915619437422));
#251281=CARTESIAN_POINT('Ctrl Pts',(173.158193840697,-6.5720382263662,130.139267102866));
#251282=CARTESIAN_POINT('Ctrl Pts',(172.879746216884,-4.11190920265221,
135.974103216695));
#251283=CARTESIAN_POINT('Ctrl Pts',(172.601298593071,2.12686350036709,137.058198437889));
#251284=CARTESIAN_POINT('Ctrl Pts',(172.322850969258,6.41115254960738,132.395322219168));
#251285=CARTESIAN_POINT('Ctrl Pts',(172.044403345445,4.80390560797255,126.270430011369));
#251286=CARTESIAN_POINT('Ctrl Pts',(171.765955721632,-1.21789590355323,
124.31199853584));
#251287=CARTESIAN_POINT('Ctrl Pts',(171.487508097819,-6.12051057723618,
128.319730643897));
#251288=CARTESIAN_POINT('Ctrl Pts',(171.209060474007,-5.39867503400336,
134.610716316833));
#251289=CARTESIAN_POINT('Ctrl Pts',(170.930612850193,0.284279125540913,
137.403847052956));
#251290=CARTESIAN_POINT('Ctrl Pts',(170.652165226381,5.70599465652041,134.13237215779));
#251291=CARTESIAN_POINT('Ctrl Pts',(170.373717602568,5.88417985149351,127.802617239562));
#251292=CARTESIAN_POINT('Ctrl Pts',(170.095269978755,0.655091221110643,
124.231317842401));
#251293=CARTESIAN_POINT('Ctrl Pts',(169.816822354942,-5.17599423848763,
126.700323644626));
#251294=CARTESIAN_POINT('Ctrl Pts',(169.538374731129,-6.25059385429175,
132.940738931629));
#251295=CARTESIAN_POINT('Ctrl Pts',(169.259927107316,-1.58120307648749,
137.217926915891));
#251296=CARTESIAN_POINT('Ctrl Pts',(168.981479483503,4.54123608254409,135.601360792124));
#251297=CARTESIAN_POINT('Ctrl Pts',(168.703031859691,6.49050113343381,129.576585854424));
#251298=CARTESIAN_POINT('Ctrl Pts',(168.424584235878,2.47531272130571,124.680075943919));
#251299=CARTESIAN_POINT('Ctrl Pts',(168.146136612065,-3.81456715595326,
125.411484460556));
#251300=CARTESIAN_POINT('Ctrl Pts',(167.867688988252,-6.59904616885666,
131.098682708838));
#251301=CARTESIAN_POINT('Ctrl Pts',(167.589241364439,-3.31932413390846,
136.515413333674));
#251302=CARTESIAN_POINT('Ctrl Pts',(167.310793740626,3.01069462210276,136.683965512842));
#251303=CARTESIAN_POINT('Ctrl Pts',(167.032346116813,6.57403210101054,131.449448027918));
#251304=CARTESIAN_POINT('Ctrl Pts',(166.753898493,4.09615523841214,125.622126727152));
#251305=CARTESIAN_POINT('Ctrl Pts',(166.475450869187,-2.14588817997888,
124.557025205477));
#251306=CARTESIAN_POINT('Ctrl Pts',(166.197003245374,-6.41596519343492,
129.232919728208));
#251307=CARTESIAN_POINT('Ctrl Pts',(165.918555621562,-4.79008363144905,
135.352891659104));
#251308=CARTESIAN_POINT('Ctrl Pts',(165.640107997748,1.23765077924384,137.292985770921));
#251309=CARTESIAN_POINT('Ctrl Pts',(165.361660373936,6.12804458641347,133.270350353765));
#251310=CARTESIAN_POINT('Ctrl Pts',(165.083212750123,5.38706479029029,126.981590839339));
#251311=CARTESIAN_POINT('Ctrl Pts',(164.80476512631,-0.304364375363971,
124.205769998417));
#251312=CARTESIAN_POINT('Ctrl Pts',(164.526317502497,-5.71609754908509,
127.493731577419));
#251313=CARTESIAN_POINT('Ctrl Pts',(164.247869878684,-5.8750163220866,133.823999511097));
#251314=CARTESIAN_POINT('Ctrl Pts',(163.969422254871,-0.635082105593798,
137.37936681918));
#251315=CARTESIAN_POINT('Ctrl Pts',(163.690974631059,5.18846154045405,134.892624634889));
#251316=CARTESIAN_POINT('Ctrl Pts',(163.412527007245,6.24406250126218,128.648967541478));
#251317=CARTESIAN_POINT('Ctrl Pts',(163.134079383433,1.56167506282176,124.386011388187));
#251318=CARTESIAN_POINT('Ctrl Pts',(162.85563175962,-4.55581546628373,126.021204622902));
#251319=CARTESIAN_POINT('Ctrl Pts',(162.577184135807,-6.48673414583306,
132.051884546553));
#251320=CARTESIAN_POINT('Ctrl Pts',(162.298736511994,-2.45666103994207,
136.936150924396));
#251321=CARTESIAN_POINT('Ctrl Pts',(162.020288888181,3.83096354709181,136.185601564872));
#251322=CARTESIAN_POINT('Ctrl Pts',(161.741841264368,6.59811978732212,130.489954663008));
#251323=CARTESIAN_POINT('Ctrl Pts',(161.463393640556,3.30192627907479,125.083231473798));
#251324=CARTESIAN_POINT('Ctrl Pts',(161.184946016742,-3.02857617157586,
124.933946475014));
#251325=CARTESIAN_POINT('Ctrl Pts',(160.90649839293,-6.57596507471956,130.179285287561));
#251326=CARTESIAN_POINT('Ctrl Pts',(160.628050769116,-4.08036332794952,
135.999037791754));
#251327=CARTESIAN_POINT('Ctrl Pts',(160.349603145304,2.16489298037573,137.045135746957));
#251328=CARTESIAN_POINT('Ctrl Pts',(160.07115552149,6.42071840063739,132.356266237063));
#251329=CARTESIAN_POINT('Ctrl Pts',(159.792707897678,4.77621728024515,126.241271277656));
#251330=CARTESIAN_POINT('Ctrl Pts',(159.514260273865,-1.25739418950663,
124.319532502318));
#251331=CARTESIAN_POINT('Ctrl Pts',(159.235812650052,-6.13552182622286,
128.357033963427));
#251332=CARTESIAN_POINT('Ctrl Pts',(158.957365026239,-5.37540464154493,
134.643509061136));
#251333=CARTESIAN_POINT('Ctrl Pts',(158.678917402427,0.324446805597038,
137.401994292032));
#251334=CARTESIAN_POINT('Ctrl Pts',(158.400469778613,5.72614748850293,134.097576488416));
#251335=CARTESIAN_POINT('Ctrl Pts',(158.122022154801,5.86579836733105,127.766854182028));
#251336=CARTESIAN_POINT('Ctrl Pts',(157.843574530988,0.615067106763091,
124.22745189946));
#251337=CARTESIAN_POINT('Ctrl Pts',(157.565126907175,-5.20088077722156,
126.731907428977));
#251338=CARTESIAN_POINT('Ctrl Pts',(157.286679283362,-6.23747330409059,
132.978748488409));
#251339=CARTESIAN_POINT('Ctrl Pts',(157.008231659549,-1.54213258201158,
137.227433319288));
#251340=CARTESIAN_POINT('Ctrl Pts',(156.729784035736,4.5703526455712,135.57362812183));
#251341=CARTESIAN_POINT('Ctrl Pts',(156.451336411923,6.48290706601333,129.537099079623));
#251342=CARTESIAN_POINT('Ctrl Pts',(156.172888788111,2.43798660040623,124.665121481617));
#251343=CARTESIAN_POINT('Ctrl Pts',(155.894441164297,-3.84732444870741,
125.434804731043));
#251344=CARTESIAN_POINT('Ctrl Pts',(155.615993540485,-6.59713228170722,
131.138847522794));
#251345=CARTESIAN_POINT('Ctrl Pts',(155.337545916672,-3.28449783564716,
136.535513189234));
#251346=CARTESIAN_POINT('Ctrl Pts',(155.059098292859,3.04642966473303,136.665529624679));
#251347=CARTESIAN_POINT('Ctrl Pts',(154.780650669046,6.57783712958646,131.409418076611));
#251348=CARTESIAN_POINT('Ctrl Pts',(154.502203045233,4.06453361755842,125.597288282381));
#251349=CARTESIAN_POINT('Ctrl Pts',(154.22375542142,-2.18387772549973,124.57020358456));
#251350=CARTESIAN_POINT('Ctrl Pts',(153.945307797607,-6.42541212718171,
129.272004644569));
#251351=CARTESIAN_POINT('Ctrl Pts',(153.666860173794,-4.76230668281685,
135.381965984011));
#251352=CARTESIAN_POINT('Ctrl Pts',(153.388412549982,1.27712595144142,137.285331620145));
#251353=CARTESIAN_POINT('Ctrl Pts',(153.109964926169,6.14294222739622,133.233001517943));
#251354=CARTESIAN_POINT('Ctrl Pts',(152.831517302356,5.36369469578529,126.948869073999));
#251355=CARTESIAN_POINT('Ctrl Pts',(152.553069678543,-0.344526230199219,
124.207745007359));
#251356=CARTESIAN_POINT('Ctrl Pts',(152.27462205473,-5.73614438167267,127.528588423912));
#251357=CARTESIAN_POINT('Ctrl Pts',(151.996174430917,-5.85652607262075,
133.859706456064));
#251358=CARTESIAN_POINT('Ctrl Pts',(151.717726807104,-0.595046410034728,
137.383110924578));
#251359=CARTESIAN_POINT('Ctrl Pts',(151.439279183291,5.21325183374003,134.860965250768));
#251360=CARTESIAN_POINT('Ctrl Pts',(151.160831559478,6.23082632381839,128.610998095198));
#251361=CARTESIAN_POINT('Ctrl Pts',(150.882383935665,1.52257581509584,124.376623945969));
#251362=CARTESIAN_POINT('Ctrl Pts',(150.603936311853,-4.58484748573611,
126.049025785542));
#251363=CARTESIAN_POINT('Ctrl Pts',(150.32548868804,-6.47901992942814,132.091348024725));
#251364=CARTESIAN_POINT('Ctrl Pts',(150.047041064227,-2.41928957569559,
136.950991709558));
#251365=CARTESIAN_POINT('Ctrl Pts',(149.768593440414,3.8636497092349,136.162181700472));
#251366=CARTESIAN_POINT('Ctrl Pts',(149.490145816601,6.59608366116008,130.449795860306));
#251367=CARTESIAN_POINT('Ctrl Pts',(149.211698192788,3.26703896508027,125.06323771061));
#251368=CARTESIAN_POINT('Ctrl Pts',(148.933250568975,-3.06425493618196,
124.95249104296));
#251369=CARTESIAN_POINT('Ctrl Pts',(148.654802945162,-6.57964824826877,
130.219326634649));
#251370=CARTESIAN_POINT('Ctrl Pts',(148.376355321349,-4.04866625388314,
136.02377987614));
#251371=CARTESIAN_POINT('Ctrl Pts',(148.097907697537,2.20284223947883,137.031841801807));
#251372=CARTESIAN_POINT('Ctrl Pts',(147.819460073724,6.43004632958585,132.317152748525));
#251373=CARTESIAN_POINT('Ctrl Pts',(147.541012449911,4.74835196802999,126.212281630895));
#251374=CARTESIAN_POINT('Ctrl Pts',(147.262564826098,-1.29684588225586,
124.327306766486));
#251375=CARTESIAN_POINT('Ctrl Pts',(146.984117202285,-6.15030572119196,
128.394427969547));
#251376=CARTESIAN_POINT('Ctrl Pts',(146.705669578472,-5.35193506149072,
134.676159544383));
#251377=CARTESIAN_POINT('Ctrl Pts',(146.427221954659,0.364602463157475,
137.399897053366));
#251378=CARTESIAN_POINT('Ctrl Pts',(146.148774330846,5.74608813598446,134.062658787717));
#251379=CARTESIAN_POINT('Ctrl Pts',(145.870326707034,5.84719952385297,127.731203680413));
#251380=CARTESIAN_POINT('Ctrl Pts',(145.59187908322,0.575020200877703,124.22382966629));
#251381=CARTESIAN_POINT('Ctrl Pts',(145.313431459408,-5.22557459540567,
126.76364211958));
#251382=CARTESIAN_POINT('Ctrl Pts',(145.034983835595,-6.22412162202233,
133.016677472446));
#251383=CARTESIAN_POINT('Ctrl Pts',(144.756536211782,-1.50300494324566,
137.236701713364));
#251384=CARTESIAN_POINT('Ctrl Pts',(144.478088587969,4.59929985250025,135.545718724575));
#251385=CARTESIAN_POINT('Ctrl Pts',(144.199640964156,6.47507277208744,129.497659263665));
#251386=CARTESIAN_POINT('Ctrl Pts',(143.921193340343,2.40057013901678,124.65039451108));
#251387=CARTESIAN_POINT('Ctrl Pts',(143.64274571653,-3.87993917743928,125.458323972397));
#251388=CARTESIAN_POINT('Ctrl Pts',(143.364298092718,-6.594973935395,131.178999942215));
#251389=CARTESIAN_POINT('Ctrl Pts',(143.085850468904,-3.2495498291107,136.555400674828));
#251390=CARTESIAN_POINT('Ctrl Pts',(142.807402845092,3.08205182079176,136.646876548744));
#251391=CARTESIAN_POINT('Ctrl Pts',(142.528955221279,6.58139841398854,131.369365704677));
#251392=CARTESIAN_POINT('Ctrl Pts',(142.250507597466,4.03276138391676,125.572642787588));
#251393=CARTESIAN_POINT('Ctrl Pts',(141.972059973653,-2.2217863466284,124.583612972623));
#251394=CARTESIAN_POINT('Ctrl Pts',(141.69361234984,-6.43462096491922,129.311146342943));
#251395=CARTESIAN_POINT('Ctrl Pts',(141.415164726027,-4.7343532651591,135.410870684068));
#251396=CARTESIAN_POINT('Ctrl Pts',(141.136717102214,1.31655379926713,137.277437314604));
#251397=CARTESIAN_POINT('Ctrl Pts',(140.858269478402,6.15761223939561,133.195562687939));
#251398=CARTESIAN_POINT('Ctrl Pts',(140.579821854588,5.34012584760095,126.916290175316));
#251399=CARTESIAN_POINT('Ctrl Pts',(140.301374230776,-0.384675318488256,
124.20996445632));
#251400=CARTESIAN_POINT('Ctrl Pts',(140.022926606963,-5.75597865932068,
127.563566655346));
#251401=CARTESIAN_POINT('Ctrl Pts',(139.74447898315,-5.83781880742758,133.895300184066));
#251402=CARTESIAN_POINT('Ctrl Pts',(139.466031359337,-0.554988664812238,
137.386611251964));
#251403=CARTESIAN_POINT('Ctrl Pts',(139.187583735524,5.23784894806212,134.829155547671));
#251404=CARTESIAN_POINT('Ctrl Pts',(138.909136111711,6.21735926081381,128.573109924773));
#251405=CARTESIAN_POINT('Ctrl Pts',(138.630688487898,1.48342014776303,124.367474685896));
#251406=CARTESIAN_POINT('Ctrl Pts',(138.352240864086,-4.61370961197883,
126.077023158863));
#251407=CARTESIAN_POINT('Ctrl Pts',(138.073793240272,-6.47106563055709,
132.130763813104));
#251408=CARTESIAN_POINT('Ctrl Pts',(137.79534561646,-2.38182846378423,136.965604729043));
#251409=CARTESIAN_POINT('Ctrl Pts',(137.516897992647,3.89619270241722,136.138563300043));
#251410=CARTESIAN_POINT('Ctrl Pts',(137.238450368834,6.59380311469226,130.409650196134));
#251411=CARTESIAN_POINT('Ctrl Pts',(136.960002745021,3.23203058975544,125.043456686844));
#251412=CARTESIAN_POINT('Ctrl Pts',(136.681555121208,-3.09982015369448,
124.971252454085));
#251413=CARTESIAN_POINT('Ctrl Pts',(136.403107497395,-6.58308761053252,
130.259389660389));
#251414=CARTESIAN_POINT('Ctrl Pts',(136.124659873582,-4.01681915499975,
136.048328553027));
#251415=CARTESIAN_POINT('Ctrl Pts',(135.846212249769,2.24070987145278,137.018317095051));
#251416=CARTESIAN_POINT('Ctrl Pts',(135.567764625956,6.43913599080291,132.277983202917));
#251417=CARTESIAN_POINT('Ctrl Pts',(135.289317002144,4.72031070388647,126.183462145311));
#251418=CARTESIAN_POINT('Ctrl Pts',(135.010869378331,-1.33624951990408,
124.335321040266));
#251419=CARTESIAN_POINT('Ctrl Pts',(134.732421754518,-6.16486171432077,
128.431911276607));
#251420=CARTESIAN_POINT('Ctrl Pts',(134.453974130705,-5.32826716351462,
134.708666556695));
#251421=CARTESIAN_POINT('Ctrl Pts',(134.175526506892,0.404744610239488,
137.397555414672));
#251422=CARTESIAN_POINT('Ctrl Pts',(133.897078883079,5.76581586005707,134.027620349581));
#251423=CARTESIAN_POINT('Ctrl Pts',(133.618631259266,5.82838401024617,127.695667055759));
#251424=CARTESIAN_POINT('Ctrl Pts',(133.340183635453,0.534951987407334,
124.220451277114));
#251425=CARTESIAN_POINT('Ctrl Pts',(133.06173601164,-5.25007477800144,126.795526540492));
#251426=CARTESIAN_POINT('Ctrl Pts',(132.783288387828,-6.21053930283845,
133.054524478268));
#251427=CARTESIAN_POINT('Ctrl Pts',(132.504840764015,-1.46382161007886,
137.245731754674));
#251428=CARTESIAN_POINT('Ctrl Pts',(132.226393140202,4.62807663068185,135.517633634551));
#251429=CARTESIAN_POINT('Ctrl Pts',(131.947945516389,6.46699854195874,129.458267868007));
#251430=CARTESIAN_POINT('Ctrl Pts',(131.669497892576,2.3630647236181,124.635895578019));
#251431=CARTESIAN_POINT('Ctrl Pts',(131.391050268763,-3.91241013359816,
125.482041313105));
#251432=CARTESIAN_POINT('Ctrl Pts',(131.11260264495,-6.59257120989826,131.219138479237));
#251433=CARTESIAN_POINT('Ctrl Pts',(130.834155021138,-3.2144814093103,136.575075053519));
#251434=CARTESIAN_POINT('Ctrl Pts',(130.555707397324,3.1175597702868,136.628006976231));
#251435=CARTESIAN_POINT('Ctrl Pts',(130.277259773512,6.58471582225214,131.329292396271));
#251436=CARTESIAN_POINT('Ctrl Pts',(129.998812149698,4.0008397148189,125.548191156024));
#251437=CARTESIAN_POINT('Ctrl Pts',(129.720364525886,-2.25961263864694,
124.59725287278));
#251438=CARTESIAN_POINT('Ctrl Pts',(129.441916902073,-6.44359136541048,
129.350343372922));
#251439=CARTESIAN_POINT('Ctrl Pts',(129.16346927826,-4.70622441430021,135.439604688201));
#251440=CARTESIAN_POINT('Ctrl Pts',(128.885021654447,1.35593286170785,137.269303146827));
#251441=CARTESIAN_POINT('Ctrl Pts',(128.606574030634,6.17205407880915,133.158035251063));
#251442=CARTESIAN_POINT('Ctrl Pts',(128.328126406821,5.31635911908928,126.883855350513));
#251443=CARTESIAN_POINT('Ctrl Pts',(128.049678783009,-0.424810152491945,
124.212428263054));
#251444=CARTESIAN_POINT('Ctrl Pts',(127.771231159195,-5.77559964706288,
127.598664975593));
#251445=CARTESIAN_POINT('Ctrl Pts',(127.492783535383,-5.81889521971155,
133.930779376167));
#251446=CARTESIAN_POINT('Ctrl Pts',(127.21433591157,-0.514910354280421,
137.389867671632));
#251447=CARTESIAN_POINT('Ctrl Pts',(126.935888287757,5.26225197196523,134.797196704317));
#251448=CARTESIAN_POINT('Ctrl Pts',(126.657440663944,6.20366181127538,128.535304434163));
#251449=CARTESIAN_POINT('Ctrl Pts',(126.378993040131,1.44420951175126,124.358563947));
#251450=CARTESIAN_POINT('Ctrl Pts',(126.100545416318,-4.64240077551519,
126.105195705413));
#251451=CARTESIAN_POINT('Ctrl Pts',(125.822097792505,-6.46287154396936,
132.170130451126));
#251452=CARTESIAN_POINT('Ctrl Pts',(125.543650168692,-2.34427909234318,
136.979989441362));
#251453=CARTESIAN_POINT('Ctrl Pts',(125.26520254488,3.92859132074607,136.114747238771));
#251454=CARTESIAN_POINT('Ctrl Pts',(124.986754921067,6.59127823242518,130.369519158099));
#251455=CARTESIAN_POINT('Ctrl Pts',(124.708307297254,3.19690245034852,125.023889135492));
#251456=CARTESIAN_POINT('Ctrl Pts',(124.429859673441,-3.13527050623128,
124.990230013179));
#251457=CARTESIAN_POINT('Ctrl Pts',(124.151412049628,-6.58628303406391,
130.299472880227));
#251458=CARTESIAN_POINT('Ctrl Pts',(123.872964425815,-3.98482321140548,
136.072682912751));
#251459=CARTESIAN_POINT('Ctrl Pts',(123.594516802002,2.2784944730983,137.004562127853));
#251460=CARTESIAN_POINT('Ctrl Pts',(123.316069178189,6.44798704746787,132.238759051683));
#251461=CARTESIAN_POINT('Ctrl Pts',(123.037621554376,4.6920945268939,126.154813888819));
#251462=CARTESIAN_POINT('Ctrl Pts',(122.759173930564,-1.37560364233486,
124.343575026687));
#251463=CARTESIAN_POINT('Ctrl Pts',(122.480726306751,-6.17918926623166,
128.46948249565));
#251464=CARTESIAN_POINT('Ctrl Pts',(122.202278682938,-5.30440182463932,
134.741028893516));
#251465=CARTESIAN_POINT('Ctrl Pts',(121.923831059125,0.444871759361186,
137.394969462721));
#251466=CARTESIAN_POINT('Ctrl Pts',(121.645383435312,5.78532992970255,133.992462472369));
#251467=CARTESIAN_POINT('Ctrl Pts',(121.366935811499,5.80935252372653,127.660245624887));
#251468=CARTESIAN_POINT('Ctrl Pts',(121.088488187686,0.494863951094175,
124.21731685712));
#251469=CARTESIAN_POINT('Ctrl Pts',(120.810040563873,-5.27438041714564,
126.827559510225));
#251470=CARTESIAN_POINT('Ctrl Pts',(120.53159294006,-6.19672684983677,133.092288103441));
#251471=CARTESIAN_POINT('Ctrl Pts',(120.253145316248,-1.42458403446405,
137.254523108609));
#251472=CARTESIAN_POINT('Ctrl Pts',(119.974697692435,4.65668191378195,135.489373892464));
#251473=CARTESIAN_POINT('Ctrl Pts',(119.696250068622,6.45868467482089,129.418926352309));
#251474=CARTESIAN_POINT('Ctrl Pts',(119.417802444809,2.32547174398699,124.621625219699));
#251475=CARTESIAN_POINT('Ctrl Pts',(119.139354820996,-3.94473611396066,
125.505955874312));
#251476=CARTESIAN_POINT('Ctrl Pts',(118.860907197183,-6.58992419425096,
131.259261646514));
#251477=CARTESIAN_POINT('Ctrl Pts',(118.58245957337,-3.17929387571916,136.594535596262));
#251478=CARTESIAN_POINT('Ctrl Pts',(118.304011949557,3.15295219745811,136.608921606362));
#251479=CARTESIAN_POINT('Ctrl Pts',(118.025564325744,6.58778923144938,131.289199636326));
#251480=CARTESIAN_POINT('Ctrl Pts',(117.747116701932,3.96876979313418,125.523934293753));
#251481=CARTESIAN_POINT('Ctrl Pts',(117.468669078118,-2.29735519988813,
124.611122779595));
#251482=CARTESIAN_POINT('Ctrl Pts',(117.190221454306,-6.45232299625411,
129.389594282045));
#251483=CARTESIAN_POINT('Ctrl Pts',(116.911773830493,-4.67792117256487,
135.468166931659));
#251484=CARTESIAN_POINT('Ctrl Pts',(116.63332620668,1.39526167955762,137.260929418227));
#251485=CARTESIAN_POINT('Ctrl Pts',(116.354878582867,6.18626721048894,133.120420597908));
#251486=CARTESIAN_POINT('Ctrl Pts',(116.076430959054,5.29239539093549,126.851565801475));
#251487=CARTESIAN_POINT('Ctrl Pts',(115.797983335241,-0.464929244999223,
124.215136336267));
#251488=CARTESIAN_POINT('Ctrl Pts',(115.519535711428,-5.79500661783607,
127.633882084071));
#251489=CARTESIAN_POINT('Ctrl Pts',(115.241088087616,-5.79975601069334,
133.96614271767));
#251490=CARTESIAN_POINT('Ctrl Pts',(114.962640463802,-0.474812963556037,
137.392880062915));
#251491=CARTESIAN_POINT('Ctrl Pts',(114.68419283999,5.28646000118636,134.765089904953));
#251492=CARTESIAN_POINT('Ctrl Pts',(114.405745216177,6.18973448276714,128.497583024264));
#251493=CARTESIAN_POINT('Ctrl Pts',(114.127297592364,1.40494536002493,124.349892059469));
#251494=CARTESIAN_POINT('Ctrl Pts',(113.848849968551,-4.67091991318358,
126.133542381245));
#251495=CARTESIAN_POINT('Ctrl Pts',(113.570402344738,-6.45443797329988,
132.209446480045));
#251496=CARTESIAN_POINT('Ctrl Pts',(113.291954720925,-2.30664285277824,
136.994145313484));
#251497=CARTESIAN_POINT('Ctrl Pts',(113.013507097112,3.96084436367879,136.09073439917));
#251498=CARTESIAN_POINT('Ctrl Pts',(112.735059473299,6.58850910791926,130.329404233275));
#251499=CARTESIAN_POINT('Ctrl Pts',(112.456611849487,3.16165584854565,125.004535781636));
#251500=CARTESIAN_POINT('Ctrl Pts',(112.178164225674,-3.1706046801665,125.00942301702));
#251501=CARTESIAN_POINT('Ctrl Pts',(111.899716601861,-6.58923440045535,
130.339574808866));
#251502=CARTESIAN_POINT('Ctrl Pts',(111.621268978048,-3.9526796087217,136.096842052857));
#251503=CARTESIAN_POINT('Ctrl Pts',(111.342821354235,2.31619464429322,136.990577409908));
#251504=CARTESIAN_POINT('Ctrl Pts',(111.064373730422,6.45659917160154,132.199481748287));
#251505=CARTESIAN_POINT('Ctrl Pts',(110.785926106609,4.66370448261314,126.12633792299));
#251506=CARTESIAN_POINT('Ctrl Pts',(110.507478482796,-1.41490679126679,
124.352068419894));
#251507=CARTESIAN_POINT('Ctrl Pts',(110.229030858983,-6.19328784601188,
128.50714023446));
#251508=CARTESIAN_POINT('Ctrl Pts',(109.950583235171,-5.28033992920373,
134.773245355646));
#251509=CARTESIAN_POINT('Ctrl Pts',(109.672135611358,0.484982423596243,
137.392139293334));
#251510=CARTESIAN_POINT('Ctrl Pts',(109.393687987545,5.80462962181993,133.957186458871));
#251511=CARTESIAN_POINT('Ctrl Pts',(109.115240363732,5.79010576951274,127.624940700352));
#251512=CARTESIAN_POINT('Ctrl Pts',(108.836792739919,0.454757577415474,
124.214426522456));
#251513=CARTESIAN_POINT('Ctrl Pts',(108.558345116106,-5.29849061218381,
126.859739841786));
#251514=CARTESIAN_POINT('Ctrl Pts',(108.279897492293,-6.18268477484283,
133.12996694862));
#251515=CARTESIAN_POINT('Ctrl Pts',(108.00144986848,-1.38529367036394,137.2630754494));
#251516=CARTESIAN_POINT('Ctrl Pts',(107.723002244667,4.68511464182123,135.460940545486));
#251517=CARTESIAN_POINT('Ctrl Pts',(107.444554620855,6.45013147874722,129.379636174388));
#251518=CARTESIAN_POINT('Ctrl Pts',(107.166106997042,2.28779259314522,124.607583964913));
#251519=CARTESIAN_POINT('Ctrl Pts',(106.887659373229,-3.97691592067581,
125.530066769856));
#251520=CARTESIAN_POINT('Ctrl Pts',(106.609211749416,-6.58703298653922,
131.299367957265));
#251521=CARTESIAN_POINT('Ctrl Pts',(106.330764125603,-3.14398853222427,
136.613781581943));
#251522=CARTESIAN_POINT('Ctrl Pts',(106.05231650179,3.18822779082625,136.589621146351));
#251523=CARTESIAN_POINT('Ctrl Pts',(105.773868877977,6.59061852769399,131.249088910493));
#251524=CARTESIAN_POINT('Ctrl Pts',(105.495421254164,3.93655280722527,125.49987309962));
#251525=CARTESIAN_POINT('Ctrl Pts',(105.216973630351,-2.33501263178752,
124.625222179118));
#251526=CARTESIAN_POINT('Ctrl Pts',(104.938526006539,-6.46081553389627,
129.428897615854));
#251527=CARTESIAN_POINT('Ctrl Pts',(104.660078382726,-4.64944458874018,
135.49655635606));
#251528=CARTESIAN_POINT('Ctrl Pts',(104.381630758913,1.43453879547275,137.252316439095));
#251529=CARTESIAN_POINT('Ctrl Pts',(104.1031831351,6.20025110776228,133.082720122298));
#251530=CARTESIAN_POINT('Ctrl Pts',(103.824735511287,5.26823555112421,126.819422724701));
#251531=CARTESIAN_POINT('Ctrl Pts',(103.546287887474,-0.505031109382345,
124.218088575609));
#251532=CARTESIAN_POINT('Ctrl Pts',(103.267840263661,-5.81419885250792,
127.669216675797));
#251533=CARTESIAN_POINT('Ctrl Pts',(102.989392639848,-5.78040188958328,
134.001388898174));
#251534=CARTESIAN_POINT('Ctrl Pts',(102.710945016035,-0.434697978462825,
137.395648314187));
#251535=CARTESIAN_POINT('Ctrl Pts',(102.432497392222,5.31047213868803,134.732836339309));
#251536=CARTESIAN_POINT('Ctrl Pts',(102.15404976841,6.17557779137139,128.459947092858));
#251537=CARTESIAN_POINT('Ctrl Pts',(101.875602144597,1.3656291475316,124.341459344644));
#251538=CARTESIAN_POINT('Ctrl Pts',(101.597154520784,-4.69926596819684,
126.162062135967));
#251539=CARTESIAN_POINT('Ctrl Pts',(101.318706896971,-6.44576523105769,
132.248710442988));
#251540=CARTESIAN_POINT('Ctrl Pts',(101.040259273158,-2.26892113971413,
137.008071820859));
#251541=CARTESIAN_POINT('Ctrl Pts',(100.761811649345,3.99295063606701,136.066525671043));
#251542=CARTESIAN_POINT('Ctrl Pts',(100.483364025532,6.58549584378548,130.289306908136));
#251543=CARTESIAN_POINT('Ctrl Pts',(100.204916401719,3.12629209042249,124.985397342422));
#251544=CARTESIAN_POINT('Ctrl Pts',(99.9264687779064,-3.20582136617937,
125.028830754405));
#251545=CARTESIAN_POINT('Ctrl Pts',(99.6480211540935,-6.5919416003429,130.379693960313));
#251546=CARTESIAN_POINT('Ctrl Pts',(99.3695735302808,-3.92038953804142,
136.120805078117));
#251547=CARTESIAN_POINT('Ctrl Pts',(99.0911259064677,2.35380898804382,136.976363459425));
#251548=CARTESIAN_POINT('Ctrl Pts',(98.812678282655,6.46497204407849,132.160152748165));
#251549=CARTESIAN_POINT('Ctrl Pts',(98.5342306588419,4.63514162304771,126.098035303012));
#251550=CARTESIAN_POINT('Ctrl Pts',(98.2557830350292,-1.45415751030726,
124.36080090516));
#251551=CARTESIAN_POINT('Ctrl Pts',(97.9773354112161,-6.20715693123341,
128.544883097616));
#251552=CARTESIAN_POINT('Ctrl Pts',(97.6988877874034,-5.25608236883021,
134.805314749293));
#251553=CARTESIAN_POINT('Ctrl Pts',(97.4204401635904,0.525075116629235,
137.389065011387));
#251554=CARTESIAN_POINT('Ctrl Pts',(97.1419925397775,5.82371422125203,133.921793616252));
#251555=CARTESIAN_POINT('Ctrl Pts',(96.8635449159648,5.77064446080036,127.589753590393));
#251556=CARTESIAN_POINT('Ctrl Pts',(96.5850972921516,0.414634352527504,
124.211780380221));
#251557=CARTESIAN_POINT('Ctrl Pts',(96.306649668339,-5.32240446970382,126.89206634272));
#251558=CARTESIAN_POINT('Ctrl Pts',(96.0282020445258,-6.16841359819089,
133.1675596176));
#251559=CARTESIAN_POINT('Ctrl Pts',(95.7497544207132,-1.34595197369742,
137.271388460138));
#251560=CARTESIAN_POINT('Ctrl Pts',(95.4713067969001,4.7133737612145,135.432334647225));
#251561=CARTESIAN_POINT('Ctrl Pts',(95.1928591730874,6.44133927067958,129.340398790155));
#251562=CARTESIAN_POINT('Ctrl Pts',(94.9144115492744,2.25002866730758,124.593772333964));
#251563=CARTESIAN_POINT('Ctrl Pts',(94.6359639254615,-4.008948361309,125.554373106298));
#251564=CARTESIAN_POINT('Ctrl Pts',(94.3575163016487,-6.58389769389783,
131.339455925338));
#251565=CARTESIAN_POINT('Ctrl Pts',(94.0790686778357,-3.10856668707799,
136.632812297395));
#251566=CARTESIAN_POINT('Ctrl Pts',(93.8006210540229,3.22338524324122,136.570106311383));
#251567=CARTESIAN_POINT('Ctrl Pts',(93.52217343021,6.59320360614536,131.208961705089));
#251568=CARTESIAN_POINT('Ctrl Pts',(93.2437258063971,3.90418995090443,125.476008465224));
#251569=CARTESIAN_POINT('Ctrl Pts',(92.9652781825842,-2.37258353893516,
124.639550548886));
#251570=CARTESIAN_POINT('Ctrl Pts',(92.6868305587713,-6.46906866364288,
129.468251917951));
#251571=CARTESIAN_POINT('Ctrl Pts',(92.4083829349583,-4.62079571803641,
135.524771909422));
#251572=CARTESIAN_POINT('Ctrl Pts',(92.1299353111456,1.47376275402524,137.24346452859));
#251573=CARTESIAN_POINT('Ctrl Pts',(91.8514876873325,6.21400525245068,133.04493522124));
#251574=CARTESIAN_POINT('Ctrl Pts',(91.5730400635199,5.24388049490719,126.787427311268));
#251575=CARTESIAN_POINT('Ctrl Pts',(91.2945924397067,-0.545114259651984,
124.221284871682));
#251576=CARTESIAN_POINT('Ctrl Pts',(91.016144815894,-5.83317563990314,127.704667441434));
#251577=CARTESIAN_POINT('Ctrl Pts',(90.7376971920811,-5.76083357355547,
134.036516611621));
#251578=CARTESIAN_POINT('Ctrl Pts',(90.4592495682681,-0.394566885476172,
137.398172322869));
#251579=CARTESIAN_POINT('Ctrl Pts',(90.1808019444553,5.33428749469169,134.700437202553));
#251580=CARTESIAN_POINT('Ctrl Pts',(89.9023543206424,6.16119226166949,128.422398034556));
#251581=CARTESIAN_POINT('Ctrl Pts',(89.6239066968295,1.32626233114802,124.333266115003));
#251582=CARTESIAN_POINT('Ctrl Pts',(89.3454590730166,-4.72743789018152,
126.190753912764));
#251583=CARTESIAN_POINT('Ctrl Pts',(89.0670114492037,-6.43685363861442,
132.28792088502));
#251584=CARTESIAN_POINT('Ctrl Pts',(88.7885638253908,-2.23111535094281,
137.021768447433));
#251585=CARTESIAN_POINT('Ctrl Pts',(88.5101162015778,4.02490894820102,136.042121951457));
#251586=CARTESIAN_POINT('Ctrl Pts',(88.2316685777651,6.58223855168135,130.2492286685));
#251587=CARTESIAN_POINT('Ctrl Pts',(87.9532209539521,3.09081248639635,124.966474527032));
#251588=CARTESIAN_POINT('Ctrl Pts',(87.6747733301392,-3.2409192593025,125.048452506173));
#251589=CARTESIAN_POINT('Ctrl Pts',(87.3963257063264,-6.59440453341028,
130.41982884794));
#251590=CARTESIAN_POINT('Ctrl Pts',(87.1178780825135,-3.88795419588509,
136.144571100572));
#251591=CARTESIAN_POINT('Ctrl Pts',(86.8394304587006,2.39133611053674,136.961920803106));
#251592=CARTESIAN_POINT('Ctrl Pts',(86.5609828348878,6.47310535463887,132.120773508667));
#251593=CARTESIAN_POINT('Ctrl Pts',(86.2825352110747,4.60640700660486,126.06990707765));
#251594=CARTESIAN_POINT('Ctrl Pts',(86.004087587262,-1.49335434500641,124.369772158902));
#251595=CARTESIAN_POINT('Ctrl Pts',(85.725639963449,-6.22079600797217,128.582709686544));
#251596=CARTESIAN_POINT('Ctrl Pts',(85.4471923396362,-5.23163004239161,
134.837235886113));
#251597=CARTESIAN_POINT('Ctrl Pts',(85.1687447158232,0.565148352810691,
137.385746730796));
#251598=CARTESIAN_POINT('Ctrl Pts',(84.8902970920103,5.842583020812,133.886285256006));
#251599=CARTESIAN_POINT('Ctrl Pts',(84.6118494681974,5.75096931873532,127.554685598878));
#251600=CARTESIAN_POINT('Ctrl Pts',(84.3334018443846,0.374495763211118,
124.209378528473));
#251601=CARTESIAN_POINT('Ctrl Pts',(84.0549542205716,-5.34612110356891,
126.924537815158));
#251602=CARTESIAN_POINT('Ctrl Pts',(83.7765065967588,-6.15391384870464,
133.205064717373));
#251603=CARTESIAN_POINT('Ctrl Pts',(83.498058972946,-1.30656040228555,137.279461832782));
#251604=CARTESIAN_POINT('Ctrl Pts',(83.2196113491328,4.74145822480973,135.403557257686));
#251605=CARTESIAN_POINT('Ctrl Pts',(82.9411637253203,6.43230837641647,129.301215653567));
#251606=CARTESIAN_POINT('Ctrl Pts',(82.6627161015071,2.21218136583022,124.580190838648));
#251607=CARTESIAN_POINT('Ctrl Pts',(82.3842684776944,-4.04083224888638,
125.578873982957));
#251608=CARTESIAN_POINT('Ctrl Pts',(82.1058208538814,-6.58051843250612,
131.379524065257));
#251609=CARTESIAN_POINT('Ctrl Pts',(81.8273732300686,-3.07302965285007,
136.651627037425));
#251610=CARTESIAN_POINT('Ctrl Pts',(81.5489256062556,3.25842325193051,136.550377824588));
#251611=CARTESIAN_POINT('Ctrl Pts',(81.270477982443,6.59554437101248,131.168819507043));
#251612=CARTESIAN_POINT('Ctrl Pts',(80.9920303586297,3.87168242338918,125.452341274876));
#251613=CARTESIAN_POINT('Ctrl Pts',(80.713582734817,-2.41006652912724,124.654107357959));
#251614=CARTESIAN_POINT('Ctrl Pts',(80.435135111004,-6.47708207967116,129.507655730047));
#251615=CARTESIAN_POINT('Ctrl Pts',(80.1566874871913,-4.59197562204804,
135.552812546207));
#251616=CARTESIAN_POINT('Ctrl Pts',(79.8782398633782,1.51293210175691,137.234374014721));
#251617=CARTESIAN_POINT('Ctrl Pts',(79.5997922395654,6.22752913488936,133.007067294864));
#251618=CARTESIAN_POINT('Ctrl Pts',(79.3213446157525,5.2193311247699,126.755580746775));
#251619=CARTESIAN_POINT('Ctrl Pts',(79.0428969919396,-0.585177210512381,
124.224725106049));
#251620=CARTESIAN_POINT('Ctrl Pts',(78.7644493681267,-5.85193627682986,
127.740233067343));
#251621=CARTESIAN_POINT('Ctrl Pts',(78.4860017443139,-5.74105178772106,
134.071524556339));
#251622=CARTESIAN_POINT('Ctrl Pts',(78.2075541205009,-0.354421171668466,
137.400451995434));
#251623=CARTESIAN_POINT('Ctrl Pts',(77.9291064966881,5.35790518671055,134.667893695246));
#251624=CARTESIAN_POINT('Ctrl Pts',(77.6506588728751,6.14657842672258,128.384937240753));
#251625=CARTESIAN_POINT('Ctrl Pts',(77.3722112490624,1.28684636962602,124.325312674148));
#251626=CARTESIAN_POINT('Ctrl Pts',(77.0937636252493,-4.75543463521666,
126.219616648455));
#251627=CARTESIAN_POINT('Ctrl Pts',(76.8153160014366,-6.42770352619243,
132.327076353179));
#251628=CARTESIAN_POINT('Ctrl Pts',(76.5368683776235,-2.19322688737167,
137.035234685673));
#251629=CARTESIAN_POINT('Ctrl Pts',(76.2584207538107,4.05671811585379,136.017524144697));
#251630=CARTESIAN_POINT('Ctrl Pts',(75.9799731299978,6.57873735230709,130.209170999483));
#251631=CARTESIAN_POINT('Ctrl Pts',(75.7015255061849,3.05521835117689,124.947768036657));
#251632=CARTESIAN_POINT('Ctrl Pts',(75.423077882372,-3.27589705897064,125.068287545233));
#251633=CARTESIAN_POINT('Ctrl Pts',(75.1446302585591,-6.5966231083926,130.459977984534));
#251634=CARTESIAN_POINT('Ctrl Pts',(74.8661826347462,-3.85537478415624,
136.168139239563));
#251635=CARTESIAN_POINT('Ctrl Pts',(74.5877350109334,2.42877462119068,136.94724997613));
#251636=CARTESIAN_POINT('Ctrl Pts',(74.3092873871204,6.48099880189986,132.081345489005));
#251637=CARTESIAN_POINT('Ctrl Pts',(74.0308397633076,4.57750169805637,126.041954289206));
#251638=CARTESIAN_POINT('Ctrl Pts',(73.7523921394947,-1.53249584291112,
124.378981848686));
#251639=CARTESIAN_POINT('Ctrl Pts',(73.4739445156818,-6.23420457082727,
128.620618599563));
#251640=CARTESIAN_POINT('Ctrl Pts',(73.1954968918689,-5.20698385597775,
134.869007583256));
#251641=CARTESIAN_POINT('Ctrl Pts',(72.917049268056,0.605200647212208,137.382184574524));
#251642=CARTESIAN_POINT('Ctrl Pts',(72.6386016442432,5.86123532130951,133.850662693911));
#251643=CARTESIAN_POINT('Ctrl Pts',(72.3601540204302,5.73108107238729,127.519738025268));
#251644=CARTESIAN_POINT('Ctrl Pts',(72.0817063966174,0.334343296816498,
124.207221056211));
#251645=CARTESIAN_POINT('Ctrl Pts',(71.8032587728044,-5.36963963495047,
126.957153055855));
#251646=CARTESIAN_POINT('Ctrl Pts',(71.5248111489915,-6.13918606367764,
133.242480858172));
#251647=CARTESIAN_POINT('Ctrl Pts',(71.2463635251787,-1.26712041579749,
137.287295268168));
#251648=CARTESIAN_POINT('Ctrl Pts',(70.9679159013657,4.76936699192676,135.374609443224));
#251649=CARTESIAN_POINT('Ctrl Pts',(70.689468277553,6.423039130601,129.262088216567));
#251650=CARTESIAN_POINT('Ctrl Pts',(70.4110206537399,2.17425209115883,124.566839982233));
#251651=CARTESIAN_POINT('Ctrl Pts',(70.1325730299272,-4.07256640193864,
125.603568491945));
#251652=CARTESIAN_POINT('Ctrl Pts',(69.8541254061142,-6.57689532758393,
131.419570892283));
#251653=CARTESIAN_POINT('Ctrl Pts',(69.5756777823013,-3.03737874637841,
136.670225104848));
#251654=CARTESIAN_POINT('Ctrl Pts',(69.2972301584884,3.2933405185478,136.530436417012));
#251655=CARTESIAN_POINT('Ctrl Pts',(69.0187825346755,6.5976407355574,131.128663803839));
#251656=CARTESIAN_POINT('Ctrl Pts',(68.7403349108627,3.83903142925813,125.428872405572));
#251657=CARTESIAN_POINT('Ctrl Pts',(68.4618872870498,-2.44746021341752,
124.668892066929));
#251658=CARTESIAN_POINT('Ctrl Pts',(68.1834396632368,-6.48485548504104,
129.547107592018));
#251659=CARTESIAN_POINT('Ctrl Pts',(67.904992039424,-4.56298536871445,135.580677227361));
#251660=CARTESIAN_POINT('Ctrl Pts',(67.6265444156111,1.55204538723279,137.225045234339));
#251661=CARTESIAN_POINT('Ctrl Pts',(67.3480967917982,6.2408222539455,132.969117746385));
#251662=CARTESIAN_POINT('Ctrl Pts',(67.0696491679854,5.19458835039884,126.723884211309));
#251663=CARTESIAN_POINT('Ctrl Pts',(66.7912015441724,-0.625218477415679,
124.228409151229));
#251664=CARTESIAN_POINT('Ctrl Pts',(66.5127539203596,-5.87048006810572,
127.775912235624));
#251665=CARTESIAN_POINT('Ctrl Pts',(66.2343062965465,-5.72105726510147,
134.106411435094));
#251666=CARTESIAN_POINT('Ctrl Pts',(65.9558586727338,-0.314262324654327,
137.402487247406));
#251667=CARTESIAN_POINT('Ctrl Pts',(65.6774110489208,5.3813243395822,134.6352070233));
#251668=CARTESIAN_POINT('Ctrl Pts',(65.398963425108,6.13173682805169,128.347566099575));
#251669=CARTESIAN_POINT('Ctrl Pts',(65.120515801295,1.24738272353907,124.317599316798));
#251670=CARTESIAN_POINT('Ctrl Pts',(64.8420681774823,-4.78325516587229,
126.248649273519));
#251671=CARTESIAN_POINT('Ctrl Pts',(64.5636205536692,-6.41831523285262,
132.366175396547));
#251672=CARTESIAN_POINT('Ctrl Pts',(64.2851729298565,-2.15525715297185,
137.048470036584));
#251673=CARTESIAN_POINT('Ctrl Pts',(64.0067253060435,4.08837696032456,135.992733162246));
#251674=CARTESIAN_POINT('Ctrl Pts',(63.7282776822307,6.57499237540094,130.169135385437));
#251675=CARTESIAN_POINT('Ctrl Pts',(63.4498300584178,3.01951100371835,124.929278564476));
#251676=CARTESIAN_POINT('Ctrl Pts',(63.1713824346048,-3.31075346906837,
125.088335136589));
#251677=CARTESIAN_POINT('Ctrl Pts',(62.892934810792,-6.59859724307971,130.500139882352));
#251678=CARTESIAN_POINT('Ctrl Pts',(62.614487186979,-3.82265251009718,136.191508621766));
#251679=CARTESIAN_POINT('Ctrl Pts',(62.3360395631662,2.46612313270748,136.932351522132));
#251680=CARTESIAN_POINT('Ctrl Pts',(62.0575919393533,6.48865209336687,132.041870150199));
#251681=CARTESIAN_POINT('Ctrl Pts',(61.7791443155403,4.5484267684992,126.014177973478));
#251682=CARTESIAN_POINT('Ctrl Pts',(61.5006966917276,-1.57158055361859,
124.388429633243));
#251683=CARTESIAN_POINT('Ctrl Pts',(61.2222490679146,-6.24738212293903,
128.658608431946));
#251684=CARTESIAN_POINT('Ctrl Pts',(60.9438014441017,-5.18214472286266,
134.900628663412));
#251685=CARTESIAN_POINT('Ctrl Pts',(60.6653538202889,0.645230515680748,
137.378378674564));
#251686=CARTESIAN_POINT('Ctrl Pts',(60.3869061964759,5.87967043157647,133.814927249971));
#251687=CARTESIAN_POINT('Ctrl Pts',(60.108458572663,5.71098045872276,127.484912164554));
#251688=CARTESIAN_POINT('Ctrl Pts',(59.8300109488502,0.294178441208572,
124.205308043382));
#251689=CARTESIAN_POINT('Ctrl Pts',(59.5515633250373,-5.39295919236059,
126.989910856244));
#251690=CARTESIAN_POINT('Ctrl Pts',(59.2731157012244,-6.12423078885343,
133.27980665353));
#251691=CARTESIAN_POINT('Ctrl Pts',(58.9946680774115,-1.2276334756968,137.294888476026));
#251692=CARTESIAN_POINT('Ctrl Pts',(58.7162204535986,4.79709902839574,135.345492276511));
#251693=CARTESIAN_POINT('Ctrl Pts',(58.4377728297857,6.41353187670863,129.223017929039));
#251694=CARTESIAN_POINT('Ctrl Pts',(58.1593252059728,2.13624224877676,124.553720259438));
#251695=CARTESIAN_POINT('Ctrl Pts',(57.8808775821599,-4.10414964454526,
125.628455718198));
#251696=CARTESIAN_POINT('Ctrl Pts',(57.602429958347,-6.57302851338661,131.459594922466));
#251697=CARTESIAN_POINT('Ctrl Pts',(57.3239823345341,-3.00161528872044,
136.688605810505));
#251698=CARTESIAN_POINT('Ctrl Pts',(57.0455347107212,3.32813574922106,136.510282827592));
#251699=CARTESIAN_POINT('Ctrl Pts',(56.7670870869083,6.59949262209846,131.088496083461));
#251700=CARTESIAN_POINT('Ctrl Pts',(56.4886394630955,3.80623817840574,125.405602726962));
#251701=CARTESIAN_POINT('Ctrl Pts',(56.2101918392826,-2.48476320616966,
124.683904127941));
#251702=CARTESIAN_POINT('Ctrl Pts',(55.9317442154696,-6.49238859170611,
129.586606041964));
#251703=CARTESIAN_POINT('Ctrl Pts',(55.6532965916568,-4.53382603227983,
135.608364920346));
#251704=CARTESIAN_POINT('Ctrl Pts',(55.3748489678439,1.59110116109648,137.215478533129));
#251705=CARTESIAN_POINT('Ctrl Pts',(55.096401344031,6.25388411703813,132.931087982032));
#251706=CARTESIAN_POINT('Ctrl Pts',(54.8179537202181,5.1696530886458,126.692338879397));
#251707=CARTESIAN_POINT('Ctrl Pts',(54.5395060964052,-0.665236576618623,
124.23233687071));
#251708=CARTESIAN_POINT('Ctrl Pts',(54.2610584725923,-5.88880632658389,
127.811703624173));
#251709=CARTESIAN_POINT('Ctrl Pts',(53.9826108487795,-5.70085074660091,
134.141175955143));
#251710=CARTESIAN_POINT('Ctrl Pts',(53.7041632249665,-0.274091832533765,
137.40427800337));
#251711=CARTESIAN_POINT('Ctrl Pts',(53.4257156011537,5.40454408550164,134.602378397932));
#251712=CARTESIAN_POINT('Ctrl Pts',(53.1472679773408,6.11666801561766,128.310285995821));
#251713=CARTESIAN_POINT('Ctrl Pts',(52.8688203535278,1.20787285522606,124.310126328773));
#251714=CARTESIAN_POINT('Ctrl Pts',(52.590372729715,-4.81089845124901,126.277850712144));
#251715=CARTESIAN_POINT('Ctrl Pts',(52.3119251059021,-6.40868910648141,
132.405216566294));
#251716=CARTESIAN_POINT('Ctrl Pts',(52.0334774820892,-2.11720755472543,
137.061474009724));
#251717=CARTESIAN_POINT('Ctrl Pts',(51.7550298582764,4.11988430848393,135.967749922743));
#251718=CARTESIAN_POINT('Ctrl Pts',(51.4765822344634,6.57100375973434,130.129123309894));
#251719=CARTESIAN_POINT('Ctrl Pts',(51.1981346106506,2.98369176716867,124.91100679562));
#251720=CARTESIAN_POINT('Ctrl Pts',(50.9196869868376,-3.34548719797895,
125.108594537373));
#251721=CARTESIAN_POINT('Ctrl Pts',(50.6412393630248,-6.60032686431936,
130.540313053181));
#251722=CARTESIAN_POINT('Ctrl Pts',(50.3627917392119,-3.78978858624336,
136.214678381218));
#251723=CARTESIAN_POINT('Ctrl Pts',(50.0843441153989,2.50338026112505,136.917225993175));
#251724=CARTESIAN_POINT('Ctrl Pts',(49.8058964915862,6.49606494544435,132.002348955022));
#251725=CARTESIAN_POINT('Ctrl Pts',(49.5274488677731,4.51918329531533,125.986579159731));
#251726=CARTESIAN_POINT('Ctrl Pts',(49.2490012439603,-1.6106070288309,124.39811516248));
#251727=CARTESIAN_POINT('Ctrl Pts',(48.9705536201474,-6.26032817600901,
128.696677775965));
#251728=CARTESIAN_POINT('Ctrl Pts',(48.6921059963345,-5.15711356346882,
134.932097954848));
#251729=CARTESIAN_POINT('Ctrl Pts',(48.4136583725217,0.685236474895564,
137.374329171949));
#251730=CARTESIAN_POINT('Ctrl Pts',(48.1352107487087,5.89788766849362,133.779080248378));
#251731=CARTESIAN_POINT('Ctrl Pts',(47.8567631248959,5.69066822257687,127.450209307224));
#251732=CARTESIAN_POINT('Ctrl Pts',(47.578315501083,0.254002684709825,124.203639560873));
#251733=CARTESIAN_POINT('Ctrl Pts',(47.29986787727,-5.41607891168467,127.022810002472));
#251734=CARTESIAN_POINT('Ctrl Pts',(47.0214202534572,-6.10904857840509,
133.317040720324));
#251735=CARTESIAN_POINT('Ctrl Pts',(46.7429726296443,-1.18810104518584,
137.302241174989));
#251736=CARTESIAN_POINT('Ctrl Pts',(46.4645250058313,4.82465330659632,135.316206836494));
#251737=CARTESIAN_POINT('Ctrl Pts',(46.1860773820186,6.40378696703385,129.184006238746));
#251738=CARTESIAN_POINT('Ctrl Pts',(45.9076297582056,2.09815324715241,124.54083215642));
#251739=CARTESIAN_POINT('Ctrl Pts',(45.6291821343927,-4.13558080637756,
125.653534739511));
#251740=CARTESIAN_POINT('Ctrl Pts',(45.3507345105798,-6.56891813320061,
131.499594672701));
#251741=CARTESIAN_POINT('Ctrl Pts',(45.072286886767,-2.96574060510383,136.706768473292));
#251742=CARTESIAN_POINT('Ctrl Pts',(44.793839262954,3.36280765460034,136.489917803126));
#251743=CARTESIAN_POINT('Ctrl Pts',(44.5153916391412,6.60109996201359,131.048317834339));
#251744=CARTESIAN_POINT('Ctrl Pts',(44.2369440153282,3.77330388599763,125.38253310131));
#251745=CARTESIAN_POINT('Ctrl Pts',(43.9584963915154,-2.52197412510756,
124.699142984721));
#251746=CARTESIAN_POINT('Ctrl Pts',(43.6800487677024,-6.49968112052436,
129.626149616253));
#251747=CARTESIAN_POINT('Ctrl Pts',(43.4016011438896,-4.50449869325427,
135.635874599185));
#251748=CARTESIAN_POINT('Ctrl Pts',(43.1231535200766,1.6300979761215,137.205674265588));
#251749=CARTESIAN_POINT('Ctrl Pts',(42.8447058962639,6.26671424015497,132.892979411015));
#251750=CARTESIAN_POINT('Ctrl Pts',(42.5662582724509,5.14452626349642,126.660945919963));
#251751=CARTESIAN_POINT('Ctrl Pts',(42.287810648638,-0.705230025235587,
124.236508118946));
#251752=CARTESIAN_POINT('Ctrl Pts',(42.0093630248251,-5.90691437317801,
127.847605906729));
#251753=CARTESIAN_POINT('Ctrl Pts',(41.7309154010123,-5.68043298097947,
134.175816828272));
#251754=CARTESIAN_POINT('Ctrl Pts',(41.4524677771993,-0.233911183839542,
137.405824196969));
#251755=CARTESIAN_POINT('Ctrl Pts',(41.1740201533865,5.42756356405245,134.569409035618));
#251756=CARTESIAN_POINT('Ctrl Pts',(40.8955725295735,6.10137254780096,128.273098310918));
#251757=CARTESIAN_POINT('Ctrl Pts',(40.6171249057607,1.1683182287399,124.302893986988));
#251758=CARTESIAN_POINT('Ctrl Pts',(40.3386772819477,-4.83836346701448,
126.307219882257));
#251759=CARTESIAN_POINT('Ctrl Pts',(40.060229658135,-6.39882550377857,132.444198415735));
#251760=CARTESIAN_POINT('Ctrl Pts',(39.781782034322,-2.07907950257448,137.074246123225));
#251761=CARTESIAN_POINT('Ctrl Pts',(39.5033344105091,4.15123899281517,135.94257535195));
#251762=CARTESIAN_POINT('Ctrl Pts',(39.2248867866962,6.56677165310695,130.089136255519));
#251763=CARTESIAN_POINT('Ctrl Pts',(38.9464391628834,2.94776196882331,124.892953407157));
#251764=CARTESIAN_POINT('Ctrl Pts',(38.6679915390704,-3.38009695863112,
125.129064996863));
#251765=CARTESIAN_POINT('Ctrl Pts',(38.3895439152575,-6.6018119080198,130.58049600839));
#251766=CARTESIAN_POINT('Ctrl Pts',(38.1110962914447,-3.75678423037978,
136.237647659355));
#251767=CARTESIAN_POINT('Ctrl Pts',(37.8326486676317,2.54054462586645,136.901873949744));
#251768=CARTESIAN_POINT('Ctrl Pts',(37.5542010438189,6.50323708344635,131.962783367948));
#251769=CARTESIAN_POINT('Ctrl Pts',(37.275753420006,4.48977236213255,125.959158870647));
#251770=CARTESIAN_POINT('Ctrl Pts',(36.9973057961931,-1.64957382240749,
124.4080380775));
#251771=CARTESIAN_POINT('Ctrl Pts',(36.7188581723802,-6.27304225031618,
128.734825220947));
#251772=CARTESIAN_POINT('Ctrl Pts',(36.4404105485673,-5.13189130533538,
134.96341429146));
#251773=CARTESIAN_POINT('Ctrl Pts',(36.1619629247544,0.725217042420823,
137.370036216732));
#251774=CARTESIAN_POINT('Ctrl Pts',(35.8835153009416,5.91588635701427,133.743123017455));
#251775=CARTESIAN_POINT('Ctrl Pts',(35.6050676771286,5.67014511662727,127.415630739204));
#251776=CARTESIAN_POINT('Ctrl Pts',(35.3266200533158,0.213817516048174,
124.202215670509));
#251777=CARTESIAN_POINT('Ctrl Pts',(35.0481724295028,-5.43899793621292,
127.055849275448));
#251778=CARTESIAN_POINT('Ctrl Pts',(34.76972480569,-6.09363999491508,133.354181678833));
#251779=CARTESIAN_POINT('Ctrl Pts',(34.4912771818771,-1.14852458915375,
137.309353092597));
#251780=CARTESIAN_POINT('Ctrl Pts',(34.2128295580642,4.85202880549439,135.286754208357));
#251781=CARTESIAN_POINT('Ctrl Pts',(33.9343819342512,6.393804762678,129.145054591279));
#251782=CARTESIAN_POINT('Ctrl Pts',(33.6559343104384,2.05998649768791,124.528176150753));
#251783=CARTESIAN_POINT('Ctrl Pts',(33.3774866866255,-4.16685872274224,
125.678804626571));
#251784=CARTESIAN_POINT('Ctrl Pts',(33.0990390628127,-6.56456433933747,
131.539568660782));
#251785=CARTESIAN_POINT('Ctrl Pts',(32.8205914389997,-2.92975602487846,
136.724712420187));
#251786=CARTESIAN_POINT('Ctrl Pts',(32.5421438151868,3.39735494990529,136.469342098247));
#251787=CARTESIAN_POINT('Ctrl Pts',(32.263696191374,6.60246269574222,131.008130545292));
#251788=CARTESIAN_POINT('Ctrl Pts',(31.985248567561,3.74022977242616,125.359664383471));
#251789=CARTESIAN_POINT('Ctrl Pts',(31.7068009437482,-2.55909159136699,
124.714608072585));
#251790=CARTESIAN_POINT('Ctrl Pts',(31.4283533199352,-6.50673280126843,
129.665736849585));
#251791=CARTESIAN_POINT('Ctrl Pts',(31.1499056961224,-4.47500443837311,
135.663205244496));
#251792=CARTESIAN_POINT('Ctrl Pts',(30.8714580723094,1.66903438726656,137.195632795014));
#251793=CARTESIAN_POINT('Ctrl Pts',(30.5930104484966,6.27931214787105,132.854793445461));
#251794=CARTESIAN_POINT('Ctrl Pts',(30.3145628246837,5.11920880603445,126.629706496284));
#251795=CARTESIAN_POINT('Ctrl Pts',(30.0361152008708,-0.745197341294603,
124.240922741373));
#251796=CARTESIAN_POINT('Ctrl Pts',(29.7576675770579,-5.9248035368878,127.883617752917));
#251797=CARTESIAN_POINT('Ctrl Pts',(29.4792199532451,-5.65980472482494,
134.210332770852));
#251798=CARTESIAN_POINT('Ctrl Pts',(29.2007723294321,-0.193721867480399,
137.407125770907));
#251799=CARTESIAN_POINT('Ctrl Pts',(28.9223247056193,5.45038192223944,134.536300158051));
#251800=CARTESIAN_POINT('Ctrl Pts',(28.6438770818064,6.08585099138068,128.236004422871));
#251801=CARTESIAN_POINT('Ctrl Pts',(28.3654294579935,1.12872030979243,124.29590255944));
#251802=CARTESIAN_POINT('Ctrl Pts',(28.0869818341806,-4.86564919544231,
126.336755695574));
#251803=CARTESIAN_POINT('Ctrl Pts',(27.8085342103677,-6.38872479024353,
132.483119500384));
#251804=CARTESIAN_POINT('Ctrl Pts',(27.5300865865548,-2.04087440936798,
137.086785903815));
#251805=CARTESIAN_POINT('Ctrl Pts',(27.2516389627419,4.18243985145892,135.91721038272));
#251806=CARTESIAN_POINT('Ctrl Pts',(26.973191338929,6.56229621234102,130.049175704046));
#251807=CARTESIAN_POINT('Ctrl Pts',(26.6947437151162,2.91172294007416,124.875119068062));
#251808=CARTESIAN_POINT('Ctrl Pts',(26.4162960913032,-3.41458146854746,
125.149745756519));
#251809=CARTESIAN_POINT('Ctrl Pts',(26.1378484674903,-6.60305231915217,
130.620687258984));
#251810=CARTESIAN_POINT('Ctrl Pts',(25.8594008436774,-3.72364066549499,
136.260415605043));
#251811=CARTESIAN_POINT('Ctrl Pts',(25.5809532198646,2.57761484979243,136.886295960714));
#251812=CARTESIAN_POINT('Ctrl Pts',(25.3025055960517,6.51016824160669,131.92317485509));
#251813=CARTESIAN_POINT('Ctrl Pts',(25.0240579722387,4.46019505878377,125.931918122295));
#251814=CARTESIAN_POINT('Ctrl Pts',(24.7456103484259,-1.68847949041943,
124.418198010604));
#251815=CARTESIAN_POINT('Ctrl Pts',(24.467162724613,-6.28552387473587,128.773049353324));
#251816=CARTESIAN_POINT('Ctrl Pts',(24.1887151008001,-5.10647888308236,
134.994576512808));
#251817=CARTESIAN_POINT('Ctrl Pts',(23.9102674769872,0.765170736761864,
137.365499967992));
#251818=CARTESIAN_POINT('Ctrl Pts',(23.6318198531744,5.93366583019039,133.707056889611));
#251819=CARTESIAN_POINT('Ctrl Pts',(23.3533722293614,5.64941190136517,127.381177741815));
#251820=CARTESIAN_POINT('Ctrl Pts',(23.0749246055485,0.173624424299845,
124.201036425055));
#251821=CARTESIAN_POINT('Ctrl Pts',(22.7964769817356,-5.46171541667246,
127.08902745089));
#251822=CARTESIAN_POINT('Ctrl Pts',(22.5180293579228,-6.07800560935413,
133.391228152785));
#251823=CARTESIAN_POINT('Ctrl Pts',(22.2395817341099,-1.10890557412062,
137.316223965318));
#251824=CARTESIAN_POINT('Ctrl Pts',(21.9611341102969,4.87922451068073,135.257135483476));
#251825=CARTESIAN_POINT('Ctrl Pts',(21.6826864864842,6.38358563353538,129.106164430008));
#251826=CARTESIAN_POINT('Ctrl Pts',(21.4042388626712,2.02174341466617,124.515752711409));
#251827=CARTESIAN_POINT('Ctrl Pts',(21.1257912388583,-4.19798223462457,
125.704264442993));
#251828=CARTESIAN_POINT('Ctrl Pts',(20.8473436150454,-6.55996729312864,
131.579515405459));
#251829=CARTESIAN_POINT('Ctrl Pts',(20.5688959912325,-2.89366288146616,
136.742436986267));
#251830=CARTESIAN_POINT('Ctrl Pts',(20.2904483674196,3.43177635497322,136.448556475397));
#251831=CARTESIAN_POINT('Ctrl Pts',(20.0120007436067,6.60358077278748,130.967935705476));
#251832=CARTESIAN_POINT('Ctrl Pts',(19.7335531197938,3.70701706326526,125.336997420853));
#251833=CARTESIAN_POINT('Ctrl Pts',(19.455105495981,-2.59611422954622,124.730298818468));
#251834=CARTESIAN_POINT('Ctrl Pts',(19.176657872168,-6.51354337263571,129.705366275038));
#251835=CARTESIAN_POINT('Ctrl Pts',(18.8982102483552,-4.4453443605568,135.690355843533));
#251836=CARTESIAN_POINT('Ctrl Pts',(18.6197626245423,1.70790895172861,137.1853544935));
#251837=CARTESIAN_POINT('Ctrl Pts',(18.3413150007294,6.29167737336628,132.816531500364));
#251838=CARTESIAN_POINT('Ctrl Pts',(18.0628673769165,5.09370165440758,126.598621765949));
#251839=CARTESIAN_POINT('Ctrl Pts',(17.7844197531036,-0.785137043792105,
124.245580574404));
#251840=CARTESIAN_POINT('Ctrl Pts',(17.5059721292907,-5.94247315482366,
127.919737828307));
#251841=CARTESIAN_POINT('Ctrl Pts',(17.2275245054778,-5.63896674252494,
134.244722503881));
#251842=CARTESIAN_POINT('Ctrl Pts',(16.949076881665,-0.15352537268619,137.408182676953));
#251843=CARTESIAN_POINT('Ctrl Pts',(16.6706292578521,5.47299831451989,134.503052992091));
#251844=CARTESIAN_POINT('Ctrl Pts',(16.3921816340391,6.07010392151387,128.199005706208));
#251845=CARTESIAN_POINT('Ctrl Pts',(16.1137340102263,1.08908056569879,124.289152305198));
#251846=CARTESIAN_POINT('Ctrl Pts',(15.8352863864134,-4.89275462544986,
126.366457057635));
#251847=CARTESIAN_POINT('Ctrl Pts',(15.5568387626005,-6.37838734016194,
132.521978378005));
#251848=CARTESIAN_POINT('Ctrl Pts',(15.2783911387876,-2.00259369080969,
137.099092886824));
#251849=CARTESIAN_POINT('Ctrl Pts',(14.9999435149747,4.21348572825588,135.891655954962));
#251850=CARTESIAN_POINT('Ctrl Pts',(14.7214958911618,6.55757760327567,130.009243136227));
#251851=CARTESIAN_POINT('Ctrl Pts',(14.4430482673489,2.87557601636067,124.857504439193));
#251852=CARTESIAN_POINT('Ctrl Pts',(14.164600643536,-3.44893944989177,125.170636050008));
#251853=CARTESIAN_POINT('Ctrl Pts',(13.8861530197231,-6.60404805175259,
130.660885315664));
#251854=CARTESIAN_POINT('Ctrl Pts',(13.6077053959103,-3.69035911973598,
136.282981374608));
#251855=CARTESIAN_POINT('Ctrl Pts',(13.3292577720973,2.61458955925225,136.870492603333));
#251856=CARTESIAN_POINT('Ctrl Pts',(13.0508101482845,6.5168581630887,131.883524884162));
#251857=CARTESIAN_POINT('Ctrl Pts',(12.7723625244716,4.43045248126686,125.904857924092));
#251858=CARTESIAN_POINT('Ctrl Pts',(12.4939149006587,-1.72732259120293,
124.428594585312));
#251859=CARTESIAN_POINT('Ctrl Pts',(12.2154672768458,-6.29777258675688,
128.811348756686));
#251860=CARTESIAN_POINT('Ctrl Pts',(11.9370196530329,-5.08087723837641,
135.025583464166));
#251861=CARTESIAN_POINT('Ctrl Pts',(11.65857202922,0.805096077419857,137.36072059382));
#251862=CARTESIAN_POINT('Ctrl Pts',(11.3801244054071,5.95122542919731,133.670883201288));
#251863=CARTESIAN_POINT('Ctrl Pts',(11.1016767815943,5.62846934506734,127.346851591727));
#251864=CARTESIAN_POINT('Ctrl Pts',(10.8232291577813,0.13342489883439,124.200101868207));
#251865=CARTESIAN_POINT('Ctrl Pts',(10.5447815339684,-5.4842305112587,127.12234329937));
#251866=CARTESIAN_POINT('Ctrl Pts',(10.2663339101556,-6.06214600106014,
133.428178769409));
#251867=CARTESIAN_POINT('Ctrl Pts',(9.98788628634267,-1.06924546818365,
137.322853538546));
#251868=CARTESIAN_POINT('Ctrl Pts',(9.70943866252976,4.90623941440849,135.227351759386));
#251869=CARTESIAN_POINT('Ctrl Pts',(9.43099103871685,6.37312995827954,129.067337196021));
#251870=CARTESIAN_POINT('Ctrl Pts',(9.15254341490403,1.98342541519871,124.503562298745));
#251871=CARTESIAN_POINT('Ctrl Pts',(8.87409579109107,-4.22895018873139,
125.729913245354));
#251872=CARTESIAN_POINT('Ctrl Pts',(8.59564816727821,-6.55512716491932,
131.61943342649));
#251873=CARTESIAN_POINT('Ctrl Pts',(8.31720054346528,-2.85746251231165,
136.759941514744));
#251874=CARTESIAN_POINT('Ctrl Pts',(8.03875291965246,3.46607059430627,136.427561704794));
#251875=CARTESIAN_POINT('Ctrl Pts',(7.76030529583951,6.60445415171875,130.927734804324));
#251876=CARTESIAN_POINT('Ctrl Pts',(7.48185767202662,3.67366698922382,125.314533053388));
#251877=CARTESIAN_POINT('Ctrl Pts',(7.20341004821377,-2.63304066775796,
124.746214640945));
#251878=CARTESIAN_POINT('Ctrl Pts',(6.92496242440086,-6.52011258225796,
129.745036424131));
#251879=CARTESIAN_POINT('Ctrl Pts',(6.64651480058794,-4.41551955887045,
135.71732539022));
#251880=CARTESIAN_POINT('Ctrl Pts',(6.36806717677509,1.74672022899638,137.174839741911));
#251881=CARTESIAN_POINT('Ctrl Pts',(6.08961955296221,6.30380945844269,132.778194993536));
#251882=CARTESIAN_POINT('Ctrl Pts',(5.81117192914928,5.06800575379271,126.567692880813));
#251883=CARTESIAN_POINT('Ctrl Pts',(5.53272430533639,-0.825047652747706,
124.250481445441));
#251884=CARTESIAN_POINT('Ctrl Pts',(5.25427668152353,-5.95992257223146,
127.955964794454));
#251885=CARTESIAN_POINT('Ctrl Pts',(4.97582905771062,-5.61791980623858,
134.278984753035));
#251886=CARTESIAN_POINT('Ctrl Pts',(4.69738143389771,-0.113323188952861,
137.408994875945));
#251887=CARTESIAN_POINT('Ctrl Pts',(4.41893381008486,5.49541190283514,134.469668769726));
#251888=CARTESIAN_POINT('Ctrl Pts',(4.14048618627195,6.05413192171396,128.162103531929));
#251889=CARTESIAN_POINT('Ctrl Pts',(3.86203856245905,1.0494004653243,124.282643474398));
#251890=CARTESIAN_POINT('Ctrl Pts',(3.58359093864613,-4.91967875263547,
126.396322867843));
#251891=CARTESIAN_POINT('Ctrl Pts',(3.30514331483329,-6.36781353659179,
132.560773608667));
#251892=CARTESIAN_POINT('Ctrl Pts',(3.02669569102039,-1.96423876540577,
137.111166616214));
#251893=CARTESIAN_POINT('Ctrl Pts',(2.74824806720748,4.24437547278969,135.865913015604));
#251894=CARTESIAN_POINT('Ctrl Pts',(2.46980044339459,6.55261600076067,129.969340031779));
#251895=CARTESIAN_POINT('Ctrl Pts',(2.19135281958173,2.83932253712042,124.840110173268));
#251896=CARTESIAN_POINT('Ctrl Pts',(1.91290519576881,-3.48316962951642,
125.191735103234));
#251897=CARTESIAN_POINT('Ctrl Pts',(1.6344575719559,-6.60479906892382,130.701088688872));
#251898=CARTESIAN_POINT('Ctrl Pts',(1.35600994814304,-3.65694082636265,
136.305344131865));
#251899=CARTESIAN_POINT('Ctrl Pts',(1.07756232433016,2.65146738413444,136.854464463202));
#251900=CARTESIAN_POINT('Ctrl Pts',(0.799114700517227,6.52330659999492,
131.843834924404));
#251901=CARTESIAN_POINT('Ctrl Pts',(0.520667076704378,4.40054573170394,
125.877979278764));
#251902=CARTESIAN_POINT('Ctrl Pts',(0.242219452891471,-1.76610168541259,
124.439227416375));
#251903=CARTESIAN_POINT('Ctrl Pts',(-0.03622817092143,-6.30978793249869,
128.849722011837));
#251904=CARTESIAN_POINT('Ctrl Pts',(-0.314675794734322,-5.05508731989592,
135.056433996558));
#251905=CARTESIAN_POINT('Ctrl Pts',(-0.593123418547181,0.844991584946641,
137.355698271319));
#251906=CARTESIAN_POINT('Ctrl Pts',(-0.871571042360099,5.96856450335716,
133.634603292916));
#251907=CARTESIAN_POINT('Ctrl Pts',(-1.15001866617301,5.60731822376822,
127.312653560908));
#251908=CARTESIAN_POINT('Ctrl Pts',(-1.42846628998586,0.0932204292604712,
124.199412034595));
#251909=CARTESIAN_POINT('Ctrl Pts',(-1.70691391379876,-5.50654238566651,
127.155795586355));
#251910=CARTESIAN_POINT('Ctrl Pts',(-1.98536153761166,-6.04606175771675,
133.465032159487));
#251911=CARTESIAN_POINT('Ctrl Pts',(-2.26380916142456,-1.02954574096264,
137.329241566624));
#251912=CARTESIAN_POINT('Ctrl Pts',(-2.5422567852374,4.9330725156305,135.197404139731));
#251913=CARTESIAN_POINT('Ctrl Pts',(-2.82070440905033,6.36243812434939,
129.028574328076));
#251914=CARTESIAN_POINT('Ctrl Pts',(-3.09915203286324,1.94503391917308,
124.491605364478));
#251915=CARTESIAN_POINT('Ctrl Pts',(-3.3775996566761,-4.25976143753379,
125.755750083229));
#251916=CARTESIAN_POINT('Ctrl Pts',(-3.65604728048899,-6.55004413406227,
131.659321244699));
#251917=CARTESIAN_POINT('Ctrl Pts',(-3.9344949043019,-2.82115625883292,
136.777225356981));
#251918=CARTESIAN_POINT('Ctrl Pts',(-4.2129425281148,3.50023639711881,136.406358564405));
#251919=CARTESIAN_POINT('Ctrl Pts',(-4.49139015192765,6.60508280017262,
130.887529331496));
#251920=CARTESIAN_POINT('Ctrl Pts',(-4.76983777574057,3.64018078610111,
125.292272113504));
#251921=CARTESIAN_POINT('Ctrl Pts',(-5.04828539955349,-2.66986953767946,
124.762354950249));
#251922=CARTESIAN_POINT('Ctrl Pts',(-5.32673302336633,-6.52644018671072,
129.784745826872));
#251923=CARTESIAN_POINT('Ctrl Pts',(-5.60518064717923,-4.38553113848304,
135.74411288519));
#251924=CARTESIAN_POINT('Ctrl Pts',(-5.88362827099213,1.7854667809037,137.164088929876));
#251925=CARTESIAN_POINT('Ctrl Pts',(-6.16207589480503,6.31570795354138,
132.739785345549));
#251926=CARTESIAN_POINT('Ctrl Pts',(-6.44052351861788,5.04212205636089,
126.536920986959));
#251927=CARTESIAN_POINT('Ctrl Pts',(-6.71897114243081,-0.864927689259141,
124.255625172881));
#251928=CARTESIAN_POINT('Ctrl Pts',(-6.99741876624371,-5.97715114251656,
127.992297308957));
#251929=CARTESIAN_POINT('Ctrl Pts',(-7.27586639005655,-5.59666469586782,
134.313118248714));
#251930=CARTESIAN_POINT('Ctrl Pts',(-7.55431401386947,-0.0731168059870705,
137.409562337785));
#251931=CARTESIAN_POINT('Ctrl Pts',(-7.83276163768236,5.51762185664139,
134.436148728019));
#251932=CARTESIAN_POINT('Ctrl Pts',(-8.11120926149529,6.03793558382929,
128.125299267457));
#251933=CARTESIAN_POINT('Ctrl Pts',(-8.38965688530811,1.00968147902963,
124.276376308223));
#251934=CARTESIAN_POINT('Ctrl Pts',(-8.66810450912106,-4.94642057931569,
126.426352019512));
#251935=CARTESIAN_POINT('Ctrl Pts',(-8.94655213293394,-6.3570037713493,
132.599503754801));
#251936=CARTESIAN_POINT('Ctrl Pts',(-9.22499975674682,-1.92581105441205,
137.123006644589));
#251937=CARTESIAN_POINT('Ctrl Pts',(-9.50344738055969,4.27510794042973,
135.839982518561));
#251938=CARTESIAN_POINT('Ctrl Pts',(-9.78189500437264,6.54741158865002,
129.929467869325));
#251939=CARTESIAN_POINT('Ctrl Pts',(-10.0603426281855,2.80296384573913,
124.822936914835));
#251940=CARTESIAN_POINT('Ctrl Pts',(-10.3387902519984,-3.51727073900952,
125.213042134361));
#251941=CARTESIAN_POINT('Ctrl Pts',(-10.6172378758113,-6.60530534283666,
130.74129588886));
#251942=CARTESIAN_POINT('Ctrl Pts',(-10.8956854996242,-3.62338702370218,
136.327503048155));
#251943=CARTESIAN_POINT('Ctrl Pts',(-11.174133123437,2.68824695791763,136.838212134247));
#251944=CARTESIAN_POINT('Ctrl Pts',(-11.4525807472499,6.52951331337615,
131.804106446543));
#251945=CARTESIAN_POINT('Ctrl Pts',(-11.7310283710628,4.37047591830066,
125.851283182307));
#251946=CARTESIAN_POINT('Ctrl Pts',(-12.0094759948757,-1.80481533607482,
124.450096109789));
#251947=CARTESIAN_POINT('Ctrl Pts',(-12.2879236186886,-6.32156946672825,
128.88816769684));
#251948=CARTESIAN_POINT('Ctrl Pts',(-12.5663712425015,-5.02911008329581,
135.087126966809));
#251949=CARTESIAN_POINT('Ctrl Pts',(-12.8448188663144,0.884855780999501,
137.350433186591));
#251950=CARTESIAN_POINT('Ctrl Pts',(-13.1232664901273,5.98568241016441,
133.598218508862));
#251951=CARTESIAN_POINT('Ctrl Pts',(-13.4017141139402,5.58595932123025,
127.278584916578));
#251952=CARTESIAN_POINT('Ctrl Pts',(-13.6801617377531,0.0530125053692662,
124.198966949783));
#251953=CARTESIAN_POINT('Ctrl Pts',(-13.958609361566,-5.5286502131212,127.189383072259));
#251954=CARTESIAN_POINT('Ctrl Pts',(-14.2370569853788,-6.02975347533148,
133.501786957402));
#251955=CARTESIAN_POINT('Ctrl Pts',(-14.5155046091917,-0.989807863545592,
137.335387812837));
#251956=CARTESIAN_POINT('Ctrl Pts',(-14.7939522330047,4.95972282003631,
135.167293734234));
#251957=CARTESIAN_POINT('Ctrl Pts',(-15.0723998568175,6.35151052793477,
128.989877262545));
#251958=CARTESIAN_POINT('Ctrl Pts',(-15.3508474806304,1.9065703492003,124.479882351679));
#251959=CARTESIAN_POINT('Ctrl Pts',(-15.6292951044433,-4.29041483930959,
125.781773999224));
#251960=CARTESIAN_POINT('Ctrl Pts',(-15.9077427282562,-6.54471838891106,
131.699177382027));
#251961=CARTESIAN_POINT('Ctrl Pts',(-16.186190352069,-2.78474546637155,
136.794287872519));
#251962=CARTESIAN_POINT('Ctrl Pts',(-16.464637975882,3.53427249738445,136.384947839923));
#251963=CARTESIAN_POINT('Ctrl Pts',(-16.7430855996949,6.60546669485434,
130.847320776822));
#251964=CARTESIAN_POINT('Ctrl Pts',(-17.0215332235078,3.6065596947407,125.270215426085));
#251965=CARTESIAN_POINT('Ctrl Pts',(-17.2999808473206,-2.7065994746034,
124.778719148295));
#251966=CARTESIAN_POINT('Ctrl Pts',(-17.5784284711336,-6.53252595152224,
129.824493011814));
#251967=CARTESIAN_POINT('Ctrl Pts',(-17.8568760949464,-4.35538021062653,
135.770717335825));
#251968=CARTESIAN_POINT('Ctrl Pts',(-18.1353237187593,1.82414717168286,
137.153102455769));
#251969=CARTESIAN_POINT('Ctrl Pts',(-18.4137713425722,6.32737241775927,
132.701303979686));
#251970=CARTESIAN_POINT('Ctrl Pts',(-18.6922189663851,5.01605152124203,
126.506307224649));
#251971=CARTESIAN_POINT('Ctrl Pts',(-18.9706665901979,-0.904775675556959,
124.261011566121));
#251972=CARTESIAN_POINT('Ctrl Pts',(-19.2491142140109,-5.99415822726801,
128.028734025499));
#251973=CARTESIAN_POINT('Ctrl Pts',(-19.5275618378238,-5.57520219902858,
134.347121726088));
#251974=CARTESIAN_POINT('Ctrl Pts',(-19.8060094616367,-0.0329077136511566,
137.409885041447));
#251975=CARTESIAN_POINT('Ctrl Pts',(-20.0844570854496,5.53962735294063,
134.402494109067));
#251976=CARTESIAN_POINT('Ctrl Pts',(-20.3629047092624,6.02151550802112,
128.08859427659));
#251977=CARTESIAN_POINT('Ctrl Pts',(-20.6413523330754,0.969925078616457,
124.270351038909));
#251978=CARTESIAN_POINT('Ctrl Pts',(-20.9197999568882,-4.9729791145623,
126.456543399899));
#251979=CARTESIAN_POINT('Ctrl Pts',(-21.1982475807011,-6.34595844499429,
132.638167381246));
#251980=CARTESIAN_POINT('Ctrl Pts',(-21.476695204514,-1.88731198178147,
137.134612533211));
#251981=CARTESIAN_POINT('Ctrl Pts',(-21.7551428283269,4.30568199237261,
135.813865424697));
#251982=CARTESIAN_POINT('Ctrl Pts',(-22.0335904521398,6.54196455979519,
129.889628126344));
#251983=CARTESIAN_POINT('Ctrl Pts',(-22.3120380759527,2.766501289502,124.805985300257));
#251984=CARTESIAN_POINT('Ctrl Pts',(-22.5904856997656,-3.5512415147419,
125.234556353852));
#251985=CARTESIAN_POINT('Ctrl Pts',(-22.8689333235784,-6.60556685473091,
130.781505425734));
#251986=CARTESIAN_POINT('Ctrl Pts',(-23.1473809473914,-3.58969895510304,
136.349457302372));
#251987=CARTESIAN_POINT('Ctrl Pts',(-23.4258285712042,2.7249269177212,136.821736218705));
#251988=CARTESIAN_POINT('Ctrl Pts',(-23.7042761950172,6.53547807324032,
131.764340922733));
#251989=CARTESIAN_POINT('Ctrl Pts',(-23.98272381883,4.34024415530499,125.824770623956));
#251990=CARTESIAN_POINT('Ctrl Pts',(-24.2611714426429,-1.84346210864104,
124.461200262812));
#251991=CARTESIAN_POINT('Ctrl Pts',(-24.5396190664558,-6.33311675287646,
128.926684387076));
#251992=CARTESIAN_POINT('Ctrl Pts',(-24.8180666902687,-5.00294649117208,
135.117661237576));
#251993=CARTESIAN_POINT('Ctrl Pts',(-25.0965143140816,0.924687188395989,
137.344925534737));
#251994=CARTESIAN_POINT('Ctrl Pts',(-25.3749619378945,6.00257851530871,
133.561730197376));
#251995=CARTESIAN_POINT('Ctrl Pts',(-25.6534095617074,5.56439342891538,
127.244646921163));
#251996=CARTESIAN_POINT('Ctrl Pts',(-25.9318571855203,0.0128026170801758,
124.198766630261));
#251997=CARTESIAN_POINT('Ctrl Pts',(-26.2103048093331,-5.5505531744091,
127.223104512485));
#251998=CARTESIAN_POINT('Ctrl Pts',(-26.4887524331461,-6.01322175821376,
133.538441801192));
#251999=CARTESIAN_POINT('Ctrl Pts',(-26.7672000569589,-0.950033308434149,
137.341292049436));
#252000=CARTESIAN_POINT('Ctrl Pts',(-27.0456476807718,4.98618934008908,
135.137021658645));
#252001=CARTESIAN_POINT('Ctrl Pts',(-27.3240953045847,6.34034757396176,
128.951247433362));
#252002=CARTESIAN_POINT('Ctrl Pts',(-27.6025429283976,1.86803613056208,
124.468393694749));
#252003=CARTESIAN_POINT('Ctrl Pts',(-27.8809905522105,-4.32090925818572,
125.807984029013));
#252004=CARTESIAN_POINT('Ctrl Pts',(-28.1594381760234,-6.53915012681315,
131.739000361591));
#252005=CARTESIAN_POINT('Ctrl Pts',(-28.4378857998363,-2.74823148414282,
136.811128429099));
#252006=CARTESIAN_POINT('Ctrl Pts',(-28.7163334236492,3.56817763388296,
136.36333032473));
#252007=CARTESIAN_POINT('Ctrl Pts',(-28.994781047462,6.60560582153853,130.807110630244));
#252008=CARTESIAN_POINT('Ctrl Pts',(-29.273228671275,3.5728049609845,125.248363808452));
#252009=CARTESIAN_POINT('Ctrl Pts',(-29.5516762950878,-2.74322911748845,
124.795306628702));
#252010=CARTESIAN_POINT('Ctrl Pts',(-29.8301239189007,-6.53836965118233,
129.86427650611));
#252011=CARTESIAN_POINT('Ctrl Pts',(-30.1085715427137,-4.32506789255462,
135.797137756284));
#252012=CARTESIAN_POINT('Ctrl Pts',(-30.3870191665265,1.862759968018,137.141880726698));
#252013=CARTESIAN_POINT('Ctrl Pts',(-30.6654667903394,6.33880241886542,
132.662752321889));
#252014=CARTESIAN_POINT('Ctrl Pts',(-30.9439144141524,4.98979511448915,
126.475852728289));
#252015=CARTESIAN_POINT('Ctrl Pts',(-31.2223620379652,-0.944590135059391,
124.266640425567));
#252016=CARTESIAN_POINT('Ctrl Pts',(-31.5008096617781,-6.01094319628198,
128.065273593905));
#252017=CARTESIAN_POINT('Ctrl Pts',(-31.7792572855909,-5.55353311102158,
134.380993925146));
#252018=CARTESIAN_POINT('Ctrl Pts',(-32.0577049094039,0.00730259809219468,
137.409962974972));
#252019=CARTESIAN_POINT('Ctrl Pts',(-32.3361525332168,5.56142757631112,
134.368706159956));
#252020=CARTESIAN_POINT('Ctrl Pts',(-32.6146001570296,6.0048723027414,128.051989919443));
#252021=CARTESIAN_POINT('Ctrl Pts',(-32.8930477808425,0.930132737272799,
124.264567889721));
#252022=CARTESIAN_POINT('Ctrl Pts',(-33.1714954046555,-4.99935337423901,
126.486895890252));
#252023=CARTESIAN_POINT('Ctrl Pts',(-33.4499430284683,-6.33467796681538,
132.676763055306));
#252024=CARTESIAN_POINT('Ctrl Pts',(-33.7283906522812,-1.84874297411136,
137.145983852021));
#252025=CARTESIAN_POINT('Ctrl Pts',(-34.0068382760941,4.33609649568588,
135.787562701789));
#252026=CARTESIAN_POINT('Ctrl Pts',(-34.285285899907,6.53627511603778,129.849822279112));
#252027=CARTESIAN_POINT('Ctrl Pts',(-34.5637335237199,2.72993621954223,
124.789255957683));
#252028=CARTESIAN_POINT('Ctrl Pts',(-34.8421811475328,-3.58508069791401,
125.256276964487));
#252029=CARTESIAN_POINT('Ctrl Pts',(-35.1206287713457,-6.60558359491616,
130.821715809516));
#252030=CARTESIAN_POINT('Ctrl Pts',(-35.3990763951586,-3.55587786888901,
136.37120608099));
#252031=CARTESIAN_POINT('Ctrl Pts',(-35.6775240189714,2.76150590435573,
136.805037327097));
#252032=CARTESIAN_POINT('Ctrl Pts',(-35.9559716427844,6.54120065856107,
131.724539826499));
#252033=CARTESIAN_POINT('Ctrl Pts',(-36.2344192665972,4.30985156296601,
125.798442586144));
#252034=CARTESIAN_POINT('Ctrl Pts',(-36.5128668904101,-1.8820405710409,
124.472539463974));
#252035=CARTESIAN_POINT('Ctrl Pts',(-36.791314514223,-6.3444293630544,128.965270655295));
#252036=CARTESIAN_POINT('Ctrl Pts',(-37.0697621380359,-4.9765975130263,
135.148035677403));
#252037=CARTESIAN_POINT('Ctrl Pts',(-37.3482097618488,0.964484331168655,
137.339175519844));
#252038=CARTESIAN_POINT('Ctrl Pts',(-37.6266573856617,6.0192521926987,133.525139710547));
#252039=CARTESIAN_POINT('Ctrl Pts',(-37.9051050094746,5.54262134595571,
127.210840832248));
#252040=CARTESIAN_POINT('Ctrl Pts',(-38.1835526332875,-0.0274077456145885,
124.198811083455));
#252041=CARTESIAN_POINT('Ctrl Pts',(-38.4620002571004,-5.5722504579079,
127.256958657474));
#252042=CARTESIAN_POINT('Ctrl Pts',(-38.7404478809132,-5.99646721895241,
133.574995332598));
#252043=CARTESIAN_POINT('Ctrl Pts',(-39.0188955047262,-0.910223549489097,
137.346954057637));
#252044=CARTESIAN_POINT('Ctrl Pts',(-39.297343128539,5.0124710950622,135.106589034709));
#252045=CARTESIAN_POINT('Ctrl Pts',(-39.5757907523519,6.32894967607775,
128.912686271968));
#252046=CARTESIAN_POINT('Ctrl Pts',(-39.8542383761648,1.82943269115809,
124.457139819403));
#252047=CARTESIAN_POINT('Ctrl Pts',(-40.1326859999777,-4.35124356418029,
125.834379201373));
#252048=CARTESIAN_POINT('Ctrl Pts',(-40.4111336237906,-6.53333955410249,
131.778788707735));
#252049=CARTESIAN_POINT('Ctrl Pts',(-40.6895812476035,-2.7116156651858,
136.827746402689));
#252050=CARTESIAN_POINT('Ctrl Pts',(-40.9680288714165,3.60195055024708,
136.34150681987));
#252051=CARTESIAN_POINT('Ctrl Pts',(-41.2464764952292,6.60550017506977,
130.766900381762));
#252052=CARTESIAN_POINT('Ctrl Pts',(-41.5249241190422,3.53891783562657,
125.226718070324));
#252053=CARTESIAN_POINT('Ctrl Pts',(-41.803371742855,-2.77975710900975,
124.812116776814));
#252054=CARTESIAN_POINT('Ctrl Pts',(-42.081819366668,-6.5439710691505,129.904094835568));
#252055=CARTESIAN_POINT('Ctrl Pts',(-42.3602669904808,-4.2945953075014,
135.82337316755));
#252056=CARTESIAN_POINT('Ctrl Pts',(-42.6387146142937,1.90130373909722,
137.130424158489));
#252057=CARTESIAN_POINT('Ctrl Pts',(-42.9171622381066,6.34999753331677,
132.624131800705));
#252058=CARTESIAN_POINT('Ctrl Pts',(-43.1956098619195,4.96335380904355,
126.44555862638));
#252059=CARTESIAN_POINT('Ctrl Pts',(-43.4740574857324,-0.984369592426984,
124.272511542639));
#252060=CARTESIAN_POINT('Ctrl Pts',(-43.7525051095453,-6.02750542758532,
128.101914660188));
#252061=CARTESIAN_POINT('Ctrl Pts',(-44.0309527333582,-5.53165823480283,
134.414733590743));
#252062=CARTESIAN_POINT('Ctrl Pts',(-44.3094003571711,0.0475126392350714,
137.409796135472));
#252063=CARTESIAN_POINT('Ctrl Pts',(-44.5878479809839,5.58302171893757,
134.334786132711));
#252064=CARTESIAN_POINT('Ctrl Pts',(-44.8662956047969,5.98800658471021,
128.015487552405));
#252065=CARTESIAN_POINT('Ctrl Pts',(-45.1447432286098,0.890305929518511,
124.259027074959));
#252066=CARTESIAN_POINT('Ctrl Pts',(-45.4231908524226,-5.02554238103793,
126.517408365848));
#252067=CARTESIAN_POINT('Ctrl Pts',(-45.7016384762356,-6.32316275481482,
132.715289346806));
#252068=CARTESIAN_POINT('Ctrl Pts',(-45.9800861000484,-1.81010546059046,
137.15712017965));
#252069=CARTESIAN_POINT('Ctrl Pts',(-46.2585337238614,4.36635032334889,
135.761075324496));
#252070=CARTESIAN_POINT('Ctrl Pts',(-46.5369813476741,6.53034346820225,
129.810051802649));
#252071=CARTESIAN_POINT('Ctrl Pts',(-46.8154289714873,2.6932699907919,124.772749507024));
#252072=CARTESIAN_POINT('Ctrl Pts',(-47.0938765952999,-3.61878703460243,
125.278203161403));
#252073=CARTESIAN_POINT('Ctrl Pts',(-47.3723242191129,-6.60535556277213,
130.861925550195));
#252074=CARTESIAN_POINT('Ctrl Pts',(-47.6507718429257,-3.52192501831287,
136.392748578105));
#252075=CARTESIAN_POINT('Ctrl Pts',(-47.9292194667387,2.79798256237344,
136.788116078208));
#252076=CARTESIAN_POINT('Ctrl Pts',(-48.2076670905515,6.54668085728591,
131.684704632686));
#252077=CARTESIAN_POINT('Ctrl Pts',(-48.4861147143645,4.27929926749242,
125.772300044465));
#252078=CARTESIAN_POINT('Ctrl Pts',(-48.7645623381774,-1.92054929373528,
124.484113293097));
#252079=CARTESIAN_POINT('Ctrl Pts',(-49.0430099619902,-6.35550687806913,
129.003925071669));
#252080=CARTESIAN_POINT('Ctrl Pts',(-49.3214575858032,-4.95006412522954,
135.178249160753));
#252081=CARTESIAN_POINT('Ctrl Pts',(-49.5999052096159,1.00424573461974,
137.333183354982));
#252082=CARTESIAN_POINT('Ctrl Pts',(-49.878352833429,6.03570282448511,133.488448404247));
#252083=CARTESIAN_POINT('Ctrl Pts',(-50.1568004572417,5.52064387912377,
127.17716790253));
#252084=CARTESIAN_POINT('Ctrl Pts',(-50.4352480810547,-0.0676170927052693,
124.199100307716));
#252085=CARTESIAN_POINT('Ctrl Pts',(-50.7136957048675,-5.5937412596168,
127.290944252747));
#252086=CARTESIAN_POINT('Ctrl Pts',(-50.9921433286805,-5.97949047839309,
133.611446197116));
#252087=CARTESIAN_POINT('Ctrl Pts',(-51.2705909524933,-0.870380061875472,
137.352373627632));
#252088=CARTESIAN_POINT('Ctrl Pts',(-51.5490385763063,5.03856711107574,
135.075996990117));
#252089=CARTESIAN_POINT('Ctrl Pts',(-51.8274862001192,6.31731725663583,
128.874195207264));
#252090=CARTESIAN_POINT('Ctrl Pts',(-52.105933823932,1.79076146145295,124.446121142656));
#252091=CARTESIAN_POINT('Ctrl Pts',(-52.3843814477449,-4.38141663324442,
125.860958538224));
#252092=CARTESIAN_POINT('Ctrl Pts',(-52.6628290715579,-6.52728688609205,
131.818540946088));
#252093=CARTESIAN_POINT('Ctrl Pts',(-52.9412766953706,-2.67489936631311,
136.844141177504));
#252094=CARTESIAN_POINT('Ctrl Pts',(-53.2197243191836,3.63558999500893,
136.319478134021));
#252095=CARTESIAN_POINT('Ctrl Pts',(-53.4981719429964,6.60514975936288,
130.726691521383));
#252096=CARTESIAN_POINT('Ctrl Pts',(-53.7766195668094,3.50489957436681,
125.205279013792));
#252097=CARTESIAN_POINT('Ctrl Pts',(-54.0550671906223,-2.8161820956091,
124.829148969725));
#252098=CARTESIAN_POINT('Ctrl Pts',(-54.3335148144351,-6.54932999786417,
129.943946524707));
#252099=CARTESIAN_POINT('Ctrl Pts',(-54.6119624382481,-4.26396358463975,
135.849422597461));
#252100=CARTESIAN_POINT('Ctrl Pts',(-54.890410062061,1.93977705666721,137.11873317567));
#252101=CARTESIAN_POINT('Ctrl Pts',(-55.1688576858738,6.3609573462743,132.58544384723));
#252102=CARTESIAN_POINT('Ctrl Pts',(-55.4473053096868,4.93672858469731,
126.415426041482));
#252103=CARTESIAN_POINT('Ctrl Pts',(-55.7257529334997,-1.02411257361735,
124.278624699781));
#252104=CARTESIAN_POINT('Ctrl Pts',(-56.0042005573125,-6.0438443074584,
128.138655866601));
#252105=CARTESIAN_POINT('Ctrl Pts',(-56.2826481811254,-5.50957838095395,
134.448339472641));
#252106=CARTESIAN_POINT('Ctrl Pts',(-56.5610958049383,0.0877209197796484,
137.40938452913));
#252107=CARTESIAN_POINT('Ctrl Pts',(-56.8395434287512,5.60440898064107,
134.300735284249));
#252108=CARTESIAN_POINT('Ctrl Pts',(-57.117991052564,5.97091897889293,127.979088528083));
#252109=CARTESIAN_POINT('Ctrl Pts',(-57.396438676377,0.850446131150592,
124.253728799937));
#252110=CARTESIAN_POINT('Ctrl Pts',(-57.6748863001899,-5.05154516451579,
126.548079696037));
#252111=CARTESIAN_POINT('Ctrl Pts',(-57.9533339240027,-6.31141323569307,
132.753744828139));
#252112=CARTESIAN_POINT('Ctrl Pts',(-58.2317815478157,-1.77140087294607,
137.168021103437));
#252113=CARTESIAN_POINT('Ctrl Pts',(-58.5102291716285,4.39644235429495,
135.734404274317));
#252114=CARTESIAN_POINT('Ctrl Pts',(-58.7886767954414,6.52416983608798,
129.770318170665));
#252115=CARTESIAN_POINT('Ctrl Pts',(-59.0671244192543,2.65650396193163,
124.756466559932));
#252116=CARTESIAN_POINT('Ctrl Pts',(-59.3455720430672,-3.6523592758065,
125.300334132115));
#252117=CARTESIAN_POINT('Ctrl Pts',(-59.62401966688,-6.60488276674858,130.902133157784));
#252118=CARTESIAN_POINT('Ctrl Pts',(-59.902467290693,-3.48784166150989,
136.414083995446));
#252119=CARTESIAN_POINT('Ctrl Pts',(-60.1809149145059,2.83435554011865,
136.770973099059));
#252120=CARTESIAN_POINT('Ctrl Pts',(-60.4593625383188,6.55191846634393,
131.644836817403));
#252121=CARTESIAN_POINT('Ctrl Pts',(-60.7378101621316,4.24858840101079,
125.746343967642));
#252122=CARTESIAN_POINT('Ctrl Pts',(-61.0162577859445,-1.95898684976931,
124.49592132131));
#252123=CARTESIAN_POINT('Ctrl Pts',(-61.2947054097575,-6.36634888743926,
129.042646203845));
#252124=CARTESIAN_POINT('Ctrl Pts',(-61.5731530335703,-4.92334731098624,
135.208300568055));
#252125=CARTESIAN_POINT('Ctrl Pts',(-61.8516006573832,1.04396992537583,
137.326949262193));
#252126=CARTESIAN_POINT('Ctrl Pts',(-62.1300482811962,6.05192980108374,
133.451657638088));
#252127=CARTESIAN_POINT('Ctrl Pts',(-62.408495905009,5.49846184280268,127.143629379772));
#252128=CARTESIAN_POINT('Ctrl Pts',(-62.6869435288219,-0.107823934219708,
124.199634292325));
#252129=CARTESIAN_POINT('Ctrl Pts',(-62.9653911526347,-5.61502478318622,
127.325060038955));
#252130=CARTESIAN_POINT('Ctrl Pts',(-63.2438387764477,-5.96229216561512,
133.647793044045));
#252131=CARTESIAN_POINT('Ctrl Pts',(-63.5222864002605,-0.830504322008783,
137.357550558596));
#252132=CARTESIAN_POINT('Ctrl Pts',(-63.8007340240734,5.06447642113188,
135.045246658467));
#252133=CARTESIAN_POINT('Ctrl Pts',(-64.0791816478864,6.30545074667997,
128.835775665549));
#252134=CARTESIAN_POINT('Ctrl Pts',(-64.3576292716992,1.75202387442331,
124.435338072814));
#252135=CARTESIAN_POINT('Ctrl Pts',(-64.6360768955121,-4.41142734730395,
125.887721054655));
#252136=CARTESIAN_POINT('Ctrl Pts',(-64.914524519325,-6.52099234706562,
131.858255603616));
#252137=CARTESIAN_POINT('Ctrl Pts',(-65.1929721431379,-2.63808394806071,
136.860312146029));
#252138=CARTESIAN_POINT('Ctrl Pts',(-65.4714197669508,3.66909472164654,
136.297245083462));
#252139=CARTESIAN_POINT('Ctrl Pts',(-65.7498673907637,6.60455458740261,
130.686485539062));
#252140=CARTESIAN_POINT('Ctrl Pts',(-66.0283150145766,3.4707514377644,125.184047433287));
#252141=CARTESIAN_POINT('Ctrl Pts',(-66.3067626383895,-2.85250272754526,
124.846402576302));
#252142=CARTESIAN_POINT('Ctrl Pts',(-66.5852102622024,-6.55444623874626,
129.983830096806));
#252143=CARTESIAN_POINT('Ctrl Pts',(-66.8636578860152,-4.23317385903938,
135.875285080744));
#252144=CARTESIAN_POINT('Ctrl Pts',(-67.1421055098281,1.978178495085,137.106808211453));
#252145=CARTESIAN_POINT('Ctrl Pts',(-67.4205531336411,6.37168145161813,
132.546689895061));
#252146=CARTESIAN_POINT('Ctrl Pts',(-67.6990007574539,4.90992042805787,
126.385456090168));
#252147=CARTESIAN_POINT('Ctrl Pts',(-67.9774483812669,-1.06381760593968,
124.284979670466));
#252148=CARTESIAN_POINT('Ctrl Pts',(-68.2558960050797,-6.05995923045808,
128.175495851683));
#252149=CARTESIAN_POINT('Ctrl Pts',(-68.5343436288926,-5.48729436765201,
134.481810325563));
#252150=CARTESIAN_POINT('Ctrl Pts',(-68.8127912527054,0.12792594979327,
137.408728171199));
#252151=CARTESIAN_POINT('Ctrl Pts',(-69.0912388765185,5.62558856890878,
134.266554876337));
#252152=CARTESIAN_POINT('Ctrl Pts',(-69.3696865003312,5.9536101184771,127.942794195258));
#252153=CARTESIAN_POINT('Ctrl Pts',(-69.6481341241442,0.810554819188534,
124.248673260987));
#252154=CARTESIAN_POINT('Ctrl Pts',(-69.9265817479571,-5.07736076112986,
126.578908744281));
#252155=CARTESIAN_POINT('Ctrl Pts',(-70.2050293717699,-6.29942984483285,
132.792128074323));
#252156=CARTESIAN_POINT('Ctrl Pts',(-70.4834769955829,-1.73263064539088,
137.178686219444));
#252157=CARTESIAN_POINT('Ctrl Pts',(-70.7619246193956,4.42637147345276,
135.707550539556));
#252158=CARTESIAN_POINT('Ctrl Pts',(-71.0403722432087,6.51775444846118,
129.730622855503));
#252159=CARTESIAN_POINT('Ctrl Pts',(-71.3188198670216,2.6196394953401,124.740407719779));
#252160=CARTESIAN_POINT('Ctrl Pts',(-71.5972674908343,-3.68579617749442,
125.322669056552));
#252161=CARTESIAN_POINT('Ctrl Pts',(-71.8757151146474,-6.6041652243652,
130.942337142376));
#252162=CARTESIAN_POINT('Ctrl Pts',(-72.1541627384602,-3.45362906145158,
136.435211542427));
#252163=CARTESIAN_POINT('Ctrl Pts',(-72.4326103622731,2.87062348977667,
136.753609024891));
#252164=CARTESIAN_POINT('Ctrl Pts',(-72.711057986086,6.55691329165398,131.604937857965));
#252165=CARTESIAN_POINT('Ctrl Pts',(-72.9895056098989,4.21772010152317,
125.720575317484));
#252166=CARTESIAN_POINT('Ctrl Pts',(-73.2679532337117,-1.99735181482566,
124.50796311106));
#252167=CARTESIAN_POINT('Ctrl Pts',(-73.5464008575247,-6.37695498941029,
129.081432616995));
#252168=CARTESIAN_POINT('Ctrl Pts',(-73.8248484813376,-4.89644806029751,
135.238188785743));
#252169=CARTESIAN_POINT('Ctrl Pts',(-74.1032961051504,1.08365543144292,
137.320473472483));
#252170=CARTESIAN_POINT('Ctrl Pts',(-74.3817437289633,6.06793252119795,
133.414768775364));
#252171=CARTESIAN_POINT('Ctrl Pts',(-74.6601913527762,5.47607605895596,
127.110226506756));
#252172=CARTESIAN_POINT('Ctrl Pts',(-74.9386389765891,-0.148026780279403,
124.200413017498));
#252173=CARTESIAN_POINT('Ctrl Pts',(-75.217086600402,-5.63610023994771,
127.359304751927));
#252174=CARTESIAN_POINT('Ctrl Pts',(-75.4955342242149,-5.94487291790794,
133.684034526541));
#252175=CARTESIAN_POINT('Ctrl Pts',(-75.7739818480278,-0.790597807498519,
137.362484658699));
#252176=CARTESIAN_POINT('Ctrl Pts',(-76.0524294718406,5.09019806515201,
135.014339179226));
#252177=CARTESIAN_POINT('Ctrl Pts',(-76.3308770956536,6.29335058592772,
128.797429070474));
#252178=CARTESIAN_POINT('Ctrl Pts',(-76.6093247194664,1.71322136550425,
124.424791009442));
#252179=CARTESIAN_POINT('Ctrl Pts',(-76.8877723432794,-4.44127459430165,
125.914665758975));
#252180=CARTESIAN_POINT('Ctrl Pts',(-77.1662199670922,-6.51445617026952,
131.89793120868));
#252181=CARTESIAN_POINT('Ctrl Pts',(-77.4446675909052,-2.60117077463652,
136.876258709042));
#252182=CARTESIAN_POINT('Ctrl Pts',(-77.7231152147181,3.7024634886308,136.274808492052));
#252183=CARTESIAN_POINT('Ctrl Pts',(-78.0015628385308,6.60371468124315,
130.646283924643));
#252184=CARTESIAN_POINT('Ctrl Pts',(-78.2800104623438,3.43647469119047,
125.163024115555));
#252185=CARTESIAN_POINT('Ctrl Pts',(-78.5584580861567,-2.88871765894464,
124.863876957204));
#252186=CARTESIAN_POINT('Ctrl Pts',(-78.8369057099696,-6.55931960221255,
130.023744073965));
#252187=CARTESIAN_POINT('Ctrl Pts',(-79.1153533337825,-4.20222727162433,
135.900959659057));
#252188=CARTESIAN_POINT('Ctrl Pts',(-79.3938009575953,2.01650663137172,
137.094649707722));
#252189=CARTESIAN_POINT('Ctrl Pts',(-79.6722485814083,6.38216945196263,
132.507871380239));
#252190=CARTESIAN_POINT('Ctrl Pts',(-79.9506962052212,4.88293033251105,
126.355649882987));
#252191=CARTESIAN_POINT('Ctrl Pts',(-80.229143829034,-1.10348321810992,
124.29157621921));
#252192=CARTESIAN_POINT('Ctrl Pts',(-80.507591452847,-6.07584959944043,
128.212433250316));
#252193=CARTESIAN_POINT('Ctrl Pts',(-80.7860390766598,-5.46480702063872,
134.515144909234));
#252194=CARTESIAN_POINT('Ctrl Pts',(-81.0644867004727,0.168126239464741,
137.407827085998));
#252195=CARTESIAN_POINT('Ctrl Pts',(-81.3429343242857,5.64655969892388,
134.232246175545));
#252196=CARTESIAN_POINT('Ctrl Pts',(-81.6213819480984,5.93608064484842,
127.906605898828));
#252197=CARTESIAN_POINT('Ctrl Pts',(-81.8998295719115,0.770633471818905,
124.243860645443));
#252198=CARTESIAN_POINT('Ctrl Pts',(-82.1782771957242,-5.10298821427442,
126.609894368197));
#252199=CARTESIAN_POINT('Ctrl Pts',(-82.4567248195372,-6.28721302628274,
132.830437663053));
#252200=CARTESIAN_POINT('Ctrl Pts',(-82.7351724433501,-1.69379621456928,
137.189115132473));
#252201=CARTESIAN_POINT('Ctrl Pts',(-83.0136200671628,4.45613657178832,
135.680515115291));
#252202=CARTESIAN_POINT('Ctrl Pts',(-83.2920676909759,6.51109754304618,
129.690967328089));
#252203=CARTESIAN_POINT('Ctrl Pts',(-83.5705153147887,2.58267795704331,
124.724573581631));
#252204=CARTESIAN_POINT('Ctrl Pts',(-83.8489629386017,-3.71909650065006,
125.345207107088));
#252205=CARTESIAN_POINT('Ctrl Pts',(-84.1274105624144,-6.60320296221082,
130.982536014198));
#252206=CARTESIAN_POINT('Ctrl Pts',(-84.4058581862275,-3.41928848589759,
136.456130436155));
#252207=CARTESIAN_POINT('Ctrl Pts',(-84.6843058100402,2.90678506742617,
136.736024499134));
#252208=CARTESIAN_POINT('Ctrl Pts',(-84.9627534338533,6.56166514813073,
131.565009232842));
#252209=CARTESIAN_POINT('Ctrl Pts',(-85.241201057666,4.1866955128661,125.694995048862));
#252210=CARTESIAN_POINT('Ctrl Pts',(-85.519648681479,-2.03564276727566,
124.520238216135));
#252211=CARTESIAN_POINT('Ctrl Pts',(-85.7980963052919,-6.38732479096924,
129.120282873878));
#252212=CARTESIAN_POINT('Ctrl Pts',(-86.0765439291047,-4.8693673699251,
135.267912706297));
#252213=CARTESIAN_POINT('Ctrl Pts',(-86.3549915529177,1.12330078225909,
137.313756225814));
#252214=CARTESIAN_POINT('Ctrl Pts',(-86.6334391767305,6.08371039184151,
133.377783183006));
#252215=CARTESIAN_POINT('Ctrl Pts',(-86.9118868005434,5.45348735709659,
127.076960521238));
#252216=CARTESIAN_POINT('Ctrl Pts',(-87.1903344243564,-0.188224141151809,
124.201436454379));
#252217=CARTESIAN_POINT('Ctrl Pts',(-87.4687820481692,-5.65696684894189,
127.39367712271));
#252218=CARTESIAN_POINT('Ctrl Pts',(-87.7472296719821,-5.92723338074904,
133.720169301662));
#252219=CARTESIAN_POINT('Ctrl Pts',(-88.0256772957949,-0.750661997095914,
137.367175745102));
#252220=CARTESIAN_POINT('Ctrl Pts',(-88.3041249196079,5.11573109001074,
134.983275697681));
#252221=CARTESIAN_POINT('Ctrl Pts',(-88.5825725434208,6.28101722275544,
128.759156842984));
#252222=CARTESIAN_POINT('Ctrl Pts',(-88.8610201672337,1.67435537253749,
124.414480343369));
#252223=CARTESIAN_POINT('Ctrl Pts',(-89.1394677910466,-4.47095726823472,
125.941791652735));
#252224=CARTESIAN_POINT('Ctrl Pts',(-89.4179154148595,-6.50767859790483,
131.93756629108));
#252225=CARTESIAN_POINT('Ctrl Pts',(-89.6963630386723,-2.56416121387375,
136.891980275641));
#252226=CARTESIAN_POINT('Ctrl Pts',(-89.9748106624853,3.73569505946763,
136.252169191183));
#252227=CARTESIAN_POINT('Ctrl Pts',(-90.253258286298,6.60263007200808,130.606088167816));
#252228=CARTESIAN_POINT('Ctrl Pts',(-90.5317059101111,3.40207060478355,
125.142209839621));
#252229=CARTESIAN_POINT('Ctrl Pts',(-90.8101535339238,-2.9248255478482,
124.881571464914));
#252230=CARTESIAN_POINT('Ctrl Pts',(-91.0886011577368,-6.56394990767886,
130.063686977158));
#252231=CARTESIAN_POINT('Ctrl Pts',(-91.3670487815497,-4.17112496913288,
135.926445381018));
#252232=CARTESIAN_POINT('Ctrl Pts',(-91.6454964053626,2.05476004526333,
137.082258115016));
#252233=CARTESIAN_POINT('Ctrl Pts',(-91.9239440291755,6.39242095867105,
132.468989741201));
#252234=CARTESIAN_POINT('Ctrl Pts',(-92.2023916529884,4.85575929818535,
126.326008524418));
#252235=CARTESIAN_POINT('Ctrl Pts',(-92.4808392768012,-1.14310794030347,
124.298414101576));
#252236=CARTESIAN_POINT('Ctrl Pts',(-92.7592869006141,-6.09151482558059,
128.249466693771));
#252237=CARTESIAN_POINT('Ctrl Pts',(-93.0377345244271,-5.44211717319261,
134.548341988427));
#252238=CARTESIAN_POINT('Ctrl Pts',(-93.3161821482399,0.208320299155509,
137.406681306919));
#252239=CARTESIAN_POINT('Ctrl Pts',(-93.5946297720528,5.6673215935918,134.197810453193));
#252240=CARTESIAN_POINT('Ctrl Pts',(-93.8730773958657,5.91833120756931,
127.870524979765));
#252241=CARTESIAN_POINT('Ctrl Pts',(-94.1515250196785,0.730683568342929,
124.239291131637));
#252242=CARTESIAN_POINT('Ctrl Pts',(-94.4299726434915,-5.12842657431339,
126.641035419604));
#252243=CARTESIAN_POINT('Ctrl Pts',(-94.7084202673044,-6.27476323274215,
132.868672174754));
#252244=CARTESIAN_POINT('Ctrl Pts',(-94.9868678911172,-1.6548990195065,
137.199307456074));
#252245=CARTESIAN_POINT('Ctrl Pts',(-95.2653155149302,4.48573654634406,
135.653299003326));
#252246=CARTESIAN_POINT('Ctrl Pts',(-95.543763138743,6.50419936651746,129.651353057874));
#252247=CARTESIAN_POINT('Ctrl Pts',(-95.822210762556,2.54562071666526,124.708964732227));
#252248=CARTESIAN_POINT('Ctrl Pts',(-96.1006583863688,-3.75225901131679,
125.367947448562));
#252249=CARTESIAN_POINT('Ctrl Pts',(-96.3791060101818,-6.60199601594203,
131.022728283664));
#252250=CARTESIAN_POINT('Ctrl Pts',(-96.6575536339946,-3.38482120735248,
136.476839901474));
#252251=CARTESIAN_POINT('Ctrl Pts',(-96.9360012578075,2.94283893308538,
136.718220173391));
#252252=CARTESIAN_POINT('Ctrl Pts',(-97.2144488816204,6.5661738596919,131.525052421605));
#252253=CARTESIAN_POINT('Ctrl Pts',(-97.4928965054334,4.15551578466796,
125.669604109659));
#252254=CARTESIAN_POINT('Ctrl Pts',(-97.771344129246,-2.07385828823457,
124.532746181678));
#252255=CARTESIAN_POINT('Ctrl Pts',(-98.0497917530593,-6.39745790785863,
129.15919553488));
#252256=CARTESIAN_POINT('Ctrl Pts',(-98.3282393768718,-4.84210624335443,
135.297471228287));
#252257=CARTESIAN_POINT('Ctrl Pts',(-98.606687000685,1.16290450875192,137.306797771098));
#252258=CARTESIAN_POINT('Ctrl Pts',(-98.8851346244975,6.09926282835875,
133.340702231527));
#252259=CARTESIAN_POINT('Ctrl Pts',(-99.1635822483109,5.43069657425812,
127.043832655902));
#252260=CARTESIAN_POINT('Ctrl Pts',(-99.4420298721233,-0.228414527308866,
124.202704565042));
#252261=CARTESIAN_POINT('Ctrl Pts',(-99.7204774959365,-5.67762383694899,
127.428175877623));
#252262=CARTESIAN_POINT('Ctrl Pts',(-99.9989251197493,-5.90937420777732,
133.756196030418));
#252263=CARTESIAN_POINT('Ctrl Pts',(-100.277372743562,-0.710698370637635,
137.371623643978));
#252264=CARTESIAN_POINT('Ctrl Pts',(-100.555820367375,5.14107454957247,
134.9520573649));
#252265=CARTESIAN_POINT('Ctrl Pts',(-100.834267991188,6.26845111417983,
128.720960401273));
#252266=CARTESIAN_POINT('Ctrl Pts',(-101.112715615001,1.63542733571746,
124.404406456659));
#252267=CARTESIAN_POINT('Ctrl Pts',(-101.391163238814,-4.50047426920288,
125.969097730777));
#252268=CARTESIAN_POINT('Ctrl Pts',(-101.669610862627,-6.50065988111587,
131.977159382129));
#252269=CARTESIAN_POINT('Ctrl Pts',(-101.94805848644,-2.52705663717401,
136.907476263252));
#252270=CARTESIAN_POINT('Ctrl Pts',(-102.226506110253,3.76878820275105,
136.229328019765));
#252271=CARTESIAN_POINT('Ctrl Pts',(-102.504953734065,6.60130079988703,
130.565899758046));
#252272=CARTESIAN_POINT('Ctrl Pts',(-102.783401357878,3.36754045339959,
125.121605376767));
#252273=CARTESIAN_POINT('Ctrl Pts',(-103.061848981691,-2.96082505626518,
124.899485443752));
#252274=CARTESIAN_POINT('Ctrl Pts',(-103.340296605504,-6.56833698356739,
130.103657326284));
#252275=CARTESIAN_POINT('Ctrl Pts',(-103.618744229317,-4.13986810407194,
135.951741302244));
#252276=CARTESIAN_POINT('Ctrl Pts',(-103.89719185313,2.0929373192654,137.06963389251));
#252277=CARTESIAN_POINT('Ctrl Pts',(-104.175639476943,6.40243559186997,
132.430046418718));
#252278=CARTESIAN_POINT('Ctrl Pts',(-104.454087100755,4.82840833191319,
126.296533112833));
#252279=CARTESIAN_POINT('Ctrl Pts',(-104.732534724569,-1.18269030421136,
124.305493064181));
#252280=CARTESIAN_POINT('Ctrl Pts',(-105.010982348381,-6.10695432839948,
128.286594809759));
#252281=CARTESIAN_POINT('Ctrl Pts',(-105.289429972194,-5.41922566609253,
134.581400333014));
#252282=CARTESIAN_POINT('Ctrl Pts',(-105.567877596007,0.248506639461218,
137.40529087642));
#252283=CARTESIAN_POINT('Ctrl Pts',(-105.84632521982,5.68787348357469,134.163248985309));
#252284=CARTESIAN_POINT('Ctrl Pts',(-106.124772843633,5.90036246435008,
127.834552775061));
#252285=CARTESIAN_POINT('Ctrl Pts',(-106.403220467446,0.690706589119241,
124.234964888896));
#252286=CARTESIAN_POINT('Ctrl Pts',(-106.681668091259,-5.1536748986197,
126.672330744555));
#252287=CARTESIAN_POINT('Ctrl Pts',(-106.960115715072,-6.26208092554253,
132.906830192629));
#252288=CARTESIAN_POINT('Ctrl Pts',(-107.238563338885,-1.61594050155245,
137.209262812568));
#252289=CARTESIAN_POINT('Ctrl Pts',(-107.517010962697,4.51517030028232,
135.625903212168));
#252290=CARTESIAN_POINT('Ctrl Pts',(-107.79545858651,6.49706017448951,129.611781512777));
#252291=CARTESIAN_POINT('Ctrl Pts',(-108.073906210323,2.50846914737518,
124.69358174996));
#252292=CARTESIAN_POINT('Ctrl Pts',(-108.352353834136,-3.78528248064593,
125.390889238328));
#252293=CARTESIAN_POINT('Ctrl Pts',(-108.630801457949,-6.60054443028347,
131.062912461436));
#252294=CARTESIAN_POINT('Ctrl Pts',(-108.909249081762,-3.35022850301195,
136.497339170987));
#252295=CARTESIAN_POINT('Ctrl Pts',(-109.187696705575,2.97878375076591,
136.700196707408));
#252296=CARTESIAN_POINT('Ctrl Pts',(-109.466144329388,6.57043925926657,
131.485068904869));
#252297=CARTESIAN_POINT('Ctrl Pts',(-109.7445919532,4.12418207230337,125.644403440746));
#252298=CARTESIAN_POINT('Ctrl Pts',(-110.023039577014,-2.11199696161116,
124.5454865442));
#252299=CARTESIAN_POINT('Ctrl Pts',(-110.301487200826,-6.40735396459295,
129.198169158078));
#252300=CARTESIAN_POINT('Ctrl Pts',(-110.579934824639,-4.81466569075636,
135.326863256411));
#252301=CARTESIAN_POINT('Ctrl Pts',(-110.858382448452,1.20246514338981,
137.299598366182));
#252302=CARTESIAN_POINT('Ctrl Pts',(-111.136830072265,6.11458925444912,
133.303527294979));
#252303=CARTESIAN_POINT('Ctrl Pts',(-111.415277696078,5.407704554961,127.010844138312));
#252304=CARTESIAN_POINT('Ctrl Pts',(-111.693725319891,-0.268596449482207,
124.204217302498));
#252305=CARTESIAN_POINT('Ctrl Pts',(-111.972172943703,-5.69807043851701,
127.462799738304));
#252306=CARTESIAN_POINT('Ctrl Pts',(-112.250620567517,-5.89129606077132,
133.792113377828));
#252307=CARTESIAN_POINT('Ctrl Pts',(-112.529068191329,-0.670708408989202,
137.375828190507));
#252308=CARTESIAN_POINT('Ctrl Pts',(-112.807515815142,5.16622750472631,
134.920685337692));
#252309=CARTESIAN_POINT('Ctrl Pts',(-113.085963438955,6.25565272584325,
128.682841160722));
#252310=CARTESIAN_POINT('Ctrl Pts',(-113.364411062768,1.5964386975353,124.394569722605));
#252311=CARTESIAN_POINT('Ctrl Pts',(-113.642858686581,-4.52982450344111,
125.996582981263));
#252312=CARTESIAN_POINT('Ctrl Pts',(-113.921306310394,-6.49340027998504,
132.016709014688));
#252313=CARTESIAN_POINT('Ctrl Pts',(-114.199753934207,-2.48985841946147,
136.922746097669));
#252314=CARTESIAN_POINT('Ctrl Pts',(-114.47820155802,3.80174169220082,136.206285824184));
#252315=CARTESIAN_POINT('Ctrl Pts',(-114.756649181833,6.59972691413776,
130.525720184532));
#252316=CARTESIAN_POINT('Ctrl Pts',(-115.035096805645,3.3328855165654,125.101211490497));
#252317=CARTESIAN_POINT('Ctrl Pts',(-115.313544429458,-2.99671485022117,
124.917618229914));
#252318=CARTESIAN_POINT('Ctrl Pts',(-115.591992053271,-6.57248066731354,
130.143653640229));
#252319=CARTESIAN_POINT('Ctrl Pts',(-115.870439677084,-4.10845783467579,
135.976846485386));
#252320=CARTESIAN_POINT('Ctrl Pts',(-116.148887300897,2.13103703870585,
137.056777507999));
#252321=CARTESIAN_POINT('Ctrl Pts',(-116.42733492471,6.41221298046361,132.391042855849));
#252322=CARTESIAN_POINT('Ctrl Pts',(-116.705782548523,4.8008784471946,126.267224740454));
#252323=CARTESIAN_POINT('Ctrl Pts',(-116.984230172336,-1.22222884309565,
124.312812844714));
#252324=CARTESIAN_POINT('Ctrl Pts',(-117.262677796149,-6.12216753577917,
128.323816222486));
#252325=CARTESIAN_POINT('Ctrl Pts',(-117.541125419961,-5.39613334759327,
134.614318718005));
#252326=CARTESIAN_POINT('Ctrl Pts',(-117.819573043774,0.288683771261777,
137.403655846021));
#252327=CARTESIAN_POINT('Ctrl Pts',(-118.098020667587,5.70821460731317,
134.128563052582));
#252328=CARTESIAN_POINT('Ctrl Pts',(-118.3764682914,5.88217508103065,127.79869061768));
#252329=CARTESIAN_POINT('Ctrl Pts',(-118.654915915213,0.650704015508265,
124.230882077529));
#252330=CARTESIAN_POINT('Ctrl Pts',(-118.933363539026,-5.17873225160735,
126.703779183394));
#252331=CARTESIAN_POINT('Ctrl Pts',(-119.211811162839,-6.24916657463125,
132.944910302722));
#252332=CARTESIAN_POINT('Ctrl Pts',(-119.490258786652,-1.57692210432836,
137.218980833058));
#252333=CARTESIAN_POINT('Ctrl Pts',(-119.768706410464,4.54443674292479,
135.598328756974));
#252334=CARTESIAN_POINT('Ctrl Pts',(-120.047154034278,6.48968023150711,
129.572254159139));
#252335=CARTESIAN_POINT('Ctrl Pts',(-120.32560165809,2.47122462583917,124.67842520485));
#252336=CARTESIAN_POINT('Ctrl Pts',(-120.604049281903,-3.81816568494053,
125.414031626265));
#252337=CARTESIAN_POINT('Ctrl Pts',(-120.882496905716,-6.59884825902321,
131.103087058474));
#252338=CARTESIAN_POINT('Ctrl Pts',(-121.160944529529,-3.31551165472302,
136.517627485086));
#252339=CARTESIAN_POINT('Ctrl Pts',(-121.439392153342,3.0146181885189,136.68195476905));
#252340=CARTESIAN_POINT('Ctrl Pts',(-121.717839777155,6.57446118879764,
131.445060164237));
#252341=CARTESIAN_POINT('Ctrl Pts',(-121.996287400968,4.0926955368563,125.619393975946));
#252342=CARTESIAN_POINT('Ctrl Pts',(-122.274735024781,-2.15005737416446,
124.5584588316));
#252343=CARTESIAN_POINT('Ctrl Pts',(-122.553182648593,-6.41701259446945,
129.237202299292));
#252344=CARTESIAN_POINT('Ctrl Pts',(-122.831630272406,-4.7870467289504,
135.356087701536));
#252345=CARTESIAN_POINT('Ctrl Pts',(-123.110077896219,1.24198122024032,
137.292158277842));
#252346=CARTESIAN_POINT('Ctrl Pts',(-123.388525520032,6.1296891021858,133.266259750888));
#252347=CARTESIAN_POINT('Ctrl Pts',(-123.666973143845,5.38451215118288,
126.97799619087));
#252348=CARTESIAN_POINT('Ctrl Pts',(-123.945420767658,-0.30876841871475,
124.20597461069));
#252349=CARTESIAN_POINT('Ctrl Pts',(-124.223868391471,-5.71830589598935,
127.497547421752));
#252350=CARTESIAN_POINT('Ctrl Pts',(-124.502316015284,-5.87299960962311,
133.827920012961));
#252351=CARTESIAN_POINT('Ctrl Pts',(-124.780763639097,-0.630693593994696,
137.379789228888));
#252352=CARTESIAN_POINT('Ctrl Pts',(-125.059211262909,5.19118902341993,
134.889160778557));
#252353=CARTESIAN_POINT('Ctrl Pts',(-125.337658886723,6.24262253199412,
128.644800533857));
#252354=CARTESIAN_POINT('Ctrl Pts',(-125.616106510535,1.55739090273089,
124.384970505708));
#252355=CARTESIAN_POINT('Ctrl Pts',(-125.894554134348,-4.55900688336737,
126.024246385717));
#252356=CARTESIAN_POINT('Ctrl Pts',(-126.173001758161,-6.48590006351826,
132.056213723232));
#252357=CARTESIAN_POINT('Ctrl Pts',(-126.451449381974,-2.45256793912933,
136.937789213063));
#252358=CARTESIAN_POINT('Ctrl Pts',(-126.729897005787,3.83455430671493,
136.183043458277));
#252359=CARTESIAN_POINT('Ctrl Pts',(-127.0083446296,6.5979084730801,130.485550936142));
#252360=CARTESIAN_POINT('Ctrl Pts',(-127.286792253413,3.29810707843306,
125.081028936517));
#252361=CARTESIAN_POINT('Ctrl Pts',(-127.565239877225,-3.03249359980603,
124.935969151478));
#252362=CARTESIAN_POINT('Ctrl Pts',(-127.843687501038,-6.57638080537151,
130.183674436914));
#252363=CARTESIAN_POINT('Ctrl Pts',(-128.122135124851,-4.07689532486387,
136.001760000162));
#252364=CARTESIAN_POINT('Ctrl Pts',(-128.400582748664,2.1690577917847,137.043689437881));
#252365=CARTESIAN_POINT('Ctrl Pts',(-128.679030372477,6.42175276214748,
132.351980497887));
#252366=CARTESIAN_POINT('Ctrl Pts',(-128.95747799629,4.77317066415926,126.238084493312));
#252367=CARTESIAN_POINT('Ctrl Pts',(-129.235925620103,-1.26172209184052,
124.320373171937));
#252368=CARTESIAN_POINT('Ctrl Pts',(-129.514373243916,-6.13715388399014,
128.361129552696));
#252369=CARTESIAN_POINT('Ctrl Pts',(-129.792820867728,-5.37284107338758,
134.647095923599));
#252370=CARTESIAN_POINT('Ctrl Pts',(-130.071268491542,0.328850205779251,
137.401776276312));
#252371=CARTESIAN_POINT('Ctrl Pts',(-130.349716115354,5.72834421106097,
134.093753940311));
#252372=CARTESIAN_POINT('Ctrl Pts',(-130.628163739167,5.86376973154965,
127.762939836503));
#252373=CARTESIAN_POINT('Ctrl Pts',(-130.90661136298,0.610677329821333,
124.227042848828));
#252374=CARTESIAN_POINT('Ctrl Pts',(-131.185058986793,-5.20359770476699,
126.735379570785));
#252375=CARTESIAN_POINT('Ctrl Pts',(-131.463506610606,-6.23602065855449,
132.982911093959));
#252376=CARTESIAN_POINT('Ctrl Pts',(-131.741954234419,-1.53784527367628,
137.228461157434));
#252377=CARTESIAN_POINT('Ctrl Pts',(-132.020401858232,4.57353478979242,
135.57057665953));
#252378=CARTESIAN_POINT('Ctrl Pts',(-132.298849482045,6.48205981103755,
129.532772461657));
#252379=CARTESIAN_POINT('Ctrl Pts',(-132.577297105858,2.43388853216508,
124.66349565853));
#252380=CARTESIAN_POINT('Ctrl Pts',(-132.85574472967,-3.85090740570176,
125.437373754826));
#252381=CARTESIAN_POINT('Ctrl Pts',(-133.134192353483,-6.59690756501448,
131.143250586095));
#252382=CARTESIAN_POINT('Ctrl Pts',(-133.412639977296,-3.28067194892964,
136.53770409198));
#252383=CARTESIAN_POINT('Ctrl Pts',(-133.691087601109,3.0503409184865,136.663495034279));
#252384=CARTESIAN_POINT('Ctrl Pts',(-133.969535224922,6.5782394992522,131.405027682246));
#252385=CARTESIAN_POINT('Ctrl Pts',(-134.247982848735,4.06105734507014,
125.59457664199));
#252386=CARTESIAN_POINT('Ctrl Pts',(-134.526430472548,-2.18803811555026,
124.57166256319));
#252387=CARTESIAN_POINT('Ctrl Pts',(-134.804878096361,-6.42643343958478,
129.276293512134));
#252388=CARTESIAN_POINT('Ctrl Pts',(-135.083325720174,-4.75925038136761,
135.385143480741));
#252389=CARTESIAN_POINT('Ctrl Pts',(-135.361773343986,1.28145127501926,
137.284477781773));
#252390=CARTESIAN_POINT('Ctrl Pts',(-135.640220967799,6.14456181203885,
133.228900980221));
#252391=CARTESIAN_POINT('Ctrl Pts',(-135.918668591612,5.36112022232688,
126.945290030769));
#252392=CARTESIAN_POINT('Ctrl Pts',(-136.197116215425,-0.348928946420584,
124.207976424505));
#252393=CARTESIAN_POINT('Ctrl Pts',(-136.475563839238,-5.73832945953392,
127.53241764038));
#252394=CARTESIAN_POINT('Ctrl Pts',(-136.754011463051,-5.85448553231475,
133.863614608987));
#252395=CARTESIAN_POINT('Ctrl Pts',(-137.032459086864,-0.590655408416443,
137.383506612345));
#252396=CARTESIAN_POINT('Ctrl Pts',(-137.310906710677,5.21595818069537,
134.857484855651));
#252397=CARTESIAN_POINT('Ctrl Pts',(-137.58935433449,6.22936101547165,128.606839930282));
#252398=CARTESIAN_POINT('Ctrl Pts',(-137.867801958302,1.51828539823306,
124.375609161675));
#252399=CARTESIAN_POINT('Ctrl Pts',(-138.146249582115,-4.58802032761614,
126.052086919061));
#252400=CARTESIAN_POINT('Ctrl Pts',(-138.424697205928,-6.47815950964009,
132.095672043897));
#252401=CARTESIAN_POINT('Ctrl Pts',(-138.703144829741,-2.41518657799051,
136.952605052004));
#252402=CARTESIAN_POINT('Ctrl Pts',(-138.981592453554,3.86722483040823,
136.159601783301));
#252403=CARTESIAN_POINT('Ctrl Pts',(-139.260040077367,6.59584554409815,
130.445393501362));
#252404=CARTESIAN_POINT('Ctrl Pts',(-139.53848770118,3.26320642772972,125.061058462695));
#252405=CARTESIAN_POINT('Ctrl Pts',(-139.816935324993,-3.06815997922566,
124.954537528447));
#252406=CARTESIAN_POINT('Ctrl Pts',(-140.095382948806,-6.58003725322031,
130.223718233352));
#252407=CARTESIAN_POINT('Ctrl Pts',(-140.373830572619,-4.04518174419624,
136.026480923393));
#252408=CARTESIAN_POINT('Ctrl Pts',(-140.652278196431,2.20699816962987,
137.030370167137));
#252409=CARTESIAN_POINT('Ctrl Pts',(-140.930725820244,6.43105458342049,
132.312860792301));
#252410=CARTESIAN_POINT('Ctrl Pts',(-141.209173444057,4.74528600953044,
126.209113451214));
#252411=CARTESIAN_POINT('Ctrl Pts',(-141.48762106787,-1.30116858700904,
124.328173765698));
#252412=CARTESIAN_POINT('Ctrl Pts',(-141.766068691683,-6.15191281770628,
128.398533417733));
#252413=CARTESIAN_POINT('Ctrl Pts',(-142.044516315496,-5.34934970658085,
134.679730735221));
#252414=CARTESIAN_POINT('Ctrl Pts',(-142.322963939309,0.369004454631186,
137.399652236939));
#252415=CARTESIAN_POINT('Ctrl Pts',(-142.601411563122,5.74826154890666,
134.058822938361));
#252416=CARTESIAN_POINT('Ctrl Pts',(-142.879859186934,5.84514709792562,
127.727301756295));
#252417=CARTESIAN_POINT('Ctrl Pts',(-143.158306810748,0.570628015260733,
124.223447345055));
#252418=CARTESIAN_POINT('Ctrl Pts',(-143.43675443456,-5.22827033670001,
126.767130735766));
#252419=CARTESIAN_POINT('Ctrl Pts',(-143.715202058373,-6.22264366443886,
133.020831158207));
#252420=CARTESIAN_POINT('Ctrl Pts',(-143.993649682186,-1.49871145760156,
137.237703434405));
#252421=CARTESIAN_POINT('Ctrl Pts',(-144.272097305999,4.60246336264661,
135.542647948195));
#252422=CARTESIAN_POINT('Ctrl Pts',(-144.550544929812,6.47419919545755,
129.493337883343));
#252423=CARTESIAN_POINT('Ctrl Pts',(-144.828992553625,2.39646224985712,
124.648793664219));
#252424=CARTESIAN_POINT('Ctrl Pts',(-145.107440177438,-3.8835064296727,
125.460914759058));
#252425=CARTESIAN_POINT('Ctrl Pts',(-145.38588780125,-6.59472242016944,
131.183401556022));
#252426=CARTESIAN_POINT('Ctrl Pts',(-145.664335425064,-3.24571067663155,
136.557568247724));
#252427=CARTESIAN_POINT('Ctrl Pts',(-145.942783048876,3.08595061694992,
136.644818187128));
#252428=CARTESIAN_POINT('Ctrl Pts',(-146.221230672689,6.58177405062243,
131.364972942318));
#252429=CARTESIAN_POINT('Ctrl Pts',(-146.499678296502,4.02926866931097,
125.569952358496));
#252430=CARTESIAN_POINT('Ctrl Pts',(-146.778125920315,-2.22593777837984,
124.585097249699));
#252431=CARTESIAN_POINT('Ctrl Pts',(-147.056573544128,-6.43561615084533,
129.315441348065));
#252432=CARTESIAN_POINT('Ctrl Pts',(-147.335021167941,-4.73127767801157,
135.414029517352));
#252433=CARTESIAN_POINT('Ctrl Pts',(-147.613468791753,1.32087384515067,
137.276557162581));
#252434=CARTESIAN_POINT('Ctrl Pts',(-147.891916415567,6.15920683289404,
133.191452367319));
#252435=CARTESIAN_POINT('Ctrl Pts',(-148.170364039379,5.33752963518947,
126.91272686995));
#252436=CARTESIAN_POINT('Ctrl Pts',(-148.448811663193,-0.389076544435395,
124.210222669761));
#252437=CARTESIAN_POINT('Ctrl Pts',(-148.727259287005,-5.75814038716998,
127.567409102056));
#252438=CARTESIAN_POINT('Ctrl Pts',(-149.005706910818,-5.83575451489182,
133.899195843233));
#252439=CARTESIAN_POINT('Ctrl Pts',(-149.284154534631,-0.550595335885521,
137.386980203127));
#252440=CARTESIAN_POINT('Ctrl Pts',(-149.562602158444,5.24053405872261,
134.825658742734));
#252441=CARTESIAN_POINT('Ctrl Pts',(-149.841049782257,6.21586866768539,
128.568960756646));
#252442=CARTESIAN_POINT('Ctrl Pts',(-150.119497406069,1.47912363311174,
124.366486037389));
#252443=CARTESIAN_POINT('Ctrl Pts',(-150.397945029883,-4.61686376108527,
126.080103549656));
#252444=CARTESIAN_POINT('Ctrl Pts',(-150.676392653695,-6.4701789051783,
132.135082514543));
#252445=CARTESIAN_POINT('Ctrl Pts',(-150.954840277509,-2.37771572122463,
136.967193065487));
#252446=CARTESIAN_POINT('Ctrl Pts',(-151.233287901321,3.89975205266408,
136.135961667893));
#252447=CARTESIAN_POINT('Ctrl Pts',(-151.511735525134,6.59353820363339,
130.405249368239));
#252448=CARTESIAN_POINT('Ctrl Pts',(-151.790183148947,3.22818485771248,
125.041300809049));
#252449=CARTESIAN_POINT('Ctrl Pts',(-152.06863077276,-3.10371266684865,
124.97332267276));
#252450=CARTESIAN_POINT('Ctrl Pts',(-152.347078396573,-6.58344987536885,
130.263783545709));
#252451=CARTESIAN_POINT('Ctrl Pts',(-152.625526020386,-4.01331826783166,
136.051008339035));
#252452=CARTESIAN_POINT('Ctrl Pts',(-152.903973644199,2.24485676634579,
137.016820189321));
#252453=CARTESIAN_POINT('Ctrl Pts',(-153.182421268012,6.44011809960154,
132.273685188686));
#252454=CARTESIAN_POINT('Ctrl Pts',(-153.460868891824,4.71722551658265,
126.180312687687));
#252455=CARTESIAN_POINT('Ctrl Pts',(-153.739316515637,-1.34056686689732,
124.336214336947));
#252456=CARTESIAN_POINT('Ctrl Pts',(-154.01776413945,-6.16644379003131,
128.436026431582));
#252457=CARTESIAN_POINT('Ctrl Pts',(-154.296211763263,-5.32566011765276,
134.712221943579));
#252458=CARTESIAN_POINT('Ctrl Pts',(-154.574659387076,0.409145029887599,
137.397283806609));
#252459=CARTESIAN_POINT('Ctrl Pts',(-154.853107010889,5.7679658828075,134.023771341112));
#252460=CARTESIAN_POINT('Ctrl Pts',(-155.131554634702,5.82630787022557,
127.691777697632));
#252461=CARTESIAN_POINT('Ctrl Pts',(-155.410002258515,0.530557555869813,
124.220095699443));
#252462=CARTESIAN_POINT('Ctrl Pts',(-155.688449882327,-5.25274923315307,
126.799031501784));
#252463=CARTESIAN_POINT('Ctrl Pts',(-155.96689750614,-6.20903608797397,
133.058669090323));
#252464=CARTESIAN_POINT('Ctrl Pts',(-156.245345129953,-1.4595221062231,
137.246707321489));
#252465=CARTESIAN_POINT('Ctrl Pts',(-156.523792753766,4.63122138952822,
135.514543657883));
#252466=CARTESIAN_POINT('Ctrl Pts',(-156.802240377579,6.46609867604585,
129.453951885458));
#252467=CARTESIAN_POINT('Ctrl Pts',(-157.080688001392,2.35894716575843,
124.634319766706));
#252468=CARTESIAN_POINT('Ctrl Pts',(-157.359135625205,-3.9159615488849,
125.484653766641));
#252469=CARTESIAN_POINT('Ctrl Pts',(-157.637583249018,-6.59229290546042,
131.223538480449));
#252470=CARTESIAN_POINT('Ctrl Pts',(-157.916030872831,-3.21062913332988,
136.577219216243));
#252471=CARTESIAN_POINT('Ctrl Pts',(-158.194478496644,3.12144596437753,
136.625924919674));
#252472=CARTESIAN_POINT('Ctrl Pts',(-158.472926120456,6.58506471193526,
131.324897428694));
#252473=CARTESIAN_POINT('Ctrl Pts',(-158.751373744269,3.99733068751967,
125.545522037924));
#252474=CARTESIAN_POINT('Ctrl Pts',(-159.029821368082,-2.26375495826568,
124.598762393297));
#252475=CARTESIAN_POINT('Ctrl Pts',(-159.308268991895,-6.44456038798308,
129.354644356446));
#252476=CARTESIAN_POINT('Ctrl Pts',(-159.586716615708,-4.7031296554214,
135.442744740987));
#252477=CARTESIAN_POINT('Ctrl Pts',(-159.865164239521,1.36024746981527,
137.268396713766));
#252478=CARTESIAN_POINT('Ctrl Pts',(-160.143611863334,6.17362362207528,
133.153915299856));
#252479=CARTESIAN_POINT('Ctrl Pts',(-160.422059487147,5.31374126392856,
126.880307915048));
#252480=CARTESIAN_POINT('Ctrl Pts',(-160.70050711096,-0.429209725076344,
124.212713263223));
#252481=CARTESIAN_POINT('Ctrl Pts',(-160.978954734773,-5.77773794479658,
127.602520510164));
#252482=CARTESIAN_POINT('Ctrl Pts',(-161.257402358585,-5.81680725143943,
133.934662397221));
#252483=CARTESIAN_POINT('Ctrl Pts',(-161.535849982398,-0.51051486084124,
137.390209872519));
#252484=CARTESIAN_POINT('Ctrl Pts',(-161.814297606211,5.26491574683228,
134.793683619137));
#252485=CARTESIAN_POINT('Ctrl Pts',(-162.092745230024,6.20214598860049,
128.531164416574));
#252486=CARTESIAN_POINT('Ctrl Pts',(-162.371192853837,1.43990705852047,
124.357601470914));
#252487=CARTESIAN_POINT('Ctrl Pts',(-162.64964047765,-4.64553611496906,
126.108295239334));
#252488=CARTESIAN_POINT('Ctrl Pts',(-162.928088101462,-6.46195854585841,
132.1744436748));
#252489=CARTESIAN_POINT('Ctrl Pts',(-163.206535725276,-2.34015675732853,
136.981552712947));
#252490=CARTESIAN_POINT('Ctrl Pts',(-163.484983349088,3.93213476817268,
136.112123988049));
#252491=CARTESIAN_POINT('Ctrl Pts',(-163.763430972902,6.5909865371863,130.365120024332));
#252492=CARTESIAN_POINT('Ctrl Pts',(-164.041878596714,3.19304366611785,
125.021756707701));
#252493=CARTESIAN_POINT('Ctrl Pts',(-164.320326220527,-3.13915034525769,
124.99232388833));
#252494=CARTESIAN_POINT('Ctrl Pts',(-164.59877384434,-6.58661854536123,
130.303868889347));
#252495=CARTESIAN_POINT('Ctrl Pts',(-164.877221468153,-3.98130607648258,
136.075341338217));
#252496=CARTESIAN_POINT('Ctrl Pts',(-165.155669091966,2.28263217906914,
137.003040006531));
#252497=CARTESIAN_POINT('Ctrl Pts',(-165.434116715779,6.44894297483741,
132.23445513871));
#252498=CARTESIAN_POINT('Ctrl Pts',(-165.712564339591,4.6889902251094,126.151683269957));
#252499=CARTESIAN_POINT('Ctrl Pts',(-165.991011963405,-1.37991547158711,
124.344494587733));
#252500=CARTESIAN_POINT('Ctrl Pts',(-166.269459587217,-6.18074626251326,
128.473607204924));
#252501=CARTESIAN_POINT('Ctrl Pts',(-166.54790721103,-5.3017731844313,134.744568344699));
#252502=CARTESIAN_POINT('Ctrl Pts',(-166.826354834843,0.449270444124704,
137.394671073086));
#252503=CARTESIAN_POINT('Ctrl Pts',(-167.104802458656,5.78745648261092,
133.988600447415));
#252504=CARTESIAN_POINT('Ctrl Pts',(-167.383250082469,5.8072527465451,127.656368976875));
#252505=CARTESIAN_POINT('Ctrl Pts',(-167.661697706282,0.490467436472931,
124.216988036188));
#252506=CARTESIAN_POINT('Ctrl Pts',(-167.940145330095,-5.27703348705155,
126.831080686747));
#252507=CARTESIAN_POINT('Ctrl Pts',(-168.218592953908,-6.19519843339338,
133.096423488211));
#252508=CARTESIAN_POINT('Ctrl Pts',(-168.49704057772,-1.42027867171577,
137.255472485049));
#252509=CARTESIAN_POINT('Ctrl Pts',(-168.775488201534,4.65980780479824,
135.486264830004));
#252510=CARTESIAN_POINT('Ctrl Pts',(-169.053935825346,6.45775855296945,
129.414615927465));
#252511=CARTESIAN_POINT('Ctrl Pts',(-169.332383449159,2.32134467000579,
124.620074502325));
#252512=CARTESIAN_POINT('Ctrl Pts',(-169.610831072972,-3.94827156070164,
125.508589897919));
#252513=CARTESIAN_POINT('Ctrl Pts',(-169.889278696785,-6.58961911091297,
131.263659872085));
#252514=CARTESIAN_POINT('Ctrl Pts',(-170.167726320598,-3.17542861898582,
136.596656269364));
#252515=CARTESIAN_POINT('Ctrl Pts',(-170.446173944411,3.15682564547787,
136.606815932013));
#252516=CARTESIAN_POINT('Ctrl Pts',(-170.724621568223,6.58811136125304,
131.284802626386));
#252517=CARTESIAN_POINT('Ctrl Pts',(-171.003069192037,3.96524458316956,
125.521286585549));
#252518=CARTESIAN_POINT('Ctrl Pts',(-171.28151681585,-2.30148825387982,
124.612657487621));
#252519=CARTESIAN_POINT('Ctrl Pts',(-171.559964439662,-6.45326581956532,
129.393901084596));
#252520=CARTESIAN_POINT('Ctrl Pts',(-171.838412063475,-4.67480735663214,
135.471288087592));
#252521=CARTESIAN_POINT('Ctrl Pts',(-172.116859687288,1.39957069001038,
137.259996737715));
#252522=CARTESIAN_POINT('Ctrl Pts',(-172.395307311101,6.18781164536257,
133.116291168777));
#252523=CARTESIAN_POINT('Ctrl Pts',(-172.673754934914,5.289755990031,126.848034367363));
#252524=CARTESIAN_POINT('Ctrl Pts',(-172.952202558727,-0.469327001192524,
124.215448112602));
#252525=CARTESIAN_POINT('Ctrl Pts',(-173.23065018254,-5.79712140621875,
127.637750563632));
#252526=CARTESIAN_POINT('Ctrl Pts',(-173.509097806352,-5.79764444405506,
133.970012956726));
#252527=CARTESIAN_POINT('Ctrl Pts',(-173.787545430165,-0.470415468481743,
137.393195500846));
#252528=CARTESIAN_POINT('Ctrl Pts',(-174.065993053978,5.28910234155359,
134.76156066971));
#252529=CARTESIAN_POINT('Ctrl Pts',(-174.344440677791,6.18819348671444,
128.493452310623));
#252530=CARTESIAN_POINT('Ctrl Pts',(-174.622888301604,1.40063712764339,
124.34895579147));
#252531=CARTESIAN_POINT('Ctrl Pts',(-174.901335925417,-4.67403632680454,
126.13666094344));
#252532=CARTESIAN_POINT('Ctrl Pts',(-175.17978354923,-6.45349873628761,
132.213754066126));
#252533=CARTESIAN_POINT('Ctrl Pts',(-175.458231173043,-2.30251107806296,
136.995683462282));
#252534=CARTESIAN_POINT('Ctrl Pts',(-175.736678796856,3.96437177698222,
136.088089627079));
#252535=CARTESIAN_POINT('Ctrl Pts',(-176.015126420669,6.58819063930867,
130.325006956645));
#252536=CARTESIAN_POINT('Ctrl Pts',(-176.293574044481,3.15778415511627,
125.002426882869));
#252537=CARTESIAN_POINT('Ctrl Pts',(-176.572021668294,-3.17447170129595,
125.011540471058));
#252538=CARTESIAN_POINT('Ctrl Pts',(-176.850469292107,-6.58954314578118,
130.343972778891));
#252539=CARTESIAN_POINT('Ctrl Pts',(-177.12891691592,-3.94914635637289,
136.099479019269));
#252540=CARTESIAN_POINT('Ctrl Pts',(-177.407364539733,2.32032300801719,
136.989030129397));
#252541=CARTESIAN_POINT('Ctrl Pts',(-177.685812163546,6.45752888212044,
132.195172096054));
#252542=CARTESIAN_POINT('Ctrl Pts',(-177.964259787359,4.66058118137817,
126.123226258898));
#252543=CARTESIAN_POINT('Ctrl Pts',(-178.242707411172,-1.41921294300185,
124.353014211231));
#252544=CARTESIAN_POINT('Ctrl Pts',(-178.521155034985,-6.19481970517025,
128.511274345191));
#252545=CARTESIAN_POINT('Ctrl Pts',(-178.799602658797,-5.27768979205393,
134.776768739972));
#252546=CARTESIAN_POINT('Ctrl Pts',(-179.078050282611,0.489379210479558,
137.391814133187));
#252547=CARTESIAN_POINT('Ctrl Pts',(-179.356497906423,5.80673262608622,
133.95331156054));
#252548=CARTESIAN_POINT('Ctrl Pts',(-179.634945530236,5.7879824329786,127.621076906106));
#252549=CARTESIAN_POINT('Ctrl Pts',(-179.913393154049,0.450359142625426,
124.214124470449));
#252550=CARTESIAN_POINT('Ctrl Pts',(-180.191840777862,-5.30112219853358,
126.863277103057));
#252551=CARTESIAN_POINT('Ctrl Pts',(-180.470288401675,-6.18113121345664,
133.134092952866));
#252552=CARTESIAN_POINT('Ctrl Pts',(-180.748736025488,-1.38098260826046,
137.263998600285));
#252553=CARTESIAN_POINT('Ctrl Pts',(-181.0271836493,4.68822154917632,135.457812512445));
#252554=CARTESIAN_POINT('Ctrl Pts',(-181.305631273113,6.44917913527537,
129.375331466973));
#252555=CARTESIAN_POINT('Ctrl Pts',(-181.584078896926,2.28365615597197,
124.606058398942));
#252556=CARTESIAN_POINT('Ctrl Pts',(-181.862526520739,-3.98043526786393,
125.532722265928));
#252557=CARTESIAN_POINT('Ctrl Pts',(-182.140974144552,-6.58670113560653,
131.303764244219));
#252558=CARTESIAN_POINT('Ctrl Pts',(-182.419421768365,-3.14011043796568,
136.615878686839));
#252559=CARTESIAN_POINT('Ctrl Pts',(-182.697869392178,3.19208834924215,
136.587491932238));
#252560=CARTESIAN_POINT('Ctrl Pts',(-182.976317015991,6.59091388568205,
131.244690021124));
#252561=CARTESIAN_POINT('Ctrl Pts',(-183.254764639804,3.93301154522339,
125.497246899427));
#252562=CARTESIAN_POINT('Ctrl Pts',(-183.533212263617,-2.33913626699958,
124.626782017781));
#252563=CARTESIAN_POINT('Ctrl Pts',(-183.811659887429,-6.46173212300977,
129.433210077844));
#252564=CARTESIAN_POINT('Ctrl Pts',(-184.090107511242,-4.64631183113728,
135.499658499484));
#252565=CARTESIAN_POINT('Ctrl Pts',(-184.368555135055,1.43884204859816,
137.251357545694));
#252566=CARTESIAN_POINT('Ctrl Pts',(-184.647002758868,6.20177037701405,
133.078581368264));
#252567=CARTESIAN_POINT('Ctrl Pts',(-184.925450382681,5.26557470227994,
126.815907422802));
#252568=CARTESIAN_POINT('Ctrl Pts',(-185.203898006494,-0.50942688622466,
124.218427116558));
#252569=CARTESIAN_POINT('Ctrl Pts',(-185.482345630307,-5.81629005317544,
127.673097957001));
#252570=CARTESIAN_POINT('Ctrl Pts',(-185.76079325412,-5.77826680282389,
134.005246211819));
#252571=CARTESIAN_POINT('Ctrl Pts',(-186.039240877932,-0.430298644703365,
137.395936977472));
#252572=CARTESIAN_POINT('Ctrl Pts',(-186.317688501746,5.31309294664177,
134.729291084778));
#252573=CARTESIAN_POINT('Ctrl Pts',(-186.596136125558,6.17401167904375,
128.455825836229));
#252574=CARTESIAN_POINT('Ctrl Pts',(-186.874583749371,1.36131529564269,
124.340549319425));
#252575=CARTESIAN_POINT('Ctrl Pts',(-187.153031373184,-4.70236334050424,
126.165199610876));
#252576=CARTESIAN_POINT('Ctrl Pts',(-187.431478996997,-6.44479978994851,
132.253012231859));
#252577=CARTESIAN_POINT('Ctrl Pts',(-187.70992662081,-2.26478007840253,
137.009584789872));
#252578=CARTESIAN_POINT('Ctrl Pts',(-187.988374244623,3.99646188453734,
136.063859475589));
#252579=CARTESIAN_POINT('Ctrl Pts',(-188.266821868436,6.58515061360439,
130.284911651585));
#252580=CARTESIAN_POINT('Ctrl Pts',(-188.545269492249,3.12240763126122,
124.983312050825));
#252581=CARTESIAN_POINT('Ctrl Pts',(-188.823717116061,-3.20967542611822,
125.030971708867));
#252582=CARTESIAN_POINT('Ctrl Pts',(-189.102164739874,-6.59222356825658,
130.384093728275));
#252583=CARTESIAN_POINT('Ctrl Pts',(-189.380612363687,-3.91684029919248,
136.123420487763));
#252584=CARTESIAN_POINT('Ctrl Pts',(-189.6590599875,2.35792785654334,136.974791077059));
#252585=CARTESIAN_POINT('Ctrl Pts',(-189.937507611313,6.46587550329532,
132.155837516369));
#252586=CARTESIAN_POINT('Ctrl Pts',(-190.215955235126,4.63199943809816,
126.094942708994));
#252587=CARTESIAN_POINT('Ctrl Pts',(-190.494402858939,-1.45845782495887,
124.361772891742));
#252588=CARTESIAN_POINT('Ctrl Pts',(-190.772850482752,-6.2086635965042,
128.549026456613));
#252589=CARTESIAN_POINT('Ctrl Pts',(-191.051298106565,-5.25341083294129,
134.808821936201));
#252590=CARTESIAN_POINT('Ctrl Pts',(-191.329745730377,0.529469842708527,
137.388713092773));
#252591=CARTESIAN_POINT('Ctrl Pts',(-191.60819335419,5.82579359894846,133.91790598813));
#252592=CARTESIAN_POINT('Ctrl Pts',(-191.886640978003,5.76849764359442,
127.585902793086));
#252593=CARTESIAN_POINT('Ctrl Pts',(-192.165088601816,0.410234160553658,
124.211505108333));
#252594=CARTESIAN_POINT('Ctrl Pts',(-192.443536225629,-5.32501447498302,
126.895619557667));
#252595=CARTESIAN_POINT('Ctrl Pts',(-192.721983849442,-6.16683494942961,
133.171676088433));
#252596=CARTESIAN_POINT('Ctrl Pts',(-193.000431473255,-1.34163537198624,
137.272285351261));
#252597=CARTESIAN_POINT('Ctrl Pts',(-193.278879097068,4.71646156978089,
135.429187759513));
#252598=CARTESIAN_POINT('Ctrl Pts',(-193.557326720881,6.44036074087642,
129.336099959682));
#252599=CARTESIAN_POINT('Ctrl Pts',(-193.835774344694,2.24588302022023,
124.592271975924));
#252600=CARTESIAN_POINT('Ctrl Pts',(-194.114221968506,-4.01245147853337,
125.557049976435));
#252601=CARTESIAN_POINT('Ctrl Pts',(-194.392669592319,-6.58353908766677,
131.343850110767));
#252602=CARTESIAN_POINT('Ctrl Pts',(-194.671117216133,-3.10467589899933,
136.634885756375));
#252603=CARTESIAN_POINT('Ctrl Pts',(-194.949564839945,3.22723276899961,
136.567953636405));
#252604=CARTESIAN_POINT('Ctrl Pts',(-195.228012463758,6.59347218137276,
131.204561099293));
#252605=CARTESIAN_POINT('Ctrl Pts',(-195.506460087571,3.90063276808784,
125.473403870355));
#252606=CARTESIAN_POINT('Ctrl Pts',(-195.784907711384,-2.3766976025655,
124.641135460387));
#252607=CARTESIAN_POINT('Ctrl Pts',(-196.063355335197,-6.46995898459376,
129.472569879579));
#252608=CARTESIAN_POINT('Ctrl Pts',(-196.34180295901,-4.61764413484867,
135.527854925386));
#252609=CARTESIAN_POINT('Ctrl Pts',(-196.620250582823,1.47806009036541,
137.242479457832));
#252610=CARTESIAN_POINT('Ctrl Pts',(-196.898698206635,6.21549929978325,
133.040787295662));
#252611=CARTESIAN_POINT('Ctrl Pts',(-197.177145830448,5.24119829672186,
126.783928271841));
#252612=CARTESIAN_POINT('Ctrl Pts',(-197.455593454261,-0.5495078942556,
124.2216501647));
#252613=CARTESIAN_POINT('Ctrl Pts',(-197.734041078074,-5.83524317536515,
127.708561380459));
#252614=CARTESIAN_POINT('Ctrl Pts',(-198.012488701887,-5.75867504579123,
134.040360856918));
#252615=CARTESIAN_POINT('Ctrl Pts',(-198.2909363257,-0.390165876051177,
137.398434200813));
#252616=CARTESIAN_POINT('Ctrl Pts',(-198.569383949513,5.33688667311775,
134.696876060105));
#252617=CARTESIAN_POINT('Ctrl Pts',(-198.847831573325,6.15960109109908,
128.418286387655));
#252618=CARTESIAN_POINT('Ctrl Pts',(-199.126279197139,1.32194301960288,
124.332382366286));
#252619=CARTESIAN_POINT('Ctrl Pts',(-199.404726820951,-4.73051610640191,
126.193910184127));
#252620=CARTESIAN_POINT('Ctrl Pts',(-199.683174444764,-6.43586202918244,
132.292216717274));
#252621=CARTESIAN_POINT('Ctrl Pts',(-199.961622068577,-2.22696515648391,
137.023256180599));
#252622=CARTESIAN_POINT('Ctrl Pts',(-200.24006969239,4.02840390172748,136.039434431435));
#252623=CARTESIAN_POINT('Ctrl Pts',(-200.518517316203,6.58186657272242,
130.244835594899));
#252624=CARTESIAN_POINT('Ctrl Pts',(-200.796964940016,3.08691540544346,
124.964412919876));
#252625=CARTESIAN_POINT('Ctrl Pts',(-201.075412563829,-3.24476021523692,
125.050616881724));
#252626=CARTESIAN_POINT('Ctrl Pts',(-201.353860187642,-6.59465971346335,
130.424230250803));
#252627=CARTESIAN_POINT('Ctrl Pts',(-201.632307811455,-3.88438910205457,
136.147164856536));
#252628=CARTESIAN_POINT('Ctrl Pts',(-201.910755435267,2.39544533118521,
136.960323377152));
#252629=CARTESIAN_POINT('Ctrl Pts',(-202.18920305908,6.47398252907625,132.116452857208));
#252630=CARTESIAN_POINT('Ctrl Pts',(-202.467650682893,4.60324605437475,
126.066833668302));
#252631=CARTESIAN_POINT('Ctrl Pts',(-202.746098306706,-1.49764866322506,
124.370770304711));
#252632=CARTESIAN_POINT('Ctrl Pts',(-203.024545930519,-6.22227742352606,
128.586862140274));
#252633=CARTESIAN_POINT('Ctrl Pts',(-203.302993554332,-5.22893720675747,
134.840726745644));
#252634=CARTESIAN_POINT('Ctrl Pts',(-203.581441178145,0.569540855237039,
137.385368066758));
#252635=CARTESIAN_POINT('Ctrl Pts',(-203.859888801958,5.84463869488665,
133.882385042152));
#252636=CARTESIAN_POINT('Ctrl Pts',(-204.138336425771,5.7487991004088,127.550847941203));
#252637=CARTESIAN_POINT('Ctrl Pts',(-204.416784049583,0.370093977104817,
124.209130046901));
#252638=CARTESIAN_POINT('Ctrl Pts',(-204.695231673396,-5.34870943106288,
126.928106852114));
#252639=CARTESIAN_POINT('Ctrl Pts',(-204.973679297209,-6.15231017106575,
133.209171502253));
#252640=CARTESIAN_POINT('Ctrl Pts',(-205.252126921022,-1.30223842092043,
137.280332430907));
#252641=CARTESIAN_POINT('Ctrl Pts',(-205.530574544835,4.74452682016742,
135.400391631911));
#252642=CARTESIAN_POINT('Ctrl Pts',(-205.809022168648,6.43130369654214,
129.296922859329));
#252643=CARTESIAN_POINT('Ctrl Pts',(-206.087469792461,2.20802666244648,
124.578715744137));
#252644=CARTESIAN_POINT('Ctrl Pts',(-206.365917416273,-4.04431900633787,
125.581572127967));
#252645=CARTESIAN_POINT('Ctrl Pts',(-206.644365040087,-6.58013308426553,
131.383915986335));
#252646=CARTESIAN_POINT('Ctrl Pts',(-206.922812663899,-3.06912631512495,
136.653676773657));
#252647=CARTESIAN_POINT('Ctrl Pts',(-207.201260287713,3.26225760245914,
136.548201768512));
#252648=CARTESIAN_POINT('Ctrl Pts',(-207.479707911525,6.59578615352751,
131.164417347887));
#252649=CARTESIAN_POINT('Ctrl Pts',(-207.758155535338,3.86810945157081,
125.449758381845));
#252650=CARTESIAN_POINT('Ctrl Pts',(-208.036603159151,-2.41417086872696,
124.655717283569));
#252651=CARTESIAN_POINT('Ctrl Pts',(-208.315050782964,-6.47794609946865,
129.511979031309));
#252652=CARTESIAN_POINT('Ctrl Pts',(-208.593498406777,-4.58880533005852,
135.555876320469));
#252653=CARTESIAN_POINT('Ctrl Pts',(-208.87194603059,1.51722336207232,137.233362803106));
#252654=CARTESIAN_POINT('Ctrl Pts',(-209.150393654402,6.22899790494034,
133.00291035145));
#252655=CARTESIAN_POINT('Ctrl Pts',(-209.428841278216,5.21662767663345,
126.752098099478));
#252656=CARTESIAN_POINT('Ctrl Pts',(-209.707288902028,-0.589568540070009,
124.225117137599));
#252657=CARTESIAN_POINT('Ctrl Pts',(-209.985736525842,-5.85398007047323,
127.744139519898));
#252658=CARTESIAN_POINT('Ctrl Pts',(-210.264184149654,-5.73886989893714,
134.07535559084));
#252659=CARTESIAN_POINT('Ctrl Pts',(-210.542631773467,-0.350018649658268,
137.400687078332));
#252660=CARTESIAN_POINT('Ctrl Pts',(-210.82107939728,5.36048263929459,134.664316796842));
#252661=CARTESIAN_POINT('Ctrl Pts',(-211.099527021093,6.14496225687153,
128.38083535594));
#252662=CARTESIAN_POINT('Ctrl Pts',(-211.377974644906,1.28252175847855,
124.324455234681));
#252663=CARTESIAN_POINT('Ctrl Pts',(-211.656422268719,-4.75849358128477,
126.222791599316));
#252664=CARTESIAN_POINT('Ctrl Pts',(-211.934869892531,-6.4266857851828,
132.331366069634));
#252665=CARTESIAN_POINT('Ctrl Pts',(-212.213317516344,-2.18906771355195,
137.036697127864));
#252666=CARTESIAN_POINT('Ctrl Pts',(-212.491765140157,4.06019664492976,
136.014815399695));
#252667=CARTESIAN_POINT('Ctrl Pts',(-212.770212763971,6.57833863835413,
130.204780271616));
#252668=CARTESIAN_POINT('Ctrl Pts',(-213.048660387783,3.05130879283982,
124.945730190337));
#252669=CARTESIAN_POINT('Ctrl Pts',(-213.327108011596,-3.27972476857289,
125.070475261673));
#252670=CARTESIAN_POINT('Ctrl Pts',(-213.605555635409,-6.59685149112928,
130.464380859201));
#252671=CARTESIAN_POINT('Ctrl Pts',(-213.884003259222,-3.85179396744981,
136.170711245733));
#252672=CARTESIAN_POINT('Ctrl Pts',(-214.162450883035,2.43287404171984,
136.94562756578));
#252673=CARTESIAN_POINT('Ctrl Pts',(-214.440898506847,6.48184965905313,
132.077019577989));
#252674=CARTESIAN_POINT('Ctrl Pts',(-214.71934613066,4.57432209567675,126.038900178414));
#252675=CARTESIAN_POINT('Ctrl Pts',(-214.997793754473,-1.53678400556905,
124.380006116735));
#252676=CARTESIAN_POINT('Ctrl Pts',(-215.276241378286,-6.23566068176903,
128.624779994154));
#252677=CARTESIAN_POINT('Ctrl Pts',(-215.554689002099,-5.20426982038336,
134.872481986055));
#252678=CARTESIAN_POINT('Ctrl Pts',(-215.833136625912,0.609590763220439,
137.381779179092));
#252679=CARTESIAN_POINT('Ctrl Pts',(-216.111584249725,5.86326721558844,
133.846750038845));
#252680=CARTESIAN_POINT('Ctrl Pts',(-216.390031873537,5.72888753335829,
127.51591364943));
#252681=CARTESIAN_POINT('Ctrl Pts',(-216.668479497351,0.329940079686948,
124.206999374164));
#252682=CARTESIAN_POINT('Ctrl Pts',(-216.946927121163,-5.37220618874772,
126.960737782571));
#252683=CARTESIAN_POINT('Ctrl Pts',(-217.225374744977,-6.13755741658593,
133.246577804923));
#252684=CARTESIAN_POINT('Ctrl Pts',(-217.503822368789,-1.26279321493052,
137.288139541036));
#252685=CARTESIAN_POINT('Ctrl Pts',(-217.782269992602,4.77241626036792,
135.37142519669));
#252686=CARTESIAN_POINT('Ctrl Pts',(-218.060717616415,6.4220083378839,129.257801617636));
#252687=CARTESIAN_POINT('Ctrl Pts',(-218.339165240228,2.17008848543354,
124.565390205911));
#252688=CARTESIAN_POINT('Ctrl Pts',(-218.617612864041,-4.07603667041411,
125.606287811847));
#252689=CARTESIAN_POINT('Ctrl Pts',(-218.896060487854,-6.57648325161253,
131.423960386264));
#252690=CARTESIAN_POINT('Ctrl Pts',(-219.174508111666,-3.03346300364714,
136.672251042379));
#252691=CARTESIAN_POINT('Ctrl Pts',(-219.45295573548,3.29716155176439,136.528237060474));
#252692=CARTESIAN_POINT('Ctrl Pts',(-219.731403359293,6.59785571640026,
131.124260254445));
#252693=CARTESIAN_POINT('Ctrl Pts',(-220.009850983105,3.83544280083539,
125.426311310091));
#252694=CARTESIAN_POINT('Ctrl Pts',(-220.288298606918,-2.45155467689987,
124.67052694699));
#252695=CARTESIAN_POINT('Ctrl Pts',(-220.566746230731,-6.48569317166813,
129.551436072715));
#252696=CARTESIAN_POINT('Ctrl Pts',(-220.845193854544,-4.55979648539947,
135.58372164639));
#252697=CARTESIAN_POINT('Ctrl Pts',(-221.123641478357,1.55633041250914,
137.224007919343));
#252698=CARTESIAN_POINT('Ctrl Pts',(-221.40208910217,6.24226569228925,132.964951939167));
#252699=CARTESIAN_POINT('Ctrl Pts',(-221.680536725983,5.19186375248807,
126.720418085194));
#252700=CARTESIAN_POINT('Ctrl Pts',(-221.958984349796,-0.629607339204784,
124.228827906785));
#252701=CARTESIAN_POINT('Ctrl Pts',(-222.237431973609,-5.87250004419688,
127.779831056953));
#252702=CARTESIAN_POINT('Ctrl Pts',(-222.515879597421,-5.71885209614835,
134.110229116839));
#252703=CARTESIAN_POINT('Ctrl Pts',(-222.794327221234,-0.309858453196267,
137.402695526548));
#252704=CARTESIAN_POINT('Ctrl Pts',(-223.072774845047,5.38387997081673,
134.631614501482));
#252705=CARTESIAN_POINT('Ctrl Pts',(-223.35122246886,6.13009571880702,128.343474128844));
#252706=CARTESIAN_POINT('Ctrl Pts',(-223.629670092673,1.24305297303857,
124.316768218352));
#252707=CARTESIAN_POINT('Ctrl Pts',(-223.908117716486,-4.78629472843886,
126.25184278623));
#252708=CARTESIAN_POINT('Ctrl Pts',(-224.186565340298,-6.41727139797729,
132.370458838244));
#252709=CARTESIAN_POINT('Ctrl Pts',(-224.465012964112,-2.15108915391133,
137.049907133607));
#252710=CARTESIAN_POINT('Ctrl Pts',(-224.743460587925,4.09183893605206,
135.990003292637));
#252711=CARTESIAN_POINT('Ctrl Pts',(-225.021908211737,6.57456694122844,
130.164747166004));
#252712=CARTESIAN_POINT('Ctrl Pts',(-225.300355835551,3.01558911286705,
124.927264554503));
#252713=CARTESIAN_POINT('Ctrl Pts',(-225.578803459363,-3.31456779050113,
125.090546112851));
#252714=CARTESIAN_POINT('Ctrl Pts',(-225.857251083176,-6.5987988200372,
130.504544065675));
#252715=CARTESIAN_POINT('Ctrl Pts',(-226.135698706989,-3.8190561032033,
136.194058782834));
#252716=CARTESIAN_POINT('Ctrl Pts',(-226.414146330802,2.47021260121173,
136.930704187504));
#252717=CARTESIAN_POINT('Ctrl Pts',(-226.692593954615,6.48947660170784,
132.037539139922));
#252718=CARTESIAN_POINT('Ctrl Pts',(-226.971041578427,4.54522863379049,
126.011143274415));
#252719=CARTESIAN_POINT('Ctrl Pts',(-227.24948920224,-1.57586240181677,
124.389479985577));
#252720=CARTESIAN_POINT('Ctrl Pts',(-227.527936826054,-6.24881287531301,
128.662778613197));
#252721=CARTESIAN_POINT('Ctrl Pts',(-227.806384449866,-5.17940958787633,
134.904086480733));
#252722=CARTESIAN_POINT('Ctrl Pts',(-228.084832073679,0.649618082593193,
137.377946562762));
#252723=CARTESIAN_POINT('Ctrl Pts',(-228.363279697492,5.88167847076755,
133.811002298682));
#252724=CARTESIAN_POINT('Ctrl Pts',(-228.641727321305,5.70876368027354,
127.481101212267));
#252725=CARTESIAN_POINT('Ctrl Pts',(-228.920174945118,0.289773956218704,
124.205113169075));
#252726=CARTESIAN_POINT('Ctrl Pts',(-229.198622568931,-5.39550387735667,
126.993511139885));
#252727=CARTESIAN_POINT('Ctrl Pts',(-229.477070192744,-6.12257723265909,
133.283893610337));
#252728=CARTESIAN_POINT('Ctrl Pts',(-229.755517816557,-1.22330121567356,
137.295706392352));
#252729=CARTESIAN_POINT('Ctrl Pts',(-230.033965440369,4.80012885692891,
135.34228952721));
#252730=CARTESIAN_POINT('Ctrl Pts',(-230.312413064183,6.41247500934538,
129.218737684256));
#252731=CARTESIAN_POINT('Ctrl Pts',(-230.590860687995,2.13206989499296,
124.552295855027));
#252732=CARTESIAN_POINT('Ctrl Pts',(-230.869308311808,-4.10760329545278,
125.631196112227));
#252733=CARTESIAN_POINT('Ctrl Pts',(-231.147755935621,-6.5725897249546,
131.463981826697));
#252734=CARTESIAN_POINT('Ctrl Pts',(-231.426203559434,-2.99768728608136,
136.690607874263));
#252735=CARTESIAN_POINT('Ctrl Pts',(-231.704651183247,3.33194332353496,
136.508060252089));
#252736=CARTESIAN_POINT('Ctrl Pts',(-231.98309880706,6.59968079330357,131.084091307006));
#252737=CARTESIAN_POINT('Ctrl Pts',(-232.261546430872,3.80263402635669,
125.403063523931));
#252738=CARTESIAN_POINT('Ctrl Pts',(-232.539994054686,-2.48884764181187,
124.685563901874));
#252739=CARTESIAN_POINT('Ctrl Pts',(-232.818441678498,-6.49319991412244,
129.5909395417));
#252740=CARTESIAN_POINT('Ctrl Pts',(-233.096889302311,-4.53061867580467,
135.611389871331));
#252741=CARTESIAN_POINT('Ctrl Pts',(-233.375336926124,1.59537979255065,
137.214415153187));
#252742=CARTESIAN_POINT('Ctrl Pts',(-233.653784549937,6.25530217018742,
132.926913465378));
#252743=CARTESIAN_POINT('Ctrl Pts',(-233.93223217375,5.16690744192206,126.688889402902));
#252744=CARTESIAN_POINT('Ctrl Pts',(-234.210679797563,-0.669622808008655,
124.232782334755));
#252745=CARTESIAN_POINT('Ctrl Pts',(-234.489127421376,-5.89080241027189,
127.815634669064));
#252746=CARTESIAN_POINT('Ctrl Pts',(-234.767575045188,-5.69862237919218,
134.144980142666));
#252747=CARTESIAN_POINT('Ctrl Pts',(-235.046022669002,-0.269686774814632,
137.404459471037));
#252748=CARTESIAN_POINT('Ctrl Pts',(-235.324470292814,5.40707780068583,
134.598770385822));
#252749=CARTESIAN_POINT('Ctrl Pts',(-235.602917916627,6.11500202779203,
128.306204090801));
#252750=CARTESIAN_POINT('Ctrl Pts',(-235.88136554044,1.20353812581378,124.309321602146));
#252751=CARTESIAN_POINT('Ctrl Pts',(-236.159813164253,-4.81391851768082,
126.281062668365));
#252752=CARTESIAN_POINT('Ctrl Pts',(-236.438260788066,-6.40761921642086,
132.40949357451));
#252753=CARTESIAN_POINT('Ctrl Pts',(-236.716708411879,-2.11303088487057,
137.062885708328));
#252754=CARTESIAN_POINT('Ctrl Pts',(-236.995156035692,4.12332960257798,
135.964999029683));
#252755=CARTESIAN_POINT('Ctrl Pts',(-237.273603659505,6.57055162110693,
130.124737761504));
#252756=CARTESIAN_POINT('Ctrl Pts',(-237.552051283318,2.97975768913041,
124.909016696624));
#252757=CARTESIAN_POINT('Ctrl Pts',(-237.83049890713,-3.34928798990126,
125.110828691528));
#252758=CARTESIAN_POINT('Ctrl Pts',(-238.108946530943,-6.60050162802816,
130.544718381962));
#252759=CARTESIAN_POINT('Ctrl Pts',(-238.387394154756,-3.7861767224282,
136.217206602688));
#252760=CARTESIAN_POINT('Ctrl Pts',(-238.665841778569,2.5074596260677,136.915553795314));
#252761=CARTESIAN_POINT('Ctrl Pts',(-238.944289402382,6.49686307441993,
131.998013005973));
#252762=CARTESIAN_POINT('Ctrl Pts',(-239.222737026195,4.51596674678651,
125.983563984846));
#252763=CARTESIAN_POINT('Ctrl Pts',(-239.501184650008,-1.61488240390346,
124.399191560181));
#252764=CARTESIAN_POINT('Ctrl Pts',(-239.77963227382,-6.26173351679718,
128.700856589348));
#252765=CARTESIAN_POINT('Ctrl Pts',(-240.058079897633,-5.15435743044315,
134.935539058562));
#252766=CARTESIAN_POINT('Ctrl Pts',(-240.336527521446,0.689621330129741,
137.373870359787));
#252767=CARTESIAN_POINT('Ctrl Pts',(-240.614975145259,5.89987177818775,
133.775143146303));
#252768=CARTESIAN_POINT('Ctrl Pts',(-240.893422769072,5.68842828685113,
127.446411919705));
#252769=CARTESIAN_POINT('Ctrl Pts',(-241.171870392886,0.249597095069331,
124.203471501526));
#252770=CARTESIAN_POINT('Ctrl Pts',(-241.450318016698,-5.41860163358522,
127.026425709627));
#252771=CARTESIAN_POINT('Ctrl Pts',(-241.728765640511,-6.10737017438111,
133.321117535742));
#252772=CARTESIAN_POINT('Ctrl Pts',(-242.007213264324,-1.18376388654087,
137.303032704464));
#252773=CARTESIAN_POINT('Ctrl Pts',(-242.285660888137,4.82766358294966,
135.312985703106));
#252774=CARTESIAN_POINT('Ctrl Pts',(-242.56410851195,6.40270406418687,129.179732506718));
#252775=CARTESIAN_POINT('Ctrl Pts',(-242.842556135762,2.09397229991911,
124.539433176702));
#252776=CARTESIAN_POINT('Ctrl Pts',(-243.121003759575,-4.13901771174057,
125.65629610612));
#252777=CARTESIAN_POINT('Ctrl Pts',(-243.399451383388,-6.56845264856689,
131.503978824623));
#252778=CARTESIAN_POINT('Ctrl Pts',(-243.677899007202,-2.9618004881116,
136.70874658909));
#252779=CARTESIAN_POINT('Ctrl Pts',(-243.956346631013,3.36660162892119,
136.487672091016));
#252780=CARTESIAN_POINT('Ctrl Pts',(-244.234794254827,6.60126131660758,
131.043911994042));
#252781=CARTESIAN_POINT('Ctrl Pts',(-244.513241878639,3.76968434387551,
125.380015884821));
#252782=CARTESIAN_POINT('Ctrl Pts',(-244.791689502453,-2.52604838156001,
124.70082759102));
#252783=CARTESIAN_POINT('Ctrl Pts',(-245.070137126265,-6.50046604866569,
129.630487974449));
#252784=CARTESIAN_POINT('Ctrl Pts',(-245.348584750079,-4.50127298246883,
135.638879970036));
#252785=CARTESIAN_POINT('Ctrl Pts',(-245.627032373891,1.63437005520677,
137.204584860103));
#252786=CARTESIAN_POINT('Ctrl Pts',(-245.905479997704,6.26810685556324,
132.888796339615));
#252787=CARTESIAN_POINT('Ctrl Pts',(-246.183927621517,5.14175966970064,
126.65751322091));
#252788=CARTESIAN_POINT('Ctrl Pts',(-246.46237524533,-0.709613463692526,
124.236980274974));
#252789=CARTESIAN_POINT('Ctrl Pts',(-246.740822869143,-5.90888649049716,
127.851549029514));
#252790=CARTESIAN_POINT('Ctrl Pts',(-247.019270492956,-5.67818149768794,
134.179607380607));
#252791=CARTESIAN_POINT('Ctrl Pts',(-247.297718116769,-0.229505103091092,
137.405978846438));
#252792=CARTESIAN_POINT('Ctrl Pts',(-247.576165740581,5.43007526929941,
134.565785666913));
#252793=CARTESIAN_POINT('Ctrl Pts',(-247.854613364394,6.09968174312738,
128.269026622868));
#252794=CARTESIAN_POINT('Ctrl Pts',(-248.133060988207,1.16397868104094,
124.302115661998));
#252795=CARTESIAN_POINT('Ctrl Pts',(-248.41150861202,-4.84136392540264,
126.31045016297));
#252796=CARTESIAN_POINT('Ctrl Pts',(-248.689956235833,-6.39772959817725,
132.448468831983));
#252797=CARTESIAN_POINT('Ctrl Pts',(-248.968403859646,-2.07489431669385,
137.075632371099));
#252798=CARTESIAN_POINT('Ctrl Pts',(-249.246851483459,4.15466747760909,
135.939803537374));
#252799=CARTESIAN_POINT('Ctrl Pts',(-249.525299107272,6.56629282677857,
130.08475354068));
#252800=CARTESIAN_POINT('Ctrl Pts',(-249.803746731085,2.94381584937754,
124.890987292882));
#252801=CARTESIAN_POINT('Ctrl Pts',(-250.082194354898,-3.38388408020374,
125.131322246124));
#252802=CARTESIAN_POINT('Ctrl Pts',(-250.36064197871,-6.60195985200274,
130.584902319384));
#252803=CARTESIAN_POINT('Ctrl Pts',(-250.639089602524,-3.75315704348482,
136.240153847548));
#252804=CARTESIAN_POINT('Ctrl Pts',(-250.917537226336,2.54461373609029,
136.900176950603));
#252805=CARTESIAN_POINT('Ctrl Pts',(-251.19598485015,6.50400880347224,131.958442640812));
#252806=CARTESIAN_POINT('Ctrl Pts',(-251.474432473962,4.48653751899202,
125.956163331638));
#252807=CARTESIAN_POINT('Ctrl Pts',(-251.752880097775,-1.65384256596459,
124.409140480742));
#252808=CARTESIAN_POINT('Ctrl Pts',(-252.031327721588,-6.27442212737671,
128.739012511497));
#252809=CARTESIAN_POINT('Ctrl Pts',(-252.309775345401,-5.12911427652582,
134.966838554275));
#252810=CARTESIAN_POINT('Ctrl Pts',(-252.588222969213,0.729599023732927,
137.369550720794));
#252811=CARTESIAN_POINT('Ctrl Pts',(-252.866670593027,5.91784646323776,
133.739173911277));
#252812=CARTESIAN_POINT('Ctrl Pts',(-253.145118216839,5.66788210748017,
127.411847055674));
#252813=CARTESIAN_POINT('Ctrl Pts',(-253.423565840652,0.209410983396998,
124.20207443517));
#252814=CARTESIAN_POINT('Ctrl Pts',(-253.702013464465,-5.44149859849489,
127.059480266814));
#252815=CARTESIAN_POINT('Ctrl Pts',(-253.980461088278,-6.0919368110008,
133.358248211846));
#252816=CARTESIAN_POINT('Ctrl Pts',(-254.258908712091,-1.1441826817532,
137.310118186916));
#252817=CARTESIAN_POINT('Ctrl Pts',(-254.537356335904,4.85501939763767,
135.283514846073));
#252818=CARTESIAN_POINT('Ctrl Pts',(-254.815803959717,6.39269590315201,
129.140787462715));
#252819=CARTESIAN_POINT('Ctrl Pts',(-255.09425158353,2.05579703890082,124.526802775315));
#252820=CARTESIAN_POINT('Ctrl Pts',(-255.372699207342,-4.17027861730954,
125.681586622223));
#252821=CARTESIAN_POINT('Ctrl Pts',(-255.651146831155,-6.5640724361261,
131.5439503534));
#252822=CARTESIAN_POINT('Ctrl Pts',(-255.929594454968,-2.925803447894,136.726665654721));
#252823=CARTESIAN_POINT('Ctrl Pts',(-256.208042078781,3.40113425532747,
136.467074956607));
#252824=CARTESIAN_POINT('Ctrl Pts',(-256.486489702594,6.60259898059897,
131.003720738236));
#252825=CARTESIAN_POINT('Ctrl Pts',(-256.764937326407,3.73659166461274,
125.357175036369));
#252826=CARTESIAN_POINT('Ctrl Pts',(-257.04338495022,-2.56314926818932,
124.716306516944));
#252827=CARTESIAN_POINT('Ctrl Pts',(-257.321832574033,-6.5075031063131,
129.670100547101));
#252828=CARTESIAN_POINT('Ctrl Pts',(-257.600280197845,-4.47173821150659,
135.666151948257));
#252829=CARTESIAN_POINT('Ctrl Pts',(-257.878727821659,1.67325768403046,
137.194590998305));
#252830=CARTESIAN_POINT('Ctrl Pts',(-258.157175445471,6.28075871394982,
132.850463013089));
#252831=CARTESIAN_POINT('Ctrl Pts',(-258.435623069284,5.1162713672671,126.626553096149));
#252832=CARTESIAN_POINT('Ctrl Pts',(-258.714070693097,-0.749294580734974,
124.240926059104));
#252833=CARTESIAN_POINT('Ctrl Pts',(-258.99251831691,-5.92728653745133,
127.888508918958));
#252834=CARTESIAN_POINT('Ctrl Pts',(-259.270965940723,-5.656519339957,134.212338033208));
#252835=CARTESIAN_POINT('Ctrl Pts',(-259.549413564536,-0.191230405826049,
137.41063083554));
#252836=CARTESIAN_POINT('Ctrl Pts',(-259.827861188349,5.45654320709978,
134.526020746857));
#252837=CARTESIAN_POINT('Ctrl Pts',(-260.059900874859,5.97341346954355,
129.293215926205));
#252838=CARTESIAN_POINT('Ctrl Pts',(-260.245542550368,3.60742224527213,
126.247226657536));
#252839=CARTESIAN_POINT('Ctrl Pts',(-260.338368351272,1.86717727106152,
125.459413119698));
#252840=CARTESIAN_POINT('Ctrl Pts',(-260.384786214875,0.950008195528324,
125.301089073499));
#252841=CARTESIAN_POINT('Ctrl Pts',(209.997886486728,-2.58542267678463,
125.478296443779));
#252842=CARTESIAN_POINT('Ctrl Pts',(209.951476810375,-3.47289965896197,
125.909102290886));
#252843=CARTESIAN_POINT('Ctrl Pts',(209.85865919672,-5.01373755653622,127.222906143875));
#252844=CARTESIAN_POINT('Ctrl Pts',(209.67302570846,-6.52844908712303,131.020616473957));
#252845=CARTESIAN_POINT('Ctrl Pts',(209.440986021949,-4.4641631800594,136.198709217918));
#252846=CARTESIAN_POINT('Ctrl Pts',(209.162538398136,2.13623200523086,137.47712630299));
#252847=CARTESIAN_POINT('Ctrl Pts',(208.884090774324,6.76311047611758,132.61329501932));
#252848=CARTESIAN_POINT('Ctrl Pts',(208.60564315051,5.180460236421,126.09244423763));
#252849=CARTESIAN_POINT('Ctrl Pts',(208.327195526698,-1.16565068102074,
123.898824768668));
#252850=CARTESIAN_POINT('Ctrl Pts',(208.048747902884,-6.43906639651766,
128.052530506575));
#252851=CARTESIAN_POINT('Ctrl Pts',(207.770300279072,-5.79609906993421,
134.734252735451));
#252852=CARTESIAN_POINT('Ctrl Pts',(207.491852655259,0.173626147510206,
137.805009652024));
#252853=CARTESIAN_POINT('Ctrl Pts',(207.213405031446,5.98357180802623,134.442293088818));
#252854=CARTESIAN_POINT('Ctrl Pts',(206.934957407633,6.29502677410122,127.736610299611));
#252855=CARTESIAN_POINT('Ctrl Pts',(206.65650978382,0.821596385081328,123.849978754804));
#252856=CARTESIAN_POINT('Ctrl Pts',(206.378062160007,-5.40680743188727,
126.354116934927));
#252857=CARTESIAN_POINT('Ctrl Pts',(206.099614536195,-6.66663710465116,
132.947794423038));
#252858=CARTESIAN_POINT('Ctrl Pts',(205.821166912381,-1.80014356190772,
137.571770081489));
#252859=CARTESIAN_POINT('Ctrl Pts',(205.542719288569,4.72058899422897,135.976822216287));
#252860=CARTESIAN_POINT('Ctrl Pts',(205.264271664756,6.90333351468265,129.628637390042));
#252861=CARTESIAN_POINT('Ctrl Pts',(204.985824040943,2.74225038547515,124.360883417158));
#252862=CARTESIAN_POINT('Ctrl Pts',(204.70737641713,-3.93882614214087,125.014370927945));
#252863=CARTESIAN_POINT('Ctrl Pts',(204.428928793317,-7.00031425910704,
130.988575726592));
#252864=CARTESIAN_POINT('Ctrl Pts',(204.150481169504,-3.62885534891233,
136.793496040797));
#252865=CARTESIAN_POINT('Ctrl Pts',(203.872033545692,3.07734423765085,137.09469337995));
#252866=CARTESIAN_POINT('Ctrl Pts',(203.593585921878,6.95561486460971,131.615382266785));
#252867=CARTESIAN_POINT('Ctrl Pts',(203.315138298066,4.44201520086038,125.390781848689));
#252868=CARTESIAN_POINT('Ctrl Pts',(203.036690674253,-2.15357941165663,
124.140995867004));
#252869=CARTESIAN_POINT('Ctrl Pts',(202.75824305044,-6.77013976170558,129.014516559232));
#252870=CARTESIAN_POINT('Ctrl Pts',(202.479795426627,-5.16527240588502,
135.532816506767));
#252871=CARTESIAN_POINT('Ctrl Pts',(202.201347802814,1.18622795093483,137.705896487686));
#252872=CARTESIAN_POINT('Ctrl Pts',(201.922900179001,6.44764277258624,133.536802163981));
#252873=CARTESIAN_POINT('Ctrl Pts',(201.644452555188,5.78398887041165,126.856727545651));
#252874=CARTESIAN_POINT('Ctrl Pts',(201.366004931376,-0.194868239746226,
123.804334868162));
#252875=CARTESIAN_POINT('Ctrl Pts',(201.087557307562,-5.99465095761073,
127.184623883922));
#252876=CARTESIAN_POINT('Ctrl Pts',(200.80910968375,-6.2856423003101,133.891274124028));
#252877=CARTESIAN_POINT('Ctrl Pts',(200.530662059936,-0.80043543977546,
137.76120165575));
#252878=CARTESIAN_POINT('Ctrl Pts',(200.252214436124,5.42033248649604,135.238132133988));
#252879=CARTESIAN_POINT('Ctrl Pts',(199.973766812311,6.66007965562565,128.640643190398));
#252880=CARTESIAN_POINT('Ctrl Pts',(199.695319188498,1.77953898422249,124.031504858911));
#252881=CARTESIAN_POINT('Ctrl Pts',(199.416871564685,-4.73631107837294,
125.646290097223));
#252882=CARTESIAN_POINT('Ctrl Pts',(199.138423940872,-6.89972264160091,
132.00109015798));
#252883=CARTESIAN_POINT('Ctrl Pts',(198.859976317059,-2.72262616738874,
137.256154234582));
#252884=CARTESIAN_POINT('Ctrl Pts',(198.581528693247,3.95643074697165,136.582335164788));
#252885=CARTESIAN_POINT('Ctrl Pts',(198.303081069434,6.999721087252,130.598839755845));
#252886=CARTESIAN_POINT('Ctrl Pts',(198.024633445621,3.61060970373355,124.804207978572));
#252887=CARTESIAN_POINT('Ctrl Pts',(197.746185821808,-3.09647560942607,
124.523423352781));
#252888=CARTESIAN_POINT('Ctrl Pts',(197.467738197995,-6.9580511087663,130.014513232485));
#252889=CARTESIAN_POINT('Ctrl Pts',(197.189290574182,-4.4255175588443,136.231434272887));
#252890=CARTESIAN_POINT('Ctrl Pts',(196.910842950369,2.17385042910367,137.461139751337));
#252891=CARTESIAN_POINT('Ctrl Pts',(196.632395326556,6.77555607120273,132.573590407591));
#252892=CARTESIAN_POINT('Ctrl Pts',(196.353947702743,5.15085668818228,126.060205318492));
#252893=CARTESIAN_POINT('Ctrl Pts',(196.07550007893,-1.20722835793932,123.90646718437));
#252894=CARTESIAN_POINT('Ctrl Pts',(195.797052455118,-6.45592951949867,
128.091556134528));
#252895=CARTESIAN_POINT('Ctrl Pts',(195.518604831305,-5.77194684232935,
134.769579876729));
#252896=CARTESIAN_POINT('Ctrl Pts',(195.240157207492,0.216173007661386,
137.80376083149));
#252897=CARTESIAN_POINT('Ctrl Pts',(194.961709583679,6.00564042424985,134.405834929363));
#252898=CARTESIAN_POINT('Ctrl Pts',(194.683261959866,6.2762176827981,127.698330076496));
#252899=CARTESIAN_POINT('Ctrl Pts',(194.404814336053,0.779257501134259,
123.845115552844));
#252900=CARTESIAN_POINT('Ctrl Pts',(194.12636671224,-5.43380225522669,126.387107265649));
#252901=CARTESIAN_POINT('Ctrl Pts',(193.847919088427,-6.65346319503207,
132.988339014042));
#252902=CARTESIAN_POINT('Ctrl Pts',(193.569471464615,-1.75891649835014,
137.58260130935));
#252903=CARTESIAN_POINT('Ctrl Pts',(193.291023840801,4.75198853246758,135.947991544374));
#252904=CARTESIAN_POINT('Ctrl Pts',(193.012576216989,6.89604824949333,129.586636238002));
#252905=CARTESIAN_POINT('Ctrl Pts',(192.734128593176,2.70297651592057,124.344310147306));
#252906=CARTESIAN_POINT('Ctrl Pts',(192.455680969363,-3.97399858803937,
125.038454847768));
#252907=CARTESIAN_POINT('Ctrl Pts',(192.17723334555,-6.99906313021511,131.031185270517));
#252908=CARTESIAN_POINT('Ctrl Pts',(191.898785721737,-3.59233057896577,
136.815474918205));
#252909=CARTESIAN_POINT('Ctrl Pts',(191.620338097924,3.11557827924791,137.075844182864));
#252910=CARTESIAN_POINT('Ctrl Pts',(191.341890474111,6.96042290329331,131.573026430018));
#252911=CARTESIAN_POINT('Ctrl Pts',(191.063442850298,4.40897891477476,125.363842346942));
#252912=CARTESIAN_POINT('Ctrl Pts',(190.784995226486,-2.19410130582752,
124.154228770475));
#252913=CARTESIAN_POINT('Ctrl Pts',(190.506547602672,-6.78090961418206,
129.055761484483));
#252914=CARTESIAN_POINT('Ctrl Pts',(190.22809997886,-5.13639325295408,135.564171377977));
#252915=CARTESIAN_POINT('Ctrl Pts',(189.949652355047,1.22821758097839,137.698547712335));
#252916=CARTESIAN_POINT('Ctrl Pts',(189.671204731234,6.46415645975623,133.497502906364));
#252917=CARTESIAN_POINT('Ctrl Pts',(189.392757107421,5.75985134361714,126.821591904301));
#252918=CARTESIAN_POINT('Ctrl Pts',(189.114309483608,-0.237475772924818,
123.80565078066));
#252919=CARTESIAN_POINT('Ctrl Pts',(188.835861859795,-6.01657425548534,
127.221182091151));
#252920=CARTESIAN_POINT('Ctrl Pts',(188.557414235982,-6.2667349232476,133.929479419415));
#252921=CARTESIAN_POINT('Ctrl Pts',(188.278966612169,-0.758072343566082,
137.76594523932));
#252922=CARTESIAN_POINT('Ctrl Pts',(188.000518988357,5.44722168595988,135.205054884148));
#252923=CARTESIAN_POINT('Ctrl Pts',(187.722071364544,6.64678509766207,128.600141483854));
#252924=CARTESIAN_POINT('Ctrl Pts',(187.443623740731,1.73827771811677,124.02079778535));
#252925=CARTESIAN_POINT('Ctrl Pts',(187.165176116918,-4.76762196479028,
125.675216934184));
#252926=CARTESIAN_POINT('Ctrl Pts',(186.886728493105,-6.89230997333645,
132.043068555446));
#252927=CARTESIAN_POINT('Ctrl Pts',(186.608280869292,-2.68330182444739,
137.272608096043));
#252928=CARTESIAN_POINT('Ctrl Pts',(186.329833245479,3.99152961452714,136.558144195375));
#252929=CARTESIAN_POINT('Ctrl Pts',(186.051385621667,6.99834033481346,130.556234274655));
#252930=CARTESIAN_POINT('Ctrl Pts',(185.772937997853,3.5740181753383,124.782340341422));
#252931=CARTESIAN_POINT('Ctrl Pts',(185.494490374041,-3.13465208677821,
124.542388849921));
#252932=CARTESIAN_POINT('Ctrl Pts',(185.216042750227,-6.96273021741339,
130.056883498557));
#252933=CARTESIAN_POINT('Ctrl Pts',(184.937595126415,-4.39239942652681,
136.258273103275));
#252934=CARTESIAN_POINT('Ctrl Pts',(184.659147502602,2.21433185669671,137.447783572063));
#252935=CARTESIAN_POINT('Ctrl Pts',(184.380699878789,6.78620033974098,132.532312894923));
#252936=CARTESIAN_POINT('Ctrl Pts',(184.102252254976,5.12188223488049,126.028938490053));
#252937=CARTESIAN_POINT('Ctrl Pts',(183.823804631163,-1.24919542597752,
123.913943728027));
#252938=CARTESIAN_POINT('Ctrl Pts',(183.54535700735,-6.47232351695142,128.130905471908));
#252939=CARTESIAN_POINT('Ctrl Pts',(183.266909383538,-5.74770248642891,
134.804641889104));
#252940=CARTESIAN_POINT('Ctrl Pts',(182.988461759724,0.258776338245136,
137.80231524236));
#252941=CARTESIAN_POINT('Ctrl Pts',(182.710014135912,6.02745234999885,134.369210164519));
#252942=CARTESIAN_POINT('Ctrl Pts',(182.431566512099,6.25719410952084,127.66018250561));
#252943=CARTESIAN_POINT('Ctrl Pts',(182.153118888286,0.73688016331929,123.840500929948));
#252944=CARTESIAN_POINT('Ctrl Pts',(181.874671264473,-5.46059065437546,
126.420266203747));
#252945=CARTESIAN_POINT('Ctrl Pts',(181.59622364066,-6.64004542538295,133.028800068927));
#252946=CARTESIAN_POINT('Ctrl Pts',(181.317776016847,-1.71762283471616,
137.593182748215));
#252947=CARTESIAN_POINT('Ctrl Pts',(181.039328393035,4.78321123051439,135.918969541833));
#252948=CARTESIAN_POINT('Ctrl Pts',(180.760880769221,6.88850784776155,129.544680596588));
#252949=CARTESIAN_POINT('Ctrl Pts',(180.482433145409,2.66360227523266,124.32797605183));
#252950=CARTESIAN_POINT('Ctrl Pts',(180.203985521595,-4.00902366402984,
125.062752534008));
#252951=CARTESIAN_POINT('Ctrl Pts',(179.925537897783,-6.99755270774298,
131.073786351827));
#252952=CARTESIAN_POINT('Ctrl Pts',(179.64709027397,-3.5556726624947,136.837231082039));
#252953=CARTESIAN_POINT('Ctrl Pts',(179.368642650157,3.15369685531979,137.056762577506));
#252954=CARTESIAN_POINT('Ctrl Pts',(179.090195026344,6.96497302975191,131.530642118605));
#252955=CARTESIAN_POINT('Ctrl Pts',(178.811747402531,4.37577924769062,125.337104441072));
#252956=CARTESIAN_POINT('Ctrl Pts',(178.533299778718,-2.23454189429802,
124.167708099424));
#252957=CARTESIAN_POINT('Ctrl Pts',(178.254852154906,-6.79142819886702,
129.097071203448));
#252958=CARTESIAN_POINT('Ctrl Pts',(177.976404531092,-5.10732376838957,
135.595349873321));
#252959=CARTESIAN_POINT('Ctrl Pts',(177.69795690728,1.27016169860089,137.690943469992));
#252960=CARTESIAN_POINT('Ctrl Pts',(177.419509283467,6.48043061542571,133.458103853558));
#252961=CARTESIAN_POINT('Ctrl Pts',(177.141061659654,5.73550038331004,126.786603845811));
#252962=CARTESIAN_POINT('Ctrl Pts',(176.862614035841,-0.280074506296806,
123.807226032976));
#252963=CARTESIAN_POINT('Ctrl Pts',(176.584166412028,-6.0382746070172,127.257873074351));
#252964=CARTESIAN_POINT('Ctrl Pts',(176.305718788215,-6.24759533000263,
133.967568912391));
#252965=CARTESIAN_POINT('Ctrl Pts',(176.027271164402,-0.71568115671533,
137.770430858802));
#252966=CARTESIAN_POINT('Ctrl Pts',(175.748823540589,5.4739090366252,135.171814564968));
#252967=CARTESIAN_POINT('Ctrl Pts',(175.470375916777,6.63324424063007,128.559721455457));
#252968=CARTESIAN_POINT('Ctrl Pts',(175.191928292964,1.69695203949225,124.010342079205));
#252969=CARTESIAN_POINT('Ctrl Pts',(174.913480669151,-4.79875618522306,
125.704333833448));
#252970=CARTESIAN_POINT('Ctrl Pts',(174.635033045338,-6.88464190799096,
132.085001052137));
#252971=CARTESIAN_POINT('Ctrl Pts',(174.356585421525,-2.64387805077028,
137.288822274217));
#252972=CARTESIAN_POINT('Ctrl Pts',(174.078137797712,4.02648057448505,136.533740017397));
#252973=CARTESIAN_POINT('Ctrl Pts',(173.799690173899,6.99670025630013,130.513637987877));
#252974=CARTESIAN_POINT('Ctrl Pts',(173.521242550086,3.53729421038521,124.76069585245));
#252975=CARTESIAN_POINT('Ctrl Pts',(173.242794926273,-3.17271240844464,
124.561586386726));
#252976=CARTESIAN_POINT('Ctrl Pts',(172.96434730246,-6.96715131953175,130.099281462668));
#252977=CARTESIAN_POINT('Ctrl Pts',(172.685899678648,-4.35911853223319,
136.284909836929));
#252978=CARTESIAN_POINT('Ctrl Pts',(172.407452054835,2.25473123140845,137.434181218309));
#252979=CARTESIAN_POINT('Ctrl Pts',(172.129004431022,6.79659314313001,132.490971352347));
#252980=CARTESIAN_POINT('Ctrl Pts',(171.850556807209,5.09271798834896,125.997848616637));
#252981=CARTESIAN_POINT('Ctrl Pts',(171.572109183396,-1.29111620461978,
123.921675598615));
#252982=CARTESIAN_POINT('Ctrl Pts',(171.293661559583,-6.48847768007612,
128.170353875152));
#252983=CARTESIAN_POINT('Ctrl Pts',(171.01521393577,-5.72324514729908,134.839555669585));
#252984=CARTESIAN_POINT('Ctrl Pts',(170.736766311957,0.301370079776633,
137.800610341449));
#252985=CARTESIAN_POINT('Ctrl Pts',(170.458318688145,6.04904092628448,134.332453302864));
#252986=CARTESIAN_POINT('Ctrl Pts',(170.179871064331,6.23793867361471,127.6221514434));
#252987=CARTESIAN_POINT('Ctrl Pts',(169.901423440519,0.694475520138818,
123.836144355433));
#252988=CARTESIAN_POINT('Ctrl Pts',(169.622975816706,-5.4871767093294,126.453587596077));
#252989=CARTESIAN_POINT('Ctrl Pts',(169.344528192893,-6.62638160640872,
133.06917869639));
#252990=CARTESIAN_POINT('Ctrl Pts',(169.06608056908,-1.67626552393645,137.603512624779));
#252991=CARTESIAN_POINT('Ctrl Pts',(168.787632945267,4.81425668490999,135.88975801558));
#252992=CARTESIAN_POINT('Ctrl Pts',(168.509185321454,6.88071218983824,129.50277163308));
#252993=CARTESIAN_POINT('Ctrl Pts',(168.230737697641,2.62412933378287,124.311881941165));
#252994=CARTESIAN_POINT('Ctrl Pts',(167.952290073828,-4.0439001841742,125.087262977647));
#252995=CARTESIAN_POINT('Ctrl Pts',(167.673842450016,-6.99578298838191,
131.116377449467));
#252996=CARTESIAN_POINT('Ctrl Pts',(167.395394826203,-3.51888298926545,
136.858763695638));
#252997=CARTESIAN_POINT('Ctrl Pts',(167.11694720239,3.19169856999505,137.037449287095));
#252998=CARTESIAN_POINT('Ctrl Pts',(166.838499578577,6.96926506657354,131.488230894564));
#252999=CARTESIAN_POINT('Ctrl Pts',(166.560051954764,4.34241743449723,125.310569126392));
#253000=CARTESIAN_POINT('Ctrl Pts',(166.281604330951,-2.27489968099678,
124.181433351974));
#253001=CARTESIAN_POINT('Ctrl Pts',(166.003156707138,-6.80169512468258,
129.13844418665));
#253002=CARTESIAN_POINT('Ctrl Pts',(165.724709083325,-5.0780650300646,135.626350836796));
#253003=CARTESIAN_POINT('Ctrl Pts',(165.446261459512,1.31205874991464,137.683084042787));
#253004=CARTESIAN_POINT('Ctrl Pts',(165.1678138357,6.49646463635559,133.418606465321));
#253005=CARTESIAN_POINT('Ctrl Pts',(164.889366211887,5.71093689192698,126.751764666776));
#253006=CARTESIAN_POINT('Ctrl Pts',(164.610918588074,-0.322662861405092,
123.809060566689));
#253007=CARTESIAN_POINT('Ctrl Pts',(164.332470964261,-6.05975120806294,
127.29469547395));
#253008=CARTESIAN_POINT('Ctrl Pts',(164.054023340448,-6.22822422981513,
134.00554119152));
#253009=CARTESIAN_POINT('Ctrl Pts',(163.775575716635,-0.673263450036036,
137.774658347991));
#253010=CARTESIAN_POINT('Ctrl Pts',(163.497128092822,5.50039354957815,135.138412408175));
#253011=CARTESIAN_POINT('Ctrl Pts',(163.218680469009,6.61945758629338,128.51938460299));
#253012=CARTESIAN_POINT('Ctrl Pts',(162.940232845196,1.65556347968583,124.000138127916));
#253013=CARTESIAN_POINT('Ctrl Pts',(162.661785221384,-4.82971258598073,
125.733639716082));
#253014=CARTESIAN_POINT('Ctrl Pts',(162.383337597571,-6.87671872970774,
132.126886094224));
#253015=CARTESIAN_POINT('Ctrl Pts',(162.104889973758,-2.60435630721971,
137.304796168278));
#253016=CARTESIAN_POINT('Ctrl Pts',(161.826442349945,4.06128233172446,136.509123535159));
#253017=CARTESIAN_POINT('Ctrl Pts',(161.547994726132,6.99480091248578,130.471052473933));
#253018=CARTESIAN_POINT('Ctrl Pts',(161.269547102319,3.50043916969439,124.739275313697));
#253019=CARTESIAN_POINT('Ctrl Pts',(160.991099478506,-3.21065516408591,
124.581015251828));
#253020=CARTESIAN_POINT('Ctrl Pts',(160.712651854693,-6.97131425129578,
130.141705553748));
#253021=CARTESIAN_POINT('Ctrl Pts',(160.434204230881,-4.32567610919938,
136.311343486817));
#253022=CARTESIAN_POINT('Ctrl Pts',(160.155756607067,2.29504705622523,137.420333194114));
#253023=CARTESIAN_POINT('Ctrl Pts',(159.877308983254,6.80673409626067,132.449567311792));
#253024=CARTESIAN_POINT('Ctrl Pts',(159.598861359442,5.06336502927952,125.966936850291));
#253025=CARTESIAN_POINT('Ctrl Pts',(159.320413735629,-1.33298914047637,
123.929662509627));
#253026=CARTESIAN_POINT('Ctrl Pts',(159.041966111816,-6.50439141027418,
128.209899882485));
#253027=CARTESIAN_POINT('Ctrl Pts',(158.763518488003,-5.69857573121565,
134.874319924428));
#253028=CARTESIAN_POINT('Ctrl Pts',(158.48507086419,0.343952653928878,137.798646191931));
#253029=CARTESIAN_POINT('Ctrl Pts',(158.206623240377,6.07040535313402,134.295565706438));
#253030=CARTESIAN_POINT('Ctrl Pts',(157.928175616564,6.2184520885971,127.584238299121));
#253031=CARTESIAN_POINT('Ctrl Pts',(157.649727992752,0.652045142912632,
123.832045990734));
#253032=CARTESIAN_POINT('Ctrl Pts',(157.371280368939,-5.51355943493244,
126.487070207899));
#253033=CARTESIAN_POINT('Ctrl Pts',(157.092832745126,-6.61247224442723,
133.109473400187));
#253034=CARTESIAN_POINT('Ctrl Pts',(156.814385121313,-1.63484609852131,
137.613590556265));
#253035=CARTESIAN_POINT('Ctrl Pts',(156.5359374975,4.84512374525377,135.860358048054));
#253036=CARTESIAN_POINT('Ctrl Pts',(156.257489873687,6.87266156459436,129.46091090043));
#253037=CARTESIAN_POINT('Ctrl Pts',(155.979042249874,2.58455915425555,124.296028411687));
#253038=CARTESIAN_POINT('Ctrl Pts',(155.700594626061,-4.07862685611001,
125.111985270442));
#253039=CARTESIAN_POINT('Ctrl Pts',(155.422147002248,-6.99375403770952,
131.158956985208));
#253040=CARTESIAN_POINT('Ctrl Pts',(155.143699378435,-3.48196292253304,
136.880071961106));
#253041=CARTESIAN_POINT('Ctrl Pts',(154.865251754623,3.22958201510593,137.017905027291));
#253042=CARTESIAN_POINT('Ctrl Pts',(154.58680413081,6.97329885471516,131.445794329457));
#253043=CARTESIAN_POINT('Ctrl Pts',(154.308356506997,4.30889471142897,125.284237386175));
#253044=CARTESIAN_POINT('Ctrl Pts',(154.029908883184,-2.31517317045128,
124.195404019528));
#253045=CARTESIAN_POINT('Ctrl Pts',(153.751461259371,-6.81171001118396,
129.179878900999));
#253046=CARTESIAN_POINT('Ctrl Pts',(153.473013635558,-5.04861812217248,
135.65717311965));
#253047=CARTESIAN_POINT('Ctrl Pts',(153.194566011745,1.3539071824088,137.674969721956));
#253048=CARTESIAN_POINT('Ctrl Pts',(152.916118387933,6.51225792839928,133.379012205241));
#253049=CARTESIAN_POINT('Ctrl Pts',(152.637670764119,5.68616177967723,126.717075658174));
#253050=CARTESIAN_POINT('Ctrl Pts',(152.359223140307,-0.365239260122265,
123.811154313817));
#253051=CARTESIAN_POINT('Ctrl Pts',(152.080775516494,-6.08100326279917,
127.331647925483));
#253052=CARTESIAN_POINT('Ctrl Pts',(151.802327892681,-6.20862234048841,
134.043394849727));
#253053=CARTESIAN_POINT('Ctrl Pts',(151.523880268868,-0.630820795332096,
137.778627550233));
#253054=CARTESIAN_POINT('Ctrl Pts',(151.245432645055,5.52667424342534,135.104849651499));
#253055=CARTESIAN_POINT('Ctrl Pts',(150.966985021242,6.60542564552152,128.479132421149));
#253056=CARTESIAN_POINT('Ctrl Pts',(150.688537397429,1.61411357236584,123.990186309594));
#253057=CARTESIAN_POINT('Ctrl Pts',(150.410089773616,-4.86049001996232,
125.763133496143));
#253058=CARTESIAN_POINT('Ctrl Pts',(150.131642149803,-6.8685407320831,132.168722129643));
#253059=CARTESIAN_POINT('Ctrl Pts',(149.853194525991,-2.56473805828847,
137.32052918631));
#253060=CARTESIAN_POINT('Ctrl Pts',(149.574746902178,4.09593359665354,136.484295660832));
#253061=CARTESIAN_POINT('Ctrl Pts',(149.296299278365,6.99264237375128,130.428479310845));
#253062=CARTESIAN_POINT('Ctrl Pts',(149.017851654552,3.46345441894284,124.718079518912));
#253063=CARTESIAN_POINT('Ctrl Pts',(148.739404030739,-3.24847894771935,
124.600674725279));
#253064=CARTESIAN_POINT('Ctrl Pts',(148.460956406926,-6.97521885844655,
130.184154199754));
#253065=CARTESIAN_POINT('Ctrl Pts',(148.182508783113,-4.29207339664657,
136.337573073429));
#253066=CARTESIAN_POINT('Ctrl Pts',(147.9040611593,2.33527783722936,137.406240012622));
#253067=CARTESIAN_POINT('Ctrl Pts',(147.625613535487,6.81662282335624,132.408102307496));
#253068=CARTESIAN_POINT('Ctrl Pts',(147.347165911675,5.03382444535687,125.936204336462));
#253069=CARTESIAN_POINT('Ctrl Pts',(147.068718287862,-1.37481268193005,
123.937904165105));
#253070=CARTESIAN_POINT('Ctrl Pts',(146.790270664049,-6.52006411785656,
128.249542028514));
#253071=CARTESIAN_POINT('Ctrl Pts',(146.511823040236,-5.67369515231286,
134.908933365434));
#253072=CARTESIAN_POINT('Ctrl Pts',(146.233375416423,0.386522482789046,
137.796422866589));
#253073=CARTESIAN_POINT('Ctrl Pts',(145.95492779261,6.09154483888081,134.258548742122));
#253074=CARTESIAN_POINT('Ctrl Pts',(145.676480168797,6.19873507655051,127.546444477659));
#253075=CARTESIAN_POINT('Ctrl Pts',(145.398032544984,0.609590603913882,
123.828205987717));
#253076=CARTESIAN_POINT('Ctrl Pts',(145.119584921171,-5.53973785356302,
126.520712798507));
#253077=CARTESIAN_POINT('Ctrl Pts',(144.841137297358,-6.59831785485502,
133.149682687181));
#253078=CARTESIAN_POINT('Ctrl Pts',(144.562689673546,-1.59336609328267,
137.623416169231));
#253079=CARTESIAN_POINT('Ctrl Pts',(144.284242049733,4.87581126775532,135.830770728684));
#253080=CARTESIAN_POINT('Ctrl Pts',(144.00579442592,6.86435627034879,129.419099949804));
#253081=CARTESIAN_POINT('Ctrl Pts',(143.727346802107,2.54489320293839,124.280416050852));
#253082=CARTESIAN_POINT('Ctrl Pts',(143.448899178294,-4.11320239302776,
125.136918496298));
#253083=CARTESIAN_POINT('Ctrl Pts',(143.170451554481,-6.99146593090932,
131.201523381251));
#253084=CARTESIAN_POINT('Ctrl Pts',(142.892003930668,-3.44491383038404,
136.901155088855));
#253085=CARTESIAN_POINT('Ctrl Pts',(142.613556306855,3.26734578686757,136.998130522314));
#253086=CARTESIAN_POINT('Ctrl Pts',(142.335108683042,6.97707424470332,131.403333995789));
#253087=CARTESIAN_POINT('Ctrl Pts',(142.05666105923,4.27521232068256,125.258110196154));
#253088=CARTESIAN_POINT('Ctrl Pts',(141.778213435417,-2.35536087031262,
124.209619584399));
#253089=CARTESIAN_POINT('Ctrl Pts',(141.499765811604,-6.8214724872659,129.221373811115));
#253090=CARTESIAN_POINT('Ctrl Pts',(141.221318187791,-5.01898413587917,
135.687815579753));
#253091=CARTESIAN_POINT('Ctrl Pts',(140.942870563978,1.39570544537436,137.666600808179));
#253092=CARTESIAN_POINT('Ctrl Pts',(140.664422940165,6.52780990633047,133.339322540502));
#253093=CARTESIAN_POINT('Ctrl Pts',(140.385975316352,5.66117596461176,126.68253810542));
#253094=CARTESIAN_POINT('Ctrl Pts',(140.10752769254,-0.407802124764288,
123.813507196776));
#253095=CARTESIAN_POINT('Ctrl Pts',(139.829080068726,-6.10202998372316,
127.368729059661));
#253096=CARTESIAN_POINT('Ctrl Pts',(139.550632444914,-6.18879038837768,
134.081128484328));
#253097=CARTESIAN_POINT('Ctrl Pts',(139.272184821101,-0.588354765331746,
137.78233831845));
#253098=CARTESIAN_POINT('Ctrl Pts',(138.993737197288,5.55275014432601,135.071127538621));
#253099=CARTESIAN_POINT('Ctrl Pts',(138.715289573475,6.59114893827324,128.438966401494));
#253100=CARTESIAN_POINT('Ctrl Pts',(138.436841949662,1.57260385347371,123.980486993006));
#253101=CARTESIAN_POINT('Ctrl Pts',(138.158394325849,-4.8910873466988,125.792814080728));
#253102=CARTESIAN_POINT('Ctrl Pts',(137.879946702036,-6.86010821815569,
132.210507608145));
#253103=CARTESIAN_POINT('Ctrl Pts',(137.601499078223,-2.52502477204539,
137.336020745319));
#253104=CARTESIAN_POINT('Ctrl Pts',(137.32305145441,4.13043308525698,136.459257314423));
#253105=CARTESIAN_POINT('Ctrl Pts',(137.044603830598,6.99022472008204,130.385920076178));
#253106=CARTESIAN_POINT('Ctrl Pts',(136.766156206785,3.42634132861412,124.69710925351));
#253107=CARTESIAN_POINT('Ctrl Pts',(136.487708582972,-3.28618235777073,
124.620564078594));
#253108=CARTESIAN_POINT('Ctrl Pts',(136.209260959159,-6.97886499629743,
130.226625827737));
#253109=CARTESIAN_POINT('Ctrl Pts',(135.930813335346,-4.25831163973555,
136.363597624819));
#253110=CARTESIAN_POINT('Ctrl Pts',(135.652365711533,2.37542208365453,137.391902196061));
#253111=CARTESIAN_POINT('Ctrl Pts',(135.37391808772,6.82625895798624,132.366577875963));
#253112=CARTESIAN_POINT('Ctrl Pts',(135.095470463907,5.00409733121823,125.905652213954));
#253113=CARTESIAN_POINT('Ctrl Pts',(134.817022840094,-1.4165852791943,123.946400259653));
#253114=CARTESIAN_POINT('Ctrl Pts',(134.538575216282,-6.53549522206528,
128.289278844285));
#253115=CARTESIAN_POINT('Ctrl Pts',(134.260127592469,-5.64860433254967,
134.943394709987));
#253116=CARTESIAN_POINT('Ctrl Pts',(133.981679968656,0.429077988916399,
137.793940447809));
#253117=CARTESIAN_POINT('Ctrl Pts',(133.703232344843,6.1124586001935,134.221403781595));
#253118=CARTESIAN_POINT('Ctrl Pts',(133.42478472103,6.17878836809604,127.508771379477));
#253119=CARTESIAN_POINT('Ctrl Pts',(133.146337097217,0.567113476311158,
123.824624488677));
#253120=CARTESIAN_POINT('Ctrl Pts',(132.867889473404,-5.5657109951702,126.554514121259));
#253121=CARTESIAN_POINT('Ctrl Pts',(132.589441849591,-6.58391896218814,
133.189805067404));
#253122=CARTESIAN_POINT('Ctrl Pts',(132.310994225778,-1.55182704527753,
137.632989099587));
#253123=CARTESIAN_POINT('Ctrl Pts',(132.032546601965,4.90631811527725,135.800997153839));
#253124=CARTESIAN_POINT('Ctrl Pts',(131.754098978153,6.85579661485726,129.377340330521));
#253125=CARTESIAN_POINT('Ctrl Pts',(131.47565135434,2.50513294966777,124.265045437181));
#253126=CARTESIAN_POINT('Ctrl Pts',(131.197203730527,-4.14762551371829,
125.162061731307));
#253127=CARTESIAN_POINT('Ctrl Pts',(130.918756106714,-6.98891875276791,
131.244075060281));
#253128=CARTESIAN_POINT('Ctrl Pts',(130.640308482901,-3.4077370856862,136.922012297644));
#253129=CARTESIAN_POINT('Ctrl Pts',(130.361860859088,3.30498848592948,136.978126504915));
#253130=CARTESIAN_POINT('Ctrl Pts',(130.083413235275,6.98059109663955,131.360851466943));
#253131=CARTESIAN_POINT('Ctrl Pts',(129.804965611462,4.24137151037132,125.232188524482));
#253132=CARTESIAN_POINT('Ctrl Pts',(129.526517987649,-2.39546129141071,
124.224079519825));
#253133=CARTESIAN_POINT('Ctrl Pts',(129.248070363836,-6.83098219117618,
129.262927379388));
#253134=CARTESIAN_POINT('Ctrl Pts',(128.969622740024,-4.98916416928312,
135.718277081636));
#253135=CARTESIAN_POINT('Ctrl Pts',(128.691175116211,1.43745198996158,137.657977611568));
#253136=CARTESIAN_POINT('Ctrl Pts',(128.412727492398,6.54311999386511,133.299538941816));
#253137=CARTESIAN_POINT('Ctrl Pts',(128.134279868585,5.63598037258881,126.648153288314));
#253138=CARTESIAN_POINT('Ctrl Pts',(127.855832244772,-0.450349878148651,
123.81611912838));
#253139=CARTESIAN_POINT('Ctrl Pts',(127.577384620959,-6.12283059168226,
127.40593750243));
#253140=CARTESIAN_POINT('Ctrl Pts',(127.298936997146,-6.16872910836309,
134.118740697091));
#253141=CARTESIAN_POINT('Ctrl Pts',(127.020489373333,-0.545866933628919,
137.785790515136));
#253142=CARTESIAN_POINT('Ctrl Pts',(126.742041749521,5.57862028602806,135.037247319125));
#253143=CARTESIAN_POINT('Ctrl Pts',(126.463594125708,6.57662799357718,128.398888032392));
#253144=CARTESIAN_POINT('Ctrl Pts',(126.185146501895,1.53103586116759,123.971040537565));
#253145=CARTESIAN_POINT('Ctrl Pts',(125.906698878082,-4.92150343239493,
125.822680370014));
#253146=CARTESIAN_POINT('Ctrl Pts',(125.628251254269,-6.85142150039552,
132.252240981353));
#253147=CARTESIAN_POINT('Ctrl Pts',(125.349803630456,-2.48521792008072,
137.351270271259));
#253148=CARTESIAN_POINT('Ctrl Pts',(125.071356006643,4.16477951914341,136.434009423738));
#253149=CARTESIAN_POINT('Ctrl Pts',(124.79290838283,6.98754804106521,130.343376346978));
#253150=CARTESIAN_POINT('Ctrl Pts',(124.514460759018,3.38910127394743,124.676365294554));
#253151=CARTESIAN_POINT('Ctrl Pts',(124.236013135205,-3.32376399712637,
124.640682574762));
#253152=CARTESIAN_POINT('Ctrl Pts',(123.957565511392,-6.98225252973936,
130.269118863895));
#253153=CARTESIAN_POINT('Ctrl Pts',(123.679117887579,-4.22439208952083,
136.389416176637));
#253154=CARTESIAN_POINT('Ctrl Pts',(123.400670263766,2.41547830794073,137.377320275725));
#253155=CARTESIAN_POINT('Ctrl Pts',(123.122222639953,6.83564214308024,132.324995555895));
#253156=CARTESIAN_POINT('Ctrl Pts',(122.84377501614,4.97418478841272,125.875281614887));
#253157=CARTESIAN_POINT('Ctrl Pts',(122.565327392328,-1.45830538437,123.955150478444));
#253158=CARTESIAN_POINT('Ctrl Pts',(122.286879768514,-6.55068415109515,
128.329108857337));
#253159=CARTESIAN_POINT('Ctrl Pts',(122.008432144702,-5.62330420167569,
134.977702681109));
#253160=CARTESIAN_POINT('Ctrl Pts',(121.729984520888,0.471617595401148,
137.791199027578));
#253161=CARTESIAN_POINT('Ctrl Pts',(121.451536897076,6.13314586210485,134.184132201278));
#253162=CARTESIAN_POINT('Ctrl Pts',(121.173089273263,6.15861270236637,127.471220400567));
#253163=CARTESIAN_POINT('Ctrl Pts',(120.89464164945,0.52461533410983,123.821301626325));
#253164=CARTESIAN_POINT('Ctrl Pts',(120.616194025637,-5.5914778973097,126.588472923636));
#253165=CARTESIAN_POINT('Ctrl Pts',(120.337746401824,-6.56927609998288,
133.229839054105));
#253166=CARTESIAN_POINT('Ctrl Pts',(120.059298778011,-1.51023049375061,
137.642308992603));
#253167=CARTESIAN_POINT('Ctrl Pts',(119.780851154198,4.93664315737715,135.77103842679));
#253168=CARTESIAN_POINT('Ctrl Pts',(119.502403530385,6.84698291530094,129.33563359));
#253169=CARTESIAN_POINT('Ctrl Pts',(119.223955906573,2.46527986777437,124.249917140239));
#253170=CARTESIAN_POINT('Ctrl Pts',(118.94550828276,-4.18189494262004,125.187414043775));
#253171=CARTESIAN_POINT('Ctrl Pts',(118.667060658947,-6.98611259767199,
131.28661044553));
#253172=CARTESIAN_POINT('Ctrl Pts',(118.388613035134,-3.37043406603744,
136.942642814599));
#253173=CARTESIAN_POINT('Ctrl Pts',(118.110165411321,3.34250871742766,136.95789371635));
#253174=CARTESIAN_POINT('Ctrl Pts',(117.831717787508,6.98384928020556,131.318348317123));
#253175=CARTESIAN_POINT('Ctrl Pts',(117.553270163695,4.20737353447909,125.206473331696));
#253176=CARTESIAN_POINT('Ctrl Pts',(117.274822539882,-2.43547294780967,
124.238783289987));
#253177=CARTESIAN_POINT('Ctrl Pts',(116.99637491607,-6.84023877052931,129.304538066038));
#253178=CARTESIAN_POINT('Ctrl Pts',(116.717927292256,-4.95915932737393,
135.748556496538));
#253179=CARTESIAN_POINT('Ctrl Pts',(116.439479668444,1.47914526923655,137.649100451659));
#253180=CARTESIAN_POINT('Ctrl Pts',(116.161032044631,6.55818762368211,133.259662883379));
#253181=CARTESIAN_POINT('Ctrl Pts',(115.882584420818,5.61057593724064,126.613922481));
#253182=CARTESIAN_POINT('Ctrl Pts',(115.604136797005,-0.49288094365267,
123.818990011842));
#253183=CARTESIAN_POINT('Ctrl Pts',(115.325689173192,-6.14340431590201,
127.443271875017));
#253184=CARTESIAN_POINT('Ctrl Pts',(115.047241549379,-6.14843924382291,
134.156230094282));
#253185=CARTESIAN_POINT('Ctrl Pts',(114.768793925566,-0.5033588746261,137.78898401237));
#253186=CARTESIAN_POINT('Ctrl Pts',(114.490346301753,5.60428370990391,135.003210248456));
#253187=CARTESIAN_POINT('Ctrl Pts',(114.211898677941,6.56186334951224,128.358898798961));
#253188=CARTESIAN_POINT('Ctrl Pts',(113.933451054127,1.48941113576461,123.961847293312));
#253189=CARTESIAN_POINT('Ctrl Pts',(113.655003430315,-4.95173714997151,
125.852731257293));
#253190=CARTESIAN_POINT('Ctrl Pts',(113.376555806502,-6.84248090069202,
132.293920702821));
#253191=CARTESIAN_POINT('Ctrl Pts',(113.098108182689,-2.4453189774521,137.366277199056));
#253192=CARTESIAN_POINT('Ctrl Pts',(112.819660558876,4.19897162559319,136.408552924347));
#253193=CARTESIAN_POINT('Ctrl Pts',(112.541212935063,6.98461243588604,130.300849699721));
#253194=CARTESIAN_POINT('Ctrl Pts',(112.26276531125,3.35173563488669,124.655848410718));
#253195=CARTESIAN_POINT('Ctrl Pts',(111.984317687437,-3.3612224731848,124.661029468288));
#253196=CARTESIAN_POINT('Ctrl Pts',(111.705870063624,-6.98538133324609,
130.311631733633));
#253197=CARTESIAN_POINT('Ctrl Pts',(111.427422439812,-4.1903160029037,136.415027772168));
#253198=CARTESIAN_POINT('Ctrl Pts',(111.148974815999,2.45544502578993,137.362494791951));
#253199=CARTESIAN_POINT('Ctrl Pts',(110.870527192186,6.84477203094083,132.28335688814));
#253200=CARTESIAN_POINT('Ctrl Pts',(110.592079568373,4.94408792536061,125.845093664656));
#253201=CARTESIAN_POINT('Ctrl Pts',(110.31363194456,-1.49997145150339,123.964154497236));
#253202=CARTESIAN_POINT('Ctrl Pts',(110.035184320747,-6.56563034211481,
128.369030591753));
#253203=CARTESIAN_POINT('Ctrl Pts',(109.756736696934,-5.59779569719655,
135.011856007506));
#253204=CARTESIAN_POINT('Ctrl Pts',(109.478289073121,0.514139725922464,
137.788198707481));
#253205=CARTESIAN_POINT('Ctrl Pts',(109.199841449309,6.15360585804082,134.146735382281));
#253206=CARTESIAN_POINT('Ctrl Pts',(108.921393825496,6.13820882697821,127.433792932393));
#253207=CARTESIAN_POINT('Ctrl Pts',(108.642946201683,0.482097752094529,
123.818237523792));
#253208=CARTESIAN_POINT('Ctrl Pts',(108.36449857787,-5.61703760517944,126.622587947283));
#253209=CARTESIAN_POINT('Ctrl Pts',(108.086050954057,-6.5543898108359,133.26978316381));
#253210=CARTESIAN_POINT('Ctrl Pts',(107.807603330244,-1.46857798007734,
137.651375502926));
#253211=CARTESIAN_POINT('Ctrl Pts',(107.529155706431,4.96678527034939,135.740895657668));
#253212=CARTESIAN_POINT('Ctrl Pts',(107.250708082618,6.83791549827476,129.2939812737));
#253213=CARTESIAN_POINT('Ctrl Pts',(106.972260458805,2.42533543402888,124.23503172061));
#253214=CARTESIAN_POINT('Ctrl Pts',(106.693812834992,-4.21600940986681,
125.212974494265));
#253215=CARTESIAN_POINT('Ctrl Pts',(106.415365211179,-6.98304756960462,
131.329127960835));
#253216=CARTESIAN_POINT('Ctrl Pts',(106.136917587367,-3.33300615371489,
136.96304587525));
#253217=CARTESIAN_POINT('Ctrl Pts',(105.858469963554,3.37990509103613,136.937432906355));
#253218=CARTESIAN_POINT('Ctrl Pts',(105.580022339741,6.98684867466819,131.275826121299));
#253219=CARTESIAN_POINT('Ctrl Pts',(105.301574715928,4.1732196528133,125.180965570684));
#253220=CARTESIAN_POINT('Ctrl Pts',(105.023127092115,-2.4753943568629,124.253730350031));
#253221=CARTESIAN_POINT('Ctrl Pts',(104.744679468302,-6.84924188231931,
129.346204329164));
#253222=CARTESIAN_POINT('Ctrl Pts',(104.466231844489,-4.92897072199215,
135.778652702442));
#253223=CARTESIAN_POINT('Ctrl Pts',(104.187784220676,1.52078373823962,137.639969657397));
#253224=CARTESIAN_POINT('Ctrl Pts',(103.909336596864,6.57301223744494,133.219695842813));
#253225=CARTESIAN_POINT('Ctrl Pts',(103.63088897305,5.58496359993783,126.579846951912));
#253226=CARTESIAN_POINT('Ctrl Pts',(103.352441349238,-0.535393745272065,
123.82211974078));
#253227=CARTESIAN_POINT('Ctrl Pts',(103.073993725425,-6.1637503940156,127.480730793984));
#253228=CARTESIAN_POINT('Ctrl Pts',(102.795546101612,-6.12792154660547,
134.193595286717));
#253229=CARTESIAN_POINT('Ctrl Pts',(102.517098477799,-0.460832163475232,
137.791918691816));
#253230=CARTESIAN_POINT('Ctrl Pts',(102.238650853986,5.6297394649859,134.96901758787));
#253231=CARTESIAN_POINT('Ctrl Pts',(101.960203230173,6.54685555318778,128.319000183017));
#253232=CARTESIAN_POINT('Ctrl Pts',(101.68175560636,1.44773121968427,123.952907600908));
#253233=CARTESIAN_POINT('Ctrl Pts',(101.403307982548,-4.981787379107,125.882965629019));
#253234=CARTESIAN_POINT('Ctrl Pts',(101.124860358735,-6.83328675034245,
132.335545228093));
#253235=CARTESIAN_POINT('Ctrl Pts',(100.846412734922,-2.4053294226295,137.38104097262));
#253236=CARTESIAN_POINT('Ctrl Pts',(100.567965111109,4.23300813760519,136.382888759548));
#253237=CARTESIAN_POINT('Ctrl Pts',(100.289517487296,6.98141801332452,130.258341710245));
#253238=CARTESIAN_POINT('Ctrl Pts',(100.011069863483,3.31424579602927,124.635559362262));
#253239=CARTESIAN_POINT('Ctrl Pts',(99.7326222396699,-3.39855639790849,
124.681604005209));
#253240=CARTESIAN_POINT('Ctrl Pts',(99.4541746158571,-6.98825129087862,
130.354162861621));
#253241=CARTESIAN_POINT('Ctrl Pts',(99.1757269920442,-4.15608464258612,
136.440431462363));
#253242=CARTESIAN_POINT('Ctrl Pts',(98.8972793682313,2.49532075622072,137.347426294104));
#253243=CARTESIAN_POINT('Ctrl Pts',(98.6188317444184,6.85364828325664,132.241663415635));
#253244=CARTESIAN_POINT('Ctrl Pts',(98.3403841206056,4.91380785731226,125.815089481885));
#253245=CARTESIAN_POINT('Ctrl Pts',(98.0619364967926,-1.54158193664305,
123.97341198238));
#253246=CARTESIAN_POINT('Ctrl Pts',(97.7834888729798,-6.58033324128762,
128.409042568218));
#253247=CARTESIAN_POINT('Ctrl Pts',(97.5050412491668,-5.57207976433927,
135.045853423614));
#253248=CARTESIAN_POINT('Ctrl Pts',(97.226593625354,0.55664280480716,137.784939598694));
#253249=CARTESIAN_POINT('Ctrl Pts',(96.948146001541,6.17383782984873,134.109214710358));
#253250=CARTESIAN_POINT('Ctrl Pts',(96.6696983777281,6.11757749800464,127.396490361844));
#253251=CARTESIAN_POINT('Ctrl Pts',(96.3912507539153,0.43956230576973,123.815432294619));
#253252=CARTESIAN_POINT('Ctrl Pts',(96.1128031301024,-5.64238917165504,
126.656857928054));
#253253=CARTESIAN_POINT('Ctrl Pts',(95.8343555062895,-6.53926064636413,
133.309635916377));
#253254=CARTESIAN_POINT('Ctrl Pts',(95.5559078824767,-1.42687104770695,
137.660188294596));
#253255=CARTESIAN_POINT('Ctrl Pts',(95.2774602586637,4.99674333726689,135.710569963425));
#253256=CARTESIAN_POINT('Ctrl Pts',(94.9990126348508,6.82859469977515,129.252384925061));
#253257=CARTESIAN_POINT('Ctrl Pts',(94.720565011038,2.38530112858694,124.22038972988));
#253258=CARTESIAN_POINT('Ctrl Pts',(94.442117387225,-4.24996765133445,125.238742135624));
#253259=CARTESIAN_POINT('Ctrl Pts',(94.1636697634123,-6.97972378214161,
131.371626030693));
#253260=CARTESIAN_POINT('Ctrl Pts',(93.885222139599,-3.29545473562348,136.983220723554));
#253261=CARTESIAN_POINT('Ctrl Pts',(93.6067745157866,3.41717622101856,136.91674483311));
#253262=CARTESIAN_POINT('Ctrl Pts',(93.3283268919733,6.98958916888377,131.233286455149));
#253263=CARTESIAN_POINT('Ctrl Pts',(93.0498792681607,4.13891113095855,125.155666186642));
#253264=CARTESIAN_POINT('Ctrl Pts',(92.7714316443476,-2.51522403926791,
124.268920146089));
#253265=CARTESIAN_POINT('Ctrl Pts',(92.4929840205349,-6.85799119293255,
129.387924624807));
#253266=CARTESIAN_POINT('Ctrl Pts',(92.2145363967218,-4.89859947178764,
135.808564584124));
#253267=CARTESIAN_POINT('Ctrl Pts',(91.9360887729091,1.562365854042,137.63058556713));
#253268=CARTESIAN_POINT('Ctrl Pts',(91.6576411490961,6.58759328582208,133.179639301113));
#253269=CARTESIAN_POINT('Ctrl Pts',(91.3791935252832,5.55914430975498,126.545927963732));
#253270=CARTESIAN_POINT('Ctrl Pts',(91.1007459014705,-0.57788670767935,
123.825508199223));
#253271=CARTESIAN_POINT('Ctrl Pts',(90.8222982776573,-6.18386807209161,
127.518312871276));
#253272=CARTESIAN_POINT('Ctrl Pts',(90.5438506538447,-6.10717677700159,
134.230834889814));
#253273=CARTESIAN_POINT('Ctrl Pts',(90.2654030300316,-0.41828837601907,
137.794594444728));
#253274=CARTESIAN_POINT('Ctrl Pts',(89.9869554062187,5.65498660800168,134.934670604388));
#253275=CARTESIAN_POINT('Ctrl Pts',(89.708507782406,6.53160516072318,128.279193663018));
#253276=CARTESIAN_POINT('Ctrl Pts',(89.430060158593,1.40599765739116,123.944221791613));
#253277=CARTESIAN_POINT('Ctrl Pts',(89.1516125347801,-5.01165300627911,
125.913382364846));
#253278=CARTESIAN_POINT('Ctrl Pts',(88.8731649109673,-6.82383939003939,
132.377113014756));
#253279=CARTESIAN_POINT('Ctrl Pts',(88.5947172871542,-2.36525073744058,
137.395561044874));
#253280=CARTESIAN_POINT('Ctrl Pts',(88.3162696633415,4.26688779394398,136.357017880338));
#253281=CARTESIAN_POINT('Ctrl Pts',(88.0378220395285,6.97796489175107,130.2158539537));
#253282=CARTESIAN_POINT('Ctrl Pts',(87.7593744157156,3.2766331465752,124.615498901007));
#253283=CARTESIAN_POINT('Ctrl Pts',(87.4809267919028,-3.43576438787495,
124.702405423128));
#253284=CARTESIAN_POINT('Ctrl Pts',(87.2024791680898,-6.99086229628967,
130.396710671853));
#253285=CARTESIAN_POINT('Ctrl Pts',(86.924031544277,-4.1216992770237,136.465626305881));
#253286=CARTESIAN_POINT('Ctrl Pts',(86.6455839204641,2.53510402162323,137.332115340552));
#253287=CARTESIAN_POINT('Ctrl Pts',(86.3671362966513,6.8622705711149,132.199916683345));
#253288=CARTESIAN_POINT('Ctrl Pts',(86.0886886728382,4.88334570630671,125.785270178391));
#253289=CARTESIAN_POINT('Ctrl Pts',(85.8102410490255,-1.58313529789712,
123.982922590838));
#253290=CARTESIAN_POINT('Ctrl Pts',(85.5317934252125,-6.59479230379227,
128.449143304076));
#253291=CARTESIAN_POINT('Ctrl Pts',(85.2533458013996,-5.5461573560172,135.079693669646));
#253292=CARTESIAN_POINT('Ctrl Pts',(84.9748981775869,0.599125257088023,
137.781421821987));
#253293=CARTESIAN_POINT('Ctrl Pts',(84.6964505537737,6.19384102782544,134.071571575853));
#253294=CARTESIAN_POINT('Ctrl Pts',(84.418002929961,6.09671947994716,127.359314071181));
#253295=CARTESIAN_POINT('Ctrl Pts',(84.1395553061481,0.397010571302045,
123.812886042756));
#253296=CARTESIAN_POINT('Ctrl Pts',(83.8611076823352,-5.66753165732491,
126.691281596061));
#253297=CARTESIAN_POINT('Ctrl Pts',(83.5826600585222,-6.52388916718428,
133.349395835046));
#253298=CARTESIAN_POINT('Ctrl Pts',(83.3042124347095,-1.38511124210516,
137.66874704105));
#253299=CARTESIAN_POINT('Ctrl Pts',(83.0257648108964,5.02651624802251,135.68006246779));
#253300=CARTESIAN_POINT('Ctrl Pts',(82.7473171870836,6.81902086518772,129.210846085452));
#253301=CARTESIAN_POINT('Ctrl Pts',(82.4688695632707,2.34517843493451,124.205991710613));
#253302=CARTESIAN_POINT('Ctrl Pts',(82.1904219394578,-4.28376840868787,
125.264716013022));
#253303=CARTESIAN_POINT('Ctrl Pts',(81.9119743156449,-6.97614135844701,
131.414103080323));
#253304=CARTESIAN_POINT('Ctrl Pts',(81.6335266918322,-3.25778120324508,
137.003166611925));
#253305=CARTESIAN_POINT('Ctrl Pts',(81.355079068019,3.45432072627939,136.895830263219));
#253306=CARTESIAN_POINT('Ctrl Pts',(81.0766314442065,6.99207066130227,131.190730894994));
#253307=CARTESIAN_POINT('Ctrl Pts',(80.7981838203932,4.10444924022979,125.130576117049));
#253308=CARTESIAN_POINT('Ctrl Pts',(80.5197361965806,-2.55496051912119,
124.284352115297));
#253309=CARTESIAN_POINT('Ctrl Pts',(80.2412885727675,-6.86648637816013,
129.429697407007));
#253310=CARTESIAN_POINT('Ctrl Pts',(79.9628409489547,-4.86804670217826,
135.838291033188));
#253311=CARTESIAN_POINT('Ctrl Pts',(79.6843933251418,1.6038900758031,137.620948528586));
#253312=CARTESIAN_POINT('Ctrl Pts',(79.405945701329,6.60193022850756,133.139494742587));
#253313=CARTESIAN_POINT('Ctrl Pts',(79.1274980775159,5.53311902343524,126.512166773338));
#253314=CARTESIAN_POINT('Ctrl Pts',(78.8490504537032,-0.620358256282274,
123.829155261608));
#253315=CARTESIAN_POINT('Ctrl Pts',(78.5706028298902,-6.2037566046621,127.556016714277));
#253316=CARTESIAN_POINT('Ctrl Pts',(78.2921552060774,-6.08620570371632,
134.267947523646));
#253317=CARTESIAN_POINT('Ctrl Pts',(78.0137075822645,-0.375729088733312,
137.797011171955));
#253318=CARTESIAN_POINT('Ctrl Pts',(77.7352599584516,5.68002420340909,134.90017057075));
#253319=CARTESIAN_POINT('Ctrl Pts',(77.4568123346387,6.51611273722737,128.23948071401));
#253320=CARTESIAN_POINT('Ctrl Pts',(77.1783647108257,1.36421199533782,123.935790187287));
#253321=CARTESIAN_POINT('Ctrl Pts',(76.8999170870129,-5.04133292480603,
125.94398033767));
#253322=CARTESIAN_POINT('Ctrl Pts',(76.6214694632,-6.81413916985829,132.418622522501));
#253323=CARTESIAN_POINT('Ctrl Pts',(76.3430218393871,-2.32508440701577,
137.409836877774));
#253324=CARTESIAN_POINT('Ctrl Pts',(76.0645742155741,4.30060933918641,136.33094124537));
#253325=CARTESIAN_POINT('Ctrl Pts',(75.7861265917614,6.97425319912241,130.173388004487));
#253326=CARTESIAN_POINT('Ctrl Pts',(75.5076789679483,3.23889908027492,124.595667770297));
#253327=CARTESIAN_POINT('Ctrl Pts',(75.2292313441357,-3.47284506432852,
124.72343295124));
#253328=CARTESIAN_POINT('Ctrl Pts',(74.9507837203226,-6.99321425272744,
130.439273587703));
#253329=CARTESIAN_POINT('Ctrl Pts',(74.6723360965098,-4.08716118037883,
136.490611369118));
#253330=CARTESIAN_POINT('Ctrl Pts',(74.3938884726969,2.57479334781394,137.316562498648));
#253331=CARTESIAN_POINT('Ctrl Pts',(74.1154408488841,6.87063857501356,132.158118238212));
#253332=CARTESIAN_POINT('Ctrl Pts',(73.836993225071,4.85270260113016,125.755636859138));
#253333=CARTESIAN_POINT('Ctrl Pts',(73.5585456012583,-1.62462999549052,
123.992685970191));
#253334=CARTESIAN_POINT('Ctrl Pts',(73.2800979774453,-6.60900699384299,
128.489331313375));
#253335=CARTESIAN_POINT('Ctrl Pts',(73.0016503536324,-5.52002943279461,
135.113375491641));
#253336=CARTESIAN_POINT('Ctrl Pts',(72.7232027298196,0.641585508562261,
137.777645507711));
#253337=CARTESIAN_POINT('Ctrl Pts',(72.4447551060067,6.21361471074508,134.033807373642));
#253338=CARTESIAN_POINT('Ctrl Pts',(72.1663074821937,6.07563554570727,127.322265437984));
#253339=CARTESIAN_POINT('Ctrl Pts',(71.8878598583809,0.354444125461637,
123.810598862555));
#253340=CARTESIAN_POINT('Ctrl Pts',(71.609412234568,-5.69246413052499,126.725857675724));
#253341=CARTESIAN_POINT('Ctrl Pts',(71.330964610755,-6.5082759428922,133.3890614465));
#253342=CARTESIAN_POINT('Ctrl Pts',(71.0525169869423,-1.34330011069692,
137.677051425141));
#253343=CARTESIAN_POINT('Ctrl Pts',(70.7740693631292,5.05610289937005,135.649374301231));
#253344=CARTESIAN_POINT('Ctrl Pts',(70.4956217393166,6.80919434927445,129.16936629411));
#253345=CARTESIAN_POINT('Ctrl Pts',(70.2171741155033,2.30496883983272,124.191838196331));
#253346=CARTESIAN_POINT('Ctrl Pts',(69.9387264916908,-4.31741042942741,
125.290895163988));
#253347=CARTESIAN_POINT('Ctrl Pts',(69.6602788678776,-6.97230043126892,
131.456557535721));
#253348=CARTESIAN_POINT('Ctrl Pts',(69.3818312440649,-3.21998695258627,
137.02288280126));
#253349=CARTESIAN_POINT('Ctrl Pts',(69.1033836202519,3.49133723041524,136.874689971681));
#253350=CARTESIAN_POINT('Ctrl Pts',(68.8249359964391,6.9942930599711,131.148161017746));
#253351=CARTESIAN_POINT('Ctrl Pts',(68.5464883726262,4.0698352576252,125.105696291628));
#253352=CARTESIAN_POINT('Ctrl Pts',(68.2680407488133,-2.59460232397255,
124.300025685817));
#253353=CARTESIAN_POINT('Ctrl Pts',(67.9895931250004,-6.87472712320984,
129.471521127857));
#253354=CARTESIAN_POINT('Ctrl Pts',(67.7111455011875,-4.83731354530826,
135.867830948109));
#253355=CARTESIAN_POINT('Ctrl Pts',(67.4326978773747,1.64535486482719,137.61105889887));
#253356=CARTESIAN_POINT('Ctrl Pts',(67.1542502535617,6.61602253424027,133.099263654809));
#253357=CARTESIAN_POINT('Ctrl Pts',(66.8758026297489,5.50688870535577,126.478564631767));
#253358=CARTESIAN_POINT('Ctrl Pts',(66.5973550059358,-0.662806817281494,
123.833060792792));
#253359=CARTESIAN_POINT('Ctrl Pts',(66.3189073821232,-6.22341525475008,
127.593840925854));
#253360=CARTESIAN_POINT('Ctrl Pts',(66.0404597583101,-6.0650091038406,134.304931812993));
#253361=CARTESIAN_POINT('Ctrl Pts',(65.7620121344974,-0.333155878668442,
137.799168783944));
#253362=CARTESIAN_POINT('Ctrl Pts',(65.4835645106842,5.70485132343066,134.865518765369));
#253363=CARTESIAN_POINT('Ctrl Pts',(65.2051168868716,6.50037885677781,128.199862807569));
#253364=CARTESIAN_POINT('Ctrl Pts',(64.9266692630585,1.32237578190785,123.927613100363));
#253365=CARTESIAN_POINT('Ctrl Pts',(64.6482216392459,-5.07082603488719,
125.974758413674));
#253366=CARTESIAN_POINT('Ctrl Pts',(64.3697740154327,-6.80418644924447,
132.460072213177));
#253367=CARTESIAN_POINT('Ctrl Pts',(64.09132639162,-2.28483191973344,137.423867942321));
#253368=CARTESIAN_POINT('Ctrl Pts',(63.812878767807,4.33417152376786,136.304659820925));
#253369=CARTESIAN_POINT('Ctrl Pts',(63.5344311439942,6.97028307297671,130.130945436197));
#253370=CARTESIAN_POINT('Ctrl Pts',(63.2559835201813,3.20104499537862,124.576066704985));
#253371=CARTESIAN_POINT('Ctrl Pts',(62.9775358963684,-3.5097970532309,124.744685810362));
#253372=CARTESIAN_POINT('Ctrl Pts',(62.6990882725555,-6.9953070730393,130.481850031987));
#253373=CARTESIAN_POINT('Ctrl Pts',(62.4206406487427,-4.05247163247362,
136.51538572624));
#253374=CARTESIAN_POINT('Ctrl Pts',(62.1421930249296,2.61438726408988,137.300768344709));
#253375=CARTESIAN_POINT('Ctrl Pts',(61.8637454011169,6.87875198487314,132.116269629093));
#253376=CARTESIAN_POINT('Ctrl Pts',(61.5852977773038,4.82187967727427,125.726190622201));
#253377=CARTESIAN_POINT('Ctrl Pts',(61.3068501534911,-1.66606449182178,
124.002701758653));
#253378=CARTESIAN_POINT('Ctrl Pts',(61.0284025296781,-6.62297678470872,
128.529605106938));
#253379=CARTESIAN_POINT('Ctrl Pts',(60.7499549058653,-5.49369696285183,
135.146897641504));
#253380=CARTESIAN_POINT('Ctrl Pts',(60.4715072820523,0.684021985849089,
137.773610795799));
#253381=CARTESIAN_POINT('Ctrl Pts',(60.1930596582395,6.23315814588628,133.995923503096));
#253382=CARTESIAN_POINT('Ctrl Pts',(59.9146120344266,6.05432647655821,127.285345835106));
#253383=CARTESIAN_POINT('Ctrl Pts',(59.6361644106137,0.311864545564345,
123.808570838767));
#253384=CARTESIAN_POINT('Ctrl Pts',(59.3577167868007,-5.71718566737322,
126.760584885814));
#253385=CARTESIAN_POINT('Ctrl Pts',(59.0792691629879,-6.49242155204172,
133.428631280914));
#253386=CARTESIAN_POINT('Ctrl Pts',(58.800821539175,-1.30143920280946,137.685101139145));
#253387=CARTESIAN_POINT('Ctrl Pts',(58.5223739153621,5.08550219496502,135.618506600908));
#253388=CARTESIAN_POINT('Ctrl Pts',(58.2439262915492,6.79911551616065,129.127947088084));
#253389=CARTESIAN_POINT('Ctrl Pts',(57.9654786677363,2.26467383326308,124.1779297115));
#253390=CARTESIAN_POINT('Ctrl Pts',(57.6870310439234,-4.35089246693584,
125.317278618444));
#253391=CARTESIAN_POINT('Ctrl Pts',(57.4085834201106,-6.96820114293417,
131.498987823723));
#253392=CARTESIAN_POINT('Ctrl Pts',(57.1301357962976,-3.18207338412696,
137.042368560968));
#253393=CARTESIAN_POINT('Ctrl Pts',(56.8516881724848,3.52822436176609,136.853324741857));
#253394=CARTESIAN_POINT('Ctrl Pts',(56.5732405486719,6.9962562825383,131.105578400848));
#253395=CARTESIAN_POINT('Ctrl Pts',(56.294792924859,4.03507046577855,125.081027632309));
#253396=CARTESIAN_POINT('Ctrl Pts',(56.0163453010462,-2.63414798488075,
124.315940276861));
#253397=CARTESIAN_POINT('Ctrl Pts',(55.7378976772331,-6.8827131227178,129.513394237565));
#253398=CARTESIAN_POINT('Ctrl Pts',(55.4594500534204,-4.80640114000575,
135.897183234276));
#253399=CARTESIAN_POINT('Ctrl Pts',(55.1810024296073,1.68675868462211,137.600917044446));
#253400=CARTESIAN_POINT('Ctrl Pts',(54.9025548057946,6.62986968082513,133.058947528554));
#253401=CARTESIAN_POINT('Ctrl Pts',(54.6241071819816,5.4804543274898,126.445122784157));
#253402=CARTESIAN_POINT('Ctrl Pts',(54.3456595581689,-0.705230817730614,
123.837224648055));
#253403=CARTESIAN_POINT('Ctrl Pts',(54.0672119343557,-6.24284329389726,
127.63178410442));
#253404=CARTESIAN_POINT('Ctrl Pts',(53.7887643105431,-6.04358776282204,
134.341786387386));
#253405=CARTESIAN_POINT('Ctrl Pts',(53.51031668673,-0.290570323389535,137.801067200743));
#253406=CARTESIAN_POINT('Ctrl Pts',(53.2318690629172,5.72946704808866,134.830716472279));
#253407=CARTESIAN_POINT('Ctrl Pts',(52.9534214391043,6.48440410239917,128.160341411752));
#253408=CARTESIAN_POINT('Ctrl Pts',(52.6749738152913,1.28049056735643,123.919690833848));
#253409=CARTESIAN_POINT('Ctrl Pts',(52.3965261914786,-5.10013124364513,
126.005715452363));
#253410=CARTESIAN_POINT('Ctrl Pts',(52.1180785676656,-6.79398159699943,
132.501460550851));
#253411=CARTESIAN_POINT('Ctrl Pts',(51.8396309438527,-2.24449476716385,
137.43765371859));
#253412=CARTESIAN_POINT('Ctrl Pts',(51.5611833200399,4.36757310402998,136.278174580871));
#253413=CARTESIAN_POINT('Ctrl Pts',(51.2827356962269,6.96605466042841,130.088527821552));
#253414=CARTESIAN_POINT('Ctrl Pts',(51.0042880724141,3.16307229458231,124.556696431394));
#253415=CARTESIAN_POINT('Ctrl Pts',(50.7258404486012,-3.54661898531293,
124.766163212963));
#253416=CARTESIAN_POINT('Ctrl Pts',(50.4473928247883,-6.99714067967511,
130.52443842702));
#253417=CARTESIAN_POINT('Ctrl Pts',(50.1689452009753,-4.0176319187415,136.539948459229));
#253418=CARTESIAN_POINT('Ctrl Pts',(49.8904975771625,2.65388430328469,137.284733463992));
#253419=CARTESIAN_POINT('Ctrl Pts',(49.6120499533496,6.88661050004828,132.074372406703));
#253420=CARTESIAN_POINT('Ctrl Pts',(49.3336023295367,4.79087807689359,125.696932558722));
#253421=CARTESIAN_POINT('Ctrl Pts',(49.0551547057238,-1.7074372515208,124.012969585086));
#253422=CARTESIAN_POINT('Ctrl Pts',(48.776707081911,-6.63670115873435,128.569963192402));
#253423=CARTESIAN_POINT('Ctrl Pts',(48.498259458098,-5.46716092194746,135.180258877061));
#253424=CARTESIAN_POINT('Ctrl Pts',(48.2198118342852,0.72643311645002,137.769317835757));
#253425=CARTESIAN_POINT('Ctrl Pts',(47.9413642104722,6.25247060906043,133.957921368012));
#253426=CARTESIAN_POINT('Ctrl Pts',(47.6629165866595,6.03279306211481,127.248556630613));
#253427=CARTESIAN_POINT('Ctrl Pts',(47.3844689628464,0.269273409411107,
123.806802046542));
#253428=CARTESIAN_POINT('Ctrl Pts',(47.1060213390337,-5.74169535180415,
126.7954619395));
#253429=CARTESIAN_POINT('Ctrl Pts',(46.8275737152206,-6.47632658212296,
133.468103872012));
#253430=CARTESIAN_POINT('Ctrl Pts',(46.5491260914079,-1.25953006961336,
137.69289588478));
#253431=CARTESIAN_POINT('Ctrl Pts',(46.2706784675948,5.11471304540623,135.587460510634));
#253432=CARTESIAN_POINT('Ctrl Pts',(45.9922308437821,6.78878473932087,129.086590002178));
#253433=CARTESIAN_POINT('Ctrl Pts',(45.7137832199691,2.22429490837156,124.164266771503));
#253434=CARTESIAN_POINT('Ctrl Pts',(45.4353355961562,-4.38421328052394,
125.343865398741));
#253435=CARTESIAN_POINT('Ctrl Pts',(45.1568879723434,-6.96384364534361,
131.541392372057));
#253436=CARTESIAN_POINT('Ctrl Pts',(44.8784403485304,-3.1440419027679,137.061623168999));
#253437=CARTESIAN_POINT('Ctrl Pts',(44.5999927247176,3.56498075346585,136.831735365442));
#253438=CARTESIAN_POINT('Ctrl Pts',(44.3215451009046,6.99796025625624,131.062984622213));
#253439=CARTESIAN_POINT('Ctrl Pts',(44.0430974770918,4.00015615291162,125.056571053198));
#253440=CARTESIAN_POINT('Ctrl Pts',(43.7646498532789,-2.67359603646683,
124.332095298706));
#253441=CARTESIAN_POINT('Ctrl Pts',(43.486202229466,-6.8904440807599,129.555315184507));
#253442=CARTESIAN_POINT('Ctrl Pts',(43.2077546056531,-4.77531063174146,
135.926346804027));
#253443=CARTESIAN_POINT('Ctrl Pts',(42.9293069818402,1.72810000095366,137.590523341125));
#253444=CARTESIAN_POINT('Ctrl Pts',(42.6508593580274,6.64347115515083,133.018547857752));
#253445=CARTESIAN_POINT('Ctrl Pts',(42.3724117342144,5.4538168693733,126.411842469708));
#253446=CARTESIAN_POINT('Ctrl Pts',(42.0939641104015,-0.74762868559244,
123.841646673103));
#253447=CARTESIAN_POINT('Ctrl Pts',(41.8155164865887,-6.26204000219037,
127.669844843974));
#253448=CARTESIAN_POINT('Ctrl Pts',(41.5370688627757,-6.02194247443641,
134.378509881167));
#253449=CARTESIAN_POINT('Ctrl Pts',(41.2586212389629,-0.247974000920424,
137.802706352008));
#253450=CARTESIAN_POINT('Ctrl Pts',(40.9801736151499,5.75387046523817,134.795764981093));
#253451=CARTESIAN_POINT('Ctrl Pts',(40.7017259913371,6.46818906604193,128.120917991039));
#253452=CARTESIAN_POINT('Ctrl Pts',(40.4232783675241,1.23855790375582,123.912023681303));
#253453=CARTESIAN_POINT('Ctrl Pts',(40.1448307437113,-5.12924746516435,
126.036850306614));
#253454=CARTESIAN_POINT('Ctrl Pts',(39.8663831198984,-6.78352499126783,
132.542786001862));
#253455=CARTESIAN_POINT('Ctrl Pts',(39.5879354960856,-2.20407444401526,
137.451193695743));
#253456=CARTESIAN_POINT('Ctrl Pts',(39.3094878722726,4.40081284226458,136.251486506627));
#253457=CARTESIAN_POINT('Ctrl Pts',(39.0310402484598,6.96156811816289,130.046136732356));
#253458=CARTESIAN_POINT('Ctrl Pts',(38.7525926246468,3.12498238497894,124.537557667297));
#253459=CARTESIAN_POINT('Ctrl Pts',(38.474145000834,-3.58330949612422,124.78786436319));
#253460=CARTESIAN_POINT('Ctrl Pts',(38.195697377021,-6.9987150046898,130.567037194673));
#253461=CARTESIAN_POINT('Ctrl Pts',(37.9172497532082,-3.98264333018119,
136.564298657899));
#253462=CARTESIAN_POINT('Ctrl Pts',(37.6388021293952,2.69328300182069,137.268458450676));
#253463=CARTESIAN_POINT('Ctrl Pts',(37.3603545055824,6.89421382933879,132.032428123559));
#253464=CARTESIAN_POINT('Ctrl Pts',(37.0819068817695,4.7596989487639,125.667863752866));
#253465=CARTESIAN_POINT('Ctrl Pts',(36.8034592579566,-1.74874674150458,
124.02348906901));
#253466=CARTESIAN_POINT('Ctrl Pts',(36.5250116341437,-6.65017960735793,
128.610404074285));
#253467=CARTESIAN_POINT('Ctrl Pts',(36.2465640103308,-5.44042229338459,
135.213457962098));
#253468=CARTESIAN_POINT('Ctrl Pts',(35.968116386518,0.768817328804687,137.764766786667));
#253469=CARTESIAN_POINT('Ctrl Pts',(35.689668762705,6.27155138463682,133.919802376575));
#253470=CARTESIAN_POINT('Ctrl Pts',(35.4112211388921,6.01103610030595,127.211899187745));
#253471=CARTESIAN_POINT('Ctrl Pts',(35.1327735150793,0.226672295232647,
123.805292551423));
#253472=CARTESIAN_POINT('Ctrl Pts',(34.8543258912663,-5.76599227560232,
126.830487544402));
#253473=CARTESIAN_POINT('Ctrl Pts',(34.5758782674535,-6.45999162954105,
133.507477757125));
#253474=CARTESIAN_POINT('Ctrl Pts',(34.2974306436406,-1.21757426406734,
137.700435373207));
#253475=CARTESIAN_POINT('Ctrl Pts',(34.0189830198277,5.1437343682746,135.556237180835));
#253476=CARTESIAN_POINT('Ctrl Pts',(33.7405353960148,6.778202401566,129.045296568894));
#253477=CARTESIAN_POINT('Ctrl Pts',(33.4620877722019,2.18383356141425,124.150849882625));
#253478=CARTESIAN_POINT('Ctrl Pts',(33.1836401483891,-4.41737163547663,
125.370654519698));
#253479=CARTESIAN_POINT('Ctrl Pts',(32.9051925245761,-6.95922809996586,
131.58376960941));
#253480=CARTESIAN_POINT('Ctrl Pts',(32.6267449007632,-3.10589391777991,
137.080645911863));
#253481=CARTESIAN_POINT('Ctrl Pts',(32.3482972769504,3.60160504349277,136.80992264244));
#253482=CARTESIAN_POINT('Ctrl Pts',(32.0698496531375,6.99940491798352,131.020381260171));
#253483=CARTESIAN_POINT('Ctrl Pts',(31.7914020293246,3.96509361278713,125.032327460544));
#253484=CARTESIAN_POINT('Ctrl Pts',(31.5129544055117,-2.71294501696876,
124.348490152723));
#253485=CARTESIAN_POINT('Ctrl Pts',(31.2345067816988,-6.89791971086261,
129.597282415287));
#253486=CARTESIAN_POINT('Ctrl Pts',(30.9560591578859,-4.74404317258561,
135.955320576696));
#253487=CARTESIAN_POINT('Ctrl Pts',(30.677611534073,1.76937728190418,137.579878174048));
#253488=CARTESIAN_POINT('Ctrl Pts',(30.3991639102601,6.65682645320975,132.978066139427));
#253489=CARTESIAN_POINT('Ctrl Pts',(30.1207162864473,5.42697731806706,126.378724921634));
#253490=CARTESIAN_POINT('Ctrl Pts',(29.8422686626343,-0.789998849798377,
123.846326704078));
#253491=CARTESIAN_POINT('Ctrl Pts',(29.5638210388214,-6.28100466828836,
127.708021734164));
#253492=CARTESIAN_POINT('Ctrl Pts',(29.2853734150086,-6.00007404075783,
134.415100933532));
#253493=CARTESIAN_POINT('Ctrl Pts',(29.0069257911957,-0.205368489683527,
137.804086176998));
#253494=CARTESIAN_POINT('Ctrl Pts',(28.7284781673828,5.77806067060162,134.760665586949));
#253495=CARTESIAN_POINT('Ctrl Pts',(28.4500305435699,6.45173434856014,128.08159400628));
#253496=CARTESIAN_POINT('Ctrl Pts',(28.171582919757,1.19657934493693,123.904611926838));
#253497=CARTESIAN_POINT('Ctrl Pts',(27.8931352959441,-5.15817362053239,
126.068161822712));
#253498=CARTESIAN_POINT('Ctrl Pts',(27.6146876721312,-6.77281701952304,
132.584047034882));
#253499=CARTESIAN_POINT('Ctrl Pts',(27.3362400483183,-2.16357244807759,
137.464487372053));
#253500=CARTESIAN_POINT('Ctrl Pts',(27.0577924245054,4.4338895067609,136.22459658713));
#253501=CARTESIAN_POINT('Ctrl Pts',(26.7793448006925,6.95682361243065,130.003773739425));
#253502=CARTESIAN_POINT('Ctrl Pts',(26.5008971768797,3.08677667800406,124.518651121888));
#253503=CARTESIAN_POINT('Ctrl Pts',(26.2224495530668,-3.61986722608435,
124.809788456898));
#253504=CARTESIAN_POINT('Ctrl Pts',(25.9440019292538,-7.00002998974624,
130.609644756432));
#253505=CARTESIAN_POINT('Ctrl Pts',(25.665554305441,-3.94750716330764,136.588435419948));
#253506=CARTESIAN_POINT('Ctrl Pts',(25.3871066816281,2.7325818997646,137.251943907838));
#253507=CARTESIAN_POINT('Ctrl Pts',(25.1086590578152,6.90156169100052,131.990438333922));
#253508=CARTESIAN_POINT('Ctrl Pts',(24.8302114340022,4.72834344823931,125.638985281792));
#253509=CARTESIAN_POINT('Ctrl Pts',(24.5517638101894,-1.78999143103474,
124.034259820624));
#253510=CARTESIAN_POINT('Ctrl Pts',(24.2733161863765,-6.66341163113055,
128.650926254035));
#253511=CARTESIAN_POINT('Ctrl Pts',(23.9948685625636,-5.41348206797292,
135.246493666413));
#253512=CARTESIAN_POINT('Ctrl Pts',(23.7164209387507,0.811173052350488,
137.759957817164));
#253513=CARTESIAN_POINT('Ctrl Pts',(23.4379733149379,6.29039976557031,133.881567941299));
#253514=CARTESIAN_POINT('Ctrl Pts',(23.159525691125,5.98905639734383,127.175374864857));
#253515=CARTESIAN_POINT('Ctrl Pts',(22.8810780673121,0.184062781628937,
123.804042409345));
#253516=CARTESIAN_POINT('Ctrl Pts',(22.6026304434992,-5.79007553843628,
126.865660402631));
#253517=CARTESIAN_POINT('Ctrl Pts',(22.3241828196863,-6.44341729959363,
133.546751477239));
#253518=CARTESIAN_POINT('Ctrl Pts',(22.0457351958734,-1.17557334085921,
137.707719325048));
#253519=CARTESIAN_POINT('Ctrl Pts',(21.7672875720605,5.17256508817436,135.524837768503));
#253520=CARTESIAN_POINT('Ctrl Pts',(21.4888399482477,6.76736889502847,129.004068318375));
#253521=CARTESIAN_POINT('Ctrl Pts',(21.2103923244347,2.14329129170119,124.137679542035));
#253522=CARTESIAN_POINT('Ctrl Pts',(20.9319447006219,-4.45036630309889,
125.397644988631));
#253523=CARTESIAN_POINT('Ctrl Pts',(20.6534970768089,-6.95435467783159,
131.626117965476));
#253524=CARTESIAN_POINT('Ctrl Pts',(20.3750494529961,-3.06763084275059,
137.099436084669));
#253525=CARTESIAN_POINT('Ctrl Pts',(20.0966018291831,3.6380958747203,136.787887381128));
#253526=CARTESIAN_POINT('Ctrl Pts',(19.8181542053702,7.00059021418742,130.977769893405));
#253527=CARTESIAN_POINT('Ctrl Pts',(19.5397065815574,3.92988414466092,125.0082977527));
#253528=CARTESIAN_POINT('Ctrl Pts',(19.2612589577445,-2.75219346829522,
124.365124231394));
#253529=CARTESIAN_POINT('Ctrl Pts',(18.9828113339316,-6.90513973601376,
129.639294374793));
#253530=CARTESIAN_POINT('Ctrl Pts',(18.7043637101187,-4.71259992116536,
135.98410347865));
#253531=CARTESIAN_POINT('Ctrl Pts',(18.4259160863058,1.81058899792882,137.568981937677));
#253532=CARTESIAN_POINT('Ctrl Pts',(18.1474684624929,6.6699350801164,132.937503873645));
#253533=CARTESIAN_POINT('Ctrl Pts',(17.86902083868,5.39993666812053,126.345771367118));
#253534=CARTESIAN_POINT('Ctrl Pts',(17.5905732148672,-0.832339740306418,
123.851264567558));
#253535=CARTESIAN_POINT('Ctrl Pts',(17.3121255910542,-6.29973658944851,
127.746313360329));
#253536=CARTESIAN_POINT('Ctrl Pts',(17.0336779672413,-5.97798327212915,
134.451558188587));
#253537=CARTESIAN_POINT('Ctrl Pts',(16.7552303434285,-0.162755368441711,
137.805206624583));
#253538=CARTESIAN_POINT('Ctrl Pts',(16.4767827196156,5.80203676780203,134.72541959047));
#253539=CARTESIAN_POINT('Ctrl Pts',(16.1983350958026,6.43504055968944,128.042370914639));
#253540=CARTESIAN_POINT('Ctrl Pts',(15.9198874719898,1.15455644643036,123.897455845098));
#253541=CARTESIAN_POINT('Ctrl Pts',(15.6414398481769,-5.18690863788001,
126.0996488404));
#253542=CARTESIAN_POINT('Ctrl Pts',(15.362992224364,-6.7618580785529,132.625242120967));
#253543=CARTESIAN_POINT('Ctrl Pts',(15.0845446005511,-2.12299028016722,
137.477534254917));
#253544=CARTESIAN_POINT('Ctrl Pts',(14.8060969767383,4.466801871851,136.197505818795));
#253545=CARTESIAN_POINT('Ctrl Pts',(14.5276493529253,6.95182131904109,129.961440412534));
#253546=CARTESIAN_POINT('Ctrl Pts',(14.2492017291125,3.04845658938423,124.499977495755));
#253547=CARTESIAN_POINT('Ctrl Pts',(13.9707541052995,-3.65629082053323,
124.831934681683));
#253548=CARTESIAN_POINT('Ctrl Pts',(13.6923064814867,-7.00108558611715,
130.652259533458));
#253549=CARTESIAN_POINT('Ctrl Pts',(13.4138588576738,-3.91222472010448,
136.612357850978));
#253550=CARTESIAN_POINT('Ctrl Pts',(13.1354112338608,2.77177954088132,137.23519044743));
#253551=CARTESIAN_POINT('Ctrl Pts',(12.856963610048,6.90865381275575,131.94840459374));
#253552=CARTESIAN_POINT('Ctrl Pts',(12.5785159862351,4.6968127372094,125.6102982156));
#253553=CARTESIAN_POINT('Ctrl Pts',(12.3000683624222,-1.83116979177416,
124.045281440813));
#253554=CARTESIAN_POINT('Ctrl Pts',(12.0216207386093,-6.67639673973472,
128.691528230086));
#253555=CARTESIAN_POINT('Ctrl Pts',(11.7431731147965,-5.38634124399241,
135.279364765853));
#253556=CARTESIAN_POINT('Ctrl Pts',(11.4647254909835,0.853498717580522,
137.75489110545));
#253557=CARTESIAN_POINT('Ctrl Pts',(11.1862778671706,6.30901505342741,133.843219478972));
#253558=CARTESIAN_POINT('Ctrl Pts',(10.9078302433578,5.96685476769427,127.13898501537));
#253559=CARTESIAN_POINT('Ctrl Pts',(10.6293826195448,0.141446447510913,
123.803051666633));
#253560=CARTESIAN_POINT('Ctrl Pts',(10.350934995732,-5.81394424789186,126.900979210845));
#253561=CARTESIAN_POINT('Ctrl Pts',(10.0724873719191,-6.42660420644864,
133.585923577051));
#253562=CARTESIAN_POINT('Ctrl Pts',(9.79403974810624,-1.1335288563486,137.714747470394));
#253563=CARTESIAN_POINT('Ctrl Pts',(9.51559212429333,5.20120413677258,135.493263437154));
#253564=CARTESIAN_POINT('Ctrl Pts',(9.23714450048043,6.75628462114785,128.962906778349));
#253565=CARTESIAN_POINT('Ctrl Pts',(8.95869687666756,2.10266960154115,124.124756237763));
#253566=CARTESIAN_POINT('Ctrl Pts',(8.68024925285465,-4.48319606076117,
125.4248358054));
#253567=CARTESIAN_POINT('Ctrl Pts',(8.40180162904178,-6.94922355952728,
131.66843587102));
#253568=CARTESIAN_POINT('Ctrl Pts',(8.12335400522884,-3.0292540955323,137.117992991138));
#253569=CARTESIAN_POINT('Ctrl Pts',(7.84490638141603,3.67445189496732,136.765630398031));
#253570=CARTESIAN_POINT('Ctrl Pts',(7.56645875760307,7.00151610094645,130.935152100895));
#253571=CARTESIAN_POINT('Ctrl Pts',(7.2880111337902,3.89452905323253,124.984482820099));
#253572=CARTESIAN_POINT('Ctrl Pts',(7.00956350997733,-2.79133993608059,
124.381996918337));
#253573=CARTESIAN_POINT('Ctrl Pts',(6.73111588616443,-6.91210388867261,
129.681349506257));
#253574=CARTESIAN_POINT('Ctrl Pts',(6.45266826235151,-4.68098204262199,
136.012694443327));
#253575=CARTESIAN_POINT('Ctrl Pts',(6.17422063853866,1.85173362191231,137.557835035774));
#253576=CARTESIAN_POINT('Ctrl Pts',(5.89577301472578,6.68279655012581,132.896862563455));
#253577=CARTESIAN_POINT('Ctrl Pts',(5.61732539091285,5.37269592153495,126.312983027266));
#253578=CARTESIAN_POINT('Ctrl Pts',(5.33887776709996,-0.874649788159289,
123.856460080569));
#253579=CARTESIAN_POINT('Ctrl Pts',(5.06043014328709,-6.31823507155263,
127.784718303561));
#253580=CARTESIAN_POINT('Ctrl Pts',(4.7819825194742,-5.95567098713191,134.487880295395));
#253581=CARTESIAN_POINT('Ctrl Pts',(4.50353489566127,-0.120136216239877,
137.806067653244));
#253582=CARTESIAN_POINT('Ctrl Pts',(4.22508727184843,5.82579786839633,134.690028297709));
#253583=CARTESIAN_POINT('Ctrl Pts',(3.94663964803551,6.41810831802433,128.003250169541));
#253584=CARTESIAN_POINT('Ctrl Pts',(3.66819202422262,1.11249076541009,123.890555701254));
#253585=CARTESIAN_POINT('Ctrl Pts',(3.3897444004097,-5.21545145242058,126.131310192911));
#253586=CARTESIAN_POINT('Ctrl Pts',(3.11129677659686,-6.75064857444498,
132.666369733619));
#253587=CARTESIAN_POINT('Ctrl Pts',(2.83284915278395,-2.08232944407128,
137.490333860877));
#253588=CARTESIAN_POINT('Ctrl Pts',(2.55440152897106,4.49954871795507,136.170215205482));
#253589=CARTESIAN_POINT('Ctrl Pts',(2.27595390515816,6.94656142335602,129.919138320362));
#253590=CARTESIAN_POINT('Ctrl Pts',(1.9975062813453,3.01002353908442,124.481537480858));
#253591=CARTESIAN_POINT('Ctrl Pts',(1.71905865753238,-3.69257892978116,
124.854302216906));
#253592=CARTESIAN_POINT('Ctrl Pts',(1.44061103371947,-7.00188175468703,
130.694879946647));
#253593=CARTESIAN_POINT('Ctrl Pts',(1.16216340990662,-3.87679730797559,
136.636065064534));
#253594=CARTESIAN_POINT('Ctrl Pts',(0.883715786093727,2.81087447268782,
137.218198690258));
#253595=CARTESIAN_POINT('Ctrl Pts',(0.605268162280799,6.91548993180329,
131.906328460586));
#253596=CARTESIAN_POINT('Ctrl Pts',(0.326820538467947,4.66510798405627,
125.5818036173));
#253597=CARTESIAN_POINT('Ctrl Pts',(0.0483729146550416,-1.87228029784353,
124.056553521165));
#253598=CARTESIAN_POINT('Ctrl Pts',(-0.23007470915786,-6.68913445200245,
128.732208497919));
#253599=CARTESIAN_POINT('Ctrl Pts',(-0.508522332970751,-5.35900082715629,
135.312070042369));
#253600=CARTESIAN_POINT('Ctrl Pts',(-0.786969956783612,0.895792756101716,
137.749566839272));
#253601=CARTESIAN_POINT('Ctrl Pts',(-1.06541758059653,6.32739655841135,
133.804758410613));
#253602=CARTESIAN_POINT('Ctrl Pts',(-1.34386520440944,5.94443203404716,
127.102730987725));
#253603=CARTESIAN_POINT('Ctrl Pts',(-1.62231282822229,0.0988248720430084,
123.802320359999));
#253604=CARTESIAN_POINT('Ctrl Pts',(-1.90076045203519,-5.83759751950527,
126.936442660293));
#253605=CARTESIAN_POINT('Ctrl Pts',(-2.17920807584809,-6.40955297312139,
133.624992605024));
#253606=CARTESIAN_POINT('Ctrl Pts',(-2.45765569966099,-1.09144236850938,
137.721519548813));
#253607=CARTESIAN_POINT('Ctrl Pts',(-2.73610332347384,5.22965045283876,
135.461515356786));
#253608=CARTESIAN_POINT('Ctrl Pts',(-3.01455094728676,6.74494999065597,
128.921813474073));
#253609=CARTESIAN_POINT('Ctrl Pts',(-3.29299857109967,2.06196999618574,
124.112080448687));
#253610=CARTESIAN_POINT('Ctrl Pts',(-3.57144619491253,-4.51585969194472,
125.452225962441));
#253611=CARTESIAN_POINT('Ctrl Pts',(-3.84989381872542,-6.94383493518842,
131.710721757939));
#253612=CARTESIAN_POINT('Ctrl Pts',(-4.12834144253832,-2.99076509818949,
137.136315943637));
#253613=CARTESIAN_POINT('Ctrl Pts',(-4.40678906635123,3.71067175704807,
136.743152517891));
#253614=CARTESIAN_POINT('Ctrl Pts',(-4.68523669016409,7.00218254395157,
130.892529461858));
#253615=CARTESIAN_POINT('Ctrl Pts',(-4.963684313977,3.85902964859785,124.960883545208));
#253616=CARTESIAN_POINT('Ctrl Pts',(-5.24213193778992,-2.83038296973812,
124.399107588329));
#253617=CARTESIAN_POINT('Ctrl Pts',(-5.52057956160276,-6.91881191077996,
129.723446251312));
#253618=CARTESIAN_POINT('Ctrl Pts',(-5.79902718541567,-4.6491907085676,
136.041092411279));
#253619=CARTESIAN_POINT('Ctrl Pts',(-6.07747480922856,1.89280962922548,
137.546437881394));
#253620=CARTESIAN_POINT('Ctrl Pts',(-6.35592243304147,6.69541038665145,
132.856143714835));
#253621=CARTESIAN_POINT('Ctrl Pts',(-6.63437005685431,5.34525608772619,
126.280361117063));
#253622=CARTESIAN_POINT('Ctrl Pts',(-6.91281768066725,-0.916927425542613,
123.86191305059));
#253623=CARTESIAN_POINT('Ctrl Pts',(-7.19126530448013,-6.33649942913263,
127.823235140749));
#253624=CARTESIAN_POINT('Ctrl Pts',(-7.469712928293,-5.93313801255607,134.524065908027));
#253625=CARTESIAN_POINT('Ctrl Pts',(-7.74816055210589,-0.0775126123463511,
137.806669231077));
#253626=CARTESIAN_POINT('Ctrl Pts',(-8.02660817591882,5.84934309190818,
134.654493020103));
#253627=CARTESIAN_POINT('Ctrl Pts',(-8.3050557997317,6.40093825099524,127.964233220621));
#253628=CARTESIAN_POINT('Ctrl Pts',(-8.58350342354456,1.07038386063539,
123.883911750995));
#253629=CARTESIAN_POINT('Ctrl Pts',(-8.86195104735747,-5.2438010064896,
126.163144707024));
#253630=CARTESIAN_POINT('Ctrl Pts',(-9.14039867117038,-6.73918892257159,
132.707428348838));
#253631=CARTESIAN_POINT('Ctrl Pts',(-9.41884629498326,-2.04159144649203,
137.50288571564));
#253632=CARTESIAN_POINT('Ctrl Pts',(-9.69729391879612,4.53212883162697,
136.142725758454));
#253633=CARTESIAN_POINT('Ctrl Pts',(-9.97574154260907,6.94104412028278,
129.876869030427));
#253634=CARTESIAN_POINT('Ctrl Pts',(-10.254189166422,2.97147895125515,124.463331760497));
#253635=CARTESIAN_POINT('Ctrl Pts',(-10.5326367902348,-3.72873020915888,
124.876890233732));
#253636=CARTESIAN_POINT('Ctrl Pts',(-10.8110844140478,-7.00241846595355,
130.737504416682));
#253637=CARTESIAN_POINT('Ctrl Pts',(-11.0895320378606,-3.84122623969676,
136.659556182137));
#253638=CARTESIAN_POINT('Ctrl Pts',(-11.3679796616735,2.84986524650705,
137.200969265957));
#253639=CARTESIAN_POINT('Ctrl Pts',(-11.6464272854864,6.92206979482823,
131.864211493609));
#253640=CARTESIAN_POINT('Ctrl Pts',(-11.9248749092993,4.6332303636112,125.553502542771));
#253641=CARTESIAN_POINT('Ctrl Pts',(-12.2033225331122,-1.91332142587795,
124.068075643991));
#253642=CARTESIAN_POINT('Ctrl Pts',(-12.4817701569251,-6.70162429593314,
128.77296555011));
#253643=CARTESIAN_POINT('Ctrl Pts',(-12.760217780738,-5.33146183057377,
135.344608284054));
#253644=CARTESIAN_POINT('Ctrl Pts',(-13.0386654045509,0.938053600692905,
137.743985215925));
#253645=CARTESIAN_POINT('Ctrl Pts',(-13.3171130283637,6.34554359938892,
133.766186161411));
#253646=CARTESIAN_POINT('Ctrl Pts',(-13.5955606521767,5.92178902728497,
127.066614125326));
#253647=CARTESIAN_POINT('Ctrl Pts',(-13.8740082759896,0.0561996345831295,
123.801848516541));
#253648=CARTESIAN_POINT('Ctrl Pts',(-14.1524558998025,-5.86103447679583,
126.972049436864));
#253649=CARTESIAN_POINT('Ctrl Pts',(-14.4309035236153,-6.39226423145161,
133.663957113442));
#253650=CARTESIAN_POINT('Ctrl Pts',(-14.7093511474282,-1.04931543687181,
137.728035309365));
#253651=CARTESIAN_POINT('Ctrl Pts',(-14.9877987712411,5.25790298228423,
135.429594703837));
#253652=CARTESIAN_POINT('Ctrl Pts',(-15.266246395054,6.73336542356173,128.880789928272));
#253653=CARTESIAN_POINT('Ctrl Pts',(-15.5446940188669,2.02119398377386,
124.099652644515));
#253654=CARTESIAN_POINT('Ctrl Pts',(-15.8231416426798,-4.54835598628669,
125.479814444798));
#253655=CARTESIAN_POINT('Ctrl Pts',(-16.1015892664927,-6.93818900449243,
131.752974059312));
#253656=CARTESIAN_POINT('Ctrl Pts',(-16.3800368903055,-2.95216527694612,
137.154404263204));
#253657=CARTESIAN_POINT('Ctrl Pts',(-16.6584845141185,3.74675411882228,
136.720454573632));
#253658=CARTESIAN_POINT('Ctrl Pts',(-16.9369321379314,7.00258951850748,
130.849903555692));
#253659=CARTESIAN_POINT('Ctrl Pts',(-17.2153797617442,3.82338724620039,
124.93750080251));
#253660=CARTESIAN_POINT('Ctrl Pts',(-17.4938273855571,-2.86932112251383,
124.416455607327));
#253661=CARTESIAN_POINT('Ctrl Pts',(-17.77227500937,-6.92526355376757,129.765583050046));
#253662=CARTESIAN_POINT('Ctrl Pts',(-18.0507226331829,-4.61722709704176,
136.069296330209));
#253663=CARTESIAN_POINT('Ctrl Pts',(-18.3291702569958,1.93381549778173,
137.534790896862));
#253664=CARTESIAN_POINT('Ctrl Pts',(-18.6076178808087,6.70777612228299,
132.81534883664));
#253665=CARTESIAN_POINT('Ctrl Pts',(-18.8860655046216,5.31761818348739,
126.247906845325));
#253666=CARTESIAN_POINT('Ctrl Pts',(-19.1645131284344,-0.959171085842972,
123.867623275557));
#253667=CARTESIAN_POINT('Ctrl Pts',(-19.4429607522474,-6.35452898539608,
127.861862444637));
#253668=CARTESIAN_POINT('Ctrl Pts',(-19.7214083760603,-5.91038518336925,
134.560113685611));
#253669=CARTESIAN_POINT('Ctrl Pts',(-19.9998559998732,-0.0348861361944895,
137.807011335788));
#253670=CARTESIAN_POINT('Ctrl Pts',(-20.278303623686,5.87267156586067,134.618815074426));
#253671=CARTESIAN_POINT('Ctrl Pts',(-20.5567512474989,6.38353099484532,
127.925321513668));
#253672=CARTESIAN_POINT('Ctrl Pts',(-20.8351988713118,1.02823729239309,
123.877524240513));
#253673=CARTESIAN_POINT('Ctrl Pts',(-21.1136464951247,-5.27195624958391,
126.1951512031));
#253674=CARTESIAN_POINT('Ctrl Pts',(-21.3920941189376,-6.72747954757436,
132.748416445183));
#253675=CARTESIAN_POINT('Ctrl Pts',(-21.6705417427505,-2.00077779699093,
137.515189354092));
#253676=CARTESIAN_POINT('Ctrl Pts',(-21.9489893665634,4.56454100559805,
136.115038496344));
#253677=CARTESIAN_POINT('Ctrl Pts',(-22.2274369903762,6.93526961426714,
129.834634109035));
#253678=CARTESIAN_POINT('Ctrl Pts',(-22.5058846141892,2.93282425418085,
124.445361009293));
#253679=CARTESIAN_POINT('Ctrl Pts',(-22.784332238002,-3.76474331906749,
124.899697895151));
#253680=CARTESIAN_POINT('Ctrl Pts',(-23.062779861815,-7.0026957000287,130.780131364099));
#253681=CARTESIAN_POINT('Ctrl Pts',(-23.3412274856278,-3.80551283336702,
136.682830333316));
#253682=CARTESIAN_POINT('Ctrl Pts',(-23.6196751094408,2.88875041752152,
137.183502812971));
#253683=CARTESIAN_POINT('Ctrl Pts',(-23.8981227332536,6.92839315801137,
131.822055253468));
#253684=CARTESIAN_POINT('Ctrl Pts',(-24.1765703570665,4.60118105711114,
125.525396040718));
#253685=CARTESIAN_POINT('Ctrl Pts',(-24.4550179808794,-1.95429165508329,
124.079847382335));
#253686=CARTESIAN_POINT('Ctrl Pts',(-24.7334656046923,-6.71386580871103,
128.813797876394));
#253687=CARTESIAN_POINT('Ctrl Pts',(-25.0119132285052,-5.30372527471246,
135.376978285193));
#253688=CARTESIAN_POINT('Ctrl Pts',(-25.290360852318,0.980279685362951,
137.738146442235));
#253689=CARTESIAN_POINT('Ctrl Pts',(-25.568808476131,6.36345550391485,133.727504160674));
#253690=CARTESIAN_POINT('Ctrl Pts',(-25.8472560999438,5.89892658645264,
127.030635766497));
#253691=CARTESIAN_POINT('Ctrl Pts',(-26.1257037237567,0.0135723146251221,
123.801636153745));
#253692=CARTESIAN_POINT('Ctrl Pts',(-26.4041513475696,-5.88425425129846,
127.007798221134));
#253693=CARTESIAN_POINT('Ctrl Pts',(-26.6825989713826,-6.37473862207999,
133.70281565846));
#253694=CARTESIAN_POINT('Ctrl Pts',(-26.9610465951954,-1.00714962246484,
137.734294510605));
#253695=CARTESIAN_POINT('Ctrl Pts',(-27.2394942190083,5.28596067820108,
135.397502661138));
#253696=CARTESIAN_POINT('Ctrl Pts',(-27.5179418428212,6.72153134913555,
128.839837661092));
#253697=CARTESIAN_POINT('Ctrl Pts',(-27.7963894666341,1.98034307527561,
124.087473285763));
#253698=CARTESIAN_POINT('Ctrl Pts',(-28.0748370904469,-4.58068373962494,
125.507600230172));
#253699=CARTESIAN_POINT('Ctrl Pts',(-28.3532847142599,-6.93228597665136,
131.795191209466));
#253700=CARTESIAN_POINT('Ctrl Pts',(-28.6317323380727,-2.91345606213275,
137.172257279568));
#253701=CARTESIAN_POINT('Ctrl Pts',(-28.9101799618857,3.78269764324474,
136.697537406337));
#253702=CARTESIAN_POINT('Ctrl Pts',(-29.1886275856985,7.00273700953358,
130.807275961916));
#253703=CARTESIAN_POINT('Ctrl Pts',(-29.4670752095115,3.78760316678249,
124.914335458459));
#253704=CARTESIAN_POINT('Ctrl Pts',(-29.7455228333243,-2.90815295154017,
124.434040332496));
#253705=CARTESIAN_POINT('Ctrl Pts',(-30.0239704571372,-6.93145857856742,
129.807758341064));
#253706=CARTESIAN_POINT('Ctrl Pts',(-30.3024180809501,-4.5850923924679,
136.097305155009));
#253707=CARTESIAN_POINT('Ctrl Pts',(-30.580865704763,1.97474970809384,137.52289451376));
#253708=CARTESIAN_POINT('Ctrl Pts',(-30.8593133285759,6.71989329880362,
132.774479440534));
#253709=CARTESIAN_POINT('Ctrl Pts',(-31.1377609523888,5.28978323295099,
126.215621414657));
#253710=CARTESIAN_POINT('Ctrl Pts',(-31.4162085762017,-1.00137920370602,
123.873590543879));
#253711=CARTESIAN_POINT('Ctrl Pts',(-31.6946562000146,-6.37232307225107,
127.900598783877));
#253712=CARTESIAN_POINT('Ctrl Pts',(-31.9731038238274,-5.88741334268594,
134.596022292384));
#253713=CARTESIAN_POINT('Ctrl Pts',(-32.2515514476404,0.00774163267598956,
137.807093954702));
#253714=CARTESIAN_POINT('Ctrl Pts',(-32.5299990714533,5.89578242580862,
134.582995782735));
#253715=CARTESIAN_POINT('Ctrl Pts',(-32.8084466952661,6.36588719460685,
127.886516490566));
#253716=CARTESIAN_POINT('Ctrl Pts',(-33.086894319079,0.9860526224398,123.8713934065));
#253717=CARTESIAN_POINT('Ctrl Pts',(-33.365341942892,-5.29991613840065,
126.227328495126));
#253718=CARTESIAN_POINT('Ctrl Pts',(-33.6437895667048,-6.71552088334846,
132.789332503824));
#253719=CARTESIAN_POINT('Ctrl Pts',(-33.9222371905177,-1.95989000793276,
137.527244320318));
#253720=CARTESIAN_POINT('Ctrl Pts',(-34.2006848143306,4.59678403882356,
136.08715444511));
#253721=CARTESIAN_POINT('Ctrl Pts',(-34.4791324381435,6.9292381192855,129.792435121214));
#253722=CARTESIAN_POINT('Ctrl Pts',(-34.7575800619564,2.89406088022529,
124.427625893158));
#253723=CARTESIAN_POINT('Ctrl Pts',(-35.0360276857693,-3.80061692502793,
124.922724356021));
#253724=CARTESIAN_POINT('Ctrl Pts',(-35.3144753095821,-7.00271344663942,
130.822759209339));
#253725=CARTESIAN_POINT('Ctrl Pts',(-35.592922933395,-3.76965841235978,
136.705886655638));
#253726=CARTESIAN_POINT('Ctrl Pts',(-35.8713705572079,2.92752854482695,
137.165799978524));
#253727=CARTESIAN_POINT('Ctrl Pts',(-36.1498181810209,6.9344597870381,131.779861302279));
#253728=CARTESIAN_POINT('Ctrl Pts',(-36.4282658048337,4.56896125215494,
125.49748515264));
#253729=CARTESIAN_POINT('Ctrl Pts',(-36.7067134286466,-1.99518946729269,
124.091868299989));
#253730=CARTESIAN_POINT('Ctrl Pts',(-36.9851610524595,-6.72585853672236,
128.854703963711));
#253731=CARTESIAN_POINT('Ctrl Pts',(-37.2636086762724,-5.27579218736066,
135.409178846303));
#253732=CARTESIAN_POINT('Ctrl Pts',(-37.5420563000852,1.02246944540875,
137.732050734562));
#253733=CARTESIAN_POINT('Ctrl Pts',(-37.8205039238982,6.38113160825695,
133.688713841779));
#253734=CARTESIAN_POINT('Ctrl Pts',(-38.0989515477111,5.87584555872632,
126.994797244432));
#253735=CARTESIAN_POINT('Ctrl Pts',(-38.377399171524,-0.0290555082599903,
123.801683279478));
#253736=CARTESIAN_POINT('Ctrl Pts',(-38.6558467953367,-5.90725598259587,
127.04368768842));
#253737=CARTESIAN_POINT('Ctrl Pts',(-38.9342944191497,-6.35697679442443,
133.741566800161));
#253738=CARTESIAN_POINT('Ctrl Pts',(-39.2127420429625,-0.964946487758246,
137.740296920595));
#253739=CARTESIAN_POINT('Ctrl Pts',(-39.4911896667755,5.31382250090111,
135.365240417872));
#253740=CARTESIAN_POINT('Ctrl Pts',(-39.7696372905882,6.70944820589337,
128.798958190032));
#253741=CARTESIAN_POINT('Ctrl Pts',(-40.0480849144012,1.93941878443644,
124.07554282374));
#253742=CARTESIAN_POINT('Ctrl Pts',(-40.3265325382142,-4.61284175404266,
125.535582288951));
#253743=CARTESIAN_POINT('Ctrl Pts',(-40.604980162027,-6.9261260704041,131.837371644027));
#253744=CARTESIAN_POINT('Ctrl Pts',(-40.8834277858398,-2.87463888813357,
137.18987433118));
#253745=CARTESIAN_POINT('Ctrl Pts',(-41.1618754096529,3.81850099841496,
136.674401865208));
#253746=CARTESIAN_POINT('Ctrl Pts',(-41.4403230334656,7.00262501156454,
130.76464826011));
#253747=CARTESIAN_POINT('Ctrl Pts',(-41.7187706572786,3.75167873633635,
124.891388371457));
#253748=CARTESIAN_POINT('Ctrl Pts',(-41.9972182810916,-2.94687701788942,
124.451861112224));
#253749=CARTESIAN_POINT('Ctrl Pts',(-42.2756659049044,-6.93739675562063,
129.849970561546));
#253750=CARTESIAN_POINT('Ctrl Pts',(-42.5541135287174,-4.55278778560923,
136.125117847804));
#253751=CARTESIAN_POINT('Ctrl Pts',(-42.8325611525302,2.01561074332903,
137.510749172913));
#253752=CARTESIAN_POINT('Ctrl Pts',(-43.1110087763431,6.73176146720674,
132.733537040953));
#253753=CARTESIAN_POINT('Ctrl Pts',(-43.389456400156,5.26175226755184,126.183506021407));
#253754=CARTESIAN_POINT('Ctrl Pts',(-43.6679040239687,-1.0435502150944,
123.879814634434));
#253755=CARTESIAN_POINT('Ctrl Pts',(-43.9463516477818,-6.38988103033122,
127.93944272308));
#253756=CARTESIAN_POINT('Ctrl Pts',(-44.2247992715946,-5.86422334173611,
134.631790397739));
#253757=CARTESIAN_POINT('Ctrl Pts',(-44.5032468954075,0.050369114677416,
137.806917084757));
#253758=CARTESIAN_POINT('Ctrl Pts',(-44.7816945192204,5.91867481537061,
134.547036472328));
#253759=CARTESIAN_POINT('Ctrl Pts',(-45.0601421430334,6.34800750407734,
127.847819589252));
#253760=CARTESIAN_POINT('Ctrl Pts',(-45.3385897668461,0.943831413943965,
123.865519476137));
#253761=CARTESIAN_POINT('Ctrl Pts',(-45.6170373906592,-5.32767963687585,
126.25967539076));
#253762=CARTESIAN_POINT('Ctrl Pts',(-45.895485014472,-6.7033133730266,132.830175008601));
#253763=CARTESIAN_POINT('Ctrl Pts',(-46.1739326382849,-1.91892959442962,
137.539050167615));
#253764=CARTESIAN_POINT('Ctrl Pts',(-46.4523802620978,4.62885673652604,
136.059074638009));
#253765=CARTESIAN_POINT('Ctrl Pts',(-46.7308278859106,6.92294985883713,
129.750273630666));
#253766=CARTESIAN_POINT('Ctrl Pts',(-47.0092755097235,2.8551902657795,124.410127069272));
#253767=CARTESIAN_POINT('Ctrl Pts',(-47.2877231335364,-3.83634969773052,
124.945968763085));
#253768=CARTESIAN_POINT('Ctrl Pts',(-47.5661707573492,-7.00247170512816,
130.865386372813));
#253769=CARTESIAN_POINT('Ctrl Pts',(-47.8446183811622,-3.73366430527375,
136.728724294741));
#253770=CARTESIAN_POINT('Ctrl Pts',(-48.123066004975,2.96619819148554,137.147861418602));
#253771=CARTESIAN_POINT('Ctrl Pts',(-48.4015136287881,6.9402694571073,131.737631203552));
#253772=CARTESIAN_POINT('Ctrl Pts',(-48.6799612526008,4.53657214265928,
125.469770912784));
#253773=CARTESIAN_POINT('Ctrl Pts',(-48.9584088764139,-2.03601334702262,
124.104137951514));
#253774=CARTESIAN_POINT('Ctrl Pts',(-49.2368565002267,-6.7376020355722,
128.895682296272));
#253775=CARTESIAN_POINT('Ctrl Pts',(-49.5153041240395,-5.24766360358919,
135.441208774179));
#253776=CARTESIAN_POINT('Ctrl Pts',(-49.7937517478526,1.06462131747325,
137.725698318783));
#253777=CARTESIAN_POINT('Ctrl Pts',(-50.0721993716652,6.39857125742062,
133.649816642113));
#253778=CARTESIAN_POINT('Ctrl Pts',(-50.3506469954783,5.85254679938199,
126.959099887138));
#253779=CARTESIAN_POINT('Ctrl Pts',(-50.6290946192911,-0.0716822544825644,
123.801989891996));
#253780=CARTESIAN_POINT('Ctrl Pts',(-50.907542243104,-5.93003881835047,
127.079716508824));
#253781=CARTESIAN_POINT('Ctrl Pts',(-51.1859898669169,-6.33897940665598,
133.780209102606));
#253782=CARTESIAN_POINT('Ctrl Pts',(-51.4644374907297,-0.922707596604453,
137.746042316915));
#253783=CARTESIAN_POINT('Ctrl Pts',(-51.7428851145428,5.34148741795441,
135.332809169526));
#253784=CARTESIAN_POINT('Ctrl Pts',(-52.0213327383556,6.69711644158035,
128.758153029896));
#253785=CARTESIAN_POINT('Ctrl Pts',(-52.2997803621686,1.89842262772099,
124.063861700536));
#253786=CARTESIAN_POINT('Ctrl Pts',(-52.5782279859813,-4.64482883791282,
125.563759584248));
#253787=CARTESIAN_POINT('Ctrl Pts',(-52.8566756097944,-6.91970951400822,
131.879513799985));
#253788=CARTESIAN_POINT('Ctrl Pts',(-53.135123233607,-2.83571519333325,
137.207254765232));
#253789=CARTESIAN_POINT('Ctrl Pts',(-53.4135708574202,3.85416285762642,
136.651048807542));
#253790=CARTESIAN_POINT('Ctrl Pts',(-53.6920184812329,7.0022535287505,130.72202202986));
#253791=CARTESIAN_POINT('Ctrl Pts',(-53.9704661050458,3.71561528605495,
124.868660391816));
#253792=CARTESIAN_POINT('Ctrl Pts',(-54.2489137288587,-2.98549188662705,
124.469917286158));
#253793=CARTESIAN_POINT('Ctrl Pts',(-54.5273613526715,-6.94307786488582,
129.892218147303));
#253794=CARTESIAN_POINT('Ctrl Pts',(-54.8058089764845,-4.5203144735249,
136.152733377983));
#253795=CARTESIAN_POINT('Ctrl Pts',(-55.0842566002972,2.05639708936689,
137.498355324372));
#253796=CARTESIAN_POINT('Ctrl Pts',(-55.3627042241104,6.74338018771311,
132.69252315503));
#253797=CARTESIAN_POINT('Ctrl Pts',(-55.6411518479232,5.23352632598741,
126.151561855625));
#253798=CARTESIAN_POINT('Ctrl Pts',(-55.919599471736,-1.08568255734582,
123.886295316588));
#253799=CARTESIAN_POINT('Ctrl Pts',(-56.1980470955489,-6.40720220901991,
127.978392822871));
#253800=CARTESIAN_POINT('Ctrl Pts',(-56.4764947193619,-5.8408160398338,
134.667416676276));
#253801=CARTESIAN_POINT('Ctrl Pts',(-56.7549423431748,0.0929947302327828,
137.806480732508));
#253802=CARTESIAN_POINT('Ctrl Pts',(-57.0333899669875,5.94134788626073,
134.510938475691));
#253803=CARTESIAN_POINT('Ctrl Pts',(-57.3118375908005,6.32989258579528,
127.809232243652));
#253804=CARTESIAN_POINT('Ctrl Pts',(-57.5902852146133,0.901575231427987,
123.859902667085));
#253805=CARTESIAN_POINT('Ctrl Pts',(-57.8687328384263,-5.35524571622284,
126.292190691378));
#253806=CARTESIAN_POINT('Ctrl Pts',(-58.1471804622391,-6.69085746896258,
132.870942446081));
#253807=CARTESIAN_POINT('Ctrl Pts',(-58.4256280860521,-1.87789807428466,
137.550606458515));
#253808=CARTESIAN_POINT('Ctrl Pts',(-58.7040757098649,4.6607579102399,136.030800115547));
#253809=CARTESIAN_POINT('Ctrl Pts',(-58.9825233336777,6.91640506593584,
129.708151199698));
#253810=CARTESIAN_POINT('Ctrl Pts',(-59.2609709574908,2.81621385120844,
124.392865186062));
#253811=CARTESIAN_POINT('Ctrl Pts',(-59.5394185813036,-3.87194031308425,
124.969430255013));
#253812=CARTESIAN_POINT('Ctrl Pts',(-59.8178662051166,-7.00197048445272,
130.908011274954));
#253813=CARTESIAN_POINT('Ctrl Pts',(-60.0963138289294,-3.69753184588372,
136.751342404371));
#253814=CARTESIAN_POINT('Ctrl Pts',(-60.3747614527424,3.00475792457964,
137.129687797925));
#253815=CARTESIAN_POINT('Ctrl Pts',(-60.6532090765552,6.94582195293937,
131.695366522141));
#253816=CARTESIAN_POINT('Ctrl Pts',(-60.9316567003681,4.50401492881459,
125.442254348109));
#253817=CARTESIAN_POINT('Ctrl Pts',(-61.210104324181,-2.07676178152925,
124.116655882255));
#253818=CARTESIAN_POINT('Ctrl Pts',(-61.4885519479939,-6.74909587010084,
128.93673135561));
#253819=CARTESIAN_POINT('Ctrl Pts',(-61.7669995718066,-5.21934056571308,
135.473066881942));
#253820=CARTESIAN_POINT('Ctrl Pts',(-62.0454471956197,1.10673373960332,
137.719089430292));
#253821=CARTESIAN_POINT('Ctrl Pts',(-62.3238948194324,6.41577380517329,
133.610814003028));
#253822=CARTESIAN_POINT('Ctrl Pts',(-62.6023424432454,5.82903117176375,
126.923545017394));
#253823=CARTESIAN_POINT('Ctrl Pts',(-62.8807900670583,-0.114306344492842,
123.802555979936));
#253824=CARTESIAN_POINT('Ctrl Pts',(-63.1592376908712,-5.95260191433588,
127.115883347286));
#253825=CARTESIAN_POINT('Ctrl Pts',(-63.4376853146842,-6.32074712567447,
133.818741133891));
#253826=CARTESIAN_POINT('Ctrl Pts',(-63.716132938497,-0.880434514181572,
137.751530486667));
#253827=CARTESIAN_POINT('Ctrl Pts',(-63.99458056231,5.36895440422691,135.300210117855));
#253828=CARTESIAN_POINT('Ctrl Pts',(-64.2730281861228,6.6845365131549,128.717423692735));
#253829=CARTESIAN_POINT('Ctrl Pts',(-64.5514758099358,1.85735612425694,
124.052430348997));
#253830=CARTESIAN_POINT('Ctrl Pts',(-64.8299234337484,-4.67664380594228,
125.592131071942));
#253831=CARTESIAN_POINT('Ctrl Pts',(-65.1083710575615,-6.91303654523158,
131.921616115747));
#253832=CARTESIAN_POINT('Ctrl Pts',(-65.3868186813742,-2.79668642006362,
137.224397937687));
#253833=CARTESIAN_POINT('Ctrl Pts',(-65.6652663051872,3.88968189941585,
136.627479098696));
#253834=CARTESIAN_POINT('Ctrl Pts',(-65.9437139290001,7.00162257485687,
130.679398850698));
#253835=CARTESIAN_POINT('Ctrl Pts',(-66.2221615528129,3.67941415228271,
124.846152361731));
#253836=CARTESIAN_POINT('Ctrl Pts',(-66.500609176626,-3.02399612686491,
124.48820818522));
#253837=CARTESIAN_POINT('Ctrl Pts',(-66.7790568004388,-6.94850169584742,
129.934499532835));
#253838=CARTESIAN_POINT('Ctrl Pts',(-67.0575044242516,-4.48767365952541,
136.180150722241));
#253839=CARTESIAN_POINT('Ctrl Pts',(-67.3359520480646,2.09710723485436,
137.485713427398));
#253840=CARTESIAN_POINT('Ctrl Pts',(-67.6143996718775,6.75474902978674,
132.651439302549));
#253841=CARTESIAN_POINT('Ctrl Pts',(-67.8928472956903,5.20510645418034,
126.119790101011));
#253842=CARTESIAN_POINT('Ctrl Pts',(-68.1712949195033,-1.12777466923081,
123.893032350195));
#253843=CARTESIAN_POINT('Ctrl Pts',(-68.449742543316,-6.42428596647451,
128.017447639935));
#253844=CARTESIAN_POINT('Ctrl Pts',(-68.728190167129,-5.81719230434518,
134.702899807851));
#253845=CARTESIAN_POINT('Ctrl Pts',(-69.0066377909419,0.135616899834216,
137.805784914121));
#253846=CARTESIAN_POINT('Ctrl Pts',(-69.2850854147548,5.96380079832,134.474703130449));
#253847=CARTESIAN_POINT('Ctrl Pts',(-69.5635330385676,6.31154311101565,
127.770755883637));
#253848=CARTESIAN_POINT('Ctrl Pts',(-69.8419806623805,0.859285640710264,
123.854543187474));
#253849=CARTESIAN_POINT('Ctrl Pts',(-70.1204282861936,-5.38261335497044,
126.324873192109));
#253850=CARTESIAN_POINT('Ctrl Pts',(-70.3988759100064,-6.67815363271447,
132.911633305611));
#253851=CARTESIAN_POINT('Ctrl Pts',(-70.6773235338194,-1.83679696793597,
137.561912764793));
#253852=CARTESIAN_POINT('Ctrl Pts',(-70.9557711576322,4.69248637785542,
136.002331925448));
#253853=CARTESIAN_POINT('Ctrl Pts',(-71.2342187814451,6.90960398310133,
129.666069389173));
#253854=CARTESIAN_POINT('Ctrl Pts',(-71.5126664052579,2.77713308079745,
124.375840883174));
#253855=CARTESIAN_POINT('Ctrl Pts',(-71.7911140290708,-3.90738745226578,
124.993107962432));
#253856=CARTESIAN_POINT('Ctrl Pts',(-72.0695616528837,-7.00120980318599,
130.950632336283));
#253857=CARTESIAN_POINT('Ctrl Pts',(-72.3480092766965,-3.66126237309149,
136.773740146404));
#253858=CARTESIAN_POINT('Ctrl Pts',(-72.6264569005095,3.04320631526353,
137.111279789924));
#253859=CARTESIAN_POINT('Ctrl Pts',(-72.9049045243223,6.95111706878496,
131.653068824177));
#253860=CARTESIAN_POINT('Ctrl Pts',(-73.1833521481353,4.47129081703998,
125.414936478256));
#253861=CARTESIAN_POINT('Ctrl Pts',(-73.4617997719481,-2.11743326086482,
124.129421628353));
#253862=CARTESIAN_POINT('Ctrl Pts',(-73.7402473957612,-6.76033961440018,
128.977849620639));
#253863=CARTESIAN_POINT('Ctrl Pts',(-74.018695019574,-5.19082412325261,
135.504751989078));
#253864=CARTESIAN_POINT('Ctrl Pts',(-74.2971426433868,1.14880515130821,
137.712224313981));
#253865=CARTESIAN_POINT('Ctrl Pts',(-74.5755902671998,6.43273861406817,
133.571707369781));
#253866=CARTESIAN_POINT('Ctrl Pts',(-74.8540378910127,5.80529954725181,
126.8881339527));
#253867=CARTESIAN_POINT('Ctrl Pts',(-75.1324855148255,-0.156926198840311,
123.803381522322));
#253868=CARTESIAN_POINT('Ctrl Pts',(-75.4109331386384,-5.97494443446864,
127.15218686363));
#253869=CARTESIAN_POINT('Ctrl Pts',(-75.6893807624512,-6.30228062708332,
133.857161466198));
#253870=CARTESIAN_POINT('Ctrl Pts',(-75.9678283862644,-0.838128806933456,
137.756761226486));
#253871=CARTESIAN_POINT('Ctrl Pts',(-76.2462760100769,5.3962224419198,135.267444470826));
#253872=CARTESIAN_POINT('Ctrl Pts',(-76.52472363389,6.67170888677059,128.676771687789));
#253873=CARTESIAN_POINT('Ctrl Pts',(-76.8031712577027,1.81622079577817,
124.041249192718));
#253874=CARTESIAN_POINT('Ctrl Pts',(-77.0816188815158,-4.70828547921653,
125.620695700721));
#253875=CARTESIAN_POINT('Ctrl Pts',(-77.3600665053286,-6.90610741134329,
131.963677031195));
#253876=CARTESIAN_POINT('Ctrl Pts',(-77.6385141291417,-2.75755401454922,
137.241303213299));
#253877=CARTESIAN_POINT('Ctrl Pts',(-77.9169617529544,3.92505680761298,
136.603693612052));
#253878=CARTESIAN_POINT('Ctrl Pts',(-78.1954093767674,7.00073217326374,
130.636780302039));
#253879=CARTESIAN_POINT('Ctrl Pts',(-78.4738570005803,3.6430766764653,124.823865115242));
#253880=CARTESIAN_POINT('Ctrl Pts',(-78.7523046243931,-3.06238831181505,
124.506733131632));
#253881=CARTESIAN_POINT('Ctrl Pts',(-79.0307522482061,-6.95366804752337,
129.976813151389));
#253882=CARTESIAN_POINT('Ctrl Pts',(-79.3091998720188,-4.45486655312747,
136.207368864621));
#253883=CARTESIAN_POINT('Ctrl Pts',(-79.5876474958318,2.13773967126259,
137.472823950436));
#253884=CARTESIAN_POINT('Ctrl Pts',(-79.8660951196445,6.76586757215105,
132.610287005887));
#253885=CARTESIAN_POINT('Ctrl Pts',(-80.1445427434577,5.17649370523912,
126.08819193488));
#253886=CARTESIAN_POINT('Ctrl Pts',(-80.4229903672703,-1.16982499101125,
123.900025485612));
#253887=CARTESIAN_POINT('Ctrl Pts',(-80.7014379910835,-6.44113166965063,
128.056605727087));
#253888=CARTESIAN_POINT('Ctrl Pts',(-80.9798856148961,-5.7933530106558,
134.738238477622));
#253889=CARTESIAN_POINT('Ctrl Pts',(-81.2583332387092,0.17823404410257,
137.804829655383));
#253890=CARTESIAN_POINT('Ctrl Pts',(-81.5367808625219,5.98603271954817,
134.438331779315));
#253891=CARTESIAN_POINT('Ctrl Pts',(-81.815228486335,6.29295975968447,127.732391934959));
#253892=CARTESIAN_POINT('Ctrl Pts',(-82.0936761101477,0.816964208846405,
123.849441235906));
#253893=CARTESIAN_POINT('Ctrl Pts',(-82.3721237339607,-5.40978153900143,
126.357721681897));
#253894=CARTESIAN_POINT('Ctrl Pts',(-82.6505713577735,-6.66520233502723,
132.952246079378));
#253895=CARTESIAN_POINT('Ctrl Pts',(-82.9290189815866,-1.79562779839943,
137.572968667493));
#253896=CARTESIAN_POINT('Ctrl Pts',(-83.2074666053992,4.72404096366304,
135.97367112261));
#253897=CARTESIAN_POINT('Ctrl Pts',(-83.4859142292123,6.90254686235,129.624029758449));
#253898=CARTESIAN_POINT('Ctrl Pts',(-83.7643618530252,2.73794940269844,
124.359054791448));
#253899=CARTESIAN_POINT('Ctrl Pts',(-84.0428094768383,-3.94268980176888,
125.017001007954));
#253900=CARTESIAN_POINT('Ctrl Pts',(-84.3212571006508,-7.00018968951541,
130.99324797746));
#253901=CARTESIAN_POINT('Ctrl Pts',(-84.5997047244641,-3.62485723087481,
136.795916690882));
#253902=CARTESIAN_POINT('Ctrl Pts',(-84.8781523482765,3.08154193881888,
137.092638076712));
#253903=CARTESIAN_POINT('Ctrl Pts',(-85.1565999720898,6.95615460843127,
131.61073967702));
#253904=CARTESIAN_POINT('Ctrl Pts',(-85.4350475959023,4.4384010199398,125.387818315495));
#253905=CARTESIAN_POINT('Ctrl Pts',(-85.7134952197154,-2.1580262779319,
124.142434716771));
#253906=CARTESIAN_POINT('Ctrl Pts',(-85.9919428435283,-6.7713328518292,
129.019035567703));
#253907=CARTESIAN_POINT('Ctrl Pts',(-86.2703904673411,-5.16211533289519,
135.536262921482));
#253908=CARTESIAN_POINT('Ctrl Pts',(-86.5488380911541,1.19083399361533,
137.70510322424));
#253909=CARTESIAN_POINT('Ctrl Pts',(-86.827285714967,6.4494650554685,133.532498191482));
#253910=CARTESIAN_POINT('Ctrl Pts',(-87.1057333387799,5.78135280522977,
126.852868005224));
#253911=CARTESIAN_POINT('Ctrl Pts',(-87.3841809625928,-0.199540238229241,
123.804466488563));
#253912=CARTESIAN_POINT('Ctrl Pts',(-87.6626285864056,-5.99706555083783,
127.188625712615));
#253913=CARTESIAN_POINT('Ctrl Pts',(-87.9410762102187,-6.28358059516641,
133.895468675847));
#253914=CARTESIAN_POINT('Ctrl Pts',(-88.2195238340314,-0.795792042514341,
137.761734342542));
#253915=CARTESIAN_POINT('Ctrl Pts',(-88.4979714578443,5.42329052060546,
135.234513442586));
#253916=CARTESIAN_POINT('Ctrl Pts',(-88.7764190816572,6.65863403776028,
128.636198521433));
#253917=CARTESIAN_POINT('Ctrl Pts',(-89.0548667054699,1.77501816656995,
124.03031864602));
#253918=CARTESIAN_POINT('Ctrl Pts',(-89.3333143292831,-4.73975268523957,
125.649452412109));
#253919=CARTESIAN_POINT('Ctrl Pts',(-89.6117619530957,-6.8989223691057,
132.005694987746));
#253920=CARTESIAN_POINT('Ctrl Pts',(-89.8902095769088,-2.71831942685781,
137.257969965635));
#253921=CARTESIAN_POINT('Ctrl Pts',(-90.1686572007216,3.9602862713853,136.579693228991));
#253922=CARTESIAN_POINT('Ctrl Pts',(-90.4471048245344,6.99958235696585,
130.59416796313));
#253923=CARTESIAN_POINT('Ctrl Pts',(-90.7255524483476,3.60660420510239,
124.801799478213));
#253924=CARTESIAN_POINT('Ctrl Pts',(-91.0040000721602,-3.10066701883943,
124.525491438947));
#253925=CARTESIAN_POINT('Ctrl Pts',(-91.2824476959735,-6.95857672847263,
130.019157435019));
#253926=CARTESIAN_POINT('Ctrl Pts',(-91.560895319786,-4.4218943700117,136.234386796543));
#253927=CARTESIAN_POINT('Ctrl Pts',(-91.8393429435991,2.17829289294083,
137.459687371113));
#253928=CARTESIAN_POINT('Ctrl Pts',(-92.1177905674117,6.77673540280433,
132.56906778996));
#253929=CARTESIAN_POINT('Ctrl Pts',(-92.3962381912249,5.14768913942031,
126.056768528114));
#253930=CARTESIAN_POINT('Ctrl Pts',(-92.6746858150375,-1.21183196449619,
123.907274463707));
#253931=CARTESIAN_POINT('Ctrl Pts',(-92.9531334388505,-6.45773869432309,
128.095865633305));
#253932=CARTESIAN_POINT('Ctrl Pts',(-93.2315810626634,-5.76929904214118,
134.773431376103));
#253933=CARTESIAN_POINT('Ctrl Pts',(-93.5100286864763,0.220844583841736,
137.803614991691));
#253934=CARTESIAN_POINT('Ctrl Pts',(-93.7884763102892,6.00804282613147,
134.401825770043));
#253935=CARTESIAN_POINT('Ctrl Pts',(-94.0669239341021,6.27414322041607,
127.694141819211));
#253936=CARTESIAN_POINT('Ctrl Pts',(-94.3453715579151,0.774612504073732,
123.844597001431));
#253937=CARTESIAN_POINT('Ctrl Pts',(-94.6238191817278,-5.43674926158731,
126.390734943524));
#253938=CARTESIAN_POINT('Ctrl Pts',(-94.9022668055408,-6.65200405581671,
132.99277926246));
#253939=CARTESIAN_POINT('Ctrl Pts',(-95.1807144293538,-1.75439209121494,
137.583773756932));
#253940=CARTESIAN_POINT('Ctrl Pts',(-95.4591620531666,4.75542049839504,
135.94481876907));
#253941=CARTESIAN_POINT('Ctrl Pts',(-95.7376096769794,6.89523396518648,
129.582033865318));
#253942=CARTESIAN_POINT('Ctrl Pts',(-96.0160573007924,2.69866426887766,
124.342507532899));
#253943=CARTESIAN_POINT('Ctrl Pts',(-96.2945049246052,-3.97784605345104,
125.041108506217));
#253944=CARTESIAN_POINT('Ctrl Pts',(-96.5729525484182,-6.99891018124123,
131.035856619345));
#253945=CARTESIAN_POINT('Ctrl Pts',(-96.8514001722308,-3.58831776824163,
136.817871216047));
#253946=CARTESIAN_POINT('Ctrl Pts',(-97.129847796044,3.11976337470375,137.073763349068));
#253947=CARTESIAN_POINT('Ctrl Pts',(-97.4082954198568,6.96093438520996,
131.56838064919));
#253948=CARTESIAN_POINT('Ctrl Pts',(-97.6867430436697,4.40534675625846,
125.360900864701));
#253949=CARTESIAN_POINT('Ctrl Pts',(-97.9651906674826,-2.1985393285419,
124.155694665303));
#253950=CARTESIAN_POINT('Ctrl Pts',(-98.2436382912955,-6.78207517502872,
129.060287670645));
#253951=CARTESIAN_POINT('Ctrl Pts',(-98.5220859151084,-5.13321525845608,
135.567598511506));
#253952=CARTESIAN_POINT('Ctrl Pts',(-98.8005335389213,1.23281870913114,
137.697726424945));
#253953=CARTESIAN_POINT('Ctrl Pts',(-99.0789811627341,6.4659525095689,133.493187921042));
#253954=CARTESIAN_POINT('Ctrl Pts',(-99.3574287865471,5.7571918330539,126.817748481762));
#253955=CARTESIAN_POINT('Ctrl Pts',(-99.6358764103599,-0.242146883580649,
123.805810838454));
#253956=CARTESIAN_POINT('Ctrl Pts',(-99.9143240341728,-6.01896444373747,
127.225198543987));
#253957=CARTESIAN_POINT('Ctrl Pts',(-100.192771657986,-6.26464772285957,
133.93366134335));
#253958=CARTESIAN_POINT('Ctrl Pts',(-100.471219281798,-0.753425789729175,
137.766449650557));
#253959=CARTESIAN_POINT('Ctrl Pts',(-100.749666905611,5.45015763726631,
135.201418253402));
#253960=CARTESIAN_POINT('Ctrl Pts',(-101.028114529424,6.64531245061667,
128.595705697122));
#253961=CARTESIAN_POINT('Ctrl Pts',(-101.306562153237,1.73374976341167,
124.019639113937));
#253962=CARTESIAN_POINT('Ctrl Pts',(-101.58500977705,-4.77104425798471,
125.678400140516));
#253963=CARTESIAN_POINT('Ctrl Pts',(-101.863457400863,-6.89148168476197,
132.047668428412));
#253964=CARTESIAN_POINT('Ctrl Pts',(-102.141905024676,-2.67898411084018,
137.274397577103));
#253965=CARTESIAN_POINT('Ctrl Pts',(-102.420352648489,3.99536898529432,
136.555478838857));
#253966=CARTESIAN_POINT('Ctrl Pts',(-102.698800272302,6.99817316856906,
130.551563412989));
#253967=CARTESIAN_POINT('Ctrl Pts',(-102.977247896115,3.56999808969468,
124.779956268296));
#253968=CARTESIAN_POINT('Ctrl Pts',(-103.255695519928,-3.13883082950684,
124.544482412068));
#253969=CARTESIAN_POINT('Ctrl Pts',(-103.53414314374,-6.96322755680218,
130.061530814641));
#253970=CARTESIAN_POINT('Ctrl Pts',(-103.812590767553,-4.38875833197407,
136.261203516848));
#253971=CARTESIAN_POINT('Ctrl Pts',(-104.091038391366,2.21876539717438,
137.44630417621));
#253972=CARTESIAN_POINT('Ctrl Pts',(-104.369486015179,6.78735211903507,
132.52778318216));
#253973=CARTESIAN_POINT('Ctrl Pts',(-104.647933638992,5.11869382408742,
126.02552104512));
#253974=CARTESIAN_POINT('Ctrl Pts',(-104.926381262805,-1.25379403310144,
123.914779015865));
#253975=CARTESIAN_POINT('Ctrl Pts',(-105.204828886617,-6.47410642511416,
128.135225903801));
#253976=CARTESIAN_POINT('Ctrl Pts',(-105.483276510431,-5.74503129012806,
134.808477199207));
#253977=CARTESIAN_POINT('Ctrl Pts',(-105.761724134243,0.263446940103889,
137.802140968053));
#253978=CARTESIAN_POINT('Ctrl Pts',(-106.040171758056,6.02983030247923,
134.365186455377));
#253979=CARTESIAN_POINT('Ctrl Pts',(-106.318619381869,6.25509419046252,
127.656006953765));
#253980=CARTESIAN_POINT('Ctrl Pts',(-106.597067005682,0.732232095750508,
123.840010663559));
#253981=CARTESIAN_POINT('Ctrl Pts',(-106.875514629495,-5.46351552342998,
126.423911753675));
#253982=CARTESIAN_POINT('Ctrl Pts',(-107.153962253308,-6.63855928414971,
133.033231352883));
#253983=CARTESIAN_POINT('Ctrl Pts',(-107.432409877121,-1.71309137438684,
137.594327632723));
#253984=CARTESIAN_POINT('Ctrl Pts',(-107.710857500934,4.78662381927155,
135.915775933963));
#253985=CARTESIAN_POINT('Ctrl Pts',(-107.989305124746,6.8876655625929,129.540083265954));
#253986=CARTESIAN_POINT('Ctrl Pts',(-108.26775274856,2.65927913505975,124.326199720693));
#253987=CARTESIAN_POINT('Ctrl Pts',(-108.546200372372,-4.0128549045848,
125.065429563905));
#253988=CARTESIAN_POINT('Ctrl Pts',(-108.824647996185,-6.99737132577695,
131.078456683062));
#253989=CARTESIAN_POINT('Ctrl Pts',(-109.103095619998,-3.5516453391731,
136.839602908365));
#253990=CARTESIAN_POINT('Ctrl Pts',(-109.381543243811,3.1578692066097,137.054656306401));
#253991=CARTESIAN_POINT('Ctrl Pts',(-109.659990867624,6.96545622200577,
131.525993310316));
#253992=CARTESIAN_POINT('Ctrl Pts',(-109.938438491437,4.37212925083209,
125.334185123311));
#253993=CARTESIAN_POINT('Ctrl Pts',(-110.21688611525,-2.23897091146772,
124.169200982596));
#253994=CARTESIAN_POINT('Ctrl Pts',(-110.495333739063,-6.79256618593892,
129.10160440085));
#253995=CARTESIAN_POINT('Ctrl Pts',(-110.773781362875,-5.10412497083799,
135.598757597999));
#253996=CARTESIAN_POINT('Ctrl Pts',(-111.052228986688,1.27475774209554,
137.690094189444));
#253997=CARTESIAN_POINT('Ctrl Pts',(-111.330676610501,6.48220036542147,
133.453778015119));
#253998=CARTESIAN_POINT('Ctrl Pts',(-111.609124234314,5.73281752601749,
126.782776683677));
#253999=CARTESIAN_POINT('Ctrl Pts',(-111.887571858127,-0.284744556090853,
123.807414522182));
#254000=CARTESIAN_POINT('Ctrl Pts',(-112.16601948194,-6.04064030169634,
127.261904002525));
#254001=CARTESIAN_POINT('Ctrl Pts',(-112.444467105753,-6.24548271172772,
133.971738053464));
#254002=CARTESIAN_POINT('Ctrl Pts',(-112.722914729566,-0.71103161847358,
137.770906975801));
#254003=CARTESIAN_POINT('Ctrl Pts',(-113.001362353379,5.47682279633179,
135.16816012963));
#254004=CARTESIAN_POINT('Ctrl Pts',(-113.279809977192,6.63174461897671,
128.55529471533));
#254005=CARTESIAN_POINT('Ctrl Pts',(-113.558257601004,1.69241711551747,
124.009210992206));
#254006=CARTESIAN_POINT('Ctrl Pts',(-113.836705224817,-4.80215903792943,
125.707537813274));
#254007=CARTESIAN_POINT('Ctrl Pts',(-114.11515284863,-6.88378563403075,
132.089595797848));
#254008=CARTESIAN_POINT('Ctrl Pts',(-114.393600472443,-2.63954952408134,
137.290585438973));
#254009=CARTESIAN_POINT('Ctrl Pts',(-114.672048096256,4.03030364933543,
136.531051338922));
#254010=CARTESIAN_POINT('Ctrl Pts',(-114.950495720069,6.99650466029252,
130.508968230339));
#254011=CARTESIAN_POINT('Ctrl Pts',(-115.228943343882,3.53325968669456,
124.758336294896));
#254012=CARTESIAN_POINT('Ctrl Pts',(-115.507390967695,-3.17687832964389,
124.563705347279));
#254013=CARTESIAN_POINT('Ctrl Pts',(-115.785838591507,-6.96762036017394,
130.103931720095));
#254014=CARTESIAN_POINT('Ctrl Pts',(-116.06428621532,-4.35545966688232,
136.287818031834));
#254015=CARTESIAN_POINT('Ctrl Pts',(-116.342733839133,2.25915568424066,
137.432674861647));
#254016=CARTESIAN_POINT('Ctrl Pts',(-116.621181462946,6.79771732743703,
132.486434712303));
#254017=CARTESIAN_POINT('Ctrl Pts',(-116.899629086759,5.08950883367243,
125.994450643782));
#254018=CARTESIAN_POINT('Ctrl Pts',(-117.178076710572,-1.2957096419083,
123.922538864004));
#254019=CARTESIAN_POINT('Ctrl Pts',(-117.456524334385,-6.49023425551004,
128.174685080065));
#254020=CARTESIAN_POINT('Ctrl Pts',(-117.734971958198,-5.7205506538686,
134.843374648297));
#254021=CARTESIAN_POINT('Ctrl Pts',(-118.013419582011,0.306039534242538,
137.800407639092));
#254022=CARTESIAN_POINT('Ctrl Pts',(-118.291867205823,6.05139434124684,
134.328415193001));
#254023=CARTESIAN_POINT('Ctrl Pts',(-118.570314829636,6.23581337569426,
127.617988751722));
#254024=CARTESIAN_POINT('Ctrl Pts',(-118.848762453449,0.689824554297045,
123.835682392233));
#254025=CARTESIAN_POINT('Ctrl Pts',(-119.127210077262,-5.49007933269568,
126.457250882969));
#254026=CARTESIAN_POINT('Ctrl Pts',(-119.405657701075,-6.62486851822702,
133.073600851681));
#254027=CARTESIAN_POINT('Ctrl Pts',(-119.684105324888,-1.67172717832737,
137.60462990379));
#254028=CARTESIAN_POINT('Ctrl Pts',(-119.962552948701,4.81764977004229,
135.886543693482));
#254029=CARTESIAN_POINT('Ctrl Pts',(-120.241000572514,6.87984193501854,
129.498179514853));
#254030=CARTESIAN_POINT('Ctrl Pts',(-120.519448196327,2.61979546067638,
124.310131959122));
#254031=CARTESIAN_POINT('Ctrl Pts',(-120.79789582014,-4.04771505790416,
125.089963279793));
#254032=CARTESIAN_POINT('Ctrl Pts',(-121.076343443952,-6.9955731801444,
131.121046590047));
#254033=CARTESIAN_POINT('Ctrl Pts',(-121.354791067765,-3.51484130258126,
136.86111096256));
#254034=CARTESIAN_POINT('Ctrl Pts',(-121.633238691578,3.19585802251066,
137.035317656727));
#254035=CARTESIAN_POINT('Ctrl Pts',(-121.911686315391,6.96971995125911,
131.483579231079));
#254036=CARTESIAN_POINT('Ctrl Pts',(-122.190133939204,4.3387497345494,125.307672081285));
#254037=CARTESIAN_POINT('Ctrl Pts',(-122.468581563017,-2.2793195285039,
124.182953168171));
#254038=CARTESIAN_POINT('Ctrl Pts',(-122.74702918683,-6.80280549581075,
129.142984227312));
#254039=CARTESIAN_POINT('Ctrl Pts',(-123.025476810643,-5.07484554799192,
135.629739026348));
#254040=CARTESIAN_POINT('Ctrl Pts',(-123.303924434456,1.31664953844379,
137.682206800553));
#254041=CARTESIAN_POINT('Ctrl Pts',(-123.582372058268,6.49820802095541,
133.414269934058));
#254042=CARTESIAN_POINT('Ctrl Pts',(-123.860819682081,5.7082307873194,126.747953906865));
#254043=CARTESIAN_POINT('Ctrl Pts',(-124.139267305894,-0.327331677286216,
123.809277480321));
#254044=CARTESIAN_POINT('Ctrl Pts',(-124.417714929707,-6.06209232150722,
127.298740728095));
#254045=CARTESIAN_POINT('Ctrl Pts',(-124.69616255352,-6.22608627193705,
134.009697395242));
#254046=CARTESIAN_POINT('Ctrl Pts',(-124.974610177333,-0.668611099680587,
137.77510615311));
#254047=CARTESIAN_POINT('Ctrl Pts',(-125.253057801146,5.50328500971429,
135.134740303665));
#254048=CARTESIAN_POINT('Ctrl Pts',(-125.531505424959,6.61793104560076,
128.514967073503));
#254049=CARTESIAN_POINT('Ctrl Pts',(-125.809953048772,1.6510217544855,123.999034667242));
#254050=CARTESIAN_POINT('Ctrl Pts',(-126.088400672584,-4.8330958721059,
125.736864350674));
#254051=CARTESIAN_POINT('Ctrl Pts',(-126.366848296398,-6.87583450209069,
132.131475542423));
#254052=CARTESIAN_POINT('Ctrl Pts',(-126.64529592021,-2.60001712784396,
137.306532951397));
#254053=CARTESIAN_POINT('Ctrl Pts',(-126.923743544023,4.06508896899354,
136.506411634357));
#254054=CARTESIAN_POINT('Ctrl Pts',(-127.202191167836,6.99457689396224,
130.466383993564));
#254055=CARTESIAN_POINT('Ctrl Pts',(-127.480638791649,3.49639035745773,
124.736940359153));
#254056=CARTESIAN_POINT('Ctrl Pts',(-127.759086415462,-3.21480810938582,
124.583159532264));
#254057=CARTESIAN_POINT('Ctrl Pts',(-128.037534039275,-6.97175497581086,
130.146358580199));
#254058=CARTESIAN_POINT('Ctrl Pts',(-128.315981663087,-4.32199960863106,
136.314229355287));
#254059=CARTESIAN_POINT('Ctrl Pts',(-128.594429286901,2.29946225746178,
137.418799932461));
#254060=CARTESIAN_POINT('Ctrl Pts',(-128.872876910713,6.80783064392392,
132.44502391257));
#254061=CARTESIAN_POINT('Ctrl Pts',(-129.151324534526,5.06013524963555,
125.963558475429));
#254062=CARTESIAN_POINT('Ctrl Pts',(-129.429772158339,-1.33757723771771,
123.930553720578));
#254063=CARTESIAN_POINT('Ctrl Pts',(-129.708219782152,-6.50612158788957,
128.214241699924));
#254064=CARTESIAN_POINT('Ctrl Pts',(-129.986667405965,-5.69585804050008,
134.878122430239));
#254065=CARTESIAN_POINT('Ctrl Pts',(-130.265115029778,0.348620787973942,
137.798415069035));
#254066=CARTESIAN_POINT('Ctrl Pts',(-130.543562653591,6.07273414337257,
134.291513345486));
#254067=CARTESIAN_POINT('Ctrl Pts',(-130.822010277403,6.21630149056731,
127.58008862186));
#254068=CARTESIAN_POINT('Ctrl Pts',(-131.100457901217,0.647391451141708,
123.831612347843));
#254069=CARTESIAN_POINT('Ctrl Pts',(-131.378905525029,-5.5164397050528,
126.490751096011));
#254070=CARTESIAN_POINT('Ctrl Pts',(-131.657353148842,-6.61093226536518,
133.113886262947));
#254071=CARTESIAN_POINT('Ctrl Pts',(-131.935800772655,-1.63030103580305,
137.614680188378));
#254072=CARTESIAN_POINT('Ctrl Pts',(-132.214248396468,4.848497201029,135.857123130838));
#254073=CARTESIAN_POINT('Ctrl Pts',(-132.492696020281,6.87176337237162,
129.456324164773));
#254074=CARTESIAN_POINT('Ctrl Pts',(-132.771143644094,2.58021470880796,
124.294304843582));
#254075=CARTESIAN_POINT('Ctrl Pts',(-133.049591267907,-4.08242522165371,
125.114708744776));
#254076=CARTESIAN_POINT('Ctrl Pts',(-133.32803889172,-6.99351581097555,
131.163624762118));
#254077=CARTESIAN_POINT('Ctrl Pts',(-133.606486515532,-3.47790702225152,
136.882394581644));
#254078=CARTESIAN_POINT('Ctrl Pts',(-133.884934139345,3.23372841471757,
137.015748116649));
#254079=CARTESIAN_POINT('Ctrl Pts',(-134.163381763158,6.97372541497715,
131.441139983145));
#254080=CARTESIAN_POINT('Ctrl Pts',(-134.441829386971,4.30520944429882,
125.281362721075));
#254081=CARTESIAN_POINT('Ctrl Pts',(-134.720277010784,-2.31958368451587,
124.196950712432));
#254082=CARTESIAN_POINT('Ctrl Pts',(-134.998724634597,-6.81279272522359,
129.184425616688));
#254083=CARTESIAN_POINT('Ctrl Pts',(-135.27717225841,-5.04537807487797,
135.660541648527));
#254084=CARTESIAN_POINT('Ctrl Pts',(-135.555619882223,1.35849254585843,
137.674064550544));
#254085=CARTESIAN_POINT('Ctrl Pts',(-135.834067506036,6.51397488300169,
133.374665141848));
#254086=CARTESIAN_POINT('Ctrl Pts',(-136.112515129848,5.68343252803032,
126.713281441693));
#254087=CARTESIAN_POINT('Ctrl Pts',(-136.390962753662,-0.369906669086523,
123.811399643837));
#254088=CARTESIAN_POINT('Ctrl Pts',(-136.669410377474,-6.08331970825794,
127.335707355701));
#254089=CARTESIAN_POINT('Ctrl Pts',(-136.947858001288,-6.20645912223011,
134.047537962086));
#254090=CARTESIAN_POINT('Ctrl Pts',(-137.2263056251,-0.626165805256695,
137.779047026878));
#254091=CARTESIAN_POINT('Ctrl Pts',(-137.504753248913,5.52954329684707,
135.101160013885));
#254092=CARTESIAN_POINT('Ctrl Pts',(-137.783200872726,6.60387224235649,
128.474724265995));
#254093=CARTESIAN_POINT('Ctrl Pts',(-138.061648496539,1.60956521423443,
123.989110516135));
#254094=CARTESIAN_POINT('Ctrl Pts',(-138.340096120352,-4.86385361413656,
125.766378666012));
#254095=CARTESIAN_POINT('Ctrl Pts',(-138.618543744165,-6.86762858357524,
132.173306110266));
#254096=CARTESIAN_POINT('Ctrl Pts',(-138.896991367977,-2.56038838701599,
137.322239523433));
#254097=CARTESIAN_POINT('Ctrl Pts',(-139.17543899179,4.09972365528409,136.481560638194));
#254098=CARTESIAN_POINT('Ctrl Pts',(-139.453886615603,6.99238994101352,
130.423812280637));
#254099=CARTESIAN_POINT('Ctrl Pts',(-139.732334239416,3.45939146819007,
124.715769253897));
#254100=CARTESIAN_POINT('Ctrl Pts',(-140.010781863229,-3.25261876323132,
124.602844246145));
#254101=CARTESIAN_POINT('Ctrl Pts',(-140.289229487042,-6.97563125050334,
130.188809822811));
#254102=CARTESIAN_POINT('Ctrl Pts',(-140.567677110855,-4.28837939709471,
136.340436508528));
#254103=CARTESIAN_POINT('Ctrl Pts',(-140.846124734668,2.33968362326381,
137.404679902793));
#254104=CARTESIAN_POINT('Ctrl Pts',(-141.124572358481,6.81769169374202,
132.403552317457));
#254105=CARTESIAN_POINT('Ctrl Pts',(-141.403019982293,5.03057416042698,
125.932845684778));
#254106=CARTESIAN_POINT('Ctrl Pts',(-141.681467606106,-1.37939526911043,
123.938823288595));
#254107=CARTESIAN_POINT('Ctrl Pts',(-141.959915229919,-6.52176783354029,
128.253894297592));
#254108=CARTESIAN_POINT('Ctrl Pts',(-142.238362853732,-5.67095436501806,
134.912719257437));
#254109=CARTESIAN_POINT('Ctrl Pts',(-142.516810477545,0.39118912343359,
137.796163331718));
#254110=CARTESIAN_POINT('Ctrl Pts',(-142.795258101358,6.09384891810056,
134.254482280245));
#254111=CARTESIAN_POINT('Ctrl Pts',(-143.073705725171,6.19655925810344,
127.542307968582));
#254112=CARTESIAN_POINT('Ctrl Pts',(-143.352153348984,0.604934358657401,
123.827800681205));
#254113=CARTESIAN_POINT('Ctrl Pts',(-143.630600972796,-5.54259566370794,
126.524411151443));
#254114=CARTESIAN_POINT('Ctrl Pts',(-143.90904859661,-6.59675104197701,
133.154086093891));
#254115=CARTESIAN_POINT('Ctrl Pts',(-144.187496220422,-1.58881448187379,
137.624478114069));
#254116=CARTESIAN_POINT('Ctrl Pts',(-144.465943844235,4.87916496916901,
135.827515336221));
#254117=CARTESIAN_POINT('Ctrl Pts',(-144.744391468048,6.86343017400547,
129.41451876668));
#254118=CARTESIAN_POINT('Ctrl Pts',(-145.022839091861,2.54053834613545,
124.278718960552));
#254119=CARTESIAN_POINT('Ctrl Pts',(-145.301286715674,-4.11698410963516,
125.139665041902));
#254120=CARTESIAN_POINT('Ctrl Pts',(-145.579734339487,-6.99119929450595,
131.206189621523));
#254121=CARTESIAN_POINT('Ctrl Pts',(-145.8581819633,-3.44084386679896,136.903452976945));
#254122=CARTESIAN_POINT('Ctrl Pts',(-146.136629587113,3.27147897992919,
136.995948411323));
#254123=CARTESIAN_POINT('Ctrl Pts',(-146.415077210925,6.97747246473481,
131.398677139117));
#254124=CARTESIAN_POINT('Ctrl Pts',(-146.693524834738,4.27150962292939,
125.255258017582));
#254125=CARTESIAN_POINT('Ctrl Pts',(-146.971972458551,-2.35976188750221,
124.211193096699));
#254126=CARTESIAN_POINT('Ctrl Pts',(-147.250420082364,-6.82252750409623,
129.225927033352));
#254127=CARTESIAN_POINT('Ctrl Pts',(-147.528867706177,-5.01572364342383,
135.69116432313));
#254128=CARTESIAN_POINT('Ctrl Pts',(-147.80731532999,1.40028521383297,137.665667741127));
#254129=CARTESIAN_POINT('Ctrl Pts',(-148.085762953803,6.52950036731291,
133.334965106058));
#254130=CARTESIAN_POINT('Ctrl Pts',(-148.364210577616,5.65842366705879,
126.678760572968));
#254131=CARTESIAN_POINT('Ctrl Pts',(-148.642658201429,-0.412467953858535,
123.813780934094));
#254132=CARTESIAN_POINT('Ctrl Pts',(-148.921105825242,-6.10432167535963,
127.372802515528));
#254133=CARTESIAN_POINT('Ctrl Pts',(-149.199553449054,-6.18660198989778,
134.085258351801));
#254134=CARTESIAN_POINT('Ctrl Pts',(-149.478001072867,-0.583697308029368,
137.782729451077));
#254135=CARTESIAN_POINT('Ctrl Pts',(-149.75644869668,5.55559668471987,135.067420504625));
#254136=CARTESIAN_POINT('Ctrl Pts',(-150.034896320493,6.58956873019717,
128.434567784019));
#254137=CARTESIAN_POINT('Ctrl Pts',(-150.313343944306,1.56804903095274,
123.979438906626));
#254138=CARTESIAN_POINT('Ctrl Pts',(-150.591791568119,-4.89443112428377,
125.796079665625));
#254139=CARTESIAN_POINT('Ctrl Pts',(-150.870239191931,-6.85916818255639,
132.21508595133));
#254140=CARTESIAN_POINT('Ctrl Pts',(-151.148686815745,-2.52066477005453,
137.33770457307));
#254141=CARTESIAN_POINT('Ctrl Pts',(-151.427134439557,4.13420642480782,
136.456499271296));
#254142=CARTESIAN_POINT('Ctrl Pts',(-151.705582063371,6.98994388248347,
130.381254669068));
#254143=CARTESIAN_POINT('Ctrl Pts',(-151.984029687183,3.42226438989971,
124.694823763634));
#254144=CARTESIAN_POINT('Ctrl Pts',(-152.262477310996,-3.29030889009209,
124.622758759495));
#254145=CARTESIAN_POINT('Ctrl Pts',(-152.540924934809,-6.97924904061452,
130.231283874884));
#254146=CARTESIAN_POINT('Ctrl Pts',(-152.819372558622,-4.25460027808296,
136.366438520441));
#254147=CARTESIAN_POINT('Ctrl Pts',(-153.097820182435,2.37981829122829,
137.390315295868));
#254148=CARTESIAN_POINT('Ctrl Pts',(-153.376267806248,6.82730011148789,
132.362021463707));
#254149=CARTESIAN_POINT('Ctrl Pts',(-153.654715430061,5.00082666144207,
125.902313409905));
#254150=CARTESIAN_POINT('Ctrl Pts',(-153.933163053873,-1.42116218650446,
123.947347261623));
#254151=CARTESIAN_POINT('Ctrl Pts',(-154.211610677687,-6.53717241268631,
128.293641403726));
#254152=CARTESIAN_POINT('Ctrl Pts',(-154.490058301499,-5.64584055023574,
134.947163847896));
#254153=CARTESIAN_POINT('Ctrl Pts',(-154.768505925312,0.433742963236675,
137.79365251058));
#254154=CARTESIAN_POINT('Ctrl Pts',(-155.046953549125,6.11473788301669,
134.217323369476));
#254155=CARTESIAN_POINT('Ctrl Pts',(-155.325401172938,6.17658740985663,
127.504648191865));
#254156=CARTESIAN_POINT('Ctrl Pts',(-155.603848796751,0.562454850108638,
123.824247533559));
#254157=CARTESIAN_POINT('Ctrl Pts',(-155.882296420564,-5.5685462394425,
126.558229801974));
#254158=CARTESIAN_POINT('Ctrl Pts',(-156.160744044376,-6.5823253735531,
133.194198854895));
#254159=CARTESIAN_POINT('Ctrl Pts',(-156.43919166819,-1.54726905384013,
137.634023317798));
#254160=CARTESIAN_POINT('Ctrl Pts',(-156.717639292002,4.90965193805665,
135.79772140676));
#254161=CARTESIAN_POINT('Ctrl Pts',(-156.996086915816,6.8548426487106,129.372764869687));
#254162=CARTESIAN_POINT('Ctrl Pts',(-157.274534539628,2.50076784287941,
124.263374887574));
#254163=CARTESIAN_POINT('Ctrl Pts',(-157.552982163441,-4.15139044125659,
125.164831246407));
#254164=CARTESIAN_POINT('Ctrl Pts',(-157.831429787254,-6.98862371657603,
131.248739591007));
#254165=CARTESIAN_POINT('Ctrl Pts',(-158.109877411067,-3.40365320961064,
136.924285368134));
#254166=CARTESIAN_POINT('Ctrl Pts',(-158.38832503488,3.30910831928323,136.975919274434));
#254167=CARTESIAN_POINT('Ctrl Pts',(-158.666772658693,6.98096096168483,
131.356192272474));
#254168=CARTESIAN_POINT('Ctrl Pts',(-158.945220282506,4.23765151920024,
125.229358938127));
#254169=CARTESIAN_POINT('Ctrl Pts',(-159.223667906319,-2.39985264864321,
124.225679793212));
#254170=CARTESIAN_POINT('Ctrl Pts',(-159.502115530131,-6.8320094717036,
129.267486939452));
#254171=CARTESIAN_POINT('Ctrl Pts',(-159.780563153944,-4.98588335248574,
135.721605915426));
#254172=CARTESIAN_POINT('Ctrl Pts',(-160.059010777757,1.44202599372318,
137.657016683454));
#254173=CARTESIAN_POINT('Ctrl Pts',(-160.33745840157,6.54478389858708,133.295171297791));
#254174=CARTESIAN_POINT('Ctrl Pts',(-160.615906025383,5.63320513111742,
126.644392579866));
#254175=CARTESIAN_POINT('Ctrl Pts',(-160.894353649196,-0.455013954479453,
123.816421262852));
#254176=CARTESIAN_POINT('Ctrl Pts',(-161.172801273009,-6.12509744457689,
127.410024833003));
#254177=CARTESIAN_POINT('Ctrl Pts',(-161.451248896821,-6.16651561075379,
134.122857166646));
#254178=CARTESIAN_POINT('Ctrl Pts',(-161.729696520635,-0.541207181682879,
137.786153289251));
#254179=CARTESIAN_POINT('Ctrl Pts',(-162.008144144447,5.58144420791359,
135.033523026113));
#254180=CARTESIAN_POINT('Ctrl Pts',(-162.286591768261,6.57502103914602,
128.394499115588));
#254181=CARTESIAN_POINT('Ctrl Pts',(-162.565039392073,1.52647474303778,
123.970020197102));
#254182=CARTESIAN_POINT('Ctrl Pts',(-162.843487015886,-4.92482726948487,
125.825966248931));
#254183=CARTESIAN_POINT('Ctrl Pts',(-163.121934639699,-6.85045361253876,
132.256813517449));
#254184=CARTESIAN_POINT('Ctrl Pts',(-163.400382263512,-2.48084774893327,
137.352927527244));
#254185=CARTESIAN_POINT('Ctrl Pts',(-163.678829887325,4.16853599979124,
136.431228462323));
#254186=CARTESIAN_POINT('Ctrl Pts',(-163.957277511138,6.98723880901292,
130.338712735846));
#254187=CARTESIAN_POINT('Ctrl Pts',(-164.23572513495,3.3850104983435,124.674104664506));
#254188=CARTESIAN_POINT('Ctrl Pts',(-164.514172758764,-3.32787709334726,
124.642902334375));
#254189=CARTESIAN_POINT('Ctrl Pts',(-164.792620382576,-6.98260821208591,
130.273779162525));
#254190=CARTESIAN_POINT('Ctrl Pts',(-165.07106800639,-4.22066350329308,
136.392234427513));
#254191=CARTESIAN_POINT('Ctrl Pts',(-165.349515630202,2.4198647741513,137.37570664397));
#254192=CARTESIAN_POINT('Ctrl Pts',(-165.627963254015,6.83665554111671,
132.320432890263));
#254193=CARTESIAN_POINT('Ctrl Pts',(-165.906410877828,4.97089385498702,
125.871962782194));
#254194=CARTESIAN_POINT('Ctrl Pts',(-166.184858501641,-1.46287644221077,
123.956125323802));
#254195=CARTESIAN_POINT('Ctrl Pts',(-166.463306125454,-6.55233475450377,
128.333481545486));
#254196=CARTESIAN_POINT('Ctrl Pts',(-166.741753749267,-5.62051752675643,
134.981454925258));
#254197=CARTESIAN_POINT('Ctrl Pts',(-167.020201373079,0.476280730534997,
137.790882698662));
#254198=CARTESIAN_POINT('Ctrl Pts',(-167.298648996893,6.13540026407138,
134.180037990117));
#254199=CARTESIAN_POINT('Ctrl Pts',(-167.577096620705,6.15638668589229,
127.467110687205));
#254200=CARTESIAN_POINT('Ctrl Pts',(-167.855544244518,0.519954499587912,
123.820953036571));
#254201=CARTESIAN_POINT('Ctrl Pts',(-168.133991868331,-5.5942904706483,
126.592205794446));
#254202=CARTESIAN_POINT('Ctrl Pts',(-168.412439492144,-6.56765579464175,
133.234223059563));
#254203=CARTESIAN_POINT('Ctrl Pts',(-168.690887115956,-1.50566629118217,
137.643315445865));
#254204=CARTESIAN_POINT('Ctrl Pts',(-168.96933473977,4.93995697798634,135.767742446477));
#254205=CARTESIAN_POINT('Ctrl Pts',(-169.247782363582,6.84600111470013,
129.331064021001));
#254206=CARTESIAN_POINT('Ctrl Pts',(-169.526229987396,2.46090467275213,
124.248273193229));
#254207=CARTESIAN_POINT('Ctrl Pts',(-169.804677611208,-4.18564294157836,
125.190206425745));
#254208=CARTESIAN_POINT('Ctrl Pts',(-170.083125235021,-6.98578917262369,
131.291273093865));
#254209=CARTESIAN_POINT('Ctrl Pts',(-170.361572858834,-3.36633642880185,
136.944890983262));
#254210=CARTESIAN_POINT('Ctrl Pts',(-170.640020482647,3.34661503841248,
136.955661448171));
#254211=CARTESIAN_POINT('Ctrl Pts',(-170.91846810646,6.98419077655865,131.313686957504));
#254212=CARTESIAN_POINT('Ctrl Pts',(-171.196915730273,4.20363638773547,
125.203666442409));
#254213=CARTESIAN_POINT('Ctrl Pts',(-171.475363354086,-2.43985448236259,
124.240410265162));
#254214=CARTESIAN_POINT('Ctrl Pts',(-171.753810977898,-6.84123827668714,
129.309103794972));
#254215=CARTESIAN_POINT('Ctrl Pts',(-172.032258601712,-4.9558583078063,
135.751865297389));
#254216=CARTESIAN_POINT('Ctrl Pts',(-172.310706225524,1.48371333881067,
137.648111698089));
#254217=CARTESIAN_POINT('Ctrl Pts',(-172.589153849337,6.55982491048677,
133.255285191615));
#254218=CARTESIAN_POINT('Ctrl Pts',(-172.86760147315,5.60777785468832,126.610178735912));
#254219=CARTESIAN_POINT('Ctrl Pts',(-173.146049096963,-0.497543094390354,
123.819320532272));
#254220=CARTESIAN_POINT('Ctrl Pts',(-173.424496720776,-6.14564624605571,
127.447372928838));
#254221=CARTESIAN_POINT('Ctrl Pts',(-173.702944344589,-6.14620072910595,
134.160333013378));
#254222=CARTESIAN_POINT('Ctrl Pts',(-173.981391968402,-0.498697000705985,
137.789318414533));
#254223=CARTESIAN_POINT('Ctrl Pts',(-174.259839592215,5.60708490864046,
134.999468834432));
#254224=CARTESIAN_POINT('Ctrl Pts',(-174.538287216028,6.56022970827155,
128.354519745462));
#254225=CARTESIAN_POINT('Ctrl Pts',(-174.81673483984,1.48484389103961,123.960854736574));
#254226=CARTESIAN_POINT('Ctrl Pts',(-175.095182463654,-4.95504092340126,
125.85603730847));
#254227=CARTESIAN_POINT('Ctrl Pts',(-175.373630087466,-6.8414851964426,
132.298487262391));
#254228=CARTESIAN_POINT('Ctrl Pts',(-175.652077711279,-2.44093879908611,
137.367907821863));
#254229=CARTESIAN_POINT('Ctrl Pts',(-175.930525335092,4.20271110814107,
136.405749147692));
#254230=CARTESIAN_POINT('Ctrl Pts',(-176.208972958905,6.98427482083815,
130.296188057377));
#254231=CARTESIAN_POINT('Ctrl Pts',(-176.487420582718,3.3476311739788,124.653612724266));
#254232=CARTESIAN_POINT('Ctrl Pts',(-176.765868206531,-3.36532198089259,
124.663274224357));
#254233=CARTESIAN_POINT('Ctrl Pts',(-177.044315830343,-6.98570864044213,
130.316294111058));
#254234=CARTESIAN_POINT('Ctrl Pts',(-177.322763454156,-4.18657033026512,
136.417823273865));
#254235=CARTESIAN_POINT('Ctrl Pts',(-177.601211077969,2.4598215880947,137.360854488428));
#254236=CARTESIAN_POINT('Ctrl Pts',(-177.879658701782,6.84575763596098,
132.278788138201));
#254237=CARTESIAN_POINT('Ctrl Pts',(-178.158106325595,4.94077685023126,
125.841794926299));
#254238=CARTESIAN_POINT('Ctrl Pts',(-178.436553949408,-1.50453649049278,
123.965157149858));
#254239=CARTESIAN_POINT('Ctrl Pts',(-178.715001573221,-6.56725429714808,
128.373413246577));
#254240=CARTESIAN_POINT('Ctrl Pts',(-178.993449197033,-5.59498623293233,
135.015591218853));
#254241=CARTESIAN_POINT('Ctrl Pts',(-179.271896820847,0.518800849074927,
137.787853998597));
#254242=CARTESIAN_POINT('Ctrl Pts',(-179.550344444659,6.15583529561319,
134.142627523792));
#254243=CARTESIAN_POINT('Ctrl Pts',(-179.828792068472,6.13595783475539,
127.429696845569));
#254244=CARTESIAN_POINT('Ctrl Pts',(-180.107239692285,0.477434881962636,
123.81791731232));
#254245=CARTESIAN_POINT('Ctrl Pts',(-180.385687316098,-5.61982740336347,
126.626337869861));
#254246=CARTESIAN_POINT('Ctrl Pts',(-180.664134939911,-6.55274284882976,
133.274157224785));
#254247=CARTESIAN_POINT('Ctrl Pts',(-180.942582563724,-1.4640077355066,
137.652354153945));
#254248=CARTESIAN_POINT('Ctrl Pts',(-181.221030187537,4.97007896599344,
135.737579566256));
#254249=CARTESIAN_POINT('Ctrl Pts',(-181.499477811349,6.83690589960112,
129.289417765863));
#254250=CARTESIAN_POINT('Ctrl Pts',(-181.777925435163,2.42095031289641,
124.233414437113));
#254251=CARTESIAN_POINT('Ctrl Pts',(-182.056373058975,-4.21974034136189,
125.215789639631));
#254252=CARTESIAN_POINT('Ctrl Pts',(-182.334820682789,-6.98269576768506,
131.333788554001));
#254253=CARTESIAN_POINT('Ctrl Pts',(-182.613268306601,-3.32889490715784,
136.965269058779));
#254254=CARTESIAN_POINT('Ctrl Pts',(-182.891715930414,3.38399774748988,
136.935175683191));
#254255=CARTESIAN_POINT('Ctrl Pts',(-183.170163554227,6.98716178967534,
131.27116276926));
#254256=CARTESIAN_POINT('Ctrl Pts',(-183.44861117804,4.16946548897866,125.178181482475));
#254257=CARTESIAN_POINT('Ctrl Pts',(-183.727058801853,-2.47976590637605,
124.255383966707));
#254258=CARTESIAN_POINT('Ctrl Pts',(-184.005506425666,-6.85021357707087,
129.350776057783));
#254259=CARTESIAN_POINT('Ctrl Pts',(-184.283954049479,-4.92564962197493,
135.781941347746));
#254260=CARTESIAN_POINT('Ctrl Pts',(-184.562401673291,1.52534570435398,
137.63895311501));
#254261=CARTESIAN_POINT('Ctrl Pts',(-184.840849297105,6.5746228456623,133.215308265529));
#254262=CARTESIAN_POINT('Ctrl Pts',(-185.119296920917,5.58214277998856,
126.576120308909));
#254263=CARTESIAN_POINT('Ctrl Pts',(-185.39774454473,-0.540053797659538,
123.822478634922));
#254264=CARTESIAN_POINT('Ctrl Pts',(-185.676192168543,-6.16596731835295,
127.484845419088));
#254265=CARTESIAN_POINT('Ctrl Pts',(-185.954639792356,-6.12565809773001,
134.197684503321));
#254266=CARTESIAN_POINT('Ctrl Pts',(-186.233087416169,-0.456168340327589,
137.792224709632));
#254267=CARTESIAN_POINT('Ctrl Pts',(-186.511535039982,5.63251783677319,
134.965259191474));
#254268=CARTESIAN_POINT('Ctrl Pts',(-186.789982663795,6.54519528567348,
128.314631155089));
#254269=CARTESIAN_POINT('Ctrl Pts',(-187.068430287608,1.44315801760525,
123.951942864674));
#254270=CARTESIAN_POINT('Ctrl Pts',(-187.346877911421,-4.98507096645316,
125.886291729948));
#254271=CARTESIAN_POINT('Ctrl Pts',(-187.625325535233,-6.83226326659722,
132.340105641921));
#254272=CARTESIAN_POINT('Ctrl Pts',(-187.903773159046,-2.40093939935397,
137.382644901827));
#254273=CARTESIAN_POINT('Ctrl Pts',(-188.182220782859,4.23673048348491,
136.380062271549));
#254274=CARTESIAN_POINT('Ctrl Pts',(-188.460668406672,6.98105202779173,
130.25368220943));
#254275=CARTESIAN_POINT('Ctrl Pts',(-188.739116030485,3.31012780190951,
124.633348702251));
#254276=CARTESIAN_POINT('Ctrl Pts',(-189.017563654298,-3.40264216519462,
124.683873674555));
#254277=CARTESIAN_POINT('Ctrl Pts',(-189.296011278111,-6.98855021079573,
130.358827145076));
#254278=CARTESIAN_POINT('Ctrl Pts',(-189.574458901924,-4.15232202233378,
136.443204111294));
#254279=CARTESIAN_POINT('Ctrl Pts',(-189.852906525736,2.49968725244504,
137.345759379595));
#254280=CARTESIAN_POINT('Ctrl Pts',(-190.13135414955,6.85460605873784,132.237088750687));
#254281=CARTESIAN_POINT('Ctrl Pts',(-190.409801773362,4.91047676317321,
125.8118109601));
#254282=CARTESIAN_POINT('Ctrl Pts',(-190.688249397175,-1.5461407876216,
123.974442405114));
#254283=CARTESIAN_POINT('Ctrl Pts',(-190.966697020988,-6.58193048776853,
128.413435027317));
#254284=CARTESIAN_POINT('Ctrl Pts',(-191.245144644801,-5.56924761483672,
135.049571463749));
#254285=CARTESIAN_POINT('Ctrl Pts',(-191.523592268614,0.561301743259386,
137.784566522618));
#254286=CARTESIAN_POINT('Ctrl Pts',(-191.802039892427,6.17604222041412,
134.105093356759));
#254287=CARTESIAN_POINT('Ctrl Pts',(-192.08048751624,6.11530161344434,127.39240805334));
#254288=CARTESIAN_POINT('Ctrl Pts',(-192.358935140053,0.43489757281158,
123.815140473294));
#254289=CARTESIAN_POINT('Ctrl Pts',(-192.637382763865,-5.64515609130746,
126.660624763449));
#254290=CARTESIAN_POINT('Ctrl Pts',(-192.915830387678,-6.53758708872167,
133.313999870785));
#254291=CARTESIAN_POINT('Ctrl Pts',(-193.194278011491,-1.42229493048546,
137.661139107108));
#254292=CARTESIAN_POINT('Ctrl Pts',(-193.472725635304,5.00001678589681,
135.707233883791));
#254293=CARTESIAN_POINT('Ctrl Pts',(-193.751173259117,6.82755734043935,
129.247827647489));
#254294=CARTESIAN_POINT('Ctrl Pts',(-194.02962088293,2.38090624383734,124.218799169824));
#254295=CARTESIAN_POINT('Ctrl Pts',(-194.308068506743,-4.25368137711504,
125.241579940071));
#254296=CARTESIAN_POINT('Ctrl Pts',(-194.586516130556,-6.97934361638637,
131.376284395991));
#254297=CARTESIAN_POINT('Ctrl Pts',(-194.864963754369,-3.29133003208973,
136.985418839569));
#254298=CARTESIAN_POINT('Ctrl Pts',(-195.143411378181,3.42125506128717,
136.914462738605));
#254299=CARTESIAN_POINT('Ctrl Pts',(-195.421859001994,6.98987389094189,
131.22862128349));
#254300=CARTESIAN_POINT('Ctrl Pts',(-195.700306625807,4.13514008914463,
125.152905002676));
#254301=CARTESIAN_POINT('Ctrl Pts',(-195.97875424962,-2.51958544175274,
124.270600342989));
#254302=CARTESIAN_POINT('Ctrl Pts',(-196.257201873433,-6.85893504027095,
129.392502183704));
#254303=CARTESIAN_POINT('Ctrl Pts',(-196.535649497246,-4.89525841438522,
135.811832952018));
#254304=CARTESIAN_POINT('Ctrl Pts',(-196.814097121059,1.56692154765205,
137.629541273595));
#254305=CARTESIAN_POINT('Ctrl Pts',(-197.092544744872,6.58917715577019,
133.175242000891));
#254306=CARTESIAN_POINT('Ctrl Pts',(-197.370992368684,5.55630085693524,
126.542218560906));
#254307=CARTESIAN_POINT('Ctrl Pts',(-197.649439992498,-0.582544489036021,
123.825895453776));
#254308=CARTESIAN_POINT('Ctrl Pts',(-197.92788761631,-6.18605990846357,
127.522440915193));
#254309=CARTESIAN_POINT('Ctrl Pts',(-198.206335240123,-6.10488847784037,
134.234910252398));
#254310=CARTESIAN_POINT('Ctrl Pts',(-198.484782863936,-0.413622776464342,
137.79487206686));
#254311=CARTESIAN_POINT('Ctrl Pts',(-198.763230487749,5.657742049887,134.930895364888));
#254312=CARTESIAN_POINT('Ctrl Pts',(-199.041678111562,6.52991832845634,
128.274834822558));
#254313=CARTESIAN_POINT('Ctrl Pts',(-199.320125735375,1.40141866741961,
123.943284911633));
#254314=CARTESIAN_POINT('Ctrl Pts',(-199.598573359188,-5.01491628586802,
125.916728392279));
#254315=CARTESIAN_POINT('Ctrl Pts',(-199.877020983,-6.82278816472322,132.381667113854));
#254316=CARTESIAN_POINT('Ctrl Pts',(-200.155468606814,-2.36085103192995,
137.397138221046));
#254317=CARTESIAN_POINT('Ctrl Pts',(-200.433916230626,4.27059286522247,
136.354168785731));
#254318=CARTESIAN_POINT('Ctrl Pts',(-200.712363854439,6.97757054929515,
130.211196767073));
#254319=CARTESIAN_POINT('Ctrl Pts',(-200.990811478252,3.27250177183757,
124.613313349352));
#254320=CARTESIAN_POINT('Ctrl Pts',(-201.269259102065,-3.43983626333961,
124.704699921646));
#254321=CARTESIAN_POINT('Ctrl Pts',(-201.547706725878,-6.9911328178512,
130.401376688499));
#254322=CARTESIAN_POINT('Ctrl Pts',(-201.826154349691,-4.1179198485831,
136.468375999304));
#254323=CARTESIAN_POINT('Ctrl Pts',(-202.104601973504,2.53946028996452,
137.330421876826));
#254324=CARTESIAN_POINT('Ctrl Pts',(-202.383049597317,6.86320048156709,
132.195336272904));
#254325=CARTESIAN_POINT('Ctrl Pts',(-202.66149722113,4.87999471659204,125.782011994664));
#254326=CARTESIAN_POINT('Ctrl Pts',(-202.939944844942,-1.5876877919352,
123.983980745501));
#254327=CARTESIAN_POINT('Ctrl Pts',(-203.218392468755,-6.59636278253501,
128.453545404684));
#254328=CARTESIAN_POINT('Ctrl Pts',(-203.496840092568,-5.54330262622176,
135.083394400798));
#254329=CARTESIAN_POINT('Ctrl Pts',(-203.775287716381,0.603781838200554,
137.781020392543));
#254330=CARTESIAN_POINT('Ctrl Pts',(-204.053735340194,6.19602028969954,
134.067436879861));
#254331=CARTESIAN_POINT('Ctrl Pts',(-204.332182964007,6.09441878738321,
127.355245692268));
#254332=CARTESIAN_POINT('Ctrl Pts',(-204.61063058782,0.392344148371673,
123.812622622391));
#254333=CARTESIAN_POINT('Ctrl Pts',(-204.889078211633,-5.67027559591653,
126.69506520469));
#254334=CARTESIAN_POINT('Ctrl Pts',(-205.167525835445,-6.5221890759199,
133.353749521179));
#254335=CARTESIAN_POINT('Ctrl Pts',(-205.445973459259,-1.38052942180316,
137.66966997982));
#254336=CARTESIAN_POINT('Ctrl Pts',(-205.724421083071,5.02976932833932,
135.676706523556));
#254337=CARTESIAN_POINT('Ctrl Pts',(-206.002868706884,6.8179557836299,129.206295207017));
#254338=CARTESIAN_POINT('Ctrl Pts',(-206.281316330697,2.340773949421,124.204427932937));
#254339=CARTESIAN_POINT('Ctrl Pts',(-206.55976395451,-4.28746479114066,
125.267576371395));
#254340=CARTESIAN_POINT('Ctrl Pts',(-206.838211578323,-6.97573284294384,
131.418759045136));
#254341=CARTESIAN_POINT('Ctrl Pts',(-207.116659202136,-3.253643195576,137.005339578972));
#254342=CARTESIAN_POINT('Ctrl Pts',(-207.395106825949,3.4583855992191,136.893523381939));
#254343=CARTESIAN_POINT('Ctrl Pts',(-207.673554449762,6.99232697986142,
131.186064076586));
#254344=CARTESIAN_POINT('Ctrl Pts',(-207.952002073574,4.10066146017411,
125.127837939644));
#254345=CARTESIAN_POINT('Ctrl Pts',(-208.230449697387,-2.55931161296347,
124.286058830161));
#254346=CARTESIAN_POINT('Ctrl Pts',(-208.5088973212,-6.86740234311116,129.434280626559));
#254347=CARTESIAN_POINT('Ctrl Pts',(-208.787344945013,-4.86468581119477,
135.841539002563));
#254348=CARTESIAN_POINT('Ctrl Pts',(-209.065792568826,1.60843932809579,
137.619876522599));
#254349=CARTESIAN_POINT('Ctrl Pts',(-209.344240192639,6.60348730149562,
133.135087882371));
#254350=CARTESIAN_POINT('Ctrl Pts',(-209.622687816452,5.53025304311036,
126.508474748144));
#254351=CARTESIAN_POINT('Ctrl Pts',(-209.901135440264,-0.625013594012848,
123.829570862223));
#254352=CARTESIAN_POINT('Ctrl Pts',(-210.179583064078,-6.20592327184948,
127.56015802404));
#254353=CARTESIAN_POINT('Ctrl Pts',(-210.45803068789,-6.08389263906328,
134.272008881199));
#254354=CARTESIAN_POINT('Ctrl Pts',(-210.736478311703,-0.371061885656257,
137.797260388114));
#254355=CARTESIAN_POINT('Ctrl Pts',(-211.014925935516,5.68275661328764,
134.896378628042));
#254356=CARTESIAN_POINT('Ctrl Pts',(-211.293373559329,6.51439940271492,
128.235132222534));
#254357=CARTESIAN_POINT('Ctrl Pts',(-211.571821183142,1.35962738715011,
123.934881198276));
#254358=CARTESIAN_POINT('Ctrl Pts',(-211.850268806955,-5.04457577571481,
125.947346167619));
#254359=CARTESIAN_POINT('Ctrl Pts',(-212.128716430768,-6.81306024192543,
132.423170138115));
#254360=CARTESIAN_POINT('Ctrl Pts',(-212.40716405458,-2.32067518230222,
137.411387242468));
#254361=CARTESIAN_POINT('Ctrl Pts',(-212.685611678394,4.30429699857105,
136.32806964973));
#254362=CARTESIAN_POINT('Ctrl Pts',(-212.964059302206,6.97383051435588,
130.168733304621));
#254363=CARTESIAN_POINT('Ctrl Pts',(-213.24250692602,3.23475447800865,124.593507407987));
#254364=CARTESIAN_POINT('Ctrl Pts',(-213.520954549832,-3.47690289708716,
124.725752193909));
#254365=CARTESIAN_POINT('Ctrl Pts',(-213.799402173646,-6.99345636590915,
130.443941164641));
#254366=CARTESIAN_POINT('Ctrl Pts',(-214.077849797458,-4.08336508379785,
136.49333800514));
#254367=CARTESIAN_POINT('Ctrl Pts',(-214.356297421271,2.57913922684953,
137.314842548456));
#254368=CARTESIAN_POINT('Ctrl Pts',(-214.634745045084,6.87154058597789,
132.153532252007));
#254369=CARTESIAN_POINT('Ctrl Pts',(-214.913192668897,4.84933184001288,
125.752399134204));
#254370=CARTESIAN_POINT('Ctrl Pts',(-215.19164029271,-1.62917596389355,
123.993771817573));
#254371=CARTESIAN_POINT('Ctrl Pts',(-215.470087916522,-6.61055064665203,
128.493742892374));
#254372=CARTESIAN_POINT('Ctrl Pts',(-215.748535540335,-5.51715222849034,
135.117058776675));
#254373=CARTESIAN_POINT('Ctrl Pts',(-216.026983164148,0.646239559784443,
137.777215739773));
#254374=CARTESIAN_POINT('Ctrl Pts',(-216.305430787961,6.21576876317433,
134.029659488472));
#254375=CARTESIAN_POINT('Ctrl Pts',(-216.583878411774,6.0733101303926,127.318211139417));
#254376=CARTESIAN_POINT('Ctrl Pts',(-216.862326035587,0.349776185474419,
123.810363852911));
#254377=CARTESIAN_POINT('Ctrl Pts',(-217.1407736594,-5.69518498637811,126.729657917385));
#254378=CARTESIAN_POINT('Ctrl Pts',(-217.419221283213,-6.50654938100331,
133.393404703032));
#254379=CARTESIAN_POINT('Ctrl Pts',(-217.697668907026,-1.33871275709491,
137.67794645597));
#254380=CARTESIAN_POINT('Ctrl Pts',(-217.976116530838,5.05933549082977,
135.64599861675));
#254381=CARTESIAN_POINT('Ctrl Pts',(-218.254564154652,6.80810158496121,
129.164821983446));
#254382=CARTESIAN_POINT('Ctrl Pts',(-218.533011778464,2.30055491676597,
124.190301258982));
#254383=CARTESIAN_POINT('Ctrl Pts',(-218.811459402277,-4.32108933158155,
125.293777970294));
#254384=CARTESIAN_POINT('Ctrl Pts',(-219.08990702609,-6.97186358115499,
131.461210927519));
#254385=CARTESIAN_POINT('Ctrl Pts',(-219.368354649903,-3.21583579411804,
137.02503053882));
#254386=CARTESIAN_POINT('Ctrl Pts',(-219.646802273716,3.49538798540175,
136.872358389107));
#254387=CARTESIAN_POINT('Ctrl Pts',(-219.925249897529,6.99452096553273,
131.143492725519));
#254388=CARTESIAN_POINT('Ctrl Pts',(-220.203697521342,4.06603087968498,
125.102981222246));
#254389=CARTESIAN_POINT('Ctrl Pts',(-220.482145145155,-2.59894294794204,
124.301758855404));
#254390=CARTESIAN_POINT('Ctrl Pts',(-220.760592768967,-6.87561517183164,
129.476109838232));
#254391=CARTESIAN_POINT('Ctrl Pts',(-221.03904039278,-4.83393294528274,
135.87105839861));
#254392=CARTESIAN_POINT('Ctrl Pts',(-221.317488016593,1.64989750722823,
137.609959220154));
#254393=CARTESIAN_POINT('Ctrl Pts',(-221.595935640406,6.61755275257056,
133.094847397895));
#254394=CARTESIAN_POINT('Ctrl Pts',(-221.874383264219,5.5040003037252,126.474890121013));
#254395=CARTESIAN_POINT('Ctrl Pts',(-222.152830888031,-0.667459538880483,
123.83350472407));
#254396=CARTESIAN_POINT('Ctrl Pts',(-222.431278511845,-6.22555667246622,
127.597995348007));
#254397=CARTESIAN_POINT('Ctrl Pts',(-222.709726135657,-6.06267135940695,
134.308979015016));
#254398=CARTESIAN_POINT('Ctrl Pts',(-222.988173759471,-0.328487245014279,
137.799389584896));
#254399=CARTESIAN_POINT('Ctrl Pts',(-223.266621383283,5.70756060005303,
134.861710259961));
#254400=CARTESIAN_POINT('Ctrl Pts',(-223.545069007096,6.49863908350723,
128.195524826214));
#254401=CARTESIAN_POINT('Ctrl Pts',(-223.823516630909,1.31778572538753,
123.926732036005));
#254402=CARTESIAN_POINT('Ctrl Pts',(-224.101964254722,-5.07404833695195,
125.978143921416));
#254403=CARTESIAN_POINT('Ctrl Pts',(-224.380411878535,-6.80307985867417,
132.464613176793));
#254404=CARTESIAN_POINT('Ctrl Pts',(-224.658859502348,-2.28041333920269,
137.425391438088));
#254405=CARTESIAN_POINT('Ctrl Pts',(-224.937307126161,4.33784163461131,
136.30176583066));
#254406=CARTESIAN_POINT('Ctrl Pts',(-225.215754749974,6.96983206156226,
130.126293395573));
#254407=CARTESIAN_POINT('Ctrl Pts',(-225.494202373786,3.19688731916334,
124.573931612073));
#254408=CARTESIAN_POINT('Ctrl Pts',(-225.7726499976,-3.51384069291894,124.747029711241));
#254409=CARTESIAN_POINT('Ctrl Pts',(-226.051097621412,-6.9955207688696,
130.486518996257));
#254410=CARTESIAN_POINT('Ctrl Pts',(-226.329545245225,-4.04865900841799,
136.518089203828));
#254411=CARTESIAN_POINT('Ctrl Pts',(-226.607992869038,2.61872259278156,
137.299021971784));
#254412=CARTESIAN_POINT('Ctrl Pts',(-226.886440492851,6.87962606292594,
132.111678237058));
#254413=CARTESIAN_POINT('Ctrl Pts',(-227.164888116664,4.81848926965818,
125.722973476035));
#254414=CARTESIAN_POINT('Ctrl Pts',(-227.443335740477,-1.67060376613766,
124.003815258517));
#254415=CARTESIAN_POINT('Ctrl Pts',(-227.72178336429,-6.62449355438458,
128.534026000853));
#254416=CARTESIAN_POINT('Ctrl Pts',(-228.000230988102,-5.49079739065326,
135.150563343936));
#254417=CARTESIAN_POINT('Ctrl Pts',(-228.278678611916,0.688673334723007,
137.773152705292));
#254418=CARTESIAN_POINT('Ctrl Pts',(-228.557126235728,6.23528690905198,
133.991762582447));
#254419=CARTESIAN_POINT('Ctrl Pts',(-228.835573859542,6.05197642466173,
127.281305767118));
#254420=CARTESIAN_POINT('Ctrl Pts',(-229.114021483354,0.307195261492642,
123.808364248553));
#254421=CARTESIAN_POINT('Ctrl Pts',(-229.392469107167,-5.7198833396657,
126.764401619687));
#254422=CARTESIAN_POINT('Ctrl Pts',(-229.670916730979,-6.49066858350677,
133.432963946903));
#254423=CARTESIAN_POINT('Ctrl Pts',(-229.949364354793,-1.29684648589306,
137.685968228869));
#254424=CARTESIAN_POINT('Ctrl Pts',(-230.227811978605,5.0887141777831,135.615111301269));
#254425=CARTESIAN_POINT('Ctrl Pts',(-230.506259602419,6.79799510958498,
129.123409513582));
#254426=CARTESIAN_POINT('Ctrl Pts',(-230.784707226231,2.26025063620168,
124.176419671429));
#254427=CARTESIAN_POINT('Ctrl Pts',(-231.063154850045,-4.35455375246839,
125.32018376586));
#254428=CARTESIAN_POINT('Ctrl Pts',(-231.341602473857,-6.96773597439774,
131.503638470075));
#254429=CARTESIAN_POINT('Ctrl Pts',(-231.62005009767,-3.17790922868121,
137.044490989456));
#254430=CARTESIAN_POINT('Ctrl Pts',(-231.898497721483,3.53226084869627,
136.850968544386));
#254431=CARTESIAN_POINT('Ctrl Pts',(-232.176945345296,6.99645576665798,
131.100908807788));
#254432=CARTESIAN_POINT('Ctrl Pts',(-232.455392969109,4.03124963092651,
125.078335771559));
#254433=CARTESIAN_POINT('Ctrl Pts',(-232.733840592922,-2.63847797813309,
124.317699836946));
#254434=CARTESIAN_POINT('Ctrl Pts',(-233.012288216734,-6.88357322210384,
129.517988268725));
#254435=CARTESIAN_POINT('Ctrl Pts',(-233.290735840548,-4.80300095620762,
135.900390046307));
#254436=CARTESIAN_POINT('Ctrl Pts',(-233.56918346436,1.6912945488023,137.599789733751));
#254437=CARTESIAN_POINT('Ctrl Pts',(-233.847631088173,6.63137298779474,
133.05452203859));
#254438=CARTESIAN_POINT('Ctrl Pts',(-234.126078711986,5.47754361158473,
126.441465924004));
#254439=CARTESIAN_POINT('Ctrl Pts',(-234.404526335799,-0.709880750790079,
123.837696893545));
#254440=CARTESIAN_POINT('Ctrl Pts',(-234.682973959612,-6.24495938279112,
127.635951485018));
#254441=CARTESIAN_POINT('Ctrl Pts',(-234.961421583425,-6.04122542523402,
134.345819283911));
#254442=CARTESIAN_POINT('Ctrl Pts',(-235.239869207238,-0.285900432155891,
137.801259578306));
#254443=CARTESIAN_POINT('Ctrl Pts',(-235.518316831051,5.73215309106056,
134.826891545298));
#254444=CARTESIAN_POINT('Ctrl Pts',(-235.796764454864,6.48263795483918,
128.156014101264));
#254445=CARTESIAN_POINT('Ctrl Pts',(-236.075212078676,1.27589523259052,
123.918837726791));
#254446=CARTESIAN_POINT('Ctrl Pts',(-236.353659702489,-5.10333287746112,
126.009120512446));
#254447=CARTESIAN_POINT('Ctrl Pts',(-236.632107326302,-6.79284738479763,
132.505994694203));
#254448=CARTESIAN_POINT('Ctrl Pts',(-236.910554950115,-2.24006699454776,
137.439150288976));
#254449=CARTESIAN_POINT('Ctrl Pts',(-237.189002573928,4.3712255303347,136.275258303218));
#254450=CARTESIAN_POINT('Ctrl Pts',(-237.467450197741,6.96557533907847,
130.083878612554));
#254451=CARTESIAN_POINT('Ctrl Pts',(-237.745897821554,3.15890169848239,
124.554586686994));
#254452=CARTESIAN_POINT('Ctrl Pts',(-238.024345445366,-3.55064828209192,
124.768531685198));
#254453=CARTESIAN_POINT('Ctrl Pts',(-238.30279306918,-6.99732595023538,
130.529108605612));
#254454=CARTESIAN_POINT('Ctrl Pts',(-238.581240692992,-4.01380290848946,
136.542628678202));
#254455=CARTESIAN_POINT('Ctrl Pts',(-238.859688316805,2.65820892098533,
137.282960733047));
#254456=CARTESIAN_POINT('Ctrl Pts',(-239.138135940618,6.88745661279959,
132.069775778975));
#254457=CARTESIAN_POINT('Ctrl Pts',(-239.416583564431,4.78746814841248,
125.693736110535));
#254458=CARTESIAN_POINT('Ctrl Pts',(-239.695031188244,-1.71196966354462,
124.014110696169));
#254459=CARTESIAN_POINT('Ctrl Pts',(-239.973478812057,-6.63819098907155,
128.574393237416));
#254460=CARTESIAN_POINT('Ctrl Pts',(-240.25192643587,-5.46423908930053,
135.183906861057));
#254461=CARTESIAN_POINT('Ctrl Pts',(-240.530374059683,0.731081590618679,
137.768831439659));
#254462=CARTESIAN_POINT('Ctrl Pts',(-240.808821683496,6.25457400407998,
133.95374756607));
#254463=CARTESIAN_POINT('Ctrl Pts',(-241.087269307308,6.03041846071876,
127.244530942912));
#254464=CARTESIAN_POINT('Ctrl Pts',(-241.365716931122,0.264602954276818,
123.806623883412));
#254465=CARTESIAN_POINT('Ctrl Pts',(-241.644164554934,-5.74436974057257,
126.799295024156));
#254466=CARTESIAN_POINT('Ctrl Pts',(-241.922612178747,-6.47454727189872,
133.472425786911));
#254467=CARTESIAN_POINT('Ctrl Pts',(-242.20105980256,-1.25493215956847,
137.693735001267));
#254468=CARTESIAN_POINT('Ctrl Pts',(-242.479507426373,5.11790430056101,
135.584045721651));
#254469=CARTESIAN_POINT('Ctrl Pts',(-242.757955050186,6.78763673199965,
129.082059331979));
#254470=CARTESIAN_POINT('Ctrl Pts',(-243.036402673998,2.21986260121965,
124.162783684665));
#254471=CARTESIAN_POINT('Ctrl Pts',(-243.314850297812,-4.38785681376436,
125.346792779616));
#254472=CARTESIAN_POINT('Ctrl Pts',(-243.593297921624,-6.96335017562108,
131.54604010063));
#254473=CARTESIAN_POINT('Ctrl Pts',(-243.871745545438,-3.13986490465013,
137.063720209766));
#254474=CARTESIAN_POINT('Ctrl Pts',(-244.15019316925,3.56900282276695,136.829354640385));
#254475=CARTESIAN_POINT('Ctrl Pts',(-244.428640793064,6.99813131154132,
131.058313901354));
#254476=CARTESIAN_POINT('Ctrl Pts',(-244.707088416876,3.99631900273028,
125.053902500829));
#254477=CARTESIAN_POINT('Ctrl Pts',(-244.985536040689,-2.67791523855318,
124.333881184089));
#254478=CARTESIAN_POINT('Ctrl Pts',(-245.263983664501,-6.89127619903846,
129.559914366219));
#254479=CARTESIAN_POINT('Ctrl Pts',(-245.542431288315,-4.7718909901659,
135.929532858758));
#254480=CARTESIAN_POINT('Ctrl Pts',(-245.820878912128,1.73262891883438,
137.589368440225));
#254481=CARTESIAN_POINT('Ctrl Pts',(-246.09932653594,6.6449474950541,133.014113298726));
#254482=CARTESIAN_POINT('Ctrl Pts',(-246.377774159753,5.45088394705135,
126.408203395661));
#254483=CARTESIAN_POINT('Ctrl Pts',(-246.656221783566,-0.752275657806765,
123.842147215306));
#254484=CARTESIAN_POINT('Ctrl Pts',(-246.934669407379,-6.26413068384941,
127.674025028594));
#254485=CARTESIAN_POINT('Ctrl Pts',(-247.213117031192,-6.01955563123113,
134.382528322752));
#254486=CARTESIAN_POINT('Ctrl Pts',(-247.491564655005,-0.243303025152602,
137.802870299053));
#254487=CARTESIAN_POINT('Ctrl Pts',(-247.770012278818,5.75653317502817,
134.791923774272));
#254488=CARTESIAN_POINT('Ctrl Pts',(-248.048459902631,6.46639660963695,
128.116601511768));
#254489=CARTESIAN_POINT('Ctrl Pts',(-248.326907526444,1.23395746102625,
123.91119856316));
#254490=CARTESIAN_POINT('Ctrl Pts',(-248.605355150257,-5.13242831209467,
126.040274792862));
#254491=CARTESIAN_POINT('Ctrl Pts',(-248.883802774069,-6.78236319946242,
132.547313156937));
#254492=CARTESIAN_POINT('Ctrl Pts',(-249.162250397883,-2.19963764338714,
137.452663285294));
#254493=CARTESIAN_POINT('Ctrl Pts',(-249.440698021695,4.40444744868852,
136.24854804965));
#254494=CARTESIAN_POINT('Ctrl Pts',(-249.719145645508,6.96106050463867,
130.041490527264));
#254495=CARTESIAN_POINT('Ctrl Pts',(-249.997593269321,3.12079902353814,
124.535473349588));
#254496=CARTESIAN_POINT('Ctrl Pts',(-250.276040893134,-3.58732430068758,
124.790257319018));
#254497=CARTESIAN_POINT('Ctrl Pts',(-250.554488516946,-6.99887184311352,
130.571708414529));
#254498=CARTESIAN_POINT('Ctrl Pts',(-250.83293614076,-3.97879807562073,
136.566955518948));
#254499=CARTESIAN_POINT('Ctrl Pts',(-251.111383764572,2.69759674828547,
137.26665942739));
#254500=CARTESIAN_POINT('Ctrl Pts',(-251.389831388386,6.89503194542569,
132.027826430486));
#254501=CARTESIAN_POINT('Ctrl Pts',(-251.668279012198,4.75626962579305,
125.66468812107));
#254502=CARTESIAN_POINT('Ctrl Pts',(-251.946726636011,-1.75327212332407,
124.024657749096));
#254503=CARTESIAN_POINT('Ctrl Pts',(-252.225174259824,-6.65164244307981,
128.614843106116));
#254504=CARTESIAN_POINT('Ctrl Pts',(-252.503621883637,-5.43747830869239,
135.217088092717));
#254505=CARTESIAN_POINT('Ctrl Pts',(-252.78206950745,0.773462756270139,
137.764252102553));
#254506=CARTESIAN_POINT('Ctrl Pts',(-253.060517131263,6.2736293330892,133.91561584884));
#254507=CARTESIAN_POINT('Ctrl Pts',(-253.338964755075,6.00863703830687,
127.207888027921));
#254508=CARTESIAN_POINT('Ctrl Pts',(-253.617412378889,0.222000840393564,
123.805142824969));
#254509=CARTESIAN_POINT('Ctrl Pts',(-253.895860002702,-5.76864327852066,
126.83433683216));
#254510=CARTESIAN_POINT('Ctrl Pts',(-254.174307626514,-6.45818604965135,
133.511788771436));
#254511=CARTESIAN_POINT('Ctrl Pts',(-254.452755250327,-1.21297131977014,
137.701246465247));
#254512=CARTESIAN_POINT('Ctrl Pts',(-254.73120287414,5.14690475579816,135.55280306703));
#254513=CARTESIAN_POINT('Ctrl Pts',(-255.009650497953,6.7770268770417,129.040772899161));
#254514=CARTESIAN_POINT('Ctrl Pts',(-255.288098121766,2.17939223099114,
124.149393939406));
#254515=CARTESIAN_POINT('Ctrl Pts',(-255.566545745579,-4.42099713522674,
125.37360376984));
#254516=CARTESIAN_POINT('Ctrl Pts',(-255.844993369392,-6.95870662337211,
131.588414730824));
#254517=CARTESIAN_POINT('Ctrl Pts',(-256.123440993205,-3.10170371057109,
137.082716575498));
#254518=CARTESIAN_POINT('Ctrl Pts',(-256.401888617018,3.60561156199617,
136.807519199501));
#254519=CARTESIAN_POINT('Ctrl Pts',(-256.68033624083,6.99954939633056,131.01570633407));
#254520=CARTESIAN_POINT('Ctrl Pts',(-256.958783864643,3.96123678073902,
125.029688453078));
#254521=CARTESIAN_POINT('Ctrl Pts',(-257.237231488456,-2.71724664265218,
124.350290708114));
#254522=CARTESIAN_POINT('Ctrl Pts',(-257.515679112269,-6.89873632689917,
129.601908459729));
#254523=CARTESIAN_POINT('Ctrl Pts',(-257.794126736082,-4.74058057908887,
135.958444437253));
#254524=CARTESIAN_POINT('Ctrl Pts',(-258.072574359895,1.77385448465437,
137.578773744179));
#254525=CARTESIAN_POINT('Ctrl Pts',(-258.351021983707,6.6583599873155,132.973475360041));
#254526=CARTESIAN_POINT('Ctrl Pts',(-258.629469607521,5.42386327951784,
126.375381938049));
#254527=CARTESIAN_POINT('Ctrl Pts',(-258.907917231333,-0.794342416617398,
123.846330221273));
#254528=CARTESIAN_POINT('Ctrl Pts',(-259.186364855146,-6.28363694765996,
127.713206958712));
#254529=CARTESIAN_POINT('Ctrl Pts',(-259.464812478959,-5.99659113747434,
134.41722675292));
#254530=CARTESIAN_POINT('Ctrl Pts',(-259.743260102772,-0.202727240537578,
137.807801967267));
#254531=CARTESIAN_POINT('Ctrl Pts',(-260.021707726585,5.7845923739281,134.749768174183));
#254532=CARTESIAN_POINT('Ctrl Pts',(-260.253747413096,6.33253704604016,
129.202365411857));
#254533=CARTESIAN_POINT('Ctrl Pts',(-260.439389088604,3.82430165355141,
125.973250269562));
#254534=CARTESIAN_POINT('Ctrl Pts',(-260.532214889509,1.97943258085903,
125.138073123498));
#254535=CARTESIAN_POINT('Ctrl Pts',(-260.578632753112,1.00712299976162,
124.970230583726));
#254536=CARTESIAN_POINT('',(-177.785171091631,5.06474445112881,133.863166627639));
#254537=CARTESIAN_POINT('',(-177.476367722506,5.12014273339247,130.804360617566));
#254538=CARTESIAN_POINT('Ctrl Pts',(-177.786046227816,5.06143466734273,
133.861215740604));
#254539=CARTESIAN_POINT('Ctrl Pts',(-177.742821434039,5.08507708225877,
133.650067943741));
#254540=CARTESIAN_POINT('Ctrl Pts',(-177.704041383372,5.10684921384841,
133.437850811182));
#254541=CARTESIAN_POINT('Ctrl Pts',(-177.627101194856,5.14805987156466,
132.959434264776));
#254542=CARTESIAN_POINT('Ctrl Pts',(-177.591430156013,5.16562332921322,
132.692970957434));
#254543=CARTESIAN_POINT('Ctrl Pts',(-177.51826800244,5.18983313181224,132.008875337098));
#254544=CARTESIAN_POINT('Ctrl Pts',(-177.491889782598,5.18373170393937,
131.607069645772));
#254545=CARTESIAN_POINT('Ctrl Pts',(-177.478015568181,5.14508328177199,
131.063381533424));
#254546=CARTESIAN_POINT('Ctrl Pts',(-177.476367722506,5.13366996699167,
130.933750143363));
#254547=CARTESIAN_POINT('Ctrl Pts',(-177.476367722506,5.1201427333925,130.804360617566));
#254548=CARTESIAN_POINT('',(-178.183936147798,3.7463393230346,126.224944438273));
#254549=CARTESIAN_POINT('Ctrl Pts',(-177.785171091631,5.06474445112881,
133.863166627639));
#254550=CARTESIAN_POINT('Ctrl Pts',(-177.792868498275,5.14945412057303,
133.722905091974));
#254551=CARTESIAN_POINT('Ctrl Pts',(-177.800565904919,5.228288425839,133.579195727341));
#254552=CARTESIAN_POINT('Ctrl Pts',(-177.808263311562,5.30097891580062,
133.43258303904));
#254553=CARTESIAN_POINT('Ctrl Pts',(-177.815673272437,5.37095491050639,
133.291445337178));
#254554=CARTESIAN_POINT('Ctrl Pts',(-177.823083233312,5.43523756743315,
133.147617601296));
#254555=CARTESIAN_POINT('Ctrl Pts',(-177.830493194186,5.49363698048319,
133.001605093988));
#254556=CARTESIAN_POINT('Ctrl Pts',(-177.837908263093,5.552076650981,132.855491933428));
#254557=CARTESIAN_POINT('Ctrl Pts',(-177.845323332,5.60462487314325,132.707191351285));
#254558=CARTESIAN_POINT('Ctrl Pts',(-177.852738400907,5.65114171470356,
132.557223385394));
#254559=CARTESIAN_POINT('Ctrl Pts',(-177.86016325716,5.69771995507294,132.407057472819));
#254560=CARTESIAN_POINT('Ctrl Pts',(-177.867588113413,5.73825082931068,
132.255220142398));
#254561=CARTESIAN_POINT('Ctrl Pts',(-177.875012969665,5.77264542002059,
132.102241743562));
#254562=CARTESIAN_POINT('Ctrl Pts',(-177.875855303563,5.77654741201243,
132.084886674789));
#254563=CARTESIAN_POINT('Ctrl Pts',(-177.87669763746,5.78037048244532,132.067516925213));
#254564=CARTESIAN_POINT('Ctrl Pts',(-177.877539971357,5.78411454368991,
132.050133272578));
#254565=CARTESIAN_POINT('Ctrl Pts',(-177.884963237763,5.8171099676497,131.8969357282));
#254566=CARTESIAN_POINT('Ctrl Pts',(-177.892386504168,5.8440647157557,131.742194755227));
#254567=CARTESIAN_POINT('Ctrl Pts',(-177.899809770574,5.8648359806621,131.586428058668));
#254568=CARTESIAN_POINT('Ctrl Pts',(-177.907224263295,5.88558269565839,
131.430845465408));
#254569=CARTESIAN_POINT('Ctrl Pts',(-177.914638756016,5.90016042593303,
131.2742399281));
#254570=CARTESIAN_POINT('Ctrl Pts',(-177.922053248737,5.9084768456705,131.117141573948));
#254571=CARTESIAN_POINT('Ctrl Pts',(-177.929460595091,5.91678524972953,
130.960194637105));
#254572=CARTESIAN_POINT('Ctrl Pts',(-177.936867941444,5.91884433792154,
130.802756199313));
#254573=CARTESIAN_POINT('Ctrl Pts',(-177.944275287798,5.91461330392028,
130.645363675491));
#254574=CARTESIAN_POINT('Ctrl Pts',(-177.951677109474,5.91038542558379,
130.488088540951));
#254575=CARTESIAN_POINT('Ctrl Pts',(-177.959078931149,5.89987677627349,
130.330859623753));
#254576=CARTESIAN_POINT('Ctrl Pts',(-177.966480752825,5.88309857495091,
130.174216411919));
#254577=CARTESIAN_POINT('Ctrl Pts',(-177.973878667136,5.86632923071016,
130.017655890817));
#254578=CARTESIAN_POINT('Ctrl Pts',(-177.981276581447,5.84329696543529,
129.861680829548));
#254579=CARTESIAN_POINT('Ctrl Pts',(-177.988674495759,5.81406499171618,
129.706827549909));
#254580=CARTESIAN_POINT('Ctrl Pts',(-177.996071180671,5.78483787582098,
129.552000004077));
#254581=CARTESIAN_POINT('Ctrl Pts',(-178.003467865583,5.74941316545811,
129.398294236346));
#254582=CARTESIAN_POINT('Ctrl Pts',(-178.010864550496,5.7079055513191,129.246238420907));
#254583=CARTESIAN_POINT('Ctrl Pts',(-178.018260907431,5.66639977767119,
129.094189347783));
#254584=CARTESIAN_POINT('Ctrl Pts',(-178.025657264366,5.61881173485076,
128.943790441604));
#254585=CARTESIAN_POINT('Ctrl Pts',(-178.033053621302,5.56530649258155,
128.7955564444));
#254586=CARTESIAN_POINT('Ctrl Pts',(-178.040451110638,5.51179305852316,
128.647299752193));
#254587=CARTESIAN_POINT('Ctrl Pts',(-178.047848599975,5.45236074791929,
128.501208980075));
#254588=CARTESIAN_POINT('Ctrl Pts',(-178.055246089312,5.38722339221779,
128.357780415561));
#254589=CARTESIAN_POINT('Ctrl Pts',(-178.062646171827,5.3220632027175,128.214301572387));
#254590=CARTESIAN_POINT('Ctrl Pts',(-178.070046254342,5.25119414060659,
128.073487134552));
#254591=CARTESIAN_POINT('Ctrl Pts',(-178.077446336857,5.1748766688598,127.935810108234));
#254592=CARTESIAN_POINT('Ctrl Pts',(-178.084854556523,5.0984752782071,127.797981691871));
#254593=CARTESIAN_POINT('Ctrl Pts',(-178.09226277619,5.01661369441823,127.663297903407));
#254594=CARTESIAN_POINT('Ctrl Pts',(-178.099670995856,4.92959690775233,
127.532204617376));
#254595=CARTESIAN_POINT('Ctrl Pts',(-178.107083775158,4.84252656370595,
127.401030645615));
#254596=CARTESIAN_POINT('Ctrl Pts',(-178.11449655446,4.75029491249686,127.273451881598));
#254597=CARTESIAN_POINT('Ctrl Pts',(-178.121909333762,4.65324782702301,
127.14988182808));
#254598=CARTESIAN_POINT('Ctrl Pts',(-178.129332704791,4.55606207612225,
127.026135211873));
#254599=CARTESIAN_POINT('Ctrl Pts',(-178.13675607582,4.45404739048349,126.906409029321));
#254600=CARTESIAN_POINT('Ctrl Pts',(-178.144179446849,4.34758769447436,
126.791081185312));
#254601=CARTESIAN_POINT('Ctrl Pts',(-178.148115496289,4.29114020918847,
126.729931595168));
#254602=CARTESIAN_POINT('Ctrl Pts',(-178.15205154573,4.23344365617117,126.670017889433));
#254603=CARTESIAN_POINT('Ctrl Pts',(-178.15598759517,4.17455901249308,126.611391787046));
#254604=CARTESIAN_POINT('Ctrl Pts',(-178.163412098033,4.0634859144098,126.500806370986));
#254605=CARTESIAN_POINT('Ctrl Pts',(-178.170836600896,3.94784763173947,
126.394470301888));
#254606=CARTESIAN_POINT('Ctrl Pts',(-178.178261103759,3.82800271599344,
126.292783756994));
#254607=CARTESIAN_POINT('Ctrl Pts',(-178.1797891116,3.80333790351263,126.271856047662));
#254608=CARTESIAN_POINT('Ctrl Pts',(-178.18131711944,3.77849505168981,126.251125163909));
#254609=CARTESIAN_POINT('Ctrl Pts',(-178.18284512728,3.75347749648132,126.230594418261));
#254610=CARTESIAN_POINT('Ctrl Pts',(-177.476367722506,5.1201427333925,130.804360617566));
#254611=CARTESIAN_POINT('Ctrl Pts',(-177.476367722506,5.0948783866862,130.5627042718));
#254612=CARTESIAN_POINT('Ctrl Pts',(-177.48211809202,5.06224363656916,130.321891244269));
#254613=CARTESIAN_POINT('Ctrl Pts',(-177.495355899915,5.01616195097393,
130.042752414703));
#254614=CARTESIAN_POINT('Ctrl Pts',(-177.497386085719,5.00943885560551,
130.003205734465));
#254615=CARTESIAN_POINT('Ctrl Pts',(-177.499617454833,5.00237413411682,
129.962810309717));
#254616=CARTESIAN_POINT('Ctrl Pts',(-177.499666670813,5.00221846150168,
129.961920748202));
#254617=CARTESIAN_POINT('Ctrl Pts',(-177.499730694524,5.00201614547379,
129.960765378705));
#254618=CARTESIAN_POINT('Ctrl Pts',(-177.499745432065,5.00196958791774,
129.960499551648));
#254619=CARTESIAN_POINT('Ctrl Pts',(-177.499769029077,5.00189506362177,
129.960074124391));
#254620=CARTESIAN_POINT('Ctrl Pts',(-177.499777884095,5.00186710242369,
129.959914523897));
#254621=CARTESIAN_POINT('Ctrl Pts',(-177.499794570173,5.00181442238816,
129.95961386397));
#254622=CARTESIAN_POINT('Ctrl Pts',(-177.499802400734,5.00178970407401,
129.959472803585));
#254623=CARTESIAN_POINT('Ctrl Pts',(-177.499820020531,5.00173409303354,
129.959155478821));
#254624=CARTESIAN_POINT('Ctrl Pts',(-177.499829810846,5.00170319900482,
129.958979214899));
#254625=CARTESIAN_POINT('Ctrl Pts',(-177.49985857684,5.00161244305434,129.958461477023));
#254626=CARTESIAN_POINT('Ctrl Pts',(-177.499877560812,5.00155257106515,
129.958120006032));
#254627=CARTESIAN_POINT('Ctrl Pts',(-177.500018881264,5.00110703522932,
129.955579570966));
#254628=CARTESIAN_POINT('Ctrl Pts',(-177.500141677395,5.00072080907722,
129.953380730883));
#254629=CARTESIAN_POINT('Ctrl Pts',(-177.500536626073,4.99948149158206,
129.94633603335));
#254630=CARTESIAN_POINT('Ctrl Pts',(-177.500810594968,4.99862617902564,
129.941490668575));
#254631=CARTESIAN_POINT('Ctrl Pts',(-177.505780023924,4.98319006347085,
129.854340602474));
#254632=CARTESIAN_POINT('Ctrl Pts',(-177.511132903343,4.96780601042822,
129.772215719214));
#254633=CARTESIAN_POINT('Ctrl Pts',(-177.529349382818,4.91874040928095,
129.523654579321));
#254634=CARTESIAN_POINT('Ctrl Pts',(-177.544257370828,4.88258806682499,
129.357846583682));
#254635=CARTESIAN_POINT('Ctrl Pts',(-177.614171330561,4.72588974921601,
128.700200073337));
#254636=CARTESIAN_POINT('Ctrl Pts',(-177.690013732162,4.58067706950535,
128.216337619616));
#254637=CARTESIAN_POINT('Ctrl Pts',(-177.84225534922,4.31179323860895,127.473090897716));
#254638=CARTESIAN_POINT('Ctrl Pts',(-177.904956701624,4.2047636979896,127.204993718243));
#254639=CARTESIAN_POINT('Ctrl Pts',(-178.037928907979,3.98269005161135,
126.69739203434));
#254640=CARTESIAN_POINT('Ctrl Pts',(-178.106102869168,3.87028467230515,
126.461623567896));
#254641=CARTESIAN_POINT('Ctrl Pts',(-178.179024752208,3.75385310384345,
126.229852392558));
#254642=CARTESIAN_POINT('Ctrl Pts',(210.579426101437,-2.14555810197798,
126.384433368448));
#254643=CARTESIAN_POINT('Ctrl Pts',(210.533016425084,-2.88204635455982,
126.741945114569));
#254644=CARTESIAN_POINT('Ctrl Pts',(210.440198811428,-4.16073755837059,
127.832228156677));
#254645=CARTESIAN_POINT('Ctrl Pts',(210.254565323169,-5.41774734084591,
130.983824311839));
#254646=CARTESIAN_POINT('Ctrl Pts',(210.022525636658,-3.70466367662459,
135.280954889074));
#254647=CARTESIAN_POINT('Ctrl Pts',(209.744078012845,1.77278938863763,136.341871604603));
#254648=CARTESIAN_POINT('Ctrl Pts',(209.465630389032,5.61248518735455,132.305536381355));
#254649=CARTESIAN_POINT('Ctrl Pts',(209.187182765219,4.2990952821384,126.894094626803));
#254650=CARTESIAN_POINT('Ctrl Pts',(208.908735141406,-0.967335548355457,
125.073681250508));
#254651=CARTESIAN_POINT('Ctrl Pts',(208.630287517594,-5.34357155608916,
128.520706403956));
#254652=CARTESIAN_POINT('Ctrl Pts',(208.351839893781,-4.80999390579215,
134.065650134797));
#254653=CARTESIAN_POINT('Ctrl Pts',(208.073392269968,0.144086686833323,
136.613971320579));
#254654=CARTESIAN_POINT('Ctrl Pts',(207.794944646155,4.96557142732685,133.823362329787));
#254655=CARTESIAN_POINT('Ctrl Pts',(207.516497022342,5.22403776314189,128.258534510045));
#254656=CARTESIAN_POINT('Ctrl Pts',(207.238049398529,0.681816090004523,
125.033145533949));
#254657=CARTESIAN_POINT('Ctrl Pts',(206.959601774716,-4.48693345015888,
127.111248278652));
#254658=CARTESIAN_POINT('Ctrl Pts',(206.681154150904,-5.53242507739068,
132.583126545744));
#254659=CARTESIAN_POINT('Ctrl Pts',(206.40270652709,-1.49388053201802,136.420413394932));
#254660=CARTESIAN_POINT('Ctrl Pts',(206.124258903278,3.91746311099657,135.0968180907));
#254661=CARTESIAN_POINT('Ctrl Pts',(205.845811279465,5.72885172159717,129.828666190814));
#254662=CARTESIAN_POINT('Ctrl Pts',(205.567363655652,2.27570431130586,125.457128678938));
#254663=CARTESIAN_POINT('Ctrl Pts',(205.288916031839,-3.26870357308214,
125.999436687584));
#254664=CARTESIAN_POINT('Ctrl Pts',(205.010468408026,-5.80933288384994,
130.9572347388));
#254665=CARTESIAN_POINT('Ctrl Pts',(204.732020784213,-3.01146890392974,
135.774549108008));
#254666=CARTESIAN_POINT('Ctrl Pts',(204.4535731604,2.5537877891123,136.024502973214));
#254667=CARTESIAN_POINT('Ctrl Pts',(204.175125536587,5.77223831170541,131.477401078575));
#254668=CARTESIAN_POINT('Ctrl Pts',(203.896677912775,3.6862837897924,126.311807855303));
#254669=CARTESIAN_POINT('Ctrl Pts',(203.618230288961,-1.78718543642468,
125.274651160291));
#254670=CARTESIAN_POINT('Ctrl Pts',(203.339782665149,-5.61831856260093,
129.319027308227));
#254671=CARTESIAN_POINT('Ctrl Pts',(203.061335041336,-4.28649139606962,
134.728352208566));
#254672=CARTESIAN_POINT('Ctrl Pts',(202.782887417523,0.984411954691954,
136.531720532469));
#254673=CARTESIAN_POINT('Ctrl Pts',(202.50443979371,5.3506888113544,133.071924892697));
#254674=CARTESIAN_POINT('Ctrl Pts',(202.225992169897,4.79994404549834,127.528348460205));
#254675=CARTESIAN_POINT('Ctrl Pts',(201.947544546084,-0.161714807569177,
124.995267158526));
#254676=CARTESIAN_POINT('Ctrl Pts',(201.669096922271,-4.97476565284641,
127.800458955558));
#254677=CARTESIAN_POINT('Ctrl Pts',(201.390649298458,-5.21624989388704,
133.366089631302));
#254678=CARTESIAN_POINT('Ctrl Pts',(201.112201674645,-0.664255310463968,
136.577616490799));
#254679=CARTESIAN_POINT('Ctrl Pts',(200.833754050833,4.49815745262305,134.483803242045));
#254680=CARTESIAN_POINT('Ctrl Pts',(200.55530642702,5.52698326394509,129.008761972148));
#254681=CARTESIAN_POINT('Ctrl Pts',(200.276858803207,1.47678146385132,125.183788137525));
#254682=CARTESIAN_POINT('Ctrl Pts',(199.998411179394,-3.93051035674001,
126.523845831826));
#254683=CARTESIAN_POINT('Ctrl Pts',(199.719963555581,-5.7258551755912,131.79748749945));
#254684=CARTESIAN_POINT('Ctrl Pts',(199.441515931768,-2.25941881165118,
136.158494079568));
#254685=CARTESIAN_POINT('Ctrl Pts',(199.163068307955,3.28331306145151,135.599313572066));
#254686=CARTESIAN_POINT('Ctrl Pts',(198.884620684142,5.80884062984016,130.633805545853));
#254687=CARTESIAN_POINT('Ctrl Pts',(198.606173060329,2.99632743704681,125.825029298466));
#254688=CARTESIAN_POINT('Ctrl Pts',(198.327725436517,-2.56966429165962,
125.592015279473));
#254689=CARTESIAN_POINT('Ctrl Pts',(198.049277812704,-5.77426007141042,
130.148891988961));
#254690=CARTESIAN_POINT('Ctrl Pts',(197.770830188891,-3.6725929338218,135.308112346714));
#254691=CARTESIAN_POINT('Ctrl Pts',(197.492382565078,1.80400769380988,136.328604885883));
#254692=CARTESIAN_POINT('Ctrl Pts',(197.213934941265,5.62281338150559,132.272586816804));
#254693=CARTESIAN_POINT('Ctrl Pts',(196.935487317452,4.27452826130232,126.867340597462));
#254694=CARTESIAN_POINT('Ctrl Pts',(196.657039693639,-1.00183950872307,
125.080023442474));
#254695=CARTESIAN_POINT('Ctrl Pts',(196.378592069827,-5.35756571281285,
128.553092501978));
#254696=CARTESIAN_POINT('Ctrl Pts',(196.100144446013,-4.78995075846325,
134.094966979145));
#254697=CARTESIAN_POINT('Ctrl Pts',(195.821696822201,0.179394940810534,
136.612934965078));
#254698=CARTESIAN_POINT('Ctrl Pts',(195.543249198387,4.98388545340951,133.79310689028));
#254699=CARTESIAN_POINT('Ctrl Pts',(195.264801574575,5.20842871066526,128.22676699923));
#254700=CARTESIAN_POINT('Ctrl Pts',(194.986353950762,0.64668042870769,125.029109720981));
#254701=CARTESIAN_POINT('Ctrl Pts',(194.70790632695,-4.50933557513701,127.138625880003));
#254702=CARTESIAN_POINT('Ctrl Pts',(194.429458703136,-5.52149247872048,
132.616773181746));
#254703=CARTESIAN_POINT('Ctrl Pts',(194.151011079324,-1.4596675342632,136.429401878284));
#254704=CARTESIAN_POINT('Ctrl Pts',(193.87256345551,3.9435205654586,135.072892454764));
#254705=CARTESIAN_POINT('Ctrl Pts',(193.594115831698,5.72280591721378,129.793810802232));
#254706=CARTESIAN_POINT('Ctrl Pts',(193.315668207884,2.24311220566103,125.443375061888));
#254707=CARTESIAN_POINT('Ctrl Pts',(193.037220584072,-3.29789204077089,
126.019423148508));
#254708=CARTESIAN_POINT('Ctrl Pts',(192.758772960259,-5.80829461271728,
130.992595012001));
#254709=CARTESIAN_POINT('Ctrl Pts',(192.480325336446,-2.98115818654302,
135.792788662769));
#254710=CARTESIAN_POINT('Ctrl Pts',(192.201877712633,2.58551697539033,136.008860638253));
#254711=CARTESIAN_POINT('Ctrl Pts',(191.92343008882,5.77622834646622,131.442251348686));
#254712=CARTESIAN_POINT('Ctrl Pts',(191.644982465007,3.658868051582,126.289451639914));
#254713=CARTESIAN_POINT('Ctrl Pts',(191.366534841194,-1.82081323706467,
125.285632716038));
#254714=CARTESIAN_POINT('Ctrl Pts',(191.088087217381,-5.6272561125207,129.35325512882));
#254715=CARTESIAN_POINT('Ctrl Pts',(190.809639593569,-4.26252552731426,
134.754372595315));
#254716=CARTESIAN_POINT('Ctrl Pts',(190.531191969755,1.01925778154541,136.525622023071));
#254717=CARTESIAN_POINT('Ctrl Pts',(190.252744345943,5.36439298267566,133.039311718326));
#254718=CARTESIAN_POINT('Ctrl Pts',(189.974296722129,4.77991309789331,127.499190535413));
#254719=CARTESIAN_POINT('Ctrl Pts',(189.695849098317,-0.197073412116412,
124.996359191464));
#254720=CARTESIAN_POINT('Ctrl Pts',(189.417401474504,-4.99295908396257,
127.830797421458));
#254721=CARTESIAN_POINT('Ctrl Pts',(189.138953850692,-5.20055927725872,
133.397794962038));
#254722=CARTESIAN_POINT('Ctrl Pts',(188.860506226878,-0.629099556198964,
136.581553036358));
#254723=CARTESIAN_POINT('Ctrl Pts',(188.582058603065,4.52047192378579,134.456353509349));
#254724=CARTESIAN_POINT('Ctrl Pts',(188.303610979253,5.51595054314194,128.975150924561));
#254725=CARTESIAN_POINT('Ctrl Pts',(188.02516335544,1.44254008251539,125.174902685784));
#254726=CARTESIAN_POINT('Ctrl Pts',(187.746715731627,-3.95649424194195,
126.547851272005));
#254727=CARTESIAN_POINT('Ctrl Pts',(187.468268107814,-5.71970364354381,
131.832324004755));
#254728=CARTESIAN_POINT('Ctrl Pts',(187.189820484001,-2.22678481978599,
136.172148603481));
#254729=CARTESIAN_POINT('Ctrl Pts',(186.911372860188,3.312440468869,135.579238274173));
#254730=CARTESIAN_POINT('Ctrl Pts',(186.632925236375,5.80769478834652,130.598448644184));
#254731=CARTESIAN_POINT('Ctrl Pts',(186.354477612562,2.96596131899707,125.806882058373));
#254732=CARTESIAN_POINT('Ctrl Pts',(186.076029988749,-2.60134570724499,
125.607754128061));
#254733=CARTESIAN_POINT('Ctrl Pts',(185.797582364937,-5.7781431113317,130.184053693262));
#254734=CARTESIAN_POINT('Ctrl Pts',(185.519134741124,-3.64510927408837,
135.33038501822));
#254735=CARTESIAN_POINT('Ctrl Pts',(185.240687117311,1.83760191255446,136.317521027561));
#254736=CARTESIAN_POINT('Ctrl Pts',(184.962239493498,5.63164671340385,132.238331952975));
#254737=CARTESIAN_POINT('Ctrl Pts',(184.683791869685,4.25048330587202,126.841393274542));
#254738=CARTESIAN_POINT('Ctrl Pts',(184.405344245872,-1.03666661210287,
125.086227982629));
#254739=CARTESIAN_POINT('Ctrl Pts',(184.126896622059,-5.37117055753467,
128.585747235914));
#254740=CARTESIAN_POINT('Ctrl Pts',(183.848448998247,-4.7698311568614,134.124063801647));
#254741=CARTESIAN_POINT('Ctrl Pts',(183.570001374433,0.214750057761129,
136.611735317726));
#254742=CARTESIAN_POINT('Ctrl Pts',(183.291553750621,5.00198646042476,133.762713190383));
#254743=CARTESIAN_POINT('Ctrl Pts',(183.013106126807,5.19264166658148,128.195109572179));
#254744=CARTESIAN_POINT('Ctrl Pts',(182.734658502995,0.611512855797894,
125.025280195685));
#254745=CARTESIAN_POINT('Ctrl Pts',(182.456210879182,-4.53156639540017,
127.166143403126));
#254746=CARTESIAN_POINT('Ctrl Pts',(182.177763255369,-5.5103575085511,132.650350493844));
#254747=CARTESIAN_POINT('Ctrl Pts',(181.899315631556,-1.42539926727337,
136.438183069882));
#254748=CARTESIAN_POINT('Ctrl Pts',(181.620868007743,3.96943126600311,135.048808039769));
#254749=CARTESIAN_POINT('Ctrl Pts',(181.34242038393,5.71654838332065,129.758993181434));
#254750=CARTESIAN_POINT('Ctrl Pts',(181.063972760118,2.21043680528058,125.429819927867));
#254751=CARTESIAN_POINT('Ctrl Pts',(180.785525136304,-3.32695821097111,
126.039587007222));
#254752=CARTESIAN_POINT('Ctrl Pts',(180.507077512492,-5.80704116228462,
131.027948262352));
#254753=CARTESIAN_POINT('Ctrl Pts',(180.228629888679,-2.95073697519064,
135.810843394787));
#254754=CARTESIAN_POINT('Ctrl Pts',(179.950182264866,2.61715034058839,135.993025435236));
#254755=CARTESIAN_POINT('Ctrl Pts',(179.671734641053,5.78000434826875,131.407077988614));
#254756=CARTESIAN_POINT('Ctrl Pts',(179.39328701724,3.63131672880039,126.26726272238));
#254757=CARTESIAN_POINT('Ctrl Pts',(179.114839393428,-1.8543735647511,125.296818772266));
#254758=CARTESIAN_POINT('Ctrl Pts',(178.836391769614,-5.63598514348121,
129.387536719606));
#254759=CARTESIAN_POINT('Ctrl Pts',(178.557944145802,-4.23840170853308,
134.780246613475));
#254760=CARTESIAN_POINT('Ctrl Pts',(178.279496521988,1.05406583912245,136.519311509933));
#254761=CARTESIAN_POINT('Ctrl Pts',(178.001048898175,5.3778983746034,133.006615727177));
#254762=CARTESIAN_POINT('Ctrl Pts',(177.722601274363,4.75970502876524,127.470155084831));
#254763=CARTESIAN_POINT('Ctrl Pts',(177.44415365055,-0.232424713990654,
124.997666442073));
#254764=CARTESIAN_POINT('Ctrl Pts',(177.165706026737,-5.01096749916768,
127.861246073811));
#254765=CARTESIAN_POINT('Ctrl Pts',(176.887258402924,-5.18467595198119,
133.429404192122));
#254766=CARTESIAN_POINT('Ctrl Pts',(176.608810779111,-0.593920490425269,
136.585275505922));
#254767=CARTESIAN_POINT('Ctrl Pts',(176.330363155298,4.54261888720253,134.428768450716));
#254768=CARTESIAN_POINT('Ctrl Pts',(176.051915531486,5.50471342676105,128.941607659011));
#254769=CARTESIAN_POINT('Ctrl Pts',(175.773467907672,1.40824524732727,125.166225835676));
#254770=CARTESIAN_POINT('Ctrl Pts',(175.49502028386,-3.98233151779528,126.572014438702));
#254771=CARTESIAN_POINT('Ctrl Pts',(175.216572660047,-5.7133401657742,131.867122418498));
#254772=CARTESIAN_POINT('Ctrl Pts',(174.938125036234,-2.19406831359054,
136.185604222037));
#254773=CARTESIAN_POINT('Ctrl Pts',(174.659677412421,3.34144513258691,135.558986041432));
#254774=CARTESIAN_POINT('Ctrl Pts',(174.381229788608,5.80633374058666,130.563099372659));
#254775=CARTESIAN_POINT('Ctrl Pts',(174.102782164795,2.93548529615992,125.788920001687));
#254776=CARTESIAN_POINT('Ctrl Pts',(173.824334540982,-2.63293072900865,
125.623685538813));
#254777=CARTESIAN_POINT('Ctrl Pts',(173.54588691717,-5.7818120400351,130.219238383264));
#254778=CARTESIAN_POINT('Ctrl Pts',(173.267439293356,-3.61749054349026,
135.352489976228));
#254779=CARTESIAN_POINT('Ctrl Pts',(172.988991669544,1.87112803828436,136.306232877052));
#254780=CARTESIAN_POINT('Ctrl Pts',(172.71054404573,5.64027136256211,132.204023952811));
#254781=CARTESIAN_POINT('Ctrl Pts',(172.432096421918,4.22628084721974,126.815592800833));
#254782=CARTESIAN_POINT('Ctrl Pts',(172.153648798105,-1.07145530142008,
125.092644410292));
#254783=CARTESIAN_POINT('Ctrl Pts',(171.875201174292,-5.38457637155629,
128.618484181386));
#254784=CARTESIAN_POINT('Ctrl Pts',(171.596753550479,-4.74953480741189,
134.153037611328));
#254785=CARTESIAN_POINT('Ctrl Pts',(171.318305926666,0.25009721706947,136.610320475968));
#254786=CARTESIAN_POINT('Ctrl Pts',(171.039858302853,5.01990211699227,133.732209867644));
#254787=CARTESIAN_POINT('Ctrl Pts',(170.76141067904,5.1766622072511,128.163548831885));
#254788=CARTESIAN_POINT('Ctrl Pts',(170.482963055228,0.576322623054293,
125.021664816339));
#254789=CARTESIAN_POINT('Ctrl Pts',(170.204515431414,-4.55362929680409,
127.193795741725));
#254790=CARTESIAN_POINT('Ctrl Pts',(169.926067807602,-5.4990183500578,132.683859402108));
#254791=CARTESIAN_POINT('Ctrl Pts',(169.647620183788,-1.39107818158956,
136.446755498118));
#254792=CARTESIAN_POINT('Ctrl Pts',(169.369172559976,3.99519487781229,135.024566345214));
#254793=CARTESIAN_POINT('Ctrl Pts',(169.090724936163,5.71007902062496,129.724214297113));
#254794=CARTESIAN_POINT('Ctrl Pts',(168.81227731235,2.17767949635139,125.416463949427));
#254795=CARTESIAN_POINT('Ctrl Pts',(168.533829688537,-3.35590109951139,
126.059927426375));
#254796=CARTESIAN_POINT('Ctrl Pts',(168.255382064725,-5.80557252980615,
131.063293227581));
#254797=CARTESIAN_POINT('Ctrl Pts',(167.976934440911,-2.92020642319446,
135.828712609743));
#254798=CARTESIAN_POINT('Ctrl Pts',(167.698486817099,2.64868672631821,135.976997964335));
#254799=CARTESIAN_POINT('Ctrl Pts',(167.420039193286,5.78356616988455,131.371882294628));
#254800=CARTESIAN_POINT('Ctrl Pts',(167.141591569473,3.60363084624196,126.245241928676));
#254801=CARTESIAN_POINT('Ctrl Pts',(166.86314394566,-1.88786517794308,125.308208912483));
#254802=CARTESIAN_POINT('Ctrl Pts',(166.584696321847,-5.64450533093961,
129.421870811324));
#254803=CARTESIAN_POINT('Ctrl Pts',(166.306248698034,-4.21412083421794,
134.805973303719));
#254804=CARTESIAN_POINT('Ctrl Pts',(166.027801074221,1.08883483790225,136.512789227187));
#254805=CARTESIAN_POINT('Ctrl Pts',(165.749353450409,5.3912044865292,132.973838130654));
#254806=CARTESIAN_POINT('Ctrl Pts',(165.470905826595,4.73932058701693,127.441243184462));
#254807=CARTESIAN_POINT('Ctrl Pts',(165.192458202783,-0.267767403281747,
124.999188861871));
#254808=CARTESIAN_POINT('Ctrl Pts',(164.914010578969,-5.02879023112935,
127.891803784357));
#254809=CARTESIAN_POINT('Ctrl Pts',(164.635562955157,-5.16860050662956,
133.46091615025));
#254810=CARTESIAN_POINT('Ctrl Pts',(164.357115331344,-0.55871941670932,
136.588783761558));
#254811=CARTESIAN_POINT('Ctrl Pts',(164.078667707531,4.56459752220588,134.401049088318));
#254812=CARTESIAN_POINT('Ctrl Pts',(163.800220083718,5.49327233119978,128.908133418456));
#254813=CARTESIAN_POINT('Ctrl Pts',(163.521772459905,1.37389822909362,125.157757908727));
#254814=CARTESIAN_POINT('Ctrl Pts',(163.243324836092,-4.00802122688977,
126.596334436543));
#254815=CARTESIAN_POINT('Ctrl Pts',(162.964877212279,-5.70676497808368,
131.901881451211));
#254816=CARTESIAN_POINT('Ctrl Pts',(162.686429588467,-2.16127050538683,
136.198860436632));
#254817=CARTESIAN_POINT('Ctrl Pts',(162.407981964654,3.37032597782655,135.538557624299));
#254818=CARTESIAN_POINT('Ctrl Pts',(162.129534340841,5.80475753699479,130.527759041158));
#254819=CARTESIAN_POINT('Ctrl Pts',(161.851086717028,2.90490049783562,125.771143793998));
#254820=CARTESIAN_POINT('Ctrl Pts',(161.572639093215,-2.66441818655578,
125.639808921385));
#254821=CARTESIAN_POINT('Ctrl Pts',(161.294191469402,-5.7852667215671,130.254444755185));
#254822=CARTESIAN_POINT('Ctrl Pts',(161.015743845589,-3.58973776544978,
135.37442640163));
#254823=CARTESIAN_POINT('Ctrl Pts',(160.737296221776,1.90458482867669,136.294740852644));
#254824=CARTESIAN_POINT('Ctrl Pts',(160.458848597964,5.64868700939082,132.169664087608));
#254825=CARTESIAN_POINT('Ctrl Pts',(160.18040097415,4.20192178217643,126.789940132385));
#254826=CARTESIAN_POINT('Ctrl Pts',(159.901953350338,-1.10620428756715,
125.099272487699));
#254827=CARTESIAN_POINT('Ctrl Pts',(159.623505726525,-5.39778265812024,
128.651302125312));
#254828=CARTESIAN_POINT('Ctrl Pts',(159.345058102712,-4.72906246220349,
134.18188733455));
#254829=CARTESIAN_POINT('Ctrl Pts',(159.066610478899,0.285435108933367,
136.608690492233));
#254830=CARTESIAN_POINT('Ctrl Pts',(158.788162855086,5.03763175924073,133.701598052375));
#254831=CARTESIAN_POINT('Ctrl Pts',(158.509715231273,5.16049092479898,128.132085947844));
#254832=CARTESIAN_POINT('Ctrl Pts',(158.23126760746,0.541111034464008,125.018263716911));
#254833=CARTESIAN_POINT('Ctrl Pts',(157.952819983648,-4.57552346179978,
127.221581871133));
#254834=CARTESIAN_POINT('Ctrl Pts',(157.674372359834,-5.48747542341729,
132.717298664853));
#254835=CARTESIAN_POINT('Ctrl Pts',(157.395924736022,-1.35670554899215,
136.455118845335));
#254836=CARTESIAN_POINT('Ctrl Pts',(157.117477112209,4.02081044620608,135.000168269382));
#254837=CARTESIAN_POINT('Ctrl Pts',(156.839029488396,5.70339806885126,129.68947543801));
#254838=CARTESIAN_POINT('Ctrl Pts',(156.560581864583,2.1448414927076,125.403307621479));
#254839=CARTESIAN_POINT('Ctrl Pts',(156.28213424077,-3.38471963390224,126.080443652244));
#254840=CARTESIAN_POINT('Ctrl Pts',(156.003686616957,-5.8038887697026,131.098628597966));
#254841=CARTESIAN_POINT('Ctrl Pts',(155.725238993144,-2.88956766187541,
135.846395645489));
#254842=CARTESIAN_POINT('Ctrl Pts',(155.446791369331,2.68012496398725,135.960778819456));
#254843=CARTESIAN_POINT('Ctrl Pts',(155.168343745519,5.78691367932904,131.336665570917));
#254844=CARTESIAN_POINT('Ctrl Pts',(154.889896121706,3.57581142981733,126.223390074792));
#254845=CARTESIAN_POINT('Ctrl Pts',(154.611448497893,-1.92128683559663,
125.319802714623));
#254846=CARTESIAN_POINT('Ctrl Pts',(154.33300087408,-5.65281635917722,129.456256131708));
#254847=CARTESIAN_POINT('Ctrl Pts',(154.054553250267,-4.18968380410554,
134.831551712731));
#254848=CARTESIAN_POINT('Ctrl Pts',(153.776105626454,1.12356348950664,136.50605541652));
#254849=CARTESIAN_POINT('Ctrl Pts',(153.497658002641,5.40431082539012,132.940980143345));
#254850=CARTESIAN_POINT('Ctrl Pts',(153.219210378828,4.71876052800142,127.412455905645));
#254851=CARTESIAN_POINT('Ctrl Pts',(152.940762755016,-0.303100170353132,
125.000926394444));
#254852=CARTESIAN_POINT('Ctrl Pts',(152.662315131202,-5.04642661941966,
127.922469420767));
#254853=CARTESIAN_POINT('Ctrl Pts',(152.38386750739,-5.15233353688545,133.492329668737));
#254854=CARTESIAN_POINT('Ctrl Pts',(152.105419883576,-0.523497639439988,
136.592077673268));
#254855=CARTESIAN_POINT('Ctrl Pts',(151.826972259764,4.58640701436939,134.373196449306));
#254856=CARTESIAN_POINT('Ctrl Pts',(151.548524635951,5.48162768041213,128.874729443297));
#254857=CARTESIAN_POINT('Ctrl Pts',(151.270077012138,1.33950030055583,125.149499218718));
#254858=CARTESIAN_POINT('Ctrl Pts',(150.991629388325,-4.03356241728369,
126.620810364342));
#254859=CARTESIAN_POINT('Ctrl Pts',(150.713181764512,-5.69997832411825,
131.936599814887));
#254860=CARTESIAN_POINT('Ctrl Pts',(150.434734140699,-2.1283926105098,136.211916756054));
#254861=CARTESIAN_POINT('Ctrl Pts',(150.156286516886,3.39908193439765,135.517953779753));
#254862=CARTESIAN_POINT('Ctrl Pts',(149.877838893074,5.8029662359777,130.49242895923));
#254863=CARTESIAN_POINT('Ctrl Pts',(149.599391269261,2.87420805735513,125.753554094008));
#254864=CARTESIAN_POINT('Ctrl Pts',(149.320943645448,-2.69580691310719,
125.65612367832));
#254865=CARTESIAN_POINT('Ctrl Pts',(149.042496021635,-5.7885070279132,130.289671504441));
#254866=CARTESIAN_POINT('Ctrl Pts',(148.764048397822,-3.56185196835627,
135.396193481562));
#254867=CARTESIAN_POINT('Ctrl Pts',(148.485600774009,1.93797104397778,136.283045380177));
#254868=CARTESIAN_POINT('Ctrl Pts',(148.207153150196,5.6568933420451,132.135253630582));
#254869=CARTESIAN_POINT('Ctrl Pts',(147.928705526383,4.17740701337624,126.764436219762));
#254870=CARTESIAN_POINT('Ctrl Pts',(147.65025790257,-1.14091228290746,125.106111969245));
#254871=CARTESIAN_POINT('Ctrl Pts',(147.371810278758,-5.41078892786276,
128.684199851613));
#254872=CARTESIAN_POINT('Ctrl Pts',(147.093362654945,-4.70841487984645,
134.210611902278));
#254873=CARTESIAN_POINT('Ctrl Pts',(146.814915031132,0.320762423894332,
136.60684542692));
#254874=CARTESIAN_POINT('Ctrl Pts',(146.536467407319,5.05517473019176,133.670878878906));
#254875=CARTESIAN_POINT('Ctrl Pts',(146.258019783506,5.14412841845787,128.100722085923));
#254876=CARTESIAN_POINT('Ctrl Pts',(145.979572159693,0.505879394805349,
125.015077023433));
#254877=CARTESIAN_POINT('Ctrl Pts',(145.70112453588,-4.59724807909095,127.249500761725));
#254878=CARTESIAN_POINT('Ctrl Pts',(145.422676912067,-5.47572915635697,
132.750667042976));
#254879=CARTESIAN_POINT('Ctrl Pts',(145.144229288255,-1.32228264317164,
136.463272801628));
#254880=CARTESIAN_POINT('Ctrl Pts',(144.865781664442,4.0462770219901,134.975614716357));
#254881=CARTESIAN_POINT('Ctrl Pts',(144.587334040629,5.69650577556471,129.654777891387));
#254882=CARTESIAN_POINT('Ctrl Pts',(144.308886416816,2.11192401117359,125.390351431538));
#254883=CARTESIAN_POINT('Ctrl Pts',(144.030438793003,-3.41341274626234,
126.101134924595));
#254884=CARTESIAN_POINT('Ctrl Pts',(143.75199116919,-5.80198994436631,131.133953064144));
#254885=CARTESIAN_POINT('Ctrl Pts',(143.473543545377,-2.85882182656403,
135.863891846773));
#254886=CARTESIAN_POINT('Ctrl Pts',(143.195095921564,2.71146388864014,135.944368601604));
#254887=CARTESIAN_POINT('Ctrl Pts',(142.916648297751,5.790046752559,131.301429122451));
#254888=CARTESIAN_POINT('Ctrl Pts',(142.638200673938,3.54785951038517,126.201707970457));
#254889=CARTESIAN_POINT('Ctrl Pts',(142.359753050125,-1.95463729925998,
125.331599749072));
#254890=CARTESIAN_POINT('Ctrl Pts',(142.081305426313,-5.66091792022584,
129.490691406602));
#254891=CARTESIAN_POINT('Ctrl Pts',(141.8028578025,-4.16509152371897,134.856980892698));
#254892=CARTESIAN_POINT('Ctrl Pts',(141.524410178687,1.15825050705268,136.499110327454));
#254893=CARTESIAN_POINT('Ctrl Pts',(141.245962554874,5.41721690552589,132.908042982814));
#254894=CARTESIAN_POINT('Ctrl Pts',(140.967514931061,4.69802561357932,127.383794315106));
#254895=CARTESIAN_POINT('Ctrl Pts',(140.689067307248,-0.338421705936203,
125.002878975406));
#254896=CARTESIAN_POINT('Ctrl Pts',(140.410619683435,-5.06387601051571,
127.953241846716));
#254897=CARTESIAN_POINT('Ctrl Pts',(140.132172059623,-5.13587564552739,
133.523643583541));
#254898=CARTESIAN_POINT('Ctrl Pts',(139.85372443581,-0.48825646377323,136.595157118993));
#254899=CARTESIAN_POINT('Ctrl Pts',(139.575276811997,4.60804655553434,134.34521156577));
#254900=CARTESIAN_POINT('Ctrl Pts',(139.296829188184,5.46977990589493,128.841396971331));
#254901=CARTESIAN_POINT('Ctrl Pts',(139.018381564371,1.30505273634171,125.141450071677));
#254902=CARTESIAN_POINT('Ctrl Pts',(138.739933940558,-4.05895414253892,
126.645441315135));
#254903=CARTESIAN_POINT('Ctrl Pts',(138.461486316745,-5.69298045535984,
131.971276223022));
#254904=CARTESIAN_POINT('Ctrl Pts',(138.183038692932,-2.09543584726193,
136.224772696493));
#254905=CARTESIAN_POINT('Ctrl Pts',(137.904591069119,3.42771193673771,135.49717527128));
#254906=CARTESIAN_POINT('Ctrl Pts',(137.626143445306,5.80095990391266,130.457110436044));
#254907=CARTESIAN_POINT('Ctrl Pts',(137.347695821494,2.84340911203807,125.736151553513));
#254908=CARTESIAN_POINT('Ctrl Pts',(137.069248197681,-2.727095745542,125.672629205068));
#254909=CARTESIAN_POINT('Ctrl Pts',(136.790800573868,-5.7915328390027,130.324917325691));
#254910=CARTESIAN_POINT('Ctrl Pts',(136.512352950055,-3.53383418552815,
135.417790409441));
#254911=CARTESIAN_POINT('Ctrl Pts',(136.233905326242,1.97128544704926,136.271146893031));
#254912=CARTESIAN_POINT('Ctrl Pts',(135.955457702429,5.66489005643625,132.100793856825));
#254913=CARTESIAN_POINT('Ctrl Pts',(135.677010078616,4.15273744922295,126.739082008025));
#254914=CARTESIAN_POINT('Ctrl Pts',(135.398562454803,-1.17557800132362,
125.113162601491));
#254915=CARTESIAN_POINT('Ctrl Pts',(135.12011483099,-5.42359469883174,128.717176141249));
#254916=CARTESIAN_POINT('Ctrl Pts',(134.841667207177,-4.68759282544451,
134.239210250113));
#254917=CARTESIAN_POINT('Ctrl Pts',(134.563219583365,0.356077852885664,
136.604785348398));
#254918=CARTESIAN_POINT('Ctrl Pts',(134.284771959552,5.0725303797842,133.640053485549));
#254919=CARTESIAN_POINT('Ctrl Pts',(134.006324335739,5.12757529454644,128.069458408322));
#254920=CARTESIAN_POINT('Ctrl Pts',(133.727876711926,0.470629009599695,
125.012104853988));
#254921=CARTESIAN_POINT('Ctrl Pts',(133.449429088113,-4.61880234366392,
127.277551378957));
#254922=CARTESIAN_POINT('Ctrl Pts',(133.1709814643,-5.46377998413907,132.783963299997));
#254923=CARTESIAN_POINT('Ctrl Pts',(132.892533840487,-1.28781073968153,
136.47121706485));
#254924=CARTESIAN_POINT('Ctrl Pts',(132.614086216674,4.07159366149105,134.950906595976));
#254925=CARTESIAN_POINT('Ctrl Pts',(132.335638592862,5.68940239616175,129.620122942976));
#254926=CARTESIAN_POINT('Ctrl Pts',(132.057190969048,2.07892827151876,125.377595859696));
#254927=CARTESIAN_POINT('Ctrl Pts',(131.778743345236,-3.44197937335791,
126.122000476702));
#254928=CARTESIAN_POINT('Ctrl Pts',(131.500295721423,-5.79987612415893,
131.169265317152));
#254929=CARTESIAN_POINT('Ctrl Pts',(131.22184809761,-2.82797005655853,135.881200565267));
#254930=CARTESIAN_POINT('Ctrl Pts',(130.943400473797,2.74270233900145,135.927767918864));
#254931=CARTESIAN_POINT('Ctrl Pts',(130.664952849984,5.79296527347731,131.26617425493));
#254932=CARTESIAN_POINT('Ctrl Pts',(130.386505226171,3.51977612371406,126.180196419108));
#254933=CARTESIAN_POINT('Ctrl Pts',(130.108057602358,-1.98791533311939,
125.343599578688));
#254934=CARTESIAN_POINT('Ctrl Pts',(129.829609978546,-5.66880971387908,
129.52517535999));
#254935=CARTESIAN_POINT('Ctrl Pts',(129.551162354732,-4.14034490433441,
134.882259901329));
#254936=CARTESIAN_POINT('Ctrl Pts',(129.27271473092,1.19289460520041,136.491954217345));
#254937=CARTESIAN_POINT('Ctrl Pts',(128.994267107107,5.42992224869717,132.875027869557));
#254938=CARTESIAN_POINT('Ctrl Pts',(128.715819483294,4.67711661209022,127.355259474909));
#254939=CARTESIAN_POINT('Ctrl Pts',(128.437371859481,-0.373730701178542,
125.005046532403));
#254940=CARTESIAN_POINT('Ctrl Pts',(128.158924235668,-5.0811377578241,127.984119921918));
#254941=CARTESIAN_POINT('Ctrl Pts',(127.880476611855,-5.11922744240848,
133.554856734316));
#254942=CARTESIAN_POINT('Ctrl Pts',(127.602028988042,-0.452997195583419,
136.598021984625));
#254943=CARTESIAN_POINT('Ctrl Pts',(127.323581364229,4.62951534383955,134.3170954747));
#254944=CARTESIAN_POINT('Ctrl Pts',(127.045133740417,5.45772944667181,128.808137237705));
#254945=CARTESIAN_POINT('Ctrl Pts',(126.766686116604,1.2705568129186,125.133610765869));
#254946=CARTESIAN_POINT('Ctrl Pts',(126.488238492791,-4.08419546175569,
126.67022637621));
#254947=CARTESIAN_POINT('Ctrl Pts',(126.209790868978,-5.68577163111709,
132.005909390672));
#254948=CARTESIAN_POINT('Ctrl Pts',(125.931343245165,-2.06240143686808,
136.237427781569));
#254949=CARTESIAN_POINT('Ctrl Pts',(125.652895621352,3.45621492395137,135.476222868834));
#254950=CARTESIAN_POINT('Ctrl Pts',(125.374447997539,5.79873861514512,130.421804780342));
#254951=CARTESIAN_POINT('Ctrl Pts',(125.096000373726,2.8125048031507,125.718936817367));
#254952=CARTESIAN_POINT('Ctrl Pts',(124.817552749914,-2.75828352444112,
125.68932489001));
#254953=CARTESIAN_POINT('Ctrl Pts',(124.5391051261,-5.79434404271298,130.36018091289));
#254954=CARTESIAN_POINT('Ctrl Pts',(124.260657502288,-3.50568545517477,
135.439216384981));
#254955=CARTESIAN_POINT('Ctrl Pts',(123.982209878475,2.00452680341345,136.25904583211));
#254956=CARTESIAN_POINT('Ctrl Pts',(123.703762254662,5.67267685624313,132.066286043259));
#254957=CARTESIAN_POINT('Ctrl Pts',(123.425314630849,4.12791400385628,126.71387843668));
#254958=CARTESIAN_POINT('Ctrl Pts',(123.146867007036,-1.21020015826455,
125.120424123171));
#254959=CARTESIAN_POINT('Ctrl Pts',(122.868419383223,-5.43619949650465,
128.750229772276));
#254960=CARTESIAN_POINT('Ctrl Pts',(122.58997175941,-4.66659707056658,134.267681318331));
#254961=CARTESIAN_POINT('Ctrl Pts',(122.311524135597,0.391380087281262,
136.602510333005));
#254962=CARTESIAN_POINT('Ctrl Pts',(122.033076511785,5.08969806489794,133.609123014551));
#254963=CARTESIAN_POINT('Ctrl Pts',(121.754628887972,5.11083216644683,128.038296073528));
#254964=CARTESIAN_POINT('Ctrl Pts',(121.476181264159,0.435361185062875,
125.00934731871));
#254965=CARTESIAN_POINT('Ctrl Pts',(121.197733640346,-4.64018545681751,
127.305732683402));
#254966=CARTESIAN_POINT('Ctrl Pts',(120.919286016533,-5.45162834954452,
132.817186202114));
#254967=CARTESIAN_POINT('Ctrl Pts',(120.64083839272,-1.25329111589093,136.478951340622));
#254968=CARTESIAN_POINT('Ctrl Pts',(120.362390768907,4.09675942659154,134.92604482381));
#254969=CARTESIAN_POINT('Ctrl Pts',(120.083943145094,5.68208819386074,129.585511876926));
#254970=CARTESIAN_POINT('Ctrl Pts',(119.805495521281,2.04585549641223,125.36504137862));
#254971=CARTESIAN_POINT('Ctrl Pts',(119.527047897469,-3.47041845664194,
126.143039535386));
#254972=CARTESIAN_POINT('Ctrl Pts',(119.248600273655,-5.79754738740892,
131.204564048482));
#254973=CARTESIAN_POINT('Ctrl Pts',(118.970152649843,-2.7970134950826,135.898321159589));
#254974=CARTESIAN_POINT('Ctrl Pts',(118.69170502603,2.77383915751901,135.910977386384));
#254975=CARTESIAN_POINT('Ctrl Pts',(118.413257402217,5.795669133937,131.230902274733));
#254976=CARTESIAN_POINT('Ctrl Pts',(118.134809778404,3.49156231044436,126.158856217863));
#254977=CARTESIAN_POINT('Ctrl Pts',(117.856362154591,-2.02111970404504,
125.355801758813));
#254978=CARTESIAN_POINT('Ctrl Pts',(117.577914530778,-5.67649144770371,
129.559706714059));
#254979=CARTESIAN_POINT('Ctrl Pts',(117.299466906965,-4.11544486294674,
134.907387801903));
#254980=CARTESIAN_POINT('Ctrl Pts',(117.021019283153,1.22749450019975,136.484587351363));
#254981=CARTESIAN_POINT('Ctrl Pts',(116.74257165934,5.44242638410263,132.841936026965));
#254982=CARTESIAN_POINT('Ctrl Pts',(116.464124035527,4.65603429832517,127.326852442422));
#254983=CARTESIAN_POINT('Ctrl Pts',(116.185676411714,-0.409025847692317,
125.007428985116));
#254984=CARTESIAN_POINT('Ctrl Pts',(115.907228787901,-5.09821122170419,
128.015102502178));
#254985=CARTESIAN_POINT('Ctrl Pts',(115.628781164088,-5.10238954443416,
133.585967964446));
#254986=CARTESIAN_POINT('Ctrl Pts',(115.350333540275,-0.417721141415912,
136.600672164005));
#254987=CARTESIAN_POINT('Ctrl Pts',(115.071885916462,4.65081258375125,134.288849217947));
#254988=CARTESIAN_POINT('Ctrl Pts',(114.793438292649,5.44547674927697,128.77495147487));
#254989=CARTESIAN_POINT('Ctrl Pts',(114.514990668836,1.23601380854556,125.125981591782));
#254990=CARTESIAN_POINT('Ctrl Pts',(114.236543045024,-4.10928543960769,
126.695164629152));
#254991=CARTESIAN_POINT('Ctrl Pts',(113.958095421211,-5.67835211851559,
132.040498034489));
#254992=CARTESIAN_POINT('Ctrl Pts',(113.679647797398,-2.02929060343055,
136.249881542344));
#254993=CARTESIAN_POINT('Ctrl Pts',(113.401200173585,3.48458983985001,135.455097348814));
#254994=CARTESIAN_POINT('Ctrl Pts',(113.122752549772,5.79630245198571,130.386513300387));
#254995=CARTESIAN_POINT('Ctrl Pts',(112.844304925959,2.78149627586357,125.701910523471));
#254996=CARTESIAN_POINT('Ctrl Pts',(112.565857302146,-2.78936909412988,
125.706210114483));
#254997=CARTESIAN_POINT('Ctrl Pts',(112.287409678333,-5.7969405348739,130.395460959329));
#254998=CARTESIAN_POINT('Ctrl Pts',(112.008962054521,-3.47740682035766,
135.460470614237));
#254999=CARTESIAN_POINT('Ctrl Pts',(111.730514430707,2.03769388129978,136.246742645822));
#255000=CARTESIAN_POINT('Ctrl Pts',(111.452066806895,5.68025345292297,132.031731468582));
#255001=CARTESIAN_POINT('Ctrl Pts',(111.173619183082,4.10293759711819,126.688826439658));
#255002=CARTESIAN_POINT('Ctrl Pts',(110.895171559269,-1.24477747079359,
125.127896265209));
#255003=CARTESIAN_POINT('Ctrl Pts',(110.616723935456,-5.44860285380605,
128.783359519875));
#255004=CARTESIAN_POINT('Ctrl Pts',(110.338276311643,-4.64542839321807,
134.296024051927));
#255005=CARTESIAN_POINT('Ctrl Pts',(110.05982868783,0.426667818943798,136.600020465042));
#255006=CARTESIAN_POINT('Ctrl Pts',(109.781381064017,5.10667714937814,133.57808861205));
#255007=CARTESIAN_POINT('Ctrl Pts',(109.502933440204,5.0938996545818,128.007236236273));
#255008=CARTESIAN_POINT('Ctrl Pts',(109.224485816392,0.400077228057368,
125.006804519781));
#255009=CARTESIAN_POINT('Ctrl Pts',(108.946038192578,-4.66139662619255,
127.334043630792));
#255010=CARTESIAN_POINT('Ctrl Pts',(108.667590568766,-5.43927470285667,
132.850334518237));
#255011=CARTESIAN_POINT('Ctrl Pts',(108.389142944953,-1.21872505093712,
136.486475342347));
#255012=CARTESIAN_POINT('Ctrl Pts',(108.11069532114,4.1217733847649,134.901030321119));
#255013=CARTESIAN_POINT('Ctrl Pts',(107.832247697327,5.67456343969215,129.550945975765));
#255014=CARTESIAN_POINT('Ctrl Pts',(107.553800073514,2.01270691137792,125.352688453517));
#255015=CARTESIAN_POINT('Ctrl Pts',(107.275352449701,-3.49872894229381,
126.164251321038));
#255016=CARTESIAN_POINT('Ctrl Pts',(106.996904825888,-5.7950038204084,131.239847950126));
#255017=CARTESIAN_POINT('Ctrl Pts',(106.718457202076,-2.76595328924301,
135.91525299533));
#255018=CARTESIAN_POINT('Ctrl Pts',(106.440009578262,2.80487319040651,135.893997626342));
#255019=CARTESIAN_POINT('Ctrl Pts',(106.16156195445,5.7981582337456,131.195614488879));
#255020=CARTESIAN_POINT('Ctrl Pts',(105.883114330637,3.46321911604922,126.137688157493));
#255021=CARTESIAN_POINT('Ctrl Pts',(105.604666706824,-2.05424918163679,
125.36820583729));
#255022=CARTESIAN_POINT('Ctrl Pts',(105.326219083011,-5.68396283705021,
129.594284189235));
#255023=CARTESIAN_POINT('Ctrl Pts',(105.047771459198,-4.09039232223623,
134.932363663296));
#255024=CARTESIAN_POINT('Ctrl Pts',(104.769323835385,1.26204890993897,136.47701000249));
#255025=CARTESIAN_POINT('Ctrl Pts',(104.490876211572,5.45472884839698,132.808768681268));
#255026=CARTESIAN_POINT('Ctrl Pts',(104.21242858776,4.63477945349693,127.29857427028));
#255027=CARTESIAN_POINT('Ctrl Pts',(103.933980963947,-0.444305837602887,
125.010026245263));
#255028=CARTESIAN_POINT('Ctrl Pts',(103.655533340134,-5.1150957694926,128.046188439421));
#255029=CARTESIAN_POINT('Ctrl Pts',(103.377085716321,-5.08536257553889,
133.616976121092));
#255030=CARTESIAN_POINT('Ctrl Pts',(103.098638092508,-0.38242960843803,
136.603107558928));
#255031=CARTESIAN_POINT('Ctrl Pts',(102.820190468695,4.6719374860923,134.260473842188));
#255032=CARTESIAN_POINT('Ctrl Pts',(102.541742844882,5.4330222677386,128.741840912539));
#255033=CARTESIAN_POINT('Ctrl Pts',(102.263295221069,1.2014250032263,125.118562832119));
#255034=CARTESIAN_POINT('Ctrl Pts',(101.984847597256,-4.13422314637653,
126.720255149861));
#255035=CARTESIAN_POINT('Ctrl Pts',(101.706399973443,-5.67072219248816,
132.07504087278));
#255036=CARTESIAN_POINT('Ctrl Pts',(101.427952349631,-1.99610457388343,
136.262133517338));
#255037=CARTESIAN_POINT('Ctrl Pts',(101.149504725818,3.51283563299066,135.433799494034));
#255038=CARTESIAN_POINT('Ctrl Pts',(100.871057102005,5.7936515047074,130.351237303918));
#255039=CARTESIAN_POINT('Ctrl Pts',(100.592609478192,2.75038467920892,125.685073302739));
#255040=CARTESIAN_POINT('Ctrl Pts',(100.314161854379,-2.82035130272114,
125.723284252797));
#255041=CARTESIAN_POINT('Ctrl Pts',(100.035714230566,-5.79932221927147,
130.430756157697));
#255042=CARTESIAN_POINT('Ctrl Pts',(99.7572666067534,-3.44899932895201,
135.481552309624));
#255043=CARTESIAN_POINT('Ctrl Pts',(99.4788189829407,2.07078545168999,136.234237790066));
#255044=CARTESIAN_POINT('Ctrl Pts',(99.2003713591278,5.6876195657222,131.997131413226));
#255045=CARTESIAN_POINT('Ctrl Pts',(98.9219237353147,4.07780915451857,126.663926945268));
#255046=CARTESIAN_POINT('Ctrl Pts',(98.6434761115021,-1.27930865763567,
125.13557875072));
#255047=CARTESIAN_POINT('Ctrl Pts',(98.3650284876889,-5.460804311125,128.816564156414));
#255048=CARTESIAN_POINT('Ctrl Pts',(98.0865808638763,-4.62408757781209,
134.324237400649));
#255049=CARTESIAN_POINT('Ctrl Pts',(97.8081332400632,0.461939740273397,
136.597315836771));
#255050=CARTESIAN_POINT('Ctrl Pts',(97.5296856162504,5.12346700405862,133.546951428038));
#255051=CARTESIAN_POINT('Ctrl Pts',(97.2512379924375,5.07677838639178,127.97628004749));
#255052=CARTESIAN_POINT('Ctrl Pts',(96.9727903686245,0.364778446043045,
125.004476551425));
#255053=CARTESIAN_POINT('Ctrl Pts',(96.6943427448119,-4.68243506580139,
127.362483172053));
#255054=CARTESIAN_POINT('Ctrl Pts',(96.4158951209985,-5.42671950184442,
132.883407020047));
#255055=CARTESIAN_POINT('Ctrl Pts',(96.1374474971861,-1.18411382567837,
136.493788791223));
#255056=CARTESIAN_POINT('Ctrl Pts',(95.8589998733729,4.14663460910971,134.875864014826));
#255057=CARTESIAN_POINT('Ctrl Pts',(95.5805522495601,5.66682841248846,129.516426520346));
#255058=CARTESIAN_POINT('Ctrl Pts',(95.3021046257473,1.97948374474885,125.340537542131));
#255059=CARTESIAN_POINT('Ctrl Pts',(95.0236570019342,-3.52690978125809,
126.185635047646));
#255060=CARTESIAN_POINT('Ctrl Pts',(94.7452093781216,-5.79224551741027,
131.275115714627));
#255061=CARTESIAN_POINT('Ctrl Pts',(94.4667617543085,-2.73479058998699,
135.931995445075));
#255062=CARTESIAN_POINT('Ctrl Pts',(94.1883141304955,2.8358032876865,135.876829267928));
#255063=CARTESIAN_POINT('Ctrl Pts',(93.909866506683,5.80043248066857,131.160312204968));
#255064=CARTESIAN_POINT('Ctrl Pts',(93.6314188828698,3.43474759079615,126.116693022386));
#255065=CARTESIAN_POINT('Ctrl Pts',(93.352971259057,-2.08730253826965,125.380811354481));
#255066=CARTESIAN_POINT('Ctrl Pts',(93.0745236352441,-5.69122360506351,
129.628906504239));
#255067=CARTESIAN_POINT('Ctrl Pts',(92.7960760114314,-4.06518821053398,
134.957186560018));
#255068=CARTESIAN_POINT('Ctrl Pts',(92.5176283876181,1.29655655399172,136.469222451509));
#255069=CARTESIAN_POINT('Ctrl Pts',(92.2391807638055,5.46682918570788,132.775527061492));
#255070=CARTESIAN_POINT('Ctrl Pts',(91.9607331399925,4.61335286521161,127.270426006341));
#255071=CARTESIAN_POINT('Ctrl Pts',(91.6822855161797,-0.479569363597252,
125.012838216602));
#255072=CARTESIAN_POINT('Ctrl Pts',(91.4038378923669,-5.13179077552621,
128.077376581749));
#255073=CARTESIAN_POINT('Ctrl Pts',(91.1253902685539,-5.06814716666323,
133.647880055237));
#255074=CARTESIAN_POINT('Ctrl Pts',(90.846942644741,-0.347123904390365,
136.605328079151));
#255075=CARTESIAN_POINT('Ctrl Pts',(90.5684950209282,4.69288926807169,134.231970398883));
#255076=CARTESIAN_POINT('Ctrl Pts',(90.2900473971151,5.42036646356212,128.708806777632));
#255077=CARTESIAN_POINT('Ctrl Pts',(90.0115997733025,1.16679167866171,125.111354761782));
#255078=CARTESIAN_POINT('Ctrl Pts',(89.7331521494893,-4.15900765798632,
126.7454970086));
#255079=CARTESIAN_POINT('Ctrl Pts',(89.4547045256766,-5.66288213576447,
132.109536625546));
#255080=CARTESIAN_POINT('Ctrl Pts',(89.1762569018636,-1.96284457794726,
136.274183252551));
#255081=CARTESIAN_POINT('Ctrl Pts',(88.8978092780507,3.5409512567151,135.412330093694));
#255082=CARTESIAN_POINT('Ctrl Pts',(88.619361654238,5.79078587154194,130.3159780981));
#255083=CARTESIAN_POINT('Ctrl Pts',(88.3409140304249,2.71917116603865,125.668425779081));
#255084=CARTESIAN_POINT('Ctrl Pts',(88.0624664066122,-2.85122900215762,
125.740546672265));
#255085=CARTESIAN_POINT('Ctrl Pts',(87.7840187827991,-5.80148900765152,
130.466065200115));
#255086=CARTESIAN_POINT('Ctrl Pts',(87.5055711589863,-3.42046403360785,
135.502460689953));
#255087=CARTESIAN_POINT('Ctrl Pts',(87.2271235351733,2.10380028836375,136.221531728214));
#255088=CARTESIAN_POINT('Ctrl Pts',(86.9486759113605,5.69477492168681,131.962487159311));
#255089=CARTESIAN_POINT('Ctrl Pts',(86.6702282875477,4.05252960720113,126.63918087617));
#255090=CARTESIAN_POINT('Ctrl Pts',(86.3917806637346,-1.31379243922498,
125.14347129503));
#255091=CARTESIAN_POINT('Ctrl Pts',(86.113333039922,-5.47280341633199,128.849842451481));
#255092=CARTESIAN_POINT('Ctrl Pts',(85.8348854161089,-4.6025754151404,134.352320319043));
#255093=CARTESIAN_POINT('Ctrl Pts',(85.5564377922961,0.497194544256039,
136.594396548415));
#255094=CARTESIAN_POINT('Ctrl Pts',(85.2779901684829,5.1400670067851,133.515712616316));
#255095=CARTESIAN_POINT('Ctrl Pts',(84.9995425446705,5.05946899631168,127.945428654274));
#255096=CARTESIAN_POINT('Ctrl Pts',(84.7210949208572,0.329466147029263,
125.002363499906));
#255097=CARTESIAN_POINT('Ctrl Pts',(84.4426472970446,-4.70329999605691,
127.391050253351));
#255098=CARTESIAN_POINT('Ctrl Pts',(84.1641996732315,-5.41396321174535,
132.916402482027));
#255099=CARTESIAN_POINT('Ctrl Pts',(83.8857520494189,-1.14945872264635,
136.500891416245));
#255100=CARTESIAN_POINT('Ctrl Pts',(83.6073044256056,4.17134217838416,134.850546837477));
#255101=CARTESIAN_POINT('Ctrl Pts',(83.328856801793,5.65888339887398,129.481954789796));
#255102=CARTESIAN_POINT('Ctrl Pts',(83.05040917798,1.94618722762166,125.328589094719));
#255103=CARTESIAN_POINT('Ctrl Pts',(82.7719615541671,-3.5549599292834,126.207189922827));
#255104=CARTESIAN_POINT('Ctrl Pts',(82.4935139303543,-5.78927258062435,
131.310366035126));
#255105=CARTESIAN_POINT('Ctrl Pts',(82.2150663065413,-2.70352655206008,
135.948547888425));
#255106=CARTESIAN_POINT('Ctrl Pts',(81.9366186827285,2.86662830323276,135.859472947324));
#255107=CARTESIAN_POINT('Ctrl Pts',(81.6581710589156,5.80249179043285,131.124996731141));
#255108=CARTESIAN_POINT('Ctrl Pts',(81.3797234351026,3.40614878970799,126.095871590527));
#255109=CARTESIAN_POINT('Ctrl Pts',(81.1012758112897,-2.12027854913937,
125.393617843285));
#255110=CARTESIAN_POINT('Ctrl Pts',(80.822828187477,-5.6982734826932,129.663572376127));
#255111=CARTESIAN_POINT('Ctrl Pts',(80.5443805636639,-4.03983346178761,
134.981855572247));
#255112=CARTESIAN_POINT('Ctrl Pts',(80.2659329398512,1.33101615366455,136.461224986989));
#255113=CARTESIAN_POINT('Ctrl Pts',(79.9874853160382,5.47872694765296,132.742212399419));
#255114=CARTESIAN_POINT('Ctrl Pts',(79.7090376922254,4.59175532743923,127.242408693648));
#255115=CARTESIAN_POINT('Ctrl Pts',(79.4305900684125,-0.514815118972584,
125.015864794932));
#255116=CARTESIAN_POINT('Ctrl Pts',(79.1521424445996,-5.1482956211654,128.108665773475));
#255117=CARTESIAN_POINT('Ctrl Pts',(78.8736948207867,-5.05074395573051,
133.678678621723));
#255118=CARTESIAN_POINT('Ctrl Pts',(78.5952471969738,-0.31180533753877,
136.607333642391));
#255119=CARTESIAN_POINT('Ctrl Pts',(78.3167995731609,4.71366715331346,134.203339944237));
#255120=CARTESIAN_POINT('Ctrl Pts',(78.0383519493481,5.407509805713,128.675850294243));
#255121=CARTESIAN_POINT('Ctrl Pts',(77.7599043255351,1.1321151182024,125.104357647873));
#255122=CARTESIAN_POINT('Ctrl Pts',(77.4814567017223,-4.18363805603787,
126.770889270024));
#255123=CARTESIAN_POINT('Ctrl Pts',(77.2030090779094,-5.65483223886072,
132.143984014535));
#255124=CARTESIAN_POINT('Ctrl Pts',(76.9245614540965,-1.92951184808342,
136.286030301474));
#255125=CARTESIAN_POINT('Ctrl Pts',(76.6461138302835,3.56893566918854,135.390689943351));
#255126=CARTESIAN_POINT('Ctrl Pts',(76.3676662064707,5.78770565867644,130.280736989476));
#255127=CARTESIAN_POINT('Ctrl Pts',(76.0892185826578,2.68785689298084,125.651968569378));
#255128=CARTESIAN_POINT('Ctrl Pts',(75.8107709588449,-2.8820010482549,125.75799673322));
#255129=CARTESIAN_POINT('Ctrl Pts',(75.532323335032,-5.8034408197229,130.501386778194));
#255130=CARTESIAN_POINT('Ctrl Pts',(75.2538757112192,-3.39180199171105,
135.523194980456));
#255131=CARTESIAN_POINT('Ctrl Pts',(74.9754280874062,2.13673716794415,136.208624931095));
#255132=CARTESIAN_POINT('Ctrl Pts',(74.6969804635933,5.70171925567246,131.92779999059));
#255133=CARTESIAN_POINT('Ctrl Pts',(74.4185328397805,4.02709989190878,126.61458914934));
#255134=CARTESIAN_POINT('Ctrl Pts',(74.1400852159675,-1.34822753775231,
125.151573605674));
#255135=CARTESIAN_POINT('Ctrl Pts',(73.8616375921548,-5.48459972479585,
128.883193171938));
#255136=CARTESIAN_POINT('Ctrl Pts',(73.5831899683417,-4.58089270234404,
134.380271766487));
#255137=CARTESIAN_POINT('Ctrl Pts',(73.3047423445289,0.532430924512096,
136.591262708148));
#255138=CARTESIAN_POINT('Ctrl Pts',(73.026294720716,5.15647654243839,133.484373334449));
#255139=CARTESIAN_POINT('Ctrl Pts',(72.7478470969032,5.04197212574731,127.914683199832));
#255140=CARTESIAN_POINT('Ctrl Pts',(72.46939947309,0.294141639526237,125.000465443524));
#255141=CARTESIAN_POINT('Ctrl Pts',(72.1909518492774,-4.72399064380143,
127.419743816117));
#255142=CARTESIAN_POINT('Ctrl Pts',(71.9125042254643,-5.40100630524849,
132.949319681519));
#255143=CARTESIAN_POINT('Ctrl Pts',(71.6340566016516,-1.11476102599866,
136.507782954223));
#255144=CARTESIAN_POINT('Ctrl Pts',(71.3556089778387,4.19589517704018,134.82507972721));
#255145=CARTESIAN_POINT('Ctrl Pts',(71.0771613540258,5.65072869325411,129.447532061481));
#255146=CARTESIAN_POINT('Ctrl Pts',(70.7987137302128,1.91281859381102,125.316843554035));
#255147=CARTESIAN_POINT('Ctrl Pts',(70.5202661064001,-3.58287834696108,
126.22891514786));
#255148=CARTESIAN_POINT('Ctrl Pts',(70.241818482587,-5.78608512021397,131.345597605407));
#255149=CARTESIAN_POINT('Ctrl Pts',(69.9633708587742,-2.67216233396265,
135.964909712024));
#255150=CARTESIAN_POINT('Ctrl Pts',(69.6849232349613,2.89734709481291,135.841929307673));
#255151=CARTESIAN_POINT('Ctrl Pts',(69.4064756111484,5.80433608672999,131.089669376025));
#255152=CARTESIAN_POINT('Ctrl Pts',(69.1280279873355,3.37742377252397,126.07522463346));
#255153=CARTESIAN_POINT('Ctrl Pts',(68.8495803635227,-2.15317599230747,
125.406624829152));
#255154=CARTESIAN_POINT('Ctrl Pts',(68.5711327397097,-5.70511220870344,
129.698280520343));
#255155=CARTESIAN_POINT('Ctrl Pts',(68.2926851158969,-4.01432901552682,
135.006369785865));
#255156=CARTESIAN_POINT('Ctrl Pts',(68.014237492084,1.36542643204398,136.45301790528));
#255157=CARTESIAN_POINT('Ctrl Pts',(67.735789868271,5.49042169335597,132.708825929535));
#255158=CARTESIAN_POINT('Ctrl Pts',(67.4573422444582,4.56998764048497,127.214523370394));
#255159=CARTESIAN_POINT('Ctrl Pts',(67.1788946206453,-0.550041797684044,
125.019105868103));
#255160=CARTESIAN_POINT('Ctrl Pts',(66.9004469968323,-5.164609694817,128.140054855163));
#255161=CARTESIAN_POINT('Ctrl Pts',(66.6219993730196,-5.03315358762317,
133.709370679297));
#255162=CARTESIAN_POINT('Ctrl Pts',(66.3435517492066,-0.2764752166261,136.609124174332));
#255163=CARTESIAN_POINT('Ctrl Pts',(66.0651041253938,4.73427037188528,134.174583539162));
#255164=CARTESIAN_POINT('Ctrl Pts',(65.7866565015808,5.39445277059944,128.642972683589));
#255165=CARTESIAN_POINT('Ctrl Pts',(65.508208877768,1.0973966068015,125.097571749668));
#255166=CARTESIAN_POINT('Ctrl Pts',(65.2297612539551,-4.20811342784249,
126.796430993211));
#255167=CARTESIAN_POINT('Ctrl Pts',(64.9513136301422,-5.64657280006891,
132.178381763287));
#255168=CARTESIAN_POINT('Ctrl Pts',(64.6728660063292,-1.89610761944867,
136.297674225111));
#255169=CARTESIAN_POINT('Ctrl Pts',(64.3944183825164,3.59678783343796,135.368879844889));
#255170=CARTESIAN_POINT('Ctrl Pts',(64.1159707587035,5.78441098024938,130.245515283918));
#255171=CARTESIAN_POINT('Ctrl Pts',(63.8375231348906,2.65644302039782,125.635702283457));
#255172=CARTESIAN_POINT('Ctrl Pts',(63.5590755110777,-2.91266630074331,
125.775633789045));
#255173=CARTESIAN_POINT('Ctrl Pts',(63.2806278872649,-5.80517758316048,
130.53671958308));
#255174=CARTESIAN_POINT('Ctrl Pts',(63.0021802634519,-3.36301426534433,
135.543754412816));
#255175=CARTESIAN_POINT('Ctrl Pts',(62.723732639639,2.16959486994269,136.195517876976));
#255176=CARTESIAN_POINT('Ctrl Pts',(62.4452850158262,5.70845231035428,131.893071192411));
#255177=CARTESIAN_POINT('Ctrl Pts',(62.1668373920132,4.00152095094907,126.590152676031));
#255178=CARTESIAN_POINT('Ctrl Pts',(61.8883897682004,-1.38261267721222,
125.159885382419));
#255179=CARTESIAN_POINT('Ctrl Pts',(61.6099421443874,-5.49619279939966,
128.916615081961));
#255180=CARTESIAN_POINT('Ctrl Pts',(61.3314945205747,-4.55904024288434,
134.408090707227));
#255181=CARTESIAN_POINT('Ctrl Pts',(61.0530468967616,0.567647575344072,
136.587914432096));
#255182=CARTESIAN_POINT('Ctrl Pts',(60.7745992729488,5.17269500295686,133.452934743723));
#255183=CARTESIAN_POINT('Ctrl Pts',(60.496151649136,5.02428842305186,127.884044823451));
#255184=CARTESIAN_POINT('Ctrl Pts',(60.2177040253229,0.258806232497024,
124.998782452612));
#255185=CARTESIAN_POINT('Ctrl Pts',(59.9392564015102,-4.74450624233532,
127.448562797104));
#255186=CARTESIAN_POINT('Ctrl Pts',(59.6608087776971,-5.38784926247686,
132.982157398764));
#255187=CARTESIAN_POINT('Ctrl Pts',(59.3823611538844,-1.08002202147149,
136.514463149789));
#255188=CARTESIAN_POINT('Ctrl Pts',(59.1039135300714,4.22029269525717,134.799463627718));
#255189=CARTESIAN_POINT('Ctrl Pts',(58.8254659062585,5.64236459780459,129.413159610949));
#255190=CARTESIAN_POINT('Ctrl Pts',(58.5470182824457,1.8793790798041,125.305301355313));
#255191=CARTESIAN_POINT('Ctrl Pts',(58.2685706586328,-3.61066399976409,
126.250809917708));
#255192=CARTESIAN_POINT('Ctrl Pts',(57.9901230348199,-5.78268325429153,
131.380809119953));
#255193=CARTESIAN_POINT('Ctrl Pts',(57.711675411007,-2.64069909790739,135.981080309579));
#255194=CARTESIAN_POINT('Ctrl Pts',(57.4332277871941,2.92795852413098,135.824198999061));
#255195=CARTESIAN_POINT('Ctrl Pts',(57.1547801633813,5.80596530121877,131.054331448687));
#255196=CARTESIAN_POINT('Ctrl Pts',(56.8763325395683,3.34857360366007,126.054752916266));
#255197=CARTESIAN_POINT('Ctrl Pts',(56.5978849157555,-2.18599364874745,
125.419831830104));
#255198=CARTESIAN_POINT('Ctrl Pts',(56.3194372919424,-5.71173952968275,
129.733029650764));
#255199=CARTESIAN_POINT('Ctrl Pts',(56.0409896681298,-3.98867581682796,
135.030728292487));
#255200=CARTESIAN_POINT('Ctrl Pts',(55.7625420443167,1.39978611404518,136.444601510497));
#255201=CARTESIAN_POINT('Ctrl Pts',(55.4840944205039,5.50191298946419,132.675368888989));
#255202=CARTESIAN_POINT('Ctrl Pts',(55.2056467966909,4.54805061095778,127.186771069878));
#255203=CARTESIAN_POINT('Ctrl Pts',(54.9271991728781,-0.585248094394635,
125.022561316018));
#255204=CARTESIAN_POINT('Ctrl Pts',(54.6487515490652,-5.18073239195715,
128.171542663682));
#255205=CARTESIAN_POINT('Ctrl Pts',(54.3703039252523,-5.01537671415865,
133.739955090657));
#255206=CARTESIAN_POINT('Ctrl Pts',(54.0918563014394,-0.241134850822232,
136.610699608625));
#255207=CARTESIAN_POINT('Ctrl Pts',(53.8134086776265,4.75469816032759,134.145702249237));
#255208=CARTESIAN_POINT('Ctrl Pts',(53.5349610538137,5.38119584205463,128.610175163959));
#255209=CARTESIAN_POINT('Ctrl Pts',(53.2565134300007,1.06263743096531,125.090997318624));
#255210=CARTESIAN_POINT('Ctrl Pts',(52.9780658061879,-4.23243286645675,
126.822121231705));
#255211=CARTESIAN_POINT('Ctrl Pts',(52.6996181823749,-5.63810412544538,
132.21272859718));
#255212=CARTESIAN_POINT('Ctrl Pts',(52.4211705585621,-1.86263312984859,
136.309114591992));
#255213=CARTESIAN_POINT('Ctrl Pts',(52.1427229347491,3.62450671739182,135.346900606486));
#255214=CARTESIAN_POINT('Ctrl Pts',(51.8642753109363,5.7809019583462,130.210314286579));
#255215=CARTESIAN_POINT('Ctrl Pts',(51.5858276871234,2.62493071234137,125.619627524071));
#255216=CARTESIAN_POINT('Ctrl Pts',(51.3073800633105,-2.94322362331098,
125.793457186192));
#255217=CARTESIAN_POINT('Ctrl Pts',(51.0289324394976,-5.80669923360788,
130.572062305503));
#255218=CARTESIAN_POINT('Ctrl Pts',(50.7504848156848,-3.33410192124705,
135.564138225197));
#255219=CARTESIAN_POINT('Ctrl Pts',(50.4720371918718,2.20237217680579,136.182211051539));
#255220=CARTESIAN_POINT('Ctrl Pts',(50.193589568059,5.71497383623647,131.858302051661));
#255221=CARTESIAN_POINT('Ctrl Pts',(49.915141944246,3.97579373215887,126.565872361749));
#255222=CARTESIAN_POINT('Ctrl Pts',(49.6366943204332,-1.41694658345112,
125.168406317271));
#255223=CARTESIAN_POINT('Ctrl Pts',(49.3582466966203,-5.50758221055828,
128.950106943089));
#255224=CARTESIAN_POINT('Ctrl Pts',(49.0797990728074,-4.53701884651156,
134.435776110423));
#255225=CARTESIAN_POINT('Ctrl Pts',(48.8013514489945,0.602843191786665,
136.584351844331));
#255226=CARTESIAN_POINT('Ctrl Pts',(48.5229038251815,5.18872178735999,133.421398009111));
#255227=CARTESIAN_POINT('Ctrl Pts',(48.2444562013688,5.006418543501,127.853514660444));
#255228=CARTESIAN_POINT('Ctrl Pts',(47.9660085775558,0.223461235307256,
124.997314589534));
#255229=CARTESIAN_POINT('Ctrl Pts',(47.6875609537429,-4.7648460314457,127.477506128414));
#255230=CARTESIAN_POINT('Ctrl Pts',(47.40911332993,-5.37449257096935,133.014914416948));
#255231=CARTESIAN_POINT('Ctrl Pts',(47.1306657061172,-1.04524299633083,
136.520931755405));
#255232=CARTESIAN_POINT('Ctrl Pts',(46.8522180823042,4.24453382897653,134.773699488214));
#255233=CARTESIAN_POINT('Ctrl Pts',(46.5737704584914,5.6337914224598,129.378838711881));
#255234=CARTESIAN_POINT('Ctrl Pts',(46.2953228346785,1.84586992471411,125.293962926255));
#255235=CARTESIAN_POINT('Ctrl Pts',(46.0168752108656,-3.63831585808481,
126.272873421051));
#255236=CARTESIAN_POINT('Ctrl Pts',(45.7384275870526,-5.77906710891461,
131.415999273987));
#255237=CARTESIAN_POINT('Ctrl Pts',(45.4599799632399,-2.60913800977569,
135.997059081882));
#255238=CARTESIAN_POINT('Ctrl Pts',(45.1815323394269,2.95846145686929,135.806282678493));
#255239=CARTESIAN_POINT('Ctrl Pts',(44.903084715614,5.80737937352832,131.018984258588));
#255240=CARTESIAN_POINT('Ctrl Pts',(44.6246370918012,3.31959935216964,126.034457197533));
#255241=CARTESIAN_POINT('Ctrl Pts',(44.3461894679882,-2.21873030238901,
125.43323835675));
#255242=CARTESIAN_POINT('Ctrl Pts',(44.0677418441753,-5.7181552000533,129.767818479747));
#255243=CARTESIAN_POINT('Ctrl Pts',(43.7892942203624,-3.96287481627985,
135.054930189501));
#255244=CARTESIAN_POINT('Ctrl Pts',(43.5108465965496,1.43409392645716,136.435976114513));
#255245=CARTESIAN_POINT('Ctrl Pts',(43.2323989727367,5.51320041016325,132.641842517543));
#255246=CARTESIAN_POINT('Ctrl Pts',(42.9539513489238,4.52594505174265,127.159152820475));
#255247=CARTESIAN_POINT('Ctrl Pts',(42.6755037251109,-0.620432704521861,
125.026231010632));
#255248=CARTESIAN_POINT('Ctrl Pts',(42.397056101298,-5.19666311515333,128.203128032237));
#255249=CARTESIAN_POINT('Ctrl Pts',(42.1186084774851,-4.99741399406557,
133.770430722483));
#255250=CARTESIAN_POINT('Ctrl Pts',(41.8401608536722,-0.205785549677785,
136.612059886891));
#255251=CARTESIAN_POINT('Ctrl Pts',(41.5617132298594,4.77494976168102,134.11669714467));
#255252=CARTESIAN_POINT('Ctrl Pts',(41.2832656060464,5.36773951131901,128.577458950676));
#255253=CARTESIAN_POINT('Ctrl Pts',(41.0048179822336,1.02783887870806,125.084634598359));
#255254=CARTESIAN_POINT('Ctrl Pts',(40.7263703584206,-4.25659547071474,
126.847959033542));
#255255=CARTESIAN_POINT('Ctrl Pts',(40.4479227346078,-5.62942652880005,
132.24702324348));
#255256=CARTESIAN_POINT('Ctrl Pts',(40.1694751107948,-1.82908961969292,
136.320350978189));
#255257=CARTESIAN_POINT('Ctrl Pts',(39.891027486982,3.65209129391637,135.324753042595));
#255258=CARTESIAN_POINT('Ctrl Pts',(39.6125798631691,5.77717872299504,130.175135301845));
#255259=CARTESIAN_POINT('Ctrl Pts',(39.3341322393562,2.59332113651206,125.603744886877));
#255260=CARTESIAN_POINT('Ctrl Pts',(39.0556846155433,-2.97367188364494,
125.811466264208));
#255261=CARTESIAN_POINT('Ctrl Pts',(38.7772369917304,-5.80800571467979,
130.607413635826));
#255262=CARTESIAN_POINT('Ctrl Pts',(38.4987893679175,-3.30506603077697,
135.584345662267));
#255263=CARTESIAN_POINT('Ctrl Pts',(38.2203417441046,2.23506787395795,136.16870494788));
#255264=CARTESIAN_POINT('Ctrl Pts',(37.9418941202917,5.72128359166147,131.823493856722));
#255265=CARTESIAN_POINT('Ctrl Pts',(37.6634464964789,3.94991918886983,126.541749106207));
#255266=CARTESIAN_POINT('Ctrl Pts',(37.3849988726659,-1.45122798421329,
125.177136094481));
#255267=CARTESIAN_POINT('Ctrl Pts',(37.1065512488531,-5.51876753623267,
128.983667514269));
#255268=CARTESIAN_POINT('Ctrl Pts',(36.8281036250402,-4.51482932923697,
134.463326950183));
#255269=CARTESIAN_POINT('Ctrl Pts',(36.5496560012273,0.6380164696531,136.580575076865));
#255270=CARTESIAN_POINT('Ctrl Pts',(36.2712083774144,5.20455630176915,133.389764299214));
#255271=CARTESIAN_POINT('Ctrl Pts',(35.9927607536015,4.9883631492699,127.82309384212));
#255272=CARTESIAN_POINT('Ctrl Pts',(35.7143131297886,0.188107957679239,
124.996061908681));
#255273=CARTESIAN_POINT('Ctrl Pts',(35.4358655059757,-4.78500925743413,
127.50657273754));
#255274=CARTESIAN_POINT('Ctrl Pts',(35.1574178821628,-5.36093672566315,
133.047589522248));
#255275=CARTESIAN_POINT('Ctrl Pts',(34.87897025835,-1.01042523932657,136.527188531377));
#255276=CARTESIAN_POINT('Ctrl Pts',(34.6005226345371,4.26861767993396,134.747788263399));
#255277=CARTESIAN_POINT('Ctrl Pts',(34.3220750107242,5.62500948490202,129.34457063605));
#255278=CARTESIAN_POINT('Ctrl Pts',(34.0436273869112,1.81229237023524,125.282828687009));
#255279=CARTESIAN_POINT('Ctrl Pts',(33.7651797630984,-3.66583289727342,
126.295104840318));
#255280=CARTESIAN_POINT('Ctrl Pts',(33.4867321392855,-5.77523681808073,
131.451166763527));
#255281=CARTESIAN_POINT('Ctrl Pts',(33.2082845154725,-2.57748023907555,
136.012845436834));
#255282=CARTESIAN_POINT('Ctrl Pts',(32.9298368916598,2.98885476273036,135.788181009863));
#255283=CARTESIAN_POINT('Ctrl Pts',(32.6513892678468,5.80857825125962,130.983629115531));
#255284=CARTESIAN_POINT('Ctrl Pts',(32.3729416440339,3.29050209170421,126.014338229324));
#255285=CARTESIAN_POINT('Ctrl Pts',(32.094494020221,-2.25138474016344,125.446843912307));
#255286=CARTESIAN_POINT('Ctrl Pts',(31.8160463964081,-5.72435898208005,
129.802645718181));
#255287=CARTESIAN_POINT('Ctrl Pts',(31.5375987725953,-3.93692696994811,
135.078974580096));
#255288=CARTESIAN_POINT('Ctrl Pts',(31.2591511487823,1.46834859799131,136.427142036947));
#255289=CARTESIAN_POINT('Ctrl Pts',(30.9807035249695,5.52428353719365,132.608248057529));
#255290=CARTESIAN_POINT('Ctrl Pts',(30.7022559011566,4.50367178196922,127.131669645585));
#255291=CARTESIAN_POINT('Ctrl Pts',(30.4238082773436,-0.655594324287056,
125.030114815962));
#255292=CARTESIAN_POINT('Ctrl Pts',(30.1453606535308,-5.21240127408669,
128.234809790423));
#255293=CARTESIAN_POINT('Ctrl Pts',(29.8669130297179,-4.97926609295916,
133.80079644549));
#255294=CARTESIAN_POINT('Ctrl Pts',(29.588465405905,-0.170428623074124,
136.613204958723));
#255295=CARTESIAN_POINT('Ctrl Pts',(29.3100177820921,4.79502442551506,134.087569300254));
#255296=CARTESIAN_POINT('Ctrl Pts',(29.0315701582792,5.35408427702179,128.544825256054));
#255297=CARTESIAN_POINT('Ctrl Pts',(28.7531225344664,0.99300223950345,125.078483824645));
#255298=CARTESIAN_POINT('Ctrl Pts',(28.4746749106534,-4.28060034526213,
126.873943441297));
#255299=CARTESIAN_POINT('Ctrl Pts',(28.1962272868406,-5.6205403316845,132.281264431386));
#255300=CARTESIAN_POINT('Ctrl Pts',(27.9177796630277,-1.79547833194873,
136.331382967337));
#255301=CARTESIAN_POINT('Ctrl Pts',(27.6393320392148,3.67954054085496,135.3024379739));
#255302=CARTESIAN_POINT('Ctrl Pts',(27.3608844154018,5.77324141216173,130.139979633288));
#255303=CARTESIAN_POINT('Ctrl Pts',(27.082436791589,2.56161546421434,125.58805496041));
#255304=CARTESIAN_POINT('Ctrl Pts',(26.8039891677761,-3.00400995347367,
125.82966035576));
#255305=CARTESIAN_POINT('Ctrl Pts',(26.5255415439632,-5.80909697796402,
130.642772264091));
#255306=CARTESIAN_POINT('Ctrl Pts',(26.2470939201503,-3.27590766986969,
135.604375975235));
#255307=CARTESIAN_POINT('Ctrl Pts',(25.9686462963375,2.2676807498481,136.155000066467));
#255308=CARTESIAN_POINT('Ctrl Pts',(25.6901986725246,5.727381342819,131.788647897428));
#255309=CARTESIAN_POINT('Ctrl Pts',(25.4117510487116,3.92389827987267,126.517783803302));
#255310=CARTESIAN_POINT('Ctrl Pts',(25.1333034248988,-1.48545560918882,
125.186074390566));
#255311=CARTESIAN_POINT('Ctrl Pts',(24.8548558010858,-5.5297483619465,129.017295551901));
#255312=CARTESIAN_POINT('Ctrl Pts',(24.576408177273,-4.49247251330123,134.490742205601));
#255313=CARTESIAN_POINT('Ctrl Pts',(24.2979605534601,0.673166105584617,
136.576584269648));
#255314=CARTESIAN_POINT('Ctrl Pts',(24.0195129296472,5.22019795943058,133.358034786234));
#255315=CARTESIAN_POINT('Ctrl Pts',(23.7410653058343,4.97012290940784,127.792783495733));
#255316=CARTESIAN_POINT('Ctrl Pts',(23.4626176820214,0.152747709641667,
124.995024456474));
#255317=CARTESIAN_POINT('Ctrl Pts',(23.1841700582085,-4.80499517314482,
127.53576154741));
#255318=CARTESIAN_POINT('Ctrl Pts',(22.9057224343956,-5.34718222887511,
133.080181503877));
#255319=CARTESIAN_POINT('Ctrl Pts',(22.6272748105827,-0.975570040643468,
136.533233245855));
#255320=CARTESIAN_POINT('Ctrl Pts',(22.3488271867698,4.29254335569345,134.721730913422));
#255321=CARTESIAN_POINT('Ctrl Pts',(22.070379562957,5.61601911054919,129.310356653276));
#255322=CARTESIAN_POINT('Ctrl Pts',(21.791931939144,1.77864766059611,125.27189905016));
#255323=CARTESIAN_POINT('Ctrl Pts',(21.5134843153312,-3.69321409767591,
126.317503351717));
#255324=CARTESIAN_POINT('Ctrl Pts',(21.2350366915183,-5.77119252372273,
131.486310285425));
#255325=CARTESIAN_POINT('Ctrl Pts',(20.9565890677054,-2.54572695889727,
136.028438789465));
#255326=CARTESIAN_POINT('Ctrl Pts',(20.6781414438925,3.01913731547902,135.769894663934));
#255327=CARTESIAN_POINT('Ctrl Pts',(20.3996938200796,5.80956188998761,130.948267329615));
#255328=CARTESIAN_POINT('Ctrl Pts',(20.1212461962667,3.26128290047392,125.994396757156));
#255329=CARTESIAN_POINT('Ctrl Pts',(19.8427985724538,-2.28395575204823,
125.460647992615));
#255330=CARTESIAN_POINT('Ctrl Pts',(19.5643509486409,-5.7303506458796,129.837510075529));
#255331=CARTESIAN_POINT('Ctrl Pts',(19.285903324828,-3.91083323933969,135.102860573299));
#255332=CARTESIAN_POINT('Ctrl Pts',(19.0074557010152,1.50254885932817,136.418099605148));
#255333=CARTESIAN_POINT('Ctrl Pts',(18.7290080772022,5.53516195986603,132.574586753804));
#255334=CARTESIAN_POINT('Ctrl Pts',(18.4505604533894,4.48123162698169,127.104322563612));
#255335=CARTESIAN_POINT('Ctrl Pts',(18.1721128295765,-0.690731650763477,
125.034212588094));
#255336=CARTESIAN_POINT('Ctrl Pts',(17.8936652057636,-5.22794628557398,
128.26658676426));
#255337=CARTESIAN_POINT('Ctrl Pts',(17.6152175819507,-4.96093368331654,
133.831051134467));
#255338=CARTESIAN_POINT('Ctrl Pts',(17.3367699581378,-0.135065381175154,
136.614134781694));
#255339=CARTESIAN_POINT('Ctrl Pts',(17.0583223343249,4.81492140795562,134.058319795333));
#255340=CARTESIAN_POINT('Ctrl Pts',(16.779874710512,5.34023064516271,128.512275289347));
#255341=CARTESIAN_POINT('Ctrl Pts',(16.5014270866992,0.958128804235671,
125.0725452254));
#255342=CARTESIAN_POINT('Ctrl Pts',(16.2229794628862,-4.30444660058956,
126.900073492105));
#255343=CARTESIAN_POINT('Ctrl Pts',(15.9445318390734,-5.61144586338,132.315450892077));
#255344=CARTESIAN_POINT('Ctrl Pts',(15.6660842152604,-1.76180051209467,
136.342210150638));
#255345=CARTESIAN_POINT('Ctrl Pts',(15.3876365914476,3.70685344106567,135.279956227294));
#255346=CARTESIAN_POINT('Ctrl Pts',(15.1091889676347,5.76909017174479,130.104848583611));
#255347=CARTESIAN_POINT('Ctrl Pts',(14.8307413438218,2.52981487031356,125.572558326068));
#255348=CARTESIAN_POINT('Ctrl Pts',(14.5522937200089,-3.03423670860886,
125.848038786661));
#255349=CARTESIAN_POINT('Ctrl Pts',(14.273846096196,-5.80997298302346,130.678136880072));
#255350=CARTESIAN_POINT('Ctrl Pts',(13.9953984723831,-3.24662791899898,
135.624228421867));
#255351=CARTESIAN_POINT('Ctrl Pts',(13.7169508485702,2.30020959599411,136.141096915141));
#255352=CARTESIAN_POINT('Ctrl Pts',(13.4385032247574,5.73326686375462,131.753765465006));
#255353=CARTESIAN_POINT('Ctrl Pts',(13.1600556009444,3.89773196938174,126.493977341077));
#255354=CARTESIAN_POINT('Ctrl Pts',(12.8816079771316,-1.51962819006047,
125.195220874312));
#255355=CARTESIAN_POINT('Ctrl Pts',(12.6031603533186,-5.54052428080121,
129.050989809886));
#255356=CARTESIAN_POINT('Ctrl Pts',(12.3247127295058,-4.46994922714442,
134.518020860792));
#255357=CARTESIAN_POINT('Ctrl Pts',(12.0462651056929,0.708290797098533,
136.572379570561));
#255358=CARTESIAN_POINT('Ctrl Pts',(11.76781748188,5.23564618073708,133.326210645918));
#255359=CARTESIAN_POINT('Ctrl Pts',(11.4893698580671,4.95169849981347,127.762584744442));
#255360=CARTESIAN_POINT('Ctrl Pts',(11.2109222342542,0.117381801481337,
124.994202271355));
#255361=CARTESIAN_POINT('Ctrl Pts',(10.9324746104413,-4.82480303799234,
127.565071476419));
#255362=CARTESIAN_POINT('Ctrl Pts',(10.6540269866284,-5.33322959028317,
133.112689154126));
#255363=CARTESIAN_POINT('Ctrl Pts',(10.3755793628155,-0.940678691853753,
136.539065674851));
#255364=CARTESIAN_POINT('Ctrl Pts',(10.0971317390026,4.31630996968034,134.695528403849));
#255365=CARTESIAN_POINT('Ctrl Pts',(9.81868411518972,5.60682063254294,129.276198031366));
#255366=CARTESIAN_POINT('Ctrl Pts',(9.54023649137686,1.74493704251384,125.261174420708));
#255367=CARTESIAN_POINT('Ctrl Pts',(9.26178886756394,-3.72045844467185,
126.340068125262));
#255368=CARTESIAN_POINT('Ctrl Pts',(8.98334124375105,-5.76693437570339,
131.52142853743));
#255369=CARTESIAN_POINT('Ctrl Pts',(8.70489361993813,-2.51387934587036,
136.043838561958));
#255370=CARTESIAN_POINT('Ctrl Pts',(8.42644599612531,3.0493079929842,135.751424318317));
#255371=CARTESIAN_POINT('Ctrl Pts',(8.14799837231237,5.81033025326331,130.912900211183));
#255372=CARTESIAN_POINT('Ctrl Pts',(7.86955074849947,3.23194286120641,125.974633519968));
#255373=CARTESIAN_POINT('Ctrl Pts',(7.59110312468663,-2.3164421311127,125.47465008616));
#255374=CARTESIAN_POINT('Ctrl Pts',(7.31265550087371,-5.73612996942864,
129.872410259879));
#255375=CARTESIAN_POINT('Ctrl Pts',(7.0342078770608,-3.88459459136738,135.126587284006));
#255376=CARTESIAN_POINT('Ctrl Pts',(6.75576025324794,1.53669344316449,136.408849154185));
#255377=CARTESIAN_POINT('Ctrl Pts',(6.47731262943506,5.54583527507644,132.540859853697));
#255378=CARTESIAN_POINT('Ctrl Pts',(6.19886500562214,4.45862541830825,127.077112587908));
#255379=CARTESIAN_POINT('Ctrl Pts',(5.92041738180924,-0.725843381924555,
125.038524175185));
#255380=CARTESIAN_POINT('Ctrl Pts',(5.64196975799638,-5.24329757358911,
128.29845777624));
#255381=CARTESIAN_POINT('Ctrl Pts',(5.36352213418349,-4.94241744445191,
133.861193668313));
#255382=CARTESIAN_POINT('Ctrl Pts',(5.08507451037056,-0.0996971343788212,
136.614849321347));
#255383=CARTESIAN_POINT('Ctrl Pts',(4.80662688655771,4.83463997171276,134.028949713759));
#255384=CARTESIAN_POINT('Ctrl Pts',(4.5281792627448,5.32617912909322,128.479810256704));
#255385=CARTESIAN_POINT('Ctrl Pts',(4.24973163893191,0.923219865152705,
125.066819020683));
#255386=CARTESIAN_POINT('Ctrl Pts',(3.97128401511898,-4.32813335306523,
126.926348217707));
#255387=CARTESIAN_POINT('Ctrl Pts',(3.69283639130614,-5.60214346088543,
132.349581358763));
#255388=CARTESIAN_POINT('Ctrl Pts',(3.41438876749324,-1.72805740807474,
136.352832126888));
#255389=CARTESIAN_POINT('Ctrl Pts',(3.13594114368033,3.73402898245891,135.257308635848));
#255390=CARTESIAN_POINT('Ctrl Pts',(2.85749351986744,5.76472515556999,130.06974345461));
#255391=CARTESIAN_POINT('Ctrl Pts',(2.5790458960546,2.49792053319242,125.557255558086));
#255392=CARTESIAN_POINT('Ctrl Pts',(2.30059827224166,-3.06435102898697,
125.866600875889));
#255393=CARTESIAN_POINT('Ctrl Pts',(2.02215064842876,-5.81063369739741,
130.713506173321));
#255394=CARTESIAN_POINT('Ctrl Pts',(1.74370302461591,-3.21722786313679,
135.643902266527));
#255395=CARTESIAN_POINT('Ctrl Pts',(1.46525540080302,2.33265320702766,136.12699600909));
#255396=CARTESIAN_POINT('Ctrl Pts',(1.18680777699008,5.73893993637821,131.718847852038));
#255397=CARTESIAN_POINT('Ctrl Pts',(0.908360153177235,3.87142122699929,
126.47033060169));
#255398=CARTESIAN_POINT('Ctrl Pts',(0.629912529364331,-1.55374446055069,
125.204575206795));
#255399=CARTESIAN_POINT('Ctrl Pts',(0.351464905551429,-5.55109489349118,
129.084749039672));
#255400=CARTESIAN_POINT('Ctrl Pts',(0.0730172817385382,-4.44726030537518,
134.545161904937));
#255401=CARTESIAN_POINT('Ctrl Pts',(-0.205430342074321,0.743389242636492,
136.56796113541));
#255402=CARTESIAN_POINT('Ctrl Pts',(-0.48387796588724,5.25090039324876,
133.294293057522));
#255403=CARTESIAN_POINT('Ctrl Pts',(-0.762325589700153,4.93309060321035,
127.732498707276));
#255404=CARTESIAN_POINT('Ctrl Pts',(-1.040773213513,0.0820115436953976,
124.993595383789));
#255405=CARTESIAN_POINT('Ctrl Pts',(-1.3192208373259,-4.84443211798899,
127.594501438479));
#255406=CARTESIAN_POINT('Ctrl Pts',(-1.5976684611388,-5.31907932690746,
133.145111268411));
#255407=CARTESIAN_POINT('Ctrl Pts',(-1.8761160849517,-0.905752485869179,
136.544685602242));
#255408=CARTESIAN_POINT('Ctrl Pts',(-2.15456370876455,4.33991664121397,
134.669181705622));
#255409=CARTESIAN_POINT('Ctrl Pts',(-2.43301133257747,5.59741439173625,
129.242096036083));
#255410=CARTESIAN_POINT('Ctrl Pts',(-2.71145895639038,1.71116176514775,
125.250655196059));
#255411=CARTESIAN_POINT('Ctrl Pts',(-2.98990658020324,-3.74756492871192,
126.362798324807));
#255412=CARTESIAN_POINT('Ctrl Pts',(-3.26835420401613,-5.76246253181,131.556520218218));
#255413=CARTESIAN_POINT('Ctrl Pts',(-3.54680182782904,-2.48193858011979,
136.059044183669));
#255414=CARTESIAN_POINT('Ctrl Pts',(-3.82524945164193,3.0793656772603,135.732770657435));
#255415=CARTESIAN_POINT('Ctrl Pts',(-4.1036970754548,5.81088331261472,130.877529070775));
#255416=CARTESIAN_POINT('Ctrl Pts',(-4.38214469926771,3.20248306110764,
125.955049250094));
#255417=CARTESIAN_POINT('Ctrl Pts',(-4.66059232308062,-2.34884267356213,
125.488849674089));
#255418=CARTESIAN_POINT('Ctrl Pts',(-4.93903994689347,-5.7416967385722,
129.907344977992));
#255419=CARTESIAN_POINT('Ctrl Pts',(-5.21748757070636,-3.85821199831392,
135.150153833014));
#255420=CARTESIAN_POINT('Ctrl Pts',(-5.49593519451928,1.57078108426016,
136.399391026839));
#255421=CARTESIAN_POINT('Ctrl Pts',(-5.77438281833216,5.55630308732125,
132.507068606974));
#255422=CARTESIAN_POINT('Ctrl Pts',(-6.05283044214503,4.43585399363028,
127.050040726751));
#255423=CARTESIAN_POINT('Ctrl Pts',(-6.33127806595794,-0.76092821669219,
125.043049417465));
#255424=CARTESIAN_POINT('Ctrl Pts',(-6.60972568977086,-5.25845456928442,
128.330421645371));
#255425=CARTESIAN_POINT('Ctrl Pts',(-6.88817331358369,-4.92371806249131,
133.891222930087));
#255426=CARTESIAN_POINT('Ctrl Pts',(-7.16662093739661,-0.0643251932685087,
136.615348551203));
#255427=CARTESIAN_POINT('Ctrl Pts',(-7.44506856120951,4.8541793861078,133.999460143849));
#255428=CARTESIAN_POINT('Ctrl Pts',(-7.72351618502242,5.3119302494974,128.44743136113));
#255429=CARTESIAN_POINT('Ctrl Pts',(-8.00196380883526,0.888276715818123,
125.06130542268));
#255430=CARTESIAN_POINT('Ctrl Pts',(-8.28041143264819,-4.35165972496785,
126.952766644486));
#255431=CARTESIAN_POINT('Ctrl Pts',(-8.55885905646108,-5.59263346890473,
132.383654566726));
#255432=CARTESIAN_POINT('Ctrl Pts',(-8.83730668027396,-1.69425027025207,
136.363248502487));
#255433=CARTESIAN_POINT('Ctrl Pts',(-9.11575430408684,3.76106615803527,
135.234496038775));
#255434=CARTESIAN_POINT('Ctrl Pts',(-9.39420192789976,5.7601465253845,130.034665547118));
#255435=CARTESIAN_POINT('Ctrl Pts',(-9.67264955171265,2.4659336347071,125.542147223509));
#255436=CARTESIAN_POINT('Ctrl Pts',(-9.95109717552551,-3.09435179871079,
125.885345935621));
#255437=CARTESIAN_POINT('Ctrl Pts',(-10.2295447993384,-5.81107909660284,
130.748878833214));
#255438=CARTESIAN_POINT('Ctrl Pts',(-10.5079924231513,-3.18770859171301,
135.663396780189));
#255439=CARTESIAN_POINT('Ctrl Pts',(-10.7864400469642,2.36501038073878,
136.112697870828));
#255440=CARTESIAN_POINT('Ctrl Pts',(-11.0648876707771,5.74440035047196,
131.683896352409));
#255441=CARTESIAN_POINT('Ctrl Pts',(-11.34333529459,3.84496702767957,126.446844461378));
#255442=CARTESIAN_POINT('Ctrl Pts',(-11.6217829184029,-1.58780315646856,
125.214137041385));
#255443=CARTESIAN_POINT('Ctrl Pts',(-11.9002305422157,-5.56145980831845,
129.118571990297));
#255444=CARTESIAN_POINT('Ctrl Pts',(-12.1786781660286,-4.42440658873985,
134.572164332316));
#255445=CARTESIAN_POINT('Ctrl Pts',(-12.4571257898416,0.778460141612691,
136.563329127923));
#255446=CARTESIAN_POINT('Ctrl Pts',(-12.7355734136544,5.26596003171537,
133.262283203764));
#255447=CARTESIAN_POINT('Ctrl Pts',(-13.0140210374673,4.91429990912079,
127.702526499083));
#255448=CARTESIAN_POINT('Ctrl Pts',(-13.2924686612802,0.0466382469415425,
124.993203816266));
#255449=CARTESIAN_POINT('Ctrl Pts',(-13.5709162850931,-4.86388168577195,
127.624050343051));
#255450=CARTESIAN_POINT('Ctrl Pts',(-13.849363908906,-5.30473196309121,
133.177446645321));
#255451=CARTESIAN_POINT('Ctrl Pts',(-14.1278115327188,-0.87079271689315,
136.550092819781));
#255452=CARTESIAN_POINT('Ctrl Pts',(-14.4062591565318,4.36336249554048,
134.642691795028));
#255453=CARTESIAN_POINT('Ctrl Pts',(-14.6847067803446,5.58780073668082,
129.20805193109));
#255454=CARTESIAN_POINT('Ctrl Pts',(-14.9631544041576,1.67732308005318,
125.240341766008));
#255455=CARTESIAN_POINT('Ctrl Pts',(-15.2416020279704,-3.77453254535539,
126.385693108075));
#255456=CARTESIAN_POINT('Ctrl Pts',(-15.5200496517834,-5.75777715774833,
131.591584027456));
#255457=CARTESIAN_POINT('Ctrl Pts',(-15.7984972755962,-2.44990584522241,
136.074055091149));
#255458=CARTESIAN_POINT('Ctrl Pts',(-16.0769448994091,3.1093092545088,135.713934372506));
#255459=CARTESIAN_POINT('Ctrl Pts',(-16.355392523222,5.81122104754806,130.842155219084));
#255460=CARTESIAN_POINT('Ctrl Pts',(-16.6338401470349,3.17290459182133,
125.935644673236));
#255461=CARTESIAN_POINT('Ctrl Pts',(-16.9122877708478,-2.38115617878252,
125.50324623023));
#255462=CARTESIAN_POINT('Ctrl Pts',(-17.1907353946607,-5.74705074703162,
129.94231293535));
#255463=CARTESIAN_POINT('Ctrl Pts',(-17.4691830184736,-3.83168643779603,
135.173559347056));
#255464=CARTESIAN_POINT('Ctrl Pts',(-17.7476306422864,1.6048105194851,136.389725573584));
#255465=CARTESIAN_POINT('Ctrl Pts',(-18.0260782660994,5.56656500871184,
132.473214265779));
#255466=CARTESIAN_POINT('Ctrl Pts',(-18.3045258899123,4.4129181967513,127.023107983299));
#255467=CARTESIAN_POINT('Ctrl Pts',(-18.5829735137251,-0.795984854984928,
125.047788147249));
#255468=CARTESIAN_POINT('Ctrl Pts',(-18.861421137538,-5.27341671101187,
128.362477187221));
#255469=CARTESIAN_POINT('Ctrl Pts',(-19.1398687613509,-4.90483623034722,
133.921137807042));
#255470=CARTESIAN_POINT('Ctrl Pts',(-19.4183163851638,-0.0289508685644962,
136.615632452765));
#255471=CARTESIAN_POINT('Ctrl Pts',(-19.6967640089767,4.87353892710056,
133.969852178351));
#255472=CARTESIAN_POINT('Ctrl Pts',(-19.9752116327896,5.29748453437273,
128.415139802436));
#255473=CARTESIAN_POINT('Ctrl Pts',(-20.2536592566025,0.853300651063172,
125.056004635698));
#255474=CARTESIAN_POINT('Ctrl Pts',(-20.5321068804154,-4.37502484451904,
126.979327793496));
#255475=CARTESIAN_POINT('Ctrl Pts',(-20.8105545042282,-5.58291623983416,
132.417669253371));
#255476=CARTESIAN_POINT('Ctrl Pts',(-21.0890021280412,-1.66038035136256,
136.37345889145));
#255477=CARTESIAN_POINT('Ctrl Pts',(-21.367449751854,3.78796396592178,135.211519281404));
#255478=CARTESIAN_POINT('Ctrl Pts',(-21.6458973756669,5.75535445085128,
129.999616160961));
#255479=CARTESIAN_POINT('Ctrl Pts',(-21.9243449994798,2.43385536014432,
125.527233882186));
#255480=CARTESIAN_POINT('Ctrl Pts',(-22.2027926232928,-3.12423790609075,
125.904273271251));
#255481=CARTESIAN_POINT('Ctrl Pts',(-22.4812402471056,-5.81130916413533,
130.784253549004));
#255482=CARTESIAN_POINT('Ctrl Pts',(-22.7596878709185,-3.15807119857507,
135.682711240481));
#255483=CARTESIAN_POINT('Ctrl Pts',(-23.0381354947314,2.39727991812053,
136.098203030175));
#255484=CARTESIAN_POINT('Ctrl Pts',(-23.3165831185443,5.74964790369824,
131.648912261261));
#255485=CARTESIAN_POINT('Ctrl Pts',(-23.5950307423572,3.81837035169266,
126.423519790431));
#255486=CARTESIAN_POINT('Ctrl Pts',(-23.8734783661701,-1.62180301575654,
125.223906023766));
#255487=CARTESIAN_POINT('Ctrl Pts',(-24.151925989983,-5.57161864120731,
129.15245740844));
#255488=CARTESIAN_POINT('Ctrl Pts',(-24.4303736137958,-4.4013889240913,
134.599027142342));
#255489=CARTESIAN_POINT('Ctrl Pts',(-24.7088212376087,0.813502194462058,
136.558483719739));
#255490=CARTESIAN_POINT('Ctrl Pts',(-24.9872688614217,5.28082453809644,
133.230182270781));
#255491=CARTESIAN_POINT('Ctrl Pts',(-25.2657164852345,4.89532711384086,
127.672669230493));
#255492=CARTESIAN_POINT('Ctrl Pts',(-25.5441641090475,0.0112632219902977,
124.993027583295));
#255493=CARTESIAN_POINT('Ctrl Pts',(-25.8226117328602,-4.88315102063038,
127.65371709519));
#255494=CARTESIAN_POINT('Ctrl Pts',(-26.1010593566733,-5.29018803048126,
133.209694086655));
#255495=CARTESIAN_POINT('Ctrl Pts',(-26.3795069804861,-0.835800680372761,
136.555287127099));
#255496=CARTESIAN_POINT('Ctrl Pts',(-26.6579546042989,4.38664666386508,
134.616059653661));
#255497=CARTESIAN_POINT('Ctrl Pts',(-26.9364022281119,5.57798002361419,
129.174066977901));
#255498=CARTESIAN_POINT('Ctrl Pts',(-27.2148498519247,1.64342224113504,
125.23023451272));
#255499=CARTESIAN_POINT('Ctrl Pts',(-27.4932974757377,-3.80136029530733,
126.408751626694));
#255500=CARTESIAN_POINT('Ctrl Pts',(-27.7717450995505,-5.75287842713667,
131.626618665841));
#255501=CARTESIAN_POINT('Ctrl Pts',(-28.0501927233634,-2.41778232816299,
136.088870728161));
#255502=CARTESIAN_POINT('Ctrl Pts',(-28.3286403471763,3.13913761515943,
135.694916161515));
#255503=CARTESIAN_POINT('Ctrl Pts',(-28.6070879709892,5.8113434455484,130.8067799669));
#255504=CARTESIAN_POINT('Ctrl Pts',(-28.8855355948021,3.14320854938853,
125.916420508438));
#255505=CARTESIAN_POINT('Ctrl Pts',(-29.163983218615,-2.41338144938502,
125.517839221114));
#255506=CARTESIAN_POINT('Ctrl Pts',(-29.4424308424279,-5.75219179641212,
129.977312836202));
#255507=CARTESIAN_POINT('Ctrl Pts',(-29.7208784662408,-3.80501889272807,
135.196802958832));
#255508=CARTESIAN_POINT('Ctrl Pts',(-29.9993260900537,1.6387804878663,136.379853152576));
#255509=CARTESIAN_POINT('Ctrl Pts',(-30.2777737138665,5.576620658989,132.439298084597));
#255510=CARTESIAN_POINT('Ctrl Pts',(-30.5562213376795,4.38981887756547,
126.996315355552));
#255511=CARTESIAN_POINT('Ctrl Pts',(-30.8346689614924,-0.831011997766135,
125.052740188944));
#255512=CARTESIAN_POINT('Ctrl Pts',(-31.1131165853052,-5.2881834443438,
128.394623213959));
#255513=CARTESIAN_POINT('Ctrl Pts',(-31.3915642091181,-4.88577264769286,
133.950937190672));
#255514=CARTESIAN_POINT('Ctrl Pts',(-31.670011832931,0.00642452892459172,
136.615701015511));
#255515=CARTESIAN_POINT('Ctrl Pts',(-31.9484594567439,4.89271787731614,
133.940126914399));
#255516=CARTESIAN_POINT('Ctrl Pts',(-32.2269070805568,5.28284251901049,
128.382936777197));
#255517=CARTESIAN_POINT('Ctrl Pts',(-32.5053547043697,0.818292966938792,
125.050916856162));
#255518=CARTESIAN_POINT('Ctrl Pts',(-32.7838023281826,-4.3982278459157,
127.006030680504));
#255519=CARTESIAN_POINT('Ctrl Pts',(-33.0622499519955,-5.57299213374921,
132.451624158271));
#255520=CARTESIAN_POINT('Ctrl Pts',(-33.3406975758084,-1.62644890646854,
136.383462915428));
#255521=CARTESIAN_POINT('Ctrl Pts',(-33.6191451996212,3.81472140941051,
135.188379215148));
#255522=CARTESIAN_POINT('Ctrl Pts',(-33.8975928234342,5.75034910954236,
129.964596594906));
#255523=CARTESIAN_POINT('Ctrl Pts',(-34.176040447247,2.40168689817613,125.512516086734));
#255524=CARTESIAN_POINT('Ctrl Pts',(-34.4544880710599,-3.15400824368619,
125.923382181419));
#255525=CARTESIAN_POINT('Ctrl Pts',(-34.7329356948729,-5.81132389146964,
130.81962900987));
#255526=CARTESIAN_POINT('Ctrl Pts',(-35.0113833186857,-3.1283167819475,
135.701844931696));
#255527=CARTESIAN_POINT('Ctrl Pts',(-35.2898309424986,2.42946062341331,
136.083512024245));
#255528=CARTESIAN_POINT('Ctrl Pts',(-35.5682785663115,5.75468240160701,
131.613896874941));
#255529=CARTESIAN_POINT('Ctrl Pts',(-35.8467261901244,3.79163218458816,
126.400357453152));
#255530=CARTESIAN_POINT('Ctrl Pts',(-36.1251738139373,-1.65574277853735,
125.233881791944));
#255531=CARTESIAN_POINT('Ctrl Pts',(-36.4036214377501,-5.58157101571846,
129.186404038463));
#255532=CARTESIAN_POINT('Ctrl Pts',(-36.6820690615631,-4.37820816435757,
134.625749339604));
#255533=CARTESIAN_POINT('Ctrl Pts',(-36.960516685376,0.848514102688449,
136.553425090409));
#255534=CARTESIAN_POINT('Ctrl Pts',(-37.2389643091888,5.29549336158222,
133.197991448084));
#255535=CARTESIAN_POINT('Ctrl Pts',(-37.5174119330018,4.87617292041449,
127.64292800788));
#255536=CARTESIAN_POINT('Ctrl Pts',(-37.7958595568146,-0.0241122203237842,
124.993066691407));
#255537=CARTESIAN_POINT('Ctrl Pts',(-38.0743071806275,-4.90223940853195,
127.683500595584));
#255538=CARTESIAN_POINT('Ctrl Pts',(-38.3527548044404,-5.27544806800837,
133.241852397473));
#255539=CARTESIAN_POINT('Ctrl Pts',(-38.6312024282533,-0.800777672950798,
136.560268331721));
#255540=CARTESIAN_POINT('Ctrl Pts',(-38.9096500520661,4.40976828338437,
134.589286268384));
#255541=CARTESIAN_POINT('Ctrl Pts',(-39.1880976758791,5.56795261644649,
129.140142435842));
#255542=CARTESIAN_POINT('Ctrl Pts',(-39.4665452996919,1.6094605046014,125.220333810727));
#255543=CARTESIAN_POINT('Ctrl Pts',(-39.7449929235049,-3.82804718445556,
126.43197302622));
#255544=CARTESIAN_POINT('Ctrl Pts',(-40.0234405473177,-5.74776652149929,
131.661622835152));
#255545=CARTESIAN_POINT('Ctrl Pts',(-40.3018881711306,-2.38556921929025,
136.103490545709));
#255546=CARTESIAN_POINT('Ctrl Pts',(-40.5803357949436,3.16884965391132,
135.675716729192));
#255547=CARTESIAN_POINT('Ctrl Pts',(-40.8587834187564,5.81125050208024,
130.771404625066));
#255548=CARTESIAN_POINT('Ctrl Pts',(-41.1372310425694,3.11339603420704,
125.897377468058));
#255549=CARTESIAN_POINT('Ctrl Pts',(-41.4156786663821,-2.4455172912504,
125.532628105994));
#255550=CARTESIAN_POINT('Ctrl Pts',(-41.6941262901951,-5.75711969621025,
130.012343383614));
#255551=CARTESIAN_POINT('Ctrl Pts',(-41.9725739140079,-3.77821035128576,
135.219883807042));
#255552=CARTESIAN_POINT('Ctrl Pts',(-42.2510215378209,1.67268973063362,
136.369774129642));
#255553=CARTESIAN_POINT('Ctrl Pts',(-42.5294691616338,5.58646966553678,
132.405321320208));
#255554=CARTESIAN_POINT('Ctrl Pts',(-42.8079167854466,4.366556892027,126.969663836325));
#255555=CARTESIAN_POINT('Ctrl Pts',(-43.0863644092596,-0.866008347092154,
125.057905359049));
#255556=CARTESIAN_POINT('Ctrl Pts',(-43.3648120330724,-5.3027542220935,
128.426858534403));
#255557=CARTESIAN_POINT('Ctrl Pts',(-43.6432596568854,-4.86652802093628,
133.98061997675));
#255558=CARTESIAN_POINT('Ctrl Pts',(-43.9217072806982,0.0417996883503892,
136.615554236903));
#255559=CARTESIAN_POINT('Ctrl Pts',(-44.2001549045111,4.9117155260715,133.910285453475));
#255560=CARTESIAN_POINT('Ctrl Pts',(-44.478602528324,5.26800474597596,128.350823478709));
#255561=CARTESIAN_POINT('Ctrl Pts',(-44.7570501521369,0.783254960667603,
125.046042272601));
#255562=CARTESIAN_POINT('Ctrl Pts',(-45.0354977759497,-4.42126786936209,
127.032874316024));
#255563=CARTESIAN_POINT('Ctrl Pts',(-45.3139453997627,-5.56286151839129,
132.485518023215));
#255564=CARTESIAN_POINT('Ctrl Pts',(-45.5923930235756,-1.59245719291215,
136.393260203719));
#255565=CARTESIAN_POINT('Ctrl Pts',(-45.8708406473885,3.84133749699455,
135.165076697471));
#255566=CARTESIAN_POINT('Ctrl Pts',(-46.1492882712014,5.74513068693249,
129.929608146614));
#255567=CARTESIAN_POINT('Ctrl Pts',(-46.4277358950142,2.3694294408167,125.497994382526));
#255568=CARTESIAN_POINT('Ctrl Pts',(-46.7061835188271,-3.18366170834627,
125.942671958037));
#255569=CARTESIAN_POINT('Ctrl Pts',(-46.98463114264,-5.81112327806003,130.85500390496));
#255570=CARTESIAN_POINT('Ctrl Pts',(-47.263078766453,-3.09844644439114,
135.720797144829));
#255571=CARTESIAN_POINT('Ctrl Pts',(-47.5415263902657,2.46155130414924,
136.068625397419));
#255572=CARTESIAN_POINT('Ctrl Pts',(-47.8199740140787,5.75950365764311,
131.578851490957));
#255573=CARTESIAN_POINT('Ctrl Pts',(-48.0984216378915,3.76475351715869,
126.377358307829));
#255574=CARTESIAN_POINT('Ctrl Pts',(-48.3768692617045,-1.6896211871606,
125.244063976264));
#255575=CARTESIAN_POINT('Ctrl Pts',(-48.6553168855173,-5.59131656306301,
129.220410622463));
#255576=CARTESIAN_POINT('Ctrl Pts',(-48.9337645093303,-4.35486516851022,
134.652329933902));
#255577=CARTESIAN_POINT('Ctrl Pts',(-49.2122121331431,0.883494568912716,
136.548153427379));
#255578=CARTESIAN_POINT('Ctrl Pts',(-49.4906597569561,5.3099659586141,133.165711928516));
#255579=CARTESIAN_POINT('Ctrl Pts',(-49.7691073807689,4.85683803860733,
127.613303933314));
#255580=CARTESIAN_POINT('Ctrl Pts',(-50.0475550045819,-0.0594867691506708,
124.993321139153));
#255581=CARTESIAN_POINT('Ctrl Pts',(-50.3260026283946,-4.92114614214944,
127.713399740592));
#255582=CARTESIAN_POINT('Ctrl Pts',(-50.6044502522077,-5.26051262186729,
133.273920386136));
#255583=CARTESIAN_POINT('Ctrl Pts',(-50.8828978760204,-0.765724992417492,
136.565036249065));
#255584=CARTESIAN_POINT('Ctrl Pts',(-51.1613454998334,4.4327264973184,134.562372631296));
#255585=CARTESIAN_POINT('Ctrl Pts',(-51.4397931236463,5.55771888674681,
129.106279562002));
#255586=CARTESIAN_POINT('Ctrl Pts',(-51.7182407474591,1.57543912891688,
125.210640026899));
#255587=CARTESIAN_POINT('Ctrl Pts',(-51.9966883712721,-3.85459222390762,
126.455356446176));
#255588=CARTESIAN_POINT('Ctrl Pts',(-52.2751359950849,-5.7424416302597,
131.696595238295));
#255589=CARTESIAN_POINT('Ctrl Pts',(-52.5535836188979,-2.35326771227282,
136.117914002047));
#255590=CARTESIAN_POINT('Ctrl Pts',(-52.8320312427106,3.19844426977395,
135.656336786975));
#255591=CARTESIAN_POINT('Ctrl Pts',(-53.1104788665238,5.81094222058764,
130.736030504428));
#255592=CARTESIAN_POINT('Ctrl Pts',(-53.3889264903363,3.08346815099054,
125.878516257743));
#255593=CARTESIAN_POINT('Ctrl Pts',(-53.6673741141495,-2.47756251357323,
125.547612336859));
#255594=CARTESIAN_POINT('Ctrl Pts',(-53.9458217379622,-5.76183426382087,
130.047403279515));
#255595=CARTESIAN_POINT('Ctrl Pts',(-54.2242693617753,-3.75126180686946,
135.242801036416));
#255596=CARTESIAN_POINT('Ctrl Pts',(-54.502716985588,1.70653699126786,136.359488878264));
#255597=CARTESIAN_POINT('Ctrl Pts',(-54.7811646094011,5.59611166339667,
132.371285231631));
#255598=CARTESIAN_POINT('Ctrl Pts',(-55.0596122332138,4.3431331021171,126.943154413196));
#255599=CARTESIAN_POINT('Ctrl Pts',(-55.3380598570268,-0.900972606160421,
125.063283466166));
#255600=CARTESIAN_POINT('Ctrl Pts',(-55.6165074808396,-5.31712850433539,
128.459181954061));
#255601=CARTESIAN_POINT('Ctrl Pts',(-55.8949551046525,-4.84710306319425,
134.01018506537));
#255602=CARTESIAN_POINT('Ctrl Pts',(-56.1734027284654,0.0771732988733811,
136.615192122377));
#255603=CARTESIAN_POINT('Ctrl Pts',(-56.4518503522783,4.93053116940174,
133.880328901363));
#255604=CARTESIAN_POINT('Ctrl Pts',(-56.7302979760911,5.25297176508825,
128.318801096944));
#255605=CARTESIAN_POINT('Ctrl Pts',(-57.0087455999042,0.748187930595796,
125.041381065643));
#255606=CARTESIAN_POINT('Ctrl Pts',(-57.2871932237169,-4.44414406110167,
127.059857705357));
#255607=CARTESIAN_POINT('Ctrl Pts',(-57.5656408475299,-5.55252476915405,
132.519349592253));
#255608=CARTESIAN_POINT('Ctrl Pts',(-57.8440884713427,-1.55840647026886,
136.402850393281));
#255609=CARTESIAN_POINT('Ctrl Pts',(-58.1225360951557,3.867811242405,135.141612591857));
#255610=CARTESIAN_POINT('Ctrl Pts',(-58.4009837189685,5.73969937639226,
129.894652112598));
#255611=CARTESIAN_POINT('Ctrl Pts',(-58.6794313427815,2.33708418337799,
125.483669307672));
#255612=CARTESIAN_POINT('Ctrl Pts',(-58.9578789665944,-3.21319720125095,
125.962141886319));
#255613=CARTESIAN_POINT('Ctrl Pts',(-59.2363265904072,-5.81070733134035,
130.890376923444));
#255614=CARTESIAN_POINT('Ctrl Pts',(-59.5147742142201,-3.06846129276222,
135.739567177598));
#255615=CARTESIAN_POINT('Ctrl Pts',(-59.793221838033,2.49355077119662,136.053543701326));
#255616=CARTESIAN_POINT('Ctrl Pts',(-60.071669461846,5.76411149315304,131.543777407928));
#255617=CARTESIAN_POINT('Ctrl Pts',(-60.3501170856587,3.73773534540316,
126.354523206705));
#255618=CARTESIAN_POINT('Ctrl Pts',(-60.6285647094717,-1.72343698624942,
125.254452199421));
#255619=CARTESIAN_POINT('Ctrl Pts',(-60.9070123332846,-5.6008549221161,
129.254475900312));
#255620=CARTESIAN_POINT('Ctrl Pts',(-61.1854599570975,-4.33136080153256,
134.678767940282));
#255621=CARTESIAN_POINT('Ctrl Pts',(-61.4639075809103,0.918442296920838,
136.542668925995));
#255622=CARTESIAN_POINT('Ctrl Pts',(-61.7423552047232,5.32424179290464,
133.133344908207));
#255623=CARTESIAN_POINT('Ctrl Pts',(-62.0208028285362,4.83732318488056,
127.583798104527));
#255624=CARTESIAN_POINT('Ctrl Pts',(-62.299250452349,-0.0948591136734494,
124.993790917104));
#255625=CARTESIAN_POINT('Ctrl Pts',(-62.5776980761619,-4.93987052088691,
127.743413422294));
#255626=CARTESIAN_POINT('Ctrl Pts',(-62.8561456999749,-5.24538224549645,
133.305896864355));
#255627=CARTESIAN_POINT('Ctrl Pts',(-63.1345933237877,-0.730643937663188,
136.569590702456));
#255628=CARTESIAN_POINT('Ctrl Pts',(-63.4130409476006,4.45552045494177,
134.53531973969));
#255629=CARTESIAN_POINT('Ctrl Pts',(-63.6914885714135,5.5472792137301,129.072479611178));
#255630=CARTESIAN_POINT('Ctrl Pts',(-63.9699361952264,1.54135937475606,
125.201153520444));
#255631=CARTESIAN_POINT('Ctrl Pts',(-64.2483838190392,-3.88099443002729,
126.478901020081));
#255632=CARTESIAN_POINT('Ctrl Pts',(-64.5268314428522,-5.73690395073373,
131.731534579357));
#255633=CARTESIAN_POINT('Ctrl Pts',(-64.805279066665,-2.32087900405488,
136.132140562712));
#255634=CARTESIAN_POINT('Ctrl Pts',(-65.083726690478,3.22792036610792,135.636777052998));
#255635=CARTESIAN_POINT('Ctrl Pts',(-65.3621743142908,5.81041861249411,
130.700658915789));
#255636=CARTESIAN_POINT('Ctrl Pts',(-65.6406219381037,3.05342600872776,
125.859837576403));
#255637=CARTESIAN_POINT('Ctrl Pts',(-65.9190695619166,-2.50951592890599,
125.562791358466));
#255638=CARTESIAN_POINT('Ctrl Pts',(-66.1975171857295,-5.76633532454392,
130.082491224748));
#255639=CARTESIAN_POINT('Ctrl Pts',(-66.4759648095424,-3.72417425806736,
135.26555379775));
#255640=CARTESIAN_POINT('Ctrl Pts',(-66.7544124333553,1.74032101554631,
136.348997779564));
#255641=CARTESIAN_POINT('Ctrl Pts',(-67.0328600571681,5.60554629528092,
132.337191080086));
#255642=CARTESIAN_POINT('Ctrl Pts',(-67.3113076809811,4.31954837581292,
126.916788068483));
#255643=CARTESIAN_POINT('Ctrl Pts',(-67.5897553047939,-0.935903479357421,
125.068874311009));
#255644=CARTESIAN_POINT('Ctrl Pts',(-67.8682029286069,-5.33130575842519,
128.491592275178));
#255645=CARTESIAN_POINT('Ctrl Pts',(-68.1466505524197,-4.82749849426569,
134.039631360986));
#255646=CARTESIAN_POINT('Ctrl Pts',(-68.4250981762326,0.112544049711387,
136.614614685353));
#255647=CARTESIAN_POINT('Ctrl Pts',(-68.7035458000455,4.94916411008632,
133.850258368115));
#255648=CARTESIAN_POINT('Ctrl Pts',(-68.9819934238584,5.23774413340002,
128.286870818499));
#255649=CARTESIAN_POINT('Ctrl Pts',(-69.2604410476712,0.713093176145084,
125.036933408012));
#255650=CARTESIAN_POINT('Ctrl Pts',(-69.5388886714842,-4.46685557344872,
127.086979848621));
#255651=CARTESIAN_POINT('Ctrl Pts',(-69.8173362952971,-5.54198226906957,
132.553117611744));
#255652=CARTESIAN_POINT('Ctrl Pts',(-70.09578391911,-1.52429800030071,136.412233128746));
#255653=CARTESIAN_POINT('Ctrl Pts',(-70.3742315429229,3.89414166464747,
135.117987767775));
#255654=CARTESIAN_POINT('Ctrl Pts',(-70.6526791667357,5.73405537918087,
129.859729788164));
#255655=CARTESIAN_POINT('Ctrl Pts',(-70.9311267905487,2.3046523244254,125.469541392991));
#255656=CARTESIAN_POINT('Ctrl Pts',(-71.2095744143614,-3.24261362795168,
125.981791244794));
#255657=CARTESIAN_POINT('Ctrl Pts',(-71.4880220381746,-5.81007606672361,
130.925746754563));
#255658=CARTESIAN_POINT('Ctrl Pts',(-71.7664696619872,-3.03836243817177,
135.758154334473));
#255659=CARTESIAN_POINT('Ctrl Pts',(-72.0449172858002,2.52545783880292,
136.038267494822));
#255660=CARTESIAN_POINT('Ctrl Pts',(-72.3233649096131,5.76850573739207,
131.508675925537));
#255661=CARTESIAN_POINT('Ctrl Pts',(-72.601812533426,3.71057867048956,126.331852995942));
#255662=CARTESIAN_POINT('Ctrl Pts',(-72.8802601572389,-1.75718892274731,
125.265046076474));
#255663=CARTESIAN_POINT('Ctrl Pts',(-73.1587077810518,-5.61018573943046,
129.28859860971));
#255664=CARTESIAN_POINT('Ctrl Pts',(-73.4371554048648,-4.30769593438731,
134.705062379074));
#255665=CARTESIAN_POINT('Ctrl Pts',(-73.7156030286775,0.953355991712339,
136.536971789486));
#255666=CARTESIAN_POINT('Ctrl Pts',(-73.9940506524905,5.33832033545752,
133.100891586529));
#255667=CARTESIAN_POINT('Ctrl Pts',(-74.2724982763033,4.81762908236426,
127.554411614868));
#255668=CARTESIAN_POINT('Ctrl Pts',(-74.5509459001162,-0.130227943157576,
124.994476007852));
#255669=CARTESIAN_POINT('Ctrl Pts',(-74.8293935239292,-4.95841185090586,
127.77354052852));
#255670=CARTESIAN_POINT('Ctrl Pts',(-75.107841147742,-5.23005749955717,
133.337780647228));
#255671=CARTESIAN_POINT('Ctrl Pts',(-75.3862887715549,-0.695535808628632,
136.573931523126));
#255672=CARTESIAN_POINT('Ctrl Pts',(-75.6647363953679,4.4781493116164,134.508128596022));
#255673=CARTESIAN_POINT('Ctrl Pts',(-75.9431840191806,5.53663398424198,
129.038743835842));
#255674=CARTESIAN_POINT('Ctrl Pts',(-76.2216316429937,1.50722250495638,
125.191874642891));
#255675=CARTESIAN_POINT('Ctrl Pts',(-76.5000792668064,-3.90725282447187,
126.502605875483));
#255676=CARTESIAN_POINT('Ctrl Pts',(-76.7785268906195,-5.73115368812196,
131.766439563647));
#255677=CARTESIAN_POINT('Ctrl Pts',(-77.0569745144322,-2.28840429481114,
136.146169700531));
#255678=CARTESIAN_POINT('Ctrl Pts',(-77.3354221382452,3.25727685066645,
135.617038252052));
#255679=CARTESIAN_POINT('Ctrl Pts',(-77.613869762058,5.80967969720196,130.665291169852));
#255680=CARTESIAN_POINT('Ctrl Pts',(-77.8923173858709,3.0232707206408,125.841342116181));
#255681=CARTESIAN_POINT('Ctrl Pts',(-78.1707650096839,-2.54137635320382,
125.57816460835));
#255682=CARTESIAN_POINT('Ctrl Pts',(-78.4492126334967,-5.77062271159095,
130.117605919119));
#255683=CARTESIAN_POINT('Ctrl Pts',(-78.7276602573096,-3.69694870861804,
135.288141247929));
#255684=CARTESIAN_POINT('Ctrl Pts',(-79.0061078811224,1.77404055158998,
136.338301222296));
#255685=CARTESIAN_POINT('Ctrl Pts',(-79.2845555049354,5.61477321158579,
132.303040128944));
#255686=CARTESIAN_POINT('Ctrl Pts',(-79.5630031287483,4.29580358705489,
126.8905657792));
#255687=CARTESIAN_POINT('Ctrl Pts',(-79.8414507525611,-0.970799672307275,
125.074677686406));
#255688=CARTESIAN_POINT('Ctrl Pts',(-80.1198983763742,-5.34528545901998,
128.524088296775));
#255689=CARTESIAN_POINT('Ctrl Pts',(-80.3983460001869,-4.80771504060458,
134.068957772455));
#255690=CARTESIAN_POINT('Ctrl Pts',(-80.6767936239998,0.147910630189091,
136.613821947228));
#255691=CARTESIAN_POINT('Ctrl Pts',(-80.9552412478128,4.96761365767528,
133.820074968005));
#255692=CARTESIAN_POINT('Ctrl Pts',(-81.2336888716256,5.22232241517632,
128.255033826564));
#255693=CARTESIAN_POINT('Ctrl Pts',(-81.5121364954386,0.6779719977639,125.032699464516));
#255694=CARTESIAN_POINT('Ctrl Pts',(-81.7905841192513,-4.48940156482041,
127.114239740797));
#255695=CARTESIAN_POINT('Ctrl Pts',(-82.0690317430644,-5.53123440879372,
132.586820830401));
#255696=CARTESIAN_POINT('Ctrl Pts',(-82.3474793668772,-1.490133046909,136.421408062431));
#255697=CARTESIAN_POINT('Ctrl Pts',(-82.62592699069,3.92032778803891,135.094203100652));
#255698=CARTESIAN_POINT('Ctrl Pts',(-82.9043746145031,5.72819890443852,
129.824842467372));
#255699=CARTESIAN_POINT('Ctrl Pts',(-83.1828222383158,2.27213506573304,
125.455611161998));
#255700=CARTESIAN_POINT('Ctrl Pts',(-83.4612698621288,-3.27190989841242,
126.001619305352));
#255701=CARTESIAN_POINT('Ctrl Pts',(-83.7397174859417,-5.80922950760163,
130.961112087674));
#255702=CARTESIAN_POINT('Ctrl Pts',(-84.0181651097544,-3.00815099594316,
135.776557926701));
#255703=CARTESIAN_POINT('Ctrl Pts',(-84.2966127335676,2.55727132464077,
136.022797343974));
#255704=CARTESIAN_POINT('Ctrl Pts',(-84.5750603573801,5.77268622752965,
131.473548344486));
#255705=CARTESIAN_POINT('Ctrl Pts',(-84.8535079811934,3.68328449871872,
126.309348515594));
#255706=CARTESIAN_POINT('Ctrl Pts',(-85.131955605006,-1.79087574596318,
125.275845214866));
#255707=CARTESIAN_POINT('Ctrl Pts',(-85.4104032288191,-5.61930866924928,
129.322777486226));
#255708=CARTESIAN_POINT('Ctrl Pts',(-85.6888508526319,-4.28387144398495,
134.731212275928));
#255709=CARTESIAN_POINT('Ctrl Pts',(-85.9672984764448,0.98823435954663,
136.531062228962));
#255710=CARTESIAN_POINT('Ctrl Pts',(-86.2457461002577,5.35220106458756,
133.068353166051));
#255711=CARTESIAN_POINT('Ctrl Pts',(-86.5241937240705,4.79775646083024,
127.525145553266));
#255712=CARTESIAN_POINT('Ctrl Pts',(-86.8026413478836,-0.165591946996939,
124.995376386011));
#255713=CARTESIAN_POINT('Ctrl Pts',(-87.0810889716963,-4.97676944515001,
127.803779942897));
#255714=CARTESIAN_POINT('Ctrl Pts',(-87.3595365955093,-5.21453895191432,
133.36957055329));
#255715=CARTESIAN_POINT('Ctrl Pts',(-87.6379842193221,-0.660401906259044,
136.578058550223));
#255716=CARTESIAN_POINT('Ctrl Pts',(-87.916431843135,4.50061222882128,134.480800207869));
#255717=CARTESIAN_POINT('Ctrl Pts',(-88.1948794669479,5.52578359274576,
129.005073486085));
#255718=CARTESIAN_POINT('Ctrl Pts',(-88.4733270907608,1.47302978447255,
125.182803738068));
#255719=CARTESIAN_POINT('Ctrl Pts',(-88.7517747145737,-3.93336643422502,
126.526470133988));
#255720=CARTESIAN_POINT('Ctrl Pts',(-89.0302223383866,-5.7251910555031,
131.801308897747));
#255721=CARTESIAN_POINT('Ctrl Pts',(-89.3086699621995,-2.25584478790559,
136.16000089565));
#255722=CARTESIAN_POINT('Ctrl Pts',(-89.5871175860123,3.28651263563227,
135.597121115567));
#255723=CARTESIAN_POINT('Ctrl Pts',(-89.8655652098253,5.80872550209253,
130.629928577187));
#255724=CARTESIAN_POINT('Ctrl Pts',(-90.1440128336381,2.99300340414587,
125.823030562435));
#255725=CARTESIAN_POINT('Ctrl Pts',(-90.4224604574511,-2.57314260586573,
125.593731516848));
#255726=CARTESIAN_POINT('Ctrl Pts',(-90.7009080812639,-5.77469626609129,
130.152746061436));
#255727=CARTESIAN_POINT('Ctrl Pts',(-90.9793557050769,-3.66958616737523,
135.310562549967));
#255728=CARTESIAN_POINT('Ctrl Pts',(-91.2578033288896,1.80769434990835,
136.327399602824));
#255729=CARTESIAN_POINT('Ctrl Pts',(-91.5362509527026,5.62379207040447,
132.268833643682));
#255730=CARTESIAN_POINT('Ctrl Pts',(-91.8146985765155,4.27189961571542,
126.864488517025));
#255731=CARTESIAN_POINT('Ctrl Pts',(-92.0931462003284,-1.00565989191805,
125.080693377311));
#255732=CARTESIAN_POINT('Ctrl Pts',(-92.3715938241412,-5.3590670880956,
128.556668814702));
#255733=CARTESIAN_POINT('Ctrl Pts',(-92.6500414479542,-4.78775343529548,
134.098163213075));
#255734=CARTESIAN_POINT('Ctrl Pts',(-92.928489071767,0.183271729783054,
136.612813937377));
#255735=CARTESIAN_POINT('Ctrl Pts',(-93.2069366955801,4.98587912851244,
133.789779819492));
#255736=CARTESIAN_POINT('Ctrl Pts',(-93.4853843193926,5.2067071818758,128.223291300872));
#255737=CARTESIAN_POINT('Ctrl Pts',(-93.7638319432059,0.642825696881324,
125.028679392048));
#255738=CARTESIAN_POINT('Ctrl Pts',(-94.0422795670186,-4.51178119976554,
127.14163637176));
#255739=CARTESIAN_POINT('Ctrl Pts',(-94.3207271908314,-5.52028158659305,
132.62045799934));
#255740=CARTESIAN_POINT('Ctrl Pts',(-94.5991748146444,-1.45591287608963,
136.430374854359));
#255741=CARTESIAN_POINT('Ctrl Pts',(-94.8776224384574,3.94636864224209,
135.07025947184));
#255742=CARTESIAN_POINT('Ctrl Pts',(-95.1560700622702,5.7221301691794,129.789991442987));
#255743=CARTESIAN_POINT('Ctrl Pts',(-95.4345176860831,2.23953361224044,
125.441879130882));
#255744=CARTESIAN_POINT('Ctrl Pts',(-95.7129653098959,-3.30108492704829,
126.021625333256));
#255745=CARTESIAN_POINT('Ctrl Pts',(-95.9914129337089,-5.80816768534362,
130.996471612301));
#255746=CARTESIAN_POINT('Ctrl Pts',(-96.2698605575217,-2.97782808557417,
135.794777272329));
#255747=CARTESIAN_POINT('Ctrl Pts',(-96.5483081813347,2.58899004984866,
136.007133822036));
#255748=CARTESIAN_POINT('Ctrl Pts',(-96.8267558051475,5.77665280865574,
131.438395966436));
#255749=CARTESIAN_POINT('Ctrl Pts',(-97.1052034289604,3.65585384148698,
126.287010599573));
#255750=CARTESIAN_POINT('Ctrl Pts',(-97.3836510527732,-1.82449620761995,
125.286849214428));
#255751=CARTESIAN_POINT('Ctrl Pts',(-97.6620986765863,-5.62822337351841,
129.35701126335));
#255752=CARTESIAN_POINT('Ctrl Pts',(-97.9405463003989,-4.25988821315111,
134.757216661848));
#255753=CARTESIAN_POINT('Ctrl Pts',(-98.2189939242121,1.02307610799351,
136.524940463405));
#255754=CARTESIAN_POINT('Ctrl Pts',(-98.4974415480248,5.36588346593846,
133.035730852497));
#255755=CARTESIAN_POINT('Ctrl Pts',(-98.7758891718378,4.77770605666655,
127.496001004183));
#255756=CARTESIAN_POINT('Ctrl Pts',(-99.0543367956506,-0.200949814765295,
124.996492018215));
#255757=CARTESIAN_POINT('Ctrl Pts',(-99.3327844194636,-4.99494262337204,
127.834130544897));
#255758=CARTESIAN_POINT('Ctrl Pts',(-99.6112320432764,-5.19882717761281,
133.401265404553));
#255759=CARTESIAN_POINT('Ctrl Pts',(-99.8896796670892,-0.625243532454567,
136.581971630822));
#255760=CARTESIAN_POINT('Ctrl Pts',(-100.168127290903,4.5229083741848,134.453335587896));
#255761=CARTESIAN_POINT('Ctrl Pts',(-100.446574914715,5.51472844130613,
128.971469809575));
#255762=CARTESIAN_POINT('Ctrl Pts',(-100.725022538528,1.43878248032906,
125.173941142103));
#255763=CARTESIAN_POINT('Ctrl Pts',(-101.003470162341,-3.95933429163924,
126.550492911299));
#255764=CARTESIAN_POINT('Ctrl Pts',(-101.281917786154,-5.71901627382367,
131.836141289563));
#255765=CARTESIAN_POINT('Ctrl Pts',(-101.560365409967,-2.22320168984167,
136.17363363555));
#255766=CARTESIAN_POINT('Ctrl Pts',(-101.83881303378,3.31562663766449,135.577026381578));
#255767=CARTESIAN_POINT('Ctrl Pts',(-102.117260657593,5.80755606252295,
130.594572448163));
#255768=CARTESIAN_POINT('Ctrl Pts',(-102.395708281405,2.96262518080941,
125.804903593708));
#255769=CARTESIAN_POINT('Ctrl Pts',(-102.674155905219,-2.60481350978186,
125.609491507123));
#255770=CARTESIAN_POINT('Ctrl Pts',(-102.952603529031,-5.77855583709781,
130.187910349571));
#255771=CARTESIAN_POINT('Ctrl Pts',(-103.231051152844,-3.64208764826766,
135.332816873036));
#255772=CARTESIAN_POINT('Ctrl Pts',(-103.509498776657,1.84128116344741,
136.316293325111));
#255773=CARTESIAN_POINT('Ctrl Pts',(-103.78794640047,5.63260253753978,132.234572891835));
#255774=CARTESIAN_POINT('Ctrl Pts',(-104.066394024283,4.24783734756473,
126.838557248259));
#255775=CARTESIAN_POINT('Ctrl Pts',(-104.344841648096,-1.04048284643121,
125.086921160811));
#255776=CARTESIAN_POINT('Ctrl Pts',(-104.623289271909,-5.3726501349701,
128.589332621676));
#255777=CARTESIAN_POINT('Ctrl Pts',(-104.901736895722,-4.76761441802147,
134.12724660063));
#255778=CARTESIAN_POINT('Ctrl Pts',(-105.180184519534,0.218626038175886,
136.611590693152));
#255779=CARTESIAN_POINT('Ctrl Pts',(-105.458632143348,5.00395984576562,
133.759374045173));
#255780=CARTESIAN_POINT('Ctrl Pts',(-105.73707976716,5.1908990121252,128.191644417652));
#255781=CARTESIAN_POINT('Ctrl Pts',(-106.015527390973,0.607655575856702,
125.024873339572));
#255782=CARTESIAN_POINT('Ctrl Pts',(-106.293975014786,-4.53399364899913,
127.169168726316));
#255783=CARTESIAN_POINT('Ctrl Pts',(-106.572422638599,-5.50912420832816,
132.654027872123));
#255784=CARTESIAN_POINT('Ctrl Pts',(-106.850870262412,-1.42163875588365,
136.43913317226));
#255785=CARTESIAN_POINT('Ctrl Pts',(-107.129317886225,3.97226326230387,
135.046157768576));
#255786=CARTESIAN_POINT('Ctrl Pts',(-107.407765510038,5.71584939828273,
129.755178006424));
#255787=CARTESIAN_POINT('Ctrl Pts',(-107.686213133851,2.20684917200607,
125.428345808491));
#255788=CARTESIAN_POINT('Ctrl Pts',(-107.964660757664,-3.3301376327682,
126.041808587174));
#255789=CARTESIAN_POINT('Ctrl Pts',(-108.243108381476,-5.80689063929651,
131.031824018185));
#255790=CARTESIAN_POINT('Ctrl Pts',(-108.521556005289,-2.94739483068967,
135.812811696231));
#255791=CARTESIAN_POINT('Ctrl Pts',(-108.800003629102,2.62061283907833,
135.991277509423));
#255792=CARTESIAN_POINT('Ctrl Pts',(-109.078451252915,5.7804053337882,131.403220093974));
#255793=CARTESIAN_POINT('Ctrl Pts',(-109.356898876728,3.62828771524594,
126.264840075618));
#255794=CARTESIAN_POINT('Ctrl Pts',(-109.635346500541,-1.85804906189805,
125.298057667405));
#255795=CARTESIAN_POINT('Ctrl Pts',(-109.913794124354,-5.636929521901,129.391298672536));
#255796=CARTESIAN_POINT('Ctrl Pts',(-110.192241748167,-4.2357471305931,
134.783074573235));
#255797=CARTESIAN_POINT('Ctrl Pts',(-110.470689371979,1.05787994597834,
136.518606719657));
#255798=CARTESIAN_POINT('Ctrl Pts',(-110.749136995792,5.37936703250445,
133.003025854698));
#255799=CARTESIAN_POINT('Ctrl Pts',(-111.027584619605,4.75747861284798,
127.466979047582));
#255800=CARTESIAN_POINT('Ctrl Pts',(-111.306032243418,-0.23630023626489,
124.997822863128));
#255801=CARTESIAN_POINT('Ctrl Pts',(-111.584479867231,-5.01293071215839,
127.864591209862));
#255802=CARTESIAN_POINT('Ctrl Pts',(-111.862927491044,-5.18292275885852,
133.432864026556));
#255803=CARTESIAN_POINT('Ctrl Pts',(-112.141375114857,-0.590061990020461,
136.585670619917));
#255804=CARTESIAN_POINT('Ctrl Pts',(-112.41982273867,4.54503692151536,134.425735753813));
#255805=CARTESIAN_POINT('Ctrl Pts',(-112.698270362483,5.50346893957634,
128.937934051507));
#255806=CARTESIAN_POINT('Ctrl Pts',(-112.976717986295,1.40448186157095,
125.165287183403));
#255807=CARTESIAN_POINT('Ctrl Pts',(-113.255165610108,-3.98515543446448,
126.574673317241));
#255808=CARTESIAN_POINT('Ctrl Pts',(-113.533613233921,-5.71262957189362,
131.870935448366));
#255809=CARTESIAN_POINT('Ctrl Pts',(-113.812060857734,-2.19047621022174,
136.187067415062));
#255810=CARTESIAN_POINT('Ctrl Pts',(-114.090508481547,3.34461777793161,
135.556754794705));
#255811=CARTESIAN_POINT('Ctrl Pts',(-114.36895610536,5.80617142182825,130.559224092919));
#255812=CARTESIAN_POINT('Ctrl Pts',(-114.647403729173,2.9321371763071,125.786961881698));
#255813=CARTESIAN_POINT('Ctrl Pts',(-114.925851352986,-2.63638789137572,
125.625443995184));
#255814=CARTESIAN_POINT('Ctrl Pts',(-115.204298976799,-5.78220128159277,
130.223097480497));
#255815=CARTESIAN_POINT('Ctrl Pts',(-115.482746600612,-3.61445417026275,
135.354903392492));
#255816=CARTESIAN_POINT('Ctrl Pts',(-115.761194224424,1.87479974763623,
136.304982800703));
#255817=CARTESIAN_POINT('Ctrl Pts',(-116.039641848237,5.64120428651674,
132.200259142944));
#255818=CARTESIAN_POINT('Ctrl Pts',(-116.31808947205,4.22361767423897,126.812772933795));
#255819=CARTESIAN_POINT('Ctrl Pts',(-116.596537095863,-1.07526724547036,
125.093360806132));
#255820=CARTESIAN_POINT('Ctrl Pts',(-116.874984719676,-5.38603409631742,
128.622078507325));
#255821=CARTESIAN_POINT('Ctrl Pts',(-117.153432343489,-4.7472987350426,
134.156206857421));
#255822=CARTESIAN_POINT('Ctrl Pts',(-117.431879967302,0.253972245300257,
136.610152259881));
#255823=CARTESIAN_POINT('Ctrl Pts',(-117.710327591115,5.02185513944583,
133.728858771743));
#255824=CARTESIAN_POINT('Ctrl Pts',(-117.988775214928,5.17489849170343,
128.160094349593));
#255825=CARTESIAN_POINT('Ctrl Pts',(-118.26722283874,0.572462937930709,
125.021281448121));
#255826=CARTESIAN_POINT('Ctrl Pts',(-118.545670462553,-4.55603808943068,
127.196835784245));
#255827=CARTESIAN_POINT('Ctrl Pts',(-118.824118086366,-5.49776268743969,
132.687529204804));
#255828=CARTESIAN_POINT('Ctrl Pts',(-119.102565710179,-1.38731195633035,
136.447682691592));
#255829=CARTESIAN_POINT('Ctrl Pts',(-119.381013333992,3.99801068868978,
135.021898883958));
#255830=CARTESIAN_POINT('Ctrl Pts',(-119.659460957805,5.70935682448427,
129.720403447709));
#255831=CARTESIAN_POINT('Ctrl Pts',(-119.937908581618,2.17408295616475,
125.415011696306));
#255832=CARTESIAN_POINT('Ctrl Pts',(-120.216356205431,-3.3590669390133,
126.062168319208));
#255833=CARTESIAN_POINT('Ctrl Pts',(-120.494803829244,-5.80539841678086,
131.067167995328));
#255834=CARTESIAN_POINT('Ctrl Pts',(-120.773251453056,-2.91685235900652,
135.830660530138));
#255835=CARTESIAN_POINT('Ctrl Pts',(-121.051699076869,2.65213852053535,
135.975228993696));
#255836=CARTESIAN_POINT('Ctrl Pts',(-121.330146700682,5.78394366387473,
131.368022030553));
#255837=CARTESIAN_POINT('Ctrl Pts',(-121.608594324495,3.60058714147007,
126.242837765265));
#255838=CARTESIAN_POINT('Ctrl Pts',(-121.887041948308,-1.89153306548558,
125.309470158462));
#255839=CARTESIAN_POINT('Ctrl Pts',(-122.165489572121,-5.64542679178685,
129.425638443252));
#255840=CARTESIAN_POINT('Ctrl Pts',(-122.443937195934,-4.21144909086733,
134.808785051914));
#255841=CARTESIAN_POINT('Ctrl Pts',(-122.722384819747,1.09264458383337,
136.512061232418));
#255842=CARTESIAN_POINT('Ctrl Pts',(-123.00083244356,5.39265126464657,132.97023938455));
#255843=CARTESIAN_POINT('Ctrl Pts',(-123.279280067372,4.73707487890982,
127.438080758883));
#255844=CARTESIAN_POINT('Ctrl Pts',(-123.557727691185,-0.27164190157181,
124.999368871432));
#255845=CARTESIAN_POINT('Ctrl Pts',(-123.836175314998,-5.03073304495359,
127.895160809065));
#255846=CARTESIAN_POINT('Ctrl Pts',(-124.114622938811,-5.16682628499523,
133.464365248398));
#255847=CARTESIAN_POINT('Ctrl Pts',(-124.393070562624,-0.554858582622917,
136.589155380447));
#255848=CARTESIAN_POINT('Ctrl Pts',(-124.671518186437,4.56699705083122,
134.398001728342));
#255849=CARTESIAN_POINT('Ctrl Pts',(-124.94996581025,5.49200550478084,128.904467454562));
#255850=CARTESIAN_POINT('Ctrl Pts',(-125.228413434063,1.37012919922165,
125.156842182641));
#255851=CARTESIAN_POINT('Ctrl Pts',(-125.506861057876,-4.0108289058903,
126.599010455801));
#255852=CARTESIAN_POINT('Ctrl Pts',(-125.785308681688,-5.70603118637341,
131.905690084846));
#255853=CARTESIAN_POINT('Ctrl Pts',(-126.063756305501,-2.1576695617001,
136.200301736396));
#255854=CARTESIAN_POINT('Ctrl Pts',(-126.342203929314,3.37348498215772,
135.536307106118));
#255855=CARTESIAN_POINT('Ctrl Pts',(-126.620651553127,5.8045716313158,130.523884821299));
#255856=CARTESIAN_POINT('Ctrl Pts',(-126.89909917694,2.90154052038371,125.769206091244));
#255857=CARTESIAN_POINT('Ctrl Pts',(-127.177546800753,-2.66786458064647,
125.641588389905));
#255858=CARTESIAN_POINT('Ctrl Pts',(-127.455994424566,-5.7856324644928,
130.258306150342));
#255859=CARTESIAN_POINT('Ctrl Pts',(-127.734442048379,-3.5866867573295,
135.376821289913));
#255860=CARTESIAN_POINT('Ctrl Pts',(-128.012889672192,1.90824886043053,
136.293468448719));
#255861=CARTESIAN_POINT('Ctrl Pts',(-128.291337296005,5.64959699859458,
132.16589366852));
#255862=CARTESIAN_POINT('Ctrl Pts',(-128.569784919818,4.19924149320669,
126.787136529081));
#255863=CARTESIAN_POINT('Ctrl Pts',(-128.84823254363,-1.11001180008614,
125.100012074652));
#255864=CARTESIAN_POINT('Ctrl Pts',(-129.126680167443,-5.39921847619124,
128.654905258242));
#255865=CARTESIAN_POINT('Ctrl Pts',(-129.405127791256,-4.72680713916258,
134.185042910317));
#255866=CARTESIAN_POINT('Ctrl Pts',(-129.683575415069,0.289309041389885,
136.608498690867));
#255867=CARTESIAN_POINT('Ctrl Pts',(-129.962023038882,5.03956434643776,
133.69823512996));
#255868=CARTESIAN_POINT('Ctrl Pts',(-130.240470662695,5.15870621351431,
128.128642265792));
#255869=CARTESIAN_POINT('Ctrl Pts',(-130.518918286508,0.537249087180579,
125.017903850796));
#255870=CARTESIAN_POINT('Ctrl Pts',(-130.79736591032,-4.57791370419536,
127.224636520332));
#255871=CARTESIAN_POINT('Ctrl Pts',(-131.075813534134,-5.4861974449331,
132.720960755981));
#255872=CARTESIAN_POINT('Ctrl Pts',(-131.354261157946,-1.35293374942274,
136.456023095549));
#255873=CARTESIAN_POINT('Ctrl Pts',(-131.632708781759,4.02360996731925,
134.99748371691));
#255874=CARTESIAN_POINT('Ctrl Pts',(-131.911156405572,5.7026526883694,129.685669055425));
#255875=CARTESIAN_POINT('Ctrl Pts',(-132.189604029385,2.1412361788793,125.401877288427));
#255876=CARTESIAN_POINT('Ctrl Pts',(-132.468051653198,-3.38787177379785,
126.082703774923));
#255877=CARTESIAN_POINT('Ctrl Pts',(-132.746499277011,-5.80369107309236,
131.102502234048));
#255878=CARTESIAN_POINT('Ctrl Pts',(-133.024946900823,-2.88620180228584,
135.848323112653));
#255879=CARTESIAN_POINT('Ctrl Pts',(-133.303394524637,2.68356592602436,
135.95898886954));
#255880=CARTESIAN_POINT('Ctrl Pts',(-133.581842148449,5.78726766780228,
131.332803080451));
#255881=CARTESIAN_POINT('Ctrl Pts',(-133.860289772262,3.57275314661281,
126.221004483821));
#255882=CARTESIAN_POINT('Ctrl Pts',(-134.138737396075,-1.92494697761906,
125.321086264707));
#255883=CARTESIAN_POINT('Ctrl Pts',(-134.417185019888,-5.65371486830715,
129.460029303025));
#255884=CARTESIAN_POINT('Ctrl Pts',(-134.695632643701,-4.1869949943469,
134.834347145171));
#255885=CARTESIAN_POINT('Ctrl Pts',(-134.974080267514,1.1273687333409,136.505304244234));
#255886=CARTESIAN_POINT('Ctrl Pts',(-135.252527891327,5.40573567011315,
132.937372656969));
#255887=CARTESIAN_POINT('Ctrl Pts',(-135.53097551514,4.71649561092,127.409307208922));
#255888=CARTESIAN_POINT('Ctrl Pts',(-135.809423138953,-0.306973501088704,
125.001129985841));
#255889=CARTESIAN_POINT('Ctrl Pts',(-136.087870762765,-5.04834896208586,
127.925838209736));
#255890=CARTESIAN_POINT('Ctrl Pts',(-136.366318386578,-5.15053835248403,
133.49576790279));
#255891=CARTESIAN_POINT('Ctrl Pts',(-136.644766010391,-0.519634614735935,
136.592425783278));
#255892=CARTESIAN_POINT('Ctrl Pts',(-136.923213634204,4.58878794839197,
134.37013453918));
#255893=CARTESIAN_POINT('Ctrl Pts',(-137.201661258017,5.48033856170195,
128.871071258858));
#255894=CARTESIAN_POINT('Ctrl Pts',(-137.48010888183,1.33572576623031,125.148606452753));
#255895=CARTESIAN_POINT('Ctrl Pts',(-137.758556505643,-4.03635375457527,
126.623503425159));
#255896=CARTESIAN_POINT('Ctrl Pts',(-138.037004129456,-5.69922136176977,
131.940403911158));
#255897=CARTESIAN_POINT('Ctrl Pts',(-138.315451753269,-2.12478295993955,
136.213336109146));
#255898=CARTESIAN_POINT('Ctrl Pts',(-138.593899377082,3.40222718065648,
135.515684073514));
#255899=CARTESIAN_POINT('Ctrl Pts',(-138.872347000894,5.80275675026745,
130.488555942812));
#255900=CARTESIAN_POINT('Ctrl Pts',(-139.150794624707,2.870836346809,125.751636880291));
#255901=CARTESIAN_POINT('Ctrl Pts',(-139.42924224852,-2.69924241121433,
125.65792409305));
#255902=CARTESIAN_POINT('Ctrl Pts',(-139.707689872333,-5.78884925865424,
130.293535054436));
#255903=CARTESIAN_POINT('Ctrl Pts',(-139.986137496146,-3.55878643839929,
135.398569753122));
#255904=CARTESIAN_POINT('Ctrl Pts',(-140.264585119959,1.94162726236197,
136.281750695826));
#255905=CARTESIAN_POINT('Ctrl Pts',(-140.543032743772,5.65778036277742,
132.131477741989));
#255906=CARTESIAN_POINT('Ctrl Pts',(-140.821480367585,4.17470970773734,
126.761648984083));
#255907=CARTESIAN_POINT('Ctrl Pts',(-141.099927991397,-1.14471522280625,
125.106874719905));
#255908=CARTESIAN_POINT('Ctrl Pts',(-141.37837561521,-5.41220278603824,
128.687811658017));
#255909=CARTESIAN_POINT('Ctrl Pts',(-141.656823239023,-4.70614038970644,
134.213753690789));
#255910=CARTESIAN_POINT('Ctrl Pts',(-141.935270862836,0.324635117026387,
136.60663004738));
#255911=CARTESIAN_POINT('Ctrl Pts',(-142.213718486649,5.05708681051884,
133.667504254592));
#255912=CARTESIAN_POINT('Ctrl Pts',(-142.492166110462,5.14232277757003,
128.097289331719));
#255913=CARTESIAN_POINT('Ctrl Pts',(-142.770613734275,0.502015328467386,
125.014740672754));
#255914=CARTESIAN_POINT('Ctrl Pts',(-143.049061358088,-4.59961968268416,
127.252569904414));
#255915=CARTESIAN_POINT('Ctrl Pts',(-143.327508981901,-5.4744289093626,
132.754321286837));
#255916=CARTESIAN_POINT('Ctrl Pts',(-143.605956605714,-1.31850540905707,
136.464154075075));
#255917=CARTESIAN_POINT('Ctrl Pts',(-143.884404229526,4.04906014960179,
134.972913172143));
#255918=CARTESIAN_POINT('Ctrl Pts',(-144.162851853339,5.69573723836169,
129.650976116669));
#255919=CARTESIAN_POINT('Ctrl Pts',(-144.441299477152,2.10831005730047,
125.388943071553));
#255920=CARTESIAN_POINT('Ctrl Pts',(-144.719747100965,-3.41655106974776,
126.103414193369));
#255921=CARTESIAN_POINT('Ctrl Pts',(-144.998194724778,-5.80176867149642,
131.13782542502));
#255922=CARTESIAN_POINT('Ctrl Pts',(-145.276642348591,-2.85544429629671,
135.865798789283));
#255923=CARTESIAN_POINT('Ctrl Pts',(-145.555089972404,2.71489389099137,
135.942557738738));
#255924=CARTESIAN_POINT('Ctrl Pts',(-145.833537596217,5.79037722239768,
131.29756454872));
#255925=CARTESIAN_POINT('Ctrl Pts',(-146.111985220029,3.54478676207412,
126.199341040322));
#255926=CARTESIAN_POINT('Ctrl Pts',(-146.390432843843,-1.95828956013508,
125.332905555698));
#255927=CARTESIAN_POINT('Ctrl Pts',(-146.668880467655,-5.66179344434354,
129.49446997749));
#255928=CARTESIAN_POINT('Ctrl Pts',(-146.947328091469,-4.16238574718705,
134.859759905796));
#255929=CARTESIAN_POINT('Ctrl Pts',(-147.225775715281,1.16205110778606,
136.498336005488));
#255930=CARTESIAN_POINT('Ctrl Pts',(-147.504223339094,5.41861976405632,
132.904426889841));
#255931=CARTESIAN_POINT('Ctrl Pts',(-147.782670962907,4.6957415714508,127.380659463914));
#255932=CARTESIAN_POINT('Ctrl Pts',(-148.06111858672,-0.342293725589094,
125.003106141093));
#255933=CARTESIAN_POINT('Ctrl Pts',(-148.339566210533,-5.06577781079073,
127.956622275114));
#255934=CARTESIAN_POINT('Ctrl Pts',(-148.618013834346,-5.1340595648799,
133.527070826096));
#255935=CARTESIAN_POINT('Ctrl Pts',(-148.896461458158,-0.48439139159784,
136.595481707227));
#255936=CARTESIAN_POINT('Ctrl Pts',(-149.174909081971,4.61040880672808,
134.342135218952));
#255937=CARTESIAN_POINT('Ctrl Pts',(-149.453356705784,5.4684685426618,128.837746701901));
#255938=CARTESIAN_POINT('Ctrl Pts',(-149.731804329597,1.30127283742975,
125.140580298914));
#255939=CARTESIAN_POINT('Ctrl Pts',(-150.01025195341,-4.06172903468827,
126.648151317718));
#255940=CARTESIAN_POINT('Ctrl Pts',(-150.288699577223,-5.69220035042211,
131.975075640969));
#255941=CARTESIAN_POINT('Ctrl Pts',(-150.567147201036,-2.09181762356486,
136.226170050321));
#255942=CARTESIAN_POINT('Ctrl Pts',(-150.845594824849,3.43084330837664,
135.494886461086));
#255943=CARTESIAN_POINT('Ctrl Pts',(-151.124042448661,5.80072684593324,
130.453238766583));
#255944=CARTESIAN_POINT('Ctrl Pts',(-151.402490072475,2.84002579333802,
125.734254899877));
#255945=CARTESIAN_POINT('Ctrl Pts',(-151.680937696287,-2.73052022036177,
125.674450499292));
#255946=CARTESIAN_POINT('Ctrl Pts',(-151.9593853201,-5.79185154487752,130.32878288736));
#255947=CARTESIAN_POINT('Ctrl Pts',(-152.237832943913,-3.53075424732904,
135.420147976222));
#255948=CARTESIAN_POINT('Ctrl Pts',(-152.516280567726,1.97493371658077,
136.269829976228));
#255949=CARTESIAN_POINT('Ctrl Pts',(-152.794728191539,5.66575407582884,
132.097012638644));
#255950=CARTESIAN_POINT('Ctrl Pts',(-153.073175815352,4.15002322686382,
126.736311243251));
#255951=CARTESIAN_POINT('Ctrl Pts',(-153.351623439165,-1.17937622768304,
125.113948487592));
#255952=CARTESIAN_POINT('Ctrl Pts',(-153.630071062978,-5.42498654472129,
128.720796487292));
#255953=CARTESIAN_POINT('Ctrl Pts',(-153.90851868679,-4.6852992524868,134.242338134946));
#255954=CARTESIAN_POINT('Ctrl Pts',(-154.186966310604,0.359949163189457,
136.604546398667));
#255955=CARTESIAN_POINT('Ctrl Pts',(-154.465413934416,5.0744218823891,133.636667284384));
#255956=CARTESIAN_POINT('Ctrl Pts',(-154.743861558229,5.12574879096345,
128.066036709167));
#255957=CARTESIAN_POINT('Ctrl Pts',(-155.022309182042,0.466762967392146,
125.011792031209));
#255958=CARTESIAN_POINT('Ctrl Pts',(-155.300756805855,-4.62115522057418,
127.280634901405));
#255959=CARTESIAN_POINT('Ctrl Pts',(-155.579204429668,-5.46245751681569,
132.787609561181));
#255960=CARTESIAN_POINT('Ctrl Pts',(-155.857652053481,-1.28402821098903,
136.472075328871));
#255961=CARTESIAN_POINT('Ctrl Pts',(-156.136099677293,4.07436029247137,
134.948188160129));
#255962=CARTESIAN_POINT('Ctrl Pts',(-156.414547301107,5.68861073071636,
129.616325916999));
#255963=CARTESIAN_POINT('Ctrl Pts',(-156.692994924919,2.07530581151645,
125.376209524969));
#255964=CARTESIAN_POINT('Ctrl Pts',(-156.971442548732,-3.44510376414151,
126.124298807112));
#255965=CARTESIAN_POINT('Ctrl Pts',(-157.249890172545,-5.79963128322921,
131.173136259331));
#255966=CARTESIAN_POINT('Ctrl Pts',(-157.528337796358,-2.82458098076833,
135.883086912459));
#255967=CARTESIAN_POINT('Ctrl Pts',(-157.806785420171,2.74612125456611,
135.925936210153));
#255968=CARTESIAN_POINT('Ctrl Pts',(-158.085233043984,5.79327221243612,
131.262307741136));
#255969=CARTESIAN_POINT('Ctrl Pts',(-158.363680667797,3.51668902415852,
126.177848237519));
#255970=CARTESIAN_POINT('Ctrl Pts',(-158.64212829161,-1.9915595775106,125.344927593469));
#255971=CARTESIAN_POINT('Ctrl Pts',(-158.920575915422,-5.66966222054205,
129.528959190434));
#255972=CARTESIAN_POINT('Ctrl Pts',(-159.199023539236,-4.13762226129274,
134.885022392109));
#255973=CARTESIAN_POINT('Ctrl Pts',(-159.477471163048,1.19669042199943,
136.491156774389));
#255974=CARTESIAN_POINT('Ctrl Pts',(-159.755918786861,5.43130306905165,
132.871403303985));
#255975=CARTESIAN_POINT('Ctrl Pts',(-160.034366410674,4.67481352955083,
127.352138585409));
#255976=CARTESIAN_POINT('Ctrl Pts',(-160.312814034487,-0.377601266270116,
125.005297263965));
#255977=CARTESIAN_POINT('Ctrl Pts',(-160.5912616583,-5.08301894523598,127.987511864483));
#255978=CARTESIAN_POINT('Ctrl Pts',(-160.869709282113,-5.1173905328107,
133.558272858373));
#255979=CARTESIAN_POINT('Ctrl Pts',(-161.148156905926,-0.449130219157962,
136.598323039052));
#255980=CARTESIAN_POINT('Ctrl Pts',(-161.426604529739,4.63185882466967,
134.314004805186));
#255981=CARTESIAN_POINT('Ctrl Pts',(-161.705052153551,5.45639588750942,
128.804495018547));
#255982=CARTESIAN_POINT('Ctrl Pts',(-161.983499777364,1.26677168948586,
125.13276401854));
#255983=CARTESIAN_POINT('Ctrl Pts',(-162.261947401177,-4.08695380593746,
126.67295322014));
#255984=CARTESIAN_POINT('Ctrl Pts',(-162.54039502499,-5.68496841249774,
132.009703989503));
#255985=CARTESIAN_POINT('Ctrl Pts',(-162.818842648803,-2.05877477411906,
136.238803084352));
#255986=CARTESIAN_POINT('Ctrl Pts',(-163.097290272616,3.45933230493559,
135.473915039499));
#255987=CARTESIAN_POINT('Ctrl Pts',(-163.375737896429,5.79848199353304,
130.417934601304));
#255988=CARTESIAN_POINT('Ctrl Pts',(-163.654185520242,2.80911000166655,
125.717060794092));
#255989=CARTESIAN_POINT('Ctrl Pts',(-163.932633144055,-2.76169684907854,
125.691166996241));
#255990=CARTESIAN_POINT('Ctrl Pts',(-164.211080767867,-5.79463921191188,
130.36404834299));
#255991=CARTESIAN_POINT('Ctrl Pts',(-164.489528391681,-3.50259122286156,
135.441555159625));
#255992=CARTESIAN_POINT('Ctrl Pts',(-164.767976015493,2.00816698890481,
136.257706731653));
#255993=CARTESIAN_POINT('Ctrl Pts',(-165.046423639306,5.67351784227885,
132.062499635604));
#255994=CARTESIAN_POINT('Ctrl Pts',(-165.324871263119,4.12518296535417,
126.711124245485));
#255995=CARTESIAN_POINT('Ctrl Pts',(-165.603318886932,-1.21399353033979,
125.121233115594));
#255996=CARTESIAN_POINT('Ctrl Pts',(-165.881766510745,-5.43756927853226,
128.753858523801));
#255997=CARTESIAN_POINT('Ctrl Pts',(-166.160214134558,-4.66428449978105,
134.270795183582));
#255998=CARTESIAN_POINT('Ctrl Pts',(-166.438661758371,0.395249871304121,
136.602247821935));
#255999=CARTESIAN_POINT('Ctrl Pts',(-166.717109382183,5.09156891968999,
133.60572536201));
#256000=CARTESIAN_POINT('Ctrl Pts',(-166.995557005996,5.10898486785074,
128.034885556215));
#256001=CARTESIAN_POINT('Ctrl Pts',(-167.274004629809,0.431493310242956,
125.009058035423));
#256002=CARTESIAN_POINT('Ctrl Pts',(-167.552452253622,-4.64251951985801,
127.30883047135));
#256003=CARTESIAN_POINT('Ctrl Pts',(-167.830899877435,-5.45028371089662,
132.820824345507));
#256004=CARTESIAN_POINT('Ctrl Pts',(-168.109347501248,-1.24950343278299,
136.479786563416));
#256005=CARTESIAN_POINT('Ctrl Pts',(-168.387795125061,4.09950945842204,
134.923309597059));
#256006=CARTESIAN_POINT('Ctrl Pts',(-168.666242748874,5.68127342950807,
129.581719740392));
#256007=CARTESIAN_POINT('Ctrl Pts',(-168.944690372687,2.04222466451309,
125.36367712052));
#256008=CARTESIAN_POINT('Ctrl Pts',(-169.223137996499,-3.47352879894819,
126.145356842267));
#256009=CARTESIAN_POINT('Ctrl Pts',(-169.501585620313,-5.79727898749155,
131.208433428525));
#256010=CARTESIAN_POINT('Ctrl Pts',(-169.780033244125,-2.79361299935373,
135.900186841566));
#256011=CARTESIAN_POINT('Ctrl Pts',(-170.058480867939,2.77724685960862,
135.909124899701));
#256012=CARTESIAN_POINT('Ctrl Pts',(-170.336928491751,5.79595253064181,
131.227033964152));
#256013=CARTESIAN_POINT('Ctrl Pts',(-170.615376115564,3.48846097403773,
126.156526871832));
#256014=CARTESIAN_POINT('Ctrl Pts',(-170.893823739377,-2.02475579691427,
125.357151932539));
#256015=CARTESIAN_POINT('Ctrl Pts',(-171.17227136319,-5.67732090532164,
129.563495663847));
#256016=CARTESIAN_POINT('Ctrl Pts',(-171.450718987003,-4.11270545428381,
134.910133667999));
#256017=CARTESIAN_POINT('Ctrl Pts',(-171.729166610815,1.23128539240979,
136.483766816968));
#256018=CARTESIAN_POINT('Ctrl Pts',(-172.007614234629,5.44378511511418,
132.838303123102));
#256019=CARTESIAN_POINT('Ctrl Pts',(-172.286061858441,4.65371226071637,
127.323745630264));
#256020=CARTESIAN_POINT('Ctrl Pts',(-172.564509482254,-0.412894814796852,
125.00770327326));
#256021=CARTESIAN_POINT('Ctrl Pts',(-172.842957106067,-5.10007172654484,
128.018505833219));
#256022=CARTESIAN_POINT('Ctrl Pts',(-173.12140472988,-5.10053187395325,
133.589372843419));
#256023=CARTESIAN_POINT('Ctrl Pts',(-173.399852353693,-0.413852404033268,
136.600949673471));
#256024=CARTESIAN_POINT('Ctrl Pts',(-173.678299977506,4.65313720737985,
134.285744340263));
#256025=CARTESIAN_POINT('Ctrl Pts',(-173.956747601319,5.44412104360021,
128.771317440947));
#256026=CARTESIAN_POINT('Ctrl Pts',(-174.235195225131,1.23222360085094,
125.125157901261));
#256027=CARTESIAN_POINT('Ctrl Pts',(-174.513642848945,-4.11202713361109,
126.697908213384));
#256028=CARTESIAN_POINT('Ctrl Pts',(-174.792090472757,-5.67752581597763,
132.044287673595));
#256029=CARTESIAN_POINT('Ctrl Pts',(-175.070538096571,-2.02565563601667,
136.251234743121));
#256030=CARTESIAN_POINT('Ctrl Pts',(-175.348985720383,3.48769311466452,
135.452770585855));
#256031=CARTESIAN_POINT('Ctrl Pts',(-175.627433344196,5.79602227624969,
130.382644755183));
#256032=CARTESIAN_POINT('Ctrl Pts',(-175.905880968009,2.77809011739122,
125.700055200075));
#256033=CARTESIAN_POINT('Ctrl Pts',(-176.184328591822,-2.79277114210269,
125.708072964459));
#256034=CARTESIAN_POINT('Ctrl Pts',(-176.462776215635,-5.79721215645926,
130.399330114555));
#256035=CARTESIAN_POINT('Ctrl Pts',(-176.741223839448,-3.47429840858841,
135.462790510077));
#256036=CARTESIAN_POINT('Ctrl Pts',(-177.019671463261,2.04132584786218,
136.245381411334));
#256037=CARTESIAN_POINT('Ctrl Pts',(-177.298119087073,5.68107137443935,
132.02794001176));
#256038=CARTESIAN_POINT('Ctrl Pts',(-177.576566710886,4.10018984367198,
126.686088924097));
#256039=CARTESIAN_POINT('Ctrl Pts',(-177.855014334699,-1.24856584802001,
125.128728333976));
#256040=CARTESIAN_POINT('Ctrl Pts',(-178.133461958512,-5.4499505212146,
128.786996542421));
#256041=CARTESIAN_POINT('Ctrl Pts',(-178.411909582325,-4.64309691029714,
134.29912378221));
#256042=CARTESIAN_POINT('Ctrl Pts',(-178.690357206138,0.430535933288815,
136.599734402363));
#256043=CARTESIAN_POINT('Ctrl Pts',(-178.968804829951,5.10852728703229,
133.574679634036));
#256044=CARTESIAN_POINT('Ctrl Pts',(-179.247252453763,5.09203162942501,
128.00383702718));
#256045=CARTESIAN_POINT('Ctrl Pts',(-179.525700077576,0.396207663951002,
125.006538786706));
#256046=CARTESIAN_POINT('Ctrl Pts',(-179.80414770139,-4.66371178887382,
127.337155569449));
#256047=CARTESIAN_POINT('Ctrl Pts',(-180.082595325202,-5.43790794271038,
132.853964409027));
#256048=CARTESIAN_POINT('Ctrl Pts',(-180.361042949015,-1.2149323537682,
136.487287492965));
#256049=CARTESIAN_POINT('Ctrl Pts',(-180.639490572828,4.12450671554208,
134.898278404822));
#256050=CARTESIAN_POINT('Ctrl Pts',(-180.917938196641,5.67372560662389,
129.547158869193));
#256051=CARTESIAN_POINT('Ctrl Pts',(-181.196385820454,2.00906784212309,
125.351346322599));
#256052=CARTESIAN_POINT('Ctrl Pts',(-181.474833444267,-3.50182512086801,
126.166587518521));
#256053=CARTESIAN_POINT('Ctrl Pts',(-181.75328106808,-5.79471187144949,
131.243715624654));
#256054=CARTESIAN_POINT('Ctrl Pts',(-182.031728691892,-2.76254149958135,
135.917097942958));
#256055=CARTESIAN_POINT('Ctrl Pts',(-182.310176315705,2.80826955274668,
135.892124430331));
#256056=CARTESIAN_POINT('Ctrl Pts',(-182.588623939518,5.79841807769547,
131.191744524852));
#256057=CARTESIAN_POINT('Ctrl Pts',(-182.867071563331,3.46010365771282,
126.135377733334));
#256058=CARTESIAN_POINT('Ctrl Pts',(-183.145519187144,-2.05787698824661,
125.369578119929));
#256059=CARTESIAN_POINT('Ctrl Pts',(-183.423966810957,-5.68476921488759,
129.598078117967));
#256060=CARTESIAN_POINT('Ctrl Pts',(-183.70241443477,-4.08763624946197,
134.93509280296));
#256061=CARTESIAN_POINT('Ctrl Pts',(-183.980862058583,1.26583473708647,
136.476166407061));
#256062=CARTESIAN_POINT('Ctrl Pts',(-184.259309682396,5.45606543971754,
132.805127573733));
#256063=CARTESIAN_POINT('Ctrl Pts',(-184.537757306209,4.63243854686269,
127.295481650585));
#256064=CARTESIAN_POINT('Ctrl Pts',(-184.816204930021,-0.448173063354899,
125.010324079826));
#256065=CARTESIAN_POINT('Ctrl Pts',(-185.094652553834,-5.11693552282041,
128.049603032828));
#256066=CARTESIAN_POINT('Ctrl Pts',(-185.373100177647,-5.08348421301165,
133.620369628814));
#256067=CARTESIAN_POINT('Ctrl Pts',(-185.65154780146,-0.378559253454916,
136.60336151315));
#256068=CARTESIAN_POINT('Ctrl Pts',(-185.929995425273,4.67424316637891,
134.257354871388));
#256069=CARTESIAN_POINT('Ctrl Pts',(-186.208443049086,5.4316444657843,128.73821519851));
#256070=CARTESIAN_POINT('Ctrl Pts',(-186.486890672899,1.19762985171755,
125.117762228929));
#256071=CARTESIAN_POINT('Ctrl Pts',(-186.765338296712,-4.13694808860639,
126.72301537273));
#256072=CARTESIAN_POINT('Ctrl Pts',(-187.043785920525,-5.66987283665109,
132.078825411735));
#256073=CARTESIAN_POINT('Ctrl Pts',(-187.322233544337,-1.99246143649967,
136.263464565965));
#256074=CARTESIAN_POINT('Ctrl Pts',(-187.600681168151,3.51592468664221,
135.43145388367));
#256075=CARTESIAN_POINT('Ctrl Pts',(-187.879128791963,5.79334778522967,
130.347370535898));
#256076=CARTESIAN_POINT('Ctrl Pts',(-188.157576415776,2.74696728996466,
125.683238747971));
#256077=CARTESIAN_POINT('Ctrl Pts',(-188.436024039589,-2.82374194796541,
125.72516777749));
#256078=CARTESIAN_POINT('Ctrl Pts',(-188.714471663402,-5.79957028317828,
130.434626894674));
#256079=CARTESIAN_POINT('Ctrl Pts',(-188.992919287215,-3.44587685290989,
135.483853240698));
#256080=CARTESIAN_POINT('Ctrl Pts',(-189.271366911028,2.07440906473995,
136.232854471987));
#256081=CARTESIAN_POINT('Ctrl Pts',(-189.54981453484,5.68841439241029,131.993335047731));
#256082=CARTESIAN_POINT('Ctrl Pts',(-189.828262158654,4.07504478794802,
126.661206206783));
#256083=CARTESIAN_POINT('Ctrl Pts',(-190.106709782466,-1.28309189963338,
125.136433864998));
#256084=CARTESIAN_POINT('Ctrl Pts',(-190.385157406279,-5.46212981397553,
128.820209315208));
#256085=CARTESIAN_POINT('Ctrl Pts',(-190.663605030092,-4.62173726915045,
134.327322881104));
#256086=CARTESIAN_POINT('Ctrl Pts',(-190.942052653905,0.465806041606811,
136.597006233083));
#256087=CARTESIAN_POINT('Ctrl Pts',(-191.220500277718,5.12529635601715,
133.543531250871));
#256088=CARTESIAN_POINT('Ctrl Pts',(-191.49894790153,5.07488970389458,127.972892272577));
#256089=CARTESIAN_POINT('Ctrl Pts',(-191.777395525344,0.360907336037817,
125.004234378408));
#256090=CARTESIAN_POINT('Ctrl Pts',(-192.055843149156,-4.68473124233415,
127.365609146106));
#256091=CARTESIAN_POINT('Ctrl Pts',(-192.33429077297,-5.42533067084548,
132.887028523726));
#256092=CARTESIAN_POINT('Ctrl Pts',(-192.612738396782,-1.1803162549878,
136.494577839569));
#256093=CARTESIAN_POINT('Ctrl Pts',(-192.891186020595,4.14935113754904,
134.873095510955));
#256094=CARTESIAN_POINT('Ctrl Pts',(-193.169633644408,5.66596754175055,
129.512644584067));
#256095=CARTESIAN_POINT('Ctrl Pts',(-193.448081268221,1.97583657298603,
125.339217588127));
#256096=CARTESIAN_POINT('Ctrl Pts',(-193.726528892034,-3.52999168137001,
126.187990049162));
#256097=CARTESIAN_POINT('Ctrl Pts',(-194.004976515847,-5.79193003022761,
131.27898154032));
#256098=CARTESIAN_POINT('Ctrl Pts',(-194.28342413966,-2.73136763281852,
135.933819589987));
#256099=CARTESIAN_POINT('Ctrl Pts',(-194.561871763472,2.83918818442447,
135.874935432001));
#256100=CARTESIAN_POINT('Ctrl Pts',(-194.840319387286,5.80066876223446,
131.156440730899));
#256101=CARTESIAN_POINT('Ctrl Pts',(-195.118767011098,3.43161812597426,
126.114401605713));
#256102=CARTESIAN_POINT('Ctrl Pts',(-195.397214634911,-2.09092192419104,
125.382205695184));
#256103=CARTESIAN_POINT('Ctrl Pts',(-195.675662258724,-5.69200687323938,
129.63270527133));
#256104=CARTESIAN_POINT('Ctrl Pts',(-195.954109882537,-4.06241557577554,
134.95989887212));
#256105=CARTESIAN_POINT('Ctrl Pts',(-196.23255750635,1.30033717579212,136.468355826305));
#256106=CARTESIAN_POINT('Ctrl Pts',(-196.511005130163,5.46814358780935,
132.771877885207));
#256107=CARTESIAN_POINT('Ctrl Pts',(-196.789452753976,4.61099317629508,
127.267347693709));
#256108=CARTESIAN_POINT('Ctrl Pts',(-197.067900377789,-0.483434704694746,
125.013159586548));
#256109=CARTESIAN_POINT('Ctrl Pts',(-197.346348001602,-5.13360970916836,
128.080802310993));
#256110=CARTESIAN_POINT('Ctrl Pts',(-197.624795625414,-5.06624818169292,
133.651262065958));
#256111=CARTESIAN_POINT('Ctrl Pts',(-197.903243249227,-0.343252075224855,
136.605558468718));
#256112=CARTESIAN_POINT('Ctrl Pts',(-198.18169087304,4.69517591957924,134.228837450539));
#256113=CARTESIAN_POINT('Ctrl Pts',(-198.460138496853,5.41896661638458,
128.705189517851));
#256114=CARTESIAN_POINT('Ctrl Pts',(-198.738586120666,1.1629917239694,125.110577275591));
#256115=CARTESIAN_POINT('Ctrl Pts',(-199.017033744479,-4.16171574746965,
126.748273767825));
#256116=CARTESIAN_POINT('Ctrl Pts',(-199.295481368292,-5.6620097581009,
132.113315924113));
#256117=CARTESIAN_POINT('Ctrl Pts',(-199.573928992105,-1.95919340559182,
136.275492099704));
#256118=CARTESIAN_POINT('Ctrl Pts',(-199.852376615917,3.54402597473752,
135.409965722843));
#256119=CARTESIAN_POINT('Ctrl Pts',(-200.13082423973,5.79045861957696,130.312113250549));
#256120=CARTESIAN_POINT('Ctrl Pts',(-200.409271863544,2.71574267265526,
125.666612060922));
#256121=CARTESIAN_POINT('Ctrl Pts',(-200.687719487356,-2.85460811903155,
125.742450801881));
#256122=CARTESIAN_POINT('Ctrl Pts',(-200.966167111169,-5.80171350468764,
130.469937375411));
#256123=CARTESIAN_POINT('Ctrl Pts',(-201.244614734982,-3.41732760899753,
135.504742570997));
#256124=CARTESIAN_POINT('Ctrl Pts',(-201.523062358795,2.10741541362659,
136.220126377805));
#256125=CARTESIAN_POINT('Ctrl Pts',(-201.801509982608,5.69554662409457,
131.958686025817));
#256126=CARTESIAN_POINT('Ctrl Pts',(-202.079957606421,4.04974872994014,
126.636477015578));
#256127=CARTESIAN_POINT('Ctrl Pts',(-202.358405230234,-1.31757040580477,
125.144349423131));
#256128=CARTESIAN_POINT('Ctrl Pts',(-202.636852854047,-5.47410670550813,
128.853495611451));
#256129=CARTESIAN_POINT('Ctrl Pts',(-202.915300477859,-4.6002063678289,
134.355391435336));
#256130=CARTESIAN_POINT('Ctrl Pts',(-203.193748101672,0.501058889310003,
136.594063415189));
#256131=CARTESIAN_POINT('Ctrl Pts',(-203.472195725485,5.14187550526088,
133.512281366733));
#256132=CARTESIAN_POINT('Ctrl Pts',(-203.750643349298,5.05755972645996,
127.942052439074));
#256133=CARTESIAN_POINT('Ctrl Pts',(-204.029090973111,0.325593634571106,
125.002144895921));
#256134=CARTESIAN_POINT('Ctrl Pts',(-204.307538596924,-4.70557710135553,
127.394190146963));
#256135=CARTESIAN_POINT('Ctrl Pts',(-204.585986220737,-5.41255236135747,
132.920015464399));
#256136=CARTESIAN_POINT('Ctrl Pts',(-204.864433844549,-1.14565641915494,
136.50165733308));
#256137=CARTESIAN_POINT('Ctrl Pts',(-205.142881468362,4.17404180382362,
134.847761848621));
#256138=CARTESIAN_POINT('Ctrl Pts',(-205.421329092175,5.6579995223666,129.478178163952));
#256139=CARTESIAN_POINT('Ctrl Pts',(-205.699776715988,1.94253208849746,
125.327291366541));
#256140=CARTESIAN_POINT('Ctrl Pts',(-205.978224339801,-3.55802743673226,
126.209563641112));
#256141=CARTESIAN_POINT('Ctrl Pts',(-206.256671963614,-5.78893356690891,
131.314229868733));
#256142=CARTESIAN_POINT('Ctrl Pts',(-206.535119587427,-2.70009255422283,
135.950351163029));
#256143=CARTESIAN_POINT('Ctrl Pts',(-206.81356721124,2.87000160893922,135.857558541658));
#256144=CARTESIAN_POINT('Ctrl Pts',(-207.092014835053,5.80270450085972,
131.121123890489));
#256145=CARTESIAN_POINT('Ctrl Pts',(-207.370462458865,3.40300543436423,
126.09359926625));
#256146=CARTESIAN_POINT('Ctrl Pts',(-207.648910082679,-2.12388938025395,
125.395034190384));
#256147=CARTESIAN_POINT('Ctrl Pts',(-207.927357706491,-5.69903361218359,
129.667375840811));
#256148=CARTESIAN_POINT('Ctrl Pts',(-208.205805330304,-4.03704436778601,
134.984550956282));
#256149=CARTESIAN_POINT('Ctrl Pts',(-208.484252954117,1.33479143002538,
136.460335364123));
#256150=CARTESIAN_POINT('Ctrl Pts',(-208.76270057793,5.48001911182977,132.738555289606));
#256151=CARTESIAN_POINT('Ctrl Pts',(-209.041148201743,4.58937694367963,
127.239344802146));
#256152=CARTESIAN_POINT('Ctrl Pts',(-209.319595825556,-0.518678432184342,
125.016209688352));
#256153=CARTESIAN_POINT('Ctrl Pts',(-209.598043449369,-5.15009366772074,
128.112102511612));
#256154=CARTESIAN_POINT('Ctrl Pts',(-209.876491073182,-5.04882441868487,
133.682049010123));
#256155=CARTESIAN_POINT('Ctrl Pts',(-210.154938696994,-0.307932177662294,
136.607540458767));
#256156=CARTESIAN_POINT('Ctrl Pts',(-210.433386320807,4.71593469130848,
134.200193134443));
#256157=CARTESIAN_POINT('Ctrl Pts',(-210.71183394462,5.40608796518471,128.672241622749));
#256158=CARTESIAN_POINT('Ctrl Pts',(-210.990281568433,1.12831050113542,
125.103603307488));
#256159=CARTESIAN_POINT('Ctrl Pts',(-211.268729192246,-4.18632919242468,
126.773682462711));
#256160=CARTESIAN_POINT('Ctrl Pts',(-211.547176816059,-5.65393687169752,
132.14775793267));
#256161=CARTESIAN_POINT('Ctrl Pts',(-211.825624439872,-1.92585277605142,
136.287316898656));
#256162=CARTESIAN_POINT('Ctrl Pts',(-212.104072063685,3.57199593764717,
135.388306899624));
#256163=CARTESIAN_POINT('Ctrl Pts',(-212.382519687498,5.78735488635066,
130.276874205606));
#256164=CARTESIAN_POINT('Ctrl Pts',(-212.660967311311,2.68441742250212,
125.650175755035));
#256165=CARTESIAN_POINT('Ctrl Pts',(-212.939414935123,-2.88536851154432,
125.759921397201));
#256166=CARTESIAN_POINT('Ctrl Pts',(-213.217862558936,-5.80364174156953,
130.505260248325));
#256167=CARTESIAN_POINT('Ctrl Pts',(-213.496310182749,-3.38865173475374,
135.525457726916));
#256168=CARTESIAN_POINT('Ctrl Pts',(-213.774757806562,2.14034367146046,
136.20719760043));
#256169=CARTESIAN_POINT('Ctrl Pts',(-214.053205430375,5.7024678052036,131.923994229952));
#256170=CARTESIAN_POINT('Ctrl Pts',(-214.331653054188,4.02430260700449,
126.611902266833));
#256171=CARTESIAN_POINT('Ctrl Pts',(-214.610100678001,-1.35200008892003,
125.152474715061));
#256172=CARTESIAN_POINT('Ctrl Pts',(-214.888548301814,-5.48588075200302,
128.886854197714));
#256173=CARTESIAN_POINT('Ctrl Pts',(-215.166995925626,-4.5785050041694,
134.383328404815));
#256174=CARTESIAN_POINT('Ctrl Pts',(-215.445443549439,0.536293170092427,
136.59090605773));
#256175=CARTESIAN_POINT('Ctrl Pts',(-215.723891173253,5.15826412041666,
133.480931139593));
#256176=CARTESIAN_POINT('Ctrl Pts',(-216.002338797065,5.04004233928969,
127.911318669453));
#256177=CARTESIAN_POINT('Ctrl Pts',(-216.280786420879,0.290267868112,125.000270416672));
#256178=CARTESIAN_POINT('Ctrl Pts',(-216.559234044691,-4.72624859348692,
127.422897512942));
#256179=CARTESIAN_POINT('Ctrl Pts',(-216.837681668504,-5.39957348775117,
132.952924008705));
#256180=CARTESIAN_POINT('Ctrl Pts',(-217.116129292317,-1.11095413060172,
136.508525711168));
#256181=CARTESIAN_POINT('Ctrl Pts',(-217.39457691613,4.19857779944424,134.822278356567));
#256182=CARTESIAN_POINT('Ctrl Pts',(-217.673024539943,5.64982184372931,
129.443760886018));
#256183=CARTESIAN_POINT('Ctrl Pts',(-217.951472163756,1.90915562276867,
125.315568099769));
#256184=CARTESIAN_POINT('Ctrl Pts',(-218.229919787568,-3.58593134807924,
126.231307494954));
#256185=CARTESIAN_POINT('Ctrl Pts',(-218.508367411381,-5.78572259252759,
131.349459303753));
#256186=CARTESIAN_POINT('Ctrl Pts',(-218.786815035194,-2.66871742270537,
135.966692049498));
#256187=CARTESIAN_POINT('Ctrl Pts',(-219.065262659007,2.90070868448967,
135.839994403207));
#256188=CARTESIAN_POINT('Ctrl Pts',(-219.34371028282,5.80452521813531,131.085795312298));
#256189=CARTESIAN_POINT('Ctrl Pts',(-219.622157906633,3.37426664313623,
126.07297148578));
#256190=CARTESIAN_POINT('Ctrl Pts',(-219.900605530446,-2.15677813481551,
125.408063130162));
#256191=CARTESIAN_POINT('Ctrl Pts',(-220.179053154259,-5.70584917134113,
129.702088541682));
#256192=CARTESIAN_POINT('Ctrl Pts',(-220.457500778071,-4.01152356563293,
135.009048141953));
#256193=CARTESIAN_POINT('Ctrl Pts',(-220.735948401884,1.36919622307095,
136.452105317718));
#256194=CARTESIAN_POINT('Ctrl Pts',(-221.014396025697,5.49169157172664,
132.705161021709));
#256195=CARTESIAN_POINT('Ctrl Pts',(-221.29284364951,4.56759065001379,127.211474013555));
#256196=CARTESIAN_POINT('Ctrl Pts',(-221.571291273323,-0.553902939853376,
125.019474272218));
#256197=CARTESIAN_POINT('Ctrl Pts',(-221.849738897136,-5.16638678765824,
128.143502474846));
#256198=CARTESIAN_POINT('Ctrl Pts',(-222.128186520948,-5.03121356963114,
133.712729320486));
#256199=CARTESIAN_POINT('Ctrl Pts',(-222.406634144762,-0.272600869560251,
136.609307409853));
#256200=CARTESIAN_POINT('Ctrl Pts',(-222.685081768574,4.73651871234416,
134.171422984523));
#256201=CARTESIAN_POINT('Ctrl Pts',(-222.963529392388,5.39300898940659,
128.639372734101));
#256202=CARTESIAN_POINT('Ctrl Pts',(-223.2419770162,1.09358746834067,125.096840583045));
#256203=CARTESIAN_POINT('Ctrl Pts',(-223.520424640014,-4.21078751141269,
126.799240515859));
#256204=CARTESIAN_POINT('Ctrl Pts',(-223.798872263826,-5.64565447658353,
132.182150161146));
#256205=CARTESIAN_POINT('Ctrl Pts',(-224.077319887639,-1.89244078332859,
136.298938524645));
#256206=CARTESIAN_POINT('Ctrl Pts',(-224.355767511452,3.59983353893359,
135.366478216591));
#256207=CARTESIAN_POINT('Ctrl Pts',(-224.634215135265,5.78403670056078,
130.241654706868));
#256208=CARTESIAN_POINT('Ctrl Pts',(-224.912662759078,2.65299270027449,
125.633930439363));
#256209=CARTESIAN_POINT('Ctrl Pts',(-225.191110382891,-2.91602198566553,
125.77757891607));
#256210=CARTESIAN_POINT('Ctrl Pts',(-225.469558006704,-5.8053549223724,
130.540594204513));
#256211=CARTESIAN_POINT('Ctrl Pts',(-225.748005630516,-3.35985029277391,
135.545997940844));
#256212=CARTESIAN_POINT('Ctrl Pts',(-226.026453254329,2.17319261807209,
136.194068618944));
#256213=CARTESIAN_POINT('Ctrl Pts',(-226.304900878142,5.7091776792716,131.88926094565));
#256214=CARTESIAN_POINT('Ctrl Pts',(-226.583348501955,3.99870736205508,
126.587482871174));
#256215=CARTESIAN_POINT('Ctrl Pts',(-226.861796125768,-1.38637967317499,
125.160809439701));
#256216=CARTESIAN_POINT('Ctrl Pts',(-227.140243749581,-5.49745151716988,
128.920283837883));
#256217=CARTESIAN_POINT('Ctrl Pts',(-227.418691373394,-4.55663398232247,
134.411132754326));
#256218=CARTESIAN_POINT('Ctrl Pts',(-227.697138997207,0.571507578333558,
136.5875342777));
#256219=CARTESIAN_POINT('Ctrl Pts',(-227.97558662102,5.17446159419872,133.44948173115));
#256220=CARTESIAN_POINT('Ctrl Pts',(-228.254034244832,5.02233819149715,
127.880692102567));
#256221=CARTESIAN_POINT('Ctrl Pts',(-228.532481868645,0.254931345670833,
124.998611010119));
#256222=CARTESIAN_POINT('Ctrl Pts',(-228.810929492458,-4.74674495273865,
127.451730180279));
#256223=CARTESIAN_POINT('Ctrl Pts',(-229.089377116271,-5.38639453096373,
132.985752937203));
#256224=CARTESIAN_POINT('Ctrl Pts',(-229.367824740084,-1.07621067523457,
136.515182719319));
#256225=CARTESIAN_POINT('Ctrl Pts',(-229.646272363897,4.22295821522052,
134.796645979094));
#256226=CARTESIAN_POINT('Ctrl Pts',(-229.92471998771,5.64143480886619,129.409394025606));
#256227=CARTESIAN_POINT('Ctrl Pts',(-230.203167611523,1.87570841257552,
125.304048222223));
#256228=CARTESIAN_POINT('Ctrl Pts',(-230.481615235336,-3.61370238142155,
126.25322080496));
#256229=CARTESIAN_POINT('Ctrl Pts',(-230.760062859148,-5.78229722606833,
131.384668539942));
#256230=CARTESIAN_POINT('Ctrl Pts',(-231.038510482961,-2.63724340088164,
135.982841643878));
#256231=CARTESIAN_POINT('Ctrl Pts',(-231.316958106774,2.93130827321233,
135.822243667495));
#256232=CARTESIAN_POINT('Ctrl Pts',(-231.595405730587,5.80613084659478,
131.050456305442));
#256233=CARTESIAN_POINT('Ctrl Pts',(-231.8738533544,3.34540281721704,126.052519028673));
#256234=CARTESIAN_POINT('Ctrl Pts',(-232.152300978213,-2.18958696916944,
125.42129203173));
#256235=CARTESIAN_POINT('Ctrl Pts',(-232.430748602025,-5.71245329815966,
129.736842087648));
#256236=CARTESIAN_POINT('Ctrl Pts',(-232.709196225839,-3.98585411499877,
135.033389521383));
#256237=CARTESIAN_POINT('Ctrl Pts',(-232.987643849651,1.40355028004735,
136.443665992055));
#256238=CARTESIAN_POINT('Ctrl Pts',(-233.266091473464,5.50316053497282,
132.671696318956));
#256239=CARTESIAN_POINT('Ctrl Pts',(-233.544539097277,4.5456351025967,127.183736360699));
#256240=CARTESIAN_POINT('Ctrl Pts',(-233.82298672109,-0.589106922445798,
125.022953217175));
#256241=CARTESIAN_POINT('Ctrl Pts',(-234.101434344904,-5.18248846523346,
128.175001037157));
#256242=CARTESIAN_POINT('Ctrl Pts',(-234.379881968716,-5.01341628710851,
133.743301860178));
#256243=CARTESIAN_POINT('Ctrl Pts',(-234.658329592529,-0.237259460132118,
136.610859256499));
#256244=CARTESIAN_POINT('Ctrl Pts',(-234.936777216342,4.75692721993639,
134.14252806687));
#256245=CARTESIAN_POINT('Ctrl Pts',(-235.215224840155,5.37973017369771,
128.606584069875));
#256246=CARTESIAN_POINT('Ctrl Pts',(-235.493672463967,1.05882391226032,
125.090289352854));
#256247=CARTESIAN_POINT('Ctrl Pts',(-235.772120087781,-4.23508979812022,
126.824946980203));
#256248=CARTESIAN_POINT('Ctrl Pts',(-236.050567711593,-5.63716287966734,
132.216491335124));
#256249=CARTESIAN_POINT('Ctrl Pts',(-236.329015335406,-1.85895866551617,
136.310356547029));
#256250=CARTESIAN_POINT('Ctrl Pts',(-236.607462959219,3.62753774706455,
135.344480482612));
#256251=CARTESIAN_POINT('Ctrl Pts',(-236.885910583032,5.78050418516386,
130.206456059403));
#256252=CARTESIAN_POINT('Ctrl Pts',(-237.164358206845,2.62146967042642,
125.617876715884));
#256253=CARTESIAN_POINT('Ctrl Pts',(-237.442805830658,-2.94656740551997,
125.795422704185));
#256254=CARTESIAN_POINT('Ctrl Pts',(-237.72125345447,-5.80685298361372,
130.575937934662));
#256255=CARTESIAN_POINT('Ctrl Pts',(-237.999701078284,-3.33092435030571,
135.566362451659));
#256256=CARTESIAN_POINT('Ctrl Pts',(-238.278148702096,2.20596103623244,
136.180739919846));
#256257=CARTESIAN_POINT('Ctrl Pts',(-238.55659632591,5.7156759976606,131.854487459968));
#256258=CARTESIAN_POINT('Ctrl Pts',(-238.835043949722,3.97296394353457,
126.56321973347));
#256259=CARTESIAN_POINT('Ctrl Pts',(-239.113491573535,-1.42070788462113,
125.169353288205));
#256260=CARTESIAN_POINT('Ctrl Pts',(-239.391939197348,-5.50881857224844,
128.95378329321));
#256261=CARTESIAN_POINT('Ctrl Pts',(-239.670386821161,-4.53459411272838,
134.438803453569));
#256262=CARTESIAN_POINT('Ctrl Pts',(-239.948834444974,0.606700809151854,
136.583948200045));
#256263=CARTESIAN_POINT('Ctrl Pts',(-240.227282068787,5.1904673264033,133.417934306771));
#256264=CARTESIAN_POINT('Ctrl Pts',(-240.5057296926,5.00444793911587,127.850173873291));
#256265=CARTESIAN_POINT('Ctrl Pts',(-240.784177316413,0.21958537665436,
124.997166737753));
#256266=CARTESIAN_POINT('Ctrl Pts',(-241.062624940225,-4.76706541961049,
127.48068708057));
#256267=CARTESIAN_POINT('Ctrl Pts',(-241.341072564039,-5.37301597934592,
133.018501033406));
#256268=CARTESIAN_POINT('Ctrl Pts',(-241.619520187851,-1.04142734048567,
136.521628110858));
#256269=CARTESIAN_POINT('Ctrl Pts',(-241.897967811664,4.24718214772698,
134.770865666018));
#256270=CARTESIAN_POINT('Ctrl Pts',(-242.176415435477,5.63283872856131,
129.375078856195));
#256271=CARTESIAN_POINT('Ctrl Pts',(-242.45486305929,1.84219169731802,125.292732160775));
#256272=CARTESIAN_POINT('Ctrl Pts',(-242.733310683103,-3.64133950769301,
126.275302759127));
#256273=CARTESIAN_POINT('Ctrl Pts',(-243.011758306915,-5.77865759445851,
131.419856272607));
#256274=CARTESIAN_POINT('Ctrl Pts',(-243.290205930729,-2.60567165503458,
135.998799347738));
#256275=CARTESIAN_POINT('Ctrl Pts',(-243.568653554541,2.96179924122969,
135.80430699228));
#256276=CARTESIAN_POINT('Ctrl Pts',(-243.847101178355,5.80752132674009,
131.015108179419));
#256277=CARTESIAN_POINT('Ctrl Pts',(-244.125548802166,3.31641502616601,
126.032242652805));
#256278=CARTESIAN_POINT('Ctrl Pts',(-244.403996425981,-2.22231466757369,
125.434720404883));
#256279=CARTESIAN_POINT('Ctrl Pts',(-244.682444049792,-5.71884574792013,
129.771635190908));
#256280=CARTESIAN_POINT('Ctrl Pts',(-244.960891673606,-3.96003696707471,
135.05757419259));
#256281=CARTESIAN_POINT('Ctrl Pts',(-245.239339297418,1.43785232795156,
136.435017699859));
#256282=CARTESIAN_POINT('Ctrl Pts',(-245.517786921232,5.51442557658153,
132.638162421391));
#256283=CARTESIAN_POINT('Ctrl Pts',(-245.796234545044,4.52351111499922,
127.156132871406));
#256284=CARTESIAN_POINT('Ctrl Pts',(-246.074682168857,-0.624289075464052,
125.026646394309));
#256285=CARTESIAN_POINT('Ctrl Pts',(-246.353129792671,-5.19839810379266,
128.206597031353));
#256286=CARTESIAN_POINT('Ctrl Pts',(-246.631577416483,-4.99543323060155,
133.773765496319));
#256287=CARTESIAN_POINT('Ctrl Pts',(-246.910025040296,-0.201909258968066,
136.612195941205));
#256288=CARTESIAN_POINT('Ctrl Pts',(-247.188472664109,4.77715945784187,
134.113509452194));
#256289=CARTESIAN_POINT('Ctrl Pts',(-247.466920287922,5.36625201010822,
128.573876845067));
#256290=CARTESIAN_POINT('Ctrl Pts',(-247.745367911734,1.02402112107033,
125.083949859676));
#256291=CARTESIAN_POINT('Ctrl Pts',(-248.023815535548,-4.25923515201858,
126.850800903184));
#256292=CARTESIAN_POINT('Ctrl Pts',(-248.30226315936,-5.62846239560694,
132.250780182078));
#256293=CARTESIAN_POINT('Ctrl Pts',(-248.580710783174,-1.82540766330725,
136.32157054271));
#256294=CARTESIAN_POINT('Ctrl Pts',(-248.859158406986,3.65510753545023,
135.322314512822));
#256295=CARTESIAN_POINT('Ctrl Pts',(-249.137606030799,5.7767574710584,130.171279567513));
#256296=CARTESIAN_POINT('Ctrl Pts',(-249.416053654612,2.58984950105633,
125.602015179472));
#256297=CARTESIAN_POINT('Ctrl Pts',(-249.694501278425,-2.97700363923603,
125.813452100338));
#256298=CARTESIAN_POINT('Ctrl Pts',(-249.972948902238,-5.80813586978118,
130.611290129096));
#256299=CARTESIAN_POINT('Ctrl Pts',(-250.251396526051,-3.30187497921299,
135.586550504748));
#256300=CARTESIAN_POINT('Ctrl Pts',(-250.529844149864,2.23864771169993,
136.167211997028));
#256301=CARTESIAN_POINT('Ctrl Pts',(-250.808291773676,5.72196251956533,
131.819675061465));
#256302=CARTESIAN_POINT('Ctrl Pts',(-251.08673939749,3.94707330538994,126.539113752772));
#256303=CARTESIAN_POINT('Ctrl Pts',(-251.365187021302,-1.45498345124562,
125.178105944033));
#256304=CARTESIAN_POINT('Ctrl Pts',(-251.643634645115,-5.5199814959705,
128.987351322257));
#256305=CARTESIAN_POINT('Ctrl Pts',(-251.922082268928,-4.51238621219265,
134.466339477392));
#256306=CARTESIAN_POINT('Ctrl Pts',(-252.200529892741,0.641871558658502,
136.580147957277));
#256307=CARTESIAN_POINT('Ctrl Pts',(-252.478977516554,5.20628072353487,
133.386290036154));
#256308=CARTESIAN_POINT('Ctrl Pts',(-252.757425140367,4.98637224582674,
127.819765111179));
#256309=CARTESIAN_POINT('Ctrl Pts',(-253.035872764179,0.184231269403876,
124.995937655572));
#256310=CARTESIAN_POINT('Ctrl Pts',(-253.314320387993,-4.78720923844335,
127.509767136124));
#256311=CARTESIAN_POINT('Ctrl Pts',(-253.592768011806,-5.35943833369967,
133.051167092665));
#256312=CARTESIAN_POINT('Ctrl Pts',(-253.871215635618,-1.00660540571931,
136.527861630253));
#256313=CARTESIAN_POINT('Ctrl Pts',(-254.149663259431,4.27124868131666,
134.744938404161));
#256314=CARTESIAN_POINT('Ctrl Pts',(-254.428110883244,5.62403395537261,
129.340816589823));
#256315=CARTESIAN_POINT('Ctrl Pts',(-254.706558507057,1.80860665472018,
125.281620447135));
#256316=CARTESIAN_POINT('Ctrl Pts',(-254.98500613087,-3.66884158147516,
126.297552326988));
#256317=CARTESIAN_POINT('Ctrl Pts',(-255.263453754682,-5.77480406163408,
131.45502159855));
#256318=CARTESIAN_POINT('Ctrl Pts',(-255.541901378496,-2.57400292253984,
136.014563813166));
#256319=CARTESIAN_POINT('Ctrl Pts',(-255.820349002309,2.99217964199006,
135.78618647082));
#256320=CARTESIAN_POINT('Ctrl Pts',(-256.098796626121,5.80869814913581,
130.979749546569));
#256321=CARTESIAN_POINT('Ctrl Pts',(-256.377244249934,3.28730143236016,
126.01214820295));
#256322=CARTESIAN_POINT('Ctrl Pts',(-256.655691873747,-2.25495451926359,
125.448338134603));
#256323=CARTESIAN_POINT('Ctrl Pts',(-256.93413949756,-5.72503666514098,
129.806484721847));
#256324=CARTESIAN_POINT('Ctrl Pts',(-257.212587121373,-3.93405347634203,
135.081566970265));
#256325=CARTESIAN_POINT('Ctrl Pts',(-257.491034745186,1.47206408278265,
136.426225506557));
#256326=CARTESIAN_POINT('Ctrl Pts',(-257.769482368999,5.52555616721843,
132.604438319186));
#256327=CARTESIAN_POINT('Ctrl Pts',(-258.047929992812,4.50108754276566,
127.128895412351));
#256328=CARTESIAN_POINT('Ctrl Pts',(-258.326377616624,-0.659198908970111,
125.030117734768));
#256329=CARTESIAN_POINT('Ctrl Pts',(-258.604825240438,-5.21458571703409,
128.239112839452));
#256330=CARTESIAN_POINT('Ctrl Pts',(-258.883272864251,-4.97637574492231,
133.802560593787));
#256331=CARTESIAN_POINT('Ctrl Pts',(-259.161720488063,-0.168236736403017,
136.616288572087));
#256332=CARTESIAN_POINT('Ctrl Pts',(-259.440168111876,4.80044487344316,
134.078525892203));
#256333=CARTESIAN_POINT('Ctrl Pts',(-259.672207798387,5.25516631655033,
129.4749169549));
#256334=CARTESIAN_POINT('Ctrl Pts',(-259.857849473896,3.17366342871357,
126.795179433485));
#256335=CARTESIAN_POINT('Ctrl Pts',(-259.9506752748,1.64266665146648,126.102093112095));
#256336=CARTESIAN_POINT('Ctrl Pts',(-259.997093138402,0.835778587061721,
125.962806053044));
#256337=CARTESIAN_POINT('Ctrl Pts',(210.385579563201,-2.29217962691353,
126.082387726892));
#256338=CARTESIAN_POINT('Ctrl Pts',(210.339169886847,-3.0789974560272,126.464330840008));
#256339=CARTESIAN_POINT('Ctrl Pts',(210.246352273192,-4.44507089109247,
127.629120819077));
#256340=CARTESIAN_POINT('Ctrl Pts',(210.060718784933,-5.78798125627161,
130.996088365878));
#256341=CARTESIAN_POINT('Ctrl Pts',(209.828679098422,-3.95783017776954,
135.586872998689));
#256342=CARTESIAN_POINT('Ctrl Pts',(209.550231474609,1.89393692750204,136.720289837399));
#256343=CARTESIAN_POINT('Ctrl Pts',(209.271783850796,5.99602695027556,132.40812259401));
#256344=CARTESIAN_POINT('Ctrl Pts',(208.993336226983,4.59288360023261,126.626877830413));
#256345=CARTESIAN_POINT('Ctrl Pts',(208.71488860317,-1.03344059257722,124.682062423228));
#256346=CARTESIAN_POINT('Ctrl Pts',(208.436440979357,-5.70873650289865,
128.364647771496));
#256347=CARTESIAN_POINT('Ctrl Pts',(208.157993355544,-5.13869562717284,
134.288517668348));
#256348=CARTESIAN_POINT('Ctrl Pts',(207.879545731732,0.153933173725622,
137.010984097728));
#256349=CARTESIAN_POINT('Ctrl Pts',(207.601098107919,5.30490488755997,134.029672582798));
#256350=CARTESIAN_POINT('Ctrl Pts',(207.322650484106,5.58103410012833,128.084559773234));
#256351=CARTESIAN_POINT('Ctrl Pts',(207.044202860293,0.728409521696789,
124.638756607567));
#256352=CARTESIAN_POINT('Ctrl Pts',(206.76575523648,-4.79355811073501,126.858871164077));
#256353=CARTESIAN_POINT('Ctrl Pts',(206.487307612667,-5.91049575314416,
132.704682504842));
#256354=CARTESIAN_POINT('Ctrl Pts',(206.208859988854,-1.59596820864792,
136.804198957117));
#256355=CARTESIAN_POINT('Ctrl Pts',(205.930412365042,4.1851717387407,135.390152799229));
#256356=CARTESIAN_POINT('Ctrl Pts',(205.651964741228,6.12034565262566,129.76198992389));
#256357=CARTESIAN_POINT('Ctrl Pts',(205.373517117416,2.43121966936229,125.091713591677));
#256358=CARTESIAN_POINT('Ctrl Pts',(205.095069493603,-3.49207776276838,
125.671081434371));
#256359=CARTESIAN_POINT('Ctrl Pts',(204.81662186979,-6.20632667560231,130.96768173473));
#256360=CARTESIAN_POINT('Ctrl Pts',(204.538174245977,-3.21726438559061,
136.114198085604));
#256361=CARTESIAN_POINT('Ctrl Pts',(204.259726622164,2.72830660529182,136.381233108793));
#256362=CARTESIAN_POINT('Ctrl Pts',(203.981278998351,6.16669716267351,131.523394807979));
#256363=CARTESIAN_POINT('Ctrl Pts',(203.702831374538,3.9381942601484,126.004799186432));
#256364=CARTESIAN_POINT('Ctrl Pts',(203.424383750725,-1.909316761502,124.896766062528));
#256365=CARTESIAN_POINT('Ctrl Pts',(203.145936126912,-6.00225896230248,
129.217523725228));
#256366=CARTESIAN_POINT('Ctrl Pts',(202.867488503099,-4.57941839934143,
134.996506974633));
#256367=CARTESIAN_POINT('Ctrl Pts',(202.589040879287,1.05168395343957,136.923112517541));
#256368=CARTESIAN_POINT('Ctrl Pts',(202.310593255474,5.71634013176502,133.226883983125));
#256369=CARTESIAN_POINT('Ctrl Pts',(202.032145631661,5.12795898713612,127.30447482202));
#256370=CARTESIAN_POINT('Ctrl Pts',(201.753698007848,-0.172765951628197,
124.598289728405));
#256371=CARTESIAN_POINT('Ctrl Pts',(201.475250384035,-5.31472742110118,
127.595180598346));
#256372=CARTESIAN_POINT('Ctrl Pts',(201.196802760222,-5.57271402936141,
133.541151128878));
#256373=CARTESIAN_POINT('Ctrl Pts',(200.918355136409,-0.709648686901125,
136.972144879116));
#256374=CARTESIAN_POINT('Ctrl Pts',(200.639907512596,4.80554913058071,134.735246206027));
#256375=CARTESIAN_POINT('Ctrl Pts',(200.361459888783,5.90468206117194,128.886055711564));
#256376=CARTESIAN_POINT('Ctrl Pts',(200.083012264971,1.57770063730838,124.799693711321));
#256377=CARTESIAN_POINT('Ctrl Pts',(199.804564641158,-4.19911059728431,
126.231327253625));
#256378=CARTESIAN_POINT('Ctrl Pts',(199.526117017345,-6.11714433092778,
131.865355052293));
#256379=CARTESIAN_POINT('Ctrl Pts',(199.247669393532,-2.4138212635637,136.524380797905));
#256380=CARTESIAN_POINT('Ctrl Pts',(198.969221769719,3.50768562329156,135.926987436306));
#256381=CARTESIAN_POINT('Ctrl Pts',(198.690774145906,6.20580078231077,130.622150282517));
#256382=CARTESIAN_POINT('Ctrl Pts',(198.412326522093,3.20108819260905,125.484755525167));
#256383=CARTESIAN_POINT('Ctrl Pts',(198.13387889828,-2.74526806424844,125.235817970576));
#256384=CARTESIAN_POINT('Ctrl Pts',(197.855431274468,-6.16885708386238,
130.104099070135));
#256385=CARTESIAN_POINT('Ctrl Pts',(197.576983650655,-3.92356780882929,
135.615886322105));
#256386=CARTESIAN_POINT('Ctrl Pts',(197.298536026841,1.92728860557448,136.706116507701));
#256387=CARTESIAN_POINT('Ctrl Pts',(197.020088403029,6.00706094473797,132.372921347066));
#256388=CARTESIAN_POINT('Ctrl Pts',(196.741640779216,4.56663773692898,126.598295504472));
#256389=CARTESIAN_POINT('Ctrl Pts',(196.463193155403,-1.07030245846182,
124.688838023107));
#256390=CARTESIAN_POINT('Ctrl Pts',(196.184745531591,-5.72368698170812,
128.399247046161));
#256391=CARTESIAN_POINT('Ctrl Pts',(195.906297907777,-5.11728278641862,
134.319837945007));
#256392=CARTESIAN_POINT('Ctrl Pts',(195.627850283965,0.191654296427489,
137.009876920548));
#256393=CARTESIAN_POINT('Ctrl Pts',(195.349402660151,5.32447044368961,133.997349569974));
#256394=CARTESIAN_POINT('Ctrl Pts',(195.070955036339,5.56435836804288,128.050621358318));
#256395=CARTESIAN_POINT('Ctrl Pts',(194.792507412526,0.690872786183208,
124.634444998269));
#256396=CARTESIAN_POINT('Ctrl Pts',(194.514059788713,-4.81749113516689,
126.888119675218));
#256397=CARTESIAN_POINT('Ctrl Pts',(194.2356121649,-5.89881605082435,132.740628459178));
#256398=CARTESIAN_POINT('Ctrl Pts',(193.957164541087,-1.55941718895885,
136.81380168864));
#256399=CARTESIAN_POINT('Ctrl Pts',(193.678716917274,4.21300988779493,135.364592151301));
#256400=CARTESIAN_POINT('Ctrl Pts',(193.400269293461,6.11388669464029,129.724752614155));
#256401=CARTESIAN_POINT('Ctrl Pts',(193.121821669648,2.39640030908087,125.077020090361));
#256402=CARTESIAN_POINT('Ctrl Pts',(192.843374045836,-3.52326088986039,
125.692433714928));
#256403=CARTESIAN_POINT('Ctrl Pts',(192.564926422022,-6.20521745188322,
131.005458431507));
#256404=CARTESIAN_POINT('Ctrl Pts',(192.28647879821,-3.1848823173506,136.133684081248));
#256405=CARTESIAN_POINT('Ctrl Pts',(192.008031174397,2.76220407667619,136.36452181979));
#256406=CARTESIAN_POINT('Ctrl Pts',(191.729583550584,6.17095986540858,131.485843042463));
#256407=CARTESIAN_POINT('Ctrl Pts',(191.451135926771,3.90890500597959,125.980915208923));
#256408=CARTESIAN_POINT('Ctrl Pts',(191.172688302958,-1.94524259331895,
124.908498067517));
#256409=CARTESIAN_POINT('Ctrl Pts',(190.894240679145,-6.01180727974115,
129.254090580708));
#256410=CARTESIAN_POINT('Ctrl Pts',(190.615793055332,-4.5538147691942,135.024305522869));
#256411=CARTESIAN_POINT('Ctrl Pts',(190.337345431519,1.08891104802307,136.916597252826));
#256412=CARTESIAN_POINT('Ctrl Pts',(190.058897807707,5.73098080836918,133.192042114338));
#256413=CARTESIAN_POINT('Ctrl Pts',(189.780450183893,5.10655917980125,127.273324325042));
#256414=CARTESIAN_POINT('Ctrl Pts',(189.502002560081,-0.210540865719208,
124.599456387862));
#256415=CARTESIAN_POINT('Ctrl Pts',(189.223554936268,-5.33416414113684,
127.627592311355));
#256416=CARTESIAN_POINT('Ctrl Pts',(188.945107312455,-5.55595115925501,
133.575023114497));
#256417=CARTESIAN_POINT('Ctrl Pts',(188.666659688642,-0.672090485321342,
136.976350437346));
#256418=CARTESIAN_POINT('Ctrl Pts',(188.388212064829,4.82938851117716,134.705920634282));
#256419=CARTESIAN_POINT('Ctrl Pts',(188.109764441016,5.89289539464864,128.850147777659));
#256420=CARTESIAN_POINT('Ctrl Pts',(187.831316817203,1.54111929438253,124.790201052305));
#256421=CARTESIAN_POINT('Ctrl Pts',(187.552869193391,-4.22687014955807,
126.256973159398));
#256422=CARTESIAN_POINT('Ctrl Pts',(187.274421569578,-6.11057242014135,
131.902572188318));
#256423=CARTESIAN_POINT('Ctrl Pts',(186.995973945765,-2.37895715467313,
136.538968434335));
#256424=CARTESIAN_POINT('Ctrl Pts',(186.717526321952,3.53880351742172,135.905540247907));
#256425=CARTESIAN_POINT('Ctrl Pts',(186.439078698139,6.20457663716883,130.584377187674));
#256426=CARTESIAN_POINT('Ctrl Pts',(186.160631074326,3.16864693777749,125.465368152723));
#256427=CARTESIAN_POINT('Ctrl Pts',(185.882183450513,-2.77911450042273,
125.25263236868));
#256428=CARTESIAN_POINT('Ctrl Pts',(185.6037358267,-6.17300548002561,130.14166362836));
#256429=CARTESIAN_POINT('Ctrl Pts',(185.325288202887,-3.89420599156785,
135.639681046572));
#256430=CARTESIAN_POINT('Ctrl Pts',(185.046840579075,1.96317856060187,136.694275209062));
#256431=CARTESIAN_POINT('Ctrl Pts',(184.768392955261,6.0164979221829,132.336325600291));
#256432=CARTESIAN_POINT('Ctrl Pts',(184.489945331449,4.54094961554151,126.570575013045));
#256433=CARTESIAN_POINT('Ctrl Pts',(184.211497707636,-1.10750955006109,
124.695466564429));
#256434=CARTESIAN_POINT('Ctrl Pts',(183.933050083823,-5.73822154400692,
128.434133314579));
#256435=CARTESIAN_POINT('Ctrl Pts',(183.65460246001,-5.09578826671723,134.350923164133));
#256436=CARTESIAN_POINT('Ctrl Pts',(183.376154836197,0.229425484589131,
137.008595292604));
#256437=CARTESIAN_POINT('Ctrl Pts',(183.097707212384,5.34380842361613,133.964878848429));
#256438=CARTESIAN_POINT('Ctrl Pts',(182.819259588571,5.54749248089459,128.016800549989));
#256439=CARTESIAN_POINT('Ctrl Pts',(182.540811964758,0.653301958305029,
124.630353773773));
#256440=CARTESIAN_POINT('Ctrl Pts',(182.262364340946,-4.84124114839195,
126.917517669999));
#256441=CARTESIAN_POINT('Ctrl Pts',(181.983916717133,-5.88692014749505,
132.776500352206));
#256442=CARTESIAN_POINT('Ctrl Pts',(181.70546909332,-1.52280712308763,136.82318296266));
#256443=CARTESIAN_POINT('Ctrl Pts',(181.427021469507,4.24069125417353,135.33886187379));
#256444=CARTESIAN_POINT('Ctrl Pts',(181.148573845694,6.10720153813428,129.687555653153));
#256445=CARTESIAN_POINT('Ctrl Pts',(180.870126221881,2.36149196193127,125.062538635854));
#256446=CARTESIAN_POINT('Ctrl Pts',(180.591678598068,-3.55431336199069,
125.713975516152));
#256447=CARTESIAN_POINT('Ctrl Pts',(180.313230974255,-6.20387834410407,
131.04322762551));
#256448=CARTESIAN_POINT('Ctrl Pts',(180.034783350442,-3.15238220429199,
136.15297262387));
#256449=CARTESIAN_POINT('Ctrl Pts',(179.75633572663,2.79599917883219,136.347604482659));
#256450=CARTESIAN_POINT('Ctrl Pts',(179.477888102817,6.17499390876314,131.448266031944));
#256451=CARTESIAN_POINT('Ctrl Pts',(179.199440479004,3.8794709017638,125.957209961944));
#256452=CARTESIAN_POINT('Ctrl Pts',(178.920992855191,-1.98109634126673,
124.920448547985));
#256453=CARTESIAN_POINT('Ctrl Pts',(178.642545231378,-6.02113282860982,
129.290714880887));
#256454=CARTESIAN_POINT('Ctrl Pts',(178.364097607565,-4.52804239515191,
135.051947700091));
#256455=CARTESIAN_POINT('Ctrl Pts',(178.085649983752,1.12609779228193,136.909855496619));
#256456=CARTESIAN_POINT('Ctrl Pts',(177.807202359939,5.74540912154417,133.157111769304));
#256457=CARTESIAN_POINT('Ctrl Pts',(177.528754736127,5.08497014694685,127.242304671825));
#256458=CARTESIAN_POINT('Ctrl Pts',(177.250307112313,-0.248307978092709,
124.600852972375));
#256459=CARTESIAN_POINT('Ctrl Pts',(176.971859488501,-5.35340320178418,
127.660121740658));
#256460=CARTESIAN_POINT('Ctrl Pts',(176.693411864688,-5.53898241132168,
133.608792432211));
#256461=CARTESIAN_POINT('Ctrl Pts',(176.414964240875,-0.634507379188621,
136.980327290216));
#256462=CARTESIAN_POINT('Ctrl Pts',(176.136516617062,4.85304893701009,134.676450488799));
#256463=CARTESIAN_POINT('Ctrl Pts',(175.858068993249,5.88089036471739,128.814312257825));
#256464=CARTESIAN_POINT('Ctrl Pts',(175.579621369436,1.50448084471559,124.780931250186));
#256465=CARTESIAN_POINT('Ctrl Pts',(175.301173745623,-4.25447307360455,
126.282787570284));
#256466=CARTESIAN_POINT('Ctrl Pts',(175.02272612181,-6.10377407984646,131.939748629711));
#256467=CARTESIAN_POINT('Ctrl Pts',(174.744278497998,-2.34400489265046,
136.553343572764));
#256468=CARTESIAN_POINT('Ctrl Pts',(174.465830874185,3.56979027988629,135.883904033421));
#256469=CARTESIAN_POINT('Ctrl Pts',(174.187383250372,6.20312257915782,130.546612244398));
#256470=CARTESIAN_POINT('Ctrl Pts',(173.908935626559,3.13608826756835,125.446178618609));
#256471=CARTESIAN_POINT('Ctrl Pts',(173.630488002746,-2.81285795548731,
125.269652488117));
#256472=CARTESIAN_POINT('Ctrl Pts',(173.352040378933,-6.17692513320066,
130.179252743065));
#256473=CARTESIAN_POINT('Ctrl Pts',(173.07359275512,-3.86469987307124,135.663296596462));
#256474=CARTESIAN_POINT('Ctrl Pts',(172.795145131307,1.99899576932572,136.682215657471));
#256475=CARTESIAN_POINT('Ctrl Pts',(172.516697507494,6.02571195608475,132.29967308599));
#256476=CARTESIAN_POINT('Ctrl Pts',(172.238249883681,4.51509322759614,126.543011406101));
#256477=CARTESIAN_POINT('Ctrl Pts',(171.959802259869,-1.14467560248665,
124.702321473066));
#256478=CARTESIAN_POINT('Ctrl Pts',(171.681354636056,-5.75254347439624,
128.469107412642));
#256479=CARTESIAN_POINT('Ctrl Pts',(171.402907012243,-5.07410492070761,
134.38187696408));
#256480=CARTESIAN_POINT('Ctrl Pts',(171.12445938843,0.267188171305193,137.007083764462));
#256481=CARTESIAN_POINT('Ctrl Pts',(170.846011764617,5.36294838675633,133.932291012718));
#256482=CARTESIAN_POINT('Ctrl Pts',(170.567564140804,5.53042102937231,127.983083035723));
#256483=CARTESIAN_POINT('Ctrl Pts',(170.289116516991,0.615706922082464,
124.62649132937));
#256484=CARTESIAN_POINT('Ctrl Pts',(170.010668893178,-4.86481176764585,
126.947059693175));
#256485=CARTESIAN_POINT('Ctrl Pts',(169.732221269365,-5.87480610217478,
132.812299166869));
#256486=CARTESIAN_POINT('Ctrl Pts',(169.453773645553,-1.48614062903852,
136.832341207004));
#256487=CARTESIAN_POINT('Ctrl Pts',(169.17532602174,4.26821548017818,135.312963568669));
#256488=CARTESIAN_POINT('Ctrl Pts',(168.896878397927,6.10029007702938,129.650400075769));
#256489=CARTESIAN_POINT('Ctrl Pts',(168.618430774114,2.32649610882855,125.048269946673));
#256490=CARTESIAN_POINT('Ctrl Pts',(168.339983150301,-3.58523412773234,
125.735705943466));
#256491=CARTESIAN_POINT('Ctrl Pts',(168.061535526488,-6.2023093493314,131.08098796821));
#256492=CARTESIAN_POINT('Ctrl Pts',(167.783087902675,-3.11976527855146,
136.172062971709));
#256493=CARTESIAN_POINT('Ctrl Pts',(167.504640278862,2.82969067421049,136.330481738588));
#256494=CARTESIAN_POINT('Ctrl Pts',(167.22619265505,6.17879913544756,131.410665161273));
#256495=CARTESIAN_POINT('Ctrl Pts',(166.947745031236,3.84989304232704,125.933684327914));
#256496=CARTESIAN_POINT('Ctrl Pts',(166.669297407424,-2.01687667896098,
124.93261705898));
#256497=CARTESIAN_POINT('Ctrl Pts',(166.39084978361,-6.03023526218728,129.327395269766));
#256498=CARTESIAN_POINT('Ctrl Pts',(166.112402159798,-4.50210223283349,
135.079432481411));
#256499=CARTESIAN_POINT('Ctrl Pts',(165.833954535985,1.16324280857304,136.902887499053));
#256500=CARTESIAN_POINT('Ctrl Pts',(165.555506912173,5.75962453647134,133.122094242209));
#256501=CARTESIAN_POINT('Ctrl Pts',(165.277059288359,5.06319268865361,127.2114170119));
#256502=CARTESIAN_POINT('Ctrl Pts',(164.998611664547,-0.286065889322858,
124.602479430144));
#256503=CARTESIAN_POINT('Ctrl Pts',(164.720164040733,-5.37244389010723,
127.692767680889));
#256504=CARTESIAN_POINT('Ctrl Pts',(164.441716416921,-5.52180841435808,
133.642457830674));
#256505=CARTESIAN_POINT('Ctrl Pts',(164.163268793108,-0.596900761151562,
136.984075290369));
#256506=CARTESIAN_POINT('Ctrl Pts',(163.884821169295,4.87652953132996,134.646836861603));
#256507=CARTESIAN_POINT('Ctrl Pts',(163.606373545482,5.86866741623098,128.778550479967));
#256508=CARTESIAN_POINT('Ctrl Pts',(163.327925921669,1.46778664595768,124.771884648456));
#256509=CARTESIAN_POINT('Ctrl Pts',(163.049478297856,-4.28191834658676,
126.308769529723));
#256510=CARTESIAN_POINT('Ctrl Pts',(162.771030674043,-6.09674956195837,
131.976882998882));
#256511=CARTESIAN_POINT('Ctrl Pts',(162.49258305023,-2.30896577266445,136.567505680515));
#256512=CARTESIAN_POINT('Ctrl Pts',(162.214135426418,3.60064476245918,135.862079594585));
#256513=CARTESIAN_POINT('Ctrl Pts',(161.935687802605,6.20143866215845,130.508856852083));
#256514=CARTESIAN_POINT('Ctrl Pts',(161.657240178792,3.10341338845521,125.427187633898));
#256515=CARTESIAN_POINT('Ctrl Pts',(161.378792554979,-2.84649717906582,
125.2868776982));
#256516=CARTESIAN_POINT('Ctrl Pts',(161.100344931166,-6.18061589814333,
130.216865021372));
#256517=CARTESIAN_POINT('Ctrl Pts',(160.821897307353,-3.83505054669964,
135.686732096692));
#256518=CARTESIAN_POINT('Ctrl Pts',(160.54344968354,2.0347389045262,136.6699382998));
#256519=CARTESIAN_POINT('Ctrl Pts',(160.265002059727,6.03470270501411,132.262965162335));
#256520=CARTESIAN_POINT('Ctrl Pts',(159.986554435914,4.48906953121078,126.51560570502));
#256521=CARTESIAN_POINT('Ctrl Pts',(159.708106812101,-1.18179923853688,
124.709402495009));
#256522=CARTESIAN_POINT('Ctrl Pts',(159.429659188289,-5.76665224217155,
128.50416804437));
#256523=CARTESIAN_POINT('Ctrl Pts',(159.151211564475,-5.05223355187421,
134.412698197843));
#256524=CARTESIAN_POINT('Ctrl Pts',(158.872763940663,0.304940957265202,
137.005342392132));
#256525=CARTESIAN_POINT('Ctrl Pts',(158.59431631685,5.38188962387183,133.899587270395));
#256526=CARTESIAN_POINT('Ctrl Pts',(158.315868693037,5.51314464606502,127.949470064936));
#256527=CARTESIAN_POINT('Ctrl Pts',(158.037421069224,0.57808907061355,124.622857808186));
#256528=CARTESIAN_POINT('Ctrl Pts',(157.758973445411,-4.88820211951067,
126.976744650055));
#256529=CARTESIAN_POINT('Ctrl Pts',(157.480525821598,-5.86247436375394,
132.848023576631));
#256530=CARTESIAN_POINT('Ctrl Pts',(157.202078197785,-1.44941906550188,
136.841276082311));
#256531=CARTESIAN_POINT('Ctrl Pts',(156.923630573973,4.29558154588865,135.286898195607));
#256532=CARTESIAN_POINT('Ctrl Pts',(156.645182950159,6.09315256743229,129.613287258817));
#256533=CARTESIAN_POINT('Ctrl Pts',(156.366735326347,2.29141404655692,125.034214551549));
#256534=CARTESIAN_POINT('Ctrl Pts',(156.088287702534,-3.61602204130483,
125.757624191644));
#256535=CARTESIAN_POINT('Ctrl Pts',(155.809840078721,-6.2005105257049,131.11873806038));
#256536=CARTESIAN_POINT('Ctrl Pts',(155.531392454908,-3.08703274876129,
136.190954417361));
#256537=CARTESIAN_POINT('Ctrl Pts',(155.252944831095,2.86327731436015,136.313154222067));
#256538=CARTESIAN_POINT('Ctrl Pts',(154.974497207282,6.18237540445775,131.373041823765));
#256539=CARTESIAN_POINT('Ctrl Pts',(154.696049583469,3.82017252368788,125.910339178587));
#256540=CARTESIAN_POINT('Ctrl Pts',(154.417601959656,-2.05258228054818,
124.945003149591));
#256541=CARTESIAN_POINT('Ctrl Pts',(154.139154335844,-6.03911424317947,
129.364130388138));
#256542=CARTESIAN_POINT('Ctrl Pts',(153.860706712031,-4.47599524346119,
135.106758848372));
#256543=CARTESIAN_POINT('Ctrl Pts',(153.582259088218,1.20034472047403,136.895693518332));
#256544=CARTESIAN_POINT('Ctrl Pts',(153.303811464405,5.77362652639317,133.086990830643));
#256545=CARTESIAN_POINT('Ctrl Pts',(153.025363840592,5.04122761189337,127.180662489822));
#256546=CARTESIAN_POINT('Ctrl Pts',(152.746916216779,-0.323813200276178,
124.604335700902));
#256547=CARTESIAN_POINT('Ctrl Pts',(152.468468592966,-5.39128550054617,
127.725528922339));
#256548=CARTESIAN_POINT('Ctrl Pts',(152.190020969154,-5.5044298047531,133.6760180624));
#256549=CARTESIAN_POINT('Ctrl Pts',(151.91157334534,-0.55927202473736,136.987594298923));
#256550=CARTESIAN_POINT('Ctrl Pts',(151.633125721528,4.89982942405471,134.617080850036));
#256551=CARTESIAN_POINT('Ctrl Pts',(151.354678097715,5.85622700211526,128.742863769248));
#256552=CARTESIAN_POINT('Ctrl Pts',(151.076230473902,1.43103805782584,124.763061582343));
#256553=CARTESIAN_POINT('Ctrl Pts',(150.797782850089,-4.3092049515099,126.334918074943));
#256554=CARTESIAN_POINT('Ctrl Pts',(150.519335226276,-6.0894991267732,132.013973919806));
#256555=CARTESIAN_POINT('Ctrl Pts',(150.240887602463,-2.27384109310269,
136.581454232806));
#256556=CARTESIAN_POINT('Ctrl Pts',(149.96243997865,3.63136582181627,135.840067740113));
#256557=CARTESIAN_POINT('Ctrl Pts',(149.683992354837,6.19952494856889,130.471112409769));
#256558=CARTESIAN_POINT('Ctrl Pts',(149.405544731024,3.0706235112177,125.40839590231));
#256559=CARTESIAN_POINT('Ctrl Pts',(149.127097107212,-2.88003092464457,
125.30430736064));
#256560=CARTESIAN_POINT('Ctrl Pts',(148.848649483398,-6.18407763809098,
130.254499069545));
#256561=CARTESIAN_POINT('Ctrl Pts',(148.570201859586,-3.80525911111971,
135.709986678852));
#256562=CARTESIAN_POINT('Ctrl Pts',(148.291754235773,2.07040664172831,136.657443590992));
#256563=CARTESIAN_POINT('Ctrl Pts',(148.01330661196,6.04346983581547,132.226203189553));
#256564=CARTESIAN_POINT('Ctrl Pts',(147.734858988147,4.46287949070312,126.488358925329));
#256565=CARTESIAN_POINT('Ctrl Pts',(147.456411364334,-1.21887908258166,
124.716709367866));
#256566=CARTESIAN_POINT('Ctrl Pts',(147.177963740522,-5.78054732452736,
128.53931391058));
#256567=CARTESIAN_POINT('Ctrl Pts',(146.899516116708,-5.03017497066859,
134.44338572333));
#256568=CARTESIAN_POINT('Ctrl Pts',(146.621068492896,0.342682443525903,
137.003371240143));
#256569=CARTESIAN_POINT('Ctrl Pts',(146.342620869082,5.40063143308812,133.866768833311));
#256570=CARTESIAN_POINT('Ctrl Pts',(146.06417324527,5.49566397115542,127.915962883168));
#256571=CARTESIAN_POINT('Ctrl Pts',(145.785725621457,0.540449797841529,
124.619453344862));
#256572=CARTESIAN_POINT('Ctrl Pts',(145.507277997644,-4.91141133724831,
127.006571440652));
#256573=CARTESIAN_POINT('Ctrl Pts',(145.228830373831,-5.84992538918966,
132.883672257711));
#256574=CARTESIAN_POINT('Ctrl Pts',(144.950382750018,-1.41264379320865,
136.849987257496));
#256575=CARTESIAN_POINT('Ctrl Pts',(144.671935126205,4.32278843724517,135.260666720466));
#256576=CARTESIAN_POINT('Ctrl Pts',(144.393487502392,6.08578927382608,129.576218577526));
#256577=CARTESIAN_POINT('Ctrl Pts',(144.11503987858,2.25624707509518,125.020372971309));
#256578=CARTESIAN_POINT('Ctrl Pts',(143.836592254767,-3.64667596185081,
125.779729448496));
#256579=CARTESIAN_POINT('Ctrl Pts',(143.558144630954,-6.19848193988065,
131.156476503179));
#256580=CARTESIAN_POINT('Ctrl Pts',(143.279697007141,-3.05418582783736,
136.209646260801));
#256581=CARTESIAN_POINT('Ctrl Pts',(143.001249383328,2.89675785471595,136.295622575173));
#256582=CARTESIAN_POINT('Ctrl Pts',(142.722801759515,6.18572258327378,131.335397413564));
#256583=CARTESIAN_POINT('Ctrl Pts',(142.444354135702,3.79031044715096,125.887175379022));
#256584=CARTESIAN_POINT('Ctrl Pts',(142.165906511889,-2.0882118229442,124.957606360848));
#256585=CARTESIAN_POINT('Ctrl Pts',(141.887458888076,-6.04776944257254,
129.400918874772));
#256586=CARTESIAN_POINT('Ctrl Pts',(141.609011264264,-4.44972239443904,
135.133925788383));
#256587=CARTESIAN_POINT('Ctrl Pts',(141.33056364045,1.2374021531599,136.888273821029));
#256588=CARTESIAN_POINT('Ctrl Pts',(141.052116016638,5.78741457246075,133.051802835376));
#256589=CARTESIAN_POINT('Ctrl Pts',(140.773668392825,5.01907573059014,127.15004224521));
#256590=CARTESIAN_POINT('Ctrl Pts',(140.495220769012,-0.361548512212229,
124.606421715863));
#256591=CARTESIAN_POINT('Ctrl Pts',(140.216773145199,-5.4099273349182,127.758404251031));
#256592=CARTESIAN_POINT('Ctrl Pts',(139.938325521386,-5.48684722647749,
133.709471883804));
#256593=CARTESIAN_POINT('Ctrl Pts',(139.659877897573,-0.521622564292735,
136.990884185479));
#256594=CARTESIAN_POINT('Ctrl Pts',(139.38143027376,4.92294775179823,134.58718355672));
#256595=CARTESIAN_POINT('Ctrl Pts',(139.102982649947,5.84356958335437,128.707253448052));
#256596=CARTESIAN_POINT('Ctrl Pts',(138.824535026135,1.39423644205237,124.754462378786));
#256597=CARTESIAN_POINT('Ctrl Pts',(138.546087402322,-4.33633187725888,
126.361232236999));
#256598=CARTESIAN_POINT('Ctrl Pts',(138.267639778509,-6.08202304295846,
132.051020018064));
#256599=CARTESIAN_POINT('Ctrl Pts',(137.989192154696,-2.23863215552307,
136.595188712768));
#256600=CARTESIAN_POINT('Ctrl Pts',(137.710744530883,3.66195231957746,135.817869285661));
#256601=CARTESIAN_POINT('Ctrl Pts',(137.43229690707,6.19738150930245,130.433380316089));
#256602=CARTESIAN_POINT('Ctrl Pts',(137.153849283257,3.03771985089675,125.389804120178));
#256603=CARTESIAN_POINT('Ctrl Pts',(136.875401659444,-2.91345794961824,
125.321940829576));
#256604=CARTESIAN_POINT('Ctrl Pts',(136.596954035631,-6.1873102247676,130.29215349304));
#256605=CARTESIAN_POINT('Ctrl Pts',(136.318506411819,-3.77532667026395,
135.733059481234));
#256606=CARTESIAN_POINT('Ctrl Pts',(136.040058788006,2.10599765925102,136.644731994041));
#256607=CARTESIAN_POINT('Ctrl Pts',(135.761611164193,6.05201302361958,132.189388529871));
#256608=CARTESIAN_POINT('Ctrl Pts',(135.48316354038,4.4365240765547,126.461272076668));
#256609=CARTESIAN_POINT('Ctrl Pts',(135.204715916567,-1.25591376061384,
124.724241820878));
#256610=CARTESIAN_POINT('Ctrl Pts',(134.926268292754,-5.79422820657625,
128.574543708929));
#256611=CARTESIAN_POINT('Ctrl Pts',(134.647820668941,-5.00792999447956,
134.473938403405));
#256612=CARTESIAN_POINT('Ctrl Pts',(134.369373045128,0.380411231562576,
137.001170381535));
#256613=CARTESIAN_POINT('Ctrl Pts',(134.090925421316,5.41917311992063,133.833836917565));
#256614=CARTESIAN_POINT('Ctrl Pts',(133.812477797503,5.4779796523963,127.88256273204));
#256615=CARTESIAN_POINT('Ctrl Pts',(133.53403017369,0.502790498503515,124.616278065551));
#256616=CARTESIAN_POINT('Ctrl Pts',(133.255582549877,-4.93443856083268,
127.036538959725));
#256617=CARTESIAN_POINT('Ctrl Pts',(132.977134926064,-5.83715964348875,
132.919243889133));
#256618=CARTESIAN_POINT('Ctrl Pts',(132.698687302251,-1.37581617488021,
136.858474409763));
#256619=CARTESIAN_POINT('Ctrl Pts',(132.420239678438,4.34983514608645,135.234270115264));
#256620=CARTESIAN_POINT('Ctrl Pts',(132.141792054625,6.07820046906025,129.539195405491));
#256621=CARTESIAN_POINT('Ctrl Pts',(131.863344430812,2.22099649756843,125.006745718858));
#256622=CARTESIAN_POINT('Ctrl Pts',(131.584896806999,-3.67719475347803,
125.802020894903));
#256623=CARTESIAN_POINT('Ctrl Pts',(131.306449183186,-6.1962236670286,131.194201898194));
#256624=CARTESIAN_POINT('Ctrl Pts',(131.028001559374,-3.02122573293442,
136.228137809392));
#256625=CARTESIAN_POINT('Ctrl Pts',(130.749553935561,2.93013105464412,136.277887447547));
#256626=CARTESIAN_POINT('Ctrl Pts',(130.471106311748,6.18884054786473,131.2977333256));
#256627=CARTESIAN_POINT('Ctrl Pts',(130.192658687935,3.76030791926647,125.864193787566));
#256628=CARTESIAN_POINT('Ctrl Pts',(129.914211064122,-2.12376398588317,
124.970426225734));
#256629=CARTESIAN_POINT('Ctrl Pts',(129.635763440309,-6.05620053964477,
129.437759366456));
#256630=CARTESIAN_POINT('Ctrl Pts',(129.357315816496,-4.42328465931731,
135.160932294765));
#256631=CARTESIAN_POINT('Ctrl Pts',(129.078868192683,1.27441373345414,136.880628682086));
#256632=CARTESIAN_POINT('Ctrl Pts',(128.800420568871,5.80098816375315,133.01653156031));
#256633=CARTESIAN_POINT('Ctrl Pts',(128.521972945058,4.99673786558976,127.11955741271));
#256634=CARTESIAN_POINT('Ctrl Pts',(128.243525321245,-0.399270426835251,
124.608737397728));
#256635=CARTESIAN_POINT('Ctrl Pts',(127.965077697432,-5.42836870244348,
127.791392448756));
#256636=CARTESIAN_POINT('Ctrl Pts',(127.686630073619,-5.46906133106002,
133.742818055242));
#256637=CARTESIAN_POINT('Ctrl Pts',(127.408182449806,-0.483953774931917,
136.993944828129));
#256638=CARTESIAN_POINT('Ctrl Pts',(127.129734825993,4.9458836579024,134.557146089508));
#256639=CARTESIAN_POINT('Ctrl Pts',(126.85128720218,5.8306956289736,128.671720835934));
#256640=CARTESIAN_POINT('Ctrl Pts',(126.572839578367,1.35738316233494,124.746087356435));
#256641=CARTESIAN_POINT('Ctrl Pts',(126.294391954555,-4.36329811863544,
126.387711040812));
#256642=CARTESIAN_POINT('Ctrl Pts',(126.015944330741,-6.07432158754323,
132.088019920899));
#256643=CARTESIAN_POINT('Ctrl Pts',(125.737496706929,-2.20334026460562,
136.608708611466));
#256644=CARTESIAN_POINT('Ctrl Pts',(125.459049083116,3.69240312234872,135.795485053802));
#256645=CARTESIAN_POINT('Ctrl Pts',(125.180601459303,6.19500842378515,130.39566196922));
#256646=CARTESIAN_POINT('Ctrl Pts',(124.90215383549,3.00470362674961,125.371412976429));
#256647=CARTESIAN_POINT('Ctrl Pts',(124.623706211677,-2.9467770153362,125.339777451594));
#256648=CARTESIAN_POINT('Ctrl Pts',(124.345258587864,-6.19031353838844,
130.329826896558));
#256649=CARTESIAN_POINT('Ctrl Pts',(124.066810964051,-3.74525433329013,
135.755949648866));
#256650=CARTESIAN_POINT('Ctrl Pts',(123.788363340238,2.14151063825588,136.631803979981));
#256651=CARTESIAN_POINT('Ctrl Pts',(123.509915716426,6.0603319518555,132.152522547471));
#256652=CARTESIAN_POINT('Ctrl Pts',(123.231468092613,4.4100042653751,126.43434616275));
#256653=CARTESIAN_POINT('Ctrl Pts',(122.9530204688,-1.29290190029971,124.731999574929));
#256654=CARTESIAN_POINT('Ctrl Pts',(122.674572844987,-5.80769438136815,
128.609856133963));
#256655=CARTESIAN_POINT('Ctrl Pts',(122.396125221174,-4.98549944760296,
134.504355105923));
#256656=CARTESIAN_POINT('Ctrl Pts',(122.117677597361,0.418125923321227,
136.998739897863));
#256657=CARTESIAN_POINT('Ctrl Pts',(121.839229973548,5.43751399730024,133.80079274346));
#256658=CARTESIAN_POINT('Ctrl Pts',(121.560782349735,5.46009234508668,127.849270849208));
#256659=CARTESIAN_POINT('Ctrl Pts',(121.282334725922,0.465112568078527,
124.613332087916));
#256660=CARTESIAN_POINT('Ctrl Pts',(121.00388710211,-4.95728293698158,127.066646096814));
#256661=CARTESIAN_POINT('Ctrl Pts',(120.725439478297,-5.82417759969065,
132.954737152777));
#256662=CARTESIAN_POINT('Ctrl Pts',(120.446991854484,-1.33893757517749,
136.866737224615));
#256663=CARTESIAN_POINT('Ctrl Pts',(120.168544230671,4.37672067018674,135.207709358136));
#256664=CARTESIAN_POINT('Ctrl Pts',(119.890096606858,6.07038643434081,129.502219114618));
#256665=CARTESIAN_POINT('Ctrl Pts',(119.611648983045,2.18566362019961,124.993333299159));
#256666=CARTESIAN_POINT('Ctrl Pts',(119.333201359232,-3.7075772853013,125.82449770485));
#256667=CARTESIAN_POINT('Ctrl Pts',(119.054753735419,-6.19373579082994,
131.231912847497));
#256668=CARTESIAN_POINT('Ctrl Pts',(118.776306111606,-2.98815368540088,
136.246428377926));
#256669=CARTESIAN_POINT('Ctrl Pts',(118.497858487794,2.96339567748857,136.259949496373));
#256670=CARTESIAN_POINT('Ctrl Pts',(118.219410863981,6.1917291826932,131.26005095553));
#256671=CARTESIAN_POINT('Ctrl Pts',(117.940963240168,3.73016605178927,125.841395255808));
#256672=CARTESIAN_POINT('Ctrl Pts',(117.662515616355,-2.15923745196658,
124.983462269205));
#256673=CARTESIAN_POINT('Ctrl Pts',(117.384067992542,-6.06440722197891,
129.474650498052));
#256674=CARTESIAN_POINT('Ctrl Pts',(117.105620368729,-4.39668301775581,
135.187777366781));
#256675=CARTESIAN_POINT('Ctrl Pts',(116.827172744916,1.31137808987868,136.872758384795));
#256676=CARTESIAN_POINT('Ctrl Pts',(116.548725121103,5.81434679729579,132.981178312436));
#256677=CARTESIAN_POINT('Ctrl Pts',(116.27027749729,4.97421484463032,127.089209121948));
#256678=CARTESIAN_POINT('Ctrl Pts',(115.991829873478,-0.436977546345769,
124.611282660692));
#256679=CARTESIAN_POINT('Ctrl Pts',(115.713382249665,-5.44660891977013,
127.824492293124));
#256680=CARTESIAN_POINT('Ctrl Pts',(115.434934625852,-5.45107277756375,
133.776055341058));
#256681=CARTESIAN_POINT('Ctrl Pts',(115.156487002039,-0.446267052485976,
136.99677611346));
#256682=CARTESIAN_POINT('Ctrl Pts',(114.878039378226,4.9686362924688,134.526969561451));
#256683=CARTESIAN_POINT('Ctrl Pts',(114.599591754413,5.81760561602206,128.636267249567));
#256684=CARTESIAN_POINT('Ctrl Pts',(114.3211441306,1.32047958428524,124.737936825626));
#256685=CARTESIAN_POINT('Ctrl Pts',(114.042696506787,-4.39010267639563,
126.414353505198));
#256686=CARTESIAN_POINT('Ctrl Pts',(113.764248882975,-6.06639504590774,
132.124972257267));
#256687=CARTESIAN_POINT('Ctrl Pts',(113.485801259161,-2.16796672810439,
136.622013427915));
#256688=CARTESIAN_POINT('Ctrl Pts',(113.207353635349,3.72271710176439,135.772915873991));
#256689=CARTESIAN_POINT('Ctrl Pts',(112.928906011536,6.19240577995249,130.357958766832));
#256690=CARTESIAN_POINT('Ctrl Pts',(112.650458387723,2.97157606220462,125.353223152553));
#256691=CARTESIAN_POINT('Ctrl Pts',(112.37201076391,-2.9799868871482,125.357816565752));
#256692=CARTESIAN_POINT('Ctrl Pts',(112.093563140097,-6.19308746766462,
130.367517884098));
#256693=CARTESIAN_POINT('Ctrl Pts',(111.815115516284,-3.71504321453968,
135.778656333547));
#256694=CARTESIAN_POINT('Ctrl Pts',(111.536667892471,2.1769442627965,136.618660027865));
#256695=CARTESIAN_POINT('Ctrl Pts',(111.258220268658,6.06842631226225,132.115606608435));
#256696=CARTESIAN_POINT('Ctrl Pts',(110.979772644846,4.38332103986566,126.407582181323));
#256697=CARTESIAN_POINT('Ctrl Pts',(110.701325021032,-1.32984213103019,
124.739982342551));
#256698=CARTESIAN_POINT('Ctrl Pts',(110.42287739722,-5.82094534990898,128.645249877167));
#256699=CARTESIAN_POINT('Ctrl Pts',(110.144429773407,-4.96288416121089,
134.534634703787));
#256700=CARTESIAN_POINT('Ctrl Pts',(109.865982149594,0.455825121270016,
136.996079879188));
#256701=CARTESIAN_POINT('Ctrl Pts',(109.587534525781,5.45565338559904,133.767637535461));
#256702=CARTESIAN_POINT('Ctrl Pts',(109.309086901968,5.44200271204727,127.816088468313));
#256703=CARTESIAN_POINT('Ctrl Pts',(109.030639278155,0.427417402736423,
124.610615521118));
#256704=CARTESIAN_POINT('Ctrl Pts',(108.752191654342,-4.97994361918818,
127.096891736289));
#256705=CARTESIAN_POINT('Ctrl Pts',(108.473744030529,-5.81097973884976,
132.990150733429));
#256706=CARTESIAN_POINT('Ctrl Pts',(108.195296406717,-1.30200936065053,
136.874775395874));
#256707=CARTESIAN_POINT('Ctrl Pts',(107.916848782904,4.40344401329306,135.180985433302));
#256708=CARTESIAN_POINT('Ctrl Pts',(107.638401159091,6.06234745921968,129.465291075077));
#256709=CARTESIAN_POINT('Ctrl Pts',(107.359953535278,2.15024975226158,124.980136209215));
#256710=CARTESIAN_POINT('Ctrl Pts',(107.081505911465,-3.73782243148481,
125.847159045447));
#256711=CARTESIAN_POINT('Ctrl Pts',(106.803058287652,-6.19101840347381,
131.269607953695));
#256712=CARTESIAN_POINT('Ctrl Pts',(106.524610663839,-2.95497091073364,
136.264517288637));
#256713=CARTESIAN_POINT('Ctrl Pts',(106.246163040026,2.99655049061638,136.241809386346));
#256714=CARTESIAN_POINT('Ctrl Pts',(105.967715416213,6.1943883807198,131.222351699685));
#256715=CARTESIAN_POINT('Ctrl Pts',(105.689267792401,3.69988596163724,125.818780628557));
#256716=CARTESIAN_POINT('Ctrl Pts',(105.410820168588,-2.19463090671215,
124.996714008204));
#256717=CARTESIAN_POINT('Ctrl Pts',(105.132372544775,-6.07238918547325,
129.511590902545));
#256718=CARTESIAN_POINT('Ctrl Pts',(104.853924920962,-4.36991845548819,
135.214460009678));
#256719=CARTESIAN_POINT('Ctrl Pts',(104.575477297149,1.34829385270585,136.864663220793));
#256720=CARTESIAN_POINT('Ctrl Pts',(104.297029673336,5.82748997807964,132.945744401783));
#256721=CARTESIAN_POINT('Ctrl Pts',(104.018582049523,4.95150750231056,127.058998497491));
#256722=CARTESIAN_POINT('Ctrl Pts',(103.74013442571,-0.474668473492613,
124.614057410436));
#256723=CARTESIAN_POINT('Ctrl Pts',(103.461686801897,-5.46464731100027,
127.857702557609));
#256724=CARTESIAN_POINT('Ctrl Pts',(103.183239178085,-5.43288223256107,
133.809182509633));
#256725=CARTESIAN_POINT('Ctrl Pts',(102.904791554272,-0.408563793450433,
136.999377936557));
#256726=CARTESIAN_POINT('Ctrl Pts',(102.626343930459,4.99120481239017,134.496655090749));
#256727=CARTESIAN_POINT('Ctrl Pts',(102.347896306646,5.80430002955499,128.600894002697));
#256728=CARTESIAN_POINT('Ctrl Pts',(102.069448682833,1.28352707537895,124.730011088381));
#256729=CARTESIAN_POINT('Ctrl Pts',(101.79100105902,-4.41674455728669,126.441158642913));
#256730=CARTESIAN_POINT('Ctrl Pts',(101.512553435207,-6.05824371177293,
132.161875657885));
#256731=CARTESIAN_POINT('Ctrl Pts',(101.234105811394,-2.13251285679878,
136.635102669099));
#256732=CARTESIAN_POINT('Ctrl Pts',(100.955658187581,3.75289313452884,135.750162582539));
#256733=CARTESIAN_POINT('Ctrl Pts',(100.677210563769,6.18957367424645,130.320272106026));
#256734=CARTESIAN_POINT('Ctrl Pts',(100.398762939956,2.93833838481571,125.33523532258));
#256735=CARTESIAN_POINT('Ctrl Pts',(100.120315316143,-3.01308633445025,
125.376057503601));
#256736=CARTESIAN_POINT('Ctrl Pts',(99.8418676923298,-6.19563190980719,
130.405225059005));
#256737=CARTESIAN_POINT('Ctrl Pts',(99.5634200685172,-3.68469443349671,
135.801178693871));
#256738=CARTESIAN_POINT('Ctrl Pts',(99.2849724447041,2.2122972198669,136.605300624745));
#256739=CARTESIAN_POINT('Ctrl Pts',(99.0065248208913,6.07629580490035,132.078642080696));
#256740=CARTESIAN_POINT('Ctrl Pts',(98.7280771970783,4.35647538878314,126.380981124141));
#256741=CARTESIAN_POINT('Ctrl Pts',(98.4496295732656,-1.36673308397146,
124.748189827941));
#256742=CARTESIAN_POINT('Ctrl Pts',(98.1711819494526,-5.8339806211792,128.680723627015));
#256743=CARTESIAN_POINT('Ctrl Pts',(97.8927343256397,-4.94008497332115,
134.564776074971));
#256744=CARTESIAN_POINT('Ctrl Pts',(97.6142867018267,0.493507428451318,
136.993190424079));
#256745=CARTESIAN_POINT('Ctrl Pts',(97.3358390780141,5.47359061265531,133.734372522146));
#256746=CARTESIAN_POINT('Ctrl Pts',(97.0573914542009,5.42371142359607,127.783016818942));
#256747=CARTESIAN_POINT('Ctrl Pts',(96.7789438303882,0.389706399285272,
124.608128465823));
#256748=CARTESIAN_POINT('Ctrl Pts',(96.5004962065753,-5.0024197677526,127.127274757387));
#256749=CARTESIAN_POINT('Ctrl Pts',(96.2220485827623,-5.79756655001767,
133.025483318824));
#256750=CARTESIAN_POINT('Ctrl Pts',(95.9436009589496,-1.26503289968789,
136.882588625681));
#256751=CARTESIAN_POINT('Ctrl Pts',(95.6651533351365,4.4300041851621,135.154099331026));
#256752=CARTESIAN_POINT('Ctrl Pts',(95.3867057113237,6.05408384158403,129.428412655251));
#256753=CARTESIAN_POINT('Ctrl Pts',(95.1082580875108,2.11475620602821,124.967154938047));
#256754=CARTESIAN_POINT('Ctrl Pts',(94.8298104636979,-3.76792907128354,
125.870004076972));
#256755=CARTESIAN_POINT('Ctrl Pts',(94.5513628398851,-6.18807160565406,
131.307285819983));
#256756=CARTESIAN_POINT('Ctrl Pts',(94.2729152160721,-2.92167863853249,
136.282403871234));
#256757=CARTESIAN_POINT('Ctrl Pts',(93.9944675922592,3.02959426546386,136.223467789656));
#256758=CARTESIAN_POINT('Ctrl Pts',(93.7160199684464,6.19681804340696,131.184636955029));
#256759=CARTESIAN_POINT('Ctrl Pts',(93.4375723446334,3.66946877085029,125.796350743805));
#256760=CARTESIAN_POINT('Ctrl Pts',(93.1591247208205,-2.22994303860241,
125.010180951684));
#256761=CARTESIAN_POINT('Ctrl Pts',(92.8806770970077,-6.08014613435319,
129.548579211095));
#256762=CARTESIAN_POINT('Ctrl Pts',(92.6022294731947,-4.3429919642852,135.24097923472));
#256763=CARTESIAN_POINT('Ctrl Pts',(92.323781849382,1.38515965400848,136.856343490049));
#256764=CARTESIAN_POINT('Ctrl Pts',(92.045334225569,5.84041721907928,132.910231141365));
#256765=CARTESIAN_POINT('Ctrl Pts',(91.7668866017561,4.9286166800594,127.028926658805));
#256766=CARTESIAN_POINT('Ctrl Pts',(91.4884389779432,-0.512341811624615,
124.617061544141));
#256767=CARTESIAN_POINT('Ctrl Pts',(91.2099913541303,-5.48248320771468,
127.891022011592));
#256768=CARTESIAN_POINT('Ctrl Pts',(90.9315437303175,-5.41449037010934,
133.842198333429));
#256769=CARTESIAN_POINT('Ctrl Pts',(90.6530961065044,-0.370845394933272,
137.00175020101));
#256770=CARTESIAN_POINT('Ctrl Pts',(90.3746484826917,5.01358838138169,134.466203800718));
#256771=CARTESIAN_POINT('Ctrl Pts',(90.0962008588786,5.79077936261581,128.565602406094));
#256772=CARTESIAN_POINT('Ctrl Pts',(89.817753235066,1.24652700490487,124.722310438393));
#256773=CARTESIAN_POINT('Ctrl Pts',(89.5393056112528,-4.44322277408392,
126.468125460682));
#256774=CARTESIAN_POINT('Ctrl Pts',(89.2608579874402,-6.04986788718945,
132.198728755283));
#256775=CARTESIAN_POINT('Ctrl Pts',(88.9824103636271,-2.09697996444503,
136.647975849991));
#256776=CARTESIAN_POINT('Ctrl Pts',(88.7039627398144,3.78293010245805,135.727226022576));
#256777=CARTESIAN_POINT('Ctrl Pts',(88.4255151160013,6.18651221161165,130.282603383299));
#256778=CARTESIAN_POINT('Ctrl Pts',(88.1470674921886,2.9049918262175,125.317450153056));
#256779=CARTESIAN_POINT('Ctrl Pts',(87.8686198683756,-3.04607413073006,
125.394499589218));
#256780=CARTESIAN_POINT('Ctrl Pts',(87.5901722445627,-6.19794677053091,
130.442947024027));
#256781=CARTESIAN_POINT('Ctrl Pts',(87.3117246207499,-3.65420911474647,
135.823515895262));
#256782=CARTESIAN_POINT('Ctrl Pts',(87.033276996937,2.24756819945024,136.59172626566));
#256783=CARTESIAN_POINT('Ctrl Pts',(86.754829373124,6.08394013816284,132.041630333989));
#256784=CARTESIAN_POINT('Ctrl Pts',(86.4763817493112,4.32946830690299,126.35454397691));
#256785=CARTESIAN_POINT('Ctrl Pts',(86.1979341254982,-1.40357339211569,
124.756621726966));
#256786=CARTESIAN_POINT('Ctrl Pts',(85.9194865016854,-5.84679971215209,
128.716276069012));
#256787=CARTESIAN_POINT('Ctrl Pts',(85.6410388778725,-4.91710272876601,
134.594778102578));
#256788=CARTESIAN_POINT('Ctrl Pts',(85.3625912540596,0.531171448533366,
136.990071639606));
#256789=CARTESIAN_POINT('Ctrl Pts',(85.0841436302467,5.49132501379855,133.700998936161));
#256790=CARTESIAN_POINT('Ctrl Pts',(84.8056960064338,5.4052191575235,127.750057126576));
#256791=CARTESIAN_POINT('Ctrl Pts',(84.527248382621,0.351980955120191,124.60587101419));
#256792=CARTESIAN_POINT('Ctrl Pts',(84.2488007588079,-5.02471054981291,
127.157794034254));
#256793=CARTESIAN_POINT('Ctrl Pts',(83.9703531349953,-5.78393853022499,
133.0607335997));
#256794=CARTESIAN_POINT('Ctrl Pts',(83.6919055111822,-1.22800956246596,
136.890176624513));
#256795=CARTESIAN_POINT('Ctrl Pts',(83.4134578873695,4.45640020159694,135.127052047582));
#256796=CARTESIAN_POINT('Ctrl Pts',(83.1350102635564,6.04559588764522,129.391585221682));
#256797=CARTESIAN_POINT('Ctrl Pts',(82.8565626397436,2.07918429672594,124.954389966684));
#256798=CARTESIAN_POINT('Ctrl Pts',(82.5781150159307,-3.79789608908488,
125.893031952893));
#256799=CARTESIAN_POINT('Ctrl Pts',(82.2996673921181,-6.18489550656524,
131.344945050191));
#256800=CARTESIAN_POINT('Ctrl Pts',(82.0212197683047,-2.88827810245507,
136.300087462925));
#256801=CARTESIAN_POINT('Ctrl Pts',(81.7427721444922,3.06252577758164,136.204925385956));
#256802=CARTESIAN_POINT('Ctrl Pts',(81.464324520679,6.19901808072266,131.146908119091));
#256803=CARTESIAN_POINT('Ctrl Pts',(81.1858768968663,3.6389156065486,125.774106432701));
#256804=CARTESIAN_POINT('Ctrl Pts',(80.9074292730533,-2.26517253913331,
125.023862600622));
#256805=CARTESIAN_POINT('Ctrl Pts',(80.6289816492404,-6.08767778118217,
129.585614053086));
#256806=CARTESIAN_POINT('Ctrl Pts',(80.3505340254275,-4.31590454191782,
135.267334059228));
#256807=CARTESIAN_POINT('Ctrl Pts',(80.0720864016147,1.42197412771073,136.847799500855));
#256808=CARTESIAN_POINT('Ctrl Pts',(79.7936387778018,5.85312804127117,132.874639847142));
#256809=CARTESIAN_POINT('Ctrl Pts',(79.5151911539889,4.90554322610457,126.998994720211));
#256810=CARTESIAN_POINT('Ctrl Pts',(79.236743530176,-0.54999616474248,124.62029495049));
#256811=CARTESIAN_POINT('Ctrl Pts',(78.9582959063631,-5.50011594899764,
127.924449420408));
#256812=CARTESIAN_POINT('Ctrl Pts',(78.6798482825503,-5.39589787172579,
133.87510158903));
#256813=CARTESIAN_POINT('Ctrl Pts',(78.4014006587372,-0.333113254603616,
137.003892818912));
#256814=CARTESIAN_POINT('Ctrl Pts',(78.1229530349246,5.035786170012,134.435616819741));
#256815=CARTESIAN_POINT('Ctrl Pts',(77.8445054111114,5.77704411621779,128.530393767498));
#256816=CARTESIAN_POINT('Ctrl Pts',(77.5660577872988,1.20948074391421,124.71483516101));
#256817=CARTESIAN_POINT('Ctrl Pts',(77.2876101634857,-4.46953634562727,
126.49525295924));
#256818=CARTESIAN_POINT('Ctrl Pts',(77.009162539673,-6.04126788252658,132.235530183857));
#256819=CARTESIAN_POINT('Ctrl Pts',(76.73071491586,-2.06136936772754,136.660632493573));
#256820=CARTESIAN_POINT('Ctrl Pts',(76.4522672920471,3.81282689252116,135.704107044024));
#256821=CARTESIAN_POINT('Ctrl Pts',(76.1738196682342,6.18322150549176,130.244953994479));
#256822=CARTESIAN_POINT('Ctrl Pts',(75.8953720444213,2.87153762207887,125.299868303017));
#256823=CARTESIAN_POINT('Ctrl Pts',(75.6169244206085,-3.07894905361277,
125.413142139227));
#256824=CARTESIAN_POINT('Ctrl Pts',(75.3384767967955,-6.20003196405775,
130.480682381363));
#256825=CARTESIAN_POINT('Ctrl Pts',(75.0600291729826,-3.62358838793365,
135.84566711001));
#256826=CARTESIAN_POINT('Ctrl Pts',(74.7815815491698,2.28275589456742,136.577937453613));
#256827=CARTESIAN_POINT('Ctrl Pts',(74.5031339253568,6.09135902878616,132.004572739798));
#256828=CARTESIAN_POINT('Ctrl Pts',(74.224686301544,4.30230079498258,126.328271719272));
#256829=CARTESIAN_POINT('Ctrl Pts',(73.946238677731,-1.44036169033171,124.76527772718));
#256830=CARTESIAN_POINT('Ctrl Pts',(73.6677910539182,-5.85940214781156,
128.75190588575));
#256831=CARTESIAN_POINT('Ctrl Pts',(73.3893434301052,-4.89393827916089,
134.624639674871));
#256832=CARTESIAN_POINT('Ctrl Pts',(73.1108958062924,0.56881578586215,136.986723641335));
#256833=CARTESIAN_POINT('Ctrl Pts',(72.8324481824796,5.50885593187395,133.66751801418));
#256834=CARTESIAN_POINT('Ctrl Pts',(72.5540005586665,5.38652659906729,127.717210612549));
#256835=CARTESIAN_POINT('Ctrl Pts',(72.2755529348538,0.314242468171368,
124.603843249867));
#256836=CARTESIAN_POINT('Ctrl Pts',(71.9971053110409,-5.04681513937595,
127.188448435987));
#256837=CARTESIAN_POINT('Ctrl Pts',(71.7186576872279,-5.77009618446306,
133.095900269846));
#256838=CARTESIAN_POINT('Ctrl Pts',(71.4402100634152,-1.19094072089807,
136.897539111196));
#256839=CARTESIAN_POINT('Ctrl Pts',(71.1617624396021,4.48263108448347,135.099844585217));
#256840=CARTESIAN_POINT('Ctrl Pts',(70.8833148157894,6.03688391192757,129.354810139024));
#256841=CARTESIAN_POINT('Ctrl Pts',(70.6048671919763,2.04353534248492,124.941841768133));
#256842=CARTESIAN_POINT('Ctrl Pts',(70.3264195681636,-3.82772237444985,
125.916241819903));
#256843=CARTESIAN_POINT('Ctrl Pts',(70.0479719443506,-6.18149022389895,
131.382584248845));
#256844=CARTESIAN_POINT('Ctrl Pts',(69.7695243205378,-2.85477054017052,
136.317567408437));
#256845=CARTESIAN_POINT('Ctrl Pts',(69.4910766967249,3.09534380668036,136.186182862342));
#256846=CARTESIAN_POINT('Ctrl Pts',(69.2126290729119,6.20098841114368,131.109166589932));
#256847=CARTESIAN_POINT('Ctrl Pts',(68.934181449099,3.60822760089105,125.752048519516));
#256848=CARTESIAN_POINT('Ctrl Pts',(68.6557338252862,-2.30031810286251,
125.037758448041));
#256849=CARTESIAN_POINT('Ctrl Pts',(68.3772862014732,-6.09498384687224,
129.622694056181));
#256850=CARTESIAN_POINT('Ctrl Pts',(68.0988385776604,-4.28865719212064,
135.293523506613));
#256851=CARTESIAN_POINT('Ctrl Pts',(67.8203909538475,1.45873590963839,136.83903156981));
#256852=CARTESIAN_POINT('Ctrl Pts',(67.5419433300346,5.86562197365073,132.83897183796));
#256853=CARTESIAN_POINT('Ctrl Pts',(67.2634957062218,4.88228799544191,126.969203790852));
#256854=CARTESIAN_POINT('Ctrl Pts',(66.9850480824087,-0.587630137549865,
124.623757509667));
#256855=CARTESIAN_POINT('Ctrl Pts',(66.706600458596,-5.51754488146136,127.957983545393));
#256856=CARTESIAN_POINT('Ctrl Pts',(66.428152834783,-5.37710542636232,133.907891057196));
#256857=CARTESIAN_POINT('Ctrl Pts',(66.1497052109702,-0.295368770640213,
137.00580571087));
#256858=CARTESIAN_POINT('Ctrl Pts',(65.8712575871573,5.05779735573374,134.404895281231));
#256859=CARTESIAN_POINT('Ctrl Pts',(65.5928099633443,5.76309479932555,128.495269391582));
#256860=CARTESIAN_POINT('Ctrl Pts',(65.3143623395316,1.17238966517029,124.707585533234));
#256861=CARTESIAN_POINT('Ctrl Pts',(65.0359147157185,-4.49568429685739,
126.522540133366));
#256862=CARTESIAN_POINT('Ctrl Pts',(64.7574670919057,-6.03244401646077,
132.272278579917));
#256863=CARTESIAN_POINT('Ctrl Pts',(64.4790194680927,-2.02568238621027,
136.673072130848));
#256864=CARTESIAN_POINT('Ctrl Pts',(64.20057184428,3.84258239688126,135.680806503568));
#256865=CARTESIAN_POINT('Ctrl Pts',(63.922124220467,6.17970167782515,130.207325334677));
#256866=CARTESIAN_POINT('Ctrl Pts',(63.6436765966542,2.8379770120581,125.282490423967));
#256867=CARTESIAN_POINT('Ctrl Pts',(63.3652289728412,-3.11170988490585,
125.431984462817));
#256868=CARTESIAN_POINT('Ctrl Pts',(63.0867813490283,-6.20188741312008,
130.518429732716));
#256869=CARTESIAN_POINT('Ctrl Pts',(62.8083337252156,-3.59283338772076,
135.86763151729));
#256870=CARTESIAN_POINT('Ctrl Pts',(62.5298861014024,2.31785900132509,136.563934699553));
#256871=CARTESIAN_POINT('Ctrl Pts',(62.2514384775899,6.09855220186056,131.967470671305));
#256872=CARTESIAN_POINT('Ctrl Pts',(61.9729908537767,4.27497385972414,126.302165324755));
#256873=CARTESIAN_POINT('Ctrl Pts',(61.6945432299639,-1.47709661541541,
124.774157507831));
#256874=CARTESIAN_POINT('Ctrl Pts',(61.416095606151,-5.87178746116934,128.787611756953));
#256875=CARTESIAN_POINT('Ctrl Pts',(61.1376479823382,-4.8705924828735,134.65435968532));
#256876=CARTESIAN_POINT('Ctrl Pts',(60.8592003585251,0.606439045512412,
136.983146553331));
#256877=CARTESIAN_POINT('Ctrl Pts',(60.5807527347125,5.52618271726667,133.633930996847));
#256878=CARTESIAN_POINT('Ctrl Pts',(60.3023051108993,5.36763444088732,127.684478494003));
#256879=CARTESIAN_POINT('Ctrl Pts',(60.0238574870866,0.276492336852797,
124.602045247997));
#256880=CARTESIAN_POINT('Ctrl Pts',(59.7454098632736,-5.06873271734795,
127.219236826675));
#256881=CARTESIAN_POINT('Ctrl Pts',(59.4669622394608,-5.75604002566515,
133.130982026147));
#256882=CARTESIAN_POINT('Ctrl Pts',(59.1885146156479,-1.15382774858414,
136.904675812908));
#256883=CARTESIAN_POINT('Ctrl Pts',(58.9100669918351,4.50869586182645,135.072477952114));
#256884=CARTESIAN_POINT('Ctrl Pts',(58.6316193680221,6.02794823725661,129.318088769994));
#256885=CARTESIAN_POINT('Ctrl Pts',(58.3531717442092,2.00781066429043,124.929510807376));
#256886=CARTESIAN_POINT('Ctrl Pts',(58.0747241203963,-3.85740682215468,
125.939632817953));
#256887=CARTESIAN_POINT('Ctrl Pts',(57.7962764965834,-6.17785588383907,
131.42020202121));
#256888=CARTESIAN_POINT('Ctrl Pts',(57.5178288727705,-2.82115719331391,
136.334843060042));
#256889=CARTESIAN_POINT('Ctrl Pts',(57.2393812489577,3.12804713667602,136.167240913326));
#256890=CARTESIAN_POINT('Ctrl Pts',(56.9609336251447,6.20272896165862,131.071413766074));
#256891=CARTESIAN_POINT('Ctrl Pts',(56.6824860013319,3.57740589103289,125.730177821614));
#256892=CARTESIAN_POINT('Ctrl Pts',(56.404038377519,-2.33537842745856,125.051867979023));
#256893=CARTESIAN_POINT('Ctrl Pts',(56.125590753706,-6.10206406069443,129.659817846364));
#256894=CARTESIAN_POINT('Ctrl Pts',(55.8471431298932,-4.26125092455389,
135.319546606417));
#256895=CARTESIAN_POINT('Ctrl Pts',(55.5686955060803,1.49544363757083,136.830040021814));
#256896=CARTESIAN_POINT('Ctrl Pts',(55.2902478822675,5.87789855325116,132.80322843551));
#256897=CARTESIAN_POINT('Ctrl Pts',(55.0118002584545,4.85885184980179,126.939554974638));
#256898=CARTESIAN_POINT('Ctrl Pts',(54.7333526346416,-0.625242335506623,
124.627449093364));
#256899=CARTESIAN_POINT('Ctrl Pts',(54.4549050108287,-5.53476935927053,
127.991623143927));
#256900=CARTESIAN_POINT('Ctrl Pts',(54.1764573870159,-5.35811373037978,
133.9405655229));
#256901=CARTESIAN_POINT('Ctrl Pts',(53.8980097632029,-0.257613341678002,
137.007488805997));
#256902=CARTESIAN_POINT('Ctrl Pts',(53.61956213939,5.07962112291461,134.374040323585));
#256903=CARTESIAN_POINT('Ctrl Pts',(53.3411145155772,5.74893192883615,128.460230579889));
#256904=CARTESIAN_POINT('Ctrl Pts',(53.0626668917642,1.13525514309568,124.7005618237));
#256905=CARTESIAN_POINT('Ctrl Pts',(52.7842192679514,-4.52166565885288,
126.549985971924));
#256906=CARTESIAN_POINT('Ctrl Pts',(52.5057716441385,-6.0233966159634,132.308972581737));
#256907=CARTESIAN_POINT('Ctrl Pts',(52.2273240203255,-1.98992034228702,
136.685294300858));
#256908=CARTESIAN_POINT('Ctrl Pts',(51.9488763965128,3.87219551293788,135.657325264614));
#256909=CARTESIAN_POINT('Ctrl Pts',(51.6704287726998,6.17595285904027,130.169718798237));
#256910=CARTESIAN_POINT('Ctrl Pts',(51.391981148887,2.80431123975502,125.265317159845));
#256911=CARTESIAN_POINT('Ctrl Pts',(51.113533525074,-3.14435541064497,125.451025861782));
#256912=CARTESIAN_POINT('Ctrl Pts',(50.8350859012611,-6.20351304896362,
130.556187679343));
#256913=CARTESIAN_POINT('Ctrl Pts',(50.5566382774483,-3.5619452537452,135.889408303207));
#256914=CARTESIAN_POINT('Ctrl Pts',(50.2781906536353,2.35287621896542,136.549718522358));
#256915=CARTESIAN_POINT('Ctrl Pts',(49.9997430298226,6.10551939084041,131.930325503341));
#256916=CARTESIAN_POINT('Ctrl Pts',(49.7212954060095,4.2474885137371,126.27622576074));
#256917=CARTESIAN_POINT('Ctrl Pts',(49.4428477821967,-1.51377680614101,
124.783260739875));
#256918=CARTESIAN_POINT('Ctrl Pts',(49.1644001583838,-5.88395519328364,
128.823392359526));
#256919=CARTESIAN_POINT('Ctrl Pts',(48.8859525345709,-4.84706620499019,
134.683937032636));
#256920=CARTESIAN_POINT('Ctrl Pts',(48.607504910758,0.644039833341117,136.97934050814));
#256921=CARTESIAN_POINT('Ctrl Pts',(48.3290572869451,5.54330472792681,133.600239128744));
#256922=CARTESIAN_POINT('Ctrl Pts',(48.0506096631323,5.34854338303893,127.651861983834));
#256923=CARTESIAN_POINT('Ctrl Pts',(47.7721620393193,0.23873196000854,124.600477075203));
#256924=CARTESIAN_POINT('Ctrl Pts',(47.4937144155065,-5.09046247156518,
127.250158065443));
#256925=CARTESIAN_POINT('Ctrl Pts',(47.2152667916935,-5.74177057468722,
133.165977568637));
#256926=CARTESIAN_POINT('Ctrl Pts',(46.9368191678807,-1.11667202075834,
136.911586465198));
#256927=CARTESIAN_POINT('Ctrl Pts',(46.6583715440677,4.53459356778643,135.044953162355));
#256928=CARTESIAN_POINT('Ctrl Pts',(46.379923920255,6.01878919474683,129.281422475313));
#256929=CARTESIAN_POINT('Ctrl Pts',(46.101476296442,1.97201158593325,124.917397541337));
#256930=CARTESIAN_POINT('Ctrl Pts',(45.8230286726291,-3.88694833223118,
125.963204080281));
#256931=CARTESIAN_POINT('Ctrl Pts',(45.5445810488162,-6.17399262105761,
131.457796973343));
#256932=CARTESIAN_POINT('Ctrl Pts',(45.2661334250033,-2.78743930743976,
136.351913777587));
#256933=CARTESIAN_POINT('Ctrl Pts',(44.9876858011905,3.16063455573481,136.148100240809));
#256934=CARTESIAN_POINT('Ctrl Pts',(44.7092381773775,6.20423966777097,131.033651046464));
#256935=CARTESIAN_POINT('Ctrl Pts',(44.4307905535647,3.54645161908363,125.708495149421));
#256936=CARTESIAN_POINT('Ctrl Pts',(44.1523429297517,-2.37035221374829,
125.066190670735));
#256937=CARTESIAN_POINT('Ctrl Pts',(43.8738953059389,-6.10891816028884,
129.696984048001));
#256938=CARTESIAN_POINT('Ctrl Pts',(43.5954476821259,-4.23368675476706,
135.345402394343));
#256939=CARTESIAN_POINT('Ctrl Pts',(43.3170000583131,1.53209595128933,136.820825190051));
#256940=CARTESIAN_POINT('Ctrl Pts',(43.0385524345002,5.88995732515911,132.767410964279));
#256941=CARTESIAN_POINT('Ctrl Pts',(42.7601048106873,4.83523565761953,126.910049370218));
#256942=CARTESIAN_POINT('Ctrl Pts',(42.4816571868744,-0.662831364878718,
124.631369564788));
#256943=CARTESIAN_POINT('Ctrl Pts',(42.2032095630615,-5.55178874416567,
128.025366969483));
#256944=CARTESIAN_POINT('Ctrl Pts',(41.9247619392486,-5.33892348752252,
133.973123775378));
#256945=CARTESIAN_POINT('Ctrl Pts',(41.6463143154357,-0.219848366758665,
137.008942041929));
#256946=CARTESIAN_POINT('Ctrl Pts',(41.3678666916229,5.10125666286673,134.343053090145));
#256947=CARTESIAN_POINT('Ctrl Pts',(41.0894190678099,5.73455602955998,128.425278630796));
#256948=CARTESIAN_POINT('Ctrl Pts',(40.8109714439971,1.09807855372398,124.693764292674));
#256949=CARTESIAN_POINT('Ctrl Pts',(40.5325238201841,-4.5474794688646,126.5775894579));
#256950=CARTESIAN_POINT('Ctrl Pts',(40.2540761963713,-6.01412601628932,
132.345610829607));
#256951=CARTESIAN_POINT('Ctrl Pts',(39.9756285725584,-1.95408456113369,
136.697298550707));
#256952=CARTESIAN_POINT('Ctrl Pts',(39.6971809487455,3.90166514336576,135.633664197272));
#256953=CARTESIAN_POINT('Ctrl Pts',(39.4187333249326,6.171975188051,130.132135778682));
#256954=CARTESIAN_POINT('Ctrl Pts',(39.1402857011198,2.77054155266769,125.248349147017));
#256955=CARTESIAN_POINT('Ctrl Pts',(38.8618380773068,-3.17688442113803,
125.470265630536));
#256956=CARTESIAN_POINT('Ctrl Pts',(38.583390453494,-6.20490881134979,130.593954822108));
#256957=CARTESIAN_POINT('Ctrl Pts',(38.304942829681,-3.53092513057837,135.910996660811));
#256958=CARTESIAN_POINT('Ctrl Pts',(38.0264952058682,2.38780624991219,136.535289448812));
#256959=CARTESIAN_POINT('Ctrl Pts',(37.7480475820552,6.11226033755391,131.893138612335));
#256960=CARTESIAN_POINT('Ctrl Pts',(37.4695999582424,4.21984577550119,126.250453988427));
#256961=CARTESIAN_POINT('Ctrl Pts',(37.1911523344295,-1.55040090331038,
124.792587085991));
#256962=CARTESIAN_POINT('Ctrl Pts',(36.9127047106166,-5.89590489327443,
128.859246367608));
#256963=CARTESIAN_POINT('Ctrl Pts',(36.6342570868037,-4.82336031728617,
134.713370620821));
#256964=CARTESIAN_POINT('Ctrl Pts',(36.3558094629908,0.681616756036961,
136.975305646799));
#256965=CARTESIAN_POINT('Ctrl Pts',(36.0773618391779,5.56022132939171,133.566443658335));
#256966=CARTESIAN_POINT('Ctrl Pts',(35.798914215365,5.32925413294858,127.619362290662));
#256967=CARTESIAN_POINT('Ctrl Pts',(35.5204665915522,0.200962736863706,
124.599138789596));
#256968=CARTESIAN_POINT('Ctrl Pts',(35.2420189677392,-5.11200359682353,
127.281211006494));
#256969=CARTESIAN_POINT('Ctrl Pts',(34.9635713439263,-5.72728836028912,
133.200885600541));
#256970=CARTESIAN_POINT('Ctrl Pts',(34.6851237201134,-1.07947491424015,
136.918270811987));
#256971=CARTESIAN_POINT('Ctrl Pts',(34.4066760963006,4.56032324271418,135.017271235878));
#256972=CARTESIAN_POINT('Ctrl Pts',(34.1282284724876,6.00940712379002,129.244812613665));
#256973=CARTESIAN_POINT('Ctrl Pts',(33.8497808486748,1.93613943396156,124.905502418881));
#256974=CARTESIAN_POINT('Ctrl Pts',(33.5713332248619,-3.91634581000783,
125.986954733445));
#256975=CARTESIAN_POINT('Ctrl Pts',(33.292885601049,-6.16990057870911,131.495367712155));
#256976=CARTESIAN_POINT('Ctrl Pts',(33.0144379772361,-2.753618131977,136.368778928511));
#256977=CARTESIAN_POINT('Ctrl Pts',(32.7359903534233,3.19310485631782,136.128761554055));
#256978=CARTESIAN_POINT('Ctrl Pts',(32.4575427296103,6.20552047350092,130.995879830412));
#256979=CARTESIAN_POINT('Ctrl Pts',(32.1790951057975,3.51536593206519,125.687001306397));
#256980=CARTESIAN_POINT('Ctrl Pts',(31.9006474819845,-2.40523816576522,
125.080725992446));
#256981=CARTESIAN_POINT('Ctrl Pts',(31.6221998581717,-6.11554589167424,
129.734191283883));
#256982=CARTESIAN_POINT('Ctrl Pts',(31.3437522343588,-4.20596570416061,
135.371089912296));
#256983=CARTESIAN_POINT('Ctrl Pts',(31.0653046105458,1.56869149262894,136.811387415981));
#256984=CARTESIAN_POINT('Ctrl Pts',(30.786856986733,5.90179784253235,132.731520751495));
#256985=CARTESIAN_POINT('Ctrl Pts',(30.5084093629201,4.81144029400183,126.880688070935));
#256986=CARTESIAN_POINT('Ctrl Pts',(30.2299617391072,-0.700395832790832,
124.635518778667));
#256987=CARTESIAN_POINT('Ctrl Pts',(29.9515141152943,-5.56860240548724,
128.05921377167));
#256988=CARTESIAN_POINT('Ctrl Pts',(29.6730664914815,-5.31953540889204,
134.005564608172));
#256989=CARTESIAN_POINT('Ctrl Pts',(29.3946188676685,-0.182075245277261,
137.010165364815));
#256990=CARTESIAN_POINT('Ctrl Pts',(29.1161712438556,5.12270317387725,134.311934729152));
#256991=CARTESIAN_POINT('Ctrl Pts',(28.8377236200427,5.71996763420123,128.390414839463));
#256992=CARTESIAN_POINT('Ctrl Pts',(28.5592759962298,1.06086127464794,124.687193192043));
#256993=CARTESIAN_POINT('Ctrl Pts',(28.280828372417,-4.57312477035222,126.605349568435));
#256994=CARTESIAN_POINT('Ctrl Pts',(28.0023807486041,-6.00463256096402,
132.382191965885));
#256995=CARTESIAN_POINT('Ctrl Pts',(27.7239331247912,-1.91817637065835,
136.709084435575));
#256996=CARTESIAN_POINT('Ctrl Pts',(27.4454855009783,3.93099019615694,135.60982417831));
#256997=CARTESIAN_POINT('Ctrl Pts',(27.1670378771654,6.16776881225138,130.094577668667));
#256998=CARTESIAN_POINT('Ctrl Pts',(26.8885902533525,2.73666920214424,125.231587014236));
#256999=CARTESIAN_POINT('Ctrl Pts',(26.6101426295396,-3.20929571101057,
125.48970305614));
#257000=CARTESIAN_POINT('Ctrl Pts',(26.3316950057267,-6.2060746485581,130.631729761538));
#257001=CARTESIAN_POINT('Ctrl Pts',(26.0532473819138,-3.49977416768234,
135.932395790139));
#257002=CARTESIAN_POINT('Ctrl Pts',(25.774799758101,2.42264779982026,136.52064801359));
#257003=CARTESIAN_POINT('Ctrl Pts',(25.4963521342881,6.11877479221284,131.85591137626));
#257004=CARTESIAN_POINT('Ctrl Pts',(25.2179045104751,4.19204666932822,126.224850962798));
#257005=CARTESIAN_POINT('Ctrl Pts',(24.9394568866623,-1.58696754980412,
124.802136200585));
#257006=CARTESIAN_POINT('Ctrl Pts',(24.6610092628494,-5.90763611834117,
128.895172452612));
#257007=CARTESIAN_POINT('Ctrl Pts',(24.3825616390365,-4.79947569819179,
134.742659359205));
#257008=CARTESIAN_POINT('Ctrl Pts',(24.1041140152236,0.719168421173241,
136.97104211882));
#257009=CARTESIAN_POINT('Ctrl Pts',(23.8256663914108,5.57693189481048,133.532545837923));
#257010=CARTESIAN_POINT('Ctrl Pts',(23.5472187675978,5.3097674053865,127.586980618775));
#257011=CARTESIAN_POINT('Ctrl Pts',(23.2687711437849,0.163186066970757,
124.598030440764));
#257012=CARTESIAN_POINT('Ctrl Pts',(22.990323519972,-5.13335529490864,127.312394499151));
#257013=CARTESIAN_POINT('Ctrl Pts',(22.7118758961592,-5.71259391911463,
133.235704828331));
#257014=CARTESIAN_POINT('Ctrl Pts',(22.4334282723462,-1.04223780738205,
136.924728605587));
#257015=CARTESIAN_POINT('Ctrl Pts',(22.1549806485334,4.58588393318709,134.98943319845));
#257016=CARTESIAN_POINT('Ctrl Pts',(21.8765330247205,5.9998023720423,129.208260541641));
#257017=CARTESIAN_POINT('Ctrl Pts',(21.5980854009075,1.90019553763114,124.893825880784));
#257018=CARTESIAN_POINT('Ctrl Pts',(21.3196377770947,-3.94559816615024,
126.010883897355));
#257019=CARTESIAN_POINT('Ctrl Pts',(21.0411901532818,-6.16557990842568,
131.532912845442));
#257020=CARTESIAN_POINT('Ctrl Pts',(20.7627425294689,-2.71969492018171,
136.385437887866));
#257021=CARTESIAN_POINT('Ctrl Pts',(20.484294905656,3.22545683522612,136.109225569666));
#257022=CARTESIAN_POINT('Ctrl Pts',(20.2058472818431,6.20657133138755,130.958101517545));
#257023=CARTESIAN_POINT('Ctrl Pts',(19.9273996580302,3.48414998186958,125.665697089004));
#257024=CARTESIAN_POINT('Ctrl Pts',(19.6489520342174,-2.44003499079723,
125.095473405541));
#257025=CARTESIAN_POINT('Ctrl Pts',(19.3705044104044,-6.12194700925765,
129.771438175283));
#257026=CARTESIAN_POINT('Ctrl Pts',(19.0920567865916,-4.17808879994825,
135.396608208416));
#257027=CARTESIAN_POINT('Ctrl Pts',(18.8136091627787,1.60522890552839,136.801727049323));
#257028=CARTESIAN_POINT('Ctrl Pts',(18.5351615389658,5.91341966661616,132.695559127084));
#257029=CARTESIAN_POINT('Ctrl Pts',(18.2567139151529,4.78746664069464,126.85147216478));
#257030=CARTESIAN_POINT('Ctrl Pts',(17.97826629134,-0.737934347277788,124.63989658125));
#257031=CARTESIAN_POINT('Ctrl Pts',(17.6998186675271,-5.58520972019883,
128.093162296283));
#257032=CARTESIAN_POINT('Ctrl Pts',(17.4213710437142,-5.29995021292075,
134.037886819174));
#257033=CARTESIAN_POINT('Ctrl Pts',(17.1429234199013,-0.144295376930669,
137.011158729324));
#257034=CARTESIAN_POINT('Ctrl Pts',(16.8644757960885,5.14395986123776,134.280686393713));
#257035=CARTESIAN_POINT('Ctrl Pts',(16.5860281722755,5.70516728333829,128.355640497777));
#257036=CARTESIAN_POINT('Ctrl Pts',(16.3075805484627,1.02360468496723,124.6808487653));
#257037=CARTESIAN_POINT('Ctrl Pts',(16.0291329246498,-4.5986006130197,126.633265274869));
#257038=CARTESIAN_POINT('Ctrl Pts',(15.7506853008369,-5.99491660177097,
132.418714635041));
#257039=CARTESIAN_POINT('Ctrl Pts',(15.472237677024,-1.88219710145218,136.720651518731));
#257040=CARTESIAN_POINT('Ctrl Pts',(15.1937900532111,3.96016958466077,135.585806091128));
#257041=CARTESIAN_POINT('Ctrl Pts',(14.9153424293982,6.16333388751023,130.057045859918));
#257042=CARTESIAN_POINT('Ctrl Pts',(14.6368948055853,2.70269544333712,125.215031382631));
#257043=CARTESIAN_POINT('Ctrl Pts',(14.3584471817724,-3.24158807925031,
125.509337418335));
#257044=CARTESIAN_POINT('Ctrl Pts',(14.0799995579596,-6.20701051738803,
130.669511097867));
#257045=CARTESIAN_POINT('Ctrl Pts',(13.8015519341466,-3.46849351936748,
135.953604898237));
#257046=CARTESIAN_POINT('Ctrl Pts',(13.5231043103337,2.45739957762318,136.505794759238));
#257047=CARTESIAN_POINT('Ctrl Pts',(13.2446566865208,6.12506251342167,131.818645174584));
#257048=CARTESIAN_POINT('Ctrl Pts',(12.966209062708,4.16409222532429,126.199417632585));
#257049=CARTESIAN_POINT('Ctrl Pts',(12.687761438895,-1.62347539063169,124.811907729812));
#257050=CARTESIAN_POINT('Ctrl Pts',(12.4093138150822,-5.91914843377905,
128.931169283287));
#257051=CARTESIAN_POINT('Ctrl Pts',(12.1308661912693,-4.77541323276041,
134.771802162479));
#257052=CARTESIAN_POINT('Ctrl Pts',(11.8524185674564,0.756693437259193,
136.96655008219));
#257053=CARTESIAN_POINT('Ctrl Pts',(11.5739709436435,5.59343580496719,133.498546923603));
#257054=CARTESIAN_POINT('Ctrl Pts',(11.2955233198306,5.2900839224404,127.554718168085));
#257055=CARTESIAN_POINT('Ctrl Pts',(11.0170756960177,0.125403350157864,
124.597152069781));
#257056=CARTESIAN_POINT('Ctrl Pts',(10.7386280722048,-5.15451677462551,
127.343707387895));
#257057=CARTESIAN_POINT('Ctrl Pts',(10.460180448392,-5.69768779567166,133.270433961767));
#257058=CARTESIAN_POINT('Ctrl Pts',(10.1817328245791,-1.0049620800187,136.930959606699));
#257059=CARTESIAN_POINT('Ctrl Pts',(9.90328520076621,4.61127469204443,134.961440081617));
#257060=CARTESIAN_POINT('Ctrl Pts',(9.62483757695328,5.98997529541125,129.171767613693));
#257061=CARTESIAN_POINT('Ctrl Pts',(9.34638995314043,1.86418122885626,124.882368359726));
#257062=CARTESIAN_POINT('Ctrl Pts',(9.0679423293275,-3.97470431670162,126.034990685308));
#257063=CARTESIAN_POINT('Ctrl Pts',(8.78949470551463,-6.16103077031137,
131.57043098196));
#257064=CARTESIAN_POINT('Ctrl Pts',(8.5110470817017,-2.68567092909101,136.401890038352));
#257065=CARTESIAN_POINT('Ctrl Pts',(8.2325994578889,3.25768929364524,136.089493011555));
#257066=CARTESIAN_POINT('Ctrl Pts',(7.95415183407592,6.20739220249103,130.920317507753));
#257067=CARTESIAN_POINT('Ctrl Pts',(7.67570421026306,3.45280492521512,125.644583286679));
#257068=CARTESIAN_POINT('Ctrl Pts',(7.39725658645018,-2.47474139943534,
125.110432363552));
#257069=CARTESIAN_POINT('Ctrl Pts',(7.11880896263729,-6.1281212758433,129.808723342005));
#257070=CARTESIAN_POINT('Ctrl Pts',(6.84036133882437,-4.15005707511893,
135.421956337113));
#257071=CARTESIAN_POINT('Ctrl Pts',(6.56191371501151,1.64170683608044,136.791844448048));
#257072=CARTESIAN_POINT('Ctrl Pts',(6.28346609119863,5.92482236675955,132.659527423617));
#257073=CARTESIAN_POINT('Ctrl Pts',(6.00501846738572,4.76331558605049,126.822402734361));
#257074=CARTESIAN_POINT('Ctrl Pts',(5.72657084357281,-0.775445517336138,
124.644502810313));
#257075=CARTESIAN_POINT('Ctrl Pts',(5.44812321975995,-5.60161007291028,
128.127211285347));
#257076=CARTESIAN_POINT('Ctrl Pts',(5.16967559594705,-5.28016862534525,
134.070089210674));
#257077=CARTESIAN_POINT('Ctrl Pts',(4.89122797213414,-0.106510161665837,
137.011922098645));
#257078=CARTESIAN_POINT('Ctrl Pts',(4.6127803483213,5.16502593727395,134.249309241742));
#257079=CARTESIAN_POINT('Ctrl Pts',(4.33433272450837,5.69015552540359,128.320956894316));
#257080=CARTESIAN_POINT('Ctrl Pts',(4.05588510069549,0.986310165238503,
124.674731247541));
#257081=CARTESIAN_POINT('Ctrl Pts',(3.77743747688256,-4.62390605285035,
126.661335542776));
#257082=CARTESIAN_POINT('Ctrl Pts',(3.49898985306972,-5.98497849873861,
132.455177483715));
#257083=CARTESIAN_POINT('Ctrl Pts',(3.22054222925682,-1.84614808674025,
136.731999371551));
#257084=CARTESIAN_POINT('Ctrl Pts',(2.94209460544391,3.9892022276243,135.561610825727));
#257085=CARTESIAN_POINT('Ctrl Pts',(2.66364698163102,6.15867057816533,130.019541743194));
#257086=CARTESIAN_POINT('Ctrl Pts',(2.38519935781816,2.66862153515642,125.198682865676));
#257087=CARTESIAN_POINT('Ctrl Pts',(2.10675173400524,-3.27376032925169,
125.529167989562));
#257088=CARTESIAN_POINT('Ctrl Pts',(1.82830411019233,-6.20771638316062,
130.707297431096));
#257089=CARTESIAN_POINT('Ctrl Pts',(1.54985648637947,-3.43708434474973,
135.974623199195));
#257090=CARTESIAN_POINT('Ctrl Pts',(1.27140886256659,2.49206029558105,136.490730236146));
#257091=CARTESIAN_POINT('Ctrl Pts',(0.992961238753657,6.13112326818657,
131.78134138822));
#257092=CARTESIAN_POINT('Ctrl Pts',(0.714513614940807,4.13598347935162,
126.174154940227));
#257093=CARTESIAN_POINT('Ctrl Pts',(0.436065991127901,-1.65992307298164,
124.821901311585));
#257094=CARTESIAN_POINT('Ctrl Pts',(0.157618367314999,-5.93044141299494,
128.967235525755));
#257095=CARTESIAN_POINT('Ctrl Pts',(-0.120829256497892,-4.75117381263555,
134.800797950748));
#257096=CARTESIAN_POINT('Ctrl Pts',(-0.399276880310752,0.794190413791566,
136.961829703365));
#257097=CARTESIAN_POINT('Ctrl Pts',(-0.67772450412367,5.60973244830296,
133.464448175219));
#257098=CARTESIAN_POINT('Ctrl Pts',(-0.956172127936585,5.27020441348929,
127.522576134092));
#257099=CARTESIAN_POINT('Ctrl Pts',(-1.23461975174943,0.0876159864779326,
124.596503709192));
#257100=CARTESIAN_POINT('Ctrl Pts',(-1.51306737556233,-5.17548725182775,
127.375148512417));
#257101=CARTESIAN_POINT('Ctrl Pts',(-1.79151499937523,-5.6825705423121,
133.305071713949));
#257102=CARTESIAN_POINT('Ctrl Pts',(-2.06996262318813,-0.967649113415911,
136.936963584433));
#257103=CARTESIAN_POINT('Ctrl Pts',(-2.34841024700098,4.63649457842225,
134.933292922676));
#257104=CARTESIAN_POINT('Ctrl Pts',(-2.62685787081389,5.97992625804282,
129.13533518208));
#257105=CARTESIAN_POINT('Ctrl Pts',(-2.90530549462681,1.82809784216042,
124.871130280269));
#257106=CARTESIAN_POINT('Ctrl Pts',(-3.18375311843967,-4.00366318312286,
126.059274204017));
#257107=CARTESIAN_POINT('Ctrl Pts',(-3.46220074225256,-6.15625333293613,
131.607920731459));
#257108=CARTESIAN_POINT('Ctrl Pts',(-3.74064836606547,-2.65154741947636,
136.418134770325));
#257109=CARTESIAN_POINT('Ctrl Pts',(-4.01909598987837,3.28980103718956,
136.06956461092));
#257110=CARTESIAN_POINT('Ctrl Pts',(-4.29754361369122,6.20798305639367,
130.882529201136));
#257111=CARTESIAN_POINT('Ctrl Pts',(-4.57599123750414,3.42133192360438,
125.623660681799));
#257112=CARTESIAN_POINT('Ctrl Pts',(-4.85443886131705,-2.5093561056208,
125.125602312169));
#257113=CARTESIAN_POINT('Ctrl Pts',(-5.13288648512991,-6.13406846264146,
129.846045402432));
#257114=CARTESIAN_POINT('Ctrl Pts',(-5.41133410894279,-4.12187156839848,
135.447133359102));
#257115=CARTESIAN_POINT('Ctrl Pts',(-5.68978173275571,1.67812393258193,
136.781739978358));
#257116=CARTESIAN_POINT('Ctrl Pts',(-5.9682293565686,5.93600552043131,132.623426976261));
#257117=CARTESIAN_POINT('Ctrl Pts',(-6.24667698038146,4.73898802499559,
126.793480856855));
#257118=CARTESIAN_POINT('Ctrl Pts',(-6.52512460419438,-0.812927952975666,
124.649337295173));
#257119=CARTESIAN_POINT('Ctrl Pts',(-6.80357222800728,-5.61780285590049,
128.161359477164));
#257120=CARTESIAN_POINT('Ctrl Pts',(-7.08201985182013,-5.26019137917956,
134.1021705894));
#257121=CARTESIAN_POINT('Ctrl Pts',(-7.36046747563304,-0.0687209996277829,
137.012455444495));
#257122=CARTESIAN_POINT('Ctrl Pts',(-7.63891509944595,5.18590062137458,
134.217804435933));
#257123=CARTESIAN_POINT('Ctrl Pts',(-7.91736272325884,5.67493291666336,
128.286365314294));
#257124=CARTESIAN_POINT('Ctrl Pts',(-8.1958103470717,0.948979097423875,
124.668840865451));
#257125=CARTESIAN_POINT('Ctrl Pts',(-8.47425797088461,-4.64904015214177,
126.689559331999));
#257126=CARTESIAN_POINT('Ctrl Pts',(-8.75270559469752,-5.97481862012702,
132.491579160764));
#257127=CARTESIAN_POINT('Ctrl Pts',(-9.03115321851038,-1.81003066233205,
136.743127573537));
#257128=CARTESIAN_POINT('Ctrl Pts',(-9.30960084232328,4.0180870492325,135.537239278668));
#257129=CARTESIAN_POINT('Ctrl Pts',(-9.58804846613619,6.15377905701727,
129.982066708221));
#257130=CARTESIAN_POINT('Ctrl Pts',(-9.86649608994908,2.63444874022312,
125.182542069172));
#257131=CARTESIAN_POINT('Ctrl Pts',(-10.144943713762,-3.30581126886015,
125.549194034992));
#257132=CARTESIAN_POINT('Ctrl Pts',(-10.4233913375749,-6.20819221971975,
130.745087361036));
#257133=CARTESIAN_POINT('Ctrl Pts',(-10.7018389613878,-3.40554780770759,
135.995449914173));
#257134=CARTESIAN_POINT('Ctrl Pts',(-10.9802865852006,2.52662866932821,
136.475455002538));
#257135=CARTESIAN_POINT('Ctrl Pts',(-11.2587342090136,6.13695683192405,
131.744001399476));
#257136=CARTESIAN_POINT('Ctrl Pts',(-11.5371818328265,4.10772147299012,
126.149063821843));
#257137=CARTESIAN_POINT('Ctrl Pts',(-11.8156294566394,-1.69630924627168,
124.832116575588));
#257138=CARTESIAN_POINT('Ctrl Pts',(-12.0940770804522,-5.94151463752335,
129.003369843568));
#257139=CARTESIAN_POINT('Ctrl Pts',(-12.3725247042651,-4.72675833601782,
134.829645649562));
#257140=CARTESIAN_POINT('Ctrl Pts',(-12.6509723280781,0.83165796130609,
136.956881157257));
#257141=CARTESIAN_POINT('Ctrl Pts',(-12.9294199518909,5.62582122093989,
133.430250856313));
#257142=CARTESIAN_POINT('Ctrl Pts',(-13.2078675757038,5.25012961517551,
127.490555707831));
#257143=CARTESIAN_POINT('Ctrl Pts',(-13.4863151995167,0.0498253761554086,
124.596085383024));
#257144=CARTESIAN_POINT('Ctrl Pts',(-13.7647628233296,-5.19626594944658,
127.406716707655));
#257145=CARTESIAN_POINT('Ctrl Pts',(-14.0432104471424,-5.66724271921134,
133.339616801361));
#257146=CARTESIAN_POINT('Ctrl Pts',(-14.3216580709554,-0.930300290219375,
136.942740316309));
#257147=CARTESIAN_POINT('Ctrl Pts',(-14.6001056947683,4.6615426577884,134.904992764631));
#257148=CARTESIAN_POINT('Ctrl Pts',(-14.8785533185811,5.96965563230779,
129.098964596818));
#257149=CARTESIAN_POINT('Ctrl Pts',(-15.157000942394,1.79194671462675,124.860112058844));
#257150=CARTESIAN_POINT('Ctrl Pts',(-15.4354485662069,-4.03247369233249,
126.08373355365));
#257151=CARTESIAN_POINT('Ctrl Pts',(-15.7138961900198,-6.15124777332969,
131.645380704742));
#257152=CARTESIAN_POINT('Ctrl Pts',(-15.9923438138327,-2.61732565579698,
136.434171481834));
#257153=CARTESIAN_POINT('Ctrl Pts',(-16.2707914376456,3.32179087594663,
136.049441106215));
#257154=CARTESIAN_POINT('Ctrl Pts',(-16.5492390614585,6.2083438712012,130.844737997954));
#257155=CARTESIAN_POINT('Ctrl Pts',(-16.8276866852714,3.38973214328102,
125.602930049661));
#257156=CARTESIAN_POINT('Ctrl Pts',(-17.1061343090842,-2.54387782669295,
125.140982689263));
#257157=CARTESIAN_POINT('Ctrl Pts',(-17.3845819328972,-6.13978834927694,
129.883402973582));
#257158=CARTESIAN_POINT('Ctrl Pts',(-17.66302955671,-4.09353332421128,135.47213834144));
#257159=CARTESIAN_POINT('Ctrl Pts',(-17.9414771805229,1.71447884558397,
136.771414014676));
#257160=CARTESIAN_POINT('Ctrl Pts',(-18.2199248043358,5.94696871323555,
132.587259122732));
#257161=CARTESIAN_POINT('Ctrl Pts',(-18.4983724281487,4.71448485899666,
126.764707603974));
#257162=CARTESIAN_POINT('Ctrl Pts',(-18.7768200519616,-0.850380265270943,
124.654399856686));
#257163=CARTESIAN_POINT('Ctrl Pts',(-19.0552676757745,-5.63378746913994,
128.19560560636));
#257164=CARTESIAN_POINT('Ctrl Pts',(-19.3337152995874,-5.24001921468789,
134.134129766565));
#257165=CARTESIAN_POINT('Ctrl Pts',(-19.6121629234003,-0.0309292911078312,
137.012758747106));
#257166=CARTESIAN_POINT('Ctrl Pts',(-19.8906105472132,5.2065831400206,134.18617314371));
#257167=CARTESIAN_POINT('Ctrl Pts',(-20.1690581710261,5.65950002119693,
128.251867039513));
#257168=CARTESIAN_POINT('Ctrl Pts',(-20.447505794839,0.911612864839816,
124.663177837304));
#257169=CARTESIAN_POINT('Ctrl Pts',(-20.7259534186518,-4.67400197954067,
126.717935596697));
#257170=CARTESIAN_POINT('Ctrl Pts',(-21.0044010424647,-5.96443734241423,
132.527918317308));
#257171=CARTESIAN_POINT('Ctrl Pts',(-21.2828486662776,-1.77384616657202,
136.754035712331));
#257172=CARTESIAN_POINT('Ctrl Pts',(-21.5612962900905,4.0468229791472,135.512692353051));
#257173=CARTESIAN_POINT('Ctrl Pts',(-21.8397439139034,6.14865950532324,
129.944622143653));
#257174=CARTESIAN_POINT('Ctrl Pts',(-22.1181915377163,2.60017832482316,
125.166609591221));
#257175=CARTESIAN_POINT('Ctrl Pts',(-22.3966391615293,-3.33773971041633,
125.569414812551));
#257176=CARTESIAN_POINT('Ctrl Pts',(-22.6750867853421,-6.20843800943312,
130.782879487369));
#257177=CARTESIAN_POINT('Ctrl Pts',(-22.953534409155,-3.37388507683905,
136.016084271426));
#257178=CARTESIAN_POINT('Ctrl Pts',(-23.2319820329679,2.56110341792085,
136.45996962444));
#257179=CARTESIAN_POINT('Ctrl Pts',(-23.5104296567807,6.14256298846929,
131.706626591997));
#257180=CARTESIAN_POINT('Ctrl Pts',(-23.7888772805937,4.07930725349882,
126.124145207193));
#257181=CARTESIAN_POINT('Ctrl Pts',(-24.0673249044065,-1.73263256219878,
124.842553143289));
#257182=CARTESIAN_POINT('Ctrl Pts',(-24.3457725282195,-5.95236769704188,
129.039570897758));
#257183=CARTESIAN_POINT('Ctrl Pts',(-24.6242201520323,-4.70216770763169,
134.858344189959));
#257184=CARTESIAN_POINT('Ctrl Pts',(-24.9026677758452,0.86909469142902,
136.951704627238));
#257185=CARTESIAN_POINT('Ctrl Pts',(-25.1811153996581,5.64170152670257,
133.395956234079));
#257186=CARTESIAN_POINT('Ctrl Pts',(-25.459563023471,5.22986027137813,127.458658075828));
#257187=CARTESIAN_POINT('Ctrl Pts',(-25.7380106472839,0.0120329195352371,
124.595897106778));
#257188=CARTESIAN_POINT('Ctrl Pts',(-26.0164582710968,-5.21685209751974,
127.438410803838));
#257189=CARTESIAN_POINT('Ctrl Pts',(-26.2949058949097,-5.6517048943475,
133.374067943923));
#257190=CARTESIAN_POINT('Ctrl Pts',(-26.5733535187226,-0.892916994403456,
136.948289588268));
#257191=CARTESIAN_POINT('Ctrl Pts',(-26.8518011425354,4.68641800197708,
134.876540656153));
#257192=CARTESIAN_POINT('Ctrl Pts',(-27.1302487663484,5.95916379878798,
129.062657205632));
#257193=CARTESIAN_POINT('Ctrl Pts',(-27.4086963901612,1.75572918584856,
124.849314103734));
#257194=CARTESIAN_POINT('Ctrl Pts',(-27.6871440139742,-4.06113477674652,
126.108367827853));
#257195=CARTESIAN_POINT('Ctrl Pts',(-27.965591637787,-6.1460142769749,131.682809513716));
#257196=CARTESIAN_POINT('Ctrl Pts',(-28.2440392616,-2.5830069061529,136.449999578631));
#257197=CARTESIAN_POINT('Ctrl Pts',(-28.5224868854127,3.3536576245212,136.029123243122));
#257198=CARTESIAN_POINT('Ctrl Pts',(-28.8009345092257,6.20847463354345,
130.806945298572));
#257199=CARTESIAN_POINT('Ctrl Pts',(-29.0793821330386,3.35800675518651,
125.582392158445));
#257200=CARTESIAN_POINT('Ctrl Pts',(-29.3578297568515,-2.57830528343674,
125.156572924908));
#257201=CARTESIAN_POINT('Ctrl Pts',(-29.6362773806644,-6.14528072379723,
129.920794671155));
#257202=CARTESIAN_POINT('Ctrl Pts',(-29.9147250044772,-4.06504339264135,
135.496970357558));
#257203=CARTESIAN_POINT('Ctrl Pts',(-30.1931726282902,1.75077022794215,
136.760866939637));
#257204=CARTESIAN_POINT('Ctrl Pts',(-30.471620252103,5.95771153892721,132.551025203244));
#257205=CARTESIAN_POINT('Ctrl Pts',(-30.750067875916,4.68980699602731,126.736084041921));
#257206=CARTESIAN_POINT('Ctrl Pts',(-31.0285154997288,-0.887801066412759,
124.659690307256));
#257207=CARTESIAN_POINT('Ctrl Pts',(-31.3069631235417,-5.6495633203129,
128.229948403933));
#257208=CARTESIAN_POINT('Ctrl Pts',(-31.5854107473546,-5.21965287935721,
134.16596555791));
#257209=CARTESIAN_POINT('Ctrl Pts',(-31.8638583711675,0.00686356350839004,
137.012831995241));
#257210=CARTESIAN_POINT('Ctrl Pts',(-32.1423059949804,5.22707272681363,
134.154416537178));
#257211=CARTESIAN_POINT('Ctrl Pts',(-32.4207536187933,5.64385741087595,
128.217463348321));
#257212=CARTESIAN_POINT('Ctrl Pts',(-32.6992012426062,0.874212852105795,
124.657742372942));
#257213=CARTESIAN_POINT('Ctrl Pts',(-32.9776488664191,-4.69879061007736,
126.746463285377));
#257214=CARTESIAN_POINT('Ctrl Pts',(-33.2560964902319,-5.9538350502823,
132.564193606789));
#257215=CARTESIAN_POINT('Ctrl Pts',(-33.5345441140448,-1.73759594028995,
136.764723383724));
#257216=CARTESIAN_POINT('Ctrl Pts',(-33.8129917378578,4.07540895254819,
135.487970958469));
#257217=CARTESIAN_POINT('Ctrl Pts',(-34.0914393616706,6.14331211279008,
129.907209437008));
#257218=CARTESIAN_POINT('Ctrl Pts',(-34.3698869854835,2.56581155885918,
125.150886022208));
#257219=CARTESIAN_POINT('Ctrl Pts',(-34.6483346092964,-3.3695444708001,
125.589829572953));
#257220=CARTESIAN_POINT('Ctrl Pts',(-34.9267822331094,-6.2084537431929,
130.820672409693));
#257221=CARTESIAN_POINT('Ctrl Pts',(-35.2052298569221,-3.34209732541825,
136.036525506343));
#257222=CARTESIAN_POINT('Ctrl Pts',(-35.4836774807351,2.59548326388451,
136.444274675672));
#257223=CARTESIAN_POINT('Ctrl Pts',(-35.7621251045479,6.14794153008404,
131.66921835072));
#257224=CARTESIAN_POINT('Ctrl Pts',(-36.0405727283609,4.05074187377708,
126.099400019648));
#257225=CARTESIAN_POINT('Ctrl Pts',(-36.3190203521737,-1.76889167478912,
124.85321062796));
#257226=CARTESIAN_POINT('Ctrl Pts',(-36.5974679759867,-5.96300018938643,
129.075837346879));
#257227=CARTESIAN_POINT('Ctrl Pts',(-36.8759155997995,-4.67740283869194,
134.886892508504));
#257228=CARTESIAN_POINT('Ctrl Pts',(-37.1543632236125,0.906499216928551,
136.946300305126));
#257229=CARTESIAN_POINT('Ctrl Pts',(-37.4328108474252,5.65737277714046,
133.361565579315));
#257230=CARTESIAN_POINT('Ctrl Pts',(-37.7112584712383,5.2093971331851,127.426884420063));
#257231=CARTESIAN_POINT('Ctrl Pts',(-37.9897060950511,-0.0257599829691867,
124.595938887431));
#257232=CARTESIAN_POINT('Ctrl Pts',(-38.268153718864,-5.23724493321992,
127.470229626529));
#257233=CARTESIAN_POINT('Ctrl Pts',(-38.5466013426768,-5.63595764348039,
133.408423865036));
#257234=CARTESIAN_POINT('Ctrl Pts',(-38.8250489664898,-0.855500611219946,
136.953611194679));
#257235=CARTESIAN_POINT('Ctrl Pts',(-39.1034965903026,4.71111968922328,
134.847937651547));
#257236=CARTESIAN_POINT('Ctrl Pts',(-39.3819442141156,5.94845114626212,
129.026414353905));
#257237=CARTESIAN_POINT('Ctrl Pts',(-39.6603918379284,1.71944659787975,
124.838736815064));
#257238=CARTESIAN_POINT('Ctrl Pts',(-39.9388394617414,-4.08964537431793,
126.133176113797));
#257239=CARTESIAN_POINT('Ctrl Pts',(-40.2172870855541,-6.14055303780089,
131.720205771443));
#257240=CARTESIAN_POINT('Ctrl Pts',(-40.495734709367,-2.54859244223803,
136.465618474199));
#257241=CARTESIAN_POINT('Ctrl Pts',(-40.7741823331801,3.3854001020792,136.008611774531));
#257242=CARTESIAN_POINT('Ctrl Pts',(-41.0526299569928,6.20837533857501,
130.769152503414));
#257243=CARTESIAN_POINT('Ctrl Pts',(-41.3310775808058,3.3261569349168,125.562047769191));
#257244=CARTESIAN_POINT('Ctrl Pts',(-41.6095252046187,-2.61263720013008,
125.172372441404));
#257245=CARTESIAN_POINT('Ctrl Pts',(-41.8879728284316,-6.15054538268038,
129.958219109591));
#257246=CARTESIAN_POINT('Ctrl Pts',(-42.1664204522444,-4.03640282939359,
135.521628487296));
#257247=CARTESIAN_POINT('Ctrl Pts',(-42.4448680760573,1.78699673486542,
136.750099144066));
#257248=CARTESIAN_POINT('Ctrl Pts',(-42.7233156998703,5.96823359942677,
132.514726560457));
#257249=CARTESIAN_POINT('Ctrl Pts',(-43.0017633236831,4.66495535053527,
126.707611231352));
#257250=CARTESIAN_POINT('Ctrl Pts',(-43.2802109474961,-0.925188969759574,
124.665208450844));
#257251=CARTESIAN_POINT('Ctrl Pts',(-43.5586585713089,-5.6651298248394,
128.264386597296));
#257252=CARTESIAN_POINT('Ctrl Pts',(-43.8371061951219,-5.19909312786956,
134.197676783747));
#257253=CARTESIAN_POINT('Ctrl Pts',(-44.1155538189346,0.0446561637927345,
137.012675186187));
#257254=CARTESIAN_POINT('Ctrl Pts',(-44.3940014427476,5.24736862250453,
134.122535793092));
#257255=CARTESIAN_POINT('Ctrl Pts',(-44.6724490665605,5.62800566534308,
128.183155515557));
#257256=CARTESIAN_POINT('Ctrl Pts',(-44.9508966903734,0.836780445093053,
124.65253467378));
#257257=CARTESIAN_POINT('Ctrl Pts',(-45.2293443141862,-4.72340512520001,
126.775141340936));
#257258=CARTESIAN_POINT('Ctrl Pts',(-45.5077919379991,-5.94301213660306,
132.600403685011));
#257259=CARTESIAN_POINT('Ctrl Pts',(-45.7862395618121,-1.7012813267513,
136.775190191685));
#257260=CARTESIAN_POINT('Ctrl Pts',(-46.0646871856249,4.10384391017172,
135.463076010984));
#257261=CARTESIAN_POINT('Ctrl Pts',(-46.3431348094379,6.13773707756737,
129.869829974632));
#257262=CARTESIAN_POINT('Ctrl Pts',(-46.6215824332507,2.5313497158043,125.135371944775));
#257263=CARTESIAN_POINT('Ctrl Pts',(-46.9000300570636,-3.40122437147435,
125.610437559721));
#257264=CARTESIAN_POINT('Ctrl Pts',(-47.1784776808764,-6.20823942041608,
130.858464727578));
#257265=CARTESIAN_POINT('Ctrl Pts',(-47.4569253046894,-3.31018573135201,
136.056772861467));
#257266=CARTESIAN_POINT('Ctrl Pts',(-47.7353729285023,2.62976693326135,
136.428370737814));
#257267=CARTESIAN_POINT('Ctrl Pts',(-48.0138205523151,6.15309225746451,
131.631778061822));
#257268=CARTESIAN_POINT('Ctrl Pts',(-48.2922681761281,4.02202639232555,
126.074829176147));
#257269=CARTESIAN_POINT('Ctrl Pts',(-48.570715799941,-1.80508524044794,
124.864088634681));
#257270=CARTESIAN_POINT('Ctrl Pts',(-48.8491634237538,-5.97341172056607,
129.112167847066));
#257271=CARTESIAN_POINT('Ctrl Pts',(-49.1276110475668,-4.65246464686987,
134.915289547327));
#257272=CARTESIAN_POINT('Ctrl Pts',(-49.4060586713796,0.943870151766231,
136.940668391181));
#257273=CARTESIAN_POINT('Ctrl Pts',(-49.6845062951925,5.6728343915496,133.327080166382));
#257274=CARTESIAN_POINT('Ctrl Pts',(-49.9629539190054,5.18874095886556,
127.395235917922));
#257275=CARTESIAN_POINT('Ctrl Pts',(-50.2414015428183,-0.0635519309279763,
124.596210723434));
#257276=CARTESIAN_POINT('Ctrl Pts',(-50.5198491666312,-5.25744370088312,
127.50217199667));
#257277=CARTESIAN_POINT('Ctrl Pts',(-50.798296790444,-5.6200015501302,133.442683291627));
#257278=CARTESIAN_POINT('Ctrl Pts',(-51.076744414257,-0.818052527146474,
136.958704938348));
#257279=CARTESIAN_POINT('Ctrl Pts',(-51.3551920380699,4.73564680419706,
134.819184810706));
#257280=CARTESIAN_POINT('Ctrl Pts',(-51.6336396618827,5.93751807169133,
128.990237384633));
#257281=CARTESIAN_POINT('Ctrl Pts',(-51.9120872856956,1.68310029518491,
124.828380584778));
#257282=CARTESIAN_POINT('Ctrl Pts',(-52.1905349095086,-4.11800442857602,
126.1581574922));
#257283=CARTESIAN_POINT('Ctrl Pts',(-52.4689825333214,-6.13486425817587,
131.757568092191));
#257284=CARTESIAN_POINT('Ctrl Pts',(-52.7474301571343,-2.51408353929296,
136.481027589776));
#257285=CARTESIAN_POINT('Ctrl Pts',(-53.0258777809472,3.41701713239144,
135.987907460498));
#257286=CARTESIAN_POINT('Ctrl Pts',(-53.3043254047601,6.20804598997526,
130.731361012906));
#257287=CARTESIAN_POINT('Ctrl Pts',(-53.5827730285729,3.29418386267868,
125.541897635768));
#257288=CARTESIAN_POINT('Ctrl Pts',(-53.8612206523859,-2.64687230459117,
125.188380653292));
#257289=CARTESIAN_POINT('Ctrl Pts',(-54.1396682761987,-6.15558213084251,
129.995674902111));
#257290=CARTESIAN_POINT('Ctrl Pts',(-54.4181159000117,-4.0076126957546,
135.546111816938));
#257291=CARTESIAN_POINT('Ctrl Pts',(-54.6965635238244,1.82315702396754,
136.739111026966));
#257292=CARTESIAN_POINT('Ctrl Pts',(-54.9750111476374,5.97853450483549,
132.478364539431));
#257293=CARTESIAN_POINT('Ctrl Pts',(-55.2534587714502,4.63993084340721,
126.679290227339));
#257294=CARTESIAN_POINT('Ctrl Pts',(-55.5319063952633,-0.962542589888887,
124.670954082973));
#257295=CARTESIAN_POINT('Ctrl Pts',(-55.810354019076,-5.68048640589689,
128.298918910331));
#257296=CARTESIAN_POINT('Ctrl Pts',(-56.088801642889,-5.1783407220741,134.229262269005));
#257297=CARTESIAN_POINT('Ctrl Pts',(-56.3672492667019,0.0824471093265141,
137.012288325754));
#257298=CARTESIAN_POINT('Ctrl Pts',(-56.6456968905149,5.26747007502141,
134.090532092806));
#257299=CARTESIAN_POINT('Ctrl Pts',(-56.9241445143275,5.6119453719906,128.148944812513));
#257300=CARTESIAN_POINT('Ctrl Pts',(-57.2025921381407,0.799317030873196,
124.64755493279));
#257301=CARTESIAN_POINT('Ctrl Pts',(-57.4810397619534,-4.74784461280872,
126.803968700697));
#257302=CARTESIAN_POINT('Ctrl Pts',(-57.7594873857663,-5.93196900242356,
132.636547210196));
#257303=CARTESIAN_POINT('Ctrl Pts',(-58.0379350095792,-1.66490367160747,
136.785435748359));
#257304=CARTESIAN_POINT('Ctrl Pts',(-58.3163826333922,4.13212679834998,
135.438008433087));
#257305=CARTESIAN_POINT('Ctrl Pts',(-58.5948302572049,6.13193460624012,
129.832485141631));
#257306=CARTESIAN_POINT('Ctrl Pts',(-58.873277881018,2.49679407265481,125.120067933803));
#257307=CARTESIAN_POINT('Ctrl Pts',(-59.1517255048308,-3.43277823852872,
125.631238009216));
#257308=CARTESIAN_POINT('Ctrl Pts',(-59.4301731286437,-6.20779504904446,
130.896255040614));
#257309=CARTESIAN_POINT('Ctrl Pts',(-59.7086207524566,-3.27815147713605,
136.076825586523));
#257310=CARTESIAN_POINT('Ctrl Pts',(-59.9870683762695,2.66395315565763,
136.412258400192));
#257311=CARTESIAN_POINT('Ctrl Pts',(-60.2655160000824,6.15801497974849,
131.594307112665));
#257312=CARTESIAN_POINT('Ctrl Pts',(-60.5439636238952,3.99316187320697,
126.050433587173));
#257313=CARTESIAN_POINT('Ctrl Pts',(-60.8224112477081,-1.84121191800936,
124.875186760365));
#257314=CARTESIAN_POINT('Ctrl Pts',(-61.1008588715211,-5.98360190477769,
129.148561052078));
#257315=CARTESIAN_POINT('Ctrl Pts',(-61.3793064953339,-4.62735405625939,
134.943534254169));
#257316=CARTESIAN_POINT('Ctrl Pts',(-61.6577541191468,0.981206111148332,
136.934809094094));
#257317=CARTESIAN_POINT('Ctrl Pts',(-61.9362017429597,5.68808579699418,
133.292501273148));
#257318=CARTESIAN_POINT('Ctrl Pts',(-62.2146493667725,5.16789251384163,
127.36371374215));
#257319=CARTESIAN_POINT('Ctrl Pts',(-62.4930969905855,-0.10134152394658,
124.596712604715));
#257320=CARTESIAN_POINT('Ctrl Pts',(-62.7715446143984,-5.27744765203657,
127.534236730624));
#257321=CARTESIAN_POINT('Ctrl Pts',(-63.0499922382113,-5.60383720555579,
133.476844954201));
#257322=CARTESIAN_POINT('Ctrl Pts',(-63.3284398620242,-0.780574129835986,
136.963570630527));
#257323=CARTESIAN_POINT('Ctrl Pts',(-63.606887485837,4.75999843803683,134.790283199078));
#257324=CARTESIAN_POINT('Ctrl Pts',(-63.88533510965,5.92636498020503,128.954127638363));
#257325=CARTESIAN_POINT('Ctrl Pts',(-64.1637827334628,1.64669162458969,
124.818245796629));
#257326=CARTESIAN_POINT('Ctrl Pts',(-64.4422303572757,-4.14621088866563,
126.183311037368));
#257327=CARTESIAN_POINT('Ctrl Pts',(-64.7206779810887,-6.12894814889968,
131.794895091487));
#257328=CARTESIAN_POINT('Ctrl Pts',(-64.9991256049015,-2.47948147605779,
136.49622635437));
#257329=CARTESIAN_POINT('Ctrl Pts',(-65.2775732287142,3.44850754387722,
135.967011068231));
#257330=CARTESIAN_POINT('Ctrl Pts',(-65.5560208525274,6.20748659994837,
130.693572227424));
#257331=CARTESIAN_POINT('Ctrl Pts',(-65.83446847634,3.26208872324607,125.521942504845));
#257332=CARTESIAN_POINT('Ctrl Pts',(-66.1129161001531,-2.68100932822562,
125.204596967384));
#257333=CARTESIAN_POINT('Ctrl Pts',(-66.3913637239659,-6.1603907816451,
130.033160660777));
#257334=CARTESIAN_POINT('Ctrl Pts',(-66.6698113477789,-3.97867405855336,
135.570419439246));
#257335=CARTESIAN_POINT('Ctrl Pts',(-66.9482589715917,1.85924975531565,
136.727902995508));
#257336=CARTESIAN_POINT('Ctrl Pts',(-67.2267065954047,5.98861387344954,
132.441940487574));
#257337=CARTESIAN_POINT('Ctrl Pts',(-67.5051542192175,4.61473440193538,
126.651122079325));
#257338=CARTESIAN_POINT('Ctrl Pts',(-67.7836018430304,-0.999860542648545,
124.676926990737));
#257339=CARTESIAN_POINT('Ctrl Pts',(-68.0620494668433,-5.69563249444164,
128.33354406343));
#257340=CARTESIAN_POINT('Ctrl Pts',(-68.3404970906562,-5.15739643095884,
134.260720843274));
#257341=CARTESIAN_POINT('Ctrl Pts',(-68.618944714469,0.120234999752325,
137.011671428276));
#257342=CARTESIAN_POINT('Ctrl Pts',(-68.8973923382821,5.28737633949755,
134.058406622227));
#257343=CARTESIAN_POINT('Ctrl Pts',(-69.1758399620947,5.59567712593856,
128.114832506878));
#257344=CARTESIAN_POINT('Ctrl Pts',(-69.4542875859078,0.761823997666808,
124.642803334499));
#257345=CARTESIAN_POINT('Ctrl Pts',(-69.7327352097205,-4.77210816728929,
126.832944296451));
#257346=CARTESIAN_POINT('Ctrl Pts',(-70.0111828335336,-5.92070605695121,
132.672622843033));
#257347=CARTESIAN_POINT('Ctrl Pts',(-70.2896304573463,-1.62846432284579,
136.795459674095));
#257348=CARTESIAN_POINT('Ctrl Pts',(-70.5680780811594,4.16025656905012,
135.412769153666));
#257349=CARTESIAN_POINT('Ctrl Pts',(-70.8465257049722,6.12590491382102,
129.795176321834));
#257350=CARTESIAN_POINT('Ctrl Pts',(-71.1249733287852,2.46214590988275,
125.104974556385));
#257351=CARTESIAN_POINT('Ctrl Pts',(-71.4034209525978,-3.46420490272305,
125.652230150673));
#257352=CARTESIAN_POINT('Ctrl Pts',(-71.681868576411,-6.20712064554441,
130.93404194847));
#257353=CARTESIAN_POINT('Ctrl Pts',(-71.9603162002238,-3.24599574981168,
136.09668293845));
#257354=CARTESIAN_POINT('Ctrl Pts',(-72.2387638240367,2.69804066428979,
136.395938259856));
#257355=CARTESIAN_POINT('Ctrl Pts',(-72.5172114478495,6.16270951452303,
131.556806891751));
#257356=CARTESIAN_POINT('Ctrl Pts',(-72.7956590716624,3.96414938600637,
126.026214156713));
#257357=CARTESIAN_POINT('Ctrl Pts',(-73.0741066954753,-1.87727036878649,
124.886504593767));
#257358=CARTESIAN_POINT('Ctrl Pts',(-73.3525543192881,-5.99357036442037,
129.185015613353));
#257359=CARTESIAN_POINT('Ctrl Pts',(-73.6310019431012,-4.60207199734241,
134.971625582408));
#257360=CARTESIAN_POINT('Ctrl Pts',(-73.909449566914,1.01850571157763,136.928722630985));
#257361=CARTESIAN_POINT('Ctrl Pts',(-74.187897190727,5.70312642832773,133.257830180947));
#257362=CARTESIAN_POINT('Ctrl Pts',(-74.4663448145398,5.14685257066011,
127.332319060812));
#257363=CARTESIAN_POINT('Ctrl Pts',(-74.7447924383527,-0.139127361718492,
124.597444512675));
#257364=CARTESIAN_POINT('Ctrl Pts',(-75.0232400621657,-5.29725604542678,
127.566422640223));
#257365=CARTESIAN_POINT('Ctrl Pts',(-75.3016876859784,-5.58746520873256,
133.510907586884));
#257366=CARTESIAN_POINT('Ctrl Pts',(-75.5801353097915,-0.743066808063574,
136.968208090913));
#257367=CARTESIAN_POINT('Ctrl Pts',(-75.8585829336042,4.7841736883842,134.761233887624));
#257368=CARTESIAN_POINT('Ctrl Pts',(-76.1370305574171,5.91499228508486,
128.918086453158));
#257369=CARTESIAN_POINT('Ctrl Pts',(-76.41547818123,1.61022193523031,124.808332826166));
#257370=CARTESIAN_POINT('Ctrl Pts',(-76.693925805043,-4.17426370938676,
126.208635817229));
#257371=CARTESIAN_POINT('Ctrl Pts',(-76.9723734288558,-6.12280492919574,
131.832185386163));
#257372=CARTESIAN_POINT('Ctrl Pts',(-77.2508210526686,-2.44478753472383,
136.511214204787));
#257373=CARTESIAN_POINT('Ctrl Pts',(-77.5292686764817,3.47987016964863,
135.945923372052));
#257374=CARTESIAN_POINT('Ctrl Pts',(-77.8077163002943,6.20669718922256,
130.655787547247));
#257375=CARTESIAN_POINT('Ctrl Pts',(-78.0861639241075,3.22987270591563,
125.502183115868));
#257376=CARTESIAN_POINT('Ctrl Pts',(-78.3646115479203,-2.71504700607423,
125.221020782777));
#257377=CARTESIAN_POINT('Ctrl Pts',(-78.6430591717333,-6.16497115690175,
130.070674996542));
#257378=CARTESIAN_POINT('Ctrl Pts',(-78.921506795546,-3.94958799012119,
135.594550453492));
#257379=CARTESIAN_POINT('Ctrl Pts',(-79.199954419359,1.89527359148086,136.71647546501));
#257380=CARTESIAN_POINT('Ctrl Pts',(-79.4784020431719,5.9984713317742,132.405455754592));
#257381=CARTESIAN_POINT('Ctrl Pts',(-79.7568496669848,4.58936695978296,
126.623107831093));
#257382=CARTESIAN_POINT('Ctrl Pts',(-80.0352972907976,-1.0371414452086,
124.683126952807));
#257383=CARTESIAN_POINT('Ctrl Pts',(-80.3137449146107,-5.71056752923021,
128.368260773546));
#257384=CARTESIAN_POINT('Ctrl Pts',(-80.5921925384234,-5.13626103062165,
134.292051340844));
#257385=CARTESIAN_POINT('Ctrl Pts',(-80.8706401622364,0.158018434826916,
137.010824516613));
#257386=CARTESIAN_POINT('Ctrl Pts',(-81.1490877860493,5.30708667829958,
134.026160571776));
#257387=CARTESIAN_POINT('Ctrl Pts',(-81.4275354098621,5.57920153001237,
128.080819862696));
#257388=CARTESIAN_POINT('Ctrl Pts',(-81.705983033675,0.724302734791404,
124.63828005498));
#257389=CARTESIAN_POINT('Ctrl Pts',(-81.984430657488,-4.79619488954742,
126.862067054498));
#257390=CARTESIAN_POINT('Ctrl Pts',(-82.2628782813007,-5.90922371753823,
132.708629246728));
#257391=CARTESIAN_POINT('Ctrl Pts',(-82.5413259051138,-1.59196463073914,
136.805261597452));
#257392=CARTESIAN_POINT('Ctrl Pts',(-82.8197735289264,4.18823217991362,
135.387359107972));
#257393=CARTESIAN_POINT('Ctrl Pts',(-83.0982211527395,6.11964822374235,
129.757904897731));
#257394=CARTESIAN_POINT('Ctrl Pts',(-83.3766687765523,2.42740651138818,
125.090092371815));
#257395=CARTESIAN_POINT('Ctrl Pts',(-83.6551164003652,-3.49550319953123,
125.67341320622));
#257396=CARTESIAN_POINT('Ctrl Pts',(-83.9335640241781,-6.20621623490623,
130.971824050937));
#257397=CARTESIAN_POINT('Ctrl Pts',(-84.2120116479911,-3.21371974092037,
136.116344181428));
#257398=CARTESIAN_POINT('Ctrl Pts',(-84.4904592718038,2.73202819603347,
136.379410921554));
#257399=CARTESIAN_POINT('Ctrl Pts',(-84.7689068956169,6.16717568783019,
131.519278788663));
#257400=CARTESIAN_POINT('Ctrl Pts',(-85.0473545194296,3.9349900057924,126.002171782228));
#257401=CARTESIAN_POINT('Ctrl Pts',(-85.3258021432425,-1.91325925661942,
124.898041715501));
#257402=CARTESIAN_POINT('Ctrl Pts',(-85.6042497670555,-6.00331673010926,
129.221530180052));
#257403=CARTESIAN_POINT('Ctrl Pts',(-85.8826973908683,-4.57661940695503,
134.999562491112));
#257404=CARTESIAN_POINT('Ctrl Pts',(-86.1611450146813,1.05576757090286,
136.922409227389));
#257405=CARTESIAN_POINT('Ctrl Pts',(-86.4395926384942,5.71795572821454,
133.223068174528));
#257406=CARTESIAN_POINT('Ctrl Pts',(-86.718040262307,5.12562190896342,127.301053037252));
#257407=CARTESIAN_POINT('Ctrl Pts',(-86.9964878861199,-0.176908044074368,
124.598406420195));
#257408=CARTESIAN_POINT('Ctrl Pts',(-87.2749355099329,-5.31686814704595,
127.598728532803));
#257409=CARTESIAN_POINT('Ctrl Pts',(-87.5533831337457,-5.57088616633168,
133.544869927476));
#257410=CARTESIAN_POINT('Ctrl Pts',(-87.8318307575586,-0.70553195167748,
136.972617147663));
#257411=CARTESIAN_POINT('Ctrl Pts',(-88.1102783813713,4.80817165941601,
134.732037952774));
#257412=CARTESIAN_POINT('Ctrl Pts',(-88.3887260051845,5.90340040775061,
128.882115164534));
#257413=CARTESIAN_POINT('Ctrl Pts',(-88.6671736289971,1.57369257850503,
124.798642040718));
#257414=CARTESIAN_POINT('Ctrl Pts',(-88.9456212528103,-4.20216185122988,
126.234130893362));
#257415=CARTESIAN_POINT('Ctrl Pts',(-89.2240688766231,-6.11643482670397,
131.869437594414));
#257416=CARTESIAN_POINT('Ctrl Pts',(-89.5025165004358,-2.41000300088966,
136.525990585645));
#257417=CARTESIAN_POINT('Ctrl Pts',(-89.7809641242489,3.51110384754994,
135.924645153375));
#257418=CARTESIAN_POINT('Ctrl Pts',(-90.0594117480617,6.20567778705031,
130.618008372501));
#257419=CARTESIAN_POINT('Ctrl Pts',(-90.3378593718745,3.19753700446471,
125.482620201028));
#257420=CARTESIAN_POINT('Ctrl Pts',(-90.6163069956876,-2.74898407685696,
125.237651490881));
#257421=CARTESIAN_POINT('Ctrl Pts',(-90.8947546195002,-6.16932308688508,
130.108216519297));
#257422=CARTESIAN_POINT('Ctrl Pts',(-91.1732022433134,-3.92035556825405,
135.618503965492));
#257423=CARTESIAN_POINT('Ctrl Pts',(-91.4516498671261,1.93122719758584,
136.70482885892));
#257424=CARTESIAN_POINT('Ctrl Pts',(-91.7300974909391,6.00810651453776,
132.368911692441));
#257425=CARTESIAN_POINT('Ctrl Pts',(-92.0085451147519,4.56382945695037,
126.595248520721));
#257426=CARTESIAN_POINT('Ctrl Pts',(-92.2869927385648,-1.07438391611076,
124.689553739443));
#257427=CARTESIAN_POINT('Ctrl Pts',(-92.5654403623776,-5.72529095683809,
128.403067754236));
#257428=CARTESIAN_POINT('Ctrl Pts',(-92.8438879861907,-5.11493530424405,
134.323252600751));
#257429=CARTESIAN_POINT('Ctrl Pts',(-93.1223356100035,0.195796014469281,
137.009747622148));
#257430=CARTESIAN_POINT('Ctrl Pts',(-93.4007832338166,5.32660036105212,
133.993795136343));
#257431=CARTESIAN_POINT('Ctrl Pts',(-93.6792308576291,5.56251919472255,
128.046908140318));
#257432=CARTESIAN_POINT('Ctrl Pts',(-93.9576784814422,0.686754632612129,
124.633985261843));
#257433=CARTESIAN_POINT('Ctrl Pts',(-94.2361261052551,-4.82010388703947,
126.891335895681));
#257434=CARTESIAN_POINT('Ctrl Pts',(-94.5145737290679,-5.8975224096676,
132.744565087048));
#257435=CARTESIAN_POINT('Ctrl Pts',(-94.7930213528811,-1.55540594779807,
136.814841155217));
#257436=CARTESIAN_POINT('Ctrl Pts',(-95.0714689766937,4.21605259429308,
135.361779237583));
#257437=CARTESIAN_POINT('Ctrl Pts',(-95.3499166005066,6.11316476784841,
129.720672250431));
#257438=CARTESIAN_POINT('Ctrl Pts',(-95.6283642243196,2.39257716445285,
125.075421931555));
#257439=CARTESIAN_POINT('Ctrl Pts',(-95.9068118481323,-3.52667196918255,
125.694786390909));
#257440=CARTESIAN_POINT('Ctrl Pts',(-96.1852594719453,-6.20508185064282,
131.009599947983));
#257441=CARTESIAN_POINT('Ctrl Pts',(-96.4637070957582,-3.18132464646333,
136.135808586901));
#257442=CARTESIAN_POINT('Ctrl Pts',(-96.742154719571,2.76591449146702,136.362676997713));
#257443=CARTESIAN_POINT('Ctrl Pts',(-97.020602343384,6.17141333417382,131.481724194021));
#257444=CARTESIAN_POINT('Ctrl Pts',(-97.299049967197,3.90568481307747,125.978307354616));
#257445=CARTESIAN_POINT('Ctrl Pts',(-97.5774975910097,-1.94917724792726,
124.909797698053));
#257446=CARTESIAN_POINT('Ctrl Pts',(-97.8559452148228,-6.01284064068852,
129.258103399115));
#257447=CARTESIAN_POINT('Ctrl Pts',(-98.1343928386354,-4.55099722825276,
135.027343945068));
#257448=CARTESIAN_POINT('Ctrl Pts',(-98.4128404624484,1.09299030837272,
136.915869117251));
#257449=CARTESIAN_POINT('Ctrl Pts',(-98.6912880862614,5.73257314714861,
133.188216542011));
#257450=CARTESIAN_POINT('Ctrl Pts',(-98.9697357100741,5.10420131546234,
127.269916830042));
#257451=CARTESIAN_POINT('Ctrl Pts',(-99.2481833338871,-0.214682171037078,
124.599598291628));
#257452=CARTESIAN_POINT('Ctrl Pts',(-99.5266309576999,-5.33628323016052,
127.631153211259));
#257453=CARTESIAN_POINT('Ctrl Pts',(-99.8050785815131,-5.55410069269506,
133.578730717485));
#257454=CARTESIAN_POINT('Ctrl Pts',(-100.083526205326,-0.667970951546107,
136.976797637399));
#257455=CARTESIAN_POINT('Ctrl Pts',(-100.361973829139,4.83199146187865,
134.702696476397));
#257456=CARTESIAN_POINT('Ctrl Pts',(-100.640421452952,5.89158977774298,
128.846215105423));
#257457=CARTESIAN_POINT('Ctrl Pts',(-100.918869076765,1.53710490802326,
124.789173799381));
#257458=CARTESIAN_POINT('Ctrl Pts',(-101.197316700577,-4.22990428042106,
126.259795321038));
#257459=CARTESIAN_POINT('Ctrl Pts',(-101.47576432439,-6.10983807746976,
131.906650335846));
#257460=CARTESIAN_POINT('Ctrl Pts',(-101.754211948203,-2.37512916350784,
136.540554949401));
#257461=CARTESIAN_POINT('Ctrl Pts',(-102.032659572016,3.54220742020778,
135.903177200671));
#257462=CARTESIAN_POINT('Ctrl Pts',(-102.311107195829,6.20442843120499,
130.580236103105));
#257463=CARTESIAN_POINT('Ctrl Pts',(-102.589554819642,3.16508281710451,
125.463254485237));
#257464=CARTESIAN_POINT('Ctrl Pts',(-102.868002443455,-2.78281928302352,
125.254488475437));
#257465=CARTESIAN_POINT('Ctrl Pts',(-103.146450067268,-6.1734464103326,
130.145783837928));
#257466=CARTESIAN_POINT('Ctrl Pts',(-103.424897691081,-3.8909778761698,
135.642279087639));
#257467=CARTESIAN_POINT('Ctrl Pts',(-103.703345314893,1.96710924135641,
136.69296360881));
#257468=CARTESIAN_POINT('Ctrl Pts',(-103.981792938706,6.01751906470488,
132.332309655276));
#257469=CARTESIAN_POINT('Ctrl Pts',(-104.260240562519,4.53812283973896,
126.567545180546));
#257470=CARTESIAN_POINT('Ctrl Pts',(-104.538688186332,-1.11158657532129,
124.696207112496));
#257471=CARTESIAN_POINT('Ctrl Pts',(-104.817135810145,-5.73980223168479,
128.437963715717));
#257472=CARTESIAN_POINT('Ctrl Pts',(-105.095583433958,-5.093420042057,134.354323466822));
#257473=CARTESIAN_POINT('Ctrl Pts',(-105.374031057771,0.233566338818549,
137.008440784786));
#257474=CARTESIAN_POINT('Ctrl Pts',(-105.652478681584,5.34591666467016,
133.961311515241));
#257475=CARTESIAN_POINT('Ctrl Pts',(-105.930926305397,5.54563073823764,
128.013098596357));
#257476=CARTESIAN_POINT('Ctrl Pts',(-106.20937392921,0.649181082487974,
124.629919114234));
#257477=CARTESIAN_POINT('Ctrl Pts',(-106.487821553022,-4.84383427380942,
126.920749735436));
#257478=CARTESIAN_POINT('Ctrl Pts',(-106.766269176835,-5.88560256693534,
132.780429032376));
#257479=CARTESIAN_POINT('Ctrl Pts',(-107.044716800648,-1.51878962871805,
136.824197992414));
#257480=CARTESIAN_POINT('Ctrl Pts',(-107.323164424461,4.2437167812931,135.336030490371));
#257481=CARTESIAN_POINT('Ctrl Pts',(-107.601612048274,6.10645478638612,
129.683479759601));
#257482=CARTESIAN_POINT('Ctrl Pts',(-107.880059672087,2.35765915969063,
125.060963779225));
#257483=CARTESIAN_POINT('Ctrl Pts',(-108.1585072959,-3.55771005670707,125.716348912751));
#257484=CARTESIAN_POINT('Ctrl Pts',(-108.436954919713,-6.20371753478999,
131.04736823981));
#257485=CARTESIAN_POINT('Ctrl Pts',(-108.715402543526,-3.14881166685081,
136.155075433609));
#257486=CARTESIAN_POINT('Ctrl Pts',(-108.993850167338,2.79969829492213,
136.345737108415));
#257487=CARTESIAN_POINT('Ctrl Pts',(-109.272297791151,6.17542229652738,
131.444144499421));
#257488=CARTESIAN_POINT('Ctrl Pts',(-109.550745414964,3.87623489377466,
125.954621758183));
#257489=CARTESIAN_POINT('Ctrl Pts',(-109.829193038777,-1.98502301175461,
124.921772105802));
#257490=CARTESIAN_POINT('Ctrl Pts',(-110.10764066259,-6.02214174324697,
129.294733915307));
#257491=CARTESIAN_POINT('Ctrl Pts',(-110.386088286403,-4.52520641067474,
135.054968914823));
#257492=CARTESIAN_POINT('Ctrl Pts',(-110.664535910216,1.13017254468408,
136.909102542919));
#257493=CARTESIAN_POINT('Ctrl Pts',(-110.942983534029,5.74697814347679,
133.153276574838));
#257494=CARTESIAN_POINT('Ctrl Pts',(-111.221431157841,5.08259158390449,
127.238911592946));
#257495=CARTESIAN_POINT('Ctrl Pts',(-111.499878781655,-0.252448342873548,
124.601020082813));
#257496=CARTESIAN_POINT('Ctrl Pts',(-111.778326405467,-5.3555005753377,
127.663695474083));
#257497=CARTESIAN_POINT('Ctrl Pts',(-112.05677402928,-5.53710940981492,
133.612488702192));
#257498=CARTESIAN_POINT('Ctrl Pts',(-112.335221653093,-0.630385199504834,
136.980749405212));
#257499=CARTESIAN_POINT('Ctrl Pts',(-112.613669276906,4.85563221312083,
134.673210545752));
#257500=CARTESIAN_POINT('Ctrl Pts',(-112.892116900719,5.8795608327098,128.810387606114));
#257501=CARTESIAN_POINT('Ctrl Pts',(-113.170564524532,1.50046027955312,
124.779928453004));
#257502=CARTESIAN_POINT('Ctrl Pts',(-113.449012148345,-4.25748996895278,
126.285628149252));
#257503=CARTESIAN_POINT('Ctrl Pts',(-113.727459772158,-6.10301492593933,
131.943822231527));
#257504=CARTESIAN_POINT('Ctrl Pts',(-114.00590739597,-2.3401673148416,136.554906756366));
#257505=CARTESIAN_POINT('Ctrl Pts',(-114.284355019783,3.57317973506622,
135.881520309444));
#257506=CARTESIAN_POINT('Ctrl Pts',(-114.562802643596,6.202949167983,130.542472138726));
#257507=CARTESIAN_POINT('Ctrl Pts',(-114.841250267409,3.13251134643626,
125.444086686097));
#257508=CARTESIAN_POINT('Ctrl Pts',(-115.119697891222,-2.81655137079845,
125.271531112549));
#257509=CARTESIAN_POINT('Ctrl Pts',(-115.398145515035,-6.17734097445314,
130.183375560363));
#257510=CARTESIAN_POINT('Ctrl Pts',(-115.676593138848,-3.86145600246928,
135.665874938939));
#257511=CARTESIAN_POINT('Ctrl Pts',(-115.955040762661,2.00291839317105,
136.680880154352));
#257512=CARTESIAN_POINT('Ctrl Pts',(-116.233488386474,6.02670863349017,
132.295650999397));
#257513=CARTESIAN_POINT('Ctrl Pts',(-116.511936010287,4.51224806071678,
126.539998837124));
#257514=CARTESIAN_POINT('Ctrl Pts',(-116.790383634099,-1.14874804428301,
124.703086825424));
#257515=CARTESIAN_POINT('Ctrl Pts',(-117.068831257912,-5.75410081604829,
128.472947364906));
#257516=CARTESIAN_POINT('Ctrl Pts',(-117.347278881725,-5.07171604131793,
134.385262787713));
#257517=CARTESIAN_POINT('Ctrl Pts',(-117.625726505538,0.271328008281021,
137.006904052952));
#257518=CARTESIAN_POINT('Ctrl Pts',(-117.904174129351,5.3650348733795,133.928710912162));
#257519=CARTESIAN_POINT('Ctrl Pts',(-118.182621753164,5.52853678636705,
127.979392483636));
#257520=CARTESIAN_POINT('Ctrl Pts',(-118.461069376977,0.611583476719488,
124.626081762825));
#257521=CARTESIAN_POINT('Ctrl Pts',(-118.73951700079,-4.86738517051901,
126.95030748382));
#257522=CARTESIAN_POINT('Ctrl Pts',(-119.017964624603,-5.87346463103546,
132.816219753764));
#257523=CARTESIAN_POINT('Ctrl Pts',(-119.296412248415,-1.48211703032935,
136.833331762325));
#257524=CARTESIAN_POINT('Ctrl Pts',(-119.574859872228,4.27122371580729,
135.310113820466));
#257525=CARTESIAN_POINT('Ctrl Pts',(-119.853307496041,6.09951852799569,
129.646328803424));
#257526=CARTESIAN_POINT('Ctrl Pts',(-120.131755119854,2.32265379100196,
125.046718450578));
#257527=CARTESIAN_POINT('Ctrl Pts',(-120.410202743667,-3.58861631197691,
125.738099972737));
#257528=CARTESIAN_POINT('Ctrl Pts',(-120.68865036748,-6.20212333790203,
131.085127526901));
#257529=CARTESIAN_POINT('Ctrl Pts',(-120.967097991293,-3.11618200686478,
136.174144007612));
#257530=CARTESIAN_POINT('Ctrl Pts',(-121.245545615105,2.83337835452712,
136.328591881372));
#257531=CARTESIAN_POINT('Ctrl Pts',(-121.523993238919,6.17920242633619,
131.406541097396));
#257532=CARTESIAN_POINT('Ctrl Pts',(-121.802440862731,3.84664133916317,
125.931115870606));
#257533=CARTESIAN_POINT('Ctrl Pts',(-122.080888486544,-2.02079521982502,
124.933964495032));
#257534=CARTESIAN_POINT('Ctrl Pts',(-122.359336110357,-6.03121969312815,
129.331420371272));
#257535=CARTESIAN_POINT('Ctrl Pts',(-122.63778373417,-4.49924790990888,
135.082436376724));
#257536=CARTESIAN_POINT('Ctrl Pts',(-122.916231357983,1.16731290203685,
136.90210975513));
#257537=CARTESIAN_POINT('Ctrl Pts',(-123.194678981796,5.76117018341619,
133.118249567719));
#257538=CARTESIAN_POINT('Ctrl Pts',(-123.473126605609,5.06079351504635,
127.208038474877));
#257539=CARTESIAN_POINT('Ctrl Pts',(-123.751574229422,-0.290205160143283,
124.602671741062));
#257540=CARTESIAN_POINT('Ctrl Pts',(-124.030021853235,-5.37451947047147,
127.696354115408));
#257541=CARTESIAN_POINT('Ctrl Pts',(-124.308469477047,-5.51991294730918,
133.646142630679));
#257542=CARTESIAN_POINT('Ctrl Pts',(-124.58691710086,-0.592776088308802,
136.984472304668));
#257543=CARTESIAN_POINT('Ctrl Pts',(-124.865364724673,4.87909303712557,
134.64358125345));
#257544=CARTESIAN_POINT('Ctrl Pts',(-125.143812348486,5.86731401838748,
128.774633994209));
#257545=CARTESIAN_POINT('Ctrl Pts',(-125.422259972299,1.46376005097626,
124.770906344175));
#257546=CARTESIAN_POINT('Ctrl Pts',(-125.700707596112,-4.28491789462882,
126.311628420759));
#257547=CARTESIAN_POINT('Ctrl Pts',(-125.979155219925,-6.09596562494584,
131.980951904039));
#257548=CARTESIAN_POINT('Ctrl Pts',(-126.257602843738,-2.30511875041471,
136.569045474729));
#257549=CARTESIAN_POINT('Ctrl Pts',(-126.536050467551,3.60401964443632,
135.859675282198));
#257550=CARTESIAN_POINT('Ctrl Pts',(-126.814498091363,6.20124005219796,
130.50471787872));
#257551=CARTESIAN_POINT('Ctrl Pts',(-127.092945715177,3.09982379940838,
125.42511751388));
#257552=CARTESIAN_POINT('Ctrl Pts',(-127.371393338989,-2.85017909022625,
125.288778770691));
#257553=CARTESIAN_POINT('Ctrl Pts',(-127.649840962802,-6.18100663493216,
130.220990293627));
#257554=CARTESIAN_POINT('Ctrl Pts',(-127.928288586615,-3.83179104109667,
135.689290645038));
#257555=CARTESIAN_POINT('Ctrl Pts',(-128.206736210428,2.03865332610762,
136.6685789433));
#257556=CARTESIAN_POINT('Ctrl Pts',(-128.485183834241,6.03567488037103,
132.258937083203));
#257557=CARTESIAN_POINT('Ctrl Pts',(-128.763631458054,4.48620607868298,
126.512610511197));
#257558=CARTESIAN_POINT('Ctrl Pts',(-129.042079081867,-1.18586694596332,
124.710192623294));
#257559=CARTESIAN_POINT('Ctrl Pts',(-129.32052670568,-5.76818618009069,
128.508017405469));
#257560=CARTESIAN_POINT('Ctrl Pts',(-129.598974329492,-5.04982410627509,
134.416069416958));
#257561=CARTESIAN_POINT('Ctrl Pts',(-129.877421953305,0.30907962358457,
137.005137483589));
#257562=CARTESIAN_POINT('Ctrl Pts',(-130.155869577118,5.38395427874936,
133.895994535135));
#257563=CARTESIAN_POINT('Ctrl Pts',(-130.434317200931,5.51123797253198,
127.945791051148));
#257564=CARTESIAN_POINT('Ctrl Pts',(-130.712764824744,0.573963208500954,
124.622473349811));
#257565=CARTESIAN_POINT('Ctrl Pts',(-130.991212448557,-4.89075570448117,
126.980008045559));
#257566=CARTESIAN_POINT('Ctrl Pts',(-131.26966007237,-5.8611090517438,132.851935924971));
#257567=CARTESIAN_POINT('Ctrl Pts',(-131.548107696183,-1.44538951154951,
136.842242126491));
#257568=CARTESIAN_POINT('Ctrl Pts',(-131.826555319995,4.29857237855583,
135.28403018822));
#257569=CARTESIAN_POINT('Ctrl Pts',(-132.105002943808,6.09235624970348,
129.609220758541));
#257570=CARTESIAN_POINT('Ctrl Pts',(-132.383450567622,2.28756235552218,
125.032686473479));
#257571=CARTESIAN_POINT('Ctrl Pts',(-132.661898191434,-3.6193895897498,
125.760038764874));
#257572=CARTESIAN_POINT('Ctrl Pts',(-132.940345815247,-6.20029931905343,
131.122876410071));
#257573=CARTESIAN_POINT('Ctrl Pts',(-133.21879343906,-3.08343687560774,
136.193013602317));
#257574=CARTESIAN_POINT('Ctrl Pts',(-133.497241062873,2.86695342225543,
136.311241951909));
#257575=CARTESIAN_POINT('Ctrl Pts',(-133.775688686686,6.18275358352724,
131.368915381349));
#257576=CARTESIAN_POINT('Ctrl Pts',(-134.054136310499,3.81690524584148,
125.907790562906));
#257577=CARTESIAN_POINT('Ctrl Pts',(-134.332583934311,-2.05649254658467,
124.946374413949));
#257578=CARTESIAN_POINT('Ctrl Pts',(-134.611031558124,-6.04007415394596,
129.36816140758));
#257579=CARTESIAN_POINT('Ctrl Pts',(-134.889479181937,-4.47312268785726,
135.109745312956));
#257580=CARTESIAN_POINT('Ctrl Pts',(-135.16792680575,1.20441000418008,136.894891013003));
#257581=CARTESIAN_POINT('Ctrl Pts',(-135.446374429563,5.775148741076,133.083136818595));
#257582=CARTESIAN_POINT('Ctrl Pts',(-135.724822053376,5.03880791662344,
127.177298619846));
#257583=CARTESIAN_POINT('Ctrl Pts',(-136.003269677189,-0.327951223754644,
124.604553205172));
#257584=CARTESIAN_POINT('Ctrl Pts',(-136.281717301002,-5.39333921080989,
127.729127925058));
#257585=CARTESIAN_POINT('Ctrl Pts',(-136.560164924815,-5.50251194239939,
133.679691255889));
#257586=CARTESIAN_POINT('Ctrl Pts',(-136.838612548628,-0.555145011576188,
136.987966197812));
#257587=CARTESIAN_POINT('Ctrl Pts',(-137.117060172441,4.90237306454367,
134.613809697415));
#257588=CARTESIAN_POINT('Ctrl Pts',(-137.395507796253,5.8548497885868,128.73895559457));
#257589=CARTESIAN_POINT('Ctrl Pts',(-137.673955420066,1.42700558223168,
124.762107807213));
#257590=CARTESIAN_POINT('Ctrl Pts',(-137.952403043879,-4.3121870410957,
126.33779517211));
#257591=CARTESIAN_POINT('Ctrl Pts',(-138.230850667692,-6.08869043570493,
132.018037977528));
#257592=CARTESIAN_POINT('Ctrl Pts',(-138.509298291505,-2.26998476896503,
136.582970580575));
#257593=CARTESIAN_POINT('Ctrl Pts',(-138.787745915318,3.63472600553235,
135.837642928407));
#257594=CARTESIAN_POINT('Ctrl Pts',(-139.066193539131,6.1993011471828,130.466974722087));
#257595=CARTESIAN_POINT('Ctrl Pts',(-139.344641162943,3.06702138726935,
125.406347671494));
#257596=CARTESIAN_POINT('Ctrl Pts',(-139.623088786757,-2.88370119522,125.306230810748));
#257597=CARTESIAN_POINT('Ctrl Pts',(-139.901536410569,-6.18444325593727,
130.258626643894));
#257598=CARTESIAN_POINT('Ctrl Pts',(-140.179984034382,-3.80198409129777,
135.712525338258));
#257599=CARTESIAN_POINT('Ctrl Pts',(-140.458431658195,2.07431271599591,
136.656060431482));
#257600=CARTESIAN_POINT('Ctrl Pts',(-140.736879282008,6.04441747309895,
132.222169267145));
#257601=CARTESIAN_POINT('Ctrl Pts',(-141.015326905821,4.45999785863389,
126.485381217648));
#257602=CARTESIAN_POINT('Ctrl Pts',(-141.293774529634,-1.22294190490765,
124.717524242802));
#257603=CARTESIAN_POINT('Ctrl Pts',(-141.572222153447,-5.78205780187226,
128.543172537875));
#257604=CARTESIAN_POINT('Ctrl Pts',(-141.85066977726,-5.02774504814366,
134.446742213005));
#257605=CARTESIAN_POINT('Ctrl Pts',(-142.129117401072,0.346819785828787,
137.003141142159));
#257606=CARTESIAN_POINT('Ctrl Pts',(-142.407565024885,5.40267417971275,
133.863163596476));
#257607=CARTESIAN_POINT('Ctrl Pts',(-142.686012648698,5.49373493774783,
127.912295544006));
#257608=CARTESIAN_POINT('Ctrl Pts',(-142.964460272511,0.536321671864061,
124.619094008905));
#257609=CARTESIAN_POINT('Ctrl Pts',(-143.242907896324,-4.91394500969209,
127.00985032009));
#257610=CARTESIAN_POINT('Ctrl Pts',(-143.521355520137,-5.84853628690073,
132.887576222521));
#257611=CARTESIAN_POINT('Ctrl Pts',(-143.79980314395,-1.40860843332932,
136.850928754739));
#257612=CARTESIAN_POINT('Ctrl Pts',(-144.078250767763,4.32576175612421,
135.257780560169));
#257613=CARTESIAN_POINT('Ctrl Pts',(-144.356698391576,6.08496821690962,
129.572157000006));
#257614=CARTESIAN_POINT('Ctrl Pts',(-144.635146015388,2.2523861535788,125.018868367886));
#257615=CARTESIAN_POINT('Ctrl Pts',(-144.913593639201,-3.65002874971022,
125.782164476213));
#257616=CARTESIAN_POINT('Ctrl Pts',(-145.192041263014,-6.19824554583293,
131.160613490521));
#257617=CARTESIAN_POINT('Ctrl Pts',(-145.470488886827,-3.05057748646412,
136.211683518503));
#257618=CARTESIAN_POINT('Ctrl Pts',(-145.74893651064,2.90042225397064,136.293687962933));
#257619=CARTESIAN_POINT('Ctrl Pts',(-146.027384134453,6.18607563651005,
131.33126874552));
#257620=CARTESIAN_POINT('Ctrl Pts',(-146.305831758266,3.78702771569254,
125.884646699409));
#257621=CARTESIAN_POINT('Ctrl Pts',(-146.584279382079,-2.09211366925746,
124.959001402698));
#257622=CARTESIAN_POINT('Ctrl Pts',(-146.862727005891,-6.04870479759444,
129.404955662777));
#257623=CARTESIAN_POINT('Ctrl Pts',(-147.141174629705,-4.4468317125993,
135.136894711575));
#257624=CARTESIAN_POINT('Ctrl Pts',(-147.419622253517,1.24146247646836,
136.887446584034));
#257625=CARTESIAN_POINT('Ctrl Pts',(-147.69806987733,5.78891329847519,133.04793962858));
#257626=CARTESIAN_POINT('Ctrl Pts',(-147.976517501143,5.01663560332014,
127.146693166932));
#257627=CARTESIAN_POINT('Ctrl Pts',(-148.254965124956,-0.365685135012239,
124.606664405427));
#257628=CARTESIAN_POINT('Ctrl Pts',(-148.533412748769,-5.41195909898036,
127.762015688586));
#257629=CARTESIAN_POINT('Ctrl Pts',(-148.811860372582,-5.48490703988586,
133.713133334664));
#257630=CARTESIAN_POINT('Ctrl Pts',(-149.090307996395,-0.517493363741682,
136.991230955176));
#257631=CARTESIAN_POINT('Ctrl Pts',(-149.368755620208,4.92547143272535,
134.583896980843));
#257632=CARTESIAN_POINT('Ctrl Pts',(-149.647203244021,5.84216860517359,
128.703353729273));
#257633=CARTESIAN_POINT('Ctrl Pts',(-149.925650867833,1.39019823527075,
124.753533168151));
#257634=CARTESIAN_POINT('Ctrl Pts',(-150.204098491647,-4.33929639788676,
126.364127433687));
#257635=CARTESIAN_POINT('Ctrl Pts',(-150.482546115459,-6.08118962780021,
132.055079077756));
#257636=CARTESIAN_POINT('Ctrl Pts',(-150.760993739272,-2.23476667239474,
136.596681557904));
#257637=CARTESIAN_POINT('Ctrl Pts',(-151.039441363085,3.66529768052036,
135.81542406449));
#257638=CARTESIAN_POINT('Ctrl Pts',(-151.317888986898,6.19713252478332,
130.429244067412));
#257639=CARTESIAN_POINT('Ctrl Pts',(-151.596336610711,3.03410532552526,
125.387777854462));
#257640=CARTESIAN_POINT('Ctrl Pts',(-151.874784234524,-2.91711644360522,
125.323886586026));
#257641=CARTESIAN_POINT('Ctrl Pts',(-152.153231858337,-6.18765071012318,
130.296283216534));
#257642=CARTESIAN_POINT('Ctrl Pts',(-152.431679482149,-3.77203625758034,
135.735578157629));
#257643=CARTESIAN_POINT('Ctrl Pts',(-152.710127105962,2.10989524146327,
136.643325082775));
#257644=CARTESIAN_POINT('Ctrl Pts',(-152.988574729775,6.0529360877152,132.185348913665));
#257645=CARTESIAN_POINT('Ctrl Pts',(-153.267022353588,4.43362437172323,
126.458311965469));
#257646=CARTESIAN_POINT('Ctrl Pts',(-153.545469977401,-1.25997154729018,
124.725081412269));
#257647=CARTESIAN_POINT('Ctrl Pts',(-153.823917601214,-5.79571516737629,
128.578411459437));
#257648=CARTESIAN_POINT('Ctrl Pts',(-154.102365225027,-5.00547968506979,
134.477280039263));
#257649=CARTESIAN_POINT('Ctrl Pts',(-154.38081284884,0.38454709653853,137.000915102638));
#257650=CARTESIAN_POINT('Ctrl Pts',(-154.659260472653,5.4211938825983,133.830219312748));
#257651=CARTESIAN_POINT('Ctrl Pts',(-154.937708096465,5.47602833059452,
127.8789072034));
#257652=CARTESIAN_POINT('Ctrl Pts',(-155.216155720278,0.498660261630971,
124.615943865326));
#257653=CARTESIAN_POINT('Ctrl Pts',(-155.494603344091,-4.93695222686361,
127.039833201595));
#257654=CARTESIAN_POINT('Ctrl Pts',(-155.773050967904,-5.83574680239484,
132.923139325752));
#257655=CARTESIAN_POINT('Ctrl Pts',(-156.051498591717,-1.37177515860606,
136.85939132518));
#257656=CARTESIAN_POINT('Ctrl Pts',(-156.32994621553,4.3527908409998,135.231365909006));
#257657=CARTESIAN_POINT('Ctrl Pts',(-156.608393839343,6.0773547033811,129.535138901228));
#257658=CARTESIAN_POINT('Ctrl Pts',(-156.886841463156,2.21712648863745,
125.005264645838));
#257659=CARTESIAN_POINT('Ctrl Pts',(-157.165289086968,-3.68053265651321,
125.804476286877));
#257660=CARTESIAN_POINT('Ctrl Pts',(-157.443736710782,-6.19596209434481,
131.19833736989));
#257661=CARTESIAN_POINT('Ctrl Pts',(-157.722184334594,-3.0176050570491,
136.230153064351));
#257662=CARTESIAN_POINT('Ctrl Pts',(-158.000631958407,2.93378360947182,
136.275930564914));
#257663=CARTESIAN_POINT('Ctrl Pts',(-158.27907958222,6.18916846218569,131.293602584915));
#257664=CARTESIAN_POINT('Ctrl Pts',(-158.557527206033,3.7570098558391,125.861685137721));
#257665=CARTESIAN_POINT('Ctrl Pts',(-158.835974829846,-2.12765726788813,
124.971844993383));
#257666=CARTESIAN_POINT('Ctrl Pts',(-159.114422453659,-6.05711130426257,
129.44180177344));
#257667=CARTESIAN_POINT('Ctrl Pts',(-159.392870077472,-4.42037595835707,
135.163883566548));
#257668=CARTESIAN_POINT('Ctrl Pts',(-159.671317701285,1.27846894590735,
136.879776744077));
#257669=CARTESIAN_POINT('Ctrl Pts',(-159.949765325097,5.80246334556346,
133.01265930192));
#257670=CARTESIAN_POINT('Ctrl Pts',(-160.22821294891,4.9942773967397,127.116223250229));
#257671=CARTESIAN_POINT('Ctrl Pts',(-160.506660572723,-0.403405495673234,
124.609005263594));
#257672=CARTESIAN_POINT('Ctrl Pts',(-160.785108196536,-5.43037844501628,
127.795016187323));
#257673=CARTESIAN_POINT('Ctrl Pts',(-161.063555820349,-5.46709889212507,
133.746467627798));
#257674=CARTESIAN_POINT('Ctrl Pts',(-161.342003444162,-0.479822539999598,
136.994266455786));
#257675=CARTESIAN_POINT('Ctrl Pts',(-161.620451067975,4.94838728575097,
134.553844212161));
#257676=CARTESIAN_POINT('Ctrl Pts',(-161.898898691787,5.82927093805496,
128.66782971756));
#257677=CARTESIAN_POINT('Ctrl Pts',(-162.177346315601,1.35333937400316,
124.745182744726));
#257678=CARTESIAN_POINT('Ctrl Pts',(-162.455793939413,-4.36624496045326,
126.390624229737));
#257679=CARTESIAN_POINT('Ctrl Pts',(-162.734241563226,-6.07346347917808,
132.092073832152));
#257680=CARTESIAN_POINT('Ctrl Pts',(-163.012689187039,-2.19946576572379,
136.61017789865));
#257681=CARTESIAN_POINT('Ctrl Pts',(-163.291136810852,3.69573353655413,
135.793019513774));
#257682=CARTESIAN_POINT('Ctrl Pts',(-163.569584434665,6.19473426535967,
130.391527312818));
#257683=CARTESIAN_POINT('Ctrl Pts',(-163.848032058478,3.0010768338922,125.369408750896));
#257684=CARTESIAN_POINT('Ctrl Pts',(-164.126479682291,-2.95042359716811,
125.341745442286));
#257685=CARTESIAN_POINT('Ctrl Pts',(-164.404927306104,-6.19062887863655,
130.333958616169));
#257686=CARTESIAN_POINT('Ctrl Pts',(-164.683374929917,-3.74194864967208,
135.758448248921));
#257687=CARTESIAN_POINT('Ctrl Pts',(-164.961822553729,2.14539958398697,
136.630373369092));
#257688=CARTESIAN_POINT('Ctrl Pts',(-165.240270177542,6.06123040855813,
132.148477387157));
#257689=CARTESIAN_POINT('Ctrl Pts',(-165.518717801355,4.40708659523179,
126.431403757722));
#257690=CARTESIAN_POINT('Ctrl Pts',(-165.797165425168,-1.29695450096345,
124.732863851664));
#257691=CARTESIAN_POINT('Ctrl Pts',(-166.075613048981,-5.80915777052276,
128.613732864363));
#257692=CARTESIAN_POINT('Ctrl Pts',(-166.354060672794,-4.98302884210618,
134.50768176414));
#257693=CARTESIAN_POINT('Ctrl Pts',(-166.632508296607,0.422260157714416,
136.998459447511));
#257694=CARTESIAN_POINT('Ctrl Pts',(-166.91095592042,5.43951270115045,133.797162904712));
#257695=CARTESIAN_POINT('Ctrl Pts',(-167.189403544233,5.45811880719792,
127.845627266545));
#257696=CARTESIAN_POINT('Ctrl Pts',(-167.467851168046,0.460980373357943,
124.613023035806));
#257697=CARTESIAN_POINT('Ctrl Pts',(-167.746298791858,-4.95977650345479,
127.069955579048));
#257698=CARTESIAN_POINT('Ctrl Pts',(-168.024746415672,-5.822741072145,132.958623916859));
#257699=CARTESIAN_POINT('Ctrl Pts',(-168.303194039484,-1.33489105224939,
136.867629524233));
#257700=CARTESIAN_POINT('Ctrl Pts',(-168.581641663297,4.37965863161014,
135.204787213532));
#257701=CARTESIAN_POINT('Ctrl Pts',(-168.86008928711,6.06951599123876,129.498167833929));
#257702=CARTESIAN_POINT('Ctrl Pts',(-169.138536910923,2.18178466725943,
124.991875811423));
#257703=CARTESIAN_POINT('Ctrl Pts',(-169.416984534736,-3.71090017982492,
125.826973370093));
#257704=CARTESIAN_POINT('Ctrl Pts',(-169.695432158549,-6.19344904920226,
131.236046650305));
#257705=CARTESIAN_POINT('Ctrl Pts',(-169.973879782361,-2.98452080916978,
136.248421555465));
#257706=CARTESIAN_POINT('Ctrl Pts',(-170.252327406175,2.96703625254325,
136.257970415857));
#257707=CARTESIAN_POINT('Ctrl Pts',(-170.530775029987,6.19203194594742,
131.25591829527));
#257708=CARTESIAN_POINT('Ctrl Pts',(-170.8092226538,3.72685277860365,125.838906728691));
#257709=CARTESIAN_POINT('Ctrl Pts',(-171.087670277614,-2.16312202539704,
124.984904710079));
#257710=CARTESIAN_POINT('Ctrl Pts',(-171.366117901426,-6.06529336244348,
129.478698374222));
#257711=CARTESIAN_POINT('Ctrl Pts',(-171.644565525239,-4.39375640545797,
135.190710877796));
#257712=CARTESIAN_POINT('Ctrl Pts',(-171.923013149052,1.31542804121008,
136.871881777341));
#257713=CARTESIAN_POINT('Ctrl Pts',(-172.201460772865,5.81579838023838,
132.977297145939));
#257714=CARTESIAN_POINT('Ctrl Pts',(-172.479908396678,4.97173412537368,
127.085889998814));
#257715=CARTESIAN_POINT('Ctrl Pts',(-172.75835602049,-0.441110907994683,
124.611575692932));
#257716=CARTESIAN_POINT('Ctrl Pts',(-173.036803644304,-5.4485965663818,
127.828128198426));
#257717=CARTESIAN_POINT('Ctrl Pts',(-173.315251268116,-5.44908815900415,
133.779692900072));
#257718=CARTESIAN_POINT('Ctrl Pts',(-173.593698891929,-0.442133936257506,
136.997072587158));
#257719=CARTESIAN_POINT('Ctrl Pts',(-173.872146515742,4.97111977446672,
134.523652504987));
#257720=CARTESIAN_POINT('Ctrl Pts',(-174.150594139555,5.81615726515733,
128.632384875785));
#257721=CARTESIAN_POINT('Ctrl Pts',(-174.429041763368,1.31643036424716,
124.737056846366));
#257722=CARTESIAN_POINT('Ctrl Pts',(-174.707489387181,-4.39303173020782,
126.417284578411));
#257723=CARTESIAN_POINT('Ctrl Pts',(-174.985937010994,-6.06551227613263,
132.129020869861));
#257724=CARTESIAN_POINT('Ctrl Pts',(-175.264384634806,-2.16408335703982,
136.623459102702));
#257725=CARTESIAN_POINT('Ctrl Pts',(-175.542832258619,3.72603244582337,
135.770430106468));
#257726=CARTESIAN_POINT('Ctrl Pts',(-175.821279882432,6.19210645777918,
130.353825855915));
#257727=CARTESIAN_POINT('Ctrl Pts',(-176.099727506245,2.96793713625374,
125.351241041473));
#257728=CARTESIAN_POINT('Ctrl Pts',(-176.378175130058,-2.98362142169932,
125.359806717758));
#257729=CARTESIAN_POINT('Ctrl Pts',(-176.656622753871,-6.19337765112022,
130.371651446723));
#257730=CARTESIAN_POINT('Ctrl Pts',(-176.935070377684,-3.71172238248064,
135.781134764673));
#257731=CARTESIAN_POINT('Ctrl Pts',(-177.213518001496,2.18082442793968,
136.617205770365));
#257732=CARTESIAN_POINT('Ctrl Pts',(-177.49196562531,6.06930012827989,132.111556053907));
#257733=CARTESIAN_POINT('Ctrl Pts',(-177.770413249122,4.38038551252508,
126.404657591498));
#257734=CARTESIAN_POINT('Ctrl Pts',(-178.048860872936,-1.33388939551094,
124.740871272604));
#257735=CARTESIAN_POINT('Ctrl Pts',(-178.327308496748,-5.82238511319243,
128.649135443807));
#257736=CARTESIAN_POINT('Ctrl Pts',(-178.605756120561,-4.96039335117553,
134.537946261091));
#257737=CARTESIAN_POINT('Ctrl Pts',(-178.884203744374,0.459957571884186,
136.995774267775));
#257738=CARTESIAN_POINT('Ctrl Pts',(-179.162651368187,5.45762995655925,
133.763995597288));
#257739=CARTESIAN_POINT('Ctrl Pts',(-179.441098991999,5.44000703120181,
127.812456966643));
#257740=CARTESIAN_POINT('Ctrl Pts',(-179.719546615813,0.423283403288203,
124.610331628578));
#257741=CARTESIAN_POINT('Ctrl Pts',(-179.997994239625,-4.98241699370369,
127.100216336253));
#257742=CARTESIAN_POINT('Ctrl Pts',(-180.276441863438,-5.80951957808352,
132.994028680947));
#257743=CARTESIAN_POINT('Ctrl Pts',(-180.554889487251,-1.29795748101432,
136.875643046625));
#257744=CARTESIAN_POINT('Ctrl Pts',(-180.833337111064,4.40636413235919,
135.178045458633));
#257745=CARTESIAN_POINT('Ctrl Pts',(-181.111784734877,6.06145237094964,
129.461245168083));
#257746=CARTESIAN_POINT('Ctrl Pts',(-181.39023235869,2.14636199904753,124.97870236077));
#257747=CARTESIAN_POINT('Ctrl Pts',(-181.668679982503,-3.74113019436597,
125.849654892224));
#257748=CARTESIAN_POINT('Ctrl Pts',(-181.947127606316,-6.19070650352801,
131.273739934436));
#257749=CARTESIAN_POINT('Ctrl Pts',(-182.225575230128,-2.95132596877351,
136.266488314898));
#257750=CARTESIAN_POINT('Ctrl Pts',(-182.504022853942,3.00017895099442,
136.239808181284));
#257751=CARTESIAN_POINT('Ctrl Pts',(-182.782470477755,6.19466598168877,
131.218217272988));
#257752=CARTESIAN_POINT('Ctrl Pts',(-183.060918101567,3.6965576014681,125.81631231638));
#257753=CARTESIAN_POINT('Ctrl Pts',(-183.33936572538,-2.19850662762309,
124.998180068855));
#257754=CARTESIAN_POINT('Ctrl Pts',(-183.617813349193,-6.07325066894868,
129.515644097905));
#257755=CARTESIAN_POINT('Ctrl Pts',(-183.896260973006,-4.36697404029963,
135.217375651221));
#257756=CARTESIAN_POINT('Ctrl Pts',(-184.174708596819,1.35233839284232,
136.863761976378));
#257757=CARTESIAN_POINT('Ctrl Pts',(-184.453156220632,5.8289179083658,132.941854470998));
#257758=CARTESIAN_POINT('Ctrl Pts',(-184.731603844444,4.94900662457131,
127.055694536694));
#257759=CARTESIAN_POINT('Ctrl Pts',(-185.010051468258,-0.478799974789776,
124.614375598192));
#257760=CARTESIAN_POINT('Ctrl Pts',(-185.28849909207,-5.46661278799793,
127.861350494915));
#257761=CARTESIAN_POINT('Ctrl Pts',(-185.566946715884,-5.43087550791776,
133.812807920317));
#257762=CARTESIAN_POINT('Ctrl Pts',(-185.845394339696,-0.404428949079144,
136.999649245311));
#257763=CARTESIAN_POINT('Ctrl Pts',(-186.123841963509,4.99366805651034,
134.493322978084));
#257764=CARTESIAN_POINT('Ctrl Pts',(-186.402289587322,5.80282807241402,
128.59702051737));
#257765=CARTESIAN_POINT('Ctrl Pts',(-186.680737211135,1.27947257368013,
124.729155774178));
#257766=CARTESIAN_POINT('Ctrl Pts',(-186.959184834948,-4.41965571455532,
126.444107491802));
#257767=CARTESIAN_POINT('Ctrl Pts',(-187.237632458761,-6.0573363132998,
132.165918821797));
#257768=CARTESIAN_POINT('Ctrl Pts',(-187.516080082574,-2.12862075745111,
136.636524677919));
#257769=CARTESIAN_POINT('Ctrl Pts',(-187.794527706387,3.75619328558978,
135.74765667963));
#257770=CARTESIAN_POINT('Ctrl Pts',(-188.072975330199,6.18924919941703,
130.316141093742));
#257771=CARTESIAN_POINT('Ctrl Pts',(-188.351422954013,2.93468746061294,
125.333275399398));
#257772=CARTESIAN_POINT('Ctrl Pts',(-188.629870577825,-3.01670868704181,
125.378069743179));
#257773=CARTESIAN_POINT('Ctrl Pts',(-188.908318201638,-6.19589692571743,
130.409360311474));
#257774=CARTESIAN_POINT('Ctrl Pts',(-189.186765825451,-3.68135857605119,
135.80363686423));
#257775=CARTESIAN_POINT('Ctrl Pts',(-189.465213449264,2.21616846064164,
136.603822774524));
#257776=CARTESIAN_POINT('Ctrl Pts',(-189.743661073077,6.07714494785282,
132.07458628205));
#257777=CARTESIAN_POINT('Ctrl Pts',(-190.02210869689,4.35352211302309,126.378074457888));
#257778=CARTESIAN_POINT('Ctrl Pts',(-190.300556320702,-1.37077486229612,
124.749103378371));
#257779=CARTESIAN_POINT('Ctrl Pts',(-190.579003944516,-5.83539670523986,
128.684617885911));
#257780=CARTESIAN_POINT('Ctrl Pts',(-190.857451568328,-4.93757405104588,
134.568072408653));
#257781=CARTESIAN_POINT('Ctrl Pts',(-191.135899192141,0.497637942157669,
136.992859662928));
#257782=CARTESIAN_POINT('Ctrl Pts',(-191.414346815954,5.47554497748281,
133.730718619501));
#257783=CARTESIAN_POINT('Ctrl Pts',(-191.692794439767,5.42169367374449,
127.779397532831));
#257784=CARTESIAN_POINT('Ctrl Pts',(-191.97124206358,0.385570748295746,
124.60786974337));
#257785=CARTESIAN_POINT('Ctrl Pts',(-192.249689687393,-5.00487285865859,
127.130614351886));
#257786=CARTESIAN_POINT('Ctrl Pts',(-192.528137311206,-5.79608281013753,
133.029352306079));
#257787=CARTESIAN_POINT('Ctrl Pts',(-192.806584935019,-1.26097581348702,
136.883431595415));
#257788=CARTESIAN_POINT('Ctrl Pts',(-193.085032558831,4.43290635366497,
135.151141635234));
#257789=CARTESIAN_POINT('Ctrl Pts',(-193.363480182644,6.05316414131348,
129.424372271875));
#257790=CARTESIAN_POINT('Ctrl Pts',(-193.641927806457,2.11085979660312,
124.965744782026));
#257791=CARTESIAN_POINT('Ctrl Pts',(-193.92037543027,-3.77122157995168,
125.872520012798));
#257792=CARTESIAN_POINT('Ctrl Pts',(-194.198823054083,-6.1877345589472,
131.311415825543));
#257793=CARTESIAN_POINT('Ctrl Pts',(-194.477270677896,-2.91802176590892,
136.284352673182));
#257794=CARTESIAN_POINT('Ctrl Pts',(-194.755718301709,3.03321047671203,
136.221444534203));
#257795=CARTESIAN_POINT('Ctrl Pts',(-195.034165925522,6.19707047180361,
131.180500915096));
#257796=CARTESIAN_POINT('Ctrl Pts',(-195.312613549334,3.66612544703105,
125.793902738034));
#257797=CARTESIAN_POINT('Ctrl Pts',(-195.591061173148,-2.23380976337827,
125.011670577786));
#257798=CARTESIAN_POINT('Ctrl Pts',(-195.86950879696,-6.08098292891658,
129.552637575454));
#257799=CARTESIAN_POINT('Ctrl Pts',(-196.147956420774,-4.3400298553121,
135.243876898752));
#257800=CARTESIAN_POINT('Ctrl Pts',(-196.426404044586,1.38919863307876,
136.855417642068));
#257801=CARTESIAN_POINT('Ctrl Pts',(-196.704851668399,5.84182144379631,
132.906332590435));
#257802=CARTESIAN_POINT('Ctrl Pts',(-196.983299292212,4.92609573650846,
127.025637982775));
#257803=CARTESIAN_POINT('Ctrl Pts',(-197.261746916025,-0.516471299475173,
124.617404875624));
#257804=CARTESIAN_POINT('Ctrl Pts',(-197.540194539838,-5.48442644226676,
127.894681845726));
#257805=CARTESIAN_POINT('Ctrl Pts',(-197.81864216365,-5.41246161374207,
133.845811461438));
#257806=CARTESIAN_POINT('Ctrl Pts',(-198.097089787464,-0.36670897563802,
137.001996334766));
#257807=CARTESIAN_POINT('Ctrl Pts',(-198.375537411276,5.01603129634849,
134.462856755322));
#257808=CARTESIAN_POINT('Ctrl Pts',(-198.65398503509,5.78928385374183,128.561737952753));
#257809=CARTESIAN_POINT('Ctrl Pts',(-198.932432658902,1.24246737178614,
124.721479820939));
#257810=CARTESIAN_POINT('Ctrl Pts',(-199.210880282716,-4.44611592693577,
126.471091975977));
#257811=CARTESIAN_POINT('Ctrl Pts',(-199.489327906528,-6.04893589364168,
132.202766320694));
#257812=CARTESIAN_POINT('Ctrl Pts',(-199.767775530341,-2.09307928103787,
136.649374140152));
#257813=CARTESIAN_POINT('Ctrl Pts',(-200.046223154153,3.7862149382325,135.724700077139));
#257814=CARTESIAN_POINT('Ctrl Pts',(-200.324670777967,6.18616259614969,
130.278474422724));
#257815=CARTESIAN_POINT('Ctrl Pts',(-200.603118401779,2.90132903904936,
125.315512490399));
#257816=CARTESIAN_POINT('Ctrl Pts',(-200.881566025592,-3.04968416713424,
125.396533841802));
#257817=CARTESIAN_POINT('Ctrl Pts',(-201.160013649405,-6.1981866090755,
130.447083813107));
#257818=CARTESIAN_POINT('Ctrl Pts',(-201.438461273218,-3.65085835552605,
135.825953713766));
#257819=CARTESIAN_POINT('Ctrl Pts',(-201.716908897031,2.2514303724059,136.590224877478));
#257820=CARTESIAN_POINT('Ctrl Pts',(-201.995356520844,6.08476457658541,
132.037569441512));
#257821=CARTESIAN_POINT('Ctrl Pts',(-202.273804144657,4.32649739215744,
126.35165534194));
#257822=CARTESIAN_POINT('Ctrl Pts',(-202.55225176847,-1.40760953451491,
124.757559863922));
#257823=CARTESIAN_POINT('Ctrl Pts',(-202.830699392283,-5.84819206451709,
128.720178875862));
#257824=CARTESIAN_POINT('Ctrl Pts',(-203.109147016096,-4.91457178729319,
134.59805909049));
#257825=CARTESIAN_POINT('Ctrl Pts',(-203.387594639908,0.535299872273523,
136.989715740974));
#257826=CARTESIAN_POINT('Ctrl Pts',(-203.666042263721,5.49325710007376,
133.697333204442));
#257827=CARTESIAN_POINT('Ctrl Pts',(-203.944489887534,5.40317941343439,
127.746450190138));
#257828=CARTESIAN_POINT('Ctrl Pts',(-204.222937511347,0.347843805837959,
124.605637471411));
#257829=CARTESIAN_POINT('Ctrl Pts',(-204.50138513516,-5.0271432662092,127.161148499539));
#257830=CARTESIAN_POINT('Ctrl Pts',(-204.779832758973,-5.78243126621161,
133.064593483327));
#257831=CARTESIAN_POINT('Ctrl Pts',(-205.058280382786,-1.22394742003769,
136.890994881994));
#257832=CARTESIAN_POINT('Ctrl Pts',(-205.336728006599,4.45928431199552,
135.124076740266));
#257833=CARTESIAN_POINT('Ctrl Pts',(-205.615175630412,6.04465160945437,
129.387550511641));
#257834=CARTESIAN_POINT('Ctrl Pts',(-205.893623254225,2.07527937547198,
124.953003555339));
#257835=CARTESIAN_POINT('Ctrl Pts',(-206.172070878037,-3.80117322153507,
125.89556788454));
#257836=CARTESIAN_POINT('Ctrl Pts',(-206.45051850185,-6.18453332558722,
131.349072927534));
#257837=CARTESIAN_POINT('Ctrl Pts',(-206.728966125663,-2.8846094346739,
136.302013968343));
#257838=CARTESIAN_POINT('Ctrl Pts',(-207.007413749476,3.06612960569919,
136.202880155086));
#257839=CARTESIAN_POINT('Ctrl Pts',(-207.285861373289,6.19924532719362,
131.142770619188));
#257840=CARTESIAN_POINT('Ctrl Pts',(-207.564308997102,3.63555744296752,
125.771678824048));
#257841=CARTESIAN_POINT('Ctrl Pts',(-207.842756620915,-2.26903012449045,
125.025375736976));
#257842=CARTESIAN_POINT('Ctrl Pts',(-208.121204244728,-6.08848985582611,
129.58967743606));
#257843=CARTESIAN_POINT('Ctrl Pts',(-208.399651868541,-4.31292484892225,
135.270213638376));
#257844=CARTESIAN_POINT('Ctrl Pts',(-208.678099492353,1.42600739604885,
136.846849083615));
#257845=CARTESIAN_POINT('Ctrl Pts',(-208.956547116166,5.85450850838505,
132.870732820528));
#257846=CARTESIAN_POINT('Ctrl Pts',(-209.234994739979,4.90300231015654,
126.995721450812));
#257847=CARTESIAN_POINT('Ctrl Pts',(-209.513442363792,-0.554123486127181,
124.620663412976));
#257848=CARTESIAN_POINT('Ctrl Pts',(-209.791889987605,-5.50203686909699,
127.928121015754));
#257849=CARTESIAN_POINT('Ctrl Pts',(-210.070337611418,-5.393847158811,133.878702300482));
#257850=CARTESIAN_POINT('Ctrl Pts',(-210.348785235231,-0.328975413660277,
137.004113768549));
#257851=CARTESIAN_POINT('Ctrl Pts',(-210.627232859043,5.03820866530154,
134.432254965643));
#257852=CARTESIAN_POINT('Ctrl Pts',(-210.905680482857,5.77552511102812,
128.526538489345));
#257853=CARTESIAN_POINT('Ctrl Pts',(-211.184128106669,1.20541612980698,
124.714029271085));
#257854=CARTESIAN_POINT('Ctrl Pts',(-211.462575730482,-4.47241138685473,
126.498237031013));
#257855=CARTESIAN_POINT('Ctrl Pts',(-211.741023354295,-6.04031132844015,
132.239562001151));
#257856=CARTESIAN_POINT('Ctrl Pts',(-212.019470978108,-2.05746024480169,
136.66200701326));
#257857=CARTESIAN_POINT('Ctrl Pts',(-212.297918601921,3.81609629128846,
135.701561149659));
#257858=CARTESIAN_POINT('Ctrl Pts',(-212.576366225734,6.1828467623524,130.240827238612));
#257859=CARTESIAN_POINT('Ctrl Pts',(-212.854813849547,2.86786310767097,
125.297952972686));
#257860=CARTESIAN_POINT('Ctrl Pts',(-213.133261473359,-3.0825466400586,
125.415198329437));
#257861=CARTESIAN_POINT('Ctrl Pts',(-213.411709097173,-6.20024661634941,
130.484820553763));
#257862=CARTESIAN_POINT('Ctrl Pts',(-213.690156720985,-3.62022285110177,
135.848084486325));
#257863=CARTESIAN_POINT('Ctrl Pts',(-213.968604344798,2.28660885659016,
136.576412583105));
#257864=CARTESIAN_POINT('Ctrl Pts',(-214.247051968611,6.09215873212836,
132.00050690397));
#257865=CARTESIAN_POINT('Ctrl Pts',(-214.525499592424,4.29931235134063,
126.325401222624));
#257866=CARTESIAN_POINT('Ctrl Pts',(-214.803947216237,-1.44439204724454,
124.766240415898));
#257867=CARTESIAN_POINT('Ctrl Pts',(-215.08239484005,-5.86077071688603,
128.755817095934));
#257868=CARTESIAN_POINT('Ctrl Pts',(-215.360842463863,-4.89138741227638,
134.627905195436));
#257869=CARTESIAN_POINT('Ctrl Pts',(-215.639290087675,0.572941966656434,
136.986342618411));
#257870=CARTESIAN_POINT('Ctrl Pts',(-215.917737711489,5.51076566800256,
133.66384058922));
#257871=CARTESIAN_POINT('Ctrl Pts',(-216.196185335301,5.38446493632399,
127.713616159441));
#257872=CARTESIAN_POINT('Ctrl Pts',(-216.474632959115,0.310103973899474,
124.603634895418));
#257873=CARTESIAN_POINT('Ctrl Pts',(-216.753080582927,-5.04922739111732,
127.191817647757));
#257874=CARTESIAN_POINT('Ctrl Pts',(-217.031528206741,-5.76856545216855,
133.099750906814));
#257875=CARTESIAN_POINT('Ctrl Pts',(-217.309975830553,-1.18687367276612,
136.898332626102));
#257876=CARTESIAN_POINT('Ctrl Pts',(-217.588423454366,4.48549702990607,
135.096851776628));
#257877=CARTESIAN_POINT('Ctrl Pts',(-217.866871078179,6.03591509080661,
129.350781251827));
#257878=CARTESIAN_POINT('Ctrl Pts',(-218.145318701992,2.03962205410111,
124.94047915284));
#257879=CARTESIAN_POINT('Ctrl Pts',(-218.423766325804,-3.83098400924668,
125.9187976534));
#257880=CARTESIAN_POINT('Ctrl Pts',(-218.702213949618,-6.18110292207006,
131.386709845009));
#257881=CARTESIAN_POINT('Ctrl Pts',(-218.98066157343,-2.85109021317626,
136.319471545938));
#257882=CARTESIAN_POINT('Ctrl Pts',(-219.259109197243,3.09893511812703,
136.18411573184));
#257883=CARTESIAN_POINT('Ctrl Pts',(-219.537556821056,6.20119046726778,
131.105027783371));
#257884=CARTESIAN_POINT('Ctrl Pts',(-219.816004444869,3.6048547219858,125.749641397935));
#257885=CARTESIAN_POINT('Ctrl Pts',(-220.094452068682,-2.30416640585769,
125.039295038577));
#257886=CARTESIAN_POINT('Ctrl Pts',(-220.372899692494,-6.09577117150464,
129.626762307198));
#257887=CARTESIAN_POINT('Ctrl Pts',(-220.651347316308,-4.28566002551621,
135.296384894171));
#257888=CARTESIAN_POINT('Ctrl Pts',(-220.929794940121,1.46276331779004,
136.83805661853));
#257889=CARTESIAN_POINT('Ctrl Pts',(-221.208242563933,5.86697863200795,
132.835056480438));
#257890=CARTESIAN_POINT('Ctrl Pts',(-221.486690187747,4.87972720125093,
126.965946049375));
#257891=CARTESIAN_POINT('Ctrl Pts',(-221.765137811559,-0.591755139529082,
124.624151089502));
#257892=CARTESIAN_POINT('Ctrl Pts',(-222.043585435373,-5.51944341592756,
127.961666765899));
#257893=CARTESIAN_POINT('Ctrl Pts',(-222.322033059185,-5.37503283288975,
133.911479218663));
#257894=CARTESIAN_POINT('Ctrl Pts',(-222.600480682998,-0.29122966137826,
137.006001468201));
#257895=CARTESIAN_POINT('Ctrl Pts',(-222.878928306811,5.06019934158045,
134.401518743003));
#257896=CARTESIAN_POINT('Ctrl Pts',(-223.157375930624,5.7615523541068,128.491423431472));
#257897=CARTESIAN_POINT('Ctrl Pts',(-223.435823554437,1.16832022068962,
124.706804400699));
#257898=CARTESIAN_POINT('Ctrl Pts',(-223.71427117825,-4.49854111992577,
126.525541651043));
#257899=CARTESIAN_POINT('Ctrl Pts',(-223.992718802062,-6.03146293728042,
132.276304499695));
#257900=CARTESIAN_POINT('Ctrl Pts',(-224.271166425875,-2.02176496861996,
136.674422829126));
#257901=CARTESIAN_POINT('Ctrl Pts',(-224.549614049688,3.84583623749284,
135.678240754614));
#257902=CARTESIAN_POINT('Ctrl Pts',(-224.828061673501,6.1793018208946,130.203200936436));
#257903=CARTESIAN_POINT('Ctrl Pts',(-225.106509297314,2.83429090657077,
125.280597496933));
#257904=CARTESIAN_POINT('Ctrl Pts',(-225.384956921127,-3.11529488808334,
125.434062514461));
#257905=CARTESIAN_POINT('Ctrl Pts',(-225.66340454494,-6.20207687120481,
130.522569135094));
#257906=CARTESIAN_POINT('Ctrl Pts',(-225.941852168753,-3.5894531979886,
135.87002836184));
#257907=CARTESIAN_POINT('Ctrl Pts',(-226.220299792565,2.32170260964191,
136.562386403224));
#257908=CARTESIAN_POINT('Ctrl Pts',(-226.498747416378,6.09932714048972,
131.963400042786));
#257909=CARTESIAN_POINT('Ctrl Pts',(-226.777195040191,4.27196799792278,
126.299313072794));
#257910=CARTESIAN_POINT('Ctrl Pts',(-227.055642664004,-1.48112103749588,
124.775144712639));
#257911=CARTESIAN_POINT('Ctrl Pts',(-227.334090287817,-5.87313219624144,
128.79153122554));
#257912=CARTESIAN_POINT('Ctrl Pts',(-227.61253791163,-4.8680217850994,134.65760961753));
#257913=CARTESIAN_POINT('Ctrl Pts',(-227.890985535443,0.610562830463375,
136.982740420231));
#257914=CARTESIAN_POINT('Ctrl Pts',(-228.169433159256,5.52807003248314,
133.630242014917));
#257915=CARTESIAN_POINT('Ctrl Pts',(-228.447880783069,5.36555093588535,
127.680896657417));
#257916=CARTESIAN_POINT('Ctrl Pts',(-228.726328406882,0.272352650944771,
124.601862089598));
#257917=CARTESIAN_POINT('Ctrl Pts',(-229.004776030695,-5.07112441504767,
127.222620660081));
#257918=CARTESIAN_POINT('Ctrl Pts',(-229.283223654507,-5.75448588181141,
133.134823273769));
#257919=CARTESIAN_POINT('Ctrl Pts',(-229.561671278321,-1.14975594545406,
136.905444555836));
#257920=CARTESIAN_POINT('Ctrl Pts',(-229.840118902133,4.51154353607471,
135.069467753152));
#257921=CARTESIAN_POINT('Ctrl Pts',(-230.118566525947,6.0269549091058,129.314065854931));
#257922=CARTESIAN_POINT('Ctrl Pts',(-230.397014149759,2.00388915378425,
124.928172038625));
#257923=CARTESIAN_POINT('Ctrl Pts',(-230.675461773572,-3.86065283843716,
125.942208458593));
#257924=CARTESIAN_POINT('Ctrl Pts',(-230.953909397385,-6.17744347551146,
131.424325183319));
#257925=CARTESIAN_POINT('Ctrl Pts',(-231.232357021197,-2.81746534348149,
136.33672475907));
#257926=CARTESIAN_POINT('Ctrl Pts',(-231.510804645011,3.13162579837364,
136.165151959792));
#257927=CARTESIAN_POINT('Ctrl Pts',(-231.789252268823,6.20290581994918,
131.067273806224));
#257928=CARTESIAN_POINT('Ctrl Pts',(-232.067699892636,3.57401842178686,
125.727791276302));
#257929=CARTESIAN_POINT('Ctrl Pts',(-232.346147516449,-2.33921730549066,
125.053427966802));
#257930=CARTESIAN_POINT('Ctrl Pts',(-232.624595140262,-6.10282660614105,
129.663890814674));
#257931=CARTESIAN_POINT('Ctrl Pts',(-232.903042764075,-4.25823639540172,
135.322389696357));
#257932=CARTESIAN_POINT('Ctrl Pts',(-233.181490387888,1.499465036299,136.829040572621));
#257933=CARTESIAN_POINT('Ctrl Pts',(-233.459938011701,5.87923135258013,
132.799304892167));
#257934=CARTESIAN_POINT('Ctrl Pts',(-233.738385635514,4.85627127225937,
126.9363128818));
#257935=CARTESIAN_POINT('Ctrl Pts',(-234.016833259326,-0.629364865227224,
124.627867775965));
#257936=CARTESIAN_POINT('Ctrl Pts',(-234.29528088314,-5.53664543775268,
127.99531785311));
#257937=CARTESIAN_POINT('Ctrl Pts',(-234.573728506952,-5.35601933315035,
133.944141001422));
#257938=CARTESIAN_POINT('Ctrl Pts',(-234.852176130765,-0.253473117473377,
137.007659363768));
#257939=CARTESIAN_POINT('Ctrl Pts',(-235.130623754578,5.08200251031112,
134.370649226346));
#257940=CARTESIAN_POINT('Ctrl Pts',(-235.409071378391,5.74736610074488,
128.456394080338));
#257941=CARTESIAN_POINT('Ctrl Pts',(-235.687519002204,1.13118101903705,
124.699805477501));
#257942=CARTESIAN_POINT('Ctrl Pts',(-235.965966626017,-4.52450415790052,
126.553004824284));
#257943=CARTESIAN_POINT('Ctrl Pts',(-236.24441424983,-6.0223910480441,132.312992454817));
#257944=CARTESIAN_POINT('Ctrl Pts',(-236.522861873642,-1.98599477519336,
136.686621127679));
#257945=CARTESIAN_POINT('Ctrl Pts',(-236.801309497456,3.87543367482126,
135.654739756147));
#257946=CARTESIAN_POINT('Ctrl Pts',(-237.079757121268,6.1755279031354,130.165596910454));
#257947=CARTESIAN_POINT('Ctrl Pts',(-237.358204745081,2.80061367977841,
125.263446706254));
#257948=CARTESIAN_POINT('Ctrl Pts',(-237.636652368894,-3.14792769771062,
125.453125697856));
#257949=CARTESIAN_POINT('Ctrl Pts',(-237.915099992707,-6.20367730582095,
130.560328158313));
#257950=CARTESIAN_POINT('Ctrl Pts',(-238.19354761652,-3.55855053636696,
135.891784527174));
#257951=CARTESIAN_POINT('Ctrl Pts',(-238.471995240333,2.35671033115007,
136.54814685758));
#257952=CARTESIAN_POINT('Ctrl Pts',(-238.750442864146,6.10626953604027,
131.92625023297));
#257953=CARTESIAN_POINT('Ctrl Pts',(-239.028890487959,4.24446534516054,
126.273391859158));
#257954=CARTESIAN_POINT('Ctrl Pts',(-239.307338111771,-1.51779514426229,
124.784272424193));
#257955=CARTESIAN_POINT('Ctrl Pts',(-239.585785735585,-5.88527604452282,
128.827319941278));
#257956=CARTESIAN_POINT('Ctrl Pts',(-239.864233359397,-4.84447577158576,
134.687171256065));
#257957=CARTESIAN_POINT('Ctrl Pts',(-240.14268098321,0.648161069640796,
136.978909279916));
#257958=CARTESIAN_POINT('Ctrl Pts',(-240.421128607023,5.54516955229552,
133.596538726537));
#257959=CARTESIAN_POINT('Ctrl Pts',(-240.699576230836,5.34643811298351,
127.648292896498));
#257960=CARTESIAN_POINT('Ctrl Pts',(-240.978023854649,0.234591235861842,
124.600319119639));
#257961=CARTESIAN_POINT('Ctrl Pts',(-241.256471478461,-5.09283352659785,
127.253556395099));
#257962=CARTESIAN_POINT('Ctrl Pts',(-241.534919102275,-5.74019307686353,
133.169809284574));
#257963=CARTESIAN_POINT('Ctrl Pts',(-241.813366726087,-1.11259561351327,
136.912330407661));
#257964=CARTESIAN_POINT('Ctrl Pts',(-242.0918143499,4.53742286533832,135.041925684563));
#257965=CARTESIAN_POINT('Ctrl Pts',(-242.370261973713,6.01777139637409,
129.277405681456));
#257966=CARTESIAN_POINT('Ctrl Pts',(-242.648709597526,1.96808199861856,
124.916082668738));
#257967=CARTESIAN_POINT('Ctrl Pts',(-242.927157221339,-3.89017860971679,
125.965799432623));
#257968=CARTESIAN_POINT('Ctrl Pts',(-243.205604845152,-6.1735551215127,
131.461917548614));
#257969=CARTESIAN_POINT('Ctrl Pts',(-243.484052468965,-2.78373607157309,
136.353772968415));
#257970=CARTESIAN_POINT('Ctrl Pts',(-243.762500092778,3.16420043507544,
136.145989541648));
#257971=CARTESIAN_POINT('Ctrl Pts',(-244.040947716591,6.20439132167383,
131.029510086731));
#257972=CARTESIAN_POINT('Ctrl Pts',(-244.319395340403,3.54304968502077,
125.706129268813));
#257973=CARTESIAN_POINT('Ctrl Pts',(-244.597842964216,-2.37418152456686,
125.067773997952));
#257974=CARTESIAN_POINT('Ctrl Pts',(-244.876290588029,-6.10965589829292,
129.701061582678));
#257975=CARTESIAN_POINT('Ctrl Pts',(-245.154738211842,-4.23065497477177,
135.348227081313));
#257976=CARTESIAN_POINT('Ctrl Pts',(-245.433185835655,1.53611119157916,
136.819801279981));
#257977=CARTESIAN_POINT('Ctrl Pts',(-245.711633459468,5.89126621607239,
132.763479380503));
#257978=CARTESIAN_POINT('Ctrl Pts',(-245.990081083281,4.83263539234992,
126.906823046158));
#257979=CARTESIAN_POINT('Ctrl Pts',(-246.268528707094,-0.666951269578287,
124.631813334641));
#257980=CARTESIAN_POINT('Ctrl Pts',(-246.546976330906,-5.55364229714491,
128.029073030433));
#257981=CARTESIAN_POINT('Ctrl Pts',(-246.825423954719,-5.33680736414475,
133.976686438464));
#257982=CARTESIAN_POINT('Ctrl Pts',(-247.103871578532,-0.215707181029578,
137.009087393821));
#257983=CARTESIAN_POINT('Ctrl Pts',(-247.382319202345,5.10361736357064,
134.339647559554));
#257984=CARTESIAN_POINT('Ctrl Pts',(-247.660766826158,5.73296687661779,
128.421451733968));
#257985=CARTESIAN_POINT('Ctrl Pts',(-247.939214449971,1.09399990105564,
124.693032760838));
#257986=CARTESIAN_POINT('Ctrl Pts',(-248.217662073784,-4.55029953871062,
126.580625533077));
#257987=CARTESIAN_POINT('Ctrl Pts',(-248.496109697597,-6.01309599689209,
132.349624507031));
#257988=CARTESIAN_POINT('Ctrl Pts',(-248.77455732141,-1.95015099000055,
136.698601456905));
#257989=CARTESIAN_POINT('Ctrl Pts',(-249.053004945222,3.90488750652966,
135.631059025098));
#257990=CARTESIAN_POINT('Ctrl Pts',(-249.331452569036,6.17152514891849,
130.128016554096));
#257991=CARTESIAN_POINT('Ctrl Pts',(-249.609900192848,2.76683267521693,
125.246501236177));
#257992=CARTESIAN_POINT('Ctrl Pts',(-249.888347816661,-3.18044385971988,
125.472387173231));
#257993=CARTESIAN_POINT('Ctrl Pts',(-250.166795440474,-6.20504786089197,
130.598096224241));
#257994=CARTESIAN_POINT('Ctrl Pts',(-250.445243064287,-3.5275160113489,
135.913352176149));
#257995=CARTESIAN_POINT('Ctrl Pts',(-250.7236906881,2.39163072389511,136.533694473816));
#257996=CARTESIAN_POINT('Ctrl Pts',(-251.002138311913,6.11298566151878,
131.889058851139));
#257997=CARTESIAN_POINT('Ctrl Pts',(-251.280585935725,4.21680541219097,
126.247638542206));
#257998=CARTESIAN_POINT('Ctrl Pts',(-251.559033559539,-1.5544130086051,
124.793623212388));
#257999=CARTESIAN_POINT('Ctrl Pts',(-251.837481183351,-5.89720181167361,
128.863181916876));
#258000=CARTESIAN_POINT('Ctrl Pts',(-252.115928807165,-4.82075024435922,
134.716589015834));
#258001=CARTESIAN_POINT('Ctrl Pts',(-252.394376430977,0.685735291195708,
136.974849339035));
#258002=CARTESIAN_POINT('Ctrl Pts',(-252.67282405479,5.56206359338632,133.562731973716));
#258003=CARTESIAN_POINT('Ctrl Pts',(-252.951271678603,5.32712717665345,
127.615806083426));
#258004=CARTESIAN_POINT('Ctrl Pts',(-253.229719302416,0.196821126400439,
124.599006045371));
#258005=CARTESIAN_POINT('Ctrl Pts',(-253.508166926229,-5.11435391846912,
127.284623701469));
#258006=CARTESIAN_POINT('Ctrl Pts',(-253.786614550041,-5.72568757235024,
133.204707652256));
#258007=CARTESIAN_POINT('Ctrl Pts',(-254.065062173855,-1.07539404373626,
136.918989908584));
#258008=CARTESIAN_POINT('Ctrl Pts',(-254.343509797667,4.56313403947717,
135.014226625117));
#258009=CARTESIAN_POINT('Ctrl Pts',(-254.621957421481,6.00836492926231,
129.240802026269));
#258010=CARTESIAN_POINT('Ctrl Pts',(-254.900405045293,1.9322018468105,124.904211611225));
#258011=CARTESIAN_POINT('Ctrl Pts',(-255.178852669106,-3.91956009939235,
125.989569474605));
#258012=CARTESIAN_POINT('Ctrl Pts',(-255.457300292919,-6.16943824888009,
131.499485975975));
#258013=CARTESIAN_POINT('Ctrl Pts',(-255.735747916732,-2.74990318521692,
136.370614733943));
#258014=CARTESIAN_POINT('Ctrl Pts',(-256.014195540545,3.19665694865877,
136.126630713714));
#258015=CARTESIAN_POINT('Ctrl Pts',(-256.292643164358,6.20564856486739,
130.991735142402));
#258016=CARTESIAN_POINT('Ctrl Pts',(-256.571090788171,3.51194654848645,
125.68466161966));
#258017=CARTESIAN_POINT('Ctrl Pts',(-256.849538411983,-2.40905189372645,
125.082322325773));
#258018=CARTESIAN_POINT('Ctrl Pts',(-257.127986035797,-6.11626988572704,
129.738292634474));
#258019=CARTESIAN_POINT('Ctrl Pts',(-257.406433659609,-4.20289584392431,
135.373859459261));
#258020=CARTESIAN_POINT('Ctrl Pts',(-257.684881283423,1.57266088340656,
136.810408252432));
#258021=CARTESIAN_POINT('Ctrl Pts',(-257.963328907235,5.90315744058412,
132.727450666138));
#258022=CARTESIAN_POINT('Ctrl Pts',(-258.241776531048,4.80867945501638,
126.87772425425));
#258023=CARTESIAN_POINT('Ctrl Pts',(-258.520224154861,-0.704246744852541,
124.635521896935));
#258024=CARTESIAN_POINT('Ctrl Pts',(-258.798671778674,-5.5709361272427,
128.063810879205));
#258025=CARTESIAN_POINT('Ctrl Pts',(-259.077119402487,-5.31644754243966,
134.007449313497));
#258026=CARTESIAN_POINT('Ctrl Pts',(-259.355567026299,-0.179733571114533,
137.013459703814));
#258027=CARTESIAN_POINT('Ctrl Pts',(-259.634014650113,5.12849404027147,
134.30227331953));
#258028=CARTESIAN_POINT('Ctrl Pts',(-259.866054336623,5.61428989304695,
129.384066440553));
#258029=CARTESIAN_POINT('Ctrl Pts',(-260.051696012132,3.39054283699284,
126.521203045511));
#258030=CARTESIAN_POINT('Ctrl Pts',(-260.144521813036,1.754921961264,125.780753115897));
#258031=CARTESIAN_POINT('Ctrl Pts',(-260.190939676638,0.892893391295023,
125.631947563271));
#258032=CARTESIAN_POINT('Ctrl Pts',(210.191733024964,-2.43880115184907,
125.780342085335));
#258033=CARTESIAN_POINT('Ctrl Pts',(210.145323348611,-3.27594855749458,
126.186716565447));
#258034=CARTESIAN_POINT('Ctrl Pts',(210.052505734956,-4.72940422381435,
127.426013481475));
#258035=CARTESIAN_POINT('Ctrl Pts',(209.866872246696,-6.15821517169733,
131.008352419918));
#258036=CARTESIAN_POINT('Ctrl Pts',(209.634832560185,-4.21099667891447,
135.892791108304));
#258037=CARTESIAN_POINT('Ctrl Pts',(209.356384936373,2.01508446636645,137.098708070195));
#258038=CARTESIAN_POINT('Ctrl Pts',(209.07793731256,6.37956871319657,132.510708806665));
#258039=CARTESIAN_POINT('Ctrl Pts',(208.799489688747,4.8866719183268,126.359661034021));
#258040=CARTESIAN_POINT('Ctrl Pts',(208.521042064934,-1.09954563679898,
124.290443595948));
#258041=CARTESIAN_POINT('Ctrl Pts',(208.242594441121,-6.07390144970816,
128.208589139036));
#258042=CARTESIAN_POINT('Ctrl Pts',(207.964146817309,-5.46739734855352,
134.511385201899));
#258043=CARTESIAN_POINT('Ctrl Pts',(207.685699193495,0.163779660617915,
137.407996874876));
#258044=CARTESIAN_POINT('Ctrl Pts',(207.407251569682,5.6442383477931,134.235982835808));
#258045=CARTESIAN_POINT('Ctrl Pts',(207.128803945869,5.93803043711477,127.910585036422));
#258046=CARTESIAN_POINT('Ctrl Pts',(206.850356322057,0.775002953389061,
124.244367681185));
#258047=CARTESIAN_POINT('Ctrl Pts',(206.571908698243,-5.10018277131114,
126.606494049502));
#258048=CARTESIAN_POINT('Ctrl Pts',(206.293461074431,-6.28856642889766,
132.82623846394));
#258049=CARTESIAN_POINT('Ctrl Pts',(206.015013450618,-1.69805588527783,
137.187984519302));
#258050=CARTESIAN_POINT('Ctrl Pts',(205.736565826805,4.45288036648484,135.683487507757));
#258051=CARTESIAN_POINT('Ctrl Pts',(205.458118202992,6.51183958365415,129.695313656966));
#258052=CARTESIAN_POINT('Ctrl Pts',(205.179670579179,2.58673502741873,124.726298504418));
#258053=CARTESIAN_POINT('Ctrl Pts',(204.901222955366,-3.71545195245463,
125.342726181157));
#258054=CARTESIAN_POINT('Ctrl Pts',(204.622775331554,-6.60332046735468,
130.978128730661));
#258055=CARTESIAN_POINT('Ctrl Pts',(204.344327707741,-3.42305986725146,
136.4538470632));
#258056=CARTESIAN_POINT('Ctrl Pts',(204.065880083927,2.90282542147133,136.737963244372));
#258057=CARTESIAN_POINT('Ctrl Pts',(203.787432460115,6.56115601364161,131.569388537382));
#258058=CARTESIAN_POINT('Ctrl Pts',(203.508984836302,4.1901047305044,125.69779051756));
#258059=CARTESIAN_POINT('Ctrl Pts',(203.230537212489,-2.03144808657932,
124.518880964767));
#258060=CARTESIAN_POINT('Ctrl Pts',(202.952089588676,-6.38619936200403,
129.116020142231));
#258061=CARTESIAN_POINT('Ctrl Pts',(202.673641964863,-4.87234540261322,
135.2646617407));
#258062=CARTESIAN_POINT('Ctrl Pts',(202.39519434105,1.1189559521872,137.314504502614));
#258063=CARTESIAN_POINT('Ctrl Pts',(202.116746717238,6.08199145217563,133.381843073553));
#258064=CARTESIAN_POINT('Ctrl Pts',(201.838299093424,5.45597392877388,127.080601183836));
#258065=CARTESIAN_POINT('Ctrl Pts',(201.559851469612,-0.183817095687214,
124.201312298284));
#258066=CARTESIAN_POINT('Ctrl Pts',(201.281403845799,-5.65468918935595,
127.389902241135));
#258067=CARTESIAN_POINT('Ctrl Pts',(201.002956221986,-5.92917816483575,
133.716212626452));
#258068=CARTESIAN_POINT('Ctrl Pts',(200.724508598173,-0.755042063338292,
137.366673267433));
#258069=CARTESIAN_POINT('Ctrl Pts',(200.44606097436,5.11294080853837,134.986689170007));
#258070=CARTESIAN_POINT('Ctrl Pts',(200.167613350547,6.2823808583988,128.763349450982));
#258071=CARTESIAN_POINT('Ctrl Pts',(199.889165726734,1.67861981076543,124.415599285115));
#258072=CARTESIAN_POINT('Ctrl Pts',(199.610718102921,-4.46771083782862,
125.938808675424));
#258073=CARTESIAN_POINT('Ctrl Pts',(199.332270479108,-6.50843348626435,
131.933222605136));
#258074=CARTESIAN_POINT('Ctrl Pts',(199.053822855296,-2.56822371547623,
136.890267516244));
#258075=CARTESIAN_POINT('Ctrl Pts',(198.775375231483,3.73205818513161,136.254661300547));
#258076=CARTESIAN_POINT('Ctrl Pts',(198.49692760767,6.60276093478139,130.610495019181));
#258077=CARTESIAN_POINT('Ctrl Pts',(198.218479983857,3.4058489481713,125.14448175187));
#258078=CARTESIAN_POINT('Ctrl Pts',(197.940032360044,-2.92087183683725,
124.879620661678));
#258079=CARTESIAN_POINT('Ctrl Pts',(197.661584736231,-6.56345409631434,
130.05930615131));
#258080=CARTESIAN_POINT('Ctrl Pts',(197.383137112418,-4.1745426838368,135.923660297497));
#258081=CARTESIAN_POINT('Ctrl Pts',(197.104689488605,2.05056951733907,137.083628129519));
#258082=CARTESIAN_POINT('Ctrl Pts',(196.826241864792,6.39130850797037,132.473255877329));
#258083=CARTESIAN_POINT('Ctrl Pts',(196.54779424098,4.85874721255563,126.329250411482));
#258084=CARTESIAN_POINT('Ctrl Pts',(196.269346617166,-1.13876540820057,
124.297652603739));
#258085=CARTESIAN_POINT('Ctrl Pts',(195.990898993354,-6.0898082506034,128.245401590344));
#258086=CARTESIAN_POINT('Ctrl Pts',(195.712451369541,-5.44461481437399,
134.544708910868));
#258087=CARTESIAN_POINT('Ctrl Pts',(195.434003745728,0.203913652044436,
137.406818876019));
#258088=CARTESIAN_POINT('Ctrl Pts',(195.155556121915,5.66505543396973,134.201592249669));
#258089=CARTESIAN_POINT('Ctrl Pts',(194.877108498102,5.92028802542049,127.874475717408));
#258090=CARTESIAN_POINT('Ctrl Pts',(194.59866087429,0.735065143658737,124.239780275557));
#258091=CARTESIAN_POINT('Ctrl Pts',(194.320213250476,-5.1256466951968,126.637613470433));
#258092=CARTESIAN_POINT('Ctrl Pts',(194.041765626664,-6.2761396229282,132.86448373661));
#258093=CARTESIAN_POINT('Ctrl Pts',(193.763318002851,-1.6591668436545,137.198201498994));
#258094=CARTESIAN_POINT('Ctrl Pts',(193.484870379038,4.48249921013125,135.656291847837));
#258095=CARTESIAN_POINT('Ctrl Pts',(193.206422755225,6.50496747206681,129.655694426079));
#258096=CARTESIAN_POINT('Ctrl Pts',(192.927975131412,2.54968841250072,124.710665118833));
#258097=CARTESIAN_POINT('Ctrl Pts',(192.649527507599,-3.74862973894988,
125.365444281348));
#258098=CARTESIAN_POINT('Ctrl Pts',(192.371079883787,-6.60214029104917,
131.018321851013));
#258099=CARTESIAN_POINT('Ctrl Pts',(192.092632259973,-3.38860644815819,
136.474579499726));
#258100=CARTESIAN_POINT('Ctrl Pts',(191.814184636161,2.93889117796205,136.720183001327));
#258101=CARTESIAN_POINT('Ctrl Pts',(191.535737012347,6.56569138435095,131.529434736241));
#258102=CARTESIAN_POINT('Ctrl Pts',(191.257289388535,4.15894196037717,125.672378777932));
#258103=CARTESIAN_POINT('Ctrl Pts',(190.978841764722,-2.06967194957323,
124.531363418996));
#258104=CARTESIAN_POINT('Ctrl Pts',(190.700394140909,-6.3963584469616,129.154926032595));
#258105=CARTESIAN_POINT('Ctrl Pts',(190.421946517096,-4.84510401107414,
135.294238450423));
#258106=CARTESIAN_POINT('Ctrl Pts',(190.143498893283,1.15856431450073,137.307572482581));
#258107=CARTESIAN_POINT('Ctrl Pts',(189.86505126947,6.09756863406271,133.344772510351));
#258108=CARTESIAN_POINT('Ctrl Pts',(189.586603645657,5.4332052617092,127.047458114672));
#258109=CARTESIAN_POINT('Ctrl Pts',(189.308156021844,-0.224008319322015,
124.202553584261));
#258110=CARTESIAN_POINT('Ctrl Pts',(189.029708398032,-5.67536919831109,
127.424387201254));
#258111=CARTESIAN_POINT('Ctrl Pts',(188.751260774218,-5.91134304125131,
133.752251266956));
#258112=CARTESIAN_POINT('Ctrl Pts',(188.472813150406,-0.71508141444371,
137.371147838333));
#258113=CARTESIAN_POINT('Ctrl Pts',(188.194365526593,5.13830509856852,134.955487759214));
#258114=CARTESIAN_POINT('Ctrl Pts',(187.91591790278,6.26984024615536,128.725144630756));
#258115=CARTESIAN_POINT('Ctrl Pts',(187.637470278967,1.63969850624965,124.405499418827));
#258116=CARTESIAN_POINT('Ctrl Pts',(187.359022655154,-4.49724605717418,
125.966095046791));
#258117=CARTESIAN_POINT('Ctrl Pts',(187.080575031341,-6.5014411967389,131.972820371883));
#258118=CARTESIAN_POINT('Ctrl Pts',(186.802127407528,-2.53112948956026,
136.905788265189));
#258119=CARTESIAN_POINT('Ctrl Pts',(186.523679783716,3.76516656597443,136.231842221641));
#258120=CARTESIAN_POINT('Ctrl Pts',(186.245232159903,6.60145848599114,130.570305731164));
#258121=CARTESIAN_POINT('Ctrl Pts',(185.96678453609,3.3713325565579,125.123854247073));
#258122=CARTESIAN_POINT('Ctrl Pts',(185.688336912277,-2.95688329360047,
124.897510609301));
#258123=CARTESIAN_POINT('Ctrl Pts',(185.409889288464,-6.5678678487195,130.099273563458));
#258124=CARTESIAN_POINT('Ctrl Pts',(185.131441664651,-4.14330270904733,
135.948977074923));
#258125=CARTESIAN_POINT('Ctrl Pts',(184.852994040838,2.08875520864929,137.071029390563));
#258126=CARTESIAN_POINT('Ctrl Pts',(184.574546417025,6.40134913096194,132.434319247607));
#258127=CARTESIAN_POINT('Ctrl Pts',(184.296098793212,4.831415925211,126.299756751549));
#258128=CARTESIAN_POINT('Ctrl Pts',(184.017651169399,-1.17835248801931,
124.304705146227));
#258129=CARTESIAN_POINT('Ctrl Pts',(183.739203545587,-6.10527253047917,
128.282519393244));
#258130=CARTESIAN_POINT('Ctrl Pts',(183.460755921774,-5.42174537657308,
134.577782526619));
#258131=CARTESIAN_POINT('Ctrl Pts',(183.182308297961,0.244100911417136,
137.405455267482));
#258132=CARTESIAN_POINT('Ctrl Pts',(182.903860674148,5.68563038680749,134.167044506474));
#258133=CARTESIAN_POINT('Ctrl Pts',(182.625413050335,5.90234329520773,127.838491527799));
#258134=CARTESIAN_POINT('Ctrl Pts',(182.346965426522,0.695091060812155,
124.23542735186));
#258135=CARTESIAN_POINT('Ctrl Pts',(182.068517802709,-5.15091590138369,
126.668891936874));
#258136=CARTESIAN_POINT('Ctrl Pts',(181.790070178896,-6.263482786439,132.902650210566));
#258137=CARTESIAN_POINT('Ctrl Pts',(181.511622555083,-1.62021497890189,
137.208182855437));
#258138=CARTESIAN_POINT('Ctrl Pts',(181.233174931271,4.51195124234396,135.628915707812));
#258139=CARTESIAN_POINT('Ctrl Pts',(180.954727307458,6.49785469294791,129.61611812487));
#258140=CARTESIAN_POINT('Ctrl Pts',(180.676279683645,2.51254711858197,124.695257343842));
#258141=CARTESIAN_POINT('Ctrl Pts',(180.397832059832,-3.78166851301026,
125.388364025079));
#258142=CARTESIAN_POINT('Ctrl Pts',(180.119384436019,-6.60071552592353,
131.058506988669));
#258143=CARTESIAN_POINT('Ctrl Pts',(179.840936812206,-3.35402743339335,
136.495101852955));
#258144=CARTESIAN_POINT('Ctrl Pts',(179.562489188393,2.97484801707599,136.702183530083));
#258145=CARTESIAN_POINT('Ctrl Pts',(179.28404156458,6.56998346925752,131.489454075275));
#258146=CARTESIAN_POINT('Ctrl Pts',(179.005593940767,4.12762507472721,125.647157201507));
#258147=CARTESIAN_POINT('Ctrl Pts',(178.727146316955,-2.10781911778238,
124.544078323705));
#258148=CARTESIAN_POINT('Ctrl Pts',(178.448698693142,-6.40628051373842,
129.193893042167));
#258149=CARTESIAN_POINT('Ctrl Pts',(178.170251069329,-4.81768308177075,
135.323648786705));
#258150=CARTESIAN_POINT('Ctrl Pts',(177.891803445516,1.19812974544141,137.300399483306));
#258151=CARTESIAN_POINT('Ctrl Pts',(177.613355821703,6.11291986848493,133.307607811431));
#258152=CARTESIAN_POINT('Ctrl Pts',(177.33490819789,5.41023526512845,127.014454258818));
#258153=CARTESIAN_POINT('Ctrl Pts',(177.056460574078,-0.264191242194762,
124.204039502676));
#258154=CARTESIAN_POINT('Ctrl Pts',(176.778012950264,-5.69583890440069,
127.458997407505));
#258155=CARTESIAN_POINT('Ctrl Pts',(176.499565326452,-5.89328887066216,
133.788180672302));
#258156=CARTESIAN_POINT('Ctrl Pts',(176.221117702638,-0.675094267951971,
137.375379074508));
#258157=CARTESIAN_POINT('Ctrl Pts',(175.942670078826,5.16347898681764,134.924132526884));
#258158=CARTESIAN_POINT('Ctrl Pts',(175.664222455013,6.25706730267374,128.687016856641));
#258159=CARTESIAN_POINT('Ctrl Pts',(175.3857748312,1.60071644210391,124.395636664696));
#258160=CARTESIAN_POINT('Ctrl Pts',(175.107327207387,-4.5266146294138,125.993560701866));
#258161=CARTESIAN_POINT('Ctrl Pts',(174.828879583574,-6.49420799391872,
132.012374840923));
#258162=CARTESIAN_POINT('Ctrl Pts',(174.550431959762,-2.49394147171037,
136.92108292349));
#258163=CARTESIAN_POINT('Ctrl Pts',(174.271984335948,3.79813542718566,136.208822025409));
#258164=CARTESIAN_POINT('Ctrl Pts',(173.993536712136,6.59991141772898,130.530125116137));
#258165=CARTESIAN_POINT('Ctrl Pts',(173.715089088322,3.33669123897678,125.103437235529));
#258166=CARTESIAN_POINT('Ctrl Pts',(173.43664146451,-2.99278518196597,124.915619437422));
#258167=CARTESIAN_POINT('Ctrl Pts',(173.158193840697,-6.5720382263662,130.139267102866));
#258168=CARTESIAN_POINT('Ctrl Pts',(172.879746216884,-4.11190920265221,
135.974103216695));
#258169=CARTESIAN_POINT('Ctrl Pts',(172.601298593071,2.12686350036709,137.058198437889));
#258170=CARTESIAN_POINT('Ctrl Pts',(172.322850969258,6.41115254960738,132.395322219168));
#258171=CARTESIAN_POINT('Ctrl Pts',(172.044403345445,4.80390560797255,126.270430011369));
#258172=CARTESIAN_POINT('Ctrl Pts',(171.765955721632,-1.21789590355323,
124.31199853584));
#258173=CARTESIAN_POINT('Ctrl Pts',(171.487508097819,-6.12051057723618,
128.319730643897));
#258174=CARTESIAN_POINT('Ctrl Pts',(171.209060474007,-5.39867503400336,
134.610716316833));
#258175=CARTESIAN_POINT('Ctrl Pts',(170.930612850193,0.284279125540913,
137.403847052956));
#258176=CARTESIAN_POINT('Ctrl Pts',(170.652165226381,5.70599465652041,134.13237215779));
#258177=CARTESIAN_POINT('Ctrl Pts',(170.373717602568,5.88417985149351,127.802617239562));
#258178=CARTESIAN_POINT('Ctrl Pts',(170.095269978755,0.655091221110643,
124.231317842401));
#258179=CARTESIAN_POINT('Ctrl Pts',(169.816822354942,-5.17599423848763,
126.700323644626));
#258180=CARTESIAN_POINT('Ctrl Pts',(169.538374731129,-6.25059385429175,
132.940738931629));
#258181=CARTESIAN_POINT('Ctrl Pts',(169.259927107316,-1.58120307648749,
137.217926915891));
#258182=CARTESIAN_POINT('Ctrl Pts',(168.981479483503,4.54123608254409,135.601360792124));
#258183=CARTESIAN_POINT('Ctrl Pts',(168.703031859691,6.49050113343381,129.576585854424));
#258184=CARTESIAN_POINT('Ctrl Pts',(168.424584235878,2.47531272130571,124.680075943919));
#258185=CARTESIAN_POINT('Ctrl Pts',(168.146136612065,-3.81456715595326,
125.411484460556));
#258186=CARTESIAN_POINT('Ctrl Pts',(167.867688988252,-6.59904616885666,
131.098682708838));
#258187=CARTESIAN_POINT('Ctrl Pts',(167.589241364439,-3.31932413390846,
136.515413333674));
#258188=CARTESIAN_POINT('Ctrl Pts',(167.310793740626,3.01069462210276,136.683965512842));
#258189=CARTESIAN_POINT('Ctrl Pts',(167.032346116813,6.57403210101054,131.449448027918));
#258190=CARTESIAN_POINT('Ctrl Pts',(166.753898493,4.09615523841214,125.622126727152));
#258191=CARTESIAN_POINT('Ctrl Pts',(166.475450869187,-2.14588817997888,
124.557025205477));
#258192=CARTESIAN_POINT('Ctrl Pts',(166.197003245374,-6.41596519343492,
129.232919728208));
#258193=CARTESIAN_POINT('Ctrl Pts',(165.918555621562,-4.79008363144905,
135.352891659104));
#258194=CARTESIAN_POINT('Ctrl Pts',(165.640107997748,1.23765077924384,137.292985770921));
#258195=CARTESIAN_POINT('Ctrl Pts',(165.361660373936,6.12804458641347,133.270350353765));
#258196=CARTESIAN_POINT('Ctrl Pts',(165.083212750123,5.38706479029029,126.981590839339));
#258197=CARTESIAN_POINT('Ctrl Pts',(164.80476512631,-0.304364375363971,
124.205769998417));
#258198=CARTESIAN_POINT('Ctrl Pts',(164.526317502497,-5.71609754908509,
127.493731577419));
#258199=CARTESIAN_POINT('Ctrl Pts',(164.247869878684,-5.8750163220866,133.823999511097));
#258200=CARTESIAN_POINT('Ctrl Pts',(163.969422254871,-0.635082105593798,
137.37936681918));
#258201=CARTESIAN_POINT('Ctrl Pts',(163.690974631059,5.18846154045405,134.892624634889));
#258202=CARTESIAN_POINT('Ctrl Pts',(163.412527007245,6.24406250126218,128.648967541478));
#258203=CARTESIAN_POINT('Ctrl Pts',(163.134079383433,1.56167506282176,124.386011388187));
#258204=CARTESIAN_POINT('Ctrl Pts',(162.85563175962,-4.55581546628373,126.021204622902));
#258205=CARTESIAN_POINT('Ctrl Pts',(162.577184135807,-6.48673414583306,
132.051884546553));
#258206=CARTESIAN_POINT('Ctrl Pts',(162.298736511994,-2.45666103994207,
136.936150924396));
#258207=CARTESIAN_POINT('Ctrl Pts',(162.020288888181,3.83096354709181,136.185601564872));
#258208=CARTESIAN_POINT('Ctrl Pts',(161.741841264368,6.59811978732212,130.489954663008));
#258209=CARTESIAN_POINT('Ctrl Pts',(161.463393640556,3.30192627907479,125.083231473798));
#258210=CARTESIAN_POINT('Ctrl Pts',(161.184946016742,-3.02857617157586,
124.933946475014));
#258211=CARTESIAN_POINT('Ctrl Pts',(160.90649839293,-6.57596507471956,130.179285287561));
#258212=CARTESIAN_POINT('Ctrl Pts',(160.628050769116,-4.08036332794952,
135.999037791754));
#258213=CARTESIAN_POINT('Ctrl Pts',(160.349603145304,2.16489298037573,137.045135746957));
#258214=CARTESIAN_POINT('Ctrl Pts',(160.07115552149,6.42071840063739,132.356266237063));
#258215=CARTESIAN_POINT('Ctrl Pts',(159.792707897678,4.77621728024515,126.241271277656));
#258216=CARTESIAN_POINT('Ctrl Pts',(159.514260273865,-1.25739418950663,
124.319532502318));
#258217=CARTESIAN_POINT('Ctrl Pts',(159.235812650052,-6.13552182622286,
128.357033963427));
#258218=CARTESIAN_POINT('Ctrl Pts',(158.957365026239,-5.37540464154493,
134.643509061136));
#258219=CARTESIAN_POINT('Ctrl Pts',(158.678917402427,0.324446805597038,
137.401994292032));
#258220=CARTESIAN_POINT('Ctrl Pts',(158.400469778613,5.72614748850293,134.097576488416));
#258221=CARTESIAN_POINT('Ctrl Pts',(158.122022154801,5.86579836733105,127.766854182028));
#258222=CARTESIAN_POINT('Ctrl Pts',(157.843574530988,0.615067106763091,
124.22745189946));
#258223=CARTESIAN_POINT('Ctrl Pts',(157.565126907175,-5.20088077722156,
126.731907428977));
#258224=CARTESIAN_POINT('Ctrl Pts',(157.286679283362,-6.23747330409059,
132.978748488409));
#258225=CARTESIAN_POINT('Ctrl Pts',(157.008231659549,-1.54213258201158,
137.227433319288));
#258226=CARTESIAN_POINT('Ctrl Pts',(156.729784035736,4.5703526455712,135.57362812183));
#258227=CARTESIAN_POINT('Ctrl Pts',(156.451336411923,6.48290706601333,129.537099079623));
#258228=CARTESIAN_POINT('Ctrl Pts',(156.172888788111,2.43798660040623,124.665121481617));
#258229=CARTESIAN_POINT('Ctrl Pts',(155.894441164297,-3.84732444870741,
125.434804731043));
#258230=CARTESIAN_POINT('Ctrl Pts',(155.615993540485,-6.59713228170722,
131.138847522794));
#258231=CARTESIAN_POINT('Ctrl Pts',(155.337545916672,-3.28449783564716,
136.535513189234));
#258232=CARTESIAN_POINT('Ctrl Pts',(155.059098292859,3.04642966473303,136.665529624679));
#258233=CARTESIAN_POINT('Ctrl Pts',(154.780650669046,6.57783712958646,131.409418076611));
#258234=CARTESIAN_POINT('Ctrl Pts',(154.502203045233,4.06453361755842,125.597288282381));
#258235=CARTESIAN_POINT('Ctrl Pts',(154.22375542142,-2.18387772549973,124.57020358456));
#258236=CARTESIAN_POINT('Ctrl Pts',(153.945307797607,-6.42541212718171,
129.272004644569));
#258237=CARTESIAN_POINT('Ctrl Pts',(153.666860173794,-4.76230668281685,
135.381965984011));
#258238=CARTESIAN_POINT('Ctrl Pts',(153.388412549982,1.27712595144142,137.285331620145));
#258239=CARTESIAN_POINT('Ctrl Pts',(153.109964926169,6.14294222739622,133.233001517943));
#258240=CARTESIAN_POINT('Ctrl Pts',(152.831517302356,5.36369469578529,126.948869073999));
#258241=CARTESIAN_POINT('Ctrl Pts',(152.553069678543,-0.344526230199219,
124.207745007359));
#258242=CARTESIAN_POINT('Ctrl Pts',(152.27462205473,-5.73614438167267,127.528588423912));
#258243=CARTESIAN_POINT('Ctrl Pts',(151.996174430917,-5.85652607262075,
133.859706456064));
#258244=CARTESIAN_POINT('Ctrl Pts',(151.717726807104,-0.595046410034728,
137.383110924578));
#258245=CARTESIAN_POINT('Ctrl Pts',(151.439279183291,5.21325183374003,134.860965250768));
#258246=CARTESIAN_POINT('Ctrl Pts',(151.160831559478,6.23082632381839,128.610998095198));
#258247=CARTESIAN_POINT('Ctrl Pts',(150.882383935665,1.52257581509584,124.376623945969));
#258248=CARTESIAN_POINT('Ctrl Pts',(150.603936311853,-4.58484748573611,
126.049025785542));
#258249=CARTESIAN_POINT('Ctrl Pts',(150.32548868804,-6.47901992942814,132.091348024725));
#258250=CARTESIAN_POINT('Ctrl Pts',(150.047041064227,-2.41928957569559,
136.950991709558));
#258251=CARTESIAN_POINT('Ctrl Pts',(149.768593440414,3.8636497092349,136.162181700472));
#258252=CARTESIAN_POINT('Ctrl Pts',(149.490145816601,6.59608366116008,130.449795860306));
#258253=CARTESIAN_POINT('Ctrl Pts',(149.211698192788,3.26703896508027,125.06323771061));
#258254=CARTESIAN_POINT('Ctrl Pts',(148.933250568975,-3.06425493618196,
124.95249104296));
#258255=CARTESIAN_POINT('Ctrl Pts',(148.654802945162,-6.57964824826877,
130.219326634649));
#258256=CARTESIAN_POINT('Ctrl Pts',(148.376355321349,-4.04866625388314,
136.02377987614));
#258257=CARTESIAN_POINT('Ctrl Pts',(148.097907697537,2.20284223947883,137.031841801807));
#258258=CARTESIAN_POINT('Ctrl Pts',(147.819460073724,6.43004632958585,132.317152748525));
#258259=CARTESIAN_POINT('Ctrl Pts',(147.541012449911,4.74835196802999,126.212281630895));
#258260=CARTESIAN_POINT('Ctrl Pts',(147.262564826098,-1.29684588225586,
124.327306766486));
#258261=CARTESIAN_POINT('Ctrl Pts',(146.984117202285,-6.15030572119196,
128.394427969547));
#258262=CARTESIAN_POINT('Ctrl Pts',(146.705669578472,-5.35193506149072,
134.676159544383));
#258263=CARTESIAN_POINT('Ctrl Pts',(146.427221954659,0.364602463157475,
137.399897053366));
#258264=CARTESIAN_POINT('Ctrl Pts',(146.148774330846,5.74608813598446,134.062658787717));
#258265=CARTESIAN_POINT('Ctrl Pts',(145.870326707034,5.84719952385297,127.731203680413));
#258266=CARTESIAN_POINT('Ctrl Pts',(145.59187908322,0.575020200877703,124.22382966629));
#258267=CARTESIAN_POINT('Ctrl Pts',(145.313431459408,-5.22557459540567,
126.76364211958));
#258268=CARTESIAN_POINT('Ctrl Pts',(145.034983835595,-6.22412162202233,
133.016677472446));
#258269=CARTESIAN_POINT('Ctrl Pts',(144.756536211782,-1.50300494324566,
137.236701713364));
#258270=CARTESIAN_POINT('Ctrl Pts',(144.478088587969,4.59929985250025,135.545718724575));
#258271=CARTESIAN_POINT('Ctrl Pts',(144.199640964156,6.47507277208744,129.497659263665));
#258272=CARTESIAN_POINT('Ctrl Pts',(143.921193340343,2.40057013901678,124.65039451108));
#258273=CARTESIAN_POINT('Ctrl Pts',(143.64274571653,-3.87993917743928,125.458323972397));
#258274=CARTESIAN_POINT('Ctrl Pts',(143.364298092718,-6.594973935395,131.178999942215));
#258275=CARTESIAN_POINT('Ctrl Pts',(143.085850468904,-3.2495498291107,136.555400674828));
#258276=CARTESIAN_POINT('Ctrl Pts',(142.807402845092,3.08205182079176,136.646876548744));
#258277=CARTESIAN_POINT('Ctrl Pts',(142.528955221279,6.58139841398854,131.369365704677));
#258278=CARTESIAN_POINT('Ctrl Pts',(142.250507597466,4.03276138391676,125.572642787588));
#258279=CARTESIAN_POINT('Ctrl Pts',(141.972059973653,-2.2217863466284,124.583612972623));
#258280=CARTESIAN_POINT('Ctrl Pts',(141.69361234984,-6.43462096491922,129.311146342943));
#258281=CARTESIAN_POINT('Ctrl Pts',(141.415164726027,-4.7343532651591,135.410870684068));
#258282=CARTESIAN_POINT('Ctrl Pts',(141.136717102214,1.31655379926713,137.277437314604));
#258283=CARTESIAN_POINT('Ctrl Pts',(140.858269478402,6.15761223939561,133.195562687939));
#258284=CARTESIAN_POINT('Ctrl Pts',(140.579821854588,5.34012584760095,126.916290175316));
#258285=CARTESIAN_POINT('Ctrl Pts',(140.301374230776,-0.384675318488256,
124.20996445632));
#258286=CARTESIAN_POINT('Ctrl Pts',(140.022926606963,-5.75597865932068,
127.563566655346));
#258287=CARTESIAN_POINT('Ctrl Pts',(139.74447898315,-5.83781880742758,133.895300184066));
#258288=CARTESIAN_POINT('Ctrl Pts',(139.466031359337,-0.554988664812238,
137.386611251964));
#258289=CARTESIAN_POINT('Ctrl Pts',(139.187583735524,5.23784894806212,134.829155547671));
#258290=CARTESIAN_POINT('Ctrl Pts',(138.909136111711,6.21735926081381,128.573109924773));
#258291=CARTESIAN_POINT('Ctrl Pts',(138.630688487898,1.48342014776303,124.367474685896));
#258292=CARTESIAN_POINT('Ctrl Pts',(138.352240864086,-4.61370961197883,
126.077023158863));
#258293=CARTESIAN_POINT('Ctrl Pts',(138.073793240272,-6.47106563055709,
132.130763813104));
#258294=CARTESIAN_POINT('Ctrl Pts',(137.79534561646,-2.38182846378423,136.965604729043));
#258295=CARTESIAN_POINT('Ctrl Pts',(137.516897992647,3.89619270241722,136.138563300043));
#258296=CARTESIAN_POINT('Ctrl Pts',(137.238450368834,6.59380311469226,130.409650196134));
#258297=CARTESIAN_POINT('Ctrl Pts',(136.960002745021,3.23203058975544,125.043456686844));
#258298=CARTESIAN_POINT('Ctrl Pts',(136.681555121208,-3.09982015369448,
124.971252454085));
#258299=CARTESIAN_POINT('Ctrl Pts',(136.403107497395,-6.58308761053252,
130.259389660389));
#258300=CARTESIAN_POINT('Ctrl Pts',(136.124659873582,-4.01681915499975,
136.048328553027));
#258301=CARTESIAN_POINT('Ctrl Pts',(135.846212249769,2.24070987145278,137.018317095051));
#258302=CARTESIAN_POINT('Ctrl Pts',(135.567764625956,6.43913599080291,132.277983202917));
#258303=CARTESIAN_POINT('Ctrl Pts',(135.289317002144,4.72031070388647,126.183462145311));
#258304=CARTESIAN_POINT('Ctrl Pts',(135.010869378331,-1.33624951990408,
124.335321040266));
#258305=CARTESIAN_POINT('Ctrl Pts',(134.732421754518,-6.16486171432077,
128.431911276607));
#258306=CARTESIAN_POINT('Ctrl Pts',(134.453974130705,-5.32826716351462,
134.708666556695));
#258307=CARTESIAN_POINT('Ctrl Pts',(134.175526506892,0.404744610239488,
137.397555414672));
#258308=CARTESIAN_POINT('Ctrl Pts',(133.897078883079,5.76581586005707,134.027620349581));
#258309=CARTESIAN_POINT('Ctrl Pts',(133.618631259266,5.82838401024617,127.695667055759));
#258310=CARTESIAN_POINT('Ctrl Pts',(133.340183635453,0.534951987407334,
124.220451277114));
#258311=CARTESIAN_POINT('Ctrl Pts',(133.06173601164,-5.25007477800144,126.795526540492));
#258312=CARTESIAN_POINT('Ctrl Pts',(132.783288387828,-6.21053930283845,
133.054524478268));
#258313=CARTESIAN_POINT('Ctrl Pts',(132.504840764015,-1.46382161007886,
137.245731754674));
#258314=CARTESIAN_POINT('Ctrl Pts',(132.226393140202,4.62807663068185,135.517633634551));
#258315=CARTESIAN_POINT('Ctrl Pts',(131.947945516389,6.46699854195874,129.458267868007));
#258316=CARTESIAN_POINT('Ctrl Pts',(131.669497892576,2.3630647236181,124.635895578019));
#258317=CARTESIAN_POINT('Ctrl Pts',(131.391050268763,-3.91241013359816,
125.482041313105));
#258318=CARTESIAN_POINT('Ctrl Pts',(131.11260264495,-6.59257120989826,131.219138479237));
#258319=CARTESIAN_POINT('Ctrl Pts',(130.834155021138,-3.2144814093103,136.575075053519));
#258320=CARTESIAN_POINT('Ctrl Pts',(130.555707397324,3.1175597702868,136.628006976231));
#258321=CARTESIAN_POINT('Ctrl Pts',(130.277259773512,6.58471582225214,131.329292396271));
#258322=CARTESIAN_POINT('Ctrl Pts',(129.998812149698,4.0008397148189,125.548191156024));
#258323=CARTESIAN_POINT('Ctrl Pts',(129.720364525886,-2.25961263864694,
124.59725287278));
#258324=CARTESIAN_POINT('Ctrl Pts',(129.441916902073,-6.44359136541048,
129.350343372922));
#258325=CARTESIAN_POINT('Ctrl Pts',(129.16346927826,-4.70622441430021,135.439604688201));
#258326=CARTESIAN_POINT('Ctrl Pts',(128.885021654447,1.35593286170785,137.269303146827));
#258327=CARTESIAN_POINT('Ctrl Pts',(128.606574030634,6.17205407880915,133.158035251063));
#258328=CARTESIAN_POINT('Ctrl Pts',(128.328126406821,5.31635911908928,126.883855350513));
#258329=CARTESIAN_POINT('Ctrl Pts',(128.049678783009,-0.424810152491945,
124.212428263054));
#258330=CARTESIAN_POINT('Ctrl Pts',(127.771231159195,-5.77559964706288,
127.598664975593));
#258331=CARTESIAN_POINT('Ctrl Pts',(127.492783535383,-5.81889521971155,
133.930779376167));
#258332=CARTESIAN_POINT('Ctrl Pts',(127.21433591157,-0.514910354280421,
137.389867671632));
#258333=CARTESIAN_POINT('Ctrl Pts',(126.935888287757,5.26225197196523,134.797196704317));
#258334=CARTESIAN_POINT('Ctrl Pts',(126.657440663944,6.20366181127538,128.535304434163));
#258335=CARTESIAN_POINT('Ctrl Pts',(126.378993040131,1.44420951175126,124.358563947));
#258336=CARTESIAN_POINT('Ctrl Pts',(126.100545416318,-4.64240077551519,
126.105195705413));
#258337=CARTESIAN_POINT('Ctrl Pts',(125.822097792505,-6.46287154396936,
132.170130451126));
#258338=CARTESIAN_POINT('Ctrl Pts',(125.543650168692,-2.34427909234318,
136.979989441362));
#258339=CARTESIAN_POINT('Ctrl Pts',(125.26520254488,3.92859132074607,136.114747238771));
#258340=CARTESIAN_POINT('Ctrl Pts',(124.986754921067,6.59127823242518,130.369519158099));
#258341=CARTESIAN_POINT('Ctrl Pts',(124.708307297254,3.19690245034852,125.023889135492));
#258342=CARTESIAN_POINT('Ctrl Pts',(124.429859673441,-3.13527050623128,
124.990230013179));
#258343=CARTESIAN_POINT('Ctrl Pts',(124.151412049628,-6.58628303406391,
130.299472880227));
#258344=CARTESIAN_POINT('Ctrl Pts',(123.872964425815,-3.98482321140548,
136.072682912751));
#258345=CARTESIAN_POINT('Ctrl Pts',(123.594516802002,2.2784944730983,137.004562127853));
#258346=CARTESIAN_POINT('Ctrl Pts',(123.316069178189,6.44798704746787,132.238759051683));
#258347=CARTESIAN_POINT('Ctrl Pts',(123.037621554376,4.6920945268939,126.154813888819));
#258348=CARTESIAN_POINT('Ctrl Pts',(122.759173930564,-1.37560364233486,
124.343575026687));
#258349=CARTESIAN_POINT('Ctrl Pts',(122.480726306751,-6.17918926623166,
128.46948249565));
#258350=CARTESIAN_POINT('Ctrl Pts',(122.202278682938,-5.30440182463932,
134.741028893516));
#258351=CARTESIAN_POINT('Ctrl Pts',(121.923831059125,0.444871759361186,
137.394969462721));
#258352=CARTESIAN_POINT('Ctrl Pts',(121.645383435312,5.78532992970255,133.992462472369));
#258353=CARTESIAN_POINT('Ctrl Pts',(121.366935811499,5.80935252372653,127.660245624887));
#258354=CARTESIAN_POINT('Ctrl Pts',(121.088488187686,0.494863951094175,
124.21731685712));
#258355=CARTESIAN_POINT('Ctrl Pts',(120.810040563873,-5.27438041714564,
126.827559510225));
#258356=CARTESIAN_POINT('Ctrl Pts',(120.53159294006,-6.19672684983677,133.092288103441));
#258357=CARTESIAN_POINT('Ctrl Pts',(120.253145316248,-1.42458403446405,
137.254523108609));
#258358=CARTESIAN_POINT('Ctrl Pts',(119.974697692435,4.65668191378195,135.489373892464));
#258359=CARTESIAN_POINT('Ctrl Pts',(119.696250068622,6.45868467482089,129.418926352309));
#258360=CARTESIAN_POINT('Ctrl Pts',(119.417802444809,2.32547174398699,124.621625219699));
#258361=CARTESIAN_POINT('Ctrl Pts',(119.139354820996,-3.94473611396066,
125.505955874312));
#258362=CARTESIAN_POINT('Ctrl Pts',(118.860907197183,-6.58992419425096,
131.259261646514));
#258363=CARTESIAN_POINT('Ctrl Pts',(118.58245957337,-3.17929387571916,136.594535596262));
#258364=CARTESIAN_POINT('Ctrl Pts',(118.304011949557,3.15295219745811,136.608921606362));
#258365=CARTESIAN_POINT('Ctrl Pts',(118.025564325744,6.58778923144938,131.289199636326));
#258366=CARTESIAN_POINT('Ctrl Pts',(117.747116701932,3.96876979313418,125.523934293753));
#258367=CARTESIAN_POINT('Ctrl Pts',(117.468669078118,-2.29735519988813,
124.611122779595));
#258368=CARTESIAN_POINT('Ctrl Pts',(117.190221454306,-6.45232299625411,
129.389594282045));
#258369=CARTESIAN_POINT('Ctrl Pts',(116.911773830493,-4.67792117256487,
135.468166931659));
#258370=CARTESIAN_POINT('Ctrl Pts',(116.63332620668,1.39526167955762,137.260929418227));
#258371=CARTESIAN_POINT('Ctrl Pts',(116.354878582867,6.18626721048894,133.120420597908));
#258372=CARTESIAN_POINT('Ctrl Pts',(116.076430959054,5.29239539093549,126.851565801475));
#258373=CARTESIAN_POINT('Ctrl Pts',(115.797983335241,-0.464929244999223,
124.215136336267));
#258374=CARTESIAN_POINT('Ctrl Pts',(115.519535711428,-5.79500661783607,
127.633882084071));
#258375=CARTESIAN_POINT('Ctrl Pts',(115.241088087616,-5.79975601069334,
133.96614271767));
#258376=CARTESIAN_POINT('Ctrl Pts',(114.962640463802,-0.474812963556037,
137.392880062915));
#258377=CARTESIAN_POINT('Ctrl Pts',(114.68419283999,5.28646000118636,134.765089904953));
#258378=CARTESIAN_POINT('Ctrl Pts',(114.405745216177,6.18973448276714,128.497583024264));
#258379=CARTESIAN_POINT('Ctrl Pts',(114.127297592364,1.40494536002493,124.349892059469));
#258380=CARTESIAN_POINT('Ctrl Pts',(113.848849968551,-4.67091991318358,
126.133542381245));
#258381=CARTESIAN_POINT('Ctrl Pts',(113.570402344738,-6.45443797329988,
132.209446480045));
#258382=CARTESIAN_POINT('Ctrl Pts',(113.291954720925,-2.30664285277824,
136.994145313484));
#258383=CARTESIAN_POINT('Ctrl Pts',(113.013507097112,3.96084436367879,136.09073439917));
#258384=CARTESIAN_POINT('Ctrl Pts',(112.735059473299,6.58850910791926,130.329404233275));
#258385=CARTESIAN_POINT('Ctrl Pts',(112.456611849487,3.16165584854565,125.004535781636));
#258386=CARTESIAN_POINT('Ctrl Pts',(112.178164225674,-3.1706046801665,125.00942301702));
#258387=CARTESIAN_POINT('Ctrl Pts',(111.899716601861,-6.58923440045535,
130.339574808866));
#258388=CARTESIAN_POINT('Ctrl Pts',(111.621268978048,-3.9526796087217,136.096842052857));
#258389=CARTESIAN_POINT('Ctrl Pts',(111.342821354235,2.31619464429322,136.990577409908));
#258390=CARTESIAN_POINT('Ctrl Pts',(111.064373730422,6.45659917160154,132.199481748287));
#258391=CARTESIAN_POINT('Ctrl Pts',(110.785926106609,4.66370448261314,126.12633792299));
#258392=CARTESIAN_POINT('Ctrl Pts',(110.507478482796,-1.41490679126679,
124.352068419894));
#258393=CARTESIAN_POINT('Ctrl Pts',(110.229030858983,-6.19328784601188,
128.50714023446));
#258394=CARTESIAN_POINT('Ctrl Pts',(109.950583235171,-5.28033992920373,
134.773245355646));
#258395=CARTESIAN_POINT('Ctrl Pts',(109.672135611358,0.484982423596243,
137.392139293334));
#258396=CARTESIAN_POINT('Ctrl Pts',(109.393687987545,5.80462962181993,133.957186458871));
#258397=CARTESIAN_POINT('Ctrl Pts',(109.115240363732,5.79010576951274,127.624940700352));
#258398=CARTESIAN_POINT('Ctrl Pts',(108.836792739919,0.454757577415474,
124.214426522456));
#258399=CARTESIAN_POINT('Ctrl Pts',(108.558345116106,-5.29849061218381,
126.859739841786));
#258400=CARTESIAN_POINT('Ctrl Pts',(108.279897492293,-6.18268477484283,
133.12996694862));
#258401=CARTESIAN_POINT('Ctrl Pts',(108.00144986848,-1.38529367036394,137.2630754494));
#258402=CARTESIAN_POINT('Ctrl Pts',(107.723002244667,4.68511464182123,135.460940545486));
#258403=CARTESIAN_POINT('Ctrl Pts',(107.444554620855,6.45013147874722,129.379636174388));
#258404=CARTESIAN_POINT('Ctrl Pts',(107.166106997042,2.28779259314522,124.607583964913));
#258405=CARTESIAN_POINT('Ctrl Pts',(106.887659373229,-3.97691592067581,
125.530066769856));
#258406=CARTESIAN_POINT('Ctrl Pts',(106.609211749416,-6.58703298653922,
131.299367957265));
#258407=CARTESIAN_POINT('Ctrl Pts',(106.330764125603,-3.14398853222427,
136.613781581943));
#258408=CARTESIAN_POINT('Ctrl Pts',(106.05231650179,3.18822779082625,136.589621146351));
#258409=CARTESIAN_POINT('Ctrl Pts',(105.773868877977,6.59061852769399,131.249088910493));
#258410=CARTESIAN_POINT('Ctrl Pts',(105.495421254164,3.93655280722527,125.49987309962));
#258411=CARTESIAN_POINT('Ctrl Pts',(105.216973630351,-2.33501263178752,
124.625222179118));
#258412=CARTESIAN_POINT('Ctrl Pts',(104.938526006539,-6.46081553389627,
129.428897615854));
#258413=CARTESIAN_POINT('Ctrl Pts',(104.660078382726,-4.64944458874018,
135.49655635606));
#258414=CARTESIAN_POINT('Ctrl Pts',(104.381630758913,1.43453879547275,137.252316439095));
#258415=CARTESIAN_POINT('Ctrl Pts',(104.1031831351,6.20025110776228,133.082720122298));
#258416=CARTESIAN_POINT('Ctrl Pts',(103.824735511287,5.26823555112421,126.819422724701));
#258417=CARTESIAN_POINT('Ctrl Pts',(103.546287887474,-0.505031109382345,
124.218088575609));
#258418=CARTESIAN_POINT('Ctrl Pts',(103.267840263661,-5.81419885250792,
127.669216675797));
#258419=CARTESIAN_POINT('Ctrl Pts',(102.989392639848,-5.78040188958328,
134.001388898174));
#258420=CARTESIAN_POINT('Ctrl Pts',(102.710945016035,-0.434697978462825,
137.395648314187));
#258421=CARTESIAN_POINT('Ctrl Pts',(102.432497392222,5.31047213868803,134.732836339309));
#258422=CARTESIAN_POINT('Ctrl Pts',(102.15404976841,6.17557779137139,128.459947092858));
#258423=CARTESIAN_POINT('Ctrl Pts',(101.875602144597,1.3656291475316,124.341459344644));
#258424=CARTESIAN_POINT('Ctrl Pts',(101.597154520784,-4.69926596819684,
126.162062135967));
#258425=CARTESIAN_POINT('Ctrl Pts',(101.318706896971,-6.44576523105769,
132.248710442988));
#258426=CARTESIAN_POINT('Ctrl Pts',(101.040259273158,-2.26892113971413,
137.008071820859));
#258427=CARTESIAN_POINT('Ctrl Pts',(100.761811649345,3.99295063606701,136.066525671043));
#258428=CARTESIAN_POINT('Ctrl Pts',(100.483364025532,6.58549584378548,130.289306908136));
#258429=CARTESIAN_POINT('Ctrl Pts',(100.204916401719,3.12629209042249,124.985397342422));
#258430=CARTESIAN_POINT('Ctrl Pts',(99.9264687779064,-3.20582136617937,
125.028830754405));
#258431=CARTESIAN_POINT('Ctrl Pts',(99.6480211540935,-6.5919416003429,130.379693960313));
#258432=CARTESIAN_POINT('Ctrl Pts',(99.3695735302808,-3.92038953804142,
136.120805078117));
#258433=CARTESIAN_POINT('Ctrl Pts',(99.0911259064677,2.35380898804382,136.976363459425));
#258434=CARTESIAN_POINT('Ctrl Pts',(98.812678282655,6.46497204407849,132.160152748165));
#258435=CARTESIAN_POINT('Ctrl Pts',(98.5342306588419,4.63514162304771,126.098035303012));
#258436=CARTESIAN_POINT('Ctrl Pts',(98.2557830350292,-1.45415751030726,
124.36080090516));
#258437=CARTESIAN_POINT('Ctrl Pts',(97.9773354112161,-6.20715693123341,
128.544883097616));
#258438=CARTESIAN_POINT('Ctrl Pts',(97.6988877874034,-5.25608236883021,
134.805314749293));
#258439=CARTESIAN_POINT('Ctrl Pts',(97.4204401635904,0.525075116629235,
137.389065011387));
#258440=CARTESIAN_POINT('Ctrl Pts',(97.1419925397775,5.82371422125203,133.921793616252));
#258441=CARTESIAN_POINT('Ctrl Pts',(96.8635449159648,5.77064446080036,127.589753590393));
#258442=CARTESIAN_POINT('Ctrl Pts',(96.5850972921516,0.414634352527504,
124.211780380221));
#258443=CARTESIAN_POINT('Ctrl Pts',(96.306649668339,-5.32240446970382,126.89206634272));
#258444=CARTESIAN_POINT('Ctrl Pts',(96.0282020445258,-6.16841359819089,
133.1675596176));
#258445=CARTESIAN_POINT('Ctrl Pts',(95.7497544207132,-1.34595197369742,
137.271388460138));
#258446=CARTESIAN_POINT('Ctrl Pts',(95.4713067969001,4.7133737612145,135.432334647225));
#258447=CARTESIAN_POINT('Ctrl Pts',(95.1928591730874,6.44133927067958,129.340398790155));
#258448=CARTESIAN_POINT('Ctrl Pts',(94.9144115492744,2.25002866730758,124.593772333964));
#258449=CARTESIAN_POINT('Ctrl Pts',(94.6359639254615,-4.008948361309,125.554373106298));
#258450=CARTESIAN_POINT('Ctrl Pts',(94.3575163016487,-6.58389769389783,
131.339455925338));
#258451=CARTESIAN_POINT('Ctrl Pts',(94.0790686778357,-3.10856668707799,
136.632812297395));
#258452=CARTESIAN_POINT('Ctrl Pts',(93.8006210540229,3.22338524324122,136.570106311383));
#258453=CARTESIAN_POINT('Ctrl Pts',(93.52217343021,6.59320360614536,131.208961705089));
#258454=CARTESIAN_POINT('Ctrl Pts',(93.2437258063971,3.90418995090443,125.476008465224));
#258455=CARTESIAN_POINT('Ctrl Pts',(92.9652781825842,-2.37258353893516,
124.639550548886));
#258456=CARTESIAN_POINT('Ctrl Pts',(92.6868305587713,-6.46906866364288,
129.468251917951));
#258457=CARTESIAN_POINT('Ctrl Pts',(92.4083829349583,-4.62079571803641,
135.524771909422));
#258458=CARTESIAN_POINT('Ctrl Pts',(92.1299353111456,1.47376275402524,137.24346452859));
#258459=CARTESIAN_POINT('Ctrl Pts',(91.8514876873325,6.21400525245068,133.04493522124));
#258460=CARTESIAN_POINT('Ctrl Pts',(91.5730400635199,5.24388049490719,126.787427311268));
#258461=CARTESIAN_POINT('Ctrl Pts',(91.2945924397067,-0.545114259651984,
124.221284871682));
#258462=CARTESIAN_POINT('Ctrl Pts',(91.016144815894,-5.83317563990314,127.704667441434));
#258463=CARTESIAN_POINT('Ctrl Pts',(90.7376971920811,-5.76083357355547,
134.036516611621));
#258464=CARTESIAN_POINT('Ctrl Pts',(90.4592495682681,-0.394566885476172,
137.398172322869));
#258465=CARTESIAN_POINT('Ctrl Pts',(90.1808019444553,5.33428749469169,134.700437202553));
#258466=CARTESIAN_POINT('Ctrl Pts',(89.9023543206424,6.16119226166949,128.422398034556));
#258467=CARTESIAN_POINT('Ctrl Pts',(89.6239066968295,1.32626233114802,124.333266115003));
#258468=CARTESIAN_POINT('Ctrl Pts',(89.3454590730166,-4.72743789018152,
126.190753912764));
#258469=CARTESIAN_POINT('Ctrl Pts',(89.0670114492037,-6.43685363861442,
132.28792088502));
#258470=CARTESIAN_POINT('Ctrl Pts',(88.7885638253908,-2.23111535094281,
137.021768447433));
#258471=CARTESIAN_POINT('Ctrl Pts',(88.5101162015778,4.02490894820102,136.042121951457));
#258472=CARTESIAN_POINT('Ctrl Pts',(88.2316685777651,6.58223855168135,130.2492286685));
#258473=CARTESIAN_POINT('Ctrl Pts',(87.9532209539521,3.09081248639635,124.966474527032));
#258474=CARTESIAN_POINT('Ctrl Pts',(87.6747733301392,-3.2409192593025,125.048452506173));
#258475=CARTESIAN_POINT('Ctrl Pts',(87.3963257063264,-6.59440453341028,
130.41982884794));
#258476=CARTESIAN_POINT('Ctrl Pts',(87.1178780825135,-3.88795419588509,
136.144571100572));
#258477=CARTESIAN_POINT('Ctrl Pts',(86.8394304587006,2.39133611053674,136.961920803106));
#258478=CARTESIAN_POINT('Ctrl Pts',(86.5609828348878,6.47310535463887,132.120773508667));
#258479=CARTESIAN_POINT('Ctrl Pts',(86.2825352110747,4.60640700660486,126.06990707765));
#258480=CARTESIAN_POINT('Ctrl Pts',(86.004087587262,-1.49335434500641,124.369772158902));
#258481=CARTESIAN_POINT('Ctrl Pts',(85.725639963449,-6.22079600797217,128.582709686544));
#258482=CARTESIAN_POINT('Ctrl Pts',(85.4471923396362,-5.23163004239161,
134.837235886113));
#258483=CARTESIAN_POINT('Ctrl Pts',(85.1687447158232,0.565148352810691,
137.385746730796));
#258484=CARTESIAN_POINT('Ctrl Pts',(84.8902970920103,5.842583020812,133.886285256006));
#258485=CARTESIAN_POINT('Ctrl Pts',(84.6118494681974,5.75096931873532,127.554685598878));
#258486=CARTESIAN_POINT('Ctrl Pts',(84.3334018443846,0.374495763211118,
124.209378528473));
#258487=CARTESIAN_POINT('Ctrl Pts',(84.0549542205716,-5.34612110356891,
126.924537815158));
#258488=CARTESIAN_POINT('Ctrl Pts',(83.7765065967588,-6.15391384870464,
133.205064717373));
#258489=CARTESIAN_POINT('Ctrl Pts',(83.498058972946,-1.30656040228555,137.279461832782));
#258490=CARTESIAN_POINT('Ctrl Pts',(83.2196113491328,4.74145822480973,135.403557257686));
#258491=CARTESIAN_POINT('Ctrl Pts',(82.9411637253203,6.43230837641647,129.301215653567));
#258492=CARTESIAN_POINT('Ctrl Pts',(82.6627161015071,2.21218136583022,124.580190838648));
#258493=CARTESIAN_POINT('Ctrl Pts',(82.3842684776944,-4.04083224888638,
125.578873982957));
#258494=CARTESIAN_POINT('Ctrl Pts',(82.1058208538814,-6.58051843250612,
131.379524065257));
#258495=CARTESIAN_POINT('Ctrl Pts',(81.8273732300686,-3.07302965285007,
136.651627037425));
#258496=CARTESIAN_POINT('Ctrl Pts',(81.5489256062556,3.25842325193051,136.550377824588));
#258497=CARTESIAN_POINT('Ctrl Pts',(81.270477982443,6.59554437101248,131.168819507043));
#258498=CARTESIAN_POINT('Ctrl Pts',(80.9920303586297,3.87168242338918,125.452341274876));
#258499=CARTESIAN_POINT('Ctrl Pts',(80.713582734817,-2.41006652912724,124.654107357959));
#258500=CARTESIAN_POINT('Ctrl Pts',(80.435135111004,-6.47708207967116,129.507655730047));
#258501=CARTESIAN_POINT('Ctrl Pts',(80.1566874871913,-4.59197562204804,
135.552812546207));
#258502=CARTESIAN_POINT('Ctrl Pts',(79.8782398633782,1.51293210175691,137.234374014721));
#258503=CARTESIAN_POINT('Ctrl Pts',(79.5997922395654,6.22752913488936,133.007067294864));
#258504=CARTESIAN_POINT('Ctrl Pts',(79.3213446157525,5.2193311247699,126.755580746775));
#258505=CARTESIAN_POINT('Ctrl Pts',(79.0428969919396,-0.585177210512381,
124.224725106049));
#258506=CARTESIAN_POINT('Ctrl Pts',(78.7644493681267,-5.85193627682986,
127.740233067343));
#258507=CARTESIAN_POINT('Ctrl Pts',(78.4860017443139,-5.74105178772106,
134.071524556339));
#258508=CARTESIAN_POINT('Ctrl Pts',(78.2075541205009,-0.354421171668466,
137.400451995434));
#258509=CARTESIAN_POINT('Ctrl Pts',(77.9291064966881,5.35790518671055,134.667893695246));
#258510=CARTESIAN_POINT('Ctrl Pts',(77.6506588728751,6.14657842672258,128.384937240753));
#258511=CARTESIAN_POINT('Ctrl Pts',(77.3722112490624,1.28684636962602,124.325312674148));
#258512=CARTESIAN_POINT('Ctrl Pts',(77.0937636252493,-4.75543463521666,
126.219616648455));
#258513=CARTESIAN_POINT('Ctrl Pts',(76.8153160014366,-6.42770352619243,
132.327076353179));
#258514=CARTESIAN_POINT('Ctrl Pts',(76.5368683776235,-2.19322688737167,
137.035234685673));
#258515=CARTESIAN_POINT('Ctrl Pts',(76.2584207538107,4.05671811585379,136.017524144697));
#258516=CARTESIAN_POINT('Ctrl Pts',(75.9799731299978,6.57873735230709,130.209170999483));
#258517=CARTESIAN_POINT('Ctrl Pts',(75.7015255061849,3.05521835117689,124.947768036657));
#258518=CARTESIAN_POINT('Ctrl Pts',(75.423077882372,-3.27589705897064,125.068287545233));
#258519=CARTESIAN_POINT('Ctrl Pts',(75.1446302585591,-6.5966231083926,130.459977984534));
#258520=CARTESIAN_POINT('Ctrl Pts',(74.8661826347462,-3.85537478415624,
136.168139239563));
#258521=CARTESIAN_POINT('Ctrl Pts',(74.5877350109334,2.42877462119068,136.94724997613));
#258522=CARTESIAN_POINT('Ctrl Pts',(74.3092873871204,6.48099880189986,132.081345489005));
#258523=CARTESIAN_POINT('Ctrl Pts',(74.0308397633076,4.57750169805637,126.041954289206));
#258524=CARTESIAN_POINT('Ctrl Pts',(73.7523921394947,-1.53249584291112,
124.378981848686));
#258525=CARTESIAN_POINT('Ctrl Pts',(73.4739445156818,-6.23420457082727,
128.620618599563));
#258526=CARTESIAN_POINT('Ctrl Pts',(73.1954968918689,-5.20698385597775,
134.869007583256));
#258527=CARTESIAN_POINT('Ctrl Pts',(72.917049268056,0.605200647212208,137.382184574524));
#258528=CARTESIAN_POINT('Ctrl Pts',(72.6386016442432,5.86123532130951,133.850662693911));
#258529=CARTESIAN_POINT('Ctrl Pts',(72.3601540204302,5.73108107238729,127.519738025268));
#258530=CARTESIAN_POINT('Ctrl Pts',(72.0817063966174,0.334343296816498,
124.207221056211));
#258531=CARTESIAN_POINT('Ctrl Pts',(71.8032587728044,-5.36963963495047,
126.957153055855));
#258532=CARTESIAN_POINT('Ctrl Pts',(71.5248111489915,-6.13918606367764,
133.242480858172));
#258533=CARTESIAN_POINT('Ctrl Pts',(71.2463635251787,-1.26712041579749,
137.287295268168));
#258534=CARTESIAN_POINT('Ctrl Pts',(70.9679159013657,4.76936699192676,135.374609443224));
#258535=CARTESIAN_POINT('Ctrl Pts',(70.689468277553,6.423039130601,129.262088216567));
#258536=CARTESIAN_POINT('Ctrl Pts',(70.4110206537399,2.17425209115883,124.566839982233));
#258537=CARTESIAN_POINT('Ctrl Pts',(70.1325730299272,-4.07256640193864,
125.603568491945));
#258538=CARTESIAN_POINT('Ctrl Pts',(69.8541254061142,-6.57689532758393,
131.419570892283));
#258539=CARTESIAN_POINT('Ctrl Pts',(69.5756777823013,-3.03737874637841,
136.670225104848));
#258540=CARTESIAN_POINT('Ctrl Pts',(69.2972301584884,3.2933405185478,136.530436417012));
#258541=CARTESIAN_POINT('Ctrl Pts',(69.0187825346755,6.5976407355574,131.128663803839));
#258542=CARTESIAN_POINT('Ctrl Pts',(68.7403349108627,3.83903142925813,125.428872405572));
#258543=CARTESIAN_POINT('Ctrl Pts',(68.4618872870498,-2.44746021341752,
124.668892066929));
#258544=CARTESIAN_POINT('Ctrl Pts',(68.1834396632368,-6.48485548504104,
129.547107592018));
#258545=CARTESIAN_POINT('Ctrl Pts',(67.904992039424,-4.56298536871445,135.580677227361));
#258546=CARTESIAN_POINT('Ctrl Pts',(67.6265444156111,1.55204538723279,137.225045234339));
#258547=CARTESIAN_POINT('Ctrl Pts',(67.3480967917982,6.2408222539455,132.969117746385));
#258548=CARTESIAN_POINT('Ctrl Pts',(67.0696491679854,5.19458835039884,126.723884211309));
#258549=CARTESIAN_POINT('Ctrl Pts',(66.7912015441724,-0.625218477415679,
124.228409151229));
#258550=CARTESIAN_POINT('Ctrl Pts',(66.5127539203596,-5.87048006810572,
127.775912235624));
#258551=CARTESIAN_POINT('Ctrl Pts',(66.2343062965465,-5.72105726510147,
134.106411435094));
#258552=CARTESIAN_POINT('Ctrl Pts',(65.9558586727338,-0.314262324654327,
137.402487247406));
#258553=CARTESIAN_POINT('Ctrl Pts',(65.6774110489208,5.3813243395822,134.6352070233));
#258554=CARTESIAN_POINT('Ctrl Pts',(65.398963425108,6.13173682805169,128.347566099575));
#258555=CARTESIAN_POINT('Ctrl Pts',(65.120515801295,1.24738272353907,124.317599316798));
#258556=CARTESIAN_POINT('Ctrl Pts',(64.8420681774823,-4.78325516587229,
126.248649273519));
#258557=CARTESIAN_POINT('Ctrl Pts',(64.5636205536692,-6.41831523285262,
132.366175396547));
#258558=CARTESIAN_POINT('Ctrl Pts',(64.2851729298565,-2.15525715297185,
137.048470036584));
#258559=CARTESIAN_POINT('Ctrl Pts',(64.0067253060435,4.08837696032456,135.992733162246));
#258560=CARTESIAN_POINT('Ctrl Pts',(63.7282776822307,6.57499237540094,130.169135385437));
#258561=CARTESIAN_POINT('Ctrl Pts',(63.4498300584178,3.01951100371835,124.929278564476));
#258562=CARTESIAN_POINT('Ctrl Pts',(63.1713824346048,-3.31075346906837,
125.088335136589));
#258563=CARTESIAN_POINT('Ctrl Pts',(62.892934810792,-6.59859724307971,130.500139882352));
#258564=CARTESIAN_POINT('Ctrl Pts',(62.614487186979,-3.82265251009718,136.191508621766));
#258565=CARTESIAN_POINT('Ctrl Pts',(62.3360395631662,2.46612313270748,136.932351522132));
#258566=CARTESIAN_POINT('Ctrl Pts',(62.0575919393533,6.48865209336687,132.041870150199));
#258567=CARTESIAN_POINT('Ctrl Pts',(61.7791443155403,4.5484267684992,126.014177973478));
#258568=CARTESIAN_POINT('Ctrl Pts',(61.5006966917276,-1.57158055361859,
124.388429633243));
#258569=CARTESIAN_POINT('Ctrl Pts',(61.2222490679146,-6.24738212293903,
128.658608431946));
#258570=CARTESIAN_POINT('Ctrl Pts',(60.9438014441017,-5.18214472286266,
134.900628663412));
#258571=CARTESIAN_POINT('Ctrl Pts',(60.6653538202889,0.645230515680748,
137.378378674564));
#258572=CARTESIAN_POINT('Ctrl Pts',(60.3869061964759,5.87967043157647,133.814927249971));
#258573=CARTESIAN_POINT('Ctrl Pts',(60.108458572663,5.71098045872276,127.484912164554));
#258574=CARTESIAN_POINT('Ctrl Pts',(59.8300109488502,0.294178441208572,
124.205308043382));
#258575=CARTESIAN_POINT('Ctrl Pts',(59.5515633250373,-5.39295919236059,
126.989910856244));
#258576=CARTESIAN_POINT('Ctrl Pts',(59.2731157012244,-6.12423078885343,
133.27980665353));
#258577=CARTESIAN_POINT('Ctrl Pts',(58.9946680774115,-1.2276334756968,137.294888476026));
#258578=CARTESIAN_POINT('Ctrl Pts',(58.7162204535986,4.79709902839574,135.345492276511));
#258579=CARTESIAN_POINT('Ctrl Pts',(58.4377728297857,6.41353187670863,129.223017929039));
#258580=CARTESIAN_POINT('Ctrl Pts',(58.1593252059728,2.13624224877676,124.553720259438));
#258581=CARTESIAN_POINT('Ctrl Pts',(57.8808775821599,-4.10414964454526,
125.628455718198));
#258582=CARTESIAN_POINT('Ctrl Pts',(57.602429958347,-6.57302851338661,131.459594922466));
#258583=CARTESIAN_POINT('Ctrl Pts',(57.3239823345341,-3.00161528872044,
136.688605810505));
#258584=CARTESIAN_POINT('Ctrl Pts',(57.0455347107212,3.32813574922106,136.510282827592));
#258585=CARTESIAN_POINT('Ctrl Pts',(56.7670870869083,6.59949262209846,131.088496083461));
#258586=CARTESIAN_POINT('Ctrl Pts',(56.4886394630955,3.80623817840574,125.405602726962));
#258587=CARTESIAN_POINT('Ctrl Pts',(56.2101918392826,-2.48476320616966,
124.683904127941));
#258588=CARTESIAN_POINT('Ctrl Pts',(55.9317442154696,-6.49238859170611,
129.586606041964));
#258589=CARTESIAN_POINT('Ctrl Pts',(55.6532965916568,-4.53382603227983,
135.608364920346));
#258590=CARTESIAN_POINT('Ctrl Pts',(55.3748489678439,1.59110116109648,137.215478533129));
#258591=CARTESIAN_POINT('Ctrl Pts',(55.096401344031,6.25388411703813,132.931087982032));
#258592=CARTESIAN_POINT('Ctrl Pts',(54.8179537202181,5.1696530886458,126.692338879397));
#258593=CARTESIAN_POINT('Ctrl Pts',(54.5395060964052,-0.665236576618623,
124.23233687071));
#258594=CARTESIAN_POINT('Ctrl Pts',(54.2610584725923,-5.88880632658389,
127.811703624173));
#258595=CARTESIAN_POINT('Ctrl Pts',(53.9826108487795,-5.70085074660091,
134.141175955143));
#258596=CARTESIAN_POINT('Ctrl Pts',(53.7041632249665,-0.274091832533765,
137.40427800337));
#258597=CARTESIAN_POINT('Ctrl Pts',(53.4257156011537,5.40454408550164,134.602378397932));
#258598=CARTESIAN_POINT('Ctrl Pts',(53.1472679773408,6.11666801561766,128.310285995821));
#258599=CARTESIAN_POINT('Ctrl Pts',(52.8688203535278,1.20787285522606,124.310126328773));
#258600=CARTESIAN_POINT('Ctrl Pts',(52.590372729715,-4.81089845124901,126.277850712144));
#258601=CARTESIAN_POINT('Ctrl Pts',(52.3119251059021,-6.40868910648141,
132.405216566294));
#258602=CARTESIAN_POINT('Ctrl Pts',(52.0334774820892,-2.11720755472543,
137.061474009724));
#258603=CARTESIAN_POINT('Ctrl Pts',(51.7550298582764,4.11988430848393,135.967749922743));
#258604=CARTESIAN_POINT('Ctrl Pts',(51.4765822344634,6.57100375973434,130.129123309894));
#258605=CARTESIAN_POINT('Ctrl Pts',(51.1981346106506,2.98369176716867,124.91100679562));
#258606=CARTESIAN_POINT('Ctrl Pts',(50.9196869868376,-3.34548719797895,
125.108594537373));
#258607=CARTESIAN_POINT('Ctrl Pts',(50.6412393630248,-6.60032686431936,
130.540313053181));
#258608=CARTESIAN_POINT('Ctrl Pts',(50.3627917392119,-3.78978858624336,
136.214678381218));
#258609=CARTESIAN_POINT('Ctrl Pts',(50.0843441153989,2.50338026112505,136.917225993175));
#258610=CARTESIAN_POINT('Ctrl Pts',(49.8058964915862,6.49606494544435,132.002348955022));
#258611=CARTESIAN_POINT('Ctrl Pts',(49.5274488677731,4.51918329531533,125.986579159731));
#258612=CARTESIAN_POINT('Ctrl Pts',(49.2490012439603,-1.6106070288309,124.39811516248));
#258613=CARTESIAN_POINT('Ctrl Pts',(48.9705536201474,-6.26032817600901,
128.696677775965));
#258614=CARTESIAN_POINT('Ctrl Pts',(48.6921059963345,-5.15711356346882,
134.932097954848));
#258615=CARTESIAN_POINT('Ctrl Pts',(48.4136583725217,0.685236474895564,
137.374329171949));
#258616=CARTESIAN_POINT('Ctrl Pts',(48.1352107487087,5.89788766849362,133.779080248378));
#258617=CARTESIAN_POINT('Ctrl Pts',(47.8567631248959,5.69066822257687,127.450209307224));
#258618=CARTESIAN_POINT('Ctrl Pts',(47.578315501083,0.254002684709825,124.203639560873));
#258619=CARTESIAN_POINT('Ctrl Pts',(47.29986787727,-5.41607891168467,127.022810002472));
#258620=CARTESIAN_POINT('Ctrl Pts',(47.0214202534572,-6.10904857840509,
133.317040720324));
#258621=CARTESIAN_POINT('Ctrl Pts',(46.7429726296443,-1.18810104518584,
137.302241174989));
#258622=CARTESIAN_POINT('Ctrl Pts',(46.4645250058313,4.82465330659632,135.316206836494));
#258623=CARTESIAN_POINT('Ctrl Pts',(46.1860773820186,6.40378696703385,129.184006238746));
#258624=CARTESIAN_POINT('Ctrl Pts',(45.9076297582056,2.09815324715241,124.54083215642));
#258625=CARTESIAN_POINT('Ctrl Pts',(45.6291821343927,-4.13558080637756,
125.653534739511));
#258626=CARTESIAN_POINT('Ctrl Pts',(45.3507345105798,-6.56891813320061,
131.499594672701));
#258627=CARTESIAN_POINT('Ctrl Pts',(45.072286886767,-2.96574060510383,136.706768473292));
#258628=CARTESIAN_POINT('Ctrl Pts',(44.793839262954,3.36280765460034,136.489917803126));
#258629=CARTESIAN_POINT('Ctrl Pts',(44.5153916391412,6.60109996201359,131.048317834339));
#258630=CARTESIAN_POINT('Ctrl Pts',(44.2369440153282,3.77330388599763,125.38253310131));
#258631=CARTESIAN_POINT('Ctrl Pts',(43.9584963915154,-2.52197412510756,
124.699142984721));
#258632=CARTESIAN_POINT('Ctrl Pts',(43.6800487677024,-6.49968112052436,
129.626149616253));
#258633=CARTESIAN_POINT('Ctrl Pts',(43.4016011438896,-4.50449869325427,
135.635874599185));
#258634=CARTESIAN_POINT('Ctrl Pts',(43.1231535200766,1.6300979761215,137.205674265588));
#258635=CARTESIAN_POINT('Ctrl Pts',(42.8447058962639,6.26671424015497,132.892979411015));
#258636=CARTESIAN_POINT('Ctrl Pts',(42.5662582724509,5.14452626349642,126.660945919963));
#258637=CARTESIAN_POINT('Ctrl Pts',(42.287810648638,-0.705230025235587,
124.236508118946));
#258638=CARTESIAN_POINT('Ctrl Pts',(42.0093630248251,-5.90691437317801,
127.847605906729));
#258639=CARTESIAN_POINT('Ctrl Pts',(41.7309154010123,-5.68043298097947,
134.175816828272));
#258640=CARTESIAN_POINT('Ctrl Pts',(41.4524677771993,-0.233911183839542,
137.405824196969));
#258641=CARTESIAN_POINT('Ctrl Pts',(41.1740201533865,5.42756356405245,134.569409035618));
#258642=CARTESIAN_POINT('Ctrl Pts',(40.8955725295735,6.10137254780096,128.273098310918));
#258643=CARTESIAN_POINT('Ctrl Pts',(40.6171249057607,1.1683182287399,124.302893986988));
#258644=CARTESIAN_POINT('Ctrl Pts',(40.3386772819477,-4.83836346701448,
126.307219882257));
#258645=CARTESIAN_POINT('Ctrl Pts',(40.060229658135,-6.39882550377857,132.444198415735));
#258646=CARTESIAN_POINT('Ctrl Pts',(39.781782034322,-2.07907950257448,137.074246123225));
#258647=CARTESIAN_POINT('Ctrl Pts',(39.5033344105091,4.15123899281517,135.94257535195));
#258648=CARTESIAN_POINT('Ctrl Pts',(39.2248867866962,6.56677165310695,130.089136255519));
#258649=CARTESIAN_POINT('Ctrl Pts',(38.9464391628834,2.94776196882331,124.892953407157));
#258650=CARTESIAN_POINT('Ctrl Pts',(38.6679915390704,-3.38009695863112,
125.129064996863));
#258651=CARTESIAN_POINT('Ctrl Pts',(38.3895439152575,-6.6018119080198,130.58049600839));
#258652=CARTESIAN_POINT('Ctrl Pts',(38.1110962914447,-3.75678423037978,
136.237647659355));
#258653=CARTESIAN_POINT('Ctrl Pts',(37.8326486676317,2.54054462586645,136.901873949744));
#258654=CARTESIAN_POINT('Ctrl Pts',(37.5542010438189,6.50323708344635,131.962783367948));
#258655=CARTESIAN_POINT('Ctrl Pts',(37.275753420006,4.48977236213255,125.959158870647));
#258656=CARTESIAN_POINT('Ctrl Pts',(36.9973057961931,-1.64957382240749,
124.4080380775));
#258657=CARTESIAN_POINT('Ctrl Pts',(36.7188581723802,-6.27304225031618,
128.734825220947));
#258658=CARTESIAN_POINT('Ctrl Pts',(36.4404105485673,-5.13189130533538,
134.96341429146));
#258659=CARTESIAN_POINT('Ctrl Pts',(36.1619629247544,0.725217042420823,
137.370036216732));
#258660=CARTESIAN_POINT('Ctrl Pts',(35.8835153009416,5.91588635701427,133.743123017455));
#258661=CARTESIAN_POINT('Ctrl Pts',(35.6050676771286,5.67014511662727,127.415630739204));
#258662=CARTESIAN_POINT('Ctrl Pts',(35.3266200533158,0.213817516048174,
124.202215670509));
#258663=CARTESIAN_POINT('Ctrl Pts',(35.0481724295028,-5.43899793621292,
127.055849275448));
#258664=CARTESIAN_POINT('Ctrl Pts',(34.76972480569,-6.09363999491508,133.354181678833));
#258665=CARTESIAN_POINT('Ctrl Pts',(34.4912771818771,-1.14852458915375,
137.309353092597));
#258666=CARTESIAN_POINT('Ctrl Pts',(34.2128295580642,4.85202880549439,135.286754208357));
#258667=CARTESIAN_POINT('Ctrl Pts',(33.9343819342512,6.393804762678,129.145054591279));
#258668=CARTESIAN_POINT('Ctrl Pts',(33.6559343104384,2.05998649768791,124.528176150753));
#258669=CARTESIAN_POINT('Ctrl Pts',(33.3774866866255,-4.16685872274224,
125.678804626571));
#258670=CARTESIAN_POINT('Ctrl Pts',(33.0990390628127,-6.56456433933747,
131.539568660782));
#258671=CARTESIAN_POINT('Ctrl Pts',(32.8205914389997,-2.92975602487846,
136.724712420187));
#258672=CARTESIAN_POINT('Ctrl Pts',(32.5421438151868,3.39735494990529,136.469342098247));
#258673=CARTESIAN_POINT('Ctrl Pts',(32.263696191374,6.60246269574222,131.008130545292));
#258674=CARTESIAN_POINT('Ctrl Pts',(31.985248567561,3.74022977242616,125.359664383471));
#258675=CARTESIAN_POINT('Ctrl Pts',(31.7068009437482,-2.55909159136699,
124.714608072585));
#258676=CARTESIAN_POINT('Ctrl Pts',(31.4283533199352,-6.50673280126843,
129.665736849585));
#258677=CARTESIAN_POINT('Ctrl Pts',(31.1499056961224,-4.47500443837311,
135.663205244496));
#258678=CARTESIAN_POINT('Ctrl Pts',(30.8714580723094,1.66903438726656,137.195632795014));
#258679=CARTESIAN_POINT('Ctrl Pts',(30.5930104484966,6.27931214787105,132.854793445461));
#258680=CARTESIAN_POINT('Ctrl Pts',(30.3145628246837,5.11920880603445,126.629706496284));
#258681=CARTESIAN_POINT('Ctrl Pts',(30.0361152008708,-0.745197341294603,
124.240922741373));
#258682=CARTESIAN_POINT('Ctrl Pts',(29.7576675770579,-5.9248035368878,127.883617752917));
#258683=CARTESIAN_POINT('Ctrl Pts',(29.4792199532451,-5.65980472482494,
134.210332770852));
#258684=CARTESIAN_POINT('Ctrl Pts',(29.2007723294321,-0.193721867480399,
137.407125770907));
#258685=CARTESIAN_POINT('Ctrl Pts',(28.9223247056193,5.45038192223944,134.536300158051));
#258686=CARTESIAN_POINT('Ctrl Pts',(28.6438770818064,6.08585099138068,128.236004422871));
#258687=CARTESIAN_POINT('Ctrl Pts',(28.3654294579935,1.12872030979243,124.29590255944));
#258688=CARTESIAN_POINT('Ctrl Pts',(28.0869818341806,-4.86564919544231,
126.336755695574));
#258689=CARTESIAN_POINT('Ctrl Pts',(27.8085342103677,-6.38872479024353,
132.483119500384));
#258690=CARTESIAN_POINT('Ctrl Pts',(27.5300865865548,-2.04087440936798,
137.086785903815));
#258691=CARTESIAN_POINT('Ctrl Pts',(27.2516389627419,4.18243985145892,135.91721038272));
#258692=CARTESIAN_POINT('Ctrl Pts',(26.973191338929,6.56229621234102,130.049175704046));
#258693=CARTESIAN_POINT('Ctrl Pts',(26.6947437151162,2.91172294007416,124.875119068062));
#258694=CARTESIAN_POINT('Ctrl Pts',(26.4162960913032,-3.41458146854746,
125.149745756519));
#258695=CARTESIAN_POINT('Ctrl Pts',(26.1378484674903,-6.60305231915217,
130.620687258984));
#258696=CARTESIAN_POINT('Ctrl Pts',(25.8594008436774,-3.72364066549499,
136.260415605043));
#258697=CARTESIAN_POINT('Ctrl Pts',(25.5809532198646,2.57761484979243,136.886295960714));
#258698=CARTESIAN_POINT('Ctrl Pts',(25.3025055960517,6.51016824160669,131.92317485509));
#258699=CARTESIAN_POINT('Ctrl Pts',(25.0240579722387,4.46019505878377,125.931918122295));
#258700=CARTESIAN_POINT('Ctrl Pts',(24.7456103484259,-1.68847949041943,
124.418198010604));
#258701=CARTESIAN_POINT('Ctrl Pts',(24.467162724613,-6.28552387473587,128.773049353324));
#258702=CARTESIAN_POINT('Ctrl Pts',(24.1887151008001,-5.10647888308236,
134.994576512808));
#258703=CARTESIAN_POINT('Ctrl Pts',(23.9102674769872,0.765170736761864,
137.365499967992));
#258704=CARTESIAN_POINT('Ctrl Pts',(23.6318198531744,5.93366583019039,133.707056889611));
#258705=CARTESIAN_POINT('Ctrl Pts',(23.3533722293614,5.64941190136517,127.381177741815));
#258706=CARTESIAN_POINT('Ctrl Pts',(23.0749246055485,0.173624424299845,
124.201036425055));
#258707=CARTESIAN_POINT('Ctrl Pts',(22.7964769817356,-5.46171541667246,
127.08902745089));
#258708=CARTESIAN_POINT('Ctrl Pts',(22.5180293579228,-6.07800560935413,
133.391228152785));
#258709=CARTESIAN_POINT('Ctrl Pts',(22.2395817341099,-1.10890557412062,
137.316223965318));
#258710=CARTESIAN_POINT('Ctrl Pts',(21.9611341102969,4.87922451068073,135.257135483476));
#258711=CARTESIAN_POINT('Ctrl Pts',(21.6826864864842,6.38358563353538,129.106164430008));
#258712=CARTESIAN_POINT('Ctrl Pts',(21.4042388626712,2.02174341466617,124.515752711409));
#258713=CARTESIAN_POINT('Ctrl Pts',(21.1257912388583,-4.19798223462457,
125.704264442993));
#258714=CARTESIAN_POINT('Ctrl Pts',(20.8473436150454,-6.55996729312864,
131.579515405459));
#258715=CARTESIAN_POINT('Ctrl Pts',(20.5688959912325,-2.89366288146616,
136.742436986267));
#258716=CARTESIAN_POINT('Ctrl Pts',(20.2904483674196,3.43177635497322,136.448556475397));
#258717=CARTESIAN_POINT('Ctrl Pts',(20.0120007436067,6.60358077278748,130.967935705476));
#258718=CARTESIAN_POINT('Ctrl Pts',(19.7335531197938,3.70701706326526,125.336997420853));
#258719=CARTESIAN_POINT('Ctrl Pts',(19.455105495981,-2.59611422954622,124.730298818468));
#258720=CARTESIAN_POINT('Ctrl Pts',(19.176657872168,-6.51354337263571,129.705366275038));
#258721=CARTESIAN_POINT('Ctrl Pts',(18.8982102483552,-4.4453443605568,135.690355843533));
#258722=CARTESIAN_POINT('Ctrl Pts',(18.6197626245423,1.70790895172861,137.1853544935));
#258723=CARTESIAN_POINT('Ctrl Pts',(18.3413150007294,6.29167737336628,132.816531500364));
#258724=CARTESIAN_POINT('Ctrl Pts',(18.0628673769165,5.09370165440758,126.598621765949));
#258725=CARTESIAN_POINT('Ctrl Pts',(17.7844197531036,-0.785137043792105,
124.245580574404));
#258726=CARTESIAN_POINT('Ctrl Pts',(17.5059721292907,-5.94247315482366,
127.919737828307));
#258727=CARTESIAN_POINT('Ctrl Pts',(17.2275245054778,-5.63896674252494,
134.244722503881));
#258728=CARTESIAN_POINT('Ctrl Pts',(16.949076881665,-0.15352537268619,137.408182676953));
#258729=CARTESIAN_POINT('Ctrl Pts',(16.6706292578521,5.47299831451989,134.503052992091));
#258730=CARTESIAN_POINT('Ctrl Pts',(16.3921816340391,6.07010392151387,128.199005706208));
#258731=CARTESIAN_POINT('Ctrl Pts',(16.1137340102263,1.08908056569879,124.289152305198));
#258732=CARTESIAN_POINT('Ctrl Pts',(15.8352863864134,-4.89275462544986,
126.366457057635));
#258733=CARTESIAN_POINT('Ctrl Pts',(15.5568387626005,-6.37838734016194,
132.521978378005));
#258734=CARTESIAN_POINT('Ctrl Pts',(15.2783911387876,-2.00259369080969,
137.099092886824));
#258735=CARTESIAN_POINT('Ctrl Pts',(14.9999435149747,4.21348572825588,135.891655954962));
#258736=CARTESIAN_POINT('Ctrl Pts',(14.7214958911618,6.55757760327567,130.009243136227));
#258737=CARTESIAN_POINT('Ctrl Pts',(14.4430482673489,2.87557601636067,124.857504439193));
#258738=CARTESIAN_POINT('Ctrl Pts',(14.164600643536,-3.44893944989177,125.170636050008));
#258739=CARTESIAN_POINT('Ctrl Pts',(13.8861530197231,-6.60404805175259,
130.660885315664));
#258740=CARTESIAN_POINT('Ctrl Pts',(13.6077053959103,-3.69035911973598,
136.282981374608));
#258741=CARTESIAN_POINT('Ctrl Pts',(13.3292577720973,2.61458955925225,136.870492603333));
#258742=CARTESIAN_POINT('Ctrl Pts',(13.0508101482845,6.5168581630887,131.883524884162));
#258743=CARTESIAN_POINT('Ctrl Pts',(12.7723625244716,4.43045248126686,125.904857924092));
#258744=CARTESIAN_POINT('Ctrl Pts',(12.4939149006587,-1.72732259120293,
124.428594585312));
#258745=CARTESIAN_POINT('Ctrl Pts',(12.2154672768458,-6.29777258675688,
128.811348756686));
#258746=CARTESIAN_POINT('Ctrl Pts',(11.9370196530329,-5.08087723837641,
135.025583464166));
#258747=CARTESIAN_POINT('Ctrl Pts',(11.65857202922,0.805096077419857,137.36072059382));
#258748=CARTESIAN_POINT('Ctrl Pts',(11.3801244054071,5.95122542919731,133.670883201288));
#258749=CARTESIAN_POINT('Ctrl Pts',(11.1016767815943,5.62846934506734,127.346851591727));
#258750=CARTESIAN_POINT('Ctrl Pts',(10.8232291577813,0.13342489883439,124.200101868207));
#258751=CARTESIAN_POINT('Ctrl Pts',(10.5447815339684,-5.4842305112587,127.12234329937));
#258752=CARTESIAN_POINT('Ctrl Pts',(10.2663339101556,-6.06214600106014,
133.428178769409));
#258753=CARTESIAN_POINT('Ctrl Pts',(9.98788628634267,-1.06924546818365,
137.322853538546));
#258754=CARTESIAN_POINT('Ctrl Pts',(9.70943866252976,4.90623941440849,135.227351759386));
#258755=CARTESIAN_POINT('Ctrl Pts',(9.43099103871685,6.37312995827954,129.067337196021));
#258756=CARTESIAN_POINT('Ctrl Pts',(9.15254341490403,1.98342541519871,124.503562298745));
#258757=CARTESIAN_POINT('Ctrl Pts',(8.87409579109107,-4.22895018873139,
125.729913245354));
#258758=CARTESIAN_POINT('Ctrl Pts',(8.59564816727821,-6.55512716491932,
131.61943342649));
#258759=CARTESIAN_POINT('Ctrl Pts',(8.31720054346528,-2.85746251231165,
136.759941514744));
#258760=CARTESIAN_POINT('Ctrl Pts',(8.03875291965246,3.46607059430627,136.427561704794));
#258761=CARTESIAN_POINT('Ctrl Pts',(7.76030529583951,6.60445415171875,130.927734804324));
#258762=CARTESIAN_POINT('Ctrl Pts',(7.48185767202662,3.67366698922382,125.314533053388));
#258763=CARTESIAN_POINT('Ctrl Pts',(7.20341004821377,-2.63304066775796,
124.746214640945));
#258764=CARTESIAN_POINT('Ctrl Pts',(6.92496242440086,-6.52011258225796,
129.745036424131));
#258765=CARTESIAN_POINT('Ctrl Pts',(6.64651480058794,-4.41551955887045,
135.71732539022));
#258766=CARTESIAN_POINT('Ctrl Pts',(6.36806717677509,1.74672022899638,137.174839741911));
#258767=CARTESIAN_POINT('Ctrl Pts',(6.08961955296221,6.30380945844269,132.778194993536));
#258768=CARTESIAN_POINT('Ctrl Pts',(5.81117192914928,5.06800575379271,126.567692880813));
#258769=CARTESIAN_POINT('Ctrl Pts',(5.53272430533639,-0.825047652747706,
124.250481445441));
#258770=CARTESIAN_POINT('Ctrl Pts',(5.25427668152353,-5.95992257223146,
127.955964794454));
#258771=CARTESIAN_POINT('Ctrl Pts',(4.97582905771062,-5.61791980623858,
134.278984753035));
#258772=CARTESIAN_POINT('Ctrl Pts',(4.69738143389771,-0.113323188952861,
137.408994875945));
#258773=CARTESIAN_POINT('Ctrl Pts',(4.41893381008486,5.49541190283514,134.469668769726));
#258774=CARTESIAN_POINT('Ctrl Pts',(4.14048618627195,6.05413192171396,128.162103531929));
#258775=CARTESIAN_POINT('Ctrl Pts',(3.86203856245905,1.0494004653243,124.282643474398));
#258776=CARTESIAN_POINT('Ctrl Pts',(3.58359093864613,-4.91967875263547,
126.396322867843));
#258777=CARTESIAN_POINT('Ctrl Pts',(3.30514331483329,-6.36781353659179,
132.560773608667));
#258778=CARTESIAN_POINT('Ctrl Pts',(3.02669569102039,-1.96423876540577,
137.111166616214));
#258779=CARTESIAN_POINT('Ctrl Pts',(2.74824806720748,4.24437547278969,135.865913015604));
#258780=CARTESIAN_POINT('Ctrl Pts',(2.46980044339459,6.55261600076067,129.969340031779));
#258781=CARTESIAN_POINT('Ctrl Pts',(2.19135281958173,2.83932253712042,124.840110173268));
#258782=CARTESIAN_POINT('Ctrl Pts',(1.91290519576881,-3.48316962951642,
125.191735103234));
#258783=CARTESIAN_POINT('Ctrl Pts',(1.6344575719559,-6.60479906892382,130.701088688872));
#258784=CARTESIAN_POINT('Ctrl Pts',(1.35600994814304,-3.65694082636265,
136.305344131865));
#258785=CARTESIAN_POINT('Ctrl Pts',(1.07756232433016,2.65146738413444,136.854464463202));
#258786=CARTESIAN_POINT('Ctrl Pts',(0.799114700517227,6.52330659999492,
131.843834924404));
#258787=CARTESIAN_POINT('Ctrl Pts',(0.520667076704378,4.40054573170394,
125.877979278764));
#258788=CARTESIAN_POINT('Ctrl Pts',(0.242219452891471,-1.76610168541259,
124.439227416375));
#258789=CARTESIAN_POINT('Ctrl Pts',(-0.03622817092143,-6.30978793249869,
128.849722011837));
#258790=CARTESIAN_POINT('Ctrl Pts',(-0.314675794734322,-5.05508731989592,
135.056433996558));
#258791=CARTESIAN_POINT('Ctrl Pts',(-0.593123418547181,0.844991584946641,
137.355698271319));
#258792=CARTESIAN_POINT('Ctrl Pts',(-0.871571042360099,5.96856450335716,
133.634603292916));
#258793=CARTESIAN_POINT('Ctrl Pts',(-1.15001866617301,5.60731822376822,
127.312653560908));
#258794=CARTESIAN_POINT('Ctrl Pts',(-1.42846628998586,0.0932204292604712,
124.199412034595));
#258795=CARTESIAN_POINT('Ctrl Pts',(-1.70691391379876,-5.50654238566651,
127.155795586355));
#258796=CARTESIAN_POINT('Ctrl Pts',(-1.98536153761166,-6.04606175771675,
133.465032159487));
#258797=CARTESIAN_POINT('Ctrl Pts',(-2.26380916142456,-1.02954574096264,
137.329241566624));
#258798=CARTESIAN_POINT('Ctrl Pts',(-2.5422567852374,4.9330725156305,135.197404139731));
#258799=CARTESIAN_POINT('Ctrl Pts',(-2.82070440905033,6.36243812434939,
129.028574328076));
#258800=CARTESIAN_POINT('Ctrl Pts',(-3.09915203286324,1.94503391917308,
124.491605364478));
#258801=CARTESIAN_POINT('Ctrl Pts',(-3.3775996566761,-4.25976143753379,
125.755750083229));
#258802=CARTESIAN_POINT('Ctrl Pts',(-3.65604728048899,-6.55004413406227,
131.659321244699));
#258803=CARTESIAN_POINT('Ctrl Pts',(-3.9344949043019,-2.82115625883292,
136.777225356981));
#258804=CARTESIAN_POINT('Ctrl Pts',(-4.2129425281148,3.50023639711881,136.406358564405));
#258805=CARTESIAN_POINT('Ctrl Pts',(-4.49139015192765,6.60508280017262,
130.887529331496));
#258806=CARTESIAN_POINT('Ctrl Pts',(-4.76983777574057,3.64018078610111,
125.292272113504));
#258807=CARTESIAN_POINT('Ctrl Pts',(-5.04828539955349,-2.66986953767946,
124.762354950249));
#258808=CARTESIAN_POINT('Ctrl Pts',(-5.32673302336633,-6.52644018671072,
129.784745826872));
#258809=CARTESIAN_POINT('Ctrl Pts',(-5.60518064717923,-4.38553113848304,
135.74411288519));
#258810=CARTESIAN_POINT('Ctrl Pts',(-5.88362827099213,1.7854667809037,137.164088929876));
#258811=CARTESIAN_POINT('Ctrl Pts',(-6.16207589480503,6.31570795354138,
132.739785345549));
#258812=CARTESIAN_POINT('Ctrl Pts',(-6.44052351861788,5.04212205636089,
126.536920986959));
#258813=CARTESIAN_POINT('Ctrl Pts',(-6.71897114243081,-0.864927689259141,
124.255625172881));
#258814=CARTESIAN_POINT('Ctrl Pts',(-6.99741876624371,-5.97715114251656,
127.992297308957));
#258815=CARTESIAN_POINT('Ctrl Pts',(-7.27586639005655,-5.59666469586782,
134.313118248714));
#258816=CARTESIAN_POINT('Ctrl Pts',(-7.55431401386947,-0.0731168059870705,
137.409562337785));
#258817=CARTESIAN_POINT('Ctrl Pts',(-7.83276163768236,5.51762185664139,
134.436148728019));
#258818=CARTESIAN_POINT('Ctrl Pts',(-8.11120926149529,6.03793558382929,
128.125299267457));
#258819=CARTESIAN_POINT('Ctrl Pts',(-8.38965688530811,1.00968147902963,
124.276376308223));
#258820=CARTESIAN_POINT('Ctrl Pts',(-8.66810450912106,-4.94642057931569,
126.426352019512));
#258821=CARTESIAN_POINT('Ctrl Pts',(-8.94655213293394,-6.3570037713493,
132.599503754801));
#258822=CARTESIAN_POINT('Ctrl Pts',(-9.22499975674682,-1.92581105441205,
137.123006644589));
#258823=CARTESIAN_POINT('Ctrl Pts',(-9.50344738055969,4.27510794042973,
135.839982518561));
#258824=CARTESIAN_POINT('Ctrl Pts',(-9.78189500437264,6.54741158865002,
129.929467869325));
#258825=CARTESIAN_POINT('Ctrl Pts',(-10.0603426281855,2.80296384573913,
124.822936914835));
#258826=CARTESIAN_POINT('Ctrl Pts',(-10.3387902519984,-3.51727073900952,
125.213042134361));
#258827=CARTESIAN_POINT('Ctrl Pts',(-10.6172378758113,-6.60530534283666,
130.74129588886));
#258828=CARTESIAN_POINT('Ctrl Pts',(-10.8956854996242,-3.62338702370218,
136.327503048155));
#258829=CARTESIAN_POINT('Ctrl Pts',(-11.174133123437,2.68824695791763,136.838212134247));
#258830=CARTESIAN_POINT('Ctrl Pts',(-11.4525807472499,6.52951331337615,
131.804106446543));
#258831=CARTESIAN_POINT('Ctrl Pts',(-11.7310283710628,4.37047591830066,
125.851283182307));
#258832=CARTESIAN_POINT('Ctrl Pts',(-12.0094759948757,-1.80481533607482,
124.450096109789));
#258833=CARTESIAN_POINT('Ctrl Pts',(-12.2879236186886,-6.32156946672825,
128.88816769684));
#258834=CARTESIAN_POINT('Ctrl Pts',(-12.5663712425015,-5.02911008329581,
135.087126966809));
#258835=CARTESIAN_POINT('Ctrl Pts',(-12.8448188663144,0.884855780999501,
137.350433186591));
#258836=CARTESIAN_POINT('Ctrl Pts',(-13.1232664901273,5.98568241016441,
133.598218508862));
#258837=CARTESIAN_POINT('Ctrl Pts',(-13.4017141139402,5.58595932123025,
127.278584916578));
#258838=CARTESIAN_POINT('Ctrl Pts',(-13.6801617377531,0.0530125053692662,
124.198966949783));
#258839=CARTESIAN_POINT('Ctrl Pts',(-13.958609361566,-5.5286502131212,127.189383072259));
#258840=CARTESIAN_POINT('Ctrl Pts',(-14.2370569853788,-6.02975347533148,
133.501786957402));
#258841=CARTESIAN_POINT('Ctrl Pts',(-14.5155046091917,-0.989807863545592,
137.335387812837));
#258842=CARTESIAN_POINT('Ctrl Pts',(-14.7939522330047,4.95972282003631,
135.167293734234));
#258843=CARTESIAN_POINT('Ctrl Pts',(-15.0723998568175,6.35151052793477,
128.989877262545));
#258844=CARTESIAN_POINT('Ctrl Pts',(-15.3508474806304,1.9065703492003,124.479882351679));
#258845=CARTESIAN_POINT('Ctrl Pts',(-15.6292951044433,-4.29041483930959,
125.781773999224));
#258846=CARTESIAN_POINT('Ctrl Pts',(-15.9077427282562,-6.54471838891106,
131.699177382027));
#258847=CARTESIAN_POINT('Ctrl Pts',(-16.186190352069,-2.78474546637155,
136.794287872519));
#258848=CARTESIAN_POINT('Ctrl Pts',(-16.464637975882,3.53427249738445,136.384947839923));
#258849=CARTESIAN_POINT('Ctrl Pts',(-16.7430855996949,6.60546669485434,
130.847320776822));
#258850=CARTESIAN_POINT('Ctrl Pts',(-17.0215332235078,3.6065596947407,125.270215426085));
#258851=CARTESIAN_POINT('Ctrl Pts',(-17.2999808473206,-2.7065994746034,
124.778719148295));
#258852=CARTESIAN_POINT('Ctrl Pts',(-17.5784284711336,-6.53252595152224,
129.824493011814));
#258853=CARTESIAN_POINT('Ctrl Pts',(-17.8568760949464,-4.35538021062653,
135.770717335825));
#258854=CARTESIAN_POINT('Ctrl Pts',(-18.1353237187593,1.82414717168286,
137.153102455769));
#258855=CARTESIAN_POINT('Ctrl Pts',(-18.4137713425722,6.32737241775927,
132.701303979686));
#258856=CARTESIAN_POINT('Ctrl Pts',(-18.6922189663851,5.01605152124203,
126.506307224649));
#258857=CARTESIAN_POINT('Ctrl Pts',(-18.9706665901979,-0.904775675556959,
124.261011566121));
#258858=CARTESIAN_POINT('Ctrl Pts',(-19.2491142140109,-5.99415822726801,
128.028734025499));
#258859=CARTESIAN_POINT('Ctrl Pts',(-19.5275618378238,-5.57520219902858,
134.347121726088));
#258860=CARTESIAN_POINT('Ctrl Pts',(-19.8060094616367,-0.0329077136511566,
137.409885041447));
#258861=CARTESIAN_POINT('Ctrl Pts',(-20.0844570854496,5.53962735294063,
134.402494109067));
#258862=CARTESIAN_POINT('Ctrl Pts',(-20.3629047092624,6.02151550802112,
128.08859427659));
#258863=CARTESIAN_POINT('Ctrl Pts',(-20.6413523330754,0.969925078616457,
124.270351038909));
#258864=CARTESIAN_POINT('Ctrl Pts',(-20.9197999568882,-4.9729791145623,
126.456543399899));
#258865=CARTESIAN_POINT('Ctrl Pts',(-21.1982475807011,-6.34595844499429,
132.638167381246));
#258866=CARTESIAN_POINT('Ctrl Pts',(-21.476695204514,-1.88731198178147,
137.134612533211));
#258867=CARTESIAN_POINT('Ctrl Pts',(-21.7551428283269,4.30568199237261,
135.813865424697));
#258868=CARTESIAN_POINT('Ctrl Pts',(-22.0335904521398,6.54196455979519,
129.889628126344));
#258869=CARTESIAN_POINT('Ctrl Pts',(-22.3120380759527,2.766501289502,124.805985300257));
#258870=CARTESIAN_POINT('Ctrl Pts',(-22.5904856997656,-3.5512415147419,
125.234556353852));
#258871=CARTESIAN_POINT('Ctrl Pts',(-22.8689333235784,-6.60556685473091,
130.781505425734));
#258872=CARTESIAN_POINT('Ctrl Pts',(-23.1473809473914,-3.58969895510304,
136.349457302372));
#258873=CARTESIAN_POINT('Ctrl Pts',(-23.4258285712042,2.7249269177212,136.821736218705));
#258874=CARTESIAN_POINT('Ctrl Pts',(-23.7042761950172,6.53547807324032,
131.764340922733));
#258875=CARTESIAN_POINT('Ctrl Pts',(-23.98272381883,4.34024415530499,125.824770623956));
#258876=CARTESIAN_POINT('Ctrl Pts',(-24.2611714426429,-1.84346210864104,
124.461200262812));
#258877=CARTESIAN_POINT('Ctrl Pts',(-24.5396190664558,-6.33311675287646,
128.926684387076));
#258878=CARTESIAN_POINT('Ctrl Pts',(-24.8180666902687,-5.00294649117208,
135.117661237576));
#258879=CARTESIAN_POINT('Ctrl Pts',(-25.0965143140816,0.924687188395989,
137.344925534737));
#258880=CARTESIAN_POINT('Ctrl Pts',(-25.3749619378945,6.00257851530871,
133.561730197376));
#258881=CARTESIAN_POINT('Ctrl Pts',(-25.6534095617074,5.56439342891538,
127.244646921163));
#258882=CARTESIAN_POINT('Ctrl Pts',(-25.9318571855203,0.0128026170801758,
124.198766630261));
#258883=CARTESIAN_POINT('Ctrl Pts',(-26.2103048093331,-5.5505531744091,
127.223104512485));
#258884=CARTESIAN_POINT('Ctrl Pts',(-26.4887524331461,-6.01322175821376,
133.538441801192));
#258885=CARTESIAN_POINT('Ctrl Pts',(-26.7672000569589,-0.950033308434149,
137.341292049436));
#258886=CARTESIAN_POINT('Ctrl Pts',(-27.0456476807718,4.98618934008908,
135.137021658645));
#258887=CARTESIAN_POINT('Ctrl Pts',(-27.3240953045847,6.34034757396176,
128.951247433362));
#258888=CARTESIAN_POINT('Ctrl Pts',(-27.6025429283976,1.86803613056208,
124.468393694749));
#258889=CARTESIAN_POINT('Ctrl Pts',(-27.8809905522105,-4.32090925818572,
125.807984029013));
#258890=CARTESIAN_POINT('Ctrl Pts',(-28.1594381760234,-6.53915012681315,
131.739000361591));
#258891=CARTESIAN_POINT('Ctrl Pts',(-28.4378857998363,-2.74823148414282,
136.811128429099));
#258892=CARTESIAN_POINT('Ctrl Pts',(-28.7163334236492,3.56817763388296,
136.36333032473));
#258893=CARTESIAN_POINT('Ctrl Pts',(-28.994781047462,6.60560582153853,130.807110630244));
#258894=CARTESIAN_POINT('Ctrl Pts',(-29.273228671275,3.5728049609845,125.248363808452));
#258895=CARTESIAN_POINT('Ctrl Pts',(-29.5516762950878,-2.74322911748845,
124.795306628702));
#258896=CARTESIAN_POINT('Ctrl Pts',(-29.8301239189007,-6.53836965118233,
129.86427650611));
#258897=CARTESIAN_POINT('Ctrl Pts',(-30.1085715427137,-4.32506789255462,
135.797137756284));
#258898=CARTESIAN_POINT('Ctrl Pts',(-30.3870191665265,1.862759968018,137.141880726698));
#258899=CARTESIAN_POINT('Ctrl Pts',(-30.6654667903394,6.33880241886542,
132.662752321889));
#258900=CARTESIAN_POINT('Ctrl Pts',(-30.9439144141524,4.98979511448915,
126.475852728289));
#258901=CARTESIAN_POINT('Ctrl Pts',(-31.2223620379652,-0.944590135059391,
124.266640425567));
#258902=CARTESIAN_POINT('Ctrl Pts',(-31.5008096617781,-6.01094319628198,
128.065273593905));
#258903=CARTESIAN_POINT('Ctrl Pts',(-31.7792572855909,-5.55353311102158,
134.380993925146));
#258904=CARTESIAN_POINT('Ctrl Pts',(-32.0577049094039,0.00730259809219468,
137.409962974972));
#258905=CARTESIAN_POINT('Ctrl Pts',(-32.3361525332168,5.56142757631112,
134.368706159956));
#258906=CARTESIAN_POINT('Ctrl Pts',(-32.6146001570296,6.0048723027414,128.051989919443));
#258907=CARTESIAN_POINT('Ctrl Pts',(-32.8930477808425,0.930132737272799,
124.264567889721));
#258908=CARTESIAN_POINT('Ctrl Pts',(-33.1714954046555,-4.99935337423901,
126.486895890252));
#258909=CARTESIAN_POINT('Ctrl Pts',(-33.4499430284683,-6.33467796681538,
132.676763055306));
#258910=CARTESIAN_POINT('Ctrl Pts',(-33.7283906522812,-1.84874297411136,
137.145983852021));
#258911=CARTESIAN_POINT('Ctrl Pts',(-34.0068382760941,4.33609649568588,
135.787562701789));
#258912=CARTESIAN_POINT('Ctrl Pts',(-34.285285899907,6.53627511603778,129.849822279112));
#258913=CARTESIAN_POINT('Ctrl Pts',(-34.5637335237199,2.72993621954223,
124.789255957683));
#258914=CARTESIAN_POINT('Ctrl Pts',(-34.8421811475328,-3.58508069791401,
125.256276964487));
#258915=CARTESIAN_POINT('Ctrl Pts',(-35.1206287713457,-6.60558359491616,
130.821715809516));
#258916=CARTESIAN_POINT('Ctrl Pts',(-35.3990763951586,-3.55587786888901,
136.37120608099));
#258917=CARTESIAN_POINT('Ctrl Pts',(-35.6775240189714,2.76150590435573,
136.805037327097));
#258918=CARTESIAN_POINT('Ctrl Pts',(-35.9559716427844,6.54120065856107,
131.724539826499));
#258919=CARTESIAN_POINT('Ctrl Pts',(-36.2344192665972,4.30985156296601,
125.798442586144));
#258920=CARTESIAN_POINT('Ctrl Pts',(-36.5128668904101,-1.8820405710409,
124.472539463974));
#258921=CARTESIAN_POINT('Ctrl Pts',(-36.791314514223,-6.3444293630544,128.965270655295));
#258922=CARTESIAN_POINT('Ctrl Pts',(-37.0697621380359,-4.9765975130263,
135.148035677403));
#258923=CARTESIAN_POINT('Ctrl Pts',(-37.3482097618488,0.964484331168655,
137.339175519844));
#258924=CARTESIAN_POINT('Ctrl Pts',(-37.6266573856617,6.0192521926987,133.525139710547));
#258925=CARTESIAN_POINT('Ctrl Pts',(-37.9051050094746,5.54262134595571,
127.210840832248));
#258926=CARTESIAN_POINT('Ctrl Pts',(-38.1835526332875,-0.0274077456145885,
124.198811083455));
#258927=CARTESIAN_POINT('Ctrl Pts',(-38.4620002571004,-5.5722504579079,
127.256958657474));
#258928=CARTESIAN_POINT('Ctrl Pts',(-38.7404478809132,-5.99646721895241,
133.574995332598));
#258929=CARTESIAN_POINT('Ctrl Pts',(-39.0188955047262,-0.910223549489097,
137.346954057637));
#258930=CARTESIAN_POINT('Ctrl Pts',(-39.297343128539,5.0124710950622,135.106589034709));
#258931=CARTESIAN_POINT('Ctrl Pts',(-39.5757907523519,6.32894967607775,
128.912686271968));
#258932=CARTESIAN_POINT('Ctrl Pts',(-39.8542383761648,1.82943269115809,
124.457139819403));
#258933=CARTESIAN_POINT('Ctrl Pts',(-40.1326859999777,-4.35124356418029,
125.834379201373));
#258934=CARTESIAN_POINT('Ctrl Pts',(-40.4111336237906,-6.53333955410249,
131.778788707735));
#258935=CARTESIAN_POINT('Ctrl Pts',(-40.6895812476035,-2.7116156651858,
136.827746402689));
#258936=CARTESIAN_POINT('Ctrl Pts',(-40.9680288714165,3.60195055024708,
136.34150681987));
#258937=CARTESIAN_POINT('Ctrl Pts',(-41.2464764952292,6.60550017506977,
130.766900381762));
#258938=CARTESIAN_POINT('Ctrl Pts',(-41.5249241190422,3.53891783562657,
125.226718070324));
#258939=CARTESIAN_POINT('Ctrl Pts',(-41.803371742855,-2.77975710900975,
124.812116776814));
#258940=CARTESIAN_POINT('Ctrl Pts',(-42.081819366668,-6.5439710691505,129.904094835568));
#258941=CARTESIAN_POINT('Ctrl Pts',(-42.3602669904808,-4.2945953075014,
135.82337316755));
#258942=CARTESIAN_POINT('Ctrl Pts',(-42.6387146142937,1.90130373909722,
137.130424158489));
#258943=CARTESIAN_POINT('Ctrl Pts',(-42.9171622381066,6.34999753331677,
132.624131800705));
#258944=CARTESIAN_POINT('Ctrl Pts',(-43.1956098619195,4.96335380904355,
126.44555862638));
#258945=CARTESIAN_POINT('Ctrl Pts',(-43.4740574857324,-0.984369592426984,
124.272511542639));
#258946=CARTESIAN_POINT('Ctrl Pts',(-43.7525051095453,-6.02750542758532,
128.101914660188));
#258947=CARTESIAN_POINT('Ctrl Pts',(-44.0309527333582,-5.53165823480283,
134.414733590743));
#258948=CARTESIAN_POINT('Ctrl Pts',(-44.3094003571711,0.0475126392350714,
137.409796135472));
#258949=CARTESIAN_POINT('Ctrl Pts',(-44.5878479809839,5.58302171893757,
134.334786132711));
#258950=CARTESIAN_POINT('Ctrl Pts',(-44.8662956047969,5.98800658471021,
128.015487552405));
#258951=CARTESIAN_POINT('Ctrl Pts',(-45.1447432286098,0.890305929518511,
124.259027074959));
#258952=CARTESIAN_POINT('Ctrl Pts',(-45.4231908524226,-5.02554238103793,
126.517408365848));
#258953=CARTESIAN_POINT('Ctrl Pts',(-45.7016384762356,-6.32316275481482,
132.715289346806));
#258954=CARTESIAN_POINT('Ctrl Pts',(-45.9800861000484,-1.81010546059046,
137.15712017965));
#258955=CARTESIAN_POINT('Ctrl Pts',(-46.2585337238614,4.36635032334889,
135.761075324496));
#258956=CARTESIAN_POINT('Ctrl Pts',(-46.5369813476741,6.53034346820225,
129.810051802649));
#258957=CARTESIAN_POINT('Ctrl Pts',(-46.8154289714873,2.6932699907919,124.772749507024));
#258958=CARTESIAN_POINT('Ctrl Pts',(-47.0938765952999,-3.61878703460243,
125.278203161403));
#258959=CARTESIAN_POINT('Ctrl Pts',(-47.3723242191129,-6.60535556277213,
130.861925550195));
#258960=CARTESIAN_POINT('Ctrl Pts',(-47.6507718429257,-3.52192501831287,
136.392748578105));
#258961=CARTESIAN_POINT('Ctrl Pts',(-47.9292194667387,2.79798256237344,
136.788116078208));
#258962=CARTESIAN_POINT('Ctrl Pts',(-48.2076670905515,6.54668085728591,
131.684704632686));
#258963=CARTESIAN_POINT('Ctrl Pts',(-48.4861147143645,4.27929926749242,
125.772300044465));
#258964=CARTESIAN_POINT('Ctrl Pts',(-48.7645623381774,-1.92054929373528,
124.484113293097));
#258965=CARTESIAN_POINT('Ctrl Pts',(-49.0430099619902,-6.35550687806913,
129.003925071669));
#258966=CARTESIAN_POINT('Ctrl Pts',(-49.3214575858032,-4.95006412522954,
135.178249160753));
#258967=CARTESIAN_POINT('Ctrl Pts',(-49.5999052096159,1.00424573461974,
137.333183354982));
#258968=CARTESIAN_POINT('Ctrl Pts',(-49.878352833429,6.03570282448511,133.488448404247));
#258969=CARTESIAN_POINT('Ctrl Pts',(-50.1568004572417,5.52064387912377,
127.17716790253));
#258970=CARTESIAN_POINT('Ctrl Pts',(-50.4352480810547,-0.0676170927052693,
124.199100307716));
#258971=CARTESIAN_POINT('Ctrl Pts',(-50.7136957048675,-5.5937412596168,
127.290944252747));
#258972=CARTESIAN_POINT('Ctrl Pts',(-50.9921433286805,-5.97949047839309,
133.611446197116));
#258973=CARTESIAN_POINT('Ctrl Pts',(-51.2705909524933,-0.870380061875472,
137.352373627632));
#258974=CARTESIAN_POINT('Ctrl Pts',(-51.5490385763063,5.03856711107574,
135.075996990117));
#258975=CARTESIAN_POINT('Ctrl Pts',(-51.8274862001192,6.31731725663583,
128.874195207264));
#258976=CARTESIAN_POINT('Ctrl Pts',(-52.105933823932,1.79076146145295,124.446121142656));
#258977=CARTESIAN_POINT('Ctrl Pts',(-52.3843814477449,-4.38141663324442,
125.860958538224));
#258978=CARTESIAN_POINT('Ctrl Pts',(-52.6628290715579,-6.52728688609205,
131.818540946088));
#258979=CARTESIAN_POINT('Ctrl Pts',(-52.9412766953706,-2.67489936631311,
136.844141177504));
#258980=CARTESIAN_POINT('Ctrl Pts',(-53.2197243191836,3.63558999500893,
136.319478134021));
#258981=CARTESIAN_POINT('Ctrl Pts',(-53.4981719429964,6.60514975936288,
130.726691521383));
#258982=CARTESIAN_POINT('Ctrl Pts',(-53.7766195668094,3.50489957436681,
125.205279013792));
#258983=CARTESIAN_POINT('Ctrl Pts',(-54.0550671906223,-2.8161820956091,
124.829148969725));
#258984=CARTESIAN_POINT('Ctrl Pts',(-54.3335148144351,-6.54932999786417,
129.943946524707));
#258985=CARTESIAN_POINT('Ctrl Pts',(-54.6119624382481,-4.26396358463975,
135.849422597461));
#258986=CARTESIAN_POINT('Ctrl Pts',(-54.890410062061,1.93977705666721,137.11873317567));
#258987=CARTESIAN_POINT('Ctrl Pts',(-55.1688576858738,6.3609573462743,132.58544384723));
#258988=CARTESIAN_POINT('Ctrl Pts',(-55.4473053096868,4.93672858469731,
126.415426041482));
#258989=CARTESIAN_POINT('Ctrl Pts',(-55.7257529334997,-1.02411257361735,
124.278624699781));
#258990=CARTESIAN_POINT('Ctrl Pts',(-56.0042005573125,-6.0438443074584,
128.138655866601));
#258991=CARTESIAN_POINT('Ctrl Pts',(-56.2826481811254,-5.50957838095395,
134.448339472641));
#258992=CARTESIAN_POINT('Ctrl Pts',(-56.5610958049383,0.0877209197796484,
137.40938452913));
#258993=CARTESIAN_POINT('Ctrl Pts',(-56.8395434287512,5.60440898064107,
134.300735284249));
#258994=CARTESIAN_POINT('Ctrl Pts',(-57.117991052564,5.97091897889293,127.979088528083));
#258995=CARTESIAN_POINT('Ctrl Pts',(-57.396438676377,0.850446131150592,
124.253728799937));
#258996=CARTESIAN_POINT('Ctrl Pts',(-57.6748863001899,-5.05154516451579,
126.548079696037));
#258997=CARTESIAN_POINT('Ctrl Pts',(-57.9533339240027,-6.31141323569307,
132.753744828139));
#258998=CARTESIAN_POINT('Ctrl Pts',(-58.2317815478157,-1.77140087294607,
137.168021103437));
#258999=CARTESIAN_POINT('Ctrl Pts',(-58.5102291716285,4.39644235429495,
135.734404274317));
#259000=CARTESIAN_POINT('Ctrl Pts',(-58.7886767954414,6.52416983608798,
129.770318170665));
#259001=CARTESIAN_POINT('Ctrl Pts',(-59.0671244192543,2.65650396193163,
124.756466559932));
#259002=CARTESIAN_POINT('Ctrl Pts',(-59.3455720430672,-3.6523592758065,
125.300334132115));
#259003=CARTESIAN_POINT('Ctrl Pts',(-59.62401966688,-6.60488276674858,130.902133157784));
#259004=CARTESIAN_POINT('Ctrl Pts',(-59.902467290693,-3.48784166150989,
136.414083995446));
#259005=CARTESIAN_POINT('Ctrl Pts',(-60.1809149145059,2.83435554011865,
136.770973099059));
#259006=CARTESIAN_POINT('Ctrl Pts',(-60.4593625383188,6.55191846634393,
131.644836817403));
#259007=CARTESIAN_POINT('Ctrl Pts',(-60.7378101621316,4.24858840101079,
125.746343967642));
#259008=CARTESIAN_POINT('Ctrl Pts',(-61.0162577859445,-1.95898684976931,
124.49592132131));
#259009=CARTESIAN_POINT('Ctrl Pts',(-61.2947054097575,-6.36634888743926,
129.042646203845));
#259010=CARTESIAN_POINT('Ctrl Pts',(-61.5731530335703,-4.92334731098624,
135.208300568055));
#259011=CARTESIAN_POINT('Ctrl Pts',(-61.8516006573832,1.04396992537583,
137.326949262193));
#259012=CARTESIAN_POINT('Ctrl Pts',(-62.1300482811962,6.05192980108374,
133.451657638088));
#259013=CARTESIAN_POINT('Ctrl Pts',(-62.408495905009,5.49846184280268,127.143629379772));
#259014=CARTESIAN_POINT('Ctrl Pts',(-62.6869435288219,-0.107823934219708,
124.199634292325));
#259015=CARTESIAN_POINT('Ctrl Pts',(-62.9653911526347,-5.61502478318622,
127.325060038955));
#259016=CARTESIAN_POINT('Ctrl Pts',(-63.2438387764477,-5.96229216561512,
133.647793044045));
#259017=CARTESIAN_POINT('Ctrl Pts',(-63.5222864002605,-0.830504322008783,
137.357550558596));
#259018=CARTESIAN_POINT('Ctrl Pts',(-63.8007340240734,5.06447642113188,
135.045246658467));
#259019=CARTESIAN_POINT('Ctrl Pts',(-64.0791816478864,6.30545074667997,
128.835775665549));
#259020=CARTESIAN_POINT('Ctrl Pts',(-64.3576292716992,1.75202387442331,
124.435338072814));
#259021=CARTESIAN_POINT('Ctrl Pts',(-64.6360768955121,-4.41142734730395,
125.887721054655));
#259022=CARTESIAN_POINT('Ctrl Pts',(-64.914524519325,-6.52099234706562,
131.858255603616));
#259023=CARTESIAN_POINT('Ctrl Pts',(-65.1929721431379,-2.63808394806071,
136.860312146029));
#259024=CARTESIAN_POINT('Ctrl Pts',(-65.4714197669508,3.66909472164654,
136.297245083462));
#259025=CARTESIAN_POINT('Ctrl Pts',(-65.7498673907637,6.60455458740261,
130.686485539062));
#259026=CARTESIAN_POINT('Ctrl Pts',(-66.0283150145766,3.4707514377644,125.184047433287));
#259027=CARTESIAN_POINT('Ctrl Pts',(-66.3067626383895,-2.85250272754526,
124.846402576302));
#259028=CARTESIAN_POINT('Ctrl Pts',(-66.5852102622024,-6.55444623874626,
129.983830096806));
#259029=CARTESIAN_POINT('Ctrl Pts',(-66.8636578860152,-4.23317385903938,
135.875285080744));
#259030=CARTESIAN_POINT('Ctrl Pts',(-67.1421055098281,1.978178495085,137.106808211453));
#259031=CARTESIAN_POINT('Ctrl Pts',(-67.4205531336411,6.37168145161813,
132.546689895061));
#259032=CARTESIAN_POINT('Ctrl Pts',(-67.6990007574539,4.90992042805787,
126.385456090168));
#259033=CARTESIAN_POINT('Ctrl Pts',(-67.9774483812669,-1.06381760593968,
124.284979670466));
#259034=CARTESIAN_POINT('Ctrl Pts',(-68.2558960050797,-6.05995923045808,
128.175495851683));
#259035=CARTESIAN_POINT('Ctrl Pts',(-68.5343436288926,-5.48729436765201,
134.481810325563));
#259036=CARTESIAN_POINT('Ctrl Pts',(-68.8127912527054,0.12792594979327,
137.408728171199));
#259037=CARTESIAN_POINT('Ctrl Pts',(-69.0912388765185,5.62558856890878,
134.266554876337));
#259038=CARTESIAN_POINT('Ctrl Pts',(-69.3696865003312,5.9536101184771,127.942794195258));
#259039=CARTESIAN_POINT('Ctrl Pts',(-69.6481341241442,0.810554819188534,
124.248673260987));
#259040=CARTESIAN_POINT('Ctrl Pts',(-69.9265817479571,-5.07736076112986,
126.578908744281));
#259041=CARTESIAN_POINT('Ctrl Pts',(-70.2050293717699,-6.29942984483285,
132.792128074323));
#259042=CARTESIAN_POINT('Ctrl Pts',(-70.4834769955829,-1.73263064539088,
137.178686219444));
#259043=CARTESIAN_POINT('Ctrl Pts',(-70.7619246193956,4.42637147345276,
135.707550539556));
#259044=CARTESIAN_POINT('Ctrl Pts',(-71.0403722432087,6.51775444846118,
129.730622855503));
#259045=CARTESIAN_POINT('Ctrl Pts',(-71.3188198670216,2.6196394953401,124.740407719779));
#259046=CARTESIAN_POINT('Ctrl Pts',(-71.5972674908343,-3.68579617749442,
125.322669056552));
#259047=CARTESIAN_POINT('Ctrl Pts',(-71.8757151146474,-6.6041652243652,
130.942337142376));
#259048=CARTESIAN_POINT('Ctrl Pts',(-72.1541627384602,-3.45362906145158,
136.435211542427));
#259049=CARTESIAN_POINT('Ctrl Pts',(-72.4326103622731,2.87062348977667,
136.753609024891));
#259050=CARTESIAN_POINT('Ctrl Pts',(-72.711057986086,6.55691329165398,131.604937857965));
#259051=CARTESIAN_POINT('Ctrl Pts',(-72.9895056098989,4.21772010152317,
125.720575317484));
#259052=CARTESIAN_POINT('Ctrl Pts',(-73.2679532337117,-1.99735181482566,
124.50796311106));
#259053=CARTESIAN_POINT('Ctrl Pts',(-73.5464008575247,-6.37695498941029,
129.081432616995));
#259054=CARTESIAN_POINT('Ctrl Pts',(-73.8248484813376,-4.89644806029751,
135.238188785743));
#259055=CARTESIAN_POINT('Ctrl Pts',(-74.1032961051504,1.08365543144292,
137.320473472483));
#259056=CARTESIAN_POINT('Ctrl Pts',(-74.3817437289633,6.06793252119795,
133.414768775364));
#259057=CARTESIAN_POINT('Ctrl Pts',(-74.6601913527762,5.47607605895596,
127.110226506756));
#259058=CARTESIAN_POINT('Ctrl Pts',(-74.9386389765891,-0.148026780279403,
124.200413017498));
#259059=CARTESIAN_POINT('Ctrl Pts',(-75.217086600402,-5.63610023994771,
127.359304751927));
#259060=CARTESIAN_POINT('Ctrl Pts',(-75.4955342242149,-5.94487291790794,
133.684034526541));
#259061=CARTESIAN_POINT('Ctrl Pts',(-75.7739818480278,-0.790597807498519,
137.362484658699));
#259062=CARTESIAN_POINT('Ctrl Pts',(-76.0524294718406,5.09019806515201,
135.014339179226));
#259063=CARTESIAN_POINT('Ctrl Pts',(-76.3308770956536,6.29335058592772,
128.797429070474));
#259064=CARTESIAN_POINT('Ctrl Pts',(-76.6093247194664,1.71322136550425,
124.424791009442));
#259065=CARTESIAN_POINT('Ctrl Pts',(-76.8877723432794,-4.44127459430165,
125.914665758975));
#259066=CARTESIAN_POINT('Ctrl Pts',(-77.1662199670922,-6.51445617026952,
131.89793120868));
#259067=CARTESIAN_POINT('Ctrl Pts',(-77.4446675909052,-2.60117077463652,
136.876258709042));
#259068=CARTESIAN_POINT('Ctrl Pts',(-77.7231152147181,3.7024634886308,136.274808492052));
#259069=CARTESIAN_POINT('Ctrl Pts',(-78.0015628385308,6.60371468124315,
130.646283924643));
#259070=CARTESIAN_POINT('Ctrl Pts',(-78.2800104623438,3.43647469119047,
125.163024115555));
#259071=CARTESIAN_POINT('Ctrl Pts',(-78.5584580861567,-2.88871765894464,
124.863876957204));
#259072=CARTESIAN_POINT('Ctrl Pts',(-78.8369057099696,-6.55931960221255,
130.023744073965));
#259073=CARTESIAN_POINT('Ctrl Pts',(-79.1153533337825,-4.20222727162433,
135.900959659057));
#259074=CARTESIAN_POINT('Ctrl Pts',(-79.3938009575953,2.01650663137172,
137.094649707722));
#259075=CARTESIAN_POINT('Ctrl Pts',(-79.6722485814083,6.38216945196263,
132.507871380239));
#259076=CARTESIAN_POINT('Ctrl Pts',(-79.9506962052212,4.88293033251105,
126.355649882987));
#259077=CARTESIAN_POINT('Ctrl Pts',(-80.229143829034,-1.10348321810992,
124.29157621921));
#259078=CARTESIAN_POINT('Ctrl Pts',(-80.507591452847,-6.07584959944043,
128.212433250316));
#259079=CARTESIAN_POINT('Ctrl Pts',(-80.7860390766598,-5.46480702063872,
134.515144909234));
#259080=CARTESIAN_POINT('Ctrl Pts',(-81.0644867004727,0.168126239464741,
137.407827085998));
#259081=CARTESIAN_POINT('Ctrl Pts',(-81.3429343242857,5.64655969892388,
134.232246175545));
#259082=CARTESIAN_POINT('Ctrl Pts',(-81.6213819480984,5.93608064484842,
127.906605898828));
#259083=CARTESIAN_POINT('Ctrl Pts',(-81.8998295719115,0.770633471818905,
124.243860645443));
#259084=CARTESIAN_POINT('Ctrl Pts',(-82.1782771957242,-5.10298821427442,
126.609894368197));
#259085=CARTESIAN_POINT('Ctrl Pts',(-82.4567248195372,-6.28721302628274,
132.830437663053));
#259086=CARTESIAN_POINT('Ctrl Pts',(-82.7351724433501,-1.69379621456928,
137.189115132473));
#259087=CARTESIAN_POINT('Ctrl Pts',(-83.0136200671628,4.45613657178832,
135.680515115291));
#259088=CARTESIAN_POINT('Ctrl Pts',(-83.2920676909759,6.51109754304618,
129.690967328089));
#259089=CARTESIAN_POINT('Ctrl Pts',(-83.5705153147887,2.58267795704331,
124.724573581631));
#259090=CARTESIAN_POINT('Ctrl Pts',(-83.8489629386017,-3.71909650065006,
125.345207107088));
#259091=CARTESIAN_POINT('Ctrl Pts',(-84.1274105624144,-6.60320296221082,
130.982536014198));
#259092=CARTESIAN_POINT('Ctrl Pts',(-84.4058581862275,-3.41928848589759,
136.456130436155));
#259093=CARTESIAN_POINT('Ctrl Pts',(-84.6843058100402,2.90678506742617,
136.736024499134));
#259094=CARTESIAN_POINT('Ctrl Pts',(-84.9627534338533,6.56166514813073,
131.565009232842));
#259095=CARTESIAN_POINT('Ctrl Pts',(-85.241201057666,4.1866955128661,125.694995048862));
#259096=CARTESIAN_POINT('Ctrl Pts',(-85.519648681479,-2.03564276727566,
124.520238216135));
#259097=CARTESIAN_POINT('Ctrl Pts',(-85.7980963052919,-6.38732479096924,
129.120282873878));
#259098=CARTESIAN_POINT('Ctrl Pts',(-86.0765439291047,-4.8693673699251,
135.267912706297));
#259099=CARTESIAN_POINT('Ctrl Pts',(-86.3549915529177,1.12330078225909,
137.313756225814));
#259100=CARTESIAN_POINT('Ctrl Pts',(-86.6334391767305,6.08371039184151,
133.377783183006));
#259101=CARTESIAN_POINT('Ctrl Pts',(-86.9118868005434,5.45348735709659,
127.076960521238));
#259102=CARTESIAN_POINT('Ctrl Pts',(-87.1903344243564,-0.188224141151809,
124.201436454379));
#259103=CARTESIAN_POINT('Ctrl Pts',(-87.4687820481692,-5.65696684894189,
127.39367712271));
#259104=CARTESIAN_POINT('Ctrl Pts',(-87.7472296719821,-5.92723338074904,
133.720169301662));
#259105=CARTESIAN_POINT('Ctrl Pts',(-88.0256772957949,-0.750661997095914,
137.367175745102));
#259106=CARTESIAN_POINT('Ctrl Pts',(-88.3041249196079,5.11573109001074,
134.983275697681));
#259107=CARTESIAN_POINT('Ctrl Pts',(-88.5825725434208,6.28101722275544,
128.759156842984));
#259108=CARTESIAN_POINT('Ctrl Pts',(-88.8610201672337,1.67435537253749,
124.414480343369));
#259109=CARTESIAN_POINT('Ctrl Pts',(-89.1394677910466,-4.47095726823472,
125.941791652735));
#259110=CARTESIAN_POINT('Ctrl Pts',(-89.4179154148595,-6.50767859790483,
131.93756629108));
#259111=CARTESIAN_POINT('Ctrl Pts',(-89.6963630386723,-2.56416121387375,
136.891980275641));
#259112=CARTESIAN_POINT('Ctrl Pts',(-89.9748106624853,3.73569505946763,
136.252169191183));
#259113=CARTESIAN_POINT('Ctrl Pts',(-90.253258286298,6.60263007200808,130.606088167816));
#259114=CARTESIAN_POINT('Ctrl Pts',(-90.5317059101111,3.40207060478355,
125.142209839621));
#259115=CARTESIAN_POINT('Ctrl Pts',(-90.8101535339238,-2.9248255478482,
124.881571464914));
#259116=CARTESIAN_POINT('Ctrl Pts',(-91.0886011577368,-6.56394990767886,
130.063686977158));
#259117=CARTESIAN_POINT('Ctrl Pts',(-91.3670487815497,-4.17112496913288,
135.926445381018));
#259118=CARTESIAN_POINT('Ctrl Pts',(-91.6454964053626,2.05476004526333,
137.082258115016));
#259119=CARTESIAN_POINT('Ctrl Pts',(-91.9239440291755,6.39242095867105,
132.468989741201));
#259120=CARTESIAN_POINT('Ctrl Pts',(-92.2023916529884,4.85575929818535,
126.326008524418));
#259121=CARTESIAN_POINT('Ctrl Pts',(-92.4808392768012,-1.14310794030347,
124.298414101576));
#259122=CARTESIAN_POINT('Ctrl Pts',(-92.7592869006141,-6.09151482558059,
128.249466693771));
#259123=CARTESIAN_POINT('Ctrl Pts',(-93.0377345244271,-5.44211717319261,
134.548341988427));
#259124=CARTESIAN_POINT('Ctrl Pts',(-93.3161821482399,0.208320299155509,
137.406681306919));
#259125=CARTESIAN_POINT('Ctrl Pts',(-93.5946297720528,5.6673215935918,134.197810453193));
#259126=CARTESIAN_POINT('Ctrl Pts',(-93.8730773958657,5.91833120756931,
127.870524979765));
#259127=CARTESIAN_POINT('Ctrl Pts',(-94.1515250196785,0.730683568342929,
124.239291131637));
#259128=CARTESIAN_POINT('Ctrl Pts',(-94.4299726434915,-5.12842657431339,
126.641035419604));
#259129=CARTESIAN_POINT('Ctrl Pts',(-94.7084202673044,-6.27476323274215,
132.868672174754));
#259130=CARTESIAN_POINT('Ctrl Pts',(-94.9868678911172,-1.6548990195065,
137.199307456074));
#259131=CARTESIAN_POINT('Ctrl Pts',(-95.2653155149302,4.48573654634406,
135.653299003326));
#259132=CARTESIAN_POINT('Ctrl Pts',(-95.543763138743,6.50419936651746,129.651353057874));
#259133=CARTESIAN_POINT('Ctrl Pts',(-95.822210762556,2.54562071666526,124.708964732227));
#259134=CARTESIAN_POINT('Ctrl Pts',(-96.1006583863688,-3.75225901131679,
125.367947448562));
#259135=CARTESIAN_POINT('Ctrl Pts',(-96.3791060101818,-6.60199601594203,
131.022728283664));
#259136=CARTESIAN_POINT('Ctrl Pts',(-96.6575536339946,-3.38482120735248,
136.476839901474));
#259137=CARTESIAN_POINT('Ctrl Pts',(-96.9360012578075,2.94283893308538,
136.718220173391));
#259138=CARTESIAN_POINT('Ctrl Pts',(-97.2144488816204,6.5661738596919,131.525052421605));
#259139=CARTESIAN_POINT('Ctrl Pts',(-97.4928965054334,4.15551578466796,
125.669604109659));
#259140=CARTESIAN_POINT('Ctrl Pts',(-97.771344129246,-2.07385828823457,
124.532746181678));
#259141=CARTESIAN_POINT('Ctrl Pts',(-98.0497917530593,-6.39745790785863,
129.15919553488));
#259142=CARTESIAN_POINT('Ctrl Pts',(-98.3282393768718,-4.84210624335443,
135.297471228287));
#259143=CARTESIAN_POINT('Ctrl Pts',(-98.606687000685,1.16290450875192,137.306797771098));
#259144=CARTESIAN_POINT('Ctrl Pts',(-98.8851346244975,6.09926282835875,
133.340702231527));
#259145=CARTESIAN_POINT('Ctrl Pts',(-99.1635822483109,5.43069657425812,
127.043832655902));
#259146=CARTESIAN_POINT('Ctrl Pts',(-99.4420298721233,-0.228414527308866,
124.202704565042));
#259147=CARTESIAN_POINT('Ctrl Pts',(-99.7204774959365,-5.67762383694899,
127.428175877623));
#259148=CARTESIAN_POINT('Ctrl Pts',(-99.9989251197493,-5.90937420777732,
133.756196030418));
#259149=CARTESIAN_POINT('Ctrl Pts',(-100.277372743562,-0.710698370637635,
137.371623643978));
#259150=CARTESIAN_POINT('Ctrl Pts',(-100.555820367375,5.14107454957247,
134.9520573649));
#259151=CARTESIAN_POINT('Ctrl Pts',(-100.834267991188,6.26845111417983,
128.720960401273));
#259152=CARTESIAN_POINT('Ctrl Pts',(-101.112715615001,1.63542733571746,
124.404406456659));
#259153=CARTESIAN_POINT('Ctrl Pts',(-101.391163238814,-4.50047426920288,
125.969097730777));
#259154=CARTESIAN_POINT('Ctrl Pts',(-101.669610862627,-6.50065988111587,
131.977159382129));
#259155=CARTESIAN_POINT('Ctrl Pts',(-101.94805848644,-2.52705663717401,
136.907476263252));
#259156=CARTESIAN_POINT('Ctrl Pts',(-102.226506110253,3.76878820275105,
136.229328019765));
#259157=CARTESIAN_POINT('Ctrl Pts',(-102.504953734065,6.60130079988703,
130.565899758046));
#259158=CARTESIAN_POINT('Ctrl Pts',(-102.783401357878,3.36754045339959,
125.121605376767));
#259159=CARTESIAN_POINT('Ctrl Pts',(-103.061848981691,-2.96082505626518,
124.899485443752));
#259160=CARTESIAN_POINT('Ctrl Pts',(-103.340296605504,-6.56833698356739,
130.103657326284));
#259161=CARTESIAN_POINT('Ctrl Pts',(-103.618744229317,-4.13986810407194,
135.951741302244));
#259162=CARTESIAN_POINT('Ctrl Pts',(-103.89719185313,2.0929373192654,137.06963389251));
#259163=CARTESIAN_POINT('Ctrl Pts',(-104.175639476943,6.40243559186997,
132.430046418718));
#259164=CARTESIAN_POINT('Ctrl Pts',(-104.454087100755,4.82840833191319,
126.296533112833));
#259165=CARTESIAN_POINT('Ctrl Pts',(-104.732534724569,-1.18269030421136,
124.305493064181));
#259166=CARTESIAN_POINT('Ctrl Pts',(-105.010982348381,-6.10695432839948,
128.286594809759));
#259167=CARTESIAN_POINT('Ctrl Pts',(-105.289429972194,-5.41922566609253,
134.581400333014));
#259168=CARTESIAN_POINT('Ctrl Pts',(-105.567877596007,0.248506639461218,
137.40529087642));
#259169=CARTESIAN_POINT('Ctrl Pts',(-105.84632521982,5.68787348357469,134.163248985309));
#259170=CARTESIAN_POINT('Ctrl Pts',(-106.124772843633,5.90036246435008,
127.834552775061));
#259171=CARTESIAN_POINT('Ctrl Pts',(-106.403220467446,0.690706589119241,
124.234964888896));
#259172=CARTESIAN_POINT('Ctrl Pts',(-106.681668091259,-5.1536748986197,
126.672330744555));
#259173=CARTESIAN_POINT('Ctrl Pts',(-106.960115715072,-6.26208092554253,
132.906830192629));
#259174=CARTESIAN_POINT('Ctrl Pts',(-107.238563338885,-1.61594050155245,
137.209262812568));
#259175=CARTESIAN_POINT('Ctrl Pts',(-107.517010962697,4.51517030028232,
135.625903212168));
#259176=CARTESIAN_POINT('Ctrl Pts',(-107.79545858651,6.49706017448951,129.611781512777));
#259177=CARTESIAN_POINT('Ctrl Pts',(-108.073906210323,2.50846914737518,
124.69358174996));
#259178=CARTESIAN_POINT('Ctrl Pts',(-108.352353834136,-3.78528248064593,
125.390889238328));
#259179=CARTESIAN_POINT('Ctrl Pts',(-108.630801457949,-6.60054443028347,
131.062912461436));
#259180=CARTESIAN_POINT('Ctrl Pts',(-108.909249081762,-3.35022850301195,
136.497339170987));
#259181=CARTESIAN_POINT('Ctrl Pts',(-109.187696705575,2.97878375076591,
136.700196707408));
#259182=CARTESIAN_POINT('Ctrl Pts',(-109.466144329388,6.57043925926657,
131.485068904869));
#259183=CARTESIAN_POINT('Ctrl Pts',(-109.7445919532,4.12418207230337,125.644403440746));
#259184=CARTESIAN_POINT('Ctrl Pts',(-110.023039577014,-2.11199696161116,
124.5454865442));
#259185=CARTESIAN_POINT('Ctrl Pts',(-110.301487200826,-6.40735396459295,
129.198169158078));
#259186=CARTESIAN_POINT('Ctrl Pts',(-110.579934824639,-4.81466569075636,
135.326863256411));
#259187=CARTESIAN_POINT('Ctrl Pts',(-110.858382448452,1.20246514338981,
137.299598366182));
#259188=CARTESIAN_POINT('Ctrl Pts',(-111.136830072265,6.11458925444912,
133.303527294979));
#259189=CARTESIAN_POINT('Ctrl Pts',(-111.415277696078,5.407704554961,127.010844138312));
#259190=CARTESIAN_POINT('Ctrl Pts',(-111.693725319891,-0.268596449482207,
124.204217302498));
#259191=CARTESIAN_POINT('Ctrl Pts',(-111.972172943703,-5.69807043851701,
127.462799738304));
#259192=CARTESIAN_POINT('Ctrl Pts',(-112.250620567517,-5.89129606077132,
133.792113377828));
#259193=CARTESIAN_POINT('Ctrl Pts',(-112.529068191329,-0.670708408989202,
137.375828190507));
#259194=CARTESIAN_POINT('Ctrl Pts',(-112.807515815142,5.16622750472631,
134.920685337692));
#259195=CARTESIAN_POINT('Ctrl Pts',(-113.085963438955,6.25565272584325,
128.682841160722));
#259196=CARTESIAN_POINT('Ctrl Pts',(-113.364411062768,1.5964386975353,124.394569722605));
#259197=CARTESIAN_POINT('Ctrl Pts',(-113.642858686581,-4.52982450344111,
125.996582981263));
#259198=CARTESIAN_POINT('Ctrl Pts',(-113.921306310394,-6.49340027998504,
132.016709014688));
#259199=CARTESIAN_POINT('Ctrl Pts',(-114.199753934207,-2.48985841946147,
136.922746097669));
#259200=CARTESIAN_POINT('Ctrl Pts',(-114.47820155802,3.80174169220082,136.206285824184));
#259201=CARTESIAN_POINT('Ctrl Pts',(-114.756649181833,6.59972691413776,
130.525720184532));
#259202=CARTESIAN_POINT('Ctrl Pts',(-115.035096805645,3.3328855165654,125.101211490497));
#259203=CARTESIAN_POINT('Ctrl Pts',(-115.313544429458,-2.99671485022117,
124.917618229914));
#259204=CARTESIAN_POINT('Ctrl Pts',(-115.591992053271,-6.57248066731354,
130.143653640229));
#259205=CARTESIAN_POINT('Ctrl Pts',(-115.870439677084,-4.10845783467579,
135.976846485386));
#259206=CARTESIAN_POINT('Ctrl Pts',(-116.148887300897,2.13103703870585,
137.056777507999));
#259207=CARTESIAN_POINT('Ctrl Pts',(-116.42733492471,6.41221298046361,132.391042855849));
#259208=CARTESIAN_POINT('Ctrl Pts',(-116.705782548523,4.8008784471946,126.267224740454));
#259209=CARTESIAN_POINT('Ctrl Pts',(-116.984230172336,-1.22222884309565,
124.312812844714));
#259210=CARTESIAN_POINT('Ctrl Pts',(-117.262677796149,-6.12216753577917,
128.323816222486));
#259211=CARTESIAN_POINT('Ctrl Pts',(-117.541125419961,-5.39613334759327,
134.614318718005));
#259212=CARTESIAN_POINT('Ctrl Pts',(-117.819573043774,0.288683771261777,
137.403655846021));
#259213=CARTESIAN_POINT('Ctrl Pts',(-118.098020667587,5.70821460731317,
134.128563052582));
#259214=CARTESIAN_POINT('Ctrl Pts',(-118.3764682914,5.88217508103065,127.79869061768));
#259215=CARTESIAN_POINT('Ctrl Pts',(-118.654915915213,0.650704015508265,
124.230882077529));
#259216=CARTESIAN_POINT('Ctrl Pts',(-118.933363539026,-5.17873225160735,
126.703779183394));
#259217=CARTESIAN_POINT('Ctrl Pts',(-119.211811162839,-6.24916657463125,
132.944910302722));
#259218=CARTESIAN_POINT('Ctrl Pts',(-119.490258786652,-1.57692210432836,
137.218980833058));
#259219=CARTESIAN_POINT('Ctrl Pts',(-119.768706410464,4.54443674292479,
135.598328756974));
#259220=CARTESIAN_POINT('Ctrl Pts',(-120.047154034278,6.48968023150711,
129.572254159139));
#259221=CARTESIAN_POINT('Ctrl Pts',(-120.32560165809,2.47122462583917,124.67842520485));
#259222=CARTESIAN_POINT('Ctrl Pts',(-120.604049281903,-3.81816568494053,
125.414031626265));
#259223=CARTESIAN_POINT('Ctrl Pts',(-120.882496905716,-6.59884825902321,
131.103087058474));
#259224=CARTESIAN_POINT('Ctrl Pts',(-121.160944529529,-3.31551165472302,
136.517627485086));
#259225=CARTESIAN_POINT('Ctrl Pts',(-121.439392153342,3.0146181885189,136.68195476905));
#259226=CARTESIAN_POINT('Ctrl Pts',(-121.717839777155,6.57446118879764,
131.445060164237));
#259227=CARTESIAN_POINT('Ctrl Pts',(-121.996287400968,4.0926955368563,125.619393975946));
#259228=CARTESIAN_POINT('Ctrl Pts',(-122.274735024781,-2.15005737416446,
124.5584588316));
#259229=CARTESIAN_POINT('Ctrl Pts',(-122.553182648593,-6.41701259446945,
129.237202299292));
#259230=CARTESIAN_POINT('Ctrl Pts',(-122.831630272406,-4.7870467289504,
135.356087701536));
#259231=CARTESIAN_POINT('Ctrl Pts',(-123.110077896219,1.24198122024032,
137.292158277842));
#259232=CARTESIAN_POINT('Ctrl Pts',(-123.388525520032,6.1296891021858,133.266259750888));
#259233=CARTESIAN_POINT('Ctrl Pts',(-123.666973143845,5.38451215118288,
126.97799619087));
#259234=CARTESIAN_POINT('Ctrl Pts',(-123.945420767658,-0.30876841871475,
124.20597461069));
#259235=CARTESIAN_POINT('Ctrl Pts',(-124.223868391471,-5.71830589598935,
127.497547421752));
#259236=CARTESIAN_POINT('Ctrl Pts',(-124.502316015284,-5.87299960962311,
133.827920012961));
#259237=CARTESIAN_POINT('Ctrl Pts',(-124.780763639097,-0.630693593994696,
137.379789228888));
#259238=CARTESIAN_POINT('Ctrl Pts',(-125.059211262909,5.19118902341993,
134.889160778557));
#259239=CARTESIAN_POINT('Ctrl Pts',(-125.337658886723,6.24262253199412,
128.644800533857));
#259240=CARTESIAN_POINT('Ctrl Pts',(-125.616106510535,1.55739090273089,
124.384970505708));
#259241=CARTESIAN_POINT('Ctrl Pts',(-125.894554134348,-4.55900688336737,
126.024246385717));
#259242=CARTESIAN_POINT('Ctrl Pts',(-126.173001758161,-6.48590006351826,
132.056213723232));
#259243=CARTESIAN_POINT('Ctrl Pts',(-126.451449381974,-2.45256793912933,
136.937789213063));
#259244=CARTESIAN_POINT('Ctrl Pts',(-126.729897005787,3.83455430671493,
136.183043458277));
#259245=CARTESIAN_POINT('Ctrl Pts',(-127.0083446296,6.5979084730801,130.485550936142));
#259246=CARTESIAN_POINT('Ctrl Pts',(-127.286792253413,3.29810707843306,
125.081028936517));
#259247=CARTESIAN_POINT('Ctrl Pts',(-127.565239877225,-3.03249359980603,
124.935969151478));
#259248=CARTESIAN_POINT('Ctrl Pts',(-127.843687501038,-6.57638080537151,
130.183674436914));
#259249=CARTESIAN_POINT('Ctrl Pts',(-128.122135124851,-4.07689532486387,
136.001760000162));
#259250=CARTESIAN_POINT('Ctrl Pts',(-128.400582748664,2.1690577917847,137.043689437881));
#259251=CARTESIAN_POINT('Ctrl Pts',(-128.679030372477,6.42175276214748,
132.351980497887));
#259252=CARTESIAN_POINT('Ctrl Pts',(-128.95747799629,4.77317066415926,126.238084493312));
#259253=CARTESIAN_POINT('Ctrl Pts',(-129.235925620103,-1.26172209184052,
124.320373171937));
#259254=CARTESIAN_POINT('Ctrl Pts',(-129.514373243916,-6.13715388399014,
128.361129552696));
#259255=CARTESIAN_POINT('Ctrl Pts',(-129.792820867728,-5.37284107338758,
134.647095923599));
#259256=CARTESIAN_POINT('Ctrl Pts',(-130.071268491542,0.328850205779251,
137.401776276312));
#259257=CARTESIAN_POINT('Ctrl Pts',(-130.349716115354,5.72834421106097,
134.093753940311));
#259258=CARTESIAN_POINT('Ctrl Pts',(-130.628163739167,5.86376973154965,
127.762939836503));
#259259=CARTESIAN_POINT('Ctrl Pts',(-130.90661136298,0.610677329821333,
124.227042848828));
#259260=CARTESIAN_POINT('Ctrl Pts',(-131.185058986793,-5.20359770476699,
126.735379570785));
#259261=CARTESIAN_POINT('Ctrl Pts',(-131.463506610606,-6.23602065855449,
132.982911093959));
#259262=CARTESIAN_POINT('Ctrl Pts',(-131.741954234419,-1.53784527367628,
137.228461157434));
#259263=CARTESIAN_POINT('Ctrl Pts',(-132.020401858232,4.57353478979242,
135.57057665953));
#259264=CARTESIAN_POINT('Ctrl Pts',(-132.298849482045,6.48205981103755,
129.532772461657));
#259265=CARTESIAN_POINT('Ctrl Pts',(-132.577297105858,2.43388853216508,
124.66349565853));
#259266=CARTESIAN_POINT('Ctrl Pts',(-132.85574472967,-3.85090740570176,
125.437373754826));
#259267=CARTESIAN_POINT('Ctrl Pts',(-133.134192353483,-6.59690756501448,
131.143250586095));
#259268=CARTESIAN_POINT('Ctrl Pts',(-133.412639977296,-3.28067194892964,
136.53770409198));
#259269=CARTESIAN_POINT('Ctrl Pts',(-133.691087601109,3.0503409184865,136.663495034279));
#259270=CARTESIAN_POINT('Ctrl Pts',(-133.969535224922,6.5782394992522,131.405027682246));
#259271=CARTESIAN_POINT('Ctrl Pts',(-134.247982848735,4.06105734507014,
125.59457664199));
#259272=CARTESIAN_POINT('Ctrl Pts',(-134.526430472548,-2.18803811555026,
124.57166256319));
#259273=CARTESIAN_POINT('Ctrl Pts',(-134.804878096361,-6.42643343958478,
129.276293512134));
#259274=CARTESIAN_POINT('Ctrl Pts',(-135.083325720174,-4.75925038136761,
135.385143480741));
#259275=CARTESIAN_POINT('Ctrl Pts',(-135.361773343986,1.28145127501926,
137.284477781773));
#259276=CARTESIAN_POINT('Ctrl Pts',(-135.640220967799,6.14456181203885,
133.228900980221));
#259277=CARTESIAN_POINT('Ctrl Pts',(-135.918668591612,5.36112022232688,
126.945290030769));
#259278=CARTESIAN_POINT('Ctrl Pts',(-136.197116215425,-0.348928946420584,
124.207976424505));
#259279=CARTESIAN_POINT('Ctrl Pts',(-136.475563839238,-5.73832945953392,
127.53241764038));
#259280=CARTESIAN_POINT('Ctrl Pts',(-136.754011463051,-5.85448553231475,
133.863614608987));
#259281=CARTESIAN_POINT('Ctrl Pts',(-137.032459086864,-0.590655408416443,
137.383506612345));
#259282=CARTESIAN_POINT('Ctrl Pts',(-137.310906710677,5.21595818069537,
134.857484855651));
#259283=CARTESIAN_POINT('Ctrl Pts',(-137.58935433449,6.22936101547165,128.606839930282));
#259284=CARTESIAN_POINT('Ctrl Pts',(-137.867801958302,1.51828539823306,
124.375609161675));
#259285=CARTESIAN_POINT('Ctrl Pts',(-138.146249582115,-4.58802032761614,
126.052086919061));
#259286=CARTESIAN_POINT('Ctrl Pts',(-138.424697205928,-6.47815950964009,
132.095672043897));
#259287=CARTESIAN_POINT('Ctrl Pts',(-138.703144829741,-2.41518657799051,
136.952605052004));
#259288=CARTESIAN_POINT('Ctrl Pts',(-138.981592453554,3.86722483040823,
136.159601783301));
#259289=CARTESIAN_POINT('Ctrl Pts',(-139.260040077367,6.59584554409815,
130.445393501362));
#259290=CARTESIAN_POINT('Ctrl Pts',(-139.53848770118,3.26320642772972,125.061058462695));
#259291=CARTESIAN_POINT('Ctrl Pts',(-139.816935324993,-3.06815997922566,
124.954537528447));
#259292=CARTESIAN_POINT('Ctrl Pts',(-140.095382948806,-6.58003725322031,
130.223718233352));
#259293=CARTESIAN_POINT('Ctrl Pts',(-140.373830572619,-4.04518174419624,
136.026480923393));
#259294=CARTESIAN_POINT('Ctrl Pts',(-140.652278196431,2.20699816962987,
137.030370167137));
#259295=CARTESIAN_POINT('Ctrl Pts',(-140.930725820244,6.43105458342049,
132.312860792301));
#259296=CARTESIAN_POINT('Ctrl Pts',(-141.209173444057,4.74528600953044,
126.209113451214));
#259297=CARTESIAN_POINT('Ctrl Pts',(-141.48762106787,-1.30116858700904,
124.328173765698));
#259298=CARTESIAN_POINT('Ctrl Pts',(-141.766068691683,-6.15191281770628,
128.398533417733));
#259299=CARTESIAN_POINT('Ctrl Pts',(-142.044516315496,-5.34934970658085,
134.679730735221));
#259300=CARTESIAN_POINT('Ctrl Pts',(-142.322963939309,0.369004454631186,
137.399652236939));
#259301=CARTESIAN_POINT('Ctrl Pts',(-142.601411563122,5.74826154890666,
134.058822938361));
#259302=CARTESIAN_POINT('Ctrl Pts',(-142.879859186934,5.84514709792562,
127.727301756295));
#259303=CARTESIAN_POINT('Ctrl Pts',(-143.158306810748,0.570628015260733,
124.223447345055));
#259304=CARTESIAN_POINT('Ctrl Pts',(-143.43675443456,-5.22827033670001,
126.767130735766));
#259305=CARTESIAN_POINT('Ctrl Pts',(-143.715202058373,-6.22264366443886,
133.020831158207));
#259306=CARTESIAN_POINT('Ctrl Pts',(-143.993649682186,-1.49871145760156,
137.237703434405));
#259307=CARTESIAN_POINT('Ctrl Pts',(-144.272097305999,4.60246336264661,
135.542647948195));
#259308=CARTESIAN_POINT('Ctrl Pts',(-144.550544929812,6.47419919545755,
129.493337883343));
#259309=CARTESIAN_POINT('Ctrl Pts',(-144.828992553625,2.39646224985712,
124.648793664219));
#259310=CARTESIAN_POINT('Ctrl Pts',(-145.107440177438,-3.8835064296727,
125.460914759058));
#259311=CARTESIAN_POINT('Ctrl Pts',(-145.38588780125,-6.59472242016944,
131.183401556022));
#259312=CARTESIAN_POINT('Ctrl Pts',(-145.664335425064,-3.24571067663155,
136.557568247724));
#259313=CARTESIAN_POINT('Ctrl Pts',(-145.942783048876,3.08595061694992,
136.644818187128));
#259314=CARTESIAN_POINT('Ctrl Pts',(-146.221230672689,6.58177405062243,
131.364972942318));
#259315=CARTESIAN_POINT('Ctrl Pts',(-146.499678296502,4.02926866931097,
125.569952358496));
#259316=CARTESIAN_POINT('Ctrl Pts',(-146.778125920315,-2.22593777837984,
124.585097249699));
#259317=CARTESIAN_POINT('Ctrl Pts',(-147.056573544128,-6.43561615084533,
129.315441348065));
#259318=CARTESIAN_POINT('Ctrl Pts',(-147.335021167941,-4.73127767801157,
135.414029517352));
#259319=CARTESIAN_POINT('Ctrl Pts',(-147.613468791753,1.32087384515067,
137.276557162581));
#259320=CARTESIAN_POINT('Ctrl Pts',(-147.891916415567,6.15920683289404,
133.191452367319));
#259321=CARTESIAN_POINT('Ctrl Pts',(-148.170364039379,5.33752963518947,
126.91272686995));
#259322=CARTESIAN_POINT('Ctrl Pts',(-148.448811663193,-0.389076544435395,
124.210222669761));
#259323=CARTESIAN_POINT('Ctrl Pts',(-148.727259287005,-5.75814038716998,
127.567409102056));
#259324=CARTESIAN_POINT('Ctrl Pts',(-149.005706910818,-5.83575451489182,
133.899195843233));
#259325=CARTESIAN_POINT('Ctrl Pts',(-149.284154534631,-0.550595335885521,
137.386980203127));
#259326=CARTESIAN_POINT('Ctrl Pts',(-149.562602158444,5.24053405872261,
134.825658742734));
#259327=CARTESIAN_POINT('Ctrl Pts',(-149.841049782257,6.21586866768539,
128.568960756646));
#259328=CARTESIAN_POINT('Ctrl Pts',(-150.119497406069,1.47912363311174,
124.366486037389));
#259329=CARTESIAN_POINT('Ctrl Pts',(-150.397945029883,-4.61686376108527,
126.080103549656));
#259330=CARTESIAN_POINT('Ctrl Pts',(-150.676392653695,-6.4701789051783,
132.135082514543));
#259331=CARTESIAN_POINT('Ctrl Pts',(-150.954840277509,-2.37771572122463,
136.967193065487));
#259332=CARTESIAN_POINT('Ctrl Pts',(-151.233287901321,3.89975205266408,
136.135961667893));
#259333=CARTESIAN_POINT('Ctrl Pts',(-151.511735525134,6.59353820363339,
130.405249368239));
#259334=CARTESIAN_POINT('Ctrl Pts',(-151.790183148947,3.22818485771248,
125.041300809049));
#259335=CARTESIAN_POINT('Ctrl Pts',(-152.06863077276,-3.10371266684865,
124.97332267276));
#259336=CARTESIAN_POINT('Ctrl Pts',(-152.347078396573,-6.58344987536885,
130.263783545709));
#259337=CARTESIAN_POINT('Ctrl Pts',(-152.625526020386,-4.01331826783166,
136.051008339035));
#259338=CARTESIAN_POINT('Ctrl Pts',(-152.903973644199,2.24485676634579,
137.016820189321));
#259339=CARTESIAN_POINT('Ctrl Pts',(-153.182421268012,6.44011809960154,
132.273685188686));
#259340=CARTESIAN_POINT('Ctrl Pts',(-153.460868891824,4.71722551658265,
126.180312687687));
#259341=CARTESIAN_POINT('Ctrl Pts',(-153.739316515637,-1.34056686689732,
124.336214336947));
#259342=CARTESIAN_POINT('Ctrl Pts',(-154.01776413945,-6.16644379003131,
128.436026431582));
#259343=CARTESIAN_POINT('Ctrl Pts',(-154.296211763263,-5.32566011765276,
134.712221943579));
#259344=CARTESIAN_POINT('Ctrl Pts',(-154.574659387076,0.409145029887599,
137.397283806609));
#259345=CARTESIAN_POINT('Ctrl Pts',(-154.853107010889,5.7679658828075,134.023771341112));
#259346=CARTESIAN_POINT('Ctrl Pts',(-155.131554634702,5.82630787022557,
127.691777697632));
#259347=CARTESIAN_POINT('Ctrl Pts',(-155.410002258515,0.530557555869813,
124.220095699443));
#259348=CARTESIAN_POINT('Ctrl Pts',(-155.688449882327,-5.25274923315307,
126.799031501784));
#259349=CARTESIAN_POINT('Ctrl Pts',(-155.96689750614,-6.20903608797397,
133.058669090323));
#259350=CARTESIAN_POINT('Ctrl Pts',(-156.245345129953,-1.4595221062231,
137.246707321489));
#259351=CARTESIAN_POINT('Ctrl Pts',(-156.523792753766,4.63122138952822,
135.514543657883));
#259352=CARTESIAN_POINT('Ctrl Pts',(-156.802240377579,6.46609867604585,
129.453951885458));
#259353=CARTESIAN_POINT('Ctrl Pts',(-157.080688001392,2.35894716575843,
124.634319766706));
#259354=CARTESIAN_POINT('Ctrl Pts',(-157.359135625205,-3.9159615488849,
125.484653766641));
#259355=CARTESIAN_POINT('Ctrl Pts',(-157.637583249018,-6.59229290546042,
131.223538480449));
#259356=CARTESIAN_POINT('Ctrl Pts',(-157.916030872831,-3.21062913332988,
136.577219216243));
#259357=CARTESIAN_POINT('Ctrl Pts',(-158.194478496644,3.12144596437753,
136.625924919674));
#259358=CARTESIAN_POINT('Ctrl Pts',(-158.472926120456,6.58506471193526,
131.324897428694));
#259359=CARTESIAN_POINT('Ctrl Pts',(-158.751373744269,3.99733068751967,
125.545522037924));
#259360=CARTESIAN_POINT('Ctrl Pts',(-159.029821368082,-2.26375495826568,
124.598762393297));
#259361=CARTESIAN_POINT('Ctrl Pts',(-159.308268991895,-6.44456038798308,
129.354644356446));
#259362=CARTESIAN_POINT('Ctrl Pts',(-159.586716615708,-4.7031296554214,
135.442744740987));
#259363=CARTESIAN_POINT('Ctrl Pts',(-159.865164239521,1.36024746981527,
137.268396713766));
#259364=CARTESIAN_POINT('Ctrl Pts',(-160.143611863334,6.17362362207528,
133.153915299856));
#259365=CARTESIAN_POINT('Ctrl Pts',(-160.422059487147,5.31374126392856,
126.880307915048));
#259366=CARTESIAN_POINT('Ctrl Pts',(-160.70050711096,-0.429209725076344,
124.212713263223));
#259367=CARTESIAN_POINT('Ctrl Pts',(-160.978954734773,-5.77773794479658,
127.602520510164));
#259368=CARTESIAN_POINT('Ctrl Pts',(-161.257402358585,-5.81680725143943,
133.934662397221));
#259369=CARTESIAN_POINT('Ctrl Pts',(-161.535849982398,-0.51051486084124,
137.390209872519));
#259370=CARTESIAN_POINT('Ctrl Pts',(-161.814297606211,5.26491574683228,
134.793683619137));
#259371=CARTESIAN_POINT('Ctrl Pts',(-162.092745230024,6.20214598860049,
128.531164416574));
#259372=CARTESIAN_POINT('Ctrl Pts',(-162.371192853837,1.43990705852047,
124.357601470914));
#259373=CARTESIAN_POINT('Ctrl Pts',(-162.64964047765,-4.64553611496906,
126.108295239334));
#259374=CARTESIAN_POINT('Ctrl Pts',(-162.928088101462,-6.46195854585841,
132.1744436748));
#259375=CARTESIAN_POINT('Ctrl Pts',(-163.206535725276,-2.34015675732853,
136.981552712947));
#259376=CARTESIAN_POINT('Ctrl Pts',(-163.484983349088,3.93213476817268,
136.112123988049));
#259377=CARTESIAN_POINT('Ctrl Pts',(-163.763430972902,6.5909865371863,130.365120024332));
#259378=CARTESIAN_POINT('Ctrl Pts',(-164.041878596714,3.19304366611785,
125.021756707701));
#259379=CARTESIAN_POINT('Ctrl Pts',(-164.320326220527,-3.13915034525769,
124.99232388833));
#259380=CARTESIAN_POINT('Ctrl Pts',(-164.59877384434,-6.58661854536123,
130.303868889347));
#259381=CARTESIAN_POINT('Ctrl Pts',(-164.877221468153,-3.98130607648258,
136.075341338217));
#259382=CARTESIAN_POINT('Ctrl Pts',(-165.155669091966,2.28263217906914,
137.003040006531));
#259383=CARTESIAN_POINT('Ctrl Pts',(-165.434116715779,6.44894297483741,
132.23445513871));
#259384=CARTESIAN_POINT('Ctrl Pts',(-165.712564339591,4.6889902251094,126.151683269957));
#259385=CARTESIAN_POINT('Ctrl Pts',(-165.991011963405,-1.37991547158711,
124.344494587733));
#259386=CARTESIAN_POINT('Ctrl Pts',(-166.269459587217,-6.18074626251326,
128.473607204924));
#259387=CARTESIAN_POINT('Ctrl Pts',(-166.54790721103,-5.3017731844313,134.744568344699));
#259388=CARTESIAN_POINT('Ctrl Pts',(-166.826354834843,0.449270444124704,
137.394671073086));
#259389=CARTESIAN_POINT('Ctrl Pts',(-167.104802458656,5.78745648261092,
133.988600447415));
#259390=CARTESIAN_POINT('Ctrl Pts',(-167.383250082469,5.8072527465451,127.656368976875));
#259391=CARTESIAN_POINT('Ctrl Pts',(-167.661697706282,0.490467436472931,
124.216988036188));
#259392=CARTESIAN_POINT('Ctrl Pts',(-167.940145330095,-5.27703348705155,
126.831080686747));
#259393=CARTESIAN_POINT('Ctrl Pts',(-168.218592953908,-6.19519843339338,
133.096423488211));
#259394=CARTESIAN_POINT('Ctrl Pts',(-168.49704057772,-1.42027867171577,
137.255472485049));
#259395=CARTESIAN_POINT('Ctrl Pts',(-168.775488201534,4.65980780479824,
135.486264830004));
#259396=CARTESIAN_POINT('Ctrl Pts',(-169.053935825346,6.45775855296945,
129.414615927465));
#259397=CARTESIAN_POINT('Ctrl Pts',(-169.332383449159,2.32134467000579,
124.620074502325));
#259398=CARTESIAN_POINT('Ctrl Pts',(-169.610831072972,-3.94827156070164,
125.508589897919));
#259399=CARTESIAN_POINT('Ctrl Pts',(-169.889278696785,-6.58961911091297,
131.263659872085));
#259400=CARTESIAN_POINT('Ctrl Pts',(-170.167726320598,-3.17542861898582,
136.596656269364));
#259401=CARTESIAN_POINT('Ctrl Pts',(-170.446173944411,3.15682564547787,
136.606815932013));
#259402=CARTESIAN_POINT('Ctrl Pts',(-170.724621568223,6.58811136125304,
131.284802626386));
#259403=CARTESIAN_POINT('Ctrl Pts',(-171.003069192037,3.96524458316956,
125.521286585549));
#259404=CARTESIAN_POINT('Ctrl Pts',(-171.28151681585,-2.30148825387982,
124.612657487621));
#259405=CARTESIAN_POINT('Ctrl Pts',(-171.559964439662,-6.45326581956532,
129.393901084596));
#259406=CARTESIAN_POINT('Ctrl Pts',(-171.838412063475,-4.67480735663214,
135.471288087592));
#259407=CARTESIAN_POINT('Ctrl Pts',(-172.116859687288,1.39957069001038,
137.259996737715));
#259408=CARTESIAN_POINT('Ctrl Pts',(-172.395307311101,6.18781164536257,
133.116291168777));
#259409=CARTESIAN_POINT('Ctrl Pts',(-172.673754934914,5.289755990031,126.848034367363));
#259410=CARTESIAN_POINT('Ctrl Pts',(-172.952202558727,-0.469327001192524,
124.215448112602));
#259411=CARTESIAN_POINT('Ctrl Pts',(-173.23065018254,-5.79712140621875,
127.637750563632));
#259412=CARTESIAN_POINT('Ctrl Pts',(-173.509097806352,-5.79764444405506,
133.970012956726));
#259413=CARTESIAN_POINT('Ctrl Pts',(-173.787545430165,-0.470415468481743,
137.393195500846));
#259414=CARTESIAN_POINT('Ctrl Pts',(-174.065993053978,5.28910234155359,
134.76156066971));
#259415=CARTESIAN_POINT('Ctrl Pts',(-174.344440677791,6.18819348671444,
128.493452310623));
#259416=CARTESIAN_POINT('Ctrl Pts',(-174.622888301604,1.40063712764339,
124.34895579147));
#259417=CARTESIAN_POINT('Ctrl Pts',(-174.901335925417,-4.67403632680454,
126.13666094344));
#259418=CARTESIAN_POINT('Ctrl Pts',(-175.17978354923,-6.45349873628761,
132.213754066126));
#259419=CARTESIAN_POINT('Ctrl Pts',(-175.458231173043,-2.30251107806296,
136.995683462282));
#259420=CARTESIAN_POINT('Ctrl Pts',(-175.736678796856,3.96437177698222,
136.088089627079));
#259421=CARTESIAN_POINT('Ctrl Pts',(-176.015126420669,6.58819063930867,
130.325006956645));
#259422=CARTESIAN_POINT('Ctrl Pts',(-176.293574044481,3.15778415511627,
125.002426882869));
#259423=CARTESIAN_POINT('Ctrl Pts',(-176.572021668294,-3.17447170129595,
125.011540471058));
#259424=CARTESIAN_POINT('Ctrl Pts',(-176.850469292107,-6.58954314578118,
130.343972778891));
#259425=CARTESIAN_POINT('Ctrl Pts',(-177.12891691592,-3.94914635637289,
136.099479019269));
#259426=CARTESIAN_POINT('Ctrl Pts',(-177.407364539733,2.32032300801719,
136.989030129397));
#259427=CARTESIAN_POINT('Ctrl Pts',(-177.685812163546,6.45752888212044,
132.195172096054));
#259428=CARTESIAN_POINT('Ctrl Pts',(-177.964259787359,4.66058118137817,
126.123226258898));
#259429=CARTESIAN_POINT('Ctrl Pts',(-178.242707411172,-1.41921294300185,
124.353014211231));
#259430=CARTESIAN_POINT('Ctrl Pts',(-178.521155034985,-6.19481970517025,
128.511274345191));
#259431=CARTESIAN_POINT('Ctrl Pts',(-178.799602658797,-5.27768979205393,
134.776768739972));
#259432=CARTESIAN_POINT('Ctrl Pts',(-179.078050282611,0.489379210479558,
137.391814133187));
#259433=CARTESIAN_POINT('Ctrl Pts',(-179.356497906423,5.80673262608622,
133.95331156054));
#259434=CARTESIAN_POINT('Ctrl Pts',(-179.634945530236,5.7879824329786,127.621076906106));
#259435=CARTESIAN_POINT('Ctrl Pts',(-179.913393154049,0.450359142625426,
124.214124470449));
#259436=CARTESIAN_POINT('Ctrl Pts',(-180.191840777862,-5.30112219853358,
126.863277103057));
#259437=CARTESIAN_POINT('Ctrl Pts',(-180.470288401675,-6.18113121345664,
133.134092952866));
#259438=CARTESIAN_POINT('Ctrl Pts',(-180.748736025488,-1.38098260826046,
137.263998600285));
#259439=CARTESIAN_POINT('Ctrl Pts',(-181.0271836493,4.68822154917632,135.457812512445));
#259440=CARTESIAN_POINT('Ctrl Pts',(-181.305631273113,6.44917913527537,
129.375331466973));
#259441=CARTESIAN_POINT('Ctrl Pts',(-181.584078896926,2.28365615597197,
124.606058398942));
#259442=CARTESIAN_POINT('Ctrl Pts',(-181.862526520739,-3.98043526786393,
125.532722265928));
#259443=CARTESIAN_POINT('Ctrl Pts',(-182.140974144552,-6.58670113560653,
131.303764244219));
#259444=CARTESIAN_POINT('Ctrl Pts',(-182.419421768365,-3.14011043796568,
136.615878686839));
#259445=CARTESIAN_POINT('Ctrl Pts',(-182.697869392178,3.19208834924215,
136.587491932238));
#259446=CARTESIAN_POINT('Ctrl Pts',(-182.976317015991,6.59091388568205,
131.244690021124));
#259447=CARTESIAN_POINT('Ctrl Pts',(-183.254764639804,3.93301154522339,
125.497246899427));
#259448=CARTESIAN_POINT('Ctrl Pts',(-183.533212263617,-2.33913626699958,
124.626782017781));
#259449=CARTESIAN_POINT('Ctrl Pts',(-183.811659887429,-6.46173212300977,
129.433210077844));
#259450=CARTESIAN_POINT('Ctrl Pts',(-184.090107511242,-4.64631183113728,
135.499658499484));
#259451=CARTESIAN_POINT('Ctrl Pts',(-184.368555135055,1.43884204859816,
137.251357545694));
#259452=CARTESIAN_POINT('Ctrl Pts',(-184.647002758868,6.20177037701405,
133.078581368264));
#259453=CARTESIAN_POINT('Ctrl Pts',(-184.925450382681,5.26557470227994,
126.815907422802));
#259454=CARTESIAN_POINT('Ctrl Pts',(-185.203898006494,-0.50942688622466,
124.218427116558));
#259455=CARTESIAN_POINT('Ctrl Pts',(-185.482345630307,-5.81629005317544,
127.673097957001));
#259456=CARTESIAN_POINT('Ctrl Pts',(-185.76079325412,-5.77826680282389,
134.005246211819));
#259457=CARTESIAN_POINT('Ctrl Pts',(-186.039240877932,-0.430298644703365,
137.395936977472));
#259458=CARTESIAN_POINT('Ctrl Pts',(-186.317688501746,5.31309294664177,
134.729291084778));
#259459=CARTESIAN_POINT('Ctrl Pts',(-186.596136125558,6.17401167904375,
128.455825836229));
#259460=CARTESIAN_POINT('Ctrl Pts',(-186.874583749371,1.36131529564269,
124.340549319425));
#259461=CARTESIAN_POINT('Ctrl Pts',(-187.153031373184,-4.70236334050424,
126.165199610876));
#259462=CARTESIAN_POINT('Ctrl Pts',(-187.431478996997,-6.44479978994851,
132.253012231859));
#259463=CARTESIAN_POINT('Ctrl Pts',(-187.70992662081,-2.26478007840253,
137.009584789872));
#259464=CARTESIAN_POINT('Ctrl Pts',(-187.988374244623,3.99646188453734,
136.063859475589));
#259465=CARTESIAN_POINT('Ctrl Pts',(-188.266821868436,6.58515061360439,
130.284911651585));
#259466=CARTESIAN_POINT('Ctrl Pts',(-188.545269492249,3.12240763126122,
124.983312050825));
#259467=CARTESIAN_POINT('Ctrl Pts',(-188.823717116061,-3.20967542611822,
125.030971708867));
#259468=CARTESIAN_POINT('Ctrl Pts',(-189.102164739874,-6.59222356825658,
130.384093728275));
#259469=CARTESIAN_POINT('Ctrl Pts',(-189.380612363687,-3.91684029919248,
136.123420487763));
#259470=CARTESIAN_POINT('Ctrl Pts',(-189.6590599875,2.35792785654334,136.974791077059));
#259471=CARTESIAN_POINT('Ctrl Pts',(-189.937507611313,6.46587550329532,
132.155837516369));
#259472=CARTESIAN_POINT('Ctrl Pts',(-190.215955235126,4.63199943809816,
126.094942708994));
#259473=CARTESIAN_POINT('Ctrl Pts',(-190.494402858939,-1.45845782495887,
124.361772891742));
#259474=CARTESIAN_POINT('Ctrl Pts',(-190.772850482752,-6.2086635965042,
128.549026456613));
#259475=CARTESIAN_POINT('Ctrl Pts',(-191.051298106565,-5.25341083294129,
134.808821936201));
#259476=CARTESIAN_POINT('Ctrl Pts',(-191.329745730377,0.529469842708527,
137.388713092773));
#259477=CARTESIAN_POINT('Ctrl Pts',(-191.60819335419,5.82579359894846,133.91790598813));
#259478=CARTESIAN_POINT('Ctrl Pts',(-191.886640978003,5.76849764359442,
127.585902793086));
#259479=CARTESIAN_POINT('Ctrl Pts',(-192.165088601816,0.410234160553658,
124.211505108333));
#259480=CARTESIAN_POINT('Ctrl Pts',(-192.443536225629,-5.32501447498302,
126.895619557667));
#259481=CARTESIAN_POINT('Ctrl Pts',(-192.721983849442,-6.16683494942961,
133.171676088433));
#259482=CARTESIAN_POINT('Ctrl Pts',(-193.000431473255,-1.34163537198624,
137.272285351261));
#259483=CARTESIAN_POINT('Ctrl Pts',(-193.278879097068,4.71646156978089,
135.429187759513));
#259484=CARTESIAN_POINT('Ctrl Pts',(-193.557326720881,6.44036074087642,
129.336099959682));
#259485=CARTESIAN_POINT('Ctrl Pts',(-193.835774344694,2.24588302022023,
124.592271975924));
#259486=CARTESIAN_POINT('Ctrl Pts',(-194.114221968506,-4.01245147853337,
125.557049976435));
#259487=CARTESIAN_POINT('Ctrl Pts',(-194.392669592319,-6.58353908766677,
131.343850110767));
#259488=CARTESIAN_POINT('Ctrl Pts',(-194.671117216133,-3.10467589899933,
136.634885756375));
#259489=CARTESIAN_POINT('Ctrl Pts',(-194.949564839945,3.22723276899961,
136.567953636405));
#259490=CARTESIAN_POINT('Ctrl Pts',(-195.228012463758,6.59347218137276,
131.204561099293));
#259491=CARTESIAN_POINT('Ctrl Pts',(-195.506460087571,3.90063276808784,
125.473403870355));
#259492=CARTESIAN_POINT('Ctrl Pts',(-195.784907711384,-2.3766976025655,
124.641135460387));
#259493=CARTESIAN_POINT('Ctrl Pts',(-196.063355335197,-6.46995898459376,
129.472569879579));
#259494=CARTESIAN_POINT('Ctrl Pts',(-196.34180295901,-4.61764413484867,
135.527854925386));
#259495=CARTESIAN_POINT('Ctrl Pts',(-196.620250582823,1.47806009036541,
137.242479457832));
#259496=CARTESIAN_POINT('Ctrl Pts',(-196.898698206635,6.21549929978325,
133.040787295662));
#259497=CARTESIAN_POINT('Ctrl Pts',(-197.177145830448,5.24119829672186,
126.783928271841));
#259498=CARTESIAN_POINT('Ctrl Pts',(-197.455593454261,-0.5495078942556,
124.2216501647));
#259499=CARTESIAN_POINT('Ctrl Pts',(-197.734041078074,-5.83524317536515,
127.708561380459));
#259500=CARTESIAN_POINT('Ctrl Pts',(-198.012488701887,-5.75867504579123,
134.040360856918));
#259501=CARTESIAN_POINT('Ctrl Pts',(-198.2909363257,-0.390165876051177,
137.398434200813));
#259502=CARTESIAN_POINT('Ctrl Pts',(-198.569383949513,5.33688667311775,
134.696876060105));
#259503=CARTESIAN_POINT('Ctrl Pts',(-198.847831573325,6.15960109109908,
128.418286387655));
#259504=CARTESIAN_POINT('Ctrl Pts',(-199.126279197139,1.32194301960288,
124.332382366286));
#259505=CARTESIAN_POINT('Ctrl Pts',(-199.404726820951,-4.73051610640191,
126.193910184127));
#259506=CARTESIAN_POINT('Ctrl Pts',(-199.683174444764,-6.43586202918244,
132.292216717274));
#259507=CARTESIAN_POINT('Ctrl Pts',(-199.961622068577,-2.22696515648391,
137.023256180599));
#259508=CARTESIAN_POINT('Ctrl Pts',(-200.24006969239,4.02840390172748,136.039434431435));
#259509=CARTESIAN_POINT('Ctrl Pts',(-200.518517316203,6.58186657272242,
130.244835594899));
#259510=CARTESIAN_POINT('Ctrl Pts',(-200.796964940016,3.08691540544346,
124.964412919876));
#259511=CARTESIAN_POINT('Ctrl Pts',(-201.075412563829,-3.24476021523692,
125.050616881724));
#259512=CARTESIAN_POINT('Ctrl Pts',(-201.353860187642,-6.59465971346335,
130.424230250803));
#259513=CARTESIAN_POINT('Ctrl Pts',(-201.632307811455,-3.88438910205457,
136.147164856536));
#259514=CARTESIAN_POINT('Ctrl Pts',(-201.910755435267,2.39544533118521,
136.960323377152));
#259515=CARTESIAN_POINT('Ctrl Pts',(-202.18920305908,6.47398252907625,132.116452857208));
#259516=CARTESIAN_POINT('Ctrl Pts',(-202.467650682893,4.60324605437475,
126.066833668302));
#259517=CARTESIAN_POINT('Ctrl Pts',(-202.746098306706,-1.49764866322506,
124.370770304711));
#259518=CARTESIAN_POINT('Ctrl Pts',(-203.024545930519,-6.22227742352606,
128.586862140274));
#259519=CARTESIAN_POINT('Ctrl Pts',(-203.302993554332,-5.22893720675747,
134.840726745644));
#259520=CARTESIAN_POINT('Ctrl Pts',(-203.581441178145,0.569540855237039,
137.385368066758));
#259521=CARTESIAN_POINT('Ctrl Pts',(-203.859888801958,5.84463869488665,
133.882385042152));
#259522=CARTESIAN_POINT('Ctrl Pts',(-204.138336425771,5.7487991004088,127.550847941203));
#259523=CARTESIAN_POINT('Ctrl Pts',(-204.416784049583,0.370093977104817,
124.209130046901));
#259524=CARTESIAN_POINT('Ctrl Pts',(-204.695231673396,-5.34870943106288,
126.928106852114));
#259525=CARTESIAN_POINT('Ctrl Pts',(-204.973679297209,-6.15231017106575,
133.209171502253));
#259526=CARTESIAN_POINT('Ctrl Pts',(-205.252126921022,-1.30223842092043,
137.280332430907));
#259527=CARTESIAN_POINT('Ctrl Pts',(-205.530574544835,4.74452682016742,
135.400391631911));
#259528=CARTESIAN_POINT('Ctrl Pts',(-205.809022168648,6.43130369654214,
129.296922859329));
#259529=CARTESIAN_POINT('Ctrl Pts',(-206.087469792461,2.20802666244648,
124.578715744137));
#259530=CARTESIAN_POINT('Ctrl Pts',(-206.365917416273,-4.04431900633787,
125.581572127967));
#259531=CARTESIAN_POINT('Ctrl Pts',(-206.644365040087,-6.58013308426553,
131.383915986335));
#259532=CARTESIAN_POINT('Ctrl Pts',(-206.922812663899,-3.06912631512495,
136.653676773657));
#259533=CARTESIAN_POINT('Ctrl Pts',(-207.201260287713,3.26225760245914,
136.548201768512));
#259534=CARTESIAN_POINT('Ctrl Pts',(-207.479707911525,6.59578615352751,
131.164417347887));
#259535=CARTESIAN_POINT('Ctrl Pts',(-207.758155535338,3.86810945157081,
125.449758381845));
#259536=CARTESIAN_POINT('Ctrl Pts',(-208.036603159151,-2.41417086872696,
124.655717283569));
#259537=CARTESIAN_POINT('Ctrl Pts',(-208.315050782964,-6.47794609946865,
129.511979031309));
#259538=CARTESIAN_POINT('Ctrl Pts',(-208.593498406777,-4.58880533005852,
135.555876320469));
#259539=CARTESIAN_POINT('Ctrl Pts',(-208.87194603059,1.51722336207232,137.233362803106));
#259540=CARTESIAN_POINT('Ctrl Pts',(-209.150393654402,6.22899790494034,
133.00291035145));
#259541=CARTESIAN_POINT('Ctrl Pts',(-209.428841278216,5.21662767663345,
126.752098099478));
#259542=CARTESIAN_POINT('Ctrl Pts',(-209.707288902028,-0.589568540070009,
124.225117137599));
#259543=CARTESIAN_POINT('Ctrl Pts',(-209.985736525842,-5.85398007047323,
127.744139519898));
#259544=CARTESIAN_POINT('Ctrl Pts',(-210.264184149654,-5.73886989893714,
134.07535559084));
#259545=CARTESIAN_POINT('Ctrl Pts',(-210.542631773467,-0.350018649658268,
137.400687078332));
#259546=CARTESIAN_POINT('Ctrl Pts',(-210.82107939728,5.36048263929459,134.664316796842));
#259547=CARTESIAN_POINT('Ctrl Pts',(-211.099527021093,6.14496225687153,
128.38083535594));
#259548=CARTESIAN_POINT('Ctrl Pts',(-211.377974644906,1.28252175847855,
124.324455234681));
#259549=CARTESIAN_POINT('Ctrl Pts',(-211.656422268719,-4.75849358128477,
126.222791599316));
#259550=CARTESIAN_POINT('Ctrl Pts',(-211.934869892531,-6.4266857851828,
132.331366069634));
#259551=CARTESIAN_POINT('Ctrl Pts',(-212.213317516344,-2.18906771355195,
137.036697127864));
#259552=CARTESIAN_POINT('Ctrl Pts',(-212.491765140157,4.06019664492976,
136.014815399695));
#259553=CARTESIAN_POINT('Ctrl Pts',(-212.770212763971,6.57833863835413,
130.204780271616));
#259554=CARTESIAN_POINT('Ctrl Pts',(-213.048660387783,3.05130879283982,
124.945730190337));
#259555=CARTESIAN_POINT('Ctrl Pts',(-213.327108011596,-3.27972476857289,
125.070475261673));
#259556=CARTESIAN_POINT('Ctrl Pts',(-213.605555635409,-6.59685149112928,
130.464380859201));
#259557=CARTESIAN_POINT('Ctrl Pts',(-213.884003259222,-3.85179396744981,
136.170711245733));
#259558=CARTESIAN_POINT('Ctrl Pts',(-214.162450883035,2.43287404171984,
136.94562756578));
#259559=CARTESIAN_POINT('Ctrl Pts',(-214.440898506847,6.48184965905313,
132.077019577989));
#259560=CARTESIAN_POINT('Ctrl Pts',(-214.71934613066,4.57432209567675,126.038900178414));
#259561=CARTESIAN_POINT('Ctrl Pts',(-214.997793754473,-1.53678400556905,
124.380006116735));
#259562=CARTESIAN_POINT('Ctrl Pts',(-215.276241378286,-6.23566068176903,
128.624779994154));
#259563=CARTESIAN_POINT('Ctrl Pts',(-215.554689002099,-5.20426982038336,
134.872481986055));
#259564=CARTESIAN_POINT('Ctrl Pts',(-215.833136625912,0.609590763220439,
137.381779179092));
#259565=CARTESIAN_POINT('Ctrl Pts',(-216.111584249725,5.86326721558844,
133.846750038845));
#259566=CARTESIAN_POINT('Ctrl Pts',(-216.390031873537,5.72888753335829,
127.51591364943));
#259567=CARTESIAN_POINT('Ctrl Pts',(-216.668479497351,0.329940079686948,
124.206999374164));
#259568=CARTESIAN_POINT('Ctrl Pts',(-216.946927121163,-5.37220618874772,
126.960737782571));
#259569=CARTESIAN_POINT('Ctrl Pts',(-217.225374744977,-6.13755741658593,
133.246577804923));
#259570=CARTESIAN_POINT('Ctrl Pts',(-217.503822368789,-1.26279321493052,
137.288139541036));
#259571=CARTESIAN_POINT('Ctrl Pts',(-217.782269992602,4.77241626036792,
135.37142519669));
#259572=CARTESIAN_POINT('Ctrl Pts',(-218.060717616415,6.4220083378839,129.257801617636));
#259573=CARTESIAN_POINT('Ctrl Pts',(-218.339165240228,2.17008848543354,
124.565390205911));
#259574=CARTESIAN_POINT('Ctrl Pts',(-218.617612864041,-4.07603667041411,
125.606287811847));
#259575=CARTESIAN_POINT('Ctrl Pts',(-218.896060487854,-6.57648325161253,
131.423960386264));
#259576=CARTESIAN_POINT('Ctrl Pts',(-219.174508111666,-3.03346300364714,
136.672251042379));
#259577=CARTESIAN_POINT('Ctrl Pts',(-219.45295573548,3.29716155176439,136.528237060474));
#259578=CARTESIAN_POINT('Ctrl Pts',(-219.731403359293,6.59785571640026,
131.124260254445));
#259579=CARTESIAN_POINT('Ctrl Pts',(-220.009850983105,3.83544280083539,
125.426311310091));
#259580=CARTESIAN_POINT('Ctrl Pts',(-220.288298606918,-2.45155467689987,
124.67052694699));
#259581=CARTESIAN_POINT('Ctrl Pts',(-220.566746230731,-6.48569317166813,
129.551436072715));
#259582=CARTESIAN_POINT('Ctrl Pts',(-220.845193854544,-4.55979648539947,
135.58372164639));
#259583=CARTESIAN_POINT('Ctrl Pts',(-221.123641478357,1.55633041250914,
137.224007919343));
#259584=CARTESIAN_POINT('Ctrl Pts',(-221.40208910217,6.24226569228925,132.964951939167));
#259585=CARTESIAN_POINT('Ctrl Pts',(-221.680536725983,5.19186375248807,
126.720418085194));
#259586=CARTESIAN_POINT('Ctrl Pts',(-221.958984349796,-0.629607339204784,
124.228827906785));
#259587=CARTESIAN_POINT('Ctrl Pts',(-222.237431973609,-5.87250004419688,
127.779831056953));
#259588=CARTESIAN_POINT('Ctrl Pts',(-222.515879597421,-5.71885209614835,
134.110229116839));
#259589=CARTESIAN_POINT('Ctrl Pts',(-222.794327221234,-0.309858453196267,
137.402695526548));
#259590=CARTESIAN_POINT('Ctrl Pts',(-223.072774845047,5.38387997081673,
134.631614501482));
#259591=CARTESIAN_POINT('Ctrl Pts',(-223.35122246886,6.13009571880702,128.343474128844));
#259592=CARTESIAN_POINT('Ctrl Pts',(-223.629670092673,1.24305297303857,
124.316768218352));
#259593=CARTESIAN_POINT('Ctrl Pts',(-223.908117716486,-4.78629472843886,
126.25184278623));
#259594=CARTESIAN_POINT('Ctrl Pts',(-224.186565340298,-6.41727139797729,
132.370458838244));
#259595=CARTESIAN_POINT('Ctrl Pts',(-224.465012964112,-2.15108915391133,
137.049907133607));
#259596=CARTESIAN_POINT('Ctrl Pts',(-224.743460587925,4.09183893605206,
135.990003292637));
#259597=CARTESIAN_POINT('Ctrl Pts',(-225.021908211737,6.57456694122844,
130.164747166004));
#259598=CARTESIAN_POINT('Ctrl Pts',(-225.300355835551,3.01558911286705,
124.927264554503));
#259599=CARTESIAN_POINT('Ctrl Pts',(-225.578803459363,-3.31456779050113,
125.090546112851));
#259600=CARTESIAN_POINT('Ctrl Pts',(-225.857251083176,-6.5987988200372,
130.504544065675));
#259601=CARTESIAN_POINT('Ctrl Pts',(-226.135698706989,-3.8190561032033,
136.194058782834));
#259602=CARTESIAN_POINT('Ctrl Pts',(-226.414146330802,2.47021260121173,
136.930704187504));
#259603=CARTESIAN_POINT('Ctrl Pts',(-226.692593954615,6.48947660170784,
132.037539139922));
#259604=CARTESIAN_POINT('Ctrl Pts',(-226.971041578427,4.54522863379049,
126.011143274415));
#259605=CARTESIAN_POINT('Ctrl Pts',(-227.24948920224,-1.57586240181677,
124.389479985577));
#259606=CARTESIAN_POINT('Ctrl Pts',(-227.527936826054,-6.24881287531301,
128.662778613197));
#259607=CARTESIAN_POINT('Ctrl Pts',(-227.806384449866,-5.17940958787633,
134.904086480733));
#259608=CARTESIAN_POINT('Ctrl Pts',(-228.084832073679,0.649618082593193,
137.377946562762));
#259609=CARTESIAN_POINT('Ctrl Pts',(-228.363279697492,5.88167847076755,
133.811002298682));
#259610=CARTESIAN_POINT('Ctrl Pts',(-228.641727321305,5.70876368027354,
127.481101212267));
#259611=CARTESIAN_POINT('Ctrl Pts',(-228.920174945118,0.289773956218704,
124.205113169075));
#259612=CARTESIAN_POINT('Ctrl Pts',(-229.198622568931,-5.39550387735667,
126.993511139885));
#259613=CARTESIAN_POINT('Ctrl Pts',(-229.477070192744,-6.12257723265909,
133.283893610337));
#259614=CARTESIAN_POINT('Ctrl Pts',(-229.755517816557,-1.22330121567356,
137.295706392352));
#259615=CARTESIAN_POINT('Ctrl Pts',(-230.033965440369,4.80012885692891,
135.34228952721));
#259616=CARTESIAN_POINT('Ctrl Pts',(-230.312413064183,6.41247500934538,
129.218737684256));
#259617=CARTESIAN_POINT('Ctrl Pts',(-230.590860687995,2.13206989499296,
124.552295855027));
#259618=CARTESIAN_POINT('Ctrl Pts',(-230.869308311808,-4.10760329545278,
125.631196112227));
#259619=CARTESIAN_POINT('Ctrl Pts',(-231.147755935621,-6.5725897249546,
131.463981826697));
#259620=CARTESIAN_POINT('Ctrl Pts',(-231.426203559434,-2.99768728608136,
136.690607874263));
#259621=CARTESIAN_POINT('Ctrl Pts',(-231.704651183247,3.33194332353496,
136.508060252089));
#259622=CARTESIAN_POINT('Ctrl Pts',(-231.98309880706,6.59968079330357,131.084091307006));
#259623=CARTESIAN_POINT('Ctrl Pts',(-232.261546430872,3.80263402635669,
125.403063523931));
#259624=CARTESIAN_POINT('Ctrl Pts',(-232.539994054686,-2.48884764181187,
124.685563901874));
#259625=CARTESIAN_POINT('Ctrl Pts',(-232.818441678498,-6.49319991412244,
129.5909395417));
#259626=CARTESIAN_POINT('Ctrl Pts',(-233.096889302311,-4.53061867580467,
135.611389871331));
#259627=CARTESIAN_POINT('Ctrl Pts',(-233.375336926124,1.59537979255065,
137.214415153187));
#259628=CARTESIAN_POINT('Ctrl Pts',(-233.653784549937,6.25530217018742,
132.926913465378));
#259629=CARTESIAN_POINT('Ctrl Pts',(-233.93223217375,5.16690744192206,126.688889402902));
#259630=CARTESIAN_POINT('Ctrl Pts',(-234.210679797563,-0.669622808008655,
124.232782334755));
#259631=CARTESIAN_POINT('Ctrl Pts',(-234.489127421376,-5.89080241027189,
127.815634669064));
#259632=CARTESIAN_POINT('Ctrl Pts',(-234.767575045188,-5.69862237919218,
134.144980142666));
#259633=CARTESIAN_POINT('Ctrl Pts',(-235.046022669002,-0.269686774814632,
137.404459471037));
#259634=CARTESIAN_POINT('Ctrl Pts',(-235.324470292814,5.40707780068583,
134.598770385822));
#259635=CARTESIAN_POINT('Ctrl Pts',(-235.602917916627,6.11500202779203,
128.306204090801));
#259636=CARTESIAN_POINT('Ctrl Pts',(-235.88136554044,1.20353812581378,124.309321602146));
#259637=CARTESIAN_POINT('Ctrl Pts',(-236.159813164253,-4.81391851768082,
126.281062668365));
#259638=CARTESIAN_POINT('Ctrl Pts',(-236.438260788066,-6.40761921642086,
132.40949357451));
#259639=CARTESIAN_POINT('Ctrl Pts',(-236.716708411879,-2.11303088487057,
137.062885708328));
#259640=CARTESIAN_POINT('Ctrl Pts',(-236.995156035692,4.12332960257798,
135.964999029683));
#259641=CARTESIAN_POINT('Ctrl Pts',(-237.273603659505,6.57055162110693,
130.124737761504));
#259642=CARTESIAN_POINT('Ctrl Pts',(-237.552051283318,2.97975768913041,
124.909016696624));
#259643=CARTESIAN_POINT('Ctrl Pts',(-237.83049890713,-3.34928798990126,
125.110828691528));
#259644=CARTESIAN_POINT('Ctrl Pts',(-238.108946530943,-6.60050162802816,
130.544718381962));
#259645=CARTESIAN_POINT('Ctrl Pts',(-238.387394154756,-3.7861767224282,
136.217206602688));
#259646=CARTESIAN_POINT('Ctrl Pts',(-238.665841778569,2.5074596260677,136.915553795314));
#259647=CARTESIAN_POINT('Ctrl Pts',(-238.944289402382,6.49686307441993,
131.998013005973));
#259648=CARTESIAN_POINT('Ctrl Pts',(-239.222737026195,4.51596674678651,
125.983563984846));
#259649=CARTESIAN_POINT('Ctrl Pts',(-239.501184650008,-1.61488240390346,
124.399191560181));
#259650=CARTESIAN_POINT('Ctrl Pts',(-239.77963227382,-6.26173351679718,
128.700856589348));
#259651=CARTESIAN_POINT('Ctrl Pts',(-240.058079897633,-5.15435743044315,
134.935539058562));
#259652=CARTESIAN_POINT('Ctrl Pts',(-240.336527521446,0.689621330129741,
137.373870359787));
#259653=CARTESIAN_POINT('Ctrl Pts',(-240.614975145259,5.89987177818775,
133.775143146303));
#259654=CARTESIAN_POINT('Ctrl Pts',(-240.893422769072,5.68842828685113,
127.446411919705));
#259655=CARTESIAN_POINT('Ctrl Pts',(-241.171870392886,0.249597095069331,
124.203471501526));
#259656=CARTESIAN_POINT('Ctrl Pts',(-241.450318016698,-5.41860163358522,
127.026425709627));
#259657=CARTESIAN_POINT('Ctrl Pts',(-241.728765640511,-6.10737017438111,
133.321117535742));
#259658=CARTESIAN_POINT('Ctrl Pts',(-242.007213264324,-1.18376388654087,
137.303032704464));
#259659=CARTESIAN_POINT('Ctrl Pts',(-242.285660888137,4.82766358294966,
135.312985703106));
#259660=CARTESIAN_POINT('Ctrl Pts',(-242.56410851195,6.40270406418687,129.179732506718));
#259661=CARTESIAN_POINT('Ctrl Pts',(-242.842556135762,2.09397229991911,
124.539433176702));
#259662=CARTESIAN_POINT('Ctrl Pts',(-243.121003759575,-4.13901771174057,
125.65629610612));
#259663=CARTESIAN_POINT('Ctrl Pts',(-243.399451383388,-6.56845264856689,
131.503978824623));
#259664=CARTESIAN_POINT('Ctrl Pts',(-243.677899007202,-2.9618004881116,
136.70874658909));
#259665=CARTESIAN_POINT('Ctrl Pts',(-243.956346631013,3.36660162892119,
136.487672091016));
#259666=CARTESIAN_POINT('Ctrl Pts',(-244.234794254827,6.60126131660758,
131.043911994042));
#259667=CARTESIAN_POINT('Ctrl Pts',(-244.513241878639,3.76968434387551,
125.380015884821));
#259668=CARTESIAN_POINT('Ctrl Pts',(-244.791689502453,-2.52604838156001,
124.70082759102));
#259669=CARTESIAN_POINT('Ctrl Pts',(-245.070137126265,-6.50046604866569,
129.630487974449));
#259670=CARTESIAN_POINT('Ctrl Pts',(-245.348584750079,-4.50127298246883,
135.638879970036));
#259671=CARTESIAN_POINT('Ctrl Pts',(-245.627032373891,1.63437005520677,
137.204584860103));
#259672=CARTESIAN_POINT('Ctrl Pts',(-245.905479997704,6.26810685556324,
132.888796339615));
#259673=CARTESIAN_POINT('Ctrl Pts',(-246.183927621517,5.14175966970064,
126.65751322091));
#259674=CARTESIAN_POINT('Ctrl Pts',(-246.46237524533,-0.709613463692526,
124.236980274974));
#259675=CARTESIAN_POINT('Ctrl Pts',(-246.740822869143,-5.90888649049716,
127.851549029514));
#259676=CARTESIAN_POINT('Ctrl Pts',(-247.019270492956,-5.67818149768794,
134.179607380607));
#259677=CARTESIAN_POINT('Ctrl Pts',(-247.297718116769,-0.229505103091092,
137.405978846438));
#259678=CARTESIAN_POINT('Ctrl Pts',(-247.576165740581,5.43007526929941,
134.565785666913));
#259679=CARTESIAN_POINT('Ctrl Pts',(-247.854613364394,6.09968174312738,
128.269026622868));
#259680=CARTESIAN_POINT('Ctrl Pts',(-248.133060988207,1.16397868104094,
124.302115661998));
#259681=CARTESIAN_POINT('Ctrl Pts',(-248.41150861202,-4.84136392540264,
126.31045016297));
#259682=CARTESIAN_POINT('Ctrl Pts',(-248.689956235833,-6.39772959817725,
132.448468831983));
#259683=CARTESIAN_POINT('Ctrl Pts',(-248.968403859646,-2.07489431669385,
137.075632371099));
#259684=CARTESIAN_POINT('Ctrl Pts',(-249.246851483459,4.15466747760909,
135.939803537374));
#259685=CARTESIAN_POINT('Ctrl Pts',(-249.525299107272,6.56629282677857,
130.08475354068));
#259686=CARTESIAN_POINT('Ctrl Pts',(-249.803746731085,2.94381584937754,
124.890987292882));
#259687=CARTESIAN_POINT('Ctrl Pts',(-250.082194354898,-3.38388408020374,
125.131322246124));
#259688=CARTESIAN_POINT('Ctrl Pts',(-250.36064197871,-6.60195985200274,
130.584902319384));
#259689=CARTESIAN_POINT('Ctrl Pts',(-250.639089602524,-3.75315704348482,
136.240153847548));
#259690=CARTESIAN_POINT('Ctrl Pts',(-250.917537226336,2.54461373609029,
136.900176950603));
#259691=CARTESIAN_POINT('Ctrl Pts',(-251.19598485015,6.50400880347224,131.958442640812));
#259692=CARTESIAN_POINT('Ctrl Pts',(-251.474432473962,4.48653751899202,
125.956163331638));
#259693=CARTESIAN_POINT('Ctrl Pts',(-251.752880097775,-1.65384256596459,
124.409140480742));
#259694=CARTESIAN_POINT('Ctrl Pts',(-252.031327721588,-6.27442212737671,
128.739012511497));
#259695=CARTESIAN_POINT('Ctrl Pts',(-252.309775345401,-5.12911427652582,
134.966838554275));
#259696=CARTESIAN_POINT('Ctrl Pts',(-252.588222969213,0.729599023732927,
137.369550720794));
#259697=CARTESIAN_POINT('Ctrl Pts',(-252.866670593027,5.91784646323776,
133.739173911277));
#259698=CARTESIAN_POINT('Ctrl Pts',(-253.145118216839,5.66788210748017,
127.411847055674));
#259699=CARTESIAN_POINT('Ctrl Pts',(-253.423565840652,0.209410983396998,
124.20207443517));
#259700=CARTESIAN_POINT('Ctrl Pts',(-253.702013464465,-5.44149859849489,
127.059480266814));
#259701=CARTESIAN_POINT('Ctrl Pts',(-253.980461088278,-6.0919368110008,
133.358248211846));
#259702=CARTESIAN_POINT('Ctrl Pts',(-254.258908712091,-1.1441826817532,
137.310118186916));
#259703=CARTESIAN_POINT('Ctrl Pts',(-254.537356335904,4.85501939763767,
135.283514846073));
#259704=CARTESIAN_POINT('Ctrl Pts',(-254.815803959717,6.39269590315201,
129.140787462715));
#259705=CARTESIAN_POINT('Ctrl Pts',(-255.09425158353,2.05579703890082,124.526802775315));
#259706=CARTESIAN_POINT('Ctrl Pts',(-255.372699207342,-4.17027861730954,
125.681586622223));
#259707=CARTESIAN_POINT('Ctrl Pts',(-255.651146831155,-6.5640724361261,
131.5439503534));
#259708=CARTESIAN_POINT('Ctrl Pts',(-255.929594454968,-2.925803447894,136.726665654721));
#259709=CARTESIAN_POINT('Ctrl Pts',(-256.208042078781,3.40113425532747,
136.467074956607));
#259710=CARTESIAN_POINT('Ctrl Pts',(-256.486489702594,6.60259898059897,
131.003720738236));
#259711=CARTESIAN_POINT('Ctrl Pts',(-256.764937326407,3.73659166461274,
125.357175036369));
#259712=CARTESIAN_POINT('Ctrl Pts',(-257.04338495022,-2.56314926818932,
124.716306516944));
#259713=CARTESIAN_POINT('Ctrl Pts',(-257.321832574033,-6.5075031063131,
129.670100547101));
#259714=CARTESIAN_POINT('Ctrl Pts',(-257.600280197845,-4.47173821150659,
135.666151948257));
#259715=CARTESIAN_POINT('Ctrl Pts',(-257.878727821659,1.67325768403046,
137.194590998305));
#259716=CARTESIAN_POINT('Ctrl Pts',(-258.157175445471,6.28075871394982,
132.850463013089));
#259717=CARTESIAN_POINT('Ctrl Pts',(-258.435623069284,5.1162713672671,126.626553096149));
#259718=CARTESIAN_POINT('Ctrl Pts',(-258.714070693097,-0.749294580734974,
124.240926059104));
#259719=CARTESIAN_POINT('Ctrl Pts',(-258.99251831691,-5.92728653745133,
127.888508918958));
#259720=CARTESIAN_POINT('Ctrl Pts',(-259.270965940723,-5.656519339957,134.212338033208));
#259721=CARTESIAN_POINT('Ctrl Pts',(-259.549413564536,-0.191230405826049,
137.41063083554));
#259722=CARTESIAN_POINT('Ctrl Pts',(-259.827861188349,5.45654320709978,
134.526020746857));
#259723=CARTESIAN_POINT('Ctrl Pts',(-260.059900874859,5.97341346954355,
129.293215926205));
#259724=CARTESIAN_POINT('Ctrl Pts',(-260.245542550368,3.60742224527213,
126.247226657536));
#259725=CARTESIAN_POINT('Ctrl Pts',(-260.338368351272,1.86717727106152,
125.459413119698));
#259726=CARTESIAN_POINT('Ctrl Pts',(-260.384786214875,0.950008195528324,
125.301089073499));
#259727=CARTESIAN_POINT('Ctrl Pts',(209.997886486728,-2.58542267678463,
125.478296443779));
#259728=CARTESIAN_POINT('Ctrl Pts',(209.951476810375,-3.47289965896197,
125.909102290886));
#259729=CARTESIAN_POINT('Ctrl Pts',(209.85865919672,-5.01373755653622,127.222906143875));
#259730=CARTESIAN_POINT('Ctrl Pts',(209.67302570846,-6.52844908712303,131.020616473957));
#259731=CARTESIAN_POINT('Ctrl Pts',(209.440986021949,-4.4641631800594,136.198709217918));
#259732=CARTESIAN_POINT('Ctrl Pts',(209.162538398136,2.13623200523086,137.47712630299));
#259733=CARTESIAN_POINT('Ctrl Pts',(208.884090774324,6.76311047611758,132.61329501932));
#259734=CARTESIAN_POINT('Ctrl Pts',(208.60564315051,5.180460236421,126.09244423763));
#259735=CARTESIAN_POINT('Ctrl Pts',(208.327195526698,-1.16565068102074,
123.898824768668));
#259736=CARTESIAN_POINT('Ctrl Pts',(208.048747902884,-6.43906639651766,
128.052530506575));
#259737=CARTESIAN_POINT('Ctrl Pts',(207.770300279072,-5.79609906993421,
134.734252735451));
#259738=CARTESIAN_POINT('Ctrl Pts',(207.491852655259,0.173626147510206,
137.805009652024));
#259739=CARTESIAN_POINT('Ctrl Pts',(207.213405031446,5.98357180802623,134.442293088818));
#259740=CARTESIAN_POINT('Ctrl Pts',(206.934957407633,6.29502677410122,127.736610299611));
#259741=CARTESIAN_POINT('Ctrl Pts',(206.65650978382,0.821596385081328,123.849978754804));
#259742=CARTESIAN_POINT('Ctrl Pts',(206.378062160007,-5.40680743188727,
126.354116934927));
#259743=CARTESIAN_POINT('Ctrl Pts',(206.099614536195,-6.66663710465116,
132.947794423038));
#259744=CARTESIAN_POINT('Ctrl Pts',(205.821166912381,-1.80014356190772,
137.571770081489));
#259745=CARTESIAN_POINT('Ctrl Pts',(205.542719288569,4.72058899422897,135.976822216287));
#259746=CARTESIAN_POINT('Ctrl Pts',(205.264271664756,6.90333351468265,129.628637390042));
#259747=CARTESIAN_POINT('Ctrl Pts',(204.985824040943,2.74225038547515,124.360883417158));
#259748=CARTESIAN_POINT('Ctrl Pts',(204.70737641713,-3.93882614214087,125.014370927945));
#259749=CARTESIAN_POINT('Ctrl Pts',(204.428928793317,-7.00031425910704,
130.988575726592));
#259750=CARTESIAN_POINT('Ctrl Pts',(204.150481169504,-3.62885534891233,
136.793496040797));
#259751=CARTESIAN_POINT('Ctrl Pts',(203.872033545692,3.07734423765085,137.09469337995));
#259752=CARTESIAN_POINT('Ctrl Pts',(203.593585921878,6.95561486460971,131.615382266785));
#259753=CARTESIAN_POINT('Ctrl Pts',(203.315138298066,4.44201520086038,125.390781848689));
#259754=CARTESIAN_POINT('Ctrl Pts',(203.036690674253,-2.15357941165663,
124.140995867004));
#259755=CARTESIAN_POINT('Ctrl Pts',(202.75824305044,-6.77013976170558,129.014516559232));
#259756=CARTESIAN_POINT('Ctrl Pts',(202.479795426627,-5.16527240588502,
135.532816506767));
#259757=CARTESIAN_POINT('Ctrl Pts',(202.201347802814,1.18622795093483,137.705896487686));
#259758=CARTESIAN_POINT('Ctrl Pts',(201.922900179001,6.44764277258624,133.536802163981));
#259759=CARTESIAN_POINT('Ctrl Pts',(201.644452555188,5.78398887041165,126.856727545651));
#259760=CARTESIAN_POINT('Ctrl Pts',(201.366004931376,-0.194868239746226,
123.804334868162));
#259761=CARTESIAN_POINT('Ctrl Pts',(201.087557307562,-5.99465095761073,
127.184623883922));
#259762=CARTESIAN_POINT('Ctrl Pts',(200.80910968375,-6.2856423003101,133.891274124028));
#259763=CARTESIAN_POINT('Ctrl Pts',(200.530662059936,-0.80043543977546,
137.76120165575));
#259764=CARTESIAN_POINT('Ctrl Pts',(200.252214436124,5.42033248649604,135.238132133988));
#259765=CARTESIAN_POINT('Ctrl Pts',(199.973766812311,6.66007965562565,128.640643190398));
#259766=CARTESIAN_POINT('Ctrl Pts',(199.695319188498,1.77953898422249,124.031504858911));
#259767=CARTESIAN_POINT('Ctrl Pts',(199.416871564685,-4.73631107837294,
125.646290097223));
#259768=CARTESIAN_POINT('Ctrl Pts',(199.138423940872,-6.89972264160091,
132.00109015798));
#259769=CARTESIAN_POINT('Ctrl Pts',(198.859976317059,-2.72262616738874,
137.256154234582));
#259770=CARTESIAN_POINT('Ctrl Pts',(198.581528693247,3.95643074697165,136.582335164788));
#259771=CARTESIAN_POINT('Ctrl Pts',(198.303081069434,6.999721087252,130.598839755845));
#259772=CARTESIAN_POINT('Ctrl Pts',(198.024633445621,3.61060970373355,124.804207978572));
#259773=CARTESIAN_POINT('Ctrl Pts',(197.746185821808,-3.09647560942607,
124.523423352781));
#259774=CARTESIAN_POINT('Ctrl Pts',(197.467738197995,-6.9580511087663,130.014513232485));
#259775=CARTESIAN_POINT('Ctrl Pts',(197.189290574182,-4.4255175588443,136.231434272887));
#259776=CARTESIAN_POINT('Ctrl Pts',(196.910842950369,2.17385042910367,137.461139751337));
#259777=CARTESIAN_POINT('Ctrl Pts',(196.632395326556,6.77555607120273,132.573590407591));
#259778=CARTESIAN_POINT('Ctrl Pts',(196.353947702743,5.15085668818228,126.060205318492));
#259779=CARTESIAN_POINT('Ctrl Pts',(196.07550007893,-1.20722835793932,123.90646718437));
#259780=CARTESIAN_POINT('Ctrl Pts',(195.797052455118,-6.45592951949867,
128.091556134528));
#259781=CARTESIAN_POINT('Ctrl Pts',(195.518604831305,-5.77194684232935,
134.769579876729));
#259782=CARTESIAN_POINT('Ctrl Pts',(195.240157207492,0.216173007661386,
137.80376083149));
#259783=CARTESIAN_POINT('Ctrl Pts',(194.961709583679,6.00564042424985,134.405834929363));
#259784=CARTESIAN_POINT('Ctrl Pts',(194.683261959866,6.2762176827981,127.698330076496));
#259785=CARTESIAN_POINT('Ctrl Pts',(194.404814336053,0.779257501134259,
123.845115552844));
#259786=CARTESIAN_POINT('Ctrl Pts',(194.12636671224,-5.43380225522669,126.387107265649));
#259787=CARTESIAN_POINT('Ctrl Pts',(193.847919088427,-6.65346319503207,
132.988339014042));
#259788=CARTESIAN_POINT('Ctrl Pts',(193.569471464615,-1.75891649835014,
137.58260130935));
#259789=CARTESIAN_POINT('Ctrl Pts',(193.291023840801,4.75198853246758,135.947991544374));
#259790=CARTESIAN_POINT('Ctrl Pts',(193.012576216989,6.89604824949333,129.586636238002));
#259791=CARTESIAN_POINT('Ctrl Pts',(192.734128593176,2.70297651592057,124.344310147306));
#259792=CARTESIAN_POINT('Ctrl Pts',(192.455680969363,-3.97399858803937,
125.038454847768));
#259793=CARTESIAN_POINT('Ctrl Pts',(192.17723334555,-6.99906313021511,131.031185270517));
#259794=CARTESIAN_POINT('Ctrl Pts',(191.898785721737,-3.59233057896577,
136.815474918205));
#259795=CARTESIAN_POINT('Ctrl Pts',(191.620338097924,3.11557827924791,137.075844182864));
#259796=CARTESIAN_POINT('Ctrl Pts',(191.341890474111,6.96042290329331,131.573026430018));
#259797=CARTESIAN_POINT('Ctrl Pts',(191.063442850298,4.40897891477476,125.363842346942));
#259798=CARTESIAN_POINT('Ctrl Pts',(190.784995226486,-2.19410130582752,
124.154228770475));
#259799=CARTESIAN_POINT('Ctrl Pts',(190.506547602672,-6.78090961418206,
129.055761484483));
#259800=CARTESIAN_POINT('Ctrl Pts',(190.22809997886,-5.13639325295408,135.564171377977));
#259801=CARTESIAN_POINT('Ctrl Pts',(189.949652355047,1.22821758097839,137.698547712335));
#259802=CARTESIAN_POINT('Ctrl Pts',(189.671204731234,6.46415645975623,133.497502906364));
#259803=CARTESIAN_POINT('Ctrl Pts',(189.392757107421,5.75985134361714,126.821591904301));
#259804=CARTESIAN_POINT('Ctrl Pts',(189.114309483608,-0.237475772924818,
123.80565078066));
#259805=CARTESIAN_POINT('Ctrl Pts',(188.835861859795,-6.01657425548534,
127.221182091151));
#259806=CARTESIAN_POINT('Ctrl Pts',(188.557414235982,-6.2667349232476,133.929479419415));
#259807=CARTESIAN_POINT('Ctrl Pts',(188.278966612169,-0.758072343566082,
137.76594523932));
#259808=CARTESIAN_POINT('Ctrl Pts',(188.000518988357,5.44722168595988,135.205054884148));
#259809=CARTESIAN_POINT('Ctrl Pts',(187.722071364544,6.64678509766207,128.600141483854));
#259810=CARTESIAN_POINT('Ctrl Pts',(187.443623740731,1.73827771811677,124.02079778535));
#259811=CARTESIAN_POINT('Ctrl Pts',(187.165176116918,-4.76762196479028,
125.675216934184));
#259812=CARTESIAN_POINT('Ctrl Pts',(186.886728493105,-6.89230997333645,
132.043068555446));
#259813=CARTESIAN_POINT('Ctrl Pts',(186.608280869292,-2.68330182444739,
137.272608096043));
#259814=CARTESIAN_POINT('Ctrl Pts',(186.329833245479,3.99152961452714,136.558144195375));
#259815=CARTESIAN_POINT('Ctrl Pts',(186.051385621667,6.99834033481346,130.556234274655));
#259816=CARTESIAN_POINT('Ctrl Pts',(185.772937997853,3.5740181753383,124.782340341422));
#259817=CARTESIAN_POINT('Ctrl Pts',(185.494490374041,-3.13465208677821,
124.542388849921));
#259818=CARTESIAN_POINT('Ctrl Pts',(185.216042750227,-6.96273021741339,
130.056883498557));
#259819=CARTESIAN_POINT('Ctrl Pts',(184.937595126415,-4.39239942652681,
136.258273103275));
#259820=CARTESIAN_POINT('Ctrl Pts',(184.659147502602,2.21433185669671,137.447783572063));
#259821=CARTESIAN_POINT('Ctrl Pts',(184.380699878789,6.78620033974098,132.532312894923));
#259822=CARTESIAN_POINT('Ctrl Pts',(184.102252254976,5.12188223488049,126.028938490053));
#259823=CARTESIAN_POINT('Ctrl Pts',(183.823804631163,-1.24919542597752,
123.913943728027));
#259824=CARTESIAN_POINT('Ctrl Pts',(183.54535700735,-6.47232351695142,128.130905471908));
#259825=CARTESIAN_POINT('Ctrl Pts',(183.266909383538,-5.74770248642891,
134.804641889104));
#259826=CARTESIAN_POINT('Ctrl Pts',(182.988461759724,0.258776338245136,
137.80231524236));
#259827=CARTESIAN_POINT('Ctrl Pts',(182.710014135912,6.02745234999885,134.369210164519));
#259828=CARTESIAN_POINT('Ctrl Pts',(182.431566512099,6.25719410952084,127.66018250561));
#259829=CARTESIAN_POINT('Ctrl Pts',(182.153118888286,0.73688016331929,123.840500929948));
#259830=CARTESIAN_POINT('Ctrl Pts',(181.874671264473,-5.46059065437546,
126.420266203747));
#259831=CARTESIAN_POINT('Ctrl Pts',(181.59622364066,-6.64004542538295,133.028800068927));
#259832=CARTESIAN_POINT('Ctrl Pts',(181.317776016847,-1.71762283471616,
137.593182748215));
#259833=CARTESIAN_POINT('Ctrl Pts',(181.039328393035,4.78321123051439,135.918969541833));
#259834=CARTESIAN_POINT('Ctrl Pts',(180.760880769221,6.88850784776155,129.544680596588));
#259835=CARTESIAN_POINT('Ctrl Pts',(180.482433145409,2.66360227523266,124.32797605183));
#259836=CARTESIAN_POINT('Ctrl Pts',(180.203985521595,-4.00902366402984,
125.062752534008));
#259837=CARTESIAN_POINT('Ctrl Pts',(179.925537897783,-6.99755270774298,
131.073786351827));
#259838=CARTESIAN_POINT('Ctrl Pts',(179.64709027397,-3.5556726624947,136.837231082039));
#259839=CARTESIAN_POINT('Ctrl Pts',(179.368642650157,3.15369685531979,137.056762577506));
#259840=CARTESIAN_POINT('Ctrl Pts',(179.090195026344,6.96497302975191,131.530642118605));
#259841=CARTESIAN_POINT('Ctrl Pts',(178.811747402531,4.37577924769062,125.337104441072));
#259842=CARTESIAN_POINT('Ctrl Pts',(178.533299778718,-2.23454189429802,
124.167708099424));
#259843=CARTESIAN_POINT('Ctrl Pts',(178.254852154906,-6.79142819886702,
129.097071203448));
#259844=CARTESIAN_POINT('Ctrl Pts',(177.976404531092,-5.10732376838957,
135.595349873321));
#259845=CARTESIAN_POINT('Ctrl Pts',(177.69795690728,1.27016169860089,137.690943469992));
#259846=CARTESIAN_POINT('Ctrl Pts',(177.419509283467,6.48043061542571,133.458103853558));
#259847=CARTESIAN_POINT('Ctrl Pts',(177.141061659654,5.73550038331004,126.786603845811));
#259848=CARTESIAN_POINT('Ctrl Pts',(176.862614035841,-0.280074506296806,
123.807226032976));
#259849=CARTESIAN_POINT('Ctrl Pts',(176.584166412028,-6.0382746070172,127.257873074351));
#259850=CARTESIAN_POINT('Ctrl Pts',(176.305718788215,-6.24759533000263,
133.967568912391));
#259851=CARTESIAN_POINT('Ctrl Pts',(176.027271164402,-0.71568115671533,
137.770430858802));
#259852=CARTESIAN_POINT('Ctrl Pts',(175.748823540589,5.4739090366252,135.171814564968));
#259853=CARTESIAN_POINT('Ctrl Pts',(175.470375916777,6.63324424063007,128.559721455457));
#259854=CARTESIAN_POINT('Ctrl Pts',(175.191928292964,1.69695203949225,124.010342079205));
#259855=CARTESIAN_POINT('Ctrl Pts',(174.913480669151,-4.79875618522306,
125.704333833448));
#259856=CARTESIAN_POINT('Ctrl Pts',(174.635033045338,-6.88464190799096,
132.085001052137));
#259857=CARTESIAN_POINT('Ctrl Pts',(174.356585421525,-2.64387805077028,
137.288822274217));
#259858=CARTESIAN_POINT('Ctrl Pts',(174.078137797712,4.02648057448505,136.533740017397));
#259859=CARTESIAN_POINT('Ctrl Pts',(173.799690173899,6.99670025630013,130.513637987877));
#259860=CARTESIAN_POINT('Ctrl Pts',(173.521242550086,3.53729421038521,124.76069585245));
#259861=CARTESIAN_POINT('Ctrl Pts',(173.242794926273,-3.17271240844464,
124.561586386726));
#259862=CARTESIAN_POINT('Ctrl Pts',(172.96434730246,-6.96715131953175,130.099281462668));
#259863=CARTESIAN_POINT('Ctrl Pts',(172.685899678648,-4.35911853223319,
136.284909836929));
#259864=CARTESIAN_POINT('Ctrl Pts',(172.407452054835,2.25473123140845,137.434181218309));
#259865=CARTESIAN_POINT('Ctrl Pts',(172.129004431022,6.79659314313001,132.490971352347));
#259866=CARTESIAN_POINT('Ctrl Pts',(171.850556807209,5.09271798834896,125.997848616637));
#259867=CARTESIAN_POINT('Ctrl Pts',(171.572109183396,-1.29111620461978,
123.921675598615));
#259868=CARTESIAN_POINT('Ctrl Pts',(171.293661559583,-6.48847768007612,
128.170353875152));
#259869=CARTESIAN_POINT('Ctrl Pts',(171.01521393577,-5.72324514729908,134.839555669585));
#259870=CARTESIAN_POINT('Ctrl Pts',(170.736766311957,0.301370079776633,
137.800610341449));
#259871=CARTESIAN_POINT('Ctrl Pts',(170.458318688145,6.04904092628448,134.332453302864));
#259872=CARTESIAN_POINT('Ctrl Pts',(170.179871064331,6.23793867361471,127.6221514434));
#259873=CARTESIAN_POINT('Ctrl Pts',(169.901423440519,0.694475520138818,
123.836144355433));
#259874=CARTESIAN_POINT('Ctrl Pts',(169.622975816706,-5.4871767093294,126.453587596077));
#259875=CARTESIAN_POINT('Ctrl Pts',(169.344528192893,-6.62638160640872,
133.06917869639));
#259876=CARTESIAN_POINT('Ctrl Pts',(169.06608056908,-1.67626552393645,137.603512624779));
#259877=CARTESIAN_POINT('Ctrl Pts',(168.787632945267,4.81425668490999,135.88975801558));
#259878=CARTESIAN_POINT('Ctrl Pts',(168.509185321454,6.88071218983824,129.50277163308));
#259879=CARTESIAN_POINT('Ctrl Pts',(168.230737697641,2.62412933378287,124.311881941165));
#259880=CARTESIAN_POINT('Ctrl Pts',(167.952290073828,-4.0439001841742,125.087262977647));
#259881=CARTESIAN_POINT('Ctrl Pts',(167.673842450016,-6.99578298838191,
131.116377449467));
#259882=CARTESIAN_POINT('Ctrl Pts',(167.395394826203,-3.51888298926545,
136.858763695638));
#259883=CARTESIAN_POINT('Ctrl Pts',(167.11694720239,3.19169856999505,137.037449287095));
#259884=CARTESIAN_POINT('Ctrl Pts',(166.838499578577,6.96926506657354,131.488230894564));
#259885=CARTESIAN_POINT('Ctrl Pts',(166.560051954764,4.34241743449723,125.310569126392));
#259886=CARTESIAN_POINT('Ctrl Pts',(166.281604330951,-2.27489968099678,
124.181433351974));
#259887=CARTESIAN_POINT('Ctrl Pts',(166.003156707138,-6.80169512468258,
129.13844418665));
#259888=CARTESIAN_POINT('Ctrl Pts',(165.724709083325,-5.0780650300646,135.626350836796));
#259889=CARTESIAN_POINT('Ctrl Pts',(165.446261459512,1.31205874991464,137.683084042787));
#259890=CARTESIAN_POINT('Ctrl Pts',(165.1678138357,6.49646463635559,133.418606465321));
#259891=CARTESIAN_POINT('Ctrl Pts',(164.889366211887,5.71093689192698,126.751764666776));
#259892=CARTESIAN_POINT('Ctrl Pts',(164.610918588074,-0.322662861405092,
123.809060566689));
#259893=CARTESIAN_POINT('Ctrl Pts',(164.332470964261,-6.05975120806294,
127.29469547395));
#259894=CARTESIAN_POINT('Ctrl Pts',(164.054023340448,-6.22822422981513,
134.00554119152));
#259895=CARTESIAN_POINT('Ctrl Pts',(163.775575716635,-0.673263450036036,
137.774658347991));
#259896=CARTESIAN_POINT('Ctrl Pts',(163.497128092822,5.50039354957815,135.138412408175));
#259897=CARTESIAN_POINT('Ctrl Pts',(163.218680469009,6.61945758629338,128.51938460299));
#259898=CARTESIAN_POINT('Ctrl Pts',(162.940232845196,1.65556347968583,124.000138127916));
#259899=CARTESIAN_POINT('Ctrl Pts',(162.661785221384,-4.82971258598073,
125.733639716082));
#259900=CARTESIAN_POINT('Ctrl Pts',(162.383337597571,-6.87671872970774,
132.126886094224));
#259901=CARTESIAN_POINT('Ctrl Pts',(162.104889973758,-2.60435630721971,
137.304796168278));
#259902=CARTESIAN_POINT('Ctrl Pts',(161.826442349945,4.06128233172446,136.509123535159));
#259903=CARTESIAN_POINT('Ctrl Pts',(161.547994726132,6.99480091248578,130.471052473933));
#259904=CARTESIAN_POINT('Ctrl Pts',(161.269547102319,3.50043916969439,124.739275313697));
#259905=CARTESIAN_POINT('Ctrl Pts',(160.991099478506,-3.21065516408591,
124.581015251828));
#259906=CARTESIAN_POINT('Ctrl Pts',(160.712651854693,-6.97131425129578,
130.141705553748));
#259907=CARTESIAN_POINT('Ctrl Pts',(160.434204230881,-4.32567610919938,
136.311343486817));
#259908=CARTESIAN_POINT('Ctrl Pts',(160.155756607067,2.29504705622523,137.420333194114));
#259909=CARTESIAN_POINT('Ctrl Pts',(159.877308983254,6.80673409626067,132.449567311792));
#259910=CARTESIAN_POINT('Ctrl Pts',(159.598861359442,5.06336502927952,125.966936850291));
#259911=CARTESIAN_POINT('Ctrl Pts',(159.320413735629,-1.33298914047637,
123.929662509627));
#259912=CARTESIAN_POINT('Ctrl Pts',(159.041966111816,-6.50439141027418,
128.209899882485));
#259913=CARTESIAN_POINT('Ctrl Pts',(158.763518488003,-5.69857573121565,
134.874319924428));
#259914=CARTESIAN_POINT('Ctrl Pts',(158.48507086419,0.343952653928878,137.798646191931));
#259915=CARTESIAN_POINT('Ctrl Pts',(158.206623240377,6.07040535313402,134.295565706438));
#259916=CARTESIAN_POINT('Ctrl Pts',(157.928175616564,6.2184520885971,127.584238299121));
#259917=CARTESIAN_POINT('Ctrl Pts',(157.649727992752,0.652045142912632,
123.832045990734));
#259918=CARTESIAN_POINT('Ctrl Pts',(157.371280368939,-5.51355943493244,
126.487070207899));
#259919=CARTESIAN_POINT('Ctrl Pts',(157.092832745126,-6.61247224442723,
133.109473400187));
#259920=CARTESIAN_POINT('Ctrl Pts',(156.814385121313,-1.63484609852131,
137.613590556265));
#259921=CARTESIAN_POINT('Ctrl Pts',(156.5359374975,4.84512374525377,135.860358048054));
#259922=CARTESIAN_POINT('Ctrl Pts',(156.257489873687,6.87266156459436,129.46091090043));
#259923=CARTESIAN_POINT('Ctrl Pts',(155.979042249874,2.58455915425555,124.296028411687));
#259924=CARTESIAN_POINT('Ctrl Pts',(155.700594626061,-4.07862685611001,
125.111985270442));
#259925=CARTESIAN_POINT('Ctrl Pts',(155.422147002248,-6.99375403770952,
131.158956985208));
#259926=CARTESIAN_POINT('Ctrl Pts',(155.143699378435,-3.48196292253304,
136.880071961106));
#259927=CARTESIAN_POINT('Ctrl Pts',(154.865251754623,3.22958201510593,137.017905027291));
#259928=CARTESIAN_POINT('Ctrl Pts',(154.58680413081,6.97329885471516,131.445794329457));
#259929=CARTESIAN_POINT('Ctrl Pts',(154.308356506997,4.30889471142897,125.284237386175));
#259930=CARTESIAN_POINT('Ctrl Pts',(154.029908883184,-2.31517317045128,
124.195404019528));
#259931=CARTESIAN_POINT('Ctrl Pts',(153.751461259371,-6.81171001118396,
129.179878900999));
#259932=CARTESIAN_POINT('Ctrl Pts',(153.473013635558,-5.04861812217248,
135.65717311965));
#259933=CARTESIAN_POINT('Ctrl Pts',(153.194566011745,1.3539071824088,137.674969721956));
#259934=CARTESIAN_POINT('Ctrl Pts',(152.916118387933,6.51225792839928,133.379012205241));
#259935=CARTESIAN_POINT('Ctrl Pts',(152.637670764119,5.68616177967723,126.717075658174));
#259936=CARTESIAN_POINT('Ctrl Pts',(152.359223140307,-0.365239260122265,
123.811154313817));
#259937=CARTESIAN_POINT('Ctrl Pts',(152.080775516494,-6.08100326279917,
127.331647925483));
#259938=CARTESIAN_POINT('Ctrl Pts',(151.802327892681,-6.20862234048841,
134.043394849727));
#259939=CARTESIAN_POINT('Ctrl Pts',(151.523880268868,-0.630820795332096,
137.778627550233));
#259940=CARTESIAN_POINT('Ctrl Pts',(151.245432645055,5.52667424342534,135.104849651499));
#259941=CARTESIAN_POINT('Ctrl Pts',(150.966985021242,6.60542564552152,128.479132421149));
#259942=CARTESIAN_POINT('Ctrl Pts',(150.688537397429,1.61411357236584,123.990186309594));
#259943=CARTESIAN_POINT('Ctrl Pts',(150.410089773616,-4.86049001996232,
125.763133496143));
#259944=CARTESIAN_POINT('Ctrl Pts',(150.131642149803,-6.8685407320831,132.168722129643));
#259945=CARTESIAN_POINT('Ctrl Pts',(149.853194525991,-2.56473805828847,
137.32052918631));
#259946=CARTESIAN_POINT('Ctrl Pts',(149.574746902178,4.09593359665354,136.484295660832));
#259947=CARTESIAN_POINT('Ctrl Pts',(149.296299278365,6.99264237375128,130.428479310845));
#259948=CARTESIAN_POINT('Ctrl Pts',(149.017851654552,3.46345441894284,124.718079518912));
#259949=CARTESIAN_POINT('Ctrl Pts',(148.739404030739,-3.24847894771935,
124.600674725279));
#259950=CARTESIAN_POINT('Ctrl Pts',(148.460956406926,-6.97521885844655,
130.184154199754));
#259951=CARTESIAN_POINT('Ctrl Pts',(148.182508783113,-4.29207339664657,
136.337573073429));
#259952=CARTESIAN_POINT('Ctrl Pts',(147.9040611593,2.33527783722936,137.406240012622));
#259953=CARTESIAN_POINT('Ctrl Pts',(147.625613535487,6.81662282335624,132.408102307496));
#259954=CARTESIAN_POINT('Ctrl Pts',(147.347165911675,5.03382444535687,125.936204336462));
#259955=CARTESIAN_POINT('Ctrl Pts',(147.068718287862,-1.37481268193005,
123.937904165105));
#259956=CARTESIAN_POINT('Ctrl Pts',(146.790270664049,-6.52006411785656,
128.249542028514));
#259957=CARTESIAN_POINT('Ctrl Pts',(146.511823040236,-5.67369515231286,
134.908933365434));
#259958=CARTESIAN_POINT('Ctrl Pts',(146.233375416423,0.386522482789046,
137.796422866589));
#259959=CARTESIAN_POINT('Ctrl Pts',(145.95492779261,6.09154483888081,134.258548742122));
#259960=CARTESIAN_POINT('Ctrl Pts',(145.676480168797,6.19873507655051,127.546444477659));
#259961=CARTESIAN_POINT('Ctrl Pts',(145.398032544984,0.609590603913882,
123.828205987717));
#259962=CARTESIAN_POINT('Ctrl Pts',(145.119584921171,-5.53973785356302,
126.520712798507));
#259963=CARTESIAN_POINT('Ctrl Pts',(144.841137297358,-6.59831785485502,
133.149682687181));
#259964=CARTESIAN_POINT('Ctrl Pts',(144.562689673546,-1.59336609328267,
137.623416169231));
#259965=CARTESIAN_POINT('Ctrl Pts',(144.284242049733,4.87581126775532,135.830770728684));
#259966=CARTESIAN_POINT('Ctrl Pts',(144.00579442592,6.86435627034879,129.419099949804));
#259967=CARTESIAN_POINT('Ctrl Pts',(143.727346802107,2.54489320293839,124.280416050852));
#259968=CARTESIAN_POINT('Ctrl Pts',(143.448899178294,-4.11320239302776,
125.136918496298));
#259969=CARTESIAN_POINT('Ctrl Pts',(143.170451554481,-6.99146593090932,
131.201523381251));
#259970=CARTESIAN_POINT('Ctrl Pts',(142.892003930668,-3.44491383038404,
136.901155088855));
#259971=CARTESIAN_POINT('Ctrl Pts',(142.613556306855,3.26734578686757,136.998130522314));
#259972=CARTESIAN_POINT('Ctrl Pts',(142.335108683042,6.97707424470332,131.403333995789));
#259973=CARTESIAN_POINT('Ctrl Pts',(142.05666105923,4.27521232068256,125.258110196154));
#259974=CARTESIAN_POINT('Ctrl Pts',(141.778213435417,-2.35536087031262,
124.209619584399));
#259975=CARTESIAN_POINT('Ctrl Pts',(141.499765811604,-6.8214724872659,129.221373811115));
#259976=CARTESIAN_POINT('Ctrl Pts',(141.221318187791,-5.01898413587917,
135.687815579753));
#259977=CARTESIAN_POINT('Ctrl Pts',(140.942870563978,1.39570544537436,137.666600808179));
#259978=CARTESIAN_POINT('Ctrl Pts',(140.664422940165,6.52780990633047,133.339322540502));
#259979=CARTESIAN_POINT('Ctrl Pts',(140.385975316352,5.66117596461176,126.68253810542));
#259980=CARTESIAN_POINT('Ctrl Pts',(140.10752769254,-0.407802124764288,
123.813507196776));
#259981=CARTESIAN_POINT('Ctrl Pts',(139.829080068726,-6.10202998372316,
127.368729059661));
#259982=CARTESIAN_POINT('Ctrl Pts',(139.550632444914,-6.18879038837768,
134.081128484328));
#259983=CARTESIAN_POINT('Ctrl Pts',(139.272184821101,-0.588354765331746,
137.78233831845));
#259984=CARTESIAN_POINT('Ctrl Pts',(138.993737197288,5.55275014432601,135.071127538621));
#259985=CARTESIAN_POINT('Ctrl Pts',(138.715289573475,6.59114893827324,128.438966401494));
#259986=CARTESIAN_POINT('Ctrl Pts',(138.436841949662,1.57260385347371,123.980486993006));
#259987=CARTESIAN_POINT('Ctrl Pts',(138.158394325849,-4.8910873466988,125.792814080728));
#259988=CARTESIAN_POINT('Ctrl Pts',(137.879946702036,-6.86010821815569,
132.210507608145));
#259989=CARTESIAN_POINT('Ctrl Pts',(137.601499078223,-2.52502477204539,
137.336020745319));
#259990=CARTESIAN_POINT('Ctrl Pts',(137.32305145441,4.13043308525698,136.459257314423));
#259991=CARTESIAN_POINT('Ctrl Pts',(137.044603830598,6.99022472008204,130.385920076178));
#259992=CARTESIAN_POINT('Ctrl Pts',(136.766156206785,3.42634132861412,124.69710925351));
#259993=CARTESIAN_POINT('Ctrl Pts',(136.487708582972,-3.28618235777073,
124.620564078594));
#259994=CARTESIAN_POINT('Ctrl Pts',(136.209260959159,-6.97886499629743,
130.226625827737));
#259995=CARTESIAN_POINT('Ctrl Pts',(135.930813335346,-4.25831163973555,
136.363597624819));
#259996=CARTESIAN_POINT('Ctrl Pts',(135.652365711533,2.37542208365453,137.391902196061));
#259997=CARTESIAN_POINT('Ctrl Pts',(135.37391808772,6.82625895798624,132.366577875963));
#259998=CARTESIAN_POINT('Ctrl Pts',(135.095470463907,5.00409733121823,125.905652213954));
#259999=CARTESIAN_POINT('Ctrl Pts',(134.817022840094,-1.4165852791943,123.946400259653));
#260000=CARTESIAN_POINT('Ctrl Pts',(134.538575216282,-6.53549522206528,
128.289278844285));
#260001=CARTESIAN_POINT('Ctrl Pts',(134.260127592469,-5.64860433254967,
134.943394709987));
#260002=CARTESIAN_POINT('Ctrl Pts',(133.981679968656,0.429077988916399,
137.793940447809));
#260003=CARTESIAN_POINT('Ctrl Pts',(133.703232344843,6.1124586001935,134.221403781595));
#260004=CARTESIAN_POINT('Ctrl Pts',(133.42478472103,6.17878836809604,127.508771379477));
#260005=CARTESIAN_POINT('Ctrl Pts',(133.146337097217,0.567113476311158,
123.824624488677));
#260006=CARTESIAN_POINT('Ctrl Pts',(132.867889473404,-5.5657109951702,126.554514121259));
#260007=CARTESIAN_POINT('Ctrl Pts',(132.589441849591,-6.58391896218814,
133.189805067404));
#260008=CARTESIAN_POINT('Ctrl Pts',(132.310994225778,-1.55182704527753,
137.632989099587));
#260009=CARTESIAN_POINT('Ctrl Pts',(132.032546601965,4.90631811527725,135.800997153839));
#260010=CARTESIAN_POINT('Ctrl Pts',(131.754098978153,6.85579661485726,129.377340330521));
#260011=CARTESIAN_POINT('Ctrl Pts',(131.47565135434,2.50513294966777,124.265045437181));
#260012=CARTESIAN_POINT('Ctrl Pts',(131.197203730527,-4.14762551371829,
125.162061731307));
#260013=CARTESIAN_POINT('Ctrl Pts',(130.918756106714,-6.98891875276791,
131.244075060281));
#260014=CARTESIAN_POINT('Ctrl Pts',(130.640308482901,-3.4077370856862,136.922012297644));
#260015=CARTESIAN_POINT('Ctrl Pts',(130.361860859088,3.30498848592948,136.978126504915));
#260016=CARTESIAN_POINT('Ctrl Pts',(130.083413235275,6.98059109663955,131.360851466943));
#260017=CARTESIAN_POINT('Ctrl Pts',(129.804965611462,4.24137151037132,125.232188524482));
#260018=CARTESIAN_POINT('Ctrl Pts',(129.526517987649,-2.39546129141071,
124.224079519825));
#260019=CARTESIAN_POINT('Ctrl Pts',(129.248070363836,-6.83098219117618,
129.262927379388));
#260020=CARTESIAN_POINT('Ctrl Pts',(128.969622740024,-4.98916416928312,
135.718277081636));
#260021=CARTESIAN_POINT('Ctrl Pts',(128.691175116211,1.43745198996158,137.657977611568));
#260022=CARTESIAN_POINT('Ctrl Pts',(128.412727492398,6.54311999386511,133.299538941816));
#260023=CARTESIAN_POINT('Ctrl Pts',(128.134279868585,5.63598037258881,126.648153288314));
#260024=CARTESIAN_POINT('Ctrl Pts',(127.855832244772,-0.450349878148651,
123.81611912838));
#260025=CARTESIAN_POINT('Ctrl Pts',(127.577384620959,-6.12283059168226,
127.40593750243));
#260026=CARTESIAN_POINT('Ctrl Pts',(127.298936997146,-6.16872910836309,
134.118740697091));
#260027=CARTESIAN_POINT('Ctrl Pts',(127.020489373333,-0.545866933628919,
137.785790515136));
#260028=CARTESIAN_POINT('Ctrl Pts',(126.742041749521,5.57862028602806,135.037247319125));
#260029=CARTESIAN_POINT('Ctrl Pts',(126.463594125708,6.57662799357718,128.398888032392));
#260030=CARTESIAN_POINT('Ctrl Pts',(126.185146501895,1.53103586116759,123.971040537565));
#260031=CARTESIAN_POINT('Ctrl Pts',(125.906698878082,-4.92150343239493,
125.822680370014));
#260032=CARTESIAN_POINT('Ctrl Pts',(125.628251254269,-6.85142150039552,
132.252240981353));
#260033=CARTESIAN_POINT('Ctrl Pts',(125.349803630456,-2.48521792008072,
137.351270271259));
#260034=CARTESIAN_POINT('Ctrl Pts',(125.071356006643,4.16477951914341,136.434009423738));
#260035=CARTESIAN_POINT('Ctrl Pts',(124.79290838283,6.98754804106521,130.343376346978));
#260036=CARTESIAN_POINT('Ctrl Pts',(124.514460759018,3.38910127394743,124.676365294554));
#260037=CARTESIAN_POINT('Ctrl Pts',(124.236013135205,-3.32376399712637,
124.640682574762));
#260038=CARTESIAN_POINT('Ctrl Pts',(123.957565511392,-6.98225252973936,
130.269118863895));
#260039=CARTESIAN_POINT('Ctrl Pts',(123.679117887579,-4.22439208952083,
136.389416176637));
#260040=CARTESIAN_POINT('Ctrl Pts',(123.400670263766,2.41547830794073,137.377320275725));
#260041=CARTESIAN_POINT('Ctrl Pts',(123.122222639953,6.83564214308024,132.324995555895));
#260042=CARTESIAN_POINT('Ctrl Pts',(122.84377501614,4.97418478841272,125.875281614887));
#260043=CARTESIAN_POINT('Ctrl Pts',(122.565327392328,-1.45830538437,123.955150478444));
#260044=CARTESIAN_POINT('Ctrl Pts',(122.286879768514,-6.55068415109515,
128.329108857337));
#260045=CARTESIAN_POINT('Ctrl Pts',(122.008432144702,-5.62330420167569,
134.977702681109));
#260046=CARTESIAN_POINT('Ctrl Pts',(121.729984520888,0.471617595401148,
137.791199027578));
#260047=CARTESIAN_POINT('Ctrl Pts',(121.451536897076,6.13314586210485,134.184132201278));
#260048=CARTESIAN_POINT('Ctrl Pts',(121.173089273263,6.15861270236637,127.471220400567));
#260049=CARTESIAN_POINT('Ctrl Pts',(120.89464164945,0.52461533410983,123.821301626325));
#260050=CARTESIAN_POINT('Ctrl Pts',(120.616194025637,-5.5914778973097,126.588472923636));
#260051=CARTESIAN_POINT('Ctrl Pts',(120.337746401824,-6.56927609998288,
133.229839054105));
#260052=CARTESIAN_POINT('Ctrl Pts',(120.059298778011,-1.51023049375061,
137.642308992603));
#260053=CARTESIAN_POINT('Ctrl Pts',(119.780851154198,4.93664315737715,135.77103842679));
#260054=CARTESIAN_POINT('Ctrl Pts',(119.502403530385,6.84698291530094,129.33563359));
#260055=CARTESIAN_POINT('Ctrl Pts',(119.223955906573,2.46527986777437,124.249917140239));
#260056=CARTESIAN_POINT('Ctrl Pts',(118.94550828276,-4.18189494262004,125.187414043775));
#260057=CARTESIAN_POINT('Ctrl Pts',(118.667060658947,-6.98611259767199,
131.28661044553));
#260058=CARTESIAN_POINT('Ctrl Pts',(118.388613035134,-3.37043406603744,
136.942642814599));
#260059=CARTESIAN_POINT('Ctrl Pts',(118.110165411321,3.34250871742766,136.95789371635));
#260060=CARTESIAN_POINT('Ctrl Pts',(117.831717787508,6.98384928020556,131.318348317123));
#260061=CARTESIAN_POINT('Ctrl Pts',(117.553270163695,4.20737353447909,125.206473331696));
#260062=CARTESIAN_POINT('Ctrl Pts',(117.274822539882,-2.43547294780967,
124.238783289987));
#260063=CARTESIAN_POINT('Ctrl Pts',(116.99637491607,-6.84023877052931,129.304538066038));
#260064=CARTESIAN_POINT('Ctrl Pts',(116.717927292256,-4.95915932737393,
135.748556496538));
#260065=CARTESIAN_POINT('Ctrl Pts',(116.439479668444,1.47914526923655,137.649100451659));
#260066=CARTESIAN_POINT('Ctrl Pts',(116.161032044631,6.55818762368211,133.259662883379));
#260067=CARTESIAN_POINT('Ctrl Pts',(115.882584420818,5.61057593724064,126.613922481));
#260068=CARTESIAN_POINT('Ctrl Pts',(115.604136797005,-0.49288094365267,
123.818990011842));
#260069=CARTESIAN_POINT('Ctrl Pts',(115.325689173192,-6.14340431590201,
127.443271875017));
#260070=CARTESIAN_POINT('Ctrl Pts',(115.047241549379,-6.14843924382291,
134.156230094282));
#260071=CARTESIAN_POINT('Ctrl Pts',(114.768793925566,-0.5033588746261,137.78898401237));
#260072=CARTESIAN_POINT('Ctrl Pts',(114.490346301753,5.60428370990391,135.003210248456));
#260073=CARTESIAN_POINT('Ctrl Pts',(114.211898677941,6.56186334951224,128.358898798961));
#260074=CARTESIAN_POINT('Ctrl Pts',(113.933451054127,1.48941113576461,123.961847293312));
#260075=CARTESIAN_POINT('Ctrl Pts',(113.655003430315,-4.95173714997151,
125.852731257293));
#260076=CARTESIAN_POINT('Ctrl Pts',(113.376555806502,-6.84248090069202,
132.293920702821));
#260077=CARTESIAN_POINT('Ctrl Pts',(113.098108182689,-2.4453189774521,137.366277199056));
#260078=CARTESIAN_POINT('Ctrl Pts',(112.819660558876,4.19897162559319,136.408552924347));
#260079=CARTESIAN_POINT('Ctrl Pts',(112.541212935063,6.98461243588604,130.300849699721));
#260080=CARTESIAN_POINT('Ctrl Pts',(112.26276531125,3.35173563488669,124.655848410718));
#260081=CARTESIAN_POINT('Ctrl Pts',(111.984317687437,-3.3612224731848,124.661029468288));
#260082=CARTESIAN_POINT('Ctrl Pts',(111.705870063624,-6.98538133324609,
130.311631733633));
#260083=CARTESIAN_POINT('Ctrl Pts',(111.427422439812,-4.1903160029037,136.415027772168));
#260084=CARTESIAN_POINT('Ctrl Pts',(111.148974815999,2.45544502578993,137.362494791951));
#260085=CARTESIAN_POINT('Ctrl Pts',(110.870527192186,6.84477203094083,132.28335688814));
#260086=CARTESIAN_POINT('Ctrl Pts',(110.592079568373,4.94408792536061,125.845093664656));
#260087=CARTESIAN_POINT('Ctrl Pts',(110.31363194456,-1.49997145150339,123.964154497236));
#260088=CARTESIAN_POINT('Ctrl Pts',(110.035184320747,-6.56563034211481,
128.369030591753));
#260089=CARTESIAN_POINT('Ctrl Pts',(109.756736696934,-5.59779569719655,
135.011856007506));
#260090=CARTESIAN_POINT('Ctrl Pts',(109.478289073121,0.514139725922464,
137.788198707481));
#260091=CARTESIAN_POINT('Ctrl Pts',(109.199841449309,6.15360585804082,134.146735382281));
#260092=CARTESIAN_POINT('Ctrl Pts',(108.921393825496,6.13820882697821,127.433792932393));
#260093=CARTESIAN_POINT('Ctrl Pts',(108.642946201683,0.482097752094529,
123.818237523792));
#260094=CARTESIAN_POINT('Ctrl Pts',(108.36449857787,-5.61703760517944,126.622587947283));
#260095=CARTESIAN_POINT('Ctrl Pts',(108.086050954057,-6.5543898108359,133.26978316381));
#260096=CARTESIAN_POINT('Ctrl Pts',(107.807603330244,-1.46857798007734,
137.651375502926));
#260097=CARTESIAN_POINT('Ctrl Pts',(107.529155706431,4.96678527034939,135.740895657668));
#260098=CARTESIAN_POINT('Ctrl Pts',(107.250708082618,6.83791549827476,129.2939812737));
#260099=CARTESIAN_POINT('Ctrl Pts',(106.972260458805,2.42533543402888,124.23503172061));
#260100=CARTESIAN_POINT('Ctrl Pts',(106.693812834992,-4.21600940986681,
125.212974494265));
#260101=CARTESIAN_POINT('Ctrl Pts',(106.415365211179,-6.98304756960462,
131.329127960835));
#260102=CARTESIAN_POINT('Ctrl Pts',(106.136917587367,-3.33300615371489,
136.96304587525));
#260103=CARTESIAN_POINT('Ctrl Pts',(105.858469963554,3.37990509103613,136.937432906355));
#260104=CARTESIAN_POINT('Ctrl Pts',(105.580022339741,6.98684867466819,131.275826121299));
#260105=CARTESIAN_POINT('Ctrl Pts',(105.301574715928,4.1732196528133,125.180965570684));
#260106=CARTESIAN_POINT('Ctrl Pts',(105.023127092115,-2.4753943568629,124.253730350031));
#260107=CARTESIAN_POINT('Ctrl Pts',(104.744679468302,-6.84924188231931,
129.346204329164));
#260108=CARTESIAN_POINT('Ctrl Pts',(104.466231844489,-4.92897072199215,
135.778652702442));
#260109=CARTESIAN_POINT('Ctrl Pts',(104.187784220676,1.52078373823962,137.639969657397));
#260110=CARTESIAN_POINT('Ctrl Pts',(103.909336596864,6.57301223744494,133.219695842813));
#260111=CARTESIAN_POINT('Ctrl Pts',(103.63088897305,5.58496359993783,126.579846951912));
#260112=CARTESIAN_POINT('Ctrl Pts',(103.352441349238,-0.535393745272065,
123.82211974078));
#260113=CARTESIAN_POINT('Ctrl Pts',(103.073993725425,-6.1637503940156,127.480730793984));
#260114=CARTESIAN_POINT('Ctrl Pts',(102.795546101612,-6.12792154660547,
134.193595286717));
#260115=CARTESIAN_POINT('Ctrl Pts',(102.517098477799,-0.460832163475232,
137.791918691816));
#260116=CARTESIAN_POINT('Ctrl Pts',(102.238650853986,5.6297394649859,134.96901758787));
#260117=CARTESIAN_POINT('Ctrl Pts',(101.960203230173,6.54685555318778,128.319000183017));
#260118=CARTESIAN_POINT('Ctrl Pts',(101.68175560636,1.44773121968427,123.952907600908));
#260119=CARTESIAN_POINT('Ctrl Pts',(101.403307982548,-4.981787379107,125.882965629019));
#260120=CARTESIAN_POINT('Ctrl Pts',(101.124860358735,-6.83328675034245,
132.335545228093));
#260121=CARTESIAN_POINT('Ctrl Pts',(100.846412734922,-2.4053294226295,137.38104097262));
#260122=CARTESIAN_POINT('Ctrl Pts',(100.567965111109,4.23300813760519,136.382888759548));
#260123=CARTESIAN_POINT('Ctrl Pts',(100.289517487296,6.98141801332452,130.258341710245));
#260124=CARTESIAN_POINT('Ctrl Pts',(100.011069863483,3.31424579602927,124.635559362262));
#260125=CARTESIAN_POINT('Ctrl Pts',(99.7326222396699,-3.39855639790849,
124.681604005209));
#260126=CARTESIAN_POINT('Ctrl Pts',(99.4541746158571,-6.98825129087862,
130.354162861621));
#260127=CARTESIAN_POINT('Ctrl Pts',(99.1757269920442,-4.15608464258612,
136.440431462363));
#260128=CARTESIAN_POINT('Ctrl Pts',(98.8972793682313,2.49532075622072,137.347426294104));
#260129=CARTESIAN_POINT('Ctrl Pts',(98.6188317444184,6.85364828325664,132.241663415635));
#260130=CARTESIAN_POINT('Ctrl Pts',(98.3403841206056,4.91380785731226,125.815089481885));
#260131=CARTESIAN_POINT('Ctrl Pts',(98.0619364967926,-1.54158193664305,
123.97341198238));
#260132=CARTESIAN_POINT('Ctrl Pts',(97.7834888729798,-6.58033324128762,
128.409042568218));
#260133=CARTESIAN_POINT('Ctrl Pts',(97.5050412491668,-5.57207976433927,
135.045853423614));
#260134=CARTESIAN_POINT('Ctrl Pts',(97.226593625354,0.55664280480716,137.784939598694));
#260135=CARTESIAN_POINT('Ctrl Pts',(96.948146001541,6.17383782984873,134.109214710358));
#260136=CARTESIAN_POINT('Ctrl Pts',(96.6696983777281,6.11757749800464,127.396490361844));
#260137=CARTESIAN_POINT('Ctrl Pts',(96.3912507539153,0.43956230576973,123.815432294619));
#260138=CARTESIAN_POINT('Ctrl Pts',(96.1128031301024,-5.64238917165504,
126.656857928054));
#260139=CARTESIAN_POINT('Ctrl Pts',(95.8343555062895,-6.53926064636413,
133.309635916377));
#260140=CARTESIAN_POINT('Ctrl Pts',(95.5559078824767,-1.42687104770695,
137.660188294596));
#260141=CARTESIAN_POINT('Ctrl Pts',(95.2774602586637,4.99674333726689,135.710569963425));
#260142=CARTESIAN_POINT('Ctrl Pts',(94.9990126348508,6.82859469977515,129.252384925061));
#260143=CARTESIAN_POINT('Ctrl Pts',(94.720565011038,2.38530112858694,124.22038972988));
#260144=CARTESIAN_POINT('Ctrl Pts',(94.442117387225,-4.24996765133445,125.238742135624));
#260145=CARTESIAN_POINT('Ctrl Pts',(94.1636697634123,-6.97972378214161,
131.371626030693));
#260146=CARTESIAN_POINT('Ctrl Pts',(93.885222139599,-3.29545473562348,136.983220723554));
#260147=CARTESIAN_POINT('Ctrl Pts',(93.6067745157866,3.41717622101856,136.91674483311));
#260148=CARTESIAN_POINT('Ctrl Pts',(93.3283268919733,6.98958916888377,131.233286455149));
#260149=CARTESIAN_POINT('Ctrl Pts',(93.0498792681607,4.13891113095855,125.155666186642));
#260150=CARTESIAN_POINT('Ctrl Pts',(92.7714316443476,-2.51522403926791,
124.268920146089));
#260151=CARTESIAN_POINT('Ctrl Pts',(92.4929840205349,-6.85799119293255,
129.387924624807));
#260152=CARTESIAN_POINT('Ctrl Pts',(92.2145363967218,-4.89859947178764,
135.808564584124));
#260153=CARTESIAN_POINT('Ctrl Pts',(91.9360887729091,1.562365854042,137.63058556713));
#260154=CARTESIAN_POINT('Ctrl Pts',(91.6576411490961,6.58759328582208,133.179639301113));
#260155=CARTESIAN_POINT('Ctrl Pts',(91.3791935252832,5.55914430975498,126.545927963732));
#260156=CARTESIAN_POINT('Ctrl Pts',(91.1007459014705,-0.57788670767935,
123.825508199223));
#260157=CARTESIAN_POINT('Ctrl Pts',(90.8222982776573,-6.18386807209161,
127.518312871276));
#260158=CARTESIAN_POINT('Ctrl Pts',(90.5438506538447,-6.10717677700159,
134.230834889814));
#260159=CARTESIAN_POINT('Ctrl Pts',(90.2654030300316,-0.41828837601907,
137.794594444728));
#260160=CARTESIAN_POINT('Ctrl Pts',(89.9869554062187,5.65498660800168,134.934670604388));
#260161=CARTESIAN_POINT('Ctrl Pts',(89.708507782406,6.53160516072318,128.279193663018));
#260162=CARTESIAN_POINT('Ctrl Pts',(89.430060158593,1.40599765739116,123.944221791613));
#260163=CARTESIAN_POINT('Ctrl Pts',(89.1516125347801,-5.01165300627911,
125.913382364846));
#260164=CARTESIAN_POINT('Ctrl Pts',(88.8731649109673,-6.82383939003939,
132.377113014756));
#260165=CARTESIAN_POINT('Ctrl Pts',(88.5947172871542,-2.36525073744058,
137.395561044874));
#260166=CARTESIAN_POINT('Ctrl Pts',(88.3162696633415,4.26688779394398,136.357017880338));
#260167=CARTESIAN_POINT('Ctrl Pts',(88.0378220395285,6.97796489175107,130.2158539537));
#260168=CARTESIAN_POINT('Ctrl Pts',(87.7593744157156,3.2766331465752,124.615498901007));
#260169=CARTESIAN_POINT('Ctrl Pts',(87.4809267919028,-3.43576438787495,
124.702405423128));
#260170=CARTESIAN_POINT('Ctrl Pts',(87.2024791680898,-6.99086229628967,
130.396710671853));
#260171=CARTESIAN_POINT('Ctrl Pts',(86.924031544277,-4.1216992770237,136.465626305881));
#260172=CARTESIAN_POINT('Ctrl Pts',(86.6455839204641,2.53510402162323,137.332115340552));
#260173=CARTESIAN_POINT('Ctrl Pts',(86.3671362966513,6.8622705711149,132.199916683345));
#260174=CARTESIAN_POINT('Ctrl Pts',(86.0886886728382,4.88334570630671,125.785270178391));
#260175=CARTESIAN_POINT('Ctrl Pts',(85.8102410490255,-1.58313529789712,
123.982922590838));
#260176=CARTESIAN_POINT('Ctrl Pts',(85.5317934252125,-6.59479230379227,
128.449143304076));
#260177=CARTESIAN_POINT('Ctrl Pts',(85.2533458013996,-5.5461573560172,135.079693669646));
#260178=CARTESIAN_POINT('Ctrl Pts',(84.9748981775869,0.599125257088023,
137.781421821987));
#260179=CARTESIAN_POINT('Ctrl Pts',(84.6964505537737,6.19384102782544,134.071571575853));
#260180=CARTESIAN_POINT('Ctrl Pts',(84.418002929961,6.09671947994716,127.359314071181));
#260181=CARTESIAN_POINT('Ctrl Pts',(84.1395553061481,0.397010571302045,
123.812886042756));
#260182=CARTESIAN_POINT('Ctrl Pts',(83.8611076823352,-5.66753165732491,
126.691281596061));
#260183=CARTESIAN_POINT('Ctrl Pts',(83.5826600585222,-6.52388916718428,
133.349395835046));
#260184=CARTESIAN_POINT('Ctrl Pts',(83.3042124347095,-1.38511124210516,
137.66874704105));
#260185=CARTESIAN_POINT('Ctrl Pts',(83.0257648108964,5.02651624802251,135.68006246779));
#260186=CARTESIAN_POINT('Ctrl Pts',(82.7473171870836,6.81902086518772,129.210846085452));
#260187=CARTESIAN_POINT('Ctrl Pts',(82.4688695632707,2.34517843493451,124.205991710613));
#260188=CARTESIAN_POINT('Ctrl Pts',(82.1904219394578,-4.28376840868787,
125.264716013022));
#260189=CARTESIAN_POINT('Ctrl Pts',(81.9119743156449,-6.97614135844701,
131.414103080323));
#260190=CARTESIAN_POINT('Ctrl Pts',(81.6335266918322,-3.25778120324508,
137.003166611925));
#260191=CARTESIAN_POINT('Ctrl Pts',(81.355079068019,3.45432072627939,136.895830263219));
#260192=CARTESIAN_POINT('Ctrl Pts',(81.0766314442065,6.99207066130227,131.190730894994));
#260193=CARTESIAN_POINT('Ctrl Pts',(80.7981838203932,4.10444924022979,125.130576117049));
#260194=CARTESIAN_POINT('Ctrl Pts',(80.5197361965806,-2.55496051912119,
124.284352115297));
#260195=CARTESIAN_POINT('Ctrl Pts',(80.2412885727675,-6.86648637816013,
129.429697407007));
#260196=CARTESIAN_POINT('Ctrl Pts',(79.9628409489547,-4.86804670217826,
135.838291033188));
#260197=CARTESIAN_POINT('Ctrl Pts',(79.6843933251418,1.6038900758031,137.620948528586));
#260198=CARTESIAN_POINT('Ctrl Pts',(79.405945701329,6.60193022850756,133.139494742587));
#260199=CARTESIAN_POINT('Ctrl Pts',(79.1274980775159,5.53311902343524,126.512166773338));
#260200=CARTESIAN_POINT('Ctrl Pts',(78.8490504537032,-0.620358256282274,
123.829155261608));
#260201=CARTESIAN_POINT('Ctrl Pts',(78.5706028298902,-6.2037566046621,127.556016714277));
#260202=CARTESIAN_POINT('Ctrl Pts',(78.2921552060774,-6.08620570371632,
134.267947523646));
#260203=CARTESIAN_POINT('Ctrl Pts',(78.0137075822645,-0.375729088733312,
137.797011171955));
#260204=CARTESIAN_POINT('Ctrl Pts',(77.7352599584516,5.68002420340909,134.90017057075));
#260205=CARTESIAN_POINT('Ctrl Pts',(77.4568123346387,6.51611273722737,128.23948071401));
#260206=CARTESIAN_POINT('Ctrl Pts',(77.1783647108257,1.36421199533782,123.935790187287));
#260207=CARTESIAN_POINT('Ctrl Pts',(76.8999170870129,-5.04133292480603,
125.94398033767));
#260208=CARTESIAN_POINT('Ctrl Pts',(76.6214694632,-6.81413916985829,132.418622522501));
#260209=CARTESIAN_POINT('Ctrl Pts',(76.3430218393871,-2.32508440701577,
137.409836877774));
#260210=CARTESIAN_POINT('Ctrl Pts',(76.0645742155741,4.30060933918641,136.33094124537));
#260211=CARTESIAN_POINT('Ctrl Pts',(75.7861265917614,6.97425319912241,130.173388004487));
#260212=CARTESIAN_POINT('Ctrl Pts',(75.5076789679483,3.23889908027492,124.595667770297));
#260213=CARTESIAN_POINT('Ctrl Pts',(75.2292313441357,-3.47284506432852,
124.72343295124));
#260214=CARTESIAN_POINT('Ctrl Pts',(74.9507837203226,-6.99321425272744,
130.439273587703));
#260215=CARTESIAN_POINT('Ctrl Pts',(74.6723360965098,-4.08716118037883,
136.490611369118));
#260216=CARTESIAN_POINT('Ctrl Pts',(74.3938884726969,2.57479334781394,137.316562498648));
#260217=CARTESIAN_POINT('Ctrl Pts',(74.1154408488841,6.87063857501356,132.158118238212));
#260218=CARTESIAN_POINT('Ctrl Pts',(73.836993225071,4.85270260113016,125.755636859138));
#260219=CARTESIAN_POINT('Ctrl Pts',(73.5585456012583,-1.62462999549052,
123.992685970191));
#260220=CARTESIAN_POINT('Ctrl Pts',(73.2800979774453,-6.60900699384299,
128.489331313375));
#260221=CARTESIAN_POINT('Ctrl Pts',(73.0016503536324,-5.52002943279461,
135.113375491641));
#260222=CARTESIAN_POINT('Ctrl Pts',(72.7232027298196,0.641585508562261,
137.777645507711));
#260223=CARTESIAN_POINT('Ctrl Pts',(72.4447551060067,6.21361471074508,134.033807373642));
#260224=CARTESIAN_POINT('Ctrl Pts',(72.1663074821937,6.07563554570727,127.322265437984));
#260225=CARTESIAN_POINT('Ctrl Pts',(71.8878598583809,0.354444125461637,
123.810598862555));
#260226=CARTESIAN_POINT('Ctrl Pts',(71.609412234568,-5.69246413052499,126.725857675724));
#260227=CARTESIAN_POINT('Ctrl Pts',(71.330964610755,-6.5082759428922,133.3890614465));
#260228=CARTESIAN_POINT('Ctrl Pts',(71.0525169869423,-1.34330011069692,
137.677051425141));
#260229=CARTESIAN_POINT('Ctrl Pts',(70.7740693631292,5.05610289937005,135.649374301231));
#260230=CARTESIAN_POINT('Ctrl Pts',(70.4956217393166,6.80919434927445,129.16936629411));
#260231=CARTESIAN_POINT('Ctrl Pts',(70.2171741155033,2.30496883983272,124.191838196331));
#260232=CARTESIAN_POINT('Ctrl Pts',(69.9387264916908,-4.31741042942741,
125.290895163988));
#260233=CARTESIAN_POINT('Ctrl Pts',(69.6602788678776,-6.97230043126892,
131.456557535721));
#260234=CARTESIAN_POINT('Ctrl Pts',(69.3818312440649,-3.21998695258627,
137.02288280126));
#260235=CARTESIAN_POINT('Ctrl Pts',(69.1033836202519,3.49133723041524,136.874689971681));
#260236=CARTESIAN_POINT('Ctrl Pts',(68.8249359964391,6.9942930599711,131.148161017746));
#260237=CARTESIAN_POINT('Ctrl Pts',(68.5464883726262,4.0698352576252,125.105696291628));
#260238=CARTESIAN_POINT('Ctrl Pts',(68.2680407488133,-2.59460232397255,
124.300025685817));
#260239=CARTESIAN_POINT('Ctrl Pts',(67.9895931250004,-6.87472712320984,
129.471521127857));
#260240=CARTESIAN_POINT('Ctrl Pts',(67.7111455011875,-4.83731354530826,
135.867830948109));
#260241=CARTESIAN_POINT('Ctrl Pts',(67.4326978773747,1.64535486482719,137.61105889887));
#260242=CARTESIAN_POINT('Ctrl Pts',(67.1542502535617,6.61602253424027,133.099263654809));
#260243=CARTESIAN_POINT('Ctrl Pts',(66.8758026297489,5.50688870535577,126.478564631767));
#260244=CARTESIAN_POINT('Ctrl Pts',(66.5973550059358,-0.662806817281494,
123.833060792792));
#260245=CARTESIAN_POINT('Ctrl Pts',(66.3189073821232,-6.22341525475008,
127.593840925854));
#260246=CARTESIAN_POINT('Ctrl Pts',(66.0404597583101,-6.0650091038406,134.304931812993));
#260247=CARTESIAN_POINT('Ctrl Pts',(65.7620121344974,-0.333155878668442,
137.799168783944));
#260248=CARTESIAN_POINT('Ctrl Pts',(65.4835645106842,5.70485132343066,134.865518765369));
#260249=CARTESIAN_POINT('Ctrl Pts',(65.2051168868716,6.50037885677781,128.199862807569));
#260250=CARTESIAN_POINT('Ctrl Pts',(64.9266692630585,1.32237578190785,123.927613100363));
#260251=CARTESIAN_POINT('Ctrl Pts',(64.6482216392459,-5.07082603488719,
125.974758413674));
#260252=CARTESIAN_POINT('Ctrl Pts',(64.3697740154327,-6.80418644924447,
132.460072213177));
#260253=CARTESIAN_POINT('Ctrl Pts',(64.09132639162,-2.28483191973344,137.423867942321));
#260254=CARTESIAN_POINT('Ctrl Pts',(63.812878767807,4.33417152376786,136.304659820925));
#260255=CARTESIAN_POINT('Ctrl Pts',(63.5344311439942,6.97028307297671,130.130945436197));
#260256=CARTESIAN_POINT('Ctrl Pts',(63.2559835201813,3.20104499537862,124.576066704985));
#260257=CARTESIAN_POINT('Ctrl Pts',(62.9775358963684,-3.5097970532309,124.744685810362));
#260258=CARTESIAN_POINT('Ctrl Pts',(62.6990882725555,-6.9953070730393,130.481850031987));
#260259=CARTESIAN_POINT('Ctrl Pts',(62.4206406487427,-4.05247163247362,
136.51538572624));
#260260=CARTESIAN_POINT('Ctrl Pts',(62.1421930249296,2.61438726408988,137.300768344709));
#260261=CARTESIAN_POINT('Ctrl Pts',(61.8637454011169,6.87875198487314,132.116269629093));
#260262=CARTESIAN_POINT('Ctrl Pts',(61.5852977773038,4.82187967727427,125.726190622201));
#260263=CARTESIAN_POINT('Ctrl Pts',(61.3068501534911,-1.66606449182178,
124.002701758653));
#260264=CARTESIAN_POINT('Ctrl Pts',(61.0284025296781,-6.62297678470872,
128.529605106938));
#260265=CARTESIAN_POINT('Ctrl Pts',(60.7499549058653,-5.49369696285183,
135.146897641504));
#260266=CARTESIAN_POINT('Ctrl Pts',(60.4715072820523,0.684021985849089,
137.773610795799));
#260267=CARTESIAN_POINT('Ctrl Pts',(60.1930596582395,6.23315814588628,133.995923503096));
#260268=CARTESIAN_POINT('Ctrl Pts',(59.9146120344266,6.05432647655821,127.285345835106));
#260269=CARTESIAN_POINT('Ctrl Pts',(59.6361644106137,0.311864545564345,
123.808570838767));
#260270=CARTESIAN_POINT('Ctrl Pts',(59.3577167868007,-5.71718566737322,
126.760584885814));
#260271=CARTESIAN_POINT('Ctrl Pts',(59.0792691629879,-6.49242155204172,
133.428631280914));
#260272=CARTESIAN_POINT('Ctrl Pts',(58.800821539175,-1.30143920280946,137.685101139145));
#260273=CARTESIAN_POINT('Ctrl Pts',(58.5223739153621,5.08550219496502,135.618506600908));
#260274=CARTESIAN_POINT('Ctrl Pts',(58.2439262915492,6.79911551616065,129.127947088084));
#260275=CARTESIAN_POINT('Ctrl Pts',(57.9654786677363,2.26467383326308,124.1779297115));
#260276=CARTESIAN_POINT('Ctrl Pts',(57.6870310439234,-4.35089246693584,
125.317278618444));
#260277=CARTESIAN_POINT('Ctrl Pts',(57.4085834201106,-6.96820114293417,
131.498987823723));
#260278=CARTESIAN_POINT('Ctrl Pts',(57.1301357962976,-3.18207338412696,
137.042368560968));
#260279=CARTESIAN_POINT('Ctrl Pts',(56.8516881724848,3.52822436176609,136.853324741857));
#260280=CARTESIAN_POINT('Ctrl Pts',(56.5732405486719,6.9962562825383,131.105578400848));
#260281=CARTESIAN_POINT('Ctrl Pts',(56.294792924859,4.03507046577855,125.081027632309));
#260282=CARTESIAN_POINT('Ctrl Pts',(56.0163453010462,-2.63414798488075,
124.315940276861));
#260283=CARTESIAN_POINT('Ctrl Pts',(55.7378976772331,-6.8827131227178,129.513394237565));
#260284=CARTESIAN_POINT('Ctrl Pts',(55.4594500534204,-4.80640114000575,
135.897183234276));
#260285=CARTESIAN_POINT('Ctrl Pts',(55.1810024296073,1.68675868462211,137.600917044446));
#260286=CARTESIAN_POINT('Ctrl Pts',(54.9025548057946,6.62986968082513,133.058947528554));
#260287=CARTESIAN_POINT('Ctrl Pts',(54.6241071819816,5.4804543274898,126.445122784157));
#260288=CARTESIAN_POINT('Ctrl Pts',(54.3456595581689,-0.705230817730614,
123.837224648055));
#260289=CARTESIAN_POINT('Ctrl Pts',(54.0672119343557,-6.24284329389726,
127.63178410442));
#260290=CARTESIAN_POINT('Ctrl Pts',(53.7887643105431,-6.04358776282204,
134.341786387386));
#260291=CARTESIAN_POINT('Ctrl Pts',(53.51031668673,-0.290570323389535,137.801067200743));
#260292=CARTESIAN_POINT('Ctrl Pts',(53.2318690629172,5.72946704808866,134.830716472279));
#260293=CARTESIAN_POINT('Ctrl Pts',(52.9534214391043,6.48440410239917,128.160341411752));
#260294=CARTESIAN_POINT('Ctrl Pts',(52.6749738152913,1.28049056735643,123.919690833848));
#260295=CARTESIAN_POINT('Ctrl Pts',(52.3965261914786,-5.10013124364513,
126.005715452363));
#260296=CARTESIAN_POINT('Ctrl Pts',(52.1180785676656,-6.79398159699943,
132.501460550851));
#260297=CARTESIAN_POINT('Ctrl Pts',(51.8396309438527,-2.24449476716385,
137.43765371859));
#260298=CARTESIAN_POINT('Ctrl Pts',(51.5611833200399,4.36757310402998,136.278174580871));
#260299=CARTESIAN_POINT('Ctrl Pts',(51.2827356962269,6.96605466042841,130.088527821552));
#260300=CARTESIAN_POINT('Ctrl Pts',(51.0042880724141,3.16307229458231,124.556696431394));
#260301=CARTESIAN_POINT('Ctrl Pts',(50.7258404486012,-3.54661898531293,
124.766163212963));
#260302=CARTESIAN_POINT('Ctrl Pts',(50.4473928247883,-6.99714067967511,
130.52443842702));
#260303=CARTESIAN_POINT('Ctrl Pts',(50.1689452009753,-4.0176319187415,136.539948459229));
#260304=CARTESIAN_POINT('Ctrl Pts',(49.8904975771625,2.65388430328469,137.284733463992));
#260305=CARTESIAN_POINT('Ctrl Pts',(49.6120499533496,6.88661050004828,132.074372406703));
#260306=CARTESIAN_POINT('Ctrl Pts',(49.3336023295367,4.79087807689359,125.696932558722));
#260307=CARTESIAN_POINT('Ctrl Pts',(49.0551547057238,-1.7074372515208,124.012969585086));
#260308=CARTESIAN_POINT('Ctrl Pts',(48.776707081911,-6.63670115873435,128.569963192402));
#260309=CARTESIAN_POINT('Ctrl Pts',(48.498259458098,-5.46716092194746,135.180258877061));
#260310=CARTESIAN_POINT('Ctrl Pts',(48.2198118342852,0.72643311645002,137.769317835757));
#260311=CARTESIAN_POINT('Ctrl Pts',(47.9413642104722,6.25247060906043,133.957921368012));
#260312=CARTESIAN_POINT('Ctrl Pts',(47.6629165866595,6.03279306211481,127.248556630613));
#260313=CARTESIAN_POINT('Ctrl Pts',(47.3844689628464,0.269273409411107,
123.806802046542));
#260314=CARTESIAN_POINT('Ctrl Pts',(47.1060213390337,-5.74169535180415,
126.7954619395));
#260315=CARTESIAN_POINT('Ctrl Pts',(46.8275737152206,-6.47632658212296,
133.468103872012));
#260316=CARTESIAN_POINT('Ctrl Pts',(46.5491260914079,-1.25953006961336,
137.69289588478));
#260317=CARTESIAN_POINT('Ctrl Pts',(46.2706784675948,5.11471304540623,135.587460510634));
#260318=CARTESIAN_POINT('Ctrl Pts',(45.9922308437821,6.78878473932087,129.086590002178));
#260319=CARTESIAN_POINT('Ctrl Pts',(45.7137832199691,2.22429490837156,124.164266771503));
#260320=CARTESIAN_POINT('Ctrl Pts',(45.4353355961562,-4.38421328052394,
125.343865398741));
#260321=CARTESIAN_POINT('Ctrl Pts',(45.1568879723434,-6.96384364534361,
131.541392372057));
#260322=CARTESIAN_POINT('Ctrl Pts',(44.8784403485304,-3.1440419027679,137.061623168999));
#260323=CARTESIAN_POINT('Ctrl Pts',(44.5999927247176,3.56498075346585,136.831735365442));
#260324=CARTESIAN_POINT('Ctrl Pts',(44.3215451009046,6.99796025625624,131.062984622213));
#260325=CARTESIAN_POINT('Ctrl Pts',(44.0430974770918,4.00015615291162,125.056571053198));
#260326=CARTESIAN_POINT('Ctrl Pts',(43.7646498532789,-2.67359603646683,
124.332095298706));
#260327=CARTESIAN_POINT('Ctrl Pts',(43.486202229466,-6.8904440807599,129.555315184507));
#260328=CARTESIAN_POINT('Ctrl Pts',(43.2077546056531,-4.77531063174146,
135.926346804027));
#260329=CARTESIAN_POINT('Ctrl Pts',(42.9293069818402,1.72810000095366,137.590523341125));
#260330=CARTESIAN_POINT('Ctrl Pts',(42.6508593580274,6.64347115515083,133.018547857752));
#260331=CARTESIAN_POINT('Ctrl Pts',(42.3724117342144,5.4538168693733,126.411842469708));
#260332=CARTESIAN_POINT('Ctrl Pts',(42.0939641104015,-0.74762868559244,
123.841646673103));
#260333=CARTESIAN_POINT('Ctrl Pts',(41.8155164865887,-6.26204000219037,
127.669844843974));
#260334=CARTESIAN_POINT('Ctrl Pts',(41.5370688627757,-6.02194247443641,
134.378509881167));
#260335=CARTESIAN_POINT('Ctrl Pts',(41.2586212389629,-0.247974000920424,
137.802706352008));
#260336=CARTESIAN_POINT('Ctrl Pts',(40.9801736151499,5.75387046523817,134.795764981093));
#260337=CARTESIAN_POINT('Ctrl Pts',(40.7017259913371,6.46818906604193,128.120917991039));
#260338=CARTESIAN_POINT('Ctrl Pts',(40.4232783675241,1.23855790375582,123.912023681303));
#260339=CARTESIAN_POINT('Ctrl Pts',(40.1448307437113,-5.12924746516435,
126.036850306614));
#260340=CARTESIAN_POINT('Ctrl Pts',(39.8663831198984,-6.78352499126783,
132.542786001862));
#260341=CARTESIAN_POINT('Ctrl Pts',(39.5879354960856,-2.20407444401526,
137.451193695743));
#260342=CARTESIAN_POINT('Ctrl Pts',(39.3094878722726,4.40081284226458,136.251486506627));
#260343=CARTESIAN_POINT('Ctrl Pts',(39.0310402484598,6.96156811816289,130.046136732356));
#260344=CARTESIAN_POINT('Ctrl Pts',(38.7525926246468,3.12498238497894,124.537557667297));
#260345=CARTESIAN_POINT('Ctrl Pts',(38.474145000834,-3.58330949612422,124.78786436319));
#260346=CARTESIAN_POINT('Ctrl Pts',(38.195697377021,-6.9987150046898,130.567037194673));
#260347=CARTESIAN_POINT('Ctrl Pts',(37.9172497532082,-3.98264333018119,
136.564298657899));
#260348=CARTESIAN_POINT('Ctrl Pts',(37.6388021293952,2.69328300182069,137.268458450676));
#260349=CARTESIAN_POINT('Ctrl Pts',(37.3603545055824,6.89421382933879,132.032428123559));
#260350=CARTESIAN_POINT('Ctrl Pts',(37.0819068817695,4.7596989487639,125.667863752866));
#260351=CARTESIAN_POINT('Ctrl Pts',(36.8034592579566,-1.74874674150458,
124.02348906901));
#260352=CARTESIAN_POINT('Ctrl Pts',(36.5250116341437,-6.65017960735793,
128.610404074285));
#260353=CARTESIAN_POINT('Ctrl Pts',(36.2465640103308,-5.44042229338459,
135.213457962098));
#260354=CARTESIAN_POINT('Ctrl Pts',(35.968116386518,0.768817328804687,137.764766786667));
#260355=CARTESIAN_POINT('Ctrl Pts',(35.689668762705,6.27155138463682,133.919802376575));
#260356=CARTESIAN_POINT('Ctrl Pts',(35.4112211388921,6.01103610030595,127.211899187745));
#260357=CARTESIAN_POINT('Ctrl Pts',(35.1327735150793,0.226672295232647,
123.805292551423));
#260358=CARTESIAN_POINT('Ctrl Pts',(34.8543258912663,-5.76599227560232,
126.830487544402));
#260359=CARTESIAN_POINT('Ctrl Pts',(34.5758782674535,-6.45999162954105,
133.507477757125));
#260360=CARTESIAN_POINT('Ctrl Pts',(34.2974306436406,-1.21757426406734,
137.700435373207));
#260361=CARTESIAN_POINT('Ctrl Pts',(34.0189830198277,5.1437343682746,135.556237180835));
#260362=CARTESIAN_POINT('Ctrl Pts',(33.7405353960148,6.778202401566,129.045296568894));
#260363=CARTESIAN_POINT('Ctrl Pts',(33.4620877722019,2.18383356141425,124.150849882625));
#260364=CARTESIAN_POINT('Ctrl Pts',(33.1836401483891,-4.41737163547663,
125.370654519698));
#260365=CARTESIAN_POINT('Ctrl Pts',(32.9051925245761,-6.95922809996586,
131.58376960941));
#260366=CARTESIAN_POINT('Ctrl Pts',(32.6267449007632,-3.10589391777991,
137.080645911863));
#260367=CARTESIAN_POINT('Ctrl Pts',(32.3482972769504,3.60160504349277,136.80992264244));
#260368=CARTESIAN_POINT('Ctrl Pts',(32.0698496531375,6.99940491798352,131.020381260171));
#260369=CARTESIAN_POINT('Ctrl Pts',(31.7914020293246,3.96509361278713,125.032327460544));
#260370=CARTESIAN_POINT('Ctrl Pts',(31.5129544055117,-2.71294501696876,
124.348490152723));
#260371=CARTESIAN_POINT('Ctrl Pts',(31.2345067816988,-6.89791971086261,
129.597282415287));
#260372=CARTESIAN_POINT('Ctrl Pts',(30.9560591578859,-4.74404317258561,
135.955320576696));
#260373=CARTESIAN_POINT('Ctrl Pts',(30.677611534073,1.76937728190418,137.579878174048));
#260374=CARTESIAN_POINT('Ctrl Pts',(30.3991639102601,6.65682645320975,132.978066139427));
#260375=CARTESIAN_POINT('Ctrl Pts',(30.1207162864473,5.42697731806706,126.378724921634));
#260376=CARTESIAN_POINT('Ctrl Pts',(29.8422686626343,-0.789998849798377,
123.846326704078));
#260377=CARTESIAN_POINT('Ctrl Pts',(29.5638210388214,-6.28100466828836,
127.708021734164));
#260378=CARTESIAN_POINT('Ctrl Pts',(29.2853734150086,-6.00007404075783,
134.415100933532));
#260379=CARTESIAN_POINT('Ctrl Pts',(29.0069257911957,-0.205368489683527,
137.804086176998));
#260380=CARTESIAN_POINT('Ctrl Pts',(28.7284781673828,5.77806067060162,134.760665586949));
#260381=CARTESIAN_POINT('Ctrl Pts',(28.4500305435699,6.45173434856014,128.08159400628));
#260382=CARTESIAN_POINT('Ctrl Pts',(28.171582919757,1.19657934493693,123.904611926838));
#260383=CARTESIAN_POINT('Ctrl Pts',(27.8931352959441,-5.15817362053239,
126.068161822712));
#260384=CARTESIAN_POINT('Ctrl Pts',(27.6146876721312,-6.77281701952304,
132.584047034882));
#260385=CARTESIAN_POINT('Ctrl Pts',(27.3362400483183,-2.16357244807759,
137.464487372053));
#260386=CARTESIAN_POINT('Ctrl Pts',(27.0577924245054,4.4338895067609,136.22459658713));
#260387=CARTESIAN_POINT('Ctrl Pts',(26.7793448006925,6.95682361243065,130.003773739425));
#260388=CARTESIAN_POINT('Ctrl Pts',(26.5008971768797,3.08677667800406,124.518651121888));
#260389=CARTESIAN_POINT('Ctrl Pts',(26.2224495530668,-3.61986722608435,
124.809788456898));
#260390=CARTESIAN_POINT('Ctrl Pts',(25.9440019292538,-7.00002998974624,
130.609644756432));
#260391=CARTESIAN_POINT('Ctrl Pts',(25.665554305441,-3.94750716330764,136.588435419948));
#260392=CARTESIAN_POINT('Ctrl Pts',(25.3871066816281,2.7325818997646,137.251943907838));
#260393=CARTESIAN_POINT('Ctrl Pts',(25.1086590578152,6.90156169100052,131.990438333922));
#260394=CARTESIAN_POINT('Ctrl Pts',(24.8302114340022,4.72834344823931,125.638985281792));
#260395=CARTESIAN_POINT('Ctrl Pts',(24.5517638101894,-1.78999143103474,
124.034259820624));
#260396=CARTESIAN_POINT('Ctrl Pts',(24.2733161863765,-6.66341163113055,
128.650926254035));
#260397=CARTESIAN_POINT('Ctrl Pts',(23.9948685625636,-5.41348206797292,
135.246493666413));
#260398=CARTESIAN_POINT('Ctrl Pts',(23.7164209387507,0.811173052350488,
137.759957817164));
#260399=CARTESIAN_POINT('Ctrl Pts',(23.4379733149379,6.29039976557031,133.881567941299));
#260400=CARTESIAN_POINT('Ctrl Pts',(23.159525691125,5.98905639734383,127.175374864857));
#260401=CARTESIAN_POINT('Ctrl Pts',(22.8810780673121,0.184062781628937,
123.804042409345));
#260402=CARTESIAN_POINT('Ctrl Pts',(22.6026304434992,-5.79007553843628,
126.865660402631));
#260403=CARTESIAN_POINT('Ctrl Pts',(22.3241828196863,-6.44341729959363,
133.546751477239));
#260404=CARTESIAN_POINT('Ctrl Pts',(22.0457351958734,-1.17557334085921,
137.707719325048));
#260405=CARTESIAN_POINT('Ctrl Pts',(21.7672875720605,5.17256508817436,135.524837768503));
#260406=CARTESIAN_POINT('Ctrl Pts',(21.4888399482477,6.76736889502847,129.004068318375));
#260407=CARTESIAN_POINT('Ctrl Pts',(21.2103923244347,2.14329129170119,124.137679542035));
#260408=CARTESIAN_POINT('Ctrl Pts',(20.9319447006219,-4.45036630309889,
125.397644988631));
#260409=CARTESIAN_POINT('Ctrl Pts',(20.6534970768089,-6.95435467783159,
131.626117965476));
#260410=CARTESIAN_POINT('Ctrl Pts',(20.3750494529961,-3.06763084275059,
137.099436084669));
#260411=CARTESIAN_POINT('Ctrl Pts',(20.0966018291831,3.6380958747203,136.787887381128));
#260412=CARTESIAN_POINT('Ctrl Pts',(19.8181542053702,7.00059021418742,130.977769893405));
#260413=CARTESIAN_POINT('Ctrl Pts',(19.5397065815574,3.92988414466092,125.0082977527));
#260414=CARTESIAN_POINT('Ctrl Pts',(19.2612589577445,-2.75219346829522,
124.365124231394));
#260415=CARTESIAN_POINT('Ctrl Pts',(18.9828113339316,-6.90513973601376,
129.639294374793));
#260416=CARTESIAN_POINT('Ctrl Pts',(18.7043637101187,-4.71259992116536,
135.98410347865));
#260417=CARTESIAN_POINT('Ctrl Pts',(18.4259160863058,1.81058899792882,137.568981937677));
#260418=CARTESIAN_POINT('Ctrl Pts',(18.1474684624929,6.6699350801164,132.937503873645));
#260419=CARTESIAN_POINT('Ctrl Pts',(17.86902083868,5.39993666812053,126.345771367118));
#260420=CARTESIAN_POINT('Ctrl Pts',(17.5905732148672,-0.832339740306418,
123.851264567558));
#260421=CARTESIAN_POINT('Ctrl Pts',(17.3121255910542,-6.29973658944851,
127.746313360329));
#260422=CARTESIAN_POINT('Ctrl Pts',(17.0336779672413,-5.97798327212915,
134.451558188587));
#260423=CARTESIAN_POINT('Ctrl Pts',(16.7552303434285,-0.162755368441711,
137.805206624583));
#260424=CARTESIAN_POINT('Ctrl Pts',(16.4767827196156,5.80203676780203,134.72541959047));
#260425=CARTESIAN_POINT('Ctrl Pts',(16.1983350958026,6.43504055968944,128.042370914639));
#260426=CARTESIAN_POINT('Ctrl Pts',(15.9198874719898,1.15455644643036,123.897455845098));
#260427=CARTESIAN_POINT('Ctrl Pts',(15.6414398481769,-5.18690863788001,
126.0996488404));
#260428=CARTESIAN_POINT('Ctrl Pts',(15.362992224364,-6.7618580785529,132.625242120967));
#260429=CARTESIAN_POINT('Ctrl Pts',(15.0845446005511,-2.12299028016722,
137.477534254917));
#260430=CARTESIAN_POINT('Ctrl Pts',(14.8060969767383,4.466801871851,136.197505818795));
#260431=CARTESIAN_POINT('Ctrl Pts',(14.5276493529253,6.95182131904109,129.961440412534));
#260432=CARTESIAN_POINT('Ctrl Pts',(14.2492017291125,3.04845658938423,124.499977495755));
#260433=CARTESIAN_POINT('Ctrl Pts',(13.9707541052995,-3.65629082053323,
124.831934681683));
#260434=CARTESIAN_POINT('Ctrl Pts',(13.6923064814867,-7.00108558611715,
130.652259533458));
#260435=CARTESIAN_POINT('Ctrl Pts',(13.4138588576738,-3.91222472010448,
136.612357850978));
#260436=CARTESIAN_POINT('Ctrl Pts',(13.1354112338608,2.77177954088132,137.23519044743));
#260437=CARTESIAN_POINT('Ctrl Pts',(12.856963610048,6.90865381275575,131.94840459374));
#260438=CARTESIAN_POINT('Ctrl Pts',(12.5785159862351,4.6968127372094,125.6102982156));
#260439=CARTESIAN_POINT('Ctrl Pts',(12.3000683624222,-1.83116979177416,
124.045281440813));
#260440=CARTESIAN_POINT('Ctrl Pts',(12.0216207386093,-6.67639673973472,
128.691528230086));
#260441=CARTESIAN_POINT('Ctrl Pts',(11.7431731147965,-5.38634124399241,
135.279364765853));
#260442=CARTESIAN_POINT('Ctrl Pts',(11.4647254909835,0.853498717580522,
137.75489110545));
#260443=CARTESIAN_POINT('Ctrl Pts',(11.1862778671706,6.30901505342741,133.843219478972));
#260444=CARTESIAN_POINT('Ctrl Pts',(10.9078302433578,5.96685476769427,127.13898501537));
#260445=CARTESIAN_POINT('Ctrl Pts',(10.6293826195448,0.141446447510913,
123.803051666633));
#260446=CARTESIAN_POINT('Ctrl Pts',(10.350934995732,-5.81394424789186,126.900979210845));
#260447=CARTESIAN_POINT('Ctrl Pts',(10.0724873719191,-6.42660420644864,
133.585923577051));
#260448=CARTESIAN_POINT('Ctrl Pts',(9.79403974810624,-1.1335288563486,137.714747470394));
#260449=CARTESIAN_POINT('Ctrl Pts',(9.51559212429333,5.20120413677258,135.493263437154));
#260450=CARTESIAN_POINT('Ctrl Pts',(9.23714450048043,6.75628462114785,128.962906778349));
#260451=CARTESIAN_POINT('Ctrl Pts',(8.95869687666756,2.10266960154115,124.124756237763));
#260452=CARTESIAN_POINT('Ctrl Pts',(8.68024925285465,-4.48319606076117,
125.4248358054));
#260453=CARTESIAN_POINT('Ctrl Pts',(8.40180162904178,-6.94922355952728,
131.66843587102));
#260454=CARTESIAN_POINT('Ctrl Pts',(8.12335400522884,-3.0292540955323,137.117992991138));
#260455=CARTESIAN_POINT('Ctrl Pts',(7.84490638141603,3.67445189496732,136.765630398031));
#260456=CARTESIAN_POINT('Ctrl Pts',(7.56645875760307,7.00151610094645,130.935152100895));
#260457=CARTESIAN_POINT('Ctrl Pts',(7.2880111337902,3.89452905323253,124.984482820099));
#260458=CARTESIAN_POINT('Ctrl Pts',(7.00956350997733,-2.79133993608059,
124.381996918337));
#260459=CARTESIAN_POINT('Ctrl Pts',(6.73111588616443,-6.91210388867261,
129.681349506257));
#260460=CARTESIAN_POINT('Ctrl Pts',(6.45266826235151,-4.68098204262199,
136.012694443327));
#260461=CARTESIAN_POINT('Ctrl Pts',(6.17422063853866,1.85173362191231,137.557835035774));
#260462=CARTESIAN_POINT('Ctrl Pts',(5.89577301472578,6.68279655012581,132.896862563455));
#260463=CARTESIAN_POINT('Ctrl Pts',(5.61732539091285,5.37269592153495,126.312983027266));
#260464=CARTESIAN_POINT('Ctrl Pts',(5.33887776709996,-0.874649788159289,
123.856460080569));
#260465=CARTESIAN_POINT('Ctrl Pts',(5.06043014328709,-6.31823507155263,
127.784718303561));
#260466=CARTESIAN_POINT('Ctrl Pts',(4.7819825194742,-5.95567098713191,134.487880295395));
#260467=CARTESIAN_POINT('Ctrl Pts',(4.50353489566127,-0.120136216239877,
137.806067653244));
#260468=CARTESIAN_POINT('Ctrl Pts',(4.22508727184843,5.82579786839633,134.690028297709));
#260469=CARTESIAN_POINT('Ctrl Pts',(3.94663964803551,6.41810831802433,128.003250169541));
#260470=CARTESIAN_POINT('Ctrl Pts',(3.66819202422262,1.11249076541009,123.890555701254));
#260471=CARTESIAN_POINT('Ctrl Pts',(3.3897444004097,-5.21545145242058,126.131310192911));
#260472=CARTESIAN_POINT('Ctrl Pts',(3.11129677659686,-6.75064857444498,
132.666369733619));
#260473=CARTESIAN_POINT('Ctrl Pts',(2.83284915278395,-2.08232944407128,
137.490333860877));
#260474=CARTESIAN_POINT('Ctrl Pts',(2.55440152897106,4.49954871795507,136.170215205482));
#260475=CARTESIAN_POINT('Ctrl Pts',(2.27595390515816,6.94656142335602,129.919138320362));
#260476=CARTESIAN_POINT('Ctrl Pts',(1.9975062813453,3.01002353908442,124.481537480858));
#260477=CARTESIAN_POINT('Ctrl Pts',(1.71905865753238,-3.69257892978116,
124.854302216906));
#260478=CARTESIAN_POINT('Ctrl Pts',(1.44061103371947,-7.00188175468703,
130.694879946647));
#260479=CARTESIAN_POINT('Ctrl Pts',(1.16216340990662,-3.87679730797559,
136.636065064534));
#260480=CARTESIAN_POINT('Ctrl Pts',(0.883715786093727,2.81087447268782,
137.218198690258));
#260481=CARTESIAN_POINT('Ctrl Pts',(0.605268162280799,6.91548993180329,
131.906328460586));
#260482=CARTESIAN_POINT('Ctrl Pts',(0.326820538467947,4.66510798405627,
125.5818036173));
#260483=CARTESIAN_POINT('Ctrl Pts',(0.0483729146550416,-1.87228029784353,
124.056553521165));
#260484=CARTESIAN_POINT('Ctrl Pts',(-0.23007470915786,-6.68913445200245,
128.732208497919));
#260485=CARTESIAN_POINT('Ctrl Pts',(-0.508522332970751,-5.35900082715629,
135.312070042369));
#260486=CARTESIAN_POINT('Ctrl Pts',(-0.786969956783612,0.895792756101716,
137.749566839272));
#260487=CARTESIAN_POINT('Ctrl Pts',(-1.06541758059653,6.32739655841135,
133.804758410613));
#260488=CARTESIAN_POINT('Ctrl Pts',(-1.34386520440944,5.94443203404716,
127.102730987725));
#260489=CARTESIAN_POINT('Ctrl Pts',(-1.62231282822229,0.0988248720430084,
123.802320359999));
#260490=CARTESIAN_POINT('Ctrl Pts',(-1.90076045203519,-5.83759751950527,
126.936442660293));
#260491=CARTESIAN_POINT('Ctrl Pts',(-2.17920807584809,-6.40955297312139,
133.624992605024));
#260492=CARTESIAN_POINT('Ctrl Pts',(-2.45765569966099,-1.09144236850938,
137.721519548813));
#260493=CARTESIAN_POINT('Ctrl Pts',(-2.73610332347384,5.22965045283876,
135.461515356786));
#260494=CARTESIAN_POINT('Ctrl Pts',(-3.01455094728676,6.74494999065597,
128.921813474073));
#260495=CARTESIAN_POINT('Ctrl Pts',(-3.29299857109967,2.06196999618574,
124.112080448687));
#260496=CARTESIAN_POINT('Ctrl Pts',(-3.57144619491253,-4.51585969194472,
125.452225962441));
#260497=CARTESIAN_POINT('Ctrl Pts',(-3.84989381872542,-6.94383493518842,
131.710721757939));
#260498=CARTESIAN_POINT('Ctrl Pts',(-4.12834144253832,-2.99076509818949,
137.136315943637));
#260499=CARTESIAN_POINT('Ctrl Pts',(-4.40678906635123,3.71067175704807,
136.743152517891));
#260500=CARTESIAN_POINT('Ctrl Pts',(-4.68523669016409,7.00218254395157,
130.892529461858));
#260501=CARTESIAN_POINT('Ctrl Pts',(-4.963684313977,3.85902964859785,124.960883545208));
#260502=CARTESIAN_POINT('Ctrl Pts',(-5.24213193778992,-2.83038296973812,
124.399107588329));
#260503=CARTESIAN_POINT('Ctrl Pts',(-5.52057956160276,-6.91881191077996,
129.723446251312));
#260504=CARTESIAN_POINT('Ctrl Pts',(-5.79902718541567,-4.6491907085676,
136.041092411279));
#260505=CARTESIAN_POINT('Ctrl Pts',(-6.07747480922856,1.89280962922548,
137.546437881394));
#260506=CARTESIAN_POINT('Ctrl Pts',(-6.35592243304147,6.69541038665145,
132.856143714835));
#260507=CARTESIAN_POINT('Ctrl Pts',(-6.63437005685431,5.34525608772619,
126.280361117063));
#260508=CARTESIAN_POINT('Ctrl Pts',(-6.91281768066725,-0.916927425542613,
123.86191305059));
#260509=CARTESIAN_POINT('Ctrl Pts',(-7.19126530448013,-6.33649942913263,
127.823235140749));
#260510=CARTESIAN_POINT('Ctrl Pts',(-7.469712928293,-5.93313801255607,134.524065908027));
#260511=CARTESIAN_POINT('Ctrl Pts',(-7.74816055210589,-0.0775126123463511,
137.806669231077));
#260512=CARTESIAN_POINT('Ctrl Pts',(-8.02660817591882,5.84934309190818,
134.654493020103));
#260513=CARTESIAN_POINT('Ctrl Pts',(-8.3050557997317,6.40093825099524,127.964233220621));
#260514=CARTESIAN_POINT('Ctrl Pts',(-8.58350342354456,1.07038386063539,
123.883911750995));
#260515=CARTESIAN_POINT('Ctrl Pts',(-8.86195104735747,-5.2438010064896,
126.163144707024));
#260516=CARTESIAN_POINT('Ctrl Pts',(-9.14039867117038,-6.73918892257159,
132.707428348838));
#260517=CARTESIAN_POINT('Ctrl Pts',(-9.41884629498326,-2.04159144649203,
137.50288571564));
#260518=CARTESIAN_POINT('Ctrl Pts',(-9.69729391879612,4.53212883162697,
136.142725758454));
#260519=CARTESIAN_POINT('Ctrl Pts',(-9.97574154260907,6.94104412028278,
129.876869030427));
#260520=CARTESIAN_POINT('Ctrl Pts',(-10.254189166422,2.97147895125515,124.463331760497));
#260521=CARTESIAN_POINT('Ctrl Pts',(-10.5326367902348,-3.72873020915888,
124.876890233732));
#260522=CARTESIAN_POINT('Ctrl Pts',(-10.8110844140478,-7.00241846595355,
130.737504416682));
#260523=CARTESIAN_POINT('Ctrl Pts',(-11.0895320378606,-3.84122623969676,
136.659556182137));
#260524=CARTESIAN_POINT('Ctrl Pts',(-11.3679796616735,2.84986524650705,
137.200969265957));
#260525=CARTESIAN_POINT('Ctrl Pts',(-11.6464272854864,6.92206979482823,
131.864211493609));
#260526=CARTESIAN_POINT('Ctrl Pts',(-11.9248749092993,4.6332303636112,125.553502542771));
#260527=CARTESIAN_POINT('Ctrl Pts',(-12.2033225331122,-1.91332142587795,
124.068075643991));
#260528=CARTESIAN_POINT('Ctrl Pts',(-12.4817701569251,-6.70162429593314,
128.77296555011));
#260529=CARTESIAN_POINT('Ctrl Pts',(-12.760217780738,-5.33146183057377,
135.344608284054));
#260530=CARTESIAN_POINT('Ctrl Pts',(-13.0386654045509,0.938053600692905,
137.743985215925));
#260531=CARTESIAN_POINT('Ctrl Pts',(-13.3171130283637,6.34554359938892,
133.766186161411));
#260532=CARTESIAN_POINT('Ctrl Pts',(-13.5955606521767,5.92178902728497,
127.066614125326));
#260533=CARTESIAN_POINT('Ctrl Pts',(-13.8740082759896,0.0561996345831295,
123.801848516541));
#260534=CARTESIAN_POINT('Ctrl Pts',(-14.1524558998025,-5.86103447679583,
126.972049436864));
#260535=CARTESIAN_POINT('Ctrl Pts',(-14.4309035236153,-6.39226423145161,
133.663957113442));
#260536=CARTESIAN_POINT('Ctrl Pts',(-14.7093511474282,-1.04931543687181,
137.728035309365));
#260537=CARTESIAN_POINT('Ctrl Pts',(-14.9877987712411,5.25790298228423,
135.429594703837));
#260538=CARTESIAN_POINT('Ctrl Pts',(-15.266246395054,6.73336542356173,128.880789928272));
#260539=CARTESIAN_POINT('Ctrl Pts',(-15.5446940188669,2.02119398377386,
124.099652644515));
#260540=CARTESIAN_POINT('Ctrl Pts',(-15.8231416426798,-4.54835598628669,
125.479814444798));
#260541=CARTESIAN_POINT('Ctrl Pts',(-16.1015892664927,-6.93818900449243,
131.752974059312));
#260542=CARTESIAN_POINT('Ctrl Pts',(-16.3800368903055,-2.95216527694612,
137.154404263204));
#260543=CARTESIAN_POINT('Ctrl Pts',(-16.6584845141185,3.74675411882228,
136.720454573632));
#260544=CARTESIAN_POINT('Ctrl Pts',(-16.9369321379314,7.00258951850748,
130.849903555692));
#260545=CARTESIAN_POINT('Ctrl Pts',(-17.2153797617442,3.82338724620039,
124.93750080251));
#260546=CARTESIAN_POINT('Ctrl Pts',(-17.4938273855571,-2.86932112251383,
124.416455607327));
#260547=CARTESIAN_POINT('Ctrl Pts',(-17.77227500937,-6.92526355376757,129.765583050046));
#260548=CARTESIAN_POINT('Ctrl Pts',(-18.0507226331829,-4.61722709704176,
136.069296330209));
#260549=CARTESIAN_POINT('Ctrl Pts',(-18.3291702569958,1.93381549778173,
137.534790896862));
#260550=CARTESIAN_POINT('Ctrl Pts',(-18.6076178808087,6.70777612228299,
132.81534883664));
#260551=CARTESIAN_POINT('Ctrl Pts',(-18.8860655046216,5.31761818348739,
126.247906845325));
#260552=CARTESIAN_POINT('Ctrl Pts',(-19.1645131284344,-0.959171085842972,
123.867623275557));
#260553=CARTESIAN_POINT('Ctrl Pts',(-19.4429607522474,-6.35452898539608,
127.861862444637));
#260554=CARTESIAN_POINT('Ctrl Pts',(-19.7214083760603,-5.91038518336925,
134.560113685611));
#260555=CARTESIAN_POINT('Ctrl Pts',(-19.9998559998732,-0.0348861361944895,
137.807011335788));
#260556=CARTESIAN_POINT('Ctrl Pts',(-20.278303623686,5.87267156586067,134.618815074426));
#260557=CARTESIAN_POINT('Ctrl Pts',(-20.5567512474989,6.38353099484532,
127.925321513668));
#260558=CARTESIAN_POINT('Ctrl Pts',(-20.8351988713118,1.02823729239309,
123.877524240513));
#260559=CARTESIAN_POINT('Ctrl Pts',(-21.1136464951247,-5.27195624958391,
126.1951512031));
#260560=CARTESIAN_POINT('Ctrl Pts',(-21.3920941189376,-6.72747954757436,
132.748416445183));
#260561=CARTESIAN_POINT('Ctrl Pts',(-21.6705417427505,-2.00077779699093,
137.515189354092));
#260562=CARTESIAN_POINT('Ctrl Pts',(-21.9489893665634,4.56454100559805,
136.115038496344));
#260563=CARTESIAN_POINT('Ctrl Pts',(-22.2274369903762,6.93526961426714,
129.834634109035));
#260564=CARTESIAN_POINT('Ctrl Pts',(-22.5058846141892,2.93282425418085,
124.445361009293));
#260565=CARTESIAN_POINT('Ctrl Pts',(-22.784332238002,-3.76474331906749,
124.899697895151));
#260566=CARTESIAN_POINT('Ctrl Pts',(-23.062779861815,-7.0026957000287,130.780131364099));
#260567=CARTESIAN_POINT('Ctrl Pts',(-23.3412274856278,-3.80551283336702,
136.682830333316));
#260568=CARTESIAN_POINT('Ctrl Pts',(-23.6196751094408,2.88875041752152,
137.183502812971));
#260569=CARTESIAN_POINT('Ctrl Pts',(-23.8981227332536,6.92839315801137,
131.822055253468));
#260570=CARTESIAN_POINT('Ctrl Pts',(-24.1765703570665,4.60118105711114,
125.525396040718));
#260571=CARTESIAN_POINT('Ctrl Pts',(-24.4550179808794,-1.95429165508329,
124.079847382335));
#260572=CARTESIAN_POINT('Ctrl Pts',(-24.7334656046923,-6.71386580871103,
128.813797876394));
#260573=CARTESIAN_POINT('Ctrl Pts',(-25.0119132285052,-5.30372527471246,
135.376978285193));
#260574=CARTESIAN_POINT('Ctrl Pts',(-25.290360852318,0.980279685362951,
137.738146442235));
#260575=CARTESIAN_POINT('Ctrl Pts',(-25.568808476131,6.36345550391485,133.727504160674));
#260576=CARTESIAN_POINT('Ctrl Pts',(-25.8472560999438,5.89892658645264,
127.030635766497));
#260577=CARTESIAN_POINT('Ctrl Pts',(-26.1257037237567,0.0135723146251221,
123.801636153745));
#260578=CARTESIAN_POINT('Ctrl Pts',(-26.4041513475696,-5.88425425129846,
127.007798221134));
#260579=CARTESIAN_POINT('Ctrl Pts',(-26.6825989713826,-6.37473862207999,
133.70281565846));
#260580=CARTESIAN_POINT('Ctrl Pts',(-26.9610465951954,-1.00714962246484,
137.734294510605));
#260581=CARTESIAN_POINT('Ctrl Pts',(-27.2394942190083,5.28596067820108,
135.397502661138));
#260582=CARTESIAN_POINT('Ctrl Pts',(-27.5179418428212,6.72153134913555,
128.839837661092));
#260583=CARTESIAN_POINT('Ctrl Pts',(-27.7963894666341,1.98034307527561,
124.087473285763));
#260584=CARTESIAN_POINT('Ctrl Pts',(-28.0748370904469,-4.58068373962494,
125.507600230172));
#260585=CARTESIAN_POINT('Ctrl Pts',(-28.3532847142599,-6.93228597665136,
131.795191209466));
#260586=CARTESIAN_POINT('Ctrl Pts',(-28.6317323380727,-2.91345606213275,
137.172257279568));
#260587=CARTESIAN_POINT('Ctrl Pts',(-28.9101799618857,3.78269764324474,
136.697537406337));
#260588=CARTESIAN_POINT('Ctrl Pts',(-29.1886275856985,7.00273700953358,
130.807275961916));
#260589=CARTESIAN_POINT('Ctrl Pts',(-29.4670752095115,3.78760316678249,
124.914335458459));
#260590=CARTESIAN_POINT('Ctrl Pts',(-29.7455228333243,-2.90815295154017,
124.434040332496));
#260591=CARTESIAN_POINT('Ctrl Pts',(-30.0239704571372,-6.93145857856742,
129.807758341064));
#260592=CARTESIAN_POINT('Ctrl Pts',(-30.3024180809501,-4.5850923924679,
136.097305155009));
#260593=CARTESIAN_POINT('Ctrl Pts',(-30.580865704763,1.97474970809384,137.52289451376));
#260594=CARTESIAN_POINT('Ctrl Pts',(-30.8593133285759,6.71989329880362,
132.774479440534));
#260595=CARTESIAN_POINT('Ctrl Pts',(-31.1377609523888,5.28978323295099,
126.215621414657));
#260596=CARTESIAN_POINT('Ctrl Pts',(-31.4162085762017,-1.00137920370602,
123.873590543879));
#260597=CARTESIAN_POINT('Ctrl Pts',(-31.6946562000146,-6.37232307225107,
127.900598783877));
#260598=CARTESIAN_POINT('Ctrl Pts',(-31.9731038238274,-5.88741334268594,
134.596022292384));
#260599=CARTESIAN_POINT('Ctrl Pts',(-32.2515514476404,0.00774163267598956,
137.807093954702));
#260600=CARTESIAN_POINT('Ctrl Pts',(-32.5299990714533,5.89578242580862,
134.582995782735));
#260601=CARTESIAN_POINT('Ctrl Pts',(-32.8084466952661,6.36588719460685,
127.886516490566));
#260602=CARTESIAN_POINT('Ctrl Pts',(-33.086894319079,0.9860526224398,123.8713934065));
#260603=CARTESIAN_POINT('Ctrl Pts',(-33.365341942892,-5.29991613840065,
126.227328495126));
#260604=CARTESIAN_POINT('Ctrl Pts',(-33.6437895667048,-6.71552088334846,
132.789332503824));
#260605=CARTESIAN_POINT('Ctrl Pts',(-33.9222371905177,-1.95989000793276,
137.527244320318));
#260606=CARTESIAN_POINT('Ctrl Pts',(-34.2006848143306,4.59678403882356,
136.08715444511));
#260607=CARTESIAN_POINT('Ctrl Pts',(-34.4791324381435,6.9292381192855,129.792435121214));
#260608=CARTESIAN_POINT('Ctrl Pts',(-34.7575800619564,2.89406088022529,
124.427625893158));
#260609=CARTESIAN_POINT('Ctrl Pts',(-35.0360276857693,-3.80061692502793,
124.922724356021));
#260610=CARTESIAN_POINT('Ctrl Pts',(-35.3144753095821,-7.00271344663942,
130.822759209339));
#260611=CARTESIAN_POINT('Ctrl Pts',(-35.592922933395,-3.76965841235978,
136.705886655638));
#260612=CARTESIAN_POINT('Ctrl Pts',(-35.8713705572079,2.92752854482695,
137.165799978524));
#260613=CARTESIAN_POINT('Ctrl Pts',(-36.1498181810209,6.9344597870381,131.779861302279));
#260614=CARTESIAN_POINT('Ctrl Pts',(-36.4282658048337,4.56896125215494,
125.49748515264));
#260615=CARTESIAN_POINT('Ctrl Pts',(-36.7067134286466,-1.99518946729269,
124.091868299989));
#260616=CARTESIAN_POINT('Ctrl Pts',(-36.9851610524595,-6.72585853672236,
128.854703963711));
#260617=CARTESIAN_POINT('Ctrl Pts',(-37.2636086762724,-5.27579218736066,
135.409178846303));
#260618=CARTESIAN_POINT('Ctrl Pts',(-37.5420563000852,1.02246944540875,
137.732050734562));
#260619=CARTESIAN_POINT('Ctrl Pts',(-37.8205039238982,6.38113160825695,
133.688713841779));
#260620=CARTESIAN_POINT('Ctrl Pts',(-38.0989515477111,5.87584555872632,
126.994797244432));
#260621=CARTESIAN_POINT('Ctrl Pts',(-38.377399171524,-0.0290555082599903,
123.801683279478));
#260622=CARTESIAN_POINT('Ctrl Pts',(-38.6558467953367,-5.90725598259587,
127.04368768842));
#260623=CARTESIAN_POINT('Ctrl Pts',(-38.9342944191497,-6.35697679442443,
133.741566800161));
#260624=CARTESIAN_POINT('Ctrl Pts',(-39.2127420429625,-0.964946487758246,
137.740296920595));
#260625=CARTESIAN_POINT('Ctrl Pts',(-39.4911896667755,5.31382250090111,
135.365240417872));
#260626=CARTESIAN_POINT('Ctrl Pts',(-39.7696372905882,6.70944820589337,
128.798958190032));
#260627=CARTESIAN_POINT('Ctrl Pts',(-40.0480849144012,1.93941878443644,
124.07554282374));
#260628=CARTESIAN_POINT('Ctrl Pts',(-40.3265325382142,-4.61284175404266,
125.535582288951));
#260629=CARTESIAN_POINT('Ctrl Pts',(-40.604980162027,-6.9261260704041,131.837371644027));
#260630=CARTESIAN_POINT('Ctrl Pts',(-40.8834277858398,-2.87463888813357,
137.18987433118));
#260631=CARTESIAN_POINT('Ctrl Pts',(-41.1618754096529,3.81850099841496,
136.674401865208));
#260632=CARTESIAN_POINT('Ctrl Pts',(-41.4403230334656,7.00262501156454,
130.76464826011));
#260633=CARTESIAN_POINT('Ctrl Pts',(-41.7187706572786,3.75167873633635,
124.891388371457));
#260634=CARTESIAN_POINT('Ctrl Pts',(-41.9972182810916,-2.94687701788942,
124.451861112224));
#260635=CARTESIAN_POINT('Ctrl Pts',(-42.2756659049044,-6.93739675562063,
129.849970561546));
#260636=CARTESIAN_POINT('Ctrl Pts',(-42.5541135287174,-4.55278778560923,
136.125117847804));
#260637=CARTESIAN_POINT('Ctrl Pts',(-42.8325611525302,2.01561074332903,
137.510749172913));
#260638=CARTESIAN_POINT('Ctrl Pts',(-43.1110087763431,6.73176146720674,
132.733537040953));
#260639=CARTESIAN_POINT('Ctrl Pts',(-43.389456400156,5.26175226755184,126.183506021407));
#260640=CARTESIAN_POINT('Ctrl Pts',(-43.6679040239687,-1.0435502150944,
123.879814634434));
#260641=CARTESIAN_POINT('Ctrl Pts',(-43.9463516477818,-6.38988103033122,
127.93944272308));
#260642=CARTESIAN_POINT('Ctrl Pts',(-44.2247992715946,-5.86422334173611,
134.631790397739));
#260643=CARTESIAN_POINT('Ctrl Pts',(-44.5032468954075,0.050369114677416,
137.806917084757));
#260644=CARTESIAN_POINT('Ctrl Pts',(-44.7816945192204,5.91867481537061,
134.547036472328));
#260645=CARTESIAN_POINT('Ctrl Pts',(-45.0601421430334,6.34800750407734,
127.847819589252));
#260646=CARTESIAN_POINT('Ctrl Pts',(-45.3385897668461,0.943831413943965,
123.865519476137));
#260647=CARTESIAN_POINT('Ctrl Pts',(-45.6170373906592,-5.32767963687585,
126.25967539076));
#260648=CARTESIAN_POINT('Ctrl Pts',(-45.895485014472,-6.7033133730266,132.830175008601));
#260649=CARTESIAN_POINT('Ctrl Pts',(-46.1739326382849,-1.91892959442962,
137.539050167615));
#260650=CARTESIAN_POINT('Ctrl Pts',(-46.4523802620978,4.62885673652604,
136.059074638009));
#260651=CARTESIAN_POINT('Ctrl Pts',(-46.7308278859106,6.92294985883713,
129.750273630666));
#260652=CARTESIAN_POINT('Ctrl Pts',(-47.0092755097235,2.8551902657795,124.410127069272));
#260653=CARTESIAN_POINT('Ctrl Pts',(-47.2877231335364,-3.83634969773052,
124.945968763085));
#260654=CARTESIAN_POINT('Ctrl Pts',(-47.5661707573492,-7.00247170512816,
130.865386372813));
#260655=CARTESIAN_POINT('Ctrl Pts',(-47.8446183811622,-3.73366430527375,
136.728724294741));
#260656=CARTESIAN_POINT('Ctrl Pts',(-48.123066004975,2.96619819148554,137.147861418602));
#260657=CARTESIAN_POINT('Ctrl Pts',(-48.4015136287881,6.9402694571073,131.737631203552));
#260658=CARTESIAN_POINT('Ctrl Pts',(-48.6799612526008,4.53657214265928,
125.469770912784));
#260659=CARTESIAN_POINT('Ctrl Pts',(-48.9584088764139,-2.03601334702262,
124.104137951514));
#260660=CARTESIAN_POINT('Ctrl Pts',(-49.2368565002267,-6.7376020355722,
128.895682296272));
#260661=CARTESIAN_POINT('Ctrl Pts',(-49.5153041240395,-5.24766360358919,
135.441208774179));
#260662=CARTESIAN_POINT('Ctrl Pts',(-49.7937517478526,1.06462131747325,
137.725698318783));
#260663=CARTESIAN_POINT('Ctrl Pts',(-50.0721993716652,6.39857125742062,
133.649816642113));
#260664=CARTESIAN_POINT('Ctrl Pts',(-50.3506469954783,5.85254679938199,
126.959099887138));
#260665=CARTESIAN_POINT('Ctrl Pts',(-50.6290946192911,-0.0716822544825644,
123.801989891996));
#260666=CARTESIAN_POINT('Ctrl Pts',(-50.907542243104,-5.93003881835047,
127.079716508824));
#260667=CARTESIAN_POINT('Ctrl Pts',(-51.1859898669169,-6.33897940665598,
133.780209102606));
#260668=CARTESIAN_POINT('Ctrl Pts',(-51.4644374907297,-0.922707596604453,
137.746042316915));
#260669=CARTESIAN_POINT('Ctrl Pts',(-51.7428851145428,5.34148741795441,
135.332809169526));
#260670=CARTESIAN_POINT('Ctrl Pts',(-52.0213327383556,6.69711644158035,
128.758153029896));
#260671=CARTESIAN_POINT('Ctrl Pts',(-52.2997803621686,1.89842262772099,
124.063861700536));
#260672=CARTESIAN_POINT('Ctrl Pts',(-52.5782279859813,-4.64482883791282,
125.563759584248));
#260673=CARTESIAN_POINT('Ctrl Pts',(-52.8566756097944,-6.91970951400822,
131.879513799985));
#260674=CARTESIAN_POINT('Ctrl Pts',(-53.135123233607,-2.83571519333325,
137.207254765232));
#260675=CARTESIAN_POINT('Ctrl Pts',(-53.4135708574202,3.85416285762642,
136.651048807542));
#260676=CARTESIAN_POINT('Ctrl Pts',(-53.6920184812329,7.0022535287505,130.72202202986));
#260677=CARTESIAN_POINT('Ctrl Pts',(-53.9704661050458,3.71561528605495,
124.868660391816));
#260678=CARTESIAN_POINT('Ctrl Pts',(-54.2489137288587,-2.98549188662705,
124.469917286158));
#260679=CARTESIAN_POINT('Ctrl Pts',(-54.5273613526715,-6.94307786488582,
129.892218147303));
#260680=CARTESIAN_POINT('Ctrl Pts',(-54.8058089764845,-4.5203144735249,
136.152733377983));
#260681=CARTESIAN_POINT('Ctrl Pts',(-55.0842566002972,2.05639708936689,
137.498355324372));
#260682=CARTESIAN_POINT('Ctrl Pts',(-55.3627042241104,6.74338018771311,
132.69252315503));
#260683=CARTESIAN_POINT('Ctrl Pts',(-55.6411518479232,5.23352632598741,
126.151561855625));
#260684=CARTESIAN_POINT('Ctrl Pts',(-55.919599471736,-1.08568255734582,
123.886295316588));
#260685=CARTESIAN_POINT('Ctrl Pts',(-56.1980470955489,-6.40720220901991,
127.978392822871));
#260686=CARTESIAN_POINT('Ctrl Pts',(-56.4764947193619,-5.8408160398338,
134.667416676276));
#260687=CARTESIAN_POINT('Ctrl Pts',(-56.7549423431748,0.0929947302327828,
137.806480732508));
#260688=CARTESIAN_POINT('Ctrl Pts',(-57.0333899669875,5.94134788626073,
134.510938475691));
#260689=CARTESIAN_POINT('Ctrl Pts',(-57.3118375908005,6.32989258579528,
127.809232243652));
#260690=CARTESIAN_POINT('Ctrl Pts',(-57.5902852146133,0.901575231427987,
123.859902667085));
#260691=CARTESIAN_POINT('Ctrl Pts',(-57.8687328384263,-5.35524571622284,
126.292190691378));
#260692=CARTESIAN_POINT('Ctrl Pts',(-58.1471804622391,-6.69085746896258,
132.870942446081));
#260693=CARTESIAN_POINT('Ctrl Pts',(-58.4256280860521,-1.87789807428466,
137.550606458515));
#260694=CARTESIAN_POINT('Ctrl Pts',(-58.7040757098649,4.6607579102399,136.030800115547));
#260695=CARTESIAN_POINT('Ctrl Pts',(-58.9825233336777,6.91640506593584,
129.708151199698));
#260696=CARTESIAN_POINT('Ctrl Pts',(-59.2609709574908,2.81621385120844,
124.392865186062));
#260697=CARTESIAN_POINT('Ctrl Pts',(-59.5394185813036,-3.87194031308425,
124.969430255013));
#260698=CARTESIAN_POINT('Ctrl Pts',(-59.8178662051166,-7.00197048445272,
130.908011274954));
#260699=CARTESIAN_POINT('Ctrl Pts',(-60.0963138289294,-3.69753184588372,
136.751342404371));
#260700=CARTESIAN_POINT('Ctrl Pts',(-60.3747614527424,3.00475792457964,
137.129687797925));
#260701=CARTESIAN_POINT('Ctrl Pts',(-60.6532090765552,6.94582195293937,
131.695366522141));
#260702=CARTESIAN_POINT('Ctrl Pts',(-60.9316567003681,4.50401492881459,
125.442254348109));
#260703=CARTESIAN_POINT('Ctrl Pts',(-61.210104324181,-2.07676178152925,
124.116655882255));
#260704=CARTESIAN_POINT('Ctrl Pts',(-61.4885519479939,-6.74909587010084,
128.93673135561));
#260705=CARTESIAN_POINT('Ctrl Pts',(-61.7669995718066,-5.21934056571308,
135.473066881942));
#260706=CARTESIAN_POINT('Ctrl Pts',(-62.0454471956197,1.10673373960332,
137.719089430292));
#260707=CARTESIAN_POINT('Ctrl Pts',(-62.3238948194324,6.41577380517329,
133.610814003028));
#260708=CARTESIAN_POINT('Ctrl Pts',(-62.6023424432454,5.82903117176375,
126.923545017394));
#260709=CARTESIAN_POINT('Ctrl Pts',(-62.8807900670583,-0.114306344492842,
123.802555979936));
#260710=CARTESIAN_POINT('Ctrl Pts',(-63.1592376908712,-5.95260191433588,
127.115883347286));
#260711=CARTESIAN_POINT('Ctrl Pts',(-63.4376853146842,-6.32074712567447,
133.818741133891));
#260712=CARTESIAN_POINT('Ctrl Pts',(-63.716132938497,-0.880434514181572,
137.751530486667));
#260713=CARTESIAN_POINT('Ctrl Pts',(-63.99458056231,5.36895440422691,135.300210117855));
#260714=CARTESIAN_POINT('Ctrl Pts',(-64.2730281861228,6.6845365131549,128.717423692735));
#260715=CARTESIAN_POINT('Ctrl Pts',(-64.5514758099358,1.85735612425694,
124.052430348997));
#260716=CARTESIAN_POINT('Ctrl Pts',(-64.8299234337484,-4.67664380594228,
125.592131071942));
#260717=CARTESIAN_POINT('Ctrl Pts',(-65.1083710575615,-6.91303654523158,
131.921616115747));
#260718=CARTESIAN_POINT('Ctrl Pts',(-65.3868186813742,-2.79668642006362,
137.224397937687));
#260719=CARTESIAN_POINT('Ctrl Pts',(-65.6652663051872,3.88968189941585,
136.627479098696));
#260720=CARTESIAN_POINT('Ctrl Pts',(-65.9437139290001,7.00162257485687,
130.679398850698));
#260721=CARTESIAN_POINT('Ctrl Pts',(-66.2221615528129,3.67941415228271,
124.846152361731));
#260722=CARTESIAN_POINT('Ctrl Pts',(-66.500609176626,-3.02399612686491,
124.48820818522));
#260723=CARTESIAN_POINT('Ctrl Pts',(-66.7790568004388,-6.94850169584742,
129.934499532835));
#260724=CARTESIAN_POINT('Ctrl Pts',(-67.0575044242516,-4.48767365952541,
136.180150722241));
#260725=CARTESIAN_POINT('Ctrl Pts',(-67.3359520480646,2.09710723485436,
137.485713427398));
#260726=CARTESIAN_POINT('Ctrl Pts',(-67.6143996718775,6.75474902978674,
132.651439302549));
#260727=CARTESIAN_POINT('Ctrl Pts',(-67.8928472956903,5.20510645418034,
126.119790101011));
#260728=CARTESIAN_POINT('Ctrl Pts',(-68.1712949195033,-1.12777466923081,
123.893032350195));
#260729=CARTESIAN_POINT('Ctrl Pts',(-68.449742543316,-6.42428596647451,
128.017447639935));
#260730=CARTESIAN_POINT('Ctrl Pts',(-68.728190167129,-5.81719230434518,
134.702899807851));
#260731=CARTESIAN_POINT('Ctrl Pts',(-69.0066377909419,0.135616899834216,
137.805784914121));
#260732=CARTESIAN_POINT('Ctrl Pts',(-69.2850854147548,5.96380079832,134.474703130449));
#260733=CARTESIAN_POINT('Ctrl Pts',(-69.5635330385676,6.31154311101565,
127.770755883637));
#260734=CARTESIAN_POINT('Ctrl Pts',(-69.8419806623805,0.859285640710264,
123.854543187474));
#260735=CARTESIAN_POINT('Ctrl Pts',(-70.1204282861936,-5.38261335497044,
126.324873192109));
#260736=CARTESIAN_POINT('Ctrl Pts',(-70.3988759100064,-6.67815363271447,
132.911633305611));
#260737=CARTESIAN_POINT('Ctrl Pts',(-70.6773235338194,-1.83679696793597,
137.561912764793));
#260738=CARTESIAN_POINT('Ctrl Pts',(-70.9557711576322,4.69248637785542,
136.002331925448));
#260739=CARTESIAN_POINT('Ctrl Pts',(-71.2342187814451,6.90960398310133,
129.666069389173));
#260740=CARTESIAN_POINT('Ctrl Pts',(-71.5126664052579,2.77713308079745,
124.375840883174));
#260741=CARTESIAN_POINT('Ctrl Pts',(-71.7911140290708,-3.90738745226578,
124.993107962432));
#260742=CARTESIAN_POINT('Ctrl Pts',(-72.0695616528837,-7.00120980318599,
130.950632336283));
#260743=CARTESIAN_POINT('Ctrl Pts',(-72.3480092766965,-3.66126237309149,
136.773740146404));
#260744=CARTESIAN_POINT('Ctrl Pts',(-72.6264569005095,3.04320631526353,
137.111279789924));
#260745=CARTESIAN_POINT('Ctrl Pts',(-72.9049045243223,6.95111706878496,
131.653068824177));
#260746=CARTESIAN_POINT('Ctrl Pts',(-73.1833521481353,4.47129081703998,
125.414936478256));
#260747=CARTESIAN_POINT('Ctrl Pts',(-73.4617997719481,-2.11743326086482,
124.129421628353));
#260748=CARTESIAN_POINT('Ctrl Pts',(-73.7402473957612,-6.76033961440018,
128.977849620639));
#260749=CARTESIAN_POINT('Ctrl Pts',(-74.018695019574,-5.19082412325261,
135.504751989078));
#260750=CARTESIAN_POINT('Ctrl Pts',(-74.2971426433868,1.14880515130821,
137.712224313981));
#260751=CARTESIAN_POINT('Ctrl Pts',(-74.5755902671998,6.43273861406817,
133.571707369781));
#260752=CARTESIAN_POINT('Ctrl Pts',(-74.8540378910127,5.80529954725181,
126.8881339527));
#260753=CARTESIAN_POINT('Ctrl Pts',(-75.1324855148255,-0.156926198840311,
123.803381522322));
#260754=CARTESIAN_POINT('Ctrl Pts',(-75.4109331386384,-5.97494443446864,
127.15218686363));
#260755=CARTESIAN_POINT('Ctrl Pts',(-75.6893807624512,-6.30228062708332,
133.857161466198));
#260756=CARTESIAN_POINT('Ctrl Pts',(-75.9678283862644,-0.838128806933456,
137.756761226486));
#260757=CARTESIAN_POINT('Ctrl Pts',(-76.2462760100769,5.3962224419198,135.267444470826));
#260758=CARTESIAN_POINT('Ctrl Pts',(-76.52472363389,6.67170888677059,128.676771687789));
#260759=CARTESIAN_POINT('Ctrl Pts',(-76.8031712577027,1.81622079577817,
124.041249192718));
#260760=CARTESIAN_POINT('Ctrl Pts',(-77.0816188815158,-4.70828547921653,
125.620695700721));
#260761=CARTESIAN_POINT('Ctrl Pts',(-77.3600665053286,-6.90610741134329,
131.963677031195));
#260762=CARTESIAN_POINT('Ctrl Pts',(-77.6385141291417,-2.75755401454922,
137.241303213299));
#260763=CARTESIAN_POINT('Ctrl Pts',(-77.9169617529544,3.92505680761298,
136.603693612052));
#260764=CARTESIAN_POINT('Ctrl Pts',(-78.1954093767674,7.00073217326374,
130.636780302039));
#260765=CARTESIAN_POINT('Ctrl Pts',(-78.4738570005803,3.6430766764653,124.823865115242));
#260766=CARTESIAN_POINT('Ctrl Pts',(-78.7523046243931,-3.06238831181505,
124.506733131632));
#260767=CARTESIAN_POINT('Ctrl Pts',(-79.0307522482061,-6.95366804752337,
129.976813151389));
#260768=CARTESIAN_POINT('Ctrl Pts',(-79.3091998720188,-4.45486655312747,
136.207368864621));
#260769=CARTESIAN_POINT('Ctrl Pts',(-79.5876474958318,2.13773967126259,
137.472823950436));
#260770=CARTESIAN_POINT('Ctrl Pts',(-79.8660951196445,6.76586757215105,
132.610287005887));
#260771=CARTESIAN_POINT('Ctrl Pts',(-80.1445427434577,5.17649370523912,
126.08819193488));
#260772=CARTESIAN_POINT('Ctrl Pts',(-80.4229903672703,-1.16982499101125,
123.900025485612));
#260773=CARTESIAN_POINT('Ctrl Pts',(-80.7014379910835,-6.44113166965063,
128.056605727087));
#260774=CARTESIAN_POINT('Ctrl Pts',(-80.9798856148961,-5.7933530106558,
134.738238477622));
#260775=CARTESIAN_POINT('Ctrl Pts',(-81.2583332387092,0.17823404410257,
137.804829655383));
#260776=CARTESIAN_POINT('Ctrl Pts',(-81.5367808625219,5.98603271954817,
134.438331779315));
#260777=CARTESIAN_POINT('Ctrl Pts',(-81.815228486335,6.29295975968447,127.732391934959));
#260778=CARTESIAN_POINT('Ctrl Pts',(-82.0936761101477,0.816964208846405,
123.849441235906));
#260779=CARTESIAN_POINT('Ctrl Pts',(-82.3721237339607,-5.40978153900143,
126.357721681897));
#260780=CARTESIAN_POINT('Ctrl Pts',(-82.6505713577735,-6.66520233502723,
132.952246079378));
#260781=CARTESIAN_POINT('Ctrl Pts',(-82.9290189815866,-1.79562779839943,
137.572968667493));
#260782=CARTESIAN_POINT('Ctrl Pts',(-83.2074666053992,4.72404096366304,
135.97367112261));
#260783=CARTESIAN_POINT('Ctrl Pts',(-83.4859142292123,6.90254686235,129.624029758449));
#260784=CARTESIAN_POINT('Ctrl Pts',(-83.7643618530252,2.73794940269844,
124.359054791448));
#260785=CARTESIAN_POINT('Ctrl Pts',(-84.0428094768383,-3.94268980176888,
125.017001007954));
#260786=CARTESIAN_POINT('Ctrl Pts',(-84.3212571006508,-7.00018968951541,
130.99324797746));
#260787=CARTESIAN_POINT('Ctrl Pts',(-84.5997047244641,-3.62485723087481,
136.795916690882));
#260788=CARTESIAN_POINT('Ctrl Pts',(-84.8781523482765,3.08154193881888,
137.092638076712));
#260789=CARTESIAN_POINT('Ctrl Pts',(-85.1565999720898,6.95615460843127,
131.61073967702));
#260790=CARTESIAN_POINT('Ctrl Pts',(-85.4350475959023,4.4384010199398,125.387818315495));
#260791=CARTESIAN_POINT('Ctrl Pts',(-85.7134952197154,-2.1580262779319,
124.142434716771));
#260792=CARTESIAN_POINT('Ctrl Pts',(-85.9919428435283,-6.7713328518292,
129.019035567703));
#260793=CARTESIAN_POINT('Ctrl Pts',(-86.2703904673411,-5.16211533289519,
135.536262921482));
#260794=CARTESIAN_POINT('Ctrl Pts',(-86.5488380911541,1.19083399361533,
137.70510322424));
#260795=CARTESIAN_POINT('Ctrl Pts',(-86.827285714967,6.4494650554685,133.532498191482));
#260796=CARTESIAN_POINT('Ctrl Pts',(-87.1057333387799,5.78135280522977,
126.852868005224));
#260797=CARTESIAN_POINT('Ctrl Pts',(-87.3841809625928,-0.199540238229241,
123.804466488563));
#260798=CARTESIAN_POINT('Ctrl Pts',(-87.6626285864056,-5.99706555083783,
127.188625712615));
#260799=CARTESIAN_POINT('Ctrl Pts',(-87.9410762102187,-6.28358059516641,
133.895468675847));
#260800=CARTESIAN_POINT('Ctrl Pts',(-88.2195238340314,-0.795792042514341,
137.761734342542));
#260801=CARTESIAN_POINT('Ctrl Pts',(-88.4979714578443,5.42329052060546,
135.234513442586));
#260802=CARTESIAN_POINT('Ctrl Pts',(-88.7764190816572,6.65863403776028,
128.636198521433));
#260803=CARTESIAN_POINT('Ctrl Pts',(-89.0548667054699,1.77501816656995,
124.03031864602));
#260804=CARTESIAN_POINT('Ctrl Pts',(-89.3333143292831,-4.73975268523957,
125.649452412109));
#260805=CARTESIAN_POINT('Ctrl Pts',(-89.6117619530957,-6.8989223691057,
132.005694987746));
#260806=CARTESIAN_POINT('Ctrl Pts',(-89.8902095769088,-2.71831942685781,
137.257969965635));
#260807=CARTESIAN_POINT('Ctrl Pts',(-90.1686572007216,3.9602862713853,136.579693228991));
#260808=CARTESIAN_POINT('Ctrl Pts',(-90.4471048245344,6.99958235696585,
130.59416796313));
#260809=CARTESIAN_POINT('Ctrl Pts',(-90.7255524483476,3.60660420510239,
124.801799478213));
#260810=CARTESIAN_POINT('Ctrl Pts',(-91.0040000721602,-3.10066701883943,
124.525491438947));
#260811=CARTESIAN_POINT('Ctrl Pts',(-91.2824476959735,-6.95857672847263,
130.019157435019));
#260812=CARTESIAN_POINT('Ctrl Pts',(-91.560895319786,-4.4218943700117,136.234386796543));
#260813=CARTESIAN_POINT('Ctrl Pts',(-91.8393429435991,2.17829289294083,
137.459687371113));
#260814=CARTESIAN_POINT('Ctrl Pts',(-92.1177905674117,6.77673540280433,
132.56906778996));
#260815=CARTESIAN_POINT('Ctrl Pts',(-92.3962381912249,5.14768913942031,
126.056768528114));
#260816=CARTESIAN_POINT('Ctrl Pts',(-92.6746858150375,-1.21183196449619,
123.907274463707));
#260817=CARTESIAN_POINT('Ctrl Pts',(-92.9531334388505,-6.45773869432309,
128.095865633305));
#260818=CARTESIAN_POINT('Ctrl Pts',(-93.2315810626634,-5.76929904214118,
134.773431376103));
#260819=CARTESIAN_POINT('Ctrl Pts',(-93.5100286864763,0.220844583841736,
137.803614991691));
#260820=CARTESIAN_POINT('Ctrl Pts',(-93.7884763102892,6.00804282613147,
134.401825770043));
#260821=CARTESIAN_POINT('Ctrl Pts',(-94.0669239341021,6.27414322041607,
127.694141819211));
#260822=CARTESIAN_POINT('Ctrl Pts',(-94.3453715579151,0.774612504073732,
123.844597001431));
#260823=CARTESIAN_POINT('Ctrl Pts',(-94.6238191817278,-5.43674926158731,
126.390734943524));
#260824=CARTESIAN_POINT('Ctrl Pts',(-94.9022668055408,-6.65200405581671,
132.99277926246));
#260825=CARTESIAN_POINT('Ctrl Pts',(-95.1807144293538,-1.75439209121494,
137.583773756932));
#260826=CARTESIAN_POINT('Ctrl Pts',(-95.4591620531666,4.75542049839504,
135.94481876907));
#260827=CARTESIAN_POINT('Ctrl Pts',(-95.7376096769794,6.89523396518648,
129.582033865318));
#260828=CARTESIAN_POINT('Ctrl Pts',(-96.0160573007924,2.69866426887766,
124.342507532899));
#260829=CARTESIAN_POINT('Ctrl Pts',(-96.2945049246052,-3.97784605345104,
125.041108506217));
#260830=CARTESIAN_POINT('Ctrl Pts',(-96.5729525484182,-6.99891018124123,
131.035856619345));
#260831=CARTESIAN_POINT('Ctrl Pts',(-96.8514001722308,-3.58831776824163,
136.817871216047));
#260832=CARTESIAN_POINT('Ctrl Pts',(-97.129847796044,3.11976337470375,137.073763349068));
#260833=CARTESIAN_POINT('Ctrl Pts',(-97.4082954198568,6.96093438520996,
131.56838064919));
#260834=CARTESIAN_POINT('Ctrl Pts',(-97.6867430436697,4.40534675625846,
125.360900864701));
#260835=CARTESIAN_POINT('Ctrl Pts',(-97.9651906674826,-2.1985393285419,
124.155694665303));
#260836=CARTESIAN_POINT('Ctrl Pts',(-98.2436382912955,-6.78207517502872,
129.060287670645));
#260837=CARTESIAN_POINT('Ctrl Pts',(-98.5220859151084,-5.13321525845608,
135.567598511506));
#260838=CARTESIAN_POINT('Ctrl Pts',(-98.8005335389213,1.23281870913114,
137.697726424945));
#260839=CARTESIAN_POINT('Ctrl Pts',(-99.0789811627341,6.4659525095689,133.493187921042));
#260840=CARTESIAN_POINT('Ctrl Pts',(-99.3574287865471,5.7571918330539,126.817748481762));
#260841=CARTESIAN_POINT('Ctrl Pts',(-99.6358764103599,-0.242146883580649,
123.805810838454));
#260842=CARTESIAN_POINT('Ctrl Pts',(-99.9143240341728,-6.01896444373747,
127.225198543987));
#260843=CARTESIAN_POINT('Ctrl Pts',(-100.192771657986,-6.26464772285957,
133.93366134335));
#260844=CARTESIAN_POINT('Ctrl Pts',(-100.471219281798,-0.753425789729175,
137.766449650557));
#260845=CARTESIAN_POINT('Ctrl Pts',(-100.749666905611,5.45015763726631,
135.201418253402));
#260846=CARTESIAN_POINT('Ctrl Pts',(-101.028114529424,6.64531245061667,
128.595705697122));
#260847=CARTESIAN_POINT('Ctrl Pts',(-101.306562153237,1.73374976341167,
124.019639113937));
#260848=CARTESIAN_POINT('Ctrl Pts',(-101.58500977705,-4.77104425798471,
125.678400140516));
#260849=CARTESIAN_POINT('Ctrl Pts',(-101.863457400863,-6.89148168476197,
132.047668428412));
#260850=CARTESIAN_POINT('Ctrl Pts',(-102.141905024676,-2.67898411084018,
137.274397577103));
#260851=CARTESIAN_POINT('Ctrl Pts',(-102.420352648489,3.99536898529432,
136.555478838857));
#260852=CARTESIAN_POINT('Ctrl Pts',(-102.698800272302,6.99817316856906,
130.551563412989));
#260853=CARTESIAN_POINT('Ctrl Pts',(-102.977247896115,3.56999808969468,
124.779956268296));
#260854=CARTESIAN_POINT('Ctrl Pts',(-103.255695519928,-3.13883082950684,
124.544482412068));
#260855=CARTESIAN_POINT('Ctrl Pts',(-103.53414314374,-6.96322755680218,
130.061530814641));
#260856=CARTESIAN_POINT('Ctrl Pts',(-103.812590767553,-4.38875833197407,
136.261203516848));
#260857=CARTESIAN_POINT('Ctrl Pts',(-104.091038391366,2.21876539717438,
137.44630417621));
#260858=CARTESIAN_POINT('Ctrl Pts',(-104.369486015179,6.78735211903507,
132.52778318216));
#260859=CARTESIAN_POINT('Ctrl Pts',(-104.647933638992,5.11869382408742,
126.02552104512));
#260860=CARTESIAN_POINT('Ctrl Pts',(-104.926381262805,-1.25379403310144,
123.914779015865));
#260861=CARTESIAN_POINT('Ctrl Pts',(-105.204828886617,-6.47410642511416,
128.135225903801));
#260862=CARTESIAN_POINT('Ctrl Pts',(-105.483276510431,-5.74503129012806,
134.808477199207));
#260863=CARTESIAN_POINT('Ctrl Pts',(-105.761724134243,0.263446940103889,
137.802140968053));
#260864=CARTESIAN_POINT('Ctrl Pts',(-106.040171758056,6.02983030247923,
134.365186455377));
#260865=CARTESIAN_POINT('Ctrl Pts',(-106.318619381869,6.25509419046252,
127.656006953765));
#260866=CARTESIAN_POINT('Ctrl Pts',(-106.597067005682,0.732232095750508,
123.840010663559));
#260867=CARTESIAN_POINT('Ctrl Pts',(-106.875514629495,-5.46351552342998,
126.423911753675));
#260868=CARTESIAN_POINT('Ctrl Pts',(-107.153962253308,-6.63855928414971,
133.033231352883));
#260869=CARTESIAN_POINT('Ctrl Pts',(-107.432409877121,-1.71309137438684,
137.594327632723));
#260870=CARTESIAN_POINT('Ctrl Pts',(-107.710857500934,4.78662381927155,
135.915775933963));
#260871=CARTESIAN_POINT('Ctrl Pts',(-107.989305124746,6.8876655625929,129.540083265954));
#260872=CARTESIAN_POINT('Ctrl Pts',(-108.26775274856,2.65927913505975,124.326199720693));
#260873=CARTESIAN_POINT('Ctrl Pts',(-108.546200372372,-4.0128549045848,
125.065429563905));
#260874=CARTESIAN_POINT('Ctrl Pts',(-108.824647996185,-6.99737132577695,
131.078456683062));
#260875=CARTESIAN_POINT('Ctrl Pts',(-109.103095619998,-3.5516453391731,
136.839602908365));
#260876=CARTESIAN_POINT('Ctrl Pts',(-109.381543243811,3.1578692066097,137.054656306401));
#260877=CARTESIAN_POINT('Ctrl Pts',(-109.659990867624,6.96545622200577,
131.525993310316));
#260878=CARTESIAN_POINT('Ctrl Pts',(-109.938438491437,4.37212925083209,
125.334185123311));
#260879=CARTESIAN_POINT('Ctrl Pts',(-110.21688611525,-2.23897091146772,
124.169200982596));
#260880=CARTESIAN_POINT('Ctrl Pts',(-110.495333739063,-6.79256618593892,
129.10160440085));
#260881=CARTESIAN_POINT('Ctrl Pts',(-110.773781362875,-5.10412497083799,
135.598757597999));
#260882=CARTESIAN_POINT('Ctrl Pts',(-111.052228986688,1.27475774209554,
137.690094189444));
#260883=CARTESIAN_POINT('Ctrl Pts',(-111.330676610501,6.48220036542147,
133.453778015119));
#260884=CARTESIAN_POINT('Ctrl Pts',(-111.609124234314,5.73281752601749,
126.782776683677));
#260885=CARTESIAN_POINT('Ctrl Pts',(-111.887571858127,-0.284744556090853,
123.807414522182));
#260886=CARTESIAN_POINT('Ctrl Pts',(-112.16601948194,-6.04064030169634,
127.261904002525));
#260887=CARTESIAN_POINT('Ctrl Pts',(-112.444467105753,-6.24548271172772,
133.971738053464));
#260888=CARTESIAN_POINT('Ctrl Pts',(-112.722914729566,-0.71103161847358,
137.770906975801));
#260889=CARTESIAN_POINT('Ctrl Pts',(-113.001362353379,5.47682279633179,
135.16816012963));
#260890=CARTESIAN_POINT('Ctrl Pts',(-113.279809977192,6.63174461897671,
128.55529471533));
#260891=CARTESIAN_POINT('Ctrl Pts',(-113.558257601004,1.69241711551747,
124.009210992206));
#260892=CARTESIAN_POINT('Ctrl Pts',(-113.836705224817,-4.80215903792943,
125.707537813274));
#260893=CARTESIAN_POINT('Ctrl Pts',(-114.11515284863,-6.88378563403075,
132.089595797848));
#260894=CARTESIAN_POINT('Ctrl Pts',(-114.393600472443,-2.63954952408134,
137.290585438973));
#260895=CARTESIAN_POINT('Ctrl Pts',(-114.672048096256,4.03030364933543,
136.531051338922));
#260896=CARTESIAN_POINT('Ctrl Pts',(-114.950495720069,6.99650466029252,
130.508968230339));
#260897=CARTESIAN_POINT('Ctrl Pts',(-115.228943343882,3.53325968669456,
124.758336294896));
#260898=CARTESIAN_POINT('Ctrl Pts',(-115.507390967695,-3.17687832964389,
124.563705347279));
#260899=CARTESIAN_POINT('Ctrl Pts',(-115.785838591507,-6.96762036017394,
130.103931720095));
#260900=CARTESIAN_POINT('Ctrl Pts',(-116.06428621532,-4.35545966688232,
136.287818031834));
#260901=CARTESIAN_POINT('Ctrl Pts',(-116.342733839133,2.25915568424066,
137.432674861647));
#260902=CARTESIAN_POINT('Ctrl Pts',(-116.621181462946,6.79771732743703,
132.486434712303));
#260903=CARTESIAN_POINT('Ctrl Pts',(-116.899629086759,5.08950883367243,
125.994450643782));
#260904=CARTESIAN_POINT('Ctrl Pts',(-117.178076710572,-1.2957096419083,
123.922538864004));
#260905=CARTESIAN_POINT('Ctrl Pts',(-117.456524334385,-6.49023425551004,
128.174685080065));
#260906=CARTESIAN_POINT('Ctrl Pts',(-117.734971958198,-5.7205506538686,
134.843374648297));
#260907=CARTESIAN_POINT('Ctrl Pts',(-118.013419582011,0.306039534242538,
137.800407639092));
#260908=CARTESIAN_POINT('Ctrl Pts',(-118.291867205823,6.05139434124684,
134.328415193001));
#260909=CARTESIAN_POINT('Ctrl Pts',(-118.570314829636,6.23581337569426,
127.617988751722));
#260910=CARTESIAN_POINT('Ctrl Pts',(-118.848762453449,0.689824554297045,
123.835682392233));
#260911=CARTESIAN_POINT('Ctrl Pts',(-119.127210077262,-5.49007933269568,
126.457250882969));
#260912=CARTESIAN_POINT('Ctrl Pts',(-119.405657701075,-6.62486851822702,
133.073600851681));
#260913=CARTESIAN_POINT('Ctrl Pts',(-119.684105324888,-1.67172717832737,
137.60462990379));
#260914=CARTESIAN_POINT('Ctrl Pts',(-119.962552948701,4.81764977004229,
135.886543693482));
#260915=CARTESIAN_POINT('Ctrl Pts',(-120.241000572514,6.87984193501854,
129.498179514853));
#260916=CARTESIAN_POINT('Ctrl Pts',(-120.519448196327,2.61979546067638,
124.310131959122));
#260917=CARTESIAN_POINT('Ctrl Pts',(-120.79789582014,-4.04771505790416,
125.089963279793));
#260918=CARTESIAN_POINT('Ctrl Pts',(-121.076343443952,-6.9955731801444,
131.121046590047));
#260919=CARTESIAN_POINT('Ctrl Pts',(-121.354791067765,-3.51484130258126,
136.86111096256));
#260920=CARTESIAN_POINT('Ctrl Pts',(-121.633238691578,3.19585802251066,
137.035317656727));
#260921=CARTESIAN_POINT('Ctrl Pts',(-121.911686315391,6.96971995125911,
131.483579231079));
#260922=CARTESIAN_POINT('Ctrl Pts',(-122.190133939204,4.3387497345494,125.307672081285));
#260923=CARTESIAN_POINT('Ctrl Pts',(-122.468581563017,-2.2793195285039,
124.182953168171));
#260924=CARTESIAN_POINT('Ctrl Pts',(-122.74702918683,-6.80280549581075,
129.142984227312));
#260925=CARTESIAN_POINT('Ctrl Pts',(-123.025476810643,-5.07484554799192,
135.629739026348));
#260926=CARTESIAN_POINT('Ctrl Pts',(-123.303924434456,1.31664953844379,
137.682206800553));
#260927=CARTESIAN_POINT('Ctrl Pts',(-123.582372058268,6.49820802095541,
133.414269934058));
#260928=CARTESIAN_POINT('Ctrl Pts',(-123.860819682081,5.7082307873194,126.747953906865));
#260929=CARTESIAN_POINT('Ctrl Pts',(-124.139267305894,-0.327331677286216,
123.809277480321));
#260930=CARTESIAN_POINT('Ctrl Pts',(-124.417714929707,-6.06209232150722,
127.298740728095));
#260931=CARTESIAN_POINT('Ctrl Pts',(-124.69616255352,-6.22608627193705,
134.009697395242));
#260932=CARTESIAN_POINT('Ctrl Pts',(-124.974610177333,-0.668611099680587,
137.77510615311));
#260933=CARTESIAN_POINT('Ctrl Pts',(-125.253057801146,5.50328500971429,
135.134740303665));
#260934=CARTESIAN_POINT('Ctrl Pts',(-125.531505424959,6.61793104560076,
128.514967073503));
#260935=CARTESIAN_POINT('Ctrl Pts',(-125.809953048772,1.6510217544855,123.999034667242));
#260936=CARTESIAN_POINT('Ctrl Pts',(-126.088400672584,-4.8330958721059,
125.736864350674));
#260937=CARTESIAN_POINT('Ctrl Pts',(-126.366848296398,-6.87583450209069,
132.131475542423));
#260938=CARTESIAN_POINT('Ctrl Pts',(-126.64529592021,-2.60001712784396,
137.306532951397));
#260939=CARTESIAN_POINT('Ctrl Pts',(-126.923743544023,4.06508896899354,
136.506411634357));
#260940=CARTESIAN_POINT('Ctrl Pts',(-127.202191167836,6.99457689396224,
130.466383993564));
#260941=CARTESIAN_POINT('Ctrl Pts',(-127.480638791649,3.49639035745773,
124.736940359153));
#260942=CARTESIAN_POINT('Ctrl Pts',(-127.759086415462,-3.21480810938582,
124.583159532264));
#260943=CARTESIAN_POINT('Ctrl Pts',(-128.037534039275,-6.97175497581086,
130.146358580199));
#260944=CARTESIAN_POINT('Ctrl Pts',(-128.315981663087,-4.32199960863106,
136.314229355287));
#260945=CARTESIAN_POINT('Ctrl Pts',(-128.594429286901,2.29946225746178,
137.418799932461));
#260946=CARTESIAN_POINT('Ctrl Pts',(-128.872876910713,6.80783064392392,
132.44502391257));
#260947=CARTESIAN_POINT('Ctrl Pts',(-129.151324534526,5.06013524963555,
125.963558475429));
#260948=CARTESIAN_POINT('Ctrl Pts',(-129.429772158339,-1.33757723771771,
123.930553720578));
#260949=CARTESIAN_POINT('Ctrl Pts',(-129.708219782152,-6.50612158788957,
128.214241699924));
#260950=CARTESIAN_POINT('Ctrl Pts',(-129.986667405965,-5.69585804050008,
134.878122430239));
#260951=CARTESIAN_POINT('Ctrl Pts',(-130.265115029778,0.348620787973942,
137.798415069035));
#260952=CARTESIAN_POINT('Ctrl Pts',(-130.543562653591,6.07273414337257,
134.291513345486));
#260953=CARTESIAN_POINT('Ctrl Pts',(-130.822010277403,6.21630149056731,
127.58008862186));
#260954=CARTESIAN_POINT('Ctrl Pts',(-131.100457901217,0.647391451141708,
123.831612347843));
#260955=CARTESIAN_POINT('Ctrl Pts',(-131.378905525029,-5.5164397050528,
126.490751096011));
#260956=CARTESIAN_POINT('Ctrl Pts',(-131.657353148842,-6.61093226536518,
133.113886262947));
#260957=CARTESIAN_POINT('Ctrl Pts',(-131.935800772655,-1.63030103580305,
137.614680188378));
#260958=CARTESIAN_POINT('Ctrl Pts',(-132.214248396468,4.848497201029,135.857123130838));
#260959=CARTESIAN_POINT('Ctrl Pts',(-132.492696020281,6.87176337237162,
129.456324164773));
#260960=CARTESIAN_POINT('Ctrl Pts',(-132.771143644094,2.58021470880796,
124.294304843582));
#260961=CARTESIAN_POINT('Ctrl Pts',(-133.049591267907,-4.08242522165371,
125.114708744776));
#260962=CARTESIAN_POINT('Ctrl Pts',(-133.32803889172,-6.99351581097555,
131.163624762118));
#260963=CARTESIAN_POINT('Ctrl Pts',(-133.606486515532,-3.47790702225152,
136.882394581644));
#260964=CARTESIAN_POINT('Ctrl Pts',(-133.884934139345,3.23372841471757,
137.015748116649));
#260965=CARTESIAN_POINT('Ctrl Pts',(-134.163381763158,6.97372541497715,
131.441139983145));
#260966=CARTESIAN_POINT('Ctrl Pts',(-134.441829386971,4.30520944429882,
125.281362721075));
#260967=CARTESIAN_POINT('Ctrl Pts',(-134.720277010784,-2.31958368451587,
124.196950712432));
#260968=CARTESIAN_POINT('Ctrl Pts',(-134.998724634597,-6.81279272522359,
129.184425616688));
#260969=CARTESIAN_POINT('Ctrl Pts',(-135.27717225841,-5.04537807487797,
135.660541648527));
#260970=CARTESIAN_POINT('Ctrl Pts',(-135.555619882223,1.35849254585843,
137.674064550544));
#260971=CARTESIAN_POINT('Ctrl Pts',(-135.834067506036,6.51397488300169,
133.374665141848));
#260972=CARTESIAN_POINT('Ctrl Pts',(-136.112515129848,5.68343252803032,
126.713281441693));
#260973=CARTESIAN_POINT('Ctrl Pts',(-136.390962753662,-0.369906669086523,
123.811399643837));
#260974=CARTESIAN_POINT('Ctrl Pts',(-136.669410377474,-6.08331970825794,
127.335707355701));
#260975=CARTESIAN_POINT('Ctrl Pts',(-136.947858001288,-6.20645912223011,
134.047537962086));
#260976=CARTESIAN_POINT('Ctrl Pts',(-137.2263056251,-0.626165805256695,
137.779047026878));
#260977=CARTESIAN_POINT('Ctrl Pts',(-137.504753248913,5.52954329684707,
135.101160013885));
#260978=CARTESIAN_POINT('Ctrl Pts',(-137.783200872726,6.60387224235649,
128.474724265995));
#260979=CARTESIAN_POINT('Ctrl Pts',(-138.061648496539,1.60956521423443,
123.989110516135));
#260980=CARTESIAN_POINT('Ctrl Pts',(-138.340096120352,-4.86385361413656,
125.766378666012));
#260981=CARTESIAN_POINT('Ctrl Pts',(-138.618543744165,-6.86762858357524,
132.173306110266));
#260982=CARTESIAN_POINT('Ctrl Pts',(-138.896991367977,-2.56038838701599,
137.322239523433));
#260983=CARTESIAN_POINT('Ctrl Pts',(-139.17543899179,4.09972365528409,136.481560638194));
#260984=CARTESIAN_POINT('Ctrl Pts',(-139.453886615603,6.99238994101352,
130.423812280637));
#260985=CARTESIAN_POINT('Ctrl Pts',(-139.732334239416,3.45939146819007,
124.715769253897));
#260986=CARTESIAN_POINT('Ctrl Pts',(-140.010781863229,-3.25261876323132,
124.602844246145));
#260987=CARTESIAN_POINT('Ctrl Pts',(-140.289229487042,-6.97563125050334,
130.188809822811));
#260988=CARTESIAN_POINT('Ctrl Pts',(-140.567677110855,-4.28837939709471,
136.340436508528));
#260989=CARTESIAN_POINT('Ctrl Pts',(-140.846124734668,2.33968362326381,
137.404679902793));
#260990=CARTESIAN_POINT('Ctrl Pts',(-141.124572358481,6.81769169374202,
132.403552317457));
#260991=CARTESIAN_POINT('Ctrl Pts',(-141.403019982293,5.03057416042698,
125.932845684778));
#260992=CARTESIAN_POINT('Ctrl Pts',(-141.681467606106,-1.37939526911043,
123.938823288595));
#260993=CARTESIAN_POINT('Ctrl Pts',(-141.959915229919,-6.52176783354029,
128.253894297592));
#260994=CARTESIAN_POINT('Ctrl Pts',(-142.238362853732,-5.67095436501806,
134.912719257437));
#260995=CARTESIAN_POINT('Ctrl Pts',(-142.516810477545,0.39118912343359,
137.796163331718));
#260996=CARTESIAN_POINT('Ctrl Pts',(-142.795258101358,6.09384891810056,
134.254482280245));
#260997=CARTESIAN_POINT('Ctrl Pts',(-143.073705725171,6.19655925810344,
127.542307968582));
#260998=CARTESIAN_POINT('Ctrl Pts',(-143.352153348984,0.604934358657401,
123.827800681205));
#260999=CARTESIAN_POINT('Ctrl Pts',(-143.630600972796,-5.54259566370794,
126.524411151443));
#261000=CARTESIAN_POINT('Ctrl Pts',(-143.90904859661,-6.59675104197701,
133.154086093891));
#261001=CARTESIAN_POINT('Ctrl Pts',(-144.187496220422,-1.58881448187379,
137.624478114069));
#261002=CARTESIAN_POINT('Ctrl Pts',(-144.465943844235,4.87916496916901,
135.827515336221));
#261003=CARTESIAN_POINT('Ctrl Pts',(-144.744391468048,6.86343017400547,
129.41451876668));
#261004=CARTESIAN_POINT('Ctrl Pts',(-145.022839091861,2.54053834613545,
124.278718960552));
#261005=CARTESIAN_POINT('Ctrl Pts',(-145.301286715674,-4.11698410963516,
125.139665041902));
#261006=CARTESIAN_POINT('Ctrl Pts',(-145.579734339487,-6.99119929450595,
131.206189621523));
#261007=CARTESIAN_POINT('Ctrl Pts',(-145.8581819633,-3.44084386679896,136.903452976945));
#261008=CARTESIAN_POINT('Ctrl Pts',(-146.136629587113,3.27147897992919,
136.995948411323));
#261009=CARTESIAN_POINT('Ctrl Pts',(-146.415077210925,6.97747246473481,
131.398677139117));
#261010=CARTESIAN_POINT('Ctrl Pts',(-146.693524834738,4.27150962292939,
125.255258017582));
#261011=CARTESIAN_POINT('Ctrl Pts',(-146.971972458551,-2.35976188750221,
124.211193096699));
#261012=CARTESIAN_POINT('Ctrl Pts',(-147.250420082364,-6.82252750409623,
129.225927033352));
#261013=CARTESIAN_POINT('Ctrl Pts',(-147.528867706177,-5.01572364342383,
135.69116432313));
#261014=CARTESIAN_POINT('Ctrl Pts',(-147.80731532999,1.40028521383297,137.665667741127));
#261015=CARTESIAN_POINT('Ctrl Pts',(-148.085762953803,6.52950036731291,
133.334965106058));
#261016=CARTESIAN_POINT('Ctrl Pts',(-148.364210577616,5.65842366705879,
126.678760572968));
#261017=CARTESIAN_POINT('Ctrl Pts',(-148.642658201429,-0.412467953858535,
123.813780934094));
#261018=CARTESIAN_POINT('Ctrl Pts',(-148.921105825242,-6.10432167535963,
127.372802515528));
#261019=CARTESIAN_POINT('Ctrl Pts',(-149.199553449054,-6.18660198989778,
134.085258351801));
#261020=CARTESIAN_POINT('Ctrl Pts',(-149.478001072867,-0.583697308029368,
137.782729451077));
#261021=CARTESIAN_POINT('Ctrl Pts',(-149.75644869668,5.55559668471987,135.067420504625));
#261022=CARTESIAN_POINT('Ctrl Pts',(-150.034896320493,6.58956873019717,
128.434567784019));
#261023=CARTESIAN_POINT('Ctrl Pts',(-150.313343944306,1.56804903095274,
123.979438906626));
#261024=CARTESIAN_POINT('Ctrl Pts',(-150.591791568119,-4.89443112428377,
125.796079665625));
#261025=CARTESIAN_POINT('Ctrl Pts',(-150.870239191931,-6.85916818255639,
132.21508595133));
#261026=CARTESIAN_POINT('Ctrl Pts',(-151.148686815745,-2.52066477005453,
137.33770457307));
#261027=CARTESIAN_POINT('Ctrl Pts',(-151.427134439557,4.13420642480782,
136.456499271296));
#261028=CARTESIAN_POINT('Ctrl Pts',(-151.705582063371,6.98994388248347,
130.381254669068));
#261029=CARTESIAN_POINT('Ctrl Pts',(-151.984029687183,3.42226438989971,
124.694823763634));
#261030=CARTESIAN_POINT('Ctrl Pts',(-152.262477310996,-3.29030889009209,
124.622758759495));
#261031=CARTESIAN_POINT('Ctrl Pts',(-152.540924934809,-6.97924904061452,
130.231283874884));
#261032=CARTESIAN_POINT('Ctrl Pts',(-152.819372558622,-4.25460027808296,
136.366438520441));
#261033=CARTESIAN_POINT('Ctrl Pts',(-153.097820182435,2.37981829122829,
137.390315295868));
#261034=CARTESIAN_POINT('Ctrl Pts',(-153.376267806248,6.82730011148789,
132.362021463707));
#261035=CARTESIAN_POINT('Ctrl Pts',(-153.654715430061,5.00082666144207,
125.902313409905));
#261036=CARTESIAN_POINT('Ctrl Pts',(-153.933163053873,-1.42116218650446,
123.947347261623));
#261037=CARTESIAN_POINT('Ctrl Pts',(-154.211610677687,-6.53717241268631,
128.293641403726));
#261038=CARTESIAN_POINT('Ctrl Pts',(-154.490058301499,-5.64584055023574,
134.947163847896));
#261039=CARTESIAN_POINT('Ctrl Pts',(-154.768505925312,0.433742963236675,
137.79365251058));
#261040=CARTESIAN_POINT('Ctrl Pts',(-155.046953549125,6.11473788301669,
134.217323369476));
#261041=CARTESIAN_POINT('Ctrl Pts',(-155.325401172938,6.17658740985663,
127.504648191865));
#261042=CARTESIAN_POINT('Ctrl Pts',(-155.603848796751,0.562454850108638,
123.824247533559));
#261043=CARTESIAN_POINT('Ctrl Pts',(-155.882296420564,-5.5685462394425,
126.558229801974));
#261044=CARTESIAN_POINT('Ctrl Pts',(-156.160744044376,-6.5823253735531,
133.194198854895));
#261045=CARTESIAN_POINT('Ctrl Pts',(-156.43919166819,-1.54726905384013,
137.634023317798));
#261046=CARTESIAN_POINT('Ctrl Pts',(-156.717639292002,4.90965193805665,
135.79772140676));
#261047=CARTESIAN_POINT('Ctrl Pts',(-156.996086915816,6.8548426487106,129.372764869687));
#261048=CARTESIAN_POINT('Ctrl Pts',(-157.274534539628,2.50076784287941,
124.263374887574));
#261049=CARTESIAN_POINT('Ctrl Pts',(-157.552982163441,-4.15139044125659,
125.164831246407));
#261050=CARTESIAN_POINT('Ctrl Pts',(-157.831429787254,-6.98862371657603,
131.248739591007));
#261051=CARTESIAN_POINT('Ctrl Pts',(-158.109877411067,-3.40365320961064,
136.924285368134));
#261052=CARTESIAN_POINT('Ctrl Pts',(-158.38832503488,3.30910831928323,136.975919274434));
#261053=CARTESIAN_POINT('Ctrl Pts',(-158.666772658693,6.98096096168483,
131.356192272474));
#261054=CARTESIAN_POINT('Ctrl Pts',(-158.945220282506,4.23765151920024,
125.229358938127));
#261055=CARTESIAN_POINT('Ctrl Pts',(-159.223667906319,-2.39985264864321,
124.225679793212));
#261056=CARTESIAN_POINT('Ctrl Pts',(-159.502115530131,-6.8320094717036,
129.267486939452));
#261057=CARTESIAN_POINT('Ctrl Pts',(-159.780563153944,-4.98588335248574,
135.721605915426));
#261058=CARTESIAN_POINT('Ctrl Pts',(-160.059010777757,1.44202599372318,
137.657016683454));
#261059=CARTESIAN_POINT('Ctrl Pts',(-160.33745840157,6.54478389858708,133.295171297791));
#261060=CARTESIAN_POINT('Ctrl Pts',(-160.615906025383,5.63320513111742,
126.644392579866));
#261061=CARTESIAN_POINT('Ctrl Pts',(-160.894353649196,-0.455013954479453,
123.816421262852));
#261062=CARTESIAN_POINT('Ctrl Pts',(-161.172801273009,-6.12509744457689,
127.410024833003));
#261063=CARTESIAN_POINT('Ctrl Pts',(-161.451248896821,-6.16651561075379,
134.122857166646));
#261064=CARTESIAN_POINT('Ctrl Pts',(-161.729696520635,-0.541207181682879,
137.786153289251));
#261065=CARTESIAN_POINT('Ctrl Pts',(-162.008144144447,5.58144420791359,
135.033523026113));
#261066=CARTESIAN_POINT('Ctrl Pts',(-162.286591768261,6.57502103914602,
128.394499115588));
#261067=CARTESIAN_POINT('Ctrl Pts',(-162.565039392073,1.52647474303778,
123.970020197102));
#261068=CARTESIAN_POINT('Ctrl Pts',(-162.843487015886,-4.92482726948487,
125.825966248931));
#261069=CARTESIAN_POINT('Ctrl Pts',(-163.121934639699,-6.85045361253876,
132.256813517449));
#261070=CARTESIAN_POINT('Ctrl Pts',(-163.400382263512,-2.48084774893327,
137.352927527244));
#261071=CARTESIAN_POINT('Ctrl Pts',(-163.678829887325,4.16853599979124,
136.431228462323));
#261072=CARTESIAN_POINT('Ctrl Pts',(-163.957277511138,6.98723880901292,
130.338712735846));
#261073=CARTESIAN_POINT('Ctrl Pts',(-164.23572513495,3.3850104983435,124.674104664506));
#261074=CARTESIAN_POINT('Ctrl Pts',(-164.514172758764,-3.32787709334726,
124.642902334375));
#261075=CARTESIAN_POINT('Ctrl Pts',(-164.792620382576,-6.98260821208591,
130.273779162525));
#261076=CARTESIAN_POINT('Ctrl Pts',(-165.07106800639,-4.22066350329308,
136.392234427513));
#261077=CARTESIAN_POINT('Ctrl Pts',(-165.349515630202,2.4198647741513,137.37570664397));
#261078=CARTESIAN_POINT('Ctrl Pts',(-165.627963254015,6.83665554111671,
132.320432890263));
#261079=CARTESIAN_POINT('Ctrl Pts',(-165.906410877828,4.97089385498702,
125.871962782194));
#261080=CARTESIAN_POINT('Ctrl Pts',(-166.184858501641,-1.46287644221077,
123.956125323802));
#261081=CARTESIAN_POINT('Ctrl Pts',(-166.463306125454,-6.55233475450377,
128.333481545486));
#261082=CARTESIAN_POINT('Ctrl Pts',(-166.741753749267,-5.62051752675643,
134.981454925258));
#261083=CARTESIAN_POINT('Ctrl Pts',(-167.020201373079,0.476280730534997,
137.790882698662));
#261084=CARTESIAN_POINT('Ctrl Pts',(-167.298648996893,6.13540026407138,
134.180037990117));
#261085=CARTESIAN_POINT('Ctrl Pts',(-167.577096620705,6.15638668589229,
127.467110687205));
#261086=CARTESIAN_POINT('Ctrl Pts',(-167.855544244518,0.519954499587912,
123.820953036571));
#261087=CARTESIAN_POINT('Ctrl Pts',(-168.133991868331,-5.5942904706483,
126.592205794446));
#261088=CARTESIAN_POINT('Ctrl Pts',(-168.412439492144,-6.56765579464175,
133.234223059563));
#261089=CARTESIAN_POINT('Ctrl Pts',(-168.690887115956,-1.50566629118217,
137.643315445865));
#261090=CARTESIAN_POINT('Ctrl Pts',(-168.96933473977,4.93995697798634,135.767742446477));
#261091=CARTESIAN_POINT('Ctrl Pts',(-169.247782363582,6.84600111470013,
129.331064021001));
#261092=CARTESIAN_POINT('Ctrl Pts',(-169.526229987396,2.46090467275213,
124.248273193229));
#261093=CARTESIAN_POINT('Ctrl Pts',(-169.804677611208,-4.18564294157836,
125.190206425745));
#261094=CARTESIAN_POINT('Ctrl Pts',(-170.083125235021,-6.98578917262369,
131.291273093865));
#261095=CARTESIAN_POINT('Ctrl Pts',(-170.361572858834,-3.36633642880185,
136.944890983262));
#261096=CARTESIAN_POINT('Ctrl Pts',(-170.640020482647,3.34661503841248,
136.955661448171));
#261097=CARTESIAN_POINT('Ctrl Pts',(-170.91846810646,6.98419077655865,131.313686957504));
#261098=CARTESIAN_POINT('Ctrl Pts',(-171.196915730273,4.20363638773547,
125.203666442409));
#261099=CARTESIAN_POINT('Ctrl Pts',(-171.475363354086,-2.43985448236259,
124.240410265162));
#261100=CARTESIAN_POINT('Ctrl Pts',(-171.753810977898,-6.84123827668714,
129.309103794972));
#261101=CARTESIAN_POINT('Ctrl Pts',(-172.032258601712,-4.9558583078063,
135.751865297389));
#261102=CARTESIAN_POINT('Ctrl Pts',(-172.310706225524,1.48371333881067,
137.648111698089));
#261103=CARTESIAN_POINT('Ctrl Pts',(-172.589153849337,6.55982491048677,
133.255285191615));
#261104=CARTESIAN_POINT('Ctrl Pts',(-172.86760147315,5.60777785468832,126.610178735912));
#261105=CARTESIAN_POINT('Ctrl Pts',(-173.146049096963,-0.497543094390354,
123.819320532272));
#261106=CARTESIAN_POINT('Ctrl Pts',(-173.424496720776,-6.14564624605571,
127.447372928838));
#261107=CARTESIAN_POINT('Ctrl Pts',(-173.702944344589,-6.14620072910595,
134.160333013378));
#261108=CARTESIAN_POINT('Ctrl Pts',(-173.981391968402,-0.498697000705985,
137.789318414533));
#261109=CARTESIAN_POINT('Ctrl Pts',(-174.259839592215,5.60708490864046,
134.999468834432));
#261110=CARTESIAN_POINT('Ctrl Pts',(-174.538287216028,6.56022970827155,
128.354519745462));
#261111=CARTESIAN_POINT('Ctrl Pts',(-174.81673483984,1.48484389103961,123.960854736574));
#261112=CARTESIAN_POINT('Ctrl Pts',(-175.095182463654,-4.95504092340126,
125.85603730847));
#261113=CARTESIAN_POINT('Ctrl Pts',(-175.373630087466,-6.8414851964426,
132.298487262391));
#261114=CARTESIAN_POINT('Ctrl Pts',(-175.652077711279,-2.44093879908611,
137.367907821863));
#261115=CARTESIAN_POINT('Ctrl Pts',(-175.930525335092,4.20271110814107,
136.405749147692));
#261116=CARTESIAN_POINT('Ctrl Pts',(-176.208972958905,6.98427482083815,
130.296188057377));
#261117=CARTESIAN_POINT('Ctrl Pts',(-176.487420582718,3.3476311739788,124.653612724266));
#261118=CARTESIAN_POINT('Ctrl Pts',(-176.765868206531,-3.36532198089259,
124.663274224357));
#261119=CARTESIAN_POINT('Ctrl Pts',(-177.044315830343,-6.98570864044213,
130.316294111058));
#261120=CARTESIAN_POINT('Ctrl Pts',(-177.322763454156,-4.18657033026512,
136.417823273865));
#261121=CARTESIAN_POINT('Ctrl Pts',(-177.601211077969,2.4598215880947,137.360854488428));
#261122=CARTESIAN_POINT('Ctrl Pts',(-177.879658701782,6.84575763596098,
132.278788138201));
#261123=CARTESIAN_POINT('Ctrl Pts',(-178.158106325595,4.94077685023126,
125.841794926299));
#261124=CARTESIAN_POINT('Ctrl Pts',(-178.436553949408,-1.50453649049278,
123.965157149858));
#261125=CARTESIAN_POINT('Ctrl Pts',(-178.715001573221,-6.56725429714808,
128.373413246577));
#261126=CARTESIAN_POINT('Ctrl Pts',(-178.993449197033,-5.59498623293233,
135.015591218853));
#261127=CARTESIAN_POINT('Ctrl Pts',(-179.271896820847,0.518800849074927,
137.787853998597));
#261128=CARTESIAN_POINT('Ctrl Pts',(-179.550344444659,6.15583529561319,
134.142627523792));
#261129=CARTESIAN_POINT('Ctrl Pts',(-179.828792068472,6.13595783475539,
127.429696845569));
#261130=CARTESIAN_POINT('Ctrl Pts',(-180.107239692285,0.477434881962636,
123.81791731232));
#261131=CARTESIAN_POINT('Ctrl Pts',(-180.385687316098,-5.61982740336347,
126.626337869861));
#261132=CARTESIAN_POINT('Ctrl Pts',(-180.664134939911,-6.55274284882976,
133.274157224785));
#261133=CARTESIAN_POINT('Ctrl Pts',(-180.942582563724,-1.4640077355066,
137.652354153945));
#261134=CARTESIAN_POINT('Ctrl Pts',(-181.221030187537,4.97007896599344,
135.737579566256));
#261135=CARTESIAN_POINT('Ctrl Pts',(-181.499477811349,6.83690589960112,
129.289417765863));
#261136=CARTESIAN_POINT('Ctrl Pts',(-181.777925435163,2.42095031289641,
124.233414437113));
#261137=CARTESIAN_POINT('Ctrl Pts',(-182.056373058975,-4.21974034136189,
125.215789639631));
#261138=CARTESIAN_POINT('Ctrl Pts',(-182.334820682789,-6.98269576768506,
131.333788554001));
#261139=CARTESIAN_POINT('Ctrl Pts',(-182.613268306601,-3.32889490715784,
136.965269058779));
#261140=CARTESIAN_POINT('Ctrl Pts',(-182.891715930414,3.38399774748988,
136.935175683191));
#261141=CARTESIAN_POINT('Ctrl Pts',(-183.170163554227,6.98716178967534,
131.27116276926));
#261142=CARTESIAN_POINT('Ctrl Pts',(-183.44861117804,4.16946548897866,125.178181482475));
#261143=CARTESIAN_POINT('Ctrl Pts',(-183.727058801853,-2.47976590637605,
124.255383966707));
#261144=CARTESIAN_POINT('Ctrl Pts',(-184.005506425666,-6.85021357707087,
129.350776057783));
#261145=CARTESIAN_POINT('Ctrl Pts',(-184.283954049479,-4.92564962197493,
135.781941347746));
#261146=CARTESIAN_POINT('Ctrl Pts',(-184.562401673291,1.52534570435398,
137.63895311501));
#261147=CARTESIAN_POINT('Ctrl Pts',(-184.840849297105,6.5746228456623,133.215308265529));
#261148=CARTESIAN_POINT('Ctrl Pts',(-185.119296920917,5.58214277998856,
126.576120308909));
#261149=CARTESIAN_POINT('Ctrl Pts',(-185.39774454473,-0.540053797659538,
123.822478634922));
#261150=CARTESIAN_POINT('Ctrl Pts',(-185.676192168543,-6.16596731835295,
127.484845419088));
#261151=CARTESIAN_POINT('Ctrl Pts',(-185.954639792356,-6.12565809773001,
134.197684503321));
#261152=CARTESIAN_POINT('Ctrl Pts',(-186.233087416169,-0.456168340327589,
137.792224709632));
#261153=CARTESIAN_POINT('Ctrl Pts',(-186.511535039982,5.63251783677319,
134.965259191474));
#261154=CARTESIAN_POINT('Ctrl Pts',(-186.789982663795,6.54519528567348,
128.314631155089));
#261155=CARTESIAN_POINT('Ctrl Pts',(-187.068430287608,1.44315801760525,
123.951942864674));
#261156=CARTESIAN_POINT('Ctrl Pts',(-187.346877911421,-4.98507096645316,
125.886291729948));
#261157=CARTESIAN_POINT('Ctrl Pts',(-187.625325535233,-6.83226326659722,
132.340105641921));
#261158=CARTESIAN_POINT('Ctrl Pts',(-187.903773159046,-2.40093939935397,
137.382644901827));
#261159=CARTESIAN_POINT('Ctrl Pts',(-188.182220782859,4.23673048348491,
136.380062271549));
#261160=CARTESIAN_POINT('Ctrl Pts',(-188.460668406672,6.98105202779173,
130.25368220943));
#261161=CARTESIAN_POINT('Ctrl Pts',(-188.739116030485,3.31012780190951,
124.633348702251));
#261162=CARTESIAN_POINT('Ctrl Pts',(-189.017563654298,-3.40264216519462,
124.683873674555));
#261163=CARTESIAN_POINT('Ctrl Pts',(-189.296011278111,-6.98855021079573,
130.358827145076));
#261164=CARTESIAN_POINT('Ctrl Pts',(-189.574458901924,-4.15232202233378,
136.443204111294));
#261165=CARTESIAN_POINT('Ctrl Pts',(-189.852906525736,2.49968725244504,
137.345759379595));
#261166=CARTESIAN_POINT('Ctrl Pts',(-190.13135414955,6.85460605873784,132.237088750687));
#261167=CARTESIAN_POINT('Ctrl Pts',(-190.409801773362,4.91047676317321,
125.8118109601));
#261168=CARTESIAN_POINT('Ctrl Pts',(-190.688249397175,-1.5461407876216,
123.974442405114));
#261169=CARTESIAN_POINT('Ctrl Pts',(-190.966697020988,-6.58193048776853,
128.413435027317));
#261170=CARTESIAN_POINT('Ctrl Pts',(-191.245144644801,-5.56924761483672,
135.049571463749));
#261171=CARTESIAN_POINT('Ctrl Pts',(-191.523592268614,0.561301743259386,
137.784566522618));
#261172=CARTESIAN_POINT('Ctrl Pts',(-191.802039892427,6.17604222041412,
134.105093356759));
#261173=CARTESIAN_POINT('Ctrl Pts',(-192.08048751624,6.11530161344434,127.39240805334));
#261174=CARTESIAN_POINT('Ctrl Pts',(-192.358935140053,0.43489757281158,
123.815140473294));
#261175=CARTESIAN_POINT('Ctrl Pts',(-192.637382763865,-5.64515609130746,
126.660624763449));
#261176=CARTESIAN_POINT('Ctrl Pts',(-192.915830387678,-6.53758708872167,
133.313999870785));
#261177=CARTESIAN_POINT('Ctrl Pts',(-193.194278011491,-1.42229493048546,
137.661139107108));
#261178=CARTESIAN_POINT('Ctrl Pts',(-193.472725635304,5.00001678589681,
135.707233883791));
#261179=CARTESIAN_POINT('Ctrl Pts',(-193.751173259117,6.82755734043935,
129.247827647489));
#261180=CARTESIAN_POINT('Ctrl Pts',(-194.02962088293,2.38090624383734,124.218799169824));
#261181=CARTESIAN_POINT('Ctrl Pts',(-194.308068506743,-4.25368137711504,
125.241579940071));
#261182=CARTESIAN_POINT('Ctrl Pts',(-194.586516130556,-6.97934361638637,
131.376284395991));
#261183=CARTESIAN_POINT('Ctrl Pts',(-194.864963754369,-3.29133003208973,
136.985418839569));
#261184=CARTESIAN_POINT('Ctrl Pts',(-195.143411378181,3.42125506128717,
136.914462738605));
#261185=CARTESIAN_POINT('Ctrl Pts',(-195.421859001994,6.98987389094189,
131.22862128349));
#261186=CARTESIAN_POINT('Ctrl Pts',(-195.700306625807,4.13514008914463,
125.152905002676));
#261187=CARTESIAN_POINT('Ctrl Pts',(-195.97875424962,-2.51958544175274,
124.270600342989));
#261188=CARTESIAN_POINT('Ctrl Pts',(-196.257201873433,-6.85893504027095,
129.392502183704));
#261189=CARTESIAN_POINT('Ctrl Pts',(-196.535649497246,-4.89525841438522,
135.811832952018));
#261190=CARTESIAN_POINT('Ctrl Pts',(-196.814097121059,1.56692154765205,
137.629541273595));
#261191=CARTESIAN_POINT('Ctrl Pts',(-197.092544744872,6.58917715577019,
133.175242000891));
#261192=CARTESIAN_POINT('Ctrl Pts',(-197.370992368684,5.55630085693524,
126.542218560906));
#261193=CARTESIAN_POINT('Ctrl Pts',(-197.649439992498,-0.582544489036021,
123.825895453776));
#261194=CARTESIAN_POINT('Ctrl Pts',(-197.92788761631,-6.18605990846357,
127.522440915193));
#261195=CARTESIAN_POINT('Ctrl Pts',(-198.206335240123,-6.10488847784037,
134.234910252398));
#261196=CARTESIAN_POINT('Ctrl Pts',(-198.484782863936,-0.413622776464342,
137.79487206686));
#261197=CARTESIAN_POINT('Ctrl Pts',(-198.763230487749,5.657742049887,134.930895364888));
#261198=CARTESIAN_POINT('Ctrl Pts',(-199.041678111562,6.52991832845634,
128.274834822558));
#261199=CARTESIAN_POINT('Ctrl Pts',(-199.320125735375,1.40141866741961,
123.943284911633));
#261200=CARTESIAN_POINT('Ctrl Pts',(-199.598573359188,-5.01491628586802,
125.916728392279));
#261201=CARTESIAN_POINT('Ctrl Pts',(-199.877020983,-6.82278816472322,132.381667113854));
#261202=CARTESIAN_POINT('Ctrl Pts',(-200.155468606814,-2.36085103192995,
137.397138221046));
#261203=CARTESIAN_POINT('Ctrl Pts',(-200.433916230626,4.27059286522247,
136.354168785731));
#261204=CARTESIAN_POINT('Ctrl Pts',(-200.712363854439,6.97757054929515,
130.211196767073));
#261205=CARTESIAN_POINT('Ctrl Pts',(-200.990811478252,3.27250177183757,
124.613313349352));
#261206=CARTESIAN_POINT('Ctrl Pts',(-201.269259102065,-3.43983626333961,
124.704699921646));
#261207=CARTESIAN_POINT('Ctrl Pts',(-201.547706725878,-6.9911328178512,
130.401376688499));
#261208=CARTESIAN_POINT('Ctrl Pts',(-201.826154349691,-4.1179198485831,
136.468375999304));
#261209=CARTESIAN_POINT('Ctrl Pts',(-202.104601973504,2.53946028996452,
137.330421876826));
#261210=CARTESIAN_POINT('Ctrl Pts',(-202.383049597317,6.86320048156709,
132.195336272904));
#261211=CARTESIAN_POINT('Ctrl Pts',(-202.66149722113,4.87999471659204,125.782011994664));
#261212=CARTESIAN_POINT('Ctrl Pts',(-202.939944844942,-1.5876877919352,
123.983980745501));
#261213=CARTESIAN_POINT('Ctrl Pts',(-203.218392468755,-6.59636278253501,
128.453545404684));
#261214=CARTESIAN_POINT('Ctrl Pts',(-203.496840092568,-5.54330262622176,
135.083394400798));
#261215=CARTESIAN_POINT('Ctrl Pts',(-203.775287716381,0.603781838200554,
137.781020392543));
#261216=CARTESIAN_POINT('Ctrl Pts',(-204.053735340194,6.19602028969954,
134.067436879861));
#261217=CARTESIAN_POINT('Ctrl Pts',(-204.332182964007,6.09441878738321,
127.355245692268));
#261218=CARTESIAN_POINT('Ctrl Pts',(-204.61063058782,0.392344148371673,
123.812622622391));
#261219=CARTESIAN_POINT('Ctrl Pts',(-204.889078211633,-5.67027559591653,
126.69506520469));
#261220=CARTESIAN_POINT('Ctrl Pts',(-205.167525835445,-6.5221890759199,
133.353749521179));
#261221=CARTESIAN_POINT('Ctrl Pts',(-205.445973459259,-1.38052942180316,
137.66966997982));
#261222=CARTESIAN_POINT('Ctrl Pts',(-205.724421083071,5.02976932833932,
135.676706523556));
#261223=CARTESIAN_POINT('Ctrl Pts',(-206.002868706884,6.8179557836299,129.206295207017));
#261224=CARTESIAN_POINT('Ctrl Pts',(-206.281316330697,2.340773949421,124.204427932937));
#261225=CARTESIAN_POINT('Ctrl Pts',(-206.55976395451,-4.28746479114066,
125.267576371395));
#261226=CARTESIAN_POINT('Ctrl Pts',(-206.838211578323,-6.97573284294384,
131.418759045136));
#261227=CARTESIAN_POINT('Ctrl Pts',(-207.116659202136,-3.253643195576,137.005339578972));
#261228=CARTESIAN_POINT('Ctrl Pts',(-207.395106825949,3.4583855992191,136.893523381939));
#261229=CARTESIAN_POINT('Ctrl Pts',(-207.673554449762,6.99232697986142,
131.186064076586));
#261230=CARTESIAN_POINT('Ctrl Pts',(-207.952002073574,4.10066146017411,
125.127837939644));
#261231=CARTESIAN_POINT('Ctrl Pts',(-208.230449697387,-2.55931161296347,
124.286058830161));
#261232=CARTESIAN_POINT('Ctrl Pts',(-208.5088973212,-6.86740234311116,129.434280626559));
#261233=CARTESIAN_POINT('Ctrl Pts',(-208.787344945013,-4.86468581119477,
135.841539002563));
#261234=CARTESIAN_POINT('Ctrl Pts',(-209.065792568826,1.60843932809579,
137.619876522599));
#261235=CARTESIAN_POINT('Ctrl Pts',(-209.344240192639,6.60348730149562,
133.135087882371));
#261236=CARTESIAN_POINT('Ctrl Pts',(-209.622687816452,5.53025304311036,
126.508474748144));
#261237=CARTESIAN_POINT('Ctrl Pts',(-209.901135440264,-0.625013594012848,
123.829570862223));
#261238=CARTESIAN_POINT('Ctrl Pts',(-210.179583064078,-6.20592327184948,
127.56015802404));
#261239=CARTESIAN_POINT('Ctrl Pts',(-210.45803068789,-6.08389263906328,
134.272008881199));
#261240=CARTESIAN_POINT('Ctrl Pts',(-210.736478311703,-0.371061885656257,
137.797260388114));
#261241=CARTESIAN_POINT('Ctrl Pts',(-211.014925935516,5.68275661328764,
134.896378628042));
#261242=CARTESIAN_POINT('Ctrl Pts',(-211.293373559329,6.51439940271492,
128.235132222534));
#261243=CARTESIAN_POINT('Ctrl Pts',(-211.571821183142,1.35962738715011,
123.934881198276));
#261244=CARTESIAN_POINT('Ctrl Pts',(-211.850268806955,-5.04457577571481,
125.947346167619));
#261245=CARTESIAN_POINT('Ctrl Pts',(-212.128716430768,-6.81306024192543,
132.423170138115));
#261246=CARTESIAN_POINT('Ctrl Pts',(-212.40716405458,-2.32067518230222,
137.411387242468));
#261247=CARTESIAN_POINT('Ctrl Pts',(-212.685611678394,4.30429699857105,
136.32806964973));
#261248=CARTESIAN_POINT('Ctrl Pts',(-212.964059302206,6.97383051435588,
130.168733304621));
#261249=CARTESIAN_POINT('Ctrl Pts',(-213.24250692602,3.23475447800865,124.593507407987));
#261250=CARTESIAN_POINT('Ctrl Pts',(-213.520954549832,-3.47690289708716,
124.725752193909));
#261251=CARTESIAN_POINT('Ctrl Pts',(-213.799402173646,-6.99345636590915,
130.443941164641));
#261252=CARTESIAN_POINT('Ctrl Pts',(-214.077849797458,-4.08336508379785,
136.49333800514));
#261253=CARTESIAN_POINT('Ctrl Pts',(-214.356297421271,2.57913922684953,
137.314842548456));
#261254=CARTESIAN_POINT('Ctrl Pts',(-214.634745045084,6.87154058597789,
132.153532252007));
#261255=CARTESIAN_POINT('Ctrl Pts',(-214.913192668897,4.84933184001288,
125.752399134204));
#261256=CARTESIAN_POINT('Ctrl Pts',(-215.19164029271,-1.62917596389355,
123.993771817573));
#261257=CARTESIAN_POINT('Ctrl Pts',(-215.470087916522,-6.61055064665203,
128.493742892374));
#261258=CARTESIAN_POINT('Ctrl Pts',(-215.748535540335,-5.51715222849034,
135.117058776675));
#261259=CARTESIAN_POINT('Ctrl Pts',(-216.026983164148,0.646239559784443,
137.777215739773));
#261260=CARTESIAN_POINT('Ctrl Pts',(-216.305430787961,6.21576876317433,
134.029659488472));
#261261=CARTESIAN_POINT('Ctrl Pts',(-216.583878411774,6.0733101303926,127.318211139417));
#261262=CARTESIAN_POINT('Ctrl Pts',(-216.862326035587,0.349776185474419,
123.810363852911));
#261263=CARTESIAN_POINT('Ctrl Pts',(-217.1407736594,-5.69518498637811,126.729657917385));
#261264=CARTESIAN_POINT('Ctrl Pts',(-217.419221283213,-6.50654938100331,
133.393404703032));
#261265=CARTESIAN_POINT('Ctrl Pts',(-217.697668907026,-1.33871275709491,
137.67794645597));
#261266=CARTESIAN_POINT('Ctrl Pts',(-217.976116530838,5.05933549082977,
135.64599861675));
#261267=CARTESIAN_POINT('Ctrl Pts',(-218.254564154652,6.80810158496121,
129.164821983446));
#261268=CARTESIAN_POINT('Ctrl Pts',(-218.533011778464,2.30055491676597,
124.190301258982));
#261269=CARTESIAN_POINT('Ctrl Pts',(-218.811459402277,-4.32108933158155,
125.293777970294));
#261270=CARTESIAN_POINT('Ctrl Pts',(-219.08990702609,-6.97186358115499,
131.461210927519));
#261271=CARTESIAN_POINT('Ctrl Pts',(-219.368354649903,-3.21583579411804,
137.02503053882));
#261272=CARTESIAN_POINT('Ctrl Pts',(-219.646802273716,3.49538798540175,
136.872358389107));
#261273=CARTESIAN_POINT('Ctrl Pts',(-219.925249897529,6.99452096553273,
131.143492725519));
#261274=CARTESIAN_POINT('Ctrl Pts',(-220.203697521342,4.06603087968498,
125.102981222246));
#261275=CARTESIAN_POINT('Ctrl Pts',(-220.482145145155,-2.59894294794204,
124.301758855404));
#261276=CARTESIAN_POINT('Ctrl Pts',(-220.760592768967,-6.87561517183164,
129.476109838232));
#261277=CARTESIAN_POINT('Ctrl Pts',(-221.03904039278,-4.83393294528274,
135.87105839861));
#261278=CARTESIAN_POINT('Ctrl Pts',(-221.317488016593,1.64989750722823,
137.609959220154));
#261279=CARTESIAN_POINT('Ctrl Pts',(-221.595935640406,6.61755275257056,
133.094847397895));
#261280=CARTESIAN_POINT('Ctrl Pts',(-221.874383264219,5.5040003037252,126.474890121013));
#261281=CARTESIAN_POINT('Ctrl Pts',(-222.152830888031,-0.667459538880483,
123.83350472407));
#261282=CARTESIAN_POINT('Ctrl Pts',(-222.431278511845,-6.22555667246622,
127.597995348007));
#261283=CARTESIAN_POINT('Ctrl Pts',(-222.709726135657,-6.06267135940695,
134.308979015016));
#261284=CARTESIAN_POINT('Ctrl Pts',(-222.988173759471,-0.328487245014279,
137.799389584896));
#261285=CARTESIAN_POINT('Ctrl Pts',(-223.266621383283,5.70756060005303,
134.861710259961));
#261286=CARTESIAN_POINT('Ctrl Pts',(-223.545069007096,6.49863908350723,
128.195524826214));
#261287=CARTESIAN_POINT('Ctrl Pts',(-223.823516630909,1.31778572538753,
123.926732036005));
#261288=CARTESIAN_POINT('Ctrl Pts',(-224.101964254722,-5.07404833695195,
125.978143921416));
#261289=CARTESIAN_POINT('Ctrl Pts',(-224.380411878535,-6.80307985867417,
132.464613176793));
#261290=CARTESIAN_POINT('Ctrl Pts',(-224.658859502348,-2.28041333920269,
137.425391438088));
#261291=CARTESIAN_POINT('Ctrl Pts',(-224.937307126161,4.33784163461131,
136.30176583066));
#261292=CARTESIAN_POINT('Ctrl Pts',(-225.215754749974,6.96983206156226,
130.126293395573));
#261293=CARTESIAN_POINT('Ctrl Pts',(-225.494202373786,3.19688731916334,
124.573931612073));
#261294=CARTESIAN_POINT('Ctrl Pts',(-225.7726499976,-3.51384069291894,124.747029711241));
#261295=CARTESIAN_POINT('Ctrl Pts',(-226.051097621412,-6.9955207688696,
130.486518996257));
#261296=CARTESIAN_POINT('Ctrl Pts',(-226.329545245225,-4.04865900841799,
136.518089203828));
#261297=CARTESIAN_POINT('Ctrl Pts',(-226.607992869038,2.61872259278156,
137.299021971784));
#261298=CARTESIAN_POINT('Ctrl Pts',(-226.886440492851,6.87962606292594,
132.111678237058));
#261299=CARTESIAN_POINT('Ctrl Pts',(-227.164888116664,4.81848926965818,
125.722973476035));
#261300=CARTESIAN_POINT('Ctrl Pts',(-227.443335740477,-1.67060376613766,
124.003815258517));
#261301=CARTESIAN_POINT('Ctrl Pts',(-227.72178336429,-6.62449355438458,
128.534026000853));
#261302=CARTESIAN_POINT('Ctrl Pts',(-228.000230988102,-5.49079739065326,
135.150563343936));
#261303=CARTESIAN_POINT('Ctrl Pts',(-228.278678611916,0.688673334723007,
137.773152705292));
#261304=CARTESIAN_POINT('Ctrl Pts',(-228.557126235728,6.23528690905198,
133.991762582447));
#261305=CARTESIAN_POINT('Ctrl Pts',(-228.835573859542,6.05197642466173,
127.281305767118));
#261306=CARTESIAN_POINT('Ctrl Pts',(-229.114021483354,0.307195261492642,
123.808364248553));
#261307=CARTESIAN_POINT('Ctrl Pts',(-229.392469107167,-5.7198833396657,
126.764401619687));
#261308=CARTESIAN_POINT('Ctrl Pts',(-229.670916730979,-6.49066858350677,
133.432963946903));
#261309=CARTESIAN_POINT('Ctrl Pts',(-229.949364354793,-1.29684648589306,
137.685968228869));
#261310=CARTESIAN_POINT('Ctrl Pts',(-230.227811978605,5.0887141777831,135.615111301269));
#261311=CARTESIAN_POINT('Ctrl Pts',(-230.506259602419,6.79799510958498,
129.123409513582));
#261312=CARTESIAN_POINT('Ctrl Pts',(-230.784707226231,2.26025063620168,
124.176419671429));
#261313=CARTESIAN_POINT('Ctrl Pts',(-231.063154850045,-4.35455375246839,
125.32018376586));
#261314=CARTESIAN_POINT('Ctrl Pts',(-231.341602473857,-6.96773597439774,
131.503638470075));
#261315=CARTESIAN_POINT('Ctrl Pts',(-231.62005009767,-3.17790922868121,
137.044490989456));
#261316=CARTESIAN_POINT('Ctrl Pts',(-231.898497721483,3.53226084869627,
136.850968544386));
#261317=CARTESIAN_POINT('Ctrl Pts',(-232.176945345296,6.99645576665798,
131.100908807788));
#261318=CARTESIAN_POINT('Ctrl Pts',(-232.455392969109,4.03124963092651,
125.078335771559));
#261319=CARTESIAN_POINT('Ctrl Pts',(-232.733840592922,-2.63847797813309,
124.317699836946));
#261320=CARTESIAN_POINT('Ctrl Pts',(-233.012288216734,-6.88357322210384,
129.517988268725));
#261321=CARTESIAN_POINT('Ctrl Pts',(-233.290735840548,-4.80300095620762,
135.900390046307));
#261322=CARTESIAN_POINT('Ctrl Pts',(-233.56918346436,1.6912945488023,137.599789733751));
#261323=CARTESIAN_POINT('Ctrl Pts',(-233.847631088173,6.63137298779474,
133.05452203859));
#261324=CARTESIAN_POINT('Ctrl Pts',(-234.126078711986,5.47754361158473,
126.441465924004));
#261325=CARTESIAN_POINT('Ctrl Pts',(-234.404526335799,-0.709880750790079,
123.837696893545));
#261326=CARTESIAN_POINT('Ctrl Pts',(-234.682973959612,-6.24495938279112,
127.635951485018));
#261327=CARTESIAN_POINT('Ctrl Pts',(-234.961421583425,-6.04122542523402,
134.345819283911));
#261328=CARTESIAN_POINT('Ctrl Pts',(-235.239869207238,-0.285900432155891,
137.801259578306));
#261329=CARTESIAN_POINT('Ctrl Pts',(-235.518316831051,5.73215309106056,
134.826891545298));
#261330=CARTESIAN_POINT('Ctrl Pts',(-235.796764454864,6.48263795483918,
128.156014101264));
#261331=CARTESIAN_POINT('Ctrl Pts',(-236.075212078676,1.27589523259052,
123.918837726791));
#261332=CARTESIAN_POINT('Ctrl Pts',(-236.353659702489,-5.10333287746112,
126.009120512446));
#261333=CARTESIAN_POINT('Ctrl Pts',(-236.632107326302,-6.79284738479763,
132.505994694203));
#261334=CARTESIAN_POINT('Ctrl Pts',(-236.910554950115,-2.24006699454776,
137.439150288976));
#261335=CARTESIAN_POINT('Ctrl Pts',(-237.189002573928,4.3712255303347,136.275258303218));
#261336=CARTESIAN_POINT('Ctrl Pts',(-237.467450197741,6.96557533907847,
130.083878612554));
#261337=CARTESIAN_POINT('Ctrl Pts',(-237.745897821554,3.15890169848239,
124.554586686994));
#261338=CARTESIAN_POINT('Ctrl Pts',(-238.024345445366,-3.55064828209192,
124.768531685198));
#261339=CARTESIAN_POINT('Ctrl Pts',(-238.30279306918,-6.99732595023538,
130.529108605612));
#261340=CARTESIAN_POINT('Ctrl Pts',(-238.581240692992,-4.01380290848946,
136.542628678202));
#261341=CARTESIAN_POINT('Ctrl Pts',(-238.859688316805,2.65820892098533,
137.282960733047));
#261342=CARTESIAN_POINT('Ctrl Pts',(-239.138135940618,6.88745661279959,
132.069775778975));
#261343=CARTESIAN_POINT('Ctrl Pts',(-239.416583564431,4.78746814841248,
125.693736110535));
#261344=CARTESIAN_POINT('Ctrl Pts',(-239.695031188244,-1.71196966354462,
124.014110696169));
#261345=CARTESIAN_POINT('Ctrl Pts',(-239.973478812057,-6.63819098907155,
128.574393237416));
#261346=CARTESIAN_POINT('Ctrl Pts',(-240.25192643587,-5.46423908930053,
135.183906861057));
#261347=CARTESIAN_POINT('Ctrl Pts',(-240.530374059683,0.731081590618679,
137.768831439659));
#261348=CARTESIAN_POINT('Ctrl Pts',(-240.808821683496,6.25457400407998,
133.95374756607));
#261349=CARTESIAN_POINT('Ctrl Pts',(-241.087269307308,6.03041846071876,
127.244530942912));
#261350=CARTESIAN_POINT('Ctrl Pts',(-241.365716931122,0.264602954276818,
123.806623883412));
#261351=CARTESIAN_POINT('Ctrl Pts',(-241.644164554934,-5.74436974057257,
126.799295024156));
#261352=CARTESIAN_POINT('Ctrl Pts',(-241.922612178747,-6.47454727189872,
133.472425786911));
#261353=CARTESIAN_POINT('Ctrl Pts',(-242.20105980256,-1.25493215956847,
137.693735001267));
#261354=CARTESIAN_POINT('Ctrl Pts',(-242.479507426373,5.11790430056101,
135.584045721651));
#261355=CARTESIAN_POINT('Ctrl Pts',(-242.757955050186,6.78763673199965,
129.082059331979));
#261356=CARTESIAN_POINT('Ctrl Pts',(-243.036402673998,2.21986260121965,
124.162783684665));
#261357=CARTESIAN_POINT('Ctrl Pts',(-243.314850297812,-4.38785681376436,
125.346792779616));
#261358=CARTESIAN_POINT('Ctrl Pts',(-243.593297921624,-6.96335017562108,
131.54604010063));
#261359=CARTESIAN_POINT('Ctrl Pts',(-243.871745545438,-3.13986490465013,
137.063720209766));
#261360=CARTESIAN_POINT('Ctrl Pts',(-244.15019316925,3.56900282276695,136.829354640385));
#261361=CARTESIAN_POINT('Ctrl Pts',(-244.428640793064,6.99813131154132,
131.058313901354));
#261362=CARTESIAN_POINT('Ctrl Pts',(-244.707088416876,3.99631900273028,
125.053902500829));
#261363=CARTESIAN_POINT('Ctrl Pts',(-244.985536040689,-2.67791523855318,
124.333881184089));
#261364=CARTESIAN_POINT('Ctrl Pts',(-245.263983664501,-6.89127619903846,
129.559914366219));
#261365=CARTESIAN_POINT('Ctrl Pts',(-245.542431288315,-4.7718909901659,
135.929532858758));
#261366=CARTESIAN_POINT('Ctrl Pts',(-245.820878912128,1.73262891883438,
137.589368440225));
#261367=CARTESIAN_POINT('Ctrl Pts',(-246.09932653594,6.6449474950541,133.014113298726));
#261368=CARTESIAN_POINT('Ctrl Pts',(-246.377774159753,5.45088394705135,
126.408203395661));
#261369=CARTESIAN_POINT('Ctrl Pts',(-246.656221783566,-0.752275657806765,
123.842147215306));
#261370=CARTESIAN_POINT('Ctrl Pts',(-246.934669407379,-6.26413068384941,
127.674025028594));
#261371=CARTESIAN_POINT('Ctrl Pts',(-247.213117031192,-6.01955563123113,
134.382528322752));
#261372=CARTESIAN_POINT('Ctrl Pts',(-247.491564655005,-0.243303025152602,
137.802870299053));
#261373=CARTESIAN_POINT('Ctrl Pts',(-247.770012278818,5.75653317502817,
134.791923774272));
#261374=CARTESIAN_POINT('Ctrl Pts',(-248.048459902631,6.46639660963695,
128.116601511768));
#261375=CARTESIAN_POINT('Ctrl Pts',(-248.326907526444,1.23395746102625,
123.91119856316));
#261376=CARTESIAN_POINT('Ctrl Pts',(-248.605355150257,-5.13242831209467,
126.040274792862));
#261377=CARTESIAN_POINT('Ctrl Pts',(-248.883802774069,-6.78236319946242,
132.547313156937));
#261378=CARTESIAN_POINT('Ctrl Pts',(-249.162250397883,-2.19963764338714,
137.452663285294));
#261379=CARTESIAN_POINT('Ctrl Pts',(-249.440698021695,4.40444744868852,
136.24854804965));
#261380=CARTESIAN_POINT('Ctrl Pts',(-249.719145645508,6.96106050463867,
130.041490527264));
#261381=CARTESIAN_POINT('Ctrl Pts',(-249.997593269321,3.12079902353814,
124.535473349588));
#261382=CARTESIAN_POINT('Ctrl Pts',(-250.276040893134,-3.58732430068758,
124.790257319018));
#261383=CARTESIAN_POINT('Ctrl Pts',(-250.554488516946,-6.99887184311352,
130.571708414529));
#261384=CARTESIAN_POINT('Ctrl Pts',(-250.83293614076,-3.97879807562073,
136.566955518948));
#261385=CARTESIAN_POINT('Ctrl Pts',(-251.111383764572,2.69759674828547,
137.26665942739));
#261386=CARTESIAN_POINT('Ctrl Pts',(-251.389831388386,6.89503194542569,
132.027826430486));
#261387=CARTESIAN_POINT('Ctrl Pts',(-251.668279012198,4.75626962579305,
125.66468812107));
#261388=CARTESIAN_POINT('Ctrl Pts',(-251.946726636011,-1.75327212332407,
124.024657749096));
#261389=CARTESIAN_POINT('Ctrl Pts',(-252.225174259824,-6.65164244307981,
128.614843106116));
#261390=CARTESIAN_POINT('Ctrl Pts',(-252.503621883637,-5.43747830869239,
135.217088092717));
#261391=CARTESIAN_POINT('Ctrl Pts',(-252.78206950745,0.773462756270139,
137.764252102553));
#261392=CARTESIAN_POINT('Ctrl Pts',(-253.060517131263,6.2736293330892,133.91561584884));
#261393=CARTESIAN_POINT('Ctrl Pts',(-253.338964755075,6.00863703830687,
127.207888027921));
#261394=CARTESIAN_POINT('Ctrl Pts',(-253.617412378889,0.222000840393564,
123.805142824969));
#261395=CARTESIAN_POINT('Ctrl Pts',(-253.895860002702,-5.76864327852066,
126.83433683216));
#261396=CARTESIAN_POINT('Ctrl Pts',(-254.174307626514,-6.45818604965135,
133.511788771436));
#261397=CARTESIAN_POINT('Ctrl Pts',(-254.452755250327,-1.21297131977014,
137.701246465247));
#261398=CARTESIAN_POINT('Ctrl Pts',(-254.73120287414,5.14690475579816,135.55280306703));
#261399=CARTESIAN_POINT('Ctrl Pts',(-255.009650497953,6.7770268770417,129.040772899161));
#261400=CARTESIAN_POINT('Ctrl Pts',(-255.288098121766,2.17939223099114,
124.149393939406));
#261401=CARTESIAN_POINT('Ctrl Pts',(-255.566545745579,-4.42099713522674,
125.37360376984));
#261402=CARTESIAN_POINT('Ctrl Pts',(-255.844993369392,-6.95870662337211,
131.588414730824));
#261403=CARTESIAN_POINT('Ctrl Pts',(-256.123440993205,-3.10170371057109,
137.082716575498));
#261404=CARTESIAN_POINT('Ctrl Pts',(-256.401888617018,3.60561156199617,
136.807519199501));
#261405=CARTESIAN_POINT('Ctrl Pts',(-256.68033624083,6.99954939633056,131.01570633407));
#261406=CARTESIAN_POINT('Ctrl Pts',(-256.958783864643,3.96123678073902,
125.029688453078));
#261407=CARTESIAN_POINT('Ctrl Pts',(-257.237231488456,-2.71724664265218,
124.350290708114));
#261408=CARTESIAN_POINT('Ctrl Pts',(-257.515679112269,-6.89873632689917,
129.601908459729));
#261409=CARTESIAN_POINT('Ctrl Pts',(-257.794126736082,-4.74058057908887,
135.958444437253));
#261410=CARTESIAN_POINT('Ctrl Pts',(-258.072574359895,1.77385448465437,
137.578773744179));
#261411=CARTESIAN_POINT('Ctrl Pts',(-258.351021983707,6.6583599873155,132.973475360041));
#261412=CARTESIAN_POINT('Ctrl Pts',(-258.629469607521,5.42386327951784,
126.375381938049));
#261413=CARTESIAN_POINT('Ctrl Pts',(-258.907917231333,-0.794342416617398,
123.846330221273));
#261414=CARTESIAN_POINT('Ctrl Pts',(-259.186364855146,-6.28363694765996,
127.713206958712));
#261415=CARTESIAN_POINT('Ctrl Pts',(-259.464812478959,-5.99659113747434,
134.41722675292));
#261416=CARTESIAN_POINT('Ctrl Pts',(-259.743260102772,-0.202727240537578,
137.807801967267));
#261417=CARTESIAN_POINT('Ctrl Pts',(-260.021707726585,5.7845923739281,134.749768174183));
#261418=CARTESIAN_POINT('Ctrl Pts',(-260.253747413096,6.33253704604016,
129.202365411857));
#261419=CARTESIAN_POINT('Ctrl Pts',(-260.439389088604,3.82430165355141,
125.973250269562));
#261420=CARTESIAN_POINT('Ctrl Pts',(-260.532214889509,1.97943258085903,
125.138073123498));
#261421=CARTESIAN_POINT('Ctrl Pts',(-260.578632753112,1.00712299976162,
124.970230583726));
#261422=CARTESIAN_POINT('',(-207.496424161897,4.58867628645328,134.536649434892));
#261423=CARTESIAN_POINT('',(-207.098616372022,-3.0618288645252,135.866570130891));
#261424=CARTESIAN_POINT('Ctrl Pts',(-207.495564181254,4.5776766096747,134.540053362101));
#261425=CARTESIAN_POINT('Ctrl Pts',(-207.425200105323,4.24191465405194,
134.818390223685));
#261426=CARTESIAN_POINT('Ctrl Pts',(-207.354706723523,3.87623645141089,
135.064257236424));
#261427=CARTESIAN_POINT('Ctrl Pts',(-207.211655246581,3.02401286069414,
135.53061445367));
#261428=CARTESIAN_POINT('Ctrl Pts',(-207.102465536533,2.31383710832897,
135.85051720249));
#261429=CARTESIAN_POINT('Ctrl Pts',(-207.017121680554,1.17680919028678,
136.083357503381));
#261430=CARTESIAN_POINT('Ctrl Pts',(-207.006414015297,1.01191707037494,
136.112213427934));
#261431=CARTESIAN_POINT('Ctrl Pts',(-206.996499081377,0.830830033328691,
136.138764692487));
#261432=CARTESIAN_POINT('Ctrl Pts',(-206.99566378727,0.815305079975026,
136.140999872962));
#261433=CARTESIAN_POINT('Ctrl Pts',(-206.994721821372,0.797482985899804,
136.143518759038));
#261434=CARTESIAN_POINT('Ctrl Pts',(-206.994601057751,0.795192058160855,
136.14384165627));
#261435=CARTESIAN_POINT('Ctrl Pts',(-206.994400925956,0.791385379449218,
136.144376712743));
#261436=CARTESIAN_POINT('Ctrl Pts',(-206.994321381524,0.789869706459846,
136.144589361887));
#261437=CARTESIAN_POINT('Ctrl Pts',(-206.994102307967,0.785688008384046,
136.145174979795));
#261438=CARTESIAN_POINT('Ctrl Pts',(-206.993963066015,0.783021855901667,
136.145547150697));
#261439=CARTESIAN_POINT('Ctrl Pts',(-206.993788136427,0.779661891522758,
136.146014653447));
#261440=CARTESIAN_POINT('Ctrl Pts',(-206.993752052949,0.778968252786303,
136.146111084266));
#261441=CARTESIAN_POINT('Ctrl Pts',(-206.993692234991,0.777817424895901,
136.146270939059));
#261442=CARTESIAN_POINT('Ctrl Pts',(-206.993668484286,0.777360243378844,
136.146334408072));
#261443=CARTESIAN_POINT('Ctrl Pts',(-206.993631449345,0.776646967855322,
136.146433374546));
#261444=CARTESIAN_POINT('Ctrl Pts',(-206.993618156518,0.776390877127087,
136.146468895845));
#261445=CARTESIAN_POINT('Ctrl Pts',(-206.993593676555,0.775919120366145,
136.146534310839));
#261446=CARTESIAN_POINT('Ctrl Pts',(-206.993582488265,0.775703454517646,
136.146564207738));
#261447=CARTESIAN_POINT('Ctrl Pts',(-206.993558003594,0.77523136736309,
136.14662963406));
#261448=CARTESIAN_POINT('Ctrl Pts',(-206.993544708385,0.774974945987442,
136.146665160236));
#261449=CARTESIAN_POINT('Ctrl Pts',(-206.993507616273,0.774259343522897,
136.146764273078));
#261450=CARTESIAN_POINT('Ctrl Pts',(-206.993483828071,0.773800159351325,
136.146827835603));
#261451=CARTESIAN_POINT('Ctrl Pts',(-206.99334996496,0.771214797369116,
136.147185513093));
#261452=CARTESIAN_POINT('Ctrl Pts',(-206.99324014741,0.769088506791007,
136.147478913998));
#261453=CARTESIAN_POINT('Ctrl Pts',(-206.992930672986,0.763081351255442,
136.148305663398));
#261454=CARTESIAN_POINT('Ctrl Pts',(-206.99273164549,0.759200212159492,
136.148837266646));
#261455=CARTESIAN_POINT('Ctrl Pts',(-206.986814011646,0.64326756001477,
136.164640627143));
#261456=CARTESIAN_POINT('Ctrl Pts',(-206.98184368946,0.530869304321618,
136.177840879035));
#261457=CARTESIAN_POINT('Ctrl Pts',(-206.96770201674,0.152471010400863,
136.215289979218));
#261458=CARTESIAN_POINT('Ctrl Pts',(-206.962007786316,-0.114938494561283,
136.230190105475));
#261459=CARTESIAN_POINT('Ctrl Pts',(-206.956679741253,-1.16160653569181,
136.244166478728));
#261460=CARTESIAN_POINT('Ctrl Pts',(-206.990483565803,-2.08084265314269,
136.163862496972));
#261461=CARTESIAN_POINT('Ctrl Pts',(-207.093821477621,-3.06040702803123,
135.870644567327));
#261462=CARTESIAN_POINT('',(-207.794902692642,5.47563200354658,128.562623629372));
#261463=CARTESIAN_POINT('Ctrl Pts',(-207.496674502688,4.59187829781673,
134.535658549994));
#261464=CARTESIAN_POINT('Ctrl Pts',(-207.504071625027,4.69122528656847,
134.41339833656));
#261465=CARTESIAN_POINT('Ctrl Pts',(-207.511468747366,4.78572386629805,
134.287121160146));
#261466=CARTESIAN_POINT('Ctrl Pts',(-207.518865869706,4.87504241186802,
134.157253703393));
#261467=CARTESIAN_POINT('Ctrl Pts',(-207.526262173893,4.96435107844546,
134.027400610507));
#261468=CARTESIAN_POINT('Ctrl Pts',(-207.53365847808,5.04848063920308,133.89395833482));
#261469=CARTESIAN_POINT('Ctrl Pts',(-207.541054782268,5.12714203594177,
133.757383662816));
#261470=CARTESIAN_POINT('Ctrl Pts',(-207.548451728743,5.20581026355275,
133.620797130813));
#261471=CARTESIAN_POINT('Ctrl Pts',(-207.555848675217,5.27900919514005,
133.481077984293));
#261472=CARTESIAN_POINT('Ctrl Pts',(-207.563245621692,5.34649516678223,
133.338708658794));
#261473=CARTESIAN_POINT('Ctrl Pts',(-207.570644671,5.4140003236014,133.196298859983));
#261474=CARTESIAN_POINT('Ctrl Pts',(-207.578043720307,5.47578912705761,
133.051237719391));
#261475=CARTESIAN_POINT('Ctrl Pts',(-207.585442769615,5.5316656567057,132.904028597253));
#261476=CARTESIAN_POINT('Ctrl Pts',(-207.59284975434,5.58760211345569,132.756661594586));
#261477=CARTESIAN_POINT('Ctrl Pts',(-207.600256739065,5.6376134973471,132.607142358003));
#261478=CARTESIAN_POINT('Ctrl Pts',(-207.60766372379,5.6815532323365,132.455991154528));
#261479=CARTESIAN_POINT('Ctrl Pts',(-207.615074827247,5.72551740048127,
132.304755901825));
#261480=CARTESIAN_POINT('Ctrl Pts',(-207.622485930705,5.763403101635,132.151887235657));
#261481=CARTESIAN_POINT('Ctrl Pts',(-207.629897034162,5.79511482293229,
131.997916125923));
#261482=CARTESIAN_POINT('Ctrl Pts',(-207.637319414593,5.8268747978075,131.843710728783));
#261483=CARTESIAN_POINT('Ctrl Pts',(-207.644741795025,5.85244196061352,
131.688399904348));
#261484=CARTESIAN_POINT('Ctrl Pts',(-207.652164175456,5.87177252105169,
131.532521330268));
#261485=CARTESIAN_POINT('Ctrl Pts',(-207.658588023416,5.88850254215265,
131.397613093029));
#261486=CARTESIAN_POINT('Ctrl Pts',(-207.665011871376,5.90056194097322,
131.262279799072));
#261487=CARTESIAN_POINT('Ctrl Pts',(-207.671435719336,5.90795384954832,
131.126869336994));
#261488=CARTESIAN_POINT('Ctrl Pts',(-207.67885957275,5.91649646233298,130.970379422006));
#261489=CARTESIAN_POINT('Ctrl Pts',(-207.686283426164,5.91883003966297,
130.813313207788));
#261490=CARTESIAN_POINT('Ctrl Pts',(-207.693707279578,5.91489478641788,
130.656204523845));
#261491=CARTESIAN_POINT('Ctrl Pts',(-207.701122589545,5.91096406190258,
130.499276642187));
#261492=CARTESIAN_POINT('Ctrl Pts',(-207.708537899512,5.90077887436122,
130.34230675777));
#261493=CARTESIAN_POINT('Ctrl Pts',(-207.715953209479,5.88433125073,130.185833096608));
#261494=CARTESIAN_POINT('Ctrl Pts',(-207.723359919502,5.86790270231684,
130.029540906599));
#261495=CARTESIAN_POINT('Ctrl Pts',(-207.730766629524,5.84522622595717,
129.873744162186));
#261496=CARTESIAN_POINT('Ctrl Pts',(-207.738173339547,5.81634586531258,
129.718979883648));
#261497=CARTESIAN_POINT('Ctrl Pts',(-207.745575077389,5.78748489227169,
129.564319499536));
#261498=CARTESIAN_POINT('Ctrl Pts',(-207.752976815231,5.75242839154114,
129.410690567196));
#261499=CARTESIAN_POINT('Ctrl Pts',(-207.760378553073,5.71127211818421,
129.258624108794));
#261500=CARTESIAN_POINT('Ctrl Pts',(-207.767776495132,5.67013695072318,
129.106635633615));
#261501=CARTESIAN_POINT('Ctrl Pts',(-207.77517443719,5.62290833687531,128.956208396221));
#261502=CARTESIAN_POINT('Ctrl Pts',(-207.782572379249,5.56973288860237,
128.807862154726));
#261503=CARTESIAN_POINT('Ctrl Pts',(-207.786682483713,5.54018999064428,
128.725444835883));
#261504=CARTESIAN_POINT('Ctrl Pts',(-207.790792588177,5.50881243015012,
128.643669624847));
#261505=CARTESIAN_POINT('Ctrl Pts',(-207.794902692642,5.47563200354658,
128.562623629372));
#261506=CARTESIAN_POINT('Ctrl Pts',(-207.386269723983,2.6533283127961,126.660259061981));
#261507=CARTESIAN_POINT('Ctrl Pts',(-207.393495255289,2.73186345863168,
126.685833507559));
#261508=CARTESIAN_POINT('Ctrl Pts',(-207.401071667583,2.80988843464172,
126.712904578486));
#261509=CARTESIAN_POINT('Ctrl Pts',(-207.437853940591,3.17010229530851,
126.845902326529));
#261510=CARTESIAN_POINT('Ctrl Pts',(-207.471155685021,3.44464862169167,
126.970579878808));
#261511=CARTESIAN_POINT('Ctrl Pts',(-207.539861816086,3.95135827120292,
127.245868129711));
#261512=CARTESIAN_POINT('Ctrl Pts',(-207.575105779606,4.18647404634928,
127.394611394059));
#261513=CARTESIAN_POINT('Ctrl Pts',(-207.673664526471,4.8027720530598,127.846802047319));
#261514=CARTESIAN_POINT('Ctrl Pts',(-207.738601360219,5.1630678639706,128.184811296776));
#261515=CARTESIAN_POINT('Ctrl Pts',(-207.795193373066,5.46743686141374,
128.565993481731));
#261516=CARTESIAN_POINT('',(-178.235140563957,-4.91824875847738,130.800866016629));
#261517=CARTESIAN_POINT('Ctrl Pts',(-178.235140564012,-4.91824875847807,
130.800866017606));
#261518=CARTESIAN_POINT('Ctrl Pts',(-178.242912059243,-4.91834661808309,
130.938592191243));
#261519=CARTESIAN_POINT('Ctrl Pts',(-178.250683554473,-4.91265502275465,
131.076364389796));
#261520=CARTESIAN_POINT('Ctrl Pts',(-178.258455049704,-4.90118910695513,
131.213662951256));
#261521=CARTESIAN_POINT('Ctrl Pts',(-178.266226229677,-4.8897236562809,
131.350955943075));
#261522=CARTESIAN_POINT('Ctrl Pts',(-178.27399740965,-4.87248438266389,
131.487774950232));
#261523=CARTESIAN_POINT('Ctrl Pts',(-178.281768589622,-4.84953840587296,
131.623604361798));
#261524=CARTESIAN_POINT('Ctrl Pts',(-178.289541094918,-4.82658851579851,
131.759456938165));
#261525=CARTESIAN_POINT('Ctrl Pts',(-178.297313600214,-4.79793004946218,
131.894319201245));
#261526=CARTESIAN_POINT('Ctrl Pts',(-178.30508610551,-4.76368139923051,
132.027685018175));
#261527=CARTESIAN_POINT('Ctrl Pts',(-178.31286157721,-4.72941967788061,
132.161101734639));
#261528=CARTESIAN_POINT('Ctrl Pts',(-178.32063704891,-4.68956362187731,
132.293020493378));
#261529=CARTESIAN_POINT('Ctrl Pts',(-178.328412520609,-4.64428160317825,
132.422949957973));
#261530=CARTESIAN_POINT('Ctrl Pts',(-178.33619753434,-4.59894401455087,
132.553038871534));
#261531=CARTESIAN_POINT('Ctrl Pts',(-178.34398254807,-4.54816729194925,
132.68113324938));
#261532=CARTESIAN_POINT('Ctrl Pts',(-178.351767561801,-4.49216835570908,
132.806760808953));
#261533=CARTESIAN_POINT('Ctrl Pts',(-178.359557729245,-4.43613234792204,
132.932471534533));
#261534=CARTESIAN_POINT('Ctrl Pts',(-178.36734789669,-4.37486741040936,
133.055711842143));
#261535=CARTESIAN_POINT('Ctrl Pts',(-178.375138064134,-4.30863618326705,
133.176034562851));
#261536=CARTESIAN_POINT('Ctrl Pts',(-178.38294095569,-4.24229677699919,
133.296553813311));
#261537=CARTESIAN_POINT('Ctrl Pts',(-178.390743847245,-4.17097507715918,
133.414145626664));
#261538=CARTESIAN_POINT('Ctrl Pts',(-178.398546738801,-4.09497718847947,
133.528391617451));
#261539=CARTESIAN_POINT('Ctrl Pts',(-178.403979900142,-4.04205978115932,
133.607941217238));
#261540=CARTESIAN_POINT('Ctrl Pts',(-178.409413061482,-3.98687607958372,
133.685869291158));
#261541=CARTESIAN_POINT('Ctrl Pts',(-178.414846222822,-3.92954049509117,
133.76204460338));
#261542=CARTESIAN_POINT('Ctrl Pts',(-178.422620556941,-3.84749875864512,
133.871044187919));
#261543=CARTESIAN_POINT('Ctrl Pts',(-178.430394891061,-3.76078840842461,
133.976800260166));
#261544=CARTESIAN_POINT('Ctrl Pts',(-178.43816922518,-3.66969498233147,
134.078886812171));
#261545=CARTESIAN_POINT('Ctrl Pts',(-178.445933978127,-3.57871382074449,
134.180847551624));
#261546=CARTESIAN_POINT('Ctrl Pts',(-178.453698731074,-3.48336058895814,
134.279147480063));
#261547=CARTESIAN_POINT('Ctrl Pts',(-178.461463484021,-3.38396310956101,
134.373390840978));
#261548=CARTESIAN_POINT('Ctrl Pts',(-178.469220524906,-3.28466435314195,
134.467540598059));
#261549=CARTESIAN_POINT('Ctrl Pts',(-178.476977565791,-3.18132962460898,
134.557641538328));
#261550=CARTESIAN_POINT('Ctrl Pts',(-178.484734606676,-3.07432564361539,
134.643332472049));
#261551=CARTESIAN_POINT('Ctrl Pts',(-178.492485797916,-2.96740235515608,
134.728958785569));
#261552=CARTESIAN_POINT('Ctrl Pts',(-178.500236989156,-2.856815625741,134.81018146859));
#261553=CARTESIAN_POINT('Ctrl Pts',(-178.507988180396,-2.74296724005992,
134.886677825042));
#261554=CARTESIAN_POINT('Ctrl Pts',(-178.515736077173,-2.6291672429796,
134.963141668503));
#261555=CARTESIAN_POINT('Ctrl Pts',(-178.523483973951,-2.51210867069543,
135.034882963187));
#261556=CARTESIAN_POINT('Ctrl Pts',(-178.531231870728,-2.39222425946025,
135.101620925594));
#261557=CARTESIAN_POINT('Ctrl Pts',(-178.538978146812,-2.27236492545981,
135.168344927857));
#261558=CARTESIAN_POINT('Ctrl Pts',(-178.546724422896,-2.14968126963242,
135.230067489522));
#261559=CARTESIAN_POINT('Ctrl Pts',(-178.55447069898,-2.0246323815396,135.286552802437));
#261560=CARTESIAN_POINT('Ctrl Pts',(-178.562217032245,-1.89958257036413,
135.343038532314));
#261561=CARTESIAN_POINT('Ctrl Pts',(-178.569963365511,-1.77216784838562,
135.394286775354));
#261562=CARTESIAN_POINT('Ctrl Pts',(-178.577709698776,-1.64286875422958,
135.440109243072));
#261563=CARTESIAN_POINT('Ctrl Pts',(-178.585457766779,-1.51354070443772,
135.485941972413));
#261564=CARTESIAN_POINT('Ctrl Pts',(-178.593205834782,-1.38232781119079,
135.526346378023));
#261565=CARTESIAN_POINT('Ctrl Pts',(-178.600953902785,-1.24972691011741,
135.561183686866));
#261566=CARTESIAN_POINT('Ctrl Pts',(-178.608710205527,-1.11698507922857,
135.596058021216));
#261567=CARTESIAN_POINT('Ctrl Pts',(-178.616466508269,-0.982852672395769,
135.625353339897));
#261568=CARTESIAN_POINT('Ctrl Pts',(-178.62422281101,-0.847838434771901,
135.648981660643));
#261569=CARTESIAN_POINT('Ctrl Pts',(-178.631983253525,-0.712752135984214,
135.672622592535));
#261570=CARTESIAN_POINT('Ctrl Pts',(-178.639743696039,-0.576783455982213,
135.690590448432));
#261571=CARTESIAN_POINT('Ctrl Pts',(-178.647504138553,-0.440446459232609,
135.702849157825));
#261572=CARTESIAN_POINT('Ctrl Pts',(-178.655277038818,-0.303890602232393,
135.715127545987));
#261573=CARTESIAN_POINT('Ctrl Pts',(-178.663049939084,-0.166965637712462,
135.721678454702));
#261574=CARTESIAN_POINT('Ctrl Pts',(-178.670822839349,-0.03018673474577,
135.722517978158));
#261575=CARTESIAN_POINT('Ctrl Pts',(-178.678313175112,0.101619910576147,
135.723326982821));
#261576=CARTESIAN_POINT('Ctrl Pts',(-178.685803510874,0.233290621547758,
135.718832649925));
#261577=CARTESIAN_POINT('Ctrl Pts',(-178.693293846636,0.364370681277128,
135.709094766236));
#261578=CARTESIAN_POINT('Ctrl Pts',(-178.701068180755,0.500420681308806,
135.698987667727));
#261579=CARTESIAN_POINT('Ctrl Pts',(-178.708842514874,0.63626532236978,
135.683199534606));
#261580=CARTESIAN_POINT('Ctrl Pts',(-178.716616848993,0.77139185169714,
135.661740330295));
#261581=CARTESIAN_POINT('Ctrl Pts',(-178.72438160194,0.906351849653709,
135.640307572536));
#261582=CARTESIAN_POINT('Ctrl Pts',(-178.732146354887,1.04059511436018,
135.61321771052));
#261583=CARTESIAN_POINT('Ctrl Pts',(-178.739911107835,1.17361148854135,
135.580532634617));
#261584=CARTESIAN_POINT('Ctrl Pts',(-178.74766814872,1.30649574898521,135.547880021992));
#261585=CARTESIAN_POINT('Ctrl Pts',(-178.755425189605,1.43815516668883,
135.509643347339));
#261586=CARTESIAN_POINT('Ctrl Pts',(-178.76318223049,1.56808764156665,135.465935910411));
#261587=CARTESIAN_POINT('Ctrl Pts',(-178.77093342173,1.6979221333539,135.422261433602));
#261588=CARTESIAN_POINT('Ctrl Pts',(-178.77868461297,1.82603190540451,135.373124530313));
#261589=CARTESIAN_POINT('Ctrl Pts',(-178.78643580421,1.95192828993981,135.318688808275));
#261590=CARTESIAN_POINT('Ctrl Pts',(-178.794183700987,2.07777116515346,
135.264276222872));
#261591=CARTESIAN_POINT('Ctrl Pts',(-178.801931597764,2.20140216582424,
135.204569452893));
#261592=CARTESIAN_POINT('Ctrl Pts',(-178.809679494541,2.32235115632627,
135.139780801263));
#261593=CARTESIAN_POINT('Ctrl Pts',(-178.817425770625,2.44327484690683,
135.075005702023));
#261594=CARTESIAN_POINT('Ctrl Pts',(-178.82517204671,2.56151729879949,135.005151020031));
#261595=CARTESIAN_POINT('Ctrl Pts',(-178.832918322794,2.6766319708055,134.93047554027));
#261596=CARTESIAN_POINT('Ctrl Pts',(-178.840664656059,2.79174749256172,
134.855799509272));
#261597=CARTESIAN_POINT('Ctrl Pts',(-178.848410989325,2.90373486036354,
134.77630282227));
#261598=CARTESIAN_POINT('Ctrl Pts',(-178.85615732259,3.01217591891128,134.692287995493));
#261599=CARTESIAN_POINT('Ctrl Pts',(-178.863905390593,3.12064126208234,
134.608254354177));
#261600=CARTESIAN_POINT('Ctrl Pts',(-178.871653458596,3.22555840668735,
134.519700799111));
#261601=CARTESIAN_POINT('Ctrl Pts',(-178.879401526599,3.32654204724801,
134.426970321963));
#261602=CARTESIAN_POINT('Ctrl Pts',(-178.887157829341,3.42763301442343,
134.334141289761));
#261603=CARTESIAN_POINT('Ctrl Pts',(-178.894914132082,3.52478183797542,
134.23712673239));
#261604=CARTESIAN_POINT('Ctrl Pts',(-178.902670434824,3.61763950674951,
134.136307114991));
#261605=CARTESIAN_POINT('Ctrl Pts',(-178.910430877338,3.71054673645731,
134.035433687128));
#261606=CARTESIAN_POINT('Ctrl Pts',(-178.918191319852,3.79915799525986,
133.93075145081));
#261607=CARTESIAN_POINT('Ctrl Pts',(-178.925951762367,3.88316507161623,
133.822673406042));
#261608=CARTESIAN_POINT('Ctrl Pts',(-178.933724662632,3.96730700358959,
133.714421864802));
#261609=CARTESIAN_POINT('Ctrl Pts',(-178.941497562898,4.04682975652453,
133.60276394041));
#261610=CARTESIAN_POINT('Ctrl Pts',(-178.949270463163,4.12146840944813,
133.488141758498));
#261611=CARTESIAN_POINT('Ctrl Pts',(-178.956760798925,4.19339375933312,
133.377686381616));
#261612=CARTESIAN_POINT('Ctrl Pts',(-178.964251134687,4.26078378529405,
133.264478786661));
#261613=CARTESIAN_POINT('Ctrl Pts',(-178.971741470449,4.32344300204487,
133.14893385604));
#261614=CARTESIAN_POINT('Ctrl Pts',(-178.979515804568,4.38847796204466,
133.029008004254));
#261615=CARTESIAN_POINT('Ctrl Pts',(-178.987290138687,4.44862230519032,
132.906184188811));
#261616=CARTESIAN_POINT('Ctrl Pts',(-178.995064472806,4.50360725859762,
132.780899188606));
#261617=CARTESIAN_POINT('Ctrl Pts',(-179.002829225753,4.55852444796399,
132.655768590966));
#261618=CARTESIAN_POINT('Ctrl Pts',(-179.0105939787,4.60829474347329,132.528183198275));
#261619=CARTESIAN_POINT('Ctrl Pts',(-179.018358731647,4.65269446277708,
132.398605673554));
#261620=CARTESIAN_POINT('Ctrl Pts',(-179.026115772532,4.69705008365385,
132.269156847057));
#261621=CARTESIAN_POINT('Ctrl Pts',(-179.033872813417,4.73604561757761,
132.137720193522));
#261622=CARTESIAN_POINT('Ctrl Pts',(-179.041629854302,4.76950498948021,
132.004779385256));
#261623=CARTESIAN_POINT('Ctrl Pts',(-179.049381045542,4.80293912941014,
131.871938828688));
#261624=CARTESIAN_POINT('Ctrl Pts',(-179.057132236782,4.83084532209175,
131.737596752741));
#261625=CARTESIAN_POINT('Ctrl Pts',(-179.064883428023,4.85309707847332,
131.602252721433));
#261626=CARTESIAN_POINT('Ctrl Pts',(-179.0726313248,4.87533937726481,131.466966214949));
#261627=CARTESIAN_POINT('Ctrl Pts',(-179.080379221577,4.89193195641557,
131.330678985081));
#261628=CARTESIAN_POINT('Ctrl Pts',(-179.088127118354,4.90279931259945,
131.193901325162));
#261629=CARTESIAN_POINT('Ctrl Pts',(-179.095873394438,4.91366439556669,
131.057152276181));
#261630=CARTESIAN_POINT('Ctrl Pts',(-179.103619670522,4.91880660669958,
130.919913390691));
#261631=CARTESIAN_POINT('Ctrl Pts',(-179.111365946606,4.91820230270907,
130.782700236056));
#261632=CARTESIAN_POINT('Ctrl Pts',(-179.119112279871,4.91759799425773,
130.645486068543));
#261633=CARTESIAN_POINT('Ctrl Pts',(-179.126858613137,4.91124708775985,
130.508298023225));
#261634=CARTESIAN_POINT('Ctrl Pts',(-179.134604946402,4.89917807553393,
130.371651423409));
#261635=CARTESIAN_POINT('Ctrl Pts',(-179.142353014405,4.88710636053639,
130.234974222535));
#261636=CARTESIAN_POINT('Ctrl Pts',(-179.150101082408,4.86931402609475,
130.098839097816));
#261637=CARTESIAN_POINT('Ctrl Pts',(-179.157849150411,4.84588137379236,
129.963755613041));
#261638=CARTESIAN_POINT('Ctrl Pts',(-179.165605453153,4.82242381698827,
129.828528559931));
#261639=CARTESIAN_POINT('Ctrl Pts',(-179.173361755895,4.79331403439889,
129.694355765308));
#261640=CARTESIAN_POINT('Ctrl Pts',(-179.181118058636,4.75868347306896,
129.561736512842));
#261641=CARTESIAN_POINT('Ctrl Pts',(-179.188878501151,4.72403442836585,
129.429046477489));
#261642=CARTESIAN_POINT('Ctrl Pts',(-179.196638943665,4.68385884803004,
129.297912010122));
#261643=CARTESIAN_POINT('Ctrl Pts',(-179.204399386179,4.63833760479553,
129.16881565443));
#261644=CARTESIAN_POINT('Ctrl Pts',(-179.212172286444,4.59274328682007,
129.039512061807));
#261645=CARTESIAN_POINT('Ctrl Pts',(-179.21994518671,4.54178630312496,128.912253482031));
#261646=CARTESIAN_POINT('Ctrl Pts',(-179.227718086975,4.48569543026932,
128.787501780324));
#261647=CARTESIAN_POINT('Ctrl Pts',(-179.235208422737,4.43164360192636,
128.667285117205));
#261648=CARTESIAN_POINT('Ctrl Pts',(-179.242698758499,4.37282480120875,
128.549396509455));
#261649=CARTESIAN_POINT('Ctrl Pts',(-179.250189094261,4.30948241586416,
128.434224678457));
#261650=CARTESIAN_POINT('Ctrl Pts',(-179.25796342838,4.24373838472681,128.314686072481));
#261651=CARTESIAN_POINT('Ctrl Pts',(-179.265737762499,4.17291271682093,
128.197695660831));
#261652=CARTESIAN_POINT('Ctrl Pts',(-179.273512096618,4.09722760829128,
128.083715659407));
#261653=CARTESIAN_POINT('Ctrl Pts',(-179.281276849565,4.02163577489393,
127.969876128149));
#261654=CARTESIAN_POINT('Ctrl Pts',(-179.289041602512,3.94119663104747,
127.859039947773));
#261655=CARTESIAN_POINT('Ctrl Pts',(-179.29680635546,3.85617852248092,127.751645389239));
#261656=CARTESIAN_POINT('Ctrl Pts',(-179.304563396344,3.77124485509857,
127.644357496495));
#261657=CARTESIAN_POINT('Ctrl Pts',(-179.31232043723,3.6817415146055,127.540504727641));
#261658=CARTESIAN_POINT('Ctrl Pts',(-179.320077478115,3.58798025533687,
127.440496656314));
#261659=CARTESIAN_POINT('Ctrl Pts',(-179.327828669355,3.49428970216282,
127.340564001851));
#261660=CARTESIAN_POINT('Ctrl Pts',(-179.335579860595,3.39634788769476,
127.244470558066));
#261661=CARTESIAN_POINT('Ctrl Pts',(-179.343331051835,3.29450673886711,
127.152592770336));
#261662=CARTESIAN_POINT('Ctrl Pts',(-179.351078948612,3.19270887524427,
127.060754033117));
#261663=CARTESIAN_POINT('Ctrl Pts',(-179.358826845389,3.08701526322851,
126.973127649607));
#261664=CARTESIAN_POINT('Ctrl Pts',(-179.366574742166,2.97781441566159,
126.890052968903));
#261665=CARTESIAN_POINT('Ctrl Pts',(-179.37432101825,2.86863641055788,126.806995665632));
#261666=CARTESIAN_POINT('Ctrl Pts',(-179.382067294334,2.75595294011129,
126.728488407918));
#261667=CARTESIAN_POINT('Ctrl Pts',(-179.389813570418,2.64018498597006,
126.654829764282));
#261668=CARTESIAN_POINT('Ctrl Pts',(-179.397559903684,2.52441617725656,
126.581170576914));
#261669=CARTESIAN_POINT('Ctrl Pts',(-179.405306236949,2.40556316927225,
126.512360284919));
#261670=CARTESIAN_POINT('Ctrl Pts',(-179.413052570214,2.28407491890505,
126.448653461738));
#261671=CARTESIAN_POINT('Ctrl Pts',(-179.420800638217,2.16255946208602,
126.384932371855));
#261672=CARTESIAN_POINT('Ctrl Pts',(-179.42854870622,2.03840793474619,126.326317206531));
#261673=CARTESIAN_POINT('Ctrl Pts',(-179.436296774223,1.9120924522984,126.273015837441));
#261674=CARTESIAN_POINT('Ctrl Pts',(-179.444053076965,1.78564272025286,
126.219657819023));
#261675=CARTESIAN_POINT('Ctrl Pts',(-179.451809379707,1.65702479963027,
126.1716250307));
#261676=CARTESIAN_POINT('Ctrl Pts',(-179.459565682449,1.52672980226203,
126.129076757373));
#261677=CARTESIAN_POINT('Ctrl Pts',(-179.467326124963,1.39636526253059,
126.08650577475));
#261678=CARTESIAN_POINT('Ctrl Pts',(-179.475086567477,1.26432223869915,
126.049425245569));
#261679=CARTESIAN_POINT('Ctrl Pts',(-179.482847009991,1.13110447457022,
126.017943823125));
#261680=CARTESIAN_POINT('Ctrl Pts',(-179.490619910257,0.997672857459797,
125.986411863907));
#261681=CARTESIAN_POINT('Ctrl Pts',(-179.498392810522,0.863063115764055,
125.960497046634));
#261682=CARTESIAN_POINT('Ctrl Pts',(-179.506165710787,0.727787489092654,
125.940256544541));
#261683=CARTESIAN_POINT('Ctrl Pts',(-179.51365604655,0.597429472185839,
125.920751835681));
#261684=CARTESIAN_POINT('Ctrl Pts',(-179.521146382312,0.466453449186646,
125.906516086481));
#261685=CARTESIAN_POINT('Ctrl Pts',(-179.528636718074,0.335318019426584,
125.897554641338));
#261686=CARTESIAN_POINT('Ctrl Pts',(-179.536411052193,0.199210549992686,
125.888253420279));
#261687=CARTESIAN_POINT('Ctrl Pts',(-179.544185386312,0.0625001998143731,
125.884604885428));
#261688=CARTESIAN_POINT('Ctrl Pts',(-179.551959720431,-0.074304053336741,
125.886671935862));
#261689=CARTESIAN_POINT('Ctrl Pts',(-179.559724473378,-0.210939707472022,
125.888736438841));
#261690=CARTESIAN_POINT('Ctrl Pts',(-179.567489226326,-0.347668647150042,
125.896502505897));
#261691=CARTESIAN_POINT('Ctrl Pts',(-179.575253979273,-0.483977095179842,
125.909981266326));
#261692=CARTESIAN_POINT('Ctrl Pts',(-179.583011020158,-0.620150159737818,
125.923446639461));
#261693=CARTESIAN_POINT('Ctrl Pts',(-179.590768061043,-0.75590317721648,
125.942613376373));
#261694=CARTESIAN_POINT('Ctrl Pts',(-179.598525101928,-0.890723050881356,
125.967440573868));
#261695=CARTESIAN_POINT('Ctrl Pts',(-179.606276293168,-1.0254412558302,
125.99224904898));
#261696=CARTESIAN_POINT('Ctrl Pts',(-179.614027484408,-1.15922733467526,
126.02270941777));
#261697=CARTESIAN_POINT('Ctrl Pts',(-179.621778675648,-1.29157434815609,
126.058729072062));
#261698=CARTESIAN_POINT('Ctrl Pts',(-179.629526572425,-1.42386511062591,
126.09473341704));
#261699=CARTESIAN_POINT('Ctrl Pts',(-179.637274469202,-1.55471764778564,
126.136292245547));
#261700=CARTESIAN_POINT('Ctrl Pts',(-179.645022365979,-1.68363645494728,
126.183262117201));
#261701=CARTESIAN_POINT('Ctrl Pts',(-179.652768642063,-1.81252829507363,
126.230222163771));
#261702=CARTESIAN_POINT('Ctrl Pts',(-179.660514918148,-1.9394868426528,
126.282590868379));
#261703=CARTESIAN_POINT('Ctrl Pts',(-179.668261194232,-2.06403335266789,
126.340175430819));
#261704=CARTESIAN_POINT('Ctrl Pts',(-179.676007527497,-2.18858078205719,
126.397760418335));
#261705=CARTESIAN_POINT('Ctrl Pts',(-179.683753860762,-2.31071578348326,
126.460561176436));
#261706=CARTESIAN_POINT('Ctrl Pts',(-179.691500194028,-2.429981504936,126.528337588141));
#261707=CARTESIAN_POINT('Ctrl Pts',(-179.699248262031,-2.54927393512061,
126.596129177904));
#261708=CARTESIAN_POINT('Ctrl Pts',(-179.706996330034,-2.66569546687332,
126.668898445397));
#261709=CARTESIAN_POINT('Ctrl Pts',(-179.714744398037,-2.77881602195207,
126.746360546269));
#261710=CARTESIAN_POINT('Ctrl Pts',(-179.722500700779,-2.89205680290245,
126.823904974785));
#261711=CARTESIAN_POINT('Ctrl Pts',(-179.73025700352,-3.00198927584127,
126.906151978699));
#261712=CARTESIAN_POINT('Ctrl Pts',(-179.738013306262,-3.10821397193136,
126.992774469098));
#261713=CARTESIAN_POINT('Ctrl Pts',(-179.745773748776,-3.21449536334011,
127.079443192529));
#261714=CARTESIAN_POINT('Ctrl Pts',(-179.753534191291,-3.31706474242677,
127.170491796366));
#261715=CARTESIAN_POINT('Ctrl Pts',(-179.761294633805,-3.41555841026557,
127.265555196444));
#261716=CARTESIAN_POINT('Ctrl Pts',(-179.76906753407,-3.51421018888385,
127.36077120073));
#261717=CARTESIAN_POINT('Ctrl Pts',(-179.776840434336,-3.60877291201382,
127.460014597025));
#261718=CARTESIAN_POINT('Ctrl Pts',(-179.784613334601,-3.69892160017226,
127.562885327165));
#261719=CARTESIAN_POINT('Ctrl Pts',(-179.792103670363,-3.78579315644455,
127.662016447149));
#261720=CARTESIAN_POINT('Ctrl Pts',(-179.799594006125,-3.86856583511938,
127.764515514558));
#261721=CARTESIAN_POINT('Ctrl Pts',(-179.807084341887,-3.94698725566329,
127.869999585564));
#261722=CARTESIAN_POINT('Ctrl Pts',(-179.81489938152,-4.02880822192404,
127.980056360295));
#261723=CARTESIAN_POINT('Ctrl Pts',(-179.822714421154,-4.10615277853036,
128.093713091792));
#261724=CARTESIAN_POINT('Ctrl Pts',(-179.830529460787,-4.17868931704032,
128.210572142352));
#261725=CARTESIAN_POINT('Ctrl Pts',(-179.838331509096,-4.25110527449914,
128.327236932372));
#261726=CARTESIAN_POINT('Ctrl Pts',(-179.846133557405,-4.31872893195353,
128.447093113703));
#261727=CARTESIAN_POINT('Ctrl Pts',(-179.853935605714,-4.38126988870761,
128.569711377796));
#261728=CARTESIAN_POINT('Ctrl Pts',(-179.861730173332,-4.44375088049264,
128.692212074126));
#261729=CARTESIAN_POINT('Ctrl Pts',(-179.86952474095,-4.50115869139553,
128.817469244293));
#261730=CARTESIAN_POINT('Ctrl Pts',(-179.877319308568,-4.55324684430206,
128.945025726441));
#261731=CARTESIAN_POINT('Ctrl Pts',(-179.885106751938,-4.60528738855242,
129.072465621758));
#261732=CARTESIAN_POINT('Ctrl Pts',(-179.892894195309,-4.65201781159595,
129.202200288788));
#261733=CARTESIAN_POINT('Ctrl Pts',(-179.900681638679,-4.6932383823034,
129.333749673307));
#261734=CARTESIAN_POINT('Ctrl Pts',(-179.90555036806,-4.71900958783941,
129.415994682738));
#261735=CARTESIAN_POINT('Ctrl Pts',(-179.910419097441,-4.74262803915595,
129.498948563585));
#261736=CARTESIAN_POINT('Ctrl Pts',(-179.915287826822,-4.76405452823417,
129.582490119309));
#261737=CARTESIAN_POINT('Ctrl Pts',(-178.165366640417,-4.76405452823403,
129.582490119308));
#261738=CARTESIAN_POINT('Ctrl Pts',(-178.174286102188,-4.80301964378508,
129.734414513464));
#261739=CARTESIAN_POINT('Ctrl Pts',(-178.18320556396,-4.83475684527663,
129.888373267217));
#261740=CARTESIAN_POINT('Ctrl Pts',(-178.192125025732,-4.85907467737619,
130.043718558394));
#261741=CARTESIAN_POINT('Ctrl Pts',(-178.200980669897,-4.88321851850083,
130.197952373904));
#261742=CARTESIAN_POINT('Ctrl Pts',(-178.209836314062,-4.90004869699476,
130.353552808266));
#261743=CARTESIAN_POINT('Ctrl Pts',(-178.218691958226,-4.9094252417917,
130.509866376946));
#261744=CARTESIAN_POINT('Ctrl Pts',(-178.224174826803,-4.91523061990645,
130.606646095947));
#261745=CARTESIAN_POINT('Ctrl Pts',(-178.22965769538,-4.91817971751586,
130.70369880656));
#261746=CARTESIAN_POINT('Ctrl Pts',(-178.235140563957,-4.91824875847738,
130.80086601663));
#261747=CARTESIAN_POINT('',(-178.485270545702,-2.29572256715808,125.351142443209));
#261748=CARTESIAN_POINT('Ctrl Pts',(-178.48283591081,-2.30474777596774,
125.357501197005));
#261749=CARTESIAN_POINT('Ctrl Pts',(-178.439259969146,-2.35809653341986,
125.471388554306));
#261750=CARTESIAN_POINT('Ctrl Pts',(-178.397030602778,-2.41201111853674,
125.585847534594));
#261751=CARTESIAN_POINT('Ctrl Pts',(-178.311610003403,-2.52439778012099,
125.826246106787));
#261752=CARTESIAN_POINT('Ctrl Pts',(-178.268672143037,-2.58283994140754,
125.952273103513));
#261753=CARTESIAN_POINT('Ctrl Pts',(-178.183448400479,-2.70162741425541,
126.21363850387));
#261754=CARTESIAN_POINT('Ctrl Pts',(-178.141394739096,-2.76182193325093,
126.348942022816));
#261755=CARTESIAN_POINT('Ctrl Pts',(-178.059030111423,-2.88183628638349,
126.627709334455));
#261756=CARTESIAN_POINT('Ctrl Pts',(-178.018924422453,-2.94145364433504,
126.771074158801));
#261757=CARTESIAN_POINT('Ctrl Pts',(-177.980719892801,-2.99891973414341,
126.915872442133));
#261758=CARTESIAN_POINT('',(-178.811624764632,-5.91430460988513,130.800157362323));
#261759=CARTESIAN_POINT('Ctrl Pts',(-178.485270545702,-2.29572256715808,
125.351142443209));
#261760=CARTESIAN_POINT('Ctrl Pts',(-178.492676155995,-2.44062366529699,
125.412143619096));
#261761=CARTESIAN_POINT('Ctrl Pts',(-178.500081766289,-2.58322966273536,
125.478982251567));
#261762=CARTESIAN_POINT('Ctrl Pts',(-178.507487376582,-2.72303992747434,
125.551458170739));
#261763=CARTESIAN_POINT('Ctrl Pts',(-178.514887922563,-2.86275458323872,
125.623884527396));
#261764=CARTESIAN_POINT('Ctrl Pts',(-178.522288468545,-2.99967698309288,
125.701940323268));
#261765=CARTESIAN_POINT('Ctrl Pts',(-178.529689014526,-3.13332760890747,
125.785377786577));
#261766=CARTESIAN_POINT('Ctrl Pts',(-178.537322090704,-3.27117762843923,
125.871436911829));
#261767=CARTESIAN_POINT('Ctrl Pts',(-178.544955166882,-3.40554653031744,
125.963221272439));
#261768=CARTESIAN_POINT('Ctrl Pts',(-178.55258824306,-3.53593626550598,
126.060408121094));
#261769=CARTESIAN_POINT('Ctrl Pts',(-178.559984666331,-3.6622834483718,
126.154581826727));
#261770=CARTESIAN_POINT('Ctrl Pts',(-178.567381089602,-3.78489421730117,
126.253827766868));
#261771=CARTESIAN_POINT('Ctrl Pts',(-178.574777512873,-3.90334590563519,
126.357808998225));
#261772=CARTESIAN_POINT('Ctrl Pts',(-178.582174070057,-4.02179973853031,
126.461792112157));
#261773=CARTESIAN_POINT('Ctrl Pts',(-178.58957062724,-4.13609406001072,
126.570510442079));
#261774=CARTESIAN_POINT('Ctrl Pts',(-178.596967184423,-4.24584063293858,
126.683587888794));
#261775=CARTESIAN_POINT('Ctrl Pts',(-178.604365335927,-4.35561086164749,
126.796689709258));
#261776=CARTESIAN_POINT('Ctrl Pts',(-178.611763487432,-4.46083113010824,
126.91415224943));
#261777=CARTESIAN_POINT('Ctrl Pts',(-178.619161638937,-4.56115140711873,
127.03556393907));
#261778=CARTESIAN_POINT('Ctrl Pts',(-178.62656284585,-4.66151311601725,
127.157025771272));
#261779=CARTESIAN_POINT('Ctrl Pts',(-178.633964052763,-4.7569705667546,
127.282439712767));
#261780=CARTESIAN_POINT('Ctrl Pts',(-178.641365259675,-4.84721530679233,
127.411362779061));
#261781=CARTESIAN_POINT('Ctrl Pts',(-178.648774778471,-4.9375613956671,
127.540430631664));
#261782=CARTESIAN_POINT('Ctrl Pts',(-178.656184297267,-5.02268287156556,
127.673015171635));
#261783=CARTESIAN_POINT('Ctrl Pts',(-178.663593816062,-5.10231539881571,
127.808645655573));
#261784=CARTESIAN_POINT('Ctrl Pts',(-178.67100831022,-5.18200139790702,
127.944367212995));
#261785=CARTESIAN_POINT('Ctrl Pts',(-178.678422804377,-5.25619092940608,
128.083138461444));
#261786=CARTESIAN_POINT('Ctrl Pts',(-178.685837298534,-5.32466681106959,
128.224466450436));
#261787=CARTESIAN_POINT('Ctrl Pts',(-178.693261769769,-5.393234835119,128.365984612928));
#261788=CARTESIAN_POINT('Ctrl Pts',(-178.700686241004,-5.45607371265313,
128.510066043443));
#261789=CARTESIAN_POINT('Ctrl Pts',(-178.708110712239,-5.51301510408258,
128.656199770549));
#261790=CARTESIAN_POINT('Ctrl Pts',(-178.709701422424,-5.52521492929238,
128.687509260591));
#261791=CARTESIAN_POINT('Ctrl Pts',(-178.71129213261,-5.53714422039791,
128.718912912318));
#261792=CARTESIAN_POINT('Ctrl Pts',(-178.712882842796,-5.54880162463143,
128.750405629503));
#261793=CARTESIAN_POINT('Ctrl Pts',(-178.721434613827,-5.6114726584305,
128.919712715677));
#261794=CARTESIAN_POINT('Ctrl Pts',(-178.729986384858,-5.66643819996979,
129.092017853483));
#261795=CARTESIAN_POINT('Ctrl Pts',(-178.738538155888,-5.71344087978109,
129.266659776783));
#261796=CARTESIAN_POINT('Ctrl Pts',(-178.747059185309,-5.76027459598887,
129.440673903352));
#261797=CARTESIAN_POINT('Ctrl Pts',(-178.75558021473,-5.79920250282132,
129.617007918382));
#261798=CARTESIAN_POINT('Ctrl Pts',(-178.764101244151,-5.8300165114818,
129.79498554439));
#261799=CARTESIAN_POINT('Ctrl Pts',(-178.772561766365,-5.86061171211978,
129.971699364288));
#261800=CARTESIAN_POINT('Ctrl Pts',(-178.781022288578,-5.88320776267822,
130.150033394033));
#261801=CARTESIAN_POINT('Ctrl Pts',(-178.789482810792,-5.89764813416367,
130.329305833256));
#261802=CARTESIAN_POINT('Ctrl Pts',(-178.796863453485,-5.91024537338731,
130.485696394633));
#261803=CARTESIAN_POINT('Ctrl Pts',(-178.804244096178,-5.91663666015527,
130.642800748583));
#261804=CARTESIAN_POINT('Ctrl Pts',(-178.811624738871,-5.91674850538075,
130.800155076613));
#261805=CARTESIAN_POINT('',(-180.561624807791,-5.90996050472777,130.808431327307));
#261806=CARTESIAN_POINT('Ctrl Pts',(-178.811624807791,-5.91021030986751,
130.800161191611));
#261807=CARTESIAN_POINT('Ctrl Pts',(-178.871526694064,-5.90189013011824,
132.075856832088));
#261808=CARTESIAN_POINT('Ctrl Pts',(-179.024244454939,-4.86928404315109,
135.340473970702));
#261809=CARTESIAN_POINT('Ctrl Pts',(-179.269778090423,0.518479272423054,
137.783525307874));
#261810=CARTESIAN_POINT('Ctrl Pts',(-179.548225714233,6.15201962547423,
134.140558312264));
#261811=CARTESIAN_POINT('Ctrl Pts',(-179.826673338048,6.13215448558245,
127.431788617551));
#261812=CARTESIAN_POINT('Ctrl Pts',(-180.10512096186,0.477138945842835,
123.822247831545));
#261813=CARTESIAN_POINT('Ctrl Pts',(-180.350104785108,-4.88402996107005,
126.29162117749));
#261814=CARTESIAN_POINT('Ctrl Pts',(-180.502272733752,-5.90199055707381,
129.544310586215));
#261815=CARTESIAN_POINT('Ctrl Pts',(-180.561624807791,-5.90996050472777,
130.808431327307));
#261816=CARTESIAN_POINT('',(-182.311624807792,-5.92507812272359,130.807023572335));
#261817=CARTESIAN_POINT('Ctrl Pts',(-180.561624807791,-5.90996050472777,
130.808431327307));
#261818=CARTESIAN_POINT('Ctrl Pts',(-180.595088608356,-5.9144541090899,
131.521166055697));
#261819=CARTESIAN_POINT('Ctrl Pts',(-180.721368283525,-5.46467200361853,
134.2052756912));
#261820=CARTESIAN_POINT('Ctrl Pts',(-180.9404638333,-1.46310027610978,137.648109452265));
#261821=CARTESIAN_POINT('Ctrl Pts',(-181.218911457112,4.96699828222215,
135.734521730019));
#261822=CARTESIAN_POINT('Ctrl Pts',(-181.497359080924,6.83266807054414,
129.290356797193));
#261823=CARTESIAN_POINT('Ctrl Pts',(-181.775806704738,2.41944969642949,
124.23748741209));
#261824=CARTESIAN_POINT('Ctrl Pts',(-182.047228613693,-4.04967250708035,
125.19448203293));
#261825=CARTESIAN_POINT('Ctrl Pts',(-182.225834648045,-5.91491065230807,
128.991748760208));
#261826=CARTESIAN_POINT('Ctrl Pts',(-182.311624807792,-5.92507812272359,
130.807023572335));
#261827=CARTESIAN_POINT('',(-184.061624807792,-5.91793140692411,130.798997977614));
#261828=CARTESIAN_POINT('Ctrl Pts',(-182.311624807792,-5.92507812272359,
130.807023572335));
#261829=CARTESIAN_POINT('Ctrl Pts',(-182.318650522649,-5.92591077938457,
130.955684016088));
#261830=CARTESIAN_POINT('Ctrl Pts',(-182.325676237506,-5.920802909146,131.104286291747));
#261831=CARTESIAN_POINT('Ctrl Pts',(-182.425517826968,-5.76118888251318,
133.209457008152));
#261832=CARTESIAN_POINT('Ctrl Pts',(-182.611149576176,-3.32683150482748,
136.961450244072));
#261833=CARTESIAN_POINT('Ctrl Pts',(-182.88959719999,3.38190018988211,136.931375521743));
#261834=CARTESIAN_POINT('Ctrl Pts',(-183.168044823802,6.98283082510118,
131.270873423793));
#261835=CARTESIAN_POINT('Ctrl Pts',(-183.446492447615,4.16688106229984,
125.181668847338));
#261836=CARTESIAN_POINT('Ctrl Pts',(-183.724940071428,-2.47822883329544,
124.259443323958));
#261837=CARTESIAN_POINT('Ctrl Pts',(-183.929984191486,-5.69455770389321,
128.0092781062));
#261838=CARTESIAN_POINT('Ctrl Pts',(-184.042212436941,-5.92199600856727,
130.386992623478));
#261839=CARTESIAN_POINT('Ctrl Pts',(-184.061624807792,-5.9181658456461,
130.798997765173));
#261840=CARTESIAN_POINT('',(-185.811624807754,-5.91674999671234,130.804163375351));
#261841=CARTESIAN_POINT('Ctrl Pts',(-184.061624807792,-5.91674757076024,
130.798999050368));
#261842=CARTESIAN_POINT('Ctrl Pts',(-184.068928931162,-5.91688801138847,
130.953982046063));
#261843=CARTESIAN_POINT('Ctrl Pts',(-184.076233054531,-5.91093487072381,
131.109156665659));
#261844=CARTESIAN_POINT('Ctrl Pts',(-184.083537177901,-5.89886979863471,
131.263997062221));
#261845=CARTESIAN_POINT('Ctrl Pts',(-184.090835650274,-5.88681406095517,
131.41871766309));
#261846=CARTESIAN_POINT('Ctrl Pts',(-184.098134122647,-5.86865583195702,
131.57310417378));
#261847=CARTESIAN_POINT('Ctrl Pts',(-184.10543259502,-5.84442882662681,
131.726630780259));
#261848=CARTESIAN_POINT('Ctrl Pts',(-184.112782708521,-5.8200304005078,
131.881243680798));
#261849=CARTESIAN_POINT('Ctrl Pts',(-184.120132822023,-5.78947697807806,
132.034984065929));
#261850=CARTESIAN_POINT('Ctrl Pts',(-184.127482935524,-5.75285625138199,
132.187319587831));
#261851=CARTESIAN_POINT('Ctrl Pts',(-184.134776202234,-5.71651875443688,
132.338476925796));
#261852=CARTESIAN_POINT('Ctrl Pts',(-184.142069468944,-5.67420758047763,
132.488250678532));
#261853=CARTESIAN_POINT('Ctrl Pts',(-184.149362735654,-5.62605967323285,
132.636131104205));
#261854=CARTESIAN_POINT('Ctrl Pts',(-184.1566557956,-5.57791313097582,132.784007337485));
#261855=CARTESIAN_POINT('Ctrl Pts',(-184.163948855547,-5.52393030354824,
132.929989984487));
#261856=CARTESIAN_POINT('Ctrl Pts',(-184.171241915494,-5.46429776820347,
133.073585256712));
#261857=CARTESIAN_POINT('Ctrl Pts',(-184.178536303616,-5.40465437287707,
133.217206679795));
#261858=CARTESIAN_POINT('Ctrl Pts',(-184.185830691739,-5.33935937028289,
133.358439507777));
#261859=CARTESIAN_POINT('Ctrl Pts',(-184.193125079861,-5.26864703532705,
133.49681098473));
#261860=CARTESIAN_POINT('Ctrl Pts',(-184.200517599794,-5.19698340338551,
133.637043980879));
#261861=CARTESIAN_POINT('Ctrl Pts',(-184.207910119727,-5.11975580564257,
133.774337715552));
#261862=CARTESIAN_POINT('Ctrl Pts',(-184.215302639659,-5.03725512909461,
133.908227774342));
#261863=CARTESIAN_POINT('Ctrl Pts',(-184.222607901079,-4.95572825936504,
134.040537445459));
#261864=CARTESIAN_POINT('Ctrl Pts',(-184.2299131625,-4.86905238698824,134.16952307254));
#261865=CARTESIAN_POINT('Ctrl Pts',(-184.23721842392,-4.7775502821432,134.294768024172));
#261866=CARTESIAN_POINT('Ctrl Pts',(-184.244654573109,-4.68440874160218,
134.422256979315));
#261867=CARTESIAN_POINT('Ctrl Pts',(-184.252090722298,-4.58626664978123,
134.545869616373));
#261868=CARTESIAN_POINT('Ctrl Pts',(-184.259526871487,-4.48350479392226,
134.665204479389));
#261869=CARTESIAN_POINT('Ctrl Pts',(-184.266963020676,-4.38074293806359,
134.784539342404));
#261870=CARTESIAN_POINT('Ctrl Pts',(-184.274399169865,-4.27336164917223,
134.899596175744));
#261871=CARTESIAN_POINT('Ctrl Pts',(-184.281835319054,-4.161777721421,135.010015948187));
#261872=CARTESIAN_POINT('Ctrl Pts',(-184.289258585459,-4.05038710764862,
135.120244423497));
#261873=CARTESIAN_POINT('Ctrl Pts',(-184.296681851865,-3.93444578121529,
135.226211097442));
#261874=CARTESIAN_POINT('Ctrl Pts',(-184.30410511827,-3.81431332688993,
135.327517082559));
#261875=CARTESIAN_POINT('Ctrl Pts',(-184.311519610991,-3.6943228591492,
135.428703332415));
#261876=CARTESIAN_POINT('Ctrl Pts',(-184.318934103712,-3.57015140620211,
135.525239619935));
#261877=CARTESIAN_POINT('Ctrl Pts',(-184.326348596433,-3.44219618145469,
135.616762929393));
#261878=CARTESIAN_POINT('Ctrl Pts',(-184.333755942787,-3.31436428477031,
135.70819802524));
#261879=CARTESIAN_POINT('Ctrl Pts',(-184.341163289141,-3.18275617821301,
135.794629546266));
#261880=CARTESIAN_POINT('Ctrl Pts',(-184.348570635494,-3.04780293399889,
135.8757339856));
#261881=CARTESIAN_POINT('Ctrl Pts',(-184.35597245717,-2.91295034300579,
135.956777934184));
#261882=CARTESIAN_POINT('Ctrl Pts',(-184.363374278845,-2.77475790068248,
136.032502520666));
#261883=CARTESIAN_POINT('Ctrl Pts',(-184.370776100521,-2.63368641439405,
136.102626978663));
#261884=CARTESIAN_POINT('Ctrl Pts',(-184.378174014832,-2.49268939864553,
136.172714418505));
#261885=CARTESIAN_POINT('Ctrl Pts',(-184.385571929143,-2.34881669916657,
136.237207451659));
#261886=CARTESIAN_POINT('Ctrl Pts',(-184.392969843455,-2.20255442484518,
136.295870844097));
#261887=CARTESIAN_POINT('Ctrl Pts',(-184.400366528367,-2.05631645666011,
136.354524487743));
#261888=CARTESIAN_POINT('Ctrl Pts',(-184.407763213279,-1.90769004789607,
136.407350274588));
#261889=CARTESIAN_POINT('Ctrl Pts',(-184.415159898191,-1.75718213247968,
136.454160748172));
#261890=CARTESIAN_POINT('Ctrl Pts',(-184.422556255127,-1.60668089074197,
136.50096914613));
#261891=CARTESIAN_POINT('Ctrl Pts',(-184.429952612062,-1.45429866469017,
136.541762650303));
#261892=CARTESIAN_POINT('Ctrl Pts',(-184.437348968997,-1.30055816731291,
136.576403498205));
#261893=CARTESIAN_POINT('Ctrl Pts',(-184.444746458334,-1.14679413187302,
136.611049649709));
#261894=CARTESIAN_POINT('Ctrl Pts',(-184.45214394767,-0.991671775233469,
136.63954118726));
#261895=CARTESIAN_POINT('Ctrl Pts',(-184.459541437007,-0.835724485702392,
136.661791380836));
#261896=CARTESIAN_POINT('Ctrl Pts',(-184.466941519522,-0.679722529091387,
136.684049374182));
#261897=CARTESIAN_POINT('Ctrl Pts',(-184.474341602037,-0.522895433160513,
136.70006161478));
#261898=CARTESIAN_POINT('Ctrl Pts',(-184.481741684552,-0.365782046711605,
136.709793206022));
#261899=CARTESIAN_POINT('Ctrl Pts',(-184.489149904218,-0.208495897941526,
136.71953549815));
#261900=CARTESIAN_POINT('Ctrl Pts',(-184.496558123885,-0.0509232027779254,
136.722983325656));
#261901=CARTESIAN_POINT('Ctrl Pts',(-184.503966343551,0.106396107174741,
136.720153922853));
#261902=CARTESIAN_POINT('Ctrl Pts',(-184.511379122853,0.263812244537669,
136.717322778599));
#261903=CARTESIAN_POINT('Ctrl Pts',(-184.518791902155,0.420974314123582,
136.708206727033));
#261904=CARTESIAN_POINT('Ctrl Pts',(-184.526204681458,0.577347679482734,
136.692874880052));
#261905=CARTESIAN_POINT('Ctrl Pts',(-184.533628052486,0.733944478439272,
136.677521126208));
#261906=CARTESIAN_POINT('Ctrl Pts',(-184.541051423515,0.889749953635859,
136.655933889856));
#261907=CARTESIAN_POINT('Ctrl Pts',(-184.548474794544,1.04423900632314,
136.628233509394));
#261908=CARTESIAN_POINT('Ctrl Pts',(-184.552410843985,1.1261528089723,136.613546103012));
#261909=CARTESIAN_POINT('Ctrl Pts',(-184.556346893425,1.20769674862925,
136.59714091264));
#261910=CARTESIAN_POINT('Ctrl Pts',(-184.560282942866,1.28879442450105,
136.579041517311));
#261911=CARTESIAN_POINT('Ctrl Pts',(-184.567706209272,1.44174211022288,
136.544906622583));
#261912=CARTESIAN_POINT('Ctrl Pts',(-184.575129475677,1.59356399310633,
136.504639476673));
#261913=CARTESIAN_POINT('Ctrl Pts',(-184.582552742083,1.74373011348117,
136.458327000013));
#261914=CARTESIAN_POINT('Ctrl Pts',(-184.589967234804,1.89371874997225,
136.412069260854));
#261915=CARTESIAN_POINT('Ctrl Pts',(-184.597381727525,2.04205516608679,
136.359780522206));
#261916=CARTESIAN_POINT('Ctrl Pts',(-184.604796220246,2.18821924286488,
136.301598752089));
#261917=CARTESIAN_POINT('Ctrl Pts',(-184.612203566599,2.33424244120238,
136.243473059753));
#261918=CARTESIAN_POINT('Ctrl Pts',(-184.619610912953,2.47809712401023,
136.179465780693));
#261919=CARTESIAN_POINT('Ctrl Pts',(-184.627018259307,2.6192781107327,136.109764724808));
#261920=CARTESIAN_POINT('Ctrl Pts',(-184.634420080982,2.76035379934881,
136.040115654599));
#261921=CARTESIAN_POINT('Ctrl Pts',(-184.641821902658,2.89875942920178,
135.964781427729));
#261922=CARTESIAN_POINT('Ctrl Pts',(-184.649223724333,3.03400970594374,
135.883997973396));
#261923=CARTESIAN_POINT('Ctrl Pts',(-184.656621638644,3.16918858511778,
135.803257164018));
#261924=CARTESIAN_POINT('Ctrl Pts',(-184.664019552956,3.30121510880317,
135.71707304701));
#261925=CARTESIAN_POINT('Ctrl Pts',(-184.671417467267,3.42962861422033,
135.625727449806));
#261926=CARTESIAN_POINT('Ctrl Pts',(-184.678814152179,3.55802077964237,
135.534397032583));
#261927=CARTESIAN_POINT('Ctrl Pts',(-184.686210837092,3.68280081455794,
135.437907053702));
#261928=CARTESIAN_POINT('Ctrl Pts',(-184.693607522004,3.80353699636812,
135.336582686238));
#261929=CARTESIAN_POINT('Ctrl Pts',(-184.701003878939,3.92426782460947,
135.235262811603));
#261930=CARTESIAN_POINT('Ctrl Pts',(-184.708400235875,4.04095487032625,
135.129109214579));
#261931=CARTESIAN_POINT('Ctrl Pts',(-184.71579659281,4.15319969089864,135.018487204419));
#261932=CARTESIAN_POINT('Ctrl Pts',(-184.723194082147,4.2654616964396,134.907848257747));
#261933=CARTESIAN_POINT('Ctrl Pts',(-184.730591571483,4.37327985674116,
134.792739797803));
#261934=CARTESIAN_POINT('Ctrl Pts',(-184.73798906082,4.47629289397063,134.673563699583));
#261935=CARTESIAN_POINT('Ctrl Pts',(-184.745389143335,4.57934204226076,
134.554345824366));
#261936=CARTESIAN_POINT('Ctrl Pts',(-184.75278922585,4.67758246983172,134.431057754148));
#261937=CARTESIAN_POINT('Ctrl Pts',(-184.760189308365,4.77069355624095,
134.304133975219));
#261938=CARTESIAN_POINT('Ctrl Pts',(-184.767597528031,4.86390702786161,
134.177070630548));
#261939=CARTESIAN_POINT('Ctrl Pts',(-184.775005747698,4.95197967345292,
134.046363894402));
#261940=CARTESIAN_POINT('Ctrl Pts',(-184.782413967364,5.03463414650848,
133.912477342097));
#261941=CARTESIAN_POINT('Ctrl Pts',(-184.789826746667,5.11733949201328,
133.778508384854));
#261942=CARTESIAN_POINT('Ctrl Pts',(-184.797239525968,5.194619837159,133.641356036106));
#261943=CARTESIAN_POINT('Ctrl Pts',(-184.804652305271,5.26624434368106,
133.501507457311));
#261944=CARTESIAN_POINT('Ctrl Pts',(-184.812075676299,5.3379711906568,133.361459056308));
#261945=CARTESIAN_POINT('Ctrl Pts',(-184.819499047328,5.4040259024361,133.21870706884));
#261946=CARTESIAN_POINT('Ctrl Pts',(-184.826922418357,5.46422589442022,
133.073758321197));
#261947=CARTESIAN_POINT('Ctrl Pts',(-184.830858467798,5.49614537464935,
132.9969030172));
#261948=CARTESIAN_POINT('Ctrl Pts',(-184.834794517239,5.52641971457611,
132.919430385207));
#261949=CARTESIAN_POINT('Ctrl Pts',(-184.838730566679,5.55502745541382,
132.841417448413));
#261950=CARTESIAN_POINT('Ctrl Pts',(-184.846153833085,5.60898076181651,
132.69428748432));
#261951=CARTESIAN_POINT('Ctrl Pts',(-184.85357709949,5.65716630769147,132.544790058487));
#261952=CARTESIAN_POINT('Ctrl Pts',(-184.861000365896,5.69937076551409,
132.39341802361));
#261953=CARTESIAN_POINT('Ctrl Pts',(-184.868414858617,5.74152534117242,
132.242224897908));
#261954=CARTESIAN_POINT('Ctrl Pts',(-184.875829351338,5.7777128006819,132.089161929462));
#261955=CARTESIAN_POINT('Ctrl Pts',(-184.883243844059,5.80776808344369,
131.93474128417));
#261956=CARTESIAN_POINT('Ctrl Pts',(-184.890651190412,5.83779439779231,
131.78046947531));
#261957=CARTESIAN_POINT('Ctrl Pts',(-184.898058536766,5.86170023104261,
131.624842958691));
#261958=CARTESIAN_POINT('Ctrl Pts',(-184.90546588312,5.87937053055049,131.468388272859));
#261959=CARTESIAN_POINT('Ctrl Pts',(-184.912867704795,5.89702765088234,
131.312050276835));
#261960=CARTESIAN_POINT('Ctrl Pts',(-184.920269526471,5.9084584559214,131.154885710824));
#261961=CARTESIAN_POINT('Ctrl Pts',(-184.927671348146,5.91359912613479,
130.997430392202));
#261962=CARTESIAN_POINT('Ctrl Pts',(-184.935069262458,5.91873708262841,
130.840058193015));
#261963=CARTESIAN_POINT('Ctrl Pts',(-184.942467176769,5.91759150510721,
130.682395919046));
#261964=CARTESIAN_POINT('Ctrl Pts',(-184.94986509108,5.91015050348987,130.52498347355));
#261965=CARTESIAN_POINT('Ctrl Pts',(-184.957261775993,5.90271073843201,
130.367597187147));
#261966=CARTESIAN_POINT('Ctrl Pts',(-184.964658460905,5.88897764325531,
130.210461019335));
#261967=CARTESIAN_POINT('Ctrl Pts',(-184.972055145817,5.86899143866611,
130.054113954552));
#261968=CARTESIAN_POINT('Ctrl Pts',(-184.979451502752,5.84900612028617,
129.897773822362));
#261969=CARTESIAN_POINT('Ctrl Pts',(-184.986847859688,5.82276829113332,
129.742223093914));
#261970=CARTESIAN_POINT('Ctrl Pts',(-184.994244216623,5.79036992825915,
129.587994448844));
#261971=CARTESIAN_POINT('Ctrl Pts',(-185.00164170596,5.75796660511301,129.433742190975));
#261972=CARTESIAN_POINT('Ctrl Pts',(-185.009039195297,5.71940094696954,
129.280812784864));
#261973=CARTESIAN_POINT('Ctrl Pts',(-185.016436684633,5.67481578315034,
129.129727407037));
#261974=CARTESIAN_POINT('Ctrl Pts',(-185.023836767148,5.63021499007076,
128.978589066463));
#261975=CARTESIAN_POINT('Ctrl Pts',(-185.031236849663,5.57959059565481,
128.829296399002));
#261976=CARTESIAN_POINT('Ctrl Pts',(-185.038636932178,5.52313484234269,
128.682354002166));
#261977=CARTESIAN_POINT('Ctrl Pts',(-185.046045151844,5.46661701012626,
128.535250027059));
#261978=CARTESIAN_POINT('Ctrl Pts',(-185.053453371511,5.40425514743527,
128.3905018324));
#261979=CARTESIAN_POINT('Ctrl Pts',(-185.060861591177,5.33628936075163,
128.248593331441));
#261980=CARTESIAN_POINT('Ctrl Pts',(-185.06827437048,5.26828174226036,128.106597488167));
#261981=CARTESIAN_POINT('Ctrl Pts',(-185.075687149781,5.19466350113199,
127.967445150473));
#261982=CARTESIAN_POINT('Ctrl Pts',(-185.083099929084,5.11571972637515,
127.831593851794));
#261983=CARTESIAN_POINT('Ctrl Pts',(-185.090523300112,5.03666315305096,
127.69554844241));
#261984=CARTESIAN_POINT('Ctrl Pts',(-185.097946671141,4.95226604824019,
127.562813806486));
#261985=CARTESIAN_POINT('Ctrl Pts',(-185.10537004217,4.86285612782121,127.433817509607));
#261986=CARTESIAN_POINT('Ctrl Pts',(-185.109306091611,4.81544884265258,
127.365420577777));
#261987=CARTESIAN_POINT('Ctrl Pts',(-185.113242141051,4.76663294343972,
127.298074068215));
#261988=CARTESIAN_POINT('Ctrl Pts',(-185.117178190492,4.71646163297881,
127.231837667725));
#261989=CARTESIAN_POINT('Ctrl Pts',(-185.124601456898,4.62184010724392,
127.10691788357));
#261990=CARTESIAN_POINT('Ctrl Pts',(-185.132024723303,4.52210915344613,
126.9855710088));
#261991=CARTESIAN_POINT('Ctrl Pts',(-185.139447989709,4.41756811377999,
126.868242920823));
#261992=CARTESIAN_POINT('Ctrl Pts',(-185.14686248243,4.31315063294114,126.751053504903));
#261993=CARTESIAN_POINT('Ctrl Pts',(-185.154276975151,4.20393462841209,
126.637873697119));
#261994=CARTESIAN_POINT('Ctrl Pts',(-185.161691467872,4.09026178058174,
126.529119205808));
#261995=CARTESIAN_POINT('Ctrl Pts',(-185.169098814225,3.97669849492183,
126.420469536169));
#261996=CARTESIAN_POINT('Ctrl Pts',(-185.176506160579,3.85868718572215,
126.316236947986));
#261997=CARTESIAN_POINT('Ctrl Pts',(-185.183913506933,3.73660865600951,
126.21680284525));
#261998=CARTESIAN_POINT('Ctrl Pts',(-185.191315328609,3.61462117706974,
126.11744290422));
#261999=CARTESIAN_POINT('Ctrl Pts',(-185.198717150284,3.48857280588916,
126.022874557316));
#262000=CARTESIAN_POINT('Ctrl Pts',(-185.206118971959,3.35887984478284,
125.933441120098));
#262001=CARTESIAN_POINT('Ctrl Pts',(-185.213516886271,3.2292553475808,125.844054894095));
#262002=CARTESIAN_POINT('Ctrl Pts',(-185.220914800582,3.09599039862963,
125.759798390713));
#262003=CARTESIAN_POINT('Ctrl Pts',(-185.228312714894,2.95953280695017,
125.68097344431));
#262004=CARTESIAN_POINT('Ctrl Pts',(-185.235709399806,2.82309789204744,
125.602161597183));
#262005=CARTESIAN_POINT('Ctrl Pts',(-185.243106084718,2.68347171034644,
125.52877970213));
#262006=CARTESIAN_POINT('Ctrl Pts',(-185.25050276963,2.54112946499453,125.461085254585));
#262007=CARTESIAN_POINT('Ctrl Pts',(-185.257899126566,2.39879353124695,
125.393393808683));
#262008=CARTESIAN_POINT('Ctrl Pts',(-185.265295483501,2.25374211042627,
125.33138946918));
#262009=CARTESIAN_POINT('Ctrl Pts',(-185.272691840437,2.10647307683844,
125.275282779531));
#262010=CARTESIAN_POINT('Ctrl Pts',(-185.280089329773,1.95918149598603,
125.219167499804));
#262011=CARTESIAN_POINT('Ctrl Pts',(-185.28748681911,1.80967197519407,125.168951800726));
#262012=CARTESIAN_POINT('Ctrl Pts',(-185.294884308446,1.65846019776952,
125.124797224583));
#262013=CARTESIAN_POINT('Ctrl Pts',(-185.302284390961,1.50719541329015,
125.080627170122));
#262014=CARTESIAN_POINT('Ctrl Pts',(-185.309684473476,1.35422754221607,
125.042522573463));
#262015=CARTESIAN_POINT('Ctrl Pts',(-185.317084555991,1.2000850284593,125.010594442877));
#262016=CARTESIAN_POINT('Ctrl Pts',(-185.324492775658,1.04577301916263,
124.97863120403));
#262017=CARTESIAN_POINT('Ctrl Pts',(-185.331900995324,0.890284153455571,
124.952858070407));
#262018=CARTESIAN_POINT('Ctrl Pts',(-185.339309214991,0.734155344681294,
124.933334600559));
#262019=CARTESIAN_POINT('Ctrl Pts',(-185.346721994293,0.577930441230811,
124.913799114341));
#262020=CARTESIAN_POINT('Ctrl Pts',(-185.354134773595,0.421065180974498,
124.900520988071));
#262021=CARTESIAN_POINT('Ctrl Pts',(-185.361547552897,0.264098597322687,
124.89350767629));
#262022=CARTESIAN_POINT('Ctrl Pts',(-185.368970923926,0.106907732454928,
124.88648434356));
#262023=CARTESIAN_POINT('Ctrl Pts',(-185.376394294955,-0.0503843726528677,
124.885743705147));
#262024=CARTESIAN_POINT('Ctrl Pts',(-185.383817665983,-0.207240856527645,
124.891241154044));
#262025=CARTESIAN_POINT('Ctrl Pts',(-185.387753715424,-0.290409927994593,
124.894156033358));
#262026=CARTESIAN_POINT('Ctrl Pts',(-185.391689764865,-0.373456639755591,
124.898823798456));
#262027=CARTESIAN_POINT('Ctrl Pts',(-185.395625814305,-0.456302018202181,
124.905231950493));
#262028=CARTESIAN_POINT('Ctrl Pts',(-185.403049080711,-0.612545816442367,
124.917317525243));
#262029=CARTESIAN_POINT('Ctrl Pts',(-185.410472347116,-0.768545395500247,
124.935633051325));
#262030=CARTESIAN_POINT('Ctrl Pts',(-185.417895613522,-0.923763824315242,
124.960167691303));
#262031=CARTESIAN_POINT('Ctrl Pts',(-185.425310106243,-1.07879879783747,
124.984673333373));
#262032=CARTESIAN_POINT('Ctrl Pts',(-185.432724598964,-1.23305409374088,
125.015383400464));
#262033=CARTESIAN_POINT('Ctrl Pts',(-185.440139091685,-1.38599527823421,
125.052235127696));
#262034=CARTESIAN_POINT('Ctrl Pts',(-185.447546438038,-1.53878905225622,
125.089051335846));
#262035=CARTESIAN_POINT('Ctrl Pts',(-185.454953784392,-1.69027087592442,
125.131997332593));
#262036=CARTESIAN_POINT('Ctrl Pts',(-185.462361130746,-1.83991402991944,
125.180958895743));
#262037=CARTESIAN_POINT('Ctrl Pts',(-185.469762952421,-1.98944557440407,
125.229883941511));
#262038=CARTESIAN_POINT('Ctrl Pts',(-185.477164774097,-2.1371408264938,
125.284815504598));
#262039=CARTESIAN_POINT('Ctrl Pts',(-185.484566595772,-2.28248592351566,
125.345588908523));
#262040=CARTESIAN_POINT('Ctrl Pts',(-185.491964510084,-2.42775429399301,
125.40633023064));
#262041=CARTESIAN_POINT('Ctrl Pts',(-185.499362424395,-2.57067463664222,
125.472907108294));
#262042=CARTESIAN_POINT('Ctrl Pts',(-185.506760338706,-2.7107509579538,
125.545105935916));
#262043=CARTESIAN_POINT('Ctrl Pts',(-185.514157023618,-2.85080400112102,
125.617292765403));
#262044=CARTESIAN_POINT('Ctrl Pts',(-185.521553708531,-2.98801362948039,
125.695099519758));
#262045=CARTESIAN_POINT('Ctrl Pts',(-185.528950393443,-3.12190634592099,
125.778265579686));
#262046=CARTESIAN_POINT('Ctrl Pts',(-185.536346750378,-3.25579312541823,
125.861427951945));
#262047=CARTESIAN_POINT('Ctrl Pts',(-185.543743107314,-3.38636296832752,
125.949948960309));
#262048=CARTESIAN_POINT('Ctrl Pts',(-185.551139464249,-3.51316962525318,
126.043523532903));
#262049=CARTESIAN_POINT('Ctrl Pts',(-185.558536953586,-3.6399956966021,
126.137112432005));
#262050=CARTESIAN_POINT('Ctrl Pts',(-185.565934442922,-3.7630571343807,
126.235756214237));
#262051=CARTESIAN_POINT('Ctrl Pts',(-185.573331932259,-3.88193928906325,
126.339108338184));
#262052=CARTESIAN_POINT('Ctrl Pts',(-185.580732014774,-4.00086311770033,
126.442496692057));
#262053=CARTESIAN_POINT('Ctrl Pts',(-185.588132097289,-4.1156044648104,
126.550596429015));
#262054=CARTESIAN_POINT('Ctrl Pts',(-185.595532179804,-4.22578429914888,
126.66302295691));
#262055=CARTESIAN_POINT('Ctrl Pts',(-185.60294039947,-4.33608528754245,
126.775573109331));
#262056=CARTESIAN_POINT('Ctrl Pts',(-185.610348619137,-4.44181448473375,
126.892459287456));
#262057=CARTESIAN_POINT('Ctrl Pts',(-185.617756838803,-4.54263156765102,
127.013261963735));
#262058=CARTESIAN_POINT('Ctrl Pts',(-185.625169618105,-4.64351070180004,
127.134138992044));
#262059=CARTESIAN_POINT('Ctrl Pts',(-185.632582397407,-4.73947147030228,
127.258937026566));
#262060=CARTESIAN_POINT('Ctrl Pts',(-185.639995176709,-4.8302162407166,
127.387206592589));
#262061=CARTESIAN_POINT('Ctrl Pts',(-185.647418547738,-4.92109067151479,
127.515659436183));
#262062=CARTESIAN_POINT('Ctrl Pts',(-185.654841918766,-5.00673401647177,
127.6475934058));
#262063=CARTESIAN_POINT('Ctrl Pts',(-185.662265289795,-5.08689361798639,
127.7825327135));
#262064=CARTESIAN_POINT('Ctrl Pts',(-185.666201339236,-5.12939616211485,
127.854080772271));
#262065=CARTESIAN_POINT('Ctrl Pts',(-185.670137388677,-5.17035781537923,
127.926473363939));
#262066=CARTESIAN_POINT('Ctrl Pts',(-185.674073438118,-5.20974640624689,
127.999637289839));
#262067=CARTESIAN_POINT('Ctrl Pts',(-185.681900715772,-5.288075055757,128.145131997376));
#262068=CARTESIAN_POINT('Ctrl Pts',(-185.689727993426,-5.36039597288839,
128.294079034415));
#262069=CARTESIAN_POINT('Ctrl Pts',(-185.69755527108,-5.42640910216598,
128.445968195082));
#262070=CARTESIAN_POINT('Ctrl Pts',(-185.705369342796,-5.49231085616024,
128.597601093116));
#262071=CARTESIAN_POINT('Ctrl Pts',(-185.713183414512,-5.55192591167538,
128.752165934091));
#262072=CARTESIAN_POINT('Ctrl Pts',(-185.720997486229,-5.60499975256745,
128.909127561655));
#262073=CARTESIAN_POINT('Ctrl Pts',(-185.728793533698,-5.6579511712372,
129.065727135315));
#262074=CARTESIAN_POINT('Ctrl Pts',(-185.736589581167,-5.70439137034077,
129.22471217246));
#262075=CARTESIAN_POINT('Ctrl Pts',(-185.744385628636,-5.7441138651048,
129.38552783418));
#262076=CARTESIAN_POINT('Ctrl Pts',(-185.752171064916,-5.78378229363978,
129.54612460994));
#262077=CARTESIAN_POINT('Ctrl Pts',(-185.759956501197,-5.81675116516731,
129.708546741938));
#262078=CARTESIAN_POINT('Ctrl Pts',(-185.767741937477,-5.842863099156,129.872222555356));
#262079=CARTESIAN_POINT('Ctrl Pts',(-185.775512714118,-5.86892586550339,
130.035590174303));
#262080=CARTESIAN_POINT('Ctrl Pts',(-185.783283490759,-5.88815739778654,
130.200206457726));
#262081=CARTESIAN_POINT('Ctrl Pts',(-185.7910542674,-5.90045097199386,130.365488324528));
#262082=CARTESIAN_POINT('Ctrl Pts',(-185.797911114185,-5.9112986849928,
130.511331203479));
#262083=CARTESIAN_POINT('Ctrl Pts',(-185.804767960969,-5.91674511390588,
130.657691966486));
#262084=CARTESIAN_POINT('Ctrl Pts',(-185.811624807754,-5.91674999671234,
130.804163375351));
#262085=CARTESIAN_POINT('',(-187.561624807792,-5.91674750900767,130.809789904034));
#262086=CARTESIAN_POINT('Ctrl Pts',(-185.811624807791,-5.91674999671237,
130.804163376133));
#262087=CARTESIAN_POINT('Ctrl Pts',(-185.819353984328,-5.91675550068887,
130.969268914026));
#262088=CARTESIAN_POINT('Ctrl Pts',(-185.827083160864,-5.90984584058032,
131.134248349692));
#262089=CARTESIAN_POINT('Ctrl Pts',(-185.834812337401,-5.89607849221174,
131.298515427497));
#262090=CARTESIAN_POINT('Ctrl Pts',(-185.84255057446,-5.88229500507678,
131.462975067292));
#262091=CARTESIAN_POINT('Ctrl Pts',(-185.85028881152,-5.86163781335462,
131.626720362507));
#262092=CARTESIAN_POINT('Ctrl Pts',(-185.858027048579,-5.83421588616898,
131.789173064722));
#262093=CARTESIAN_POINT('Ctrl Pts',(-185.865901549692,-5.80631108117604,
131.954486426734));
#262094=CARTESIAN_POINT('Ctrl Pts',(-185.873776050805,-5.77140116501924,
132.118460904788));
#262095=CARTESIAN_POINT('Ctrl Pts',(-185.881650551917,-5.72965398230494,
132.28050282127));
#262096=CARTESIAN_POINT('Ctrl Pts',(-185.889414944337,-5.68849054802612,
132.44027891503));
#262097=CARTESIAN_POINT('Ctrl Pts',(-185.897179336757,-5.64067998075974,
132.59817586172));
#262098=CARTESIAN_POINT('Ctrl Pts',(-185.904943729177,-5.58643216126939,
132.753644144925));
#262099=CARTESIAN_POINT('Ctrl Pts',(-185.912873284636,-5.53103038996559,
132.91241952709));
#262100=CARTESIAN_POINT('Ctrl Pts',(-185.920802840095,-5.46891459747241,
133.068661436369));
#262101=CARTESIAN_POINT('Ctrl Pts',(-185.928732395554,-5.40035816938212,
133.221810142352));
#262102=CARTESIAN_POINT('Ctrl Pts',(-185.936661951013,-5.33180174129202,
133.374958848335));
#262103=CARTESIAN_POINT('Ctrl Pts',(-185.944591506471,-5.25680489255712,
133.525014066598));
#262104=CARTESIAN_POINT('Ctrl Pts',(-185.95252106193,-5.17568835721522,
133.671446349016));
#262105=CARTESIAN_POINT('Ctrl Pts',(-185.959944328336,-5.09975097902817,
133.808529171427));
#262106=CARTESIAN_POINT('Ctrl Pts',(-185.967367594741,-5.01824886787116,
133.942800289093));
#262107=CARTESIAN_POINT('Ctrl Pts',(-185.974790861147,-4.93141506493196,
134.073775858838));
#262108=CARTESIAN_POINT('Ctrl Pts',(-185.982205353868,-4.84468389233649,
134.204596626337));
#262109=CARTESIAN_POINT('Ctrl Pts',(-185.989619846589,-4.75263377562075,
134.332129290969));
#262110=CARTESIAN_POINT('Ctrl Pts',(-185.99703433931,-4.65554394683494,
134.455913865376));
#262111=CARTESIAN_POINT('Ctrl Pts',(-186.004441685664,-4.55854769688175,
134.579579131549));
#262112=CARTESIAN_POINT('Ctrl Pts',(-186.011849032018,-4.45652163394964,
134.699503207619));
#262113=CARTESIAN_POINT('Ctrl Pts',(-186.019256378371,-4.34978858474558,
134.815254511764));
#262114=CARTESIAN_POINT('Ctrl Pts',(-186.026658200047,-4.24313514107611,
134.930919484221));
#262115=CARTESIAN_POINT('Ctrl Pts',(-186.034060021722,-4.13178195327352,
135.042417608329));
#262116=CARTESIAN_POINT('Ctrl Pts',(-186.041461843398,-4.0160923929967,
135.149349967773));
#262117=CARTESIAN_POINT('Ctrl Pts',(-186.048859757709,-3.90046390433854,
135.256225878457));
#262118=CARTESIAN_POINT('Ctrl Pts',(-186.056257672021,-3.78050387557164,
135.358540571827));
#262119=CARTESIAN_POINT('Ctrl Pts',(-186.063655586332,-3.65661275257442,
135.455931722065));
#262120=CARTESIAN_POINT('Ctrl Pts',(-186.071052271244,-3.53274221803405,
135.553306687661));
#262121=CARTESIAN_POINT('Ctrl Pts',(-186.078448956157,-3.4049421790122,
135.645759503541));
#262122=CARTESIAN_POINT('Ctrl Pts',(-186.085845641069,-3.27364649016796,
135.732967846785));
#262123=CARTESIAN_POINT('Ctrl Pts',(-186.093241998004,-3.14235662311216,
135.820172323119));
#262124=CARTESIAN_POINT('Ctrl Pts',(-186.10063835494,-3.00757172538186,
135.902132582656));
#262125=CARTESIAN_POINT('Ctrl Pts',(-186.108034711876,-2.86975475604621,
135.978569562192));
#262126=CARTESIAN_POINT('Ctrl Pts',(-186.115432201212,-2.73191668658033,
136.055018244425));
#262127=CARTESIAN_POINT('Ctrl Pts',(-186.122829690549,-2.59104594766015,
136.125941781829));
#262128=CARTESIAN_POINT('Ctrl Pts',(-186.130227179886,-2.44763008059823,
136.191107089329));
#262129=CARTESIAN_POINT('Ctrl Pts',(-186.137627262401,-2.30416393932624,
136.256295240426));
#262130=CARTESIAN_POINT('Ctrl Pts',(-186.145027344916,-2.15815123321437,
136.315720988395));
#262131=CARTESIAN_POINT('Ctrl Pts',(-186.152427427431,-2.01009930602779,
136.369199460013));
#262132=CARTESIAN_POINT('Ctrl Pts',(-186.159835647097,-1.8618845805278,
136.422736736708));
#262133=CARTESIAN_POINT('Ctrl Pts',(-186.167243866764,-1.71162650717714,
136.47031355006));
#262134=CARTESIAN_POINT('Ctrl Pts',(-186.174652086431,-1.5598481143866,
136.511794754071));
#262135=CARTESIAN_POINT('Ctrl Pts',(-186.182064865733,-1.40797630452743,
136.553301489072));
#262136=CARTESIAN_POINT('Ctrl Pts',(-186.189477645035,-1.25458267355879,
136.588705055152));
#262137=CARTESIAN_POINT('Ctrl Pts',(-186.196890424337,-1.10019974227204,
136.617921582208));
#262138=CARTESIAN_POINT('Ctrl Pts',(-186.204313795366,-0.94559622141344,
136.647179855207));
#262139=CARTESIAN_POINT('Ctrl Pts',(-186.211737166394,-0.790000945331487,
136.67023337849));
#262140=CARTESIAN_POINT('Ctrl Pts',(-186.219160537423,-0.633951672601608,
136.687050124867));
#262141=CARTESIAN_POINT('Ctrl Pts',(-186.223096586864,-0.551210603860005,
136.695966767307));
#262142=CARTESIAN_POINT('Ctrl Pts',(-186.227032636304,-0.468341915081361,
136.703130899092));
#262143=CARTESIAN_POINT('Ctrl Pts',(-186.230968685744,-0.385425554330736,
136.708543685914));
#262144=CARTESIAN_POINT('Ctrl Pts',(-186.23839195215,-0.229047885666553,
136.718752032934));
#262145=CARTESIAN_POINT('Ctrl Pts',(-186.245815218555,-0.0720279097393259,
136.72275881741));
#262146=CARTESIAN_POINT('Ctrl Pts',(-186.253238484961,0.0851013380298015,
136.72049857444));
#262147=CARTESIAN_POINT('Ctrl Pts',(-186.260652977682,0.242044872077285,
136.718241002889));
#262148=CARTESIAN_POINT('Ctrl Pts',(-186.268067470403,0.399097051278048,
136.709731153093));
#262149=CARTESIAN_POINT('Ctrl Pts',(-186.275481963124,0.555719943496593,
136.694955316482));
#262150=CARTESIAN_POINT('Ctrl Pts',(-186.282889309477,0.712191876675316,
136.680193721379));
#262151=CARTESIAN_POINT('Ctrl Pts',(-186.290296655831,0.868234977439624,
136.65917819753));
#262152=CARTESIAN_POINT('Ctrl Pts',(-186.297704002185,1.02331164805928,
136.631947067671));
#262153=CARTESIAN_POINT('Ctrl Pts',(-186.30510582386,1.1782726566464,136.604736247816));
#262154=CARTESIAN_POINT('Ctrl Pts',(-186.312507645536,1.33226830420908,
136.571319116806));
#262155=CARTESIAN_POINT('Ctrl Pts',(-186.319909467211,1.48476655989437,
136.531785765494));
#262156=CARTESIAN_POINT('Ctrl Pts',(-186.327307381523,1.63718431293841,
136.492273283531));
#262157=CARTESIAN_POINT('Ctrl Pts',(-186.334705295834,1.78810588790865,
136.446651104826));
#262158=CARTESIAN_POINT('Ctrl Pts',(-186.342103210145,1.93700999905407,
136.395060289885));
#262159=CARTESIAN_POINT('Ctrl Pts',(-186.349499895057,2.08588936503698,
136.343478048401));
#262160=CARTESIAN_POINT('Ctrl Pts',(-186.35689657997,2.23275158021718,136.285929261356));
#262161=CARTESIAN_POINT('Ctrl Pts',(-186.364293264882,2.37709095615206,
136.22260471955));
#262162=CARTESIAN_POINT('Ctrl Pts',(-186.371689621817,2.52142393192816,
136.15928298562));
#262163=CARTESIAN_POINT('Ctrl Pts',(-186.379085978753,2.66323394903901,
136.090186156123));
#262164=CARTESIAN_POINT('Ctrl Pts',(-186.386482335688,2.80203598302284,
136.015552891158));
#262165=CARTESIAN_POINT('Ctrl Pts',(-186.393879825025,2.94085926795201,
135.94090819965));
#262166=CARTESIAN_POINT('Ctrl Pts',(-186.401277314361,3.07667332397372,
135.860725561701));
#262167=CARTESIAN_POINT('Ctrl Pts',(-186.408674803698,3.20901852202426,
135.775289171449));
#262168=CARTESIAN_POINT('Ctrl Pts',(-186.416074886213,3.34141011347863,
135.689822831602));
#262169=CARTESIAN_POINT('Ctrl Pts',(-186.423474968728,3.47033011248045,
135.599099274988));
#262170=CARTESIAN_POINT('Ctrl Pts',(-186.430875051243,3.59534874825436,
135.503445415793));
#262171=CARTESIAN_POINT('Ctrl Pts',(-186.438283270909,3.72050485487072,
135.407686375345));
#262172=CARTESIAN_POINT('Ctrl Pts',(-186.445691490576,3.84175073429224,
135.306986432451));
#262173=CARTESIAN_POINT('Ctrl Pts',(-186.453099710242,3.95868997473241,
135.201712576012));
#262174=CARTESIAN_POINT('Ctrl Pts',(-186.460512489544,4.07570118932416,
135.096373925272));
#262175=CARTESIAN_POINT('Ctrl Pts',(-186.467925268846,4.18840021653473,
134.986456011451));
#262176=CARTESIAN_POINT('Ctrl Pts',(-186.475338048148,4.29642865357484,
134.872361525536));
#262177=CARTESIAN_POINT('Ctrl Pts',(-186.482761419177,4.40461144671197,
134.758104016068));
#262178=CARTESIAN_POINT('Ctrl Pts',(-186.490184790206,4.50811007610825,
134.639658296061));
#262179=CARTESIAN_POINT('Ctrl Pts',(-186.497608161235,4.60660692473589,
134.517459485557));
#262180=CARTESIAN_POINT('Ctrl Pts',(-186.501544210675,4.65883231727349,
134.452666744113));
#262181=CARTESIAN_POINT('Ctrl Pts',(-186.505480260116,4.7096522547113,134.386819357501));
#262182=CARTESIAN_POINT('Ctrl Pts',(-186.509416309556,4.75902450389532,
134.319985218377));
#262183=CARTESIAN_POINT('Ctrl Pts',(-186.516839575961,4.85213902500785,
134.193938117801));
#262184=CARTESIAN_POINT('Ctrl Pts',(-186.524262842367,4.94038317868034,
134.063998529898));
#262185=CARTESIAN_POINT('Ctrl Pts',(-186.531686108772,5.02341376877007,
133.930579527085));
#262186=CARTESIAN_POINT('Ctrl Pts',(-186.539100601493,5.10634622359734,
133.797318214453));
#262187=CARTESIAN_POINT('Ctrl Pts',(-186.546515094214,5.18407718502282,
133.660585986465));
#262188=CARTESIAN_POINT('Ctrl Pts',(-186.553929586935,5.25630435417878,
133.520828010844));
#262189=CARTESIAN_POINT('Ctrl Pts',(-186.561336933289,5.3284619080698,133.381204739222));
#262190=CARTESIAN_POINT('Ctrl Pts',(-186.568744279642,5.39512606019245,
133.238561855208));
#262191=CARTESIAN_POINT('Ctrl Pts',(-186.576151625996,5.45603846784417,
133.093372369372));
#262192=CARTESIAN_POINT('Ctrl Pts',(-186.583553447672,5.51690544472435,
132.948291171332));
#262193=CARTESIAN_POINT('Ctrl Pts',(-186.590955269347,5.57202907504359,
132.800667496085));
#262194=CARTESIAN_POINT('Ctrl Pts',(-186.598357091022,5.6211975791176,132.650997652563));
#262195=CARTESIAN_POINT('Ctrl Pts',(-186.605755005334,5.67034012752104,
132.501406818586));
#262196=CARTESIAN_POINT('Ctrl Pts',(-186.613152919645,5.71353369422572,
132.349772321271));
#262197=CARTESIAN_POINT('Ctrl Pts',(-186.620550833956,5.75061518974696,
132.196608979731));
#262198=CARTESIAN_POINT('Ctrl Pts',(-186.627947518869,5.78769052299643,
132.043471091159));
#262199=CARTESIAN_POINT('Ctrl Pts',(-186.635344203781,5.81865571320347,
131.88880522507));
#262200=CARTESIAN_POINT('Ctrl Pts',(-186.642740888693,5.84339794111647,
131.733139958559));
#262201=CARTESIAN_POINT('Ctrl Pts',(-186.650137245628,5.86813907193316,
131.577481594409));
#262202=CARTESIAN_POINT('Ctrl Pts',(-186.657533602564,5.88665773050493,
131.42082428662));
#262203=CARTESIAN_POINT('Ctrl Pts',(-186.664929959499,5.89889254076296,
131.26370510162));
#262204=CARTESIAN_POINT('Ctrl Pts',(-186.672327448836,5.91112922420171,
131.106561861272));
#262205=CARTESIAN_POINT('Ctrl Pts',(-186.679724938173,5.91708011472825,
130.948956975106));
#262206=CARTESIAN_POINT('Ctrl Pts',(-186.687122427509,5.91673587218311,
130.791430755944));
#262207=CARTESIAN_POINT('Ctrl Pts',(-186.694522510024,5.91639150896428,
130.633849316211));
#262208=CARTESIAN_POINT('Ctrl Pts',(-186.701922592539,5.90974761986768,
130.47634697145));
#262209=CARTESIAN_POINT('Ctrl Pts',(-186.709322675054,5.89684694545481,
130.319462005091));
#262210=CARTESIAN_POINT('Ctrl Pts',(-186.716730894721,5.88393208542427,
130.162404527584));
#262211=CARTESIAN_POINT('Ctrl Pts',(-186.724139114387,5.86474673092027,
130.005966156498));
#262212=CARTESIAN_POINT('Ctrl Pts',(-186.731547334054,5.83938536984659,
129.850678770763));
#262213=CARTESIAN_POINT('Ctrl Pts',(-186.738960113356,5.81400839927836,
129.695295808233));
#262214=CARTESIAN_POINT('Ctrl Pts',(-186.746372892658,5.78244792237959,
129.541065607525));
#262215=CARTESIAN_POINT('Ctrl Pts',(-186.75378567196,5.7448490090175,129.38850736737));
#262216=CARTESIAN_POINT('Ctrl Pts',(-186.761209042988,5.70719637256474,
129.235731144846));
#262217=CARTESIAN_POINT('Ctrl Pts',(-186.768632414017,5.66348817105071,
129.084632011842));
#262218=CARTESIAN_POINT('Ctrl Pts',(-186.776055785046,5.61391880352735,
128.935712381567));
#262219=CARTESIAN_POINT('Ctrl Pts',(-186.779991834487,5.58763593546334,
128.856751620311));
#262220=CARTESIAN_POINT('Ctrl Pts',(-186.783927883928,5.55970608173856,
128.77840324676));
#262221=CARTESIAN_POINT('Ctrl Pts',(-186.787863933369,5.53016353431541,
128.700739490502));
#262222=CARTESIAN_POINT('Ctrl Pts',(-186.795287199775,5.47444721187183,
128.554268070017));
#262223=CARTESIAN_POINT('Ctrl Pts',(-186.80271046618,5.41282347703181,128.409790243116));
#262224=CARTESIAN_POINT('Ctrl Pts',(-186.810133732586,5.34545435342012,
128.267818026163));
#262225=CARTESIAN_POINT('Ctrl Pts',(-186.817548225307,5.27816485451769,
128.12601360858));
#262226=CARTESIAN_POINT('Ctrl Pts',(-186.824962718028,5.20514364198745,
127.986709240179));
#262227=CARTESIAN_POINT('Ctrl Pts',(-186.832377210749,5.12660184812075,
127.850399877586));
#262228=CARTESIAN_POINT('Ctrl Pts',(-186.839784557103,5.04813575579202,
127.714221895088));
#262229=CARTESIAN_POINT('Ctrl Pts',(-186.847191903456,4.96415986019837,
127.581033492824));
#262230=CARTESIAN_POINT('Ctrl Pts',(-186.85459924981,4.87493247798782,127.451307695592));
#262231=CARTESIAN_POINT('Ctrl Pts',(-186.862001071486,4.78577164492528,
127.321678652754));
#262232=CARTESIAN_POINT('Ctrl Pts',(-186.869402893161,4.69136733467664,
127.195507379004));
#262233=CARTESIAN_POINT('Ctrl Pts',(-186.876804714836,4.59202263391012,
127.073240317689));
#262234=CARTESIAN_POINT('Ctrl Pts',(-186.884202629148,4.4927303764384,126.951037800204));
#262235=CARTESIAN_POINT('Ctrl Pts',(-186.891600543459,4.38850315720013,
126.832735679553));
#262236=CARTESIAN_POINT('Ctrl Pts',(-186.89899845777,4.27968595424607,126.718749439844));
#262237=CARTESIAN_POINT('Ctrl Pts',(-186.906395142683,4.17088683473652,
126.604782142579));
#262238=CARTESIAN_POINT('Ctrl Pts',(-186.913791827595,4.05749950290368,
126.495129572533));
#262239=CARTESIAN_POINT('Ctrl Pts',(-186.921188512507,3.93990768406763,
126.390172356569));
#262240=CARTESIAN_POINT('Ctrl Pts',(-186.928584869443,3.82232107937571,
126.285219794517));
#262241=CARTESIAN_POINT('Ctrl Pts',(-186.935981226378,3.70053063686753,
126.184962421158));
#262242=CARTESIAN_POINT('Ctrl Pts',(-186.943377583313,3.57495503047606,
126.089742171438));
#262243=CARTESIAN_POINT('Ctrl Pts',(-186.95077507265,3.4493601981394,125.994507343255));
#262244=CARTESIAN_POINT('Ctrl Pts',(-186.958172561986,3.31997934549403,
125.904311399832));
#262245=CARTESIAN_POINT('Ctrl Pts',(-186.965570051323,3.18726200443501,
125.819454251586));
#262246=CARTESIAN_POINT('Ctrl Pts',(-186.972970133838,3.05449813951574,
125.734567356798));
#262247=CARTESIAN_POINT('Ctrl Pts',(-186.980370216353,2.91839577182612,
125.655023184307));
#262248=CARTESIAN_POINT('Ctrl Pts',(-186.987770298868,2.77943087677651,
125.581076730611));
#262249=CARTESIAN_POINT('Ctrl Pts',(-186.995178518535,2.64031317554104,
125.507048965188));
#262250=CARTESIAN_POINT('Ctrl Pts',(-187.002586738201,2.49832699064388,
125.438631386499));
#262251=CARTESIAN_POINT('Ctrl Pts',(-187.009994957867,2.35397087991152,
125.376031992747));
#262252=CARTESIAN_POINT('Ctrl Pts',(-187.017407737169,2.20952592040129,
125.313394070112));
#262253=CARTESIAN_POINT('Ctrl Pts',(-187.024820516472,2.06270847584779,
125.256581602402));
#262254=CARTESIAN_POINT('Ctrl Pts',(-187.032233295774,1.91403377665382,
125.205753177825));
#262255=CARTESIAN_POINT('Ctrl Pts',(-187.039656666802,1.76514664407727,
125.15485212721));
#262256=CARTESIAN_POINT('Ctrl Pts',(-187.047080037831,1.61439731357947,
125.109952302834));
#262257=CARTESIAN_POINT('Ctrl Pts',(-187.05450340886,1.46231355706026,125.071161717882));
#262258=CARTESIAN_POINT('Ctrl Pts',(-187.058439458301,1.38167510015412,
125.050594018973));
#262259=CARTESIAN_POINT('Ctrl Pts',(-187.062375507741,1.30066162638929,
125.031742986259));
#262260=CARTESIAN_POINT('Ctrl Pts',(-187.066311557182,1.21935244020638,
125.014618810796));
#262261=CARTESIAN_POINT('Ctrl Pts',(-187.073734823588,1.06600585263888,
124.9823231503));
#262262=CARTESIAN_POINT('Ctrl Pts',(-187.081158089993,0.911143431117751,
124.956075149189));
#262263=CARTESIAN_POINT('Ctrl Pts',(-187.088581356398,0.755283527239422,
124.936015249749));
#262264=CARTESIAN_POINT('Ctrl Pts',(-187.095995849119,0.599607836824118,
124.915979059444));
#262265=CARTESIAN_POINT('Ctrl Pts',(-187.10341034184,0.442937377369268,
124.902116459795));
#262266=CARTESIAN_POINT('Ctrl Pts',(-187.110824834561,0.285802692063943,
124.894517355371));
#262267=CARTESIAN_POINT('Ctrl Pts',(-187.118232180915,0.128819459083885,
124.88692557525));
#262268=CARTESIAN_POINT('Ctrl Pts',(-187.125639527269,-0.0286267386259374,
124.885585289803));
#262269=CARTESIAN_POINT('Ctrl Pts',(-187.133046873623,-0.185998305446971,
124.890534851374));
#262270=CARTESIAN_POINT('Ctrl Pts',(-187.140448695298,-0.343252498615732,
124.895480721376));
#262271=CARTESIAN_POINT('Ctrl Pts',(-187.147850516973,-0.500431800219757,
124.906707085891));
#262272=CARTESIAN_POINT('Ctrl Pts',(-187.155252338649,-0.656996779079823,
124.924200263054));
#262273=CARTESIAN_POINT('Ctrl Pts',(-187.16265025296,-0.813479108507141,
124.941684205705));
#262274=CARTESIAN_POINT('Ctrl Pts',(-187.170048167272,-0.969347390991606,
124.965428331216));
#262275=CARTESIAN_POINT('Ctrl Pts',(-187.177446081583,-1.12406559892257,
124.995366979093));
#262276=CARTESIAN_POINT('Ctrl Pts',(-187.184842766495,-1.27875809549403,
125.02530065171));
#262277=CARTESIAN_POINT('Ctrl Pts',(-187.192239451407,-1.43230053069113,
125.061426732754));
#262278=CARTESIAN_POINT('Ctrl Pts',(-187.199636136319,-1.58416525944525,
125.103628121363));
#262279=CARTESIAN_POINT('Ctrl Pts',(-187.207032493255,-1.73602325435815,
125.145827638718));
#262280=CARTESIAN_POINT('Ctrl Pts',(-187.21442885019,-1.88620333107437,
125.194101828061));
#262281=CARTESIAN_POINT('Ctrl Pts',(-187.221825207126,-2.03419150655014,
125.248283271346));
#262282=CARTESIAN_POINT('Ctrl Pts',(-187.229222696462,-2.18220233939295,
125.302473009948));
#262283=CARTESIAN_POINT('Ctrl Pts',(-187.236620185799,-2.32802025223464,
125.362571674956));
#262284=CARTESIAN_POINT('Ctrl Pts',(-187.244017675135,-2.4711499389764,
125.428363171362));
#262285=CARTESIAN_POINT('Ctrl Pts',(-187.25141775765,-2.61432979960858,
125.494177730874));
#262286=CARTESIAN_POINT('Ctrl Pts',(-187.258817840165,-2.75481921895261,
125.565688939224));
#262287=CARTESIAN_POINT('Ctrl Pts',(-187.26621792268,-2.89214638489867,
125.642634176653));
#262288=CARTESIAN_POINT('Ctrl Pts',(-187.273626142347,-3.02962455618108,
125.719664023281));
#262289=CARTESIAN_POINT('Ctrl Pts',(-187.281034362013,-3.16393320396151,
125.802139649419));
#262290=CARTESIAN_POINT('Ctrl Pts',(-187.28844258168,-3.29462785077745,
125.889754032357));
#262291=CARTESIAN_POINT('Ctrl Pts',(-187.295855360982,-3.42540293796775,
125.977422340486));
#262292=CARTESIAN_POINT('Ctrl Pts',(-187.303268140284,-3.55255929106162,
126.070235488155));
#262293=CARTESIAN_POINT('Ctrl Pts',(-187.310680919586,-3.67568499069044,
126.167845718236));
#262294=CARTESIAN_POINT('Ctrl Pts',(-187.318104290615,-3.79898661809308,
126.26559541839));
#262295=CARTESIAN_POINT('Ctrl Pts',(-187.325527661644,-3.91824580736076,
126.368155647766));
#262296=CARTESIAN_POINT('Ctrl Pts',(-187.332951032672,-4.03308641033856,
126.475140760682));
#262297=CARTESIAN_POINT('Ctrl Pts',(-187.336887082113,-4.09397765360244,
126.531866834624));
#262298=CARTESIAN_POINT('Ctrl Pts',(-187.340823131554,-4.1536273227506,
126.589836320882));
#262299=CARTESIAN_POINT('Ctrl Pts',(-187.344759180995,-4.21198397777087,
126.648988006897));
#262300=CARTESIAN_POINT('Ctrl Pts',(-187.352082400964,-4.32055949944319,
126.759042724129));
#262301=CARTESIAN_POINT('Ctrl Pts',(-187.359405620933,-4.42500455681407,
126.873544452405));
#262302=CARTESIAN_POINT('Ctrl Pts',(-187.366728840903,-4.52492539990628,
126.992145947878));
#262303=CARTESIAN_POINT('Ctrl Pts',(-187.374043222144,-4.62472564397862,
127.1106042978));
#262304=CARTESIAN_POINT('Ctrl Pts',(-187.381357603385,-4.72001229335793,
127.233152278661));
#262305=CARTESIAN_POINT('Ctrl Pts',(-187.388671984626,-4.81042708213411,
127.3594046164));
#262306=CARTESIAN_POINT('Ctrl Pts',(-187.395978017208,-4.90073867116098,
127.485512849288));
#262307=CARTESIAN_POINT('Ctrl Pts',(-187.403284049789,-4.98618925122516,
127.615316708677));
#262308=CARTESIAN_POINT('Ctrl Pts',(-187.410590082371,-5.06645997052641,
127.748396951297));
#262309=CARTESIAN_POINT('Ctrl Pts',(-187.417891395085,-5.14667883307661,
127.881391220987));
#262310=CARTESIAN_POINT('Ctrl Pts',(-187.4251927078,-5.22172429356674,128.017657336095));
#262311=CARTESIAN_POINT('Ctrl Pts',(-187.432494020514,-5.29131999812529,
128.156745985498));
#262312=CARTESIAN_POINT('Ctrl Pts',(-187.439792150053,-5.36088536083589,
128.295773996006));
#262313=CARTESIAN_POINT('Ctrl Pts',(-187.447090279593,-5.42500552334415,
128.437621749531));
#262314=CARTESIAN_POINT('Ctrl Pts',(-187.454388409132,-5.48344955540227,
128.581814434501));
#262315=CARTESIAN_POINT('Ctrl Pts',(-187.461684889562,-5.54188038124945,
128.725974537204));
#262316=CARTESIAN_POINT('Ctrl Pts',(-187.468981369991,-5.59463748570317,
128.87247816067));
#262317=CARTESIAN_POINT('Ctrl Pts',(-187.47627785042,-5.64153778312993,
129.020829848553));
#262318=CARTESIAN_POINT('Ctrl Pts',(-187.483576690867,-5.68845325027215,
129.169229520201));
#262319=CARTESIAN_POINT('Ctrl Pts',(-187.490875531314,-5.7295080036463,
129.319478085701));
#262320=CARTESIAN_POINT('Ctrl Pts',(-187.498174371761,-5.76456856275173,
129.471064008467));
#262321=CARTESIAN_POINT('Ctrl Pts',(-187.505474224208,-5.79963398307961,
129.62267094895));
#262322=CARTESIAN_POINT('Ctrl Pts',(-187.512774076655,-5.82870347565599,
129.775615239507));
#262323=CARTESIAN_POINT('Ctrl Pts',(-187.520073929102,-5.85169470676966,
129.929375119821));
#262324=CARTESIAN_POINT('Ctrl Pts',(-187.527380321913,-5.87470653706738,
130.083272762574));
#262325=CARTESIAN_POINT('Ctrl Pts',(-187.534686714723,-5.89162917731749,
130.237987073307));
#262326=CARTESIAN_POINT('Ctrl Pts',(-187.541993107533,-5.9024321476053,
130.392990582907));
#262327=CARTESIAN_POINT('Ctrl Pts',(-187.54853700762,-5.91210772350591,
130.531817977784));
#262328=CARTESIAN_POINT('Ctrl Pts',(-187.555080907706,-5.91687497723714,
130.670877114353));
#262329=CARTESIAN_POINT('Ctrl Pts',(-187.561624807792,-5.91674750900767,
130.809789904034));
#262330=CARTESIAN_POINT('',(-189.311624807792,-5.92158926949562,130.802089018337));
#262331=CARTESIAN_POINT('Ctrl Pts',(-187.561624807792,-5.91744066498834,
130.809790540083));
#262332=CARTESIAN_POINT('Ctrl Pts',(-187.582152140131,-5.92149194206913,
131.245596366776));
#262333=CARTESIAN_POINT('Ctrl Pts',(-187.695495347076,-5.67831340457064,
133.64744955503));
#262334=CARTESIAN_POINT('Ctrl Pts',(-187.90165442862,-2.39945118657061,
137.378567378342));
#262335=CARTESIAN_POINT('Ctrl Pts',(-188.180102052435,4.23410436286723,
136.376606194958));
#262336=CARTESIAN_POINT('Ctrl Pts',(-188.458549676247,6.97672485032798,
130.254023545258));
#262337=CARTESIAN_POINT('Ctrl Pts',(-188.73699730006,3.3080760322958,124.637173779559));
#262338=CARTESIAN_POINT('Ctrl Pts',(-189.015444923873,-3.40053305091948,
124.687667434156));
#262339=CARTESIAN_POINT('Ctrl Pts',(-189.20698742645,-5.86572937063765,
128.589015218929));
#262340=CARTESIAN_POINT('Ctrl Pts',(-189.305714054423,-5.92609167912231,
130.677041554188));
#262341=CARTESIAN_POINT('Ctrl Pts',(-189.311624807792,-5.92547957657923,
130.802087525964));
#262342=CARTESIAN_POINT('',(-191.061624793292,-5.91313729896144,130.80003214728));
#262343=CARTESIAN_POINT('Ctrl Pts',(-189.311624807792,-5.91674956464851,
130.802090874911));
#262344=CARTESIAN_POINT('Ctrl Pts',(-189.318977448973,-5.91680914766334,
130.957411468767));
#262345=CARTESIAN_POINT('Ctrl Pts',(-189.326330090154,-5.91074854494049,
131.112981837623));
#262346=CARTESIAN_POINT('Ctrl Pts',(-189.333682731335,-5.89853497471983,
131.268274094959));
#262347=CARTESIAN_POINT('Ctrl Pts',(-189.341027006048,-5.88633530215123,
131.42338964739));
#262348=CARTESIAN_POINT('Ctrl Pts',(-189.348371280761,-5.86799662359575,
131.578227341974));
#262349=CARTESIAN_POINT('Ctrl Pts',(-189.355715555474,-5.8435381292413,
131.732257537813));
#262350=CARTESIAN_POINT('Ctrl Pts',(-189.363053149278,-5.81910188418644,
131.886147616115));
#262351=CARTESIAN_POINT('Ctrl Pts',(-189.370390743082,-5.78855696232474,
132.039231283816));
#262352=CARTESIAN_POINT('Ctrl Pts',(-189.377728336886,-5.75197447447406,
132.190982486533));
#262353=CARTESIAN_POINT('Ctrl Pts',(-189.385060929245,-5.71541692194747,
132.342630252726));
#262354=CARTESIAN_POINT('Ctrl Pts',(-189.392393521605,-5.67283008434618,
132.492946992982));
#262355=CARTESIAN_POINT('Ctrl Pts',(-189.399726113965,-5.62433638296606,
132.641415546996));
#262356=CARTESIAN_POINT('Ctrl Pts',(-189.407056104548,-5.57585988828992,
132.789831420881));
#262357=CARTESIAN_POINT('Ctrl Pts',(-189.414386095132,-5.52148081560047,
132.936400051107));
#262358=CARTESIAN_POINT('Ctrl Pts',(-189.421716085716,-5.46137178798303,
133.080618238294));
#262359=CARTESIAN_POINT('Ctrl Pts',(-189.429044866575,-5.40127268062225,
133.224812624041));
#262360=CARTESIAN_POINT('Ctrl Pts',(-189.436373647433,-5.33544564582625,
133.366656986859));
#262361=CARTESIAN_POINT('Ctrl Pts',(-189.443702428292,-5.26411181390032,
133.505667222388));
#262362=CARTESIAN_POINT('Ctrl Pts',(-189.45103151263,-5.19277502809146,
133.644683214231));
#262363=CARTESIAN_POINT('Ctrl Pts',(-189.458360596969,-5.11593116510898,
133.780864506177));
#262364=CARTESIAN_POINT('Ctrl Pts',(-189.465689681307,-5.03384764105057,
133.913750990162));
#262365=CARTESIAN_POINT('Ctrl Pts',(-189.473020582319,-4.95174377079516,
134.046670412968));
#262366=CARTESIAN_POINT('Ctrl Pts',(-189.480351483332,-4.86439785503814,
134.176293078574));
#262367=CARTESIAN_POINT('Ctrl Pts',(-189.487682384344,-4.77212086708803,
134.302187513283));
#262368=CARTESIAN_POINT('Ctrl Pts',(-189.495020896959,-4.6797480688371,
134.428212662962));
#262369=CARTESIAN_POINT('Ctrl Pts',(-189.502359409575,-4.5824341979447,
134.550501542638));
#262370=CARTESIAN_POINT('Ctrl Pts',(-189.509697922191,-4.48053120714239,
134.668654946978));
#262371=CARTESIAN_POINT('Ctrl Pts',(-189.517040396452,-4.37857320471192,
134.78687213562));
#262372=CARTESIAN_POINT('Ctrl Pts',(-189.524382870713,-4.27202140698691,
134.900949123779));
#262373=CARTESIAN_POINT('Ctrl Pts',(-189.531725344974,-4.16126441642406,
135.010523835881));
#262374=CARTESIAN_POINT('Ctrl Pts',(-189.539078893906,-4.05034037083163,
135.120263819778));
#262375=CARTESIAN_POINT('Ctrl Pts',(-189.546432442839,-3.93519874240669,
135.225487704928));
#262376=CARTESIAN_POINT('Ctrl Pts',(-189.553785991771,-3.81626167847011,
135.325873347167));
#262377=CARTESIAN_POINT('Ctrl Pts',(-189.559970718347,-3.71622926868426,
135.410303022565));
#262378=CARTESIAN_POINT('Ctrl Pts',(-189.566155444922,-3.61351273278213,
135.491310933321));
#262379=CARTESIAN_POINT('Ctrl Pts',(-189.572340171498,-3.50837810462016,
135.568729792758));
#262380=CARTESIAN_POINT('Ctrl Pts',(-189.579763437904,-3.38218944555196,
135.661652383818));
#262381=CARTESIAN_POINT('Ctrl Pts',(-189.587186704309,-3.25211571553351,
135.749698689375));
#262382=CARTESIAN_POINT('Ctrl Pts',(-189.594609970715,-3.11857050878932,
135.832526142309));
#262383=CARTESIAN_POINT('Ctrl Pts',(-189.602024463436,-2.98518314138887,
135.915255700071));
#262384=CARTESIAN_POINT('Ctrl Pts',(-189.609438956157,-2.84833277843893,
135.992778488313));
#262385=CARTESIAN_POINT('Ctrl Pts',(-189.616853448878,-2.70846504719477,
136.064792885985));
#262386=CARTESIAN_POINT('Ctrl Pts',(-189.624260795232,-2.5687321257355,
136.13673787347));
#262387=CARTESIAN_POINT('Ctrl Pts',(-189.631668141586,-2.42598795540314,
136.203184870211));
#262388=CARTESIAN_POINT('Ctrl Pts',(-189.63907548794,-2.28070593937386,
136.263876253646));
#262389=CARTESIAN_POINT('Ctrl Pts',(-189.646477309616,-2.13553228015454,
136.324522371158));
#262390=CARTESIAN_POINT('Ctrl Pts',(-189.653879131291,-1.98782488706824,
136.379421279541));
#262391=CARTESIAN_POINT('Ctrl Pts',(-189.661280952967,-1.83808039076475,
136.428361954656));
#262392=CARTESIAN_POINT('Ctrl Pts',(-189.668678867278,-1.68841494341483,
136.477276794369));
#262393=CARTESIAN_POINT('Ctrl Pts',(-189.67607678159,-1.53671488843013,
136.520239549164));
#262394=CARTESIAN_POINT('Ctrl Pts',(-189.683474695901,-1.38349529252278,
136.557087913212));
#262395=CARTESIAN_POINT('Ctrl Pts',(-189.690871380814,-1.23030115893236,
136.59393015373));
#262396=CARTESIAN_POINT('Ctrl Pts',(-189.698268065726,-1.07558834819108,
136.62465993296));
#262397=CARTESIAN_POINT('Ctrl Pts',(-189.705664750638,-0.919885608475016,
136.649165236184));
#262398=CARTESIAN_POINT('Ctrl Pts',(-189.713061107574,-0.7641897727816,
136.673669452817));
#262399=CARTESIAN_POINT('Ctrl Pts',(-189.72045746451,-0.607504464148897,
136.691949684189));
#262400=CARTESIAN_POINT('Ctrl Pts',(-189.727853821445,-0.450366841788114,
136.703945371624));
#262401=CARTESIAN_POINT('Ctrl Pts',(-189.735251310782,-0.293205161256196,
136.71594289563));
#262402=CARTESIAN_POINT('Ctrl Pts',(-189.742648800119,-0.135591401348304,
136.721653931456));
#262403=CARTESIAN_POINT('Ctrl Pts',(-189.750046289455,0.021934111525369,
136.721069961217));
#262404=CARTESIAN_POINT('Ctrl Pts',(-189.75744637197,0.179514844723607,
136.720485786269));
#262405=CARTESIAN_POINT('Ctrl Pts',(-189.764846454486,0.337006896234077,
136.713602213106));
#262406=CARTESIAN_POINT('Ctrl Pts',(-189.772246537001,0.493872048296028,
136.700462801417));
#262407=CARTESIAN_POINT('Ctrl Pts',(-189.779654756667,0.650909689718572,
136.687308941594));
#262408=CARTESIAN_POINT('Ctrl Pts',(-189.787062976334,0.807318682811136,
136.667885536733));
#262409=CARTESIAN_POINT('Ctrl Pts',(-189.794471196001,0.962567293055188,
136.642287884057));
#262410=CARTESIAN_POINT('Ctrl Pts',(-189.801883975303,1.11791145622882,
136.616674476453));
#262411=CARTESIAN_POINT('Ctrl Pts',(-189.809296754605,1.27209344867101,
136.584879323986));
#262412=CARTESIAN_POINT('Ctrl Pts',(-189.816709533907,1.4245942930246,136.547048286487));
#262413=CARTESIAN_POINT('Ctrl Pts',(-189.824132904936,1.57731303773595,
136.509163194228));
#262414=CARTESIAN_POINT('Ctrl Pts',(-189.831556275965,1.72834547933129,
136.465225096164));
#262415=CARTESIAN_POINT('Ctrl Pts',(-189.838979646994,1.87718950102327,
136.41542915571));
#262416=CARTESIAN_POINT('Ctrl Pts',(-189.842915696433,1.95611017275407,
136.389026153255));
#262417=CARTESIAN_POINT('Ctrl Pts',(-189.846851745872,2.03441595105685,
136.360977098998));
#262418=CARTESIAN_POINT('Ctrl Pts',(-189.850787795312,2.11203465861468,
136.331316394783));
#262419=CARTESIAN_POINT('Ctrl Pts',(-189.858211061717,2.25842111873141,
136.275377232289));
#262420=CARTESIAN_POINT('Ctrl Pts',(-189.865634328123,2.40280499749717,
136.213533698149));
#262421=CARTESIAN_POINT('Ctrl Pts',(-189.873057594528,2.54467452571146,
136.145948595003));
#262422=CARTESIAN_POINT('Ctrl Pts',(-189.880472087249,2.68637637592454,
136.078443371836));
#262423=CARTESIAN_POINT('Ctrl Pts',(-189.88788657997,2.82556945715901,136.005210246327));
#262424=CARTESIAN_POINT('Ctrl Pts',(-189.895301072691,2.96175913466819,
135.926461103764));
#262425=CARTESIAN_POINT('Ctrl Pts',(-189.902708419045,3.09781754743913,
135.847787862589));
#262426=CARTESIAN_POINT('Ctrl Pts',(-189.910115765399,3.23087799845622,
135.763609374162));
#262427=CARTESIAN_POINT('Ctrl Pts',(-189.917523111753,3.36046785658173,
135.674184674694));
#262428=CARTESIAN_POINT('Ctrl Pts',(-189.924924933428,3.48996106170153,
135.584826671541));
#262429=CARTESIAN_POINT('Ctrl Pts',(-189.932326755103,3.61598852205761,
135.49023045941));
#262430=CARTESIAN_POINT('Ctrl Pts',(-189.939728576779,3.73810425606627,
135.390699804028));
#262431=CARTESIAN_POINT('Ctrl Pts',(-189.94712649109,3.86015552612914,135.291221690105));
#262432=CARTESIAN_POINT('Ctrl Pts',(-189.954524405402,3.97829889370356,
135.18681455587));
#262433=CARTESIAN_POINT('Ctrl Pts',(-189.961922319713,4.09211940015992,
135.077824011271));
#262434=CARTESIAN_POINT('Ctrl Pts',(-189.969319004625,4.20592099171351,
134.968851578922));
#262435=CARTESIAN_POINT('Ctrl Pts',(-189.976715689538,4.31540087856674,
134.855297505843));
#262436=CARTESIAN_POINT('Ctrl Pts',(-189.98411237445,4.42017901826155,134.73754609616));
#262437=CARTESIAN_POINT('Ctrl Pts',(-189.991508731385,4.52495251198384,
134.619799907697));
#262438=CARTESIAN_POINT('Ctrl Pts',(-189.998905088321,4.62502442492598,
134.497857031564));
#262439=CARTESIAN_POINT('Ctrl Pts',(-190.006301445256,4.72005345968584,
134.372136661575));
#262440=CARTESIAN_POINT('Ctrl Pts',(-190.013698934593,4.81509704363352,
134.246397043477));
#262441=CARTESIAN_POINT('Ctrl Pts',(-190.02109642393,4.90509598697833,134.11687907778));
#262442=CARTESIAN_POINT('Ctrl Pts',(-190.028493913266,4.98975106375987,
133.984032752269));
#262443=CARTESIAN_POINT('Ctrl Pts',(-190.035893995781,5.07443581624746,
133.851139857685));
#262444=CARTESIAN_POINT('Ctrl Pts',(-190.043294078296,5.15377277199098,
133.71491659491));
#262445=CARTESIAN_POINT('Ctrl Pts',(-190.050694160811,5.22750765914304,
133.575839326866));
#262446=CARTESIAN_POINT('Ctrl Pts',(-190.058102380478,5.30132362538356,
133.436609129067));
#262447=CARTESIAN_POINT('Ctrl Pts',(-190.065510600145,5.36952504604308,
133.294518988678));
#262448=CARTESIAN_POINT('Ctrl Pts',(-190.072918819811,5.43190468187914,
133.150067779485));
#262449=CARTESIAN_POINT('Ctrl Pts',(-190.080331599113,5.49432271134037,
133.005527662983));
#262450=CARTESIAN_POINT('Ctrl Pts',(-190.087744378416,5.55091168210434,
132.858623929535));
#262451=CARTESIAN_POINT('Ctrl Pts',(-190.095157157718,5.60151379023981,
132.709872050293));
#262452=CARTESIAN_POINT('Ctrl Pts',(-190.102580528747,5.65218820104032,
132.56090762739));
#262453=CARTESIAN_POINT('Ctrl Pts',(-190.110003899775,5.69685855860319,
132.410090141567));
#262454=CARTESIAN_POINT('Ctrl Pts',(-190.117427270804,5.73541765304766,
132.25794752849));
#262455=CARTESIAN_POINT('Ctrl Pts',(-190.121363320244,5.7558626101311,132.17727786444));
#262456=CARTESIAN_POINT('Ctrl Pts',(-190.125299369684,5.77459033229658,
132.096235796439));
#262457=CARTESIAN_POINT('Ctrl Pts',(-190.129235419124,5.79159074918677,
132.014900644345));
#262458=CARTESIAN_POINT('Ctrl Pts',(-190.13665868553,5.82365300488208,131.861505085854));
#262459=CARTESIAN_POINT('Ctrl Pts',(-190.144081951935,5.84966530135562,
131.706602898674));
#262460=CARTESIAN_POINT('Ctrl Pts',(-190.15150521834,5.86948798532478,131.550712647528));
#262461=CARTESIAN_POINT('Ctrl Pts',(-190.158919711061,5.88928724052766,
131.395006645713));
#262462=CARTESIAN_POINT('Ctrl Pts',(-190.166334203782,5.90291139835537,
131.238315271165));
#262463=CARTESIAN_POINT('Ctrl Pts',(-190.173748696503,5.9102713617377,131.081169203277));
#262464=CARTESIAN_POINT('Ctrl Pts',(-190.181156042857,5.91762423131021,
130.924174598686));
#262465=CARTESIAN_POINT('Ctrl Pts',(-190.18856338921,5.91872490889553,130.766726543612));
#262466=CARTESIAN_POINT('Ctrl Pts',(-190.195970735564,5.91353586032059,
130.609362691417));
#262467=CARTESIAN_POINT('Ctrl Pts',(-190.203372557239,5.90835068193385,
130.45211620712));
#262468=CARTESIAN_POINT('Ctrl Pts',(-190.210774378915,5.8968851302798,130.294954172144));
#262469=CARTESIAN_POINT('Ctrl Pts',(-190.21817620059,5.8791537081288,130.138415996223));
#262470=CARTESIAN_POINT('Ctrl Pts',(-190.225574114901,5.86143164625758,
129.981960455587));
#262471=CARTESIAN_POINT('Ctrl Pts',(-190.232972029212,5.83745034325019,
129.826128488115));
#262472=CARTESIAN_POINT('Ctrl Pts',(-190.240369943524,5.80727627526828,
129.671456020874));
#262473=CARTESIAN_POINT('Ctrl Pts',(-190.247766628436,5.77710722166901,
129.51680925739));
#262474=CARTESIAN_POINT('Ctrl Pts',(-190.255163313348,5.74074751701105,
129.36332197774));
#262475=CARTESIAN_POINT('Ctrl Pts',(-190.26255999826,5.69831506500718,129.211521648174));
#262476=CARTESIAN_POINT('Ctrl Pts',(-190.269956355195,5.6558844945027,129.059728049594));
#262477=CARTESIAN_POINT('Ctrl Pts',(-190.277352712131,5.60738181255083,
128.909621611885));
#262478=CARTESIAN_POINT('Ctrl Pts',(-190.284749069066,5.55297521919776,
128.761716062712));
#262479=CARTESIAN_POINT('Ctrl Pts',(-190.292146558402,5.49856029605635,
128.613787868822));
#262480=CARTESIAN_POINT('Ctrl Pts',(-190.299544047739,5.43823979060307,
128.468061584774));
#262481=CARTESIAN_POINT('Ctrl Pts',(-190.306941537075,5.37223055136691,
128.325032187232));
#262482=CARTESIAN_POINT('Ctrl Pts',(-190.31434161959,5.30619817269379,128.181952650957));
#262483=CARTESIAN_POINT('Ctrl Pts',(-190.321741702105,5.23447324617382,
128.041572222184));
#262484=CARTESIAN_POINT('Ctrl Pts',(-190.32914178462,5.15731910927882,127.904362312813));
#262485=CARTESIAN_POINT('Ctrl Pts',(-190.336550004286,5.08008013347921,
127.767001527043));
#262486=CARTESIAN_POINT('Ctrl Pts',(-190.343958223952,4.99740020795088,
127.632818548654));
#262487=CARTESIAN_POINT('Ctrl Pts',(-190.351366443619,4.90958703146701,
127.502257387358));
#262488=CARTESIAN_POINT('Ctrl Pts',(-190.358779222921,4.82171980743826,
127.371615867845));
#262489=CARTESIAN_POINT('Ctrl Pts',(-190.366192002223,4.72871325692401,
127.244600907808));
#262490=CARTESIAN_POINT('Ctrl Pts',(-190.373604781525,4.63091576352256,
127.121623896911));
#262491=CARTESIAN_POINT('Ctrl Pts',(-190.381028152553,4.53297853247616,
126.998471170694));
#262492=CARTESIAN_POINT('Ctrl Pts',(-190.388451523582,4.43023692968165,
126.879368198737));
#262493=CARTESIAN_POINT('Ctrl Pts',(-190.395874894611,4.32307717280776,
126.764690541873));
#262494=CARTESIAN_POINT('Ctrl Pts',(-190.399810944053,4.26625849842815,
126.703885696528));
#262495=CARTESIAN_POINT('Ctrl Pts',(-190.403746993495,4.20819830263757,
126.644324316123));
#262496=CARTESIAN_POINT('Ctrl Pts',(-190.407683042937,4.14895787620481,
126.586057747456));
#262497=CARTESIAN_POINT('Ctrl Pts',(-190.415106309343,4.03723228082388,
126.476168817428));
#262498=CARTESIAN_POINT('Ctrl Pts',(-190.422529575748,3.92096896531795,
126.370555519829));
#262499=CARTESIAN_POINT('Ctrl Pts',(-190.429952842154,3.80052872686658,
126.269615645822));
#262500=CARTESIAN_POINT('Ctrl Pts',(-190.437367334875,3.68023083877513,
126.168795074362));
#262501=CARTESIAN_POINT('Ctrl Pts',(-190.444781827596,3.55576613772917,
126.072637169181));
#262502=CARTESIAN_POINT('Ctrl Pts',(-190.452196320317,3.42753294018989,
125.981503735342));
#262503=CARTESIAN_POINT('Ctrl Pts',(-190.459603666671,3.29942333863392,
125.890458139337));
#262504=CARTESIAN_POINT('Ctrl Pts',(-190.467011013024,3.16755277385676,
125.804427588461));
#262505=CARTESIAN_POINT('Ctrl Pts',(-190.474418359378,3.03235330072144,
125.72373427605));
#262506=CARTESIAN_POINT('Ctrl Pts',(-190.481820181054,2.89725466445357,
125.643101147756));
#262507=CARTESIAN_POINT('Ctrl Pts',(-190.489222002729,2.75883238263387,
125.567797522283));
#262508=CARTESIAN_POINT('Ctrl Pts',(-190.496623824405,2.61754811504931,
125.498102762175));
#262509=CARTESIAN_POINT('Ctrl Pts',(-190.504021738716,2.47633843033066,
125.428444793389));
#262510=CARTESIAN_POINT('Ctrl Pts',(-190.511419653028,2.33227010265108,
125.364389957968));
#262511=CARTESIAN_POINT('Ctrl Pts',(-190.518817567339,2.18582995461846,
125.306172009307));
#262512=CARTESIAN_POINT('Ctrl Pts',(-190.526214252251,2.03941414228153,
125.247963735412));
#262513=CARTESIAN_POINT('Ctrl Pts',(-190.533610937163,1.89062763842013,
125.195590560915));
#262514=CARTESIAN_POINT('Ctrl Pts',(-190.541007622076,1.73997794516578,
125.149238398477));
#262515=CARTESIAN_POINT('Ctrl Pts',(-190.548403979011,1.58933493187669,
125.102888291342));
#262516=CARTESIAN_POINT('Ctrl Pts',(-190.555800335947,1.43682925025374,
125.0625587752));
#262517=CARTESIAN_POINT('Ctrl Pts',(-190.563196692882,1.28298403016603,
125.028386020943));
#262518=CARTESIAN_POINT('Ctrl Pts',(-190.570594182219,1.12911525598238,
124.994208034749));
#262519=CARTESIAN_POINT('Ctrl Pts',(-190.577991671555,0.97390689941849,
124.966188768263));
#262520=CARTESIAN_POINT('Ctrl Pts',(-190.585389160892,0.817892610288261,
124.944413327655));
#262521=CARTESIAN_POINT('Ctrl Pts',(-190.592789243407,0.661823630589273,
124.9226302537));
#262522=CARTESIAN_POINT('Ctrl Pts',(-190.600189325922,0.50494852531532,
124.907095415004));
#262523=CARTESIAN_POINT('Ctrl Pts',(-190.607589408437,0.347806246985612,
124.897842067942));
#262524=CARTESIAN_POINT('Ctrl Pts',(-190.614997628104,0.190491174567385,
124.888578545873));
#262525=CARTESIAN_POINT('Ctrl Pts',(-190.62240584777,0.0329087152680474,
124.885610331419));
#262526=CARTESIAN_POINT('Ctrl Pts',(-190.629814067437,-0.124401254264218,
124.888918546982));
#262527=CARTESIAN_POINT('Ctrl Pts',(-190.637226846739,-0.281808045457423,
124.892228798696));
#262528=CARTESIAN_POINT('Ctrl Pts',(-190.644639626041,-0.438941640954478,
124.901823155316));
#262529=CARTESIAN_POINT('Ctrl Pts',(-190.652052405343,-0.59526761713485,
124.917630878017));
#262530=CARTESIAN_POINT('Ctrl Pts',(-190.659475776372,-0.75181695920117,
124.933461187533));
#262531=CARTESIAN_POINT('Ctrl Pts',(-190.666899147401,-0.907556008596329,
124.955522542167));
#262532=CARTESIAN_POINT('Ctrl Pts',(-190.67432251843,-1.06196003527188,
124.983693005858));
#262533=CARTESIAN_POINT('Ctrl Pts',(-190.67825856787,-1.14382875507758,
124.998629661646));
#262534=CARTESIAN_POINT('Ctrl Pts',(-190.68219461731,-1.22532238526077,
125.015282967731));
#262535=CARTESIAN_POINT('Ctrl Pts',(-190.68613066675,-1.3063645971489,125.033629112651));
#262536=CARTESIAN_POINT('Ctrl Pts',(-190.693553933156,-1.45920767955153,
125.068229369412));
#262537=CARTESIAN_POINT('Ctrl Pts',(-190.700977199561,-1.61090629986719,
125.108958422396));
#262538=CARTESIAN_POINT('Ctrl Pts',(-190.708400465967,-1.76093076543627,
125.155727738555));
#262539=CARTESIAN_POINT('Ctrl Pts',(-190.715814958688,-1.91077791454581,
125.202441777267));
#262540=CARTESIAN_POINT('Ctrl Pts',(-190.723229451409,-2.05895449464387,
125.255181758744));
#262541=CARTESIAN_POINT('Ctrl Pts',(-190.73064394413,-2.20494080910687,
125.313808132539));
#262542=CARTESIAN_POINT('Ctrl Pts',(-190.738051290484,-2.35078641646454,
125.372378000029));
#262543=CARTESIAN_POINT('Ctrl Pts',(-190.745458636838,-2.49444561681005,
125.436822826783));
#262544=CARTESIAN_POINT('Ctrl Pts',(-190.752865983192,-2.63541380355637,
125.506953266179));
#262545=CARTESIAN_POINT('Ctrl Pts',(-190.760267804868,-2.7762768509102,
125.577031399648));
#262546=CARTESIAN_POINT('Ctrl Pts',(-190.767669626543,-2.91445254820704,
125.652786536705));
#262547=CARTESIAN_POINT('Ctrl Pts',(-190.775071448219,-3.04945632143417,
125.733981272175));
#262548=CARTESIAN_POINT('Ctrl Pts',(-190.78246936253,-3.18438882722145,
125.815133145578));
#262549=CARTESIAN_POINT('Ctrl Pts',(-190.789867276842,-3.31615242456538,
125.901718706713));
#262550=CARTESIAN_POINT('Ctrl Pts',(-190.797265191153,-3.44428731060594,
125.993454727352));
#262551=CARTESIAN_POINT('Ctrl Pts',(-190.804661876065,-3.5724009029514,
126.085175503127));
#262552=CARTESIAN_POINT('Ctrl Pts',(-190.812058560978,-3.69688667759057,
126.182044822578));
#262553=CARTESIAN_POINT('Ctrl Pts',(-190.81945524589,-3.81731390363919,
126.283736200123));
#262554=CARTESIAN_POINT('Ctrl Pts',(-190.826851602826,-3.9377357898191,
126.385423068566));
#262555=CARTESIAN_POINT('Ctrl Pts',(-190.834247959761,-4.05409920001659,
126.491931329125));
#262556=CARTESIAN_POINT('Ctrl Pts',(-190.841644316697,-4.16600680533306,
126.602894461518));
#262557=CARTESIAN_POINT('Ctrl Pts',(-190.849041806034,-4.27793154398928,
126.713874582649));
#262558=CARTESIAN_POINT('Ctrl Pts',(-190.85643929537,-4.38539885432859,
126.829310670813));
#262559=CARTESIAN_POINT('Ctrl Pts',(-190.863836784707,-4.48804868336094,
126.948799753271));
#262560=CARTESIAN_POINT('Ctrl Pts',(-190.871236867222,-4.59073449613216,
127.068330722442));
#262561=CARTESIAN_POINT('Ctrl Pts',(-190.878636949737,-4.68859922218421,
127.19191723167));
#262562=CARTESIAN_POINT('Ctrl Pts',(-190.886037032252,-4.78132356498639,
127.319123820818));
#262563=CARTESIAN_POINT('Ctrl Pts',(-190.893445251919,-4.87414986773537,
127.446470286688));
#262564=CARTESIAN_POINT('Ctrl Pts',(-190.900853471586,-4.9618242790364,
127.57744448025));
#262565=CARTESIAN_POINT('Ctrl Pts',(-190.908261691252,-5.04407086463152,
127.711581984189));
#262566=CARTESIAN_POINT('Ctrl Pts',(-190.915674470554,-5.12636807162771,
127.845802047523));
#262567=CARTESIAN_POINT('Ctrl Pts',(-190.923087249857,-5.20323061424422,
127.98318897578));
#262568=CARTESIAN_POINT('Ctrl Pts',(-190.930500029159,-5.27442913803752,
128.123254907169));
#262569=CARTESIAN_POINT('Ctrl Pts',(-190.937923400188,-5.3457293936204,
128.26352097133));
#262570=CARTESIAN_POINT('Ctrl Pts',(-190.945346771217,-5.41134931149239,
128.406473345405));
#262571=CARTESIAN_POINT('Ctrl Pts',(-190.952770142245,-5.47110785050535,
128.551604649726));
#262572=CARTESIAN_POINT('Ctrl Pts',(-190.956706191685,-5.50279326176559,
128.628556749628));
#262573=CARTESIAN_POINT('Ctrl Pts',(-190.960642241124,-5.53283166141068,
128.706121167425));
#262574=CARTESIAN_POINT('Ctrl Pts',(-190.964578290564,-5.56120182518544,
128.784220814965));
#262575=CARTESIAN_POINT('Ctrl Pts',(-190.973177240122,-5.62318112981626,
128.954842383627));
#262576=CARTESIAN_POINT('Ctrl Pts',(-190.98177618968,-5.67735007641122,
129.128443962409));
#262577=CARTESIAN_POINT('Ctrl Pts',(-190.990375139238,-5.72345280997876,
129.304354452763));
#262578=CARTESIAN_POINT('Ctrl Pts',(-190.998941388787,-5.76938022448008,
129.479595992265));
#262579=CARTESIAN_POINT('Ctrl Pts',(-191.007507638336,-5.80730256775135,
129.657128801406));
#262580=CARTESIAN_POINT('Ctrl Pts',(-191.016073887885,-5.83701346337239,
129.836267444927));
#262581=CARTESIAN_POINT('Ctrl Pts',(-191.024576231815,-5.8665027108652,
130.014069684944));
#262582=CARTESIAN_POINT('Ctrl Pts',(-191.033078575745,-5.88790249831863,
130.19345375926));
#262583=CARTESIAN_POINT('Ctrl Pts',(-191.041580919675,-5.90105816818685,
130.373729617549));
#262584=CARTESIAN_POINT('Ctrl Pts',(-191.048262204323,-5.91139611450565,
130.515393414546));
#262585=CARTESIAN_POINT('Ctrl Pts',(-191.054943488972,-5.9166441504911,
130.657607486087));
#262586=CARTESIAN_POINT('Ctrl Pts',(-191.06162477362,-5.91674841448608,
130.80002908476));
#262587=CARTESIAN_POINT('',(-192.811624807792,-5.9097125884178,130.808293688258));
#262588=CARTESIAN_POINT('Ctrl Pts',(-191.061624807792,-5.91047567621124,
130.800034404554));
#262589=CARTESIAN_POINT('Ctrl Pts',(-191.12209184332,-5.90179870917759,
132.087620467717));
#262590=CARTESIAN_POINT('Ctrl Pts',(-191.275374753451,-4.85401633074215,
135.36448301843));
#262591=CARTESIAN_POINT('Ctrl Pts',(-191.52147353819,0.560953822592365,
137.780239869629));
#262592=CARTESIAN_POINT('Ctrl Pts',(-191.799921162001,6.17221402509524,
134.103047410633));
#262593=CARTESIAN_POINT('Ctrl Pts',(-192.078368785815,6.11151106794695,
127.394522938632));
#262594=CARTESIAN_POINT('Ctrl Pts',(-192.356816409627,0.434628003272854,
123.819472713731));
#262595=CARTESIAN_POINT('Ctrl Pts',(-192.601235083619,-4.89907710821755,
126.315663527414));
#262596=CARTESIAN_POINT('Ctrl Pts',(-192.752837883008,-5.902105290066,129.556078088356));
#262597=CARTESIAN_POINT('Ctrl Pts',(-192.811624807792,-5.9097125884178,
130.808293688258));
#262598=CARTESIAN_POINT('',(-194.561624807792,-5.92485436802142,130.807214191615));
#262599=CARTESIAN_POINT('Ctrl Pts',(-192.811624807792,-5.9097125884178,
130.808293688258));
#262600=CARTESIAN_POINT('Ctrl Pts',(-192.845653757612,-5.91411609097954,
131.533141636508));
#262601=CARTESIAN_POINT('Ctrl Pts',(-192.972498582038,-5.45424420182938,
134.22966001815));
#262602=CARTESIAN_POINT('Ctrl Pts',(-193.192159281066,-1.42141332660588,
137.656888960118));
#262603=CARTESIAN_POINT('Ctrl Pts',(-193.47060690488,4.99691754528912,135.704194857198));
#262604=CARTESIAN_POINT('Ctrl Pts',(-193.749054528692,6.82332530604844,
129.248792458293));
#262605=CARTESIAN_POINT('Ctrl Pts',(-194.027502152505,2.37943044852847,
124.222881204015));
#262606=CARTESIAN_POINT('Ctrl Pts',(-194.298358912204,-4.07028890202498,
125.217162883923));
#262607=CARTESIAN_POINT('Ctrl Pts',(-194.476399797301,-5.91415325007818,
129.003717447568));
#262608=CARTESIAN_POINT('Ctrl Pts',(-194.561624807792,-5.92485436802142,
130.807214191615));
#262609=CARTESIAN_POINT('',(-196.311624807792,-5.91811478187531,130.799043979201));
#262610=CARTESIAN_POINT('Ctrl Pts',(-194.561624807792,-5.92485436802142,
130.807214191615));
#262611=CARTESIAN_POINT('Ctrl Pts',(-194.569215671905,-5.92580750057834,
130.96784894699));
#262612=CARTESIAN_POINT('Ctrl Pts',(-194.576806536018,-5.91984348713247,
131.128411830021));
#262613=CARTESIAN_POINT('Ctrl Pts',(-194.677213274735,-5.74644163664981,
133.244482439234));
#262614=CARTESIAN_POINT('Ctrl Pts',(-194.862845023943,-3.28928991419861,
136.981587535098));
#262615=CARTESIAN_POINT('Ctrl Pts',(-195.141292647756,3.41913440987934,
136.910675415994));
#262616=CARTESIAN_POINT('Ctrl Pts',(-195.419740271569,6.98554124528268,
131.228358307197));
#262617=CARTESIAN_POINT('Ctrl Pts',(-195.698187895382,4.13257693892937,
125.156408035065));
#262618=CARTESIAN_POINT('Ctrl Pts',(-195.976635519195,-2.5180236866903,
124.27465026843));
#262619=CARTESIAN_POINT('Ctrl Pts',(-196.181114489998,-5.70266478639503,
128.033605093401));
#262620=CARTESIAN_POINT('Ctrl Pts',(-196.292777586197,-5.92224318811939,
130.39909676226));
#262621=CARTESIAN_POINT('Ctrl Pts',(-196.311624807792,-5.91853255389597,
130.799043603888));
#262622=CARTESIAN_POINT('',(-198.061624807755,-5.91674998668501,130.803963675558));
#262623=CARTESIAN_POINT('Ctrl Pts',(-196.311624807792,-5.91674761240624,
130.79904520742));
#262624=CARTESIAN_POINT('Ctrl Pts',(-196.318927817343,-5.91688679200283,
130.953970325757));
#262625=CARTESIAN_POINT('Ctrl Pts',(-196.326230826894,-5.91093694148842,
131.109091464218));
#262626=CARTESIAN_POINT('Ctrl Pts',(-196.333533836445,-5.89887867729289,
131.263883101324));
#262627=CARTESIAN_POINT('Ctrl Pts',(-196.340831042499,-5.88682999546239,
131.41855172985));
#262628=CARTESIAN_POINT('Ctrl Pts',(-196.348128248553,-5.86868258965433,
131.572890996276));
#262629=CARTESIAN_POINT('Ctrl Pts',(-196.355425454607,-5.84446913863302,
131.726375286683));
#262630=CARTESIAN_POINT('Ctrl Pts',(-196.362846509282,-5.81984473545903,
131.882464521733));
#262631=CARTESIAN_POINT('Ctrl Pts',(-196.370267563958,-5.78894650617216,
132.037669091922));
#262632=CARTESIAN_POINT('Ctrl Pts',(-196.377688618634,-5.75186394852528,
132.191440889272));
#262633=CARTESIAN_POINT('Ctrl Pts',(-196.3849802672,-5.71542802531407,132.342531260482));
#262634=CARTESIAN_POINT('Ctrl Pts',(-196.392271915766,-5.67302179942338,
132.492238033825));
#262635=CARTESIAN_POINT('Ctrl Pts',(-196.399563564333,-5.62478171151197,
132.640051566593));
#262636=CARTESIAN_POINT('Ctrl Pts',(-196.40685488677,-5.57654378120929,
132.787858488184));
#262637=CARTESIAN_POINT('Ctrl Pts',(-196.414146209206,-5.52247262718137,
132.933771971568));
#262638=CARTESIAN_POINT('Ctrl Pts',(-196.421437531643,-5.46275434354564,
133.077298263999));
#262639=CARTESIAN_POINT('Ctrl Pts',(-196.428730063846,-5.40302615153141,
133.220848370123));
#262640=CARTESIAN_POINT('Ctrl Pts',(-196.43602259605,-5.3376491138028,133.362010141883));
#262641=CARTESIAN_POINT('Ctrl Pts',(-196.443315128253,-5.26685704862626,
133.500310801052));
#262642=CARTESIAN_POINT('Ctrl Pts',(-196.450833098134,-5.19387655310716,
133.642886817326));
#262643=CARTESIAN_POINT('Ctrl Pts',(-196.458351068014,-5.11514103364721,
133.782421580859));
#262644=CARTESIAN_POINT('Ctrl Pts',(-196.465869037895,-5.03095663489101,
133.918426432597));
#262645=CARTESIAN_POINT('Ctrl Pts',(-196.473172341532,-4.9491760165358,
134.050547835598));
#262646=CARTESIAN_POINT('Ctrl Pts',(-196.480475645169,-4.86225370657967,
134.179337872425));
#262647=CARTESIAN_POINT('Ctrl Pts',(-196.487778948806,-4.77051280347123,
134.304380353856));
#262648=CARTESIAN_POINT('Ctrl Pts',(-196.495404251808,-4.67472708529593,
134.434935901931));
#262649=CARTESIAN_POINT('Ctrl Pts',(-196.503029554811,-4.57368851682401,
134.561405546719));
#262650=CARTESIAN_POINT('Ctrl Pts',(-196.510654857813,-4.467808907599,134.683357153744));
#262651=CARTESIAN_POINT('Ctrl Pts',(-196.518280160816,-4.361929298374,134.805308760768));
#262652=CARTESIAN_POINT('Ctrl Pts',(-196.525905463818,-4.25120902523955,
134.922742040811));
#262653=CARTESIAN_POINT('Ctrl Pts',(-196.53353076682,-4.13609959561202,
135.035271949381));
#262654=CARTESIAN_POINT('Ctrl Pts',(-196.540954033226,-4.024040053635,135.144820316129));
#262655=CARTESIAN_POINT('Ctrl Pts',(-196.548377299631,-3.90745582610583,
135.250079258993));
#262656=CARTESIAN_POINT('Ctrl Pts',(-196.555800566037,-3.78670891927233,
135.350652086797));
#262657=CARTESIAN_POINT('Ctrl Pts',(-196.563215058758,-3.66610472525497,
135.451106045871));
#262658=CARTESIAN_POINT('Ctrl Pts',(-196.570629551479,-3.5413479291358,
135.546884677918));
#262659=CARTESIAN_POINT('Ctrl Pts',(-196.578044044199,-3.41283794674118,
135.63762739189));
#262660=CARTESIAN_POINT('Ctrl Pts',(-196.585451390553,-3.28445182710626,
135.728282644617));
#262661=CARTESIAN_POINT('Ctrl Pts',(-196.592858736907,-3.15232002574301,
135.813911428368));
#262662=CARTESIAN_POINT('Ctrl Pts',(-196.60026608326,-3.0168755761589,135.894192866322));
#262663=CARTESIAN_POINT('Ctrl Pts',(-196.607667904936,-2.88153214615492,
135.974414427351));
#262664=CARTESIAN_POINT('Ctrl Pts',(-196.615069726611,-2.74288130716737,
136.049296394212));
#262665=CARTESIAN_POINT('Ctrl Pts',(-196.622471548287,-2.60138556712834,
136.118560810788));
#262666=CARTESIAN_POINT('Ctrl Pts',(-196.629869462598,-2.45996452158867,
136.187788663217));
#262667=CARTESIAN_POINT('Ctrl Pts',(-196.637267376909,-2.31570190033966,
136.251404707507));
#262668=CARTESIAN_POINT('Ctrl Pts',(-196.644665291221,-2.1690852351992,
136.309176673071));
#262669=CARTESIAN_POINT('Ctrl Pts',(-196.652061976133,-2.02249293508921,
136.366939037981));
#262670=CARTESIAN_POINT('Ctrl Pts',(-196.659458661045,-1.87354771447102,
136.418859114951));
#262671=CARTESIAN_POINT('Ctrl Pts',(-196.666855345957,-1.72275763897961,
136.464752536845));
#262672=CARTESIAN_POINT('Ctrl Pts',(-196.674251702893,-1.57197424967773,
136.510643923776));
#262673=CARTESIAN_POINT('Ctrl Pts',(-196.681648059828,-1.41934652527773,
136.550509078279));
#262674=CARTESIAN_POINT('Ctrl Pts',(-196.689044416763,-1.26539800768293,
136.584213422323));
#262675=CARTESIAN_POINT('Ctrl Pts',(-196.6964419061,-1.11142592017751,136.617922926587));
#262676=CARTESIAN_POINT('Ctrl Pts',(-196.703839395436,-0.956133001520995,
136.645469662442));
#262677=CARTESIAN_POINT('Ctrl Pts',(-196.711236884773,-0.800053158089319,
136.666770148359));
#262678=CARTESIAN_POINT('Ctrl Pts',(-196.718636967288,-0.643918601110704,
136.688078101128));
#262679=CARTESIAN_POINT('Ctrl Pts',(-196.726037049803,-0.486996939769862,
136.703135394011));
#262680=CARTESIAN_POINT('Ctrl Pts',(-196.733437132318,-0.329827225310558,
136.711910411173));
#262681=CARTESIAN_POINT('Ctrl Pts',(-196.740845351984,-0.172484686592092,
136.720695077368));
#262682=CARTESIAN_POINT('Ctrl Pts',(-196.748253571651,-0.0148939229818671,
136.723183651275));
#262683=CARTESIAN_POINT('Ctrl Pts',(-196.755661791317,0.142405248829505,
136.719396653602));
#262684=CARTESIAN_POINT('Ctrl Pts',(-196.763074570619,0.299801235656451,
136.715607325096));
#262685=CARTESIAN_POINT('Ctrl Pts',(-196.770487349921,0.456904901399012,
136.705534752304));
#262686=CARTESIAN_POINT('Ctrl Pts',(-196.777900129223,0.613182040216748,
136.689251300328));
#262687=CARTESIAN_POINT('Ctrl Pts',(-196.785323500252,0.769682475138877,
136.672944581791));
#262688=CARTESIAN_POINT('Ctrl Pts',(-196.792746871281,0.925353655985176,
136.650409313252));
#262689=CARTESIAN_POINT('Ctrl Pts',(-196.80017024231,1.07967122626914,136.621769027302));
#262690=CARTESIAN_POINT('Ctrl Pts',(-196.804106291751,1.16149410484353,
136.606583260475));
#262691=CARTESIAN_POINT('Ctrl Pts',(-196.808042341192,1.24293667063961,
136.589681992946));
#262692=CARTESIAN_POINT('Ctrl Pts',(-196.811978390633,1.32392266781222,
136.571089268383));
#262693=CARTESIAN_POINT('Ctrl Pts',(-196.819401657039,1.47665973097384,
136.536023970121));
#262694=CARTESIAN_POINT('Ctrl Pts',(-196.826824923444,1.62823368340216,
136.494833387375));
#262695=CARTESIAN_POINT('Ctrl Pts',(-196.83424818985,1.7781151043552,136.447607664982));
#262696=CARTESIAN_POINT('Ctrl Pts',(-196.841662682571,1.92781937791556,
136.40043775947));
#262697=CARTESIAN_POINT('Ctrl Pts',(-196.849077175292,2.07583474930553,
136.347247023744));
#262698=CARTESIAN_POINT('Ctrl Pts',(-196.856491668013,2.22164194905233,
136.288176589379));
#262699=CARTESIAN_POINT('Ctrl Pts',(-196.863899014366,2.36730861433047,
136.229163089323));
#262700=CARTESIAN_POINT('Ctrl Pts',(-196.87130636072,2.51077100136879,136.164281311885));
#262701=CARTESIAN_POINT('Ctrl Pts',(-196.878713707074,2.65152508222352,
136.093722138661));
#262702=CARTESIAN_POINT('Ctrl Pts',(-196.886115528749,2.79217418337481,
136.02321559113));
#262703=CARTESIAN_POINT('Ctrl Pts',(-196.893517350425,2.93011866807073,
135.947040245676));
#262704=CARTESIAN_POINT('Ctrl Pts',(-196.9009191721,3.06487468712279,135.865434981249));
#262705=CARTESIAN_POINT('Ctrl Pts',(-196.908317086411,3.19955956952096,
135.783872795607));
#262706=CARTESIAN_POINT('Ctrl Pts',(-196.915715000723,3.33105901987783,
135.696886592468));
#262707=CARTESIAN_POINT('Ctrl Pts',(-196.923112915034,3.45891409951243,
135.604760998232));
#262708=CARTESIAN_POINT('Ctrl Pts',(-196.930509599946,3.5867479319525,135.512650713597));
#262709=CARTESIAN_POINT('Ctrl Pts',(-196.937906284858,3.7109382930943,135.415402950964));
#262710=CARTESIAN_POINT('Ctrl Pts',(-196.94530296977,3.83105544775849,135.313345505398));
#262711=CARTESIAN_POINT('Ctrl Pts',(-196.952699326706,3.95116727630217,
135.211292585167));
#262712=CARTESIAN_POINT('Ctrl Pts',(-196.960095683641,4.0672059730031,135.104430647757));
#262713=CARTESIAN_POINT('Ctrl Pts',(-196.967492040577,4.17877532636475,
134.993127421085));
#262714=CARTESIAN_POINT('Ctrl Pts',(-196.974889529913,4.29036176127955,
134.881807153605));
#262715=CARTESIAN_POINT('Ctrl Pts',(-196.98228701925,4.39747722609323,134.766044506611));
#262716=CARTESIAN_POINT('Ctrl Pts',(-196.989684508586,4.49976289599391,
134.646243546852));
#262717=CARTESIAN_POINT('Ctrl Pts',(-196.997084591101,4.60208442197746,
134.526400591052));
#262718=CARTESIAN_POINT('Ctrl Pts',(-197.004484673616,4.69957253990412,
134.40251678771));
#262719=CARTESIAN_POINT('Ctrl Pts',(-197.011884756131,4.79190928011303,
134.275028566775));
#262720=CARTESIAN_POINT('Ctrl Pts',(-197.019292975798,4.88434755406011,
134.147400159435));
#262721=CARTESIAN_POINT('Ctrl Pts',(-197.026701195464,4.97162291886746,
134.01615972179));
#262722=CARTESIAN_POINT('Ctrl Pts',(-197.034109415131,5.05346085508178,
133.881772508856));
#262723=CARTESIAN_POINT('Ctrl Pts',(-197.041522194433,5.13534916118031,
133.747302582836));
#262724=CARTESIAN_POINT('Ctrl Pts',(-197.048934973735,5.2117931892249,133.609682347809));
#262725=CARTESIAN_POINT('Ctrl Pts',(-197.056347753037,5.28256507071789,
133.469400361384));
#262726=CARTESIAN_POINT('Ctrl Pts',(-197.063771124065,5.35343807439412,
133.328917933479));
#262727=CARTESIAN_POINT('Ctrl Pts',(-197.071194495094,5.41862259046731,
133.185766497095));
#262728=CARTESIAN_POINT('Ctrl Pts',(-197.078617866123,5.47793912291705,
133.04045398058));
#262729=CARTESIAN_POINT('Ctrl Pts',(-197.082553915564,5.50939017170535,
132.963405797591));
#262730=CARTESIAN_POINT('Ctrl Pts',(-197.086489965005,5.53919235282093,
132.88575031248));
#262731=CARTESIAN_POINT('Ctrl Pts',(-197.090426014446,5.56732467673674,
132.80756467764));
#262732=CARTESIAN_POINT('Ctrl Pts',(-197.097849280852,5.62038136165785,
132.660109010435));
#262733=CARTESIAN_POINT('Ctrl Pts',(-197.105272547257,5.66765598150285,
132.510321035348));
#262734=CARTESIAN_POINT('Ctrl Pts',(-197.112695813663,5.70893821283385,
132.35869489453));
#262735=CARTESIAN_POINT('Ctrl Pts',(-197.120110306384,5.75017165199582,
132.207247963219));
#262736=CARTESIAN_POINT('Ctrl Pts',(-197.127524799105,5.7854267033022,132.053967547337));
#262737=CARTESIAN_POINT('Ctrl Pts',(-197.134939291826,5.81454142691153,
131.899366808064));
#262738=CARTESIAN_POINT('Ctrl Pts',(-197.14234663818,5.84362808865393,131.744915078805));
#262739=CARTESIAN_POINT('Ctrl Pts',(-197.149753984533,5.86658613620568,
131.589145923993));
#262740=CARTESIAN_POINT('Ctrl Pts',(-197.157161330887,5.88330372424391,
131.432586572775));
#262741=CARTESIAN_POINT('Ctrl Pts',(-197.164563152563,5.90000884367436,
131.276143989427));
#262742=CARTESIAN_POINT('Ctrl Pts',(-197.171964974238,5.91048273160501,
131.118912752756));
#262743=CARTESIAN_POINT('Ctrl Pts',(-197.179366795914,5.91466483135784,
130.961429058695));
#262744=CARTESIAN_POINT('Ctrl Pts',(-197.186764710225,5.91884472341276,
130.804028499051));
#262745=CARTESIAN_POINT('Ctrl Pts',(-197.194162624536,5.91673943210462,
130.646376119654));
#262746=CARTESIAN_POINT('Ctrl Pts',(-197.201560538848,5.90834035411677,
130.489011886135));
#262747=CARTESIAN_POINT('Ctrl Pts',(-197.20895722376,5.8999426719033,130.331673803696));
#262748=CARTESIAN_POINT('Ctrl Pts',(-197.216353908672,5.8852532987146,130.1746241445));
#262749=CARTESIAN_POINT('Ctrl Pts',(-197.223750593585,5.86431573546309,
130.018401638166));
#262750=CARTESIAN_POINT('Ctrl Pts',(-197.23114695052,5.84337910060514,129.862186058901));
#262751=CARTESIAN_POINT('Ctrl Pts',(-197.238543307455,5.81619487614345,
129.706797929561));
#262752=CARTESIAN_POINT('Ctrl Pts',(-197.245939664391,5.7828582799976,129.552769360021));
#262753=CARTESIAN_POINT('Ctrl Pts',(-197.253337153727,5.74951657993387,
129.398717208314));
#262754=CARTESIAN_POINT('Ctrl Pts',(-197.260734643064,5.71002071162072,
129.246025395738));
#262755=CARTESIAN_POINT('Ctrl Pts',(-197.268132132401,5.66451667428286,
129.09521421972));
#262756=CARTESIAN_POINT('Ctrl Pts',(-197.275532214916,5.61899668557493,
128.944350177076));
#262757=CARTESIAN_POINT('Ctrl Pts',(-197.282932297431,5.56746444227009,
128.79536844072));
#262758=CARTESIAN_POINT('Ctrl Pts',(-197.290332379946,5.51011525487502,
128.648772428581));
#262759=CARTESIAN_POINT('Ctrl Pts',(-197.297740599612,5.45270300615285,
128.502015219055));
#262760=CARTESIAN_POINT('Ctrl Pts',(-197.305148819279,5.38946117553666,
128.357649320603));
#262761=CARTESIAN_POINT('Ctrl Pts',(-197.312557038945,5.32063281077705,
128.216157175913));
#262762=CARTESIAN_POINT('Ctrl Pts',(-197.319969818248,5.2517620833074,128.07457794517));
#262763=CARTESIAN_POINT('Ctrl Pts',(-197.32738259755,5.17729814637798,127.935876320775));
#262764=CARTESIAN_POINT('Ctrl Pts',(-197.334795376852,5.09752886885128,
127.80050809227));
#262765=CARTESIAN_POINT('Ctrl Pts',(-197.34221874788,5.01764561323994,127.664946443292));
#262766=CARTESIAN_POINT('Ctrl Pts',(-197.349642118909,4.93244207870739,
127.532728015764));
#262767=CARTESIAN_POINT('Ctrl Pts',(-197.357065489938,4.84224857777326,
127.40427837245));
#262768=CARTESIAN_POINT('Ctrl Pts',(-197.361001539378,4.79442581941926,
127.336171289465));
#262769=CARTESIAN_POINT('Ctrl Pts',(-197.364937588819,4.74520086733818,
127.26912318392));
#262770=CARTESIAN_POINT('Ctrl Pts',(-197.368873638259,4.69462728667099,
127.203193417651));
#262771=CARTESIAN_POINT('Ctrl Pts',(-197.376296904665,4.59924709187124,
127.078851936054));
#262772=CARTESIAN_POINT('Ctrl Pts',(-197.38372017107,4.49877931298799,126.958114400183));
#262773=CARTESIAN_POINT('Ctrl Pts',(-197.391143437476,4.39352600085202,
126.841424857004));
#262774=CARTESIAN_POINT('Ctrl Pts',(-197.398557930197,4.28839708939024,
126.724873231176));
#262775=CARTESIAN_POINT('Ctrl Pts',(-197.405972422918,4.17849415076658,
126.612360349171));
#262776=CARTESIAN_POINT('Ctrl Pts',(-197.413386915639,4.06416138957402,
126.504299831717));
#262777=CARTESIAN_POINT('Ctrl Pts',(-197.420794261992,3.94993882660157,
126.396343467059));
#262778=CARTESIAN_POINT('Ctrl Pts',(-197.428201608346,3.83129521052947,
126.292831178398));
#262779=CARTESIAN_POINT('Ctrl Pts',(-197.4356089547,3.70861365904349,126.194142044607));
#262780=CARTESIAN_POINT('Ctrl Pts',(-197.443010776375,3.58602360808748,
126.095526516895));
#262781=CARTESIAN_POINT('Ctrl Pts',(-197.450412598051,3.45940190792309,
126.001727214337));
#262782=CARTESIAN_POINT('Ctrl Pts',(-197.457814419726,3.32916694301156,
125.91308491198));
#262783=CARTESIAN_POINT('Ctrl Pts',(-197.465212334038,3.19900072812314,
125.824489403203));
#262784=CARTESIAN_POINT('Ctrl Pts',(-197.472610248349,3.06522535501235,
125.741045682467));
#262785=CARTESIAN_POINT('Ctrl Pts',(-197.48000816266,2.92829046175452,125.6630528526));
#262786=CARTESIAN_POINT('Ctrl Pts',(-197.487404847572,2.79137832459229,
125.585072983727));
#262787=CARTESIAN_POINT('Ctrl Pts',(-197.494801532485,2.65130803341802,
125.512542392469));
#262788=CARTESIAN_POINT('Ctrl Pts',(-197.502198217397,2.50855635002252,
125.445715676794));
#262789=CARTESIAN_POINT('Ctrl Pts',(-197.509594574332,2.36581099638625,
125.378891924286));
#262790=CARTESIAN_POINT('Ctrl Pts',(-197.516990931268,2.22038482501944,
125.317771702748));
#262791=CARTESIAN_POINT('Ctrl Pts',(-197.524387288203,2.0727769826413,125.262562521033));
#262792=CARTESIAN_POINT('Ctrl Pts',(-197.53178477754,1.9251465411261,125.207344886652));
#262793=CARTESIAN_POINT('Ctrl Pts',(-197.539182266876,1.77533411318653,
125.158040224843));
#262794=CARTESIAN_POINT('Ctrl Pts',(-197.546579756213,1.62385635592891,
125.11480693579));
#262795=CARTESIAN_POINT('Ctrl Pts',(-197.553979838728,1.47232549837808,
125.071558491375));
#262796=CARTESIAN_POINT('Ctrl Pts',(-197.561379921243,1.31912850795002,
125.034385759555));
#262797=CARTESIAN_POINT('Ctrl Pts',(-197.568780003758,1.16479449450476,
125.003396529755));
#262798=CARTESIAN_POINT('Ctrl Pts',(-197.576188223424,1.01029077494556,
124.972373224112));
#262799=CARTESIAN_POINT('Ctrl Pts',(-197.583596443091,0.854647901707854,
124.947547072864));
#262800=CARTESIAN_POINT('Ctrl Pts',(-197.591004662757,0.698403140736846,
124.928974365113));
#262801=CARTESIAN_POINT('Ctrl Pts',(-197.598417442059,0.542062213722543,
124.910390226172));
#262802=CARTESIAN_POINT('Ctrl Pts',(-197.605830221361,0.38511903209279,
124.898067229277));
#262803=CARTESIAN_POINT('Ctrl Pts',(-197.613243000663,0.228112664648767,
124.892009547583));
#262804=CARTESIAN_POINT('Ctrl Pts',(-197.620666371692,0.0708819591442937,
124.88594321039));
#262805=CARTESIAN_POINT('Ctrl Pts',(-197.628089742721,-0.0864117401809329,
124.886160067387));
#262806=CARTESIAN_POINT('Ctrl Pts',(-197.63551311375,-0.243231853336173,
124.892612244367));
#262807=CARTESIAN_POINT('Ctrl Pts',(-197.639449163191,-0.326381640180508,
124.896033343419));
#262808=CARTESIAN_POINT('Ctrl Pts',(-197.643385212631,-0.409398399272633,
124.901206550941));
#262809=CARTESIAN_POINT('Ctrl Pts',(-197.647321262072,-0.492203234551277,
124.908118887583));
#262810=CARTESIAN_POINT('Ctrl Pts',(-197.654744528478,-0.64837056963286,
124.921155338763));
#262811=CARTESIAN_POINT('Ctrl Pts',(-197.662167794883,-0.804255766574924,
124.940420139216));
#262812=CARTESIAN_POINT('Ctrl Pts',(-197.669591061289,-0.959321970235522,
124.965899183256));
#262813=CARTESIAN_POINT('Ctrl Pts',(-197.67700555401,-1.11420489852084,
124.991348113182));
#262814=CARTESIAN_POINT('Ctrl Pts',(-197.684420046731,-1.26827039553683,
125.022996607056));
#262815=CARTESIAN_POINT('Ctrl Pts',(-197.691834539452,-1.42098441946168,
125.060778647911));
#262816=CARTESIAN_POINT('Ctrl Pts',(-197.699241885806,-1.57355125186026,
125.098524273012));
#262817=CARTESIAN_POINT('Ctrl Pts',(-197.706649232159,-1.72476884444938,
125.142391586927));
#262818=CARTESIAN_POINT('Ctrl Pts',(-197.714056578513,-1.87411118297151,
125.192263163284));
#262819=CARTESIAN_POINT('Ctrl Pts',(-197.721458400189,-2.02334213634406,
125.242097543538));
#262820=CARTESIAN_POINT('Ctrl Pts',(-197.728860221864,-2.17070026796815,
125.297927151792));
#262821=CARTESIAN_POINT('Ctrl Pts',(-197.73626204354,-2.31567272712397,
125.359584186586));
#262822=CARTESIAN_POINT('Ctrl Pts',(-197.743659957851,-2.46056865644708,
125.421208673112));
#262823=CARTESIAN_POINT('Ctrl Pts',(-197.751057872162,-2.60308107876267,
125.488654313942));
#262824=CARTESIAN_POINT('Ctrl Pts',(-197.758455786474,-2.74271531002859,
125.561704488214));
#262825=CARTESIAN_POINT('Ctrl Pts',(-197.765852471386,-2.88232633661789,
125.634742522872));
#262826=CARTESIAN_POINT('Ctrl Pts',(-197.773249156298,-3.01905979100342,
125.713383069601));
#262827=CARTESIAN_POINT('Ctrl Pts',(-197.780645841211,-3.15244377131063,
125.797362631624));
#262828=CARTESIAN_POINT('Ctrl Pts',(-197.788042198146,-3.28582183723238,
125.881338469906));
#262829=CARTESIAN_POINT('Ctrl Pts',(-197.795438555081,-3.41585040848234,
125.970652653875));
#262830=CARTESIAN_POINT('Ctrl Pts',(-197.802834912017,-3.54208510099192,
126.064997400864));
#262831=CARTESIAN_POINT('Ctrl Pts',(-197.810232401353,-3.66833912035446,
126.159356592273));
#262832=CARTESIAN_POINT('Ctrl Pts',(-197.81762989069,-3.79079780538828,
126.258747656766));
#262833=CARTESIAN_POINT('Ctrl Pts',(-197.825027380027,-3.90904862374609,
126.362821535256));
#262834=CARTESIAN_POINT('Ctrl Pts',(-197.832427462542,-4.02734089474615,
126.466931896683));
#262835=CARTESIAN_POINT('Ctrl Pts',(-197.839827545057,-4.14142208218471,
126.575728093952));
#262836=CARTESIAN_POINT('Ctrl Pts',(-197.847227627572,-4.2509155029613,
126.688823234771));
#262837=CARTESIAN_POINT('Ctrl Pts',(-197.854635847238,-4.36052932300976,
126.802042735323));
#262838=CARTESIAN_POINT('Ctrl Pts',(-197.862044066905,-4.46554504194146,
126.919570351452));
#262839=CARTESIAN_POINT('Ctrl Pts',(-197.869452286571,-4.56562489677327,
127.040984491736));
#262840=CARTESIAN_POINT('Ctrl Pts',(-197.876865065873,-4.66576634908582,
127.162473360399));
#262841=CARTESIAN_POINT('Ctrl Pts',(-197.884277845175,-4.76096565859968,
127.287853223139));
#262842=CARTESIAN_POINT('Ctrl Pts',(-197.891690624478,-4.8509279344683,
127.416672801799));
#262843=CARTESIAN_POINT('Ctrl Pts',(-197.899113995506,-4.94101875265536,
127.545676443914));
#262844=CARTESIAN_POINT('Ctrl Pts',(-197.906537366535,-5.02585739131891,
127.678129304451));
#262845=CARTESIAN_POINT('Ctrl Pts',(-197.913960737564,-5.10519409379517,
127.813554066286));
#262846=CARTESIAN_POINT('Ctrl Pts',(-197.917896787004,-5.14726031710364,
127.88535952448));
#262847=CARTESIAN_POINT('Ctrl Pts',(-197.921832836445,-5.18778053718604,
127.958000120082));
#262848=CARTESIAN_POINT('Ctrl Pts',(-197.925768885886,-5.22672302868686,
128.031402459949));
#262849=CARTESIAN_POINT('Ctrl Pts',(-197.933618442971,-5.30438498764153,
128.177786763732));
#262850=CARTESIAN_POINT('Ctrl Pts',(-197.941468000057,-5.37598238513895,
128.327603249052));
#262851=CARTESIAN_POINT('Ctrl Pts',(-197.949317557143,-5.44121712518422,
128.480336788277));
#262852=CARTESIAN_POINT('Ctrl Pts',(-197.957153559567,-5.50633921749837,
128.632806586333));
#262853=CARTESIAN_POINT('Ctrl Pts',(-197.964989561992,-5.56512043354741,
128.788183113502));
#262854=CARTESIAN_POINT('Ctrl Pts',(-197.972825564417,-5.6173084054525,
128.94592664227));
#262855=CARTESIAN_POINT('Ctrl Pts',(-197.98064289557,-5.66937202622657,
129.103294306917));
#262856=CARTESIAN_POINT('Ctrl Pts',(-197.988460226724,-5.71487364188634,
129.263017430468));
#262857=CARTESIAN_POINT('Ctrl Pts',(-197.996277557878,-5.75360906848479,
129.424536987695));
#262858=CARTESIAN_POINT('Ctrl Pts',(-198.004083819218,-5.79228964337747,
129.585827823465));
#262859=CARTESIAN_POINT('Ctrl Pts',(-198.011890080558,-5.82422305311737,
129.748909723495));
#262860=CARTESIAN_POINT('Ctrl Pts',(-198.019696341898,-5.84925431259238,
129.913207123986));
#262861=CARTESIAN_POINT('Ctrl Pts',(-198.027487193755,-5.87423616060821,
130.07718020303));
#262862=CARTESIAN_POINT('Ctrl Pts',(-198.035278045612,-5.89234298762165,
130.242363691703));
#262863=CARTESIAN_POINT('Ctrl Pts',(-198.04306889747,-5.90347053031272,
130.40817094048));
#262864=CARTESIAN_POINT('Ctrl Pts',(-198.049254200898,-5.91230489518304,
130.539808425459));
#262865=CARTESIAN_POINT('Ctrl Pts',(-198.055439504327,-5.91674112270733,
130.671838733572));
#262866=CARTESIAN_POINT('Ctrl Pts',(-198.061624807755,-5.91674998668501,
130.803963675558));
#262867=CARTESIAN_POINT('',(-199.811624807792,-5.91674748832781,130.809812394026));
#262868=CARTESIAN_POINT('Ctrl Pts',(-198.061624807792,-5.91674998668506,
130.803963676344));
#262869=CARTESIAN_POINT('Ctrl Pts',(-198.069335284224,-5.91676103632174,
130.96866800542));
#262870=CARTESIAN_POINT('Ctrl Pts',(-198.077045760657,-5.90989046074581,
131.133254346916));
#262871=CARTESIAN_POINT('Ctrl Pts',(-198.084756237089,-5.89619368993992,
131.297138999004));
#262872=CARTESIAN_POINT('Ctrl Pts',(-198.09247513413,-5.88248196089642,
131.461202629451));
#262873=CARTESIAN_POINT('Ctrl Pts',(-198.10019403117,-5.86192918777857,
131.624562717793));
#262874=CARTESIAN_POINT('Ctrl Pts',(-198.107912928211,-5.83464232566053,
131.786643414988));
#262875=CARTESIAN_POINT('Ctrl Pts',(-198.115938226668,-5.80627231226227,
131.955157901231));
#262876=CARTESIAN_POINT('Ctrl Pts',(-198.123963525126,-5.77062274114287,
132.122288952053));
#262877=CARTESIAN_POINT('Ctrl Pts',(-198.131988823583,-5.72787106095795,
132.287406021976));
#262878=CARTESIAN_POINT('Ctrl Pts',(-198.13973298131,-5.68661704950663,
132.446738742092));
#262879=CARTESIAN_POINT('Ctrl Pts',(-198.147477139037,-5.63875026118319,
132.604195921967));
#262880=CARTESIAN_POINT('Ctrl Pts',(-198.155221296764,-5.58447970808055,
132.759230677835));
#262881=CARTESIAN_POINT('Ctrl Pts',(-198.162974554244,-5.53014538450852,
132.914447606882));
#262882=CARTESIAN_POINT('Ctrl Pts',(-198.170727811723,-5.46939239828204,
133.067236130232));
#262883=CARTESIAN_POINT('Ctrl Pts',(-198.178481069202,-5.40247702272164,
133.217071247017));
#262884=CARTESIAN_POINT('Ctrl Pts',(-198.186248543322,-5.33543894881967,
133.367181106642));
#262885=CARTESIAN_POINT('Ctrl Pts',(-198.194016017441,-5.26221604894185,
133.514326447479));
#262886=CARTESIAN_POINT('Ctrl Pts',(-198.201783491561,-5.18311009938688,
133.658007452781));
#262887=CARTESIAN_POINT('Ctrl Pts',(-198.202594497607,-5.17485060571508,
133.673009261883));
#262888=CARTESIAN_POINT('Ctrl Pts',(-198.203405503652,-5.16652701566992,
133.687973331658));
#262889=CARTESIAN_POINT('Ctrl Pts',(-198.204216509698,-5.15813969907268,
133.702899112627));
#262890=CARTESIAN_POINT('Ctrl Pts',(-198.211639776104,-5.08136926578121,
133.839517142834));
#262891=CARTESIAN_POINT('Ctrl Pts',(-198.219063042509,-4.9990513182663,
133.973289646283));
#262892=CARTESIAN_POINT('Ctrl Pts',(-198.226486308914,-4.91142183868873,
134.103734207348));
#262893=CARTESIAN_POINT('Ctrl Pts',(-198.233900801635,-4.82389592987909,
134.234024593775));
#262894=CARTESIAN_POINT('Ctrl Pts',(-198.241315294356,-4.73107119111244,
134.360994560333));
#262895=CARTESIAN_POINT('Ctrl Pts',(-198.248729787077,-4.63322964933905,
134.484185827951));
#262896=CARTESIAN_POINT('Ctrl Pts',(-198.256137133431,-4.53548241092728,
134.607258359188));
#262897=CARTESIAN_POINT('Ctrl Pts',(-198.263544479785,-4.43272822641348,
134.726559151738));
#262898=CARTESIAN_POINT('Ctrl Pts',(-198.270951826138,-4.32529254368441,
134.841658596914));
#262899=CARTESIAN_POINT('Ctrl Pts',(-198.278353647814,-4.21793699054084,
134.956672196582));
#262900=CARTESIAN_POINT('Ctrl Pts',(-198.285755469489,-4.10590714512817,
135.067490416427));
#262901=CARTESIAN_POINT('Ctrl Pts',(-198.293157291165,-3.98956880068971,
135.173716559471));
#262902=CARTESIAN_POINT('Ctrl Pts',(-198.300555205476,-3.87329187035737,
135.279886626562));
#262903=CARTESIAN_POINT('Ctrl Pts',(-198.307953119787,-3.75271124559411,
135.381469193533));
#262904=CARTESIAN_POINT('Ctrl Pts',(-198.315351034099,-3.62822957043913,
135.478104378909));
#262905=CARTESIAN_POINT('Ctrl Pts',(-198.322747719011,-3.50376858188041,
135.57472350527));
#262906=CARTESIAN_POINT('Ctrl Pts',(-198.330144403923,-3.37540812416725,
135.666396653101));
#262907=CARTESIAN_POINT('Ctrl Pts',(-198.337541088835,-3.24358400599151,
135.752804146452));
#262908=CARTESIAN_POINT('Ctrl Pts',(-198.344937445771,-3.11176573303569,
135.839207808404));
#262909=CARTESIAN_POINT('Ctrl Pts',(-198.352333802706,-2.97648441719638,
135.920346075478));
#262910=CARTESIAN_POINT('Ctrl Pts',(-198.359730159642,-2.83820470770205,
135.995942707804));
#262911=CARTESIAN_POINT('Ctrl Pts',(-198.367127648978,-2.69990382723119,
136.071550914167));
#262912=CARTESIAN_POINT('Ctrl Pts',(-198.374525138315,-2.55860396661923,
136.141615617351));
#262913=CARTESIAN_POINT('Ctrl Pts',(-198.381922627651,-2.41479407700068,
136.205906704399));
#262914=CARTESIAN_POINT('Ctrl Pts',(-198.389322710166,-2.27093377504764,
136.270220328589));
#262915=CARTESIAN_POINT('Ctrl Pts',(-198.396722792681,-2.12456203282009,
136.328756154751));
#262916=CARTESIAN_POINT('Ctrl Pts',(-198.404122875196,-1.97618731005907,
136.381332401434));
#262917=CARTESIAN_POINT('Ctrl Pts',(-198.411531094863,-1.82764943403772,
136.433966461105));
#262918=CARTESIAN_POINT('Ctrl Pts',(-198.418939314529,-1.67710453105635,
136.480627729429));
#262919=CARTESIAN_POINT('Ctrl Pts',(-198.426347534195,-1.52507644250729,
136.521184246734));
#262920=CARTESIAN_POINT('Ctrl Pts',(-198.433760313498,-1.37295478320602,
136.561765725898));
#262921=CARTESIAN_POINT('Ctrl Pts',(-198.441173092799,-1.21934848271258,
136.596234885463));
#262922=CARTESIAN_POINT('Ctrl Pts',(-198.448585872102,-1.06479056249309,
136.624511098484));
#262923=CARTESIAN_POINT('Ctrl Pts',(-198.45600924313,-0.910011802669364,
136.652827713883));
#262924=CARTESIAN_POINT('Ctrl Pts',(-198.463432614159,-0.754279076069821,
136.67493365743));
#262925=CARTESIAN_POINT('Ctrl Pts',(-198.470855985188,-0.598130326265068,
136.690800176017));
#262926=CARTESIAN_POINT('Ctrl Pts',(-198.474792034629,-0.515336512371863,
136.699212984885));
#262927=CARTESIAN_POINT('Ctrl Pts',(-198.47872808407,-0.432425748835829,
136.705872538709));
#262928=CARTESIAN_POINT('Ctrl Pts',(-198.482664133511,-0.349477975144942,
136.710780489823));
#262929=CARTESIAN_POINT('Ctrl Pts',(-198.490087399917,-0.193041062691021,
136.720036732451));
#262930=CARTESIAN_POINT('Ctrl Pts',(-198.497510666322,-0.0359996055459115,
136.72308761753));
#262931=CARTESIAN_POINT('Ctrl Pts',(-198.504933932728,0.1211129722417,136.719870926107));
#262932=CARTESIAN_POINT('Ctrl Pts',(-198.512348425449,0.278039856009755,
136.716658036546));
#262933=CARTESIAN_POINT('Ctrl Pts',(-198.51976291817,0.435037323525875,
136.707192323227));
#262934=CARTESIAN_POINT('Ctrl Pts',(-198.527177410891,0.591567369173254,
136.691463352378));
#262935=CARTESIAN_POINT('Ctrl Pts',(-198.534584757244,0.74794654526894,
136.675749541703));
#262936=CARTESIAN_POINT('Ctrl Pts',(-198.541992103598,0.903858827456171,
136.653784528579));
#262937=CARTESIAN_POINT('Ctrl Pts',(-198.549399449952,1.05876686124651,
136.62560990754));
#262938=CARTESIAN_POINT('Ctrl Pts',(-198.556801271627,1.2135593587809,136.597456300197));
#262939=CARTESIAN_POINT('Ctrl Pts',(-198.564203093303,1.36734873359921,
136.563102373113));
#262940=CARTESIAN_POINT('Ctrl Pts',(-198.571604914978,1.5196035131144,136.522641454096));
#262941=CARTESIAN_POINT('Ctrl Pts',(-198.57900282929,1.67177791851663,136.482201894084));
#262942=CARTESIAN_POINT('Ctrl Pts',(-198.586400743601,1.82241898210764,
136.43566185819));
#262943=CARTESIAN_POINT('Ctrl Pts',(-198.593798657912,1.97100628646992,
136.383165577519));
#262944=CARTESIAN_POINT('Ctrl Pts',(-198.601195342825,2.11956889831808,
136.330678020777));
#262945=CARTESIAN_POINT('Ctrl Pts',(-198.608592027737,2.26607807668035,
136.27223630799));
#262946=CARTESIAN_POINT('Ctrl Pts',(-198.615988712649,2.41002930388112,
136.208034304692));
#262947=CARTESIAN_POINT('Ctrl Pts',(-198.623385069584,2.55397414813362,
136.143835148178));
#262948=CARTESIAN_POINT('Ctrl Pts',(-198.63078142652,2.6953609258196,136.073876361061));
#262949=CARTESIAN_POINT('Ctrl Pts',(-198.638177783455,2.83370607425544,
135.998399551501));
#262950=CARTESIAN_POINT('Ctrl Pts',(-198.645575272792,2.97207240368668,
135.922911186248));
#262951=CARTESIAN_POINT('Ctrl Pts',(-198.652972762128,3.10739584891269,
135.84190329519));
#262952=CARTESIAN_POINT('Ctrl Pts',(-198.660370251465,3.23921851935599,
135.755662865093));
#262953=CARTESIAN_POINT('Ctrl Pts',(-198.66777033398,3.37108740003226,135.669392203545));
#262954=CARTESIAN_POINT('Ctrl Pts',(-198.675170416495,3.49945275040591,
135.577885555203));
#262955=CARTESIAN_POINT('Ctrl Pts',(-198.68257049901,3.62388679768368,135.481472444332));
#262956=CARTESIAN_POINT('Ctrl Pts',(-198.689978718676,3.74845767298839,
135.384953317334));
#262957=CARTESIAN_POINT('Ctrl Pts',(-198.697386938343,3.86908831687014,
135.283517182095));
#262958=CARTESIAN_POINT('Ctrl Pts',(-198.704795158009,3.98538455885265,
135.17753343379));
#262959=CARTESIAN_POINT('Ctrl Pts',(-198.712207937311,4.10175237923126,
135.071484454256));
#262960=CARTESIAN_POINT('Ctrl Pts',(-198.719620716613,4.21378021684949,
134.960882545995));
#262961=CARTESIAN_POINT('Ctrl Pts',(-198.727033495915,4.32111212685275,
134.846132574229));
#262962=CARTESIAN_POINT('Ctrl Pts',(-198.734456866944,4.42859739772255,
134.731218642321));
#262963=CARTESIAN_POINT('Ctrl Pts',(-198.741880237973,4.53137309681198,
134.612145091307));
#262964=CARTESIAN_POINT('Ctrl Pts',(-198.749303609002,4.62912426167716,
134.489348966591));
#262965=CARTESIAN_POINT('Ctrl Pts',(-198.753239658442,4.68095427479721,
134.424239514812));
#262966=CARTESIAN_POINT('Ctrl Pts',(-198.757175707883,4.73137243893255,
134.35808399281));
#262967=CARTESIAN_POINT('Ctrl Pts',(-198.761111757324,4.78033693499349,
134.290950549066));
#262968=CARTESIAN_POINT('Ctrl Pts',(-198.76853502373,4.87268244643274,134.164338969331));
#262969=CARTESIAN_POINT('Ctrl Pts',(-198.775958290135,4.9601339859933,134.033864621697));
#262970=CARTESIAN_POINT('Ctrl Pts',(-198.783381556541,5.04235087838011,
133.899942660058));
#262971=CARTESIAN_POINT('Ctrl Pts',(-198.790796049262,5.12447059722781,
133.766178983056));
#262972=CARTESIAN_POINT('Ctrl Pts',(-198.798210541983,5.20136779059828,
133.628976117973));
#262973=CARTESIAN_POINT('Ctrl Pts',(-198.805625034704,5.27274287508696,
133.488781064463));
#262974=CARTESIAN_POINT('Ctrl Pts',(-198.813032381058,5.34404916558199,
133.348721136224));
#262975=CARTESIAN_POINT('Ctrl Pts',(-198.820439727411,5.40984377485081,
133.205675091435));
#262976=CARTESIAN_POINT('Ctrl Pts',(-198.827847073765,5.46987124432698,
133.060117504508));
#262977=CARTESIAN_POINT('Ctrl Pts',(-198.835248895441,5.52985394305153,
132.914668479921));
#262978=CARTESIAN_POINT('Ctrl Pts',(-198.842650717116,5.58407792484558,
132.766711986614));
#262979=CARTESIAN_POINT('Ctrl Pts',(-198.850052538791,5.63233443512196,
132.616745613487));
#262980=CARTESIAN_POINT('Ctrl Pts',(-198.857450453103,5.68056547116234,
132.46685840644));
#262981=CARTESIAN_POINT('Ctrl Pts',(-198.864848367414,5.7228351953659,132.314963787059));
#262982=CARTESIAN_POINT('Ctrl Pts',(-198.872246281726,5.7589836551197,132.161577557692));
#262983=CARTESIAN_POINT('Ctrl Pts',(-198.879642966638,5.79512610765524,
132.008216818333));
#262984=CARTESIAN_POINT('Ctrl Pts',(-198.88703965155,5.82514922912225,131.853365323941));
#262985=CARTESIAN_POINT('Ctrl Pts',(-198.894436336462,5.84894341995819,
131.697552328582));
#262986=CARTESIAN_POINT('Ctrl Pts',(-198.901832693398,5.87273655573477,
131.541746242135));
#262987=CARTESIAN_POINT('Ctrl Pts',(-198.909229050333,5.89030125370091,
131.384979108511));
#262988=CARTESIAN_POINT('Ctrl Pts',(-198.916625407269,5.90157940820071,
131.227788357802));
#262989=CARTESIAN_POINT('Ctrl Pts',(-198.924022896605,5.9128592894148,131.070573540788));
#262990=CARTESIAN_POINT('Ctrl Pts',(-198.931420385942,5.91785068400867,
130.912935349915));
#262991=CARTESIAN_POINT('Ctrl Pts',(-198.938817875279,5.91654754103343,
130.75541414485));
#262992=CARTESIAN_POINT('Ctrl Pts',(-198.946217957794,5.91524394124343,
130.597837720972));
#262993=CARTESIAN_POINT('Ctrl Pts',(-198.953618040309,5.90764141376477,
130.440378737603));
#262994=CARTESIAN_POINT('Ctrl Pts',(-198.961018122824,5.89378597505109,
130.283575208025));
#262995=CARTESIAN_POINT('Ctrl Pts',(-198.96842634249,5.87991530085824,130.126599256847));
#262996=CARTESIAN_POINT('Ctrl Pts',(-198.975834562157,5.85977801704612,
129.970280570899));
#262997=CARTESIAN_POINT('Ctrl Pts',(-198.983242781823,5.83347184746589,
129.815150444083));
#262998=CARTESIAN_POINT('Ctrl Pts',(-198.990655561125,5.80714948687722,
129.659924837261));
#262999=CARTESIAN_POINT('Ctrl Pts',(-198.998068340427,5.77465075171243,
129.505889611662));
#263000=CARTESIAN_POINT('Ctrl Pts',(-199.005481119729,5.73612386966094,
129.353563073315));
#263001=CARTESIAN_POINT('Ctrl Pts',(-199.012904490758,5.6975419385936,129.201018883665));
#263002=CARTESIAN_POINT('Ctrl Pts',(-199.020327861787,5.65291476358045,
129.050188614405));
#263003=CARTESIAN_POINT('Ctrl Pts',(-199.027751232816,5.60243979840348,
128.901573486076));
#263004=CARTESIAN_POINT('Ctrl Pts',(-199.031687282256,5.57567676073842,
128.82277417907));
#263005=CARTESIAN_POINT('Ctrl Pts',(-199.035623331697,5.54727049570574,
128.744597274093));
#263006=CARTESIAN_POINT('Ctrl Pts',(-199.039559381137,5.51725573431446,
128.667114790649));
#263007=CARTESIAN_POINT('Ctrl Pts',(-199.046982647543,5.46064883105527,
128.520985245009));
#263008=CARTESIAN_POINT('Ctrl Pts',(-199.054405913948,5.39814676042029,
128.376885216112));
#263009=CARTESIAN_POINT('Ctrl Pts',(-199.061829180354,5.32991465982133,
128.235325724552));
#263010=CARTESIAN_POINT('Ctrl Pts',(-199.069243673075,5.26176320389876,
128.093933544556));
#263011=CARTESIAN_POINT('Ctrl Pts',(-199.076658165796,5.18789535905273,
127.955076257988));
#263012=CARTESIAN_POINT('Ctrl Pts',(-199.084072658517,5.10852526660425,
127.819247527084));
#263013=CARTESIAN_POINT('Ctrl Pts',(-199.09148000487,5.02923167403911,127.683549713025));
#263014=CARTESIAN_POINT('Ctrl Pts',(-199.098887351224,4.94444657871635,
127.550874963544));
#263015=CARTESIAN_POINT('Ctrl Pts',(-199.106294697578,4.85443117193422,
127.421694722232));
#263016=CARTESIAN_POINT('Ctrl Pts',(-199.113696519254,4.7644829020383,127.292610828418));
#263017=CARTESIAN_POINT('Ctrl Pts',(-199.121098340929,4.66931230052762,
127.16701655816));
#263018=CARTESIAN_POINT('Ctrl Pts',(-199.128500162604,4.56922516608224,
127.045356501561));
#263019=CARTESIAN_POINT('Ctrl Pts',(-199.135898076916,4.46919086685664,
126.92376066836));
#263020=CARTESIAN_POINT('Ctrl Pts',(-199.143295991227,4.36424544012047,
126.806095200239));
#263021=CARTESIAN_POINT('Ctrl Pts',(-199.150693905538,4.25473638670253,
126.692773473631));
#263022=CARTESIAN_POINT('Ctrl Pts',(-199.158090590451,4.14524553170241,
126.579470579038));
#263023=CARTESIAN_POINT('Ctrl Pts',(-199.165487275363,4.0311928143572,126.470510261472));
#263024=CARTESIAN_POINT('Ctrl Pts',(-199.172883960275,3.91296426986117,
126.3662708049));
#263025=CARTESIAN_POINT('Ctrl Pts',(-199.18028031721,3.79474096774303,126.262035970415));
#263026=CARTESIAN_POINT('Ctrl Pts',(-199.187676674146,3.67234248664227,
126.162521827584));
#263027=CARTESIAN_POINT('Ctrl Pts',(-199.195073031081,3.5461895741899,126.068067756434));
#263028=CARTESIAN_POINT('Ctrl Pts',(-199.202470520418,3.42001734740458,
125.973599224125));
#263029=CARTESIAN_POINT('Ctrl Pts',(-199.209868009754,3.29008984357849,
125.884192529796));
#263030=CARTESIAN_POINT('Ctrl Pts',(-199.217265499091,3.15685841191773,
125.800144841882));
#263031=CARTESIAN_POINT('Ctrl Pts',(-199.224665581606,3.02358027618456,
125.716067691181));
#263032=CARTESIAN_POINT('Ctrl Pts',(-199.232065664121,2.8869962222029,125.637353486203));
#263033=CARTESIAN_POINT('Ctrl Pts',(-199.239465746636,2.74758376880045,
125.564254321323));
#263034=CARTESIAN_POINT('Ctrl Pts',(-199.246873966302,2.60801801707374,
125.491074776397));
#263035=CARTESIAN_POINT('Ctrl Pts',(-199.254282185969,2.4656179856307,125.423522775534));
#263036=CARTESIAN_POINT('Ctrl Pts',(-199.261690405635,2.32088348920477,
125.361803278223));
#263037=CARTESIAN_POINT('Ctrl Pts',(-199.269103184937,2.1760599111109,125.300045793591));
#263038=CARTESIAN_POINT('Ctrl Pts',(-199.276515964239,2.028899353128,125.24412809794));
#263039=CARTESIAN_POINT('Ctrl Pts',(-199.283928743541,1.87991800148424,
125.194205640188));
#263040=CARTESIAN_POINT('Ctrl Pts',(-199.29135211457,1.73072377829936,125.144211850888));
#263041=CARTESIAN_POINT('Ctrl Pts',(-199.298775485599,1.57970392286291,
125.100230512364));
#263042=CARTESIAN_POINT('Ctrl Pts',(-199.306198856628,1.42738685480326,
125.062366423104));
#263043=CARTESIAN_POINT('Ctrl Pts',(-199.310134906068,1.34662469051819,
125.042289974441));
#263044=CARTESIAN_POINT('Ctrl Pts',(-199.314070955509,1.26549796615698,
125.023932443002));
#263045=CARTESIAN_POINT('Ctrl Pts',(-199.31800700495,1.18408604672678,125.007303536905));
#263046=CARTESIAN_POINT('Ctrl Pts',(-199.325430271356,1.03054570746349,
124.975941938976));
#263047=CARTESIAN_POINT('Ctrl Pts',(-199.332853537761,0.875526376150656,
124.950637115694));
#263048=CARTESIAN_POINT('Ctrl Pts',(-199.340276804166,0.719547249692918,
124.931526351391));
#263049=CARTESIAN_POINT('Ctrl Pts',(-199.347691296887,0.563752477609392,
124.912438174424));
#263050=CARTESIAN_POINT('Ctrl Pts',(-199.355105789608,0.407000535315681,
124.899529529172));
#263051=CARTESIAN_POINT('Ctrl Pts',(-199.362520282329,0.24982250344574,
124.892887088972));
#263052=CARTESIAN_POINT('Ctrl Pts',(-199.369927628683,0.0927959656810105,
124.886251051005));
#263053=CARTESIAN_POINT('Ctrl Pts',(-199.377334975037,-0.0646554736133486,
124.885869210084));
#263054=CARTESIAN_POINT('Ctrl Pts',(-199.38474232139,-0.221993995317587,
124.891776645347));
#263055=CARTESIAN_POINT('Ctrl Pts',(-199.392144143066,-0.379215168016295,
124.897679674621));
#263056=CARTESIAN_POINT('Ctrl Pts',(-199.399545964741,-0.536323219385118,
124.909862626159));
#263057=CARTESIAN_POINT('Ctrl Pts',(-199.406947786417,-0.692778811524635,
124.928308534679));
#263058=CARTESIAN_POINT('Ctrl Pts',(-199.414345700728,-0.84915181197491,
124.946744705747));
#263059=CARTESIAN_POINT('Ctrl Pts',(-199.421743615039,-1.00487266934929,
124.971437205811));
#263060=CARTESIAN_POINT('Ctrl Pts',(-199.429141529351,-1.15940576566253,
125.00231711264));
#263061=CARTESIAN_POINT('Ctrl Pts',(-199.436538214263,-1.3139131813789,
125.033191887789));
#263062=CARTESIAN_POINT('Ctrl Pts',(-199.443934899175,-1.46723286208119,
125.070251955885));
#263063=CARTESIAN_POINT('Ctrl Pts',(-199.451331584087,-1.61883788530298,
125.113377006308));
#263064=CARTESIAN_POINT('Ctrl Pts',(-199.458727941023,-1.7704361861996,
125.156500144521));
#263065=CARTESIAN_POINT('Ctrl Pts',(-199.466124297958,-1.92031962173487,
125.205687628209));
#263066=CARTESIAN_POINT('Ctrl Pts',(-199.473520654893,-2.06797523750912,
125.260768913666));
#263067=CARTESIAN_POINT('Ctrl Pts',(-199.48091814423,-2.21565345973426,
125.315858632208));
#263068=CARTESIAN_POINT('Ctrl Pts',(-199.488315633567,-2.36110283327585,
125.376843818751));
#263069=CARTESIAN_POINT('Ctrl Pts',(-199.495713122903,-2.50382937664356,
125.443505367221));
#263070=CARTESIAN_POINT('Ctrl Pts',(-199.503113205418,-2.64660595258121,
125.510190283794));
#263071=CARTESIAN_POINT('Ctrl Pts',(-199.510513287933,-2.78665745995995,
125.582555366178));
#263072=CARTESIAN_POINT('Ctrl Pts',(-199.517913370448,-2.92351369405257,
125.660335127428));
#263073=CARTESIAN_POINT('Ctrl Pts',(-199.525321590115,-3.06052041564315,
125.738200415521));
#263074=CARTESIAN_POINT('Ctrl Pts',(-199.532729809781,-3.1943245224501,
125.821492088438));
#263075=CARTESIAN_POINT('Ctrl Pts',(-199.540138029447,-3.3244834141804,
125.909900423496));
#263076=CARTESIAN_POINT('Ctrl Pts',(-199.54755080875,-3.45472241653674,
125.998363172409));
#263077=CARTESIAN_POINT('Ctrl Pts',(-199.554963588052,-3.58131143374482,
126.091948637279));
#263078=CARTESIAN_POINT('Ctrl Pts',(-199.562376367354,-3.7038406709643,
126.190306559949));
#263079=CARTESIAN_POINT('Ctrl Pts',(-199.569799738382,-3.82654498370379,
126.288805021032));
#263080=CARTESIAN_POINT('Ctrl Pts',(-199.577223109411,-3.94517765014855,
126.39208931474));
#263081=CARTESIAN_POINT('Ctrl Pts',(-199.58464648044,-4.05936487664758,
126.499771512815));
#263082=CARTESIAN_POINT('Ctrl Pts',(-199.588582529881,-4.11990968402192,
126.556867198033));
#263083=CARTESIAN_POINT('Ctrl Pts',(-199.592518579321,-4.17920537128048,
126.615198714714));
#263084=CARTESIAN_POINT('Ctrl Pts',(-199.596454628762,-4.23720087198234,
126.674704538306));
#263085=CARTESIAN_POINT('Ctrl Pts',(-199.603780504856,-4.3451435842251,
126.785458302217));
#263086=CARTESIAN_POINT('Ctrl Pts',(-199.611106380951,-4.44892529945081,
126.900636519193));
#263087=CARTESIAN_POINT('Ctrl Pts',(-199.618432257045,-4.54815423714637,
127.01988924132));
#263088=CARTESIAN_POINT('Ctrl Pts',(-199.625749275158,-4.64726319356173,
127.138997770688));
#263089=CARTESIAN_POINT('Ctrl Pts',(-199.633066293272,-4.74183008260889,
127.262170710391));
#263090=CARTESIAN_POINT('Ctrl Pts',(-199.640383311386,-4.83149884976926,
127.389020308435));
#263091=CARTESIAN_POINT('Ctrl Pts',(-199.647691937754,-4.9210647775684,
127.515724425147));
#263092=CARTESIAN_POINT('Ctrl Pts',(-199.655000564122,-5.00574355056634,
127.646096491343));
#263093=CARTESIAN_POINT('Ctrl Pts',(-199.66230919049,-5.08521874467687,
127.779715038116));
#263094=CARTESIAN_POINT('Ctrl Pts',(-199.669613071836,-5.1646423406467,
127.913246834945));
#263095=CARTESIAN_POINT('Ctrl Pts',(-199.676916953183,-5.23886888252049,
128.050020591129));
#263096=CARTESIAN_POINT('Ctrl Pts',(-199.684220834529,-5.30762463042162,
128.18958503541));
#263097=CARTESIAN_POINT('Ctrl Pts',(-199.691521506071,-5.37635016253885,
128.329088145923));
#263098=CARTESIAN_POINT('Ctrl Pts',(-199.698822177613,-5.43960951509057,
128.471379160608));
#263099=CARTESIAN_POINT('Ctrl Pts',(-199.706122849155,-5.49717452749041,
128.615981588053));
#263100=CARTESIAN_POINT('Ctrl Pts',(-199.713421843476,-5.55472631518357,
128.760550795239));
#263101=CARTESIAN_POINT('Ctrl Pts',(-199.720720837798,-5.60658622516097,
128.907430001561));
#263102=CARTESIAN_POINT('Ctrl Pts',(-199.728019832119,-5.6525740654497,
129.05612236232));
#263103=CARTESIAN_POINT('Ctrl Pts',(-199.735321043721,-5.69857587587576,
129.204859892687));
#263104=CARTESIAN_POINT('Ctrl Pts',(-199.742622255322,-5.73870193341256,
129.355411312575));
#263105=CARTESIAN_POINT('Ctrl Pts',(-199.749923466924,-5.77282175169358,
129.50726401913));
#263106=CARTESIAN_POINT('Ctrl Pts',(-199.757225668922,-5.80694619826219,
129.659137324213));
#263107=CARTESIAN_POINT('Ctrl Pts',(-199.764527870919,-5.83506270707501,
129.81231189086));
#263108=CARTESIAN_POINT('Ctrl Pts',(-199.771830072916,-5.85709199383315,
129.966265194433));
#263109=CARTESIAN_POINT('Ctrl Pts',(-199.779138508574,-5.87914008630182,
130.120349923109));
#263110=CARTESIAN_POINT('Ctrl Pts',(-199.786446944231,-5.8950905299074,
130.275214335113));
#263111=CARTESIAN_POINT('Ctrl Pts',(-199.793755379889,-5.90491592475032,
130.430330559776));
#263112=CARTESIAN_POINT('Ctrl Pts',(-199.799711855857,-5.91292375720509,
130.556752424544));
#263113=CARTESIAN_POINT('Ctrl Pts',(-199.805668331824,-5.9168640205334,
130.683341391447));
#263114=CARTESIAN_POINT('Ctrl Pts',(-199.811624807792,-5.91674748832781,
130.809812394026));
#263115=CARTESIAN_POINT('',(-201.561624807792,-5.9216802870108,130.802292919862));
#263116=CARTESIAN_POINT('Ctrl Pts',(-199.811624807792,-5.91707319532089,
130.809812694137));
#263117=CARTESIAN_POINT('Ctrl Pts',(-199.832717289386,-5.92122840583984,
131.257688120002));
#263118=CARTESIAN_POINT('Ctrl Pts',(-199.946625645587,-5.66995203506684,
133.671789078785));
#263119=CARTESIAN_POINT('Ctrl Pts',(-200.153349876387,-2.35938766776408,
137.393051713948));
#263120=CARTESIAN_POINT('Ctrl Pts',(-200.431797500202,4.26794575514161,
136.350728759107));
#263121=CARTESIAN_POINT('Ctrl Pts',(-200.710245124014,6.97324552981307,
130.211564437336));
#263122=CARTESIAN_POINT('Ctrl Pts',(-200.988692747828,3.27047332456854,
124.617150845494));
#263123=CARTESIAN_POINT('Ctrl Pts',(-201.26714037164,-3.43770409444905,
124.708480772182));
#263124=CARTESIAN_POINT('Ctrl Pts',(-201.458117724962,-5.87190273225,128.613207570693));
#263125=CARTESIAN_POINT('Ctrl Pts',(-201.556279203679,-5.9261716932185,
130.689210903785));
#263126=CARTESIAN_POINT('Ctrl Pts',(-201.561624807792,-5.92566153694035,
130.802291529712));
#263127=CARTESIAN_POINT('',(-203.31162480776,-5.91674832526764,130.799908882784));
#263128=CARTESIAN_POINT('Ctrl Pts',(-201.561624807792,-5.91674963930729,
130.802294641516));
#263129=CARTESIAN_POINT('Ctrl Pts',(-201.568982881734,-5.91680390723813,
130.957712590457));
#263130=CARTESIAN_POINT('Ctrl Pts',(-201.576340955677,-5.91073031198679,
131.113380258586));
#263131=CARTESIAN_POINT('Ctrl Pts',(-201.583699029619,-5.89849601535624,
131.26876918696));
#263132=CARTESIAN_POINT('Ctrl Pts',(-201.591048671187,-5.88627573926641,
131.423980039155));
#263133=CARTESIAN_POINT('Ctrl Pts',(-201.598398312754,-5.86790884059778,
131.578912411785));
#263134=CARTESIAN_POINT('Ctrl Pts',(-201.605747954322,-5.84341445076555,
131.733036082454));
#263135=CARTESIAN_POINT('Ctrl Pts',(-201.61309084544,-5.81894255837628,
131.887018194647));
#263136=CARTESIAN_POINT('Ctrl Pts',(-201.620433736558,-5.78835443516488,
132.040192709969));
#263137=CARTESIAN_POINT('Ctrl Pts',(-201.627776627676,-5.75172113270748,
132.192032975893));
#263138=CARTESIAN_POINT('Ctrl Pts',(-201.635114444198,-5.71511314714554,
132.343768306585));
#263139=CARTESIAN_POINT('Ctrl Pts',(-201.64245226072,-5.67246838760474,
132.494170855111));
#263140=CARTESIAN_POINT('Ctrl Pts',(-201.649790077242,-5.62390921912543,
132.642722839093));
#263141=CARTESIAN_POINT('Ctrl Pts',(-201.65712519342,-5.57536792060671,
132.791220155373));
#263142=CARTESIAN_POINT('Ctrl Pts',(-201.664460309597,-5.52091665958435,
132.937867900585));
#263143=CARTESIAN_POINT('Ctrl Pts',(-201.671795425774,-5.46072800920963,
133.082162226999));
#263144=CARTESIAN_POINT('Ctrl Pts',(-201.679129259572,-5.40054988146438,
133.2264313268));
#263145=CARTESIAN_POINT('Ctrl Pts',(-201.68646309337,-5.33463650595489,
133.368347475309));
#263146=CARTESIAN_POINT('Ctrl Pts',(-201.693796927167,-5.2632089776057,
133.507425881401));
#263147=CARTESIAN_POINT('Ctrl Pts',(-201.701130988438,-5.19177923379931,
133.646508601267));
#263148=CARTESIAN_POINT('Ctrl Pts',(-201.708465049707,-5.11483517035096,
133.782753065024));
#263149=CARTESIAN_POINT('Ctrl Pts',(-201.715799110978,-5.03264419073689,
133.915698434638));
#263150=CARTESIAN_POINT('Ctrl Pts',(-201.723134909502,-4.95043374214518,
134.04867529567));
#263151=CARTESIAN_POINT('Ctrl Pts',(-201.730470708027,-4.86297410395734,
134.178351183875));
#263152=CARTESIAN_POINT('Ctrl Pts',(-201.737806506552,-4.77057626898022,
134.304293848978));
#263153=CARTESIAN_POINT('Ctrl Pts',(-201.745149895269,-4.67808283196083,
134.430366824234));
#263154=CARTESIAN_POINT('Ctrl Pts',(-201.752493283986,-4.58064121767003,
134.55269855382));
#263155=CARTESIAN_POINT('Ctrl Pts',(-201.759836672703,-4.4786034494646,
134.67088899648));
#263156=CARTESIAN_POINT('Ctrl Pts',(-201.767183945264,-4.3765117145283,
134.789141948854));
#263157=CARTESIAN_POINT('Ctrl Pts',(-201.774531217824,-4.26981924252526,
134.903248973441));
#263158=CARTESIAN_POINT('Ctrl Pts',(-201.781878490384,-4.15891476263121,
135.012847110317));
#263159=CARTESIAN_POINT('Ctrl Pts',(-201.789236993135,-4.04784076697534,
135.12261276623));
#263160=CARTESIAN_POINT('Ctrl Pts',(-201.796595495886,-3.93254218153233,
135.227855508902));
#263161=CARTESIAN_POINT('Ctrl Pts',(-201.803953998638,-3.81344138899068,
135.328252231567));
#263162=CARTESIAN_POINT('Ctrl Pts',(-201.81064787218,-3.70509792958346,
135.419580996176));
#263163=CARTESIAN_POINT('Ctrl Pts',(-201.817341745723,-3.5936086492963,
135.506900002018));
#263164=CARTESIAN_POINT('Ctrl Pts',(-201.824035619266,-3.47931103503038,
135.589998013359));
#263165=CARTESIAN_POINT('Ctrl Pts',(-201.831458885672,-3.35255906776189,
135.682150736593));
#263166=CARTESIAN_POINT('Ctrl Pts',(-201.838882152077,-3.22195178485856,
135.769403615139));
#263167=CARTESIAN_POINT('Ctrl Pts',(-201.846305418483,-3.0879048581852,
135.851416605892));
#263168=CARTESIAN_POINT('Ctrl Pts',(-201.853719911204,-2.95401636384689,
135.933332664101));
#263169=CARTESIAN_POINT('Ctrl Pts',(-201.861134403924,-2.8166966332044,
136.010020969021));
#263170=CARTESIAN_POINT('Ctrl Pts',(-201.868548896646,-2.67639312130945,
136.081182617852));
#263171=CARTESIAN_POINT('Ctrl Pts',(-201.875956242999,-2.53622483922201,
136.152275678408));
#263172=CARTESIAN_POINT('Ctrl Pts',(-201.883363589353,-2.39307883188319,
136.217852519758));
#263173=CARTESIAN_POINT('Ctrl Pts',(-201.890770935707,-2.24743006191977,
136.277658405854));
#263174=CARTESIAN_POINT('Ctrl Pts',(-201.898172757382,-2.10188992230359,
136.337419686464));
#263175=CARTESIAN_POINT('Ctrl Pts',(-201.905574579058,-1.95385108065789,
136.391418440872));
#263176=CARTESIAN_POINT('Ctrl Pts',(-201.912976400733,-1.80381144299486,
136.439446671977));
#263177=CARTESIAN_POINT('Ctrl Pts',(-201.920374315044,-1.65385101008865,
136.487449549353));
#263178=CARTESIAN_POINT('Ctrl Pts',(-201.927772229356,-1.50189223927456,
136.529488066856));
#263179=CARTESIAN_POINT('Ctrl Pts',(-201.935170143667,-1.34845117572333,
136.56540305702));
#263180=CARTESIAN_POINT('Ctrl Pts',(-201.942566828579,-1.19503561129339,
136.601312078765));
#263181=CARTESIAN_POINT('Ctrl Pts',(-201.949963513491,-1.04013860613695,
136.631099507851));
#263182=CARTESIAN_POINT('Ctrl Pts',(-201.957360198404,-0.884289580498989,
136.654656550279));
#263183=CARTESIAN_POINT('Ctrl Pts',(-201.964756555339,-0.728447465370143,
136.678212548163));
#263184=CARTESIAN_POINT('Ctrl Pts',(-201.972152912275,-0.571653782799518,
136.695538652899));
#263185=CARTESIAN_POINT('Ctrl Pts',(-201.97954926921,-0.414446050683824,
136.706577576775));
#263186=CARTESIAN_POINT('Ctrl Pts',(-201.986946758547,-0.25721424966346,
136.717618190738));
#263187=CARTESIAN_POINT('Ctrl Pts',(-201.994344247883,-0.0995686452809479,
136.722369681061));
#263188=CARTESIAN_POINT('Ctrl Pts',(-202.00174173722,0.0579503942137365,
136.720826819135));
#263189=CARTESIAN_POINT('Ctrl Pts',(-202.009141819735,0.215524651763755,
136.719283416362));
#263190=CARTESIAN_POINT('Ctrl Pts',(-202.016541902249,0.372971883044187,
136.711441271919));
#263191=CARTESIAN_POINT('Ctrl Pts',(-202.023941984764,0.529754145426437,
136.69734722097));
#263192=CARTESIAN_POINT('Ctrl Pts',(-202.031350204431,0.686708806024008,
136.683237672164));
#263193=CARTESIAN_POINT('Ctrl Pts',(-202.038758424097,0.842996665438895,
136.662862521241));
#263194=CARTESIAN_POINT('Ctrl Pts',(-202.046166643764,0.998086579105648,
136.636320300478));
#263195=CARTESIAN_POINT('Ctrl Pts',(-202.053579423066,1.15327194802645,
136.609761743421));
#263196=CARTESIAN_POINT('Ctrl Pts',(-202.060992202368,1.30725753771265,
136.577028630497));
#263197=CARTESIAN_POINT('Ctrl Pts',(-202.06840498167,1.45952526831276,136.538269977999));
#263198=CARTESIAN_POINT('Ctrl Pts',(-202.075828352699,1.61201056618677,
136.49945594532));
#263199=CARTESIAN_POINT('Ctrl Pts',(-202.083251723727,1.76277274582379,
136.454599283991));
#263200=CARTESIAN_POINT('Ctrl Pts',(-202.090675094756,1.91131088775466,
136.403898210337));
#263201=CARTESIAN_POINT('Ctrl Pts',(-202.094611144197,1.99006937472724,
136.377015284531));
#263202=CARTESIAN_POINT('Ctrl Pts',(-202.098547193638,2.06820295967937,
136.34849008045));
#263203=CARTESIAN_POINT('Ctrl Pts',(-202.102483243078,2.14563967604513,
136.318357438664));
#263204=CARTESIAN_POINT('Ctrl Pts',(-202.109906509484,2.29168290639948,
136.261528216662));
#263205=CARTESIAN_POINT('Ctrl Pts',(-202.117329775889,2.43568765092004,
136.198806922689));
#263206=CARTESIAN_POINT('Ctrl Pts',(-202.124753042294,2.5771431409141,136.130359471653));
#263207=CARTESIAN_POINT('Ctrl Pts',(-202.132167535015,2.71843144226654,
136.06199291982));
#263208=CARTESIAN_POINT('Ctrl Pts',(-202.139582027737,2.85717615375475,
135.987913843359));
#263209=CARTESIAN_POINT('Ctrl Pts',(-202.146996520458,2.99288393960237,
135.908337134613));
#263210=CARTESIAN_POINT('Ctrl Pts',(-202.154403866811,3.12846092517669,
135.828837124895));
#263211=CARTESIAN_POINT('Ctrl Pts',(-202.161811213165,3.26100649253989,
135.743850219369));
#263212=CARTESIAN_POINT('Ctrl Pts',(-202.169218559519,3.39004959613795,
135.653638326486));
#263213=CARTESIAN_POINT('Ctrl Pts',(-202.176620381194,3.51899645452082,
135.563493717036));
#263214=CARTESIAN_POINT('Ctrl Pts',(-202.18402220287,3.64444574588738,135.468132092632));
#263215=CARTESIAN_POINT('Ctrl Pts',(-202.191424024545,3.76595334602514,
135.36785992819));
#263216=CARTESIAN_POINT('Ctrl Pts',(-202.198821938857,3.88739680324591,
135.267640696643));
#263217=CARTESIAN_POINT('Ctrl Pts',(-202.206219853168,4.00490242603697,
135.16251632462));
#263218=CARTESIAN_POINT('Ctrl Pts',(-202.213617767479,4.11805736728282,
135.052834941634));
#263219=CARTESIAN_POINT('Ctrl Pts',(-202.221014452392,4.23119350423076,
134.943171785704));
#263220=CARTESIAN_POINT('Ctrl Pts',(-202.228411137304,4.33998012680202,
134.828953381375));
#263221=CARTESIAN_POINT('Ctrl Pts',(-202.235807822216,4.44403953894811,
134.710566339077));
#263222=CARTESIAN_POINT('Ctrl Pts',(-202.243204179152,4.54809433699053,
134.592184546185));
#263223=CARTESIAN_POINT('Ctrl Pts',(-202.250600536087,4.64742209493324,
134.469634763234));
#263224=CARTESIAN_POINT('Ctrl Pts',(-202.257996893022,4.74168407344933,
134.343338253847));
#263225=CARTESIAN_POINT('Ctrl Pts',(-202.265394382359,4.83596048371523,
134.217022408141));
#263226=CARTESIAN_POINT('Ctrl Pts',(-202.272791871696,4.92516934696955,
134.086958992999));
#263227=CARTESIAN_POINT('Ctrl Pts',(-202.280189361032,5.00901418199923,
133.953599809344));
#263228=CARTESIAN_POINT('Ctrl Pts',(-202.287589443547,5.09288840870597,
133.820193876833));
#263229=CARTESIAN_POINT('Ctrl Pts',(-202.294989526062,5.17139466485451,
133.683490191393));
#263230=CARTESIAN_POINT('Ctrl Pts',(-202.302389608577,5.24428158306487,
133.543966654942));
#263231=CARTESIAN_POINT('Ctrl Pts',(-202.309797828244,5.31724864793465,
133.40428969802));
#263232=CARTESIAN_POINT('Ctrl Pts',(-202.31720604791,5.3845838619657,133.261787028827));
#263233=CARTESIAN_POINT('Ctrl Pts',(-202.324614267577,5.44608302654156,
133.116958773432));
#263234=CARTESIAN_POINT('Ctrl Pts',(-202.332027046879,5.50762004282705,
132.972041378663));
#263235=CARTESIAN_POINT('Ctrl Pts',(-202.339439826181,5.56331372040708,
132.824795893876));
#263236=CARTESIAN_POINT('Ctrl Pts',(-202.346852605483,5.61300939609337,
132.675738741267));
#263237=CARTESIAN_POINT('Ctrl Pts',(-202.354275976512,5.66277607929151,
132.526468608809));
#263238=CARTESIAN_POINT('Ctrl Pts',(-202.361699347541,5.70652754037334,
132.375381996141));
#263239=CARTESIAN_POINT('Ctrl Pts',(-202.36912271857,5.74415978513868,132.223007481763));
#263240=CARTESIAN_POINT('Ctrl Pts',(-202.37305876801,5.76411330428583,132.142214858066));
#263241=CARTESIAN_POINT('Ctrl Pts',(-202.376994817451,5.78234735340238,
132.061060290616));
#263242=CARTESIAN_POINT('Ctrl Pts',(-202.380930866892,5.79885234516005,
131.9796231591));
#263243=CARTESIAN_POINT('Ctrl Pts',(-202.388354133297,5.82998024451299,
131.82603527062));
#263244=CARTESIAN_POINT('Ctrl Pts',(-202.395777399702,5.85504912545923,
131.670977609184));
#263245=CARTESIAN_POINT('Ctrl Pts',(-202.403200666108,5.87392249395432,
131.514969580018));
#263246=CARTESIAN_POINT('Ctrl Pts',(-202.410615158829,5.89277355569518,
131.359145939387));
#263247=CARTESIAN_POINT('Ctrl Pts',(-202.41802965155,5.90544363622744,131.202374533849));
#263248=CARTESIAN_POINT('Ctrl Pts',(-202.425444144271,5.91184687052777,
131.045186575326));
#263249=CARTESIAN_POINT('Ctrl Pts',(-202.432851490625,5.91824393314985,
130.888150120474));
#263250=CARTESIAN_POINT('Ctrl Pts',(-202.440258836978,5.91838615934132,
130.730698282408));
#263251=CARTESIAN_POINT('Ctrl Pts',(-202.447666183332,5.91223928847316,
130.573368933009));
#263252=CARTESIAN_POINT('Ctrl Pts',(-202.455068005008,5.90609700217325,
130.416156925776));
#263253=CARTESIAN_POINT('Ctrl Pts',(-202.462469826683,5.8936749730336,130.259067596714));
#263254=CARTESIAN_POINT('Ctrl Pts',(-202.469871648358,5.87499098709605,
130.10264025728));
#263255=CARTESIAN_POINT('Ctrl Pts',(-202.47726956267,5.85631686428913,129.94629549462));
#263256=CARTESIAN_POINT('Ctrl Pts',(-202.484667476981,5.83138741218186,
129.790612395348));
#263257=CARTESIAN_POINT('Ctrl Pts',(-202.492065391293,5.80027236804441,
129.636126471943));
#263258=CARTESIAN_POINT('Ctrl Pts',(-202.499462076205,5.76916249466294,
129.481666221295));
#263259=CARTESIAN_POINT('Ctrl Pts',(-202.506858761117,5.73186914302823,
129.328403117249));
#263260=CARTESIAN_POINT('Ctrl Pts',(-202.514255446029,5.68851342550535,
129.176863898569));
#263261=CARTESIAN_POINT('Ctrl Pts',(-202.521651802964,5.64515963042055,
129.025331399297));
#263262=CARTESIAN_POINT('Ctrl Pts',(-202.5290481599,5.59574410661747,128.875522992302));
#263263=CARTESIAN_POINT('Ctrl Pts',(-202.536444516835,5.54043817823208,
128.727951371852));
#263264=CARTESIAN_POINT('Ctrl Pts',(-202.543842006172,5.48512378236803,
128.580357157809));
#263265=CARTESIAN_POINT('Ctrl Pts',(-202.551239495508,5.42391731725896,
128.435000761769));
#263266=CARTESIAN_POINT('Ctrl Pts',(-202.558636984845,5.35703864047963,
128.292375831205));
#263267=CARTESIAN_POINT('Ctrl Pts',(-202.56603706736,5.29013651948354,128.149700903693));
#263268=CARTESIAN_POINT('Ctrl Pts',(-202.573437149875,5.21755838634373,
128.009759685829));
#263269=CARTESIAN_POINT('Ctrl Pts',(-202.58083723239,5.13957044327107,127.873021977771));
#263270=CARTESIAN_POINT('Ctrl Pts',(-202.588245452056,5.06149674443775,
127.736133912546));
#263271=CARTESIAN_POINT('Ctrl Pts',(-202.595653671723,4.9780015408993,127.60245671643));
#263272=CARTESIAN_POINT('Ctrl Pts',(-202.603061891389,4.8893952285411,127.472432517859));
#263273=CARTESIAN_POINT('Ctrl Pts',(-202.610474670691,4.80073438047586,
127.342328291562));
#263274=CARTESIAN_POINT('Ctrl Pts',(-202.617887449993,4.70695637704169,
127.215881842089));
#263275=CARTESIAN_POINT('Ctrl Pts',(-202.625300229295,4.60841209962781,
127.093502430771));
#263276=CARTESIAN_POINT('Ctrl Pts',(-202.632723600324,4.50972701752896,
126.970948158011));
#263277=CARTESIAN_POINT('Ctrl Pts',(-202.640146971353,4.40626230469941,
126.852472810054));
#263278=CARTESIAN_POINT('Ctrl Pts',(-202.647570342382,4.29840645779756,
126.738449589756));
#263279=CARTESIAN_POINT('Ctrl Pts',(-202.651506391822,4.24121869980284,
126.677991742403));
#263280=CARTESIAN_POINT('Ctrl Pts',(-202.655442441263,4.18279701272454,
126.618784894444));
#263281=CARTESIAN_POINT('Ctrl Pts',(-202.659378490704,4.12320299875834,
126.560880018632));
#263282=CARTESIAN_POINT('Ctrl Pts',(-202.66680175711,4.01081054828672,126.451673230002));
#263283=CARTESIAN_POINT('Ctrl Pts',(-202.674225023515,3.89390648875168,
126.346769616974));
#263284=CARTESIAN_POINT('Ctrl Pts',(-202.681648289921,3.77285403211578,
126.246564767065));
#263285=CARTESIAN_POINT('Ctrl Pts',(-202.689062782642,3.65194464943049,
126.146478350966));
#263286=CARTESIAN_POINT('Ctrl Pts',(-202.696477275363,3.52689691396513,
126.051079879331));
#263287=CARTESIAN_POINT('Ctrl Pts',(-202.703891768084,3.39811133721108,
125.960728725853));
#263288=CARTESIAN_POINT('Ctrl Pts',(-202.711299114438,3.2694498888457,125.87046465622));
#263289=CARTESIAN_POINT('Ctrl Pts',(-202.718706460791,3.13705807494424,
125.785238432848));
#263290=CARTESIAN_POINT('Ctrl Pts',(-202.726113807145,3.00136990364706,
125.705369613065));
#263291=CARTESIAN_POINT('Ctrl Pts',(-202.733515628821,2.86578293370648,
125.625560362461));
#263292=CARTESIAN_POINT('Ctrl Pts',(-202.740917450496,2.7269048219899,125.551100747908));
#263293=CARTESIAN_POINT('Ctrl Pts',(-202.748319272171,2.5851989202899,125.482267316521));
#263294=CARTESIAN_POINT('Ctrl Pts',(-202.755717186483,2.44356782403319,
125.413470221767));
#263295=CARTESIAN_POINT('Ctrl Pts',(-202.763115100794,2.29911224564274,
125.350293557936));
#263296=CARTESIAN_POINT('Ctrl Pts',(-202.770513015105,2.15232042163001,
125.292968110664));
#263297=CARTESIAN_POINT('Ctrl Pts',(-202.777909700018,2.00555299175515,
125.235652189841));
#263298=CARTESIAN_POINT('Ctrl Pts',(-202.78530638493,1.85645043418548,125.184185691378));
#263299=CARTESIAN_POINT('Ctrl Pts',(-202.792703069842,1.70552137335281,
125.13875143518));
#263300=CARTESIAN_POINT('Ctrl Pts',(-202.800099426778,1.55459900487243,
125.093319193584));
#263301=CARTESIAN_POINT('Ctrl Pts',(-202.807495783713,1.40185065161534,
125.053918770026));
#263302=CARTESIAN_POINT('Ctrl Pts',(-202.814892140649,1.2478002626691,125.020683148431));
#263303=CARTESIAN_POINT('Ctrl Pts',(-202.822289629985,1.09372628821504,
124.987442438377));
#263304=CARTESIAN_POINT('Ctrl Pts',(-202.829687119322,0.938350246075035,
124.960368488343));
#263305=CARTESIAN_POINT('Ctrl Pts',(-202.837084608658,0.782206294241051,
124.939543154443));
#263306=CARTESIAN_POINT('Ctrl Pts',(-202.844484691173,0.626007606387029,
124.918710520255));
#263307=CARTESIAN_POINT('Ctrl Pts',(-202.851884773688,0.469040842675188,
124.904130912675));
#263308=CARTESIAN_POINT('Ctrl Pts',(-202.859284856203,0.311845148080142,
124.895834306707));
#263309=CARTESIAN_POINT('Ctrl Pts',(-202.86669307587,0.154476600659004,
124.887528577766));
#263310=CARTESIAN_POINT('Ctrl Pts',(-202.874101295536,-0.00312100736494086,
124.885519667463));
#263311=CARTESIAN_POINT('Ctrl Pts',(-202.881509515203,-0.160407924259452,
124.889785412166));
#263312=CARTESIAN_POINT('Ctrl Pts',(-202.888922294505,-0.317791648627735,
124.894053782363));
#263313=CARTESIAN_POINT('Ctrl Pts',(-202.896335073807,-0.474863929231365,
124.904604478017));
#263314=CARTESIAN_POINT('Ctrl Pts',(-202.903747853109,-0.631090782958744,
124.921363508425));
#263315=CARTESIAN_POINT('Ctrl Pts',(-202.911171224138,-0.787540860940819,
124.938146484921));
#263316=CARTESIAN_POINT('Ctrl Pts',(-202.918594595167,-0.943142731124381,
124.961155458605));
#263317=CARTESIAN_POINT('Ctrl Pts',(-202.926017966195,-1.09737241544244,
124.990265301498));
#263318=CARTESIAN_POINT('Ctrl Pts',(-202.929954015636,-1.17914869475504,
125.00570003868));
#263319=CARTESIAN_POINT('Ctrl Pts',(-202.933890065077,-1.260539441657,125.022849111077));
#263320=CARTESIAN_POINT('Ctrl Pts',(-202.937826114517,-1.34146847383707,
125.041688243033));
#263321=CARTESIAN_POINT('Ctrl Pts',(-202.945249380923,-1.49409810282559,
125.077218257956));
#263322=CARTESIAN_POINT('Ctrl Pts',(-202.952672647328,-1.64554598320926,
125.118869988883));
#263323=CARTESIAN_POINT('Ctrl Pts',(-202.960095913734,-1.79528297106824,
125.166551680018));
#263324=CARTESIAN_POINT('Ctrl Pts',(-202.967510406455,-1.94484298224202,
125.214177015355));
#263325=CARTESIAN_POINT('Ctrl Pts',(-202.974924899176,-2.0926957737322,
125.267818012581));
#263326=CARTESIAN_POINT('Ctrl Pts',(-202.982339391897,-2.23832250802715,
125.327331960296));
#263327=CARTESIAN_POINT('Ctrl Pts',(-202.98974673825,-2.38380888179367,
125.386788546228));
#263328=CARTESIAN_POINT('Ctrl Pts',(-202.997154084604,-2.52707312651263,
125.452106673295));
#263329=CARTESIAN_POINT('Ctrl Pts',(-203.004561430958,-2.66761179755283,
125.523093926699));
#263330=CARTESIAN_POINT('Ctrl Pts',(-203.011963252633,-2.80804564954954,
125.594028235132));
#263331=CARTESIAN_POINT('Ctrl Pts',(-203.019365074309,-2.94575764374757,
125.670623083307));
#263332=CARTESIAN_POINT('Ctrl Pts',(-203.026766895984,-3.08026466026495,
125.752638120712));
#263333=CARTESIAN_POINT('Ctrl Pts',(-203.034164810295,-3.21470067157453,
125.834609863016));
#263334=CARTESIAN_POINT('Ctrl Pts',(-203.041562724607,-3.34593475675407,
125.921995902334));
#263335=CARTESIAN_POINT('Ctrl Pts',(-203.048960638918,-3.47350884555318,
126.014510216733));
#263336=CARTESIAN_POINT('Ctrl Pts',(-203.05635732383,-3.60106173385371,
126.107009156931));
#263337=CARTESIAN_POINT('Ctrl Pts',(-203.063754008742,-3.72495553101644,
126.20463446186));
#263338=CARTESIAN_POINT('Ctrl Pts',(-203.071150693655,-3.84476150154799,
126.307057030002));
#263339=CARTESIAN_POINT('Ctrl Pts',(-203.07854705059,-3.96456215975726,
126.409475056621));
#263340=CARTESIAN_POINT('Ctrl Pts',(-203.085943407525,-4.08027506799617,
126.516689680931));
#263341=CARTESIAN_POINT('Ctrl Pts',(-203.093339764461,-4.19150513584072,
126.628331970787));
#263342=CARTESIAN_POINT('Ctrl Pts',(-203.100737253797,-4.3027522332923,
126.739991353362));
#263343=CARTESIAN_POINT('Ctrl Pts',(-203.108134743134,-4.40951486027692,
126.85607948678));
#263344=CARTESIAN_POINT('Ctrl Pts',(-203.11553223247,-4.51143542348493,
126.976191214023));
#263345=CARTESIAN_POINT('Ctrl Pts',(-203.122932314985,-4.61339171478823,
127.096345046245));
#263346=CARTESIAN_POINT('Ctrl Pts',(-203.1303323975,-4.71050232147278,127.220524996061));
#263347=CARTESIAN_POINT('Ctrl Pts',(-203.137732480015,-4.80245060369318,
127.348293667753));
#263348=CARTESIAN_POINT('Ctrl Pts',(-203.145140699682,-4.89449999250279,
127.476202834236));
#263349=CARTESIAN_POINT('Ctrl Pts',(-203.152548919348,-4.98137550230915,
127.607708300172));
#263350=CARTESIAN_POINT('Ctrl Pts',(-203.159957139014,-5.06280403100677,
127.74234397716));
#263351=CARTESIAN_POINT('Ctrl Pts',(-203.167369918316,-5.14428267760486,
127.87706252016));
#263352=CARTESIAN_POINT('Ctrl Pts',(-203.174782697619,-5.22030748290961,
128.014914787064));
#263353=CARTESIAN_POINT('Ctrl Pts',(-203.182195476921,-5.29065206648016,
128.155411528975));
#263354=CARTESIAN_POINT('Ctrl Pts',(-203.189618847949,-5.36109716169105,
128.296109019219));
#263355=CARTESIAN_POINT('Ctrl Pts',(-203.197042218978,-5.42584567210385,
128.43945819178));
#263356=CARTESIAN_POINT('Ctrl Pts',(-203.204465590007,-5.48471964848875,
128.584950574338));
#263357=CARTESIAN_POINT('Ctrl Pts',(-203.208401639448,-5.51593604343254,
128.662094126619));
#263358=CARTESIAN_POINT('Ctrl Pts',(-203.212337688889,-5.54550172992229,
128.739839959623));
#263359=CARTESIAN_POINT('Ctrl Pts',(-203.21627373833,-5.5733959533535,128.818110857429));
#263360=CARTESIAN_POINT('Ctrl Pts',(-203.224921721089,-5.63468297906373,
128.990081607504));
#263361=CARTESIAN_POINT('Ctrl Pts',(-203.233569703848,-5.68805083248295,
129.165014549172));
#263362=CARTESIAN_POINT('Ctrl Pts',(-203.242217686606,-5.73324512702968,
129.342228313056));
#263363=CARTESIAN_POINT('Ctrl Pts',(-203.250830811819,-5.77825725629626,
129.518727778925));
#263364=CARTESIAN_POINT('Ctrl Pts',(-203.259443937031,-5.81516149890193,
129.697489615715));
#263365=CARTESIAN_POINT('Ctrl Pts',(-203.268057062243,-5.84375315109936,
129.877818836794));
#263366=CARTESIAN_POINT('Ctrl Pts',(-203.276602616523,-5.87212049858119,
130.056733354925));
#263367=CARTESIAN_POINT('Ctrl Pts',(-203.285148170803,-5.89230509977486,
130.237190643914));
#263368=CARTESIAN_POINT('Ctrl Pts',(-203.293693725083,-5.90415413278233,
130.418492066309));
#263369=CARTESIAN_POINT('Ctrl Pts',(-203.299670752642,-5.91244171653796,
130.545299943557));
#263370=CARTESIAN_POINT('Ctrl Pts',(-203.305647780201,-5.91665247871619,
130.672520358863));
#263371=CARTESIAN_POINT('Ctrl Pts',(-203.31162480776,-5.91674832526764,
130.799908882784));
#263372=CARTESIAN_POINT('',(-205.061626015508,-5.91263662896126,130.80817859488));
#263373=CARTESIAN_POINT('Ctrl Pts',(-203.311624807792,-5.91674832526815,
130.799908883463));
#263374=CARTESIAN_POINT('Ctrl Pts',(-203.31925383089,-5.91687066290775,
130.962506425771));
#263375=CARTESIAN_POINT('Ctrl Pts',(-203.326882853988,-5.91028565918037,
131.125172439786));
#263376=CARTESIAN_POINT('Ctrl Pts',(-203.334511877086,-5.8970065749038,
131.287314050147));
#263377=CARTESIAN_POINT('Ctrl Pts',(-203.341914747701,-5.88412113183752,
131.444649183011));
#263378=CARTESIAN_POINT('Ctrl Pts',(-203.349317618315,-5.86493289222459,
131.601490170919));
#263379=CARTESIAN_POINT('Ctrl Pts',(-203.35672048893,-5.83950678773434,
131.757298725999));
#263380=CARTESIAN_POINT('Ctrl Pts',(-203.364124032299,-5.81407837258119,
131.913121440585));
#263381=CARTESIAN_POINT('Ctrl Pts',(-203.371527575669,-5.78241102307281,
132.067911168375));
#263382=CARTESIAN_POINT('Ctrl Pts',(-203.378931119038,-5.7446210682295,
132.22113842123));
#263383=CARTESIAN_POINT('Ctrl Pts',(-203.386336782644,-5.70682029105092,
132.374409555499));
#263384=CARTESIAN_POINT('Ctrl Pts',(-203.39374244625,-5.66289350593888,
132.526116962837));
#263385=CARTESIAN_POINT('Ctrl Pts',(-203.401148109856,-5.61300728187641,
132.675745082635));
#263386=CARTESIAN_POINT('Ctrl Pts',(-203.40894588088,-5.56047973361094,
132.833295557386));
#263387=CARTESIAN_POINT('Ctrl Pts',(-203.416743651903,-5.5013446649065,
132.988540125356));
#263388=CARTESIAN_POINT('Ctrl Pts',(-203.424541422927,-5.43585428549973,
133.1409005272));
#263389=CARTESIAN_POINT('Ctrl Pts',(-203.431959917198,-5.37354930079099,
133.285850252536));
#263390=CARTESIAN_POINT('Ctrl Pts',(-203.439378411468,-5.305492808283,133.428189425049));
#263391=CARTESIAN_POINT('Ctrl Pts',(-203.446796905739,-5.23194910023918,
133.567445700405));
#263392=CARTESIAN_POINT('Ctrl Pts',(-203.454220864128,-5.15835122331424,
133.706804545468));
#263393=CARTESIAN_POINT('Ctrl Pts',(-203.461644822517,-5.07925826396159,
133.84307564888));
#263394=CARTESIAN_POINT('Ctrl Pts',(-203.469068780906,-4.99497801599823,
133.975815359825));
#263395=CARTESIAN_POINT('Ctrl Pts',(-203.47650313371,-4.91057976578007,
134.108740921968));
#263396=CARTESIAN_POINT('Ctrl Pts',(-203.483937486513,-4.82097993977899,
134.238124918073));
#263397=CARTESIAN_POINT('Ctrl Pts',(-203.491371839317,-4.72652713722884,
134.363556001854));
#263398=CARTESIAN_POINT('Ctrl Pts',(-203.492488346925,-4.71234200565376,
134.382393520477));
#263399=CARTESIAN_POINT('Ctrl Pts',(-203.493604854534,-4.69804748499611,
134.401141949454));
#263400=CARTESIAN_POINT('Ctrl Pts',(-203.494721362142,-4.68364482727004,
134.419799967699));
#263401=CARTESIAN_POINT('Ctrl Pts',(-203.502144628548,-4.58788662156608,
134.543850568851));
#263402=CARTESIAN_POINT('Ctrl Pts',(-203.509567894953,-4.48705182451503,
134.664281756115));
#263403=CARTESIAN_POINT('Ctrl Pts',(-203.516991161359,-4.38144383707481,
134.78065040392));
#263404=CARTESIAN_POINT('Ctrl Pts',(-203.52440565408,-4.27596066950554,
134.896881513646));
#263405=CARTESIAN_POINT('Ctrl Pts',(-203.531820146801,-4.16571578943428,
135.009059367759));
#263406=CARTESIAN_POINT('Ctrl Pts',(-203.539234639522,-4.05105465877887,
135.116771395088));
#263407=CARTESIAN_POINT('Ctrl Pts',(-203.546641985876,-3.93650404283811,
135.22437960551));
#263408=CARTESIAN_POINT('Ctrl Pts',(-203.55404933223,-3.81754592051431,
135.327530304353));
#263409=CARTESIAN_POINT('Ctrl Pts',(-203.561456678584,-3.69456456150438,
135.425845580581));
#263410=CARTESIAN_POINT('Ctrl Pts',(-203.568858500259,-3.57167492663218,
135.524087529567));
#263411=CARTESIAN_POINT('Ctrl Pts',(-203.576260321934,-3.44476832015857,
135.617501004755));
#263412=CARTESIAN_POINT('Ctrl Pts',(-203.58366214361,-3.31426416180886,
135.705746506093));
#263413=CARTESIAN_POINT('Ctrl Pts',(-203.591060057921,-3.18382889558812,
135.793945423318));
#263414=CARTESIAN_POINT('Ctrl Pts',(-203.598457972233,-3.04980016813304,
135.876981591329));
#263415=CARTESIAN_POINT('Ctrl Pts',(-203.605855886544,-2.91262852580243,
135.954557277227));
#263416=CARTESIAN_POINT('Ctrl Pts',(-203.613252571456,-2.77547967891002,
136.032120071453));
#263417=CARTESIAN_POINT('Ctrl Pts',(-203.620649256369,-2.63518927836053,
136.104224000971));
#263418=CARTESIAN_POINT('Ctrl Pts',(-203.628045941281,-2.49223485864503,
136.170615920089));
#263419=CARTESIAN_POINT('Ctrl Pts',(-203.635442298216,-2.3492867776783,
136.23700489532));
#263420=CARTESIAN_POINT('Ctrl Pts',(-203.642838655152,-2.20367525098471,
136.297682206512));
#263421=CARTESIAN_POINT('Ctrl Pts',(-203.650235012087,-2.05590005455707,
136.352441865004));
#263422=CARTESIAN_POINT('Ctrl Pts',(-203.657632501424,-1.90810223337002,
136.40720990734));
#263423=CARTESIAN_POINT('Ctrl Pts',(-203.665029990761,-1.75814043291998,
136.456058363276));
#263424=CARTESIAN_POINT('Ctrl Pts',(-203.672427480097,-1.60653179003577,
136.498830405887));
#263425=CARTESIAN_POINT('Ctrl Pts',(-203.679827562612,-1.45487000097703,
136.541617442172));
#263426=CARTESIAN_POINT('Ctrl Pts',(-203.687227645127,-1.30156057913766,
136.578323722869));
#263427=CARTESIAN_POINT('Ctrl Pts',(-203.694627727642,-1.14713296000083,
136.60884306948));
#263428=CARTESIAN_POINT('Ctrl Pts',(-203.702035947309,-0.992535531820553,
136.63939597525));
#263429=CARTESIAN_POINT('Ctrl Pts',(-203.709444166976,-0.836817817244495,
136.663748288138));
#263430=CARTESIAN_POINT('Ctrl Pts',(-203.716852386642,-0.680517251053971,
136.681845354553));
#263431=CARTESIAN_POINT('Ctrl Pts',(-203.724265165944,-0.524120484472526,
136.699953559411));
#263432=CARTESIAN_POINT('Ctrl Pts',(-203.731677945247,-0.367140522827894,
136.711798818167));
#263433=CARTESIAN_POINT('Ctrl Pts',(-203.739090724549,-0.210116445125973,
136.717378598427));
#263434=CARTESIAN_POINT('Ctrl Pts',(-203.746514095577,-0.0528680040588055,
136.722966351339));
#263435=CARTESIAN_POINT('Ctrl Pts',(-203.753937466606,0.104424306655523,
136.722270747431));
#263436=CARTESIAN_POINT('Ctrl Pts',(-203.761360837635,0.261224055224296,
136.715341293856));
#263437=CARTESIAN_POINT('Ctrl Pts',(-203.765296887076,0.344363044267299,
136.711667131301));
#263438=CARTESIAN_POINT('Ctrl Pts',(-203.769232936516,0.427363673358813,
136.706241273284));
#263439=CARTESIAN_POINT('Ctrl Pts',(-203.773168985957,0.510147086307701,
136.699076939225));
#263440=CARTESIAN_POINT('Ctrl Pts',(-203.780592252362,0.666274019559398,
136.68556522878));
#263441=CARTESIAN_POINT('Ctrl Pts',(-203.788015518767,0.822099859025682,
136.665826056643));
#263442=CARTESIAN_POINT('Ctrl Pts',(-203.795438785173,0.977087794984135,
136.639875162436));
#263443=CARTESIAN_POINT('Ctrl Pts',(-203.802853277894,1.13189254807323,
136.613954940032));
#263444=CARTESIAN_POINT('Ctrl Pts',(-203.810267770615,1.28586100433918,
136.581837670375));
#263445=CARTESIAN_POINT('Ctrl Pts',(-203.817682263336,1.43845932536675,
136.543590995567));
#263446=CARTESIAN_POINT('Ctrl Pts',(-203.82508960969,1.59091056638773,136.505381184343));
#263447=CARTESIAN_POINT('Ctrl Pts',(-203.832496956044,1.74199394153385,
136.461053819284));
#263448=CARTESIAN_POINT('Ctrl Pts',(-203.839904302397,1.8911837963895,136.410727927222));
#263449=CARTESIAN_POINT('Ctrl Pts',(-203.847306124073,2.04026237982279,
136.360439570108));
#263450=CARTESIAN_POINT('Ctrl Pts',(-203.854707945748,2.18744990277064,
136.30416171299));
#263451=CARTESIAN_POINT('Ctrl Pts',(-203.862109767424,2.33223402761866,
136.24206371749));
#263452=CARTESIAN_POINT('Ctrl Pts',(-203.869507681735,2.47694172205335,
136.179998503038));
#263453=CARTESIAN_POINT('Ctrl Pts',(-203.876905596046,2.61924820292951,
136.112119415821));
#263454=CARTESIAN_POINT('Ctrl Pts',(-203.884303510358,2.7586594478157,136.038644581345));
#263455=CARTESIAN_POINT('Ctrl Pts',(-203.89170019527,2.89804752508276,135.965181957054));
#263456=CARTESIAN_POINT('Ctrl Pts',(-203.899096880182,3.03454099135519,
135.886125604982));
#263457=CARTESIAN_POINT('Ctrl Pts',(-203.906493565094,3.16766874893783,
135.801740456992));
#263458=CARTESIAN_POINT('Ctrl Pts',(-203.91388992203,3.30079060349657,135.717359050728));
#263459=CARTESIAN_POINT('Ctrl Pts',(-203.921286278965,3.43054673081018,
135.627649518213));
#263460=CARTESIAN_POINT('Ctrl Pts',(-203.928682635901,3.55649368565297,
135.532920993242));
#263461=CARTESIAN_POINT('Ctrl Pts',(-203.936080125237,3.68245992329573,
135.438177965092));
#263462=CARTESIAN_POINT('Ctrl Pts',(-203.943477614574,3.80461552889866,
135.338414638858));
#263463=CARTESIAN_POINT('Ctrl Pts',(-203.95087510391,3.92254903444112,135.233981327616));
#263464=CARTESIAN_POINT('Ctrl Pts',(-203.958275186425,4.04052388139095,
135.12951140744));
#263465=CARTESIAN_POINT('Ctrl Pts',(-203.96567526894,4.15427340221235,135.020368490215));
#263466=CARTESIAN_POINT('Ctrl Pts',(-203.973075351455,4.26342209311666,
134.906940612938));
#263467=CARTESIAN_POINT('Ctrl Pts',(-203.980483571122,4.37269080422754,
134.793388010048));
#263468=CARTESIAN_POINT('Ctrl Pts',(-203.987891790788,4.47734832309786,
134.675541306575));
#263469=CARTESIAN_POINT('Ctrl Pts',(-203.995300010455,4.57705817148828,
134.55382312002));
#263470=CARTESIAN_POINT('Ctrl Pts',(-204.002712789757,4.6768293896272,134.432030017952));
#263471=CARTESIAN_POINT('Ctrl Pts',(-204.010125569059,4.77164664501153,
134.306360982011));
#263472=CARTESIAN_POINT('Ctrl Pts',(-204.017538348361,4.8612164216961,134.177268185812));
#263473=CARTESIAN_POINT('Ctrl Pts',(-204.02496171939,4.95091417987762,134.047990935772));
#263474=CARTESIAN_POINT('Ctrl Pts',(-204.032385090419,5.03534928462894,
133.915280469116));
#263475=CARTESIAN_POINT('Ctrl Pts',(-204.039808461447,5.11427343323228,
133.779614860926));
#263476=CARTESIAN_POINT('Ctrl Pts',(-204.043744510888,5.15612091057836,
133.707681700217));
#263477=CARTESIAN_POINT('Ctrl Pts',(-204.047680560328,5.19641984998835,
133.634918111469));
#263478=CARTESIAN_POINT('Ctrl Pts',(-204.051616609769,5.23513874963715,
133.561397584048));
#263479=CARTESIAN_POINT('Ctrl Pts',(-204.059039876174,5.30816138600291,
133.422740163822));
#263480=CARTESIAN_POINT('Ctrl Pts',(-204.06646314258,5.3757819339304,133.280969967167));
#263481=CARTESIAN_POINT('Ctrl Pts',(-204.073886408985,5.437723476843,133.136547134955));
#263482=CARTESIAN_POINT('Ctrl Pts',(-204.081300901706,5.49959180999563,
132.992294998537));
#263483=CARTESIAN_POINT('Ctrl Pts',(-204.088715394427,5.5557943529252,132.845396806912));
#263484=CARTESIAN_POINT('Ctrl Pts',(-204.096129887148,5.60609946214324,
132.696338255663));
#263485=CARTESIAN_POINT('Ctrl Pts',(-204.103537233502,5.65635608540307,
132.547423372657));
#263486=CARTESIAN_POINT('Ctrl Pts',(-204.110944579855,5.70072647244532,
132.396352626674));
#263487=CARTESIAN_POINT('Ctrl Pts',(-204.118351926209,5.73902663486398,
132.243632602572));
#263488=CARTESIAN_POINT('Ctrl Pts',(-204.125753747884,5.77729823157674,
132.091026482824));
#263489=CARTESIAN_POINT('Ctrl Pts',(-204.13315556956,5.80950852791993,131.936773894766));
#263490=CARTESIAN_POINT('Ctrl Pts',(-204.140557391235,5.83552308162863,
131.781397426637));
#263491=CARTESIAN_POINT('Ctrl Pts',(-204.147955305546,5.86152390245685,
131.626102980537));
#263492=CARTESIAN_POINT('Ctrl Pts',(-204.155353219858,5.88133543288823,
131.469686203167));
#263493=CARTESIAN_POINT('Ctrl Pts',(-204.162751134169,5.89487415689882,
131.312680631756));
#263494=CARTESIAN_POINT('Ctrl Pts',(-204.170147819081,5.90841063101912,
131.155701151823));
#263495=CARTESIAN_POINT('Ctrl Pts',(-204.177544503993,5.9156763355876,130.998133443599));
#263496=CARTESIAN_POINT('Ctrl Pts',(-204.184941188905,5.91663952547246,
130.840517057061));
#263497=CARTESIAN_POINT('Ctrl Pts',(-204.192337545841,5.91760267264848,
130.682907659399));
#263498=CARTESIAN_POINT('Ctrl Pts',(-204.199733902776,5.91226385852082,
130.525249961006));
#263499=CARTESIAN_POINT('Ctrl Pts',(-204.207130259712,5.90064347312982,
130.368084139275));
#263500=CARTESIAN_POINT('Ctrl Pts',(-204.214527749048,5.8890213086282,130.210894255055));
#263501=CARTESIAN_POINT('Ctrl Pts',(-204.221925238385,5.87111568546889,
130.054196769752));
#263502=CARTESIAN_POINT('Ctrl Pts',(-204.229322727721,5.84699892344906,
129.898527215838));
#263503=CARTESIAN_POINT('Ctrl Pts',(-204.236722810236,5.82287370733566,
129.742803092204));
#263504=CARTESIAN_POINT('Ctrl Pts',(-204.244122892751,5.79253307447818,
129.58810798606));
#263505=CARTESIAN_POINT('Ctrl Pts',(-204.251522975266,5.75610052241988,
129.434967562853));
#263506=CARTESIAN_POINT('Ctrl Pts',(-204.258931194933,5.71962790902519,
129.281658746007));
#263507=CARTESIAN_POINT('Ctrl Pts',(-204.266339414599,5.67705008515344,
129.129908389533));
#263508=CARTESIAN_POINT('Ctrl Pts',(-204.273747634265,5.62854073617138,
128.980228017189));
#263509=CARTESIAN_POINT('Ctrl Pts',(-204.281160413567,5.58000153049444,
128.830455519072));
#263510=CARTESIAN_POINT('Ctrl Pts',(-204.288573192869,5.52552365400217,
128.682755893192));
#263511=CARTESIAN_POINT('Ctrl Pts',(-204.295985972171,5.46532888062469,
128.537620493708));
#263512=CARTESIAN_POINT('Ctrl Pts',(-204.3034093432,5.40504809813207,128.392277717958));
#263513=CARTESIAN_POINT('Ctrl Pts',(-204.310832714229,5.33903426053937,
128.249506824144));
#263514=CARTESIAN_POINT('Ctrl Pts',(-204.318256085258,5.26755537227114,
128.109775127633));
#263515=CARTESIAN_POINT('Ctrl Pts',(-204.322192134699,5.22965555059476,
128.035686029319));
#263516=CARTESIAN_POINT('Ctrl Pts',(-204.32612818414,5.19022004371018,127.962450893188));
#263517=CARTESIAN_POINT('Ctrl Pts',(-204.330064233581,5.14929365279669,
127.890135945416));
#263518=CARTESIAN_POINT('Ctrl Pts',(-204.337487499987,5.07210775681115,
127.753752210805));
#263519=CARTESIAN_POINT('Ctrl Pts',(-204.344910766392,4.98938303310252,
127.620230874498));
#263520=CARTESIAN_POINT('Ctrl Pts',(-204.352334032798,4.90135693104575,
127.490053631635));
#263521=CARTESIAN_POINT('Ctrl Pts',(-204.359748525519,4.81343486853123,
127.360030247463));
#263522=CARTESIAN_POINT('Ctrl Pts',(-204.367163018239,4.72022410681939,
127.233343395595));
#263523=CARTESIAN_POINT('Ctrl Pts',(-204.374577510961,4.62200806639798,
127.110450494586));
#263524=CARTESIAN_POINT('Ctrl Pts',(-204.381984857314,4.52388669029411,
126.987676042383));
#263525=CARTESIAN_POINT('Ctrl Pts',(-204.389392203668,4.42076987115514,
126.868688550817));
#263526=CARTESIAN_POINT('Ctrl Pts',(-204.396799550022,4.31298436294144,
126.753916636035));
#263527=CARTESIAN_POINT('Ctrl Pts',(-204.404201371697,4.20527924522689,
126.639230322478));
#263528=CARTESIAN_POINT('Ctrl Pts',(-204.411603193373,4.09291262618729,
126.528753596247));
#263529=CARTESIAN_POINT('Ctrl Pts',(-204.419005015048,3.97625150478076,
126.422882039137));
#263530=CARTESIAN_POINT('Ctrl Pts',(-204.42640292936,3.85965196787114,126.317066370797));
#263531=CARTESIAN_POINT('Ctrl Pts',(-204.433800843671,3.73876271923734,
126.215851280293));
#263532=CARTESIAN_POINT('Ctrl Pts',(-204.441198757982,3.61398749640891,
126.119595421924));
#263533=CARTESIAN_POINT('Ctrl Pts',(-204.448595442894,3.48923300895941,
126.023355559533));
#263534=CARTESIAN_POINT('Ctrl Pts',(-204.455992127807,3.36059412427482,
125.932073521404));
#263535=CARTESIAN_POINT('Ctrl Pts',(-204.463388812719,3.22850762201203,
125.846067655557));
#263536=CARTESIAN_POINT('Ctrl Pts',(-204.470785169654,3.0964269766028,125.7600656033));
#263537=CARTESIAN_POINT('Ctrl Pts',(-204.47818152659,2.9608993304014,125.679339461843));
#263538=CARTESIAN_POINT('Ctrl Pts',(-204.485577883525,2.82239017126325,
125.604164055545));
#263539=CARTESIAN_POINT('Ctrl Pts',(-204.492975372862,2.68385980601923,
125.5289771397));
#263540=CARTESIAN_POINT('Ctrl Pts',(-204.500372862198,2.54234734704194,
125.459342829222));
#263541=CARTESIAN_POINT('Ctrl Pts',(-204.507770351535,2.39834244358581,
125.395489747801));
#263542=CARTESIAN_POINT('Ctrl Pts',(-204.51517043405,2.25428705943503,125.331614282781));
#263543=CARTESIAN_POINT('Ctrl Pts',(-204.522570516565,2.1077378322723,125.273524232987));
#263544=CARTESIAN_POINT('Ctrl Pts',(-204.52997059908,1.95920377276374,125.221399831452));
#263545=CARTESIAN_POINT('Ctrl Pts',(-204.537378818746,1.81050638478601,
125.169218113778));
#263546=CARTESIAN_POINT('Ctrl Pts',(-204.544787038413,1.65982015826697,
125.123015268486));
#263547=CARTESIAN_POINT('Ctrl Pts',(-204.552195258079,1.5076693338124,125.082921660242));
#263548=CARTESIAN_POINT('Ctrl Pts',(-204.559608037382,1.35542486306415,
125.042803375052));
#263549=CARTESIAN_POINT('Ctrl Pts',(-204.567020816684,1.2017143617988,125.008801899886));
#263550=CARTESIAN_POINT('Ctrl Pts',(-204.574433595986,1.04707109441425,
124.980996238984));
#263551=CARTESIAN_POINT('Ctrl Pts',(-204.581856967014,0.89220686547698,
124.953150848049));
#263552=CARTESIAN_POINT('Ctrl Pts',(-204.589280338043,0.73640757733136,
124.931519003745));
#263553=CARTESIAN_POINT('Ctrl Pts',(-204.596703709072,0.580211258570826,
124.916127821733));
#263554=CARTESIAN_POINT('Ctrl Pts',(-204.600639758513,0.497392222485452,
124.907967047723));
#263555=CARTESIAN_POINT('Ctrl Pts',(-204.604575807954,0.414461573604239,
124.901559876592));
#263556=CARTESIAN_POINT('Ctrl Pts',(-204.608511857394,0.331499246015727,
124.896904412702));
#263557=CARTESIAN_POINT('Ctrl Pts',(-204.6159351238,0.175034885349205,124.888124353097));
#263558=CARTESIAN_POINT('Ctrl Pts',(-204.623358390205,0.017984869765548,
124.885551462325));
#263559=CARTESIAN_POINT('Ctrl Pts',(-204.630781656611,-0.139117189784255,
124.889246335491));
#263560=CARTESIAN_POINT('Ctrl Pts',(-204.638196149331,-0.296033567746183,
124.892936841624));
#263561=CARTESIAN_POINT('Ctrl Pts',(-204.645610642053,-0.453001497684593,
124.902880357385));
#263562=CARTESIAN_POINT('Ctrl Pts',(-204.653025134774,-0.609482944717867,
124.919085678993));
#263563=CARTESIAN_POINT('Ctrl Pts',(-204.660432481127,-0.765813569041512,
124.935275381302));
#263564=CARTESIAN_POINT('Ctrl Pts',(-204.667839827481,-0.92165827510939,
124.957714836041));
#263565=CARTESIAN_POINT('Ctrl Pts',(-204.675247173835,-1.07647983752149,
124.986360813346));
#263566=CARTESIAN_POINT('Ctrl Pts',(-204.68264899551,-1.23118592817213,
125.0149854254));
#263567=CARTESIAN_POINT('Ctrl Pts',(-204.690050817186,-1.38487002911259,
125.049807275314));
#263568=CARTESIAN_POINT('Ctrl Pts',(-204.697452638861,-1.53700095427533,
125.090731418094));
#263569=CARTESIAN_POINT('Ctrl Pts',(-204.704850553172,-1.689051570706,125.131633957337));
#263570=CARTESIAN_POINT('Ctrl Pts',(-204.712248467484,-1.83955028467765,
125.17863227724));
#263571=CARTESIAN_POINT('Ctrl Pts',(-204.719646381795,-1.98797712017319,
125.231580563395));
#263572=CARTESIAN_POINT('Ctrl Pts',(-204.727043066707,-2.1363792898212,
125.284520050505));
#263573=CARTESIAN_POINT('Ctrl Pts',(-204.734439751619,-2.28270991309183,
125.343407416136));
#263574=CARTESIAN_POINT('Ctrl Pts',(-204.741836436532,-2.42646506470635,
125.408047260073));
#263575=CARTESIAN_POINT('Ctrl Pts',(-204.749232793467,-2.57021384206722,
125.472684237812));
#263576=CARTESIAN_POINT('Ctrl Pts',(-204.756629150402,-2.711387034376,125.5430730336));
#263577=CARTESIAN_POINT('Ctrl Pts',(-204.764025507338,-2.84950181656107,
125.6189705686));
#263578=CARTESIAN_POINT('Ctrl Pts',(-204.771422996674,-2.98763774447108,
125.694879723706));
#263579=CARTESIAN_POINT('Ctrl Pts',(-204.778820486011,-3.12271400273242,
125.776299117558));
#263580=CARTESIAN_POINT('Ctrl Pts',(-204.786217975348,-3.25427357637751,
125.862940371059));
#263581=CARTESIAN_POINT('Ctrl Pts',(-204.793618057863,-3.38587926802739,
125.949611996517));
#263582=CARTESIAN_POINT('Ctrl Pts',(-204.801018140377,-3.5139655090601,
126.041508920977));
#263583=CARTESIAN_POINT('Ctrl Pts',(-204.808418222892,-3.63810553162232,
126.138300319705));
#263584=CARTESIAN_POINT('Ctrl Pts',(-204.815826442559,-3.76238205890143,
126.235198150526));
#263585=CARTESIAN_POINT('Ctrl Pts',(-204.823234662225,-3.88270340732681,
126.337000974104));
#263586=CARTESIAN_POINT('Ctrl Pts',(-204.830642881892,-3.99867653255975,
126.443338197255));
#263587=CARTESIAN_POINT('Ctrl Pts',(-204.838055661194,-4.11472103731682,
126.549740869193));
#263588=CARTESIAN_POINT('Ctrl Pts',(-204.845468440496,-4.22641172186707,
126.660683239356));
#263589=CARTESIAN_POINT('Ctrl Pts',(-204.852881219798,-4.33339387527508,
126.775759361022));
#263590=CARTESIAN_POINT('Ctrl Pts',(-204.860304590827,-4.44052888980039,
126.890999908847));
#263591=CARTESIAN_POINT('Ctrl Pts',(-204.867727961855,-4.54294169391004,
127.010385722194));
#263592=CARTESIAN_POINT('Ctrl Pts',(-204.875151332884,-4.64031865683491,
127.133478799047));
#263593=CARTESIAN_POINT('Ctrl Pts',(-204.879087382325,-4.69195025910903,
127.198745701977));
#263594=CARTESIAN_POINT('Ctrl Pts',(-204.883023431766,-4.74216683506,127.265054373102));
#263595=CARTESIAN_POINT('Ctrl Pts',(-204.886959481207,-4.79092677321238,
127.332336536973));
#263596=CARTESIAN_POINT('Ctrl Pts',(-204.894439644792,-4.88359133935193,
127.460201188986));
#263597=CARTESIAN_POINT('Ctrl Pts',(-204.901919808376,-4.97127200205635,
127.591969048914));
#263598=CARTESIAN_POINT('Ctrl Pts',(-204.909399971961,-5.05362495660158,
127.727218215838));
#263599=CARTESIAN_POINT('Ctrl Pts',(-204.916871063548,-5.13587803287105,
127.862303351566));
#263600=CARTESIAN_POINT('Ctrl Pts',(-204.924342155134,-5.21281607482848,
128.000861080831));
#263601=CARTESIAN_POINT('Ctrl Pts',(-204.931813246721,-5.28413634723124,
128.142437698628));
#263602=CARTESIAN_POINT('Ctrl Pts',(-204.939276676359,-5.35538347741398,
128.28386912309));
#263603=CARTESIAN_POINT('Ctrl Pts',(-204.946740105998,-5.42102414483629,
128.428312948119));
#263604=CARTESIAN_POINT('Ctrl Pts',(-204.954203535636,-5.48079969101944,
128.575287871014));
#263605=CARTESIAN_POINT('Ctrl Pts',(-204.961660708341,-5.5405251246347,
128.722139578124));
#263606=CARTESIAN_POINT('Ctrl Pts',(-204.969117881046,-5.59439509099741,
128.871517820658));
#263607=CARTESIAN_POINT('Ctrl Pts',(-204.976575053751,-5.64219757205847,
129.022918190667));
#263608=CARTESIAN_POINT('Ctrl Pts',(-204.984026968987,-5.68996635133299,
129.174211820128));
#263609=CARTESIAN_POINT('Ctrl Pts',(-204.991478884223,-5.73167605837681,
129.327524388969));
#263610=CARTESIAN_POINT('Ctrl Pts',(-204.99893079946,-5.76716343358339,
129.482333199984));
#263611=CARTESIAN_POINT('Ctrl Pts',(-205.006379560772,-5.80263578923023,
129.637076490228));
#263612=CARTESIAN_POINT('Ctrl Pts',(-205.013828322084,-5.83189097662629,
129.793314405558));
#263613=CARTESIAN_POINT('Ctrl Pts',(-205.021277083396,-5.85481604611657,
129.95051073109));
#263614=CARTESIAN_POINT('Ctrl Pts',(-205.028725022292,-5.87773858445527,
130.107689700612));
#263615=CARTESIAN_POINT('Ctrl Pts',(-205.036172961189,-5.89433233816279,
130.265826508781));
#263616=CARTESIAN_POINT('Ctrl Pts',(-205.043620900085,-5.90453575298649,
130.424376270251));
#263617=CARTESIAN_POINT('Ctrl Pts',(-205.049622202654,-5.91275732682686,
130.552130418624));
#263618=CARTESIAN_POINT('Ctrl Pts',(-205.055623505223,-5.91683088167834,
130.680152436099));
#263619=CARTESIAN_POINT('Ctrl Pts',(-205.061624807792,-5.91674878301709,
130.808155504365));
#263620=CARTESIAN_POINT('',(-206.811623324931,-5.92153837798521,130.807366761688));
#263621=CARTESIAN_POINT('Ctrl Pts',(-205.061626944303,-5.90947417380247,
130.808196352657));
#263622=CARTESIAN_POINT('Ctrl Pts',(-205.096220331209,-5.91377200472859,
131.545141902329));
#263623=CARTESIAN_POINT('Ctrl Pts',(-205.223629592719,-5.44370849995411,
134.254054771831));
#263624=CARTESIAN_POINT('Ctrl Pts',(-205.443854728833,-1.37967370610466,
137.665414544981));
#263625=CARTESIAN_POINT('Ctrl Pts',(-205.722302352646,5.0266516457322,135.673686419238));
#263626=CARTESIAN_POINT('Ctrl Pts',(-206.000749976459,6.813729700728,129.207285761534));
#263627=CARTESIAN_POINT('Ctrl Pts',(-206.279197600272,2.3393230299546,124.208518875085));
#263628=CARTESIAN_POINT('Ctrl Pts',(-206.549488398635,-4.09076040919075,
125.239883832662));
#263629=CARTESIAN_POINT('Ctrl Pts',(-206.726963322394,-5.91340440505827,
129.015638925646));
#263630=CARTESIAN_POINT('Ctrl Pts',(-206.811622371547,-5.92461749863669,
130.807348163968));
#263631=CARTESIAN_POINT('Ctrl Pts',(-206.811624807792,-5.91674922156144,
130.807395687932));
#263632=CARTESIAN_POINT('Ctrl Pts',(-206.819780821161,-5.91666079577132,
130.979778256311));
#263633=CARTESIAN_POINT('Ctrl Pts',(-206.827936834529,-5.90903961803116,
131.151962513016));
#263634=CARTESIAN_POINT('Ctrl Pts',(-206.836092847897,-5.89393313865187,
131.323477867907));
#263635=CARTESIAN_POINT('Ctrl Pts',(-206.843516422095,-5.88018327514893,
131.479590530506));
#263636=CARTESIAN_POINT('Ctrl Pts',(-206.850939996293,-5.86020589862519,
131.635392596784));
#263637=CARTESIAN_POINT('Ctrl Pts',(-206.858363570491,-5.83401756875813,
131.790347214798));
#263638=CARTESIAN_POINT('Ctrl Pts',(-206.865778303408,-5.80786042849981,
131.945117285957));
#263639=CARTESIAN_POINT('Ctrl Pts',(-206.873193036325,-5.77550712091378,
132.099041553354));
#263640=CARTESIAN_POINT('Ctrl Pts',(-206.880607769242,-5.73702611008395,
132.251586230494));
#263641=CARTESIAN_POINT('Ctrl Pts',(-206.888015288472,-5.69858253687992,
132.403982499097));
#263642=CARTESIAN_POINT('Ctrl Pts',(-206.895422807702,-5.65402321989905,
132.555001489991));
#263643=CARTESIAN_POINT('Ctrl Pts',(-206.902830326931,-5.60346799857048,
132.704117694536));
#263644=CARTESIAN_POINT('Ctrl Pts',(-206.910232254374,-5.55295094035424,
132.853121334279));
#263645=CARTESIAN_POINT('Ctrl Pts',(-206.917634181817,-5.49644710986732,
133.000224695794));
#263646=CARTESIAN_POINT('Ctrl Pts',(-206.925036109261,-5.43412666074035,
133.144915679412));
#263647=CARTESIAN_POINT('Ctrl Pts',(-206.932434348698,-5.37183726273652,
133.289534570841));
#263648=CARTESIAN_POINT('Ctrl Pts',(-206.939832588136,-5.30373716364741,
133.431743135487));
#263649=CARTESIAN_POINT('Ctrl Pts',(-206.947230827574,-5.23004527582684,
133.57104762106));
#263650=CARTESIAN_POINT('Ctrl Pts',(-206.954627182734,-5.15637215678872,
133.710316626804));
#263651=CARTESIAN_POINT('Ctrl Pts',(-206.962023537895,-5.07711025803544,
133.846682695997));
#263652=CARTESIAN_POINT('Ctrl Pts',(-206.969419893055,-4.99252519862058,
133.97967520098));
#263653=CARTESIAN_POINT('Ctrl Pts',(-206.976815824747,-4.9079449820142,
134.112660091648));
#263654=CARTESIAN_POINT('Ctrl Pts',(-206.984211756438,-4.81804241190689,
134.242271487812));
#263655=CARTESIAN_POINT('Ctrl Pts',(-206.99160768813,-4.72312724667466,
134.368066494069));
#263656=CARTESIAN_POINT('Ctrl Pts',(-206.999004656617,-4.62819877580896,
134.493879134833));
#263657=CARTESIAN_POINT('Ctrl Pts',(-207.006401625103,-4.52825653613315,
134.615874023046));
#263658=CARTESIAN_POINT('Ctrl Pts',(-207.01379859359,-4.42365139311575,
134.733640311694));
#263659=CARTESIAN_POINT('Ctrl Pts',(-207.021201700528,-4.31895944243015,
134.851504329924));
#263660=CARTESIAN_POINT('Ctrl Pts',(-207.028604807466,-4.20959710649542,
134.965132459073));
#263661=CARTESIAN_POINT('Ctrl Pts',(-207.036007914404,-4.09595347651789,
135.074149333732));
#263662=CARTESIAN_POINT('Ctrl Pts',(-207.043414228711,-3.98226061085117,
135.183213439556));
#263663=CARTESIAN_POINT('Ctrl Pts',(-207.050820543018,-3.86428303275637,
135.287662060798));
#263664=CARTESIAN_POINT('Ctrl Pts',(-207.058226857325,-3.74244355311888,
135.387159632821));
#263665=CARTESIAN_POINT('Ctrl Pts',(-207.065642606406,-3.62044886429578,
135.486783953063));
#263666=CARTESIAN_POINT('Ctrl Pts',(-207.073058355488,-3.49458274227156,
135.581444397463));
#263667=CARTESIAN_POINT('Ctrl Pts',(-207.08047410457,-3.36529835974214,
135.670847801605));
#263668=CARTESIAN_POINT('Ctrl Pts',(-207.086208830725,-3.26532052582677,
135.73998498984));
#263669=CARTESIAN_POINT('Ctrl Pts',(-207.091943556881,-3.16329913061462,
135.805979224788));
#263670=CARTESIAN_POINT('Ctrl Pts',(-207.097678283037,-3.05945365335209,
135.868713873954));
#263671=CARTESIAN_POINT('Origin',(210.,0.,130.804360617566));
#263672=CARTESIAN_POINT('',(-178.530629926805,1.98348391145776,125.240348466903));
#263673=CARTESIAN_POINT('Ctrl Pts',(-178.18410255161,3.73285074851184,126.213744553045));
#263674=CARTESIAN_POINT('Ctrl Pts',(-178.294692878395,3.30225397105088,
125.863605599916));
#263675=CARTESIAN_POINT('Ctrl Pts',(-178.403686871865,2.806068509165,125.563687251781));
#263676=CARTESIAN_POINT('Ctrl Pts',(-178.503050604127,2.18460962668051,
125.30481172624));
#263677=CARTESIAN_POINT('Ctrl Pts',(-178.516849507463,2.09302951709462,
125.269308805648));
#263678=CARTESIAN_POINT('Ctrl Pts',(-178.529878634857,2.00062638375932,
125.236109129432));
#263679=CARTESIAN_POINT('',(-177.987180129183,4.43101178267811,134.710827119055));
#263680=CARTESIAN_POINT('Ctrl Pts',(-177.98715711374,4.43823075232565,134.717165027655));
#263681=CARTESIAN_POINT('Ctrl Pts',(-177.917823106101,4.66836223140131,
134.456130613341));
#263682=CARTESIAN_POINT('Ctrl Pts',(-177.848712438811,4.88126271378723,
134.167633593295));
#263683=CARTESIAN_POINT('Ctrl Pts',(-177.785458995272,5.06765282954142,
133.85834577826));
#263684=CARTESIAN_POINT('Ctrl Pts',(-178.529931596729,1.99775342761758,
125.244229456078));
#263685=CARTESIAN_POINT('Ctrl Pts',(-178.491569805427,2.76854523389136,
125.517184209005));
#263686=CARTESIAN_POINT('Ctrl Pts',(-178.36039213952,5.21384277720883,126.968629961239));
#263687=CARTESIAN_POINT('Ctrl Pts',(-178.179474983672,6.55706668978598,
131.115450305371));
#263688=CARTESIAN_POINT('Ctrl Pts',(-178.036919619125,5.13087667649733,
133.913851480684));
#263689=CARTESIAN_POINT('Ctrl Pts',(-177.987180129183,4.43101178267811,
134.710827119055));
#263690=CARTESIAN_POINT('Origin',(210.,0.,130.804360617566));
#263691=CARTESIAN_POINT('',(-207.299567498839,-3.90840034609305,135.243902605346));
#263692=CARTESIAN_POINT('Ctrl Pts',(-207.097024439715,-3.07128565518615,
135.861547087012));
#263693=CARTESIAN_POINT('Ctrl Pts',(-207.161528107063,-3.37326783662078,
135.678149945624));
#263694=CARTESIAN_POINT('Ctrl Pts',(-207.230903561036,-3.65533760795257,
135.469418255391));
#263695=CARTESIAN_POINT('Ctrl Pts',(-207.299550587757,-3.91125355034577,
135.243958147456));
#263696=CARTESIAN_POINT('',(-178.657321351531,-0.670823532967099,124.921705606293));
#263697=CARTESIAN_POINT('Ctrl Pts',(-178.656496695459,-0.652296033834956,
124.923676945854));
#263698=CARTESIAN_POINT('Ctrl Pts',(-178.631041117028,-1.20105617910375,
124.984546410404));
#263699=CARTESIAN_POINT('Ctrl Pts',(-178.571675042675,-1.75540607403642,
125.126022270676));
#263700=CARTESIAN_POINT('Ctrl Pts',(-178.487473351945,-2.28203573490688,
125.345395642053));
#263701=CARTESIAN_POINT('Ctrl Pts',(-178.486373882786,-2.28888204220153,
125.348262685419));
#263702=CARTESIAN_POINT('Ctrl Pts',(-178.485270545702,-2.29572256715809,
125.351142443209));
#263703=CARTESIAN_POINT('',(-179.063374001572,-5.91358993803376,130.79964208133));
#263704=CARTESIAN_POINT('Ctrl Pts',(-179.063373167743,-5.91137817917409,
130.799626087985));
#263705=CARTESIAN_POINT('Ctrl Pts',(-179.032829268644,-5.91617425954304,
130.149473536606));
#263706=CARTESIAN_POINT('Ctrl Pts',(-178.909469494942,-5.51702945710787,
127.529389957826));
#263707=CARTESIAN_POINT('Ctrl Pts',(-178.774255230047,-3.11548842989244,
125.328065259864));
#263708=CARTESIAN_POINT('Ctrl Pts',(-178.66958486425,-0.929687989411222,
124.947409885417));
#263709=CARTESIAN_POINT('Ctrl Pts',(-178.657730373058,-0.680012995400244,
124.920727840718));
#263710=CARTESIAN_POINT('',(-180.813376354123,-5.91239331584027,130.807847145143));
#263711=CARTESIAN_POINT('Ctrl Pts',(-180.813375192208,-5.91674898580156,
130.807824938015));
#263712=CARTESIAN_POINT('Ctrl Pts',(-180.80590436759,-5.91684231226662,
130.648431696059));
#263713=CARTESIAN_POINT('Ctrl Pts',(-180.798433542972,-5.91049037800369,
130.489025468643));
#263714=CARTESIAN_POINT('Ctrl Pts',(-180.790962718354,-5.89771667312605,
130.330157490171));
#263715=CARTESIAN_POINT('Ctrl Pts',(-180.783490770938,-5.88494104847493,
130.171265635264));
#263716=CARTESIAN_POINT('Ctrl Pts',(-180.776018823522,-5.86574175873066,
130.012912552212));
#263717=CARTESIAN_POINT('Ctrl Pts',(-180.768546876106,-5.84019423006307,
129.855644686616));
#263718=CARTESIAN_POINT('Ctrl Pts',(-180.761072443837,-5.81463820537227,
129.698324520407));
#263719=CARTESIAN_POINT('Ctrl Pts',(-180.753598011569,-5.78272979363846,
129.542090648727));
#263720=CARTESIAN_POINT('Ctrl Pts',(-180.7461235793,-5.74459562263046,129.3874796434));
#263721=CARTESIAN_POINT('Ctrl Pts',(-180.738645298881,-5.70644181855295,
129.232789037847));
#263722=CARTESIAN_POINT('Ctrl Pts',(-180.731167018461,-5.66205595596423,
129.079723315102));
#263723=CARTESIAN_POINT('Ctrl Pts',(-180.723688738042,-5.61161462016539,
128.928804188864));
#263724=CARTESIAN_POINT('Ctrl Pts',(-180.716200537055,-5.56110636969527,
128.777684855721));
#263725=CARTESIAN_POINT('Ctrl Pts',(-180.708712336068,-5.50452671422177,
128.628718151764));
#263726=CARTESIAN_POINT('Ctrl Pts',(-180.701224135081,-5.4421008949015,
128.482407040896));
#263727=CARTESIAN_POINT('Ctrl Pts',(-180.693730469935,-5.37962952330192,
128.335989166437));
#263728=CARTESIAN_POINT('Ctrl Pts',(-180.686236804789,-5.31130363918635,
128.192231074739));
#263729=CARTESIAN_POINT('Ctrl Pts',(-180.678743139642,-5.23739446975496,
128.051611131928));
#263730=CARTESIAN_POINT('Ctrl Pts',(-180.67123737861,-5.16336599996819,
127.910764207684));
#263731=CARTESIAN_POINT('Ctrl Pts',(-180.663731617577,-5.0837364204128,
127.773065865971));
#263732=CARTESIAN_POINT('Ctrl Pts',(-180.656225856544,-4.99882089239424,
127.638966448073));
#263733=CARTESIAN_POINT('Ctrl Pts',(-180.651626308805,-4.9467844602118,
127.556790014292));
#263734=CARTESIAN_POINT('Ctrl Pts',(-180.647026761065,-4.89276383469503,
127.475964459253));
#263735=CARTESIAN_POINT('Ctrl Pts',(-180.642427213326,-4.83683886899804,
127.396587104281));
#263736=CARTESIAN_POINT('Ctrl Pts',(-180.63500394692,-4.74658088221714,
127.26847901934));
#263737=CARTESIAN_POINT('Ctrl Pts',(-180.627580680515,-4.65109331048002,
127.143765544506));
#263738=CARTESIAN_POINT('Ctrl Pts',(-180.62015741411,-4.55065994398724,
127.022902613477));
#263739=CARTESIAN_POINT('Ctrl Pts',(-180.612742921389,-4.45034528139318,
126.902182532395));
#263740=CARTESIAN_POINT('Ctrl Pts',(-180.605328428668,-4.34509669582955,
126.785304220586));
#263741=CARTESIAN_POINT('Ctrl Pts',(-180.597913935947,-4.23524133075553,
126.672694920446));
#263742=CARTESIAN_POINT('Ctrl Pts',(-180.590506589593,-4.12549184841834,
126.560194157389));
#263743=CARTESIAN_POINT('Ctrl Pts',(-180.583099243239,-4.01114468503391,
126.451954479988));
#263744=CARTESIAN_POINT('Ctrl Pts',(-180.575691896886,-3.89256726626094,
126.348370195658));
#263745=CARTESIAN_POINT('Ctrl Pts',(-180.56829007521,-3.77407828700056,
126.244863168396));
#263746=CARTESIAN_POINT('Ctrl Pts',(-180.560888253535,-3.65136561447588,
126.146004865181));
#263747=CARTESIAN_POINT('Ctrl Pts',(-180.55348643186,-3.52483346582677,
126.05215275167));
#263748=CARTESIAN_POINT('Ctrl Pts',(-180.546088517549,-3.39836811251472,
125.958350181959));
#263749=CARTESIAN_POINT('Ctrl Pts',(-180.538690603237,-3.26808759764599,
125.869548760655));
#263750=CARTESIAN_POINT('Ctrl Pts',(-180.531292688926,-3.13442905661681,
125.78606558324));
#263751=CARTESIAN_POINT('Ctrl Pts',(-180.523896004014,-3.00079272721176,
125.702596279216));
#263752=CARTESIAN_POINT('Ctrl Pts',(-180.516499319102,-2.86377980209576,
125.624443662571));
#263753=CARTESIAN_POINT('Ctrl Pts',(-180.50910263419,-2.72385632332298,
125.551881460787));
#263754=CARTESIAN_POINT('Ctrl Pts',(-180.501706277254,-2.58393904890388,
125.479322476488));
#263755=CARTESIAN_POINT('Ctrl Pts',(-180.494309920319,-2.44111180882452,
125.412353586024));
#263756=CARTESIAN_POINT('Ctrl Pts',(-180.486913563384,-2.29586492173638,
125.351202374526));
#263757=CARTESIAN_POINT('Ctrl Pts',(-180.479516074047,-2.15059579697861,
125.29004180062));
#263758=CARTESIAN_POINT('Ctrl Pts',(-180.472118584711,-2.0029066316598,
125.234700824044));
#263759=CARTESIAN_POINT('Ctrl Pts',(-180.464721095374,-1.85330723241896,
125.185358671956));
#263760=CARTESIAN_POINT('Ctrl Pts',(-180.457321012859,-1.70365539134041,
125.135999223054));
#263761=CARTESIAN_POINT('Ctrl Pts',(-180.449920930344,-1.55209233740366,
125.092642902312));
#263762=CARTESIAN_POINT('Ctrl Pts',(-180.442520847829,-1.39914237269438,
125.055418872912));
#263763=CARTESIAN_POINT('Ctrl Pts',(-180.435112628163,-1.24602422377592,
125.018153911864));
#263764=CARTESIAN_POINT('Ctrl Pts',(-180.427704408496,-1.0915164813912,
124.987034796868));
#263765=CARTESIAN_POINT('Ctrl Pts',(-180.42029618883,-0.936153686024078,
124.962139564007));
#263766=CARTESIAN_POINT('Ctrl Pts',(-180.412883409528,-0.780695267448333,
124.937229008546));
#263767=CARTESIAN_POINT('Ctrl Pts',(-180.405470630226,-0.624381117031028,
124.91855001255));
#263768=CARTESIAN_POINT('Ctrl Pts',(-180.398057850924,-0.467749690625702,
124.906128612175));
#263769=CARTESIAN_POINT('Ctrl Pts',(-180.390634479895,-0.310894461893262,
124.893689463521));
#263770=CARTESIAN_POINT('Ctrl Pts',(-180.383211108867,-0.153721423776527,
124.887525782551));
#263771=CARTESIAN_POINT('Ctrl Pts',(-180.375787737838,0.00323134341759472,
124.887611499941));
#263772=CARTESIAN_POINT('Ctrl Pts',(-180.371851688396,0.0864514666357916,
124.887656949358));
#263773=CARTESIAN_POINT('Ctrl Pts',(-180.367915638954,0.169609742978011,
124.889458461255));
#263774=CARTESIAN_POINT('Ctrl Pts',(-180.363979589513,0.252626814831058,
124.893006267256));
#263775=CARTESIAN_POINT('Ctrl Pts',(-180.356556323107,0.409194421432122,
124.899697318649));
#263776=CARTESIAN_POINT('Ctrl Pts',(-180.349133056702,0.565732764817981,
124.912623037657));
#263777=CARTESIAN_POINT('Ctrl Pts',(-180.341709790296,0.721704859521438,
124.931791106846));
#263778=CARTESIAN_POINT('Ctrl Pts',(-180.334295297575,0.877492608161631,
124.950936520968));
#263779=CARTESIAN_POINT('Ctrl Pts',(-180.326880804854,1.03271507339061,
124.976309554354));
#263780=CARTESIAN_POINT('Ctrl Pts',(-180.319466312133,1.18683597505039,
125.007865906896));
#263781=CARTESIAN_POINT('Ctrl Pts',(-180.31205896578,1.34080832918305,125.039391844237));
#263782=CARTESIAN_POINT('Ctrl Pts',(-180.304651619426,1.49368087018309,
125.077089161737));
#263783=CARTESIAN_POINT('Ctrl Pts',(-180.297244273072,1.6449232535122,125.120861866572));
#263784=CARTESIAN_POINT('Ctrl Pts',(-180.289842451397,1.79605283456535,
125.164601924071));
#263785=CARTESIAN_POINT('Ctrl Pts',(-180.282440629721,1.94555432179695,
125.214408243235));
#263786=CARTESIAN_POINT('Ctrl Pts',(-180.275038808046,2.09290847999003,
125.270133963653));
#263787=CARTESIAN_POINT('Ctrl Pts',(-180.267640893735,2.24018485107,125.325830266896));
#263788=CARTESIAN_POINT('Ctrl Pts',(-180.260242979423,2.38531580236709,
125.387439616482));
#263789=CARTESIAN_POINT('Ctrl Pts',(-180.252845065112,2.52779827011158,
125.454765635876));
#263790=CARTESIAN_POINT('Ctrl Pts',(-180.2454483802,2.67025705985461,125.522080466907));
#263791=CARTESIAN_POINT('Ctrl Pts',(-180.238051695287,2.81006790238803,
125.595109922935));
#263792=CARTESIAN_POINT('Ctrl Pts',(-180.230655010375,2.94674859591522,
125.673609865973));
#263793=CARTESIAN_POINT('Ctrl Pts',(-180.22325865344,3.08342322887723,125.752106328241));
#263794=CARTESIAN_POINT('Ctrl Pts',(-180.215862296504,3.21696766509498,
125.836072609297));
#263795=CARTESIAN_POINT('Ctrl Pts',(-180.208465939569,3.34692540154562,
125.925219205495));
#263796=CARTESIAN_POINT('Ctrl Pts',(-180.201068450232,3.47690303485747,
126.014379450264));
#263797=CARTESIAN_POINT('Ctrl Pts',(-180.193670960896,3.60329256715243,
126.108721378205));
#263798=CARTESIAN_POINT('Ctrl Pts',(-180.186273471559,3.72566764660411,
126.20791295121));
#263799=CARTESIAN_POINT('Ctrl Pts',(-180.178873389044,3.84808562445071,
126.307139295668));
#263800=CARTESIAN_POINT('Ctrl Pts',(-180.171473306529,3.96648605779236,
126.411218435038));
#263801=CARTESIAN_POINT('Ctrl Pts',(-180.164073224014,4.08047687990288,
126.519779074979));
#263802=CARTESIAN_POINT('Ctrl Pts',(-180.156665004348,4.19459304664037,
126.628459088503));
#263803=CARTESIAN_POINT('Ctrl Pts',(-180.149256784681,4.30428964824568,
126.741630186279));
#263804=CARTESIAN_POINT('Ctrl Pts',(-180.141848565015,4.40921209856459,
126.858884824665));
#263805=CARTESIAN_POINT('Ctrl Pts',(-180.134435785713,4.51419912690065,
126.976211631324));
#263806=CARTESIAN_POINT('Ctrl Pts',(-180.127023006411,4.61440591173413,
127.097626699522));
#263807=CARTESIAN_POINT('Ctrl Pts',(-180.119610227109,4.7095194995687,127.222691084278));
#263808=CARTESIAN_POINT('Ctrl Pts',(-180.11218685608,4.80476899015836,127.347934166893));
#263809=CARTESIAN_POINT('Ctrl Pts',(-180.104763485052,4.89491053578961,
127.476836675114));
#263810=CARTESIAN_POINT('Ctrl Pts',(-180.097340114023,4.97967522377445,
127.608931815632));
#263811=CARTESIAN_POINT('Ctrl Pts',(-180.093404064582,5.02461949524755,
127.678971828719));
#263812=CARTESIAN_POINT('Ctrl Pts',(-180.089468015141,5.06805291187504,
127.749909002942));
#263813=CARTESIAN_POINT('Ctrl Pts',(-180.0855319657,5.10994079734045,127.821671292448));
#263814=CARTESIAN_POINT('Ctrl Pts',(-180.078108699294,5.18894004204775,
127.957012730823));
#263815=CARTESIAN_POINT('Ctrl Pts',(-180.070685432889,5.2626780668334,128.095699539363));
#263816=CARTESIAN_POINT('Ctrl Pts',(-180.063262166483,5.33085815437477,
128.2372840896));
#263817=CARTESIAN_POINT('Ctrl Pts',(-180.055847673762,5.39895765871467,
128.378701298656));
#263818=CARTESIAN_POINT('Ctrl Pts',(-180.048433181041,5.46151214110167,
128.523009099099));
#263819=CARTESIAN_POINT('Ctrl Pts',(-180.04101868832,5.51826899994545,128.669732357952));
#263820=CARTESIAN_POINT('Ctrl Pts',(-180.033611341967,5.57497115439181,
128.816314199405));
#263821=CARTESIAN_POINT('Ctrl Pts',(-180.026203995613,5.62588667606558,
128.965306518641));
#263822=CARTESIAN_POINT('Ctrl Pts',(-180.018796649259,5.67080966227076,
129.116211235314));
#263823=CARTESIAN_POINT('Ctrl Pts',(-180.011394827583,5.71569914321786,
129.267003401556));
#263824=CARTESIAN_POINT('Ctrl Pts',(-180.003993005908,5.75460488194266,
129.419704768962));
#263825=CARTESIAN_POINT('Ctrl Pts',(-179.996591184232,5.78736977694945,
129.573799108599));
#263826=CARTESIAN_POINT('Ctrl Pts',(-179.989193269921,5.8201173756232,129.727812103033));
#263827=CARTESIAN_POINT('Ctrl Pts',(-179.98179535561,5.84673050914526,129.883216241026));
#263828=CARTESIAN_POINT('Ctrl Pts',(-179.974397441298,5.86710247640078,
130.039482134464));
#263829=CARTESIAN_POINT('Ctrl Pts',(-179.967000756386,5.88747105820495,
130.195722059347));
#263830=CARTESIAN_POINT('Ctrl Pts',(-179.959604071474,5.90160048400506,
130.352823085647));
#263831=CARTESIAN_POINT('Ctrl Pts',(-179.952207386562,5.9094355121563,130.51024756079));
#263832=CARTESIAN_POINT('Ctrl Pts',(-179.944811029626,5.91727019289419,
130.667665055567));
#263833=CARTESIAN_POINT('Ctrl Pts',(-179.937414672691,5.91881101237257,
130.825405597834));
#263834=CARTESIAN_POINT('Ctrl Pts',(-179.930018315755,5.91405478717383,
130.982928634877));
#263835=CARTESIAN_POINT('Ctrl Pts',(-179.922620826419,5.90929783378486,
131.140475789099));
#263836=CARTESIAN_POINT('Ctrl Pts',(-179.915223337082,5.89824192734704,
131.297804998638));
#263837=CARTESIAN_POINT('Ctrl Pts',(-179.907825847746,5.88093596734664,
131.454378086923));
#263838=CARTESIAN_POINT('Ctrl Pts',(-179.900425765231,5.86362394076881,
131.61100606166));
#263839=CARTESIAN_POINT('Ctrl Pts',(-179.893025682716,5.84005753945498,
131.766877016608));
#263840=CARTESIAN_POINT('Ctrl Pts',(-179.885625600201,5.81033722220633,
131.921460401266));
#263841=CARTESIAN_POINT('Ctrl Pts',(-179.878217380534,5.78058422441342,
132.076213766249));
#263842=CARTESIAN_POINT('Ctrl Pts',(-179.870809160868,5.74466386733851,
132.229676366655));
#263843=CARTESIAN_POINT('Ctrl Pts',(-179.863400941201,5.70272736651028,
132.381329591818));
#263844=CARTESIAN_POINT('Ctrl Pts',(-179.855988161899,5.66076505446567,
132.533076157011));
#263845=CARTESIAN_POINT('Ctrl Pts',(-179.848575382597,5.61277933382527,
132.683010773186));
#263846=CARTESIAN_POINT('Ctrl Pts',(-179.841162603295,5.55897034242447,
132.830632883217));
#263847=CARTESIAN_POINT('Ctrl Pts',(-179.833739232266,5.50508446621329,
132.978465922642));
#263848=CARTESIAN_POINT('Ctrl Pts',(-179.826315861237,5.44535884258079,
133.123979512235));
#263849=CARTESIAN_POINT('Ctrl Pts',(-179.818892490209,5.380040844081,133.266695094951));
#263850=CARTESIAN_POINT('Ctrl Pts',(-179.814956440768,5.34540767399451,
133.342366321317));
#263851=CARTESIAN_POINT('Ctrl Pts',(-179.811020391327,5.30920304288685,
133.417251360219));
#263852=CARTESIAN_POINT('Ctrl Pts',(-179.807084341887,5.27146882157906,
133.491282094949));
#263853=CARTESIAN_POINT('Ctrl Pts',(-179.799661075481,5.20030325783337,
133.630901750236));
#263854=CARTESIAN_POINT('Ctrl Pts',(-179.792237809076,5.12347932154279,
133.767903246486));
#263855=CARTESIAN_POINT('Ctrl Pts',(-179.784814542671,5.04121323225327,
133.901794992893));
#263856=CARTESIAN_POINT('Ctrl Pts',(-179.77740004995,4.95904437464975,134.035528490373));
#263857=CARTESIAN_POINT('Ctrl Pts',(-179.769985557229,4.87144636083707,
134.166159239093));
#263858=CARTESIAN_POINT('Ctrl Pts',(-179.762571064508,4.77868239631381,
134.293217897201));
#263859=CARTESIAN_POINT('Ctrl Pts',(-179.755163718154,4.68600784119206,
134.42015409139));
#263860=CARTESIAN_POINT('Ctrl Pts',(-179.7477563718,4.5881774664831,134.543524749663));
#263861=CARTESIAN_POINT('Ctrl Pts',(-179.740349025446,4.485499025852,134.662887415656));
#263862=CARTESIAN_POINT('Ctrl Pts',(-179.732947203771,4.38289716667605,
134.78216105647));
#263863=CARTESIAN_POINT('Ctrl Pts',(-179.725545382096,4.27545468365737,
134.897432375347));
#263864=CARTESIAN_POINT('Ctrl Pts',(-179.71814356042,4.16352097762122,135.008290164003));
#263865=CARTESIAN_POINT('Ctrl Pts',(-179.710745646109,4.05164636051687,
135.119089431696));
#263866=CARTESIAN_POINT('Ctrl Pts',(-179.703347731798,3.93528550668121,
135.225479547193));
#263867=CARTESIAN_POINT('Ctrl Pts',(-179.695949817487,3.81482613076614,
135.32708459262));
#263868=CARTESIAN_POINT('Ctrl Pts',(-179.688553132574,3.69438677301383,
135.428672753131));
#263869=CARTESIAN_POINT('Ctrl Pts',(-179.681156447662,3.56985053003108,
135.525477181344));
#263870=CARTESIAN_POINT('Ctrl Pts',(-179.67375976275,3.44163988469777,135.617160786548));
#263871=CARTESIAN_POINT('Ctrl Pts',(-179.666363405815,3.31343492435919,
135.708840326406));
#263872=CARTESIAN_POINT('Ctrl Pts',(-179.658967048879,3.18155618927124,
135.795399277593));
#263873=CARTESIAN_POINT('Ctrl Pts',(-179.651570691944,3.04645674102676,
135.876542779866));
#263874=CARTESIAN_POINT('Ctrl Pts',(-179.644173202607,2.91133660871186,
135.957698705416));
#263875=CARTESIAN_POINT('Ctrl Pts',(-179.636775713271,2.77299510144716,
136.033437338946));
#263876=CARTESIAN_POINT('Ctrl Pts',(-179.629378223934,2.63191143379257,
136.103508923395));
#263877=CARTESIAN_POINT('Ctrl Pts',(-179.621978141419,2.49077830947559,
136.17360507133));
#263878=CARTESIAN_POINT('Ctrl Pts',(-179.614578058904,2.3469014450307,136.23803004898));
#263879=CARTESIAN_POINT('Ctrl Pts',(-179.607177976389,2.20078150805586,
136.296581599673));
#263880=CARTESIAN_POINT('Ctrl Pts',(-179.599769756723,2.05450089718987,
136.355197533815));
#263881=CARTESIAN_POINT('Ctrl Pts',(-179.592361537056,1.90597263478008,
136.407927004143));
#263882=CARTESIAN_POINT('Ctrl Pts',(-179.58495331739,1.75571477835447,136.45461691083));
#263883=CARTESIAN_POINT('Ctrl Pts',(-179.577540538088,1.60536444072542,
136.501335554375));
#263884=CARTESIAN_POINT('Ctrl Pts',(-179.570127758786,1.45328274764712,
136.542007130973));
#263885=CARTESIAN_POINT('Ctrl Pts',(-179.562714979484,1.29999901139323,
136.576529458901));
#263886=CARTESIAN_POINT('Ctrl Pts',(-179.555291608455,1.14649625614847,
136.611101113949));
#263887=CARTESIAN_POINT('Ctrl Pts',(-179.547868237426,0.991788393612213,
136.639505904812));
#263888=CARTESIAN_POINT('Ctrl Pts',(-179.540444866397,0.836411758288183,
136.661693281253));
#263889=CARTESIAN_POINT('Ctrl Pts',(-179.536508816957,0.754027338025988,
136.673457560621));
#263890=CARTESIAN_POINT('Ctrl Pts',(-179.532572767516,0.671454946475021,
136.683474771799));
#263891=CARTESIAN_POINT('Ctrl Pts',(-179.528636718075,0.588774524354783,
136.691743323147));
#263892=CARTESIAN_POINT('Ctrl Pts',(-179.521213451669,0.432841828606704,
136.707337552936));
#263893=CARTESIAN_POINT('Ctrl Pts',(-179.513790185264,0.276053375632314,
136.716756054739));
#263894=CARTESIAN_POINT('Ctrl Pts',(-179.506366918858,0.118939626646369,
136.719915023343));
#263895=CARTESIAN_POINT('Ctrl Pts',(-179.498952426137,-0.0379884269357607,
136.723070258309));
#263896=CARTESIAN_POINT('Ctrl Pts',(-179.491537933416,-0.195240641656169,
136.7199806789));
#263897=CARTESIAN_POINT('Ctrl Pts',(-179.484123440695,-0.352279877922297,
136.710614036622));
#263898=CARTESIAN_POINT('Ctrl Pts',(-179.476716094341,-0.509167753859644,
136.701256422266));
#263899=CARTESIAN_POINT('Ctrl Pts',(-179.469308747988,-0.665842689874027,
136.685633811616));
#263900=CARTESIAN_POINT('Ctrl Pts',(-179.461901401634,-0.821766086522907,
136.663765968072));
#263901=CARTESIAN_POINT('Ctrl Pts',(-179.454499579958,-0.977573189619913,
136.641914434392));
#263902=CARTESIAN_POINT('Ctrl Pts',(-179.447097758283,-1.13262950134629,
136.61382699401));
#263903=CARTESIAN_POINT('Ctrl Pts',(-179.439695936607,-1.28640020084502,
136.579575339615));
#263904=CARTESIAN_POINT('Ctrl Pts',(-179.432298022296,-1.44008972598887,
136.545341766401));
#263905=CARTESIAN_POINT('Ctrl Pts',(-179.424900107985,-1.59249462705246,
136.504950540707));
#263906=CARTESIAN_POINT('Ctrl Pts',(-179.417502193673,-1.74308906444127,
136.458524665056));
#263907=CARTESIAN_POINT('Ctrl Pts',(-179.410105508761,-1.89365847576642,
136.412106504543));
#263908=CARTESIAN_POINT('Ctrl Pts',(-179.402708823849,-2.04241766416558,
136.3596557943));
#263909=CARTESIAN_POINT('Ctrl Pts',(-179.395312138936,-2.18885466336137,
136.301345775376));
#263910=CARTESIAN_POINT('Ctrl Pts',(-179.387915782001,-2.33528516938715,
136.243038341979));
#263911=CARTESIAN_POINT('Ctrl Pts',(-179.380519425065,-2.47939334413142,
136.178872254585));
#263912=CARTESIAN_POINT('Ctrl Pts',(-179.37312306813,-2.62068622246135,
136.109069307579));
#263913=CARTESIAN_POINT('Ctrl Pts',(-179.365725578793,-2.76200073309085,
136.039255673564));
#263914=CARTESIAN_POINT('Ctrl Pts',(-179.358328089457,-2.90049875436519,
135.963803626908));
#263915=CARTESIAN_POINT('Ctrl Pts',(-179.35093060012,-3.03571113142043,
135.882981344601));
#263916=CARTESIAN_POINT('Ctrl Pts',(-179.343530517605,-3.17097090696619,
135.802130730167));
#263917=CARTESIAN_POINT('Ctrl Pts',(-179.33613043509,-3.30294242489327,
135.715906323391));
#263918=CARTESIAN_POINT('Ctrl Pts',(-179.328730352575,-3.43118489787047,
135.624620025433));
#263919=CARTESIAN_POINT('Ctrl Pts',(-179.321322132908,-3.55956838662981,
135.533233348805));
#263920=CARTESIAN_POINT('Ctrl Pts',(-179.313913913242,-3.6842143372299,
135.4367738818));
#263921=CARTESIAN_POINT('Ctrl Pts',(-179.306505693575,-3.80471391970313,
135.335594726693));
#263922=CARTESIAN_POINT('Ctrl Pts',(-179.299092914273,-3.92528766765873,
135.234353297504));
#263923=CARTESIAN_POINT('Ctrl Pts',(-179.291680134971,-4.04170968684056,
135.128386642548));
#263924=CARTESIAN_POINT('Ctrl Pts',(-179.284267355669,-4.15360790265782,
135.018084855515));
#263925=CARTESIAN_POINT('Ctrl Pts',(-179.27684398464,-4.26566600389351,
134.907625464115));
#263926=CARTESIAN_POINT('Ctrl Pts',(-179.269420613611,-4.37318713756271,
134.792818841095));
#263927=CARTESIAN_POINT('Ctrl Pts',(-179.261997242582,-4.47583887241952,
134.674088896223));
#263928=CARTESIAN_POINT('Ctrl Pts',(-179.258061193142,-4.53026728532872,
134.611135430574));
#263929=CARTESIAN_POINT('Ctrl Pts',(-179.254125143702,-4.58332744336295,
134.547079486324));
#263930=CARTESIAN_POINT('Ctrl Pts',(-179.250189094261,-4.63497479752016,
134.481987459546));
#263931=CARTESIAN_POINT('Ctrl Pts',(-179.242405181676,-4.73711235857636,
134.35326177809));
#263932=CARTESIAN_POINT('Ctrl Pts',(-179.23462126909,-4.83405257557669,
134.220064488449));
#263933=CARTESIAN_POINT('Ctrl Pts',(-179.226837356504,-4.92538181691207,
134.082857913605));
#263934=CARTESIAN_POINT('Ctrl Pts',(-179.21943360423,-5.01225060826353,
133.952352402468));
#263935=CARTESIAN_POINT('Ctrl Pts',(-179.212029851955,-5.09404316262776,
133.818220254166));
#263936=CARTESIAN_POINT('Ctrl Pts',(-179.20462609968,-5.17044286712766,
133.680895185456));
#263937=CARTESIAN_POINT('Ctrl Pts',(-179.197229304088,-5.24677078525505,
133.543699149556));
#263938=CARTESIAN_POINT('Ctrl Pts',(-179.189832508496,-5.31771575753479,
133.403316488217));
#263939=CARTESIAN_POINT('Ctrl Pts',(-179.182435712904,-5.38300406071346,
133.260210337081));
#263940=CARTESIAN_POINT('Ctrl Pts',(-179.175044399858,-5.44824397184658,
133.117210257003));
#263941=CARTESIAN_POINT('Ctrl Pts',(-179.167653086811,-5.50783540530376,
132.971491044007));
#263942=CARTESIAN_POINT('Ctrl Pts',(-179.160261773764,-5.56155032784516,
132.82354077628));
#263943=CARTESIAN_POINT('Ctrl Pts',(-179.152874472875,-5.61523609281154,
132.67567081903));
#263944=CARTESIAN_POINT('Ctrl Pts',(-179.145487171987,-5.66305157103681,
132.525572568989));
#263945=CARTESIAN_POINT('Ctrl Pts',(-179.138099871098,-5.70481673901178,
132.373754302016));
#263946=CARTESIAN_POINT('Ctrl Pts',(-179.130714471695,-5.74657115666838,
132.221975112935));
#263947=CARTESIAN_POINT('Ctrl Pts',(-179.123329072291,-5.78227826278416,
132.068477147734));
#263948=CARTESIAN_POINT('Ctrl Pts',(-179.115943672887,-5.81180782512948,
131.913784056233));
#263949=CARTESIAN_POINT('Ctrl Pts',(-179.108559362774,-5.84133303208765,
131.759113780793));
#263950=CARTESIAN_POINT('Ctrl Pts',(-179.101175052661,-5.86468244308912,
131.603249097923));
#263951=CARTESIAN_POINT('Ctrl Pts',(-179.093790742548,-5.88177695426642,
131.446723772456));
#263952=CARTESIAN_POINT('Ctrl Pts',(-179.086404697669,-5.89887548138718,
131.290161675136));
#263953=CARTESIAN_POINT('Ctrl Pts',(-179.079018652791,-5.90971613497904,
131.132938997188));
#263954=CARTESIAN_POINT('Ctrl Pts',(-179.071632607912,-5.91427167588424,
130.975594686412));
#263955=CARTESIAN_POINT('Ctrl Pts',(-179.068880136011,-5.91596933661368,
130.916959002315));
#263956=CARTESIAN_POINT('Ctrl Pts',(-179.066127664109,-5.91679467625972,
130.858306445919));
#263957=CARTESIAN_POINT('Ctrl Pts',(-179.063375192208,-5.91674813668029,
130.799664918431));
#263958=CARTESIAN_POINT('',(-182.56337376072,-5.92087641190242,130.807755266905));
#263959=CARTESIAN_POINT('Ctrl Pts',(-182.56337265757,-5.92405711974599,
130.807733754196));
#263960=CARTESIAN_POINT('Ctrl Pts',(-182.479952757115,-5.91188579994225,
129.041809576944));
#263961=CARTESIAN_POINT('Ctrl Pts',(-182.303716982053,-4.13524844748988,
125.289854803609));
#263962=CARTESIAN_POINT('Ctrl Pts',(-182.034665332392,2.25108434336954,
124.177884947263));
#263963=CARTESIAN_POINT('Ctrl Pts',(-181.756217708577,6.79180772637146,
129.116489669186));
#263964=CARTESIAN_POINT('Ctrl Pts',(-181.477770084765,5.09119160707943,
135.60616533563));
#263965=CARTESIAN_POINT('Ctrl Pts',(-181.199322460952,-1.28798088058456,
137.683217047348));
#263966=CARTESIAN_POINT('Ctrl Pts',(-180.977858187196,-5.42030405385856,
134.307513343875));
#263967=CARTESIAN_POINT('Ctrl Pts',(-180.849209788043,-5.91302735279117,
131.571366059404));
#263968=CARTESIAN_POINT('Ctrl Pts',(-180.813377263496,-5.90898434920711,
130.80786452556));
#263969=CARTESIAN_POINT('',(-184.313376079986,-5.91869333543885,130.799262689142));
#263970=CARTESIAN_POINT('Ctrl Pts',(-184.313375192208,-5.91674778898835,
130.799245541667));
#263971=CARTESIAN_POINT('Ctrl Pts',(-184.30222306504,-5.91654340696533,
130.56283128179));
#263972=CARTESIAN_POINT('Ctrl Pts',(-184.291070937872,-5.90216644403423,
130.327006005632));
#263973=CARTESIAN_POINT('Ctrl Pts',(-184.279918810703,-5.87384581741895,
130.093118130302));
#263974=CARTESIAN_POINT('Ctrl Pts',(-184.274027981434,-5.85888616230683,
129.969572772447));
#263975=CARTESIAN_POINT('Ctrl Pts',(-184.268137152164,-5.84003663158251,
129.846567305077));
#263976=CARTESIAN_POINT('Ctrl Pts',(-184.262246322894,-5.81733560061832,
129.724297160042));
#263977=CARTESIAN_POINT('Ctrl Pts',(-184.254823056489,-5.78872913575387,
129.570219725698));
#263978=CARTESIAN_POINT('Ctrl Pts',(-184.247399790083,-5.75395386469645,
129.417046595923));
#263979=CARTESIAN_POINT('Ctrl Pts',(-184.239976523677,-5.71307757234325,
129.265310516079));
#263980=CARTESIAN_POINT('Ctrl Pts',(-184.232562030956,-5.67224959237304,
129.11375377568));
#263981=CARTESIAN_POINT('Ctrl Pts',(-184.225147538235,-5.6253350405974,
128.963631061319));
#263982=CARTESIAN_POINT('Ctrl Pts',(-184.217733045514,-5.5724530706871,
128.815467121803));
#263983=CARTESIAN_POINT('Ctrl Pts',(-184.21032569916,-5.51962207041052,
128.66744598827));
#263984=CARTESIAN_POINT('Ctrl Pts',(-184.202918352807,-5.46083522698721,
128.521380220278));
#263985=CARTESIAN_POINT('Ctrl Pts',(-184.195511006453,-5.39626204145504,
128.377781432282));
#263986=CARTESIAN_POINT('Ctrl Pts',(-184.188109184777,-5.33173701704084,
128.23428974568));
#263987=CARTESIAN_POINT('Ctrl Pts',(-184.180707363102,-5.26143439604173,
128.093261714445));
#263988=CARTESIAN_POINT('Ctrl Pts',(-184.173305541426,-5.18557248352986,
127.955190812069));
#263989=CARTESIAN_POINT('Ctrl Pts',(-184.165907627115,-5.1097506179311,
127.817192796247));
#263990=CARTESIAN_POINT('Ctrl Pts',(-184.158509712804,-5.02837548473259,
127.682149126725));
#263991=CARTESIAN_POINT('Ctrl Pts',(-184.151111798492,-4.94171214425669,
127.550530313785));
#263992=CARTESIAN_POINT('Ctrl Pts',(-184.14371511358,-4.85506320565538,
127.418933373503));
#263993=CARTESIAN_POINT('Ctrl Pts',(-184.136318428668,-4.76312800903145,
127.290760471687));
#263994=CARTESIAN_POINT('Ctrl Pts',(-184.128921743756,-4.66621597412815,
127.166454757694));
#263995=CARTESIAN_POINT('Ctrl Pts',(-184.12152538682,-4.56930823640603,
127.042154555547));
#263996=CARTESIAN_POINT('Ctrl Pts',(-184.114129029885,-4.46742432870891,
126.921721494671));
#263997=CARTESIAN_POINT('Ctrl Pts',(-184.106732672949,-4.36091497905957,
126.80556691097));
#263998=CARTESIAN_POINT('Ctrl Pts',(-184.099335183613,-4.25438932255719,
126.689394543706));
#263999=CARTESIAN_POINT('Ctrl Pts',(-184.091937694276,-4.14323706635495,
126.577502233055));
#264000=CARTESIAN_POINT('Ctrl Pts',(-184.084540204939,-4.02784681849153,
126.470265490637));
#264001=CARTESIAN_POINT('Ctrl Pts',(-184.077140122424,-3.91241612075543,
126.362991156545));
#264002=CARTESIAN_POINT('Ctrl Pts',(-184.069740039909,-3.79274474677175,
126.260375893956));
#264003=CARTESIAN_POINT('Ctrl Pts',(-184.062339957394,-3.66925535844911,
126.1627557575));
#264004=CARTESIAN_POINT('Ctrl Pts',(-184.054931737728,-3.54563018084883,
126.065028277668));
#264005=CARTESIAN_POINT('Ctrl Pts',(-184.047523518061,-3.41817889765681,
125.972307124804));
#264006=CARTESIAN_POINT('Ctrl Pts',(-184.040115298395,-3.28735479886558,
125.884886154895));
#264007=CARTESIAN_POINT('Ctrl Pts',(-184.032702519093,-3.15645018002447,
125.797411378838));
#264008=CARTESIAN_POINT('Ctrl Pts',(-184.025289739791,-3.02216892674676,
125.715243480416));
#264009=CARTESIAN_POINT('Ctrl Pts',(-184.017876960489,-2.88498957422633,
125.638630686655));
#264010=CARTESIAN_POINT('Ctrl Pts',(-184.01045358946,-2.74761421341414,
125.561908424942));
#264011=CARTESIAN_POINT('Ctrl Pts',(-184.003030218431,-2.60733281501413,
125.490757289058));
#264012=CARTESIAN_POINT('Ctrl Pts',(-183.995606847402,-2.46464530350015,
125.425377991601));
#264013=CARTESIAN_POINT('Ctrl Pts',(-183.991670797962,-2.38898896116109,
125.390712319337));
#264014=CARTESIAN_POINT('Ctrl Pts',(-183.987734748521,-2.31265646397017,
125.357668496352));
#264015=CARTESIAN_POINT('Ctrl Pts',(-183.983798699081,-2.23572401264854,
125.326270740449));
#264016=CARTESIAN_POINT('Ctrl Pts',(-183.976375432675,-2.09063181042523,
125.267055552704));
#264017=CARTESIAN_POINT('Ctrl Pts',(-183.96895216627,-1.94296603481777,
125.213519155027));
#264018=CARTESIAN_POINT('Ctrl Pts',(-183.961528899864,-1.79321153898064,
125.165892479945));
#264019=CARTESIAN_POINT('Ctrl Pts',(-183.954114407143,-1.64363404052125,
125.118322095638));
#264020=CARTESIAN_POINT('Ctrl Pts',(-183.946699914422,-1.49197308804768,
125.076647642673));
#264021=CARTESIAN_POINT('Ctrl Pts',(-183.939285421701,-1.33873457306213,
125.04105251324));
#264022=CARTESIAN_POINT('Ctrl Pts',(-183.931878075348,-1.18564375512665,
125.005491691733));
#264023=CARTESIAN_POINT('Ctrl Pts',(-183.924470728994,-1.03097876289946,
124.975998612581));
#264024=CARTESIAN_POINT('Ctrl Pts',(-183.91706338264,-0.875261651561804,
124.95270720987));
#264025=CARTESIAN_POINT('Ctrl Pts',(-183.909661560965,-0.71966067992065,
124.929433178765));
#264026=CARTESIAN_POINT('Ctrl Pts',(-183.902259739289,-0.563009519234663,
124.912351669202));
#264027=CARTESIAN_POINT('Ctrl Pts',(-183.894857917614,-0.405841341951333,
124.901545749415));
#264028=CARTESIAN_POINT('Ctrl Pts',(-183.887460003302,-0.248756132525396,
124.890745533989));
#264029=CARTESIAN_POINT('Ctrl Pts',(-183.880062088991,-0.091154821529368,
124.886214336211));
#264030=CARTESIAN_POINT('Ctrl Pts',(-183.87266417468,0.066423465832265,
124.887983475625));
#264031=CARTESIAN_POINT('Ctrl Pts',(-183.865267489768,0.223975566541075,
124.889752321039));
#264032=CARTESIAN_POINT('Ctrl Pts',(-183.857870804855,0.38150427830029,
124.89781942147));
#264033=CARTESIAN_POINT('Ctrl Pts',(-183.850474119943,0.538469518075691,
124.912163986376));
#264034=CARTESIAN_POINT('Ctrl Pts',(-183.843077763008,0.695427797847872,
124.92650791523));
#264035=CARTESIAN_POINT('Ctrl Pts',(-183.835681406072,0.851822283566282,
124.947128721133));
#264036=CARTESIAN_POINT('Ctrl Pts',(-183.828285049137,1.00711732962266,
124.97395366377));
#264037=CARTESIAN_POINT('Ctrl Pts',(-183.8208875598,1.16243615174704,125.000782713374));
#264038=CARTESIAN_POINT('Ctrl Pts',(-183.813490070464,1.31665483117389,
125.033817727484));
#264039=CARTESIAN_POINT('Ctrl Pts',(-183.806092581127,1.46924738720576,
125.072934732353));
#264040=CARTESIAN_POINT('Ctrl Pts',(-183.798692498612,1.6218934343218,125.112065449627));
#264041=CARTESIAN_POINT('Ctrl Pts',(-183.791292416097,1.77291186172737,
125.157282309882));
#264042=CARTESIAN_POINT('Ctrl Pts',(-183.783892333582,1.92179147805772,
125.20841136142));
#264043=CARTESIAN_POINT('Ctrl Pts',(-183.776484113915,2.07083480283121,
125.259596634606));
#264044=CARTESIAN_POINT('Ctrl Pts',(-183.769075894249,2.21773426647063,
125.316706960799));
#264045=CARTESIAN_POINT('Ctrl Pts',(-183.761667674582,2.3619976252977,125.379519810631));
#264046=CARTESIAN_POINT('Ctrl Pts',(-183.75425489528,2.50634977581538,125.442371320724));
#264047=CARTESIAN_POINT('Ctrl Pts',(-183.746842115978,2.64806225327137,
125.510932185989));
#264048=CARTESIAN_POINT('Ctrl Pts',(-183.739429336676,2.7866675572784,125.584933973986));
#264049=CARTESIAN_POINT('Ctrl Pts',(-183.732005965648,2.92547090704354,
125.659041499208));
#264050=CARTESIAN_POINT('Ctrl Pts',(-183.724582594619,3.06115789516633,
125.738605285748));
#264051=CARTESIAN_POINT('Ctrl Pts',(-183.71715922359,3.19328943506455,125.823313223051));
#264052=CARTESIAN_POINT('Ctrl Pts',(-183.713223174149,3.26334874797098,
125.868227403948));
#264053=CARTESIAN_POINT('Ctrl Pts',(-183.709287124708,3.33240903135922,
125.914587102222));
#264054=CARTESIAN_POINT('Ctrl Pts',(-183.705351075268,3.40040872175365,
125.962341298364));
#264055=CARTESIAN_POINT('Ctrl Pts',(-183.697927808862,3.52865401564075,
126.052404221932));
#264056=CARTESIAN_POINT('Ctrl Pts',(-183.690504542457,3.65351266188925,
126.147701890419));
#264057=CARTESIAN_POINT('Ctrl Pts',(-183.683081276051,3.77452829544996,
126.247951207806));
#264058=CARTESIAN_POINT('Ctrl Pts',(-183.67566678333,3.89540089858187,126.348082038826));
#264059=CARTESIAN_POINT('Ctrl Pts',(-183.668252290609,4.01243924548009,
126.453152633621));
#264060=CARTESIAN_POINT('Ctrl Pts',(-183.660837797888,4.12521559638735,
126.562836499301));
#264061=CARTESIAN_POINT('Ctrl Pts',(-183.653430451534,4.23788324920132,
126.672414647542));
#264062=CARTESIAN_POINT('Ctrl Pts',(-183.646023105181,4.34629681818062,
126.786596956152));
#264063=CARTESIAN_POINT('Ctrl Pts',(-183.638615758827,4.45006143720835,
126.905016599969));
#264064=CARTESIAN_POINT('Ctrl Pts',(-183.631213937151,4.55374866466839,
127.023347921947));
#264065=CARTESIAN_POINT('Ctrl Pts',(-183.623812115476,4.65279360120558,
127.145910006866));
#264066=CARTESIAN_POINT('Ctrl Pts',(-183.616410293801,4.74683816642942,
127.272299182054));
#264067=CARTESIAN_POINT('Ctrl Pts',(-183.609012379489,4.84083308625904,
127.398621637381));
#264068=CARTESIAN_POINT('Ctrl Pts',(-183.601614465178,4.92983266949919,
127.528766860743));
#264069=CARTESIAN_POINT('Ctrl Pts',(-183.594216550867,5.01351915578842,
127.662298199815));
#264070=CARTESIAN_POINT('Ctrl Pts',(-183.586819865954,5.09719173490199,
127.795807348402));
#264071=CARTESIAN_POINT('Ctrl Pts',(-183.579423181042,5.17555277139587,
127.932701179883));
#264072=CARTESIAN_POINT('Ctrl Pts',(-183.57202649613,5.24832782886879,128.072514069309));
#264073=CARTESIAN_POINT('Ctrl Pts',(-183.564630139194,5.32109965941941,
128.212320759286));
#264074=CARTESIAN_POINT('Ctrl Pts',(-183.557233782259,5.38828583108009,
128.355045918725));
#264075=CARTESIAN_POINT('Ctrl Pts',(-183.549837425324,5.44965801280331,
128.500199575888));
#264076=CARTESIAN_POINT('Ctrl Pts',(-183.542439935987,5.5110395907644,128.645375456446));
#264077=CARTESIAN_POINT('Ctrl Pts',(-183.53504244665,5.56660526102463,128.7929802312));
#264078=CARTESIAN_POINT('Ctrl Pts',(-183.527644957314,5.61617502079312,
128.942504366853));
#264079=CARTESIAN_POINT('Ctrl Pts',(-183.520244874799,5.665762157164,129.09208091796));
#264080=CARTESIAN_POINT('Ctrl Pts',(-183.512844792284,5.70934908086662,
129.243577815451));
#264081=CARTESIAN_POINT('Ctrl Pts',(-183.505444709769,5.74680583097126,
129.396470954412));
#264082=CARTESIAN_POINT('Ctrl Pts',(-183.498036490102,5.78430376862334,
129.549532215098));
#264083=CARTESIAN_POINT('Ctrl Pts',(-183.490628270436,5.81565798206432,
129.703992420572));
#264084=CARTESIAN_POINT('Ctrl Pts',(-183.483220050769,5.84078962182305,
129.859317149728));
#264085=CARTESIAN_POINT('Ctrl Pts',(-183.475807271467,5.8659367296867,130.014737478662));
#264086=CARTESIAN_POINT('Ctrl Pts',(-183.468394492165,5.88485358757889,
130.17102302182));
#264087=CARTESIAN_POINT('Ctrl Pts',(-183.460981712863,5.89751333993616,
130.327635363594));
#264088=CARTESIAN_POINT('Ctrl Pts',(-183.453558341834,5.91019118114126,
130.484471480425));
#264089=CARTESIAN_POINT('Ctrl Pts',(-183.446134970806,5.91659404558043,
130.641634956467));
#264090=CARTESIAN_POINT('Ctrl Pts',(-183.438711599777,5.91674718368156,
130.798587672361));
#264091=CARTESIAN_POINT('Ctrl Pts',(-183.434775550336,5.91682838117727,
130.881807768356));
#264092=CARTESIAN_POINT('Ctrl Pts',(-183.430839500895,5.9151534241066,130.964968689975));
#264093=CARTESIAN_POINT('Ctrl Pts',(-183.426903451455,5.91173196006602,
131.04799106483));
#264094=CARTESIAN_POINT('Ctrl Pts',(-183.419480185049,5.90527918566564,
131.204568672769));
#264095=CARTESIAN_POINT('Ctrl Pts',(-183.412056918644,5.8925917063369,131.36112650563));
#264096=CARTESIAN_POINT('Ctrl Pts',(-183.404633652238,5.87366102232141,
131.517127590259));
#264097=CARTESIAN_POINT('Ctrl Pts',(-183.397219159517,5.85475271280228,
131.672944294561));
#264098=CARTESIAN_POINT('Ctrl Pts',(-183.389804666796,5.82961593096655,
131.828205193483));
#264099=CARTESIAN_POINT('Ctrl Pts',(-183.382390174075,5.79829416074255,
131.982373940071));
#264100=CARTESIAN_POINT('Ctrl Pts',(-183.374982827722,5.76700257961994,
132.136394093016));
#264101=CARTESIAN_POINT('Ctrl Pts',(-183.367575481368,5.72953795175678,
132.289323825892));
#264102=CARTESIAN_POINT('Ctrl Pts',(-183.360168135014,5.68599546277168,
132.44063264869));
#264103=CARTESIAN_POINT('Ctrl Pts',(-183.352766313339,5.64248544941762,
132.59182861966));
#264104=CARTESIAN_POINT('Ctrl Pts',(-183.345364491663,5.59290670374262,
132.741405730511));
#264105=CARTESIAN_POINT('Ctrl Pts',(-183.337962669988,5.5374052957988,132.888844523131));
#264106=CARTESIAN_POINT('Ctrl Pts',(-183.330564755676,5.48193318661622,
133.03620548396));
#264107=CARTESIAN_POINT('Ctrl Pts',(-183.323166841365,5.42054477297452,
133.181430026141));
#264108=CARTESIAN_POINT('Ctrl Pts',(-183.315768927054,5.35343566560404,
133.324014787634));
#264109=CARTESIAN_POINT('Ctrl Pts',(-183.308372242142,5.28633771054982,
133.466575854126));
#264110=CARTESIAN_POINT('Ctrl Pts',(-183.300975557229,5.21352110739003,
133.606497673161));
#264111=CARTESIAN_POINT('Ctrl Pts',(-183.293578872317,5.13522926000215,
133.743297671965));
#264112=CARTESIAN_POINT('Ctrl Pts',(-183.286182515382,5.05694088415682,
133.880091604913));
#264113=CARTESIAN_POINT('Ctrl Pts',(-183.278786158446,4.97317793223063,
134.013763668875));
#264114=CARTESIAN_POINT('Ctrl Pts',(-183.271389801511,4.88422921281487,
134.143856920781));
#264115=CARTESIAN_POINT('Ctrl Pts',(-183.263992312174,4.7952668751231,134.273970090296));
#264116=CARTESIAN_POINT('Ctrl Pts',(-183.256594822838,4.70111739978136,
134.400503048588));
#264117=CARTESIAN_POINT('Ctrl Pts',(-183.249197333501,4.60211217567657,
134.523028939021));
#264118=CARTESIAN_POINT('Ctrl Pts',(-183.241797250986,4.50307224544381,
134.645597780714));
#264119=CARTESIAN_POINT('Ctrl Pts',(-183.234397168471,4.39917341190046,
134.764156467682));
#264120=CARTESIAN_POINT('Ctrl Pts',(-183.226997085956,4.29078637229727,
134.878312368607));
#264121=CARTESIAN_POINT('Ctrl Pts',(-183.219588866289,4.18228015000174,
134.99259379568));
#264122=CARTESIAN_POINT('Ctrl Pts',(-183.212180646623,4.06927612283048,
135.102462497404));
#264123=CARTESIAN_POINT('Ctrl Pts',(-183.204772426956,3.95218129433147,
135.207563267824));
#264124=CARTESIAN_POINT('Ctrl Pts',(-183.197359647654,3.83501439591901,
135.312728726014));
#264125=CARTESIAN_POINT('Ctrl Pts',(-183.189946868352,3.71375196598444,
135.413120167876));
#264126=CARTESIAN_POINT('Ctrl Pts',(-183.18253408905,3.58883247273898,135.508423972275));
#264127=CARTESIAN_POINT('Ctrl Pts',(-183.175110718021,3.46373448866361,
135.603863951219));
#264128=CARTESIAN_POINT('Ctrl Pts',(-183.167687346993,3.33496930979695,
135.694201560142));
#264129=CARTESIAN_POINT('Ctrl Pts',(-183.160263975964,3.20300331966732,
135.779167176288));
#264130=CARTESIAN_POINT('Ctrl Pts',(-183.156327926523,3.13303178521975,
135.82421798469));
#264131=CARTESIAN_POINT('Ctrl Pts',(-183.152391877082,3.06216079141112,
135.867759305324));
#264132=CARTESIAN_POINT('Ctrl Pts',(-183.148455827642,2.99046233124018,
135.90975635227));
#264133=CARTESIAN_POINT('Ctrl Pts',(-183.141032561236,2.85524127299102,
135.988961472127));
#264134=CARTESIAN_POINT('Ctrl Pts',(-183.133609294831,2.71666684177059,
136.062910469239));
#264135=CARTESIAN_POINT('Ctrl Pts',(-183.126186028425,2.57518621397406,
136.131305945412));
#264136=CARTESIAN_POINT('Ctrl Pts',(-183.118771535704,2.43387280453034,
136.199620583812));
#264137=CARTESIAN_POINT('Ctrl Pts',(-183.111357042983,2.28966036846826,
136.262394605668));
#264138=CARTESIAN_POINT('Ctrl Pts',(-183.103942550262,2.14302365379594,
136.319374686612));
#264139=CARTESIAN_POINT('Ctrl Pts',(-183.096535203909,1.99652827310958,
136.376299848008));
#264140=CARTESIAN_POINT('Ctrl Pts',(-183.089127857555,1.84761361116126,
136.427442051669));
#264141=CARTESIAN_POINT('Ctrl Pts',(-183.081720511201,1.69677743437165,
136.472594637145));
#264142=CARTESIAN_POINT('Ctrl Pts',(-183.074318689525,1.54605375689342,
136.517713546118));
#264143=CARTESIAN_POINT('Ctrl Pts',(-183.06691686785,1.39341177422502,136.556851625278));
#264144=CARTESIAN_POINT('Ctrl Pts',(-183.059515046175,1.23936747561927,
136.589850987697));
#264145=CARTESIAN_POINT('Ctrl Pts',(-183.052117131863,1.08540449579967,
136.622832930009));
#264146=CARTESIAN_POINT('Ctrl Pts',(-183.044719217552,0.930041038421735,
136.649682531358));
#264147=CARTESIAN_POINT('Ctrl Pts',(-183.037321303241,0.773806328602494,
136.670292285112));
#264148=CARTESIAN_POINT('Ctrl Pts',(-183.029924618328,0.617597582157862,
136.690898613898));
#264149=CARTESIAN_POINT('Ctrl Pts',(-183.022527933416,0.460518240359305,
136.705267104356));
#264150=CARTESIAN_POINT('Ctrl Pts',(-183.015131248504,0.303105871090587,
136.713341696687));
#264151=CARTESIAN_POINT('Ctrl Pts',(-183.007734891569,0.145700481651279,
136.721415930983));
#264152=CARTESIAN_POINT('Ctrl Pts',(-183.000338534633,-0.012037533089414,
136.72319680293));
#264153=CARTESIAN_POINT('Ctrl Pts',(-182.992942177698,-0.169567625887687,
136.718680306486));
#264154=CARTESIAN_POINT('Ctrl Pts',(-182.985544688361,-0.327121836945322,
136.714163118556));
#264155=CARTESIAN_POINT('Ctrl Pts',(-182.978147199025,-0.484467689507502,
136.703346653195));
#264156=CARTESIAN_POINT('Ctrl Pts',(-182.970749709688,-0.641066933207348,
136.686278990822));
#264157=CARTESIAN_POINT('Ctrl Pts',(-182.963349627173,-0.797721072529536,
136.669205345406));
#264158=CARTESIAN_POINT('Ctrl Pts',(-182.955949544658,-0.953627711032837,
136.645876180442));
#264159=CARTESIAN_POINT('Ctrl Pts',(-182.948549462143,-1.10825614594989,
136.616391147206));
#264160=CARTESIAN_POINT('Ctrl Pts',(-182.941141242476,-1.26305461072711,
136.586873692145));
#264161=CARTESIAN_POINT('Ctrl Pts',(-182.93373302281,-1.41657169809388,
136.551186920619));
#264162=CARTESIAN_POINT('Ctrl Pts',(-182.926324803144,-1.56828856786049,
136.509481258746));
#264163=CARTESIAN_POINT('Ctrl Pts',(-182.918912023842,-1.7200988168289,
136.467749927734));
#264164=CARTESIAN_POINT('Ctrl Pts',(-182.911499244539,-1.8701062854791,
136.419992437623));
#264165=CARTESIAN_POINT('Ctrl Pts',(-182.904086465237,-2.01781011269092,
136.366408164254));
#264166=CARTESIAN_POINT('Ctrl Pts',(-182.896663094209,-2.1657249860579,
136.312747327163));
#264167=CARTESIAN_POINT('Ctrl Pts',(-182.88923972318,-2.31132929938075,
136.253243219605));
#264168=CARTESIAN_POINT('Ctrl Pts',(-182.881816352151,-2.45414411970913,
136.188142485565));
#264169=CARTESIAN_POINT('Ctrl Pts',(-182.87788030271,-2.52986796424262,
136.153624514306));
#264170=CARTESIAN_POINT('Ctrl Pts',(-182.873944253269,-2.60480801371997,
136.117533887402));
#264171=CARTESIAN_POINT('Ctrl Pts',(-182.870008203829,-2.67889608778898,
136.079912371964));
#264172=CARTESIAN_POINT('Ctrl Pts',(-182.862584937423,-2.81862388327062,
136.008959367975));
#264173=CARTESIAN_POINT('Ctrl Pts',(-182.855161671018,-2.95574213382726,
135.932344013602));
#264174=CARTESIAN_POINT('Ctrl Pts',(-182.847738404613,-3.08975892017157,
135.850281780022));
#264175=CARTESIAN_POINT('Ctrl Pts',(-182.840323911892,-3.22361730980421,
135.768316537187));
#264176=CARTESIAN_POINT('Ctrl Pts',(-182.832909419171,-3.35438121652008,
135.680917422574));
#264177=CARTESIAN_POINT('Ctrl Pts',(-182.82549492645,-3.48158089845803,
135.588346927119));
#264178=CARTESIAN_POINT('Ctrl Pts',(-182.818087580096,-3.60865798055354,
135.495865654593));
#264179=CARTESIAN_POINT('Ctrl Pts',(-182.810680233742,-3.7321773771412,
135.398223142311));
#264180=CARTESIAN_POINT('Ctrl Pts',(-182.803272887389,-3.85169616402163,
135.295726470239));
#264181=CARTESIAN_POINT('Ctrl Pts',(-182.795871065713,-3.97112580928161,
135.193306244053));
#264182=CARTESIAN_POINT('Ctrl Pts',(-182.788469244038,-4.08656050384569,
135.086039308776));
#264183=CARTESIAN_POINT('Ctrl Pts',(-182.781067422363,-4.19758850817627,
134.974274439041));
#264184=CARTESIAN_POINT('Ctrl Pts',(-182.773669508051,-4.30855790168761,
134.86256856911));
#264185=CARTESIAN_POINT('Ctrl Pts',(-182.76627159374,-4.4151249753976,134.746369757665));
#264186=CARTESIAN_POINT('Ctrl Pts',(-182.758873679429,-4.51691322183099,
134.626065146824));
#264187=CARTESIAN_POINT('Ctrl Pts',(-182.751476994517,-4.61868455290431,
134.505780528426));
#264188=CARTESIAN_POINT('Ctrl Pts',(-182.744080309604,-4.71567839198069,
134.381391749517));
#264189=CARTESIAN_POINT('Ctrl Pts',(-182.736683624692,-4.80755700579362,
134.253320779491));
#264190=CARTESIAN_POINT('Ctrl Pts',(-182.729287267757,-4.89943154561279,
134.125255488265));
#264191=CARTESIAN_POINT('Ctrl Pts',(-182.721890910821,-4.98619109355161,
133.993508633881));
#264192=CARTESIAN_POINT('Ctrl Pts',(-182.714494553886,-5.06754010022365,
133.858532828677));
#264193=CARTESIAN_POINT('Ctrl Pts',(-182.70709706455,-5.14890156163604,
133.723536358334));
#264194=CARTESIAN_POINT('Ctrl Pts',(-182.699699575213,-5.22485063968611,
133.585310272575));
#264195=CARTESIAN_POINT('Ctrl Pts',(-182.692302085877,-5.29513684831921,
133.444333405318));
#264196=CARTESIAN_POINT('Ctrl Pts',(-182.684902003362,-5.36544769567369,
133.303307118839));
#264197=CARTESIAN_POINT('Ctrl Pts',(-182.677501920847,-5.43009155481507,
133.159528464853));
#264198=CARTESIAN_POINT('Ctrl Pts',(-182.670101838332,-5.48886540737634,
133.013497802579));
#264199=CARTESIAN_POINT('Ctrl Pts',(-182.662693618666,-5.54770388783085,
132.867306564579));
#264200=CARTESIAN_POINT('Ctrl Pts',(-182.655285398999,-5.6006593318303,
132.718858719442));
#264201=CARTESIAN_POINT('Ctrl Pts',(-182.647877179333,-5.6475778513308,
132.568672091104));
#264202=CARTESIAN_POINT('Ctrl Pts',(-182.640464400031,-5.69452524839718,
132.418393025403));
#264203=CARTESIAN_POINT('Ctrl Pts',(-182.633051620729,-5.73542822034687,
132.26637340365));
#264204=CARTESIAN_POINT('Ctrl Pts',(-182.625638841427,-5.77018378005181,
132.113142382005));
#264205=CARTESIAN_POINT('Ctrl Pts',(-182.618215470398,-5.80498900013038,
131.959692416689));
#264206=CARTESIAN_POINT('Ctrl Pts',(-182.61079209937,-5.83362919713295,
131.80502796056));
#264207=CARTESIAN_POINT('Ctrl Pts',(-182.603368728341,-5.85605300467136,
131.649685270572));
#264208=CARTESIAN_POINT('Ctrl Pts',(-182.5994326789,-5.86794264548235,131.567318848928));
#264209=CARTESIAN_POINT('Ctrl Pts',(-182.595496629458,-5.87808550618547,
131.484761797472));
#264210=CARTESIAN_POINT('Ctrl Pts',(-182.591560580017,-5.88647987348797,
131.40209405441));
#264211=CARTESIAN_POINT('Ctrl Pts',(-182.582165450747,-5.90651675745441,
131.204770788007));
#264212=CARTESIAN_POINT('Ctrl Pts',(-182.572770321477,-5.91663410596626,
131.006423364004));
#264213=CARTESIAN_POINT('Ctrl Pts',(-182.563375192208,-5.91674901010249,
130.807783182575));
#264214=CARTESIAN_POINT('',(-186.063375192208,-5.90709598019638,130.803332506185));
#264215=CARTESIAN_POINT('Ctrl Pts',(-186.063375192208,-5.90709598019638,
130.803332506185));
#264216=CARTESIAN_POINT('Ctrl Pts',(-186.019894150062,-5.90852920600748,
129.876120039144));
#264217=CARTESIAN_POINT('Ctrl Pts',(-185.883597233311,-5.26549744303905,
126.971533866971));
#264218=CARTESIAN_POINT('Ctrl Pts',(-185.654484441958,-0.717600748298859,
123.842851463917));
#264219=CARTESIAN_POINT('Ctrl Pts',(-185.376036818144,5.46903407832205,
126.437757042646));
#264220=CARTESIAN_POINT('Ctrl Pts',(-185.097589194332,6.62989376413611,
133.045357986287));
#264221=CARTESIAN_POINT('Ctrl Pts',(-184.819141570519,1.69820496902565,
137.593591826879));
#264222=CARTESIAN_POINT('Ctrl Pts',(-184.557737350984,-4.39666896695656,
136.006341653894));
#264223=CARTESIAN_POINT('Ctrl Pts',(-184.389149006053,-5.90500976629783,
132.406387652391));
#264224=CARTESIAN_POINT('Ctrl Pts',(-184.313376535726,-5.91969208008458,
130.799271491783));
#264225=CARTESIAN_POINT('',(-187.813375192208,-5.91590714834001,130.809830359851));
#264226=CARTESIAN_POINT('Ctrl Pts',(-187.813375192208,-5.91590714834001,
130.809830359851));
#264227=CARTESIAN_POINT('Ctrl Pts',(-187.743456064355,-5.90233112363404,
129.324427893846));
#264228=CARTESIAN_POINT('Ctrl Pts',(-187.580721061896,-4.58174601807203,
125.845682237925));
#264229=CARTESIAN_POINT('Ctrl Pts',(-187.325170184835,1.26703804199676,
123.92161587942));
#264230=CARTESIAN_POINT('Ctrl Pts',(-187.046722561023,6.47551308848548,
128.150063955324));
#264231=CARTESIAN_POINT('Ctrl Pts',(-186.768274937209,5.73330795305963,
134.817680994228));
#264232=CARTESIAN_POINT('Ctrl Pts',(-186.489827313397,-0.277527103565456,
137.797252668579));
#264233=CARTESIAN_POINT('Ctrl Pts',(-186.254860731729,-5.1345300677341,
134.88889554915));
#264234=CARTESIAN_POINT('Ctrl Pts',(-186.112710024666,-5.90546980125088,
131.855374257204));
#264235=CARTESIAN_POINT('Ctrl Pts',(-186.063375192208,-5.90709598019638,
130.803332506185));
#264236=CARTESIAN_POINT('',(-189.563375998339,-5.92191640313042,130.80298505409));
#264237=CARTESIAN_POINT('Ctrl Pts',(-189.563375192208,-5.91674983639772,
130.802969219882));
#264238=CARTESIAN_POINT('Ctrl Pts',(-189.559833853251,-5.91673225127943,
130.728190637922));
#264239=CARTESIAN_POINT('Ctrl Pts',(-189.556292514295,-5.91529709555501,
130.653430419199));
#264240=CARTESIAN_POINT('Ctrl Pts',(-189.552751175338,-5.91244610460354,
130.578724577319));
#264241=CARTESIAN_POINT('Ctrl Pts',(-189.545327908933,-5.90646992847011,
130.42212805461));
#264242=CARTESIAN_POINT('Ctrl Pts',(-189.537904642528,-5.89425901609847,
130.265532330591));
#264243=CARTESIAN_POINT('Ctrl Pts',(-189.530481376122,-5.87580323340804,
130.109474350058));
#264244=CARTESIAN_POINT('Ctrl Pts',(-189.523066883401,-5.85736926392009,
129.953600817098));
#264245=CARTESIAN_POINT('Ctrl Pts',(-189.51565239068,-5.832705159285,129.798264129616));
#264246=CARTESIAN_POINT('Ctrl Pts',(-189.508237897959,-5.80185277077408,
129.644000764434));
#264247=CARTESIAN_POINT('Ctrl Pts',(-189.500830551605,-5.77103011895677,
129.48988608409));
#264248=CARTESIAN_POINT('Ctrl Pts',(-189.493423205251,-5.73403113012844,
129.336843030134));
#264249=CARTESIAN_POINT('Ctrl Pts',(-189.486015858898,-5.69094937483769,
129.18540237983));
#264250=CARTESIAN_POINT('Ctrl Pts',(-189.478614037222,-5.64789975154543,
129.034074679676));
#264251=CARTESIAN_POINT('Ctrl Pts',(-189.471212215547,-5.59877649678882,
128.884347361008));
#264252=CARTESIAN_POINT('Ctrl Pts',(-189.463810393871,-5.54372409889164,
128.73674032412));
#264253=CARTESIAN_POINT('Ctrl Pts',(-189.45641247956,-5.48870076272677,
128.589211207839));
#264254=CARTESIAN_POINT('Ctrl Pts',(-189.449014565249,-5.42775464698324,
128.443800493114));
#264255=CARTESIAN_POINT('Ctrl Pts',(-189.441616650937,-5.36107982942442,
128.301012135025));
#264256=CARTESIAN_POINT('Ctrl Pts',(-189.434219966025,-5.29441609201077,
128.158247505772));
#264257=CARTESIAN_POINT('Ctrl Pts',(-189.426823281113,-5.22202570001855,
128.018104706153));
#264258=CARTESIAN_POINT('Ctrl Pts',(-189.419426596201,-5.14415058741227,
127.881067047545));
#264259=CARTESIAN_POINT('Ctrl Pts',(-189.412030239265,-5.06627892787009,
127.744035465331));
#264260=CARTESIAN_POINT('Ctrl Pts',(-189.40463388233,-4.98292321570959,
127.610109074916));
#264261=CARTESIAN_POINT('Ctrl Pts',(-189.397237525395,-4.89437086740681,
127.479745696289));
#264262=CARTESIAN_POINT('Ctrl Pts',(-189.389840036058,-4.80580496151345,
127.349362358695));
#264263=CARTESIAN_POINT('Ctrl Pts',(-189.382442546721,-4.71204104506515,
127.222543427878));
#264264=CARTESIAN_POINT('Ctrl Pts',(-189.375045057385,-4.61340920620913,
127.099716767131));
#264265=CARTESIAN_POINT('Ctrl Pts',(-189.36764497487,-4.51474279211475,
126.976847049689));
#264266=CARTESIAN_POINT('Ctrl Pts',(-189.360244892355,-4.41120529168435,
126.857972679567));
#264267=CARTESIAN_POINT('Ctrl Pts',(-189.35284480984,-4.30316620541695,
126.74348741454));
#264268=CARTESIAN_POINT('Ctrl Pts',(-189.345436590173,-4.19500831906767,
126.628876261194));
#264269=CARTESIAN_POINT('Ctrl Pts',(-189.338028370507,-4.08233921785816,
126.518664122988));
#264270=CARTESIAN_POINT('Ctrl Pts',(-189.33062015084,-3.96556482232641,
126.413207443008));
#264271=CARTESIAN_POINT('Ctrl Pts',(-189.323207371538,-3.84871855410236,
126.307685856202));
#264272=CARTESIAN_POINT('Ctrl Pts',(-189.315794592236,-3.72776224286292,
126.206925798223));
#264273=CARTESIAN_POINT('Ctrl Pts',(-189.308381812934,-3.6031334002335,
126.111242223297));
#264274=CARTESIAN_POINT('Ctrl Pts',(-189.300958441905,-3.4783264820694,
126.015421931193));
#264275=CARTESIAN_POINT('Ctrl Pts',(-189.293535070877,-3.349836856241,125.924692823797));
#264276=CARTESIAN_POINT('Ctrl Pts',(-189.286111699848,-3.21813008347746,
125.839325942126));
#264277=CARTESIAN_POINT('Ctrl Pts',(-189.282175650407,-3.14829599229798,
125.794062373115));
#264278=CARTESIAN_POINT('Ctrl Pts',(-189.278239600966,-3.07755785156217,
125.750305547236));
#264279=CARTESIAN_POINT('Ctrl Pts',(-189.274303551526,-3.00598754805893,
125.708090469368));
#264280=CARTESIAN_POINT('Ctrl Pts',(-189.26688028512,-2.8710081892836,125.628474149996));
#264281=CARTESIAN_POINT('Ctrl Pts',(-189.259457018715,-2.73265947523997,
125.55410372251));
#264282=CARTESIAN_POINT('Ctrl Pts',(-189.252033752309,-2.59138767507411,
125.485277944776));
#264283=CARTESIAN_POINT('Ctrl Pts',(-189.244619259588,-2.45028284644415,
125.416533513396));
#264284=CARTESIAN_POINT('Ctrl Pts',(-189.237204766867,-2.30626214089305,
125.353320849256));
#264285=CARTESIAN_POINT('Ctrl Pts',(-189.229790274146,-2.15979953319767,
125.295894720522));
#264286=CARTESIAN_POINT('Ctrl Pts',(-189.222382927793,-2.01347809167781,
125.238523941253));
#264287=CARTESIAN_POINT('Ctrl Pts',(-189.214975581439,-1.86471977876785,
125.186928729472));
#264288=CARTESIAN_POINT('Ctrl Pts',(-189.207568235085,-1.71402172957951,
125.141317259704));
#264289=CARTESIAN_POINT('Ctrl Pts',(-189.20016641341,-1.56343607668177,
125.09573980869));
#264290=CARTESIAN_POINT('Ctrl Pts',(-189.192764591734,-1.4109139238907,
125.056137321127));
#264291=CARTESIAN_POINT('Ctrl Pts',(-189.185362770059,-1.25697077751556,
125.022669253703));
#264292=CARTESIAN_POINT('Ctrl Pts',(-189.177964855747,-1.10310889652911,
124.989218853811));
#264293=CARTESIAN_POINT('Ctrl Pts',(-189.170566941436,-0.94782787973478,
124.961896503906));
#264294=CARTESIAN_POINT('Ctrl Pts',(-189.163169027125,-0.791656622585064,
124.940811320901));
#264295=CARTESIAN_POINT('Ctrl Pts',(-189.155772342213,-0.635511318265274,
124.919729641871));
#264296=CARTESIAN_POINT('Ctrl Pts',(-189.1483756573,-0.478476436789943,
124.904883122484));
#264297=CARTESIAN_POINT('Ctrl Pts',(-189.140978972388,-0.321089372926129,
124.896329458449));
#264298=CARTESIAN_POINT('Ctrl Pts',(-189.133582615453,-0.163709287769656,
124.887776173693));
#264299=CARTESIAN_POINT('Ctrl Pts',(-189.126186258517,-0.00597742402233353,
124.885515209737));
#264300=CARTESIAN_POINT('Ctrl Pts',(-189.118789901582,0.151565685768833,
124.889552217846));
#264301=CARTESIAN_POINT('Ctrl Pts',(-189.111392412245,0.309132915812747,
124.893589844031));
#264302=CARTESIAN_POINT('Ctrl Pts',(-189.103994922909,0.466510961159943,
124.90392735264));
#264303=CARTESIAN_POINT('Ctrl Pts',(-189.096597433572,0.623161427596432,
124.920518301727));
#264304=CARTESIAN_POINT('Ctrl Pts',(-189.089197351057,0.779866807610867,
124.937115066746));
#264305=CARTESIAN_POINT('Ctrl Pts',(-189.081797268542,0.935843729918489,
124.959969597473));
#264306=CARTESIAN_POINT('Ctrl Pts',(-189.074397186027,1.09056119090591,
124.988983858371));
#264307=CARTESIAN_POINT('Ctrl Pts',(-189.06698896636,1.24544877964724,125.018030023431));
#264308=CARTESIAN_POINT('Ctrl Pts',(-189.059580746694,1.39907377419055,
125.053249376451));
#264309=CARTESIAN_POINT('Ctrl Pts',(-189.052172527027,1.55091687890397,
125.094493071184));
#264310=CARTESIAN_POINT('Ctrl Pts',(-189.044759747725,1.7028534405147,125.135762150722));
#264311=CARTESIAN_POINT('Ctrl Pts',(-189.037346968423,1.85300557171295,
125.183062848489));
#264312=CARTESIAN_POINT('Ctrl Pts',(-189.029934189121,2.00087180686703,
125.236197314017));
#264313=CARTESIAN_POINT('Ctrl Pts',(-189.022510818092,2.14894932023193,
125.289407700562));
#264314=CARTESIAN_POINT('Ctrl Pts',(-189.015087447064,2.29473406916035,
125.348468363057));
#264315=CARTESIAN_POINT('Ctrl Pts',(-189.007664076035,2.43774637222091,
125.413134116368));
#264316=CARTESIAN_POINT('Ctrl Pts',(-189.003728026594,2.5135749268355,125.447421450406));
#264317=CARTESIAN_POINT('Ctrl Pts',(-188.999791977153,2.58862447664729,
125.483283818407));
#264318=CARTESIAN_POINT('Ctrl Pts',(-188.995855927713,2.66282671449517,
125.520679660972));
#264319=CARTESIAN_POINT('Ctrl Pts',(-188.988432661307,2.80276981930618,
125.591207052967));
#264320=CARTESIAN_POINT('Ctrl Pts',(-188.981009394902,2.94012062552616,
125.667404711676));
#264321=CARTESIAN_POINT('Ctrl Pts',(-188.973586128496,3.07438656032618,
125.749058664153));
#264322=CARTESIAN_POINT('Ctrl Pts',(-188.966171635775,3.20849380394173,
125.830616108438));
#264323=CARTESIAN_POINT('Ctrl Pts',(-188.958757143054,3.33952311781041,
125.917616817874));
#264324=CARTESIAN_POINT('Ctrl Pts',(-188.951342650333,3.46700396331473,
126.009799732473));
#264325=CARTESIAN_POINT('Ctrl Pts',(-188.943935303979,3.59436193798021,
126.101893797708));
#264326=CARTESIAN_POINT('Ctrl Pts',(-188.936527957626,3.71817795265517,
126.199159907163));
#264327=CARTESIAN_POINT('Ctrl Pts',(-188.929120611272,3.83800815054602,
126.301292330404));
#264328=CARTESIAN_POINT('Ctrl Pts',(-188.921718789596,3.95774897455468,
126.403348579431));
#264329=CARTESIAN_POINT('Ctrl Pts',(-188.914316967921,4.07350961808697,
126.510263674354));
#264330=CARTESIAN_POINT('Ctrl Pts',(-188.906915146246,4.1848772819624,126.62169009535));
#264331=CARTESIAN_POINT('Ctrl Pts',(-188.899517231934,4.29618615571496,
126.733057695206));
#264332=CARTESIAN_POINT('Ctrl Pts',(-188.892119317623,4.40310640502578,
126.848931614914));
#264333=CARTESIAN_POINT('Ctrl Pts',(-188.884721403311,4.50526034583612,
126.968925860105));
#264334=CARTESIAN_POINT('Ctrl Pts',(-188.877324718399,4.60739731051461,
127.08890016443));
#264335=CARTESIAN_POINT('Ctrl Pts',(-188.869928033487,4.70476929697789,
127.2129931513));
#264336=CARTESIAN_POINT('Ctrl Pts',(-188.862531348575,4.79703728919411,
127.340783881217));
#264337=CARTESIAN_POINT('Ctrl Pts',(-188.855134991639,4.88930119015086,
127.468568944758));
#264338=CARTESIAN_POINT('Ctrl Pts',(-188.847738634704,4.97646132833132,
127.600051122683));
#264339=CARTESIAN_POINT('Ctrl Pts',(-188.840342277768,5.05822077812171,
127.734778704295));
#264340=CARTESIAN_POINT('Ctrl Pts',(-188.832944788432,5.13999274549259,
127.869526913045));
#264341=CARTESIAN_POINT('Ctrl Pts',(-188.825547299095,5.21636218440918,
128.007521195684));
#264342=CARTESIAN_POINT('Ctrl Pts',(-188.818149809759,5.28707715257132,
128.148283482907));
#264343=CARTESIAN_POINT('Ctrl Pts',(-188.810749727244,5.35781690975603,
128.289095114132));
#264344=CARTESIAN_POINT('Ctrl Pts',(-188.803349644729,5.42289808223647,
128.432676348477));
#264345=CARTESIAN_POINT('Ctrl Pts',(-188.795949562214,5.48211612966465,
128.57852744696));
#264346=CARTESIAN_POINT('Ctrl Pts',(-188.788541342547,5.54139929342365,
128.724538923719));
#264347=CARTESIAN_POINT('Ctrl Pts',(-188.781133122881,5.59480631631315,
128.872824903103));
#264348=CARTESIAN_POINT('Ctrl Pts',(-188.773724903214,5.64218173492415,
129.022868031955));
#264349=CARTESIAN_POINT('Ctrl Pts',(-188.766312123912,5.68958631231479,
129.173003509849));
#264350=CARTESIAN_POINT('Ctrl Pts',(-188.75889934461,5.73095179023987,129.324897932882));
#264351=CARTESIAN_POINT('Ctrl Pts',(-188.751486565308,5.76617357147899,
129.478022460806));
#264352=CARTESIAN_POINT('Ctrl Pts',(-188.744063194279,5.80144567925094,
129.631365780237));
#264353=CARTESIAN_POINT('Ctrl Pts',(-188.73663982325,5.83055648899496,129.785942349065));
#264354=CARTESIAN_POINT('Ctrl Pts',(-188.729216452221,5.85345300237912,
129.941216069162));
#264355=CARTESIAN_POINT('Ctrl Pts',(-188.725280402781,5.86559328316901,
130.023545921295));
#264356=CARTESIAN_POINT('Ctrl Pts',(-188.72134435334,5.8759873721544,130.106071718954));
#264357=CARTESIAN_POINT('Ctrl Pts',(-188.7174083039,5.88463331274603,130.18871352952));
#264358=CARTESIAN_POINT('Ctrl Pts',(-188.709985037494,5.90093928687214,
130.344573405092));
#264359=CARTESIAN_POINT('Ctrl Pts',(-188.702561771089,5.91107350431225,
130.501317224105));
#264360=CARTESIAN_POINT('Ctrl Pts',(-188.695138504683,5.91494973892084,
130.658414913483));
#264361=CARTESIAN_POINT('Ctrl Pts',(-188.687724011962,5.91882139214203,
130.815326926438));
#264362=CARTESIAN_POINT('Ctrl Pts',(-188.680309519241,5.91644977602051,
130.972591607699));
#264363=CARTESIAN_POINT('Ctrl Pts',(-188.67289502652,5.90780019010058,131.1296719705));
#264364=CARTESIAN_POINT('Ctrl Pts',(-188.665487680167,5.89915894097722,
131.286600933333));
#264365=CARTESIAN_POINT('Ctrl Pts',(-188.658080333813,5.88425178867966,
131.443345561147));
#264366=CARTESIAN_POINT('Ctrl Pts',(-188.650672987459,5.86309603744215,
131.599367169885));
#264367=CARTESIAN_POINT('Ctrl Pts',(-188.643271165784,5.84195606496208,
131.75527241182));
#264368=CARTESIAN_POINT('Ctrl Pts',(-188.635869344108,5.81457682305113,
131.910455340087));
#264369=CARTESIAN_POINT('Ctrl Pts',(-188.628467522433,5.78102756193813,
132.064380812091));
#264370=CARTESIAN_POINT('Ctrl Pts',(-188.621069608122,5.74749601121893,
132.218225028037));
#264371=CARTESIAN_POINT('Ctrl Pts',(-188.61367169381,5.70780100727417,132.3708127459));
#264372=CARTESIAN_POINT('Ctrl Pts',(-188.606273779499,5.66206315063794,
132.521617570001));
#264373=CARTESIAN_POINT('Ctrl Pts',(-188.598877094587,5.61633289480377,
132.672397333077));
#264374=CARTESIAN_POINT('Ctrl Pts',(-188.591480409675,5.56456188758136,
132.821394433549));
#264375=CARTESIAN_POINT('Ctrl Pts',(-188.584083724762,5.50692103084546,
132.968096119547));
#264376=CARTESIAN_POINT('Ctrl Pts',(-188.576687367827,5.44928272996555,
133.114791300639));
#264377=CARTESIAN_POINT('Ctrl Pts',(-188.569291010892,5.38577523360099,
133.259190922191));
#264378=CARTESIAN_POINT('Ctrl Pts',(-188.561894653956,5.3166180832047,133.400801011613));
#264379=CARTESIAN_POINT('Ctrl Pts',(-188.55449716462,5.24745034467193,133.542432781902));
#264380=CARTESIAN_POINT('Ctrl Pts',(-188.547099675283,5.17263139364863,
133.681273834221));
#264381=CARTESIAN_POINT('Ctrl Pts',(-188.539702185946,5.09242726241424,
133.816853794242));
#264382=CARTESIAN_POINT('Ctrl Pts',(-188.532302103431,5.0121950157461,133.952481281607));
#264383=CARTESIAN_POINT('Ctrl Pts',(-188.524902020916,4.92657402028228,
134.084845079539));
#264384=CARTESIAN_POINT('Ctrl Pts',(-188.517501938401,4.83587416152764,
134.213502981324));
#264385=CARTESIAN_POINT('Ctrl Pts',(-188.510093718735,4.74507456895399,
134.342302355698));
#264386=CARTESIAN_POINT('Ctrl Pts',(-188.502685499068,4.64918517523304,
134.467387390564));
#264387=CARTESIAN_POINT('Ctrl Pts',(-188.495277279402,4.54855721245665,
134.588347648134));
#264388=CARTESIAN_POINT('Ctrl Pts',(-188.4878645001,4.44786731484825,134.709382354725));
#264389=CARTESIAN_POINT('Ctrl Pts',(-188.480451720798,4.34243328610366,
134.826286948712));
#264390=CARTESIAN_POINT('Ctrl Pts',(-188.473038941496,4.23264351714947,
134.938687578419));
#264391=CARTESIAN_POINT('Ctrl Pts',(-188.465615570467,4.12269687542492,
135.051248811416));
#264392=CARTESIAN_POINT('Ctrl Pts',(-188.458192199438,4.00838233397257,
135.159292971309));
#264393=CARTESIAN_POINT('Ctrl Pts',(-188.45076882841,3.89012228043788,135.262485694966));
#264394=CARTESIAN_POINT('Ctrl Pts',(-188.446832778969,3.82741796243955,
135.317200953127));
#264395=CARTESIAN_POINT('Ctrl Pts',(-188.442896729528,3.76360493059685,
135.370553004011));
#264396=CARTESIAN_POINT('Ctrl Pts',(-188.438960680087,3.69874937690234,
135.422496995951));
#264397=CARTESIAN_POINT('Ctrl Pts',(-188.431537413681,3.57643382671275,
135.520461743629));
#264398=CARTESIAN_POINT('Ctrl Pts',(-188.424114147276,3.45003860462953,
135.613711810634));
#264399=CARTESIAN_POINT('Ctrl Pts',(-188.41669088087,3.31996306880589,135.701888135025));
#264400=CARTESIAN_POINT('Ctrl Pts',(-188.409276388149,3.1900412714635,135.789960242322));
#264401=CARTESIAN_POINT('Ctrl Pts',(-188.401861895428,3.05644812470781,
135.872970336136));
#264402=CARTESIAN_POINT('Ctrl Pts',(-188.394447402707,2.91961665426848,
135.950598967528));
#264403=CARTESIAN_POINT('Ctrl Pts',(-188.387040056353,2.78291706715196,
136.028152777522));
#264404=CARTESIAN_POINT('Ctrl Pts',(-188.37963271,2.64298569258825,136.100335268136));
#264405=CARTESIAN_POINT('Ctrl Pts',(-188.372225363646,2.50028509409351,
136.16686982602));
#264406=CARTESIAN_POINT('Ctrl Pts',(-188.36482354197,2.35769092708891,136.233354759921));
#264407=CARTESIAN_POINT('Ctrl Pts',(-188.357421720295,2.2123319855006,136.294199991563));
#264408=CARTESIAN_POINT('Ctrl Pts',(-188.35001989862,2.06469593138949,136.349174525481));
#264409=CARTESIAN_POINT('Ctrl Pts',(-188.342621984308,1.91713781320257,
136.40412003877));
#264410=CARTESIAN_POINT('Ctrl Pts',(-188.335224069997,1.76730532541907,
136.453200896397));
#264411=CARTESIAN_POINT('Ctrl Pts',(-188.327826155686,1.61570652716677,
136.496234033285));
#264412=CARTESIAN_POINT('Ctrl Pts',(-188.320429470773,1.46413292188381,
136.539260018847));
#264413=CARTESIAN_POINT('Ctrl Pts',(-188.313032785861,1.31079394745819,
136.576240176501));
#264414=CARTESIAN_POINT('Ctrl Pts',(-188.305636100949,1.15621337319739,
136.607041135925));
#264415=CARTESIAN_POINT('Ctrl Pts',(-188.298239744013,1.00163965320169,
136.637840729602));
#264416=CARTESIAN_POINT('Ctrl Pts',(-188.290843387078,0.845824808937177,
136.662461596891));
#264417=CARTESIAN_POINT('Ctrl Pts',(-188.283447030143,0.689303101053426,
136.680821439981));
#264418=CARTESIAN_POINT('Ctrl Pts',(-188.276049540806,0.53275742929617,
136.69918409401));
#264419=CARTESIAN_POINT('Ctrl Pts',(-188.268652051469,0.375505049213833,
136.711283771691));
#264420=CARTESIAN_POINT('Ctrl Pts',(-188.261254562133,0.21808549699706,
136.7170900447));
#264421=CARTESIAN_POINT('Ctrl Pts',(-188.253854479618,0.060610761600514,
136.722898353089));
#264422=CARTESIAN_POINT('Ctrl Pts',(-188.246454397103,-0.0970308897949569,
136.72240885064));
#264423=CARTESIAN_POINT('Ctrl Pts',(-188.239054314588,-0.254299915471865,
136.715643229275));
#264424=CARTESIAN_POINT('Ctrl Pts',(-188.231646094921,-0.411741874610377,
136.708870168413));
#264425=CARTESIAN_POINT('Ctrl Pts',(-188.224237875255,-0.568810016570274,
136.695807222463));
#264426=CARTESIAN_POINT('Ctrl Pts',(-188.216829655588,-0.724969178892556,
136.676528041282));
#264427=CARTESIAN_POINT('Ctrl Pts',(-188.209416876286,-0.881224454573593,
136.657236994087));
#264428=CARTESIAN_POINT('Ctrl Pts',(-188.202004096984,-1.03656926831098,
136.631722148261));
#264429=CARTESIAN_POINT('Ctrl Pts',(-188.194591317682,-1.19047915331876,
136.600108192126));
#264430=CARTESIAN_POINT('Ctrl Pts',(-188.187167946653,-1.34460895198768,
136.568449064488));
#264431=CARTESIAN_POINT('Ctrl Pts',(-188.179744575625,-1.49729936561825,
136.530673510755));
#264432=CARTESIAN_POINT('Ctrl Pts',(-188.172321204596,-1.648040774199,136.486956166176));
#264433=CARTESIAN_POINT('Ctrl Pts',(-188.168385155155,-1.72796748601767,
136.463776181097));
#264434=CARTESIAN_POINT('Ctrl Pts',(-188.164449105714,-1.80734657986099,
136.438926556829));
#264435=CARTESIAN_POINT('Ctrl Pts',(-188.160513056274,-1.88610454236212,
136.412438739149));
#264436=CARTESIAN_POINT('Ctrl Pts',(-188.153089789868,-2.03463960169,136.36248354166));
#264437=CARTESIAN_POINT('Ctrl Pts',(-188.145666523463,-2.18141322895194,
136.306547600599));
#264438=CARTESIAN_POINT('Ctrl Pts',(-188.138243257057,-2.32590747232902,
136.244772825539));
#264439=CARTESIAN_POINT('Ctrl Pts',(-188.130828764336,-2.47023093550992,
136.183071063134));
#264440=CARTESIAN_POINT('Ctrl Pts',(-188.123414271615,-2.61228003741925,
136.115544348554));
#264441=CARTESIAN_POINT('Ctrl Pts',(-188.115999778894,-2.75155195563308,
136.042384328657));
#264442=CARTESIAN_POINT('Ctrl Pts',(-188.10859243254,-2.89068963832824,
135.969294823142));
#264443=CARTESIAN_POINT('Ctrl Pts',(-188.101185086187,-3.02705513796119,
135.890582993991));
#264444=CARTESIAN_POINT('Ctrl Pts',(-188.093777739833,-3.16016570500775,
135.80648849272));
#264445=CARTESIAN_POINT('Ctrl Pts',(-188.086375918158,-3.29317699317143,
135.722456712301));
#264446=CARTESIAN_POINT('Ctrl Pts',(-188.078974096482,-3.42293786829595,
135.633050451894));
#264447=CARTESIAN_POINT('Ctrl Pts',(-188.071572274807,-3.5489903940987,
135.53855513671));
#264448=CARTESIAN_POINT('Ctrl Pts',(-188.064174360495,-3.67497637775464,
135.444109704868));
#264449=CARTESIAN_POINT('Ctrl Pts',(-188.056776446184,-3.79725761282802,
135.344580791833));
#264450=CARTESIAN_POINT('Ctrl Pts',(-188.049378531873,-3.91540546311575,
135.240296890993));
#264451=CARTESIAN_POINT('Ctrl Pts',(-188.041981846961,-4.03353367937402,
135.136030320245));
#264452=CARTESIAN_POINT('Ctrl Pts',(-188.034585162048,-4.1475295945303,
135.027010576778));
#264453=CARTESIAN_POINT('Ctrl Pts',(-188.027188477136,-4.2569978902504,
134.913606232628));
#264454=CARTESIAN_POINT('Ctrl Pts',(-188.019792120201,-4.36646133203156,
134.800206916945));
#264455=CARTESIAN_POINT('Ctrl Pts',(-188.012395763265,-4.4713972942949,
134.682423655727));
#264456=CARTESIAN_POINT('Ctrl Pts',(-188.00499940633,-4.5714477566311,134.560661453614));
#264457=CARTESIAN_POINT('Ctrl Pts',(-187.997601916993,-4.67151353694821,
134.438880609397));
#264458=CARTESIAN_POINT('Ctrl Pts',(-187.990204427657,-4.76669209099886,
134.313119899753));
#264459=CARTESIAN_POINT('Ctrl Pts',(-187.98280693832,-4.85666618608259,
134.183816804508));
#264460=CARTESIAN_POINT('Ctrl Pts',(-187.975406855805,-4.94667182144627,
134.054468382263));
#264461=CARTESIAN_POINT('Ctrl Pts',(-187.96800677329,-5.03146915236339,
133.92157540827));
#264462=CARTESIAN_POINT('Ctrl Pts',(-187.960606690775,-5.11078479338413,
133.785603539271));
#264463=CARTESIAN_POINT('Ctrl Pts',(-187.953198471109,-5.19018765010589,
133.649482155223));
#264464=CARTESIAN_POINT('Ctrl Pts',(-187.945790251442,-5.26409659104829,
133.510275437626));
#264465=CARTESIAN_POINT('Ctrl Pts',(-187.938382031776,-5.3322843115409,
133.368473443359));
#264466=CARTESIAN_POINT('Ctrl Pts',(-187.930969252474,-5.40051400043771,
133.226584172331));
#264467=CARTESIAN_POINT('Ctrl Pts',(-187.923556473172,-5.46301530435872,
133.082096783536));
#264468=CARTESIAN_POINT('Ctrl Pts',(-187.91614369387,-5.51960964001329,
132.93551992282));
#264469=CARTESIAN_POINT('Ctrl Pts',(-187.908720322841,-5.57628484030872,
132.788733626212));
#264470=CARTESIAN_POINT('Ctrl Pts',(-187.901296951812,-5.62703609533202,
132.639852247296));
#264471=CARTESIAN_POINT('Ctrl Pts',(-187.893873580783,-5.67173486859993,
132.489398938438));
#264472=CARTESIAN_POINT('Ctrl Pts',(-187.889937531343,-5.6954352307193,
132.409624984003));
#264473=CARTESIAN_POINT('Ctrl Pts',(-187.886001481902,-5.71743487721036,
132.329409275315));
#264474=CARTESIAN_POINT('Ctrl Pts',(-187.882065432461,-5.73772052852476,
132.248830658462));
#264475=CARTESIAN_POINT('Ctrl Pts',(-187.872272656446,-5.78819063633813,
132.048353413881));
#264476=CARTESIAN_POINT('Ctrl Pts',(-187.862479880431,-5.82817280781611,
131.845137610024));
#264477=CARTESIAN_POINT('Ctrl Pts',(-187.852687104416,-5.85742459265489,
131.640128350768));
#264478=CARTESIAN_POINT('Ctrl Pts',(-187.843111607346,-5.88602734836112,
131.43966777059));
#264479=CARTESIAN_POINT('Ctrl Pts',(-187.833536110275,-5.90437066060156,
131.237492158579));
#264480=CARTESIAN_POINT('Ctrl Pts',(-187.823960613204,-5.91227224031638,
131.034507350944));
#264481=CARTESIAN_POINT('Ctrl Pts',(-187.820432147727,-5.915183885637,130.959709679258));
#264482=CARTESIAN_POINT('Ctrl Pts',(-187.81690368225,-5.91667814734567,
130.88480237372));
#264483=CARTESIAN_POINT('Ctrl Pts',(-187.813375216773,-5.91674747054566,
130.809831658736));
#264484=CARTESIAN_POINT('',(-191.313375192208,-5.91167657527647,130.799567797019));
#264485=CARTESIAN_POINT('Ctrl Pts',(-191.313375192208,-5.91167657527647,
130.799567797019));
#264486=CARTESIAN_POINT('Ctrl Pts',(-191.283395767544,-5.91650671956634,
130.161511730902));
#264487=CARTESIAN_POINT('Ctrl Pts',(-191.160600468276,-5.52689340955663,
127.553783705044));
#264488=CARTESIAN_POINT('Ctrl Pts',(-190.944989294402,-1.71886118746277,
124.020329607269));
#264489=CARTESIAN_POINT('Ctrl Pts',(-190.66654167059,4.77851096535738,125.691299549647));
#264490=CARTESIAN_POINT('Ctrl Pts',(-190.388094046777,6.88466498425298,
132.060922826512));
#264491=CARTESIAN_POINT('Ctrl Pts',(-190.109646422965,2.66414821720038,
137.275826819836));
#264492=CARTESIAN_POINT('Ctrl Pts',(-189.834740626303,-3.91976489026385,
136.553081220811));
#264493=CARTESIAN_POINT('Ctrl Pts',(-189.65265070425,-5.9201422633631,132.691092662961));
#264494=CARTESIAN_POINT('Ctrl Pts',(-189.563376656799,-5.92613653540298,
130.802997987718));
#264495=CARTESIAN_POINT('',(-193.063375192208,-5.90877653025682,130.807662282052));
#264496=CARTESIAN_POINT('Ctrl Pts',(-193.063375192208,-5.90877653025682,
130.807662282052));
#264497=CARTESIAN_POINT('Ctrl Pts',(-193.006957681836,-5.90270635330487,
129.605440343458));
#264498=CARTESIAN_POINT('Ctrl Pts',(-192.857724296862,-4.96095598029521,
126.416633059624));
#264499=CARTESIAN_POINT('Ctrl Pts',(-192.61567503728,0.256241860122023,
123.810656260109));
#264500=CARTESIAN_POINT('Ctrl Pts',(-192.337227413466,6.02250653238034,
127.239676115707));
#264501=CARTESIAN_POINT('Ctrl Pts',(-192.058779789655,6.25438191717603,
133.944466883987));
#264502=CARTESIAN_POINT('Ctrl Pts',(-191.780332165841,0.738785863635208,
137.763653396148));
#264503=CARTESIAN_POINT('Ctrl Pts',(-191.531863966693,-4.78877897888325,
135.464945051595));
#264504=CARTESIAN_POINT('Ctrl Pts',(-191.376211642148,-5.90155266118287,
132.136924284238));
#264505=CARTESIAN_POINT('Ctrl Pts',(-191.313375192208,-5.91167657527647,
130.799567797019));
#264506=CARTESIAN_POINT('',(-194.813375192208,-5.92378430407072,130.807954965743));
#264507=CARTESIAN_POINT('Ctrl Pts',(-194.813375192208,-5.92378430407072,
130.807954965743));
#264508=CARTESIAN_POINT('Ctrl Pts',(-194.730519596129,-5.91124949145352,
129.053764187153));
#264509=CARTESIAN_POINT('Ctrl Pts',(-194.554848125446,-4.15536005181142,
125.312715685492));
#264510=CARTESIAN_POINT('Ctrl Pts',(-194.286360780158,2.21070539777845,
124.164304731159));
#264511=CARTESIAN_POINT('Ctrl Pts',(-194.007913156345,6.78140734036955,
129.075177280167));
#264512=CARTESIAN_POINT('Ctrl Pts',(-193.729465532532,5.12032722732323,
135.575084840937));
#264513=CARTESIAN_POINT('Ctrl Pts',(-193.451017908719,-1.24608346573943,
137.690929903266));
#264514=CARTESIAN_POINT('Ctrl Pts',(-193.228987795278,-5.40948930689292,
134.331882897925));
#264515=CARTESIAN_POINT('Ctrl Pts',(-193.099773556441,-5.91269277027163,
131.5832887094));
#264516=CARTESIAN_POINT('Ctrl Pts',(-193.063375192208,-5.90877653025682,
130.807662282052));
#264517=CARTESIAN_POINT('',(-196.563375192208,-5.91754067440713,130.799324060973));
#264518=CARTESIAN_POINT('Ctrl Pts',(-196.563375192208,-5.92005028606524,
130.799321924984));
#264519=CARTESIAN_POINT('Ctrl Pts',(-196.546897385026,-5.92321501407519,
130.449886125491));
#264520=CARTESIAN_POINT('Ctrl Pts',(-196.530419577843,-5.89494931063627,
130.100961680412));
#264521=CARTESIAN_POINT('Ctrl Pts',(-196.421125896056,-5.48691602341415,
127.826183567757));
#264522=CARTESIAN_POINT('Ctrl Pts',(-196.235494146848,-2.68383279408233,
124.341033141431));
#264523=CARTESIAN_POINT('Ctrl Pts',(-195.957046523035,3.98710327515676,
125.052789701408));
#264524=CARTESIAN_POINT('Ctrl Pts',(-195.678598899222,6.99408621534913,
131.049958953475));
#264525=CARTESIAN_POINT('Ctrl Pts',(-195.400151275409,3.57384560374378,
136.821435332985));
#264526=CARTESIAN_POINT('Ctrl Pts',(-195.121703651596,-3.13058452563971,
137.063513999468));
#264527=CARTESIAN_POINT('Ctrl Pts',(-194.926111623863,-5.81921701947016,
133.19324015144));
#264528=CARTESIAN_POINT('Ctrl Pts',(-194.823335470733,-5.92529114525991,
131.018830628555));
#264529=CARTESIAN_POINT('Ctrl Pts',(-194.813375192208,-5.92378430407072,
130.807954965743));
#264530=CARTESIAN_POINT('',(-198.313375158537,-5.91281518750731,130.803135099679));
#264531=CARTESIAN_POINT('Ctrl Pts',(-198.313375135094,-5.91674987280848,
130.803133783915));
#264532=CARTESIAN_POINT('Ctrl Pts',(-198.305494209198,-5.91671497079014,
130.634808997274));
#264533=CARTESIAN_POINT('Ctrl Pts',(-198.297613283303,-5.90949285436914,
130.466668773567));
#264534=CARTESIAN_POINT('Ctrl Pts',(-198.289732357408,-5.89515605919228,
130.29932042088));
#264535=CARTESIAN_POINT('Ctrl Pts',(-198.281836630896,-5.88079233908077,
130.131657782929));
#264536=CARTESIAN_POINT('Ctrl Pts',(-198.273940904384,-5.85928727531646,
129.964790277688));
#264537=CARTESIAN_POINT('Ctrl Pts',(-198.266045177872,-5.83076466142615,
129.799316327217));
#264538=CARTESIAN_POINT('Ctrl Pts',(-198.258126453544,-5.80215896996073,
129.633360402175));
#264539=CARTESIAN_POINT('Ctrl Pts',(-198.250207729216,-5.76649488777139,
129.468806441626));
#264540=CARTESIAN_POINT('Ctrl Pts',(-198.242289004889,-5.72394703223156,
129.306241485218));
#264541=CARTESIAN_POINT('Ctrl Pts',(-198.234357905677,-5.6813326855795,
129.143422482521));
#264542=CARTESIAN_POINT('Ctrl Pts',(-198.226426806465,-5.63181316657086,
128.982598970972));
#264543=CARTESIAN_POINT('Ctrl Pts',(-198.218495707253,-5.57561197482526,
128.824339994268));
#264544=CARTESIAN_POINT('Ctrl Pts',(-198.210545405859,-5.51927471297368,
128.665697852811));
#264545=CARTESIAN_POINT('Ctrl Pts',(-198.202595104465,-5.45622353317009,
128.509632936207));
#264546=CARTESIAN_POINT('Ctrl Pts',(-198.194644803071,-5.38672971531874,
128.356693659706));
#264547=CARTESIAN_POINT('Ctrl Pts',(-198.19130570656,-5.35754257470302,
128.292459742115));
#264548=CARTESIAN_POINT('Ctrl Pts',(-198.187966610049,-5.32721951801162,
128.228776855833));
#264549=CARTESIAN_POINT('Ctrl Pts',(-198.184627513538,-5.29578296029053,
128.165684169042));
#264550=CARTESIAN_POINT('Ctrl Pts',(-198.177204247133,-5.22589521009871,
128.025420531639));
#264551=CARTESIAN_POINT('Ctrl Pts',(-198.169780980727,-5.15032541721235,
127.887723278348));
#264552=CARTESIAN_POINT('Ctrl Pts',(-198.162357714322,-5.06928530351928,
127.753085953754));
#264553=CARTESIAN_POINT('Ctrl Pts',(-198.154943221601,-4.98834097251064,
127.618607759295));
#264554=CARTESIAN_POINT('Ctrl Pts',(-198.14752872888,-4.90193938086913,
127.487182611414));
#264555=CARTESIAN_POINT('Ctrl Pts',(-198.14011423616,-4.8103394376285,127.359282235686));
#264556=CARTESIAN_POINT('Ctrl Pts',(-198.132706889806,-4.71882778186184,
127.231505135156));
#264557=CARTESIAN_POINT('Ctrl Pts',(-198.125299543452,-4.62212796504708,
127.107246344862));
#264558=CARTESIAN_POINT('Ctrl Pts',(-198.117892197099,-4.52054368801486,
126.986951112778));
#264559=CARTESIAN_POINT('Ctrl Pts',(-198.110490375423,-4.41903517636901,
126.866745601416));
#264560=CARTESIAN_POINT('Ctrl Pts',(-198.103088553748,-4.31264969804995,
126.750498046109));
#264561=CARTESIAN_POINT('Ctrl Pts',(-198.095686732073,-4.20173288463405,
126.638622828328));
#264562=CARTESIAN_POINT('Ctrl Pts',(-198.088288817762,-4.09087462334089,
126.526806668604));
#264563=CARTESIAN_POINT('Ctrl Pts',(-198.080890903451,-3.97549005300435,
126.419358514093));
#264564=CARTESIAN_POINT('Ctrl Pts',(-198.07349298914,-3.85596343966191,
126.316657807164));
#264565=CARTESIAN_POINT('Ctrl Pts',(-198.066096304228,-3.736456689474,126.213974167229));
#264566=CARTESIAN_POINT('Ctrl Pts',(-198.058699619315,-3.61280954527593,
126.116036652106));
#264567=CARTESIAN_POINT('Ctrl Pts',(-198.051302934403,-3.48544139440895,
126.023186196083));
#264568=CARTESIAN_POINT('Ctrl Pts',(-198.043906577468,-3.35807889117926,
125.930339857147));
#264569=CARTESIAN_POINT('Ctrl Pts',(-198.036510220533,-3.22699601099537,
125.842580348711));
#264570=CARTESIAN_POINT('Ctrl Pts',(-198.029113863598,-3.09264310423706,
125.76020665557));
#264571=CARTESIAN_POINT('Ctrl Pts',(-198.021716374261,-2.95826962770573,
125.677820350807));
#264572=CARTESIAN_POINT('Ctrl Pts',(-198.014318884925,-2.82062544600519,
125.600821698323));
#264573=CARTESIAN_POINT('Ctrl Pts',(-198.006921395588,-2.68018747322264,
125.529464820407));
#264574=CARTESIAN_POINT('Ctrl Pts',(-197.999521313073,-2.53970027012625,
125.458082928449));
#264575=CARTESIAN_POINT('Ctrl Pts',(-197.992121230558,-2.39641765864562,
125.392346917666));
#264576=CARTESIAN_POINT('Ctrl Pts',(-197.984721148044,-2.2508384387309,
125.332463607823));
#264577=CARTESIAN_POINT('Ctrl Pts',(-197.977312928377,-2.10509913949819,
125.272514450125));
#264578=CARTESIAN_POINT('Ctrl Pts',(-197.969904708711,-1.95705853397072,
125.21843098787));
#264579=CARTESIAN_POINT('Ctrl Pts',(-197.962496489045,-1.80723326014781,
125.170371044811));
#264580=CARTESIAN_POINT('Ctrl Pts',(-197.955083709743,-1.65731577136839,
125.122281521658));
#264581=CARTESIAN_POINT('Ctrl Pts',(-197.947670930441,-1.50561178442189,
125.080223004612));
#264582=CARTESIAN_POINT('Ctrl Pts',(-197.940258151139,-1.35264965650991,
125.04430250421));
#264583=CARTESIAN_POINT('Ctrl Pts',(-197.93283478011,-1.19946896913657,
125.008330678912));
#264584=CARTESIAN_POINT('Ctrl Pts',(-197.925411409082,-1.04502691596486,
124.97851445706));
#264585=CARTESIAN_POINT('Ctrl Pts',(-197.917988038053,-0.889859347573362,
124.954909283976));
#264586=CARTESIAN_POINT('Ctrl Pts',(-197.91405198861,-0.807585779573266,
124.942393254802));
#264587=CARTESIAN_POINT('Ctrl Pts',(-197.910115939167,-0.725108295893379,
124.931622504652));
#264588=CARTESIAN_POINT('Ctrl Pts',(-197.906179889724,-0.642506819387798,
124.922599355024));
#264589=CARTESIAN_POINT('Ctrl Pts',(-197.898756623319,-0.486723012682509,
124.905581976438));
#264590=CARTESIAN_POINT('Ctrl Pts',(-197.891333356914,-0.330027094746583,
124.894732254595));
#264591=CARTESIAN_POINT('Ctrl Pts',(-197.883910090508,-0.172948739468105,
124.890138834777));
#264592=CARTESIAN_POINT('Ctrl Pts',(-197.876495597787,-0.0160560377610202,
124.885550844));
#264593=CARTESIAN_POINT('Ctrl Pts',(-197.869081105066,0.141217832067213,
124.887204447401));
#264594=CARTESIAN_POINT('Ctrl Pts',(-197.861666612345,0.298336047272165,
124.895136796674));
#264595=CARTESIAN_POINT('Ctrl Pts',(-197.854259265991,0.455302826025905,
124.90306150045));
#264596=CARTESIAN_POINT('Ctrl Pts',(-197.846851919638,0.612113878507934,
124.917252883675));
#264597=CARTESIAN_POINT('Ctrl Pts',(-197.839444573284,0.768230447271629,
124.937696101643));
#264598=CARTESIAN_POINT('Ctrl Pts',(-197.832042751609,0.924230578407954,
124.958124072289));
#264599=CARTESIAN_POINT('Ctrl Pts',(-197.824640929933,1.07953688863353,
124.984794545045));
#264600=CARTESIAN_POINT('Ctrl Pts',(-197.817239108258,1.23361392477094,
125.017640713587));
#264601=CARTESIAN_POINT('Ctrl Pts',(-197.809841193946,1.38760962484074,
125.050469542891));
#264602=CARTESIAN_POINT('Ctrl Pts',(-197.802443279635,1.54037697901615,
125.089467497698));
#264603=CARTESIAN_POINT('Ctrl Pts',(-197.795045365324,1.69138904650517,
125.134516381975));
#264604=CARTESIAN_POINT('Ctrl Pts',(-197.787648680412,1.84237601852799,
125.179557779945));
#264605=CARTESIAN_POINT('Ctrl Pts',(-197.780251995499,1.99160792542631,
125.23064800505));
#264606=CARTESIAN_POINT('Ctrl Pts',(-197.772855310587,2.1385712404262,125.287618498152));
#264607=CARTESIAN_POINT('Ctrl Pts',(-197.765458953652,2.2855280389187,125.344586465122));
#264608=CARTESIAN_POINT('Ctrl Pts',(-197.758062596717,2.43021609746273,
125.407434046729));
#264609=CARTESIAN_POINT('Ctrl Pts',(-197.750666239781,2.57214044630336,
125.475943959028));
#264610=CARTESIAN_POINT('Ctrl Pts',(-197.743268750445,2.71408652412452,
125.544464360369));
#264611=CARTESIAN_POINT('Ctrl Pts',(-197.735871261108,2.8532677135316,125.618648656259));
#264612=CARTESIAN_POINT('Ctrl Pts',(-197.728473771771,2.98921243053313,
125.698232964672));
#264613=CARTESIAN_POINT('Ctrl Pts',(-197.721073689256,3.12520480274389,
125.777845171241));
#264614=CARTESIAN_POINT('Ctrl Pts',(-197.713673606741,3.25795812173416,
125.862860970739));
#264615=CARTESIAN_POINT('Ctrl Pts',(-197.706273524226,3.38702877062359,
125.952972499772));
#264616=CARTESIAN_POINT('Ctrl Pts',(-197.69886530456,3.51624134596045,126.043183115696));
#264617=CARTESIAN_POINT('Ctrl Pts',(-197.691457084894,3.64176285786007,
126.138500437448));
#264618=CARTESIAN_POINT('Ctrl Pts',(-197.684048865227,3.76318126927204,
126.238575110438));
#264619=CARTESIAN_POINT('Ctrl Pts',(-197.676636085925,3.88467441169026,
126.33871137772));
#264620=CARTESIAN_POINT('Ctrl Pts',(-197.669223306623,4.002059143761,126.443610582622));
#264621=CARTESIAN_POINT('Ctrl Pts',(-197.661810527321,4.11495984451519,
126.552886045076));
#264622=CARTESIAN_POINT('Ctrl Pts',(-197.654387156293,4.2280218630853,126.662317645436));
#264623=CARTESIAN_POINT('Ctrl Pts',(-197.646963785264,4.33658679716489,
126.776137722587));
#264624=CARTESIAN_POINT('Ctrl Pts',(-197.639540414235,4.4403183587074,126.893925419813));
#264625=CARTESIAN_POINT('Ctrl Pts',(-197.635604364794,4.49531932164588,
126.956379283164));
#264626=CARTESIAN_POINT('Ctrl Pts',(-197.631668315353,4.54896215332004,
127.019948072493));
#264627=CARTESIAN_POINT('Ctrl Pts',(-197.627732265912,4.60120170033201,
127.084565801267));
#264628=CARTESIAN_POINT('Ctrl Pts',(-197.620308999507,4.69972385564997,
127.206432821078));
#264629=CARTESIAN_POINT('Ctrl Pts',(-197.612885733101,4.79355000507247,
127.332400995022));
#264630=CARTESIAN_POINT('Ctrl Pts',(-197.605462466696,4.88231926713834,
127.462072608398));
#264631=CARTESIAN_POINT('Ctrl Pts',(-197.598047973975,4.97098361130828,
127.591590960695));
#264632=CARTESIAN_POINT('Ctrl Pts',(-197.590633481254,5.05460275620507,
127.72480373464));
#264633=CARTESIAN_POINT('Ctrl Pts',(-197.583218988533,5.13285527925053,
127.861279367452));
#264634=CARTESIAN_POINT('Ctrl Pts',(-197.575811642179,5.21103237956813,
127.997623459912));
#264635=CARTESIAN_POINT('Ctrl Pts',(-197.568404295825,5.28385297112994,
128.137223828763));
#264636=CARTESIAN_POINT('Ctrl Pts',(-197.560996949471,5.35103833164711,
128.279619178182));
#264637=CARTESIAN_POINT('Ctrl Pts',(-197.553595127796,5.41817358278764,
128.421908323777));
#264638=CARTESIAN_POINT('Ctrl Pts',(-197.54619330612,5.47968181295513,128.566987963062));
#264639=CARTESIAN_POINT('Ctrl Pts',(-197.538791484445,5.53532980268285,
128.714371493663));
#264640=CARTESIAN_POINT('Ctrl Pts',(-197.531393570133,5.59094841626997,
128.861677221646));
#264641=CARTESIAN_POINT('Ctrl Pts',(-197.523995655822,5.64071281889356,
129.011284070463));
#264642=CARTESIAN_POINT('Ctrl Pts',(-197.516597741511,5.6844376278525,129.162684822059));
#264643=CARTESIAN_POINT('Ctrl Pts',(-197.509201056598,5.72815517054139,
129.314060413596));
#264644=CARTESIAN_POINT('Ctrl Pts',(-197.501804371686,5.76583500808062,
129.467228957956));
#264645=CARTESIAN_POINT('Ctrl Pts',(-197.494407686774,5.79734138028169,
129.621667300187));
#264646=CARTESIAN_POINT('Ctrl Pts',(-197.487011329838,5.82884635545729,
129.77609879446));
#264647=CARTESIAN_POINT('Ctrl Pts',(-197.479614972903,5.85417833496008,
129.93179960889));
#264648=CARTESIAN_POINT('Ctrl Pts',(-197.472218615968,5.87325258268416,
130.088235864123));
#264649=CARTESIAN_POINT('Ctrl Pts',(-197.464821126631,5.89232975072421,
130.244696070146));
#264650=CARTESIAN_POINT('Ctrl Pts',(-197.457423637294,5.90514723414698,
130.401891570591));
#264651=CARTESIAN_POINT('Ctrl Pts',(-197.450026147958,5.91167214170678,
130.559282973812));
#264652=CARTESIAN_POINT('Ctrl Pts',(-197.442626065443,5.91819933656282,
130.716729550346));
#264653=CARTESIAN_POINT('Ctrl Pts',(-197.435225982928,5.9184295482666,130.874371793638));
#264654=CARTESIAN_POINT('Ctrl Pts',(-197.427825900413,5.91238200524872,
131.03167006856));
#264655=CARTESIAN_POINT('Ctrl Pts',(-197.420417680746,5.9063278123356,131.189141309106));
#264656=CARTESIAN_POINT('Ctrl Pts',(-197.41300946108,5.89398209323351,131.346267452684));
#264657=CARTESIAN_POINT('Ctrl Pts',(-197.405601241413,5.87541605376114,
131.502513006165));
#264658=CARTESIAN_POINT('Ctrl Pts',(-197.398188462111,5.85683858720126,
131.658854726177));
#264659=CARTESIAN_POINT('Ctrl Pts',(-197.390775682809,5.83203323018161,
131.814314408332));
#264660=CARTESIAN_POINT('Ctrl Pts',(-197.383362903507,5.80112227528612,
131.96836702205));
#264661=CARTESIAN_POINT('Ctrl Pts',(-197.375939532478,5.77016715336866,
132.122639753366));
#264662=CARTESIAN_POINT('Ctrl Pts',(-197.368516161449,5.73308909762374,
132.275501039037));
#264663=CARTESIAN_POINT('Ctrl Pts',(-197.361092790421,5.69006041482304,
132.426440467069));
#264664=CARTESIAN_POINT('Ctrl Pts',(-197.35715674098,5.66724557474622,132.506472173542));
#264665=CARTESIAN_POINT('Ctrl Pts',(-197.35322069154,5.64275861274537,132.585963890444));
#264666=CARTESIAN_POINT('Ctrl Pts',(-197.3492846421,5.6166306386455,132.664841961608));
#264667=CARTESIAN_POINT('Ctrl Pts',(-197.341861375694,5.56735409491276,
132.813603542143));
#264668=CARTESIAN_POINT('Ctrl Pts',(-197.334438109289,5.51208882816386,
132.960631013906));
#264669=CARTESIAN_POINT('Ctrl Pts',(-197.327014842883,5.45097438179734,
133.105405782592));
#264670=CARTESIAN_POINT('Ctrl Pts',(-197.319600350162,5.38993216763119,
133.250009439524));
#264671=CARTESIAN_POINT('Ctrl Pts',(-197.312185857442,5.32305467845807,
133.392365352562));
#264672=CARTESIAN_POINT('Ctrl Pts',(-197.304771364721,5.25053126351302,
133.531969829563));
#264673=CARTESIAN_POINT('Ctrl Pts',(-197.297364018367,5.17807774936575,
133.671439750514));
#264674=CARTESIAN_POINT('Ctrl Pts',(-197.289956672013,5.09998931384532,
133.808163185873));
#264675=CARTESIAN_POINT('Ctrl Pts',(-197.282549325659,5.01650340198775,
133.941656297024));
#264676=CARTESIAN_POINT('Ctrl Pts',(-197.275147503984,4.93307975707299,
134.075049843976));
#264677=CARTESIAN_POINT('Ctrl Pts',(-197.267745682308,4.84426684850198,
134.20521754882));
#264678=CARTESIAN_POINT('Ctrl Pts',(-197.260343860633,4.75034800781524,
134.331700176943));
#264679=CARTESIAN_POINT('Ctrl Pts',(-197.252945946322,4.65647874615343,
134.458116035871));
#264680=CARTESIAN_POINT('Ctrl Pts',(-197.24554803201,4.55750914234047,134.580850393335));
#264681=CARTESIAN_POINT('Ctrl Pts',(-197.238150117699,4.453765729412,134.699473117869));
#264682=CARTESIAN_POINT('Ctrl Pts',(-197.230753432787,4.3500395567568,134.818076129458));
#264683=CARTESIAN_POINT('Ctrl Pts',(-197.223356747875,4.24154139500116,
134.932568583504));
#264684=CARTESIAN_POINT('Ctrl Pts',(-197.215960062963,4.12863800752296,
135.042553483085));
#264685=CARTESIAN_POINT('Ctrl Pts',(-197.208563706027,4.01573962629928,
135.152533505821));
#264686=CARTESIAN_POINT('Ctrl Pts',(-197.201167349092,3.89843667513432,
135.258006111018));
#264687=CARTESIAN_POINT('Ctrl Pts',(-197.193770992156,3.77713251991294,
135.35861143296));
#264688=CARTESIAN_POINT('Ctrl Pts',(-197.18637350282,3.65580979271537,135.459232157834));
#264689=CARTESIAN_POINT('Ctrl Pts',(-197.178976013483,3.53048492905807,
135.554983877352));
#264690=CARTESIAN_POINT('Ctrl Pts',(-197.171578524146,3.40159395588911,
135.645547364817));
#264691=CARTESIAN_POINT('Ctrl Pts',(-197.164178441631,3.27265780018913,
135.736142599172));
#264692=CARTESIAN_POINT('Ctrl Pts',(-197.156778359116,3.14015335129741,
135.821545765924));
#264693=CARTESIAN_POINT('Ctrl Pts',(-197.149378276601,3.00454501296717,
135.901481356528));
#264694=CARTESIAN_POINT('Ctrl Pts',(-197.141970056935,2.86878755932826,
135.981504844531));
#264695=CARTESIAN_POINT('Ctrl Pts',(-197.134561837268,2.72991972195824,
136.056048560025));
#264696=CARTESIAN_POINT('Ctrl Pts',(-197.127153617602,2.58843051487615,
136.124882963366));
#264697=CARTESIAN_POINT('Ctrl Pts',(-197.1197408383,2.44685422354838,136.193759733134));
#264698=CARTESIAN_POINT('Ctrl Pts',(-197.112328058998,2.3026536887318,136.256920039268));
#264699=CARTESIAN_POINT('Ctrl Pts',(-197.104915279696,2.15633673565307,
136.31418297813));
#264700=CARTESIAN_POINT('Ctrl Pts',(-197.097491908667,2.00981071804999,
136.371527736965));
#264701=CARTESIAN_POINT('Ctrl Pts',(-197.090068537638,1.86116259434809,
136.422958177311));
#264702=CARTESIAN_POINT('Ctrl Pts',(-197.08264516661,1.71091492463178,136.468343375588));
#264703=CARTESIAN_POINT('Ctrl Pts',(-197.078709117169,1.63125000500077,
136.492407696719));
#264704=CARTESIAN_POINT('Ctrl Pts',(-197.074773067728,1.55113557114578,
136.514773336763));
#264705=CARTESIAN_POINT('Ctrl Pts',(-197.070837018287,1.47065040770534,
136.535426656342));
#264706=CARTESIAN_POINT('Ctrl Pts',(-197.063413751881,1.31885790131885,
136.574378172499));
#264707=CARTESIAN_POINT('Ctrl Pts',(-197.055990485476,1.16528729868185,
136.607353878223));
#264708=CARTESIAN_POINT('Ctrl Pts',(-197.04856721907,1.01045033448641,136.634190862439));
#264709=CARTESIAN_POINT('Ctrl Pts',(-197.041152726349,0.855796374724231,
136.660996127568));
#264710=CARTESIAN_POINT('Ctrl Pts',(-197.033738233628,0.699879396883509,
136.681677050091));
#264711=CARTESIAN_POINT('Ctrl Pts',(-197.026323740907,0.543225519315743,
136.696120676976));
#264712=CARTESIAN_POINT('Ctrl Pts',(-197.018916394553,0.38672263065309,
136.71055038255));
#264713=CARTESIAN_POINT('Ctrl Pts',(-197.011509048199,0.229484625460507,
136.718754726634));
#264714=CARTESIAN_POINT('Ctrl Pts',(-197.004101701846,0.072046915710644,
136.720671951872));
#264715=CARTESIAN_POINT('Ctrl Pts',(-196.99669988017,-0.0852733710555033,
136.722587747171));
#264716=CARTESIAN_POINT('Ctrl Pts',(-196.989298058495,-0.242792694141263,
136.718225755868));
#264717=CARTESIAN_POINT('Ctrl Pts',(-196.981896236819,-0.399971538843124,
136.707576125289));
#264718=CARTESIAN_POINT('Ctrl Pts',(-196.974498322508,-0.557067410055896,
136.696932116566));
#264719=CARTESIAN_POINT('Ctrl Pts',(-196.967100408196,-0.71382278933619,
136.680007104075));
#264720=CARTESIAN_POINT('Ctrl Pts',(-196.959702493885,-0.869699295819346,
136.656843312743));
#264721=CARTESIAN_POINT('Ctrl Pts',(-196.952305808973,-1.02554989845523,
136.633683370814));
#264722=CARTESIAN_POINT('Ctrl Pts',(-196.944909124061,-1.18052154928376,
136.604286762546));
#264723=CARTESIAN_POINT('Ctrl Pts',(-196.937512439148,-1.33408199898751,
136.568747469823));
#264724=CARTESIAN_POINT('Ctrl Pts',(-196.930116082213,-1.48763563966,136.533209752951));
#264725=CARTESIAN_POINT('Ctrl Pts',(-196.922719725277,-1.63977783994152,
136.491529977363));
#264726=CARTESIAN_POINT('Ctrl Pts',(-196.915323368342,-1.7899878054991,
136.443852989993));
#264727=CARTESIAN_POINT('Ctrl Pts',(-196.907925879005,-1.94022076858587,
136.396168703155));
#264728=CARTESIAN_POINT('Ctrl Pts',(-196.900528389669,-2.08852055208359,
136.34248548924));
#264729=CARTESIAN_POINT('Ctrl Pts',(-196.893130900332,-2.23438289831461,
136.28299764024));
#264730=CARTESIAN_POINT('Ctrl Pts',(-196.885730817817,-2.38029637636477,
136.223488937868));
#264731=CARTESIAN_POINT('Ctrl Pts',(-196.878330735302,-2.52377037052379,
136.158171690011));
#264732=CARTESIAN_POINT('Ctrl Pts',(-196.870930652787,-2.66432206607766,
136.087287693602));
#264733=CARTESIAN_POINT('Ctrl Pts',(-196.86352243312,-2.80502831267005,
136.016325752951));
#264734=CARTESIAN_POINT('Ctrl Pts',(-196.856114213454,-2.9428055098375,
135.939785007485));
#264735=CARTESIAN_POINT('Ctrl Pts',(-196.848705993787,-3.07719621535446,
135.857952806763));
#264736=CARTESIAN_POINT('Ctrl Pts',(-196.841293214485,-3.21166963610861,
135.776070239686));
#264737=CARTESIAN_POINT('Ctrl Pts',(-196.833880435183,-3.3427521018158,
135.688889934013));
#264738=CARTESIAN_POINT('Ctrl Pts',(-196.826467655881,-3.47001692118132,
135.596741354654));
#264739=CARTESIAN_POINT('Ctrl Pts',(-196.819044284852,-3.59746358248833,
135.504461109084));
#264740=CARTESIAN_POINT('Ctrl Pts',(-196.811620913823,-3.72108141033138,
135.407198641944));
#264741=CARTESIAN_POINT('Ctrl Pts',(-196.804197542794,-3.84047779850241,
135.305322830439));
#264742=CARTESIAN_POINT('Ctrl Pts',(-196.800261493354,-3.90378462838005,
135.251305830709));
#264743=CARTESIAN_POINT('Ctrl Pts',(-196.796325443914,-3.96590528316954,
135.195992463312));
#264744=CARTESIAN_POINT('Ctrl Pts',(-196.792389394474,-4.02678570265285,
135.139441639578));
#264745=CARTESIAN_POINT('Ctrl Pts',(-196.78507668251,-4.13989428490648,
135.034376931548));
#264746=CARTESIAN_POINT('Ctrl Pts',(-196.777763970547,-4.24908372070728,
134.924700531894));
#264747=CARTESIAN_POINT('Ctrl Pts',(-196.770451258584,-4.35394615139191,
134.810740963125));
#264748=CARTESIAN_POINT('Ctrl Pts',(-196.763147289429,-4.45868321243069,
134.696917640204));
#264749=CARTESIAN_POINT('Ctrl Pts',(-196.755843320274,-4.55910330236656,
134.578821616739));
#264750=CARTESIAN_POINT('Ctrl Pts',(-196.748539351119,-4.65483230230702,
134.456820993792));
#264751=CARTESIAN_POINT('Ctrl Pts',(-196.741242407847,-4.75046921796755,
134.3349377265));
#264752=CARTESIAN_POINT('Ctrl Pts',(-196.733945464575,-4.84142378676094,
134.209157634796));
#264753=CARTESIAN_POINT('Ctrl Pts',(-196.726648521302,-4.92735958258975,
134.079884714006));
#264754=CARTESIAN_POINT('Ctrl Pts',(-196.719357248112,-5.01322860210467,
133.950712244595));
#264755=CARTESIAN_POINT('Ctrl Pts',(-196.712065974921,-5.09408640058275,
133.818052669374));
#264756=CARTESIAN_POINT('Ctrl Pts',(-196.704774701731,-5.16963782844034,
133.682341730301));
#264757=CARTESIAN_POINT('Ctrl Pts',(-196.697486477277,-5.24515766559986,
133.546687536724));
#264758=CARTESIAN_POINT('Ctrl Pts',(-196.690198252823,-5.31537535882009,
133.407984853367));
#264759=CARTESIAN_POINT('Ctrl Pts',(-196.682910028369,-5.38004001794075,
133.266696900013));
#264760=CARTESIAN_POINT('Ctrl Pts',(-196.675623313027,-5.44469128748668,
133.125438201984));
#264761=CARTESIAN_POINT('Ctrl Pts',(-196.668336597685,-5.50379165095616,
132.98159564949));
#264762=CARTESIAN_POINT('Ctrl Pts',(-196.661049882344,-5.5571371184965,
132.835655182303));
#264763=CARTESIAN_POINT('Ctrl Pts',(-196.653763137853,-5.61048279943774,
132.689714131302));
#264764=CARTESIAN_POINT('Ctrl Pts',(-196.646476393361,-5.65807340793315,
132.541675511368));
#264765=CARTESIAN_POINT('Ctrl Pts',(-196.63918964887,-5.69975396984224,
132.392042967965));
#264766=CARTESIAN_POINT('Ctrl Pts',(-196.631898500147,-5.74145972418876,
132.242319984118));
#264767=CARTESIAN_POINT('Ctrl Pts',(-196.624607351424,-5.77724819432482,
132.091001524323));
#264768=CARTESIAN_POINT('Ctrl Pts',(-196.617316202701,-5.80701487487784,
131.938604332756));
#264769=CARTESIAN_POINT('Ctrl Pts',(-196.61002256742,-5.83679170699883,
131.786155167962));
#264770=CARTESIAN_POINT('Ctrl Pts',(-196.602728932139,-5.86054259825711,
131.632626918938));
#264771=CARTESIAN_POINT('Ctrl Pts',(-196.595435296857,-5.87821471232728,
131.478543351162));
#264772=CARTESIAN_POINT('Ctrl Pts',(-196.58813424297,-5.89590480130939,
131.324303059717));
#264773=CARTESIAN_POINT('Ctrl Pts',(-196.580833189082,-5.90750373817299,
131.169506705419));
#264774=CARTESIAN_POINT('Ctrl Pts',(-196.573532135195,-5.91301075271542,
131.014680375962));
#264775=CARTESIAN_POINT('Ctrl Pts',(-196.570146487533,-5.91556446772689,
130.942884247832));
#264776=CARTESIAN_POINT('Ctrl Pts',(-196.56676083987,-5.91680893090054,
130.871081648203));
#264777=CARTESIAN_POINT('Ctrl Pts',(-196.563375192208,-5.91674785692228,
130.799324735758));
#264778=CARTESIAN_POINT('',(-200.063375194059,-5.91567330630329,130.809819562943));
#264779=CARTESIAN_POINT('Ctrl Pts',(-200.063375192208,-5.91554583036233,
130.809819405987));
#264780=CARTESIAN_POINT('Ctrl Pts',(-199.994021213611,-5.90217632497919,
129.336193982877));
#264781=CARTESIAN_POINT('Ctrl Pts',(-199.831851360409,-4.59893760167832,
125.869330780398));
#264782=CARTESIAN_POINT('Ctrl Pts',(-199.576865632603,1.22511734593415,
123.91403058054));
#264783=CARTESIAN_POINT('Ctrl Pts',(-199.298418008789,6.45923565506566,
128.110694847157));
#264784=CARTESIAN_POINT('Ctrl Pts',(-199.019970384977,5.7576319483906,134.782706363876));
#264785=CARTESIAN_POINT('Ctrl Pts',(-198.741522761164,-0.234954242897439,
137.798812492739));
#264786=CARTESIAN_POINT('Ctrl Pts',(-198.505991030241,-5.12129580041003,
134.913151181637));
#264787=CARTESIAN_POINT('Ctrl Pts',(-198.363275173922,-5.90520520611573,
131.867199701326));
#264788=CARTESIAN_POINT('Ctrl Pts',(-198.313375192208,-5.90716405999748,
130.803136989425));
#264789=CARTESIAN_POINT('',(-201.813375867204,-5.92197308054016,130.803199987403));
#264790=CARTESIAN_POINT('Ctrl Pts',(-201.813375192208,-5.91674988355362,
130.803186748634));
#264791=CARTESIAN_POINT('Ctrl Pts',(-201.810399002507,-5.91673741614191,
130.740346209347));
#264792=CARTESIAN_POINT('Ctrl Pts',(-201.807422812807,-5.9157238558129,
130.677516728804));
#264793=CARTESIAN_POINT('Ctrl Pts',(-201.804446623105,-5.91371007129092,
130.614719495411));
#264794=CARTESIAN_POINT('Ctrl Pts',(-201.7970233567,-5.90868725336307,130.458089495395));
#264795=CARTESIAN_POINT('Ctrl Pts',(-201.789600090295,-5.89742980985056,
130.301422341445));
#264796=CARTESIAN_POINT('Ctrl Pts',(-201.782176823889,-5.87992433832519,
130.145254906719));
#264797=CARTESIAN_POINT('Ctrl Pts',(-201.774762331168,-5.86243955681343,
129.989272048933));
#264798=CARTESIAN_POINT('Ctrl Pts',(-201.767347838447,-5.83872148765387,
129.833788102077));
#264799=CARTESIAN_POINT('Ctrl Pts',(-201.759933345726,-5.80880871565572,
129.679339787793));
#264800=CARTESIAN_POINT('Ctrl Pts',(-201.752525999373,-5.77892477471341,
129.52504033661));
#264801=CARTESIAN_POINT('Ctrl Pts',(-201.745118653019,-5.74285808789947,
129.371774894843));
#264802=CARTESIAN_POINT('Ctrl Pts',(-201.737711306665,-5.70069899303698,
129.220074799512));
#264803=CARTESIAN_POINT('Ctrl Pts',(-201.73030948499,-5.658571342018,129.068487847836));
#264804=CARTESIAN_POINT('Ctrl Pts',(-201.722907663315,-5.6103604300888,
128.918464276076));
#264805=CARTESIAN_POINT('Ctrl Pts',(-201.715505841639,-5.55620757811541,
128.770524854434));
#264806=CARTESIAN_POINT('Ctrl Pts',(-201.708107927328,-5.50208331301106,
128.622663528862));
#264807=CARTESIAN_POINT('Ctrl Pts',(-201.700710013017,-5.44202348275199,
128.476884511958));
#264808=CARTESIAN_POINT('Ctrl Pts',(-201.693312098705,-5.37621909378814,
128.333692930869));
#264809=CARTESIAN_POINT('Ctrl Pts',(-201.685915413793,-5.31042564032021,
128.190525145624));
#264810=CARTESIAN_POINT('Ctrl Pts',(-201.678518728881,-5.23888967855432,
128.049944281665));
#264811=CARTESIAN_POINT('Ctrl Pts',(-201.671122043969,-5.16185019591898,
127.912435114136));
#264812=CARTESIAN_POINT('Ctrl Pts',(-201.663725687034,-5.08481412929481,
127.774932043906));
#264813=CARTESIAN_POINT('Ctrl Pts',(-201.656329330098,-5.00227520947535,
127.640500724959));
#264814=CARTESIAN_POINT('Ctrl Pts',(-201.648932973163,-4.91451806073126,
127.509600718386));
#264815=CARTESIAN_POINT('Ctrl Pts',(-201.641535483827,-4.82674747614365,
127.378680670687));
#264816=CARTESIAN_POINT('Ctrl Pts',(-201.63413799449,-4.73375727975254,
127.251293321958));
#264817=CARTESIAN_POINT('Ctrl Pts',(-201.626740505153,-4.635874949064,127.127868536908));
#264818=CARTESIAN_POINT('Ctrl Pts',(-201.619340422639,-4.53795830587631,
127.004400485491));
#264819=CARTESIAN_POINT('Ctrl Pts',(-201.611940340124,-4.43514634578947,
126.884898055683));
#264820=CARTESIAN_POINT('Ctrl Pts',(-201.604540257609,-4.32780616554116,
126.76975724722));
#264821=CARTESIAN_POINT('Ctrl Pts',(-201.597132037942,-4.22034795372998,
126.654489829602));
#264822=CARTESIAN_POINT('Ctrl Pts',(-201.589723818276,-4.10835183258725,
126.543593884573));
#264823=CARTESIAN_POINT('Ctrl Pts',(-201.58231559861,-3.99222154535993,
126.437428319572));
#264824=CARTESIAN_POINT('Ctrl Pts',(-201.574902819308,-3.87601978187823,
126.331197411437));
#264825=CARTESIAN_POINT('Ctrl Pts',(-201.567490040006,-3.7556790667533,
126.22970292491));
#264826=CARTESIAN_POINT('Ctrl Pts',(-201.560077260704,-3.63163498628868,
126.133262471641));
#264827=CARTESIAN_POINT('Ctrl Pts',(-201.552653889675,-3.50741366582499,
126.03668421973));
#264828=CARTESIAN_POINT('Ctrl Pts',(-201.545230518646,-3.3794787144427,
125.945174640511));
#264829=CARTESIAN_POINT('Ctrl Pts',(-201.537807147618,-3.24829403434159,
125.859007603982));
#264830=CARTESIAN_POINT('Ctrl Pts',(-201.533871098176,-3.17873676920309,
125.813319773655));
#264831=CARTESIAN_POINT('Ctrl Pts',(-201.529935048734,-3.10826629928466,
125.769133155338));
#264832=CARTESIAN_POINT('Ctrl Pts',(-201.525998999293,-3.03695429695874,
125.726483190857));
#264833=CARTESIAN_POINT('Ctrl Pts',(-201.518575732887,-2.90246208617211,
125.646046688922));
#264834=CARTESIAN_POINT('Ctrl Pts',(-201.511152466482,-2.76456864931066,
125.570835471457));
#264835=CARTESIAN_POINT('Ctrl Pts',(-201.503729200076,-2.6237184286282,
125.50115100736));
#264836=CARTESIAN_POINT('Ctrl Pts',(-201.496314707355,-2.4830346812097,
125.431548904513));
#264837=CARTESIAN_POINT('Ctrl Pts',(-201.488900214634,-2.3394014374572,
125.367460716645));
#264838=CARTESIAN_POINT('Ctrl Pts',(-201.481485721913,-2.1932911125198,
125.30914409242));
#264839=CARTESIAN_POINT('Ctrl Pts',(-201.47407837556,-2.04732161421452,
125.250883675953));
#264840=CARTESIAN_POINT('Ctrl Pts',(-201.466671029206,-1.89888013215013,
125.198383886038));
#264841=CARTESIAN_POINT('Ctrl Pts',(-201.459263682852,-1.74846252501016,
125.151855919546));
#264842=CARTESIAN_POINT('Ctrl Pts',(-201.451861861177,-1.5981571049961,
125.105362655367));
#264843=CARTESIAN_POINT('Ctrl Pts',(-201.444460039501,-1.44587884966913,
125.064832455911));
#264844=CARTESIAN_POINT('Ctrl Pts',(-201.437058217826,-1.29214228512928,
125.030427912946));
#264845=CARTESIAN_POINT('Ctrl Pts',(-201.429660303514,-1.13848687692604,
124.996041531872));
#264846=CARTESIAN_POINT('Ctrl Pts',(-201.422262389203,-0.983375056028614,
124.967774448564));
#264847=CARTESIAN_POINT('Ctrl Pts',(-201.414864474892,-0.827335043864665,
124.94573899745));
#264848=CARTESIAN_POINT('Ctrl Pts',(-201.40746778998,-0.67132096271966,
124.923707208227));
#264849=CARTESIAN_POINT('Ctrl Pts',(-201.400071105067,-0.514379365714424,
124.907905048017));
#264850=CARTESIAN_POINT('Ctrl Pts',(-201.392674420155,-0.357047286449173,
124.898393482732));
#264851=CARTESIAN_POINT('Ctrl Pts',(-201.38527806322,-0.199722183453189,
124.8888823392));
#264852=CARTESIAN_POINT('Ctrl Pts',(-201.377881706284,-0.0420070052413085,
124.88566125851));
#264853=CARTESIAN_POINT('Ctrl Pts',(-201.370485349349,0.115557760055124,
124.888739182198));
#264854=CARTESIAN_POINT('Ctrl Pts',(-201.363087860012,0.273146648919818,
124.891817577123));
#264855=CARTESIAN_POINT('Ctrl Pts',(-201.355690370676,0.430584705765377,
124.90119688937));
#264856=CARTESIAN_POINT('Ctrl Pts',(-201.348292881339,0.587333263647712,
124.916833955213));
#264857=CARTESIAN_POINT('Ctrl Pts',(-201.340892798824,0.744136769493798,
124.932476502606));
#264858=CARTESIAN_POINT('Ctrl Pts',(-201.333492716309,0.900249923925743,
124.954381134094));
#264859=CARTESIAN_POINT('Ctrl Pts',(-201.326092633794,1.05514113639827,
124.982453048325));
#264860=CARTESIAN_POINT('Ctrl Pts',(-201.318684414127,1.21020266768233,
125.010555830512));
#264861=CARTESIAN_POINT('Ctrl Pts',(-201.311276194461,1.36403920610859,
125.044839372054));
#264862=CARTESIAN_POINT('Ctrl Pts',(-201.303867974794,1.51613055959717,
125.08515799056));
#264863=CARTESIAN_POINT('Ctrl Pts',(-201.296455195492,1.66831552277604,
125.125501424502));
#264864=CARTESIAN_POINT('Ctrl Pts',(-201.28904241619,1.81875280477592,125.171887227256));
#264865=CARTESIAN_POINT('Ctrl Pts',(-201.281629636888,1.96693974488418,
125.224120604583));
#264866=CARTESIAN_POINT('Ctrl Pts',(-201.274206265859,2.11533842144153,
125.276428615409));
#264867=CARTESIAN_POINT('Ctrl Pts',(-201.266782894831,2.26147998833225,
125.334600750501));
#264868=CARTESIAN_POINT('Ctrl Pts',(-201.259359523802,2.4048832805008,125.398394749225));
#264869=CARTESIAN_POINT('Ctrl Pts',(-201.255423474361,2.48091914692211,
125.432219858064));
#264870=CARTESIAN_POINT('Ctrl Pts',(-201.25148742492,2.55618561065255,125.467624713707));
#264871=CARTESIAN_POINT('Ctrl Pts',(-201.24755137548,2.63061411281273,125.504568173331));
#264872=CARTESIAN_POINT('Ctrl Pts',(-201.240128109074,2.77098394505528,
125.574242385217));
#264873=CARTESIAN_POINT('Ctrl Pts',(-201.232704842669,2.908796043259,125.649602538817));
#264874=CARTESIAN_POINT('Ctrl Pts',(-201.225281576263,3.04355654120713,
125.730437663581));
#264875=CARTESIAN_POINT('Ctrl Pts',(-201.217867083542,3.17815776343784,
125.81117724794));
#264876=CARTESIAN_POINT('Ctrl Pts',(-201.210452590821,3.30971424764855,
125.89737873283));
#264877=CARTESIAN_POINT('Ctrl Pts',(-201.2030380981,3.43775387479355,125.988783927403));
#264878=CARTESIAN_POINT('Ctrl Pts',(-201.195630751746,3.56567009252529,
126.080101022208));
#264879=CARTESIAN_POINT('Ctrl Pts',(-201.188223405393,3.69007589959199,
126.176611626323));
#264880=CARTESIAN_POINT('Ctrl Pts',(-201.180816059039,3.81052558635577,
126.27801271686));
#264881=CARTESIAN_POINT('Ctrl Pts',(-201.173414237363,3.93088543719886,
126.379338178638));
#264882=CARTESIAN_POINT('Ctrl Pts',(-201.166012415688,4.04729475848319,
126.485546624777));
#264883=CARTESIAN_POINT('Ctrl Pts',(-201.158610594013,4.15933864322472,
126.59629305472));
#264884=CARTESIAN_POINT('Ctrl Pts',(-201.151212679701,4.27132338087164,
126.706981022484));
#264885=CARTESIAN_POINT('Ctrl Pts',(-201.14381476539,4.37894700663587,126.822201941411));
#264886=CARTESIAN_POINT('Ctrl Pts',(-201.136416851079,4.48182949379902,
126.941572123354));
#264887=CARTESIAN_POINT('Ctrl Pts',(-201.129020166166,4.58469488375913,
127.060922468139));
#264888=CARTESIAN_POINT('Ctrl Pts',(-201.121623481254,4.68282045537774,
127.184420424934));
#264889=CARTESIAN_POINT('Ctrl Pts',(-201.114226796342,4.77586463652599,
127.311647125726));
#264890=CARTESIAN_POINT('Ctrl Pts',(-201.106830439406,4.86890469199773,
127.438868185153));
#264891=CARTESIAN_POINT('Ctrl Pts',(-201.099434082471,4.95686358463872,
127.569817358517));
#264892=CARTESIAN_POINT('Ctrl Pts',(-201.092037725536,5.03944164464534,
127.704044750962));
#264893=CARTESIAN_POINT('Ctrl Pts',(-201.084640236199,5.12203234756399,
127.838292693965));
#264894=CARTESIAN_POINT('Ctrl Pts',(-201.077242746863,5.19924038189781,
127.975819537438));
#264895=CARTESIAN_POINT('Ctrl Pts',(-201.069845257526,5.27081089987097,
128.11614875458));
#264896=CARTESIAN_POINT('Ctrl Pts',(-201.062445175011,5.34240650677816,
128.25652716391));
#264897=CARTESIAN_POINT('Ctrl Pts',(-201.055045092496,5.40836049318189,
128.399709570458));
#264898=CARTESIAN_POINT('Ctrl Pts',(-201.047645009981,5.46846528047079,
128.545197489595));
#264899=CARTESIAN_POINT('Ctrl Pts',(-201.040236790314,5.52863615915231,
128.690845387655));
#264900=CARTESIAN_POINT('Ctrl Pts',(-201.032828570648,5.58294485137867,
128.838803515936));
#264901=CARTESIAN_POINT('Ctrl Pts',(-201.025420350982,5.63123274734572,
128.988555477216));
#264902=CARTESIAN_POINT('Ctrl Pts',(-201.01800757168,5.67955036370688,129.138399608329));
#264903=CARTESIAN_POINT('Ctrl Pts',(-201.010594792377,5.72183969969134,
129.290039413705));
#264904=CARTESIAN_POINT('Ctrl Pts',(-201.003182013075,5.75799294081597,
129.442946699607));
#264905=CARTESIAN_POINT('Ctrl Pts',(-200.995758642047,5.79419783938699,
129.596072466609));
#264906=CARTESIAN_POINT('Ctrl Pts',(-200.988335271018,5.82424906122381,
129.750468965729));
#264907=CARTESIAN_POINT('Ctrl Pts',(-200.980911899989,5.84809034559499,
129.905600431388));
#264908=CARTESIAN_POINT('Ctrl Pts',(-200.976975850548,5.86073156663221,
129.987854856808));
#264909=CARTESIAN_POINT('Ctrl Pts',(-200.973039801108,5.8716278209937,130.070315853689));
#264910=CARTESIAN_POINT('Ctrl Pts',(-200.969103751667,5.88077666555392,
130.152903502802));
#264911=CARTESIAN_POINT('Ctrl Pts',(-200.961680485262,5.898031100869,130.308661231559));
#264912=CARTESIAN_POINT('Ctrl Pts',(-200.954257218856,5.90911927466106,
130.465340456614));
#264913=CARTESIAN_POINT('Ctrl Pts',(-200.946833952451,5.91395173567687,
130.622411639596));
#264914=CARTESIAN_POINT('Ctrl Pts',(-200.93941945973,5.91877848512508,130.779297177483));
#264915=CARTESIAN_POINT('Ctrl Pts',(-200.932004967009,5.91736422769598,
130.936573381693));
#264916=CARTESIAN_POINT('Ctrl Pts',(-200.924590474288,5.90967099478593,
131.093703486643));
#264917=CARTESIAN_POINT('Ctrl Pts',(-200.917183127934,5.90198517690339,
131.250682143683));
#264918=CARTESIAN_POINT('Ctrl Pts',(-200.90977578158,5.88803244983971,131.40751461145));
#264919=CARTESIAN_POINT('Ctrl Pts',(-200.902368435227,5.86782683838578,
131.563662110531));
#264920=CARTESIAN_POINT('Ctrl Pts',(-200.894966613551,5.84763629703924,
131.719693148917));
#264921=CARTESIAN_POINT('Ctrl Pts',(-200.887564791876,5.82120220493272,
131.87503986722));
#264922=CARTESIAN_POINT('Ctrl Pts',(-200.880162970201,5.78859055344715,
132.029166711216));
#264923=CARTESIAN_POINT('Ctrl Pts',(-200.872765055889,5.75599611739846,
132.183212192852));
#264924=CARTESIAN_POINT('Ctrl Pts',(-200.865367141578,5.71723069365822,
132.336038718374));
#264925=CARTESIAN_POINT('Ctrl Pts',(-200.857969227266,5.67241167620617,
132.487119167727));
#264926=CARTESIAN_POINT('Ctrl Pts',(-200.850572542354,5.62760010686179,
132.63817451025));
#264927=CARTESIAN_POINT('Ctrl Pts',(-200.843175857442,5.57673704647701,
132.787483994966));
#264928=CARTESIAN_POINT('Ctrl Pts',(-200.83577917253,5.51999027249402,132.934533839178));
#264929=CARTESIAN_POINT('Ctrl Pts',(-200.828382815595,5.46324601472245,
133.081577163045));
#264930=CARTESIAN_POINT('Ctrl Pts',(-200.820986458659,5.40061869648633,
133.226360697364));
#264931=CARTESIAN_POINT('Ctrl Pts',(-200.813590101724,5.33232484821961,
133.368389142282));
#264932=CARTESIAN_POINT('Ctrl Pts',(-200.806192612387,5.26402054399037,
133.510439332119));
#264933=CARTESIAN_POINT('Ctrl Pts',(-200.79879512305,5.1900481440821,133.649733256226));
#264934=CARTESIAN_POINT('Ctrl Pts',(-200.791397633714,5.11067081254324,
133.785798929576));
#264935=CARTESIAN_POINT('Ctrl Pts',(-200.783997551199,5.03126565540398,
133.921912300536));
#264936=CARTESIAN_POINT('Ctrl Pts',(-200.776597468684,4.94645198230616,
134.054794845375));
#264937=CARTESIAN_POINT('Ctrl Pts',(-200.769197386169,4.85653698117537,
134.18400247921));
#264938=CARTESIAN_POINT('Ctrl Pts',(-200.761789166503,4.76652310925724,
134.313352190122));
#264939=CARTESIAN_POINT('Ctrl Pts',(-200.754380946836,4.67139692025517,
134.439018613408));
#264940=CARTESIAN_POINT('Ctrl Pts',(-200.74697272717,4.57150714130225,134.560589180836));
#264941=CARTESIAN_POINT('Ctrl Pts',(-200.739559947868,4.47155588185713,
134.682234572919));
#264942=CARTESIAN_POINT('Ctrl Pts',(-200.732147168566,4.36683543800591,
134.799778807794));
#264943=CARTESIAN_POINT('Ctrl Pts',(-200.724734389264,4.25773191773792,
134.912845676462));
#264944=CARTESIAN_POINT('Ctrl Pts',(-200.717311018235,4.14847250524356,
135.026074100376));
#264945=CARTESIAN_POINT('Ctrl Pts',(-200.709887647206,4.03481777724236,
135.134812123521));
#264946=CARTESIAN_POINT('Ctrl Pts',(-200.702464276177,3.91718807819064,
135.238722817768));
#264947=CARTESIAN_POINT('Ctrl Pts',(-200.698528226736,3.85481798926586,
135.293818761162));
#264948=CARTESIAN_POINT('Ctrl Pts',(-200.694592177296,3.79133090880903,
135.347558271593));
#264949=CARTESIAN_POINT('Ctrl Pts',(-200.690656127855,3.72679275456151,
135.399896095293));
#264950=CARTESIAN_POINT('Ctrl Pts',(-200.683232861449,3.60507580982061,
135.498603597382));
#264951=CARTESIAN_POINT('Ctrl Pts',(-200.675809595044,3.4792505691735,135.592621340272));
#264952=CARTESIAN_POINT('Ctrl Pts',(-200.668386328638,3.34971419766227,
135.681587837666));
#264953=CARTESIAN_POINT('Ctrl Pts',(-200.660971835917,3.22033092738485,
135.770449184047));
#264954=CARTESIAN_POINT('Ctrl Pts',(-200.653557343196,3.08724556180289,
135.854270959279));
#264955=CARTESIAN_POINT('Ctrl Pts',(-200.646142850475,2.95088917404671,
135.93273108439));
#264956=CARTESIAN_POINT('Ctrl Pts',(-200.638735504121,2.81466421171077,
136.011115586678));
#264957=CARTESIAN_POINT('Ctrl Pts',(-200.631328157768,2.67517482505955,
136.084148541912));
#264958=CARTESIAN_POINT('Ctrl Pts',(-200.623920811414,2.53288188521501,
136.151550526111));
#264959=CARTESIAN_POINT('Ctrl Pts',(-200.616518989738,2.3906950728134,136.218902239368));
#264960=CARTESIAN_POINT('Ctrl Pts',(-200.609117168063,2.24570920658458,
136.280631184824));
#264961=CARTESIAN_POINT('Ctrl Pts',(-200.601715346387,2.09841053341921,
136.336503402757));
#264962=CARTESIAN_POINT('Ctrl Pts',(-200.594317432076,1.95118961807727,
136.39234612618));
#264963=CARTESIAN_POINT('Ctrl Pts',(-200.586919517765,1.80165867545395,
136.442338147334));
#264964=CARTESIAN_POINT('Ctrl Pts',(-200.579521603453,1.65032464089478,
136.486293311831));
#264965=CARTESIAN_POINT('Ctrl Pts',(-200.572124918541,1.49901575530602,
136.530241171777));
#264966=CARTESIAN_POINT('Ctrl Pts',(-200.564728233629,1.34590473061233,
136.568154062135));
#264967=CARTESIAN_POINT('Ctrl Pts',(-200.557331548716,1.19151451455393,
136.599895426719));
#264968=CARTESIAN_POINT('Ctrl Pts',(-200.549935191781,1.03713114431951,
136.631635383858));
#264969=CARTESIAN_POINT('Ctrl Pts',(-200.542538834845,0.881469061150174,
136.657204284162));
#264970=CARTESIAN_POINT('Ctrl Pts',(-200.53514247791,0.725062014826754,
136.676516579149));
#264971=CARTESIAN_POINT('Ctrl Pts',(-200.527744988573,0.568631022185253,
136.695831830898));
#264972=CARTESIAN_POINT('Ctrl Pts',(-200.520347499237,0.411455209797665,
136.708888524271));
#264973=CARTESIAN_POINT('Ctrl Pts',(-200.5129500099,0.254073918632435,136.715652947198));
#264974=CARTESIAN_POINT('Ctrl Pts',(-200.505549927385,0.0966374576993343,
136.722419741384));
#264975=CARTESIAN_POINT('Ctrl Pts',(-200.49814984487,-0.0610042527022276,
136.72288985748));
#264976=CARTESIAN_POINT('Ctrl Pts',(-200.490749762355,-0.218311548806333,
136.717081702664));
#264977=CARTESIAN_POINT('Ctrl Pts',(-200.483341542688,-0.375791820453863,
136.711267161183));
#264978=CARTESIAN_POINT('Ctrl Pts',(-200.475933323022,-0.532936570164552,
136.699160575621));
#264979=CARTESIAN_POINT('Ctrl Pts',(-200.468525103355,-0.689210197067142,
136.680832336783));
#264980=CARTESIAN_POINT('Ctrl Pts',(-200.461112324053,-0.845580007779526,
136.66249281722));
#264981=CARTESIAN_POINT('Ctrl Pts',(-200.453699544751,-1.00107725944581,
136.637924072098));
#264982=CARTESIAN_POINT('Ctrl Pts',(-200.446286765449,-1.15517673598396,
136.607247594851));
#264983=CARTESIAN_POINT('Ctrl Pts',(-200.43886339442,-1.30949639708053,
136.576527285615));
#264984=CARTESIAN_POINT('Ctrl Pts',(-200.431440023392,-1.4624139322289,
136.539681901662));
#264985=CARTESIAN_POINT('Ctrl Pts',(-200.424016652363,-1.61341866780536,
136.496882972803));
#264986=CARTESIAN_POINT('Ctrl Pts',(-200.420080602922,-1.69348500191474,
136.474189953777));
#264987=CARTESIAN_POINT('Ctrl Pts',(-200.416144553482,-1.77301389176252,
136.449823992991));
#264988=CARTESIAN_POINT('Ctrl Pts',(-200.412208504041,-1.85193163392452,
136.423816088141));
#264989=CARTESIAN_POINT('Ctrl Pts',(-200.404785237635,-2.00076803270955,
136.37476599127));
#264990=CARTESIAN_POINT('Ctrl Pts',(-200.39736197123,-2.14787943854751,
136.3197245393));
#264991=CARTESIAN_POINT('Ctrl Pts',(-200.389938704824,-2.29274704537207,
136.258830486255));
#264992=CARTESIAN_POINT('Ctrl Pts',(-200.382524212103,-2.43744343071588,
136.198008404924));
#264993=CARTESIAN_POINT('Ctrl Pts',(-200.375109719382,-2.57990095506391,
136.131347634659));
#264994=CARTESIAN_POINT('Ctrl Pts',(-200.367695226661,-2.71961563869954,
136.059036757942));
#264995=CARTESIAN_POINT('Ctrl Pts',(-200.360287880307,-2.85919566006293,
135.986795577171));
#264996=CARTESIAN_POINT('Ctrl Pts',(-200.352880533953,-2.99603777440594,
135.908915301869));
#264997=CARTESIAN_POINT('Ctrl Pts',(-200.3454731876,-3.1296577823218,135.825632640475));
#264998=CARTESIAN_POINT('Ctrl Pts',(-200.338071365924,-3.26317813139457,
135.742412094433));
#264999=CARTESIAN_POINT('Ctrl Pts',(-200.330669544249,-3.39348084363586,
135.653797381792));
#265000=CARTESIAN_POINT('Ctrl Pts',(-200.323267722573,-3.52010625378327,
135.560071134889));
#265001=CARTESIAN_POINT('Ctrl Pts',(-200.315869808262,-3.64666481936232,
135.466394365342));
#265002=CARTESIAN_POINT('Ctrl Pts',(-200.30847189395,-3.76954964959203,
135.367611656931));
#265003=CARTESIAN_POINT('Ctrl Pts',(-200.301073979639,-3.88833011657844,
135.264048887727));
#265004=CARTESIAN_POINT('Ctrl Pts',(-200.293677294726,-4.00709084440596,
135.160503328776));
#265005=CARTESIAN_POINT('Ctrl Pts',(-200.286280609814,-4.12174828160482,
135.052179530682));
#265006=CARTESIAN_POINT('Ctrl Pts',(-200.278883924902,-4.23190487356255,
134.939443652236));
#265007=CARTESIAN_POINT('Ctrl Pts',(-200.271487567967,-4.34205658106188,
134.826712772617));
#265008=CARTESIAN_POINT('Ctrl Pts',(-200.264091211031,-4.44770757924775,
134.709570468634));
#265009=CARTESIAN_POINT('Ctrl Pts',(-200.256694854095,-4.5484973889659,
134.588419558052));
#265010=CARTESIAN_POINT('Ctrl Pts',(-200.249297364759,-4.64930262986123,
134.467250098956));
#265011=CARTESIAN_POINT('Ctrl Pts',(-200.241899875422,-4.74524496160936,
134.342071098237));
#265012=CARTESIAN_POINT('Ctrl Pts',(-200.234502386085,-4.83600449432356,
134.21331809653));
#265013=CARTESIAN_POINT('Ctrl Pts',(-200.22710230357,-4.92679584265112,
134.084519960658));
#265014=CARTESIAN_POINT('Ctrl Pts',(-200.219702221055,-5.01240055972236,
133.952145634283));
#265015=CARTESIAN_POINT('Ctrl Pts',(-200.21230213854,-5.09254243056786,
133.816659101343));
#265016=CARTESIAN_POINT('Ctrl Pts',(-200.204893918873,-5.17277242563903,
133.681023587033));
#265017=CARTESIAN_POINT('Ctrl Pts',(-200.197485699207,-5.24752738802124,
133.542269353312));
#265018=CARTESIAN_POINT('Ctrl Pts',(-200.19007747954,-5.31657703414016,
133.400885064313));
#265019=CARTESIAN_POINT('Ctrl Pts',(-200.182664700238,-5.38566917916411,
133.259413755643));
#265020=CARTESIAN_POINT('Ctrl Pts',(-200.175251920936,-5.44904886082607,
133.115309507039));
#265021=CARTESIAN_POINT('Ctrl Pts',(-200.167839141634,-5.50653440287247,
132.969079867834));
#265022=CARTESIAN_POINT('Ctrl Pts',(-200.160415770605,-5.56410208295706,
132.822641288864));
#265023=CARTESIAN_POINT('Ctrl Pts',(-200.152992399576,-5.615758680887,132.674071605666));
#265024=CARTESIAN_POINT('Ctrl Pts',(-200.145569028547,-5.66137247798355,
132.523893178476));
#265025=CARTESIAN_POINT('Ctrl Pts',(-200.141632979107,-5.68555800768561,
132.44426497292));
#265026=CARTESIAN_POINT('Ctrl Pts',(-200.137696929668,-5.70804554235413,
132.364184668557));
#265027=CARTESIAN_POINT('Ctrl Pts',(-200.133760880228,-5.7288213227283,
132.283731029178));
#265028=CARTESIAN_POINT('Ctrl Pts',(-200.124071939592,-5.77996277961027,
132.085687140804));
#265029=CARTESIAN_POINT('Ctrl Pts',(-200.114382998956,-5.82085499360012,
131.88489595805));
#265030=CARTESIAN_POINT('Ctrl Pts',(-200.10469405832,-5.85125580823402,
131.682276347638));
#265031=CARTESIAN_POINT('Ctrl Pts',(-200.095203709521,-5.88103350483466,
131.483809781632));
#265032=CARTESIAN_POINT('Ctrl Pts',(-200.085713360723,-5.90074552551159,
131.283588737847));
#265033=CARTESIAN_POINT('Ctrl Pts',(-200.076223011924,-5.91020894769956,
131.082498635521));
#265034=CARTESIAN_POINT('Ctrl Pts',(-200.071940411166,-5.91447939759482,
130.991755013462));
#265035=CARTESIAN_POINT('Ctrl Pts',(-200.067657810408,-5.91666348839728,
130.900834742462));
#265036=CARTESIAN_POINT('Ctrl Pts',(-200.06337520965,-5.91674748049752,
130.809820885532));
#265037=CARTESIAN_POINT('',(-203.563375192208,-5.91198242686231,130.79947290462));
#265038=CARTESIAN_POINT('Ctrl Pts',(-203.563375192208,-5.91198242686231,
130.79947290462));
#265039=CARTESIAN_POINT('Ctrl Pts',(-203.5339609168,-5.91683243646446,130.173526639722));
#265040=CARTESIAN_POINT('Ctrl Pts',(-203.504546641391,-5.82534361100667,
129.54896166662));
#265041=CARTESIAN_POINT('Ctrl Pts',(-203.382316491379,-5.02009495809496,
127.092968345155));
#265042=CARTESIAN_POINT('Ctrl Pts',(-203.196684742167,-1.76012566321133,
124.030918495546));
#265043=CARTESIAN_POINT('Ctrl Pts',(-202.918237118359,4.74729777661893,
125.662306130287));
#265044=CARTESIAN_POINT('Ctrl Pts',(-202.639789494544,6.89218647818192,
132.018990635446));
#265045=CARTESIAN_POINT('Ctrl Pts',(-202.361341870732,2.70349250829908,
137.25948949219));
#265046=CARTESIAN_POINT('Ctrl Pts',(-202.085870845849,-3.89824401710562,
136.575431840637));
#265047=CARTESIAN_POINT('Ctrl Pts',(-201.90321569557,-5.92108948216704,
132.703162475868));
#265048=CARTESIAN_POINT('Ctrl Pts',(-201.813376419895,-5.92624986544025,
130.803210827386));
#265049=CARTESIAN_POINT('',(-205.313375192208,-5.90857914829821,130.807499840963));
#265050=CARTESIAN_POINT('Ctrl Pts',(-205.313375192208,-5.90857914829821,
130.807499840963));
#265051=CARTESIAN_POINT('Ctrl Pts',(-205.257522831092,-5.90287670038602,
129.617221394239));
#265052=CARTESIAN_POINT('Ctrl Pts',(-205.108854595372,-4.97542928644342,
126.440754491598));
#265053=CARTESIAN_POINT('Ctrl Pts',(-204.867370485048,0.213664449080756,
123.809226020325));
#265054=CARTESIAN_POINT('Ctrl Pts',(-204.588922861234,6.00069570294186,
127.203081454398));
#265055=CARTESIAN_POINT('Ctrl Pts',(-204.310475237422,6.27338075607734,
133.906336507158));
#265056=CARTESIAN_POINT('Ctrl Pts',(-204.032027613609,0.781135366069192,
137.759027257328));
#265057=CARTESIAN_POINT('Ctrl Pts',(-203.782994265204,-4.77292417967637,
135.488857499412));
#265058=CARTESIAN_POINT('Ctrl Pts',(-203.626776791404,-5.90152837485451,
132.148681533904));
#265059=CARTESIAN_POINT('Ctrl Pts',(-203.563375192208,-5.91198242686231,
130.79947290462));
#265060=CARTESIAN_POINT('',(-207.063375192208,-5.92350094233479,130.808116397466));
#265061=CARTESIAN_POINT('Ctrl Pts',(-207.063375192208,-5.92350094233479,
130.808116397466));
#265062=CARTESIAN_POINT('Ctrl Pts',(-206.981084745385,-5.91062028060458,
129.06567203012));
#265063=CARTESIAN_POINT('Ctrl Pts',(-206.805978423956,-4.17532705327718,
125.335613429113));
#265064=CARTESIAN_POINT('Ctrl Pts',(-206.538056227925,2.17024453367553,
124.150970564787));
#265065=CARTESIAN_POINT('Ctrl Pts',(-206.259608604111,6.77075566682168,
129.033928966654));
#265066=CARTESIAN_POINT('Ctrl Pts',(-205.981160980299,5.14927311196064,
135.543827565311));
#265067=CARTESIAN_POINT('Ctrl Pts',(-205.702713356486,-1.20413987681471,
137.698387574825));
#265068=CARTESIAN_POINT('Ctrl Pts',(-205.480118093789,-5.39856531937876,
134.356261281287));
#265069=CARTESIAN_POINT('Ctrl Pts',(-205.350338705697,-5.91235307129998,
131.595235086907));
#265070=CARTESIAN_POINT('Ctrl Pts',(-205.313375192208,-5.90857914829821,
130.807499840963));
#265071=CARTESIAN_POINT('Ctrl Pts',(-207.299567498839,-3.90840034609405,
135.243902605345));
#265072=CARTESIAN_POINT('Ctrl Pts',(-207.231362157743,-4.98707972514044,
134.275313217871));
#265073=CARTESIAN_POINT('Ctrl Pts',(-207.152631388866,-5.83925384327957,
132.696773286164));
#265074=CARTESIAN_POINT('Ctrl Pts',(-207.073900619989,-5.92514845404535,
131.030985187931));
#265075=CARTESIAN_POINT('Ctrl Pts',(-207.063375192208,-5.92350094233479,
130.808116397466));
#265076=CARTESIAN_POINT('Origin',(213.235140564004,0.,130.804360617566));
#265077=CARTESIAN_POINT('',(-177.889859436045,-4.91824981877161,130.80302545727));
#265078=CARTESIAN_POINT('Ctrl Pts',(-177.889859436045,-4.91824981877161,
130.80302545727));
#265079=CARTESIAN_POINT('Ctrl Pts',(-177.897578984021,-4.91828660513675,
130.938533181825));
#265080=CARTESIAN_POINT('Ctrl Pts',(-177.905298531998,-4.91271888509105,
131.074267759702));
#265081=CARTESIAN_POINT('Ctrl Pts',(-177.913018079974,-4.90151653121722,
131.209723117934));
#265082=CARTESIAN_POINT('Ctrl Pts',(-177.920728283118,-4.89032773825667,
131.345014501845));
#265083=CARTESIAN_POINT('Ctrl Pts',(-177.928438486262,-4.87351791200395,
131.480026946718));
#265084=CARTESIAN_POINT('Ctrl Pts',(-177.936148689406,-4.85110890292581,
131.614252878582));
#265085=CARTESIAN_POINT('Ctrl Pts',(-177.943851468977,-4.82872146979285,
131.748349574418));
#265086=CARTESIAN_POINT('Ctrl Pts',(-177.951554248548,-4.80074564454809,
131.881660874833));
#265087=CARTESIAN_POINT('Ctrl Pts',(-177.959257028118,-4.76725516232351,
132.013683270872));
#265088=CARTESIAN_POINT('Ctrl Pts',(-177.966954298254,-4.73378863426308,
132.145611237511));
#265089=CARTESIAN_POINT('Ctrl Pts',(-177.974651568389,-4.69481539576988,
132.276251751023));
#265090=CARTESIAN_POINT('Ctrl Pts',(-177.982348838524,-4.65046036686952,
132.405110891243));
#265091=CARTESIAN_POINT('Ctrl Pts',(-177.990043303124,-4.60612150469107,
132.533923064299));
#265092=CARTESIAN_POINT('Ctrl Pts',(-177.997737767723,-4.55640488027498,
132.660954780006));
#265093=CARTESIAN_POINT('Ctrl Pts',(-178.005432232323,-4.5014853573474,
132.785726974424));
#265094=CARTESIAN_POINT('Ctrl Pts',(-178.013125478951,-4.44657452773564,
132.910479418413));
#265095=CARTESIAN_POINT('Ctrl Pts',(-178.020818725579,-4.38646259723445,
133.03297268916));
#265096=CARTESIAN_POINT('Ctrl Pts',(-178.028511972207,-4.32137249872143,
133.152747891802));
#265097=CARTESIAN_POINT('Ctrl Pts',(-178.036205725472,-4.25627811371228,
133.272530982217));
#265098=CARTESIAN_POINT('Ctrl Pts',(-178.043899478737,-4.18620509819149,
133.389595299688));
#265099=CARTESIAN_POINT('Ctrl Pts',(-178.051593232003,-4.11142201299136,
133.503507166679));
#265100=CARTESIAN_POINT('Ctrl Pts',(-178.059289216561,-4.03661723967682,
133.617452069665));
#265101=CARTESIAN_POINT('Ctrl Pts',(-178.06698520112,-3.95709989735997,
133.72824237193));
#265102=CARTESIAN_POINT('Ctrl Pts',(-178.074681185679,-3.87318119104158,
133.835474360708));
#265103=CARTESIAN_POINT('Ctrl Pts',(-178.082385491664,-3.78917174605771,
133.942822296072));
#265104=CARTESIAN_POINT('Ctrl Pts',(-178.09008979765,-3.70075168025727,
134.046603923423));
#265105=CARTESIAN_POINT('Ctrl Pts',(-178.097794103635,-3.60827196007457,
134.146449264601));
#265106=CARTESIAN_POINT('Ctrl Pts',(-178.105503084718,-3.5157361216954,
134.246355193554));
#265107=CARTESIAN_POINT('Ctrl Pts',(-178.113212065802,-3.41913600421425,
134.342319800581));
#265108=CARTESIAN_POINT('Ctrl Pts',(-178.120921046885,-3.31885770099228,
134.434011650801));
#265109=CARTESIAN_POINT('Ctrl Pts',(-178.128641384245,-3.21843167550299,
134.525838574388));
#265110=CARTESIAN_POINT('Ctrl Pts',(-178.136361721606,-3.11431694878514,
134.61337991927));
#265111=CARTESIAN_POINT('Ctrl Pts',(-178.144082058966,-3.00693114976664,
134.696345730983));
#265112=CARTESIAN_POINT('Ctrl Pts',(-178.148050571034,-2.9517312511805,
134.738992937919));
#265113=CARTESIAN_POINT('Ctrl Pts',(-178.152019083102,-2.89566748822361,
134.780431866513));
#265114=CARTESIAN_POINT('Ctrl Pts',(-178.15598759517,-2.83879919740751,
134.820627812275));
#265115=CARTESIAN_POINT('Ctrl Pts',(-178.163761929289,-2.72739394374767,
134.899371862246));
#265116=CARTESIAN_POINT('Ctrl Pts',(-178.171536263408,-2.61253338564665,
134.973601801254));
#265117=CARTESIAN_POINT('Ctrl Pts',(-178.179310597527,-2.49461950041102,
135.04299915024));
#265118=CARTESIAN_POINT('Ctrl Pts',(-178.187075350474,-2.37685093350067,
135.112310973196));
#265119=CARTESIAN_POINT('Ctrl Pts',(-178.194840103421,-2.25603686031665,
135.176801859868));
#265120=CARTESIAN_POINT('Ctrl Pts',(-178.202604856368,-2.13261028670629,
135.236195048988));
#265121=CARTESIAN_POINT('Ctrl Pts',(-178.210361897253,-2.00930630210852,
135.295529247955));
#265122=CARTESIAN_POINT('Ctrl Pts',(-178.218118938138,-1.88339533081727,
135.349775656748));
#265123=CARTESIAN_POINT('Ctrl Pts',(-178.225875979023,-1.75533686375186,
135.39870230678));
#265124=CARTESIAN_POINT('Ctrl Pts',(-178.233627170264,-1.6273749665728,
135.447592060845));
#265125=CARTESIAN_POINT('Ctrl Pts',(-178.241378361504,-1.49726916076229,
135.491169902165));
#265126=CARTESIAN_POINT('Ctrl Pts',(-178.249129552744,-1.36550057426087,
135.529251224151));
#265127=CARTESIAN_POINT('Ctrl Pts',(-178.256877449521,-1.23378799292357,
135.567316360559));
#265128=CARTESIAN_POINT('Ctrl Pts',(-178.264625346298,-1.10041441132796,
135.599889515772));
#265129=CARTESIAN_POINT('Ctrl Pts',(-178.272373243075,-0.965877633492174,
135.626835444833));
#265130=CARTESIAN_POINT('Ctrl Pts',(-178.280119519159,-0.831368997850033,
135.653775737386));
#265131=CARTESIAN_POINT('Ctrl Pts',(-178.287865795243,-0.695698033044637,
135.675091068361));
#265132=CARTESIAN_POINT('Ctrl Pts',(-178.295612071327,-0.559373905331694,
135.690697066945));
#265133=CARTESIAN_POINT('Ctrl Pts',(-178.303358404593,-0.423048771305566,
135.706303180729));
#265134=CARTESIAN_POINT('Ctrl Pts',(-178.311104737858,-0.286070853179251,
135.716199833558));
#265135=CARTESIAN_POINT('Ctrl Pts',(-178.318851071123,-0.148955232533464,
135.720354454137));
#265136=CARTESIAN_POINT('Ctrl Pts',(-178.326599139126,-0.01180890579494,
135.724510005114));
#265137=CARTESIAN_POINT('Ctrl Pts',(-178.334347207129,0.125474794115099,
135.722920953233));
#265138=CARTESIAN_POINT('Ctrl Pts',(-178.342095275132,0.262380385697254,
135.715606854083));
#265139=CARTESIAN_POINT('Ctrl Pts',(-178.349851577874,0.399431482171527,
135.708284981421));
#265140=CARTESIAN_POINT('Ctrl Pts',(-178.357607880616,0.536103276532238,
135.695225927641));
#265141=CARTESIAN_POINT('Ctrl Pts',(-178.365364183358,0.671884454715865,
135.676501249979));
#265142=CARTESIAN_POINT('Ctrl Pts',(-178.373124625872,0.807738103402582,
135.657766578393));
#265143=CARTESIAN_POINT('Ctrl Pts',(-178.380885068386,0.942699804202917,
135.63336032706));
#265144=CARTESIAN_POINT('Ctrl Pts',(-178.3886455109,1.0762690282611,135.603405110098));
#265145=CARTESIAN_POINT('Ctrl Pts',(-178.396418411166,1.21005266949546,
135.573401806363));
#265146=CARTESIAN_POINT('Ctrl Pts',(-178.404191311431,1.34243898930015,
135.537831838098));
#265147=CARTESIAN_POINT('Ctrl Pts',(-178.411964211697,1.47294233469106,
135.496867830259));
#265148=CARTESIAN_POINT('Ctrl Pts',(-178.419454547459,1.59870155475822,
135.457392967287));
#265149=CARTESIAN_POINT('Ctrl Pts',(-178.426944883221,1.72271203539251,
135.412909533879));
#265150=CARTESIAN_POINT('Ctrl Pts',(-178.434435218983,1.8445590297808,135.363613302837));
#265151=CARTESIAN_POINT('Ctrl Pts',(-178.442209553102,1.97102588999646,
135.312447990212));
#265152=CARTESIAN_POINT('Ctrl Pts',(-178.449983887221,2.09556257726352,
135.255935644863));
#265153=CARTESIAN_POINT('Ctrl Pts',(-178.45775822134,2.21768386757729,135.194242315971));
#265154=CARTESIAN_POINT('Ctrl Pts',(-178.465522974287,2.33965465431505,
135.132625018593));
#265155=CARTESIAN_POINT('Ctrl Pts',(-178.473287727234,2.45921562135268,
135.065839616714));
#265156=CARTESIAN_POINT('Ctrl Pts',(-178.481052480181,2.57589987136006,
134.994100814192));
#265157=CARTESIAN_POINT('Ctrl Pts',(-178.488809521066,2.69246822892538,
134.922433263661));
#265158=CARTESIAN_POINT('Ctrl Pts',(-178.496566561951,2.80616522451045,
134.845822306524));
#265159=CARTESIAN_POINT('Ctrl Pts',(-178.504323602836,2.91654733030766,
134.76452914082));
#265160=CARTESIAN_POINT('Ctrl Pts',(-178.512074794076,3.02684619610039,
134.683297278925));
#265161=CARTESIAN_POINT('Ctrl Pts',(-178.519825985316,3.13383483424316,
134.59739046739));
#265162=CARTESIAN_POINT('Ctrl Pts',(-178.527577176556,3.23709786857969,
134.507113708408));
#265163=CARTESIAN_POINT('Ctrl Pts',(-178.535325073334,3.34031701337215,
134.416875319456));
#265164=CARTESIAN_POINT('Ctrl Pts',(-178.543072970111,3.43981341005556,
134.322270933959));
#265165=CARTESIAN_POINT('Ctrl Pts',(-178.550820866888,3.53520419798672,
134.223646265335));
#265166=CARTESIAN_POINT('Ctrl Pts',(-178.558567142972,3.63057503222116,
134.125042226865));
#265167=CARTESIAN_POINT('Ctrl Pts',(-178.566313419056,3.72184169427708,
134.022419858821));
#265168=CARTESIAN_POINT('Ctrl Pts',(-178.57405969514,3.80865798380126,133.916161932709));
#265169=CARTESIAN_POINT('Ctrl Pts',(-178.581806028405,3.89547491418369,
133.809903222225));
#265170=CARTESIAN_POINT('Ctrl Pts',(-178.589552361671,3.97784115911567,
133.700009202882));
#265171=CARTESIAN_POINT('Ctrl Pts',(-178.597298694936,4.05545090126791,
133.586895621821));
#265172=CARTESIAN_POINT('Ctrl Pts',(-178.605046762939,4.1330780235839,133.473756709758));
#265173=CARTESIAN_POINT('Ctrl Pts',(-178.612794830942,4.20594630237465,
133.357397123591));
#265174=CARTESIAN_POINT('Ctrl Pts',(-178.620542898945,4.27379355996916,
133.238261122777));
#265175=CARTESIAN_POINT('Ctrl Pts',(-178.628299201687,4.34171292643635,
133.118998502804));
#265176=CARTESIAN_POINT('Ctrl Pts',(-178.636055504429,4.40460041788537,
132.996953913909));
#265177=CARTESIAN_POINT('Ctrl Pts',(-178.643811807171,4.46223985970607,
132.872596217528));
#265178=CARTESIAN_POINT('Ctrl Pts',(-178.651572249685,4.51991006543252,
132.7481721477));
#265179=CARTESIAN_POINT('Ctrl Pts',(-178.659332692199,4.57232649087066,
132.621432871501));
#265180=CARTESIAN_POINT('Ctrl Pts',(-178.667093134713,4.6193217466782,132.492865773959));
#265181=CARTESIAN_POINT('Ctrl Pts',(-178.674866034979,4.66639244344228,
132.364092289099));
#265182=CARTESIAN_POINT('Ctrl Pts',(-178.682638935244,4.70802446131689,
132.233485492179));
#265183=CARTESIAN_POINT('Ctrl Pts',(-178.69041183551,4.7441005272662,132.101547284817));
#265184=CARTESIAN_POINT('Ctrl Pts',(-178.697902171271,4.77886513734783,
131.974405363625));
#265185=CARTESIAN_POINT('Ctrl Pts',(-178.705392507033,4.80847065889238,
131.846027451783));
#265186=CARTESIAN_POINT('Ctrl Pts',(-178.712882842795,4.83285762032032,
131.716868307513));
#265187=CARTESIAN_POINT('Ctrl Pts',(-178.720657176914,4.85816922080323,
131.58281205503));
#265188=CARTESIAN_POINT('Ctrl Pts',(-178.728431511034,4.87793890559331,
131.447489509917));
#265189=CARTESIAN_POINT('Ctrl Pts',(-178.736205845153,4.89204410114357,
131.311398658512));
#265190=CARTESIAN_POINT('Ctrl Pts',(-178.7439705981,4.90613191330093,131.175475526918));
#265191=CARTESIAN_POINT('Ctrl Pts',(-178.751735351047,4.91456908636255,
131.038786358168));
#265192=CARTESIAN_POINT('Ctrl Pts',(-178.759500103994,4.91728388735268,
130.901840018886));
#265193=CARTESIAN_POINT('Ctrl Pts',(-178.767257144879,4.9199959919642,130.765029696639));
#265194=CARTESIAN_POINT('Ctrl Pts',(-178.775014185764,4.91699702730776,
130.627963100528));
#265195=CARTESIAN_POINT('Ctrl Pts',(-178.782771226649,4.90826700907514,
130.491154566979));
#265196=CARTESIAN_POINT('Ctrl Pts',(-178.790522417889,4.89954357421716,
130.354449201808));
#265197=CARTESIAN_POINT('Ctrl Pts',(-178.798273609129,4.88509771292451,
130.218001900438));
#265198=CARTESIAN_POINT('Ctrl Pts',(-178.806024800369,4.86496151122054,
130.082326991727));
#265199=CARTESIAN_POINT('Ctrl Pts',(-178.813772697147,4.84483386793941,
129.946709748471));
#265200=CARTESIAN_POINT('Ctrl Pts',(-178.821520593924,4.81902075182776,
129.811864630855));
#265201=CARTESIAN_POINT('Ctrl Pts',(-178.829268490701,4.78760607584458,
129.678300616928));
#265202=CARTESIAN_POINT('Ctrl Pts',(-178.837014766785,4.75619797113449,
129.544764541714));
#265203=CARTESIAN_POINT('Ctrl Pts',(-178.844761042869,4.71919072663617,
129.412509417502));
#265204=CARTESIAN_POINT('Ctrl Pts',(-178.852507318953,4.67671924911073,
129.282033409802));
#265205=CARTESIAN_POINT('Ctrl Pts',(-178.860253652219,4.63424745807043,
129.151556438958));
#265206=CARTESIAN_POINT('Ctrl Pts',(-178.867999985484,4.58631147452994,
129.022858982598));
#265207=CARTESIAN_POINT('Ctrl Pts',(-178.875746318749,4.53309577659699,
128.896423054987));
#265208=CARTESIAN_POINT('Ctrl Pts',(-178.883494386752,4.47986816137724,
128.769958812926));
#265209=CARTESIAN_POINT('Ctrl Pts',(-178.891242454755,4.42135863065274,
128.645757467678));
#265210=CARTESIAN_POINT('Ctrl Pts',(-178.898990522758,4.35779923905243,
128.524279729831));
#265211=CARTESIAN_POINT('Ctrl Pts',(-178.9067468255,4.29417229577462,128.402672883999));
#265212=CARTESIAN_POINT('Ctrl Pts',(-178.914503128242,4.22548495189499,
128.283795774974));
#265213=CARTESIAN_POINT('Ctrl Pts',(-178.922259430984,4.15201482616275,
128.168083707637));
#265214=CARTESIAN_POINT('Ctrl Pts',(-178.930019873498,4.07850548721226,
128.052309881286));
#265215=CARTESIAN_POINT('Ctrl Pts',(-178.937780316012,4.00020850299509,
127.93970478349));
#265216=CARTESIAN_POINT('Ctrl Pts',(-178.945540758526,3.91744344631057,
127.830672687157));
#265217=CARTESIAN_POINT('Ctrl Pts',(-178.953313658792,3.83454552780952,
127.721465562824));
#265218=CARTESIAN_POINT('Ctrl Pts',(-178.961086559057,3.74716545316439,
127.615843203123));
#265219=CARTESIAN_POINT('Ctrl Pts',(-178.968859459323,3.65566209747847,
127.514175563263));
#265220=CARTESIAN_POINT('Ctrl Pts',(-178.976349795085,3.56748511925551,
127.416203798198));
#265221=CARTESIAN_POINT('Ctrl Pts',(-178.983840130847,3.47547965372134,
127.321904437295));
#265222=CARTESIAN_POINT('Ctrl Pts',(-178.991330466609,3.37999615600626,
127.231573323606));
#265223=CARTESIAN_POINT('Ctrl Pts',(-178.999104800728,3.28089237245302,
127.137817278285));
#265224=CARTESIAN_POINT('Ctrl Pts',(-179.006879134847,3.17772768024682,
127.048039341494));
#265225=CARTESIAN_POINT('Ctrl Pts',(-179.014653468966,3.07085479539997,
126.962611811609));
#265226=CARTESIAN_POINT('Ctrl Pts',(-179.022418221913,2.9641136218319,126.87728956352));
#265227=CARTESIAN_POINT('Ctrl Pts',(-179.03018297486,2.85367365105237,126.796307296342));
#265228=CARTESIAN_POINT('Ctrl Pts',(-179.037947727807,2.73992423354038,
126.720000415899));
#265229=CARTESIAN_POINT('Ctrl Pts',(-179.045704768692,2.62628779355376,
126.643769324527));
#265230=CARTESIAN_POINT('Ctrl Pts',(-179.053461809577,2.50934877066748,
126.572204595192));
#265231=CARTESIAN_POINT('Ctrl Pts',(-179.061218850462,2.38952908867568,
126.50560105266));
#265232=CARTESIAN_POINT('Ctrl Pts',(-179.068970041702,2.26979976363732,
126.439047736377));
#265233=CARTESIAN_POINT('Ctrl Pts',(-179.076721232943,2.14719444371695,
126.377448349309));
#265234=CARTESIAN_POINT('Ctrl Pts',(-179.084472424183,2.02216319162956,
126.321053903887));
#265235=CARTESIAN_POINT('Ctrl Pts',(-179.09222032096,1.89718508116047,126.264683427609));
#265236=CARTESIAN_POINT('Ctrl Pts',(-179.099968217737,1.76978344491984,
126.213513653413));
#265237=CARTESIAN_POINT('Ctrl Pts',(-179.107716114514,1.64043185755897,
126.167749098018));
#265238=CARTESIAN_POINT('Ctrl Pts',(-179.115462390598,1.51110732776167,
126.121994115581));
#265239=CARTESIAN_POINT('Ctrl Pts',(-179.123208666682,1.37983402649866,
126.08164223333));
#265240=CARTESIAN_POINT('Ctrl Pts',(-179.130954942766,1.24710399492245,
126.046849221011));
#265241=CARTESIAN_POINT('Ctrl Pts',(-179.138701276032,1.11437298356347,
126.012055951859));
#265242=CARTESIAN_POINT('Ctrl Pts',(-179.146447609297,0.980185598621585,
125.982821733656));
#265243=CARTESIAN_POINT('Ctrl Pts',(-179.154193942562,0.845047087272823,
125.959251900231));
#265244=CARTESIAN_POINT('Ctrl Pts',(-179.161942010565,0.709878312591245,
125.935676788506));
#265245=CARTESIAN_POINT('Ctrl Pts',(-179.169690078568,0.573758372738378,
125.917768652887));
#265246=CARTESIAN_POINT('Ctrl Pts',(-179.177438146571,0.437200307775627,
125.905581284571));
#265247=CARTESIAN_POINT('Ctrl Pts',(-179.185194449313,0.300497107276185,
125.893380963375));
#265248=CARTESIAN_POINT('Ctrl Pts',(-179.192950752055,0.163355241530021,
125.886913589944));
#265249=CARTESIAN_POINT('Ctrl Pts',(-179.200707054797,0.0262910045776176,
125.886180888685));
#265250=CARTESIAN_POINT('Ctrl Pts',(-179.208467497311,-0.110846387685345,
125.885447796361));
#265251=CARTESIAN_POINT('Ctrl Pts',(-179.216227939825,-0.247905678082787,
125.890455460777));
#265252=CARTESIAN_POINT('Ctrl Pts',(-179.223988382339,-0.384374003464339,
125.901153535669));
#265253=CARTESIAN_POINT('Ctrl Pts',(-179.231761282605,-0.52106139991651,
125.911868784061));
#265254=CARTESIAN_POINT('Ctrl Pts',(-179.23953418287,-0.657155547236459,
125.928292650204));
#265255=CARTESIAN_POINT('Ctrl Pts',(-179.247307083135,-0.792151210869699,
125.950323172138));
#265256=CARTESIAN_POINT('Ctrl Pts',(-179.254797418897,-0.922239442095216,
125.971552829108));
#265257=CARTESIAN_POINT('Ctrl Pts',(-179.262287754659,-1.05130736659908,
125.997988525034));
#265258=CARTESIAN_POINT('Ctrl Pts',(-179.269778090421,-1.17891665368521,
126.029495322486));
#265259=CARTESIAN_POINT('Ctrl Pts',(-179.27755242454,-1.31136428567816,
126.062196709739));
#265260=CARTESIAN_POINT('Ctrl Pts',(-179.285326758659,-1.44266004261855,
126.100464919285));
#265261=CARTESIAN_POINT('Ctrl Pts',(-179.293101092779,-1.57230004771894,
126.144204437518));
#265262=CARTESIAN_POINT('Ctrl Pts',(-179.300865845726,-1.70178028309931,
126.187890050703));
#265263=CARTESIAN_POINT('Ctrl Pts',(-179.308630598673,-1.8296084598658,
126.237033432431));
#265264=CARTESIAN_POINT('Ctrl Pts',(-179.31639535162,-1.95529193815402,
126.291488306156));
#265265=CARTESIAN_POINT('Ctrl Pts',(-179.324152392505,-2.08085058584013,
126.345889094533));
#265266=CARTESIAN_POINT('Ctrl Pts',(-179.33190943339,-2.20426841771294,
126.405590722102));
#265267=CARTESIAN_POINT('Ctrl Pts',(-179.339666474275,-2.32506932923065,
126.470397572411));
#265268=CARTESIAN_POINT('Ctrl Pts',(-179.347417665515,-2.44577914384112,
126.53515555137));
#265269=CARTESIAN_POINT('Ctrl Pts',(-179.355168856755,-2.56387562298451,
126.605010906023));
#265270=CARTESIAN_POINT('Ctrl Pts',(-179.362920047995,-2.67890431290246,
126.679720664211));
#265271=CARTESIAN_POINT('Ctrl Pts',(-179.370667944772,-2.79388411255856,
126.754398668759));
#265272=CARTESIAN_POINT('Ctrl Pts',(-179.378415841549,-2.90579838913901,
126.833926760686));
#265273=CARTESIAN_POINT('Ctrl Pts',(-179.386163738326,-3.01421909826937,
126.918017054507));
#265274=CARTESIAN_POINT('Ctrl Pts',(-179.393910014411,-3.12261712812466,
127.002089758452));
#265275=CARTESIAN_POINT('Ctrl Pts',(-179.401656290495,-3.22752273534894,
127.090722526651));
#265276=CARTESIAN_POINT('Ctrl Pts',(-179.409402566579,-3.32853890617992,
127.183585588301));
#265277=CARTESIAN_POINT('Ctrl Pts',(-179.417148899844,-3.42955582268919,
127.276449335445));
#265278=CARTESIAN_POINT('Ctrl Pts',(-179.424895233109,-3.52668295768921,
127.373543173757));
#265279=CARTESIAN_POINT('Ctrl Pts',(-179.432641566375,-3.61955859240775,
127.474498959985));
#265280=CARTESIAN_POINT('Ctrl Pts',(-179.440389634378,-3.71245502598061,
127.575477354561));
#265281=CARTESIAN_POINT('Ctrl Pts',(-179.448137702381,-3.80109780006598,
127.680319130344));
#265282=CARTESIAN_POINT('Ctrl Pts',(-179.455885770384,-3.88516434792299,
127.788621727654));
#265283=CARTESIAN_POINT('Ctrl Pts',(-179.463642073126,-3.96932024270782,
127.897039430254));
#265284=CARTESIAN_POINT('Ctrl Pts',(-179.471398375867,-4.04888995545252,
128.008924992652));
#265285=CARTESIAN_POINT('Ctrl Pts',(-179.479154678609,-4.12359296582618,
128.123844974133));
#265286=CARTESIAN_POINT('Ctrl Pts',(-179.486915121123,-4.19833584744553,
128.238826291868));
#265287=CARTESIAN_POINT('Ctrl Pts',(-179.494675563638,-4.26820665186612,
128.356844919536));
#265288=CARTESIAN_POINT('Ctrl Pts',(-179.502436006152,-4.33297052176697,
128.477442157456));
#265289=CARTESIAN_POINT('Ctrl Pts',(-179.510208906417,-4.39783835638142,
128.59823298877));
#265290=CARTESIAN_POINT('Ctrl Pts',(-179.517981806683,-4.45758270355803,
128.721610350122));
#265291=CARTESIAN_POINT('Ctrl Pts',(-179.525754706948,-4.5120162551646,
128.847094060443));
#265292=CARTESIAN_POINT('Ctrl Pts',(-179.53324504271,-4.56447101006087,
128.968016121821));
#265293=CARTESIAN_POINT('Ctrl Pts',(-179.540735378472,-4.6119942762349,
129.090893761478));
#265294=CARTESIAN_POINT('Ctrl Pts',(-179.548225714234,-4.65446265192088,
129.215285262407));
#265295=CARTESIAN_POINT('Ctrl Pts',(-179.555502049297,-4.69571769586986,
129.336122868151));
#265296=CARTESIAN_POINT('Ctrl Pts',(-179.562778384359,-4.73228882758073,
129.458636134573));
#265297=CARTESIAN_POINT('Ctrl Pts',(-179.570054719422,-4.76405452823393,
129.582490119308));
#265298=CARTESIAN_POINT('Ctrl Pts',(-177.819765072025,-4.76405452823413,
129.582490119309));
#265299=CARTESIAN_POINT('Ctrl Pts',(-177.827528067606,-4.79810789403888,
129.715263675749));
#265300=CARTESIAN_POINT('Ctrl Pts',(-177.835291063187,-4.82657512862265,
129.849339500209));
#265301=CARTESIAN_POINT('Ctrl Pts',(-177.843054058769,-4.84938475087329,
129.984207826619));
#265302=CARTESIAN_POINT('Ctrl Pts',(-177.850828440854,-4.87222782952152,
130.119273973419));
#265303=CARTESIAN_POINT('Ctrl Pts',(-177.85860282294,-4.88939667628526,
130.255134556517));
#265304=CARTESIAN_POINT('Ctrl Pts',(-177.866377205026,-4.90087174218342,
130.39127560311));
#265305=CARTESIAN_POINT('Ctrl Pts',(-177.870098127136,-4.90636386052154,
130.456434508968));
#265306=CARTESIAN_POINT('Ctrl Pts',(-177.873819049247,-4.91055247038314,
130.52165766879));
#265307=CARTESIAN_POINT('Ctrl Pts',(-177.877539971357,-4.91343964523087,
130.586888975338));
#265308=CARTESIAN_POINT('Ctrl Pts',(-177.88164645957,-4.91662599235856,
130.658879622671));
#265309=CARTESIAN_POINT('Ctrl Pts',(-177.885752947782,-4.91823024989552,
130.730940811616));
#265310=CARTESIAN_POINT('Ctrl Pts',(-177.889859435994,-4.91824981877137,
130.803025456376));
#265311=CARTESIAN_POINT('Origin',(213.235140564004,0.,130.804360617566));
#265312=CARTESIAN_POINT('',(-207.7784959754,-4.32025079610558,133.152443722346));
#265313=CARTESIAN_POINT('',(-207.934947426862,-4.83864761984552,129.923070498784));
#265314=CARTESIAN_POINT('Ctrl Pts',(-207.778555181163,-4.32174403853603,
133.152064075816));
#265315=CARTESIAN_POINT('Ctrl Pts',(-207.801743821445,-4.40255038673971,
133.003312600242));
#265316=CARTESIAN_POINT('Ctrl Pts',(-207.823415744591,-4.47600032780121,
132.849732400647));
#265317=CARTESIAN_POINT('Ctrl Pts',(-207.918593342393,-4.79298445822066,
132.087388166203));
#265318=CARTESIAN_POINT('Ctrl Pts',(-207.96044672069,-4.91825,131.426623044073));
#265319=CARTESIAN_POINT('Ctrl Pts',(-207.96044672069,-4.91825,130.515843321034));
#265320=CARTESIAN_POINT('Ctrl Pts',(-207.9520747996,-4.89250964418619,130.218795312125));
#265321=CARTESIAN_POINT('Ctrl Pts',(-207.934947426862,-4.83864761984552,
129.923070498784));
#265322=CARTESIAN_POINT('',(-207.639859435957,-4.91824901139309,130.80747901955));
#265323=CARTESIAN_POINT('Ctrl Pts',(-207.639859435995,-4.91824901139267,
130.807479020212));
#265324=CARTESIAN_POINT('Ctrl Pts',(-207.650384863776,-4.91813168363402,
130.992524762711));
#265325=CARTESIAN_POINT('Ctrl Pts',(-207.660910291556,-4.90757161966847,
131.177239249296));
#265326=CARTESIAN_POINT('Ctrl Pts',(-207.671435719336,-4.88667662202955,
131.360754950939));
#265327=CARTESIAN_POINT('Ctrl Pts',(-207.679211362107,-4.87124047627466,
131.496326879103));
#265328=CARTESIAN_POINT('Ctrl Pts',(-207.686987004878,-4.85013380583299,
131.63147072125));
#265329=CARTESIAN_POINT('Ctrl Pts',(-207.694762647649,-4.82338668994206,
131.765674250981));
#265330=CARTESIAN_POINT('Ctrl Pts',(-207.702526426575,-4.79668038400811,
131.899673016942));
#265331=CARTESIAN_POINT('Ctrl Pts',(-207.7102902055,-4.76435084676709,132.032733947661));
#265332=CARTESIAN_POINT('Ctrl Pts',(-207.718053984426,-4.72647989782645,
132.164349896179));
#265333=CARTESIAN_POINT('Ctrl Pts',(-207.72581092684,-4.68864229671419,
132.295849948313));
#265334=CARTESIAN_POINT('Ctrl Pts',(-207.733567869255,-4.64527309585006,
132.425907175703));
#265335=CARTESIAN_POINT('Ctrl Pts',(-207.741324811669,-4.59650519091897,
132.554024325927));
#265336=CARTESIAN_POINT('Ctrl Pts',(-207.749075720058,-4.54777522191265,
132.682041815471));
#265337=CARTESIAN_POINT('Ctrl Pts',(-207.756826628447,-4.49365504758959,
132.808121868315));
#265338=CARTESIAN_POINT('Ctrl Pts',(-207.764577536836,-4.43432729007962,
132.931782660075));
#265339=CARTESIAN_POINT('Ctrl Pts',(-207.769236751612,-4.3986642747871,
133.006117455334));
#265340=CARTESIAN_POINT('Ctrl Pts',(-207.773895966387,-4.36112049094283,
133.079578367346));
#265341=CARTESIAN_POINT('Ctrl Pts',(-207.778555181163,-4.32174403853604,
133.152064075816));
#265342=CARTESIAN_POINT('',(-207.345738387465,-2.41370886482958,126.51939632007));
#265343=CARTESIAN_POINT('Ctrl Pts',(-207.344683452294,-2.4077731095894,
126.515793057735));
#265344=CARTESIAN_POINT('Ctrl Pts',(-207.352734226166,-2.53162780530793,
126.585330030555));
#265345=CARTESIAN_POINT('Ctrl Pts',(-207.360785000037,-2.65233540086029,
126.660162464917));
#265346=CARTESIAN_POINT('Ctrl Pts',(-207.368835773908,-2.76943374285605,
126.73995170526));
#265347=CARTESIAN_POINT('Ctrl Pts',(-207.37688654778,-2.88653208485212,
126.819740945603));
#265348=CARTESIAN_POINT('Ctrl Pts',(-207.384937321651,-3.00002084366859,
126.904486660409));
#265349=CARTESIAN_POINT('Ctrl Pts',(-207.392988095523,-3.10947838849646,
126.993805905457));
#265350=CARTESIAN_POINT('Ctrl Pts',(-207.400658416081,-3.21376332677892,
127.078904214322));
#265351=CARTESIAN_POINT('Ctrl Pts',(-207.408328736639,-3.31473885798247,
127.168439200213));
#265352=CARTESIAN_POINT('Ctrl Pts',(-207.415999057197,-3.41199622474628,
127.262120531855));
#265353=CARTESIAN_POINT('Ctrl Pts',(-207.423659876097,-3.5091331133442,
127.355685815167));
#265354=CARTESIAN_POINT('Ctrl Pts',(-207.431320694998,-3.6025607104101,
127.453386953501));
#265355=CARTESIAN_POINT('Ctrl Pts',(-207.438981513899,-3.69190164243585,
127.554892149481));
#265356=CARTESIAN_POINT('Ctrl Pts',(-207.446634794044,-3.78115465703662,
127.65629745759));
#265357=CARTESIAN_POINT('Ctrl Pts',(-207.454288074189,-3.86632874177754,
127.761499077257));
#265358=CARTESIAN_POINT('Ctrl Pts',(-207.461941354334,-3.94708224177111,
127.870127354992));
#265359=CARTESIAN_POINT('Ctrl Pts',(-207.469588971909,-4.02777599322606,
127.978675259977));
#265360=CARTESIAN_POINT('Ctrl Pts',(-207.477236589484,-4.10405542874681,
128.090644456684));
#265361=CARTESIAN_POINT('Ctrl Pts',(-207.48488420706,-4.17561853151846,
128.205631516305));
#265362=CARTESIAN_POINT('Ctrl Pts',(-207.492528815864,-4.24715347950354,
128.320573337026));
#265363=CARTESIAN_POINT('Ctrl Pts',(-207.500173424667,-4.31397557168506,
128.438530319058));
#265364=CARTESIAN_POINT('Ctrl Pts',(-207.507818033471,-4.37582579382953,
128.559069615367));
#265365=CARTESIAN_POINT('Ctrl Pts',(-207.515461394372,-4.43766591957205,
128.679589234896));
#265366=CARTESIAN_POINT('Ctrl Pts',(-207.523104755273,-4.49453560601694,
128.802689972396));
#265367=CARTESIAN_POINT('Ctrl Pts',(-207.530748116175,-4.54622180435359,
128.927914410471));
#265368=CARTESIAN_POINT('Ctrl Pts',(-207.538391988785,-4.59791146298729,
129.053147232095));
#265369=CARTESIAN_POINT('Ctrl Pts',(-207.546035861395,-4.64441679099704,
129.180503664702));
#265370=CARTESIAN_POINT('Ctrl Pts',(-207.553679734006,-4.68557310654164,
129.309506870287));
#265371=CARTESIAN_POINT('Ctrl Pts',(-207.561329824708,-4.72676290167804,
129.438615016623));
#265372=CARTESIAN_POINT('Ctrl Pts',(-207.568979915409,-4.76259487138462,
129.569372227599));
#265373=CARTESIAN_POINT('Ctrl Pts',(-207.576630006111,-4.79295434605128,
129.701286867009));
#265374=CARTESIAN_POINT('Ctrl Pts',(-207.584283333495,-4.82332666552696,
129.833257318266));
#265375=CARTESIAN_POINT('Ctrl Pts',(-207.591936660878,-4.84822180430393,
129.966385778011));
#265376=CARTESIAN_POINT('Ctrl Pts',(-207.599589988262,-4.86757658728517,
130.100172269598));
#265377=CARTESIAN_POINT('Ctrl Pts',(-207.607253582638,-4.88695733484313,
130.2341382367));
#265378=CARTESIAN_POINT('Ctrl Pts',(-207.614917177013,-4.9007828403537,
130.368763598783));
#265379=CARTESIAN_POINT('Ctrl Pts',(-207.622580771389,-4.90904194574255,
130.503544664797));
#265380=CARTESIAN_POINT('Ctrl Pts',(-207.628340326245,-4.91524905538563,
130.604839032065));
#265381=CARTESIAN_POINT('Ctrl Pts',(-207.634099881101,-4.91831321358352,
130.7062212724));
#265382=CARTESIAN_POINT('Ctrl Pts',(-207.639859435958,-4.91824901139309,
130.80747901955));
#265383=CARTESIAN_POINT('Ctrl Pts',(-207.934947426862,-4.83864761984552,
129.923070498784));
#265384=CARTESIAN_POINT('Ctrl Pts',(-207.915135175363,-4.77634221032461,
129.580988005111));
#265385=CARTESIAN_POINT('Ctrl Pts',(-207.88355659529,-4.67629636070848,
129.240699151234));
#265386=CARTESIAN_POINT('Ctrl Pts',(-207.767461666534,-4.28964812743423,
128.310813320659));
#265387=CARTESIAN_POINT('Ctrl Pts',(-207.660120443156,-3.91181434973351,
127.760719114158));
#265388=CARTESIAN_POINT('Ctrl Pts',(-207.48661174168,-3.17142674355786,
127.020331507982));
#265389=CARTESIAN_POINT('Ctrl Pts',(-207.410631570968,-2.80838203606073,
126.740710909013));
#265390=CARTESIAN_POINT('Ctrl Pts',(-207.344683452294,-2.40777310958941,
126.515793057735));
#265391=CARTESIAN_POINT('Ctrl Pts',(210.578629502474,3.43871735229388,135.623751273273));
#265392=CARTESIAN_POINT('Ctrl Pts',(210.532211638871,4.24191310225744,135.050661598608));
#265393=CARTESIAN_POINT('Ctrl Pts',(210.439385837966,5.5417116830592,133.497735776206));
#265394=CARTESIAN_POINT('Ctrl Pts',(210.253744162458,6.40049231640402,129.500124813146));
#265395=CARTESIAN_POINT('Ctrl Pts',(210.021704475947,3.49988613106459,124.739836436729));
#265396=CARTESIAN_POINT('Ctrl Pts',(209.743256852134,-3.22132718841443,
124.582443963435));
#265397=CARTESIAN_POINT('Ctrl Pts',(209.464809228321,-6.97029916743427,
130.151104711613));
#265398=CARTESIAN_POINT('Ctrl Pts',(209.186361604508,-4.320155850937,136.315756482887));
#265399=CARTESIAN_POINT('Ctrl Pts',(208.907913980696,2.30329626696544,137.417975354914));
#265400=CARTESIAN_POINT('Ctrl Pts',(208.629466356883,6.80838731381026,132.441404887444));
#265401=CARTESIAN_POINT('Ctrl Pts',(208.35101873307,5.05782663488002,125.961106241921));
#265402=CARTESIAN_POINT('Ctrl Pts',(208.072571109257,-1.34111875541754,
123.931185212061));
#265403=CARTESIAN_POINT('Ctrl Pts',(207.794123485444,-6.50738248846785,
128.217554840719));
#265404=CARTESIAN_POINT('Ctrl Pts',(207.515675861631,-5.69381680528821,
134.880978212762));
#265405=CARTESIAN_POINT('Ctrl Pts',(207.237228237818,0.352161018465804,
137.798239159538));
#265406=CARTESIAN_POINT('Ctrl Pts',(206.958780614005,6.07448159193836,134.288440920842));
#265407=CARTESIAN_POINT('Ctrl Pts',(206.680332990192,6.21467071562046,127.576957111676));
#265408=CARTESIAN_POINT('Ctrl Pts',(206.40188536638,0.643870262773591,123.831292031177));
#265409=CARTESIAN_POINT('Ctrl Pts',(206.123437742567,-5.51860979104455,
126.493540260974));
#265410=CARTESIAN_POINT('Ctrl Pts',(205.844990118754,-6.60976007302988,
133.117219720399));
#265411=CARTESIAN_POINT('Ctrl Pts',(205.566542494941,-1.62686214948821,
137.615495756827));
#265412=CARTESIAN_POINT('Ctrl Pts',(205.288094871128,4.8510417637676,135.85467075854));
#265413=CARTESIAN_POINT('Ctrl Pts',(205.009647247315,6.87107573233629,129.452857771449));
#265414=CARTESIAN_POINT('Ctrl Pts',(204.731199623502,2.57692653546199,124.293009711503));
#265415=CARTESIAN_POINT('Ctrl Pts',(204.452751999689,-4.08529213152394,
125.116775123829));
#265416=CARTESIAN_POINT('Ctrl Pts',(204.174304375876,-6.9933269740478,131.167153704944));
#265417=CARTESIAN_POINT('Ctrl Pts',(203.895856752063,-3.47483593506387,
136.884143186524));
#265418=CARTESIAN_POINT('Ctrl Pts',(203.617409128251,3.23685955433703,137.014109488232));
#265419=CARTESIAN_POINT('Ctrl Pts',(203.338961504438,6.97403925260401,131.437619947721));
#265420=CARTESIAN_POINT('Ctrl Pts',(203.060513880625,4.30241757323156,125.27919601562));
#265421=CARTESIAN_POINT('Ctrl Pts',(202.782066256812,-2.32291566837452,
124.198128435325));
#265422=CARTESIAN_POINT('Ctrl Pts',(202.503618632999,-6.81360289295739,
129.18786549711));
#265423=CARTESIAN_POINT('Ctrl Pts',(202.225171009186,-5.0429219211382,135.663082604955));
#265424=CARTESIAN_POINT('Ctrl Pts',(201.946723385373,1.36195793536179,137.673371567868));
#265425=CARTESIAN_POINT('Ctrl Pts',(201.66827576156,6.51526498482727,133.371375037445));
#265426=CARTESIAN_POINT('Ctrl Pts',(201.389828137747,5.6813618015098,126.710417660699));
#265427=CARTESIAN_POINT('Ctrl Pts',(201.111380513935,-0.373435327379839,
123.811593861123));
#265428=CARTESIAN_POINT('Ctrl Pts',(200.832932890122,-6.08506363376988,
127.338781095048));
#265429=CARTESIAN_POINT('Ctrl Pts',(200.554485266309,-6.20481573259303,
134.050666607207));
#265430=CARTESIAN_POINT('Ctrl Pts',(200.276037642496,-0.622645295272457,
137.779355505743));
#265431=CARTESIAN_POINT('Ctrl Pts',(199.997590018683,5.53170575049466,135.098364849491));
#265432=CARTESIAN_POINT('Ctrl Pts',(199.71914239487,6.60268945040398,128.471394077867));
#265433=CARTESIAN_POINT('Ctrl Pts',(199.440694771057,1.60612410470526,123.988305584475));
#265434=CARTESIAN_POINT('Ctrl Pts',(199.162247147244,-4.86639082969376,
125.768838683693));
#265435=CARTESIAN_POINT('Ctrl Pts',(198.883799523432,-6.86693032801245,
132.176770441218));
#265436=CARTESIAN_POINT('Ctrl Pts',(198.605351899619,-2.5570963230842,137.323524616753));
#265437=CARTESIAN_POINT('Ctrl Pts',(198.326904275806,4.10258428165832,136.479485555902));
#265438=CARTESIAN_POINT('Ctrl Pts',(198.048456651993,6.99219035394115,130.420283921986));
#265439=CARTESIAN_POINT('Ctrl Pts',(197.77000902818,3.45631507844086,124.714030008118));
#265440=CARTESIAN_POINT('Ctrl Pts',(197.491561404367,-3.25574490376804,
124.604492395141));
#265441=CARTESIAN_POINT('Ctrl Pts',(197.213113780554,-6.97593437139489,
130.192330798173));
#265442=CARTESIAN_POINT('Ctrl Pts',(196.934666156741,-4.28558094504976,
136.342594705906));
#265443=CARTESIAN_POINT('Ctrl Pts',(196.656218532928,2.3430120075278,137.403492044232));
#265444=CARTESIAN_POINT('Ctrl Pts',(196.377770909115,6.81849138768721,132.400109986944));
#265445=CARTESIAN_POINT('Ctrl Pts',(196.099323285303,5.02811028438465,125.930312215887));
#265446=CARTESIAN_POINT('Ctrl Pts',(195.82087566149,-1.38285853342424,123.939526815472));
#265447=CARTESIAN_POINT('Ctrl Pts',(195.542428037677,-6.5230479154113,128.257188313404));
#265448=CARTESIAN_POINT('Ctrl Pts',(195.263980413864,-5.66887493174189,
134.915576722577));
#265449=CARTESIAN_POINT('Ctrl Pts',(194.985532790051,0.394717174261835,
137.795958375315));
#265450=CARTESIAN_POINT('Ctrl Pts',(194.707085166238,6.09558348012494,134.251403247221));
#265451=CARTESIAN_POINT('Ctrl Pts',(194.428637542425,6.19490635356113,127.539184339867));
#265452=CARTESIAN_POINT('Ctrl Pts',(194.150189918612,0.601412926074683,
123.827502918989));
#265453=CARTESIAN_POINT('Ctrl Pts',(193.871742294799,-5.54474959981957,
126.527212884656));
#265454=CARTESIAN_POINT('Ctrl Pts',(193.593294670987,-6.59555811955654,
133.157412666584));
#265455=CARTESIAN_POINT('Ctrl Pts',(193.314847047174,-1.58537093834796,
137.625272568447));
#265456=CARTESIAN_POINT('Ctrl Pts',(193.036399423361,4.88169468552635,135.825047607524));
#265457=CARTESIAN_POINT('Ctrl Pts',(192.757951799548,6.86272137744547,129.411056577024));
#265458=CARTESIAN_POINT('Ctrl Pts',(192.479504175735,2.53724238606986,124.277443893095));
#265459=CARTESIAN_POINT('Ctrl Pts',(192.201056551922,-4.11983840692253,
125.141748821346));
#265460=CARTESIAN_POINT('Ctrl Pts',(191.922608928109,-6.99098896924831,
131.209717356357));
#265461=CARTESIAN_POINT('Ctrl Pts',(191.644161304296,-3.43776219763276,
136.905182851196));
#265462=CARTESIAN_POINT('Ctrl Pts',(191.365713680483,3.27460008958736,136.994290755064));
#265463=CARTESIAN_POINT('Ctrl Pts',(191.08726605667,6.9777648675845,131.395155257469));
#265464=CARTESIAN_POINT('Ctrl Pts',(190.808818432858,4.26870461503614,125.253108347726));
#265465=CARTESIAN_POINT('Ctrl Pts',(190.530370809044,-2.36308664091672,
124.212391080215));
#265466=CARTESIAN_POINT('Ctrl Pts',(190.251923185232,-6.82331671706736,
129.229371781915));
#265467=CARTESIAN_POINT('Ctrl Pts',(189.973475561419,-5.01325206778612,
135.693690281095));
#265468=CARTESIAN_POINT('Ctrl Pts',(189.695027937606,1.40374632081163,137.664953676525));
#265469=CARTESIAN_POINT('Ctrl Pts',(189.416580313793,6.53077041740369,133.331667209374));
#265470=CARTESIAN_POINT('Ctrl Pts',(189.13813268998,5.65633554627347,126.675909450142));
#265471=CARTESIAN_POINT('Ctrl Pts',(188.859685066167,-0.41599536452862,
123.81399662772));
#265472=CARTESIAN_POINT('Ctrl Pts',(188.581237442354,-6.10604685783229,
127.375886813701));
#265473=CARTESIAN_POINT('Ctrl Pts',(188.302789818542,-6.18493958576042,
134.088376935175));
#265474=CARTESIAN_POINT('Ctrl Pts',(188.024342194729,-0.580174985471077,
137.783016493883));
#265475=CARTESIAN_POINT('Ctrl Pts',(187.745894570916,5.55774208334242,135.064612228548));
#265476=CARTESIAN_POINT('Ctrl Pts',(187.467446947103,6.58836568835925,128.431244857581));
#265477=CARTESIAN_POINT('Ctrl Pts',(187.18899932329,1.56460308533104,123.97865493689));
#265478=CARTESIAN_POINT('Ctrl Pts',(186.910551699478,-4.89695331800637,
125.798555082479));
#265479=CARTESIAN_POINT('Ctrl Pts',(186.632104075664,-6.85844885156509,
132.218545967617));
#265480=CARTESIAN_POINT('Ctrl Pts',(186.353656451852,-2.51736494438869,
137.338969602853));
#265481=CARTESIAN_POINT('Ctrl Pts',(186.075208828038,4.13705436656654,136.454406814005));
#265482=CARTESIAN_POINT('Ctrl Pts',(185.796761204226,6.98972282098866,130.377727590732));
#265483=CARTESIAN_POINT('Ctrl Pts',(185.518313580413,3.41917746986535,124.693103276936));
#265484=CARTESIAN_POINT('Ctrl Pts',(185.2398659566,-3.29342493995873,124.62442590766));
#265485=CARTESIAN_POINT('Ctrl Pts',(184.961418332787,-6.97953072271363,
130.234806630193));
#265486=CARTESIAN_POINT('Ctrl Pts',(184.682970708974,-4.25178874032612,
136.368579642862));
#265487=CARTESIAN_POINT('Ctrl Pts',(184.404523085161,2.38313938299372,137.389107198495));
#265488=CARTESIAN_POINT('Ctrl Pts',(184.126075461348,6.82807883617355,132.358574329007));
#265489=CARTESIAN_POINT('Ctrl Pts',(183.847627837535,4.99834740910532,125.899794986266));
#265490=CARTESIAN_POINT('Ctrl Pts',(183.569180213722,-1.42462110408482,
123.948071857337));
#265491=CARTESIAN_POINT('Ctrl Pts',(183.290732589909,-6.53843241923107,
128.296943150732));
#265492=CARTESIAN_POINT('Ctrl Pts',(183.012284966097,-5.64374376128527,
134.950008601993));
#265493=CARTESIAN_POINT('Ctrl Pts',(182.733837342284,0.437269701071178,
137.793426081729));
#265494=CARTESIAN_POINT('Ctrl Pts',(182.455389718471,6.11645366995566,134.214233834728));
#265495=CARTESIAN_POINT('Ctrl Pts',(182.176942094658,6.17491552152431,127.501534682722));
#265496=CARTESIAN_POINT('Ctrl Pts',(181.898494470845,0.558931670205695,
123.82397121282));
#265497=CARTESIAN_POINT('Ctrl Pts',(181.620046847032,-5.57068308070185,
126.561044594899));
#265498=CARTESIAN_POINT('Ctrl Pts',(181.341599223219,-6.58111222344223,
133.197518104296));
#265499=CARTESIAN_POINT('Ctrl Pts',(181.063151599407,-1.54382073804491,
137.634796795631));
#265500=CARTESIAN_POINT('Ctrl Pts',(180.784703975594,4.91216658577983,135.795238324681));
#265501=CARTESIAN_POINT('Ctrl Pts',(180.506256351781,6.85411278995147,129.369307058824));
#265502=CARTESIAN_POINT('Ctrl Pts',(180.227808727968,2.49746418218255,124.262119907186));
#265503=CARTESIAN_POINT('Ctrl Pts',(179.949361104155,-4.15423200110403,
125.16693236216));
#265504=CARTESIAN_POINT('Ctrl Pts',(179.670913480342,-6.98839192089168,
131.252265980172));
#265505=CARTESIAN_POINT('Ctrl Pts',(179.392465856529,-3.40056106730489,
136.925996451342));
#265506=CARTESIAN_POINT('Ctrl Pts',(179.114018232716,3.31221928049139,136.974242649806));
#265507=CARTESIAN_POINT('Ctrl Pts',(178.835570608904,6.98123192042358,131.352668676138));
#265508=CARTESIAN_POINT('Ctrl Pts',(178.55712298509,4.23483347762603,125.227226382977));
#265509=CARTESIAN_POINT('Ctrl Pts',(178.278675361277,-2.40317004799311,
124.22689799325));
#265510=CARTESIAN_POINT('Ctrl Pts',(178.000227737465,-6.83277770089014,
129.270936428355));
#265511=CARTESIAN_POINT('Ctrl Pts',(177.721780113652,-4.98339644641697,
135.724116781409));
#265512=CARTESIAN_POINT('Ctrl Pts',(177.443332489839,1.44548268986267,137.65628156334));
#265513=CARTESIAN_POINT('Ctrl Pts',(177.164884866026,6.54603384991367,133.291865731052));
#265514=CARTESIAN_POINT('Ctrl Pts',(176.886437242213,5.63109969342586,126.64155422085));
#265515=CARTESIAN_POINT('Ctrl Pts',(176.6079896184,-0.458539986806858,123.816658424832));
#265516=CARTESIAN_POINT('Ctrl Pts',(176.329541994587,-6.12680382008778,
127.413119575705));
#265517=CARTESIAN_POINT('Ctrl Pts',(176.051094370774,-6.16483425371434,
134.125965572714));
#265518=CARTESIAN_POINT('Ctrl Pts',(175.772646746962,-0.537683177073775,
137.786418885364));
#265519=CARTESIAN_POINT('Ctrl Pts',(175.494199123148,5.58357247201413,135.030701742416));
#265520=CARTESIAN_POINT('Ctrl Pts',(175.215751499336,6.57379779200069,128.391183573973));
#265521=CARTESIAN_POINT('Ctrl Pts',(174.937303875523,1.5230240890144,123.969257218339));
#265522=CARTESIAN_POINT('Ctrl Pts',(174.65885625171,-4.92733434791298,125.82845697323));
#265523=CARTESIAN_POINT('Ctrl Pts',(174.380408627897,-6.84971323277332,
132.260269090858));
#265524=CARTESIAN_POINT('Ctrl Pts',(174.101961004084,-2.4775402838095,137.354172446613));
#265525=CARTESIAN_POINT('Ctrl Pts',(173.823513380271,4.1713711514037,136.429118707571));
#265526=CARTESIAN_POINT('Ctrl Pts',(173.545065756458,6.98699628128659,130.335187068521));
#265527=CARTESIAN_POINT('Ctrl Pts',(173.266618132645,3.38191316241135,124.672403000642));
#265528=CARTESIAN_POINT('Ctrl Pts',(172.988170508833,-3.33098293707706,
124.644588419932));
#265529=CARTESIAN_POINT('Ctrl Pts',(172.709722885019,-6.98286844495469,
130.277303567246));
#265530=CARTESIAN_POINT('Ctrl Pts',(172.431275261207,-4.21783898400718,
136.394358395635));
#265531=CARTESIAN_POINT('Ctrl Pts',(172.152827637394,2.42317845035331,137.374478352552));
#265532=CARTESIAN_POINT('Ctrl Pts',(171.874380013581,6.83741326768756,132.316981079111));
#265533=CARTESIAN_POINT('Ctrl Pts',(171.595932389768,4.96839931822471,125.869459497128));
#265534=CARTESIAN_POINT('Ctrl Pts',(171.317484765955,-1.46633088488636,
123.956870961504));
#265535=CARTESIAN_POINT('Ctrl Pts',(171.039037142142,-6.55357463903296,
128.336790901335));
#265536=CARTESIAN_POINT('Ctrl Pts',(170.760589518329,-5.61840345982816,
134.984286862899));
#265537=CARTESIAN_POINT('Ctrl Pts',(170.482141894517,0.479806024690783,
137.79063480575));
#265538=CARTESIAN_POINT('Ctrl Pts',(170.203694270703,6.13709721234627,134.176938068128));
#265539=CARTESIAN_POINT('Ctrl Pts',(169.925246646891,6.15469587572206,127.464007413007));
#265540=CARTESIAN_POINT('Ctrl Pts',(169.646799023078,0.51642970291829,123.820698167548));
#265541=CARTESIAN_POINT('Ctrl Pts',(169.368351399265,-5.59641013787386,
126.595033542778));
#265542=CARTESIAN_POINT('Ctrl Pts',(169.089903775452,-6.56642246179436,
133.237534862678));
#265543=CARTESIAN_POINT('Ctrl Pts',(168.811456151639,-1.50221333089678,
137.644067918489));
#265544=CARTESIAN_POINT('Ctrl Pts',(168.533008527826,4.94245646389391,135.76524410303));
#265545=CARTESIAN_POINT('Ctrl Pts',(168.254560904013,6.84525022078748,129.32761071706));
#265546=CARTESIAN_POINT('Ctrl Pts',(167.976113280201,2.45759343384159,124.247038346411));
#265547=CARTESIAN_POINT('Ctrl Pts',(167.697665656387,-4.1884716586909,125.192324799951));
#265548=CARTESIAN_POINT('Ctrl Pts',(167.419218032575,-6.98553591510243,
131.294798006688));
#265549=CARTESIAN_POINT('Ctrl Pts',(167.140770408762,-3.36323392793624,
136.946583212019));
#265550=CARTESIAN_POINT('Ctrl Pts',(166.862322784949,3.34971573589186,136.953965917302));
#265551=CARTESIAN_POINT('Ctrl Pts',(166.583875161136,6.98444028114645,131.310161777048));
#265552=CARTESIAN_POINT('Ctrl Pts',(166.305427537323,4.20080541690416,125.20155108099));
#265553=CARTESIAN_POINT('Ctrl Pts',(166.02697991351,-2.44316440471955,124.241648636582));
#265554=CARTESIAN_POINT('Ctrl Pts',(165.748532289697,-6.84198549362249,
129.312557896394));
#265555=CARTESIAN_POINT('Ctrl Pts',(165.470084665885,-4.95335616345982,
135.754360978348));
#265556=CARTESIAN_POINT('Ctrl Pts',(165.191637042072,1.48716549602113,137.647355549705));
#265557=CARTESIAN_POINT('Ctrl Pts',(164.913189418259,6.56105471673207,133.251972077313));
#265558=CARTESIAN_POINT('Ctrl Pts',(164.634741794446,5.60565517810829,126.60735324588));
#265559=CARTESIAN_POINT('Ctrl Pts',(164.356294170633,-0.501067617717217,
123.819579153818));
#265560=CARTESIAN_POINT('Ctrl Pts',(164.07784654682,-6.1473337513746,127.450478001396));
#265561=CARTESIAN_POINT('Ctrl Pts',(163.799398923007,-6.14450048146789,
134.163431126959));
#265562=CARTESIAN_POINT('Ctrl Pts',(163.520951299194,-0.495171444628521,
137.789562554107));
#265563=CARTESIAN_POINT('Ctrl Pts',(163.242503675381,5.60919595935461,134.996634647659));
#265564=CARTESIAN_POINT('Ctrl Pts',(162.964056051569,6.55898630114736,128.351211711527));
#265565=CARTESIAN_POINT('Ctrl Pts',(162.685608427755,1.48138865648,123.960112777059));
#265566=CARTESIAN_POINT('Ctrl Pts',(162.407160803943,-4.95753279363329,
125.85854324792));
#265567=CARTESIAN_POINT('Ctrl Pts',(162.12871318013,-6.84072379533872,132.301938264875));
#265568=CARTESIAN_POINT('Ctrl Pts',(161.850265556317,-2.4376238170639,137.369132584688));
#265569=CARTESIAN_POINT('Ctrl Pts',(161.571817932504,4.20553336454888,136.403622173655));
#265570=CARTESIAN_POINT('Ctrl Pts',(161.293370308691,6.98401083586784,130.292663931709));
#265571=CARTESIAN_POINT('Ctrl Pts',(161.014922684878,3.34452353692138,124.651929946293));
#265572=CARTESIAN_POINT('Ctrl Pts',(160.736475061065,-3.36841750339773,
124.664979184829));
#265573=CARTESIAN_POINT('Ctrl Pts',(160.458027437253,-6.98594741443756,
130.319820034592));
#265574=CARTESIAN_POINT('Ctrl Pts',(160.179579813439,-4.18373293411359,
136.419930008985));
#265575=CARTESIAN_POINT('Ctrl Pts',(159.901132189627,2.46312772594441,137.35960604848));
#265576=CARTESIAN_POINT('Ctrl Pts',(159.622684565814,6.84649433633851,132.275331778507));
#265577=CARTESIAN_POINT('Ctrl Pts',(159.344236942001,4.93826712148011,125.839306872565));
#265578=CARTESIAN_POINT('Ctrl Pts',(159.065789318188,-1.50798633025781,
123.965923801919));
#265579=CARTESIAN_POINT('Ctrl Pts',(158.787341694375,-6.56847401371661,
128.376730088641));
#265580=CARTESIAN_POINT('Ctrl Pts',(158.508894070562,-5.59285496636459,
135.018410235101));
#265581=CARTESIAN_POINT('Ctrl Pts',(158.230446446749,0.522324568921774,
137.787584650814));
#265582=CARTESIAN_POINT('Ctrl Pts',(157.951998822937,6.15751334234277,134.139517329431));
#265583=CARTESIAN_POINT('Ctrl Pts',(157.673551199123,6.13424816540071,127.426603921307));
#265584=CARTESIAN_POINT('Ctrl Pts',(157.395103575311,0.473908599138188,
123.817683904457));
#265585=CARTESIAN_POINT('Ctrl Pts',(157.116655951498,-5.62192981801017,
126.62917846882));
#265586=CARTESIAN_POINT('Ctrl Pts',(156.838208327685,-6.55148937894732,
133.277461458893));
#265587=CARTESIAN_POINT('Ctrl Pts',(156.559760703872,-1.46055025868114,
137.653085593479));
#265588=CARTESIAN_POINT('Ctrl Pts',(156.281313080059,4.97256319746619,135.735066054016));
#265589=CARTESIAN_POINT('Ctrl Pts',(156.002865456246,6.83613399835919,129.285969096806));
#265590=CARTESIAN_POINT('Ctrl Pts',(155.724417832433,2.4176316184721,124.232199769625));
#265591=CARTESIAN_POINT('Ctrl Pts',(155.44597020862,-4.2225561109203,125.217925193794));
#265592=CARTESIAN_POINT('Ctrl Pts',(155.167522584808,-6.98242105771092,
131.337311859867));
#265593=CARTESIAN_POINT('Ctrl Pts',(154.889074960995,-3.3257821626974,136.96694237038));
#265594=CARTESIAN_POINT('Ctrl Pts',(154.610627337182,3.38708806634394,136.933461308912));
#265595=CARTESIAN_POINT('Ctrl Pts',(154.332179713369,6.98738983086623,131.267636135312));
#265596=CARTESIAN_POINT('Ctrl Pts',(154.053732089556,4.1666216937926,125.17608339317));
#265597=CARTESIAN_POINT('Ctrl Pts',(153.775284465743,-2.48306822909056,
124.256642463619));
#265598=CARTESIAN_POINT('Ctrl Pts',(153.49683684193,-6.85093975406627,129.354234643731));
#265599=CARTESIAN_POINT('Ctrl Pts',(153.218389218117,-4.92313233206838,
135.784421751204));
#265600=CARTESIAN_POINT('Ctrl Pts',(152.939941594304,1.52879319471521,137.638175966376));
#265601=CARTESIAN_POINT('Ctrl Pts',(152.661493970491,6.57583246125511,133.21198772643));
#265602=CARTESIAN_POINT('Ctrl Pts',(152.383046346679,5.58000294317656,126.573307792561));
#265603=CARTESIAN_POINT('Ctrl Pts',(152.104598722866,-0.543576681382813,
123.822758706449));
#265604=CARTESIAN_POINT('Ctrl Pts',(151.826151099053,-6.16763589094857,
127.487960706439));
#265605=CARTESIAN_POINT('Ctrl Pts',(151.54770347524,-6.12393902249645,134.200772209611));
#265606=CARTESIAN_POINT('Ctrl Pts',(151.269255851427,-0.452641363423277,
137.792447383624));
#265607=CARTESIAN_POINT('Ctrl Pts',(150.990808227614,5.63461159587598,134.962412206646));
#265608=CARTESIAN_POINT('Ctrl Pts',(150.712360603801,6.54393176464461,128.311330751416));
#265609=CARTESIAN_POINT('Ctrl Pts',(150.433912979988,1.4396983305442,123.951221951899));
#265610=CARTESIAN_POINT('Ctrl Pts',(150.155465356176,-4.98754753615285,
125.888812791691));
#265611=CARTESIAN_POINT('Ctrl Pts',(149.877017732362,-6.83148087236823,
132.343551945603));
#265612=CARTESIAN_POINT('Ctrl Pts',(149.59857010855,-2.39761702327129,137.383849462723));
#265613=CARTESIAN_POINT('Ctrl Pts',(149.320122484737,4.23953974010866,136.377918157044));
#265614=CARTESIAN_POINT('Ctrl Pts',(149.041674860924,6.98076659535922,130.250159756006));
#265615=CARTESIAN_POINT('Ctrl Pts',(148.763227237111,3.30700997888175,124.631684872525));
#265616=CARTESIAN_POINT('Ctrl Pts',(148.484779613298,-3.40572725176907,
124.685597446761));
#265617=CARTESIAN_POINT('Ctrl Pts',(148.206331989485,-6.98876751706998,
130.362354456768));
#265618=CARTESIAN_POINT('Ctrl Pts',(147.927884365672,-4.14947185445744,
136.445293535346));
#265619=CARTESIAN_POINT('Ctrl Pts',(147.649436741859,2.50298572943186,137.344490837378));
#265620=CARTESIAN_POINT('Ctrl Pts',(147.370989118047,6.85532170562399,132.233627970525));
#265621=CARTESIAN_POINT('Ctrl Pts',(147.092541494233,4.90795193543132,125.809338229895));
#265622=CARTESIAN_POINT('Ctrl Pts',(146.814093870421,-1.54958589664124,
123.975230043125));
#265623=CARTESIAN_POINT('Ctrl Pts',(146.535646246608,-6.58312999118006,
128.41675923269));
#265624=CARTESIAN_POINT('Ctrl Pts',(146.257198622795,-5.56709922760349,
135.052377454143));
#265625=CARTESIAN_POINT('Ctrl Pts',(145.978750998982,0.564823758223794,
137.784275729942));
#265626=CARTESIAN_POINT('Ctrl Pts',(145.700303375169,6.17770130341801,134.101973005276));
#265627=CARTESIAN_POINT('Ctrl Pts',(145.421855751356,6.11357314825767,127.389325593625));
#265628=CARTESIAN_POINT('Ctrl Pts',(145.143408127543,0.431369934500661,
123.81492853524));
#265629=CARTESIAN_POINT('Ctrl Pts',(144.864960503731,-5.64724117546963,
126.663478107772));
#265630=CARTESIAN_POINT('Ctrl Pts',(144.586512879918,-6.53631352825206,
133.317296413447));
#265631=CARTESIAN_POINT('Ctrl Pts',(144.308065256105,-1.41883306523854,
137.661849486446));
#265632=CARTESIAN_POINT('Ctrl Pts',(144.029617632292,5.00248567088053,135.704705295899));
#265633=CARTESIAN_POINT('Ctrl Pts',(143.751170008479,6.82676446047164,129.244383741109));
#265634=CARTESIAN_POINT('Ctrl Pts',(143.472722384666,2.37758021687388,124.217604726676));
#265635=CARTESIAN_POINT('Ctrl Pts',(143.194274760853,-4.25648409478009,
125.243732595056));
#265636=CARTESIAN_POINT('Ctrl Pts',(142.91582713704,-6.97904746413934,131.379805964341));
#265637=CARTESIAN_POINT('Ctrl Pts',(142.637379513228,-3.28820715937746,
136.987073172008));
#265638=CARTESIAN_POINT('Ctrl Pts',(142.358931889414,3.42433488700229,136.912729584442));
#265639=CARTESIAN_POINT('Ctrl Pts',(142.080484265602,6.99008046028611,131.225093326731));
#265640=CARTESIAN_POINT('Ctrl Pts',(141.802036641788,4.13228357498186,125.150824263232));
#265641=CARTESIAN_POINT('Ctrl Pts',(141.523589017976,-2.52288004245522,
124.271878918761));
#265642=CARTESIAN_POINT('Ctrl Pts',(141.245141394163,-6.859640150418,129.395965126019));
#265643=CARTESIAN_POINT('Ctrl Pts',(140.96669377035,-4.89272607219785,135.814297986063));
#265644=CARTESIAN_POINT('Ctrl Pts',(140.688246146537,1.57036424341533,137.628743153505));
#265645=CARTESIAN_POINT('Ctrl Pts',(140.409798522724,6.59036653588803,133.17191416004));
#265646=CARTESIAN_POINT('Ctrl Pts',(140.131350898911,5.55414393918375,126.539419122461));
#265647=CARTESIAN_POINT('Ctrl Pts',(139.852903275098,-0.586065602614643,
123.826196964908));
#265648=CARTESIAN_POINT('Ctrl Pts',(139.574455651286,-6.18770948650656,
127.525566301902));
#265649=CARTESIAN_POINT('Ctrl Pts',(139.296008027473,-6.10315063871238,
134.237987436982));
#265650=CARTESIAN_POINT('Ctrl Pts',(139.01756040366,-0.410094509425858,
137.795073267016));
#265651=CARTESIAN_POINT('Ctrl Pts',(138.739112779847,5.65981843979252,134.928035687503));
#265652=CARTESIAN_POINT('Ctrl Pts',(138.460665156034,6.52863474034383,128.271542171445));
#265653=CARTESIAN_POINT('Ctrl Pts',(138.182217532221,1.39795465605713,123.942585072312));
#265654=CARTESIAN_POINT('Ctrl Pts',(137.903769908408,-5.01737746326431,
125.919264482896));
#265655=CARTESIAN_POINT('Ctrl Pts',(137.625322284595,-6.82198480636163,
132.385108591028));
#265656=CARTESIAN_POINT('Ctrl Pts',(137.346874660782,-2.35752138489827,
137.39832253538));
#265657=CARTESIAN_POINT('Ctrl Pts',(137.06842703697,4.27338901796432,136.352007610208));
#265658=CARTESIAN_POINT('Ctrl Pts',(136.789979413157,6.9772636799772,130.20767611642));
#265659=CARTESIAN_POINT('Ctrl Pts',(136.511531789344,3.26937387837121,124.611668529527));
#265660=CARTESIAN_POINT('Ctrl Pts',(136.233084165531,-3.44291079966457,
124.706442441713));
#265661=CARTESIAN_POINT('Ctrl Pts',(135.954636541718,-6.99132864835187,
130.404905257644));
#265662=CARTESIAN_POINT('Ctrl Pts',(135.676188917905,-4.1150570145959,136.470448034864));
#265663=CARTESIAN_POINT('Ctrl Pts',(135.397741294092,2.54275098386259,137.329133279345));
#265664=CARTESIAN_POINT('Ctrl Pts',(135.11929367028,6.8638950484427,132.191871200516));
#265665=CARTESIAN_POINT('Ctrl Pts',(134.840846046466,4.87745488341857,125.779554679616));
#265666=CARTESIAN_POINT('Ctrl Pts',(134.562398422654,-1.59112804254939,
123.984789340275));
#265667=CARTESIAN_POINT('Ctrl Pts',(134.283950798841,-6.59754202834077,
128.456876850186));
#265668=CARTESIAN_POINT('Ctrl Pts',(134.005503175028,-5.54113719793324,
135.086187261361));
#265669=CARTESIAN_POINT('Ctrl Pts',(133.727055551215,0.607302017773813,
137.780708165749));
#265670=CARTESIAN_POINT('Ctrl Pts',(133.448607927402,6.19766034749954,134.064306486881));
#265671=CARTESIAN_POINT('Ctrl Pts',(133.170160303589,6.09267159041341,127.352173811322));
#265672=CARTESIAN_POINT('Ctrl Pts',(132.891712679776,0.388815285291658,
123.812432161999));
#265673=CARTESIAN_POINT('Ctrl Pts',(132.613265055963,-5.67234327233058,
126.697931188648));
#265674=CARTESIAN_POINT('Ctrl Pts',(132.334817432151,-6.52089547205522,
133.357038250242));
#265675=CARTESIAN_POINT('Ctrl Pts',(132.056369808337,-1.37706329641493,
137.670359272641));
#265676=CARTESIAN_POINT('Ctrl Pts',(131.777922184525,5.0322227753486,135.674162953708));
#265677=CARTESIAN_POINT('Ctrl Pts',(131.499474560712,6.81714195431646,129.20285619093));
#265678=CARTESIAN_POINT('Ctrl Pts',(131.221026936899,2.33744071316646,124.203253758389));
#265679=CARTESIAN_POINT('Ctrl Pts',(130.942579313086,-4.29025435305649,
125.269746047434));
#265680=CARTESIAN_POINT('Ctrl Pts',(130.664131689273,-6.97541525939744,
131.422278745477));
#265681=CARTESIAN_POINT('Ctrl Pts',(130.38568406546,-3.25051031033198,137.006974870947));
#265682=CARTESIAN_POINT('Ctrl Pts',(130.107236441647,3.46145481767177,136.891771512113));
#265683=CARTESIAN_POINT('Ctrl Pts',(129.828788817834,6.99251206970404,131.182534927744));
#265684=CARTESIAN_POINT('Ctrl Pts',(129.550341194022,4.09779233288376,125.125774627163));
#265685=CARTESIAN_POINT('Ctrl Pts',(129.271893570209,-2.5625983695722,124.287357437414));
#265686=CARTESIAN_POINT('Ctrl Pts',(128.993445946396,-6.86808636028122,
129.43774779692));
#265687=CARTESIAN_POINT('Ctrl Pts',(128.714998322583,-4.86213851056362,
135.84398857585));
#265688=CARTESIAN_POINT('Ctrl Pts',(128.43655069877,1.61187710169066,137.61905746063));
#265689=CARTESIAN_POINT('Ctrl Pts',(128.158103074957,6.60465640206541,133.131752863082));
#265690=CARTESIAN_POINT('Ctrl Pts',(127.879655451144,5.52807912434469,126.505688491336));
#265691=CARTESIAN_POINT('Ctrl Pts',(127.601207827331,-0.628532806970051,
123.829893801787));
#265692=CARTESIAN_POINT('Ctrl Pts',(127.322760203518,-6.20755379421381,
127.563293394292));
#265693=CARTESIAN_POINT('Ctrl Pts',(127.044312579706,-6.08213610043705,
134.275075430049));
#265694=CARTESIAN_POINT('Ctrl Pts',(126.765864955893,-0.367532459225645,
137.797440106979));
#265695=CARTESIAN_POINT('Ctrl Pts',(126.48741733208,5.68481555705546,134.893506364063));
#265696=CARTESIAN_POINT('Ctrl Pts',(126.208969708267,6.51309579508176,128.231847445991));
#265697=CARTESIAN_POINT('Ctrl Pts',(125.930522084454,1.35615917984635,123.934202458341));
#265698=CARTESIAN_POINT('Ctrl Pts',(125.652074460641,-5.04702146960864,
125.949897193134));
#265699=CARTESIAN_POINT('Ctrl Pts',(125.373626836828,-6.81223594919939,
132.426606661257));
#265700=CARTESIAN_POINT('Ctrl Pts',(125.095179213015,-2.3173383877032,137.412551266352));
#265701=CARTESIAN_POINT('Ctrl Pts',(124.816731589202,4.3070799438184,136.325891493273));
#265702=CARTESIAN_POINT('Ctrl Pts',(124.538283965389,6.97350221952356,130.165214587198));
#265703=CARTESIAN_POINT('Ctrl Pts',(124.259836341577,3.2316166300094,124.591881659011));
#265704=CARTESIAN_POINT('Ctrl Pts',(123.981388717764,-3.47996676923432,
124.727513397266));
#265705=CARTESIAN_POINT('Ctrl Pts',(123.702941093951,-6.99363071337966,
130.447470860486));
#265706=CARTESIAN_POINT('Ctrl Pts',(123.424493470138,-4.08048968978323,
136.495392575427));
#265707=CARTESIAN_POINT('Ctrl Pts',(123.146045846325,2.58242201572056,137.313533943462));
#265708=CARTESIAN_POINT('Ctrl Pts',(122.867598222512,6.87221404710605,132.150063015792));
#265709=CARTESIAN_POINT('Ctrl Pts',(122.589150598699,4.84677709552158,125.749957325369));
#265710=CARTESIAN_POINT('Ctrl Pts',(122.310702974886,-1.63261122862275,
123.994601339147));
#265711=CARTESIAN_POINT('Ctrl Pts',(122.032255351073,-6.6117095911554,128.497081454556));
#265712=CARTESIAN_POINT('Ctrl Pts',(121.753807727261,-5.51496983938628,
135.119838403918));
#265713=CARTESIAN_POINT('Ctrl Pts',(121.475360103447,0.649757773524084,
137.776882090432));
#265714=CARTESIAN_POINT('Ctrl Pts',(121.196912479635,6.21738973499768,134.026519169992));
#265715=CARTESIAN_POINT('Ctrl Pts',(120.918464855822,6.07154426638285,127.315149951069));
#265716=CARTESIAN_POINT('Ctrl Pts',(120.640017232009,0.346246228389124,
123.810194877238));
#265717=CARTESIAN_POINT('Ctrl Pts',(120.361569608196,-5.69723517842559,
126.732536434776));
#265718=CARTESIAN_POINT('Ctrl Pts',(120.083121984383,-6.50523578167861,
133.396685496627));
#265719=CARTESIAN_POINT('Ctrl Pts',(119.80467436057,-1.3352425000044,137.678614636731));
#265720=CARTESIAN_POINT('Ctrl Pts',(119.526226736757,5.06177340895125,135.6434401592));
#265721=CARTESIAN_POINT('Ctrl Pts',(119.247779112945,6.8072668364591,129.161387985085));
#265722=CARTESIAN_POINT('Ctrl Pts',(118.969331489131,2.29721459473369,124.189147396544));
#265723=CARTESIAN_POINT('Ctrl Pts',(118.690883865319,-4.32386563438011,
125.29596458699));
#265724=CARTESIAN_POINT('Ctrl Pts',(118.412436241506,-6.97152457807781,
131.464728629428));
#265725=CARTESIAN_POINT('Ctrl Pts',(118.133988617693,-3.21269301243169,
137.026646729736));
#265726=CARTESIAN_POINT('Ctrl Pts',(117.85554099388,3.49844648286018,136.870587868534));
#265727=CARTESIAN_POINT('Ctrl Pts',(117.577093370067,6.99468456901571,131.139962515369));
#265728=CARTESIAN_POINT('Ctrl Pts',(117.298645746254,4.06314924558364,125.100935413187));
#265729=CARTESIAN_POINT('Ctrl Pts',(117.020198122441,-2.60222173866402,
124.303077446017));
#265730=CARTESIAN_POINT('Ctrl Pts',(116.741750498628,-6.8762780706787,129.479581108162));
#265731=CARTESIAN_POINT('Ctrl Pts',(116.463302874816,-4.83137078059878,
135.873492420371));
#265732=CARTESIAN_POINT('Ctrl Pts',(116.184855251003,1.65333023126747,137.609119246659));
#265733=CARTESIAN_POINT('Ctrl Pts',(115.90640762719,6.61870153027093,133.09150532375));
#265734=CARTESIAN_POINT('Ctrl Pts',(115.627960003377,5.5018094645007,126.472117149089));
#265735=CARTESIAN_POINT('Ctrl Pts',(115.349512379564,-0.670976720811003,
123.833849080098));
#265736=CARTESIAN_POINT('Ctrl Pts',(115.071064755751,-6.22716807873245,
127.601140585621));
#265737=CARTESIAN_POINT('Ctrl Pts',(114.792617131938,-6.06089618637186,
134.312034814502));
#265738=CARTESIAN_POINT('Ctrl Pts',(114.514169508125,-0.324956789974863,
137.79954781581));
#265739=CARTESIAN_POINT('Ctrl Pts',(114.235721884312,5.70960202138734,134.858825515823));
#265740=CARTESIAN_POINT('Ctrl Pts',(113.957274260499,6.4973155046598,128.192248045959));
#265741=CARTESIAN_POINT('Ctrl Pts',(113.678826636687,1.31431345065849,123.926074420608));
#265742=CARTESIAN_POINT('Ctrl Pts',(113.400379012874,-5.07647845671644,
125.980709787299));
#265743=CARTESIAN_POINT('Ctrl Pts',(113.121931389061,-6.80223466212876,
132.468044618562));
#265744=CARTESIAN_POINT('Ctrl Pts',(112.843483765248,-2.27706952068197,
137.42653512839));
#265745=CARTESIAN_POINT('Ctrl Pts',(112.565036141435,4.34061126924124,136.299570773982));
#265746=CARTESIAN_POINT('Ctrl Pts',(112.286588517622,6.96948235338073,130.122776741767));
#265747=CARTESIAN_POINT('Ctrl Pts',(112.008140893809,3.1937396329048,124.572324994188));
#265748=CARTESIAN_POINT('Ctrl Pts',(111.729693269996,-3.51689378735575,
124.748809532627));
#265749=CARTESIAN_POINT('Ctrl Pts',(111.451245646184,-6.99567362684944,
130.490049688009));
#265750=CARTESIAN_POINT('Ctrl Pts',(111.172798022371,-4.0457711609245,136.52012623271));
#265751=CARTESIAN_POINT('Ctrl Pts',(110.894350398558,2.62199735498092,137.297693407768));
#265752=CARTESIAN_POINT('Ctrl Pts',(110.615902774745,6.88027839335069,132.108204965571));
#265753=CARTESIAN_POINT('Ctrl Pts',(110.337455150932,4.81591970851693,125.720547263895));
#265754=CARTESIAN_POINT('Ctrl Pts',(110.059007527119,-1.67403391768677,
124.004665676154));
#265755=CARTESIAN_POINT('Ctrl Pts',(109.780559903306,-6.62563215463966,
128.537371556004));
#265756=CARTESIAN_POINT('Ctrl Pts',(109.502112279493,-5.48859812160383,
135.153329634858));
#265757=CARTESIAN_POINT('Ctrl Pts',(109.22366465568,0.692189452261082,137.772797645767));
#265758=CARTESIAN_POINT('Ctrl Pts',(108.945217031867,6.23688873483282,133.988612454835));
#265759=CARTESIAN_POINT('Ctrl Pts',(108.666769408055,6.05019195904657,127.278255384801));
#265760=CARTESIAN_POINT('Ctrl Pts',(108.388321784241,0.303664341205276,
123.808216763862));
#265761=CARTESIAN_POINT('Ctrl Pts',(108.109874160429,-5.72191597137591,
126.767292563848));
#265762=CARTESIAN_POINT('Ctrl Pts',(107.831426536616,-6.48933503739778,
133.436236683461));
#265763=CARTESIAN_POINT('Ctrl Pts',(107.552978912803,-1.29337222569216,
137.68661527281));
#265764=CARTESIAN_POINT('Ctrl Pts',(107.27453128899,5.09113647667873,135.612538050821));
#265765=CARTESIAN_POINT('Ctrl Pts',(106.996083665177,6.79713947282576,129.119980660195));
#265766=CARTESIAN_POINT('Ctrl Pts',(106.717636041364,2.25690335216928,124.175286163858));
#265767=CARTESIAN_POINT('Ctrl Pts',(106.439188417551,-4.35731669327239,
125.322387242187));
#265768=CARTESIAN_POINT('Ctrl Pts',(106.160740793739,-6.96737556435125,
131.5071540432));
#265769=CARTESIAN_POINT('Ctrl Pts',(105.882293169926,-3.17475666701035,
137.046088019424));
#265770=CARTESIAN_POINT('Ctrl Pts',(105.603845546113,3.53530851182771,136.849179438675));
#265771=CARTESIAN_POINT('Ctrl Pts',(105.3253979223,6.99659787771835,131.097377667143));
#265772=CARTESIAN_POINT('Ctrl Pts',(105.046950298487,4.02835559679407,125.076307541727));
#265773=CARTESIAN_POINT('Ctrl Pts',(104.768502674674,-2.64174868147234,
124.319038362058));
#265774=CARTESIAN_POINT('Ctrl Pts',(104.490055050861,-6.88421497806359,
129.521463509594));
#265775=CARTESIAN_POINT('Ctrl Pts',(104.211607427049,-4.80042402241278,
135.902808426348));
#265776=CARTESIAN_POINT('Ctrl Pts',(103.933159803235,1.69472209608453,137.598928879852));
#265777=CARTESIAN_POINT('Ctrl Pts',(103.654712179423,6.63250140005722,133.051173033428));
#265778=CARTESIAN_POINT('Ctrl Pts',(103.37626455561,5.47533593308374,126.438706339714));
#265779=CARTESIAN_POINT('Ctrl Pts',(103.097816931797,-0.713395771362793,
123.838062653278));
#265780=CARTESIAN_POINT('Ctrl Pts',(102.819369307984,-6.24655161324796,
127.639106473447));
#265781=CARTESIAN_POINT('Ctrl Pts',(102.540921684171,-6.03943168356949,
134.348864220799));
#265782=CARTESIAN_POINT('Ctrl Pts',(102.262474060358,-0.282369079330704,
137.801396315408));
#265783=CARTESIAN_POINT('Ctrl Pts',(101.984026436545,5.73417691431645,134.823994427897));
#265784=CARTESIAN_POINT('Ctrl Pts',(101.705578812732,6.48129445382252,128.15274543872));
#265785=CARTESIAN_POINT('Ctrl Pts',(101.427131188919,1.27241901910234,123.9182012603));
#265786=CARTESIAN_POINT('Ctrl Pts',(101.148683565106,-5.1057473330482,126.01170112362));
#265787=CARTESIAN_POINT('Ctrl Pts',(100.870235941294,-6.7919813157512,132.509420927444));
#265788=CARTESIAN_POINT('Ctrl Pts',(100.591788317481,-2.23671627601227,
137.440273603317));
#265789=CARTESIAN_POINT('Ctrl Pts',(100.313340693668,4.37398175171709,136.273046427655));
#265790=CARTESIAN_POINT('Ctrl Pts',(100.034893069855,6.96520423050629,130.080364152676));
#265791=CARTESIAN_POINT('Ctrl Pts',(99.7564454460421,3.15574429060373,124.552999259737));
#265792=CARTESIAN_POINT('Ctrl Pts',(99.4779978222292,-3.55369048568456,
124.770330058661));
#265793=CARTESIAN_POINT('Ctrl Pts',(99.1995501984162,-6.99745731306031,
130.532640162439));
#265794=CARTESIAN_POINT('Ctrl Pts',(98.9211025746034,-4.01090271452764,
136.544648090195));
#265795=CARTESIAN_POINT('Ctrl Pts',(98.6426549507905,2.66147553516503,137.281612259238));
#265796=CARTESIAN_POINT('Ctrl Pts',(98.3642073269776,6.88808778834931,132.066298600918));
#265797=CARTESIAN_POINT('Ctrl Pts',(98.0857597031646,4.78488386583629,125.691325584995));
#265798=CARTESIAN_POINT('Ctrl Pts',(97.8073120793519,-1.71539457480834,
124.014981978356));
#265799=CARTESIAN_POINT('Ctrl Pts',(97.5288644555388,-6.63930920288774,
128.577745661565));
#265800=CARTESIAN_POINT('Ctrl Pts',(97.2504168317261,-5.46202302179963,
135.186659713151));
#265801=CARTESIAN_POINT('Ctrl Pts',(96.9719692079131,0.734595481663425,
137.768454983106));
#265802=CARTESIAN_POINT('Ctrl Pts',(96.6935215841003,6.25615662446226,133.950587746053));
#265803=CARTESIAN_POINT('Ctrl Pts',(96.4150739602873,6.0286154596223,127.24149147966));
#265804=CARTESIAN_POINT('Ctrl Pts',(96.1366263364746,0.26107120162757,123.806497895168));
#265805=CARTESIAN_POINT('Ctrl Pts',(95.8581787126614,-5.74638473662552,
126.80219828796));
#265806=CARTESIAN_POINT('Ctrl Pts',(95.5797310888487,-6.47319382842077,
133.47569034516));
#265807=CARTESIAN_POINT('Ctrl Pts',(95.3012834650358,-1.25145402499642,
137.694360884412));
#265808=CARTESIAN_POINT('Ctrl Pts',(95.0228358412229,5.12031089047184,135.581457773658));
#265809=CARTESIAN_POINT('Ctrl Pts',(94.7443882174101,6.78676023868958,129.078635750625));
#265810=CARTESIAN_POINT('Ctrl Pts',(94.465940593597,2.21650847922131,124.161670573963));
#265811=CARTESIAN_POINT('Ctrl Pts',(94.1874929697842,-4.39060629019222,
125.349013033923));
#265812=CARTESIAN_POINT('Ctrl Pts',(93.9090453459715,-6.96296837196094,
131.549553414704));
#265813=CARTESIAN_POINT('Ctrl Pts',(93.6305977221583,-3.13670267981308,
137.065298019608));
#265814=CARTESIAN_POINT('Ctrl Pts',(93.3521500983456,3.5720395386382,136.82754701583));
#265815=CARTESIAN_POINT('Ctrl Pts',(93.0737024745325,6.99825192491364,131.054781961061));
#265816=CARTESIAN_POINT('Ctrl Pts',(92.7952548507199,3.99341267580637,125.051891925383));
#265817=CARTESIAN_POINT('Ctrl Pts',(92.5168072269068,-2.68117773331193,
124.335239594101));
#265818=CARTESIAN_POINT('Ctrl Pts',(92.238359603094,-6.89189678833074,129.563393449252));
#265819=CARTESIAN_POINT('Ctrl Pts',(91.959911979281,-4.7692993827493,135.931935507467));
#265820=CARTESIAN_POINT('Ctrl Pts',(91.6814643554683,1.73605116235111,137.588486737821));
#265821=CARTESIAN_POINT('Ctrl Pts',(91.4030167316553,6.6460555000649,133.010757486647));
#265822=CARTESIAN_POINT('Ctrl Pts',(91.1245691078424,5.44865951108031,126.405457301267));
#265823=CARTESIAN_POINT('Ctrl Pts',(90.8461214840295,-0.755788386771977,
123.84253436519));
#265824=CARTESIAN_POINT('Ctrl Pts',(90.5676738602166,-6.26570367949625,
127.677189650927));
#265825=CARTESIAN_POINT('Ctrl Pts',(90.2892262364038,-6.01774338740505,
134.38556228421));
#265826=CARTESIAN_POINT('Ctrl Pts',(90.0107786125907,-0.239770905396614,
137.802985537273));
#265827=CARTESIAN_POINT('Ctrl Pts',(89.7323309887781,5.75853932521132,134.78901439096));
#265828=CARTESIAN_POINT('Ctrl Pts',(89.453883364965,6.46503323623579,128.113341088056));
#265829=CARTESIAN_POINT('Ctrl Pts',(89.1754357411521,1.23047743759138,123.910583269158));
#265830=CARTESIAN_POINT('Ctrl Pts',(88.8969881173393,-5.13482701403487,
126.042870053701));
#265831=CARTESIAN_POINT('Ctrl Pts',(88.6185404935264,-6.78147629000823,
132.550734054689));
#265832=CARTESIAN_POINT('Ctrl Pts',(88.3400928697134,-2.19628014899849,
137.453766182047));
#265833=CARTESIAN_POINT('Ctrl Pts',(88.0616452459006,4.4071901546906,136.246319437167));
#265834=CARTESIAN_POINT('Ctrl Pts',(87.7831976220877,6.96066800942769,130.037978391542));
#265835=CARTESIAN_POINT('Ctrl Pts',(87.5047499982748,3.1176320110373,124.533905171779));
#265836=CARTESIAN_POINT('Ctrl Pts',(87.2263023744621,-3.59035550070555,
124.792074177916));
#265837=CARTESIAN_POINT('Ctrl Pts',(86.9478547506488,-6.99898170591706,
130.57524070557));
#265838=CARTESIAN_POINT('Ctrl Pts',(86.6694071268362,-3.97588564265574,
136.568957239218));
#265839=CARTESIAN_POINT('Ctrl Pts',(86.3909595030232,2.70085509339449,137.265291093768));
#265840=CARTESIAN_POINT('Ctrl Pts',(86.1125118792103,6.89564194272181,132.024345474689));
#265841=CARTESIAN_POINT('Ctrl Pts',(85.8340642553976,4.75367071752436,125.662293371487));
#265842=CARTESIAN_POINT('Ctrl Pts',(85.5556166315845,-1.75669166735309,
124.025549863481));
#265843=CARTESIAN_POINT('Ctrl Pts',(85.2771690077717,-6.65274022909182,
128.618202275162));
#265844=CARTESIAN_POINT('Ctrl Pts',(84.9987213839588,-5.4352455247236,135.21982740374));
#265845=CARTESIAN_POINT('Ctrl Pts',(84.7202737601459,0.776974290360158,
137.763854263368));
#265846=CARTESIAN_POINT('Ctrl Pts',(84.4418261363329,6.27519268990729,133.912446452669));
#265847=CARTESIAN_POINT('Ctrl Pts',(84.1633785125202,6.00681556763514,127.204859597945));
#265848=CARTESIAN_POINT('Ctrl Pts',(83.8849308887072,0.218468387960617,
123.805038334852));
#265849=CARTESIAN_POINT('Ctrl Pts',(83.6064832648944,-5.77064056747553,
126.837252313669));
#265850=CARTESIAN_POINT('Ctrl Pts',(83.3280356410814,-6.45681275286598,
133.515045019753));
#265851=CARTESIAN_POINT('Ctrl Pts',(83.0495880172686,-1.20948945121144,
137.701851184522));
#265852=CARTESIAN_POINT('Ctrl Pts',(82.7711403934555,5.14929556926191,135.550200479404));
#265853=CARTESIAN_POINT('Ctrl Pts',(82.4926927696429,6.77612951865689,129.037354788424));
#265854=CARTESIAN_POINT('Ctrl Pts',(82.2142451458298,2.17603147273656,124.148301131391));
#265855=CARTESIAN_POINT('Ctrl Pts',(81.9357975220171,-4.42373319158141,
125.375840975569));
#265856=CARTESIAN_POINT('Ctrl Pts',(81.6573498982041,-6.95830316421689,
131.591925172815));
#265857=CARTESIAN_POINT('Ctrl Pts',(81.3789022743912,-3.09853246094448,
137.084276018453));
#265858=CARTESIAN_POINT('Ctrl Pts',(81.1004546505783,3.60863820220999,136.805691401599));
#265859=CARTESIAN_POINT('Ctrl Pts',(80.8220070267654,6.99964664931016,131.012176975526));
#265860=CARTESIAN_POINT('Ctrl Pts',(80.5435594029525,3.95832177744353,125.02768946888));
#265861=CARTESIAN_POINT('Ctrl Pts',(80.2651117791397,-2.72050743312451,
124.351680541802));
#265862=CARTESIAN_POINT('Ctrl Pts',(79.9866641553267,-6.89932321682792,
129.605369373404));
#265863=CARTESIAN_POINT('Ctrl Pts',(79.7082165315139,-4.73799801494326,
135.960872584412));
#265864=CARTESIAN_POINT('Ctrl Pts',(79.4297689077009,1.77731589860328,137.577793207502));
#265865=CARTESIAN_POINT('Ctrl Pts',(79.1513212838881,6.65936332804202,132.970260181018));
#265866=CARTESIAN_POINT('Ctrl Pts',(78.8728736600752,5.42178118699497,126.372371265798));
#265867=CARTESIAN_POINT('Ctrl Pts',(78.5944260362623,-0.798152996164653,
123.847264050135));
#265868=CARTESIAN_POINT('Ctrl Pts',(78.3159784124494,-6.28462356779051,
127.715388706879));
#265869=CARTESIAN_POINT('Ctrl Pts',(78.0375307886365,-5.99583210154638,
134.422127644877));
#265870=CARTESIAN_POINT('Ctrl Pts',(77.7590831648237,-0.197163846663491,
137.804315422519));
#265871=CARTESIAN_POINT('Ctrl Pts',(77.4806355410107,5.78268835131386,134.753886701214));
#265872=CARTESIAN_POINT('Ctrl Pts',(77.2021879171979,6.44853245446487,128.07403645411));
#265873=CARTESIAN_POINT('Ctrl Pts',(76.9237402933849,1.18849026028645,123.903220729472));
#265874=CARTESIAN_POINT('Ctrl Pts',(76.6452926695721,-5.16371642211823,
126.074215422566));
#265875=CARTESIAN_POINT('Ctrl Pts',(76.3668450457591,-6.77071997416741,
132.591982469425));
#265876=CARTESIAN_POINT('Ctrl Pts',(76.0883974219463,-2.15576263801617,
137.467012364608));
#265877=CARTESIAN_POINT('Ctrl Pts',(75.8099497981334,4.44023524761227,136.219390792892));
#265878=CARTESIAN_POINT('Ctrl Pts',(75.5315021743204,6.95587385823614,129.995621028982));
#265879=CARTESIAN_POINT('Ctrl Pts',(75.2530545505077,3.0794042064702,124.515043437855));
#265880=CARTESIAN_POINT('Ctrl Pts',(74.9746069266946,-3.62688747378295,
124.814041084656));
#265881=CARTESIAN_POINT('Ctrl Pts',(74.6961593028819,-7.0002467489329,130.617849738824));
#265882=CARTESIAN_POINT('Ctrl Pts',(74.4177116790688,-3.94072124287924,
136.593052778991));
#265883=CARTESIAN_POINT('Ctrl Pts',(74.1392640552561,2.74013457044532,137.248730516143));
#265884=CARTESIAN_POINT('Ctrl Pts',(73.860816431443,6.90294057654623,131.982347141473));
#265885=CARTESIAN_POINT('Ctrl Pts',(73.5823688076304,4.72228142019582,125.633451699173));
#265886=CARTESIAN_POINT('Ctrl Pts',(73.3039211838172,-1.79792366504193,
124.036368939932));
#265887=CARTESIAN_POINT('Ctrl Pts',(73.0254735600045,-6.66592473556012,
128.658739897661));
#265888=CARTESIAN_POINT('Ctrl Pts',(72.7470259361915,-5.40826662262595,
135.252831477583));
#265889=CARTESIAN_POINT('Ctrl Pts',(72.4685783123786,0.819324307988826,
137.758995657032));
#265890=CARTESIAN_POINT('Ctrl Pts',(72.1901306885658,6.2939962257795,133.87418998802));
#265891=CARTESIAN_POINT('Ctrl Pts',(71.9116830647529,5.98479309088811,127.168361097063));
#265892=CARTESIAN_POINT('Ctrl Pts',(71.63323544094,0.17585747886725,123.803838136996));
#265893=CARTESIAN_POINT('Ctrl Pts',(71.3547878171271,-5.79468256511725,
126.872453342036));
#265894=CARTESIAN_POINT('Ctrl Pts',(71.0763401933142,-6.44019241774003,
133.554299248939));
#265895=CARTESIAN_POINT('Ctrl Pts',(70.7978925695013,-1.16748005934989,
137.709085895581));
#265896=CARTESIAN_POINT('Ctrl Pts',(70.5194449456884,5.17808943901089,135.518767326308));
#265897=CARTESIAN_POINT('Ctrl Pts',(70.2409973218756,6.76524770665308,128.996139303274));
#265898=CARTESIAN_POINT('Ctrl Pts',(69.9625496980626,2.1354738326052,124.135178331551));
#265899=CARTESIAN_POINT('Ctrl Pts',(69.6841020742497,-4.45669616991057,
125.402870073008));
#265900=CARTESIAN_POINT('Ctrl Pts',(69.4056544504369,-6.95338011399016,
131.634267747431));
#265901=CARTESIAN_POINT('Ctrl Pts',(69.1272068266238,-3.06024742481583,
137.103021312725));
#265902=CARTESIAN_POINT('Ctrl Pts',(68.8487592028112,3.64510314636624,136.783613405848));
#265903=CARTESIAN_POINT('Ctrl Pts',(68.5703115789981,7.00078199922599,130.969564289278));
#265904=CARTESIAN_POINT('Ctrl Pts',(68.2918639551854,3.92308420201135,125.003701069051));
#265905=CARTESIAN_POINT('Ctrl Pts',(68.0134163313723,-2.75973632353393,
124.368360595937));
#265906=CARTESIAN_POINT('Ctrl Pts',(67.7349687075595,-6.90649398836592,
129.647389726619));
#265907=CARTESIAN_POINT('Ctrl Pts',(67.4565210837467,-4.70652107887851,
135.98961858491));
#265908=CARTESIAN_POINT('Ctrl Pts',(67.1780734599337,1.81851477576126,137.566848685147));
#265909=CARTESIAN_POINT('Ctrl Pts',(66.8996258361208,6.67242439086218,132.929682617185));
#265910=CARTESIAN_POINT('Ctrl Pts',(66.6211782123079,5.39470195681365,126.339449459324));
#265911=CARTESIAN_POINT('Ctrl Pts',(66.3427305884951,-0.840488029704522,
123.852251532852));
#265912=CARTESIAN_POINT('Ctrl Pts',(66.0642829646821,-6.30331057704718,
127.753702225821));
#265913=CARTESIAN_POINT('Ctrl Pts',(65.7858353408693,-5.97369863792435,
134.458558947856));
#265914=CARTESIAN_POINT('Ctrl Pts',(65.5073877170563,-0.154549481951222,
137.805385921867));
#265915=CARTESIAN_POINT('Ctrl Pts',(65.2289400932435,5.80662309777304,134.718612660325));
#265916=CARTESIAN_POINT('Ctrl Pts',(64.9504924694306,6.43179271995227,128.03483299333));
#265917=CARTESIAN_POINT('Ctrl Pts',(64.6720448456177,1.14645904303803,123.896113914062));
#265918=CARTESIAN_POINT('Ctrl Pts',(64.3935972218049,-5.19241448679041,
126.1057360687));
#265919=CARTESIAN_POINT('Ctrl Pts',(64.1151495979918,-6.75971276680813,
132.633164643176));
#265920=CARTESIAN_POINT('Ctrl Pts',(63.8367019741791,-2.11516524445634,
137.480011660159));
#265921=CARTESIAN_POINT('Ctrl Pts',(63.5582543503661,4.47311580598391,136.192261492683));
#265922=CARTESIAN_POINT('Ctrl Pts',(63.2798067265533,6.95082195458075,129.953293634565));
#265923=CARTESIAN_POINT('Ctrl Pts',(63.0013591027403,3.041062293448,124.496414756892));
#265924=CARTESIAN_POINT('Ctrl Pts',(62.7229114789275,-3.66328505121137,
124.836229964889));
#265925=CARTESIAN_POINT('Ctrl Pts',(62.4444638551145,-7.00125239523119,
130.660465683307));
#265926=CARTESIAN_POINT('Ctrl Pts',(62.1660162313017,-3.90541081822766,
136.616933816649));
#265927=CARTESIAN_POINT('Ctrl Pts',(61.8875686074887,2.77931251080179,137.231931140021));
#265928=CARTESIAN_POINT('Ctrl Pts',(61.609120983676,6.909983419369,131.940305157533));
#265929=CARTESIAN_POINT('Ctrl Pts',(61.3306733598629,4.69071713699276,125.604801636791));
#265930=CARTESIAN_POINT('Ctrl Pts',(61.0522257360502,-1.83908904000824,
124.047438806804));
#265931=CARTESIAN_POINT('Ctrl Pts',(60.7737781122372,-6.67886223373588,
128.699357026925));
#265932=CARTESIAN_POINT('Ctrl Pts',(60.4953304884244,-5.38108731521968,
135.285670711703));
#265933=CARTESIAN_POINT('Ctrl Pts',(60.2168828646114,0.861643965253713,
137.753879344138));
#265934=CARTESIAN_POINT('Ctrl Pts',(59.9384352407986,6.31256653530686,133.835819769716));
#265935=CARTESIAN_POINT('Ctrl Pts',(59.6599876169856,5.96254884543232,127.131997329482));
#265936=CARTESIAN_POINT('Ctrl Pts',(59.3815399931728,0.133240053310041,
123.802897346075));
#265937=CARTESIAN_POINT('Ctrl Pts',(59.1030923693598,-5.81850983866561,
126.907800068673));
#265938=CARTESIAN_POINT('Ctrl Pts',(58.824644745547,-6.42333343891552,133.593451578138));
#265939=CARTESIAN_POINT('Ctrl Pts',(58.5461971217341,-1.12542740608588,
137.716064749505));
#265940=CARTESIAN_POINT('Ctrl Pts',(58.2677494979212,5.20669143275151,135.487159479138));
#265941=CARTESIAN_POINT('Ctrl Pts',(57.9893018741083,6.75411520590753,128.954990822428));
#265942=CARTESIAN_POINT('Ctrl Pts',(57.7108542502954,2.09483706170563,124.122302660713));
#265943=CARTESIAN_POINT('Ctrl Pts',(57.4324066264825,-4.48949400372376,
125.430099324666));
#265944=CARTESIAN_POINT('Ctrl Pts',(57.1539590026696,-6.94819940370625,
131.676579569534));
#265945=CARTESIAN_POINT('Ctrl Pts',(56.8755113788568,-3.02184899009409,
137.121533207807));
#265946=CARTESIAN_POINT('Ctrl Pts',(56.5970637550437,3.68143301988451,136.761313846687));
#265947=CARTESIAN_POINT('Ctrl Pts',(56.318616131231,7.00165793259049,130.926945481348));
#265948=CARTESIAN_POINT('Ctrl Pts',(56.040168507418,3.88770125525153,124.979927614796));
#265949=CARTESIAN_POINT('Ctrl Pts',(55.7617208836052,-2.79886295089852,
124.385279138419));
#265950=CARTESIAN_POINT('Ctrl Pts',(55.4832732597923,-6.91340883722955,
129.689452951814));
#265951=CARTESIAN_POINT('Ctrl Pts',(55.2048256359794,-4.67486974094423,
136.018172443767));
#265952=CARTESIAN_POINT('Ctrl Pts',(54.9263780121665,1.85964626718557,137.555653576309));
#265953=CARTESIAN_POINT('Ctrl Pts',(54.6479303883536,6.68523820454244,132.889026298762));
#265954=CARTESIAN_POINT('Ctrl Pts',(54.3694827645407,5.36742282396772,126.306693101776));
#265955=CARTESIAN_POINT('Ctrl Pts',(54.0910351407278,-0.882791918651148,
123.857496628527));
#265956=CARTESIAN_POINT('Ctrl Pts',(53.8125875169149,-6.32176401481248,
127.792128788032));
#265957=CARTESIAN_POINT('Ctrl Pts',(53.534139893102,-5.95134381670231,134.494854843172));
#265958=CARTESIAN_POINT('Ctrl Pts',(53.2556922692892,-0.111929390351441,
137.806196995646));
#265959=CARTESIAN_POINT('Ctrl Pts',(52.9772446454762,5.83034267767769,134.683193575387));
#265960=CARTESIAN_POINT('Ctrl Pts',(52.6987970216634,6.41481465299549,127.995732158415));
#265961=CARTESIAN_POINT('Ctrl Pts',(52.4203493978505,1.10438534332797,123.889263086274));
#265962=CARTESIAN_POINT('Ctrl Pts',(52.1419017740376,-5.22092014463445,
126.137430824095));
#265963=CARTESIAN_POINT('Ctrl Pts',(51.8634541502246,-6.74845507580631,
132.674279049921));
#265964=CARTESIAN_POINT('Ctrl Pts',(51.5850065264118,-2.07448947267055,
137.492763587005));
#265965=CARTESIAN_POINT('Ctrl Pts',(51.3065589025989,4.50583061140446,136.164932541826));
#265966=CARTESIAN_POINT('Ctrl Pts',(51.028111278786,6.94551248566166,129.910997776748));
#265967=CARTESIAN_POINT('Ctrl Pts',(50.7496636549731,3.00260769274395,124.478019819181));
#265968=CARTESIAN_POINT('Ctrl Pts',(50.4712160311602,-3.69954688426507,
124.858639996399));
#265969=CARTESIAN_POINT('Ctrl Pts',(50.1927684073473,-7.00199860754717,
130.70308695987));
#265970=CARTESIAN_POINT('Ctrl Pts',(49.9143207835345,-3.86995567714208,
136.640599467269));
#265971=CARTESIAN_POINT('Ctrl Pts',(49.6358731597215,2.81838746271124,137.214893587909));
#265972=CARTESIAN_POINT('Ctrl Pts',(49.3574255359087,6.91677021021505,131.89822108075));
#265973=CARTESIAN_POINT('Ctrl Pts',(49.0789779120958,4.65897903754105,125.576344245977));
#265974=CARTESIAN_POINT('Ctrl Pts',(48.8005302882828,-1.88018626685394,
124.058759053897));
#265975=CARTESIAN_POINT('Ctrl Pts',(48.5220826644701,-6.69155224421552,
128.740052157871));
#265976=CARTESIAN_POINT('Ctrl Pts',(48.243635040657,-5.35370860964396,135.318343889229));
#265977=CARTESIAN_POINT('Ctrl Pts',(47.9651874168443,0.903931693984841,
137.748505514272));
#265978=CARTESIAN_POINT('Ctrl Pts',(47.6867397930313,6.33090293035988,133.797337219578));
#265979=CARTESIAN_POINT('Ctrl Pts',(47.4082921692184,5.94008365553619,127.095769642671));
#265980=CARTESIAN_POINT('Ctrl Pts',(47.1298445454056,0.0906176904940206,
123.80221599695));
#265981=CARTESIAN_POINT('Ctrl Pts',(46.8513969215926,-5.84212150519187,
126.943291183793));
#265982=CARTESIAN_POINT('Ctrl Pts',(46.5729492977799,-6.40623644110861,
133.632500556544));
#265983=CARTESIAN_POINT('Ctrl Pts',(46.2945016739667,-1.08333304969514,
137.722787487691));
#265984=CARTESIAN_POINT('Ctrl Pts',(46.016054050154,5.23510049062639,135.455378109134));
#265985=CARTESIAN_POINT('Ctrl Pts',(45.737606426341,6.7427324289391,128.913910870662));
#265986=CARTESIAN_POINT('Ctrl Pts',(45.4591588025282,2.0541226658487,124.10967459599));
#265987=CARTESIAN_POINT('Ctrl Pts',(45.1807111787153,-4.5221254776858,125.457527721552));
#265988=CARTESIAN_POINT('Ctrl Pts',(44.9022635549024,-6.94276122533821,
131.718859071242));
#265989=CARTESIAN_POINT('Ctrl Pts',(44.6238159310895,-2.98333857964632,
137.139811017737));
#265990=CARTESIAN_POINT('Ctrl Pts',(44.3453683072766,3.71762647654865,136.738793550433));
#265991=CARTESIAN_POINT('Ctrl Pts',(44.0669206834637,7.00227441694529,130.88432213099));
#265992=CARTESIAN_POINT('Ctrl Pts',(43.7884730596509,3.85217424829189,124.956369987047));
#265993=CARTESIAN_POINT('Ctrl Pts',(43.5100254358379,-2.8378858653675,124.402435542326));
#265994=CARTESIAN_POINT('Ctrl Pts',(43.2315778120251,-6.92006750718621,
129.731557490323));
#265995=CARTESIAN_POINT('Ctrl Pts',(42.9531301882121,-4.64304517399252,
136.04653310291));
#265996=CARTESIAN_POINT('Ctrl Pts',(42.6746825643993,1.90070884873357,137.544208295828));
#265997=CARTESIAN_POINT('Ctrl Pts',(42.3962349405864,6.69780429426274,132.848292732287));
#265998=CARTESIAN_POINT('Ctrl Pts',(42.1177873167735,5.33994479929498,126.274103406951));
#265999=CARTESIAN_POINT('Ctrl Pts',(41.8393396929606,-0.925063095418803,
123.862999142802));
#266000=CARTESIAN_POINT('Ctrl Pts',(41.5608920691476,-6.33998319728738,
127.8306669696));
#266001=CARTESIAN_POINT('Ctrl Pts',(41.2824444453348,-5.92876846624656,
134.531013985867));
#266002=CARTESIAN_POINT('Ctrl Pts',(41.0039968215219,-0.069305151166692,
137.806748613804));
#266003=CARTESIAN_POINT('Ctrl Pts',(40.725549197709,5.85384621209049,134.647630758868));
#266004=CARTESIAN_POINT('Ctrl Pts',(40.4471015738961,6.39759888272248,127.956735398261));
#266005=CARTESIAN_POINT('Ctrl Pts',(40.1686539500832,1.06227072021291,123.882668499967));
#266006=CARTESIAN_POINT('Ctrl Pts',(39.8902063262704,-5.24923233936253,
126.169298514289));
#266007=CARTESIAN_POINT('Ctrl Pts',(39.6117587024575,-6.73694731831984,
132.715324166149));
#266008=CARTESIAN_POINT('Ctrl Pts',(39.3333110786445,-2.03373682991476,
137.505267672621));
#266009=CARTESIAN_POINT('Ctrl Pts',(39.0548634548317,4.53837845161457,136.137404953004));
#266010=CARTESIAN_POINT('Ctrl Pts',(38.7764158310188,6.9399456482232,129.86873502282));
#266011=CARTESIAN_POINT('Ctrl Pts',(38.4979682072059,2.96404182930761,124.459859306355));
#266012=CARTESIAN_POINT('Ctrl Pts',(38.219520583393,-3.73567162924815,124.881270348773));
#266013=CARTESIAN_POINT('Ctrl Pts',(37.9410729595801,-7.00248535822977,
130.745711989165));
#266014=CARTESIAN_POINT('Ctrl Pts',(37.6626253357672,-3.83435713342598,
136.664048853912));
#266015=CARTESIAN_POINT('Ctrl Pts',(37.3841777119543,2.8573579782368,137.197618491141));
#266016=CARTESIAN_POINT('Ctrl Pts',(37.1057300881414,6.92330069759731,131.856096470565));
#266017=CARTESIAN_POINT('Ctrl Pts',(36.8272824643285,4.62706829790778,125.548080581235));
#266018=CARTESIAN_POINT('Ctrl Pts',(36.5488348405156,-1.92121382270608,
124.070329261737));
#266019=CARTESIAN_POINT('Ctrl Pts',(36.2703872167028,-6.70399429676593,
128.780823782526));
#266020=CARTESIAN_POINT('Ctrl Pts',(35.9919395928899,-5.32613152042688,
135.350849799446));
#266021=CARTESIAN_POINT('Ctrl Pts',(35.7134919690769,0.946185927194629,
137.742874366562));
#266022=CARTESIAN_POINT('Ctrl Pts',(35.4350443452641,6.34900473147662,133.758743763591));
#266023=CARTESIAN_POINT('Ctrl Pts',(35.1565967214512,5.91739835365575,127.059679379064));
#266024=CARTESIAN_POINT('Ctrl Pts',(34.8781490976383,0.0479919698059151,
123.80179411487));
#266025=CARTESIAN_POINT('Ctrl Pts',(34.5997014738253,-5.8655166897575,126.978925372262));
#266026=CARTESIAN_POINT('Ctrl Pts',(34.3212538500126,-6.38890205785425,
133.671444737187));
#266027=CARTESIAN_POINT('Ctrl Pts',(34.0428062261996,-1.04119854999986,
137.729253861025));
#266028=CARTESIAN_POINT('Ctrl Pts',(33.7643586023867,5.26331555992738,135.423424393967));
#266029=CARTESIAN_POINT('Ctrl Pts',(33.4859109785738,6.73109979754094,128.872900970206));
#266030=CARTESIAN_POINT('Ctrl Pts',(33.207463354761,2.01333215372067,124.097294605319));
#266031=CARTESIAN_POINT('Ctrl Pts',(32.9290157309481,-4.55458938262534,
125.485154247296));
#266032=CARTESIAN_POINT('Ctrl Pts',(32.6505681071352,-6.93706578039975,
131.761104685873));
#266033=CARTESIAN_POINT('Ctrl Pts',(32.3721204833222,-2.94471762049033,
137.157854065221));
#266034=CARTESIAN_POINT('Ctrl Pts',(32.0936728595094,3.75368217519627,136.716053351584));
#266035=CARTESIAN_POINT('Ctrl Pts',(31.8152252356965,7.00263142944649,130.84169581763));
#266036=CARTESIAN_POINT('Ctrl Pts',(31.5367776118836,3.8165044975991,124.933029058741));
#266037=CARTESIAN_POINT('Ctrl Pts',(31.2583299880707,-2.87680362093211,
124.41982917192));
#266038=CARTESIAN_POINT('Ctrl Pts',(30.9798823642578,-6.92646975149653,
129.773701781947));
#266039=CARTESIAN_POINT('Ctrl Pts',(30.7014347404449,-4.6110485572945,136.074699511423));
#266040=CARTESIAN_POINT('Ctrl Pts',(30.422987116632,1.94170099881587,137.532513267813));
#266041=CARTESIAN_POINT('Ctrl Pts',(30.1445394928192,6.71012219438185,132.807483427156));
#266042=CARTESIAN_POINT('Ctrl Pts',(29.8660918690062,5.31226890100394,126.241681582474));
#266043=CARTESIAN_POINT('Ctrl Pts',(29.5876442451933,-0.967299993633269,
123.868758871779));
#266044=CARTESIAN_POINT('Ctrl Pts',(29.3091966213805,-6.35796744935336,
127.869315342481));
#266045=CARTESIAN_POINT('Ctrl Pts',(29.0307489975676,-5.90597342309497,
134.567035036052));
#266046=CARTESIAN_POINT('Ctrl Pts',(28.7523013737546,-0.026678343854083,
137.807040755898));
#266047=CARTESIAN_POINT('Ctrl Pts',(28.4738537499418,5.87713283007914,134.611925528561));
#266048=CARTESIAN_POINT('Ctrl Pts',(28.1954061261289,6.38014604707014,127.917844157905));
#266049=CARTESIAN_POINT('Ctrl Pts',(27.916958502316,1.02011673426565,123.876330399509));
#266050=CARTESIAN_POINT('Ctrl Pts',(27.6385108785031,-5.27735002185588,
126.201337958415));
#266051=CARTESIAN_POINT('Ctrl Pts',(27.3600632546902,-6.72518992077305,
132.756298470923));
#266052=CARTESIAN_POINT('Ctrl Pts',(27.0816156308773,-1.99290882629253,
137.51752345366));
#266053=CARTESIAN_POINT('Ctrl Pts',(26.8031680070644,4.57075812054227,136.109679746264));
#266054=CARTESIAN_POINT('Ctrl Pts',(26.5247203832516,6.93412164854658,129.826506938842));
#266055=CARTESIAN_POINT('Ctrl Pts',(26.2462727594386,2.92536613221128,124.441933891359));
#266056=CARTESIAN_POINT('Ctrl Pts',(25.9678251356258,-3.7716579475455,124.904120183435));
#266057=CARTESIAN_POINT('Ctrl Pts',(25.6893775118128,-7.00271262924226,
130.788339191706));
#266058=CARTESIAN_POINT('Ctrl Pts',(25.410929888,-3.79861650619593,136.687281107654));
#266059=CARTESIAN_POINT('Ctrl Pts',(25.1324822641871,2.89622261331168,137.180106489852));
#266060=CARTESIAN_POINT('Ctrl Pts',(24.8540346403742,6.92957463952618,131.813932887921));
#266061=CARTESIAN_POINT('Ctrl Pts',(24.5755870165613,4.59498610055721,125.520011689881));
#266062=CARTESIAN_POINT('Ctrl Pts',(24.2971393927484,-1.96217018727317,
124.082149001586));
#266063=CARTESIAN_POINT('Ctrl Pts',(24.0186917689355,-6.71618793034234,
128.821670390082));
#266064=CARTESIAN_POINT('Ctrl Pts',(23.7402441451226,-5.29835706944761,
135.383187237832));
#266065=CARTESIAN_POINT('Ctrl Pts',(23.4617965213097,0.988405099136929,
137.736986109674));
#266066=CARTESIAN_POINT('Ctrl Pts',(23.1833488974968,6.36687126788796,133.720040831851));
#266067=CARTESIAN_POINT('Ctrl Pts',(22.9049012736839,5.89449378040337,127.023727875996));
#266068=CARTESIAN_POINT('Ctrl Pts',(22.6264536498711,0.00536447075796404,
123.801631715467));
#266069=CARTESIAN_POINT('Ctrl Pts',(22.3480060260581,-5.88869452544514,
127.01470131364));
#266070=CARTESIAN_POINT('Ctrl Pts',(22.0695584022453,-6.3713309314846,133.710282676972));
#266071=CARTESIAN_POINT('Ctrl Pts',(21.7911107784324,-0.999025468309402,
137.735463629893));
#266072=CARTESIAN_POINT('Ctrl Pts',(21.5126631546195,5.29133559513472,135.391299517692));
#266073=CARTESIAN_POINT('Ctrl Pts',(21.2342155308066,6.71921774276442,128.831962640697));
#266074=CARTESIAN_POINT('Ctrl Pts',(20.9557679069937,1.97246703682929,124.085163147446));
#266075=CARTESIAN_POINT('Ctrl Pts',(20.6773202831809,-4.58688451558038,
125.51297787819));
#266076=CARTESIAN_POINT('Ctrl Pts',(20.3988726593679,-6.93111327993769,
131.803314848003));
#266077=CARTESIAN_POINT('Ctrl Pts',(20.120425035555,-2.90598754374001,137.175661681671));
#266078=CARTESIAN_POINT('Ctrl Pts',(19.8419774117421,3.78959877977074,136.693094092787));
#266079=CARTESIAN_POINT('Ctrl Pts',(19.5635297879293,7.00272895686486,130.799068120799));
#266080=CARTESIAN_POINT('Ctrl Pts',(19.2850821641163,3.78069332492835,124.909905694786));
#266081=CARTESIAN_POINT('Ctrl Pts',(19.0066345403035,-2.91561477548059,
124.437459382677));
#266082=CARTESIAN_POINT('Ctrl Pts',(18.7281869164906,-6.932615332923,129.815884265012));
#266083=CARTESIAN_POINT('Ctrl Pts',(18.4497392926777,-4.57888107649638,
136.102670625591));
#266084=CARTESIAN_POINT('Ctrl Pts',(18.1712916688647,1.98262119845391,137.520568925627));
#266085=CARTESIAN_POINT('Ctrl Pts',(17.892844045052,6.72219144845534,132.766599895572));
#266086=CARTESIAN_POINT('Ctrl Pts',(17.614396421239,5.28439615463518,126.209428829746));
#266087=CARTESIAN_POINT('Ctrl Pts',(17.3359487974261,-1.00950104819076,
123.87477560203));
#266088=CARTESIAN_POINT('Ctrl Pts',(17.0575011736132,-6.37571610459714,
127.908072474542));
#266089=CARTESIAN_POINT('Ctrl Pts',(16.7790535498004,-5.88295953192644,
134.602916658952));
#266090=CARTESIAN_POINT('Ctrl Pts',(16.5006059259874,0.0159494520341194,
137.807073411106));
#266091=CARTESIAN_POINT('Ctrl Pts',(16.2221583021745,5.90020166874948,134.576079207535));
#266092=CARTESIAN_POINT('Ctrl Pts',(15.9437106783617,6.3624567927597,127.879059878479));
#266093=CARTESIAN_POINT('Ctrl Pts',(15.6652630545488,0.977924947517885,
123.870249019757));
#266094=CARTESIAN_POINT('Ctrl Pts',(15.3868154307359,-5.3052721502032,126.233547969238));
#266095=CARTESIAN_POINT('Ctrl Pts',(15.108367806923,-6.71318331884074,132.797200445919));
#266096=CARTESIAN_POINT('Ctrl Pts',(14.8299201831101,-1.95200697470083,
137.529530475982));
#266097=CARTESIAN_POINT('Ctrl Pts',(14.5514725592972,4.6029684183469,136.081757948972));
#266098=CARTESIAN_POINT('Ctrl Pts',(14.2730249354843,6.92804070244224,129.784315089592));
#266099=CARTESIAN_POINT('Ctrl Pts',(13.9945773116714,2.88658203459712,124.424244238425));
#266100=CARTESIAN_POINT('Ctrl Pts',(13.7161296878585,-3.80750450567058,
124.927188653676));
#266101=CARTESIAN_POINT('Ctrl Pts',(13.4376820640456,-7.00268041216303,
130.830966987928));
#266102=CARTESIAN_POINT('Ctrl Pts',(13.1592344402328,-3.7627351198343,136.710295367612));
#266103=CARTESIAN_POINT('Ctrl Pts',(12.8807868164199,2.93497992779253,137.162358232954));
#266104=CARTESIAN_POINT('Ctrl Pts',(12.602339192607,6.93559180351842,131.771731895206));
#266105=CARTESIAN_POINT('Ctrl Pts',(12.323891568794,4.56273363430679,125.49213861202));
#266106=CARTESIAN_POINT('Ctrl Pts',(12.0454439449812,-2.00305384290271,
124.094217835458));
#266107=CARTESIAN_POINT('Ctrl Pts',(11.7669963211683,-6.72813269310505,
128.862590466954));
#266108=CARTESIAN_POINT('Ctrl Pts',(11.4885486973554,-5.27038628589867,
135.415355006116));
#266109=CARTESIAN_POINT('Ctrl Pts',(11.2101010735425,1.03058764536478,137.730840961799));
#266110=CARTESIAN_POINT('Ctrl Pts',(10.9316534497296,6.38450187754329,133.681229858508));
#266111=CARTESIAN_POINT('Ctrl Pts',(10.6532058259167,5.87137078451608,126.987916465666));
#266112=CARTESIAN_POINT('Ctrl Pts',(10.3747582021038,-0.0372632270726686,
123.801728804758));
#266113=CARTESIAN_POINT('Ctrl Pts',(10.0963105782909,-5.91165415339157,
127.050617682238));
#266114=CARTESIAN_POINT('Ctrl Pts',(9.81786295447806,-6.35352371310424,
133.749012936746));
#266115=CARTESIAN_POINT('Ctrl Pts',(9.53941533066515,-0.956815367363035,
137.741416564191));
#266116=CARTESIAN_POINT('Ctrl Pts',(9.26096770685226,5.31915955795546,135.35900467071));
#266117=CARTESIAN_POINT('Ctrl Pts',(8.98252008303941,6.70708670490366,128.791097399121));
#266118=CARTESIAN_POINT('Ctrl Pts',(8.70407245922646,1.93152882944647,124.073280671906));
#266119=CARTESIAN_POINT('Ctrl Pts',(8.42562483541358,-4.61900967984285,
125.540997583217));
#266120=CARTESIAN_POINT('Ctrl Pts',(8.14717721160073,-6.92490394452403,
131.845487993513));
#266121=CARTESIAN_POINT('Ctrl Pts',(7.86872958778781,-2.86714978455288,
137.193233207215));
#266122=CARTESIAN_POINT('Ctrl Pts',(7.59028196397491,3.82537495936868,136.669916624805));
#266123=CARTESIAN_POINT('Ctrl Pts',(7.31183434016203,7.00256699558648,130.756440620084));
#266124=CARTESIAN_POINT('Ctrl Pts',(7.03338671634916,3.7447420572761,124.887000752025));
#266125=CARTESIAN_POINT('Ctrl Pts',(6.75493909253623,-2.95431789085107,
124.455325521299));
#266126=CARTESIAN_POINT('Ctrl Pts',(6.47649146872337,-6.9385040237388,129.858103376433));
#266127=CARTESIAN_POINT('Ctrl Pts',(6.19804384491048,-4.54654392357636,
136.130445408932));
#266128=CARTESIAN_POINT('Ctrl Pts',(5.91959622109758,2.02346793133434,137.508375711873));
#266129=CARTESIAN_POINT('Ctrl Pts',(5.64114859728465,6.73401160925262,132.725643652489));
#266130=CARTESIAN_POINT('Ctrl Pts',(5.36270097347181,5.25632759302358,126.177346343905));
#266131=CARTESIAN_POINT('Ctrl Pts',(5.08425334965889,-1.05166469531565,
123.881049110601));
#266132=CARTESIAN_POINT('Ctrl Pts',(4.80580572584599,-6.39322850533622,
127.946936929627));
#266133=CARTESIAN_POINT('Ctrl Pts',(4.5273581020331,-5.85972764552883,134.638657524961));
#266134=CARTESIAN_POINT('Ctrl Pts',(4.24891047822024,0.0585766569097649,
137.806846578216));
#266135=CARTESIAN_POINT('Ctrl Pts',(3.97046285440732,5.92305187327717,134.54009312409));
#266136=CARTESIAN_POINT('Ctrl Pts',(3.69201523059441,6.34453177527304,127.840383997147));
#266137=CARTESIAN_POINT('Ctrl Pts',(3.41356760678156,0.935696923401329,
123.864424586062));
#266138=CARTESIAN_POINT('Ctrl Pts',(3.13511998296867,-5.33299768974021,
126.265927353204));
#266139=CARTESIAN_POINT('Ctrl Pts',(2.85667235915575,-6.70092795743158,
132.838028575505));
#266140=CARTESIAN_POINT('Ctrl Pts',(2.57822473534285,-1.91103279077285,
137.541288294661));
#266141=CARTESIAN_POINT('Ctrl Pts',(2.29977711153,4.63500815146407,136.053640595781));
#266142=CARTESIAN_POINT('Ctrl Pts',(2.02132948771708,6.92170303524179,129.742161038504));
#266143=CARTESIAN_POINT('Ctrl Pts',(1.74288186390418,2.84769097362441,124.40679100305));
#266144=CARTESIAN_POINT('Ctrl Pts',(1.46443424009131,-3.84320997531586,
124.950474904685));
#266145=CARTESIAN_POINT('Ctrl Pts',(1.18598661627842,-7.00238870818588,
130.873593798241));
#266146=CARTESIAN_POINT('Ctrl Pts',(0.907538992465495,-3.72671430393905,
136.733090780986));
#266147=CARTESIAN_POINT('Ctrl Pts',(0.629091368652655,2.97362848551254,
137.144374378117));
#266148=CARTESIAN_POINT('Ctrl Pts',(0.350643744839755,6.94135196660579,
131.729495056193));
#266149=CARTESIAN_POINT('Ctrl Pts',(0.0721961210268491,4.53031209428387,
125.4644623805));
#266150=CARTESIAN_POINT('Ctrl Pts',(-0.206251502786054,-2.04386327463549,
124.106535316138));
#266151=CARTESIAN_POINT('Ctrl Pts',(-0.484699126598912,-6.73982814243653,
128.903582496833));
#266152=CARTESIAN_POINT('Ctrl Pts',(-0.763146750411823,-5.24222020624778,
135.447351912307));
#266153=CARTESIAN_POINT('Ctrl Pts',(-1.04159437422473,1.07273200278813,
137.724439150648));
#266154=CARTESIAN_POINT('Ctrl Pts',(-1.32004199803759,6.40189590713365,
133.642312281717));
#266155=CARTESIAN_POINT('Ctrl Pts',(-1.59848962185049,5.84803022282516,
126.952246475077));
#266156=CARTESIAN_POINT('Ctrl Pts',(-1.87693724566341,-0.0798895441007186,
123.802085379146));
#266157=CARTESIAN_POINT('Ctrl Pts',(-2.1553848694763,-5.93439472281934,
127.08667314716));
#266158=CARTESIAN_POINT('Ctrl Pts',(-2.43383249328916,-6.33548106256618,
133.787634081347));
#266159=CARTESIAN_POINT('Ctrl Pts',(-2.71228011710207,-0.914569811271147,
137.747112443329));
#266160=CARTESIAN_POINT('Ctrl Pts',(-2.99072774091498,5.34678641736288,
135.326541049718));
#266161=CARTESIAN_POINT('Ctrl Pts',(-3.26917536472784,6.6947071334783,128.750306759754));
#266162=CARTESIAN_POINT('Ctrl Pts',(-3.54762298854074,1.89051904855254,
124.061647619009));
#266163=CARTESIAN_POINT('Ctrl Pts',(-3.82607061235365,-4.65096368500298,
125.569212324096));
#266164=CARTESIAN_POINT('Ctrl Pts',(-4.10451823616654,-6.91843800424817,
131.887622559669));
#266165=CARTESIAN_POINT('Ctrl Pts',(-4.38296585997939,-2.82820578207579,
137.210567990736));
#266166=CARTESIAN_POINT('Ctrl Pts',(-4.66141348379231,3.86100938829084,
136.646521806489));
#266167=CARTESIAN_POINT('Ctrl Pts',(-4.93986110760522,7.00214555161287,
130.713814895061));
#266168=CARTESIAN_POINT('Ctrl Pts',(-5.21830873141809,3.70865202682979,
124.864315079211));
#266169=CARTESIAN_POINT('Ctrl Pts',(-5.49675635523098,-2.99291153288594,
124.473426925751));
#266170=CARTESIAN_POINT('Ctrl Pts',(-5.77520397904388,-6.9441356057364,
129.900357551763));
#266171=CARTESIAN_POINT('Ctrl Pts',(-6.05365160285679,-4.51403829679898,
136.158022832244));
#266172=CARTESIAN_POINT('Ctrl Pts',(-6.33209922666964,2.06423968386644,
137.495934078373));
#266173=CARTESIAN_POINT('Ctrl Pts',(-6.61054685048256,6.74558223877327,
132.684616215558));
#266174=CARTESIAN_POINT('Ctrl Pts',(-6.88899447429547,5.22806425626005,
126.145435313781));
#266175=CARTESIAN_POINT('Ctrl Pts',(-7.16744209810832,-1.09378937261818,
123.887579165027));
#266176=CARTESIAN_POINT('Ctrl Pts',(-7.44588972192122,-6.41050400264194,
127.985907267597));
#266177=CARTESIAN_POINT('Ctrl Pts',(-7.72433734573414,-5.8362786247684,
134.674256309687));
#266178=CARTESIAN_POINT('Ctrl Pts',(-8.002784969547,0.101201691205851,137.806360265633));
#266179=CARTESIAN_POINT('Ctrl Pts',(-8.28123259335988,5.94568259693924,
134.503968611703));
#266180=CARTESIAN_POINT('Ctrl Pts',(-8.55968021717279,6.32637165882838,
127.80181794706));
#266181=CARTESIAN_POINT('Ctrl Pts',(-8.8381278409857,0.893434226691435,
123.858857314246));
#266182=CARTESIAN_POINT('Ctrl Pts',(-9.11657546479855,-5.3605256130866,
126.298474910485));
#266183=CARTESIAN_POINT('Ctrl Pts',(-9.39502308861147,-6.68842429067269,
132.878781346775));
#266184=CARTESIAN_POINT('Ctrl Pts',(-9.67347071242438,-1.86998779282204,
137.552796474009));
#266185=CARTESIAN_POINT('Ctrl Pts',(-9.95191833623725,4.66687613264966,
136.025328728591));
#266186=CARTESIAN_POINT('Ctrl Pts',(-10.2303659600501,6.91510888178999,
129.700046347612));
#266187=CARTESIAN_POINT('Ctrl Pts',(-10.508813583863,2.80869439041515,124.389574831969));
#266188=CARTESIAN_POINT('Ctrl Pts',(-10.787261207676,-3.87877303340228,
124.973978073582));
#266189=CARTESIAN_POINT('Ctrl Pts',(-11.0657088314888,-7.00183752812002,
130.916218043094));
#266190=CARTESIAN_POINT('Ctrl Pts',(-11.3441564553017,-3.69055539327479,
136.755666503084));
#266191=CARTESIAN_POINT('Ctrl Pts',(-11.6226040791146,3.01216685433575,
137.126155591738));
#266192=CARTESIAN_POINT('Ctrl Pts',(-11.9010517029275,6.94685491534338,
131.687223935982));
#266193=CARTESIAN_POINT('Ctrl Pts',(-12.1794993267404,4.49772268187999,
125.436984020872));
#266194=CARTESIAN_POINT('Ctrl Pts',(-12.4579469505533,-2.08459697026297,
124.119100987199));
#266195=CARTESIAN_POINT('Ctrl Pts',(-12.7363945743662,-6.75127384495765,
128.944644960744));
#266196=CARTESIAN_POINT('Ctrl Pts',(-13.0148421981791,-5.21385987419926,
135.479176770748));
#266197=CARTESIAN_POINT('Ctrl Pts',(-13.2932898219919,1.11483660973293,
137.717780913442));
#266198=CARTESIAN_POINT('Ctrl Pts',(-13.5717374458049,6.41905271211686,
133.603289543584));
#266199=CARTESIAN_POINT('Ctrl Pts',(-13.8501850696177,5.82447296022373,
126.916719225995));
#266200=CARTESIAN_POINT('Ctrl Pts',(-14.1286326934306,-0.122512900792341,
123.802701425419));
#266201=CARTESIAN_POINT('Ctrl Pts',(-14.4070803172435,-5.95691539106803,
127.122866372359));
#266202=CARTESIAN_POINT('Ctrl Pts',(-14.6855279410564,-6.31720364844761,
133.826144679651));
#266203=CARTESIAN_POINT('Ctrl Pts',(-14.9639755648693,-0.872290365458834,
137.752551056246));
#266204=CARTESIAN_POINT('Ctrl Pts',(-15.2424231886822,5.37421514963333,
135.293909857666));
#266205=CARTESIAN_POINT('Ctrl Pts',(-15.5208708124951,6.68207948721813,
128.709592234107));
#266206=CARTESIAN_POINT('Ctrl Pts',(-15.799318436308,1.84943921378025,124.050264419823));
#266207=CARTESIAN_POINT('Ctrl Pts',(-16.0777660601209,-4.68274534699314,
125.59762105532));
#266208=CARTESIAN_POINT('Ctrl Pts',(-16.3562136839338,-6.91171569870797,
131.929716985153));
#266209=CARTESIAN_POINT('Ctrl Pts',(-16.6346613077467,-2.78915697939336,
137.227665389888));
#266210=CARTESIAN_POINT('Ctrl Pts',(-16.9131089315595,3.89650074609022,
136.622910504741));
#266211=CARTESIAN_POINT('Ctrl Pts',(-17.1915565553724,7.00146464056082,
130.671192525245));
#266212=CARTESIAN_POINT('Ctrl Pts',(-17.4700041791854,3.67242457091876,
124.841849516969));
#266213=CARTESIAN_POINT('Ctrl Pts',(-17.7484518029982,-3.0313942714833,
124.491762925279));
#266214=CARTESIAN_POINT('Ctrl Pts',(-18.0268994268111,-6.94950987023543,
129.942645225261));
#266215=CARTESIAN_POINT('Ctrl Pts',(-18.305347050624,-4.48136540067248,
136.185401873632));
#266216=CARTESIAN_POINT('Ctrl Pts',(-18.5837946744369,2.10493494523792,
137.483244486159));
#266217=CARTESIAN_POINT('Ctrl Pts',(-18.8622422982498,6.75690290826339,
132.643519105064));
#266218=CARTESIAN_POINT('Ctrl Pts',(-19.1406899220627,5.19960719165284,
126.113696921846));
#266219=CARTESIAN_POINT('Ctrl Pts',(-19.4191375458756,-1.1358735191536,
123.894365523333));
#266220=CARTESIAN_POINT('Ctrl Pts',(-19.6975851696885,-6.42754195636435,
128.024982044393));
#266221=CARTESIAN_POINT('Ctrl Pts',(-19.9760327935014,-5.81261333855723,
134.709711694007));
#266222=CARTESIAN_POINT('Ctrl Pts',(-20.2544804173143,0.143822975436045,
137.805614491377));
#266223=CARTESIAN_POINT('Ctrl Pts',(-20.5329280411272,5.96809300114641,
134.467707008981));
#266224=CARTESIAN_POINT('Ctrl Pts',(-20.81137566494,6.30797711635522,127.763363157294));
#266225=CARTESIAN_POINT('Ctrl Pts',(-21.089823288753,0.851138423447451,
123.853547410611));
#266226=CARTESIAN_POINT('Ctrl Pts',(-21.3682709125658,-5.38785490018508,
126.331189435016));
#266227=CARTESIAN_POINT('Ctrl Pts',(-21.6467185363787,-6.67567278189203,
132.919457249623));
#266228=CARTESIAN_POINT('Ctrl Pts',(-21.9251661601916,-1.82887350178604,
137.564054587584));
#266229=CARTESIAN_POINT('Ctrl Pts',(-22.2036137840045,4.69857118102365,
135.996823396506));
#266230=CARTESIAN_POINT('Ctrl Pts',(-22.4820614078173,6.90825848643574,
129.657972577492));
#266231=CARTESIAN_POINT('Ctrl Pts',(-22.7605090316303,2.76959373000234,
124.372596363135));
#266232=CARTESIAN_POINT('Ctrl Pts',(-23.0389566554432,-3.91419236212754,
124.997697289448));
#266233=CARTESIAN_POINT('Ctrl Pts',(-23.3174042792561,-7.0010268923895,
130.958838143028));
#266234=CARTESIAN_POINT('Ctrl Pts',(-23.5958519030689,-3.65425972772349,
136.778021697354));
#266235=CARTESIAN_POINT('Ctrl Pts',(-23.8742995268818,3.05059360620828,
137.107702548922));
#266236=CARTESIAN_POINT('Ctrl Pts',(-24.1527471506948,6.95210044581739,
131.644920100946));
#266237=CARTESIAN_POINT('Ctrl Pts',(-24.4311947745076,4.4649666047081,125.409704551357));
#266238=CARTESIAN_POINT('Ctrl Pts',(-24.7096423983205,-2.12525342038311,
124.131914383013));
#266239=CARTESIAN_POINT('Ctrl Pts',(-24.9880900221334,-6.76246937654364,
128.985776337104));
#266240=CARTESIAN_POINT('Ctrl Pts',(-25.2665376459463,-5.18530634065569,
135.510828402156));
#266241=CARTESIAN_POINT('Ctrl Pts',(-25.5449852697592,1.15689990599717,
137.710866496904));
#266242=CARTESIAN_POINT('Ctrl Pts',(-25.8234328935721,6.43597165674122,
133.564163090109));
#266243=CARTESIAN_POINT('Ctrl Pts',(-26.101880517385,5.8006998696348,126.881336034893));
#266244=CARTESIAN_POINT('Ctrl Pts',(-26.3803281411979,-0.165131717723356,
123.803576920747));
#266245=CARTESIAN_POINT('Ctrl Pts',(-26.6587757650107,-5.9792153236265,
127.15919601668));
#266246=CARTESIAN_POINT('Ctrl Pts',(-26.9372233888237,-6.29869214802456,
133.864543304637));
#266247=CARTESIAN_POINT('Ctrl Pts',(-27.2156710126366,-0.829978596605981,
137.75773220141));
#266248=CARTESIAN_POINT('Ctrl Pts',(-27.4941186364494,5.40144473838504,
135.261112303716));
#266249=CARTESIAN_POINT('Ctrl Pts',(-27.7725662602623,6.66920423404522,
128.668955330874));
#266250=CARTESIAN_POINT('Ctrl Pts',(-28.0510138840753,1.80829084735756,
124.039131496154));
#266251=CARTESIAN_POINT('Ctrl Pts',(-28.3294615078881,-4.71435348813263,
125.626222724194));
#266252=CARTESIAN_POINT('Ctrl Pts',(-28.607909131701,-6.9047372770006,131.971769710144));
#266253=CARTESIAN_POINT('Ctrl Pts',(-28.8863567555139,-2.75000482347336,
137.244524771118));
#266254=CARTESIAN_POINT('Ctrl Pts',(-29.1648043793268,3.93184771762154,
136.599083594488));
#266255=CARTESIAN_POINT('Ctrl Pts',(-29.4432520031397,7.00052428766157,
130.628575090021));
#266256=CARTESIAN_POINT('Ctrl Pts',(-29.7216996269525,3.63606103196502,
124.819604897767));
#266257=CARTESIAN_POINT('Ctrl Pts',(-30.0001472507655,-3.06976468065099,
124.510332840438));
#266258=CARTESIAN_POINT('Ctrl Pts',(-30.2785948745783,-6.95462661809053,
129.984964829937));
#266259=CARTESIAN_POINT('Ctrl Pts',(-30.5570424983912,-4.44852644590303,
136.212581518559));
#266260=CARTESIAN_POINT('Ctrl Pts',(-30.8354901222041,2.14555220747066,
137.470307405446));
#266261=CARTESIAN_POINT('Ctrl Pts',(-31.113937746017,6.7679731982313,132.602353843876));
#266262=CARTESIAN_POINT('Ctrl Pts',(-31.3923853698299,5.17095745368924,
126.082132344179));
#266263=CARTESIAN_POINT('Ctrl Pts',(-31.6708329936428,-1.17791557547805,
123.901407934047));
#266264=CARTESIAN_POINT('Ctrl Pts',(-31.9492806174558,-6.44434173515584,
128.064159812084));
#266265=CARTESIAN_POINT('Ctrl Pts',(-32.2277282412685,-5.78873266382121,
134.745022364106));
#266266=CARTESIAN_POINT('Ctrl Pts',(-32.5061758650815,0.186438930252996,
137.804609283086));
#266267=CARTESIAN_POINT('Ctrl Pts',(-32.7846234888944,5.99028225547263,
134.431309659613));
#266268=CARTESIAN_POINT('Ctrl Pts',(-33.0630711127073,6.28934882947028,
127.725021052809));
#266269=CARTESIAN_POINT('Ctrl Pts',(-33.3415187365202,0.808811080956172,
123.848495071916));
#266270=CARTESIAN_POINT('Ctrl Pts',(-33.619966360333,-5.41498453833882,
126.364069714552));
#266271=CARTESIAN_POINT('Ctrl Pts',(-33.898413984146,-6.66267390360147,
132.960054776787));
#266272=CARTESIAN_POINT('Ctrl Pts',(-34.1768616079588,-1.78769144116968,
137.575062218212));
#266273=CARTESIAN_POINT('Ctrl Pts',(-34.4553092317717,4.73009212211488,
135.968125655805));
#266274=CARTESIAN_POINT('Ctrl Pts',(-34.7337568555846,6.90115210302259,
129.615941287202));
#266275=CARTESIAN_POINT('Ctrl Pts',(-35.0122044793975,2.73039044127535,
124.355856225691));
#266276=CARTESIAN_POINT('Ctrl Pts',(-35.2906521032104,-3.94946664901538,
125.02163167336));
#266277=CARTESIAN_POINT('Ctrl Pts',(-35.5690997270233,-6.99995683103299,
131.00145251874));
#266278=CARTESIAN_POINT('Ctrl Pts',(-35.8475473508362,-3.61782865223385,
136.800155535415));
#266279=CARTESIAN_POINT('Ctrl Pts',(-36.125994974649,3.08890731721304,137.089015933453));
#266280=CARTESIAN_POINT('Ctrl Pts',(-36.404442598462,6.95708836365274,131.60258511867));
#266281=CARTESIAN_POINT('Ctrl Pts',(-36.6828902222748,4.43204507655667,
125.382624982808));
#266282=CARTESIAN_POINT('Ctrl Pts',(-36.9613378460878,-2.16583111845593,
124.144975028777));
#266283=CARTESIAN_POINT('Ctrl Pts',(-37.2397854699006,-6.7734143223399,
129.026975101771));
#266284=CARTESIAN_POINT('Ctrl Pts',(-37.5182330937135,-5.15656066367905,
135.54230563367));
#266285=CARTESIAN_POINT('Ctrl Pts',(-37.7966807175264,1.19892033290996,
137.703696157251));
#266286=CARTESIAN_POINT('Ctrl Pts',(-38.0751283413393,6.45265211406898,
133.524934371139));
#266287=CARTESIAN_POINT('Ctrl Pts',(-38.3535759651522,5.77671183197903,
126.846098212911));
#266288=CARTESIAN_POINT('Ctrl Pts',(-38.6320235889651,-0.207744415637528,
123.80471183269));
#266289=CARTESIAN_POINT('Ctrl Pts',(-38.910471212778,-6.00129369416227,
127.195660733917));
#266290=CARTESIAN_POINT('Ctrl Pts',(-39.1889188365908,-6.27994724724761,
133.902828533427));
#266291=CARTESIAN_POINT('Ctrl Pts',(-39.4673664604039,-0.787636072591,137.762655686833));
#266292=CARTESIAN_POINT('Ctrl Pts',(-39.7458140842166,5.42847417461558,
135.228149603194));
#266293=CARTESIAN_POINT('Ctrl Pts',(-40.0242617080296,6.65608185105682,
128.628397555869));
#266294=CARTESIAN_POINT('Ctrl Pts',(-40.3027093318424,1.76707547405252,
124.028249260538));
#266295=CARTESIAN_POINT('Ctrl Pts',(-40.5811569556554,-4.7457869371699,
125.655016270872));
#266296=CARTESIAN_POINT('Ctrl Pts',(-40.8596045794682,-6.89750299771422,
132.013779176361));
#266297=CARTESIAN_POINT('Ctrl Pts',(-41.1380522032811,-2.7107507651133,
137.261145509698));
#266298=CARTESIAN_POINT('Ctrl Pts',(-41.416499827094,3.96704899308973,136.575041958643));
#266299=CARTESIAN_POINT('Ctrl Pts',(-41.694947450907,6.99932452776054,130.585964168594));
#266300=CARTESIAN_POINT('Ctrl Pts',(-41.9733950747197,3.59956275743227,
124.79758204589));
#266301=CARTESIAN_POINT('Ctrl Pts',(-42.2518426985328,-3.10802133855968,
124.529135983109));
#266302=CARTESIAN_POINT('Ctrl Pts',(-42.5302903223456,-6.95948565969872,
130.027314797628));
#266303=CARTESIAN_POINT('Ctrl Pts',(-42.8087379461585,-4.41552264935019,
136.23956075987));
#266304=CARTESIAN_POINT('Ctrl Pts',(-43.0871855699714,2.18608996547759,
137.457123315624));
#266305=CARTESIAN_POINT('Ctrl Pts',(-43.3656331937842,6.77879269846351,
132.561121957388));
#266306=CARTESIAN_POINT('Ctrl Pts',(-43.6440808175972,5.14211610399531,
126.050742750417));
#266307=CARTESIAN_POINT('Ctrl Pts',(-43.92252844141,-1.21991398370768,123.908706136214));
#266308=CARTESIAN_POINT('Ctrl Pts',(-44.200976065223,-6.46090271649442,
128.103439118922));
#266309=CARTESIAN_POINT('Ctrl Pts',(-44.4794236890358,-5.76463748546755,
134.780187011534));
#266310=CARTESIAN_POINT('Ctrl Pts',(-44.7578713128487,0.229047976506494,
137.803344678006));
#266311=CARTESIAN_POINT('Ctrl Pts',(-45.0363189366615,6.01224953768695,
134.394777912313));
#266312=CARTESIAN_POINT('Ctrl Pts',(-45.3147665604746,6.27048748845154,
127.686793054383));
#266313=CARTESIAN_POINT('Ctrl Pts',(-45.5932141842873,0.766453767672844,
123.843700485376));
#266314=CARTESIAN_POINT('Ctrl Pts',(-45.8716618081003,-5.44191352224889,
126.397114530699));
#266315=CARTESIAN_POINT('Ctrl Pts',(-46.1501094319132,-6.6494281374793,
133.000572423912));
#266316=CARTESIAN_POINT('Ctrl Pts',(-46.4285570557261,-1.74644313698983,
137.585818958004));
#266317=CARTESIAN_POINT('Ctrl Pts',(-46.7070046795389,4.76143778790304,
135.93923656989));
#266318=CARTESIAN_POINT('Ctrl Pts',(-46.9854523033519,6.89378999488032,
129.573954034227));
#266319=CARTESIAN_POINT('Ctrl Pts',(-47.2638999271647,2.69108597692664,
124.339355039948));
#266320=CARTESIAN_POINT('Ctrl Pts',(-47.5423475509777,-3.98459458696386,
125.045780338419));
#266321=CARTESIAN_POINT('Ctrl Pts',(-47.8207951747905,-6.998627383702,131.044059591139));
#266322=CARTESIAN_POINT('Ctrl Pts',(-48.0992427986034,-3.58126351677304,
136.822067197091));
#266323=CARTESIAN_POINT('Ctrl Pts',(-48.3776904224163,3.1271065676212,137.070096437769));
#266324=CARTESIAN_POINT('Ctrl Pts',(-48.6561380462292,6.9618184840203,131.560220557891));
#266325=CARTESIAN_POINT('Ctrl Pts',(-48.9345856700421,4.39895931734504,
125.355746318666));
#266326=CARTESIAN_POINT('Ctrl Pts',(-49.213033293855,-2.20632856086043,
124.158282440523));
#266327=CARTESIAN_POINT('Ctrl Pts',(-49.4914809176678,-6.78410827677761,
129.068239728113));
#266328=CARTESIAN_POINT('Ctrl Pts',(-49.7699285414808,-5.12762390845042,
135.573607298891));
#266329=CARTESIAN_POINT('Ctrl Pts',(-50.0483761652936,1.2408963333889,137.696270160183));
#266330=CARTESIAN_POINT('Ctrl Pts',(-50.3268237891066,6.46909346599971,
133.485604840309));
#266331=CARTESIAN_POINT('Ctrl Pts',(-50.6052714129194,5.7525097361419,126.811007065796));
#266332=CARTESIAN_POINT('Ctrl Pts',(-50.8837190367324,-0.250349415506305,
123.806106119193));
#266333=CARTESIAN_POINT('Ctrl Pts',(-51.1621666605453,-6.02314968455324,
127.232259172855));
#266334=CARTESIAN_POINT('Ctrl Pts',(-51.4406142843581,-6.26096964071598,
133.94099894735));
#266335=CARTESIAN_POINT('Ctrl Pts',(-51.719061908171,-0.745264362431691,
137.767321330073));
#266336=CARTESIAN_POINT('Ctrl Pts',(-51.997509531984,5.45530245673899,135.195022977544));
#266337=CARTESIAN_POINT('Ctrl Pts',(-52.2759571557968,6.64271282450778,
128.587920411975));
#266338=CARTESIAN_POINT('Ctrl Pts',(-52.5544047796097,1.72579462111621,
124.01761811622));
#266339=CARTESIAN_POINT('Ctrl Pts',(-52.8328524034226,-4.77704452932697,
125.684000628399));
#266340=CARTESIAN_POINT('Ctrl Pts',(-53.1113000272355,-6.89001312891767,
132.05574382713));
#266341=CARTESIAN_POINT('Ctrl Pts',(-53.3897476510484,-2.67139625888694,
137.277526989739));
#266342=CARTESIAN_POINT('Ctrl Pts',(-53.6681952748612,4.00210326809833,
136.550786488079));
#266343=CARTESIAN_POINT('Ctrl Pts',(-53.9466428986742,6.99786540531528,
130.543361339928));
#266344=CARTESIAN_POINT('Ctrl Pts',(-54.225090522487,3.56293109977782,124.775781777402));
#266345=CARTESIAN_POINT('Ctrl Pts',(-54.5035381462999,-3.14616282759469,
124.548171656537));
#266346=CARTESIAN_POINT('Ctrl Pts',(-54.7819857701128,-6.9640868150063,
130.069693559035));
#266347=CARTESIAN_POINT('Ctrl Pts',(-55.0604333939257,-4.382355233982,136.266338597842));
#266348=CARTESIAN_POINT('Ctrl Pts',(-55.3388810177386,2.22654671711671,
137.443692705233));
#266349=CARTESIAN_POINT('Ctrl Pts',(-55.6173286415515,6.78936100803939,
132.519824973462));
#266350=CARTESIAN_POINT('Ctrl Pts',(-55.8957762653644,5.11308421129812,
126.019529303714));
#266351=CARTESIAN_POINT('Ctrl Pts',(-56.1742238891773,-1.26186718757599,
123.916259859391));
#266352=CARTESIAN_POINT('Ctrl Pts',(-56.4526715129901,-6.47722428670686,
128.142818509401));
#266353=CARTESIAN_POINT('Ctrl Pts',(-56.7311191368031,-5.74032869635189,
134.815204333253));
#266354=CARTESIAN_POINT('Ctrl Pts',(-57.0095667606159,0.271648535303317,
137.801820722997));
#266355=CARTESIAN_POINT('Ctrl Pts',(-57.2880143844289,6.03399403378365,
134.358113120779));
#266356=CARTESIAN_POINT('Ctrl Pts',(-57.5664620082417,6.25139379221294,
127.64868057857));
#266357=CARTESIAN_POINT('Ctrl Pts',(-57.8449096320546,0.724068053163303,
123.839163828657));
#266358=CARTESIAN_POINT('Ctrl Pts',(-58.1233572558676,-5.46864085405239,
126.430322658971));
#266359=CARTESIAN_POINT('Ctrl Pts',(-58.4018048796803,-6.63593597435208,
133.0410086896));
#266360=CARTESIAN_POINT('Ctrl Pts',(-58.6802525034934,-1.705130117717,137.596324408362));
#266361=CARTESIAN_POINT('Ctrl Pts',(-58.9587001273061,4.79260701686295,
135.910157209259));
#266362=CARTESIAN_POINT('Ctrl Pts',(-59.2371477511191,6.88617243481463,
129.532012374421));
#266363=CARTESIAN_POINT('Ctrl Pts',(-59.515595374932,2.65168179339722,124.323093417365));
#266364=CARTESIAN_POINT('Ctrl Pts',(-59.7940429987449,-4.01957487429483,
125.070142389788));
#266365=CARTESIAN_POINT('Ctrl Pts',(-60.0724906225578,-6.99703859965941,
131.086657781405));
#266366=CARTESIAN_POINT('Ctrl Pts',(-60.3509382463707,-3.5445656762756,
136.843755870437));
#266367=CARTESIAN_POINT('Ctrl Pts',(-60.6293858701835,3.16518994194552,
137.050944762941));
#266368=CARTESIAN_POINT('Ctrl Pts',(-60.9078334939965,6.96629063164357,
131.517827988445));
#266369=CARTESIAN_POINT('Ctrl Pts',(-61.1862811178092,4.36571055307847,
125.32906955493));
#266370=CARTESIAN_POINT('Ctrl Pts',(-61.4647287416223,-2.24674424694855,
124.171836125139));
#266371=CARTESIAN_POINT('Ctrl Pts',(-61.743176365435,-6.79455084358828,
129.109568687053));
#266372=CARTESIAN_POINT('Ctrl Pts',(-62.0216239892481,-5.09849714723216,
135.60473223792));
#266373=CARTESIAN_POINT('Ctrl Pts',(-62.3000716130609,1.2828263519976,137.688588780872));
#266374=CARTESIAN_POINT('Ctrl Pts',(-62.5785192368738,6.48529510329292,
133.446175954988));
#266375=CARTESIAN_POINT('Ctrl Pts',(-62.8569668606868,5.72809447894126,
126.776063893867));
#266376=CARTESIAN_POINT('Ctrl Pts',(-63.1354144844995,-0.292945138585431,
123.80775972859));
#266377=CARTESIAN_POINT('Ctrl Pts',(-63.4138621083125,-6.04478248491762,
127.268989977326));
#266378=CARTESIAN_POINT('Ctrl Pts',(-63.6923097321254,-6.24176003165182,
133.979053131985));
#266379=CARTESIAN_POINT('Ctrl Pts',(-63.9707573559382,-0.702865036227365,
137.771728958244));
#266380=CARTESIAN_POINT('Ctrl Pts',(-64.2492049797512,5.48192859062395,
135.161733654286));
#266381=CARTESIAN_POINT('Ctrl Pts',(-64.527652603564,6.62909764979204,128.547525399088));
#266382=CARTESIAN_POINT('Ctrl Pts',(-64.806100227377,1.68444981822529,124.007238457143));
#266383=CARTESIAN_POINT('Ctrl Pts',(-65.0845478511898,-4.80812510634223,
125.713174722747));
#266384=CARTESIAN_POINT('Ctrl Pts',(-65.3629954750027,-6.88226794815085,
132.097662107432));
#266385=CARTESIAN_POINT('Ctrl Pts',(-65.6414430988157,-2.63194276308962,
137.29366860422));
#266386=CARTESIAN_POINT('Ctrl Pts',(-65.9198907226284,4.03700924369883,
136.526318081592));
#266387=CARTESIAN_POINT('Ctrl Pts',(-66.1983383464414,6.99614697439381,
130.500768182686));
#266388=CARTESIAN_POINT('Ctrl Pts',(-66.4767859702543,3.5261674164012,124.75420490012));
#266389=CARTESIAN_POINT('Ctrl Pts',(-66.7552335940671,-3.18418773440913,
124.567439155348));
#266390=CARTESIAN_POINT('Ctrl Pts',(-67.0336812178801,-6.96842991351606,
130.112099543802));
#266391=CARTESIAN_POINT('Ctrl Pts',(-67.3121288416929,-4.34902542882876,
136.292914040211));
#266392=CARTESIAN_POINT('Ctrl Pts',(-67.5905764655059,2.26692096324861,
137.43001607195));
#266393=CARTESIAN_POINT('Ctrl Pts',(-67.8690240893187,6.79967773534632,
132.478464422373));
#266394=CARTESIAN_POINT('Ctrl Pts',(-68.1474717131316,5.08386285138514,
125.988493160695));
#266395=CARTESIAN_POINT('Ctrl Pts',(-68.4259193369445,-1.30377363249137,
123.924068823677));
#266396=CARTESIAN_POINT('Ctrl Pts',(-68.7043669607574,-6.49330584099122,
128.182296524302));
#266397=CARTESIAN_POINT('Ctrl Pts',(-68.9828145845703,-5.71580719724563,
134.850073031684));
#266398=CARTESIAN_POINT('Ctrl Pts',(-69.2612622083832,0.314239028063776,
137.800037474531));
#266399=CARTESIAN_POINT('Ctrl Pts',(-69.5397098321961,6.05551493801243,
134.32131664364));
#266400=CARTESIAN_POINT('Ctrl Pts',(-69.818157456009,6.23206844827842,127.610685037641));
#266401=CARTESIAN_POINT('Ctrl Pts',(-70.0966050798218,0.681655508046095,
123.834885269867));
#266402=CARTESIAN_POINT('Ctrl Pts',(-70.3750527036349,-5.49516554335789,
126.463692868828));
#266403=CARTESIAN_POINT('Ctrl Pts',(-70.6535003274475,-6.62219791417695,
133.081362075471));
#266404=CARTESIAN_POINT('Ctrl Pts',(-70.9319479512606,-1.66375391422059,
137.606578180005));
#266405=CARTESIAN_POINT('Ctrl Pts',(-71.2103955750734,4.82359865400735,
135.880888651457));
#266406=CARTESIAN_POINT('Ctrl Pts',(-71.4888431988863,6.87829970509706,
129.490117861946));
#266407=CARTESIAN_POINT('Ctrl Pts',(-71.7672908226993,2.6121793508235,124.307071960521));
#266408=CARTESIAN_POINT('Ctrl Pts',(-72.045738446512,-4.05440621480077,
125.094716924722));
#266409=CARTESIAN_POINT('Ctrl Pts',(-72.3241860703251,-6.99519053777849,
131.129245511046));
#266410=CARTESIAN_POINT('Ctrl Pts',(-72.6026336941378,-3.5077364905931,
136.865220751771));
#266411=CARTESIAN_POINT('Ctrl Pts',(-72.8810813179508,3.20315602899298,
137.031561618638));
#266412=CARTESIAN_POINT('Ctrl Pts',(-73.1595289417638,6.97050464080582,
131.475408981201));
#266413=CARTESIAN_POINT('Ctrl Pts',(-73.4379765655765,4.33230001580124,
125.302595680118));
#266414=CARTESIAN_POINT('Ctrl Pts',(-73.7164241893894,-2.28707667910305,
124.18563558039));
#266415=CARTESIAN_POINT('Ctrl Pts',(-73.9948718132024,-6.80474163581863,
129.150960447132));
#266416=CARTESIAN_POINT('Ctrl Pts',(-74.2733194370152,-5.0691814593271,
135.635679297414));
#266417=CARTESIAN_POINT('Ctrl Pts',(-74.5517670608282,1.32470883500465,
137.680652303954));
#266418=CARTESIAN_POINT('Ctrl Pts',(-74.830214684641,6.5012564255912,133.406649176227));
#266419=CARTESIAN_POINT('Ctrl Pts',(-75.108662308454,5.70346696509291,126.741269991954));
#266420=CARTESIAN_POINT('Ctrl Pts',(-75.3871099322667,-0.335530006474783,
123.809672599606));
#266421=CARTESIAN_POINT('Ctrl Pts',(-75.6655575560798,-6.06619129364391,
127.305851786256));
#266422=CARTESIAN_POINT('Ctrl Pts',(-75.9440051798925,-6.22231913187452,
134.016989677222));
#266423=CARTESIAN_POINT('Ctrl Pts',(-76.2224528037055,-0.66043966510086,
137.775878408018));
#266424=CARTESIAN_POINT('Ctrl Pts',(-76.5009004275184,5.50835158962877,
135.128282866967));
#266425=CARTESIAN_POINT('Ctrl Pts',(-76.7793480513312,6.61523683142527,
128.507214014061));
#266426=CARTESIAN_POINT('Ctrl Pts',(-77.0577956751442,1.64304259742666,
123.997110667925));
#266427=CARTESIAN_POINT('Ctrl Pts',(-77.336243298957,-4.83902751651344,
125.742537472861));
#266428=CARTESIAN_POINT('Ctrl Pts',(-77.6146909227699,-6.87426774241415,
132.139532463972));
#266429=CARTESIAN_POINT('Ctrl Pts',(-77.8931385465828,-2.59239173968542,
137.309569755007));
#266430=CARTESIAN_POINT('Ctrl Pts',(-78.1715861703958,4.07176562643718,
136.501637645866));
#266431=CARTESIAN_POINT('Ctrl Pts',(-78.4500337942086,6.99416929867323,
130.458186275174));
#266432=CARTESIAN_POINT('Ctrl Pts',(-78.7284814180215,3.48927306959449,
124.732852213582));
#266433=CARTESIAN_POINT('Ctrl Pts',(-79.0069290418344,-3.22209464997582,
124.586937765577));
#266434=CARTESIAN_POINT('Ctrl Pts',(-79.2853766656473,-6.97251479429268,
130.154531180556));
#266435=CARTESIAN_POINT('Ctrl Pts',(-79.5638242894601,-4.3155344689392,
136.319286102215));
#266436=CARTESIAN_POINT('Ctrl Pts',(-79.8422719132732,2.30721120779087,
137.416093922569));
#266437=CARTESIAN_POINT('Ctrl Pts',(-80.1207195370859,6.80974249809405,
132.437041836753));
#266438=CARTESIAN_POINT('Ctrl Pts',(-80.3991671608989,5.0544531070646,125.957635471416));
#266439=CARTESIAN_POINT('Ctrl Pts',(-80.6776147847117,-1.34563176559565,
123.932132739704));
#266440=CARTESIAN_POINT('Ctrl Pts',(-80.9560624085247,-6.50914678343976,
128.221871700751));
#266441=CARTESIAN_POINT('Ctrl Pts',(-81.2345100323374,-5.69107389680138,
134.884791814753));
#266442=CARTESIAN_POINT('Ctrl Pts',(-81.5129576561506,0.356817876581242,
137.797994998686));
#266443=CARTESIAN_POINT('Ctrl Pts',(-81.7914052799631,6.07681145290804,
134.284389844403));
#266444=CARTESIAN_POINT('Ctrl Pts',(-82.0698529037763,6.21251217275584,
127.572807839535));
#266445=CARTESIAN_POINT('Ctrl Pts',(-82.348300527589,0.639217703933302,
123.830864967548));
#266446=CARTESIAN_POINT('Ctrl Pts',(-82.626748151402,-5.52148660728364,
126.497223923725));
#266447=CARTESIAN_POINT('Ctrl Pts',(-82.9051957752149,-6.60821446602265,
133.121631086217));
#266448=CARTESIAN_POINT('Ctrl Pts',(-83.1836433990278,-1.62231605971109,
137.616579892973));
#266449=CARTESIAN_POINT('Ctrl Pts',(-83.4620910228406,4.85441155092967,
135.851431981043));
#266450=CARTESIAN_POINT('Ctrl Pts',(-83.7405386466535,6.87017209745416,
129.448272049221));
#266451=CARTESIAN_POINT('Ctrl Pts',(-84.0189862704665,2.57258011298421,
124.291291263097));
#266452=CARTESIAN_POINT('Ctrl Pts',(-84.2974338942792,-4.08908731779306,
125.119503032603));
#266453=CARTESIAN_POINT('Ctrl Pts',(-84.5758815180923,-6.99308326653956,
131.171821201958));
#266454=CARTESIAN_POINT('Ctrl Pts',(-84.8543291419051,-3.47077732444568,
136.886461045702));
#266455=CARTESIAN_POINT('Ctrl Pts',(-85.132776765718,3.2410034219148,137.011947723114));
#266456=CARTESIAN_POINT('Ctrl Pts',(-85.4112243895309,6.97446035535538,
131.432965108015));
#266457=CARTESIAN_POINT('Ctrl Pts',(-85.6896720133437,4.29872894355427,
125.27632567523));
#266458=CARTESIAN_POINT('Ctrl Pts',(-85.9681196371569,-2.327324362789,124.19968029493));
#266459=CARTESIAN_POINT('Ctrl Pts',(-86.2465672609694,-6.81468027584547,
129.192413474561));
#266460=CARTESIAN_POINT('Ctrl Pts',(-86.5250148847825,-5.03967793103904,
135.666447330617));
#266461=CARTESIAN_POINT('Ctrl Pts',(-86.8034625085954,1.36654223043768,
137.672461023519));
#266462=CARTESIAN_POINT('Ctrl Pts',(-87.0819101324082,6.51697684144191,
133.367025968708));
#266463=CARTESIAN_POINT('Ctrl Pts',(-87.3603577562212,5.67862810717874,
126.706626649358));
#266464=CARTESIAN_POINT('Ctrl Pts',(-87.638805380034,-0.378102441176264,
123.811844661359));
#266465=CARTESIAN_POINT('Ctrl Pts',(-87.917253003847,-6.08737531742114,
127.342843233717));
#266466=CARTESIAN_POINT('Ctrl Pts',(-88.1957006276599,-6.20264766177327,
134.054807177307));
#266467=CARTESIAN_POINT('Ctrl Pts',(-88.4741482514726,-0.617989821139493,
137.779769525637));
#266468=CARTESIAN_POINT('Ctrl Pts',(-88.7525958752857,5.53457047463998,
135.094671855119));
#266469=CARTESIAN_POINT('Ctrl Pts',(-89.0310434990984,6.6011308830247,128.466987750645));
#266470=CARTESIAN_POINT('Ctrl Pts',(-89.3094911229114,1.60157449308101,
123.987235123859));
#266471=CARTESIAN_POINT('Ctrl Pts',(-89.5879387467241,-4.86975061474005,
125.772087790693));
#266472=CARTESIAN_POINT('Ctrl Pts',(-89.8663863705374,-6.8660128081587,
132.181353345229));
#266473=CARTESIAN_POINT('Ctrl Pts',(-90.1448339943499,-2.55274465425183,
137.325229852876));
#266474=CARTESIAN_POINT('Ctrl Pts',(-90.4232816181632,4.10637112840284,
136.476746095445));
#266475=CARTESIAN_POINT('Ctrl Pts',(-90.7017292419757,6.99193245143733,
130.415617195278));
#266476=CARTESIAN_POINT('Ctrl Pts',(-90.9801768657889,3.45224942649073,
124.711724509022));
#266477=CARTESIAN_POINT('Ctrl Pts',(-91.2586244896016,-3.2598821696406,
124.606666764696));
#266478=CARTESIAN_POINT('Ctrl Pts',(-91.5370721134145,-6.97634130596949,
130.196986896981));
#266479=CARTESIAN_POINT('Ctrl Pts',(-91.8155197372274,-4.28188359533257,
136.345453806627));
#266480=CARTESIAN_POINT('Ctrl Pts',(-92.0939673610402,2.34741595777304,
137.401926772977));
#266481=CARTESIAN_POINT('Ctrl Pts',(-92.3724149848533,6.81955492332935,
132.395558751529));
#266482=CARTESIAN_POINT('Ctrl Pts',(-92.650862608666,5.02485606812542,125.926957379319));
#266483=CARTESIAN_POINT('Ctrl Pts',(-92.929310232479,-1.38744003581995,
123.940451308663));
#266484=CARTESIAN_POINT('Ctrl Pts',(-93.2077578562919,-6.52474652706058,
128.261542572277));
#266485=CARTESIAN_POINT('Ctrl Pts',(-93.4862054801047,-5.66612971152105,
134.919359395943));
#266486=CARTESIAN_POINT('Ctrl Pts',(-93.7646531039176,0.39938350308132,
137.795693371147));
#266487=CARTESIAN_POINT('Ctrl Pts',(-94.0431007277306,6.09788278932073,
134.247334091402));
#266488=CARTESIAN_POINT('Ctrl Pts',(-94.3215483515434,6.19272569030992,
127.535050387806));
#266489=CARTESIAN_POINT('Ctrl Pts',(-94.5999959753563,0.596756213373149,
123.827103070676));
#266490=CARTESIAN_POINT('Ctrl Pts',(-94.8784435991693,-5.54760307049237,
126.530914581157));
#266491=CARTESIAN_POINT('Ctrl Pts',(-95.1568912229821,-6.59398614805128,
133.161814229653));
#266492=CARTESIAN_POINT('Ctrl Pts',(-95.4353388467949,-1.58081808968337,
137.626329176652));
#266493=CARTESIAN_POINT('Ctrl Pts',(-95.7137864706081,4.88504456584684,
135.821788289543));
#266494=CARTESIAN_POINT('Ctrl Pts',(-95.9922340944205,6.86178991305786,
129.406476486855));
#266495=CARTESIAN_POINT('Ctrl Pts',(-96.2706817182339,2.53288554724217,
124.275751909854));
#266496=CARTESIAN_POINT('Ctrl Pts',(-96.5491293420464,-4.12361689815126,
125.144499794972));
#266497=CARTESIAN_POINT('Ctrl Pts',(-96.8275769658595,-6.99071686402826,
131.214383276482));
#266498=CARTESIAN_POINT('Ctrl Pts',(-97.1060245896722,-3.4336895473684,
136.907475965166));
#266499=CARTESIAN_POINT('Ctrl Pts',(-97.3844722134854,3.27873071826322,
136.992103803166));
#266500=CARTESIAN_POINT('Ctrl Pts',(-97.6629198372979,6.9781576287114,131.390497941658));
#266501=CARTESIAN_POINT('Ctrl Pts',(-97.9413674611112,4.26499858032525,
125.250260513709));
#266502=CARTESIAN_POINT('Ctrl Pts',(-98.2198150849237,-2.36748580661544,
124.21396974833));
#266503=CARTESIAN_POINT('Ctrl Pts',(-98.498262708737,-6.82436639538843,
129.233926233285));
#266504=CARTESIAN_POINT('Ctrl Pts',(-98.7767103325495,-5.00998765563179,
135.69703519741));
#266505=CARTESIAN_POINT('Ctrl Pts',(-99.0551579563628,1.40832498814648,
137.664015243098));
#266506=CARTESIAN_POINT('Ctrl Pts',(-99.3336055801754,6.53245576831905,
133.327307800681));
#266507=CARTESIAN_POINT('Ctrl Pts',(-99.6120532039884,5.65357882561176,
126.672135149802));
#266508=CARTESIAN_POINT('Ctrl Pts',(-99.8905008278013,-0.420660865152761,
123.814275833361));
#266509=CARTESIAN_POINT('Ctrl Pts',(-100.168948451614,-6.10833377126732,
127.379962948978));
#266510=CARTESIAN_POINT('Ctrl Pts',(-100.447396075427,-6.18274635028192,
134.092504230901));
#266511=CARTESIAN_POINT('Ctrl Pts',(-100.72584369924,-0.575517077338011,
137.783402166914));
#266512=CARTESIAN_POINT('Ctrl Pts',(-101.004291323053,5.56058427410689,
135.060901864211));
#266513=CARTESIAN_POINT('Ctrl Pts',(-101.282738946866,6.58678032729173,
128.426848099441));
#266514=CARTESIAN_POINT('Ctrl Pts',(-101.561186570679,1.56004704180311,
123.977612190885));
#266515=CARTESIAN_POINT('Ctrl Pts',(-101.839634194492,-4.90029326256724,
125.801824581246));
#266516=CARTESIAN_POINT('Ctrl Pts',(-102.118081818304,-6.85750345127332,
132.223123201514));
#266517=CARTESIAN_POINT('Ctrl Pts',(-102.396529442117,-2.51300297592632,
137.340648317539));
#266518=CARTESIAN_POINT('Ctrl Pts',(-102.67497706593,4.14082446727623,136.451644352694));
#266519=CARTESIAN_POINT('Ctrl Pts',(-102.953424689743,6.98943651557314,
130.373062520413));
#266520=CARTESIAN_POINT('Ctrl Pts',(-103.231872313556,3.41509785901489,
124.690822569333));
#266521=CARTESIAN_POINT('Ctrl Pts',(-103.510319937369,-3.29754889317273,
124.626625421641));
#266522=CARTESIAN_POINT('Ctrl Pts',(-103.788767561182,-6.97990930675369,
130.239465119861));
#266523=CARTESIAN_POINT('Ctrl Pts',(-104.067215184995,-4.24807405495459,
136.371416183792));
#266524=CARTESIAN_POINT('Ctrl Pts',(-104.345662808808,2.38753372339306,
137.387515148146));
#266525=CARTESIAN_POINT('Ctrl Pts',(-104.62411043262,6.82911464744894,132.354016703874));
#266526=CARTESIAN_POINT('Ctrl Pts',(-104.902558056433,4.99507283129728,
125.896460021193));
#266527=CARTESIAN_POINT('Ctrl Pts',(-105.181005680246,-1.42919689394351,
123.949024222305));
#266528=CARTESIAN_POINT('Ctrl Pts',(-105.459453304059,-6.54010449379936,
128.301307668861));
#266529=CARTESIAN_POINT('Ctrl Pts',(-105.737900927872,-5.64097556572054,
134.953774494342));
#266530=CARTESIAN_POINT('Ctrl Pts',(-106.016348551685,0.441934330278796,
137.793132677202));
#266531=CARTESIAN_POINT('Ctrl Pts',(-106.294796175498,6.11872816644418,
134.210150757753));
#266532=CARTESIAN_POINT('Ctrl Pts',(-106.573243799311,6.17270973413615,
127.49741408157));
#266533=CARTESIAN_POINT('Ctrl Pts',(-106.851691423124,0.554272609792058,
123.823599718647));
#266534=CARTESIAN_POINT('Ctrl Pts',(-107.130139046936,-5.57351396522919,
126.564763592701));
#266535=CARTESIAN_POINT('Ctrl Pts',(-107.40858667075,-6.57951348749827,
133.201910016778));
#266536=CARTESIAN_POINT('Ctrl Pts',(-107.687034294562,-1.53926154185996,
137.635825669776));
#266537=CARTESIAN_POINT('Ctrl Pts',(-107.965481918375,4.91549656364115,
135.791958675416));
#266538=CARTESIAN_POINT('Ctrl Pts',(-108.243929542188,6.85315346251289,
129.364732723601));
#266539=CARTESIAN_POINT('Ctrl Pts',(-108.522377166001,2.49309712449469,
124.260454476607));
#266540=CARTESIAN_POINT('Ctrl Pts',(-108.800824789814,-4.15799367636883,
125.169706285567));
#266541=CARTESIAN_POINT('Ctrl Pts',(-109.079272413627,-6.98809141793296,
131.256930157466));
#266542=CARTESIAN_POINT('Ctrl Pts',(-109.35772003744,-3.39647453366164,
136.928264731447));
#266543=CARTESIAN_POINT('Ctrl Pts',(-109.636167661252,3.31633652003941,
136.97203059412));
#266544=CARTESIAN_POINT('Ctrl Pts',(-109.914615285065,6.98159632387027,
131.348009055767));
#266545=CARTESIAN_POINT('Ctrl Pts',(-110.193062908878,4.23111017600536,
125.22440116141));
#266546=CARTESIAN_POINT('Ctrl Pts',(-110.471510532691,-2.40755952238467,
124.228503411086));
#266547=CARTESIAN_POINT('Ctrl Pts',(-110.749958156504,-6.83379963552497,
129.275497185033));
#266548=CARTESIAN_POINT('Ctrl Pts',(-111.028405780317,-4.98011173328953,
135.727441764346));
#266549=CARTESIAN_POINT('Ctrl Pts',(-111.30685340413,1.45005555985492,137.655315275653));
#266550=CARTESIAN_POINT('Ctrl Pts',(-111.585301027943,6.54769263264538,
133.287496143919));
#266551=CARTESIAN_POINT('Ctrl Pts',(-111.863748651756,5.62832004860235,
126.63779677138));
#266552=CARTESIAN_POINT('Ctrl Pts',(-112.142196275568,-0.463203701385527,
123.816966025527));
#266553=CARTESIAN_POINT('Ctrl Pts',(-112.420643899382,-6.12906587855929,
127.417209556553));
#266554=CARTESIAN_POINT('Ctrl Pts',(-112.699091523194,-6.16261593485082,
134.130079441122));
#266555=CARTESIAN_POINT('Ctrl Pts',(-112.977539147007,-0.533023007539609,
137.786776197239));
#266556=CARTESIAN_POINT('Ctrl Pts',(-113.25598677082,5.58639202407863,135.026974145601));
#266557=CARTESIAN_POINT('Ctrl Pts',(-113.534434394633,6.57218569599142,
128.386796547837));
#266558=CARTESIAN_POINT('Ctrl Pts',(-113.812882018446,1.5184617824084,123.968242225583));
#266559=CARTESIAN_POINT('Ctrl Pts',(-114.091329642259,-4.93065432822552,
125.831746742611));
#266560=CARTESIAN_POINT('Ctrl Pts',(-114.369777266072,-6.84873998707567,
132.26484048503));
#266561=CARTESIAN_POINT('Ctrl Pts',(-114.648224889884,-2.4731681773514,
137.355824577657));
#266562=CARTESIAN_POINT('Ctrl Pts',(-114.926672513697,4.17512436637621,
136.426333347767));
#266563=CARTESIAN_POINT('Ctrl Pts',(-115.20512013751,6.98668158356849,130.330523827459));
#266564=CARTESIAN_POINT('Ctrl Pts',(-115.483567761323,3.377819743832,124.670147169045));
#266565=CARTESIAN_POINT('Ctrl Pts',(-115.762015385136,-3.33509342481799,
124.646812996834));
#266566=CARTESIAN_POINT('Ctrl Pts',(-116.040463008949,-6.98321866443162,
130.281964275151));
#266567=CARTESIAN_POINT('Ctrl Pts',(-116.318910632762,-4.21410710063033,
136.397172271667));
#266568=CARTESIAN_POINT('Ctrl Pts',(-116.597358256575,2.42756301807353,
137.372859582102));
#266569=CARTESIAN_POINT('Ctrl Pts',(-116.875805880388,6.83842131621399,
132.312417233142));
#266570=CARTESIAN_POINT('Ctrl Pts',(-117.154253504201,4.96510450020791,
125.866144527128));
#266571=CARTESIAN_POINT('Ctrl Pts',(-117.432701128013,-1.47090079265054,
123.957851162959));
#266572=CARTESIAN_POINT('Ctrl Pts',(-117.711148751826,-6.55522011456102,
128.341165516992));
#266573=CARTESIAN_POINT('Ctrl Pts',(-117.989596375639,-5.61561239149597,
134.988035834682));
#266574=CARTESIAN_POINT('Ctrl Pts',(-118.268043999452,0.484468781437156,
137.790313011739));
#266575=CARTESIAN_POINT('Ctrl Pts',(-118.546491623265,6.13934681184524,
134.172841221298));
#266576=CARTESIAN_POINT('Ctrl Pts',(-118.824939247078,6.15246504593319,
127.459900315453));
#266577=CARTESIAN_POINT('Ctrl Pts',(-119.103386870891,0.511768467435545,
123.820355041281));
#266578=CARTESIAN_POINT('Ctrl Pts',(-119.381834494704,-5.59921833135585,
126.598769704074));
#266579=CARTESIAN_POINT('Ctrl Pts',(-119.660282118516,-6.56479702065358,
133.241916961827));
#266580=CARTESIAN_POINT('Ctrl Pts',(-119.93872974233,-1.49764795613459,
137.645069020452));
#266581=CARTESIAN_POINT('Ctrl Pts',(-120.217177366142,4.94576641590264,
135.761944244007));
#266582=CARTESIAN_POINT('Ctrl Pts',(-120.495624989955,6.84426306584611,
129.323042306287));
#266583=CARTESIAN_POINT('Ctrl Pts',(-120.774072613768,2.45321631911644,
124.245399530209));
#266584=CARTESIAN_POINT('Ctrl Pts',(-121.052520237581,-4.19221637860163,
125.195121570349));
#266585=CARTESIAN_POINT('Ctrl Pts',(-121.330967861394,-6.98520702554029,
131.299460268319));
#266586=CARTESIAN_POINT('Ctrl Pts',(-121.609415485207,-3.35913366234199,
136.948826574209));
#266587=CARTESIAN_POINT('Ctrl Pts',(-121.88786310902,3.3538194337463,136.951728839794));
#266588=CARTESIAN_POINT('Ctrl Pts',(-122.166310732833,6.98477631340985,
131.305500024783));
#266589=CARTESIAN_POINT('Ctrl Pts',(-122.444758356646,4.19706498634193,
125.198748576561));
#266590=CARTESIAN_POINT('Ctrl Pts',(-122.723205980458,-2.44754402515043,
124.24328074465));
#266591=CARTESIAN_POINT('Ctrl Pts',(-123.001653604271,-6.84297964670285,
129.317124789377));
#266592=CARTESIAN_POINT('Ctrl Pts',(-123.280101228084,-4.95005127107555,
135.7576659047));
#266593=CARTESIAN_POINT('Ctrl Pts',(-123.558548851897,1.49173239922134,
137.646361443563));
#266594=CARTESIAN_POINT('Ctrl Pts',(-123.83699647571,6.5626868698133,133.247592473656));
#266595=CARTESIAN_POINT('Ctrl Pts',(-124.115444099523,5.60285271212367,
126.603612786514));
#266596=CARTESIAN_POINT('Ctrl Pts',(-124.393891723336,-0.505729373435472,
123.819915138168));
#266597=CARTESIAN_POINT('Ctrl Pts',(-124.672339347149,-6.14957087106115,
127.454581676257));
#266598=CARTESIAN_POINT('Ctrl Pts',(-124.950786970961,-6.14225716141998,
134.167531415611));
#266599=CARTESIAN_POINT('Ctrl Pts',(-125.229234594775,-0.490509186377616,
137.789891491587));
#266600=CARTESIAN_POINT('Ctrl Pts',(-125.507682218587,5.6119927682395,134.992889956494));
#266601=CARTESIAN_POINT('Ctrl Pts',(-125.786129842401,6.55734752993325,
128.346834579959));
#266602=CARTESIAN_POINT('Ctrl Pts',(-126.064577466213,1.47682025585389,
123.959125575163));
#266603=CARTESIAN_POINT('Ctrl Pts',(-126.343025090026,-4.9608326866744,
125.861853166013));
#266604=CARTESIAN_POINT('Ctrl Pts',(-126.621472713839,-6.8397227402992,
132.306503649927));
#266605=CARTESIAN_POINT('Ctrl Pts',(-126.899920337652,-2.43324173462049,
137.370758070868));
#266606=CARTESIAN_POINT('Ctrl Pts',(-127.178367961465,4.20926955470684,
136.400814018573));
#266607=CARTESIAN_POINT('Ctrl Pts',(-127.456815585278,6.98366775750873,
130.288002692701));
#266608=CARTESIAN_POINT('Ctrl Pts',(-127.73526320909,3.34041646229627,124.649699074291));
#266609=CARTESIAN_POINT('Ctrl Pts',(-128.013710832904,-3.37251437334987,
124.66722874222));
#266610=CARTESIAN_POINT('Ctrl Pts',(-128.292158456716,-6.9862692563739,
130.324482788031));
#266611=CARTESIAN_POINT('Ctrl Pts',(-128.570606080529,-4.17998399101771,
136.422721115849));
#266612=CARTESIAN_POINT('Ctrl Pts',(-128.849053704342,2.46750235851359,
137.357960617914));
#266613=CARTESIAN_POINT('Ctrl Pts',(-129.127501328155,6.84747458476236,
132.270761880817));
#266614=CARTESIAN_POINT('Ctrl Pts',(-129.405948951968,4.93495218534535,
125.836012020477));
#266615=CARTESIAN_POINT('Ctrl Pts',(-129.684396575781,-1.51255018658779,
123.966931803538));
#266616=CARTESIAN_POINT('Ctrl Pts',(-129.962844199593,-6.57009282923063,
128.381114639724));
#266617=CARTESIAN_POINT('Ctrl Pts',(-130.241291823406,-5.59004112868908,
135.022142147398));
#266618=CARTESIAN_POINT('Ctrl Pts',(-130.519739447219,0.52698528042665,
137.78723447924));
#266619=CARTESIAN_POINT('Ctrl Pts',(-130.798187071032,6.15973796149245,
134.135406864555));
#266620=CARTESIAN_POINT('Ctrl Pts',(-131.076634694845,6.13199237587537,
127.422510479544));
#266621=CARTESIAN_POINT('Ctrl Pts',(-131.355082318658,0.4692453613103,123.81736915881));
#266622=CARTESIAN_POINT('Ctrl Pts',(-131.633529942471,-5.62471521638866,
126.632931655165));
#266623=CARTESIAN_POINT('Ctrl Pts',(-131.911977566284,-6.54983729284086,
133.281833582332));
#266624=CARTESIAN_POINT('Ctrl Pts',(-132.190425190097,-1.45597887451291,
137.654058886162));
#266625=CARTESIAN_POINT('Ctrl Pts',(-132.46887281391,4.97585300097076,135.731746107516));
#266626=CARTESIAN_POINT('Ctrl Pts',(-132.747320437723,6.83511905249447,
129.281406779768));
#266627=CARTESIAN_POINT('Ctrl Pts',(-133.025768061535,2.4132446089053,124.230587628526));
#266628=CARTESIAN_POINT('Ctrl Pts',(-133.304215685348,-4.22628373671482,
125.220744707546));
#266629=CARTESIAN_POINT('Ctrl Pts',(-133.582663309161,-6.98206379373247,
131.341972033073));
#266630=CARTESIAN_POINT('Ctrl Pts',(-133.861110932974,-3.32166831708915,
136.969160731525));
#266631=CARTESIAN_POINT('Ctrl Pts',(-134.139558556787,3.39117807044069,
136.931199292478));
#266632=CARTESIAN_POINT('Ctrl Pts',(-134.4180061806,6.98769747949419,131.262972423894));
#266633=CARTESIAN_POINT('Ctrl Pts',(-134.696453804413,4.16286427289247,
125.173303709728));
#266634=CARTESIAN_POINT('Ctrl Pts',(-134.974901428226,-2.48743783327188,
124.25830120144));
#266635=CARTESIAN_POINT('Ctrl Pts',(-135.253349052039,-6.85190608875344,
129.358807503792));
#266636=CARTESIAN_POINT('Ctrl Pts',(-135.531796675851,-4.91980738289134,
135.787706498505));
#266637=CARTESIAN_POINT('Ctrl Pts',(-135.810244299665,1.53335396189511,
137.637154078616));
#266638=CARTESIAN_POINT('Ctrl Pts',(-136.088691923477,6.57743792420584,
133.207598268539));
#266639=CARTESIAN_POINT('Ctrl Pts',(-136.36713954729,5.57717775987727,126.569584461903));
#266640=CARTESIAN_POINT('Ctrl Pts',(-136.645587171103,-0.548236305497475,
123.823123062006));
#266641=CARTESIAN_POINT('Ctrl Pts',(-136.924034794916,-6.1698479889529,
127.492077923251));
#266642=CARTESIAN_POINT('Ctrl Pts',(-137.202482418729,-6.12167078439119,
134.204858766568));
#266643=CARTESIAN_POINT('Ctrl Pts',(-137.480930042542,-0.447977189217358,
137.792747934521));
#266644=CARTESIAN_POINT('Ctrl Pts',(-137.759377666354,5.63738555794455,
134.958650559891));
#266645=CARTESIAN_POINT('Ctrl Pts',(-138.037825290167,6.54226637895086,
128.306963676612));
#266646=CARTESIAN_POINT('Ctrl Pts',(-138.31627291398,1.43512400518173,123.950262577445));
#266647=CARTESIAN_POINT('Ctrl Pts',(-138.594720537793,-4.99082721964375,
125.892142735845));
#266648=CARTESIAN_POINT('Ctrl Pts',(-138.873168161606,-6.83045204508126,
132.348111152362));
#266649=CARTESIAN_POINT('Ctrl Pts',(-139.151615785419,-2.39322512722196,
137.385448243807));
#266650=CARTESIAN_POINT('Ctrl Pts',(-139.430063409232,4.24325876700673,
136.375087310741));
#266651=CARTESIAN_POINT('Ctrl Pts',(-139.708511033045,6.98039514907165,
130.245500691775));
#266652=CARTESIAN_POINT('Ctrl Pts',(-139.986958656858,3.30288940040013,
124.629479042785));
#266653=CARTESIAN_POINT('Ctrl Pts',(-140.26540628067,-3.40981035212143,
124.687871901284));
#266654=CARTESIAN_POINT('Ctrl Pts',(-140.543853904484,-6.98906096953965,
130.36701908296));
#266655=CARTESIAN_POINT('Ctrl Pts',(-140.822301528296,-4.1457059905611,
136.448061769617));
#266656=CARTESIAN_POINT('Ctrl Pts',(-141.100749152109,2.50735026474636,
137.342818807668));
#266657=CARTESIAN_POINT('Ctrl Pts',(-141.379196775922,6.85627411762182,
132.229052190456));
#266658=CARTESIAN_POINT('Ctrl Pts',(-141.657644399735,4.90461700401472,
125.80606361781));
#266659=CARTESIAN_POINT('Ctrl Pts',(-141.936092023548,-1.5541435324211,
123.976265807557));
#266660=CARTESIAN_POINT('Ctrl Pts',(-142.214539647361,-6.58472208669408,
128.421153556726));
#266661=CARTESIAN_POINT('Ctrl Pts',(-142.492987271174,-5.56426272485295,
135.056092168669));
#266662=CARTESIAN_POINT('Ctrl Pts',(-142.771434894987,0.569482251782813,
137.783897193782));
#266663=CARTESIAN_POINT('Ctrl Pts',(-143.0498825188,6.17990085978423,134.097849074668));
#266664=CARTESIAN_POINT('Ctrl Pts',(-143.328330142612,6.11129248258502,
127.385245959334));
#266665=CARTESIAN_POINT('Ctrl Pts',(-143.606777766425,0.426704867125613,
123.814642181877));
#266666=CARTESIAN_POINT('Ctrl Pts',(-143.885225390238,-5.65000367553061,
126.667248180088));
#266667=CARTESIAN_POINT('Ctrl Pts',(-144.163673014051,-6.53463485839856,
133.321658399163));
#266668=CARTESIAN_POINT('Ctrl Pts',(-144.442120637864,-1.4142558410586,
137.662794933783));
#266669=CARTESIAN_POINT('Ctrl Pts',(-144.720568261677,5.00575520397605,
135.701365384942));
#266670=CARTESIAN_POINT('Ctrl Pts',(-144.99901588549,6.82572176129271,129.239827686864));
#266671=CARTESIAN_POINT('Ctrl Pts',(-145.277463509303,2.37318347502772,
124.216019320419));
#266672=CARTESIAN_POINT('Ctrl Pts',(-145.555911133116,-4.26019448832994,
125.246574747685));
#266673=CARTESIAN_POINT('Ctrl Pts',(-145.834358756928,-6.97866183898313,
131.384463876438));
#266674=CARTESIAN_POINT('Ctrl Pts',(-146.112806380741,-3.28407988619528,
136.989266449907));
#266675=CARTESIAN_POINT('Ctrl Pts',(-146.391254004554,3.42841104578457,
136.910442712901));
#266676=CARTESIAN_POINT('Ctrl Pts',(-146.669701628367,6.99035971387901,
131.220427828976));
#266677=CARTESIAN_POINT('Ctrl Pts',(-146.94814925218,4.12850930297597,125.148067503779));
#266678=CARTESIAN_POINT('Ctrl Pts',(-147.226596875993,-2.52723946847004,
124.27356422487));
#266679=CARTESIAN_POINT('Ctrl Pts',(-147.505044499806,-6.86057863090408,
129.400543783708));
#266680=CARTESIAN_POINT('Ctrl Pts',(-147.783492123619,-4.88938118943532,
135.817562432597));
#266681=CARTESIAN_POINT('Ctrl Pts',(-148.061939747432,1.57491870557395,
137.627693521995));
#266682=CARTESIAN_POINT('Ctrl Pts',(-148.340387371245,6.5919452492172,133.167515010566));
#266683=CARTESIAN_POINT('Ctrl Pts',(-148.618834995057,5.55129614325799,
126.535713058481));
#266684=CARTESIAN_POINT('Ctrl Pts',(-148.89728261887,-0.590722922461593,
123.826589678167));
#266685=CARTESIAN_POINT('Ctrl Pts',(-149.175730242683,-6.18989648085842,
127.529696908099));
#266686=CARTESIAN_POINT('Ctrl Pts',(-149.454177866496,-6.10085756660025,
134.242060110815));
#266687=CARTESIAN_POINT('Ctrl Pts',(-149.732625490309,-0.405428592098244,
137.795345420191));
#266688=CARTESIAN_POINT('Ctrl Pts',(-150.011073114122,5.66256945225453,
134.924257224548));
#266689=CARTESIAN_POINT('Ctrl Pts',(-150.289520737935,6.52694280188189,
128.267185315226));
#266690=CARTESIAN_POINT('Ctrl Pts',(-150.567968361748,1.39337457546175,
123.94165356085));
#266691=CARTESIAN_POINT('Ctrl Pts',(-150.84641598556,-5.02063681567507,
125.922614329717));
#266692=CARTESIAN_POINT('Ctrl Pts',(-151.124863609373,-6.8209282449509,
132.389661450552));
#266693=CARTESIAN_POINT('Ctrl Pts',(-151.403311233186,-2.35311983798619,
137.399894552124));
#266694=CARTESIAN_POINT('Ctrl Pts',(-151.681758856999,4.2770907437925,136.349154177582));
#266695=CARTESIAN_POINT('Ctrl Pts',(-151.960206480812,6.97686387952531,
130.20301939961));
#266696=CARTESIAN_POINT('Ctrl Pts',(-152.238654104625,3.26523994872261,
124.609487823786));
#266697=CARTESIAN_POINT('Ctrl Pts',(-152.517101728438,-3.44697997911642,
124.708741709087));
#266698=CARTESIAN_POINT('Ctrl Pts',(-152.795549352251,-6.99159370048095,
130.40957158374));
#266699=CARTESIAN_POINT('Ctrl Pts',(-153.073996976064,-4.11127436944443,
136.473193293963));
#266700=CARTESIAN_POINT('Ctrl Pts',(-153.352444599876,2.54710526019297,
137.327434712448));
#266701=CARTESIAN_POINT('Ctrl Pts',(-153.63089222369,6.86481958872245,132.187289707623));
#266702=CARTESIAN_POINT('Ctrl Pts',(-153.909339847502,4.87410008029735,
125.776300428876));
#266703=CARTESIAN_POINT('Ctrl Pts',(-154.187787471315,-1.5956792888948,
123.98585282914));
#266704=CARTESIAN_POINT('Ctrl Pts',(-154.466235095128,-6.5991073448593,
128.461280784342));
#266705=CARTESIAN_POINT('Ctrl Pts',(-154.744682718941,-5.53827813521478,
135.089884640464));
#266706=CARTESIAN_POINT('Ctrl Pts',(-155.023130342754,0.611958120764675,
137.78030127903));
#266707=CARTESIAN_POINT('Ctrl Pts',(-155.301577966567,6.19983475957701,
134.060169243357));
#266708=CARTESIAN_POINT('Ctrl Pts',(-155.58002559038,6.0903661331043,127.348108135675));
#266709=CARTESIAN_POINT('Ctrl Pts',(-155.858473214192,0.38414856123516,
123.812174211531));
#266710=CARTESIAN_POINT('Ctrl Pts',(-156.136920838005,-5.67508277170857,
126.701718007236));
#266711=CARTESIAN_POINT('Ctrl Pts',(-156.415368461818,-6.51919028065846,
133.3613899366));
#266712=CARTESIAN_POINT('Ctrl Pts',(-156.693816085631,-1.37248040183399,
137.671276839599));
#266713=CARTESIAN_POINT('Ctrl Pts',(-156.972263709444,5.03547191688086,
135.670803202055));
#266714=CARTESIAN_POINT('Ctrl Pts',(-157.250711333257,6.81607154046107,
129.198306568304));
#266715=CARTESIAN_POINT('Ctrl Pts',(-157.52915895707,2.33303440196427,124.201695145721));
#266716=CARTESIAN_POINT('Ctrl Pts',(-157.807606580883,-4.29394737687161,
125.272610733624));
#266717=CARTESIAN_POINT('Ctrl Pts',(-158.086054204696,-6.97500128735293,
131.426934223863));
#266718=CARTESIAN_POINT('Ctrl Pts',(-158.364501828508,-3.2463697625135,
137.009142984327));
#266719=CARTESIAN_POINT('Ctrl Pts',(-158.642949452322,3.46551698009634,
136.889459870208));
#266720=CARTESIAN_POINT('Ctrl Pts',(-158.921397076134,6.99276291791392,
131.177867816534));
#266721=CARTESIAN_POINT('Ctrl Pts',(-159.199844699947,4.09400134962899,
125.123040893851));
#266722=CARTESIAN_POINT('Ctrl Pts',(-159.47829232376,-2.56694745588028,
124.289069249361));
#266723=CARTESIAN_POINT('Ctrl Pts',(-159.756739947573,-6.86899695179061,
129.442332082575));
#266724=CARTESIAN_POINT('Ctrl Pts',(-160.035187571386,-4.85877381816122,
135.84723260065));
#266725=CARTESIAN_POINT('Ctrl Pts',(-160.313635195198,1.61642509006095,
137.617980124263));
#266726=CARTESIAN_POINT('Ctrl Pts',(-160.592082819012,6.60620830727321,
133.12734418504));
#266727=CARTESIAN_POINT('Ctrl Pts',(-160.870530442824,5.52520882131862,
126.501999831362));
#266728=CARTESIAN_POINT('Ctrl Pts',(-161.148978066638,-0.633187649970563,
123.830314858198));
#266729=CARTESIAN_POINT('Ctrl Pts',(-161.42742569045,-6.20971560387352,
127.567437236815));
#266730=CARTESIAN_POINT('Ctrl Pts',(-161.705873314263,-6.07981827928859,
134.279134069845));
#266731=CARTESIAN_POINT('Ctrl Pts',(-161.984320938076,-0.362864971672915,
137.79768385235));
#266732=CARTESIAN_POINT('Ctrl Pts',(-162.262768561889,5.68754351797111,
134.889711224922));
#266733=CARTESIAN_POINT('Ctrl Pts',(-162.541216185702,6.5113773665471,128.227500969805));
#266734=CARTESIAN_POINT('Ctrl Pts',(-162.819663809515,1.35157351373451,
123.93329884439));
#266735=CARTESIAN_POINT('Ctrl Pts',(-163.098111433328,-5.05026037016286,
125.953266818493));
#266736=CARTESIAN_POINT('Ctrl Pts',(-163.376559057141,-6.81115169281603,
132.431153004838));
#266737=CARTESIAN_POINT('Ctrl Pts',(-163.655006680953,-2.31292735302948,
137.414096460505));
#266738=CARTESIAN_POINT('Ctrl Pts',(-163.933454304766,4.31076423140788,
136.323015580059));
#266739=CARTESIAN_POINT('Ctrl Pts',(-164.211901928579,6.97307407972212,
130.160560390364));
#266740=CARTESIAN_POINT('Ctrl Pts',(-164.490349552392,3.2274695023783,124.589726158078));
#266741=CARTESIAN_POINT('Ctrl Pts',(-164.768797176205,-3.4840218770001,
124.729837392289));
#266742=CARTESIAN_POINT('Ctrl Pts',(-165.047244800018,-6.99386735534677,
130.452138713572));
#266743=CARTESIAN_POINT('Ctrl Pts',(-165.325692423831,-4.07669040354407,
136.498114757629));
#266744=CARTESIAN_POINT('Ctrl Pts',(-165.604140047644,2.58676587171747,
137.31180890232));
#266745=CARTESIAN_POINT('Ctrl Pts',(-165.882587671457,6.87311068140868,
132.145475979844));
#266746=CARTESIAN_POINT('Ctrl Pts',(-166.161035295269,4.84340254500906,
125.746723556562));
#266747=CARTESIAN_POINT('Ctrl Pts',(-166.439482919082,-1.63715591688565,
123.995692513036));
#266748=CARTESIAN_POINT('Ctrl Pts',(-166.717930542895,-6.61324807067504,
128.501494835643));
#266749=CARTESIAN_POINT('Ctrl Pts',(-166.996378166708,-5.5120883226436,
135.12351831059));
#266750=CARTESIAN_POINT('Ctrl Pts',(-167.274825790521,0.654411313413328,
137.776446868231));
#266751=CARTESIAN_POINT('Ctrl Pts',(-167.553273414334,6.21953892221278,
134.022368766858));
#266752=CARTESIAN_POINT('Ctrl Pts',(-167.831721038147,6.06921410286677,
127.311098384725));
#266753=CARTESIAN_POINT('Ctrl Pts',(-168.11016866196,0.3415780205785,123.809965339223));
#266754=CARTESIAN_POINT('Ctrl Pts',(-168.388616285773,-5.69995157560742,
126.736339859314));
#266755=CARTESIAN_POINT('Ctrl Pts',(-168.667063909585,-6.50350413192509,
133.401026722375));
#266756=CARTESIAN_POINT('Ctrl Pts',(-168.945511533399,-1.33065410484337,
137.679504289309));
#266757=CARTESIAN_POINT('Ctrl Pts',(-169.223959157211,5.06500203852252,
135.640060691349));
#266758=CARTESIAN_POINT('Ctrl Pts',(-169.502406781024,6.80616874759175,
129.156844962666));
#266759=CARTESIAN_POINT('Ctrl Pts',(-169.780854404837,2.29279887745254,
124.18761563522));
#266760=CARTESIAN_POINT('Ctrl Pts',(-170.05930202865,-4.32754115161411,
125.298851700587));
#266761=CARTESIAN_POINT('Ctrl Pts',(-170.337749652463,-6.97108227448498,
131.469381501595));
#266762=CARTESIAN_POINT('Ctrl Pts',(-170.616197276276,-3.20853934340632,
137.028789598255));
#266763=CARTESIAN_POINT('Ctrl Pts',(-170.894644900089,3.50249449840198,
136.868251541923));
#266764=CARTESIAN_POINT('Ctrl Pts',(-171.173092523901,6.99490700254731,
131.135293963646));
#266765=CARTESIAN_POINT('Ctrl Pts',(-171.451540147715,4.05934169155642,
125.098224807315));
#266766=CARTESIAN_POINT('Ctrl Pts',(-171.729987771527,-2.60656032410858,
124.304815700371));
#266767=CARTESIAN_POINT('Ctrl Pts',(-172.00843539534,-6.87716073946864,
129.484170851909));
#266768=CARTESIAN_POINT('Ctrl Pts',(-172.286883019153,-4.82798640323697,
135.876715903229));
#266769=CARTESIAN_POINT('Ctrl Pts',(-172.565330642966,1.65787157732142,
137.608014245356));
#266770=CARTESIAN_POINT('Ctrl Pts',(-172.843778266779,6.62022656985093,
133.087087280501));
#266771=CARTESIAN_POINT('Ctrl Pts',(-173.122225890592,5.49891676073447,
126.468446029806));
#266772=CARTESIAN_POINT('Ctrl Pts',(-173.400673514405,-0.675628914478315,
123.834298464058));
#266773=CARTESIAN_POINT('Ctrl Pts',(-173.679121138218,-6.22930462359329,
127.605297510917));
#266774=CARTESIAN_POINT('Ctrl Pts',(-173.95756876203,-6.05855370207473,
134.316079269865));
#266775=CARTESIAN_POINT('Ctrl Pts',(-174.236016385844,-0.320287905152608,
137.799763144343));
#266776=CARTESIAN_POINT('Ctrl Pts',(-174.514464009656,5.71230682967103,
134.855013841124));
#266777=CARTESIAN_POINT('Ctrl Pts',(-174.792911633469,6.49557064972945,
128.187912110866));
#266778=CARTESIAN_POINT('Ctrl Pts',(-175.071359257282,1.30972236895365,
123.925198737649));
#266779=CARTESIAN_POINT('Ctrl Pts',(-175.349806881095,-5.07969678539539,
125.984099066334));
#266780=CARTESIAN_POINT('Ctrl Pts',(-175.628254504908,-6.80112275095037,
132.472584277733));
#266781=CARTESIAN_POINT('Ctrl Pts',(-175.906702128721,-2.27264916169912,
137.428053442694));
#266782=CARTESIAN_POINT('Ctrl Pts',(-176.185149752534,4.34427798206938,
136.296672486746));
#266783=CARTESIAN_POINT('Ctrl Pts',(-176.463597376347,6.96902589009458,
130.118125237372));
#266784=CARTESIAN_POINT('Ctrl Pts',(-176.742045000159,3.18957946096438,
124.570194777934));
#266785=CARTESIAN_POINT('Ctrl Pts',(-177.020492623972,-3.52093467317244,
124.751158169184));
#266786=CARTESIAN_POINT('Ctrl Pts',(-177.298940247785,-6.99588184988549,
130.494718895118));
#266787=CARTESIAN_POINT('Ctrl Pts',(-177.577387871598,-4.04195537438161,
136.522825237142));
#266788=CARTESIAN_POINT('Ctrl Pts',(-177.855835495411,2.62633062968132,
137.295941956302));
#266789=CARTESIAN_POINT('Ctrl Pts',(-178.134283119224,6.88114708845103,
132.103612556543));
#266790=CARTESIAN_POINT('Ctrl Pts',(-178.412730743037,4.81252553565828,
125.717334096849));
#266791=CARTESIAN_POINT('Ctrl Pts',(-178.69117836685,-1.67857187946192,
124.005784494632));
#266792=CARTESIAN_POINT('Ctrl Pts',(-178.969625990663,-6.62714374015151,
128.541794220484));
#266793=CARTESIAN_POINT('Ctrl Pts',(-179.248073614475,-5.48569425761253,
135.15699193274));
#266794=CARTESIAN_POINT('Ctrl Pts',(-179.526521238288,0.696840256609583,
137.772334104211));
#266795=CARTESIAN_POINT('Ctrl Pts',(-179.804968862101,6.23901261754625,
133.984449045885));
#266796=CARTESIAN_POINT('Ctrl Pts',(-180.083416485914,6.0478371756692,127.27421807789));
#266797=CARTESIAN_POINT('Ctrl Pts',(-180.361864109727,0.298994822622653,
123.808015646805));
#266798=CARTESIAN_POINT('Ctrl Pts',(-180.64031173354,-5.72460916570447,
126.771112453397));
#266799=CARTESIAN_POINT('Ctrl Pts',(-180.918759357353,-6.48757699345442,
133.440567287733));
#266800=CARTESIAN_POINT('Ctrl Pts',(-181.197206981166,-1.28877849997557,
137.687476978041));
#266801=CARTESIAN_POINT('Ctrl Pts',(-181.475654604978,5.094344474651,135.609138992));
#266802=CARTESIAN_POINT('Ctrl Pts',(-181.754102228792,6.79601374963652,
129.115444406326));
#266803=CARTESIAN_POINT('Ctrl Pts',(-182.032549852604,2.25247839243521,
124.173781310638));
#266804=CARTESIAN_POINT('Ctrl Pts',(-182.310997476417,-4.36097456772779,
125.32529667621));
#266805=CARTESIAN_POINT('Ctrl Pts',(-182.58944510023,-6.96690494559973,
131.511804136733));
#266806=CARTESIAN_POINT('Ctrl Pts',(-182.867892724043,-3.17059003069381,
137.048205563678));
#266807=CARTESIAN_POINT('Ctrl Pts',(-183.146340347856,3.53934223048593,
136.84681851393));
#266808=CARTESIAN_POINT('Ctrl Pts',(-183.424787971669,6.99679188832936,
131.092707847901));
#266809=CARTESIAN_POINT('Ctrl Pts',(-183.703235595482,4.02453161308464,
125.07362016374));
#266810=CARTESIAN_POINT('Ctrl Pts',(-183.981683219295,-2.64607660528548,
124.320802994409));
#266811=CARTESIAN_POINT('Ctrl Pts',(-184.260130843107,-6.88506969142675,
129.52605854136));
#266812=CARTESIAN_POINT('Ctrl Pts',(-184.53857846692,-4.79702008550057,
135.906011247817));
#266813=CARTESIAN_POINT('Ctrl Pts',(-184.817026090733,1.6992566315413,137.597796254561));
#266814=CARTESIAN_POINT('Ctrl Pts',(-185.095473714546,6.63399951749853,
133.046745788687));
#266815=CARTESIAN_POINT('Ctrl Pts',(-185.373921338359,5.47242093576752,
126.435052897159));
#266816=CARTESIAN_POINT('Ctrl Pts',(-185.652368962172,-0.718045143308166,
123.838540348135));
#266817=CARTESIAN_POINT('Ctrl Pts',(-185.930816585985,-6.24866281413942,
127.64327632748));
#266818=CARTESIAN_POINT('Ctrl Pts',(-186.209264209798,-6.03706462292539,
134.35289434186));
#266819=CARTESIAN_POINT('Ctrl Pts',(-186.487711833611,-0.277698970246197,
137.801583219124));
#266820=CARTESIAN_POINT('Ctrl Pts',(-186.766159457423,5.73685846974069,
134.820166358884));
#266821=CARTESIAN_POINT('Ctrl Pts',(-187.044607081237,6.47952323715255,
128.148420205389));
#266822=CARTESIAN_POINT('Ctrl Pts',(-187.323054705049,1.2678226919294,123.917353540782));
#266823=CARTESIAN_POINT('Ctrl Pts',(-187.601502328862,-5.10894497059535,
126.01510993074));
#266824=CARTESIAN_POINT('Ctrl Pts',(-187.879949952675,-6.79084179098006,
132.513953733987));
#266825=CARTESIAN_POINT('Ctrl Pts',(-188.158397576488,-2.23228675651833,
137.44176498151));
#266826=CARTESIAN_POINT('Ctrl Pts',(-188.436845200301,4.37763075391265,
136.270125873797));
#266827=CARTESIAN_POINT('Ctrl Pts',(-188.715292824114,6.96471946064982,
130.075715513085));
#266828=CARTESIAN_POINT('Ctrl Pts',(-188.993740447926,3.15157122851057,
124.550894407098));
#266829=CARTESIAN_POINT('Ctrl Pts',(-189.27218807174,-3.55771699981564,
124.772703249722));
#266830=CARTESIAN_POINT('Ctrl Pts',(-189.550635695553,-6.99763710944952,
130.53731055055));
#266831=CARTESIAN_POINT('Ctrl Pts',(-189.829083319365,-4.00707056907658,
136.547323816845));
#266832=CARTESIAN_POINT('Ctrl Pts',(-190.107530943179,2.66579806799723,
137.279834462351));
#266833=CARTESIAN_POINT('Ctrl Pts',(-190.385978566991,6.88892851205765,
132.061700988983));
#266834=CARTESIAN_POINT('Ctrl Pts',(-190.664426190804,4.78147019640398,
125.688133138775));
#266835=CARTESIAN_POINT('Ctrl Pts',(-190.942873814617,-1.71992564193992,
124.016128399968));
#266836=CARTESIAN_POINT('Ctrl Pts',(-191.22132143843,-6.64079383837953,
128.582177445553));
#266837=CARTESIAN_POINT('Ctrl Pts',(-191.499769062243,-5.45909691816341,
135.190304266535));
#266838=CARTESIAN_POINT('Ctrl Pts',(-191.778216686055,0.739243378134395,
137.767963139373));
#266839=CARTESIAN_POINT('Ctrl Pts',(-192.056664309869,6.25825512397307,
133.946411485565));
#266840=CARTESIAN_POINT('Ctrl Pts',(-192.335111933681,6.0262361436405,127.237468581785));
#266841=CARTESIAN_POINT('Ctrl Pts',(-192.613559557494,0.256400545303713,
123.806325206523));
#266842=CARTESIAN_POINT('Ctrl Pts',(-192.892007181307,-5.74905462830365,
126.806034500975));
#266843=CARTESIAN_POINT('Ctrl Pts',(-193.17045480512,-6.47140945543246,
133.480010167483));
#266844=CARTESIAN_POINT('Ctrl Pts',(-193.448902428933,-1.24685513894648,
137.695194610365));
#266845=CARTESIAN_POINT('Ctrl Pts',(-193.727350052746,5.12349813797151,
135.578039249819));
#266846=CARTESIAN_POINT('Ctrl Pts',(-194.005797676559,6.78560692289256,
129.074106433399));
#266847=CARTESIAN_POINT('Ctrl Pts',(-194.284245300372,2.2120744410027,124.160192684611));
#266848=CARTESIAN_POINT('Ctrl Pts',(-194.562692924184,-4.39424638632456,
125.35194468056));
#266849=CARTESIAN_POINT('Ctrl Pts',(-194.841140547997,-6.9624694554897,
131.554200557291));
#266850=CARTESIAN_POINT('Ctrl Pts',(-195.11958817181,-3.13252323060231,
137.067390161131));
#266851=CARTESIAN_POINT('Ctrl Pts',(-195.398035795623,3.57605881094196,
136.825161580438));
#266852=CARTESIAN_POINT('Ctrl Pts',(-195.676483419436,6.99841750541489,
131.050111047343));
#266853=CARTESIAN_POINT('Ctrl Pts',(-195.954931043249,3.98957240411393,
125.04922787486));
#266854=CARTESIAN_POINT('Ctrl Pts',(-196.233378667062,-2.68549483512068,
124.337030539057));
#266855=CARTESIAN_POINT('Ctrl Pts',(-196.511826290875,-6.89272351459547,
129.567993598765));
#266856=CARTESIAN_POINT('Ctrl Pts',(-196.790273914688,-4.76587601242081,
135.935117548864));
#266857=CARTESIAN_POINT('Ctrl Pts',(-197.0687215385,1.74057871918182,137.58732653051));
#266858=CARTESIAN_POINT('Ctrl Pts',(-197.347169162313,6.64752663985393,
133.006321204467));
#266859=CARTESIAN_POINT('Ctrl Pts',(-197.625616786126,5.44572232823074,
126.401821670817));
#266860=CARTESIAN_POINT('Ctrl Pts',(-197.904064409939,-0.760434764710735,
123.843040353244));
#266861=CARTESIAN_POINT('Ctrl Pts',(-198.182512033752,-6.26778945818702,
127.681372279183));
#266862=CARTESIAN_POINT('Ctrl Pts',(-198.460959657565,-6.01535183812634,
134.389577921633));
#266863=CARTESIAN_POINT('Ctrl Pts',(-198.739407281378,-0.235099745102313,
137.803144009248));
#266864=CARTESIAN_POINT('Ctrl Pts',(-199.017854905191,5.76119752841001,
134.785170069484));
#266865=CARTESIAN_POINT('Ctrl Pts',(-199.296302529004,6.46323572345932,
128.10902671676));
#266866=CARTESIAN_POINT('Ctrl Pts',(-199.574750152817,1.22587603526843,
123.909763544495));
#266867=CARTESIAN_POINT('Ctrl Pts',(-199.853197776629,-5.13800384196074,
126.04629826259));
#266868=CARTESIAN_POINT('Ctrl Pts',(-200.131645400443,-6.78030919386985,
132.555259840639));
#266869=CARTESIAN_POINT('Ctrl Pts',(-200.410093024255,-2.19184163313082,
137.455230568865));
#266870=CARTESIAN_POINT('Ctrl Pts',(-200.688540648069,4.41082131103843,
136.243376724908));
#266871=CARTESIAN_POINT('Ctrl Pts',(-200.96698827188,6.96015495096418,130.03333278901));
#266872=CARTESIAN_POINT('Ctrl Pts',(-201.245435895694,3.11344621342587,
124.531825760752));
#266873=CARTESIAN_POINT('Ctrl Pts',(-201.523883519507,-3.59436749394705,
124.794471835542));
#266874=CARTESIAN_POINT('Ctrl Pts',(-201.80233114332,-6.99913306899709,
130.579912101622));
#266875=CARTESIAN_POINT('Ctrl Pts',(-202.080778767133,-3.97203728029775,
136.571609588935));
#266876=CARTESIAN_POINT('Ctrl Pts',(-202.359226390945,2.705166724186,137.263487017335));
#266877=CARTESIAN_POINT('Ctrl Pts',(-202.637674014758,6.89645466388467,
132.019742830214));
#266878=CARTESIAN_POINT('Ctrl Pts',(-202.916121638571,4.75023767801316,
125.659121764391));
#266879=CARTESIAN_POINT('Ctrl Pts',(-203.194569262384,-1.76121567194074,
124.026723845744));
#266880=CARTESIAN_POINT('Ctrl Pts',(-203.473016886197,-6.65419785954973,
128.622643014438));
#266881=CARTESIAN_POINT('Ctrl Pts',(-203.75146451001,-5.43229728987039,
135.223454077576));
#266882=CARTESIAN_POINT('Ctrl Pts',(-204.029912133822,0.781619106723946,
137.763334135682));
#266883=CARTESIAN_POINT('Ctrl Pts',(-204.308359757636,6.27726572845484,
133.908257495395));
#266884=CARTESIAN_POINT('Ctrl Pts',(-204.586807381448,6.00441180721532,
127.200851258176));
#266885=CARTESIAN_POINT('Ctrl Pts',(-204.865255005262,0.213796766968775,
123.804894081017));
#266886=CARTESIAN_POINT('Ctrl Pts',(-205.143702629074,-5.77328705756903,
126.841104707996));
#266887=CARTESIAN_POINT('Ctrl Pts',(-205.422150252887,-6.4550021169537,
133.519353900054));
#266888=CARTESIAN_POINT('Ctrl Pts',(-205.7005978767,-1.20488557524167,137.702656900301));
#266889=CARTESIAN_POINT('Ctrl Pts',(-205.979045500513,5.15246194818434,
135.546762617222));
#266890=CARTESIAN_POINT('Ctrl Pts',(-206.257493124326,6.77494865298866,
129.032832575676));
#266891=CARTESIAN_POINT('Ctrl Pts',(-206.535940748139,2.17158852033829,
124.14685026067));
#266892=CARTESIAN_POINT('Ctrl Pts',(-206.814388371952,-4.42735537450605,
125.378794726189));
#266893=CARTESIAN_POINT('Ctrl Pts',(-207.092835995765,-6.9577759685135,
131.596569192254));
#266894=CARTESIAN_POINT('Ctrl Pts',(-207.371283619578,-3.09434035370993,
137.086342679721));
#266895=CARTESIAN_POINT('Ctrl Pts',(-207.64973124339,3.61264287922363,136.803281543952));
#266896=CARTESIAN_POINT('Ctrl Pts',(-207.928178867203,6.99978379356611,
131.007505140413));
#266897=CARTESIAN_POINT('Ctrl Pts',(-208.206626491016,3.95446536007061,
125.025048844539));
#266898=CARTESIAN_POINT('Ctrl Pts',(-208.485074114829,-2.72481355295718,
124.353497733001));
#266899=CARTESIAN_POINT('Ctrl Pts',(-208.763521738642,-6.90012192535954,
129.609974470206));
#266900=CARTESIAN_POINT('Ctrl Pts',(-209.041969362455,-4.73455533805275,
135.964033727826));
#266901=CARTESIAN_POINT('Ctrl Pts',(-209.320416986268,1.78183630903778,
137.576605461163));
#266902=CARTESIAN_POINT('Ctrl Pts',(-209.598864610081,6.66080743566547,
132.965815025787));
#266903=CARTESIAN_POINT('Ctrl Pts',(-209.877312233893,5.41882192745001,
126.368753582173));
#266904=CARTESIAN_POINT('Ctrl Pts',(-210.155759857706,-0.802796207923886,
123.847798312635));
#266905=CARTESIAN_POINT('Ctrl Pts',(-210.434207481519,-6.28668384699127,
127.719583954367));
#266906=CARTESIAN_POINT('Ctrl Pts',(-210.712655105332,-5.99341615225276,
134.42612864986));
#266907=CARTESIAN_POINT('Ctrl Pts',(-210.991102729145,-0.19249180825093,
137.804445456879));
#266908=CARTESIAN_POINT('Ctrl Pts',(-211.269550352958,5.78532310378624,
134.750026269725));
#266909=CARTESIAN_POINT('Ctrl Pts',(-211.547997976771,6.44670871218949,
128.069733104719));
#266910=CARTESIAN_POINT('Ctrl Pts',(-211.826445600584,1.18388395332015,
123.902429030038));
#266911=CARTESIAN_POINT('Ctrl Pts',(-212.104893224396,-5.16687232270428,
126.077662906191));
#266912=CARTESIAN_POINT('Ctrl Pts',(-212.38334084821,-6.76952534990887,
132.596501067076));
#266913=CARTESIAN_POINT('Ctrl Pts',(-212.661788472022,-2.15131529024619,
137.468449705789));
#266914=CARTESIAN_POINT('Ctrl Pts',(-212.940236095835,4.44384842355829,
136.216426031276));
#266915=CARTESIAN_POINT('Ctrl Pts',(-213.218683719648,6.95533253017721,
129.990978635656));
#266916=CARTESIAN_POINT('Ctrl Pts',(-213.497131343461,3.0752058284468,124.512989545492));
#266917=CARTESIAN_POINT('Ctrl Pts',(-213.775578967274,-3.63088479746918,
124.81646312));
#266918=CARTESIAN_POINT('Ctrl Pts',(-214.054026591087,-7.00036967309483,
130.622521969716));
#266919=CARTESIAN_POINT('Ctrl Pts',(-214.3324742149,-3.93685680621679,136.595681653493));
#266920=CARTESIAN_POINT('Ctrl Pts',(-214.610921838713,2.74443513942699,
137.246900227015));
#266921=CARTESIAN_POINT('Ctrl Pts',(-214.889369462525,6.90372526504794,
131.977739635008));
#266922=CARTESIAN_POINT('Ctrl Pts',(-215.167817086339,4.71882913781829,
125.630301048724));
#266923=CARTESIAN_POINT('Ctrl Pts',(-215.446264710151,-1.80244043944716,
124.037570439344));
#266924=CARTESIAN_POINT('Ctrl Pts',(-215.724712333964,-6.66735530697114,
128.66318942767));
#266925=CARTESIAN_POINT('Ctrl Pts',(-216.003159957777,-5.40529636580357,
135.256440137483));
#266926=CARTESIAN_POINT('Ctrl Pts',(-216.28160758159,0.823965872130078,
137.758447264668));
#266927=CARTESIAN_POINT('Ctrl Pts',(-216.560055205403,6.29604372654653,
133.869988489185));
#266928=CARTESIAN_POINT('Ctrl Pts',(-216.838502829216,5.98236497510254,
127.164367463932));
#266929=CARTESIAN_POINT('Ctrl Pts',(-217.116950453029,0.171185066315507,
123.803722323317));
#266930=CARTESIAN_POINT('Ctrl Pts',(-217.395398076842,-5.79730555555969,
126.876321774922));
#266931=CARTESIAN_POINT('Ctrl Pts',(-217.673845700654,-6.43835558599724,
133.558597027552));
#266932=CARTESIAN_POINT('Ctrl Pts',(-217.952293324468,-1.16287136405879,
137.709863571333));
#266933=CARTESIAN_POINT('Ctrl Pts',(-218.23074094828,5.18123483202488,135.515310253174));
#266934=CARTESIAN_POINT('Ctrl Pts',(-218.509188572093,6.76403933487094,
128.991624362576));
#266935=CARTESIAN_POINT('Ctrl Pts',(-218.787636195906,2.13102213066266,
124.133754533223));
#266936=CARTESIAN_POINT('Ctrl Pts',(-219.066083819719,-4.46030030540597,
125.405845818157));
#266937=CARTESIAN_POINT('Ctrl Pts',(-219.344531443532,-6.95282465859006,
131.638908471637));
#266938=CARTESIAN_POINT('Ctrl Pts',(-219.622979067345,-3.0560428148978,
137.105062417155));
#266939=CARTESIAN_POINT('Ctrl Pts',(-219.901426691158,3.6490930796943,136.781179215245));
#266940=CARTESIAN_POINT('Ctrl Pts',(-220.179874314971,7.00089070215466,
130.964891705888));
#266941=CARTESIAN_POINT('Ctrl Pts',(-220.458321938783,3.91921178185968,
125.001083968743));
#266942=CARTESIAN_POINT('Ctrl Pts',(-220.736769562596,-2.76403130182543,
124.370203966041));
#266943=CARTESIAN_POINT('Ctrl Pts',(-221.015217186409,-6.90726464956813,
129.651999600063));
#266944=CARTESIAN_POINT('Ctrl Pts',(-221.293664810222,-4.7030592229955,
135.992758713204));
#266945=CARTESIAN_POINT('Ctrl Pts',(-221.572112434035,1.82302787229404,
137.565633443793));
#266946=CARTESIAN_POINT('Ctrl Pts',(-221.850560057848,6.67384141280798,
132.925228753618));
#266947=CARTESIAN_POINT('Ctrl Pts',(-222.129007681661,5.39172073022998,
126.33584985658));
#266948=CARTESIAN_POINT('Ctrl Pts',(-222.407455305474,-0.845127903228338,
123.85281405));
#266949=CARTESIAN_POINT('Ctrl Pts',(-222.685902929286,-6.30534528041361,
127.757909937084));
#266950=CARTESIAN_POINT('Ctrl Pts',(-222.964350553099,-5.9712583781396,
134.462545172141));
#266951=CARTESIAN_POINT('Ctrl Pts',(-223.242798176912,-0.14987673854478,
137.805487513793));
#266952=CARTESIAN_POINT('Ctrl Pts',(-223.521245800725,5.80923430188729,
134.714736261875));
#266953=CARTESIAN_POINT('Ctrl Pts',(-223.799693424538,6.42994281575757,
128.030540825308));
#266954=CARTESIAN_POINT('Ctrl Pts',(-224.078141048351,1.1418480021166,123.895350269195));
#266955=CARTESIAN_POINT('Ctrl Pts',(-224.356588672164,-5.19554934309376,
126.109202699315));
#266956=CARTESIAN_POINT('Ctrl Pts',(-224.635036295977,-6.75849065869668,
132.637675885092));
#266957=CARTESIAN_POINT('Ctrl Pts',(-224.913483919789,-2.11070922958169,
137.481421902441));
#266958=CARTESIAN_POINT('Ctrl Pts',(-225.191931543603,4.47671086764076,
136.189274791569));
#266959=CARTESIAN_POINT('Ctrl Pts',(-225.470379167415,6.95025237698553,
129.948654622468));
#266960=CARTESIAN_POINT('Ctrl Pts',(-225.748826791228,3.03685149058481,
124.494386459301));
#266961=CARTESIAN_POINT('Ctrl Pts',(-226.027274415041,-3.66726755721984,
124.838676288203));
#266962=CARTESIAN_POINT('Ctrl Pts',(-226.305722038854,-7.00134687591997,
130.665138575908));
#266963=CARTESIAN_POINT('Ctrl Pts',(-226.584169662667,-3.9015304504591,
136.619539118521));
#266964=CARTESIAN_POINT('Ctrl Pts',(-226.86261728648,2.78360185861461,137.230074706019));
#266965=CARTESIAN_POINT('Ctrl Pts',(-227.141064910293,6.91074004613266,
131.935692959814));
#266966=CARTESIAN_POINT('Ctrl Pts',(-227.419512534106,4.68724573967455,
125.601672059739));
#266967=CARTESIAN_POINT('Ctrl Pts',(-227.697960157918,-1.8435984168596,
124.048667778841));
#266968=CARTESIAN_POINT('Ctrl Pts',(-227.976407781732,-6.68026569308986,
128.703815182788));
#266969=CARTESIAN_POINT('Ctrl Pts',(-228.254855405544,-5.37809514649209,
135.289261223946));
#266970=CARTESIAN_POINT('Ctrl Pts',(-228.533303029357,0.86628210517778,
137.753302707416));
#266971=CARTESIAN_POINT('Ctrl Pts',(-228.81175065317,6.31458842242258,133.831605885006));
#266972=CARTESIAN_POINT('Ctrl Pts',(-229.090198276983,5.96009646425557,
127.128018550972));
#266973=CARTESIAN_POINT('Ctrl Pts',(-229.368645900796,0.128567022336676,
123.802809976843));
#266974=CARTESIAN_POINT('Ctrl Pts',(-229.647093524609,-5.82110923226107,
126.911684396774));
#266975=CARTESIAN_POINT('Ctrl Pts',(-229.925541148421,-6.42147047940683,
133.597738095807));
#266976=CARTESIAN_POINT('Ctrl Pts',(-230.203988772235,-1.12081406224988,
137.716814356412));
#266977=CARTESIAN_POINT('Ctrl Pts',(-230.482436396047,5.20981572330331,
135.483683323156));
#266978=CARTESIAN_POINT('Ctrl Pts',(-230.76088401986,6.75287937278817,128.950483321085));
#266979=CARTESIAN_POINT('Ctrl Pts',(-231.039331643673,2.0903767751783,124.120905987538));
#266980=CARTESIAN_POINT('Ctrl Pts',(-231.317779267486,-4.49307995823781,
125.433096954076));
#266981=CARTESIAN_POINT('Ctrl Pts',(-231.596226891299,-6.94761570919197,
131.681216826544));
#266982=CARTESIAN_POINT('Ctrl Pts',(-231.874674515112,-3.01763203329532,
137.123548679767));
#266983=CARTESIAN_POINT('Ctrl Pts',(-232.153122138925,3.68540806167951,
136.758855413326));
#266984=CARTESIAN_POINT('Ctrl Pts',(-232.431569762738,7.00173819016367,
130.922272322824));
#266985=CARTESIAN_POINT('Ctrl Pts',(-232.71001738655,3.88381297581431,124.977334135496));
#266986=CARTESIAN_POINT('Ctrl Pts',(-232.988465010364,-2.80314662849731,
124.38714861912));
#266987=CARTESIAN_POINT('Ctrl Pts',(-233.266912634176,-6.914151422545,129.694067431082));
#266988=CARTESIAN_POINT('Ctrl Pts',(-233.545360257989,-4.67138883434919,
136.021291440583));
#266989=CARTESIAN_POINT('Ctrl Pts',(-233.823807881803,1.86415188258208,
137.554410884971));
#266990=CARTESIAN_POINT('Ctrl Pts',(-234.102255505615,6.68662808830262,
132.884563891901));
#266991=CARTESIAN_POINT('Ctrl Pts',(-234.380703129428,5.36441974081549,
126.303111713297));
#266992=CARTESIAN_POINT('Ctrl Pts',(-234.659150753241,-0.887428282007554,
123.858087379481));
#266993=CARTESIAN_POINT('Ctrl Pts',(-234.937598377053,-6.32377306694735,
127.796348807152));
#266994=CARTESIAN_POINT('Ctrl Pts',(-235.216046000867,-5.94887933685163,
134.498826139047));
#266995=CARTESIAN_POINT('Ctrl Pts',(-235.494493624679,-0.107256115101469,
137.806270141374));
#266996=CARTESIAN_POINT('Ctrl Pts',(-235.772941248493,5.83293023667497,
134.679301353618));
#266997=CARTESIAN_POINT('Ctrl Pts',(-236.051388872305,6.41293865542997,
127.991451330808));
#266998=CARTESIAN_POINT('Ctrl Pts',(-236.329836496118,1.09976973931543,
123.88852752427));
#266999=CARTESIAN_POINT('Ctrl Pts',(-236.608284119931,-5.22403384049169,
126.140916473241));
#267000=CARTESIAN_POINT('Ctrl Pts',(-236.886731743744,-6.7472055291277,
132.678782768935));
#267001=CARTESIAN_POINT('Ctrl Pts',(-237.165179367557,-2.07002495581049,
137.494146678133));
#267002=CARTESIAN_POINT('Ctrl Pts',(-237.44362699137,4.50940742555574,136.161924011888));
#267003=CARTESIAN_POINT('Ctrl Pts',(-237.722074615182,6.94491467963605,
129.906362317783));
#267004=CARTESIAN_POINT('Ctrl Pts',(-238.000522238996,2.99838462107406,
124.476017191522));
#267005=CARTESIAN_POINT('Ctrl Pts',(-238.278969862808,-3.70351442502255,
124.861110517033));
#267006=CARTESIAN_POINT('Ctrl Pts',(-238.557417486622,-7.00206464126185,
130.707760341024));
#267007=CARTESIAN_POINT('Ctrl Pts',(-238.835865110434,-3.86605952205578,
136.64318109997));
#267008=CARTESIAN_POINT('Ctrl Pts',(-239.114312734247,2.82266543041169,
137.213011077826));
#267009=CARTESIAN_POINT('Ctrl Pts',(-239.39276035806,6.91749874720356,131.893604362681));
#267010=CARTESIAN_POINT('Ctrl Pts',(-239.671207981873,4.655488653916,125.573235858291));
#267011=CARTESIAN_POINT('Ctrl Pts',(-239.949655605686,-1.88468807905538,
124.060015453022));
#267012=CARTESIAN_POINT('Ctrl Pts',(-240.228103229498,-6.69292853950653,
128.74451877439));
#267013=CARTESIAN_POINT('Ctrl Pts',(-240.506550853312,-5.35069463988719,
135.321916120768));
#267014=CARTESIAN_POINT('Ctrl Pts',(-240.784998477124,0.908566237823527,
137.747900654559));
#267015=CARTESIAN_POINT('Ctrl Pts',(-241.063446100938,6.33289912890243,
133.79311110514));
#267016=CARTESIAN_POINT('Ctrl Pts',(-241.34189372475,5.9376070998423,127.091805866219));
#267017=CARTESIAN_POINT('Ctrl Pts',(-241.620341348563,0.0859442142595387,
123.802157075403));
#267018=CARTESIAN_POINT('Ctrl Pts',(-241.898788972376,-5.84469720561911,
126.947191263173));
#267019=CARTESIAN_POINT('Ctrl Pts',(-242.177236596189,-6.40434742286629,
133.636775654432));
#267020=CARTESIAN_POINT('Ctrl Pts',(-242.455684220002,-1.07871522826414,
137.723508997977));
#267021=CARTESIAN_POINT('Ctrl Pts',(-242.734131843815,5.23820356294377,
135.451882999115));
#267022=CARTESIAN_POINT('Ctrl Pts',(-243.012579467628,6.74146918027728,
128.909410975699));
#267023=CARTESIAN_POINT('Ctrl Pts',(-243.29102709144,2.04965396001378,124.108305099723));
#267024=CARTESIAN_POINT('Ctrl Pts',(-243.569474715254,-4.52569311833944,
125.460547124147));
#267025=CARTESIAN_POINT('Ctrl Pts',(-243.847922339066,-6.94214931333881,
131.72349268922));
#267026=CARTESIAN_POINT('Ctrl Pts',(-244.12636996288,-2.9791094322281,137.141800782542));
#267027=CARTESIAN_POINT('Ctrl Pts',(-244.404817586691,3.72158647951367,
136.736310965414));
#267028=CARTESIAN_POINT('Ctrl Pts',(-244.683265210505,7.00232622618917,
130.879648570499));
#267029=CARTESIAN_POINT('Ctrl Pts',(-244.961712834317,3.84827025365086,
124.953800224859));
#267030=CARTESIAN_POINT('Ctrl Pts',(-245.240160458131,-2.84215808354001,
124.404331064352));
#267031=CARTESIAN_POINT('Ctrl Pts',(-245.518608081943,-6.92078198909823,
129.736176404423));
#267032=CARTESIAN_POINT('Ctrl Pts',(-245.797055705757,-4.63954534567172,
136.049630852671));
#267033=CARTESIAN_POINT('Ctrl Pts',(-246.075503329569,1.90520681603656,
137.542938200555));
#267034=CARTESIAN_POINT('Ctrl Pts',(-246.353950953382,6.69916698833444,
132.843821947487));
#267035=CARTESIAN_POINT('Ctrl Pts',(-246.632398577195,5.33691997085474,
126.270540365447));
#267036=CARTESIAN_POINT('Ctrl Pts',(-246.910846201008,-0.929695776805409,
123.86361810567));
#267037=CARTESIAN_POINT('Ctrl Pts',(-247.189293824821,-6.34196652374499,
127.834899140205));
#267038=CARTESIAN_POINT('Ctrl Pts',(-247.467741448634,-5.9262798576518,
134.534970206175));
#267039=CARTESIAN_POINT('Ctrl Pts',(-247.746189072447,-0.0646315172428821,
137.806793310625));
#267040=CARTESIAN_POINT('Ctrl Pts',(-248.024636696259,5.85641003008765,
134.643722858007));
#267041=CARTESIAN_POINT('Ctrl Pts',(-248.303084320073,6.39569686130214,
127.952466069697));
#267042=CARTESIAN_POINT('Ctrl Pts',(-248.581531943885,1.05765072414216,
123.881961048084));
#267043=CARTESIAN_POINT('Ctrl Pts',(-248.859979567699,-5.25232475939459,
126.172803052805));
#267044=CARTESIAN_POINT('Ctrl Pts',(-249.138427191511,-6.73567037937639,
132.719820195375));
#267045=CARTESIAN_POINT('Ctrl Pts',(-249.416874815324,-2.02926397650361,
137.506623561341));
#267046=CARTESIAN_POINT('Ctrl Pts',(-249.695322439137,4.54193688572079,
136.134374705723));
#267047=CARTESIAN_POINT('Ctrl Pts',(-249.97377006295,6.93931963591783,129.864103288757));
#267048=CARTESIAN_POINT('Ctrl Pts',(-250.252217686763,2.95980664532115,
124.457882422832));
#267049=CARTESIAN_POINT('Ctrl Pts',(-250.530665310576,-3.73962405773988,
124.883764975191));
#267050=CARTESIAN_POINT('Ctrl Pts',(-250.809112934388,-7.00252294251614,
130.750385685678));
#267051=CARTESIAN_POINT('Ctrl Pts',(-251.087560558202,-3.83044533540895,
136.666606721818));
#267052=CARTESIAN_POINT('Ctrl Pts',(-251.366008182014,2.86162440732935,
137.195709974661));
#267053=CARTESIAN_POINT('Ctrl Pts',(-251.644455805827,6.9240011177651,131.851475403357));
#267054=CARTESIAN_POINT('Ctrl Pts',(-251.92290342964,4.62355905740654,125.54499349784));
#267055=CARTESIAN_POINT('Ctrl Pts',(-252.201351053453,-1.92570790361727,
124.071613041873));
#267056=CARTESIAN_POINT('Ctrl Pts',(-252.479798677266,-6.70534337666252,
128.785298693283));
#267057=CARTESIAN_POINT('Ctrl Pts',(-252.758246301079,-5.3230958619522,
135.354403619622));
#267058=CARTESIAN_POINT('Ctrl Pts',(-253.036693924892,0.950816704398073,
137.74224130304));
#267059=CARTESIAN_POINT('Ctrl Pts',(-253.315141548704,6.35097516523885,
133.754505582129));
#267060=CARTESIAN_POINT('Ctrl Pts',(-253.593589172518,5.91489771943887,
127.055730740027));
#267061=CARTESIAN_POINT('Ctrl Pts',(-253.87203679633,0.0433182135112656,
123.801763664947));
#267062=CARTESIAN_POINT('Ctrl Pts',(-254.150484420143,-5.86806858651122,
126.982841017323));
#267063=CARTESIAN_POINT('Ctrl Pts',(-254.428932043956,-6.38698707931617,
133.675708334441));
#267064=CARTESIAN_POINT('Ctrl Pts',(-254.707379667769,-1.03657636838919,
137.729947101491));
#267065=CARTESIAN_POINT('Ctrl Pts',(-254.985827291582,5.26639719763008,
135.41991073597));
#267066=CARTESIAN_POINT('Ctrl Pts',(-255.264274915395,6.72980937160111,
128.868408326187));
#267067=CARTESIAN_POINT('Ctrl Pts',(-255.542722539208,2.00885483266244,
124.095953322692));
#267068=CARTESIAN_POINT('Ctrl Pts',(-255.821170163021,-4.5581378946222,
125.488193449449));
#267069=CARTESIAN_POINT('Ctrl Pts',(-256.099617786833,-6.93642696247006,
131.765738008466));
#267070=CARTESIAN_POINT('Ctrl Pts',(-256.378065410647,-2.94047400549736,
137.159811411449));
#267071=CARTESIAN_POINT('Ctrl Pts',(-256.656513034459,3.7576223973322,136.713559240208));
#267072=CARTESIAN_POINT('Ctrl Pts',(-256.934960658272,7.0026634652268,130.836998362911));
#267073=CARTESIAN_POINT('Ctrl Pts',(-257.213408282085,3.81256854888166,
124.930527794066));
#267074=CARTESIAN_POINT('Ctrl Pts',(-257.491855905898,-2.88103328591622,
124.421666290213));
#267075=CARTESIAN_POINT('Ctrl Pts',(-257.770303529711,-6.92721451599304,
129.778484277494));
#267076=CARTESIAN_POINT('Ctrl Pts',(-258.048751153524,-4.60741964202412,
136.077475067175));
#267077=CARTESIAN_POINT('Ctrl Pts',(-258.327198777336,1.94598288966397,
137.53178391186));
#267078=CARTESIAN_POINT('Ctrl Pts',(-258.60564640115,6.71185090883407,132.801931226644));
#267079=CARTESIAN_POINT('Ctrl Pts',(-258.884094024962,5.30847971878909,
126.240167716581));
#267080=CARTESIAN_POINT('Ctrl Pts',(-259.162541648776,-0.970525071554103,
123.86553674091));
#267081=CARTESIAN_POINT('Ctrl Pts',(-259.440989272588,-6.36258613651914,
127.881151058581));
#267082=CARTESIAN_POINT('Ctrl Pts',(-259.673028959099,-5.97575359986218,
133.442106215535));
#267083=CARTESIAN_POINT('Ctrl Pts',(-259.858689921174,-2.9628379271774,
136.206922793942));
#267084=CARTESIAN_POINT('Ctrl Pts',(-259.951535008647,-1.00384119663989,
136.721969923993));
#267085=CARTESIAN_POINT('Ctrl Pts',(-259.997972158816,-0.016740685831905,
136.724751058381));
#267086=CARTESIAN_POINT('Ctrl Pts',(210.384788400103,3.2437100417032,135.350446923363));
#267087=CARTESIAN_POINT('Ctrl Pts',(210.338370536501,4.00135710969089,134.809856772425));
#267088=CARTESIAN_POINT('Ctrl Pts',(210.245544735596,5.2274450014198,133.344996311945));
#267089=CARTESIAN_POINT('Ctrl Pts',(210.059903060087,6.03752477204218,129.574087134129));
#267090=CARTESIAN_POINT('Ctrl Pts',(209.827863373576,3.30140998082846,125.08375145776));
#267091=CARTESIAN_POINT('Ctrl Pts',(209.549415749763,-3.03864792542705,
124.935284604053));
#267092=CARTESIAN_POINT('Ctrl Pts',(209.27096812595,-6.57501826603042,130.18815040753));
#267093=CARTESIAN_POINT('Ctrl Pts',(208.992520502138,-4.0751627655632,136.003208990552));
#267094=CARTESIAN_POINT('Ctrl Pts',(208.714072878324,2.17267791003586,137.042921783734));
#267095=CARTESIAN_POINT('Ctrl Pts',(208.435625254512,6.42228832295553,132.348569225854));
#267096=CARTESIAN_POINT('Ctrl Pts',(208.157177630698,4.77100074356668,126.235763887068));
#267097=CARTESIAN_POINT('Ctrl Pts',(207.878730006886,-1.26506482749479,
124.320958291314));
#267098=CARTESIAN_POINT('Ctrl Pts',(207.600282383073,-6.13835327551471,
128.364250828182));
#267099=CARTESIAN_POINT('Ctrl Pts',(207.32183475926,-5.37092434612766,134.649796015418));
#267100=CARTESIAN_POINT('Ctrl Pts',(207.043387135447,0.332190207827403,
137.40162108792));
#267101=CARTESIAN_POINT('Ctrl Pts',(206.764939511634,5.73000189292936,134.090861108297));
#267102=CARTESIAN_POINT('Ctrl Pts',(206.486491887821,5.86224098722307,127.759980958474));
#267103=CARTESIAN_POINT('Ctrl Pts',(206.208044264008,0.607356820266201,
124.226729984437));
#267104=CARTESIAN_POINT('Ctrl Pts',(205.929596640195,-5.20565320191231,
126.738003936844));
#267105=CARTESIAN_POINT('Ctrl Pts',(205.651149016382,-6.23492509722864,
132.986059061584));
#267106=CARTESIAN_POINT('Ctrl Pts',(205.37270139257,-1.53460390898592,137.229240938669));
#267107=CARTESIAN_POINT('Ctrl Pts',(205.094253768756,4.57594250116295,135.568271122458));
#267108=CARTESIAN_POINT('Ctrl Pts',(204.815806144944,6.48142172411287,129.529500574057));
#267109=CARTESIAN_POINT('Ctrl Pts',(204.537358521131,2.43079079302514,124.662263970705));
#267110=CARTESIAN_POINT('Ctrl Pts',(204.258910897318,-3.85361800715474,
125.439314209572));
#267111=CARTESIAN_POINT('Ctrl Pts',(203.980463273505,-6.5967401814699,131.146579956944));
#267112=CARTESIAN_POINT('Ctrl Pts',(203.702015649692,-3.27778036432047,
136.539362872731));
#267113=CARTESIAN_POINT('Ctrl Pts',(203.42356802588,3.05329946149495,136.661958874297));
#267114=CARTESIAN_POINT('Ctrl Pts',(203.145120402066,6.5785462535266,131.40170824395));
#267115=CARTESIAN_POINT('Ctrl Pts',(202.866672778254,4.05843041346184,125.592524323598));
#267116=CARTESIAN_POINT('Ctrl Pts',(202.58822515444,-2.19118470860141,124.572763346851));
#267117=CARTESIAN_POINT('Ctrl Pts',(202.309777530628,-6.42720813017419,
129.279535830482));
#267118=CARTESIAN_POINT('Ctrl Pts',(202.031329906815,-4.75694126595338,
135.387547802118));
#267119=CARTESIAN_POINT('Ctrl Pts',(201.752882283002,1.28472223178851,137.283834652022));
#267120=CARTESIAN_POINT('Ctrl Pts',(201.474434659189,6.14578876089344,133.225801404307));
#267121=CARTESIAN_POINT('Ctrl Pts',(201.195987035376,5.35917565710019,126.94258236746));
#267122=CARTESIAN_POINT('Ctrl Pts',(200.917539411563,-0.352258065224466,
124.208148884143));
#267123=CARTESIAN_POINT('Ctrl Pts',(200.63909178775,-5.73998383440169,127.535311740963));
#267124=CARTESIAN_POINT('Ctrl Pts',(200.360644163938,-5.85294487354697,
133.866570813476));
#267125=CARTESIAN_POINT('Ctrl Pts',(200.082196540124,-0.587335506164227,
137.383808313225));
#267126=CARTESIAN_POINT('Ctrl Pts',(199.803748916312,5.2180064984534,134.854854804556));
#267127=CARTESIAN_POINT('Ctrl Pts',(199.525301292498,6.22825544477889,128.603695015683));
#267128=CARTESIAN_POINT('Ctrl Pts',(199.246853668687,1.51504190454761,124.374839406449));
#267129=CARTESIAN_POINT('Ctrl Pts',(198.968406044873,-4.5904211320519,126.054399690658));
#267130=CARTESIAN_POINT('Ctrl Pts',(198.689958421061,-6.47751140283473,
132.098942018204));
#267131=CARTESIAN_POINT('Ctrl Pts',(198.411510797247,-2.41208513843682,
136.95382728238));
#267132=CARTESIAN_POINT('Ctrl Pts',(198.133063173434,3.86992953127461,136.15765309974));
#267133=CARTESIAN_POINT('Ctrl Pts',(197.854615549622,6.59566801831256,130.442064648858));
#267134=CARTESIAN_POINT('Ctrl Pts',(197.576167925809,3.26030981281707,125.059408494076));
#267135=CARTESIAN_POINT('Ctrl Pts',(197.297720301996,-3.07111383566833,
124.956082684267));
#267136=CARTESIAN_POINT('Ctrl Pts',(197.019272678183,-6.58033390142619,
130.227038590899));
#267137=CARTESIAN_POINT('Ctrl Pts',(196.74082505437,-4.04254857895594,136.028525236289));
#267138=CARTESIAN_POINT('Ctrl Pts',(196.462377430557,2.21014139809766,137.029259811701));
#267139=CARTESIAN_POINT('Ctrl Pts',(196.183929806745,6.43181940170927,132.309616130935));
#267140=CARTESIAN_POINT('Ctrl Pts',(195.905482182931,4.74296958699597,126.206716169203));
#267141=CARTESIAN_POINT('Ctrl Pts',(195.627034559119,-1.30443757122094,
124.328826848098));
#267142=CARTESIAN_POINT('Ctrl Pts',(195.348586935305,-6.15313032680387,
128.401636713722));
#267143=CARTESIAN_POINT('Ctrl Pts',(195.070139311493,-5.34739690918169,
134.682432467391));
#267144=CARTESIAN_POINT('Ctrl Pts',(194.791691687679,0.372333033116476,
137.399469645412));
#267145=CARTESIAN_POINT('Ctrl Pts',(194.513244063867,5.74990710746052,134.055923815831));
#267146=CARTESIAN_POINT('Ctrl Pts',(194.234796440054,5.84359744862664,127.724350254736));
#267147=CARTESIAN_POINT('Ctrl Pts',(193.956348816241,0.567307210110782,
124.223155750211));
#267148=CARTESIAN_POINT('Ctrl Pts',(193.677901192428,-5.23031063999889,
126.769767009054));
#267149=CARTESIAN_POINT('Ctrl Pts',(193.399453568615,-6.22152852682933,
133.023972693263));
#267150=CARTESIAN_POINT('Ctrl Pts',(193.121005944802,-1.49546563606909,
137.238463313985));
#267151=CARTESIAN_POINT('Ctrl Pts',(192.84255832099,4.60485711668079,135.540327880088));
#267152=CARTESIAN_POINT('Ctrl Pts',(192.564110697177,6.47354113897745,129.490069896797));
#267153=CARTESIAN_POINT('Ctrl Pts',(192.285663073364,2.39335710461987,124.64758087922));
#267154=CARTESIAN_POINT('Ctrl Pts',(192.007215449551,-3.88620518688872,
125.462871665772));
#267155=CARTESIAN_POINT('Ctrl Pts',(191.728767825738,-6.59453476332446,
131.18672985278));
#267156=CARTESIAN_POINT('Ctrl Pts',(191.450320201925,-3.24280905319821,
136.559209392401));
#267157=CARTESIAN_POINT('Ctrl Pts',(191.171872578112,3.08889975678785,136.643264047941));
#267158=CARTESIAN_POINT('Ctrl Pts',(190.893424954299,6.58206059142805,131.361651697256));
#267159=CARTESIAN_POINT('Ctrl Pts',(190.614977330486,4.02662929408197,125.567916069518));
#267160=CARTESIAN_POINT('Ctrl Pts',(190.336529706674,-2.22907761274862,
124.586217166899));
#267161=CARTESIAN_POINT('Ctrl Pts',(190.05808208286,-6.43637108995848,129.318688322246));
#267162=CARTESIAN_POINT('Ctrl Pts',(189.779634459048,-4.72895396970476,
135.416419737866));
#267163=CARTESIAN_POINT('Ctrl Pts',(189.501186835235,1.32414082646293,137.275894133543));
#267164=CARTESIAN_POINT('Ctrl Pts',(189.222739211422,6.16041489098677,133.188345380025));
#267165=CARTESIAN_POINT('Ctrl Pts',(188.944291587609,5.33556862369218,126.910031093937));
#267166=CARTESIAN_POINT('Ctrl Pts',(188.665843963796,-0.392404551757433,
124.210415391489));
#267167=CARTESIAN_POINT('Ctrl Pts',(188.387396339983,-5.75977711417006,
127.570313219673));
#267168=CARTESIAN_POINT('Ctrl Pts',(188.10894871617,-5.83419588941534,133.902142614521));
#267169=CARTESIAN_POINT('Ctrl Pts',(187.830501092358,-0.547273658602122,
137.387261689231));
#267170=CARTESIAN_POINT('Ctrl Pts',(187.552053468544,5.24256632866185,134.823016271676));
#267171=CARTESIAN_POINT('Ctrl Pts',(187.273605844732,6.214743973489,128.565822630237));
#267172=CARTESIAN_POINT('Ctrl Pts',(186.995158220918,1.47587551380139,124.365736040492));
#267173=CARTESIAN_POINT('Ctrl Pts',(186.716710597106,-4.61925044254253,
126.082430892781));
#267174=CARTESIAN_POINT('Ctrl Pts',(186.438262973293,-6.46951090511933,
132.138348483055));
#267175=CARTESIAN_POINT('Ctrl Pts',(186.15981534948,-2.37460689906969,136.968396393875));
#267176=CARTESIAN_POINT('Ctrl Pts',(185.881367725667,3.90244484122886,136.133996556155));
#267177=CARTESIAN_POINT('Ctrl Pts',(185.602920101854,6.59334041746713,130.401921658061));
#267178=CARTESIAN_POINT('Ctrl Pts',(185.324472478041,3.22527825263932,125.039668503516));
#267179=CARTESIAN_POINT('Ctrl Pts',(185.046024854228,-3.10665706276191,
124.974885780916));
#267180=CARTESIAN_POINT('Ctrl Pts',(184.767577230416,-6.5837263061198,130.26710564752));
#267181=CARTESIAN_POINT('Ctrl Pts',(184.489129606603,-4.01067270706429,
136.05303658523));
#267182=CARTESIAN_POINT('Ctrl Pts',(184.21068198279,2.247993177529,137.015690720733));
#267183=CARTESIAN_POINT('Ctrl Pts',(183.932234358977,6.44086315254518,132.270435931769));
#267184=CARTESIAN_POINT('Ctrl Pts',(183.653786735164,4.71489454403,126.177929550814));
#267185=CARTESIAN_POINT('Ctrl Pts',(183.375339111351,-1.34383181504516,
124.33688730648));
#267186=CARTESIAN_POINT('Ctrl Pts',(183.096891487538,-6.16764238592767,
128.439137081397));
#267187=CARTESIAN_POINT('Ctrl Pts',(182.818443863726,-5.32369091022383,
134.71491173846));
#267188=CARTESIAN_POINT('Ctrl Pts',(182.539996239912,0.412472435216218,
137.397080956463));
#267189=CARTESIAN_POINT('Ctrl Pts',(182.2615486161,5.76959376309122,134.020862255314));
#267190=CARTESIAN_POINT('Ctrl Pts',(181.983100992287,5.82474028301032,127.688835683913));
#267191=CARTESIAN_POINT('Ctrl Pts',(181.704653368474,0.527235037225083,
124.219824324685));
#267192=CARTESIAN_POINT('Ctrl Pts',(181.426205744661,-5.25477345090652,
126.801680146133));
#267193=CARTESIAN_POINT('Ctrl Pts',(181.147758120848,-6.20790184760947,
133.061803779016));
#267194=CARTESIAN_POINT('Ctrl Pts',(180.869310497035,-1.45627171922457,
137.247447428754));
#267195=CARTESIAN_POINT('Ctrl Pts',(180.590862873222,4.63360097629919,135.5122090613));
#267196=CARTESIAN_POINT('Ctrl Pts',(180.31241524941,6.46542073859599,129.450687965235));
#267197=CARTESIAN_POINT('Ctrl Pts',(180.033967625596,2.35583469548556,124.633125906077));
#267198=CARTESIAN_POINT('Ctrl Pts',(179.755520001784,-3.91864834385308,
125.4866270652));
#267199=CARTESIAN_POINT('Ctrl Pts',(179.477072377971,-6.59208499180493,
131.226865573221));
#267200=CARTESIAN_POINT('Ctrl Pts',(179.198624754158,-3.20771757354326,
136.578842667508));
#267201=CARTESIAN_POINT('Ctrl Pts',(178.920177130345,3.12438558908937,136.62435285703));
#267202=CARTESIAN_POINT('Ctrl Pts',(178.641729506532,6.58533103007041,131.32157450091));
#267203=CARTESIAN_POINT('Ctrl Pts',(178.363281882719,3.99467896572256,125.5435018533));
#267204=CARTESIAN_POINT('Ctrl Pts',(178.084834258906,-2.26688791720775,
124.599901402811));
#267205=CARTESIAN_POINT('Ctrl Pts',(177.806386635093,-6.44529554785546,
129.357895865998));
#267206=CARTESIAN_POINT('Ctrl Pts',(177.527939011281,-4.70079144021631,
135.445120772143));
#267207=CARTESIAN_POINT('Ctrl Pts',(177.249491387467,1.36351035455298,137.26771380997));
#267208=CARTESIAN_POINT('Ctrl Pts',(176.971043763655,6.17481274467203,133.150801016333));
#267209=CARTESIAN_POINT('Ctrl Pts',(176.692596139842,5.31176387881016,126.877624126216));
#267210=CARTESIAN_POINT('Ctrl Pts',(176.414148516029,-0.432536497586617,
124.212926239906));
#267211=CARTESIAN_POINT('Ctrl Pts',(176.135700892216,-5.77935696328393,
127.605434537195));
#267212=CARTESIAN_POINT('Ctrl Pts',(175.857253268403,-5.81523071700703,
133.937599626117));
#267213=CARTESIAN_POINT('Ctrl Pts',(175.57880564459,-0.50719153161477,137.390471133416));
#267214=CARTESIAN_POINT('Ctrl Pts',(175.300358020777,5.2669318936477,134.791028826034));
#267215=CARTESIAN_POINT('Ctrl Pts',(175.021910396965,6.20100221257536,128.528033194638));
#267216=CARTESIAN_POINT('Ctrl Pts',(174.743462773151,1.43665443394553,124.356871260137));
#267217=CARTESIAN_POINT('Ctrl Pts',(174.465015149339,-4.64790858500931,
126.110637067746));
#267218=CARTESIAN_POINT('Ctrl Pts',(174.186567525525,-6.46127067729819,
132.177705516496));
#267219=CARTESIAN_POINT('Ctrl Pts',(173.908119901713,-2.33704066777073,
136.982737094758));
#267220=CARTESIAN_POINT('Ctrl Pts',(173.6296722779,3.93481554465429,136.11014252095));
#267221=CARTESIAN_POINT('Ctrl Pts',(173.351224654087,6.59076849796787,130.361793579788));
#267222=CARTESIAN_POINT('Ctrl Pts',(173.072777030274,3.1901271785899,125.020142125741));
#267223=CARTESIAN_POINT('Ctrl Pts',(172.794329406461,-3.14208517153551,
124.993904890899));
#267224=CARTESIAN_POINT('Ctrl Pts',(172.515881782648,-6.58687474841394,
130.30719261232));
#267225=CARTESIAN_POINT('Ctrl Pts',(172.237434158836,-3.97864821822065,
136.077353442554));
#267226=CARTESIAN_POINT('Ctrl Pts',(171.958986535022,2.28576165674636,137.001891466644));
#267227=CARTESIAN_POINT('Ctrl Pts',(171.68053891121,6.44966823482829,132.231201406644));
#267228=CARTESIAN_POINT('Ctrl Pts',(171.402091287397,4.68664478891289,126.149314366529));
#267229=CARTESIAN_POINT('Ctrl Pts',(171.123643663584,-1.38317626268716,
124.345187419464));
#267230=CARTESIAN_POINT('Ctrl Pts',(170.845196039771,-6.18192590079466,
128.476725093301));
#267231=CARTESIAN_POINT('Ctrl Pts',(170.566748415958,-5.29978763994156,
134.747246102621));
#267232=CARTESIAN_POINT('Ctrl Pts',(170.288300792145,0.452596552998033,
137.394447971839));
#267233=CARTESIAN_POINT('Ctrl Pts',(170.009853168332,5.78906662430322,133.985681506144));
#267234=CARTESIAN_POINT('Ctrl Pts',(169.73140554452,5.80566727950083,127.653436560012));
#267235=CARTESIAN_POINT('Ctrl Pts',(169.452957920706,0.487143327451347,
124.216736891574));
#267236=CARTESIAN_POINT('Ctrl Pts',(169.174510296894,-5.27904154425138,
126.833741604011));
#267237=CARTESIAN_POINT('Ctrl Pts',(168.896062673081,-6.19404513230377,
133.099551214382));
#267238=CARTESIAN_POINT('Ctrl Pts',(168.617615049268,-1.41702383969606,
137.256192792574));
#267239=CARTESIAN_POINT('Ctrl Pts',(168.339167425455,4.66217313612931,135.483915791456));
#267240=CARTESIAN_POINT('Ctrl Pts',(168.060719801642,6.45706075967145,129.411356194513));
#267241=CARTESIAN_POINT('Ctrl Pts',(167.782272177829,2.3182249900303,124.618899610305));
#267242=CARTESIAN_POINT('Ctrl Pts',(167.503824554016,-3.95094629386185,
125.510579515201));
#267243=CARTESIAN_POINT('Ctrl Pts',(167.225376930203,-6.58939094815179,
131.266985637585));
#267244=CARTESIAN_POINT('Ctrl Pts',(166.946929306391,-3.1725072307341,136.59826196706));
#267245=CARTESIAN_POINT('Ctrl Pts',(166.668481682578,3.15975564613386,136.605226004165));
#267246=CARTESIAN_POINT('Ctrl Pts',(166.390034058765,6.58835744684964,131.281478139015));
#267247=CARTESIAN_POINT('Ctrl Pts',(166.111586434952,3.96258061306513,125.519282580138));
#267248=CARTESIAN_POINT('Ctrl Pts',(165.833138811139,-2.30461422130139,
124.613815547242));
#267249=CARTESIAN_POINT('Ctrl Pts',(165.554691187326,-6.45398117295568,
129.397157009033));
#267250=CARTESIAN_POINT('Ctrl Pts',(165.276243563513,-4.67245472117232,
135.473649841348));
#267251=CARTESIAN_POINT('Ctrl Pts',(164.9977959397,1.40282935726546,137.259293984466));
#267252=CARTESIAN_POINT('Ctrl Pts',(164.719348315888,6.18898178840028,133.11316970443));
#267253=CARTESIAN_POINT('Ctrl Pts',(164.440900692075,5.2877623045642,126.845362665158));
#267254=CARTESIAN_POINT('Ctrl Pts',(164.162453068262,-0.472652415616787,
124.215681336348));
#267255=CARTESIAN_POINT('Ctrl Pts',(163.884005444449,-5.79872265620017,
127.640674392099));
#267256=CARTESIAN_POINT('Ctrl Pts',(163.605557820636,-5.79605005908598,
133.97294053439));
#267257=CARTESIAN_POINT('Ctrl Pts',(163.327110196823,-0.467090610458611,
137.393436526853));
#267258=CARTESIAN_POINT('Ctrl Pts',(163.04866257301,5.29110229053537,134.758893652935));
#267259=CARTESIAN_POINT('Ctrl Pts',(162.770214949197,6.18703067124424,128.49032810919));
#267260=CARTESIAN_POINT('Ctrl Pts',(162.491767325384,1.39738011833125,124.34824539387));
#267261=CARTESIAN_POINT('Ctrl Pts',(162.213319701571,-4.67639449751423,
126.139017170363));
#267262=CARTESIAN_POINT('Ctrl Pts',(161.934872077759,-6.45279102471594,
132.217011660137));
#267263=CARTESIAN_POINT('Ctrl Pts',(161.656424453946,-2.29938783657033,
136.996848853628));
#267264=CARTESIAN_POINT('Ctrl Pts',(161.377976830133,3.96704044204275,136.086091878046));
#267265=CARTESIAN_POINT('Ctrl Pts',(161.09952920632,6.58795235511813,130.321681900999));
#267266=CARTESIAN_POINT('Ctrl Pts',(160.821081582507,3.15485789320466,125.000830084311));
#267267=CARTESIAN_POINT('Ctrl Pts',(160.542633958694,-3.17739684918762,
125.013139309456));
#267268=CARTESIAN_POINT('Ctrl Pts',(160.264186334881,-6.58977911164196,
130.347297999864));
#267269=CARTESIAN_POINT('Ctrl Pts',(159.985738711068,-3.94647629910411,
136.10147490719));
#267270=CARTESIAN_POINT('Ctrl Pts',(159.707291087255,2.32344543622502,136.98786256077));
#267271=CARTESIAN_POINT('Ctrl Pts',(159.428843463442,6.45823432228318,132.191914009409));
#267272=CARTESIAN_POINT('Ctrl Pts',(159.15039583963,4.65822136844951,126.120871676696));
#267273=CARTESIAN_POINT('Ctrl Pts',(158.871948215817,-1.42246945622416,
124.353726879487));
#267274=CARTESIAN_POINT('Ctrl Pts',(158.593500592004,-6.19598034212407,
128.514399356595));
#267275=CARTESIAN_POINT('Ctrl Pts',(158.315052968191,-5.2756879840792,134.779434361708));
#267276=CARTESIAN_POINT('Ctrl Pts',(158.036605344378,0.49270389964821,137.391570789103));
#267277=CARTESIAN_POINT('Ctrl Pts',(157.758157720565,5.80832496952254,133.950382871961));
#267278=CARTESIAN_POINT('Ctrl Pts',(157.479710096752,5.78637914485521,127.618154194761));
#267279=CARTESIAN_POINT('Ctrl Pts',(157.201262472939,0.447033566402335,
124.213893565282));
#267280=CARTESIAN_POINT('Ctrl Pts',(156.922814849126,-5.3031140207705,126.865950194636));
#267281=CARTESIAN_POINT('Ctrl Pts',(156.644367225313,-6.17995889437779,
133.137213600617));
#267282=CARTESIAN_POINT('Ctrl Pts',(156.365919601501,-1.37772345182797,
137.264699081378));
#267283=CARTESIAN_POINT('Ctrl Pts',(156.087471977688,4.69057253741941,135.455449118975));
#267284=CARTESIAN_POINT('Ctrl Pts',(155.809024353875,6.44846151198586,129.372076042081));
#267285=CARTESIAN_POINT('Ctrl Pts',(155.530576730062,2.28052938189546,124.604902519066));
#267286=CARTESIAN_POINT('Ctrl Pts',(155.252129106249,-3.98309784010292,
125.534728128207));
#267287=CARTESIAN_POINT('Ctrl Pts',(154.973681482436,-6.58645273219382,
131.307088559209));
#267288=CARTESIAN_POINT('Ctrl Pts',(154.695233858623,-3.13717932950269,
136.617466571466));
#267289=CARTESIAN_POINT('Ctrl Pts',(154.41678623481,3.19500861727094,136.585884198101));
#267290=CARTESIAN_POINT('Ctrl Pts',(154.138338610998,6.59113972962085,131.241364097354));
#267291=CARTESIAN_POINT('Ctrl Pts',(153.859890987185,3.93033542552574,125.495259147487));
#267292=CARTESIAN_POINT('Ctrl Pts',(153.581443363372,-2.3422551270676,124.627959084596));
#267293=CARTESIAN_POINT('Ctrl Pts',(153.302995739559,-6.46242764341012,
129.436470296516));
#267294=CARTESIAN_POINT('Ctrl Pts',(153.024548115746,-4.64394486260028,
135.502005888322));
#267295=CARTESIAN_POINT('Ctrl Pts',(152.746100491933,1.44209637762021,137.250634969033));
#267296=CARTESIAN_POINT('Ctrl Pts',(152.46765286812,6.20292149713234,133.075452838754));
#267297=CARTESIAN_POINT('Ctrl Pts',(152.189205244307,5.26356479034146,126.813247906226));
#267298=CARTESIAN_POINT('Ctrl Pts',(151.910757620494,-0.512750819337957,
124.218680578724));
#267299=CARTESIAN_POINT('Ctrl Pts',(151.632309996682,-5.8178734753159,127.676031478561));
#267300=CARTESIAN_POINT('Ctrl Pts',(151.353862372869,-5.77665462639848,
134.008164029768));
#267301=CARTESIAN_POINT('Ctrl Pts',(151.075414749056,-0.4269723810881,137.39615775966));
#267302=CARTESIAN_POINT('Ctrl Pts',(150.796967125243,5.31507662368183,134.72661194316));
#267303=CARTESIAN_POINT('Ctrl Pts',(150.51851950143,6.17282986721635,128.452708771068));
#267304=CARTESIAN_POINT('Ctrl Pts',(150.240071877617,1.35805402228283,124.339858761329));
#267305=CARTESIAN_POINT('Ctrl Pts',(149.961624253804,-4.70470712450132,
126.167570148998));
#267306=CARTESIAN_POINT('Ctrl Pts',(149.683176629991,-6.44407226158927,
132.256265457474));
#267307=CARTESIAN_POINT('Ctrl Pts',(149.404729006178,-2.26164980070799,
137.010731147569));
#267308=CARTESIAN_POINT('Ctrl Pts',(149.126281382365,3.99911833928874,136.061845518646));
#267309=CARTESIAN_POINT('Ctrl Pts',(148.847833758553,6.58489209327119,130.281588108047));
#267310=CARTESIAN_POINT('Ctrl Pts',(148.56938613474,3.11947170339994,124.981733094838));
#267311=CARTESIAN_POINT('Ctrl Pts',(148.290938510927,-3.21259078723097,
125.032588323847));
#267312=CARTESIAN_POINT('Ctrl Pts',(148.012490887114,-6.59243928818165,
130.387420324031));
#267313=CARTESIAN_POINT('Ctrl Pts',(147.734043263301,-3.91415814185689,
136.125400085308));
#267314=CARTESIAN_POINT('Ctrl Pts',(147.455595639488,2.36104311957866,136.973604522958));
#267315=CARTESIAN_POINT('Ctrl Pts',(147.177148015675,6.46656109749016,132.152575195872));
#267316=CARTESIAN_POINT('Ctrl Pts',(146.898700391862,4.6296253358803,126.092602535266));
#267317=CARTESIAN_POINT('Ctrl Pts',(146.62025276805,-1.46170993963237,124.362505370115));
#267318=CARTESIAN_POINT('Ctrl Pts',(146.341805144237,-6.20980518912327,
128.552158475246));
#267319=CARTESIAN_POINT('Ctrl Pts',(146.063357520424,-5.2513928356585,134.811475322978));
#267320=CARTESIAN_POINT('Ctrl Pts',(145.784909896611,0.532792988974217,
137.388449514872));
#267321=CARTESIAN_POINT('Ctrl Pts',(145.506462272798,5.82736808512415,133.914967660766));
#267322=CARTESIAN_POINT('Ctrl Pts',(145.228014648985,5.76687659380242,127.582989895561));
#267323=CARTESIAN_POINT('Ctrl Pts',(144.949567025172,0.406907240360106,
124.211294451169));
#267324=CARTESIAN_POINT('Ctrl Pts',(144.671119401359,-5.32698998844935,
126.898304724507));
#267325=CARTESIAN_POINT('Ctrl Pts',(144.392671777546,-6.16564365580234,
133.174789542127));
#267326=CARTESIAN_POINT('Ctrl Pts',(144.114224153734,-1.33837201191069,
137.272965979966));
#267327=CARTESIAN_POINT('Ctrl Pts',(143.83577652992,4.71879812781917,135.426810098699));
#267328=CARTESIAN_POINT('Ctrl Pts',(143.557328906108,6.43962331418753,129.332848963481));
#267329=CARTESIAN_POINT('Ctrl Pts',(143.278881282295,2.24274926790569,124.591135151027));
#267330=CARTESIAN_POINT('Ctrl Pts',(143.000433658482,-4.01510179118866,
125.559072009383));
#267331=CARTESIAN_POINT('Ctrl Pts',(142.721986034669,-6.58327045280769,
131.347172852065));
#267332=CARTESIAN_POINT('Ctrl Pts',(142.443538410856,-3.10173517893752,
136.636455769093));
#267333=CARTESIAN_POINT('Ctrl Pts',(142.165090787043,3.23014319618891,136.566328155556));
#267334=CARTESIAN_POINT('Ctrl Pts',(141.886643163231,6.5936777752854,131.201233862367));
#267335=CARTESIAN_POINT('Ctrl Pts',(141.608195539417,3.89794459796173,125.471432445543));
#267336=CARTESIAN_POINT('Ctrl Pts',(141.329747915605,-2.37980923970876,
124.642331490782));
#267337=CARTESIAN_POINT('Ctrl Pts',(141.051300291792,-6.47063464623165,
129.475834271677));
#267338=CARTESIAN_POINT('Ctrl Pts',(140.772852667979,-4.61526292094352,
135.530187862324));
#267339=CARTESIAN_POINT('Ctrl Pts',(140.494405044166,1.48130996056343,137.241737084533));
#267340=CARTESIAN_POINT('Ctrl Pts',(140.215957420353,6.21663135432719,133.037651816923));
#267341=CARTESIAN_POINT('Ctrl Pts',(139.93750979654,5.23917223278974,126.781281039444));
#267342=CARTESIAN_POINT('Ctrl Pts',(139.659062172727,-0.552830222889001,
124.221923855894));
#267343=CARTESIAN_POINT('Ctrl Pts',(139.380614548914,-5.83680871099059,
127.711504486408));
#267344=CARTESIAN_POINT('Ctrl Pts',(139.102166925101,-5.75704513764935,
134.043268807033));
#267345=CARTESIAN_POINT('Ctrl Pts',(138.823719301288,-0.386838330098996,
137.398634730999));
#267346=CARTESIAN_POINT('Ctrl Pts',(138.545271677476,5.33885400470937,134.694184892919));
#267347=CARTESIAN_POINT('Ctrl Pts',(138.266824053663,6.15840032670771,128.41517657427));
#267348=CARTESIAN_POINT('Ctrl Pts',(137.98837642985,1.31867760304303,124.331711673279));
#267349=CARTESIAN_POINT('Ctrl Pts',(137.709928806037,-4.7328454168358,126.196294945608));
#267350=CARTESIAN_POINT('Ctrl Pts',(137.431481182224,-6.43511471099507,
132.295465453942));
#267351=CARTESIAN_POINT('Ctrl Pts',(137.153033558411,-2.22382795858067,
137.024383462168));
#267352=CARTESIAN_POINT('Ctrl Pts',(136.874585934598,4.03104804773404,136.037404341212));
#267353=CARTESIAN_POINT('Ctrl Pts',(136.596138310785,6.5815878258261,130.241513686623));
#267354=CARTESIAN_POINT('Ctrl Pts',(136.317690686972,3.08396992042408,124.96285186497));
#267355=CARTESIAN_POINT('Ctrl Pts',(136.03924306316,-3.24766568154122,125.052251213384));
#267356=CARTESIAN_POINT('Ctrl Pts',(135.760795439346,-6.5948551794591,130.427558098075));
#267357=CARTESIAN_POINT('Ctrl Pts',(135.482347815534,-3.88169494404043,
136.149128090351));
#267358=CARTESIAN_POINT('Ctrl Pts',(135.203900191721,2.3985533136112,136.959117881544));
#267359=CARTESIAN_POINT('Ctrl Pts',(134.925452567908,6.47464825189767,132.113186423748));
#267360=CARTESIAN_POINT('Ctrl Pts',(134.647004944095,4.60085775084163,126.064507989766));
#267361=CARTESIAN_POINT('Ctrl Pts',(134.368557320282,-1.50089625884118,
124.371522566057));
#267362=CARTESIAN_POINT('Ctrl Pts',(134.090109696469,-6.22339992950755,
128.590001050074));
#267363=CARTESIAN_POINT('Ctrl Pts',(133.811662072656,-5.22690309494509,
134.843367799137));
#267364=CARTESIAN_POINT('Ctrl Pts',(133.533214448844,0.572862335460145,
137.385084264805));
#267365=CARTESIAN_POINT('Ctrl Pts',(133.25476682503,5.84619526545829,133.879437184883));
#267366=CARTESIAN_POINT('Ctrl Pts',(132.976319201218,5.7471603490167,127.547944965438));
#267367=CARTESIAN_POINT('Ctrl Pts',(132.697871577405,0.366765836220533,
124.208939645549));
#267368=CARTESIAN_POINT('Ctrl Pts',(132.419423953592,-5.35066856255522,
126.930803994717));
#267369=CARTESIAN_POINT('Ctrl Pts',(132.140976329779,-6.15109994703373,
133.212277646521));
#267370=CARTESIAN_POINT('Ctrl Pts',(131.862528705966,-1.29897097812634,
137.280993182001));
#267371=CARTESIAN_POINT('Ctrl Pts',(131.584081082153,4.74684886141891,135.397999791857));
#267372=CARTESIAN_POINT('Ctrl Pts',(131.30563345834,6.43054649377913,129.293676412286));
#267373=CARTESIAN_POINT('Ctrl Pts',(131.027185834528,2.20488604801711,124.577598016342));
#267374=CARTESIAN_POINT('Ctrl Pts',(130.748738210715,-4.04695696120101,
125.583610256657));
#267375=CARTESIAN_POINT('Ctrl Pts',(130.470290586902,-6.57984422791396,
131.387237030814));
#267376=CARTESIAN_POINT('Ctrl Pts',(130.191842963089,-3.06617609243459,
136.65522885629));
#267377=CARTESIAN_POINT('Ctrl Pts',(129.913395339276,3.26515808096253,136.546558601182));
#267378=CARTESIAN_POINT('Ctrl Pts',(129.634947715463,6.59597148979528,131.161088921098));
#267379=CARTESIAN_POINT('Ctrl Pts',(129.35650009165,3.86540933062731,125.447803357213));
#267380=CARTESIAN_POINT('Ctrl Pts',(129.078052467837,-2.41727516764341,
124.656932233223));
#267381=CARTESIAN_POINT('Ctrl Pts',(128.799604844024,-6.47860187730669,
129.515247475871));
#267382=CARTESIAN_POINT('Ctrl Pts',(128.521157220212,-4.58640995902212,
135.558194719059));
#267383=CARTESIAN_POINT('Ctrl Pts',(128.242709596398,1.52046865302106,137.232600660681));
#267384=CARTESIAN_POINT('Ctrl Pts',(127.964261972586,6.23011085196111,132.999768039666));
#267385=CARTESIAN_POINT('Ctrl Pts',(127.685814348773,5.2145855357842,126.749463249355));
#267386=CARTESIAN_POINT('Ctrl Pts',(127.40736672496,-0.592889141112855,
124.225411047681));
#267387=CARTESIAN_POINT('Ctrl Pts',(127.128919101147,-5.85552766157182,
127.747092101177));
#267388=CARTESIAN_POINT('Ctrl Pts',(126.850471477334,-5.7372223194756,134.078253565364));
#267389=CARTESIAN_POINT('Ctrl Pts',(126.572023853521,-0.346689944673359,
137.400867349086));
#267390=CARTESIAN_POINT('Ctrl Pts',(126.293576229708,5.36243355253846,134.66161370381));
#267391=CARTESIAN_POINT('Ctrl Pts',(126.015128605896,6.14374258441013,128.377732909565));
#267392=CARTESIAN_POINT('Ctrl Pts',(125.736680982083,1.27925231971985,124.323804431618));
#267393=CARTESIAN_POINT('Ctrl Pts',(125.45823335827,-4.76080833184274,126.225190495787));
#267394=CARTESIAN_POINT('Ctrl Pts',(125.179785734457,-6.42591870485886,
132.334610196974));
#267395=CARTESIAN_POINT('Ctrl Pts',(124.901338110644,-2.1859237116904,137.037805291532));
#267396=CARTESIAN_POINT('Ctrl Pts',(124.622890486831,4.06282838421153,136.012769251418));
#267397=CARTESIAN_POINT('Ctrl Pts',(124.344442863018,6.5780396752237,130.201460121699));
#267398=CARTESIAN_POINT('Ctrl Pts',(124.065995239205,3.04835385980878,124.944187094356));
#267399=CARTESIAN_POINT('Ctrl Pts',(123.787547615392,-3.28262023240536,
125.07212724945));
#267400=CARTESIAN_POINT('Ctrl Pts',(123.509099991579,-6.59702669595264,
130.467709834674));
#267401=CARTESIAN_POINT('Ctrl Pts',(123.230652367767,-3.84908790859021,
136.17265804307));
#267402=CARTESIAN_POINT('Ctrl Pts',(122.952204743954,2.43597462836867,136.944403173336));
#267403=CARTESIAN_POINT('Ctrl Pts',(122.673757120141,6.48249548583303,132.073749152604));
#267404=CARTESIAN_POINT('Ctrl Pts',(122.395309496328,4.57191967932717,126.036589081248));
#267405=CARTESIAN_POINT('Ctrl Pts',(122.116861872515,-1.54002696178715,
124.380778133181));
#267406=CARTESIAN_POINT('Ctrl Pts',(121.838414248702,-6.23676405951882,
128.627925678811));
#267407=CARTESIAN_POINT('Ctrl Pts',(121.559966624889,-5.20221966941523,
134.8751106084));
#267408=CARTESIAN_POINT('Ctrl Pts',(121.281519001076,0.612910454321425,
137.381475163605));
#267409=CARTESIAN_POINT('Ctrl Pts',(121.003071377263,5.86480581287692,133.843792760907));
#267410=CARTESIAN_POINT('Ctrl Pts',(120.724623753451,5.72723114109079,127.513020702994));
#267411=CARTESIAN_POINT('Ctrl Pts',(120.446176129638,0.326610841437887,
124.206829235678));
#267412=CARTESIAN_POINT('Ctrl Pts',(120.167728505825,-5.3741488656698,126.963446800991));
#267413=CARTESIAN_POINT('Ctrl Pts',(119.889280882012,-6.13632830699453,
133.249676524665));
#267414=CARTESIAN_POINT('Ctrl Pts',(119.610833258199,-1.25952181049465,
137.288780390037));
#267415=CARTESIAN_POINT('Ctrl Pts',(119.332385634386,4.77472369878856,135.369019266025));
#267416=CARTESIAN_POINT('Ctrl Pts',(119.053938010573,6.42123138710552,129.254559840052));
#267417=CARTESIAN_POINT('Ctrl Pts',(118.77549038676,2.16694112526505,124.564291616636));
#267418=CARTESIAN_POINT('Ctrl Pts',(118.497042762948,-4.07866216973492,
125.608341960757));
#267419=CARTESIAN_POINT('Ctrl Pts',(118.218595139134,-6.57617418447253,
131.427279610862));
#267420=CARTESIAN_POINT('Ctrl Pts',(117.940147515322,-3.03050338764912,
136.673785137412));
#267421=CARTESIAN_POINT('Ctrl Pts',(117.661699891509,3.30005197410286,136.526576267552));
#267422=CARTESIAN_POINT('Ctrl Pts',(117.383252267696,6.59802078815589,131.120930761129));
#267423=CARTESIAN_POINT('Ctrl Pts',(117.104804643883,3.83273082912851,125.424372758082));
#267424=CARTESIAN_POINT('Ctrl Pts',(116.82635702007,-2.45465152255762,124.671760770883));
#267425=CARTESIAN_POINT('Ctrl Pts',(116.547909396257,-6.48632904140672,
129.554708448625));
#267426=CARTESIAN_POINT('Ctrl Pts',(116.269461772444,-4.55738704599302,
135.586025420722));
#267427=CARTESIAN_POINT('Ctrl Pts',(115.991014148631,1.55957100395386,137.223226036031));
#267428=CARTESIAN_POINT('Ctrl Pts',(115.712566524818,6.24335949054626,132.961802910777));
#267429=CARTESIAN_POINT('Ctrl Pts',(115.434118901006,5.18980561039392,126.717795714978));
#267430=CARTESIAN_POINT('Ctrl Pts',(115.155671277193,-0.632926089611396,
124.229142024863));
#267431=CARTESIAN_POINT('Ctrl Pts',(114.87722365338,-5.87402963342224,127.782793004156));
#267432=CARTESIAN_POINT('Ctrl Pts',(114.598776029567,-5.71718690641897,
134.113117008387));
#267433=CARTESIAN_POINT('Ctrl Pts',(114.320328405754,-0.306528712524212,
137.40285553119));
#267434=CARTESIAN_POINT('Ctrl Pts',(114.041880781941,5.38581439342023,134.628899582769));
#267435=CARTESIAN_POINT('Ctrl Pts',(113.763433158128,6.12885718347172,128.340379164441));
#267436=CARTESIAN_POINT('Ctrl Pts',(113.484985534315,1.23977963323159,124.316137329349));
#267437=CARTESIAN_POINT('Ctrl Pts',(113.206537910502,-4.78859483334625,
126.254255728798));
#267438=CARTESIAN_POINT('Ctrl Pts',(112.92809028669,-6.41648458394181,132.373698236044));
#267439=CARTESIAN_POINT('Ctrl Pts',(112.649642662877,-2.14793846459313,
137.050996138312));
#267440=CARTESIAN_POINT('Ctrl Pts',(112.371195039064,4.09445817108915,135.987941162125));
#267441=CARTESIAN_POINT('Ctrl Pts',(112.092747415251,6.57424777294209,130.161428897475));
#267442=CARTESIAN_POINT('Ctrl Pts',(111.814299791438,3.01262484132005,124.925739474628));
#267443=CARTESIAN_POINT('Ctrl Pts',(111.535852167625,-3.31745314456969,
125.092215695531));
#267444=CARTESIAN_POINT('Ctrl Pts',(111.257404543812,-6.59895375719588,
130.507874045991));
#267445=CARTESIAN_POINT('Ctrl Pts',(110.978956919999,-3.816338243772,136.195989071554));
#267446=CARTESIAN_POINT('Ctrl Pts',(110.700509296186,2.47330567719032,136.929460943594));
#267447=CARTESIAN_POINT('Ctrl Pts',(110.422061672374,6.49010250851429,132.0342648438));
#267448=CARTESIAN_POINT('Ctrl Pts',(110.143614048561,4.54281219364771,126.008846844259));
#267449=CARTESIAN_POINT('Ctrl Pts',(109.865166424748,-1.57910059846782,
124.390271728514));
#267450=CARTESIAN_POINT('Ctrl Pts',(109.586718800935,-6.24989708394428,
128.665930956147));
#267451=CARTESIAN_POINT('Ctrl Pts',(109.308271177122,-5.17734347372243,
134.906702574525));
#267452=CARTESIAN_POINT('Ctrl Pts',(109.029823553309,0.652935861560398,
137.377622345005));
#267453=CARTESIAN_POINT('Ctrl Pts',(108.751375929496,5.88319903775945,133.808035709655));
#267454=CARTESIAN_POINT('Ctrl Pts',(108.472928305683,5.70708970850866,127.478218402361));
#267455=CARTESIAN_POINT('Ctrl Pts',(108.19448068187,0.286443743970404,124.204963299759));
#267456=CARTESIAN_POINT('Ctrl Pts',(107.916033058058,-5.39743002772183,
126.996231933739));
#267457=CARTESIAN_POINT('Ctrl Pts',(107.637585434244,-6.12132928305326,
133.286984790727));
#267458=CARTESIAN_POINT('Ctrl Pts',(107.359137810432,-1.22002597081922,
137.296327315513));
#267459=CARTESIAN_POINT('Ctrl Pts',(107.080690186619,4.80242160701559,135.339869595089));
#267460=CARTESIAN_POINT('Ctrl Pts',(106.802242562806,6.41167833934146,129.215500696253));
#267461=CARTESIAN_POINT('Ctrl Pts',(106.523794938993,2.12891590571267,124.551216444981));
#267462=CARTESIAN_POINT('Ctrl Pts',(106.24534731518,-4.11021624194206,125.633266205238));
#267463=CARTESIAN_POINT('Ctrl Pts',(105.966899691367,-6.57226045847839,
131.467299108419));
#267464=CARTESIAN_POINT('Ctrl Pts',(105.688452067554,-2.99471838644612,
136.692123924851));
#267465=CARTESIAN_POINT('Ctrl Pts',(105.410004443742,3.33482358260376,136.506381895117));
#267466=CARTESIAN_POINT('Ctrl Pts',(105.131556819929,6.59982559442975,131.080760870538));
#267467=CARTESIAN_POINT('Ctrl Pts',(104.853109196116,3.79991030437941,125.401141516381));
#267468=CARTESIAN_POINT('Ctrl Pts',(104.574661572303,-2.49193691945696,
124.686816554284));
#267469=CARTESIAN_POINT('Ctrl Pts',(104.29621394849,-6.49381585219884,129.594215727701));
#267470=CARTESIAN_POINT('Ctrl Pts',(104.017766324677,-4.52819525731082,
135.613678936038));
#267471=CARTESIAN_POINT('Ctrl Pts',(103.739318700864,1.59861556440955,137.213613557961));
#267472=CARTESIAN_POINT('Ctrl Pts',(103.460871077051,6.25637677914949,132.923757837073));
#267473=CARTESIAN_POINT('Ctrl Pts',(103.182423453238,5.16483337484823,126.686279609768));
#267474=CARTESIAN_POINT('Ctrl Pts',(102.903975829425,-0.672939584800916,
124.233116649188));
#267475=CARTESIAN_POINT('Ctrl Pts',(102.625528205613,-5.89231394094447,
127.818605872432));
#267476=CARTESIAN_POINT('Ctrl Pts',(102.347080581799,-5.69693964089892,
134.147857844226));
#267477=CARTESIAN_POINT('Ctrl Pts',(102.068632957987,-0.266356121840884,
137.40459920364));
#267478=CARTESIAN_POINT('Ctrl Pts',(101.790185334174,5.40899566096888,134.59604374203));
#267479=CARTESIAN_POINT('Ctrl Pts',(101.511737710361,6.11374467547657,128.303116723058));
#267480=CARTESIAN_POINT('Ctrl Pts',(101.233290086548,1.20026100625305,124.308710650579));
#267481=CARTESIAN_POINT('Ctrl Pts',(100.954842462735,-4.81620389170723,
126.28348956762));
#267482=CARTESIAN_POINT('Ctrl Pts',(100.676394838922,-6.40681269782886,
132.412728122731));
#267483=CARTESIAN_POINT('Ctrl Pts',(100.397947215109,-2.10987362484612,
137.063955513716));
#267484=CARTESIAN_POINT('Ctrl Pts',(100.119499591297,4.12593623631335,135.962920993349));
#267485=CARTESIAN_POINT('Ctrl Pts',(99.8410519674839,6.5702122594916,130.121421497322));
#267486=CARTESIAN_POINT('Ctrl Pts',(99.5626043436712,2.97678418891005,124.907509689368));
#267487=CARTESIAN_POINT('Ctrl Pts',(99.2841567198582,-3.35216312728773,
125.112515807244));
#267488=CARTESIAN_POINT('Ctrl Pts',(99.0057090960455,-6.6006362917809,130.548049243728));
#267489=CARTESIAN_POINT('Ctrl Pts',(98.7272614722323,-3.78344716313679,
136.219120311263));
#267490=CARTESIAN_POINT('Ctrl Pts',(98.4488138484198,2.51054507676055,136.914291746006));
#267491=CARTESIAN_POINT('Ctrl Pts',(98.1703662246066,6.49746903806041,131.994734960442));
#267492=CARTESIAN_POINT('Ctrl Pts',(97.8919186007939,4.51353637239165,125.981282306795));
#267493=CARTESIAN_POINT('Ctrl Pts',(97.6134709769809,-1.61811572099509,
124.400003000271));
#267494=CARTESIAN_POINT('Ctrl Pts',(97.335023353168,-6.26279851613479,128.704015473778));
#267495=CARTESIAN_POINT('Ctrl Pts',(97.0565757293552,-5.15227542966332,
134.938142526861));
#267496=CARTESIAN_POINT('Ctrl Pts',(96.7781281055422,0.692937074020952,
137.373525951775));
#267497=CARTESIAN_POINT('Ctrl Pts',(96.4996804817294,5.90137425853808,133.772167356118));
#267498=CARTESIAN_POINT('Ctrl Pts',(96.2212328579164,5.6867367976186,127.443539353151));
#267499=CARTESIAN_POINT('Ctrl Pts',(95.9427852341037,0.246266032224636,
124.203341906934));
#267500=CARTESIAN_POINT('Ctrl Pts',(95.6643376102905,-5.42051118601915,
127.029158178097));
#267501=CARTESIAN_POINT('Ctrl Pts',(95.3858899864779,-6.10610343100435,
133.324201062238));
#267502=CARTESIAN_POINT('Ctrl Pts',(95.1074423626648,-1.18048492263276,
137.303633678775));
#267503=CARTESIAN_POINT('Ctrl Pts',(94.828994738852,4.82994155974394,135.3105518592));
#267504=CARTESIAN_POINT('Ctrl Pts',(94.5505471150391,6.40188770447863,129.176500428244));
#267505=CARTESIAN_POINT('Ctrl Pts',(94.2720994912261,2.09081179839861,124.538372985881));
#267506=CARTESIAN_POINT('Ctrl Pts',(93.9936518674133,-4.14161800857485,
125.658382066524));
#267507=CARTESIAN_POINT('Ctrl Pts',(93.7152042436005,-6.56810319495607,
131.507294040545));
#267508=CARTESIAN_POINT('Ctrl Pts',(93.4367566197874,-2.95882241485189,
136.710244539055));
#267509=CARTESIAN_POINT('Ctrl Pts',(93.1583089959747,3.36947161799043,136.485976232185));
#267510=CARTESIAN_POINT('Ctrl Pts',(92.8798613721617,6.60138584173913,131.040580737834));
#267511=CARTESIAN_POINT('Ctrl Pts',(92.6014137483489,3.76694897255651,125.37811049295));
#267512=CARTESIAN_POINT('Ctrl Pts',(92.3229661245359,-2.5291299767175,124.702099025532));
#267513=CARTESIAN_POINT('Ctrl Pts',(92.044518500723,-6.50106203225643,129.633767849141));
#267514=CARTESIAN_POINT('Ctrl Pts',(91.7660708769102,-4.49883567468812,
135.641154240296));
#267515=CARTESIAN_POINT('Ctrl Pts',(91.4876232530973,1.63760088757763,137.203763582666));
#267516=CARTESIAN_POINT('Ctrl Pts',(91.2091756292845,6.26916223541028,132.885634228324));
#267517=CARTESIAN_POINT('Ctrl Pts',(90.9307280054714,5.13966975450256,126.654916101563));
#267518=CARTESIAN_POINT('Ctrl Pts',(90.6522803816587,-0.71292814396669,
124.237334773374));
#267519=CARTESIAN_POINT('Ctrl Pts',(90.3738327578456,-5.91037990660673,
127.85452937895));
#267520=CARTESIAN_POINT('Ctrl Pts',(90.0953851340328,-5.67648127318543,
134.182474785545));
#267521=CARTESIAN_POINT('Ctrl Pts',(89.8169375102199,-0.226173661233629,
137.406098301819));
#267522=CARTESIAN_POINT('Ctrl Pts',(89.5384898864071,5.43197649619419,134.563047399079));
#267523=CARTESIAN_POINT('Ctrl Pts',(89.260042262594,6.09840562042418,128.265946966186));
#267524=CARTESIAN_POINT('Ctrl Pts',(88.9815946387814,1.1606979031614,124.301524670509));
#267525=CARTESIAN_POINT('Ctrl Pts',(88.7031470149683,-4.84363448386183,
126.312890928981));
#267526=CARTESIAN_POINT('Ctrl Pts',(88.4246993911556,-6.39690340491527,
132.45169841077));
#267527=CARTESIAN_POINT('Ctrl Pts',(88.1462517673426,-2.07173060295614,
137.076682937528));
#267528=CARTESIAN_POINT('Ctrl Pts',(87.8678041435297,4.15726141345302,135.937709672222));
#267529=CARTESIAN_POINT('Ctrl Pts',(87.5893565197169,6.5659332844097,130.081439403729));
#267530=CARTESIAN_POINT('Ctrl Pts',(87.3109088959039,2.94083323066708,124.889498414087));
#267531=CARTESIAN_POINT('Ctrl Pts',(87.032461272091,-3.38674889436835,125.133026832359));
#267532=CARTESIAN_POINT('Ctrl Pts',(86.7540136482781,-6.60207423736065,
130.588233939178));
#267533=CARTESIAN_POINT('Ctrl Pts',(86.4755660244652,-3.75041588547566,
136.242050905059));
#267534=CARTESIAN_POINT('Ctrl Pts',(86.1971184006524,2.54769144715974,136.898896142674));
#267535=CARTESIAN_POINT('Ctrl Pts',(85.9186707768394,6.50459480150186,131.955160967326));
#267536=CARTESIAN_POINT('Ctrl Pts',(85.6402231530266,4.48409330038545,125.953896490271));
#267537=CARTESIAN_POINT('Ctrl Pts',(85.3617755292137,-1.65707088364924,
124.409971587854));
#267538=CARTESIAN_POINT('Ctrl Pts',(85.0833279054008,-6.27546787802325,
128.742177820471));
#267539=CARTESIAN_POINT('Ctrl Pts',(84.8048802815879,-5.12701646614329,
134.969429300388));
#267540=CARTESIAN_POINT('Ctrl Pts',(84.526432657775,0.732912609443495,137.369186135708));
#267541=CARTESIAN_POINT('Ctrl Pts',(84.2479850339622,5.91933080172332,133.73618902941));
#267542=CARTESIAN_POINT('Ctrl Pts',(83.9695374101491,5.6661731626052,127.408984840408));
#267543=CARTESIAN_POINT('Ctrl Pts',(83.6910897863363,0.206079195000604,
124.201965117285));
#267544=CARTESIAN_POINT('Ctrl Pts',(83.4126421625234,-5.44339148528112,
127.062224313968));
#267545=CARTESIAN_POINT('Ctrl Pts',(83.1341945387106,-6.09065131504733,
133.361323960135));
#267546=CARTESIAN_POINT('Ctrl Pts',(82.8557469148977,-1.14090013114324,
137.310699209084));
#267547=CARTESIAN_POINT('Ctrl Pts',(82.5772992910847,4.85728253721157,135.281067144739));
#267548=CARTESIAN_POINT('Ctrl Pts',(82.2988516672719,6.39185984531258,129.137560481192));
#267549=CARTESIAN_POINT('Ctrl Pts',(82.0204040434589,2.05263021528453,124.52576171526));
#267550=CARTESIAN_POINT('Ctrl Pts',(81.7419564196462,-4.17286630602932,
125.683688613938));
#267551=CARTESIAN_POINT('Ctrl Pts',(81.4635087958331,-6.56370254795435,
131.547262925216));
#267552=CARTESIAN_POINT('Ctrl Pts',(81.1850611720204,-2.92281680300497,
136.728146308557));
#267553=CARTESIAN_POINT('Ctrl Pts',(80.9066135482074,3.40399479636718,136.465360034899));
#267554=CARTESIAN_POINT('Ctrl Pts',(80.6281659243945,6.60270147226842,131.000391851905));
#267555=CARTESIAN_POINT('Ctrl Pts',(80.3497183005816,3.73384805505426,125.355280541214));
#267556=CARTESIAN_POINT('Ctrl Pts',(80.0712706767688,-2.56622931613655,
124.717607618327));
#267557=CARTESIAN_POINT('Ctrl Pts',(79.7928230529558,-6.50806731306963,
129.673363347327));
#267558=CARTESIAN_POINT('Ctrl Pts',(79.514375429143,-4.46930938605503,135.668450315387));
#267559=CARTESIAN_POINT('Ctrl Pts',(79.23592780533,1.67652552884245,137.193676475141));
#267560=CARTESIAN_POINT('Ctrl Pts',(78.9574801815173,6.28171538555901,132.847433497217));
#267561=CARTESIAN_POINT('Ctrl Pts',(78.6790325577042,5.11431568180404,126.62370635255));
#267562=CARTESIAN_POINT('Ctrl Pts',(78.4005849338915,-0.752890285318027,
124.241796241119));
#267563=CARTESIAN_POINT('Ctrl Pts',(78.1221373100785,-5.92822686096799,
127.890562192549));
#267564=CARTESIAN_POINT('Ctrl Pts',(77.8436896862655,-5.65581256137084,
134.216966549603));
#267565=CARTESIAN_POINT('Ctrl Pts',(77.5652420624528,-0.185982819678218,
137.407352770183));
#267566=CARTESIAN_POINT('Ctrl Pts',(77.2867944386398,5.45475604753291,134.529911776607));
#267567=CARTESIAN_POINT('Ctrl Pts',(77.008346814827,6.08284058670873,128.228871271165));
#267568=CARTESIAN_POINT('Ctrl Pts',(76.729899191014,1.12109178998211,124.294579655415));
#267569=CARTESIAN_POINT('Ctrl Pts',(76.4514515672013,-4.8708855933594,126.342458723402));
#267570=CARTESIAN_POINT('Ctrl Pts',(76.1730039433881,-6.38675707239351,
132.4906076561));
#267571=CARTESIAN_POINT('Ctrl Pts',(75.8945563195755,-2.03351081232684,
137.089177938131));
#267572=CARTESIAN_POINT('Ctrl Pts',(75.6161086957625,4.18843254174224,135.912308132958));
#267573=CARTESIAN_POINT('Ctrl Pts',(75.3376610719495,6.56141100625526,130.041484098248));
#267574=CARTESIAN_POINT('Ctrl Pts',(75.0592134481368,2.90477329876725,124.871706316201));
#267575=CARTESIAN_POINT('Ctrl Pts',(74.7807658243238,-3.42120916422307,
125.153748010832));
#267576=CARTESIAN_POINT('Ctrl Pts',(74.5023182005109,-6.60326754065171,
130.628426643279));
#267577=CARTESIAN_POINT('Ctrl Pts',(74.223870576698,-3.71724563477466,136.264780003243));
#267578=CARTESIAN_POINT('Ctrl Pts',(73.9454229528852,2.58474341191554,136.883274704086));
#267579=CARTESIAN_POINT('Ctrl Pts',(73.6669753290721,6.51147953479087,131.915544330879));
#267580=CARTESIAN_POINT('Ctrl Pts',(73.3885277052595,4.45448406865298,125.926690409479));
#267581=CARTESIAN_POINT('Ctrl Pts',(73.1100800814464,-1.6959646429323,124.420177121874));
#267582=CARTESIAN_POINT('Ctrl Pts',(72.8316324576336,-6.28790470014163,
128.780416582107));
#267583=CARTESIAN_POINT('Ctrl Pts',(72.5531848338207,-5.1015675191428,135.000561735763));
#267584=CARTESIAN_POINT('Ctrl Pts',(72.2747372100078,0.772860986519783,
137.364603057617));
#267585=CARTESIAN_POINT('Ctrl Pts',(71.996289586195,5.93706800192887,133.700102062723));
#267586=CARTESIAN_POINT('Ctrl Pts',(71.7178419623819,5.64539956546153,127.374556144564));
#267587=CARTESIAN_POINT('Ctrl Pts',(71.4393943385692,0.165884721436248,
124.20083298183));
#267588=CARTESIAN_POINT('Ctrl Pts',(71.1609467147562,-5.46607007766984,
127.095429116077));
#267589=CARTESIAN_POINT('Ctrl Pts',(70.8824990909434,-6.07497350776591,
133.398352108815));
#267590=CARTESIAN_POINT('Ctrl Pts',(70.6040514671303,-1.10127306317963,
137.317523644624));
#267591=CARTESIAN_POINT('Ctrl Pts',(70.3256038433176,4.88444352628841,135.251416544269));
#267592=CARTESIAN_POINT('Ctrl Pts',(70.0471562195047,6.38159513342946,129.098682298033));
#267593=CARTESIAN_POINT('Ctrl Pts',(69.7687085956917,2.01437257120279,124.513383100429));
#267594=CARTESIAN_POINT('Ctrl Pts',(69.4902609718789,-4.20395997638847,
125.709184909736));
#267595=CARTESIAN_POINT('Ctrl Pts',(69.211813348066,-6.5590586805409,131.587204281367));
#267596=CARTESIAN_POINT('Ctrl Pts',(68.9333657242531,-2.88670288510633,
136.745828570004));
#267597=CARTESIAN_POINT('Ctrl Pts',(68.6549181004402,3.43839183846502,136.444534067195));
#267598=CARTESIAN_POINT('Ctrl Pts',(68.3764704766273,6.60377243726651,130.960195701968));
#267599=CARTESIAN_POINT('Ctrl Pts',(68.0980228528144,3.70060877843901,125.332652507142));
#267600=CARTESIAN_POINT('Ctrl Pts',(67.8195752290015,-2.6032335629848,124.733341757993));
#267601=CARTESIAN_POINT('Ctrl Pts',(67.5411276051886,-6.51483143505509,
129.713000755032));
#267602=CARTESIAN_POINT('Ctrl Pts',(67.2626799813758,-4.43961748551916,
135.695566149845));
#267603=CARTESIAN_POINT('Ctrl Pts',(66.9842323575627,1.71538804583728,137.183352609169));
#267604=CARTESIAN_POINT('Ctrl Pts',(66.7057847337499,6.29403576443417,132.809157059292));
#267605=CARTESIAN_POINT('Ctrl Pts',(66.4273371099371,5.08877209625689,126.592651519219));
#267606=CARTESIAN_POINT('Ctrl Pts',(66.1488894861241,-0.792824528042931,
124.246500887099));
#267607=CARTESIAN_POINT('Ctrl Pts',(65.8704418623113,-5.94585414270274,
127.92670297802));
#267608=CARTESIAN_POINT('Ctrl Pts',(65.5919942384984,-5.63493427134196,
134.251331858291));
#267609=CARTESIAN_POINT('Ctrl Pts',(65.3135466146855,-0.145785086460763,
137.408362562243));
#267610=CARTESIAN_POINT('Ctrl Pts',(65.0350989908726,5.47733347088038,134.496638102466));
#267611=CARTESIAN_POINT('Ctrl Pts',(64.7566513670597,6.06705015109826,128.191891011849));
#267612=CARTESIAN_POINT('Ctrl Pts',(64.4782037432468,1.0814441343344,124.28787586265));
#267613=CARTESIAN_POINT('Ctrl Pts',(64.199756119434,-4.89795621039988,126.37219185524));
#267614=CARTESIAN_POINT('Ctrl Pts',(63.921308495621,-6.37637407623982,132.529454416925));
#267615=CARTESIAN_POINT('Ctrl Pts',(63.6428608718081,-1.99521566920641,
137.101440052517));
#267616=CARTESIAN_POINT('Ctrl Pts',(63.3644132479953,4.21944846612332,135.886717316821));
#267617=CARTESIAN_POINT('Ctrl Pts',(63.0859656241823,6.556645592603,130.001557061437));
#267618=CARTESIAN_POINT('Ctrl Pts',(62.8075180003696,2.86860572942485,124.854134055001));
#267619=CARTESIAN_POINT('Ctrl Pts',(62.5290703765565,-3.4555426599142,125.174678574835));
#267620=CARTESIAN_POINT('Ctrl Pts',(62.2506227527437,-6.60421615743575,
130.66862586668));
#267621=CARTESIAN_POINT('Ctrl Pts',(61.9721751289308,-3.68393764016947,
136.287306763578));
#267622=CARTESIAN_POINT('Ctrl Pts',(61.6937275051179,2.62169959805353,136.867428009101));
#267623=CARTESIAN_POINT('Ctrl Pts',(61.415279881305,6.51812298281107,131.875886519111));
#267624=CARTESIAN_POINT('Ctrl Pts',(61.1368322574921,4.42470977437533,125.899665072552));
#267625=CARTESIAN_POINT('Ctrl Pts',(60.8583846336791,-1.73479555762186,
124.430619224162));
#267626=CARTESIAN_POINT('Ctrl Pts',(60.5799370098664,-6.30010852163892,
128.818730341733));
#267627=CARTESIAN_POINT('Ctrl Pts',(60.3014893860534,-5.07592953168175,
135.031538679362));
#267628=CARTESIAN_POINT('Ctrl Pts',(60.0230417622406,0.81278072494776,137.35977688733));
#267629=CARTESIAN_POINT('Ctrl Pts',(59.7445941384276,5.95458520189618,133.663907793273));
#267630=CARTESIAN_POINT('Ctrl Pts',(59.4661465146148,5.62441677596096,127.340254541386));
#267631=CARTESIAN_POINT('Ctrl Pts',(59.1876988908018,0.125684100952275,
124.199945542519));
#267632=CARTESIAN_POINT('Ctrl Pts',(58.909251266989,-5.48854612282181,127.128771354006));
#267633=CARTESIAN_POINT('Ctrl Pts',(58.6308036431761,-6.05907059010694,
133.435284136186));
#267634=CARTESIAN_POINT('Ctrl Pts',(58.3523560193632,-1.06160518713815,
137.324106732513));
#267635=CARTESIAN_POINT('Ctrl Pts',(58.0739083955504,4.91142352051418,135.221601156507));
#267636=CARTESIAN_POINT('Ctrl Pts',(57.7954607717374,6.37109394919177,129.059867319411));
#267637=CARTESIAN_POINT('Ctrl Pts',(57.5170131479246,1.97604028380464,124.501237600083));
#267638=CARTESIAN_POINT('Ctrl Pts',(57.2385655241116,-4.23489786746425,
125.734870009144));
#267639=CARTESIAN_POINT('Ctrl Pts',(56.9601179002987,-6.554171764796,131.627116628959));
#267640=CARTESIAN_POINT('Ctrl Pts',(56.6816702764859,-2.85048199937133,
136.76329066817));
#267641=CARTESIAN_POINT('Ctrl Pts',(56.4032226526729,3.47266146968847,136.423499100792));
#267642=CARTESIAN_POINT('Ctrl Pts',(56.1247750288601,6.60459869704857,130.919993777505));
#267643=CARTESIAN_POINT('Ctrl Pts',(55.8463274050471,3.66723237440476,125.310227229228));
#267644=CARTESIAN_POINT('Ctrl Pts',(55.5678797812343,-2.6401413460556,124.749300861495));
#267645=CARTESIAN_POINT('Ctrl Pts',(55.2894321574214,-6.5213541475661,129.752678603477));
#267646=CARTESIAN_POINT('Ctrl Pts',(55.0109845336085,-4.40976107332459,
135.722500738884));
#267647=CARTESIAN_POINT('Ctrl Pts',(54.7325369097956,1.75418699849736,137.172792367301));
#267648=CARTESIAN_POINT('Ctrl Pts',(54.4540892859827,6.30612291549916,132.770806332897));
#267649=CARTESIAN_POINT('Ctrl Pts',(54.1756416621698,5.06303994438864,126.561752752318));
#267650=CARTESIAN_POINT('Ctrl Pts',(53.897194038357,-0.832729392363195,
124.251448536985));
#267651=CARTESIAN_POINT('Ctrl Pts',(53.618746414544,-5.96326109862574,127.962950396153));
#267652=CARTESIAN_POINT('Ctrl Pts',(53.3402987907312,-5.61384717675129,
134.285569438194));
#267653=CARTESIAN_POINT('Ctrl Pts',(53.0618511669183,-0.105581951123662,
137.409127640582));
#267654=CARTESIAN_POINT('Ctrl Pts',(52.7834035431054,5.49970792962155,134.463227609627));
#267655=CARTESIAN_POINT('Ctrl Pts',(52.5049559192925,6.05103489871361,128.155007558556));
#267656=CARTESIAN_POINT('Ctrl Pts',(52.2265082954796,1.04175640537643,124.281413540623));
#267657=CARTESIAN_POINT('Ctrl Pts',(51.9480606716666,-4.9248453318719,126.402089222721));
#267658=CARTESIAN_POINT('Ctrl Pts',(51.6696130478539,-6.36575480119974,
132.568237253767));
#267659=CARTESIAN_POINT('Ctrl Pts',(51.3911654240409,-1.95684659263562,
137.113468826308));
#267660=CARTESIAN_POINT('Ctrl Pts',(51.112717800228,4.25030803728985,135.860938172086));
#267661=CARTESIAN_POINT('Ctrl Pts',(50.8342701764151,6.55163722003711,129.961659772806));
#267662=CARTESIAN_POINT('Ctrl Pts',(50.5558225526023,2.83233186284197,124.836782281636));
#267663=CARTESIAN_POINT('Ctrl Pts',(50.2773749287893,-3.48974810920128,
125.195817748775));
#267664=CARTESIAN_POINT('Ctrl Pts',(49.9989273049765,-6.60492005256131,
130.708830119782));
#267665=CARTESIAN_POINT('Ctrl Pts',(49.7204796811635,-3.65049313590031,
136.309630351328));
#267666=CARTESIAN_POINT('Ctrl Pts',(49.4420320573507,2.65855863614892,136.851356644924));
#267667=CARTESIAN_POINT('Ctrl Pts',(49.1635844335378,6.52452489938715,131.836189001557));
#267668=CARTESIAN_POINT('Ctrl Pts',(48.8851368097249,4.39477152084969,125.87282148092));
#267669=CARTESIAN_POINT('Ctrl Pts',(48.606689185912,-1.77356218882415,124.441297507781));
#267670=CARTESIAN_POINT('Ctrl Pts',(48.3282415620992,-6.31207889029818,
128.857117679619));
#267671=CARTESIAN_POINT('Ctrl Pts',(48.0497939382862,-5.05010345378512,
135.062358983324));
#267672=CARTESIAN_POINT('Ctrl Pts',(47.7713463144734,0.852670345487299,
137.354707803682));
#267673=CARTESIAN_POINT('Ctrl Pts',(47.4928986906604,5.97188175251911,133.627607562248));
#267674=CARTESIAN_POINT('Ctrl Pts',(47.2144510668476,5.60322557162828,127.306081301933));
#267675=CARTESIAN_POINT('Ctrl Pts',(46.9360034430346,0.0854788231980546,
124.199302832238));
#267676=CARTESIAN_POINT('Ctrl Pts',(46.6575558192218,-5.5108187878785,127.162249792247));
#267677=CARTESIAN_POINT('Ctrl Pts',(46.3791081954089,-6.04294315135938,
133.47211867372));
#267678=CARTESIAN_POINT('Ctrl Pts',(46.100660571596,-1.02189797292572,137.330448228811));
#267679=CARTESIAN_POINT('Ctrl Pts',(45.822212947783,4.93822152013526,135.191622086273));
#267680=CARTESIAN_POINT('Ctrl Pts',(45.5437653239702,6.36035668172477,129.02111698363));
#267681=CARTESIAN_POINT('Ctrl Pts',(45.2653177001572,1.9376347735074,124.489325664279));
#267682=CARTESIAN_POINT('Ctrl Pts',(44.9868700763445,-4.26567883284234,
125.76074296039));
#267683=CARTESIAN_POINT('Ctrl Pts',(44.7084224525315,-6.54904198180601,
131.666998489025));
#267684=CARTESIAN_POINT('Ctrl Pts',(44.4299748287186,-2.81415548797717,
136.780531955991));
#267685=CARTESIAN_POINT('Ctrl Pts',(44.1515272049057,3.50680242016433,136.402255915145));
#267686=CARTESIAN_POINT('Ctrl Pts',(43.8730795810928,6.60518022099696,130.879787568212));
#267687=CARTESIAN_POINT('Ctrl Pts',(43.59463195728,3.63372007972613,125.288005538446));
#267688=CARTESIAN_POINT('Ctrl Pts',(43.316184333467,-2.6769512977182,124.765484337463));
#267689=CARTESIAN_POINT('Ctrl Pts',(43.0377367096542,-6.52763520890084,
129.792395422388));
#267690=CARTESIAN_POINT('Ctrl Pts',(42.7592890858413,-4.37974125581177,
135.749253084432));
#267691=CARTESIAN_POINT('Ctrl Pts',(42.4808414620283,1.79292094911309,137.161996140853));
#267692=CARTESIAN_POINT('Ctrl Pts',(42.2023938382155,6.31797639086063,132.732382739134));
#267693=CARTESIAN_POINT('Ctrl Pts',(41.9239462144025,5.0371201797131,126.531011196811));
#267694=CARTESIAN_POINT('Ctrl Pts',(41.6454985905898,-0.872603399589798,
124.256639007436));
#267695=CARTESIAN_POINT('Ctrl Pts',(41.3670509667768,-5.98044708371573,
127.999303103786));
#267696=CARTESIAN_POINT('Ctrl Pts',(41.0886033429639,-5.592552058989,134.319678020622));
#267697=CARTESIAN_POINT('Ctrl Pts',(40.810155719151,-0.0653749034083074,
137.409647976851));
#267698=CARTESIAN_POINT('Ctrl Pts',(40.5317080953382,5.52187859466303,134.429681536124));
#267699=CARTESIAN_POINT('Ctrl Pts',(40.2532604715252,6.03479542300531,128.118222278014));
#267700=CARTESIAN_POINT('Ctrl Pts',(39.9748128477124,1.00203007375177,124.275192928799));
#267701=CARTESIAN_POINT('Ctrl Pts',(39.6963652238994,-4.95155196138904,
126.432149717987));
#267702=CARTESIAN_POINT('Ctrl Pts',(39.4179176000866,-6.35489964077443,
132.60695472951));
#267703=CARTESIAN_POINT('Ctrl Pts',(39.1394699762736,-1.91840500439501,
137.125263813774));
#267704=CARTESIAN_POINT('Ctrl Pts',(38.8610223524608,4.28101011172891,135.834971654011));
#267705=CARTESIAN_POINT('Ctrl Pts',(38.5825747286478,6.54638607414467,129.921793710766));
#267706=CARTESIAN_POINT('Ctrl Pts',(38.304127104835,2.79595304316033,124.819651639079));
#267707=CARTESIAN_POINT('Ctrl Pts',(38.0256794810221,-3.52382424458856,
125.217164749334));
#267708=CARTESIAN_POINT('Ctrl Pts',(37.7472318572093,-6.60537919994535,
130.749037912801));
#267709=CARTESIAN_POINT('Ctrl Pts',(37.4687842333963,-3.61691336126579,
136.331749939282));
#267710=CARTESIAN_POINT('Ctrl Pts',(37.1903366095834,2.69531916037638,136.835061207086));
#267711=CARTESIAN_POINT('Ctrl Pts',(36.9118889857706,6.53068504729366,131.796453249222));
#267712=CARTESIAN_POINT('Ctrl Pts',(36.6334413619576,4.36467041744916,125.846160629286));
#267713=CARTESIAN_POINT('Ctrl Pts',(36.3549937381448,-1.8122631000273,124.452211577043));
#267714=CARTESIAN_POINT('Ctrl Pts',(36.0765461143319,-6.32381536255287,
128.895577173308));
#267715=CARTESIAN_POINT('Ctrl Pts',(35.798098490519,-5.02409024244786,135.093021505591));
#267716=CARTESIAN_POINT('Ctrl Pts',(35.5196508667061,0.892528370013623,
137.34939599451));
#267717=CARTESIAN_POINT('Ctrl Pts',(35.2412032428932,5.98895701286753,133.591202714771));
#267718=CARTESIAN_POINT('Ctrl Pts',(34.9627556190803,5.58182673771145,127.272037692505));
#267719=CARTESIAN_POINT('Ctrl Pts',(34.6843079952674,0.0452703779943793,
124.198904874802));
#267720=CARTESIAN_POINT('Ctrl Pts',(34.4058603714545,-5.53288724751859,
127.195863190245));
#267721=CARTESIAN_POINT('Ctrl Pts',(34.1274127476417,-6.02659178913083,
133.508854356496));
#267722=CARTESIAN_POINT('Ctrl Pts',(33.8489651238287,-0.982152891908117,
137.336547898535));
#267723=CARTESIAN_POINT('Ctrl Pts',(33.5705175000158,4.96483653214189,135.161480444452));
#267724=CARTESIAN_POINT('Ctrl Pts',(33.292069876203,6.34938372890195,128.982432726597));
#267725=CARTESIAN_POINT('Ctrl Pts',(33.0136222523901,1.89915746344075,124.477647734417));
#267726=CARTESIAN_POINT('Ctrl Pts',(32.7351746285772,-4.29630173192265,
125.786802804744));
#267727=CARTESIAN_POINT('Ctrl Pts',(32.4567270047643,-6.543669521657,131.706848383727));
#267728=CARTESIAN_POINT('Ctrl Pts',(32.1782793809514,-2.77772469701646,
136.797551794587));
#267729=CARTESIAN_POINT('Ctrl Pts',(31.8998317571386,3.54081342478663,136.380805297429));
#267730=CARTESIAN_POINT('Ctrl Pts',(31.6213841333256,6.60551698756319,130.839578563946));
#267731=CARTESIAN_POINT('Ctrl Pts',(31.3429365095127,3.6000731362139,125.26598825823));
#267732=CARTESIAN_POINT('Ctrl Pts',(31.0644888856998,-2.71366205396602,
124.781891586214));
#267733=CARTESIAN_POINT('Ctrl Pts',(30.7860412618869,-6.53367438631237,
129.83214974004));
#267734=CARTESIAN_POINT('Ctrl Pts',(30.507593638074,-4.34955914537615,135.775822195171));
#267735=CARTESIAN_POINT('Ctrl Pts',(30.2291460142612,1.83158846238341,137.150964329883));
#267736=CARTESIAN_POINT('Ctrl Pts',(29.9506983904483,6.32959575128355,132.693887701803));
#267737=CARTESIAN_POINT('Ctrl Pts',(29.6722507666353,5.01101376269691,126.500427991838));
#267738=CARTESIAN_POINT('Ctrl Pts',(29.3938031428225,-0.912445072176531,
124.26207210612));
#267739=CARTESIAN_POINT('Ctrl Pts',(29.1153555190096,-5.99741146113971,
128.035759753857));
#267740=CARTESIAN_POINT('Ctrl Pts',(28.8369078951967,-5.57104970715349,
134.353656341672));
#267741=CARTESIAN_POINT('Ctrl Pts',(28.5584602713837,-0.0251654332018655,
137.409923551768));
#267742=CARTESIAN_POINT('Ctrl Pts',(28.280012647571,5.54384464446253,134.396001125022));
#267743=CARTESIAN_POINT('Ctrl Pts',(28.001565023758,6.0183323257333,128.081536533317));
#267744=CARTESIAN_POINT('Ctrl Pts',(27.7231173999451,0.962266611534229,
124.269214257685));
#267745=CARTESIAN_POINT('Ctrl Pts',(27.4446697761322,-4.97807510932732,
126.462372227135));
#267746=CARTESIAN_POINT('Ctrl Pts',(27.1662221523194,-6.34380899720599,
132.645605409466));
#267747=CARTESIAN_POINT('Ctrl Pts',(26.8877745285064,-1.87989232895117,
137.136824577849));
#267748=CARTESIAN_POINT('Ctrl Pts',(26.6093269046936,4.31155355176403,135.808818724794));
#267749=CARTESIAN_POINT('Ctrl Pts',(26.3308792808807,6.5408923495088,129.881960352566));
#267750=CARTESIAN_POINT('Ctrl Pts',(26.0524316570678,2.75947061841045,124.802742762115));
#267751=CARTESIAN_POINT('Ctrl Pts',(25.7739840332549,-3.55776980337282,
125.238718785491));
#267752=CARTESIAN_POINT('Ctrl Pts',(25.4955364094419,-6.60559358257403,
130.789247755823));
#267753=CARTESIAN_POINT('Ctrl Pts',(25.2170887856292,-3.58319956057628,
136.353664707793));
#267754=CARTESIAN_POINT('Ctrl Pts',(24.9386411618162,2.73197980856112,136.81854229942));
#267755=CARTESIAN_POINT('Ctrl Pts',(24.6601935380033,6.5366031982641,131.756680734531));
#267756=CARTESIAN_POINT('Ctrl Pts',(24.3817459141905,4.3344075795813,125.819683505575));
#267757=CARTESIAN_POINT('Ctrl Pts',(24.1032982903775,-1.85089685715453,
124.463361027524));
#267758=CARTESIAN_POINT('Ctrl Pts',(23.8248506665647,-6.33531750350378,
128.934107397669));
#267759=CARTESIAN_POINT('Ctrl Pts',(23.5464030427517,-4.99789086159903,
135.123525109951));
#267760=CARTESIAN_POINT('Ctrl Pts',(23.2679554189389,0.932353321572971,
137.343841656646));
#267761=CARTESIAN_POINT('Ctrl Pts',(22.9895077951259,6.00581035021119,133.554694599836));
#267762=CARTESIAN_POINT('Ctrl Pts',(22.7110601713131,5.56022106715229,127.238124974604));
#267763=CARTESIAN_POINT('Ctrl Pts',(22.4326125475002,0.00506025528043594,
124.198751684957));
#267764=CARTESIAN_POINT('Ctrl Pts',(22.1541649236873,-5.554750683987,127.229610302442));
#267765=CARTESIAN_POINT('Ctrl Pts',(21.8757172998744,-6.01001710932725,
133.545489823263));
#267766=CARTESIAN_POINT('Ctrl Pts',(21.5972696760615,-0.942371416853923,
137.342405515655));
#267767=CARTESIAN_POINT('Ctrl Pts',(21.3188220522486,4.99126757030501,135.131177347952));
#267768=CARTESIAN_POINT('Ctrl Pts',(21.0403744284357,6.33817549733007,128.943815981773));
#267769=CARTESIAN_POINT('Ctrl Pts',(20.7619268046228,1.86060977939589,124.466204243228));
#267770=CARTESIAN_POINT('Ctrl Pts',(20.48347918081,-4.32676542996233,125.813048576547));
#267771=CARTESIAN_POINT('Ctrl Pts',(20.205031556997,-6.5380545834274,131.746664836412));
#267772=CARTESIAN_POINT('Ctrl Pts',(19.9265839331841,-2.74119097644563,
136.814349553278));
#267773=CARTESIAN_POINT('Ctrl Pts',(19.6481363093713,3.57469322326559,136.359148042506));
#267774=CARTESIAN_POINT('Ctrl Pts',(19.3696886855584,6.60560898426828,130.799368254665));
#267775=CARTESIAN_POINT('Ctrl Pts',(19.0912410617455,3.56629279066743,125.244176204439));
#267776=CARTESIAN_POINT('Ctrl Pts',(18.8127934379326,-2.75027225446848,
124.798521999768));
#267777=CARTESIAN_POINT('Ctrl Pts',(18.5343458141197,-6.53947145601676,
129.871940083324));
#267778=CARTESIAN_POINT('Ctrl Pts',(18.2558981903068,-4.31921586042675,
135.802207086573));
#267779=CARTESIAN_POINT('Ctrl Pts',(17.9774505664939,1.87018810546999,137.139697343177));
#267780=CARTESIAN_POINT('Ctrl Pts',(17.6990029426811,6.34098056620813,132.65532264735));
#267781=CARTESIAN_POINT('Ctrl Pts',(17.4205553188681,4.98472166072295,126.470004270672));
#267782=CARTESIAN_POINT('Ctrl Pts',(17.1421076950552,-0.95225293377558,
124.26774763171));
#267783=CARTESIAN_POINT('Ctrl Pts',(16.8636600712423,-6.01415360227624,
128.072318995452));
#267784=CARTESIAN_POINT('Ctrl Pts',(16.5852124474295,-5.54934091802252,
134.387503142263));
#267785=CARTESIAN_POINT('Ctrl Pts',(16.3067648236166,0.0150449695187284,
137.409954355121));
#267786=CARTESIAN_POINT('Ctrl Pts',(16.0283171998036,5.56560526505998,134.362187624359));
#267787=CARTESIAN_POINT('Ctrl Pts',(15.7498695759908,6.00164621694371,128.044951683866));
#267788=CARTESIAN_POINT('Ctrl Pts',(15.4714219521779,0.922467492173741,
124.263477748823));
#267789=CARTESIAN_POINT('Ctrl Pts',(15.192974328365,-5.00441379286154,126.492755630261));
#267790=CARTESIAN_POINT('Ctrl Pts',(14.9145267045521,-6.33248328146239,
132.684187861418));
#267791=CARTESIAN_POINT('Ctrl Pts',(14.6360790807393,-1.84130999340576,
137.148150690142));
#267792=CARTESIAN_POINT('Ctrl Pts',(14.3576314569263,4.34193722559672,135.782480353541));
#267793=CARTESIAN_POINT('Ctrl Pts',(14.0791838331134,6.53515624970152,129.842161174248));
#267794=CARTESIAN_POINT('Ctrl Pts',(13.8007362093005,2.72288594046203,124.786056277307));
#267795=CARTESIAN_POINT('Ctrl Pts',(13.5222885854877,-3.59158352768866,
125.260479058552));
#267796=CARTESIAN_POINT('Ctrl Pts',(13.2438409616747,-6.60556319250329,
130.829458158858));
#267797=CARTESIAN_POINT('Ctrl Pts',(12.9653933378619,-3.54935298310934,
136.375373844801));
#267798=CARTESIAN_POINT('Ctrl Pts',(12.686945714049,2.76853922222938,136.801800534039));
#267799=CARTESIAN_POINT('Ctrl Pts',(12.4084980902361,6.5422791329992,131.716872931266));
#267800=CARTESIAN_POINT('Ctrl Pts',(12.1300504664232,4.30398412864651,125.793391090908));
#267801=CARTESIAN_POINT('Ctrl Pts',(11.8516028426103,-1.88946202861834,
124.474745446076));
#267802=CARTESIAN_POINT('Ctrl Pts',(11.5731552187974,-6.34658488693473,
128.972706924952));
#267803=CARTESIAN_POINT('Ctrl Pts',(11.2947075949845,-4.97150628206636,
135.153868666082));
#267804=CARTESIAN_POINT('Ctrl Pts',(11.0162599711716,0.972143724437105,
137.338044995907));
#267805=CARTESIAN_POINT('Ctrl Pts',(10.7378123473587,6.0224411400439,133.518084570262));
#267806=CARTESIAN_POINT('Ctrl Pts',(10.4593647235458,5.53840936055655,127.204344404875));
#267807=CARTESIAN_POINT('Ctrl Pts',(10.1809170997329,-0.0351500549433496,
124.198843268382));
#267808=CARTESIAN_POINT('Ctrl Pts',(9.90246947592002,-5.57640828712608,
127.263489878326));
#267809=CARTESIAN_POINT('Ctrl Pts',(9.62402185210712,-5.99321972612948,
133.582023716479));
#267810=CARTESIAN_POINT('Ctrl Pts',(9.34557422829421,-0.902555021880531,
137.348020863117));
#267811=CARTESIAN_POINT('Ctrl Pts',(9.06712660448133,5.01751365521256,135.100713919668));
#267812=CARTESIAN_POINT('Ctrl Pts',(8.78867898066847,6.32673240233446,128.905268180115));
#267813=CARTESIAN_POINT('Ctrl Pts',(8.51023135685555,1.82199314977141,124.454995614755));
#267814=CARTESIAN_POINT('Ctrl Pts',(8.23178373304265,-4.35706879811783,
125.839479303254));
#267815=CARTESIAN_POINT('Ctrl Pts',(7.9533361092298,-6.53219737518076,131.786446371669));
#267816=CARTESIAN_POINT('Ctrl Pts',(7.67488848541689,-2.70455568003535,
136.83092460962));
#267817=CARTESIAN_POINT('Ctrl Pts',(7.39644086160398,3.60844056017245,136.337284952891));
#267818=CARTESIAN_POINT('Ctrl Pts',(7.1179932377911,6.60545620770325,130.759158130379));
#267819=CARTESIAN_POINT('Ctrl Pts',(6.83954561397822,3.53238029483008,125.222570185327));
#267820=CARTESIAN_POINT('Ctrl Pts',(6.5610979901653,-2.78678054262086,124.815374961881));
#267821=CARTESIAN_POINT('Ctrl Pts',(6.28265036635242,-6.54502620320144,
129.911764977794));
#267822=CARTESIAN_POINT('Ctrl Pts',(6.00420274253956,-4.28871252534551,
135.828406780936));
#267823=CARTESIAN_POINT('Ctrl Pts',(5.72575511872663,1.90871844804856,137.128195598241));
#267824=CARTESIAN_POINT('Ctrl Pts',(5.44730749491374,6.35213041376593,132.616689004818));
#267825=CARTESIAN_POINT('Ctrl Pts',(5.16885987110085,4.95824484805471,126.439741160674));
#267826=CARTESIAN_POINT('Ctrl Pts',(4.89041224728798,-0.992025509291961,
124.273665373899));
#267827=CARTESIAN_POINT('Ctrl Pts',(4.61196462347505,-6.03067288673954,
128.108979473854));
#267828=CARTESIAN_POINT('Ctrl Pts',(4.33351699966218,-5.52742649602286,
134.421217168191));
#267829=CARTESIAN_POINT('Ctrl Pts',(4.05506937584931,0.0552548147426717,
137.409740385768));
#267830=CARTESIAN_POINT('Ctrl Pts',(3.77662175203639,5.58715965010757,134.328242287108));
#267831=CARTESIAN_POINT('Ctrl Pts',(3.49817412822347,5.98473771494644,128.008469085329));
#267832=CARTESIAN_POINT('Ctrl Pts',(3.21972650441063,0.882634190440881,
124.25798361478));
#267833=CARTESIAN_POINT('Ctrl Pts',(2.94127888059773,-5.03056703600248,
126.523298801495));
#267834=CARTESIAN_POINT('Ctrl Pts',(2.66283125678483,-6.32092291322184,
132.722700655682));
#267835=CARTESIAN_POINT('Ctrl Pts',(2.38438363297192,-1.80265942744139,
137.159241730961));
#267836=CARTESIAN_POINT('Ctrl Pts',(2.10593600915906,4.37216000734877,135.755957516231));
#267837=CARTESIAN_POINT('Ctrl Pts',(1.82748838534615,6.529177987276,129.802397650584));
#267838=CARTESIAN_POINT('Ctrl Pts',(1.54904076153325,2.68620036497402,124.769592802981));
#267839=CARTESIAN_POINT('Ctrl Pts',(1.27059313772038,-3.62526416455594,
125.282444762183));
#267840=CARTESIAN_POINT('Ctrl Pts',(0.992145513907496,-6.60528803085927,
130.869667631896));
#267841=CARTESIAN_POINT('Ctrl Pts',(0.713697890094564,-3.51537488306232,
136.396876545864));
#267842=CARTESIAN_POINT('Ctrl Pts',(0.435250266281723,2.80499604665836,
136.784836531317));
#267843=CARTESIAN_POINT('Ctrl Pts',(0.156802642468823,6.54771264117505,
131.677031314524));
#267844=CARTESIAN_POINT('Ctrl Pts',(-0.121644981344083,4.27340119199728,
125.767284359559));
#267845=CARTESIAN_POINT('Ctrl Pts',(-0.400092605156985,-1.92795718537184,
124.486364410847));
#267846=CARTESIAN_POINT('Ctrl Pts',(-0.678540228969845,-6.35761709532873,
129.011374324836));
#267847=CARTESIAN_POINT('Ctrl Pts',(-0.956987852782752,-4.94493748154019,
135.184051049593));
#267848=CARTESIAN_POINT('Ctrl Pts',(-1.23543547659566,1.01189810415772,
137.332006227089));
#267849=CARTESIAN_POINT('Ctrl Pts',(-1.51388310040852,6.03884876610542,
133.48137398265));
#267850=CARTESIAN_POINT('Ctrl Pts',(-1.79233072422142,5.51639242616521,
127.170697235071));
#267851=CARTESIAN_POINT('Ctrl Pts',(-2.07077834803434,-0.0753590626689394,
124.19917962168));
#267852=CARTESIAN_POINT('Ctrl Pts',(-2.34922597184723,-5.59785925440532,
127.297500662476));
#267853=CARTESIAN_POINT('Ctrl Pts',(-2.6276735956601,-5.97620026197078,
133.618454682368));
#267854=CARTESIAN_POINT('Ctrl Pts',(-2.906121219473,-0.862705182398668,
137.353393732843));
#267855=CARTESIAN_POINT('Ctrl Pts',(-3.18456884328591,5.04357381430661,
135.070091288433));
#267856=CARTESIAN_POINT('Ctrl Pts',(-3.46301646709877,6.31505486794284,
128.866790750024));
#267857=CARTESIAN_POINT('Ctrl Pts',(-3.74146409091167,1.78330900552073,
124.444022264336));
#267858=CARTESIAN_POINT('Ctrl Pts',(-4.01991171472458,-4.38721071348669,
125.866094005463));
#267859=CARTESIAN_POINT('Ctrl Pts',(-4.29835933853748,-6.52609811395827,
131.826191515377));
#267860=CARTESIAN_POINT('Ctrl Pts',(-4.57680696235032,-2.66782016531947,
136.847276349416));
#267861=CARTESIAN_POINT('Ctrl Pts',(-4.85525458616324,3.64205418498746,
136.31521683873));
#267862=CARTESIAN_POINT('Ctrl Pts',(-5.13370220997616,6.60505866352928,
130.718949681087));
#267863=CARTESIAN_POINT('Ctrl Pts',(-5.41214983378902,3.49833690534187,
125.201171001511));
#267864=CARTESIAN_POINT('Ctrl Pts',(-5.69059745760191,-2.82318556559566,
124.832449848059));
#267865=CARTESIAN_POINT('Ctrl Pts',(-5.96904508141481,-6.55033842203324,
129.951622947723));
#267866=CARTESIAN_POINT('Ctrl Pts',(-6.24749270522772,-4.2580502704442,
135.854420307421));
#267867=CARTESIAN_POINT('Ctrl Pts',(-6.52594032904057,1.9471780623631,137.116459521273));
#267868=CARTESIAN_POINT('Ctrl Pts',(-6.80438795285348,6.36304488079526,
132.577988205793));
#267869=CARTESIAN_POINT('Ctrl Pts',(-7.0828355766664,4.93158430580029,126.409639783256));
#267870=CARTESIAN_POINT('Ctrl Pts',(-7.36128320047925,-1.03176132493798,
124.279825113401));
#267871=CARTESIAN_POINT('Ctrl Pts',(-7.63973082429214,-6.04696870240127,
128.145739830595));
#267872=CARTESIAN_POINT('Ctrl Pts',(-7.91817844810507,-5.50530725320171,
134.454797170168));
#267873=CARTESIAN_POINT('Ctrl Pts',(-8.19662607191793,0.09546261247915,
137.40928165164));
#267874=CARTESIAN_POINT('Ctrl Pts',(-8.47507369573082,5.60850700089942,
134.294166371127));
#267875=CARTESIAN_POINT('Ctrl Pts',(-8.75352131954372,5.96760744629241,
127.972090089581));
#267876=CARTESIAN_POINT('Ctrl Pts',(-9.03196894335663,0.842768182373745,
124.252732059145));
#267877=CARTESIAN_POINT('Ctrl Pts',(-9.31041656716948,-5.05653386963193,
126.554000609049));
#267878=CARTESIAN_POINT('Ctrl Pts',(-9.5888641909824,-6.30912832085822,
132.76114236515));
#267879=CARTESIAN_POINT('Ctrl Pts',(-9.86731181479532,-1.76394206326903,
137.170097289323));
#267880=CARTESIAN_POINT('Ctrl Pts',(-10.1457594386081,4.40222077710389,
135.729251195677));
#267881=CARTESIAN_POINT('Ctrl Pts',(-10.424207062421,6.52295778375913,129.762671255026));
#267882=CARTESIAN_POINT('Ctrl Pts',(-10.7026546862339,2.64941525134336,
124.753352949195));
#267883=CARTESIAN_POINT('Ctrl Pts',(-10.9811023100469,-3.65881046592654,
125.304615082438));
#267884=CARTESIAN_POINT('Ctrl Pts',(-11.2595499338597,-6.60476810783814,
130.909874684957));
#267885=CARTESIAN_POINT('Ctrl Pts',(-11.5379975576726,-3.48126651950624,
136.418172014193));
#267886=CARTESIAN_POINT('Ctrl Pts',(-11.8164451814855,2.84134893092756,
136.767650919861));
#267887=CARTESIAN_POINT('Ctrl Pts',(-12.0948928052984,6.5529035214511,131.637157360647));
#267888=CARTESIAN_POINT('Ctrl Pts',(-12.3733404291112,4.2426599028951,125.741364278924));
#267889=CARTESIAN_POINT('Ctrl Pts',(-12.6517880529242,-1.96638090096281,
124.498217491291));
#267890=CARTESIAN_POINT('Ctrl Pts',(-12.9302356767371,-6.36841371988325,
129.050108164486));
#267891=CARTESIAN_POINT('Ctrl Pts',(-13.2086833005499,-4.91818544453708,
135.214071142064));
#267892=CARTESIAN_POINT('Ctrl Pts',(-13.4871309243628,1.05161498762227,
137.325725573964));
#267893=CARTESIAN_POINT('Ctrl Pts',(-13.7655785481758,6.05503262040511,
133.444564197323));
#267894=CARTESIAN_POINT('Ctrl Pts',(-14.0440261719886,5.49417107982388,
127.137184712));
#267895=CARTESIAN_POINT('Ctrl Pts',(-14.3224737958015,-0.115565277936756,
124.199760732389));
#267896=CARTESIAN_POINT('Ctrl Pts',(-14.6009214196144,-5.61910279095105,
127.331641394614));
#267897=CARTESIAN_POINT('Ctrl Pts',(-14.8793690434273,-5.95895934751375,
133.654781370965));
#267898=CARTESIAN_POINT('Ctrl Pts',(-15.1578166672402,-0.822823375059262,
137.358523925738));
#267899=CARTESIAN_POINT('Ctrl Pts',(-15.4362642910531,5.06944708191823,
135.039310588977));
#267900=CARTESIAN_POINT('Ctrl Pts',(-15.714711914866,6.3031433268707,128.828385117298));
#267901=CARTESIAN_POINT('Ctrl Pts',(-15.9931595386788,1.74455878009922,
124.433284598595));
#267902=CARTESIAN_POINT('Ctrl Pts',(-16.2716071624918,-4.41719005914895,
125.892891696959));
#267903=CARTESIAN_POINT('Ctrl Pts',(-16.5500547863046,-6.51975702577033,
131.865898794765));
#267904=CARTESIAN_POINT('Ctrl Pts',(-16.8285024101176,-2.63098579354628,
136.863404166748));
#267905=CARTESIAN_POINT('Ctrl Pts',(-17.1069500339304,3.67553285214529,
136.292944517765));
#267906=CARTESIAN_POINT('Ctrl Pts',(-17.3853976577434,6.60441636647752,
130.678744396729));
#267907=CARTESIAN_POINT('Ctrl Pts',(-17.6638452815562,3.46416388369313,
125.179979445948));
#267908=CARTESIAN_POINT('Ctrl Pts',(-17.9422929053691,-2.8594859743911,
124.849746025587));
#267909=CARTESIAN_POINT('Ctrl Pts',(-18.220740529182,-6.55540791566593,
129.991512516161));
#267910=CARTESIAN_POINT('Ctrl Pts',(-18.4991881529949,-4.22723023192423,
135.880246702087));
#267911=CARTESIAN_POINT('Ctrl Pts',(-18.7776357768078,1.98556552327847,
137.104489547159));
#267912=CARTESIAN_POINT('Ctrl Pts',(-19.0560834006207,6.37372356285652,
132.539221684343));
#267913=CARTESIAN_POINT('Ctrl Pts',(-19.3345310244336,4.90474102187576,
126.379701253833));
#267914=CARTESIAN_POINT('Ctrl Pts',(-19.6129786482465,-1.07145890828896,
124.286226621967));
#267915=CARTESIAN_POINT('Ctrl Pts',(-19.8914262720594,-6.06304044541393,
128.182598703507));
#267916=CARTESIAN_POINT('Ctrl Pts',(-20.1698738958722,-5.48298400919569,
134.488241903877));
#267917=CARTESIAN_POINT('Ctrl Pts',(-20.4483215196851,0.135666872813404,
137.408578169733));
#267918=CARTESIAN_POINT('Ctrl Pts',(-20.7267691434981,5.62964652640204,
134.25996113911));
#267919=CARTESIAN_POINT('Ctrl Pts',(-21.0052167673109,5.95025604574973,
127.935816044659));
#267920=CARTESIAN_POINT('Ctrl Pts',(-21.2836643911238,0.802870945221437,
124.247723276515));
#267921=CARTESIAN_POINT('Ctrl Pts',(-21.5621120149367,-5.08231333153929,
126.584859915257));
#267922=CARTESIAN_POINT('Ctrl Pts',(-21.8405596387496,-6.29709994142449,
132.79951156535));
#267923=CARTESIAN_POINT('Ctrl Pts',(-22.1190072625625,-1.725159335575,137.180716962973));
#267924=CARTESIAN_POINT('Ctrl Pts',(-22.3974548863754,4.43211842094896,
135.702362381491));
#267925=CARTESIAN_POINT('Ctrl Pts',(-22.6759025101882,6.51649586964294,
129.722983459651));
#267926=CARTESIAN_POINT('Ctrl Pts',(-22.9543501340012,2.61253196265622,
124.737337317723));
#267927=CARTESIAN_POINT('Ctrl Pts',(-23.232797757814,-3.6922211887298,125.326989197785));
#267928=CARTESIAN_POINT('Ctrl Pts',(-23.511245381627,-6.60400344270576,
130.950077828156));
#267929=CARTESIAN_POINT('Ctrl Pts',(-23.7896930054398,-3.4470291563393,
136.439259460675));
#267930=CARTESIAN_POINT('Ctrl Pts',(-24.0681406292527,2.87759652796706,
136.75024433649));
#267931=CARTESIAN_POINT('Ctrl Pts',(-24.3465882530656,6.55785158147733,
131.597252547181));
#267932=CARTESIAN_POINT('Ctrl Pts',(-24.6250358768785,4.21176140046998,
125.715631809479));
#267933=CARTESIAN_POINT('Ctrl Pts',(-24.9034835006914,-2.00473175158637,
124.510304248187));
#267934=CARTESIAN_POINT('Ctrl Pts',(-25.1819311245043,-6.3789743605254,
129.088907008606));
#267935=CARTESIAN_POINT('Ctrl Pts',(-25.4603787483172,-4.89125116236366,
135.24392783109));
#267936=CARTESIAN_POINT('Ctrl Pts',(-25.73882637213,1.09129290310671,137.319203269261));
#267937=CARTESIAN_POINT('Ctrl Pts',(-26.017273995943,6.07099210324431,133.407656578282));
#267938=CARTESIAN_POINT('Ctrl Pts',(-26.2957216197559,5.47174614495268,
127.103808077481));
#267939=CARTESIAN_POINT('Ctrl Pts',(-26.5741692435687,-0.155767210890682,
124.200586578976));
#267940=CARTESIAN_POINT('Ctrl Pts',(-26.8526168673816,-5.64013810957666,
127.365910809639));
#267941=CARTESIAN_POINT('Ctrl Pts',(-27.1310644911945,-5.94149762162655,
133.691002436174));
#267942=CARTESIAN_POINT('Ctrl Pts',(-27.4095121150075,-0.782911077696857,
137.363411251701));
#267943=CARTESIAN_POINT('Ctrl Pts',(-27.6879597388203,5.09513249930392,
135.008372961895));
#267944=CARTESIAN_POINT('Ctrl Pts',(-27.9664073626332,6.29099822050462,
128.79005270507));
#267945=CARTESIAN_POINT('Ctrl Pts',(-28.2448549864461,1.70574390941038,
124.422783015417));
#267946=CARTESIAN_POINT('Ctrl Pts',(-28.523302610259,-4.44700572420938,
125.919871384741));
#267947=CARTESIAN_POINT('Ctrl Pts',(-28.8017502340719,-6.51317434558802,
131.905566738465));
#267948=CARTESIAN_POINT('Ctrl Pts',(-29.0801978578848,-2.59405392962697,
136.879307463993));
#267949=CARTESIAN_POINT('Ctrl Pts',(-29.3586454816977,3.7088753210816,136.270468815306));
#267950=CARTESIAN_POINT('Ctrl Pts',(-29.6370931055106,6.6035293403484,130.638543767126));
#267951=CARTESIAN_POINT('Ctrl Pts',(-29.9155407293234,3.42986249617799,
125.158996303897));
#267952=CARTESIAN_POINT('Ctrl Pts',(-30.1939883531365,-2.89568042388203,
124.86726285355));
#267953=CARTESIAN_POINT('Ctrl Pts',(-30.4724359769491,-6.56023449624756,
130.031432204983));
#267954=CARTESIAN_POINT('Ctrl Pts',(-30.7508836007622,-4.19625355183344,
135.905885007927));
#267955=CARTESIAN_POINT('Ctrl Pts',(-31.029331224575,2.02387940833292,137.092286119451));
#267956=CARTESIAN_POINT('Ctrl Pts',(-31.3077788483879,6.38416606424714,
132.50039087698));
#267957=CARTESIAN_POINT('Ctrl Pts',(-31.5862264722008,4.8777159909692,126.349926681791));
#267958=CARTESIAN_POINT('Ctrl Pts',(-31.8646740960137,-1.11111678833609,
124.292869662384));
#267959=CARTESIAN_POINT('Ctrl Pts',(-32.1431217198266,-6.07888752023319,
128.219554726771));
#267960=CARTESIAN_POINT('Ctrl Pts',(-32.4215693436394,-5.46045759120085,
134.52155013001));
#267961=CARTESIAN_POINT('Ctrl Pts',(-32.7000169674524,0.175866105961793,
137.407629966116));
#267962=CARTESIAN_POINT('Ctrl Pts',(-32.9784645912652,5.65057744328232,
134.225627858545));
#267963=CARTESIAN_POINT('Ctrl Pts',(-33.2569122150782,5.93268415628106,
127.89964829471));
#267964=CARTESIAN_POINT('Ctrl Pts',(-33.535359838891,0.762943957391,124.242957452493));
#267965=CARTESIAN_POINT('Ctrl Pts',(-33.813807462704,-5.10790446645711,
126.615875576613));
#267966=CARTESIAN_POINT('Ctrl Pts',(-34.0922550865168,-6.28483822063666,
132.837806834499));
#267967=CARTESIAN_POINT('Ctrl Pts',(-34.3707027103298,-1.68631268146717,
137.191100358392));
#267968=CARTESIAN_POINT('Ctrl Pts',(-34.6491503341426,4.46185183101625,
135.675292070049));
#267969=CARTESIAN_POINT('Ctrl Pts',(-34.9275979579556,6.5097924843757,129.683335735103));
#267970=CARTESIAN_POINT('Ctrl Pts',(-35.2060455817684,2.57555186563646,
124.721546502031));
#267971=CARTESIAN_POINT('Ctrl Pts',(-35.4844932055813,-3.72549509491909,
125.349566279145));
#267972=CARTESIAN_POINT('Ctrl Pts',(-35.7629408293942,-6.60299406379731,
130.990275571749));
#267973=CARTESIAN_POINT('Ctrl Pts',(-36.0413884532071,-3.41266406223907,
136.460138103909));
#267974=CARTESIAN_POINT('Ctrl Pts',(-36.3198360770199,2.91373749460914,
136.73261742621));
#267975=CARTESIAN_POINT('Ctrl Pts',(-36.5982837008328,6.56255663790157,
131.557318352812));
#267976=CARTESIAN_POINT('Ctrl Pts',(-36.8767313246458,4.18070682967726,
125.690087904753));
#267977=CARTESIAN_POINT('Ctrl Pts',(-37.1551789484586,-2.04300831613737,
124.522624233657));
#267978=CARTESIAN_POINT('Ctrl Pts',(-37.4336265722715,-6.38929862592666,
129.12776941949));
#267979=CARTESIAN_POINT('Ctrl Pts',(-37.7120741960844,-4.86413563307991,
135.273620010322));
#267980=CARTESIAN_POINT('Ctrl Pts',(-37.9905218198973,1.13093038033133,
137.312439554669));
#267981=CARTESIAN_POINT('Ctrl Pts',(-38.2689694437102,6.0867266232385,133.370652493151));
#267982=CARTESIAN_POINT('Ctrl Pts',(-38.5474170675231,5.44911845251588,
127.070568568297));
#267983=CARTESIAN_POINT('Ctrl Pts',(-38.825864691336,-0.195963371833029,
124.201657130839));
#267984=CARTESIAN_POINT('Ctrl Pts',(-39.1043123151489,-5.66096443081045,
127.400307637685));
#267985=CARTESIAN_POINT('Ctrl Pts',(-39.3827599389617,-5.92381573136,133.727116535809));
#267986=CARTESIAN_POINT('Ctrl Pts',(-39.6612075627747,-0.742969769276543,
137.368055529631));
#267987=CARTESIAN_POINT('Ctrl Pts',(-39.9396551865875,5.12062911468111,
134.977279553588));
#267988=CARTESIAN_POINT('Ctrl Pts',(-40.2181028104005,6.27861999888597,
128.751794933764));
#267989=CARTESIAN_POINT('Ctrl Pts',(-40.4965504342133,1.66686583175366,
124.412517903944));
#267990=CARTESIAN_POINT('Ctrl Pts',(-40.7749980580263,-4.47665660383728,
125.947032069068));
#267991=CARTESIAN_POINT('Ctrl Pts',(-41.0534456818391,-6.5063503173351,
131.945193876568));
#267992=CARTESIAN_POINT('Ctrl Pts',(-41.3318933056519,-2.55702594208532,
136.894985651848));
#267993=CARTESIAN_POINT('Ctrl Pts',(-41.6103409294649,3.74208035627896,
136.247790564197));
#267994=CARTESIAN_POINT('Ctrl Pts',(-41.8887885532778,6.60239761801125,
130.598349281928));
#267995=CARTESIAN_POINT('Ctrl Pts',(-42.1672361770906,3.39543401384647,
125.138222352896));
#267996=CARTESIAN_POINT('Ctrl Pts',(-42.4456838009036,-2.93176757287012,
124.884999682853));
#267997=CARTESIAN_POINT('Ctrl Pts',(-42.7241314247165,-6.56481798492739,
130.071380534953));
#267998=CARTESIAN_POINT('Ctrl Pts',(-43.0025790485293,-4.16512137802412,
135.931334274905));
#267999=CARTESIAN_POINT('Ctrl Pts',(-43.2810266723423,2.06211829779186,
137.079849690351));
#268000=CARTESIAN_POINT('Ctrl Pts',(-43.5594742961552,6.39437199801655,
132.461497222591));
#268001=CARTESIAN_POINT('Ctrl Pts',(-43.837921919968,4.85051021450257,126.320317170437));
#268002=CARTESIAN_POINT('Ctrl Pts',(-44.116369543781,-1.150733495542,124.299753988494));
#268003=CARTESIAN_POINT('Ctrl Pts',(-44.3948171675938,-6.09450933963988,
128.256606530968));
#268004=CARTESIAN_POINT('Ctrl Pts',(-44.6732647914067,-5.43772883394191,
134.554720614319));
#268005=CARTESIAN_POINT('Ctrl Pts',(-44.9517124152196,0.216058822326645,
137.406437075925));
#268006=CARTESIAN_POINT('Ctrl Pts',(-45.2301600390324,5.67129897593744,
134.191167801664));
#268007=CARTESIAN_POINT('Ctrl Pts',(-45.5086076628454,5.91489242901924,
127.863588179946));
#268008=CARTESIAN_POINT('Ctrl Pts',(-45.7870552866582,0.722988698391639,
124.238434763679));
#268009=CARTESIAN_POINT('Ctrl Pts',(-46.0655029104712,-5.13330632609627,
126.647046443824));
#268010=CARTESIAN_POINT('Ctrl Pts',(-46.343950534284,-6.27234361285742,
132.876026753548));
#268011=CARTESIAN_POINT('Ctrl Pts',(-46.622398158097,-1.64740354042306,
137.201247090823));
#268012=CARTESIAN_POINT('Ctrl Pts',(-46.9008457819097,4.49141990552312,
135.64804126445));
#268013=CARTESIAN_POINT('Ctrl Pts',(-47.1792934057228,6.50284787635396,
129.643729550545));
#268014=CARTESIAN_POINT('Ctrl Pts',(-47.4577410295356,2.53847633059532,
124.705981087252));
#268015=CARTESIAN_POINT('Ctrl Pts',(-47.7361886533485,-3.75863095151733,
125.372345489915));
#268016=CARTESIAN_POINT('Ctrl Pts',(-48.0146362771614,-6.60174000851572,
131.030466426196));
#268017=CARTESIAN_POINT('Ctrl Pts',(-48.2930839009743,-3.37817251061699,
136.480807170229));
#268018=CARTESIAN_POINT('Ctrl Pts',(-48.5715315247872,2.94977049163681,
136.714770842195));
#268019=CARTESIAN_POINT('Ctrl Pts',(-48.8499791486,6.56701851637621,131.517356257317));
#268020=CARTESIAN_POINT('Ctrl Pts',(-49.128426772413,4.14949734125552,125.664733511282));
#268021=CARTESIAN_POINT('Ctrl Pts',(-49.4068743962258,-2.08120917626415,
124.535176991179));
#268022=CARTESIAN_POINT('Ctrl Pts',(-49.6853220200388,-6.39938613351776,
129.166693957078));
#268023=CARTESIAN_POINT('Ctrl Pts',(-49.9637696438516,-4.83683986146123,
135.303146579501));
#268024=CARTESIAN_POINT('Ctrl Pts',(-50.2422172676646,1.17052595051479,
137.305434680818));
#268025=CARTESIAN_POINT('Ctrl Pts',(-50.5206648914774,6.10223559733929,
133.333553313131));
#268026=CARTESIAN_POINT('Ctrl Pts',(-50.7991125152903,5.42628884099088,
127.03746741615));
#268027=CARTESIAN_POINT('Ctrl Pts',(-51.0775601391032,-0.236152271280866,
124.202972348307));
#268028=CARTESIAN_POINT('Ctrl Pts',(-51.3560077629162,-5.68158098292544,
127.434830604167));
#268029=CARTESIAN_POINT('Ctrl Pts',(-51.634455386729,-5.90591433192304,
133.763122331648));
#268030=CARTESIAN_POINT('Ctrl Pts',(-51.9129030105419,-0.703000929838195,
137.372456587432));
#268031=CARTESIAN_POINT('Ctrl Pts',(-52.1913506343548,5.14593598326309,
134.946031516236));
#268032=CARTESIAN_POINT('Ctrl Pts',(-52.4697982581677,6.26600912069438,
128.713613221033));
#268033=CARTESIAN_POINT('Ctrl Pts',(-52.7482458819806,1.62792598777083,
124.402489644555));
#268034=CARTESIAN_POINT('Ctrl Pts',(-53.0266935057934,-4.50614159930848,
125.97437274349));
#268035=CARTESIAN_POINT('Ctrl Pts',(-53.3051411296064,-6.49928519387843,
131.984778740675));
#268036=CARTESIAN_POINT('Ctrl Pts',(-53.5835887534191,-2.51990320300721,
136.910438149353));
#268037=CARTESIAN_POINT('Ctrl Pts',(-53.8620363772322,3.7751467273123,136.22491060479));
#268038=CARTESIAN_POINT('Ctrl Pts',(-54.140484001045,6.60102124140245,130.558162430556));
#268039=CARTESIAN_POINT('Ctrl Pts',(-54.418931624858,3.36087971245889,125.117658362733));
#268040=CARTESIAN_POINT('Ctrl Pts',(-54.6973792486707,-2.96774608413265,
124.902955856252));
#268041=CARTESIAN_POINT('Ctrl Pts',(-54.9758268724838,-6.56915821186243,
130.111356025769));
#268042=CARTESIAN_POINT('Ctrl Pts',(-55.2542744962966,-4.13383486411065,
135.956593559989));
#268043=CARTESIAN_POINT('Ctrl Pts',(-55.5327221201095,2.10028077469877,
137.067180720695));
#268044=CARTESIAN_POINT('Ctrl Pts',(-55.8111697439224,6.40434098598004,
132.422542162396));
#268045=CARTESIAN_POINT('Ctrl Pts',(-56.0896173677353,4.82312470059616,
126.29087381696));
#268046=CARTESIAN_POINT('Ctrl Pts',(-56.3680649915482,-1.19030756189505,
124.306879345194));
#268047=CARTESIAN_POINT('Ctrl Pts',(-56.646512615361,-6.10990532476174,
128.293752743129));
#268048=CARTESIAN_POINT('Ctrl Pts',(-56.924960239174,-5.41479857964128,
134.587752127659));
#268049=CARTESIAN_POINT('Ctrl Pts',(-57.2034078629868,0.256243532552689,
137.404999543363));
#268050=CARTESIAN_POINT('Ctrl Pts',(-57.4818554867998,5.69181035652338,
134.156582245398));
#268051=CARTESIAN_POINT('Ctrl Pts',(-57.7603031106126,5.89688152324325,
127.827637036585));
#268052=CARTESIAN_POINT('Ctrl Pts',(-58.0387507344255,0.683006648780185,
124.234155377662));
#268053=CARTESIAN_POINT('Ctrl Pts',(-58.3171983582384,-5.15851796918197,
126.67837136184));
#268054=CARTESIAN_POINT('Ctrl Pts',(-58.5956459820513,-6.25961658107885,
132.91416990625));
#268055=CARTESIAN_POINT('Ctrl Pts',(-58.8740936058642,-1.60843335423465,
137.211156784272));
#268056=CARTESIAN_POINT('Ctrl Pts',(-59.1525412296771,4.52082154881365,
135.620610974484));
#268057=CARTESIAN_POINT('Ctrl Pts',(-59.4309888534899,6.49566230291273,
129.604166373598));
#268058=CARTESIAN_POINT('Ctrl Pts',(-59.7094364773029,2.50130673138007,
124.69064165017));
#268059=CARTESIAN_POINT('Ctrl Pts',(-59.9878841011157,-3.79162753066369,
125.395325986002));
#268060=CARTESIAN_POINT('Ctrl Pts',(-60.2663317249287,-6.60024132333016,
131.070648902209));
#268061=CARTESIAN_POINT('Ctrl Pts',(-60.5447793487415,-3.34355577957023,
136.501265893734));
#268062=CARTESIAN_POINT('Ctrl Pts',(-60.8232269725544,2.98569418383416,
136.696705245755));
#268063=CARTESIAN_POINT('Ctrl Pts',(-61.1016745963673,6.57123705156454,
131.477367741508));
#268064=CARTESIAN_POINT('Ctrl Pts',(-61.3801222201802,4.11813409168408,
125.639569568584));
#268065=CARTESIAN_POINT('Ctrl Pts',(-61.6585698439931,-2.11933291641938,
124.547962055604));
#268066=CARTESIAN_POINT('Ctrl Pts',(-61.937017467806,-6.40923650950231,
129.205679179005));
#268067=CARTESIAN_POINT('Ctrl Pts',(-62.2154650916189,-4.80936485896274,
135.332506444514));
#268068=CARTESIAN_POINT('Ctrl Pts',(-62.4939127154318,1.21007814642843,
137.298188907278));
#268069=CARTESIAN_POINT('Ctrl Pts',(-62.7723603392447,6.1175184508558,133.296360412945));
#268070=CARTESIAN_POINT('Ctrl Pts',(-63.0508079630576,5.40325815633759,
127.004505847616));
#268071=CARTESIAN_POINT('Ctrl Pts',(-63.3292555868704,-0.276332420019459,
124.204532182646));
#268072=CARTESIAN_POINT('Ctrl Pts',(-63.6077032106833,-5.70198700196771,
127.469478429822));
#268073=CARTESIAN_POINT('Ctrl Pts',(-63.8861508344962,-5.8877940866586,
133.799018489484));
#268074=CARTESIAN_POINT('Ctrl Pts',(-64.1645984583092,-0.663006040441876,
137.376614262022));
#268075=CARTESIAN_POINT('Ctrl Pts',(-64.4430460821219,5.17105216729505,
134.914630007745));
#268076=CARTESIAN_POINT('Ctrl Pts',(-64.721493705935,6.25316605323042,128.675508981716));
#268077=CARTESIAN_POINT('Ctrl Pts',(-64.9999413297477,1.58892582039159,
124.392698608848));
#268078=CARTESIAN_POINT('Ctrl Pts',(-65.2783889535607,-4.53545961804555,
126.00189239489));
#268079=CARTESIAN_POINT('Ctrl Pts',(-65.5568365773735,-6.49197923701883,
132.024319863954));
#268080=CARTESIAN_POINT('Ctrl Pts',(-65.8352842011867,-2.48268708798906,
136.92566438391));
#268081=CARTESIAN_POINT('Ctrl Pts',(-66.1137318249993,3.80807320889562,
136.201829784909));
#268082=CARTESIAN_POINT('Ctrl Pts',(-66.3921794488124,6.59940026152389,
130.517984702147));
#268083=CARTESIAN_POINT('Ctrl Pts',(-66.6706270726251,3.3262008724376,125.097305095413));
#268084=CARTESIAN_POINT('Ctrl Pts',(-66.9490746964381,-3.00361462447264,
124.921130708376));
#268085=CARTESIAN_POINT('Ctrl Pts',(-67.227522320251,-6.57325501622426,
130.151357196124));
#268086=CARTESIAN_POINT('Ctrl Pts',(-67.5059699440638,-4.10239516942585,
135.981661927186));
#268087=CARTESIAN_POINT('Ctrl Pts',(-67.7844175678767,2.13836542492937,
137.054279679937));
#268088=CARTESIAN_POINT('Ctrl Pts',(-68.0628651916897,6.41407265873309,
132.383527139888));
#268089=CARTESIAN_POINT('Ctrl Pts',(-68.3413128155024,4.79556046403026,
126.261597712398));
#268090=CARTESIAN_POINT('Ctrl Pts',(-68.6197604393155,-1.22983752096341,
124.314245468451));
#268091=CARTESIAN_POINT('Ctrl Pts',(-68.8982080631282,-6.12507490509475,
128.330991986789));
#268092=CARTESIAN_POINT('Ctrl Pts',(-69.1766556869413,-5.39166767798822,
134.620643446035));
#268093=CARTESIAN_POINT('Ctrl Pts',(-69.455103310754,0.296418747580413,
137.403317421698));
#268094=CARTESIAN_POINT('Ctrl Pts',(-69.733550934567,5.7121108249834,134.121872471326));
#268095=CARTESIAN_POINT('Ctrl Pts',(-70.0119985583799,5.87865210635384,
127.791796196812));
#268096=CARTESIAN_POINT('Ctrl Pts',(-70.2904461821926,0.642999290106501,
124.230119453016));
#268097=CARTESIAN_POINT('Ctrl Pts',(-70.5688938060058,-5.18353846148724,
126.709849169906));
#268098=CARTESIAN_POINT('Ctrl Pts',(-70.8473414298183,-6.24665759690589,
132.95223487919));
#268099=CARTESIAN_POINT('Ctrl Pts',(-71.1257890536316,-1.56940356695681,
137.220829071533));
#268100=CARTESIAN_POINT('Ctrl Pts',(-71.4042366774442,4.55005567139915,
135.593002216589));
#268101=CARTESIAN_POINT('Ctrl Pts',(-71.6826843012574,6.48823603031619,
129.56464767029));
#268102=CARTESIAN_POINT('Ctrl Pts',(-71.9611319250699,2.46404444532374,
124.675528759193));
#268103=CARTESIAN_POINT('Ctrl Pts',(-72.2395795488831,-3.82448360965763,
125.418506915858));
#268104=CARTESIAN_POINT('Ctrl Pts',(-72.518027172696,-6.59849806377525,
131.110821510811));
#268105=CARTESIAN_POINT('Ctrl Pts',(-72.7964747965087,-3.30881515183405,
136.52151351632));
#268106=CARTESIAN_POINT('Ctrl Pts',(-73.0749224203217,3.02150724003593,
136.678421306317));
#268107=CARTESIAN_POINT('Ctrl Pts',(-73.3533700441346,6.57521208714753,
131.437354287172));
#268108=CARTESIAN_POINT('Ctrl Pts',(-73.6318176679474,4.08661824313884,
125.614597009117));
#268109=CARTESIAN_POINT('Ctrl Pts',(-73.9102652917603,-2.15737812391465,
124.56097895318));
#268110=CARTESIAN_POINT('Ctrl Pts',(-74.1887129155733,-6.41884938887091,
129.244723640663));
#268111=CARTESIAN_POINT('Ctrl Pts',(-74.4671605393861,-4.78171164368069,
135.361698517417));
#268112=CARTESIAN_POINT('Ctrl Pts',(-74.745608163199,1.24958550245192,137.290702502541));
#268113=CARTESIAN_POINT('Ctrl Pts',(-75.0240557870119,6.13257461747648,
133.25907517079));
#268114=CARTESIAN_POINT('Ctrl Pts',(-75.3025034108249,5.380027251966,126.971685084098));
#268115=CARTESIAN_POINT('Ctrl Pts',(-75.5809510346376,-0.31650232915867,
124.206336576053));
#268116=CARTESIAN_POINT('Ctrl Pts',(-75.8593986584506,-5.72218173178456,
127.504249830764));
#268117=CARTESIAN_POINT('Ctrl Pts',(-76.1378462822634,-5.86945566701928,
133.83480367917));
#268118=CARTESIAN_POINT('Ctrl Pts',(-76.4162939060764,-0.622986583113102,
137.380528399336));
#268119=CARTESIAN_POINT('Ctrl Pts',(-76.6947415298893,5.19597673608708,
134.88307619171));
#268120=CARTESIAN_POINT('Ctrl Pts',(-76.9731891537022,6.24009127239896,
128.637483627779));
#268121=CARTESIAN_POINT('Ctrl Pts',(-77.2516367775151,1.54986677478153,
124.383145159635));
#268122=CARTESIAN_POINT('Ctrl Pts',(-77.5300844013279,-4.56460957365852,
126.029590003516));
#268123=CARTESIAN_POINT('Ctrl Pts',(-77.8085320251407,-6.48443271748106,
132.063815781194));
#268124=CARTESIAN_POINT('Ctrl Pts',(-78.0869796489538,-2.44537897608793,
136.940663791305));
#268125=CARTESIAN_POINT('Ctrl Pts',(-78.3654272727665,3.84085858092573,
136.178548959823));
#268126=CARTESIAN_POINT('Ctrl Pts',(-78.6438748965796,6.5975347384416,130.477817585504));
#268127=CARTESIAN_POINT('Ctrl Pts',(-78.9223225203923,3.29139877882003,
125.077163305135));
#268128=CARTESIAN_POINT('Ctrl Pts',(-79.2007701442053,-3.03937186476788,
124.939523565746));
#268129=CARTESIAN_POINT('Ctrl Pts',(-79.4792177680182,-6.57710824620412,
130.191382563762));
#268130=CARTESIAN_POINT('Ctrl Pts',(-79.7576653918309,-4.07080345897965,
136.00653844758));
#268131=CARTESIAN_POINT('Ctrl Pts',(-80.036113015644,2.17637083724304,137.041147046131));
#268132=CARTESIAN_POINT('Ctrl Pts',(-80.314560639457,6.42356665566488,132.344453600785));
#268133=CARTESIAN_POINT('Ctrl Pts',(-80.5930082632696,4.76781852620778,
126.232489941585));
#268134=CARTESIAN_POINT('Ctrl Pts',(-80.8714558870828,-1.26932190795047,
124.321852085313));
#268135=CARTESIAN_POINT('Ctrl Pts',(-81.1499035108954,-6.14001751852468,
128.368322882032));
#268136=CARTESIAN_POINT('Ctrl Pts',(-81.4283511347085,-5.36833698610627,
134.653393350648));
#268137=CARTESIAN_POINT('Ctrl Pts',(-81.7067987585213,0.336582978702201,
137.401390773263));
#268138=CARTESIAN_POINT('Ctrl Pts',(-81.9852463823341,5.73219962907597,
134.087039765632));
#268139=CARTESIAN_POINT('Ctrl Pts',(-82.2636940061471,5.86020485384888,
127.756066988721));
#268140=CARTESIAN_POINT('Ctrl Pts',(-82.54214162996,0.602968104857597,124.226327139294));
#268141=CARTESIAN_POINT('Ctrl Pts',(-82.8205892537728,-5.20836687586887,
126.741478701599));
#268142=CARTESIAN_POINT('Ctrl Pts',(-83.0990368775859,-6.23346714053832,
132.990220261861));
#268143=CARTESIAN_POINT('Ctrl Pts',(-83.3774845013985,-1.53031562485268,
137.230263594196));
#268144=CARTESIAN_POINT('Ctrl Pts',(-83.6559321252116,4.57912118999838,
135.56521601382));
#268145=CARTESIAN_POINT('Ctrl Pts',(-83.9343797490243,6.48056933374724,
129.525174905002));
#268146=CARTESIAN_POINT('Ctrl Pts',(-84.2128273728376,2.42669085319518,
124.660642974335));
#268147=CARTESIAN_POINT('Ctrl Pts',(-84.4912749966499,-3.85719797100462,
125.441887420503));
#268148=CARTESIAN_POINT('Ctrl Pts',(-84.7697226204634,-6.59651029444787,
131.150982763393));
#268149=CARTESIAN_POINT('Ctrl Pts',(-85.0481702442759,-3.27395191473627,
136.541549287701));
#268150=CARTESIAN_POINT('Ctrl Pts',(-85.326617868089,3.05720833317481,136.659919701402));
#268151=CARTESIAN_POINT('Ctrl Pts',(-85.6050654919017,6.57894347582879,
131.397317377022));
#268152=CARTESIAN_POINT('Ctrl Pts',(-85.8835131157147,4.05495096345227,
125.58981675825));
#268153=CARTESIAN_POINT('Ctrl Pts',(-86.1619607395276,-2.19534338896908,
124.574227201559));
#268154=CARTESIAN_POINT('Ctrl Pts',(-86.4404083633404,-6.42822441541511,
129.283825895241));
#268155=CARTESIAN_POINT('Ctrl Pts',(-86.7188559871533,-4.75388124031539,
135.390721716488));
#268156=CARTESIAN_POINT('Ctrl Pts',(-86.9973036109663,1.28904655462414,
137.282975744021));
#268157=CARTESIAN_POINT('Ctrl Pts',(-87.2757512347791,6.14740353928957,
133.221698968287));
#268158=CARTESIAN_POINT('Ctrl Pts',(-87.554198858592,5.35659698870609,126.939006341782));
#268159=CARTESIAN_POINT('Ctrl Pts',(-87.8326464824051,-0.356660510187587,
124.208385461669));
#268160=CARTESIAN_POINT('Ctrl Pts',(-88.1110941062178,-5.74216442405318,
127.539143518524));
#268161=CARTESIAN_POINT('Ctrl Pts',(-88.3895417300309,-5.85089975254147,
133.870476574676));
#268162=CARTESIAN_POINT('Ctrl Pts',(-88.6679893538435,-0.582944040787213,
137.384198854334));
#268163=CARTESIAN_POINT('Ctrl Pts',(-88.9464369776566,5.22070876605056,
134.851371237371));
#268164=CARTESIAN_POINT('Ctrl Pts',(-89.2248846014694,6.22678526269035,
128.599538568266));
#268165=CARTESIAN_POINT('Ctrl Pts',(-89.5033322252823,1.51075029828878,
124.373829650922));
#268166=CARTESIAN_POINT('Ctrl Pts',(-89.7817798490951,-4.59359038598471,
126.057464543021));
#268167=CARTESIAN_POINT('Ctrl Pts',(-90.0602274729082,-6.47664591490472,
132.103265028861));
#268168=CARTESIAN_POINT('Ctrl Pts',(-90.338675096721,-2.40798024976945,
136.955435815729));
#268169=CARTESIAN_POINT('Ctrl Pts',(-90.6171227205338,3.87350162852866,
136.155068992212));
#268170=CARTESIAN_POINT('Ctrl Pts',(-90.8955703443469,6.59542474128344,
130.437662569033));
#268171=CARTESIAN_POINT('Ctrl Pts',(-91.1740179681596,3.25647472121003,
125.057233738258));
#268172=CARTESIAN_POINT('Ctrl Pts',(-91.4524655919725,-3.07501648002118,
124.958133746811));
#268173=CARTESIAN_POINT('Ctrl Pts',(-91.7309132157855,-6.58071775901922,
130.231430645527));
#268174=CARTESIAN_POINT('Ctrl Pts',(-92.0093608395982,-4.03906090341396,
136.031222199361));
#268175=CARTESIAN_POINT('Ctrl Pts',(-92.2878084634112,2.21429560333469,
137.027783305909));
#268176=CARTESIAN_POINT('Ctrl Pts',(-92.5662560872241,6.4328226249721,132.305322992969));
#268177=CARTESIAN_POINT('Ctrl Pts',(-92.844703711037,4.73989991511645,126.203551583122));
#268178=CARTESIAN_POINT('Ctrl Pts',(-93.1231513348499,-1.30875925974737,
124.329698913911));
#268179=CARTESIAN_POINT('Ctrl Pts',(-93.4015989586628,-6.15473261134757,
128.40574404555));
#268180=CARTESIAN_POINT('Ctrl Pts',(-93.6800465824757,-5.34480736852315,
134.686000627937));
#268181=CARTESIAN_POINT('Ctrl Pts',(-93.9584942062885,0.37673473761816,
137.399219669449));
#268182=CARTESIAN_POINT('Ctrl Pts',(-94.2369418301014,5.75207602440345,
134.052085419056));
#268183=CARTESIAN_POINT('Ctrl Pts',(-94.5153894539144,5.84154044929785,
127.720450736271));
#268184=CARTESIAN_POINT('Ctrl Pts',(-94.7938370777271,0.56291457640357,
124.222778577022));
#268185=CARTESIAN_POINT('Ctrl Pts',(-95.0722847015402,-5.23300229230026,
126.773258784876));
#268186=CARTESIAN_POINT('Ctrl Pts',(-95.350732325353,-6.22004570075364,
133.028124646699));
#268187=CARTESIAN_POINT('Ctrl Pts',(-95.6291799491659,-1.49117097634027,
137.239460002661));
#268188=CARTESIAN_POINT('Ctrl Pts',(-95.9076275729788,4.60801702757804,
135.537253395802));
#268189=CARTESIAN_POINT('Ctrl Pts',(-96.1860751967916,6.47266249729856,
129.48574954041));
#268190=CARTESIAN_POINT('Ctrl Pts',(-96.4645228206046,2.38924733914408,
124.645984847192));
#268191=CARTESIAN_POINT('Ctrl Pts',(-96.7429704444176,-3.88976940246256,
125.465466633565));
#268192=CARTESIAN_POINT('Ctrl Pts',(-97.0214180682302,-6.59427808900543,
131.191131171763));
#268193=CARTESIAN_POINT('Ctrl Pts',(-97.2998656920433,-3.23896736014657,
136.561372465446));
#268194=CARTESIAN_POINT('Ctrl Pts',(-97.5783133158561,3.09279614033489,
136.641201116591));
#268195=CARTESIAN_POINT('Ctrl Pts',(-97.856760939669,6.58243107933991,131.357258494642));
#268196=CARTESIAN_POINT('Ctrl Pts',(-98.135208563482,4.02313342606635,125.565229734223));
#268197=CARTESIAN_POINT('Ctrl Pts',(-98.4136561872948,-2.2332273047675,
124.587706309824));
#268198=CARTESIAN_POINT('Ctrl Pts',(-98.6921038111079,-6.43736124173946,
129.322984493793));
#268199=CARTESIAN_POINT('Ctrl Pts',(-98.9705514349205,-4.72587468013238,
135.419574966262));
#268200=CARTESIAN_POINT('Ctrl Pts',(-99.2489990587337,1.32845984070286,
137.275008918035));
#268201=CARTESIAN_POINT('Ctrl Pts',(-99.5274466825463,6.16200466680371,
133.184233190419));
#268202=CARTESIAN_POINT('Ctrl Pts',(-99.8058943063594,5.3329682347749,126.906470831589));
#268203=CARTESIAN_POINT('Ctrl Pts',(-100.084341930172,-0.396805475030165,
124.210678763569));
#268204=CARTESIAN_POINT('Ctrl Pts',(-100.362789553985,-5.76193433830736,
127.574158200105));
#268205=CARTESIAN_POINT('Ctrl Pts',(-100.641237177798,-5.83212703082168,
133.906035854126));
#268206=CARTESIAN_POINT('Ctrl Pts',(-100.919684801611,-0.542879897255484,
137.387625491007));
#268207=CARTESIAN_POINT('Ctrl Pts',(-101.198132425424,5.24524734073077,
134.819516319564));
#268208=CARTESIAN_POINT('Ctrl Pts',(-101.476580049237,6.21324851716398,
128.561675209245));
#268209=CARTESIAN_POINT('Ctrl Pts',(-101.75502767305,1.47157784038775,124.3647524279));
#268210=CARTESIAN_POINT('Ctrl Pts',(-102.033475296863,-4.62240098113028,
126.085514980508));
#268211=CARTESIAN_POINT('Ctrl Pts',(-102.311922920676,-6.4686191178319,
132.142666145147));
#268212=CARTESIAN_POINT('Ctrl Pts',(-102.590370544489,-2.3704922948573,
136.969979909799));
#268213=CARTESIAN_POINT('Ctrl Pts',(-102.868818168302,3.90600114210426,
136.131390752135));
#268214=CARTESIAN_POINT('Ctrl Pts',(-103.147265792114,6.59307034823604,
130.397521140692));
#268215=CARTESIAN_POINT('Ctrl Pts',(-103.425713415927,3.22142999373166,
125.037517133282));
#268216=CARTESIAN_POINT('Ctrl Pts',(-103.70416103974,-3.11054714940797,
124.976960561963));
#268217=CARTESIAN_POINT('Ctrl Pts',(-103.982608663553,-6.58408342091771,
130.271499957422));
#268218=CARTESIAN_POINT('Ctrl Pts',(-104.261056287366,-4.00716867896111,
136.055712267864));
#268219=CARTESIAN_POINT('Ctrl Pts',(-104.539503911179,2.25213831788793,
137.014188954471));
#268220=CARTESIAN_POINT('Ctrl Pts',(-104.817951534992,6.44184022367115,
132.266136766442));
#268221=CARTESIAN_POINT('Ctrl Pts',(-105.096399158805,4.71180566529118,
126.17478370933));
#268222=CARTESIAN_POINT('Ctrl Pts',(-105.374846782618,-1.34814811498862,
124.337785663482));
#268223=CARTESIAN_POINT('Ctrl Pts',(-105.65329440643,-6.16921963829011,
128.443254090687));
#268224=CARTESIAN_POINT('Ctrl Pts',(-105.931742030243,-5.32107969713743,
134.718464069627));
#268225=CARTESIAN_POINT('Ctrl Pts',(-106.210189654056,0.416872536489867,
137.396804190707));
#268226=CARTESIAN_POINT('Ctrl Pts',(-106.488637277869,5.77173927443855,
134.017010726842));
#268227=CARTESIAN_POINT('Ctrl Pts',(-106.767084901682,5.82265958431723,
127.684948759235));
#268228=CARTESIAN_POINT('Ctrl Pts',(-107.045532525495,0.52284018894291,
124.219473897692));
#268229=CARTESIAN_POINT('Ctrl Pts',(-107.323980149308,-5.25744379790729,
126.805188242113));
#268230=CARTESIAN_POINT('Ctrl Pts',(-107.602427773121,-6.20639377488812,
133.065946629143));
#268231=CARTESIAN_POINT('Ctrl Pts',(-107.880875396933,-1.45197107193893,
137.248417956151));
#268232=CARTESIAN_POINT('Ctrl Pts',(-108.159323020746,4.63674211339212,
135.509115398702));
#268233=CARTESIAN_POINT('Ctrl Pts',(-108.437770644559,6.46451581396073,
129.446373037437));
#268234=CARTESIAN_POINT('Ctrl Pts',(-108.716218268372,2.35171529065418,
124.631554920928));
#268235=CARTESIAN_POINT('Ctrl Pts',(-108.994665892185,-3.92219669708481,
125.489243681306));
#268236=CARTESIAN_POINT('Ctrl Pts',(-109.273113515998,-6.59180153016358,
131.231265248209));
#268237=CARTESIAN_POINT('Ctrl Pts',(-109.551561139811,-3.20386278442967,
136.580982315001));
#268238=CARTESIAN_POINT('Ctrl Pts',(-109.830008763624,3.12826934279688,
136.622266245509));
#268239=CARTESIAN_POINT('Ctrl Pts',(-110.108456387437,6.5856747684467,131.317179124427));
#268240=CARTESIAN_POINT('Ctrl Pts',(-110.38690401125,3.99116680999183,125.540836848117));
#268241=CARTESIAN_POINT('Ctrl Pts',(-110.665351635062,-2.27102846750687,
124.601415778499));
#268242=CARTESIAN_POINT('Ctrl Pts',(-110.943799258875,-6.44625952927566,
129.362197985281));
#268243=CARTESIAN_POINT('Ctrl Pts',(-111.222246882688,-4.69769300092514,
135.448257197571));
#268244=CARTESIAN_POINT('Ctrl Pts',(-111.500694506501,1.36782390021364,
137.266802319797));
#268245=CARTESIAN_POINT('Ctrl Pts',(-111.779142130314,6.17637745896884,
133.1466792255));
#268246=CARTESIAN_POINT('Ctrl Pts',(-112.057589754127,5.30914186574463,
126.874079759138));
#268247=CARTESIAN_POINT('Ctrl Pts',(-112.33603737794,-0.436935736099303,
124.213216396775));
#268248=CARTESIAN_POINT('Ctrl Pts',(-112.614485001753,-5.78149074196569,
127.609292578024));
#268249=CARTESIAN_POINT('Ctrl Pts',(-112.892932625565,-5.81313819748998,
133.94148019986));
#268250=CARTESIAN_POINT('Ctrl Pts',(-113.171380249379,-0.502795637109545,
137.390808182378));
#268251=CARTESIAN_POINT('Ctrl Pts',(-113.449827873191,5.26959155084185,
134.787512618686));
#268252=CARTESIAN_POINT('Ctrl Pts',(-113.728275497004,6.19948153742887,
128.523894953756));
#268253=CARTESIAN_POINT('Ctrl Pts',(-114.006723120817,1.43235085262869,
124.355913826926));
#268254=CARTESIAN_POINT('Ctrl Pts',(-114.28517074463,-4.65104029150761,
126.113740276555));
#268255=CARTESIAN_POINT('Ctrl Pts',(-114.563618368443,-6.46035262369882,
132.182017670029));
#268256=CARTESIAN_POINT('Ctrl Pts',(-114.842065992256,-2.33291650048142,
136.984295534578));
#268257=CARTESIAN_POINT('Ctrl Pts',(-115.120513616069,3.93835591737112,
136.107515116997));
#268258=CARTESIAN_POINT('Ctrl Pts',(-115.398961239881,6.59047164654225,
130.357394787938));
#268259=CARTESIAN_POINT('Ctrl Pts',(-115.677408863695,3.18626589498021,
125.018014220813));
#268260=CARTESIAN_POINT('Ctrl Pts',(-115.955856487507,-3.14596255632626,
124.996003313566));
#268261=CARTESIAN_POINT('Ctrl Pts',(-116.23430411132,-6.58720510718372,
130.311589014666));
#268262=CARTESIAN_POINT('Ctrl Pts',(-116.512751735133,-3.97512796739924,
136.0800077456));
#268263=CARTESIAN_POINT('Ctrl Pts',(-116.791199358946,2.28989757862811,
137.00036449556));
#268264=CARTESIAN_POINT('Ctrl Pts',(-117.069646982759,6.45061911761184,
132.226896373261));
#268265=CARTESIAN_POINT('Ctrl Pts',(-117.348094606572,4.68353681777373,
126.146187386213));
#268266=CARTESIAN_POINT('Ctrl Pts',(-117.626542230384,-1.38748701410568,
124.346112034364));
#268267=CARTESIAN_POINT('Ctrl Pts',(-117.904989854198,-6.18347806253024,
128.480851627495));
#268268=CARTESIAN_POINT('Ctrl Pts',(-118.18343747801,-5.29715485118671,
134.750782472776));
#268269=CARTESIAN_POINT('Ctrl Pts',(-118.461885101824,0.45699488799644,
137.394144426544));
#268270=CARTESIAN_POINT('Ctrl Pts',(-118.740332725636,5.79118865055225,
133.981816988697));
#268271=CARTESIAN_POINT('Ctrl Pts',(-119.018780349449,5.80356295854445,
127.649562373154));
#268272=CARTESIAN_POINT('Ctrl Pts',(-119.297227973262,0.482746427446748,
124.216413223762));
#268273=CARTESIAN_POINT('Ctrl Pts',(-119.575675597075,-5.28169048700048,
126.837265890154));
#268274=CARTESIAN_POINT('Ctrl Pts',(-119.854123220888,-6.19251186881905,
133.103684807684));
#268275=CARTESIAN_POINT('Ctrl Pts',(-120.132570844701,-1.41271736421608,
137.257137122728));
#268276=CARTESIAN_POINT('Ctrl Pts',(-120.411018468513,4.66529538302207,
135.480803065184));
#268277=CARTESIAN_POINT('Ctrl Pts',(-120.689466092327,6.45612958561205,
129.407046855192));
#268278=CARTESIAN_POINT('Ctrl Pts',(-120.967913716139,2.31409609848935,
124.61735373025));
#268279=CARTESIAN_POINT('Ctrl Pts',(-121.246361339953,-3.95447865326606,
125.51321768266));
#268280=CARTESIAN_POINT('Ctrl Pts',(-121.524808963765,-6.5890807096919,
131.271383505546));
#268281=CARTESIAN_POINT('Ctrl Pts',(-121.803256587578,-3.16863948839908,
136.600378109714));
#268282=CARTESIAN_POINT('Ctrl Pts',(-122.081704211391,3.16362662608795,
136.603115789794));
#268283=CARTESIAN_POINT('Ctrl Pts',(-122.360151835204,6.58867442295306,
131.277080751534));
#268284=CARTESIAN_POINT('Ctrl Pts',(-122.638599459017,3.9590522997634,125.51663900382));
#268285=CARTESIAN_POINT('Ctrl Pts',(-122.91704708283,-2.30874547645122,
124.615355099576));
#268286=CARTESIAN_POINT('Ctrl Pts',(-123.195494706643,-6.45491894829438,
129.401464916637));
#268287=CARTESIAN_POINT('Ctrl Pts',(-123.473942330455,-4.66933724697619,
135.476767347585));
#268288=CARTESIAN_POINT('Ctrl Pts',(-123.752389954268,1.40713727450679,
137.258356253404));
#268289=CARTESIAN_POINT('Ctrl Pts',(-124.030837578081,6.19052138319586,
133.109038465103));
#268290=CARTESIAN_POINT('Ctrl Pts',(-124.309285201894,5.28511876451003,
126.841834324687));
#268291=CARTESIAN_POINT('Ctrl Pts',(-124.587732825707,-0.477049806354697,
124.215998267256));
#268292=CARTESIAN_POINT('Ctrl Pts',(-124.86618044952,-5.80083291035842,
127.644545350364));
#268293=CARTESIAN_POINT('Ctrl Pts',(-125.144628073333,-5.79393395618462,
133.976808298475));
#268294=CARTESIAN_POINT('Ctrl Pts',(-125.423075697146,-0.462692745686338,
137.393746810514));
#268295=CARTESIAN_POINT('Ctrl Pts',(-125.701523320958,5.2937404943001,134.755361320645));
#268296=CARTESIAN_POINT('Ctrl Pts',(-125.979970944772,6.18548483362552,
128.486199201761));
#268297=CARTESIAN_POINT('Ctrl Pts',(-126.258418568584,1.39307078858202,
124.34731417552));
#268298=CARTESIAN_POINT('Ctrl Pts',(-126.536866192397,-4.67950725587653,
126.142139385264));
#268299=CARTESIAN_POINT('Ctrl Pts',(-126.81531381621,-6.45184673882346,
132.221318145323));
#268300=CARTESIAN_POINT('Ctrl Pts',(-127.093761440023,-2.29525425902701,
136.998382159598));
#268301=CARTESIAN_POINT('Ctrl Pts',(-127.372209063836,3.97056475541062,
136.083442971518));
#268302=CARTESIAN_POINT('Ctrl Pts',(-127.650656687649,6.58762873249828,
130.317284997668));
#268303=CARTESIAN_POINT('Ctrl Pts',(-127.929104311462,3.15098372797424,
124.998725723536));
#268304=CARTESIAN_POINT('Ctrl Pts',(-128.207551935275,-3.18126138844507,
125.015261295985));
#268305=CARTESIAN_POINT('Ctrl Pts',(-128.485999559087,-6.59008270214206,
130.351696331743));
#268306=CARTESIAN_POINT('Ctrl Pts',(-128.764447182901,-3.94293995600869,
136.104107732291));
#268307=CARTESIAN_POINT('Ctrl Pts',(-129.042894806713,2.32757198637139,
136.986310441447));
#268308=CARTESIAN_POINT('Ctrl Pts',(-129.321342430526,6.45915898148892,
132.187603267495));
#268309=CARTESIAN_POINT('Ctrl Pts',(-129.599790054339,4.6550944200771,126.117763673416));
#268310=CARTESIAN_POINT('Ctrl Pts',(-129.878237678152,-1.42677449938118,
124.354677718024));
#268311=CARTESIAN_POINT('Ctrl Pts',(-130.156685301965,-6.19750735571679,
128.518535262782));
#268312=CARTESIAN_POINT('Ctrl Pts',(-130.435132925778,-5.27303371721495,
134.782954639811));
#268313=CARTESIAN_POINT('Ctrl Pts',(-130.713580549591,0.497100305389368,
137.391240475519));
#268314=CARTESIAN_POINT('Ctrl Pts',(-130.992028173403,5.81042343204081,
133.946505508738));
#268315=CARTESIAN_POINT('Ctrl Pts',(-131.270475797217,5.78425127961196,
127.614292889281));
#268316=CARTESIAN_POINT('Ctrl Pts',(-131.548923421029,0.442634777604211,
124.213596668645));
#268317=CARTESIAN_POINT('Ctrl Pts',(-131.827371044842,-5.30574146111081,
126.869490540348));
#268318=CARTESIAN_POINT('Ctrl Pts',(-132.105818668655,-6.17840049694519,
133.141337783923));
#268319=CARTESIAN_POINT('Ctrl Pts',(-132.384266292468,-1.37341130773126,
137.265617179298));
#268320=CARTESIAN_POINT('Ctrl Pts',(-132.662713916281,4.69367577841589,
135.45231744437));
#268321=CARTESIAN_POINT('Ctrl Pts',(-132.941161540094,6.44750412300737,
129.367772450924));
#268322=CARTESIAN_POINT('Ctrl Pts',(-133.219609163907,2.27639115664257,
124.603381801387));
#268323=CARTESIAN_POINT('Ctrl Pts',(-133.49805678772,-3.98661407478655,
125.537387749261));
#268324=CARTESIAN_POINT('Ctrl Pts',(-133.776504411532,-6.58611572841139,
131.311484457178));
#268325=CARTESIAN_POINT('Ctrl Pts',(-134.054952035345,-3.13329877726696,
136.619559130867));
#268326=CARTESIAN_POINT('Ctrl Pts',(-134.333399659158,3.19886668003099,
136.583750459073));
#268327=CARTESIAN_POINT('Ctrl Pts',(-134.611847282971,6.59142993170542,
131.236964861823));
#268328=CARTESIAN_POINT('Ctrl Pts',(-134.890294906784,3.92679108539655,
125.492637097993));
#268329=CARTESIAN_POINT('Ctrl Pts',(-135.168742530597,-2.34637693398254,
124.629523756529));
#268330=CARTESIAN_POINT('Ctrl Pts',(-135.44719015441,-6.46333917791768,
129.440783832808));
#268331=CARTESIAN_POINT('Ctrl Pts',(-135.725637778223,-4.64080846901838,
135.505104359849));
#268332=CARTESIAN_POINT('Ctrl Pts',(-136.004085402036,1.44639850681073,
137.24967103183));
#268333=CARTESIAN_POINT('Ctrl Pts',(-136.282533025848,6.20443591537649,
133.07131230402));
#268334=CARTESIAN_POINT('Ctrl Pts',(-136.560980649661,5.26089982125598,
126.809735723105));
#268335=CARTESIAN_POINT('Ctrl Pts',(-136.839428273474,-0.517146199354053,
124.219024271924));
#268336=CARTESIAN_POINT('Ctrl Pts',(-137.117875897287,-5.81996012675442,
127.679915210822));
#268337=CARTESIAN_POINT('Ctrl Pts',(-137.3963235211,-5.77451501852576,134.012018840873));
#268338=CARTESIAN_POINT('Ctrl Pts',(-137.674771144913,-0.422572709013315,
137.396441266521));
#268339=CARTESIAN_POINT('Ctrl Pts',(-137.953218768726,5.31769327625758,
134.723063616821));
#268340=CARTESIAN_POINT('Ctrl Pts',(-138.231666392539,6.17125892440694,
128.448589350091));
#268341=CARTESIAN_POINT('Ctrl Pts',(-138.510114016352,1.35373910378499,
124.338953792345));
#268342=CARTESIAN_POINT('Ctrl Pts',(-138.788561640165,-4.70780081938319,
126.170711254294));
#268343=CARTESIAN_POINT('Ctrl Pts',(-139.067009263977,-6.44310177839452,
132.260566114734));
#268344=CARTESIAN_POINT('Ctrl Pts',(-139.34545688779,-2.25750696608163,
137.012239262869));
#268345=CARTESIAN_POINT('Ctrl Pts',(-139.623904511603,4.00262646271346,
136.059175207703));
#268346=CARTESIAN_POINT('Ctrl Pts',(-139.902352135416,6.5845417114487,130.277193256163));
#268347=CARTESIAN_POINT('Ctrl Pts',(-140.180799759229,3.11558480010749,
124.979652356196));
#268348=CARTESIAN_POINT('Ctrl Pts',(-140.459247383042,-3.21644233775325,
125.034733795609));
#268349=CARTESIAN_POINT('Ctrl Pts',(-140.737695006855,-6.59271609916233,
130.391820422461));
#268350=CARTESIAN_POINT('Ctrl Pts',(-141.016142630668,-3.91060583752806,
136.128011334905));
#268351=CARTESIAN_POINT('Ctrl Pts',(-141.294590254481,2.36516014507876,
136.97202731291));
#268352=CARTESIAN_POINT('Ctrl Pts',(-141.573037878293,6.46745949885459,
132.148258905163));
#268353=CARTESIAN_POINT('Ctrl Pts',(-141.851485502106,4.62647952614482,
126.089513624195));
#268354=CARTESIAN_POINT('Ctrl Pts',(-142.129933125919,-1.4660091150024,
124.363482397054));
#268355=CARTESIAN_POINT('Ctrl Pts',(-142.408380749732,-6.21130699798892,
128.556303600169));
#268356=CARTESIAN_POINT('Ctrl Pts',(-142.686828373545,-5.24871718904012,
134.814979378581));
#268357=CARTESIAN_POINT('Ctrl Pts',(-142.965275997358,0.537187302547703,
137.388092445238));
#268358=CARTESIAN_POINT('Ctrl Pts',(-143.243723621171,5.82944290615228,
133.911077595444));
#268359=CARTESIAN_POINT('Ctrl Pts',(-143.522171244983,5.76472526312116,
127.579141614542));
#268360=CARTESIAN_POINT('Ctrl Pts',(-143.800618868797,0.402506725767204,
124.21102433671));
#268361=CARTESIAN_POINT('Ctrl Pts',(-144.079066492609,-5.32959582902011,
126.901860998601));
#268362=CARTESIAN_POINT('Ctrl Pts',(-144.357514116423,-6.1640601821688,
133.178904162615));
#268363=CARTESIAN_POINT('Ctrl Pts',(-144.635961740235,-1.33405435898536,
137.27385781163));
#268364=CARTESIAN_POINT('Ctrl Pts',(-144.914409364048,4.72188224792766,
135.423659591808));
#268365=CARTESIAN_POINT('Ctrl Pts',(-145.192856987861,6.43863974576633,
129.328551279958));
#268366=CARTESIAN_POINT('Ctrl Pts',(-145.471304611674,2.23860186228433,
124.589639652074));
#268367=CARTESIAN_POINT('Ctrl Pts',(-145.749752235487,-4.01860177085642,
125.56175298548));
#268368=CARTESIAN_POINT('Ctrl Pts',(-146.0281998593,-6.58290669619051,131.35156661715));
#268369=CARTESIAN_POINT('Ctrl Pts',(-146.306647483113,-3.09784196059638,
136.638524667701));
#268370=CARTESIAN_POINT('Ctrl Pts',(-146.585095106925,3.2339881987928,136.564170970937));
#268371=CARTESIAN_POINT('Ctrl Pts',(-146.863542730738,6.59394119259793,
131.196832941802));
#268372=CARTESIAN_POINT('Ctrl Pts',(-147.141990354551,3.89438436234147,
125.468832020033));
#268373=CARTESIAN_POINT('Ctrl Pts',(-147.420437978364,-2.38392144565404,
124.643921224334));
#268374=CARTESIAN_POINT('Ctrl Pts',(-147.698885602177,-6.47151990613084,
129.480153276819));
#268375=CARTESIAN_POINT('Ctrl Pts',(-147.97733322599,-4.61210772419611,
135.533267184325));
#268376=CARTESIAN_POINT('Ctrl Pts',(-148.255780849803,1.48560614228611,
137.240746976909));
#268377=CARTESIAN_POINT('Ctrl Pts',(-148.534228473616,6.21812053990256,
133.033502140209));
#268378=CARTESIAN_POINT('Ctrl Pts',(-148.812676097428,5.23648593342438,
126.777785143819));
#268379=CARTESIAN_POINT('Ctrl Pts',(-149.091123721242,-0.557223429310831,
124.222294298654));
#268380=CARTESIAN_POINT('Ctrl Pts',(-149.369571345054,-5.83887168238761,
127.715400848752));
#268381=CARTESIAN_POINT('Ctrl Pts',(-149.648018968867,-5.75488210408933,
134.047110522317));
#268382=CARTESIAN_POINT('Ctrl Pts',(-149.92646659268,-0.382437013753756,
137.398891450554));
#268383=CARTESIAN_POINT('Ctrl Pts',(-150.204914216493,5.34144900913504,
134.690620704017));
#268384=CARTESIAN_POINT('Ctrl Pts',(-150.483361840306,6.15680433691945,
128.411066792389));
#268385=CARTESIAN_POINT('Ctrl Pts',(-150.761809464119,1.31435725568762,
124.330832987197));
#268386=CARTESIAN_POINT('Ctrl Pts',(-151.040257087932,-4.73591993359918,
126.199454824906));
#268387=CARTESIAN_POINT('Ctrl Pts',(-151.318704711745,-6.43411806645975,
132.299760123916));
#268388=CARTESIAN_POINT('Ctrl Pts',(-151.597152335558,-2.21967602038541,
137.025866330917));
#268389=CARTESIAN_POINT('Ctrl Pts',(-151.87559995937,4.03453985122072,136.034712724799));
#268390=CARTESIAN_POINT('Ctrl Pts',(-152.154047583183,6.58121069778455,
130.237121049039));
#268391=CARTESIAN_POINT('Ctrl Pts',(-152.432495206996,3.08007042310019,
124.960794825562));
#268392=CARTESIAN_POINT('Ctrl Pts',(-152.710942830809,-3.25150410060774,
125.054420090877));
#268393=CARTESIAN_POINT('Ctrl Pts',(-152.989390454622,-6.59510520066311,
130.431959800007));
#268394=CARTESIAN_POINT('Ctrl Pts',(-153.267838078435,-3.87812681010997,
136.151717667683));
#268395=CARTESIAN_POINT('Ctrl Pts',(-153.546285702248,2.40266066190714,
136.957515639215));
#268396=CARTESIAN_POINT('Ctrl Pts',(-153.824733326061,6.47552036213011,
132.108864744186));
#268397=CARTESIAN_POINT('Ctrl Pts',(-154.103180949873,4.59769319631231,
126.061438285362));
#268398=CARTESIAN_POINT('Ctrl Pts',(-154.381628573686,-1.50518940711724,
124.372525745196));
#268399=CARTESIAN_POINT('Ctrl Pts',(-154.660076197499,-6.22487647799626,
128.594155240135));
#268400=CARTESIAN_POINT('Ctrl Pts',(-154.938523821312,-5.22420616771914,
134.846855502398));
#268401=CARTESIAN_POINT('Ctrl Pts',(-155.216971445125,0.577254394032953,
137.384700452354));
#268402=CARTESIAN_POINT('Ctrl Pts',(-155.495419068938,5.84824636811312,
133.87553456161));
#268403=CARTESIAN_POINT('Ctrl Pts',(-155.773866692751,5.74498563261573,
127.544109851479));
#268404=CARTESIAN_POINT('Ctrl Pts',(-156.052314316564,0.362363758895462,
124.208696323275));
#268405=CARTESIAN_POINT('Ctrl Pts',(-156.330761940377,-5.353252706796,126.934376065411));
#268406=CARTESIAN_POINT('Ctrl Pts',(-156.60920956419,-6.14949145587554,
133.216382551721));
#268407=CARTESIAN_POINT('Ctrl Pts',(-156.887657188002,-1.29464797636456,
137.281858714364));
#268408=CARTESIAN_POINT('Ctrl Pts',(-157.166104811815,4.74991374635575,
135.394830569423));
#268409=CARTESIAN_POINT('Ctrl Pts',(-157.444552435628,6.42953678236183,
129.28938479565));
#268410=CARTESIAN_POINT('Ctrl Pts',(-157.723000059441,2.20072961571137,
124.576127791533));
#268411=CARTESIAN_POINT('Ctrl Pts',(-158.001447683254,-4.05044055615985,
125.586312488451));
#268412=CARTESIAN_POINT('Ctrl Pts',(-158.279895307067,-6.57945373194114,
131.391628500203));
#268413=CARTESIAN_POINT('Ctrl Pts',(-158.55834293088,-3.06227035225273,
136.657274017441));
#268414=CARTESIAN_POINT('Ctrl Pts',(-158.836790554693,3.2689898809326,136.54437805091));
#268415=CARTESIAN_POINT('Ctrl Pts',(-159.115238178505,6.59620811257463,
131.156686478575));
#268416=CARTESIAN_POINT('Ctrl Pts',(-159.393685802319,3.86183333144169,
125.445224652049));
#268417=CARTESIAN_POINT('Ctrl Pts',(-159.672133426131,-2.42137762023968,
124.658546969484));
#268418=CARTESIAN_POINT('Ctrl Pts',(-159.950581049944,-6.47946082979399,
129.519571789819));
#268419=CARTESIAN_POINT('Ctrl Pts',(-160.229028673757,-4.58323607602601,
135.56125477743));
#268420=CARTESIAN_POINT('Ctrl Pts',(-160.50747629757,1.52475872807955,137.231584419323));
#268421=CARTESIAN_POINT('Ctrl Pts',(-160.785923921383,6.23157474968534,
132.99560937474));
#268422=CARTESIAN_POINT('Ctrl Pts',(-161.064371545196,5.2118780056808,126.745983770767));
#268423=CARTESIAN_POINT('Ctrl Pts',(-161.342819169009,-0.597280011148509,
124.225808226271));
#268424=CARTESIAN_POINT('Ctrl Pts',(-161.621266792821,-5.85756687648338,
127.751000949223));
#268425=CARTESIAN_POINT('Ctrl Pts',(-161.899714416635,-5.73503594038016,
134.08208204247));
#268426=CARTESIAN_POINT('Ctrl Pts',(-162.178162040447,-0.342287147149402,
137.401097271823));
#268427=CARTESIAN_POINT('Ctrl Pts',(-162.45660966426,5.36500681265522,134.658033784415));
#268428=CARTESIAN_POINT('Ctrl Pts',(-162.735057288073,6.14212160678308,
128.373632919072));
#268429=CARTESIAN_POINT('Ctrl Pts',(-163.013504911886,1.27492670359879,
124.322952060995));
#268430=CARTESIAN_POINT('Ctrl Pts',(-163.291952535699,-4.76386355656041,
126.228369031995));
#268431=CARTESIAN_POINT('Ctrl Pts',(-163.570400159512,-6.42489593591386,
132.338898720518));
#268432=CARTESIAN_POINT('Ctrl Pts',(-163.848847783325,-2.18176282377798,
137.039262858781));
#268433=CARTESIAN_POINT('Ctrl Pts',(-164.127295407138,4.06630373837012,
136.010056429275));
#268434=CARTESIAN_POINT('Ctrl Pts',(-164.405743030951,6.57763581493773,
130.197069861187));
#268435=CARTESIAN_POINT('Ctrl Pts',(-164.684190654763,3.04444191295097,
124.942153830408));
#268436=CARTESIAN_POINT('Ctrl Pts',(-164.962638278576,-3.28644537778151,
125.074319452304));
#268437=CARTESIAN_POINT('Ctrl Pts',(-165.241085902389,-6.59724991811553,
130.472112977002));
#268438=CARTESIAN_POINT('Ctrl Pts',(-165.519533526202,-3.84550407727676,
136.175225852179));
#268439=CARTESIAN_POINT('Ctrl Pts',(-165.797981150015,2.44007214726114,
136.942775958099));
#268440=CARTESIAN_POINT('Ctrl Pts',(-166.076428773828,6.48334127261722,
132.069422244329));
#268441=CARTESIAN_POINT('Ctrl Pts',(-166.354876397641,4.56873649726763,
126.03353869726));
#268442=CARTESIAN_POINT('Ctrl Pts',(-166.633324021454,-1.54431392388507,
124.381807427344));
#268443=CARTESIAN_POINT('Ctrl Pts',(-166.911771645267,-6.23821529291649,
128.632088780075));
#268444=CARTESIAN_POINT('Ctrl Pts',(-167.19021926908,-5.19950156151742,
134.878581830081));
#268445=CARTESIAN_POINT('Ctrl Pts',(-167.468666892892,0.617300095144361,
137.381064622557));
#268446=CARTESIAN_POINT('Ctrl Pts',(-167.747114516705,5.86683312115408,
133.839877724298));
#268447=CARTESIAN_POINT('Ctrl Pts',(-168.025562140518,5.72503311955499,
127.509198898206));
#268448=CARTESIAN_POINT('Ctrl Pts',(-168.304009764331,0.32220736450136,
124.206612714607));
#268449=CARTESIAN_POINT('Ctrl Pts',(-168.582457388144,-5.37671121782417,
126.967034535923));
#268450=CARTESIAN_POINT('Ctrl Pts',(-168.860905011957,-6.1346948579149,
133.253771562468));
#268451=CARTESIAN_POINT('Ctrl Pts',(-169.13935263577,-1.25519362008691,
137.289619591024));
#268452=CARTESIAN_POINT('Ctrl Pts',(-169.417800259582,4.77776923498369,
135.365831445486));
#268453=CARTESIAN_POINT('Ctrl Pts',(-169.696247883396,6.42019557010726,
129.250274449328));
#268454=CARTESIAN_POINT('Ctrl Pts',(-169.974695507208,2.16277582029264,
124.562846720449));
#268455=CARTESIAN_POINT('Ctrl Pts',(-170.253143131021,-4.08212925089891,
125.611065348116));
#268456=CARTESIAN_POINT('Ctrl Pts',(-170.531590754834,-6.57575696361412,
131.431668621828));
#268457=CARTESIAN_POINT('Ctrl Pts',(-170.810038378647,-3.02658527035502,
136.675806485322));
#268458=CARTESIAN_POINT('Ctrl Pts',(-171.08848600246,3.30387042945021,136.524372432426));
#268459=CARTESIAN_POINT('Ctrl Pts',(-171.366933626273,6.59823060763395,
131.116526959784));
#268460=CARTESIAN_POINT('Ctrl Pts',(-171.645381250086,3.82913919888762,
125.421815868818));
#268461=CARTESIAN_POINT('Ctrl Pts',(-171.923828873899,-2.45874406978715,
124.673400450021));
#268462=CARTESIAN_POINT('Ctrl Pts',(-172.202276497711,-6.48716165465291,
129.559037911142));
#268463=CARTESIAN_POINT('Ctrl Pts',(-172.480724121525,-4.55419459435809,
135.589066102071));
#268464=CARTESIAN_POINT('Ctrl Pts',(-172.759171745337,1.5638548133772,137.222183698596));
#268465=CARTESIAN_POINT('Ctrl Pts',(-173.03761936915,6.24479804617409,132.957635411742));
#268466=CARTESIAN_POINT('Ctrl Pts',(-173.316066992963,5.18707694988104,
126.714332782362));
#268467=CARTESIAN_POINT('Ctrl Pts',(-173.594514616776,-0.637314460555731,
124.229565924566));
#268468=CARTESIAN_POINT('Ctrl Pts',(-173.872962240589,-5.8760450162844,
127.786714193059));
#268469=CARTESIAN_POINT('Ctrl Pts',(-174.151409864401,-5.71497726280517,
134.11693210545));
#268470=CARTESIAN_POINT('Ctrl Pts',(-174.429857488215,-0.302124596968923,
137.403058648589));
#268471=CARTESIAN_POINT('Ctrl Pts',(-174.708305112027,5.38836581387496,
134.625304065538));
#268472=CARTESIAN_POINT('Ctrl Pts',(-174.98675273584,6.1272112780718,128.336289117263));
#268473=CARTESIAN_POINT('Ctrl Pts',(-175.265200359654,1.2354489086321,124.315311305772));
#268474=CARTESIAN_POINT('Ctrl Pts',(-175.543647983466,-4.79163065280562,
126.257452804136));
#268475=CARTESIAN_POINT('Ctrl Pts',(-175.822095607279,-6.41543572848632,
132.377980454247));
#268476=CARTESIAN_POINT('Ctrl Pts',(-176.100543231092,-2.14376878114676,
137.05242835005));
#268477=CARTESIAN_POINT('Ctrl Pts',(-176.378990854905,4.09791694713909,
135.985207234778));
#268478=CARTESIAN_POINT('Ctrl Pts',(-176.657438478718,6.57381719537689,
130.157041176716));
#268479=CARTESIAN_POINT('Ctrl Pts',(-176.93588610253,3.00870058988678,124.923730061481));
#268480=CARTESIAN_POINT('Ctrl Pts',(-177.214333726344,-3.32126487451375,
125.094431142515));
#268481=CARTESIAN_POINT('Ctrl Pts',(-177.492781350156,-6.59915017204588,
130.512278465557));
#268482=CARTESIAN_POINT('Ctrl Pts',(-177.771228973969,-3.81273884787578,
136.198535017289));
#268483=CARTESIAN_POINT('Ctrl Pts',(-178.049676597782,2.47739321484437,
136.927808815745));
#268484=CARTESIAN_POINT('Ctrl Pts',(-178.328124221595,6.49092194050925,
132.029932867148));
#268485=CARTESIAN_POINT('Ctrl Pts',(-178.606571845408,4.53961050201187,
126.005815893719));
#268486=CARTESIAN_POINT('Ctrl Pts',(-178.885019469221,-1.58338121553252,
124.391327099562));
#268487=CARTESIAN_POINT('Ctrl Pts',(-179.163467093034,-6.25132294847495,
128.670102814346));
#268488=CARTESIAN_POINT('Ctrl Pts',(-179.441914716847,-5.1746042858732,
134.910157185999));
#268489=CARTESIAN_POINT('Ctrl Pts',(-179.72036234066,0.657322921973241,
137.377185090575));
#268490=CARTESIAN_POINT('Ctrl Pts',(-179.998809964472,5.88520247653593,
133.804108404782));
#268491=CARTESIAN_POINT('Ctrl Pts',(-180.277257588285,5.70486846328706,
127.474410048364));
#268492=CARTESIAN_POINT('Ctrl Pts',(-180.555705212098,0.282039030594865,
124.204773587913));
#268493=CARTESIAN_POINT('Ctrl Pts',(-180.834152835911,-5.39997049284089,
126.999835199963));
#268494=CARTESIAN_POINT('Ctrl Pts',(-181.112600459724,-6.11967093658025,
133.291069809391));
#268495=CARTESIAN_POINT('Ctrl Pts',(-181.391048083537,-1.21569275214809,
137.297140154028));
#268496=CARTESIAN_POINT('Ctrl Pts',(-181.669495707349,4.8054476816156,135.336663294571));
#268497=CARTESIAN_POINT('Ctrl Pts',(-181.947943331163,6.41061645514481,
129.21122169024));
#268498=CARTESIAN_POINT('Ctrl Pts',(-182.226390954976,2.12474188242055,
124.549796930959));
#268499=CARTESIAN_POINT('Ctrl Pts',(-182.504838578788,-4.11366668083735,
125.636010647245));
#268500=CARTESIAN_POINT('Ctrl Pts',(-182.783286202602,-6.5718165281946,
131.471685498325));
#268501=CARTESIAN_POINT('Ctrl Pts',(-183.061733826414,-2.99078803722709,
136.694121384618));
#268502=CARTESIAN_POINT('Ctrl Pts',(-183.340181450227,3.33862855183402,
136.5041548568));
#268503=CARTESIAN_POINT('Ctrl Pts',(-183.61862907404,6.60000860283161,131.076355873553));
#268504=CARTESIAN_POINT('Ctrl Pts',(-183.897076697853,3.79630317617236,
125.398606537762));
#268505=CARTESIAN_POINT('Ctrl Pts',(-184.175524321666,-2.49601940966891,
124.68848111554));
#268506=CARTESIAN_POINT('Ctrl Pts',(-184.453971945479,-6.49462209535141,
129.598550178357));
#268507=CARTESIAN_POINT('Ctrl Pts',(-184.732419569291,-4.52498435533419,
135.616700127691));
#268508=CARTESIAN_POINT('Ctrl Pts',(-185.010867193105,1.60289294946002,
137.212545163075));
#268509=CARTESIAN_POINT('Ctrl Pts',(-185.289314816917,6.25778993937471,
132.919581658354));
#268510=CARTESIAN_POINT('Ctrl Pts',(-185.56776244073,5.16208368503734,126.682833351442));
#268511=CARTESIAN_POINT('Ctrl Pts',(-185.846210064543,-0.677325294041226,
124.233567254297));
#268512=CARTESIAN_POINT('Ctrl Pts',(-186.124657688356,-5.89430541707644,
127.822539256894));
#268513=CARTESIAN_POINT('Ctrl Pts',(-186.403105312169,-5.69470681464601,
134.151659419877));
#268514=CARTESIAN_POINT('Ctrl Pts',(-186.681552935982,-0.261950851450417,
137.404775508174));
#268515=CARTESIAN_POINT('Ctrl Pts',(-186.960000559794,5.41152514721792,
134.592432760195));
#268516=CARTESIAN_POINT('Ctrl Pts',(-187.238448183608,6.11207390329327,
128.299036770752));
#268517=CARTESIAN_POINT('Ctrl Pts',(-187.51689580742,1.19592533365239,124.307911004657));
#268518=CARTESIAN_POINT('Ctrl Pts',(-187.795343431234,-4.81922019341476,
126.286705063617));
#268519=CARTESIAN_POINT('Ctrl Pts',(-188.073791055046,-6.40573779472858,
132.417003876913));
#268520=CARTESIAN_POINT('Ctrl Pts',(-188.352238678859,-2.10569530037498,
137.065362316871));
#268521=CARTESIAN_POINT('Ctrl Pts',(-188.630686302672,4.12937830608858,
135.960166062105));
#268522=CARTESIAN_POINT('Ctrl Pts',(-188.909133926485,6.56975498060235,
130.117036478904));
#268523=CARTESIAN_POINT('Ctrl Pts',(-189.187581550298,2.97284777831579,
124.905524201484));
#268524=CARTESIAN_POINT('Ctrl Pts',(-189.466029174111,-3.35596130055467,
125.114754416262));
#268525=CARTESIAN_POINT('Ctrl Pts',(-189.744476797923,-6.60080589203976,
130.552454777323));
#268526=CARTESIAN_POINT('Ctrl Pts',(-190.022924421737,-3.77983233603489,
136.221644299282));
#268527=CARTESIAN_POINT('Ctrl Pts',(-190.301372045549,2.5146224817104,136.912614766765));
#268528=CARTESIAN_POINT('Ctrl Pts',(-190.579819669362,6.49826208490189,
131.990398075938));
#268529=CARTESIAN_POINT('Ctrl Pts',(-190.858267293175,4.51031628981952,
125.978270902017));
#268530=CARTESIAN_POINT('Ctrl Pts',(-191.136714916988,-1.62238983440674,
124.401084409096));
#268531=CARTESIAN_POINT('Ctrl Pts',(-191.415162540801,-6.26419895896261,
128.708195934325));
#268532=CARTESIAN_POINT('Ctrl Pts',(-191.693610164614,-5.14951526336424,
134.941580400114));
#268533=CARTESIAN_POINT('Ctrl Pts',(-191.972057788427,0.697321391460013,
137.373062000163));
#268534=CARTESIAN_POINT('Ctrl Pts',(-192.25050541224,5.90335375357599,133.768227928508));
#268535=CARTESIAN_POINT('Ctrl Pts',(-192.528953036052,5.68449241101982,
127.439744591064));
#268536=CARTESIAN_POINT('Ctrl Pts',(-192.807400659866,0.241860245628379,
124.203179011344));
#268537=CARTESIAN_POINT('Ctrl Pts',(-193.085848283678,-5.42302966996514,
127.032776842093));
#268538=CARTESIAN_POINT('Ctrl Pts',(-193.364295907491,-6.10442024858855,
133.32827591039));
#268539=CARTESIAN_POINT('Ctrl Pts',(-193.642743531304,-1.17614683626724,
137.304420124699));
#268540=CARTESIAN_POINT('Ctrl Pts',(-193.921191155117,4.83294806061645,
135.307327197512));
#268541=CARTESIAN_POINT('Ctrl Pts',(-194.19963877893,6.40079979243214,129.172227965502));
#268542=CARTESIAN_POINT('Ctrl Pts',(-194.478086402743,2.08662921145659,
124.536978906625));
#268543=CARTESIAN_POINT('Ctrl Pts',(-194.756534026555,-4.14505167734362,
125.661147461485));
#268544=CARTESIAN_POINT('Ctrl Pts',(-195.034981650369,-6.5676325716969,
131.511677646851));
#268545=CARTESIAN_POINT('Ctrl Pts',(-195.313429274181,-2.95487997934909,
136.712218036662));
#268546=CARTESIAN_POINT('Ctrl Pts',(-195.591876897994,3.3732629601091,136.483726073203));
#268547=CARTESIAN_POINT('Ctrl Pts',(-195.870324521807,6.60154203228333,
131.03617470844));
#268548=CARTESIAN_POINT('Ctrl Pts',(-196.14877214562,3.76332648004682,125.375597518911));
#268549=CARTESIAN_POINT('Ctrl Pts',(-196.427219769433,-2.53320225863353,
124.703788407225));
#268550=CARTESIAN_POINT('Ctrl Pts',(-196.705667393246,-6.50184187543975,
129.63810712732));
#268551=CARTESIAN_POINT('Ctrl Pts',(-196.984115017059,-4.49560644135098,
135.644155830301));
#268552=CARTESIAN_POINT('Ctrl Pts',(-197.262562640871,1.64187168975517,
137.202669169918));
#268553=CARTESIAN_POINT('Ctrl Pts',(-197.541010264685,6.27054994786743,
132.881449524674));
#268554=CARTESIAN_POINT('Ctrl Pts',(-197.819457888497,5.13689913728475,
126.651486645231));
#268555=CARTESIAN_POINT('Ctrl Pts',(-198.097905512311,-0.717311028988463,
124.237812067191));
#268556=CARTESIAN_POINT('Ctrl Pts',(-198.376353136123,-5.91234740221361,
127.858474813215));
#268557=CARTESIAN_POINT('Ctrl Pts',(-198.654800759936,-5.67422534703162,
134.186262698915));
#268558=CARTESIAN_POINT('Ctrl Pts',(-198.933248383749,-0.221767399246752,
137.406247786956));
#268559=CARTESIAN_POINT('Ctrl Pts',(-199.211696007562,5.43448395450644,
134.559421086446));
#268560=CARTESIAN_POINT('Ctrl Pts',(-199.490143631375,6.09671004336861,
128.261877259937));
#268561=CARTESIAN_POINT('Ctrl Pts',(-199.768591255188,1.15635744321901,
124.300751431872));
#268562=CARTESIAN_POINT('Ctrl Pts',(-200.047038879001,-4.84663115604747,
126.316124726487));
#268563=CARTESIAN_POINT('Ctrl Pts',(-200.325486502814,-6.39580249400115,
132.455967542492));
#268564=CARTESIAN_POINT('Ctrl Pts',(-200.603934126626,-2.06754379228947,
137.078064279972));
#268565=CARTESIAN_POINT('Ctrl Pts',(-200.882381750439,4.16068664940635,
135.934933839164));
#268566=CARTESIAN_POINT('Ctrl Pts',(-201.160829374253,6.56544932114097,
130.077057250143));
#268567=CARTESIAN_POINT('Ctrl Pts',(-201.439276998065,2.9368848067771,124.887536925038));
#268568=CARTESIAN_POINT('Ctrl Pts',(-201.717724621878,-3.39053337021544,
125.13528852046));
#268569=CARTESIAN_POINT('Ctrl Pts',(-201.996172245691,-6.60221701674386,
130.592640423553));
#268570=CARTESIAN_POINT('Ctrl Pts',(-202.274619869504,-3.74678576111652,
136.244552841837));
#268571=CARTESIAN_POINT('Ctrl Pts',(-202.553067493317,2.55175856831618,
136.897194374181));
#268572=CARTESIAN_POINT('Ctrl Pts',(-202.83151511713,6.50536143380309,131.950819335672));
#268573=CARTESIAN_POINT('Ctrl Pts',(-203.109962740942,4.48085494619837,
125.950904742844));
#268574=CARTESIAN_POINT('Ctrl Pts',(-203.388410364755,-1.66133833502902,
124.411078994385));
#268575=CARTESIAN_POINT('Ctrl Pts',(-203.666857988568,-6.27684284725421,
128.746366728457));
#268576=CARTESIAN_POINT('Ctrl Pts',(-203.945305612381,-5.12423542367342,
134.97285030803));
#268577=CARTESIAN_POINT('Ctrl Pts',(-204.223753236194,0.737294021446153,
137.368695504108));
#268578=CARTESIAN_POINT('Ctrl Pts',(-204.502200860007,5.9212862796718,133.732237625041));
#268579=CARTESIAN_POINT('Ctrl Pts',(-204.78064848382,5.66390571779574,127.405203810847));
#268580=CARTESIAN_POINT('Ctrl Pts',(-205.059096107633,0.20167249844203,
124.201829043986));
#268581=CARTESIAN_POINT('Ctrl Pts',(-205.337543731446,-5.44588789473034,
127.065858241646));
#268582=CARTESIAN_POINT('Ctrl Pts',(-205.615991355258,-6.08894335906002,
133.36538848678));
#268583=CARTESIAN_POINT('Ctrl Pts',(-205.894438979071,-1.13655733783284,
137.311459233274));
#268584=CARTESIAN_POINT('Ctrl Pts',(-206.172886602884,4.86026935294961,
135.277824241371));
#268585=CARTESIAN_POINT('Ctrl Pts',(-206.451334226697,6.39074594572923,
129.133294720038));
#268586=CARTESIAN_POINT('Ctrl Pts',(-206.72978185051,2.04843921967989,124.524393122426));
#268587=CARTESIAN_POINT('Ctrl Pts',(-207.008229474323,-4.17628307743617,
125.686474859378));
#268588=CARTESIAN_POINT('Ctrl Pts',(-207.286677098136,-6.56320524915893,
131.551643585487));
#268589=CARTESIAN_POINT('Ctrl Pts',(-207.565124721949,-2.9188624273063,
136.730095770877));
#268590=CARTESIAN_POINT('Ctrl Pts',(-207.843572345762,3.40777237088467,
136.463086838631));
#268591=CARTESIAN_POINT('Ctrl Pts',(-208.122019969575,6.60283083916734,
130.995984953369));
#268592=CARTESIAN_POINT('Ctrl Pts',(-208.400467593387,3.73021033247459,
125.352789664874));
#268593=CARTESIAN_POINT('Ctrl Pts',(-208.678915217201,-2.57029123885685,
124.719321757855));
#268594=CARTESIAN_POINT('Ctrl Pts',(-208.957362841013,-6.50882072738636,
129.677707292235));
#268595=CARTESIAN_POINT('Ctrl Pts',(-209.235810464827,-4.4660619410178,
135.671432192519));
#268596=CARTESIAN_POINT('Ctrl Pts',(-209.514258088639,1.68078958989102,
137.192556085085));
#268597=CARTESIAN_POINT('Ctrl Pts',(-209.792705712452,6.28307759882623,
132.8432404237));
#268598=CARTESIAN_POINT('Ctrl Pts',(-210.071153336265,5.11152423984512,
126.620293825292));
#268599=CARTESIAN_POINT('Ctrl Pts',(-210.349600960078,-0.757270183712145,
124.242300205957));
#268600=CARTESIAN_POINT('Ctrl Pts',(-210.62804858389,-5.93017030314353,
127.894519530418));
#268601=CARTESIAN_POINT('Ctrl Pts',(-210.906496207704,-5.65353361891029,
134.220740660327));
#268602=CARTESIAN_POINT('Ctrl Pts',(-211.184943831516,-0.181575729370575,
137.407475430382));
#268603=CARTESIAN_POINT('Ctrl Pts',(-211.463391455329,5.4572413849935,134.52627026755));
#268604=CARTESIAN_POINT('Ctrl Pts',(-211.741839079142,6.08112026761121,
128.224811961777));
#268605=CARTESIAN_POINT('Ctrl Pts',(-212.020286702955,1.11674670353533,
124.293832852717));
#268606=CARTESIAN_POINT('Ctrl Pts',(-212.298734326768,-4.87386252498038,
126.345710702588));
#268607=CARTESIAN_POINT('Ctrl Pts',(-212.577181950581,-6.38563019446009,
132.494870007167));
#268608=CARTESIAN_POINT('Ctrl Pts',(-212.855629574394,-2.02931567060901,
137.090533768676));
#268609=CARTESIAN_POINT('Ctrl Pts',(-213.134077198207,4.19184081695006,
135.909511500946));
#268610=CARTESIAN_POINT('Ctrl Pts',(-213.412524822019,6.56090037654053,
130.037104971874));
#268611=CARTESIAN_POINT('Ctrl Pts',(-213.690972445832,2.90081300789186,
124.869768898671));
#268612=CARTESIAN_POINT('Ctrl Pts',(-213.969420069645,-3.42497980241531,
125.156032694208));
#268613=CARTESIAN_POINT('Ctrl Pts',(-214.247867693459,-6.60338349386843,
130.632833915152));
#268614=CARTESIAN_POINT('Ctrl Pts',(-214.52631531727,-3.71360034767391,
136.267259796069));
#268615=CARTESIAN_POINT('Ctrl Pts',(-214.804762941084,2.58880009856982,
136.881548209402));
#268616=CARTESIAN_POINT('Ctrl Pts',(-215.083210564897,6.51221972414398,
131.911198112957));
#268617=CARTESIAN_POINT('Ctrl Pts',(-215.36165818871,4.45122756284936,125.923718430264));
#268618=CARTESIAN_POINT('Ctrl Pts',(-215.640105812523,-1.70022527414834,
124.421310485075));
#268619=CARTESIAN_POINT('Ctrl Pts',(-215.918553436335,-6.28925414482577,
128.784613782311));
#268620=CARTESIAN_POINT('Ctrl Pts',(-216.197001060149,-5.09876570355457,
135.003965751026));
#268621=CARTESIAN_POINT('Ctrl Pts',(-216.475448683961,0.77723933073121,
137.364085764208));
#268622=CARTESIAN_POINT('Ctrl Pts',(-216.753896307774,5.93899939032692,
133.696138828015));
#268623=CARTESIAN_POINT('Ctrl Pts',(-217.032343931587,5.64310914646246,
127.370788987637));
#268624=CARTESIAN_POINT('Ctrl Pts',(-217.3107915554,0.161477278206604,124.200723735865));
#268625=CARTESIAN_POINT('Ctrl Pts',(-217.589239179213,-5.46854432011718,
127.099078172778));
#268626=CARTESIAN_POINT('Ctrl Pts',(-217.867686803026,-6.07324084149572,
133.402406163341));
#268627=CARTESIAN_POINT('Ctrl Pts',(-218.146134426838,-1.09692572384833,
137.318257218917));
#268628=CARTESIAN_POINT('Ctrl Pts',(-218.424582050652,4.88741054621452,
135.24815551939));
#268629=CARTESIAN_POINT('Ctrl Pts',(-218.703029674464,6.38045528758512,
129.094423396537));
#268630=CARTESIAN_POINT('Ctrl Pts',(-218.981477298277,2.01017332223456,
124.512040044732));
#268631=CARTESIAN_POINT('Ctrl Pts',(-219.25992492209,-4.20735972382344,
125.711991902411));
#268632=CARTESIAN_POINT('Ctrl Pts',(-219.538372545903,-6.55853472463687,
131.591581833275));
#268633=CARTESIAN_POINT('Ctrl Pts',(-219.816820169716,-2.8827367157428,
136.747753924796));
#268634=CARTESIAN_POINT('Ctrl Pts',(-220.095267793529,3.44215550540127,
136.442237917877));
#268635=CARTESIAN_POINT('Ctrl Pts',(-220.373715417342,6.60387497572639,
130.955788097589));
#268636=CARTESIAN_POINT('Ctrl Pts',(-220.652163041155,3.69695596058723,
125.330183820803));
#268637=CARTESIAN_POINT('Ctrl Pts',(-220.930610664968,-2.60728497599312,
124.735080591838));
#268638=CARTESIAN_POINT('Ctrl Pts',(-221.20905828878,-6.51555839258729,
129.717349205704));
#268639=CARTESIAN_POINT('Ctrl Pts',(-221.487505912593,-4.43635194911701,
135.698528203611));
#268640=CARTESIAN_POINT('Ctrl Pts',(-221.765953536406,1.71964520775051,
137.182206283321));
#268641=CARTESIAN_POINT('Ctrl Pts',(-222.044401160219,6.295372428034,132.804955771283));
#268642=CARTESIAN_POINT('Ctrl Pts',(-222.322848784032,5.08595993299503,
126.589256047487));
#268643=CARTESIAN_POINT('Ctrl Pts',(-222.601296407845,-0.797201277510683,
124.247031504286));
#268644=CARTESIAN_POINT('Ctrl Pts',(-222.879744031658,-5.94777345943203,
127.930672072853));
#268645=CARTESIAN_POINT('Ctrl Pts',(-223.158191655471,-5.63263239702162,
134.255092026522));
#268646=CARTESIAN_POINT('Ctrl Pts',(-223.436639279283,-0.141377331138957,
137.40845839296));
#268647=CARTESIAN_POINT('Ctrl Pts',(-223.715086903097,5.47979659539413,
134.492981531924));
#268648=CARTESIAN_POINT('Ctrl Pts',(-223.993534526909,6.06530515370598,
128.187842249741));
#268649=CARTESIAN_POINT('Ctrl Pts',(-224.271982150722,1.07709458239186,
124.287155523561));
#268650=CARTESIAN_POINT('Ctrl Pts',(-224.550429774535,-4.90091329114502,
126.375461895601));
#268651=CARTESIAN_POINT('Ctrl Pts',(-224.828877398348,-6.37522127304402,
132.533709829396));
#268652=CARTESIAN_POINT('Ctrl Pts',(-225.107325022161,-1.99101235188949,
137.102770320923));
#268653=CARTESIAN_POINT('Ctrl Pts',(-225.385772645974,4.22283965429091,
135.883899989486));
#268654=CARTESIAN_POINT('Ctrl Pts',(-225.664220269787,6.55610831536389,
129.997181124546));
#268655=CARTESIAN_POINT('Ctrl Pts',(-225.9426678936,2.86463371831382,124.852220780782));
#268656=CARTESIAN_POINT('Ctrl Pts',(-226.221115517412,-3.45929932072906,
125.176986168825));
#268657=CARTESIAN_POINT('Ctrl Pts',(-226.499563141226,-6.60430528018926,
130.673033762736));
#268658=CARTESIAN_POINT('Ctrl Pts',(-226.778010765038,-3.68027732540471,
136.289764320562));
#268659=CARTESIAN_POINT('Ctrl Pts',(-227.056458388851,2.62574569988376,
136.865676852203));
#268660=CARTESIAN_POINT('Ctrl Pts',(-227.334906012664,6.51883670178814,
131.871535875972));
#268661=CARTESIAN_POINT('Ctrl Pts',(-227.613353636477,4.42143523762624,
125.896712971676));
#268662=CARTESIAN_POINT('Ctrl Pts',(-227.89180126029,-1.73904921079426,
124.431778502036));
#268663=CARTESIAN_POINT('Ctrl Pts',(-228.170248884103,-6.30143239177224,
128.822935678624));
#268664=CARTESIAN_POINT('Ctrl Pts',(-228.448696507916,-5.07310704679746,
135.034925576111));
#268665=CARTESIAN_POINT('Ctrl Pts',(-228.727144131728,0.81715583912702,
137.359232951281));
#268666=CARTESIAN_POINT('Ctrl Pts',(-229.005591755541,5.95649242917557,
133.659932875084));
#268667=CARTESIAN_POINT('Ctrl Pts',(-229.284039379354,5.62210346764449,
127.336501396687));
#268668=CARTESIAN_POINT('Ctrl Pts',(-229.562487003167,0.121276074371264,
124.199863127936));
#268669=CARTESIAN_POINT('Ctrl Pts',(-229.84093462698,-5.4909981065832,127.132435404515));
#268670=CARTESIAN_POINT('Ctrl Pts',(-230.119382250793,-6.0573132777586,
133.439327568368));
#268671=CARTESIAN_POINT('Ctrl Pts',(-230.397829874606,-1.05725346287773,
137.324813829725));
#268672=CARTESIAN_POINT('Ctrl Pts',(-230.676277498418,4.91437063468431,
135.218322130955));
#268673=CARTESIAN_POINT('Ctrl Pts',(-230.954725122232,6.3699281993239,129.055615435388));
#268674=CARTESIAN_POINT('Ctrl Pts',(-231.233172746044,1.97183293707754,
124.49992013129));
#268675=CARTESIAN_POINT('Ctrl Pts',(-231.511620369858,-4.23828046494889,
125.73769764504));
#268676=CARTESIAN_POINT('Ctrl Pts',(-231.79006799367,-6.55362117119865,
131.631490910294));
#268677=CARTESIAN_POINT('Ctrl Pts',(-232.068515617483,-2.84650418331021,
136.765191844092));
#268678=CARTESIAN_POINT('Ctrl Pts',(-232.346963241296,3.47641108958031,
136.421180083507));
#268679=CARTESIAN_POINT('Ctrl Pts',(-232.625410865109,6.60467440326965,
130.915585630608));
#268680=CARTESIAN_POINT('Ctrl Pts',(-232.903858488922,3.66356459663667,
125.307780824367));
#268681=CARTESIAN_POINT('Ctrl Pts',(-233.182306112735,-2.64418209922576,
124.751064325225));
#268682=CARTESIAN_POINT('Ctrl Pts',(-233.460753736548,-6.52205462137589,
129.75703139878));
#268683=CARTESIAN_POINT('Ctrl Pts',(-233.73920136036,-4.40647756656326,
135.725442859523));
#268684=CARTESIAN_POINT('Ctrl Pts',(-234.017648984174,1.75843710352442,
137.17162014814));
#268685=CARTESIAN_POINT('Ctrl Pts',(-234.296096607986,6.30743397990132,
132.766596986079));
#268686=CARTESIAN_POINT('Ctrl Pts',(-234.574544231799,5.06020716402928,
126.558374461932));
#268687=CARTESIAN_POINT('Ctrl Pts',(-234.852991855612,-0.837102830722735,
124.252005786856));
#268688=CARTESIAN_POINT('Ctrl Pts',(-235.131439479425,-5.96515621878728,
127.966931100874));
#268689=CARTESIAN_POINT('Ctrl Pts',(-235.409887103238,-5.6115224558684,
134.289315524594));
#268690=CARTESIAN_POINT('Ctrl Pts',(-235.688334727051,-0.101173694118813,
137.409196638266));
#268691=CARTESIAN_POINT('Ctrl Pts',(-235.966782350864,5.50214874991674,
134.459556113093));
#268692=CARTESIAN_POINT('Ctrl Pts',(-236.245229974676,6.04926528768773,
128.150969493757));
#268693=CARTESIAN_POINT('Ctrl Pts',(-236.52367759849,1.03740254911254,124.280719691838));
#268694=CARTESIAN_POINT('Ctrl Pts',(-236.802125222302,-4.92778245216537,
126.405377203086));
#268695=CARTESIAN_POINT('Ctrl Pts',(-237.080572846115,-6.36457611545918,
132.572485569954));
#268696=CARTESIAN_POINT('Ctrl Pts',(-237.359020469928,-1.95263525547508,
137.114773483282));
#268697=CARTESIAN_POINT('Ctrl Pts',(-237.637468093741,4.25368201275546,
135.858100253825));
#268698=CARTESIAN_POINT('Ctrl Pts',(-237.915915717553,6.55107331518259,
129.957287187551));
#268699=CARTESIAN_POINT('Ctrl Pts',(-238.194363341367,2.8283482786799,124.834893221623));
#268700=CARTESIAN_POINT('Ctrl Pts',(-238.47281096518,-3.49349065343433,
125.198148167872));
#268701=CARTESIAN_POINT('Ctrl Pts',(-238.751258588993,-6.60498234154917,
130.713238476685));
#268702=CARTESIAN_POINT('Ctrl Pts',(-239.029706212805,-3.64681792910581,
136.312065581403));
#268703=CARTESIAN_POINT('Ctrl Pts',(-239.308153836619,2.66259400322518,
136.8495808907));
#268704=CARTESIAN_POINT('Ctrl Pts',(-239.586601460431,6.52521212154101,
131.831834094415));
#268705=CARTESIAN_POINT('Ctrl Pts',(-239.865049084244,4.39147907449425,
125.869889367774));
#268706=CARTESIAN_POINT('Ctrl Pts',(-240.143496708057,-1.77780870633274,
124.44248265737));
#268707=CARTESIAN_POINT('Ctrl Pts',(-240.42194433187,-6.31337713682396,
128.861330997368));
#268708=CARTESIAN_POINT('Ctrl Pts',(-240.700391955683,-5.04726040419313,
135.065728636055));
#268709=CARTESIAN_POINT('Ctrl Pts',(-240.978839579496,0.857042067512721,
137.354137245149));
#268710=CARTESIAN_POINT('Ctrl Pts',(-241.257287203309,5.97376474800676,
133.623621107872));
#268711=CARTESIAN_POINT('Ctrl Pts',(-241.535734827122,5.60088945971499,
127.302342308534));
#268712=CARTESIAN_POINT('Ctrl Pts',(-241.814182450934,0.0810703766063902,
124.199247252091));
#268713=CARTESIAN_POINT('Ctrl Pts',(-242.092630074747,-5.51324842209508,
127.165928700792));
#268714=CARTESIAN_POINT('Ctrl Pts',(-242.37107769856,-6.04116125805038,
133.476151333726));
#268715=CARTESIAN_POINT('Ctrl Pts',(-242.649525322373,-1.01754202499167,
137.331128822742));
#268716=CARTESIAN_POINT('Ctrl Pts',(-242.927972946186,4.94114861934255,
135.188325181553));
#268717=CARTESIAN_POINT('Ctrl Pts',(-243.206420569999,6.35916507103108,
129.016872274634));
#268718=CARTESIAN_POINT('Ctrl Pts',(-243.484868193812,1.93341948492588,
124.488033831209));
#268719=CARTESIAN_POINT('Ctrl Pts',(-243.763315817625,-4.26904415503308,
125.763591134728));
#268720=CARTESIAN_POINT('Ctrl Pts',(-244.041763441437,-6.54846477091785,
131.671369337695));
#268721=CARTESIAN_POINT('Ctrl Pts',(-244.320211065251,-2.8101661726183,
136.782408882594));
#268722=CARTESIAN_POINT('Ctrl Pts',(-244.598658689063,3.51053785406796,
136.399914115825));
#268723=CARTESIAN_POINT('Ctrl Pts',(-244.877106312876,6.60522909217403,
130.875379042142));
#268724=CARTESIAN_POINT('Ctrl Pts',(-245.155553936689,3.6300374779527,125.285581505715));
#268725=CARTESIAN_POINT('Ctrl Pts',(-245.434001560502,-2.68098124131831,
124.767272365732));
#268726=CARTESIAN_POINT('Ctrl Pts',(-245.712449184315,-6.528309173032,129.796752401026));
#268727=CARTESIAN_POINT('Ctrl Pts',(-245.990896808128,-4.37643990036281,
135.752175162922));
#268728=CARTESIAN_POINT('Ctrl Pts',(-246.269344431941,1.79716383976481,
137.160798071814));
#268729=CARTESIAN_POINT('Ctrl Pts',(-246.547792055753,6.31926180748295,
132.728165489484));
#268730=CARTESIAN_POINT('Ctrl Pts',(-246.826239679567,5.03426688722615,
126.527650212955));
#268731=CARTESIAN_POINT('Ctrl Pts',(-247.104687303379,-0.876973364781528,
124.257222869343));
#268732=CARTESIAN_POINT('Ctrl Pts',(-247.383134927193,-5.98231793708558,
128.003295270889));
#268733=CARTESIAN_POINT('Ctrl Pts',(-247.661582551005,-5.59020457768662,
134.32340988638));
#268734=CARTESIAN_POINT('Ctrl Pts',(-247.940030174818,-0.0609663080697638,
137.409690138946));
#268735=CARTESIAN_POINT('Ctrl Pts',(-248.218477798631,5.524297020294,134.425995249648));
#268736=CARTESIAN_POINT('Ctrl Pts',(-248.496925422444,6.03300126391963,
128.114195060156));
#268737=CARTESIAN_POINT('Ctrl Pts',(-248.775373046256,0.997672074500306,
124.274525596028));
#268738=CARTESIAN_POINT('Ctrl Pts',(-249.05382067007,-4.95446901239483,
126.435455516518));
#268739=CARTESIAN_POINT('Ctrl Pts',(-249.332268293882,-6.35369511616563,
132.611195791991));
#268740=CARTESIAN_POINT('Ctrl Pts',(-249.610715917695,-1.91418580344349,
137.126542810973));
#268741=CARTESIAN_POINT('Ctrl Pts',(-249.889163541508,4.28436674946925,
135.832113249982));
#268742=CARTESIAN_POINT('Ctrl Pts',(-250.167611165321,6.54579556256923,
129.917424639176));
#268743=CARTESIAN_POINT('Ctrl Pts',(-250.446058789134,2.79195803356287,
124.817786863269));
#268744=CARTESIAN_POINT('Ctrl Pts',(-250.724506412947,-3.52755253356211,
125.219517907192));
#268745=CARTESIAN_POINT('Ctrl Pts',(-251.00295403676,-6.60541465285253,
130.75344656718));
#268746=CARTESIAN_POINT('Ctrl Pts',(-251.281401660573,-3.61322339864049,
136.334162752248));
#268747=CARTESIAN_POINT('Ctrl Pts',(-251.559849284386,2.6993436431913,136.83326092127));
#268748=CARTESIAN_POINT('Ctrl Pts',(-251.838296908198,6.53134574711249,
131.792094239578));
#268749=CARTESIAN_POINT('Ctrl Pts',(-252.116744532012,4.3613601835781,125.843248612281));
#268750=CARTESIAN_POINT('Ctrl Pts',(-252.395192155824,-1.81650232468185,
124.453422554885));
#268751=CARTESIAN_POINT('Ctrl Pts',(-252.673639779637,-6.32508793705065,
128.899798314935));
#268752=CARTESIAN_POINT('Ctrl Pts',(-252.95208740345,-5.02122673409033,
135.096373791053));
#268753=CARTESIAN_POINT('Ctrl Pts',(-253.230535027263,0.896896539007115,
137.348798831588));
#268754=CARTESIAN_POINT('Ctrl Pts',(-253.508982651076,5.99081570467794,
133.587204877683));
#268755=CARTESIAN_POINT('Ctrl Pts',(-253.787430274889,5.57946791275175,
127.26831297809));
#268756=CARTESIAN_POINT('Ctrl Pts',(-254.065877898701,0.0408616672245685,
124.198876151673));
#268757=CARTESIAN_POINT('Ctrl Pts',(-254.344325522515,-5.53529442795169,
127.199556781751));
#268758=CARTESIAN_POINT('Ctrl Pts',(-254.622773146327,-6.0247854077167,
133.512876168065));
#268759=CARTESIAN_POINT('Ctrl Pts',(-254.90122077014,-0.977792831057213,
137.337201825807));
#268760=CARTESIAN_POINT('Ctrl Pts',(-255.179668393953,4.96774341227684,
135.158166043599));
#268761=CARTESIAN_POINT('Ctrl Pts',(-255.458116017766,6.34816648213513,
128.97819485735));
#268762=CARTESIAN_POINT('Ctrl Pts',(-255.736563641579,1.89493404819936,
124.476382515012));
#268763=CARTESIAN_POINT('Ctrl Pts',(-256.015011265392,-4.29964901022966,
125.789669655819));
#268764=CARTESIAN_POINT('Ctrl Pts',(-256.293458889205,-6.54306693065544,
131.711218953762));
#268765=CARTESIAN_POINT('Ctrl Pts',(-256.571906513018,-2.77372173452912,
136.799398141047));
#268766=CARTESIAN_POINT('Ctrl Pts',(-256.85035413683,3.54453019961847,136.378452625405));
#268767=CARTESIAN_POINT('Ctrl Pts',(-257.128801760644,6.60554720661629,
130.835147498674));
#268768=CARTESIAN_POINT('Ctrl Pts',(-257.407249384456,3.5963603924579,125.263628838565));
#268769=CARTESIAN_POINT('Ctrl Pts',(-257.685697008269,-2.71765185753996,
124.783624522784));
#268770=CARTESIAN_POINT('Ctrl Pts',(-257.964144632082,-6.53437691572335,
129.836661023534));
#268771=CARTESIAN_POINT('Ctrl Pts',(-258.242592255895,-4.34613602341029,
135.778440351053));
#268772=CARTESIAN_POINT('Ctrl Pts',(-258.521039879708,1.83562753012831,
137.150276335207));
#268773=CARTESIAN_POINT('Ctrl Pts',(-258.799487503521,6.33122643152078,
132.688650362788));
#268774=CARTESIAN_POINT('Ctrl Pts',(-259.077935127334,5.00743946241547,
126.498999976245));
#268775=CARTESIAN_POINT('Ctrl Pts',(-259.356382751147,-0.915487258132909,
124.259032700089));
#268776=CARTESIAN_POINT('Ctrl Pts',(-259.634830374959,-6.00176822571329,
128.046924274587));
#268777=CARTESIAN_POINT('Ctrl Pts',(-259.86687006147,-5.63687269779404,
133.292521465648));
#268778=CARTESIAN_POINT('Ctrl Pts',(-260.052531023546,-2.79481741349804,
135.900547185714));
#268779=CARTESIAN_POINT('Ctrl Pts',(-260.145376111017,-0.946914048523564,
136.386386345067));
#268780=CARTESIAN_POINT('Ctrl Pts',(-260.191813261187,-0.0157913329746497,
136.389009763222));
#268781=CARTESIAN_POINT('Ctrl Pts',(210.190947297731,3.04870273111253,135.077142573452));
#268782=CARTESIAN_POINT('Ctrl Pts',(210.144529434129,3.76080111712433,134.569051946243));
#268783=CARTESIAN_POINT('Ctrl Pts',(210.051703633225,4.91317831978039,133.192256847685));
#268784=CARTESIAN_POINT('Ctrl Pts',(209.866061957716,5.67455722768035,129.648049455111));
#268785=CARTESIAN_POINT('Ctrl Pts',(209.634022271206,3.10293383059235,125.427666478792));
#268786=CARTESIAN_POINT('Ctrl Pts',(209.355574647392,-2.85596866243967,
125.28812524467));
#268787=CARTESIAN_POINT('Ctrl Pts',(209.07712702358,-6.17973736462657,130.225196103446));
#268788=CARTESIAN_POINT('Ctrl Pts',(208.798679399767,-3.83016968018938,
135.690661498217));
#268789=CARTESIAN_POINT('Ctrl Pts',(208.520231775954,2.04205955310628,136.667868212554));
#268790=CARTESIAN_POINT('Ctrl Pts',(208.241784152142,6.03618933210081,132.255733564264));
#268791=CARTESIAN_POINT('Ctrl Pts',(207.963336528328,4.48417485225333,126.510421532214));
#268792=CARTESIAN_POINT('Ctrl Pts',(207.684888904515,-1.18901089957204,
124.710731370568));
#268793=CARTESIAN_POINT('Ctrl Pts',(207.406441280703,-5.76932406256156,
128.510946815645));
#268794=CARTESIAN_POINT('Ctrl Pts',(207.12799365689,-5.04803188696711,134.418613818075));
#268795=CARTESIAN_POINT('Ctrl Pts',(206.849546033077,0.312219397189005,
137.005003016302));
#268796=CARTESIAN_POINT('Ctrl Pts',(206.571098409264,5.38552219392035,133.893281295751));
#268797=CARTESIAN_POINT('Ctrl Pts',(206.292650785451,5.50981125882569,127.943004805273));
#268798=CARTESIAN_POINT('Ctrl Pts',(206.014203161638,0.570843377758803,
124.622167937696));
#268799=CARTESIAN_POINT('Ctrl Pts',(205.735755537825,-4.89269661278007,
126.982467612715));
#268800=CARTESIAN_POINT('Ctrl Pts',(205.457307914013,-5.86009012142741,
132.854898402769));
#268801=CARTESIAN_POINT('Ctrl Pts',(205.178860290199,-1.44234566848361,
136.842986120511));
#268802=CARTESIAN_POINT('Ctrl Pts',(204.900412666387,4.30084323855829,135.281871486376));
#268803=CARTESIAN_POINT('Ctrl Pts',(204.621965042573,6.09176771588946,129.606143376667));
#268804=CARTESIAN_POINT('Ctrl Pts',(204.343517418761,2.28465505058828,125.031518229909));
#268805=CARTESIAN_POINT('Ctrl Pts',(204.065069794948,-3.62194388278553,
125.761853295313));
#268806=CARTESIAN_POINT('Ctrl Pts',(203.786622171135,-6.20015338889199,
131.126006208945));
#268807=CARTESIAN_POINT('Ctrl Pts',(203.508174547322,-3.08072479357708,
136.194582558939));
#268808=CARTESIAN_POINT('Ctrl Pts',(203.229726923509,2.86973936865286,136.309808260363));
#268809=CARTESIAN_POINT('Ctrl Pts',(202.951279299696,6.1830532544492,131.365796540178));
#268810=CARTESIAN_POINT('Ctrl Pts',(202.672831675884,3.81444325369211,125.905852631576));
#268811=CARTESIAN_POINT('Ctrl Pts',(202.39438405207,-2.05945374882828,124.947398258377));
#268812=CARTESIAN_POINT('Ctrl Pts',(202.115936428258,-6.04081336739099,
129.371206163854));
#268813=CARTESIAN_POINT('Ctrl Pts',(201.837488804444,-4.47096061076856,
135.112012999282));
#268814=CARTESIAN_POINT('Ctrl Pts',(201.559041180632,1.20748652821524,136.894297736177));
#268815=CARTESIAN_POINT('Ctrl Pts',(201.280593556819,5.77631253695961,133.08022777117));
#268816=CARTESIAN_POINT('Ctrl Pts',(201.002145933006,5.03698951269057,127.174747074221));
#268817=CARTESIAN_POINT('Ctrl Pts',(200.723698309193,-0.331080803069094,
124.604703907164));
#268818=CARTESIAN_POINT('Ctrl Pts',(200.44525068538,-5.39490403503349,127.731842386878));
#268819=CARTESIAN_POINT('Ctrl Pts',(200.166803061567,-5.50107401450091,
133.682475019745));
#268820=CARTESIAN_POINT('Ctrl Pts',(199.888355437754,-0.552025717056,136.988261120707));
#268821=CARTESIAN_POINT('Ctrl Pts',(199.609907813942,4.90430724641216,134.611344759621));
#268822=CARTESIAN_POINT('Ctrl Pts',(199.331460190128,5.85382143915379,128.735995953499));
#268823=CARTESIAN_POINT('Ctrl Pts',(199.053012566316,1.42395970438994,124.761373228423));
#268824=CARTESIAN_POINT('Ctrl Pts',(198.774564942502,-4.31445143441004,
126.339960697623));
#268825=CARTESIAN_POINT('Ctrl Pts',(198.49611731869,-6.088092477657,132.02111359519));
#268826=CARTESIAN_POINT('Ctrl Pts',(198.217669694877,-2.26707395378944,
136.584129948007));
#268827=CARTESIAN_POINT('Ctrl Pts',(197.939222071064,3.6372747808909,135.835820643578));
#268828=CARTESIAN_POINT('Ctrl Pts',(197.660774447251,6.19914568268399,130.46384537573));
#268829=CARTESIAN_POINT('Ctrl Pts',(197.382326823438,3.06430454719326,125.404786980035));
#268830=CARTESIAN_POINT('Ctrl Pts',(197.103879199626,-2.88648276756863,
125.307672973393));
#268831=CARTESIAN_POINT('Ctrl Pts',(196.825431575812,-6.1847334314575,130.261746383626));
#268832=CARTESIAN_POINT('Ctrl Pts',(196.546983952,-3.79951621286212,135.71445576667));
#268833=CARTESIAN_POINT('Ctrl Pts',(196.268536328187,2.07727078866752,136.65502757917));
#268834=CARTESIAN_POINT('Ctrl Pts',(195.990088704374,6.04514741573133,132.219122274927));
#268835=CARTESIAN_POINT('Ctrl Pts',(195.711641080561,4.45782888960729,126.483120122517));
#268836=CARTESIAN_POINT('Ctrl Pts',(195.433193456748,-1.22601660901765,
124.718126880723));
#268837=CARTESIAN_POINT('Ctrl Pts',(195.154745832935,-5.78321273819644,
128.54608511404));
#268838=CARTESIAN_POINT('Ctrl Pts',(194.876298209123,-5.02591888662151,
134.449288212205));
#268839=CARTESIAN_POINT('Ctrl Pts',(194.597850585309,0.349948891971121,
137.002980915508));
#268840=CARTESIAN_POINT('Ctrl Pts',(194.319402961497,5.40423073479611,133.860444384439));
#268841=CARTESIAN_POINT('Ctrl Pts',(194.040955337684,5.49228854369214,127.909516169605));
#268842=CARTESIAN_POINT('Ctrl Pts',(193.762507713871,0.533201494146887,
124.618808581434));
#268843=CARTESIAN_POINT('Ctrl Pts',(193.484060090058,-4.91587168017823,
127.012321133451));
#268844=CARTESIAN_POINT('Ctrl Pts',(193.205612466245,-5.84749893410212,
132.890532719942));
#268845=CARTESIAN_POINT('Ctrl Pts',(192.927164842432,-1.40556033379022,
136.851654059523));
#268846=CARTESIAN_POINT('Ctrl Pts',(192.648717218619,4.32801954783523,135.255608152653));
#268847=CARTESIAN_POINT('Ctrl Pts',(192.370269594806,6.08436090050943,129.569083216569));
#268848=CARTESIAN_POINT('Ctrl Pts',(192.091821970994,2.24947182316989,125.017717865345));
#268849=CARTESIAN_POINT('Ctrl Pts',(191.81337434718,-3.65257196685492,125.783994510198));
#268850=CARTESIAN_POINT('Ctrl Pts',(191.534926723368,-6.19808055740059,
131.163742349203));
#268851=CARTESIAN_POINT('Ctrl Pts',(191.256479099555,-3.04785590876364,
136.213235933607));
#268852=CARTESIAN_POINT('Ctrl Pts',(190.978031475742,2.90319942398833,136.292237340818));
#268853=CARTESIAN_POINT('Ctrl Pts',(190.699583851929,6.18635631527163,131.328148137043));
#268854=CARTESIAN_POINT('Ctrl Pts',(190.421136228116,3.7845539731278,125.882723791311));
#268855=CARTESIAN_POINT('Ctrl Pts',(190.142688604304,-2.09506858458051,
124.960043253581));
#268856=CARTESIAN_POINT('Ctrl Pts',(189.86424098049,-6.04942546284962,129.408004862578));
#268857=CARTESIAN_POINT('Ctrl Pts',(189.585793356678,-4.44465587162338,
135.139149194637));
#268858=CARTESIAN_POINT('Ctrl Pts',(189.307345732864,1.24453533211424,136.886834590562));
#268859=CARTESIAN_POINT('Ctrl Pts',(189.028898109051,5.79005936456987,133.045023550676));
#268860=CARTESIAN_POINT('Ctrl Pts',(188.750450485239,5.01480170111087,127.144152737732));
#268861=CARTESIAN_POINT('Ctrl Pts',(188.472002861426,-0.368813738986236,
124.606834155258));
#268862=CARTESIAN_POINT('Ctrl Pts',(188.193555237613,-5.41350737050784,
127.764739625646));
#268863=CARTESIAN_POINT('Ctrl Pts',(187.9151076138,-5.48345219307025,133.715908293866));
#268864=CARTESIAN_POINT('Ctrl Pts',(187.636659989987,-0.51437233173317,
136.991506884579));
#268865=CARTESIAN_POINT('Ctrl Pts',(187.358212366174,4.92739057398128,134.581420314804));
#268866=CARTESIAN_POINT('Ctrl Pts',(187.079764742362,5.84112225861874,128.700400402891));
#268867=CARTESIAN_POINT('Ctrl Pts',(186.801317118548,1.38714794227173,124.752817144095));
#268868=CARTESIAN_POINT('Ctrl Pts',(186.522869494736,-4.34154756707868,
126.366306703083));
#268869=CARTESIAN_POINT('Ctrl Pts',(186.244421870923,-6.08057295867359,
132.058150998494));
#268870=CARTESIAN_POINT('Ctrl Pts',(185.96597424711,-2.23184885375068,136.597823184897));
#268871=CARTESIAN_POINT('Ctrl Pts',(185.687526623297,3.66783531589119,135.813586298303));
#268872=CARTESIAN_POINT('Ctrl Pts',(185.409078999484,6.19695801394562,130.42611572539));
#268873=CARTESIAN_POINT('Ctrl Pts',(185.130631375671,3.03137903541329,125.386233730096));
#268874=CARTESIAN_POINT('Ctrl Pts',(184.852183751858,-2.9198891855651,125.325345654173));
#268875=CARTESIAN_POINT('Ctrl Pts',(184.573736128045,-6.18792188952598,
130.299404664846));
#268876=CARTESIAN_POINT('Ctrl Pts',(184.295288504232,-3.76955667380246,
135.737493527599));
#268877=CARTESIAN_POINT('Ctrl Pts',(184.01684088042,2.11284697206427,136.642274242971));
#268878=CARTESIAN_POINT('Ctrl Pts',(183.738393256607,6.05364746891681,132.182297534532));
#268879=CARTESIAN_POINT('Ctrl Pts',(183.459945632794,4.43144167895468,126.456064115361));
#268880=CARTESIAN_POINT('Ctrl Pts',(183.181498008981,-1.2630425260055,124.725702755623));
#268881=CARTESIAN_POINT('Ctrl Pts',(182.903050385168,-5.79685235262429,
128.581331012064));
#268882=CARTESIAN_POINT('Ctrl Pts',(182.624602761355,-5.00363805916239,
134.479814874928));
#268883=CARTESIAN_POINT('Ctrl Pts',(182.346155137542,0.387675169361259,
137.000735831198));
#268884=CARTESIAN_POINT('Ctrl Pts',(182.06770751373,5.42273385622678,133.827490675898));
#268885=CARTESIAN_POINT('Ctrl Pts',(181.789259889916,5.47456504449634,127.876136685104));
#268886=CARTESIAN_POINT('Ctrl Pts',(181.510812266103,0.495538404244469,
124.615677436551));
#268887=CARTESIAN_POINT('Ctrl Pts',(181.232364642291,-4.93886382111119,
127.042315697369));
#268888=CARTESIAN_POINT('Ctrl Pts',(180.953917018477,-5.83469147177671,
132.926089453735));
#268889=CARTESIAN_POINT('Ctrl Pts',(180.675469394665,-1.36872270040423,
136.860098061879));
#268890=CARTESIAN_POINT('Ctrl Pts',(180.397021770852,4.35503536681857,135.229179797918));
#268891=CARTESIAN_POINT('Ctrl Pts',(180.118574147039,6.07672868724052,129.532068871648));
#268892=CARTESIAN_POINT('Ctrl Pts',(179.840126523226,2.21420520878857,125.004131904969));
#268893=CARTESIAN_POINT('Ctrl Pts',(179.561678899413,-3.68306468660213,
125.80632176824));
#268894=CARTESIAN_POINT('Ctrl Pts',(179.2832312756,-6.19577806271818,131.20146516627));
#268895=CARTESIAN_POINT('Ctrl Pts',(179.004783651788,-3.01487407978163,
136.231688883676));
#268896=CARTESIAN_POINT('Ctrl Pts',(178.726336027974,2.93655189768736,136.274463064253));
#268897=CARTESIAN_POINT('Ctrl Pts',(178.447888404162,6.18943013971724,131.290480325685));
#268898=CARTESIAN_POINT('Ctrl Pts',(178.169440780348,3.75452445381909,125.859777323623));
#268899=CARTESIAN_POINT('Ctrl Pts',(177.890993156536,-2.13060578642238,
124.972904812372));
#268900=CARTESIAN_POINT('Ctrl Pts',(177.612545532723,-6.05781339482078,
129.44485530364));
#268901=CARTESIAN_POINT('Ctrl Pts',(177.33409790891,-4.41818643401566,135.166124762878));
#268902=CARTESIAN_POINT('Ctrl Pts',(177.055650285097,1.28153801924328,136.879146056599));
#268903=CARTESIAN_POINT('Ctrl Pts',(176.777202661284,5.80359163943039,133.009736301615));
#268904=CARTESIAN_POINT('Ctrl Pts',(176.498755037472,4.99242806419446,127.113694031581));
#268905=CARTESIAN_POINT('Ctrl Pts',(176.220307413658,-0.406533008366379,
124.60919405498));
#268906=CARTESIAN_POINT('Ctrl Pts',(175.941859789846,-5.43191010648008,
127.797749498684));
#268907=CARTESIAN_POINT('Ctrl Pts',(175.663412166033,-5.46562718029972,
133.749233679521));
#268908=CARTESIAN_POINT('Ctrl Pts',(175.38496454222,-0.476699886155768,
136.994523381468));
#268909=CARTESIAN_POINT('Ctrl Pts',(175.106516918407,4.95029131528126,134.551355909651));
#268910=CARTESIAN_POINT('Ctrl Pts',(174.828069294595,5.82820663315002,128.664882815304));
#268911=CARTESIAN_POINT('Ctrl Pts',(174.549621670781,1.35028477887665,124.744485301934));
#268912=CARTESIAN_POINT('Ctrl Pts',(174.271174046969,-4.36848282210566,
126.392817162263));
#268913=CARTESIAN_POINT('Ctrl Pts',(173.992726423155,-6.07282812182305,
132.095141942134));
#268914=CARTESIAN_POINT('Ctrl Pts',(173.714278799343,-2.19654105173196,
136.611301742902));
#268915=CARTESIAN_POINT('Ctrl Pts',(173.435831175529,3.69825993790488,135.791166334329));
#268916=CARTESIAN_POINT('Ctrl Pts',(173.157383551717,6.19454071464915,130.388400091055));
#268917=CARTESIAN_POINT('Ctrl Pts',(172.878935927904,2.99834119476844,125.367881250842));
#268918=CARTESIAN_POINT('Ctrl Pts',(172.600488304091,-2.95318740599396,
125.343221361866));
#268919=CARTESIAN_POINT('Ctrl Pts',(172.322040680278,-6.1908810518732,130.337081657394));
#268920=CARTESIAN_POINT('Ctrl Pts',(172.043593056465,-3.7394574524341,135.760348489473));
#268921=CARTESIAN_POINT('Ctrl Pts',(171.765145432652,2.14834486313941,136.629304580736));
#268922=CARTESIAN_POINT('Ctrl Pts',(171.486697808839,6.06192320196904,132.145421734178));
#268923=CARTESIAN_POINT('Ctrl Pts',(171.208250185027,4.40489025960108,126.42916923593));
#268924=CARTESIAN_POINT('Ctrl Pts',(170.929802561213,-1.30002164048796,
124.733503877423));
#268925=CARTESIAN_POINT('Ctrl Pts',(170.651354937401,-5.81027716255637,
128.616659285268));
#268926=CARTESIAN_POINT('Ctrl Pts',(170.372907313588,-4.98117182005496,
134.510205342342));
#268927=CARTESIAN_POINT('Ctrl Pts',(170.094459689775,0.42538708130529,136.998261137926));
#268928=CARTESIAN_POINT('Ctrl Pts',(169.816012065962,5.44103603626017,133.794424944161));
#268929=CARTESIAN_POINT('Ctrl Pts',(169.537564442149,5.45663868327959,127.842865707018));
#268930=CARTESIAN_POINT('Ctrl Pts',(169.259116818336,0.457856951984399,
124.612775615598));
#268931=CARTESIAN_POINT('Ctrl Pts',(168.980669194523,-4.9616729506289,127.072449665244));
#268932=CARTESIAN_POINT('Ctrl Pts',(168.702221570711,-5.82166780281318,
132.961567566087));
#268933=CARTESIAN_POINT('Ctrl Pts',(168.423773946897,-1.33183434849535,
136.868317666657));
#268934=CARTESIAN_POINT('Ctrl Pts',(168.145326323085,4.38188980836473,135.202587479883));
#268935=CARTESIAN_POINT('Ctrl Pts',(167.866878699272,6.06887129855542,129.495101671966));
#268936=CARTESIAN_POINT('Ctrl Pts',(167.588431075459,2.17885654621902,124.9907608742));
#268937=CARTESIAN_POINT('Ctrl Pts',(167.309983451646,-3.71342092903282,
125.82883423045));
#268938=CARTESIAN_POINT('Ctrl Pts',(167.031535827833,-6.19324598120115,
131.239173268482));
#268939=CARTESIAN_POINT('Ctrl Pts',(166.75308820402,-2.98178053353198,136.249940722101));
#268940=CARTESIAN_POINT('Ctrl Pts',(166.474640580207,2.96979555637586,136.25648609103));
#268941=CARTESIAN_POINT('Ctrl Pts',(166.196192956395,6.19227461255283,131.252794500981));
#268942=CARTESIAN_POINT('Ctrl Pts',(165.917745332582,3.7243558092261,125.837014079288));
#268943=CARTESIAN_POINT('Ctrl Pts',(165.639297708769,-2.16606403788322,
124.985982457902));
#268944=CARTESIAN_POINT('Ctrl Pts',(165.360850084956,-6.06597685228888,
129.481756121673));
#268945=CARTESIAN_POINT('Ctrl Pts',(165.082402461143,-4.39155327888481,
135.192938704347));
#268946=CARTESIAN_POINT('Ctrl Pts',(164.80395483733,1.31849321850979,136.871232419228));
#268947=CARTESIAN_POINT('Ctrl Pts',(164.525507213517,5.81690886006848,132.974367331546));
#268948=CARTESIAN_POINT('Ctrl Pts',(164.247059589704,4.96986943102014,127.083372084437));
#268949=CARTESIAN_POINT('Ctrl Pts',(163.968611965891,-0.444237213516358,
124.611783518878));
#268950=CARTESIAN_POINT('Ctrl Pts',(163.690164342078,-5.45011156102575,
127.830870782803));
#268951=CARTESIAN_POINT('Ctrl Pts',(163.411716718265,-5.44759963670407,
133.782449941821));
#268952=CARTESIAN_POINT('Ctrl Pts',(163.133269094453,-0.439009776288703,
136.9973104996));
#268953=CARTESIAN_POINT('Ctrl Pts',(162.85482147064,4.97300862171615,134.52115265821));
#268954=CARTESIAN_POINT('Ctrl Pts',(162.576373846827,5.81507504134112,128.629444506854));
#268955=CARTESIAN_POINT('Ctrl Pts',(162.297926223014,1.31337158018249,124.736378010682));
#268956=CARTESIAN_POINT('Ctrl Pts',(162.019478599201,-4.39525620139515,
126.419491092807));
#268957=CARTESIAN_POINT('Ctrl Pts',(161.741030975388,-6.06485825409316,
132.132085055398));
#268958=CARTESIAN_POINT('Ctrl Pts',(161.462583351575,-2.16115185607673,
136.624565122567));
#268959=CARTESIAN_POINT('Ctrl Pts',(161.184135727762,3.72854751953661,135.768561582436));
#268960=CARTESIAN_POINT('Ctrl Pts',(160.905688103949,6.19189387436843,130.350699870288));
#268961=CARTESIAN_POINT('Ctrl Pts',(160.627240480137,2.96519224948793,125.349730222329));
#268962=CARTESIAN_POINT('Ctrl Pts',(160.348792856324,-2.9863761949775,125.361299434083));
#268963=CARTESIAN_POINT('Ctrl Pts',(160.070345232511,-6.19361080884636,
130.374775965136));
#268964=CARTESIAN_POINT('Ctrl Pts',(159.791897608698,-3.70921966409463,
135.783019805394));
#268965=CARTESIAN_POINT('Ctrl Pts',(159.513449984885,2.18376314650564,136.616119073061));
#268966=CARTESIAN_POINT('Ctrl Pts',(159.235002361072,6.06997430822783,132.108496240312));
#268967=CARTESIAN_POINT('Ctrl Pts',(158.956554737259,4.37817561541891,126.402436480826));
#268968=CARTESIAN_POINT('Ctrl Pts',(158.678107113446,-1.3369525821905,124.741529957054));
#268969=CARTESIAN_POINT('Ctrl Pts',(158.399659489633,-5.82348667053154,
128.652068624549));
#268970=CARTESIAN_POINT('Ctrl Pts',(158.121211865821,-4.95852100179383,
134.540458488317));
#268971=CARTESIAN_POINT('Ctrl Pts',(157.842764242008,0.463083230374652,
136.995556927392));
#268972=CARTESIAN_POINT('Ctrl Pts',(157.564316618195,5.45913659670229,133.761248414491));
#268973=CARTESIAN_POINT('Ctrl Pts',(157.285868994382,5.43851012430973,127.809704468215));
#268974=CARTESIAN_POINT('Ctrl Pts',(157.007421370569,0.420158533666468,
124.610103226106));
#268975=CARTESIAN_POINT('Ctrl Pts',(156.728973746756,-4.98429822353081,
127.102721920452));
#268976=CARTESIAN_POINT('Ctrl Pts',(156.450526122943,-5.80842840980828,
132.996965742341));
#268977=CARTESIAN_POINT('Ctrl Pts',(156.172078499131,-1.2948966449748,136.876312569277));
#268978=CARTESIAN_POINT('Ctrl Pts',(155.893630875317,4.40858187737264,135.175832183934));
#268979=CARTESIAN_POINT('Ctrl Pts',(155.615183251505,6.06078902561252,129.458182987356));
#268980=CARTESIAN_POINT('Ctrl Pts',(155.336735627692,2.14342714531882,124.977605268507));
#268981=CARTESIAN_POINT('Ctrl Pts',(155.058288003879,-3.74363956928552,
125.85153106262));
#268982=CARTESIAN_POINT('Ctrl Pts',(154.779840380066,-6.19048440667673,
131.276865258552));
#268983=CARTESIAN_POINT('Ctrl Pts',(154.501392756253,-2.94857649630798,
136.267990772552));
#268984=CARTESIAN_POINT('Ctrl Pts',(154.22294513244,3.00292916819795,136.238307087292));
#268985=CARTESIAN_POINT('Ctrl Pts',(153.944497508627,6.19488962837548,131.215092059396));
#268986=CARTESIAN_POINT('Ctrl Pts',(153.666049884815,3.69404915725887,125.814434901805));
#268987=CARTESIAN_POINT('Ctrl Pts',(153.387602261001,-2.20144202504465,
124.999275705575));
#268988=CARTESIAN_POINT('Ctrl Pts',(153.109154637189,-6.07391553275397,
129.518705949301));
#268989=CARTESIAN_POINT('Ctrl Pts',(152.830707013376,-4.36475739313218,
135.219590025439));
#268990=CARTESIAN_POINT('Ctrl Pts',(152.552259389563,1.3553995605252,136.863093971691));
#268991=CARTESIAN_POINT('Ctrl Pts',(152.27381176575,5.83001053300956,132.93891795108));
#268992=CARTESIAN_POINT('Ctrl Pts',(151.995364141937,4.94712663750637,127.053188019893));
#268993=CARTESIAN_POINT('Ctrl Pts',(151.716916518124,-0.481924957293099,
124.614602450997));
#268994=CARTESIAN_POINT('Ctrl Pts',(151.438468894311,-5.46811105968323,
127.864102250682));
#268995=CARTESIAN_POINT('Ctrl Pts',(151.160021270498,-5.4293702303005,133.815555849925));
#268996=CARTESIAN_POINT('Ctrl Pts',(150.881573646685,-0.40130339875292,
136.999868135696));
#268997=CARTESIAN_POINT('Ctrl Pts',(150.603126022873,4.99554165148768,134.490811679673));
#268998=CARTESIAN_POINT('Ctrl Pts',(150.324678399059,5.80172796978809,128.59408679072));
#268999=CARTESIAN_POINT('Ctrl Pts',(150.046230775247,1.27640971402146,124.728495570759));
#269000=CARTESIAN_POINT('Ctrl Pts',(149.767783151434,-4.42186671284978,
126.446327506304));
#269001=CARTESIAN_POINT('Ctrl Pts',(149.489335527621,-6.05666365081033,
132.168978969345));
#269002=CARTESIAN_POINT('Ctrl Pts',(149.210887903808,-2.12568257814469,
136.637612832414));
#269003=CARTESIAN_POINT('Ctrl Pts',(148.932440279995,3.75869693846883,135.74577288025));
#269004=CARTESIAN_POINT('Ctrl Pts',(148.653992656183,6.18901759118317,130.313016460088));
#269005=CARTESIAN_POINT('Ctrl Pts',(148.375545032369,2.93193342791814,125.331781317152));
#269006=CARTESIAN_POINT('Ctrl Pts',(148.097097408557,-3.01945432269288,
125.379579200934));
#269007=CARTESIAN_POINT('Ctrl Pts',(147.818649784743,-6.19611105929333,
130.412486191295));
#269008=CARTESIAN_POINT('Ctrl Pts',(147.540202160931,-3.67884442925635,
135.805506635269));
#269009=CARTESIAN_POINT('Ctrl Pts',(147.261754537118,2.21910050972548,136.602718208539));
#269010=CARTESIAN_POINT('Ctrl Pts',(146.983306913305,6.07780048935632,132.071522421221));
#269011=CARTESIAN_POINT('Ctrl Pts',(146.704859289492,4.35129873632927,126.375866840638));
#269012=CARTESIAN_POINT('Ctrl Pts',(146.426411665679,-1.37383398262348,
124.749780697104));
#269013=CARTESIAN_POINT('Ctrl Pts',(146.147964041867,-5.83648038706648,
128.687557717801));
#269014=CARTESIAN_POINT('Ctrl Pts',(145.869516418053,-4.93568644371351,
134.570573191811));
#269015=CARTESIAN_POINT('Ctrl Pts',(145.591068794241,0.500762219724632,
136.992623299802));
#269016=CARTESIAN_POINT('Ctrl Pts',(145.312621170428,5.47703486683029,133.727962316256));
#269017=CARTESIAN_POINT('Ctrl Pts',(145.034173546615,5.42018003934715,127.776654197497));
#269018=CARTESIAN_POINT('Ctrl Pts',(144.755725922802,0.382444546219556,
124.607660367099));
#269019=CARTESIAN_POINT('Ctrl Pts',(144.477278298989,-5.00673880142907,
127.133131341243));
#269020=CARTESIAN_POINT('Ctrl Pts',(144.198830675176,-5.79497378335261,
133.032282670807));
#269021=CARTESIAN_POINT('Ctrl Pts',(143.920383051363,-1.25791095858285,
136.884082473484));
#269022=CARTESIAN_POINT('Ctrl Pts',(143.64193542755,4.43511058475782,135.148914901497));
#269023=CARTESIAN_POINT('Ctrl Pts',(143.363487803737,6.05248216790344,129.421314185853));
#269024=CARTESIAN_POINT('Ctrl Pts',(143.085040179924,2.10791831893749,124.964665575378));
#269025=CARTESIAN_POINT('Ctrl Pts',(142.806592556112,-3.77371948759721,
125.87441142371));
#269026=CARTESIAN_POINT('Ctrl Pts',(142.528144932299,-6.18749344147606,
131.314539739788));
#269027=CARTESIAN_POINT('Ctrl Pts',(142.249697308486,-2.91526319849757,
136.285838366179));
#269028=CARTESIAN_POINT('Ctrl Pts',(141.971249684673,3.03595150537554,136.219926726669));
#269029=CARTESIAN_POINT('Ctrl Pts',(141.69280206086,6.19727509028471,131.177374398005));
#269030=CARTESIAN_POINT('Ctrl Pts',(141.414354437047,3.6636056209416,125.792040627854));
#269031=CARTESIAN_POINT('Ctrl Pts',(141.135906813234,-2.23673843696229,
125.012784062803));
#269032=CARTESIAN_POINT('Ctrl Pts',(140.857459189421,-6.0816291420453,129.555703417335));
#269033=CARTESIAN_POINT('Ctrl Pts',(140.579011565609,-4.33779976968917,
135.246077738584));
#269034=CARTESIAN_POINT('Ctrl Pts',(140.300563941795,1.39225567771152,136.854731015561));
#269035=CARTESIAN_POINT('Ctrl Pts',(140.022116317983,5.84289617276637,132.903389473806));
#269036=CARTESIAN_POINT('Ctrl Pts',(139.74366869417,4.92420052639575,127.023142956427));
#269037=CARTESIAN_POINT('Ctrl Pts',(139.465221070357,-0.519594843163371,
124.617650746882));
#269038=CARTESIAN_POINT('Ctrl Pts',(139.186773446544,-5.48590793547459,
127.897442670915));
#269039=CARTESIAN_POINT('Ctrl Pts',(138.908325822731,-5.41093963658633,
133.848550177083));
#269040=CARTESIAN_POINT('Ctrl Pts',(138.629878198918,-0.363582150772119,
137.002196194983));
#269041=CARTESIAN_POINT('Ctrl Pts',(138.351430575105,5.0178895696262,134.460334098336));
#269042=CARTESIAN_POINT('Ctrl Pts',(138.072982951292,5.78816591307159,128.558810977095));
#269043=CARTESIAN_POINT('Ctrl Pts',(137.79453532748,1.23940055002892,124.720838274248));
#269044=CARTESIAN_POINT('Ctrl Pts',(137.516087703667,-4.44831337040726,
126.473325408321));
#269045=CARTESIAN_POINT('Ctrl Pts',(137.237640079854,-6.0482446156285,132.205822316857));
#269046=CARTESIAN_POINT('Ctrl Pts',(136.959192456041,-2.09013453226308,
136.650444388955));
#269047=CARTESIAN_POINT('Ctrl Pts',(136.680744832228,3.78870707750376,135.722801072215));
#269048=CARTESIAN_POINT('Ctrl Pts',(136.402297208415,6.18591197167502,130.275351256826));
#269049=CARTESIAN_POINT('Ctrl Pts',(136.123849584602,2.89856596247695,125.314035200413));
#269050=CARTESIAN_POINT('Ctrl Pts',(135.845401960789,-3.05242056341787,
125.398059985055));
#269051=CARTESIAN_POINT('Ctrl Pts',(135.566954336976,-6.19838171056633,
130.450210938505));
#269052=CARTESIAN_POINT('Ctrl Pts',(135.288506713164,-3.64833287348497,
135.827808145838));
#269053=CARTESIAN_POINT('Ctrl Pts',(135.01005908935,2.25435564335981,136.589102483743));
#269054=CARTESIAN_POINT('Ctrl Pts',(134.731611465538,6.08540145535266,132.034501646982));
#269055=CARTESIAN_POINT('Ctrl Pts',(134.453163841725,4.32426061826468,126.349461299917));
#269056=CARTESIAN_POINT('Ctrl Pts',(134.174716217912,-1.41066447513297,
124.75825579184));
#269057=CARTESIAN_POINT('Ctrl Pts',(133.896268594099,-5.84925783067434,
128.723125249964));
#269058=CARTESIAN_POINT('Ctrl Pts',(133.617820970286,-4.91266899195694,
134.600548336913));
#269059=CARTESIAN_POINT('Ctrl Pts',(133.339373346473,0.538422653146471,
136.989460363863));
#269060=CARTESIAN_POINT('Ctrl Pts',(133.06092572266,5.49473018341705,133.694567882885));
#269061=CARTESIAN_POINT('Ctrl Pts',(132.782478098847,5.40164910761999,127.743716119554));
#269062=CARTESIAN_POINT('Ctrl Pts',(132.504030475035,0.344716387149417,
124.605447129098));
#269063=CARTESIAN_POINT('Ctrl Pts',(132.225582851222,-5.02899385277987,
127.163676800786));
#269064=CARTESIAN_POINT('Ctrl Pts',(131.947135227409,-5.78130442201224,
133.067517042801));
#269065=CARTESIAN_POINT('Ctrl Pts',(131.668687603596,-1.22087865983776,
136.891627091362));
#269066=CARTESIAN_POINT('Ctrl Pts',(131.390239979783,4.46147494748924,135.121836630005));
#269067=CARTESIAN_POINT('Ctrl Pts',(131.11179235597,6.04395103324181,129.384496633644));
#269068=CARTESIAN_POINT('Ctrl Pts',(130.833344732157,2.07233138286776,124.951942274296));
#269069=CARTESIAN_POINT('Ctrl Pts',(130.554897108344,-3.80365956934553,
125.897474465882));
#269070=CARTESIAN_POINT('Ctrl Pts',(130.276449484532,-6.18427319643048,
131.35219531615));
#269071=CARTESIAN_POINT('Ctrl Pts',(129.998001860718,-2.88184187453723,
136.303482841632));
#269072=CARTESIAN_POINT('Ctrl Pts',(129.719554236906,3.0688613442533,136.201345690253));
#269073=CARTESIAN_POINT('Ctrl Pts',(129.441106613093,6.1994309098865,131.139642914452));
#269074=CARTESIAN_POINT('Ctrl Pts',(129.16265898928,3.63302632837089,125.769832087263));
#269075=CARTESIAN_POINT('Ctrl Pts',(128.884211365467,-2.27195196571463,
125.026507029031));
#269076=CARTESIAN_POINT('Ctrl Pts',(128.605763741654,-6.08911739433215,
129.592747154821));
#269077=CARTESIAN_POINT('Ctrl Pts',(128.327316117841,-4.31068140748063,
135.272400862266));
#269078=CARTESIAN_POINT('Ctrl Pts',(128.048868494028,1.42906020435147,136.846143860731));
#269079=CARTESIAN_POINT('Ctrl Pts',(127.770420870216,5.85556530185681,132.867783216248));
#269080=CARTESIAN_POINT('Ctrl Pts',(127.491973246402,4.9010919472237,126.993238007373));
#269081=CARTESIAN_POINT('Ctrl Pts',(127.21352562259,-0.557245475255655,
124.620928293575));
#269082=CARTESIAN_POINT('Ctrl Pts',(126.935077998777,-5.50350152892981,
127.930890808061));
#269083=CARTESIAN_POINT('Ctrl Pts',(126.656630374964,-5.39230853851415,
133.881431700678));
#269084=CARTESIAN_POINT('Ctrl Pts',(126.378182751151,-0.325847430121078,
137.004294591193));
#269085=CARTESIAN_POINT('Ctrl Pts',(126.099735127338,5.04005154802147,134.429721043558));
#269086=CARTESIAN_POINT('Ctrl Pts',(125.821287503525,5.77438937373851,128.523618373138));
#269087=CARTESIAN_POINT('Ctrl Pts',(125.542839879712,1.20234545959337,124.713406404895));
#269088=CARTESIAN_POINT('Ctrl Pts',(125.264392255899,-4.47459519407686,
126.50048379844));
#269089=CARTESIAN_POINT('Ctrl Pts',(124.985944632086,-6.03960146051831,
132.24261373269));
#269090=CARTESIAN_POINT('Ctrl Pts',(124.707497008274,-2.05450903567761,
136.663059316712));
#269091=CARTESIAN_POINT('Ctrl Pts',(124.429049384461,3.81857682460466,135.69964700956));
#269092=CARTESIAN_POINT('Ctrl Pts',(124.150601760648,6.18257713092382,130.237705656202));
#269093=CARTESIAN_POINT('Ctrl Pts',(123.872154136835,2.86509108960817,125.296492529702));
#269094=CARTESIAN_POINT('Ctrl Pts',(123.593706513022,-3.08527369557641,
125.416741101634));
#269095=CARTESIAN_POINT('Ctrl Pts',(123.315258889209,-6.20042267852561,
130.487948808862));
#269096=CARTESIAN_POINT('Ctrl Pts',(123.036811265396,-3.61768612739718,
135.849923510712));
#269097=CARTESIAN_POINT('Ctrl Pts',(122.758363641583,2.28952724101679,136.575272403211));
#269098=CARTESIAN_POINT('Ctrl Pts',(122.47991601777,6.09277692456002,131.997435289415));
#269099=CARTESIAN_POINT('Ctrl Pts',(122.201468393958,4.29706226313277,126.323220837128));
#269100=CARTESIAN_POINT('Ctrl Pts',(121.923020770144,-1.44744269495155,
124.766954927214));
#269101=CARTESIAN_POINT('Ctrl Pts',(121.644573146332,-5.86181852788225,
128.758769903068));
#269102=CARTESIAN_POINT('Ctrl Pts',(121.366125522519,-4.88946949944416,
134.630382812884));
#269103=CARTESIAN_POINT('Ctrl Pts',(121.087677898706,0.576063135118759,
136.986068236777));
#269104=CARTESIAN_POINT('Ctrl Pts',(120.809230274893,5.51222189075617,133.661066351821));
#269105=CARTESIAN_POINT('Ctrl Pts',(120.53078265108,5.38291801579874,127.710891454918));
#269106=CARTESIAN_POINT('Ctrl Pts',(120.252335027267,0.306975454486648,
124.603463594118));
#269107=CARTESIAN_POINT('Ctrl Pts',(119.973887403454,-5.05106255291402,
127.194357167205));
#269108=CARTESIAN_POINT('Ctrl Pts',(119.695439779642,-5.76742083231046,
133.102667552701));
#269109=CARTESIAN_POINT('Ctrl Pts',(119.416992155829,-1.18380112098488,
136.898946143343));
#269110=CARTESIAN_POINT('Ctrl Pts',(119.138544532016,4.48767398862585,135.09459837285));
#269111=CARTESIAN_POINT('Ctrl Pts',(118.860096908203,6.03519593775195,129.347731695017));
#269112=CARTESIAN_POINT('Ctrl Pts',(118.58164928439,2.0366676557964,124.939435836727));
#269113=CARTESIAN_POINT('Ctrl Pts',(118.303201660577,-3.83345870508974,
125.920719334523));
#269114=CARTESIAN_POINT('Ctrl Pts',(118.024754036764,-6.18082379086727,
131.389830592295));
#269115=CARTESIAN_POINT('Ctrl Pts',(117.746306412951,-2.84831376286653,
136.320923545089));
#269116=CARTESIAN_POINT('Ctrl Pts',(117.467858789138,3.10165746534553,136.18256466657));
#269117=CARTESIAN_POINT('Ctrl Pts',(117.189411165326,6.20135700729606,131.101899006891));
#269118=CARTESIAN_POINT('Ctrl Pts',(116.910963541513,3.60231241267338,125.747810102979));
#269119=CARTESIAN_POINT('Ctrl Pts',(116.6325159177,-2.30708130645123,125.040444095748));
#269120=CARTESIAN_POINT('Ctrl Pts',(116.354068293887,-6.09638001213474,
129.62983578909));
#269121=CARTESIAN_POINT('Ctrl Pts',(116.075620670074,-4.28340331138726,
135.298558421074));
#269122=CARTESIAN_POINT('Ctrl Pts',(115.797173046261,1.46581177664024,136.837332825402));
#269123=CARTESIAN_POINT('Ctrl Pts',(115.518725422448,5.86801745082159,132.832100497806));
#269124=CARTESIAN_POINT('Ctrl Pts',(115.240277798635,4.87780175628715,126.963474280869));
#269125=CARTESIAN_POINT('Ctrl Pts',(114.961830174822,-0.594875458411799,
124.624434969628));
#269126=CARTESIAN_POINT('Ctrl Pts',(114.68338255101,-5.52089118811201,127.964445422689));
#269127=CARTESIAN_POINT('Ctrl Pts',(114.404934927196,-5.37347762646609,
133.914199202272));
#269128=CARTESIAN_POINT('Ctrl Pts',(114.126487303384,-0.288100635073559,
137.006163246571));
#269129=CARTESIAN_POINT('Ctrl Pts',(113.848039679571,5.06202676545313,134.398973649715));
#269130=CARTESIAN_POINT('Ctrl Pts',(113.569592055758,5.76039886228364,128.488510282924));
#269131=CARTESIAN_POINT('Ctrl Pts',(113.291144431945,1.16524581580469,124.706200238089));
#269132=CARTESIAN_POINT('Ctrl Pts',(113.012696808132,-4.50071120997606,
126.527801670297));
#269133=CARTESIAN_POINT('Ctrl Pts',(112.734249184319,-6.03073450575487,
132.279351853526));
#269134=CARTESIAN_POINT('Ctrl Pts',(112.455801560506,-2.01880740850426,
136.675457148234));
#269135=CARTESIAN_POINT('Ctrl Pts',(112.177353936694,3.84830507293705,135.676311550269));
#269136=CARTESIAN_POINT('Ctrl Pts',(111.898906312881,6.17901319250346,130.200081053184));
#269137=CARTESIAN_POINT('Ctrl Pts',(111.620458689068,2.8315100497353,125.279153955068));
#269138=CARTESIAN_POINT('Ctrl Pts',(111.342011065255,-3.11801250178361,
125.435621858436));
#269139=CARTESIAN_POINT('Ctrl Pts',(111.063563441442,-6.20223388754234,
130.525698403974));
#269140=CARTESIAN_POINT('Ctrl Pts',(110.785115817629,-3.58690532661952,
135.871851910398));
#269141=CARTESIAN_POINT('Ctrl Pts',(110.506668193816,2.32461399939974,136.56122847942));
#269142=CARTESIAN_POINT('Ctrl Pts',(110.228220570003,6.09992662367788,131.960324722029));
#269143=CARTESIAN_POINT('Ctrl Pts',(109.94977294619,4.26970467877848,126.297146424621));
#269144=CARTESIAN_POINT('Ctrl Pts',(109.671325322378,-1.48416727924886,
124.775877780875));
#269145=CARTESIAN_POINT('Ctrl Pts',(109.392877698565,-5.8741620132489,128.794490356288));
#269146=CARTESIAN_POINT('Ctrl Pts',(109.114430074752,-4.86608882584101,
134.660075514194));
#269147=CARTESIAN_POINT('Ctrl Pts',(108.835982450939,0.61368227085971,136.982447044243));
#269148=CARTESIAN_POINT('Ctrl Pts',(108.557534827126,5.52950934068608,133.627458964475));
#269149=CARTESIAN_POINT('Ctrl Pts',(108.279087203313,5.36398745797076,127.67818141992));
#269150=CARTESIAN_POINT('Ctrl Pts',(108.0006395795,0.269223146735527,124.601709835656));
#269151=CARTESIAN_POINT('Ctrl Pts',(107.722191955687,-5.07294408406776,
127.225171303631));
#269152=CARTESIAN_POINT('Ctrl Pts',(107.443744331874,-5.75332352870873,
133.137732897993));
#269153=CARTESIAN_POINT('Ctrl Pts',(107.165296708062,-1.14667971594628,
136.906039358215));
#269154=CARTESIAN_POINT('Ctrl Pts',(106.886849084249,4.51370673735246,135.067201139359));
#269155=CARTESIAN_POINT('Ctrl Pts',(106.608401460436,6.02621720585718,129.31102073231));
#269156=CARTESIAN_POINT('Ctrl Pts',(106.329953836623,2.00092845925606,124.927146726103));
#269157=CARTESIAN_POINT('Ctrl Pts',(106.05150621281,-3.86311579061174,125.944145168289));
#269158=CARTESIAN_POINT('Ctrl Pts',(105.773058588997,-6.17714535260555,
131.427444173636));
#269159=CARTESIAN_POINT('Ctrl Pts',(105.494610965184,-2.81468010588189,
136.338159830278));
#269160=CARTESIAN_POINT('Ctrl Pts',(105.216163341371,3.13433865337982,136.163584351558));
#269161=CARTESIAN_POINT('Ctrl Pts',(104.937715717558,6.20305331114115,131.064144073934));
#269162=CARTESIAN_POINT('Ctrl Pts',(104.659268093745,3.57146501196475,125.725975491034));
#269163=CARTESIAN_POINT('Ctrl Pts',(104.380820469933,-2.34212515744159,
125.054594746511));
#269164=CARTESIAN_POINT('Ctrl Pts',(104.10237284612,-6.10341672633411,129.666967945808));
#269165=CARTESIAN_POINT('Ctrl Pts',(103.823925222307,-4.25596649220884,
135.324549445729));
#269166=CARTESIAN_POINT('Ctrl Pts',(103.545477598494,1.50250903273456,136.828298236068));
#269167=CARTESIAN_POINT('Ctrl Pts',(103.267029974681,5.88025215824177,132.796342640716));
#269168=CARTESIAN_POINT('Ctrl Pts',(102.988582350868,4.85433081661274,126.933852879821));
#269169=CARTESIAN_POINT('Ctrl Pts',(102.710134727055,-0.63248339823904,
124.628170645098));
#269170=CARTESIAN_POINT('Ctrl Pts',(102.431687103242,-5.53807626864099,
127.998105271418));
#269171=CARTESIAN_POINT('Ctrl Pts',(102.153239479429,-5.35444759822839,
133.946851467654));
#269172=CARTESIAN_POINT('Ctrl Pts',(101.874791855617,-0.250343164351048,
137.00780209187));
#269173=CARTESIAN_POINT('Ctrl Pts',(101.596344231803,5.0838144076213,134.368093056165));
#269174=CARTESIAN_POINT('Ctrl Pts',(101.317896607991,5.74619489713063,128.453488007394));
#269175=CARTESIAN_POINT('Ctrl Pts',(101.039448984178,1.12810299340375,124.69922004086));
#269176=CARTESIAN_POINT('Ctrl Pts',(100.761001360365,-4.52666045036627,
126.55527801162));
#269177=CARTESIAN_POINT('Ctrl Pts',(100.482553736552,-6.0216440799065,132.316035318018));
#269178=CARTESIAN_POINT('Ctrl Pts',(100.204106112739,-1.98303097367997,
136.687637424115));
#269179=CARTESIAN_POINT('Ctrl Pts',(99.9256584889259,3.87789072090961,135.652795559044));
#269180=CARTESIAN_POINT('Ctrl Pts',(99.6472108651132,6.17522028847693,130.162478841968));
#269181=CARTESIAN_POINT('Ctrl Pts',(99.3687632413001,2.79782408721636,125.262020118999));
#269182=CARTESIAN_POINT('Ctrl Pts',(99.0903156174874,-3.15063576889091,
125.454701555827));
#269183=CARTESIAN_POINT('Ctrl Pts',(98.8118679936743,-6.20381527050148,
130.563458325018));
#269184=CARTESIAN_POINT('Ctrl Pts',(98.5334203698616,-3.55599161174595,
135.89359253233));
#269185=CARTESIAN_POINT('Ctrl Pts',(98.2549727460486,2.35961461835606,136.546971232774));
#269186=CARTESIAN_POINT('Ctrl Pts',(97.9765251222358,6.10685028777152,131.923171319966));
#269187=CARTESIAN_POINT('Ctrl Pts',(97.6980774984228,4.24218887894701,126.271239028595));
#269188=CARTESIAN_POINT('Ctrl Pts',(97.4196298746099,-1.52083686718185,
124.785024022185));
#269189=CARTESIAN_POINT('Ctrl Pts',(97.141182250797,-5.88628782938184,128.830285285991));
#269190=CARTESIAN_POINT('Ctrl Pts',(96.8627346269842,-4.842527837527,134.689625340572));
#269191=CARTESIAN_POINT('Ctrl Pts',(96.5842870031713,0.651278666378471,
136.978596920444));
#269192=CARTESIAN_POINT('Ctrl Pts',(96.3058393793584,5.54659189261388,133.593746966183));
#269193=CARTESIAN_POINT('Ctrl Pts',(96.0273917555454,5.34485813561491,127.645587226641));
#269194=CARTESIAN_POINT('Ctrl Pts',(95.7489441317327,0.231460862821695,
124.6001859187));
#269195=CARTESIAN_POINT('Ctrl Pts',(95.4704965079195,-5.09463763541278,
127.256118068232));
#269196=CARTESIAN_POINT('Ctrl Pts',(95.192048884107,-5.73901303358793,133.172711779316));
#269197=CARTESIAN_POINT('Ctrl Pts',(94.9136012602939,-1.10951582026908,
136.912906473138));
#269198=CARTESIAN_POINT('Ctrl Pts',(94.635153636481,4.53957222901603,135.039645944743));
#269199=CARTESIAN_POINT('Ctrl Pts',(94.3567060126683,6.01701517026768,129.274365105863));
#269200=CARTESIAN_POINT('Ctrl Pts',(94.0782583888551,1.96511511757592,124.915075397801));
#269201=CARTESIAN_POINT('Ctrl Pts',(93.7998107650425,-3.89262972695748,
125.967751099126));
#269202=CARTESIAN_POINT('Ctrl Pts',(93.5213631412293,-6.17323801795121,
131.465034666385));
#269203=CARTESIAN_POINT('Ctrl Pts',(93.2429155174167,-2.7809421498907,136.355191058501));
#269204=CARTESIAN_POINT('Ctrl Pts',(92.9644678936037,3.16690369734264,136.14440544854));
#269205=CARTESIAN_POINT('Ctrl Pts',(92.6860202697908,6.20451975856463,131.026379514606));
#269206=CARTESIAN_POINT('Ctrl Pts',(92.4075726459779,3.54048526930663,125.704329060518));
#269207=CARTESIAN_POINT('Ctrl Pts',(92.129125022165,-2.37708222012305,125.068958456964));
#269208=CARTESIAN_POINT('Ctrl Pts',(91.850677398352,-6.1102272761821,129.70414224903));
#269209=CARTESIAN_POINT('Ctrl Pts',(91.5722297745392,-4.22837196662692,
135.350372973126));
#269210=CARTESIAN_POINT('Ctrl Pts',(91.2937821507264,1.53915061280415,136.819040427511));
#269211=CARTESIAN_POINT('Ctrl Pts',(91.0153345269133,5.89226897075567,132.76051097));
#269212=CARTESIAN_POINT('Ctrl Pts',(90.7368869031008,4.8306799979248,126.90437490186));
#269213=CARTESIAN_POINT('Ctrl Pts',(90.4584392792875,-0.670067901161403,
124.632135181558));
#269214=CARTESIAN_POINT('Ctrl Pts',(90.1799916554748,-5.5550561337172,128.031869106972));
#269215=CARTESIAN_POINT('Ctrl Pts',(89.9015440316619,-5.3352191589658,133.979387286881));
#269216=CARTESIAN_POINT('Ctrl Pts',(89.6230964078489,-0.212576417070642,
137.009211066365));
#269217=CARTESIAN_POINT('Ctrl Pts',(89.3446487840362,5.10541366717708,134.337080407198));
#269218=CARTESIAN_POINT('Ctrl Pts',(89.0662011602232,5.73177800461257,128.418552844315));
#269219=CARTESIAN_POINT('Ctrl Pts',(88.7877535364103,1.09091836873142,124.69246607186));
#269220=CARTESIAN_POINT('Ctrl Pts',(88.5093059125973,-4.5524419536888,126.58291180426));
#269221=CARTESIAN_POINT('Ctrl Pts',(88.2308582887847,-6.0123305198223,132.352662766849));
#269222=CARTESIAN_POINT('Ctrl Pts',(87.9524106649715,-1.94718105691378,
136.69959969301));
#269223=CARTESIAN_POINT('Ctrl Pts',(87.6739630411587,3.90733267221543,135.629099907278));
#269224=CARTESIAN_POINT('Ctrl Pts',(87.395515417346,6.17119855939173,130.124900415918));
#269225=CARTESIAN_POINT('Ctrl Pts',(87.1170677935327,2.76403445029686,125.245091656395));
#269226=CARTESIAN_POINT('Ctrl Pts',(86.8386201697203,-3.18314228803115,
125.473979486801));
#269227=CARTESIAN_POINT('Ctrl Pts',(86.5601725459069,-6.20516676880425,
130.601227172784));
#269228=CARTESIAN_POINT('Ctrl Pts',(86.2817249220945,-3.52494612829556,
135.915144570902));
#269229=CARTESIAN_POINT('Ctrl Pts',(86.0032772982812,2.394527800925,136.532501191579));
#269230=CARTESIAN_POINT('Ctrl Pts',(85.7248296744686,6.11354766028192,131.885976459962));
#269231=CARTESIAN_POINT('Ctrl Pts',(85.4463820506556,4.21451588324655,126.245499609054));
#269232=CARTESIAN_POINT('Ctrl Pts',(85.1679344268427,-1.55745009994542,
124.794393312227));
#269233=CARTESIAN_POINT('Ctrl Pts',(84.8894868030298,-5.89819552695468,
128.86615336578));
#269234=CARTESIAN_POINT('Ctrl Pts',(84.611039179217,-4.81878740756302,134.719031197036));
#269235=CARTESIAN_POINT('Ctrl Pts',(84.332591555404,0.68885092852684,136.974518008049));
#269236=CARTESIAN_POINT('Ctrl Pts',(84.0541439315912,5.56346891353935,133.559931606153));
#269237=CARTESIAN_POINT('Ctrl Pts',(83.7756963077782,5.32553075757526,127.613110082872));
#269238=CARTESIAN_POINT('Ctrl Pts',(83.4972486839655,0.193690002040587,
124.598891899719));
#269239=CARTESIAN_POINT('Ctrl Pts',(83.2188010601524,-5.11614240308669,
127.287196314267));
#269240=CARTESIAN_POINT('Ctrl Pts',(82.9403534363397,-5.72448987722869,
133.207602900518));
#269241=CARTESIAN_POINT('Ctrl Pts',(82.6619058125266,-1.07231081107503,
136.919547233648));
#269242=CARTESIAN_POINT('Ctrl Pts',(82.3834581887138,4.56526950516122,135.011933810073));
#269243=CARTESIAN_POINT('Ctrl Pts',(82.1050105649009,6.00759017196827,129.237766173961));
#269244=CARTESIAN_POINT('Ctrl Pts',(81.826562941088,1.92922895783247,124.903222299129));
#269245=CARTESIAN_POINT('Ctrl Pts',(81.5481153172751,-3.92199942047723,
125.991536252305));
#269246=CARTESIAN_POINT('Ctrl Pts',(81.2696676934623,-6.16910193169181,
131.502600677615));
#269247=CARTESIAN_POINT('Ctrl Pts',(80.9912200696492,-2.74710114506546,
136.372016598662));
#269248=CARTESIAN_POINT('Ctrl Pts',(80.7127724458365,3.19935139052435,136.125028668197));
#269249=CARTESIAN_POINT('Ctrl Pts',(80.4343248220235,6.20575629522666,130.988606728286));
#269250=CARTESIAN_POINT('Ctrl Pts',(80.1558771982107,3.50937433266497,125.682871613546));
#269251=CARTESIAN_POINT('Ctrl Pts',(79.8774295743978,-2.41195119914859,
125.083534694853));
#269252=CARTESIAN_POINT('Ctrl Pts',(79.5989819505849,-6.11681140931136,
129.741357321249));
#269253=CARTESIAN_POINT('Ctrl Pts',(79.320534326772,-4.20062075716678,135.376028046362));
#269254=CARTESIAN_POINT('Ctrl Pts',(79.0420867029591,1.57573515908161,136.809559742781));
#269255=CARTESIAN_POINT('Ctrl Pts',(78.7636390791462,5.90406744307602,132.724606813414));
#269256=CARTESIAN_POINT('Ctrl Pts',(78.4851914553333,4.80685017661309,126.875041439303));
#269257=CARTESIAN_POINT('Ctrl Pts',(78.2067438315204,-0.707627574471386,
124.636328432103));
#269258=CARTESIAN_POINT('Ctrl Pts',(77.9282962077074,-5.57183015414549,
128.065735678218));
#269259=CARTESIAN_POINT('Ctrl Pts',(77.6498485838947,-5.31579302119528,
134.011805454327));
#269260=CARTESIAN_POINT('Ctrl Pts',(77.3714009600817,-0.174801792692954,
137.010390117845));
#269261=CARTESIAN_POINT('Ctrl Pts',(77.0929533362689,5.12682374375196,134.305936852001));
#269262=CARTESIAN_POINT('Ctrl Pts',(76.814505712456,5.7171487189526,128.38370608822));
#269263=CARTESIAN_POINT('Ctrl Pts',(76.536058088643,1.05369331967776,124.68593858136));
#269264=CARTESIAN_POINT('Ctrl Pts',(76.2576104648302,-4.57805476460059,
126.610702024239));
#269265=CARTESIAN_POINT('Ctrl Pts',(75.9791628410172,-6.00279417061961,
132.389232842773));
#269266=CARTESIAN_POINT('Ctrl Pts',(75.7007152172044,-1.91125898663751,
136.711343511654));
#269267=CARTESIAN_POINT('Ctrl Pts',(75.4222675933915,3.93662983587222,135.605225473025));
#269268=CARTESIAN_POINT('Ctrl Pts',(75.1438199695785,6.16694815427437,130.087347167514));
#269269=CARTESIAN_POINT('Ctrl Pts',(74.8653723457658,2.73014239106432,125.228369194547));
#269270=CARTESIAN_POINT('Ctrl Pts',(74.5869247219528,-3.21553085466319,
125.493454937009));
#269271=CARTESIAN_POINT('Ctrl Pts',(74.3084770981399,-6.20628833237051,
130.639003547736));
#269272=CARTESIAN_POINT('Ctrl Pts',(74.0300294743271,-3.49377002667009,
135.936507227495));
#269273=CARTESIAN_POINT('Ctrl Pts',(73.7515818505141,2.42935225338577,136.517818892029));
#269274=CARTESIAN_POINT('Ctrl Pts',(73.4731342267013,6.1200184930355,131.848741520285));
#269275=CARTESIAN_POINT('Ctrl Pts',(73.1946866028884,4.18668671711015,126.219929119786));
#269276=CARTESIAN_POINT('Ctrl Pts',(72.9162389790755,-1.59400562082267,
124.803985303816));
#269277=CARTESIAN_POINT('Ctrl Pts',(72.6377913552626,-5.90988466472314,
128.902093266552));
#269278=CARTESIAN_POINT('Ctrl Pts',(72.3593437314497,-4.79486841565966,
134.748291993943));
#269279=CARTESIAN_POINT('Ctrl Pts',(72.0808961076369,0.726397665050741,
136.970210458201));
#269280=CARTESIAN_POINT('Ctrl Pts',(71.8024484838239,5.58013977807825,133.526014137426));
#269281=CARTESIAN_POINT('Ctrl Pts',(71.524000860011,5.30600604003494,127.580751192065));
#269282=CARTESIAN_POINT('Ctrl Pts',(71.2455532361981,0.155911964005252,
124.597827826664));
#269283=CARTESIAN_POINT('Ctrl Pts',(70.9671056123853,-5.13745759022245,
127.318404890117));
#269284=CARTESIAN_POINT('Ctrl Pts',(70.6886579885723,-5.70975459779179,
133.242404968692));
#269285=CARTESIAN_POINT('Ctrl Pts',(70.4102103647595,-1.03506606700937,
136.925961393668));
#269286=CARTESIAN_POINT('Ctrl Pts',(70.1317627409465,4.59079761356593,134.98406576223));
#269287=CARTESIAN_POINT('Ctrl Pts',(69.8533151171337,5.99794256020584,129.201225292793));
#269288=CARTESIAN_POINT('Ctrl Pts',(69.5748674933208,1.89327130980037,124.891587869307));
#269289=CARTESIAN_POINT('Ctrl Pts',(69.2964198695077,-3.95122378286636,
126.015499746463));
#269290=CARTESIAN_POINT('Ctrl Pts',(69.0179722456952,-6.16473724709165,
131.540140815303));
#269291=CARTESIAN_POINT('Ctrl Pts',(68.7395246218819,-2.71315834539685,
136.388635827283));
#269292=CARTESIAN_POINT('Ctrl Pts',(68.4610769980694,3.23168053056381,136.105454728543));
#269293=CARTESIAN_POINT('Ctrl Pts',(68.1826293742561,6.20676287530703,130.950827114659));
#269294=CARTESIAN_POINT('Ctrl Pts',(67.9041817504435,3.47813335486666,125.661603945233));
#269295=CARTESIAN_POINT('Ctrl Pts',(67.6257341266304,-2.44673080243567,
125.09832292005));
#269296=CARTESIAN_POINT('Ctrl Pts',(67.3472865028177,-6.12316888174425,
129.778611783445));
#269297=CARTESIAN_POINT('Ctrl Pts',(67.0688388790048,-4.17271389215982,
135.401513714782));
#269298=CARTESIAN_POINT('Ctrl Pts',(66.7903912551918,1.61226131591331,136.799856533191));
#269299=CARTESIAN_POINT('Ctrl Pts',(66.511943631379,5.91564713800617,132.688631501398));
#269300=CARTESIAN_POINT('Ctrl Pts',(66.233496007566,4.78284223570014,126.845853579115));
#269301=CARTESIAN_POINT('Ctrl Pts',(65.9550483837533,-0.745161026381345,
124.640750241348));
#269302=CARTESIAN_POINT('Ctrl Pts',(65.6766007599402,-5.58839770835831,
128.099703730218));
#269303=CARTESIAN_POINT('Ctrl Pts',(65.3981531361275,-5.2961699047596,134.044104768727));
#269304=CARTESIAN_POINT('Ctrl Pts',(65.1197055123145,-0.137020690970298,
137.011339202618));
#269305=CARTESIAN_POINT('Ctrl Pts',(64.8412578885016,5.14804384398771,134.274663544608));
#269306=CARTESIAN_POINT('Ctrl Pts',(64.5628102646887,5.70230758224426,128.348949030369));
#269307=CARTESIAN_POINT('Ctrl Pts',(64.2843626408759,1.01642922563077,124.679637811238));
#269308=CARTESIAN_POINT('Ctrl Pts',(64.0059150170629,-4.60349793400934,
126.638647641779));
#269309=CARTESIAN_POINT('Ctrl Pts',(63.72746739325,-5.9930353856715,132.425744190676));
#269310=CARTESIAN_POINT('Ctrl Pts',(63.4490197694371,-1.87526609395646,
136.722868444874));
#269311=CARTESIAN_POINT('Ctrl Pts',(63.1705721456243,3.96578112626272,135.581173140958));
#269312=CARTESIAN_POINT('Ctrl Pts',(62.8921245218114,6.16246923062527,130.049820488308));
#269313=CARTESIAN_POINT('Ctrl Pts',(62.6136768979985,2.69614916540168,125.211853353112));
#269314=CARTESIAN_POINT('Ctrl Pts',(62.3352292741856,-3.24780026861702,
125.513127184779));
#269315=CARTESIAN_POINT('Ctrl Pts',(62.0567816503727,-6.20717991964031,
130.676786050054));
#269316=CARTESIAN_POINT('Ctrl Pts',(61.7783340265599,-3.46246446211126,
135.957679710507));
#269317=CARTESIAN_POINT('Ctrl Pts',(61.4998864027468,2.46408668530527,136.502924878181));
#269318=CARTESIAN_POINT('Ctrl Pts',(61.2214387789342,6.12626254625314,131.81146788069));
#269319=CARTESIAN_POINT('Ctrl Pts',(60.942991155121,4.15870241175792,126.194528508313));
#269320=CARTESIAN_POINT('Ctrl Pts',(60.6645435313083,-1.63050207523548,
124.813799641521));
#269321=CARTESIAN_POINT('Ctrl Pts',(60.3860959074953,-5.92135480954196,
128.938103656541));
#269322=CARTESIAN_POINT('Ctrl Pts',(60.1076482836825,-4.77077174814381,
134.777406647022));
#269323=CARTESIAN_POINT('Ctrl Pts',(59.8292006598696,0.763917484641806,
136.965674430521));
#269324=CARTESIAN_POINT('Ctrl Pts',(59.5507530360567,5.59660386848551,133.491995816827));
#269325=CARTESIAN_POINT('Ctrl Pts',(59.2723054122438,5.28628470648961,127.548511753291));
#269326=CARTESIAN_POINT('Ctrl Pts',(58.9938577884309,0.11812814859451,124.596993738963));
#269327=CARTESIAN_POINT('Ctrl Pts',(58.715410164618,-5.15858240697801,127.34974263934));
#269328=CARTESIAN_POINT('Ctrl Pts',(58.4369625408051,-5.69480774129836,
133.277116694236));
#269329=CARTESIAN_POINT('Ctrl Pts',(58.1585149169922,-0.997782968190397,
136.932148715521));
#269330=CARTESIAN_POINT('Ctrl Pts',(57.8800672931793,4.61615560827684,134.956042833877));
#269331=CARTESIAN_POINT('Ctrl Pts',(57.6016196693665,5.98807269247603,129.164743816393));
#269332=CARTESIAN_POINT('Ctrl Pts',(57.3231720455535,1.85724350590365,124.880172539454));
#269333=CARTESIAN_POINT('Ctrl Pts',(57.0447244217407,-3.98030173120474,
126.039640693622));
#269334=CARTESIAN_POINT('Ctrl Pts',(56.7662767979277,-6.16014412588574,
131.577653688385));
#269335=CARTESIAN_POINT('Ctrl Pts',(56.4878291741149,-2.67911500864857,
136.405048128532));
#269336=CARTESIAN_POINT('Ctrl Pts',(56.209381550302,3.26388991949243,136.085684354897));
#269337=CARTESIAN_POINT('Ctrl Pts',(55.9309339264891,6.20753946150667,130.913042073662));
#269338=CARTESIAN_POINT('Ctrl Pts',(55.6524863026762,3.44676349355797,125.640526843659));
#269339=CARTESIAN_POINT('Ctrl Pts',(55.3740386788633,-2.48141974121268,
125.113322584571));
#269340=CARTESIAN_POINT('Ctrl Pts',(55.0955910550504,-6.12929945790263,
129.815904255142));
#269341=CARTESIAN_POINT('Ctrl Pts',(54.8171434312375,-4.14465240570495,
135.426829034002));
#269342=CARTESIAN_POINT('Ctrl Pts',(54.5386958074246,1.64872772980914,136.789931158292));
#269343=CARTESIAN_POINT('Ctrl Pts',(54.2602481836117,5.92700762645589,132.652586367033));
#269344=CARTESIAN_POINT('Ctrl Pts',(53.9818005597989,4.75865706480954,126.81681240286));
#269345=CARTESIAN_POINT('Ctrl Pts',(53.703352935986,-0.78266686607524,124.645400445441));
#269346=CARTESIAN_POINT('Ctrl Pts',(53.4249053121731,-5.604758182439,128.133772004274));
#269347=CARTESIAN_POINT('Ctrl Pts',(53.1464576883601,-5.27635053680027,
134.076284033214));
#269348=CARTESIAN_POINT('Ctrl Pts',(52.8680100645473,-0.0992345118958833,
137.012058285519));
#269349=CARTESIAN_POINT('Ctrl Pts',(52.5895624407343,5.1690731815654,134.243261643865));
#269350=CARTESIAN_POINT('Ctrl Pts',(52.3111148169216,5.68725514443172,128.314282958697));
#269351=CARTESIAN_POINT('Ctrl Pts',(52.0326671931086,0.979127467424884,
124.673563994973));
#269352=CARTESIAN_POINT('Ctrl Pts',(51.7542195692957,-4.62877051910935,
126.666747621346));
#269353=CARTESIAN_POINT('Ctrl Pts',(51.4757719454828,-5.98305452659317,
132.462195457613));
#269354=CARTESIAN_POINT('Ctrl Pts',(51.1973243216699,-1.83920371260068,
136.734174065611));
#269355=CARTESIAN_POINT('Ctrl Pts',(50.9188766978571,3.99478546317524,135.556943802347));
#269356=CARTESIAN_POINT('Ctrl Pts',(50.6404290740441,6.15776195441257,130.012321768865));
#269357=CARTESIAN_POINT('Ctrl Pts',(50.3619814502312,2.66205603294,125.195544744091));
#269358=CARTESIAN_POINT('Ctrl Pts',(50.0835338264184,-3.27994933413751,
125.532995501151));
#269359=CARTESIAN_POINT('Ctrl Pts',(49.8050862026055,-6.20784149757545,
130.714573279694));
#269360=CARTESIAN_POINT('Ctrl Pts',(49.5266385787925,-3.43103059465853,
135.978661235386));
#269361=CARTESIAN_POINT('Ctrl Pts',(49.2481909549797,2.4987298095866,136.487819701939));
#269362=CARTESIAN_POINT('Ctrl Pts',(48.9697433311668,6.13227958855924,131.774156922365));
#269363=CARTESIAN_POINT('Ctrl Pts',(48.6912957073539,4.13056400415832,126.169298715863));
#269364=CARTESIAN_POINT('Ctrl Pts',(48.412848083541,-1.66693811079436,124.823835961664));
#269365=CARTESIAN_POINT('Ctrl Pts',(48.1344004597282,-5.93260553638082,
128.974183201367));
#269366=CARTESIAN_POINT('Ctrl Pts',(47.8559528359152,-4.7464982979263,134.806374077418));
#269367=CARTESIAN_POINT('Ctrl Pts',(47.5775052121024,0.801408996989757,
136.960910093092));
#269368=CARTESIAN_POINT('Ctrl Pts',(47.2990575882894,5.61286057467834,133.457877904919));
#269369=CARTESIAN_POINT('Ctrl Pts',(47.0206099644766,5.26636748772036,127.516392961194));
#269370=CARTESIAN_POINT('Ctrl Pts',(46.7421623406636,0.0803399559020909,
124.596389667526));
#269371=CARTESIAN_POINT('Ctrl Pts',(46.4637147168508,-5.17951607056515,
127.381208400702));
#269372=CARTESIAN_POINT('Ctrl Pts',(46.1852670930379,-5.67964986161014,
133.311736790894));
#269373=CARTESIAN_POINT('Ctrl Pts',(45.9068194692249,-0.960462896156299,
136.938108969933));
#269374=CARTESIAN_POINT('Ctrl Pts',(45.6283718454121,4.64134254964412,134.927866063412));
#269375=CARTESIAN_POINT('Ctrl Pts',(45.3499242215992,5.97798093451044,129.128323096598));
#269376=CARTESIAN_POINT('Ctrl Pts',(45.0714765977863,1.82114688116607,124.868976732569));
#269377=CARTESIAN_POINT('Ctrl Pts',(44.7930289739735,-4.00923218799886,
126.063958199228));
#269378=CARTESIAN_POINT('Ctrl Pts',(44.5145813501605,-6.15532273827383,
131.615137906808));
#269379=CARTESIAN_POINT('Ctrl Pts',(44.2361337263477,-2.644972396308,136.421252894246));
#269380=CARTESIAN_POINT('Ctrl Pts',(43.9576861025347,3.29597836378001,136.065718279858));
#269381=CARTESIAN_POINT('Ctrl Pts',(43.6792384787219,6.20808602504863,130.875253005433));
#269382=CARTESIAN_POINT('Ctrl Pts',(43.4007908549089,3.41526591116036,125.619641089845));
#269383=CARTESIAN_POINT('Ctrl Pts',(43.1223432310961,-2.5160167300689,125.128533132602));
#269384=CARTESIAN_POINT('Ctrl Pts',(42.8438956072832,-6.13520291061547,
129.853233354452));
#269385=CARTESIAN_POINT('Ctrl Pts',(42.5654479834703,-4.11643733763101,
135.451973065955));
#269386=CARTESIAN_POINT('Ctrl Pts',(42.2870003596574,1.68513304949262,136.779783985877));
#269387=CARTESIAN_POINT('Ctrl Pts',(42.0085527358444,5.93814848745852,132.616472745983));
#269388=CARTESIAN_POINT('Ctrl Pts',(41.7301051120316,4.73429556013123,126.787918986671));
#269389=CARTESIAN_POINT('Ctrl Pts',(41.4516574882187,-0.820143703760798,
124.65027887207));
#269390=CARTESIAN_POINT('Ctrl Pts',(41.1732098644058,-5.62091097014408,
128.167939237972));
#269391=CARTESIAN_POINT('Ctrl Pts',(40.8947622405929,-5.25633565173145,
134.108342055376));
#269392=CARTESIAN_POINT('Ctrl Pts',(40.61631461678,-0.0614446556499193,
137.012547339898));
#269393=CARTESIAN_POINT('Ctrl Pts',(40.3378669929672,5.18991097723558,134.211732313379));
#269394=CARTESIAN_POINT('Ctrl Pts',(40.0594193691542,5.67199196328813,128.279709157768));
#269395=CARTESIAN_POINT('Ctrl Pts',(39.7809717453414,0.941789427290636,
124.66771735763));
#269396=CARTESIAN_POINT('Ctrl Pts',(39.5025241215285,-4.65387158341555,
126.695000921683));
#269397=CARTESIAN_POINT('Ctrl Pts',(39.2240764977156,-5.97285196322902,
132.49858529287));
#269398=CARTESIAN_POINT('Ctrl Pts',(38.9456288739027,-1.80307317887526,
136.745259954929));
#269399=CARTESIAN_POINT('Ctrl Pts',(38.6671812500898,4.02364177184326,135.532538355018));
#269400=CARTESIAN_POINT('Ctrl Pts',(38.3887336262769,6.15282650006613,129.974852398711));
#269401=CARTESIAN_POINT('Ctrl Pts',(38.110286002464,2.62786425701304,125.179443971804));
#269402=CARTESIAN_POINT('Ctrl Pts',(37.8318383786511,-3.31197685992897,
125.553059149895));
#269403=CARTESIAN_POINT('Ctrl Pts',(37.5533907548383,-6.20827304166094,
130.752363836438));
#269404=CARTESIAN_POINT('Ctrl Pts',(37.2749431310254,-3.3994695891056,135.999451024653));
#269405=CARTESIAN_POINT('Ctrl Pts',(36.9964955072125,2.53328034251594,136.47250392303));
#269406=CARTESIAN_POINT('Ctrl Pts',(36.7180478833995,6.13806939699002,131.73681002788));
#269407=CARTESIAN_POINT('Ctrl Pts',(36.4396002595867,4.10227253699055,126.144240677337));
#269408=CARTESIAN_POINT('Ctrl Pts',(36.1611526357737,-1.70331237734853,
124.834093892349));
#269409=CARTESIAN_POINT('Ctrl Pts',(35.8827050119609,-5.94363642833981,
129.01033056409));
#269410=CARTESIAN_POINT('Ctrl Pts',(35.604257388148,-4.72204896446884,134.835193211735));
#269411=CARTESIAN_POINT('Ctrl Pts',(35.3258097643351,0.838870812832614,
136.955917622458));
#269412=CARTESIAN_POINT('Ctrl Pts',(35.0473621405222,5.62890929425843,133.423661665951));
#269413=CARTESIAN_POINT('Ctrl Pts',(34.7689145167094,5.24625512176713,127.484396005948));
#269414=CARTESIAN_POINT('Ctrl Pts',(34.4904668928964,0.0425487861828518,
124.596015634733));
#269415=CARTESIAN_POINT('Ctrl Pts',(34.2120192690835,-5.20025780527969,
127.412801008228));
#269416=CARTESIAN_POINT('Ctrl Pts',(33.9335716452707,-5.66428152040741,
133.346263975806));
#269417=CARTESIAN_POINT('Ctrl Pts',(33.6551240214578,-0.923107233816384,
136.943841936043));
#269418=CARTESIAN_POINT('Ctrl Pts',(33.3766763976448,4.66635750435639,134.899536494936));
#269419=CARTESIAN_POINT('Ctrl Pts',(33.098228773832,5.96766766026296,129.091964482989));
#269420=CARTESIAN_POINT('Ctrl Pts',(32.8197811500191,1.78498277316083,124.858000863516));
#269421=CARTESIAN_POINT('Ctrl Pts',(32.5413335262063,-4.03801408121996,
126.08845136219));
#269422=CARTESIAN_POINT('Ctrl Pts',(32.2628859023933,-6.15027326291425,
131.65259208158));
#269423=CARTESIAN_POINT('Ctrl Pts',(31.9844382785804,-2.6107317735426,136.437249523951));
#269424=CARTESIAN_POINT('Ctrl Pts',(31.7059906547675,3.32794467437699,136.045557243275));
#269425=CARTESIAN_POINT('Ctrl Pts',(31.4275430309546,6.20840254567991,130.837461310262));
#269426=CARTESIAN_POINT('Ctrl Pts',(31.1490954071417,3.3836417748287,125.598947457719));
#269427=CARTESIAN_POINT('Ctrl Pts',(30.8706477833288,-2.55052048699994,
125.143954000505));
#269428=CARTESIAN_POINT('Ctrl Pts',(30.5922001595159,-6.14087902112821,
129.890597698133));
#269429=CARTESIAN_POINT('Ctrl Pts',(30.3137525357031,-4.08806973345779,
135.476944878919));
#269430=CARTESIAN_POINT('Ctrl Pts',(30.0353049118902,1.72147592595096,136.769415391952));
#269431=CARTESIAN_POINT('Ctrl Pts',(29.7568572880773,5.94906930818524,132.58029197645));
#269432=CARTESIAN_POINT('Ctrl Pts',(29.4784096642643,4.70975862438989,126.759174401203));
#269433=CARTESIAN_POINT('Ctrl Pts',(29.1999620404515,-0.857590150719802,
124.65538534046));
#269434=CARTESIAN_POINT('Ctrl Pts',(28.9215144166386,-5.63685547292606,
128.202204165235));
#269435=CARTESIAN_POINT('Ctrl Pts',(28.6430667928257,-5.23612599121204,
134.140277647291));
#269436=CARTESIAN_POINT('Ctrl Pts',(28.3646191690128,-0.0236525225496446,
137.012806347637));
#269437=CARTESIAN_POINT('Ctrl Pts',(28.0861715451999,5.2105564588459,134.180076721482));
#269438=CARTESIAN_POINT('Ctrl Pts',(27.807723921387,5.65651860439647,128.245228908728));
#269439=CARTESIAN_POINT('Ctrl Pts',(27.5292762975741,0.904416488802812,
124.662098115861));
#269440=CARTESIAN_POINT('Ctrl Pts',(27.2508286737613,-4.67880019679877,
126.723406495856));
#269441=CARTESIAN_POINT('Ctrl Pts',(26.9723810499484,-5.96242807363892,
132.53491234801));
#269442=CARTESIAN_POINT('Ctrl Pts',(26.6939334261354,-1.76687583160983,
136.756125702037));
#269443=CARTESIAN_POINT('Ctrl Pts',(26.4154858023226,4.05234898298581,135.507957703324));
#269444=CARTESIAN_POINT('Ctrl Pts',(26.1370381785097,6.14766305047102,129.937413766291));
#269445=CARTESIAN_POINT('Ctrl Pts',(25.8585905546968,2.59357510460964,125.163551632871));
#269446=CARTESIAN_POINT('Ctrl Pts',(25.5801429308839,-3.34388165920016,
125.573317387547));
#269447=CARTESIAN_POINT('Ctrl Pts',(25.301695307071,-6.2084745359058,130.790156319941));
#269448=CARTESIAN_POINT('Ctrl Pts',(25.0232476832582,-3.36778261495664,
136.020048307934));
#269449=CARTESIAN_POINT('Ctrl Pts',(24.7448000594452,2.56773700381057,136.456978108987));
#269450=CARTESIAN_POINT('Ctrl Pts',(24.4663524356323,6.14363175700203,131.69942858114));
#269451=CARTESIAN_POINT('Ctrl Pts',(24.1879048118195,4.07382905860539,126.11935532127));
#269452=CARTESIAN_POINT('Ctrl Pts',(23.9094571880065,-1.73962352703587,
124.844573053462));
#269453=CARTESIAN_POINT('Ctrl Pts',(23.6310095641937,-5.95444707666522,
129.046544405257));
#269454=CARTESIAN_POINT('Ctrl Pts',(23.3525619403807,-4.69742465375045,
134.863862982068));
#269455=CARTESIAN_POINT('Ctrl Pts',(23.0741143165679,0.876301544009003,
136.950697203617));
#269456=CARTESIAN_POINT('Ctrl Pts',(22.795666692755,5.64474943253441,133.389348367819));
#269457=CARTESIAN_POINT('Ctrl Pts',(22.5172190689421,5.22594835390121,127.452522073212));
#269458=CARTESIAN_POINT('Ctrl Pts',(22.2387714451292,0.0047560398029127,
124.595871654449));
#269459=CARTESIAN_POINT('Ctrl Pts',(21.9603238213163,-5.22080684252888,
127.444519291243));
#269460=CARTESIAN_POINT('Ctrl Pts',(21.6818761975034,-5.64870328716988,
133.380696969555));
#269461=CARTESIAN_POINT('Ctrl Pts',(21.4034285736905,-0.885717365398449,
136.949347401415));
#269462=CARTESIAN_POINT('Ctrl Pts',(21.1249809498776,4.69119954547528,134.871055178212));
#269463=CARTESIAN_POINT('Ctrl Pts',(20.8465333260648,5.95713325189572,129.055669322849));
#269464=CARTESIAN_POINT('Ctrl Pts',(20.5680857022518,1.74875252196249,124.847245339011));
#269465=CARTESIAN_POINT('Ctrl Pts',(20.289638078439,-4.06664634434428,126.113119274905));
#269466=CARTESIAN_POINT('Ctrl Pts',(20.011190454626,-6.14499588691713,131.690014824823));
#269467=CARTESIAN_POINT('Ctrl Pts',(19.7327428308132,-2.57639440915122,
136.453037424885));
#269468=CARTESIAN_POINT('Ctrl Pts',(19.4542952070003,3.35978766676044,136.025201992224));
#269469=CARTESIAN_POINT('Ctrl Pts',(19.1758475831874,6.20848901167171,130.799668388532));
#269470=CARTESIAN_POINT('Ctrl Pts',(18.8973999593745,3.3518922564065,125.578446714094));
#269471=CARTESIAN_POINT('Ctrl Pts',(18.6189523355616,-2.58492973345636,
125.159584616859));
#269472=CARTESIAN_POINT('Ctrl Pts',(18.3405047117487,-6.14632757911053,
129.927995901635));
#269473=CARTESIAN_POINT('Ctrl Pts',(18.0620570879358,-4.05955064435711,
135.501743547556));
#269474=CARTESIAN_POINT('Ctrl Pts',(17.7836094641229,1.75775501248606,136.758825760728));
#269475=CARTESIAN_POINT('Ctrl Pts',(17.5051618403101,5.95976968396092,132.544045399129));
#269476=CARTESIAN_POINT('Ctrl Pts',(17.2267142164972,4.68504716681072,126.730579711598));
#269477=CARTESIAN_POINT('Ctrl Pts',(16.9482665926842,-0.8950048193604,124.660719661391));
#269478=CARTESIAN_POINT('Ctrl Pts',(16.6698189688713,-5.65259109995534,
128.236565516362));
#269479=CARTESIAN_POINT('Ctrl Pts',(16.3913713450585,-5.21572230411858,
134.172089625574));
#269480=CARTESIAN_POINT('Ctrl Pts',(16.1129237212456,0.0141404870033325,
137.012835299135));
#269481=CARTESIAN_POINT('Ctrl Pts',(15.8344760974327,5.23100886137047,134.148296041183));
#269482=CARTESIAN_POINT('Ctrl Pts',(15.5560284736198,5.64083564112771,128.210843489254));
#269483=CARTESIAN_POINT('Ctrl Pts',(15.2775808498069,0.8670100368296,124.656706477888));
#269484=CARTESIAN_POINT('Ctrl Pts',(14.999133225994,-4.70355543551987,126.751963291284));
#269485=CARTESIAN_POINT('Ctrl Pts',(14.7206856021811,-5.95178324408404,
132.571175276918));
#269486=CARTESIAN_POINT('Ctrl Pts',(14.4422379783683,-1.73061301211068,
136.766770904302));
#269487=CARTESIAN_POINT('Ctrl Pts',(14.1637903545553,4.08090603284655,135.48320275811));
#269488=CARTESIAN_POINT('Ctrl Pts',(13.8853427307424,6.14227179696077,129.900007258904));
#269489=CARTESIAN_POINT('Ctrl Pts',(13.6068951069296,2.55918984632695,125.147868316191));
#269490=CARTESIAN_POINT('Ctrl Pts',(13.3284474831167,-3.37566254970675,
125.593769463429));
#269491=CARTESIAN_POINT('Ctrl Pts',(13.0499998593037,-6.20844597284355,
130.827949329789));
#269492=CARTESIAN_POINT('Ctrl Pts',(12.7715522354909,-3.33597084638438,
136.04045232199));
#269493=CARTESIAN_POINT('Ctrl Pts',(12.493104611678,2.60209851666622,136.441242835124));
#269494=CARTESIAN_POINT('Ctrl Pts',(12.2146569878651,6.14896646247997,131.662013967328));
#269495=CARTESIAN_POINT('Ctrl Pts',(11.9362093640522,4.04523462298623,126.094643569795));
#269496=CARTESIAN_POINT('Ctrl Pts',(11.6577617402393,-1.77587021433397,
124.855273056695));
#269497=CARTESIAN_POINT('Ctrl Pts',(11.3793141164265,-5.96503708076441,
129.08282338295));
#269498=CARTESIAN_POINT('Ctrl Pts',(11.1008664926135,-4.67262627823404,
134.892382326048));
#269499=CARTESIAN_POINT('Ctrl Pts',(10.8224188688007,0.913699803509421,
136.945249030013));
#269500=CARTESIAN_POINT('Ctrl Pts',(10.5439712449878,5.6603804025445,133.354939282016));
#269501=CARTESIAN_POINT('Ctrl Pts',(10.2655236211749,5.20544793659703,127.420772344084));
#269502=CARTESIAN_POINT('Ctrl Pts',(9.98707599736195,-0.0330368828140487,
124.595957732005));
#269503=CARTESIAN_POINT('Ctrl Pts',(9.70862837354909,-5.24116242086055,
127.476362074414));
#269504=CARTESIAN_POINT('Ctrl Pts',(9.43018074973619,-5.63291573915475,
133.415034496211));
#269505=CARTESIAN_POINT('Ctrl Pts',(9.15173312592329,-0.848294676398009,
136.954625162043));
#269506=CARTESIAN_POINT('Ctrl Pts',(8.87328550211039,4.71586775246963,134.842423168626));
#269507=CARTESIAN_POINT('Ctrl Pts',(8.59483787829755,5.94637809976527,129.019438961107));
#269508=CARTESIAN_POINT('Ctrl Pts',(8.3163902544846,1.71245747009635,124.836710557603));
#269509=CARTESIAN_POINT('Ctrl Pts',(8.03794263067172,-4.09512791639282,
126.137961023291));
#269510=CARTESIAN_POINT('Ctrl Pts',(7.75949500685887,-6.1394908058375,131.727404749824));
#269511=CARTESIAN_POINT('Ctrl Pts',(7.48104738304595,-2.54196157551782,
136.468616012024));
#269512=CARTESIAN_POINT('Ctrl Pts',(7.20259975923305,3.39150616097622,136.004653280976));
#269513=CARTESIAN_POINT('Ctrl Pts',(6.92415213542018,6.20834541982004,130.761875640674));
#269514=CARTESIAN_POINT('Ctrl Pts',(6.64570451160728,3.32001853238404,125.558139618628));
#269515=CARTESIAN_POINT('Ctrl Pts',(6.36725688779438,-2.61924319439064,
125.175424402463));
#269516=CARTESIAN_POINT('Ctrl Pts',(6.08880926398148,-6.15154838266407,
129.965426579154));
#269517=CARTESIAN_POINT('Ctrl Pts',(5.81036164016863,-4.03088112711464,
135.52636815294));
#269518=CARTESIAN_POINT('Ctrl Pts',(5.53191401635571,1.79396896476278,136.748015484609));
#269519=CARTESIAN_POINT('Ctrl Pts',(5.2534663925428,5.97024921827925,132.507734357147));
#269520=CARTESIAN_POINT('Ctrl Pts',(4.97501876872993,4.66016210308585,126.702135977443));
#269521=CARTESIAN_POINT('Ctrl Pts',(4.69657114491704,-0.932386323268277,
124.666281637197));
#269522=CARTESIAN_POINT('Ctrl Pts',(4.41812352110413,-5.66811726814286,
128.27102201808));
#269523=CARTESIAN_POINT('Ctrl Pts',(4.13967589729124,-5.19512534651691,
134.203776811419));
#269524=CARTESIAN_POINT('Ctrl Pts',(3.86122827347838,0.051932972575587,
137.012634193321));
#269525=CARTESIAN_POINT('Ctrl Pts',(3.58278064966546,5.25126742693796,134.116391450127));
#269526=CARTESIAN_POINT('Ctrl Pts',(3.30433302585255,5.62494365461986,128.176554173511));
#269527=CARTESIAN_POINT('Ctrl Pts',(3.02588540203969,0.829571457480427,
124.651542643499));
#269528=CARTESIAN_POINT('Ctrl Pts',(2.74743777822681,-4.72813638226476,
126.780670249786));
#269529=CARTESIAN_POINT('Ctrl Pts',(2.46899015441389,-5.9409178690121,132.607372735859));
#269530=CARTESIAN_POINT('Ctrl Pts',(2.19054253060099,-1.69428606410994,
136.77719516726));
#269531=CARTESIAN_POINT('Ctrl Pts',(1.91209490678813,4.10931186323347,135.458274436681));
#269532=CARTESIAN_POINT('Ctrl Pts',(1.63364728297522,6.13665293931019,129.862634262664));
#269533=CARTESIAN_POINT('Ctrl Pts',(1.35519965916232,2.52470975632363,125.132394602912));
#269534=CARTESIAN_POINT('Ctrl Pts',(1.07675203534945,-3.40731835379603,
125.614414619682));
#269535=CARTESIAN_POINT('Ctrl Pts',(0.798304411536565,-6.20818735353264,
130.86574146555));
#269536=CARTESIAN_POINT('Ctrl Pts',(0.519856787723634,-3.30403546218559,
136.060662310741));
#269537=CARTESIAN_POINT('Ctrl Pts',(0.241409163910791,2.63636360780418,
136.425298684517));
#269538=CARTESIAN_POINT('Ctrl Pts',(-0.0370384599021062,6.15407331574431,
131.624567572855));
#269539=CARTESIAN_POINT('Ctrl Pts',(-0.315486083715014,4.01649028971072,
126.070106338619));
#269540=CARTESIAN_POINT('Ctrl Pts',(-0.593933707527915,-1.81205109610819,
124.866193505555));
#269541=CARTESIAN_POINT('Ctrl Pts',(-0.872381331340776,-5.97540604822092,
129.119166152838));
#269542=CARTESIAN_POINT('Ctrl Pts',(-1.15082895515369,-4.6476547568326,
134.920750186879));
#269543=CARTESIAN_POINT('Ctrl Pts',(-1.42927657896659,0.951064205527318,
136.939573303531));
#269544=CARTESIAN_POINT('Ctrl Pts',(-1.70772420277945,5.67580162507719,
133.320435683583));
#269545=CARTESIAN_POINT('Ctrl Pts',(-1.98617182659235,5.18475462950527,
127.389147995065));
#269546=CARTESIAN_POINT('Ctrl Pts',(-2.26461945040527,-0.0708285812371651,
124.596273864213));
#269547=CARTESIAN_POINT('Ctrl Pts',(-2.54306707421816,-5.26132378599129,
127.508328177794));
#269548=CARTESIAN_POINT('Ctrl Pts',(-2.82151469803103,-5.61691946137538,
133.449275283389));
#269549=CARTESIAN_POINT('Ctrl Pts',(-3.09996232184393,-0.810840553526189,
136.959675022356));
#269550=CARTESIAN_POINT('Ctrl Pts',(-3.37840994565684,4.74036121125036,
134.813641527147));
#269551=CARTESIAN_POINT('Ctrl Pts',(-3.6568575694697,5.93540260240737,128.983274740293));
#269552=CARTESIAN_POINT('Ctrl Pts',(-3.9353051932826,1.6760989624889,124.826396909662));
#269553=CARTESIAN_POINT('Ctrl Pts',(-4.21375281709551,-4.12345774197041,
126.162975686831));
#269554=CARTESIAN_POINT('Ctrl Pts',(-4.49220044090841,-6.13375822366836,
131.764760471086));
#269555=CARTESIAN_POINT('Ctrl Pts',(-4.77064806472125,-2.50743454856317,
136.483984708096));
#269556=CARTESIAN_POINT('Ctrl Pts',(-5.04909568853418,3.4230989816841,135.983911870971));
#269557=CARTESIAN_POINT('Ctrl Pts',(-5.32754331234708,6.20797177544568,
130.724084467112));
#269558=CARTESIAN_POINT('Ctrl Pts',(-5.60599093615995,3.28802178385396,
125.538026923812));
#269559=CARTESIAN_POINT('Ctrl Pts',(-5.88443855997284,-2.65345959830539,
125.191472770368));
#269560=CARTESIAN_POINT('Ctrl Pts',(-6.16288618378574,-6.15654123833006,
130.002888343683));
#269561=CARTESIAN_POINT('Ctrl Pts',(-6.44133380759864,-4.00206224408943,
135.550817782599));
#269562=CARTESIAN_POINT('Ctrl Pts',(-6.71978143141151,1.83011644085978,
136.736984964173));
#269563=CARTESIAN_POINT('Ctrl Pts',(-6.9982290552244,5.98050752281724,132.471360196026));
#269564=CARTESIAN_POINT('Ctrl Pts',(-7.27667667903734,4.63510435534053,
126.673844252731));
#269565=CARTESIAN_POINT('Ctrl Pts',(-7.55512430285017,-0.969733277257762,
124.672071061776));
#269566=CARTESIAN_POINT('Ctrl Pts',(-7.83357192666308,-5.68343340216059,
128.305572393592));
#269567=CARTESIAN_POINT('Ctrl Pts',(-8.112019550476,-5.17433588163501,134.235338030648));
#269568=CARTESIAN_POINT('Ctrl Pts',(-8.39046717428886,0.0897235337524442,
137.012203037646));
#269569=CARTESIAN_POINT('Ctrl Pts',(-8.66891479810176,5.27133140485959,
134.084364130551));
#269570=CARTESIAN_POINT('Ctrl Pts',(-8.94736242191464,5.60884323375645,
128.142362232103));
#269571=CARTESIAN_POINT('Ctrl Pts',(-9.22581004572757,0.792102138056052,
124.646606804043));
#269572=CARTESIAN_POINT('Ctrl Pts',(-9.50425766954039,-4.75254212617725,
126.809526307613));
#269573=CARTESIAN_POINT('Ctrl Pts',(-9.78270529335335,-5.92983235104376,
132.643503383524));
#269574=CARTESIAN_POINT('Ctrl Pts',(-10.0611529171662,-1.65789633371603,
136.787398104638));
#269575=CARTESIAN_POINT('Ctrl Pts',(-10.3396005409791,4.13756542155812,
135.433173662763));
#269576=CARTESIAN_POINT('Ctrl Pts',(-10.618048164792,6.13080668572826,129.82529616244));
#269577=CARTESIAN_POINT('Ctrl Pts',(-10.8964957886049,2.49013611227157,
125.11713106642));
#269578=CARTESIAN_POINT('Ctrl Pts',(-11.1749434124178,-3.4388478984508,
125.635252091294));
#269579=CARTESIAN_POINT('Ctrl Pts',(-11.4533910362307,-6.20769868755626,
130.90353132682));
#269580=CARTESIAN_POINT('Ctrl Pts',(-11.7318386600436,-3.2719776457377,
136.080677525301));
#269581=CARTESIAN_POINT('Ctrl Pts',(-12.0102862838565,2.67053100751937,
136.409146247984));
#269582=CARTESIAN_POINT('Ctrl Pts',(-12.2887339076694,6.15895212755882,
131.587090785312));
#269583=CARTESIAN_POINT('Ctrl Pts',(-12.5671815314823,3.98759712391021,
126.045744536976));
#269584=CARTESIAN_POINT('Ctrl Pts',(-12.8456291552951,-1.84816483166266,
124.877333995382));
#269585=CARTESIAN_POINT('Ctrl Pts',(-13.1240767791081,-5.98555359480885,
129.155571368227));
#269586=CARTESIAN_POINT('Ctrl Pts',(-13.4025244029209,-4.62251101487491,
134.948965513381));
#269587=CARTESIAN_POINT('Ctrl Pts',(-13.6809720267338,0.988393365511613,
136.933670234486));
#269588=CARTESIAN_POINT('Ctrl Pts',(-13.9594196505467,5.69101252869335,
133.285838851062));
#269589=CARTESIAN_POINT('Ctrl Pts',(-14.2378672743596,5.16386919942402,
127.357650198006));
#269590=CARTESIAN_POINT('Ctrl Pts',(-14.5163148981725,-0.108617655081171,
124.59682003936));
#269591=CARTESIAN_POINT('Ctrl Pts',(-14.7947625219854,-5.28129019083405,
127.540416416869));
#269592=CARTESIAN_POINT('Ctrl Pts',(-15.0732101457983,-5.60071504657988,
133.483418062279));
#269593=CARTESIAN_POINT('Ctrl Pts',(-15.3516577696111,-0.77335638465969,
136.96449679523));
#269594=CARTESIAN_POINT('Ctrl Pts',(-15.6301053934241,4.76467901420313,
134.784711320289));
#269595=CARTESIAN_POINT('Ctrl Pts',(-15.908553017237,5.92420716652329,128.947178000488));
#269596=CARTESIAN_POINT('Ctrl Pts',(-16.1870006410499,1.63967834641818,
124.816304777366));
#269597=CARTESIAN_POINT('Ctrl Pts',(-16.4654482648627,-4.15163477130477,
126.188162338596));
#269598=CARTESIAN_POINT('Ctrl Pts',(-16.7438958886757,-6.12779835283271,
131.802080604377));
#269599=CARTESIAN_POINT('Ctrl Pts',(-17.0223435124885,-2.4728146076992,
136.499142943608));
#269600=CARTESIAN_POINT('Ctrl Pts',(-17.3007911363014,3.45456495820035,
135.96297853079));
#269601=CARTESIAN_POINT('Ctrl Pts',(-17.5792387601143,6.20736809239421,
130.686296268213));
#269602=CARTESIAN_POINT('Ctrl Pts',(-17.8576863839272,3.25590319646751,
125.518109374927));
#269603=CARTESIAN_POINT('Ctrl Pts',(-18.13613400774,-2.6875776772989,125.207729125896));
#269604=CARTESIAN_POINT('Ctrl Pts',(-18.414581631553,-6.16130596109642,
130.040379807061));
#269605=CARTESIAN_POINT('Ctrl Pts',(-18.6930292553659,-3.97309506317598,
135.575091530542));
#269606=CARTESIAN_POINT('Ctrl Pts',(-18.9714768791788,1.86619610131902,
136.72573460816));
#269607=CARTESIAN_POINT('Ctrl Pts',(-19.2499245029916,5.99054421744964,
132.434924263623));
#269608=CARTESIAN_POINT('Ctrl Pts',(-19.5283721268046,4.6098748520987,126.645705585822));
#269609=CARTESIAN_POINT('Ctrl Pts',(-19.8068197506174,-1.00704429742433,
124.678087720601));
#269610=CARTESIAN_POINT('Ctrl Pts',(-20.0852673744304,-5.6985389344635,
128.340215362621));
#269611=CARTESIAN_POINT('Ctrl Pts',(-20.3637149982432,-5.15335467983417,
134.266772113748));
#269612=CARTESIAN_POINT('Ctrl Pts',(-20.6421626220562,0.127510770190762,
137.011541848088));
#269613=CARTESIAN_POINT('Ctrl Pts',(-20.920610245869,5.29120005165768,134.05221526924));
#269614=CARTESIAN_POINT('Ctrl Pts',(-21.1990578696819,5.59253497514422,
128.108268932023));
#269615=CARTESIAN_POINT('Ctrl Pts',(-21.4775054934948,0.754603466995427,
124.64189914242));
#269616=CARTESIAN_POINT('Ctrl Pts',(-21.7559531173077,-4.77677176289349,
126.838530395495));
#269617=CARTESIAN_POINT('Ctrl Pts',(-22.0344007411205,-5.91852710095694,
132.679565881077));
#269618=CARTESIAN_POINT('Ctrl Pts',(-22.3128483649335,-1.62144516936395,
136.797379338361));
#269619=CARTESIAN_POINT('Ctrl Pts',(-22.5912959887463,4.16566566087426,
135.407901366475));
#269620=CARTESIAN_POINT('Ctrl Pts',(-22.8697436125593,6.12473325285015,
129.787994341809));
#269621=CARTESIAN_POINT('Ctrl Pts',(-23.1481912363721,2.45547019531011,
125.102078272311));
#269622=CARTESIAN_POINT('Ctrl Pts',(-23.426638860185,-3.47025001533206,
125.656281106122));
#269623=CARTESIAN_POINT('Ctrl Pts',(-23.7050864839979,-6.20697999302203,
130.941317513284));
#269624=CARTESIAN_POINT('Ctrl Pts',(-23.9835341078108,-3.23979858495512,
136.100497223997));
#269625=CARTESIAN_POINT('Ctrl Pts',(-24.2619817316237,2.70459944972584,
136.392786124057));
#269626=CARTESIAN_POINT('Ctrl Pts',(-24.5404293554366,6.16360271713728,
131.549584993415));
#269627=CARTESIAN_POINT('Ctrl Pts',(-24.8188769792495,3.95855619623184,
126.021559067602));
#269628=CARTESIAN_POINT('Ctrl Pts',(-25.0973246030624,-1.88421008278963,
124.88869411336));
#269629=CARTESIAN_POINT('Ctrl Pts',(-25.3757722268753,-5.99547934450715,
129.192037680109));
#269630=CARTESIAN_POINT('Ctrl Pts',(-25.6542198506882,-4.59719598407162,
134.977027260026));
#269631=CARTESIAN_POINT('Ctrl Pts',(-25.932667474501,1.02568590021626,136.92754004162));
#269632=CARTESIAN_POINT('Ctrl Pts',(-26.211115098314,5.7060125497474,133.251150066453));
#269633=CARTESIAN_POINT('Ctrl Pts',(-26.4895627221268,5.14279242027056,
127.326280120068));
#269634=CARTESIAN_POINT('Ctrl Pts',(-26.7680103459397,-0.146402704058008,
124.597596237205));
#269635=CARTESIAN_POINT('Ctrl Pts',(-27.0464579697526,-5.30106089552683,
127.572625602596));
#269636=CARTESIAN_POINT('Ctrl Pts',(-27.3249055935655,-5.58430309522854,
133.517461567711));
#269637=CARTESIAN_POINT('Ctrl Pts',(-27.6033532173784,-0.735843558787732,
136.969090301993));
#269638=CARTESIAN_POINT('Ctrl Pts',(-27.8818008411913,4.78882026022281,
134.755633620073));
#269639=CARTESIAN_POINT('Ctrl Pts',(-28.1602484650042,5.91279220696403,
128.911150079267));
#269640=CARTESIAN_POINT('Ctrl Pts',(-28.4386960888171,1.60319697146318,
124.806434534681));
#269641=CARTESIAN_POINT('Ctrl Pts',(-28.7171437126299,-4.17965796028613,
126.213520045287));
#269642=CARTESIAN_POINT('Ctrl Pts',(-28.9955913364429,-6.12161141417542,
131.839363766787));
#269643=CARTESIAN_POINT('Ctrl Pts',(-29.2740389602557,-2.43810303578058,
136.514090156867));
#269644=CARTESIAN_POINT('Ctrl Pts',(-29.5524865840687,3.48590292454168,
135.941854036124));
#269645=CARTESIAN_POINT('Ctrl Pts',(-29.8309342078815,6.20653439303521,
130.648512444231));
#269646=CARTESIAN_POINT('Ctrl Pts',(-30.1093818316944,3.22366396039099,
125.498387710026));
#269647=CARTESIAN_POINT('Ctrl Pts',(-30.3878294555073,-2.72159616711309,
125.224192866663));
#269648=CARTESIAN_POINT('Ctrl Pts',(-30.6662770793202,-6.16584237440457,
130.077899580028));
#269649=CARTESIAN_POINT('Ctrl Pts',(-30.9447247031331,-3.94398065776386,
135.599188497297));
#269650=CARTESIAN_POINT('Ctrl Pts',(-31.2231723269461,1.90220660919519,
136.714264833456));
#269651=CARTESIAN_POINT('Ctrl Pts',(-31.5016199507588,6.00035893026297,
132.398427910084));
#269652=CARTESIAN_POINT('Ctrl Pts',(-31.7800675745718,4.58447452824918,
126.617721019404));
#269653=CARTESIAN_POINT('Ctrl Pts',(-32.0585151983846,-1.04431800119413,
124.68433139072));
#269654=CARTESIAN_POINT('Ctrl Pts',(-32.3369628221976,-5.71343330531054,
128.374949641459));
#269655=CARTESIAN_POINT('Ctrl Pts',(-32.6154104460104,-5.1321825185805,
134.298077895915));
#269656=CARTESIAN_POINT('Ctrl Pts',(-32.8938580698234,0.165293281670594,
137.010650649146));
#269657=CARTESIAN_POINT('Ctrl Pts',(-33.1723056936362,5.31087263109202,
134.019946057479));
#269658=CARTESIAN_POINT('Ctrl Pts',(-33.4507533174492,5.57601948309184,
128.074275536613));
#269659=CARTESIAN_POINT('Ctrl Pts',(-33.729200941262,0.717076833825826,
124.637419833072));
#269660=CARTESIAN_POINT('Ctrl Pts',(-34.0076485650749,-4.80082439457541,
126.867681438675));
#269661=CARTESIAN_POINT('Ctrl Pts',(-34.2860961888878,-5.90700253767186,
132.715558892209));
#269662=CARTESIAN_POINT('Ctrl Pts',(-34.5645438127007,-1.58493392176466,
136.807138498572));
#269663=CARTESIAN_POINT('Ctrl Pts',(-34.8429914365135,4.19361153991761,
135.382458484293));
#269664=CARTESIAN_POINT('Ctrl Pts',(-35.1214390603265,6.11843286572883,
129.750730183006));
#269665=CARTESIAN_POINT('Ctrl Pts',(-35.3998866841394,2.42071328999757,
125.087236778371));
#269666=CARTESIAN_POINT('Ctrl Pts',(-35.6783343079523,-3.50152354082281,
125.677500884929));
#269667=CARTESIAN_POINT('Ctrl Pts',(-35.9567819317651,-6.20603129656164,
130.979098624759));
#269668=CARTESIAN_POINT('Ctrl Pts',(-36.2352295555781,-3.2074994722443,
136.120120672404));
#269669=CARTESIAN_POINT('Ctrl Pts',(-36.5136771793909,2.73856767200523,
136.376218918968));
#269670=CARTESIAN_POINT('Ctrl Pts',(-36.7921248032039,6.1680249121504,131.512051586954));
#269671=CARTESIAN_POINT('Ctrl Pts',(-37.0705724270167,3.92936858279784,
125.997550826698));
#269672=CARTESIAN_POINT('Ctrl Pts',(-37.3490200508296,-1.92018551381882,
124.900273438536));
#269673=CARTESIAN_POINT('Ctrl Pts',(-37.6274676746425,-6.00518292951342,
129.228563737208));
#269674=CARTESIAN_POINT('Ctrl Pts',(-37.9059152984554,-4.57171060248077,
135.004934386972));
#269675=CARTESIAN_POINT('Ctrl Pts',(-38.1843629222683,1.0629404277527,136.921182952087));
#269676=CARTESIAN_POINT('Ctrl Pts',(-38.4628105460811,5.72080113240803,
133.216370615161));
#269677=CARTESIAN_POINT('Ctrl Pts',(-38.7412581698941,5.12152507305273,
127.295038923683));
#269678=CARTESIAN_POINT('Ctrl Pts',(-39.0197057937069,-0.184182328028525,
124.598602428988));
#269679=CARTESIAN_POINT('Ctrl Pts',(-39.2981534175199,-5.32063516745863,
127.604954541453));
#269680=CARTESIAN_POINT('Ctrl Pts',(-39.5766010413327,-5.56768421547239,
133.55140453819));
#269681=CARTESIAN_POINT('Ctrl Pts',(-39.8550486651457,-0.698303465962086,
136.973455372429));
#269682=CARTESIAN_POINT('Ctrl Pts',(-40.1334962889585,4.81278405474664,
134.726409503982));
#269683=CARTESIAN_POINT('Ctrl Pts',(-40.4119439127715,5.90115814671511,
128.875192311658));
#269684=CARTESIAN_POINT('Ctrl Pts',(-40.6903915365843,1.56665618945481,
124.796786547352));
#269685=CARTESIAN_POINT('Ctrl Pts',(-40.9688391603973,-4.20752627050468,
126.239047867263));
#269686=CARTESIAN_POINT('Ctrl Pts',(-41.2472867842101,-6.11519763695597,
131.876608576776));
#269687=CARTESIAN_POINT('Ctrl Pts',(-41.5257344080229,-2.40330111905734,
136.528825793999));
#269688=CARTESIAN_POINT('Ctrl Pts',(-41.8041820318359,3.51711171946819,
135.920539169751));
#269689=CARTESIAN_POINT('Ctrl Pts',(-42.0826296556488,6.20547070826194,
130.610734395262));
#269690=CARTESIAN_POINT('Ctrl Pts',(-42.3610772794617,3.19130527026066,
125.478862659902));
#269691=CARTESIAN_POINT('Ctrl Pts',(-42.6395249032745,-2.75551380718057,
125.240863382598));
#269692=CARTESIAN_POINT('Ctrl Pts',(-42.9179725270875,-6.17015031015604,
130.115446272278));
#269693=CARTESIAN_POINT('Ctrl Pts',(-43.1964201509003,-3.91472010669807,
135.623107789941));
#269694=CARTESIAN_POINT('Ctrl Pts',(-43.4748677747133,1.93814663010615,
136.702576065077));
#269695=CARTESIAN_POINT('Ctrl Pts',(-43.7533153985261,6.00995129756958,
132.361872487794));
#269696=CARTESIAN_POINT('Ctrl Pts',(-44.031763022339,4.55890432500984,126.589891590455));
#269697=CARTESIAN_POINT('Ctrl Pts',(-44.3102106461518,-1.08155300737633,
124.690801840773));
#269698=CARTESIAN_POINT('Ctrl Pts',(-44.5886582699649,-5.72811596278534,
128.409773943013));
#269699=CARTESIAN_POINT('Ctrl Pts',(-44.8671058937777,-5.11082018241628,
134.329254217104));
#269700=CARTESIAN_POINT('Ctrl Pts',(-45.1455535175906,0.2030696681468,137.009529473845));
#269701=CARTESIAN_POINT('Ctrl Pts',(-45.4240011414034,5.33034841418793,
133.987557691017));
#269702=CARTESIAN_POINT('Ctrl Pts',(-45.7024487652165,5.55929736958694,
128.040383305508));
#269703=CARTESIAN_POINT('Ctrl Pts',(-45.9808963890292,0.679523629110432,
124.633169041983));
#269704=CARTESIAN_POINT('Ctrl Pts',(-46.2593440128422,-4.82469912994364,
126.896978356949));
#269705=CARTESIAN_POINT('Ctrl Pts',(-46.537791636655,-5.89525908823553,
132.751481083186));
#269706=CARTESIAN_POINT('Ctrl Pts',(-46.816239260468,-1.54836394385628,
136.816675223641));
#269707=CARTESIAN_POINT('Ctrl Pts',(-47.0946868842807,4.22140202314317,
135.35684595901));
#269708=CARTESIAN_POINT('Ctrl Pts',(-47.3731345080937,6.11190575782758,
129.713505066864));
#269709=CARTESIAN_POINT('Ctrl Pts',(-47.6515821319066,2.38586668426401,
125.072607134557));
#269710=CARTESIAN_POINT('Ctrl Pts',(-47.9300297557195,-3.53266731607082,
125.69891064141));
#269711=CARTESIAN_POINT('Ctrl Pts',(-48.2084773795324,-6.20485263332943,
131.016873261253));
#269712=CARTESIAN_POINT('Ctrl Pts',(-48.4869250033452,-3.17508150446096,
136.139547143367));
#269713=CARTESIAN_POINT('Ctrl Pts',(-48.7653726271582,2.77243441565242,
136.359445246621));
#269714=CARTESIAN_POINT('Ctrl Pts',(-49.043820250971,6.1722185487321,131.474491956744));
#269715=CARTESIAN_POINT('Ctrl Pts',(-49.322267874784,3.900035365166,125.973720703898));
#269716=CARTESIAN_POINT('Ctrl Pts',(-49.6007154985968,-1.95608979166789,
124.912071541833));
#269717=CARTESIAN_POINT('Ctrl Pts',(-49.8791631224098,-6.0146639902579,
129.265148186042));
#269718=CARTESIAN_POINT('Ctrl Pts',(-50.1576107462225,-4.54605581447205,
135.032685860113));
#269719=CARTESIAN_POINT('Ctrl Pts',(-50.4360583700356,1.10015556764067,
136.914599201455));
#269720=CARTESIAN_POINT('Ctrl Pts',(-50.7145059938484,5.73537772867887,
133.181501785951));
#269721=CARTESIAN_POINT('Ctrl Pts',(-50.9929536176612,5.10006794583985,
127.263927766504));
#269722=CARTESIAN_POINT('Ctrl Pts',(-51.2714012414742,-0.221955127055423,
124.599838577421));
#269723=CARTESIAN_POINT('Ctrl Pts',(-51.5498488652871,-5.34001228129766,
127.637402035479));
#269724=CARTESIAN_POINT('Ctrl Pts',(-51.8282964891,-5.5508590231301,133.585245715947));
#269725=CARTESIAN_POINT('Ctrl Pts',(-52.1067441129128,-0.660737497244709,
136.977591844792));
#269726=CARTESIAN_POINT('Ctrl Pts',(-52.3851917367258,4.8365695097872,134.697040054928));
#269727=CARTESIAN_POINT('Ctrl Pts',(-52.6636393605386,5.889305416881,128.83930603009));
#269728=CARTESIAN_POINT('Ctrl Pts',(-52.9420869843516,1.53005735442545,
124.78736117289));
#269729=CARTESIAN_POINT('Ctrl Pts',(-53.2205346081644,-4.23523866929,126.264744858582));
#269730=CARTESIAN_POINT('Ctrl Pts',(-53.4989822319774,-6.1085572588392,
131.913813654221));
#269731=CARTESIAN_POINT('Ctrl Pts',(-53.7774298557902,-2.36841014712749,
136.543349308967));
#269732=CARTESIAN_POINT('Ctrl Pts',(-54.0558774796031,3.54819018652628,
135.8990347215));
#269733=CARTESIAN_POINT('Ctrl Pts',(-54.334325103416,6.20417707748961,130.572963521183));
#269734=CARTESIAN_POINT('Ctrl Pts',(-54.6127727272289,3.15882832513996,
125.459534948064));
#269735=CARTESIAN_POINT('Ctrl Pts',(-54.8912203510417,-2.7893293406706,
125.257740055968));
#269736=CARTESIAN_POINT('Ctrl Pts',(-55.1696679748547,-6.17422960871856,
130.153018492501));
#269737=CARTESIAN_POINT('Ctrl Pts',(-55.4481155986676,-3.88531449423931,
135.646848522136));
#269738=CARTESIAN_POINT('Ctrl Pts',(-55.7265632224805,1.97401483228084,
136.690668736158));
#269739=CARTESIAN_POINT('Ctrl Pts',(-56.0050108462934,6.01932096392068,
132.32525935133));
#269740=CARTESIAN_POINT('Ctrl Pts',(-56.2834584701062,4.53316518989421,
126.562218330207));
#269741=CARTESIAN_POINT('Ctrl Pts',(-56.5619060939192,-1.11874793621411,
124.697498830995));
#269742=CARTESIAN_POINT('Ctrl Pts',(-56.840353717732,-5.74258636281662,
128.444686976857));
#269743=CARTESIAN_POINT('Ctrl Pts',(-57.118801341545,-5.08926846293066,
134.360299922064));
#269744=CARTESIAN_POINT('Ctrl Pts',(-57.3972489653578,0.240838529802063,
137.00817836373));
#269745=CARTESIAN_POINT('Ctrl Pts',(-57.6756965891708,5.34962667926312,
133.955051370017));
#269746=CARTESIAN_POINT('Ctrl Pts',(-57.9541442129836,5.54236925427356,
128.0065934946));
#269747=CARTESIAN_POINT('Ctrl Pts',(-58.2325918367966,0.641945244397073,
124.629146926667));
#269748=CARTESIAN_POINT('Ctrl Pts',(-58.5110394606094,-4.84839508431156,
126.92642006471));
#269749=CARTESIAN_POINT('Ctrl Pts',(-58.7894870844223,-5.88329718780563,
132.787331122898));
#269750=CARTESIAN_POINT('Ctrl Pts',(-59.0679347082352,-1.5117365907523,
136.825989160181));
#269751=CARTESIAN_POINT('Ctrl Pts',(-59.3463823320481,4.24903608076433,
135.331064739709));
#269752=CARTESIAN_POINT('Ctrl Pts',(-59.624829955861,6.10515217101086,129.676320372777));
#269753=CARTESIAN_POINT('Ctrl Pts',(-59.9032775796738,2.3509316693629,125.058189882977));
#269754=CARTESIAN_POINT('Ctrl Pts',(-60.1817252034868,-3.56368018703254,
125.720509582217));
#269755=CARTESIAN_POINT('Ctrl Pts',(-60.4601728272995,-6.20344404700091,
131.054640023013));
#269756=CARTESIAN_POINT('Ctrl Pts',(-60.7386204511126,-3.14254588286485,
136.158775917031));
#269757=CARTESIAN_POINT('Ctrl Pts',(-61.0170680749254,2.80619842572279,
136.342465728569));
#269758=CARTESIAN_POINT('Ctrl Pts',(-61.2955156987383,6.17618347148551,
131.436907494571));
#269759=CARTESIAN_POINT('Ctrl Pts',(-61.5739633225512,3.87055763028967,
125.950069582238));
#269760=CARTESIAN_POINT('Ctrl Pts',(-61.8524109463641,-1.9919215858902,
124.924087986069));
#269761=CARTESIAN_POINT('Ctrl Pts',(-62.130858570177,-6.02392217541635,
129.301789670958));
#269762=CARTESIAN_POINT('Ctrl Pts',(-62.4093061939898,-4.5202325706933,
135.060280651108));
#269763=CARTESIAN_POINT('Ctrl Pts',(-62.6877538178028,1.13732994085927,
136.907789033684));
#269764=CARTESIAN_POINT('Ctrl Pts',(-62.9662014416156,5.74974179841868,
133.146544870902));
#269765=CARTESIAN_POINT('Ctrl Pts',(-63.2446490654287,5.0784218337339,127.232947801366));
#269766=CARTESIAN_POINT('Ctrl Pts',(-63.5230966892413,-0.25971970145348,
124.601304636701));
#269767=CARTESIAN_POINT('Ctrl Pts',(-63.8015443130544,-5.3591915190178,
127.669966882319));
#269768=CARTESIAN_POINT('Ctrl Pts',(-64.0799919368672,-5.53382814166538,
133.618983846983));
#269769=CARTESIAN_POINT('Ctrl Pts',(-64.3584395606801,-0.623147044656387,
136.9814995658));
#269770=CARTESIAN_POINT('Ctrl Pts',(-64.636887184493,4.86017574396616,134.667526361205));
#269771=CARTESIAN_POINT('Ctrl Pts',(-64.9153348083059,5.8772344566688,128.803492564343));
#269772=CARTESIAN_POINT('Ctrl Pts',(-65.1937824321189,1.4934018225579,124.778158760555));
#269773=CARTESIAN_POINT('Ctrl Pts',(-65.4722300559316,-4.26279412974889,
126.290610067033));
#269774=CARTESIAN_POINT('Ctrl Pts',(-65.7506776797446,-6.10169052588679,
131.950977620477));
#269775=CARTESIAN_POINT('Ctrl Pts',(-66.0291253035574,-2.33343141288849,
136.5576601636));
#269776=CARTESIAN_POINT('Ctrl Pts',(-66.3075729273703,3.57913717409239,
135.877341488227));
#269777=CARTESIAN_POINT('Ctrl Pts',(-66.5860205511832,6.20265354865397,
130.535201221608));
#269778=CARTESIAN_POINT('Ctrl Pts',(-66.8644681749961,3.126234328474,125.440405290707));
#269779=CARTESIAN_POINT('Ctrl Pts',(-67.142915798809,-2.82304151453613,
125.274822261403));
#269780=CARTESIAN_POINT('Ctrl Pts',(-67.421363422622,-6.17808011893247,
130.190614848446));
#269781=CARTESIAN_POINT('Ctrl Pts',(-67.6998110464348,-3.85576491002292,
135.670409814162));
#269782=CARTESIAN_POINT('Ctrl Pts',(-67.9782586702478,2.00980988661012,
136.678543287925));
#269783=CARTESIAN_POINT('Ctrl Pts',(-68.2567062940606,6.02846758211988,
132.288589857404));
#269784=CARTESIAN_POINT('Ctrl Pts',(-68.5351539178734,4.50725807667536,
126.534702264101));
#269785=CARTESIAN_POINT('Ctrl Pts',(-68.8136015416864,-1.15590140943545,
124.704422113226));
#269786=CARTESIAN_POINT('Ctrl Pts',(-69.0920491654993,-5.75684396919829,
128.479687449276));
#269787=CARTESIAN_POINT('Ctrl Pts',(-69.3704967893121,-5.0675281587308,
134.391213860386));
#269788=CARTESIAN_POINT('Ctrl Pts',(-69.648944413125,0.278598467097045,
137.006597368867));
#269789=CARTESIAN_POINT('Ctrl Pts',(-69.9273920369379,5.36870671195437,
133.922428299012));
#269790=CARTESIAN_POINT('Ctrl Pts',(-70.2058396607509,5.52523576442926,
127.972907355982));
#269791=CARTESIAN_POINT('Ctrl Pts',(-70.4842872845636,0.604343072166899,
124.625353636165));
#269792=CARTESIAN_POINT('Ctrl Pts',(-70.7627349083767,-4.87191137961658,
126.956005470983));
#269793=CARTESIAN_POINT('Ctrl Pts',(-71.0411825321895,-5.87111727963483,
132.823107682909));
#269794=CARTESIAN_POINT('Ctrl Pts',(-71.3196301560023,-1.47505321969301,
136.835079963061));
#269795=CARTESIAN_POINT('Ctrl Pts',(-71.5980777798154,4.27651268879093,
135.305115781721));
#269796=CARTESIAN_POINT('Ctrl Pts',(-71.8765254036282,6.09817235553532,
129.639177478635));
#269797=CARTESIAN_POINT('Ctrl Pts',(-72.1549730274411,2.31590953982396,
125.043985557866));
#269798=CARTESIAN_POINT('Ctrl Pts',(-72.433420651254,-3.5945610045145,125.742296906994));
#269799=CARTESIAN_POINT('Ctrl Pts',(-72.7118682750669,-6.20180558977201,
131.092397510578));
#269800=CARTESIAN_POINT('Ctrl Pts',(-72.9903158988798,-3.109893813075,136.177806280867));
#269801=CARTESIAN_POINT('Ctrl Pts',(-73.2687635226926,2.8398584510789,136.325280993997));
#269802=CARTESIAN_POINT('Ctrl Pts',(-73.5472111465057,6.17991953348924,
131.399299593141));
#269803=CARTESIAN_POINT('Ctrl Pts',(-73.8256587703184,3.84093647047644,
125.926598338115));
#269804=CARTESIAN_POINT('Ctrl Pts',(-74.1041063941314,-2.02767956872624,
124.93632232597));
#269805=CARTESIAN_POINT('Ctrl Pts',(-74.3825540179442,-6.0329571419232,
129.338486834193));
#269806=CARTESIAN_POINT('Ctrl Pts',(-74.6610016417573,-4.49424182803428,
135.08771773742));
#269807=CARTESIAN_POINT('Ctrl Pts',(-74.9394492655699,1.17446216989917,
136.900752701129));
#269808=CARTESIAN_POINT('Ctrl Pts',(-75.217896889383,5.76389280936176,133.111501165354));
#269809=CARTESIAN_POINT('Ctrl Pts',(-75.4963445131958,5.05658753883907,
127.202100176243));
#269810=CARTESIAN_POINT('Ctrl Pts',(-75.7747921370087,-0.297474651842549,
124.603000552501));
#269811=CARTESIAN_POINT('Ctrl Pts',(-76.0532397608216,-5.37817216992523,
127.702647875272));
#269812=CARTESIAN_POINT('Ctrl Pts',(-76.3316873846344,-5.51659220216403,
133.65261768112));
#269813=CARTESIAN_POINT('Ctrl Pts',(-76.6101350084474,-0.585533501125347,
136.985178390654));
#269814=CARTESIAN_POINT('Ctrl Pts',(-76.8885826322602,4.8836018825454,134.637869516455));
#269815=CARTESIAN_POINT('Ctrl Pts',(-77.1670302560731,5.86494571337264,
128.767753241497));
#269816=CARTESIAN_POINT('Ctrl Pts',(-77.4454778798861,1.4566909521364,124.769179651345));
#269817=CARTESIAN_POINT('Ctrl Pts',(-77.7239255036988,-4.29019163080361,
126.316642534169));
#269818=CARTESIAN_POINT('Ctrl Pts',(-78.0023731275119,-6.09459769254796,
131.988099098418));
#269819=CARTESIAN_POINT('Ctrl Pts',(-78.2808207513247,-2.29836621249045,
136.571757827603));
#269820=CARTESIAN_POINT('Ctrl Pts',(-78.5592683751376,3.60995153541429,
135.855460273781));
#269821=CARTESIAN_POINT('Ctrl Pts',(-78.8377159989505,6.20090017820995,
130.497448895834));
#269822=CARTESIAN_POINT('Ctrl Pts',(-79.1161636227633,3.09352448804556,
125.421474396687));
#269823=CARTESIAN_POINT('Ctrl Pts',(-79.3946112465763,-2.85664907955992,
125.292109365916));
#269824=CARTESIAN_POINT('Ctrl Pts',(-79.6730588703891,-6.18170169811556,
130.228233946967));
#269825=CARTESIAN_POINT('Ctrl Pts',(-79.9515064942021,-3.8260724490201,
135.693790792945));
#269826=CARTESIAN_POINT('Ctrl Pts',(-80.2299541180149,2.04553046669522,
136.666200169693));
#269827=CARTESIAN_POINT('Ctrl Pts',(-80.5084017418279,6.03739081323573,
132.251865364817));
#269828=CARTESIAN_POINT('Ctrl Pts',(-80.7868493656406,4.48118394535095,
126.507344411756));
#269829=CARTESIAN_POINT('Ctrl Pts',(-81.0652969894537,-1.19301205030527,
124.711571430921));
#269830=CARTESIAN_POINT('Ctrl Pts',(-81.3437446132665,-5.77088825360962,
128.514774063314));
#269831=CARTESIAN_POINT('Ctrl Pts',(-81.6221922370794,-5.04560007541116,
134.421994886542));
#269832=CARTESIAN_POINT('Ctrl Pts',(-81.9006398608923,0.316348080823153,
137.00478654784));
#269833=CARTESIAN_POINT('Ctrl Pts',(-82.179087484705,5.38758780524389,133.889689686862));
#269834=CARTESIAN_POINT('Ctrl Pts',(-82.4575351085182,5.50789753494193,
127.939326137905));
#269835=CARTESIAN_POINT('Ctrl Pts',(-82.7359827323308,0.566718505781886,
124.621789311041));
#269836=CARTESIAN_POINT('Ctrl Pts',(-83.0144303561439,-4.89524714445407,
126.985733479472));
#269837=CARTESIAN_POINT('Ctrl Pts',(-83.2928779799568,-5.858719815054,132.858809437506));
#269838=CARTESIAN_POINT('Ctrl Pts',(-83.5713256037696,-1.43831518999427,
136.843947295418));
#269839=CARTESIAN_POINT('Ctrl Pts',(-83.8497732275826,4.30383082906709,
135.279000046597));
#269840=CARTESIAN_POINT('Ctrl Pts',(-84.1282208513953,6.09096657004034,
129.602077760783));
#269841=CARTESIAN_POINT('Ctrl Pts',(-84.4066684752085,2.28080159340614,
125.029994685571));
#269842=CARTESIAN_POINT('Ctrl Pts',(-84.685116099021,-3.6253086242162,125.764271808403));
#269843=CARTESIAN_POINT('Ctrl Pts',(-84.9635637228342,-6.19993732235617,
131.130144324829));
#269844=CARTESIAN_POINT('Ctrl Pts',(-85.242011346647,-3.07712650502686,
136.196637529698));
#269845=CARTESIAN_POINT('Ctrl Pts',(-85.5204589704598,2.87341324443482,
136.307891679689));
#269846=CARTESIAN_POINT('Ctrl Pts',(-85.7989065942728,6.18342659630218,
131.361669646028));
#269847=CARTESIAN_POINT('Ctrl Pts',(-86.0773542180856,3.81117298335027,
125.903307841269));
#269848=CARTESIAN_POINT('Ctrl Pts',(-86.3558018418987,-2.06336241514917,
124.948774108188));
#269849=CARTESIAN_POINT('Ctrl Pts',(-86.6342494657113,-6.04176855498474,
129.375238315919));
#269850=CARTESIAN_POINT('Ctrl Pts',(-86.9126970895244,-4.46808454959173,
135.114996102359));
#269851=CARTESIAN_POINT('Ctrl Pts',(-87.1911447133372,1.2115508788106,136.893490464523));
#269852=CARTESIAN_POINT('Ctrl Pts',(-87.4695923371502,5.77783023713722,
133.076371967865));
#269853=CARTESIAN_POINT('Ctrl Pts',(-87.7480399609628,5.03456587023344,
127.171386034204));
#269854=CARTESIAN_POINT('Ctrl Pts',(-88.026487584776,-0.33521857919891,
124.60492626198));
#269855=CARTESIAN_POINT('Ctrl Pts',(-88.3049352085887,-5.39695353068522,
127.735443803332));
#269856=CARTESIAN_POINT('Ctrl Pts',(-88.5833828324018,-5.49915184330967,
133.686145972045));
#269857=CARTESIAN_POINT('Ctrl Pts',(-88.8618304562145,-0.547898260434929,
136.988628183031));
#269858=CARTESIAN_POINT('Ctrl Pts',(-89.1402780800275,4.90684705746115,
134.608070619623));
#269859=CARTESIAN_POINT('Ctrl Pts',(-89.4187257038403,5.85243964235601,
128.732089385887));
#269860=CARTESIAN_POINT('Ctrl Pts',(-89.6971733276532,1.41992610349655,
124.760424177987));
#269861=CARTESIAN_POINT('Ctrl Pts',(-89.9756209514662,-4.31743015722937,
126.342841295349));
#269862=CARTESIAN_POINT('Ctrl Pts',(-90.254068575279,-6.08727902165076,
132.025176712493));
#269863=CARTESIAN_POINT('Ctrl Pts',(-90.5325161990919,-2.26321584528708,
136.585641778581));
#269864=CARTESIAN_POINT('Ctrl Pts',(-90.8109638229048,3.64063212865448,
135.833391888981));
#269865=CARTESIAN_POINT('Ctrl Pts',(-91.0894114467178,6.19891703112955,
130.459707942787));
#269866=CARTESIAN_POINT('Ctrl Pts',(-91.3678590705306,3.06070001592934,
125.402742967496));
#269867=CARTESIAN_POINT('Ctrl Pts',(-91.6463066943433,-2.89015079040179,
125.309600728926));
#269868=CARTESIAN_POINT('Ctrl Pts',(-91.9247543181566,-6.18509421206894,
130.265874394073));
#269869=CARTESIAN_POINT('Ctrl Pts',(-92.2032019419691,-3.79623821149537,
135.716990592095));
#269870=CARTESIAN_POINT('Ctrl Pts',(-92.4816495657822,2.08117524889636,
136.653639838841));
#269871=CARTESIAN_POINT('Ctrl Pts',(-92.7600971895951,6.04609032661485,
132.21508723441));
#269872=CARTESIAN_POINT('Ctrl Pts',(-93.0385448134079,4.45494376210749,
126.480145786926));
#269873=CARTESIAN_POINT('Ctrl Pts',(-93.3169924372209,-1.23007848367479,
124.718946519161));
#269874=CARTESIAN_POINT('Ctrl Pts',(-93.5954400610337,-5.78471869563455,
128.549945518824));
#269875=CARTESIAN_POINT('Ctrl Pts',(-93.8738876848466,-5.02348502552524,
134.45264185993));
#269876=CARTESIAN_POINT('Ctrl Pts',(-94.1523353086595,0.354085972155003,
137.002745967751));
#269877=CARTESIAN_POINT('Ctrl Pts',(-94.4307829324724,5.40626925948619,
133.85683674671));
#269878=CARTESIAN_POINT('Ctrl Pts',(-94.7092305562852,5.49035520828578,
127.905851084735));
#269879=CARTESIAN_POINT('Ctrl Pts',(-94.9876781800983,0.529072939433998,
124.618454083368));
#269880=CARTESIAN_POINT('Ctrl Pts',(-95.2661258039109,-4.91840151410816,
127.015602988595));
#269881=CARTESIAN_POINT('Ctrl Pts',(-95.5445734277241,-5.84610525345601,
132.894435063746));
#269882=CARTESIAN_POINT('Ctrl Pts',(-95.8230210515366,-1.40152386299717,
136.85259082867));
#269883=CARTESIAN_POINT('Ctrl Pts',(-96.10146867535,4.33098948930923,135.252718502061));
#269884=CARTESIAN_POINT('Ctrl Pts',(-96.3799162991623,6.08353508153927,
129.565022593965));
#269885=CARTESIAN_POINT('Ctrl Pts',(-96.6583639229758,2.245609131046,125.01621778453));
#269886=CARTESIAN_POINT('Ctrl Pts',(-96.9368115467883,-3.65592190677386,
125.786433472156));
#269887=CARTESIAN_POINT('Ctrl Pts',(-97.2152591706015,-6.19783931398261,
131.167879067045));
#269888=CARTESIAN_POINT('Ctrl Pts',(-97.493706794414,-3.04424517292474,
136.215268965725));
#269889=CARTESIAN_POINT('Ctrl Pts',(-97.7721544182274,2.90686156240656,
136.290298430015));
#269890=CARTESIAN_POINT('Ctrl Pts',(-98.0506020420397,6.18670452996842,
131.324019047625));
#269891=CARTESIAN_POINT('Ctrl Pts',(-98.3290496658531,3.78126827180747,
125.880198954735));
#269892=CARTESIAN_POINT('Ctrl Pts',(-98.6074972896656,-2.09896880291958,
124.961442871316));
#269893=CARTESIAN_POINT('Ctrl Pts',(-98.8859449134787,-6.05035608809047,
129.412042754299));
#269894=CARTESIAN_POINT('Ctrl Pts',(-99.1643925372916,-4.44176170463296,
135.142114735114));
#269895=CARTESIAN_POINT('Ctrl Pts',(-99.4428401611044,1.24859469325925,
136.886002592972));
#269896=CARTESIAN_POINT('Ctrl Pts',(-99.7212877849174,5.79155356528836,
133.041158580159));
#269897=CARTESIAN_POINT('Ctrl Pts',(-99.9997354087301,5.01235764393804,
127.140806513377));
#269898=CARTESIAN_POINT('Ctrl Pts',(-100.278183032543,-0.37295008490757,
124.607081693777));
#269899=CARTESIAN_POINT('Ctrl Pts',(-100.556630656356,-5.41553490534739,
127.768353451233));
#269900=CARTESIAN_POINT('Ctrl Pts',(-100.835078280169,-5.48150771136145,
133.719567477352));
#269901=CARTESIAN_POINT('Ctrl Pts',(-101.113525903981,-0.510242717172956,
136.9918488151));
#269902=CARTESIAN_POINT('Ctrl Pts',(-101.391973527794,4.92991040735466,
134.578130774917));
#269903=CARTESIAN_POINT('Ctrl Pts',(-101.670421151607,5.83971670703623,
128.696502319049));
#269904=CARTESIAN_POINT('Ctrl Pts',(-101.94886877542,1.38310863897239,124.751892664915));
#269905=CARTESIAN_POINT('Ctrl Pts',(-102.227316399233,-4.34450869969331,
126.36920537977));
#269906=CARTESIAN_POINT('Ctrl Pts',(-102.505764023046,-6.07973478439049,
132.062209088779));
#269907=CARTESIAN_POINT('Ctrl Pts',(-102.784211646859,-2.22798161378826,
136.599311502058));
#269908=CARTESIAN_POINT('Ctrl Pts',(-103.062659270672,3.6711778169323,135.811137151577));
#269909=CARTESIAN_POINT('Ctrl Pts',(-103.341106894485,6.19670418089893,
130.42197976097));
#269910=CARTESIAN_POINT('Ctrl Pts',(-103.619554518298,3.02776212844844,
125.384211697232));
#269911=CARTESIAN_POINT('Ctrl Pts',(-103.89800214211,-2.92354540564323,
125.327295702285));
#269912=CARTESIAN_POINT('Ctrl Pts',(-104.176449765923,-6.18825753508174,
130.303534794984));
#269913=CARTESIAN_POINT('Ctrl Pts',(-104.454897389736,-3.76626330296762,
135.740008351935));
#269914=CARTESIAN_POINT('Ctrl Pts',(-104.733345013549,2.1167429123828,136.640862760796));
#269915=CARTESIAN_POINT('Ctrl Pts',(-105.011792637362,6.05456579989334,
132.17825682901));
#269916=CARTESIAN_POINT('Ctrl Pts',(-105.290240261175,4.42853849928509,
126.453107397468));
#269917=CARTESIAN_POINT('Ctrl Pts',(-105.568687884988,-1.26709933603374,
124.726547104658));
#269918=CARTESIAN_POINT('Ctrl Pts',(-105.847135508801,-5.79833478278087,
128.585200512514));
#269919=CARTESIAN_POINT('Ctrl Pts',(-106.125583132613,-5.00118382855433,
134.483153644914));
#269920=CARTESIAN_POINT('Ctrl Pts',(-106.404030756427,0.391810742700936,
137.000475704212));
#269921=CARTESIAN_POINT('Ctrl Pts',(-106.682478380239,5.42475038243292,
133.823870695931));
#269922=CARTESIAN_POINT('Ctrl Pts',(-106.960926004052,5.47260943449832,
127.872483436902));
#269923=CARTESIAN_POINT('Ctrl Pts',(-107.239373627865,0.491407768093767,
124.615348076738));
#269924=CARTESIAN_POINT('Ctrl Pts',(-107.517821251678,-4.94137363058539,
127.045612891524));
#269925=CARTESIAN_POINT('Ctrl Pts',(-107.796268875491,-5.83327406227795,
132.929983241508));
#269926=CARTESIAN_POINT('Ctrl Pts',(-108.074716499304,-1.36468060201792,
136.861010242526));
#269927=CARTESIAN_POINT('Ctrl Pts',(-108.353164123117,4.3579876631431,135.22627212199));
#269928=CARTESIAN_POINT('Ctrl Pts',(-108.631611746929,6.07587816540856,
129.528013351273));
#269929=CARTESIAN_POINT('Ctrl Pts',(-108.910059370743,2.21033345681367,
125.00265536525));
#269930=CARTESIAN_POINT('Ctrl Pts',(-109.188506994555,-3.68639971780079,
125.808781077045));
#269931=CARTESIAN_POINT('Ctrl Pts',(-109.466954618368,-6.19551164239422,
131.205600338952));
#269932=CARTESIAN_POINT('Ctrl Pts',(-109.745402242181,-3.01125103519769,
136.233699898554));
#269933=CARTESIAN_POINT('Ctrl Pts',(-110.023849865994,2.94020216555433,
136.272501896897));
#269934=CARTESIAN_POINT('Ctrl Pts',(-110.302297489807,6.18975321302316,
131.286349193086));
#269935=CARTESIAN_POINT('Ctrl Pts',(-110.58074511362,3.75122344397827,125.857272534824));
#269936=CARTESIAN_POINT('Ctrl Pts',(-110.859192737433,-2.13449741262907,
124.974328145912));
#269937=CARTESIAN_POINT('Ctrl Pts',(-111.137640361246,-6.05871942302636,
129.44889878553));
#269938=CARTESIAN_POINT('Ctrl Pts',(-111.416087985058,-4.41527426856075,
135.169072630797));
#269939=CARTESIAN_POINT('Ctrl Pts',(-111.694535608871,1.28559224057236,
136.878289363941));
#269940=CARTESIAN_POINT('Ctrl Pts',(-111.972983232684,5.8050622852923,133.005862307081));
#269941=CARTESIAN_POINT('Ctrl Pts',(-112.251430856497,4.9899636828869,127.110362746893));
#269942=CARTESIAN_POINT('Ctrl Pts',(-112.52987848031,-0.410667770813077,
124.609466768025));
#269943=CARTESIAN_POINT('Ctrl Pts',(-112.808326104123,-5.43391560537209,
127.801375599495));
#269944=CARTESIAN_POINT('Ctrl Pts',(-113.086773727936,-5.46366046012913,
133.752880958598));
#269945=CARTESIAN_POINT('Ctrl Pts',(-113.365221351749,-0.472568266679477,
136.994840167519));
#269946=CARTESIAN_POINT('Ctrl Pts',(-113.643668975562,4.95279107760506,
134.548051091771));
#269947=CARTESIAN_POINT('Ctrl Pts',(-113.922116599375,5.8267773788663,128.660993359675));
#269948=CARTESIAN_POINT('Ctrl Pts',(-114.200564223187,1.34623992284899,
124.74358542827));
#269949=CARTESIAN_POINT('Ctrl Pts',(-114.479011847001,-4.37142625478972,
126.395733810498));
#269950=CARTESIAN_POINT('Ctrl Pts',(-114.757459470813,-6.07196526032194,
132.099194855029));
#269951=CARTESIAN_POINT('Ctrl Pts',(-115.035907094626,-2.19266482361144,
136.612766491501));
#269952=CARTESIAN_POINT('Ctrl Pts',(-115.314354718439,3.70158746836604,
135.788696886227));
#269953=CARTESIAN_POINT('Ctrl Pts',(-115.592802342252,6.19426170951602,
130.384265748418));
#269954=CARTESIAN_POINT('Ctrl Pts',(-115.871249966065,2.99471204612843,
125.36588127258));
#269955=CARTESIAN_POINT('Ctrl Pts',(-116.149697589878,-2.95683168783455,
125.345193630298));
#269956=CARTESIAN_POINT('Ctrl Pts',(-116.428145213691,-6.19119154993583,
130.34121375418));
#269957=CARTESIAN_POINT('Ctrl Pts',(-116.706592837503,-3.73614883416816,
135.762843219532));
#269958=CARTESIAN_POINT('Ctrl Pts',(-116.985040461316,2.1522321391827,136.627869409019));
#269959=CARTESIAN_POINT('Ctrl Pts',(-117.263488085129,6.06281691900968,
132.14137551338));
#269960=CARTESIAN_POINT('Ctrl Pts',(-117.541935708942,4.40196913533955,
126.426230245297));
#269961=CARTESIAN_POINT('Ctrl Pts',(-117.820383332755,-1.30407323556081,
124.73437290577));
#269962=CARTESIAN_POINT('Ctrl Pts',(-118.098830956568,-5.81173601049948,
128.620537737998));
#269963=CARTESIAN_POINT('Ctrl Pts',(-118.377278580381,-4.97869731087745,
134.51352911087));
#269964=CARTESIAN_POINT('Ctrl Pts',(-118.655726204194,0.429520994555717,
136.997975841351));
#269965=CARTESIAN_POINT('Ctrl Pts',(-118.934173828006,5.44303048925927,
133.790792756097));
#269966=CARTESIAN_POINT('Ctrl Pts',(-119.21262145182,5.45466087115571,127.839224430854));
#269967=CARTESIAN_POINT('Ctrl Pts',(-119.491069075632,0.453724387457947,
124.612471406243));
#269968=CARTESIAN_POINT('Ctrl Pts',(-119.769516699445,-4.96416264264509,
127.075762076232));
#269969=CARTESIAN_POINT('Ctrl Pts',(-120.047964323258,-5.82022671698453,
132.965452653541));
#269970=CARTESIAN_POINT('Ctrl Pts',(-120.326411947071,-1.32778677229758,
136.869205225004));
#269971=CARTESIAN_POINT('Ctrl Pts',(-120.604859570884,4.38482435014149,
135.199661886361));
#269972=CARTESIAN_POINT('Ctrl Pts',(-120.883307194697,6.06799610537801,
129.491051404098));
#269973=CARTESIAN_POINT('Ctrl Pts',(-121.16175481851,2.17497587786225,124.989307930291));
#269974=CARTESIAN_POINT('Ctrl Pts',(-121.440202442323,-3.71674092793051,
125.831313794972));
#269975=CARTESIAN_POINT('Ctrl Pts',(-121.718650066136,-6.19295439384353,
131.243306742772));
#269976=CARTESIAN_POINT('Ctrl Pts',(-121.997097689948,-2.97814531445616,
136.251929645219));
#269977=CARTESIAN_POINT('Ctrl Pts',(-122.275545313761,2.97343381842962,
136.254502739794));
#269978=CARTESIAN_POINT('Ctrl Pts',(-122.553992937574,6.19257253249627,
131.248661478285));
#269979=CARTESIAN_POINT('Ctrl Pts',(-122.832440561387,3.72103961318487,
125.83452943108));
#269980=CARTESIAN_POINT('Ctrl Pts',(-123.1108881852,-2.16994692775201,124.987429454503));
#269981=CARTESIAN_POINT('Ctrl Pts',(-123.389335809013,-6.06685824988591,
129.485805043896));
#269982=CARTESIAN_POINT('Ctrl Pts',(-123.667783432826,-4.38862322287681,
135.19586879047));
#269983=CARTESIAN_POINT('Ctrl Pts',(-123.946231056639,1.32254214979223,
136.870351063246));
#269984=CARTESIAN_POINT('Ctrl Pts',(-124.224678680451,5.81835589657845,
132.97048445655));
#269985=CARTESIAN_POINT('Ctrl Pts',(-124.503126304264,4.96738481689638,
127.080055862859));
#269986=CARTESIAN_POINT('Ctrl Pts',(-124.781573928077,-0.448370239273912,
124.612081396343));
#269987=CARTESIAN_POINT('Ctrl Pts',(-125.06002155189,-5.4520949496557,127.834509024472));
#269988=CARTESIAN_POINT('Ctrl Pts',(-125.338469175703,-5.44561075094924,
133.786085181339));
#269989=CARTESIAN_POINT('Ctrl Pts',(-125.616916799516,-0.434876304995071,
136.997602129441));
#269990=CARTESIAN_POINT('Ctrl Pts',(-125.895364423329,4.97548822036069,
134.517832684797));
#269991=CARTESIAN_POINT('Ctrl Pts',(-126.173812047142,5.8136221373178,128.625563823564));
#269992=CARTESIAN_POINT('Ctrl Pts',(-126.452259670955,1.30932132131015,
124.735502775877));
#269993=CARTESIAN_POINT('Ctrl Pts',(-126.730707294768,-4.39818182507867,
126.422425604514));
#269994=CARTESIAN_POINT('Ctrl Pts',(-127.00915491858,-6.0639707373477,132.136132640718));
#269995=CARTESIAN_POINT('Ctrl Pts',(-127.287602542393,-2.15726678343353,
136.626006248326));
#269996=CARTESIAN_POINT('Ctrl Pts',(-127.566050166206,3.73185995611441,
135.766071924465));
#269997=CARTESIAN_POINT('Ctrl Pts',(-127.844497790019,6.19158970748781,
130.346567302635));
#269998=CARTESIAN_POINT('Ctrl Pts',(-128.122945413832,2.96155099365221,
125.34775237278));
#269999=CARTESIAN_POINT('Ctrl Pts',(-128.401393037645,-2.99000840354028,
125.363293849751));
#270000=CARTESIAN_POINT('Ctrl Pts',(-128.679840661458,-6.19389614791022,
130.378909875453));
#270001=CARTESIAN_POINT('Ctrl Pts',(-128.958288285271,-3.70589592099968,
135.785494348734));
#270002=CARTESIAN_POINT('Ctrl Pts',(-129.236735909083,2.18764161422919,
136.614660264981));
#270003=CARTESIAN_POINT('Ctrl Pts',(-129.515183532897,6.07084337821547,
132.104444654172));
#270004=CARTESIAN_POINT('Ctrl Pts',(-129.793631156709,4.37523665480886,
126.399515326358));
#270005=CARTESIAN_POINT('Ctrl Pts',(-130.072078780522,-1.34099881217456,
124.742423632508));
#270006=CARTESIAN_POINT('Ctrl Pts',(-130.350526404335,-5.82492188220296,
128.655955885842));
#270007=CARTESIAN_POINT('Ctrl Pts',(-130.628974028148,-4.95602630574081,
134.543767132223));
#270008=CARTESIAN_POINT('Ctrl Pts',(-130.907421651961,0.467215330352083,
136.995246471799));
#270009=CARTESIAN_POINT('Ctrl Pts',(-131.185869275774,5.46110890258918,
133.757604152921));
#270010=CARTESIAN_POINT('Ctrl Pts',(-131.464316899587,5.43651018334856,
127.80607529902));
#270011=CARTESIAN_POINT('Ctrl Pts',(-131.742764523399,0.416024193898128,
124.60982417848));
#270012=CARTESIAN_POINT('Ctrl Pts',(-132.021212147213,-4.98676770583297,
127.106049425532));
#270013=CARTESIAN_POINT('Ctrl Pts',(-132.299659771025,-5.80696370104951,
133.000841985516));
#270014=CARTESIAN_POINT('Ctrl Pts',(-132.578107394838,-1.2908437409496,
136.877175472434));
#270015=CARTESIAN_POINT('Ctrl Pts',(-132.856555018651,4.41149855586104,
135.172888781227));
#270016=CARTESIAN_POINT('Ctrl Pts',(-133.135002642464,6.05988919352027,
129.454138122079));
#270017=CARTESIAN_POINT('Ctrl Pts',(-133.413450266277,2.13953770437982,
124.976175974248));
#270018=CARTESIAN_POINT('Ctrl Pts',(-133.69189789009,-3.74694441285829,
125.854030790976));
#270019=CARTESIAN_POINT('Ctrl Pts',(-133.970345513903,-6.19016766309031,
131.280996881284));
#270020=CARTESIAN_POINT('Ctrl Pts',(-134.248793137716,-2.94492923744478,
136.269957530209));
#270021=CARTESIAN_POINT('Ctrl Pts',(-134.527240761528,3.00655528962129,
136.236301625668));
#270022=CARTESIAN_POINT('Ctrl Pts',(-134.805688385342,6.19516238391663,
131.210957299752));
#270023=CARTESIAN_POINT('Ctrl Pts',(-135.084136009154,3.69071789790064,
125.811970486258));
#270024=CARTESIAN_POINT('Ctrl Pts',(-135.362583632967,-2.2053160346932,
125.000746311619));
#270025=CARTESIAN_POINT('Ctrl Pts',(-135.64103125678,-6.07477226708194,
129.522760161825));
#270026=CARTESIAN_POINT('Ctrl Pts',(-135.919478880593,-4.36180955514542,
135.222502221193));
#270027=CARTESIAN_POINT('Ctrl Pts',(-136.197926504406,1.35944305172635,
136.862187985044));
#270028=CARTESIAN_POINT('Ctrl Pts',(-136.476374128219,5.83143390654715,
132.935026339502));
#270029=CARTESIAN_POINT('Ctrl Pts',(-136.754821752032,4.9446218826347,127.049886984307));
#270030=CARTESIAN_POINT('Ctrl Pts',(-137.033269375845,-0.486056093210629,
124.614925481843));
#270031=CARTESIAN_POINT('Ctrl Pts',(-137.311716999657,-5.47007226455594,
127.867752498391));
#270032=CARTESIAN_POINT('Ctrl Pts',(-137.59016462347,-5.42735925266033,
133.819178915179));
#270033=CARTESIAN_POINT('Ctrl Pts',(-137.868612247283,-0.397168228809268,
137.000134598521));
#270034=CARTESIAN_POINT('Ctrl Pts',(-138.147059871096,4.99800099457058,
134.487476673751));
#270035=CARTESIAN_POINT('Ctrl Pts',(-138.425507494909,5.80025146986304,
128.590215023569));
#270036=CARTESIAN_POINT('Ctrl Pts',(-138.703955118722,1.27235420238826,
124.727645007244));
#270037=CARTESIAN_POINT('Ctrl Pts',(-138.982402742535,-4.42477441912264,
126.449279772744));
#270038=CARTESIAN_POINT('Ctrl Pts',(-139.260850366348,-6.05575151170779,
132.173021077107));
#270039=CARTESIAN_POINT('Ctrl Pts',(-139.539297990161,-2.12178880494131,
136.639030281933));
#270040=CARTESIAN_POINT('Ctrl Pts',(-139.817745613973,3.76199415842019,
135.743263104665));
#270041=CARTESIAN_POINT('Ctrl Pts',(-140.096193237787,6.18868827382574,
130.308885820552));
#270042=CARTESIAN_POINT('Ctrl Pts',(-140.374640861599,2.92828019981485,
125.329825669606));
#270043=CARTESIAN_POINT('Ctrl Pts',(-140.653088485412,-3.02307432338508,
125.381595689934));
#270044=CARTESIAN_POINT('Ctrl Pts',(-140.931536109225,-6.19637122878504,
130.416621761961));
#270045=CARTESIAN_POINT('Ctrl Pts',(-141.209983733038,-3.675505684495,135.807960900193));
#270046=CARTESIAN_POINT('Ctrl Pts',(-141.488431356851,2.22297002541115,
136.601235818153));
#270047=CARTESIAN_POINT('Ctrl Pts',(-141.766878980664,6.07864488008735,
132.06746561987));
#270048=CARTESIAN_POINT('Ctrl Pts',(-142.045326604476,4.34834204827492,
126.372963630579));
#270049=CARTESIAN_POINT('Ctrl Pts',(-142.32377422829,-1.3778746975837,124.750698986551));
#270050=CARTESIAN_POINT('Ctrl Pts',(-142.602221852102,-5.83789190928377,
128.691453643612));
#270051=CARTESIAN_POINT('Ctrl Pts',(-142.880669475915,-4.93317165322728,
134.573866588494));
#270052=CARTESIAN_POINT('Ctrl Pts',(-143.159117099728,0.504892353312588,
136.992287696695));
#270053=CARTESIAN_POINT('Ctrl Pts',(-143.437564723541,5.47898495252035,
133.72430611622));
#270054=CARTESIAN_POINT('Ctrl Pts',(-143.716012347354,5.4181580436573,127.77303726975));
#270055=CARTESIAN_POINT('Ctrl Pts',(-143.994459971167,0.378308584408798,
124.607406491544));
#270056=CARTESIAN_POINT('Ctrl Pts',(-144.27290759498,-5.00918798250961,
127.136473817112));
#270057=CARTESIAN_POINT('Ctrl Pts',(-144.551355218793,-5.79348550593904,
133.036149926065));
#270058=CARTESIAN_POINT('Ctrl Pts',(-144.829802842605,-1.2538528769121,
136.884920689477));
#270059=CARTESIAN_POINT('Ctrl Pts',(-145.108250466418,4.43800929187927,
135.145953798675));
#270060=CARTESIAN_POINT('Ctrl Pts',(-145.386698090231,6.05155773023994,
129.417274873051));
#270061=CARTESIAN_POINT('Ctrl Pts',(-145.665145714044,2.10402024954095,
124.963259983731));
#270062=CARTESIAN_POINT('Ctrl Pts',(-145.943593337857,-3.77700905338292,
125.876931223274));
#270063=CARTESIAN_POINT('Ctrl Pts',(-146.22204096167,-6.18715155339789,
131.318669357863));
#270064=CARTESIAN_POINT('Ctrl Pts',(-146.500488585483,-2.9116040349975,
136.287782885497));
#270065=CARTESIAN_POINT('Ctrl Pts',(-146.778936209295,3.03956535180104,
136.217899228972));
#270066=CARTESIAN_POINT('Ctrl Pts',(-147.057383833109,6.19752267131684,
131.173238054629));
#270067=CARTESIAN_POINT('Ctrl Pts',(-147.335831456921,3.66025942170698,
125.789596536289));
#270068=CARTESIAN_POINT('Ctrl Pts',(-147.614279080735,-2.24060342283806,
125.014278223797));
#270069=CARTESIAN_POINT('Ctrl Pts',(-147.892726704547,-6.08246118135759,
129.559762769929));
#270070=CARTESIAN_POINT('Ctrl Pts',(-148.17117432836,-4.33483425895693,
135.248971936054));
#270071=CARTESIAN_POINT('Ctrl Pts',(-148.449621952173,1.39629357899829,
136.853800431821));
#270072=CARTESIAN_POINT('Ctrl Pts',(-148.728069575986,5.84429583058792,
132.899489269852));
#270073=CARTESIAN_POINT('Ctrl Pts',(-149.006517199799,4.9216757235908,127.019857229157));
#270074=CARTESIAN_POINT('Ctrl Pts',(-149.284964823612,-0.52372393616008,
124.617998919139));
#270075=CARTESIAN_POINT('Ctrl Pts',(-149.563412447425,-5.48784688391679,
127.901104789406));
#270076=CARTESIAN_POINT('Ctrl Pts',(-149.841860071237,-5.40890664157841,
133.852160933818));
#270077=CARTESIAN_POINT('Ctrl Pts',(-150.12030769505,-0.359445435409253,
137.002437480918));
#270078=CARTESIAN_POINT('Ctrl Pts',(-150.398755318863,5.02032856601553,
134.456984183485));
#270079=CARTESIAN_POINT('Ctrl Pts',(-150.677202942676,5.78666587195703,
128.554948269553));
#270080=CARTESIAN_POINT('Ctrl Pts',(-150.955650566489,1.23533993591347,
124.720012413542));
#270081=CARTESIAN_POINT('Ctrl Pts',(-151.234098190302,-4.45120305152329,
126.476295320094));
#270082=CARTESIAN_POINT('Ctrl Pts',(-151.512545814115,-6.0473078879686,
132.209858797279));
#270083=CARTESIAN_POINT('Ctrl Pts',(-151.790993437928,-2.08623220278462,
136.651838109709));
#270084=CARTESIAN_POINT('Ctrl Pts',(-152.069441061741,3.79198895864895,
135.720271272016));
#270085=CARTESIAN_POINT('Ctrl Pts',(-152.347888685554,6.18555751604382,
130.27122269847));
#270086=CARTESIAN_POINT('Ctrl Pts',(-152.626336309366,2.89490089747778,
125.312101827337));
#270087=CARTESIAN_POINT('Ctrl Pts',(-152.904783933179,-3.05602822209906,
125.400098472666));
#270088=CARTESIAN_POINT('Ctrl Pts',(-153.183231556992,-6.19861670084527,
130.454348016274));
#270089=CARTESIAN_POINT('Ctrl Pts',(-153.461679180805,-3.64497925077551,
135.830242041403));
#270090=CARTESIAN_POINT('Ctrl Pts',(-153.740126804618,2.25821606362131,
136.587596565983));
#270091=CARTESIAN_POINT('Ctrl Pts',(-154.018574428431,6.08622113553776,
132.030439780749));
#270092=CARTESIAN_POINT('Ctrl Pts',(-154.297022052244,4.32128631232727,
126.346576141847));
#270093=CARTESIAN_POINT('Ctrl Pts',(-154.575469676057,-1.41469952533967,
124.759198661251));
#270094=CARTESIAN_POINT('Ctrl Pts',(-154.85391729987,-5.85064561113321,
128.727029695929));
#270095=CARTESIAN_POINT('Ctrl Pts',(-155.132364923682,-4.9101342002235,
134.603826364333));
#270096=CARTESIAN_POINT('Ctrl Pts',(-155.410812547495,0.542550667301237,
136.989099625678));
#270097=CARTESIAN_POINT('Ctrl Pts',(-155.689260171308,5.49665797664923,
133.690899879866));
#270098=CARTESIAN_POINT('Ctrl Pts',(-155.967707795121,5.39960513212718,
127.740111567281));
#270099=CARTESIAN_POINT('Ctrl Pts',(-156.246155418934,0.340578956555753,
124.605218435021));
#270100=CARTESIAN_POINT('Ctrl Pts',(-156.524603042747,-5.03142264188343,
127.167034123586));
#270101=CARTESIAN_POINT('Ctrl Pts',(-156.80305066656,-5.77979263109261,
133.071375166841));
#270102=CARTESIAN_POINT('Ctrl Pts',(-157.081498290373,-1.21681555089514,
136.89244058913));
#270103=CARTESIAN_POINT('Ctrl Pts',(-157.359945914186,4.46435557583064,
135.118857936792));
#270104=CARTESIAN_POINT('Ctrl Pts',(-157.638393537999,6.04300202426259,
129.380463022997));
#270105=CARTESIAN_POINT('Ctrl Pts',(-157.916841161811,2.06842482945845,
124.950560437346));
#270106=CARTESIAN_POINT('Ctrl Pts',(-158.195288785624,-3.80693373544809,
125.900014243279));
#270107=CARTESIAN_POINT('Ctrl Pts',(-158.473736409437,-6.18390617652933,
131.356322776543));
#270108=CARTESIAN_POINT('Ctrl Pts',(-158.75218403325,-2.87817094199197,
136.305405050556));
#270109=CARTESIAN_POINT('Ctrl Pts',(-159.030631657063,3.07246278176887,
136.199296231612));
#270110=CARTESIAN_POINT('Ctrl Pts',(-159.309079280876,6.19965330723533,
131.135505140616));
#270111=CARTESIAN_POINT('Ctrl Pts',(-159.587526904689,3.62966531325439,
125.767408410247));
#270112=CARTESIAN_POINT('Ctrl Pts',(-159.865974528502,-2.27580778459908,
125.028024689608));
#270113=CARTESIAN_POINT('Ctrl Pts',(-160.144422152314,-6.08992470779737,
129.596811497064));
#270114=CARTESIAN_POINT('Ctrl Pts',(-160.422869776128,-4.3076983338908,
135.275276954208));
#270115=CARTESIAN_POINT('Ctrl Pts',(-160.70131739994,1.43309236609815,136.845188714382));
#270116=CARTESIAN_POINT('Ctrl Pts',(-160.979765023753,5.85694119209746,
132.863874564441));
#270117=CARTESIAN_POINT('Ctrl Pts',(-161.258212647566,4.89854719004298,
126.989967710171));
#270118=CARTESIAN_POINT('Ctrl Pts',(-161.536660271379,-0.561372372326459,
124.621301594343));
#270119=CARTESIAN_POINT('Ctrl Pts',(-161.815107895192,-5.50541814909322,
127.934564661631));
#270120=CARTESIAN_POINT('Ctrl Pts',(-162.093555519005,-5.39025360147175,
133.885030015096));
#270121=CARTESIAN_POINT('Ctrl Pts',(-162.372003142818,-0.32170932262588,
137.004510691297));
#270122=CARTESIAN_POINT('Ctrl Pts',(-162.650450766631,5.04247010733932,
134.426356343909));
#270123=CARTESIAN_POINT('Ctrl Pts',(-162.928898390443,5.77286584701905,
128.519764868338));
#270124=CARTESIAN_POINT('Ctrl Pts',(-163.207346014257,1.19827989346308,
124.712605277602));
#270125=CARTESIAN_POINT('Ctrl Pts',(-163.485793638069,-4.47746674295796,
126.503471245498));
#270126=CARTESIAN_POINT('Ctrl Pts',(-163.764241261882,-6.03864017901171,
132.246644436198));
#270127=CARTESIAN_POINT('Ctrl Pts',(-164.042688885695,-2.05059829452646,
136.664429257056));
#270128=CARTESIAN_POINT('Ctrl Pts',(-164.321136509508,3.82184324533235,
135.697097278492));
#270129=CARTESIAN_POINT('Ctrl Pts',(-164.599584133321,6.18219755015336,
130.23357933201));
#270130=CARTESIAN_POINT('Ctrl Pts',(-164.878031757134,2.86141432352365,
125.294581502737));
#270131=CARTESIAN_POINT('Ctrl Pts',(-165.156479380946,-3.08886887856293,
125.418801512319));
#270132=CARTESIAN_POINT('Ctrl Pts',(-165.43492700476,-6.20063248088431,
130.492087240433));
#270133=CARTESIAN_POINT('Ctrl Pts',(-165.713374628572,-3.61431775100944,
135.85233694673));
#270134=CARTESIAN_POINT('Ctrl Pts',(-165.991822252385,2.2933784228048,136.573743013877));
#270135=CARTESIAN_POINT('Ctrl Pts',(-166.270269876198,6.09357186382579,
131.993368508814));
#270136=CARTESIAN_POINT('Ctrl Pts',(-166.548717500011,4.2940704495262,126.320353837957));
#270137=CARTESIAN_POINT('Ctrl Pts',(-166.827165123824,-1.45147193088449,
124.767922341652));
#270138=CARTESIAN_POINT('Ctrl Pts',(-167.105612747637,-5.86318251515793,
128.762682724506));
#270139=CARTESIAN_POINT('Ctrl Pts',(-167.38406037145,-4.88691480039125,
134.633645349573));
#270140=CARTESIAN_POINT('Ctrl Pts',(-167.662507995262,0.580188876875391,
136.985682376883));
#270141=CARTESIAN_POINT('Ctrl Pts',(-167.940955619076,5.51412732009539,
133.657386681736));
#270142=CARTESIAN_POINT('Ctrl Pts',(-168.219403242888,5.38085213624319,
127.707299411689));
#270143=CARTESIAN_POINT('Ctrl Pts',(-168.497850866701,0.302836708424229,
124.60326008999));
#270144=CARTESIAN_POINT('Ctrl Pts',(-168.776298490514,-5.05347086004094,
127.197729212531));
#270145=CARTESIAN_POINT('Ctrl Pts',(-169.054746114327,-5.7658855839047,
133.106516402559));
#270146=CARTESIAN_POINT('Ctrl Pts',(-169.33319373814,-1.17973313533045,
136.899734892741));
#270147=CARTESIAN_POINT('Ctrl Pts',(-169.611641361953,4.49053643144484,
135.091602199623));
#270148=CARTESIAN_POINT('Ctrl Pts',(-169.890088985766,6.03422239262278,
129.34370393599));
#270149=CARTESIAN_POINT('Ctrl Pts',(-170.168536609579,2.03275276313275,
124.938077805679));
#270150=CARTESIAN_POINT('Ctrl Pts',(-170.446984233392,-3.83671735018369,
125.923278995643));
#270151=CARTESIAN_POINT('Ctrl Pts',(-170.725431857205,-6.18043165274327,
131.393955742061));
#270152=CARTESIAN_POINT('Ctrl Pts',(-171.003879481017,-2.84463119730373,
136.32282337239));
#270153=CARTESIAN_POINT('Ctrl Pts',(-171.282327104831,3.10524636049842,
136.180493322929));
#270154=CARTESIAN_POINT('Ctrl Pts',(-171.560774728643,6.20155421272058,
131.097759955922));
#270155=CARTESIAN_POINT('Ctrl Pts',(-171.839222352457,3.59893670621881,
125.745406930321));
#270156=CARTESIAN_POINT('Ctrl Pts',(-172.117669976268,-2.31092781546573,
125.04198519967));
#270157=CARTESIAN_POINT('Ctrl Pts',(-172.396117600082,-6.09716256983718,
129.633904970377));
#270158=CARTESIAN_POINT('Ctrl Pts',(-172.674565223895,-4.2804027854792,
135.301416300912));
#270159=CARTESIAN_POINT('Ctrl Pts',(-172.953012847708,1.469838049433,136.836353151837));
#270160=CARTESIAN_POINT('Ctrl Pts',(-173.23146047152,5.86936952249723,132.828183542982));
#270161=CARTESIAN_POINT('Ctrl Pts',(-173.509908095334,4.8752371390276,126.960219534917));
#270162=CARTESIAN_POINT('Ctrl Pts',(-173.788355719146,-0.599000006633149,
124.624833385073));
#270163=CARTESIAN_POINT('Ctrl Pts',(-174.06680334296,-5.5227854089755,127.968130875202));
#270164=CARTESIAN_POINT('Ctrl Pts',(-174.345250966772,-5.37140082353563,
133.917784941036));
#270165=CARTESIAN_POINT('Ctrl Pts',(-174.623698590585,-0.283961288785237,
137.006354152836));
#270166=CARTESIAN_POINT('Ctrl Pts',(-174.902146214398,5.06442479807889,
134.39559428995));
#270167=CARTESIAN_POINT('Ctrl Pts',(-175.18059383821,5.75885190641417,128.484666123661));
#270168=CARTESIAN_POINT('Ctrl Pts',(-175.459041462024,1.16117544831056,
124.705423873895));
#270169=CARTESIAN_POINT('Ctrl Pts',(-175.737489085836,-4.50356452021585,
126.530806541938));
#270170=CARTESIAN_POINT('Ctrl Pts',(-176.01593670965,-6.02974870602229,
132.28337663076));
#270171=CARTESIAN_POINT('Ctrl Pts',(-176.294384333462,-2.01488840059438,
136.676803257405));
#270172=CARTESIAN_POINT('Ctrl Pts',(-176.572831957276,3.85155591220881,
135.67374198281));
#270173=CARTESIAN_POINT('Ctrl Pts',(-176.851279581088,6.17860850065921,
130.195957116059));
#270174=CARTESIAN_POINT('Ctrl Pts',(-177.129727204901,2.82782171880919,
125.277265345029));
#270175=CARTESIAN_POINT('Ctrl Pts',(-177.408174828714,-3.12159507585506,
125.437704115845));
#270176=CARTESIAN_POINT('Ctrl Pts',(-177.686622452527,-6.20241849420629,
130.529838035997));
#270177=CARTESIAN_POINT('Ctrl Pts',(-177.965070076339,-3.58352232136993,
135.874244797437));
#270178=CARTESIAN_POINT('Ctrl Pts',(-178.243517700153,2.32845580000743,
136.559675675186));
#270179=CARTESIAN_POINT('Ctrl Pts',(-178.521965323965,6.10069679256748,
131.956253177754));
#270180=CARTESIAN_POINT('Ctrl Pts',(-178.800412947778,4.26669546836545,
126.294297690589));
#270181=CARTESIAN_POINT('Ctrl Pts',(-179.078860571591,-1.48819055160311,
124.776869704492));
#270182=CARTESIAN_POINT('Ctrl Pts',(-179.357308195404,-5.8755021567984,
128.798411408209));
#270183=CARTESIAN_POINT('Ctrl Pts',(-179.635755819217,-4.86351431413387,
134.663322439258));
#270184=CARTESIAN_POINT('Ctrl Pts',(-179.91420344303,0.617805587336893,
136.982036076937));
#270185=CARTESIAN_POINT('Ctrl Pts',(-180.192651066843,5.53139233552561,
133.623767763677));
#270186=CARTESIAN_POINT('Ctrl Pts',(-180.471098690656,5.36189975090491,
127.674602018838));
#270187=CARTESIAN_POINT('Ctrl Pts',(-180.749546314469,0.265083238567079,
124.601531529021));
#270188=CARTESIAN_POINT('Ctrl Pts',(-181.027993938281,-5.07533181997731,
127.22855794653));
#270189=CARTESIAN_POINT('Ctrl Pts',(-181.306441562095,-5.75176487970607,
133.141572331048));
#270190=CARTESIAN_POINT('Ctrl Pts',(-181.584889185907,-1.14260700432061,
136.906803330016));
#270191=CARTESIAN_POINT('Ctrl Pts',(-181.86333680972,4.5165508885802,135.064187597142));
#270192=CARTESIAN_POINT('Ctrl Pts',(-182.141784433533,6.02521916065313,
129.306998974155));
#270193=CARTESIAN_POINT('Ctrl Pts',(-182.420232057346,1.99700537240587,
124.925812551278));
#270194=CARTESIAN_POINT('Ctrl Pts',(-182.698679681159,-3.86635879394691,
125.946724618282));
#270195=CARTESIAN_POINT('Ctrl Pts',(-182.977127304972,-6.17672811078948,
131.431566859916));
#270196=CARTESIAN_POINT('Ctrl Pts',(-183.255574928785,-2.81098604376035,
136.340037205557));
#270197=CARTESIAN_POINT('Ctrl Pts',(-183.534022552597,3.13791487318212,
136.161491199671));
#270198=CARTESIAN_POINT('Ctrl Pts',(-183.81247017641,6.20322531733387,131.060003899207));
#270199=CARTESIAN_POINT('Ctrl Pts',(-184.090917800223,3.56807473926006,
125.723592911784));
#270200=CARTESIAN_POINT('Ctrl Pts',(-184.369365424036,-2.34596221405232,
125.056159236672));
#270201=CARTESIAN_POINT('Ctrl Pts',(-184.647813047849,-6.10417449927606,
129.671041815353));
#270202=CARTESIAN_POINT('Ctrl Pts',(-184.926260671662,-4.25294862516783,
135.327389007565));
#270203=CARTESIAN_POINT('Ctrl Pts',(-185.204708295475,1.50652926737877,
136.827294071589));
#270204=CARTESIAN_POINT('Ctrl Pts',(-185.483155919288,5.88158036125089,
132.792417528021));
#270205=CARTESIAN_POINT('Ctrl Pts',(-185.761603543101,4.85174643430717,
126.930613805724));
#270206=CARTESIAN_POINT('Ctrl Pts',(-186.040051166913,-0.6366054447743,
124.628594160457));
#270207=CARTESIAN_POINT('Ctrl Pts',(-186.318498790727,-5.53994802001346,
128.001802186308));
#270208=CARTESIAN_POINT('Ctrl Pts',(-186.596946414539,-5.35234900636664,
133.950424497894));
#270209=CARTESIAN_POINT('Ctrl Pts',(-186.875394038353,-0.246202732654624,
137.007967797222));
#270210=CARTESIAN_POINT('Ctrl Pts',(-187.153841662165,5.08619182469514,
134.364699161505));
#270211=CARTESIAN_POINT('Ctrl Pts',(-187.432289285978,5.744624569434,128.449653336115));
#270212=CARTESIAN_POINT('Ctrl Pts',(-187.71073690979,1.12402797537536,124.698468468532));
#270213=CARTESIAN_POINT('Ctrl Pts',(-187.989184533604,-4.52949541623416,
126.558300196495));
#270214=CARTESIAN_POINT('Ctrl Pts',(-188.267632157416,-6.0206337984771,
132.32005401984));
#270215=CARTESIAN_POINT('Ctrl Pts',(-188.54607978123,-1.97910384423165,
136.688959652232));
#270216=CARTESIAN_POINT('Ctrl Pts',(-188.824527405043,3.88112585826452,
135.650206250412));
#270217=CARTESIAN_POINT('Ctrl Pts',(-189.102975028855,6.17479050055486,
130.158357444724));
#270218=CARTESIAN_POINT('Ctrl Pts',(-189.381422652668,2.79412432812102,
125.260153995869));
#270219=CARTESIAN_POINT('Ctrl Pts',(-189.659870276481,-3.15420560129371,
125.456805582802));
#270220=CARTESIAN_POINT('Ctrl Pts',(-189.938317900294,-6.20397467462999,
130.567599004095));
#270221=CARTESIAN_POINT('Ctrl Pts',(-190.216765524107,-3.55259410299321,
135.89596478172));
#270222=CARTESIAN_POINT('Ctrl Pts',(-190.49521314792,2.36344689542356,136.545395071179));
#270223=CARTESIAN_POINT('Ctrl Pts',(-190.773660771733,6.10759565774615,
131.919095162891));
#270224=CARTESIAN_POINT('Ctrl Pts',(-191.052108395545,4.23916238323504,
126.26840866526));
#270225=CARTESIAN_POINT('Ctrl Pts',(-191.330556019359,-1.52485402687357,
124.786040418225));
#270226=CARTESIAN_POINT('Ctrl Pts',(-191.609003643171,-5.88760407954571,
128.834214423098));
#270227=CARTESIAN_POINT('Ctrl Pts',(-191.887451266984,-4.83993360856504,
134.692856533694));
#270228=CARTESIAN_POINT('Ctrl Pts',(-192.165898890797,0.655399404785621,
136.978160860955));
#270229=CARTESIAN_POINT('Ctrl Pts',(-192.44434651461,5.54845238317892,133.59004437145));
#270230=CARTESIAN_POINT('Ctrl Pts',(-192.722794138423,5.34274867839911,
127.642020600343));
#270231=CARTESIAN_POINT('Ctrl Pts',(-193.001241762236,0.227319945953055,
124.600032816164));
#270232=CARTESIAN_POINT('Ctrl Pts',(-193.279689386049,-5.09700471162664,
127.259519183211));
#270233=CARTESIAN_POINT('Ctrl Pts',(-193.558137009861,-5.73743104174462,
133.176541653297));
#270234=CARTESIAN_POINT('Ctrl Pts',(-193.836584633675,-1.105438533588,136.913645639033));
#270235=CARTESIAN_POINT('Ctrl Pts',(-194.115032257487,4.5423979832614,135.036615145204));
#270236=CARTESIAN_POINT('Ctrl Pts',(-194.3934798813,6.01599266197172,129.270349497605));
#270237=CARTESIAN_POINT('Ctrl Pts',(-194.671927505113,1.96118398191049,
124.913765128639));
#270238=CARTESIAN_POINT('Ctrl Pts',(-194.950375128926,-3.89585696836267,
125.970350242409));
#270239=CARTESIAN_POINT('Ctrl Pts',(-195.228822752739,-6.17279568790409,
131.469154736412));
#270240=CARTESIAN_POINT('Ctrl Pts',(-195.507270376552,-2.77723672809589,
136.357045912194));
#270241=CARTESIAN_POINT('Ctrl Pts',(-195.785718000365,3.17046710927626,
136.142290565968));
#270242=CARTESIAN_POINT('Ctrl Pts',(-196.064165624178,6.20466655915177,
131.022238369536));
#270243=CARTESIAN_POINT('Ctrl Pts',(-196.342613247991,3.5370805559797,125.701967162963));
#270244=CARTESIAN_POINT('Ctrl Pts',(-196.621060871803,-2.38090968214636,
125.070546275391));
#270245=CARTESIAN_POINT('Ctrl Pts',(-196.899508495616,-6.11096023628406,
129.708220655875));
#270246=CARTESIAN_POINT('Ctrl Pts',(-197.177956119429,-4.22533687028115,
135.353194111738));
#270247=CARTESIAN_POINT('Ctrl Pts',(-197.456403743242,1.54316466032852,
136.818011809327));
#270248=CARTESIAN_POINT('Ctrl Pts',(-197.734851367055,5.89357325588093,
132.75657784488));
#270249=CARTESIAN_POINT('Ctrl Pts',(-198.013298990868,4.82807594633875,
126.901151619645));
#270250=CARTESIAN_POINT('Ctrl Pts',(-198.291746614681,-0.674187293266194,
124.632583781138));
#270251=CARTESIAN_POINT('Ctrl Pts',(-198.570194238494,-5.55690534624021,
128.035577347248));
#270252=CARTESIAN_POINT('Ctrl Pts',(-198.848641862306,-5.33309885593691,
133.982947476197));
#270253=CARTESIAN_POINT('Ctrl Pts',(-199.12708948612,-0.2084350533912,137.009351564664));
#270254=CARTESIAN_POINT('Ctrl Pts',(-199.405537109932,5.10777038060287,
134.333672103408));
#270255=CARTESIAN_POINT('Ctrl Pts',(-199.683984733745,5.7301843632779,128.414727803113));
#270256=CARTESIAN_POINT('Ctrl Pts',(-199.962432357558,1.08683885116959,
124.691739319248));
#270257=CARTESIAN_POINT('Ctrl Pts',(-200.240879981371,-4.5552584701342,
126.585951190383));
#270258=CARTESIAN_POINT('Ctrl Pts',(-200.519327605184,-6.01129579413245,
132.356675244344));
#270259=CARTESIAN_POINT('Ctrl Pts',(-200.797775228997,-1.94324595144814,
136.700897991079));
#270260=CARTESIAN_POINT('Ctrl Pts',(-201.076222852809,3.91055198777426,
135.626490953421));
#270261=CARTESIAN_POINT('Ctrl Pts',(-201.354670476623,6.17074369131775,
130.120781711275));
#270262=CARTESIAN_POINT('Ctrl Pts',(-201.633118100435,2.76032340012831,
125.243248089324));
#270263=CARTESIAN_POINT('Ctrl Pts',(-201.911565724248,-3.18669924648382,
125.476105205376));
#270264=CARTESIAN_POINT('Ctrl Pts',(-202.190013348061,-6.20530096449064,
130.605368745483));
#270265=CARTESIAN_POINT('Ctrl Pts',(-202.468460971874,-3.52153424193529,
135.91749609474));
#270266=CARTESIAN_POINT('Ctrl Pts',(-202.746908595687,2.39835041244635,
136.530901731028));
#270267=CARTESIAN_POINT('Ctrl Pts',(-203.0253562195,6.11426820372151,131.881895841131));
#270268=CARTESIAN_POINT('Ctrl Pts',(-203.303803843313,4.21147221438356,
126.242687721299));
#270269=CARTESIAN_POINT('Ctrl Pts',(-203.582251467125,-1.56146099811728,
124.795434143027));
#270270=CARTESIAN_POINT('Ctrl Pts',(-203.860699090939,-5.89948783495869,
128.870090442477));
#270271=CARTESIAN_POINT('Ctrl Pts',(-204.139146714752,-4.81617355747646,
134.722246538484));
#270272=CARTESIAN_POINT('Ctrl Pts',(-204.417594338564,0.69296893616836,
136.974056872534));
#270273=CARTESIAN_POINT('Ctrl Pts',(-204.696041962377,5.56530683088876,
133.556217754686));
#270274=CARTESIAN_POINT('Ctrl Pts',(-204.97448958619,5.32339962837619,127.60955636352));
#270275=CARTESIAN_POINT('Ctrl Pts',(-205.252937210003,0.18954822991528,
124.598764006957));
#270276=CARTESIAN_POINT('Ctrl Pts',(-205.531384833816,-5.11848873189165,
127.290611775294));
#270277=CARTESIAN_POINT('Ctrl Pts',(-205.809832457629,-5.72288460116635,
133.211423073505));
#270278=CARTESIAN_POINT('Ctrl Pts',(-206.088280081441,-1.06822910042401,
136.920261566246));
#270279=CARTESIAN_POINT('Ctrl Pts',(-206.366727705255,4.56807675771487,
135.00888586552));
#270280=CARTESIAN_POINT('Ctrl Pts',(-206.645175329067,6.00654323846982,
129.233756864401));
#270281=CARTESIAN_POINT('Ctrl Pts',(-206.92362295288,1.92528991902147,124.901935984182));
#270282=CARTESIAN_POINT('Ctrl Pts',(-207.202070576693,-3.92521078036628,
125.994154992568));
#270283=CARTESIAN_POINT('Ctrl Pts',(-207.480518200506,-6.16863452980439,
131.506717978718));
#270284=CARTESIAN_POINT('Ctrl Pts',(-207.758965824319,-2.74338450090264,
136.373848862034));
#270285=CARTESIAN_POINT('Ctrl Pts',(-208.037413448132,3.20290186254569,
136.12289213331));
#270286=CARTESIAN_POINT('Ctrl Pts',(-208.315861071945,6.20587788476857,
130.984464766326));
#270287=CARTESIAN_POINT('Ctrl Pts',(-208.594308695758,3.50595530487857,
125.680530485208));
#270288=CARTESIAN_POINT('Ctrl Pts',(-208.872756319571,-2.41576892475653,
125.085145782709));
#270289=CARTESIAN_POINT('Ctrl Pts',(-209.151203943383,-6.11751952941318,
129.745440114266));
#270290=CARTESIAN_POINT('Ctrl Pts',(-209.429651567197,-4.19756854398286,
135.378830657213));
#270291=CARTESIAN_POINT('Ctrl Pts',(-209.708099191009,1.57974287074426,
136.808506709009));
#270292=CARTESIAN_POINT('Ctrl Pts',(-209.986546814822,5.90534776198698,
132.720665821612));
#270293=CARTESIAN_POINT('Ctrl Pts',(-210.264994438635,4.80422655224024,
126.87183406841));
#270294=CARTESIAN_POINT('Ctrl Pts',(-210.543442062448,-0.711744159500396,
124.63680209928));
#270295=CARTESIAN_POINT('Ctrl Pts',(-210.821889686261,-5.57365675929581,
128.06945510647));
#270296=CARTESIAN_POINT('Ctrl Pts',(-211.100337310074,-5.31365108556781,
134.015352670796));
#270297=CARTESIAN_POINT('Ctrl Pts',(-211.378784933887,-0.170659650490228,
137.010505403884));
#270298=CARTESIAN_POINT('Ctrl Pts',(-211.657232557699,5.12915966620077,
134.302514265376));
#270299=CARTESIAN_POINT('Ctrl Pts',(-211.935680181513,5.71553182303293,
128.379890818834));
#270300=CARTESIAN_POINT('Ctrl Pts',(-212.214127805325,1.04960945375051,
124.685236675394));
#270301=CARTESIAN_POINT('Ctrl Pts',(-212.492575429138,-4.58085272725645,
126.613758498985));
#270302=CARTESIAN_POINT('Ctrl Pts',(-212.771023052951,-6.00173503901134,
132.393238947258));
#270303=CARTESIAN_POINT('Ctrl Pts',(-213.049470676764,-1.90731605097184,
136.712617831564));
#270304=CARTESIAN_POINT('Ctrl Pts',(-213.327918300577,3.93983321034183,
135.602596970618));
#270305=CARTESIAN_POINT('Ctrl Pts',(-213.60636592439,6.16646822290386,130.083231308093));
#270306=CARTESIAN_POINT('Ctrl Pts',(-213.884813548203,2.72642018733693,
125.226548251849));
#270307=CARTESIAN_POINT('Ctrl Pts',(-214.163261172015,-3.21907480736146,
125.495602268416));
#270308=CARTESIAN_POINT('Ctrl Pts',(-214.441708795829,-6.20639731464204,
130.643145860587));
#270309=CARTESIAN_POINT('Ctrl Pts',(-214.720156419641,-3.49034388913101,
135.938837938644));
#270310=CARTESIAN_POINT('Ctrl Pts',(-214.998604043455,2.43316505771265,
136.516196191791));
#270311=CARTESIAN_POINT('Ctrl Pts',(-215.277051667267,6.12071418324004,
131.844656590906));
#270312=CARTESIAN_POINT('Ctrl Pts',(-215.55549929108,4.18362598788043,126.217135811804));
#270313=CARTESIAN_POINT('Ctrl Pts',(-215.833946914893,-1.59801010884951,
124.805050530808));
#270314=CARTESIAN_POINT('Ctrl Pts',(-216.112394538706,-5.91115298268039,
128.90603813695));
#270315=CARTESIAN_POINT('Ctrl Pts',(-216.390842162519,-4.79223504130557,
134.75149136457));
#270316=CARTESIAN_POINT('Ctrl Pts',(-216.669289786332,0.730512789332353,
136.969724263749));
#270317=CARTESIAN_POINT('Ctrl Pts',(-216.947737410145,5.5819550541073,133.522289166845));
#270318=CARTESIAN_POINT('Ctrl Pts',(-217.226185033957,5.3038533178224,127.577210511344));
#270319=CARTESIAN_POINT('Ctrl Pts',(-217.50463265777,0.151769490097695,
124.597725148413));
#270320=CARTESIAN_POINT('Ctrl Pts',(-217.783080281583,-5.13978308467467,
127.321834570635));
#270321=CARTESIAN_POINT('Ctrl Pts',(-218.061527905396,-5.70812609699421,
133.24621529913));
#270322=CARTESIAN_POINT('Ctrl Pts',(-218.339975529209,-1.03098008363786,
136.9266508665));
#270323=CARTESIAN_POINT('Ctrl Pts',(-218.618423153022,4.59358626040416,
134.981000785606));
#270324=CARTESIAN_POINT('Ctrl Pts',(-218.896870776835,5.99687124029931,
129.197222430498));
#270325=CARTESIAN_POINT('Ctrl Pts',(-219.175318400648,1.88932451380644,
124.890325556239));
#270326=CARTESIAN_POINT('Ctrl Pts',(-219.45376602446,-3.95441914224089,
126.018137986666));
#270327=CARTESIAN_POINT('Ctrl Pts',(-219.732213648274,-6.16424479068368,
131.544255194914));
#270328=CARTESIAN_POINT('Ctrl Pts',(-220.010661272086,-2.70943061658779,
136.390445432439));
#270329=CARTESIAN_POINT('Ctrl Pts',(-220.289108895899,3.23521793110825,
136.103296620509));
#270330=CARTESIAN_POINT('Ctrl Pts',(-220.567556519712,6.20685924929812,
130.94668448929));
#270331=CARTESIAN_POINT('Ctrl Pts',(-220.846004143525,3.47470013931478,
125.659283672863));
#270332=CARTESIAN_POINT('Ctrl Pts',(-221.124451767337,-2.45053865016082,
125.099957217636));
#270333=CARTESIAN_POINT('Ctrl Pts',(-221.402899391151,-6.12385213560643,
129.782698811345));
#270334=CARTESIAN_POINT('Ctrl Pts',(-221.681347014963,-4.16964467523852,
135.404297694017));
#270335=CARTESIAN_POINT('Ctrl Pts',(-221.959794638777,1.61626254320698,
136.79877912285));
#270336=CARTESIAN_POINT('Ctrl Pts',(-222.238242262589,5.91690344326002,
132.684682788949));
#270337=CARTESIAN_POINT('Ctrl Pts',(-222.516689886402,4.7801991357601,126.842662238393));
#270338=CARTESIAN_POINT('Ctrl Pts',(-222.795137510215,-0.749274651793031,
124.64124895857));
#270339=CARTESIAN_POINT('Ctrl Pts',(-223.073585134028,-5.59020163845046,
128.103434208622));
#270340=CARTESIAN_POINT('Ctrl Pts',(-223.352032757841,-5.29400641590365,
134.047638880903));
#270341=CARTESIAN_POINT('Ctrl Pts',(-223.630480381654,-0.132877923733138,
137.011429272127));
#270342=CARTESIAN_POINT('Ctrl Pts',(-223.908928005467,5.15035888890098,
134.271226801972));
#270343=CARTESIAN_POINT('Ctrl Pts',(-224.187375629279,5.70066749165438,
128.345143674176));
#270344=CARTESIAN_POINT('Ctrl Pts',(-224.465823253093,1.01234116266713,
124.678960777928));
#270345=CARTESIAN_POINT('Ctrl Pts',(-224.744270876905,-4.60627723919628,
126.641721091889));
#270346=CARTESIAN_POINT('Ctrl Pts',(-225.022718500718,-5.99195188739136,
132.4297437737));
#270347=CARTESIAN_POINT('Ctrl Pts',(-225.301166124531,-1.87131547419729,
136.724118739406));
#270348=CARTESIAN_POINT('Ctrl Pts',(-225.579613748344,3.96896844094108,
135.578525187401));
#270349=CARTESIAN_POINT('Ctrl Pts',(-225.858061372157,6.16196425374224,
130.045707626623));
#270350=CARTESIAN_POINT('Ctrl Pts',(-226.13650899597,2.69241594604283,125.210055102262));
#270351=CARTESIAN_POINT('Ctrl Pts',(-226.414956619783,-3.25133108423828,
125.515296049447));
#270352=CARTESIAN_POINT('Ctrl Pts',(-226.693404243596,-6.20726368445854,
130.680928949564));
#270353=CARTESIAN_POINT('Ctrl Pts',(-226.971851867408,-3.45902420035033,
135.959989522602));
#270354=CARTESIAN_POINT('Ctrl Pts',(-227.250299491222,2.46788954115291,
136.501278998386));
#270355=CARTESIAN_POINT('Ctrl Pts',(-227.528747115034,6.12693335744362,
131.80737879213));
#270356=CARTESIAN_POINT('Ctrl Pts',(-227.807194738847,4.15562473557794,
126.191753883612));
#270357=CARTESIAN_POINT('Ctrl Pts',(-228.08564236266,-1.63450000472891,
124.81488922523));
#270358=CARTESIAN_POINT('Ctrl Pts',(-228.364089986473,-5.9225990904546,
128.942056174461));
#270359=CARTESIAN_POINT('Ctrl Pts',(-228.642537610286,-4.76811894710285,
134.780589928275));
#270360=CARTESIAN_POINT('Ctrl Pts',(-228.920985234099,0.768029573076269,
136.965163195147));
#270361=CARTESIAN_POINT('Ctrl Pts',(-229.199432857912,5.59839643592858,
133.48825986516));
#270362=CARTESIAN_POINT('Ctrl Pts',(-229.477880481725,5.28411047103341,
127.544984242401));
#270363=CARTESIAN_POINT('Ctrl Pts',(-229.756328105537,0.11398512640586,
124.59691627903));
#270364=CARTESIAN_POINT('Ctrl Pts',(-230.03477572935,-5.16088698090536,
127.353186412258));
#270365=CARTESIAN_POINT('Ctrl Pts',(-230.313223353163,-5.69315607611037,
133.280917040931));
#270366=CARTESIAN_POINT('Ctrl Pts',(-230.591670976976,-0.993692863505588,
136.932813303039));
#270367=CARTESIAN_POINT('Ctrl Pts',(-230.870118600789,4.6189255460653,134.952960938754));
#270368=CARTESIAN_POINT('Ctrl Pts',(-231.148566224602,5.98697702585963,
129.160747549691));
#270369=CARTESIAN_POINT('Ctrl Pts',(-231.427013848415,1.85328909897679,
124.878934275042));
#270370=CARTESIAN_POINT('Ctrl Pts',(-231.705461472227,-3.98348097165998,
126.042298336002));
#270371=CARTESIAN_POINT('Ctrl Pts',(-231.983909096041,-6.15962663320533,
131.581764994044));
#270372=CARTESIAN_POINT('Ctrl Pts',(-232.262356719853,-2.6753763333251,
136.406835008417));
#270373=CARTESIAN_POINT('Ctrl Pts',(-232.540804343666,3.26741411748112,
136.083504753687));
#270374=CARTESIAN_POINT('Ctrl Pts',(-232.819251967479,6.20761061637562,
130.90889893839));
#270375=CARTESIAN_POINT('Ctrl Pts',(-233.097699591292,3.44331621745904,
125.638227513236));
#270376=CARTESIAN_POINT('Ctrl Pts',(-233.376147215105,-2.48521756995422,
125.114980031328));
#270377=CARTESIAN_POINT('Ctrl Pts',(-233.654594838918,-6.12995782020675,
129.819995366479));
#270378=CARTESIAN_POINT('Ctrl Pts',(-233.933042462731,-4.14156629877734,
135.429594278462));
#270379=CARTESIAN_POINT('Ctrl Pts',(-234.211490086544,1.65272232446679,
136.788829411307));
#270380=CARTESIAN_POINT('Ctrl Pts',(-234.489937710357,5.92823987150001,
132.648630080257));
#270381=CARTESIAN_POINT('Ctrl Pts',(-234.768385334169,4.75599458724306,
126.813637210565));
#270382=CARTESIAN_POINT('Ctrl Pts',(-235.046832957982,-0.786777379437916,
124.64592419423));
#270383=CARTESIAN_POINT('Ctrl Pts',(-235.325280581795,-5.6065393706272,
128.137513394595));
#270384=CARTESIAN_POINT('Ctrl Pts',(-235.603728205608,-5.27416557488518,
134.079804910139));
#270385=CARTESIAN_POINT('Ctrl Pts',(-235.882175829421,-0.0950912731361558,
137.012123135159));
#270386=CARTESIAN_POINT('Ctrl Pts',(-236.160623453234,5.17136726315852,
134.239810872567));
#270387=CARTESIAN_POINT('Ctrl Pts',(-236.439071077047,5.68559191994549,
128.310487656705));
#270388=CARTESIAN_POINT('Ctrl Pts',(-236.71751870086,0.975035358909668,
124.672911859406));
#270389=CARTESIAN_POINT('Ctrl Pts',(-236.995966324673,-4.63153106383903,
126.669837932931));
#270390=CARTESIAN_POINT('Ctrl Pts',(-237.274413948486,-5.98194670179065,
132.466188370973));
#270391=CARTESIAN_POINT('Ctrl Pts',(-237.552861572298,-1.83524555513966,
136.735400288432));
#270392=CARTESIAN_POINT('Ctrl Pts',(-237.831309196112,3.99795659995517,
135.554276495761));
#270393=CARTESIAN_POINT('Ctrl Pts',(-238.109756819924,6.15723195072914,
130.008212057319));
#270394=CARTESIAN_POINT('Ctrl Pts',(-238.388204443737,2.65831193628575,
125.193769251723));
#270395=CARTESIAN_POINT('Ctrl Pts',(-238.66665206755,-3.28346688184612,
125.535185818711));
#270396=CARTESIAN_POINT('Ctrl Pts',(-238.945099691363,-6.20790004183648,
130.718716612347));
#270397=CARTESIAN_POINT('Ctrl Pts',(-239.223547315176,-3.42757633615586,
135.980950062836));
#270398=CARTESIAN_POINT('Ctrl Pts',(-239.501994938989,2.50252257603867,
136.486150703575));
#270399=CARTESIAN_POINT('Ctrl Pts',(-239.780442562802,6.13292549587844,
131.770063826148));
#270400=CARTESIAN_POINT('Ctrl Pts',(-240.058890186614,4.12746949507249,
126.166542877259));
#270401=CARTESIAN_POINT('Ctrl Pts',(-240.337337810428,-1.67092933361012,
124.824949861719));
#270402=CARTESIAN_POINT('Ctrl Pts',(-240.61578543424,-5.93382573414137,
128.978143220346));
#270403=CARTESIAN_POINT('Ctrl Pts',(-240.894233058053,-4.74382616849909,
134.80954115134));
#270404=CARTESIAN_POINT('Ctrl Pts',(-241.172680681866,0.805517897201924,
136.960373835741));
#270405=CARTESIAN_POINT('Ctrl Pts',(-241.451128305679,5.6146303671111,133.454131110603));
#270406=CARTESIAN_POINT('Ctrl Pts',(-241.729575929492,5.26417181958768,
127.512878750849));
#270407=CARTESIAN_POINT('Ctrl Pts',(-242.008023553305,0.0761965389532375,
124.596337428779));
#270408=CARTESIAN_POINT('Ctrl Pts',(-242.286471177117,-5.18179963857104,
127.384666138411));
#270409=CARTESIAN_POINT('Ctrl Pts',(-242.564918800931,-5.67797509323448,
133.315527013022));
#270410=CARTESIAN_POINT('Ctrl Pts',(-242.843366424743,-0.956368821719198,
136.938748647509));
#270411=CARTESIAN_POINT('Ctrl Pts',(-243.121814048556,4.64409367574132,
134.924767363992));
#270412=CARTESIAN_POINT('Ctrl Pts',(-243.400261672369,5.9768609617849,129.124333573571));
#270413=CARTESIAN_POINT('Ctrl Pts',(-243.678709296182,1.81718500983798,
124.867762562695));
#270414=CARTESIAN_POINT('Ctrl Pts',(-243.957156919995,-4.01239519172672,
126.066635145309));
#270415=CARTESIAN_POINT('Ctrl Pts',(-244.235604543808,-6.15478022849689,
131.619245986169));
#270416=CARTESIAN_POINT('Ctrl Pts',(-244.514052167621,-2.64122291300849,
136.423016982646));
#270417=CARTESIAN_POINT('Ctrl Pts',(-244.792499791433,3.29948922862226,
136.063517266237));
#270418=CARTESIAN_POINT('Ctrl Pts',(-245.070947415247,6.20813195815889,
130.871109513785));
#270419=CARTESIAN_POINT('Ctrl Pts',(-245.349395039059,3.41180470225455,
125.617362786572));
#270420=CARTESIAN_POINT('Ctrl Pts',(-245.627842662872,-2.51980439909662,
125.13021366711));
#270421=CARTESIAN_POINT('Ctrl Pts',(-245.906290286685,-6.13583635696575,
129.857328397629));
#270422=CARTESIAN_POINT('Ctrl Pts',(-246.184737910498,-4.1133344550539,
135.454719473173));
#270423=CARTESIAN_POINT('Ctrl Pts',(-246.463185534311,1.68912086349306,
136.778657943074));
#270424=CARTESIAN_POINT('Ctrl Pts',(-246.741633158124,5.93935662663147,
132.612509031482));
#270425=CARTESIAN_POINT('Ctrl Pts',(-247.020080781937,4.73161380359756,
126.784760060463));
#270426=CARTESIAN_POINT('Ctrl Pts',(-247.29852840575,-0.824250952757648,
124.650827633015));
#270427=CARTESIAN_POINT('Ctrl Pts',(-247.576976029562,-5.62266935042617,
128.171691401572));
#270428=CARTESIAN_POINT('Ctrl Pts',(-247.855423653376,-5.25412929772145,
134.111849566585));
#270429=CARTESIAN_POINT('Ctrl Pts',(-248.133871277188,-0.0573010988966442,
137.012586967267));
#270430=CARTESIAN_POINT('Ctrl Pts',(-248.412318901001,5.19218401050035,
134.208267641291));
#270431=CARTESIAN_POINT('Ctrl Pts',(-248.690766524814,5.67030566653712,
128.275924050614));
#270432=CARTESIAN_POINT('Ctrl Pts',(-248.969214148627,0.937693424858449,
124.667090143972));
#270433=CARTESIAN_POINT('Ctrl Pts',(-249.24766177244,-4.65661326539506,
126.698107980232));
#270434=CARTESIAN_POINT('Ctrl Pts',(-249.526109396252,-5.97171985295489,
132.502571388608));
#270435=CARTESIAN_POINT('Ctrl Pts',(-249.804557020066,-1.79910763038337,
136.746462060605));
#270436=CARTESIAN_POINT('Ctrl Pts',(-250.083004643878,4.02679661321771,
135.52985179424));
#270437=CARTESIAN_POINT('Ctrl Pts',(-250.361452267692,6.15227148922063,
129.970745989595));
#270438=CARTESIAN_POINT('Ctrl Pts',(-250.639899891504,2.62410942180459,
125.177691303707));
#270439=CARTESIAN_POINT('Ctrl Pts',(-250.918347515317,-3.31548100938434,
125.555270839195));
#270440=CARTESIAN_POINT('Ctrl Pts',(-251.19679513913,-6.20830636318893,
130.756507448682));
#270441=CARTESIAN_POINT('Ctrl Pts',(-251.475242762943,-3.39600146187203,
136.001718782677));
#270442=CARTESIAN_POINT('Ctrl Pts',(-251.753690386756,2.53706287905323,
136.47081186788));
#270443=CARTESIAN_POINT('Ctrl Pts',(-252.032138010569,6.13869037645988,
131.732713075798));
#270444=CARTESIAN_POINT('Ctrl Pts',(-252.310585634382,4.09916130974965,
126.141503726722));
#270445=CARTESIAN_POINT('Ctrl Pts',(-252.589033258195,-1.70729674574642,
124.835232067896));
#270446=CARTESIAN_POINT('Ctrl Pts',(-252.867480882007,-5.94483249743877,
129.014297936587));
#270447=CARTESIAN_POINT('Ctrl Pts',(-253.14592850582,-4.71935760622846,
134.838343962485));
#270448=CARTESIAN_POINT('Ctrl Pts',(-253.424376129633,0.842976373616159,
136.955356360136));
#270449=CARTESIAN_POINT('Ctrl Pts',(-253.702823753446,5.63065624411703,
133.419904173236));
#270450=CARTESIAN_POINT('Ctrl Pts',(-253.981271377259,5.24403810606461,
127.480895216153));
#270451=CARTESIAN_POINT('Ctrl Pts',(-254.259719001072,0.0384051209378723,
124.595988638398));
#270452=CARTESIAN_POINT('Ctrl Pts',(-254.538166624885,-5.20252026939218,
127.416272546179));
#270453=CARTESIAN_POINT('Ctrl Pts',(-254.816614248698,-5.66258373611722,
133.350044001689));
#270454=CARTESIAN_POINT('Ctrl Pts',(-255.095061872511,-0.919009293725241,
136.944456550123));
#270455=CARTESIAN_POINT('Ctrl Pts',(-255.373509496324,4.6690896269236,134.896421351226));
#270456=CARTESIAN_POINT('Ctrl Pts',(-255.651957120136,5.96652359266914,
129.087981388513));
#270457=CARTESIAN_POINT('Ctrl Pts',(-255.93040474395,1.78101326373629,124.856811707331));
#270458=CARTESIAN_POINT('Ctrl Pts',(-256.208852367762,-4.04116012583712,
126.091145862189));
#270459=CARTESIAN_POINT('Ctrl Pts',(-256.487299991575,-6.14970689884083,
131.656699899059));
#270460=CARTESIAN_POINT('Ctrl Pts',(-256.765747615388,-2.60696946356087,
136.438984870644));
#270461=CARTESIAN_POINT('Ctrl Pts',(-257.044195239201,3.33143800190474,
136.043346010603));
#270462=CARTESIAN_POINT('Ctrl Pts',(-257.322642863014,6.2084309480058,130.833296634437));
#270463=CARTESIAN_POINT('Ctrl Pts',(-257.601090486826,3.38015223603414,
125.596729883064));
#270464=CARTESIAN_POINT('Ctrl Pts',(-257.87953811064,-2.5542704291637,125.145582755354));
#270465=CARTESIAN_POINT('Ctrl Pts',(-258.157985734452,-6.14153931545366,
129.894837769574));
#270466=CARTESIAN_POINT('Ctrl Pts',(-258.436433358265,-4.08485240479644,
135.479405634932));
#270467=CARTESIAN_POINT('Ctrl Pts',(-258.714880982078,1.72527217059264,
136.768768758555));
#270468=CARTESIAN_POINT('Ctrl Pts',(-258.993328605892,5.95060195420752,
132.575369498931));
#270469=CARTESIAN_POINT('Ctrl Pts',(-259.271776229703,4.70639920604184,
126.75783223591));
#270470=CARTESIAN_POINT('Ctrl Pts',(-259.550223853517,-0.860449444711704,
124.652528659269));
#270471=CARTESIAN_POINT('Ctrl Pts',(-259.82867147733,-5.64095031490746,
128.212697490595));
#270472=CARTESIAN_POINT('Ctrl Pts',(-260.060711163841,-5.29799179572588,
133.142936715762));
#270473=CARTESIAN_POINT('Ctrl Pts',(-260.246372125917,-2.62679689981868,
135.594171577488));
#270474=CARTESIAN_POINT('Ctrl Pts',(-260.339217213388,-0.889986900407246,
136.05080276614));
#270475=CARTESIAN_POINT('Ctrl Pts',(-260.385654363559,-0.0148419801173944,
136.053268468065));
#270476=CARTESIAN_POINT('Ctrl Pts',(209.997106195361,2.85369542052185,134.803838223542));
#270477=CARTESIAN_POINT('Ctrl Pts',(209.950688331758,3.52024512455777,134.328247120061));
#270478=CARTESIAN_POINT('Ctrl Pts',(209.857862530854,4.598911638141,133.039517383424));
#270479=CARTESIAN_POINT('Ctrl Pts',(209.672220855345,5.31158968331849,129.722011776094));
#270480=CARTESIAN_POINT('Ctrl Pts',(209.440181168834,2.90445768035623,125.771581499823));
#270481=CARTESIAN_POINT('Ctrl Pts',(209.161733545021,-2.67328939945229,
125.640965885288));
#270482=CARTESIAN_POINT('Ctrl Pts',(208.883285921209,-5.78445646322271,
130.262241799363));
#270483=CARTESIAN_POINT('Ctrl Pts',(208.604838297395,-3.58517659481558,
135.378114005881));
#270484=CARTESIAN_POINT('Ctrl Pts',(208.326390673583,1.91144119617671,136.292814641374));
#270485=CARTESIAN_POINT('Ctrl Pts',(208.04794304977,5.65009034124608,132.162897902674));
#270486=CARTESIAN_POINT('Ctrl Pts',(207.769495425957,4.19734896093999,126.785079177362));
#270487=CARTESIAN_POINT('Ctrl Pts',(207.491047802144,-1.1129569716493,125.100504449821));
#270488=CARTESIAN_POINT('Ctrl Pts',(207.212600178331,-5.4002948496084,128.657642803108));
#270489=CARTESIAN_POINT('Ctrl Pts',(206.934152554519,-4.72513942780656,
134.187431620732));
#270490=CARTESIAN_POINT('Ctrl Pts',(206.655704930705,0.292248586550605,
136.608384944684));
#270491=CARTESIAN_POINT('Ctrl Pts',(206.377257306892,5.04104249491135,133.695701483205));
#270492=CARTESIAN_POINT('Ctrl Pts',(206.09880968308,5.15738153042831,128.12602865207));
#270493=CARTESIAN_POINT('Ctrl Pts',(205.820362059267,0.534329935251406,
125.017605890956));
#270494=CARTESIAN_POINT('Ctrl Pts',(205.541914435454,-4.57974002364783,
127.226931288585));
#270495=CARTESIAN_POINT('Ctrl Pts',(205.263466811641,-5.48525514562618,
132.723737743954));
#270496=CARTESIAN_POINT('Ctrl Pts',(204.985019187828,-1.35008742798131,
136.456731302353));
#270497=CARTESIAN_POINT('Ctrl Pts',(204.706571564015,4.02574397595362,134.995471850294));
#270498=CARTESIAN_POINT('Ctrl Pts',(204.428123940202,5.70211370766606,129.682786179275));
#270499=CARTESIAN_POINT('Ctrl Pts',(204.149676316389,2.13851930815143,125.40077248911));
#270500=CARTESIAN_POINT('Ctrl Pts',(203.871228692576,-3.39026975841633,
126.084392381055));
#270501=CARTESIAN_POINT('Ctrl Pts',(203.592781068764,-5.8035665963141,131.105432460946));
#270502=CARTESIAN_POINT('Ctrl Pts',(203.314333444951,-2.88366922283368,
135.849802245147));
#270503=CARTESIAN_POINT('Ctrl Pts',(203.035885821138,2.68617927581077,135.957657646429));
#270504=CARTESIAN_POINT('Ctrl Pts',(202.757438197325,5.78756025537181,131.329884836407));
#270505=CARTESIAN_POINT('Ctrl Pts',(202.478990573512,3.57045609392238,126.219180939555));
#270506=CARTESIAN_POINT('Ctrl Pts',(202.200542949699,-1.92772278905516,
125.322033169903));
#270507=CARTESIAN_POINT('Ctrl Pts',(201.922095325886,-5.6544186046078,129.462876497226));
#270508=CARTESIAN_POINT('Ctrl Pts',(201.643647702073,-4.18497995558374,
134.836478196445));
#270509=CARTESIAN_POINT('Ctrl Pts',(201.36520007826,1.13025082464198,136.504760820331));
#270510=CARTESIAN_POINT('Ctrl Pts',(201.086752454448,5.4068363130258,132.934654138033));
#270511=CARTESIAN_POINT('Ctrl Pts',(200.808304830635,4.71480336828096,127.406911780982));
#270512=CARTESIAN_POINT('Ctrl Pts',(200.529857206822,-0.309903540913717,
125.001258930184));
#270513=CARTESIAN_POINT('Ctrl Pts',(200.251409583008,-5.04982423566531,
127.928373032793));
#270514=CARTESIAN_POINT('Ctrl Pts',(199.972961959197,-5.14920315545485,
133.498379226012));
#270515=CARTESIAN_POINT('Ctrl Pts',(199.694514335383,-0.516715927947778,
136.59271392819));
#270516=CARTESIAN_POINT('Ctrl Pts',(199.416066711571,4.59060799437092,134.367834714685));
#270517=CARTESIAN_POINT('Ctrl Pts',(199.137619087757,5.47938743352869,128.868296891315));
#270518=CARTESIAN_POINT('Ctrl Pts',(198.859171463945,1.33287750423228,125.147907050397));
#270519=CARTESIAN_POINT('Ctrl Pts',(198.580723840131,-4.03848173676817,
126.625521704588));
#270520=CARTESIAN_POINT('Ctrl Pts',(198.302276216319,-5.69867355247927,
131.943285172176));
#270521=CARTESIAN_POINT('Ctrl Pts',(198.023828592506,-2.12206276914206,
136.214432613634));
#270522=CARTESIAN_POINT('Ctrl Pts',(197.745380968693,3.4046200305072,135.513988187415));
#270523=CARTESIAN_POINT('Ctrl Pts',(197.46693334488,5.80262334705539,130.485626102603));
#270524=CARTESIAN_POINT('Ctrl Pts',(197.188485721067,2.86829928156946,125.750165465994));
#270525=CARTESIAN_POINT('Ctrl Pts',(196.910038097254,-2.70185169946893,
125.65926326252));
#270526=CARTESIAN_POINT('Ctrl Pts',(196.631590473441,-5.78913296148881,
130.296454176353));
#270527=CARTESIAN_POINT('Ctrl Pts',(196.353142849628,-3.5564838467683,135.400386297052));
#270528=CARTESIAN_POINT('Ctrl Pts',(196.074695225815,1.94440017923737,136.280795346639));
#270529=CARTESIAN_POINT('Ctrl Pts',(195.796247602003,5.6584754297534,132.128628418917));
#270530=CARTESIAN_POINT('Ctrl Pts',(195.51779997819,4.17268819221861,126.759524075833));
#270531=CARTESIAN_POINT('Ctrl Pts',(195.239352354377,-1.14759564681435,
125.107426913349));
#270532=CARTESIAN_POINT('Ctrl Pts',(194.960904730564,-5.41329514958902,
128.690533514357));
#270533=CARTESIAN_POINT('Ctrl Pts',(194.682457106751,-4.70444086406131,
134.216143957018));
#270534=CARTESIAN_POINT('Ctrl Pts',(194.404009482938,0.327564750825761,
136.606492185605));
#270535=CARTESIAN_POINT('Ctrl Pts',(194.125561859125,5.0585543621317,133.664964953048));
#270536=CARTESIAN_POINT('Ctrl Pts',(193.847114235312,5.14097963875765,128.094682084473));
#270537=CARTESIAN_POINT('Ctrl Pts',(193.568666611499,0.499095778182989,
125.014461412655));
#270538=CARTESIAN_POINT('Ctrl Pts',(193.290218987687,-4.60143272035756,
127.254875257849));
#270539=CARTESIAN_POINT('Ctrl Pts',(193.011771363874,-5.4734693413749,132.757092746623));
#270540=CARTESIAN_POINT('Ctrl Pts',(192.733323740061,-1.31565503151135,
136.464844805061));
#270541=CARTESIAN_POINT('Ctrl Pts',(192.454876116248,4.05118197898966,134.970888425217));
#270542=CARTESIAN_POINT('Ctrl Pts',(192.176428492435,5.69518066204141,129.648096536341));
#270543=CARTESIAN_POINT('Ctrl Pts',(191.897980868622,2.1055865417199,125.38785485147));
#270544=CARTESIAN_POINT('Ctrl Pts',(191.619533244809,-3.4189387468211,126.105117354624));
#270545=CARTESIAN_POINT('Ctrl Pts',(191.341085620997,-5.80162635147675,
131.140754845624));
#270546=CARTESIAN_POINT('Ctrl Pts',(191.062637997183,-2.85290276432908,
135.867262474811));
#270547=CARTESIAN_POINT('Ctrl Pts',(190.784190373371,2.71749909118881,135.941210633695));
#270548=CARTESIAN_POINT('Ctrl Pts',(190.505742749557,5.79065203911519,131.29464457683));
#270549=CARTESIAN_POINT('Ctrl Pts',(190.227295125745,3.54247865217362,126.197531513104));
#270550=CARTESIAN_POINT('Ctrl Pts',(189.948847501932,-1.96105955641241,
125.333869340265));
#270551=CARTESIAN_POINT('Ctrl Pts',(189.670399878119,-5.66247983574075,
129.497321402909));
#270552=CARTESIAN_POINT('Ctrl Pts',(189.391952254306,-4.160357773542,134.861878651407));
#270553=CARTESIAN_POINT('Ctrl Pts',(189.113504630493,1.16492983776554,136.497775047581));
#270554=CARTESIAN_POINT('Ctrl Pts',(188.83505700668,5.41970383815296,132.901701721328));
#270555=CARTESIAN_POINT('Ctrl Pts',(188.556609382867,4.69403477852959,127.378274381527));
#270556=CARTESIAN_POINT('Ctrl Pts',(188.278161759054,-0.345222926215044,
125.003252919028));
#270557=CARTESIAN_POINT('Ctrl Pts',(187.999714135242,-5.0672376268456,127.959166031618));
#270558=CARTESIAN_POINT('Ctrl Pts',(187.721266511429,-5.13270849672517,
133.529673973213));
#270559=CARTESIAN_POINT('Ctrl Pts',(187.442818887616,-0.48147100486422,
136.595752079925));
#270560=CARTESIAN_POINT('Ctrl Pts',(187.164371263803,4.61221481930072,134.339824357932));
#270561=CARTESIAN_POINT('Ctrl Pts',(186.88592363999,5.4675005437485,128.834978175547));
#270562=CARTESIAN_POINT('Ctrl Pts',(186.607476016177,1.29842037074208,125.139898247696));
#270563=CARTESIAN_POINT('Ctrl Pts',(186.329028392364,-4.06384469161484,
126.650182513385));
#270564=CARTESIAN_POINT('Ctrl Pts',(186.050580768551,-5.69163501222784,
131.977953513933));
#270565=CARTESIAN_POINT('Ctrl Pts',(185.772133144738,-2.08909080843167,
136.227249975919));
#270566=CARTESIAN_POINT('Ctrl Pts',(185.493685520926,3.4332257905535,135.493176040453));
#270567=CARTESIAN_POINT('Ctrl Pts',(185.215237897112,5.80057561042411,130.450309792719));
#270568=CARTESIAN_POINT('Ctrl Pts',(184.9367902733,2.83747981818726,125.732798956676));
#270569=CARTESIAN_POINT('Ctrl Pts',(184.658342649487,-2.73312130836828,
125.675805527429));
#270570=CARTESIAN_POINT('Ctrl Pts',(184.379895025674,-5.79211747293216,
130.331703682172));
#270571=CARTESIAN_POINT('Ctrl Pts',(184.101447401861,-3.52844064054064,
135.421950469967));
#270572=CARTESIAN_POINT('Ctrl Pts',(183.822999778048,1.97770076659953,136.26885776521));
#270573=CARTESIAN_POINT('Ctrl Pts',(183.544552154236,5.66643178528845,132.094159137294));
#270574=CARTESIAN_POINT('Ctrl Pts',(183.266104530422,4.14798881387936,126.734198679909));
#270575=CARTESIAN_POINT('Ctrl Pts',(182.98765690661,-1.18225323696583,125.114518204765));
#270576=CARTESIAN_POINT('Ctrl Pts',(182.709209282797,-5.42606231932092,
128.72352494273));
#270577=CARTESIAN_POINT('Ctrl Pts',(182.430761658984,-4.68358520810093,
134.244718011395));
#270578=CARTESIAN_POINT('Ctrl Pts',(182.152314035171,0.362877903506298,
136.604390705933));
#270579=CARTESIAN_POINT('Ctrl Pts',(181.873866411358,5.07587394936235,133.634119096483));
#270580=CARTESIAN_POINT('Ctrl Pts',(181.595418787545,5.12438980598236,128.063437686296));
#270581=CARTESIAN_POINT('Ctrl Pts',(181.316971163732,0.463841771263853,
125.011530548415));
#270582=CARTESIAN_POINT('Ctrl Pts',(181.038523539919,-4.62295419131585,
127.282951248603));
#270583=CARTESIAN_POINT('Ctrl Pts',(180.760075916106,-5.46148109594396,
132.790375128456));
#270584=CARTESIAN_POINT('Ctrl Pts',(180.481628292294,-1.2811736815839,136.472748695004));
#270585=CARTESIAN_POINT('Ctrl Pts',(180.203180668481,4.07646975733793,134.946150534538));
#270586=CARTESIAN_POINT('Ctrl Pts',(179.924733044668,5.68803663588505,129.61344977806));
#270587=CARTESIAN_POINT('Ctrl Pts',(179.646285420855,2.07257572209157,125.37513790386));
#270588=CARTESIAN_POINT('Ctrl Pts',(179.367837797042,-3.44748102935117,
126.12601647128));
#270589=CARTESIAN_POINT('Ctrl Pts',(179.089390173229,-5.79947113363144,
131.176064759319));
#270590=CARTESIAN_POINT('Ctrl Pts',(178.810942549416,-2.82203058602,135.884535099843));
#270591=CARTESIAN_POINT('Ctrl Pts',(178.532494925603,2.74871820628535,135.924573271475));
#270592=CARTESIAN_POINT('Ctrl Pts',(178.254047301791,5.79352924936408,131.259386150458));
#270593=CARTESIAN_POINT('Ctrl Pts',(177.975599677977,3.51436994191561,126.176052793945));
#270594=CARTESIAN_POINT('Ctrl Pts',(177.697152054165,-1.99432365563702,
125.345908221933));
#270595=CARTESIAN_POINT('Ctrl Pts',(177.418704430351,-5.6703312417861,129.531814741282));
#270596=CARTESIAN_POINT('Ctrl Pts',(177.140256806539,-4.135581427815,134.887128753614));
#270597=CARTESIAN_POINT('Ctrl Pts',(176.861809182726,1.19956568393359,136.490578303229));
#270598=CARTESIAN_POINT('Ctrl Pts',(176.583361558913,5.43237053418876,132.868671586896));
#270599=CARTESIAN_POINT('Ctrl Pts',(176.3049139351,4.67309224957875,127.349763936946));
#270600=CARTESIAN_POINT('Ctrl Pts',(176.026466311287,-0.380529519146142,
125.005461870054));
#270601=CARTESIAN_POINT('Ctrl Pts',(175.748018687475,-5.08446324967622,
127.990064460173));
#270602=CARTESIAN_POINT('Ctrl Pts',(175.469571063661,-5.11602364359241,
133.560867732924));
#270603=CARTESIAN_POINT('Ctrl Pts',(175.191123439849,-0.446208240696769,
136.59857562952));
#270604=CARTESIAN_POINT('Ctrl Pts',(174.912675816035,4.63365073691483,134.311682993269));
#270605=CARTESIAN_POINT('Ctrl Pts',(174.634228192223,5.45541105372469,128.801732435971));
#270606=CARTESIAN_POINT('Ctrl Pts',(174.35578056841,1.26391512380778,125.132099343732));
#270607=CARTESIAN_POINT('Ctrl Pts',(174.077332944597,-4.089057059202,126.674997256779));
#270608=CARTESIAN_POINT('Ctrl Pts',(173.798885320784,-5.68438556634791,
132.012578367773));
#270609=CARTESIAN_POINT('Ctrl Pts',(173.520437696972,-2.0560414356932,136.239866391045));
#270610=CARTESIAN_POINT('Ctrl Pts',(173.241990073158,3.46170433115548,135.472190147709));
#270611=CARTESIAN_POINT('Ctrl Pts',(172.963542449346,5.79831293133042,130.41500660232));
#270612=CARTESIAN_POINT('Ctrl Pts',(172.685094825533,2.80655521094699,125.715620375941));
#270613=CARTESIAN_POINT('Ctrl Pts',(172.40664720172,-2.76428964045241,125.692537832834));
#270614=CARTESIAN_POINT('Ctrl Pts',(172.128199577907,-5.79488735533246,
130.366970702468));
#270615=CARTESIAN_POINT('Ctrl Pts',(171.849751954094,-3.50026668664755,
135.443343536393));
#270616=CARTESIAN_POINT('Ctrl Pts',(171.571304330281,2.01092806953244,136.256717694829));
#270617=CARTESIAN_POINT('Ctrl Pts',(171.292856706468,5.6741781691098,132.059642061713));
#270618=CARTESIAN_POINT('Ctrl Pts',(171.014409082656,4.12313573028927,126.709024105332));
#270619=CARTESIAN_POINT('Ctrl Pts',(170.735961458842,-1.21686701828875,
125.121820335384));
#270620=CARTESIAN_POINT('Ctrl Pts',(170.45751383503,-5.43862842431808,128.756593477234));
#270621=CARTESIAN_POINT('Ctrl Pts',(170.179066211217,-4.66255600016836,
134.273164582064));
#270622=CARTESIAN_POINT('Ctrl Pts',(169.900618587404,0.398177609612544,
136.602074304013));
#270623=CARTESIAN_POINT('Ctrl Pts',(169.62217096359,5.09300544821711,133.603168382178));
#270624=CARTESIAN_POINT('Ctrl Pts',(169.343723339778,5.10761008705837,128.032294854024));
#270625=CARTESIAN_POINT('Ctrl Pts',(169.065275715965,0.428570576517446,
125.008814339624));
#270626=CARTESIAN_POINT('Ctrl Pts',(168.786828092152,-4.64430435700642,
127.311157726477));
#270627=CARTESIAN_POINT('Ctrl Pts',(168.508380468339,-5.4492904733226,132.823583917792));
#270628=CARTESIAN_POINT('Ctrl Pts',(168.229932844526,-1.24664485729461,
136.480442540741));
#270629=CARTESIAN_POINT('Ctrl Pts',(167.951485220714,4.10160648060013,134.92125916831));
#270630=CARTESIAN_POINT('Ctrl Pts',(167.673037596901,5.6806818374394,129.578847149419));
#270631=CARTESIAN_POINT('Ctrl Pts',(167.394589973088,2.03948810240773,125.362622138095));
#270632=CARTESIAN_POINT('Ctrl Pts',(167.116142349275,-3.47589556420378,
126.147088945699));
#270633=CARTESIAN_POINT('Ctrl Pts',(166.837694725462,-5.79710101425052,
131.21136089938));
#270634=CARTESIAN_POINT('Ctrl Pts',(166.559247101649,-2.79105383632985,
135.901619477142));
#270635=CARTESIAN_POINT('Ctrl Pts',(166.280799477836,2.77983546661788,135.907746177893));
#270636=CARTESIAN_POINT('Ctrl Pts',(166.002351854023,5.79619177825601,131.224110862948));
#270637=CARTESIAN_POINT('Ctrl Pts',(165.72390423021,3.48613100538707,126.154745578436));
#270638=CARTESIAN_POINT('Ctrl Pts',(165.445456606397,-2.02751385446508,
125.358149368562));
#270639=CARTESIAN_POINT('Ctrl Pts',(165.167008982585,-5.67797253162207,
129.566355234311));
#270640=CARTESIAN_POINT('Ctrl Pts',(164.888561358772,-4.11065183659732,
134.912227567346));
#270641=CARTESIAN_POINT('Ctrl Pts',(164.610113734959,1.23415707975413,136.483170853989));
#270642=CARTESIAN_POINT('Ctrl Pts',(164.331666111146,5.44483593173667,132.835564958663));
#270643=CARTESIAN_POINT('Ctrl Pts',(164.053218487333,4.65197655747607,127.321381503715));
#270644=CARTESIAN_POINT('Ctrl Pts',(163.77477086352,-0.415822011415935,
125.007885701408));
#270645=CARTESIAN_POINT('Ctrl Pts',(163.496323239708,-5.10150046585131,
128.021067173507));
#270646=CARTESIAN_POINT('Ctrl Pts',(163.217875615894,-5.09914921432216,
133.591959349252));
#270647=CARTESIAN_POINT('Ctrl Pts',(162.939427992082,-0.41092894211879,
136.601184472346));
#270648=CARTESIAN_POINT('Ctrl Pts',(162.660980368268,4.65491495289691,134.283411663486));
#270649=CARTESIAN_POINT('Ctrl Pts',(162.382532744456,5.443119411438,128.768560904517));
#270650=CARTESIAN_POINT('Ctrl Pts',(162.104085120643,1.22936304203373,125.124510627495));
#270651=CARTESIAN_POINT('Ctrl Pts',(161.82563749683,-4.11411790527609,126.69996501525));
#270652=CARTESIAN_POINT('Ctrl Pts',(161.547189873017,-5.67692548347038,
132.04715845066));
#270653=CARTESIAN_POINT('Ctrl Pts',(161.268742249204,-2.02291587558315,
136.252281391507));
#270654=CARTESIAN_POINT('Ctrl Pts',(160.990294625391,3.49005459703047,135.451031286826));
#270655=CARTESIAN_POINT('Ctrl Pts',(160.711847001578,5.79583539361873,130.379717839577));
#270656=CARTESIAN_POINT('Ctrl Pts',(160.433399377766,2.77552660577121,125.698630360346));
#270657=CARTESIAN_POINT('Ctrl Pts',(160.154951753952,-2.79535554076737,
125.70945955871));
#270658=CARTESIAN_POINT('Ctrl Pts',(159.87650413014,-5.79744250605075,130.402253930408));
#270659=CARTESIAN_POINT('Ctrl Pts',(159.598056506327,-3.47196302908515,
135.4645647036));
#270660=CARTESIAN_POINT('Ctrl Pts',(159.319608882514,2.04408085678626,136.244375585352));
#270661=CARTESIAN_POINT('Ctrl Pts',(159.041161258701,5.68171429417248,132.025078471215));
#270662=CARTESIAN_POINT('Ctrl Pts',(158.762713634888,4.09812986238831,126.684001284956));
#270663=CARTESIAN_POINT('Ctrl Pts',(158.484266011075,-1.25143570815684,
125.129333034622));
#270664=CARTESIAN_POINT('Ctrl Pts',(158.205818387262,-5.450992998939,128.789737892503));
#270665=CARTESIAN_POINT('Ctrl Pts',(157.927370763449,-4.64135401950845,
134.301482614925));
#270666=CARTESIAN_POINT('Ctrl Pts',(157.648923139637,0.43346256110109,136.59954306568));
#270667=CARTESIAN_POINT('Ctrl Pts',(157.370475515823,5.10994822388206,133.572113957021));
#270668=CARTESIAN_POINT('Ctrl Pts',(157.092027892011,5.09064110376424,128.001254741669));
#270669=CARTESIAN_POINT('Ctrl Pts',(156.813580268198,0.39328350093061,125.006312886931));
#270670=CARTESIAN_POINT('Ctrl Pts',(156.535132644385,-4.66548242629113,
127.339493646268));
#270671=CARTESIAN_POINT('Ctrl Pts',(156.256685020572,-5.43689792523874,
132.856717884066));
#270672=CARTESIAN_POINT('Ctrl Pts',(155.978237396759,-1.21206983812162,
136.487926057176));
#270673=CARTESIAN_POINT('Ctrl Pts',(155.699789772946,4.12659121732586,134.896215248893));
#270674=CARTESIAN_POINT('Ctrl Pts',(155.421342149133,5.67311653923917,129.544289932631));
#270675=CARTESIAN_POINT('Ctrl Pts',(155.142894525321,2.0063249087422,125.350308017949));
#270676=CARTESIAN_POINT('Ctrl Pts',(154.864446901507,-3.50418129846815,
126.168333997033));
#270677=CARTESIAN_POINT('Ctrl Pts',(154.585999277695,-5.79451608115961,
131.246641957895));
#270678=CARTESIAN_POINT('Ctrl Pts',(154.307551653882,-2.75997366311328,
135.918514973638));
#270679=CARTESIAN_POINT('Ctrl Pts',(154.029104030069,2.81084971912495,135.890729976482));
#270680=CARTESIAN_POINT('Ctrl Pts',(153.750656406256,5.79863952713012,131.188820021437));
#270681=CARTESIAN_POINT('Ctrl Pts',(153.472208782443,3.457762888992,126.133610656121));
#270682=CARTESIAN_POINT('Ctrl Pts',(153.19376115863,-2.0606289230217,125.370592326552));
#270683=CARTESIAN_POINT('Ctrl Pts',(152.915313534817,-5.68540342209783,
129.600941602086));
#270684=CARTESIAN_POINT('Ctrl Pts',(152.636865911004,-4.08556992366409,
134.937174162558));
#270685=CARTESIAN_POINT('Ctrl Pts',(152.358418287191,1.26870274343019,136.475552974349));
#270686=CARTESIAN_POINT('Ctrl Pts',(152.079970663379,5.45709956888678,132.802383063404));
#270687=CARTESIAN_POINT('Ctrl Pts',(151.801523039566,4.63068848467127,127.293128133558));
#270688=CARTESIAN_POINT('Ctrl Pts',(151.523075415753,-0.451099095248245,
125.010524323271));
#270689=CARTESIAN_POINT('Ctrl Pts',(151.24462779194,-5.11834864405056,128.052173022803));
#270690=CARTESIAN_POINT('Ctrl Pts',(150.966180168127,-5.08208583420252,
133.622947670083));
#270691=CARTESIAN_POINT('Ctrl Pts',(150.687732544314,-0.375634416417742,
136.603578511732));
#270692=CARTESIAN_POINT('Ctrl Pts',(150.409284920501,4.67600667929353,134.255011416186));
#270693=CARTESIAN_POINT('Ctrl Pts',(150.130837296688,5.43062607235983,128.735464810371));
#270694=CARTESIAN_POINT('Ctrl Pts',(149.852389672876,1.19476540576009,125.117132380189));
#270695=CARTESIAN_POINT('Ctrl Pts',(149.573942049063,-4.13902630119825,
126.725084863609));
#270696=CARTESIAN_POINT('Ctrl Pts',(149.29549442525,-5.66925504003138,132.081692481218));
#270697=CARTESIAN_POINT('Ctrl Pts',(149.017046801437,-1.98971535558138,
136.264494517259));
#270698=CARTESIAN_POINT('Ctrl Pts',(148.738599177624,3.5182755376489,135.429700241853));
#270699=CARTESIAN_POINT('Ctrl Pts',(148.460151553811,5.79314308909515,130.344444812129));
#270700=CARTESIAN_POINT('Ctrl Pts',(148.181703929998,2.74439515243632,125.681829539465));
#270701=CARTESIAN_POINT('Ctrl Pts',(147.903256306185,-2.82631785815477,
125.726570078021));
#270702=CARTESIAN_POINT('Ctrl Pts',(147.624808682372,-5.79978283040501,
130.437552058559));
#270703=CARTESIAN_POINT('Ctrl Pts',(147.346361058559,-3.4435307166558,135.48561318523));
#270704=CARTESIAN_POINT('Ctrl Pts',(147.067913434747,2.07715789987228,136.23183189412));
#270705=CARTESIAN_POINT('Ctrl Pts',(146.789465810933,5.68903988122249,131.990469646568));
#270706=CARTESIAN_POINT('Ctrl Pts',(146.511018187121,4.07297213677825,126.65913114601));
#270707=CARTESIAN_POINT('Ctrl Pts',(146.232570563308,-1.2859580256146,125.137056024094));
#270708=CARTESIAN_POINT('Ctrl Pts',(145.954122939495,-5.46315558500969,
128.822956960357));
#270709=CARTESIAN_POINT('Ctrl Pts',(145.675675315682,-4.61998005176852,
134.329671060644));
#270710=CARTESIAN_POINT('Ctrl Pts',(145.397227691869,0.468731450475054,
136.596797084732));
#270711=CARTESIAN_POINT('Ctrl Pts',(145.118780068056,5.12670164853643,133.540956971746));
#270712=CARTESIAN_POINT('Ctrl Pts',(144.840332444244,5.07348348489189,127.970318499433));
#270713=CARTESIAN_POINT('Ctrl Pts',(144.56188482043,0.357981852079004,125.004026283029));
#270714=CARTESIAN_POINT('Ctrl Pts',(144.283437196618,-4.6864876144088,127.367957957979));
#270715=CARTESIAN_POINT('Ctrl Pts',(144.004989572805,-5.42430391090288,
132.889775799486));
#270716=CARTESIAN_POINT('Ctrl Pts',(143.726541948992,-1.17744990525502,
136.495198967004));
#270717=CARTESIAN_POINT('Ctrl Pts',(143.448094325179,4.15142304169647,134.871019704297));
#270718=CARTESIAN_POINT('Ctrl Pts',(143.169646701366,5.66534102161933,129.509779408224));
#270719=CARTESIAN_POINT('Ctrl Pts',(142.891199077553,1.9730873699693,125.338195999729));
#270720=CARTESIAN_POINT('Ctrl Pts',(142.61275145374,-3.53233718400576,126.189750838038));
#270721=CARTESIAN_POINT('Ctrl Pts',(142.334303829928,-5.79171643014443,
131.281906627513));
#270722=CARTESIAN_POINT('Ctrl Pts',(142.055856206114,-2.72879121805762,
135.935220963265));
#270723=CARTESIAN_POINT('Ctrl Pts',(141.777408582302,2.84175981456215,135.873525297782));
#270724=CARTESIAN_POINT('Ctrl Pts',(141.498960958489,5.80087240528401,131.153514933643));
#270725=CARTESIAN_POINT('Ctrl Pts',(141.220513334676,3.42926664392146,126.112648810165));
#270726=CARTESIAN_POINT('Ctrl Pts',(140.942065710863,-2.09366763421581,
125.383236634823));
#270727=CARTESIAN_POINT('Ctrl Pts',(140.66361808705,-5.69262363785895,129.635572562993));
#270728=CARTESIAN_POINT('Ctrl Pts',(140.385170463237,-4.06033661843482,
134.961967614844));
#270729=CARTESIAN_POINT('Ctrl Pts',(140.106722839424,1.30320139485961,136.467724946589));
#270730=CARTESIAN_POINT('Ctrl Pts',(139.828275215611,5.46916099120554,132.769127130691));
#270731=CARTESIAN_POINT('Ctrl Pts',(139.549827591798,4.60922882000175,127.26500487341));
#270732=CARTESIAN_POINT('Ctrl Pts',(139.271379967986,-0.486359463437733,
125.013377637868));
#270733=CARTESIAN_POINT('Ctrl Pts',(138.992932344173,-5.13500715995863,
128.083380855422));
#270734=CARTESIAN_POINT('Ctrl Pts',(138.71448472036,-5.06483413552331,133.653831547135));
#270735=CARTESIAN_POINT('Ctrl Pts',(138.436037096547,-0.340325971445257,
136.605757658967));
#270736=CARTESIAN_POINT('Ctrl Pts',(138.157589472734,4.69692513454305,134.226483303753));
#270737=CARTESIAN_POINT('Ctrl Pts',(137.879141848921,5.41793149943546,128.70244537992));
#270738=CARTESIAN_POINT('Ctrl Pts',(137.600694225109,1.16012349701482,125.109964875215));
#270739=CARTESIAN_POINT('Ctrl Pts',(137.322246601295,-4.16378132397874,
126.750355871033));
#270740=CARTESIAN_POINT('Ctrl Pts',(137.043798977483,-5.66137452026194,
132.116179179772));
#270741=CARTESIAN_POINT('Ctrl Pts',(136.765351353669,-1.95644110594549,
136.276505315742));
#270742=CARTESIAN_POINT('Ctrl Pts',(136.486903729857,3.54636610727348,135.408197803219));
#270743=CARTESIAN_POINT('Ctrl Pts',(136.208456106044,5.79023611752392,130.309188827029));
#270744=CARTESIAN_POINT('Ctrl Pts',(135.930008482231,2.71316200452982,125.665218535856));
#270745=CARTESIAN_POINT('Ctrl Pts',(135.651560858418,-2.85717544529452,
125.743868756725));
#270746=CARTESIAN_POINT('Ctrl Pts',(135.373113234605,-5.80190824167357,
130.472863778936));
#270747=CARTESIAN_POINT('Ctrl Pts',(135.094665610792,-3.41497080292952,
135.506488201326));
#270748=CARTESIAN_POINT('Ctrl Pts',(134.816217986979,2.11015797310843,136.219087085943));
#270749=CARTESIAN_POINT('Ctrl Pts',(134.537770363167,5.69615465880763,131.955816870215));
#270750=CARTESIAN_POINT('Ctrl Pts',(134.259322739353,4.04766348568775,126.634414610068));
#270751=CARTESIAN_POINT('Ctrl Pts',(133.980875115541,-1.32043269142476,
125.144989017623));
#270752=CARTESIAN_POINT('Ctrl Pts',(133.702427491728,-5.47511573184112,
128.856249449853));
#270753=CARTESIAN_POINT('Ctrl Pts',(133.423979867915,-4.59843488896879,
134.357728874689));
#270754=CARTESIAN_POINT('Ctrl Pts',(133.145532244102,0.503982970832797,
136.59383646292));
#270755=CARTESIAN_POINT('Ctrl Pts',(132.867084620289,5.14326510137581,133.509698580887));
#270756=CARTESIAN_POINT('Ctrl Pts',(132.588636996476,5.05613786622328,127.93948727367));
#270757=CARTESIAN_POINT('Ctrl Pts',(132.310189372663,0.322666938078297,
125.001954612649));
#270758=CARTESIAN_POINT('Ctrl Pts',(132.03174174885,-4.70731914300451,127.396549606854));
#270759=CARTESIAN_POINT('Ctrl Pts',(131.753294125038,-5.41150889699075,
132.92275643908));
#270760=CARTESIAN_POINT('Ctrl Pts',(131.474846501225,-1.14278634154918,
136.502261000723));
#270761=CARTESIAN_POINT('Ctrl Pts',(131.196398877412,4.17610103355955,134.845673468154));
#270762=CARTESIAN_POINT('Ctrl Pts',(130.917951253599,5.65735557270449,129.475316855001));
#270763=CARTESIAN_POINT('Ctrl Pts',(130.639503629786,1.93977671771839,125.326286532249));
#270764=CARTESIAN_POINT('Ctrl Pts',(130.361056005973,-3.56036217749005,
126.211338675105));
#270765=CARTESIAN_POINT('Ctrl Pts',(130.08260838216,-5.788702164947,131.317153601487));
#270766=CARTESIAN_POINT('Ctrl Pts',(129.804160758347,-2.69750765663984,
135.951736826975));
#270767=CARTESIAN_POINT('Ctrl Pts',(129.525713134534,2.87256460754407,135.856132779323));
#270768=CARTESIAN_POINT('Ctrl Pts',(129.247265510721,5.80289032997773,131.118196907806));
#270769=CARTESIAN_POINT('Ctrl Pts',(128.968817886909,3.40064332611445,126.091860817314));
#270770=CARTESIAN_POINT('Ctrl Pts',(128.690370263096,-2.12662876378584,
125.396081824838));
#270771=CARTESIAN_POINT('Ctrl Pts',(128.411922639283,-5.69963291135762,
129.670246833772));
#270772=CARTESIAN_POINT('Ctrl Pts',(128.13347501547,-4.03495285593914,134.986607005474));
#270773=CARTESIAN_POINT('Ctrl Pts',(127.855027391657,1.33765175568188,136.459687060782));
#270774=CARTESIAN_POINT('Ctrl Pts',(127.576579767844,5.48101975175251,132.73579839283));
#270775=CARTESIAN_POINT('Ctrl Pts',(127.298132144031,4.5875983586632,127.237012765392));
#270776=CARTESIAN_POINT('Ctrl Pts',(127.019684520218,-0.521601809398458,
125.016445539469));
#270777=CARTESIAN_POINT('Ctrl Pts',(126.741236896406,-5.15147539628782,
128.114689514947));
#270778=CARTESIAN_POINT('Ctrl Pts',(126.462789272592,-5.0473947575527,133.684609835992));
#270779=CARTESIAN_POINT('Ctrl Pts',(126.18434164878,-0.305004915568794,
136.607721833301));
#270780=CARTESIAN_POINT('Ctrl Pts',(125.905894024967,4.71766954350447,134.197828383304));
#270781=CARTESIAN_POINT('Ctrl Pts',(125.627446401154,5.40503616306688,128.669503836711));
#270782=CARTESIAN_POINT('Ctrl Pts',(125.348998777341,1.12543859946687,125.10300837817));
#270783=CARTESIAN_POINT('Ctrl Pts',(125.070551153528,-4.18838205631096,
126.775777101093));
#270784=CARTESIAN_POINT('Ctrl Pts',(124.792103529715,-5.65328421617778,
132.150617268407));
#270785=CARTESIAN_POINT('Ctrl Pts',(124.513655905902,-1.9230943596648,136.288313341892));
#270786=CARTESIAN_POINT('Ctrl Pts',(124.23520828209,3.57432526499779,135.386524767704));
#270787=CARTESIAN_POINT('Ctrl Pts',(123.956760658277,5.78711458662396,130.273951190703));
#270788=CARTESIAN_POINT('Ctrl Pts',(123.678313034464,2.68182831940755,125.648797965047));
#270789=CARTESIAN_POINT('Ctrl Pts',(123.399865410651,-2.88792715874745,
125.761354953818));
#270790=CARTESIAN_POINT('Ctrl Pts',(123.121417786838,-5.8038186610986,130.50818778305));
#270791=CARTESIAN_POINT('Ctrl Pts',(122.842970163025,-3.38628434620416,
135.527188978355));
#270792=CARTESIAN_POINT('Ctrl Pts',(122.564522539212,2.1430798536649,136.206141633086));
#270793=CARTESIAN_POINT('Ctrl Pts',(122.286074915399,5.703058363287,131.921121426228));
#270794=CARTESIAN_POINT('Ctrl Pts',(122.007627291586,4.02220484693838,126.609852593007));
#270795=CARTESIAN_POINT('Ctrl Pts',(121.729179667773,-1.35485842811595,
125.153131721247));
#270796=CARTESIAN_POINT('Ctrl Pts',(121.450732043961,-5.48687299624567,
128.889614127324));
#270797=CARTESIAN_POINT('Ctrl Pts',(121.172284420148,-4.57671932947311,
134.385655017367));
#270798=CARTESIAN_POINT('Ctrl Pts',(120.893836796335,0.539215815916097,
136.59066130995));
#270799=CARTESIAN_POINT('Ctrl Pts',(120.615389172522,5.15963796863542,133.478339942736));
#270800=CARTESIAN_POINT('Ctrl Pts',(120.336941548709,5.0386048905067,127.908762206842));
#270801=CARTESIAN_POINT('Ctrl Pts',(120.058493924896,0.287340067535411,
125.000097952557));
#270802=CARTESIAN_POINT('Ctrl Pts',(119.780046301083,-4.72797624015824,
127.42526753342));
#270803=CARTESIAN_POINT('Ctrl Pts',(119.50159867727,-5.39851335762638,132.955658580739));
#270804=CARTESIAN_POINT('Ctrl Pts',(119.223151053457,-1.10808043147514,
136.509111896649));
#270805=CARTESIAN_POINT('Ctrl Pts',(118.944703429644,4.20062427846316,134.820177479675));
#270806=CARTESIAN_POINT('Ctrl Pts',(118.666255805832,5.64916048839838,129.440903549983));
#270807=CARTESIAN_POINT('Ctrl Pts',(118.387808182019,1.90639418632776,125.314580056818));
#270808=CARTESIAN_POINT('Ctrl Pts',(118.109360558206,-3.58825524044456,
126.23309670829));
#270809=CARTESIAN_POINT('Ctrl Pts',(117.830912934393,-5.785473397262,131.352381573729));
#270810=CARTESIAN_POINT('Ctrl Pts',(117.55246531058,-2.66612413808396,135.968061952766));
#270811=CARTESIAN_POINT('Ctrl Pts',(117.274017686767,2.9032629565882,135.838553065588));
#270812=CARTESIAN_POINT('Ctrl Pts',(116.995570062954,5.80469322643624,131.082867252651));
#270813=CARTESIAN_POINT('Ctrl Pts',(116.717122439142,3.37189399621826,126.071247447876));
#270814=CARTESIAN_POINT('Ctrl Pts',(116.438674815328,-2.15951109034483,
125.409127420613));
#270815=CARTESIAN_POINT('Ctrl Pts',(116.160227191516,-5.70643098286277,
129.704963129555));
#270816=CARTESIAN_POINT('Ctrl Pts',(115.881779567703,-4.00941957678149,
135.011091421425));
#270817=CARTESIAN_POINT('Ctrl Pts',(115.60333194389,1.37205254932662,136.451439614773));
#270818=CARTESIAN_POINT('Ctrl Pts',(115.324884320077,5.49267541109693,132.702398084833));
#270819=CARTESIAN_POINT('Ctrl Pts',(115.046436696264,4.56579790218037,127.20915284676));
#270820=CARTESIAN_POINT('Ctrl Pts',(114.767989072451,-0.556824827212187,
125.019727914392));
#270821=CARTESIAN_POINT('Ctrl Pts',(114.489541448638,-5.1677527428018,128.146097841224));
#270822=CARTESIAN_POINT('Ctrl Pts',(114.211093824825,-5.02976834651319,
133.715281396157));
#270823=CARTESIAN_POINT('Ctrl Pts',(113.932646201012,-0.269672557622912,
136.60947096195));
#270824=CARTESIAN_POINT('Ctrl Pts',(113.6541985772,4.73823913748602,134.169047716661));
#270825=CARTESIAN_POINT('Ctrl Pts',(113.375750953387,5.39194054109557,128.636641401405));
#270826=CARTESIAN_POINT('Ctrl Pts',(113.097303329574,1.09071199837779,125.09626314683));
#270827=CARTESIAN_POINT('Ctrl Pts',(112.818855705761,-4.21282758660586,
126.801347611796));
#270828=CARTESIAN_POINT('Ctrl Pts',(112.540408081948,-5.64498442756793,
132.185005471008));
#270829=CARTESIAN_POINT('Ctrl Pts',(112.261960458135,-1.8896763524154,136.299918158156));
#270830=CARTESIAN_POINT('Ctrl Pts',(111.983512834322,3.60215197478495,135.364681938413));
#270831=CARTESIAN_POINT('Ctrl Pts',(111.705065210509,5.78377861206482,130.238733208892));
#270832=CARTESIAN_POINT('Ctrl Pts',(111.426617586696,2.65039525815055,125.632568435507));
#270833=CARTESIAN_POINT('Ctrl Pts',(111.148169962883,-2.91857185899754,
125.77902802134));
#270834=CARTESIAN_POINT('Ctrl Pts',(110.869722339071,-5.80551401788879,
130.543522761958));
#270835=CARTESIAN_POINT('Ctrl Pts',(110.591274715258,-3.35747240946702,
135.547714749242));
#270836=CARTESIAN_POINT('Ctrl Pts',(110.312827091445,2.17592232160915,136.192996015246));
#270837=CARTESIAN_POINT('Ctrl Pts',(110.034379467632,5.70975073884148,131.886384600257));
#270838=CARTESIAN_POINT('Ctrl Pts',(109.755931843819,3.99659716390926,126.585446004984));
#270839=CARTESIAN_POINT('Ctrl Pts',(109.477484220006,-1.38923396002991,
125.161483833236));
#270840=CARTESIAN_POINT('Ctrl Pts',(109.199036596193,-5.49842694255352,
128.923049756431));
#270841=CARTESIAN_POINT('Ctrl Pts',(108.92058897238,-4.55483417795961,134.413448453863));
#270842=CARTESIAN_POINT('Ctrl Pts',(108.642141348568,0.57442868015902,136.58727174348));
#270843=CARTESIAN_POINT('Ctrl Pts',(108.363693724754,5.17581964361271,133.446882219296));
#270844=CARTESIAN_POINT('Ctrl Pts',(108.085246100942,5.02088520743284,127.878144437479));
#270845=CARTESIAN_POINT('Ctrl Pts',(107.806798477129,0.252002549500665,
124.998456371553));
#270846=CARTESIAN_POINT('Ctrl Pts',(107.528350853316,-4.74845814041369,
127.454110673523));
#270847=CARTESIAN_POINT('Ctrl Pts',(107.249903229503,-5.38531777436419,
132.988481005259));
#270848=CARTESIAN_POINT('Ctrl Pts',(106.97145560569,-1.07333346107335,136.515751400918));
#270849=CARTESIAN_POINT('Ctrl Pts',(106.693007981877,4.22499186768932,134.794532683627));
#270850=CARTESIAN_POINT('Ctrl Pts',(106.414560358064,5.64075607237289,129.406540768369));
#270851=CARTESIAN_POINT('Ctrl Pts',(106.136112734251,1.87294101279944,125.303077007226));
#270852=CARTESIAN_POINT('Ctrl Pts',(105.857665110439,-3.61601533928142,
126.25502413134));
#270853=CARTESIAN_POINT('Ctrl Pts',(105.579217486626,-5.78203024673271,
131.387589238853));
#270854=CARTESIAN_POINT('Ctrl Pts',(105.300769862813,-2.63464182531766,
135.984195735705));
#270855=CARTESIAN_POINT('Ctrl Pts',(105.022322239,2.93385372415587,135.820786808));
#270856=CARTESIAN_POINT('Ctrl Pts',(104.743874615187,5.80628102785255,131.047527277329));
#270857=CARTESIAN_POINT('Ctrl Pts',(104.465426991374,3.34301971955009,126.050809465687));
#270858=CARTESIAN_POINT('Ctrl Pts',(104.186979367561,-2.19231339542621,
125.422372938737));
#270859=CARTESIAN_POINT('Ctrl Pts',(103.908531743748,-5.71301760046937,
129.739720163916));
#270860=CARTESIAN_POINT('Ctrl Pts',(103.630084119935,-3.98373772710686,
135.03541995542));
#270861=CARTESIAN_POINT('Ctrl Pts',(103.351636496123,1.40640250105958,136.442982914176));
#270862=CARTESIAN_POINT('Ctrl Pts',(103.07318887231,5.50412753733405,132.66892744436));
#270863=CARTESIAN_POINT('Ctrl Pts',(102.794741248497,4.54382825837723,127.181426149873));
#270864=CARTESIAN_POINT('Ctrl Pts',(102.516293624684,-0.592027211677165,
125.023224641008));
#270865=CARTESIAN_POINT('Ctrl Pts',(102.237846000871,-5.18383859633749,
128.177604670405));
#270866=CARTESIAN_POINT('Ctrl Pts',(101.959398377058,-5.01195555555783,
133.745845091081));
#270867=CARTESIAN_POINT('Ctrl Pts',(101.680950753245,-0.234330206861215,
136.611004980102));
#270868=CARTESIAN_POINT('Ctrl Pts',(101.402503129432,4.75863315427373,134.140142370299));
#270869=CARTESIAN_POINT('Ctrl Pts',(101.124055505619,5.37864511878468,128.603859291732));
#270870=CARTESIAN_POINT('Ctrl Pts',(100.845607881807,1.05594498055446,125.089729431141));
#270871=CARTESIAN_POINT('Ctrl Pts',(100.567160257994,-4.23711700902531,
126.827066455619));
#270872=CARTESIAN_POINT('Ctrl Pts',(100.288712634181,-5.63647546198416,
132.219342513305));
#270873=CARTESIAN_POINT('Ctrl Pts',(100.010265010368,-1.85618832251382,
136.311319334515));
#270874=CARTESIAN_POINT('Ctrl Pts',(99.731817386555,3.62984520550588,135.342670124737));
#270875=CARTESIAN_POINT('Ctrl Pts',(99.4533697627421,5.78022831746224,130.203536186614));
#270876=CARTESIAN_POINT('Ctrl Pts',(99.1749221389292,2.61886398552269,125.616530548629));
#270877=CARTESIAN_POINT('Ctrl Pts',(98.8964745151164,-2.9491084104941,125.796887304409));
#270878=CARTESIAN_POINT('Ctrl Pts',(98.6180268913035,-5.80699424922206,
130.578867406308));
#270879=CARTESIAN_POINT('Ctrl Pts',(98.3395792674906,-3.32853606035512,
135.568064753397));
#270880=CARTESIAN_POINT('Ctrl Pts',(98.0611316436778,2.20868415995158,136.179650719541));
#270881=CARTESIAN_POINT('Ctrl Pts',(97.7826840198649,5.71623153748262,131.851607679491));
#270882=CARTESIAN_POINT('Ctrl Pts',(97.5042363960519,3.97084138550236,126.561195750394));
#270883=CARTESIAN_POINT('Ctrl Pts',(97.2257887722391,-1.42355801336861,
125.170045044101));
#270884=CARTESIAN_POINT('Ctrl Pts',(96.9473411484261,-5.50977714262889,
128.956555098203));
#270885=CARTESIAN_POINT('Ctrl Pts',(96.6688935246133,-4.53278024539068,
134.441108154283));
#270886=CARTESIAN_POINT('Ctrl Pts',(96.3904459008004,0.609620258735999,
136.583667889112));
#270887=CARTESIAN_POINT('Ctrl Pts',(96.1119982769875,5.19180952668969,133.415326576248));
#270888=CARTESIAN_POINT('Ctrl Pts',(95.8335506531746,5.00297947361121,127.847635100131));
#270889=CARTESIAN_POINT('Ctrl Pts',(95.5551030293618,0.216655693418756,
124.997029930466));
#270890=CARTESIAN_POINT('Ctrl Pts',(95.2766554055487,-4.7687640848064,127.483077958369));
#270891=CARTESIAN_POINT('Ctrl Pts',(94.9982077817361,-5.37192263617151,
133.021222496396));
#270892=CARTESIAN_POINT('Ctrl Pts',(94.7197601579228,-1.03854671790542,
136.522179267501));
#270893=CARTESIAN_POINT('Ctrl Pts',(94.4413125341102,4.24920289828813,134.768740030285));
#270894=CARTESIAN_POINT('Ctrl Pts',(94.1628649102971,5.63214263605674,129.372229783482));
#270895=CARTESIAN_POINT('Ctrl Pts',(93.8844172864844,1.83941843675322,125.29177780972));
#270896=CARTESIAN_POINT('Ctrl Pts',(93.6059696626714,-3.6436414453401,126.277120131727));
#270897=CARTESIAN_POINT('Ctrl Pts',(93.3275220388585,-5.77837284094635,
131.422775292226));
#270898=CARTESIAN_POINT('Ctrl Pts',(93.0490744150458,-2.60306188492951,
136.000137577949));
#270899=CARTESIAN_POINT('Ctrl Pts',(92.7706267912327,2.96433577669487,135.802834664895));
#270900=CARTESIAN_POINT('Ctrl Pts',(92.49217916742,5.80765367539012,131.012178291378));
#270901=CARTESIAN_POINT('Ctrl Pts',(92.213731543607,3.31402156605677,126.030547628085));
#270902=CARTESIAN_POINT('Ctrl Pts',(91.9352839197941,-2.22503446352861,
125.435817888395));
#270903=CARTESIAN_POINT('Ctrl Pts',(91.6568362959812,-5.71939252010779,
129.77451664892));
#270904=CARTESIAN_POINT('Ctrl Pts',(91.3783886721684,-3.95790825856573,
135.059591705955));
#270905=CARTESIAN_POINT('Ctrl Pts',(91.0999410483554,1.44070033803066,136.434317272356));
#270906=CARTESIAN_POINT('Ctrl Pts',(90.8214934245425,5.51537570610103,132.635387711677));
#270907=CARTESIAN_POINT('Ctrl Pts',(90.5430458007297,4.52169024134706,127.153833702157));
#270908=CARTESIAN_POINT('Ctrl Pts',(90.2645981769166,-0.627207658356129,
125.026935589742));
#270909=CARTESIAN_POINT('Ctrl Pts',(89.9861505531037,-5.19973236082766,
128.209208834995));
#270910=CARTESIAN_POINT('Ctrl Pts',(89.707702929291,-4.99395704474619,133.776299788217));
#270911=CARTESIAN_POINT('Ctrl Pts',(89.4292553054779,-0.198979172907652,
136.61232383091));
#270912=CARTESIAN_POINT('Ctrl Pts',(89.1508076816652,4.77885083815996,134.111113415317));
#270913=CARTESIAN_POINT('Ctrl Pts',(88.8723600578521,5.36515038880097,128.571158722445));
#270914=CARTESIAN_POINT('Ctrl Pts',(88.5939124340396,1.02113883430145,125.08340747321));
#270915=CARTESIAN_POINT('Ctrl Pts',(88.3154648102263,-4.26124942351577,
126.85293267954));
#270916=CARTESIAN_POINT('Ctrl Pts',(88.0370171864138,-5.62775763472933,
132.253627122929));
#270917=CARTESIAN_POINT('Ctrl Pts',(87.7585695626006,-1.82263151087143,
136.322516448493));
#270918=CARTESIAN_POINT('Ctrl Pts',(87.480121938788,3.65740393097785,135.320490142334));
#270919=CARTESIAN_POINT('Ctrl Pts',(87.2016743149749,5.77646383437373,130.168361428106));
#270920=CARTESIAN_POINT('Ctrl Pts',(86.9232266911622,2.58723566992664,125.600684898703));
#270921=CARTESIAN_POINT('Ctrl Pts',(86.6447790673492,-2.97953568169397,
125.814932141244));
#270922=CARTESIAN_POINT('Ctrl Pts',(86.3663314435363,-5.80825930024783,
130.614220406392));
#270923=CARTESIAN_POINT('Ctrl Pts',(86.0878838197235,-3.29947637111547,
135.588238236744));
#270924=CARTESIAN_POINT('Ctrl Pts',(85.8094361959104,2.24136415469026,136.166106240484));
#270925=CARTESIAN_POINT('Ctrl Pts',(85.5309885720977,5.72250051906197,131.816791952599));
#270926=CARTESIAN_POINT('Ctrl Pts',(85.2525409482847,3.94493846610766,126.537102727838));
#270927=CARTESIAN_POINT('Ctrl Pts',(84.9740933244718,-1.45782931624159,
125.178815036599));
#270928=CARTESIAN_POINT('Ctrl Pts',(84.6956457006588,-5.52092317588609,
128.990128911089));
#270929=CARTESIAN_POINT('Ctrl Pts',(84.417198076846,-4.51055834898274,134.468633093685));
#270930=CARTESIAN_POINT('Ctrl Pts',(84.138750453033,0.644789247610192,136.579849880389));
#270931=CARTESIAN_POINT('Ctrl Pts',(83.8603028292202,5.20760702535536,133.383674182895));
#270932=CARTESIAN_POINT('Ctrl Pts',(83.5818552054073,4.98488835254533,127.817235325336));
#270933=CARTESIAN_POINT('Ctrl Pts',(83.3034075815944,0.181300809080568,
124.995818682153));
#270934=CARTESIAN_POINT('Ctrl Pts',(83.0249599577814,-4.78889332089225,
127.512168314565));
#270935=CARTESIAN_POINT('Ctrl Pts',(82.7465123339688,-5.35832843941005,
133.053881840899));
#270936=CARTESIAN_POINT('Ctrl Pts',(82.4680647101557,-1.00372149100682,
136.528395258211));
#270937=CARTESIAN_POINT('Ctrl Pts',(82.1896170863428,4.27325647311088,134.742800475408));
#270938=CARTESIAN_POINT('Ctrl Pts',(81.91116946253,5.62332049862395,129.337971866731));
#270939=CARTESIAN_POINT('Ctrl Pts',(81.632721838717,1.80582770038043,125.280682882997));
#270940=CARTESIAN_POINT('Ctrl Pts',(81.3542742149043,-3.67113253492515,
126.299383890674));
#270941=CARTESIAN_POINT('Ctrl Pts',(81.0758265910913,-5.77450131542928,
131.457938430015));
#270942=CARTESIAN_POINT('Ctrl Pts',(80.7973789672785,-2.57138548712596,
136.015886888767));
#270943=CARTESIAN_POINT('Ctrl Pts',(80.5189313434656,2.99470798468153,135.784697301496));
#270944=CARTESIAN_POINT('Ctrl Pts',(80.2404837196526,5.80881111818491,130.976821604667));
#270945=CARTESIAN_POINT('Ctrl Pts',(79.9620360958398,3.2849006102757,126.010462685879));
#270946=CARTESIAN_POINT('Ctrl Pts',(79.6835884720269,-2.25767308216064,
125.449461771377));
#270947=CARTESIAN_POINT('Ctrl Pts',(79.4051408482139,-5.72555550555307,
129.809351295171));
#270948=CARTESIAN_POINT('Ctrl Pts',(79.1266932244012,-3.93193212827854,
135.083605777338));
#270949=CARTESIAN_POINT('Ctrl Pts',(78.8482456005881,1.47494478932078,136.425443010422));
#270950=CARTESIAN_POINT('Ctrl Pts',(78.5697979767754,5.526419500593,132.601780129612));
#270951=CARTESIAN_POINT('Ctrl Pts',(78.2913503529625,4.49938467142216,127.126376526057));
#270952=CARTESIAN_POINT('Ctrl Pts',(78.0129027291494,-0.662364863624755,
125.030860623086));
#270953=CARTESIAN_POINT('Ctrl Pts',(77.7344551053368,-5.21543344732299,
128.240909163888));
#270954=CARTESIAN_POINT('Ctrl Pts',(77.4560074815235,-4.97577348101974,
133.806644359053));
#270955=CARTESIAN_POINT('Ctrl Pts',(77.1775598577108,-0.163620765707691,
136.613427465507));
#270956=CARTESIAN_POINT('Ctrl Pts',(76.8991122338979,4.79889143997102,134.081961927395));
#270957=CARTESIAN_POINT('Ctrl Pts',(76.620664610085,5.35145685119646,128.538540905275));
#270958=CARTESIAN_POINT('Ctrl Pts',(76.3422169862721,0.986294849373407,
125.077297507303));
#270959=CARTESIAN_POINT('Ctrl Pts',(76.0637693624593,-4.28522393584178,
126.878945325076));
#270960=CARTESIAN_POINT('Ctrl Pts',(75.7853217386464,-5.61883126884571,
132.287858029448));
#270961=CARTESIAN_POINT('Ctrl Pts',(75.5068741148335,-1.78900716094817,
136.333509085178));
#270962=CARTESIAN_POINT('Ctrl Pts',(75.2284264910206,3.68482713000219,135.298142813091));
#270963=CARTESIAN_POINT('Ctrl Pts',(74.9499788672077,5.77248530229349,130.133210236781));
#270964=CARTESIAN_POINT('Ctrl Pts',(74.6715312433948,2.55551148336137,125.585032072894));
#270965=CARTESIAN_POINT('Ctrl Pts',(74.3930836195819,-3.0098525451033,125.833161863185));
#270966=CARTESIAN_POINT('Ctrl Pts',(74.1146359957691,-5.80930912408932,
130.649580452192));
#270967=CARTESIAN_POINT('Ctrl Pts',(73.8361883719562,-3.27029441856551,
135.608234451746));
#270968=CARTESIAN_POINT('Ctrl Pts',(73.5577407481433,2.273961094856,136.152363079971));
#270969=CARTESIAN_POINT('Ctrl Pts',(73.2792931243304,5.72855745128013,131.781938709691));
#270970=CARTESIAN_POINT('Ctrl Pts',(73.0008455005175,3.91888936556733,126.513167830092));
#270971=CARTESIAN_POINT('Ctrl Pts',(72.7223978767045,-1.49204659871303,
125.187793485758));
#270972=CARTESIAN_POINT('Ctrl Pts',(72.4439502528918,-5.53186462930466,
129.023769950998));
#270973=CARTESIAN_POINT('Ctrl Pts',(72.1655026290786,-4.48816931217651,
134.496022252122));
#270974=CARTESIAN_POINT('Ctrl Pts',(71.8870550052659,0.679934343581693,
136.575817858786));
#270975=CARTESIAN_POINT('Ctrl Pts',(71.6086073814528,5.22321155422762,133.351926212129));
#270976=CARTESIAN_POINT('Ctrl Pts',(71.3301597576401,4.96661251460835,127.786946239566));
#270977=CARTESIAN_POINT('Ctrl Pts',(71.0517121338272,0.145939206574258,
124.994822671498));
#270978=CARTESIAN_POINT('Ctrl Pts',(70.7732645100143,-4.80884510277506,
127.541380664158));
#270979=CARTESIAN_POINT('Ctrl Pts',(70.4948168862015,-5.34453568781766,
133.086457828568));
#270980=CARTESIAN_POINT('Ctrl Pts',(70.2163692623885,-0.968859070839113,
136.534399142713));
#270981=CARTESIAN_POINT('Ctrl Pts',(69.9379216385757,4.29715170084345,134.716714980192));
#270982=CARTESIAN_POINT('Ctrl Pts',(69.6594740147628,5.61428998698222,129.303768287553));
#270983=CARTESIAN_POINT('Ctrl Pts',(69.3810263909498,1.77217004839796,125.269792638185));
#270984=CARTESIAN_POINT('Ctrl Pts',(69.102578767137,-3.69848758934425,126.321814583191));
#270985=CARTESIAN_POINT('Ctrl Pts',(68.8241311433241,-5.77041581364239,
131.493077349239));
#270986=CARTESIAN_POINT('Ctrl Pts',(68.5456835195112,-2.53961380568736,
136.031443084562));
#270987=CARTESIAN_POINT('Ctrl Pts',(68.2672358956983,3.02496922266262,135.76637538989));
#270988=CARTESIAN_POINT('Ctrl Pts',(67.9887882718854,5.80975331334755,130.94145852735));
#270989=CARTESIAN_POINT('Ctrl Pts',(67.7103406480725,3.25565793129432,125.990555383323));
#270990=CARTESIAN_POINT('Ctrl Pts',(67.4318930242597,-2.29022804188655,
125.463304082106));
#270991=CARTESIAN_POINT('Ctrl Pts',(67.1534454004468,-5.73150632843341,
129.844222811859));
#270992=CARTESIAN_POINT('Ctrl Pts',(66.8749977766338,-3.90581029880048,
135.107461279717));
#270993=CARTESIAN_POINT('Ctrl Pts',(66.5965501528209,1.50913458598933,136.416360457212));
#270994=CARTESIAN_POINT('Ctrl Pts',(66.3181025290079,5.53725851157817,132.568105943505));
#270995=CARTESIAN_POINT('Ctrl Pts',(66.0396549051952,4.47691237514338,127.09905563901));
#270996=CARTESIAN_POINT('Ctrl Pts',(65.7612072813823,-0.69749752471975,
125.034999595595));
#270997=CARTESIAN_POINT('Ctrl Pts',(65.4827596575694,-5.23094127401388,
128.272704482416));
#270998=CARTESIAN_POINT('Ctrl Pts',(65.2043120337565,-4.95740553817722,
133.836877679162));
#270999=CARTESIAN_POINT('Ctrl Pts',(64.9258644099437,-0.128256295479839,
136.614315842995));
#271000=CARTESIAN_POINT('Ctrl Pts',(64.6474167861306,4.81875421709505,134.05268898675));
#271001=CARTESIAN_POINT('Ctrl Pts',(64.3689691623179,5.33756501339024,128.506007048888));
#271002=CARTESIAN_POINT('Ctrl Pts',(64.0905215385049,0.951414316927145,
125.071399759827));
#271003=CARTESIAN_POINT('Ctrl Pts',(63.8120739146922,-4.30903965761881,
126.905103428319));
#271004=CARTESIAN_POINT('Ctrl Pts',(63.5336262908791,-5.60969669510319,
132.322033964426));
#271005=CARTESIAN_POINT('Ctrl Pts',(63.2551786670663,-1.75531651870651,
136.344296837232));
#271006=CARTESIAN_POINT('Ctrl Pts',(62.9767310432534,3.71211378640213,135.275628965096));
#271007=CARTESIAN_POINT('Ctrl Pts',(62.6982834194405,5.76829286864752,130.098083915181));
#271008=CARTESIAN_POINT('Ctrl Pts',(62.4198357956276,2.52369260137852,125.569572651222));
#271009=CARTESIAN_POINT('Ctrl Pts',(62.1413881718147,-3.04005787731984,
125.851575794724));
#271010=CARTESIAN_POINT('Ctrl Pts',(61.8629405480017,-5.81014368184488,
130.684946233427));
#271011=CARTESIAN_POINT('Ctrl Pts',(61.5844929241889,-3.24099128405306,
135.628052657436));
#271012=CARTESIAN_POINT('Ctrl Pts',(61.3060453003759,2.306473772557,136.138421747261));
#271013=CARTESIAN_POINT('Ctrl Pts',(61.0275976765631,5.73440210969521,131.747049242268));
#271014=CARTESIAN_POINT('Ctrl Pts',(60.7491500527502,3.89269504914048,126.489391944074));
#271015=CARTESIAN_POINT('Ctrl Pts',(60.4707024289374,-1.5262085928491,125.196980058879));
#271016=CARTESIAN_POINT('Ctrl Pts',(60.1922548051244,-5.54260109744501,
129.057476971348));
#271017=CARTESIAN_POINT('Ctrl Pts',(59.9138071813117,-4.46561396460588,
134.52327461468));
#271018=CARTESIAN_POINT('Ctrl Pts',(59.6353595574987,0.715054244335847,
136.571571973714));
#271019=CARTESIAN_POINT('Ctrl Pts',(59.3569119336859,5.23862253507484,133.320083840384));
#271020=CARTESIAN_POINT('Ctrl Pts',(59.0784643098728,4.94815263701827,127.756768965196));
#271021=CARTESIAN_POINT('Ctrl Pts',(58.80001668606,0.110572196236736,124.994041935407));
#271022=CARTESIAN_POINT('Ctrl Pts',(58.5215690622471,-4.82861869113419,
127.570713924673));
#271023=CARTESIAN_POINT('Ctrl Pts',(58.2431214384343,-5.3305448924898,133.118949252284));
#271024=CARTESIAN_POINT('Ctrl Pts',(57.9646738146213,-0.933960749242644,
136.54019069853));
#271025=CARTESIAN_POINT('Ctrl Pts',(57.6862261908085,4.32088769603949,134.690484511247));
#271026=CARTESIAN_POINT('Ctrl Pts',(57.4077785669955,5.6050514357603,129.269620313377));
#271027=CARTESIAN_POINT('Ctrl Pts',(57.1293309431827,1.73844672800264,125.259107478825));
#271028=CARTESIAN_POINT('Ctrl Pts',(56.8508833193697,-3.72570559494523,
126.3444113781));
#271029=CARTESIAN_POINT('Ctrl Pts',(56.5724356955568,-5.76611648697549,
131.528190747811));
#271030=CARTESIAN_POINT('Ctrl Pts',(56.293988071744,-2.50774801792579,136.046805588895));
#271031=CARTESIAN_POINT('Ctrl Pts',(56.0155404479311,3.05511836929639,135.747869609001));
#271032=CARTESIAN_POINT('Ctrl Pts',(55.7370928241181,5.81048022596477,130.906090369819));
#271033=CARTESIAN_POINT('Ctrl Pts',(55.4586452003054,3.22629461271119,125.97082645809));
#271034=CARTESIAN_POINT('Ctrl Pts',(55.1801975764924,-2.32269813636975,
125.477344307648));
#271035=CARTESIAN_POINT('Ctrl Pts',(54.9017499526795,-5.73724476823917,
129.879129906805));
#271036=CARTESIAN_POINT('Ctrl Pts',(54.6233023288666,-3.87954373808533,
135.131157329118));
#271037=CARTESIAN_POINT('Ctrl Pts',(54.3448547050537,1.54326846112093,136.407069949284));
#271038=CARTESIAN_POINT('Ctrl Pts',(54.0664070812409,5.54789233741261,132.534366401168));
#271039=CARTESIAN_POINT('Ctrl Pts',(53.7879594574279,4.45427418523046,127.071872053402));
#271040=CARTESIAN_POINT('Ctrl Pts',(53.5095118336151,-0.732604339787292,
125.039352353899));
#271041=CARTESIAN_POINT('Ctrl Pts',(53.2310642098022,-5.24625526625226,
128.304593612394));
#271042=CARTESIAN_POINT('Ctrl Pts',(52.9526165859893,-4.93885389684926,
133.866998628235));
#271043=CARTESIAN_POINT('Ctrl Pts',(52.6741689621764,-0.0928870726681018,
136.614988930455));
#271044=CARTESIAN_POINT('Ctrl Pts',(52.3957213383635,4.83843843350925,134.023295678104));
#271045=CARTESIAN_POINT('Ctrl Pts',(52.1172737145507,5.32347539014984,128.473558358838));
#271046=CARTESIAN_POINT('Ctrl Pts',(51.8388260907377,0.91649852947334,125.065714449322));
#271047=CARTESIAN_POINT('Ctrl Pts',(51.5603784669247,-4.33269570634681,
126.931406019971));
#271048=CARTESIAN_POINT('Ctrl Pts',(51.2819308431118,-5.6003542519866,132.356153661459));
#271049=CARTESIAN_POINT('Ctrl Pts',(51.0034832192991,-1.72156083256576,
136.354879304913));
#271050=CARTESIAN_POINT('Ctrl Pts',(50.7250355954861,3.73926288906064,135.252949432607));
#271051=CARTESIAN_POINT('Ctrl Pts',(50.4465879716733,5.76388668878802,130.062983764924));
#271052=CARTESIAN_POINT('Ctrl Pts',(50.1681403478604,2.49178020303801,125.554307206545));
#271053=CARTESIAN_POINT('Ctrl Pts',(49.8896927240475,-3.07015055907373,
125.870173253527));
#271054=CARTESIAN_POINT('Ctrl Pts',(49.6112451002346,-5.81076294258959,
130.720316439607));
#271055=CARTESIAN_POINT('Ctrl Pts',(49.3327974764216,-3.21156805341676,
135.647692119444));
#271056=CARTESIAN_POINT('Ctrl Pts',(49.0543498526089,2.33890098302428,136.124282758954));
#271057=CARTESIAN_POINT('Ctrl Pts',(48.7759022287959,5.74003427773134,131.712124843171));
#271058=CARTESIAN_POINT('Ctrl Pts',(48.497454604983,3.86635648746696,126.465775950806));
#271059=CARTESIAN_POINT('Ctrl Pts',(48.2190069811701,-1.56031403276457,
125.206374415548));
#271060=CARTESIAN_POINT('Ctrl Pts',(47.9405593573573,-5.55313218246346,
129.091248723115));
#271061=CARTESIAN_POINT('Ctrl Pts',(47.6621117335443,-4.44289314206747,
134.550389171513));
#271062=CARTESIAN_POINT('Ctrl Pts',(47.3836641097315,0.750147648492217,
136.567112382502));
#271063=CARTESIAN_POINT('Ctrl Pts',(47.1052164859186,5.25383939683757,133.288148247589));
#271064=CARTESIAN_POINT('Ctrl Pts',(46.8267688621057,4.92950940381243,127.726704620456));
#271065=CARTESIAN_POINT('Ctrl Pts',(46.5483212382927,0.0752010886061242,
124.993476502813));
#271066=CARTESIAN_POINT('Ctrl Pts',(46.2698736144798,-4.84821335325179,
127.600167009156));
#271067=CARTESIAN_POINT('Ctrl Pts',(45.991425990667,-5.31635657186091,133.151354908068));
#271068=CARTESIAN_POINT('Ctrl Pts',(45.7129783668541,-0.899027819386881,
136.545769711054));
#271069=CARTESIAN_POINT('Ctrl Pts',(45.4345307430412,4.344463579153,134.664110040551));
#271070=CARTESIAN_POINT('Ctrl Pts',(45.1560831192283,5.5956051872961,129.235529209567));
#271071=CARTESIAN_POINT('Ctrl Pts',(44.8776354954154,1.70465898882477,125.248627800858));
#271072=CARTESIAN_POINT('Ctrl Pts',(44.5991878716026,-3.7527855431554,126.367173438067));
#271073=CARTESIAN_POINT('Ctrl Pts',(44.3207402477896,-5.76160349474165,
131.563277324591));
#271074=CARTESIAN_POINT('Ctrl Pts',(44.0422926239769,-2.47578930463884,
136.0619738325));
#271075=CARTESIAN_POINT('Ctrl Pts',(43.7638450001637,3.08515430739569,135.72918064457));
#271076=CARTESIAN_POINT('Ctrl Pts',(43.485397376351,5.8109918291003,130.870718442656));
#271077=CARTESIAN_POINT('Ctrl Pts',(43.206949752538,3.19681174259461,125.951276641244));
#271078=CARTESIAN_POINT('Ctrl Pts',(42.9285021287252,-2.3550821624196,125.491581927739));
#271079=CARTESIAN_POINT('Ctrl Pts',(42.6500545049123,-5.74277061233009,
129.914071286517));
#271080=CARTESIAN_POINT('Ctrl Pts',(42.3716068810994,-3.85313341945026,
135.154693047476));
#271081=CARTESIAN_POINT('Ctrl Pts',(42.0931592572865,1.57734514987214,136.397571830902));
#271082=CARTESIAN_POINT('Ctrl Pts',(41.8147116334736,5.5583205840564,132.50056275283));
#271083=CARTESIAN_POINT('Ctrl Pts',(41.5362640096606,4.43147094054935,127.04482677653));
#271084=CARTESIAN_POINT('Ctrl Pts',(41.2578163858478,-0.767684007931795,
125.043918736703));
#271085=CARTESIAN_POINT('Ctrl Pts',(40.9793687620349,-5.26137485657243,
128.336575372158));
#271086=CARTESIAN_POINT('Ctrl Pts',(40.700921138222,-4.9201192444739,133.897006090131));
#271087=CARTESIAN_POINT('Ctrl Pts',(40.4224735144091,-0.0575144078915333,
136.615446702946));
#271088=CARTESIAN_POINT('Ctrl Pts',(40.1440258905964,4.85794335980812,133.993783090635));
#271089=CARTESIAN_POINT('Ctrl Pts',(39.8655782667833,5.30918850357096,128.441196037522));
#271090=CARTESIAN_POINT('Ctrl Pts',(39.5871306429705,0.8815487808295,125.060241786462));
#271091=CARTESIAN_POINT('Ctrl Pts',(39.3086830191576,-4.35619120544207,
126.957852125381));
#271092=CARTESIAN_POINT('Ctrl Pts',(39.0302353953447,-5.59080428568363,
132.39021585623));
#271093=CARTESIAN_POINT('Ctrl Pts',(38.7517877715318,-1.6877413533555,136.365256096082));
#271094=CARTESIAN_POINT('Ctrl Pts',(38.4733401477189,3.76627343195761,135.230105056025));
#271095=CARTESIAN_POINT('Ctrl Pts',(38.194892523906,5.7592669259876,130.027911086658));
#271096=CARTESIAN_POINT('Ctrl Pts',(37.9164449000932,2.45977547086574,125.539236304527));
#271097=CARTESIAN_POINT('Ctrl Pts',(37.6379972762802,-3.10012947526937,
125.888953550457));
#271098=CARTESIAN_POINT('Ctrl Pts',(37.3595496524674,-5.81116688337655,
130.755689760074));
#271099=CARTESIAN_POINT('Ctrl Pts',(37.0811020286545,-3.18202581694541,
135.667152110023));
#271100=CARTESIAN_POINT('Ctrl Pts',(36.8026544048415,2.3712415246555,136.109946638975));
#271101=CARTESIAN_POINT('Ctrl Pts',(36.5242067810287,5.74545374668639,131.677166806538));
#271102=CARTESIAN_POINT('Ctrl Pts',(36.2457591572158,3.83987465653194,126.442320725389));
#271103=CARTESIAN_POINT('Ctrl Pts',(35.9673115334029,-1.59436165466975,
125.215976207654));
#271104=CARTESIAN_POINT('Ctrl Pts',(35.6888639095901,-5.56345749412674,
129.125083954872));
#271105=CARTESIAN_POINT('Ctrl Pts',(35.4104162857771,-4.42000768648982,
134.57736491788));
#271106=CARTESIAN_POINT('Ctrl Pts',(35.1319686619643,0.785213255651605,
136.562439250406));
#271107=CARTESIAN_POINT('Ctrl Pts',(34.8535210381513,5.26886157564935,133.25612061713));
#271108=CARTESIAN_POINT('Ctrl Pts',(34.5750734143385,4.91068350582282,127.69675431939));
#271109=CARTESIAN_POINT('Ctrl Pts',(34.2966257905255,0.0398271943713243,
124.993126394665));
#271110=CARTESIAN_POINT('Ctrl Pts',(34.0181781667127,-4.86762836304081,
127.629738826211));
#271111=CARTESIAN_POINT('Ctrl Pts',(33.7397305428998,-5.30197125168398,
133.183673595116));
#271112=CARTESIAN_POINT('Ctrl Pts',(33.4612829190869,-0.864061575724654,
136.551135973552));
#271113=CARTESIAN_POINT('Ctrl Pts',(33.182835295274,4.36787847657091,134.637592545421));
#271114=CARTESIAN_POINT('Ctrl Pts',(32.9043876714611,5.58595159162396,129.201496239381));
#271115=CARTESIAN_POINT('Ctrl Pts',(32.6259400476482,1.67080808288091,125.238353992614));
#271116=CARTESIAN_POINT('Ctrl Pts',(32.3474924238352,-3.77972643051725,
126.390099919638));
#271117=CARTESIAN_POINT('Ctrl Pts',(32.0690448000224,-5.75687700417149,
131.598335779433));
#271118=CARTESIAN_POINT('Ctrl Pts',(31.7905971762095,-2.44373885006871,
136.076947253315));
#271119=CARTESIAN_POINT('Ctrl Pts',(31.5121495523967,3.11507592396733,135.71030918912));
#271120=CARTESIAN_POINT('Ctrl Pts',(31.2337019285837,5.81128810379662,130.835344056578));
#271121=CARTESIAN_POINT('Ctrl Pts',(30.9552543047708,3.16721041344351,125.931906657209));
#271122=CARTESIAN_POINT('Ctrl Pts',(30.676806680958,-2.38737892003384,125.506016414799));
#271123=CARTESIAN_POINT('Ctrl Pts',(30.398359057145,-5.74808365594406,129.949045656226));
#271124=CARTESIAN_POINT('Ctrl Pts',(30.1199114333322,-3.82658032153943,
135.178067562667));
#271125=CARTESIAN_POINT('Ctrl Pts',(29.8414638095193,1.61136338951851,136.387866454021));
#271126=CARTESIAN_POINT('Ctrl Pts',(29.5630161857064,5.56854286508694,132.466696251098));
#271127=CARTESIAN_POINT('Ctrl Pts',(29.2845685618935,4.40850348608286,127.017920810568));
#271128=CARTESIAN_POINT('Ctrl Pts',(29.0061209380806,-0.802735229263066,
125.048698574801));
#271129=CARTESIAN_POINT('Ctrl Pts',(28.7276733142678,-5.27629948471241,
128.368648576612));
#271130=CARTESIAN_POINT('Ctrl Pts',(28.4492256904548,-4.90120227527057,
133.926898952911));
#271131=CARTESIAN_POINT('Ctrl Pts',(28.170778066642,-0.0221396118974229,
136.615689143506));
#271132=CARTESIAN_POINT('Ctrl Pts',(27.892330442829,4.87726827322928,133.964152317942));
#271133=CARTESIAN_POINT('Ctrl Pts',(27.6138828190162,5.29470488305963,128.408921284139));
#271134=CARTESIAN_POINT('Ctrl Pts',(27.3354351952032,0.846566366071392,
125.054981974037));
#271135=CARTESIAN_POINT('Ctrl Pts',(27.0569875713904,-4.37952528427021,
126.984440764576));
#271136=CARTESIAN_POINT('Ctrl Pts',(26.7785399475775,-5.58104715007188,
132.424219286554));
#271137=CARTESIAN_POINT('Ctrl Pts',(26.5000923237646,-1.65385933426847,
136.375426826225));
#271138=CARTESIAN_POINT('Ctrl Pts',(26.2216446999517,3.79314441420758,135.207096681855));
#271139=CARTESIAN_POINT('Ctrl Pts',(25.9431970761388,5.75443375143326,129.992867180015));
#271140=CARTESIAN_POINT('Ctrl Pts',(25.6647494523259,2.42767959080881,125.524360503627));
#271141=CARTESIAN_POINT('Ctrl Pts',(25.3863018285131,-3.12999351502748,
125.907915989602));
#271142=CARTESIAN_POINT('Ctrl Pts',(25.1078542047001,-5.81135548923757,
130.791064884058));
#271143=CARTESIAN_POINT('Ctrl Pts',(24.8294065808873,-3.152365669337,135.686431908074));
#271144=CARTESIAN_POINT('Ctrl Pts',(24.5509589570743,2.40349419906,136.095413918554));
#271145=CARTESIAN_POINT('Ctrl Pts',(24.2725113332615,5.75066031573997,131.64217642775));
#271146=CARTESIAN_POINT('Ctrl Pts',(23.9940637094486,3.81325053762949,126.419027136963));
#271147=CARTESIAN_POINT('Ctrl Pts',(23.7156160856357,-1.62835019691723,
125.2257850794));
#271148=CARTESIAN_POINT('Ctrl Pts',(23.4371684618228,-5.57357664982666,
129.158981412844));
#271149=CARTESIAN_POINT('Ctrl Pts',(23.1587208380098,-4.39695844590187,
134.604200854185));
#271150=CARTESIAN_POINT('Ctrl Pts',(22.880273214197,0.820249766445046,136.557552750588));
#271151=CARTESIAN_POINT('Ctrl Pts',(22.6018255903841,5.28368851485763,133.224002135804));
#271152=CARTESIAN_POINT('Ctrl Pts',(22.3233779665712,4.89167564065013,127.666919171818));
#271153=CARTESIAN_POINT('Ctrl Pts',(22.0449303427584,0.00445182432539013,
124.992991623939));
#271154=CARTESIAN_POINT('Ctrl Pts',(21.7664827189454,-4.88686300107076,
127.659428280044));
#271155=CARTESIAN_POINT('Ctrl Pts',(21.4880350951325,-5.28738946501251,
133.215904115845));
#271156=CARTESIAN_POINT('Ctrl Pts',(21.2095874713197,-0.829063313942982,
136.556289287176));
#271157=CARTESIAN_POINT('Ctrl Pts',(20.9311398475068,4.39113152064558,134.610933008472));
#271158=CARTESIAN_POINT('Ctrl Pts',(20.6526922236938,5.57609100646137,129.167522663925));
#271159=CARTESIAN_POINT('Ctrl Pts',(20.374244599881,1.6368952645291,125.228286434793));
#271160=CARTESIAN_POINT('Ctrl Pts',(20.0957969760681,-3.80652725872624,
126.413189973261));
#271161=CARTESIAN_POINT('Ctrl Pts',(19.8173493522552,-5.75193719040684,
131.633364813234));
#271162=CARTESIAN_POINT('Ctrl Pts',(19.5389017284423,-2.41159784185683,
136.091725296493));
#271163=CARTESIAN_POINT('Ctrl Pts',(19.2604541046294,3.14488211025528,135.691255941942));
#271164=CARTESIAN_POINT('Ctrl Pts',(18.9820064808165,5.81136903907515,130.799968522399));
#271165=CARTESIAN_POINT('Ctrl Pts',(18.7035588570036,3.13749172214556,125.912717223747));
#271166=CARTESIAN_POINT('Ctrl Pts',(18.4251112331907,-2.41958721244422,
125.52064723395));
#271167=CARTESIAN_POINT('Ctrl Pts',(18.1466636093778,-5.75318370220431,
129.984051719947));
#271168=CARTESIAN_POINT('Ctrl Pts',(17.868215985565,-3.79988542828747,135.201280008538));
#271169=CARTESIAN_POINT('Ctrl Pts',(17.589768361752,1.64532191950215,136.377954178279));
#271170=CARTESIAN_POINT('Ctrl Pts',(17.3113207379392,5.57855880171371,132.432768150908));
#271171=CARTESIAN_POINT('Ctrl Pts',(17.0328731141263,4.38537267289848,126.991155152525));
#271172=CARTESIAN_POINT('Ctrl Pts',(16.7544254903134,-0.83775670494522,
125.053691691071));
#271173=CARTESIAN_POINT('Ctrl Pts',(16.4759778665005,-5.29102859763445,
128.400812037271));
#271174=CARTESIAN_POINT('Ctrl Pts',(16.1975302426876,-4.88210369021464,
133.956676108886));
#271175=CARTESIAN_POINT('Ctrl Pts',(15.9190826188747,0.013236004487936,
136.61571624315));
#271176=CARTESIAN_POINT('Ctrl Pts',(15.6406349950618,4.89641245768097,133.934404458007));
#271177=CARTESIAN_POINT('Ctrl Pts',(15.3621873712489,5.2800250653117,128.376735294641));
#271178=CARTESIAN_POINT('Ctrl Pts',(15.0837397474361,0.811552581485459,
125.049935206953));
#271179=CARTESIAN_POINT('Ctrl Pts',(14.8052921236231,-4.40269707817821,
127.011170952307));
#271180=CARTESIAN_POINT('Ctrl Pts',(14.5268444998103,-5.57108320670569,
132.458162692417));
#271181=CARTESIAN_POINT('Ctrl Pts',(14.2483968759974,-1.6199160308156,136.385391118461));
#271182=CARTESIAN_POINT('Ctrl Pts',(13.9699492521845,3.81987484009636,135.18392516268));
#271183=CARTESIAN_POINT('Ctrl Pts',(13.6915016283715,5.74938734422005,129.95785334356));
#271184=CARTESIAN_POINT('Ctrl Pts',(13.4130540045587,2.39549375219187,125.509680355073));
#271185=CARTESIAN_POINT('Ctrl Pts',(13.1346063807458,-3.15974157172482,
125.927059868305));
#271186=CARTESIAN_POINT('Ctrl Pts',(12.8561587569329,-5.81132875318382,
130.82644050072));
#271187=CARTESIAN_POINT('Ctrl Pts',(12.57771113312,-3.12258870965941,135.705530799178));
#271188=CARTESIAN_POINT('Ctrl Pts',(12.2992635093071,2.43565781110307,136.080685136208));
#271189=CARTESIAN_POINT('Ctrl Pts',(12.0208158854942,5.75565379196074,131.607155003388));
#271190=CARTESIAN_POINT('Ctrl Pts',(11.7423682616813,3.78648511732596,126.395896048684));
#271191=CARTESIAN_POINT('Ctrl Pts',(11.4639206378685,-1.66227840004959,
125.235800667314));
#271192=CARTESIAN_POINT('Ctrl Pts',(11.1854730140555,-5.58348927459409,
129.192939840948));
#271193=CARTESIAN_POINT('Ctrl Pts',(10.9070253902426,-4.37374627440173,
134.630895986013));
#271194=CARTESIAN_POINT('Ctrl Pts',(10.6285777664298,0.855255882581734,
136.552453064119));
#271195=CARTESIAN_POINT('Ctrl Pts',(10.3501301426169,5.29831966504511,133.19179399377));
#271196=CARTESIAN_POINT('Ctrl Pts',(10.071682518804,4.87248651263752,127.637200283293));
#271197=CARTESIAN_POINT('Ctrl Pts',(9.79323489499104,-0.0309237106847325,
124.993072195629));
#271198=CARTESIAN_POINT('Ctrl Pts',(9.51478727117816,-4.90591655459505,
127.689234270502));
#271199=CARTESIAN_POINT('Ctrl Pts',(9.23633964736526,-5.27261175218,133.248045275945));
#271200=CARTESIAN_POINT('Ctrl Pts',(8.95789202355236,-0.794034330915497,
136.561229460968));
#271201=CARTESIAN_POINT('Ctrl Pts',(8.67944439973947,4.41422184972672,134.584132417584));
#271202=CARTESIAN_POINT('Ctrl Pts',(8.40099677592661,5.56602379719609,129.1336097421));
#271203=CARTESIAN_POINT('Ctrl Pts',(8.12254915211368,1.60292179042129,125.218425500451));
#271204=CARTESIAN_POINT('Ctrl Pts',(7.84410152830078,-3.83318703466779,
126.436442743329));
#271205=CARTESIAN_POINT('Ctrl Pts',(7.56565390448795,-5.74678423649425,
131.668363127979));
#271206=CARTESIAN_POINT('Ctrl Pts',(7.28720628067502,-2.37936747100029,
136.106307414428));
#271207=CARTESIAN_POINT('Ctrl Pts',(7.00875865686212,3.17457176177998,135.672021609062));
#271208=CARTESIAN_POINT('Ctrl Pts',(6.73031103304925,5.81123463193681,130.764593150968));
#271209=CARTESIAN_POINT('Ctrl Pts',(6.45186340923634,3.10765676993803,125.89370905193));
#271210=CARTESIAN_POINT('Ctrl Pts',(6.17341578542346,-2.45170584616043,
125.535473843045));
#271211=CARTESIAN_POINT('Ctrl Pts',(5.89496816161054,-5.75807056212669,
130.019088180515));
#271212=CARTESIAN_POINT('Ctrl Pts',(5.61652053779771,-3.77304972888379,
135.224329524944));
#271213=CARTESIAN_POINT('Ctrl Pts',(5.33807291398477,1.67921948147701,136.367835370977));
#271214=CARTESIAN_POINT('Ctrl Pts',(5.05962529017187,5.58836802279258,132.398779709476));
#271215=CARTESIAN_POINT('Ctrl Pts',(4.781177666359,4.36207935811697,126.964530794212));
#271216=CARTESIAN_POINT('Ctrl Pts',(4.50273004254611,-0.872747137244579,
125.058897900495));
#271217=CARTESIAN_POINT('Ctrl Pts',(4.2242824187332,-5.30556164954619,128.433064562307));
#271218=CARTESIAN_POINT('Ctrl Pts',(3.94583479492031,-4.86282419701095,
133.986336454649));
#271219=CARTESIAN_POINT('Ctrl Pts',(3.66738717110745,0.0486111304084952,
136.615528000873));
#271220=CARTESIAN_POINT('Ctrl Pts',(3.38893954729453,4.91537520376836,133.904540613147));
#271221=CARTESIAN_POINT('Ctrl Pts',(3.11049192348162,5.26514959429328,128.344639261694));
#271222=CARTESIAN_POINT('Ctrl Pts',(2.83204429966877,0.776508724519974,
125.045101672218));
#271223=CARTESIAN_POINT('Ctrl Pts',(2.55359667585587,-4.42570572852705,
127.038041698076));
#271224=CARTESIAN_POINT('Ctrl Pts',(2.27514905204296,-5.56091282480238,
132.492044816037));
#271225=CARTESIAN_POINT('Ctrl Pts',(1.99670142823006,-1.58591270077849,
136.395148603559));
#271226=CARTESIAN_POINT('Ctrl Pts',(1.7182538044172,3.84646371911817,135.160591357131));
#271227=CARTESIAN_POINT('Ctrl Pts',(1.43980618060429,5.7441278913444,129.922870874744));
#271228=CARTESIAN_POINT('Ctrl Pts',(1.16135855679139,2.36321914767325,125.495196402842));
#271229=CARTESIAN_POINT('Ctrl Pts',(0.882910932978526,-3.18937254303613,
125.946384477181));
#271230=CARTESIAN_POINT('Ctrl Pts',(0.604463309165634,-5.81108667620601,
130.861815299204));
#271231=CARTESIAN_POINT('Ctrl Pts',(0.326015685352703,-3.09269604130886,
135.724448075619));
#271232=CARTESIAN_POINT('Ctrl Pts',(0.0475680615398608,2.46773116894999,
136.065760837718));
#271233=CARTESIAN_POINT('Ctrl Pts',(-0.230879562273037,5.76043399031358,
131.572103831187));
#271234=CARTESIAN_POINT('Ctrl Pts',(-0.509327186085944,3.75957938742415,
126.37292831768));
#271235=CARTESIAN_POINT('Ctrl Pts',(-0.787774809898847,-1.69614500684454,
125.246022600264));
#271236=CARTESIAN_POINT('Ctrl Pts',(-1.06622243371171,-5.59319500111311,
129.226957980841));
#271237=CARTESIAN_POINT('Ctrl Pts',(-1.34467005752462,-4.35037203212501,
134.657449324165));
#271238=CARTESIAN_POINT('Ctrl Pts',(-1.62311768133752,0.890230306896913,
136.547140379971));
#271239=CARTESIAN_POINT('Ctrl Pts',(-1.90156530515039,5.31275448404895,
133.159497384516));
#271240=CARTESIAN_POINT('Ctrl Pts',(-2.18001292896328,4.85311683284533,
127.607598755059));
#271241=CARTESIAN_POINT('Ctrl Pts',(-2.4584605527762,-0.0662980998053887,
124.993368106748));
#271242=CARTESIAN_POINT('Ctrl Pts',(-2.73690817658909,-4.92478831757726,
127.719155693111));
#271243=CARTESIAN_POINT('Ctrl Pts',(-3.01535580040196,-5.25763866077998,
133.280095884409));
#271244=CARTESIAN_POINT('Ctrl Pts',(-3.29380342421486,-0.758975924653704,
136.565956311869));
#271245=CARTESIAN_POINT('Ctrl Pts',(-3.57225104802777,4.43714860819409,
134.557191765862));
#271246=CARTESIAN_POINT('Ctrl Pts',(-3.85069867184063,5.55575033687191,
129.099758730564));
#271247=CARTESIAN_POINT('Ctrl Pts',(-4.12914629565353,1.56888891945708,
125.208771554989));
#271248=CARTESIAN_POINT('Ctrl Pts',(-4.40759391946644,-3.85970477045413,
126.459857368199));
#271249=CARTESIAN_POINT('Ctrl Pts',(-4.68604154327934,-5.74141833337845,
131.703329426794));
#271250=CARTESIAN_POINT('Ctrl Pts',(-4.96448916709218,-2.34704893180687,
136.120693066776));
#271251=CARTESIAN_POINT('Ctrl Pts',(-5.24293679090511,3.20414377838073,
135.652606903212));
#271252=CARTESIAN_POINT('Ctrl Pts',(-5.52138441471801,5.81088488736209,
130.729219253137));
#271253=CARTESIAN_POINT('Ctrl Pts',(-5.79983203853088,3.07770666236606,
125.874882846113));
#271254=CARTESIAN_POINT('Ctrl Pts',(-6.07827966234377,-2.48373363101511,
125.550495692676));
#271255=CARTESIAN_POINT('Ctrl Pts',(-6.35672728615668,-5.7627440546269,
130.054153739642));
#271256=CARTESIAN_POINT('Ctrl Pts',(-6.63517490996957,-3.74607421773465,
135.247215257776));
#271257=CARTESIAN_POINT('Ctrl Pts',(-6.91362253378244,1.71305481935644,
136.357510407073));
#271258=CARTESIAN_POINT('Ctrl Pts',(-7.19207015759534,5.59797016483923,
132.36473218626));
#271259=CARTESIAN_POINT('Ctrl Pts',(-7.47051778140826,4.33862440488076,
126.938048722207));
#271260=CARTESIAN_POINT('Ctrl Pts',(-7.74896540522111,-0.907705229577551,
125.064317010151));
#271261=CARTESIAN_POINT('Ctrl Pts',(-8.027413029034,-5.31989810191992,128.46540495659));
#271262=CARTESIAN_POINT('Ctrl Pts',(-8.30586065284694,-4.84336451006833,
134.015878891129));
#271263=CARTESIAN_POINT('Ctrl Pts',(-8.58430827665978,0.0839844550257475,
136.615124423653));
#271264=CARTESIAN_POINT('Ctrl Pts',(-8.86275590047269,4.93415580881975,
133.874561889976));
#271265=CARTESIAN_POINT('Ctrl Pts',(-9.14120352428557,5.25007902122049,
128.312634374625));
#271266=CARTESIAN_POINT('Ctrl Pts',(-9.4196511480985,0.741436093738357,
125.040481548942));
#271267=CARTESIAN_POINT('Ctrl Pts',(-9.69809877191133,-4.44855038272257,
127.065052006178));
#271268=CARTESIAN_POINT('Ctrl Pts',(-9.97654639572428,-5.5505363812293,
132.525864401898));
#271269=CARTESIAN_POINT('Ctrl Pts',(-10.2549940195371,-1.55185060416301,
136.404698919952));
#271270=CARTESIAN_POINT('Ctrl Pts',(-10.53344164335,3.87291006601234,135.137096129849));
#271271=CARTESIAN_POINT('Ctrl Pts',(-10.8118892671629,5.7386555876974,129.887921069854));
#271272=CARTESIAN_POINT('Ctrl Pts',(-11.0903368909758,2.33085697319978,
125.480909183646));
#271273=CARTESIAN_POINT('Ctrl Pts',(-11.3687845147887,-3.21888533097506,
125.965889100148));
#271274=CARTESIAN_POINT('Ctrl Pts',(-11.6472321386015,-5.81062926727439,
130.897187968684));
#271275=CARTESIAN_POINT('Ctrl Pts',(-11.9256797624145,-3.06268877196916,
135.743183036409));
#271276=CARTESIAN_POINT('Ctrl Pts',(-12.2041273862274,2.49971308411117,
136.050641576106));
#271277=CARTESIAN_POINT('Ctrl Pts',(-12.4825750100403,5.76500073366654,
131.537024209977));
#271278=CARTESIAN_POINT('Ctrl Pts',(-12.7610226338531,3.73253434492532,
126.350124795028));
#271279=CARTESIAN_POINT('Ctrl Pts',(-13.039470257666,-1.7299487623625,125.256450499474));
#271280=CARTESIAN_POINT('Ctrl Pts',(-13.3179178814789,-5.60269346973446,
129.261034571969));
#271281=CARTESIAN_POINT('Ctrl Pts',(-13.5963655052918,-4.32683658521273,
134.683859884699));
#271282=CARTESIAN_POINT('Ctrl Pts',(-13.8748131291047,0.925171743400955,
136.541614895008));
#271283=CARTESIAN_POINT('Ctrl Pts',(-14.1532607529176,5.3269924369816,133.127113504801));
#271284=CARTESIAN_POINT('Ctrl Pts',(-14.4317083767304,4.83356731902416,
127.578115684011));
#271285=CARTESIAN_POINT('Ctrl Pts',(-14.7101560005434,-0.101670032225581,
124.99387934633));
#271286=CARTESIAN_POINT('Ctrl Pts',(-14.9886036243562,-4.94347759071707,
127.749191439124));
#271287=CARTESIAN_POINT('Ctrl Pts',(-15.2670512481692,-5.24247074564602,
133.312054753593));
#271288=CARTESIAN_POINT('Ctrl Pts',(-15.545498871982,-0.723889394260118,
136.570469664722));
#271289=CARTESIAN_POINT('Ctrl Pts',(-15.823946495795,4.45991094648802,134.530112051601));
#271290=CARTESIAN_POINT('Ctrl Pts',(-16.1023941196078,5.54527100617588,
129.065970883678));
#271291=CARTESIAN_POINT('Ctrl Pts',(-16.3808417434207,1.53479791273714,
125.199324956138));
#271292=CARTESIAN_POINT('Ctrl Pts',(-16.6592893672336,-3.88607948346057,
126.483432980235));
#271293=CARTESIAN_POINT('Ctrl Pts',(-16.9377369910465,-5.73583967989507,
131.738262413989));
#271294=CARTESIAN_POINT('Ctrl Pts',(-17.2161846148594,-2.31464342185212,
136.134881720468));
#271295=CARTESIAN_POINT('Ctrl Pts',(-17.4946322386723,3.23359706425542,
135.633012543814));
#271296=CARTESIAN_POINT('Ctrl Pts',(-17.7730798624852,5.81031981831091,
130.693848139697));
#271297=CARTESIAN_POINT('Ctrl Pts',(-18.0515274862981,3.04764250924188,
125.856239303907));
#271298=CARTESIAN_POINT('Ctrl Pts',(-18.3299751101109,-2.51566938020671,
125.565712226204));
#271299=CARTESIAN_POINT('Ctrl Pts',(-18.6084227339239,-5.76720400652691,
130.089247097961));
#271300=CARTESIAN_POINT('Ctrl Pts',(-18.8868703577367,-3.71895989442774,
135.269936358996));
#271301=CARTESIAN_POINT('Ctrl Pts',(-19.1653179815497,1.74682667935956,
136.346979669161));
#271302=CARTESIAN_POINT('Ctrl Pts',(-19.4437656053625,5.60736487204277,
132.330626842902));
#271303=CARTESIAN_POINT('Ctrl Pts',(-19.7222132291754,4.31500868232164,
126.91170991781));
#271304=CARTESIAN_POINT('Ctrl Pts',(-20.0006608529883,-0.942629686559699,
125.069948819234));
#271305=CARTESIAN_POINT('Ctrl Pts',(-20.2791084768012,-5.33403742351306,
128.497832021735));
#271306=CARTESIAN_POINT('Ctrl Pts',(-20.5575561006141,-4.82372535047263,
134.045302323618));
#271307=CARTESIAN_POINT('Ctrl Pts',(-20.836003724427,0.119354667568119,
136.614505526443));
#271308=CARTESIAN_POINT('Ctrl Pts',(-21.1144513482399,4.95275357691331,
133.844469399368));
#271309=CARTESIAN_POINT('Ctrl Pts',(-21.3928989720528,5.23481390453873,
128.280721819388));
#271310=CARTESIAN_POINT('Ctrl Pts',(-21.6713465958657,0.706335988769417,
125.036075008324));
#271311=CARTESIAN_POINT('Ctrl Pts',(-21.9497942196786,-4.47123019424771,
127.092200875735));
#271312=CARTESIAN_POINT('Ctrl Pts',(-22.2282418434914,-5.53995426048939,
132.559620196804));
#271313=CARTESIAN_POINT('Ctrl Pts',(-22.5066894673044,-1.5177310031529,
136.41404171375));
#271314=CARTESIAN_POINT('Ctrl Pts',(-22.7851370911172,3.89921290079955,
135.11344035146));
#271315=CARTESIAN_POINT('Ctrl Pts',(-23.0635847149301,5.73297063605735,
129.853005223969));
#271316=CARTESIAN_POINT('Ctrl Pts',(-23.342032338743,2.298408427964,125.466819226899));
#271317=CARTESIAN_POINT('Ctrl Pts',(-23.6204799625559,-3.24827884193431,
125.985573014458));
#271318=CARTESIAN_POINT('Ctrl Pts',(-23.8989275863688,-5.80995654333829,
130.932557198412));
#271319=CARTESIAN_POINT('Ctrl Pts',(-24.1773752101816,-3.03256801357094,
135.761734987319));
#271320=CARTESIAN_POINT('Ctrl Pts',(-24.4558228339946,2.53160237148462,
136.035327911625));
#271321=CARTESIAN_POINT('Ctrl Pts',(-24.7342704578075,5.76935385279724,
131.501917439649));
#271322=CARTESIAN_POINT('Ctrl Pts',(-25.0127180816204,3.70535099199371,
126.327486325724));
#271323=CARTESIAN_POINT('Ctrl Pts',(-25.2911657054332,-1.76368841399288,
125.267083978533));
#271324=CARTESIAN_POINT('Ctrl Pts',(-25.5696133292462,-5.61198432848891,
129.295168351611));
#271325=CARTESIAN_POINT('Ctrl Pts',(-25.8480609530591,-4.30314080577957,
134.71012668896));
#271326=CARTESIAN_POINT('Ctrl Pts',(-26.1265085768719,0.960078897325804,
136.535876813977));
#271327=CARTESIAN_POINT('Ctrl Pts',(-26.4049562006848,5.3410329962505,133.094643554625));
#271328=CARTESIAN_POINT('Ctrl Pts',(-26.6834038244978,4.81383869558843,
127.548752162656));
#271329=CARTESIAN_POINT('Ctrl Pts',(-26.9618514483106,-0.137038197225328,
124.994605895435));
#271330=CARTESIAN_POINT('Ctrl Pts',(-27.2402990721235,-4.96198368147699,
127.779340395554));
#271331=CARTESIAN_POINT('Ctrl Pts',(-27.5187466959364,-5.22710856883054,
133.343920699249));
#271332=CARTESIAN_POINT('Ctrl Pts',(-27.7971943197493,-0.688776039878604,
136.574769352283));
#271333=CARTESIAN_POINT('Ctrl Pts',(-28.0756419435621,4.48250802114168,
134.502894278251));
#271334=CARTESIAN_POINT('Ctrl Pts',(-28.3540895673751,5.53458619342344,
129.032247453463));
#271335=CARTESIAN_POINT('Ctrl Pts',(-28.632537191188,1.50065003351598,125.190086053944));
#271336=CARTESIAN_POINT('Ctrl Pts',(-28.9109848150008,-3.91231019636288,
126.507168705834));
#271337=CARTESIAN_POINT('Ctrl Pts',(-29.1894324388138,-5.73004848276283,
131.773160795109));
#271338=CARTESIAN_POINT('Ctrl Pts',(-29.4678800626266,-2.28215214193419,
136.148872849742));
#271339=CARTESIAN_POINT('Ctrl Pts',(-29.7463276864396,3.26293052800175,
135.613239256942));
#271340=CARTESIAN_POINT('Ctrl Pts',(-30.0247753102524,5.80953944572202,
130.658481121338));
#271341=CARTESIAN_POINT('Ctrl Pts',(-30.3032229340653,3.01746542460398,
125.837779116156));
#271342=CARTESIAN_POINT('Ctrl Pts',(-30.5816705578782,-2.54751191034413,
125.581122879776));
#271343=CARTESIAN_POINT('Ctrl Pts',(-30.8601181816911,-5.77145025256159,
130.124366955075));
#271344=CARTESIAN_POINT('Ctrl Pts',(-31.138565805504,-3.69170776369427,
135.292491986665));
#271345=CARTESIAN_POINT('Ctrl Pts',(-31.4170134293169,1.78053381005746,
136.336243547461));
#271346=CARTESIAN_POINT('Ctrl Pts',(-31.6954610531298,5.6165517962788,132.296464943187));
#271347=CARTESIAN_POINT('Ctrl Pts',(-31.9739086769427,4.29123306552915,
126.885515357016));
#271348=CARTESIAN_POINT('Ctrl Pts',(-32.2523563007555,-0.977519214052166,
125.075793119056));
#271349=CARTESIAN_POINT('Ctrl Pts',(-32.5308039245685,-5.34797909038788,
128.530344556146));
#271350=CARTESIAN_POINT('Ctrl Pts',(-32.8092515483813,-4.80390744596015,
134.07460566182));
#271351=CARTESIAN_POINT('Ctrl Pts',(-33.0876991721943,0.154720457379397,
136.613671332177));
#271352=CARTESIAN_POINT('Ctrl Pts',(-33.3661467960071,4.9711678189017,133.814264256411));
#271353=CARTESIAN_POINT('Ctrl Pts',(-33.64459441982,5.21935480990263,128.248902778514));
#271354=CARTESIAN_POINT('Ctrl Pts',(-33.9230420436329,0.671209710260644,
125.031882213649));
#271355=CARTESIAN_POINT('Ctrl Pts',(-34.2014896674458,-4.49374432269368,
127.119487300736));
#271356=CARTESIAN_POINT('Ctrl Pts',(-34.4799372912587,-5.52916685470707,
132.59331094992));
#271357=CARTESIAN_POINT('Ctrl Pts',(-34.7583849150716,-1.48355516206214,
136.423176638752));
#271358=CARTESIAN_POINT('Ctrl Pts',(-35.0368325388844,3.92537124881898,
135.089624898536));
#271359=CARTESIAN_POINT('Ctrl Pts',(-35.3152801626974,5.72707324708195,
129.818124630907));
#271360=CARTESIAN_POINT('Ctrl Pts',(-35.5937277865103,2.26587471435868,
125.45292705471));
#271361=CARTESIAN_POINT('Ctrl Pts',(-35.8721754103231,-3.27755198672651,
126.005435490714));
#271362=CARTESIAN_POINT('Ctrl Pts',(-36.1506230341361,-5.80906852932597,
130.967921677768));
#271363=CARTESIAN_POINT('Ctrl Pts',(-36.4290706579489,-3.00233488224952,
135.780103240898));
#271364=CARTESIAN_POINT('Ctrl Pts',(-36.7075182817618,2.56339784940132,
136.019820411726));
#271365=CARTESIAN_POINT('Ctrl Pts',(-36.9859659055747,5.77349318639923,
131.466784821096));
#271366=CARTESIAN_POINT('Ctrl Pts',(-37.2644135293876,3.67803033591843,
126.305013748643));
#271367=CARTESIAN_POINT('Ctrl Pts',(-37.5428611532005,-1.79736271150026,
125.277922643415));
#271368=CARTESIAN_POINT('Ctrl Pts',(-37.8213087770133,-5.62106723310019,
129.329358054928));
#271369=CARTESIAN_POINT('Ctrl Pts',(-38.0997564008263,-4.27928557188161,
134.736248763623));
#271370=CARTESIAN_POINT('Ctrl Pts',(-38.3782040246392,0.994950475174061,
136.529926349506));
#271371=CARTESIAN_POINT('Ctrl Pts',(-38.656651648452,5.35487564157755,133.062088737171));
#271372=CARTESIAN_POINT('Ctrl Pts',(-38.9350992722649,4.79393169358958,
127.51950927907));
#271373=CARTESIAN_POINT('Ctrl Pts',(-39.2135468960779,-0.172401284224016,
124.995547727136));
#271374=CARTESIAN_POINT('Ctrl Pts',(-39.4919945198907,-4.98030590410683,
127.809601445221));
#271375=CARTESIAN_POINT('Ctrl Pts',(-39.7704421437036,-5.21155269958477,
133.375692540572));
#271376=CARTESIAN_POINT('Ctrl Pts',(-40.0488897675166,-0.65363716264763,
136.578855215227));
#271377=CARTESIAN_POINT('Ctrl Pts',(-40.3273373913294,4.50493899481217,
134.475539454375));
#271378=CARTESIAN_POINT('Ctrl Pts',(-40.6057850151423,5.52369629454426,
128.998589689552));
#271379=CARTESIAN_POINT('Ctrl Pts',(-40.8842326389552,1.46644654715595,
125.181055190758));
#271380=CARTESIAN_POINT('Ctrl Pts',(-41.1626802627681,-3.93839593717207,
126.531063665459));
#271381=CARTESIAN_POINT('Ctrl Pts',(-41.441127886581,-5.72404495657686,
131.808023276983));
#271382=CARTESIAN_POINT('Ctrl Pts',(-41.7195755103939,-2.24957629602936,
136.162665936149));
#271383=CARTESIAN_POINT('Ctrl Pts',(-41.9980231342068,3.29214308265742,
135.593287775304));
#271384=CARTESIAN_POINT('Ctrl Pts',(-42.2764707580197,5.80854379851262,
130.623119508596));
#271385=CARTESIAN_POINT('Ctrl Pts',(-42.5549183818325,2.98717652667487,
125.81950296691));
#271386=CARTESIAN_POINT('Ctrl Pts',(-42.8333660056454,-2.57926004149102,
125.596727082342));
#271387=CARTESIAN_POINT('Ctrl Pts',(-43.1118136294584,-5.7754826353847,
130.159512009603));
#271388=CARTESIAN_POINT('Ctrl Pts',(-43.3902612532712,-3.66431883537201,
135.314881304976));
#271389=CARTESIAN_POINT('Ctrl Pts',(-43.6687088770841,1.81417496242045,
136.325302439805));
#271390=CARTESIAN_POINT('Ctrl Pts',(-43.947156500897,5.62553059712261,132.262247752997));
#271391=CARTESIAN_POINT('Ctrl Pts',(-44.2256041247099,4.26729843551711,
126.859466010475));
#271392=CARTESIAN_POINT('Ctrl Pts',(-44.5040517485228,-1.01237251921066,
125.081849693053));
#271393=CARTESIAN_POINT('Ctrl Pts',(-44.7824993723357,-5.3617225859308,
128.562941355057));
#271394=CARTESIAN_POINT('Ctrl Pts',(-45.0609469961486,-4.78391153089065,
134.103787819889));
#271395=CARTESIAN_POINT('Ctrl Pts',(-45.3393946199614,0.190080513966956,
136.612621871764));
#271396=CARTESIAN_POINT('Ctrl Pts',(-45.6178422437743,4.98939785243841,
133.783947580368));
#271397=CARTESIAN_POINT('Ctrl Pts',(-45.8962898675873,5.20370231015464,
128.217178431071));
#271398=CARTESIAN_POINT('Ctrl Pts',(-46.1747374914001,0.636058559829223,
125.027903320286));
#271399=CARTESIAN_POINT('Ctrl Pts',(-46.453185115213,-4.51609193379101,
127.146910270074));
#271400=CARTESIAN_POINT('Ctrl Pts',(-46.7316327390259,-5.51817456361365,
132.626935412823));
#271401=CARTESIAN_POINT('Ctrl Pts',(-47.0100803628388,-1.4493243472895,
136.43210335646));
#271402=CARTESIAN_POINT('Ctrl Pts',(-47.2885279866517,3.95138414076325,
135.06565065357));
#271403=CARTESIAN_POINT('Ctrl Pts',(-47.5669756104645,5.72096363930122,
129.783280583183));
#271404=CARTESIAN_POINT('Ctrl Pts',(-47.8454232342775,2.23325703793269,
125.439233181862));
#271405=CARTESIAN_POINT('Ctrl Pts',(-48.1238708580903,-3.30670368062431,
126.025475792906));
#271406=CARTESIAN_POINT('Ctrl Pts',(-48.4023184819033,-5.80796525814313,
131.00328009631));
#271407=CARTESIAN_POINT('Ctrl Pts',(-48.6807661057162,-2.97199049830493,
135.798287116504));
#271408=CARTESIAN_POINT('Ctrl Pts',(-48.9592137295291,2.59509833966803,
136.004119651047));
#271409=CARTESIAN_POINT('Ctrl Pts',(-49.2376613533419,5.77741858108801,
131.431627656171));
#271410=CARTESIAN_POINT('Ctrl Pts',(-49.5161089771548,3.65057338907646,
126.282707896514));
#271411=CARTESIAN_POINT('Ctrl Pts',(-49.7945566009678,-1.8309704070716,
125.288966092489));
#271412=CARTESIAN_POINT('Ctrl Pts',(-50.0730042247805,-5.62994184699806,
129.363602415007));
#271413=CARTESIAN_POINT('Ctrl Pts',(-50.3514518485936,-4.25527176748286,
134.762225140725));
#271414=CARTESIAN_POINT('Ctrl Pts',(-50.6298994724063,1.02978518476655,
136.52376372209));
#271415=CARTESIAN_POINT('Ctrl Pts',(-50.9083470962193,5.36851986001845,
133.029450258773));
#271416=CARTESIAN_POINT('Ctrl Pts',(-51.1867947200322,4.77384705068883,
127.490388116857));
#271417=CARTESIAN_POINT('Ctrl Pts',(-51.465242343845,-0.207757982829986,
124.996704806535));
#271418=CARTESIAN_POINT('Ctrl Pts',(-51.743689967658,-4.99844357966987,
127.839973466791));
#271419=CARTESIAN_POINT('Ctrl Pts',(-52.0221375914708,-5.19580371433717,
133.407369100245));
#271420=CARTESIAN_POINT('Ctrl Pts',(-52.3005852152837,-0.618474064651215,
136.58272710215));
#271421=CARTESIAN_POINT('Ctrl Pts',(-52.5790328390967,4.52720303631132,
134.448048593619));
#271422=CARTESIAN_POINT('Ctrl Pts',(-52.8574804629095,5.51260171306762,
128.964998839148));
#271423=CARTESIAN_POINT('Ctrl Pts',(-53.1359280867224,1.43218872108006,
125.172232701224));
#271424=CARTESIAN_POINT('Ctrl Pts',(-53.4143757105353,-3.96433573927151,
126.555116973674));
#271425=CARTESIAN_POINT('Ctrl Pts',(-53.6928233343482,-5.71782932379997,
131.842848567767));
#271426=CARTESIAN_POINT('Ctrl Pts',(-53.9712709581611,-2.21691709124776,
136.176260468582));
#271427=CARTESIAN_POINT('Ctrl Pts',(-54.249718581974,3.32123364574025,135.573158838211));
#271428=CARTESIAN_POINT('Ctrl Pts',(-54.5281662057869,5.80733291357678,
130.58776461181));
#271429=CARTESIAN_POINT('Ctrl Pts',(-54.8066138295998,2.95677693782102,
125.801411533396));
#271430=CARTESIAN_POINT('Ctrl Pts',(-55.0850614534126,-2.61091259720856,
125.612524255684));
#271431=CARTESIAN_POINT('Ctrl Pts',(-55.3635090772256,-5.77930100557468,
130.194680959234));
#271432=CARTESIAN_POINT('Ctrl Pts',(-55.6419567010384,-3.63679412436797,
135.337103484283));
#271433=CARTESIAN_POINT('Ctrl Pts',(-55.9204043248514,1.8477488898629,136.314156751619));
#271434=CARTESIAN_POINT('Ctrl Pts',(-56.1988519486642,5.63430094186134,
132.227976540264));
#271435=CARTESIAN_POINT('Ctrl Pts',(-56.4772995724772,4.24320567919224,
126.833562843453));
#271436=CARTESIAN_POINT('Ctrl Pts',(-56.7557471962901,-1.04718831053316,
125.088118316796));
#271437=CARTESIAN_POINT('Ctrl Pts',(-57.0341948201028,-5.3752674008715,
128.595621210585));
#271438=CARTESIAN_POINT('Ctrl Pts',(-57.3126424439159,-4.76373834622006,
134.13284771647));
#271439=CARTESIAN_POINT('Ctrl Pts',(-57.5910900677287,0.225433527051438,
136.611357184097));
#271440=CARTESIAN_POINT('Ctrl Pts',(-57.8695376915416,5.00744300200284,
133.753520494635));
#271441=CARTESIAN_POINT('Ctrl Pts',(-58.1479853153544,5.18785698530388,
128.185549952615));
#271442=CARTESIAN_POINT('Ctrl Pts',(-58.4264329391674,0.600883840013963,
125.024138475672));
#271443=CARTESIAN_POINT('Ctrl Pts',(-58.7048805629802,-4.53827219944114,
127.174468767579));
#271444=CARTESIAN_POINT('Ctrl Pts',(-58.9833281867932,-5.5069777945324,
132.660492339548));
#271445=CARTESIAN_POINT('Ctrl Pts',(-59.261775810606,-1.41503982726995,
136.440821536091));
#271446=CARTESIAN_POINT('Ctrl Pts',(-59.540223434419,3.97725061271504,135.041518504932));
#271447=CARTESIAN_POINT('Ctrl Pts',(-59.8186710582318,5.71464203910897,
129.748474371954));
#271448=CARTESIAN_POINT('Ctrl Pts',(-60.0971186820448,2.20055660734573,
125.425738115783));
#271449=CARTESIAN_POINT('Ctrl Pts',(-60.3755663058576,-3.3357328434014,
126.045693178431));
#271450=CARTESIAN_POINT('Ctrl Pts',(-60.6540139296705,-5.80664677067165,
131.038631143817));
#271451=CARTESIAN_POINT('Ctrl Pts',(-60.9324615534834,-2.94153598615947,
135.816285940328));
#271452=CARTESIAN_POINT('Ctrl Pts',(-61.2109091772963,2.62670266761142,
135.988226211385));
#271453=CARTESIAN_POINT('Ctrl Pts',(-61.4893568011092,5.78112989140647,
131.396447247635));
#271454=CARTESIAN_POINT('Ctrl Pts',(-61.767804424922,3.62298116889529,126.260569595891));
#271455=CARTESIAN_POINT('Ctrl Pts',(-62.046252048735,-1.86451025536104,
125.300213916535));
#271456=CARTESIAN_POINT('Ctrl Pts',(-62.3246996725479,-5.63860784133039,
129.39790016291));
#271457=CARTESIAN_POINT('Ctrl Pts',(-62.6031472963608,-4.23110028242386,
134.788054857702));
#271458=CARTESIAN_POINT('Ctrl Pts',(-62.8815949201736,1.0645817352901,136.517389160091));
#271459=CARTESIAN_POINT('Ctrl Pts',(-63.1600425439866,5.38196514598156,
132.99672932886));
#271460=CARTESIAN_POINT('Ctrl Pts',(-63.4384901677994,4.75358551113023,
127.461389755115));
#271461=CARTESIAN_POINT('Ctrl Pts',(-63.7169377916123,-0.243106982887504,
124.998077090756));
#271462=CARTESIAN_POINT('Ctrl Pts',(-63.9953854154252,-5.0163960360679,
127.870455334816));
#271463=CARTESIAN_POINT('Ctrl Pts',(-64.2738330392381,-5.17986219667218,
133.438949204482));
#271464=CARTESIAN_POINT('Ctrl Pts',(-64.552280663051,-0.583288048870894,
136.586384869579));
#271465=CARTESIAN_POINT('Ctrl Pts',(-64.8307282868638,4.54929932063727,
134.420422714664));
#271466=CARTESIAN_POINT('Ctrl Pts',(-65.1091759106768,5.50130286010717,
128.93147614697));
#271467=CARTESIAN_POINT('Ctrl Pts',(-65.3876235344896,1.39787782472419,
125.16361891226));
#271468=CARTESIAN_POINT('Ctrl Pts',(-65.6660711583025,-3.99012864145221,
126.579327739175));
#271469=CARTESIAN_POINT('Ctrl Pts',(-65.9445187821156,-5.71140181475477,
131.877635376998));
#271470=CARTESIAN_POINT('Ctrl Pts',(-66.2229664059283,-2.18417573778792,
136.189655943291));
#271471=CARTESIAN_POINT('Ctrl Pts',(-66.5014140297413,3.35020113928917,
135.552853191544));
#271472=CARTESIAN_POINT('Ctrl Pts',(-66.7798616535541,5.80590683578406,
130.552417741069));
#271473=CARTESIAN_POINT('Ctrl Pts',(-67.0583092773671,2.92626778451039,
125.783505486001));
#271474=CARTESIAN_POINT('Ctrl Pts',(-67.3367569011799,-2.64246840459962,
125.628513814431));
#271475=CARTESIAN_POINT('Ctrl Pts',(-67.6152045249929,-5.78290522164069,
130.229872500769));
#271476=CARTESIAN_POINT('Ctrl Pts',(-67.8936521488056,-3.60913465062,135.359157701137));
#271477=CARTESIAN_POINT('Ctrl Pts',(-68.1720997726187,1.88125434829088,
136.302806895912));
#271478=CARTESIAN_POINT('Ctrl Pts',(-68.4505473964314,5.64286250550667,
132.193652574919));
#271479=CARTESIAN_POINT('Ctrl Pts',(-68.7289950202444,4.21895568932047,
126.807806815805));
#271480=CARTESIAN_POINT('Ctrl Pts',(-69.0074426440573,-1.08196529790749,
125.094598758));
#271481=CARTESIAN_POINT('Ctrl Pts',(-69.2858902678701,-5.38861303330182,
128.628382911763));
#271482=CARTESIAN_POINT('Ctrl Pts',(-69.564337891683,-4.74338863947339,
134.161784274737));
#271483=CARTESIAN_POINT('Ctrl Pts',(-69.8427855154959,0.260778186613682,
136.609877316035));
#271484=CARTESIAN_POINT('Ctrl Pts',(-70.1212331393089,5.02530259892534,
133.722984126697));
#271485=CARTESIAN_POINT('Ctrl Pts',(-70.3996807631217,5.17181942250469,
128.154018515153));
#271486=CARTESIAN_POINT('Ctrl Pts',(-70.6781283869345,0.5656868542273,125.020587819316));
#271487=CARTESIAN_POINT('Ctrl Pts',(-70.9565760107477,-4.56028429774593,
127.202161772061));
#271488=CARTESIAN_POINT('Ctrl Pts',(-71.2350236345604,-5.49557696236377,
132.693980486629));
#271489=CARTESIAN_POINT('Ctrl Pts',(-71.5134712583732,-1.38070287242923,
136.449330854589));
#271490=CARTESIAN_POINT('Ctrl Pts',(-71.7919188821862,4.00296970618273,
135.017229346852));
#271491=CARTESIAN_POINT('Ctrl Pts',(-72.0703665059991,5.70810868075446,
129.71370728698));
#271492=CARTESIAN_POINT('Ctrl Pts',(-72.348814129812,2.16777463432419,125.412442356538));
#271493=CARTESIAN_POINT('Ctrl Pts',(-72.6272617536249,-3.36463839937136,
126.06608689813));
#271494=CARTESIAN_POINT('Ctrl Pts',(-72.9057093774378,-5.80511311576878,
131.073973510343));
#271495=CARTESIAN_POINT('Ctrl Pts',(-73.1841570012506,-2.91097247431594,
135.834099045416));
#271496=CARTESIAN_POINT('Ctrl Pts',(-73.4626046250635,2.65820966212185,
135.972140681676));
#271497=CARTESIAN_POINT('Ctrl Pts',(-73.7410522488765,5.78462697983096,
131.361244899111));
#271498=CARTESIAN_POINT('Ctrl Pts',(-74.0194998726893,3.59525469781404,
126.238599667113));
#271499=CARTESIAN_POINT('Ctrl Pts',(-74.2979474965022,-1.89798101353784,
125.31166569876));
#271500=CARTESIAN_POINT('Ctrl Pts',(-74.5763951203151,-5.64706489497548,
129.432250027724));
#271501=CARTESIAN_POINT('Ctrl Pts',(-74.854842744128,-4.20677201238788,
134.813736957424));
#271502=CARTESIAN_POINT('Ctrl Pts',(-75.1332903679409,1.09933883734644,
136.510802899716));
#271503=CARTESIAN_POINT('Ctrl Pts',(-75.4117379917539,5.39521100124704,
132.963927159917));
#271504=CARTESIAN_POINT('Ctrl Pts',(-75.6901856155667,4.73314782571214,
127.432515268386));
#271505=CARTESIAN_POINT('Ctrl Pts',(-75.9686332393795,-0.278446974526432,
124.99966452895));
#271506=CARTESIAN_POINT('Ctrl Pts',(-76.2470808631926,-5.03416260806588,
127.901045919781));
#271507=CARTESIAN_POINT('Ctrl Pts',(-76.5255284870053,-5.16372873730878,
133.470431683069));
#271508=CARTESIAN_POINT('Ctrl Pts',(-76.8039761108183,-0.548080419137594,
136.589828381972));
#271509=CARTESIAN_POINT('Ctrl Pts',(-77.0824237346311,4.57122702900371,
134.392662841198));
#271510=CARTESIAN_POINT('Ctrl Pts',(-77.360871358444,5.48980015434633,128.898022855216));
#271511=CARTESIAN_POINT('Ctrl Pts',(-77.639318982257,1.36351512949127,125.155214143056));
#271512=CARTESIAN_POINT('Ctrl Pts',(-77.9177666060698,-4.0157736879487,
126.603695064822));
#271513=CARTESIAN_POINT('Ctrl Pts',(-78.1962142298826,-5.70476266761487,
131.91238241564));
#271514=CARTESIAN_POINT('Ctrl Pts',(-78.4746618536957,-2.15135344889296,
136.202851863901));
#271515=CARTESIAN_POINT('Ctrl Pts',(-78.7531094775085,3.37904448990285,
135.532371587738));
#271516=CARTESIAN_POINT('Ctrl Pts',(-79.0315571013213,5.8042656179783,130.517080206165));
#271517=CARTESIAN_POINT('Ctrl Pts',(-79.3100047251342,2.8956501972711,125.765785488239));
#271518=CARTESIAN_POINT('Ctrl Pts',(-79.5884523489472,-2.67392629435197,
125.644695166086));
#271519=CARTESIAN_POINT('Ctrl Pts',(-79.8668999727601,-5.78629515002701,
130.265085330171));
#271520=CARTESIAN_POINT('Ctrl Pts',(-80.1453475965729,-3.58134143906054,
135.38104313831));
#271521=CARTESIAN_POINT('Ctrl Pts',(-80.4237952203859,1.91469009614739,
136.291253293255));
#271522=CARTESIAN_POINT('Ctrl Pts',(-80.7022428441988,5.65121497080658,
132.15927712885));
#271523=CARTESIAN_POINT('Ctrl Pts',(-80.9806904680116,4.19454936449412,
126.782198881926));
#271524=CARTESIAN_POINT('Ctrl Pts',(-81.2591380918246,-1.11670219266007,
125.10129077653));
#271525=CARTESIAN_POINT('Ctrl Pts',(-81.5375857156372,-5.40175898869456,
128.661225244595));
#271526=CARTESIAN_POINT('Ctrl Pts',(-81.8160333394505,-4.72286316471603,
134.190596422436));
#271527=CARTESIAN_POINT('Ctrl Pts',(-82.0944809632629,0.296113182944105,
136.608182322418));
#271528=CARTESIAN_POINT('Ctrl Pts',(-82.3729285870762,5.04297598141181,
133.692339608092));
#271529=CARTESIAN_POINT('Ctrl Pts',(-82.6513762108889,5.15559021603496,
128.122585287091));
#271530=CARTESIAN_POINT('Ctrl Pts',(-82.9298238347018,0.530468906706182,
125.017251482786));
#271531=CARTESIAN_POINT('Ctrl Pts',(-83.2082714585147,-4.58212741303929,
127.229988257347));
#271532=CARTESIAN_POINT('Ctrl Pts',(-83.4867190823277,-5.48397248956967,
132.72739861315));
#271533=CARTESIAN_POINT('Ctrl Pts',(-83.7651667061405,-1.34631475513585,
136.45763099664));
#271534=CARTESIAN_POINT('Ctrl Pts',(-84.0436143299535,4.02854046813582,
134.992784079373));
#271535=CARTESIAN_POINT('Ctrl Pts',(-84.3220619537663,5.70136380633342,
129.678980616565));
#271536=CARTESIAN_POINT('Ctrl Pts',(-84.6005095775792,2.13491233361711,
125.399346396808));
#271537=CARTESIAN_POINT('Ctrl Pts',(-84.8789572013921,-3.39341927742779,
126.086656196302));
#271538=CARTESIAN_POINT('Ctrl Pts',(-85.1574048252049,-5.80336435026449,
131.109305886265));
#271539=CARTESIAN_POINT('Ctrl Pts',(-85.4358524490179,-2.88030109531746,
135.851725771696));
#271540=CARTESIAN_POINT('Ctrl Pts',(-85.7143000728307,2.68961815569484,
135.955863657977));
#271541=CARTESIAN_POINT('Ctrl Pts',(-85.9927476966438,5.78790971677558,
131.326021915035));
#271542=CARTESIAN_POINT('Ctrl Pts',(-86.2711953204564,3.56739500324825,
126.216798924288));
#271543=CARTESIAN_POINT('Ctrl Pts',(-86.5496429442695,-1.93138144132926,
125.323321014816));
#271544=CARTESIAN_POINT('Ctrl Pts',(-86.8280905680822,-5.65531269455438,
129.466650736599));
#271545=CARTESIAN_POINT('Ctrl Pts',(-87.1065381918953,-4.18228785886808,
134.83927048823));
#271546=CARTESIAN_POINT('Ctrl Pts',(-87.3849858157081,1.13405520299706,
136.504005185026));
#271547=CARTESIAN_POINT('Ctrl Pts',(-87.663433439521,5.40825693498488,132.931044967442));
#271548=CARTESIAN_POINT('Ctrl Pts',(-87.9418810633338,4.71253475176078,
127.403765726628));
#271549=CARTESIAN_POINT('Ctrl Pts',(-88.2203286871468,-0.313776648210234,
125.00146706229));
#271550=CARTESIAN_POINT('Ctrl Pts',(-88.4987763109598,-5.05174263731727,
127.931744088139));
#271551=CARTESIAN_POINT('Ctrl Pts',(-88.7772239347726,-5.14740393407785,
133.501815369412));
#271552=CARTESIAN_POINT('Ctrl Pts',(-89.0556715585855,-0.512852480082647,
136.593057511728));
#271553=CARTESIAN_POINT('Ctrl Pts',(-89.3341191823985,4.59298534887173,
134.364770001874));
#271554=CARTESIAN_POINT('Ctrl Pts',(-89.6125668062112,5.47809402202166,
128.864640203508));
#271555=CARTESIAN_POINT('Ctrl Pts',(-89.8910144300243,1.32910190870433,
125.147018705051));
#271556=CARTESIAN_POINT('Ctrl Pts',(-90.169462053837,-4.04126992847403,
126.628218047677));
#271557=CARTESIAN_POINT('Ctrl Pts',(-90.44790967765,-5.69791212839678,131.947088396125));
#271558=CARTESIAN_POINT('Ctrl Pts',(-90.7263573014627,-2.1184514408047,
136.215847741432));
#271559=CARTESIAN_POINT('Ctrl Pts',(-91.0048049252757,3.40776262878029,
135.511714785749));
#271560=CARTESIAN_POINT('Ctrl Pts',(-91.2832525490887,5.80240932097568,
130.48175331654));
#271561=CARTESIAN_POINT('Ctrl Pts',(-91.5617001729014,2.86492531064864,
125.748252196732));
#271562=CARTESIAN_POINT('Ctrl Pts',(-91.8401477967144,-2.70528510078237,
125.661067711041));
#271563=CARTESIAN_POINT('Ctrl Pts',(-92.1185954205271,-5.78947066511866,
130.30031814262));
#271564=CARTESIAN_POINT('Ctrl Pts',(-92.3970430443404,-3.55341551957677,
135.402758984829));
#271565=CARTESIAN_POINT('Ctrl Pts',(-92.6754906681528,1.94805489445803,
136.279496371773));
#271566=CARTESIAN_POINT('Ctrl Pts',(-92.9539382919661,5.6593580282576,132.124851475851));
#271567=CARTESIAN_POINT('Ctrl Pts',(-93.2323859157787,4.16998760909852,
126.75673999073));
#271568=CARTESIAN_POINT('Ctrl Pts',(-93.5108335395918,-1.15139770760221,
125.10819412441));
#271569=CARTESIAN_POINT('Ctrl Pts',(-93.7892811634045,-5.41470477992152,
128.694146992097));
#271570=CARTESIAN_POINT('Ctrl Pts',(-94.0677287872175,-4.70216268252734,
134.219283091922));
#271571=CARTESIAN_POINT('Ctrl Pts',(-94.3461764110305,0.331437206691851,
136.606272266052));
#271572=CARTESIAN_POINT('Ctrl Pts',(-94.6246240348431,5.0604624945689,133.661588074364));
#271573=CARTESIAN_POINT('Ctrl Pts',(-94.9030716586564,5.13916996727372,
128.0912514332));
#271574=CARTESIAN_POINT('Ctrl Pts',(-95.1815192824688,0.495231302464415,
125.014129589715));
#271575=CARTESIAN_POINT('Ctrl Pts',(-95.459966906282,-4.60380073591605,
127.257947192314));
#271576=CARTESIAN_POINT('Ctrl Pts',(-95.7384145300948,-5.47216480615837,
132.760745480792));
#271577=CARTESIAN_POINT('Ctrl Pts',(-96.0168621539077,-1.31187674965409,
136.465721654678));
#271578=CARTESIAN_POINT('Ctrl Pts',(-96.2953097777207,4.05396195104042,
134.96818360832));
#271579=CARTESIAN_POINT('Ctrl Pts',(-96.5737574015334,5.69440766577999,
129.64429564752));
#271580=CARTESIAN_POINT('Ctrl Pts',(-96.8522050253465,2.10197092294792,
125.386450721867));
#271581=CARTESIAN_POINT('Ctrl Pts',(-97.1306526491593,-3.42207441108517,
126.107400310748));
#271582=CARTESIAN_POINT('Ctrl Pts',(-97.4091002729722,-5.80140053895979,
131.144626962327));
#271583=CARTESIAN_POINT('Ctrl Pts',(-97.6875478967851,-2.8495229857029,
135.869165466005));
#271584=CARTESIAN_POINT('Ctrl Pts',(-97.965995520598,2.72092698447821,135.93939574344));
#271585=CARTESIAN_POINT('Ctrl Pts',(-98.2444431444108,5.79097798059694,
131.290779600608));
#271586=CARTESIAN_POINT('Ctrl Pts',(-98.5228907682237,3.53940311754856,
126.195168175249));
#271587=CARTESIAN_POINT('Ctrl Pts',(-98.8013383920368,-1.96471030107164,
125.33517943281));
#271588=CARTESIAN_POINT('Ctrl Pts',(-99.0797860158496,-5.6633509344415,
129.501101014807));
#271589=CARTESIAN_POINT('Ctrl Pts',(-99.3582336396624,-4.15764872913354,
134.864654503967));
#271590=CARTESIAN_POINT('Ctrl Pts',(-99.6366812634755,1.16872954581563,
136.496996267908));
#271591=CARTESIAN_POINT('Ctrl Pts',(-99.9151288872883,5.42110246377302,
132.898083969897));
#271592=CARTESIAN_POINT('Ctrl Pts',(-100.193576511101,4.69174705310118,
127.375142195163));
#271593=CARTESIAN_POINT('Ctrl Pts',(-100.472024134914,-0.34909469478497,
125.003484623986));
#271594=CARTESIAN_POINT('Ctrl Pts',(-100.750471758727,-5.06913547238742,
127.96254870236));
#271595=CARTESIAN_POINT('Ctrl Pts',(-101.02891938254,-5.13088839190121,
133.533099100579));
#271596=CARTESIAN_POINT('Ctrl Pts',(-101.307367006353,-0.47760553709043,
136.596072139193));
#271597=CARTESIAN_POINT('Ctrl Pts',(-101.585814630166,4.61457347397855,
134.33674523027));
#271598=CARTESIAN_POINT('Ctrl Pts',(-101.864262253979,5.46618489690847,
128.831329428852));
#271599=CARTESIAN_POINT('Ctrl Pts',(-102.142709877791,1.29463943755703,
125.139032901931));
#271600=CARTESIAN_POINT('Ctrl Pts',(-102.421157501604,-4.06661641825637,
126.652895779031));
#271601=CARTESIAN_POINT('Ctrl Pts',(-102.699605125417,-5.69085045094906,
131.981752032413));
#271602=CARTESIAN_POINT('Ctrl Pts',(-102.97805274923,-2.08547093271925,
136.228643094318));
#271603=CARTESIAN_POINT('Ctrl Pts',(-103.256500373043,3.43635449176034,
135.490883551018));
#271604=CARTESIAN_POINT('Ctrl Pts',(-103.534947996856,5.80033801356182,
130.446438381249));
#271605=CARTESIAN_POINT('Ctrl Pts',(-103.813395620669,2.83409426316523,
125.730906261181));
#271606=CARTESIAN_POINT('Ctrl Pts',(-104.091843244482,-2.73654366187847,
125.677630842606));
#271607=CARTESIAN_POINT('Ctrl Pts',(-104.370290868295,-5.79243164924577,
130.335569632546));
#271608=CARTESIAN_POINT('Ctrl Pts',(-104.648738492108,-3.52535792697413,
135.424304436005));
#271609=CARTESIAN_POINT('Ctrl Pts',(-104.92718611592,1.98134750687769,136.267536567122));
#271610=CARTESIAN_POINT('Ctrl Pts',(-105.205633739733,5.66729137611554,
132.090376891579));
#271611=CARTESIAN_POINT('Ctrl Pts',(-105.484081363546,4.14527133327901,
126.731431085605));
#271612=CARTESIAN_POINT('Ctrl Pts',(-105.762528987359,-1.18605055707886,
125.115308545834));
#271613=CARTESIAN_POINT('Ctrl Pts',(-106.040976611172,-5.42744992727162,
128.72714693434));
#271614=CARTESIAN_POINT('Ctrl Pts',(-106.319424234985,-4.68128795997122,
134.247843220201));
#271615=CARTESIAN_POINT('Ctrl Pts',(-106.597871858798,0.366748948912009,
136.604147217717));
#271616=CARTESIAN_POINT('Ctrl Pts',(-106.876319482611,5.07776149042729,
133.630730665021));
#271617=CARTESIAN_POINT('Ctrl Pts',(-107.154767106424,5.12255928467941,
128.060018114567));
#271618=CARTESIAN_POINT('Ctrl Pts',(-107.433214730236,0.45997534724462,
125.011222255784));
#271619=CARTESIAN_POINT('Ctrl Pts',(-107.711662354049,-4.62530346326349,
127.286037540936));
#271620=CARTESIAN_POINT('Ctrl Pts',(-107.990109977862,-5.46015434966779,
132.794019853873));
#271621=CARTESIAN_POINT('Ctrl Pts',(-108.268557601675,-1.2773901320969,
136.473602528901));
#271622=CARTESIAN_POINT('Ctrl Pts',(-108.547005225488,4.07923321289408,
134.943428845277));
#271623=CARTESIAN_POINT('Ctrl Pts',(-108.825452849301,5.6872405168564,129.609653665109));
#271624=CARTESIAN_POINT('Ctrl Pts',(-109.103900473114,2.06895162297316,
125.373755809571));
#271625=CARTESIAN_POINT('Ctrl Pts',(-109.382348096927,-3.45060273851677,
126.128318472786));
#271626=CARTESIAN_POINT('Ctrl Pts',(-109.66079572074,-5.79922175462486,
131.179935429694));
#271627=CARTESIAN_POINT('Ctrl Pts',(-109.939243344552,-2.81863928596571,
135.886417482107));
#271628=CARTESIAN_POINT('Ctrl Pts',(-110.217690968365,2.7521349883118,135.922737548286));
#271629=CARTESIAN_POINT('Ctrl Pts',(-110.496138592178,5.79383165759959,
131.255519261747));
#271630=CARTESIAN_POINT('Ctrl Pts',(-110.774586215991,3.51128007796473,
126.17370822153));
#271631=CARTESIAN_POINT('Ctrl Pts',(-111.053033839804,-1.99796635775128,
125.347240513325));
#271632=CARTESIAN_POINT('Ctrl Pts',(-111.331481463617,-5.67117931677705,
129.535599585778));
#271633=CARTESIAN_POINT('Ctrl Pts',(-111.60992908743,-4.13285553619637,
134.889888064022));
#271634=CARTESIAN_POINT('Ctrl Pts',(-111.888376711243,1.20336058093108,
136.489776408084));
#271635=CARTESIAN_POINT('Ctrl Pts',(-112.166824335056,5.43374711161577,
132.865045388662));
#271636=CARTESIAN_POINT('Ctrl Pts',(-112.445271958868,4.67078550002918,
127.34664573465));
#271637=CARTESIAN_POINT('Ctrl Pts',(-112.723719582681,-0.384399805526852,
125.005717139274));
#271638=CARTESIAN_POINT('Ctrl Pts',(-113.002167206494,-5.08634046877848,
127.993458620965));
#271639=CARTESIAN_POINT('Ctrl Pts',(-113.280614830307,-5.11418272276831,
133.564281717336));
#271640=CARTESIAN_POINT('Ctrl Pts',(-113.55906245412,-0.442340896249408,
136.598872152659));
#271641=CARTESIAN_POINT('Ctrl Pts',(-113.837510077933,4.63599060436829,
134.308589564856));
#271642=CARTESIAN_POINT('Ctrl Pts',(-114.115957701746,5.45407322030374,
128.798091765594));
#271643=CARTESIAN_POINT('Ctrl Pts',(-114.394405325558,1.26012899306928,
125.131257029612));
#271644=CARTESIAN_POINT('Ctrl Pts',(-114.672852949372,-4.09181221807183,
126.677727344441));
#271645=CARTESIAN_POINT('Ctrl Pts',(-114.951300573184,-5.68357789694507,
132.016372040028));
#271646=CARTESIAN_POINT('Ctrl Pts',(-115.229748196997,-2.05241314674147,
136.241237448422));
#271647=CARTESIAN_POINT('Ctrl Pts',(-115.50819582081,3.46481901936097,135.469878655457));
#271648=CARTESIAN_POINT('Ctrl Pts',(-115.786643444623,5.79805177248978,
130.411136708898));
#271649=CARTESIAN_POINT('Ctrl Pts',(-116.065091068436,2.80315819727665,
125.713748324348));
#271650=CARTESIAN_POINT('Ctrl Pts',(-116.343538692249,-2.76770081934284,
125.694383947029));
#271651=CARTESIAN_POINT('Ctrl Pts',(-116.621986316062,-5.79517799268792,
130.370838493694));
#271652=CARTESIAN_POINT('Ctrl Pts',(-116.900433939875,-3.49716970093708,
135.445678693465));
#271653=CARTESIAN_POINT('Ctrl Pts',(-117.178881563688,2.0145666997373,136.255374322477));
#271654=CARTESIAN_POINT('Ctrl Pts',(-117.4573291875,5.67501472040751,132.055854653499));
#271655=CARTESIAN_POINT('Ctrl Pts',(-117.735776811314,4.12040145290537,
126.706273104381));
#271656=CARTESIAN_POINT('Ctrl Pts',(-118.014224435126,-1.22065945701595,
125.122633777175));
#271657=CARTESIAN_POINT('Ctrl Pts',(-118.29267205894,-5.43999395846872,
128.760223848501));
#271658=CARTESIAN_POINT('Ctrl Pts',(-118.571119682752,-4.6602397705682,
134.276275748964));
#271659=CARTESIAN_POINT('Ctrl Pts',(-118.849567306565,0.402047101114997,
136.601807256156));
#271660=CARTESIAN_POINT('Ctrl Pts',(-119.128014930377,5.09487232796628,
133.599768523497));
#271661=CARTESIAN_POINT('Ctrl Pts',(-119.406462554191,5.10575878376697,
128.028886488555));
#271662=CARTESIAN_POINT('Ctrl Pts',(-119.684910178003,0.424702347469154,
125.008529588725));
#271663=CARTESIAN_POINT('Ctrl Pts',(-119.963357801817,-4.64663479828973,
127.314258262312));
#271664=CARTESIAN_POINT('Ctrl Pts',(-120.241805425629,-5.44794156515001,
132.827220499399));
#271665=CARTESIAN_POINT('Ctrl Pts',(-120.520253049442,-1.24285618037906,
136.48127332728));
#271666=CARTESIAN_POINT('Ctrl Pts',(-120.798700673255,4.10435331726091,
134.918520707537));
#271667=CARTESIAN_POINT('Ctrl Pts',(-121.077148297068,5.67986262514396,
129.575055953004));
#271668=CARTESIAN_POINT('Ctrl Pts',(-121.355595920881,2.03585565723516,
125.361262130332));
#271669=CARTESIAN_POINT('Ctrl Pts',(-121.634043544694,-3.47900320259493,
126.149409907283));
#271670=CARTESIAN_POINT('Ctrl Pts',(-121.912491168507,-5.79682807799514,
131.215229979999));
#271671=CARTESIAN_POINT('Ctrl Pts',(-122.19093879232,-2.78765114051323,
135.903481180724));
#271672=CARTESIAN_POINT('Ctrl Pts',(-122.469386416133,2.78324101077128,
135.905889689793));
#271673=CARTESIAN_POINT('Ctrl Pts',(-122.747834039945,5.79647064203949,
131.220242205036));
#271674=CARTESIAN_POINT('Ctrl Pts',(-123.026281663758,3.48302692660634,
126.152419858339));
#271675=CARTESIAN_POINT('Ctrl Pts',(-123.304729287571,-2.03114837905279,
125.359503809431));
#271676=CARTESIAN_POINT('Ctrl Pts',(-123.583176911384,-5.67879755147744,
129.570145171156));
#271677=CARTESIAN_POINT('Ctrl Pts',(-123.861624535197,-4.10790919877744,
134.914970233354));
#271678=CARTESIAN_POINT('Ctrl Pts',(-124.14007215901,1.23794702507767,136.482345873087));
#271679=CARTESIAN_POINT('Ctrl Pts',(-124.418519782823,5.44619040996103,
132.831930447996));
#271680=CARTESIAN_POINT('Ctrl Pts',(-124.696967406636,4.64965086928273,
127.318277401031));
#271681=CARTESIAN_POINT('Ctrl Pts',(-124.975415030448,-0.419690672193134,
125.00816452543));
#271682=CARTESIAN_POINT('Ctrl Pts',(-125.253862654262,-5.10335698895296,
128.024472698579));
#271683=CARTESIAN_POINT('Ctrl Pts',(-125.532310278074,-5.09728754571388,
133.595362064203));
#271684=CARTESIAN_POINT('Ctrl Pts',(-125.810757901887,-0.407059864303788,
136.601457448367));
#271685=CARTESIAN_POINT('Ctrl Pts',(-126.0892055257,4.65723594642128,134.280304048949));
#271686=CARTESIAN_POINT('Ctrl Pts',(-126.367653149513,5.44175944101008,
128.764928445366));
#271687=CARTESIAN_POINT('Ctrl Pts',(-126.646100773326,1.22557185403828,
125.123691376234));
#271688=CARTESIAN_POINT('Ctrl Pts',(-126.924548397139,-4.11685639428078,
126.702711823764));
#271689=CARTESIAN_POINT('Ctrl Pts',(-127.202996020952,-5.67609473587197,
132.050947136115));
#271690=CARTESIAN_POINT('Ctrl Pts',(-127.481443644765,-2.01927930784003,
136.253630337055));
#271691=CARTESIAN_POINT('Ctrl Pts',(-127.759891268577,3.4931551568182,135.44870087741));
#271692=CARTESIAN_POINT('Ctrl Pts',(-128.038338892391,5.79555068247735,
130.375849607603));
#271693=CARTESIAN_POINT('Ctrl Pts',(-128.316786516203,2.77211825933019,
125.696779022025));
#271694=CARTESIAN_POINT('Ctrl Pts',(-128.595234140016,-2.7987554186355,
125.711326403516));
#271695=CARTESIAN_POINT('Ctrl Pts',(-128.873681763829,-5.79770959367839,
130.406123419165));
#271696=CARTESIAN_POINT('Ctrl Pts',(-129.152129387642,-3.46885188599067,
135.466880965177));
#271697=CARTESIAN_POINT('Ctrl Pts',(-129.430577011455,2.04771124208698,
136.243010088514));
#271698=CARTESIAN_POINT('Ctrl Pts',(-129.709024635268,5.68252777494204,
132.021286040849));
#271699=CARTESIAN_POINT('Ctrl Pts',(-129.98747225908,4.09537888954061,126.681266979298));
#271700=CARTESIAN_POINT('Ctrl Pts',(-130.265919882893,-1.25522312496795,
125.130169546993));
#271701=CARTESIAN_POINT('Ctrl Pts',(-130.544367506706,-5.45233640868912,
128.793376508901));
#271702=CARTESIAN_POINT('Ctrl Pts',(-130.822815130519,-4.63901889426667,
134.304579624636));
#271703=CARTESIAN_POINT('Ctrl Pts',(-131.101262754332,0.437330355314798,
136.599252468079));
#271704=CARTESIAN_POINT('Ctrl Pts',(-131.379710378145,5.11179437313754,
133.568702797104));
#271705=CARTESIAN_POINT('Ctrl Pts',(-131.658158001958,5.08876908708517,
127.997857708758));
#271706=CARTESIAN_POINT('Ctrl Pts',(-131.936605625771,0.389413610192037,
125.006051688315));
#271707=CARTESIAN_POINT('Ctrl Pts',(-132.215053249584,-4.66779395055513,
127.342608310716));
#271708=CARTESIAN_POINT('Ctrl Pts',(-132.493500873397,-5.43552690515385,
132.860346187109));
#271709=CARTESIAN_POINT('Ctrl Pts',(-132.77194849721,-1.20827617416795,
136.488733765571));
#271710=CARTESIAN_POINT('Ctrl Pts',(-133.050396121022,4.12932133330617,
134.893460118082));
#271711=CARTESIAN_POINT('Ctrl Pts',(-133.328843744835,5.67227426403318,
129.540503793235));
#271712=CARTESIAN_POINT('Ctrl Pts',(-133.607291368648,2.00268425211708,
125.348970147109));
#271713=CARTESIAN_POINT('Ctrl Pts',(-133.885738992461,-3.50727475093002,
126.170673832692));
#271714=CARTESIAN_POINT('Ctrl Pts',(-134.164186616274,-5.79421959776922,
131.25050930539));
#271715=CARTESIAN_POINT('Ctrl Pts',(-134.442634240087,-2.75655969762259,
135.920355929551));
#271716=CARTESIAN_POINT('Ctrl Pts',(-134.7210818639,2.81424389921159,135.888852792264));
#271717=CARTESIAN_POINT('Ctrl Pts',(-134.999529487713,5.79889483612785,
131.18494973768));
#271718=CARTESIAN_POINT('Ctrl Pts',(-135.277977111526,3.45464471040472,
126.131303874523));
#271719=CARTESIAN_POINT('Ctrl Pts',(-135.556424735338,-2.06425513540386,
125.371968866708));
#271720=CARTESIAN_POINT('Ctrl Pts',(-135.834872359151,-5.68620535624619,
129.604736490841));
#271721=CARTESIAN_POINT('Ctrl Pts',(-136.113319982964,-4.08281064127246,
134.939900082537));
#271722=CARTESIAN_POINT('Ctrl Pts',(-136.391767606777,1.27248759664198,
136.474704938258));
#271723=CARTESIAN_POINT('Ctrl Pts',(-136.67021523059,5.45843189771781,132.798740374984));
#271724=CARTESIAN_POINT('Ctrl Pts',(-136.948662854403,4.62834394401342,
127.290038245509));
#271725=CARTESIAN_POINT('Ctrl Pts',(-137.227110478216,-0.454965987067202,
125.010826691762));
#271726=CARTESIAN_POINT('Ctrl Pts',(-137.505558102029,-5.12018440235748,
128.055589785961));
#271727=CARTESIAN_POINT('Ctrl Pts',(-137.784005725841,-5.0802034867949,
133.626338989485));
#271728=CARTESIAN_POINT('Ctrl Pts',(-138.062453349655,-0.371763748605222,
136.603827930521));
#271729=CARTESIAN_POINT('Ctrl Pts',(-138.340900973467,4.67830871288359,
134.251889730681));
#271730=CARTESIAN_POINT('Ctrl Pts',(-138.61934859728,5.42924401531914,128.731840697047));
#271731=CARTESIAN_POINT('Ctrl Pts',(-138.897796221093,1.19096930099152,
125.116336222143));
#271732=CARTESIAN_POINT('Ctrl Pts',(-139.176243844906,-4.14174801886209,
126.727848291193));
#271733=CARTESIAN_POINT('Ctrl Pts',(-139.454691468719,-5.66840124502105,
132.085476039479));
#271734=CARTESIAN_POINT('Ctrl Pts',(-139.733139092532,-1.98607064380098,
136.265821300996));
#271735=CARTESIAN_POINT('Ctrl Pts',(-140.011586716345,3.52136185412693,
135.427351001626));
#271736=CARTESIAN_POINT('Ctrl Pts',(-140.290034340158,5.79283483620279,
130.340578384942));
#271737=CARTESIAN_POINT('Ctrl Pts',(-140.56848196397,2.7409755995222,125.679998983016));
#271738=CARTESIAN_POINT('Ctrl Pts',(-140.846929587784,-2.82970630901691,
125.72845758426));
#271739=CARTESIAN_POINT('Ctrl Pts',(-141.125377211596,-5.80002635840773,
130.441423101462));
#271740=CARTESIAN_POINT('Ctrl Pts',(-141.403824835409,-3.44040553146196,
135.487910465481));
#271741=CARTESIAN_POINT('Ctrl Pts',(-141.682272459222,2.08077990574355,
136.230444323395));
#271742=CARTESIAN_POINT('Ctrl Pts',(-141.960720083035,5.68983026132012,
131.986672334579));
#271743=CARTESIAN_POINT('Ctrl Pts',(-142.239167706848,4.07020457040501,
126.656413636965));
#271744=CARTESIAN_POINT('Ctrl Pts',(-142.517615330661,-1.289740280165,125.137915576048));
#271745=CARTESIAN_POINT('Ctrl Pts',(-142.796062954474,-5.46447682057862,
128.826603687055));
#271746=CARTESIAN_POINT('Ctrl Pts',(-143.074510578287,-4.61762611741445,
134.332753798405));
#271747=CARTESIAN_POINT('Ctrl Pts',(-143.352958202099,0.472597404077474,
136.596482948152));
#271748=CARTESIAN_POINT('Ctrl Pts',(-143.631405825913,5.12852699888841,
133.537534636997));
#271749=CARTESIAN_POINT('Ctrl Pts',(-143.909853449725,5.07159082419343,
127.966932924958));
#271750=CARTESIAN_POINT('Ctrl Pts',(-144.188301073538,0.354110443050382,
125.003788646376));
#271751=CARTESIAN_POINT('Ctrl Pts',(-144.466748697351,-4.6887801359991,
127.371086635623));
#271752=CARTESIAN_POINT('Ctrl Pts',(-144.745196321164,-5.4229108297093,
132.893395689516));
#271753=CARTESIAN_POINT('Ctrl Pts',(-145.023643944977,-1.17365139483885,
136.495983567324));
#271754=CARTESIAN_POINT('Ctrl Pts',(-145.30209156879,4.15413633583088,134.868248005541));
#271755=CARTESIAN_POINT('Ctrl Pts',(-145.580539192603,5.66447571471356,
129.505998466145));
#271756=CARTESIAN_POINT('Ctrl Pts',(-145.858986816416,1.96943863679757,
125.336880315387));
#271757=CARTESIAN_POINT('Ctrl Pts',(-146.137434440228,-3.53541633590941,
126.192109461069));
#271758=CARTESIAN_POINT('Ctrl Pts',(-146.415882064041,-5.79139641060527,
131.285772098575));
#271759=CARTESIAN_POINT('Ctrl Pts',(-146.694329687854,-2.72536610939861,
135.937041103293));
#271760=CARTESIAN_POINT('Ctrl Pts',(-146.972777311667,2.84514250480927,
135.871627487008));
#271761=CARTESIAN_POINT('Ctrl Pts',(-147.25122493548,5.80110415003576,131.149643167454));
#271762=CARTESIAN_POINT('Ctrl Pts',(-147.529672559293,3.42613448107249,
126.110361052543));
#271763=CARTESIAN_POINT('Ctrl Pts',(-147.808120183106,-2.09728540002206,
125.38463522326));
#271764=CARTESIAN_POINT('Ctrl Pts',(-148.086567806919,-5.69340245658434,
129.639372263039));
#271765=CARTESIAN_POINT('Ctrl Pts',(-148.365015430732,-4.05756079371773,
134.964676687782));
#271766=CARTESIAN_POINT('Ctrl Pts',(-148.643463054544,1.30698101571045,
136.466853886735));
#271767=CARTESIAN_POINT('Ctrl Pts',(-148.921910678358,5.47047112127328,
132.765476399497));
#271768=CARTESIAN_POINT('Ctrl Pts',(-149.20035830217,4.60686551375719,127.261929314495));
#271769=CARTESIAN_POINT('Ctrl Pts',(-149.478805925983,-0.49022444300932,
125.013703539625));
#271770=CARTESIAN_POINT('Ctrl Pts',(-149.757253549796,-5.13682208544599,
128.086808730058));
#271771=CARTESIAN_POINT('Ctrl Pts',(-150.035701173609,-5.06293117906749,
133.657211345319));
#271772=CARTESIAN_POINT('Ctrl Pts',(-150.314148797422,-0.336453857064764,
136.605983511281));
#271773=CARTESIAN_POINT('Ctrl Pts',(-150.592596421235,4.69920812289605,
134.223347662954));
#271774=CARTESIAN_POINT('Ctrl Pts',(-150.871044045047,5.41652740699458,
128.698829746717));
#271775=CARTESIAN_POINT('Ctrl Pts',(-151.14949166886,1.15632261613933,125.109191839888));
#271776=CARTESIAN_POINT('Ctrl Pts',(-151.427939292673,-4.1664861694474,
126.753135815284));
#271777=CARTESIAN_POINT('Ctrl Pts',(-151.706386916486,-5.66049770947745,
132.119957470642));
#271778=CARTESIAN_POINT('Ctrl Pts',(-151.984834540299,-1.95278838518384,
136.277809888502));
#271779=CARTESIAN_POINT('Ctrl Pts',(-152.263282164112,3.54943806607717,
135.405829819234));
#271780=CARTESIAN_POINT('Ctrl Pts',(-152.541729787925,5.78990433430307,
130.3053243479));
#271781=CARTESIAN_POINT('Ctrl Pts',(-152.820177411738,2.70973137185537,
125.663408829112));
#271782=CARTESIAN_POINT('Ctrl Pts',(-153.09862503555,-2.86055234359039,
125.745776854456));
#271783=CARTESIAN_POINT('Ctrl Pts',(-153.377072659364,-5.80212820102742,
130.476736232542));
#271784=CARTESIAN_POINT('Ctrl Pts',(-153.655520283176,-3.41183169144105,
135.508766415124));
#271785=CARTESIAN_POINT('Ctrl Pts',(-153.933967906989,2.1137714653355,136.21767749275));
#271786=CARTESIAN_POINT('Ctrl Pts',(-154.212415530802,5.69692190894542,
131.952014817313));
#271787=CARTESIAN_POINT('Ctrl Pts',(-154.490863154615,4.04487942834225,
126.631713998332));
#271788=CARTESIAN_POINT('Ctrl Pts',(-154.769310778428,-1.32420964356211,
125.145871577308));
#271789=CARTESIAN_POINT('Ctrl Pts',(-155.047758402241,-5.47641474427016,
128.859904151722));
#271790=CARTESIAN_POINT('Ctrl Pts',(-155.326206026054,-4.59606223272787,
134.360797226267));
#271791=CARTESIAN_POINT('Ctrl Pts',(-155.604653649866,0.507846940569522,
136.593498799002));
#271792=CARTESIAN_POINT('Ctrl Pts',(-155.88310127368,5.14506958518534,133.50626519812));
#271793=CARTESIAN_POINT('Ctrl Pts',(-156.161548897493,5.05422463163864,
127.936113283085));
#271794=CARTESIAN_POINT('Ctrl Pts',(-156.439996521305,0.318794154216047,
125.001740546765));
#271795=CARTESIAN_POINT('Ctrl Pts',(-156.718444145118,-4.70959257697085,
127.399692181761));
#271796=CARTESIAN_POINT('Ctrl Pts',(-156.996891768931,-5.41009380630968,
132.926367781962));
#271797=CARTESIAN_POINT('Ctrl Pts',(-157.275339392744,-1.1389831254257,
136.503022463895));
#271798=CARTESIAN_POINT('Ctrl Pts',(-157.553787016557,4.17879740530553,
134.84288530416));
#271799=CARTESIAN_POINT('Ctrl Pts',(-157.83223464037,5.65646726616335,129.471541250343));
#271800=CARTESIAN_POINT('Ctrl Pts',(-158.110682264183,1.93612004320555,
125.324993083158));
#271801=CARTESIAN_POINT('Ctrl Pts',(-158.389129887996,-3.56342691473634,
126.213715998108));
#271802=CARTESIAN_POINT('Ctrl Pts',(-158.667577511808,-5.78835862111754,
131.321017052882));
#271803=CARTESIAN_POINT('Ctrl Pts',(-158.946025135621,-2.69407153173119,
135.95353608367));
#271804=CARTESIAN_POINT('Ctrl Pts',(-159.224472759434,2.87593568260513,
135.854214412314));
#271805=CARTESIAN_POINT('Ctrl Pts',(-159.502920383247,5.80309850189603,
131.114323802656));
#271806=CARTESIAN_POINT('Ctrl Pts',(-159.78136800706,3.39749729506709,126.089592168444));
#271807=CARTESIAN_POINT('Ctrl Pts',(-160.059815630873,-2.13023794895846,
125.39750240973));
#271808=CARTESIAN_POINT('Ctrl Pts',(-160.338263254686,-5.70038858580074,
129.674051204309));
#271809=CARTESIAN_POINT('Ctrl Pts',(-160.616710878499,-4.03216059175559,
134.989299130986));
#271810=CARTESIAN_POINT('Ctrl Pts',(-160.895158502312,1.34142600411673,
136.458793009441));
#271811=CARTESIAN_POINT('Ctrl Pts',(-161.173606126125,5.48230763450959,
132.732139754142));
#271812=CARTESIAN_POINT('Ctrl Pts',(-161.452053749937,4.58521637440516,
127.233951649575));
#271813=CARTESIAN_POINT('Ctrl Pts',(-161.730501373751,-0.525464733504406,
125.016794962416));
#271814=CARTESIAN_POINT('Ctrl Pts',(-162.008948997563,-5.15326942170307,
128.118128374039));
#271815=CARTESIAN_POINT('Ctrl Pts',(-162.287396621376,-5.04547126256333,
133.687977987722));
#271816=CARTESIAN_POINT('Ctrl Pts',(-162.565844245189,-0.301131498102361,
136.607924110772));
#271817=CARTESIAN_POINT('Ctrl Pts',(-162.844291869002,4.71993340202341,
134.194678903404));
#271818=CARTESIAN_POINT('Ctrl Pts',(-163.122739492814,5.40361008725504,
128.665896817606));
#271819=CARTESIAN_POINT('Ctrl Pts',(-163.401187116628,1.12163308332736,
125.102258494207));
#271820=CARTESIAN_POINT('Ctrl Pts',(-163.67963474044,-4.19106992935549,
126.778573459));
#271821=CARTESIAN_POINT('Ctrl Pts',(-163.958082364253,-5.65238442210956,
132.154390151878));
#271822=CARTESIAN_POINT('Ctrl Pts',(-164.236529988066,-1.91943376527495,
136.289595655332));
#271823=CARTESIAN_POINT('Ctrl Pts',(-164.514977611879,3.57738275229458,
135.384138127707));
#271824=CARTESIAN_POINT('Ctrl Pts',(-164.793425235692,5.78675928536899,
130.270088802833));
#271825=CARTESIAN_POINT('Ctrl Pts',(-165.071872859505,2.67838673409632,
125.647009175068));
#271826=CARTESIAN_POINT('Ctrl Pts',(-165.350320483318,-2.89129237934434,
125.763283572333));
#271827=CARTESIAN_POINT('Ctrl Pts',(-165.628768107131,-5.80401504365309,
130.512061503863));
#271828=CARTESIAN_POINT('Ctrl Pts',(-165.907215730944,-3.38313142474212,
135.52944804128));
#271829=CARTESIAN_POINT('Ctrl Pts',(-166.185663354757,2.14668469834846,
136.204710069657));
#271830=CARTESIAN_POINT('Ctrl Pts',(-166.464110978569,5.70380245503433,
131.917314773299));
#271831=CARTESIAN_POINT('Ctrl Pts',(-166.742558602383,4.01940440178476,
126.607168978656));
#271832=CARTESIAN_POINT('Ctrl Pts',(-167.021006226195,-1.3586299378839,
125.15403725596));
#271833=CARTESIAN_POINT('Ctrl Pts',(-167.299453850008,-5.48814973739939,
128.893276668938));
#271834=CARTESIAN_POINT('Ctrl Pts',(-167.577901473821,-4.57432803926507,
134.388708869063));
#271835=CARTESIAN_POINT('Ctrl Pts',(-167.856349097634,0.543077658606429,
136.590300131209));
#271836=CARTESIAN_POINT('Ctrl Pts',(-168.134796721447,5.16142151903669,
133.474895639175));
#271837=CARTESIAN_POINT('Ctrl Pts',(-168.413244345259,5.03667115293141,
127.905399925171));
#271838=CARTESIAN_POINT('Ctrl Pts',(-168.691691969073,0.283466052347084,
124.999907465374));
#271839=CARTESIAN_POINT('Ctrl Pts',(-168.970139592885,-4.7302305022577,
127.42842388914));
#271840=CARTESIAN_POINT('Ctrl Pts',(-169.248587216698,-5.39707630989451,
132.959261242652));
#271841=CARTESIAN_POINT('Ctrl Pts',(-169.527034840511,-1.10427265057399,
136.509850194457));
#271842=CARTESIAN_POINT('Ctrl Pts',(-169.805482464324,4.20330362790601,
134.81737295376));
#271843=CARTESIAN_POINT('Ctrl Pts',(-170.083930088137,5.6482492151383,129.437133422652));
#271844=CARTESIAN_POINT('Ctrl Pts',(-170.36237771195,1.90272970597286,125.313308890908));
#271845=CARTESIAN_POINT('Ctrl Pts',(-170.640825335763,-3.59130544946847,
126.235492643171));
#271846=CARTESIAN_POINT('Ctrl Pts',(-170.919272959575,-5.78510634187241,
131.356242862295));
#271847=CARTESIAN_POINT('Ctrl Pts',(-171.197720583389,-2.66267712425244,
135.969840259458));
#271848=CARTESIAN_POINT('Ctrl Pts',(-171.476168207202,2.90662229154664,
135.836614213432));
#271849=CARTESIAN_POINT('Ctrl Pts',(-171.754615831014,5.80487781780722,
131.07899295206));
#271850=CARTESIAN_POINT('Ctrl Pts',(-172.033063454828,3.36873421355001,
126.068997991823));
#271851=CARTESIAN_POINT('Ctrl Pts',(-172.31151107864,-2.16311156114431,
125.410569949319));
#271852=CARTESIAN_POINT('Ctrl Pts',(-172.589958702453,-5.70716348502144,
129.70877202961));
#271853=CARTESIAN_POINT('Ctrl Pts',(-172.868406326266,-4.00661097660031,
135.013766499754));
#271854=CARTESIAN_POINT('Ctrl Pts',(-173.146853950079,1.3758212854888,136.450522605077));
#271855=CARTESIAN_POINT('Ctrl Pts',(-173.425301573892,5.49394099882038,
132.698731674224));
#271856=CARTESIAN_POINT('Ctrl Pts',(-173.703749197705,4.56339732817417,
127.206106287473));
#271857=CARTESIAN_POINT('Ctrl Pts',(-173.982196821517,-0.560685552710569,
125.02010084558));
#271858=CARTESIAN_POINT('Ctrl Pts',(-174.260644445331,-5.1695258016666,
128.149547557344));
#271859=CARTESIAN_POINT('Ctrl Pts',(-174.539092069143,-5.02782438426607,
133.718637776622));
#271860=CARTESIAN_POINT('Ctrl Pts',(-174.817539692956,-0.265797980601551,
136.609649657082));
#271861=CARTESIAN_POINT('Ctrl Pts',(-175.095987316769,4.74048378228282,
134.165884514362));
#271862=CARTESIAN_POINT('Ctrl Pts',(-175.374434940582,5.39049253475655,
128.633043130058));
#271863=CARTESIAN_POINT('Ctrl Pts',(-175.652882564395,1.08690198798901,
125.095536442018));
#271864=CARTESIAN_POINT('Ctrl Pts',(-175.931330188208,-4.21549838762608,
126.80416027974));
#271865=CARTESIAN_POINT('Ctrl Pts',(-176.209777812021,-5.64406168355824,
132.188772807274));
#271866=CARTESIAN_POINT('Ctrl Pts',(-176.488225435833,-1.886008020042,136.301178164761));
#271867=CARTESIAN_POINT('Ctrl Pts',(-176.766673059646,3.60519487727851,
135.362276730843));
#271868=CARTESIAN_POINT('Ctrl Pts',(-177.045120683459,5.78339980594152,
130.234873055403));
#271869=CARTESIAN_POINT('Ctrl Pts',(-177.323568307272,2.64694284773159,
125.630800628577));
#271870=CARTESIAN_POINT('Ctrl Pts',(-177.602015931085,-2.92192527719638,
125.780977089175));
#271871=CARTESIAN_POINT('Ctrl Pts',(-177.880463554898,-5.80568681636668,
130.547397606436));
#271872=CARTESIAN_POINT('Ctrl Pts',(-178.158911178711,-3.35430579486411,
135.549954577584));
#271873=CARTESIAN_POINT('Ctrl Pts',(-178.437358802524,2.17951838517049,
136.191542534628));
#271874=CARTESIAN_POINT('Ctrl Pts',(-178.715806426336,5.71047164462571,
131.88257348836));
#271875=CARTESIAN_POINT('Ctrl Pts',(-178.99425405015,3.99378043471903,126.582779487459));
#271876=CARTESIAN_POINT('Ctrl Pts',(-179.272701673962,-1.39299988767372,
125.162412309422));
#271877=CARTESIAN_POINT('Ctrl Pts',(-179.551149297775,-5.49968136512185,
128.926720002072));
#271878=CARTESIAN_POINT('Ctrl Pts',(-179.829596921588,-4.55242434239454,
134.416487692516));
#271879=CARTESIAN_POINT('Ctrl Pts',(-180.108044545401,0.578288252700551,
136.5868870633));
#271880=CARTESIAN_POINT('Ctrl Pts',(-180.386492169214,5.17758219451528,
133.443427122574));
#271881=CARTESIAN_POINT('Ctrl Pts',(-180.664939793027,5.01893103852278,
127.874793989312));
#271882=CARTESIAN_POINT('Ctrl Pts',(-180.94338741684,0.248127446539293,
124.998289470128));
#271883=CARTESIAN_POINT('Ctrl Pts',(-181.221835040653,-4.75069314711374,
127.457280693096));
#271884=CARTESIAN_POINT('Ctrl Pts',(-181.500282664465,-5.38385882283189,
132.992074852706));
#271885=CARTESIAN_POINT('Ctrl Pts',(-181.778730288279,-1.06952125649312,
136.516466506004));
#271886=CARTESIAN_POINT('Ctrl Pts',(-182.057177912091,4.22765409554481,
134.791711899713));
#271887=CARTESIAN_POINT('Ctrl Pts',(-182.335625535904,5.63982186616143,
129.402776258069));
#271888=CARTESIAN_POINT('Ctrl Pts',(-182.614073159717,1.86926886239121,
125.301828171599));
#271889=CARTESIAN_POINT('Ctrl Pts',(-182.89252078353,-3.61905090705647,
126.257438589318));
#271890=CARTESIAN_POINT('Ctrl Pts',(-183.170968407343,-5.78163969338434,
131.391448221508));
#271891=CARTESIAN_POINT('Ctrl Pts',(-183.449416031155,-2.63118405029363,
135.985953026497));
#271892=CARTESIAN_POINT('Ctrl Pts',(-183.727863654969,2.93720119453022,
135.818827542541));
#271893=CARTESIAN_POINT('Ctrl Pts',(-184.006311278781,5.80644203183612,
131.04365192486));
#271894=CARTESIAN_POINT('Ctrl Pts',(-184.284758902595,3.33984630234777,
126.048579285806));
#271895=CARTESIAN_POINT('Ctrl Pts',(-184.563206526407,-2.19590501843575,
125.423837357804));
#271896=CARTESIAN_POINT('Ctrl Pts',(-184.84165415022,-5.71372690320071,
129.743533452349));
#271897=CARTESIAN_POINT('Ctrl Pts',(-185.120101774033,-3.98091289500146,
135.03807788744));
#271898=CARTESIAN_POINT('Ctrl Pts',(-185.398549397846,1.41016558529749,
136.442042980103));
#271899=CARTESIAN_POINT('Ctrl Pts',(-185.676997021659,5.50537078312707,
132.665253397689));
#271900=CARTESIAN_POINT('Ctrl Pts',(-185.955444645472,4.54140918357699,
127.178394260007));
#271901=CARTESIAN_POINT('Ctrl Pts',(-186.233892269285,-0.595885595507362,
125.023621066618));
#271902=CARTESIAN_POINT('Ctrl Pts',(-186.512339893098,-5.18559062295048,
128.181065115723));
#271903=CARTESIAN_POINT('Ctrl Pts',(-186.79078751691,-5.00999119808726,
133.749189575911));
#271904=CARTESIAN_POINT('Ctrl Pts',(-187.069235140724,-0.230454613858838,
136.611160086272));
#271905=CARTESIAN_POINT('Ctrl Pts',(-187.347682764536,4.76085850217237,
134.136965562817));
#271906=CARTESIAN_POINT('Ctrl Pts',(-187.626130388349,5.37717523557474,
128.600269901479));
#271907=CARTESIAN_POINT('Ctrl Pts',(-187.904578012162,1.05213061709833,
125.089025932407));
#271908=CARTESIAN_POINT('Ctrl Pts',(-188.183025635975,-4.23977063905356,
126.829895329374));
#271909=CARTESIAN_POINT('Ctrl Pts',(-188.461473259788,-5.63552980222562,
132.223104162766));
#271910=CARTESIAN_POINT('Ctrl Pts',(-188.739920883601,-1.85251238808831,
136.312556987595));
#271911=CARTESIAN_POINT('Ctrl Pts',(-189.018368507414,3.63287341044046,
135.340246438718));
#271912=CARTESIAN_POINT('Ctrl Pts',(-189.296816131227,5.77982602050738,
130.199678410544));
#271913=CARTESIAN_POINT('Ctrl Pts',(-189.575263755039,2.61540087792624,
125.614783790254));
#271914=CARTESIAN_POINT('Ctrl Pts',(-189.853711378852,-2.95244990203274,
125.798856749341));
#271915=CARTESIAN_POINT('Ctrl Pts',(-190.132159002665,-5.80714345722022,
130.582743230867));
#271916=CARTESIAN_POINT('Ctrl Pts',(-190.410606626478,-3.32535586995153,
135.570285264159));
#271917=CARTESIAN_POINT('Ctrl Pts',(-190.689054250291,2.21227130913674,
136.178175375592));
#271918=CARTESIAN_POINT('Ctrl Pts',(-190.967501874104,5.7169292305904,131.847792249846));
#271919=CARTESIAN_POINT('Ctrl Pts',(-191.245949497917,3.96800847665057,
126.558546428502));
#271920=CARTESIAN_POINT('Ctrl Pts',(-191.52439712173,-1.4273182193404,125.170996427354));
#271921=CARTESIAN_POINT('Ctrl Pts',(-191.802844745543,-5.51100920012879,
128.960232911869));
#271922=CARTESIAN_POINT('Ctrl Pts',(-192.081292369355,-4.53035195376586,
134.444132667273));
#271923=CARTESIAN_POINT('Ctrl Pts',(-192.359739993168,0.613477418111232,
136.583259721745));
#271924=CARTESIAN_POINT('Ctrl Pts',(-192.638187616981,5.19355101278185,
133.411860814392));
#271925=CARTESIAN_POINT('Ctrl Pts',(-192.916635240794,5.00100494577841,
127.844296609621));
#271926=CARTESIAN_POINT('Ctrl Pts',(-193.195082864607,0.21277964627773,
124.996886620986));
#271927=CARTESIAN_POINT('Ctrl Pts',(-193.47353048842,-4.77097975328813,
127.486261524329));
#271928=CARTESIAN_POINT('Ctrl Pts',(-193.751978112233,-5.3704418349007,
133.024807396204));
#271929=CARTESIAN_POINT('Ctrl Pts',(-194.030425736046,-1.03473023090876,
136.522871153366));
#271930=CARTESIAN_POINT('Ctrl Pts',(-194.308873359859,4.25184790590635,
134.765903092897));
#271931=CARTESIAN_POINT('Ctrl Pts',(-194.587320983671,5.63118553151129,
129.368471029708));
#271932=CARTESIAN_POINT('Ctrl Pts',(-194.865768607484,1.83573875236439,
125.290551350653));
#271933=CARTESIAN_POINT('Ctrl Pts',(-195.144216231297,-3.64666225938173,
126.279553023333));
#271934=CARTESIAN_POINT('Ctrl Pts',(-195.42266385511,-5.77795880411129,
131.426631825972));
#271935=CARTESIAN_POINT('Ctrl Pts',(-195.701111478923,-2.59959347684268,
136.001873787725));
#271936=CARTESIAN_POINT('Ctrl Pts',(-195.979559102736,2.96767125844341,
135.800855058734));
#271937=CARTESIAN_POINT('Ctrl Pts',(-196.258006726549,5.80779108602021,
131.008302030633));
#271938=CARTESIAN_POINT('Ctrl Pts',(-196.536454350362,3.31083463191258,
126.028336807015));
#271939=CARTESIAN_POINT('Ctrl Pts',(-196.814901974175,-2.22861710565919,
125.437304143558));
#271940=CARTESIAN_POINT('Ctrl Pts',(-197.093349597988,-5.72007859712835,
129.778334184429));
#271941=CARTESIAN_POINT('Ctrl Pts',(-197.3717972218,-3.95506729921131,135.062232393175));
#271942=CARTESIAN_POINT('Ctrl Pts',(-197.650244845613,1.44445763090186,
136.433354448736));
#271943=CARTESIAN_POINT('Ctrl Pts',(-197.928692469426,5.51659656389443,
132.631706165088));
#271944=CARTESIAN_POINT('Ctrl Pts',(-198.207140093239,4.51925275539276,
127.150816594059));
#271945=CARTESIAN_POINT('Ctrl Pts',(-198.485587717052,-0.631063557543924,
125.027355495085));
#271946=CARTESIAN_POINT('Ctrl Pts',(-198.764035340865,-5.2014632902668,
128.212679881281));
#271947=CARTESIAN_POINT('Ctrl Pts',(-199.042482964678,-4.99197236484219,
133.779632253479));
#271948=CARTESIAN_POINT('Ctrl Pts',(-199.320930588491,-0.19510270753564,
136.612455342372));
#271949=CARTESIAN_POINT('Ctrl Pts',(-199.599378212304,4.7810568066993,134.10792312037));
#271950=CARTESIAN_POINT('Ctrl Pts',(-199.877825836116,5.36365868318719,
128.56757834629));
#271951=CARTESIAN_POINT('Ctrl Pts',(-200.156273459929,1.01732025912016,
125.082727206624));
#271952=CARTESIAN_POINT('Ctrl Pts',(-200.434721083742,-4.26388578422093,
126.855777654281));
#271953=CARTESIAN_POINT('Ctrl Pts',(-200.713168707555,-5.62678909426374,
132.257382946195));
#271954=CARTESIAN_POINT('Ctrl Pts',(-200.991616331368,-1.8189481106068,
136.323731702186));
#271955=CARTESIAN_POINT('Ctrl Pts',(-201.270063955181,3.66041732614217,
135.318048067677));
#271956=CARTESIAN_POINT('Ctrl Pts',(-201.548511578994,5.77603806149454,
130.164506172408));
#271957=CARTESIAN_POINT('Ctrl Pts',(-201.826959202806,2.58376199347953,
125.59895925361));
#271958=CARTESIAN_POINT('Ctrl Pts',(-202.10540682662,-2.9828651227522,125.816921890294));
#271959=CARTESIAN_POINT('Ctrl Pts',(-202.383854450432,-5.80838491223743,
130.618097067413));
#271960=CARTESIAN_POINT('Ctrl Pts',(-202.662302074245,-3.29628272275406,
135.590439347642));
#271961=CARTESIAN_POINT('Ctrl Pts',(-202.940749698058,2.24494225657654,
136.164609087875));
#271962=CARTESIAN_POINT('Ctrl Pts',(-203.219197321871,5.72317497363993,
131.812972346589));
#271963=CARTESIAN_POINT('Ctrl Pts',(-203.497644945684,3.94208948256877,
126.534470699752));
#271964=CARTESIAN_POINT('Ctrl Pts',(-203.776092569497,-1.46158366120557,
125.179789291667));
#271965=CARTESIAN_POINT('Ctrl Pts',(-204.05454019331,-5.52213282266317,
128.993814156497));
#271966=CARTESIAN_POINT('Ctrl Pts',(-204.332987817123,-4.5081116912795,
134.471642768938));
#271967=CARTESIAN_POINT('Ctrl Pts',(-204.611435440935,0.648643850890564,
136.579418240959));
#271968=CARTESIAN_POINT('Ctrl Pts',(-204.889883064748,5.20932738210573,
133.380197884332));
#271969=CARTESIAN_POINT('Ctrl Pts',(-205.168330688562,4.98289353895661,
127.813908916192));
#271970=CARTESIAN_POINT('Ctrl Pts',(-205.446778312374,0.177423961388546,
124.995698969927));
#271971=CARTESIAN_POINT('Ctrl Pts',(-205.725225936187,-4.79108956905296,
127.515365308944));
#271972=CARTESIAN_POINT('Ctrl Pts',(-206.00367356,-5.35682584327266,133.057457660231));
#271973=CARTESIAN_POINT('Ctrl Pts',(-206.282121183813,-0.999900863015179,
136.529063899218));
#271974=CARTESIAN_POINT('Ctrl Pts',(-206.560568807626,4.27588416248015,
134.739947489669));
#271975=CARTESIAN_POINT('Ctrl Pts',(-206.839016431439,5.62234053121038,
129.334219008764));
#271976=CARTESIAN_POINT('Ctrl Pts',(-207.117464055252,1.80214061836306,
125.279478845937));
#271977=CARTESIAN_POINT('Ctrl Pts',(-207.395911679064,-3.67413848329639,
126.301835125757));
#271978=CARTESIAN_POINT('Ctrl Pts',(-207.674359302878,-5.77406381044983,
131.461792371951));
#271979=CARTESIAN_POINT('Ctrl Pts',(-207.95280692669,-2.56790657449899,
136.01760195319));
#271980=CARTESIAN_POINT('Ctrl Pts',(-208.231254550503,2.99803135420673,
135.782697427989));
#271981=CARTESIAN_POINT('Ctrl Pts',(-208.509702174316,5.8089249303698,130.972944579282));
#271982=CARTESIAN_POINT('Ctrl Pts',(-208.788149798129,3.28170027728254,
126.008271305542));
#271983=CARTESIAN_POINT('Ctrl Pts',(-209.066597421942,-2.2612466106562,
125.450969807563));
#271984=CARTESIAN_POINT('Ctrl Pts',(-209.345045045754,-5.72621833144002,
129.813172936296));
#271985=CARTESIAN_POINT('Ctrl Pts',(-209.623492669568,-3.92907514694791,
135.086229121905));
#271986=CARTESIAN_POINT('Ctrl Pts',(-209.90194029338,1.4786961515975,136.424457332932));
#271987=CARTESIAN_POINT('Ctrl Pts',(-210.180387917194,5.52761792514773,
132.598091219525));
#271988=CARTESIAN_POINT('Ctrl Pts',(-210.458835541006,4.49692886463537,
127.123374311529));
#271989=CARTESIAN_POINT('Ctrl Pts',(-210.73728316482,-0.666218135288655,
125.031303992602));
#271990=CARTESIAN_POINT('Ctrl Pts',(-211.015730788632,-5.21714321544808,
128.244390682522));
#271991=CARTESIAN_POINT('Ctrl Pts',(-211.294178412445,-4.97376855222533,
133.809964681263));
#271992=CARTESIAN_POINT('Ctrl Pts',(-211.572626036258,-0.159743571609885,
136.613535377387));
#271993=CARTESIAN_POINT('Ctrl Pts',(-211.851073660071,4.80107794740803,
134.0787582632));
#271994=CARTESIAN_POINT('Ctrl Pts',(-212.129521283884,5.34994337845465,
128.534969675892));
#271995=CARTESIAN_POINT('Ctrl Pts',(-212.407968907697,0.982472203965689,
125.076640498072));
#271996=CARTESIAN_POINT('Ctrl Pts',(-212.686416531509,-4.28784292953254,
126.881806295382));
#271997=CARTESIAN_POINT('Ctrl Pts',(-212.964864155322,-5.61783988356258,
132.291607887347));
#271998=CARTESIAN_POINT('Ctrl Pts',(-213.243311779135,-1.78531643133465,
136.334701894451));
#271999=CARTESIAN_POINT('Ctrl Pts',(-213.521759402948,3.68782560373359,
135.295682440288));
#272000=CARTESIAN_POINT('Ctrl Pts',(-213.800207026761,5.77203606926717,
130.129357644311));
#272001=CARTESIAN_POINT('Ctrl Pts',(-214.078654650574,2.55202736678199,
125.583327605028));
#272002=CARTESIAN_POINT('Ctrl Pts',(-214.357102274386,-3.0131698123076,
125.835171842623));
#272003=CARTESIAN_POINT('Ctrl Pts',(-214.6355498982,-5.80941113541564,130.653457806023));
#272004=CARTESIAN_POINT('Ctrl Pts',(-214.913997522012,-3.26708743058812,
135.610416081219));
#272005=CARTESIAN_POINT('Ctrl Pts',(-215.192445145826,2.27753001685547,
136.15084417418));
#272006=CARTESIAN_POINT('Ctrl Pts',(-215.470892769638,5.72920864233609,
131.778115068854));
#272007=CARTESIAN_POINT('Ctrl Pts',(-215.749340393451,3.9160244129115,126.510553193344));
#272008=CARTESIAN_POINT('Ctrl Pts',(-216.027788017264,-1.49579494355069,
125.18879057654));
#272009=CARTESIAN_POINT('Ctrl Pts',(-216.306235641077,-5.53305182053502,
129.02746249159));
#272010=CARTESIAN_POINT('Ctrl Pts',(-216.58468326489,-4.48570437905656,
134.499016978113));
#272011=CARTESIAN_POINT('Ctrl Pts',(-216.863130888703,0.683786247933482,
136.57536276329));
#272012=CARTESIAN_POINT('Ctrl Pts',(-217.141578512516,5.2249107178877,133.348439505674));
#272013=CARTESIAN_POINT('Ctrl Pts',(-217.420026136328,4.96459748918233,
127.78363203505));
#272014=CARTESIAN_POINT('Ctrl Pts',(-217.698473760142,0.142061701988793,
124.994726560962));
#272015=CARTESIAN_POINT('Ctrl Pts',(-217.976921383954,-4.81102184923216,
127.544590968491));
#272016=CARTESIAN_POINT('Ctrl Pts',(-218.255369007768,-5.34301135249269,
133.090024434919));
#272017=CARTESIAN_POINT('Ctrl Pts',(-218.53381663158,-0.965034443427401,
136.535044514085));
#272018=CARTESIAN_POINT('Ctrl Pts',(-218.812264255394,4.29976197459382,
134.713846051821));
#272019=CARTESIAN_POINT('Ctrl Pts',(-219.090711879206,5.61328719301349,
129.300021464458));
#272020=CARTESIAN_POINT('Ctrl Pts',(-219.369159503019,1.76847570537835,
125.268611067748));
#272021=CARTESIAN_POINT('Ctrl Pts',(-219.647607126831,-3.70147856065836,
126.324284070919));
#272022=CARTESIAN_POINT('Ctrl Pts',(-219.926054750645,-5.76995485673049,
131.496928556552));
#272023=CARTESIAN_POINT('Ctrl Pts',(-220.204502374457,-2.5361245174328,
136.033136940081));
#272024=CARTESIAN_POINT('Ctrl Pts',(-220.48294999827,3.02828035681523,135.764355323142));
#272025=CARTESIAN_POINT('Ctrl Pts',(-220.761397622083,5.80984352286985,
130.937580880991));
#272026=CARTESIAN_POINT('Ctrl Pts',(-221.039845245896,3.25244431804234,
125.988383524923));
#272027=CARTESIAN_POINT('Ctrl Pts',(-221.318292869709,-2.29379232432851,
125.464833843433));
#272028=CARTESIAN_POINT('Ctrl Pts',(-221.596740493522,-5.73214587862558,
129.848048416986));
#272029=CARTESIAN_POINT('Ctrl Pts',(-221.875188117335,-3.90293740136003,
135.110067184424));
#272030=CARTESIAN_POINT('Ctrl Pts',(-222.153635741148,1.51287987866345,
136.415351962378));
#272031=CARTESIAN_POINT('Ctrl Pts',(-222.432083364961,5.53843445848603,
132.564409806615));
#272032=CARTESIAN_POINT('Ctrl Pts',(-222.710530988774,4.47443833852516,
127.0960684293));
#272033=CARTESIAN_POINT('Ctrl Pts',(-222.988978612586,-0.701348026075381,
125.035466412855));
#272034=CARTESIAN_POINT('Ctrl Pts',(-223.267426236399,-5.23262981746888,
128.27619634439));
#272035=CARTESIAN_POINT('Ctrl Pts',(-223.545873860212,-4.95538043478568,
133.840185735283));
#272036=CARTESIAN_POINT('Ctrl Pts',(-223.824321484025,-0.124378516327312,
136.614400151295));
#272037=CARTESIAN_POINT('Ctrl Pts',(-224.102769107838,4.82092118240782,
134.049472072021));
#272038=CARTESIAN_POINT('Ctrl Pts',(-224.381216731651,5.33602982960279,
128.502445098609));
#272039=CARTESIAN_POINT('Ctrl Pts',(-224.659664355464,0.947587742942381,
125.070766032295));
#272040=CARTESIAN_POINT('Ctrl Pts',(-224.938111979277,-4.31164118724753,
126.907980288176));
#272041=CARTESIAN_POINT('Ctrl Pts',(-225.216559603089,-5.60868250173869,
132.325777718005));
#272042=CARTESIAN_POINT('Ctrl Pts',(-225.495007226903,-1.75161859650508,
136.345467157888));
#272043=CARTESIAN_POINT('Ctrl Pts',(-225.773454850715,3.71509722759125,
135.273150385318));
#272044=CARTESIAN_POINT('Ctrl Pts',(-226.051902474528,5.7678201921206,130.0942341287));
#272045=CARTESIAN_POINT('Ctrl Pts',(-226.330350098341,2.52019817377184,
125.567889423742));
#272046=CARTESIAN_POINT('Ctrl Pts',(-226.608797722154,-3.04336284774751,
125.853605930069));
#272047=CARTESIAN_POINT('Ctrl Pts',(-226.887245345967,-5.81022208872781,
130.688824136393));
#272048=CARTESIAN_POINT('Ctrl Pts',(-227.16569296978,-3.23777107529596,
135.630214724643));
#272049=CARTESIAN_POINT('Ctrl Pts',(-227.444140593593,2.31003338242206,
136.13688114457));
#272050=CARTESIAN_POINT('Ctrl Pts',(-227.722588217406,5.73503001309909,
131.74322170829));
#272051=CARTESIAN_POINT('Ctrl Pts',(-228.001035841218,3.88981423352964,
126.486794795549));
#272052=CARTESIAN_POINT('Ctrl Pts',(-228.279483465031,-1.52995079866356,
125.197999948425));
#272053=CARTESIAN_POINT('Ctrl Pts',(-228.557931088844,-5.54376578913698,
129.061176670297));
#272054=CARTESIAN_POINT('Ctrl Pts',(-228.836378712657,-4.46313084740822,
134.526254280438));
#272055=CARTESIAN_POINT('Ctrl Pts',(-229.11482633647,0.718903307025501,
136.571093439014));
#272056=CARTESIAN_POINT('Ctrl Pts',(-229.393273960283,5.24030044268158,
133.316586855238));
#272057=CARTESIAN_POINT('Ctrl Pts',(-229.671721584096,4.94611747442232,
127.753467088116));
#272058=CARTESIAN_POINT('Ctrl Pts',(-229.950169207909,0.106694178440453,
124.993969430123));
#272059=CARTESIAN_POINT('Ctrl Pts',(-230.228616831722,-4.83077585522751,
127.57393742));
#272060=CARTESIAN_POINT('Ctrl Pts',(-230.507064455534,-5.32899887446215,
133.122506513493));
#272061=CARTESIAN_POINT('Ctrl Pts',(-230.785512079348,-0.930132264133436,
136.540812776352));
#272062=CARTESIAN_POINT('Ctrl Pts',(-231.06395970316,4.3234804574463,134.687599746553));
#272063=CARTESIAN_POINT('Ctrl Pts',(-231.342407326973,5.60402585239536,
129.265879663993));
#272064=CARTESIAN_POINT('Ctrl Pts',(-231.620854950786,1.73474526087603,
125.257948418793));
#272065=CARTESIAN_POINT('Ctrl Pts',(-231.899302574599,-3.72868147837107,
126.346899026965));
#272066=CARTESIAN_POINT('Ctrl Pts',(-232.177750198412,-5.76563209521201,
131.532039077795));
#272067=CARTESIAN_POINT('Ctrl Pts',(-232.456197822225,-2.50424848333998,
136.048478172742));
#272068=CARTESIAN_POINT('Ctrl Pts',(-232.734645446038,3.05841714538193,
135.745829423867));
#272069=CARTESIAN_POINT('Ctrl Pts',(-233.01309306985,5.81054682948159,130.902212246173));
#272070=CARTESIAN_POINT('Ctrl Pts',(-233.291540693664,3.22306783828139,
125.968674202107));
#272071=CARTESIAN_POINT('Ctrl Pts',(-233.569988317476,-2.32625304068266,
125.478895737432));
#272072=CARTESIAN_POINT('Ctrl Pts',(-233.84843594129,-5.73786101903762,
129.882959334177));
#272073=CARTESIAN_POINT('Ctrl Pts',(-234.126883565102,-3.87665503099142,
135.133745697402));
#272074=CARTESIAN_POINT('Ctrl Pts',(-234.405331188915,1.54700754540913,
136.406038674476));
#272075=CARTESIAN_POINT('Ctrl Pts',(-234.683778812728,5.54904576309872,
132.530663174436));
#272076=CARTESIAN_POINT('Ctrl Pts',(-234.962226436541,4.45178201045685,
127.0688999592));
#272077=CARTESIAN_POINT('Ctrl Pts',(-235.240674060353,-0.736451928153096,
125.039842601604));
#272078=CARTESIAN_POINT('Ctrl Pts',(-235.519121684167,-5.24792252246713,
128.308095688315));
#272079=CARTESIAN_POINT('Ctrl Pts',(-235.797569307979,-4.93680869390195,
133.870294295687));
#272080=CARTESIAN_POINT('Ctrl Pts',(-236.076016931792,-0.0890088521534987,
136.61504963205));
#272081=CARTESIAN_POINT('Ctrl Pts',(-236.354464555605,4.8405857764003,134.020065632043));
#272082=CARTESIAN_POINT('Ctrl Pts',(-236.632912179418,5.32191855220324,
128.470005819654));
#272083=CARTESIAN_POINT('Ctrl Pts',(-236.911359803231,0.912668168706789,
125.065104026974));
#272084=CARTESIAN_POINT('Ctrl Pts',(-237.189807427044,-4.33527967551271,
126.934298662776));
#272085=CARTESIAN_POINT('Ctrl Pts',(-237.468255050857,-5.59931728812211,
132.359891171993));
#272086=CARTESIAN_POINT('Ctrl Pts',(-237.74670267467,-1.71785585480426,
136.356027093583));
#272087=CARTESIAN_POINT('Ctrl Pts',(-238.025150298482,3.7422311871549,135.250452737698));
#272088=CARTESIAN_POINT('Ctrl Pts',(-238.303597922296,5.76339058627568,
130.059136927086));
#272089=CARTESIAN_POINT('Ctrl Pts',(-238.582045546108,2.48827559389159,
125.552645281824));
#272090=CARTESIAN_POINT('Ctrl Pts',(-238.860493169922,-3.07344311025789,
125.87222346955));
#272091=CARTESIAN_POINT('Ctrl Pts',(-239.138940793734,-5.81081774212379,
130.724194748009));
#272092=CARTESIAN_POINT('Ctrl Pts',(-239.417388417547,-3.20833474320591,
135.649834544268));
#272093=CARTESIAN_POINT('Ctrl Pts',(-239.69583604136,2.34245114885216,136.12272051645));
#272094=CARTESIAN_POINT('Ctrl Pts',(-239.974283665173,5.7406388702159,131.708293557882));
#272095=CARTESIAN_POINT('Ctrl Pts',(-240.252731288985,3.86345991565072,
126.463196386742));
#272096=CARTESIAN_POINT('Ctrl Pts',(-240.531178912799,-1.56404996088748,
125.207417066067));
#272097=CARTESIAN_POINT('Ctrl Pts',(-240.809626536611,-5.5542743314588,
129.094955443325));
#272098=CARTESIAN_POINT('Ctrl Pts',(-241.088074160425,-4.44039193280503,
134.553353666625));
#272099=CARTESIAN_POINT('Ctrl Pts',(-241.366521784237,0.753993726891117,
136.566610426332));
#272100=CARTESIAN_POINT('Ctrl Pts',(-241.64496940805,5.25549598621542,133.284641113335));
#272101=CARTESIAN_POINT('Ctrl Pts',(-241.923417031863,4.92745417946037,
127.723415193164));
#272102=CARTESIAN_POINT('Ctrl Pts',(-242.201864655676,0.071322701300089,
124.993427605467));
#272103=CARTESIAN_POINT('Ctrl Pts',(-242.480312279489,-4.85035085504701,
127.603403576029));
#272104=CARTESIAN_POINT('Ctrl Pts',(-242.758759903302,-5.31478892841856,
133.154902692318));
#272105=CARTESIAN_POINT('Ctrl Pts',(-243.037207527115,-0.895195618446729,
136.546368472274));
#272106=CARTESIAN_POINT('Ctrl Pts',(-243.315655150928,4.34703873214009,
134.661209546432));
#272107=CARTESIAN_POINT('Ctrl Pts',(-243.59410277474,5.59455685253872,129.231794872506));
#272108=CARTESIAN_POINT('Ctrl Pts',(-243.872550398553,1.7009505347501,125.247491294183));
#272109=CARTESIAN_POINT('Ctrl Pts',(-244.150998022366,-3.75574622842035,
126.36967915589));
#272110=CARTESIAN_POINT('Ctrl Pts',(-244.429445646179,-5.76109568607594,
131.567122634643));
#272111=CARTESIAN_POINT('Ctrl Pts',(-244.707893269992,-2.47227965339868,
136.063625082699));
#272112=CARTESIAN_POINT('Ctrl Pts',(-244.986340893805,3.08844060317656,
135.727120416648));
#272113=CARTESIAN_POINT('Ctrl Pts',(-245.264788517618,5.81103482414375,
130.866839985428));
#272114=CARTESIAN_POINT('Ctrl Pts',(-245.543236141431,3.1935719265564,125.949144067427));
#272115=CARTESIAN_POINT('Ctrl Pts',(-245.821683765243,-2.35862755687492,
125.49315496849));
#272116=CARTESIAN_POINT('Ctrl Pts',(-246.100131389057,-5.74336354089951,
129.917904394232));
#272117=CARTESIAN_POINT('Ctrl Pts',(-246.378579012869,-3.85022900974501,
135.157263783424));
#272118=CARTESIAN_POINT('Ctrl Pts',(-246.657026636682,1.58107788722132,
136.396517814333));
#272119=CARTESIAN_POINT('Ctrl Pts',(-246.935474260495,5.55945144577998,
132.496852573479));
#272120=CARTESIAN_POINT('Ctrl Pts',(-247.213921884308,4.42896071996899,
127.04186990797));
#272121=CARTESIAN_POINT('Ctrl Pts',(-247.492369508121,-0.77152854073377,
125.044432396689));
#272122=CARTESIAN_POINT('Ctrl Pts',(-247.770817131934,-5.26302076376676,
128.340087532256));
#272123=CARTESIAN_POINT('Ctrl Pts',(-248.049264755747,-4.91805401775627,
133.90028924679));
#272124=CARTESIAN_POINT('Ctrl Pts',(-248.32771237956,-0.0536358897235281,
136.615483795589));
#272125=CARTESIAN_POINT('Ctrl Pts',(-248.606160003372,4.86007100070672,
133.990540032933));
#272126=CARTESIAN_POINT('Ctrl Pts',(-248.884607627186,5.30761006915461,
128.437653041073));
#272127=CARTESIAN_POINT('Ctrl Pts',(-249.163055250998,0.877714775216597,
125.059654691916));
#272128=CARTESIAN_POINT('Ctrl Pts',(-249.441502874812,-4.35875751839529,
126.960760443945));
#272129=CARTESIAN_POINT('Ctrl Pts',(-249.719950498624,-5.58974458974414,
132.393946985223));
#272130=CARTESIAN_POINT('Ctrl Pts',(-249.998398122437,-1.68402945732324,
136.366381310236));
#272131=CARTESIAN_POINT('Ctrl Pts',(-250.27684574625,3.76922647696617,135.227590338499));
#272132=CARTESIAN_POINT('Ctrl Pts',(-250.555293370063,5.75874741587205,
130.024067340013));
#272133=CARTESIAN_POINT('Ctrl Pts',(-250.833740993876,2.45626081004631,
125.537595744144));
#272134=CARTESIAN_POINT('Ctrl Pts',(-251.112188617689,-3.10340948520656,
125.891023771197));
#272135=CARTESIAN_POINT('Ctrl Pts',(-251.390636241501,-5.81119807352532,
130.759568330183));
#272136=CARTESIAN_POINT('Ctrl Pts',(-251.669083865314,-3.17877952510356,
135.669274813107));
#272137=CARTESIAN_POINT('Ctrl Pts',(-251.947531489127,2.37478211491517,
136.10836281449));
#272138=CARTESIAN_POINT('Ctrl Pts',(-252.22597911294,5.74603500580729,131.673331912019));
#272139=CARTESIAN_POINT('Ctrl Pts',(-252.504426736753,3.83696243592119,
126.439758841162));
#272140=CARTESIAN_POINT('Ctrl Pts',(-252.782874360566,-1.59809116681098,
125.217041580908));
#272141=CARTESIAN_POINT('Ctrl Pts',(-253.061321984379,-5.5645770578269,
129.128797558239));
#272142=CARTESIAN_POINT('Ctrl Pts',(-253.339769608192,-4.41748847836656,
134.580314133917));
#272143=CARTESIAN_POINT('Ctrl Pts',(-253.618217232004,0.789056208225191,
136.561913888683));
#272144=CARTESIAN_POINT('Ctrl Pts',(-253.896664855818,5.27049678355612,
133.252603468789));
#272145=CARTESIAN_POINT('Ctrl Pts',(-254.17511247963,4.90860829937749,127.693477454216));
#272146=CARTESIAN_POINT('Ctrl Pts',(-254.453560103444,0.0359485746511809,
124.993101125124));
#272147=CARTESIAN_POINT('Ctrl Pts',(-254.732007727256,-4.86974611083267,
127.632988310607));
#272148=CARTESIAN_POINT('Ctrl Pts',(-255.010455351069,-5.30038206451776,
133.187211835313));
#272149=CARTESIAN_POINT('Ctrl Pts',(-255.288902974882,-0.860225756393269,
136.55171127444));
#272150=CARTESIAN_POINT('Ctrl Pts',(-255.567350598695,4.37043584157037,
134.634676658854));
#272151=CARTESIAN_POINT('Ctrl Pts',(-255.845798222508,5.58488070320316,
129.197767919676));
#272152=CARTESIAN_POINT('Ctrl Pts',(-256.12424584632,1.66709247927321,125.23724089965));
#272153=CARTESIAN_POINT('Ctrl Pts',(-256.402693470134,-3.78267124144458,
126.39262206856));
#272154=CARTESIAN_POINT('Ctrl Pts',(-256.681141093946,-5.75634686702621,
131.602180844355));
#272155=CARTESIAN_POINT('Ctrl Pts',(-256.95958871776,-2.44021719259262,
136.078571600242));
#272156=CARTESIAN_POINT('Ctrl Pts',(-257.238036341572,3.118345804191,135.708239395799));
#272157=CARTESIAN_POINT('Ctrl Pts',(-257.516483965385,5.81131468939531,
130.8314457702));
#272158=CARTESIAN_POINT('Ctrl Pts',(-257.794931589198,3.16394407961038,
125.929830927563));
#272159=CARTESIAN_POINT('Ctrl Pts',(-258.073379213011,-2.39088900078744,
125.507540987923));
#272160=CARTESIAN_POINT('Ctrl Pts',(-258.351826836824,-5.74870171518396,
129.953014515613));
#272161=CARTESIAN_POINT('Ctrl Pts',(-258.630274460636,-3.82356878618261,
135.180370918811));
#272162=CARTESIAN_POINT('Ctrl Pts',(-258.908722084449,1.61491681105698,
136.387261181902));
#272163=CARTESIAN_POINT('Ctrl Pts',(-259.187169708263,5.56997747689423,
132.462088635074));
#272164=CARTESIAN_POINT('Ctrl Pts',(-259.465617332075,4.40535894966821,
127.016664495574));
#272165=CARTESIAN_POINT('Ctrl Pts',(-259.744064955888,-0.805411631290512,
125.046024618449));
#272166=CARTESIAN_POINT('Ctrl Pts',(-260.022512579701,-5.28013240410161,
128.378470706602));
#272167=CARTESIAN_POINT('Ctrl Pts',(-260.254552266212,-4.95911089365773,
132.993351965875));
#272168=CARTESIAN_POINT('Ctrl Pts',(-260.440213228287,-2.45877638613931,
135.28779596926));
#272169=CARTESIAN_POINT('Ctrl Pts',(-260.53305831576,-0.833059752290926,
135.715219187214));
#272170=CARTESIAN_POINT('Ctrl Pts',(-260.579495465929,-0.013892627260139,
135.717527172907));
#272171=CARTESIAN_POINT('Ctrl Pts',(-207.299567498839,-3.90840034609179,
135.243902605347));
#272172=CARTESIAN_POINT('Ctrl Pts',(-207.309485839119,-3.91568439033028,
135.211326968109));
#272173=CARTESIAN_POINT('Ctrl Pts',(-207.319294625375,-3.92298020337359,
135.178719366898));
#272174=CARTESIAN_POINT('Ctrl Pts',(-207.373488585912,-3.96376374076592,
134.996347972705));
#272175=CARTESIAN_POINT('Ctrl Pts',(-207.415719149759,-3.99734042662899,
134.845804617557));
#272176=CARTESIAN_POINT('Ctrl Pts',(-207.499376031093,-4.06628914634799,
134.528884546366));
#272177=CARTESIAN_POINT('Ctrl Pts',(-207.540351370784,-4.10153445023782,
134.36234850031));
#272178=CARTESIAN_POINT('Ctrl Pts',(-207.656874908577,-4.20404560328433,
133.851628215195));
#272179=CARTESIAN_POINT('Ctrl Pts',(-207.723530466945,-4.26603286108595,
133.504762588803));
#272180=CARTESIAN_POINT('Ctrl Pts',(-207.778274395763,-4.31466228417799,
133.153864562742));
#272181=CARTESIAN_POINT('Ctrl Pts',(-178.531763843762,1.96089658445146,
125.231307795101));
#272182=CARTESIAN_POINT('Ctrl Pts',(-178.570801079156,1.56843596370832,
125.131935448447));
#272183=CARTESIAN_POINT('Ctrl Pts',(-178.601759745776,1.16805303801507,
125.056039372548));
#272184=CARTESIAN_POINT('Ctrl Pts',(-178.625335154052,0.72444720086025,
124.99874952163));
#272185=CARTESIAN_POINT('Ctrl Pts',(-178.627404925171,0.683646809442433,
124.993728200571));
#272186=CARTESIAN_POINT('Ctrl Pts',(-178.629486211621,0.64054918726823,
124.988685854593));
#272187=CARTESIAN_POINT('Ctrl Pts',(-178.629595291271,0.638284118533388,
124.988421607827));
#272188=CARTESIAN_POINT('Ctrl Pts',(-178.629744702131,0.635172831973636,
124.988059686924));
#272189=CARTESIAN_POINT('Ctrl Pts',(-178.629785292499,0.634326701253174,
124.987961366993));
#272190=CARTESIAN_POINT('Ctrl Pts',(-178.629858681012,0.632795262003021,
124.987783607086));
#272191=CARTESIAN_POINT('Ctrl Pts',(-178.629891493623,0.632109958282007,
124.987704131074));
#272192=CARTESIAN_POINT('Ctrl Pts',(-178.62994393397,0.631013785865012,
124.98757711741));
#272193=CARTESIAN_POINT('Ctrl Pts',(-178.62996357934,0.630602923758097,
124.98752953583));
#272194=CARTESIAN_POINT('Ctrl Pts',(-178.629994326891,0.629959541468569,
124.98745506556));
#272195=CARTESIAN_POINT('Ctrl Pts',(-178.630005435777,0.629727024217423,
124.987428160163));
#272196=CARTESIAN_POINT('Ctrl Pts',(-178.630026130574,0.629293740909809,
124.987378038377));
#272197=CARTESIAN_POINT('Ctrl Pts',(-178.630035717301,0.629092974966084,
124.987354819958));
#272198=CARTESIAN_POINT('Ctrl Pts',(-178.630056886341,0.628649540099313,
124.987303550298));
#272199=CARTESIAN_POINT('Ctrl Pts',(-178.630068467602,0.628406869994507,
124.98727550168));
#272200=CARTESIAN_POINT('Ctrl Pts',(-178.630101658504,0.627711187230269,
124.987195117429));
#272201=CARTESIAN_POINT('Ctrl Pts',(-178.630123259547,0.627258171775908,
124.987142803207));
#272202=CARTESIAN_POINT('Ctrl Pts',(-178.630259381619,0.624401810565511,
124.986813142828));
#272203=CARTESIAN_POINT('Ctrl Pts',(-178.630373575472,0.621998354980397,
124.986536611421));
#272204=CARTESIAN_POINT('Ctrl Pts',(-178.630705048662,0.615000656884468,
124.985733983766));
#272205=CARTESIAN_POINT('Ctrl Pts',(-178.630921427308,0.610406113059156,
124.985210129304));
#272206=CARTESIAN_POINT('Ctrl Pts',(-178.636268568232,0.496200348966026,
124.972266679728));
#272207=CARTESIAN_POINT('Ctrl Pts',(-178.64069439242,0.386339611214377,
124.961599087318));
#272208=CARTESIAN_POINT('Ctrl Pts',(-178.65506927048,-0.0414682925157202,
124.927025558109));
#272209=CARTESIAN_POINT('Ctrl Pts',(-178.659656383999,-0.360982716739327,
124.916125069186));
#272210=CARTESIAN_POINT('Ctrl Pts',(-178.657730373057,-0.680012995379148,
124.92072784072));
#272211=CARTESIAN_POINT('',(-177.476367722506,-5.64337912711117,130.804360617576));
#272212=CARTESIAN_POINT('Ctrl Pts',(-177.476367722506,-5.64337912711113,
130.804360617586));
#272213=CARTESIAN_POINT('Ctrl Pts',(-177.476367722506,-5.66278702247985,
131.040394557583));
#272214=CARTESIAN_POINT('Ctrl Pts',(-177.481821319387,-5.65742368675511,
131.284442682447));
#272215=CARTESIAN_POINT('Ctrl Pts',(-177.494362458831,-5.6215507189005,
131.5448204376));
#272216=CARTESIAN_POINT('Ctrl Pts',(-177.494712937718,-5.6205398291972,
131.551991505204));
#272217=CARTESIAN_POINT('Ctrl Pts',(-177.495082378428,-5.61946569039355,
131.55944266065));
#272218=CARTESIAN_POINT('Ctrl Pts',(-177.495096443372,-5.61942478425224,
131.559726172768));
#272219=CARTESIAN_POINT('Ctrl Pts',(-177.495125486698,-5.6193402891457,
131.560311279265));
#272220=CARTESIAN_POINT('Ctrl Pts',(-177.495140466066,-5.6192966956462,
131.560612872408));
#272221=CARTESIAN_POINT('Ctrl Pts',(-177.495163361027,-5.61923004398011,
131.561073561054));
#272222=CARTESIAN_POINT('Ctrl Pts',(-177.495171270364,-5.61920701437734,
131.561232661122));
#272223=CARTESIAN_POINT('Ctrl Pts',(-177.495185587491,-5.61916532000669,
131.561520565902));
#272224=CARTESIAN_POINT('Ctrl Pts',(-177.495191994478,-5.61914665895088,
131.561649371792));
#272225=CARTESIAN_POINT('Ctrl Pts',(-177.495205667846,-5.61910682818089,
131.561924190531));
#272226=CARTESIAN_POINT('Ctrl Pts',(-177.495212934609,-5.61908565661172,
131.562070201652));
#272227=CARTESIAN_POINT('Ctrl Pts',(-177.495232530402,-5.61902855560728,
131.562463826025));
#272228=CARTESIAN_POINT('Ctrl Pts',(-177.495244863336,-5.61899260850394,
131.562711438321));
#272229=CARTESIAN_POINT('Ctrl Pts',(-177.495303923655,-5.61882041779216,
131.563896629399));
#272230=CARTESIAN_POINT('Ctrl Pts',(-177.495350729054,-5.6186838181541,
131.564834152763));
#272231=CARTESIAN_POINT('Ctrl Pts',(-177.500236184812,-5.60441144589133,
131.662509836507));
#272232=CARTESIAN_POINT('Ctrl Pts',(-177.505963587261,-5.58621592287407,
131.758520867681));
#272233=CARTESIAN_POINT('Ctrl Pts',(-177.527820287702,-5.51277087162531,
132.075255600853));
#272234=CARTESIAN_POINT('Ctrl Pts',(-177.547590315895,-5.44069144148586,
132.290973448603));
#272235=CARTESIAN_POINT('Ctrl Pts',(-177.609386990917,-5.20268998524819,
132.843250606157));
#272236=CARTESIAN_POINT('Ctrl Pts',(-177.657311288753,-5.00712947277706,
133.165027679615));
#272237=CARTESIAN_POINT('Ctrl Pts',(-177.779852173243,-4.46943606900208,
133.857655628443));
#272238=CARTESIAN_POINT('Ctrl Pts',(-177.858334959518,-4.09801820021662,
134.208982373595));
#272239=CARTESIAN_POINT('Ctrl Pts',(-178.033565929287,-3.13626912879633,
134.909021435998));
#272240=CARTESIAN_POINT('Ctrl Pts',(-178.123833995731,-2.5229730614002,
135.204982366882));
#272241=CARTESIAN_POINT('Ctrl Pts',(-178.219857087681,-1.56463168596343,
135.50774809867));
#272242=CARTESIAN_POINT('Ctrl Pts',(-178.244990796156,-1.25482479666693,
135.583862452928));
#272243=CARTESIAN_POINT('Ctrl Pts',(-178.266053397623,-0.911313259705867,
135.646805482782));
#272244=CARTESIAN_POINT('Ctrl Pts',(-178.267880485167,-0.880555601331235,
135.652254596537));
#272245=CARTESIAN_POINT('Ctrl Pts',(-178.269729479139,-0.848389479458237,
135.657759390394));
#272246=CARTESIAN_POINT('Ctrl Pts',(-178.269808415561,-0.847014208584358,
135.657994379534));
#272247=CARTESIAN_POINT('Ctrl Pts',(-178.269900842308,-0.84540149531386,
135.658269506422));
#272248=CARTESIAN_POINT('Ctrl Pts',(-178.26991444318,-0.845164118492042,
135.658309991603));
#272249=CARTESIAN_POINT('Ctrl Pts',(-178.269945205294,-0.844627086959365,
135.658401558698));
#272250=CARTESIAN_POINT('Ctrl Pts',(-178.26996236452,-0.844327431044021,
135.658452634283));
#272251=CARTESIAN_POINT('Ctrl Pts',(-178.270036338938,-0.843035175886533,
135.658672820216));
#272252=CARTESIAN_POINT('Ctrl Pts',(-178.270093100188,-0.842042544645915,
135.65884176107));
#272253=CARTESIAN_POINT('Ctrl Pts',(-178.270171301912,-0.840673485715273,
135.659074502599));
#272254=CARTESIAN_POINT('Ctrl Pts',(-178.270192793215,-0.840297088128566,
135.659138462936));
#272255=CARTESIAN_POINT('Ctrl Pts',(-178.270228585886,-0.839669959618898,
135.65924498328));
#272256=CARTESIAN_POINT('Ctrl Pts',(-178.270242892027,-0.839419231083232,
135.659287558272));
#272257=CARTESIAN_POINT('Ctrl Pts',(-178.270270866443,-0.838928818979041,
135.659370808756));
#272258=CARTESIAN_POINT('Ctrl Pts',(-178.270284535031,-0.838689135834364,
135.659411485233));
#272259=CARTESIAN_POINT('Ctrl Pts',(-178.270316659246,-0.838125679795843,
135.659507082639));
#272260=CARTESIAN_POINT('Ctrl Pts',(-178.270335112011,-0.837801905327044,
135.659561994584));
#272261=CARTESIAN_POINT('Ctrl Pts',(-178.27039519559,-0.836747298356631,
135.659740788603));
#272262=CARTESIAN_POINT('Ctrl Pts',(-178.270436800547,-0.836016450446397,
135.659864589485));
#272263=CARTESIAN_POINT('Ctrl Pts',(-178.271388514283,-0.819284919468759,
135.662696415416));
#272264=CARTESIAN_POINT('Ctrl Pts',(-178.272283232261,-0.803275074011935,
135.665356129665));
#272265=CARTESIAN_POINT('Ctrl Pts',(-178.278448654202,-0.690946895868277,
135.683667854268));
#272266=CARTESIAN_POINT('Ctrl Pts',(-178.283175569697,-0.594299441116708,
135.69762350265));
#272267=CARTESIAN_POINT('Ctrl Pts',(-178.29762587154,-0.257144687268308,
135.740133838043));
#272268=CARTESIAN_POINT('Ctrl Pts',(-178.304395271029,-0.0150406824488884,
135.759773395935));
#272269=CARTESIAN_POINT('Ctrl Pts',(-178.311724226144,0.565295564888802,
135.781048775607));
#272270=CARTESIAN_POINT('Ctrl Pts',(-178.308758158221,0.904892298835856,
135.772540046965));
#272271=CARTESIAN_POINT('Ctrl Pts',(-178.284936729491,1.67857512639212,
135.702974800853));
#272272=CARTESIAN_POINT('Ctrl Pts',(-178.2591473322,2.10490618035434,135.627638776919));
#272273=CARTESIAN_POINT('Ctrl Pts',(-178.194644860972,2.84130200828785,
135.429071105338));
#272274=CARTESIAN_POINT('Ctrl Pts',(-178.161544567716,3.14862850841257,
135.324747060875));
#272275=CARTESIAN_POINT('Ctrl Pts',(-178.08287528526,3.78466764810847,135.063692269719));
#272276=CARTESIAN_POINT('Ctrl Pts',(-178.035971305646,4.11310941484443,
134.901002070262));
#272277=CARTESIAN_POINT('Ctrl Pts',(-177.986855337731,4.42643889577882,
134.716028699704));
#272278=CARTESIAN_POINT('Ctrl Pts',(-177.724568368167,-4.0763856389639,
128.064914591592));
#272279=CARTESIAN_POINT('Ctrl Pts',(-177.691585751546,-4.29769346073786,
128.245438695333));
#272280=CARTESIAN_POINT('Ctrl Pts',(-177.658565300108,-4.50476052182415,
128.444579006132));
#272281=CARTESIAN_POINT('Ctrl Pts',(-177.591983415667,-4.91024198597078,
128.913284039984));
#272282=CARTESIAN_POINT('Ctrl Pts',(-177.559170578233,-5.10202391398061,
129.189936967786));
#272283=CARTESIAN_POINT('Ctrl Pts',(-177.511016994937,-5.38947078045,129.745095435989));
#272284=CARTESIAN_POINT('Ctrl Pts',(-177.494082314589,-5.49376686443764,
130.017086379215));
#272285=CARTESIAN_POINT('Ctrl Pts',(-177.479282123345,-5.60168409655279,
130.464069607833));
#272286=CARTESIAN_POINT('Ctrl Pts',(-177.476367722506,-5.6292128072582,
130.63207340011));
#272287=CARTESIAN_POINT('Ctrl Pts',(-177.476367722506,-5.64337912711113,
130.804360617586));
#272288=CARTESIAN_POINT('Ctrl Pts',(-207.34813506021,-2.42719411321803,
126.52758245404));
#272289=CARTESIAN_POINT('Ctrl Pts',(-207.275406626519,-2.16786091358167,
126.278797702914));
#272290=CARTESIAN_POINT('Ctrl Pts',(-207.201807943886,-1.87211081777635,
126.052281281209));
#272291=CARTESIAN_POINT('Ctrl Pts',(-207.11237315121,-1.37178070646407,
125.790031492887));
#272292=CARTESIAN_POINT('Ctrl Pts',(-207.084971087936,-1.18086676444924,
125.712744191699));
#272293=CARTESIAN_POINT('Ctrl Pts',(-207.063270754911,-0.944940672522864,
125.65220001207));
#272294=CARTESIAN_POINT('Ctrl Pts',(-207.060199958288,-0.907909035294405,
125.643661607663));
#272295=CARTESIAN_POINT('Ctrl Pts',(-207.05651245521,-0.857669349578529,
125.633430886317));
#272296=CARTESIAN_POINT('Ctrl Pts',(-207.055601249506,-0.844672757306036,
125.630905093974));
#272297=CARTESIAN_POINT('Ctrl Pts',(-207.053869199003,-0.818733203357481,
125.626107588021));
#272298=CARTESIAN_POINT('Ctrl Pts',(-207.053047813369,-0.805792534069772,
125.623834345885));
#272299=CARTESIAN_POINT('Ctrl Pts',(-207.052056959923,-0.789313017632923,
125.621093920067));
#272300=CARTESIAN_POINT('Ctrl Pts',(-207.051848658496,-0.785795645827727,
125.620517927937));
#272301=CARTESIAN_POINT('Ctrl Pts',(-207.051309755514,-0.77655390024144,
125.619028033472));
#272302=CARTESIAN_POINT('Ctrl Pts',(-207.050984267124,-0.770827036641165,
125.61812844047));
#272303=CARTESIAN_POINT('Ctrl Pts',(-207.050558971052,-0.763143325302232,
125.616953324576));
#272304=CARTESIAN_POINT('Ctrl Pts',(-207.050451847101,-0.761190106292071,
125.616657364513));
#272305=CARTESIAN_POINT('Ctrl Pts',(-207.050281269822,-0.758050935866936,
125.616186141554));
#272306=CARTESIAN_POINT('Ctrl Pts',(-207.050217207391,-0.756865277556876,
125.616009178234));
#272307=CARTESIAN_POINT('Ctrl Pts',(-207.050140480006,-0.755437087963941,
125.615797241911));
#272308=CARTESIAN_POINT('Ctrl Pts',(-207.050127474191,-0.755194716525449,
125.615761317682));
#272309=CARTESIAN_POINT('Ctrl Pts',(-207.050104551004,-0.754767027640041,
125.615698000761));
#272310=CARTESIAN_POINT('Ctrl Pts',(-207.050094627378,-0.754581711618658,
125.61567059062));
#272311=CARTESIAN_POINT('Ctrl Pts',(-207.050079247226,-0.754294241125006,
125.615628109336));
#272312=CARTESIAN_POINT('Ctrl Pts',(-207.050073784885,-0.754192093897613,
125.615613021962));
#272313=CARTESIAN_POINT('Ctrl Pts',(-207.050065117715,-0.754029935148036,
125.615589082738));
#272314=CARTESIAN_POINT('Ctrl Pts',(-207.050061910961,-0.7539699207954,
125.615580225526));
#272315=CARTESIAN_POINT('Ctrl Pts',(-207.050055915098,-0.753857675590644,
125.615563664704));
#272316=CARTESIAN_POINT('Ctrl Pts',(-207.050053125904,-0.753805447395421,
125.615555960854));
#272317=CARTESIAN_POINT('Ctrl Pts',(-207.050046939125,-0.753689569362406,
125.615538872798));
#272318=CARTESIAN_POINT('Ctrl Pts',(-207.050043542009,-0.753625921891587,
125.6155294899));
#272319=CARTESIAN_POINT('Ctrl Pts',(-207.050033723883,-0.753441915123111,
125.615502372131));
#272320=CARTESIAN_POINT('Ctrl Pts',(-207.050027305447,-0.753321553335802,
125.615484644445));
#272321=CARTESIAN_POINT('Ctrl Pts',(-207.049984956323,-0.752526935601,125.615367677068));
#272322=CARTESIAN_POINT('Ctrl Pts',(-207.049949137064,-0.751852627823885,
125.615268748258));
#272323=CARTESIAN_POINT('Ctrl Pts',(-207.049848735386,-0.74995628909578,
125.614991458904));
#272324=CARTESIAN_POINT('Ctrl Pts',(-207.049784416123,-0.748734138025705,
125.614813832405));
#272325=CARTESIAN_POINT('Ctrl Pts',(-207.046900286426,-0.693599268926534,
125.606849368149));
#272326=CARTESIAN_POINT('Ctrl Pts',(-207.04482234318,-0.63943866282689,
125.601129670294));
#272327=CARTESIAN_POINT('Ctrl Pts',(-207.040659911464,-0.464929010650244,
125.589677856696));
#272328=CARTESIAN_POINT('Ctrl Pts',(-207.041642634753,-0.345181292398407,
125.592365210721));
#272329=CARTESIAN_POINT('Ctrl Pts',(-207.053450498118,-0.0530637227305841,
125.624908849078));
#272330=CARTESIAN_POINT('Ctrl Pts',(-207.068272476064,0.114378418145951,
125.665776031825));
#272331=CARTESIAN_POINT('Ctrl Pts',(-207.109163444678,0.432031775628351,
125.78146128078));
#272332=CARTESIAN_POINT('Ctrl Pts',(-207.134520331742,0.580945678162572,
125.854273005136));
#272333=CARTESIAN_POINT('Ctrl Pts',(-207.162924005066,0.722039655879066,
125.938592129034));
#272334=CARTESIAN_POINT('Origin',(210.,0.,130.804360617566));
#272335=CARTESIAN_POINT('',(-207.850862027148,5.62578014279778,132.627039335973));
#272336=CARTESIAN_POINT('Ctrl Pts',(-207.850956227665,5.62869451042201,
132.628018664143));
#272337=CARTESIAN_POINT('Ctrl Pts',(-207.832561498011,5.57924092088534,
132.78065646182));
#272338=CARTESIAN_POINT('Ctrl Pts',(-207.812041489125,5.52351902058675,
132.931423281303));
#272339=CARTESIAN_POINT('Ctrl Pts',(-207.709624216109,5.24091110965318,
133.6098729297));
#272340=CARTESIAN_POINT('Ctrl Pts',(-207.605250752705,4.94131457183235,
134.105628873409));
#272341=CARTESIAN_POINT('Ctrl Pts',(-207.496674502688,4.59187829781674,
134.535658549994));
#272342=CARTESIAN_POINT('',(-207.955976777759,5.91281439438548,130.433367747241));
#272343=CARTESIAN_POINT('Ctrl Pts',(-207.955976777759,5.91281439438548,
130.433367747241));
#272344=CARTESIAN_POINT('Ctrl Pts',(-207.947415967503,5.92542666017732,
130.614125802698));
#272345=CARTESIAN_POINT('Ctrl Pts',(-207.912377717299,5.94123870869834,
131.355802411338));
#272346=CARTESIAN_POINT('Ctrl Pts',(-207.877339467095,5.80436545607685,
132.093047857022));
#272347=CARTESIAN_POINT('Ctrl Pts',(-207.850862027148,5.62578014279735,
132.627039335975));
#272348=CARTESIAN_POINT('Ctrl Pts',(-207.794849275159,5.47606313559233,
128.563676994761));
#272349=CARTESIAN_POINT('Ctrl Pts',(-207.883928897283,5.72131300358244,
129.163049323563));
#272350=CARTESIAN_POINT('Ctrl Pts',(-207.940709210396,5.86582931839541,
129.807281383254));
#272351=CARTESIAN_POINT('Ctrl Pts',(-207.955943877287,5.9051406252583,130.43389502075));
#272352=CARTESIAN_POINT('Ctrl Pts',(210.578629502474,3.43871735229388,135.623751273273));
#272353=CARTESIAN_POINT('Ctrl Pts',(210.532211638871,4.24191310225744,135.050661598608));
#272354=CARTESIAN_POINT('Ctrl Pts',(210.439385837966,5.5417116830592,133.497735776206));
#272355=CARTESIAN_POINT('Ctrl Pts',(210.253744162458,6.40049231640402,129.500124813146));
#272356=CARTESIAN_POINT('Ctrl Pts',(210.021704475947,3.49988613106459,124.739836436729));
#272357=CARTESIAN_POINT('Ctrl Pts',(209.743256852134,-3.22132718841443,
124.582443963435));
#272358=CARTESIAN_POINT('Ctrl Pts',(209.464809228321,-6.97029916743427,
130.151104711613));
#272359=CARTESIAN_POINT('Ctrl Pts',(209.186361604508,-4.320155850937,136.315756482887));
#272360=CARTESIAN_POINT('Ctrl Pts',(208.907913980696,2.30329626696544,137.417975354914));
#272361=CARTESIAN_POINT('Ctrl Pts',(208.629466356883,6.80838731381026,132.441404887444));
#272362=CARTESIAN_POINT('Ctrl Pts',(208.35101873307,5.05782663488002,125.961106241921));
#272363=CARTESIAN_POINT('Ctrl Pts',(208.072571109257,-1.34111875541754,
123.931185212061));
#272364=CARTESIAN_POINT('Ctrl Pts',(207.794123485444,-6.50738248846785,
128.217554840719));
#272365=CARTESIAN_POINT('Ctrl Pts',(207.515675861631,-5.69381680528821,
134.880978212762));
#272366=CARTESIAN_POINT('Ctrl Pts',(207.237228237818,0.352161018465804,
137.798239159538));
#272367=CARTESIAN_POINT('Ctrl Pts',(206.958780614005,6.07448159193836,134.288440920842));
#272368=CARTESIAN_POINT('Ctrl Pts',(206.680332990192,6.21467071562046,127.576957111676));
#272369=CARTESIAN_POINT('Ctrl Pts',(206.40188536638,0.643870262773591,123.831292031177));
#272370=CARTESIAN_POINT('Ctrl Pts',(206.123437742567,-5.51860979104455,
126.493540260974));
#272371=CARTESIAN_POINT('Ctrl Pts',(205.844990118754,-6.60976007302988,
133.117219720399));
#272372=CARTESIAN_POINT('Ctrl Pts',(205.566542494941,-1.62686214948821,
137.615495756827));
#272373=CARTESIAN_POINT('Ctrl Pts',(205.288094871128,4.8510417637676,135.85467075854));
#272374=CARTESIAN_POINT('Ctrl Pts',(205.009647247315,6.87107573233629,129.452857771449));
#272375=CARTESIAN_POINT('Ctrl Pts',(204.731199623502,2.57692653546199,124.293009711503));
#272376=CARTESIAN_POINT('Ctrl Pts',(204.452751999689,-4.08529213152394,
125.116775123829));
#272377=CARTESIAN_POINT('Ctrl Pts',(204.174304375876,-6.9933269740478,131.167153704944));
#272378=CARTESIAN_POINT('Ctrl Pts',(203.895856752063,-3.47483593506387,
136.884143186524));
#272379=CARTESIAN_POINT('Ctrl Pts',(203.617409128251,3.23685955433703,137.014109488232));
#272380=CARTESIAN_POINT('Ctrl Pts',(203.338961504438,6.97403925260401,131.437619947721));
#272381=CARTESIAN_POINT('Ctrl Pts',(203.060513880625,4.30241757323156,125.27919601562));
#272382=CARTESIAN_POINT('Ctrl Pts',(202.782066256812,-2.32291566837452,
124.198128435325));
#272383=CARTESIAN_POINT('Ctrl Pts',(202.503618632999,-6.81360289295739,
129.18786549711));
#272384=CARTESIAN_POINT('Ctrl Pts',(202.225171009186,-5.0429219211382,135.663082604955));
#272385=CARTESIAN_POINT('Ctrl Pts',(201.946723385373,1.36195793536179,137.673371567868));
#272386=CARTESIAN_POINT('Ctrl Pts',(201.66827576156,6.51526498482727,133.371375037445));
#272387=CARTESIAN_POINT('Ctrl Pts',(201.389828137747,5.6813618015098,126.710417660699));
#272388=CARTESIAN_POINT('Ctrl Pts',(201.111380513935,-0.373435327379839,
123.811593861123));
#272389=CARTESIAN_POINT('Ctrl Pts',(200.832932890122,-6.08506363376988,
127.338781095048));
#272390=CARTESIAN_POINT('Ctrl Pts',(200.554485266309,-6.20481573259303,
134.050666607207));
#272391=CARTESIAN_POINT('Ctrl Pts',(200.276037642496,-0.622645295272457,
137.779355505743));
#272392=CARTESIAN_POINT('Ctrl Pts',(199.997590018683,5.53170575049466,135.098364849491));
#272393=CARTESIAN_POINT('Ctrl Pts',(199.71914239487,6.60268945040398,128.471394077867));
#272394=CARTESIAN_POINT('Ctrl Pts',(199.440694771057,1.60612410470526,123.988305584475));
#272395=CARTESIAN_POINT('Ctrl Pts',(199.162247147244,-4.86639082969376,
125.768838683693));
#272396=CARTESIAN_POINT('Ctrl Pts',(198.883799523432,-6.86693032801245,
132.176770441218));
#272397=CARTESIAN_POINT('Ctrl Pts',(198.605351899619,-2.5570963230842,137.323524616753));
#272398=CARTESIAN_POINT('Ctrl Pts',(198.326904275806,4.10258428165832,136.479485555902));
#272399=CARTESIAN_POINT('Ctrl Pts',(198.048456651993,6.99219035394115,130.420283921986));
#272400=CARTESIAN_POINT('Ctrl Pts',(197.77000902818,3.45631507844086,124.714030008118));
#272401=CARTESIAN_POINT('Ctrl Pts',(197.491561404367,-3.25574490376804,
124.604492395141));
#272402=CARTESIAN_POINT('Ctrl Pts',(197.213113780554,-6.97593437139489,
130.192330798173));
#272403=CARTESIAN_POINT('Ctrl Pts',(196.934666156741,-4.28558094504976,
136.342594705906));
#272404=CARTESIAN_POINT('Ctrl Pts',(196.656218532928,2.3430120075278,137.403492044232));
#272405=CARTESIAN_POINT('Ctrl Pts',(196.377770909115,6.81849138768721,132.400109986944));
#272406=CARTESIAN_POINT('Ctrl Pts',(196.099323285303,5.02811028438465,125.930312215887));
#272407=CARTESIAN_POINT('Ctrl Pts',(195.82087566149,-1.38285853342424,123.939526815472));
#272408=CARTESIAN_POINT('Ctrl Pts',(195.542428037677,-6.5230479154113,128.257188313404));
#272409=CARTESIAN_POINT('Ctrl Pts',(195.263980413864,-5.66887493174189,
134.915576722577));
#272410=CARTESIAN_POINT('Ctrl Pts',(194.985532790051,0.394717174261835,
137.795958375315));
#272411=CARTESIAN_POINT('Ctrl Pts',(194.707085166238,6.09558348012494,134.251403247221));
#272412=CARTESIAN_POINT('Ctrl Pts',(194.428637542425,6.19490635356113,127.539184339867));
#272413=CARTESIAN_POINT('Ctrl Pts',(194.150189918612,0.601412926074683,
123.827502918989));
#272414=CARTESIAN_POINT('Ctrl Pts',(193.871742294799,-5.54474959981957,
126.527212884656));
#272415=CARTESIAN_POINT('Ctrl Pts',(193.593294670987,-6.59555811955654,
133.157412666584));
#272416=CARTESIAN_POINT('Ctrl Pts',(193.314847047174,-1.58537093834796,
137.625272568447));
#272417=CARTESIAN_POINT('Ctrl Pts',(193.036399423361,4.88169468552635,135.825047607524));
#272418=CARTESIAN_POINT('Ctrl Pts',(192.757951799548,6.86272137744547,129.411056577024));
#272419=CARTESIAN_POINT('Ctrl Pts',(192.479504175735,2.53724238606986,124.277443893095));
#272420=CARTESIAN_POINT('Ctrl Pts',(192.201056551922,-4.11983840692253,
125.141748821346));
#272421=CARTESIAN_POINT('Ctrl Pts',(191.922608928109,-6.99098896924831,
131.209717356357));
#272422=CARTESIAN_POINT('Ctrl Pts',(191.644161304296,-3.43776219763276,
136.905182851196));
#272423=CARTESIAN_POINT('Ctrl Pts',(191.365713680483,3.27460008958736,136.994290755064));
#272424=CARTESIAN_POINT('Ctrl Pts',(191.08726605667,6.9777648675845,131.395155257469));
#272425=CARTESIAN_POINT('Ctrl Pts',(190.808818432858,4.26870461503614,125.253108347726));
#272426=CARTESIAN_POINT('Ctrl Pts',(190.530370809044,-2.36308664091672,
124.212391080215));
#272427=CARTESIAN_POINT('Ctrl Pts',(190.251923185232,-6.82331671706736,
129.229371781915));
#272428=CARTESIAN_POINT('Ctrl Pts',(189.973475561419,-5.01325206778612,
135.693690281095));
#272429=CARTESIAN_POINT('Ctrl Pts',(189.695027937606,1.40374632081163,137.664953676525));
#272430=CARTESIAN_POINT('Ctrl Pts',(189.416580313793,6.53077041740369,133.331667209374));
#272431=CARTESIAN_POINT('Ctrl Pts',(189.13813268998,5.65633554627347,126.675909450142));
#272432=CARTESIAN_POINT('Ctrl Pts',(188.859685066167,-0.41599536452862,
123.81399662772));
#272433=CARTESIAN_POINT('Ctrl Pts',(188.581237442354,-6.10604685783229,
127.375886813701));
#272434=CARTESIAN_POINT('Ctrl Pts',(188.302789818542,-6.18493958576042,
134.088376935175));
#272435=CARTESIAN_POINT('Ctrl Pts',(188.024342194729,-0.580174985471077,
137.783016493883));
#272436=CARTESIAN_POINT('Ctrl Pts',(187.745894570916,5.55774208334242,135.064612228548));
#272437=CARTESIAN_POINT('Ctrl Pts',(187.467446947103,6.58836568835925,128.431244857581));
#272438=CARTESIAN_POINT('Ctrl Pts',(187.18899932329,1.56460308533104,123.97865493689));
#272439=CARTESIAN_POINT('Ctrl Pts',(186.910551699478,-4.89695331800637,
125.798555082479));
#272440=CARTESIAN_POINT('Ctrl Pts',(186.632104075664,-6.85844885156509,
132.218545967617));
#272441=CARTESIAN_POINT('Ctrl Pts',(186.353656451852,-2.51736494438869,
137.338969602853));
#272442=CARTESIAN_POINT('Ctrl Pts',(186.075208828038,4.13705436656654,136.454406814005));
#272443=CARTESIAN_POINT('Ctrl Pts',(185.796761204226,6.98972282098866,130.377727590732));
#272444=CARTESIAN_POINT('Ctrl Pts',(185.518313580413,3.41917746986535,124.693103276936));
#272445=CARTESIAN_POINT('Ctrl Pts',(185.2398659566,-3.29342493995873,124.62442590766));
#272446=CARTESIAN_POINT('Ctrl Pts',(184.961418332787,-6.97953072271363,
130.234806630193));
#272447=CARTESIAN_POINT('Ctrl Pts',(184.682970708974,-4.25178874032612,
136.368579642862));
#272448=CARTESIAN_POINT('Ctrl Pts',(184.404523085161,2.38313938299372,137.389107198495));
#272449=CARTESIAN_POINT('Ctrl Pts',(184.126075461348,6.82807883617355,132.358574329007));
#272450=CARTESIAN_POINT('Ctrl Pts',(183.847627837535,4.99834740910532,125.899794986266));
#272451=CARTESIAN_POINT('Ctrl Pts',(183.569180213722,-1.42462110408482,
123.948071857337));
#272452=CARTESIAN_POINT('Ctrl Pts',(183.290732589909,-6.53843241923107,
128.296943150732));
#272453=CARTESIAN_POINT('Ctrl Pts',(183.012284966097,-5.64374376128527,
134.950008601993));
#272454=CARTESIAN_POINT('Ctrl Pts',(182.733837342284,0.437269701071178,
137.793426081729));
#272455=CARTESIAN_POINT('Ctrl Pts',(182.455389718471,6.11645366995566,134.214233834728));
#272456=CARTESIAN_POINT('Ctrl Pts',(182.176942094658,6.17491552152431,127.501534682722));
#272457=CARTESIAN_POINT('Ctrl Pts',(181.898494470845,0.558931670205695,
123.82397121282));
#272458=CARTESIAN_POINT('Ctrl Pts',(181.620046847032,-5.57068308070185,
126.561044594899));
#272459=CARTESIAN_POINT('Ctrl Pts',(181.341599223219,-6.58111222344223,
133.197518104296));
#272460=CARTESIAN_POINT('Ctrl Pts',(181.063151599407,-1.54382073804491,
137.634796795631));
#272461=CARTESIAN_POINT('Ctrl Pts',(180.784703975594,4.91216658577983,135.795238324681));
#272462=CARTESIAN_POINT('Ctrl Pts',(180.506256351781,6.85411278995147,129.369307058824));
#272463=CARTESIAN_POINT('Ctrl Pts',(180.227808727968,2.49746418218255,124.262119907186));
#272464=CARTESIAN_POINT('Ctrl Pts',(179.949361104155,-4.15423200110403,
125.16693236216));
#272465=CARTESIAN_POINT('Ctrl Pts',(179.670913480342,-6.98839192089168,
131.252265980172));
#272466=CARTESIAN_POINT('Ctrl Pts',(179.392465856529,-3.40056106730489,
136.925996451342));
#272467=CARTESIAN_POINT('Ctrl Pts',(179.114018232716,3.31221928049139,136.974242649806));
#272468=CARTESIAN_POINT('Ctrl Pts',(178.835570608904,6.98123192042358,131.352668676138));
#272469=CARTESIAN_POINT('Ctrl Pts',(178.55712298509,4.23483347762603,125.227226382977));
#272470=CARTESIAN_POINT('Ctrl Pts',(178.278675361277,-2.40317004799311,
124.22689799325));
#272471=CARTESIAN_POINT('Ctrl Pts',(178.000227737465,-6.83277770089014,
129.270936428355));
#272472=CARTESIAN_POINT('Ctrl Pts',(177.721780113652,-4.98339644641697,
135.724116781409));
#272473=CARTESIAN_POINT('Ctrl Pts',(177.443332489839,1.44548268986267,137.65628156334));
#272474=CARTESIAN_POINT('Ctrl Pts',(177.164884866026,6.54603384991367,133.291865731052));
#272475=CARTESIAN_POINT('Ctrl Pts',(176.886437242213,5.63109969342586,126.64155422085));
#272476=CARTESIAN_POINT('Ctrl Pts',(176.6079896184,-0.458539986806858,123.816658424832));
#272477=CARTESIAN_POINT('Ctrl Pts',(176.329541994587,-6.12680382008778,
127.413119575705));
#272478=CARTESIAN_POINT('Ctrl Pts',(176.051094370774,-6.16483425371434,
134.125965572714));
#272479=CARTESIAN_POINT('Ctrl Pts',(175.772646746962,-0.537683177073775,
137.786418885364));
#272480=CARTESIAN_POINT('Ctrl Pts',(175.494199123148,5.58357247201413,135.030701742416));
#272481=CARTESIAN_POINT('Ctrl Pts',(175.215751499336,6.57379779200069,128.391183573973));
#272482=CARTESIAN_POINT('Ctrl Pts',(174.937303875523,1.5230240890144,123.969257218339));
#272483=CARTESIAN_POINT('Ctrl Pts',(174.65885625171,-4.92733434791298,125.82845697323));
#272484=CARTESIAN_POINT('Ctrl Pts',(174.380408627897,-6.84971323277332,
132.260269090858));
#272485=CARTESIAN_POINT('Ctrl Pts',(174.101961004084,-2.4775402838095,137.354172446613));
#272486=CARTESIAN_POINT('Ctrl Pts',(173.823513380271,4.1713711514037,136.429118707571));
#272487=CARTESIAN_POINT('Ctrl Pts',(173.545065756458,6.98699628128659,130.335187068521));
#272488=CARTESIAN_POINT('Ctrl Pts',(173.266618132645,3.38191316241135,124.672403000642));
#272489=CARTESIAN_POINT('Ctrl Pts',(172.988170508833,-3.33098293707706,
124.644588419932));
#272490=CARTESIAN_POINT('Ctrl Pts',(172.709722885019,-6.98286844495469,
130.277303567246));
#272491=CARTESIAN_POINT('Ctrl Pts',(172.431275261207,-4.21783898400718,
136.394358395635));
#272492=CARTESIAN_POINT('Ctrl Pts',(172.152827637394,2.42317845035331,137.374478352552));
#272493=CARTESIAN_POINT('Ctrl Pts',(171.874380013581,6.83741326768756,132.316981079111));
#272494=CARTESIAN_POINT('Ctrl Pts',(171.595932389768,4.96839931822471,125.869459497128));
#272495=CARTESIAN_POINT('Ctrl Pts',(171.317484765955,-1.46633088488636,
123.956870961504));
#272496=CARTESIAN_POINT('Ctrl Pts',(171.039037142142,-6.55357463903296,
128.336790901335));
#272497=CARTESIAN_POINT('Ctrl Pts',(170.760589518329,-5.61840345982816,
134.984286862899));
#272498=CARTESIAN_POINT('Ctrl Pts',(170.482141894517,0.479806024690783,
137.79063480575));
#272499=CARTESIAN_POINT('Ctrl Pts',(170.203694270703,6.13709721234627,134.176938068128));
#272500=CARTESIAN_POINT('Ctrl Pts',(169.925246646891,6.15469587572206,127.464007413007));
#272501=CARTESIAN_POINT('Ctrl Pts',(169.646799023078,0.51642970291829,123.820698167548));
#272502=CARTESIAN_POINT('Ctrl Pts',(169.368351399265,-5.59641013787386,
126.595033542778));
#272503=CARTESIAN_POINT('Ctrl Pts',(169.089903775452,-6.56642246179436,
133.237534862678));
#272504=CARTESIAN_POINT('Ctrl Pts',(168.811456151639,-1.50221333089678,
137.644067918489));
#272505=CARTESIAN_POINT('Ctrl Pts',(168.533008527826,4.94245646389391,135.76524410303));
#272506=CARTESIAN_POINT('Ctrl Pts',(168.254560904013,6.84525022078748,129.32761071706));
#272507=CARTESIAN_POINT('Ctrl Pts',(167.976113280201,2.45759343384159,124.247038346411));
#272508=CARTESIAN_POINT('Ctrl Pts',(167.697665656387,-4.1884716586909,125.192324799951));
#272509=CARTESIAN_POINT('Ctrl Pts',(167.419218032575,-6.98553591510243,
131.294798006688));
#272510=CARTESIAN_POINT('Ctrl Pts',(167.140770408762,-3.36323392793624,
136.946583212019));
#272511=CARTESIAN_POINT('Ctrl Pts',(166.862322784949,3.34971573589186,136.953965917302));
#272512=CARTESIAN_POINT('Ctrl Pts',(166.583875161136,6.98444028114645,131.310161777048));
#272513=CARTESIAN_POINT('Ctrl Pts',(166.305427537323,4.20080541690416,125.20155108099));
#272514=CARTESIAN_POINT('Ctrl Pts',(166.02697991351,-2.44316440471955,124.241648636582));
#272515=CARTESIAN_POINT('Ctrl Pts',(165.748532289697,-6.84198549362249,
129.312557896394));
#272516=CARTESIAN_POINT('Ctrl Pts',(165.470084665885,-4.95335616345982,
135.754360978348));
#272517=CARTESIAN_POINT('Ctrl Pts',(165.191637042072,1.48716549602113,137.647355549705));
#272518=CARTESIAN_POINT('Ctrl Pts',(164.913189418259,6.56105471673207,133.251972077313));
#272519=CARTESIAN_POINT('Ctrl Pts',(164.634741794446,5.60565517810829,126.60735324588));
#272520=CARTESIAN_POINT('Ctrl Pts',(164.356294170633,-0.501067617717217,
123.819579153818));
#272521=CARTESIAN_POINT('Ctrl Pts',(164.07784654682,-6.1473337513746,127.450478001396));
#272522=CARTESIAN_POINT('Ctrl Pts',(163.799398923007,-6.14450048146789,
134.163431126959));
#272523=CARTESIAN_POINT('Ctrl Pts',(163.520951299194,-0.495171444628521,
137.789562554107));
#272524=CARTESIAN_POINT('Ctrl Pts',(163.242503675381,5.60919595935461,134.996634647659));
#272525=CARTESIAN_POINT('Ctrl Pts',(162.964056051569,6.55898630114736,128.351211711527));
#272526=CARTESIAN_POINT('Ctrl Pts',(162.685608427755,1.48138865648,123.960112777059));
#272527=CARTESIAN_POINT('Ctrl Pts',(162.407160803943,-4.95753279363329,
125.85854324792));
#272528=CARTESIAN_POINT('Ctrl Pts',(162.12871318013,-6.84072379533872,132.301938264875));
#272529=CARTESIAN_POINT('Ctrl Pts',(161.850265556317,-2.4376238170639,137.369132584688));
#272530=CARTESIAN_POINT('Ctrl Pts',(161.571817932504,4.20553336454888,136.403622173655));
#272531=CARTESIAN_POINT('Ctrl Pts',(161.293370308691,6.98401083586784,130.292663931709));
#272532=CARTESIAN_POINT('Ctrl Pts',(161.014922684878,3.34452353692138,124.651929946293));
#272533=CARTESIAN_POINT('Ctrl Pts',(160.736475061065,-3.36841750339773,
124.664979184829));
#272534=CARTESIAN_POINT('Ctrl Pts',(160.458027437253,-6.98594741443756,
130.319820034592));
#272535=CARTESIAN_POINT('Ctrl Pts',(160.179579813439,-4.18373293411359,
136.419930008985));
#272536=CARTESIAN_POINT('Ctrl Pts',(159.901132189627,2.46312772594441,137.35960604848));
#272537=CARTESIAN_POINT('Ctrl Pts',(159.622684565814,6.84649433633851,132.275331778507));
#272538=CARTESIAN_POINT('Ctrl Pts',(159.344236942001,4.93826712148011,125.839306872565));
#272539=CARTESIAN_POINT('Ctrl Pts',(159.065789318188,-1.50798633025781,
123.965923801919));
#272540=CARTESIAN_POINT('Ctrl Pts',(158.787341694375,-6.56847401371661,
128.376730088641));
#272541=CARTESIAN_POINT('Ctrl Pts',(158.508894070562,-5.59285496636459,
135.018410235101));
#272542=CARTESIAN_POINT('Ctrl Pts',(158.230446446749,0.522324568921774,
137.787584650814));
#272543=CARTESIAN_POINT('Ctrl Pts',(157.951998822937,6.15751334234277,134.139517329431));
#272544=CARTESIAN_POINT('Ctrl Pts',(157.673551199123,6.13424816540071,127.426603921307));
#272545=CARTESIAN_POINT('Ctrl Pts',(157.395103575311,0.473908599138188,
123.817683904457));
#272546=CARTESIAN_POINT('Ctrl Pts',(157.116655951498,-5.62192981801017,
126.62917846882));
#272547=CARTESIAN_POINT('Ctrl Pts',(156.838208327685,-6.55148937894732,
133.277461458893));
#272548=CARTESIAN_POINT('Ctrl Pts',(156.559760703872,-1.46055025868114,
137.653085593479));
#272549=CARTESIAN_POINT('Ctrl Pts',(156.281313080059,4.97256319746619,135.735066054016));
#272550=CARTESIAN_POINT('Ctrl Pts',(156.002865456246,6.83613399835919,129.285969096806));
#272551=CARTESIAN_POINT('Ctrl Pts',(155.724417832433,2.4176316184721,124.232199769625));
#272552=CARTESIAN_POINT('Ctrl Pts',(155.44597020862,-4.2225561109203,125.217925193794));
#272553=CARTESIAN_POINT('Ctrl Pts',(155.167522584808,-6.98242105771092,
131.337311859867));
#272554=CARTESIAN_POINT('Ctrl Pts',(154.889074960995,-3.3257821626974,136.96694237038));
#272555=CARTESIAN_POINT('Ctrl Pts',(154.610627337182,3.38708806634394,136.933461308912));
#272556=CARTESIAN_POINT('Ctrl Pts',(154.332179713369,6.98738983086623,131.267636135312));
#272557=CARTESIAN_POINT('Ctrl Pts',(154.053732089556,4.1666216937926,125.17608339317));
#272558=CARTESIAN_POINT('Ctrl Pts',(153.775284465743,-2.48306822909056,
124.256642463619));
#272559=CARTESIAN_POINT('Ctrl Pts',(153.49683684193,-6.85093975406627,129.354234643731));
#272560=CARTESIAN_POINT('Ctrl Pts',(153.218389218117,-4.92313233206838,
135.784421751204));
#272561=CARTESIAN_POINT('Ctrl Pts',(152.939941594304,1.52879319471521,137.638175966376));
#272562=CARTESIAN_POINT('Ctrl Pts',(152.661493970491,6.57583246125511,133.21198772643));
#272563=CARTESIAN_POINT('Ctrl Pts',(152.383046346679,5.58000294317656,126.573307792561));
#272564=CARTESIAN_POINT('Ctrl Pts',(152.104598722866,-0.543576681382813,
123.822758706449));
#272565=CARTESIAN_POINT('Ctrl Pts',(151.826151099053,-6.16763589094857,
127.487960706439));
#272566=CARTESIAN_POINT('Ctrl Pts',(151.54770347524,-6.12393902249645,134.200772209611));
#272567=CARTESIAN_POINT('Ctrl Pts',(151.269255851427,-0.452641363423277,
137.792447383624));
#272568=CARTESIAN_POINT('Ctrl Pts',(150.990808227614,5.63461159587598,134.962412206646));
#272569=CARTESIAN_POINT('Ctrl Pts',(150.712360603801,6.54393176464461,128.311330751416));
#272570=CARTESIAN_POINT('Ctrl Pts',(150.433912979988,1.4396983305442,123.951221951899));
#272571=CARTESIAN_POINT('Ctrl Pts',(150.155465356176,-4.98754753615285,
125.888812791691));
#272572=CARTESIAN_POINT('Ctrl Pts',(149.877017732362,-6.83148087236823,
132.343551945603));
#272573=CARTESIAN_POINT('Ctrl Pts',(149.59857010855,-2.39761702327129,137.383849462723));
#272574=CARTESIAN_POINT('Ctrl Pts',(149.320122484737,4.23953974010866,136.377918157044));
#272575=CARTESIAN_POINT('Ctrl Pts',(149.041674860924,6.98076659535922,130.250159756006));
#272576=CARTESIAN_POINT('Ctrl Pts',(148.763227237111,3.30700997888175,124.631684872525));
#272577=CARTESIAN_POINT('Ctrl Pts',(148.484779613298,-3.40572725176907,
124.685597446761));
#272578=CARTESIAN_POINT('Ctrl Pts',(148.206331989485,-6.98876751706998,
130.362354456768));
#272579=CARTESIAN_POINT('Ctrl Pts',(147.927884365672,-4.14947185445744,
136.445293535346));
#272580=CARTESIAN_POINT('Ctrl Pts',(147.649436741859,2.50298572943186,137.344490837378));
#272581=CARTESIAN_POINT('Ctrl Pts',(147.370989118047,6.85532170562399,132.233627970525));
#272582=CARTESIAN_POINT('Ctrl Pts',(147.092541494233,4.90795193543132,125.809338229895));
#272583=CARTESIAN_POINT('Ctrl Pts',(146.814093870421,-1.54958589664124,
123.975230043125));
#272584=CARTESIAN_POINT('Ctrl Pts',(146.535646246608,-6.58312999118006,
128.41675923269));
#272585=CARTESIAN_POINT('Ctrl Pts',(146.257198622795,-5.56709922760349,
135.052377454143));
#272586=CARTESIAN_POINT('Ctrl Pts',(145.978750998982,0.564823758223794,
137.784275729942));
#272587=CARTESIAN_POINT('Ctrl Pts',(145.700303375169,6.17770130341801,134.101973005276));
#272588=CARTESIAN_POINT('Ctrl Pts',(145.421855751356,6.11357314825767,127.389325593625));
#272589=CARTESIAN_POINT('Ctrl Pts',(145.143408127543,0.431369934500661,
123.81492853524));
#272590=CARTESIAN_POINT('Ctrl Pts',(144.864960503731,-5.64724117546963,
126.663478107772));
#272591=CARTESIAN_POINT('Ctrl Pts',(144.586512879918,-6.53631352825206,
133.317296413447));
#272592=CARTESIAN_POINT('Ctrl Pts',(144.308065256105,-1.41883306523854,
137.661849486446));
#272593=CARTESIAN_POINT('Ctrl Pts',(144.029617632292,5.00248567088053,135.704705295899));
#272594=CARTESIAN_POINT('Ctrl Pts',(143.751170008479,6.82676446047164,129.244383741109));
#272595=CARTESIAN_POINT('Ctrl Pts',(143.472722384666,2.37758021687388,124.217604726676));
#272596=CARTESIAN_POINT('Ctrl Pts',(143.194274760853,-4.25648409478009,
125.243732595056));
#272597=CARTESIAN_POINT('Ctrl Pts',(142.91582713704,-6.97904746413934,131.379805964341));
#272598=CARTESIAN_POINT('Ctrl Pts',(142.637379513228,-3.28820715937746,
136.987073172008));
#272599=CARTESIAN_POINT('Ctrl Pts',(142.358931889414,3.42433488700229,136.912729584442));
#272600=CARTESIAN_POINT('Ctrl Pts',(142.080484265602,6.99008046028611,131.225093326731));
#272601=CARTESIAN_POINT('Ctrl Pts',(141.802036641788,4.13228357498186,125.150824263232));
#272602=CARTESIAN_POINT('Ctrl Pts',(141.523589017976,-2.52288004245522,
124.271878918761));
#272603=CARTESIAN_POINT('Ctrl Pts',(141.245141394163,-6.859640150418,129.395965126019));
#272604=CARTESIAN_POINT('Ctrl Pts',(140.96669377035,-4.89272607219785,135.814297986063));
#272605=CARTESIAN_POINT('Ctrl Pts',(140.688246146537,1.57036424341533,137.628743153505));
#272606=CARTESIAN_POINT('Ctrl Pts',(140.409798522724,6.59036653588803,133.17191416004));
#272607=CARTESIAN_POINT('Ctrl Pts',(140.131350898911,5.55414393918375,126.539419122461));
#272608=CARTESIAN_POINT('Ctrl Pts',(139.852903275098,-0.586065602614643,
123.826196964908));
#272609=CARTESIAN_POINT('Ctrl Pts',(139.574455651286,-6.18770948650656,
127.525566301902));
#272610=CARTESIAN_POINT('Ctrl Pts',(139.296008027473,-6.10315063871238,
134.237987436982));
#272611=CARTESIAN_POINT('Ctrl Pts',(139.01756040366,-0.410094509425858,
137.795073267016));
#272612=CARTESIAN_POINT('Ctrl Pts',(138.739112779847,5.65981843979252,134.928035687503));
#272613=CARTESIAN_POINT('Ctrl Pts',(138.460665156034,6.52863474034383,128.271542171445));
#272614=CARTESIAN_POINT('Ctrl Pts',(138.182217532221,1.39795465605713,123.942585072312));
#272615=CARTESIAN_POINT('Ctrl Pts',(137.903769908408,-5.01737746326431,
125.919264482896));
#272616=CARTESIAN_POINT('Ctrl Pts',(137.625322284595,-6.82198480636163,
132.385108591028));
#272617=CARTESIAN_POINT('Ctrl Pts',(137.346874660782,-2.35752138489827,
137.39832253538));
#272618=CARTESIAN_POINT('Ctrl Pts',(137.06842703697,4.27338901796432,136.352007610208));
#272619=CARTESIAN_POINT('Ctrl Pts',(136.789979413157,6.9772636799772,130.20767611642));
#272620=CARTESIAN_POINT('Ctrl Pts',(136.511531789344,3.26937387837121,124.611668529527));
#272621=CARTESIAN_POINT('Ctrl Pts',(136.233084165531,-3.44291079966457,
124.706442441713));
#272622=CARTESIAN_POINT('Ctrl Pts',(135.954636541718,-6.99132864835187,
130.404905257644));
#272623=CARTESIAN_POINT('Ctrl Pts',(135.676188917905,-4.1150570145959,136.470448034864));
#272624=CARTESIAN_POINT('Ctrl Pts',(135.397741294092,2.54275098386259,137.329133279345));
#272625=CARTESIAN_POINT('Ctrl Pts',(135.11929367028,6.8638950484427,132.191871200516));
#272626=CARTESIAN_POINT('Ctrl Pts',(134.840846046466,4.87745488341857,125.779554679616));
#272627=CARTESIAN_POINT('Ctrl Pts',(134.562398422654,-1.59112804254939,
123.984789340275));
#272628=CARTESIAN_POINT('Ctrl Pts',(134.283950798841,-6.59754202834077,
128.456876850186));
#272629=CARTESIAN_POINT('Ctrl Pts',(134.005503175028,-5.54113719793324,
135.086187261361));
#272630=CARTESIAN_POINT('Ctrl Pts',(133.727055551215,0.607302017773813,
137.780708165749));
#272631=CARTESIAN_POINT('Ctrl Pts',(133.448607927402,6.19766034749954,134.064306486881));
#272632=CARTESIAN_POINT('Ctrl Pts',(133.170160303589,6.09267159041341,127.352173811322));
#272633=CARTESIAN_POINT('Ctrl Pts',(132.891712679776,0.388815285291658,
123.812432161999));
#272634=CARTESIAN_POINT('Ctrl Pts',(132.613265055963,-5.67234327233058,
126.697931188648));
#272635=CARTESIAN_POINT('Ctrl Pts',(132.334817432151,-6.52089547205522,
133.357038250242));
#272636=CARTESIAN_POINT('Ctrl Pts',(132.056369808337,-1.37706329641493,
137.670359272641));
#272637=CARTESIAN_POINT('Ctrl Pts',(131.777922184525,5.0322227753486,135.674162953708));
#272638=CARTESIAN_POINT('Ctrl Pts',(131.499474560712,6.81714195431646,129.20285619093));
#272639=CARTESIAN_POINT('Ctrl Pts',(131.221026936899,2.33744071316646,124.203253758389));
#272640=CARTESIAN_POINT('Ctrl Pts',(130.942579313086,-4.29025435305649,
125.269746047434));
#272641=CARTESIAN_POINT('Ctrl Pts',(130.664131689273,-6.97541525939744,
131.422278745477));
#272642=CARTESIAN_POINT('Ctrl Pts',(130.38568406546,-3.25051031033198,137.006974870947));
#272643=CARTESIAN_POINT('Ctrl Pts',(130.107236441647,3.46145481767177,136.891771512113));
#272644=CARTESIAN_POINT('Ctrl Pts',(129.828788817834,6.99251206970404,131.182534927744));
#272645=CARTESIAN_POINT('Ctrl Pts',(129.550341194022,4.09779233288376,125.125774627163));
#272646=CARTESIAN_POINT('Ctrl Pts',(129.271893570209,-2.5625983695722,124.287357437414));
#272647=CARTESIAN_POINT('Ctrl Pts',(128.993445946396,-6.86808636028122,
129.43774779692));
#272648=CARTESIAN_POINT('Ctrl Pts',(128.714998322583,-4.86213851056362,
135.84398857585));
#272649=CARTESIAN_POINT('Ctrl Pts',(128.43655069877,1.61187710169066,137.61905746063));
#272650=CARTESIAN_POINT('Ctrl Pts',(128.158103074957,6.60465640206541,133.131752863082));
#272651=CARTESIAN_POINT('Ctrl Pts',(127.879655451144,5.52807912434469,126.505688491336));
#272652=CARTESIAN_POINT('Ctrl Pts',(127.601207827331,-0.628532806970051,
123.829893801787));
#272653=CARTESIAN_POINT('Ctrl Pts',(127.322760203518,-6.20755379421381,
127.563293394292));
#272654=CARTESIAN_POINT('Ctrl Pts',(127.044312579706,-6.08213610043705,
134.275075430049));
#272655=CARTESIAN_POINT('Ctrl Pts',(126.765864955893,-0.367532459225645,
137.797440106979));
#272656=CARTESIAN_POINT('Ctrl Pts',(126.48741733208,5.68481555705546,134.893506364063));
#272657=CARTESIAN_POINT('Ctrl Pts',(126.208969708267,6.51309579508176,128.231847445991));
#272658=CARTESIAN_POINT('Ctrl Pts',(125.930522084454,1.35615917984635,123.934202458341));
#272659=CARTESIAN_POINT('Ctrl Pts',(125.652074460641,-5.04702146960864,
125.949897193134));
#272660=CARTESIAN_POINT('Ctrl Pts',(125.373626836828,-6.81223594919939,
132.426606661257));
#272661=CARTESIAN_POINT('Ctrl Pts',(125.095179213015,-2.3173383877032,137.412551266352));
#272662=CARTESIAN_POINT('Ctrl Pts',(124.816731589202,4.3070799438184,136.325891493273));
#272663=CARTESIAN_POINT('Ctrl Pts',(124.538283965389,6.97350221952356,130.165214587198));
#272664=CARTESIAN_POINT('Ctrl Pts',(124.259836341577,3.2316166300094,124.591881659011));
#272665=CARTESIAN_POINT('Ctrl Pts',(123.981388717764,-3.47996676923432,
124.727513397266));
#272666=CARTESIAN_POINT('Ctrl Pts',(123.702941093951,-6.99363071337966,
130.447470860486));
#272667=CARTESIAN_POINT('Ctrl Pts',(123.424493470138,-4.08048968978323,
136.495392575427));
#272668=CARTESIAN_POINT('Ctrl Pts',(123.146045846325,2.58242201572056,137.313533943462));
#272669=CARTESIAN_POINT('Ctrl Pts',(122.867598222512,6.87221404710605,132.150063015792));
#272670=CARTESIAN_POINT('Ctrl Pts',(122.589150598699,4.84677709552158,125.749957325369));
#272671=CARTESIAN_POINT('Ctrl Pts',(122.310702974886,-1.63261122862275,
123.994601339147));
#272672=CARTESIAN_POINT('Ctrl Pts',(122.032255351073,-6.6117095911554,128.497081454556));
#272673=CARTESIAN_POINT('Ctrl Pts',(121.753807727261,-5.51496983938628,
135.119838403918));
#272674=CARTESIAN_POINT('Ctrl Pts',(121.475360103447,0.649757773524084,
137.776882090432));
#272675=CARTESIAN_POINT('Ctrl Pts',(121.196912479635,6.21738973499768,134.026519169992));
#272676=CARTESIAN_POINT('Ctrl Pts',(120.918464855822,6.07154426638285,127.315149951069));
#272677=CARTESIAN_POINT('Ctrl Pts',(120.640017232009,0.346246228389124,
123.810194877238));
#272678=CARTESIAN_POINT('Ctrl Pts',(120.361569608196,-5.69723517842559,
126.732536434776));
#272679=CARTESIAN_POINT('Ctrl Pts',(120.083121984383,-6.50523578167861,
133.396685496627));
#272680=CARTESIAN_POINT('Ctrl Pts',(119.80467436057,-1.3352425000044,137.678614636731));
#272681=CARTESIAN_POINT('Ctrl Pts',(119.526226736757,5.06177340895125,135.6434401592));
#272682=CARTESIAN_POINT('Ctrl Pts',(119.247779112945,6.8072668364591,129.161387985085));
#272683=CARTESIAN_POINT('Ctrl Pts',(118.969331489131,2.29721459473369,124.189147396544));
#272684=CARTESIAN_POINT('Ctrl Pts',(118.690883865319,-4.32386563438011,
125.29596458699));
#272685=CARTESIAN_POINT('Ctrl Pts',(118.412436241506,-6.97152457807781,
131.464728629428));
#272686=CARTESIAN_POINT('Ctrl Pts',(118.133988617693,-3.21269301243169,
137.026646729736));
#272687=CARTESIAN_POINT('Ctrl Pts',(117.85554099388,3.49844648286018,136.870587868534));
#272688=CARTESIAN_POINT('Ctrl Pts',(117.577093370067,6.99468456901571,131.139962515369));
#272689=CARTESIAN_POINT('Ctrl Pts',(117.298645746254,4.06314924558364,125.100935413187));
#272690=CARTESIAN_POINT('Ctrl Pts',(117.020198122441,-2.60222173866402,
124.303077446017));
#272691=CARTESIAN_POINT('Ctrl Pts',(116.741750498628,-6.8762780706787,129.479581108162));
#272692=CARTESIAN_POINT('Ctrl Pts',(116.463302874816,-4.83137078059878,
135.873492420371));
#272693=CARTESIAN_POINT('Ctrl Pts',(116.184855251003,1.65333023126747,137.609119246659));
#272694=CARTESIAN_POINT('Ctrl Pts',(115.90640762719,6.61870153027093,133.09150532375));
#272695=CARTESIAN_POINT('Ctrl Pts',(115.627960003377,5.5018094645007,126.472117149089));
#272696=CARTESIAN_POINT('Ctrl Pts',(115.349512379564,-0.670976720811003,
123.833849080098));
#272697=CARTESIAN_POINT('Ctrl Pts',(115.071064755751,-6.22716807873245,
127.601140585621));
#272698=CARTESIAN_POINT('Ctrl Pts',(114.792617131938,-6.06089618637186,
134.312034814502));
#272699=CARTESIAN_POINT('Ctrl Pts',(114.514169508125,-0.324956789974863,
137.79954781581));
#272700=CARTESIAN_POINT('Ctrl Pts',(114.235721884312,5.70960202138734,134.858825515823));
#272701=CARTESIAN_POINT('Ctrl Pts',(113.957274260499,6.4973155046598,128.192248045959));
#272702=CARTESIAN_POINT('Ctrl Pts',(113.678826636687,1.31431345065849,123.926074420608));
#272703=CARTESIAN_POINT('Ctrl Pts',(113.400379012874,-5.07647845671644,
125.980709787299));
#272704=CARTESIAN_POINT('Ctrl Pts',(113.121931389061,-6.80223466212876,
132.468044618562));
#272705=CARTESIAN_POINT('Ctrl Pts',(112.843483765248,-2.27706952068197,
137.42653512839));
#272706=CARTESIAN_POINT('Ctrl Pts',(112.565036141435,4.34061126924124,136.299570773982));
#272707=CARTESIAN_POINT('Ctrl Pts',(112.286588517622,6.96948235338073,130.122776741767));
#272708=CARTESIAN_POINT('Ctrl Pts',(112.008140893809,3.1937396329048,124.572324994188));
#272709=CARTESIAN_POINT('Ctrl Pts',(111.729693269996,-3.51689378735575,
124.748809532627));
#272710=CARTESIAN_POINT('Ctrl Pts',(111.451245646184,-6.99567362684944,
130.490049688009));
#272711=CARTESIAN_POINT('Ctrl Pts',(111.172798022371,-4.0457711609245,136.52012623271));
#272712=CARTESIAN_POINT('Ctrl Pts',(110.894350398558,2.62199735498092,137.297693407768));
#272713=CARTESIAN_POINT('Ctrl Pts',(110.615902774745,6.88027839335069,132.108204965571));
#272714=CARTESIAN_POINT('Ctrl Pts',(110.337455150932,4.81591970851693,125.720547263895));
#272715=CARTESIAN_POINT('Ctrl Pts',(110.059007527119,-1.67403391768677,
124.004665676154));
#272716=CARTESIAN_POINT('Ctrl Pts',(109.780559903306,-6.62563215463966,
128.537371556004));
#272717=CARTESIAN_POINT('Ctrl Pts',(109.502112279493,-5.48859812160383,
135.153329634858));
#272718=CARTESIAN_POINT('Ctrl Pts',(109.22366465568,0.692189452261082,137.772797645767));
#272719=CARTESIAN_POINT('Ctrl Pts',(108.945217031867,6.23688873483282,133.988612454835));
#272720=CARTESIAN_POINT('Ctrl Pts',(108.666769408055,6.05019195904657,127.278255384801));
#272721=CARTESIAN_POINT('Ctrl Pts',(108.388321784241,0.303664341205276,
123.808216763862));
#272722=CARTESIAN_POINT('Ctrl Pts',(108.109874160429,-5.72191597137591,
126.767292563848));
#272723=CARTESIAN_POINT('Ctrl Pts',(107.831426536616,-6.48933503739778,
133.436236683461));
#272724=CARTESIAN_POINT('Ctrl Pts',(107.552978912803,-1.29337222569216,
137.68661527281));
#272725=CARTESIAN_POINT('Ctrl Pts',(107.27453128899,5.09113647667873,135.612538050821));
#272726=CARTESIAN_POINT('Ctrl Pts',(106.996083665177,6.79713947282576,129.119980660195));
#272727=CARTESIAN_POINT('Ctrl Pts',(106.717636041364,2.25690335216928,124.175286163858));
#272728=CARTESIAN_POINT('Ctrl Pts',(106.439188417551,-4.35731669327239,
125.322387242187));
#272729=CARTESIAN_POINT('Ctrl Pts',(106.160740793739,-6.96737556435125,
131.5071540432));
#272730=CARTESIAN_POINT('Ctrl Pts',(105.882293169926,-3.17475666701035,
137.046088019424));
#272731=CARTESIAN_POINT('Ctrl Pts',(105.603845546113,3.53530851182771,136.849179438675));
#272732=CARTESIAN_POINT('Ctrl Pts',(105.3253979223,6.99659787771835,131.097377667143));
#272733=CARTESIAN_POINT('Ctrl Pts',(105.046950298487,4.02835559679407,125.076307541727));
#272734=CARTESIAN_POINT('Ctrl Pts',(104.768502674674,-2.64174868147234,
124.319038362058));
#272735=CARTESIAN_POINT('Ctrl Pts',(104.490055050861,-6.88421497806359,
129.521463509594));
#272736=CARTESIAN_POINT('Ctrl Pts',(104.211607427049,-4.80042402241278,
135.902808426348));
#272737=CARTESIAN_POINT('Ctrl Pts',(103.933159803235,1.69472209608453,137.598928879852));
#272738=CARTESIAN_POINT('Ctrl Pts',(103.654712179423,6.63250140005722,133.051173033428));
#272739=CARTESIAN_POINT('Ctrl Pts',(103.37626455561,5.47533593308374,126.438706339714));
#272740=CARTESIAN_POINT('Ctrl Pts',(103.097816931797,-0.713395771362793,
123.838062653278));
#272741=CARTESIAN_POINT('Ctrl Pts',(102.819369307984,-6.24655161324796,
127.639106473447));
#272742=CARTESIAN_POINT('Ctrl Pts',(102.540921684171,-6.03943168356949,
134.348864220799));
#272743=CARTESIAN_POINT('Ctrl Pts',(102.262474060358,-0.282369079330704,
137.801396315408));
#272744=CARTESIAN_POINT('Ctrl Pts',(101.984026436545,5.73417691431645,134.823994427897));
#272745=CARTESIAN_POINT('Ctrl Pts',(101.705578812732,6.48129445382252,128.15274543872));
#272746=CARTESIAN_POINT('Ctrl Pts',(101.427131188919,1.27241901910234,123.9182012603));
#272747=CARTESIAN_POINT('Ctrl Pts',(101.148683565106,-5.1057473330482,126.01170112362));
#272748=CARTESIAN_POINT('Ctrl Pts',(100.870235941294,-6.7919813157512,132.509420927444));
#272749=CARTESIAN_POINT('Ctrl Pts',(100.591788317481,-2.23671627601227,
137.440273603317));
#272750=CARTESIAN_POINT('Ctrl Pts',(100.313340693668,4.37398175171709,136.273046427655));
#272751=CARTESIAN_POINT('Ctrl Pts',(100.034893069855,6.96520423050629,130.080364152676));
#272752=CARTESIAN_POINT('Ctrl Pts',(99.7564454460421,3.15574429060373,124.552999259737));
#272753=CARTESIAN_POINT('Ctrl Pts',(99.4779978222292,-3.55369048568456,
124.770330058661));
#272754=CARTESIAN_POINT('Ctrl Pts',(99.1995501984162,-6.99745731306031,
130.532640162439));
#272755=CARTESIAN_POINT('Ctrl Pts',(98.9211025746034,-4.01090271452764,
136.544648090195));
#272756=CARTESIAN_POINT('Ctrl Pts',(98.6426549507905,2.66147553516503,137.281612259238));
#272757=CARTESIAN_POINT('Ctrl Pts',(98.3642073269776,6.88808778834931,132.066298600918));
#272758=CARTESIAN_POINT('Ctrl Pts',(98.0857597031646,4.78488386583629,125.691325584995));
#272759=CARTESIAN_POINT('Ctrl Pts',(97.8073120793519,-1.71539457480834,
124.014981978356));
#272760=CARTESIAN_POINT('Ctrl Pts',(97.5288644555388,-6.63930920288774,
128.577745661565));
#272761=CARTESIAN_POINT('Ctrl Pts',(97.2504168317261,-5.46202302179963,
135.186659713151));
#272762=CARTESIAN_POINT('Ctrl Pts',(96.9719692079131,0.734595481663425,
137.768454983106));
#272763=CARTESIAN_POINT('Ctrl Pts',(96.6935215841003,6.25615662446226,133.950587746053));
#272764=CARTESIAN_POINT('Ctrl Pts',(96.4150739602873,6.0286154596223,127.24149147966));
#272765=CARTESIAN_POINT('Ctrl Pts',(96.1366263364746,0.26107120162757,123.806497895168));
#272766=CARTESIAN_POINT('Ctrl Pts',(95.8581787126614,-5.74638473662552,
126.80219828796));
#272767=CARTESIAN_POINT('Ctrl Pts',(95.5797310888487,-6.47319382842077,
133.47569034516));
#272768=CARTESIAN_POINT('Ctrl Pts',(95.3012834650358,-1.25145402499642,
137.694360884412));
#272769=CARTESIAN_POINT('Ctrl Pts',(95.0228358412229,5.12031089047184,135.581457773658));
#272770=CARTESIAN_POINT('Ctrl Pts',(94.7443882174101,6.78676023868958,129.078635750625));
#272771=CARTESIAN_POINT('Ctrl Pts',(94.465940593597,2.21650847922131,124.161670573963));
#272772=CARTESIAN_POINT('Ctrl Pts',(94.1874929697842,-4.39060629019222,
125.349013033923));
#272773=CARTESIAN_POINT('Ctrl Pts',(93.9090453459715,-6.96296837196094,
131.549553414704));
#272774=CARTESIAN_POINT('Ctrl Pts',(93.6305977221583,-3.13670267981308,
137.065298019608));
#272775=CARTESIAN_POINT('Ctrl Pts',(93.3521500983456,3.5720395386382,136.82754701583));
#272776=CARTESIAN_POINT('Ctrl Pts',(93.0737024745325,6.99825192491364,131.054781961061));
#272777=CARTESIAN_POINT('Ctrl Pts',(92.7952548507199,3.99341267580637,125.051891925383));
#272778=CARTESIAN_POINT('Ctrl Pts',(92.5168072269068,-2.68117773331193,
124.335239594101));
#272779=CARTESIAN_POINT('Ctrl Pts',(92.238359603094,-6.89189678833074,129.563393449252));
#272780=CARTESIAN_POINT('Ctrl Pts',(91.959911979281,-4.7692993827493,135.931935507467));
#272781=CARTESIAN_POINT('Ctrl Pts',(91.6814643554683,1.73605116235111,137.588486737821));
#272782=CARTESIAN_POINT('Ctrl Pts',(91.4030167316553,6.6460555000649,133.010757486647));
#272783=CARTESIAN_POINT('Ctrl Pts',(91.1245691078424,5.44865951108031,126.405457301267));
#272784=CARTESIAN_POINT('Ctrl Pts',(90.8461214840295,-0.755788386771977,
123.84253436519));
#272785=CARTESIAN_POINT('Ctrl Pts',(90.5676738602166,-6.26570367949625,
127.677189650927));
#272786=CARTESIAN_POINT('Ctrl Pts',(90.2892262364038,-6.01774338740505,
134.38556228421));
#272787=CARTESIAN_POINT('Ctrl Pts',(90.0107786125907,-0.239770905396614,
137.802985537273));
#272788=CARTESIAN_POINT('Ctrl Pts',(89.7323309887781,5.75853932521132,134.78901439096));
#272789=CARTESIAN_POINT('Ctrl Pts',(89.453883364965,6.46503323623579,128.113341088056));
#272790=CARTESIAN_POINT('Ctrl Pts',(89.1754357411521,1.23047743759138,123.910583269158));
#272791=CARTESIAN_POINT('Ctrl Pts',(88.8969881173393,-5.13482701403487,
126.042870053701));
#272792=CARTESIAN_POINT('Ctrl Pts',(88.6185404935264,-6.78147629000823,
132.550734054689));
#272793=CARTESIAN_POINT('Ctrl Pts',(88.3400928697134,-2.19628014899849,
137.453766182047));
#272794=CARTESIAN_POINT('Ctrl Pts',(88.0616452459006,4.4071901546906,136.246319437167));
#272795=CARTESIAN_POINT('Ctrl Pts',(87.7831976220877,6.96066800942769,130.037978391542));
#272796=CARTESIAN_POINT('Ctrl Pts',(87.5047499982748,3.1176320110373,124.533905171779));
#272797=CARTESIAN_POINT('Ctrl Pts',(87.2263023744621,-3.59035550070555,
124.792074177916));
#272798=CARTESIAN_POINT('Ctrl Pts',(86.9478547506488,-6.99898170591706,
130.57524070557));
#272799=CARTESIAN_POINT('Ctrl Pts',(86.6694071268362,-3.97588564265574,
136.568957239218));
#272800=CARTESIAN_POINT('Ctrl Pts',(86.3909595030232,2.70085509339449,137.265291093768));
#272801=CARTESIAN_POINT('Ctrl Pts',(86.1125118792103,6.89564194272181,132.024345474689));
#272802=CARTESIAN_POINT('Ctrl Pts',(85.8340642553976,4.75367071752436,125.662293371487));
#272803=CARTESIAN_POINT('Ctrl Pts',(85.5556166315845,-1.75669166735309,
124.025549863481));
#272804=CARTESIAN_POINT('Ctrl Pts',(85.2771690077717,-6.65274022909182,
128.618202275162));
#272805=CARTESIAN_POINT('Ctrl Pts',(84.9987213839588,-5.4352455247236,135.21982740374));
#272806=CARTESIAN_POINT('Ctrl Pts',(84.7202737601459,0.776974290360158,
137.763854263368));
#272807=CARTESIAN_POINT('Ctrl Pts',(84.4418261363329,6.27519268990729,133.912446452669));
#272808=CARTESIAN_POINT('Ctrl Pts',(84.1633785125202,6.00681556763514,127.204859597945));
#272809=CARTESIAN_POINT('Ctrl Pts',(83.8849308887072,0.218468387960617,
123.805038334852));
#272810=CARTESIAN_POINT('Ctrl Pts',(83.6064832648944,-5.77064056747553,
126.837252313669));
#272811=CARTESIAN_POINT('Ctrl Pts',(83.3280356410814,-6.45681275286598,
133.515045019753));
#272812=CARTESIAN_POINT('Ctrl Pts',(83.0495880172686,-1.20948945121144,
137.701851184522));
#272813=CARTESIAN_POINT('Ctrl Pts',(82.7711403934555,5.14929556926191,135.550200479404));
#272814=CARTESIAN_POINT('Ctrl Pts',(82.4926927696429,6.77612951865689,129.037354788424));
#272815=CARTESIAN_POINT('Ctrl Pts',(82.2142451458298,2.17603147273656,124.148301131391));
#272816=CARTESIAN_POINT('Ctrl Pts',(81.9357975220171,-4.42373319158141,
125.375840975569));
#272817=CARTESIAN_POINT('Ctrl Pts',(81.6573498982041,-6.95830316421689,
131.591925172815));
#272818=CARTESIAN_POINT('Ctrl Pts',(81.3789022743912,-3.09853246094448,
137.084276018453));
#272819=CARTESIAN_POINT('Ctrl Pts',(81.1004546505783,3.60863820220999,136.805691401599));
#272820=CARTESIAN_POINT('Ctrl Pts',(80.8220070267654,6.99964664931016,131.012176975526));
#272821=CARTESIAN_POINT('Ctrl Pts',(80.5435594029525,3.95832177744353,125.02768946888));
#272822=CARTESIAN_POINT('Ctrl Pts',(80.2651117791397,-2.72050743312451,
124.351680541802));
#272823=CARTESIAN_POINT('Ctrl Pts',(79.9866641553267,-6.89932321682792,
129.605369373404));
#272824=CARTESIAN_POINT('Ctrl Pts',(79.7082165315139,-4.73799801494326,
135.960872584412));
#272825=CARTESIAN_POINT('Ctrl Pts',(79.4297689077009,1.77731589860328,137.577793207502));
#272826=CARTESIAN_POINT('Ctrl Pts',(79.1513212838881,6.65936332804202,132.970260181018));
#272827=CARTESIAN_POINT('Ctrl Pts',(78.8728736600752,5.42178118699497,126.372371265798));
#272828=CARTESIAN_POINT('Ctrl Pts',(78.5944260362623,-0.798152996164653,
123.847264050135));
#272829=CARTESIAN_POINT('Ctrl Pts',(78.3159784124494,-6.28462356779051,
127.715388706879));
#272830=CARTESIAN_POINT('Ctrl Pts',(78.0375307886365,-5.99583210154638,
134.422127644877));
#272831=CARTESIAN_POINT('Ctrl Pts',(77.7590831648237,-0.197163846663491,
137.804315422519));
#272832=CARTESIAN_POINT('Ctrl Pts',(77.4806355410107,5.78268835131386,134.753886701214));
#272833=CARTESIAN_POINT('Ctrl Pts',(77.2021879171979,6.44853245446487,128.07403645411));
#272834=CARTESIAN_POINT('Ctrl Pts',(76.9237402933849,1.18849026028645,123.903220729472));
#272835=CARTESIAN_POINT('Ctrl Pts',(76.6452926695721,-5.16371642211823,
126.074215422566));
#272836=CARTESIAN_POINT('Ctrl Pts',(76.3668450457591,-6.77071997416741,
132.591982469425));
#272837=CARTESIAN_POINT('Ctrl Pts',(76.0883974219463,-2.15576263801617,
137.467012364608));
#272838=CARTESIAN_POINT('Ctrl Pts',(75.8099497981334,4.44023524761227,136.219390792892));
#272839=CARTESIAN_POINT('Ctrl Pts',(75.5315021743204,6.95587385823614,129.995621028982));
#272840=CARTESIAN_POINT('Ctrl Pts',(75.2530545505077,3.0794042064702,124.515043437855));
#272841=CARTESIAN_POINT('Ctrl Pts',(74.9746069266946,-3.62688747378295,
124.814041084656));
#272842=CARTESIAN_POINT('Ctrl Pts',(74.6961593028819,-7.0002467489329,130.617849738824));
#272843=CARTESIAN_POINT('Ctrl Pts',(74.4177116790688,-3.94072124287924,
136.593052778991));
#272844=CARTESIAN_POINT('Ctrl Pts',(74.1392640552561,2.74013457044532,137.248730516143));
#272845=CARTESIAN_POINT('Ctrl Pts',(73.860816431443,6.90294057654623,131.982347141473));
#272846=CARTESIAN_POINT('Ctrl Pts',(73.5823688076304,4.72228142019582,125.633451699173));
#272847=CARTESIAN_POINT('Ctrl Pts',(73.3039211838172,-1.79792366504193,
124.036368939932));
#272848=CARTESIAN_POINT('Ctrl Pts',(73.0254735600045,-6.66592473556012,
128.658739897661));
#272849=CARTESIAN_POINT('Ctrl Pts',(72.7470259361915,-5.40826662262595,
135.252831477583));
#272850=CARTESIAN_POINT('Ctrl Pts',(72.4685783123786,0.819324307988826,
137.758995657032));
#272851=CARTESIAN_POINT('Ctrl Pts',(72.1901306885658,6.2939962257795,133.87418998802));
#272852=CARTESIAN_POINT('Ctrl Pts',(71.9116830647529,5.98479309088811,127.168361097063));
#272853=CARTESIAN_POINT('Ctrl Pts',(71.63323544094,0.17585747886725,123.803838136996));
#272854=CARTESIAN_POINT('Ctrl Pts',(71.3547878171271,-5.79468256511725,
126.872453342036));
#272855=CARTESIAN_POINT('Ctrl Pts',(71.0763401933142,-6.44019241774003,
133.554299248939));
#272856=CARTESIAN_POINT('Ctrl Pts',(70.7978925695013,-1.16748005934989,
137.709085895581));
#272857=CARTESIAN_POINT('Ctrl Pts',(70.5194449456884,5.17808943901089,135.518767326308));
#272858=CARTESIAN_POINT('Ctrl Pts',(70.2409973218756,6.76524770665308,128.996139303274));
#272859=CARTESIAN_POINT('Ctrl Pts',(69.9625496980626,2.1354738326052,124.135178331551));
#272860=CARTESIAN_POINT('Ctrl Pts',(69.6841020742497,-4.45669616991057,
125.402870073008));
#272861=CARTESIAN_POINT('Ctrl Pts',(69.4056544504369,-6.95338011399016,
131.634267747431));
#272862=CARTESIAN_POINT('Ctrl Pts',(69.1272068266238,-3.06024742481583,
137.103021312725));
#272863=CARTESIAN_POINT('Ctrl Pts',(68.8487592028112,3.64510314636624,136.783613405848));
#272864=CARTESIAN_POINT('Ctrl Pts',(68.5703115789981,7.00078199922599,130.969564289278));
#272865=CARTESIAN_POINT('Ctrl Pts',(68.2918639551854,3.92308420201135,125.003701069051));
#272866=CARTESIAN_POINT('Ctrl Pts',(68.0134163313723,-2.75973632353393,
124.368360595937));
#272867=CARTESIAN_POINT('Ctrl Pts',(67.7349687075595,-6.90649398836592,
129.647389726619));
#272868=CARTESIAN_POINT('Ctrl Pts',(67.4565210837467,-4.70652107887851,
135.98961858491));
#272869=CARTESIAN_POINT('Ctrl Pts',(67.1780734599337,1.81851477576126,137.566848685147));
#272870=CARTESIAN_POINT('Ctrl Pts',(66.8996258361208,6.67242439086218,132.929682617185));
#272871=CARTESIAN_POINT('Ctrl Pts',(66.6211782123079,5.39470195681365,126.339449459324));
#272872=CARTESIAN_POINT('Ctrl Pts',(66.3427305884951,-0.840488029704522,
123.852251532852));
#272873=CARTESIAN_POINT('Ctrl Pts',(66.0642829646821,-6.30331057704718,
127.753702225821));
#272874=CARTESIAN_POINT('Ctrl Pts',(65.7858353408693,-5.97369863792435,
134.458558947856));
#272875=CARTESIAN_POINT('Ctrl Pts',(65.5073877170563,-0.154549481951222,
137.805385921867));
#272876=CARTESIAN_POINT('Ctrl Pts',(65.2289400932435,5.80662309777304,134.718612660325));
#272877=CARTESIAN_POINT('Ctrl Pts',(64.9504924694306,6.43179271995227,128.03483299333));
#272878=CARTESIAN_POINT('Ctrl Pts',(64.6720448456177,1.14645904303803,123.896113914062));
#272879=CARTESIAN_POINT('Ctrl Pts',(64.3935972218049,-5.19241448679041,
126.1057360687));
#272880=CARTESIAN_POINT('Ctrl Pts',(64.1151495979918,-6.75971276680813,
132.633164643176));
#272881=CARTESIAN_POINT('Ctrl Pts',(63.8367019741791,-2.11516524445634,
137.480011660159));
#272882=CARTESIAN_POINT('Ctrl Pts',(63.5582543503661,4.47311580598391,136.192261492683));
#272883=CARTESIAN_POINT('Ctrl Pts',(63.2798067265533,6.95082195458075,129.953293634565));
#272884=CARTESIAN_POINT('Ctrl Pts',(63.0013591027403,3.041062293448,124.496414756892));
#272885=CARTESIAN_POINT('Ctrl Pts',(62.7229114789275,-3.66328505121137,
124.836229964889));
#272886=CARTESIAN_POINT('Ctrl Pts',(62.4444638551145,-7.00125239523119,
130.660465683307));
#272887=CARTESIAN_POINT('Ctrl Pts',(62.1660162313017,-3.90541081822766,
136.616933816649));
#272888=CARTESIAN_POINT('Ctrl Pts',(61.8875686074887,2.77931251080179,137.231931140021));
#272889=CARTESIAN_POINT('Ctrl Pts',(61.609120983676,6.909983419369,131.940305157533));
#272890=CARTESIAN_POINT('Ctrl Pts',(61.3306733598629,4.69071713699276,125.604801636791));
#272891=CARTESIAN_POINT('Ctrl Pts',(61.0522257360502,-1.83908904000824,
124.047438806804));
#272892=CARTESIAN_POINT('Ctrl Pts',(60.7737781122372,-6.67886223373588,
128.699357026925));
#272893=CARTESIAN_POINT('Ctrl Pts',(60.4953304884244,-5.38108731521968,
135.285670711703));
#272894=CARTESIAN_POINT('Ctrl Pts',(60.2168828646114,0.861643965253713,
137.753879344138));
#272895=CARTESIAN_POINT('Ctrl Pts',(59.9384352407986,6.31256653530686,133.835819769716));
#272896=CARTESIAN_POINT('Ctrl Pts',(59.6599876169856,5.96254884543232,127.131997329482));
#272897=CARTESIAN_POINT('Ctrl Pts',(59.3815399931728,0.133240053310041,
123.802897346075));
#272898=CARTESIAN_POINT('Ctrl Pts',(59.1030923693598,-5.81850983866561,
126.907800068673));
#272899=CARTESIAN_POINT('Ctrl Pts',(58.824644745547,-6.42333343891552,133.593451578138));
#272900=CARTESIAN_POINT('Ctrl Pts',(58.5461971217341,-1.12542740608588,
137.716064749505));
#272901=CARTESIAN_POINT('Ctrl Pts',(58.2677494979212,5.20669143275151,135.487159479138));
#272902=CARTESIAN_POINT('Ctrl Pts',(57.9893018741083,6.75411520590753,128.954990822428));
#272903=CARTESIAN_POINT('Ctrl Pts',(57.7108542502954,2.09483706170563,124.122302660713));
#272904=CARTESIAN_POINT('Ctrl Pts',(57.4324066264825,-4.48949400372376,
125.430099324666));
#272905=CARTESIAN_POINT('Ctrl Pts',(57.1539590026696,-6.94819940370625,
131.676579569534));
#272906=CARTESIAN_POINT('Ctrl Pts',(56.8755113788568,-3.02184899009409,
137.121533207807));
#272907=CARTESIAN_POINT('Ctrl Pts',(56.5970637550437,3.68143301988451,136.761313846687));
#272908=CARTESIAN_POINT('Ctrl Pts',(56.318616131231,7.00165793259049,130.926945481348));
#272909=CARTESIAN_POINT('Ctrl Pts',(56.040168507418,3.88770125525153,124.979927614796));
#272910=CARTESIAN_POINT('Ctrl Pts',(55.7617208836052,-2.79886295089852,
124.385279138419));
#272911=CARTESIAN_POINT('Ctrl Pts',(55.4832732597923,-6.91340883722955,
129.689452951814));
#272912=CARTESIAN_POINT('Ctrl Pts',(55.2048256359794,-4.67486974094423,
136.018172443767));
#272913=CARTESIAN_POINT('Ctrl Pts',(54.9263780121665,1.85964626718557,137.555653576309));
#272914=CARTESIAN_POINT('Ctrl Pts',(54.6479303883536,6.68523820454244,132.889026298762));
#272915=CARTESIAN_POINT('Ctrl Pts',(54.3694827645407,5.36742282396772,126.306693101776));
#272916=CARTESIAN_POINT('Ctrl Pts',(54.0910351407278,-0.882791918651148,
123.857496628527));
#272917=CARTESIAN_POINT('Ctrl Pts',(53.8125875169149,-6.32176401481248,
127.792128788032));
#272918=CARTESIAN_POINT('Ctrl Pts',(53.534139893102,-5.95134381670231,134.494854843172));
#272919=CARTESIAN_POINT('Ctrl Pts',(53.2556922692892,-0.111929390351441,
137.806196995646));
#272920=CARTESIAN_POINT('Ctrl Pts',(52.9772446454762,5.83034267767769,134.683193575387));
#272921=CARTESIAN_POINT('Ctrl Pts',(52.6987970216634,6.41481465299549,127.995732158415));
#272922=CARTESIAN_POINT('Ctrl Pts',(52.4203493978505,1.10438534332797,123.889263086274));
#272923=CARTESIAN_POINT('Ctrl Pts',(52.1419017740376,-5.22092014463445,
126.137430824095));
#272924=CARTESIAN_POINT('Ctrl Pts',(51.8634541502246,-6.74845507580631,
132.674279049921));
#272925=CARTESIAN_POINT('Ctrl Pts',(51.5850065264118,-2.07448947267055,
137.492763587005));
#272926=CARTESIAN_POINT('Ctrl Pts',(51.3065589025989,4.50583061140446,136.164932541826));
#272927=CARTESIAN_POINT('Ctrl Pts',(51.028111278786,6.94551248566166,129.910997776748));
#272928=CARTESIAN_POINT('Ctrl Pts',(50.7496636549731,3.00260769274395,124.478019819181));
#272929=CARTESIAN_POINT('Ctrl Pts',(50.4712160311602,-3.69954688426507,
124.858639996399));
#272930=CARTESIAN_POINT('Ctrl Pts',(50.1927684073473,-7.00199860754717,
130.70308695987));
#272931=CARTESIAN_POINT('Ctrl Pts',(49.9143207835345,-3.86995567714208,
136.640599467269));
#272932=CARTESIAN_POINT('Ctrl Pts',(49.6358731597215,2.81838746271124,137.214893587909));
#272933=CARTESIAN_POINT('Ctrl Pts',(49.3574255359087,6.91677021021505,131.89822108075));
#272934=CARTESIAN_POINT('Ctrl Pts',(49.0789779120958,4.65897903754105,125.576344245977));
#272935=CARTESIAN_POINT('Ctrl Pts',(48.8005302882828,-1.88018626685394,
124.058759053897));
#272936=CARTESIAN_POINT('Ctrl Pts',(48.5220826644701,-6.69155224421552,
128.740052157871));
#272937=CARTESIAN_POINT('Ctrl Pts',(48.243635040657,-5.35370860964396,135.318343889229));
#272938=CARTESIAN_POINT('Ctrl Pts',(47.9651874168443,0.903931693984841,
137.748505514272));
#272939=CARTESIAN_POINT('Ctrl Pts',(47.6867397930313,6.33090293035988,133.797337219578));
#272940=CARTESIAN_POINT('Ctrl Pts',(47.4082921692184,5.94008365553619,127.095769642671));
#272941=CARTESIAN_POINT('Ctrl Pts',(47.1298445454056,0.0906176904940206,
123.80221599695));
#272942=CARTESIAN_POINT('Ctrl Pts',(46.8513969215926,-5.84212150519187,
126.943291183793));
#272943=CARTESIAN_POINT('Ctrl Pts',(46.5729492977799,-6.40623644110861,
133.632500556544));
#272944=CARTESIAN_POINT('Ctrl Pts',(46.2945016739667,-1.08333304969514,
137.722787487691));
#272945=CARTESIAN_POINT('Ctrl Pts',(46.016054050154,5.23510049062639,135.455378109134));
#272946=CARTESIAN_POINT('Ctrl Pts',(45.737606426341,6.7427324289391,128.913910870662));
#272947=CARTESIAN_POINT('Ctrl Pts',(45.4591588025282,2.0541226658487,124.10967459599));
#272948=CARTESIAN_POINT('Ctrl Pts',(45.1807111787153,-4.5221254776858,125.457527721552));
#272949=CARTESIAN_POINT('Ctrl Pts',(44.9022635549024,-6.94276122533821,
131.718859071242));
#272950=CARTESIAN_POINT('Ctrl Pts',(44.6238159310895,-2.98333857964632,
137.139811017737));
#272951=CARTESIAN_POINT('Ctrl Pts',(44.3453683072766,3.71762647654865,136.738793550433));
#272952=CARTESIAN_POINT('Ctrl Pts',(44.0669206834637,7.00227441694529,130.88432213099));
#272953=CARTESIAN_POINT('Ctrl Pts',(43.7884730596509,3.85217424829189,124.956369987047));
#272954=CARTESIAN_POINT('Ctrl Pts',(43.5100254358379,-2.8378858653675,124.402435542326));
#272955=CARTESIAN_POINT('Ctrl Pts',(43.2315778120251,-6.92006750718621,
129.731557490323));
#272956=CARTESIAN_POINT('Ctrl Pts',(42.9531301882121,-4.64304517399252,
136.04653310291));
#272957=CARTESIAN_POINT('Ctrl Pts',(42.6746825643993,1.90070884873357,137.544208295828));
#272958=CARTESIAN_POINT('Ctrl Pts',(42.3962349405864,6.69780429426274,132.848292732287));
#272959=CARTESIAN_POINT('Ctrl Pts',(42.1177873167735,5.33994479929498,126.274103406951));
#272960=CARTESIAN_POINT('Ctrl Pts',(41.8393396929606,-0.925063095418803,
123.862999142802));
#272961=CARTESIAN_POINT('Ctrl Pts',(41.5608920691476,-6.33998319728738,
127.8306669696));
#272962=CARTESIAN_POINT('Ctrl Pts',(41.2824444453348,-5.92876846624656,
134.531013985867));
#272963=CARTESIAN_POINT('Ctrl Pts',(41.0039968215219,-0.069305151166692,
137.806748613804));
#272964=CARTESIAN_POINT('Ctrl Pts',(40.725549197709,5.85384621209049,134.647630758868));
#272965=CARTESIAN_POINT('Ctrl Pts',(40.4471015738961,6.39759888272248,127.956735398261));
#272966=CARTESIAN_POINT('Ctrl Pts',(40.1686539500832,1.06227072021291,123.882668499967));
#272967=CARTESIAN_POINT('Ctrl Pts',(39.8902063262704,-5.24923233936253,
126.169298514289));
#272968=CARTESIAN_POINT('Ctrl Pts',(39.6117587024575,-6.73694731831984,
132.715324166149));
#272969=CARTESIAN_POINT('Ctrl Pts',(39.3333110786445,-2.03373682991476,
137.505267672621));
#272970=CARTESIAN_POINT('Ctrl Pts',(39.0548634548317,4.53837845161457,136.137404953004));
#272971=CARTESIAN_POINT('Ctrl Pts',(38.7764158310188,6.9399456482232,129.86873502282));
#272972=CARTESIAN_POINT('Ctrl Pts',(38.4979682072059,2.96404182930761,124.459859306355));
#272973=CARTESIAN_POINT('Ctrl Pts',(38.219520583393,-3.73567162924815,124.881270348773));
#272974=CARTESIAN_POINT('Ctrl Pts',(37.9410729595801,-7.00248535822977,
130.745711989165));
#272975=CARTESIAN_POINT('Ctrl Pts',(37.6626253357672,-3.83435713342598,
136.664048853912));
#272976=CARTESIAN_POINT('Ctrl Pts',(37.3841777119543,2.8573579782368,137.197618491141));
#272977=CARTESIAN_POINT('Ctrl Pts',(37.1057300881414,6.92330069759731,131.856096470565));
#272978=CARTESIAN_POINT('Ctrl Pts',(36.8272824643285,4.62706829790778,125.548080581235));
#272979=CARTESIAN_POINT('Ctrl Pts',(36.5488348405156,-1.92121382270608,
124.070329261737));
#272980=CARTESIAN_POINT('Ctrl Pts',(36.2703872167028,-6.70399429676593,
128.780823782526));
#272981=CARTESIAN_POINT('Ctrl Pts',(35.9919395928899,-5.32613152042688,
135.350849799446));
#272982=CARTESIAN_POINT('Ctrl Pts',(35.7134919690769,0.946185927194629,
137.742874366562));
#272983=CARTESIAN_POINT('Ctrl Pts',(35.4350443452641,6.34900473147662,133.758743763591));
#272984=CARTESIAN_POINT('Ctrl Pts',(35.1565967214512,5.91739835365575,127.059679379064));
#272985=CARTESIAN_POINT('Ctrl Pts',(34.8781490976383,0.0479919698059151,
123.80179411487));
#272986=CARTESIAN_POINT('Ctrl Pts',(34.5997014738253,-5.8655166897575,126.978925372262));
#272987=CARTESIAN_POINT('Ctrl Pts',(34.3212538500126,-6.38890205785425,
133.671444737187));
#272988=CARTESIAN_POINT('Ctrl Pts',(34.0428062261996,-1.04119854999986,
137.729253861025));
#272989=CARTESIAN_POINT('Ctrl Pts',(33.7643586023867,5.26331555992738,135.423424393967));
#272990=CARTESIAN_POINT('Ctrl Pts',(33.4859109785738,6.73109979754094,128.872900970206));
#272991=CARTESIAN_POINT('Ctrl Pts',(33.207463354761,2.01333215372067,124.097294605319));
#272992=CARTESIAN_POINT('Ctrl Pts',(32.9290157309481,-4.55458938262534,
125.485154247296));
#272993=CARTESIAN_POINT('Ctrl Pts',(32.6505681071352,-6.93706578039975,
131.761104685873));
#272994=CARTESIAN_POINT('Ctrl Pts',(32.3721204833222,-2.94471762049033,
137.157854065221));
#272995=CARTESIAN_POINT('Ctrl Pts',(32.0936728595094,3.75368217519627,136.716053351584));
#272996=CARTESIAN_POINT('Ctrl Pts',(31.8152252356965,7.00263142944649,130.84169581763));
#272997=CARTESIAN_POINT('Ctrl Pts',(31.5367776118836,3.8165044975991,124.933029058741));
#272998=CARTESIAN_POINT('Ctrl Pts',(31.2583299880707,-2.87680362093211,
124.41982917192));
#272999=CARTESIAN_POINT('Ctrl Pts',(30.9798823642578,-6.92646975149653,
129.773701781947));
#273000=CARTESIAN_POINT('Ctrl Pts',(30.7014347404449,-4.6110485572945,136.074699511423));
#273001=CARTESIAN_POINT('Ctrl Pts',(30.422987116632,1.94170099881587,137.532513267813));
#273002=CARTESIAN_POINT('Ctrl Pts',(30.1445394928192,6.71012219438185,132.807483427156));
#273003=CARTESIAN_POINT('Ctrl Pts',(29.8660918690062,5.31226890100394,126.241681582474));
#273004=CARTESIAN_POINT('Ctrl Pts',(29.5876442451933,-0.967299993633269,
123.868758871779));
#273005=CARTESIAN_POINT('Ctrl Pts',(29.3091966213805,-6.35796744935336,
127.869315342481));
#273006=CARTESIAN_POINT('Ctrl Pts',(29.0307489975676,-5.90597342309497,
134.567035036052));
#273007=CARTESIAN_POINT('Ctrl Pts',(28.7523013737546,-0.026678343854083,
137.807040755898));
#273008=CARTESIAN_POINT('Ctrl Pts',(28.4738537499418,5.87713283007914,134.611925528561));
#273009=CARTESIAN_POINT('Ctrl Pts',(28.1954061261289,6.38014604707014,127.917844157905));
#273010=CARTESIAN_POINT('Ctrl Pts',(27.916958502316,1.02011673426565,123.876330399509));
#273011=CARTESIAN_POINT('Ctrl Pts',(27.6385108785031,-5.27735002185588,
126.201337958415));
#273012=CARTESIAN_POINT('Ctrl Pts',(27.3600632546902,-6.72518992077305,
132.756298470923));
#273013=CARTESIAN_POINT('Ctrl Pts',(27.0816156308773,-1.99290882629253,
137.51752345366));
#273014=CARTESIAN_POINT('Ctrl Pts',(26.8031680070644,4.57075812054227,136.109679746264));
#273015=CARTESIAN_POINT('Ctrl Pts',(26.5247203832516,6.93412164854658,129.826506938842));
#273016=CARTESIAN_POINT('Ctrl Pts',(26.2462727594386,2.92536613221128,124.441933891359));
#273017=CARTESIAN_POINT('Ctrl Pts',(25.9678251356258,-3.7716579475455,124.904120183435));
#273018=CARTESIAN_POINT('Ctrl Pts',(25.6893775118128,-7.00271262924226,
130.788339191706));
#273019=CARTESIAN_POINT('Ctrl Pts',(25.410929888,-3.79861650619593,136.687281107654));
#273020=CARTESIAN_POINT('Ctrl Pts',(25.1324822641871,2.89622261331168,137.180106489852));
#273021=CARTESIAN_POINT('Ctrl Pts',(24.8540346403742,6.92957463952618,131.813932887921));
#273022=CARTESIAN_POINT('Ctrl Pts',(24.5755870165613,4.59498610055721,125.520011689881));
#273023=CARTESIAN_POINT('Ctrl Pts',(24.2971393927484,-1.96217018727317,
124.082149001586));
#273024=CARTESIAN_POINT('Ctrl Pts',(24.0186917689355,-6.71618793034234,
128.821670390082));
#273025=CARTESIAN_POINT('Ctrl Pts',(23.7402441451226,-5.29835706944761,
135.383187237832));
#273026=CARTESIAN_POINT('Ctrl Pts',(23.4617965213097,0.988405099136929,
137.736986109674));
#273027=CARTESIAN_POINT('Ctrl Pts',(23.1833488974968,6.36687126788796,133.720040831851));
#273028=CARTESIAN_POINT('Ctrl Pts',(22.9049012736839,5.89449378040337,127.023727875996));
#273029=CARTESIAN_POINT('Ctrl Pts',(22.6264536498711,0.00536447075796404,
123.801631715467));
#273030=CARTESIAN_POINT('Ctrl Pts',(22.3480060260581,-5.88869452544514,
127.01470131364));
#273031=CARTESIAN_POINT('Ctrl Pts',(22.0695584022453,-6.3713309314846,133.710282676972));
#273032=CARTESIAN_POINT('Ctrl Pts',(21.7911107784324,-0.999025468309402,
137.735463629893));
#273033=CARTESIAN_POINT('Ctrl Pts',(21.5126631546195,5.29133559513472,135.391299517692));
#273034=CARTESIAN_POINT('Ctrl Pts',(21.2342155308066,6.71921774276442,128.831962640697));
#273035=CARTESIAN_POINT('Ctrl Pts',(20.9557679069937,1.97246703682929,124.085163147446));
#273036=CARTESIAN_POINT('Ctrl Pts',(20.6773202831809,-4.58688451558038,
125.51297787819));
#273037=CARTESIAN_POINT('Ctrl Pts',(20.3988726593679,-6.93111327993769,
131.803314848003));
#273038=CARTESIAN_POINT('Ctrl Pts',(20.120425035555,-2.90598754374001,137.175661681671));
#273039=CARTESIAN_POINT('Ctrl Pts',(19.8419774117421,3.78959877977074,136.693094092787));
#273040=CARTESIAN_POINT('Ctrl Pts',(19.5635297879293,7.00272895686486,130.799068120799));
#273041=CARTESIAN_POINT('Ctrl Pts',(19.2850821641163,3.78069332492835,124.909905694786));
#273042=CARTESIAN_POINT('Ctrl Pts',(19.0066345403035,-2.91561477548059,
124.437459382677));
#273043=CARTESIAN_POINT('Ctrl Pts',(18.7281869164906,-6.932615332923,129.815884265012));
#273044=CARTESIAN_POINT('Ctrl Pts',(18.4497392926777,-4.57888107649638,
136.102670625591));
#273045=CARTESIAN_POINT('Ctrl Pts',(18.1712916688647,1.98262119845391,137.520568925627));
#273046=CARTESIAN_POINT('Ctrl Pts',(17.892844045052,6.72219144845534,132.766599895572));
#273047=CARTESIAN_POINT('Ctrl Pts',(17.614396421239,5.28439615463518,126.209428829746));
#273048=CARTESIAN_POINT('Ctrl Pts',(17.3359487974261,-1.00950104819076,
123.87477560203));
#273049=CARTESIAN_POINT('Ctrl Pts',(17.0575011736132,-6.37571610459714,
127.908072474542));
#273050=CARTESIAN_POINT('Ctrl Pts',(16.7790535498004,-5.88295953192644,
134.602916658952));
#273051=CARTESIAN_POINT('Ctrl Pts',(16.5006059259874,0.0159494520341194,
137.807073411106));
#273052=CARTESIAN_POINT('Ctrl Pts',(16.2221583021745,5.90020166874948,134.576079207535));
#273053=CARTESIAN_POINT('Ctrl Pts',(15.9437106783617,6.3624567927597,127.879059878479));
#273054=CARTESIAN_POINT('Ctrl Pts',(15.6652630545488,0.977924947517885,
123.870249019757));
#273055=CARTESIAN_POINT('Ctrl Pts',(15.3868154307359,-5.3052721502032,126.233547969238));
#273056=CARTESIAN_POINT('Ctrl Pts',(15.108367806923,-6.71318331884074,132.797200445919));
#273057=CARTESIAN_POINT('Ctrl Pts',(14.8299201831101,-1.95200697470083,
137.529530475982));
#273058=CARTESIAN_POINT('Ctrl Pts',(14.5514725592972,4.6029684183469,136.081757948972));
#273059=CARTESIAN_POINT('Ctrl Pts',(14.2730249354843,6.92804070244224,129.784315089592));
#273060=CARTESIAN_POINT('Ctrl Pts',(13.9945773116714,2.88658203459712,124.424244238425));
#273061=CARTESIAN_POINT('Ctrl Pts',(13.7161296878585,-3.80750450567058,
124.927188653676));
#273062=CARTESIAN_POINT('Ctrl Pts',(13.4376820640456,-7.00268041216303,
130.830966987928));
#273063=CARTESIAN_POINT('Ctrl Pts',(13.1592344402328,-3.7627351198343,136.710295367612));
#273064=CARTESIAN_POINT('Ctrl Pts',(12.8807868164199,2.93497992779253,137.162358232954));
#273065=CARTESIAN_POINT('Ctrl Pts',(12.602339192607,6.93559180351842,131.771731895206));
#273066=CARTESIAN_POINT('Ctrl Pts',(12.323891568794,4.56273363430679,125.49213861202));
#273067=CARTESIAN_POINT('Ctrl Pts',(12.0454439449812,-2.00305384290271,
124.094217835458));
#273068=CARTESIAN_POINT('Ctrl Pts',(11.7669963211683,-6.72813269310505,
128.862590466954));
#273069=CARTESIAN_POINT('Ctrl Pts',(11.4885486973554,-5.27038628589867,
135.415355006116));
#273070=CARTESIAN_POINT('Ctrl Pts',(11.2101010735425,1.03058764536478,137.730840961799));
#273071=CARTESIAN_POINT('Ctrl Pts',(10.9316534497296,6.38450187754329,133.681229858508));
#273072=CARTESIAN_POINT('Ctrl Pts',(10.6532058259167,5.87137078451608,126.987916465666));
#273073=CARTESIAN_POINT('Ctrl Pts',(10.3747582021038,-0.0372632270726686,
123.801728804758));
#273074=CARTESIAN_POINT('Ctrl Pts',(10.0963105782909,-5.91165415339157,
127.050617682238));
#273075=CARTESIAN_POINT('Ctrl Pts',(9.81786295447806,-6.35352371310424,
133.749012936746));
#273076=CARTESIAN_POINT('Ctrl Pts',(9.53941533066515,-0.956815367363035,
137.741416564191));
#273077=CARTESIAN_POINT('Ctrl Pts',(9.26096770685226,5.31915955795546,135.35900467071));
#273078=CARTESIAN_POINT('Ctrl Pts',(8.98252008303941,6.70708670490366,128.791097399121));
#273079=CARTESIAN_POINT('Ctrl Pts',(8.70407245922646,1.93152882944647,124.073280671906));
#273080=CARTESIAN_POINT('Ctrl Pts',(8.42562483541358,-4.61900967984285,
125.540997583217));
#273081=CARTESIAN_POINT('Ctrl Pts',(8.14717721160073,-6.92490394452403,
131.845487993513));
#273082=CARTESIAN_POINT('Ctrl Pts',(7.86872958778781,-2.86714978455288,
137.193233207215));
#273083=CARTESIAN_POINT('Ctrl Pts',(7.59028196397491,3.82537495936868,136.669916624805));
#273084=CARTESIAN_POINT('Ctrl Pts',(7.31183434016203,7.00256699558648,130.756440620084));
#273085=CARTESIAN_POINT('Ctrl Pts',(7.03338671634916,3.7447420572761,124.887000752025));
#273086=CARTESIAN_POINT('Ctrl Pts',(6.75493909253623,-2.95431789085107,
124.455325521299));
#273087=CARTESIAN_POINT('Ctrl Pts',(6.47649146872337,-6.9385040237388,129.858103376433));
#273088=CARTESIAN_POINT('Ctrl Pts',(6.19804384491048,-4.54654392357636,
136.130445408932));
#273089=CARTESIAN_POINT('Ctrl Pts',(5.91959622109758,2.02346793133434,137.508375711873));
#273090=CARTESIAN_POINT('Ctrl Pts',(5.64114859728465,6.73401160925262,132.725643652489));
#273091=CARTESIAN_POINT('Ctrl Pts',(5.36270097347181,5.25632759302358,126.177346343905));
#273092=CARTESIAN_POINT('Ctrl Pts',(5.08425334965889,-1.05166469531565,
123.881049110601));
#273093=CARTESIAN_POINT('Ctrl Pts',(4.80580572584599,-6.39322850533622,
127.946936929627));
#273094=CARTESIAN_POINT('Ctrl Pts',(4.5273581020331,-5.85972764552883,134.638657524961));
#273095=CARTESIAN_POINT('Ctrl Pts',(4.24891047822024,0.0585766569097649,
137.806846578216));
#273096=CARTESIAN_POINT('Ctrl Pts',(3.97046285440732,5.92305187327717,134.54009312409));
#273097=CARTESIAN_POINT('Ctrl Pts',(3.69201523059441,6.34453177527304,127.840383997147));
#273098=CARTESIAN_POINT('Ctrl Pts',(3.41356760678156,0.935696923401329,
123.864424586062));
#273099=CARTESIAN_POINT('Ctrl Pts',(3.13511998296867,-5.33299768974021,
126.265927353204));
#273100=CARTESIAN_POINT('Ctrl Pts',(2.85667235915575,-6.70092795743158,
132.838028575505));
#273101=CARTESIAN_POINT('Ctrl Pts',(2.57822473534285,-1.91103279077285,
137.541288294661));
#273102=CARTESIAN_POINT('Ctrl Pts',(2.29977711153,4.63500815146407,136.053640595781));
#273103=CARTESIAN_POINT('Ctrl Pts',(2.02132948771708,6.92170303524179,129.742161038504));
#273104=CARTESIAN_POINT('Ctrl Pts',(1.74288186390418,2.84769097362441,124.40679100305));
#273105=CARTESIAN_POINT('Ctrl Pts',(1.46443424009131,-3.84320997531586,
124.950474904685));
#273106=CARTESIAN_POINT('Ctrl Pts',(1.18598661627842,-7.00238870818588,
130.873593798241));
#273107=CARTESIAN_POINT('Ctrl Pts',(0.907538992465495,-3.72671430393905,
136.733090780986));
#273108=CARTESIAN_POINT('Ctrl Pts',(0.629091368652655,2.97362848551254,
137.144374378117));
#273109=CARTESIAN_POINT('Ctrl Pts',(0.350643744839755,6.94135196660579,
131.729495056193));
#273110=CARTESIAN_POINT('Ctrl Pts',(0.0721961210268491,4.53031209428387,
125.4644623805));
#273111=CARTESIAN_POINT('Ctrl Pts',(-0.206251502786054,-2.04386327463549,
124.106535316138));
#273112=CARTESIAN_POINT('Ctrl Pts',(-0.484699126598912,-6.73982814243653,
128.903582496833));
#273113=CARTESIAN_POINT('Ctrl Pts',(-0.763146750411823,-5.24222020624778,
135.447351912307));
#273114=CARTESIAN_POINT('Ctrl Pts',(-1.04159437422473,1.07273200278813,
137.724439150648));
#273115=CARTESIAN_POINT('Ctrl Pts',(-1.32004199803759,6.40189590713365,
133.642312281717));
#273116=CARTESIAN_POINT('Ctrl Pts',(-1.59848962185049,5.84803022282516,
126.952246475077));
#273117=CARTESIAN_POINT('Ctrl Pts',(-1.87693724566341,-0.0798895441007186,
123.802085379146));
#273118=CARTESIAN_POINT('Ctrl Pts',(-2.1553848694763,-5.93439472281934,
127.08667314716));
#273119=CARTESIAN_POINT('Ctrl Pts',(-2.43383249328916,-6.33548106256618,
133.787634081347));
#273120=CARTESIAN_POINT('Ctrl Pts',(-2.71228011710207,-0.914569811271147,
137.747112443329));
#273121=CARTESIAN_POINT('Ctrl Pts',(-2.99072774091498,5.34678641736288,
135.326541049718));
#273122=CARTESIAN_POINT('Ctrl Pts',(-3.26917536472784,6.6947071334783,128.750306759754));
#273123=CARTESIAN_POINT('Ctrl Pts',(-3.54762298854074,1.89051904855254,
124.061647619009));
#273124=CARTESIAN_POINT('Ctrl Pts',(-3.82607061235365,-4.65096368500298,
125.569212324096));
#273125=CARTESIAN_POINT('Ctrl Pts',(-4.10451823616654,-6.91843800424817,
131.887622559669));
#273126=CARTESIAN_POINT('Ctrl Pts',(-4.38296585997939,-2.82820578207579,
137.210567990736));
#273127=CARTESIAN_POINT('Ctrl Pts',(-4.66141348379231,3.86100938829084,
136.646521806489));
#273128=CARTESIAN_POINT('Ctrl Pts',(-4.93986110760522,7.00214555161287,
130.713814895061));
#273129=CARTESIAN_POINT('Ctrl Pts',(-5.21830873141809,3.70865202682979,
124.864315079211));
#273130=CARTESIAN_POINT('Ctrl Pts',(-5.49675635523098,-2.99291153288594,
124.473426925751));
#273131=CARTESIAN_POINT('Ctrl Pts',(-5.77520397904388,-6.9441356057364,
129.900357551763));
#273132=CARTESIAN_POINT('Ctrl Pts',(-6.05365160285679,-4.51403829679898,
136.158022832244));
#273133=CARTESIAN_POINT('Ctrl Pts',(-6.33209922666964,2.06423968386644,
137.495934078373));
#273134=CARTESIAN_POINT('Ctrl Pts',(-6.61054685048256,6.74558223877327,
132.684616215558));
#273135=CARTESIAN_POINT('Ctrl Pts',(-6.88899447429547,5.22806425626005,
126.145435313781));
#273136=CARTESIAN_POINT('Ctrl Pts',(-7.16744209810832,-1.09378937261818,
123.887579165027));
#273137=CARTESIAN_POINT('Ctrl Pts',(-7.44588972192122,-6.41050400264194,
127.985907267597));
#273138=CARTESIAN_POINT('Ctrl Pts',(-7.72433734573414,-5.8362786247684,
134.674256309687));
#273139=CARTESIAN_POINT('Ctrl Pts',(-8.002784969547,0.101201691205851,137.806360265633));
#273140=CARTESIAN_POINT('Ctrl Pts',(-8.28123259335988,5.94568259693924,
134.503968611703));
#273141=CARTESIAN_POINT('Ctrl Pts',(-8.55968021717279,6.32637165882838,
127.80181794706));
#273142=CARTESIAN_POINT('Ctrl Pts',(-8.8381278409857,0.893434226691435,
123.858857314246));
#273143=CARTESIAN_POINT('Ctrl Pts',(-9.11657546479855,-5.3605256130866,
126.298474910485));
#273144=CARTESIAN_POINT('Ctrl Pts',(-9.39502308861147,-6.68842429067269,
132.878781346775));
#273145=CARTESIAN_POINT('Ctrl Pts',(-9.67347071242438,-1.86998779282204,
137.552796474009));
#273146=CARTESIAN_POINT('Ctrl Pts',(-9.95191833623725,4.66687613264966,
136.025328728591));
#273147=CARTESIAN_POINT('Ctrl Pts',(-10.2303659600501,6.91510888178999,
129.700046347612));
#273148=CARTESIAN_POINT('Ctrl Pts',(-10.508813583863,2.80869439041515,124.389574831969));
#273149=CARTESIAN_POINT('Ctrl Pts',(-10.787261207676,-3.87877303340228,
124.973978073582));
#273150=CARTESIAN_POINT('Ctrl Pts',(-11.0657088314888,-7.00183752812002,
130.916218043094));
#273151=CARTESIAN_POINT('Ctrl Pts',(-11.3441564553017,-3.69055539327479,
136.755666503084));
#273152=CARTESIAN_POINT('Ctrl Pts',(-11.6226040791146,3.01216685433575,
137.126155591738));
#273153=CARTESIAN_POINT('Ctrl Pts',(-11.9010517029275,6.94685491534338,
131.687223935982));
#273154=CARTESIAN_POINT('Ctrl Pts',(-12.1794993267404,4.49772268187999,
125.436984020872));
#273155=CARTESIAN_POINT('Ctrl Pts',(-12.4579469505533,-2.08459697026297,
124.119100987199));
#273156=CARTESIAN_POINT('Ctrl Pts',(-12.7363945743662,-6.75127384495765,
128.944644960744));
#273157=CARTESIAN_POINT('Ctrl Pts',(-13.0148421981791,-5.21385987419926,
135.479176770748));
#273158=CARTESIAN_POINT('Ctrl Pts',(-13.2932898219919,1.11483660973293,
137.717780913442));
#273159=CARTESIAN_POINT('Ctrl Pts',(-13.5717374458049,6.41905271211686,
133.603289543584));
#273160=CARTESIAN_POINT('Ctrl Pts',(-13.8501850696177,5.82447296022373,
126.916719225995));
#273161=CARTESIAN_POINT('Ctrl Pts',(-14.1286326934306,-0.122512900792341,
123.802701425419));
#273162=CARTESIAN_POINT('Ctrl Pts',(-14.4070803172435,-5.95691539106803,
127.122866372359));
#273163=CARTESIAN_POINT('Ctrl Pts',(-14.6855279410564,-6.31720364844761,
133.826144679651));
#273164=CARTESIAN_POINT('Ctrl Pts',(-14.9639755648693,-0.872290365458834,
137.752551056246));
#273165=CARTESIAN_POINT('Ctrl Pts',(-15.2424231886822,5.37421514963333,
135.293909857666));
#273166=CARTESIAN_POINT('Ctrl Pts',(-15.5208708124951,6.68207948721813,
128.709592234107));
#273167=CARTESIAN_POINT('Ctrl Pts',(-15.799318436308,1.84943921378025,124.050264419823));
#273168=CARTESIAN_POINT('Ctrl Pts',(-16.0777660601209,-4.68274534699314,
125.59762105532));
#273169=CARTESIAN_POINT('Ctrl Pts',(-16.3562136839338,-6.91171569870797,
131.929716985153));
#273170=CARTESIAN_POINT('Ctrl Pts',(-16.6346613077467,-2.78915697939336,
137.227665389888));
#273171=CARTESIAN_POINT('Ctrl Pts',(-16.9131089315595,3.89650074609022,
136.622910504741));
#273172=CARTESIAN_POINT('Ctrl Pts',(-17.1915565553724,7.00146464056082,
130.671192525245));
#273173=CARTESIAN_POINT('Ctrl Pts',(-17.4700041791854,3.67242457091876,
124.841849516969));
#273174=CARTESIAN_POINT('Ctrl Pts',(-17.7484518029982,-3.0313942714833,
124.491762925279));
#273175=CARTESIAN_POINT('Ctrl Pts',(-18.0268994268111,-6.94950987023543,
129.942645225261));
#273176=CARTESIAN_POINT('Ctrl Pts',(-18.305347050624,-4.48136540067248,
136.185401873632));
#273177=CARTESIAN_POINT('Ctrl Pts',(-18.5837946744369,2.10493494523792,
137.483244486159));
#273178=CARTESIAN_POINT('Ctrl Pts',(-18.8622422982498,6.75690290826339,
132.643519105064));
#273179=CARTESIAN_POINT('Ctrl Pts',(-19.1406899220627,5.19960719165284,
126.113696921846));
#273180=CARTESIAN_POINT('Ctrl Pts',(-19.4191375458756,-1.1358735191536,
123.894365523333));
#273181=CARTESIAN_POINT('Ctrl Pts',(-19.6975851696885,-6.42754195636435,
128.024982044393));
#273182=CARTESIAN_POINT('Ctrl Pts',(-19.9760327935014,-5.81261333855723,
134.709711694007));
#273183=CARTESIAN_POINT('Ctrl Pts',(-20.2544804173143,0.143822975436045,
137.805614491377));
#273184=CARTESIAN_POINT('Ctrl Pts',(-20.5329280411272,5.96809300114641,
134.467707008981));
#273185=CARTESIAN_POINT('Ctrl Pts',(-20.81137566494,6.30797711635522,127.763363157294));
#273186=CARTESIAN_POINT('Ctrl Pts',(-21.089823288753,0.851138423447451,
123.853547410611));
#273187=CARTESIAN_POINT('Ctrl Pts',(-21.3682709125658,-5.38785490018508,
126.331189435016));
#273188=CARTESIAN_POINT('Ctrl Pts',(-21.6467185363787,-6.67567278189203,
132.919457249623));
#273189=CARTESIAN_POINT('Ctrl Pts',(-21.9251661601916,-1.82887350178604,
137.564054587584));
#273190=CARTESIAN_POINT('Ctrl Pts',(-22.2036137840045,4.69857118102365,
135.996823396506));
#273191=CARTESIAN_POINT('Ctrl Pts',(-22.4820614078173,6.90825848643574,
129.657972577492));
#273192=CARTESIAN_POINT('Ctrl Pts',(-22.7605090316303,2.76959373000234,
124.372596363135));
#273193=CARTESIAN_POINT('Ctrl Pts',(-23.0389566554432,-3.91419236212754,
124.997697289448));
#273194=CARTESIAN_POINT('Ctrl Pts',(-23.3174042792561,-7.0010268923895,
130.958838143028));
#273195=CARTESIAN_POINT('Ctrl Pts',(-23.5958519030689,-3.65425972772349,
136.778021697354));
#273196=CARTESIAN_POINT('Ctrl Pts',(-23.8742995268818,3.05059360620828,
137.107702548922));
#273197=CARTESIAN_POINT('Ctrl Pts',(-24.1527471506948,6.95210044581739,
131.644920100946));
#273198=CARTESIAN_POINT('Ctrl Pts',(-24.4311947745076,4.4649666047081,125.409704551357));
#273199=CARTESIAN_POINT('Ctrl Pts',(-24.7096423983205,-2.12525342038311,
124.131914383013));
#273200=CARTESIAN_POINT('Ctrl Pts',(-24.9880900221334,-6.76246937654364,
128.985776337104));
#273201=CARTESIAN_POINT('Ctrl Pts',(-25.2665376459463,-5.18530634065569,
135.510828402156));
#273202=CARTESIAN_POINT('Ctrl Pts',(-25.5449852697592,1.15689990599717,
137.710866496904));
#273203=CARTESIAN_POINT('Ctrl Pts',(-25.8234328935721,6.43597165674122,
133.564163090109));
#273204=CARTESIAN_POINT('Ctrl Pts',(-26.101880517385,5.8006998696348,126.881336034893));
#273205=CARTESIAN_POINT('Ctrl Pts',(-26.3803281411979,-0.165131717723356,
123.803576920747));
#273206=CARTESIAN_POINT('Ctrl Pts',(-26.6587757650107,-5.9792153236265,
127.15919601668));
#273207=CARTESIAN_POINT('Ctrl Pts',(-26.9372233888237,-6.29869214802456,
133.864543304637));
#273208=CARTESIAN_POINT('Ctrl Pts',(-27.2156710126366,-0.829978596605981,
137.75773220141));
#273209=CARTESIAN_POINT('Ctrl Pts',(-27.4941186364494,5.40144473838504,
135.261112303716));
#273210=CARTESIAN_POINT('Ctrl Pts',(-27.7725662602623,6.66920423404522,
128.668955330874));
#273211=CARTESIAN_POINT('Ctrl Pts',(-28.0510138840753,1.80829084735756,
124.039131496154));
#273212=CARTESIAN_POINT('Ctrl Pts',(-28.3294615078881,-4.71435348813263,
125.626222724194));
#273213=CARTESIAN_POINT('Ctrl Pts',(-28.607909131701,-6.9047372770006,131.971769710144));
#273214=CARTESIAN_POINT('Ctrl Pts',(-28.8863567555139,-2.75000482347336,
137.244524771118));
#273215=CARTESIAN_POINT('Ctrl Pts',(-29.1648043793268,3.93184771762154,
136.599083594488));
#273216=CARTESIAN_POINT('Ctrl Pts',(-29.4432520031397,7.00052428766157,
130.628575090021));
#273217=CARTESIAN_POINT('Ctrl Pts',(-29.7216996269525,3.63606103196502,
124.819604897767));
#273218=CARTESIAN_POINT('Ctrl Pts',(-30.0001472507655,-3.06976468065099,
124.510332840438));
#273219=CARTESIAN_POINT('Ctrl Pts',(-30.2785948745783,-6.95462661809053,
129.984964829937));
#273220=CARTESIAN_POINT('Ctrl Pts',(-30.5570424983912,-4.44852644590303,
136.212581518559));
#273221=CARTESIAN_POINT('Ctrl Pts',(-30.8354901222041,2.14555220747066,
137.470307405446));
#273222=CARTESIAN_POINT('Ctrl Pts',(-31.113937746017,6.7679731982313,132.602353843876));
#273223=CARTESIAN_POINT('Ctrl Pts',(-31.3923853698299,5.17095745368924,
126.082132344179));
#273224=CARTESIAN_POINT('Ctrl Pts',(-31.6708329936428,-1.17791557547805,
123.901407934047));
#273225=CARTESIAN_POINT('Ctrl Pts',(-31.9492806174558,-6.44434173515584,
128.064159812084));
#273226=CARTESIAN_POINT('Ctrl Pts',(-32.2277282412685,-5.78873266382121,
134.745022364106));
#273227=CARTESIAN_POINT('Ctrl Pts',(-32.5061758650815,0.186438930252996,
137.804609283086));
#273228=CARTESIAN_POINT('Ctrl Pts',(-32.7846234888944,5.99028225547263,
134.431309659613));
#273229=CARTESIAN_POINT('Ctrl Pts',(-33.0630711127073,6.28934882947028,
127.725021052809));
#273230=CARTESIAN_POINT('Ctrl Pts',(-33.3415187365202,0.808811080956172,
123.848495071916));
#273231=CARTESIAN_POINT('Ctrl Pts',(-33.619966360333,-5.41498453833882,
126.364069714552));
#273232=CARTESIAN_POINT('Ctrl Pts',(-33.898413984146,-6.66267390360147,
132.960054776787));
#273233=CARTESIAN_POINT('Ctrl Pts',(-34.1768616079588,-1.78769144116968,
137.575062218212));
#273234=CARTESIAN_POINT('Ctrl Pts',(-34.4553092317717,4.73009212211488,
135.968125655805));
#273235=CARTESIAN_POINT('Ctrl Pts',(-34.7337568555846,6.90115210302259,
129.615941287202));
#273236=CARTESIAN_POINT('Ctrl Pts',(-35.0122044793975,2.73039044127535,
124.355856225691));
#273237=CARTESIAN_POINT('Ctrl Pts',(-35.2906521032104,-3.94946664901538,
125.02163167336));
#273238=CARTESIAN_POINT('Ctrl Pts',(-35.5690997270233,-6.99995683103299,
131.00145251874));
#273239=CARTESIAN_POINT('Ctrl Pts',(-35.8475473508362,-3.61782865223385,
136.800155535415));
#273240=CARTESIAN_POINT('Ctrl Pts',(-36.125994974649,3.08890731721304,137.089015933453));
#273241=CARTESIAN_POINT('Ctrl Pts',(-36.404442598462,6.95708836365274,131.60258511867));
#273242=CARTESIAN_POINT('Ctrl Pts',(-36.6828902222748,4.43204507655667,
125.382624982808));
#273243=CARTESIAN_POINT('Ctrl Pts',(-36.9613378460878,-2.16583111845593,
124.144975028777));
#273244=CARTESIAN_POINT('Ctrl Pts',(-37.2397854699006,-6.7734143223399,
129.026975101771));
#273245=CARTESIAN_POINT('Ctrl Pts',(-37.5182330937135,-5.15656066367905,
135.54230563367));
#273246=CARTESIAN_POINT('Ctrl Pts',(-37.7966807175264,1.19892033290996,
137.703696157251));
#273247=CARTESIAN_POINT('Ctrl Pts',(-38.0751283413393,6.45265211406898,
133.524934371139));
#273248=CARTESIAN_POINT('Ctrl Pts',(-38.3535759651522,5.77671183197903,
126.846098212911));
#273249=CARTESIAN_POINT('Ctrl Pts',(-38.6320235889651,-0.207744415637528,
123.80471183269));
#273250=CARTESIAN_POINT('Ctrl Pts',(-38.910471212778,-6.00129369416227,
127.195660733917));
#273251=CARTESIAN_POINT('Ctrl Pts',(-39.1889188365908,-6.27994724724761,
133.902828533427));
#273252=CARTESIAN_POINT('Ctrl Pts',(-39.4673664604039,-0.787636072591,137.762655686833));
#273253=CARTESIAN_POINT('Ctrl Pts',(-39.7458140842166,5.42847417461558,
135.228149603194));
#273254=CARTESIAN_POINT('Ctrl Pts',(-40.0242617080296,6.65608185105682,
128.628397555869));
#273255=CARTESIAN_POINT('Ctrl Pts',(-40.3027093318424,1.76707547405252,
124.028249260538));
#273256=CARTESIAN_POINT('Ctrl Pts',(-40.5811569556554,-4.7457869371699,
125.655016270872));
#273257=CARTESIAN_POINT('Ctrl Pts',(-40.8596045794682,-6.89750299771422,
132.013779176361));
#273258=CARTESIAN_POINT('Ctrl Pts',(-41.1380522032811,-2.7107507651133,
137.261145509698));
#273259=CARTESIAN_POINT('Ctrl Pts',(-41.416499827094,3.96704899308973,136.575041958643));
#273260=CARTESIAN_POINT('Ctrl Pts',(-41.694947450907,6.99932452776054,130.585964168594));
#273261=CARTESIAN_POINT('Ctrl Pts',(-41.9733950747197,3.59956275743227,
124.79758204589));
#273262=CARTESIAN_POINT('Ctrl Pts',(-42.2518426985328,-3.10802133855968,
124.529135983109));
#273263=CARTESIAN_POINT('Ctrl Pts',(-42.5302903223456,-6.95948565969872,
130.027314797628));
#273264=CARTESIAN_POINT('Ctrl Pts',(-42.8087379461585,-4.41552264935019,
136.23956075987));
#273265=CARTESIAN_POINT('Ctrl Pts',(-43.0871855699714,2.18608996547759,
137.457123315624));
#273266=CARTESIAN_POINT('Ctrl Pts',(-43.3656331937842,6.77879269846351,
132.561121957388));
#273267=CARTESIAN_POINT('Ctrl Pts',(-43.6440808175972,5.14211610399531,
126.050742750417));
#273268=CARTESIAN_POINT('Ctrl Pts',(-43.92252844141,-1.21991398370768,123.908706136214));
#273269=CARTESIAN_POINT('Ctrl Pts',(-44.200976065223,-6.46090271649442,
128.103439118922));
#273270=CARTESIAN_POINT('Ctrl Pts',(-44.4794236890358,-5.76463748546755,
134.780187011534));
#273271=CARTESIAN_POINT('Ctrl Pts',(-44.7578713128487,0.229047976506494,
137.803344678006));
#273272=CARTESIAN_POINT('Ctrl Pts',(-45.0363189366615,6.01224953768695,
134.394777912313));
#273273=CARTESIAN_POINT('Ctrl Pts',(-45.3147665604746,6.27048748845154,
127.686793054383));
#273274=CARTESIAN_POINT('Ctrl Pts',(-45.5932141842873,0.766453767672844,
123.843700485376));
#273275=CARTESIAN_POINT('Ctrl Pts',(-45.8716618081003,-5.44191352224889,
126.397114530699));
#273276=CARTESIAN_POINT('Ctrl Pts',(-46.1501094319132,-6.6494281374793,
133.000572423912));
#273277=CARTESIAN_POINT('Ctrl Pts',(-46.4285570557261,-1.74644313698983,
137.585818958004));
#273278=CARTESIAN_POINT('Ctrl Pts',(-46.7070046795389,4.76143778790304,
135.93923656989));
#273279=CARTESIAN_POINT('Ctrl Pts',(-46.9854523033519,6.89378999488032,
129.573954034227));
#273280=CARTESIAN_POINT('Ctrl Pts',(-47.2638999271647,2.69108597692664,
124.339355039948));
#273281=CARTESIAN_POINT('Ctrl Pts',(-47.5423475509777,-3.98459458696386,
125.045780338419));
#273282=CARTESIAN_POINT('Ctrl Pts',(-47.8207951747905,-6.998627383702,131.044059591139));
#273283=CARTESIAN_POINT('Ctrl Pts',(-48.0992427986034,-3.58126351677304,
136.822067197091));
#273284=CARTESIAN_POINT('Ctrl Pts',(-48.3776904224163,3.1271065676212,137.070096437769));
#273285=CARTESIAN_POINT('Ctrl Pts',(-48.6561380462292,6.9618184840203,131.560220557891));
#273286=CARTESIAN_POINT('Ctrl Pts',(-48.9345856700421,4.39895931734504,
125.355746318666));
#273287=CARTESIAN_POINT('Ctrl Pts',(-49.213033293855,-2.20632856086043,
124.158282440523));
#273288=CARTESIAN_POINT('Ctrl Pts',(-49.4914809176678,-6.78410827677761,
129.068239728113));
#273289=CARTESIAN_POINT('Ctrl Pts',(-49.7699285414808,-5.12762390845042,
135.573607298891));
#273290=CARTESIAN_POINT('Ctrl Pts',(-50.0483761652936,1.2408963333889,137.696270160183));
#273291=CARTESIAN_POINT('Ctrl Pts',(-50.3268237891066,6.46909346599971,
133.485604840309));
#273292=CARTESIAN_POINT('Ctrl Pts',(-50.6052714129194,5.7525097361419,126.811007065796));
#273293=CARTESIAN_POINT('Ctrl Pts',(-50.8837190367324,-0.250349415506305,
123.806106119193));
#273294=CARTESIAN_POINT('Ctrl Pts',(-51.1621666605453,-6.02314968455324,
127.232259172855));
#273295=CARTESIAN_POINT('Ctrl Pts',(-51.4406142843581,-6.26096964071598,
133.94099894735));
#273296=CARTESIAN_POINT('Ctrl Pts',(-51.719061908171,-0.745264362431691,
137.767321330073));
#273297=CARTESIAN_POINT('Ctrl Pts',(-51.997509531984,5.45530245673899,135.195022977544));
#273298=CARTESIAN_POINT('Ctrl Pts',(-52.2759571557968,6.64271282450778,
128.587920411975));
#273299=CARTESIAN_POINT('Ctrl Pts',(-52.5544047796097,1.72579462111621,
124.01761811622));
#273300=CARTESIAN_POINT('Ctrl Pts',(-52.8328524034226,-4.77704452932697,
125.684000628399));
#273301=CARTESIAN_POINT('Ctrl Pts',(-53.1113000272355,-6.89001312891767,
132.05574382713));
#273302=CARTESIAN_POINT('Ctrl Pts',(-53.3897476510484,-2.67139625888694,
137.277526989739));
#273303=CARTESIAN_POINT('Ctrl Pts',(-53.6681952748612,4.00210326809833,
136.550786488079));
#273304=CARTESIAN_POINT('Ctrl Pts',(-53.9466428986742,6.99786540531528,
130.543361339928));
#273305=CARTESIAN_POINT('Ctrl Pts',(-54.225090522487,3.56293109977782,124.775781777402));
#273306=CARTESIAN_POINT('Ctrl Pts',(-54.5035381462999,-3.14616282759469,
124.548171656537));
#273307=CARTESIAN_POINT('Ctrl Pts',(-54.7819857701128,-6.9640868150063,
130.069693559035));
#273308=CARTESIAN_POINT('Ctrl Pts',(-55.0604333939257,-4.382355233982,136.266338597842));
#273309=CARTESIAN_POINT('Ctrl Pts',(-55.3388810177386,2.22654671711671,
137.443692705233));
#273310=CARTESIAN_POINT('Ctrl Pts',(-55.6173286415515,6.78936100803939,
132.519824973462));
#273311=CARTESIAN_POINT('Ctrl Pts',(-55.8957762653644,5.11308421129812,
126.019529303714));
#273312=CARTESIAN_POINT('Ctrl Pts',(-56.1742238891773,-1.26186718757599,
123.916259859391));
#273313=CARTESIAN_POINT('Ctrl Pts',(-56.4526715129901,-6.47722428670686,
128.142818509401));
#273314=CARTESIAN_POINT('Ctrl Pts',(-56.7311191368031,-5.74032869635189,
134.815204333253));
#273315=CARTESIAN_POINT('Ctrl Pts',(-57.0095667606159,0.271648535303317,
137.801820722997));
#273316=CARTESIAN_POINT('Ctrl Pts',(-57.2880143844289,6.03399403378365,
134.358113120779));
#273317=CARTESIAN_POINT('Ctrl Pts',(-57.5664620082417,6.25139379221294,
127.64868057857));
#273318=CARTESIAN_POINT('Ctrl Pts',(-57.8449096320546,0.724068053163303,
123.839163828657));
#273319=CARTESIAN_POINT('Ctrl Pts',(-58.1233572558676,-5.46864085405239,
126.430322658971));
#273320=CARTESIAN_POINT('Ctrl Pts',(-58.4018048796803,-6.63593597435208,
133.0410086896));
#273321=CARTESIAN_POINT('Ctrl Pts',(-58.6802525034934,-1.705130117717,137.596324408362));
#273322=CARTESIAN_POINT('Ctrl Pts',(-58.9587001273061,4.79260701686295,
135.910157209259));
#273323=CARTESIAN_POINT('Ctrl Pts',(-59.2371477511191,6.88617243481463,
129.532012374421));
#273324=CARTESIAN_POINT('Ctrl Pts',(-59.515595374932,2.65168179339722,124.323093417365));
#273325=CARTESIAN_POINT('Ctrl Pts',(-59.7940429987449,-4.01957487429483,
125.070142389788));
#273326=CARTESIAN_POINT('Ctrl Pts',(-60.0724906225578,-6.99703859965941,
131.086657781405));
#273327=CARTESIAN_POINT('Ctrl Pts',(-60.3509382463707,-3.5445656762756,
136.843755870437));
#273328=CARTESIAN_POINT('Ctrl Pts',(-60.6293858701835,3.16518994194552,
137.050944762941));
#273329=CARTESIAN_POINT('Ctrl Pts',(-60.9078334939965,6.96629063164357,
131.517827988445));
#273330=CARTESIAN_POINT('Ctrl Pts',(-61.1862811178092,4.36571055307847,
125.32906955493));
#273331=CARTESIAN_POINT('Ctrl Pts',(-61.4647287416223,-2.24674424694855,
124.171836125139));
#273332=CARTESIAN_POINT('Ctrl Pts',(-61.743176365435,-6.79455084358828,
129.109568687053));
#273333=CARTESIAN_POINT('Ctrl Pts',(-62.0216239892481,-5.09849714723216,
135.60473223792));
#273334=CARTESIAN_POINT('Ctrl Pts',(-62.3000716130609,1.2828263519976,137.688588780872));
#273335=CARTESIAN_POINT('Ctrl Pts',(-62.5785192368738,6.48529510329292,
133.446175954988));
#273336=CARTESIAN_POINT('Ctrl Pts',(-62.8569668606868,5.72809447894126,
126.776063893867));
#273337=CARTESIAN_POINT('Ctrl Pts',(-63.1354144844995,-0.292945138585431,
123.80775972859));
#273338=CARTESIAN_POINT('Ctrl Pts',(-63.4138621083125,-6.04478248491762,
127.268989977326));
#273339=CARTESIAN_POINT('Ctrl Pts',(-63.6923097321254,-6.24176003165182,
133.979053131985));
#273340=CARTESIAN_POINT('Ctrl Pts',(-63.9707573559382,-0.702865036227365,
137.771728958244));
#273341=CARTESIAN_POINT('Ctrl Pts',(-64.2492049797512,5.48192859062395,
135.161733654286));
#273342=CARTESIAN_POINT('Ctrl Pts',(-64.527652603564,6.62909764979204,128.547525399088));
#273343=CARTESIAN_POINT('Ctrl Pts',(-64.806100227377,1.68444981822529,124.007238457143));
#273344=CARTESIAN_POINT('Ctrl Pts',(-65.0845478511898,-4.80812510634223,
125.713174722747));
#273345=CARTESIAN_POINT('Ctrl Pts',(-65.3629954750027,-6.88226794815085,
132.097662107432));
#273346=CARTESIAN_POINT('Ctrl Pts',(-65.6414430988157,-2.63194276308962,
137.29366860422));
#273347=CARTESIAN_POINT('Ctrl Pts',(-65.9198907226284,4.03700924369883,
136.526318081592));
#273348=CARTESIAN_POINT('Ctrl Pts',(-66.1983383464414,6.99614697439381,
130.500768182686));
#273349=CARTESIAN_POINT('Ctrl Pts',(-66.4767859702543,3.5261674164012,124.75420490012));
#273350=CARTESIAN_POINT('Ctrl Pts',(-66.7552335940671,-3.18418773440913,
124.567439155348));
#273351=CARTESIAN_POINT('Ctrl Pts',(-67.0336812178801,-6.96842991351606,
130.112099543802));
#273352=CARTESIAN_POINT('Ctrl Pts',(-67.3121288416929,-4.34902542882876,
136.292914040211));
#273353=CARTESIAN_POINT('Ctrl Pts',(-67.5905764655059,2.26692096324861,
137.43001607195));
#273354=CARTESIAN_POINT('Ctrl Pts',(-67.8690240893187,6.79967773534632,
132.478464422373));
#273355=CARTESIAN_POINT('Ctrl Pts',(-68.1474717131316,5.08386285138514,
125.988493160695));
#273356=CARTESIAN_POINT('Ctrl Pts',(-68.4259193369445,-1.30377363249137,
123.924068823677));
#273357=CARTESIAN_POINT('Ctrl Pts',(-68.7043669607574,-6.49330584099122,
128.182296524302));
#273358=CARTESIAN_POINT('Ctrl Pts',(-68.9828145845703,-5.71580719724563,
134.850073031684));
#273359=CARTESIAN_POINT('Ctrl Pts',(-69.2612622083832,0.314239028063776,
137.800037474531));
#273360=CARTESIAN_POINT('Ctrl Pts',(-69.5397098321961,6.05551493801243,
134.32131664364));
#273361=CARTESIAN_POINT('Ctrl Pts',(-69.818157456009,6.23206844827842,127.610685037641));
#273362=CARTESIAN_POINT('Ctrl Pts',(-70.0966050798218,0.681655508046095,
123.834885269867));
#273363=CARTESIAN_POINT('Ctrl Pts',(-70.3750527036349,-5.49516554335789,
126.463692868828));
#273364=CARTESIAN_POINT('Ctrl Pts',(-70.6535003274475,-6.62219791417695,
133.081362075471));
#273365=CARTESIAN_POINT('Ctrl Pts',(-70.9319479512606,-1.66375391422059,
137.606578180005));
#273366=CARTESIAN_POINT('Ctrl Pts',(-71.2103955750734,4.82359865400735,
135.880888651457));
#273367=CARTESIAN_POINT('Ctrl Pts',(-71.4888431988863,6.87829970509706,
129.490117861946));
#273368=CARTESIAN_POINT('Ctrl Pts',(-71.7672908226993,2.6121793508235,124.307071960521));
#273369=CARTESIAN_POINT('Ctrl Pts',(-72.045738446512,-4.05440621480077,
125.094716924722));
#273370=CARTESIAN_POINT('Ctrl Pts',(-72.3241860703251,-6.99519053777849,
131.129245511046));
#273371=CARTESIAN_POINT('Ctrl Pts',(-72.6026336941378,-3.5077364905931,
136.865220751771));
#273372=CARTESIAN_POINT('Ctrl Pts',(-72.8810813179508,3.20315602899298,
137.031561618638));
#273373=CARTESIAN_POINT('Ctrl Pts',(-73.1595289417638,6.97050464080582,
131.475408981201));
#273374=CARTESIAN_POINT('Ctrl Pts',(-73.4379765655765,4.33230001580124,
125.302595680118));
#273375=CARTESIAN_POINT('Ctrl Pts',(-73.7164241893894,-2.28707667910305,
124.18563558039));
#273376=CARTESIAN_POINT('Ctrl Pts',(-73.9948718132024,-6.80474163581863,
129.150960447132));
#273377=CARTESIAN_POINT('Ctrl Pts',(-74.2733194370152,-5.0691814593271,
135.635679297414));
#273378=CARTESIAN_POINT('Ctrl Pts',(-74.5517670608282,1.32470883500465,
137.680652303954));
#273379=CARTESIAN_POINT('Ctrl Pts',(-74.830214684641,6.5012564255912,133.406649176227));
#273380=CARTESIAN_POINT('Ctrl Pts',(-75.108662308454,5.70346696509291,126.741269991954));
#273381=CARTESIAN_POINT('Ctrl Pts',(-75.3871099322667,-0.335530006474783,
123.809672599606));
#273382=CARTESIAN_POINT('Ctrl Pts',(-75.6655575560798,-6.06619129364391,
127.305851786256));
#273383=CARTESIAN_POINT('Ctrl Pts',(-75.9440051798925,-6.22231913187452,
134.016989677222));
#273384=CARTESIAN_POINT('Ctrl Pts',(-76.2224528037055,-0.66043966510086,
137.775878408018));
#273385=CARTESIAN_POINT('Ctrl Pts',(-76.5009004275184,5.50835158962877,
135.128282866967));
#273386=CARTESIAN_POINT('Ctrl Pts',(-76.7793480513312,6.61523683142527,
128.507214014061));
#273387=CARTESIAN_POINT('Ctrl Pts',(-77.0577956751442,1.64304259742666,
123.997110667925));
#273388=CARTESIAN_POINT('Ctrl Pts',(-77.336243298957,-4.83902751651344,
125.742537472861));
#273389=CARTESIAN_POINT('Ctrl Pts',(-77.6146909227699,-6.87426774241415,
132.139532463972));
#273390=CARTESIAN_POINT('Ctrl Pts',(-77.8931385465828,-2.59239173968542,
137.309569755007));
#273391=CARTESIAN_POINT('Ctrl Pts',(-78.1715861703958,4.07176562643718,
136.501637645866));
#273392=CARTESIAN_POINT('Ctrl Pts',(-78.4500337942086,6.99416929867323,
130.458186275174));
#273393=CARTESIAN_POINT('Ctrl Pts',(-78.7284814180215,3.48927306959449,
124.732852213582));
#273394=CARTESIAN_POINT('Ctrl Pts',(-79.0069290418344,-3.22209464997582,
124.586937765577));
#273395=CARTESIAN_POINT('Ctrl Pts',(-79.2853766656473,-6.97251479429268,
130.154531180556));
#273396=CARTESIAN_POINT('Ctrl Pts',(-79.5638242894601,-4.3155344689392,
136.319286102215));
#273397=CARTESIAN_POINT('Ctrl Pts',(-79.8422719132732,2.30721120779087,
137.416093922569));
#273398=CARTESIAN_POINT('Ctrl Pts',(-80.1207195370859,6.80974249809405,
132.437041836753));
#273399=CARTESIAN_POINT('Ctrl Pts',(-80.3991671608989,5.0544531070646,125.957635471416));
#273400=CARTESIAN_POINT('Ctrl Pts',(-80.6776147847117,-1.34563176559565,
123.932132739704));
#273401=CARTESIAN_POINT('Ctrl Pts',(-80.9560624085247,-6.50914678343976,
128.221871700751));
#273402=CARTESIAN_POINT('Ctrl Pts',(-81.2345100323374,-5.69107389680138,
134.884791814753));
#273403=CARTESIAN_POINT('Ctrl Pts',(-81.5129576561506,0.356817876581242,
137.797994998686));
#273404=CARTESIAN_POINT('Ctrl Pts',(-81.7914052799631,6.07681145290804,
134.284389844403));
#273405=CARTESIAN_POINT('Ctrl Pts',(-82.0698529037763,6.21251217275584,
127.572807839535));
#273406=CARTESIAN_POINT('Ctrl Pts',(-82.348300527589,0.639217703933302,
123.830864967548));
#273407=CARTESIAN_POINT('Ctrl Pts',(-82.626748151402,-5.52148660728364,
126.497223923725));
#273408=CARTESIAN_POINT('Ctrl Pts',(-82.9051957752149,-6.60821446602265,
133.121631086217));
#273409=CARTESIAN_POINT('Ctrl Pts',(-83.1836433990278,-1.62231605971109,
137.616579892973));
#273410=CARTESIAN_POINT('Ctrl Pts',(-83.4620910228406,4.85441155092967,
135.851431981043));
#273411=CARTESIAN_POINT('Ctrl Pts',(-83.7405386466535,6.87017209745416,
129.448272049221));
#273412=CARTESIAN_POINT('Ctrl Pts',(-84.0189862704665,2.57258011298421,
124.291291263097));
#273413=CARTESIAN_POINT('Ctrl Pts',(-84.2974338942792,-4.08908731779306,
125.119503032603));
#273414=CARTESIAN_POINT('Ctrl Pts',(-84.5758815180923,-6.99308326653956,
131.171821201958));
#273415=CARTESIAN_POINT('Ctrl Pts',(-84.8543291419051,-3.47077732444568,
136.886461045702));
#273416=CARTESIAN_POINT('Ctrl Pts',(-85.132776765718,3.2410034219148,137.011947723114));
#273417=CARTESIAN_POINT('Ctrl Pts',(-85.4112243895309,6.97446035535538,
131.432965108015));
#273418=CARTESIAN_POINT('Ctrl Pts',(-85.6896720133437,4.29872894355427,
125.27632567523));
#273419=CARTESIAN_POINT('Ctrl Pts',(-85.9681196371569,-2.327324362789,124.19968029493));
#273420=CARTESIAN_POINT('Ctrl Pts',(-86.2465672609694,-6.81468027584547,
129.192413474561));
#273421=CARTESIAN_POINT('Ctrl Pts',(-86.5250148847825,-5.03967793103904,
135.666447330617));
#273422=CARTESIAN_POINT('Ctrl Pts',(-86.8034625085954,1.36654223043768,
137.672461023519));
#273423=CARTESIAN_POINT('Ctrl Pts',(-87.0819101324082,6.51697684144191,
133.367025968708));
#273424=CARTESIAN_POINT('Ctrl Pts',(-87.3603577562212,5.67862810717874,
126.706626649358));
#273425=CARTESIAN_POINT('Ctrl Pts',(-87.638805380034,-0.378102441176264,
123.811844661359));
#273426=CARTESIAN_POINT('Ctrl Pts',(-87.917253003847,-6.08737531742114,
127.342843233717));
#273427=CARTESIAN_POINT('Ctrl Pts',(-88.1957006276599,-6.20264766177327,
134.054807177307));
#273428=CARTESIAN_POINT('Ctrl Pts',(-88.4741482514726,-0.617989821139493,
137.779769525637));
#273429=CARTESIAN_POINT('Ctrl Pts',(-88.7525958752857,5.53457047463998,
135.094671855119));
#273430=CARTESIAN_POINT('Ctrl Pts',(-89.0310434990984,6.6011308830247,128.466987750645));
#273431=CARTESIAN_POINT('Ctrl Pts',(-89.3094911229114,1.60157449308101,
123.987235123859));
#273432=CARTESIAN_POINT('Ctrl Pts',(-89.5879387467241,-4.86975061474005,
125.772087790693));
#273433=CARTESIAN_POINT('Ctrl Pts',(-89.8663863705374,-6.8660128081587,
132.181353345229));
#273434=CARTESIAN_POINT('Ctrl Pts',(-90.1448339943499,-2.55274465425183,
137.325229852876));
#273435=CARTESIAN_POINT('Ctrl Pts',(-90.4232816181632,4.10637112840284,
136.476746095445));
#273436=CARTESIAN_POINT('Ctrl Pts',(-90.7017292419757,6.99193245143733,
130.415617195278));
#273437=CARTESIAN_POINT('Ctrl Pts',(-90.9801768657889,3.45224942649073,
124.711724509022));
#273438=CARTESIAN_POINT('Ctrl Pts',(-91.2586244896016,-3.2598821696406,
124.606666764696));
#273439=CARTESIAN_POINT('Ctrl Pts',(-91.5370721134145,-6.97634130596949,
130.196986896981));
#273440=CARTESIAN_POINT('Ctrl Pts',(-91.8155197372274,-4.28188359533257,
136.345453806627));
#273441=CARTESIAN_POINT('Ctrl Pts',(-92.0939673610402,2.34741595777304,
137.401926772977));
#273442=CARTESIAN_POINT('Ctrl Pts',(-92.3724149848533,6.81955492332935,
132.395558751529));
#273443=CARTESIAN_POINT('Ctrl Pts',(-92.650862608666,5.02485606812542,125.926957379319));
#273444=CARTESIAN_POINT('Ctrl Pts',(-92.929310232479,-1.38744003581995,
123.940451308663));
#273445=CARTESIAN_POINT('Ctrl Pts',(-93.2077578562919,-6.52474652706058,
128.261542572277));
#273446=CARTESIAN_POINT('Ctrl Pts',(-93.4862054801047,-5.66612971152105,
134.919359395943));
#273447=CARTESIAN_POINT('Ctrl Pts',(-93.7646531039176,0.39938350308132,
137.795693371147));
#273448=CARTESIAN_POINT('Ctrl Pts',(-94.0431007277306,6.09788278932073,
134.247334091402));
#273449=CARTESIAN_POINT('Ctrl Pts',(-94.3215483515434,6.19272569030992,
127.535050387806));
#273450=CARTESIAN_POINT('Ctrl Pts',(-94.5999959753563,0.596756213373149,
123.827103070676));
#273451=CARTESIAN_POINT('Ctrl Pts',(-94.8784435991693,-5.54760307049237,
126.530914581157));
#273452=CARTESIAN_POINT('Ctrl Pts',(-95.1568912229821,-6.59398614805128,
133.161814229653));
#273453=CARTESIAN_POINT('Ctrl Pts',(-95.4353388467949,-1.58081808968337,
137.626329176652));
#273454=CARTESIAN_POINT('Ctrl Pts',(-95.7137864706081,4.88504456584684,
135.821788289543));
#273455=CARTESIAN_POINT('Ctrl Pts',(-95.9922340944205,6.86178991305786,
129.406476486855));
#273456=CARTESIAN_POINT('Ctrl Pts',(-96.2706817182339,2.53288554724217,
124.275751909854));
#273457=CARTESIAN_POINT('Ctrl Pts',(-96.5491293420464,-4.12361689815126,
125.144499794972));
#273458=CARTESIAN_POINT('Ctrl Pts',(-96.8275769658595,-6.99071686402826,
131.214383276482));
#273459=CARTESIAN_POINT('Ctrl Pts',(-97.1060245896722,-3.4336895473684,
136.907475965166));
#273460=CARTESIAN_POINT('Ctrl Pts',(-97.3844722134854,3.27873071826322,
136.992103803166));
#273461=CARTESIAN_POINT('Ctrl Pts',(-97.6629198372979,6.9781576287114,131.390497941658));
#273462=CARTESIAN_POINT('Ctrl Pts',(-97.9413674611112,4.26499858032525,
125.250260513709));
#273463=CARTESIAN_POINT('Ctrl Pts',(-98.2198150849237,-2.36748580661544,
124.21396974833));
#273464=CARTESIAN_POINT('Ctrl Pts',(-98.498262708737,-6.82436639538843,
129.233926233285));
#273465=CARTESIAN_POINT('Ctrl Pts',(-98.7767103325495,-5.00998765563179,
135.69703519741));
#273466=CARTESIAN_POINT('Ctrl Pts',(-99.0551579563628,1.40832498814648,
137.664015243098));
#273467=CARTESIAN_POINT('Ctrl Pts',(-99.3336055801754,6.53245576831905,
133.327307800681));
#273468=CARTESIAN_POINT('Ctrl Pts',(-99.6120532039884,5.65357882561176,
126.672135149802));
#273469=CARTESIAN_POINT('Ctrl Pts',(-99.8905008278013,-0.420660865152761,
123.814275833361));
#273470=CARTESIAN_POINT('Ctrl Pts',(-100.168948451614,-6.10833377126732,
127.379962948978));
#273471=CARTESIAN_POINT('Ctrl Pts',(-100.447396075427,-6.18274635028192,
134.092504230901));
#273472=CARTESIAN_POINT('Ctrl Pts',(-100.72584369924,-0.575517077338011,
137.783402166914));
#273473=CARTESIAN_POINT('Ctrl Pts',(-101.004291323053,5.56058427410689,
135.060901864211));
#273474=CARTESIAN_POINT('Ctrl Pts',(-101.282738946866,6.58678032729173,
128.426848099441));
#273475=CARTESIAN_POINT('Ctrl Pts',(-101.561186570679,1.56004704180311,
123.977612190885));
#273476=CARTESIAN_POINT('Ctrl Pts',(-101.839634194492,-4.90029326256724,
125.801824581246));
#273477=CARTESIAN_POINT('Ctrl Pts',(-102.118081818304,-6.85750345127332,
132.223123201514));
#273478=CARTESIAN_POINT('Ctrl Pts',(-102.396529442117,-2.51300297592632,
137.340648317539));
#273479=CARTESIAN_POINT('Ctrl Pts',(-102.67497706593,4.14082446727623,136.451644352694));
#273480=CARTESIAN_POINT('Ctrl Pts',(-102.953424689743,6.98943651557314,
130.373062520413));
#273481=CARTESIAN_POINT('Ctrl Pts',(-103.231872313556,3.41509785901489,
124.690822569333));
#273482=CARTESIAN_POINT('Ctrl Pts',(-103.510319937369,-3.29754889317273,
124.626625421641));
#273483=CARTESIAN_POINT('Ctrl Pts',(-103.788767561182,-6.97990930675369,
130.239465119861));
#273484=CARTESIAN_POINT('Ctrl Pts',(-104.067215184995,-4.24807405495459,
136.371416183792));
#273485=CARTESIAN_POINT('Ctrl Pts',(-104.345662808808,2.38753372339306,
137.387515148146));
#273486=CARTESIAN_POINT('Ctrl Pts',(-104.62411043262,6.82911464744894,132.354016703874));
#273487=CARTESIAN_POINT('Ctrl Pts',(-104.902558056433,4.99507283129728,
125.896460021193));
#273488=CARTESIAN_POINT('Ctrl Pts',(-105.181005680246,-1.42919689394351,
123.949024222305));
#273489=CARTESIAN_POINT('Ctrl Pts',(-105.459453304059,-6.54010449379936,
128.301307668861));
#273490=CARTESIAN_POINT('Ctrl Pts',(-105.737900927872,-5.64097556572054,
134.953774494342));
#273491=CARTESIAN_POINT('Ctrl Pts',(-106.016348551685,0.441934330278796,
137.793132677202));
#273492=CARTESIAN_POINT('Ctrl Pts',(-106.294796175498,6.11872816644418,
134.210150757753));
#273493=CARTESIAN_POINT('Ctrl Pts',(-106.573243799311,6.17270973413615,
127.49741408157));
#273494=CARTESIAN_POINT('Ctrl Pts',(-106.851691423124,0.554272609792058,
123.823599718647));
#273495=CARTESIAN_POINT('Ctrl Pts',(-107.130139046936,-5.57351396522919,
126.564763592701));
#273496=CARTESIAN_POINT('Ctrl Pts',(-107.40858667075,-6.57951348749827,
133.201910016778));
#273497=CARTESIAN_POINT('Ctrl Pts',(-107.687034294562,-1.53926154185996,
137.635825669776));
#273498=CARTESIAN_POINT('Ctrl Pts',(-107.965481918375,4.91549656364115,
135.791958675416));
#273499=CARTESIAN_POINT('Ctrl Pts',(-108.243929542188,6.85315346251289,
129.364732723601));
#273500=CARTESIAN_POINT('Ctrl Pts',(-108.522377166001,2.49309712449469,
124.260454476607));
#273501=CARTESIAN_POINT('Ctrl Pts',(-108.800824789814,-4.15799367636883,
125.169706285567));
#273502=CARTESIAN_POINT('Ctrl Pts',(-109.079272413627,-6.98809141793296,
131.256930157466));
#273503=CARTESIAN_POINT('Ctrl Pts',(-109.35772003744,-3.39647453366164,
136.928264731447));
#273504=CARTESIAN_POINT('Ctrl Pts',(-109.636167661252,3.31633652003941,
136.97203059412));
#273505=CARTESIAN_POINT('Ctrl Pts',(-109.914615285065,6.98159632387027,
131.348009055767));
#273506=CARTESIAN_POINT('Ctrl Pts',(-110.193062908878,4.23111017600536,
125.22440116141));
#273507=CARTESIAN_POINT('Ctrl Pts',(-110.471510532691,-2.40755952238467,
124.228503411086));
#273508=CARTESIAN_POINT('Ctrl Pts',(-110.749958156504,-6.83379963552497,
129.275497185033));
#273509=CARTESIAN_POINT('Ctrl Pts',(-111.028405780317,-4.98011173328953,
135.727441764346));
#273510=CARTESIAN_POINT('Ctrl Pts',(-111.30685340413,1.45005555985492,137.655315275653));
#273511=CARTESIAN_POINT('Ctrl Pts',(-111.585301027943,6.54769263264538,
133.287496143919));
#273512=CARTESIAN_POINT('Ctrl Pts',(-111.863748651756,5.62832004860235,
126.63779677138));
#273513=CARTESIAN_POINT('Ctrl Pts',(-112.142196275568,-0.463203701385527,
123.816966025527));
#273514=CARTESIAN_POINT('Ctrl Pts',(-112.420643899382,-6.12906587855929,
127.417209556553));
#273515=CARTESIAN_POINT('Ctrl Pts',(-112.699091523194,-6.16261593485082,
134.130079441122));
#273516=CARTESIAN_POINT('Ctrl Pts',(-112.977539147007,-0.533023007539609,
137.786776197239));
#273517=CARTESIAN_POINT('Ctrl Pts',(-113.25598677082,5.58639202407863,135.026974145601));
#273518=CARTESIAN_POINT('Ctrl Pts',(-113.534434394633,6.57218569599142,
128.386796547837));
#273519=CARTESIAN_POINT('Ctrl Pts',(-113.812882018446,1.5184617824084,123.968242225583));
#273520=CARTESIAN_POINT('Ctrl Pts',(-114.091329642259,-4.93065432822552,
125.831746742611));
#273521=CARTESIAN_POINT('Ctrl Pts',(-114.369777266072,-6.84873998707567,
132.26484048503));
#273522=CARTESIAN_POINT('Ctrl Pts',(-114.648224889884,-2.4731681773514,
137.355824577657));
#273523=CARTESIAN_POINT('Ctrl Pts',(-114.926672513697,4.17512436637621,
136.426333347767));
#273524=CARTESIAN_POINT('Ctrl Pts',(-115.20512013751,6.98668158356849,130.330523827459));
#273525=CARTESIAN_POINT('Ctrl Pts',(-115.483567761323,3.377819743832,124.670147169045));
#273526=CARTESIAN_POINT('Ctrl Pts',(-115.762015385136,-3.33509342481799,
124.646812996834));
#273527=CARTESIAN_POINT('Ctrl Pts',(-116.040463008949,-6.98321866443162,
130.281964275151));
#273528=CARTESIAN_POINT('Ctrl Pts',(-116.318910632762,-4.21410710063033,
136.397172271667));
#273529=CARTESIAN_POINT('Ctrl Pts',(-116.597358256575,2.42756301807353,
137.372859582102));
#273530=CARTESIAN_POINT('Ctrl Pts',(-116.875805880388,6.83842131621399,
132.312417233142));
#273531=CARTESIAN_POINT('Ctrl Pts',(-117.154253504201,4.96510450020791,
125.866144527128));
#273532=CARTESIAN_POINT('Ctrl Pts',(-117.432701128013,-1.47090079265054,
123.957851162959));
#273533=CARTESIAN_POINT('Ctrl Pts',(-117.711148751826,-6.55522011456102,
128.341165516992));
#273534=CARTESIAN_POINT('Ctrl Pts',(-117.989596375639,-5.61561239149597,
134.988035834682));
#273535=CARTESIAN_POINT('Ctrl Pts',(-118.268043999452,0.484468781437156,
137.790313011739));
#273536=CARTESIAN_POINT('Ctrl Pts',(-118.546491623265,6.13934681184524,
134.172841221298));
#273537=CARTESIAN_POINT('Ctrl Pts',(-118.824939247078,6.15246504593319,
127.459900315453));
#273538=CARTESIAN_POINT('Ctrl Pts',(-119.103386870891,0.511768467435545,
123.820355041281));
#273539=CARTESIAN_POINT('Ctrl Pts',(-119.381834494704,-5.59921833135585,
126.598769704074));
#273540=CARTESIAN_POINT('Ctrl Pts',(-119.660282118516,-6.56479702065358,
133.241916961827));
#273541=CARTESIAN_POINT('Ctrl Pts',(-119.93872974233,-1.49764795613459,
137.645069020452));
#273542=CARTESIAN_POINT('Ctrl Pts',(-120.217177366142,4.94576641590264,
135.761944244007));
#273543=CARTESIAN_POINT('Ctrl Pts',(-120.495624989955,6.84426306584611,
129.323042306287));
#273544=CARTESIAN_POINT('Ctrl Pts',(-120.774072613768,2.45321631911644,
124.245399530209));
#273545=CARTESIAN_POINT('Ctrl Pts',(-121.052520237581,-4.19221637860163,
125.195121570349));
#273546=CARTESIAN_POINT('Ctrl Pts',(-121.330967861394,-6.98520702554029,
131.299460268319));
#273547=CARTESIAN_POINT('Ctrl Pts',(-121.609415485207,-3.35913366234199,
136.948826574209));
#273548=CARTESIAN_POINT('Ctrl Pts',(-121.88786310902,3.3538194337463,136.951728839794));
#273549=CARTESIAN_POINT('Ctrl Pts',(-122.166310732833,6.98477631340985,
131.305500024783));
#273550=CARTESIAN_POINT('Ctrl Pts',(-122.444758356646,4.19706498634193,
125.198748576561));
#273551=CARTESIAN_POINT('Ctrl Pts',(-122.723205980458,-2.44754402515043,
124.24328074465));
#273552=CARTESIAN_POINT('Ctrl Pts',(-123.001653604271,-6.84297964670285,
129.317124789377));
#273553=CARTESIAN_POINT('Ctrl Pts',(-123.280101228084,-4.95005127107555,
135.7576659047));
#273554=CARTESIAN_POINT('Ctrl Pts',(-123.558548851897,1.49173239922134,
137.646361443563));
#273555=CARTESIAN_POINT('Ctrl Pts',(-123.83699647571,6.5626868698133,133.247592473656));
#273556=CARTESIAN_POINT('Ctrl Pts',(-124.115444099523,5.60285271212367,
126.603612786514));
#273557=CARTESIAN_POINT('Ctrl Pts',(-124.393891723336,-0.505729373435472,
123.819915138168));
#273558=CARTESIAN_POINT('Ctrl Pts',(-124.672339347149,-6.14957087106115,
127.454581676257));
#273559=CARTESIAN_POINT('Ctrl Pts',(-124.950786970961,-6.14225716141998,
134.167531415611));
#273560=CARTESIAN_POINT('Ctrl Pts',(-125.229234594775,-0.490509186377616,
137.789891491587));
#273561=CARTESIAN_POINT('Ctrl Pts',(-125.507682218587,5.6119927682395,134.992889956494));
#273562=CARTESIAN_POINT('Ctrl Pts',(-125.786129842401,6.55734752993325,
128.346834579959));
#273563=CARTESIAN_POINT('Ctrl Pts',(-126.064577466213,1.47682025585389,
123.959125575163));
#273564=CARTESIAN_POINT('Ctrl Pts',(-126.343025090026,-4.9608326866744,
125.861853166013));
#273565=CARTESIAN_POINT('Ctrl Pts',(-126.621472713839,-6.8397227402992,
132.306503649927));
#273566=CARTESIAN_POINT('Ctrl Pts',(-126.899920337652,-2.43324173462049,
137.370758070868));
#273567=CARTESIAN_POINT('Ctrl Pts',(-127.178367961465,4.20926955470684,
136.400814018573));
#273568=CARTESIAN_POINT('Ctrl Pts',(-127.456815585278,6.98366775750873,
130.288002692701));
#273569=CARTESIAN_POINT('Ctrl Pts',(-127.73526320909,3.34041646229627,124.649699074291));
#273570=CARTESIAN_POINT('Ctrl Pts',(-128.013710832904,-3.37251437334987,
124.66722874222));
#273571=CARTESIAN_POINT('Ctrl Pts',(-128.292158456716,-6.9862692563739,
130.324482788031));
#273572=CARTESIAN_POINT('Ctrl Pts',(-128.570606080529,-4.17998399101771,
136.422721115849));
#273573=CARTESIAN_POINT('Ctrl Pts',(-128.849053704342,2.46750235851359,
137.357960617914));
#273574=CARTESIAN_POINT('Ctrl Pts',(-129.127501328155,6.84747458476236,
132.270761880817));
#273575=CARTESIAN_POINT('Ctrl Pts',(-129.405948951968,4.93495218534535,
125.836012020477));
#273576=CARTESIAN_POINT('Ctrl Pts',(-129.684396575781,-1.51255018658779,
123.966931803538));
#273577=CARTESIAN_POINT('Ctrl Pts',(-129.962844199593,-6.57009282923063,
128.381114639724));
#273578=CARTESIAN_POINT('Ctrl Pts',(-130.241291823406,-5.59004112868908,
135.022142147398));
#273579=CARTESIAN_POINT('Ctrl Pts',(-130.519739447219,0.52698528042665,
137.78723447924));
#273580=CARTESIAN_POINT('Ctrl Pts',(-130.798187071032,6.15973796149245,
134.135406864555));
#273581=CARTESIAN_POINT('Ctrl Pts',(-131.076634694845,6.13199237587537,
127.422510479544));
#273582=CARTESIAN_POINT('Ctrl Pts',(-131.355082318658,0.4692453613103,123.81736915881));
#273583=CARTESIAN_POINT('Ctrl Pts',(-131.633529942471,-5.62471521638866,
126.632931655165));
#273584=CARTESIAN_POINT('Ctrl Pts',(-131.911977566284,-6.54983729284086,
133.281833582332));
#273585=CARTESIAN_POINT('Ctrl Pts',(-132.190425190097,-1.45597887451291,
137.654058886162));
#273586=CARTESIAN_POINT('Ctrl Pts',(-132.46887281391,4.97585300097076,135.731746107516));
#273587=CARTESIAN_POINT('Ctrl Pts',(-132.747320437723,6.83511905249447,
129.281406779768));
#273588=CARTESIAN_POINT('Ctrl Pts',(-133.025768061535,2.4132446089053,124.230587628526));
#273589=CARTESIAN_POINT('Ctrl Pts',(-133.304215685348,-4.22628373671482,
125.220744707546));
#273590=CARTESIAN_POINT('Ctrl Pts',(-133.582663309161,-6.98206379373247,
131.341972033073));
#273591=CARTESIAN_POINT('Ctrl Pts',(-133.861110932974,-3.32166831708915,
136.969160731525));
#273592=CARTESIAN_POINT('Ctrl Pts',(-134.139558556787,3.39117807044069,
136.931199292478));
#273593=CARTESIAN_POINT('Ctrl Pts',(-134.4180061806,6.98769747949419,131.262972423894));
#273594=CARTESIAN_POINT('Ctrl Pts',(-134.696453804413,4.16286427289247,
125.173303709728));
#273595=CARTESIAN_POINT('Ctrl Pts',(-134.974901428226,-2.48743783327188,
124.25830120144));
#273596=CARTESIAN_POINT('Ctrl Pts',(-135.253349052039,-6.85190608875344,
129.358807503792));
#273597=CARTESIAN_POINT('Ctrl Pts',(-135.531796675851,-4.91980738289134,
135.787706498505));
#273598=CARTESIAN_POINT('Ctrl Pts',(-135.810244299665,1.53335396189511,
137.637154078616));
#273599=CARTESIAN_POINT('Ctrl Pts',(-136.088691923477,6.57743792420584,
133.207598268539));
#273600=CARTESIAN_POINT('Ctrl Pts',(-136.36713954729,5.57717775987727,126.569584461903));
#273601=CARTESIAN_POINT('Ctrl Pts',(-136.645587171103,-0.548236305497475,
123.823123062006));
#273602=CARTESIAN_POINT('Ctrl Pts',(-136.924034794916,-6.1698479889529,
127.492077923251));
#273603=CARTESIAN_POINT('Ctrl Pts',(-137.202482418729,-6.12167078439119,
134.204858766568));
#273604=CARTESIAN_POINT('Ctrl Pts',(-137.480930042542,-0.447977189217358,
137.792747934521));
#273605=CARTESIAN_POINT('Ctrl Pts',(-137.759377666354,5.63738555794455,
134.958650559891));
#273606=CARTESIAN_POINT('Ctrl Pts',(-138.037825290167,6.54226637895086,
128.306963676612));
#273607=CARTESIAN_POINT('Ctrl Pts',(-138.31627291398,1.43512400518173,123.950262577445));
#273608=CARTESIAN_POINT('Ctrl Pts',(-138.594720537793,-4.99082721964375,
125.892142735845));
#273609=CARTESIAN_POINT('Ctrl Pts',(-138.873168161606,-6.83045204508126,
132.348111152362));
#273610=CARTESIAN_POINT('Ctrl Pts',(-139.151615785419,-2.39322512722196,
137.385448243807));
#273611=CARTESIAN_POINT('Ctrl Pts',(-139.430063409232,4.24325876700673,
136.375087310741));
#273612=CARTESIAN_POINT('Ctrl Pts',(-139.708511033045,6.98039514907165,
130.245500691775));
#273613=CARTESIAN_POINT('Ctrl Pts',(-139.986958656858,3.30288940040013,
124.629479042785));
#273614=CARTESIAN_POINT('Ctrl Pts',(-140.26540628067,-3.40981035212143,
124.687871901284));
#273615=CARTESIAN_POINT('Ctrl Pts',(-140.543853904484,-6.98906096953965,
130.36701908296));
#273616=CARTESIAN_POINT('Ctrl Pts',(-140.822301528296,-4.1457059905611,
136.448061769617));
#273617=CARTESIAN_POINT('Ctrl Pts',(-141.100749152109,2.50735026474636,
137.342818807668));
#273618=CARTESIAN_POINT('Ctrl Pts',(-141.379196775922,6.85627411762182,
132.229052190456));
#273619=CARTESIAN_POINT('Ctrl Pts',(-141.657644399735,4.90461700401472,
125.80606361781));
#273620=CARTESIAN_POINT('Ctrl Pts',(-141.936092023548,-1.5541435324211,
123.976265807557));
#273621=CARTESIAN_POINT('Ctrl Pts',(-142.214539647361,-6.58472208669408,
128.421153556726));
#273622=CARTESIAN_POINT('Ctrl Pts',(-142.492987271174,-5.56426272485295,
135.056092168669));
#273623=CARTESIAN_POINT('Ctrl Pts',(-142.771434894987,0.569482251782813,
137.783897193782));
#273624=CARTESIAN_POINT('Ctrl Pts',(-143.0498825188,6.17990085978423,134.097849074668));
#273625=CARTESIAN_POINT('Ctrl Pts',(-143.328330142612,6.11129248258502,
127.385245959334));
#273626=CARTESIAN_POINT('Ctrl Pts',(-143.606777766425,0.426704867125613,
123.814642181877));
#273627=CARTESIAN_POINT('Ctrl Pts',(-143.885225390238,-5.65000367553061,
126.667248180088));
#273628=CARTESIAN_POINT('Ctrl Pts',(-144.163673014051,-6.53463485839856,
133.321658399163));
#273629=CARTESIAN_POINT('Ctrl Pts',(-144.442120637864,-1.4142558410586,
137.662794933783));
#273630=CARTESIAN_POINT('Ctrl Pts',(-144.720568261677,5.00575520397605,
135.701365384942));
#273631=CARTESIAN_POINT('Ctrl Pts',(-144.99901588549,6.82572176129271,129.239827686864));
#273632=CARTESIAN_POINT('Ctrl Pts',(-145.277463509303,2.37318347502772,
124.216019320419));
#273633=CARTESIAN_POINT('Ctrl Pts',(-145.555911133116,-4.26019448832994,
125.246574747685));
#273634=CARTESIAN_POINT('Ctrl Pts',(-145.834358756928,-6.97866183898313,
131.384463876438));
#273635=CARTESIAN_POINT('Ctrl Pts',(-146.112806380741,-3.28407988619528,
136.989266449907));
#273636=CARTESIAN_POINT('Ctrl Pts',(-146.391254004554,3.42841104578457,
136.910442712901));
#273637=CARTESIAN_POINT('Ctrl Pts',(-146.669701628367,6.99035971387901,
131.220427828976));
#273638=CARTESIAN_POINT('Ctrl Pts',(-146.94814925218,4.12850930297597,125.148067503779));
#273639=CARTESIAN_POINT('Ctrl Pts',(-147.226596875993,-2.52723946847004,
124.27356422487));
#273640=CARTESIAN_POINT('Ctrl Pts',(-147.505044499806,-6.86057863090408,
129.400543783708));
#273641=CARTESIAN_POINT('Ctrl Pts',(-147.783492123619,-4.88938118943532,
135.817562432597));
#273642=CARTESIAN_POINT('Ctrl Pts',(-148.061939747432,1.57491870557395,
137.627693521995));
#273643=CARTESIAN_POINT('Ctrl Pts',(-148.340387371245,6.5919452492172,133.167515010566));
#273644=CARTESIAN_POINT('Ctrl Pts',(-148.618834995057,5.55129614325799,
126.535713058481));
#273645=CARTESIAN_POINT('Ctrl Pts',(-148.89728261887,-0.590722922461593,
123.826589678167));
#273646=CARTESIAN_POINT('Ctrl Pts',(-149.175730242683,-6.18989648085842,
127.529696908099));
#273647=CARTESIAN_POINT('Ctrl Pts',(-149.454177866496,-6.10085756660025,
134.242060110815));
#273648=CARTESIAN_POINT('Ctrl Pts',(-149.732625490309,-0.405428592098244,
137.795345420191));
#273649=CARTESIAN_POINT('Ctrl Pts',(-150.011073114122,5.66256945225453,
134.924257224548));
#273650=CARTESIAN_POINT('Ctrl Pts',(-150.289520737935,6.52694280188189,
128.267185315226));
#273651=CARTESIAN_POINT('Ctrl Pts',(-150.567968361748,1.39337457546175,
123.94165356085));
#273652=CARTESIAN_POINT('Ctrl Pts',(-150.84641598556,-5.02063681567507,
125.922614329717));
#273653=CARTESIAN_POINT('Ctrl Pts',(-151.124863609373,-6.8209282449509,
132.389661450552));
#273654=CARTESIAN_POINT('Ctrl Pts',(-151.403311233186,-2.35311983798619,
137.399894552124));
#273655=CARTESIAN_POINT('Ctrl Pts',(-151.681758856999,4.2770907437925,136.349154177582));
#273656=CARTESIAN_POINT('Ctrl Pts',(-151.960206480812,6.97686387952531,
130.20301939961));
#273657=CARTESIAN_POINT('Ctrl Pts',(-152.238654104625,3.26523994872261,
124.609487823786));
#273658=CARTESIAN_POINT('Ctrl Pts',(-152.517101728438,-3.44697997911642,
124.708741709087));
#273659=CARTESIAN_POINT('Ctrl Pts',(-152.795549352251,-6.99159370048095,
130.40957158374));
#273660=CARTESIAN_POINT('Ctrl Pts',(-153.073996976064,-4.11127436944443,
136.473193293963));
#273661=CARTESIAN_POINT('Ctrl Pts',(-153.352444599876,2.54710526019297,
137.327434712448));
#273662=CARTESIAN_POINT('Ctrl Pts',(-153.63089222369,6.86481958872245,132.187289707623));
#273663=CARTESIAN_POINT('Ctrl Pts',(-153.909339847502,4.87410008029735,
125.776300428876));
#273664=CARTESIAN_POINT('Ctrl Pts',(-154.187787471315,-1.5956792888948,
123.98585282914));
#273665=CARTESIAN_POINT('Ctrl Pts',(-154.466235095128,-6.5991073448593,
128.461280784342));
#273666=CARTESIAN_POINT('Ctrl Pts',(-154.744682718941,-5.53827813521478,
135.089884640464));
#273667=CARTESIAN_POINT('Ctrl Pts',(-155.023130342754,0.611958120764675,
137.78030127903));
#273668=CARTESIAN_POINT('Ctrl Pts',(-155.301577966567,6.19983475957701,
134.060169243357));
#273669=CARTESIAN_POINT('Ctrl Pts',(-155.58002559038,6.0903661331043,127.348108135675));
#273670=CARTESIAN_POINT('Ctrl Pts',(-155.858473214192,0.38414856123516,
123.812174211531));
#273671=CARTESIAN_POINT('Ctrl Pts',(-156.136920838005,-5.67508277170857,
126.701718007236));
#273672=CARTESIAN_POINT('Ctrl Pts',(-156.415368461818,-6.51919028065846,
133.3613899366));
#273673=CARTESIAN_POINT('Ctrl Pts',(-156.693816085631,-1.37248040183399,
137.671276839599));
#273674=CARTESIAN_POINT('Ctrl Pts',(-156.972263709444,5.03547191688086,
135.670803202055));
#273675=CARTESIAN_POINT('Ctrl Pts',(-157.250711333257,6.81607154046107,
129.198306568304));
#273676=CARTESIAN_POINT('Ctrl Pts',(-157.52915895707,2.33303440196427,124.201695145721));
#273677=CARTESIAN_POINT('Ctrl Pts',(-157.807606580883,-4.29394737687161,
125.272610733624));
#273678=CARTESIAN_POINT('Ctrl Pts',(-158.086054204696,-6.97500128735293,
131.426934223863));
#273679=CARTESIAN_POINT('Ctrl Pts',(-158.364501828508,-3.2463697625135,
137.009142984327));
#273680=CARTESIAN_POINT('Ctrl Pts',(-158.642949452322,3.46551698009634,
136.889459870208));
#273681=CARTESIAN_POINT('Ctrl Pts',(-158.921397076134,6.99276291791392,
131.177867816534));
#273682=CARTESIAN_POINT('Ctrl Pts',(-159.199844699947,4.09400134962899,
125.123040893851));
#273683=CARTESIAN_POINT('Ctrl Pts',(-159.47829232376,-2.56694745588028,
124.289069249361));
#273684=CARTESIAN_POINT('Ctrl Pts',(-159.756739947573,-6.86899695179061,
129.442332082575));
#273685=CARTESIAN_POINT('Ctrl Pts',(-160.035187571386,-4.85877381816122,
135.84723260065));
#273686=CARTESIAN_POINT('Ctrl Pts',(-160.313635195198,1.61642509006095,
137.617980124263));
#273687=CARTESIAN_POINT('Ctrl Pts',(-160.592082819012,6.60620830727321,
133.12734418504));
#273688=CARTESIAN_POINT('Ctrl Pts',(-160.870530442824,5.52520882131862,
126.501999831362));
#273689=CARTESIAN_POINT('Ctrl Pts',(-161.148978066638,-0.633187649970563,
123.830314858198));
#273690=CARTESIAN_POINT('Ctrl Pts',(-161.42742569045,-6.20971560387352,
127.567437236815));
#273691=CARTESIAN_POINT('Ctrl Pts',(-161.705873314263,-6.07981827928859,
134.279134069845));
#273692=CARTESIAN_POINT('Ctrl Pts',(-161.984320938076,-0.362864971672915,
137.79768385235));
#273693=CARTESIAN_POINT('Ctrl Pts',(-162.262768561889,5.68754351797111,
134.889711224922));
#273694=CARTESIAN_POINT('Ctrl Pts',(-162.541216185702,6.5113773665471,128.227500969805));
#273695=CARTESIAN_POINT('Ctrl Pts',(-162.819663809515,1.35157351373451,
123.93329884439));
#273696=CARTESIAN_POINT('Ctrl Pts',(-163.098111433328,-5.05026037016286,
125.953266818493));
#273697=CARTESIAN_POINT('Ctrl Pts',(-163.376559057141,-6.81115169281603,
132.431153004838));
#273698=CARTESIAN_POINT('Ctrl Pts',(-163.655006680953,-2.31292735302948,
137.414096460505));
#273699=CARTESIAN_POINT('Ctrl Pts',(-163.933454304766,4.31076423140788,
136.323015580059));
#273700=CARTESIAN_POINT('Ctrl Pts',(-164.211901928579,6.97307407972212,
130.160560390364));
#273701=CARTESIAN_POINT('Ctrl Pts',(-164.490349552392,3.2274695023783,124.589726158078));
#273702=CARTESIAN_POINT('Ctrl Pts',(-164.768797176205,-3.4840218770001,
124.729837392289));
#273703=CARTESIAN_POINT('Ctrl Pts',(-165.047244800018,-6.99386735534677,
130.452138713572));
#273704=CARTESIAN_POINT('Ctrl Pts',(-165.325692423831,-4.07669040354407,
136.498114757629));
#273705=CARTESIAN_POINT('Ctrl Pts',(-165.604140047644,2.58676587171747,
137.31180890232));
#273706=CARTESIAN_POINT('Ctrl Pts',(-165.882587671457,6.87311068140868,
132.145475979844));
#273707=CARTESIAN_POINT('Ctrl Pts',(-166.161035295269,4.84340254500906,
125.746723556562));
#273708=CARTESIAN_POINT('Ctrl Pts',(-166.439482919082,-1.63715591688565,
123.995692513036));
#273709=CARTESIAN_POINT('Ctrl Pts',(-166.717930542895,-6.61324807067504,
128.501494835643));
#273710=CARTESIAN_POINT('Ctrl Pts',(-166.996378166708,-5.5120883226436,
135.12351831059));
#273711=CARTESIAN_POINT('Ctrl Pts',(-167.274825790521,0.654411313413328,
137.776446868231));
#273712=CARTESIAN_POINT('Ctrl Pts',(-167.553273414334,6.21953892221278,
134.022368766858));
#273713=CARTESIAN_POINT('Ctrl Pts',(-167.831721038147,6.06921410286677,
127.311098384725));
#273714=CARTESIAN_POINT('Ctrl Pts',(-168.11016866196,0.3415780205785,123.809965339223));
#273715=CARTESIAN_POINT('Ctrl Pts',(-168.388616285773,-5.69995157560742,
126.736339859314));
#273716=CARTESIAN_POINT('Ctrl Pts',(-168.667063909585,-6.50350413192509,
133.401026722375));
#273717=CARTESIAN_POINT('Ctrl Pts',(-168.945511533399,-1.33065410484337,
137.679504289309));
#273718=CARTESIAN_POINT('Ctrl Pts',(-169.223959157211,5.06500203852252,
135.640060691349));
#273719=CARTESIAN_POINT('Ctrl Pts',(-169.502406781024,6.80616874759175,
129.156844962666));
#273720=CARTESIAN_POINT('Ctrl Pts',(-169.780854404837,2.29279887745254,
124.18761563522));
#273721=CARTESIAN_POINT('Ctrl Pts',(-170.05930202865,-4.32754115161411,
125.298851700587));
#273722=CARTESIAN_POINT('Ctrl Pts',(-170.337749652463,-6.97108227448498,
131.469381501595));
#273723=CARTESIAN_POINT('Ctrl Pts',(-170.616197276276,-3.20853934340632,
137.028789598255));
#273724=CARTESIAN_POINT('Ctrl Pts',(-170.894644900089,3.50249449840198,
136.868251541923));
#273725=CARTESIAN_POINT('Ctrl Pts',(-171.173092523901,6.99490700254731,
131.135293963646));
#273726=CARTESIAN_POINT('Ctrl Pts',(-171.451540147715,4.05934169155642,
125.098224807315));
#273727=CARTESIAN_POINT('Ctrl Pts',(-171.729987771527,-2.60656032410858,
124.304815700371));
#273728=CARTESIAN_POINT('Ctrl Pts',(-172.00843539534,-6.87716073946864,
129.484170851909));
#273729=CARTESIAN_POINT('Ctrl Pts',(-172.286883019153,-4.82798640323697,
135.876715903229));
#273730=CARTESIAN_POINT('Ctrl Pts',(-172.565330642966,1.65787157732142,
137.608014245356));
#273731=CARTESIAN_POINT('Ctrl Pts',(-172.843778266779,6.62022656985093,
133.087087280501));
#273732=CARTESIAN_POINT('Ctrl Pts',(-173.122225890592,5.49891676073447,
126.468446029806));
#273733=CARTESIAN_POINT('Ctrl Pts',(-173.400673514405,-0.675628914478315,
123.834298464058));
#273734=CARTESIAN_POINT('Ctrl Pts',(-173.679121138218,-6.22930462359329,
127.605297510917));
#273735=CARTESIAN_POINT('Ctrl Pts',(-173.95756876203,-6.05855370207473,
134.316079269865));
#273736=CARTESIAN_POINT('Ctrl Pts',(-174.236016385844,-0.320287905152608,
137.799763144343));
#273737=CARTESIAN_POINT('Ctrl Pts',(-174.514464009656,5.71230682967103,
134.855013841124));
#273738=CARTESIAN_POINT('Ctrl Pts',(-174.792911633469,6.49557064972945,
128.187912110866));
#273739=CARTESIAN_POINT('Ctrl Pts',(-175.071359257282,1.30972236895365,
123.925198737649));
#273740=CARTESIAN_POINT('Ctrl Pts',(-175.349806881095,-5.07969678539539,
125.984099066334));
#273741=CARTESIAN_POINT('Ctrl Pts',(-175.628254504908,-6.80112275095037,
132.472584277733));
#273742=CARTESIAN_POINT('Ctrl Pts',(-175.906702128721,-2.27264916169912,
137.428053442694));
#273743=CARTESIAN_POINT('Ctrl Pts',(-176.185149752534,4.34427798206938,
136.296672486746));
#273744=CARTESIAN_POINT('Ctrl Pts',(-176.463597376347,6.96902589009458,
130.118125237372));
#273745=CARTESIAN_POINT('Ctrl Pts',(-176.742045000159,3.18957946096438,
124.570194777934));
#273746=CARTESIAN_POINT('Ctrl Pts',(-177.020492623972,-3.52093467317244,
124.751158169184));
#273747=CARTESIAN_POINT('Ctrl Pts',(-177.298940247785,-6.99588184988549,
130.494718895118));
#273748=CARTESIAN_POINT('Ctrl Pts',(-177.577387871598,-4.04195537438161,
136.522825237142));
#273749=CARTESIAN_POINT('Ctrl Pts',(-177.855835495411,2.62633062968132,
137.295941956302));
#273750=CARTESIAN_POINT('Ctrl Pts',(-178.134283119224,6.88114708845103,
132.103612556543));
#273751=CARTESIAN_POINT('Ctrl Pts',(-178.412730743037,4.81252553565828,
125.717334096849));
#273752=CARTESIAN_POINT('Ctrl Pts',(-178.69117836685,-1.67857187946192,
124.005784494632));
#273753=CARTESIAN_POINT('Ctrl Pts',(-178.969625990663,-6.62714374015151,
128.541794220484));
#273754=CARTESIAN_POINT('Ctrl Pts',(-179.248073614475,-5.48569425761253,
135.15699193274));
#273755=CARTESIAN_POINT('Ctrl Pts',(-179.526521238288,0.696840256609583,
137.772334104211));
#273756=CARTESIAN_POINT('Ctrl Pts',(-179.804968862101,6.23901261754625,
133.984449045885));
#273757=CARTESIAN_POINT('Ctrl Pts',(-180.083416485914,6.0478371756692,127.27421807789));
#273758=CARTESIAN_POINT('Ctrl Pts',(-180.361864109727,0.298994822622653,
123.808015646805));
#273759=CARTESIAN_POINT('Ctrl Pts',(-180.64031173354,-5.72460916570447,
126.771112453397));
#273760=CARTESIAN_POINT('Ctrl Pts',(-180.918759357353,-6.48757699345442,
133.440567287733));
#273761=CARTESIAN_POINT('Ctrl Pts',(-181.197206981166,-1.28877849997557,
137.687476978041));
#273762=CARTESIAN_POINT('Ctrl Pts',(-181.475654604978,5.094344474651,135.609138992));
#273763=CARTESIAN_POINT('Ctrl Pts',(-181.754102228792,6.79601374963652,
129.115444406326));
#273764=CARTESIAN_POINT('Ctrl Pts',(-182.032549852604,2.25247839243521,
124.173781310638));
#273765=CARTESIAN_POINT('Ctrl Pts',(-182.310997476417,-4.36097456772779,
125.32529667621));
#273766=CARTESIAN_POINT('Ctrl Pts',(-182.58944510023,-6.96690494559973,
131.511804136733));
#273767=CARTESIAN_POINT('Ctrl Pts',(-182.867892724043,-3.17059003069381,
137.048205563678));
#273768=CARTESIAN_POINT('Ctrl Pts',(-183.146340347856,3.53934223048593,
136.84681851393));
#273769=CARTESIAN_POINT('Ctrl Pts',(-183.424787971669,6.99679188832936,
131.092707847901));
#273770=CARTESIAN_POINT('Ctrl Pts',(-183.703235595482,4.02453161308464,
125.07362016374));
#273771=CARTESIAN_POINT('Ctrl Pts',(-183.981683219295,-2.64607660528548,
124.320802994409));
#273772=CARTESIAN_POINT('Ctrl Pts',(-184.260130843107,-6.88506969142675,
129.52605854136));
#273773=CARTESIAN_POINT('Ctrl Pts',(-184.53857846692,-4.79702008550057,
135.906011247817));
#273774=CARTESIAN_POINT('Ctrl Pts',(-184.817026090733,1.6992566315413,137.597796254561));
#273775=CARTESIAN_POINT('Ctrl Pts',(-185.095473714546,6.63399951749853,
133.046745788687));
#273776=CARTESIAN_POINT('Ctrl Pts',(-185.373921338359,5.47242093576752,
126.435052897159));
#273777=CARTESIAN_POINT('Ctrl Pts',(-185.652368962172,-0.718045143308166,
123.838540348135));
#273778=CARTESIAN_POINT('Ctrl Pts',(-185.930816585985,-6.24866281413942,
127.64327632748));
#273779=CARTESIAN_POINT('Ctrl Pts',(-186.209264209798,-6.03706462292539,
134.35289434186));
#273780=CARTESIAN_POINT('Ctrl Pts',(-186.487711833611,-0.277698970246197,
137.801583219124));
#273781=CARTESIAN_POINT('Ctrl Pts',(-186.766159457423,5.73685846974069,
134.820166358884));
#273782=CARTESIAN_POINT('Ctrl Pts',(-187.044607081237,6.47952323715255,
128.148420205389));
#273783=CARTESIAN_POINT('Ctrl Pts',(-187.323054705049,1.2678226919294,123.917353540782));
#273784=CARTESIAN_POINT('Ctrl Pts',(-187.601502328862,-5.10894497059535,
126.01510993074));
#273785=CARTESIAN_POINT('Ctrl Pts',(-187.879949952675,-6.79084179098006,
132.513953733987));
#273786=CARTESIAN_POINT('Ctrl Pts',(-188.158397576488,-2.23228675651833,
137.44176498151));
#273787=CARTESIAN_POINT('Ctrl Pts',(-188.436845200301,4.37763075391265,
136.270125873797));
#273788=CARTESIAN_POINT('Ctrl Pts',(-188.715292824114,6.96471946064982,
130.075715513085));
#273789=CARTESIAN_POINT('Ctrl Pts',(-188.993740447926,3.15157122851057,
124.550894407098));
#273790=CARTESIAN_POINT('Ctrl Pts',(-189.27218807174,-3.55771699981564,
124.772703249722));
#273791=CARTESIAN_POINT('Ctrl Pts',(-189.550635695553,-6.99763710944952,
130.53731055055));
#273792=CARTESIAN_POINT('Ctrl Pts',(-189.829083319365,-4.00707056907658,
136.547323816845));
#273793=CARTESIAN_POINT('Ctrl Pts',(-190.107530943179,2.66579806799723,
137.279834462351));
#273794=CARTESIAN_POINT('Ctrl Pts',(-190.385978566991,6.88892851205765,
132.061700988983));
#273795=CARTESIAN_POINT('Ctrl Pts',(-190.664426190804,4.78147019640398,
125.688133138775));
#273796=CARTESIAN_POINT('Ctrl Pts',(-190.942873814617,-1.71992564193992,
124.016128399968));
#273797=CARTESIAN_POINT('Ctrl Pts',(-191.22132143843,-6.64079383837953,
128.582177445553));
#273798=CARTESIAN_POINT('Ctrl Pts',(-191.499769062243,-5.45909691816341,
135.190304266535));
#273799=CARTESIAN_POINT('Ctrl Pts',(-191.778216686055,0.739243378134395,
137.767963139373));
#273800=CARTESIAN_POINT('Ctrl Pts',(-192.056664309869,6.25825512397307,
133.946411485565));
#273801=CARTESIAN_POINT('Ctrl Pts',(-192.335111933681,6.0262361436405,127.237468581785));
#273802=CARTESIAN_POINT('Ctrl Pts',(-192.613559557494,0.256400545303713,
123.806325206523));
#273803=CARTESIAN_POINT('Ctrl Pts',(-192.892007181307,-5.74905462830365,
126.806034500975));
#273804=CARTESIAN_POINT('Ctrl Pts',(-193.17045480512,-6.47140945543246,
133.480010167483));
#273805=CARTESIAN_POINT('Ctrl Pts',(-193.448902428933,-1.24685513894648,
137.695194610365));
#273806=CARTESIAN_POINT('Ctrl Pts',(-193.727350052746,5.12349813797151,
135.578039249819));
#273807=CARTESIAN_POINT('Ctrl Pts',(-194.005797676559,6.78560692289256,
129.074106433399));
#273808=CARTESIAN_POINT('Ctrl Pts',(-194.284245300372,2.2120744410027,124.160192684611));
#273809=CARTESIAN_POINT('Ctrl Pts',(-194.562692924184,-4.39424638632456,
125.35194468056));
#273810=CARTESIAN_POINT('Ctrl Pts',(-194.841140547997,-6.9624694554897,
131.554200557291));
#273811=CARTESIAN_POINT('Ctrl Pts',(-195.11958817181,-3.13252323060231,
137.067390161131));
#273812=CARTESIAN_POINT('Ctrl Pts',(-195.398035795623,3.57605881094196,
136.825161580438));
#273813=CARTESIAN_POINT('Ctrl Pts',(-195.676483419436,6.99841750541489,
131.050111047343));
#273814=CARTESIAN_POINT('Ctrl Pts',(-195.954931043249,3.98957240411393,
125.04922787486));
#273815=CARTESIAN_POINT('Ctrl Pts',(-196.233378667062,-2.68549483512068,
124.337030539057));
#273816=CARTESIAN_POINT('Ctrl Pts',(-196.511826290875,-6.89272351459547,
129.567993598765));
#273817=CARTESIAN_POINT('Ctrl Pts',(-196.790273914688,-4.76587601242081,
135.935117548864));
#273818=CARTESIAN_POINT('Ctrl Pts',(-197.0687215385,1.74057871918182,137.58732653051));
#273819=CARTESIAN_POINT('Ctrl Pts',(-197.347169162313,6.64752663985393,
133.006321204467));
#273820=CARTESIAN_POINT('Ctrl Pts',(-197.625616786126,5.44572232823074,
126.401821670817));
#273821=CARTESIAN_POINT('Ctrl Pts',(-197.904064409939,-0.760434764710735,
123.843040353244));
#273822=CARTESIAN_POINT('Ctrl Pts',(-198.182512033752,-6.26778945818702,
127.681372279183));
#273823=CARTESIAN_POINT('Ctrl Pts',(-198.460959657565,-6.01535183812634,
134.389577921633));
#273824=CARTESIAN_POINT('Ctrl Pts',(-198.739407281378,-0.235099745102313,
137.803144009248));
#273825=CARTESIAN_POINT('Ctrl Pts',(-199.017854905191,5.76119752841001,
134.785170069484));
#273826=CARTESIAN_POINT('Ctrl Pts',(-199.296302529004,6.46323572345932,
128.10902671676));
#273827=CARTESIAN_POINT('Ctrl Pts',(-199.574750152817,1.22587603526843,
123.909763544495));
#273828=CARTESIAN_POINT('Ctrl Pts',(-199.853197776629,-5.13800384196074,
126.04629826259));
#273829=CARTESIAN_POINT('Ctrl Pts',(-200.131645400443,-6.78030919386985,
132.555259840639));
#273830=CARTESIAN_POINT('Ctrl Pts',(-200.410093024255,-2.19184163313082,
137.455230568865));
#273831=CARTESIAN_POINT('Ctrl Pts',(-200.688540648069,4.41082131103843,
136.243376724908));
#273832=CARTESIAN_POINT('Ctrl Pts',(-200.96698827188,6.96015495096418,130.03333278901));
#273833=CARTESIAN_POINT('Ctrl Pts',(-201.245435895694,3.11344621342587,
124.531825760752));
#273834=CARTESIAN_POINT('Ctrl Pts',(-201.523883519507,-3.59436749394705,
124.794471835542));
#273835=CARTESIAN_POINT('Ctrl Pts',(-201.80233114332,-6.99913306899709,
130.579912101622));
#273836=CARTESIAN_POINT('Ctrl Pts',(-202.080778767133,-3.97203728029775,
136.571609588935));
#273837=CARTESIAN_POINT('Ctrl Pts',(-202.359226390945,2.705166724186,137.263487017335));
#273838=CARTESIAN_POINT('Ctrl Pts',(-202.637674014758,6.89645466388467,
132.019742830214));
#273839=CARTESIAN_POINT('Ctrl Pts',(-202.916121638571,4.75023767801316,
125.659121764391));
#273840=CARTESIAN_POINT('Ctrl Pts',(-203.194569262384,-1.76121567194074,
124.026723845744));
#273841=CARTESIAN_POINT('Ctrl Pts',(-203.473016886197,-6.65419785954973,
128.622643014438));
#273842=CARTESIAN_POINT('Ctrl Pts',(-203.75146451001,-5.43229728987039,
135.223454077576));
#273843=CARTESIAN_POINT('Ctrl Pts',(-204.029912133822,0.781619106723946,
137.763334135682));
#273844=CARTESIAN_POINT('Ctrl Pts',(-204.308359757636,6.27726572845484,
133.908257495395));
#273845=CARTESIAN_POINT('Ctrl Pts',(-204.586807381448,6.00441180721532,
127.200851258176));
#273846=CARTESIAN_POINT('Ctrl Pts',(-204.865255005262,0.213796766968775,
123.804894081017));
#273847=CARTESIAN_POINT('Ctrl Pts',(-205.143702629074,-5.77328705756903,
126.841104707996));
#273848=CARTESIAN_POINT('Ctrl Pts',(-205.422150252887,-6.4550021169537,
133.519353900054));
#273849=CARTESIAN_POINT('Ctrl Pts',(-205.7005978767,-1.20488557524167,137.702656900301));
#273850=CARTESIAN_POINT('Ctrl Pts',(-205.979045500513,5.15246194818434,
135.546762617222));
#273851=CARTESIAN_POINT('Ctrl Pts',(-206.257493124326,6.77494865298866,
129.032832575676));
#273852=CARTESIAN_POINT('Ctrl Pts',(-206.535940748139,2.17158852033829,
124.14685026067));
#273853=CARTESIAN_POINT('Ctrl Pts',(-206.814388371952,-4.42735537450605,
125.378794726189));
#273854=CARTESIAN_POINT('Ctrl Pts',(-207.092835995765,-6.9577759685135,
131.596569192254));
#273855=CARTESIAN_POINT('Ctrl Pts',(-207.371283619578,-3.09434035370993,
137.086342679721));
#273856=CARTESIAN_POINT('Ctrl Pts',(-207.64973124339,3.61264287922363,136.803281543952));
#273857=CARTESIAN_POINT('Ctrl Pts',(-207.928178867203,6.99978379356611,
131.007505140413));
#273858=CARTESIAN_POINT('Ctrl Pts',(-208.206626491016,3.95446536007061,
125.025048844539));
#273859=CARTESIAN_POINT('Ctrl Pts',(-208.485074114829,-2.72481355295718,
124.353497733001));
#273860=CARTESIAN_POINT('Ctrl Pts',(-208.763521738642,-6.90012192535954,
129.609974470206));
#273861=CARTESIAN_POINT('Ctrl Pts',(-209.041969362455,-4.73455533805275,
135.964033727826));
#273862=CARTESIAN_POINT('Ctrl Pts',(-209.320416986268,1.78183630903778,
137.576605461163));
#273863=CARTESIAN_POINT('Ctrl Pts',(-209.598864610081,6.66080743566547,
132.965815025787));
#273864=CARTESIAN_POINT('Ctrl Pts',(-209.877312233893,5.41882192745001,
126.368753582173));
#273865=CARTESIAN_POINT('Ctrl Pts',(-210.155759857706,-0.802796207923886,
123.847798312635));
#273866=CARTESIAN_POINT('Ctrl Pts',(-210.434207481519,-6.28668384699127,
127.719583954367));
#273867=CARTESIAN_POINT('Ctrl Pts',(-210.712655105332,-5.99341615225276,
134.42612864986));
#273868=CARTESIAN_POINT('Ctrl Pts',(-210.991102729145,-0.19249180825093,
137.804445456879));
#273869=CARTESIAN_POINT('Ctrl Pts',(-211.269550352958,5.78532310378624,
134.750026269725));
#273870=CARTESIAN_POINT('Ctrl Pts',(-211.547997976771,6.44670871218949,
128.069733104719));
#273871=CARTESIAN_POINT('Ctrl Pts',(-211.826445600584,1.18388395332015,
123.902429030038));
#273872=CARTESIAN_POINT('Ctrl Pts',(-212.104893224396,-5.16687232270428,
126.077662906191));
#273873=CARTESIAN_POINT('Ctrl Pts',(-212.38334084821,-6.76952534990887,
132.596501067076));
#273874=CARTESIAN_POINT('Ctrl Pts',(-212.661788472022,-2.15131529024619,
137.468449705789));
#273875=CARTESIAN_POINT('Ctrl Pts',(-212.940236095835,4.44384842355829,
136.216426031276));
#273876=CARTESIAN_POINT('Ctrl Pts',(-213.218683719648,6.95533253017721,
129.990978635656));
#273877=CARTESIAN_POINT('Ctrl Pts',(-213.497131343461,3.0752058284468,124.512989545492));
#273878=CARTESIAN_POINT('Ctrl Pts',(-213.775578967274,-3.63088479746918,
124.81646312));
#273879=CARTESIAN_POINT('Ctrl Pts',(-214.054026591087,-7.00036967309483,
130.622521969716));
#273880=CARTESIAN_POINT('Ctrl Pts',(-214.3324742149,-3.93685680621679,136.595681653493));
#273881=CARTESIAN_POINT('Ctrl Pts',(-214.610921838713,2.74443513942699,
137.246900227015));
#273882=CARTESIAN_POINT('Ctrl Pts',(-214.889369462525,6.90372526504794,
131.977739635008));
#273883=CARTESIAN_POINT('Ctrl Pts',(-215.167817086339,4.71882913781829,
125.630301048724));
#273884=CARTESIAN_POINT('Ctrl Pts',(-215.446264710151,-1.80244043944716,
124.037570439344));
#273885=CARTESIAN_POINT('Ctrl Pts',(-215.724712333964,-6.66735530697114,
128.66318942767));
#273886=CARTESIAN_POINT('Ctrl Pts',(-216.003159957777,-5.40529636580357,
135.256440137483));
#273887=CARTESIAN_POINT('Ctrl Pts',(-216.28160758159,0.823965872130078,
137.758447264668));
#273888=CARTESIAN_POINT('Ctrl Pts',(-216.560055205403,6.29604372654653,
133.869988489185));
#273889=CARTESIAN_POINT('Ctrl Pts',(-216.838502829216,5.98236497510254,
127.164367463932));
#273890=CARTESIAN_POINT('Ctrl Pts',(-217.116950453029,0.171185066315507,
123.803722323317));
#273891=CARTESIAN_POINT('Ctrl Pts',(-217.395398076842,-5.79730555555969,
126.876321774922));
#273892=CARTESIAN_POINT('Ctrl Pts',(-217.673845700654,-6.43835558599724,
133.558597027552));
#273893=CARTESIAN_POINT('Ctrl Pts',(-217.952293324468,-1.16287136405879,
137.709863571333));
#273894=CARTESIAN_POINT('Ctrl Pts',(-218.23074094828,5.18123483202488,135.515310253174));
#273895=CARTESIAN_POINT('Ctrl Pts',(-218.509188572093,6.76403933487094,
128.991624362576));
#273896=CARTESIAN_POINT('Ctrl Pts',(-218.787636195906,2.13102213066266,
124.133754533223));
#273897=CARTESIAN_POINT('Ctrl Pts',(-219.066083819719,-4.46030030540597,
125.405845818157));
#273898=CARTESIAN_POINT('Ctrl Pts',(-219.344531443532,-6.95282465859006,
131.638908471637));
#273899=CARTESIAN_POINT('Ctrl Pts',(-219.622979067345,-3.0560428148978,
137.105062417155));
#273900=CARTESIAN_POINT('Ctrl Pts',(-219.901426691158,3.6490930796943,136.781179215245));
#273901=CARTESIAN_POINT('Ctrl Pts',(-220.179874314971,7.00089070215466,
130.964891705888));
#273902=CARTESIAN_POINT('Ctrl Pts',(-220.458321938783,3.91921178185968,
125.001083968743));
#273903=CARTESIAN_POINT('Ctrl Pts',(-220.736769562596,-2.76403130182543,
124.370203966041));
#273904=CARTESIAN_POINT('Ctrl Pts',(-221.015217186409,-6.90726464956813,
129.651999600063));
#273905=CARTESIAN_POINT('Ctrl Pts',(-221.293664810222,-4.7030592229955,
135.992758713204));
#273906=CARTESIAN_POINT('Ctrl Pts',(-221.572112434035,1.82302787229404,
137.565633443793));
#273907=CARTESIAN_POINT('Ctrl Pts',(-221.850560057848,6.67384141280798,
132.925228753618));
#273908=CARTESIAN_POINT('Ctrl Pts',(-222.129007681661,5.39172073022998,
126.33584985658));
#273909=CARTESIAN_POINT('Ctrl Pts',(-222.407455305474,-0.845127903228338,
123.85281405));
#273910=CARTESIAN_POINT('Ctrl Pts',(-222.685902929286,-6.30534528041361,
127.757909937084));
#273911=CARTESIAN_POINT('Ctrl Pts',(-222.964350553099,-5.9712583781396,
134.462545172141));
#273912=CARTESIAN_POINT('Ctrl Pts',(-223.242798176912,-0.14987673854478,
137.805487513793));
#273913=CARTESIAN_POINT('Ctrl Pts',(-223.521245800725,5.80923430188729,
134.714736261875));
#273914=CARTESIAN_POINT('Ctrl Pts',(-223.799693424538,6.42994281575757,
128.030540825308));
#273915=CARTESIAN_POINT('Ctrl Pts',(-224.078141048351,1.1418480021166,123.895350269195));
#273916=CARTESIAN_POINT('Ctrl Pts',(-224.356588672164,-5.19554934309376,
126.109202699315));
#273917=CARTESIAN_POINT('Ctrl Pts',(-224.635036295977,-6.75849065869668,
132.637675885092));
#273918=CARTESIAN_POINT('Ctrl Pts',(-224.913483919789,-2.11070922958169,
137.481421902441));
#273919=CARTESIAN_POINT('Ctrl Pts',(-225.191931543603,4.47671086764076,
136.189274791569));
#273920=CARTESIAN_POINT('Ctrl Pts',(-225.470379167415,6.95025237698553,
129.948654622468));
#273921=CARTESIAN_POINT('Ctrl Pts',(-225.748826791228,3.03685149058481,
124.494386459301));
#273922=CARTESIAN_POINT('Ctrl Pts',(-226.027274415041,-3.66726755721984,
124.838676288203));
#273923=CARTESIAN_POINT('Ctrl Pts',(-226.305722038854,-7.00134687591997,
130.665138575908));
#273924=CARTESIAN_POINT('Ctrl Pts',(-226.584169662667,-3.9015304504591,
136.619539118521));
#273925=CARTESIAN_POINT('Ctrl Pts',(-226.86261728648,2.78360185861461,137.230074706019));
#273926=CARTESIAN_POINT('Ctrl Pts',(-227.141064910293,6.91074004613266,
131.935692959814));
#273927=CARTESIAN_POINT('Ctrl Pts',(-227.419512534106,4.68724573967455,
125.601672059739));
#273928=CARTESIAN_POINT('Ctrl Pts',(-227.697960157918,-1.8435984168596,
124.048667778841));
#273929=CARTESIAN_POINT('Ctrl Pts',(-227.976407781732,-6.68026569308986,
128.703815182788));
#273930=CARTESIAN_POINT('Ctrl Pts',(-228.254855405544,-5.37809514649209,
135.289261223946));
#273931=CARTESIAN_POINT('Ctrl Pts',(-228.533303029357,0.86628210517778,
137.753302707416));
#273932=CARTESIAN_POINT('Ctrl Pts',(-228.81175065317,6.31458842242258,133.831605885006));
#273933=CARTESIAN_POINT('Ctrl Pts',(-229.090198276983,5.96009646425557,
127.128018550972));
#273934=CARTESIAN_POINT('Ctrl Pts',(-229.368645900796,0.128567022336676,
123.802809976843));
#273935=CARTESIAN_POINT('Ctrl Pts',(-229.647093524609,-5.82110923226107,
126.911684396774));
#273936=CARTESIAN_POINT('Ctrl Pts',(-229.925541148421,-6.42147047940683,
133.597738095807));
#273937=CARTESIAN_POINT('Ctrl Pts',(-230.203988772235,-1.12081406224988,
137.716814356412));
#273938=CARTESIAN_POINT('Ctrl Pts',(-230.482436396047,5.20981572330331,
135.483683323156));
#273939=CARTESIAN_POINT('Ctrl Pts',(-230.76088401986,6.75287937278817,128.950483321085));
#273940=CARTESIAN_POINT('Ctrl Pts',(-231.039331643673,2.0903767751783,124.120905987538));
#273941=CARTESIAN_POINT('Ctrl Pts',(-231.317779267486,-4.49307995823781,
125.433096954076));
#273942=CARTESIAN_POINT('Ctrl Pts',(-231.596226891299,-6.94761570919197,
131.681216826544));
#273943=CARTESIAN_POINT('Ctrl Pts',(-231.874674515112,-3.01763203329532,
137.123548679767));
#273944=CARTESIAN_POINT('Ctrl Pts',(-232.153122138925,3.68540806167951,
136.758855413326));
#273945=CARTESIAN_POINT('Ctrl Pts',(-232.431569762738,7.00173819016367,
130.922272322824));
#273946=CARTESIAN_POINT('Ctrl Pts',(-232.71001738655,3.88381297581431,124.977334135496));
#273947=CARTESIAN_POINT('Ctrl Pts',(-232.988465010364,-2.80314662849731,
124.38714861912));
#273948=CARTESIAN_POINT('Ctrl Pts',(-233.266912634176,-6.914151422545,129.694067431082));
#273949=CARTESIAN_POINT('Ctrl Pts',(-233.545360257989,-4.67138883434919,
136.021291440583));
#273950=CARTESIAN_POINT('Ctrl Pts',(-233.823807881803,1.86415188258208,
137.554410884971));
#273951=CARTESIAN_POINT('Ctrl Pts',(-234.102255505615,6.68662808830262,
132.884563891901));
#273952=CARTESIAN_POINT('Ctrl Pts',(-234.380703129428,5.36441974081549,
126.303111713297));
#273953=CARTESIAN_POINT('Ctrl Pts',(-234.659150753241,-0.887428282007554,
123.858087379481));
#273954=CARTESIAN_POINT('Ctrl Pts',(-234.937598377053,-6.32377306694735,
127.796348807152));
#273955=CARTESIAN_POINT('Ctrl Pts',(-235.216046000867,-5.94887933685163,
134.498826139047));
#273956=CARTESIAN_POINT('Ctrl Pts',(-235.494493624679,-0.107256115101469,
137.806270141374));
#273957=CARTESIAN_POINT('Ctrl Pts',(-235.772941248493,5.83293023667497,
134.679301353618));
#273958=CARTESIAN_POINT('Ctrl Pts',(-236.051388872305,6.41293865542997,
127.991451330808));
#273959=CARTESIAN_POINT('Ctrl Pts',(-236.329836496118,1.09976973931543,
123.88852752427));
#273960=CARTESIAN_POINT('Ctrl Pts',(-236.608284119931,-5.22403384049169,
126.140916473241));
#273961=CARTESIAN_POINT('Ctrl Pts',(-236.886731743744,-6.7472055291277,
132.678782768935));
#273962=CARTESIAN_POINT('Ctrl Pts',(-237.165179367557,-2.07002495581049,
137.494146678133));
#273963=CARTESIAN_POINT('Ctrl Pts',(-237.44362699137,4.50940742555574,136.161924011888));
#273964=CARTESIAN_POINT('Ctrl Pts',(-237.722074615182,6.94491467963605,
129.906362317783));
#273965=CARTESIAN_POINT('Ctrl Pts',(-238.000522238996,2.99838462107406,
124.476017191522));
#273966=CARTESIAN_POINT('Ctrl Pts',(-238.278969862808,-3.70351442502255,
124.861110517033));
#273967=CARTESIAN_POINT('Ctrl Pts',(-238.557417486622,-7.00206464126185,
130.707760341024));
#273968=CARTESIAN_POINT('Ctrl Pts',(-238.835865110434,-3.86605952205578,
136.64318109997));
#273969=CARTESIAN_POINT('Ctrl Pts',(-239.114312734247,2.82266543041169,
137.213011077826));
#273970=CARTESIAN_POINT('Ctrl Pts',(-239.39276035806,6.91749874720356,131.893604362681));
#273971=CARTESIAN_POINT('Ctrl Pts',(-239.671207981873,4.655488653916,125.573235858291));
#273972=CARTESIAN_POINT('Ctrl Pts',(-239.949655605686,-1.88468807905538,
124.060015453022));
#273973=CARTESIAN_POINT('Ctrl Pts',(-240.228103229498,-6.69292853950653,
128.74451877439));
#273974=CARTESIAN_POINT('Ctrl Pts',(-240.506550853312,-5.35069463988719,
135.321916120768));
#273975=CARTESIAN_POINT('Ctrl Pts',(-240.784998477124,0.908566237823527,
137.747900654559));
#273976=CARTESIAN_POINT('Ctrl Pts',(-241.063446100938,6.33289912890243,
133.79311110514));
#273977=CARTESIAN_POINT('Ctrl Pts',(-241.34189372475,5.9376070998423,127.091805866219));
#273978=CARTESIAN_POINT('Ctrl Pts',(-241.620341348563,0.0859442142595387,
123.802157075403));
#273979=CARTESIAN_POINT('Ctrl Pts',(-241.898788972376,-5.84469720561911,
126.947191263173));
#273980=CARTESIAN_POINT('Ctrl Pts',(-242.177236596189,-6.40434742286629,
133.636775654432));
#273981=CARTESIAN_POINT('Ctrl Pts',(-242.455684220002,-1.07871522826414,
137.723508997977));
#273982=CARTESIAN_POINT('Ctrl Pts',(-242.734131843815,5.23820356294377,
135.451882999115));
#273983=CARTESIAN_POINT('Ctrl Pts',(-243.012579467628,6.74146918027728,
128.909410975699));
#273984=CARTESIAN_POINT('Ctrl Pts',(-243.29102709144,2.04965396001378,124.108305099723));
#273985=CARTESIAN_POINT('Ctrl Pts',(-243.569474715254,-4.52569311833944,
125.460547124147));
#273986=CARTESIAN_POINT('Ctrl Pts',(-243.847922339066,-6.94214931333881,
131.72349268922));
#273987=CARTESIAN_POINT('Ctrl Pts',(-244.12636996288,-2.9791094322281,137.141800782542));
#273988=CARTESIAN_POINT('Ctrl Pts',(-244.404817586691,3.72158647951367,
136.736310965414));
#273989=CARTESIAN_POINT('Ctrl Pts',(-244.683265210505,7.00232622618917,
130.879648570499));
#273990=CARTESIAN_POINT('Ctrl Pts',(-244.961712834317,3.84827025365086,
124.953800224859));
#273991=CARTESIAN_POINT('Ctrl Pts',(-245.240160458131,-2.84215808354001,
124.404331064352));
#273992=CARTESIAN_POINT('Ctrl Pts',(-245.518608081943,-6.92078198909823,
129.736176404423));
#273993=CARTESIAN_POINT('Ctrl Pts',(-245.797055705757,-4.63954534567172,
136.049630852671));
#273994=CARTESIAN_POINT('Ctrl Pts',(-246.075503329569,1.90520681603656,
137.542938200555));
#273995=CARTESIAN_POINT('Ctrl Pts',(-246.353950953382,6.69916698833444,
132.843821947487));
#273996=CARTESIAN_POINT('Ctrl Pts',(-246.632398577195,5.33691997085474,
126.270540365447));
#273997=CARTESIAN_POINT('Ctrl Pts',(-246.910846201008,-0.929695776805409,
123.86361810567));
#273998=CARTESIAN_POINT('Ctrl Pts',(-247.189293824821,-6.34196652374499,
127.834899140205));
#273999=CARTESIAN_POINT('Ctrl Pts',(-247.467741448634,-5.9262798576518,
134.534970206175));
#274000=CARTESIAN_POINT('Ctrl Pts',(-247.746189072447,-0.0646315172428821,
137.806793310625));
#274001=CARTESIAN_POINT('Ctrl Pts',(-248.024636696259,5.85641003008765,
134.643722858007));
#274002=CARTESIAN_POINT('Ctrl Pts',(-248.303084320073,6.39569686130214,
127.952466069697));
#274003=CARTESIAN_POINT('Ctrl Pts',(-248.581531943885,1.05765072414216,
123.881961048084));
#274004=CARTESIAN_POINT('Ctrl Pts',(-248.859979567699,-5.25232475939459,
126.172803052805));
#274005=CARTESIAN_POINT('Ctrl Pts',(-249.138427191511,-6.73567037937639,
132.719820195375));
#274006=CARTESIAN_POINT('Ctrl Pts',(-249.416874815324,-2.02926397650361,
137.506623561341));
#274007=CARTESIAN_POINT('Ctrl Pts',(-249.695322439137,4.54193688572079,
136.134374705723));
#274008=CARTESIAN_POINT('Ctrl Pts',(-249.97377006295,6.93931963591783,129.864103288757));
#274009=CARTESIAN_POINT('Ctrl Pts',(-250.252217686763,2.95980664532115,
124.457882422832));
#274010=CARTESIAN_POINT('Ctrl Pts',(-250.530665310576,-3.73962405773988,
124.883764975191));
#274011=CARTESIAN_POINT('Ctrl Pts',(-250.809112934388,-7.00252294251614,
130.750385685678));
#274012=CARTESIAN_POINT('Ctrl Pts',(-251.087560558202,-3.83044533540895,
136.666606721818));
#274013=CARTESIAN_POINT('Ctrl Pts',(-251.366008182014,2.86162440732935,
137.195709974661));
#274014=CARTESIAN_POINT('Ctrl Pts',(-251.644455805827,6.9240011177651,131.851475403357));
#274015=CARTESIAN_POINT('Ctrl Pts',(-251.92290342964,4.62355905740654,125.54499349784));
#274016=CARTESIAN_POINT('Ctrl Pts',(-252.201351053453,-1.92570790361727,
124.071613041873));
#274017=CARTESIAN_POINT('Ctrl Pts',(-252.479798677266,-6.70534337666252,
128.785298693283));
#274018=CARTESIAN_POINT('Ctrl Pts',(-252.758246301079,-5.3230958619522,
135.354403619622));
#274019=CARTESIAN_POINT('Ctrl Pts',(-253.036693924892,0.950816704398073,
137.74224130304));
#274020=CARTESIAN_POINT('Ctrl Pts',(-253.315141548704,6.35097516523885,
133.754505582129));
#274021=CARTESIAN_POINT('Ctrl Pts',(-253.593589172518,5.91489771943887,
127.055730740027));
#274022=CARTESIAN_POINT('Ctrl Pts',(-253.87203679633,0.0433182135112656,
123.801763664947));
#274023=CARTESIAN_POINT('Ctrl Pts',(-254.150484420143,-5.86806858651122,
126.982841017323));
#274024=CARTESIAN_POINT('Ctrl Pts',(-254.428932043956,-6.38698707931617,
133.675708334441));
#274025=CARTESIAN_POINT('Ctrl Pts',(-254.707379667769,-1.03657636838919,
137.729947101491));
#274026=CARTESIAN_POINT('Ctrl Pts',(-254.985827291582,5.26639719763008,
135.41991073597));
#274027=CARTESIAN_POINT('Ctrl Pts',(-255.264274915395,6.72980937160111,
128.868408326187));
#274028=CARTESIAN_POINT('Ctrl Pts',(-255.542722539208,2.00885483266244,
124.095953322692));
#274029=CARTESIAN_POINT('Ctrl Pts',(-255.821170163021,-4.5581378946222,
125.488193449449));
#274030=CARTESIAN_POINT('Ctrl Pts',(-256.099617786833,-6.93642696247006,
131.765738008466));
#274031=CARTESIAN_POINT('Ctrl Pts',(-256.378065410647,-2.94047400549736,
137.159811411449));
#274032=CARTESIAN_POINT('Ctrl Pts',(-256.656513034459,3.7576223973322,136.713559240208));
#274033=CARTESIAN_POINT('Ctrl Pts',(-256.934960658272,7.0026634652268,130.836998362911));
#274034=CARTESIAN_POINT('Ctrl Pts',(-257.213408282085,3.81256854888166,
124.930527794066));
#274035=CARTESIAN_POINT('Ctrl Pts',(-257.491855905898,-2.88103328591622,
124.421666290213));
#274036=CARTESIAN_POINT('Ctrl Pts',(-257.770303529711,-6.92721451599304,
129.778484277494));
#274037=CARTESIAN_POINT('Ctrl Pts',(-258.048751153524,-4.60741964202412,
136.077475067175));
#274038=CARTESIAN_POINT('Ctrl Pts',(-258.327198777336,1.94598288966397,
137.53178391186));
#274039=CARTESIAN_POINT('Ctrl Pts',(-258.60564640115,6.71185090883407,132.801931226644));
#274040=CARTESIAN_POINT('Ctrl Pts',(-258.884094024962,5.30847971878909,
126.240167716581));
#274041=CARTESIAN_POINT('Ctrl Pts',(-259.162541648776,-0.970525071554103,
123.86553674091));
#274042=CARTESIAN_POINT('Ctrl Pts',(-259.440989272588,-6.36258613651914,
127.881151058581));
#274043=CARTESIAN_POINT('Ctrl Pts',(-259.673028959099,-5.97575359986218,
133.442106215535));
#274044=CARTESIAN_POINT('Ctrl Pts',(-259.858689921174,-2.9628379271774,
136.206922793942));
#274045=CARTESIAN_POINT('Ctrl Pts',(-259.951535008647,-1.00384119663989,
136.721969923993));
#274046=CARTESIAN_POINT('Ctrl Pts',(-259.997972158816,-0.016740685831905,
136.724751058381));
#274047=CARTESIAN_POINT('Ctrl Pts',(210.384788400103,3.2437100417032,135.350446923363));
#274048=CARTESIAN_POINT('Ctrl Pts',(210.338370536501,4.00135710969089,134.809856772425));
#274049=CARTESIAN_POINT('Ctrl Pts',(210.245544735596,5.2274450014198,133.344996311945));
#274050=CARTESIAN_POINT('Ctrl Pts',(210.059903060087,6.03752477204218,129.574087134129));
#274051=CARTESIAN_POINT('Ctrl Pts',(209.827863373576,3.30140998082846,125.08375145776));
#274052=CARTESIAN_POINT('Ctrl Pts',(209.549415749763,-3.03864792542705,
124.935284604053));
#274053=CARTESIAN_POINT('Ctrl Pts',(209.27096812595,-6.57501826603042,130.18815040753));
#274054=CARTESIAN_POINT('Ctrl Pts',(208.992520502138,-4.0751627655632,136.003208990552));
#274055=CARTESIAN_POINT('Ctrl Pts',(208.714072878324,2.17267791003586,137.042921783734));
#274056=CARTESIAN_POINT('Ctrl Pts',(208.435625254512,6.42228832295553,132.348569225854));
#274057=CARTESIAN_POINT('Ctrl Pts',(208.157177630698,4.77100074356668,126.235763887068));
#274058=CARTESIAN_POINT('Ctrl Pts',(207.878730006886,-1.26506482749479,
124.320958291314));
#274059=CARTESIAN_POINT('Ctrl Pts',(207.600282383073,-6.13835327551471,
128.364250828182));
#274060=CARTESIAN_POINT('Ctrl Pts',(207.32183475926,-5.37092434612766,134.649796015418));
#274061=CARTESIAN_POINT('Ctrl Pts',(207.043387135447,0.332190207827403,
137.40162108792));
#274062=CARTESIAN_POINT('Ctrl Pts',(206.764939511634,5.73000189292936,134.090861108297));
#274063=CARTESIAN_POINT('Ctrl Pts',(206.486491887821,5.86224098722307,127.759980958474));
#274064=CARTESIAN_POINT('Ctrl Pts',(206.208044264008,0.607356820266201,
124.226729984437));
#274065=CARTESIAN_POINT('Ctrl Pts',(205.929596640195,-5.20565320191231,
126.738003936844));
#274066=CARTESIAN_POINT('Ctrl Pts',(205.651149016382,-6.23492509722864,
132.986059061584));
#274067=CARTESIAN_POINT('Ctrl Pts',(205.37270139257,-1.53460390898592,137.229240938669));
#274068=CARTESIAN_POINT('Ctrl Pts',(205.094253768756,4.57594250116295,135.568271122458));
#274069=CARTESIAN_POINT('Ctrl Pts',(204.815806144944,6.48142172411287,129.529500574057));
#274070=CARTESIAN_POINT('Ctrl Pts',(204.537358521131,2.43079079302514,124.662263970705));
#274071=CARTESIAN_POINT('Ctrl Pts',(204.258910897318,-3.85361800715474,
125.439314209572));
#274072=CARTESIAN_POINT('Ctrl Pts',(203.980463273505,-6.5967401814699,131.146579956944));
#274073=CARTESIAN_POINT('Ctrl Pts',(203.702015649692,-3.27778036432047,
136.539362872731));
#274074=CARTESIAN_POINT('Ctrl Pts',(203.42356802588,3.05329946149495,136.661958874297));
#274075=CARTESIAN_POINT('Ctrl Pts',(203.145120402066,6.5785462535266,131.40170824395));
#274076=CARTESIAN_POINT('Ctrl Pts',(202.866672778254,4.05843041346184,125.592524323598));
#274077=CARTESIAN_POINT('Ctrl Pts',(202.58822515444,-2.19118470860141,124.572763346851));
#274078=CARTESIAN_POINT('Ctrl Pts',(202.309777530628,-6.42720813017419,
129.279535830482));
#274079=CARTESIAN_POINT('Ctrl Pts',(202.031329906815,-4.75694126595338,
135.387547802118));
#274080=CARTESIAN_POINT('Ctrl Pts',(201.752882283002,1.28472223178851,137.283834652022));
#274081=CARTESIAN_POINT('Ctrl Pts',(201.474434659189,6.14578876089344,133.225801404307));
#274082=CARTESIAN_POINT('Ctrl Pts',(201.195987035376,5.35917565710019,126.94258236746));
#274083=CARTESIAN_POINT('Ctrl Pts',(200.917539411563,-0.352258065224466,
124.208148884143));
#274084=CARTESIAN_POINT('Ctrl Pts',(200.63909178775,-5.73998383440169,127.535311740963));
#274085=CARTESIAN_POINT('Ctrl Pts',(200.360644163938,-5.85294487354697,
133.866570813476));
#274086=CARTESIAN_POINT('Ctrl Pts',(200.082196540124,-0.587335506164227,
137.383808313225));
#274087=CARTESIAN_POINT('Ctrl Pts',(199.803748916312,5.2180064984534,134.854854804556));
#274088=CARTESIAN_POINT('Ctrl Pts',(199.525301292498,6.22825544477889,128.603695015683));
#274089=CARTESIAN_POINT('Ctrl Pts',(199.246853668687,1.51504190454761,124.374839406449));
#274090=CARTESIAN_POINT('Ctrl Pts',(198.968406044873,-4.5904211320519,126.054399690658));
#274091=CARTESIAN_POINT('Ctrl Pts',(198.689958421061,-6.47751140283473,
132.098942018204));
#274092=CARTESIAN_POINT('Ctrl Pts',(198.411510797247,-2.41208513843682,
136.95382728238));
#274093=CARTESIAN_POINT('Ctrl Pts',(198.133063173434,3.86992953127461,136.15765309974));
#274094=CARTESIAN_POINT('Ctrl Pts',(197.854615549622,6.59566801831256,130.442064648858));
#274095=CARTESIAN_POINT('Ctrl Pts',(197.576167925809,3.26030981281707,125.059408494076));
#274096=CARTESIAN_POINT('Ctrl Pts',(197.297720301996,-3.07111383566833,
124.956082684267));
#274097=CARTESIAN_POINT('Ctrl Pts',(197.019272678183,-6.58033390142619,
130.227038590899));
#274098=CARTESIAN_POINT('Ctrl Pts',(196.74082505437,-4.04254857895594,136.028525236289));
#274099=CARTESIAN_POINT('Ctrl Pts',(196.462377430557,2.21014139809766,137.029259811701));
#274100=CARTESIAN_POINT('Ctrl Pts',(196.183929806745,6.43181940170927,132.309616130935));
#274101=CARTESIAN_POINT('Ctrl Pts',(195.905482182931,4.74296958699597,126.206716169203));
#274102=CARTESIAN_POINT('Ctrl Pts',(195.627034559119,-1.30443757122094,
124.328826848098));
#274103=CARTESIAN_POINT('Ctrl Pts',(195.348586935305,-6.15313032680387,
128.401636713722));
#274104=CARTESIAN_POINT('Ctrl Pts',(195.070139311493,-5.34739690918169,
134.682432467391));
#274105=CARTESIAN_POINT('Ctrl Pts',(194.791691687679,0.372333033116476,
137.399469645412));
#274106=CARTESIAN_POINT('Ctrl Pts',(194.513244063867,5.74990710746052,134.055923815831));
#274107=CARTESIAN_POINT('Ctrl Pts',(194.234796440054,5.84359744862664,127.724350254736));
#274108=CARTESIAN_POINT('Ctrl Pts',(193.956348816241,0.567307210110782,
124.223155750211));
#274109=CARTESIAN_POINT('Ctrl Pts',(193.677901192428,-5.23031063999889,
126.769767009054));
#274110=CARTESIAN_POINT('Ctrl Pts',(193.399453568615,-6.22152852682933,
133.023972693263));
#274111=CARTESIAN_POINT('Ctrl Pts',(193.121005944802,-1.49546563606909,
137.238463313985));
#274112=CARTESIAN_POINT('Ctrl Pts',(192.84255832099,4.60485711668079,135.540327880088));
#274113=CARTESIAN_POINT('Ctrl Pts',(192.564110697177,6.47354113897745,129.490069896797));
#274114=CARTESIAN_POINT('Ctrl Pts',(192.285663073364,2.39335710461987,124.64758087922));
#274115=CARTESIAN_POINT('Ctrl Pts',(192.007215449551,-3.88620518688872,
125.462871665772));
#274116=CARTESIAN_POINT('Ctrl Pts',(191.728767825738,-6.59453476332446,
131.18672985278));
#274117=CARTESIAN_POINT('Ctrl Pts',(191.450320201925,-3.24280905319821,
136.559209392401));
#274118=CARTESIAN_POINT('Ctrl Pts',(191.171872578112,3.08889975678785,136.643264047941));
#274119=CARTESIAN_POINT('Ctrl Pts',(190.893424954299,6.58206059142805,131.361651697256));
#274120=CARTESIAN_POINT('Ctrl Pts',(190.614977330486,4.02662929408197,125.567916069518));
#274121=CARTESIAN_POINT('Ctrl Pts',(190.336529706674,-2.22907761274862,
124.586217166899));
#274122=CARTESIAN_POINT('Ctrl Pts',(190.05808208286,-6.43637108995848,129.318688322246));
#274123=CARTESIAN_POINT('Ctrl Pts',(189.779634459048,-4.72895396970476,
135.416419737866));
#274124=CARTESIAN_POINT('Ctrl Pts',(189.501186835235,1.32414082646293,137.275894133543));
#274125=CARTESIAN_POINT('Ctrl Pts',(189.222739211422,6.16041489098677,133.188345380025));
#274126=CARTESIAN_POINT('Ctrl Pts',(188.944291587609,5.33556862369218,126.910031093937));
#274127=CARTESIAN_POINT('Ctrl Pts',(188.665843963796,-0.392404551757433,
124.210415391489));
#274128=CARTESIAN_POINT('Ctrl Pts',(188.387396339983,-5.75977711417006,
127.570313219673));
#274129=CARTESIAN_POINT('Ctrl Pts',(188.10894871617,-5.83419588941534,133.902142614521));
#274130=CARTESIAN_POINT('Ctrl Pts',(187.830501092358,-0.547273658602122,
137.387261689231));
#274131=CARTESIAN_POINT('Ctrl Pts',(187.552053468544,5.24256632866185,134.823016271676));
#274132=CARTESIAN_POINT('Ctrl Pts',(187.273605844732,6.214743973489,128.565822630237));
#274133=CARTESIAN_POINT('Ctrl Pts',(186.995158220918,1.47587551380139,124.365736040492));
#274134=CARTESIAN_POINT('Ctrl Pts',(186.716710597106,-4.61925044254253,
126.082430892781));
#274135=CARTESIAN_POINT('Ctrl Pts',(186.438262973293,-6.46951090511933,
132.138348483055));
#274136=CARTESIAN_POINT('Ctrl Pts',(186.15981534948,-2.37460689906969,136.968396393875));
#274137=CARTESIAN_POINT('Ctrl Pts',(185.881367725667,3.90244484122886,136.133996556155));
#274138=CARTESIAN_POINT('Ctrl Pts',(185.602920101854,6.59334041746713,130.401921658061));
#274139=CARTESIAN_POINT('Ctrl Pts',(185.324472478041,3.22527825263932,125.039668503516));
#274140=CARTESIAN_POINT('Ctrl Pts',(185.046024854228,-3.10665706276191,
124.974885780916));
#274141=CARTESIAN_POINT('Ctrl Pts',(184.767577230416,-6.5837263061198,130.26710564752));
#274142=CARTESIAN_POINT('Ctrl Pts',(184.489129606603,-4.01067270706429,
136.05303658523));
#274143=CARTESIAN_POINT('Ctrl Pts',(184.21068198279,2.247993177529,137.015690720733));
#274144=CARTESIAN_POINT('Ctrl Pts',(183.932234358977,6.44086315254518,132.270435931769));
#274145=CARTESIAN_POINT('Ctrl Pts',(183.653786735164,4.71489454403,126.177929550814));
#274146=CARTESIAN_POINT('Ctrl Pts',(183.375339111351,-1.34383181504516,
124.33688730648));
#274147=CARTESIAN_POINT('Ctrl Pts',(183.096891487538,-6.16764238592767,
128.439137081397));
#274148=CARTESIAN_POINT('Ctrl Pts',(182.818443863726,-5.32369091022383,
134.71491173846));
#274149=CARTESIAN_POINT('Ctrl Pts',(182.539996239912,0.412472435216218,
137.397080956463));
#274150=CARTESIAN_POINT('Ctrl Pts',(182.2615486161,5.76959376309122,134.020862255314));
#274151=CARTESIAN_POINT('Ctrl Pts',(181.983100992287,5.82474028301032,127.688835683913));
#274152=CARTESIAN_POINT('Ctrl Pts',(181.704653368474,0.527235037225083,
124.219824324685));
#274153=CARTESIAN_POINT('Ctrl Pts',(181.426205744661,-5.25477345090652,
126.801680146133));
#274154=CARTESIAN_POINT('Ctrl Pts',(181.147758120848,-6.20790184760947,
133.061803779016));
#274155=CARTESIAN_POINT('Ctrl Pts',(180.869310497035,-1.45627171922457,
137.247447428754));
#274156=CARTESIAN_POINT('Ctrl Pts',(180.590862873222,4.63360097629919,135.5122090613));
#274157=CARTESIAN_POINT('Ctrl Pts',(180.31241524941,6.46542073859599,129.450687965235));
#274158=CARTESIAN_POINT('Ctrl Pts',(180.033967625596,2.35583469548556,124.633125906077));
#274159=CARTESIAN_POINT('Ctrl Pts',(179.755520001784,-3.91864834385308,
125.4866270652));
#274160=CARTESIAN_POINT('Ctrl Pts',(179.477072377971,-6.59208499180493,
131.226865573221));
#274161=CARTESIAN_POINT('Ctrl Pts',(179.198624754158,-3.20771757354326,
136.578842667508));
#274162=CARTESIAN_POINT('Ctrl Pts',(178.920177130345,3.12438558908937,136.62435285703));
#274163=CARTESIAN_POINT('Ctrl Pts',(178.641729506532,6.58533103007041,131.32157450091));
#274164=CARTESIAN_POINT('Ctrl Pts',(178.363281882719,3.99467896572256,125.5435018533));
#274165=CARTESIAN_POINT('Ctrl Pts',(178.084834258906,-2.26688791720775,
124.599901402811));
#274166=CARTESIAN_POINT('Ctrl Pts',(177.806386635093,-6.44529554785546,
129.357895865998));
#274167=CARTESIAN_POINT('Ctrl Pts',(177.527939011281,-4.70079144021631,
135.445120772143));
#274168=CARTESIAN_POINT('Ctrl Pts',(177.249491387467,1.36351035455298,137.26771380997));
#274169=CARTESIAN_POINT('Ctrl Pts',(176.971043763655,6.17481274467203,133.150801016333));
#274170=CARTESIAN_POINT('Ctrl Pts',(176.692596139842,5.31176387881016,126.877624126216));
#274171=CARTESIAN_POINT('Ctrl Pts',(176.414148516029,-0.432536497586617,
124.212926239906));
#274172=CARTESIAN_POINT('Ctrl Pts',(176.135700892216,-5.77935696328393,
127.605434537195));
#274173=CARTESIAN_POINT('Ctrl Pts',(175.857253268403,-5.81523071700703,
133.937599626117));
#274174=CARTESIAN_POINT('Ctrl Pts',(175.57880564459,-0.50719153161477,137.390471133416));
#274175=CARTESIAN_POINT('Ctrl Pts',(175.300358020777,5.2669318936477,134.791028826034));
#274176=CARTESIAN_POINT('Ctrl Pts',(175.021910396965,6.20100221257536,128.528033194638));
#274177=CARTESIAN_POINT('Ctrl Pts',(174.743462773151,1.43665443394553,124.356871260137));
#274178=CARTESIAN_POINT('Ctrl Pts',(174.465015149339,-4.64790858500931,
126.110637067746));
#274179=CARTESIAN_POINT('Ctrl Pts',(174.186567525525,-6.46127067729819,
132.177705516496));
#274180=CARTESIAN_POINT('Ctrl Pts',(173.908119901713,-2.33704066777073,
136.982737094758));
#274181=CARTESIAN_POINT('Ctrl Pts',(173.6296722779,3.93481554465429,136.11014252095));
#274182=CARTESIAN_POINT('Ctrl Pts',(173.351224654087,6.59076849796787,130.361793579788));
#274183=CARTESIAN_POINT('Ctrl Pts',(173.072777030274,3.1901271785899,125.020142125741));
#274184=CARTESIAN_POINT('Ctrl Pts',(172.794329406461,-3.14208517153551,
124.993904890899));
#274185=CARTESIAN_POINT('Ctrl Pts',(172.515881782648,-6.58687474841394,
130.30719261232));
#274186=CARTESIAN_POINT('Ctrl Pts',(172.237434158836,-3.97864821822065,
136.077353442554));
#274187=CARTESIAN_POINT('Ctrl Pts',(171.958986535022,2.28576165674636,137.001891466644));
#274188=CARTESIAN_POINT('Ctrl Pts',(171.68053891121,6.44966823482829,132.231201406644));
#274189=CARTESIAN_POINT('Ctrl Pts',(171.402091287397,4.68664478891289,126.149314366529));
#274190=CARTESIAN_POINT('Ctrl Pts',(171.123643663584,-1.38317626268716,
124.345187419464));
#274191=CARTESIAN_POINT('Ctrl Pts',(170.845196039771,-6.18192590079466,
128.476725093301));
#274192=CARTESIAN_POINT('Ctrl Pts',(170.566748415958,-5.29978763994156,
134.747246102621));
#274193=CARTESIAN_POINT('Ctrl Pts',(170.288300792145,0.452596552998033,
137.394447971839));
#274194=CARTESIAN_POINT('Ctrl Pts',(170.009853168332,5.78906662430322,133.985681506144));
#274195=CARTESIAN_POINT('Ctrl Pts',(169.73140554452,5.80566727950083,127.653436560012));
#274196=CARTESIAN_POINT('Ctrl Pts',(169.452957920706,0.487143327451347,
124.216736891574));
#274197=CARTESIAN_POINT('Ctrl Pts',(169.174510296894,-5.27904154425138,
126.833741604011));
#274198=CARTESIAN_POINT('Ctrl Pts',(168.896062673081,-6.19404513230377,
133.099551214382));
#274199=CARTESIAN_POINT('Ctrl Pts',(168.617615049268,-1.41702383969606,
137.256192792574));
#274200=CARTESIAN_POINT('Ctrl Pts',(168.339167425455,4.66217313612931,135.483915791456));
#274201=CARTESIAN_POINT('Ctrl Pts',(168.060719801642,6.45706075967145,129.411356194513));
#274202=CARTESIAN_POINT('Ctrl Pts',(167.782272177829,2.3182249900303,124.618899610305));
#274203=CARTESIAN_POINT('Ctrl Pts',(167.503824554016,-3.95094629386185,
125.510579515201));
#274204=CARTESIAN_POINT('Ctrl Pts',(167.225376930203,-6.58939094815179,
131.266985637585));
#274205=CARTESIAN_POINT('Ctrl Pts',(166.946929306391,-3.1725072307341,136.59826196706));
#274206=CARTESIAN_POINT('Ctrl Pts',(166.668481682578,3.15975564613386,136.605226004165));
#274207=CARTESIAN_POINT('Ctrl Pts',(166.390034058765,6.58835744684964,131.281478139015));
#274208=CARTESIAN_POINT('Ctrl Pts',(166.111586434952,3.96258061306513,125.519282580138));
#274209=CARTESIAN_POINT('Ctrl Pts',(165.833138811139,-2.30461422130139,
124.613815547242));
#274210=CARTESIAN_POINT('Ctrl Pts',(165.554691187326,-6.45398117295568,
129.397157009033));
#274211=CARTESIAN_POINT('Ctrl Pts',(165.276243563513,-4.67245472117232,
135.473649841348));
#274212=CARTESIAN_POINT('Ctrl Pts',(164.9977959397,1.40282935726546,137.259293984466));
#274213=CARTESIAN_POINT('Ctrl Pts',(164.719348315888,6.18898178840028,133.11316970443));
#274214=CARTESIAN_POINT('Ctrl Pts',(164.440900692075,5.2877623045642,126.845362665158));
#274215=CARTESIAN_POINT('Ctrl Pts',(164.162453068262,-0.472652415616787,
124.215681336348));
#274216=CARTESIAN_POINT('Ctrl Pts',(163.884005444449,-5.79872265620017,
127.640674392099));
#274217=CARTESIAN_POINT('Ctrl Pts',(163.605557820636,-5.79605005908598,
133.97294053439));
#274218=CARTESIAN_POINT('Ctrl Pts',(163.327110196823,-0.467090610458611,
137.393436526853));
#274219=CARTESIAN_POINT('Ctrl Pts',(163.04866257301,5.29110229053537,134.758893652935));
#274220=CARTESIAN_POINT('Ctrl Pts',(162.770214949197,6.18703067124424,128.49032810919));
#274221=CARTESIAN_POINT('Ctrl Pts',(162.491767325384,1.39738011833125,124.34824539387));
#274222=CARTESIAN_POINT('Ctrl Pts',(162.213319701571,-4.67639449751423,
126.139017170363));
#274223=CARTESIAN_POINT('Ctrl Pts',(161.934872077759,-6.45279102471594,
132.217011660137));
#274224=CARTESIAN_POINT('Ctrl Pts',(161.656424453946,-2.29938783657033,
136.996848853628));
#274225=CARTESIAN_POINT('Ctrl Pts',(161.377976830133,3.96704044204275,136.086091878046));
#274226=CARTESIAN_POINT('Ctrl Pts',(161.09952920632,6.58795235511813,130.321681900999));
#274227=CARTESIAN_POINT('Ctrl Pts',(160.821081582507,3.15485789320466,125.000830084311));
#274228=CARTESIAN_POINT('Ctrl Pts',(160.542633958694,-3.17739684918762,
125.013139309456));
#274229=CARTESIAN_POINT('Ctrl Pts',(160.264186334881,-6.58977911164196,
130.347297999864));
#274230=CARTESIAN_POINT('Ctrl Pts',(159.985738711068,-3.94647629910411,
136.10147490719));
#274231=CARTESIAN_POINT('Ctrl Pts',(159.707291087255,2.32344543622502,136.98786256077));
#274232=CARTESIAN_POINT('Ctrl Pts',(159.428843463442,6.45823432228318,132.191914009409));
#274233=CARTESIAN_POINT('Ctrl Pts',(159.15039583963,4.65822136844951,126.120871676696));
#274234=CARTESIAN_POINT('Ctrl Pts',(158.871948215817,-1.42246945622416,
124.353726879487));
#274235=CARTESIAN_POINT('Ctrl Pts',(158.593500592004,-6.19598034212407,
128.514399356595));
#274236=CARTESIAN_POINT('Ctrl Pts',(158.315052968191,-5.2756879840792,134.779434361708));
#274237=CARTESIAN_POINT('Ctrl Pts',(158.036605344378,0.49270389964821,137.391570789103));
#274238=CARTESIAN_POINT('Ctrl Pts',(157.758157720565,5.80832496952254,133.950382871961));
#274239=CARTESIAN_POINT('Ctrl Pts',(157.479710096752,5.78637914485521,127.618154194761));
#274240=CARTESIAN_POINT('Ctrl Pts',(157.201262472939,0.447033566402335,
124.213893565282));
#274241=CARTESIAN_POINT('Ctrl Pts',(156.922814849126,-5.3031140207705,126.865950194636));
#274242=CARTESIAN_POINT('Ctrl Pts',(156.644367225313,-6.17995889437779,
133.137213600617));
#274243=CARTESIAN_POINT('Ctrl Pts',(156.365919601501,-1.37772345182797,
137.264699081378));
#274244=CARTESIAN_POINT('Ctrl Pts',(156.087471977688,4.69057253741941,135.455449118975));
#274245=CARTESIAN_POINT('Ctrl Pts',(155.809024353875,6.44846151198586,129.372076042081));
#274246=CARTESIAN_POINT('Ctrl Pts',(155.530576730062,2.28052938189546,124.604902519066));
#274247=CARTESIAN_POINT('Ctrl Pts',(155.252129106249,-3.98309784010292,
125.534728128207));
#274248=CARTESIAN_POINT('Ctrl Pts',(154.973681482436,-6.58645273219382,
131.307088559209));
#274249=CARTESIAN_POINT('Ctrl Pts',(154.695233858623,-3.13717932950269,
136.617466571466));
#274250=CARTESIAN_POINT('Ctrl Pts',(154.41678623481,3.19500861727094,136.585884198101));
#274251=CARTESIAN_POINT('Ctrl Pts',(154.138338610998,6.59113972962085,131.241364097354));
#274252=CARTESIAN_POINT('Ctrl Pts',(153.859890987185,3.93033542552574,125.495259147487));
#274253=CARTESIAN_POINT('Ctrl Pts',(153.581443363372,-2.3422551270676,124.627959084596));
#274254=CARTESIAN_POINT('Ctrl Pts',(153.302995739559,-6.46242764341012,
129.436470296516));
#274255=CARTESIAN_POINT('Ctrl Pts',(153.024548115746,-4.64394486260028,
135.502005888322));
#274256=CARTESIAN_POINT('Ctrl Pts',(152.746100491933,1.44209637762021,137.250634969033));
#274257=CARTESIAN_POINT('Ctrl Pts',(152.46765286812,6.20292149713234,133.075452838754));
#274258=CARTESIAN_POINT('Ctrl Pts',(152.189205244307,5.26356479034146,126.813247906226));
#274259=CARTESIAN_POINT('Ctrl Pts',(151.910757620494,-0.512750819337957,
124.218680578724));
#274260=CARTESIAN_POINT('Ctrl Pts',(151.632309996682,-5.8178734753159,127.676031478561));
#274261=CARTESIAN_POINT('Ctrl Pts',(151.353862372869,-5.77665462639848,
134.008164029768));
#274262=CARTESIAN_POINT('Ctrl Pts',(151.075414749056,-0.4269723810881,137.39615775966));
#274263=CARTESIAN_POINT('Ctrl Pts',(150.796967125243,5.31507662368183,134.72661194316));
#274264=CARTESIAN_POINT('Ctrl Pts',(150.51851950143,6.17282986721635,128.452708771068));
#274265=CARTESIAN_POINT('Ctrl Pts',(150.240071877617,1.35805402228283,124.339858761329));
#274266=CARTESIAN_POINT('Ctrl Pts',(149.961624253804,-4.70470712450132,
126.167570148998));
#274267=CARTESIAN_POINT('Ctrl Pts',(149.683176629991,-6.44407226158927,
132.256265457474));
#274268=CARTESIAN_POINT('Ctrl Pts',(149.404729006178,-2.26164980070799,
137.010731147569));
#274269=CARTESIAN_POINT('Ctrl Pts',(149.126281382365,3.99911833928874,136.061845518646));
#274270=CARTESIAN_POINT('Ctrl Pts',(148.847833758553,6.58489209327119,130.281588108047));
#274271=CARTESIAN_POINT('Ctrl Pts',(148.56938613474,3.11947170339994,124.981733094838));
#274272=CARTESIAN_POINT('Ctrl Pts',(148.290938510927,-3.21259078723097,
125.032588323847));
#274273=CARTESIAN_POINT('Ctrl Pts',(148.012490887114,-6.59243928818165,
130.387420324031));
#274274=CARTESIAN_POINT('Ctrl Pts',(147.734043263301,-3.91415814185689,
136.125400085308));
#274275=CARTESIAN_POINT('Ctrl Pts',(147.455595639488,2.36104311957866,136.973604522958));
#274276=CARTESIAN_POINT('Ctrl Pts',(147.177148015675,6.46656109749016,132.152575195872));
#274277=CARTESIAN_POINT('Ctrl Pts',(146.898700391862,4.6296253358803,126.092602535266));
#274278=CARTESIAN_POINT('Ctrl Pts',(146.62025276805,-1.46170993963237,124.362505370115));
#274279=CARTESIAN_POINT('Ctrl Pts',(146.341805144237,-6.20980518912327,
128.552158475246));
#274280=CARTESIAN_POINT('Ctrl Pts',(146.063357520424,-5.2513928356585,134.811475322978));
#274281=CARTESIAN_POINT('Ctrl Pts',(145.784909896611,0.532792988974217,
137.388449514872));
#274282=CARTESIAN_POINT('Ctrl Pts',(145.506462272798,5.82736808512415,133.914967660766));
#274283=CARTESIAN_POINT('Ctrl Pts',(145.228014648985,5.76687659380242,127.582989895561));
#274284=CARTESIAN_POINT('Ctrl Pts',(144.949567025172,0.406907240360106,
124.211294451169));
#274285=CARTESIAN_POINT('Ctrl Pts',(144.671119401359,-5.32698998844935,
126.898304724507));
#274286=CARTESIAN_POINT('Ctrl Pts',(144.392671777546,-6.16564365580234,
133.174789542127));
#274287=CARTESIAN_POINT('Ctrl Pts',(144.114224153734,-1.33837201191069,
137.272965979966));
#274288=CARTESIAN_POINT('Ctrl Pts',(143.83577652992,4.71879812781917,135.426810098699));
#274289=CARTESIAN_POINT('Ctrl Pts',(143.557328906108,6.43962331418753,129.332848963481));
#274290=CARTESIAN_POINT('Ctrl Pts',(143.278881282295,2.24274926790569,124.591135151027));
#274291=CARTESIAN_POINT('Ctrl Pts',(143.000433658482,-4.01510179118866,
125.559072009383));
#274292=CARTESIAN_POINT('Ctrl Pts',(142.721986034669,-6.58327045280769,
131.347172852065));
#274293=CARTESIAN_POINT('Ctrl Pts',(142.443538410856,-3.10173517893752,
136.636455769093));
#274294=CARTESIAN_POINT('Ctrl Pts',(142.165090787043,3.23014319618891,136.566328155556));
#274295=CARTESIAN_POINT('Ctrl Pts',(141.886643163231,6.5936777752854,131.201233862367));
#274296=CARTESIAN_POINT('Ctrl Pts',(141.608195539417,3.89794459796173,125.471432445543));
#274297=CARTESIAN_POINT('Ctrl Pts',(141.329747915605,-2.37980923970876,
124.642331490782));
#274298=CARTESIAN_POINT('Ctrl Pts',(141.051300291792,-6.47063464623165,
129.475834271677));
#274299=CARTESIAN_POINT('Ctrl Pts',(140.772852667979,-4.61526292094352,
135.530187862324));
#274300=CARTESIAN_POINT('Ctrl Pts',(140.494405044166,1.48130996056343,137.241737084533));
#274301=CARTESIAN_POINT('Ctrl Pts',(140.215957420353,6.21663135432719,133.037651816923));
#274302=CARTESIAN_POINT('Ctrl Pts',(139.93750979654,5.23917223278974,126.781281039444));
#274303=CARTESIAN_POINT('Ctrl Pts',(139.659062172727,-0.552830222889001,
124.221923855894));
#274304=CARTESIAN_POINT('Ctrl Pts',(139.380614548914,-5.83680871099059,
127.711504486408));
#274305=CARTESIAN_POINT('Ctrl Pts',(139.102166925101,-5.75704513764935,
134.043268807033));
#274306=CARTESIAN_POINT('Ctrl Pts',(138.823719301288,-0.386838330098996,
137.398634730999));
#274307=CARTESIAN_POINT('Ctrl Pts',(138.545271677476,5.33885400470937,134.694184892919));
#274308=CARTESIAN_POINT('Ctrl Pts',(138.266824053663,6.15840032670771,128.41517657427));
#274309=CARTESIAN_POINT('Ctrl Pts',(137.98837642985,1.31867760304303,124.331711673279));
#274310=CARTESIAN_POINT('Ctrl Pts',(137.709928806037,-4.7328454168358,126.196294945608));
#274311=CARTESIAN_POINT('Ctrl Pts',(137.431481182224,-6.43511471099507,
132.295465453942));
#274312=CARTESIAN_POINT('Ctrl Pts',(137.153033558411,-2.22382795858067,
137.024383462168));
#274313=CARTESIAN_POINT('Ctrl Pts',(136.874585934598,4.03104804773404,136.037404341212));
#274314=CARTESIAN_POINT('Ctrl Pts',(136.596138310785,6.5815878258261,130.241513686623));
#274315=CARTESIAN_POINT('Ctrl Pts',(136.317690686972,3.08396992042408,124.96285186497));
#274316=CARTESIAN_POINT('Ctrl Pts',(136.03924306316,-3.24766568154122,125.052251213384));
#274317=CARTESIAN_POINT('Ctrl Pts',(135.760795439346,-6.5948551794591,130.427558098075));
#274318=CARTESIAN_POINT('Ctrl Pts',(135.482347815534,-3.88169494404043,
136.149128090351));
#274319=CARTESIAN_POINT('Ctrl Pts',(135.203900191721,2.3985533136112,136.959117881544));
#274320=CARTESIAN_POINT('Ctrl Pts',(134.925452567908,6.47464825189767,132.113186423748));
#274321=CARTESIAN_POINT('Ctrl Pts',(134.647004944095,4.60085775084163,126.064507989766));
#274322=CARTESIAN_POINT('Ctrl Pts',(134.368557320282,-1.50089625884118,
124.371522566057));
#274323=CARTESIAN_POINT('Ctrl Pts',(134.090109696469,-6.22339992950755,
128.590001050074));
#274324=CARTESIAN_POINT('Ctrl Pts',(133.811662072656,-5.22690309494509,
134.843367799137));
#274325=CARTESIAN_POINT('Ctrl Pts',(133.533214448844,0.572862335460145,
137.385084264805));
#274326=CARTESIAN_POINT('Ctrl Pts',(133.25476682503,5.84619526545829,133.879437184883));
#274327=CARTESIAN_POINT('Ctrl Pts',(132.976319201218,5.7471603490167,127.547944965438));
#274328=CARTESIAN_POINT('Ctrl Pts',(132.697871577405,0.366765836220533,
124.208939645549));
#274329=CARTESIAN_POINT('Ctrl Pts',(132.419423953592,-5.35066856255522,
126.930803994717));
#274330=CARTESIAN_POINT('Ctrl Pts',(132.140976329779,-6.15109994703373,
133.212277646521));
#274331=CARTESIAN_POINT('Ctrl Pts',(131.862528705966,-1.29897097812634,
137.280993182001));
#274332=CARTESIAN_POINT('Ctrl Pts',(131.584081082153,4.74684886141891,135.397999791857));
#274333=CARTESIAN_POINT('Ctrl Pts',(131.30563345834,6.43054649377913,129.293676412286));
#274334=CARTESIAN_POINT('Ctrl Pts',(131.027185834528,2.20488604801711,124.577598016342));
#274335=CARTESIAN_POINT('Ctrl Pts',(130.748738210715,-4.04695696120101,
125.583610256657));
#274336=CARTESIAN_POINT('Ctrl Pts',(130.470290586902,-6.57984422791396,
131.387237030814));
#274337=CARTESIAN_POINT('Ctrl Pts',(130.191842963089,-3.06617609243459,
136.65522885629));
#274338=CARTESIAN_POINT('Ctrl Pts',(129.913395339276,3.26515808096253,136.546558601182));
#274339=CARTESIAN_POINT('Ctrl Pts',(129.634947715463,6.59597148979528,131.161088921098));
#274340=CARTESIAN_POINT('Ctrl Pts',(129.35650009165,3.86540933062731,125.447803357213));
#274341=CARTESIAN_POINT('Ctrl Pts',(129.078052467837,-2.41727516764341,
124.656932233223));
#274342=CARTESIAN_POINT('Ctrl Pts',(128.799604844024,-6.47860187730669,
129.515247475871));
#274343=CARTESIAN_POINT('Ctrl Pts',(128.521157220212,-4.58640995902212,
135.558194719059));
#274344=CARTESIAN_POINT('Ctrl Pts',(128.242709596398,1.52046865302106,137.232600660681));
#274345=CARTESIAN_POINT('Ctrl Pts',(127.964261972586,6.23011085196111,132.999768039666));
#274346=CARTESIAN_POINT('Ctrl Pts',(127.685814348773,5.2145855357842,126.749463249355));
#274347=CARTESIAN_POINT('Ctrl Pts',(127.40736672496,-0.592889141112855,
124.225411047681));
#274348=CARTESIAN_POINT('Ctrl Pts',(127.128919101147,-5.85552766157182,
127.747092101177));
#274349=CARTESIAN_POINT('Ctrl Pts',(126.850471477334,-5.7372223194756,134.078253565364));
#274350=CARTESIAN_POINT('Ctrl Pts',(126.572023853521,-0.346689944673359,
137.400867349086));
#274351=CARTESIAN_POINT('Ctrl Pts',(126.293576229708,5.36243355253846,134.66161370381));
#274352=CARTESIAN_POINT('Ctrl Pts',(126.015128605896,6.14374258441013,128.377732909565));
#274353=CARTESIAN_POINT('Ctrl Pts',(125.736680982083,1.27925231971985,124.323804431618));
#274354=CARTESIAN_POINT('Ctrl Pts',(125.45823335827,-4.76080833184274,126.225190495787));
#274355=CARTESIAN_POINT('Ctrl Pts',(125.179785734457,-6.42591870485886,
132.334610196974));
#274356=CARTESIAN_POINT('Ctrl Pts',(124.901338110644,-2.1859237116904,137.037805291532));
#274357=CARTESIAN_POINT('Ctrl Pts',(124.622890486831,4.06282838421153,136.012769251418));
#274358=CARTESIAN_POINT('Ctrl Pts',(124.344442863018,6.5780396752237,130.201460121699));
#274359=CARTESIAN_POINT('Ctrl Pts',(124.065995239205,3.04835385980878,124.944187094356));
#274360=CARTESIAN_POINT('Ctrl Pts',(123.787547615392,-3.28262023240536,
125.07212724945));
#274361=CARTESIAN_POINT('Ctrl Pts',(123.509099991579,-6.59702669595264,
130.467709834674));
#274362=CARTESIAN_POINT('Ctrl Pts',(123.230652367767,-3.84908790859021,
136.17265804307));
#274363=CARTESIAN_POINT('Ctrl Pts',(122.952204743954,2.43597462836867,136.944403173336));
#274364=CARTESIAN_POINT('Ctrl Pts',(122.673757120141,6.48249548583303,132.073749152604));
#274365=CARTESIAN_POINT('Ctrl Pts',(122.395309496328,4.57191967932717,126.036589081248));
#274366=CARTESIAN_POINT('Ctrl Pts',(122.116861872515,-1.54002696178715,
124.380778133181));
#274367=CARTESIAN_POINT('Ctrl Pts',(121.838414248702,-6.23676405951882,
128.627925678811));
#274368=CARTESIAN_POINT('Ctrl Pts',(121.559966624889,-5.20221966941523,
134.8751106084));
#274369=CARTESIAN_POINT('Ctrl Pts',(121.281519001076,0.612910454321425,
137.381475163605));
#274370=CARTESIAN_POINT('Ctrl Pts',(121.003071377263,5.86480581287692,133.843792760907));
#274371=CARTESIAN_POINT('Ctrl Pts',(120.724623753451,5.72723114109079,127.513020702994));
#274372=CARTESIAN_POINT('Ctrl Pts',(120.446176129638,0.326610841437887,
124.206829235678));
#274373=CARTESIAN_POINT('Ctrl Pts',(120.167728505825,-5.3741488656698,126.963446800991));
#274374=CARTESIAN_POINT('Ctrl Pts',(119.889280882012,-6.13632830699453,
133.249676524665));
#274375=CARTESIAN_POINT('Ctrl Pts',(119.610833258199,-1.25952181049465,
137.288780390037));
#274376=CARTESIAN_POINT('Ctrl Pts',(119.332385634386,4.77472369878856,135.369019266025));
#274377=CARTESIAN_POINT('Ctrl Pts',(119.053938010573,6.42123138710552,129.254559840052));
#274378=CARTESIAN_POINT('Ctrl Pts',(118.77549038676,2.16694112526505,124.564291616636));
#274379=CARTESIAN_POINT('Ctrl Pts',(118.497042762948,-4.07866216973492,
125.608341960757));
#274380=CARTESIAN_POINT('Ctrl Pts',(118.218595139134,-6.57617418447253,
131.427279610862));
#274381=CARTESIAN_POINT('Ctrl Pts',(117.940147515322,-3.03050338764912,
136.673785137412));
#274382=CARTESIAN_POINT('Ctrl Pts',(117.661699891509,3.30005197410286,136.526576267552));
#274383=CARTESIAN_POINT('Ctrl Pts',(117.383252267696,6.59802078815589,131.120930761129));
#274384=CARTESIAN_POINT('Ctrl Pts',(117.104804643883,3.83273082912851,125.424372758082));
#274385=CARTESIAN_POINT('Ctrl Pts',(116.82635702007,-2.45465152255762,124.671760770883));
#274386=CARTESIAN_POINT('Ctrl Pts',(116.547909396257,-6.48632904140672,
129.554708448625));
#274387=CARTESIAN_POINT('Ctrl Pts',(116.269461772444,-4.55738704599302,
135.586025420722));
#274388=CARTESIAN_POINT('Ctrl Pts',(115.991014148631,1.55957100395386,137.223226036031));
#274389=CARTESIAN_POINT('Ctrl Pts',(115.712566524818,6.24335949054626,132.961802910777));
#274390=CARTESIAN_POINT('Ctrl Pts',(115.434118901006,5.18980561039392,126.717795714978));
#274391=CARTESIAN_POINT('Ctrl Pts',(115.155671277193,-0.632926089611396,
124.229142024863));
#274392=CARTESIAN_POINT('Ctrl Pts',(114.87722365338,-5.87402963342224,127.782793004156));
#274393=CARTESIAN_POINT('Ctrl Pts',(114.598776029567,-5.71718690641897,
134.113117008387));
#274394=CARTESIAN_POINT('Ctrl Pts',(114.320328405754,-0.306528712524212,
137.40285553119));
#274395=CARTESIAN_POINT('Ctrl Pts',(114.041880781941,5.38581439342023,134.628899582769));
#274396=CARTESIAN_POINT('Ctrl Pts',(113.763433158128,6.12885718347172,128.340379164441));
#274397=CARTESIAN_POINT('Ctrl Pts',(113.484985534315,1.23977963323159,124.316137329349));
#274398=CARTESIAN_POINT('Ctrl Pts',(113.206537910502,-4.78859483334625,
126.254255728798));
#274399=CARTESIAN_POINT('Ctrl Pts',(112.92809028669,-6.41648458394181,132.373698236044));
#274400=CARTESIAN_POINT('Ctrl Pts',(112.649642662877,-2.14793846459313,
137.050996138312));
#274401=CARTESIAN_POINT('Ctrl Pts',(112.371195039064,4.09445817108915,135.987941162125));
#274402=CARTESIAN_POINT('Ctrl Pts',(112.092747415251,6.57424777294209,130.161428897475));
#274403=CARTESIAN_POINT('Ctrl Pts',(111.814299791438,3.01262484132005,124.925739474628));
#274404=CARTESIAN_POINT('Ctrl Pts',(111.535852167625,-3.31745314456969,
125.092215695531));
#274405=CARTESIAN_POINT('Ctrl Pts',(111.257404543812,-6.59895375719588,
130.507874045991));
#274406=CARTESIAN_POINT('Ctrl Pts',(110.978956919999,-3.816338243772,136.195989071554));
#274407=CARTESIAN_POINT('Ctrl Pts',(110.700509296186,2.47330567719032,136.929460943594));
#274408=CARTESIAN_POINT('Ctrl Pts',(110.422061672374,6.49010250851429,132.0342648438));
#274409=CARTESIAN_POINT('Ctrl Pts',(110.143614048561,4.54281219364771,126.008846844259));
#274410=CARTESIAN_POINT('Ctrl Pts',(109.865166424748,-1.57910059846782,
124.390271728514));
#274411=CARTESIAN_POINT('Ctrl Pts',(109.586718800935,-6.24989708394428,
128.665930956147));
#274412=CARTESIAN_POINT('Ctrl Pts',(109.308271177122,-5.17734347372243,
134.906702574525));
#274413=CARTESIAN_POINT('Ctrl Pts',(109.029823553309,0.652935861560398,
137.377622345005));
#274414=CARTESIAN_POINT('Ctrl Pts',(108.751375929496,5.88319903775945,133.808035709655));
#274415=CARTESIAN_POINT('Ctrl Pts',(108.472928305683,5.70708970850866,127.478218402361));
#274416=CARTESIAN_POINT('Ctrl Pts',(108.19448068187,0.286443743970404,124.204963299759));
#274417=CARTESIAN_POINT('Ctrl Pts',(107.916033058058,-5.39743002772183,
126.996231933739));
#274418=CARTESIAN_POINT('Ctrl Pts',(107.637585434244,-6.12132928305326,
133.286984790727));
#274419=CARTESIAN_POINT('Ctrl Pts',(107.359137810432,-1.22002597081922,
137.296327315513));
#274420=CARTESIAN_POINT('Ctrl Pts',(107.080690186619,4.80242160701559,135.339869595089));
#274421=CARTESIAN_POINT('Ctrl Pts',(106.802242562806,6.41167833934146,129.215500696253));
#274422=CARTESIAN_POINT('Ctrl Pts',(106.523794938993,2.12891590571267,124.551216444981));
#274423=CARTESIAN_POINT('Ctrl Pts',(106.24534731518,-4.11021624194206,125.633266205238));
#274424=CARTESIAN_POINT('Ctrl Pts',(105.966899691367,-6.57226045847839,
131.467299108419));
#274425=CARTESIAN_POINT('Ctrl Pts',(105.688452067554,-2.99471838644612,
136.692123924851));
#274426=CARTESIAN_POINT('Ctrl Pts',(105.410004443742,3.33482358260376,136.506381895117));
#274427=CARTESIAN_POINT('Ctrl Pts',(105.131556819929,6.59982559442975,131.080760870538));
#274428=CARTESIAN_POINT('Ctrl Pts',(104.853109196116,3.79991030437941,125.401141516381));
#274429=CARTESIAN_POINT('Ctrl Pts',(104.574661572303,-2.49193691945696,
124.686816554284));
#274430=CARTESIAN_POINT('Ctrl Pts',(104.29621394849,-6.49381585219884,129.594215727701));
#274431=CARTESIAN_POINT('Ctrl Pts',(104.017766324677,-4.52819525731082,
135.613678936038));
#274432=CARTESIAN_POINT('Ctrl Pts',(103.739318700864,1.59861556440955,137.213613557961));
#274433=CARTESIAN_POINT('Ctrl Pts',(103.460871077051,6.25637677914949,132.923757837073));
#274434=CARTESIAN_POINT('Ctrl Pts',(103.182423453238,5.16483337484823,126.686279609768));
#274435=CARTESIAN_POINT('Ctrl Pts',(102.903975829425,-0.672939584800916,
124.233116649188));
#274436=CARTESIAN_POINT('Ctrl Pts',(102.625528205613,-5.89231394094447,
127.818605872432));
#274437=CARTESIAN_POINT('Ctrl Pts',(102.347080581799,-5.69693964089892,
134.147857844226));
#274438=CARTESIAN_POINT('Ctrl Pts',(102.068632957987,-0.266356121840884,
137.40459920364));
#274439=CARTESIAN_POINT('Ctrl Pts',(101.790185334174,5.40899566096888,134.59604374203));
#274440=CARTESIAN_POINT('Ctrl Pts',(101.511737710361,6.11374467547657,128.303116723058));
#274441=CARTESIAN_POINT('Ctrl Pts',(101.233290086548,1.20026100625305,124.308710650579));
#274442=CARTESIAN_POINT('Ctrl Pts',(100.954842462735,-4.81620389170723,
126.28348956762));
#274443=CARTESIAN_POINT('Ctrl Pts',(100.676394838922,-6.40681269782886,
132.412728122731));
#274444=CARTESIAN_POINT('Ctrl Pts',(100.397947215109,-2.10987362484612,
137.063955513716));
#274445=CARTESIAN_POINT('Ctrl Pts',(100.119499591297,4.12593623631335,135.962920993349));
#274446=CARTESIAN_POINT('Ctrl Pts',(99.8410519674839,6.5702122594916,130.121421497322));
#274447=CARTESIAN_POINT('Ctrl Pts',(99.5626043436712,2.97678418891005,124.907509689368));
#274448=CARTESIAN_POINT('Ctrl Pts',(99.2841567198582,-3.35216312728773,
125.112515807244));
#274449=CARTESIAN_POINT('Ctrl Pts',(99.0057090960455,-6.6006362917809,130.548049243728));
#274450=CARTESIAN_POINT('Ctrl Pts',(98.7272614722323,-3.78344716313679,
136.219120311263));
#274451=CARTESIAN_POINT('Ctrl Pts',(98.4488138484198,2.51054507676055,136.914291746006));
#274452=CARTESIAN_POINT('Ctrl Pts',(98.1703662246066,6.49746903806041,131.994734960442));
#274453=CARTESIAN_POINT('Ctrl Pts',(97.8919186007939,4.51353637239165,125.981282306795));
#274454=CARTESIAN_POINT('Ctrl Pts',(97.6134709769809,-1.61811572099509,
124.400003000271));
#274455=CARTESIAN_POINT('Ctrl Pts',(97.335023353168,-6.26279851613479,128.704015473778));
#274456=CARTESIAN_POINT('Ctrl Pts',(97.0565757293552,-5.15227542966332,
134.938142526861));
#274457=CARTESIAN_POINT('Ctrl Pts',(96.7781281055422,0.692937074020952,
137.373525951775));
#274458=CARTESIAN_POINT('Ctrl Pts',(96.4996804817294,5.90137425853808,133.772167356118));
#274459=CARTESIAN_POINT('Ctrl Pts',(96.2212328579164,5.6867367976186,127.443539353151));
#274460=CARTESIAN_POINT('Ctrl Pts',(95.9427852341037,0.246266032224636,
124.203341906934));
#274461=CARTESIAN_POINT('Ctrl Pts',(95.6643376102905,-5.42051118601915,
127.029158178097));
#274462=CARTESIAN_POINT('Ctrl Pts',(95.3858899864779,-6.10610343100435,
133.324201062238));
#274463=CARTESIAN_POINT('Ctrl Pts',(95.1074423626648,-1.18048492263276,
137.303633678775));
#274464=CARTESIAN_POINT('Ctrl Pts',(94.828994738852,4.82994155974394,135.3105518592));
#274465=CARTESIAN_POINT('Ctrl Pts',(94.5505471150391,6.40188770447863,129.176500428244));
#274466=CARTESIAN_POINT('Ctrl Pts',(94.2720994912261,2.09081179839861,124.538372985881));
#274467=CARTESIAN_POINT('Ctrl Pts',(93.9936518674133,-4.14161800857485,
125.658382066524));
#274468=CARTESIAN_POINT('Ctrl Pts',(93.7152042436005,-6.56810319495607,
131.507294040545));
#274469=CARTESIAN_POINT('Ctrl Pts',(93.4367566197874,-2.95882241485189,
136.710244539055));
#274470=CARTESIAN_POINT('Ctrl Pts',(93.1583089959747,3.36947161799043,136.485976232185));
#274471=CARTESIAN_POINT('Ctrl Pts',(92.8798613721617,6.60138584173913,131.040580737834));
#274472=CARTESIAN_POINT('Ctrl Pts',(92.6014137483489,3.76694897255651,125.37811049295));
#274473=CARTESIAN_POINT('Ctrl Pts',(92.3229661245359,-2.5291299767175,124.702099025532));
#274474=CARTESIAN_POINT('Ctrl Pts',(92.044518500723,-6.50106203225643,129.633767849141));
#274475=CARTESIAN_POINT('Ctrl Pts',(91.7660708769102,-4.49883567468812,
135.641154240296));
#274476=CARTESIAN_POINT('Ctrl Pts',(91.4876232530973,1.63760088757763,137.203763582666));
#274477=CARTESIAN_POINT('Ctrl Pts',(91.2091756292845,6.26916223541028,132.885634228324));
#274478=CARTESIAN_POINT('Ctrl Pts',(90.9307280054714,5.13966975450256,126.654916101563));
#274479=CARTESIAN_POINT('Ctrl Pts',(90.6522803816587,-0.71292814396669,
124.237334773374));
#274480=CARTESIAN_POINT('Ctrl Pts',(90.3738327578456,-5.91037990660673,
127.85452937895));
#274481=CARTESIAN_POINT('Ctrl Pts',(90.0953851340328,-5.67648127318543,
134.182474785545));
#274482=CARTESIAN_POINT('Ctrl Pts',(89.8169375102199,-0.226173661233629,
137.406098301819));
#274483=CARTESIAN_POINT('Ctrl Pts',(89.5384898864071,5.43197649619419,134.563047399079));
#274484=CARTESIAN_POINT('Ctrl Pts',(89.260042262594,6.09840562042418,128.265946966186));
#274485=CARTESIAN_POINT('Ctrl Pts',(88.9815946387814,1.1606979031614,124.301524670509));
#274486=CARTESIAN_POINT('Ctrl Pts',(88.7031470149683,-4.84363448386183,
126.312890928981));
#274487=CARTESIAN_POINT('Ctrl Pts',(88.4246993911556,-6.39690340491527,
132.45169841077));
#274488=CARTESIAN_POINT('Ctrl Pts',(88.1462517673426,-2.07173060295614,
137.076682937528));
#274489=CARTESIAN_POINT('Ctrl Pts',(87.8678041435297,4.15726141345302,135.937709672222));
#274490=CARTESIAN_POINT('Ctrl Pts',(87.5893565197169,6.5659332844097,130.081439403729));
#274491=CARTESIAN_POINT('Ctrl Pts',(87.3109088959039,2.94083323066708,124.889498414087));
#274492=CARTESIAN_POINT('Ctrl Pts',(87.032461272091,-3.38674889436835,125.133026832359));
#274493=CARTESIAN_POINT('Ctrl Pts',(86.7540136482781,-6.60207423736065,
130.588233939178));
#274494=CARTESIAN_POINT('Ctrl Pts',(86.4755660244652,-3.75041588547566,
136.242050905059));
#274495=CARTESIAN_POINT('Ctrl Pts',(86.1971184006524,2.54769144715974,136.898896142674));
#274496=CARTESIAN_POINT('Ctrl Pts',(85.9186707768394,6.50459480150186,131.955160967326));
#274497=CARTESIAN_POINT('Ctrl Pts',(85.6402231530266,4.48409330038545,125.953896490271));
#274498=CARTESIAN_POINT('Ctrl Pts',(85.3617755292137,-1.65707088364924,
124.409971587854));
#274499=CARTESIAN_POINT('Ctrl Pts',(85.0833279054008,-6.27546787802325,
128.742177820471));
#274500=CARTESIAN_POINT('Ctrl Pts',(84.8048802815879,-5.12701646614329,
134.969429300388));
#274501=CARTESIAN_POINT('Ctrl Pts',(84.526432657775,0.732912609443495,137.369186135708));
#274502=CARTESIAN_POINT('Ctrl Pts',(84.2479850339622,5.91933080172332,133.73618902941));
#274503=CARTESIAN_POINT('Ctrl Pts',(83.9695374101491,5.6661731626052,127.408984840408));
#274504=CARTESIAN_POINT('Ctrl Pts',(83.6910897863363,0.206079195000604,
124.201965117285));
#274505=CARTESIAN_POINT('Ctrl Pts',(83.4126421625234,-5.44339148528112,
127.062224313968));
#274506=CARTESIAN_POINT('Ctrl Pts',(83.1341945387106,-6.09065131504733,
133.361323960135));
#274507=CARTESIAN_POINT('Ctrl Pts',(82.8557469148977,-1.14090013114324,
137.310699209084));
#274508=CARTESIAN_POINT('Ctrl Pts',(82.5772992910847,4.85728253721157,135.281067144739));
#274509=CARTESIAN_POINT('Ctrl Pts',(82.2988516672719,6.39185984531258,129.137560481192));
#274510=CARTESIAN_POINT('Ctrl Pts',(82.0204040434589,2.05263021528453,124.52576171526));
#274511=CARTESIAN_POINT('Ctrl Pts',(81.7419564196462,-4.17286630602932,
125.683688613938));
#274512=CARTESIAN_POINT('Ctrl Pts',(81.4635087958331,-6.56370254795435,
131.547262925216));
#274513=CARTESIAN_POINT('Ctrl Pts',(81.1850611720204,-2.92281680300497,
136.728146308557));
#274514=CARTESIAN_POINT('Ctrl Pts',(80.9066135482074,3.40399479636718,136.465360034899));
#274515=CARTESIAN_POINT('Ctrl Pts',(80.6281659243945,6.60270147226842,131.000391851905));
#274516=CARTESIAN_POINT('Ctrl Pts',(80.3497183005816,3.73384805505426,125.355280541214));
#274517=CARTESIAN_POINT('Ctrl Pts',(80.0712706767688,-2.56622931613655,
124.717607618327));
#274518=CARTESIAN_POINT('Ctrl Pts',(79.7928230529558,-6.50806731306963,
129.673363347327));
#274519=CARTESIAN_POINT('Ctrl Pts',(79.514375429143,-4.46930938605503,135.668450315387));
#274520=CARTESIAN_POINT('Ctrl Pts',(79.23592780533,1.67652552884245,137.193676475141));
#274521=CARTESIAN_POINT('Ctrl Pts',(78.9574801815173,6.28171538555901,132.847433497217));
#274522=CARTESIAN_POINT('Ctrl Pts',(78.6790325577042,5.11431568180404,126.62370635255));
#274523=CARTESIAN_POINT('Ctrl Pts',(78.4005849338915,-0.752890285318027,
124.241796241119));
#274524=CARTESIAN_POINT('Ctrl Pts',(78.1221373100785,-5.92822686096799,
127.890562192549));
#274525=CARTESIAN_POINT('Ctrl Pts',(77.8436896862655,-5.65581256137084,
134.216966549603));
#274526=CARTESIAN_POINT('Ctrl Pts',(77.5652420624528,-0.185982819678218,
137.407352770183));
#274527=CARTESIAN_POINT('Ctrl Pts',(77.2867944386398,5.45475604753291,134.529911776607));
#274528=CARTESIAN_POINT('Ctrl Pts',(77.008346814827,6.08284058670873,128.228871271165));
#274529=CARTESIAN_POINT('Ctrl Pts',(76.729899191014,1.12109178998211,124.294579655415));
#274530=CARTESIAN_POINT('Ctrl Pts',(76.4514515672013,-4.8708855933594,126.342458723402));
#274531=CARTESIAN_POINT('Ctrl Pts',(76.1730039433881,-6.38675707239351,
132.4906076561));
#274532=CARTESIAN_POINT('Ctrl Pts',(75.8945563195755,-2.03351081232684,
137.089177938131));
#274533=CARTESIAN_POINT('Ctrl Pts',(75.6161086957625,4.18843254174224,135.912308132958));
#274534=CARTESIAN_POINT('Ctrl Pts',(75.3376610719495,6.56141100625526,130.041484098248));
#274535=CARTESIAN_POINT('Ctrl Pts',(75.0592134481368,2.90477329876725,124.871706316201));
#274536=CARTESIAN_POINT('Ctrl Pts',(74.7807658243238,-3.42120916422307,
125.153748010832));
#274537=CARTESIAN_POINT('Ctrl Pts',(74.5023182005109,-6.60326754065171,
130.628426643279));
#274538=CARTESIAN_POINT('Ctrl Pts',(74.223870576698,-3.71724563477466,136.264780003243));
#274539=CARTESIAN_POINT('Ctrl Pts',(73.9454229528852,2.58474341191554,136.883274704086));
#274540=CARTESIAN_POINT('Ctrl Pts',(73.6669753290721,6.51147953479087,131.915544330879));
#274541=CARTESIAN_POINT('Ctrl Pts',(73.3885277052595,4.45448406865298,125.926690409479));
#274542=CARTESIAN_POINT('Ctrl Pts',(73.1100800814464,-1.6959646429323,124.420177121874));
#274543=CARTESIAN_POINT('Ctrl Pts',(72.8316324576336,-6.28790470014163,
128.780416582107));
#274544=CARTESIAN_POINT('Ctrl Pts',(72.5531848338207,-5.1015675191428,135.000561735763));
#274545=CARTESIAN_POINT('Ctrl Pts',(72.2747372100078,0.772860986519783,
137.364603057617));
#274546=CARTESIAN_POINT('Ctrl Pts',(71.996289586195,5.93706800192887,133.700102062723));
#274547=CARTESIAN_POINT('Ctrl Pts',(71.7178419623819,5.64539956546153,127.374556144564));
#274548=CARTESIAN_POINT('Ctrl Pts',(71.4393943385692,0.165884721436248,
124.20083298183));
#274549=CARTESIAN_POINT('Ctrl Pts',(71.1609467147562,-5.46607007766984,
127.095429116077));
#274550=CARTESIAN_POINT('Ctrl Pts',(70.8824990909434,-6.07497350776591,
133.398352108815));
#274551=CARTESIAN_POINT('Ctrl Pts',(70.6040514671303,-1.10127306317963,
137.317523644624));
#274552=CARTESIAN_POINT('Ctrl Pts',(70.3256038433176,4.88444352628841,135.251416544269));
#274553=CARTESIAN_POINT('Ctrl Pts',(70.0471562195047,6.38159513342946,129.098682298033));
#274554=CARTESIAN_POINT('Ctrl Pts',(69.7687085956917,2.01437257120279,124.513383100429));
#274555=CARTESIAN_POINT('Ctrl Pts',(69.4902609718789,-4.20395997638847,
125.709184909736));
#274556=CARTESIAN_POINT('Ctrl Pts',(69.211813348066,-6.5590586805409,131.587204281367));
#274557=CARTESIAN_POINT('Ctrl Pts',(68.9333657242531,-2.88670288510633,
136.745828570004));
#274558=CARTESIAN_POINT('Ctrl Pts',(68.6549181004402,3.43839183846502,136.444534067195));
#274559=CARTESIAN_POINT('Ctrl Pts',(68.3764704766273,6.60377243726651,130.960195701968));
#274560=CARTESIAN_POINT('Ctrl Pts',(68.0980228528144,3.70060877843901,125.332652507142));
#274561=CARTESIAN_POINT('Ctrl Pts',(67.8195752290015,-2.6032335629848,124.733341757993));
#274562=CARTESIAN_POINT('Ctrl Pts',(67.5411276051886,-6.51483143505509,
129.713000755032));
#274563=CARTESIAN_POINT('Ctrl Pts',(67.2626799813758,-4.43961748551916,
135.695566149845));
#274564=CARTESIAN_POINT('Ctrl Pts',(66.9842323575627,1.71538804583728,137.183352609169));
#274565=CARTESIAN_POINT('Ctrl Pts',(66.7057847337499,6.29403576443417,132.809157059292));
#274566=CARTESIAN_POINT('Ctrl Pts',(66.4273371099371,5.08877209625689,126.592651519219));
#274567=CARTESIAN_POINT('Ctrl Pts',(66.1488894861241,-0.792824528042931,
124.246500887099));
#274568=CARTESIAN_POINT('Ctrl Pts',(65.8704418623113,-5.94585414270274,
127.92670297802));
#274569=CARTESIAN_POINT('Ctrl Pts',(65.5919942384984,-5.63493427134196,
134.251331858291));
#274570=CARTESIAN_POINT('Ctrl Pts',(65.3135466146855,-0.145785086460763,
137.408362562243));
#274571=CARTESIAN_POINT('Ctrl Pts',(65.0350989908726,5.47733347088038,134.496638102466));
#274572=CARTESIAN_POINT('Ctrl Pts',(64.7566513670597,6.06705015109826,128.191891011849));
#274573=CARTESIAN_POINT('Ctrl Pts',(64.4782037432468,1.0814441343344,124.28787586265));
#274574=CARTESIAN_POINT('Ctrl Pts',(64.199756119434,-4.89795621039988,126.37219185524));
#274575=CARTESIAN_POINT('Ctrl Pts',(63.921308495621,-6.37637407623982,132.529454416925));
#274576=CARTESIAN_POINT('Ctrl Pts',(63.6428608718081,-1.99521566920641,
137.101440052517));
#274577=CARTESIAN_POINT('Ctrl Pts',(63.3644132479953,4.21944846612332,135.886717316821));
#274578=CARTESIAN_POINT('Ctrl Pts',(63.0859656241823,6.556645592603,130.001557061437));
#274579=CARTESIAN_POINT('Ctrl Pts',(62.8075180003696,2.86860572942485,124.854134055001));
#274580=CARTESIAN_POINT('Ctrl Pts',(62.5290703765565,-3.4555426599142,125.174678574835));
#274581=CARTESIAN_POINT('Ctrl Pts',(62.2506227527437,-6.60421615743575,
130.66862586668));
#274582=CARTESIAN_POINT('Ctrl Pts',(61.9721751289308,-3.68393764016947,
136.287306763578));
#274583=CARTESIAN_POINT('Ctrl Pts',(61.6937275051179,2.62169959805353,136.867428009101));
#274584=CARTESIAN_POINT('Ctrl Pts',(61.415279881305,6.51812298281107,131.875886519111));
#274585=CARTESIAN_POINT('Ctrl Pts',(61.1368322574921,4.42470977437533,125.899665072552));
#274586=CARTESIAN_POINT('Ctrl Pts',(60.8583846336791,-1.73479555762186,
124.430619224162));
#274587=CARTESIAN_POINT('Ctrl Pts',(60.5799370098664,-6.30010852163892,
128.818730341733));
#274588=CARTESIAN_POINT('Ctrl Pts',(60.3014893860534,-5.07592953168175,
135.031538679362));
#274589=CARTESIAN_POINT('Ctrl Pts',(60.0230417622406,0.81278072494776,137.35977688733));
#274590=CARTESIAN_POINT('Ctrl Pts',(59.7445941384276,5.95458520189618,133.663907793273));
#274591=CARTESIAN_POINT('Ctrl Pts',(59.4661465146148,5.62441677596096,127.340254541386));
#274592=CARTESIAN_POINT('Ctrl Pts',(59.1876988908018,0.125684100952275,
124.199945542519));
#274593=CARTESIAN_POINT('Ctrl Pts',(58.909251266989,-5.48854612282181,127.128771354006));
#274594=CARTESIAN_POINT('Ctrl Pts',(58.6308036431761,-6.05907059010694,
133.435284136186));
#274595=CARTESIAN_POINT('Ctrl Pts',(58.3523560193632,-1.06160518713815,
137.324106732513));
#274596=CARTESIAN_POINT('Ctrl Pts',(58.0739083955504,4.91142352051418,135.221601156507));
#274597=CARTESIAN_POINT('Ctrl Pts',(57.7954607717374,6.37109394919177,129.059867319411));
#274598=CARTESIAN_POINT('Ctrl Pts',(57.5170131479246,1.97604028380464,124.501237600083));
#274599=CARTESIAN_POINT('Ctrl Pts',(57.2385655241116,-4.23489786746425,
125.734870009144));
#274600=CARTESIAN_POINT('Ctrl Pts',(56.9601179002987,-6.554171764796,131.627116628959));
#274601=CARTESIAN_POINT('Ctrl Pts',(56.6816702764859,-2.85048199937133,
136.76329066817));
#274602=CARTESIAN_POINT('Ctrl Pts',(56.4032226526729,3.47266146968847,136.423499100792));
#274603=CARTESIAN_POINT('Ctrl Pts',(56.1247750288601,6.60459869704857,130.919993777505));
#274604=CARTESIAN_POINT('Ctrl Pts',(55.8463274050471,3.66723237440476,125.310227229228));
#274605=CARTESIAN_POINT('Ctrl Pts',(55.5678797812343,-2.6401413460556,124.749300861495));
#274606=CARTESIAN_POINT('Ctrl Pts',(55.2894321574214,-6.5213541475661,129.752678603477));
#274607=CARTESIAN_POINT('Ctrl Pts',(55.0109845336085,-4.40976107332459,
135.722500738884));
#274608=CARTESIAN_POINT('Ctrl Pts',(54.7325369097956,1.75418699849736,137.172792367301));
#274609=CARTESIAN_POINT('Ctrl Pts',(54.4540892859827,6.30612291549916,132.770806332897));
#274610=CARTESIAN_POINT('Ctrl Pts',(54.1756416621698,5.06303994438864,126.561752752318));
#274611=CARTESIAN_POINT('Ctrl Pts',(53.897194038357,-0.832729392363195,
124.251448536985));
#274612=CARTESIAN_POINT('Ctrl Pts',(53.618746414544,-5.96326109862574,127.962950396153));
#274613=CARTESIAN_POINT('Ctrl Pts',(53.3402987907312,-5.61384717675129,
134.285569438194));
#274614=CARTESIAN_POINT('Ctrl Pts',(53.0618511669183,-0.105581951123662,
137.409127640582));
#274615=CARTESIAN_POINT('Ctrl Pts',(52.7834035431054,5.49970792962155,134.463227609627));
#274616=CARTESIAN_POINT('Ctrl Pts',(52.5049559192925,6.05103489871361,128.155007558556));
#274617=CARTESIAN_POINT('Ctrl Pts',(52.2265082954796,1.04175640537643,124.281413540623));
#274618=CARTESIAN_POINT('Ctrl Pts',(51.9480606716666,-4.9248453318719,126.402089222721));
#274619=CARTESIAN_POINT('Ctrl Pts',(51.6696130478539,-6.36575480119974,
132.568237253767));
#274620=CARTESIAN_POINT('Ctrl Pts',(51.3911654240409,-1.95684659263562,
137.113468826308));
#274621=CARTESIAN_POINT('Ctrl Pts',(51.112717800228,4.25030803728985,135.860938172086));
#274622=CARTESIAN_POINT('Ctrl Pts',(50.8342701764151,6.55163722003711,129.961659772806));
#274623=CARTESIAN_POINT('Ctrl Pts',(50.5558225526023,2.83233186284197,124.836782281636));
#274624=CARTESIAN_POINT('Ctrl Pts',(50.2773749287893,-3.48974810920128,
125.195817748775));
#274625=CARTESIAN_POINT('Ctrl Pts',(49.9989273049765,-6.60492005256131,
130.708830119782));
#274626=CARTESIAN_POINT('Ctrl Pts',(49.7204796811635,-3.65049313590031,
136.309630351328));
#274627=CARTESIAN_POINT('Ctrl Pts',(49.4420320573507,2.65855863614892,136.851356644924));
#274628=CARTESIAN_POINT('Ctrl Pts',(49.1635844335378,6.52452489938715,131.836189001557));
#274629=CARTESIAN_POINT('Ctrl Pts',(48.8851368097249,4.39477152084969,125.87282148092));
#274630=CARTESIAN_POINT('Ctrl Pts',(48.606689185912,-1.77356218882415,124.441297507781));
#274631=CARTESIAN_POINT('Ctrl Pts',(48.3282415620992,-6.31207889029818,
128.857117679619));
#274632=CARTESIAN_POINT('Ctrl Pts',(48.0497939382862,-5.05010345378512,
135.062358983324));
#274633=CARTESIAN_POINT('Ctrl Pts',(47.7713463144734,0.852670345487299,
137.354707803682));
#274634=CARTESIAN_POINT('Ctrl Pts',(47.4928986906604,5.97188175251911,133.627607562248));
#274635=CARTESIAN_POINT('Ctrl Pts',(47.2144510668476,5.60322557162828,127.306081301933));
#274636=CARTESIAN_POINT('Ctrl Pts',(46.9360034430346,0.0854788231980546,
124.199302832238));
#274637=CARTESIAN_POINT('Ctrl Pts',(46.6575558192218,-5.5108187878785,127.162249792247));
#274638=CARTESIAN_POINT('Ctrl Pts',(46.3791081954089,-6.04294315135938,
133.47211867372));
#274639=CARTESIAN_POINT('Ctrl Pts',(46.100660571596,-1.02189797292572,137.330448228811));
#274640=CARTESIAN_POINT('Ctrl Pts',(45.822212947783,4.93822152013526,135.191622086273));
#274641=CARTESIAN_POINT('Ctrl Pts',(45.5437653239702,6.36035668172477,129.02111698363));
#274642=CARTESIAN_POINT('Ctrl Pts',(45.2653177001572,1.9376347735074,124.489325664279));
#274643=CARTESIAN_POINT('Ctrl Pts',(44.9868700763445,-4.26567883284234,
125.76074296039));
#274644=CARTESIAN_POINT('Ctrl Pts',(44.7084224525315,-6.54904198180601,
131.666998489025));
#274645=CARTESIAN_POINT('Ctrl Pts',(44.4299748287186,-2.81415548797717,
136.780531955991));
#274646=CARTESIAN_POINT('Ctrl Pts',(44.1515272049057,3.50680242016433,136.402255915145));
#274647=CARTESIAN_POINT('Ctrl Pts',(43.8730795810928,6.60518022099696,130.879787568212));
#274648=CARTESIAN_POINT('Ctrl Pts',(43.59463195728,3.63372007972613,125.288005538446));
#274649=CARTESIAN_POINT('Ctrl Pts',(43.316184333467,-2.6769512977182,124.765484337463));
#274650=CARTESIAN_POINT('Ctrl Pts',(43.0377367096542,-6.52763520890084,
129.792395422388));
#274651=CARTESIAN_POINT('Ctrl Pts',(42.7592890858413,-4.37974125581177,
135.749253084432));
#274652=CARTESIAN_POINT('Ctrl Pts',(42.4808414620283,1.79292094911309,137.161996140853));
#274653=CARTESIAN_POINT('Ctrl Pts',(42.2023938382155,6.31797639086063,132.732382739134));
#274654=CARTESIAN_POINT('Ctrl Pts',(41.9239462144025,5.0371201797131,126.531011196811));
#274655=CARTESIAN_POINT('Ctrl Pts',(41.6454985905898,-0.872603399589798,
124.256639007436));
#274656=CARTESIAN_POINT('Ctrl Pts',(41.3670509667768,-5.98044708371573,
127.999303103786));
#274657=CARTESIAN_POINT('Ctrl Pts',(41.0886033429639,-5.592552058989,134.319678020622));
#274658=CARTESIAN_POINT('Ctrl Pts',(40.810155719151,-0.0653749034083074,
137.409647976851));
#274659=CARTESIAN_POINT('Ctrl Pts',(40.5317080953382,5.52187859466303,134.429681536124));
#274660=CARTESIAN_POINT('Ctrl Pts',(40.2532604715252,6.03479542300531,128.118222278014));
#274661=CARTESIAN_POINT('Ctrl Pts',(39.9748128477124,1.00203007375177,124.275192928799));
#274662=CARTESIAN_POINT('Ctrl Pts',(39.6963652238994,-4.95155196138904,
126.432149717987));
#274663=CARTESIAN_POINT('Ctrl Pts',(39.4179176000866,-6.35489964077443,
132.60695472951));
#274664=CARTESIAN_POINT('Ctrl Pts',(39.1394699762736,-1.91840500439501,
137.125263813774));
#274665=CARTESIAN_POINT('Ctrl Pts',(38.8610223524608,4.28101011172891,135.834971654011));
#274666=CARTESIAN_POINT('Ctrl Pts',(38.5825747286478,6.54638607414467,129.921793710766));
#274667=CARTESIAN_POINT('Ctrl Pts',(38.304127104835,2.79595304316033,124.819651639079));
#274668=CARTESIAN_POINT('Ctrl Pts',(38.0256794810221,-3.52382424458856,
125.217164749334));
#274669=CARTESIAN_POINT('Ctrl Pts',(37.7472318572093,-6.60537919994535,
130.749037912801));
#274670=CARTESIAN_POINT('Ctrl Pts',(37.4687842333963,-3.61691336126579,
136.331749939282));
#274671=CARTESIAN_POINT('Ctrl Pts',(37.1903366095834,2.69531916037638,136.835061207086));
#274672=CARTESIAN_POINT('Ctrl Pts',(36.9118889857706,6.53068504729366,131.796453249222));
#274673=CARTESIAN_POINT('Ctrl Pts',(36.6334413619576,4.36467041744916,125.846160629286));
#274674=CARTESIAN_POINT('Ctrl Pts',(36.3549937381448,-1.8122631000273,124.452211577043));
#274675=CARTESIAN_POINT('Ctrl Pts',(36.0765461143319,-6.32381536255287,
128.895577173308));
#274676=CARTESIAN_POINT('Ctrl Pts',(35.798098490519,-5.02409024244786,135.093021505591));
#274677=CARTESIAN_POINT('Ctrl Pts',(35.5196508667061,0.892528370013623,
137.34939599451));
#274678=CARTESIAN_POINT('Ctrl Pts',(35.2412032428932,5.98895701286753,133.591202714771));
#274679=CARTESIAN_POINT('Ctrl Pts',(34.9627556190803,5.58182673771145,127.272037692505));
#274680=CARTESIAN_POINT('Ctrl Pts',(34.6843079952674,0.0452703779943793,
124.198904874802));
#274681=CARTESIAN_POINT('Ctrl Pts',(34.4058603714545,-5.53288724751859,
127.195863190245));
#274682=CARTESIAN_POINT('Ctrl Pts',(34.1274127476417,-6.02659178913083,
133.508854356496));
#274683=CARTESIAN_POINT('Ctrl Pts',(33.8489651238287,-0.982152891908117,
137.336547898535));
#274684=CARTESIAN_POINT('Ctrl Pts',(33.5705175000158,4.96483653214189,135.161480444452));
#274685=CARTESIAN_POINT('Ctrl Pts',(33.292069876203,6.34938372890195,128.982432726597));
#274686=CARTESIAN_POINT('Ctrl Pts',(33.0136222523901,1.89915746344075,124.477647734417));
#274687=CARTESIAN_POINT('Ctrl Pts',(32.7351746285772,-4.29630173192265,
125.786802804744));
#274688=CARTESIAN_POINT('Ctrl Pts',(32.4567270047643,-6.543669521657,131.706848383727));
#274689=CARTESIAN_POINT('Ctrl Pts',(32.1782793809514,-2.77772469701646,
136.797551794587));
#274690=CARTESIAN_POINT('Ctrl Pts',(31.8998317571386,3.54081342478663,136.380805297429));
#274691=CARTESIAN_POINT('Ctrl Pts',(31.6213841333256,6.60551698756319,130.839578563946));
#274692=CARTESIAN_POINT('Ctrl Pts',(31.3429365095127,3.6000731362139,125.26598825823));
#274693=CARTESIAN_POINT('Ctrl Pts',(31.0644888856998,-2.71366205396602,
124.781891586214));
#274694=CARTESIAN_POINT('Ctrl Pts',(30.7860412618869,-6.53367438631237,
129.83214974004));
#274695=CARTESIAN_POINT('Ctrl Pts',(30.507593638074,-4.34955914537615,135.775822195171));
#274696=CARTESIAN_POINT('Ctrl Pts',(30.2291460142612,1.83158846238341,137.150964329883));
#274697=CARTESIAN_POINT('Ctrl Pts',(29.9506983904483,6.32959575128355,132.693887701803));
#274698=CARTESIAN_POINT('Ctrl Pts',(29.6722507666353,5.01101376269691,126.500427991838));
#274699=CARTESIAN_POINT('Ctrl Pts',(29.3938031428225,-0.912445072176531,
124.26207210612));
#274700=CARTESIAN_POINT('Ctrl Pts',(29.1153555190096,-5.99741146113971,
128.035759753857));
#274701=CARTESIAN_POINT('Ctrl Pts',(28.8369078951967,-5.57104970715349,
134.353656341672));
#274702=CARTESIAN_POINT('Ctrl Pts',(28.5584602713837,-0.0251654332018655,
137.409923551768));
#274703=CARTESIAN_POINT('Ctrl Pts',(28.280012647571,5.54384464446253,134.396001125022));
#274704=CARTESIAN_POINT('Ctrl Pts',(28.001565023758,6.0183323257333,128.081536533317));
#274705=CARTESIAN_POINT('Ctrl Pts',(27.7231173999451,0.962266611534229,
124.269214257685));
#274706=CARTESIAN_POINT('Ctrl Pts',(27.4446697761322,-4.97807510932732,
126.462372227135));
#274707=CARTESIAN_POINT('Ctrl Pts',(27.1662221523194,-6.34380899720599,
132.645605409466));
#274708=CARTESIAN_POINT('Ctrl Pts',(26.8877745285064,-1.87989232895117,
137.136824577849));
#274709=CARTESIAN_POINT('Ctrl Pts',(26.6093269046936,4.31155355176403,135.808818724794));
#274710=CARTESIAN_POINT('Ctrl Pts',(26.3308792808807,6.5408923495088,129.881960352566));
#274711=CARTESIAN_POINT('Ctrl Pts',(26.0524316570678,2.75947061841045,124.802742762115));
#274712=CARTESIAN_POINT('Ctrl Pts',(25.7739840332549,-3.55776980337282,
125.238718785491));
#274713=CARTESIAN_POINT('Ctrl Pts',(25.4955364094419,-6.60559358257403,
130.789247755823));
#274714=CARTESIAN_POINT('Ctrl Pts',(25.2170887856292,-3.58319956057628,
136.353664707793));
#274715=CARTESIAN_POINT('Ctrl Pts',(24.9386411618162,2.73197980856112,136.81854229942));
#274716=CARTESIAN_POINT('Ctrl Pts',(24.6601935380033,6.5366031982641,131.756680734531));
#274717=CARTESIAN_POINT('Ctrl Pts',(24.3817459141905,4.3344075795813,125.819683505575));
#274718=CARTESIAN_POINT('Ctrl Pts',(24.1032982903775,-1.85089685715453,
124.463361027524));
#274719=CARTESIAN_POINT('Ctrl Pts',(23.8248506665647,-6.33531750350378,
128.934107397669));
#274720=CARTESIAN_POINT('Ctrl Pts',(23.5464030427517,-4.99789086159903,
135.123525109951));
#274721=CARTESIAN_POINT('Ctrl Pts',(23.2679554189389,0.932353321572971,
137.343841656646));
#274722=CARTESIAN_POINT('Ctrl Pts',(22.9895077951259,6.00581035021119,133.554694599836));
#274723=CARTESIAN_POINT('Ctrl Pts',(22.7110601713131,5.56022106715229,127.238124974604));
#274724=CARTESIAN_POINT('Ctrl Pts',(22.4326125475002,0.00506025528043594,
124.198751684957));
#274725=CARTESIAN_POINT('Ctrl Pts',(22.1541649236873,-5.554750683987,127.229610302442));
#274726=CARTESIAN_POINT('Ctrl Pts',(21.8757172998744,-6.01001710932725,
133.545489823263));
#274727=CARTESIAN_POINT('Ctrl Pts',(21.5972696760615,-0.942371416853923,
137.342405515655));
#274728=CARTESIAN_POINT('Ctrl Pts',(21.3188220522486,4.99126757030501,135.131177347952));
#274729=CARTESIAN_POINT('Ctrl Pts',(21.0403744284357,6.33817549733007,128.943815981773));
#274730=CARTESIAN_POINT('Ctrl Pts',(20.7619268046228,1.86060977939589,124.466204243228));
#274731=CARTESIAN_POINT('Ctrl Pts',(20.48347918081,-4.32676542996233,125.813048576547));
#274732=CARTESIAN_POINT('Ctrl Pts',(20.205031556997,-6.5380545834274,131.746664836412));
#274733=CARTESIAN_POINT('Ctrl Pts',(19.9265839331841,-2.74119097644563,
136.814349553278));
#274734=CARTESIAN_POINT('Ctrl Pts',(19.6481363093713,3.57469322326559,136.359148042506));
#274735=CARTESIAN_POINT('Ctrl Pts',(19.3696886855584,6.60560898426828,130.799368254665));
#274736=CARTESIAN_POINT('Ctrl Pts',(19.0912410617455,3.56629279066743,125.244176204439));
#274737=CARTESIAN_POINT('Ctrl Pts',(18.8127934379326,-2.75027225446848,
124.798521999768));
#274738=CARTESIAN_POINT('Ctrl Pts',(18.5343458141197,-6.53947145601676,
129.871940083324));
#274739=CARTESIAN_POINT('Ctrl Pts',(18.2558981903068,-4.31921586042675,
135.802207086573));
#274740=CARTESIAN_POINT('Ctrl Pts',(17.9774505664939,1.87018810546999,137.139697343177));
#274741=CARTESIAN_POINT('Ctrl Pts',(17.6990029426811,6.34098056620813,132.65532264735));
#274742=CARTESIAN_POINT('Ctrl Pts',(17.4205553188681,4.98472166072295,126.470004270672));
#274743=CARTESIAN_POINT('Ctrl Pts',(17.1421076950552,-0.95225293377558,
124.26774763171));
#274744=CARTESIAN_POINT('Ctrl Pts',(16.8636600712423,-6.01415360227624,
128.072318995452));
#274745=CARTESIAN_POINT('Ctrl Pts',(16.5852124474295,-5.54934091802252,
134.387503142263));
#274746=CARTESIAN_POINT('Ctrl Pts',(16.3067648236166,0.0150449695187284,
137.409954355121));
#274747=CARTESIAN_POINT('Ctrl Pts',(16.0283171998036,5.56560526505998,134.362187624359));
#274748=CARTESIAN_POINT('Ctrl Pts',(15.7498695759908,6.00164621694371,128.044951683866));
#274749=CARTESIAN_POINT('Ctrl Pts',(15.4714219521779,0.922467492173741,
124.263477748823));
#274750=CARTESIAN_POINT('Ctrl Pts',(15.192974328365,-5.00441379286154,126.492755630261));
#274751=CARTESIAN_POINT('Ctrl Pts',(14.9145267045521,-6.33248328146239,
132.684187861418));
#274752=CARTESIAN_POINT('Ctrl Pts',(14.6360790807393,-1.84130999340576,
137.148150690142));
#274753=CARTESIAN_POINT('Ctrl Pts',(14.3576314569263,4.34193722559672,135.782480353541));
#274754=CARTESIAN_POINT('Ctrl Pts',(14.0791838331134,6.53515624970152,129.842161174248));
#274755=CARTESIAN_POINT('Ctrl Pts',(13.8007362093005,2.72288594046203,124.786056277307));
#274756=CARTESIAN_POINT('Ctrl Pts',(13.5222885854877,-3.59158352768866,
125.260479058552));
#274757=CARTESIAN_POINT('Ctrl Pts',(13.2438409616747,-6.60556319250329,
130.829458158858));
#274758=CARTESIAN_POINT('Ctrl Pts',(12.9653933378619,-3.54935298310934,
136.375373844801));
#274759=CARTESIAN_POINT('Ctrl Pts',(12.686945714049,2.76853922222938,136.801800534039));
#274760=CARTESIAN_POINT('Ctrl Pts',(12.4084980902361,6.5422791329992,131.716872931266));
#274761=CARTESIAN_POINT('Ctrl Pts',(12.1300504664232,4.30398412864651,125.793391090908));
#274762=CARTESIAN_POINT('Ctrl Pts',(11.8516028426103,-1.88946202861834,
124.474745446076));
#274763=CARTESIAN_POINT('Ctrl Pts',(11.5731552187974,-6.34658488693473,
128.972706924952));
#274764=CARTESIAN_POINT('Ctrl Pts',(11.2947075949845,-4.97150628206636,
135.153868666082));
#274765=CARTESIAN_POINT('Ctrl Pts',(11.0162599711716,0.972143724437105,
137.338044995907));
#274766=CARTESIAN_POINT('Ctrl Pts',(10.7378123473587,6.0224411400439,133.518084570262));
#274767=CARTESIAN_POINT('Ctrl Pts',(10.4593647235458,5.53840936055655,127.204344404875));
#274768=CARTESIAN_POINT('Ctrl Pts',(10.1809170997329,-0.0351500549433496,
124.198843268382));
#274769=CARTESIAN_POINT('Ctrl Pts',(9.90246947592002,-5.57640828712608,
127.263489878326));
#274770=CARTESIAN_POINT('Ctrl Pts',(9.62402185210712,-5.99321972612948,
133.582023716479));
#274771=CARTESIAN_POINT('Ctrl Pts',(9.34557422829421,-0.902555021880531,
137.348020863117));
#274772=CARTESIAN_POINT('Ctrl Pts',(9.06712660448133,5.01751365521256,135.100713919668));
#274773=CARTESIAN_POINT('Ctrl Pts',(8.78867898066847,6.32673240233446,128.905268180115));
#274774=CARTESIAN_POINT('Ctrl Pts',(8.51023135685555,1.82199314977141,124.454995614755));
#274775=CARTESIAN_POINT('Ctrl Pts',(8.23178373304265,-4.35706879811783,
125.839479303254));
#274776=CARTESIAN_POINT('Ctrl Pts',(7.9533361092298,-6.53219737518076,131.786446371669));
#274777=CARTESIAN_POINT('Ctrl Pts',(7.67488848541689,-2.70455568003535,
136.83092460962));
#274778=CARTESIAN_POINT('Ctrl Pts',(7.39644086160398,3.60844056017245,136.337284952891));
#274779=CARTESIAN_POINT('Ctrl Pts',(7.1179932377911,6.60545620770325,130.759158130379));
#274780=CARTESIAN_POINT('Ctrl Pts',(6.83954561397822,3.53238029483008,125.222570185327));
#274781=CARTESIAN_POINT('Ctrl Pts',(6.5610979901653,-2.78678054262086,124.815374961881));
#274782=CARTESIAN_POINT('Ctrl Pts',(6.28265036635242,-6.54502620320144,
129.911764977794));
#274783=CARTESIAN_POINT('Ctrl Pts',(6.00420274253956,-4.28871252534551,
135.828406780936));
#274784=CARTESIAN_POINT('Ctrl Pts',(5.72575511872663,1.90871844804856,137.128195598241));
#274785=CARTESIAN_POINT('Ctrl Pts',(5.44730749491374,6.35213041376593,132.616689004818));
#274786=CARTESIAN_POINT('Ctrl Pts',(5.16885987110085,4.95824484805471,126.439741160674));
#274787=CARTESIAN_POINT('Ctrl Pts',(4.89041224728798,-0.992025509291961,
124.273665373899));
#274788=CARTESIAN_POINT('Ctrl Pts',(4.61196462347505,-6.03067288673954,
128.108979473854));
#274789=CARTESIAN_POINT('Ctrl Pts',(4.33351699966218,-5.52742649602286,
134.421217168191));
#274790=CARTESIAN_POINT('Ctrl Pts',(4.05506937584931,0.0552548147426717,
137.409740385768));
#274791=CARTESIAN_POINT('Ctrl Pts',(3.77662175203639,5.58715965010757,134.328242287108));
#274792=CARTESIAN_POINT('Ctrl Pts',(3.49817412822347,5.98473771494644,128.008469085329));
#274793=CARTESIAN_POINT('Ctrl Pts',(3.21972650441063,0.882634190440881,
124.25798361478));
#274794=CARTESIAN_POINT('Ctrl Pts',(2.94127888059773,-5.03056703600248,
126.523298801495));
#274795=CARTESIAN_POINT('Ctrl Pts',(2.66283125678483,-6.32092291322184,
132.722700655682));
#274796=CARTESIAN_POINT('Ctrl Pts',(2.38438363297192,-1.80265942744139,
137.159241730961));
#274797=CARTESIAN_POINT('Ctrl Pts',(2.10593600915906,4.37216000734877,135.755957516231));
#274798=CARTESIAN_POINT('Ctrl Pts',(1.82748838534615,6.529177987276,129.802397650584));
#274799=CARTESIAN_POINT('Ctrl Pts',(1.54904076153325,2.68620036497402,124.769592802981));
#274800=CARTESIAN_POINT('Ctrl Pts',(1.27059313772038,-3.62526416455594,
125.282444762183));
#274801=CARTESIAN_POINT('Ctrl Pts',(0.992145513907496,-6.60528803085927,
130.869667631896));
#274802=CARTESIAN_POINT('Ctrl Pts',(0.713697890094564,-3.51537488306232,
136.396876545864));
#274803=CARTESIAN_POINT('Ctrl Pts',(0.435250266281723,2.80499604665836,
136.784836531317));
#274804=CARTESIAN_POINT('Ctrl Pts',(0.156802642468823,6.54771264117505,
131.677031314524));
#274805=CARTESIAN_POINT('Ctrl Pts',(-0.121644981344083,4.27340119199728,
125.767284359559));
#274806=CARTESIAN_POINT('Ctrl Pts',(-0.400092605156985,-1.92795718537184,
124.486364410847));
#274807=CARTESIAN_POINT('Ctrl Pts',(-0.678540228969845,-6.35761709532873,
129.011374324836));
#274808=CARTESIAN_POINT('Ctrl Pts',(-0.956987852782752,-4.94493748154019,
135.184051049593));
#274809=CARTESIAN_POINT('Ctrl Pts',(-1.23543547659566,1.01189810415772,
137.332006227089));
#274810=CARTESIAN_POINT('Ctrl Pts',(-1.51388310040852,6.03884876610542,
133.48137398265));
#274811=CARTESIAN_POINT('Ctrl Pts',(-1.79233072422142,5.51639242616521,
127.170697235071));
#274812=CARTESIAN_POINT('Ctrl Pts',(-2.07077834803434,-0.0753590626689394,
124.19917962168));
#274813=CARTESIAN_POINT('Ctrl Pts',(-2.34922597184723,-5.59785925440532,
127.297500662476));
#274814=CARTESIAN_POINT('Ctrl Pts',(-2.6276735956601,-5.97620026197078,
133.618454682368));
#274815=CARTESIAN_POINT('Ctrl Pts',(-2.906121219473,-0.862705182398668,
137.353393732843));
#274816=CARTESIAN_POINT('Ctrl Pts',(-3.18456884328591,5.04357381430661,
135.070091288433));
#274817=CARTESIAN_POINT('Ctrl Pts',(-3.46301646709877,6.31505486794284,
128.866790750024));
#274818=CARTESIAN_POINT('Ctrl Pts',(-3.74146409091167,1.78330900552073,
124.444022264336));
#274819=CARTESIAN_POINT('Ctrl Pts',(-4.01991171472458,-4.38721071348669,
125.866094005463));
#274820=CARTESIAN_POINT('Ctrl Pts',(-4.29835933853748,-6.52609811395827,
131.826191515377));
#274821=CARTESIAN_POINT('Ctrl Pts',(-4.57680696235032,-2.66782016531947,
136.847276349416));
#274822=CARTESIAN_POINT('Ctrl Pts',(-4.85525458616324,3.64205418498746,
136.31521683873));
#274823=CARTESIAN_POINT('Ctrl Pts',(-5.13370220997616,6.60505866352928,
130.718949681087));
#274824=CARTESIAN_POINT('Ctrl Pts',(-5.41214983378902,3.49833690534187,
125.201171001511));
#274825=CARTESIAN_POINT('Ctrl Pts',(-5.69059745760191,-2.82318556559566,
124.832449848059));
#274826=CARTESIAN_POINT('Ctrl Pts',(-5.96904508141481,-6.55033842203324,
129.951622947723));
#274827=CARTESIAN_POINT('Ctrl Pts',(-6.24749270522772,-4.2580502704442,
135.854420307421));
#274828=CARTESIAN_POINT('Ctrl Pts',(-6.52594032904057,1.9471780623631,137.116459521273));
#274829=CARTESIAN_POINT('Ctrl Pts',(-6.80438795285348,6.36304488079526,
132.577988205793));
#274830=CARTESIAN_POINT('Ctrl Pts',(-7.0828355766664,4.93158430580029,126.409639783256));
#274831=CARTESIAN_POINT('Ctrl Pts',(-7.36128320047925,-1.03176132493798,
124.279825113401));
#274832=CARTESIAN_POINT('Ctrl Pts',(-7.63973082429214,-6.04696870240127,
128.145739830595));
#274833=CARTESIAN_POINT('Ctrl Pts',(-7.91817844810507,-5.50530725320171,
134.454797170168));
#274834=CARTESIAN_POINT('Ctrl Pts',(-8.19662607191793,0.09546261247915,
137.40928165164));
#274835=CARTESIAN_POINT('Ctrl Pts',(-8.47507369573082,5.60850700089942,
134.294166371127));
#274836=CARTESIAN_POINT('Ctrl Pts',(-8.75352131954372,5.96760744629241,
127.972090089581));
#274837=CARTESIAN_POINT('Ctrl Pts',(-9.03196894335663,0.842768182373745,
124.252732059145));
#274838=CARTESIAN_POINT('Ctrl Pts',(-9.31041656716948,-5.05653386963193,
126.554000609049));
#274839=CARTESIAN_POINT('Ctrl Pts',(-9.5888641909824,-6.30912832085822,
132.76114236515));
#274840=CARTESIAN_POINT('Ctrl Pts',(-9.86731181479532,-1.76394206326903,
137.170097289323));
#274841=CARTESIAN_POINT('Ctrl Pts',(-10.1457594386081,4.40222077710389,
135.729251195677));
#274842=CARTESIAN_POINT('Ctrl Pts',(-10.424207062421,6.52295778375913,129.762671255026));
#274843=CARTESIAN_POINT('Ctrl Pts',(-10.7026546862339,2.64941525134336,
124.753352949195));
#274844=CARTESIAN_POINT('Ctrl Pts',(-10.9811023100469,-3.65881046592654,
125.304615082438));
#274845=CARTESIAN_POINT('Ctrl Pts',(-11.2595499338597,-6.60476810783814,
130.909874684957));
#274846=CARTESIAN_POINT('Ctrl Pts',(-11.5379975576726,-3.48126651950624,
136.418172014193));
#274847=CARTESIAN_POINT('Ctrl Pts',(-11.8164451814855,2.84134893092756,
136.767650919861));
#274848=CARTESIAN_POINT('Ctrl Pts',(-12.0948928052984,6.5529035214511,131.637157360647));
#274849=CARTESIAN_POINT('Ctrl Pts',(-12.3733404291112,4.2426599028951,125.741364278924));
#274850=CARTESIAN_POINT('Ctrl Pts',(-12.6517880529242,-1.96638090096281,
124.498217491291));
#274851=CARTESIAN_POINT('Ctrl Pts',(-12.9302356767371,-6.36841371988325,
129.050108164486));
#274852=CARTESIAN_POINT('Ctrl Pts',(-13.2086833005499,-4.91818544453708,
135.214071142064));
#274853=CARTESIAN_POINT('Ctrl Pts',(-13.4871309243628,1.05161498762227,
137.325725573964));
#274854=CARTESIAN_POINT('Ctrl Pts',(-13.7655785481758,6.05503262040511,
133.444564197323));
#274855=CARTESIAN_POINT('Ctrl Pts',(-14.0440261719886,5.49417107982388,
127.137184712));
#274856=CARTESIAN_POINT('Ctrl Pts',(-14.3224737958015,-0.115565277936756,
124.199760732389));
#274857=CARTESIAN_POINT('Ctrl Pts',(-14.6009214196144,-5.61910279095105,
127.331641394614));
#274858=CARTESIAN_POINT('Ctrl Pts',(-14.8793690434273,-5.95895934751375,
133.654781370965));
#274859=CARTESIAN_POINT('Ctrl Pts',(-15.1578166672402,-0.822823375059262,
137.358523925738));
#274860=CARTESIAN_POINT('Ctrl Pts',(-15.4362642910531,5.06944708191823,
135.039310588977));
#274861=CARTESIAN_POINT('Ctrl Pts',(-15.714711914866,6.3031433268707,128.828385117298));
#274862=CARTESIAN_POINT('Ctrl Pts',(-15.9931595386788,1.74455878009922,
124.433284598595));
#274863=CARTESIAN_POINT('Ctrl Pts',(-16.2716071624918,-4.41719005914895,
125.892891696959));
#274864=CARTESIAN_POINT('Ctrl Pts',(-16.5500547863046,-6.51975702577033,
131.865898794765));
#274865=CARTESIAN_POINT('Ctrl Pts',(-16.8285024101176,-2.63098579354628,
136.863404166748));
#274866=CARTESIAN_POINT('Ctrl Pts',(-17.1069500339304,3.67553285214529,
136.292944517765));
#274867=CARTESIAN_POINT('Ctrl Pts',(-17.3853976577434,6.60441636647752,
130.678744396729));
#274868=CARTESIAN_POINT('Ctrl Pts',(-17.6638452815562,3.46416388369313,
125.179979445948));
#274869=CARTESIAN_POINT('Ctrl Pts',(-17.9422929053691,-2.8594859743911,
124.849746025587));
#274870=CARTESIAN_POINT('Ctrl Pts',(-18.220740529182,-6.55540791566593,
129.991512516161));
#274871=CARTESIAN_POINT('Ctrl Pts',(-18.4991881529949,-4.22723023192423,
135.880246702087));
#274872=CARTESIAN_POINT('Ctrl Pts',(-18.7776357768078,1.98556552327847,
137.104489547159));
#274873=CARTESIAN_POINT('Ctrl Pts',(-19.0560834006207,6.37372356285652,
132.539221684343));
#274874=CARTESIAN_POINT('Ctrl Pts',(-19.3345310244336,4.90474102187576,
126.379701253833));
#274875=CARTESIAN_POINT('Ctrl Pts',(-19.6129786482465,-1.07145890828896,
124.286226621967));
#274876=CARTESIAN_POINT('Ctrl Pts',(-19.8914262720594,-6.06304044541393,
128.182598703507));
#274877=CARTESIAN_POINT('Ctrl Pts',(-20.1698738958722,-5.48298400919569,
134.488241903877));
#274878=CARTESIAN_POINT('Ctrl Pts',(-20.4483215196851,0.135666872813404,
137.408578169733));
#274879=CARTESIAN_POINT('Ctrl Pts',(-20.7267691434981,5.62964652640204,
134.25996113911));
#274880=CARTESIAN_POINT('Ctrl Pts',(-21.0052167673109,5.95025604574973,
127.935816044659));
#274881=CARTESIAN_POINT('Ctrl Pts',(-21.2836643911238,0.802870945221437,
124.247723276515));
#274882=CARTESIAN_POINT('Ctrl Pts',(-21.5621120149367,-5.08231333153929,
126.584859915257));
#274883=CARTESIAN_POINT('Ctrl Pts',(-21.8405596387496,-6.29709994142449,
132.79951156535));
#274884=CARTESIAN_POINT('Ctrl Pts',(-22.1190072625625,-1.725159335575,137.180716962973));
#274885=CARTESIAN_POINT('Ctrl Pts',(-22.3974548863754,4.43211842094896,
135.702362381491));
#274886=CARTESIAN_POINT('Ctrl Pts',(-22.6759025101882,6.51649586964294,
129.722983459651));
#274887=CARTESIAN_POINT('Ctrl Pts',(-22.9543501340012,2.61253196265622,
124.737337317723));
#274888=CARTESIAN_POINT('Ctrl Pts',(-23.232797757814,-3.6922211887298,125.326989197785));
#274889=CARTESIAN_POINT('Ctrl Pts',(-23.511245381627,-6.60400344270576,
130.950077828156));
#274890=CARTESIAN_POINT('Ctrl Pts',(-23.7896930054398,-3.4470291563393,
136.439259460675));
#274891=CARTESIAN_POINT('Ctrl Pts',(-24.0681406292527,2.87759652796706,
136.75024433649));
#274892=CARTESIAN_POINT('Ctrl Pts',(-24.3465882530656,6.55785158147733,
131.597252547181));
#274893=CARTESIAN_POINT('Ctrl Pts',(-24.6250358768785,4.21176140046998,
125.715631809479));
#274894=CARTESIAN_POINT('Ctrl Pts',(-24.9034835006914,-2.00473175158637,
124.510304248187));
#274895=CARTESIAN_POINT('Ctrl Pts',(-25.1819311245043,-6.3789743605254,
129.088907008606));
#274896=CARTESIAN_POINT('Ctrl Pts',(-25.4603787483172,-4.89125116236366,
135.24392783109));
#274897=CARTESIAN_POINT('Ctrl Pts',(-25.73882637213,1.09129290310671,137.319203269261));
#274898=CARTESIAN_POINT('Ctrl Pts',(-26.017273995943,6.07099210324431,133.407656578282));
#274899=CARTESIAN_POINT('Ctrl Pts',(-26.2957216197559,5.47174614495268,
127.103808077481));
#274900=CARTESIAN_POINT('Ctrl Pts',(-26.5741692435687,-0.155767210890682,
124.200586578976));
#274901=CARTESIAN_POINT('Ctrl Pts',(-26.8526168673816,-5.64013810957666,
127.365910809639));
#274902=CARTESIAN_POINT('Ctrl Pts',(-27.1310644911945,-5.94149762162655,
133.691002436174));
#274903=CARTESIAN_POINT('Ctrl Pts',(-27.4095121150075,-0.782911077696857,
137.363411251701));
#274904=CARTESIAN_POINT('Ctrl Pts',(-27.6879597388203,5.09513249930392,
135.008372961895));
#274905=CARTESIAN_POINT('Ctrl Pts',(-27.9664073626332,6.29099822050462,
128.79005270507));
#274906=CARTESIAN_POINT('Ctrl Pts',(-28.2448549864461,1.70574390941038,
124.422783015417));
#274907=CARTESIAN_POINT('Ctrl Pts',(-28.523302610259,-4.44700572420938,
125.919871384741));
#274908=CARTESIAN_POINT('Ctrl Pts',(-28.8017502340719,-6.51317434558802,
131.905566738465));
#274909=CARTESIAN_POINT('Ctrl Pts',(-29.0801978578848,-2.59405392962697,
136.879307463993));
#274910=CARTESIAN_POINT('Ctrl Pts',(-29.3586454816977,3.7088753210816,136.270468815306));
#274911=CARTESIAN_POINT('Ctrl Pts',(-29.6370931055106,6.6035293403484,130.638543767126));
#274912=CARTESIAN_POINT('Ctrl Pts',(-29.9155407293234,3.42986249617799,
125.158996303897));
#274913=CARTESIAN_POINT('Ctrl Pts',(-30.1939883531365,-2.89568042388203,
124.86726285355));
#274914=CARTESIAN_POINT('Ctrl Pts',(-30.4724359769491,-6.56023449624756,
130.031432204983));
#274915=CARTESIAN_POINT('Ctrl Pts',(-30.7508836007622,-4.19625355183344,
135.905885007927));
#274916=CARTESIAN_POINT('Ctrl Pts',(-31.029331224575,2.02387940833292,137.092286119451));
#274917=CARTESIAN_POINT('Ctrl Pts',(-31.3077788483879,6.38416606424714,
132.50039087698));
#274918=CARTESIAN_POINT('Ctrl Pts',(-31.5862264722008,4.8777159909692,126.349926681791));
#274919=CARTESIAN_POINT('Ctrl Pts',(-31.8646740960137,-1.11111678833609,
124.292869662384));
#274920=CARTESIAN_POINT('Ctrl Pts',(-32.1431217198266,-6.07888752023319,
128.219554726771));
#274921=CARTESIAN_POINT('Ctrl Pts',(-32.4215693436394,-5.46045759120085,
134.52155013001));
#274922=CARTESIAN_POINT('Ctrl Pts',(-32.7000169674524,0.175866105961793,
137.407629966116));
#274923=CARTESIAN_POINT('Ctrl Pts',(-32.9784645912652,5.65057744328232,
134.225627858545));
#274924=CARTESIAN_POINT('Ctrl Pts',(-33.2569122150782,5.93268415628106,
127.89964829471));
#274925=CARTESIAN_POINT('Ctrl Pts',(-33.535359838891,0.762943957391,124.242957452493));
#274926=CARTESIAN_POINT('Ctrl Pts',(-33.813807462704,-5.10790446645711,
126.615875576613));
#274927=CARTESIAN_POINT('Ctrl Pts',(-34.0922550865168,-6.28483822063666,
132.837806834499));
#274928=CARTESIAN_POINT('Ctrl Pts',(-34.3707027103298,-1.68631268146717,
137.191100358392));
#274929=CARTESIAN_POINT('Ctrl Pts',(-34.6491503341426,4.46185183101625,
135.675292070049));
#274930=CARTESIAN_POINT('Ctrl Pts',(-34.9275979579556,6.5097924843757,129.683335735103));
#274931=CARTESIAN_POINT('Ctrl Pts',(-35.2060455817684,2.57555186563646,
124.721546502031));
#274932=CARTESIAN_POINT('Ctrl Pts',(-35.4844932055813,-3.72549509491909,
125.349566279145));
#274933=CARTESIAN_POINT('Ctrl Pts',(-35.7629408293942,-6.60299406379731,
130.990275571749));
#274934=CARTESIAN_POINT('Ctrl Pts',(-36.0413884532071,-3.41266406223907,
136.460138103909));
#274935=CARTESIAN_POINT('Ctrl Pts',(-36.3198360770199,2.91373749460914,
136.73261742621));
#274936=CARTESIAN_POINT('Ctrl Pts',(-36.5982837008328,6.56255663790157,
131.557318352812));
#274937=CARTESIAN_POINT('Ctrl Pts',(-36.8767313246458,4.18070682967726,
125.690087904753));
#274938=CARTESIAN_POINT('Ctrl Pts',(-37.1551789484586,-2.04300831613737,
124.522624233657));
#274939=CARTESIAN_POINT('Ctrl Pts',(-37.4336265722715,-6.38929862592666,
129.12776941949));
#274940=CARTESIAN_POINT('Ctrl Pts',(-37.7120741960844,-4.86413563307991,
135.273620010322));
#274941=CARTESIAN_POINT('Ctrl Pts',(-37.9905218198973,1.13093038033133,
137.312439554669));
#274942=CARTESIAN_POINT('Ctrl Pts',(-38.2689694437102,6.0867266232385,133.370652493151));
#274943=CARTESIAN_POINT('Ctrl Pts',(-38.5474170675231,5.44911845251588,
127.070568568297));
#274944=CARTESIAN_POINT('Ctrl Pts',(-38.825864691336,-0.195963371833029,
124.201657130839));
#274945=CARTESIAN_POINT('Ctrl Pts',(-39.1043123151489,-5.66096443081045,
127.400307637685));
#274946=CARTESIAN_POINT('Ctrl Pts',(-39.3827599389617,-5.92381573136,133.727116535809));
#274947=CARTESIAN_POINT('Ctrl Pts',(-39.6612075627747,-0.742969769276543,
137.368055529631));
#274948=CARTESIAN_POINT('Ctrl Pts',(-39.9396551865875,5.12062911468111,
134.977279553588));
#274949=CARTESIAN_POINT('Ctrl Pts',(-40.2181028104005,6.27861999888597,
128.751794933764));
#274950=CARTESIAN_POINT('Ctrl Pts',(-40.4965504342133,1.66686583175366,
124.412517903944));
#274951=CARTESIAN_POINT('Ctrl Pts',(-40.7749980580263,-4.47665660383728,
125.947032069068));
#274952=CARTESIAN_POINT('Ctrl Pts',(-41.0534456818391,-6.5063503173351,
131.945193876568));
#274953=CARTESIAN_POINT('Ctrl Pts',(-41.3318933056519,-2.55702594208532,
136.894985651848));
#274954=CARTESIAN_POINT('Ctrl Pts',(-41.6103409294649,3.74208035627896,
136.247790564197));
#274955=CARTESIAN_POINT('Ctrl Pts',(-41.8887885532778,6.60239761801125,
130.598349281928));
#274956=CARTESIAN_POINT('Ctrl Pts',(-42.1672361770906,3.39543401384647,
125.138222352896));
#274957=CARTESIAN_POINT('Ctrl Pts',(-42.4456838009036,-2.93176757287012,
124.884999682853));
#274958=CARTESIAN_POINT('Ctrl Pts',(-42.7241314247165,-6.56481798492739,
130.071380534953));
#274959=CARTESIAN_POINT('Ctrl Pts',(-43.0025790485293,-4.16512137802412,
135.931334274905));
#274960=CARTESIAN_POINT('Ctrl Pts',(-43.2810266723423,2.06211829779186,
137.079849690351));
#274961=CARTESIAN_POINT('Ctrl Pts',(-43.5594742961552,6.39437199801655,
132.461497222591));
#274962=CARTESIAN_POINT('Ctrl Pts',(-43.837921919968,4.85051021450257,126.320317170437));
#274963=CARTESIAN_POINT('Ctrl Pts',(-44.116369543781,-1.150733495542,124.299753988494));
#274964=CARTESIAN_POINT('Ctrl Pts',(-44.3948171675938,-6.09450933963988,
128.256606530968));
#274965=CARTESIAN_POINT('Ctrl Pts',(-44.6732647914067,-5.43772883394191,
134.554720614319));
#274966=CARTESIAN_POINT('Ctrl Pts',(-44.9517124152196,0.216058822326645,
137.406437075925));
#274967=CARTESIAN_POINT('Ctrl Pts',(-45.2301600390324,5.67129897593744,
134.191167801664));
#274968=CARTESIAN_POINT('Ctrl Pts',(-45.5086076628454,5.91489242901924,
127.863588179946));
#274969=CARTESIAN_POINT('Ctrl Pts',(-45.7870552866582,0.722988698391639,
124.238434763679));
#274970=CARTESIAN_POINT('Ctrl Pts',(-46.0655029104712,-5.13330632609627,
126.647046443824));
#274971=CARTESIAN_POINT('Ctrl Pts',(-46.343950534284,-6.27234361285742,
132.876026753548));
#274972=CARTESIAN_POINT('Ctrl Pts',(-46.622398158097,-1.64740354042306,
137.201247090823));
#274973=CARTESIAN_POINT('Ctrl Pts',(-46.9008457819097,4.49141990552312,
135.64804126445));
#274974=CARTESIAN_POINT('Ctrl Pts',(-47.1792934057228,6.50284787635396,
129.643729550545));
#274975=CARTESIAN_POINT('Ctrl Pts',(-47.4577410295356,2.53847633059532,
124.705981087252));
#274976=CARTESIAN_POINT('Ctrl Pts',(-47.7361886533485,-3.75863095151733,
125.372345489915));
#274977=CARTESIAN_POINT('Ctrl Pts',(-48.0146362771614,-6.60174000851572,
131.030466426196));
#274978=CARTESIAN_POINT('Ctrl Pts',(-48.2930839009743,-3.37817251061699,
136.480807170229));
#274979=CARTESIAN_POINT('Ctrl Pts',(-48.5715315247872,2.94977049163681,
136.714770842195));
#274980=CARTESIAN_POINT('Ctrl Pts',(-48.8499791486,6.56701851637621,131.517356257317));
#274981=CARTESIAN_POINT('Ctrl Pts',(-49.128426772413,4.14949734125552,125.664733511282));
#274982=CARTESIAN_POINT('Ctrl Pts',(-49.4068743962258,-2.08120917626415,
124.535176991179));
#274983=CARTESIAN_POINT('Ctrl Pts',(-49.6853220200388,-6.39938613351776,
129.166693957078));
#274984=CARTESIAN_POINT('Ctrl Pts',(-49.9637696438516,-4.83683986146123,
135.303146579501));
#274985=CARTESIAN_POINT('Ctrl Pts',(-50.2422172676646,1.17052595051479,
137.305434680818));
#274986=CARTESIAN_POINT('Ctrl Pts',(-50.5206648914774,6.10223559733929,
133.333553313131));
#274987=CARTESIAN_POINT('Ctrl Pts',(-50.7991125152903,5.42628884099088,
127.03746741615));
#274988=CARTESIAN_POINT('Ctrl Pts',(-51.0775601391032,-0.236152271280866,
124.202972348307));
#274989=CARTESIAN_POINT('Ctrl Pts',(-51.3560077629162,-5.68158098292544,
127.434830604167));
#274990=CARTESIAN_POINT('Ctrl Pts',(-51.634455386729,-5.90591433192304,
133.763122331648));
#274991=CARTESIAN_POINT('Ctrl Pts',(-51.9129030105419,-0.703000929838195,
137.372456587432));
#274992=CARTESIAN_POINT('Ctrl Pts',(-52.1913506343548,5.14593598326309,
134.946031516236));
#274993=CARTESIAN_POINT('Ctrl Pts',(-52.4697982581677,6.26600912069438,
128.713613221033));
#274994=CARTESIAN_POINT('Ctrl Pts',(-52.7482458819806,1.62792598777083,
124.402489644555));
#274995=CARTESIAN_POINT('Ctrl Pts',(-53.0266935057934,-4.50614159930848,
125.97437274349));
#274996=CARTESIAN_POINT('Ctrl Pts',(-53.3051411296064,-6.49928519387843,
131.984778740675));
#274997=CARTESIAN_POINT('Ctrl Pts',(-53.5835887534191,-2.51990320300721,
136.910438149353));
#274998=CARTESIAN_POINT('Ctrl Pts',(-53.8620363772322,3.7751467273123,136.22491060479));
#274999=CARTESIAN_POINT('Ctrl Pts',(-54.140484001045,6.60102124140245,130.558162430556));
#275000=CARTESIAN_POINT('Ctrl Pts',(-54.418931624858,3.36087971245889,125.117658362733));
#275001=CARTESIAN_POINT('Ctrl Pts',(-54.6973792486707,-2.96774608413265,
124.902955856252));
#275002=CARTESIAN_POINT('Ctrl Pts',(-54.9758268724838,-6.56915821186243,
130.111356025769));
#275003=CARTESIAN_POINT('Ctrl Pts',(-55.2542744962966,-4.13383486411065,
135.956593559989));
#275004=CARTESIAN_POINT('Ctrl Pts',(-55.5327221201095,2.10028077469877,
137.067180720695));
#275005=CARTESIAN_POINT('Ctrl Pts',(-55.8111697439224,6.40434098598004,
132.422542162396));
#275006=CARTESIAN_POINT('Ctrl Pts',(-56.0896173677353,4.82312470059616,
126.29087381696));
#275007=CARTESIAN_POINT('Ctrl Pts',(-56.3680649915482,-1.19030756189505,
124.306879345194));
#275008=CARTESIAN_POINT('Ctrl Pts',(-56.646512615361,-6.10990532476174,
128.293752743129));
#275009=CARTESIAN_POINT('Ctrl Pts',(-56.924960239174,-5.41479857964128,
134.587752127659));
#275010=CARTESIAN_POINT('Ctrl Pts',(-57.2034078629868,0.256243532552689,
137.404999543363));
#275011=CARTESIAN_POINT('Ctrl Pts',(-57.4818554867998,5.69181035652338,
134.156582245398));
#275012=CARTESIAN_POINT('Ctrl Pts',(-57.7603031106126,5.89688152324325,
127.827637036585));
#275013=CARTESIAN_POINT('Ctrl Pts',(-58.0387507344255,0.683006648780185,
124.234155377662));
#275014=CARTESIAN_POINT('Ctrl Pts',(-58.3171983582384,-5.15851796918197,
126.67837136184));
#275015=CARTESIAN_POINT('Ctrl Pts',(-58.5956459820513,-6.25961658107885,
132.91416990625));
#275016=CARTESIAN_POINT('Ctrl Pts',(-58.8740936058642,-1.60843335423465,
137.211156784272));
#275017=CARTESIAN_POINT('Ctrl Pts',(-59.1525412296771,4.52082154881365,
135.620610974484));
#275018=CARTESIAN_POINT('Ctrl Pts',(-59.4309888534899,6.49566230291273,
129.604166373598));
#275019=CARTESIAN_POINT('Ctrl Pts',(-59.7094364773029,2.50130673138007,
124.69064165017));
#275020=CARTESIAN_POINT('Ctrl Pts',(-59.9878841011157,-3.79162753066369,
125.395325986002));
#275021=CARTESIAN_POINT('Ctrl Pts',(-60.2663317249287,-6.60024132333016,
131.070648902209));
#275022=CARTESIAN_POINT('Ctrl Pts',(-60.5447793487415,-3.34355577957023,
136.501265893734));
#275023=CARTESIAN_POINT('Ctrl Pts',(-60.8232269725544,2.98569418383416,
136.696705245755));
#275024=CARTESIAN_POINT('Ctrl Pts',(-61.1016745963673,6.57123705156454,
131.477367741508));
#275025=CARTESIAN_POINT('Ctrl Pts',(-61.3801222201802,4.11813409168408,
125.639569568584));
#275026=CARTESIAN_POINT('Ctrl Pts',(-61.6585698439931,-2.11933291641938,
124.547962055604));
#275027=CARTESIAN_POINT('Ctrl Pts',(-61.937017467806,-6.40923650950231,
129.205679179005));
#275028=CARTESIAN_POINT('Ctrl Pts',(-62.2154650916189,-4.80936485896274,
135.332506444514));
#275029=CARTESIAN_POINT('Ctrl Pts',(-62.4939127154318,1.21007814642843,
137.298188907278));
#275030=CARTESIAN_POINT('Ctrl Pts',(-62.7723603392447,6.1175184508558,133.296360412945));
#275031=CARTESIAN_POINT('Ctrl Pts',(-63.0508079630576,5.40325815633759,
127.004505847616));
#275032=CARTESIAN_POINT('Ctrl Pts',(-63.3292555868704,-0.276332420019459,
124.204532182646));
#275033=CARTESIAN_POINT('Ctrl Pts',(-63.6077032106833,-5.70198700196771,
127.469478429822));
#275034=CARTESIAN_POINT('Ctrl Pts',(-63.8861508344962,-5.8877940866586,
133.799018489484));
#275035=CARTESIAN_POINT('Ctrl Pts',(-64.1645984583092,-0.663006040441876,
137.376614262022));
#275036=CARTESIAN_POINT('Ctrl Pts',(-64.4430460821219,5.17105216729505,
134.914630007745));
#275037=CARTESIAN_POINT('Ctrl Pts',(-64.721493705935,6.25316605323042,128.675508981716));
#275038=CARTESIAN_POINT('Ctrl Pts',(-64.9999413297477,1.58892582039159,
124.392698608848));
#275039=CARTESIAN_POINT('Ctrl Pts',(-65.2783889535607,-4.53545961804555,
126.00189239489));
#275040=CARTESIAN_POINT('Ctrl Pts',(-65.5568365773735,-6.49197923701883,
132.024319863954));
#275041=CARTESIAN_POINT('Ctrl Pts',(-65.8352842011867,-2.48268708798906,
136.92566438391));
#275042=CARTESIAN_POINT('Ctrl Pts',(-66.1137318249993,3.80807320889562,
136.201829784909));
#275043=CARTESIAN_POINT('Ctrl Pts',(-66.3921794488124,6.59940026152389,
130.517984702147));
#275044=CARTESIAN_POINT('Ctrl Pts',(-66.6706270726251,3.3262008724376,125.097305095413));
#275045=CARTESIAN_POINT('Ctrl Pts',(-66.9490746964381,-3.00361462447264,
124.921130708376));
#275046=CARTESIAN_POINT('Ctrl Pts',(-67.227522320251,-6.57325501622426,
130.151357196124));
#275047=CARTESIAN_POINT('Ctrl Pts',(-67.5059699440638,-4.10239516942585,
135.981661927186));
#275048=CARTESIAN_POINT('Ctrl Pts',(-67.7844175678767,2.13836542492937,
137.054279679937));
#275049=CARTESIAN_POINT('Ctrl Pts',(-68.0628651916897,6.41407265873309,
132.383527139888));
#275050=CARTESIAN_POINT('Ctrl Pts',(-68.3413128155024,4.79556046403026,
126.261597712398));
#275051=CARTESIAN_POINT('Ctrl Pts',(-68.6197604393155,-1.22983752096341,
124.314245468451));
#275052=CARTESIAN_POINT('Ctrl Pts',(-68.8982080631282,-6.12507490509475,
128.330991986789));
#275053=CARTESIAN_POINT('Ctrl Pts',(-69.1766556869413,-5.39166767798822,
134.620643446035));
#275054=CARTESIAN_POINT('Ctrl Pts',(-69.455103310754,0.296418747580413,
137.403317421698));
#275055=CARTESIAN_POINT('Ctrl Pts',(-69.733550934567,5.7121108249834,134.121872471326));
#275056=CARTESIAN_POINT('Ctrl Pts',(-70.0119985583799,5.87865210635384,
127.791796196812));
#275057=CARTESIAN_POINT('Ctrl Pts',(-70.2904461821926,0.642999290106501,
124.230119453016));
#275058=CARTESIAN_POINT('Ctrl Pts',(-70.5688938060058,-5.18353846148724,
126.709849169906));
#275059=CARTESIAN_POINT('Ctrl Pts',(-70.8473414298183,-6.24665759690589,
132.95223487919));
#275060=CARTESIAN_POINT('Ctrl Pts',(-71.1257890536316,-1.56940356695681,
137.220829071533));
#275061=CARTESIAN_POINT('Ctrl Pts',(-71.4042366774442,4.55005567139915,
135.593002216589));
#275062=CARTESIAN_POINT('Ctrl Pts',(-71.6826843012574,6.48823603031619,
129.56464767029));
#275063=CARTESIAN_POINT('Ctrl Pts',(-71.9611319250699,2.46404444532374,
124.675528759193));
#275064=CARTESIAN_POINT('Ctrl Pts',(-72.2395795488831,-3.82448360965763,
125.418506915858));
#275065=CARTESIAN_POINT('Ctrl Pts',(-72.518027172696,-6.59849806377525,
131.110821510811));
#275066=CARTESIAN_POINT('Ctrl Pts',(-72.7964747965087,-3.30881515183405,
136.52151351632));
#275067=CARTESIAN_POINT('Ctrl Pts',(-73.0749224203217,3.02150724003593,
136.678421306317));
#275068=CARTESIAN_POINT('Ctrl Pts',(-73.3533700441346,6.57521208714753,
131.437354287172));
#275069=CARTESIAN_POINT('Ctrl Pts',(-73.6318176679474,4.08661824313884,
125.614597009117));
#275070=CARTESIAN_POINT('Ctrl Pts',(-73.9102652917603,-2.15737812391465,
124.56097895318));
#275071=CARTESIAN_POINT('Ctrl Pts',(-74.1887129155733,-6.41884938887091,
129.244723640663));
#275072=CARTESIAN_POINT('Ctrl Pts',(-74.4671605393861,-4.78171164368069,
135.361698517417));
#275073=CARTESIAN_POINT('Ctrl Pts',(-74.745608163199,1.24958550245192,137.290702502541));
#275074=CARTESIAN_POINT('Ctrl Pts',(-75.0240557870119,6.13257461747648,
133.25907517079));
#275075=CARTESIAN_POINT('Ctrl Pts',(-75.3025034108249,5.380027251966,126.971685084098));
#275076=CARTESIAN_POINT('Ctrl Pts',(-75.5809510346376,-0.31650232915867,
124.206336576053));
#275077=CARTESIAN_POINT('Ctrl Pts',(-75.8593986584506,-5.72218173178456,
127.504249830764));
#275078=CARTESIAN_POINT('Ctrl Pts',(-76.1378462822634,-5.86945566701928,
133.83480367917));
#275079=CARTESIAN_POINT('Ctrl Pts',(-76.4162939060764,-0.622986583113102,
137.380528399336));
#275080=CARTESIAN_POINT('Ctrl Pts',(-76.6947415298893,5.19597673608708,
134.88307619171));
#275081=CARTESIAN_POINT('Ctrl Pts',(-76.9731891537022,6.24009127239896,
128.637483627779));
#275082=CARTESIAN_POINT('Ctrl Pts',(-77.2516367775151,1.54986677478153,
124.383145159635));
#275083=CARTESIAN_POINT('Ctrl Pts',(-77.5300844013279,-4.56460957365852,
126.029590003516));
#275084=CARTESIAN_POINT('Ctrl Pts',(-77.8085320251407,-6.48443271748106,
132.063815781194));
#275085=CARTESIAN_POINT('Ctrl Pts',(-78.0869796489538,-2.44537897608793,
136.940663791305));
#275086=CARTESIAN_POINT('Ctrl Pts',(-78.3654272727665,3.84085858092573,
136.178548959823));
#275087=CARTESIAN_POINT('Ctrl Pts',(-78.6438748965796,6.5975347384416,130.477817585504));
#275088=CARTESIAN_POINT('Ctrl Pts',(-78.9223225203923,3.29139877882003,
125.077163305135));
#275089=CARTESIAN_POINT('Ctrl Pts',(-79.2007701442053,-3.03937186476788,
124.939523565746));
#275090=CARTESIAN_POINT('Ctrl Pts',(-79.4792177680182,-6.57710824620412,
130.191382563762));
#275091=CARTESIAN_POINT('Ctrl Pts',(-79.7576653918309,-4.07080345897965,
136.00653844758));
#275092=CARTESIAN_POINT('Ctrl Pts',(-80.036113015644,2.17637083724304,137.041147046131));
#275093=CARTESIAN_POINT('Ctrl Pts',(-80.314560639457,6.42356665566488,132.344453600785));
#275094=CARTESIAN_POINT('Ctrl Pts',(-80.5930082632696,4.76781852620778,
126.232489941585));
#275095=CARTESIAN_POINT('Ctrl Pts',(-80.8714558870828,-1.26932190795047,
124.321852085313));
#275096=CARTESIAN_POINT('Ctrl Pts',(-81.1499035108954,-6.14001751852468,
128.368322882032));
#275097=CARTESIAN_POINT('Ctrl Pts',(-81.4283511347085,-5.36833698610627,
134.653393350648));
#275098=CARTESIAN_POINT('Ctrl Pts',(-81.7067987585213,0.336582978702201,
137.401390773263));
#275099=CARTESIAN_POINT('Ctrl Pts',(-81.9852463823341,5.73219962907597,
134.087039765632));
#275100=CARTESIAN_POINT('Ctrl Pts',(-82.2636940061471,5.86020485384888,
127.756066988721));
#275101=CARTESIAN_POINT('Ctrl Pts',(-82.54214162996,0.602968104857597,124.226327139294));
#275102=CARTESIAN_POINT('Ctrl Pts',(-82.8205892537728,-5.20836687586887,
126.741478701599));
#275103=CARTESIAN_POINT('Ctrl Pts',(-83.0990368775859,-6.23346714053832,
132.990220261861));
#275104=CARTESIAN_POINT('Ctrl Pts',(-83.3774845013985,-1.53031562485268,
137.230263594196));
#275105=CARTESIAN_POINT('Ctrl Pts',(-83.6559321252116,4.57912118999838,
135.56521601382));
#275106=CARTESIAN_POINT('Ctrl Pts',(-83.9343797490243,6.48056933374724,
129.525174905002));
#275107=CARTESIAN_POINT('Ctrl Pts',(-84.2128273728376,2.42669085319518,
124.660642974335));
#275108=CARTESIAN_POINT('Ctrl Pts',(-84.4912749966499,-3.85719797100462,
125.441887420503));
#275109=CARTESIAN_POINT('Ctrl Pts',(-84.7697226204634,-6.59651029444787,
131.150982763393));
#275110=CARTESIAN_POINT('Ctrl Pts',(-85.0481702442759,-3.27395191473627,
136.541549287701));
#275111=CARTESIAN_POINT('Ctrl Pts',(-85.326617868089,3.05720833317481,136.659919701402));
#275112=CARTESIAN_POINT('Ctrl Pts',(-85.6050654919017,6.57894347582879,
131.397317377022));
#275113=CARTESIAN_POINT('Ctrl Pts',(-85.8835131157147,4.05495096345227,
125.58981675825));
#275114=CARTESIAN_POINT('Ctrl Pts',(-86.1619607395276,-2.19534338896908,
124.574227201559));
#275115=CARTESIAN_POINT('Ctrl Pts',(-86.4404083633404,-6.42822441541511,
129.283825895241));
#275116=CARTESIAN_POINT('Ctrl Pts',(-86.7188559871533,-4.75388124031539,
135.390721716488));
#275117=CARTESIAN_POINT('Ctrl Pts',(-86.9973036109663,1.28904655462414,
137.282975744021));
#275118=CARTESIAN_POINT('Ctrl Pts',(-87.2757512347791,6.14740353928957,
133.221698968287));
#275119=CARTESIAN_POINT('Ctrl Pts',(-87.554198858592,5.35659698870609,126.939006341782));
#275120=CARTESIAN_POINT('Ctrl Pts',(-87.8326464824051,-0.356660510187587,
124.208385461669));
#275121=CARTESIAN_POINT('Ctrl Pts',(-88.1110941062178,-5.74216442405318,
127.539143518524));
#275122=CARTESIAN_POINT('Ctrl Pts',(-88.3895417300309,-5.85089975254147,
133.870476574676));
#275123=CARTESIAN_POINT('Ctrl Pts',(-88.6679893538435,-0.582944040787213,
137.384198854334));
#275124=CARTESIAN_POINT('Ctrl Pts',(-88.9464369776566,5.22070876605056,
134.851371237371));
#275125=CARTESIAN_POINT('Ctrl Pts',(-89.2248846014694,6.22678526269035,
128.599538568266));
#275126=CARTESIAN_POINT('Ctrl Pts',(-89.5033322252823,1.51075029828878,
124.373829650922));
#275127=CARTESIAN_POINT('Ctrl Pts',(-89.7817798490951,-4.59359038598471,
126.057464543021));
#275128=CARTESIAN_POINT('Ctrl Pts',(-90.0602274729082,-6.47664591490472,
132.103265028861));
#275129=CARTESIAN_POINT('Ctrl Pts',(-90.338675096721,-2.40798024976945,
136.955435815729));
#275130=CARTESIAN_POINT('Ctrl Pts',(-90.6171227205338,3.87350162852866,
136.155068992212));
#275131=CARTESIAN_POINT('Ctrl Pts',(-90.8955703443469,6.59542474128344,
130.437662569033));
#275132=CARTESIAN_POINT('Ctrl Pts',(-91.1740179681596,3.25647472121003,
125.057233738258));
#275133=CARTESIAN_POINT('Ctrl Pts',(-91.4524655919725,-3.07501648002118,
124.958133746811));
#275134=CARTESIAN_POINT('Ctrl Pts',(-91.7309132157855,-6.58071775901922,
130.231430645527));
#275135=CARTESIAN_POINT('Ctrl Pts',(-92.0093608395982,-4.03906090341396,
136.031222199361));
#275136=CARTESIAN_POINT('Ctrl Pts',(-92.2878084634112,2.21429560333469,
137.027783305909));
#275137=CARTESIAN_POINT('Ctrl Pts',(-92.5662560872241,6.4328226249721,132.305322992969));
#275138=CARTESIAN_POINT('Ctrl Pts',(-92.844703711037,4.73989991511645,126.203551583122));
#275139=CARTESIAN_POINT('Ctrl Pts',(-93.1231513348499,-1.30875925974737,
124.329698913911));
#275140=CARTESIAN_POINT('Ctrl Pts',(-93.4015989586628,-6.15473261134757,
128.40574404555));
#275141=CARTESIAN_POINT('Ctrl Pts',(-93.6800465824757,-5.34480736852315,
134.686000627937));
#275142=CARTESIAN_POINT('Ctrl Pts',(-93.9584942062885,0.37673473761816,
137.399219669449));
#275143=CARTESIAN_POINT('Ctrl Pts',(-94.2369418301014,5.75207602440345,
134.052085419056));
#275144=CARTESIAN_POINT('Ctrl Pts',(-94.5153894539144,5.84154044929785,
127.720450736271));
#275145=CARTESIAN_POINT('Ctrl Pts',(-94.7938370777271,0.56291457640357,
124.222778577022));
#275146=CARTESIAN_POINT('Ctrl Pts',(-95.0722847015402,-5.23300229230026,
126.773258784876));
#275147=CARTESIAN_POINT('Ctrl Pts',(-95.350732325353,-6.22004570075364,
133.028124646699));
#275148=CARTESIAN_POINT('Ctrl Pts',(-95.6291799491659,-1.49117097634027,
137.239460002661));
#275149=CARTESIAN_POINT('Ctrl Pts',(-95.9076275729788,4.60801702757804,
135.537253395802));
#275150=CARTESIAN_POINT('Ctrl Pts',(-96.1860751967916,6.47266249729856,
129.48574954041));
#275151=CARTESIAN_POINT('Ctrl Pts',(-96.4645228206046,2.38924733914408,
124.645984847192));
#275152=CARTESIAN_POINT('Ctrl Pts',(-96.7429704444176,-3.88976940246256,
125.465466633565));
#275153=CARTESIAN_POINT('Ctrl Pts',(-97.0214180682302,-6.59427808900543,
131.191131171763));
#275154=CARTESIAN_POINT('Ctrl Pts',(-97.2998656920433,-3.23896736014657,
136.561372465446));
#275155=CARTESIAN_POINT('Ctrl Pts',(-97.5783133158561,3.09279614033489,
136.641201116591));
#275156=CARTESIAN_POINT('Ctrl Pts',(-97.856760939669,6.58243107933991,131.357258494642));
#275157=CARTESIAN_POINT('Ctrl Pts',(-98.135208563482,4.02313342606635,125.565229734223));
#275158=CARTESIAN_POINT('Ctrl Pts',(-98.4136561872948,-2.2332273047675,
124.587706309824));
#275159=CARTESIAN_POINT('Ctrl Pts',(-98.6921038111079,-6.43736124173946,
129.322984493793));
#275160=CARTESIAN_POINT('Ctrl Pts',(-98.9705514349205,-4.72587468013238,
135.419574966262));
#275161=CARTESIAN_POINT('Ctrl Pts',(-99.2489990587337,1.32845984070286,
137.275008918035));
#275162=CARTESIAN_POINT('Ctrl Pts',(-99.5274466825463,6.16200466680371,
133.184233190419));
#275163=CARTESIAN_POINT('Ctrl Pts',(-99.8058943063594,5.3329682347749,126.906470831589));
#275164=CARTESIAN_POINT('Ctrl Pts',(-100.084341930172,-0.396805475030165,
124.210678763569));
#275165=CARTESIAN_POINT('Ctrl Pts',(-100.362789553985,-5.76193433830736,
127.574158200105));
#275166=CARTESIAN_POINT('Ctrl Pts',(-100.641237177798,-5.83212703082168,
133.906035854126));
#275167=CARTESIAN_POINT('Ctrl Pts',(-100.919684801611,-0.542879897255484,
137.387625491007));
#275168=CARTESIAN_POINT('Ctrl Pts',(-101.198132425424,5.24524734073077,
134.819516319564));
#275169=CARTESIAN_POINT('Ctrl Pts',(-101.476580049237,6.21324851716398,
128.561675209245));
#275170=CARTESIAN_POINT('Ctrl Pts',(-101.75502767305,1.47157784038775,124.3647524279));
#275171=CARTESIAN_POINT('Ctrl Pts',(-102.033475296863,-4.62240098113028,
126.085514980508));
#275172=CARTESIAN_POINT('Ctrl Pts',(-102.311922920676,-6.4686191178319,
132.142666145147));
#275173=CARTESIAN_POINT('Ctrl Pts',(-102.590370544489,-2.3704922948573,
136.969979909799));
#275174=CARTESIAN_POINT('Ctrl Pts',(-102.868818168302,3.90600114210426,
136.131390752135));
#275175=CARTESIAN_POINT('Ctrl Pts',(-103.147265792114,6.59307034823604,
130.397521140692));
#275176=CARTESIAN_POINT('Ctrl Pts',(-103.425713415927,3.22142999373166,
125.037517133282));
#275177=CARTESIAN_POINT('Ctrl Pts',(-103.70416103974,-3.11054714940797,
124.976960561963));
#275178=CARTESIAN_POINT('Ctrl Pts',(-103.982608663553,-6.58408342091771,
130.271499957422));
#275179=CARTESIAN_POINT('Ctrl Pts',(-104.261056287366,-4.00716867896111,
136.055712267864));
#275180=CARTESIAN_POINT('Ctrl Pts',(-104.539503911179,2.25213831788793,
137.014188954471));
#275181=CARTESIAN_POINT('Ctrl Pts',(-104.817951534992,6.44184022367115,
132.266136766442));
#275182=CARTESIAN_POINT('Ctrl Pts',(-105.096399158805,4.71180566529118,
126.17478370933));
#275183=CARTESIAN_POINT('Ctrl Pts',(-105.374846782618,-1.34814811498862,
124.337785663482));
#275184=CARTESIAN_POINT('Ctrl Pts',(-105.65329440643,-6.16921963829011,
128.443254090687));
#275185=CARTESIAN_POINT('Ctrl Pts',(-105.931742030243,-5.32107969713743,
134.718464069627));
#275186=CARTESIAN_POINT('Ctrl Pts',(-106.210189654056,0.416872536489867,
137.396804190707));
#275187=CARTESIAN_POINT('Ctrl Pts',(-106.488637277869,5.77173927443855,
134.017010726842));
#275188=CARTESIAN_POINT('Ctrl Pts',(-106.767084901682,5.82265958431723,
127.684948759235));
#275189=CARTESIAN_POINT('Ctrl Pts',(-107.045532525495,0.52284018894291,
124.219473897692));
#275190=CARTESIAN_POINT('Ctrl Pts',(-107.323980149308,-5.25744379790729,
126.805188242113));
#275191=CARTESIAN_POINT('Ctrl Pts',(-107.602427773121,-6.20639377488812,
133.065946629143));
#275192=CARTESIAN_POINT('Ctrl Pts',(-107.880875396933,-1.45197107193893,
137.248417956151));
#275193=CARTESIAN_POINT('Ctrl Pts',(-108.159323020746,4.63674211339212,
135.509115398702));
#275194=CARTESIAN_POINT('Ctrl Pts',(-108.437770644559,6.46451581396073,
129.446373037437));
#275195=CARTESIAN_POINT('Ctrl Pts',(-108.716218268372,2.35171529065418,
124.631554920928));
#275196=CARTESIAN_POINT('Ctrl Pts',(-108.994665892185,-3.92219669708481,
125.489243681306));
#275197=CARTESIAN_POINT('Ctrl Pts',(-109.273113515998,-6.59180153016358,
131.231265248209));
#275198=CARTESIAN_POINT('Ctrl Pts',(-109.551561139811,-3.20386278442967,
136.580982315001));
#275199=CARTESIAN_POINT('Ctrl Pts',(-109.830008763624,3.12826934279688,
136.622266245509));
#275200=CARTESIAN_POINT('Ctrl Pts',(-110.108456387437,6.5856747684467,131.317179124427));
#275201=CARTESIAN_POINT('Ctrl Pts',(-110.38690401125,3.99116680999183,125.540836848117));
#275202=CARTESIAN_POINT('Ctrl Pts',(-110.665351635062,-2.27102846750687,
124.601415778499));
#275203=CARTESIAN_POINT('Ctrl Pts',(-110.943799258875,-6.44625952927566,
129.362197985281));
#275204=CARTESIAN_POINT('Ctrl Pts',(-111.222246882688,-4.69769300092514,
135.448257197571));
#275205=CARTESIAN_POINT('Ctrl Pts',(-111.500694506501,1.36782390021364,
137.266802319797));
#275206=CARTESIAN_POINT('Ctrl Pts',(-111.779142130314,6.17637745896884,
133.1466792255));
#275207=CARTESIAN_POINT('Ctrl Pts',(-112.057589754127,5.30914186574463,
126.874079759138));
#275208=CARTESIAN_POINT('Ctrl Pts',(-112.33603737794,-0.436935736099303,
124.213216396775));
#275209=CARTESIAN_POINT('Ctrl Pts',(-112.614485001753,-5.78149074196569,
127.609292578024));
#275210=CARTESIAN_POINT('Ctrl Pts',(-112.892932625565,-5.81313819748998,
133.94148019986));
#275211=CARTESIAN_POINT('Ctrl Pts',(-113.171380249379,-0.502795637109545,
137.390808182378));
#275212=CARTESIAN_POINT('Ctrl Pts',(-113.449827873191,5.26959155084185,
134.787512618686));
#275213=CARTESIAN_POINT('Ctrl Pts',(-113.728275497004,6.19948153742887,
128.523894953756));
#275214=CARTESIAN_POINT('Ctrl Pts',(-114.006723120817,1.43235085262869,
124.355913826926));
#275215=CARTESIAN_POINT('Ctrl Pts',(-114.28517074463,-4.65104029150761,
126.113740276555));
#275216=CARTESIAN_POINT('Ctrl Pts',(-114.563618368443,-6.46035262369882,
132.182017670029));
#275217=CARTESIAN_POINT('Ctrl Pts',(-114.842065992256,-2.33291650048142,
136.984295534578));
#275218=CARTESIAN_POINT('Ctrl Pts',(-115.120513616069,3.93835591737112,
136.107515116997));
#275219=CARTESIAN_POINT('Ctrl Pts',(-115.398961239881,6.59047164654225,
130.357394787938));
#275220=CARTESIAN_POINT('Ctrl Pts',(-115.677408863695,3.18626589498021,
125.018014220813));
#275221=CARTESIAN_POINT('Ctrl Pts',(-115.955856487507,-3.14596255632626,
124.996003313566));
#275222=CARTESIAN_POINT('Ctrl Pts',(-116.23430411132,-6.58720510718372,
130.311589014666));
#275223=CARTESIAN_POINT('Ctrl Pts',(-116.512751735133,-3.97512796739924,
136.0800077456));
#275224=CARTESIAN_POINT('Ctrl Pts',(-116.791199358946,2.28989757862811,
137.00036449556));
#275225=CARTESIAN_POINT('Ctrl Pts',(-117.069646982759,6.45061911761184,
132.226896373261));
#275226=CARTESIAN_POINT('Ctrl Pts',(-117.348094606572,4.68353681777373,
126.146187386213));
#275227=CARTESIAN_POINT('Ctrl Pts',(-117.626542230384,-1.38748701410568,
124.346112034364));
#275228=CARTESIAN_POINT('Ctrl Pts',(-117.904989854198,-6.18347806253024,
128.480851627495));
#275229=CARTESIAN_POINT('Ctrl Pts',(-118.18343747801,-5.29715485118671,
134.750782472776));
#275230=CARTESIAN_POINT('Ctrl Pts',(-118.461885101824,0.45699488799644,
137.394144426544));
#275231=CARTESIAN_POINT('Ctrl Pts',(-118.740332725636,5.79118865055225,
133.981816988697));
#275232=CARTESIAN_POINT('Ctrl Pts',(-119.018780349449,5.80356295854445,
127.649562373154));
#275233=CARTESIAN_POINT('Ctrl Pts',(-119.297227973262,0.482746427446748,
124.216413223762));
#275234=CARTESIAN_POINT('Ctrl Pts',(-119.575675597075,-5.28169048700048,
126.837265890154));
#275235=CARTESIAN_POINT('Ctrl Pts',(-119.854123220888,-6.19251186881905,
133.103684807684));
#275236=CARTESIAN_POINT('Ctrl Pts',(-120.132570844701,-1.41271736421608,
137.257137122728));
#275237=CARTESIAN_POINT('Ctrl Pts',(-120.411018468513,4.66529538302207,
135.480803065184));
#275238=CARTESIAN_POINT('Ctrl Pts',(-120.689466092327,6.45612958561205,
129.407046855192));
#275239=CARTESIAN_POINT('Ctrl Pts',(-120.967913716139,2.31409609848935,
124.61735373025));
#275240=CARTESIAN_POINT('Ctrl Pts',(-121.246361339953,-3.95447865326606,
125.51321768266));
#275241=CARTESIAN_POINT('Ctrl Pts',(-121.524808963765,-6.5890807096919,
131.271383505546));
#275242=CARTESIAN_POINT('Ctrl Pts',(-121.803256587578,-3.16863948839908,
136.600378109714));
#275243=CARTESIAN_POINT('Ctrl Pts',(-122.081704211391,3.16362662608795,
136.603115789794));
#275244=CARTESIAN_POINT('Ctrl Pts',(-122.360151835204,6.58867442295306,
131.277080751534));
#275245=CARTESIAN_POINT('Ctrl Pts',(-122.638599459017,3.9590522997634,125.51663900382));
#275246=CARTESIAN_POINT('Ctrl Pts',(-122.91704708283,-2.30874547645122,
124.615355099576));
#275247=CARTESIAN_POINT('Ctrl Pts',(-123.195494706643,-6.45491894829438,
129.401464916637));
#275248=CARTESIAN_POINT('Ctrl Pts',(-123.473942330455,-4.66933724697619,
135.476767347585));
#275249=CARTESIAN_POINT('Ctrl Pts',(-123.752389954268,1.40713727450679,
137.258356253404));
#275250=CARTESIAN_POINT('Ctrl Pts',(-124.030837578081,6.19052138319586,
133.109038465103));
#275251=CARTESIAN_POINT('Ctrl Pts',(-124.309285201894,5.28511876451003,
126.841834324687));
#275252=CARTESIAN_POINT('Ctrl Pts',(-124.587732825707,-0.477049806354697,
124.215998267256));
#275253=CARTESIAN_POINT('Ctrl Pts',(-124.86618044952,-5.80083291035842,
127.644545350364));
#275254=CARTESIAN_POINT('Ctrl Pts',(-125.144628073333,-5.79393395618462,
133.976808298475));
#275255=CARTESIAN_POINT('Ctrl Pts',(-125.423075697146,-0.462692745686338,
137.393746810514));
#275256=CARTESIAN_POINT('Ctrl Pts',(-125.701523320958,5.2937404943001,134.755361320645));
#275257=CARTESIAN_POINT('Ctrl Pts',(-125.979970944772,6.18548483362552,
128.486199201761));
#275258=CARTESIAN_POINT('Ctrl Pts',(-126.258418568584,1.39307078858202,
124.34731417552));
#275259=CARTESIAN_POINT('Ctrl Pts',(-126.536866192397,-4.67950725587653,
126.142139385264));
#275260=CARTESIAN_POINT('Ctrl Pts',(-126.81531381621,-6.45184673882346,
132.221318145323));
#275261=CARTESIAN_POINT('Ctrl Pts',(-127.093761440023,-2.29525425902701,
136.998382159598));
#275262=CARTESIAN_POINT('Ctrl Pts',(-127.372209063836,3.97056475541062,
136.083442971518));
#275263=CARTESIAN_POINT('Ctrl Pts',(-127.650656687649,6.58762873249828,
130.317284997668));
#275264=CARTESIAN_POINT('Ctrl Pts',(-127.929104311462,3.15098372797424,
124.998725723536));
#275265=CARTESIAN_POINT('Ctrl Pts',(-128.207551935275,-3.18126138844507,
125.015261295985));
#275266=CARTESIAN_POINT('Ctrl Pts',(-128.485999559087,-6.59008270214206,
130.351696331743));
#275267=CARTESIAN_POINT('Ctrl Pts',(-128.764447182901,-3.94293995600869,
136.104107732291));
#275268=CARTESIAN_POINT('Ctrl Pts',(-129.042894806713,2.32757198637139,
136.986310441447));
#275269=CARTESIAN_POINT('Ctrl Pts',(-129.321342430526,6.45915898148892,
132.187603267495));
#275270=CARTESIAN_POINT('Ctrl Pts',(-129.599790054339,4.6550944200771,126.117763673416));
#275271=CARTESIAN_POINT('Ctrl Pts',(-129.878237678152,-1.42677449938118,
124.354677718024));
#275272=CARTESIAN_POINT('Ctrl Pts',(-130.156685301965,-6.19750735571679,
128.518535262782));
#275273=CARTESIAN_POINT('Ctrl Pts',(-130.435132925778,-5.27303371721495,
134.782954639811));
#275274=CARTESIAN_POINT('Ctrl Pts',(-130.713580549591,0.497100305389368,
137.391240475519));
#275275=CARTESIAN_POINT('Ctrl Pts',(-130.992028173403,5.81042343204081,
133.946505508738));
#275276=CARTESIAN_POINT('Ctrl Pts',(-131.270475797217,5.78425127961196,
127.614292889281));
#275277=CARTESIAN_POINT('Ctrl Pts',(-131.548923421029,0.442634777604211,
124.213596668645));
#275278=CARTESIAN_POINT('Ctrl Pts',(-131.827371044842,-5.30574146111081,
126.869490540348));
#275279=CARTESIAN_POINT('Ctrl Pts',(-132.105818668655,-6.17840049694519,
133.141337783923));
#275280=CARTESIAN_POINT('Ctrl Pts',(-132.384266292468,-1.37341130773126,
137.265617179298));
#275281=CARTESIAN_POINT('Ctrl Pts',(-132.662713916281,4.69367577841589,
135.45231744437));
#275282=CARTESIAN_POINT('Ctrl Pts',(-132.941161540094,6.44750412300737,
129.367772450924));
#275283=CARTESIAN_POINT('Ctrl Pts',(-133.219609163907,2.27639115664257,
124.603381801387));
#275284=CARTESIAN_POINT('Ctrl Pts',(-133.49805678772,-3.98661407478655,
125.537387749261));
#275285=CARTESIAN_POINT('Ctrl Pts',(-133.776504411532,-6.58611572841139,
131.311484457178));
#275286=CARTESIAN_POINT('Ctrl Pts',(-134.054952035345,-3.13329877726696,
136.619559130867));
#275287=CARTESIAN_POINT('Ctrl Pts',(-134.333399659158,3.19886668003099,
136.583750459073));
#275288=CARTESIAN_POINT('Ctrl Pts',(-134.611847282971,6.59142993170542,
131.236964861823));
#275289=CARTESIAN_POINT('Ctrl Pts',(-134.890294906784,3.92679108539655,
125.492637097993));
#275290=CARTESIAN_POINT('Ctrl Pts',(-135.168742530597,-2.34637693398254,
124.629523756529));
#275291=CARTESIAN_POINT('Ctrl Pts',(-135.44719015441,-6.46333917791768,
129.440783832808));
#275292=CARTESIAN_POINT('Ctrl Pts',(-135.725637778223,-4.64080846901838,
135.505104359849));
#275293=CARTESIAN_POINT('Ctrl Pts',(-136.004085402036,1.44639850681073,
137.24967103183));
#275294=CARTESIAN_POINT('Ctrl Pts',(-136.282533025848,6.20443591537649,
133.07131230402));
#275295=CARTESIAN_POINT('Ctrl Pts',(-136.560980649661,5.26089982125598,
126.809735723105));
#275296=CARTESIAN_POINT('Ctrl Pts',(-136.839428273474,-0.517146199354053,
124.219024271924));
#275297=CARTESIAN_POINT('Ctrl Pts',(-137.117875897287,-5.81996012675442,
127.679915210822));
#275298=CARTESIAN_POINT('Ctrl Pts',(-137.3963235211,-5.77451501852576,134.012018840873));
#275299=CARTESIAN_POINT('Ctrl Pts',(-137.674771144913,-0.422572709013315,
137.396441266521));
#275300=CARTESIAN_POINT('Ctrl Pts',(-137.953218768726,5.31769327625758,
134.723063616821));
#275301=CARTESIAN_POINT('Ctrl Pts',(-138.231666392539,6.17125892440694,
128.448589350091));
#275302=CARTESIAN_POINT('Ctrl Pts',(-138.510114016352,1.35373910378499,
124.338953792345));
#275303=CARTESIAN_POINT('Ctrl Pts',(-138.788561640165,-4.70780081938319,
126.170711254294));
#275304=CARTESIAN_POINT('Ctrl Pts',(-139.067009263977,-6.44310177839452,
132.260566114734));
#275305=CARTESIAN_POINT('Ctrl Pts',(-139.34545688779,-2.25750696608163,
137.012239262869));
#275306=CARTESIAN_POINT('Ctrl Pts',(-139.623904511603,4.00262646271346,
136.059175207703));
#275307=CARTESIAN_POINT('Ctrl Pts',(-139.902352135416,6.5845417114487,130.277193256163));
#275308=CARTESIAN_POINT('Ctrl Pts',(-140.180799759229,3.11558480010749,
124.979652356196));
#275309=CARTESIAN_POINT('Ctrl Pts',(-140.459247383042,-3.21644233775325,
125.034733795609));
#275310=CARTESIAN_POINT('Ctrl Pts',(-140.737695006855,-6.59271609916233,
130.391820422461));
#275311=CARTESIAN_POINT('Ctrl Pts',(-141.016142630668,-3.91060583752806,
136.128011334905));
#275312=CARTESIAN_POINT('Ctrl Pts',(-141.294590254481,2.36516014507876,
136.97202731291));
#275313=CARTESIAN_POINT('Ctrl Pts',(-141.573037878293,6.46745949885459,
132.148258905163));
#275314=CARTESIAN_POINT('Ctrl Pts',(-141.851485502106,4.62647952614482,
126.089513624195));
#275315=CARTESIAN_POINT('Ctrl Pts',(-142.129933125919,-1.4660091150024,
124.363482397054));
#275316=CARTESIAN_POINT('Ctrl Pts',(-142.408380749732,-6.21130699798892,
128.556303600169));
#275317=CARTESIAN_POINT('Ctrl Pts',(-142.686828373545,-5.24871718904012,
134.814979378581));
#275318=CARTESIAN_POINT('Ctrl Pts',(-142.965275997358,0.537187302547703,
137.388092445238));
#275319=CARTESIAN_POINT('Ctrl Pts',(-143.243723621171,5.82944290615228,
133.911077595444));
#275320=CARTESIAN_POINT('Ctrl Pts',(-143.522171244983,5.76472526312116,
127.579141614542));
#275321=CARTESIAN_POINT('Ctrl Pts',(-143.800618868797,0.402506725767204,
124.21102433671));
#275322=CARTESIAN_POINT('Ctrl Pts',(-144.079066492609,-5.32959582902011,
126.901860998601));
#275323=CARTESIAN_POINT('Ctrl Pts',(-144.357514116423,-6.1640601821688,
133.178904162615));
#275324=CARTESIAN_POINT('Ctrl Pts',(-144.635961740235,-1.33405435898536,
137.27385781163));
#275325=CARTESIAN_POINT('Ctrl Pts',(-144.914409364048,4.72188224792766,
135.423659591808));
#275326=CARTESIAN_POINT('Ctrl Pts',(-145.192856987861,6.43863974576633,
129.328551279958));
#275327=CARTESIAN_POINT('Ctrl Pts',(-145.471304611674,2.23860186228433,
124.589639652074));
#275328=CARTESIAN_POINT('Ctrl Pts',(-145.749752235487,-4.01860177085642,
125.56175298548));
#275329=CARTESIAN_POINT('Ctrl Pts',(-146.0281998593,-6.58290669619051,131.35156661715));
#275330=CARTESIAN_POINT('Ctrl Pts',(-146.306647483113,-3.09784196059638,
136.638524667701));
#275331=CARTESIAN_POINT('Ctrl Pts',(-146.585095106925,3.2339881987928,136.564170970937));
#275332=CARTESIAN_POINT('Ctrl Pts',(-146.863542730738,6.59394119259793,
131.196832941802));
#275333=CARTESIAN_POINT('Ctrl Pts',(-147.141990354551,3.89438436234147,
125.468832020033));
#275334=CARTESIAN_POINT('Ctrl Pts',(-147.420437978364,-2.38392144565404,
124.643921224334));
#275335=CARTESIAN_POINT('Ctrl Pts',(-147.698885602177,-6.47151990613084,
129.480153276819));
#275336=CARTESIAN_POINT('Ctrl Pts',(-147.97733322599,-4.61210772419611,
135.533267184325));
#275337=CARTESIAN_POINT('Ctrl Pts',(-148.255780849803,1.48560614228611,
137.240746976909));
#275338=CARTESIAN_POINT('Ctrl Pts',(-148.534228473616,6.21812053990256,
133.033502140209));
#275339=CARTESIAN_POINT('Ctrl Pts',(-148.812676097428,5.23648593342438,
126.777785143819));
#275340=CARTESIAN_POINT('Ctrl Pts',(-149.091123721242,-0.557223429310831,
124.222294298654));
#275341=CARTESIAN_POINT('Ctrl Pts',(-149.369571345054,-5.83887168238761,
127.715400848752));
#275342=CARTESIAN_POINT('Ctrl Pts',(-149.648018968867,-5.75488210408933,
134.047110522317));
#275343=CARTESIAN_POINT('Ctrl Pts',(-149.92646659268,-0.382437013753756,
137.398891450554));
#275344=CARTESIAN_POINT('Ctrl Pts',(-150.204914216493,5.34144900913504,
134.690620704017));
#275345=CARTESIAN_POINT('Ctrl Pts',(-150.483361840306,6.15680433691945,
128.411066792389));
#275346=CARTESIAN_POINT('Ctrl Pts',(-150.761809464119,1.31435725568762,
124.330832987197));
#275347=CARTESIAN_POINT('Ctrl Pts',(-151.040257087932,-4.73591993359918,
126.199454824906));
#275348=CARTESIAN_POINT('Ctrl Pts',(-151.318704711745,-6.43411806645975,
132.299760123916));
#275349=CARTESIAN_POINT('Ctrl Pts',(-151.597152335558,-2.21967602038541,
137.025866330917));
#275350=CARTESIAN_POINT('Ctrl Pts',(-151.87559995937,4.03453985122072,136.034712724799));
#275351=CARTESIAN_POINT('Ctrl Pts',(-152.154047583183,6.58121069778455,
130.237121049039));
#275352=CARTESIAN_POINT('Ctrl Pts',(-152.432495206996,3.08007042310019,
124.960794825562));
#275353=CARTESIAN_POINT('Ctrl Pts',(-152.710942830809,-3.25150410060774,
125.054420090877));
#275354=CARTESIAN_POINT('Ctrl Pts',(-152.989390454622,-6.59510520066311,
130.431959800007));
#275355=CARTESIAN_POINT('Ctrl Pts',(-153.267838078435,-3.87812681010997,
136.151717667683));
#275356=CARTESIAN_POINT('Ctrl Pts',(-153.546285702248,2.40266066190714,
136.957515639215));
#275357=CARTESIAN_POINT('Ctrl Pts',(-153.824733326061,6.47552036213011,
132.108864744186));
#275358=CARTESIAN_POINT('Ctrl Pts',(-154.103180949873,4.59769319631231,
126.061438285362));
#275359=CARTESIAN_POINT('Ctrl Pts',(-154.381628573686,-1.50518940711724,
124.372525745196));
#275360=CARTESIAN_POINT('Ctrl Pts',(-154.660076197499,-6.22487647799626,
128.594155240135));
#275361=CARTESIAN_POINT('Ctrl Pts',(-154.938523821312,-5.22420616771914,
134.846855502398));
#275362=CARTESIAN_POINT('Ctrl Pts',(-155.216971445125,0.577254394032953,
137.384700452354));
#275363=CARTESIAN_POINT('Ctrl Pts',(-155.495419068938,5.84824636811312,
133.87553456161));
#275364=CARTESIAN_POINT('Ctrl Pts',(-155.773866692751,5.74498563261573,
127.544109851479));
#275365=CARTESIAN_POINT('Ctrl Pts',(-156.052314316564,0.362363758895462,
124.208696323275));
#275366=CARTESIAN_POINT('Ctrl Pts',(-156.330761940377,-5.353252706796,126.934376065411));
#275367=CARTESIAN_POINT('Ctrl Pts',(-156.60920956419,-6.14949145587554,
133.216382551721));
#275368=CARTESIAN_POINT('Ctrl Pts',(-156.887657188002,-1.29464797636456,
137.281858714364));
#275369=CARTESIAN_POINT('Ctrl Pts',(-157.166104811815,4.74991374635575,
135.394830569423));
#275370=CARTESIAN_POINT('Ctrl Pts',(-157.444552435628,6.42953678236183,
129.28938479565));
#275371=CARTESIAN_POINT('Ctrl Pts',(-157.723000059441,2.20072961571137,
124.576127791533));
#275372=CARTESIAN_POINT('Ctrl Pts',(-158.001447683254,-4.05044055615985,
125.586312488451));
#275373=CARTESIAN_POINT('Ctrl Pts',(-158.279895307067,-6.57945373194114,
131.391628500203));
#275374=CARTESIAN_POINT('Ctrl Pts',(-158.55834293088,-3.06227035225273,
136.657274017441));
#275375=CARTESIAN_POINT('Ctrl Pts',(-158.836790554693,3.2689898809326,136.54437805091));
#275376=CARTESIAN_POINT('Ctrl Pts',(-159.115238178505,6.59620811257463,
131.156686478575));
#275377=CARTESIAN_POINT('Ctrl Pts',(-159.393685802319,3.86183333144169,
125.445224652049));
#275378=CARTESIAN_POINT('Ctrl Pts',(-159.672133426131,-2.42137762023968,
124.658546969484));
#275379=CARTESIAN_POINT('Ctrl Pts',(-159.950581049944,-6.47946082979399,
129.519571789819));
#275380=CARTESIAN_POINT('Ctrl Pts',(-160.229028673757,-4.58323607602601,
135.56125477743));
#275381=CARTESIAN_POINT('Ctrl Pts',(-160.50747629757,1.52475872807955,137.231584419323));
#275382=CARTESIAN_POINT('Ctrl Pts',(-160.785923921383,6.23157474968534,
132.99560937474));
#275383=CARTESIAN_POINT('Ctrl Pts',(-161.064371545196,5.2118780056808,126.745983770767));
#275384=CARTESIAN_POINT('Ctrl Pts',(-161.342819169009,-0.597280011148509,
124.225808226271));
#275385=CARTESIAN_POINT('Ctrl Pts',(-161.621266792821,-5.85756687648338,
127.751000949223));
#275386=CARTESIAN_POINT('Ctrl Pts',(-161.899714416635,-5.73503594038016,
134.08208204247));
#275387=CARTESIAN_POINT('Ctrl Pts',(-162.178162040447,-0.342287147149402,
137.401097271823));
#275388=CARTESIAN_POINT('Ctrl Pts',(-162.45660966426,5.36500681265522,134.658033784415));
#275389=CARTESIAN_POINT('Ctrl Pts',(-162.735057288073,6.14212160678308,
128.373632919072));
#275390=CARTESIAN_POINT('Ctrl Pts',(-163.013504911886,1.27492670359879,
124.322952060995));
#275391=CARTESIAN_POINT('Ctrl Pts',(-163.291952535699,-4.76386355656041,
126.228369031995));
#275392=CARTESIAN_POINT('Ctrl Pts',(-163.570400159512,-6.42489593591386,
132.338898720518));
#275393=CARTESIAN_POINT('Ctrl Pts',(-163.848847783325,-2.18176282377798,
137.039262858781));
#275394=CARTESIAN_POINT('Ctrl Pts',(-164.127295407138,4.06630373837012,
136.010056429275));
#275395=CARTESIAN_POINT('Ctrl Pts',(-164.405743030951,6.57763581493773,
130.197069861187));
#275396=CARTESIAN_POINT('Ctrl Pts',(-164.684190654763,3.04444191295097,
124.942153830408));
#275397=CARTESIAN_POINT('Ctrl Pts',(-164.962638278576,-3.28644537778151,
125.074319452304));
#275398=CARTESIAN_POINT('Ctrl Pts',(-165.241085902389,-6.59724991811553,
130.472112977002));
#275399=CARTESIAN_POINT('Ctrl Pts',(-165.519533526202,-3.84550407727676,
136.175225852179));
#275400=CARTESIAN_POINT('Ctrl Pts',(-165.797981150015,2.44007214726114,
136.942775958099));
#275401=CARTESIAN_POINT('Ctrl Pts',(-166.076428773828,6.48334127261722,
132.069422244329));
#275402=CARTESIAN_POINT('Ctrl Pts',(-166.354876397641,4.56873649726763,
126.03353869726));
#275403=CARTESIAN_POINT('Ctrl Pts',(-166.633324021454,-1.54431392388507,
124.381807427344));
#275404=CARTESIAN_POINT('Ctrl Pts',(-166.911771645267,-6.23821529291649,
128.632088780075));
#275405=CARTESIAN_POINT('Ctrl Pts',(-167.19021926908,-5.19950156151742,
134.878581830081));
#275406=CARTESIAN_POINT('Ctrl Pts',(-167.468666892892,0.617300095144361,
137.381064622557));
#275407=CARTESIAN_POINT('Ctrl Pts',(-167.747114516705,5.86683312115408,
133.839877724298));
#275408=CARTESIAN_POINT('Ctrl Pts',(-168.025562140518,5.72503311955499,
127.509198898206));
#275409=CARTESIAN_POINT('Ctrl Pts',(-168.304009764331,0.32220736450136,
124.206612714607));
#275410=CARTESIAN_POINT('Ctrl Pts',(-168.582457388144,-5.37671121782417,
126.967034535923));
#275411=CARTESIAN_POINT('Ctrl Pts',(-168.860905011957,-6.1346948579149,
133.253771562468));
#275412=CARTESIAN_POINT('Ctrl Pts',(-169.13935263577,-1.25519362008691,
137.289619591024));
#275413=CARTESIAN_POINT('Ctrl Pts',(-169.417800259582,4.77776923498369,
135.365831445486));
#275414=CARTESIAN_POINT('Ctrl Pts',(-169.696247883396,6.42019557010726,
129.250274449328));
#275415=CARTESIAN_POINT('Ctrl Pts',(-169.974695507208,2.16277582029264,
124.562846720449));
#275416=CARTESIAN_POINT('Ctrl Pts',(-170.253143131021,-4.08212925089891,
125.611065348116));
#275417=CARTESIAN_POINT('Ctrl Pts',(-170.531590754834,-6.57575696361412,
131.431668621828));
#275418=CARTESIAN_POINT('Ctrl Pts',(-170.810038378647,-3.02658527035502,
136.675806485322));
#275419=CARTESIAN_POINT('Ctrl Pts',(-171.08848600246,3.30387042945021,136.524372432426));
#275420=CARTESIAN_POINT('Ctrl Pts',(-171.366933626273,6.59823060763395,
131.116526959784));
#275421=CARTESIAN_POINT('Ctrl Pts',(-171.645381250086,3.82913919888762,
125.421815868818));
#275422=CARTESIAN_POINT('Ctrl Pts',(-171.923828873899,-2.45874406978715,
124.673400450021));
#275423=CARTESIAN_POINT('Ctrl Pts',(-172.202276497711,-6.48716165465291,
129.559037911142));
#275424=CARTESIAN_POINT('Ctrl Pts',(-172.480724121525,-4.55419459435809,
135.589066102071));
#275425=CARTESIAN_POINT('Ctrl Pts',(-172.759171745337,1.5638548133772,137.222183698596));
#275426=CARTESIAN_POINT('Ctrl Pts',(-173.03761936915,6.24479804617409,132.957635411742));
#275427=CARTESIAN_POINT('Ctrl Pts',(-173.316066992963,5.18707694988104,
126.714332782362));
#275428=CARTESIAN_POINT('Ctrl Pts',(-173.594514616776,-0.637314460555731,
124.229565924566));
#275429=CARTESIAN_POINT('Ctrl Pts',(-173.872962240589,-5.8760450162844,
127.786714193059));
#275430=CARTESIAN_POINT('Ctrl Pts',(-174.151409864401,-5.71497726280517,
134.11693210545));
#275431=CARTESIAN_POINT('Ctrl Pts',(-174.429857488215,-0.302124596968923,
137.403058648589));
#275432=CARTESIAN_POINT('Ctrl Pts',(-174.708305112027,5.38836581387496,
134.625304065538));
#275433=CARTESIAN_POINT('Ctrl Pts',(-174.98675273584,6.1272112780718,128.336289117263));
#275434=CARTESIAN_POINT('Ctrl Pts',(-175.265200359654,1.2354489086321,124.315311305772));
#275435=CARTESIAN_POINT('Ctrl Pts',(-175.543647983466,-4.79163065280562,
126.257452804136));
#275436=CARTESIAN_POINT('Ctrl Pts',(-175.822095607279,-6.41543572848632,
132.377980454247));
#275437=CARTESIAN_POINT('Ctrl Pts',(-176.100543231092,-2.14376878114676,
137.05242835005));
#275438=CARTESIAN_POINT('Ctrl Pts',(-176.378990854905,4.09791694713909,
135.985207234778));
#275439=CARTESIAN_POINT('Ctrl Pts',(-176.657438478718,6.57381719537689,
130.157041176716));
#275440=CARTESIAN_POINT('Ctrl Pts',(-176.93588610253,3.00870058988678,124.923730061481));
#275441=CARTESIAN_POINT('Ctrl Pts',(-177.214333726344,-3.32126487451375,
125.094431142515));
#275442=CARTESIAN_POINT('Ctrl Pts',(-177.492781350156,-6.59915017204588,
130.512278465557));
#275443=CARTESIAN_POINT('Ctrl Pts',(-177.771228973969,-3.81273884787578,
136.198535017289));
#275444=CARTESIAN_POINT('Ctrl Pts',(-178.049676597782,2.47739321484437,
136.927808815745));
#275445=CARTESIAN_POINT('Ctrl Pts',(-178.328124221595,6.49092194050925,
132.029932867148));
#275446=CARTESIAN_POINT('Ctrl Pts',(-178.606571845408,4.53961050201187,
126.005815893719));
#275447=CARTESIAN_POINT('Ctrl Pts',(-178.885019469221,-1.58338121553252,
124.391327099562));
#275448=CARTESIAN_POINT('Ctrl Pts',(-179.163467093034,-6.25132294847495,
128.670102814346));
#275449=CARTESIAN_POINT('Ctrl Pts',(-179.441914716847,-5.1746042858732,
134.910157185999));
#275450=CARTESIAN_POINT('Ctrl Pts',(-179.72036234066,0.657322921973241,
137.377185090575));
#275451=CARTESIAN_POINT('Ctrl Pts',(-179.998809964472,5.88520247653593,
133.804108404782));
#275452=CARTESIAN_POINT('Ctrl Pts',(-180.277257588285,5.70486846328706,
127.474410048364));
#275453=CARTESIAN_POINT('Ctrl Pts',(-180.555705212098,0.282039030594865,
124.204773587913));
#275454=CARTESIAN_POINT('Ctrl Pts',(-180.834152835911,-5.39997049284089,
126.999835199963));
#275455=CARTESIAN_POINT('Ctrl Pts',(-181.112600459724,-6.11967093658025,
133.291069809391));
#275456=CARTESIAN_POINT('Ctrl Pts',(-181.391048083537,-1.21569275214809,
137.297140154028));
#275457=CARTESIAN_POINT('Ctrl Pts',(-181.669495707349,4.8054476816156,135.336663294571));
#275458=CARTESIAN_POINT('Ctrl Pts',(-181.947943331163,6.41061645514481,
129.21122169024));
#275459=CARTESIAN_POINT('Ctrl Pts',(-182.226390954976,2.12474188242055,
124.549796930959));
#275460=CARTESIAN_POINT('Ctrl Pts',(-182.504838578788,-4.11366668083735,
125.636010647245));
#275461=CARTESIAN_POINT('Ctrl Pts',(-182.783286202602,-6.5718165281946,
131.471685498325));
#275462=CARTESIAN_POINT('Ctrl Pts',(-183.061733826414,-2.99078803722709,
136.694121384618));
#275463=CARTESIAN_POINT('Ctrl Pts',(-183.340181450227,3.33862855183402,
136.5041548568));
#275464=CARTESIAN_POINT('Ctrl Pts',(-183.61862907404,6.60000860283161,131.076355873553));
#275465=CARTESIAN_POINT('Ctrl Pts',(-183.897076697853,3.79630317617236,
125.398606537762));
#275466=CARTESIAN_POINT('Ctrl Pts',(-184.175524321666,-2.49601940966891,
124.68848111554));
#275467=CARTESIAN_POINT('Ctrl Pts',(-184.453971945479,-6.49462209535141,
129.598550178357));
#275468=CARTESIAN_POINT('Ctrl Pts',(-184.732419569291,-4.52498435533419,
135.616700127691));
#275469=CARTESIAN_POINT('Ctrl Pts',(-185.010867193105,1.60289294946002,
137.212545163075));
#275470=CARTESIAN_POINT('Ctrl Pts',(-185.289314816917,6.25778993937471,
132.919581658354));
#275471=CARTESIAN_POINT('Ctrl Pts',(-185.56776244073,5.16208368503734,126.682833351442));
#275472=CARTESIAN_POINT('Ctrl Pts',(-185.846210064543,-0.677325294041226,
124.233567254297));
#275473=CARTESIAN_POINT('Ctrl Pts',(-186.124657688356,-5.89430541707644,
127.822539256894));
#275474=CARTESIAN_POINT('Ctrl Pts',(-186.403105312169,-5.69470681464601,
134.151659419877));
#275475=CARTESIAN_POINT('Ctrl Pts',(-186.681552935982,-0.261950851450417,
137.404775508174));
#275476=CARTESIAN_POINT('Ctrl Pts',(-186.960000559794,5.41152514721792,
134.592432760195));
#275477=CARTESIAN_POINT('Ctrl Pts',(-187.238448183608,6.11207390329327,
128.299036770752));
#275478=CARTESIAN_POINT('Ctrl Pts',(-187.51689580742,1.19592533365239,124.307911004657));
#275479=CARTESIAN_POINT('Ctrl Pts',(-187.795343431234,-4.81922019341476,
126.286705063617));
#275480=CARTESIAN_POINT('Ctrl Pts',(-188.073791055046,-6.40573779472858,
132.417003876913));
#275481=CARTESIAN_POINT('Ctrl Pts',(-188.352238678859,-2.10569530037498,
137.065362316871));
#275482=CARTESIAN_POINT('Ctrl Pts',(-188.630686302672,4.12937830608858,
135.960166062105));
#275483=CARTESIAN_POINT('Ctrl Pts',(-188.909133926485,6.56975498060235,
130.117036478904));
#275484=CARTESIAN_POINT('Ctrl Pts',(-189.187581550298,2.97284777831579,
124.905524201484));
#275485=CARTESIAN_POINT('Ctrl Pts',(-189.466029174111,-3.35596130055467,
125.114754416262));
#275486=CARTESIAN_POINT('Ctrl Pts',(-189.744476797923,-6.60080589203976,
130.552454777323));
#275487=CARTESIAN_POINT('Ctrl Pts',(-190.022924421737,-3.77983233603489,
136.221644299282));
#275488=CARTESIAN_POINT('Ctrl Pts',(-190.301372045549,2.5146224817104,136.912614766765));
#275489=CARTESIAN_POINT('Ctrl Pts',(-190.579819669362,6.49826208490189,
131.990398075938));
#275490=CARTESIAN_POINT('Ctrl Pts',(-190.858267293175,4.51031628981952,
125.978270902017));
#275491=CARTESIAN_POINT('Ctrl Pts',(-191.136714916988,-1.62238983440674,
124.401084409096));
#275492=CARTESIAN_POINT('Ctrl Pts',(-191.415162540801,-6.26419895896261,
128.708195934325));
#275493=CARTESIAN_POINT('Ctrl Pts',(-191.693610164614,-5.14951526336424,
134.941580400114));
#275494=CARTESIAN_POINT('Ctrl Pts',(-191.972057788427,0.697321391460013,
137.373062000163));
#275495=CARTESIAN_POINT('Ctrl Pts',(-192.25050541224,5.90335375357599,133.768227928508));
#275496=CARTESIAN_POINT('Ctrl Pts',(-192.528953036052,5.68449241101982,
127.439744591064));
#275497=CARTESIAN_POINT('Ctrl Pts',(-192.807400659866,0.241860245628379,
124.203179011344));
#275498=CARTESIAN_POINT('Ctrl Pts',(-193.085848283678,-5.42302966996514,
127.032776842093));
#275499=CARTESIAN_POINT('Ctrl Pts',(-193.364295907491,-6.10442024858855,
133.32827591039));
#275500=CARTESIAN_POINT('Ctrl Pts',(-193.642743531304,-1.17614683626724,
137.304420124699));
#275501=CARTESIAN_POINT('Ctrl Pts',(-193.921191155117,4.83294806061645,
135.307327197512));
#275502=CARTESIAN_POINT('Ctrl Pts',(-194.19963877893,6.40079979243214,129.172227965502));
#275503=CARTESIAN_POINT('Ctrl Pts',(-194.478086402743,2.08662921145659,
124.536978906625));
#275504=CARTESIAN_POINT('Ctrl Pts',(-194.756534026555,-4.14505167734362,
125.661147461485));
#275505=CARTESIAN_POINT('Ctrl Pts',(-195.034981650369,-6.5676325716969,
131.511677646851));
#275506=CARTESIAN_POINT('Ctrl Pts',(-195.313429274181,-2.95487997934909,
136.712218036662));
#275507=CARTESIAN_POINT('Ctrl Pts',(-195.591876897994,3.3732629601091,136.483726073203));
#275508=CARTESIAN_POINT('Ctrl Pts',(-195.870324521807,6.60154203228333,
131.03617470844));
#275509=CARTESIAN_POINT('Ctrl Pts',(-196.14877214562,3.76332648004682,125.375597518911));
#275510=CARTESIAN_POINT('Ctrl Pts',(-196.427219769433,-2.53320225863353,
124.703788407225));
#275511=CARTESIAN_POINT('Ctrl Pts',(-196.705667393246,-6.50184187543975,
129.63810712732));
#275512=CARTESIAN_POINT('Ctrl Pts',(-196.984115017059,-4.49560644135098,
135.644155830301));
#275513=CARTESIAN_POINT('Ctrl Pts',(-197.262562640871,1.64187168975517,
137.202669169918));
#275514=CARTESIAN_POINT('Ctrl Pts',(-197.541010264685,6.27054994786743,
132.881449524674));
#275515=CARTESIAN_POINT('Ctrl Pts',(-197.819457888497,5.13689913728475,
126.651486645231));
#275516=CARTESIAN_POINT('Ctrl Pts',(-198.097905512311,-0.717311028988463,
124.237812067191));
#275517=CARTESIAN_POINT('Ctrl Pts',(-198.376353136123,-5.91234740221361,
127.858474813215));
#275518=CARTESIAN_POINT('Ctrl Pts',(-198.654800759936,-5.67422534703162,
134.186262698915));
#275519=CARTESIAN_POINT('Ctrl Pts',(-198.933248383749,-0.221767399246752,
137.406247786956));
#275520=CARTESIAN_POINT('Ctrl Pts',(-199.211696007562,5.43448395450644,
134.559421086446));
#275521=CARTESIAN_POINT('Ctrl Pts',(-199.490143631375,6.09671004336861,
128.261877259937));
#275522=CARTESIAN_POINT('Ctrl Pts',(-199.768591255188,1.15635744321901,
124.300751431872));
#275523=CARTESIAN_POINT('Ctrl Pts',(-200.047038879001,-4.84663115604747,
126.316124726487));
#275524=CARTESIAN_POINT('Ctrl Pts',(-200.325486502814,-6.39580249400115,
132.455967542492));
#275525=CARTESIAN_POINT('Ctrl Pts',(-200.603934126626,-2.06754379228947,
137.078064279972));
#275526=CARTESIAN_POINT('Ctrl Pts',(-200.882381750439,4.16068664940635,
135.934933839164));
#275527=CARTESIAN_POINT('Ctrl Pts',(-201.160829374253,6.56544932114097,
130.077057250143));
#275528=CARTESIAN_POINT('Ctrl Pts',(-201.439276998065,2.9368848067771,124.887536925038));
#275529=CARTESIAN_POINT('Ctrl Pts',(-201.717724621878,-3.39053337021544,
125.13528852046));
#275530=CARTESIAN_POINT('Ctrl Pts',(-201.996172245691,-6.60221701674386,
130.592640423553));
#275531=CARTESIAN_POINT('Ctrl Pts',(-202.274619869504,-3.74678576111652,
136.244552841837));
#275532=CARTESIAN_POINT('Ctrl Pts',(-202.553067493317,2.55175856831618,
136.897194374181));
#275533=CARTESIAN_POINT('Ctrl Pts',(-202.83151511713,6.50536143380309,131.950819335672));
#275534=CARTESIAN_POINT('Ctrl Pts',(-203.109962740942,4.48085494619837,
125.950904742844));
#275535=CARTESIAN_POINT('Ctrl Pts',(-203.388410364755,-1.66133833502902,
124.411078994385));
#275536=CARTESIAN_POINT('Ctrl Pts',(-203.666857988568,-6.27684284725421,
128.746366728457));
#275537=CARTESIAN_POINT('Ctrl Pts',(-203.945305612381,-5.12423542367342,
134.97285030803));
#275538=CARTESIAN_POINT('Ctrl Pts',(-204.223753236194,0.737294021446153,
137.368695504108));
#275539=CARTESIAN_POINT('Ctrl Pts',(-204.502200860007,5.9212862796718,133.732237625041));
#275540=CARTESIAN_POINT('Ctrl Pts',(-204.78064848382,5.66390571779574,127.405203810847));
#275541=CARTESIAN_POINT('Ctrl Pts',(-205.059096107633,0.20167249844203,
124.201829043986));
#275542=CARTESIAN_POINT('Ctrl Pts',(-205.337543731446,-5.44588789473034,
127.065858241646));
#275543=CARTESIAN_POINT('Ctrl Pts',(-205.615991355258,-6.08894335906002,
133.36538848678));
#275544=CARTESIAN_POINT('Ctrl Pts',(-205.894438979071,-1.13655733783284,
137.311459233274));
#275545=CARTESIAN_POINT('Ctrl Pts',(-206.172886602884,4.86026935294961,
135.277824241371));
#275546=CARTESIAN_POINT('Ctrl Pts',(-206.451334226697,6.39074594572923,
129.133294720038));
#275547=CARTESIAN_POINT('Ctrl Pts',(-206.72978185051,2.04843921967989,124.524393122426));
#275548=CARTESIAN_POINT('Ctrl Pts',(-207.008229474323,-4.17628307743617,
125.686474859378));
#275549=CARTESIAN_POINT('Ctrl Pts',(-207.286677098136,-6.56320524915893,
131.551643585487));
#275550=CARTESIAN_POINT('Ctrl Pts',(-207.565124721949,-2.9188624273063,
136.730095770877));
#275551=CARTESIAN_POINT('Ctrl Pts',(-207.843572345762,3.40777237088467,
136.463086838631));
#275552=CARTESIAN_POINT('Ctrl Pts',(-208.122019969575,6.60283083916734,
130.995984953369));
#275553=CARTESIAN_POINT('Ctrl Pts',(-208.400467593387,3.73021033247459,
125.352789664874));
#275554=CARTESIAN_POINT('Ctrl Pts',(-208.678915217201,-2.57029123885685,
124.719321757855));
#275555=CARTESIAN_POINT('Ctrl Pts',(-208.957362841013,-6.50882072738636,
129.677707292235));
#275556=CARTESIAN_POINT('Ctrl Pts',(-209.235810464827,-4.4660619410178,
135.671432192519));
#275557=CARTESIAN_POINT('Ctrl Pts',(-209.514258088639,1.68078958989102,
137.192556085085));
#275558=CARTESIAN_POINT('Ctrl Pts',(-209.792705712452,6.28307759882623,
132.8432404237));
#275559=CARTESIAN_POINT('Ctrl Pts',(-210.071153336265,5.11152423984512,
126.620293825292));
#275560=CARTESIAN_POINT('Ctrl Pts',(-210.349600960078,-0.757270183712145,
124.242300205957));
#275561=CARTESIAN_POINT('Ctrl Pts',(-210.62804858389,-5.93017030314353,
127.894519530418));
#275562=CARTESIAN_POINT('Ctrl Pts',(-210.906496207704,-5.65353361891029,
134.220740660327));
#275563=CARTESIAN_POINT('Ctrl Pts',(-211.184943831516,-0.181575729370575,
137.407475430382));
#275564=CARTESIAN_POINT('Ctrl Pts',(-211.463391455329,5.4572413849935,134.52627026755));
#275565=CARTESIAN_POINT('Ctrl Pts',(-211.741839079142,6.08112026761121,
128.224811961777));
#275566=CARTESIAN_POINT('Ctrl Pts',(-212.020286702955,1.11674670353533,
124.293832852717));
#275567=CARTESIAN_POINT('Ctrl Pts',(-212.298734326768,-4.87386252498038,
126.345710702588));
#275568=CARTESIAN_POINT('Ctrl Pts',(-212.577181950581,-6.38563019446009,
132.494870007167));
#275569=CARTESIAN_POINT('Ctrl Pts',(-212.855629574394,-2.02931567060901,
137.090533768676));
#275570=CARTESIAN_POINT('Ctrl Pts',(-213.134077198207,4.19184081695006,
135.909511500946));
#275571=CARTESIAN_POINT('Ctrl Pts',(-213.412524822019,6.56090037654053,
130.037104971874));
#275572=CARTESIAN_POINT('Ctrl Pts',(-213.690972445832,2.90081300789186,
124.869768898671));
#275573=CARTESIAN_POINT('Ctrl Pts',(-213.969420069645,-3.42497980241531,
125.156032694208));
#275574=CARTESIAN_POINT('Ctrl Pts',(-214.247867693459,-6.60338349386843,
130.632833915152));
#275575=CARTESIAN_POINT('Ctrl Pts',(-214.52631531727,-3.71360034767391,
136.267259796069));
#275576=CARTESIAN_POINT('Ctrl Pts',(-214.804762941084,2.58880009856982,
136.881548209402));
#275577=CARTESIAN_POINT('Ctrl Pts',(-215.083210564897,6.51221972414398,
131.911198112957));
#275578=CARTESIAN_POINT('Ctrl Pts',(-215.36165818871,4.45122756284936,125.923718430264));
#275579=CARTESIAN_POINT('Ctrl Pts',(-215.640105812523,-1.70022527414834,
124.421310485075));
#275580=CARTESIAN_POINT('Ctrl Pts',(-215.918553436335,-6.28925414482577,
128.784613782311));
#275581=CARTESIAN_POINT('Ctrl Pts',(-216.197001060149,-5.09876570355457,
135.003965751026));
#275582=CARTESIAN_POINT('Ctrl Pts',(-216.475448683961,0.77723933073121,
137.364085764208));
#275583=CARTESIAN_POINT('Ctrl Pts',(-216.753896307774,5.93899939032692,
133.696138828015));
#275584=CARTESIAN_POINT('Ctrl Pts',(-217.032343931587,5.64310914646246,
127.370788987637));
#275585=CARTESIAN_POINT('Ctrl Pts',(-217.3107915554,0.161477278206604,124.200723735865));
#275586=CARTESIAN_POINT('Ctrl Pts',(-217.589239179213,-5.46854432011718,
127.099078172778));
#275587=CARTESIAN_POINT('Ctrl Pts',(-217.867686803026,-6.07324084149572,
133.402406163341));
#275588=CARTESIAN_POINT('Ctrl Pts',(-218.146134426838,-1.09692572384833,
137.318257218917));
#275589=CARTESIAN_POINT('Ctrl Pts',(-218.424582050652,4.88741054621452,
135.24815551939));
#275590=CARTESIAN_POINT('Ctrl Pts',(-218.703029674464,6.38045528758512,
129.094423396537));
#275591=CARTESIAN_POINT('Ctrl Pts',(-218.981477298277,2.01017332223456,
124.512040044732));
#275592=CARTESIAN_POINT('Ctrl Pts',(-219.25992492209,-4.20735972382344,
125.711991902411));
#275593=CARTESIAN_POINT('Ctrl Pts',(-219.538372545903,-6.55853472463687,
131.591581833275));
#275594=CARTESIAN_POINT('Ctrl Pts',(-219.816820169716,-2.8827367157428,
136.747753924796));
#275595=CARTESIAN_POINT('Ctrl Pts',(-220.095267793529,3.44215550540127,
136.442237917877));
#275596=CARTESIAN_POINT('Ctrl Pts',(-220.373715417342,6.60387497572639,
130.955788097589));
#275597=CARTESIAN_POINT('Ctrl Pts',(-220.652163041155,3.69695596058723,
125.330183820803));
#275598=CARTESIAN_POINT('Ctrl Pts',(-220.930610664968,-2.60728497599312,
124.735080591838));
#275599=CARTESIAN_POINT('Ctrl Pts',(-221.20905828878,-6.51555839258729,
129.717349205704));
#275600=CARTESIAN_POINT('Ctrl Pts',(-221.487505912593,-4.43635194911701,
135.698528203611));
#275601=CARTESIAN_POINT('Ctrl Pts',(-221.765953536406,1.71964520775051,
137.182206283321));
#275602=CARTESIAN_POINT('Ctrl Pts',(-222.044401160219,6.295372428034,132.804955771283));
#275603=CARTESIAN_POINT('Ctrl Pts',(-222.322848784032,5.08595993299503,
126.589256047487));
#275604=CARTESIAN_POINT('Ctrl Pts',(-222.601296407845,-0.797201277510683,
124.247031504286));
#275605=CARTESIAN_POINT('Ctrl Pts',(-222.879744031658,-5.94777345943203,
127.930672072853));
#275606=CARTESIAN_POINT('Ctrl Pts',(-223.158191655471,-5.63263239702162,
134.255092026522));
#275607=CARTESIAN_POINT('Ctrl Pts',(-223.436639279283,-0.141377331138957,
137.40845839296));
#275608=CARTESIAN_POINT('Ctrl Pts',(-223.715086903097,5.47979659539413,
134.492981531924));
#275609=CARTESIAN_POINT('Ctrl Pts',(-223.993534526909,6.06530515370598,
128.187842249741));
#275610=CARTESIAN_POINT('Ctrl Pts',(-224.271982150722,1.07709458239186,
124.287155523561));
#275611=CARTESIAN_POINT('Ctrl Pts',(-224.550429774535,-4.90091329114502,
126.375461895601));
#275612=CARTESIAN_POINT('Ctrl Pts',(-224.828877398348,-6.37522127304402,
132.533709829396));
#275613=CARTESIAN_POINT('Ctrl Pts',(-225.107325022161,-1.99101235188949,
137.102770320923));
#275614=CARTESIAN_POINT('Ctrl Pts',(-225.385772645974,4.22283965429091,
135.883899989486));
#275615=CARTESIAN_POINT('Ctrl Pts',(-225.664220269787,6.55610831536389,
129.997181124546));
#275616=CARTESIAN_POINT('Ctrl Pts',(-225.9426678936,2.86463371831382,124.852220780782));
#275617=CARTESIAN_POINT('Ctrl Pts',(-226.221115517412,-3.45929932072906,
125.176986168825));
#275618=CARTESIAN_POINT('Ctrl Pts',(-226.499563141226,-6.60430528018926,
130.673033762736));
#275619=CARTESIAN_POINT('Ctrl Pts',(-226.778010765038,-3.68027732540471,
136.289764320562));
#275620=CARTESIAN_POINT('Ctrl Pts',(-227.056458388851,2.62574569988376,
136.865676852203));
#275621=CARTESIAN_POINT('Ctrl Pts',(-227.334906012664,6.51883670178814,
131.871535875972));
#275622=CARTESIAN_POINT('Ctrl Pts',(-227.613353636477,4.42143523762624,
125.896712971676));
#275623=CARTESIAN_POINT('Ctrl Pts',(-227.89180126029,-1.73904921079426,
124.431778502036));
#275624=CARTESIAN_POINT('Ctrl Pts',(-228.170248884103,-6.30143239177224,
128.822935678624));
#275625=CARTESIAN_POINT('Ctrl Pts',(-228.448696507916,-5.07310704679746,
135.034925576111));
#275626=CARTESIAN_POINT('Ctrl Pts',(-228.727144131728,0.81715583912702,
137.359232951281));
#275627=CARTESIAN_POINT('Ctrl Pts',(-229.005591755541,5.95649242917557,
133.659932875084));
#275628=CARTESIAN_POINT('Ctrl Pts',(-229.284039379354,5.62210346764449,
127.336501396687));
#275629=CARTESIAN_POINT('Ctrl Pts',(-229.562487003167,0.121276074371264,
124.199863127936));
#275630=CARTESIAN_POINT('Ctrl Pts',(-229.84093462698,-5.4909981065832,127.132435404515));
#275631=CARTESIAN_POINT('Ctrl Pts',(-230.119382250793,-6.0573132777586,
133.439327568368));
#275632=CARTESIAN_POINT('Ctrl Pts',(-230.397829874606,-1.05725346287773,
137.324813829725));
#275633=CARTESIAN_POINT('Ctrl Pts',(-230.676277498418,4.91437063468431,
135.218322130955));
#275634=CARTESIAN_POINT('Ctrl Pts',(-230.954725122232,6.3699281993239,129.055615435388));
#275635=CARTESIAN_POINT('Ctrl Pts',(-231.233172746044,1.97183293707754,
124.49992013129));
#275636=CARTESIAN_POINT('Ctrl Pts',(-231.511620369858,-4.23828046494889,
125.73769764504));
#275637=CARTESIAN_POINT('Ctrl Pts',(-231.79006799367,-6.55362117119865,
131.631490910294));
#275638=CARTESIAN_POINT('Ctrl Pts',(-232.068515617483,-2.84650418331021,
136.765191844092));
#275639=CARTESIAN_POINT('Ctrl Pts',(-232.346963241296,3.47641108958031,
136.421180083507));
#275640=CARTESIAN_POINT('Ctrl Pts',(-232.625410865109,6.60467440326965,
130.915585630608));
#275641=CARTESIAN_POINT('Ctrl Pts',(-232.903858488922,3.66356459663667,
125.307780824367));
#275642=CARTESIAN_POINT('Ctrl Pts',(-233.182306112735,-2.64418209922576,
124.751064325225));
#275643=CARTESIAN_POINT('Ctrl Pts',(-233.460753736548,-6.52205462137589,
129.75703139878));
#275644=CARTESIAN_POINT('Ctrl Pts',(-233.73920136036,-4.40647756656326,
135.725442859523));
#275645=CARTESIAN_POINT('Ctrl Pts',(-234.017648984174,1.75843710352442,
137.17162014814));
#275646=CARTESIAN_POINT('Ctrl Pts',(-234.296096607986,6.30743397990132,
132.766596986079));
#275647=CARTESIAN_POINT('Ctrl Pts',(-234.574544231799,5.06020716402928,
126.558374461932));
#275648=CARTESIAN_POINT('Ctrl Pts',(-234.852991855612,-0.837102830722735,
124.252005786856));
#275649=CARTESIAN_POINT('Ctrl Pts',(-235.131439479425,-5.96515621878728,
127.966931100874));
#275650=CARTESIAN_POINT('Ctrl Pts',(-235.409887103238,-5.6115224558684,
134.289315524594));
#275651=CARTESIAN_POINT('Ctrl Pts',(-235.688334727051,-0.101173694118813,
137.409196638266));
#275652=CARTESIAN_POINT('Ctrl Pts',(-235.966782350864,5.50214874991674,
134.459556113093));
#275653=CARTESIAN_POINT('Ctrl Pts',(-236.245229974676,6.04926528768773,
128.150969493757));
#275654=CARTESIAN_POINT('Ctrl Pts',(-236.52367759849,1.03740254911254,124.280719691838));
#275655=CARTESIAN_POINT('Ctrl Pts',(-236.802125222302,-4.92778245216537,
126.405377203086));
#275656=CARTESIAN_POINT('Ctrl Pts',(-237.080572846115,-6.36457611545918,
132.572485569954));
#275657=CARTESIAN_POINT('Ctrl Pts',(-237.359020469928,-1.95263525547508,
137.114773483282));
#275658=CARTESIAN_POINT('Ctrl Pts',(-237.637468093741,4.25368201275546,
135.858100253825));
#275659=CARTESIAN_POINT('Ctrl Pts',(-237.915915717553,6.55107331518259,
129.957287187551));
#275660=CARTESIAN_POINT('Ctrl Pts',(-238.194363341367,2.8283482786799,124.834893221623));
#275661=CARTESIAN_POINT('Ctrl Pts',(-238.47281096518,-3.49349065343433,
125.198148167872));
#275662=CARTESIAN_POINT('Ctrl Pts',(-238.751258588993,-6.60498234154917,
130.713238476685));
#275663=CARTESIAN_POINT('Ctrl Pts',(-239.029706212805,-3.64681792910581,
136.312065581403));
#275664=CARTESIAN_POINT('Ctrl Pts',(-239.308153836619,2.66259400322518,
136.8495808907));
#275665=CARTESIAN_POINT('Ctrl Pts',(-239.586601460431,6.52521212154101,
131.831834094415));
#275666=CARTESIAN_POINT('Ctrl Pts',(-239.865049084244,4.39147907449425,
125.869889367774));
#275667=CARTESIAN_POINT('Ctrl Pts',(-240.143496708057,-1.77780870633274,
124.44248265737));
#275668=CARTESIAN_POINT('Ctrl Pts',(-240.42194433187,-6.31337713682396,
128.861330997368));
#275669=CARTESIAN_POINT('Ctrl Pts',(-240.700391955683,-5.04726040419313,
135.065728636055));
#275670=CARTESIAN_POINT('Ctrl Pts',(-240.978839579496,0.857042067512721,
137.354137245149));
#275671=CARTESIAN_POINT('Ctrl Pts',(-241.257287203309,5.97376474800676,
133.623621107872));
#275672=CARTESIAN_POINT('Ctrl Pts',(-241.535734827122,5.60088945971499,
127.302342308534));
#275673=CARTESIAN_POINT('Ctrl Pts',(-241.814182450934,0.0810703766063902,
124.199247252091));
#275674=CARTESIAN_POINT('Ctrl Pts',(-242.092630074747,-5.51324842209508,
127.165928700792));
#275675=CARTESIAN_POINT('Ctrl Pts',(-242.37107769856,-6.04116125805038,
133.476151333726));
#275676=CARTESIAN_POINT('Ctrl Pts',(-242.649525322373,-1.01754202499167,
137.331128822742));
#275677=CARTESIAN_POINT('Ctrl Pts',(-242.927972946186,4.94114861934255,
135.188325181553));
#275678=CARTESIAN_POINT('Ctrl Pts',(-243.206420569999,6.35916507103108,
129.016872274634));
#275679=CARTESIAN_POINT('Ctrl Pts',(-243.484868193812,1.93341948492588,
124.488033831209));
#275680=CARTESIAN_POINT('Ctrl Pts',(-243.763315817625,-4.26904415503308,
125.763591134728));
#275681=CARTESIAN_POINT('Ctrl Pts',(-244.041763441437,-6.54846477091785,
131.671369337695));
#275682=CARTESIAN_POINT('Ctrl Pts',(-244.320211065251,-2.8101661726183,
136.782408882594));
#275683=CARTESIAN_POINT('Ctrl Pts',(-244.598658689063,3.51053785406796,
136.399914115825));
#275684=CARTESIAN_POINT('Ctrl Pts',(-244.877106312876,6.60522909217403,
130.875379042142));
#275685=CARTESIAN_POINT('Ctrl Pts',(-245.155553936689,3.6300374779527,125.285581505715));
#275686=CARTESIAN_POINT('Ctrl Pts',(-245.434001560502,-2.68098124131831,
124.767272365732));
#275687=CARTESIAN_POINT('Ctrl Pts',(-245.712449184315,-6.528309173032,129.796752401026));
#275688=CARTESIAN_POINT('Ctrl Pts',(-245.990896808128,-4.37643990036281,
135.752175162922));
#275689=CARTESIAN_POINT('Ctrl Pts',(-246.269344431941,1.79716383976481,
137.160798071814));
#275690=CARTESIAN_POINT('Ctrl Pts',(-246.547792055753,6.31926180748295,
132.728165489484));
#275691=CARTESIAN_POINT('Ctrl Pts',(-246.826239679567,5.03426688722615,
126.527650212955));
#275692=CARTESIAN_POINT('Ctrl Pts',(-247.104687303379,-0.876973364781528,
124.257222869343));
#275693=CARTESIAN_POINT('Ctrl Pts',(-247.383134927193,-5.98231793708558,
128.003295270889));
#275694=CARTESIAN_POINT('Ctrl Pts',(-247.661582551005,-5.59020457768662,
134.32340988638));
#275695=CARTESIAN_POINT('Ctrl Pts',(-247.940030174818,-0.0609663080697638,
137.409690138946));
#275696=CARTESIAN_POINT('Ctrl Pts',(-248.218477798631,5.524297020294,134.425995249648));
#275697=CARTESIAN_POINT('Ctrl Pts',(-248.496925422444,6.03300126391963,
128.114195060156));
#275698=CARTESIAN_POINT('Ctrl Pts',(-248.775373046256,0.997672074500306,
124.274525596028));
#275699=CARTESIAN_POINT('Ctrl Pts',(-249.05382067007,-4.95446901239483,
126.435455516518));
#275700=CARTESIAN_POINT('Ctrl Pts',(-249.332268293882,-6.35369511616563,
132.611195791991));
#275701=CARTESIAN_POINT('Ctrl Pts',(-249.610715917695,-1.91418580344349,
137.126542810973));
#275702=CARTESIAN_POINT('Ctrl Pts',(-249.889163541508,4.28436674946925,
135.832113249982));
#275703=CARTESIAN_POINT('Ctrl Pts',(-250.167611165321,6.54579556256923,
129.917424639176));
#275704=CARTESIAN_POINT('Ctrl Pts',(-250.446058789134,2.79195803356287,
124.817786863269));
#275705=CARTESIAN_POINT('Ctrl Pts',(-250.724506412947,-3.52755253356211,
125.219517907192));
#275706=CARTESIAN_POINT('Ctrl Pts',(-251.00295403676,-6.60541465285253,
130.75344656718));
#275707=CARTESIAN_POINT('Ctrl Pts',(-251.281401660573,-3.61322339864049,
136.334162752248));
#275708=CARTESIAN_POINT('Ctrl Pts',(-251.559849284386,2.6993436431913,136.83326092127));
#275709=CARTESIAN_POINT('Ctrl Pts',(-251.838296908198,6.53134574711249,
131.792094239578));
#275710=CARTESIAN_POINT('Ctrl Pts',(-252.116744532012,4.3613601835781,125.843248612281));
#275711=CARTESIAN_POINT('Ctrl Pts',(-252.395192155824,-1.81650232468185,
124.453422554885));
#275712=CARTESIAN_POINT('Ctrl Pts',(-252.673639779637,-6.32508793705065,
128.899798314935));
#275713=CARTESIAN_POINT('Ctrl Pts',(-252.95208740345,-5.02122673409033,
135.096373791053));
#275714=CARTESIAN_POINT('Ctrl Pts',(-253.230535027263,0.896896539007115,
137.348798831588));
#275715=CARTESIAN_POINT('Ctrl Pts',(-253.508982651076,5.99081570467794,
133.587204877683));
#275716=CARTESIAN_POINT('Ctrl Pts',(-253.787430274889,5.57946791275175,
127.26831297809));
#275717=CARTESIAN_POINT('Ctrl Pts',(-254.065877898701,0.0408616672245685,
124.198876151673));
#275718=CARTESIAN_POINT('Ctrl Pts',(-254.344325522515,-5.53529442795169,
127.199556781751));
#275719=CARTESIAN_POINT('Ctrl Pts',(-254.622773146327,-6.0247854077167,
133.512876168065));
#275720=CARTESIAN_POINT('Ctrl Pts',(-254.90122077014,-0.977792831057213,
137.337201825807));
#275721=CARTESIAN_POINT('Ctrl Pts',(-255.179668393953,4.96774341227684,
135.158166043599));
#275722=CARTESIAN_POINT('Ctrl Pts',(-255.458116017766,6.34816648213513,
128.97819485735));
#275723=CARTESIAN_POINT('Ctrl Pts',(-255.736563641579,1.89493404819936,
124.476382515012));
#275724=CARTESIAN_POINT('Ctrl Pts',(-256.015011265392,-4.29964901022966,
125.789669655819));
#275725=CARTESIAN_POINT('Ctrl Pts',(-256.293458889205,-6.54306693065544,
131.711218953762));
#275726=CARTESIAN_POINT('Ctrl Pts',(-256.571906513018,-2.77372173452912,
136.799398141047));
#275727=CARTESIAN_POINT('Ctrl Pts',(-256.85035413683,3.54453019961847,136.378452625405));
#275728=CARTESIAN_POINT('Ctrl Pts',(-257.128801760644,6.60554720661629,
130.835147498674));
#275729=CARTESIAN_POINT('Ctrl Pts',(-257.407249384456,3.5963603924579,125.263628838565));
#275730=CARTESIAN_POINT('Ctrl Pts',(-257.685697008269,-2.71765185753996,
124.783624522784));
#275731=CARTESIAN_POINT('Ctrl Pts',(-257.964144632082,-6.53437691572335,
129.836661023534));
#275732=CARTESIAN_POINT('Ctrl Pts',(-258.242592255895,-4.34613602341029,
135.778440351053));
#275733=CARTESIAN_POINT('Ctrl Pts',(-258.521039879708,1.83562753012831,
137.150276335207));
#275734=CARTESIAN_POINT('Ctrl Pts',(-258.799487503521,6.33122643152078,
132.688650362788));
#275735=CARTESIAN_POINT('Ctrl Pts',(-259.077935127334,5.00743946241547,
126.498999976245));
#275736=CARTESIAN_POINT('Ctrl Pts',(-259.356382751147,-0.915487258132909,
124.259032700089));
#275737=CARTESIAN_POINT('Ctrl Pts',(-259.634830374959,-6.00176822571329,
128.046924274587));
#275738=CARTESIAN_POINT('Ctrl Pts',(-259.86687006147,-5.63687269779404,
133.292521465648));
#275739=CARTESIAN_POINT('Ctrl Pts',(-260.052531023546,-2.79481741349804,
135.900547185714));
#275740=CARTESIAN_POINT('Ctrl Pts',(-260.145376111017,-0.946914048523564,
136.386386345067));
#275741=CARTESIAN_POINT('Ctrl Pts',(-260.191813261187,-0.0157913329746497,
136.389009763222));
#275742=CARTESIAN_POINT('Ctrl Pts',(210.190947297731,3.04870273111253,135.077142573452));
#275743=CARTESIAN_POINT('Ctrl Pts',(210.144529434129,3.76080111712433,134.569051946243));
#275744=CARTESIAN_POINT('Ctrl Pts',(210.051703633225,4.91317831978039,133.192256847685));
#275745=CARTESIAN_POINT('Ctrl Pts',(209.866061957716,5.67455722768035,129.648049455111));
#275746=CARTESIAN_POINT('Ctrl Pts',(209.634022271206,3.10293383059235,125.427666478792));
#275747=CARTESIAN_POINT('Ctrl Pts',(209.355574647392,-2.85596866243967,
125.28812524467));
#275748=CARTESIAN_POINT('Ctrl Pts',(209.07712702358,-6.17973736462657,130.225196103446));
#275749=CARTESIAN_POINT('Ctrl Pts',(208.798679399767,-3.83016968018938,
135.690661498217));
#275750=CARTESIAN_POINT('Ctrl Pts',(208.520231775954,2.04205955310628,136.667868212554));
#275751=CARTESIAN_POINT('Ctrl Pts',(208.241784152142,6.03618933210081,132.255733564264));
#275752=CARTESIAN_POINT('Ctrl Pts',(207.963336528328,4.48417485225333,126.510421532214));
#275753=CARTESIAN_POINT('Ctrl Pts',(207.684888904515,-1.18901089957204,
124.710731370568));
#275754=CARTESIAN_POINT('Ctrl Pts',(207.406441280703,-5.76932406256156,
128.510946815645));
#275755=CARTESIAN_POINT('Ctrl Pts',(207.12799365689,-5.04803188696711,134.418613818075));
#275756=CARTESIAN_POINT('Ctrl Pts',(206.849546033077,0.312219397189005,
137.005003016302));
#275757=CARTESIAN_POINT('Ctrl Pts',(206.571098409264,5.38552219392035,133.893281295751));
#275758=CARTESIAN_POINT('Ctrl Pts',(206.292650785451,5.50981125882569,127.943004805273));
#275759=CARTESIAN_POINT('Ctrl Pts',(206.014203161638,0.570843377758803,
124.622167937696));
#275760=CARTESIAN_POINT('Ctrl Pts',(205.735755537825,-4.89269661278007,
126.982467612715));
#275761=CARTESIAN_POINT('Ctrl Pts',(205.457307914013,-5.86009012142741,
132.854898402769));
#275762=CARTESIAN_POINT('Ctrl Pts',(205.178860290199,-1.44234566848361,
136.842986120511));
#275763=CARTESIAN_POINT('Ctrl Pts',(204.900412666387,4.30084323855829,135.281871486376));
#275764=CARTESIAN_POINT('Ctrl Pts',(204.621965042573,6.09176771588946,129.606143376667));
#275765=CARTESIAN_POINT('Ctrl Pts',(204.343517418761,2.28465505058828,125.031518229909));
#275766=CARTESIAN_POINT('Ctrl Pts',(204.065069794948,-3.62194388278553,
125.761853295313));
#275767=CARTESIAN_POINT('Ctrl Pts',(203.786622171135,-6.20015338889199,
131.126006208945));
#275768=CARTESIAN_POINT('Ctrl Pts',(203.508174547322,-3.08072479357708,
136.194582558939));
#275769=CARTESIAN_POINT('Ctrl Pts',(203.229726923509,2.86973936865286,136.309808260363));
#275770=CARTESIAN_POINT('Ctrl Pts',(202.951279299696,6.1830532544492,131.365796540178));
#275771=CARTESIAN_POINT('Ctrl Pts',(202.672831675884,3.81444325369211,125.905852631576));
#275772=CARTESIAN_POINT('Ctrl Pts',(202.39438405207,-2.05945374882828,124.947398258377));
#275773=CARTESIAN_POINT('Ctrl Pts',(202.115936428258,-6.04081336739099,
129.371206163854));
#275774=CARTESIAN_POINT('Ctrl Pts',(201.837488804444,-4.47096061076856,
135.112012999282));
#275775=CARTESIAN_POINT('Ctrl Pts',(201.559041180632,1.20748652821524,136.894297736177));
#275776=CARTESIAN_POINT('Ctrl Pts',(201.280593556819,5.77631253695961,133.08022777117));
#275777=CARTESIAN_POINT('Ctrl Pts',(201.002145933006,5.03698951269057,127.174747074221));
#275778=CARTESIAN_POINT('Ctrl Pts',(200.723698309193,-0.331080803069094,
124.604703907164));
#275779=CARTESIAN_POINT('Ctrl Pts',(200.44525068538,-5.39490403503349,127.731842386878));
#275780=CARTESIAN_POINT('Ctrl Pts',(200.166803061567,-5.50107401450091,
133.682475019745));
#275781=CARTESIAN_POINT('Ctrl Pts',(199.888355437754,-0.552025717056,136.988261120707));
#275782=CARTESIAN_POINT('Ctrl Pts',(199.609907813942,4.90430724641216,134.611344759621));
#275783=CARTESIAN_POINT('Ctrl Pts',(199.331460190128,5.85382143915379,128.735995953499));
#275784=CARTESIAN_POINT('Ctrl Pts',(199.053012566316,1.42395970438994,124.761373228423));
#275785=CARTESIAN_POINT('Ctrl Pts',(198.774564942502,-4.31445143441004,
126.339960697623));
#275786=CARTESIAN_POINT('Ctrl Pts',(198.49611731869,-6.088092477657,132.02111359519));
#275787=CARTESIAN_POINT('Ctrl Pts',(198.217669694877,-2.26707395378944,
136.584129948007));
#275788=CARTESIAN_POINT('Ctrl Pts',(197.939222071064,3.6372747808909,135.835820643578));
#275789=CARTESIAN_POINT('Ctrl Pts',(197.660774447251,6.19914568268399,130.46384537573));
#275790=CARTESIAN_POINT('Ctrl Pts',(197.382326823438,3.06430454719326,125.404786980035));
#275791=CARTESIAN_POINT('Ctrl Pts',(197.103879199626,-2.88648276756863,
125.307672973393));
#275792=CARTESIAN_POINT('Ctrl Pts',(196.825431575812,-6.1847334314575,130.261746383626));
#275793=CARTESIAN_POINT('Ctrl Pts',(196.546983952,-3.79951621286212,135.71445576667));
#275794=CARTESIAN_POINT('Ctrl Pts',(196.268536328187,2.07727078866752,136.65502757917));
#275795=CARTESIAN_POINT('Ctrl Pts',(195.990088704374,6.04514741573133,132.219122274927));
#275796=CARTESIAN_POINT('Ctrl Pts',(195.711641080561,4.45782888960729,126.483120122517));
#275797=CARTESIAN_POINT('Ctrl Pts',(195.433193456748,-1.22601660901765,
124.718126880723));
#275798=CARTESIAN_POINT('Ctrl Pts',(195.154745832935,-5.78321273819644,
128.54608511404));
#275799=CARTESIAN_POINT('Ctrl Pts',(194.876298209123,-5.02591888662151,
134.449288212205));
#275800=CARTESIAN_POINT('Ctrl Pts',(194.597850585309,0.349948891971121,
137.002980915508));
#275801=CARTESIAN_POINT('Ctrl Pts',(194.319402961497,5.40423073479611,133.860444384439));
#275802=CARTESIAN_POINT('Ctrl Pts',(194.040955337684,5.49228854369214,127.909516169605));
#275803=CARTESIAN_POINT('Ctrl Pts',(193.762507713871,0.533201494146887,
124.618808581434));
#275804=CARTESIAN_POINT('Ctrl Pts',(193.484060090058,-4.91587168017823,
127.012321133451));
#275805=CARTESIAN_POINT('Ctrl Pts',(193.205612466245,-5.84749893410212,
132.890532719942));
#275806=CARTESIAN_POINT('Ctrl Pts',(192.927164842432,-1.40556033379022,
136.851654059523));
#275807=CARTESIAN_POINT('Ctrl Pts',(192.648717218619,4.32801954783523,135.255608152653));
#275808=CARTESIAN_POINT('Ctrl Pts',(192.370269594806,6.08436090050943,129.569083216569));
#275809=CARTESIAN_POINT('Ctrl Pts',(192.091821970994,2.24947182316989,125.017717865345));
#275810=CARTESIAN_POINT('Ctrl Pts',(191.81337434718,-3.65257196685492,125.783994510198));
#275811=CARTESIAN_POINT('Ctrl Pts',(191.534926723368,-6.19808055740059,
131.163742349203));
#275812=CARTESIAN_POINT('Ctrl Pts',(191.256479099555,-3.04785590876364,
136.213235933607));
#275813=CARTESIAN_POINT('Ctrl Pts',(190.978031475742,2.90319942398833,136.292237340818));
#275814=CARTESIAN_POINT('Ctrl Pts',(190.699583851929,6.18635631527163,131.328148137043));
#275815=CARTESIAN_POINT('Ctrl Pts',(190.421136228116,3.7845539731278,125.882723791311));
#275816=CARTESIAN_POINT('Ctrl Pts',(190.142688604304,-2.09506858458051,
124.960043253581));
#275817=CARTESIAN_POINT('Ctrl Pts',(189.86424098049,-6.04942546284962,129.408004862578));
#275818=CARTESIAN_POINT('Ctrl Pts',(189.585793356678,-4.44465587162338,
135.139149194637));
#275819=CARTESIAN_POINT('Ctrl Pts',(189.307345732864,1.24453533211424,136.886834590562));
#275820=CARTESIAN_POINT('Ctrl Pts',(189.028898109051,5.79005936456987,133.045023550676));
#275821=CARTESIAN_POINT('Ctrl Pts',(188.750450485239,5.01480170111087,127.144152737732));
#275822=CARTESIAN_POINT('Ctrl Pts',(188.472002861426,-0.368813738986236,
124.606834155258));
#275823=CARTESIAN_POINT('Ctrl Pts',(188.193555237613,-5.41350737050784,
127.764739625646));
#275824=CARTESIAN_POINT('Ctrl Pts',(187.9151076138,-5.48345219307025,133.715908293866));
#275825=CARTESIAN_POINT('Ctrl Pts',(187.636659989987,-0.51437233173317,
136.991506884579));
#275826=CARTESIAN_POINT('Ctrl Pts',(187.358212366174,4.92739057398128,134.581420314804));
#275827=CARTESIAN_POINT('Ctrl Pts',(187.079764742362,5.84112225861874,128.700400402891));
#275828=CARTESIAN_POINT('Ctrl Pts',(186.801317118548,1.38714794227173,124.752817144095));
#275829=CARTESIAN_POINT('Ctrl Pts',(186.522869494736,-4.34154756707868,
126.366306703083));
#275830=CARTESIAN_POINT('Ctrl Pts',(186.244421870923,-6.08057295867359,
132.058150998494));
#275831=CARTESIAN_POINT('Ctrl Pts',(185.96597424711,-2.23184885375068,136.597823184897));
#275832=CARTESIAN_POINT('Ctrl Pts',(185.687526623297,3.66783531589119,135.813586298303));
#275833=CARTESIAN_POINT('Ctrl Pts',(185.409078999484,6.19695801394562,130.42611572539));
#275834=CARTESIAN_POINT('Ctrl Pts',(185.130631375671,3.03137903541329,125.386233730096));
#275835=CARTESIAN_POINT('Ctrl Pts',(184.852183751858,-2.9198891855651,125.325345654173));
#275836=CARTESIAN_POINT('Ctrl Pts',(184.573736128045,-6.18792188952598,
130.299404664846));
#275837=CARTESIAN_POINT('Ctrl Pts',(184.295288504232,-3.76955667380246,
135.737493527599));
#275838=CARTESIAN_POINT('Ctrl Pts',(184.01684088042,2.11284697206427,136.642274242971));
#275839=CARTESIAN_POINT('Ctrl Pts',(183.738393256607,6.05364746891681,132.182297534532));
#275840=CARTESIAN_POINT('Ctrl Pts',(183.459945632794,4.43144167895468,126.456064115361));
#275841=CARTESIAN_POINT('Ctrl Pts',(183.181498008981,-1.2630425260055,124.725702755623));
#275842=CARTESIAN_POINT('Ctrl Pts',(182.903050385168,-5.79685235262429,
128.581331012064));
#275843=CARTESIAN_POINT('Ctrl Pts',(182.624602761355,-5.00363805916239,
134.479814874928));
#275844=CARTESIAN_POINT('Ctrl Pts',(182.346155137542,0.387675169361259,
137.000735831198));
#275845=CARTESIAN_POINT('Ctrl Pts',(182.06770751373,5.42273385622678,133.827490675898));
#275846=CARTESIAN_POINT('Ctrl Pts',(181.789259889916,5.47456504449634,127.876136685104));
#275847=CARTESIAN_POINT('Ctrl Pts',(181.510812266103,0.495538404244469,
124.615677436551));
#275848=CARTESIAN_POINT('Ctrl Pts',(181.232364642291,-4.93886382111119,
127.042315697369));
#275849=CARTESIAN_POINT('Ctrl Pts',(180.953917018477,-5.83469147177671,
132.926089453735));
#275850=CARTESIAN_POINT('Ctrl Pts',(180.675469394665,-1.36872270040423,
136.860098061879));
#275851=CARTESIAN_POINT('Ctrl Pts',(180.397021770852,4.35503536681857,135.229179797918));
#275852=CARTESIAN_POINT('Ctrl Pts',(180.118574147039,6.07672868724052,129.532068871648));
#275853=CARTESIAN_POINT('Ctrl Pts',(179.840126523226,2.21420520878857,125.004131904969));
#275854=CARTESIAN_POINT('Ctrl Pts',(179.561678899413,-3.68306468660213,
125.80632176824));
#275855=CARTESIAN_POINT('Ctrl Pts',(179.2832312756,-6.19577806271818,131.20146516627));
#275856=CARTESIAN_POINT('Ctrl Pts',(179.004783651788,-3.01487407978163,
136.231688883676));
#275857=CARTESIAN_POINT('Ctrl Pts',(178.726336027974,2.93655189768736,136.274463064253));
#275858=CARTESIAN_POINT('Ctrl Pts',(178.447888404162,6.18943013971724,131.290480325685));
#275859=CARTESIAN_POINT('Ctrl Pts',(178.169440780348,3.75452445381909,125.859777323623));
#275860=CARTESIAN_POINT('Ctrl Pts',(177.890993156536,-2.13060578642238,
124.972904812372));
#275861=CARTESIAN_POINT('Ctrl Pts',(177.612545532723,-6.05781339482078,
129.44485530364));
#275862=CARTESIAN_POINT('Ctrl Pts',(177.33409790891,-4.41818643401566,135.166124762878));
#275863=CARTESIAN_POINT('Ctrl Pts',(177.055650285097,1.28153801924328,136.879146056599));
#275864=CARTESIAN_POINT('Ctrl Pts',(176.777202661284,5.80359163943039,133.009736301615));
#275865=CARTESIAN_POINT('Ctrl Pts',(176.498755037472,4.99242806419446,127.113694031581));
#275866=CARTESIAN_POINT('Ctrl Pts',(176.220307413658,-0.406533008366379,
124.60919405498));
#275867=CARTESIAN_POINT('Ctrl Pts',(175.941859789846,-5.43191010648008,
127.797749498684));
#275868=CARTESIAN_POINT('Ctrl Pts',(175.663412166033,-5.46562718029972,
133.749233679521));
#275869=CARTESIAN_POINT('Ctrl Pts',(175.38496454222,-0.476699886155768,
136.994523381468));
#275870=CARTESIAN_POINT('Ctrl Pts',(175.106516918407,4.95029131528126,134.551355909651));
#275871=CARTESIAN_POINT('Ctrl Pts',(174.828069294595,5.82820663315002,128.664882815304));
#275872=CARTESIAN_POINT('Ctrl Pts',(174.549621670781,1.35028477887665,124.744485301934));
#275873=CARTESIAN_POINT('Ctrl Pts',(174.271174046969,-4.36848282210566,
126.392817162263));
#275874=CARTESIAN_POINT('Ctrl Pts',(173.992726423155,-6.07282812182305,
132.095141942134));
#275875=CARTESIAN_POINT('Ctrl Pts',(173.714278799343,-2.19654105173196,
136.611301742902));
#275876=CARTESIAN_POINT('Ctrl Pts',(173.435831175529,3.69825993790488,135.791166334329));
#275877=CARTESIAN_POINT('Ctrl Pts',(173.157383551717,6.19454071464915,130.388400091055));
#275878=CARTESIAN_POINT('Ctrl Pts',(172.878935927904,2.99834119476844,125.367881250842));
#275879=CARTESIAN_POINT('Ctrl Pts',(172.600488304091,-2.95318740599396,
125.343221361866));
#275880=CARTESIAN_POINT('Ctrl Pts',(172.322040680278,-6.1908810518732,130.337081657394));
#275881=CARTESIAN_POINT('Ctrl Pts',(172.043593056465,-3.7394574524341,135.760348489473));
#275882=CARTESIAN_POINT('Ctrl Pts',(171.765145432652,2.14834486313941,136.629304580736));
#275883=CARTESIAN_POINT('Ctrl Pts',(171.486697808839,6.06192320196904,132.145421734178));
#275884=CARTESIAN_POINT('Ctrl Pts',(171.208250185027,4.40489025960108,126.42916923593));
#275885=CARTESIAN_POINT('Ctrl Pts',(170.929802561213,-1.30002164048796,
124.733503877423));
#275886=CARTESIAN_POINT('Ctrl Pts',(170.651354937401,-5.81027716255637,
128.616659285268));
#275887=CARTESIAN_POINT('Ctrl Pts',(170.372907313588,-4.98117182005496,
134.510205342342));
#275888=CARTESIAN_POINT('Ctrl Pts',(170.094459689775,0.42538708130529,136.998261137926));
#275889=CARTESIAN_POINT('Ctrl Pts',(169.816012065962,5.44103603626017,133.794424944161));
#275890=CARTESIAN_POINT('Ctrl Pts',(169.537564442149,5.45663868327959,127.842865707018));
#275891=CARTESIAN_POINT('Ctrl Pts',(169.259116818336,0.457856951984399,
124.612775615598));
#275892=CARTESIAN_POINT('Ctrl Pts',(168.980669194523,-4.9616729506289,127.072449665244));
#275893=CARTESIAN_POINT('Ctrl Pts',(168.702221570711,-5.82166780281318,
132.961567566087));
#275894=CARTESIAN_POINT('Ctrl Pts',(168.423773946897,-1.33183434849535,
136.868317666657));
#275895=CARTESIAN_POINT('Ctrl Pts',(168.145326323085,4.38188980836473,135.202587479883));
#275896=CARTESIAN_POINT('Ctrl Pts',(167.866878699272,6.06887129855542,129.495101671966));
#275897=CARTESIAN_POINT('Ctrl Pts',(167.588431075459,2.17885654621902,124.9907608742));
#275898=CARTESIAN_POINT('Ctrl Pts',(167.309983451646,-3.71342092903282,
125.82883423045));
#275899=CARTESIAN_POINT('Ctrl Pts',(167.031535827833,-6.19324598120115,
131.239173268482));
#275900=CARTESIAN_POINT('Ctrl Pts',(166.75308820402,-2.98178053353198,136.249940722101));
#275901=CARTESIAN_POINT('Ctrl Pts',(166.474640580207,2.96979555637586,136.25648609103));
#275902=CARTESIAN_POINT('Ctrl Pts',(166.196192956395,6.19227461255283,131.252794500981));
#275903=CARTESIAN_POINT('Ctrl Pts',(165.917745332582,3.7243558092261,125.837014079288));
#275904=CARTESIAN_POINT('Ctrl Pts',(165.639297708769,-2.16606403788322,
124.985982457902));
#275905=CARTESIAN_POINT('Ctrl Pts',(165.360850084956,-6.06597685228888,
129.481756121673));
#275906=CARTESIAN_POINT('Ctrl Pts',(165.082402461143,-4.39155327888481,
135.192938704347));
#275907=CARTESIAN_POINT('Ctrl Pts',(164.80395483733,1.31849321850979,136.871232419228));
#275908=CARTESIAN_POINT('Ctrl Pts',(164.525507213517,5.81690886006848,132.974367331546));
#275909=CARTESIAN_POINT('Ctrl Pts',(164.247059589704,4.96986943102014,127.083372084437));
#275910=CARTESIAN_POINT('Ctrl Pts',(163.968611965891,-0.444237213516358,
124.611783518878));
#275911=CARTESIAN_POINT('Ctrl Pts',(163.690164342078,-5.45011156102575,
127.830870782803));
#275912=CARTESIAN_POINT('Ctrl Pts',(163.411716718265,-5.44759963670407,
133.782449941821));
#275913=CARTESIAN_POINT('Ctrl Pts',(163.133269094453,-0.439009776288703,
136.9973104996));
#275914=CARTESIAN_POINT('Ctrl Pts',(162.85482147064,4.97300862171615,134.52115265821));
#275915=CARTESIAN_POINT('Ctrl Pts',(162.576373846827,5.81507504134112,128.629444506854));
#275916=CARTESIAN_POINT('Ctrl Pts',(162.297926223014,1.31337158018249,124.736378010682));
#275917=CARTESIAN_POINT('Ctrl Pts',(162.019478599201,-4.39525620139515,
126.419491092807));
#275918=CARTESIAN_POINT('Ctrl Pts',(161.741030975388,-6.06485825409316,
132.132085055398));
#275919=CARTESIAN_POINT('Ctrl Pts',(161.462583351575,-2.16115185607673,
136.624565122567));
#275920=CARTESIAN_POINT('Ctrl Pts',(161.184135727762,3.72854751953661,135.768561582436));
#275921=CARTESIAN_POINT('Ctrl Pts',(160.905688103949,6.19189387436843,130.350699870288));
#275922=CARTESIAN_POINT('Ctrl Pts',(160.627240480137,2.96519224948793,125.349730222329));
#275923=CARTESIAN_POINT('Ctrl Pts',(160.348792856324,-2.9863761949775,125.361299434083));
#275924=CARTESIAN_POINT('Ctrl Pts',(160.070345232511,-6.19361080884636,
130.374775965136));
#275925=CARTESIAN_POINT('Ctrl Pts',(159.791897608698,-3.70921966409463,
135.783019805394));
#275926=CARTESIAN_POINT('Ctrl Pts',(159.513449984885,2.18376314650564,136.616119073061));
#275927=CARTESIAN_POINT('Ctrl Pts',(159.235002361072,6.06997430822783,132.108496240312));
#275928=CARTESIAN_POINT('Ctrl Pts',(158.956554737259,4.37817561541891,126.402436480826));
#275929=CARTESIAN_POINT('Ctrl Pts',(158.678107113446,-1.3369525821905,124.741529957054));
#275930=CARTESIAN_POINT('Ctrl Pts',(158.399659489633,-5.82348667053154,
128.652068624549));
#275931=CARTESIAN_POINT('Ctrl Pts',(158.121211865821,-4.95852100179383,
134.540458488317));
#275932=CARTESIAN_POINT('Ctrl Pts',(157.842764242008,0.463083230374652,
136.995556927392));
#275933=CARTESIAN_POINT('Ctrl Pts',(157.564316618195,5.45913659670229,133.761248414491));
#275934=CARTESIAN_POINT('Ctrl Pts',(157.285868994382,5.43851012430973,127.809704468215));
#275935=CARTESIAN_POINT('Ctrl Pts',(157.007421370569,0.420158533666468,
124.610103226106));
#275936=CARTESIAN_POINT('Ctrl Pts',(156.728973746756,-4.98429822353081,
127.102721920452));
#275937=CARTESIAN_POINT('Ctrl Pts',(156.450526122943,-5.80842840980828,
132.996965742341));
#275938=CARTESIAN_POINT('Ctrl Pts',(156.172078499131,-1.2948966449748,136.876312569277));
#275939=CARTESIAN_POINT('Ctrl Pts',(155.893630875317,4.40858187737264,135.175832183934));
#275940=CARTESIAN_POINT('Ctrl Pts',(155.615183251505,6.06078902561252,129.458182987356));
#275941=CARTESIAN_POINT('Ctrl Pts',(155.336735627692,2.14342714531882,124.977605268507));
#275942=CARTESIAN_POINT('Ctrl Pts',(155.058288003879,-3.74363956928552,
125.85153106262));
#275943=CARTESIAN_POINT('Ctrl Pts',(154.779840380066,-6.19048440667673,
131.276865258552));
#275944=CARTESIAN_POINT('Ctrl Pts',(154.501392756253,-2.94857649630798,
136.267990772552));
#275945=CARTESIAN_POINT('Ctrl Pts',(154.22294513244,3.00292916819795,136.238307087292));
#275946=CARTESIAN_POINT('Ctrl Pts',(153.944497508627,6.19488962837548,131.215092059396));
#275947=CARTESIAN_POINT('Ctrl Pts',(153.666049884815,3.69404915725887,125.814434901805));
#275948=CARTESIAN_POINT('Ctrl Pts',(153.387602261001,-2.20144202504465,
124.999275705575));
#275949=CARTESIAN_POINT('Ctrl Pts',(153.109154637189,-6.07391553275397,
129.518705949301));
#275950=CARTESIAN_POINT('Ctrl Pts',(152.830707013376,-4.36475739313218,
135.219590025439));
#275951=CARTESIAN_POINT('Ctrl Pts',(152.552259389563,1.3553995605252,136.863093971691));
#275952=CARTESIAN_POINT('Ctrl Pts',(152.27381176575,5.83001053300956,132.93891795108));
#275953=CARTESIAN_POINT('Ctrl Pts',(151.995364141937,4.94712663750637,127.053188019893));
#275954=CARTESIAN_POINT('Ctrl Pts',(151.716916518124,-0.481924957293099,
124.614602450997));
#275955=CARTESIAN_POINT('Ctrl Pts',(151.438468894311,-5.46811105968323,
127.864102250682));
#275956=CARTESIAN_POINT('Ctrl Pts',(151.160021270498,-5.4293702303005,133.815555849925));
#275957=CARTESIAN_POINT('Ctrl Pts',(150.881573646685,-0.40130339875292,
136.999868135696));
#275958=CARTESIAN_POINT('Ctrl Pts',(150.603126022873,4.99554165148768,134.490811679673));
#275959=CARTESIAN_POINT('Ctrl Pts',(150.324678399059,5.80172796978809,128.59408679072));
#275960=CARTESIAN_POINT('Ctrl Pts',(150.046230775247,1.27640971402146,124.728495570759));
#275961=CARTESIAN_POINT('Ctrl Pts',(149.767783151434,-4.42186671284978,
126.446327506304));
#275962=CARTESIAN_POINT('Ctrl Pts',(149.489335527621,-6.05666365081033,
132.168978969345));
#275963=CARTESIAN_POINT('Ctrl Pts',(149.210887903808,-2.12568257814469,
136.637612832414));
#275964=CARTESIAN_POINT('Ctrl Pts',(148.932440279995,3.75869693846883,135.74577288025));
#275965=CARTESIAN_POINT('Ctrl Pts',(148.653992656183,6.18901759118317,130.313016460088));
#275966=CARTESIAN_POINT('Ctrl Pts',(148.375545032369,2.93193342791814,125.331781317152));
#275967=CARTESIAN_POINT('Ctrl Pts',(148.097097408557,-3.01945432269288,
125.379579200934));
#275968=CARTESIAN_POINT('Ctrl Pts',(147.818649784743,-6.19611105929333,
130.412486191295));
#275969=CARTESIAN_POINT('Ctrl Pts',(147.540202160931,-3.67884442925635,
135.805506635269));
#275970=CARTESIAN_POINT('Ctrl Pts',(147.261754537118,2.21910050972548,136.602718208539));
#275971=CARTESIAN_POINT('Ctrl Pts',(146.983306913305,6.07780048935632,132.071522421221));
#275972=CARTESIAN_POINT('Ctrl Pts',(146.704859289492,4.35129873632927,126.375866840638));
#275973=CARTESIAN_POINT('Ctrl Pts',(146.426411665679,-1.37383398262348,
124.749780697104));
#275974=CARTESIAN_POINT('Ctrl Pts',(146.147964041867,-5.83648038706648,
128.687557717801));
#275975=CARTESIAN_POINT('Ctrl Pts',(145.869516418053,-4.93568644371351,
134.570573191811));
#275976=CARTESIAN_POINT('Ctrl Pts',(145.591068794241,0.500762219724632,
136.992623299802));
#275977=CARTESIAN_POINT('Ctrl Pts',(145.312621170428,5.47703486683029,133.727962316256));
#275978=CARTESIAN_POINT('Ctrl Pts',(145.034173546615,5.42018003934715,127.776654197497));
#275979=CARTESIAN_POINT('Ctrl Pts',(144.755725922802,0.382444546219556,
124.607660367099));
#275980=CARTESIAN_POINT('Ctrl Pts',(144.477278298989,-5.00673880142907,
127.133131341243));
#275981=CARTESIAN_POINT('Ctrl Pts',(144.198830675176,-5.79497378335261,
133.032282670807));
#275982=CARTESIAN_POINT('Ctrl Pts',(143.920383051363,-1.25791095858285,
136.884082473484));
#275983=CARTESIAN_POINT('Ctrl Pts',(143.64193542755,4.43511058475782,135.148914901497));
#275984=CARTESIAN_POINT('Ctrl Pts',(143.363487803737,6.05248216790344,129.421314185853));
#275985=CARTESIAN_POINT('Ctrl Pts',(143.085040179924,2.10791831893749,124.964665575378));
#275986=CARTESIAN_POINT('Ctrl Pts',(142.806592556112,-3.77371948759721,
125.87441142371));
#275987=CARTESIAN_POINT('Ctrl Pts',(142.528144932299,-6.18749344147606,
131.314539739788));
#275988=CARTESIAN_POINT('Ctrl Pts',(142.249697308486,-2.91526319849757,
136.285838366179));
#275989=CARTESIAN_POINT('Ctrl Pts',(141.971249684673,3.03595150537554,136.219926726669));
#275990=CARTESIAN_POINT('Ctrl Pts',(141.69280206086,6.19727509028471,131.177374398005));
#275991=CARTESIAN_POINT('Ctrl Pts',(141.414354437047,3.6636056209416,125.792040627854));
#275992=CARTESIAN_POINT('Ctrl Pts',(141.135906813234,-2.23673843696229,
125.012784062803));
#275993=CARTESIAN_POINT('Ctrl Pts',(140.857459189421,-6.0816291420453,129.555703417335));
#275994=CARTESIAN_POINT('Ctrl Pts',(140.579011565609,-4.33779976968917,
135.246077738584));
#275995=CARTESIAN_POINT('Ctrl Pts',(140.300563941795,1.39225567771152,136.854731015561));
#275996=CARTESIAN_POINT('Ctrl Pts',(140.022116317983,5.84289617276637,132.903389473806));
#275997=CARTESIAN_POINT('Ctrl Pts',(139.74366869417,4.92420052639575,127.023142956427));
#275998=CARTESIAN_POINT('Ctrl Pts',(139.465221070357,-0.519594843163371,
124.617650746882));
#275999=CARTESIAN_POINT('Ctrl Pts',(139.186773446544,-5.48590793547459,
127.897442670915));
#276000=CARTESIAN_POINT('Ctrl Pts',(138.908325822731,-5.41093963658633,
133.848550177083));
#276001=CARTESIAN_POINT('Ctrl Pts',(138.629878198918,-0.363582150772119,
137.002196194983));
#276002=CARTESIAN_POINT('Ctrl Pts',(138.351430575105,5.0178895696262,134.460334098336));
#276003=CARTESIAN_POINT('Ctrl Pts',(138.072982951292,5.78816591307159,128.558810977095));
#276004=CARTESIAN_POINT('Ctrl Pts',(137.79453532748,1.23940055002892,124.720838274248));
#276005=CARTESIAN_POINT('Ctrl Pts',(137.516087703667,-4.44831337040726,
126.473325408321));
#276006=CARTESIAN_POINT('Ctrl Pts',(137.237640079854,-6.0482446156285,132.205822316857));
#276007=CARTESIAN_POINT('Ctrl Pts',(136.959192456041,-2.09013453226308,
136.650444388955));
#276008=CARTESIAN_POINT('Ctrl Pts',(136.680744832228,3.78870707750376,135.722801072215));
#276009=CARTESIAN_POINT('Ctrl Pts',(136.402297208415,6.18591197167502,130.275351256826));
#276010=CARTESIAN_POINT('Ctrl Pts',(136.123849584602,2.89856596247695,125.314035200413));
#276011=CARTESIAN_POINT('Ctrl Pts',(135.845401960789,-3.05242056341787,
125.398059985055));
#276012=CARTESIAN_POINT('Ctrl Pts',(135.566954336976,-6.19838171056633,
130.450210938505));
#276013=CARTESIAN_POINT('Ctrl Pts',(135.288506713164,-3.64833287348497,
135.827808145838));
#276014=CARTESIAN_POINT('Ctrl Pts',(135.01005908935,2.25435564335981,136.589102483743));
#276015=CARTESIAN_POINT('Ctrl Pts',(134.731611465538,6.08540145535266,132.034501646982));
#276016=CARTESIAN_POINT('Ctrl Pts',(134.453163841725,4.32426061826468,126.349461299917));
#276017=CARTESIAN_POINT('Ctrl Pts',(134.174716217912,-1.41066447513297,
124.75825579184));
#276018=CARTESIAN_POINT('Ctrl Pts',(133.896268594099,-5.84925783067434,
128.723125249964));
#276019=CARTESIAN_POINT('Ctrl Pts',(133.617820970286,-4.91266899195694,
134.600548336913));
#276020=CARTESIAN_POINT('Ctrl Pts',(133.339373346473,0.538422653146471,
136.989460363863));
#276021=CARTESIAN_POINT('Ctrl Pts',(133.06092572266,5.49473018341705,133.694567882885));
#276022=CARTESIAN_POINT('Ctrl Pts',(132.782478098847,5.40164910761999,127.743716119554));
#276023=CARTESIAN_POINT('Ctrl Pts',(132.504030475035,0.344716387149417,
124.605447129098));
#276024=CARTESIAN_POINT('Ctrl Pts',(132.225582851222,-5.02899385277987,
127.163676800786));
#276025=CARTESIAN_POINT('Ctrl Pts',(131.947135227409,-5.78130442201224,
133.067517042801));
#276026=CARTESIAN_POINT('Ctrl Pts',(131.668687603596,-1.22087865983776,
136.891627091362));
#276027=CARTESIAN_POINT('Ctrl Pts',(131.390239979783,4.46147494748924,135.121836630005));
#276028=CARTESIAN_POINT('Ctrl Pts',(131.11179235597,6.04395103324181,129.384496633644));
#276029=CARTESIAN_POINT('Ctrl Pts',(130.833344732157,2.07233138286776,124.951942274296));
#276030=CARTESIAN_POINT('Ctrl Pts',(130.554897108344,-3.80365956934553,
125.897474465882));
#276031=CARTESIAN_POINT('Ctrl Pts',(130.276449484532,-6.18427319643048,
131.35219531615));
#276032=CARTESIAN_POINT('Ctrl Pts',(129.998001860718,-2.88184187453723,
136.303482841632));
#276033=CARTESIAN_POINT('Ctrl Pts',(129.719554236906,3.0688613442533,136.201345690253));
#276034=CARTESIAN_POINT('Ctrl Pts',(129.441106613093,6.1994309098865,131.139642914452));
#276035=CARTESIAN_POINT('Ctrl Pts',(129.16265898928,3.63302632837089,125.769832087263));
#276036=CARTESIAN_POINT('Ctrl Pts',(128.884211365467,-2.27195196571463,
125.026507029031));
#276037=CARTESIAN_POINT('Ctrl Pts',(128.605763741654,-6.08911739433215,
129.592747154821));
#276038=CARTESIAN_POINT('Ctrl Pts',(128.327316117841,-4.31068140748063,
135.272400862266));
#276039=CARTESIAN_POINT('Ctrl Pts',(128.048868494028,1.42906020435147,136.846143860731));
#276040=CARTESIAN_POINT('Ctrl Pts',(127.770420870216,5.85556530185681,132.867783216248));
#276041=CARTESIAN_POINT('Ctrl Pts',(127.491973246402,4.9010919472237,126.993238007373));
#276042=CARTESIAN_POINT('Ctrl Pts',(127.21352562259,-0.557245475255655,
124.620928293575));
#276043=CARTESIAN_POINT('Ctrl Pts',(126.935077998777,-5.50350152892981,
127.930890808061));
#276044=CARTESIAN_POINT('Ctrl Pts',(126.656630374964,-5.39230853851415,
133.881431700678));
#276045=CARTESIAN_POINT('Ctrl Pts',(126.378182751151,-0.325847430121078,
137.004294591193));
#276046=CARTESIAN_POINT('Ctrl Pts',(126.099735127338,5.04005154802147,134.429721043558));
#276047=CARTESIAN_POINT('Ctrl Pts',(125.821287503525,5.77438937373851,128.523618373138));
#276048=CARTESIAN_POINT('Ctrl Pts',(125.542839879712,1.20234545959337,124.713406404895));
#276049=CARTESIAN_POINT('Ctrl Pts',(125.264392255899,-4.47459519407686,
126.50048379844));
#276050=CARTESIAN_POINT('Ctrl Pts',(124.985944632086,-6.03960146051831,
132.24261373269));
#276051=CARTESIAN_POINT('Ctrl Pts',(124.707497008274,-2.05450903567761,
136.663059316712));
#276052=CARTESIAN_POINT('Ctrl Pts',(124.429049384461,3.81857682460466,135.69964700956));
#276053=CARTESIAN_POINT('Ctrl Pts',(124.150601760648,6.18257713092382,130.237705656202));
#276054=CARTESIAN_POINT('Ctrl Pts',(123.872154136835,2.86509108960817,125.296492529702));
#276055=CARTESIAN_POINT('Ctrl Pts',(123.593706513022,-3.08527369557641,
125.416741101634));
#276056=CARTESIAN_POINT('Ctrl Pts',(123.315258889209,-6.20042267852561,
130.487948808862));
#276057=CARTESIAN_POINT('Ctrl Pts',(123.036811265396,-3.61768612739718,
135.849923510712));
#276058=CARTESIAN_POINT('Ctrl Pts',(122.758363641583,2.28952724101679,136.575272403211));
#276059=CARTESIAN_POINT('Ctrl Pts',(122.47991601777,6.09277692456002,131.997435289415));
#276060=CARTESIAN_POINT('Ctrl Pts',(122.201468393958,4.29706226313277,126.323220837128));
#276061=CARTESIAN_POINT('Ctrl Pts',(121.923020770144,-1.44744269495155,
124.766954927214));
#276062=CARTESIAN_POINT('Ctrl Pts',(121.644573146332,-5.86181852788225,
128.758769903068));
#276063=CARTESIAN_POINT('Ctrl Pts',(121.366125522519,-4.88946949944416,
134.630382812884));
#276064=CARTESIAN_POINT('Ctrl Pts',(121.087677898706,0.576063135118759,
136.986068236777));
#276065=CARTESIAN_POINT('Ctrl Pts',(120.809230274893,5.51222189075617,133.661066351821));
#276066=CARTESIAN_POINT('Ctrl Pts',(120.53078265108,5.38291801579874,127.710891454918));
#276067=CARTESIAN_POINT('Ctrl Pts',(120.252335027267,0.306975454486648,
124.603463594118));
#276068=CARTESIAN_POINT('Ctrl Pts',(119.973887403454,-5.05106255291402,
127.194357167205));
#276069=CARTESIAN_POINT('Ctrl Pts',(119.695439779642,-5.76742083231046,
133.102667552701));
#276070=CARTESIAN_POINT('Ctrl Pts',(119.416992155829,-1.18380112098488,
136.898946143343));
#276071=CARTESIAN_POINT('Ctrl Pts',(119.138544532016,4.48767398862585,135.09459837285));
#276072=CARTESIAN_POINT('Ctrl Pts',(118.860096908203,6.03519593775195,129.347731695017));
#276073=CARTESIAN_POINT('Ctrl Pts',(118.58164928439,2.0366676557964,124.939435836727));
#276074=CARTESIAN_POINT('Ctrl Pts',(118.303201660577,-3.83345870508974,
125.920719334523));
#276075=CARTESIAN_POINT('Ctrl Pts',(118.024754036764,-6.18082379086727,
131.389830592295));
#276076=CARTESIAN_POINT('Ctrl Pts',(117.746306412951,-2.84831376286653,
136.320923545089));
#276077=CARTESIAN_POINT('Ctrl Pts',(117.467858789138,3.10165746534553,136.18256466657));
#276078=CARTESIAN_POINT('Ctrl Pts',(117.189411165326,6.20135700729606,131.101899006891));
#276079=CARTESIAN_POINT('Ctrl Pts',(116.910963541513,3.60231241267338,125.747810102979));
#276080=CARTESIAN_POINT('Ctrl Pts',(116.6325159177,-2.30708130645123,125.040444095748));
#276081=CARTESIAN_POINT('Ctrl Pts',(116.354068293887,-6.09638001213474,
129.62983578909));
#276082=CARTESIAN_POINT('Ctrl Pts',(116.075620670074,-4.28340331138726,
135.298558421074));
#276083=CARTESIAN_POINT('Ctrl Pts',(115.797173046261,1.46581177664024,136.837332825402));
#276084=CARTESIAN_POINT('Ctrl Pts',(115.518725422448,5.86801745082159,132.832100497806));
#276085=CARTESIAN_POINT('Ctrl Pts',(115.240277798635,4.87780175628715,126.963474280869));
#276086=CARTESIAN_POINT('Ctrl Pts',(114.961830174822,-0.594875458411799,
124.624434969628));
#276087=CARTESIAN_POINT('Ctrl Pts',(114.68338255101,-5.52089118811201,127.964445422689));
#276088=CARTESIAN_POINT('Ctrl Pts',(114.404934927196,-5.37347762646609,
133.914199202272));
#276089=CARTESIAN_POINT('Ctrl Pts',(114.126487303384,-0.288100635073559,
137.006163246571));
#276090=CARTESIAN_POINT('Ctrl Pts',(113.848039679571,5.06202676545313,134.398973649715));
#276091=CARTESIAN_POINT('Ctrl Pts',(113.569592055758,5.76039886228364,128.488510282924));
#276092=CARTESIAN_POINT('Ctrl Pts',(113.291144431945,1.16524581580469,124.706200238089));
#276093=CARTESIAN_POINT('Ctrl Pts',(113.012696808132,-4.50071120997606,
126.527801670297));
#276094=CARTESIAN_POINT('Ctrl Pts',(112.734249184319,-6.03073450575487,
132.279351853526));
#276095=CARTESIAN_POINT('Ctrl Pts',(112.455801560506,-2.01880740850426,
136.675457148234));
#276096=CARTESIAN_POINT('Ctrl Pts',(112.177353936694,3.84830507293705,135.676311550269));
#276097=CARTESIAN_POINT('Ctrl Pts',(111.898906312881,6.17901319250346,130.200081053184));
#276098=CARTESIAN_POINT('Ctrl Pts',(111.620458689068,2.8315100497353,125.279153955068));
#276099=CARTESIAN_POINT('Ctrl Pts',(111.342011065255,-3.11801250178361,
125.435621858436));
#276100=CARTESIAN_POINT('Ctrl Pts',(111.063563441442,-6.20223388754234,
130.525698403974));
#276101=CARTESIAN_POINT('Ctrl Pts',(110.785115817629,-3.58690532661952,
135.871851910398));
#276102=CARTESIAN_POINT('Ctrl Pts',(110.506668193816,2.32461399939974,136.56122847942));
#276103=CARTESIAN_POINT('Ctrl Pts',(110.228220570003,6.09992662367788,131.960324722029));
#276104=CARTESIAN_POINT('Ctrl Pts',(109.94977294619,4.26970467877848,126.297146424621));
#276105=CARTESIAN_POINT('Ctrl Pts',(109.671325322378,-1.48416727924886,
124.775877780875));
#276106=CARTESIAN_POINT('Ctrl Pts',(109.392877698565,-5.8741620132489,128.794490356288));
#276107=CARTESIAN_POINT('Ctrl Pts',(109.114430074752,-4.86608882584101,
134.660075514194));
#276108=CARTESIAN_POINT('Ctrl Pts',(108.835982450939,0.61368227085971,136.982447044243));
#276109=CARTESIAN_POINT('Ctrl Pts',(108.557534827126,5.52950934068608,133.627458964475));
#276110=CARTESIAN_POINT('Ctrl Pts',(108.279087203313,5.36398745797076,127.67818141992));
#276111=CARTESIAN_POINT('Ctrl Pts',(108.0006395795,0.269223146735527,124.601709835656));
#276112=CARTESIAN_POINT('Ctrl Pts',(107.722191955687,-5.07294408406776,
127.225171303631));
#276113=CARTESIAN_POINT('Ctrl Pts',(107.443744331874,-5.75332352870873,
133.137732897993));
#276114=CARTESIAN_POINT('Ctrl Pts',(107.165296708062,-1.14667971594628,
136.906039358215));
#276115=CARTESIAN_POINT('Ctrl Pts',(106.886849084249,4.51370673735246,135.067201139359));
#276116=CARTESIAN_POINT('Ctrl Pts',(106.608401460436,6.02621720585718,129.31102073231));
#276117=CARTESIAN_POINT('Ctrl Pts',(106.329953836623,2.00092845925606,124.927146726103));
#276118=CARTESIAN_POINT('Ctrl Pts',(106.05150621281,-3.86311579061174,125.944145168289));
#276119=CARTESIAN_POINT('Ctrl Pts',(105.773058588997,-6.17714535260555,
131.427444173636));
#276120=CARTESIAN_POINT('Ctrl Pts',(105.494610965184,-2.81468010588189,
136.338159830278));
#276121=CARTESIAN_POINT('Ctrl Pts',(105.216163341371,3.13433865337982,136.163584351558));
#276122=CARTESIAN_POINT('Ctrl Pts',(104.937715717558,6.20305331114115,131.064144073934));
#276123=CARTESIAN_POINT('Ctrl Pts',(104.659268093745,3.57146501196475,125.725975491034));
#276124=CARTESIAN_POINT('Ctrl Pts',(104.380820469933,-2.34212515744159,
125.054594746511));
#276125=CARTESIAN_POINT('Ctrl Pts',(104.10237284612,-6.10341672633411,129.666967945808));
#276126=CARTESIAN_POINT('Ctrl Pts',(103.823925222307,-4.25596649220884,
135.324549445729));
#276127=CARTESIAN_POINT('Ctrl Pts',(103.545477598494,1.50250903273456,136.828298236068));
#276128=CARTESIAN_POINT('Ctrl Pts',(103.267029974681,5.88025215824177,132.796342640716));
#276129=CARTESIAN_POINT('Ctrl Pts',(102.988582350868,4.85433081661274,126.933852879821));
#276130=CARTESIAN_POINT('Ctrl Pts',(102.710134727055,-0.63248339823904,
124.628170645098));
#276131=CARTESIAN_POINT('Ctrl Pts',(102.431687103242,-5.53807626864099,
127.998105271418));
#276132=CARTESIAN_POINT('Ctrl Pts',(102.153239479429,-5.35444759822839,
133.946851467654));
#276133=CARTESIAN_POINT('Ctrl Pts',(101.874791855617,-0.250343164351048,
137.00780209187));
#276134=CARTESIAN_POINT('Ctrl Pts',(101.596344231803,5.0838144076213,134.368093056165));
#276135=CARTESIAN_POINT('Ctrl Pts',(101.317896607991,5.74619489713063,128.453488007394));
#276136=CARTESIAN_POINT('Ctrl Pts',(101.039448984178,1.12810299340375,124.69922004086));
#276137=CARTESIAN_POINT('Ctrl Pts',(100.761001360365,-4.52666045036627,
126.55527801162));
#276138=CARTESIAN_POINT('Ctrl Pts',(100.482553736552,-6.0216440799065,132.316035318018));
#276139=CARTESIAN_POINT('Ctrl Pts',(100.204106112739,-1.98303097367997,
136.687637424115));
#276140=CARTESIAN_POINT('Ctrl Pts',(99.9256584889259,3.87789072090961,135.652795559044));
#276141=CARTESIAN_POINT('Ctrl Pts',(99.6472108651132,6.17522028847693,130.162478841968));
#276142=CARTESIAN_POINT('Ctrl Pts',(99.3687632413001,2.79782408721636,125.262020118999));
#276143=CARTESIAN_POINT('Ctrl Pts',(99.0903156174874,-3.15063576889091,
125.454701555827));
#276144=CARTESIAN_POINT('Ctrl Pts',(98.8118679936743,-6.20381527050148,
130.563458325018));
#276145=CARTESIAN_POINT('Ctrl Pts',(98.5334203698616,-3.55599161174595,
135.89359253233));
#276146=CARTESIAN_POINT('Ctrl Pts',(98.2549727460486,2.35961461835606,136.546971232774));
#276147=CARTESIAN_POINT('Ctrl Pts',(97.9765251222358,6.10685028777152,131.923171319966));
#276148=CARTESIAN_POINT('Ctrl Pts',(97.6980774984228,4.24218887894701,126.271239028595));
#276149=CARTESIAN_POINT('Ctrl Pts',(97.4196298746099,-1.52083686718185,
124.785024022185));
#276150=CARTESIAN_POINT('Ctrl Pts',(97.141182250797,-5.88628782938184,128.830285285991));
#276151=CARTESIAN_POINT('Ctrl Pts',(96.8627346269842,-4.842527837527,134.689625340572));
#276152=CARTESIAN_POINT('Ctrl Pts',(96.5842870031713,0.651278666378471,
136.978596920444));
#276153=CARTESIAN_POINT('Ctrl Pts',(96.3058393793584,5.54659189261388,133.593746966183));
#276154=CARTESIAN_POINT('Ctrl Pts',(96.0273917555454,5.34485813561491,127.645587226641));
#276155=CARTESIAN_POINT('Ctrl Pts',(95.7489441317327,0.231460862821695,
124.6001859187));
#276156=CARTESIAN_POINT('Ctrl Pts',(95.4704965079195,-5.09463763541278,
127.256118068232));
#276157=CARTESIAN_POINT('Ctrl Pts',(95.192048884107,-5.73901303358793,133.172711779316));
#276158=CARTESIAN_POINT('Ctrl Pts',(94.9136012602939,-1.10951582026908,
136.912906473138));
#276159=CARTESIAN_POINT('Ctrl Pts',(94.635153636481,4.53957222901603,135.039645944743));
#276160=CARTESIAN_POINT('Ctrl Pts',(94.3567060126683,6.01701517026768,129.274365105863));
#276161=CARTESIAN_POINT('Ctrl Pts',(94.0782583888551,1.96511511757592,124.915075397801));
#276162=CARTESIAN_POINT('Ctrl Pts',(93.7998107650425,-3.89262972695748,
125.967751099126));
#276163=CARTESIAN_POINT('Ctrl Pts',(93.5213631412293,-6.17323801795121,
131.465034666385));
#276164=CARTESIAN_POINT('Ctrl Pts',(93.2429155174167,-2.7809421498907,136.355191058501));
#276165=CARTESIAN_POINT('Ctrl Pts',(92.9644678936037,3.16690369734264,136.14440544854));
#276166=CARTESIAN_POINT('Ctrl Pts',(92.6860202697908,6.20451975856463,131.026379514606));
#276167=CARTESIAN_POINT('Ctrl Pts',(92.4075726459779,3.54048526930663,125.704329060518));
#276168=CARTESIAN_POINT('Ctrl Pts',(92.129125022165,-2.37708222012305,125.068958456964));
#276169=CARTESIAN_POINT('Ctrl Pts',(91.850677398352,-6.1102272761821,129.70414224903));
#276170=CARTESIAN_POINT('Ctrl Pts',(91.5722297745392,-4.22837196662692,
135.350372973126));
#276171=CARTESIAN_POINT('Ctrl Pts',(91.2937821507264,1.53915061280415,136.819040427511));
#276172=CARTESIAN_POINT('Ctrl Pts',(91.0153345269133,5.89226897075567,132.76051097));
#276173=CARTESIAN_POINT('Ctrl Pts',(90.7368869031008,4.8306799979248,126.90437490186));
#276174=CARTESIAN_POINT('Ctrl Pts',(90.4584392792875,-0.670067901161403,
124.632135181558));
#276175=CARTESIAN_POINT('Ctrl Pts',(90.1799916554748,-5.5550561337172,128.031869106972));
#276176=CARTESIAN_POINT('Ctrl Pts',(89.9015440316619,-5.3352191589658,133.979387286881));
#276177=CARTESIAN_POINT('Ctrl Pts',(89.6230964078489,-0.212576417070642,
137.009211066365));
#276178=CARTESIAN_POINT('Ctrl Pts',(89.3446487840362,5.10541366717708,134.337080407198));
#276179=CARTESIAN_POINT('Ctrl Pts',(89.0662011602232,5.73177800461257,128.418552844315));
#276180=CARTESIAN_POINT('Ctrl Pts',(88.7877535364103,1.09091836873142,124.69246607186));
#276181=CARTESIAN_POINT('Ctrl Pts',(88.5093059125973,-4.5524419536888,126.58291180426));
#276182=CARTESIAN_POINT('Ctrl Pts',(88.2308582887847,-6.0123305198223,132.352662766849));
#276183=CARTESIAN_POINT('Ctrl Pts',(87.9524106649715,-1.94718105691378,
136.69959969301));
#276184=CARTESIAN_POINT('Ctrl Pts',(87.6739630411587,3.90733267221543,135.629099907278));
#276185=CARTESIAN_POINT('Ctrl Pts',(87.395515417346,6.17119855939173,130.124900415918));
#276186=CARTESIAN_POINT('Ctrl Pts',(87.1170677935327,2.76403445029686,125.245091656395));
#276187=CARTESIAN_POINT('Ctrl Pts',(86.8386201697203,-3.18314228803115,
125.473979486801));
#276188=CARTESIAN_POINT('Ctrl Pts',(86.5601725459069,-6.20516676880425,
130.601227172784));
#276189=CARTESIAN_POINT('Ctrl Pts',(86.2817249220945,-3.52494612829556,
135.915144570902));
#276190=CARTESIAN_POINT('Ctrl Pts',(86.0032772982812,2.394527800925,136.532501191579));
#276191=CARTESIAN_POINT('Ctrl Pts',(85.7248296744686,6.11354766028192,131.885976459962));
#276192=CARTESIAN_POINT('Ctrl Pts',(85.4463820506556,4.21451588324655,126.245499609054));
#276193=CARTESIAN_POINT('Ctrl Pts',(85.1679344268427,-1.55745009994542,
124.794393312227));
#276194=CARTESIAN_POINT('Ctrl Pts',(84.8894868030298,-5.89819552695468,
128.86615336578));
#276195=CARTESIAN_POINT('Ctrl Pts',(84.611039179217,-4.81878740756302,134.719031197036));
#276196=CARTESIAN_POINT('Ctrl Pts',(84.332591555404,0.68885092852684,136.974518008049));
#276197=CARTESIAN_POINT('Ctrl Pts',(84.0541439315912,5.56346891353935,133.559931606153));
#276198=CARTESIAN_POINT('Ctrl Pts',(83.7756963077782,5.32553075757526,127.613110082872));
#276199=CARTESIAN_POINT('Ctrl Pts',(83.4972486839655,0.193690002040587,
124.598891899719));
#276200=CARTESIAN_POINT('Ctrl Pts',(83.2188010601524,-5.11614240308669,
127.287196314267));
#276201=CARTESIAN_POINT('Ctrl Pts',(82.9403534363397,-5.72448987722869,
133.207602900518));
#276202=CARTESIAN_POINT('Ctrl Pts',(82.6619058125266,-1.07231081107503,
136.919547233648));
#276203=CARTESIAN_POINT('Ctrl Pts',(82.3834581887138,4.56526950516122,135.011933810073));
#276204=CARTESIAN_POINT('Ctrl Pts',(82.1050105649009,6.00759017196827,129.237766173961));
#276205=CARTESIAN_POINT('Ctrl Pts',(81.826562941088,1.92922895783247,124.903222299129));
#276206=CARTESIAN_POINT('Ctrl Pts',(81.5481153172751,-3.92199942047723,
125.991536252305));
#276207=CARTESIAN_POINT('Ctrl Pts',(81.2696676934623,-6.16910193169181,
131.502600677615));
#276208=CARTESIAN_POINT('Ctrl Pts',(80.9912200696492,-2.74710114506546,
136.372016598662));
#276209=CARTESIAN_POINT('Ctrl Pts',(80.7127724458365,3.19935139052435,136.125028668197));
#276210=CARTESIAN_POINT('Ctrl Pts',(80.4343248220235,6.20575629522666,130.988606728286));
#276211=CARTESIAN_POINT('Ctrl Pts',(80.1558771982107,3.50937433266497,125.682871613546));
#276212=CARTESIAN_POINT('Ctrl Pts',(79.8774295743978,-2.41195119914859,
125.083534694853));
#276213=CARTESIAN_POINT('Ctrl Pts',(79.5989819505849,-6.11681140931136,
129.741357321249));
#276214=CARTESIAN_POINT('Ctrl Pts',(79.320534326772,-4.20062075716678,135.376028046362));
#276215=CARTESIAN_POINT('Ctrl Pts',(79.0420867029591,1.57573515908161,136.809559742781));
#276216=CARTESIAN_POINT('Ctrl Pts',(78.7636390791462,5.90406744307602,132.724606813414));
#276217=CARTESIAN_POINT('Ctrl Pts',(78.4851914553333,4.80685017661309,126.875041439303));
#276218=CARTESIAN_POINT('Ctrl Pts',(78.2067438315204,-0.707627574471386,
124.636328432103));
#276219=CARTESIAN_POINT('Ctrl Pts',(77.9282962077074,-5.57183015414549,
128.065735678218));
#276220=CARTESIAN_POINT('Ctrl Pts',(77.6498485838947,-5.31579302119528,
134.011805454327));
#276221=CARTESIAN_POINT('Ctrl Pts',(77.3714009600817,-0.174801792692954,
137.010390117845));
#276222=CARTESIAN_POINT('Ctrl Pts',(77.0929533362689,5.12682374375196,134.305936852001));
#276223=CARTESIAN_POINT('Ctrl Pts',(76.814505712456,5.7171487189526,128.38370608822));
#276224=CARTESIAN_POINT('Ctrl Pts',(76.536058088643,1.05369331967776,124.68593858136));
#276225=CARTESIAN_POINT('Ctrl Pts',(76.2576104648302,-4.57805476460059,
126.610702024239));
#276226=CARTESIAN_POINT('Ctrl Pts',(75.9791628410172,-6.00279417061961,
132.389232842773));
#276227=CARTESIAN_POINT('Ctrl Pts',(75.7007152172044,-1.91125898663751,
136.711343511654));
#276228=CARTESIAN_POINT('Ctrl Pts',(75.4222675933915,3.93662983587222,135.605225473025));
#276229=CARTESIAN_POINT('Ctrl Pts',(75.1438199695785,6.16694815427437,130.087347167514));
#276230=CARTESIAN_POINT('Ctrl Pts',(74.8653723457658,2.73014239106432,125.228369194547));
#276231=CARTESIAN_POINT('Ctrl Pts',(74.5869247219528,-3.21553085466319,
125.493454937009));
#276232=CARTESIAN_POINT('Ctrl Pts',(74.3084770981399,-6.20628833237051,
130.639003547736));
#276233=CARTESIAN_POINT('Ctrl Pts',(74.0300294743271,-3.49377002667009,
135.936507227495));
#276234=CARTESIAN_POINT('Ctrl Pts',(73.7515818505141,2.42935225338577,136.517818892029));
#276235=CARTESIAN_POINT('Ctrl Pts',(73.4731342267013,6.1200184930355,131.848741520285));
#276236=CARTESIAN_POINT('Ctrl Pts',(73.1946866028884,4.18668671711015,126.219929119786));
#276237=CARTESIAN_POINT('Ctrl Pts',(72.9162389790755,-1.59400562082267,
124.803985303816));
#276238=CARTESIAN_POINT('Ctrl Pts',(72.6377913552626,-5.90988466472314,
128.902093266552));
#276239=CARTESIAN_POINT('Ctrl Pts',(72.3593437314497,-4.79486841565966,
134.748291993943));
#276240=CARTESIAN_POINT('Ctrl Pts',(72.0808961076369,0.726397665050741,
136.970210458201));
#276241=CARTESIAN_POINT('Ctrl Pts',(71.8024484838239,5.58013977807825,133.526014137426));
#276242=CARTESIAN_POINT('Ctrl Pts',(71.524000860011,5.30600604003494,127.580751192065));
#276243=CARTESIAN_POINT('Ctrl Pts',(71.2455532361981,0.155911964005252,
124.597827826664));
#276244=CARTESIAN_POINT('Ctrl Pts',(70.9671056123853,-5.13745759022245,
127.318404890117));
#276245=CARTESIAN_POINT('Ctrl Pts',(70.6886579885723,-5.70975459779179,
133.242404968692));
#276246=CARTESIAN_POINT('Ctrl Pts',(70.4102103647595,-1.03506606700937,
136.925961393668));
#276247=CARTESIAN_POINT('Ctrl Pts',(70.1317627409465,4.59079761356593,134.98406576223));
#276248=CARTESIAN_POINT('Ctrl Pts',(69.8533151171337,5.99794256020584,129.201225292793));
#276249=CARTESIAN_POINT('Ctrl Pts',(69.5748674933208,1.89327130980037,124.891587869307));
#276250=CARTESIAN_POINT('Ctrl Pts',(69.2964198695077,-3.95122378286636,
126.015499746463));
#276251=CARTESIAN_POINT('Ctrl Pts',(69.0179722456952,-6.16473724709165,
131.540140815303));
#276252=CARTESIAN_POINT('Ctrl Pts',(68.7395246218819,-2.71315834539685,
136.388635827283));
#276253=CARTESIAN_POINT('Ctrl Pts',(68.4610769980694,3.23168053056381,136.105454728543));
#276254=CARTESIAN_POINT('Ctrl Pts',(68.1826293742561,6.20676287530703,130.950827114659));
#276255=CARTESIAN_POINT('Ctrl Pts',(67.9041817504435,3.47813335486666,125.661603945233));
#276256=CARTESIAN_POINT('Ctrl Pts',(67.6257341266304,-2.44673080243567,
125.09832292005));
#276257=CARTESIAN_POINT('Ctrl Pts',(67.3472865028177,-6.12316888174425,
129.778611783445));
#276258=CARTESIAN_POINT('Ctrl Pts',(67.0688388790048,-4.17271389215982,
135.401513714782));
#276259=CARTESIAN_POINT('Ctrl Pts',(66.7903912551918,1.61226131591331,136.799856533191));
#276260=CARTESIAN_POINT('Ctrl Pts',(66.511943631379,5.91564713800617,132.688631501398));
#276261=CARTESIAN_POINT('Ctrl Pts',(66.233496007566,4.78284223570014,126.845853579115));
#276262=CARTESIAN_POINT('Ctrl Pts',(65.9550483837533,-0.745161026381345,
124.640750241348));
#276263=CARTESIAN_POINT('Ctrl Pts',(65.6766007599402,-5.58839770835831,
128.099703730218));
#276264=CARTESIAN_POINT('Ctrl Pts',(65.3981531361275,-5.2961699047596,134.044104768727));
#276265=CARTESIAN_POINT('Ctrl Pts',(65.1197055123145,-0.137020690970298,
137.011339202618));
#276266=CARTESIAN_POINT('Ctrl Pts',(64.8412578885016,5.14804384398771,134.274663544608));
#276267=CARTESIAN_POINT('Ctrl Pts',(64.5628102646887,5.70230758224426,128.348949030369));
#276268=CARTESIAN_POINT('Ctrl Pts',(64.2843626408759,1.01642922563077,124.679637811238));
#276269=CARTESIAN_POINT('Ctrl Pts',(64.0059150170629,-4.60349793400934,
126.638647641779));
#276270=CARTESIAN_POINT('Ctrl Pts',(63.72746739325,-5.9930353856715,132.425744190676));
#276271=CARTESIAN_POINT('Ctrl Pts',(63.4490197694371,-1.87526609395646,
136.722868444874));
#276272=CARTESIAN_POINT('Ctrl Pts',(63.1705721456243,3.96578112626272,135.581173140958));
#276273=CARTESIAN_POINT('Ctrl Pts',(62.8921245218114,6.16246923062527,130.049820488308));
#276274=CARTESIAN_POINT('Ctrl Pts',(62.6136768979985,2.69614916540168,125.211853353112));
#276275=CARTESIAN_POINT('Ctrl Pts',(62.3352292741856,-3.24780026861702,
125.513127184779));
#276276=CARTESIAN_POINT('Ctrl Pts',(62.0567816503727,-6.20717991964031,
130.676786050054));
#276277=CARTESIAN_POINT('Ctrl Pts',(61.7783340265599,-3.46246446211126,
135.957679710507));
#276278=CARTESIAN_POINT('Ctrl Pts',(61.4998864027468,2.46408668530527,136.502924878181));
#276279=CARTESIAN_POINT('Ctrl Pts',(61.2214387789342,6.12626254625314,131.81146788069));
#276280=CARTESIAN_POINT('Ctrl Pts',(60.942991155121,4.15870241175792,126.194528508313));
#276281=CARTESIAN_POINT('Ctrl Pts',(60.6645435313083,-1.63050207523548,
124.813799641521));
#276282=CARTESIAN_POINT('Ctrl Pts',(60.3860959074953,-5.92135480954196,
128.938103656541));
#276283=CARTESIAN_POINT('Ctrl Pts',(60.1076482836825,-4.77077174814381,
134.777406647022));
#276284=CARTESIAN_POINT('Ctrl Pts',(59.8292006598696,0.763917484641806,
136.965674430521));
#276285=CARTESIAN_POINT('Ctrl Pts',(59.5507530360567,5.59660386848551,133.491995816827));
#276286=CARTESIAN_POINT('Ctrl Pts',(59.2723054122438,5.28628470648961,127.548511753291));
#276287=CARTESIAN_POINT('Ctrl Pts',(58.9938577884309,0.11812814859451,124.596993738963));
#276288=CARTESIAN_POINT('Ctrl Pts',(58.715410164618,-5.15858240697801,127.34974263934));
#276289=CARTESIAN_POINT('Ctrl Pts',(58.4369625408051,-5.69480774129836,
133.277116694236));
#276290=CARTESIAN_POINT('Ctrl Pts',(58.1585149169922,-0.997782968190397,
136.932148715521));
#276291=CARTESIAN_POINT('Ctrl Pts',(57.8800672931793,4.61615560827684,134.956042833877));
#276292=CARTESIAN_POINT('Ctrl Pts',(57.6016196693665,5.98807269247603,129.164743816393));
#276293=CARTESIAN_POINT('Ctrl Pts',(57.3231720455535,1.85724350590365,124.880172539454));
#276294=CARTESIAN_POINT('Ctrl Pts',(57.0447244217407,-3.98030173120474,
126.039640693622));
#276295=CARTESIAN_POINT('Ctrl Pts',(56.7662767979277,-6.16014412588574,
131.577653688385));
#276296=CARTESIAN_POINT('Ctrl Pts',(56.4878291741149,-2.67911500864857,
136.405048128532));
#276297=CARTESIAN_POINT('Ctrl Pts',(56.209381550302,3.26388991949243,136.085684354897));
#276298=CARTESIAN_POINT('Ctrl Pts',(55.9309339264891,6.20753946150667,130.913042073662));
#276299=CARTESIAN_POINT('Ctrl Pts',(55.6524863026762,3.44676349355797,125.640526843659));
#276300=CARTESIAN_POINT('Ctrl Pts',(55.3740386788633,-2.48141974121268,
125.113322584571));
#276301=CARTESIAN_POINT('Ctrl Pts',(55.0955910550504,-6.12929945790263,
129.815904255142));
#276302=CARTESIAN_POINT('Ctrl Pts',(54.8171434312375,-4.14465240570495,
135.426829034002));
#276303=CARTESIAN_POINT('Ctrl Pts',(54.5386958074246,1.64872772980914,136.789931158292));
#276304=CARTESIAN_POINT('Ctrl Pts',(54.2602481836117,5.92700762645589,132.652586367033));
#276305=CARTESIAN_POINT('Ctrl Pts',(53.9818005597989,4.75865706480954,126.81681240286));
#276306=CARTESIAN_POINT('Ctrl Pts',(53.703352935986,-0.78266686607524,124.645400445441));
#276307=CARTESIAN_POINT('Ctrl Pts',(53.4249053121731,-5.604758182439,128.133772004274));
#276308=CARTESIAN_POINT('Ctrl Pts',(53.1464576883601,-5.27635053680027,
134.076284033214));
#276309=CARTESIAN_POINT('Ctrl Pts',(52.8680100645473,-0.0992345118958833,
137.012058285519));
#276310=CARTESIAN_POINT('Ctrl Pts',(52.5895624407343,5.1690731815654,134.243261643865));
#276311=CARTESIAN_POINT('Ctrl Pts',(52.3111148169216,5.68725514443172,128.314282958697));
#276312=CARTESIAN_POINT('Ctrl Pts',(52.0326671931086,0.979127467424884,
124.673563994973));
#276313=CARTESIAN_POINT('Ctrl Pts',(51.7542195692957,-4.62877051910935,
126.666747621346));
#276314=CARTESIAN_POINT('Ctrl Pts',(51.4757719454828,-5.98305452659317,
132.462195457613));
#276315=CARTESIAN_POINT('Ctrl Pts',(51.1973243216699,-1.83920371260068,
136.734174065611));
#276316=CARTESIAN_POINT('Ctrl Pts',(50.9188766978571,3.99478546317524,135.556943802347));
#276317=CARTESIAN_POINT('Ctrl Pts',(50.6404290740441,6.15776195441257,130.012321768865));
#276318=CARTESIAN_POINT('Ctrl Pts',(50.3619814502312,2.66205603294,125.195544744091));
#276319=CARTESIAN_POINT('Ctrl Pts',(50.0835338264184,-3.27994933413751,
125.532995501151));
#276320=CARTESIAN_POINT('Ctrl Pts',(49.8050862026055,-6.20784149757545,
130.714573279694));
#276321=CARTESIAN_POINT('Ctrl Pts',(49.5266385787925,-3.43103059465853,
135.978661235386));
#276322=CARTESIAN_POINT('Ctrl Pts',(49.2481909549797,2.4987298095866,136.487819701939));
#276323=CARTESIAN_POINT('Ctrl Pts',(48.9697433311668,6.13227958855924,131.774156922365));
#276324=CARTESIAN_POINT('Ctrl Pts',(48.6912957073539,4.13056400415832,126.169298715863));
#276325=CARTESIAN_POINT('Ctrl Pts',(48.412848083541,-1.66693811079436,124.823835961664));
#276326=CARTESIAN_POINT('Ctrl Pts',(48.1344004597282,-5.93260553638082,
128.974183201367));
#276327=CARTESIAN_POINT('Ctrl Pts',(47.8559528359152,-4.7464982979263,134.806374077418));
#276328=CARTESIAN_POINT('Ctrl Pts',(47.5775052121024,0.801408996989757,
136.960910093092));
#276329=CARTESIAN_POINT('Ctrl Pts',(47.2990575882894,5.61286057467834,133.457877904919));
#276330=CARTESIAN_POINT('Ctrl Pts',(47.0206099644766,5.26636748772036,127.516392961194));
#276331=CARTESIAN_POINT('Ctrl Pts',(46.7421623406636,0.0803399559020909,
124.596389667526));
#276332=CARTESIAN_POINT('Ctrl Pts',(46.4637147168508,-5.17951607056515,
127.381208400702));
#276333=CARTESIAN_POINT('Ctrl Pts',(46.1852670930379,-5.67964986161014,
133.311736790894));
#276334=CARTESIAN_POINT('Ctrl Pts',(45.9068194692249,-0.960462896156299,
136.938108969933));
#276335=CARTESIAN_POINT('Ctrl Pts',(45.6283718454121,4.64134254964412,134.927866063412));
#276336=CARTESIAN_POINT('Ctrl Pts',(45.3499242215992,5.97798093451044,129.128323096598));
#276337=CARTESIAN_POINT('Ctrl Pts',(45.0714765977863,1.82114688116607,124.868976732569));
#276338=CARTESIAN_POINT('Ctrl Pts',(44.7930289739735,-4.00923218799886,
126.063958199228));
#276339=CARTESIAN_POINT('Ctrl Pts',(44.5145813501605,-6.15532273827383,
131.615137906808));
#276340=CARTESIAN_POINT('Ctrl Pts',(44.2361337263477,-2.644972396308,136.421252894246));
#276341=CARTESIAN_POINT('Ctrl Pts',(43.9576861025347,3.29597836378001,136.065718279858));
#276342=CARTESIAN_POINT('Ctrl Pts',(43.6792384787219,6.20808602504863,130.875253005433));
#276343=CARTESIAN_POINT('Ctrl Pts',(43.4007908549089,3.41526591116036,125.619641089845));
#276344=CARTESIAN_POINT('Ctrl Pts',(43.1223432310961,-2.5160167300689,125.128533132602));
#276345=CARTESIAN_POINT('Ctrl Pts',(42.8438956072832,-6.13520291061547,
129.853233354452));
#276346=CARTESIAN_POINT('Ctrl Pts',(42.5654479834703,-4.11643733763101,
135.451973065955));
#276347=CARTESIAN_POINT('Ctrl Pts',(42.2870003596574,1.68513304949262,136.779783985877));
#276348=CARTESIAN_POINT('Ctrl Pts',(42.0085527358444,5.93814848745852,132.616472745983));
#276349=CARTESIAN_POINT('Ctrl Pts',(41.7301051120316,4.73429556013123,126.787918986671));
#276350=CARTESIAN_POINT('Ctrl Pts',(41.4516574882187,-0.820143703760798,
124.65027887207));
#276351=CARTESIAN_POINT('Ctrl Pts',(41.1732098644058,-5.62091097014408,
128.167939237972));
#276352=CARTESIAN_POINT('Ctrl Pts',(40.8947622405929,-5.25633565173145,
134.108342055376));
#276353=CARTESIAN_POINT('Ctrl Pts',(40.61631461678,-0.0614446556499193,
137.012547339898));
#276354=CARTESIAN_POINT('Ctrl Pts',(40.3378669929672,5.18991097723558,134.211732313379));
#276355=CARTESIAN_POINT('Ctrl Pts',(40.0594193691542,5.67199196328813,128.279709157768));
#276356=CARTESIAN_POINT('Ctrl Pts',(39.7809717453414,0.941789427290636,
124.66771735763));
#276357=CARTESIAN_POINT('Ctrl Pts',(39.5025241215285,-4.65387158341555,
126.695000921683));
#276358=CARTESIAN_POINT('Ctrl Pts',(39.2240764977156,-5.97285196322902,
132.49858529287));
#276359=CARTESIAN_POINT('Ctrl Pts',(38.9456288739027,-1.80307317887526,
136.745259954929));
#276360=CARTESIAN_POINT('Ctrl Pts',(38.6671812500898,4.02364177184326,135.532538355018));
#276361=CARTESIAN_POINT('Ctrl Pts',(38.3887336262769,6.15282650006613,129.974852398711));
#276362=CARTESIAN_POINT('Ctrl Pts',(38.110286002464,2.62786425701304,125.179443971804));
#276363=CARTESIAN_POINT('Ctrl Pts',(37.8318383786511,-3.31197685992897,
125.553059149895));
#276364=CARTESIAN_POINT('Ctrl Pts',(37.5533907548383,-6.20827304166094,
130.752363836438));
#276365=CARTESIAN_POINT('Ctrl Pts',(37.2749431310254,-3.3994695891056,135.999451024653));
#276366=CARTESIAN_POINT('Ctrl Pts',(36.9964955072125,2.53328034251594,136.47250392303));
#276367=CARTESIAN_POINT('Ctrl Pts',(36.7180478833995,6.13806939699002,131.73681002788));
#276368=CARTESIAN_POINT('Ctrl Pts',(36.4396002595867,4.10227253699055,126.144240677337));
#276369=CARTESIAN_POINT('Ctrl Pts',(36.1611526357737,-1.70331237734853,
124.834093892349));
#276370=CARTESIAN_POINT('Ctrl Pts',(35.8827050119609,-5.94363642833981,
129.01033056409));
#276371=CARTESIAN_POINT('Ctrl Pts',(35.604257388148,-4.72204896446884,134.835193211735));
#276372=CARTESIAN_POINT('Ctrl Pts',(35.3258097643351,0.838870812832614,
136.955917622458));
#276373=CARTESIAN_POINT('Ctrl Pts',(35.0473621405222,5.62890929425843,133.423661665951));
#276374=CARTESIAN_POINT('Ctrl Pts',(34.7689145167094,5.24625512176713,127.484396005948));
#276375=CARTESIAN_POINT('Ctrl Pts',(34.4904668928964,0.0425487861828518,
124.596015634733));
#276376=CARTESIAN_POINT('Ctrl Pts',(34.2120192690835,-5.20025780527969,
127.412801008228));
#276377=CARTESIAN_POINT('Ctrl Pts',(33.9335716452707,-5.66428152040741,
133.346263975806));
#276378=CARTESIAN_POINT('Ctrl Pts',(33.6551240214578,-0.923107233816384,
136.943841936043));
#276379=CARTESIAN_POINT('Ctrl Pts',(33.3766763976448,4.66635750435639,134.899536494936));
#276380=CARTESIAN_POINT('Ctrl Pts',(33.098228773832,5.96766766026296,129.091964482989));
#276381=CARTESIAN_POINT('Ctrl Pts',(32.8197811500191,1.78498277316083,124.858000863516));
#276382=CARTESIAN_POINT('Ctrl Pts',(32.5413335262063,-4.03801408121996,
126.08845136219));
#276383=CARTESIAN_POINT('Ctrl Pts',(32.2628859023933,-6.15027326291425,
131.65259208158));
#276384=CARTESIAN_POINT('Ctrl Pts',(31.9844382785804,-2.6107317735426,136.437249523951));
#276385=CARTESIAN_POINT('Ctrl Pts',(31.7059906547675,3.32794467437699,136.045557243275));
#276386=CARTESIAN_POINT('Ctrl Pts',(31.4275430309546,6.20840254567991,130.837461310262));
#276387=CARTESIAN_POINT('Ctrl Pts',(31.1490954071417,3.3836417748287,125.598947457719));
#276388=CARTESIAN_POINT('Ctrl Pts',(30.8706477833288,-2.55052048699994,
125.143954000505));
#276389=CARTESIAN_POINT('Ctrl Pts',(30.5922001595159,-6.14087902112821,
129.890597698133));
#276390=CARTESIAN_POINT('Ctrl Pts',(30.3137525357031,-4.08806973345779,
135.476944878919));
#276391=CARTESIAN_POINT('Ctrl Pts',(30.0353049118902,1.72147592595096,136.769415391952));
#276392=CARTESIAN_POINT('Ctrl Pts',(29.7568572880773,5.94906930818524,132.58029197645));
#276393=CARTESIAN_POINT('Ctrl Pts',(29.4784096642643,4.70975862438989,126.759174401203));
#276394=CARTESIAN_POINT('Ctrl Pts',(29.1999620404515,-0.857590150719802,
124.65538534046));
#276395=CARTESIAN_POINT('Ctrl Pts',(28.9215144166386,-5.63685547292606,
128.202204165235));
#276396=CARTESIAN_POINT('Ctrl Pts',(28.6430667928257,-5.23612599121204,
134.140277647291));
#276397=CARTESIAN_POINT('Ctrl Pts',(28.3646191690128,-0.0236525225496446,
137.012806347637));
#276398=CARTESIAN_POINT('Ctrl Pts',(28.0861715451999,5.2105564588459,134.180076721482));
#276399=CARTESIAN_POINT('Ctrl Pts',(27.807723921387,5.65651860439647,128.245228908728));
#276400=CARTESIAN_POINT('Ctrl Pts',(27.5292762975741,0.904416488802812,
124.662098115861));
#276401=CARTESIAN_POINT('Ctrl Pts',(27.2508286737613,-4.67880019679877,
126.723406495856));
#276402=CARTESIAN_POINT('Ctrl Pts',(26.9723810499484,-5.96242807363892,
132.53491234801));
#276403=CARTESIAN_POINT('Ctrl Pts',(26.6939334261354,-1.76687583160983,
136.756125702037));
#276404=CARTESIAN_POINT('Ctrl Pts',(26.4154858023226,4.05234898298581,135.507957703324));
#276405=CARTESIAN_POINT('Ctrl Pts',(26.1370381785097,6.14766305047102,129.937413766291));
#276406=CARTESIAN_POINT('Ctrl Pts',(25.8585905546968,2.59357510460964,125.163551632871));
#276407=CARTESIAN_POINT('Ctrl Pts',(25.5801429308839,-3.34388165920016,
125.573317387547));
#276408=CARTESIAN_POINT('Ctrl Pts',(25.301695307071,-6.2084745359058,130.790156319941));
#276409=CARTESIAN_POINT('Ctrl Pts',(25.0232476832582,-3.36778261495664,
136.020048307934));
#276410=CARTESIAN_POINT('Ctrl Pts',(24.7448000594452,2.56773700381057,136.456978108987));
#276411=CARTESIAN_POINT('Ctrl Pts',(24.4663524356323,6.14363175700203,131.69942858114));
#276412=CARTESIAN_POINT('Ctrl Pts',(24.1879048118195,4.07382905860539,126.11935532127));
#276413=CARTESIAN_POINT('Ctrl Pts',(23.9094571880065,-1.73962352703587,
124.844573053462));
#276414=CARTESIAN_POINT('Ctrl Pts',(23.6310095641937,-5.95444707666522,
129.046544405257));
#276415=CARTESIAN_POINT('Ctrl Pts',(23.3525619403807,-4.69742465375045,
134.863862982068));
#276416=CARTESIAN_POINT('Ctrl Pts',(23.0741143165679,0.876301544009003,
136.950697203617));
#276417=CARTESIAN_POINT('Ctrl Pts',(22.795666692755,5.64474943253441,133.389348367819));
#276418=CARTESIAN_POINT('Ctrl Pts',(22.5172190689421,5.22594835390121,127.452522073212));
#276419=CARTESIAN_POINT('Ctrl Pts',(22.2387714451292,0.0047560398029127,
124.595871654449));
#276420=CARTESIAN_POINT('Ctrl Pts',(21.9603238213163,-5.22080684252888,
127.444519291243));
#276421=CARTESIAN_POINT('Ctrl Pts',(21.6818761975034,-5.64870328716988,
133.380696969555));
#276422=CARTESIAN_POINT('Ctrl Pts',(21.4034285736905,-0.885717365398449,
136.949347401415));
#276423=CARTESIAN_POINT('Ctrl Pts',(21.1249809498776,4.69119954547528,134.871055178212));
#276424=CARTESIAN_POINT('Ctrl Pts',(20.8465333260648,5.95713325189572,129.055669322849));
#276425=CARTESIAN_POINT('Ctrl Pts',(20.5680857022518,1.74875252196249,124.847245339011));
#276426=CARTESIAN_POINT('Ctrl Pts',(20.289638078439,-4.06664634434428,126.113119274905));
#276427=CARTESIAN_POINT('Ctrl Pts',(20.011190454626,-6.14499588691713,131.690014824823));
#276428=CARTESIAN_POINT('Ctrl Pts',(19.7327428308132,-2.57639440915122,
136.453037424885));
#276429=CARTESIAN_POINT('Ctrl Pts',(19.4542952070003,3.35978766676044,136.025201992224));
#276430=CARTESIAN_POINT('Ctrl Pts',(19.1758475831874,6.20848901167171,130.799668388532));
#276431=CARTESIAN_POINT('Ctrl Pts',(18.8973999593745,3.3518922564065,125.578446714094));
#276432=CARTESIAN_POINT('Ctrl Pts',(18.6189523355616,-2.58492973345636,
125.159584616859));
#276433=CARTESIAN_POINT('Ctrl Pts',(18.3405047117487,-6.14632757911053,
129.927995901635));
#276434=CARTESIAN_POINT('Ctrl Pts',(18.0620570879358,-4.05955064435711,
135.501743547556));
#276435=CARTESIAN_POINT('Ctrl Pts',(17.7836094641229,1.75775501248606,136.758825760728));
#276436=CARTESIAN_POINT('Ctrl Pts',(17.5051618403101,5.95976968396092,132.544045399129));
#276437=CARTESIAN_POINT('Ctrl Pts',(17.2267142164972,4.68504716681072,126.730579711598));
#276438=CARTESIAN_POINT('Ctrl Pts',(16.9482665926842,-0.8950048193604,124.660719661391));
#276439=CARTESIAN_POINT('Ctrl Pts',(16.6698189688713,-5.65259109995534,
128.236565516362));
#276440=CARTESIAN_POINT('Ctrl Pts',(16.3913713450585,-5.21572230411858,
134.172089625574));
#276441=CARTESIAN_POINT('Ctrl Pts',(16.1129237212456,0.0141404870033325,
137.012835299135));
#276442=CARTESIAN_POINT('Ctrl Pts',(15.8344760974327,5.23100886137047,134.148296041183));
#276443=CARTESIAN_POINT('Ctrl Pts',(15.5560284736198,5.64083564112771,128.210843489254));
#276444=CARTESIAN_POINT('Ctrl Pts',(15.2775808498069,0.8670100368296,124.656706477888));
#276445=CARTESIAN_POINT('Ctrl Pts',(14.999133225994,-4.70355543551987,126.751963291284));
#276446=CARTESIAN_POINT('Ctrl Pts',(14.7206856021811,-5.95178324408404,
132.571175276918));
#276447=CARTESIAN_POINT('Ctrl Pts',(14.4422379783683,-1.73061301211068,
136.766770904302));
#276448=CARTESIAN_POINT('Ctrl Pts',(14.1637903545553,4.08090603284655,135.48320275811));
#276449=CARTESIAN_POINT('Ctrl Pts',(13.8853427307424,6.14227179696077,129.900007258904));
#276450=CARTESIAN_POINT('Ctrl Pts',(13.6068951069296,2.55918984632695,125.147868316191));
#276451=CARTESIAN_POINT('Ctrl Pts',(13.3284474831167,-3.37566254970675,
125.593769463429));
#276452=CARTESIAN_POINT('Ctrl Pts',(13.0499998593037,-6.20844597284355,
130.827949329789));
#276453=CARTESIAN_POINT('Ctrl Pts',(12.7715522354909,-3.33597084638438,
136.04045232199));
#276454=CARTESIAN_POINT('Ctrl Pts',(12.493104611678,2.60209851666622,136.441242835124));
#276455=CARTESIAN_POINT('Ctrl Pts',(12.2146569878651,6.14896646247997,131.662013967328));
#276456=CARTESIAN_POINT('Ctrl Pts',(11.9362093640522,4.04523462298623,126.094643569795));
#276457=CARTESIAN_POINT('Ctrl Pts',(11.6577617402393,-1.77587021433397,
124.855273056695));
#276458=CARTESIAN_POINT('Ctrl Pts',(11.3793141164265,-5.96503708076441,
129.08282338295));
#276459=CARTESIAN_POINT('Ctrl Pts',(11.1008664926135,-4.67262627823404,
134.892382326048));
#276460=CARTESIAN_POINT('Ctrl Pts',(10.8224188688007,0.913699803509421,
136.945249030013));
#276461=CARTESIAN_POINT('Ctrl Pts',(10.5439712449878,5.6603804025445,133.354939282016));
#276462=CARTESIAN_POINT('Ctrl Pts',(10.2655236211749,5.20544793659703,127.420772344084));
#276463=CARTESIAN_POINT('Ctrl Pts',(9.98707599736195,-0.0330368828140487,
124.595957732005));
#276464=CARTESIAN_POINT('Ctrl Pts',(9.70862837354909,-5.24116242086055,
127.476362074414));
#276465=CARTESIAN_POINT('Ctrl Pts',(9.43018074973619,-5.63291573915475,
133.415034496211));
#276466=CARTESIAN_POINT('Ctrl Pts',(9.15173312592329,-0.848294676398009,
136.954625162043));
#276467=CARTESIAN_POINT('Ctrl Pts',(8.87328550211039,4.71586775246963,134.842423168626));
#276468=CARTESIAN_POINT('Ctrl Pts',(8.59483787829755,5.94637809976527,129.019438961107));
#276469=CARTESIAN_POINT('Ctrl Pts',(8.3163902544846,1.71245747009635,124.836710557603));
#276470=CARTESIAN_POINT('Ctrl Pts',(8.03794263067172,-4.09512791639282,
126.137961023291));
#276471=CARTESIAN_POINT('Ctrl Pts',(7.75949500685887,-6.1394908058375,131.727404749824));
#276472=CARTESIAN_POINT('Ctrl Pts',(7.48104738304595,-2.54196157551782,
136.468616012024));
#276473=CARTESIAN_POINT('Ctrl Pts',(7.20259975923305,3.39150616097622,136.004653280976));
#276474=CARTESIAN_POINT('Ctrl Pts',(6.92415213542018,6.20834541982004,130.761875640674));
#276475=CARTESIAN_POINT('Ctrl Pts',(6.64570451160728,3.32001853238404,125.558139618628));
#276476=CARTESIAN_POINT('Ctrl Pts',(6.36725688779438,-2.61924319439064,
125.175424402463));
#276477=CARTESIAN_POINT('Ctrl Pts',(6.08880926398148,-6.15154838266407,
129.965426579154));
#276478=CARTESIAN_POINT('Ctrl Pts',(5.81036164016863,-4.03088112711464,
135.52636815294));
#276479=CARTESIAN_POINT('Ctrl Pts',(5.53191401635571,1.79396896476278,136.748015484609));
#276480=CARTESIAN_POINT('Ctrl Pts',(5.2534663925428,5.97024921827925,132.507734357147));
#276481=CARTESIAN_POINT('Ctrl Pts',(4.97501876872993,4.66016210308585,126.702135977443));
#276482=CARTESIAN_POINT('Ctrl Pts',(4.69657114491704,-0.932386323268277,
124.666281637197));
#276483=CARTESIAN_POINT('Ctrl Pts',(4.41812352110413,-5.66811726814286,
128.27102201808));
#276484=CARTESIAN_POINT('Ctrl Pts',(4.13967589729124,-5.19512534651691,
134.203776811419));
#276485=CARTESIAN_POINT('Ctrl Pts',(3.86122827347838,0.051932972575587,
137.012634193321));
#276486=CARTESIAN_POINT('Ctrl Pts',(3.58278064966546,5.25126742693796,134.116391450127));
#276487=CARTESIAN_POINT('Ctrl Pts',(3.30433302585255,5.62494365461986,128.176554173511));
#276488=CARTESIAN_POINT('Ctrl Pts',(3.02588540203969,0.829571457480427,
124.651542643499));
#276489=CARTESIAN_POINT('Ctrl Pts',(2.74743777822681,-4.72813638226476,
126.780670249786));
#276490=CARTESIAN_POINT('Ctrl Pts',(2.46899015441389,-5.9409178690121,132.607372735859));
#276491=CARTESIAN_POINT('Ctrl Pts',(2.19054253060099,-1.69428606410994,
136.77719516726));
#276492=CARTESIAN_POINT('Ctrl Pts',(1.91209490678813,4.10931186323347,135.458274436681));
#276493=CARTESIAN_POINT('Ctrl Pts',(1.63364728297522,6.13665293931019,129.862634262664));
#276494=CARTESIAN_POINT('Ctrl Pts',(1.35519965916232,2.52470975632363,125.132394602912));
#276495=CARTESIAN_POINT('Ctrl Pts',(1.07675203534945,-3.40731835379603,
125.614414619682));
#276496=CARTESIAN_POINT('Ctrl Pts',(0.798304411536565,-6.20818735353264,
130.86574146555));
#276497=CARTESIAN_POINT('Ctrl Pts',(0.519856787723634,-3.30403546218559,
136.060662310741));
#276498=CARTESIAN_POINT('Ctrl Pts',(0.241409163910791,2.63636360780418,
136.425298684517));
#276499=CARTESIAN_POINT('Ctrl Pts',(-0.0370384599021062,6.15407331574431,
131.624567572855));
#276500=CARTESIAN_POINT('Ctrl Pts',(-0.315486083715014,4.01649028971072,
126.070106338619));
#276501=CARTESIAN_POINT('Ctrl Pts',(-0.593933707527915,-1.81205109610819,
124.866193505555));
#276502=CARTESIAN_POINT('Ctrl Pts',(-0.872381331340776,-5.97540604822092,
129.119166152838));
#276503=CARTESIAN_POINT('Ctrl Pts',(-1.15082895515369,-4.6476547568326,
134.920750186879));
#276504=CARTESIAN_POINT('Ctrl Pts',(-1.42927657896659,0.951064205527318,
136.939573303531));
#276505=CARTESIAN_POINT('Ctrl Pts',(-1.70772420277945,5.67580162507719,
133.320435683583));
#276506=CARTESIAN_POINT('Ctrl Pts',(-1.98617182659235,5.18475462950527,
127.389147995065));
#276507=CARTESIAN_POINT('Ctrl Pts',(-2.26461945040527,-0.0708285812371651,
124.596273864213));
#276508=CARTESIAN_POINT('Ctrl Pts',(-2.54306707421816,-5.26132378599129,
127.508328177794));
#276509=CARTESIAN_POINT('Ctrl Pts',(-2.82151469803103,-5.61691946137538,
133.449275283389));
#276510=CARTESIAN_POINT('Ctrl Pts',(-3.09996232184393,-0.810840553526189,
136.959675022356));
#276511=CARTESIAN_POINT('Ctrl Pts',(-3.37840994565684,4.74036121125036,
134.813641527147));
#276512=CARTESIAN_POINT('Ctrl Pts',(-3.6568575694697,5.93540260240737,128.983274740293));
#276513=CARTESIAN_POINT('Ctrl Pts',(-3.9353051932826,1.6760989624889,124.826396909662));
#276514=CARTESIAN_POINT('Ctrl Pts',(-4.21375281709551,-4.12345774197041,
126.162975686831));
#276515=CARTESIAN_POINT('Ctrl Pts',(-4.49220044090841,-6.13375822366836,
131.764760471086));
#276516=CARTESIAN_POINT('Ctrl Pts',(-4.77064806472125,-2.50743454856317,
136.483984708096));
#276517=CARTESIAN_POINT('Ctrl Pts',(-5.04909568853418,3.4230989816841,135.983911870971));
#276518=CARTESIAN_POINT('Ctrl Pts',(-5.32754331234708,6.20797177544568,
130.724084467112));
#276519=CARTESIAN_POINT('Ctrl Pts',(-5.60599093615995,3.28802178385396,
125.538026923812));
#276520=CARTESIAN_POINT('Ctrl Pts',(-5.88443855997284,-2.65345959830539,
125.191472770368));
#276521=CARTESIAN_POINT('Ctrl Pts',(-6.16288618378574,-6.15654123833006,
130.002888343683));
#276522=CARTESIAN_POINT('Ctrl Pts',(-6.44133380759864,-4.00206224408943,
135.550817782599));
#276523=CARTESIAN_POINT('Ctrl Pts',(-6.71978143141151,1.83011644085978,
136.736984964173));
#276524=CARTESIAN_POINT('Ctrl Pts',(-6.9982290552244,5.98050752281724,132.471360196026));
#276525=CARTESIAN_POINT('Ctrl Pts',(-7.27667667903734,4.63510435534053,
126.673844252731));
#276526=CARTESIAN_POINT('Ctrl Pts',(-7.55512430285017,-0.969733277257762,
124.672071061776));
#276527=CARTESIAN_POINT('Ctrl Pts',(-7.83357192666308,-5.68343340216059,
128.305572393592));
#276528=CARTESIAN_POINT('Ctrl Pts',(-8.112019550476,-5.17433588163501,134.235338030648));
#276529=CARTESIAN_POINT('Ctrl Pts',(-8.39046717428886,0.0897235337524442,
137.012203037646));
#276530=CARTESIAN_POINT('Ctrl Pts',(-8.66891479810176,5.27133140485959,
134.084364130551));
#276531=CARTESIAN_POINT('Ctrl Pts',(-8.94736242191464,5.60884323375645,
128.142362232103));
#276532=CARTESIAN_POINT('Ctrl Pts',(-9.22581004572757,0.792102138056052,
124.646606804043));
#276533=CARTESIAN_POINT('Ctrl Pts',(-9.50425766954039,-4.75254212617725,
126.809526307613));
#276534=CARTESIAN_POINT('Ctrl Pts',(-9.78270529335335,-5.92983235104376,
132.643503383524));
#276535=CARTESIAN_POINT('Ctrl Pts',(-10.0611529171662,-1.65789633371603,
136.787398104638));
#276536=CARTESIAN_POINT('Ctrl Pts',(-10.3396005409791,4.13756542155812,
135.433173662763));
#276537=CARTESIAN_POINT('Ctrl Pts',(-10.618048164792,6.13080668572826,129.82529616244));
#276538=CARTESIAN_POINT('Ctrl Pts',(-10.8964957886049,2.49013611227157,
125.11713106642));
#276539=CARTESIAN_POINT('Ctrl Pts',(-11.1749434124178,-3.4388478984508,
125.635252091294));
#276540=CARTESIAN_POINT('Ctrl Pts',(-11.4533910362307,-6.20769868755626,
130.90353132682));
#276541=CARTESIAN_POINT('Ctrl Pts',(-11.7318386600436,-3.2719776457377,
136.080677525301));
#276542=CARTESIAN_POINT('Ctrl Pts',(-12.0102862838565,2.67053100751937,
136.409146247984));
#276543=CARTESIAN_POINT('Ctrl Pts',(-12.2887339076694,6.15895212755882,
131.587090785312));
#276544=CARTESIAN_POINT('Ctrl Pts',(-12.5671815314823,3.98759712391021,
126.045744536976));
#276545=CARTESIAN_POINT('Ctrl Pts',(-12.8456291552951,-1.84816483166266,
124.877333995382));
#276546=CARTESIAN_POINT('Ctrl Pts',(-13.1240767791081,-5.98555359480885,
129.155571368227));
#276547=CARTESIAN_POINT('Ctrl Pts',(-13.4025244029209,-4.62251101487491,
134.948965513381));
#276548=CARTESIAN_POINT('Ctrl Pts',(-13.6809720267338,0.988393365511613,
136.933670234486));
#276549=CARTESIAN_POINT('Ctrl Pts',(-13.9594196505467,5.69101252869335,
133.285838851062));
#276550=CARTESIAN_POINT('Ctrl Pts',(-14.2378672743596,5.16386919942402,
127.357650198006));
#276551=CARTESIAN_POINT('Ctrl Pts',(-14.5163148981725,-0.108617655081171,
124.59682003936));
#276552=CARTESIAN_POINT('Ctrl Pts',(-14.7947625219854,-5.28129019083405,
127.540416416869));
#276553=CARTESIAN_POINT('Ctrl Pts',(-15.0732101457983,-5.60071504657988,
133.483418062279));
#276554=CARTESIAN_POINT('Ctrl Pts',(-15.3516577696111,-0.77335638465969,
136.96449679523));
#276555=CARTESIAN_POINT('Ctrl Pts',(-15.6301053934241,4.76467901420313,
134.784711320289));
#276556=CARTESIAN_POINT('Ctrl Pts',(-15.908553017237,5.92420716652329,128.947178000488));
#276557=CARTESIAN_POINT('Ctrl Pts',(-16.1870006410499,1.63967834641818,
124.816304777366));
#276558=CARTESIAN_POINT('Ctrl Pts',(-16.4654482648627,-4.15163477130477,
126.188162338596));
#276559=CARTESIAN_POINT('Ctrl Pts',(-16.7438958886757,-6.12779835283271,
131.802080604377));
#276560=CARTESIAN_POINT('Ctrl Pts',(-17.0223435124885,-2.4728146076992,
136.499142943608));
#276561=CARTESIAN_POINT('Ctrl Pts',(-17.3007911363014,3.45456495820035,
135.96297853079));
#276562=CARTESIAN_POINT('Ctrl Pts',(-17.5792387601143,6.20736809239421,
130.686296268213));
#276563=CARTESIAN_POINT('Ctrl Pts',(-17.8576863839272,3.25590319646751,
125.518109374927));
#276564=CARTESIAN_POINT('Ctrl Pts',(-18.13613400774,-2.6875776772989,125.207729125896));
#276565=CARTESIAN_POINT('Ctrl Pts',(-18.414581631553,-6.16130596109642,
130.040379807061));
#276566=CARTESIAN_POINT('Ctrl Pts',(-18.6930292553659,-3.97309506317598,
135.575091530542));
#276567=CARTESIAN_POINT('Ctrl Pts',(-18.9714768791788,1.86619610131902,
136.72573460816));
#276568=CARTESIAN_POINT('Ctrl Pts',(-19.2499245029916,5.99054421744964,
132.434924263623));
#276569=CARTESIAN_POINT('Ctrl Pts',(-19.5283721268046,4.6098748520987,126.645705585822));
#276570=CARTESIAN_POINT('Ctrl Pts',(-19.8068197506174,-1.00704429742433,
124.678087720601));
#276571=CARTESIAN_POINT('Ctrl Pts',(-20.0852673744304,-5.6985389344635,
128.340215362621));
#276572=CARTESIAN_POINT('Ctrl Pts',(-20.3637149982432,-5.15335467983417,
134.266772113748));
#276573=CARTESIAN_POINT('Ctrl Pts',(-20.6421626220562,0.127510770190762,
137.011541848088));
#276574=CARTESIAN_POINT('Ctrl Pts',(-20.920610245869,5.29120005165768,134.05221526924));
#276575=CARTESIAN_POINT('Ctrl Pts',(-21.1990578696819,5.59253497514422,
128.108268932023));
#276576=CARTESIAN_POINT('Ctrl Pts',(-21.4775054934948,0.754603466995427,
124.64189914242));
#276577=CARTESIAN_POINT('Ctrl Pts',(-21.7559531173077,-4.77677176289349,
126.838530395495));
#276578=CARTESIAN_POINT('Ctrl Pts',(-22.0344007411205,-5.91852710095694,
132.679565881077));
#276579=CARTESIAN_POINT('Ctrl Pts',(-22.3128483649335,-1.62144516936395,
136.797379338361));
#276580=CARTESIAN_POINT('Ctrl Pts',(-22.5912959887463,4.16566566087426,
135.407901366475));
#276581=CARTESIAN_POINT('Ctrl Pts',(-22.8697436125593,6.12473325285015,
129.787994341809));
#276582=CARTESIAN_POINT('Ctrl Pts',(-23.1481912363721,2.45547019531011,
125.102078272311));
#276583=CARTESIAN_POINT('Ctrl Pts',(-23.426638860185,-3.47025001533206,
125.656281106122));
#276584=CARTESIAN_POINT('Ctrl Pts',(-23.7050864839979,-6.20697999302203,
130.941317513284));
#276585=CARTESIAN_POINT('Ctrl Pts',(-23.9835341078108,-3.23979858495512,
136.100497223997));
#276586=CARTESIAN_POINT('Ctrl Pts',(-24.2619817316237,2.70459944972584,
136.392786124057));
#276587=CARTESIAN_POINT('Ctrl Pts',(-24.5404293554366,6.16360271713728,
131.549584993415));
#276588=CARTESIAN_POINT('Ctrl Pts',(-24.8188769792495,3.95855619623184,
126.021559067602));
#276589=CARTESIAN_POINT('Ctrl Pts',(-25.0973246030624,-1.88421008278963,
124.88869411336));
#276590=CARTESIAN_POINT('Ctrl Pts',(-25.3757722268753,-5.99547934450715,
129.192037680109));
#276591=CARTESIAN_POINT('Ctrl Pts',(-25.6542198506882,-4.59719598407162,
134.977027260026));
#276592=CARTESIAN_POINT('Ctrl Pts',(-25.932667474501,1.02568590021626,136.92754004162));
#276593=CARTESIAN_POINT('Ctrl Pts',(-26.211115098314,5.7060125497474,133.251150066453));
#276594=CARTESIAN_POINT('Ctrl Pts',(-26.4895627221268,5.14279242027056,
127.326280120068));
#276595=CARTESIAN_POINT('Ctrl Pts',(-26.7680103459397,-0.146402704058008,
124.597596237205));
#276596=CARTESIAN_POINT('Ctrl Pts',(-27.0464579697526,-5.30106089552683,
127.572625602596));
#276597=CARTESIAN_POINT('Ctrl Pts',(-27.3249055935655,-5.58430309522854,
133.517461567711));
#276598=CARTESIAN_POINT('Ctrl Pts',(-27.6033532173784,-0.735843558787732,
136.969090301993));
#276599=CARTESIAN_POINT('Ctrl Pts',(-27.8818008411913,4.78882026022281,
134.755633620073));
#276600=CARTESIAN_POINT('Ctrl Pts',(-28.1602484650042,5.91279220696403,
128.911150079267));
#276601=CARTESIAN_POINT('Ctrl Pts',(-28.4386960888171,1.60319697146318,
124.806434534681));
#276602=CARTESIAN_POINT('Ctrl Pts',(-28.7171437126299,-4.17965796028613,
126.213520045287));
#276603=CARTESIAN_POINT('Ctrl Pts',(-28.9955913364429,-6.12161141417542,
131.839363766787));
#276604=CARTESIAN_POINT('Ctrl Pts',(-29.2740389602557,-2.43810303578058,
136.514090156867));
#276605=CARTESIAN_POINT('Ctrl Pts',(-29.5524865840687,3.48590292454168,
135.941854036124));
#276606=CARTESIAN_POINT('Ctrl Pts',(-29.8309342078815,6.20653439303521,
130.648512444231));
#276607=CARTESIAN_POINT('Ctrl Pts',(-30.1093818316944,3.22366396039099,
125.498387710026));
#276608=CARTESIAN_POINT('Ctrl Pts',(-30.3878294555073,-2.72159616711309,
125.224192866663));
#276609=CARTESIAN_POINT('Ctrl Pts',(-30.6662770793202,-6.16584237440457,
130.077899580028));
#276610=CARTESIAN_POINT('Ctrl Pts',(-30.9447247031331,-3.94398065776386,
135.599188497297));
#276611=CARTESIAN_POINT('Ctrl Pts',(-31.2231723269461,1.90220660919519,
136.714264833456));
#276612=CARTESIAN_POINT('Ctrl Pts',(-31.5016199507588,6.00035893026297,
132.398427910084));
#276613=CARTESIAN_POINT('Ctrl Pts',(-31.7800675745718,4.58447452824918,
126.617721019404));
#276614=CARTESIAN_POINT('Ctrl Pts',(-32.0585151983846,-1.04431800119413,
124.68433139072));
#276615=CARTESIAN_POINT('Ctrl Pts',(-32.3369628221976,-5.71343330531054,
128.374949641459));
#276616=CARTESIAN_POINT('Ctrl Pts',(-32.6154104460104,-5.1321825185805,
134.298077895915));
#276617=CARTESIAN_POINT('Ctrl Pts',(-32.8938580698234,0.165293281670594,
137.010650649146));
#276618=CARTESIAN_POINT('Ctrl Pts',(-33.1723056936362,5.31087263109202,
134.019946057479));
#276619=CARTESIAN_POINT('Ctrl Pts',(-33.4507533174492,5.57601948309184,
128.074275536613));
#276620=CARTESIAN_POINT('Ctrl Pts',(-33.729200941262,0.717076833825826,
124.637419833072));
#276621=CARTESIAN_POINT('Ctrl Pts',(-34.0076485650749,-4.80082439457541,
126.867681438675));
#276622=CARTESIAN_POINT('Ctrl Pts',(-34.2860961888878,-5.90700253767186,
132.715558892209));
#276623=CARTESIAN_POINT('Ctrl Pts',(-34.5645438127007,-1.58493392176466,
136.807138498572));
#276624=CARTESIAN_POINT('Ctrl Pts',(-34.8429914365135,4.19361153991761,
135.382458484293));
#276625=CARTESIAN_POINT('Ctrl Pts',(-35.1214390603265,6.11843286572883,
129.750730183006));
#276626=CARTESIAN_POINT('Ctrl Pts',(-35.3998866841394,2.42071328999757,
125.087236778371));
#276627=CARTESIAN_POINT('Ctrl Pts',(-35.6783343079523,-3.50152354082281,
125.677500884929));
#276628=CARTESIAN_POINT('Ctrl Pts',(-35.9567819317651,-6.20603129656164,
130.979098624759));
#276629=CARTESIAN_POINT('Ctrl Pts',(-36.2352295555781,-3.2074994722443,
136.120120672404));
#276630=CARTESIAN_POINT('Ctrl Pts',(-36.5136771793909,2.73856767200523,
136.376218918968));
#276631=CARTESIAN_POINT('Ctrl Pts',(-36.7921248032039,6.1680249121504,131.512051586954));
#276632=CARTESIAN_POINT('Ctrl Pts',(-37.0705724270167,3.92936858279784,
125.997550826698));
#276633=CARTESIAN_POINT('Ctrl Pts',(-37.3490200508296,-1.92018551381882,
124.900273438536));
#276634=CARTESIAN_POINT('Ctrl Pts',(-37.6274676746425,-6.00518292951342,
129.228563737208));
#276635=CARTESIAN_POINT('Ctrl Pts',(-37.9059152984554,-4.57171060248077,
135.004934386972));
#276636=CARTESIAN_POINT('Ctrl Pts',(-38.1843629222683,1.0629404277527,136.921182952087));
#276637=CARTESIAN_POINT('Ctrl Pts',(-38.4628105460811,5.72080113240803,
133.216370615161));
#276638=CARTESIAN_POINT('Ctrl Pts',(-38.7412581698941,5.12152507305273,
127.295038923683));
#276639=CARTESIAN_POINT('Ctrl Pts',(-39.0197057937069,-0.184182328028525,
124.598602428988));
#276640=CARTESIAN_POINT('Ctrl Pts',(-39.2981534175199,-5.32063516745863,
127.604954541453));
#276641=CARTESIAN_POINT('Ctrl Pts',(-39.5766010413327,-5.56768421547239,
133.55140453819));
#276642=CARTESIAN_POINT('Ctrl Pts',(-39.8550486651457,-0.698303465962086,
136.973455372429));
#276643=CARTESIAN_POINT('Ctrl Pts',(-40.1334962889585,4.81278405474664,
134.726409503982));
#276644=CARTESIAN_POINT('Ctrl Pts',(-40.4119439127715,5.90115814671511,
128.875192311658));
#276645=CARTESIAN_POINT('Ctrl Pts',(-40.6903915365843,1.56665618945481,
124.796786547352));
#276646=CARTESIAN_POINT('Ctrl Pts',(-40.9688391603973,-4.20752627050468,
126.239047867263));
#276647=CARTESIAN_POINT('Ctrl Pts',(-41.2472867842101,-6.11519763695597,
131.876608576776));
#276648=CARTESIAN_POINT('Ctrl Pts',(-41.5257344080229,-2.40330111905734,
136.528825793999));
#276649=CARTESIAN_POINT('Ctrl Pts',(-41.8041820318359,3.51711171946819,
135.920539169751));
#276650=CARTESIAN_POINT('Ctrl Pts',(-42.0826296556488,6.20547070826194,
130.610734395262));
#276651=CARTESIAN_POINT('Ctrl Pts',(-42.3610772794617,3.19130527026066,
125.478862659902));
#276652=CARTESIAN_POINT('Ctrl Pts',(-42.6395249032745,-2.75551380718057,
125.240863382598));
#276653=CARTESIAN_POINT('Ctrl Pts',(-42.9179725270875,-6.17015031015604,
130.115446272278));
#276654=CARTESIAN_POINT('Ctrl Pts',(-43.1964201509003,-3.91472010669807,
135.623107789941));
#276655=CARTESIAN_POINT('Ctrl Pts',(-43.4748677747133,1.93814663010615,
136.702576065077));
#276656=CARTESIAN_POINT('Ctrl Pts',(-43.7533153985261,6.00995129756958,
132.361872487794));
#276657=CARTESIAN_POINT('Ctrl Pts',(-44.031763022339,4.55890432500984,126.589891590455));
#276658=CARTESIAN_POINT('Ctrl Pts',(-44.3102106461518,-1.08155300737633,
124.690801840773));
#276659=CARTESIAN_POINT('Ctrl Pts',(-44.5886582699649,-5.72811596278534,
128.409773943013));
#276660=CARTESIAN_POINT('Ctrl Pts',(-44.8671058937777,-5.11082018241628,
134.329254217104));
#276661=CARTESIAN_POINT('Ctrl Pts',(-45.1455535175906,0.2030696681468,137.009529473845));
#276662=CARTESIAN_POINT('Ctrl Pts',(-45.4240011414034,5.33034841418793,
133.987557691017));
#276663=CARTESIAN_POINT('Ctrl Pts',(-45.7024487652165,5.55929736958694,
128.040383305508));
#276664=CARTESIAN_POINT('Ctrl Pts',(-45.9808963890292,0.679523629110432,
124.633169041983));
#276665=CARTESIAN_POINT('Ctrl Pts',(-46.2593440128422,-4.82469912994364,
126.896978356949));
#276666=CARTESIAN_POINT('Ctrl Pts',(-46.537791636655,-5.89525908823553,
132.751481083186));
#276667=CARTESIAN_POINT('Ctrl Pts',(-46.816239260468,-1.54836394385628,
136.816675223641));
#276668=CARTESIAN_POINT('Ctrl Pts',(-47.0946868842807,4.22140202314317,
135.35684595901));
#276669=CARTESIAN_POINT('Ctrl Pts',(-47.3731345080937,6.11190575782758,
129.713505066864));
#276670=CARTESIAN_POINT('Ctrl Pts',(-47.6515821319066,2.38586668426401,
125.072607134557));
#276671=CARTESIAN_POINT('Ctrl Pts',(-47.9300297557195,-3.53266731607082,
125.69891064141));
#276672=CARTESIAN_POINT('Ctrl Pts',(-48.2084773795324,-6.20485263332943,
131.016873261253));
#276673=CARTESIAN_POINT('Ctrl Pts',(-48.4869250033452,-3.17508150446096,
136.139547143367));
#276674=CARTESIAN_POINT('Ctrl Pts',(-48.7653726271582,2.77243441565242,
136.359445246621));
#276675=CARTESIAN_POINT('Ctrl Pts',(-49.043820250971,6.1722185487321,131.474491956744));
#276676=CARTESIAN_POINT('Ctrl Pts',(-49.322267874784,3.900035365166,125.973720703898));
#276677=CARTESIAN_POINT('Ctrl Pts',(-49.6007154985968,-1.95608979166789,
124.912071541833));
#276678=CARTESIAN_POINT('Ctrl Pts',(-49.8791631224098,-6.0146639902579,
129.265148186042));
#276679=CARTESIAN_POINT('Ctrl Pts',(-50.1576107462225,-4.54605581447205,
135.032685860113));
#276680=CARTESIAN_POINT('Ctrl Pts',(-50.4360583700356,1.10015556764067,
136.914599201455));
#276681=CARTESIAN_POINT('Ctrl Pts',(-50.7145059938484,5.73537772867887,
133.181501785951));
#276682=CARTESIAN_POINT('Ctrl Pts',(-50.9929536176612,5.10006794583985,
127.263927766504));
#276683=CARTESIAN_POINT('Ctrl Pts',(-51.2714012414742,-0.221955127055423,
124.599838577421));
#276684=CARTESIAN_POINT('Ctrl Pts',(-51.5498488652871,-5.34001228129766,
127.637402035479));
#276685=CARTESIAN_POINT('Ctrl Pts',(-51.8282964891,-5.5508590231301,133.585245715947));
#276686=CARTESIAN_POINT('Ctrl Pts',(-52.1067441129128,-0.660737497244709,
136.977591844792));
#276687=CARTESIAN_POINT('Ctrl Pts',(-52.3851917367258,4.8365695097872,134.697040054928));
#276688=CARTESIAN_POINT('Ctrl Pts',(-52.6636393605386,5.889305416881,128.83930603009));
#276689=CARTESIAN_POINT('Ctrl Pts',(-52.9420869843516,1.53005735442545,
124.78736117289));
#276690=CARTESIAN_POINT('Ctrl Pts',(-53.2205346081644,-4.23523866929,126.264744858582));
#276691=CARTESIAN_POINT('Ctrl Pts',(-53.4989822319774,-6.1085572588392,
131.913813654221));
#276692=CARTESIAN_POINT('Ctrl Pts',(-53.7774298557902,-2.36841014712749,
136.543349308967));
#276693=CARTESIAN_POINT('Ctrl Pts',(-54.0558774796031,3.54819018652628,
135.8990347215));
#276694=CARTESIAN_POINT('Ctrl Pts',(-54.334325103416,6.20417707748961,130.572963521183));
#276695=CARTESIAN_POINT('Ctrl Pts',(-54.6127727272289,3.15882832513996,
125.459534948064));
#276696=CARTESIAN_POINT('Ctrl Pts',(-54.8912203510417,-2.7893293406706,
125.257740055968));
#276697=CARTESIAN_POINT('Ctrl Pts',(-55.1696679748547,-6.17422960871856,
130.153018492501));
#276698=CARTESIAN_POINT('Ctrl Pts',(-55.4481155986676,-3.88531449423931,
135.646848522136));
#276699=CARTESIAN_POINT('Ctrl Pts',(-55.7265632224805,1.97401483228084,
136.690668736158));
#276700=CARTESIAN_POINT('Ctrl Pts',(-56.0050108462934,6.01932096392068,
132.32525935133));
#276701=CARTESIAN_POINT('Ctrl Pts',(-56.2834584701062,4.53316518989421,
126.562218330207));
#276702=CARTESIAN_POINT('Ctrl Pts',(-56.5619060939192,-1.11874793621411,
124.697498830995));
#276703=CARTESIAN_POINT('Ctrl Pts',(-56.840353717732,-5.74258636281662,
128.444686976857));
#276704=CARTESIAN_POINT('Ctrl Pts',(-57.118801341545,-5.08926846293066,
134.360299922064));
#276705=CARTESIAN_POINT('Ctrl Pts',(-57.3972489653578,0.240838529802063,
137.00817836373));
#276706=CARTESIAN_POINT('Ctrl Pts',(-57.6756965891708,5.34962667926312,
133.955051370017));
#276707=CARTESIAN_POINT('Ctrl Pts',(-57.9541442129836,5.54236925427356,
128.0065934946));
#276708=CARTESIAN_POINT('Ctrl Pts',(-58.2325918367966,0.641945244397073,
124.629146926667));
#276709=CARTESIAN_POINT('Ctrl Pts',(-58.5110394606094,-4.84839508431156,
126.92642006471));
#276710=CARTESIAN_POINT('Ctrl Pts',(-58.7894870844223,-5.88329718780563,
132.787331122898));
#276711=CARTESIAN_POINT('Ctrl Pts',(-59.0679347082352,-1.5117365907523,
136.825989160181));
#276712=CARTESIAN_POINT('Ctrl Pts',(-59.3463823320481,4.24903608076433,
135.331064739709));
#276713=CARTESIAN_POINT('Ctrl Pts',(-59.624829955861,6.10515217101086,129.676320372777));
#276714=CARTESIAN_POINT('Ctrl Pts',(-59.9032775796738,2.3509316693629,125.058189882977));
#276715=CARTESIAN_POINT('Ctrl Pts',(-60.1817252034868,-3.56368018703254,
125.720509582217));
#276716=CARTESIAN_POINT('Ctrl Pts',(-60.4601728272995,-6.20344404700091,
131.054640023013));
#276717=CARTESIAN_POINT('Ctrl Pts',(-60.7386204511126,-3.14254588286485,
136.158775917031));
#276718=CARTESIAN_POINT('Ctrl Pts',(-61.0170680749254,2.80619842572279,
136.342465728569));
#276719=CARTESIAN_POINT('Ctrl Pts',(-61.2955156987383,6.17618347148551,
131.436907494571));
#276720=CARTESIAN_POINT('Ctrl Pts',(-61.5739633225512,3.87055763028967,
125.950069582238));
#276721=CARTESIAN_POINT('Ctrl Pts',(-61.8524109463641,-1.9919215858902,
124.924087986069));
#276722=CARTESIAN_POINT('Ctrl Pts',(-62.130858570177,-6.02392217541635,
129.301789670958));
#276723=CARTESIAN_POINT('Ctrl Pts',(-62.4093061939898,-4.5202325706933,
135.060280651108));
#276724=CARTESIAN_POINT('Ctrl Pts',(-62.6877538178028,1.13732994085927,
136.907789033684));
#276725=CARTESIAN_POINT('Ctrl Pts',(-62.9662014416156,5.74974179841868,
133.146544870902));
#276726=CARTESIAN_POINT('Ctrl Pts',(-63.2446490654287,5.0784218337339,127.232947801366));
#276727=CARTESIAN_POINT('Ctrl Pts',(-63.5230966892413,-0.25971970145348,
124.601304636701));
#276728=CARTESIAN_POINT('Ctrl Pts',(-63.8015443130544,-5.3591915190178,
127.669966882319));
#276729=CARTESIAN_POINT('Ctrl Pts',(-64.0799919368672,-5.53382814166538,
133.618983846983));
#276730=CARTESIAN_POINT('Ctrl Pts',(-64.3584395606801,-0.623147044656387,
136.9814995658));
#276731=CARTESIAN_POINT('Ctrl Pts',(-64.636887184493,4.86017574396616,134.667526361205));
#276732=CARTESIAN_POINT('Ctrl Pts',(-64.9153348083059,5.8772344566688,128.803492564343));
#276733=CARTESIAN_POINT('Ctrl Pts',(-65.1937824321189,1.4934018225579,124.778158760555));
#276734=CARTESIAN_POINT('Ctrl Pts',(-65.4722300559316,-4.26279412974889,
126.290610067033));
#276735=CARTESIAN_POINT('Ctrl Pts',(-65.7506776797446,-6.10169052588679,
131.950977620477));
#276736=CARTESIAN_POINT('Ctrl Pts',(-66.0291253035574,-2.33343141288849,
136.5576601636));
#276737=CARTESIAN_POINT('Ctrl Pts',(-66.3075729273703,3.57913717409239,
135.877341488227));
#276738=CARTESIAN_POINT('Ctrl Pts',(-66.5860205511832,6.20265354865397,
130.535201221608));
#276739=CARTESIAN_POINT('Ctrl Pts',(-66.8644681749961,3.126234328474,125.440405290707));
#276740=CARTESIAN_POINT('Ctrl Pts',(-67.142915798809,-2.82304151453613,
125.274822261403));
#276741=CARTESIAN_POINT('Ctrl Pts',(-67.421363422622,-6.17808011893247,
130.190614848446));
#276742=CARTESIAN_POINT('Ctrl Pts',(-67.6998110464348,-3.85576491002292,
135.670409814162));
#276743=CARTESIAN_POINT('Ctrl Pts',(-67.9782586702478,2.00980988661012,
136.678543287925));
#276744=CARTESIAN_POINT('Ctrl Pts',(-68.2567062940606,6.02846758211988,
132.288589857404));
#276745=CARTESIAN_POINT('Ctrl Pts',(-68.5351539178734,4.50725807667536,
126.534702264101));
#276746=CARTESIAN_POINT('Ctrl Pts',(-68.8136015416864,-1.15590140943545,
124.704422113226));
#276747=CARTESIAN_POINT('Ctrl Pts',(-69.0920491654993,-5.75684396919829,
128.479687449276));
#276748=CARTESIAN_POINT('Ctrl Pts',(-69.3704967893121,-5.0675281587308,
134.391213860386));
#276749=CARTESIAN_POINT('Ctrl Pts',(-69.648944413125,0.278598467097045,
137.006597368867));
#276750=CARTESIAN_POINT('Ctrl Pts',(-69.9273920369379,5.36870671195437,
133.922428299012));
#276751=CARTESIAN_POINT('Ctrl Pts',(-70.2058396607509,5.52523576442926,
127.972907355982));
#276752=CARTESIAN_POINT('Ctrl Pts',(-70.4842872845636,0.604343072166899,
124.625353636165));
#276753=CARTESIAN_POINT('Ctrl Pts',(-70.7627349083767,-4.87191137961658,
126.956005470983));
#276754=CARTESIAN_POINT('Ctrl Pts',(-71.0411825321895,-5.87111727963483,
132.823107682909));
#276755=CARTESIAN_POINT('Ctrl Pts',(-71.3196301560023,-1.47505321969301,
136.835079963061));
#276756=CARTESIAN_POINT('Ctrl Pts',(-71.5980777798154,4.27651268879093,
135.305115781721));
#276757=CARTESIAN_POINT('Ctrl Pts',(-71.8765254036282,6.09817235553532,
129.639177478635));
#276758=CARTESIAN_POINT('Ctrl Pts',(-72.1549730274411,2.31590953982396,
125.043985557866));
#276759=CARTESIAN_POINT('Ctrl Pts',(-72.433420651254,-3.5945610045145,125.742296906994));
#276760=CARTESIAN_POINT('Ctrl Pts',(-72.7118682750669,-6.20180558977201,
131.092397510578));
#276761=CARTESIAN_POINT('Ctrl Pts',(-72.9903158988798,-3.109893813075,136.177806280867));
#276762=CARTESIAN_POINT('Ctrl Pts',(-73.2687635226926,2.8398584510789,136.325280993997));
#276763=CARTESIAN_POINT('Ctrl Pts',(-73.5472111465057,6.17991953348924,
131.399299593141));
#276764=CARTESIAN_POINT('Ctrl Pts',(-73.8256587703184,3.84093647047644,
125.926598338115));
#276765=CARTESIAN_POINT('Ctrl Pts',(-74.1041063941314,-2.02767956872624,
124.93632232597));
#276766=CARTESIAN_POINT('Ctrl Pts',(-74.3825540179442,-6.0329571419232,
129.338486834193));
#276767=CARTESIAN_POINT('Ctrl Pts',(-74.6610016417573,-4.49424182803428,
135.08771773742));
#276768=CARTESIAN_POINT('Ctrl Pts',(-74.9394492655699,1.17446216989917,
136.900752701129));
#276769=CARTESIAN_POINT('Ctrl Pts',(-75.217896889383,5.76389280936176,133.111501165354));
#276770=CARTESIAN_POINT('Ctrl Pts',(-75.4963445131958,5.05658753883907,
127.202100176243));
#276771=CARTESIAN_POINT('Ctrl Pts',(-75.7747921370087,-0.297474651842549,
124.603000552501));
#276772=CARTESIAN_POINT('Ctrl Pts',(-76.0532397608216,-5.37817216992523,
127.702647875272));
#276773=CARTESIAN_POINT('Ctrl Pts',(-76.3316873846344,-5.51659220216403,
133.65261768112));
#276774=CARTESIAN_POINT('Ctrl Pts',(-76.6101350084474,-0.585533501125347,
136.985178390654));
#276775=CARTESIAN_POINT('Ctrl Pts',(-76.8885826322602,4.8836018825454,134.637869516455));
#276776=CARTESIAN_POINT('Ctrl Pts',(-77.1670302560731,5.86494571337264,
128.767753241497));
#276777=CARTESIAN_POINT('Ctrl Pts',(-77.4454778798861,1.4566909521364,124.769179651345));
#276778=CARTESIAN_POINT('Ctrl Pts',(-77.7239255036988,-4.29019163080361,
126.316642534169));
#276779=CARTESIAN_POINT('Ctrl Pts',(-78.0023731275119,-6.09459769254796,
131.988099098418));
#276780=CARTESIAN_POINT('Ctrl Pts',(-78.2808207513247,-2.29836621249045,
136.571757827603));
#276781=CARTESIAN_POINT('Ctrl Pts',(-78.5592683751376,3.60995153541429,
135.855460273781));
#276782=CARTESIAN_POINT('Ctrl Pts',(-78.8377159989505,6.20090017820995,
130.497448895834));
#276783=CARTESIAN_POINT('Ctrl Pts',(-79.1161636227633,3.09352448804556,
125.421474396687));
#276784=CARTESIAN_POINT('Ctrl Pts',(-79.3946112465763,-2.85664907955992,
125.292109365916));
#276785=CARTESIAN_POINT('Ctrl Pts',(-79.6730588703891,-6.18170169811556,
130.228233946967));
#276786=CARTESIAN_POINT('Ctrl Pts',(-79.9515064942021,-3.8260724490201,
135.693790792945));
#276787=CARTESIAN_POINT('Ctrl Pts',(-80.2299541180149,2.04553046669522,
136.666200169693));
#276788=CARTESIAN_POINT('Ctrl Pts',(-80.5084017418279,6.03739081323573,
132.251865364817));
#276789=CARTESIAN_POINT('Ctrl Pts',(-80.7868493656406,4.48118394535095,
126.507344411756));
#276790=CARTESIAN_POINT('Ctrl Pts',(-81.0652969894537,-1.19301205030527,
124.711571430921));
#276791=CARTESIAN_POINT('Ctrl Pts',(-81.3437446132665,-5.77088825360962,
128.514774063314));
#276792=CARTESIAN_POINT('Ctrl Pts',(-81.6221922370794,-5.04560007541116,
134.421994886542));
#276793=CARTESIAN_POINT('Ctrl Pts',(-81.9006398608923,0.316348080823153,
137.00478654784));
#276794=CARTESIAN_POINT('Ctrl Pts',(-82.179087484705,5.38758780524389,133.889689686862));
#276795=CARTESIAN_POINT('Ctrl Pts',(-82.4575351085182,5.50789753494193,
127.939326137905));
#276796=CARTESIAN_POINT('Ctrl Pts',(-82.7359827323308,0.566718505781886,
124.621789311041));
#276797=CARTESIAN_POINT('Ctrl Pts',(-83.0144303561439,-4.89524714445407,
126.985733479472));
#276798=CARTESIAN_POINT('Ctrl Pts',(-83.2928779799568,-5.858719815054,132.858809437506));
#276799=CARTESIAN_POINT('Ctrl Pts',(-83.5713256037696,-1.43831518999427,
136.843947295418));
#276800=CARTESIAN_POINT('Ctrl Pts',(-83.8497732275826,4.30383082906709,
135.279000046597));
#276801=CARTESIAN_POINT('Ctrl Pts',(-84.1282208513953,6.09096657004034,
129.602077760783));
#276802=CARTESIAN_POINT('Ctrl Pts',(-84.4066684752085,2.28080159340614,
125.029994685571));
#276803=CARTESIAN_POINT('Ctrl Pts',(-84.685116099021,-3.6253086242162,125.764271808403));
#276804=CARTESIAN_POINT('Ctrl Pts',(-84.9635637228342,-6.19993732235617,
131.130144324829));
#276805=CARTESIAN_POINT('Ctrl Pts',(-85.242011346647,-3.07712650502686,
136.196637529698));
#276806=CARTESIAN_POINT('Ctrl Pts',(-85.5204589704598,2.87341324443482,
136.307891679689));
#276807=CARTESIAN_POINT('Ctrl Pts',(-85.7989065942728,6.18342659630218,
131.361669646028));
#276808=CARTESIAN_POINT('Ctrl Pts',(-86.0773542180856,3.81117298335027,
125.903307841269));
#276809=CARTESIAN_POINT('Ctrl Pts',(-86.3558018418987,-2.06336241514917,
124.948774108188));
#276810=CARTESIAN_POINT('Ctrl Pts',(-86.6342494657113,-6.04176855498474,
129.375238315919));
#276811=CARTESIAN_POINT('Ctrl Pts',(-86.9126970895244,-4.46808454959173,
135.114996102359));
#276812=CARTESIAN_POINT('Ctrl Pts',(-87.1911447133372,1.2115508788106,136.893490464523));
#276813=CARTESIAN_POINT('Ctrl Pts',(-87.4695923371502,5.77783023713722,
133.076371967865));
#276814=CARTESIAN_POINT('Ctrl Pts',(-87.7480399609628,5.03456587023344,
127.171386034204));
#276815=CARTESIAN_POINT('Ctrl Pts',(-88.026487584776,-0.33521857919891,
124.60492626198));
#276816=CARTESIAN_POINT('Ctrl Pts',(-88.3049352085887,-5.39695353068522,
127.735443803332));
#276817=CARTESIAN_POINT('Ctrl Pts',(-88.5833828324018,-5.49915184330967,
133.686145972045));
#276818=CARTESIAN_POINT('Ctrl Pts',(-88.8618304562145,-0.547898260434929,
136.988628183031));
#276819=CARTESIAN_POINT('Ctrl Pts',(-89.1402780800275,4.90684705746115,
134.608070619623));
#276820=CARTESIAN_POINT('Ctrl Pts',(-89.4187257038403,5.85243964235601,
128.732089385887));
#276821=CARTESIAN_POINT('Ctrl Pts',(-89.6971733276532,1.41992610349655,
124.760424177987));
#276822=CARTESIAN_POINT('Ctrl Pts',(-89.9756209514662,-4.31743015722937,
126.342841295349));
#276823=CARTESIAN_POINT('Ctrl Pts',(-90.254068575279,-6.08727902165076,
132.025176712493));
#276824=CARTESIAN_POINT('Ctrl Pts',(-90.5325161990919,-2.26321584528708,
136.585641778581));
#276825=CARTESIAN_POINT('Ctrl Pts',(-90.8109638229048,3.64063212865448,
135.833391888981));
#276826=CARTESIAN_POINT('Ctrl Pts',(-91.0894114467178,6.19891703112955,
130.459707942787));
#276827=CARTESIAN_POINT('Ctrl Pts',(-91.3678590705306,3.06070001592934,
125.402742967496));
#276828=CARTESIAN_POINT('Ctrl Pts',(-91.6463066943433,-2.89015079040179,
125.309600728926));
#276829=CARTESIAN_POINT('Ctrl Pts',(-91.9247543181566,-6.18509421206894,
130.265874394073));
#276830=CARTESIAN_POINT('Ctrl Pts',(-92.2032019419691,-3.79623821149537,
135.716990592095));
#276831=CARTESIAN_POINT('Ctrl Pts',(-92.4816495657822,2.08117524889636,
136.653639838841));
#276832=CARTESIAN_POINT('Ctrl Pts',(-92.7600971895951,6.04609032661485,
132.21508723441));
#276833=CARTESIAN_POINT('Ctrl Pts',(-93.0385448134079,4.45494376210749,
126.480145786926));
#276834=CARTESIAN_POINT('Ctrl Pts',(-93.3169924372209,-1.23007848367479,
124.718946519161));
#276835=CARTESIAN_POINT('Ctrl Pts',(-93.5954400610337,-5.78471869563455,
128.549945518824));
#276836=CARTESIAN_POINT('Ctrl Pts',(-93.8738876848466,-5.02348502552524,
134.45264185993));
#276837=CARTESIAN_POINT('Ctrl Pts',(-94.1523353086595,0.354085972155003,
137.002745967751));
#276838=CARTESIAN_POINT('Ctrl Pts',(-94.4307829324724,5.40626925948619,
133.85683674671));
#276839=CARTESIAN_POINT('Ctrl Pts',(-94.7092305562852,5.49035520828578,
127.905851084735));
#276840=CARTESIAN_POINT('Ctrl Pts',(-94.9876781800983,0.529072939433998,
124.618454083368));
#276841=CARTESIAN_POINT('Ctrl Pts',(-95.2661258039109,-4.91840151410816,
127.015602988595));
#276842=CARTESIAN_POINT('Ctrl Pts',(-95.5445734277241,-5.84610525345601,
132.894435063746));
#276843=CARTESIAN_POINT('Ctrl Pts',(-95.8230210515366,-1.40152386299717,
136.85259082867));
#276844=CARTESIAN_POINT('Ctrl Pts',(-96.10146867535,4.33098948930923,135.252718502061));
#276845=CARTESIAN_POINT('Ctrl Pts',(-96.3799162991623,6.08353508153927,
129.565022593965));
#276846=CARTESIAN_POINT('Ctrl Pts',(-96.6583639229758,2.245609131046,125.01621778453));
#276847=CARTESIAN_POINT('Ctrl Pts',(-96.9368115467883,-3.65592190677386,
125.786433472156));
#276848=CARTESIAN_POINT('Ctrl Pts',(-97.2152591706015,-6.19783931398261,
131.167879067045));
#276849=CARTESIAN_POINT('Ctrl Pts',(-97.493706794414,-3.04424517292474,
136.215268965725));
#276850=CARTESIAN_POINT('Ctrl Pts',(-97.7721544182274,2.90686156240656,
136.290298430015));
#276851=CARTESIAN_POINT('Ctrl Pts',(-98.0506020420397,6.18670452996842,
131.324019047625));
#276852=CARTESIAN_POINT('Ctrl Pts',(-98.3290496658531,3.78126827180747,
125.880198954735));
#276853=CARTESIAN_POINT('Ctrl Pts',(-98.6074972896656,-2.09896880291958,
124.961442871316));
#276854=CARTESIAN_POINT('Ctrl Pts',(-98.8859449134787,-6.05035608809047,
129.412042754299));
#276855=CARTESIAN_POINT('Ctrl Pts',(-99.1643925372916,-4.44176170463296,
135.142114735114));
#276856=CARTESIAN_POINT('Ctrl Pts',(-99.4428401611044,1.24859469325925,
136.886002592972));
#276857=CARTESIAN_POINT('Ctrl Pts',(-99.7212877849174,5.79155356528836,
133.041158580159));
#276858=CARTESIAN_POINT('Ctrl Pts',(-99.9997354087301,5.01235764393804,
127.140806513377));
#276859=CARTESIAN_POINT('Ctrl Pts',(-100.278183032543,-0.37295008490757,
124.607081693777));
#276860=CARTESIAN_POINT('Ctrl Pts',(-100.556630656356,-5.41553490534739,
127.768353451233));
#276861=CARTESIAN_POINT('Ctrl Pts',(-100.835078280169,-5.48150771136145,
133.719567477352));
#276862=CARTESIAN_POINT('Ctrl Pts',(-101.113525903981,-0.510242717172956,
136.9918488151));
#276863=CARTESIAN_POINT('Ctrl Pts',(-101.391973527794,4.92991040735466,
134.578130774917));
#276864=CARTESIAN_POINT('Ctrl Pts',(-101.670421151607,5.83971670703623,
128.696502319049));
#276865=CARTESIAN_POINT('Ctrl Pts',(-101.94886877542,1.38310863897239,124.751892664915));
#276866=CARTESIAN_POINT('Ctrl Pts',(-102.227316399233,-4.34450869969331,
126.36920537977));
#276867=CARTESIAN_POINT('Ctrl Pts',(-102.505764023046,-6.07973478439049,
132.062209088779));
#276868=CARTESIAN_POINT('Ctrl Pts',(-102.784211646859,-2.22798161378826,
136.599311502058));
#276869=CARTESIAN_POINT('Ctrl Pts',(-103.062659270672,3.6711778169323,135.811137151577));
#276870=CARTESIAN_POINT('Ctrl Pts',(-103.341106894485,6.19670418089893,
130.42197976097));
#276871=CARTESIAN_POINT('Ctrl Pts',(-103.619554518298,3.02776212844844,
125.384211697232));
#276872=CARTESIAN_POINT('Ctrl Pts',(-103.89800214211,-2.92354540564323,
125.327295702285));
#276873=CARTESIAN_POINT('Ctrl Pts',(-104.176449765923,-6.18825753508174,
130.303534794984));
#276874=CARTESIAN_POINT('Ctrl Pts',(-104.454897389736,-3.76626330296762,
135.740008351935));
#276875=CARTESIAN_POINT('Ctrl Pts',(-104.733345013549,2.1167429123828,136.640862760796));
#276876=CARTESIAN_POINT('Ctrl Pts',(-105.011792637362,6.05456579989334,
132.17825682901));
#276877=CARTESIAN_POINT('Ctrl Pts',(-105.290240261175,4.42853849928509,
126.453107397468));
#276878=CARTESIAN_POINT('Ctrl Pts',(-105.568687884988,-1.26709933603374,
124.726547104658));
#276879=CARTESIAN_POINT('Ctrl Pts',(-105.847135508801,-5.79833478278087,
128.585200512514));
#276880=CARTESIAN_POINT('Ctrl Pts',(-106.125583132613,-5.00118382855433,
134.483153644914));
#276881=CARTESIAN_POINT('Ctrl Pts',(-106.404030756427,0.391810742700936,
137.000475704212));
#276882=CARTESIAN_POINT('Ctrl Pts',(-106.682478380239,5.42475038243292,
133.823870695931));
#276883=CARTESIAN_POINT('Ctrl Pts',(-106.960926004052,5.47260943449832,
127.872483436902));
#276884=CARTESIAN_POINT('Ctrl Pts',(-107.239373627865,0.491407768093767,
124.615348076738));
#276885=CARTESIAN_POINT('Ctrl Pts',(-107.517821251678,-4.94137363058539,
127.045612891524));
#276886=CARTESIAN_POINT('Ctrl Pts',(-107.796268875491,-5.83327406227795,
132.929983241508));
#276887=CARTESIAN_POINT('Ctrl Pts',(-108.074716499304,-1.36468060201792,
136.861010242526));
#276888=CARTESIAN_POINT('Ctrl Pts',(-108.353164123117,4.3579876631431,135.22627212199));
#276889=CARTESIAN_POINT('Ctrl Pts',(-108.631611746929,6.07587816540856,
129.528013351273));
#276890=CARTESIAN_POINT('Ctrl Pts',(-108.910059370743,2.21033345681367,
125.00265536525));
#276891=CARTESIAN_POINT('Ctrl Pts',(-109.188506994555,-3.68639971780079,
125.808781077045));
#276892=CARTESIAN_POINT('Ctrl Pts',(-109.466954618368,-6.19551164239422,
131.205600338952));
#276893=CARTESIAN_POINT('Ctrl Pts',(-109.745402242181,-3.01125103519769,
136.233699898554));
#276894=CARTESIAN_POINT('Ctrl Pts',(-110.023849865994,2.94020216555433,
136.272501896897));
#276895=CARTESIAN_POINT('Ctrl Pts',(-110.302297489807,6.18975321302316,
131.286349193086));
#276896=CARTESIAN_POINT('Ctrl Pts',(-110.58074511362,3.75122344397827,125.857272534824));
#276897=CARTESIAN_POINT('Ctrl Pts',(-110.859192737433,-2.13449741262907,
124.974328145912));
#276898=CARTESIAN_POINT('Ctrl Pts',(-111.137640361246,-6.05871942302636,
129.44889878553));
#276899=CARTESIAN_POINT('Ctrl Pts',(-111.416087985058,-4.41527426856075,
135.169072630797));
#276900=CARTESIAN_POINT('Ctrl Pts',(-111.694535608871,1.28559224057236,
136.878289363941));
#276901=CARTESIAN_POINT('Ctrl Pts',(-111.972983232684,5.8050622852923,133.005862307081));
#276902=CARTESIAN_POINT('Ctrl Pts',(-112.251430856497,4.9899636828869,127.110362746893));
#276903=CARTESIAN_POINT('Ctrl Pts',(-112.52987848031,-0.410667770813077,
124.609466768025));
#276904=CARTESIAN_POINT('Ctrl Pts',(-112.808326104123,-5.43391560537209,
127.801375599495));
#276905=CARTESIAN_POINT('Ctrl Pts',(-113.086773727936,-5.46366046012913,
133.752880958598));
#276906=CARTESIAN_POINT('Ctrl Pts',(-113.365221351749,-0.472568266679477,
136.994840167519));
#276907=CARTESIAN_POINT('Ctrl Pts',(-113.643668975562,4.95279107760506,
134.548051091771));
#276908=CARTESIAN_POINT('Ctrl Pts',(-113.922116599375,5.8267773788663,128.660993359675));
#276909=CARTESIAN_POINT('Ctrl Pts',(-114.200564223187,1.34623992284899,
124.74358542827));
#276910=CARTESIAN_POINT('Ctrl Pts',(-114.479011847001,-4.37142625478972,
126.395733810498));
#276911=CARTESIAN_POINT('Ctrl Pts',(-114.757459470813,-6.07196526032194,
132.099194855029));
#276912=CARTESIAN_POINT('Ctrl Pts',(-115.035907094626,-2.19266482361144,
136.612766491501));
#276913=CARTESIAN_POINT('Ctrl Pts',(-115.314354718439,3.70158746836604,
135.788696886227));
#276914=CARTESIAN_POINT('Ctrl Pts',(-115.592802342252,6.19426170951602,
130.384265748418));
#276915=CARTESIAN_POINT('Ctrl Pts',(-115.871249966065,2.99471204612843,
125.36588127258));
#276916=CARTESIAN_POINT('Ctrl Pts',(-116.149697589878,-2.95683168783455,
125.345193630298));
#276917=CARTESIAN_POINT('Ctrl Pts',(-116.428145213691,-6.19119154993583,
130.34121375418));
#276918=CARTESIAN_POINT('Ctrl Pts',(-116.706592837503,-3.73614883416816,
135.762843219532));
#276919=CARTESIAN_POINT('Ctrl Pts',(-116.985040461316,2.1522321391827,136.627869409019));
#276920=CARTESIAN_POINT('Ctrl Pts',(-117.263488085129,6.06281691900968,
132.14137551338));
#276921=CARTESIAN_POINT('Ctrl Pts',(-117.541935708942,4.40196913533955,
126.426230245297));
#276922=CARTESIAN_POINT('Ctrl Pts',(-117.820383332755,-1.30407323556081,
124.73437290577));
#276923=CARTESIAN_POINT('Ctrl Pts',(-118.098830956568,-5.81173601049948,
128.620537737998));
#276924=CARTESIAN_POINT('Ctrl Pts',(-118.377278580381,-4.97869731087745,
134.51352911087));
#276925=CARTESIAN_POINT('Ctrl Pts',(-118.655726204194,0.429520994555717,
136.997975841351));
#276926=CARTESIAN_POINT('Ctrl Pts',(-118.934173828006,5.44303048925927,
133.790792756097));
#276927=CARTESIAN_POINT('Ctrl Pts',(-119.21262145182,5.45466087115571,127.839224430854));
#276928=CARTESIAN_POINT('Ctrl Pts',(-119.491069075632,0.453724387457947,
124.612471406243));
#276929=CARTESIAN_POINT('Ctrl Pts',(-119.769516699445,-4.96416264264509,
127.075762076232));
#276930=CARTESIAN_POINT('Ctrl Pts',(-120.047964323258,-5.82022671698453,
132.965452653541));
#276931=CARTESIAN_POINT('Ctrl Pts',(-120.326411947071,-1.32778677229758,
136.869205225004));
#276932=CARTESIAN_POINT('Ctrl Pts',(-120.604859570884,4.38482435014149,
135.199661886361));
#276933=CARTESIAN_POINT('Ctrl Pts',(-120.883307194697,6.06799610537801,
129.491051404098));
#276934=CARTESIAN_POINT('Ctrl Pts',(-121.16175481851,2.17497587786225,124.989307930291));
#276935=CARTESIAN_POINT('Ctrl Pts',(-121.440202442323,-3.71674092793051,
125.831313794972));
#276936=CARTESIAN_POINT('Ctrl Pts',(-121.718650066136,-6.19295439384353,
131.243306742772));
#276937=CARTESIAN_POINT('Ctrl Pts',(-121.997097689948,-2.97814531445616,
136.251929645219));
#276938=CARTESIAN_POINT('Ctrl Pts',(-122.275545313761,2.97343381842962,
136.254502739794));
#276939=CARTESIAN_POINT('Ctrl Pts',(-122.553992937574,6.19257253249627,
131.248661478285));
#276940=CARTESIAN_POINT('Ctrl Pts',(-122.832440561387,3.72103961318487,
125.83452943108));
#276941=CARTESIAN_POINT('Ctrl Pts',(-123.1108881852,-2.16994692775201,124.987429454503));
#276942=CARTESIAN_POINT('Ctrl Pts',(-123.389335809013,-6.06685824988591,
129.485805043896));
#276943=CARTESIAN_POINT('Ctrl Pts',(-123.667783432826,-4.38862322287681,
135.19586879047));
#276944=CARTESIAN_POINT('Ctrl Pts',(-123.946231056639,1.32254214979223,
136.870351063246));
#276945=CARTESIAN_POINT('Ctrl Pts',(-124.224678680451,5.81835589657845,
132.97048445655));
#276946=CARTESIAN_POINT('Ctrl Pts',(-124.503126304264,4.96738481689638,
127.080055862859));
#276947=CARTESIAN_POINT('Ctrl Pts',(-124.781573928077,-0.448370239273912,
124.612081396343));
#276948=CARTESIAN_POINT('Ctrl Pts',(-125.06002155189,-5.4520949496557,127.834509024472));
#276949=CARTESIAN_POINT('Ctrl Pts',(-125.338469175703,-5.44561075094924,
133.786085181339));
#276950=CARTESIAN_POINT('Ctrl Pts',(-125.616916799516,-0.434876304995071,
136.997602129441));
#276951=CARTESIAN_POINT('Ctrl Pts',(-125.895364423329,4.97548822036069,
134.517832684797));
#276952=CARTESIAN_POINT('Ctrl Pts',(-126.173812047142,5.8136221373178,128.625563823564));
#276953=CARTESIAN_POINT('Ctrl Pts',(-126.452259670955,1.30932132131015,
124.735502775877));
#276954=CARTESIAN_POINT('Ctrl Pts',(-126.730707294768,-4.39818182507867,
126.422425604514));
#276955=CARTESIAN_POINT('Ctrl Pts',(-127.00915491858,-6.0639707373477,132.136132640718));
#276956=CARTESIAN_POINT('Ctrl Pts',(-127.287602542393,-2.15726678343353,
136.626006248326));
#276957=CARTESIAN_POINT('Ctrl Pts',(-127.566050166206,3.73185995611441,
135.766071924465));
#276958=CARTESIAN_POINT('Ctrl Pts',(-127.844497790019,6.19158970748781,
130.346567302635));
#276959=CARTESIAN_POINT('Ctrl Pts',(-128.122945413832,2.96155099365221,
125.34775237278));
#276960=CARTESIAN_POINT('Ctrl Pts',(-128.401393037645,-2.99000840354028,
125.363293849751));
#276961=CARTESIAN_POINT('Ctrl Pts',(-128.679840661458,-6.19389614791022,
130.378909875453));
#276962=CARTESIAN_POINT('Ctrl Pts',(-128.958288285271,-3.70589592099968,
135.785494348734));
#276963=CARTESIAN_POINT('Ctrl Pts',(-129.236735909083,2.18764161422919,
136.614660264981));
#276964=CARTESIAN_POINT('Ctrl Pts',(-129.515183532897,6.07084337821547,
132.104444654172));
#276965=CARTESIAN_POINT('Ctrl Pts',(-129.793631156709,4.37523665480886,
126.399515326358));
#276966=CARTESIAN_POINT('Ctrl Pts',(-130.072078780522,-1.34099881217456,
124.742423632508));
#276967=CARTESIAN_POINT('Ctrl Pts',(-130.350526404335,-5.82492188220296,
128.655955885842));
#276968=CARTESIAN_POINT('Ctrl Pts',(-130.628974028148,-4.95602630574081,
134.543767132223));
#276969=CARTESIAN_POINT('Ctrl Pts',(-130.907421651961,0.467215330352083,
136.995246471799));
#276970=CARTESIAN_POINT('Ctrl Pts',(-131.185869275774,5.46110890258918,
133.757604152921));
#276971=CARTESIAN_POINT('Ctrl Pts',(-131.464316899587,5.43651018334856,
127.80607529902));
#276972=CARTESIAN_POINT('Ctrl Pts',(-131.742764523399,0.416024193898128,
124.60982417848));
#276973=CARTESIAN_POINT('Ctrl Pts',(-132.021212147213,-4.98676770583297,
127.106049425532));
#276974=CARTESIAN_POINT('Ctrl Pts',(-132.299659771025,-5.80696370104951,
133.000841985516));
#276975=CARTESIAN_POINT('Ctrl Pts',(-132.578107394838,-1.2908437409496,
136.877175472434));
#276976=CARTESIAN_POINT('Ctrl Pts',(-132.856555018651,4.41149855586104,
135.172888781227));
#276977=CARTESIAN_POINT('Ctrl Pts',(-133.135002642464,6.05988919352027,
129.454138122079));
#276978=CARTESIAN_POINT('Ctrl Pts',(-133.413450266277,2.13953770437982,
124.976175974248));
#276979=CARTESIAN_POINT('Ctrl Pts',(-133.69189789009,-3.74694441285829,
125.854030790976));
#276980=CARTESIAN_POINT('Ctrl Pts',(-133.970345513903,-6.19016766309031,
131.280996881284));
#276981=CARTESIAN_POINT('Ctrl Pts',(-134.248793137716,-2.94492923744478,
136.269957530209));
#276982=CARTESIAN_POINT('Ctrl Pts',(-134.527240761528,3.00655528962129,
136.236301625668));
#276983=CARTESIAN_POINT('Ctrl Pts',(-134.805688385342,6.19516238391663,
131.210957299752));
#276984=CARTESIAN_POINT('Ctrl Pts',(-135.084136009154,3.69071789790064,
125.811970486258));
#276985=CARTESIAN_POINT('Ctrl Pts',(-135.362583632967,-2.2053160346932,
125.000746311619));
#276986=CARTESIAN_POINT('Ctrl Pts',(-135.64103125678,-6.07477226708194,
129.522760161825));
#276987=CARTESIAN_POINT('Ctrl Pts',(-135.919478880593,-4.36180955514542,
135.222502221193));
#276988=CARTESIAN_POINT('Ctrl Pts',(-136.197926504406,1.35944305172635,
136.862187985044));
#276989=CARTESIAN_POINT('Ctrl Pts',(-136.476374128219,5.83143390654715,
132.935026339502));
#276990=CARTESIAN_POINT('Ctrl Pts',(-136.754821752032,4.9446218826347,127.049886984307));
#276991=CARTESIAN_POINT('Ctrl Pts',(-137.033269375845,-0.486056093210629,
124.614925481843));
#276992=CARTESIAN_POINT('Ctrl Pts',(-137.311716999657,-5.47007226455594,
127.867752498391));
#276993=CARTESIAN_POINT('Ctrl Pts',(-137.59016462347,-5.42735925266033,
133.819178915179));
#276994=CARTESIAN_POINT('Ctrl Pts',(-137.868612247283,-0.397168228809268,
137.000134598521));
#276995=CARTESIAN_POINT('Ctrl Pts',(-138.147059871096,4.99800099457058,
134.487476673751));
#276996=CARTESIAN_POINT('Ctrl Pts',(-138.425507494909,5.80025146986304,
128.590215023569));
#276997=CARTESIAN_POINT('Ctrl Pts',(-138.703955118722,1.27235420238826,
124.727645007244));
#276998=CARTESIAN_POINT('Ctrl Pts',(-138.982402742535,-4.42477441912264,
126.449279772744));
#276999=CARTESIAN_POINT('Ctrl Pts',(-139.260850366348,-6.05575151170779,
132.173021077107));
#277000=CARTESIAN_POINT('Ctrl Pts',(-139.539297990161,-2.12178880494131,
136.639030281933));
#277001=CARTESIAN_POINT('Ctrl Pts',(-139.817745613973,3.76199415842019,
135.743263104665));
#277002=CARTESIAN_POINT('Ctrl Pts',(-140.096193237787,6.18868827382574,
130.308885820552));
#277003=CARTESIAN_POINT('Ctrl Pts',(-140.374640861599,2.92828019981485,
125.329825669606));
#277004=CARTESIAN_POINT('Ctrl Pts',(-140.653088485412,-3.02307432338508,
125.381595689934));
#277005=CARTESIAN_POINT('Ctrl Pts',(-140.931536109225,-6.19637122878504,
130.416621761961));
#277006=CARTESIAN_POINT('Ctrl Pts',(-141.209983733038,-3.675505684495,135.807960900193));
#277007=CARTESIAN_POINT('Ctrl Pts',(-141.488431356851,2.22297002541115,
136.601235818153));
#277008=CARTESIAN_POINT('Ctrl Pts',(-141.766878980664,6.07864488008735,
132.06746561987));
#277009=CARTESIAN_POINT('Ctrl Pts',(-142.045326604476,4.34834204827492,
126.372963630579));
#277010=CARTESIAN_POINT('Ctrl Pts',(-142.32377422829,-1.3778746975837,124.750698986551));
#277011=CARTESIAN_POINT('Ctrl Pts',(-142.602221852102,-5.83789190928377,
128.691453643612));
#277012=CARTESIAN_POINT('Ctrl Pts',(-142.880669475915,-4.93317165322728,
134.573866588494));
#277013=CARTESIAN_POINT('Ctrl Pts',(-143.159117099728,0.504892353312588,
136.992287696695));
#277014=CARTESIAN_POINT('Ctrl Pts',(-143.437564723541,5.47898495252035,
133.72430611622));
#277015=CARTESIAN_POINT('Ctrl Pts',(-143.716012347354,5.4181580436573,127.77303726975));
#277016=CARTESIAN_POINT('Ctrl Pts',(-143.994459971167,0.378308584408798,
124.607406491544));
#277017=CARTESIAN_POINT('Ctrl Pts',(-144.27290759498,-5.00918798250961,
127.136473817112));
#277018=CARTESIAN_POINT('Ctrl Pts',(-144.551355218793,-5.79348550593904,
133.036149926065));
#277019=CARTESIAN_POINT('Ctrl Pts',(-144.829802842605,-1.2538528769121,
136.884920689477));
#277020=CARTESIAN_POINT('Ctrl Pts',(-145.108250466418,4.43800929187927,
135.145953798675));
#277021=CARTESIAN_POINT('Ctrl Pts',(-145.386698090231,6.05155773023994,
129.417274873051));
#277022=CARTESIAN_POINT('Ctrl Pts',(-145.665145714044,2.10402024954095,
124.963259983731));
#277023=CARTESIAN_POINT('Ctrl Pts',(-145.943593337857,-3.77700905338292,
125.876931223274));
#277024=CARTESIAN_POINT('Ctrl Pts',(-146.22204096167,-6.18715155339789,
131.318669357863));
#277025=CARTESIAN_POINT('Ctrl Pts',(-146.500488585483,-2.9116040349975,
136.287782885497));
#277026=CARTESIAN_POINT('Ctrl Pts',(-146.778936209295,3.03956535180104,
136.217899228972));
#277027=CARTESIAN_POINT('Ctrl Pts',(-147.057383833109,6.19752267131684,
131.173238054629));
#277028=CARTESIAN_POINT('Ctrl Pts',(-147.335831456921,3.66025942170698,
125.789596536289));
#277029=CARTESIAN_POINT('Ctrl Pts',(-147.614279080735,-2.24060342283806,
125.014278223797));
#277030=CARTESIAN_POINT('Ctrl Pts',(-147.892726704547,-6.08246118135759,
129.559762769929));
#277031=CARTESIAN_POINT('Ctrl Pts',(-148.17117432836,-4.33483425895693,
135.248971936054));
#277032=CARTESIAN_POINT('Ctrl Pts',(-148.449621952173,1.39629357899829,
136.853800431821));
#277033=CARTESIAN_POINT('Ctrl Pts',(-148.728069575986,5.84429583058792,
132.899489269852));
#277034=CARTESIAN_POINT('Ctrl Pts',(-149.006517199799,4.9216757235908,127.019857229157));
#277035=CARTESIAN_POINT('Ctrl Pts',(-149.284964823612,-0.52372393616008,
124.617998919139));
#277036=CARTESIAN_POINT('Ctrl Pts',(-149.563412447425,-5.48784688391679,
127.901104789406));
#277037=CARTESIAN_POINT('Ctrl Pts',(-149.841860071237,-5.40890664157841,
133.852160933818));
#277038=CARTESIAN_POINT('Ctrl Pts',(-150.12030769505,-0.359445435409253,
137.002437480918));
#277039=CARTESIAN_POINT('Ctrl Pts',(-150.398755318863,5.02032856601553,
134.456984183485));
#277040=CARTESIAN_POINT('Ctrl Pts',(-150.677202942676,5.78666587195703,
128.554948269553));
#277041=CARTESIAN_POINT('Ctrl Pts',(-150.955650566489,1.23533993591347,
124.720012413542));
#277042=CARTESIAN_POINT('Ctrl Pts',(-151.234098190302,-4.45120305152329,
126.476295320094));
#277043=CARTESIAN_POINT('Ctrl Pts',(-151.512545814115,-6.0473078879686,
132.209858797279));
#277044=CARTESIAN_POINT('Ctrl Pts',(-151.790993437928,-2.08623220278462,
136.651838109709));
#277045=CARTESIAN_POINT('Ctrl Pts',(-152.069441061741,3.79198895864895,
135.720271272016));
#277046=CARTESIAN_POINT('Ctrl Pts',(-152.347888685554,6.18555751604382,
130.27122269847));
#277047=CARTESIAN_POINT('Ctrl Pts',(-152.626336309366,2.89490089747778,
125.312101827337));
#277048=CARTESIAN_POINT('Ctrl Pts',(-152.904783933179,-3.05602822209906,
125.400098472666));
#277049=CARTESIAN_POINT('Ctrl Pts',(-153.183231556992,-6.19861670084527,
130.454348016274));
#277050=CARTESIAN_POINT('Ctrl Pts',(-153.461679180805,-3.64497925077551,
135.830242041403));
#277051=CARTESIAN_POINT('Ctrl Pts',(-153.740126804618,2.25821606362131,
136.587596565983));
#277052=CARTESIAN_POINT('Ctrl Pts',(-154.018574428431,6.08622113553776,
132.030439780749));
#277053=CARTESIAN_POINT('Ctrl Pts',(-154.297022052244,4.32128631232727,
126.346576141847));
#277054=CARTESIAN_POINT('Ctrl Pts',(-154.575469676057,-1.41469952533967,
124.759198661251));
#277055=CARTESIAN_POINT('Ctrl Pts',(-154.85391729987,-5.85064561113321,
128.727029695929));
#277056=CARTESIAN_POINT('Ctrl Pts',(-155.132364923682,-4.9101342002235,
134.603826364333));
#277057=CARTESIAN_POINT('Ctrl Pts',(-155.410812547495,0.542550667301237,
136.989099625678));
#277058=CARTESIAN_POINT('Ctrl Pts',(-155.689260171308,5.49665797664923,
133.690899879866));
#277059=CARTESIAN_POINT('Ctrl Pts',(-155.967707795121,5.39960513212718,
127.740111567281));
#277060=CARTESIAN_POINT('Ctrl Pts',(-156.246155418934,0.340578956555753,
124.605218435021));
#277061=CARTESIAN_POINT('Ctrl Pts',(-156.524603042747,-5.03142264188343,
127.167034123586));
#277062=CARTESIAN_POINT('Ctrl Pts',(-156.80305066656,-5.77979263109261,
133.071375166841));
#277063=CARTESIAN_POINT('Ctrl Pts',(-157.081498290373,-1.21681555089514,
136.89244058913));
#277064=CARTESIAN_POINT('Ctrl Pts',(-157.359945914186,4.46435557583064,
135.118857936792));
#277065=CARTESIAN_POINT('Ctrl Pts',(-157.638393537999,6.04300202426259,
129.380463022997));
#277066=CARTESIAN_POINT('Ctrl Pts',(-157.916841161811,2.06842482945845,
124.950560437346));
#277067=CARTESIAN_POINT('Ctrl Pts',(-158.195288785624,-3.80693373544809,
125.900014243279));
#277068=CARTESIAN_POINT('Ctrl Pts',(-158.473736409437,-6.18390617652933,
131.356322776543));
#277069=CARTESIAN_POINT('Ctrl Pts',(-158.75218403325,-2.87817094199197,
136.305405050556));
#277070=CARTESIAN_POINT('Ctrl Pts',(-159.030631657063,3.07246278176887,
136.199296231612));
#277071=CARTESIAN_POINT('Ctrl Pts',(-159.309079280876,6.19965330723533,
131.135505140616));
#277072=CARTESIAN_POINT('Ctrl Pts',(-159.587526904689,3.62966531325439,
125.767408410247));
#277073=CARTESIAN_POINT('Ctrl Pts',(-159.865974528502,-2.27580778459908,
125.028024689608));
#277074=CARTESIAN_POINT('Ctrl Pts',(-160.144422152314,-6.08992470779737,
129.596811497064));
#277075=CARTESIAN_POINT('Ctrl Pts',(-160.422869776128,-4.3076983338908,
135.275276954208));
#277076=CARTESIAN_POINT('Ctrl Pts',(-160.70131739994,1.43309236609815,136.845188714382));
#277077=CARTESIAN_POINT('Ctrl Pts',(-160.979765023753,5.85694119209746,
132.863874564441));
#277078=CARTESIAN_POINT('Ctrl Pts',(-161.258212647566,4.89854719004298,
126.989967710171));
#277079=CARTESIAN_POINT('Ctrl Pts',(-161.536660271379,-0.561372372326459,
124.621301594343));
#277080=CARTESIAN_POINT('Ctrl Pts',(-161.815107895192,-5.50541814909322,
127.934564661631));
#277081=CARTESIAN_POINT('Ctrl Pts',(-162.093555519005,-5.39025360147175,
133.885030015096));
#277082=CARTESIAN_POINT('Ctrl Pts',(-162.372003142818,-0.32170932262588,
137.004510691297));
#277083=CARTESIAN_POINT('Ctrl Pts',(-162.650450766631,5.04247010733932,
134.426356343909));
#277084=CARTESIAN_POINT('Ctrl Pts',(-162.928898390443,5.77286584701905,
128.519764868338));
#277085=CARTESIAN_POINT('Ctrl Pts',(-163.207346014257,1.19827989346308,
124.712605277602));
#277086=CARTESIAN_POINT('Ctrl Pts',(-163.485793638069,-4.47746674295796,
126.503471245498));
#277087=CARTESIAN_POINT('Ctrl Pts',(-163.764241261882,-6.03864017901171,
132.246644436198));
#277088=CARTESIAN_POINT('Ctrl Pts',(-164.042688885695,-2.05059829452646,
136.664429257056));
#277089=CARTESIAN_POINT('Ctrl Pts',(-164.321136509508,3.82184324533235,
135.697097278492));
#277090=CARTESIAN_POINT('Ctrl Pts',(-164.599584133321,6.18219755015336,
130.23357933201));
#277091=CARTESIAN_POINT('Ctrl Pts',(-164.878031757134,2.86141432352365,
125.294581502737));
#277092=CARTESIAN_POINT('Ctrl Pts',(-165.156479380946,-3.08886887856293,
125.418801512319));
#277093=CARTESIAN_POINT('Ctrl Pts',(-165.43492700476,-6.20063248088431,
130.492087240433));
#277094=CARTESIAN_POINT('Ctrl Pts',(-165.713374628572,-3.61431775100944,
135.85233694673));
#277095=CARTESIAN_POINT('Ctrl Pts',(-165.991822252385,2.2933784228048,136.573743013877));
#277096=CARTESIAN_POINT('Ctrl Pts',(-166.270269876198,6.09357186382579,
131.993368508814));
#277097=CARTESIAN_POINT('Ctrl Pts',(-166.548717500011,4.2940704495262,126.320353837957));
#277098=CARTESIAN_POINT('Ctrl Pts',(-166.827165123824,-1.45147193088449,
124.767922341652));
#277099=CARTESIAN_POINT('Ctrl Pts',(-167.105612747637,-5.86318251515793,
128.762682724506));
#277100=CARTESIAN_POINT('Ctrl Pts',(-167.38406037145,-4.88691480039125,
134.633645349573));
#277101=CARTESIAN_POINT('Ctrl Pts',(-167.662507995262,0.580188876875391,
136.985682376883));
#277102=CARTESIAN_POINT('Ctrl Pts',(-167.940955619076,5.51412732009539,
133.657386681736));
#277103=CARTESIAN_POINT('Ctrl Pts',(-168.219403242888,5.38085213624319,
127.707299411689));
#277104=CARTESIAN_POINT('Ctrl Pts',(-168.497850866701,0.302836708424229,
124.60326008999));
#277105=CARTESIAN_POINT('Ctrl Pts',(-168.776298490514,-5.05347086004094,
127.197729212531));
#277106=CARTESIAN_POINT('Ctrl Pts',(-169.054746114327,-5.7658855839047,
133.106516402559));
#277107=CARTESIAN_POINT('Ctrl Pts',(-169.33319373814,-1.17973313533045,
136.899734892741));
#277108=CARTESIAN_POINT('Ctrl Pts',(-169.611641361953,4.49053643144484,
135.091602199623));
#277109=CARTESIAN_POINT('Ctrl Pts',(-169.890088985766,6.03422239262278,
129.34370393599));
#277110=CARTESIAN_POINT('Ctrl Pts',(-170.168536609579,2.03275276313275,
124.938077805679));
#277111=CARTESIAN_POINT('Ctrl Pts',(-170.446984233392,-3.83671735018369,
125.923278995643));
#277112=CARTESIAN_POINT('Ctrl Pts',(-170.725431857205,-6.18043165274327,
131.393955742061));
#277113=CARTESIAN_POINT('Ctrl Pts',(-171.003879481017,-2.84463119730373,
136.32282337239));
#277114=CARTESIAN_POINT('Ctrl Pts',(-171.282327104831,3.10524636049842,
136.180493322929));
#277115=CARTESIAN_POINT('Ctrl Pts',(-171.560774728643,6.20155421272058,
131.097759955922));
#277116=CARTESIAN_POINT('Ctrl Pts',(-171.839222352457,3.59893670621881,
125.745406930321));
#277117=CARTESIAN_POINT('Ctrl Pts',(-172.117669976268,-2.31092781546573,
125.04198519967));
#277118=CARTESIAN_POINT('Ctrl Pts',(-172.396117600082,-6.09716256983718,
129.633904970377));
#277119=CARTESIAN_POINT('Ctrl Pts',(-172.674565223895,-4.2804027854792,
135.301416300912));
#277120=CARTESIAN_POINT('Ctrl Pts',(-172.953012847708,1.469838049433,136.836353151837));
#277121=CARTESIAN_POINT('Ctrl Pts',(-173.23146047152,5.86936952249723,132.828183542982));
#277122=CARTESIAN_POINT('Ctrl Pts',(-173.509908095334,4.8752371390276,126.960219534917));
#277123=CARTESIAN_POINT('Ctrl Pts',(-173.788355719146,-0.599000006633149,
124.624833385073));
#277124=CARTESIAN_POINT('Ctrl Pts',(-174.06680334296,-5.5227854089755,127.968130875202));
#277125=CARTESIAN_POINT('Ctrl Pts',(-174.345250966772,-5.37140082353563,
133.917784941036));
#277126=CARTESIAN_POINT('Ctrl Pts',(-174.623698590585,-0.283961288785237,
137.006354152836));
#277127=CARTESIAN_POINT('Ctrl Pts',(-174.902146214398,5.06442479807889,
134.39559428995));
#277128=CARTESIAN_POINT('Ctrl Pts',(-175.18059383821,5.75885190641417,128.484666123661));
#277129=CARTESIAN_POINT('Ctrl Pts',(-175.459041462024,1.16117544831056,
124.705423873895));
#277130=CARTESIAN_POINT('Ctrl Pts',(-175.737489085836,-4.50356452021585,
126.530806541938));
#277131=CARTESIAN_POINT('Ctrl Pts',(-176.01593670965,-6.02974870602229,
132.28337663076));
#277132=CARTESIAN_POINT('Ctrl Pts',(-176.294384333462,-2.01488840059438,
136.676803257405));
#277133=CARTESIAN_POINT('Ctrl Pts',(-176.572831957276,3.85155591220881,
135.67374198281));
#277134=CARTESIAN_POINT('Ctrl Pts',(-176.851279581088,6.17860850065921,
130.195957116059));
#277135=CARTESIAN_POINT('Ctrl Pts',(-177.129727204901,2.82782171880919,
125.277265345029));
#277136=CARTESIAN_POINT('Ctrl Pts',(-177.408174828714,-3.12159507585506,
125.437704115845));
#277137=CARTESIAN_POINT('Ctrl Pts',(-177.686622452527,-6.20241849420629,
130.529838035997));
#277138=CARTESIAN_POINT('Ctrl Pts',(-177.965070076339,-3.58352232136993,
135.874244797437));
#277139=CARTESIAN_POINT('Ctrl Pts',(-178.243517700153,2.32845580000743,
136.559675675186));
#277140=CARTESIAN_POINT('Ctrl Pts',(-178.521965323965,6.10069679256748,
131.956253177754));
#277141=CARTESIAN_POINT('Ctrl Pts',(-178.800412947778,4.26669546836545,
126.294297690589));
#277142=CARTESIAN_POINT('Ctrl Pts',(-179.078860571591,-1.48819055160311,
124.776869704492));
#277143=CARTESIAN_POINT('Ctrl Pts',(-179.357308195404,-5.8755021567984,
128.798411408209));
#277144=CARTESIAN_POINT('Ctrl Pts',(-179.635755819217,-4.86351431413387,
134.663322439258));
#277145=CARTESIAN_POINT('Ctrl Pts',(-179.91420344303,0.617805587336893,
136.982036076937));
#277146=CARTESIAN_POINT('Ctrl Pts',(-180.192651066843,5.53139233552561,
133.623767763677));
#277147=CARTESIAN_POINT('Ctrl Pts',(-180.471098690656,5.36189975090491,
127.674602018838));
#277148=CARTESIAN_POINT('Ctrl Pts',(-180.749546314469,0.265083238567079,
124.601531529021));
#277149=CARTESIAN_POINT('Ctrl Pts',(-181.027993938281,-5.07533181997731,
127.22855794653));
#277150=CARTESIAN_POINT('Ctrl Pts',(-181.306441562095,-5.75176487970607,
133.141572331048));
#277151=CARTESIAN_POINT('Ctrl Pts',(-181.584889185907,-1.14260700432061,
136.906803330016));
#277152=CARTESIAN_POINT('Ctrl Pts',(-181.86333680972,4.5165508885802,135.064187597142));
#277153=CARTESIAN_POINT('Ctrl Pts',(-182.141784433533,6.02521916065313,
129.306998974155));
#277154=CARTESIAN_POINT('Ctrl Pts',(-182.420232057346,1.99700537240587,
124.925812551278));
#277155=CARTESIAN_POINT('Ctrl Pts',(-182.698679681159,-3.86635879394691,
125.946724618282));
#277156=CARTESIAN_POINT('Ctrl Pts',(-182.977127304972,-6.17672811078948,
131.431566859916));
#277157=CARTESIAN_POINT('Ctrl Pts',(-183.255574928785,-2.81098604376035,
136.340037205557));
#277158=CARTESIAN_POINT('Ctrl Pts',(-183.534022552597,3.13791487318212,
136.161491199671));
#277159=CARTESIAN_POINT('Ctrl Pts',(-183.81247017641,6.20322531733387,131.060003899207));
#277160=CARTESIAN_POINT('Ctrl Pts',(-184.090917800223,3.56807473926006,
125.723592911784));
#277161=CARTESIAN_POINT('Ctrl Pts',(-184.369365424036,-2.34596221405232,
125.056159236672));
#277162=CARTESIAN_POINT('Ctrl Pts',(-184.647813047849,-6.10417449927606,
129.671041815353));
#277163=CARTESIAN_POINT('Ctrl Pts',(-184.926260671662,-4.25294862516783,
135.327389007565));
#277164=CARTESIAN_POINT('Ctrl Pts',(-185.204708295475,1.50652926737877,
136.827294071589));
#277165=CARTESIAN_POINT('Ctrl Pts',(-185.483155919288,5.88158036125089,
132.792417528021));
#277166=CARTESIAN_POINT('Ctrl Pts',(-185.761603543101,4.85174643430717,
126.930613805724));
#277167=CARTESIAN_POINT('Ctrl Pts',(-186.040051166913,-0.6366054447743,
124.628594160457));
#277168=CARTESIAN_POINT('Ctrl Pts',(-186.318498790727,-5.53994802001346,
128.001802186308));
#277169=CARTESIAN_POINT('Ctrl Pts',(-186.596946414539,-5.35234900636664,
133.950424497894));
#277170=CARTESIAN_POINT('Ctrl Pts',(-186.875394038353,-0.246202732654624,
137.007967797222));
#277171=CARTESIAN_POINT('Ctrl Pts',(-187.153841662165,5.08619182469514,
134.364699161505));
#277172=CARTESIAN_POINT('Ctrl Pts',(-187.432289285978,5.744624569434,128.449653336115));
#277173=CARTESIAN_POINT('Ctrl Pts',(-187.71073690979,1.12402797537536,124.698468468532));
#277174=CARTESIAN_POINT('Ctrl Pts',(-187.989184533604,-4.52949541623416,
126.558300196495));
#277175=CARTESIAN_POINT('Ctrl Pts',(-188.267632157416,-6.0206337984771,
132.32005401984));
#277176=CARTESIAN_POINT('Ctrl Pts',(-188.54607978123,-1.97910384423165,
136.688959652232));
#277177=CARTESIAN_POINT('Ctrl Pts',(-188.824527405043,3.88112585826452,
135.650206250412));
#277178=CARTESIAN_POINT('Ctrl Pts',(-189.102975028855,6.17479050055486,
130.158357444724));
#277179=CARTESIAN_POINT('Ctrl Pts',(-189.381422652668,2.79412432812102,
125.260153995869));
#277180=CARTESIAN_POINT('Ctrl Pts',(-189.659870276481,-3.15420560129371,
125.456805582802));
#277181=CARTESIAN_POINT('Ctrl Pts',(-189.938317900294,-6.20397467462999,
130.567599004095));
#277182=CARTESIAN_POINT('Ctrl Pts',(-190.216765524107,-3.55259410299321,
135.89596478172));
#277183=CARTESIAN_POINT('Ctrl Pts',(-190.49521314792,2.36344689542356,136.545395071179));
#277184=CARTESIAN_POINT('Ctrl Pts',(-190.773660771733,6.10759565774615,
131.919095162891));
#277185=CARTESIAN_POINT('Ctrl Pts',(-191.052108395545,4.23916238323504,
126.26840866526));
#277186=CARTESIAN_POINT('Ctrl Pts',(-191.330556019359,-1.52485402687357,
124.786040418225));
#277187=CARTESIAN_POINT('Ctrl Pts',(-191.609003643171,-5.88760407954571,
128.834214423098));
#277188=CARTESIAN_POINT('Ctrl Pts',(-191.887451266984,-4.83993360856504,
134.692856533694));
#277189=CARTESIAN_POINT('Ctrl Pts',(-192.165898890797,0.655399404785621,
136.978160860955));
#277190=CARTESIAN_POINT('Ctrl Pts',(-192.44434651461,5.54845238317892,133.59004437145));
#277191=CARTESIAN_POINT('Ctrl Pts',(-192.722794138423,5.34274867839911,
127.642020600343));
#277192=CARTESIAN_POINT('Ctrl Pts',(-193.001241762236,0.227319945953055,
124.600032816164));
#277193=CARTESIAN_POINT('Ctrl Pts',(-193.279689386049,-5.09700471162664,
127.259519183211));
#277194=CARTESIAN_POINT('Ctrl Pts',(-193.558137009861,-5.73743104174462,
133.176541653297));
#277195=CARTESIAN_POINT('Ctrl Pts',(-193.836584633675,-1.105438533588,136.913645639033));
#277196=CARTESIAN_POINT('Ctrl Pts',(-194.115032257487,4.5423979832614,135.036615145204));
#277197=CARTESIAN_POINT('Ctrl Pts',(-194.3934798813,6.01599266197172,129.270349497605));
#277198=CARTESIAN_POINT('Ctrl Pts',(-194.671927505113,1.96118398191049,
124.913765128639));
#277199=CARTESIAN_POINT('Ctrl Pts',(-194.950375128926,-3.89585696836267,
125.970350242409));
#277200=CARTESIAN_POINT('Ctrl Pts',(-195.228822752739,-6.17279568790409,
131.469154736412));
#277201=CARTESIAN_POINT('Ctrl Pts',(-195.507270376552,-2.77723672809589,
136.357045912194));
#277202=CARTESIAN_POINT('Ctrl Pts',(-195.785718000365,3.17046710927626,
136.142290565968));
#277203=CARTESIAN_POINT('Ctrl Pts',(-196.064165624178,6.20466655915177,
131.022238369536));
#277204=CARTESIAN_POINT('Ctrl Pts',(-196.342613247991,3.5370805559797,125.701967162963));
#277205=CARTESIAN_POINT('Ctrl Pts',(-196.621060871803,-2.38090968214636,
125.070546275391));
#277206=CARTESIAN_POINT('Ctrl Pts',(-196.899508495616,-6.11096023628406,
129.708220655875));
#277207=CARTESIAN_POINT('Ctrl Pts',(-197.177956119429,-4.22533687028115,
135.353194111738));
#277208=CARTESIAN_POINT('Ctrl Pts',(-197.456403743242,1.54316466032852,
136.818011809327));
#277209=CARTESIAN_POINT('Ctrl Pts',(-197.734851367055,5.89357325588093,
132.75657784488));
#277210=CARTESIAN_POINT('Ctrl Pts',(-198.013298990868,4.82807594633875,
126.901151619645));
#277211=CARTESIAN_POINT('Ctrl Pts',(-198.291746614681,-0.674187293266194,
124.632583781138));
#277212=CARTESIAN_POINT('Ctrl Pts',(-198.570194238494,-5.55690534624021,
128.035577347248));
#277213=CARTESIAN_POINT('Ctrl Pts',(-198.848641862306,-5.33309885593691,
133.982947476197));
#277214=CARTESIAN_POINT('Ctrl Pts',(-199.12708948612,-0.2084350533912,137.009351564664));
#277215=CARTESIAN_POINT('Ctrl Pts',(-199.405537109932,5.10777038060287,
134.333672103408));
#277216=CARTESIAN_POINT('Ctrl Pts',(-199.683984733745,5.7301843632779,128.414727803113));
#277217=CARTESIAN_POINT('Ctrl Pts',(-199.962432357558,1.08683885116959,
124.691739319248));
#277218=CARTESIAN_POINT('Ctrl Pts',(-200.240879981371,-4.5552584701342,
126.585951190383));
#277219=CARTESIAN_POINT('Ctrl Pts',(-200.519327605184,-6.01129579413245,
132.356675244344));
#277220=CARTESIAN_POINT('Ctrl Pts',(-200.797775228997,-1.94324595144814,
136.700897991079));
#277221=CARTESIAN_POINT('Ctrl Pts',(-201.076222852809,3.91055198777426,
135.626490953421));
#277222=CARTESIAN_POINT('Ctrl Pts',(-201.354670476623,6.17074369131775,
130.120781711275));
#277223=CARTESIAN_POINT('Ctrl Pts',(-201.633118100435,2.76032340012831,
125.243248089324));
#277224=CARTESIAN_POINT('Ctrl Pts',(-201.911565724248,-3.18669924648382,
125.476105205376));
#277225=CARTESIAN_POINT('Ctrl Pts',(-202.190013348061,-6.20530096449064,
130.605368745483));
#277226=CARTESIAN_POINT('Ctrl Pts',(-202.468460971874,-3.52153424193529,
135.91749609474));
#277227=CARTESIAN_POINT('Ctrl Pts',(-202.746908595687,2.39835041244635,
136.530901731028));
#277228=CARTESIAN_POINT('Ctrl Pts',(-203.0253562195,6.11426820372151,131.881895841131));
#277229=CARTESIAN_POINT('Ctrl Pts',(-203.303803843313,4.21147221438356,
126.242687721299));
#277230=CARTESIAN_POINT('Ctrl Pts',(-203.582251467125,-1.56146099811728,
124.795434143027));
#277231=CARTESIAN_POINT('Ctrl Pts',(-203.860699090939,-5.89948783495869,
128.870090442477));
#277232=CARTESIAN_POINT('Ctrl Pts',(-204.139146714752,-4.81617355747646,
134.722246538484));
#277233=CARTESIAN_POINT('Ctrl Pts',(-204.417594338564,0.69296893616836,
136.974056872534));
#277234=CARTESIAN_POINT('Ctrl Pts',(-204.696041962377,5.56530683088876,
133.556217754686));
#277235=CARTESIAN_POINT('Ctrl Pts',(-204.97448958619,5.32339962837619,127.60955636352));
#277236=CARTESIAN_POINT('Ctrl Pts',(-205.252937210003,0.18954822991528,
124.598764006957));
#277237=CARTESIAN_POINT('Ctrl Pts',(-205.531384833816,-5.11848873189165,
127.290611775294));
#277238=CARTESIAN_POINT('Ctrl Pts',(-205.809832457629,-5.72288460116635,
133.211423073505));
#277239=CARTESIAN_POINT('Ctrl Pts',(-206.088280081441,-1.06822910042401,
136.920261566246));
#277240=CARTESIAN_POINT('Ctrl Pts',(-206.366727705255,4.56807675771487,
135.00888586552));
#277241=CARTESIAN_POINT('Ctrl Pts',(-206.645175329067,6.00654323846982,
129.233756864401));
#277242=CARTESIAN_POINT('Ctrl Pts',(-206.92362295288,1.92528991902147,124.901935984182));
#277243=CARTESIAN_POINT('Ctrl Pts',(-207.202070576693,-3.92521078036628,
125.994154992568));
#277244=CARTESIAN_POINT('Ctrl Pts',(-207.480518200506,-6.16863452980439,
131.506717978718));
#277245=CARTESIAN_POINT('Ctrl Pts',(-207.758965824319,-2.74338450090264,
136.373848862034));
#277246=CARTESIAN_POINT('Ctrl Pts',(-208.037413448132,3.20290186254569,
136.12289213331));
#277247=CARTESIAN_POINT('Ctrl Pts',(-208.315861071945,6.20587788476857,
130.984464766326));
#277248=CARTESIAN_POINT('Ctrl Pts',(-208.594308695758,3.50595530487857,
125.680530485208));
#277249=CARTESIAN_POINT('Ctrl Pts',(-208.872756319571,-2.41576892475653,
125.085145782709));
#277250=CARTESIAN_POINT('Ctrl Pts',(-209.151203943383,-6.11751952941318,
129.745440114266));
#277251=CARTESIAN_POINT('Ctrl Pts',(-209.429651567197,-4.19756854398286,
135.378830657213));
#277252=CARTESIAN_POINT('Ctrl Pts',(-209.708099191009,1.57974287074426,
136.808506709009));
#277253=CARTESIAN_POINT('Ctrl Pts',(-209.986546814822,5.90534776198698,
132.720665821612));
#277254=CARTESIAN_POINT('Ctrl Pts',(-210.264994438635,4.80422655224024,
126.87183406841));
#277255=CARTESIAN_POINT('Ctrl Pts',(-210.543442062448,-0.711744159500396,
124.63680209928));
#277256=CARTESIAN_POINT('Ctrl Pts',(-210.821889686261,-5.57365675929581,
128.06945510647));
#277257=CARTESIAN_POINT('Ctrl Pts',(-211.100337310074,-5.31365108556781,
134.015352670796));
#277258=CARTESIAN_POINT('Ctrl Pts',(-211.378784933887,-0.170659650490228,
137.010505403884));
#277259=CARTESIAN_POINT('Ctrl Pts',(-211.657232557699,5.12915966620077,
134.302514265376));
#277260=CARTESIAN_POINT('Ctrl Pts',(-211.935680181513,5.71553182303293,
128.379890818834));
#277261=CARTESIAN_POINT('Ctrl Pts',(-212.214127805325,1.04960945375051,
124.685236675394));
#277262=CARTESIAN_POINT('Ctrl Pts',(-212.492575429138,-4.58085272725645,
126.613758498985));
#277263=CARTESIAN_POINT('Ctrl Pts',(-212.771023052951,-6.00173503901134,
132.393238947258));
#277264=CARTESIAN_POINT('Ctrl Pts',(-213.049470676764,-1.90731605097184,
136.712617831564));
#277265=CARTESIAN_POINT('Ctrl Pts',(-213.327918300577,3.93983321034183,
135.602596970618));
#277266=CARTESIAN_POINT('Ctrl Pts',(-213.60636592439,6.16646822290386,130.083231308093));
#277267=CARTESIAN_POINT('Ctrl Pts',(-213.884813548203,2.72642018733693,
125.226548251849));
#277268=CARTESIAN_POINT('Ctrl Pts',(-214.163261172015,-3.21907480736146,
125.495602268416));
#277269=CARTESIAN_POINT('Ctrl Pts',(-214.441708795829,-6.20639731464204,
130.643145860587));
#277270=CARTESIAN_POINT('Ctrl Pts',(-214.720156419641,-3.49034388913101,
135.938837938644));
#277271=CARTESIAN_POINT('Ctrl Pts',(-214.998604043455,2.43316505771265,
136.516196191791));
#277272=CARTESIAN_POINT('Ctrl Pts',(-215.277051667267,6.12071418324004,
131.844656590906));
#277273=CARTESIAN_POINT('Ctrl Pts',(-215.55549929108,4.18362598788043,126.217135811804));
#277274=CARTESIAN_POINT('Ctrl Pts',(-215.833946914893,-1.59801010884951,
124.805050530808));
#277275=CARTESIAN_POINT('Ctrl Pts',(-216.112394538706,-5.91115298268039,
128.90603813695));
#277276=CARTESIAN_POINT('Ctrl Pts',(-216.390842162519,-4.79223504130557,
134.75149136457));
#277277=CARTESIAN_POINT('Ctrl Pts',(-216.669289786332,0.730512789332353,
136.969724263749));
#277278=CARTESIAN_POINT('Ctrl Pts',(-216.947737410145,5.5819550541073,133.522289166845));
#277279=CARTESIAN_POINT('Ctrl Pts',(-217.226185033957,5.3038533178224,127.577210511344));
#277280=CARTESIAN_POINT('Ctrl Pts',(-217.50463265777,0.151769490097695,
124.597725148413));
#277281=CARTESIAN_POINT('Ctrl Pts',(-217.783080281583,-5.13978308467467,
127.321834570635));
#277282=CARTESIAN_POINT('Ctrl Pts',(-218.061527905396,-5.70812609699421,
133.24621529913));
#277283=CARTESIAN_POINT('Ctrl Pts',(-218.339975529209,-1.03098008363786,
136.9266508665));
#277284=CARTESIAN_POINT('Ctrl Pts',(-218.618423153022,4.59358626040416,
134.981000785606));
#277285=CARTESIAN_POINT('Ctrl Pts',(-218.896870776835,5.99687124029931,
129.197222430498));
#277286=CARTESIAN_POINT('Ctrl Pts',(-219.175318400648,1.88932451380644,
124.890325556239));
#277287=CARTESIAN_POINT('Ctrl Pts',(-219.45376602446,-3.95441914224089,
126.018137986666));
#277288=CARTESIAN_POINT('Ctrl Pts',(-219.732213648274,-6.16424479068368,
131.544255194914));
#277289=CARTESIAN_POINT('Ctrl Pts',(-220.010661272086,-2.70943061658779,
136.390445432439));
#277290=CARTESIAN_POINT('Ctrl Pts',(-220.289108895899,3.23521793110825,
136.103296620509));
#277291=CARTESIAN_POINT('Ctrl Pts',(-220.567556519712,6.20685924929812,
130.94668448929));
#277292=CARTESIAN_POINT('Ctrl Pts',(-220.846004143525,3.47470013931478,
125.659283672863));
#277293=CARTESIAN_POINT('Ctrl Pts',(-221.124451767337,-2.45053865016082,
125.099957217636));
#277294=CARTESIAN_POINT('Ctrl Pts',(-221.402899391151,-6.12385213560643,
129.782698811345));
#277295=CARTESIAN_POINT('Ctrl Pts',(-221.681347014963,-4.16964467523852,
135.404297694017));
#277296=CARTESIAN_POINT('Ctrl Pts',(-221.959794638777,1.61626254320698,
136.79877912285));
#277297=CARTESIAN_POINT('Ctrl Pts',(-222.238242262589,5.91690344326002,
132.684682788949));
#277298=CARTESIAN_POINT('Ctrl Pts',(-222.516689886402,4.7801991357601,126.842662238393));
#277299=CARTESIAN_POINT('Ctrl Pts',(-222.795137510215,-0.749274651793031,
124.64124895857));
#277300=CARTESIAN_POINT('Ctrl Pts',(-223.073585134028,-5.59020163845046,
128.103434208622));
#277301=CARTESIAN_POINT('Ctrl Pts',(-223.352032757841,-5.29400641590365,
134.047638880903));
#277302=CARTESIAN_POINT('Ctrl Pts',(-223.630480381654,-0.132877923733138,
137.011429272127));
#277303=CARTESIAN_POINT('Ctrl Pts',(-223.908928005467,5.15035888890098,
134.271226801972));
#277304=CARTESIAN_POINT('Ctrl Pts',(-224.187375629279,5.70066749165438,
128.345143674176));
#277305=CARTESIAN_POINT('Ctrl Pts',(-224.465823253093,1.01234116266713,
124.678960777928));
#277306=CARTESIAN_POINT('Ctrl Pts',(-224.744270876905,-4.60627723919628,
126.641721091889));
#277307=CARTESIAN_POINT('Ctrl Pts',(-225.022718500718,-5.99195188739136,
132.4297437737));
#277308=CARTESIAN_POINT('Ctrl Pts',(-225.301166124531,-1.87131547419729,
136.724118739406));
#277309=CARTESIAN_POINT('Ctrl Pts',(-225.579613748344,3.96896844094108,
135.578525187401));
#277310=CARTESIAN_POINT('Ctrl Pts',(-225.858061372157,6.16196425374224,
130.045707626623));
#277311=CARTESIAN_POINT('Ctrl Pts',(-226.13650899597,2.69241594604283,125.210055102262));
#277312=CARTESIAN_POINT('Ctrl Pts',(-226.414956619783,-3.25133108423828,
125.515296049447));
#277313=CARTESIAN_POINT('Ctrl Pts',(-226.693404243596,-6.20726368445854,
130.680928949564));
#277314=CARTESIAN_POINT('Ctrl Pts',(-226.971851867408,-3.45902420035033,
135.959989522602));
#277315=CARTESIAN_POINT('Ctrl Pts',(-227.250299491222,2.46788954115291,
136.501278998386));
#277316=CARTESIAN_POINT('Ctrl Pts',(-227.528747115034,6.12693335744362,
131.80737879213));
#277317=CARTESIAN_POINT('Ctrl Pts',(-227.807194738847,4.15562473557794,
126.191753883612));
#277318=CARTESIAN_POINT('Ctrl Pts',(-228.08564236266,-1.63450000472891,
124.81488922523));
#277319=CARTESIAN_POINT('Ctrl Pts',(-228.364089986473,-5.9225990904546,
128.942056174461));
#277320=CARTESIAN_POINT('Ctrl Pts',(-228.642537610286,-4.76811894710285,
134.780589928275));
#277321=CARTESIAN_POINT('Ctrl Pts',(-228.920985234099,0.768029573076269,
136.965163195147));
#277322=CARTESIAN_POINT('Ctrl Pts',(-229.199432857912,5.59839643592858,
133.48825986516));
#277323=CARTESIAN_POINT('Ctrl Pts',(-229.477880481725,5.28411047103341,
127.544984242401));
#277324=CARTESIAN_POINT('Ctrl Pts',(-229.756328105537,0.11398512640586,
124.59691627903));
#277325=CARTESIAN_POINT('Ctrl Pts',(-230.03477572935,-5.16088698090536,
127.353186412258));
#277326=CARTESIAN_POINT('Ctrl Pts',(-230.313223353163,-5.69315607611037,
133.280917040931));
#277327=CARTESIAN_POINT('Ctrl Pts',(-230.591670976976,-0.993692863505588,
136.932813303039));
#277328=CARTESIAN_POINT('Ctrl Pts',(-230.870118600789,4.6189255460653,134.952960938754));
#277329=CARTESIAN_POINT('Ctrl Pts',(-231.148566224602,5.98697702585963,
129.160747549691));
#277330=CARTESIAN_POINT('Ctrl Pts',(-231.427013848415,1.85328909897679,
124.878934275042));
#277331=CARTESIAN_POINT('Ctrl Pts',(-231.705461472227,-3.98348097165998,
126.042298336002));
#277332=CARTESIAN_POINT('Ctrl Pts',(-231.983909096041,-6.15962663320533,
131.581764994044));
#277333=CARTESIAN_POINT('Ctrl Pts',(-232.262356719853,-2.6753763333251,
136.406835008417));
#277334=CARTESIAN_POINT('Ctrl Pts',(-232.540804343666,3.26741411748112,
136.083504753687));
#277335=CARTESIAN_POINT('Ctrl Pts',(-232.819251967479,6.20761061637562,
130.90889893839));
#277336=CARTESIAN_POINT('Ctrl Pts',(-233.097699591292,3.44331621745904,
125.638227513236));
#277337=CARTESIAN_POINT('Ctrl Pts',(-233.376147215105,-2.48521756995422,
125.114980031328));
#277338=CARTESIAN_POINT('Ctrl Pts',(-233.654594838918,-6.12995782020675,
129.819995366479));
#277339=CARTESIAN_POINT('Ctrl Pts',(-233.933042462731,-4.14156629877734,
135.429594278462));
#277340=CARTESIAN_POINT('Ctrl Pts',(-234.211490086544,1.65272232446679,
136.788829411307));
#277341=CARTESIAN_POINT('Ctrl Pts',(-234.489937710357,5.92823987150001,
132.648630080257));
#277342=CARTESIAN_POINT('Ctrl Pts',(-234.768385334169,4.75599458724306,
126.813637210565));
#277343=CARTESIAN_POINT('Ctrl Pts',(-235.046832957982,-0.786777379437916,
124.64592419423));
#277344=CARTESIAN_POINT('Ctrl Pts',(-235.325280581795,-5.6065393706272,
128.137513394595));
#277345=CARTESIAN_POINT('Ctrl Pts',(-235.603728205608,-5.27416557488518,
134.079804910139));
#277346=CARTESIAN_POINT('Ctrl Pts',(-235.882175829421,-0.0950912731361558,
137.012123135159));
#277347=CARTESIAN_POINT('Ctrl Pts',(-236.160623453234,5.17136726315852,
134.239810872567));
#277348=CARTESIAN_POINT('Ctrl Pts',(-236.439071077047,5.68559191994549,
128.310487656705));
#277349=CARTESIAN_POINT('Ctrl Pts',(-236.71751870086,0.975035358909668,
124.672911859406));
#277350=CARTESIAN_POINT('Ctrl Pts',(-236.995966324673,-4.63153106383903,
126.669837932931));
#277351=CARTESIAN_POINT('Ctrl Pts',(-237.274413948486,-5.98194670179065,
132.466188370973));
#277352=CARTESIAN_POINT('Ctrl Pts',(-237.552861572298,-1.83524555513966,
136.735400288432));
#277353=CARTESIAN_POINT('Ctrl Pts',(-237.831309196112,3.99795659995517,
135.554276495761));
#277354=CARTESIAN_POINT('Ctrl Pts',(-238.109756819924,6.15723195072914,
130.008212057319));
#277355=CARTESIAN_POINT('Ctrl Pts',(-238.388204443737,2.65831193628575,
125.193769251723));
#277356=CARTESIAN_POINT('Ctrl Pts',(-238.66665206755,-3.28346688184612,
125.535185818711));
#277357=CARTESIAN_POINT('Ctrl Pts',(-238.945099691363,-6.20790004183648,
130.718716612347));
#277358=CARTESIAN_POINT('Ctrl Pts',(-239.223547315176,-3.42757633615586,
135.980950062836));
#277359=CARTESIAN_POINT('Ctrl Pts',(-239.501994938989,2.50252257603867,
136.486150703575));
#277360=CARTESIAN_POINT('Ctrl Pts',(-239.780442562802,6.13292549587844,
131.770063826148));
#277361=CARTESIAN_POINT('Ctrl Pts',(-240.058890186614,4.12746949507249,
126.166542877259));
#277362=CARTESIAN_POINT('Ctrl Pts',(-240.337337810428,-1.67092933361012,
124.824949861719));
#277363=CARTESIAN_POINT('Ctrl Pts',(-240.61578543424,-5.93382573414137,
128.978143220346));
#277364=CARTESIAN_POINT('Ctrl Pts',(-240.894233058053,-4.74382616849909,
134.80954115134));
#277365=CARTESIAN_POINT('Ctrl Pts',(-241.172680681866,0.805517897201924,
136.960373835741));
#277366=CARTESIAN_POINT('Ctrl Pts',(-241.451128305679,5.6146303671111,133.454131110603));
#277367=CARTESIAN_POINT('Ctrl Pts',(-241.729575929492,5.26417181958768,
127.512878750849));
#277368=CARTESIAN_POINT('Ctrl Pts',(-242.008023553305,0.0761965389532375,
124.596337428779));
#277369=CARTESIAN_POINT('Ctrl Pts',(-242.286471177117,-5.18179963857104,
127.384666138411));
#277370=CARTESIAN_POINT('Ctrl Pts',(-242.564918800931,-5.67797509323448,
133.315527013022));
#277371=CARTESIAN_POINT('Ctrl Pts',(-242.843366424743,-0.956368821719198,
136.938748647509));
#277372=CARTESIAN_POINT('Ctrl Pts',(-243.121814048556,4.64409367574132,
134.924767363992));
#277373=CARTESIAN_POINT('Ctrl Pts',(-243.400261672369,5.9768609617849,129.124333573571));
#277374=CARTESIAN_POINT('Ctrl Pts',(-243.678709296182,1.81718500983798,
124.867762562695));
#277375=CARTESIAN_POINT('Ctrl Pts',(-243.957156919995,-4.01239519172672,
126.066635145309));
#277376=CARTESIAN_POINT('Ctrl Pts',(-244.235604543808,-6.15478022849689,
131.619245986169));
#277377=CARTESIAN_POINT('Ctrl Pts',(-244.514052167621,-2.64122291300849,
136.423016982646));
#277378=CARTESIAN_POINT('Ctrl Pts',(-244.792499791433,3.29948922862226,
136.063517266237));
#277379=CARTESIAN_POINT('Ctrl Pts',(-245.070947415247,6.20813195815889,
130.871109513785));
#277380=CARTESIAN_POINT('Ctrl Pts',(-245.349395039059,3.41180470225455,
125.617362786572));
#277381=CARTESIAN_POINT('Ctrl Pts',(-245.627842662872,-2.51980439909662,
125.13021366711));
#277382=CARTESIAN_POINT('Ctrl Pts',(-245.906290286685,-6.13583635696575,
129.857328397629));
#277383=CARTESIAN_POINT('Ctrl Pts',(-246.184737910498,-4.1133344550539,
135.454719473173));
#277384=CARTESIAN_POINT('Ctrl Pts',(-246.463185534311,1.68912086349306,
136.778657943074));
#277385=CARTESIAN_POINT('Ctrl Pts',(-246.741633158124,5.93935662663147,
132.612509031482));
#277386=CARTESIAN_POINT('Ctrl Pts',(-247.020080781937,4.73161380359756,
126.784760060463));
#277387=CARTESIAN_POINT('Ctrl Pts',(-247.29852840575,-0.824250952757648,
124.650827633015));
#277388=CARTESIAN_POINT('Ctrl Pts',(-247.576976029562,-5.62266935042617,
128.171691401572));
#277389=CARTESIAN_POINT('Ctrl Pts',(-247.855423653376,-5.25412929772145,
134.111849566585));
#277390=CARTESIAN_POINT('Ctrl Pts',(-248.133871277188,-0.0573010988966442,
137.012586967267));
#277391=CARTESIAN_POINT('Ctrl Pts',(-248.412318901001,5.19218401050035,
134.208267641291));
#277392=CARTESIAN_POINT('Ctrl Pts',(-248.690766524814,5.67030566653712,
128.275924050614));
#277393=CARTESIAN_POINT('Ctrl Pts',(-248.969214148627,0.937693424858449,
124.667090143972));
#277394=CARTESIAN_POINT('Ctrl Pts',(-249.24766177244,-4.65661326539506,
126.698107980232));
#277395=CARTESIAN_POINT('Ctrl Pts',(-249.526109396252,-5.97171985295489,
132.502571388608));
#277396=CARTESIAN_POINT('Ctrl Pts',(-249.804557020066,-1.79910763038337,
136.746462060605));
#277397=CARTESIAN_POINT('Ctrl Pts',(-250.083004643878,4.02679661321771,
135.52985179424));
#277398=CARTESIAN_POINT('Ctrl Pts',(-250.361452267692,6.15227148922063,
129.970745989595));
#277399=CARTESIAN_POINT('Ctrl Pts',(-250.639899891504,2.62410942180459,
125.177691303707));
#277400=CARTESIAN_POINT('Ctrl Pts',(-250.918347515317,-3.31548100938434,
125.555270839195));
#277401=CARTESIAN_POINT('Ctrl Pts',(-251.19679513913,-6.20830636318893,
130.756507448682));
#277402=CARTESIAN_POINT('Ctrl Pts',(-251.475242762943,-3.39600146187203,
136.001718782677));
#277403=CARTESIAN_POINT('Ctrl Pts',(-251.753690386756,2.53706287905323,
136.47081186788));
#277404=CARTESIAN_POINT('Ctrl Pts',(-252.032138010569,6.13869037645988,
131.732713075798));
#277405=CARTESIAN_POINT('Ctrl Pts',(-252.310585634382,4.09916130974965,
126.141503726722));
#277406=CARTESIAN_POINT('Ctrl Pts',(-252.589033258195,-1.70729674574642,
124.835232067896));
#277407=CARTESIAN_POINT('Ctrl Pts',(-252.867480882007,-5.94483249743877,
129.014297936587));
#277408=CARTESIAN_POINT('Ctrl Pts',(-253.14592850582,-4.71935760622846,
134.838343962485));
#277409=CARTESIAN_POINT('Ctrl Pts',(-253.424376129633,0.842976373616159,
136.955356360136));
#277410=CARTESIAN_POINT('Ctrl Pts',(-253.702823753446,5.63065624411703,
133.419904173236));
#277411=CARTESIAN_POINT('Ctrl Pts',(-253.981271377259,5.24403810606461,
127.480895216153));
#277412=CARTESIAN_POINT('Ctrl Pts',(-254.259719001072,0.0384051209378723,
124.595988638398));
#277413=CARTESIAN_POINT('Ctrl Pts',(-254.538166624885,-5.20252026939218,
127.416272546179));
#277414=CARTESIAN_POINT('Ctrl Pts',(-254.816614248698,-5.66258373611722,
133.350044001689));
#277415=CARTESIAN_POINT('Ctrl Pts',(-255.095061872511,-0.919009293725241,
136.944456550123));
#277416=CARTESIAN_POINT('Ctrl Pts',(-255.373509496324,4.6690896269236,134.896421351226));
#277417=CARTESIAN_POINT('Ctrl Pts',(-255.651957120136,5.96652359266914,
129.087981388513));
#277418=CARTESIAN_POINT('Ctrl Pts',(-255.93040474395,1.78101326373629,124.856811707331));
#277419=CARTESIAN_POINT('Ctrl Pts',(-256.208852367762,-4.04116012583712,
126.091145862189));
#277420=CARTESIAN_POINT('Ctrl Pts',(-256.487299991575,-6.14970689884083,
131.656699899059));
#277421=CARTESIAN_POINT('Ctrl Pts',(-256.765747615388,-2.60696946356087,
136.438984870644));
#277422=CARTESIAN_POINT('Ctrl Pts',(-257.044195239201,3.33143800190474,
136.043346010603));
#277423=CARTESIAN_POINT('Ctrl Pts',(-257.322642863014,6.2084309480058,130.833296634437));
#277424=CARTESIAN_POINT('Ctrl Pts',(-257.601090486826,3.38015223603414,
125.596729883064));
#277425=CARTESIAN_POINT('Ctrl Pts',(-257.87953811064,-2.5542704291637,125.145582755354));
#277426=CARTESIAN_POINT('Ctrl Pts',(-258.157985734452,-6.14153931545366,
129.894837769574));
#277427=CARTESIAN_POINT('Ctrl Pts',(-258.436433358265,-4.08485240479644,
135.479405634932));
#277428=CARTESIAN_POINT('Ctrl Pts',(-258.714880982078,1.72527217059264,
136.768768758555));
#277429=CARTESIAN_POINT('Ctrl Pts',(-258.993328605892,5.95060195420752,
132.575369498931));
#277430=CARTESIAN_POINT('Ctrl Pts',(-259.271776229703,4.70639920604184,
126.75783223591));
#277431=CARTESIAN_POINT('Ctrl Pts',(-259.550223853517,-0.860449444711704,
124.652528659269));
#277432=CARTESIAN_POINT('Ctrl Pts',(-259.82867147733,-5.64095031490746,
128.212697490595));
#277433=CARTESIAN_POINT('Ctrl Pts',(-260.060711163841,-5.29799179572588,
133.142936715762));
#277434=CARTESIAN_POINT('Ctrl Pts',(-260.246372125917,-2.62679689981868,
135.594171577488));
#277435=CARTESIAN_POINT('Ctrl Pts',(-260.339217213388,-0.889986900407246,
136.05080276614));
#277436=CARTESIAN_POINT('Ctrl Pts',(-260.385654363559,-0.0148419801173944,
136.053268468065));
#277437=CARTESIAN_POINT('Ctrl Pts',(209.997106195361,2.85369542052185,134.803838223542));
#277438=CARTESIAN_POINT('Ctrl Pts',(209.950688331758,3.52024512455777,134.328247120061));
#277439=CARTESIAN_POINT('Ctrl Pts',(209.857862530854,4.598911638141,133.039517383424));
#277440=CARTESIAN_POINT('Ctrl Pts',(209.672220855345,5.31158968331849,129.722011776094));
#277441=CARTESIAN_POINT('Ctrl Pts',(209.440181168834,2.90445768035623,125.771581499823));
#277442=CARTESIAN_POINT('Ctrl Pts',(209.161733545021,-2.67328939945229,
125.640965885288));
#277443=CARTESIAN_POINT('Ctrl Pts',(208.883285921209,-5.78445646322271,
130.262241799363));
#277444=CARTESIAN_POINT('Ctrl Pts',(208.604838297395,-3.58517659481558,
135.378114005881));
#277445=CARTESIAN_POINT('Ctrl Pts',(208.326390673583,1.91144119617671,136.292814641374));
#277446=CARTESIAN_POINT('Ctrl Pts',(208.04794304977,5.65009034124608,132.162897902674));
#277447=CARTESIAN_POINT('Ctrl Pts',(207.769495425957,4.19734896093999,126.785079177362));
#277448=CARTESIAN_POINT('Ctrl Pts',(207.491047802144,-1.1129569716493,125.100504449821));
#277449=CARTESIAN_POINT('Ctrl Pts',(207.212600178331,-5.4002948496084,128.657642803108));
#277450=CARTESIAN_POINT('Ctrl Pts',(206.934152554519,-4.72513942780656,
134.187431620732));
#277451=CARTESIAN_POINT('Ctrl Pts',(206.655704930705,0.292248586550605,
136.608384944684));
#277452=CARTESIAN_POINT('Ctrl Pts',(206.377257306892,5.04104249491135,133.695701483205));
#277453=CARTESIAN_POINT('Ctrl Pts',(206.09880968308,5.15738153042831,128.12602865207));
#277454=CARTESIAN_POINT('Ctrl Pts',(205.820362059267,0.534329935251406,
125.017605890956));
#277455=CARTESIAN_POINT('Ctrl Pts',(205.541914435454,-4.57974002364783,
127.226931288585));
#277456=CARTESIAN_POINT('Ctrl Pts',(205.263466811641,-5.48525514562618,
132.723737743954));
#277457=CARTESIAN_POINT('Ctrl Pts',(204.985019187828,-1.35008742798131,
136.456731302353));
#277458=CARTESIAN_POINT('Ctrl Pts',(204.706571564015,4.02574397595362,134.995471850294));
#277459=CARTESIAN_POINT('Ctrl Pts',(204.428123940202,5.70211370766606,129.682786179275));
#277460=CARTESIAN_POINT('Ctrl Pts',(204.149676316389,2.13851930815143,125.40077248911));
#277461=CARTESIAN_POINT('Ctrl Pts',(203.871228692576,-3.39026975841633,
126.084392381055));
#277462=CARTESIAN_POINT('Ctrl Pts',(203.592781068764,-5.8035665963141,131.105432460946));
#277463=CARTESIAN_POINT('Ctrl Pts',(203.314333444951,-2.88366922283368,
135.849802245147));
#277464=CARTESIAN_POINT('Ctrl Pts',(203.035885821138,2.68617927581077,135.957657646429));
#277465=CARTESIAN_POINT('Ctrl Pts',(202.757438197325,5.78756025537181,131.329884836407));
#277466=CARTESIAN_POINT('Ctrl Pts',(202.478990573512,3.57045609392238,126.219180939555));
#277467=CARTESIAN_POINT('Ctrl Pts',(202.200542949699,-1.92772278905516,
125.322033169903));
#277468=CARTESIAN_POINT('Ctrl Pts',(201.922095325886,-5.6544186046078,129.462876497226));
#277469=CARTESIAN_POINT('Ctrl Pts',(201.643647702073,-4.18497995558374,
134.836478196445));
#277470=CARTESIAN_POINT('Ctrl Pts',(201.36520007826,1.13025082464198,136.504760820331));
#277471=CARTESIAN_POINT('Ctrl Pts',(201.086752454448,5.4068363130258,132.934654138033));
#277472=CARTESIAN_POINT('Ctrl Pts',(200.808304830635,4.71480336828096,127.406911780982));
#277473=CARTESIAN_POINT('Ctrl Pts',(200.529857206822,-0.309903540913717,
125.001258930184));
#277474=CARTESIAN_POINT('Ctrl Pts',(200.251409583008,-5.04982423566531,
127.928373032793));
#277475=CARTESIAN_POINT('Ctrl Pts',(199.972961959197,-5.14920315545485,
133.498379226012));
#277476=CARTESIAN_POINT('Ctrl Pts',(199.694514335383,-0.516715927947778,
136.59271392819));
#277477=CARTESIAN_POINT('Ctrl Pts',(199.416066711571,4.59060799437092,134.367834714685));
#277478=CARTESIAN_POINT('Ctrl Pts',(199.137619087757,5.47938743352869,128.868296891315));
#277479=CARTESIAN_POINT('Ctrl Pts',(198.859171463945,1.33287750423228,125.147907050397));
#277480=CARTESIAN_POINT('Ctrl Pts',(198.580723840131,-4.03848173676817,
126.625521704588));
#277481=CARTESIAN_POINT('Ctrl Pts',(198.302276216319,-5.69867355247927,
131.943285172176));
#277482=CARTESIAN_POINT('Ctrl Pts',(198.023828592506,-2.12206276914206,
136.214432613634));
#277483=CARTESIAN_POINT('Ctrl Pts',(197.745380968693,3.4046200305072,135.513988187415));
#277484=CARTESIAN_POINT('Ctrl Pts',(197.46693334488,5.80262334705539,130.485626102603));
#277485=CARTESIAN_POINT('Ctrl Pts',(197.188485721067,2.86829928156946,125.750165465994));
#277486=CARTESIAN_POINT('Ctrl Pts',(196.910038097254,-2.70185169946893,
125.65926326252));
#277487=CARTESIAN_POINT('Ctrl Pts',(196.631590473441,-5.78913296148881,
130.296454176353));
#277488=CARTESIAN_POINT('Ctrl Pts',(196.353142849628,-3.5564838467683,135.400386297052));
#277489=CARTESIAN_POINT('Ctrl Pts',(196.074695225815,1.94440017923737,136.280795346639));
#277490=CARTESIAN_POINT('Ctrl Pts',(195.796247602003,5.6584754297534,132.128628418917));
#277491=CARTESIAN_POINT('Ctrl Pts',(195.51779997819,4.17268819221861,126.759524075833));
#277492=CARTESIAN_POINT('Ctrl Pts',(195.239352354377,-1.14759564681435,
125.107426913349));
#277493=CARTESIAN_POINT('Ctrl Pts',(194.960904730564,-5.41329514958902,
128.690533514357));
#277494=CARTESIAN_POINT('Ctrl Pts',(194.682457106751,-4.70444086406131,
134.216143957018));
#277495=CARTESIAN_POINT('Ctrl Pts',(194.404009482938,0.327564750825761,
136.606492185605));
#277496=CARTESIAN_POINT('Ctrl Pts',(194.125561859125,5.0585543621317,133.664964953048));
#277497=CARTESIAN_POINT('Ctrl Pts',(193.847114235312,5.14097963875765,128.094682084473));
#277498=CARTESIAN_POINT('Ctrl Pts',(193.568666611499,0.499095778182989,
125.014461412655));
#277499=CARTESIAN_POINT('Ctrl Pts',(193.290218987687,-4.60143272035756,
127.254875257849));
#277500=CARTESIAN_POINT('Ctrl Pts',(193.011771363874,-5.4734693413749,132.757092746623));
#277501=CARTESIAN_POINT('Ctrl Pts',(192.733323740061,-1.31565503151135,
136.464844805061));
#277502=CARTESIAN_POINT('Ctrl Pts',(192.454876116248,4.05118197898966,134.970888425217));
#277503=CARTESIAN_POINT('Ctrl Pts',(192.176428492435,5.69518066204141,129.648096536341));
#277504=CARTESIAN_POINT('Ctrl Pts',(191.897980868622,2.1055865417199,125.38785485147));
#277505=CARTESIAN_POINT('Ctrl Pts',(191.619533244809,-3.4189387468211,126.105117354624));
#277506=CARTESIAN_POINT('Ctrl Pts',(191.341085620997,-5.80162635147675,
131.140754845624));
#277507=CARTESIAN_POINT('Ctrl Pts',(191.062637997183,-2.85290276432908,
135.867262474811));
#277508=CARTESIAN_POINT('Ctrl Pts',(190.784190373371,2.71749909118881,135.941210633695));
#277509=CARTESIAN_POINT('Ctrl Pts',(190.505742749557,5.79065203911519,131.29464457683));
#277510=CARTESIAN_POINT('Ctrl Pts',(190.227295125745,3.54247865217362,126.197531513104));
#277511=CARTESIAN_POINT('Ctrl Pts',(189.948847501932,-1.96105955641241,
125.333869340265));
#277512=CARTESIAN_POINT('Ctrl Pts',(189.670399878119,-5.66247983574075,
129.497321402909));
#277513=CARTESIAN_POINT('Ctrl Pts',(189.391952254306,-4.160357773542,134.861878651407));
#277514=CARTESIAN_POINT('Ctrl Pts',(189.113504630493,1.16492983776554,136.497775047581));
#277515=CARTESIAN_POINT('Ctrl Pts',(188.83505700668,5.41970383815296,132.901701721328));
#277516=CARTESIAN_POINT('Ctrl Pts',(188.556609382867,4.69403477852959,127.378274381527));
#277517=CARTESIAN_POINT('Ctrl Pts',(188.278161759054,-0.345222926215044,
125.003252919028));
#277518=CARTESIAN_POINT('Ctrl Pts',(187.999714135242,-5.0672376268456,127.959166031618));
#277519=CARTESIAN_POINT('Ctrl Pts',(187.721266511429,-5.13270849672517,
133.529673973213));
#277520=CARTESIAN_POINT('Ctrl Pts',(187.442818887616,-0.48147100486422,
136.595752079925));
#277521=CARTESIAN_POINT('Ctrl Pts',(187.164371263803,4.61221481930072,134.339824357932));
#277522=CARTESIAN_POINT('Ctrl Pts',(186.88592363999,5.4675005437485,128.834978175547));
#277523=CARTESIAN_POINT('Ctrl Pts',(186.607476016177,1.29842037074208,125.139898247696));
#277524=CARTESIAN_POINT('Ctrl Pts',(186.329028392364,-4.06384469161484,
126.650182513385));
#277525=CARTESIAN_POINT('Ctrl Pts',(186.050580768551,-5.69163501222784,
131.977953513933));
#277526=CARTESIAN_POINT('Ctrl Pts',(185.772133144738,-2.08909080843167,
136.227249975919));
#277527=CARTESIAN_POINT('Ctrl Pts',(185.493685520926,3.4332257905535,135.493176040453));
#277528=CARTESIAN_POINT('Ctrl Pts',(185.215237897112,5.80057561042411,130.450309792719));
#277529=CARTESIAN_POINT('Ctrl Pts',(184.9367902733,2.83747981818726,125.732798956676));
#277530=CARTESIAN_POINT('Ctrl Pts',(184.658342649487,-2.73312130836828,
125.675805527429));
#277531=CARTESIAN_POINT('Ctrl Pts',(184.379895025674,-5.79211747293216,
130.331703682172));
#277532=CARTESIAN_POINT('Ctrl Pts',(184.101447401861,-3.52844064054064,
135.421950469967));
#277533=CARTESIAN_POINT('Ctrl Pts',(183.822999778048,1.97770076659953,136.26885776521));
#277534=CARTESIAN_POINT('Ctrl Pts',(183.544552154236,5.66643178528845,132.094159137294));
#277535=CARTESIAN_POINT('Ctrl Pts',(183.266104530422,4.14798881387936,126.734198679909));
#277536=CARTESIAN_POINT('Ctrl Pts',(182.98765690661,-1.18225323696583,125.114518204765));
#277537=CARTESIAN_POINT('Ctrl Pts',(182.709209282797,-5.42606231932092,
128.72352494273));
#277538=CARTESIAN_POINT('Ctrl Pts',(182.430761658984,-4.68358520810093,
134.244718011395));
#277539=CARTESIAN_POINT('Ctrl Pts',(182.152314035171,0.362877903506298,
136.604390705933));
#277540=CARTESIAN_POINT('Ctrl Pts',(181.873866411358,5.07587394936235,133.634119096483));
#277541=CARTESIAN_POINT('Ctrl Pts',(181.595418787545,5.12438980598236,128.063437686296));
#277542=CARTESIAN_POINT('Ctrl Pts',(181.316971163732,0.463841771263853,
125.011530548415));
#277543=CARTESIAN_POINT('Ctrl Pts',(181.038523539919,-4.62295419131585,
127.282951248603));
#277544=CARTESIAN_POINT('Ctrl Pts',(180.760075916106,-5.46148109594396,
132.790375128456));
#277545=CARTESIAN_POINT('Ctrl Pts',(180.481628292294,-1.2811736815839,136.472748695004));
#277546=CARTESIAN_POINT('Ctrl Pts',(180.203180668481,4.07646975733793,134.946150534538));
#277547=CARTESIAN_POINT('Ctrl Pts',(179.924733044668,5.68803663588505,129.61344977806));
#277548=CARTESIAN_POINT('Ctrl Pts',(179.646285420855,2.07257572209157,125.37513790386));
#277549=CARTESIAN_POINT('Ctrl Pts',(179.367837797042,-3.44748102935117,
126.12601647128));
#277550=CARTESIAN_POINT('Ctrl Pts',(179.089390173229,-5.79947113363144,
131.176064759319));
#277551=CARTESIAN_POINT('Ctrl Pts',(178.810942549416,-2.82203058602,135.884535099843));
#277552=CARTESIAN_POINT('Ctrl Pts',(178.532494925603,2.74871820628535,135.924573271475));
#277553=CARTESIAN_POINT('Ctrl Pts',(178.254047301791,5.79352924936408,131.259386150458));
#277554=CARTESIAN_POINT('Ctrl Pts',(177.975599677977,3.51436994191561,126.176052793945));
#277555=CARTESIAN_POINT('Ctrl Pts',(177.697152054165,-1.99432365563702,
125.345908221933));
#277556=CARTESIAN_POINT('Ctrl Pts',(177.418704430351,-5.6703312417861,129.531814741282));
#277557=CARTESIAN_POINT('Ctrl Pts',(177.140256806539,-4.135581427815,134.887128753614));
#277558=CARTESIAN_POINT('Ctrl Pts',(176.861809182726,1.19956568393359,136.490578303229));
#277559=CARTESIAN_POINT('Ctrl Pts',(176.583361558913,5.43237053418876,132.868671586896));
#277560=CARTESIAN_POINT('Ctrl Pts',(176.3049139351,4.67309224957875,127.349763936946));
#277561=CARTESIAN_POINT('Ctrl Pts',(176.026466311287,-0.380529519146142,
125.005461870054));
#277562=CARTESIAN_POINT('Ctrl Pts',(175.748018687475,-5.08446324967622,
127.990064460173));
#277563=CARTESIAN_POINT('Ctrl Pts',(175.469571063661,-5.11602364359241,
133.560867732924));
#277564=CARTESIAN_POINT('Ctrl Pts',(175.191123439849,-0.446208240696769,
136.59857562952));
#277565=CARTESIAN_POINT('Ctrl Pts',(174.912675816035,4.63365073691483,134.311682993269));
#277566=CARTESIAN_POINT('Ctrl Pts',(174.634228192223,5.45541105372469,128.801732435971));
#277567=CARTESIAN_POINT('Ctrl Pts',(174.35578056841,1.26391512380778,125.132099343732));
#277568=CARTESIAN_POINT('Ctrl Pts',(174.077332944597,-4.089057059202,126.674997256779));
#277569=CARTESIAN_POINT('Ctrl Pts',(173.798885320784,-5.68438556634791,
132.012578367773));
#277570=CARTESIAN_POINT('Ctrl Pts',(173.520437696972,-2.0560414356932,136.239866391045));
#277571=CARTESIAN_POINT('Ctrl Pts',(173.241990073158,3.46170433115548,135.472190147709));
#277572=CARTESIAN_POINT('Ctrl Pts',(172.963542449346,5.79831293133042,130.41500660232));
#277573=CARTESIAN_POINT('Ctrl Pts',(172.685094825533,2.80655521094699,125.715620375941));
#277574=CARTESIAN_POINT('Ctrl Pts',(172.40664720172,-2.76428964045241,125.692537832834));
#277575=CARTESIAN_POINT('Ctrl Pts',(172.128199577907,-5.79488735533246,
130.366970702468));
#277576=CARTESIAN_POINT('Ctrl Pts',(171.849751954094,-3.50026668664755,
135.443343536393));
#277577=CARTESIAN_POINT('Ctrl Pts',(171.571304330281,2.01092806953244,136.256717694829));
#277578=CARTESIAN_POINT('Ctrl Pts',(171.292856706468,5.6741781691098,132.059642061713));
#277579=CARTESIAN_POINT('Ctrl Pts',(171.014409082656,4.12313573028927,126.709024105332));
#277580=CARTESIAN_POINT('Ctrl Pts',(170.735961458842,-1.21686701828875,
125.121820335384));
#277581=CARTESIAN_POINT('Ctrl Pts',(170.45751383503,-5.43862842431808,128.756593477234));
#277582=CARTESIAN_POINT('Ctrl Pts',(170.179066211217,-4.66255600016836,
134.273164582064));
#277583=CARTESIAN_POINT('Ctrl Pts',(169.900618587404,0.398177609612544,
136.602074304013));
#277584=CARTESIAN_POINT('Ctrl Pts',(169.62217096359,5.09300544821711,133.603168382178));
#277585=CARTESIAN_POINT('Ctrl Pts',(169.343723339778,5.10761008705837,128.032294854024));
#277586=CARTESIAN_POINT('Ctrl Pts',(169.065275715965,0.428570576517446,
125.008814339624));
#277587=CARTESIAN_POINT('Ctrl Pts',(168.786828092152,-4.64430435700642,
127.311157726477));
#277588=CARTESIAN_POINT('Ctrl Pts',(168.508380468339,-5.4492904733226,132.823583917792));
#277589=CARTESIAN_POINT('Ctrl Pts',(168.229932844526,-1.24664485729461,
136.480442540741));
#277590=CARTESIAN_POINT('Ctrl Pts',(167.951485220714,4.10160648060013,134.92125916831));
#277591=CARTESIAN_POINT('Ctrl Pts',(167.673037596901,5.6806818374394,129.578847149419));
#277592=CARTESIAN_POINT('Ctrl Pts',(167.394589973088,2.03948810240773,125.362622138095));
#277593=CARTESIAN_POINT('Ctrl Pts',(167.116142349275,-3.47589556420378,
126.147088945699));
#277594=CARTESIAN_POINT('Ctrl Pts',(166.837694725462,-5.79710101425052,
131.21136089938));
#277595=CARTESIAN_POINT('Ctrl Pts',(166.559247101649,-2.79105383632985,
135.901619477142));
#277596=CARTESIAN_POINT('Ctrl Pts',(166.280799477836,2.77983546661788,135.907746177893));
#277597=CARTESIAN_POINT('Ctrl Pts',(166.002351854023,5.79619177825601,131.224110862948));
#277598=CARTESIAN_POINT('Ctrl Pts',(165.72390423021,3.48613100538707,126.154745578436));
#277599=CARTESIAN_POINT('Ctrl Pts',(165.445456606397,-2.02751385446508,
125.358149368562));
#277600=CARTESIAN_POINT('Ctrl Pts',(165.167008982585,-5.67797253162207,
129.566355234311));
#277601=CARTESIAN_POINT('Ctrl Pts',(164.888561358772,-4.11065183659732,
134.912227567346));
#277602=CARTESIAN_POINT('Ctrl Pts',(164.610113734959,1.23415707975413,136.483170853989));
#277603=CARTESIAN_POINT('Ctrl Pts',(164.331666111146,5.44483593173667,132.835564958663));
#277604=CARTESIAN_POINT('Ctrl Pts',(164.053218487333,4.65197655747607,127.321381503715));
#277605=CARTESIAN_POINT('Ctrl Pts',(163.77477086352,-0.415822011415935,
125.007885701408));
#277606=CARTESIAN_POINT('Ctrl Pts',(163.496323239708,-5.10150046585131,
128.021067173507));
#277607=CARTESIAN_POINT('Ctrl Pts',(163.217875615894,-5.09914921432216,
133.591959349252));
#277608=CARTESIAN_POINT('Ctrl Pts',(162.939427992082,-0.41092894211879,
136.601184472346));
#277609=CARTESIAN_POINT('Ctrl Pts',(162.660980368268,4.65491495289691,134.283411663486));
#277610=CARTESIAN_POINT('Ctrl Pts',(162.382532744456,5.443119411438,128.768560904517));
#277611=CARTESIAN_POINT('Ctrl Pts',(162.104085120643,1.22936304203373,125.124510627495));
#277612=CARTESIAN_POINT('Ctrl Pts',(161.82563749683,-4.11411790527609,126.69996501525));
#277613=CARTESIAN_POINT('Ctrl Pts',(161.547189873017,-5.67692548347038,
132.04715845066));
#277614=CARTESIAN_POINT('Ctrl Pts',(161.268742249204,-2.02291587558315,
136.252281391507));
#277615=CARTESIAN_POINT('Ctrl Pts',(160.990294625391,3.49005459703047,135.451031286826));
#277616=CARTESIAN_POINT('Ctrl Pts',(160.711847001578,5.79583539361873,130.379717839577));
#277617=CARTESIAN_POINT('Ctrl Pts',(160.433399377766,2.77552660577121,125.698630360346));
#277618=CARTESIAN_POINT('Ctrl Pts',(160.154951753952,-2.79535554076737,
125.70945955871));
#277619=CARTESIAN_POINT('Ctrl Pts',(159.87650413014,-5.79744250605075,130.402253930408));
#277620=CARTESIAN_POINT('Ctrl Pts',(159.598056506327,-3.47196302908515,
135.4645647036));
#277621=CARTESIAN_POINT('Ctrl Pts',(159.319608882514,2.04408085678626,136.244375585352));
#277622=CARTESIAN_POINT('Ctrl Pts',(159.041161258701,5.68171429417248,132.025078471215));
#277623=CARTESIAN_POINT('Ctrl Pts',(158.762713634888,4.09812986238831,126.684001284956));
#277624=CARTESIAN_POINT('Ctrl Pts',(158.484266011075,-1.25143570815684,
125.129333034622));
#277625=CARTESIAN_POINT('Ctrl Pts',(158.205818387262,-5.450992998939,128.789737892503));
#277626=CARTESIAN_POINT('Ctrl Pts',(157.927370763449,-4.64135401950845,
134.301482614925));
#277627=CARTESIAN_POINT('Ctrl Pts',(157.648923139637,0.43346256110109,136.59954306568));
#277628=CARTESIAN_POINT('Ctrl Pts',(157.370475515823,5.10994822388206,133.572113957021));
#277629=CARTESIAN_POINT('Ctrl Pts',(157.092027892011,5.09064110376424,128.001254741669));
#277630=CARTESIAN_POINT('Ctrl Pts',(156.813580268198,0.39328350093061,125.006312886931));
#277631=CARTESIAN_POINT('Ctrl Pts',(156.535132644385,-4.66548242629113,
127.339493646268));
#277632=CARTESIAN_POINT('Ctrl Pts',(156.256685020572,-5.43689792523874,
132.856717884066));
#277633=CARTESIAN_POINT('Ctrl Pts',(155.978237396759,-1.21206983812162,
136.487926057176));
#277634=CARTESIAN_POINT('Ctrl Pts',(155.699789772946,4.12659121732586,134.896215248893));
#277635=CARTESIAN_POINT('Ctrl Pts',(155.421342149133,5.67311653923917,129.544289932631));
#277636=CARTESIAN_POINT('Ctrl Pts',(155.142894525321,2.0063249087422,125.350308017949));
#277637=CARTESIAN_POINT('Ctrl Pts',(154.864446901507,-3.50418129846815,
126.168333997033));
#277638=CARTESIAN_POINT('Ctrl Pts',(154.585999277695,-5.79451608115961,
131.246641957895));
#277639=CARTESIAN_POINT('Ctrl Pts',(154.307551653882,-2.75997366311328,
135.918514973638));
#277640=CARTESIAN_POINT('Ctrl Pts',(154.029104030069,2.81084971912495,135.890729976482));
#277641=CARTESIAN_POINT('Ctrl Pts',(153.750656406256,5.79863952713012,131.188820021437));
#277642=CARTESIAN_POINT('Ctrl Pts',(153.472208782443,3.457762888992,126.133610656121));
#277643=CARTESIAN_POINT('Ctrl Pts',(153.19376115863,-2.0606289230217,125.370592326552));
#277644=CARTESIAN_POINT('Ctrl Pts',(152.915313534817,-5.68540342209783,
129.600941602086));
#277645=CARTESIAN_POINT('Ctrl Pts',(152.636865911004,-4.08556992366409,
134.937174162558));
#277646=CARTESIAN_POINT('Ctrl Pts',(152.358418287191,1.26870274343019,136.475552974349));
#277647=CARTESIAN_POINT('Ctrl Pts',(152.079970663379,5.45709956888678,132.802383063404));
#277648=CARTESIAN_POINT('Ctrl Pts',(151.801523039566,4.63068848467127,127.293128133558));
#277649=CARTESIAN_POINT('Ctrl Pts',(151.523075415753,-0.451099095248245,
125.010524323271));
#277650=CARTESIAN_POINT('Ctrl Pts',(151.24462779194,-5.11834864405056,128.052173022803));
#277651=CARTESIAN_POINT('Ctrl Pts',(150.966180168127,-5.08208583420252,
133.622947670083));
#277652=CARTESIAN_POINT('Ctrl Pts',(150.687732544314,-0.375634416417742,
136.603578511732));
#277653=CARTESIAN_POINT('Ctrl Pts',(150.409284920501,4.67600667929353,134.255011416186));
#277654=CARTESIAN_POINT('Ctrl Pts',(150.130837296688,5.43062607235983,128.735464810371));
#277655=CARTESIAN_POINT('Ctrl Pts',(149.852389672876,1.19476540576009,125.117132380189));
#277656=CARTESIAN_POINT('Ctrl Pts',(149.573942049063,-4.13902630119825,
126.725084863609));
#277657=CARTESIAN_POINT('Ctrl Pts',(149.29549442525,-5.66925504003138,132.081692481218));
#277658=CARTESIAN_POINT('Ctrl Pts',(149.017046801437,-1.98971535558138,
136.264494517259));
#277659=CARTESIAN_POINT('Ctrl Pts',(148.738599177624,3.5182755376489,135.429700241853));
#277660=CARTESIAN_POINT('Ctrl Pts',(148.460151553811,5.79314308909515,130.344444812129));
#277661=CARTESIAN_POINT('Ctrl Pts',(148.181703929998,2.74439515243632,125.681829539465));
#277662=CARTESIAN_POINT('Ctrl Pts',(147.903256306185,-2.82631785815477,
125.726570078021));
#277663=CARTESIAN_POINT('Ctrl Pts',(147.624808682372,-5.79978283040501,
130.437552058559));
#277664=CARTESIAN_POINT('Ctrl Pts',(147.346361058559,-3.4435307166558,135.48561318523));
#277665=CARTESIAN_POINT('Ctrl Pts',(147.067913434747,2.07715789987228,136.23183189412));
#277666=CARTESIAN_POINT('Ctrl Pts',(146.789465810933,5.68903988122249,131.990469646568));
#277667=CARTESIAN_POINT('Ctrl Pts',(146.511018187121,4.07297213677825,126.65913114601));
#277668=CARTESIAN_POINT('Ctrl Pts',(146.232570563308,-1.2859580256146,125.137056024094));
#277669=CARTESIAN_POINT('Ctrl Pts',(145.954122939495,-5.46315558500969,
128.822956960357));
#277670=CARTESIAN_POINT('Ctrl Pts',(145.675675315682,-4.61998005176852,
134.329671060644));
#277671=CARTESIAN_POINT('Ctrl Pts',(145.397227691869,0.468731450475054,
136.596797084732));
#277672=CARTESIAN_POINT('Ctrl Pts',(145.118780068056,5.12670164853643,133.540956971746));
#277673=CARTESIAN_POINT('Ctrl Pts',(144.840332444244,5.07348348489189,127.970318499433));
#277674=CARTESIAN_POINT('Ctrl Pts',(144.56188482043,0.357981852079004,125.004026283029));
#277675=CARTESIAN_POINT('Ctrl Pts',(144.283437196618,-4.6864876144088,127.367957957979));
#277676=CARTESIAN_POINT('Ctrl Pts',(144.004989572805,-5.42430391090288,
132.889775799486));
#277677=CARTESIAN_POINT('Ctrl Pts',(143.726541948992,-1.17744990525502,
136.495198967004));
#277678=CARTESIAN_POINT('Ctrl Pts',(143.448094325179,4.15142304169647,134.871019704297));
#277679=CARTESIAN_POINT('Ctrl Pts',(143.169646701366,5.66534102161933,129.509779408224));
#277680=CARTESIAN_POINT('Ctrl Pts',(142.891199077553,1.9730873699693,125.338195999729));
#277681=CARTESIAN_POINT('Ctrl Pts',(142.61275145374,-3.53233718400576,126.189750838038));
#277682=CARTESIAN_POINT('Ctrl Pts',(142.334303829928,-5.79171643014443,
131.281906627513));
#277683=CARTESIAN_POINT('Ctrl Pts',(142.055856206114,-2.72879121805762,
135.935220963265));
#277684=CARTESIAN_POINT('Ctrl Pts',(141.777408582302,2.84175981456215,135.873525297782));
#277685=CARTESIAN_POINT('Ctrl Pts',(141.498960958489,5.80087240528401,131.153514933643));
#277686=CARTESIAN_POINT('Ctrl Pts',(141.220513334676,3.42926664392146,126.112648810165));
#277687=CARTESIAN_POINT('Ctrl Pts',(140.942065710863,-2.09366763421581,
125.383236634823));
#277688=CARTESIAN_POINT('Ctrl Pts',(140.66361808705,-5.69262363785895,129.635572562993));
#277689=CARTESIAN_POINT('Ctrl Pts',(140.385170463237,-4.06033661843482,
134.961967614844));
#277690=CARTESIAN_POINT('Ctrl Pts',(140.106722839424,1.30320139485961,136.467724946589));
#277691=CARTESIAN_POINT('Ctrl Pts',(139.828275215611,5.46916099120554,132.769127130691));
#277692=CARTESIAN_POINT('Ctrl Pts',(139.549827591798,4.60922882000175,127.26500487341));
#277693=CARTESIAN_POINT('Ctrl Pts',(139.271379967986,-0.486359463437733,
125.013377637868));
#277694=CARTESIAN_POINT('Ctrl Pts',(138.992932344173,-5.13500715995863,
128.083380855422));
#277695=CARTESIAN_POINT('Ctrl Pts',(138.71448472036,-5.06483413552331,133.653831547135));
#277696=CARTESIAN_POINT('Ctrl Pts',(138.436037096547,-0.340325971445257,
136.605757658967));
#277697=CARTESIAN_POINT('Ctrl Pts',(138.157589472734,4.69692513454305,134.226483303753));
#277698=CARTESIAN_POINT('Ctrl Pts',(137.879141848921,5.41793149943546,128.70244537992));
#277699=CARTESIAN_POINT('Ctrl Pts',(137.600694225109,1.16012349701482,125.109964875215));
#277700=CARTESIAN_POINT('Ctrl Pts',(137.322246601295,-4.16378132397874,
126.750355871033));
#277701=CARTESIAN_POINT('Ctrl Pts',(137.043798977483,-5.66137452026194,
132.116179179772));
#277702=CARTESIAN_POINT('Ctrl Pts',(136.765351353669,-1.95644110594549,
136.276505315742));
#277703=CARTESIAN_POINT('Ctrl Pts',(136.486903729857,3.54636610727348,135.408197803219));
#277704=CARTESIAN_POINT('Ctrl Pts',(136.208456106044,5.79023611752392,130.309188827029));
#277705=CARTESIAN_POINT('Ctrl Pts',(135.930008482231,2.71316200452982,125.665218535856));
#277706=CARTESIAN_POINT('Ctrl Pts',(135.651560858418,-2.85717544529452,
125.743868756725));
#277707=CARTESIAN_POINT('Ctrl Pts',(135.373113234605,-5.80190824167357,
130.472863778936));
#277708=CARTESIAN_POINT('Ctrl Pts',(135.094665610792,-3.41497080292952,
135.506488201326));
#277709=CARTESIAN_POINT('Ctrl Pts',(134.816217986979,2.11015797310843,136.219087085943));
#277710=CARTESIAN_POINT('Ctrl Pts',(134.537770363167,5.69615465880763,131.955816870215));
#277711=CARTESIAN_POINT('Ctrl Pts',(134.259322739353,4.04766348568775,126.634414610068));
#277712=CARTESIAN_POINT('Ctrl Pts',(133.980875115541,-1.32043269142476,
125.144989017623));
#277713=CARTESIAN_POINT('Ctrl Pts',(133.702427491728,-5.47511573184112,
128.856249449853));
#277714=CARTESIAN_POINT('Ctrl Pts',(133.423979867915,-4.59843488896879,
134.357728874689));
#277715=CARTESIAN_POINT('Ctrl Pts',(133.145532244102,0.503982970832797,
136.59383646292));
#277716=CARTESIAN_POINT('Ctrl Pts',(132.867084620289,5.14326510137581,133.509698580887));
#277717=CARTESIAN_POINT('Ctrl Pts',(132.588636996476,5.05613786622328,127.93948727367));
#277718=CARTESIAN_POINT('Ctrl Pts',(132.310189372663,0.322666938078297,
125.001954612649));
#277719=CARTESIAN_POINT('Ctrl Pts',(132.03174174885,-4.70731914300451,127.396549606854));
#277720=CARTESIAN_POINT('Ctrl Pts',(131.753294125038,-5.41150889699075,
132.92275643908));
#277721=CARTESIAN_POINT('Ctrl Pts',(131.474846501225,-1.14278634154918,
136.502261000723));
#277722=CARTESIAN_POINT('Ctrl Pts',(131.196398877412,4.17610103355955,134.845673468154));
#277723=CARTESIAN_POINT('Ctrl Pts',(130.917951253599,5.65735557270449,129.475316855001));
#277724=CARTESIAN_POINT('Ctrl Pts',(130.639503629786,1.93977671771839,125.326286532249));
#277725=CARTESIAN_POINT('Ctrl Pts',(130.361056005973,-3.56036217749005,
126.211338675105));
#277726=CARTESIAN_POINT('Ctrl Pts',(130.08260838216,-5.788702164947,131.317153601487));
#277727=CARTESIAN_POINT('Ctrl Pts',(129.804160758347,-2.69750765663984,
135.951736826975));
#277728=CARTESIAN_POINT('Ctrl Pts',(129.525713134534,2.87256460754407,135.856132779323));
#277729=CARTESIAN_POINT('Ctrl Pts',(129.247265510721,5.80289032997773,131.118196907806));
#277730=CARTESIAN_POINT('Ctrl Pts',(128.968817886909,3.40064332611445,126.091860817314));
#277731=CARTESIAN_POINT('Ctrl Pts',(128.690370263096,-2.12662876378584,
125.396081824838));
#277732=CARTESIAN_POINT('Ctrl Pts',(128.411922639283,-5.69963291135762,
129.670246833772));
#277733=CARTESIAN_POINT('Ctrl Pts',(128.13347501547,-4.03495285593914,134.986607005474));
#277734=CARTESIAN_POINT('Ctrl Pts',(127.855027391657,1.33765175568188,136.459687060782));
#277735=CARTESIAN_POINT('Ctrl Pts',(127.576579767844,5.48101975175251,132.73579839283));
#277736=CARTESIAN_POINT('Ctrl Pts',(127.298132144031,4.5875983586632,127.237012765392));
#277737=CARTESIAN_POINT('Ctrl Pts',(127.019684520218,-0.521601809398458,
125.016445539469));
#277738=CARTESIAN_POINT('Ctrl Pts',(126.741236896406,-5.15147539628782,
128.114689514947));
#277739=CARTESIAN_POINT('Ctrl Pts',(126.462789272592,-5.0473947575527,133.684609835992));
#277740=CARTESIAN_POINT('Ctrl Pts',(126.18434164878,-0.305004915568794,
136.607721833301));
#277741=CARTESIAN_POINT('Ctrl Pts',(125.905894024967,4.71766954350447,134.197828383304));
#277742=CARTESIAN_POINT('Ctrl Pts',(125.627446401154,5.40503616306688,128.669503836711));
#277743=CARTESIAN_POINT('Ctrl Pts',(125.348998777341,1.12543859946687,125.10300837817));
#277744=CARTESIAN_POINT('Ctrl Pts',(125.070551153528,-4.18838205631096,
126.775777101093));
#277745=CARTESIAN_POINT('Ctrl Pts',(124.792103529715,-5.65328421617778,
132.150617268407));
#277746=CARTESIAN_POINT('Ctrl Pts',(124.513655905902,-1.9230943596648,136.288313341892));
#277747=CARTESIAN_POINT('Ctrl Pts',(124.23520828209,3.57432526499779,135.386524767704));
#277748=CARTESIAN_POINT('Ctrl Pts',(123.956760658277,5.78711458662396,130.273951190703));
#277749=CARTESIAN_POINT('Ctrl Pts',(123.678313034464,2.68182831940755,125.648797965047));
#277750=CARTESIAN_POINT('Ctrl Pts',(123.399865410651,-2.88792715874745,
125.761354953818));
#277751=CARTESIAN_POINT('Ctrl Pts',(123.121417786838,-5.8038186610986,130.50818778305));
#277752=CARTESIAN_POINT('Ctrl Pts',(122.842970163025,-3.38628434620416,
135.527188978355));
#277753=CARTESIAN_POINT('Ctrl Pts',(122.564522539212,2.1430798536649,136.206141633086));
#277754=CARTESIAN_POINT('Ctrl Pts',(122.286074915399,5.703058363287,131.921121426228));
#277755=CARTESIAN_POINT('Ctrl Pts',(122.007627291586,4.02220484693838,126.609852593007));
#277756=CARTESIAN_POINT('Ctrl Pts',(121.729179667773,-1.35485842811595,
125.153131721247));
#277757=CARTESIAN_POINT('Ctrl Pts',(121.450732043961,-5.48687299624567,
128.889614127324));
#277758=CARTESIAN_POINT('Ctrl Pts',(121.172284420148,-4.57671932947311,
134.385655017367));
#277759=CARTESIAN_POINT('Ctrl Pts',(120.893836796335,0.539215815916097,
136.59066130995));
#277760=CARTESIAN_POINT('Ctrl Pts',(120.615389172522,5.15963796863542,133.478339942736));
#277761=CARTESIAN_POINT('Ctrl Pts',(120.336941548709,5.0386048905067,127.908762206842));
#277762=CARTESIAN_POINT('Ctrl Pts',(120.058493924896,0.287340067535411,
125.000097952557));
#277763=CARTESIAN_POINT('Ctrl Pts',(119.780046301083,-4.72797624015824,
127.42526753342));
#277764=CARTESIAN_POINT('Ctrl Pts',(119.50159867727,-5.39851335762638,132.955658580739));
#277765=CARTESIAN_POINT('Ctrl Pts',(119.223151053457,-1.10808043147514,
136.509111896649));
#277766=CARTESIAN_POINT('Ctrl Pts',(118.944703429644,4.20062427846316,134.820177479675));
#277767=CARTESIAN_POINT('Ctrl Pts',(118.666255805832,5.64916048839838,129.440903549983));
#277768=CARTESIAN_POINT('Ctrl Pts',(118.387808182019,1.90639418632776,125.314580056818));
#277769=CARTESIAN_POINT('Ctrl Pts',(118.109360558206,-3.58825524044456,
126.23309670829));
#277770=CARTESIAN_POINT('Ctrl Pts',(117.830912934393,-5.785473397262,131.352381573729));
#277771=CARTESIAN_POINT('Ctrl Pts',(117.55246531058,-2.66612413808396,135.968061952766));
#277772=CARTESIAN_POINT('Ctrl Pts',(117.274017686767,2.9032629565882,135.838553065588));
#277773=CARTESIAN_POINT('Ctrl Pts',(116.995570062954,5.80469322643624,131.082867252651));
#277774=CARTESIAN_POINT('Ctrl Pts',(116.717122439142,3.37189399621826,126.071247447876));
#277775=CARTESIAN_POINT('Ctrl Pts',(116.438674815328,-2.15951109034483,
125.409127420613));
#277776=CARTESIAN_POINT('Ctrl Pts',(116.160227191516,-5.70643098286277,
129.704963129555));
#277777=CARTESIAN_POINT('Ctrl Pts',(115.881779567703,-4.00941957678149,
135.011091421425));
#277778=CARTESIAN_POINT('Ctrl Pts',(115.60333194389,1.37205254932662,136.451439614773));
#277779=CARTESIAN_POINT('Ctrl Pts',(115.324884320077,5.49267541109693,132.702398084833));
#277780=CARTESIAN_POINT('Ctrl Pts',(115.046436696264,4.56579790218037,127.20915284676));
#277781=CARTESIAN_POINT('Ctrl Pts',(114.767989072451,-0.556824827212187,
125.019727914392));
#277782=CARTESIAN_POINT('Ctrl Pts',(114.489541448638,-5.1677527428018,128.146097841224));
#277783=CARTESIAN_POINT('Ctrl Pts',(114.211093824825,-5.02976834651319,
133.715281396157));
#277784=CARTESIAN_POINT('Ctrl Pts',(113.932646201012,-0.269672557622912,
136.60947096195));
#277785=CARTESIAN_POINT('Ctrl Pts',(113.6541985772,4.73823913748602,134.169047716661));
#277786=CARTESIAN_POINT('Ctrl Pts',(113.375750953387,5.39194054109557,128.636641401405));
#277787=CARTESIAN_POINT('Ctrl Pts',(113.097303329574,1.09071199837779,125.09626314683));
#277788=CARTESIAN_POINT('Ctrl Pts',(112.818855705761,-4.21282758660586,
126.801347611796));
#277789=CARTESIAN_POINT('Ctrl Pts',(112.540408081948,-5.64498442756793,
132.185005471008));
#277790=CARTESIAN_POINT('Ctrl Pts',(112.261960458135,-1.8896763524154,136.299918158156));
#277791=CARTESIAN_POINT('Ctrl Pts',(111.983512834322,3.60215197478495,135.364681938413));
#277792=CARTESIAN_POINT('Ctrl Pts',(111.705065210509,5.78377861206482,130.238733208892));
#277793=CARTESIAN_POINT('Ctrl Pts',(111.426617586696,2.65039525815055,125.632568435507));
#277794=CARTESIAN_POINT('Ctrl Pts',(111.148169962883,-2.91857185899754,
125.77902802134));
#277795=CARTESIAN_POINT('Ctrl Pts',(110.869722339071,-5.80551401788879,
130.543522761958));
#277796=CARTESIAN_POINT('Ctrl Pts',(110.591274715258,-3.35747240946702,
135.547714749242));
#277797=CARTESIAN_POINT('Ctrl Pts',(110.312827091445,2.17592232160915,136.192996015246));
#277798=CARTESIAN_POINT('Ctrl Pts',(110.034379467632,5.70975073884148,131.886384600257));
#277799=CARTESIAN_POINT('Ctrl Pts',(109.755931843819,3.99659716390926,126.585446004984));
#277800=CARTESIAN_POINT('Ctrl Pts',(109.477484220006,-1.38923396002991,
125.161483833236));
#277801=CARTESIAN_POINT('Ctrl Pts',(109.199036596193,-5.49842694255352,
128.923049756431));
#277802=CARTESIAN_POINT('Ctrl Pts',(108.92058897238,-4.55483417795961,134.413448453863));
#277803=CARTESIAN_POINT('Ctrl Pts',(108.642141348568,0.57442868015902,136.58727174348));
#277804=CARTESIAN_POINT('Ctrl Pts',(108.363693724754,5.17581964361271,133.446882219296));
#277805=CARTESIAN_POINT('Ctrl Pts',(108.085246100942,5.02088520743284,127.878144437479));
#277806=CARTESIAN_POINT('Ctrl Pts',(107.806798477129,0.252002549500665,
124.998456371553));
#277807=CARTESIAN_POINT('Ctrl Pts',(107.528350853316,-4.74845814041369,
127.454110673523));
#277808=CARTESIAN_POINT('Ctrl Pts',(107.249903229503,-5.38531777436419,
132.988481005259));
#277809=CARTESIAN_POINT('Ctrl Pts',(106.97145560569,-1.07333346107335,136.515751400918));
#277810=CARTESIAN_POINT('Ctrl Pts',(106.693007981877,4.22499186768932,134.794532683627));
#277811=CARTESIAN_POINT('Ctrl Pts',(106.414560358064,5.64075607237289,129.406540768369));
#277812=CARTESIAN_POINT('Ctrl Pts',(106.136112734251,1.87294101279944,125.303077007226));
#277813=CARTESIAN_POINT('Ctrl Pts',(105.857665110439,-3.61601533928142,
126.25502413134));
#277814=CARTESIAN_POINT('Ctrl Pts',(105.579217486626,-5.78203024673271,
131.387589238853));
#277815=CARTESIAN_POINT('Ctrl Pts',(105.300769862813,-2.63464182531766,
135.984195735705));
#277816=CARTESIAN_POINT('Ctrl Pts',(105.022322239,2.93385372415587,135.820786808));
#277817=CARTESIAN_POINT('Ctrl Pts',(104.743874615187,5.80628102785255,131.047527277329));
#277818=CARTESIAN_POINT('Ctrl Pts',(104.465426991374,3.34301971955009,126.050809465687));
#277819=CARTESIAN_POINT('Ctrl Pts',(104.186979367561,-2.19231339542621,
125.422372938737));
#277820=CARTESIAN_POINT('Ctrl Pts',(103.908531743748,-5.71301760046937,
129.739720163916));
#277821=CARTESIAN_POINT('Ctrl Pts',(103.630084119935,-3.98373772710686,
135.03541995542));
#277822=CARTESIAN_POINT('Ctrl Pts',(103.351636496123,1.40640250105958,136.442982914176));
#277823=CARTESIAN_POINT('Ctrl Pts',(103.07318887231,5.50412753733405,132.66892744436));
#277824=CARTESIAN_POINT('Ctrl Pts',(102.794741248497,4.54382825837723,127.181426149873));
#277825=CARTESIAN_POINT('Ctrl Pts',(102.516293624684,-0.592027211677165,
125.023224641008));
#277826=CARTESIAN_POINT('Ctrl Pts',(102.237846000871,-5.18383859633749,
128.177604670405));
#277827=CARTESIAN_POINT('Ctrl Pts',(101.959398377058,-5.01195555555783,
133.745845091081));
#277828=CARTESIAN_POINT('Ctrl Pts',(101.680950753245,-0.234330206861215,
136.611004980102));
#277829=CARTESIAN_POINT('Ctrl Pts',(101.402503129432,4.75863315427373,134.140142370299));
#277830=CARTESIAN_POINT('Ctrl Pts',(101.124055505619,5.37864511878468,128.603859291732));
#277831=CARTESIAN_POINT('Ctrl Pts',(100.845607881807,1.05594498055446,125.089729431141));
#277832=CARTESIAN_POINT('Ctrl Pts',(100.567160257994,-4.23711700902531,
126.827066455619));
#277833=CARTESIAN_POINT('Ctrl Pts',(100.288712634181,-5.63647546198416,
132.219342513305));
#277834=CARTESIAN_POINT('Ctrl Pts',(100.010265010368,-1.85618832251382,
136.311319334515));
#277835=CARTESIAN_POINT('Ctrl Pts',(99.731817386555,3.62984520550588,135.342670124737));
#277836=CARTESIAN_POINT('Ctrl Pts',(99.4533697627421,5.78022831746224,130.203536186614));
#277837=CARTESIAN_POINT('Ctrl Pts',(99.1749221389292,2.61886398552269,125.616530548629));
#277838=CARTESIAN_POINT('Ctrl Pts',(98.8964745151164,-2.9491084104941,125.796887304409));
#277839=CARTESIAN_POINT('Ctrl Pts',(98.6180268913035,-5.80699424922206,
130.578867406308));
#277840=CARTESIAN_POINT('Ctrl Pts',(98.3395792674906,-3.32853606035512,
135.568064753397));
#277841=CARTESIAN_POINT('Ctrl Pts',(98.0611316436778,2.20868415995158,136.179650719541));
#277842=CARTESIAN_POINT('Ctrl Pts',(97.7826840198649,5.71623153748262,131.851607679491));
#277843=CARTESIAN_POINT('Ctrl Pts',(97.5042363960519,3.97084138550236,126.561195750394));
#277844=CARTESIAN_POINT('Ctrl Pts',(97.2257887722391,-1.42355801336861,
125.170045044101));
#277845=CARTESIAN_POINT('Ctrl Pts',(96.9473411484261,-5.50977714262889,
128.956555098203));
#277846=CARTESIAN_POINT('Ctrl Pts',(96.6688935246133,-4.53278024539068,
134.441108154283));
#277847=CARTESIAN_POINT('Ctrl Pts',(96.3904459008004,0.609620258735999,
136.583667889112));
#277848=CARTESIAN_POINT('Ctrl Pts',(96.1119982769875,5.19180952668969,133.415326576248));
#277849=CARTESIAN_POINT('Ctrl Pts',(95.8335506531746,5.00297947361121,127.847635100131));
#277850=CARTESIAN_POINT('Ctrl Pts',(95.5551030293618,0.216655693418756,
124.997029930466));
#277851=CARTESIAN_POINT('Ctrl Pts',(95.2766554055487,-4.7687640848064,127.483077958369));
#277852=CARTESIAN_POINT('Ctrl Pts',(94.9982077817361,-5.37192263617151,
133.021222496396));
#277853=CARTESIAN_POINT('Ctrl Pts',(94.7197601579228,-1.03854671790542,
136.522179267501));
#277854=CARTESIAN_POINT('Ctrl Pts',(94.4413125341102,4.24920289828813,134.768740030285));
#277855=CARTESIAN_POINT('Ctrl Pts',(94.1628649102971,5.63214263605674,129.372229783482));
#277856=CARTESIAN_POINT('Ctrl Pts',(93.8844172864844,1.83941843675322,125.29177780972));
#277857=CARTESIAN_POINT('Ctrl Pts',(93.6059696626714,-3.6436414453401,126.277120131727));
#277858=CARTESIAN_POINT('Ctrl Pts',(93.3275220388585,-5.77837284094635,
131.422775292226));
#277859=CARTESIAN_POINT('Ctrl Pts',(93.0490744150458,-2.60306188492951,
136.000137577949));
#277860=CARTESIAN_POINT('Ctrl Pts',(92.7706267912327,2.96433577669487,135.802834664895));
#277861=CARTESIAN_POINT('Ctrl Pts',(92.49217916742,5.80765367539012,131.012178291378));
#277862=CARTESIAN_POINT('Ctrl Pts',(92.213731543607,3.31402156605677,126.030547628085));
#277863=CARTESIAN_POINT('Ctrl Pts',(91.9352839197941,-2.22503446352861,
125.435817888395));
#277864=CARTESIAN_POINT('Ctrl Pts',(91.6568362959812,-5.71939252010779,
129.77451664892));
#277865=CARTESIAN_POINT('Ctrl Pts',(91.3783886721684,-3.95790825856573,
135.059591705955));
#277866=CARTESIAN_POINT('Ctrl Pts',(91.0999410483554,1.44070033803066,136.434317272356));
#277867=CARTESIAN_POINT('Ctrl Pts',(90.8214934245425,5.51537570610103,132.635387711677));
#277868=CARTESIAN_POINT('Ctrl Pts',(90.5430458007297,4.52169024134706,127.153833702157));
#277869=CARTESIAN_POINT('Ctrl Pts',(90.2645981769166,-0.627207658356129,
125.026935589742));
#277870=CARTESIAN_POINT('Ctrl Pts',(89.9861505531037,-5.19973236082766,
128.209208834995));
#277871=CARTESIAN_POINT('Ctrl Pts',(89.707702929291,-4.99395704474619,133.776299788217));
#277872=CARTESIAN_POINT('Ctrl Pts',(89.4292553054779,-0.198979172907652,
136.61232383091));
#277873=CARTESIAN_POINT('Ctrl Pts',(89.1508076816652,4.77885083815996,134.111113415317));
#277874=CARTESIAN_POINT('Ctrl Pts',(88.8723600578521,5.36515038880097,128.571158722445));
#277875=CARTESIAN_POINT('Ctrl Pts',(88.5939124340396,1.02113883430145,125.08340747321));
#277876=CARTESIAN_POINT('Ctrl Pts',(88.3154648102263,-4.26124942351577,
126.85293267954));
#277877=CARTESIAN_POINT('Ctrl Pts',(88.0370171864138,-5.62775763472933,
132.253627122929));
#277878=CARTESIAN_POINT('Ctrl Pts',(87.7585695626006,-1.82263151087143,
136.322516448493));
#277879=CARTESIAN_POINT('Ctrl Pts',(87.480121938788,3.65740393097785,135.320490142334));
#277880=CARTESIAN_POINT('Ctrl Pts',(87.2016743149749,5.77646383437373,130.168361428106));
#277881=CARTESIAN_POINT('Ctrl Pts',(86.9232266911622,2.58723566992664,125.600684898703));
#277882=CARTESIAN_POINT('Ctrl Pts',(86.6447790673492,-2.97953568169397,
125.814932141244));
#277883=CARTESIAN_POINT('Ctrl Pts',(86.3663314435363,-5.80825930024783,
130.614220406392));
#277884=CARTESIAN_POINT('Ctrl Pts',(86.0878838197235,-3.29947637111547,
135.588238236744));
#277885=CARTESIAN_POINT('Ctrl Pts',(85.8094361959104,2.24136415469026,136.166106240484));
#277886=CARTESIAN_POINT('Ctrl Pts',(85.5309885720977,5.72250051906197,131.816791952599));
#277887=CARTESIAN_POINT('Ctrl Pts',(85.2525409482847,3.94493846610766,126.537102727838));
#277888=CARTESIAN_POINT('Ctrl Pts',(84.9740933244718,-1.45782931624159,
125.178815036599));
#277889=CARTESIAN_POINT('Ctrl Pts',(84.6956457006588,-5.52092317588609,
128.990128911089));
#277890=CARTESIAN_POINT('Ctrl Pts',(84.417198076846,-4.51055834898274,134.468633093685));
#277891=CARTESIAN_POINT('Ctrl Pts',(84.138750453033,0.644789247610192,136.579849880389));
#277892=CARTESIAN_POINT('Ctrl Pts',(83.8603028292202,5.20760702535536,133.383674182895));
#277893=CARTESIAN_POINT('Ctrl Pts',(83.5818552054073,4.98488835254533,127.817235325336));
#277894=CARTESIAN_POINT('Ctrl Pts',(83.3034075815944,0.181300809080568,
124.995818682153));
#277895=CARTESIAN_POINT('Ctrl Pts',(83.0249599577814,-4.78889332089225,
127.512168314565));
#277896=CARTESIAN_POINT('Ctrl Pts',(82.7465123339688,-5.35832843941005,
133.053881840899));
#277897=CARTESIAN_POINT('Ctrl Pts',(82.4680647101557,-1.00372149100682,
136.528395258211));
#277898=CARTESIAN_POINT('Ctrl Pts',(82.1896170863428,4.27325647311088,134.742800475408));
#277899=CARTESIAN_POINT('Ctrl Pts',(81.91116946253,5.62332049862395,129.337971866731));
#277900=CARTESIAN_POINT('Ctrl Pts',(81.632721838717,1.80582770038043,125.280682882997));
#277901=CARTESIAN_POINT('Ctrl Pts',(81.3542742149043,-3.67113253492515,
126.299383890674));
#277902=CARTESIAN_POINT('Ctrl Pts',(81.0758265910913,-5.77450131542928,
131.457938430015));
#277903=CARTESIAN_POINT('Ctrl Pts',(80.7973789672785,-2.57138548712596,
136.015886888767));
#277904=CARTESIAN_POINT('Ctrl Pts',(80.5189313434656,2.99470798468153,135.784697301496));
#277905=CARTESIAN_POINT('Ctrl Pts',(80.2404837196526,5.80881111818491,130.976821604667));
#277906=CARTESIAN_POINT('Ctrl Pts',(79.9620360958398,3.2849006102757,126.010462685879));
#277907=CARTESIAN_POINT('Ctrl Pts',(79.6835884720269,-2.25767308216064,
125.449461771377));
#277908=CARTESIAN_POINT('Ctrl Pts',(79.4051408482139,-5.72555550555307,
129.809351295171));
#277909=CARTESIAN_POINT('Ctrl Pts',(79.1266932244012,-3.93193212827854,
135.083605777338));
#277910=CARTESIAN_POINT('Ctrl Pts',(78.8482456005881,1.47494478932078,136.425443010422));
#277911=CARTESIAN_POINT('Ctrl Pts',(78.5697979767754,5.526419500593,132.601780129612));
#277912=CARTESIAN_POINT('Ctrl Pts',(78.2913503529625,4.49938467142216,127.126376526057));
#277913=CARTESIAN_POINT('Ctrl Pts',(78.0129027291494,-0.662364863624755,
125.030860623086));
#277914=CARTESIAN_POINT('Ctrl Pts',(77.7344551053368,-5.21543344732299,
128.240909163888));
#277915=CARTESIAN_POINT('Ctrl Pts',(77.4560074815235,-4.97577348101974,
133.806644359053));
#277916=CARTESIAN_POINT('Ctrl Pts',(77.1775598577108,-0.163620765707691,
136.613427465507));
#277917=CARTESIAN_POINT('Ctrl Pts',(76.8991122338979,4.79889143997102,134.081961927395));
#277918=CARTESIAN_POINT('Ctrl Pts',(76.620664610085,5.35145685119646,128.538540905275));
#277919=CARTESIAN_POINT('Ctrl Pts',(76.3422169862721,0.986294849373407,
125.077297507303));
#277920=CARTESIAN_POINT('Ctrl Pts',(76.0637693624593,-4.28522393584178,
126.878945325076));
#277921=CARTESIAN_POINT('Ctrl Pts',(75.7853217386464,-5.61883126884571,
132.287858029448));
#277922=CARTESIAN_POINT('Ctrl Pts',(75.5068741148335,-1.78900716094817,
136.333509085178));
#277923=CARTESIAN_POINT('Ctrl Pts',(75.2284264910206,3.68482713000219,135.298142813091));
#277924=CARTESIAN_POINT('Ctrl Pts',(74.9499788672077,5.77248530229349,130.133210236781));
#277925=CARTESIAN_POINT('Ctrl Pts',(74.6715312433948,2.55551148336137,125.585032072894));
#277926=CARTESIAN_POINT('Ctrl Pts',(74.3930836195819,-3.0098525451033,125.833161863185));
#277927=CARTESIAN_POINT('Ctrl Pts',(74.1146359957691,-5.80930912408932,
130.649580452192));
#277928=CARTESIAN_POINT('Ctrl Pts',(73.8361883719562,-3.27029441856551,
135.608234451746));
#277929=CARTESIAN_POINT('Ctrl Pts',(73.5577407481433,2.273961094856,136.152363079971));
#277930=CARTESIAN_POINT('Ctrl Pts',(73.2792931243304,5.72855745128013,131.781938709691));
#277931=CARTESIAN_POINT('Ctrl Pts',(73.0008455005175,3.91888936556733,126.513167830092));
#277932=CARTESIAN_POINT('Ctrl Pts',(72.7223978767045,-1.49204659871303,
125.187793485758));
#277933=CARTESIAN_POINT('Ctrl Pts',(72.4439502528918,-5.53186462930466,
129.023769950998));
#277934=CARTESIAN_POINT('Ctrl Pts',(72.1655026290786,-4.48816931217651,
134.496022252122));
#277935=CARTESIAN_POINT('Ctrl Pts',(71.8870550052659,0.679934343581693,
136.575817858786));
#277936=CARTESIAN_POINT('Ctrl Pts',(71.6086073814528,5.22321155422762,133.351926212129));
#277937=CARTESIAN_POINT('Ctrl Pts',(71.3301597576401,4.96661251460835,127.786946239566));
#277938=CARTESIAN_POINT('Ctrl Pts',(71.0517121338272,0.145939206574258,
124.994822671498));
#277939=CARTESIAN_POINT('Ctrl Pts',(70.7732645100143,-4.80884510277506,
127.541380664158));
#277940=CARTESIAN_POINT('Ctrl Pts',(70.4948168862015,-5.34453568781766,
133.086457828568));
#277941=CARTESIAN_POINT('Ctrl Pts',(70.2163692623885,-0.968859070839113,
136.534399142713));
#277942=CARTESIAN_POINT('Ctrl Pts',(69.9379216385757,4.29715170084345,134.716714980192));
#277943=CARTESIAN_POINT('Ctrl Pts',(69.6594740147628,5.61428998698222,129.303768287553));
#277944=CARTESIAN_POINT('Ctrl Pts',(69.3810263909498,1.77217004839796,125.269792638185));
#277945=CARTESIAN_POINT('Ctrl Pts',(69.102578767137,-3.69848758934425,126.321814583191));
#277946=CARTESIAN_POINT('Ctrl Pts',(68.8241311433241,-5.77041581364239,
131.493077349239));
#277947=CARTESIAN_POINT('Ctrl Pts',(68.5456835195112,-2.53961380568736,
136.031443084562));
#277948=CARTESIAN_POINT('Ctrl Pts',(68.2672358956983,3.02496922266262,135.76637538989));
#277949=CARTESIAN_POINT('Ctrl Pts',(67.9887882718854,5.80975331334755,130.94145852735));
#277950=CARTESIAN_POINT('Ctrl Pts',(67.7103406480725,3.25565793129432,125.990555383323));
#277951=CARTESIAN_POINT('Ctrl Pts',(67.4318930242597,-2.29022804188655,
125.463304082106));
#277952=CARTESIAN_POINT('Ctrl Pts',(67.1534454004468,-5.73150632843341,
129.844222811859));
#277953=CARTESIAN_POINT('Ctrl Pts',(66.8749977766338,-3.90581029880048,
135.107461279717));
#277954=CARTESIAN_POINT('Ctrl Pts',(66.5965501528209,1.50913458598933,136.416360457212));
#277955=CARTESIAN_POINT('Ctrl Pts',(66.3181025290079,5.53725851157817,132.568105943505));
#277956=CARTESIAN_POINT('Ctrl Pts',(66.0396549051952,4.47691237514338,127.09905563901));
#277957=CARTESIAN_POINT('Ctrl Pts',(65.7612072813823,-0.69749752471975,
125.034999595595));
#277958=CARTESIAN_POINT('Ctrl Pts',(65.4827596575694,-5.23094127401388,
128.272704482416));
#277959=CARTESIAN_POINT('Ctrl Pts',(65.2043120337565,-4.95740553817722,
133.836877679162));
#277960=CARTESIAN_POINT('Ctrl Pts',(64.9258644099437,-0.128256295479839,
136.614315842995));
#277961=CARTESIAN_POINT('Ctrl Pts',(64.6474167861306,4.81875421709505,134.05268898675));
#277962=CARTESIAN_POINT('Ctrl Pts',(64.3689691623179,5.33756501339024,128.506007048888));
#277963=CARTESIAN_POINT('Ctrl Pts',(64.0905215385049,0.951414316927145,
125.071399759827));
#277964=CARTESIAN_POINT('Ctrl Pts',(63.8120739146922,-4.30903965761881,
126.905103428319));
#277965=CARTESIAN_POINT('Ctrl Pts',(63.5336262908791,-5.60969669510319,
132.322033964426));
#277966=CARTESIAN_POINT('Ctrl Pts',(63.2551786670663,-1.75531651870651,
136.344296837232));
#277967=CARTESIAN_POINT('Ctrl Pts',(62.9767310432534,3.71211378640213,135.275628965096));
#277968=CARTESIAN_POINT('Ctrl Pts',(62.6982834194405,5.76829286864752,130.098083915181));
#277969=CARTESIAN_POINT('Ctrl Pts',(62.4198357956276,2.52369260137852,125.569572651222));
#277970=CARTESIAN_POINT('Ctrl Pts',(62.1413881718147,-3.04005787731984,
125.851575794724));
#277971=CARTESIAN_POINT('Ctrl Pts',(61.8629405480017,-5.81014368184488,
130.684946233427));
#277972=CARTESIAN_POINT('Ctrl Pts',(61.5844929241889,-3.24099128405306,
135.628052657436));
#277973=CARTESIAN_POINT('Ctrl Pts',(61.3060453003759,2.306473772557,136.138421747261));
#277974=CARTESIAN_POINT('Ctrl Pts',(61.0275976765631,5.73440210969521,131.747049242268));
#277975=CARTESIAN_POINT('Ctrl Pts',(60.7491500527502,3.89269504914048,126.489391944074));
#277976=CARTESIAN_POINT('Ctrl Pts',(60.4707024289374,-1.5262085928491,125.196980058879));
#277977=CARTESIAN_POINT('Ctrl Pts',(60.1922548051244,-5.54260109744501,
129.057476971348));
#277978=CARTESIAN_POINT('Ctrl Pts',(59.9138071813117,-4.46561396460588,
134.52327461468));
#277979=CARTESIAN_POINT('Ctrl Pts',(59.6353595574987,0.715054244335847,
136.571571973714));
#277980=CARTESIAN_POINT('Ctrl Pts',(59.3569119336859,5.23862253507484,133.320083840384));
#277981=CARTESIAN_POINT('Ctrl Pts',(59.0784643098728,4.94815263701827,127.756768965196));
#277982=CARTESIAN_POINT('Ctrl Pts',(58.80001668606,0.110572196236736,124.994041935407));
#277983=CARTESIAN_POINT('Ctrl Pts',(58.5215690622471,-4.82861869113419,
127.570713924673));
#277984=CARTESIAN_POINT('Ctrl Pts',(58.2431214384343,-5.3305448924898,133.118949252284));
#277985=CARTESIAN_POINT('Ctrl Pts',(57.9646738146213,-0.933960749242644,
136.54019069853));
#277986=CARTESIAN_POINT('Ctrl Pts',(57.6862261908085,4.32088769603949,134.690484511247));
#277987=CARTESIAN_POINT('Ctrl Pts',(57.4077785669955,5.6050514357603,129.269620313377));
#277988=CARTESIAN_POINT('Ctrl Pts',(57.1293309431827,1.73844672800264,125.259107478825));
#277989=CARTESIAN_POINT('Ctrl Pts',(56.8508833193697,-3.72570559494523,
126.3444113781));
#277990=CARTESIAN_POINT('Ctrl Pts',(56.5724356955568,-5.76611648697549,
131.528190747811));
#277991=CARTESIAN_POINT('Ctrl Pts',(56.293988071744,-2.50774801792579,136.046805588895));
#277992=CARTESIAN_POINT('Ctrl Pts',(56.0155404479311,3.05511836929639,135.747869609001));
#277993=CARTESIAN_POINT('Ctrl Pts',(55.7370928241181,5.81048022596477,130.906090369819));
#277994=CARTESIAN_POINT('Ctrl Pts',(55.4586452003054,3.22629461271119,125.97082645809));
#277995=CARTESIAN_POINT('Ctrl Pts',(55.1801975764924,-2.32269813636975,
125.477344307648));
#277996=CARTESIAN_POINT('Ctrl Pts',(54.9017499526795,-5.73724476823917,
129.879129906805));
#277997=CARTESIAN_POINT('Ctrl Pts',(54.6233023288666,-3.87954373808533,
135.131157329118));
#277998=CARTESIAN_POINT('Ctrl Pts',(54.3448547050537,1.54326846112093,136.407069949284));
#277999=CARTESIAN_POINT('Ctrl Pts',(54.0664070812409,5.54789233741261,132.534366401168));
#278000=CARTESIAN_POINT('Ctrl Pts',(53.7879594574279,4.45427418523046,127.071872053402));
#278001=CARTESIAN_POINT('Ctrl Pts',(53.5095118336151,-0.732604339787292,
125.039352353899));
#278002=CARTESIAN_POINT('Ctrl Pts',(53.2310642098022,-5.24625526625226,
128.304593612394));
#278003=CARTESIAN_POINT('Ctrl Pts',(52.9526165859893,-4.93885389684926,
133.866998628235));
#278004=CARTESIAN_POINT('Ctrl Pts',(52.6741689621764,-0.0928870726681018,
136.614988930455));
#278005=CARTESIAN_POINT('Ctrl Pts',(52.3957213383635,4.83843843350925,134.023295678104));
#278006=CARTESIAN_POINT('Ctrl Pts',(52.1172737145507,5.32347539014984,128.473558358838));
#278007=CARTESIAN_POINT('Ctrl Pts',(51.8388260907377,0.91649852947334,125.065714449322));
#278008=CARTESIAN_POINT('Ctrl Pts',(51.5603784669247,-4.33269570634681,
126.931406019971));
#278009=CARTESIAN_POINT('Ctrl Pts',(51.2819308431118,-5.6003542519866,132.356153661459));
#278010=CARTESIAN_POINT('Ctrl Pts',(51.0034832192991,-1.72156083256576,
136.354879304913));
#278011=CARTESIAN_POINT('Ctrl Pts',(50.7250355954861,3.73926288906064,135.252949432607));
#278012=CARTESIAN_POINT('Ctrl Pts',(50.4465879716733,5.76388668878802,130.062983764924));
#278013=CARTESIAN_POINT('Ctrl Pts',(50.1681403478604,2.49178020303801,125.554307206545));
#278014=CARTESIAN_POINT('Ctrl Pts',(49.8896927240475,-3.07015055907373,
125.870173253527));
#278015=CARTESIAN_POINT('Ctrl Pts',(49.6112451002346,-5.81076294258959,
130.720316439607));
#278016=CARTESIAN_POINT('Ctrl Pts',(49.3327974764216,-3.21156805341676,
135.647692119444));
#278017=CARTESIAN_POINT('Ctrl Pts',(49.0543498526089,2.33890098302428,136.124282758954));
#278018=CARTESIAN_POINT('Ctrl Pts',(48.7759022287959,5.74003427773134,131.712124843171));
#278019=CARTESIAN_POINT('Ctrl Pts',(48.497454604983,3.86635648746696,126.465775950806));
#278020=CARTESIAN_POINT('Ctrl Pts',(48.2190069811701,-1.56031403276457,
125.206374415548));
#278021=CARTESIAN_POINT('Ctrl Pts',(47.9405593573573,-5.55313218246346,
129.091248723115));
#278022=CARTESIAN_POINT('Ctrl Pts',(47.6621117335443,-4.44289314206747,
134.550389171513));
#278023=CARTESIAN_POINT('Ctrl Pts',(47.3836641097315,0.750147648492217,
136.567112382502));
#278024=CARTESIAN_POINT('Ctrl Pts',(47.1052164859186,5.25383939683757,133.288148247589));
#278025=CARTESIAN_POINT('Ctrl Pts',(46.8267688621057,4.92950940381243,127.726704620456));
#278026=CARTESIAN_POINT('Ctrl Pts',(46.5483212382927,0.0752010886061242,
124.993476502813));
#278027=CARTESIAN_POINT('Ctrl Pts',(46.2698736144798,-4.84821335325179,
127.600167009156));
#278028=CARTESIAN_POINT('Ctrl Pts',(45.991425990667,-5.31635657186091,133.151354908068));
#278029=CARTESIAN_POINT('Ctrl Pts',(45.7129783668541,-0.899027819386881,
136.545769711054));
#278030=CARTESIAN_POINT('Ctrl Pts',(45.4345307430412,4.344463579153,134.664110040551));
#278031=CARTESIAN_POINT('Ctrl Pts',(45.1560831192283,5.5956051872961,129.235529209567));
#278032=CARTESIAN_POINT('Ctrl Pts',(44.8776354954154,1.70465898882477,125.248627800858));
#278033=CARTESIAN_POINT('Ctrl Pts',(44.5991878716026,-3.7527855431554,126.367173438067));
#278034=CARTESIAN_POINT('Ctrl Pts',(44.3207402477896,-5.76160349474165,
131.563277324591));
#278035=CARTESIAN_POINT('Ctrl Pts',(44.0422926239769,-2.47578930463884,
136.0619738325));
#278036=CARTESIAN_POINT('Ctrl Pts',(43.7638450001637,3.08515430739569,135.72918064457));
#278037=CARTESIAN_POINT('Ctrl Pts',(43.485397376351,5.8109918291003,130.870718442656));
#278038=CARTESIAN_POINT('Ctrl Pts',(43.206949752538,3.19681174259461,125.951276641244));
#278039=CARTESIAN_POINT('Ctrl Pts',(42.9285021287252,-2.3550821624196,125.491581927739));
#278040=CARTESIAN_POINT('Ctrl Pts',(42.6500545049123,-5.74277061233009,
129.914071286517));
#278041=CARTESIAN_POINT('Ctrl Pts',(42.3716068810994,-3.85313341945026,
135.154693047476));
#278042=CARTESIAN_POINT('Ctrl Pts',(42.0931592572865,1.57734514987214,136.397571830902));
#278043=CARTESIAN_POINT('Ctrl Pts',(41.8147116334736,5.5583205840564,132.50056275283));
#278044=CARTESIAN_POINT('Ctrl Pts',(41.5362640096606,4.43147094054935,127.04482677653));
#278045=CARTESIAN_POINT('Ctrl Pts',(41.2578163858478,-0.767684007931795,
125.043918736703));
#278046=CARTESIAN_POINT('Ctrl Pts',(40.9793687620349,-5.26137485657243,
128.336575372158));
#278047=CARTESIAN_POINT('Ctrl Pts',(40.700921138222,-4.9201192444739,133.897006090131));
#278048=CARTESIAN_POINT('Ctrl Pts',(40.4224735144091,-0.0575144078915333,
136.615446702946));
#278049=CARTESIAN_POINT('Ctrl Pts',(40.1440258905964,4.85794335980812,133.993783090635));
#278050=CARTESIAN_POINT('Ctrl Pts',(39.8655782667833,5.30918850357096,128.441196037522));
#278051=CARTESIAN_POINT('Ctrl Pts',(39.5871306429705,0.8815487808295,125.060241786462));
#278052=CARTESIAN_POINT('Ctrl Pts',(39.3086830191576,-4.35619120544207,
126.957852125381));
#278053=CARTESIAN_POINT('Ctrl Pts',(39.0302353953447,-5.59080428568363,
132.39021585623));
#278054=CARTESIAN_POINT('Ctrl Pts',(38.7517877715318,-1.6877413533555,136.365256096082));
#278055=CARTESIAN_POINT('Ctrl Pts',(38.4733401477189,3.76627343195761,135.230105056025));
#278056=CARTESIAN_POINT('Ctrl Pts',(38.194892523906,5.7592669259876,130.027911086658));
#278057=CARTESIAN_POINT('Ctrl Pts',(37.9164449000932,2.45977547086574,125.539236304527));
#278058=CARTESIAN_POINT('Ctrl Pts',(37.6379972762802,-3.10012947526937,
125.888953550457));
#278059=CARTESIAN_POINT('Ctrl Pts',(37.3595496524674,-5.81116688337655,
130.755689760074));
#278060=CARTESIAN_POINT('Ctrl Pts',(37.0811020286545,-3.18202581694541,
135.667152110023));
#278061=CARTESIAN_POINT('Ctrl Pts',(36.8026544048415,2.3712415246555,136.109946638975));
#278062=CARTESIAN_POINT('Ctrl Pts',(36.5242067810287,5.74545374668639,131.677166806538));
#278063=CARTESIAN_POINT('Ctrl Pts',(36.2457591572158,3.83987465653194,126.442320725389));
#278064=CARTESIAN_POINT('Ctrl Pts',(35.9673115334029,-1.59436165466975,
125.215976207654));
#278065=CARTESIAN_POINT('Ctrl Pts',(35.6888639095901,-5.56345749412674,
129.125083954872));
#278066=CARTESIAN_POINT('Ctrl Pts',(35.4104162857771,-4.42000768648982,
134.57736491788));
#278067=CARTESIAN_POINT('Ctrl Pts',(35.1319686619643,0.785213255651605,
136.562439250406));
#278068=CARTESIAN_POINT('Ctrl Pts',(34.8535210381513,5.26886157564935,133.25612061713));
#278069=CARTESIAN_POINT('Ctrl Pts',(34.5750734143385,4.91068350582282,127.69675431939));
#278070=CARTESIAN_POINT('Ctrl Pts',(34.2966257905255,0.0398271943713243,
124.993126394665));
#278071=CARTESIAN_POINT('Ctrl Pts',(34.0181781667127,-4.86762836304081,
127.629738826211));
#278072=CARTESIAN_POINT('Ctrl Pts',(33.7397305428998,-5.30197125168398,
133.183673595116));
#278073=CARTESIAN_POINT('Ctrl Pts',(33.4612829190869,-0.864061575724654,
136.551135973552));
#278074=CARTESIAN_POINT('Ctrl Pts',(33.182835295274,4.36787847657091,134.637592545421));
#278075=CARTESIAN_POINT('Ctrl Pts',(32.9043876714611,5.58595159162396,129.201496239381));
#278076=CARTESIAN_POINT('Ctrl Pts',(32.6259400476482,1.67080808288091,125.238353992614));
#278077=CARTESIAN_POINT('Ctrl Pts',(32.3474924238352,-3.77972643051725,
126.390099919638));
#278078=CARTESIAN_POINT('Ctrl Pts',(32.0690448000224,-5.75687700417149,
131.598335779433));
#278079=CARTESIAN_POINT('Ctrl Pts',(31.7905971762095,-2.44373885006871,
136.076947253315));
#278080=CARTESIAN_POINT('Ctrl Pts',(31.5121495523967,3.11507592396733,135.71030918912));
#278081=CARTESIAN_POINT('Ctrl Pts',(31.2337019285837,5.81128810379662,130.835344056578));
#278082=CARTESIAN_POINT('Ctrl Pts',(30.9552543047708,3.16721041344351,125.931906657209));
#278083=CARTESIAN_POINT('Ctrl Pts',(30.676806680958,-2.38737892003384,125.506016414799));
#278084=CARTESIAN_POINT('Ctrl Pts',(30.398359057145,-5.74808365594406,129.949045656226));
#278085=CARTESIAN_POINT('Ctrl Pts',(30.1199114333322,-3.82658032153943,
135.178067562667));
#278086=CARTESIAN_POINT('Ctrl Pts',(29.8414638095193,1.61136338951851,136.387866454021));
#278087=CARTESIAN_POINT('Ctrl Pts',(29.5630161857064,5.56854286508694,132.466696251098));
#278088=CARTESIAN_POINT('Ctrl Pts',(29.2845685618935,4.40850348608286,127.017920810568));
#278089=CARTESIAN_POINT('Ctrl Pts',(29.0061209380806,-0.802735229263066,
125.048698574801));
#278090=CARTESIAN_POINT('Ctrl Pts',(28.7276733142678,-5.27629948471241,
128.368648576612));
#278091=CARTESIAN_POINT('Ctrl Pts',(28.4492256904548,-4.90120227527057,
133.926898952911));
#278092=CARTESIAN_POINT('Ctrl Pts',(28.170778066642,-0.0221396118974229,
136.615689143506));
#278093=CARTESIAN_POINT('Ctrl Pts',(27.892330442829,4.87726827322928,133.964152317942));
#278094=CARTESIAN_POINT('Ctrl Pts',(27.6138828190162,5.29470488305963,128.408921284139));
#278095=CARTESIAN_POINT('Ctrl Pts',(27.3354351952032,0.846566366071392,
125.054981974037));
#278096=CARTESIAN_POINT('Ctrl Pts',(27.0569875713904,-4.37952528427021,
126.984440764576));
#278097=CARTESIAN_POINT('Ctrl Pts',(26.7785399475775,-5.58104715007188,
132.424219286554));
#278098=CARTESIAN_POINT('Ctrl Pts',(26.5000923237646,-1.65385933426847,
136.375426826225));
#278099=CARTESIAN_POINT('Ctrl Pts',(26.2216446999517,3.79314441420758,135.207096681855));
#278100=CARTESIAN_POINT('Ctrl Pts',(25.9431970761388,5.75443375143326,129.992867180015));
#278101=CARTESIAN_POINT('Ctrl Pts',(25.6647494523259,2.42767959080881,125.524360503627));
#278102=CARTESIAN_POINT('Ctrl Pts',(25.3863018285131,-3.12999351502748,
125.907915989602));
#278103=CARTESIAN_POINT('Ctrl Pts',(25.1078542047001,-5.81135548923757,
130.791064884058));
#278104=CARTESIAN_POINT('Ctrl Pts',(24.8294065808873,-3.152365669337,135.686431908074));
#278105=CARTESIAN_POINT('Ctrl Pts',(24.5509589570743,2.40349419906,136.095413918554));
#278106=CARTESIAN_POINT('Ctrl Pts',(24.2725113332615,5.75066031573997,131.64217642775));
#278107=CARTESIAN_POINT('Ctrl Pts',(23.9940637094486,3.81325053762949,126.419027136963));
#278108=CARTESIAN_POINT('Ctrl Pts',(23.7156160856357,-1.62835019691723,
125.2257850794));
#278109=CARTESIAN_POINT('Ctrl Pts',(23.4371684618228,-5.57357664982666,
129.158981412844));
#278110=CARTESIAN_POINT('Ctrl Pts',(23.1587208380098,-4.39695844590187,
134.604200854185));
#278111=CARTESIAN_POINT('Ctrl Pts',(22.880273214197,0.820249766445046,136.557552750588));
#278112=CARTESIAN_POINT('Ctrl Pts',(22.6018255903841,5.28368851485763,133.224002135804));
#278113=CARTESIAN_POINT('Ctrl Pts',(22.3233779665712,4.89167564065013,127.666919171818));
#278114=CARTESIAN_POINT('Ctrl Pts',(22.0449303427584,0.00445182432539013,
124.992991623939));
#278115=CARTESIAN_POINT('Ctrl Pts',(21.7664827189454,-4.88686300107076,
127.659428280044));
#278116=CARTESIAN_POINT('Ctrl Pts',(21.4880350951325,-5.28738946501251,
133.215904115845));
#278117=CARTESIAN_POINT('Ctrl Pts',(21.2095874713197,-0.829063313942982,
136.556289287176));
#278118=CARTESIAN_POINT('Ctrl Pts',(20.9311398475068,4.39113152064558,134.610933008472));
#278119=CARTESIAN_POINT('Ctrl Pts',(20.6526922236938,5.57609100646137,129.167522663925));
#278120=CARTESIAN_POINT('Ctrl Pts',(20.374244599881,1.6368952645291,125.228286434793));
#278121=CARTESIAN_POINT('Ctrl Pts',(20.0957969760681,-3.80652725872624,
126.413189973261));
#278122=CARTESIAN_POINT('Ctrl Pts',(19.8173493522552,-5.75193719040684,
131.633364813234));
#278123=CARTESIAN_POINT('Ctrl Pts',(19.5389017284423,-2.41159784185683,
136.091725296493));
#278124=CARTESIAN_POINT('Ctrl Pts',(19.2604541046294,3.14488211025528,135.691255941942));
#278125=CARTESIAN_POINT('Ctrl Pts',(18.9820064808165,5.81136903907515,130.799968522399));
#278126=CARTESIAN_POINT('Ctrl Pts',(18.7035588570036,3.13749172214556,125.912717223747));
#278127=CARTESIAN_POINT('Ctrl Pts',(18.4251112331907,-2.41958721244422,
125.52064723395));
#278128=CARTESIAN_POINT('Ctrl Pts',(18.1466636093778,-5.75318370220431,
129.984051719947));
#278129=CARTESIAN_POINT('Ctrl Pts',(17.868215985565,-3.79988542828747,135.201280008538));
#278130=CARTESIAN_POINT('Ctrl Pts',(17.589768361752,1.64532191950215,136.377954178279));
#278131=CARTESIAN_POINT('Ctrl Pts',(17.3113207379392,5.57855880171371,132.432768150908));
#278132=CARTESIAN_POINT('Ctrl Pts',(17.0328731141263,4.38537267289848,126.991155152525));
#278133=CARTESIAN_POINT('Ctrl Pts',(16.7544254903134,-0.83775670494522,
125.053691691071));
#278134=CARTESIAN_POINT('Ctrl Pts',(16.4759778665005,-5.29102859763445,
128.400812037271));
#278135=CARTESIAN_POINT('Ctrl Pts',(16.1975302426876,-4.88210369021464,
133.956676108886));
#278136=CARTESIAN_POINT('Ctrl Pts',(15.9190826188747,0.013236004487936,
136.61571624315));
#278137=CARTESIAN_POINT('Ctrl Pts',(15.6406349950618,4.89641245768097,133.934404458007));
#278138=CARTESIAN_POINT('Ctrl Pts',(15.3621873712489,5.2800250653117,128.376735294641));
#278139=CARTESIAN_POINT('Ctrl Pts',(15.0837397474361,0.811552581485459,
125.049935206953));
#278140=CARTESIAN_POINT('Ctrl Pts',(14.8052921236231,-4.40269707817821,
127.011170952307));
#278141=CARTESIAN_POINT('Ctrl Pts',(14.5268444998103,-5.57108320670569,
132.458162692417));
#278142=CARTESIAN_POINT('Ctrl Pts',(14.2483968759974,-1.6199160308156,136.385391118461));
#278143=CARTESIAN_POINT('Ctrl Pts',(13.9699492521845,3.81987484009636,135.18392516268));
#278144=CARTESIAN_POINT('Ctrl Pts',(13.6915016283715,5.74938734422005,129.95785334356));
#278145=CARTESIAN_POINT('Ctrl Pts',(13.4130540045587,2.39549375219187,125.509680355073));
#278146=CARTESIAN_POINT('Ctrl Pts',(13.1346063807458,-3.15974157172482,
125.927059868305));
#278147=CARTESIAN_POINT('Ctrl Pts',(12.8561587569329,-5.81132875318382,
130.82644050072));
#278148=CARTESIAN_POINT('Ctrl Pts',(12.57771113312,-3.12258870965941,135.705530799178));
#278149=CARTESIAN_POINT('Ctrl Pts',(12.2992635093071,2.43565781110307,136.080685136208));
#278150=CARTESIAN_POINT('Ctrl Pts',(12.0208158854942,5.75565379196074,131.607155003388));
#278151=CARTESIAN_POINT('Ctrl Pts',(11.7423682616813,3.78648511732596,126.395896048684));
#278152=CARTESIAN_POINT('Ctrl Pts',(11.4639206378685,-1.66227840004959,
125.235800667314));
#278153=CARTESIAN_POINT('Ctrl Pts',(11.1854730140555,-5.58348927459409,
129.192939840948));
#278154=CARTESIAN_POINT('Ctrl Pts',(10.9070253902426,-4.37374627440173,
134.630895986013));
#278155=CARTESIAN_POINT('Ctrl Pts',(10.6285777664298,0.855255882581734,
136.552453064119));
#278156=CARTESIAN_POINT('Ctrl Pts',(10.3501301426169,5.29831966504511,133.19179399377));
#278157=CARTESIAN_POINT('Ctrl Pts',(10.071682518804,4.87248651263752,127.637200283293));
#278158=CARTESIAN_POINT('Ctrl Pts',(9.79323489499104,-0.0309237106847325,
124.993072195629));
#278159=CARTESIAN_POINT('Ctrl Pts',(9.51478727117816,-4.90591655459505,
127.689234270502));
#278160=CARTESIAN_POINT('Ctrl Pts',(9.23633964736526,-5.27261175218,133.248045275945));
#278161=CARTESIAN_POINT('Ctrl Pts',(8.95789202355236,-0.794034330915497,
136.561229460968));
#278162=CARTESIAN_POINT('Ctrl Pts',(8.67944439973947,4.41422184972672,134.584132417584));
#278163=CARTESIAN_POINT('Ctrl Pts',(8.40099677592661,5.56602379719609,129.1336097421));
#278164=CARTESIAN_POINT('Ctrl Pts',(8.12254915211368,1.60292179042129,125.218425500451));
#278165=CARTESIAN_POINT('Ctrl Pts',(7.84410152830078,-3.83318703466779,
126.436442743329));
#278166=CARTESIAN_POINT('Ctrl Pts',(7.56565390448795,-5.74678423649425,
131.668363127979));
#278167=CARTESIAN_POINT('Ctrl Pts',(7.28720628067502,-2.37936747100029,
136.106307414428));
#278168=CARTESIAN_POINT('Ctrl Pts',(7.00875865686212,3.17457176177998,135.672021609062));
#278169=CARTESIAN_POINT('Ctrl Pts',(6.73031103304925,5.81123463193681,130.764593150968));
#278170=CARTESIAN_POINT('Ctrl Pts',(6.45186340923634,3.10765676993803,125.89370905193));
#278171=CARTESIAN_POINT('Ctrl Pts',(6.17341578542346,-2.45170584616043,
125.535473843045));
#278172=CARTESIAN_POINT('Ctrl Pts',(5.89496816161054,-5.75807056212669,
130.019088180515));
#278173=CARTESIAN_POINT('Ctrl Pts',(5.61652053779771,-3.77304972888379,
135.224329524944));
#278174=CARTESIAN_POINT('Ctrl Pts',(5.33807291398477,1.67921948147701,136.367835370977));
#278175=CARTESIAN_POINT('Ctrl Pts',(5.05962529017187,5.58836802279258,132.398779709476));
#278176=CARTESIAN_POINT('Ctrl Pts',(4.781177666359,4.36207935811697,126.964530794212));
#278177=CARTESIAN_POINT('Ctrl Pts',(4.50273004254611,-0.872747137244579,
125.058897900495));
#278178=CARTESIAN_POINT('Ctrl Pts',(4.2242824187332,-5.30556164954619,128.433064562307));
#278179=CARTESIAN_POINT('Ctrl Pts',(3.94583479492031,-4.86282419701095,
133.986336454649));
#278180=CARTESIAN_POINT('Ctrl Pts',(3.66738717110745,0.0486111304084952,
136.615528000873));
#278181=CARTESIAN_POINT('Ctrl Pts',(3.38893954729453,4.91537520376836,133.904540613147));
#278182=CARTESIAN_POINT('Ctrl Pts',(3.11049192348162,5.26514959429328,128.344639261694));
#278183=CARTESIAN_POINT('Ctrl Pts',(2.83204429966877,0.776508724519974,
125.045101672218));
#278184=CARTESIAN_POINT('Ctrl Pts',(2.55359667585587,-4.42570572852705,
127.038041698076));
#278185=CARTESIAN_POINT('Ctrl Pts',(2.27514905204296,-5.56091282480238,
132.492044816037));
#278186=CARTESIAN_POINT('Ctrl Pts',(1.99670142823006,-1.58591270077849,
136.395148603559));
#278187=CARTESIAN_POINT('Ctrl Pts',(1.7182538044172,3.84646371911817,135.160591357131));
#278188=CARTESIAN_POINT('Ctrl Pts',(1.43980618060429,5.7441278913444,129.922870874744));
#278189=CARTESIAN_POINT('Ctrl Pts',(1.16135855679139,2.36321914767325,125.495196402842));
#278190=CARTESIAN_POINT('Ctrl Pts',(0.882910932978526,-3.18937254303613,
125.946384477181));
#278191=CARTESIAN_POINT('Ctrl Pts',(0.604463309165634,-5.81108667620601,
130.861815299204));
#278192=CARTESIAN_POINT('Ctrl Pts',(0.326015685352703,-3.09269604130886,
135.724448075619));
#278193=CARTESIAN_POINT('Ctrl Pts',(0.0475680615398608,2.46773116894999,
136.065760837718));
#278194=CARTESIAN_POINT('Ctrl Pts',(-0.230879562273037,5.76043399031358,
131.572103831187));
#278195=CARTESIAN_POINT('Ctrl Pts',(-0.509327186085944,3.75957938742415,
126.37292831768));
#278196=CARTESIAN_POINT('Ctrl Pts',(-0.787774809898847,-1.69614500684454,
125.246022600264));
#278197=CARTESIAN_POINT('Ctrl Pts',(-1.06622243371171,-5.59319500111311,
129.226957980841));
#278198=CARTESIAN_POINT('Ctrl Pts',(-1.34467005752462,-4.35037203212501,
134.657449324165));
#278199=CARTESIAN_POINT('Ctrl Pts',(-1.62311768133752,0.890230306896913,
136.547140379971));
#278200=CARTESIAN_POINT('Ctrl Pts',(-1.90156530515039,5.31275448404895,
133.159497384516));
#278201=CARTESIAN_POINT('Ctrl Pts',(-2.18001292896328,4.85311683284533,
127.607598755059));
#278202=CARTESIAN_POINT('Ctrl Pts',(-2.4584605527762,-0.0662980998053887,
124.993368106748));
#278203=CARTESIAN_POINT('Ctrl Pts',(-2.73690817658909,-4.92478831757726,
127.719155693111));
#278204=CARTESIAN_POINT('Ctrl Pts',(-3.01535580040196,-5.25763866077998,
133.280095884409));
#278205=CARTESIAN_POINT('Ctrl Pts',(-3.29380342421486,-0.758975924653704,
136.565956311869));
#278206=CARTESIAN_POINT('Ctrl Pts',(-3.57225104802777,4.43714860819409,
134.557191765862));
#278207=CARTESIAN_POINT('Ctrl Pts',(-3.85069867184063,5.55575033687191,
129.099758730564));
#278208=CARTESIAN_POINT('Ctrl Pts',(-4.12914629565353,1.56888891945708,
125.208771554989));
#278209=CARTESIAN_POINT('Ctrl Pts',(-4.40759391946644,-3.85970477045413,
126.459857368199));
#278210=CARTESIAN_POINT('Ctrl Pts',(-4.68604154327934,-5.74141833337845,
131.703329426794));
#278211=CARTESIAN_POINT('Ctrl Pts',(-4.96448916709218,-2.34704893180687,
136.120693066776));
#278212=CARTESIAN_POINT('Ctrl Pts',(-5.24293679090511,3.20414377838073,
135.652606903212));
#278213=CARTESIAN_POINT('Ctrl Pts',(-5.52138441471801,5.81088488736209,
130.729219253137));
#278214=CARTESIAN_POINT('Ctrl Pts',(-5.79983203853088,3.07770666236606,
125.874882846113));
#278215=CARTESIAN_POINT('Ctrl Pts',(-6.07827966234377,-2.48373363101511,
125.550495692676));
#278216=CARTESIAN_POINT('Ctrl Pts',(-6.35672728615668,-5.7627440546269,
130.054153739642));
#278217=CARTESIAN_POINT('Ctrl Pts',(-6.63517490996957,-3.74607421773465,
135.247215257776));
#278218=CARTESIAN_POINT('Ctrl Pts',(-6.91362253378244,1.71305481935644,
136.357510407073));
#278219=CARTESIAN_POINT('Ctrl Pts',(-7.19207015759534,5.59797016483923,
132.36473218626));
#278220=CARTESIAN_POINT('Ctrl Pts',(-7.47051778140826,4.33862440488076,
126.938048722207));
#278221=CARTESIAN_POINT('Ctrl Pts',(-7.74896540522111,-0.907705229577551,
125.064317010151));
#278222=CARTESIAN_POINT('Ctrl Pts',(-8.027413029034,-5.31989810191992,128.46540495659));
#278223=CARTESIAN_POINT('Ctrl Pts',(-8.30586065284694,-4.84336451006833,
134.015878891129));
#278224=CARTESIAN_POINT('Ctrl Pts',(-8.58430827665978,0.0839844550257475,
136.615124423653));
#278225=CARTESIAN_POINT('Ctrl Pts',(-8.86275590047269,4.93415580881975,
133.874561889976));
#278226=CARTESIAN_POINT('Ctrl Pts',(-9.14120352428557,5.25007902122049,
128.312634374625));
#278227=CARTESIAN_POINT('Ctrl Pts',(-9.4196511480985,0.741436093738357,
125.040481548942));
#278228=CARTESIAN_POINT('Ctrl Pts',(-9.69809877191133,-4.44855038272257,
127.065052006178));
#278229=CARTESIAN_POINT('Ctrl Pts',(-9.97654639572428,-5.5505363812293,
132.525864401898));
#278230=CARTESIAN_POINT('Ctrl Pts',(-10.2549940195371,-1.55185060416301,
136.404698919952));
#278231=CARTESIAN_POINT('Ctrl Pts',(-10.53344164335,3.87291006601234,135.137096129849));
#278232=CARTESIAN_POINT('Ctrl Pts',(-10.8118892671629,5.7386555876974,129.887921069854));
#278233=CARTESIAN_POINT('Ctrl Pts',(-11.0903368909758,2.33085697319978,
125.480909183646));
#278234=CARTESIAN_POINT('Ctrl Pts',(-11.3687845147887,-3.21888533097506,
125.965889100148));
#278235=CARTESIAN_POINT('Ctrl Pts',(-11.6472321386015,-5.81062926727439,
130.897187968684));
#278236=CARTESIAN_POINT('Ctrl Pts',(-11.9256797624145,-3.06268877196916,
135.743183036409));
#278237=CARTESIAN_POINT('Ctrl Pts',(-12.2041273862274,2.49971308411117,
136.050641576106));
#278238=CARTESIAN_POINT('Ctrl Pts',(-12.4825750100403,5.76500073366654,
131.537024209977));
#278239=CARTESIAN_POINT('Ctrl Pts',(-12.7610226338531,3.73253434492532,
126.350124795028));
#278240=CARTESIAN_POINT('Ctrl Pts',(-13.039470257666,-1.7299487623625,125.256450499474));
#278241=CARTESIAN_POINT('Ctrl Pts',(-13.3179178814789,-5.60269346973446,
129.261034571969));
#278242=CARTESIAN_POINT('Ctrl Pts',(-13.5963655052918,-4.32683658521273,
134.683859884699));
#278243=CARTESIAN_POINT('Ctrl Pts',(-13.8748131291047,0.925171743400955,
136.541614895008));
#278244=CARTESIAN_POINT('Ctrl Pts',(-14.1532607529176,5.3269924369816,133.127113504801));
#278245=CARTESIAN_POINT('Ctrl Pts',(-14.4317083767304,4.83356731902416,
127.578115684011));
#278246=CARTESIAN_POINT('Ctrl Pts',(-14.7101560005434,-0.101670032225581,
124.99387934633));
#278247=CARTESIAN_POINT('Ctrl Pts',(-14.9886036243562,-4.94347759071707,
127.749191439124));
#278248=CARTESIAN_POINT('Ctrl Pts',(-15.2670512481692,-5.24247074564602,
133.312054753593));
#278249=CARTESIAN_POINT('Ctrl Pts',(-15.545498871982,-0.723889394260118,
136.570469664722));
#278250=CARTESIAN_POINT('Ctrl Pts',(-15.823946495795,4.45991094648802,134.530112051601));
#278251=CARTESIAN_POINT('Ctrl Pts',(-16.1023941196078,5.54527100617588,
129.065970883678));
#278252=CARTESIAN_POINT('Ctrl Pts',(-16.3808417434207,1.53479791273714,
125.199324956138));
#278253=CARTESIAN_POINT('Ctrl Pts',(-16.6592893672336,-3.88607948346057,
126.483432980235));
#278254=CARTESIAN_POINT('Ctrl Pts',(-16.9377369910465,-5.73583967989507,
131.738262413989));
#278255=CARTESIAN_POINT('Ctrl Pts',(-17.2161846148594,-2.31464342185212,
136.134881720468));
#278256=CARTESIAN_POINT('Ctrl Pts',(-17.4946322386723,3.23359706425542,
135.633012543814));
#278257=CARTESIAN_POINT('Ctrl Pts',(-17.7730798624852,5.81031981831091,
130.693848139697));
#278258=CARTESIAN_POINT('Ctrl Pts',(-18.0515274862981,3.04764250924188,
125.856239303907));
#278259=CARTESIAN_POINT('Ctrl Pts',(-18.3299751101109,-2.51566938020671,
125.565712226204));
#278260=CARTESIAN_POINT('Ctrl Pts',(-18.6084227339239,-5.76720400652691,
130.089247097961));
#278261=CARTESIAN_POINT('Ctrl Pts',(-18.8868703577367,-3.71895989442774,
135.269936358996));
#278262=CARTESIAN_POINT('Ctrl Pts',(-19.1653179815497,1.74682667935956,
136.346979669161));
#278263=CARTESIAN_POINT('Ctrl Pts',(-19.4437656053625,5.60736487204277,
132.330626842902));
#278264=CARTESIAN_POINT('Ctrl Pts',(-19.7222132291754,4.31500868232164,
126.91170991781));
#278265=CARTESIAN_POINT('Ctrl Pts',(-20.0006608529883,-0.942629686559699,
125.069948819234));
#278266=CARTESIAN_POINT('Ctrl Pts',(-20.2791084768012,-5.33403742351306,
128.497832021735));
#278267=CARTESIAN_POINT('Ctrl Pts',(-20.5575561006141,-4.82372535047263,
134.045302323618));
#278268=CARTESIAN_POINT('Ctrl Pts',(-20.836003724427,0.119354667568119,
136.614505526443));
#278269=CARTESIAN_POINT('Ctrl Pts',(-21.1144513482399,4.95275357691331,
133.844469399368));
#278270=CARTESIAN_POINT('Ctrl Pts',(-21.3928989720528,5.23481390453873,
128.280721819388));
#278271=CARTESIAN_POINT('Ctrl Pts',(-21.6713465958657,0.706335988769417,
125.036075008324));
#278272=CARTESIAN_POINT('Ctrl Pts',(-21.9497942196786,-4.47123019424771,
127.092200875735));
#278273=CARTESIAN_POINT('Ctrl Pts',(-22.2282418434914,-5.53995426048939,
132.559620196804));
#278274=CARTESIAN_POINT('Ctrl Pts',(-22.5066894673044,-1.5177310031529,
136.41404171375));
#278275=CARTESIAN_POINT('Ctrl Pts',(-22.7851370911172,3.89921290079955,
135.11344035146));
#278276=CARTESIAN_POINT('Ctrl Pts',(-23.0635847149301,5.73297063605735,
129.853005223969));
#278277=CARTESIAN_POINT('Ctrl Pts',(-23.342032338743,2.298408427964,125.466819226899));
#278278=CARTESIAN_POINT('Ctrl Pts',(-23.6204799625559,-3.24827884193431,
125.985573014458));
#278279=CARTESIAN_POINT('Ctrl Pts',(-23.8989275863688,-5.80995654333829,
130.932557198412));
#278280=CARTESIAN_POINT('Ctrl Pts',(-24.1773752101816,-3.03256801357094,
135.761734987319));
#278281=CARTESIAN_POINT('Ctrl Pts',(-24.4558228339946,2.53160237148462,
136.035327911625));
#278282=CARTESIAN_POINT('Ctrl Pts',(-24.7342704578075,5.76935385279724,
131.501917439649));
#278283=CARTESIAN_POINT('Ctrl Pts',(-25.0127180816204,3.70535099199371,
126.327486325724));
#278284=CARTESIAN_POINT('Ctrl Pts',(-25.2911657054332,-1.76368841399288,
125.267083978533));
#278285=CARTESIAN_POINT('Ctrl Pts',(-25.5696133292462,-5.61198432848891,
129.295168351611));
#278286=CARTESIAN_POINT('Ctrl Pts',(-25.8480609530591,-4.30314080577957,
134.71012668896));
#278287=CARTESIAN_POINT('Ctrl Pts',(-26.1265085768719,0.960078897325804,
136.535876813977));
#278288=CARTESIAN_POINT('Ctrl Pts',(-26.4049562006848,5.3410329962505,133.094643554625));
#278289=CARTESIAN_POINT('Ctrl Pts',(-26.6834038244978,4.81383869558843,
127.548752162656));
#278290=CARTESIAN_POINT('Ctrl Pts',(-26.9618514483106,-0.137038197225328,
124.994605895435));
#278291=CARTESIAN_POINT('Ctrl Pts',(-27.2402990721235,-4.96198368147699,
127.779340395554));
#278292=CARTESIAN_POINT('Ctrl Pts',(-27.5187466959364,-5.22710856883054,
133.343920699249));
#278293=CARTESIAN_POINT('Ctrl Pts',(-27.7971943197493,-0.688776039878604,
136.574769352283));
#278294=CARTESIAN_POINT('Ctrl Pts',(-28.0756419435621,4.48250802114168,
134.502894278251));
#278295=CARTESIAN_POINT('Ctrl Pts',(-28.3540895673751,5.53458619342344,
129.032247453463));
#278296=CARTESIAN_POINT('Ctrl Pts',(-28.632537191188,1.50065003351598,125.190086053944));
#278297=CARTESIAN_POINT('Ctrl Pts',(-28.9109848150008,-3.91231019636288,
126.507168705834));
#278298=CARTESIAN_POINT('Ctrl Pts',(-29.1894324388138,-5.73004848276283,
131.773160795109));
#278299=CARTESIAN_POINT('Ctrl Pts',(-29.4678800626266,-2.28215214193419,
136.148872849742));
#278300=CARTESIAN_POINT('Ctrl Pts',(-29.7463276864396,3.26293052800175,
135.613239256942));
#278301=CARTESIAN_POINT('Ctrl Pts',(-30.0247753102524,5.80953944572202,
130.658481121338));
#278302=CARTESIAN_POINT('Ctrl Pts',(-30.3032229340653,3.01746542460398,
125.837779116156));
#278303=CARTESIAN_POINT('Ctrl Pts',(-30.5816705578782,-2.54751191034413,
125.581122879776));
#278304=CARTESIAN_POINT('Ctrl Pts',(-30.8601181816911,-5.77145025256159,
130.124366955075));
#278305=CARTESIAN_POINT('Ctrl Pts',(-31.138565805504,-3.69170776369427,
135.292491986665));
#278306=CARTESIAN_POINT('Ctrl Pts',(-31.4170134293169,1.78053381005746,
136.336243547461));
#278307=CARTESIAN_POINT('Ctrl Pts',(-31.6954610531298,5.6165517962788,132.296464943187));
#278308=CARTESIAN_POINT('Ctrl Pts',(-31.9739086769427,4.29123306552915,
126.885515357016));
#278309=CARTESIAN_POINT('Ctrl Pts',(-32.2523563007555,-0.977519214052166,
125.075793119056));
#278310=CARTESIAN_POINT('Ctrl Pts',(-32.5308039245685,-5.34797909038788,
128.530344556146));
#278311=CARTESIAN_POINT('Ctrl Pts',(-32.8092515483813,-4.80390744596015,
134.07460566182));
#278312=CARTESIAN_POINT('Ctrl Pts',(-33.0876991721943,0.154720457379397,
136.613671332177));
#278313=CARTESIAN_POINT('Ctrl Pts',(-33.3661467960071,4.9711678189017,133.814264256411));
#278314=CARTESIAN_POINT('Ctrl Pts',(-33.64459441982,5.21935480990263,128.248902778514));
#278315=CARTESIAN_POINT('Ctrl Pts',(-33.9230420436329,0.671209710260644,
125.031882213649));
#278316=CARTESIAN_POINT('Ctrl Pts',(-34.2014896674458,-4.49374432269368,
127.119487300736));
#278317=CARTESIAN_POINT('Ctrl Pts',(-34.4799372912587,-5.52916685470707,
132.59331094992));
#278318=CARTESIAN_POINT('Ctrl Pts',(-34.7583849150716,-1.48355516206214,
136.423176638752));
#278319=CARTESIAN_POINT('Ctrl Pts',(-35.0368325388844,3.92537124881898,
135.089624898536));
#278320=CARTESIAN_POINT('Ctrl Pts',(-35.3152801626974,5.72707324708195,
129.818124630907));
#278321=CARTESIAN_POINT('Ctrl Pts',(-35.5937277865103,2.26587471435868,
125.45292705471));
#278322=CARTESIAN_POINT('Ctrl Pts',(-35.8721754103231,-3.27755198672651,
126.005435490714));
#278323=CARTESIAN_POINT('Ctrl Pts',(-36.1506230341361,-5.80906852932597,
130.967921677768));
#278324=CARTESIAN_POINT('Ctrl Pts',(-36.4290706579489,-3.00233488224952,
135.780103240898));
#278325=CARTESIAN_POINT('Ctrl Pts',(-36.7075182817618,2.56339784940132,
136.019820411726));
#278326=CARTESIAN_POINT('Ctrl Pts',(-36.9859659055747,5.77349318639923,
131.466784821096));
#278327=CARTESIAN_POINT('Ctrl Pts',(-37.2644135293876,3.67803033591843,
126.305013748643));
#278328=CARTESIAN_POINT('Ctrl Pts',(-37.5428611532005,-1.79736271150026,
125.277922643415));
#278329=CARTESIAN_POINT('Ctrl Pts',(-37.8213087770133,-5.62106723310019,
129.329358054928));
#278330=CARTESIAN_POINT('Ctrl Pts',(-38.0997564008263,-4.27928557188161,
134.736248763623));
#278331=CARTESIAN_POINT('Ctrl Pts',(-38.3782040246392,0.994950475174061,
136.529926349506));
#278332=CARTESIAN_POINT('Ctrl Pts',(-38.656651648452,5.35487564157755,133.062088737171));
#278333=CARTESIAN_POINT('Ctrl Pts',(-38.9350992722649,4.79393169358958,
127.51950927907));
#278334=CARTESIAN_POINT('Ctrl Pts',(-39.2135468960779,-0.172401284224016,
124.995547727136));
#278335=CARTESIAN_POINT('Ctrl Pts',(-39.4919945198907,-4.98030590410683,
127.809601445221));
#278336=CARTESIAN_POINT('Ctrl Pts',(-39.7704421437036,-5.21155269958477,
133.375692540572));
#278337=CARTESIAN_POINT('Ctrl Pts',(-40.0488897675166,-0.65363716264763,
136.578855215227));
#278338=CARTESIAN_POINT('Ctrl Pts',(-40.3273373913294,4.50493899481217,
134.475539454375));
#278339=CARTESIAN_POINT('Ctrl Pts',(-40.6057850151423,5.52369629454426,
128.998589689552));
#278340=CARTESIAN_POINT('Ctrl Pts',(-40.8842326389552,1.46644654715595,
125.181055190758));
#278341=CARTESIAN_POINT('Ctrl Pts',(-41.1626802627681,-3.93839593717207,
126.531063665459));
#278342=CARTESIAN_POINT('Ctrl Pts',(-41.441127886581,-5.72404495657686,
131.808023276983));
#278343=CARTESIAN_POINT('Ctrl Pts',(-41.7195755103939,-2.24957629602936,
136.162665936149));
#278344=CARTESIAN_POINT('Ctrl Pts',(-41.9980231342068,3.29214308265742,
135.593287775304));
#278345=CARTESIAN_POINT('Ctrl Pts',(-42.2764707580197,5.80854379851262,
130.623119508596));
#278346=CARTESIAN_POINT('Ctrl Pts',(-42.5549183818325,2.98717652667487,
125.81950296691));
#278347=CARTESIAN_POINT('Ctrl Pts',(-42.8333660056454,-2.57926004149102,
125.596727082342));
#278348=CARTESIAN_POINT('Ctrl Pts',(-43.1118136294584,-5.7754826353847,
130.159512009603));
#278349=CARTESIAN_POINT('Ctrl Pts',(-43.3902612532712,-3.66431883537201,
135.314881304976));
#278350=CARTESIAN_POINT('Ctrl Pts',(-43.6687088770841,1.81417496242045,
136.325302439805));
#278351=CARTESIAN_POINT('Ctrl Pts',(-43.947156500897,5.62553059712261,132.262247752997));
#278352=CARTESIAN_POINT('Ctrl Pts',(-44.2256041247099,4.26729843551711,
126.859466010475));
#278353=CARTESIAN_POINT('Ctrl Pts',(-44.5040517485228,-1.01237251921066,
125.081849693053));
#278354=CARTESIAN_POINT('Ctrl Pts',(-44.7824993723357,-5.3617225859308,
128.562941355057));
#278355=CARTESIAN_POINT('Ctrl Pts',(-45.0609469961486,-4.78391153089065,
134.103787819889));
#278356=CARTESIAN_POINT('Ctrl Pts',(-45.3393946199614,0.190080513966956,
136.612621871764));
#278357=CARTESIAN_POINT('Ctrl Pts',(-45.6178422437743,4.98939785243841,
133.783947580368));
#278358=CARTESIAN_POINT('Ctrl Pts',(-45.8962898675873,5.20370231015464,
128.217178431071));
#278359=CARTESIAN_POINT('Ctrl Pts',(-46.1747374914001,0.636058559829223,
125.027903320286));
#278360=CARTESIAN_POINT('Ctrl Pts',(-46.453185115213,-4.51609193379101,
127.146910270074));
#278361=CARTESIAN_POINT('Ctrl Pts',(-46.7316327390259,-5.51817456361365,
132.626935412823));
#278362=CARTESIAN_POINT('Ctrl Pts',(-47.0100803628388,-1.4493243472895,
136.43210335646));
#278363=CARTESIAN_POINT('Ctrl Pts',(-47.2885279866517,3.95138414076325,
135.06565065357));
#278364=CARTESIAN_POINT('Ctrl Pts',(-47.5669756104645,5.72096363930122,
129.783280583183));
#278365=CARTESIAN_POINT('Ctrl Pts',(-47.8454232342775,2.23325703793269,
125.439233181862));
#278366=CARTESIAN_POINT('Ctrl Pts',(-48.1238708580903,-3.30670368062431,
126.025475792906));
#278367=CARTESIAN_POINT('Ctrl Pts',(-48.4023184819033,-5.80796525814313,
131.00328009631));
#278368=CARTESIAN_POINT('Ctrl Pts',(-48.6807661057162,-2.97199049830493,
135.798287116504));
#278369=CARTESIAN_POINT('Ctrl Pts',(-48.9592137295291,2.59509833966803,
136.004119651047));
#278370=CARTESIAN_POINT('Ctrl Pts',(-49.2376613533419,5.77741858108801,
131.431627656171));
#278371=CARTESIAN_POINT('Ctrl Pts',(-49.5161089771548,3.65057338907646,
126.282707896514));
#278372=CARTESIAN_POINT('Ctrl Pts',(-49.7945566009678,-1.8309704070716,
125.288966092489));
#278373=CARTESIAN_POINT('Ctrl Pts',(-50.0730042247805,-5.62994184699806,
129.363602415007));
#278374=CARTESIAN_POINT('Ctrl Pts',(-50.3514518485936,-4.25527176748286,
134.762225140725));
#278375=CARTESIAN_POINT('Ctrl Pts',(-50.6298994724063,1.02978518476655,
136.52376372209));
#278376=CARTESIAN_POINT('Ctrl Pts',(-50.9083470962193,5.36851986001845,
133.029450258773));
#278377=CARTESIAN_POINT('Ctrl Pts',(-51.1867947200322,4.77384705068883,
127.490388116857));
#278378=CARTESIAN_POINT('Ctrl Pts',(-51.465242343845,-0.207757982829986,
124.996704806535));
#278379=CARTESIAN_POINT('Ctrl Pts',(-51.743689967658,-4.99844357966987,
127.839973466791));
#278380=CARTESIAN_POINT('Ctrl Pts',(-52.0221375914708,-5.19580371433717,
133.407369100245));
#278381=CARTESIAN_POINT('Ctrl Pts',(-52.3005852152837,-0.618474064651215,
136.58272710215));
#278382=CARTESIAN_POINT('Ctrl Pts',(-52.5790328390967,4.52720303631132,
134.448048593619));
#278383=CARTESIAN_POINT('Ctrl Pts',(-52.8574804629095,5.51260171306762,
128.964998839148));
#278384=CARTESIAN_POINT('Ctrl Pts',(-53.1359280867224,1.43218872108006,
125.172232701224));
#278385=CARTESIAN_POINT('Ctrl Pts',(-53.4143757105353,-3.96433573927151,
126.555116973674));
#278386=CARTESIAN_POINT('Ctrl Pts',(-53.6928233343482,-5.71782932379997,
131.842848567767));
#278387=CARTESIAN_POINT('Ctrl Pts',(-53.9712709581611,-2.21691709124776,
136.176260468582));
#278388=CARTESIAN_POINT('Ctrl Pts',(-54.249718581974,3.32123364574025,135.573158838211));
#278389=CARTESIAN_POINT('Ctrl Pts',(-54.5281662057869,5.80733291357678,
130.58776461181));
#278390=CARTESIAN_POINT('Ctrl Pts',(-54.8066138295998,2.95677693782102,
125.801411533396));
#278391=CARTESIAN_POINT('Ctrl Pts',(-55.0850614534126,-2.61091259720856,
125.612524255684));
#278392=CARTESIAN_POINT('Ctrl Pts',(-55.3635090772256,-5.77930100557468,
130.194680959234));
#278393=CARTESIAN_POINT('Ctrl Pts',(-55.6419567010384,-3.63679412436797,
135.337103484283));
#278394=CARTESIAN_POINT('Ctrl Pts',(-55.9204043248514,1.8477488898629,136.314156751619));
#278395=CARTESIAN_POINT('Ctrl Pts',(-56.1988519486642,5.63430094186134,
132.227976540264));
#278396=CARTESIAN_POINT('Ctrl Pts',(-56.4772995724772,4.24320567919224,
126.833562843453));
#278397=CARTESIAN_POINT('Ctrl Pts',(-56.7557471962901,-1.04718831053316,
125.088118316796));
#278398=CARTESIAN_POINT('Ctrl Pts',(-57.0341948201028,-5.3752674008715,
128.595621210585));
#278399=CARTESIAN_POINT('Ctrl Pts',(-57.3126424439159,-4.76373834622006,
134.13284771647));
#278400=CARTESIAN_POINT('Ctrl Pts',(-57.5910900677287,0.225433527051438,
136.611357184097));
#278401=CARTESIAN_POINT('Ctrl Pts',(-57.8695376915416,5.00744300200284,
133.753520494635));
#278402=CARTESIAN_POINT('Ctrl Pts',(-58.1479853153544,5.18785698530388,
128.185549952615));
#278403=CARTESIAN_POINT('Ctrl Pts',(-58.4264329391674,0.600883840013963,
125.024138475672));
#278404=CARTESIAN_POINT('Ctrl Pts',(-58.7048805629802,-4.53827219944114,
127.174468767579));
#278405=CARTESIAN_POINT('Ctrl Pts',(-58.9833281867932,-5.5069777945324,
132.660492339548));
#278406=CARTESIAN_POINT('Ctrl Pts',(-59.261775810606,-1.41503982726995,
136.440821536091));
#278407=CARTESIAN_POINT('Ctrl Pts',(-59.540223434419,3.97725061271504,135.041518504932));
#278408=CARTESIAN_POINT('Ctrl Pts',(-59.8186710582318,5.71464203910897,
129.748474371954));
#278409=CARTESIAN_POINT('Ctrl Pts',(-60.0971186820448,2.20055660734573,
125.425738115783));
#278410=CARTESIAN_POINT('Ctrl Pts',(-60.3755663058576,-3.3357328434014,
126.045693178431));
#278411=CARTESIAN_POINT('Ctrl Pts',(-60.6540139296705,-5.80664677067165,
131.038631143817));
#278412=CARTESIAN_POINT('Ctrl Pts',(-60.9324615534834,-2.94153598615947,
135.816285940328));
#278413=CARTESIAN_POINT('Ctrl Pts',(-61.2109091772963,2.62670266761142,
135.988226211385));
#278414=CARTESIAN_POINT('Ctrl Pts',(-61.4893568011092,5.78112989140647,
131.396447247635));
#278415=CARTESIAN_POINT('Ctrl Pts',(-61.767804424922,3.62298116889529,126.260569595891));
#278416=CARTESIAN_POINT('Ctrl Pts',(-62.046252048735,-1.86451025536104,
125.300213916535));
#278417=CARTESIAN_POINT('Ctrl Pts',(-62.3246996725479,-5.63860784133039,
129.39790016291));
#278418=CARTESIAN_POINT('Ctrl Pts',(-62.6031472963608,-4.23110028242386,
134.788054857702));
#278419=CARTESIAN_POINT('Ctrl Pts',(-62.8815949201736,1.0645817352901,136.517389160091));
#278420=CARTESIAN_POINT('Ctrl Pts',(-63.1600425439866,5.38196514598156,
132.99672932886));
#278421=CARTESIAN_POINT('Ctrl Pts',(-63.4384901677994,4.75358551113023,
127.461389755115));
#278422=CARTESIAN_POINT('Ctrl Pts',(-63.7169377916123,-0.243106982887504,
124.998077090756));
#278423=CARTESIAN_POINT('Ctrl Pts',(-63.9953854154252,-5.0163960360679,
127.870455334816));
#278424=CARTESIAN_POINT('Ctrl Pts',(-64.2738330392381,-5.17986219667218,
133.438949204482));
#278425=CARTESIAN_POINT('Ctrl Pts',(-64.552280663051,-0.583288048870894,
136.586384869579));
#278426=CARTESIAN_POINT('Ctrl Pts',(-64.8307282868638,4.54929932063727,
134.420422714664));
#278427=CARTESIAN_POINT('Ctrl Pts',(-65.1091759106768,5.50130286010717,
128.93147614697));
#278428=CARTESIAN_POINT('Ctrl Pts',(-65.3876235344896,1.39787782472419,
125.16361891226));
#278429=CARTESIAN_POINT('Ctrl Pts',(-65.6660711583025,-3.99012864145221,
126.579327739175));
#278430=CARTESIAN_POINT('Ctrl Pts',(-65.9445187821156,-5.71140181475477,
131.877635376998));
#278431=CARTESIAN_POINT('Ctrl Pts',(-66.2229664059283,-2.18417573778792,
136.189655943291));
#278432=CARTESIAN_POINT('Ctrl Pts',(-66.5014140297413,3.35020113928917,
135.552853191544));
#278433=CARTESIAN_POINT('Ctrl Pts',(-66.7798616535541,5.80590683578406,
130.552417741069));
#278434=CARTESIAN_POINT('Ctrl Pts',(-67.0583092773671,2.92626778451039,
125.783505486001));
#278435=CARTESIAN_POINT('Ctrl Pts',(-67.3367569011799,-2.64246840459962,
125.628513814431));
#278436=CARTESIAN_POINT('Ctrl Pts',(-67.6152045249929,-5.78290522164069,
130.229872500769));
#278437=CARTESIAN_POINT('Ctrl Pts',(-67.8936521488056,-3.60913465062,135.359157701137));
#278438=CARTESIAN_POINT('Ctrl Pts',(-68.1720997726187,1.88125434829088,
136.302806895912));
#278439=CARTESIAN_POINT('Ctrl Pts',(-68.4505473964314,5.64286250550667,
132.193652574919));
#278440=CARTESIAN_POINT('Ctrl Pts',(-68.7289950202444,4.21895568932047,
126.807806815805));
#278441=CARTESIAN_POINT('Ctrl Pts',(-69.0074426440573,-1.08196529790749,
125.094598758));
#278442=CARTESIAN_POINT('Ctrl Pts',(-69.2858902678701,-5.38861303330182,
128.628382911763));
#278443=CARTESIAN_POINT('Ctrl Pts',(-69.564337891683,-4.74338863947339,
134.161784274737));
#278444=CARTESIAN_POINT('Ctrl Pts',(-69.8427855154959,0.260778186613682,
136.609877316035));
#278445=CARTESIAN_POINT('Ctrl Pts',(-70.1212331393089,5.02530259892534,
133.722984126697));
#278446=CARTESIAN_POINT('Ctrl Pts',(-70.3996807631217,5.17181942250469,
128.154018515153));
#278447=CARTESIAN_POINT('Ctrl Pts',(-70.6781283869345,0.5656868542273,125.020587819316));
#278448=CARTESIAN_POINT('Ctrl Pts',(-70.9565760107477,-4.56028429774593,
127.202161772061));
#278449=CARTESIAN_POINT('Ctrl Pts',(-71.2350236345604,-5.49557696236377,
132.693980486629));
#278450=CARTESIAN_POINT('Ctrl Pts',(-71.5134712583732,-1.38070287242923,
136.449330854589));
#278451=CARTESIAN_POINT('Ctrl Pts',(-71.7919188821862,4.00296970618273,
135.017229346852));
#278452=CARTESIAN_POINT('Ctrl Pts',(-72.0703665059991,5.70810868075446,
129.71370728698));
#278453=CARTESIAN_POINT('Ctrl Pts',(-72.348814129812,2.16777463432419,125.412442356538));
#278454=CARTESIAN_POINT('Ctrl Pts',(-72.6272617536249,-3.36463839937136,
126.06608689813));
#278455=CARTESIAN_POINT('Ctrl Pts',(-72.9057093774378,-5.80511311576878,
131.073973510343));
#278456=CARTESIAN_POINT('Ctrl Pts',(-73.1841570012506,-2.91097247431594,
135.834099045416));
#278457=CARTESIAN_POINT('Ctrl Pts',(-73.4626046250635,2.65820966212185,
135.972140681676));
#278458=CARTESIAN_POINT('Ctrl Pts',(-73.7410522488765,5.78462697983096,
131.361244899111));
#278459=CARTESIAN_POINT('Ctrl Pts',(-74.0194998726893,3.59525469781404,
126.238599667113));
#278460=CARTESIAN_POINT('Ctrl Pts',(-74.2979474965022,-1.89798101353784,
125.31166569876));
#278461=CARTESIAN_POINT('Ctrl Pts',(-74.5763951203151,-5.64706489497548,
129.432250027724));
#278462=CARTESIAN_POINT('Ctrl Pts',(-74.854842744128,-4.20677201238788,
134.813736957424));
#278463=CARTESIAN_POINT('Ctrl Pts',(-75.1332903679409,1.09933883734644,
136.510802899716));
#278464=CARTESIAN_POINT('Ctrl Pts',(-75.4117379917539,5.39521100124704,
132.963927159917));
#278465=CARTESIAN_POINT('Ctrl Pts',(-75.6901856155667,4.73314782571214,
127.432515268386));
#278466=CARTESIAN_POINT('Ctrl Pts',(-75.9686332393795,-0.278446974526432,
124.99966452895));
#278467=CARTESIAN_POINT('Ctrl Pts',(-76.2470808631926,-5.03416260806588,
127.901045919781));
#278468=CARTESIAN_POINT('Ctrl Pts',(-76.5255284870053,-5.16372873730878,
133.470431683069));
#278469=CARTESIAN_POINT('Ctrl Pts',(-76.8039761108183,-0.548080419137594,
136.589828381972));
#278470=CARTESIAN_POINT('Ctrl Pts',(-77.0824237346311,4.57122702900371,
134.392662841198));
#278471=CARTESIAN_POINT('Ctrl Pts',(-77.360871358444,5.48980015434633,128.898022855216));
#278472=CARTESIAN_POINT('Ctrl Pts',(-77.639318982257,1.36351512949127,125.155214143056));
#278473=CARTESIAN_POINT('Ctrl Pts',(-77.9177666060698,-4.0157736879487,
126.603695064822));
#278474=CARTESIAN_POINT('Ctrl Pts',(-78.1962142298826,-5.70476266761487,
131.91238241564));
#278475=CARTESIAN_POINT('Ctrl Pts',(-78.4746618536957,-2.15135344889296,
136.202851863901));
#278476=CARTESIAN_POINT('Ctrl Pts',(-78.7531094775085,3.37904448990285,
135.532371587738));
#278477=CARTESIAN_POINT('Ctrl Pts',(-79.0315571013213,5.8042656179783,130.517080206165));
#278478=CARTESIAN_POINT('Ctrl Pts',(-79.3100047251342,2.8956501972711,125.765785488239));
#278479=CARTESIAN_POINT('Ctrl Pts',(-79.5884523489472,-2.67392629435197,
125.644695166086));
#278480=CARTESIAN_POINT('Ctrl Pts',(-79.8668999727601,-5.78629515002701,
130.265085330171));
#278481=CARTESIAN_POINT('Ctrl Pts',(-80.1453475965729,-3.58134143906054,
135.38104313831));
#278482=CARTESIAN_POINT('Ctrl Pts',(-80.4237952203859,1.91469009614739,
136.291253293255));
#278483=CARTESIAN_POINT('Ctrl Pts',(-80.7022428441988,5.65121497080658,
132.15927712885));
#278484=CARTESIAN_POINT('Ctrl Pts',(-80.9806904680116,4.19454936449412,
126.782198881926));
#278485=CARTESIAN_POINT('Ctrl Pts',(-81.2591380918246,-1.11670219266007,
125.10129077653));
#278486=CARTESIAN_POINT('Ctrl Pts',(-81.5375857156372,-5.40175898869456,
128.661225244595));
#278487=CARTESIAN_POINT('Ctrl Pts',(-81.8160333394505,-4.72286316471603,
134.190596422436));
#278488=CARTESIAN_POINT('Ctrl Pts',(-82.0944809632629,0.296113182944105,
136.608182322418));
#278489=CARTESIAN_POINT('Ctrl Pts',(-82.3729285870762,5.04297598141181,
133.692339608092));
#278490=CARTESIAN_POINT('Ctrl Pts',(-82.6513762108889,5.15559021603496,
128.122585287091));
#278491=CARTESIAN_POINT('Ctrl Pts',(-82.9298238347018,0.530468906706182,
125.017251482786));
#278492=CARTESIAN_POINT('Ctrl Pts',(-83.2082714585147,-4.58212741303929,
127.229988257347));
#278493=CARTESIAN_POINT('Ctrl Pts',(-83.4867190823277,-5.48397248956967,
132.72739861315));
#278494=CARTESIAN_POINT('Ctrl Pts',(-83.7651667061405,-1.34631475513585,
136.45763099664));
#278495=CARTESIAN_POINT('Ctrl Pts',(-84.0436143299535,4.02854046813582,
134.992784079373));
#278496=CARTESIAN_POINT('Ctrl Pts',(-84.3220619537663,5.70136380633342,
129.678980616565));
#278497=CARTESIAN_POINT('Ctrl Pts',(-84.6005095775792,2.13491233361711,
125.399346396808));
#278498=CARTESIAN_POINT('Ctrl Pts',(-84.8789572013921,-3.39341927742779,
126.086656196302));
#278499=CARTESIAN_POINT('Ctrl Pts',(-85.1574048252049,-5.80336435026449,
131.109305886265));
#278500=CARTESIAN_POINT('Ctrl Pts',(-85.4358524490179,-2.88030109531746,
135.851725771696));
#278501=CARTESIAN_POINT('Ctrl Pts',(-85.7143000728307,2.68961815569484,
135.955863657977));
#278502=CARTESIAN_POINT('Ctrl Pts',(-85.9927476966438,5.78790971677558,
131.326021915035));
#278503=CARTESIAN_POINT('Ctrl Pts',(-86.2711953204564,3.56739500324825,
126.216798924288));
#278504=CARTESIAN_POINT('Ctrl Pts',(-86.5496429442695,-1.93138144132926,
125.323321014816));
#278505=CARTESIAN_POINT('Ctrl Pts',(-86.8280905680822,-5.65531269455438,
129.466650736599));
#278506=CARTESIAN_POINT('Ctrl Pts',(-87.1065381918953,-4.18228785886808,
134.83927048823));
#278507=CARTESIAN_POINT('Ctrl Pts',(-87.3849858157081,1.13405520299706,
136.504005185026));
#278508=CARTESIAN_POINT('Ctrl Pts',(-87.663433439521,5.40825693498488,132.931044967442));
#278509=CARTESIAN_POINT('Ctrl Pts',(-87.9418810633338,4.71253475176078,
127.403765726628));
#278510=CARTESIAN_POINT('Ctrl Pts',(-88.2203286871468,-0.313776648210234,
125.00146706229));
#278511=CARTESIAN_POINT('Ctrl Pts',(-88.4987763109598,-5.05174263731727,
127.931744088139));
#278512=CARTESIAN_POINT('Ctrl Pts',(-88.7772239347726,-5.14740393407785,
133.501815369412));
#278513=CARTESIAN_POINT('Ctrl Pts',(-89.0556715585855,-0.512852480082647,
136.593057511728));
#278514=CARTESIAN_POINT('Ctrl Pts',(-89.3341191823985,4.59298534887173,
134.364770001874));
#278515=CARTESIAN_POINT('Ctrl Pts',(-89.6125668062112,5.47809402202166,
128.864640203508));
#278516=CARTESIAN_POINT('Ctrl Pts',(-89.8910144300243,1.32910190870433,
125.147018705051));
#278517=CARTESIAN_POINT('Ctrl Pts',(-90.169462053837,-4.04126992847403,
126.628218047677));
#278518=CARTESIAN_POINT('Ctrl Pts',(-90.44790967765,-5.69791212839678,131.947088396125));
#278519=CARTESIAN_POINT('Ctrl Pts',(-90.7263573014627,-2.1184514408047,
136.215847741432));
#278520=CARTESIAN_POINT('Ctrl Pts',(-91.0048049252757,3.40776262878029,
135.511714785749));
#278521=CARTESIAN_POINT('Ctrl Pts',(-91.2832525490887,5.80240932097568,
130.48175331654));
#278522=CARTESIAN_POINT('Ctrl Pts',(-91.5617001729014,2.86492531064864,
125.748252196732));
#278523=CARTESIAN_POINT('Ctrl Pts',(-91.8401477967144,-2.70528510078237,
125.661067711041));
#278524=CARTESIAN_POINT('Ctrl Pts',(-92.1185954205271,-5.78947066511866,
130.30031814262));
#278525=CARTESIAN_POINT('Ctrl Pts',(-92.3970430443404,-3.55341551957677,
135.402758984829));
#278526=CARTESIAN_POINT('Ctrl Pts',(-92.6754906681528,1.94805489445803,
136.279496371773));
#278527=CARTESIAN_POINT('Ctrl Pts',(-92.9539382919661,5.6593580282576,132.124851475851));
#278528=CARTESIAN_POINT('Ctrl Pts',(-93.2323859157787,4.16998760909852,
126.75673999073));
#278529=CARTESIAN_POINT('Ctrl Pts',(-93.5108335395918,-1.15139770760221,
125.10819412441));
#278530=CARTESIAN_POINT('Ctrl Pts',(-93.7892811634045,-5.41470477992152,
128.694146992097));
#278531=CARTESIAN_POINT('Ctrl Pts',(-94.0677287872175,-4.70216268252734,
134.219283091922));
#278532=CARTESIAN_POINT('Ctrl Pts',(-94.3461764110305,0.331437206691851,
136.606272266052));
#278533=CARTESIAN_POINT('Ctrl Pts',(-94.6246240348431,5.0604624945689,133.661588074364));
#278534=CARTESIAN_POINT('Ctrl Pts',(-94.9030716586564,5.13916996727372,
128.0912514332));
#278535=CARTESIAN_POINT('Ctrl Pts',(-95.1815192824688,0.495231302464415,
125.014129589715));
#278536=CARTESIAN_POINT('Ctrl Pts',(-95.459966906282,-4.60380073591605,
127.257947192314));
#278537=CARTESIAN_POINT('Ctrl Pts',(-95.7384145300948,-5.47216480615837,
132.760745480792));
#278538=CARTESIAN_POINT('Ctrl Pts',(-96.0168621539077,-1.31187674965409,
136.465721654678));
#278539=CARTESIAN_POINT('Ctrl Pts',(-96.2953097777207,4.05396195104042,
134.96818360832));
#278540=CARTESIAN_POINT('Ctrl Pts',(-96.5737574015334,5.69440766577999,
129.64429564752));
#278541=CARTESIAN_POINT('Ctrl Pts',(-96.8522050253465,2.10197092294792,
125.386450721867));
#278542=CARTESIAN_POINT('Ctrl Pts',(-97.1306526491593,-3.42207441108517,
126.107400310748));
#278543=CARTESIAN_POINT('Ctrl Pts',(-97.4091002729722,-5.80140053895979,
131.144626962327));
#278544=CARTESIAN_POINT('Ctrl Pts',(-97.6875478967851,-2.8495229857029,
135.869165466005));
#278545=CARTESIAN_POINT('Ctrl Pts',(-97.965995520598,2.72092698447821,135.93939574344));
#278546=CARTESIAN_POINT('Ctrl Pts',(-98.2444431444108,5.79097798059694,
131.290779600608));
#278547=CARTESIAN_POINT('Ctrl Pts',(-98.5228907682237,3.53940311754856,
126.195168175249));
#278548=CARTESIAN_POINT('Ctrl Pts',(-98.8013383920368,-1.96471030107164,
125.33517943281));
#278549=CARTESIAN_POINT('Ctrl Pts',(-99.0797860158496,-5.6633509344415,
129.501101014807));
#278550=CARTESIAN_POINT('Ctrl Pts',(-99.3582336396624,-4.15764872913354,
134.864654503967));
#278551=CARTESIAN_POINT('Ctrl Pts',(-99.6366812634755,1.16872954581563,
136.496996267908));
#278552=CARTESIAN_POINT('Ctrl Pts',(-99.9151288872883,5.42110246377302,
132.898083969897));
#278553=CARTESIAN_POINT('Ctrl Pts',(-100.193576511101,4.69174705310118,
127.375142195163));
#278554=CARTESIAN_POINT('Ctrl Pts',(-100.472024134914,-0.34909469478497,
125.003484623986));
#278555=CARTESIAN_POINT('Ctrl Pts',(-100.750471758727,-5.06913547238742,
127.96254870236));
#278556=CARTESIAN_POINT('Ctrl Pts',(-101.02891938254,-5.13088839190121,
133.533099100579));
#278557=CARTESIAN_POINT('Ctrl Pts',(-101.307367006353,-0.47760553709043,
136.596072139193));
#278558=CARTESIAN_POINT('Ctrl Pts',(-101.585814630166,4.61457347397855,
134.33674523027));
#278559=CARTESIAN_POINT('Ctrl Pts',(-101.864262253979,5.46618489690847,
128.831329428852));
#278560=CARTESIAN_POINT('Ctrl Pts',(-102.142709877791,1.29463943755703,
125.139032901931));
#278561=CARTESIAN_POINT('Ctrl Pts',(-102.421157501604,-4.06661641825637,
126.652895779031));
#278562=CARTESIAN_POINT('Ctrl Pts',(-102.699605125417,-5.69085045094906,
131.981752032413));
#278563=CARTESIAN_POINT('Ctrl Pts',(-102.97805274923,-2.08547093271925,
136.228643094318));
#278564=CARTESIAN_POINT('Ctrl Pts',(-103.256500373043,3.43635449176034,
135.490883551018));
#278565=CARTESIAN_POINT('Ctrl Pts',(-103.534947996856,5.80033801356182,
130.446438381249));
#278566=CARTESIAN_POINT('Ctrl Pts',(-103.813395620669,2.83409426316523,
125.730906261181));
#278567=CARTESIAN_POINT('Ctrl Pts',(-104.091843244482,-2.73654366187847,
125.677630842606));
#278568=CARTESIAN_POINT('Ctrl Pts',(-104.370290868295,-5.79243164924577,
130.335569632546));
#278569=CARTESIAN_POINT('Ctrl Pts',(-104.648738492108,-3.52535792697413,
135.424304436005));
#278570=CARTESIAN_POINT('Ctrl Pts',(-104.92718611592,1.98134750687769,136.267536567122));
#278571=CARTESIAN_POINT('Ctrl Pts',(-105.205633739733,5.66729137611554,
132.090376891579));
#278572=CARTESIAN_POINT('Ctrl Pts',(-105.484081363546,4.14527133327901,
126.731431085605));
#278573=CARTESIAN_POINT('Ctrl Pts',(-105.762528987359,-1.18605055707886,
125.115308545834));
#278574=CARTESIAN_POINT('Ctrl Pts',(-106.040976611172,-5.42744992727162,
128.72714693434));
#278575=CARTESIAN_POINT('Ctrl Pts',(-106.319424234985,-4.68128795997122,
134.247843220201));
#278576=CARTESIAN_POINT('Ctrl Pts',(-106.597871858798,0.366748948912009,
136.604147217717));
#278577=CARTESIAN_POINT('Ctrl Pts',(-106.876319482611,5.07776149042729,
133.630730665021));
#278578=CARTESIAN_POINT('Ctrl Pts',(-107.154767106424,5.12255928467941,
128.060018114567));
#278579=CARTESIAN_POINT('Ctrl Pts',(-107.433214730236,0.45997534724462,
125.011222255784));
#278580=CARTESIAN_POINT('Ctrl Pts',(-107.711662354049,-4.62530346326349,
127.286037540936));
#278581=CARTESIAN_POINT('Ctrl Pts',(-107.990109977862,-5.46015434966779,
132.794019853873));
#278582=CARTESIAN_POINT('Ctrl Pts',(-108.268557601675,-1.2773901320969,
136.473602528901));
#278583=CARTESIAN_POINT('Ctrl Pts',(-108.547005225488,4.07923321289408,
134.943428845277));
#278584=CARTESIAN_POINT('Ctrl Pts',(-108.825452849301,5.6872405168564,129.609653665109));
#278585=CARTESIAN_POINT('Ctrl Pts',(-109.103900473114,2.06895162297316,
125.373755809571));
#278586=CARTESIAN_POINT('Ctrl Pts',(-109.382348096927,-3.45060273851677,
126.128318472786));
#278587=CARTESIAN_POINT('Ctrl Pts',(-109.66079572074,-5.79922175462486,
131.179935429694));
#278588=CARTESIAN_POINT('Ctrl Pts',(-109.939243344552,-2.81863928596571,
135.886417482107));
#278589=CARTESIAN_POINT('Ctrl Pts',(-110.217690968365,2.7521349883118,135.922737548286));
#278590=CARTESIAN_POINT('Ctrl Pts',(-110.496138592178,5.79383165759959,
131.255519261747));
#278591=CARTESIAN_POINT('Ctrl Pts',(-110.774586215991,3.51128007796473,
126.17370822153));
#278592=CARTESIAN_POINT('Ctrl Pts',(-111.053033839804,-1.99796635775128,
125.347240513325));
#278593=CARTESIAN_POINT('Ctrl Pts',(-111.331481463617,-5.67117931677705,
129.535599585778));
#278594=CARTESIAN_POINT('Ctrl Pts',(-111.60992908743,-4.13285553619637,
134.889888064022));
#278595=CARTESIAN_POINT('Ctrl Pts',(-111.888376711243,1.20336058093108,
136.489776408084));
#278596=CARTESIAN_POINT('Ctrl Pts',(-112.166824335056,5.43374711161577,
132.865045388662));
#278597=CARTESIAN_POINT('Ctrl Pts',(-112.445271958868,4.67078550002918,
127.34664573465));
#278598=CARTESIAN_POINT('Ctrl Pts',(-112.723719582681,-0.384399805526852,
125.005717139274));
#278599=CARTESIAN_POINT('Ctrl Pts',(-113.002167206494,-5.08634046877848,
127.993458620965));
#278600=CARTESIAN_POINT('Ctrl Pts',(-113.280614830307,-5.11418272276831,
133.564281717336));
#278601=CARTESIAN_POINT('Ctrl Pts',(-113.55906245412,-0.442340896249408,
136.598872152659));
#278602=CARTESIAN_POINT('Ctrl Pts',(-113.837510077933,4.63599060436829,
134.308589564856));
#278603=CARTESIAN_POINT('Ctrl Pts',(-114.115957701746,5.45407322030374,
128.798091765594));
#278604=CARTESIAN_POINT('Ctrl Pts',(-114.394405325558,1.26012899306928,
125.131257029612));
#278605=CARTESIAN_POINT('Ctrl Pts',(-114.672852949372,-4.09181221807183,
126.677727344441));
#278606=CARTESIAN_POINT('Ctrl Pts',(-114.951300573184,-5.68357789694507,
132.016372040028));
#278607=CARTESIAN_POINT('Ctrl Pts',(-115.229748196997,-2.05241314674147,
136.241237448422));
#278608=CARTESIAN_POINT('Ctrl Pts',(-115.50819582081,3.46481901936097,135.469878655457));
#278609=CARTESIAN_POINT('Ctrl Pts',(-115.786643444623,5.79805177248978,
130.411136708898));
#278610=CARTESIAN_POINT('Ctrl Pts',(-116.065091068436,2.80315819727665,
125.713748324348));
#278611=CARTESIAN_POINT('Ctrl Pts',(-116.343538692249,-2.76770081934284,
125.694383947029));
#278612=CARTESIAN_POINT('Ctrl Pts',(-116.621986316062,-5.79517799268792,
130.370838493694));
#278613=CARTESIAN_POINT('Ctrl Pts',(-116.900433939875,-3.49716970093708,
135.445678693465));
#278614=CARTESIAN_POINT('Ctrl Pts',(-117.178881563688,2.0145666997373,136.255374322477));
#278615=CARTESIAN_POINT('Ctrl Pts',(-117.4573291875,5.67501472040751,132.055854653499));
#278616=CARTESIAN_POINT('Ctrl Pts',(-117.735776811314,4.12040145290537,
126.706273104381));
#278617=CARTESIAN_POINT('Ctrl Pts',(-118.014224435126,-1.22065945701595,
125.122633777175));
#278618=CARTESIAN_POINT('Ctrl Pts',(-118.29267205894,-5.43999395846872,
128.760223848501));
#278619=CARTESIAN_POINT('Ctrl Pts',(-118.571119682752,-4.6602397705682,
134.276275748964));
#278620=CARTESIAN_POINT('Ctrl Pts',(-118.849567306565,0.402047101114997,
136.601807256156));
#278621=CARTESIAN_POINT('Ctrl Pts',(-119.128014930377,5.09487232796628,
133.599768523497));
#278622=CARTESIAN_POINT('Ctrl Pts',(-119.406462554191,5.10575878376697,
128.028886488555));
#278623=CARTESIAN_POINT('Ctrl Pts',(-119.684910178003,0.424702347469154,
125.008529588725));
#278624=CARTESIAN_POINT('Ctrl Pts',(-119.963357801817,-4.64663479828973,
127.314258262312));
#278625=CARTESIAN_POINT('Ctrl Pts',(-120.241805425629,-5.44794156515001,
132.827220499399));
#278626=CARTESIAN_POINT('Ctrl Pts',(-120.520253049442,-1.24285618037906,
136.48127332728));
#278627=CARTESIAN_POINT('Ctrl Pts',(-120.798700673255,4.10435331726091,
134.918520707537));
#278628=CARTESIAN_POINT('Ctrl Pts',(-121.077148297068,5.67986262514396,
129.575055953004));
#278629=CARTESIAN_POINT('Ctrl Pts',(-121.355595920881,2.03585565723516,
125.361262130332));
#278630=CARTESIAN_POINT('Ctrl Pts',(-121.634043544694,-3.47900320259493,
126.149409907283));
#278631=CARTESIAN_POINT('Ctrl Pts',(-121.912491168507,-5.79682807799514,
131.215229979999));
#278632=CARTESIAN_POINT('Ctrl Pts',(-122.19093879232,-2.78765114051323,
135.903481180724));
#278633=CARTESIAN_POINT('Ctrl Pts',(-122.469386416133,2.78324101077128,
135.905889689793));
#278634=CARTESIAN_POINT('Ctrl Pts',(-122.747834039945,5.79647064203949,
131.220242205036));
#278635=CARTESIAN_POINT('Ctrl Pts',(-123.026281663758,3.48302692660634,
126.152419858339));
#278636=CARTESIAN_POINT('Ctrl Pts',(-123.304729287571,-2.03114837905279,
125.359503809431));
#278637=CARTESIAN_POINT('Ctrl Pts',(-123.583176911384,-5.67879755147744,
129.570145171156));
#278638=CARTESIAN_POINT('Ctrl Pts',(-123.861624535197,-4.10790919877744,
134.914970233354));
#278639=CARTESIAN_POINT('Ctrl Pts',(-124.14007215901,1.23794702507767,136.482345873087));
#278640=CARTESIAN_POINT('Ctrl Pts',(-124.418519782823,5.44619040996103,
132.831930447996));
#278641=CARTESIAN_POINT('Ctrl Pts',(-124.696967406636,4.64965086928273,
127.318277401031));
#278642=CARTESIAN_POINT('Ctrl Pts',(-124.975415030448,-0.419690672193134,
125.00816452543));
#278643=CARTESIAN_POINT('Ctrl Pts',(-125.253862654262,-5.10335698895296,
128.024472698579));
#278644=CARTESIAN_POINT('Ctrl Pts',(-125.532310278074,-5.09728754571388,
133.595362064203));
#278645=CARTESIAN_POINT('Ctrl Pts',(-125.810757901887,-0.407059864303788,
136.601457448367));
#278646=CARTESIAN_POINT('Ctrl Pts',(-126.0892055257,4.65723594642128,134.280304048949));
#278647=CARTESIAN_POINT('Ctrl Pts',(-126.367653149513,5.44175944101008,
128.764928445366));
#278648=CARTESIAN_POINT('Ctrl Pts',(-126.646100773326,1.22557185403828,
125.123691376234));
#278649=CARTESIAN_POINT('Ctrl Pts',(-126.924548397139,-4.11685639428078,
126.702711823764));
#278650=CARTESIAN_POINT('Ctrl Pts',(-127.202996020952,-5.67609473587197,
132.050947136115));
#278651=CARTESIAN_POINT('Ctrl Pts',(-127.481443644765,-2.01927930784003,
136.253630337055));
#278652=CARTESIAN_POINT('Ctrl Pts',(-127.759891268577,3.4931551568182,135.44870087741));
#278653=CARTESIAN_POINT('Ctrl Pts',(-128.038338892391,5.79555068247735,
130.375849607603));
#278654=CARTESIAN_POINT('Ctrl Pts',(-128.316786516203,2.77211825933019,
125.696779022025));
#278655=CARTESIAN_POINT('Ctrl Pts',(-128.595234140016,-2.7987554186355,
125.711326403516));
#278656=CARTESIAN_POINT('Ctrl Pts',(-128.873681763829,-5.79770959367839,
130.406123419165));
#278657=CARTESIAN_POINT('Ctrl Pts',(-129.152129387642,-3.46885188599067,
135.466880965177));
#278658=CARTESIAN_POINT('Ctrl Pts',(-129.430577011455,2.04771124208698,
136.243010088514));
#278659=CARTESIAN_POINT('Ctrl Pts',(-129.709024635268,5.68252777494204,
132.021286040849));
#278660=CARTESIAN_POINT('Ctrl Pts',(-129.98747225908,4.09537888954061,126.681266979298));
#278661=CARTESIAN_POINT('Ctrl Pts',(-130.265919882893,-1.25522312496795,
125.130169546993));
#278662=CARTESIAN_POINT('Ctrl Pts',(-130.544367506706,-5.45233640868912,
128.793376508901));
#278663=CARTESIAN_POINT('Ctrl Pts',(-130.822815130519,-4.63901889426667,
134.304579624636));
#278664=CARTESIAN_POINT('Ctrl Pts',(-131.101262754332,0.437330355314798,
136.599252468079));
#278665=CARTESIAN_POINT('Ctrl Pts',(-131.379710378145,5.11179437313754,
133.568702797104));
#278666=CARTESIAN_POINT('Ctrl Pts',(-131.658158001958,5.08876908708517,
127.997857708758));
#278667=CARTESIAN_POINT('Ctrl Pts',(-131.936605625771,0.389413610192037,
125.006051688315));
#278668=CARTESIAN_POINT('Ctrl Pts',(-132.215053249584,-4.66779395055513,
127.342608310716));
#278669=CARTESIAN_POINT('Ctrl Pts',(-132.493500873397,-5.43552690515385,
132.860346187109));
#278670=CARTESIAN_POINT('Ctrl Pts',(-132.77194849721,-1.20827617416795,
136.488733765571));
#278671=CARTESIAN_POINT('Ctrl Pts',(-133.050396121022,4.12932133330617,
134.893460118082));
#278672=CARTESIAN_POINT('Ctrl Pts',(-133.328843744835,5.67227426403318,
129.540503793235));
#278673=CARTESIAN_POINT('Ctrl Pts',(-133.607291368648,2.00268425211708,
125.348970147109));
#278674=CARTESIAN_POINT('Ctrl Pts',(-133.885738992461,-3.50727475093002,
126.170673832692));
#278675=CARTESIAN_POINT('Ctrl Pts',(-134.164186616274,-5.79421959776922,
131.25050930539));
#278676=CARTESIAN_POINT('Ctrl Pts',(-134.442634240087,-2.75655969762259,
135.920355929551));
#278677=CARTESIAN_POINT('Ctrl Pts',(-134.7210818639,2.81424389921159,135.888852792264));
#278678=CARTESIAN_POINT('Ctrl Pts',(-134.999529487713,5.79889483612785,
131.18494973768));
#278679=CARTESIAN_POINT('Ctrl Pts',(-135.277977111526,3.45464471040472,
126.131303874523));
#278680=CARTESIAN_POINT('Ctrl Pts',(-135.556424735338,-2.06425513540386,
125.371968866708));
#278681=CARTESIAN_POINT('Ctrl Pts',(-135.834872359151,-5.68620535624619,
129.604736490841));
#278682=CARTESIAN_POINT('Ctrl Pts',(-136.113319982964,-4.08281064127246,
134.939900082537));
#278683=CARTESIAN_POINT('Ctrl Pts',(-136.391767606777,1.27248759664198,
136.474704938258));
#278684=CARTESIAN_POINT('Ctrl Pts',(-136.67021523059,5.45843189771781,132.798740374984));
#278685=CARTESIAN_POINT('Ctrl Pts',(-136.948662854403,4.62834394401342,
127.290038245509));
#278686=CARTESIAN_POINT('Ctrl Pts',(-137.227110478216,-0.454965987067202,
125.010826691762));
#278687=CARTESIAN_POINT('Ctrl Pts',(-137.505558102029,-5.12018440235748,
128.055589785961));
#278688=CARTESIAN_POINT('Ctrl Pts',(-137.784005725841,-5.0802034867949,
133.626338989485));
#278689=CARTESIAN_POINT('Ctrl Pts',(-138.062453349655,-0.371763748605222,
136.603827930521));
#278690=CARTESIAN_POINT('Ctrl Pts',(-138.340900973467,4.67830871288359,
134.251889730681));
#278691=CARTESIAN_POINT('Ctrl Pts',(-138.61934859728,5.42924401531914,128.731840697047));
#278692=CARTESIAN_POINT('Ctrl Pts',(-138.897796221093,1.19096930099152,
125.116336222143));
#278693=CARTESIAN_POINT('Ctrl Pts',(-139.176243844906,-4.14174801886209,
126.727848291193));
#278694=CARTESIAN_POINT('Ctrl Pts',(-139.454691468719,-5.66840124502105,
132.085476039479));
#278695=CARTESIAN_POINT('Ctrl Pts',(-139.733139092532,-1.98607064380098,
136.265821300996));
#278696=CARTESIAN_POINT('Ctrl Pts',(-140.011586716345,3.52136185412693,
135.427351001626));
#278697=CARTESIAN_POINT('Ctrl Pts',(-140.290034340158,5.79283483620279,
130.340578384942));
#278698=CARTESIAN_POINT('Ctrl Pts',(-140.56848196397,2.7409755995222,125.679998983016));
#278699=CARTESIAN_POINT('Ctrl Pts',(-140.846929587784,-2.82970630901691,
125.72845758426));
#278700=CARTESIAN_POINT('Ctrl Pts',(-141.125377211596,-5.80002635840773,
130.441423101462));
#278701=CARTESIAN_POINT('Ctrl Pts',(-141.403824835409,-3.44040553146196,
135.487910465481));
#278702=CARTESIAN_POINT('Ctrl Pts',(-141.682272459222,2.08077990574355,
136.230444323395));
#278703=CARTESIAN_POINT('Ctrl Pts',(-141.960720083035,5.68983026132012,
131.986672334579));
#278704=CARTESIAN_POINT('Ctrl Pts',(-142.239167706848,4.07020457040501,
126.656413636965));
#278705=CARTESIAN_POINT('Ctrl Pts',(-142.517615330661,-1.289740280165,125.137915576048));
#278706=CARTESIAN_POINT('Ctrl Pts',(-142.796062954474,-5.46447682057862,
128.826603687055));
#278707=CARTESIAN_POINT('Ctrl Pts',(-143.074510578287,-4.61762611741445,
134.332753798405));
#278708=CARTESIAN_POINT('Ctrl Pts',(-143.352958202099,0.472597404077474,
136.596482948152));
#278709=CARTESIAN_POINT('Ctrl Pts',(-143.631405825913,5.12852699888841,
133.537534636997));
#278710=CARTESIAN_POINT('Ctrl Pts',(-143.909853449725,5.07159082419343,
127.966932924958));
#278711=CARTESIAN_POINT('Ctrl Pts',(-144.188301073538,0.354110443050382,
125.003788646376));
#278712=CARTESIAN_POINT('Ctrl Pts',(-144.466748697351,-4.6887801359991,
127.371086635623));
#278713=CARTESIAN_POINT('Ctrl Pts',(-144.745196321164,-5.4229108297093,
132.893395689516));
#278714=CARTESIAN_POINT('Ctrl Pts',(-145.023643944977,-1.17365139483885,
136.495983567324));
#278715=CARTESIAN_POINT('Ctrl Pts',(-145.30209156879,4.15413633583088,134.868248005541));
#278716=CARTESIAN_POINT('Ctrl Pts',(-145.580539192603,5.66447571471356,
129.505998466145));
#278717=CARTESIAN_POINT('Ctrl Pts',(-145.858986816416,1.96943863679757,
125.336880315387));
#278718=CARTESIAN_POINT('Ctrl Pts',(-146.137434440228,-3.53541633590941,
126.192109461069));
#278719=CARTESIAN_POINT('Ctrl Pts',(-146.415882064041,-5.79139641060527,
131.285772098575));
#278720=CARTESIAN_POINT('Ctrl Pts',(-146.694329687854,-2.72536610939861,
135.937041103293));
#278721=CARTESIAN_POINT('Ctrl Pts',(-146.972777311667,2.84514250480927,
135.871627487008));
#278722=CARTESIAN_POINT('Ctrl Pts',(-147.25122493548,5.80110415003576,131.149643167454));
#278723=CARTESIAN_POINT('Ctrl Pts',(-147.529672559293,3.42613448107249,
126.110361052543));
#278724=CARTESIAN_POINT('Ctrl Pts',(-147.808120183106,-2.09728540002206,
125.38463522326));
#278725=CARTESIAN_POINT('Ctrl Pts',(-148.086567806919,-5.69340245658434,
129.639372263039));
#278726=CARTESIAN_POINT('Ctrl Pts',(-148.365015430732,-4.05756079371773,
134.964676687782));
#278727=CARTESIAN_POINT('Ctrl Pts',(-148.643463054544,1.30698101571045,
136.466853886735));
#278728=CARTESIAN_POINT('Ctrl Pts',(-148.921910678358,5.47047112127328,
132.765476399497));
#278729=CARTESIAN_POINT('Ctrl Pts',(-149.20035830217,4.60686551375719,127.261929314495));
#278730=CARTESIAN_POINT('Ctrl Pts',(-149.478805925983,-0.49022444300932,
125.013703539625));
#278731=CARTESIAN_POINT('Ctrl Pts',(-149.757253549796,-5.13682208544599,
128.086808730058));
#278732=CARTESIAN_POINT('Ctrl Pts',(-150.035701173609,-5.06293117906749,
133.657211345319));
#278733=CARTESIAN_POINT('Ctrl Pts',(-150.314148797422,-0.336453857064764,
136.605983511281));
#278734=CARTESIAN_POINT('Ctrl Pts',(-150.592596421235,4.69920812289605,
134.223347662954));
#278735=CARTESIAN_POINT('Ctrl Pts',(-150.871044045047,5.41652740699458,
128.698829746717));
#278736=CARTESIAN_POINT('Ctrl Pts',(-151.14949166886,1.15632261613933,125.109191839888));
#278737=CARTESIAN_POINT('Ctrl Pts',(-151.427939292673,-4.1664861694474,
126.753135815284));
#278738=CARTESIAN_POINT('Ctrl Pts',(-151.706386916486,-5.66049770947745,
132.119957470642));
#278739=CARTESIAN_POINT('Ctrl Pts',(-151.984834540299,-1.95278838518384,
136.277809888502));
#278740=CARTESIAN_POINT('Ctrl Pts',(-152.263282164112,3.54943806607717,
135.405829819234));
#278741=CARTESIAN_POINT('Ctrl Pts',(-152.541729787925,5.78990433430307,
130.3053243479));
#278742=CARTESIAN_POINT('Ctrl Pts',(-152.820177411738,2.70973137185537,
125.663408829112));
#278743=CARTESIAN_POINT('Ctrl Pts',(-153.09862503555,-2.86055234359039,
125.745776854456));
#278744=CARTESIAN_POINT('Ctrl Pts',(-153.377072659364,-5.80212820102742,
130.476736232542));
#278745=CARTESIAN_POINT('Ctrl Pts',(-153.655520283176,-3.41183169144105,
135.508766415124));
#278746=CARTESIAN_POINT('Ctrl Pts',(-153.933967906989,2.1137714653355,136.21767749275));
#278747=CARTESIAN_POINT('Ctrl Pts',(-154.212415530802,5.69692190894542,
131.952014817313));
#278748=CARTESIAN_POINT('Ctrl Pts',(-154.490863154615,4.04487942834225,
126.631713998332));
#278749=CARTESIAN_POINT('Ctrl Pts',(-154.769310778428,-1.32420964356211,
125.145871577308));
#278750=CARTESIAN_POINT('Ctrl Pts',(-155.047758402241,-5.47641474427016,
128.859904151722));
#278751=CARTESIAN_POINT('Ctrl Pts',(-155.326206026054,-4.59606223272787,
134.360797226267));
#278752=CARTESIAN_POINT('Ctrl Pts',(-155.604653649866,0.507846940569522,
136.593498799002));
#278753=CARTESIAN_POINT('Ctrl Pts',(-155.88310127368,5.14506958518534,133.50626519812));
#278754=CARTESIAN_POINT('Ctrl Pts',(-156.161548897493,5.05422463163864,
127.936113283085));
#278755=CARTESIAN_POINT('Ctrl Pts',(-156.439996521305,0.318794154216047,
125.001740546765));
#278756=CARTESIAN_POINT('Ctrl Pts',(-156.718444145118,-4.70959257697085,
127.399692181761));
#278757=CARTESIAN_POINT('Ctrl Pts',(-156.996891768931,-5.41009380630968,
132.926367781962));
#278758=CARTESIAN_POINT('Ctrl Pts',(-157.275339392744,-1.1389831254257,
136.503022463895));
#278759=CARTESIAN_POINT('Ctrl Pts',(-157.553787016557,4.17879740530553,
134.84288530416));
#278760=CARTESIAN_POINT('Ctrl Pts',(-157.83223464037,5.65646726616335,129.471541250343));
#278761=CARTESIAN_POINT('Ctrl Pts',(-158.110682264183,1.93612004320555,
125.324993083158));
#278762=CARTESIAN_POINT('Ctrl Pts',(-158.389129887996,-3.56342691473634,
126.213715998108));
#278763=CARTESIAN_POINT('Ctrl Pts',(-158.667577511808,-5.78835862111754,
131.321017052882));
#278764=CARTESIAN_POINT('Ctrl Pts',(-158.946025135621,-2.69407153173119,
135.95353608367));
#278765=CARTESIAN_POINT('Ctrl Pts',(-159.224472759434,2.87593568260513,
135.854214412314));
#278766=CARTESIAN_POINT('Ctrl Pts',(-159.502920383247,5.80309850189603,
131.114323802656));
#278767=CARTESIAN_POINT('Ctrl Pts',(-159.78136800706,3.39749729506709,126.089592168444));
#278768=CARTESIAN_POINT('Ctrl Pts',(-160.059815630873,-2.13023794895846,
125.39750240973));
#278769=CARTESIAN_POINT('Ctrl Pts',(-160.338263254686,-5.70038858580074,
129.674051204309));
#278770=CARTESIAN_POINT('Ctrl Pts',(-160.616710878499,-4.03216059175559,
134.989299130986));
#278771=CARTESIAN_POINT('Ctrl Pts',(-160.895158502312,1.34142600411673,
136.458793009441));
#278772=CARTESIAN_POINT('Ctrl Pts',(-161.173606126125,5.48230763450959,
132.732139754142));
#278773=CARTESIAN_POINT('Ctrl Pts',(-161.452053749937,4.58521637440516,
127.233951649575));
#278774=CARTESIAN_POINT('Ctrl Pts',(-161.730501373751,-0.525464733504406,
125.016794962416));
#278775=CARTESIAN_POINT('Ctrl Pts',(-162.008948997563,-5.15326942170307,
128.118128374039));
#278776=CARTESIAN_POINT('Ctrl Pts',(-162.287396621376,-5.04547126256333,
133.687977987722));
#278777=CARTESIAN_POINT('Ctrl Pts',(-162.565844245189,-0.301131498102361,
136.607924110772));
#278778=CARTESIAN_POINT('Ctrl Pts',(-162.844291869002,4.71993340202341,
134.194678903404));
#278779=CARTESIAN_POINT('Ctrl Pts',(-163.122739492814,5.40361008725504,
128.665896817606));
#278780=CARTESIAN_POINT('Ctrl Pts',(-163.401187116628,1.12163308332736,
125.102258494207));
#278781=CARTESIAN_POINT('Ctrl Pts',(-163.67963474044,-4.19106992935549,
126.778573459));
#278782=CARTESIAN_POINT('Ctrl Pts',(-163.958082364253,-5.65238442210956,
132.154390151878));
#278783=CARTESIAN_POINT('Ctrl Pts',(-164.236529988066,-1.91943376527495,
136.289595655332));
#278784=CARTESIAN_POINT('Ctrl Pts',(-164.514977611879,3.57738275229458,
135.384138127707));
#278785=CARTESIAN_POINT('Ctrl Pts',(-164.793425235692,5.78675928536899,
130.270088802833));
#278786=CARTESIAN_POINT('Ctrl Pts',(-165.071872859505,2.67838673409632,
125.647009175068));
#278787=CARTESIAN_POINT('Ctrl Pts',(-165.350320483318,-2.89129237934434,
125.763283572333));
#278788=CARTESIAN_POINT('Ctrl Pts',(-165.628768107131,-5.80401504365309,
130.512061503863));
#278789=CARTESIAN_POINT('Ctrl Pts',(-165.907215730944,-3.38313142474212,
135.52944804128));
#278790=CARTESIAN_POINT('Ctrl Pts',(-166.185663354757,2.14668469834846,
136.204710069657));
#278791=CARTESIAN_POINT('Ctrl Pts',(-166.464110978569,5.70380245503433,
131.917314773299));
#278792=CARTESIAN_POINT('Ctrl Pts',(-166.742558602383,4.01940440178476,
126.607168978656));
#278793=CARTESIAN_POINT('Ctrl Pts',(-167.021006226195,-1.3586299378839,
125.15403725596));
#278794=CARTESIAN_POINT('Ctrl Pts',(-167.299453850008,-5.48814973739939,
128.893276668938));
#278795=CARTESIAN_POINT('Ctrl Pts',(-167.577901473821,-4.57432803926507,
134.388708869063));
#278796=CARTESIAN_POINT('Ctrl Pts',(-167.856349097634,0.543077658606429,
136.590300131209));
#278797=CARTESIAN_POINT('Ctrl Pts',(-168.134796721447,5.16142151903669,
133.474895639175));
#278798=CARTESIAN_POINT('Ctrl Pts',(-168.413244345259,5.03667115293141,
127.905399925171));
#278799=CARTESIAN_POINT('Ctrl Pts',(-168.691691969073,0.283466052347084,
124.999907465374));
#278800=CARTESIAN_POINT('Ctrl Pts',(-168.970139592885,-4.7302305022577,
127.42842388914));
#278801=CARTESIAN_POINT('Ctrl Pts',(-169.248587216698,-5.39707630989451,
132.959261242652));
#278802=CARTESIAN_POINT('Ctrl Pts',(-169.527034840511,-1.10427265057399,
136.509850194457));
#278803=CARTESIAN_POINT('Ctrl Pts',(-169.805482464324,4.20330362790601,
134.81737295376));
#278804=CARTESIAN_POINT('Ctrl Pts',(-170.083930088137,5.6482492151383,129.437133422652));
#278805=CARTESIAN_POINT('Ctrl Pts',(-170.36237771195,1.90272970597286,125.313308890908));
#278806=CARTESIAN_POINT('Ctrl Pts',(-170.640825335763,-3.59130544946847,
126.235492643171));
#278807=CARTESIAN_POINT('Ctrl Pts',(-170.919272959575,-5.78510634187241,
131.356242862295));
#278808=CARTESIAN_POINT('Ctrl Pts',(-171.197720583389,-2.66267712425244,
135.969840259458));
#278809=CARTESIAN_POINT('Ctrl Pts',(-171.476168207202,2.90662229154664,
135.836614213432));
#278810=CARTESIAN_POINT('Ctrl Pts',(-171.754615831014,5.80487781780722,
131.07899295206));
#278811=CARTESIAN_POINT('Ctrl Pts',(-172.033063454828,3.36873421355001,
126.068997991823));
#278812=CARTESIAN_POINT('Ctrl Pts',(-172.31151107864,-2.16311156114431,
125.410569949319));
#278813=CARTESIAN_POINT('Ctrl Pts',(-172.589958702453,-5.70716348502144,
129.70877202961));
#278814=CARTESIAN_POINT('Ctrl Pts',(-172.868406326266,-4.00661097660031,
135.013766499754));
#278815=CARTESIAN_POINT('Ctrl Pts',(-173.146853950079,1.3758212854888,136.450522605077));
#278816=CARTESIAN_POINT('Ctrl Pts',(-173.425301573892,5.49394099882038,
132.698731674224));
#278817=CARTESIAN_POINT('Ctrl Pts',(-173.703749197705,4.56339732817417,
127.206106287473));
#278818=CARTESIAN_POINT('Ctrl Pts',(-173.982196821517,-0.560685552710569,
125.02010084558));
#278819=CARTESIAN_POINT('Ctrl Pts',(-174.260644445331,-5.1695258016666,
128.149547557344));
#278820=CARTESIAN_POINT('Ctrl Pts',(-174.539092069143,-5.02782438426607,
133.718637776622));
#278821=CARTESIAN_POINT('Ctrl Pts',(-174.817539692956,-0.265797980601551,
136.609649657082));
#278822=CARTESIAN_POINT('Ctrl Pts',(-175.095987316769,4.74048378228282,
134.165884514362));
#278823=CARTESIAN_POINT('Ctrl Pts',(-175.374434940582,5.39049253475655,
128.633043130058));
#278824=CARTESIAN_POINT('Ctrl Pts',(-175.652882564395,1.08690198798901,
125.095536442018));
#278825=CARTESIAN_POINT('Ctrl Pts',(-175.931330188208,-4.21549838762608,
126.80416027974));
#278826=CARTESIAN_POINT('Ctrl Pts',(-176.209777812021,-5.64406168355824,
132.188772807274));
#278827=CARTESIAN_POINT('Ctrl Pts',(-176.488225435833,-1.886008020042,136.301178164761));
#278828=CARTESIAN_POINT('Ctrl Pts',(-176.766673059646,3.60519487727851,
135.362276730843));
#278829=CARTESIAN_POINT('Ctrl Pts',(-177.045120683459,5.78339980594152,
130.234873055403));
#278830=CARTESIAN_POINT('Ctrl Pts',(-177.323568307272,2.64694284773159,
125.630800628577));
#278831=CARTESIAN_POINT('Ctrl Pts',(-177.602015931085,-2.92192527719638,
125.780977089175));
#278832=CARTESIAN_POINT('Ctrl Pts',(-177.880463554898,-5.80568681636668,
130.547397606436));
#278833=CARTESIAN_POINT('Ctrl Pts',(-178.158911178711,-3.35430579486411,
135.549954577584));
#278834=CARTESIAN_POINT('Ctrl Pts',(-178.437358802524,2.17951838517049,
136.191542534628));
#278835=CARTESIAN_POINT('Ctrl Pts',(-178.715806426336,5.71047164462571,
131.88257348836));
#278836=CARTESIAN_POINT('Ctrl Pts',(-178.99425405015,3.99378043471903,126.582779487459));
#278837=CARTESIAN_POINT('Ctrl Pts',(-179.272701673962,-1.39299988767372,
125.162412309422));
#278838=CARTESIAN_POINT('Ctrl Pts',(-179.551149297775,-5.49968136512185,
128.926720002072));
#278839=CARTESIAN_POINT('Ctrl Pts',(-179.829596921588,-4.55242434239454,
134.416487692516));
#278840=CARTESIAN_POINT('Ctrl Pts',(-180.108044545401,0.578288252700551,
136.5868870633));
#278841=CARTESIAN_POINT('Ctrl Pts',(-180.386492169214,5.17758219451528,
133.443427122574));
#278842=CARTESIAN_POINT('Ctrl Pts',(-180.664939793027,5.01893103852278,
127.874793989312));
#278843=CARTESIAN_POINT('Ctrl Pts',(-180.94338741684,0.248127446539293,
124.998289470128));
#278844=CARTESIAN_POINT('Ctrl Pts',(-181.221835040653,-4.75069314711374,
127.457280693096));
#278845=CARTESIAN_POINT('Ctrl Pts',(-181.500282664465,-5.38385882283189,
132.992074852706));
#278846=CARTESIAN_POINT('Ctrl Pts',(-181.778730288279,-1.06952125649312,
136.516466506004));
#278847=CARTESIAN_POINT('Ctrl Pts',(-182.057177912091,4.22765409554481,
134.791711899713));
#278848=CARTESIAN_POINT('Ctrl Pts',(-182.335625535904,5.63982186616143,
129.402776258069));
#278849=CARTESIAN_POINT('Ctrl Pts',(-182.614073159717,1.86926886239121,
125.301828171599));
#278850=CARTESIAN_POINT('Ctrl Pts',(-182.89252078353,-3.61905090705647,
126.257438589318));
#278851=CARTESIAN_POINT('Ctrl Pts',(-183.170968407343,-5.78163969338434,
131.391448221508));
#278852=CARTESIAN_POINT('Ctrl Pts',(-183.449416031155,-2.63118405029363,
135.985953026497));
#278853=CARTESIAN_POINT('Ctrl Pts',(-183.727863654969,2.93720119453022,
135.818827542541));
#278854=CARTESIAN_POINT('Ctrl Pts',(-184.006311278781,5.80644203183612,
131.04365192486));
#278855=CARTESIAN_POINT('Ctrl Pts',(-184.284758902595,3.33984630234777,
126.048579285806));
#278856=CARTESIAN_POINT('Ctrl Pts',(-184.563206526407,-2.19590501843575,
125.423837357804));
#278857=CARTESIAN_POINT('Ctrl Pts',(-184.84165415022,-5.71372690320071,
129.743533452349));
#278858=CARTESIAN_POINT('Ctrl Pts',(-185.120101774033,-3.98091289500146,
135.03807788744));
#278859=CARTESIAN_POINT('Ctrl Pts',(-185.398549397846,1.41016558529749,
136.442042980103));
#278860=CARTESIAN_POINT('Ctrl Pts',(-185.676997021659,5.50537078312707,
132.665253397689));
#278861=CARTESIAN_POINT('Ctrl Pts',(-185.955444645472,4.54140918357699,
127.178394260007));
#278862=CARTESIAN_POINT('Ctrl Pts',(-186.233892269285,-0.595885595507362,
125.023621066618));
#278863=CARTESIAN_POINT('Ctrl Pts',(-186.512339893098,-5.18559062295048,
128.181065115723));
#278864=CARTESIAN_POINT('Ctrl Pts',(-186.79078751691,-5.00999119808726,
133.749189575911));
#278865=CARTESIAN_POINT('Ctrl Pts',(-187.069235140724,-0.230454613858838,
136.611160086272));
#278866=CARTESIAN_POINT('Ctrl Pts',(-187.347682764536,4.76085850217237,
134.136965562817));
#278867=CARTESIAN_POINT('Ctrl Pts',(-187.626130388349,5.37717523557474,
128.600269901479));
#278868=CARTESIAN_POINT('Ctrl Pts',(-187.904578012162,1.05213061709833,
125.089025932407));
#278869=CARTESIAN_POINT('Ctrl Pts',(-188.183025635975,-4.23977063905356,
126.829895329374));
#278870=CARTESIAN_POINT('Ctrl Pts',(-188.461473259788,-5.63552980222562,
132.223104162766));
#278871=CARTESIAN_POINT('Ctrl Pts',(-188.739920883601,-1.85251238808831,
136.312556987595));
#278872=CARTESIAN_POINT('Ctrl Pts',(-189.018368507414,3.63287341044046,
135.340246438718));
#278873=CARTESIAN_POINT('Ctrl Pts',(-189.296816131227,5.77982602050738,
130.199678410544));
#278874=CARTESIAN_POINT('Ctrl Pts',(-189.575263755039,2.61540087792624,
125.614783790254));
#278875=CARTESIAN_POINT('Ctrl Pts',(-189.853711378852,-2.95244990203274,
125.798856749341));
#278876=CARTESIAN_POINT('Ctrl Pts',(-190.132159002665,-5.80714345722022,
130.582743230867));
#278877=CARTESIAN_POINT('Ctrl Pts',(-190.410606626478,-3.32535586995153,
135.570285264159));
#278878=CARTESIAN_POINT('Ctrl Pts',(-190.689054250291,2.21227130913674,
136.178175375592));
#278879=CARTESIAN_POINT('Ctrl Pts',(-190.967501874104,5.7169292305904,131.847792249846));
#278880=CARTESIAN_POINT('Ctrl Pts',(-191.245949497917,3.96800847665057,
126.558546428502));
#278881=CARTESIAN_POINT('Ctrl Pts',(-191.52439712173,-1.4273182193404,125.170996427354));
#278882=CARTESIAN_POINT('Ctrl Pts',(-191.802844745543,-5.51100920012879,
128.960232911869));
#278883=CARTESIAN_POINT('Ctrl Pts',(-192.081292369355,-4.53035195376586,
134.444132667273));
#278884=CARTESIAN_POINT('Ctrl Pts',(-192.359739993168,0.613477418111232,
136.583259721745));
#278885=CARTESIAN_POINT('Ctrl Pts',(-192.638187616981,5.19355101278185,
133.411860814392));
#278886=CARTESIAN_POINT('Ctrl Pts',(-192.916635240794,5.00100494577841,
127.844296609621));
#278887=CARTESIAN_POINT('Ctrl Pts',(-193.195082864607,0.21277964627773,
124.996886620986));
#278888=CARTESIAN_POINT('Ctrl Pts',(-193.47353048842,-4.77097975328813,
127.486261524329));
#278889=CARTESIAN_POINT('Ctrl Pts',(-193.751978112233,-5.3704418349007,
133.024807396204));
#278890=CARTESIAN_POINT('Ctrl Pts',(-194.030425736046,-1.03473023090876,
136.522871153366));
#278891=CARTESIAN_POINT('Ctrl Pts',(-194.308873359859,4.25184790590635,
134.765903092897));
#278892=CARTESIAN_POINT('Ctrl Pts',(-194.587320983671,5.63118553151129,
129.368471029708));
#278893=CARTESIAN_POINT('Ctrl Pts',(-194.865768607484,1.83573875236439,
125.290551350653));
#278894=CARTESIAN_POINT('Ctrl Pts',(-195.144216231297,-3.64666225938173,
126.279553023333));
#278895=CARTESIAN_POINT('Ctrl Pts',(-195.42266385511,-5.77795880411129,
131.426631825972));
#278896=CARTESIAN_POINT('Ctrl Pts',(-195.701111478923,-2.59959347684268,
136.001873787725));
#278897=CARTESIAN_POINT('Ctrl Pts',(-195.979559102736,2.96767125844341,
135.800855058734));
#278898=CARTESIAN_POINT('Ctrl Pts',(-196.258006726549,5.80779108602021,
131.008302030633));
#278899=CARTESIAN_POINT('Ctrl Pts',(-196.536454350362,3.31083463191258,
126.028336807015));
#278900=CARTESIAN_POINT('Ctrl Pts',(-196.814901974175,-2.22861710565919,
125.437304143558));
#278901=CARTESIAN_POINT('Ctrl Pts',(-197.093349597988,-5.72007859712835,
129.778334184429));
#278902=CARTESIAN_POINT('Ctrl Pts',(-197.3717972218,-3.95506729921131,135.062232393175));
#278903=CARTESIAN_POINT('Ctrl Pts',(-197.650244845613,1.44445763090186,
136.433354448736));
#278904=CARTESIAN_POINT('Ctrl Pts',(-197.928692469426,5.51659656389443,
132.631706165088));
#278905=CARTESIAN_POINT('Ctrl Pts',(-198.207140093239,4.51925275539276,
127.150816594059));
#278906=CARTESIAN_POINT('Ctrl Pts',(-198.485587717052,-0.631063557543924,
125.027355495085));
#278907=CARTESIAN_POINT('Ctrl Pts',(-198.764035340865,-5.2014632902668,
128.212679881281));
#278908=CARTESIAN_POINT('Ctrl Pts',(-199.042482964678,-4.99197236484219,
133.779632253479));
#278909=CARTESIAN_POINT('Ctrl Pts',(-199.320930588491,-0.19510270753564,
136.612455342372));
#278910=CARTESIAN_POINT('Ctrl Pts',(-199.599378212304,4.7810568066993,134.10792312037));
#278911=CARTESIAN_POINT('Ctrl Pts',(-199.877825836116,5.36365868318719,
128.56757834629));
#278912=CARTESIAN_POINT('Ctrl Pts',(-200.156273459929,1.01732025912016,
125.082727206624));
#278913=CARTESIAN_POINT('Ctrl Pts',(-200.434721083742,-4.26388578422093,
126.855777654281));
#278914=CARTESIAN_POINT('Ctrl Pts',(-200.713168707555,-5.62678909426374,
132.257382946195));
#278915=CARTESIAN_POINT('Ctrl Pts',(-200.991616331368,-1.8189481106068,
136.323731702186));
#278916=CARTESIAN_POINT('Ctrl Pts',(-201.270063955181,3.66041732614217,
135.318048067677));
#278917=CARTESIAN_POINT('Ctrl Pts',(-201.548511578994,5.77603806149454,
130.164506172408));
#278918=CARTESIAN_POINT('Ctrl Pts',(-201.826959202806,2.58376199347953,
125.59895925361));
#278919=CARTESIAN_POINT('Ctrl Pts',(-202.10540682662,-2.9828651227522,125.816921890294));
#278920=CARTESIAN_POINT('Ctrl Pts',(-202.383854450432,-5.80838491223743,
130.618097067413));
#278921=CARTESIAN_POINT('Ctrl Pts',(-202.662302074245,-3.29628272275406,
135.590439347642));
#278922=CARTESIAN_POINT('Ctrl Pts',(-202.940749698058,2.24494225657654,
136.164609087875));
#278923=CARTESIAN_POINT('Ctrl Pts',(-203.219197321871,5.72317497363993,
131.812972346589));
#278924=CARTESIAN_POINT('Ctrl Pts',(-203.497644945684,3.94208948256877,
126.534470699752));
#278925=CARTESIAN_POINT('Ctrl Pts',(-203.776092569497,-1.46158366120557,
125.179789291667));
#278926=CARTESIAN_POINT('Ctrl Pts',(-204.05454019331,-5.52213282266317,
128.993814156497));
#278927=CARTESIAN_POINT('Ctrl Pts',(-204.332987817123,-4.5081116912795,
134.471642768938));
#278928=CARTESIAN_POINT('Ctrl Pts',(-204.611435440935,0.648643850890564,
136.579418240959));
#278929=CARTESIAN_POINT('Ctrl Pts',(-204.889883064748,5.20932738210573,
133.380197884332));
#278930=CARTESIAN_POINT('Ctrl Pts',(-205.168330688562,4.98289353895661,
127.813908916192));
#278931=CARTESIAN_POINT('Ctrl Pts',(-205.446778312374,0.177423961388546,
124.995698969927));
#278932=CARTESIAN_POINT('Ctrl Pts',(-205.725225936187,-4.79108956905296,
127.515365308944));
#278933=CARTESIAN_POINT('Ctrl Pts',(-206.00367356,-5.35682584327266,133.057457660231));
#278934=CARTESIAN_POINT('Ctrl Pts',(-206.282121183813,-0.999900863015179,
136.529063899218));
#278935=CARTESIAN_POINT('Ctrl Pts',(-206.560568807626,4.27588416248015,
134.739947489669));
#278936=CARTESIAN_POINT('Ctrl Pts',(-206.839016431439,5.62234053121038,
129.334219008764));
#278937=CARTESIAN_POINT('Ctrl Pts',(-207.117464055252,1.80214061836306,
125.279478845937));
#278938=CARTESIAN_POINT('Ctrl Pts',(-207.395911679064,-3.67413848329639,
126.301835125757));
#278939=CARTESIAN_POINT('Ctrl Pts',(-207.674359302878,-5.77406381044983,
131.461792371951));
#278940=CARTESIAN_POINT('Ctrl Pts',(-207.95280692669,-2.56790657449899,
136.01760195319));
#278941=CARTESIAN_POINT('Ctrl Pts',(-208.231254550503,2.99803135420673,
135.782697427989));
#278942=CARTESIAN_POINT('Ctrl Pts',(-208.509702174316,5.8089249303698,130.972944579282));
#278943=CARTESIAN_POINT('Ctrl Pts',(-208.788149798129,3.28170027728254,
126.008271305542));
#278944=CARTESIAN_POINT('Ctrl Pts',(-209.066597421942,-2.2612466106562,
125.450969807563));
#278945=CARTESIAN_POINT('Ctrl Pts',(-209.345045045754,-5.72621833144002,
129.813172936296));
#278946=CARTESIAN_POINT('Ctrl Pts',(-209.623492669568,-3.92907514694791,
135.086229121905));
#278947=CARTESIAN_POINT('Ctrl Pts',(-209.90194029338,1.4786961515975,136.424457332932));
#278948=CARTESIAN_POINT('Ctrl Pts',(-210.180387917194,5.52761792514773,
132.598091219525));
#278949=CARTESIAN_POINT('Ctrl Pts',(-210.458835541006,4.49692886463537,
127.123374311529));
#278950=CARTESIAN_POINT('Ctrl Pts',(-210.73728316482,-0.666218135288655,
125.031303992602));
#278951=CARTESIAN_POINT('Ctrl Pts',(-211.015730788632,-5.21714321544808,
128.244390682522));
#278952=CARTESIAN_POINT('Ctrl Pts',(-211.294178412445,-4.97376855222533,
133.809964681263));
#278953=CARTESIAN_POINT('Ctrl Pts',(-211.572626036258,-0.159743571609885,
136.613535377387));
#278954=CARTESIAN_POINT('Ctrl Pts',(-211.851073660071,4.80107794740803,
134.0787582632));
#278955=CARTESIAN_POINT('Ctrl Pts',(-212.129521283884,5.34994337845465,
128.534969675892));
#278956=CARTESIAN_POINT('Ctrl Pts',(-212.407968907697,0.982472203965689,
125.076640498072));
#278957=CARTESIAN_POINT('Ctrl Pts',(-212.686416531509,-4.28784292953254,
126.881806295382));
#278958=CARTESIAN_POINT('Ctrl Pts',(-212.964864155322,-5.61783988356258,
132.291607887347));
#278959=CARTESIAN_POINT('Ctrl Pts',(-213.243311779135,-1.78531643133465,
136.334701894451));
#278960=CARTESIAN_POINT('Ctrl Pts',(-213.521759402948,3.68782560373359,
135.295682440288));
#278961=CARTESIAN_POINT('Ctrl Pts',(-213.800207026761,5.77203606926717,
130.129357644311));
#278962=CARTESIAN_POINT('Ctrl Pts',(-214.078654650574,2.55202736678199,
125.583327605028));
#278963=CARTESIAN_POINT('Ctrl Pts',(-214.357102274386,-3.0131698123076,
125.835171842623));
#278964=CARTESIAN_POINT('Ctrl Pts',(-214.6355498982,-5.80941113541564,130.653457806023));
#278965=CARTESIAN_POINT('Ctrl Pts',(-214.913997522012,-3.26708743058812,
135.610416081219));
#278966=CARTESIAN_POINT('Ctrl Pts',(-215.192445145826,2.27753001685547,
136.15084417418));
#278967=CARTESIAN_POINT('Ctrl Pts',(-215.470892769638,5.72920864233609,
131.778115068854));
#278968=CARTESIAN_POINT('Ctrl Pts',(-215.749340393451,3.9160244129115,126.510553193344));
#278969=CARTESIAN_POINT('Ctrl Pts',(-216.027788017264,-1.49579494355069,
125.18879057654));
#278970=CARTESIAN_POINT('Ctrl Pts',(-216.306235641077,-5.53305182053502,
129.02746249159));
#278971=CARTESIAN_POINT('Ctrl Pts',(-216.58468326489,-4.48570437905656,
134.499016978113));
#278972=CARTESIAN_POINT('Ctrl Pts',(-216.863130888703,0.683786247933482,
136.57536276329));
#278973=CARTESIAN_POINT('Ctrl Pts',(-217.141578512516,5.2249107178877,133.348439505674));
#278974=CARTESIAN_POINT('Ctrl Pts',(-217.420026136328,4.96459748918233,
127.78363203505));
#278975=CARTESIAN_POINT('Ctrl Pts',(-217.698473760142,0.142061701988793,
124.994726560962));
#278976=CARTESIAN_POINT('Ctrl Pts',(-217.976921383954,-4.81102184923216,
127.544590968491));
#278977=CARTESIAN_POINT('Ctrl Pts',(-218.255369007768,-5.34301135249269,
133.090024434919));
#278978=CARTESIAN_POINT('Ctrl Pts',(-218.53381663158,-0.965034443427401,
136.535044514085));
#278979=CARTESIAN_POINT('Ctrl Pts',(-218.812264255394,4.29976197459382,
134.713846051821));
#278980=CARTESIAN_POINT('Ctrl Pts',(-219.090711879206,5.61328719301349,
129.300021464458));
#278981=CARTESIAN_POINT('Ctrl Pts',(-219.369159503019,1.76847570537835,
125.268611067748));
#278982=CARTESIAN_POINT('Ctrl Pts',(-219.647607126831,-3.70147856065836,
126.324284070919));
#278983=CARTESIAN_POINT('Ctrl Pts',(-219.926054750645,-5.76995485673049,
131.496928556552));
#278984=CARTESIAN_POINT('Ctrl Pts',(-220.204502374457,-2.5361245174328,
136.033136940081));
#278985=CARTESIAN_POINT('Ctrl Pts',(-220.48294999827,3.02828035681523,135.764355323142));
#278986=CARTESIAN_POINT('Ctrl Pts',(-220.761397622083,5.80984352286985,
130.937580880991));
#278987=CARTESIAN_POINT('Ctrl Pts',(-221.039845245896,3.25244431804234,
125.988383524923));
#278988=CARTESIAN_POINT('Ctrl Pts',(-221.318292869709,-2.29379232432851,
125.464833843433));
#278989=CARTESIAN_POINT('Ctrl Pts',(-221.596740493522,-5.73214587862558,
129.848048416986));
#278990=CARTESIAN_POINT('Ctrl Pts',(-221.875188117335,-3.90293740136003,
135.110067184424));
#278991=CARTESIAN_POINT('Ctrl Pts',(-222.153635741148,1.51287987866345,
136.415351962378));
#278992=CARTESIAN_POINT('Ctrl Pts',(-222.432083364961,5.53843445848603,
132.564409806615));
#278993=CARTESIAN_POINT('Ctrl Pts',(-222.710530988774,4.47443833852516,
127.0960684293));
#278994=CARTESIAN_POINT('Ctrl Pts',(-222.988978612586,-0.701348026075381,
125.035466412855));
#278995=CARTESIAN_POINT('Ctrl Pts',(-223.267426236399,-5.23262981746888,
128.27619634439));
#278996=CARTESIAN_POINT('Ctrl Pts',(-223.545873860212,-4.95538043478568,
133.840185735283));
#278997=CARTESIAN_POINT('Ctrl Pts',(-223.824321484025,-0.124378516327312,
136.614400151295));
#278998=CARTESIAN_POINT('Ctrl Pts',(-224.102769107838,4.82092118240782,
134.049472072021));
#278999=CARTESIAN_POINT('Ctrl Pts',(-224.381216731651,5.33602982960279,
128.502445098609));
#279000=CARTESIAN_POINT('Ctrl Pts',(-224.659664355464,0.947587742942381,
125.070766032295));
#279001=CARTESIAN_POINT('Ctrl Pts',(-224.938111979277,-4.31164118724753,
126.907980288176));
#279002=CARTESIAN_POINT('Ctrl Pts',(-225.216559603089,-5.60868250173869,
132.325777718005));
#279003=CARTESIAN_POINT('Ctrl Pts',(-225.495007226903,-1.75161859650508,
136.345467157888));
#279004=CARTESIAN_POINT('Ctrl Pts',(-225.773454850715,3.71509722759125,
135.273150385318));
#279005=CARTESIAN_POINT('Ctrl Pts',(-226.051902474528,5.7678201921206,130.0942341287));
#279006=CARTESIAN_POINT('Ctrl Pts',(-226.330350098341,2.52019817377184,
125.567889423742));
#279007=CARTESIAN_POINT('Ctrl Pts',(-226.608797722154,-3.04336284774751,
125.853605930069));
#279008=CARTESIAN_POINT('Ctrl Pts',(-226.887245345967,-5.81022208872781,
130.688824136393));
#279009=CARTESIAN_POINT('Ctrl Pts',(-227.16569296978,-3.23777107529596,
135.630214724643));
#279010=CARTESIAN_POINT('Ctrl Pts',(-227.444140593593,2.31003338242206,
136.13688114457));
#279011=CARTESIAN_POINT('Ctrl Pts',(-227.722588217406,5.73503001309909,
131.74322170829));
#279012=CARTESIAN_POINT('Ctrl Pts',(-228.001035841218,3.88981423352964,
126.486794795549));
#279013=CARTESIAN_POINT('Ctrl Pts',(-228.279483465031,-1.52995079866356,
125.197999948425));
#279014=CARTESIAN_POINT('Ctrl Pts',(-228.557931088844,-5.54376578913698,
129.061176670297));
#279015=CARTESIAN_POINT('Ctrl Pts',(-228.836378712657,-4.46313084740822,
134.526254280438));
#279016=CARTESIAN_POINT('Ctrl Pts',(-229.11482633647,0.718903307025501,
136.571093439014));
#279017=CARTESIAN_POINT('Ctrl Pts',(-229.393273960283,5.24030044268158,
133.316586855238));
#279018=CARTESIAN_POINT('Ctrl Pts',(-229.671721584096,4.94611747442232,
127.753467088116));
#279019=CARTESIAN_POINT('Ctrl Pts',(-229.950169207909,0.106694178440453,
124.993969430123));
#279020=CARTESIAN_POINT('Ctrl Pts',(-230.228616831722,-4.83077585522751,
127.57393742));
#279021=CARTESIAN_POINT('Ctrl Pts',(-230.507064455534,-5.32899887446215,
133.122506513493));
#279022=CARTESIAN_POINT('Ctrl Pts',(-230.785512079348,-0.930132264133436,
136.540812776352));
#279023=CARTESIAN_POINT('Ctrl Pts',(-231.06395970316,4.3234804574463,134.687599746553));
#279024=CARTESIAN_POINT('Ctrl Pts',(-231.342407326973,5.60402585239536,
129.265879663993));
#279025=CARTESIAN_POINT('Ctrl Pts',(-231.620854950786,1.73474526087603,
125.257948418793));
#279026=CARTESIAN_POINT('Ctrl Pts',(-231.899302574599,-3.72868147837107,
126.346899026965));
#279027=CARTESIAN_POINT('Ctrl Pts',(-232.177750198412,-5.76563209521201,
131.532039077795));
#279028=CARTESIAN_POINT('Ctrl Pts',(-232.456197822225,-2.50424848333998,
136.048478172742));
#279029=CARTESIAN_POINT('Ctrl Pts',(-232.734645446038,3.05841714538193,
135.745829423867));
#279030=CARTESIAN_POINT('Ctrl Pts',(-233.01309306985,5.81054682948159,130.902212246173));
#279031=CARTESIAN_POINT('Ctrl Pts',(-233.291540693664,3.22306783828139,
125.968674202107));
#279032=CARTESIAN_POINT('Ctrl Pts',(-233.569988317476,-2.32625304068266,
125.478895737432));
#279033=CARTESIAN_POINT('Ctrl Pts',(-233.84843594129,-5.73786101903762,
129.882959334177));
#279034=CARTESIAN_POINT('Ctrl Pts',(-234.126883565102,-3.87665503099142,
135.133745697402));
#279035=CARTESIAN_POINT('Ctrl Pts',(-234.405331188915,1.54700754540913,
136.406038674476));
#279036=CARTESIAN_POINT('Ctrl Pts',(-234.683778812728,5.54904576309872,
132.530663174436));
#279037=CARTESIAN_POINT('Ctrl Pts',(-234.962226436541,4.45178201045685,
127.0688999592));
#279038=CARTESIAN_POINT('Ctrl Pts',(-235.240674060353,-0.736451928153096,
125.039842601604));
#279039=CARTESIAN_POINT('Ctrl Pts',(-235.519121684167,-5.24792252246713,
128.308095688315));
#279040=CARTESIAN_POINT('Ctrl Pts',(-235.797569307979,-4.93680869390195,
133.870294295687));
#279041=CARTESIAN_POINT('Ctrl Pts',(-236.076016931792,-0.0890088521534987,
136.61504963205));
#279042=CARTESIAN_POINT('Ctrl Pts',(-236.354464555605,4.8405857764003,134.020065632043));
#279043=CARTESIAN_POINT('Ctrl Pts',(-236.632912179418,5.32191855220324,
128.470005819654));
#279044=CARTESIAN_POINT('Ctrl Pts',(-236.911359803231,0.912668168706789,
125.065104026974));
#279045=CARTESIAN_POINT('Ctrl Pts',(-237.189807427044,-4.33527967551271,
126.934298662776));
#279046=CARTESIAN_POINT('Ctrl Pts',(-237.468255050857,-5.59931728812211,
132.359891171993));
#279047=CARTESIAN_POINT('Ctrl Pts',(-237.74670267467,-1.71785585480426,
136.356027093583));
#279048=CARTESIAN_POINT('Ctrl Pts',(-238.025150298482,3.7422311871549,135.250452737698));
#279049=CARTESIAN_POINT('Ctrl Pts',(-238.303597922296,5.76339058627568,
130.059136927086));
#279050=CARTESIAN_POINT('Ctrl Pts',(-238.582045546108,2.48827559389159,
125.552645281824));
#279051=CARTESIAN_POINT('Ctrl Pts',(-238.860493169922,-3.07344311025789,
125.87222346955));
#279052=CARTESIAN_POINT('Ctrl Pts',(-239.138940793734,-5.81081774212379,
130.724194748009));
#279053=CARTESIAN_POINT('Ctrl Pts',(-239.417388417547,-3.20833474320591,
135.649834544268));
#279054=CARTESIAN_POINT('Ctrl Pts',(-239.69583604136,2.34245114885216,136.12272051645));
#279055=CARTESIAN_POINT('Ctrl Pts',(-239.974283665173,5.7406388702159,131.708293557882));
#279056=CARTESIAN_POINT('Ctrl Pts',(-240.252731288985,3.86345991565072,
126.463196386742));
#279057=CARTESIAN_POINT('Ctrl Pts',(-240.531178912799,-1.56404996088748,
125.207417066067));
#279058=CARTESIAN_POINT('Ctrl Pts',(-240.809626536611,-5.5542743314588,
129.094955443325));
#279059=CARTESIAN_POINT('Ctrl Pts',(-241.088074160425,-4.44039193280503,
134.553353666625));
#279060=CARTESIAN_POINT('Ctrl Pts',(-241.366521784237,0.753993726891117,
136.566610426332));
#279061=CARTESIAN_POINT('Ctrl Pts',(-241.64496940805,5.25549598621542,133.284641113335));
#279062=CARTESIAN_POINT('Ctrl Pts',(-241.923417031863,4.92745417946037,
127.723415193164));
#279063=CARTESIAN_POINT('Ctrl Pts',(-242.201864655676,0.071322701300089,
124.993427605467));
#279064=CARTESIAN_POINT('Ctrl Pts',(-242.480312279489,-4.85035085504701,
127.603403576029));
#279065=CARTESIAN_POINT('Ctrl Pts',(-242.758759903302,-5.31478892841856,
133.154902692318));
#279066=CARTESIAN_POINT('Ctrl Pts',(-243.037207527115,-0.895195618446729,
136.546368472274));
#279067=CARTESIAN_POINT('Ctrl Pts',(-243.315655150928,4.34703873214009,
134.661209546432));
#279068=CARTESIAN_POINT('Ctrl Pts',(-243.59410277474,5.59455685253872,129.231794872506));
#279069=CARTESIAN_POINT('Ctrl Pts',(-243.872550398553,1.7009505347501,125.247491294183));
#279070=CARTESIAN_POINT('Ctrl Pts',(-244.150998022366,-3.75574622842035,
126.36967915589));
#279071=CARTESIAN_POINT('Ctrl Pts',(-244.429445646179,-5.76109568607594,
131.567122634643));
#279072=CARTESIAN_POINT('Ctrl Pts',(-244.707893269992,-2.47227965339868,
136.063625082699));
#279073=CARTESIAN_POINT('Ctrl Pts',(-244.986340893805,3.08844060317656,
135.727120416648));
#279074=CARTESIAN_POINT('Ctrl Pts',(-245.264788517618,5.81103482414375,
130.866839985428));
#279075=CARTESIAN_POINT('Ctrl Pts',(-245.543236141431,3.1935719265564,125.949144067427));
#279076=CARTESIAN_POINT('Ctrl Pts',(-245.821683765243,-2.35862755687492,
125.49315496849));
#279077=CARTESIAN_POINT('Ctrl Pts',(-246.100131389057,-5.74336354089951,
129.917904394232));
#279078=CARTESIAN_POINT('Ctrl Pts',(-246.378579012869,-3.85022900974501,
135.157263783424));
#279079=CARTESIAN_POINT('Ctrl Pts',(-246.657026636682,1.58107788722132,
136.396517814333));
#279080=CARTESIAN_POINT('Ctrl Pts',(-246.935474260495,5.55945144577998,
132.496852573479));
#279081=CARTESIAN_POINT('Ctrl Pts',(-247.213921884308,4.42896071996899,
127.04186990797));
#279082=CARTESIAN_POINT('Ctrl Pts',(-247.492369508121,-0.77152854073377,
125.044432396689));
#279083=CARTESIAN_POINT('Ctrl Pts',(-247.770817131934,-5.26302076376676,
128.340087532256));
#279084=CARTESIAN_POINT('Ctrl Pts',(-248.049264755747,-4.91805401775627,
133.90028924679));
#279085=CARTESIAN_POINT('Ctrl Pts',(-248.32771237956,-0.0536358897235281,
136.615483795589));
#279086=CARTESIAN_POINT('Ctrl Pts',(-248.606160003372,4.86007100070672,
133.990540032933));
#279087=CARTESIAN_POINT('Ctrl Pts',(-248.884607627186,5.30761006915461,
128.437653041073));
#279088=CARTESIAN_POINT('Ctrl Pts',(-249.163055250998,0.877714775216597,
125.059654691916));
#279089=CARTESIAN_POINT('Ctrl Pts',(-249.441502874812,-4.35875751839529,
126.960760443945));
#279090=CARTESIAN_POINT('Ctrl Pts',(-249.719950498624,-5.58974458974414,
132.393946985223));
#279091=CARTESIAN_POINT('Ctrl Pts',(-249.998398122437,-1.68402945732324,
136.366381310236));
#279092=CARTESIAN_POINT('Ctrl Pts',(-250.27684574625,3.76922647696617,135.227590338499));
#279093=CARTESIAN_POINT('Ctrl Pts',(-250.555293370063,5.75874741587205,
130.024067340013));
#279094=CARTESIAN_POINT('Ctrl Pts',(-250.833740993876,2.45626081004631,
125.537595744144));
#279095=CARTESIAN_POINT('Ctrl Pts',(-251.112188617689,-3.10340948520656,
125.891023771197));
#279096=CARTESIAN_POINT('Ctrl Pts',(-251.390636241501,-5.81119807352532,
130.759568330183));
#279097=CARTESIAN_POINT('Ctrl Pts',(-251.669083865314,-3.17877952510356,
135.669274813107));
#279098=CARTESIAN_POINT('Ctrl Pts',(-251.947531489127,2.37478211491517,
136.10836281449));
#279099=CARTESIAN_POINT('Ctrl Pts',(-252.22597911294,5.74603500580729,131.673331912019));
#279100=CARTESIAN_POINT('Ctrl Pts',(-252.504426736753,3.83696243592119,
126.439758841162));
#279101=CARTESIAN_POINT('Ctrl Pts',(-252.782874360566,-1.59809116681098,
125.217041580908));
#279102=CARTESIAN_POINT('Ctrl Pts',(-253.061321984379,-5.5645770578269,
129.128797558239));
#279103=CARTESIAN_POINT('Ctrl Pts',(-253.339769608192,-4.41748847836656,
134.580314133917));
#279104=CARTESIAN_POINT('Ctrl Pts',(-253.618217232004,0.789056208225191,
136.561913888683));
#279105=CARTESIAN_POINT('Ctrl Pts',(-253.896664855818,5.27049678355612,
133.252603468789));
#279106=CARTESIAN_POINT('Ctrl Pts',(-254.17511247963,4.90860829937749,127.693477454216));
#279107=CARTESIAN_POINT('Ctrl Pts',(-254.453560103444,0.0359485746511809,
124.993101125124));
#279108=CARTESIAN_POINT('Ctrl Pts',(-254.732007727256,-4.86974611083267,
127.632988310607));
#279109=CARTESIAN_POINT('Ctrl Pts',(-255.010455351069,-5.30038206451776,
133.187211835313));
#279110=CARTESIAN_POINT('Ctrl Pts',(-255.288902974882,-0.860225756393269,
136.55171127444));
#279111=CARTESIAN_POINT('Ctrl Pts',(-255.567350598695,4.37043584157037,
134.634676658854));
#279112=CARTESIAN_POINT('Ctrl Pts',(-255.845798222508,5.58488070320316,
129.197767919676));
#279113=CARTESIAN_POINT('Ctrl Pts',(-256.12424584632,1.66709247927321,125.23724089965));
#279114=CARTESIAN_POINT('Ctrl Pts',(-256.402693470134,-3.78267124144458,
126.39262206856));
#279115=CARTESIAN_POINT('Ctrl Pts',(-256.681141093946,-5.75634686702621,
131.602180844355));
#279116=CARTESIAN_POINT('Ctrl Pts',(-256.95958871776,-2.44021719259262,
136.078571600242));
#279117=CARTESIAN_POINT('Ctrl Pts',(-257.238036341572,3.118345804191,135.708239395799));
#279118=CARTESIAN_POINT('Ctrl Pts',(-257.516483965385,5.81131468939531,
130.8314457702));
#279119=CARTESIAN_POINT('Ctrl Pts',(-257.794931589198,3.16394407961038,
125.929830927563));
#279120=CARTESIAN_POINT('Ctrl Pts',(-258.073379213011,-2.39088900078744,
125.507540987923));
#279121=CARTESIAN_POINT('Ctrl Pts',(-258.351826836824,-5.74870171518396,
129.953014515613));
#279122=CARTESIAN_POINT('Ctrl Pts',(-258.630274460636,-3.82356878618261,
135.180370918811));
#279123=CARTESIAN_POINT('Ctrl Pts',(-258.908722084449,1.61491681105698,
136.387261181902));
#279124=CARTESIAN_POINT('Ctrl Pts',(-259.187169708263,5.56997747689423,
132.462088635074));
#279125=CARTESIAN_POINT('Ctrl Pts',(-259.465617332075,4.40535894966821,
127.016664495574));
#279126=CARTESIAN_POINT('Ctrl Pts',(-259.744064955888,-0.805411631290512,
125.046024618449));
#279127=CARTESIAN_POINT('Ctrl Pts',(-260.022512579701,-5.28013240410161,
128.378470706602));
#279128=CARTESIAN_POINT('Ctrl Pts',(-260.254552266212,-4.95911089365773,
132.993351965875));
#279129=CARTESIAN_POINT('Ctrl Pts',(-260.440213228287,-2.45877638613931,
135.28779596926));
#279130=CARTESIAN_POINT('Ctrl Pts',(-260.53305831576,-0.833059752290926,
135.715219187214));
#279131=CARTESIAN_POINT('Ctrl Pts',(-260.579495465929,-0.013892627260139,
135.717527172907));
#279132=CARTESIAN_POINT('Ctrl Pts',(-207.955946566515,5.91285886696315,
130.43400564734));
#279133=CARTESIAN_POINT('Ctrl Pts',(-207.96403085718,5.89480070884798,130.766618159613));
#279134=CARTESIAN_POINT('Ctrl Pts',(-207.961339644263,5.86589899174327,
131.093332415071));
#279135=CARTESIAN_POINT('Ctrl Pts',(-207.946271365849,5.81943915897531,
131.462598684382));
#279136=CARTESIAN_POINT('Ctrl Pts',(-207.944637644607,5.81466923197383,
131.499362911161));
#279137=CARTESIAN_POINT('Ctrl Pts',(-207.942857924687,5.80972272473499,
131.536391330104));
#279138=CARTESIAN_POINT('Ctrl Pts',(-207.942844083457,5.80968426884596,
131.536679137172));
#279139=CARTESIAN_POINT('Ctrl Pts',(-207.942816746832,5.80960834566923,
131.53724722448));
#279140=CARTESIAN_POINT('Ctrl Pts',(-207.942803251882,5.80957087889668,
131.537527504213));
#279141=CARTESIAN_POINT('Ctrl Pts',(-207.942782545224,5.80951341028276,
131.537957318521));
#279142=CARTESIAN_POINT('Ctrl Pts',(-207.942775338973,5.80949341406807,
131.538106854989));
#279143=CARTESIAN_POINT('Ctrl Pts',(-207.942762251891,5.80945710634709,
131.538378341032));
#279144=CARTESIAN_POINT('Ctrl Pts',(-207.94275637189,5.80944079587429,131.538500288738));
#279145=CARTESIAN_POINT('Ctrl Pts',(-207.942743776405,5.80940586278758,
131.538761446312));
#279146=CARTESIAN_POINT('Ctrl Pts',(-207.942737060443,5.80938723960864,
131.538900656877));
#279147=CARTESIAN_POINT('Ctrl Pts',(-207.942718928357,5.80933696868309,
131.539276397358));
#279148=CARTESIAN_POINT('Ctrl Pts',(-207.942707508596,5.80930531703825,
131.539512927819));
#279149=CARTESIAN_POINT('Ctrl Pts',(-207.942651664994,5.80915058405599,
131.540669022502));
#279150=CARTESIAN_POINT('Ctrl Pts',(-207.94260716388,5.80902742209205,131.541588572013));
#279151=CARTESIAN_POINT('Ctrl Pts',(-207.937191179903,5.79405539795786,
131.653292239375));
#279152=CARTESIAN_POINT('Ctrl Pts',(-207.930620303857,5.77795735485189,
131.763821827678));
#279153=CARTESIAN_POINT('Ctrl Pts',(-207.905019315672,5.72103221687411,
132.127689826094));
#279154=CARTESIAN_POINT('Ctrl Pts',(-207.880926532226,5.6753051964054,132.379606835433));
#279155=CARTESIAN_POINT('Ctrl Pts',(-207.850713743235,5.62477921028189,
132.630029653041));
#279156=CARTESIAN_POINT('Origin',(-192.718407221598,12.,130.804360617566));
#279157=CARTESIAN_POINT('',(-177.476367722507,12.,130.804360617566));
#279158=CARTESIAN_POINT('Origin',(-192.718407221598,12.,130.804360617566));
#279159=CARTESIAN_POINT('',(-177.476367722506,12.,130.804360617566));
#279160=CARTESIAN_POINT('',(-177.476367722507,-12.,130.804360617566));
#279161=CARTESIAN_POINT('',(-177.476367722506,12.,130.804360617566));
#279162=CARTESIAN_POINT('Origin',(-192.718407221598,-12.,130.804360617566));
#279163=CARTESIAN_POINT('Origin',(-192.718407221598,-12.,130.804360617566));
#279164=CARTESIAN_POINT('Origin',(-192.718407221598,12.,130.804360617566));
#279165=CARTESIAN_POINT('',(0.,0.,0.));
#279166=CARTESIAN_POINT('Origin',(-192.718407221598,22.,130.804360617566));
#279167=CARTESIAN_POINT('',(-186.217299572429,22.,130.804360617566));
#279168=CARTESIAN_POINT('Origin',(-192.718407221598,22.,130.804360617566));
#279169=CARTESIAN_POINT('',(-186.217299572429,17.,130.804360617566));
#279170=CARTESIAN_POINT('',(-186.217299572428,22.,130.804360617566));
#279171=CARTESIAN_POINT('Origin',(-192.718407221598,17.,130.804360617566));
#279172=CARTESIAN_POINT('Origin',(-200.401984582636,22.,117.640683052811));
#279173=CARTESIAN_POINT('',(-200.401984582636,22.,117.640683052811));
#279174=CARTESIAN_POINT('',(-27.6628184943316,22.,16.8136353382454));
#279175=CARTESIAN_POINT('',(-200.401984582636,22.,117.640683052811));
#279176=CARTESIAN_POINT('',(-27.6628184943316,17.,16.8136353382454));
#279177=CARTESIAN_POINT('',(-27.6628184943316,22.,16.8136353382454));
#279178=CARTESIAN_POINT('',(-200.401984582636,17.,117.640683052811));
#279179=CARTESIAN_POINT('',(-200.401984582636,17.,117.640683052811));
#279180=CARTESIAN_POINT('',(-200.401984582636,22.,117.640683052811));
#279181=CARTESIAN_POINT('Origin',(-192.718407221598,22.,130.804360617566));
#279182=CARTESIAN_POINT('',(-185.034829860561,22.,143.96803818232));
#279183=CARTESIAN_POINT('Origin',(-192.718407221598,22.,130.804360617566));
#279184=CARTESIAN_POINT('',(-185.034829860561,17.,143.96803818232));
#279185=CARTESIAN_POINT('Origin',(-192.718407221598,17.,130.804360617566));
#279186=CARTESIAN_POINT('',(-185.034829860561,22.,143.96803818232));
#279187=CARTESIAN_POINT('Origin',(-12.2956637722558,22.,43.1409904677544));
#279188=CARTESIAN_POINT('',(-12.2956637722558,22.,43.1409904677544));
#279189=CARTESIAN_POINT('',(-12.2956637722558,22.,43.1409904677544));
#279190=CARTESIAN_POINT('',(-12.2956637722558,17.,43.1409904677544));
#279191=CARTESIAN_POINT('',(-12.2956637722558,17.,43.1409904677544));
#279192=CARTESIAN_POINT('',(-12.2956637722558,22.,43.1409904677544));
#279193=CARTESIAN_POINT('Origin',(-106.348824177446,17.,80.3908367602827));
#279194=CARTESIAN_POINT('Origin',(-19.9792411332937,17.,29.9773129029999));
#279195=CARTESIAN_POINT('Origin',(-106.348824177446,22.,80.3908367602827));
#279196=CARTESIAN_POINT('Origin',(-19.9792411332937,22.,29.9773129029999));
#279197=CARTESIAN_POINT('',(-12.4213924902778,22.,29.9773129029999));
#279198=CARTESIAN_POINT('Origin',(-19.9792411332937,22.,29.9773129029999));
#279199=CARTESIAN_POINT('Origin',(-19.9792411332937,-22.,29.9773129029999));
#279200=CARTESIAN_POINT('',(-12.4213924902778,-22.,29.9773129029999));
#279201=CARTESIAN_POINT('',(-12.4213924902778,-22.,29.9773129029999));
#279202=CARTESIAN_POINT('Origin',(-19.9792411332937,-22.,29.9773129029999));
#279203=CARTESIAN_POINT('Origin',(-192.718407221598,-22.,130.804360617566));
#279204=CARTESIAN_POINT('',(-186.217299572429,-17.,130.804360617566));
#279205=CARTESIAN_POINT('Origin',(-192.718407221598,-17.,130.804360617566));
#279206=CARTESIAN_POINT('',(-186.217299572429,-22.,130.804360617566));
#279207=CARTESIAN_POINT('',(-186.217299572428,-22.,130.804360617566));
#279208=CARTESIAN_POINT('Origin',(-192.718407221598,-22.,130.804360617566));
#279209=CARTESIAN_POINT('Origin',(-200.401984582636,-22.,117.640683052811));
#279210=CARTESIAN_POINT('',(-200.401984582636,-22.,117.640683052811));
#279211=CARTESIAN_POINT('',(-27.6628184943316,-22.,16.8136353382454));
#279212=CARTESIAN_POINT('',(-200.401984582636,-22.,117.640683052811));
#279213=CARTESIAN_POINT('',(-200.401984582636,-17.,117.640683052811));
#279214=CARTESIAN_POINT('',(-200.401984582636,-22.,117.640683052811));
#279215=CARTESIAN_POINT('',(-27.6628184943316,-17.,16.8136353382454));
#279216=CARTESIAN_POINT('',(-200.401984582636,-17.,117.640683052811));
#279217=CARTESIAN_POINT('',(-27.6628184943316,-22.,16.8136353382454));
#279218=CARTESIAN_POINT('Origin',(-192.718407221598,-22.,130.804360617566));
#279219=CARTESIAN_POINT('',(-185.034829860561,-22.,143.96803818232));
#279220=CARTESIAN_POINT('Origin',(-192.718407221598,-22.,130.804360617566));
#279221=CARTESIAN_POINT('',(-185.034829860561,-17.,143.96803818232));
#279222=CARTESIAN_POINT('',(-185.034829860561,-22.,143.96803818232));
#279223=CARTESIAN_POINT('Origin',(-192.718407221598,-17.,130.804360617566));
#279224=CARTESIAN_POINT('Origin',(-12.2956637722558,-22.,43.1409904677544));
#279225=CARTESIAN_POINT('',(-12.2956637722558,-22.,43.1409904677544));
#279226=CARTESIAN_POINT('',(-12.2956637722558,-22.,43.1409904677544));
#279227=CARTESIAN_POINT('',(-12.2956637722558,-17.,43.1409904677544));
#279228=CARTESIAN_POINT('',(-12.2956637722558,-22.,43.1409904677544));
#279229=CARTESIAN_POINT('',(-12.2956637722558,-17.,43.1409904677544));
#279230=CARTESIAN_POINT('Origin',(-19.9792411332937,-22.,29.9773129029999));
#279231=CARTESIAN_POINT('Origin',(-19.9792411332937,-22.,29.9773129029999));
#279232=CARTESIAN_POINT('Origin',(-19.9792411332937,-17.,29.9773129029999));
#279233=CARTESIAN_POINT('',(-12.2956637722558,-22.,43.1409904677544));
#279234=CARTESIAN_POINT('Origin',(-106.348824177446,-17.,80.3908367602827));
#279235=CARTESIAN_POINT('Origin',(-106.348824177446,-22.,80.3908367602827));
#279236=CARTESIAN_POINT('',(0.,0.,0.));
#279237=CARTESIAN_POINT('',(0.,0.,0.));
#279238=CARTESIAN_POINT('',(0.,0.,0.));
#279239=CARTESIAN_POINT('',(0.,0.,0.));
#279240=CARTESIAN_POINT('',(0.,0.,0.));
#279241=CARTESIAN_POINT('',(0.,0.,0.));
#279242=CARTESIAN_POINT('',(0.,0.,0.));
#279243=CARTESIAN_POINT('',(0.,0.,0.));
#279244=CARTESIAN_POINT('',(0.,0.,0.));
#279245=UNCERTAINTY_MEASURE_WITH_UNIT(LENGTH_MEASURE(0.01),#279267,
'DISTANCE_ACCURACY_VALUE',
'Maximum model space distance between geometric entities at asserted c
onnectivities');
#279246=UNCERTAINTY_MEASURE_WITH_UNIT(LENGTH_MEASURE(0.01),#279267,
'DISTANCE_ACCURACY_VALUE',
'Maximum model space distance between geometric entities at asserted c
onnectivities');
#279247=UNCERTAINTY_MEASURE_WITH_UNIT(LENGTH_MEASURE(0.01),#279267,
'DISTANCE_ACCURACY_VALUE',
'Maximum model space distance between geometric entities at asserted c
onnectivities');
#279248=UNCERTAINTY_MEASURE_WITH_UNIT(LENGTH_MEASURE(0.01),#279267,
'DISTANCE_ACCURACY_VALUE',
'Maximum model space distance between geometric entities at asserted c
onnectivities');
#279249=UNCERTAINTY_MEASURE_WITH_UNIT(LENGTH_MEASURE(0.01),#279267,
'DISTANCE_ACCURACY_VALUE',
'Maximum model space distance between geometric entities at asserted c
onnectivities');
#279250=UNCERTAINTY_MEASURE_WITH_UNIT(LENGTH_MEASURE(0.01),#279267,
'DISTANCE_ACCURACY_VALUE',
'Maximum model space distance between geometric entities at asserted c
onnectivities');
#279251=UNCERTAINTY_MEASURE_WITH_UNIT(LENGTH_MEASURE(0.01),#279267,
'DISTANCE_ACCURACY_VALUE',
'Maximum model space distance between geometric entities at asserted c
onnectivities');
#279252=UNCERTAINTY_MEASURE_WITH_UNIT(LENGTH_MEASURE(0.01),#279267,
'DISTANCE_ACCURACY_VALUE',
'Maximum model space distance between geometric entities at asserted c
onnectivities');
#279253=UNCERTAINTY_MEASURE_WITH_UNIT(LENGTH_MEASURE(0.01),#279267,
'DISTANCE_ACCURACY_VALUE',
'Maximum model space distance between geometric entities at asserted c
onnectivities');
#279254=UNCERTAINTY_MEASURE_WITH_UNIT(LENGTH_MEASURE(0.01),#279267,
'DISTANCE_ACCURACY_VALUE',
'Maximum model space distance between geometric entities at asserted c
onnectivities');
#279255=UNCERTAINTY_MEASURE_WITH_UNIT(LENGTH_MEASURE(0.01),#279267,
'DISTANCE_ACCURACY_VALUE',
'Maximum model space distance between geometric entities at asserted c
onnectivities');
#279256=(
GEOMETRIC_REPRESENTATION_CONTEXT(3)
GLOBAL_UNCERTAINTY_ASSIGNED_CONTEXT((#279245))
GLOBAL_UNIT_ASSIGNED_CONTEXT((#279267,#279269,#279270))
REPRESENTATION_CONTEXT('','3D')
);
#279257=(
GEOMETRIC_REPRESENTATION_CONTEXT(3)
GLOBAL_UNCERTAINTY_ASSIGNED_CONTEXT((#279246))
GLOBAL_UNIT_ASSIGNED_CONTEXT((#279267,#279269,#279270))
REPRESENTATION_CONTEXT('','3D')
);
#279258=(
GEOMETRIC_REPRESENTATION_CONTEXT(3)
GLOBAL_UNCERTAINTY_ASSIGNED_CONTEXT((#279247))
GLOBAL_UNIT_ASSIGNED_CONTEXT((#279267,#279269,#279270))
REPRESENTATION_CONTEXT('','3D')
);
#279259=(
GEOMETRIC_REPRESENTATION_CONTEXT(3)
GLOBAL_UNCERTAINTY_ASSIGNED_CONTEXT((#279248))
GLOBAL_UNIT_ASSIGNED_CONTEXT((#279267,#279269,#279270))
REPRESENTATION_CONTEXT('','3D')
);
#279260=(
GEOMETRIC_REPRESENTATION_CONTEXT(3)
GLOBAL_UNCERTAINTY_ASSIGNED_CONTEXT((#279249))
GLOBAL_UNIT_ASSIGNED_CONTEXT((#279267,#279269,#279270))
REPRESENTATION_CONTEXT('','3D')
);
#279261=(
GEOMETRIC_REPRESENTATION_CONTEXT(3)
GLOBAL_UNCERTAINTY_ASSIGNED_CONTEXT((#279250))
GLOBAL_UNIT_ASSIGNED_CONTEXT((#279267,#279269,#279270))
REPRESENTATION_CONTEXT('','3D')
);
#279262=(
GEOMETRIC_REPRESENTATION_CONTEXT(3)
GLOBAL_UNCERTAINTY_ASSIGNED_CONTEXT((#279251))
GLOBAL_UNIT_ASSIGNED_CONTEXT((#279267,#279269,#279270))
REPRESENTATION_CONTEXT('','3D')
);
#279263=(
GEOMETRIC_REPRESENTATION_CONTEXT(3)
GLOBAL_UNCERTAINTY_ASSIGNED_CONTEXT((#279252))
GLOBAL_UNIT_ASSIGNED_CONTEXT((#279267,#279269,#279270))
REPRESENTATION_CONTEXT('','3D')
);
#279264=(
GEOMETRIC_REPRESENTATION_CONTEXT(3)
GLOBAL_UNCERTAINTY_ASSIGNED_CONTEXT((#279253))
GLOBAL_UNIT_ASSIGNED_CONTEXT((#279267,#279269,#279270))
REPRESENTATION_CONTEXT('','3D')
);
#279265=(
GEOMETRIC_REPRESENTATION_CONTEXT(3)
GLOBAL_UNCERTAINTY_ASSIGNED_CONTEXT((#279254))
GLOBAL_UNIT_ASSIGNED_CONTEXT((#279267,#279269,#279270))
REPRESENTATION_CONTEXT('','3D')
);
#279266=(
GEOMETRIC_REPRESENTATION_CONTEXT(3)
GLOBAL_UNCERTAINTY_ASSIGNED_CONTEXT((#279255))
GLOBAL_UNIT_ASSIGNED_CONTEXT((#279267,#279269,#279270))
REPRESENTATION_CONTEXT('','3D')
);
#279267=(
LENGTH_UNIT()
NAMED_UNIT(*)
SI_UNIT(.MILLI.,.METRE.)
);
#279268=(
LENGTH_UNIT()
NAMED_UNIT(*)
SI_UNIT($,.METRE.)
);
#279269=(
NAMED_UNIT(*)
PLANE_ANGLE_UNIT()
SI_UNIT($,.RADIAN.)
);
#279270=(
NAMED_UNIT(*)
SI_UNIT($,.STERADIAN.)
SOLID_ANGLE_UNIT()
);
#279271=SHAPE_DEFINITION_REPRESENTATION(#279281,#279300);
#279272=SHAPE_DEFINITION_REPRESENTATION(#279282,#279301);
#279273=SHAPE_DEFINITION_REPRESENTATION(#279283,#279302);
#279274=SHAPE_DEFINITION_REPRESENTATION(#279284,#279303);
#279275=SHAPE_DEFINITION_REPRESENTATION(#279285,#279304);
#279276=SHAPE_DEFINITION_REPRESENTATION(#279286,#279305);
#279277=SHAPE_DEFINITION_REPRESENTATION(#279287,#279306);
#279278=SHAPE_DEFINITION_REPRESENTATION(#279288,#279307);
#279279=SHAPE_DEFINITION_REPRESENTATION(#279289,#279308);
#279280=SHAPE_DEFINITION_REPRESENTATION(#279290,#279309);
#279281=PRODUCT_DEFINITION_SHAPE('',$,#279311);
#279282=PRODUCT_DEFINITION_SHAPE('',$,#279312);
#279283=PRODUCT_DEFINITION_SHAPE('',$,#279313);
#279284=PRODUCT_DEFINITION_SHAPE('',$,#279314);
#279285=PRODUCT_DEFINITION_SHAPE('',$,#279315);
#279286=PRODUCT_DEFINITION_SHAPE('',$,#279316);
#279287=PRODUCT_DEFINITION_SHAPE('',$,#279317);
#279288=PRODUCT_DEFINITION_SHAPE('',$,#279318);
#279289=PRODUCT_DEFINITION_SHAPE('',$,#279319);
#279290=PRODUCT_DEFINITION_SHAPE('',$,#279320);
#279291=PRODUCT_DEFINITION_SHAPE($,$,#38);
#279292=PRODUCT_DEFINITION_SHAPE($,$,#39);
#279293=PRODUCT_DEFINITION_SHAPE($,$,#40);
#279294=PRODUCT_DEFINITION_SHAPE($,$,#41);
#279295=PRODUCT_DEFINITION_SHAPE($,$,#42);
#279296=PRODUCT_DEFINITION_SHAPE($,$,#43);
#279297=PRODUCT_DEFINITION_SHAPE($,$,#44);
#279298=PRODUCT_DEFINITION_SHAPE($,$,#45);
#279299=PRODUCT_DEFINITION_SHAPE($,$,#46);
#279300=SHAPE_REPRESENTATION('',(#15047,#15665,#15666,#15667,#15668,#15669,
#15670,#15671,#15672,#15673),#279256);
#279301=SHAPE_REPRESENTATION('',(#15048),#279257);
#279302=SHAPE_REPRESENTATION('',(#15104),#279258);
#279303=SHAPE_REPRESENTATION('',(#15397),#279259);
#279304=SHAPE_REPRESENTATION('',(#15446),#279260);
#279305=SHAPE_REPRESENTATION('',(#15474),#279261);
#279306=SHAPE_REPRESENTATION('',(#15503),#279262);
#279307=SHAPE_REPRESENTATION('',(#15552),#279263);
#279308=SHAPE_REPRESENTATION('',(#15608),#279264);
#279309=SHAPE_REPRESENTATION('',(#15636),#279265);
#279310=PRODUCT_DEFINITION_CONTEXT('part definition',#279342,'design');
#279311=PRODUCT_DEFINITION('BR-355','BR-355',#279321,#279310);
#279312=PRODUCT_DEFINITION('base','Base',#279322,#279310);
#279313=PRODUCT_DEFINITION('Screw','Screw',#279323,#279310);
#279314=PRODUCT_DEFINITION('Arm_04','Arm_04',#279324,#279310);
#279315=PRODUCT_DEFINITION('Shaft_01','Shaft_01',#279325,#279310);
#279316=PRODUCT_DEFINITION('Arm_01','Arm_01',#279326,#279310);
#279317=PRODUCT_DEFINITION('Arm_03','Arm_03',#279327,#279310);
#279318=PRODUCT_DEFINITION('Top_Part','Top_Part',#279328,#279310);
#279319=PRODUCT_DEFINITION('Shaft_02','Shaft_02',#279329,#279310);
#279320=PRODUCT_DEFINITION('Arm_02','Arm_02',#279330,#279310);
#279321=PRODUCT_DEFINITION_FORMATION('',$,#279344);
#279322=PRODUCT_DEFINITION_FORMATION('',$,#279345);
#279323=PRODUCT_DEFINITION_FORMATION('',$,#279346);
#279324=PRODUCT_DEFINITION_FORMATION('',$,#279347);
#279325=PRODUCT_DEFINITION_FORMATION('',$,#279348);
#279326=PRODUCT_DEFINITION_FORMATION('',$,#279349);
#279327=PRODUCT_DEFINITION_FORMATION('',$,#279350);
#279328=PRODUCT_DEFINITION_FORMATION('',$,#279351);
#279329=PRODUCT_DEFINITION_FORMATION('',$,#279352);
#279330=PRODUCT_DEFINITION_FORMATION('',$,#279353);
#279331=PRODUCT_RELATED_PRODUCT_CATEGORY('BR-355','BR-355',(#279344));
#279332=PRODUCT_RELATED_PRODUCT_CATEGORY('Base','Base',(#279345));
#279333=PRODUCT_RELATED_PRODUCT_CATEGORY('Screw','Screw',(#279346));
#279334=PRODUCT_RELATED_PRODUCT_CATEGORY('Arm_04','Arm_04',(#279347));
#279335=PRODUCT_RELATED_PRODUCT_CATEGORY('Shaft_01','Shaft_01',(#279348));
#279336=PRODUCT_RELATED_PRODUCT_CATEGORY('Arm_01','Arm_01',(#279349));
#279337=PRODUCT_RELATED_PRODUCT_CATEGORY('Arm_03','Arm_03',(#279350));
#279338=PRODUCT_RELATED_PRODUCT_CATEGORY('Top_Part','Top_Part',(#279351));
#279339=PRODUCT_RELATED_PRODUCT_CATEGORY('Shaft_02','Shaft_02',(#279352));
#279340=PRODUCT_RELATED_PRODUCT_CATEGORY('Arm_02','Arm_02',(#279353));
#279341=APPLICATION_PROTOCOL_DEFINITION('international standard',
'automotive_design',2009,#279342);
#279342=APPLICATION_CONTEXT(
'Core Data for Automotive Mechanical Design Process');
#279343=PRODUCT_CONTEXT('part definition',#279342,'mechanical');
#279344=PRODUCT('BR-355','BR-355',$,(#279343));
#279345=PRODUCT('base','Base',$,(#279343));
#279346=PRODUCT('Screw','Screw',$,(#279343));
#279347=PRODUCT('Arm_04','Arm_04',$,(#279343));
#279348=PRODUCT('Shaft_01','Shaft_01',$,(#279343));
#279349=PRODUCT('Arm_01','Arm_01',$,(#279343));
#279350=PRODUCT('Arm_03','Arm_03',$,(#279343));
#279351=PRODUCT('Top_Part','Top_Part',$,(#279343));
#279352=PRODUCT('Shaft_02','Shaft_02',$,(#279343));
#279353=PRODUCT('Arm_02','Arm_02',$,(#279343));
#279354=PRESENTATION_STYLE_ASSIGNMENT((#279356));
#279355=PRESENTATION_STYLE_ASSIGNMENT((#279357));
#279356=SURFACE_STYLE_USAGE(.BOTH.,#279358);
#279357=SURFACE_STYLE_USAGE(.BOTH.,#279359);
#279358=SURFACE_SIDE_STYLE('',(#279360));
#279359=SURFACE_SIDE_STYLE('',(#279361));
#279360=SURFACE_STYLE_FILL_AREA(#279362);
#279361=SURFACE_STYLE_FILL_AREA(#279363);
#279362=FILL_AREA_STYLE('Steel - Satin',(#279364));
#279363=FILL_AREA_STYLE('Opaque(160,160,160)',(#279365));
#279364=FILL_AREA_STYLE_COLOUR('Steel - Satin',#279366);
#279365=FILL_AREA_STYLE_COLOUR('Opaque(160,160,160)',#279367);
#279366=COLOUR_RGB('Steel - Satin', 0.66274510, 0.83137255, 0.94901961);
#279367=COLOUR_RGB('Opaque(160,160,160)', 0.66274510, 0.83137255, 0.94901961);
ENDSEC;
END-ISO-10303-21;
